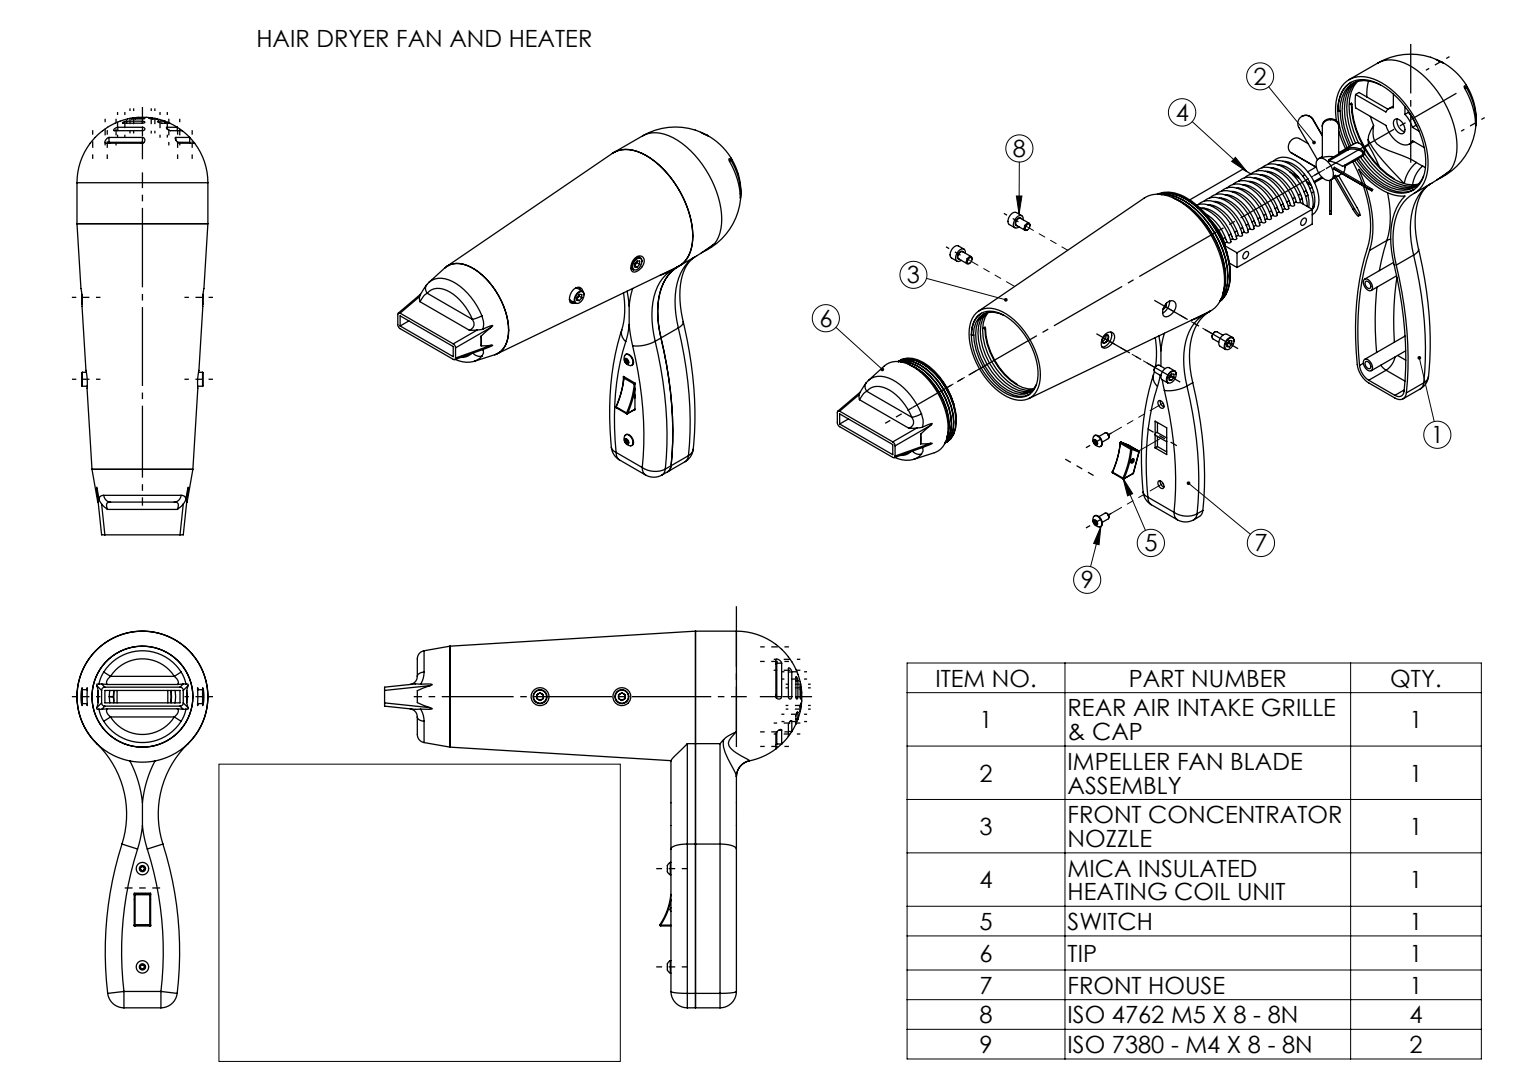
ISO-10303-21;
HEADER;
FILE_DESCRIPTION (('STEP AP214'),
    '1' );
FILE_NAME ('BR-835',
    '2026-10-04T13:31:42',
    ( '' ),
    ( '' ),
    'SwSTEP 2.0',
    'SolidWorks 2026',
    '' );
FILE_SCHEMA (( 'AUTOMOTIVE_DESIGN' ));
ENDSEC;

DATA;
#1 = CARTESIAN_POINT ( 'NONE',  ( -19.03943276465977164, 0.05219959533909376836, 71.24890960531435269 ) ) ;
#2 = CARTESIAN_POINT ( 'NONE',  ( 4.379528057220339221, -16.55341960407611168, 72.70724293864769550 ) ) ;
#3 = CARTESIAN_POINT ( 'NONE',  ( 19.05341960407617918, -5.049401038297876454, 86.04275706135233293 ) ) ;
#4 = CARTESIAN_POINT ( 'NONE',  ( 21.53943276465977519, -0.05219959533907433946, 43.74890960531435979 ) ) ;
#5 = ORIENTED_EDGE ( 'NONE', *, *, #6876, .T. ) ;
#6 = CARTESIAN_POINT ( 'NONE',  ( -19.05341960407611168, -5.049401038298163336, 21.45724293864768839 ) ) ;
#7 = CARTESIAN_POINT ( 'NONE',  ( -16.18388926212240264, -7.379444403734405356, 30.43953151366152809 ) ) ;
#9 = CARTESIAN_POINT ( 'NONE',  ( 21.53943276465977519, -0.05219959533907433946, 73.74890960531433848 ) ) ;
#8 = CARTESIAN_POINT ( 'NONE',  ( 5.049401038298161559, -19.05341960407611168, 77.70724293864765286 ) ) ;
#11 = CARTESIAN_POINT ( 'NONE',  ( -5.049401038298153566, 19.05341960407611168, 75.20724293864769550 ) ) ;
#10 = CARTESIAN_POINT ( 'NONE',  ( -8.314922557961024197, 14.29746914071037800, 97.91775706135236135 ) ) ;
#12 = CARTESIAN_POINT ( 'NONE',  ( -9.564922557961040184, 16.46253265017147172, 72.91775706135233293 ) ) ;
#13 = CARTESIAN_POINT ( 'NONE',  ( 5.823673210054444382, -21.52544592524334988, 85.20942372801901854 ) ) ;
#14 = CARTESIAN_POINT ( 'NONE',  ( -15.80617190586745835, -15.72974639402198527, 56.87390960531436690 ) ) ;
#15 = CARTESIAN_POINT ( 'NONE',  ( 21.52544592524344225, -5.823673210054117533, 23.54057627198102765 ) ) ;
#16 = CARTESIAN_POINT ( 'NONE',  ( -19.02544592524342804, 5.153800228976336051, 36.04057627198100988 ) ) ;
#17 = CARTESIAN_POINT ( 'NONE',  ( -4.379528057220086978, -16.55341960407618274, 94.79275706135234714 ) ) ;
#18 = CARTESIAN_POINT ( 'NONE',  ( -19.05341960407611168, -5.049401038298163336, 56.45724293864768129 ) ) ;
#19 = CARTESIAN_POINT ( 'NONE',  ( 14.29746914071037800, 8.314922557961029526, 26.66775706135235424 ) ) ;
#20 = CARTESIAN_POINT ( 'NONE',  ( 0.000000000000000000, 0.000000000000000000, -45.64921306006598201 ) ) ;
#21 = CARTESIAN_POINT ( 'NONE',  ( 18.67979575497194134, -10.72451020669871369, 110.8344237280190043 ) ) ;
#22 = CARTESIAN_POINT ( 'NONE',  ( -14.29746914071049879, 8.314922557960819915, 55.83224293864770260 ) ) ;
#23 = CARTESIAN_POINT ( 'NONE',  ( -0.05219959533907301413, -21.53943276465977519, 102.4989096053143811 ) ) ;
#24 = CARTESIAN_POINT ( 'NONE',  ( 10.81492255796078972, 18.62759615963270932, 99.58224293864770971 ) ) ;
#25 = CARTESIAN_POINT ( 'NONE',  ( -3.573655867282028392E-15, 2.428612866367529932E-14, -24.99999999999997868 ) ) ;
#26 = CARTESIAN_POINT ( 'NONE',  ( -15.72974639402197994, 15.80617190586746368, 40.62390960531435269 ) ) ;
#27 = CARTESIAN_POINT ( 'NONE',  ( -12.06949235617739369, -12.14591786802326823, 74.37609039468568994 ) ) ;
#28 = CARTESIAN_POINT ( 'NONE',  ( -4.483927247898539470, -16.52544592524342804, 92.29057627198103830 ) ) ;
#29 = CARTESIAN_POINT ( 'NONE',  ( 19.03943276465977164, -0.05219959533909143690, 58.74890960531435979 ) ) ;
#30 = SHAPE_REPRESENTATION_RELATIONSHIP ( 'NONE' , 'NONE' ,  #65015, #146166 ) ;
#31 = DIRECTION ( 'NONE',  ( 0.000000000000000000, 0.000000000000000000, 1.000000000000000000 ) ) ;
#32 = CARTESIAN_POINT ( 'NONE',  ( -12.06949235617739369, -12.14591786802326823, 109.3760903946857042 ) ) ;
#33 = CARTESIAN_POINT ( 'NONE',  ( -5.719274019375665041, -21.55341960407619695, 34.79275706135235424 ) ) ;
#34 = CARTESIAN_POINT ( 'NONE',  ( -19.05341960407611168, -5.049401038298163336, 91.45724293864766707 ) ) ;
#35 = CARTESIAN_POINT ( 'NONE',  ( 21.55341960407619695, -5.719274019375665929, 71.04275706135234714 ) ) ;
#36 = CARTESIAN_POINT ( 'NONE',  ( 0.000000000000000000, 0.000000000000000000, 0.000000000000000000 ) ) ;
#37 = CARTESIAN_POINT ( 'NONE',  ( 0.000000000000000000, -0.7216878364870318308, 1.249999999999999778 ) ) ;
#38 = ORIENTED_EDGE ( 'NONE', *, *, #138549, .T. ) ;
#39 = CARTESIAN_POINT ( 'NONE',  ( 10.72451020669871369, 18.67979575497193778, 57.08442372801901854 ) ) ;
#40 = CARTESIAN_POINT ( 'NONE',  ( -0.05219959533909027116, -19.03943276465977164, 57.49890960531435979 ) ) ;
#41 = CARTESIAN_POINT ( 'NONE',  ( 9.564922557960805705, 16.46253265017160317, 84.58224293864769550 ) ) ;
#42 = CARTESIAN_POINT ( 'NONE',  ( -9.564922557961040184, 16.46253265017147172, 67.91775706135233293 ) ) ;
#43 = CARTESIAN_POINT ( 'NONE',  ( 5.719274019375673035, 21.55341960407619339, 47.29275706135234003 ) ) ;
#44 = CARTESIAN_POINT ( 'NONE',  ( -19.05341960407617563, 5.049401038297882671, 103.5427570613523329 ) ) ;
#45 = CARTESIAN_POINT ( 'NONE',  ( -5.049401038297874678, -19.05341960407617918, 69.79275706135233293 ) ) ;
#46 = CARTESIAN_POINT ( 'NONE',  ( 13.89961937509977652, -13.97604488694527269, 38.12390960531436690 ) ) ;
#47 = CARTESIAN_POINT ( 'NONE',  ( 19.05341960407617918, -5.049401038297876454, 86.04275706135233293 ) ) ;
#48 = CARTESIAN_POINT ( 'NONE',  ( -16.52544592524335698, -4.483927247898792601, 98.95942372801903275 ) ) ;
#49 = CARTESIAN_POINT ( 'NONE',  ( 0.05219959533936267826, -19.03943276465977164, 80.00109039468567573 ) ) ;
#50 = CARTESIAN_POINT ( 'NONE',  ( -12.14591786802309592, -12.06949235617757132, 31.87390960531435979 ) ) ;
#51 = CARTESIAN_POINT ( 'NONE',  ( 16.51473224551083163, -9.474510206698727899, 45.83442372801900433 ) ) ;
#52 = CARTESIAN_POINT ( 'NONE',  ( 15.80617190586769283, -15.72974639402175789, 100.6260903946857184 ) ) ;
#53 = PRODUCT_DEFINITION_SHAPE ( 'NONE', 'NONE',  #200200 ) ;
#55 = EDGE_CURVE ( 'NONE', #141361, #196966, #36036, .T. ) ;
#54 = CARTESIAN_POINT ( 'NONE',  ( 19.05341960407617918, -5.049401038297876454, 21.04275706135232582 ) ) ;
#56 = CARTESIAN_POINT ( 'NONE',  ( 0.05219959533909260263, 19.03943276465977164, 24.99890960531435269 ) ) ;
#57 = CARTESIAN_POINT ( 'NONE',  ( -21.53943276465977519, -0.05219959533937600094, 83.75109039468568994 ) ) ;
#58 = CARTESIAN_POINT ( 'NONE',  ( 8.314922557961029526, -14.29746914071037800, 30.41775706135234358 ) ) ;
#59 = CARTESIAN_POINT ( 'NONE',  ( 19.02544592524343514, -5.153800228976328945, 98.54057627198100988 ) ) ;
#60 = CARTESIAN_POINT ( 'NONE',  ( -8.571926809382608425, 26.38167802310805854, 144.4750000027312069 ) ) ;
#61 = CARTESIAN_POINT ( 'NONE',  ( 0.05219959533909260263, 19.03943276465977164, 79.99890960531436690 ) ) ;
#62 = DIRECTION ( 'NONE',  ( -0.000000000000000000, -0.000000000000000000, 1.000000000000000000 ) ) ;
#63 = ORIENTED_EDGE ( 'NONE', *, *, #98272, .F. ) ;
#64 = CARTESIAN_POINT ( 'NONE',  ( -16.51473224551082808, 9.474510206698731452, 83.33442372801899012 ) ) ;
#66 = CARTESIAN_POINT ( 'NONE',  ( 0.05219959533909260263, 19.03943276465977164, 114.9989096053143669 ) ) ;
#65 = CIRCLE ( 'NONE', #138924, 4.000000000000000888 ) ;
#68 = CARTESIAN_POINT ( 'NONE',  ( -13.97604488694547697, 13.89961937509957934, 103.1260903946856473 ) ) ;
#67 = CARTESIAN_POINT ( 'NONE',  ( -10.72451020669870658, -18.67979575497194134, 109.5844237280190328 ) ) ;
#69 = CARTESIAN_POINT ( 'NONE',  ( -4.483927247898539470, -16.52544592524342804, 97.29057627198105251 ) ) ;
#70 = CARTESIAN_POINT ( 'NONE',  ( -5.153800228976328057, -19.02544592524343514, 22.29057627198102765 ) ) ;
#71 = CARTESIAN_POINT ( 'NONE',  ( -5.823673210054116645, -21.52544592524344225, 62.29057627198102409 ) ) ;
#72 =( BOUNDED_CURVE ( )  B_SPLINE_CURVE ( 2, ( #135553, #193227, #149715, #197225, #132546, #194235, #55701, #58687, #117374, #179071, #182049 ),
 .UNSPECIFIED., .F., .T. ) 
 B_SPLINE_CURVE_WITH_KNOTS ( ( 3, 2, 2, 2, 2, 3 ),
 ( 0.1000000000000000888, 0.1200000000000001343, 0.1400000000000001799, 0.1600000000000001976, 0.1800000000000002431, 0.2000000000000001776 ),
 .UNSPECIFIED. ) 
 CURVE ( )  GEOMETRIC_REPRESENTATION_ITEM ( )  RATIONAL_B_SPLINE_CURVE ( ( 0.9999999999999997780, 0.9510565162951537532, 1.000000000000000000, 0.9510565162951535312, 1.000000000000000000, 0.9510565162951535312, 1.000000000000000000, 0.9510565162951535312, 1.000000000000000000, 0.9510565162951529761, 1.000000000000000444 ) ) 
 REPRESENTATION_ITEM ( '' )  );
#73 = CARTESIAN_POINT ( 'NONE',  ( 10.72451020669898902, -18.67979575497178502, 47.91557627198102409 ) ) ;
#74 = CARTESIAN_POINT ( 'NONE',  ( 13.89961937509977652, -13.97604488694527269, 28.12390960531435624 ) ) ;
#75 = CARTESIAN_POINT ( 'NONE',  ( 27.73933785331498569, 2.768321779492822058E-14, 140.3750000027311842 ) ) ;
#76 = CARTESIAN_POINT ( 'NONE',  ( 16.51473224551083163, -9.474510206698727899, 55.83442372801899722 ) ) ;
#77 = CARTESIAN_POINT ( 'NONE',  ( -14.29746914071049879, 8.314922557960819915, 35.83224293864768839 ) ) ;
#78 = CARTESIAN_POINT ( 'NONE',  ( 9.474510206698971260, -16.51473224551069308, 112.9155762719810383 ) ) ;
#79 = CARTESIAN_POINT ( 'NONE',  ( -15.80617190586768217, 15.72974639402176855, 83.12609039468568994 ) ) ;
#80 = CARTESIAN_POINT ( 'NONE',  ( -10.72451020669898014, 18.67979575497178502, 65.41557627198102409 ) ) ;
#81 = CARTESIAN_POINT ( 'NONE',  ( 18.67979575497194134, -10.72451020669871369, 55.83442372801901854 ) ) ;
#82 = CARTESIAN_POINT ( 'NONE',  ( 15.80617190586769283, -15.72974639402175789, 45.62609039468567573 ) ) ;
#83 = CARTESIAN_POINT ( 'NONE',  ( 13.89961937509977652, -13.97604488694527269, 78.12390960531433848 ) ) ;
#84 = CARTESIAN_POINT ( 'NONE',  ( -8.314922557961024197, 14.29746914071037800, 97.91775706135236135 ) ) ;
#85 = CARTESIAN_POINT ( 'NONE',  ( -5.049401038298153566, 19.05341960407611168, 25.20724293864768484 ) ) ;
#86 = CARTESIAN_POINT ( 'NONE',  ( -31.23840969660177791, 7.314650797970922547, 96.67552899226033958 ) ) ;
#87 = CARTESIAN_POINT ( 'NONE',  ( -14.29746914071049879, 8.314922557960819915, 70.83224293864770971 ) ) ;
#88 = CARTESIAN_POINT ( 'NONE',  ( 8.224510206698953496, -14.34966873604960469, 37.91557627198102409 ) ) ;
#89 = CARTESIAN_POINT ( 'NONE',  ( 19.05341960407611168, 5.049401038298154454, 63.95724293864769550 ) ) ;
#90 = CARTESIAN_POINT ( 'NONE',  ( -19.03943276465977164, 0.05219959533909376836, 36.24890960531436690 ) ) ;
#91 = CARTESIAN_POINT ( 'NONE',  ( 15.72974639402199770, -15.80617190586745480, 43.12390960531435269 ) ) ;
#92 = CARTESIAN_POINT ( 'NONE',  ( -19.02544592524334988, -5.153800228976617603, 33.95942372801897591 ) ) ;
#94 = CARTESIAN_POINT ( 'NONE',  ( 16.55341960407611168, 4.379528057220329451, 48.95724293864770971 ) ) ;
#93 = CARTESIAN_POINT ( 'NONE',  ( 25.38276140623240096, 4.833717845876353891, 166.7901960806512136 ) ) ;
#96 = AXIS2_PLACEMENT_3D ( 'NONE', #158680, #174858, #36324 ) ;
#95 = CARTESIAN_POINT ( 'NONE',  ( -10.72451020669898014, 18.67979575497178502, 30.41557627198101699 ) ) ;
#97 = CARTESIAN_POINT ( 'NONE',  ( 7.656827144875921753, -71.74905178543389184, -15.00000000000000178 ) ) ;
#98 = CARTESIAN_POINT ( 'NONE',  ( -8.314922557961024197, 14.29746914071037800, 72.91775706135234714 ) ) ;
#99 = CARTESIAN_POINT ( 'NONE',  ( 13.97604488694548053, -13.89961937509957401, 70.62609039468567573 ) ) ;
#100 = CARTESIAN_POINT ( 'NONE',  ( 16.53943276465976808, -0.05219959533910856209, 43.74890960531435979 ) ) ;
#101 = CARTESIAN_POINT ( 'NONE',  ( 28.79475375365586132, 2.781246896534039337E-14, 145.2656553485623760 ) ) ;
#102 = CARTESIAN_POINT ( 'NONE',  ( -8.314922557960811034, -14.29746914071050412, 27.08224293864769550 ) ) ;
#103 = CARTESIAN_POINT ( 'NONE',  ( 16.46253265017160672, -9.564922557960803928, 48.33224293864769550 ) ) ;
#104 = CARTESIAN_POINT ( 'NONE',  ( 19.05341960407611168, 5.049401038298154454, 73.95724293864768129 ) ) ;
#105 = CARTESIAN_POINT ( 'NONE',  ( -5.049401038298153566, 19.05341960407611168, 35.20724293864768839 ) ) ;
#106 = CARTESIAN_POINT ( 'NONE',  ( 21.55341960407619695, -5.719274019375665929, 41.04275706135236135 ) ) ;
#107 = CARTESIAN_POINT ( 'NONE',  ( 16.46253265017160672, -9.564922557960803928, 63.33224293864769550 ) ) ;
#108 = DIRECTION ( 'NONE',  ( -0.000000000000000000, -0.000000000000000000, -1.000000000000000000 ) ) ;
#109 = CARTESIAN_POINT ( 'NONE',  ( -19.03943276465977164, 0.05219959533909376836, 46.24890960531435979 ) ) ;
#110 = CARTESIAN_POINT ( 'NONE',  ( -0.05219959533907301413, -21.53943276465977519, 32.49890960531435979 ) ) ;
#111 = B_SPLINE_CURVE_WITH_KNOTS ( 'NONE', 3,
 ( #132361, #22184, #54519, #149527, #68676, #38352 ),
 .UNSPECIFIED., .F., .F.,
 ( 4, 2, 4 ),
 ( 0.007228050697041336729, 0.007608510107494812283, 0.007988969517948286969 ),
 .UNSPECIFIED. ) ;
#113 = CARTESIAN_POINT ( 'NONE',  ( 12.06949235617757843, -12.14591786802309237, 113.1239096053143953 ) ) ;
#112 = CARTESIAN_POINT ( 'NONE',  ( 10.72451020669871369, 18.67979575497193778, 67.08442372801901854 ) ) ;
#114 = CARTESIAN_POINT ( 'NONE',  ( -21.55341960407610458, -5.719274019375992779, 31.45724293864769550 ) ) ;
#115 = CARTESIAN_POINT ( 'NONE',  ( 8.314922557961029526, -14.29746914071037800, 95.41775706135234714 ) ) ;
#116 = CARTESIAN_POINT ( 'NONE',  ( 10.81492255796106328, -18.62759615963255655, 110.4177570613523756 ) ) ;
#117 = CARTESIAN_POINT ( 'NONE',  ( -8.314922557961024197, 14.29746914071037800, 67.91775706135234714 ) ) ;
#118 = CARTESIAN_POINT ( 'NONE',  ( -9.564922557960796823, -16.46253265017161027, 112.0822429386476955 ) ) ;
#119 = CARTESIAN_POINT ( 'NONE',  ( -14.29746914071037622, -8.314922557961029526, 59.16775706135234714 ) ) ;
#120 = CARTESIAN_POINT ( 'NONE',  ( -8.314922557961024197, 14.29746914071037800, 37.91775706135235424 ) ) ;
#121 = CARTESIAN_POINT ( 'NONE',  ( -0.05219959533934338120, 16.53943276465976808, 102.5010903946856899 ) ) ;
#122 = CARTESIAN_POINT ( 'NONE',  ( -15.72974639402176322, -15.80617190586768395, 54.37609039468568994 ) ) ;
#123 = CARTESIAN_POINT ( 'NONE',  ( 4.379528057220092307, 16.55341960407617563, 22.29275706135235069 ) ) ;
#124 = CARTESIAN_POINT ( 'NONE',  ( 5.719274019375991003, -21.55341960407610458, 112.7072429386476955 ) ) ;
#125 = CARTESIAN_POINT ( 'NONE',  ( 8.224510206698742110, 14.34966873604972548, 27.08442372801901854 ) ) ;
#126 = CARTESIAN_POINT ( 'NONE',  ( -12.14591786802326823, 12.06949235617739902, 83.12609039468568994 ) ) ;
#127 = FACE_OUTER_BOUND ( 'NONE', #92552, .T. ) ;
#128 = CARTESIAN_POINT ( 'NONE',  ( 18.67979575497194134, -10.72451020669871369, 85.83442372801901854 ) ) ;
#129 = CARTESIAN_POINT ( 'NONE',  ( 16.46253265017146816, 9.564922557961045513, 81.66775706135233293 ) ) ;
#130 = CARTESIAN_POINT ( 'NONE',  ( -4.379528057220328563, 16.55341960407611168, 60.20724293864768839 ) ) ;
#131 = CARTESIAN_POINT ( 'NONE',  ( -4.379528057220328563, 16.55341960407611168, 40.20724293864769550 ) ) ;
#132 = CARTESIAN_POINT ( 'NONE',  ( -14.29746914071049879, 8.314922557960819915, 105.8322429386476955 ) ) ;
#134 = CARTESIAN_POINT ( 'NONE',  ( 9.809999999999998721, 0.000000000000000000, 1.999999999999999556 ) ) ;
#133 = CARTESIAN_POINT ( 'NONE',  ( -16.46253265017146816, -9.564922557961047289, 49.16775706135233293 ) ) ;
#135 = CARTESIAN_POINT ( 'NONE',  ( 0.05219959533937995610, -21.53943276465977519, 45.00109039468568284 ) ) ;
#136 = CARTESIAN_POINT ( 'NONE',  ( 0.05219959533934541429, -16.53943276465976808, 20.00109039468568639 ) ) ;
#137 = DIRECTION ( 'NONE',  ( 0.000000000000000000, 0.000000000000000000, -1.000000000000000000 ) ) ;
#138 = CARTESIAN_POINT ( 'NONE',  ( 16.46253265017160672, -9.564922557960803928, 108.3322429386476955 ) ) ;
#139 = CARTESIAN_POINT ( 'NONE',  ( 15.80617190586746368, 15.72974639402197994, 69.37390960531436690 ) ) ;
#140 = CARTESIAN_POINT ( 'NONE',  ( -19.02544592524334988, -5.153800228976617603, 98.95942372801900433 ) ) ;
#141 = CARTESIAN_POINT ( 'NONE',  ( -16.51473224551069308, -9.474510206698971260, 106.6655762719810383 ) ) ;
#142 = CARTESIAN_POINT ( 'NONE',  ( 1.955436445514509014, -27.87083070116242567, 139.9999999999999716 ) ) ;
#143 = CARTESIAN_POINT ( 'NONE',  ( 14.29746914071049879, -8.314922557960816363, 113.3322429386476955 ) ) ;
#144 = CARTESIAN_POINT ( 'NONE',  ( -21.55341960407619339, 5.719274019375674811, 98.54275706135234714 ) ) ;
#145 = CARTESIAN_POINT ( 'NONE',  ( 13.89961937509977652, -13.97604488694527269, 28.12390960531435624 ) ) ;
#146 = CARTESIAN_POINT ( 'NONE',  ( 21.52544592524334988, 5.823673210054432836, 51.45942372801901854 ) ) ;
#147 = CARTESIAN_POINT ( 'NONE',  ( -21.53943276465977519, -0.05219959533937600094, 93.75109039468567573 ) ) ;
#148 = CARTESIAN_POINT ( 'NONE',  ( 14.29746914071037800, 8.314922557961029526, 86.66775706135234714 ) ) ;
#149 = CARTESIAN_POINT ( 'NONE',  ( -5.719274019375665041, -21.55341960407619695, 39.79275706135235424 ) ) ;
#150 = CARTESIAN_POINT ( 'NONE',  ( 21.52544592524334988, 5.823673210054432836, 36.45942372801901143 ) ) ;
#152 = CARTESIAN_POINT ( 'NONE',  ( -16.51473224551069308, -9.474510206698971260, 81.66557627198103830 ) ) ;
#151 = CARTESIAN_POINT ( 'NONE',  ( 5.049401038297881783, 19.05341960407617563, 67.29275706135234714 ) ) ;
#153 = CARTESIAN_POINT ( 'NONE',  ( -0.05219959533910754901, -16.53943276465976808, 107.4989096053143669 ) ) ;
#154 = CARTESIAN_POINT ( 'NONE',  ( -0.05219959533907301413, -21.53943276465977519, 82.49890960531436690 ) ) ;
#155 = CARTESIAN_POINT ( 'NONE',  ( 12.14591786802309770, 12.06949235617756955, 64.37390960531435269 ) ) ;
#156 = CARTESIAN_POINT ( 'NONE',  ( -21.52544592524334988, -5.823673210054445271, 103.9594237280190185 ) ) ;
#157 = CARTESIAN_POINT ( 'NONE',  ( -8.224510206698948167, 14.34966873604960824, 90.41557627198103830 ) ) ;
#158 = CARTESIAN_POINT ( 'NONE',  ( -19.02544592524342804, 5.153800228976336051, 41.04057627198103120 ) ) ;
#159 = CARTESIAN_POINT ( 'NONE',  ( 19.02544592524334988, 5.153800228976608722, 66.45942372801899012 ) ) ;
#161 = CARTESIAN_POINT ( 'NONE',  ( -8.224510206698948167, 14.34966873604960824, 50.41557627198103120 ) ) ;
#160 = AXIS2_PLACEMENT_3D ( 'NONE', #57198, #41025, #151201 ) ;
#162 = CARTESIAN_POINT ( 'NONE',  ( 5.823673210054444382, -21.52544592524334988, 95.20942372801903275 ) ) ;
#163 = CARTESIAN_POINT ( 'NONE',  ( 13.97604488694527802, 13.89961937509977652, 89.37390960531436690 ) ) ;
#164 = CARTESIAN_POINT ( 'NONE',  ( 5.153800228976615827, -19.02544592524334988, 55.20942372801899722 ) ) ;
#165 = CARTESIAN_POINT ( 'NONE',  ( 0.05219959533907565091, 21.53943276465977519, 69.99890960531435269 ) ) ;
#166 = CARTESIAN_POINT ( 'NONE',  ( 18.67979575497178502, 10.72451020669898547, 109.1655762719810383 ) ) ;
#167 = CARTESIAN_POINT ( 'NONE',  ( 5.153800228976615827, -19.02544592524334988, 110.2094237280189901 ) ) ;
#168 = CARTESIAN_POINT ( 'NONE',  ( 0.05219959533934541429, -16.53943276465976808, 80.00109039468568994 ) ) ;
#170 = CARTESIAN_POINT ( 'NONE',  ( -10.72451020669870658, -18.67979575497194134, 24.58442372801901499 ) ) ;
#169 = CARTESIAN_POINT ( 'NONE',  ( -5.153800228976328057, -19.02544592524343514, 22.29057627198102765 ) ) ;
#171 = CARTESIAN_POINT ( 'NONE',  ( -14.29746914071049879, 8.314922557960819915, 110.8322429386476955 ) ) ;
#172 = CARTESIAN_POINT ( 'NONE',  ( -11.40812507854755609, 35.11059874428196537, -7.524999997268813523 ) ) ;
#173 = CARTESIAN_POINT ( 'NONE',  ( 8.314922557961029526, -14.29746914071037800, 45.41775706135234003 ) ) ;
#174 = APPLICATION_CONTEXT ( 'automotive_design' ) ;
#175 = CARTESIAN_POINT ( 'NONE',  ( 16.53943276465976808, -0.05219959533910856209, 78.74890960531436690 ) ) ;
#176 = CARTESIAN_POINT ( 'NONE',  ( -18.67979575497178146, -10.72451020669898902, 81.66557627198103830 ) ) ;
#177 = CARTESIAN_POINT ( 'NONE',  ( -8.224510206698735004, -14.34966873604973081, 104.5844237280190185 ) ) ;
#178 = CARTESIAN_POINT ( 'NONE',  ( -4.483927247898782831, 16.52544592524335698, 32.70942372801900433 ) ) ;
#179 = CARTESIAN_POINT ( 'NONE',  ( 19.03943276465977164, -0.05219959533909143690, 38.74890960531436690 ) ) ;
#180 = CARTESIAN_POINT ( 'NONE',  ( -16.53943276465976808, -0.05219959533934237506, 83.75109039468568994 ) ) ;
#181 = CARTESIAN_POINT ( 'NONE',  ( -5.153800228976607833, 19.02544592524334988, 77.70942372801900433 ) ) ;
#182 = CARTESIAN_POINT ( 'NONE',  ( 21.55341960407610458, 5.719274019375980345, 68.95724293864769550 ) ) ;
#183 = CARTESIAN_POINT ( 'NONE',  ( -4.379528057220086978, -16.55341960407618274, 109.7927570613523613 ) ) ;
#184 = CARTESIAN_POINT ( 'NONE',  ( 15.72974639402176855, 15.80617190586768217, 86.87609039468568994 ) ) ;
#185 = CARTESIAN_POINT ( 'NONE',  ( -18.67979575497178146, -10.72451020669898902, 41.66557627198103120 ) ) ;
#186 = EDGE_LOOP ( 'NONE', ( #96983, #147295, #14374 ) ) ;
#187 = CARTESIAN_POINT ( 'NONE',  ( -14.34966873604972548, 8.224510206698743886, 98.33442372801901854 ) ) ;
#188 = CARTESIAN_POINT ( 'NONE',  ( -18.62759615963270932, 10.81492255796079327, 50.83224293864770971 ) ) ;
#189 = ORIENTED_EDGE ( 'NONE', *, *, #119223, .F. ) ;
#190 = CARTESIAN_POINT ( 'NONE',  ( -0.05219959533907301413, -21.53943276465977519, 22.49890960531436335 ) ) ;
#191 = CARTESIAN_POINT ( 'NONE',  ( 17.50000000000000355, 3.565345528327941160, 108.0750551319352581 ) ) ;
#192 = CARTESIAN_POINT ( 'NONE',  ( -16.46253265017160317, 9.564922557960807481, 25.83224293864769194 ) ) ;
#193 = CARTESIAN_POINT ( 'NONE',  ( 15.72974639402199770, -15.80617190586745480, 78.12390960531436690 ) ) ;
#194 = CARTESIAN_POINT ( 'NONE',  ( 0.05219959533934541429, -16.53943276465976808, 105.0010903946856757 ) ) ;
#195 = CARTESIAN_POINT ( 'NONE',  ( 21.53943276465977519, 0.05219959533937863772, 61.25109039468567573 ) ) ;
#196 = CARTESIAN_POINT ( 'NONE',  ( -14.29746914071037622, -8.314922557961029526, 24.16775706135235424 ) ) ;
#197 = CARTESIAN_POINT ( 'NONE',  ( 12.14591786802309770, 12.06949235617756955, 114.3739096053143527 ) ) ;
#198 = CARTESIAN_POINT ( 'NONE',  ( -19.05341960407617563, 5.049401038297882671, 113.5427570613523471 ) ) ;
#199 = CARTESIAN_POINT ( 'NONE',  ( -5.049401038298153566, 19.05341960407611168, 35.20724293864768839 ) ) ;
#200 = CARTESIAN_POINT ( 'NONE',  ( -23.31738231874055245, -16.94106989632524574, 144.1999999999999886 ) ) ;
#201 = CARTESIAN_POINT ( 'NONE',  ( -19.03943276465977164, 0.05219959533909376836, 111.2489096053143669 ) ) ;
#202 = CARTESIAN_POINT ( 'NONE',  ( 0.05219959533934541429, -16.53943276465976808, 85.00109039468568994 ) ) ;
#203 = CARTESIAN_POINT ( 'NONE',  ( -9.564922557961040184, 16.46253265017147172, 82.91775706135233293 ) ) ;
#204 = CARTESIAN_POINT ( 'NONE',  ( 9.564922557961047289, -16.46253265017146816, 30.41775706135232937 ) ) ;
#205 = CARTESIAN_POINT ( 'NONE',  ( 0.05219959533907565091, 21.53943276465977519, 59.99890960531436690 ) ) ;
#206 = CARTESIAN_POINT ( 'NONE',  ( -14.34966873604972548, 8.224510206698743886, 83.33442372801903275 ) ) ;
#207 = CARTESIAN_POINT ( 'NONE',  ( -16.46253265017146816, -9.564922557961047289, 99.16775706135233293 ) ) ;
#208 = CARTESIAN_POINT ( 'NONE',  ( 19.05341960407611168, 5.049401038298154454, 53.95724293864770260 ) ) ;
#209 = CARTESIAN_POINT ( 'NONE',  ( 16.46253265017160672, -9.564922557960803928, 98.33224293864769550 ) ) ;
#210 = CARTESIAN_POINT ( 'NONE',  ( -0.05219959533937732626, 21.53943276465977519, 47.50109039468568994 ) ) ;
#211 = CARTESIAN_POINT ( 'NONE',  ( -19.05341960407611168, -5.049401038298163336, 41.45724293864769550 ) ) ;
#212 = SPHERICAL_SURFACE ( 'NONE', #37950, 10.00000000000000000 ) ;
#213 = CARTESIAN_POINT ( 'NONE',  ( -13.89961937509977652, 13.97604488694528158, 110.6239096053143243 ) ) ;
#214 = CARTESIAN_POINT ( 'NONE',  ( 8.314922557960818139, 14.29746914071049879, 64.58224293864769550 ) ) ;
#215 = CARTESIAN_POINT ( 'NONE',  ( -5.719274019375978568, 21.55341960407610458, 55.20724293864770260 ) ) ;
#216 = CARTESIAN_POINT ( 'NONE',  ( 23.29544513554940011, 16.92513159979228021, 143.4656553485623647 ) ) ;
#217 = CARTESIAN_POINT ( 'NONE',  ( -16.46253265017146816, -9.564922557961047289, 49.16775706135233293 ) ) ;
#218 = CARTESIAN_POINT ( 'NONE',  ( 19.76513836702801186, -12.18681594171306237, 170.0000000000000000 ) ) ;
#220 = CARTESIAN_POINT ( 'NONE',  ( 5.049401038298161559, -19.05341960407611168, 67.70724293864769550 ) ) ;
#219 = CARTESIAN_POINT ( 'NONE',  ( -16.46253265017160317, 9.564922557960807481, 60.83224293864769550 ) ) ;
#221 = EDGE_CURVE ( 'NONE', #165210, #193478, #178958, .T. ) ;
#222 = CARTESIAN_POINT ( 'NONE',  ( 12.06949235617739724, 12.14591786802326823, 46.87609039468568994 ) ) ;
#223 = CARTESIAN_POINT ( 'NONE',  ( 15.64208950468054127, -40.81369178264755959, -21.33727593494802122 ) ) ;
#224 = CARTESIAN_POINT ( 'NONE',  ( 16.51473224551083163, -9.474510206698727899, 30.83442372801900433 ) ) ;
#225 = CYLINDRICAL_SURFACE ( 'NONE', #105054, 10.00000000000000178 ) ;
#226 = CARTESIAN_POINT ( 'NONE',  ( -0.05219959533934338120, 16.53943276465976808, 92.50109039468567573 ) ) ;
#227 = CARTESIAN_POINT ( 'NONE',  ( 69.65682714487590488, -71.74905178543389184, -4.999999999999999112 ) ) ;
#228 = CARTESIAN_POINT ( 'NONE',  ( 16.52544592524335698, 4.483927247898782831, 81.45942372801900433 ) ) ;
#229 = CARTESIAN_POINT ( 'NONE',  ( 4.483927247898790824, -16.52544592524335698, 60.20942372801902565 ) ) ;
#230 = CARTESIAN_POINT ( 'NONE',  ( -5.823673210054431948, 21.52544592524334988, 112.7094237280190328 ) ) ;
#232 = CARTESIAN_POINT ( 'NONE',  ( 17.25602135761909395, -17.10936820804715808, -56.77278709839602300 ) ) ;
#231 = CARTESIAN_POINT ( 'NONE',  ( -5.049401038298153566, 19.05341960407611168, 50.20724293864770260 ) ) ;
#233 = CARTESIAN_POINT ( 'NONE',  ( -10.72451020669870658, -18.67979575497194134, 69.58442372801900433 ) ) ;
#234 = CARTESIAN_POINT ( 'NONE',  ( -19.03943276465977164, -0.05219959533935918106, 73.75109039468566152 ) ) ;
#235 = CARTESIAN_POINT ( 'NONE',  ( -18.67979575497193778, 10.72451020669871902, 113.3344237280190328 ) ) ;
#236 = CARTESIAN_POINT ( 'NONE',  ( 16.51473224551069308, 9.474510206698969483, 29.16557627198103475 ) ) ;
#237 = CARTESIAN_POINT ( 'NONE',  ( 17.50000000000006750, 5.663021631379938192, 23.82188452050911209 ) ) ;
#238 = CARTESIAN_POINT ( 'NONE',  ( -10.72451020669898014, 18.67979575497178502, 70.41557627198102409 ) ) ;
#239 = CARTESIAN_POINT ( 'NONE',  ( 18.67979575497178502, 10.72451020669898547, 24.16557627198103120 ) ) ;
#240 = CARTESIAN_POINT ( 'NONE',  ( 0.05219959533910956823, 16.53943276465976808, 114.9989096053143669 ) ) ;
#241 = CARTESIAN_POINT ( 'NONE',  ( 4.379528057220092307, 16.55341960407617563, 37.29275706135235424 ) ) ;
#242 = CARTESIAN_POINT ( 'NONE',  ( 14.34966873604960469, 8.224510206698951720, 24.16557627198103120 ) ) ;
#243 = VERTEX_POINT ( 'NONE', #159375 ) ;
#244 = CARTESIAN_POINT ( 'NONE',  ( -15.72974639402176322, -15.80617190586768395, 24.37609039468567573 ) ) ;
#246 = CARTESIAN_POINT ( 'NONE',  ( -30.74264578624800492, -22.33583958711396278, -7.800000000000000711 ) ) ;
#245 = CARTESIAN_POINT ( 'NONE',  ( 4.483927247898545687, 16.52544592524342804, 34.79057627198103120 ) ) ;
#247 = CARTESIAN_POINT ( 'NONE',  ( -13.89961937509957401, -13.97604488694547875, 109.3760903946856331 ) ) ;
#248 = CARTESIAN_POINT ( 'NONE',  ( 16.46253265017146816, 9.564922557961045513, 21.66775706135233648 ) ) ;
#249 = CARTESIAN_POINT ( 'NONE',  ( 12.14591786802309770, 12.06949235617756955, 49.37390960531436690 ) ) ;
#250 = CARTESIAN_POINT ( 'NONE',  ( 18.67979575497178502, 10.72451020669898547, 99.16557627198100988 ) ) ;
#252 = CARTESIAN_POINT ( 'NONE',  ( -15.72974639402197994, 15.80617190586746368, 60.62390960531437401 ) ) ;
#251 = CARTESIAN_POINT ( 'NONE',  ( 17.50000000000000355, 5.622605283950888655, 33.81207310596111881 ) ) ;
#253 = CARTESIAN_POINT ( 'NONE',  ( -0.05219959533909027116, -19.03943276465977164, 77.49890960531435269 ) ) ;
#254 = CARTESIAN_POINT ( 'NONE',  ( 8.314922557960818139, 14.29746914071049879, 49.58224293864769550 ) ) ;
#255 = CARTESIAN_POINT ( 'NONE',  ( 0.05219959533909260263, 19.03943276465977164, 89.99890960531436690 ) ) ;
#256 = B_SPLINE_CURVE_WITH_KNOTS ( 'NONE', 3,
 ( #135702, #179228, #194389, #162034, #102364, #70032, #58838, #148877, #56868, #196396, #118543, #180233, #23530, #41702, #119537, #146865, #181220, #193382, #54858, #116532, #178220, #17313, #108315, #14325, #1126, #186178, #60815, #44673, #78968, #169995, #75990, #62800 ),
 .UNSPECIFIED., .F., .F.,
 ( 4, 2, 2, 2, 2, 2, 2, 2, 2, 2, 2, 2, 2, 2, 2, 4 ),
 ( 1.646036181032119693E-15, 0.0003712461730052185930, 0.0007424923460087911502, 0.001113738519012363653, 0.001484984692015936265, 0.002227477038023079753, 0.002598723211026658653, 0.002969969384030237119, 0.003341215557033815585, 0.003712461730037394485, 0.004083707903040972517, 0.004454954076044551417, 0.004826200249048129449, 0.005197446422051708349, 0.005568692595055286382, 0.005939938768058865282 ),
 .UNSPECIFIED. ) ;
#257 = CARTESIAN_POINT ( 'NONE',  ( -36.88729982035408739, 1.776435236410510043, 50.21758054017369233 ) ) ;
#258 = CARTESIAN_POINT ( 'NONE',  ( 0.05219959533936267826, -19.03943276465977164, 60.00109039468566863 ) ) ;
#259 = CARTESIAN_POINT ( 'NONE',  ( 5.823673210054125526, 21.52544592524343514, 99.79057627198103830 ) ) ;
#260 = CARTESIAN_POINT ( 'NONE',  ( 19.05341960407611168, 5.049401038298154454, 43.95724293864769550 ) ) ;
#261 = CARTESIAN_POINT ( 'NONE',  ( -0.05219959533910754901, -16.53943276465976808, 102.4989096053143811 ) ) ;
#262 = CARTESIAN_POINT ( 'NONE',  ( -10.81492255796105439, 18.62759615963255655, 47.91775706135234714 ) ) ;
#263 = CARTESIAN_POINT ( 'NONE',  ( 22.44159573604009239, 16.30477369853692693, 146.0750000027311728 ) ) ;
#264 = CARTESIAN_POINT ( 'NONE',  ( -16.52544592524342804, 4.483927247898546575, 26.04057627198103475 ) ) ;
#265 = CARTESIAN_POINT ( 'NONE',  ( -13.89961937509977652, 13.97604488694528158, 55.62390960531434558 ) ) ;
#266 = CARTESIAN_POINT ( 'NONE',  ( -13.89961937509977652, 13.97604488694528158, 105.6239096053143527 ) ) ;
#267 = CARTESIAN_POINT ( 'NONE',  ( 5.823673210054125526, 21.52544592524343514, 59.79057627198103120 ) ) ;
#268 = CARTESIAN_POINT ( 'NONE',  ( -5.359611314223446995E-15, 29.16686587814335496, 140.3750000027311842 ) ) ;
#269 = CARTESIAN_POINT ( 'NONE',  ( 0.05219959533909260263, 19.03943276465977164, 34.99890960531435979 ) ) ;
#270 = CARTESIAN_POINT ( 'NONE',  ( -15.72974639402197994, 15.80617190586746368, 50.62390960531435979 ) ) ;
#271 = CARTESIAN_POINT ( 'NONE',  ( 15.72974639402176855, 15.80617190586768217, 91.87609039468568994 ) ) ;
#273 = CARTESIAN_POINT ( 'NONE',  ( -16.52544592524335698, -4.483927247898792601, 83.95942372801900433 ) ) ;
#272 = CARTESIAN_POINT ( 'NONE',  ( 14.16830335033699662, -40.16376294013230819, -20.11902964094307933 ) ) ;
#274 = CARTESIAN_POINT ( 'NONE',  ( 12.06949235617739724, 12.14591786802326823, 91.87609039468568994 ) ) ;
#275 = CARTESIAN_POINT ( 'NONE',  ( 5.153800228976335163, 19.02544592524342804, 54.79057627198103120 ) ) ;
#276 = CARTESIAN_POINT ( 'NONE',  ( 13.89961937509977652, -13.97604488694527269, 68.12390960531436690 ) ) ;
#277 = EDGE_LOOP ( 'NONE', ( #133276, #198078, #94972, #136074, #147190 ) ) ;
#278 = CARTESIAN_POINT ( 'NONE',  ( -19.03943276465977164, -0.05219959533935918106, 28.75109039468566507 ) ) ;
#279 = CARTESIAN_POINT ( 'NONE',  ( 14.29746914071037800, 8.314922557961029526, 76.66775706135234714 ) ) ;
#280 = CARTESIAN_POINT ( 'NONE',  ( -18.67979575497193778, 10.72451020669871902, 113.3344237280190328 ) ) ;
#281 = CARTESIAN_POINT ( 'NONE',  ( -19.05341960407611168, -5.049401038298163336, 71.45724293864766707 ) ) ;
#282 = CARTESIAN_POINT ( 'NONE',  ( -21.52544592524343514, 5.823673210054127303, 36.04057627198102409 ) ) ;
#283 = CARTESIAN_POINT ( 'NONE',  ( 14.34966873604972726, -8.224510206698740333, 25.83442372801901499 ) ) ;
#284 = CARTESIAN_POINT ( 'NONE',  ( 0.05219959533937995610, -21.53943276465977519, 80.00109039468568994 ) ) ;
#285 = CARTESIAN_POINT ( 'NONE',  ( -0.05219959533934338120, 16.53943276465976808, 52.50109039468567573 ) ) ;
#286 = CARTESIAN_POINT ( 'NONE',  ( 10.72451020669898902, -18.67979575497178502, 97.91557627198103830 ) ) ;
#287 = CARTESIAN_POINT ( 'NONE',  ( -16.51473224551082808, 9.474510206698731452, 113.3344237280190043 ) ) ;
#288 = CARTESIAN_POINT ( 'NONE',  ( 13.89961937509977652, -13.97604488694527269, 73.12390960531436690 ) ) ;
#289 = CARTESIAN_POINT ( 'NONE',  ( 4.483927247898790824, -16.52544592524335698, 25.20942372801901854 ) ) ;
#290 = CARTESIAN_POINT ( 'NONE',  ( 13.97604488694527802, 13.89961937509977652, 44.37390960531435269 ) ) ;
#291 = CARTESIAN_POINT ( 'NONE',  ( 16.46253265017146816, 9.564922557961045513, 111.6677570613523329 ) ) ;
#292 = CARTESIAN_POINT ( 'NONE',  ( -12.06949235617756955, 12.14591786802309770, 75.62390960531439532 ) ) ;
#293 = CARTESIAN_POINT ( 'NONE',  ( 4.379528057220092307, 16.55341960407617563, 87.29275706135236135 ) ) ;
#294 = EDGE_CURVE ( 'NONE', #2008, #55198, #134552, .T. ) ;
#296 = CARTESIAN_POINT ( 'NONE',  ( 0.05219959533909260263, 19.03943276465977164, 69.99890960531435269 ) ) ;
#295 = CARTESIAN_POINT ( 'NONE',  ( 21.52544592524334988, 5.823673210054432836, 31.45942372801901854 ) ) ;
#297 = CARTESIAN_POINT ( 'NONE',  ( 13.89961937509977652, -13.97604488694527269, 63.12390960531435979 ) ) ;
#298 = CARTESIAN_POINT ( 'NONE',  ( 4.483927247898790824, -16.52544592524335698, 80.20942372801901854 ) ) ;
#300 = ORIENTED_EDGE ( 'NONE', *, *, #146255, .F. ) ;
#299 = CARTESIAN_POINT ( 'NONE',  ( 33.78191506369888941, -21.41920200728860380, -24.99999999999997868 ) ) ;
#301 = EDGE_LOOP ( 'NONE', ( #33851, #130611, #76912, #84363 ) ) ;
#302 = CARTESIAN_POINT ( 'NONE',  ( -19.02544592524334988, -5.153800228976617603, 28.95942372801900433 ) ) ;
#303 = CARTESIAN_POINT ( 'NONE',  ( -5.049401038298153566, 19.05341960407611168, 35.20724293864768839 ) ) ;
#305 = ORIENTED_EDGE ( 'NONE', *, *, #5230, .T. ) ;
#304 = CARTESIAN_POINT ( 'NONE',  ( 0.05219959533909260263, 19.03943276465977164, 109.9989096053143669 ) ) ;
#306 = CARTESIAN_POINT ( 'NONE',  ( -12.14591786802326823, 12.06949235617739902, 33.12609039468569705 ) ) ;
#308 = CARTESIAN_POINT ( 'NONE',  ( -16.52544592524335698, -4.483927247898792601, 38.95942372801901854 ) ) ;
#307 = CARTESIAN_POINT ( 'NONE',  ( 9.474510206698729675, 16.51473224551082808, 52.08442372801900433 ) ) ;
#309 = CARTESIAN_POINT ( 'NONE',  ( 0.05219959533909260263, 19.03943276465977164, 109.9989096053143669 ) ) ;
#310 = CARTESIAN_POINT ( 'NONE',  ( -0.05219959533909027116, -19.03943276465977164, 67.49890960531436690 ) ) ;
#311 = CARTESIAN_POINT ( 'NONE',  ( 15.80617190586746368, 15.72974639402197994, 99.37390960531436690 ) ) ;
#313 = CARTESIAN_POINT ( 'NONE',  ( 19.02544592524343514, -5.153800228976328945, 23.54057627198102054 ) ) ;
#312 = CARTESIAN_POINT ( 'NONE',  ( 16.51473224551069308, 9.474510206698969483, 94.16557627198103830 ) ) ;
#314 = CARTESIAN_POINT ( 'NONE',  ( -9.564922557960796823, -16.46253265017161027, 67.08224293864769550 ) ) ;
#316 = CARTESIAN_POINT ( 'NONE',  ( 9.474510206698971260, -16.51473224551069308, 27.91557627198103120 ) ) ;
#315 = CARTESIAN_POINT ( 'NONE',  ( -12.06949235617739369, -12.14591786802326823, 109.3760903946857042 ) ) ;
#317 = CARTESIAN_POINT ( 'NONE',  ( -9.474510206698720793, -16.51473224551083518, 34.58442372801899722 ) ) ;
#318 = CARTESIAN_POINT ( 'NONE',  ( 12.14591786802309770, 12.06949235617756955, 59.37390960531436690 ) ) ;
#319 = CARTESIAN_POINT ( 'NONE',  ( 21.55341960407619695, -5.719274019375665929, 101.0427570613523756 ) ) ;
#320 = CARTESIAN_POINT ( 'NONE',  ( 19.05341960407611168, 5.049401038298154454, 38.95724293864767418 ) ) ;
#321 = CARTESIAN_POINT ( 'NONE',  ( -8.224510206698735004, -14.34966873604973081, 54.58442372801901143 ) ) ;
#323 = CARTESIAN_POINT ( 'NONE',  ( 18.67979575497194134, -10.72451020669871369, 85.83442372801901854 ) ) ;
#322 = CARTESIAN_POINT ( 'NONE',  ( -8.224510206698948167, 14.34966873604960824, 45.41557627198103830 ) ) ;
#324 = CARTESIAN_POINT ( 'NONE',  ( 13.89961937509977652, -13.97604488694527269, 83.12390960531436690 ) ) ;
#325 = CARTESIAN_POINT ( 'NONE',  ( 5.049401038298161559, -19.05341960407611168, 92.70724293864769550 ) ) ;
#326 = CARTESIAN_POINT ( 'NONE',  ( 16.53943276465976808, -0.05219959533910856209, 103.7489096053143669 ) ) ;
#327 = CARTESIAN_POINT ( 'NONE',  ( 14.29746914071049879, -8.314922557960816363, 78.33224293864770971 ) ) ;
#328 = CARTESIAN_POINT ( 'NONE',  ( 15.80617190586746368, 15.72974639402197994, 84.37390960531438111 ) ) ;
#329 = CARTESIAN_POINT ( 'NONE',  ( 19.02544592524343514, -5.153800228976328945, 78.54057627198099567 ) ) ;
#330 = CARTESIAN_POINT ( 'NONE',  ( 21.52544592524344225, -5.823673210054117533, 93.54057627198103830 ) ) ;
#331 = CARTESIAN_POINT ( 'NONE',  ( 16.46253265017146816, 9.564922557961045513, 71.66775706135233293 ) ) ;
#333 = CARTESIAN_POINT ( 'NONE',  ( -12.14591786802309592, -12.06949235617757132, 91.87390960531436690 ) ) ;
#332 = CARTESIAN_POINT ( 'NONE',  ( 19.53037848336981952, -5.499999999999893419, 47.35532783611446916 ) ) ;
#334 = CARTESIAN_POINT ( 'NONE',  ( 5.049401038298161559, -19.05341960407611168, 57.70724293864769550 ) ) ;
#335 = CARTESIAN_POINT ( 'NONE',  ( 21.52544592524344225, -5.823673210054117533, 63.54057627198103830 ) ) ;
#336 = CARTESIAN_POINT ( 'NONE',  ( -18.09867054820431775, -5.499999999999926281, 83.98393025253589883 ) ) ;
#338 = CARTESIAN_POINT ( 'NONE',  ( -30.82560697742735911, 2.051108057200722688E-14, 150.0000000000000000 ) ) ;
#337 = CARTESIAN_POINT ( 'NONE',  ( 16.53943276465976808, -0.05219959533910856209, 23.74890960531435269 ) ) ;
#339 = CARTESIAN_POINT ( 'NONE',  ( -0.05219959533934338120, 16.53943276465976808, 22.50109039468567573 ) ) ;
#340 = CARTESIAN_POINT ( 'NONE',  ( -8.314922557960811034, -14.29746914071050412, 77.08224293864769550 ) ) ;
#341 = CARTESIAN_POINT ( 'NONE',  ( -19.20446147854526231, -5.499999999999955591, 94.38999695167676407 ) ) ;
#342 = CARTESIAN_POINT ( 'NONE',  ( -19.03943276465977164, 0.05219959533909376836, 76.24890960531435269 ) ) ;
#343 = CARTESIAN_POINT ( 'NONE',  ( -16.46253265017160317, 9.564922557960807481, 35.83224293864768839 ) ) ;
#344 = CARTESIAN_POINT ( 'NONE',  ( -8.224510206698948167, 14.34966873604960824, 65.41557627198102409 ) ) ;
#345 = CARTESIAN_POINT ( 'NONE',  ( -10.81492255796078084, -18.62759615963271287, 22.08224293864769194 ) ) ;
#346 = CARTESIAN_POINT ( 'NONE',  ( 5.153800228976615827, -19.02544592524334988, 95.20942372801897591 ) ) ;
#347 = CARTESIAN_POINT ( 'NONE',  ( -19.03943276465977164, 0.05219959533909376836, 96.24890960531436690 ) ) ;
#348 = CARTESIAN_POINT ( 'NONE',  ( -10.72451020669898014, 18.67979575497178502, 70.41557627198102409 ) ) ;
#349 = CARTESIAN_POINT ( 'NONE',  ( 8.314922557961029526, -14.29746914071037800, 75.41775706135233293 ) ) ;
#350 = CARTESIAN_POINT ( 'NONE',  ( -16.29526858892909758, 7.335722546919977383, 94.20329402199732272 ) ) ;
#351 = CARTESIAN_POINT ( 'NONE',  ( 16.51473224551069308, 9.474510206698969483, 69.16557627198102409 ) ) ;
#352 = CARTESIAN_POINT ( 'NONE',  ( 18.67979575497178502, 10.72451020669898547, 64.16557627198102409 ) ) ;
#353 = CARTESIAN_POINT ( 'NONE',  ( 19.02544592524334988, 5.153800228976608722, 106.4594237280190185 ) ) ;
#355 = CARTESIAN_POINT ( 'NONE',  ( 18.67979575497194134, -10.72451020669871369, 40.83442372801901854 ) ) ;
#354 = CARTESIAN_POINT ( 'NONE',  ( -8.314922557960811034, -14.29746914071050412, 37.08224293864768129 ) ) ;
#356 = CARTESIAN_POINT ( 'NONE',  ( -23.31738231874055245, -16.94106989632524574, 144.4500000054623854 ) ) ;
#358 = CARTESIAN_POINT ( 'NONE',  ( -0.05219959533909027116, -19.03943276465977164, 102.4989096053143669 ) ) ;
#357 = CARTESIAN_POINT ( 'NONE',  ( 16.53943276465976808, 0.05219959533934440121, 76.25109039468568994 ) ) ;
#359 = CARTESIAN_POINT ( 'NONE',  ( 9.564922557960805705, 16.46253265017160317, 104.5822429386476955 ) ) ;
#360 = CARTESIAN_POINT ( 'NONE',  ( 0.2500000000000002220, 0.000000000000000000, 0.000000000000000000 ) ) ;
#361 = CARTESIAN_POINT ( 'NONE',  ( -12.06949235617739369, -12.14591786802326823, 99.37609039468568994 ) ) ;
#362 = CARTESIAN_POINT ( 'NONE',  ( 12.06949235617739724, 12.14591786802326823, 51.87609039468568284 ) ) ;
#363 = CARTESIAN_POINT ( 'NONE',  ( -19.02544592524342804, 5.153800228976336051, 61.04057627198103120 ) ) ;
#364 = CARTESIAN_POINT ( 'NONE',  ( 0.05219959533909260263, 19.03943276465977164, 69.99890960531435269 ) ) ;
#365 = CARTESIAN_POINT ( 'NONE',  ( -18.62759615963255300, -10.81492255796106328, 54.16775706135235424 ) ) ;
#366 = CARTESIAN_POINT ( 'NONE',  ( 14.34966873604972726, -8.224510206698740333, 65.83442372801900433 ) ) ;
#367 = CARTESIAN_POINT ( 'NONE',  ( -0.05219959533910754901, -16.53943276465976808, 32.49890960531435979 ) ) ;
#368 = CARTESIAN_POINT ( 'NONE',  ( -16.46253265017160317, 9.564922557960807481, 40.83224293864769550 ) ) ;
#369 = CARTESIAN_POINT ( 'NONE',  ( -9.474510206698964154, 16.51473224551069663, 30.41557627198102054 ) ) ;
#370 = CARTESIAN_POINT ( 'NONE',  ( -12.06949235617739369, -12.14591786802326823, 24.37609039468567573 ) ) ;
#371 = CARTESIAN_POINT ( 'NONE',  ( 19.05341960407617918, -5.049401038297876454, 76.04275706135230450 ) ) ;
#372 = CARTESIAN_POINT ( 'NONE',  ( -14.34966873604960291, -8.224510206698953496, 81.66557627198103830 ) ) ;
#373 = CARTESIAN_POINT ( 'NONE',  ( -16.46253265017160317, 9.564922557960807481, 55.83224293864769550 ) ) ;
#375 = CYLINDRICAL_SURFACE ( 'NONE', #121053, 37.99626262588765968 ) ;
#374 = CARTESIAN_POINT ( 'NONE',  ( 0.05219959533936267826, -19.03943276465977164, 85.00109039468567573 ) ) ;
#376 = CARTESIAN_POINT ( 'NONE',  ( -21.52544592524334988, -5.823673210054445271, 93.95942372801903275 ) ) ;
#377 = CARTESIAN_POINT ( 'NONE',  ( -14.34966873604972548, 8.224510206698743886, 48.33442372801902565 ) ) ;
#378 = FACE_OUTER_BOUND ( 'NONE', #8839, .T. ) ;
#379 = CARTESIAN_POINT ( 'NONE',  ( -15.80617190586745835, -15.72974639402198527, 51.87390960531437401 ) ) ;
#380 = CARTESIAN_POINT ( 'NONE',  ( 16.55341960407618274, -4.379528057220086978, 36.04275706135234714 ) ) ;
#381 = CARTESIAN_POINT ( 'NONE',  ( -19.35633801406909527, 5.499999999999580780, 69.13373818172763663 ) ) ;
#382 = CARTESIAN_POINT ( 'NONE',  ( 9.564922557961047289, -16.46253265017146816, 45.41775706135232582 ) ) ;
#383 = CARTESIAN_POINT ( 'NONE',  ( -19.03943276465977164, 0.05219959533909376836, 76.24890960531435269 ) ) ;
#384 = CARTESIAN_POINT ( 'NONE',  ( 13.89961937509977652, -13.97604488694527269, 58.12390960531436690 ) ) ;
#385 = CARTESIAN_POINT ( 'NONE',  ( 16.46253265017160672, -9.564922557960803928, 73.33224293864769550 ) ) ;
#386 = CARTESIAN_POINT ( 'NONE',  ( -16.51473224551069308, -9.474510206698971260, 91.66557627198103830 ) ) ;
#387 = CARTESIAN_POINT ( 'NONE',  ( -9.474510206698720793, -16.51473224551083518, 39.58442372801899722 ) ) ;
#388 = CARTESIAN_POINT ( 'NONE',  ( 9.564922557961047289, -16.46253265017146816, 20.41775706135233293 ) ) ;
#389 = CARTESIAN_POINT ( 'NONE',  ( -14.34966873604960291, -8.224510206698953496, 41.66557627198103120 ) ) ;
#390 = CARTESIAN_POINT ( 'NONE',  ( 13.89961937509977652, -13.97604488694527269, 38.12390960531436690 ) ) ;
#391 = CARTESIAN_POINT ( 'NONE',  ( -5.049401038298153566, 19.05341960407611168, 105.2072429386476671 ) ) ;
#392 = CARTESIAN_POINT ( 'NONE',  ( -0.05219959533937732626, 21.53943276465977519, 82.50109039468568994 ) ) ;
#393 = CARTESIAN_POINT ( 'NONE',  ( -13.97604488694527625, -13.89961937509977652, 56.87390960531434558 ) ) ;
#394 = ADVANCED_FACE ( 'NONE', ( #34064 ), #127044, .F. ) ;
#395 = CARTESIAN_POINT ( 'NONE',  ( 18.67979575497194134, -10.72451020669871369, 85.83442372801901854 ) ) ;
#396 = CARTESIAN_POINT ( 'NONE',  ( 18.67979575497178502, 10.72451020669898547, 39.16557627198102409 ) ) ;
#397 = CARTESIAN_POINT ( 'NONE',  ( -15.80617190586768217, 15.72974639402176855, 23.12609039468567573 ) ) ;
#398 = CARTESIAN_POINT ( 'NONE',  ( 19.05341960407617918, -5.049401038297876454, 51.04275706135231871 ) ) ;
#399 = CARTESIAN_POINT ( 'NONE',  ( -0.05219959533909027116, -19.03943276465977164, 22.49890960531436690 ) ) ;
#400 = CARTESIAN_POINT ( 'NONE',  ( 19.05341960407611168, 5.049401038298154454, 78.95724293864769550 ) ) ;
#401 = CARTESIAN_POINT ( 'NONE',  ( 12.14591786802327356, -12.06949235617739191, 30.62609039468567929 ) ) ;
#402 = CARTESIAN_POINT ( 'NONE',  ( -12.06949235617756955, 12.14591786802309770, 90.62390960531436690 ) ) ;
#403 = CARTESIAN_POINT ( 'NONE',  ( -19.03943276465977164, 0.05219959533909376836, 56.24890960531435979 ) ) ;
#404 = CARTESIAN_POINT ( 'NONE',  ( 0.05219959533907565091, 21.53943276465977519, 34.99890960531435979 ) ) ;
#405 = CARTESIAN_POINT ( 'NONE',  ( -16.51473224551082808, 9.474510206698731452, 103.3344237280190043 ) ) ;
#406 = CARTESIAN_POINT ( 'NONE',  ( -21.55341960407610458, -5.719274019375992779, 101.4572429386476955 ) ) ;
#407 = CARTESIAN_POINT ( 'NONE',  ( 18.62759615963255655, 10.81492255796105972, 61.66775706135235424 ) ) ;
#408 = CARTESIAN_POINT ( 'NONE',  ( -8.314922557961024197, 14.29746914071037800, 52.91775706135235424 ) ) ;
#409 = CARTESIAN_POINT ( 'NONE',  ( -16.53943276465976808, -0.05219959533934237506, 73.75109039468567573 ) ) ;
#410 = CARTESIAN_POINT ( 'NONE',  ( -13.89961937509977652, 13.97604488694528158, 60.62390960531436690 ) ) ;
#411 = CARTESIAN_POINT ( 'NONE',  ( -16.53943276465976808, -0.05219959533934237506, 83.75109039468568994 ) ) ;
#412 = CARTESIAN_POINT ( 'NONE',  ( -10.72451020669898014, 18.67979575497178502, 115.4155762719810241 ) ) ;
#413 = CARTESIAN_POINT ( 'NONE',  ( -14.34966873604960291, -8.224510206698953496, 66.66557627198102409 ) ) ;
#414 = CARTESIAN_POINT ( 'NONE',  ( 9.564922557960805705, 16.46253265017160317, 84.58224293864769550 ) ) ;
#415 = CARTESIAN_POINT ( 'NONE',  ( 0.05219959533934541429, -16.53943276465976808, 75.00109039468568994 ) ) ;
#416 = CARTESIAN_POINT ( 'NONE',  ( -5.719274019375665041, -21.55341960407619695, 54.79275706135235424 ) ) ;
#417 = CARTESIAN_POINT ( 'NONE',  ( -0.05219959533934338120, 16.53943276465976808, 22.50109039468567573 ) ) ;
#418 = CARTESIAN_POINT ( 'NONE',  ( -21.53943276465977519, -0.05219959533937600094, 18.75109039468568639 ) ) ;
#419 = CARTESIAN_POINT ( 'NONE',  ( -4.379528057220328563, 16.55341960407611168, 60.20724293864768839 ) ) ;
#420 = ORIENTED_EDGE ( 'NONE', *, *, #46651, .T. ) ;
#421 = CARTESIAN_POINT ( 'NONE',  ( -17.26058549869091863, 6.457015423128480869, 73.62254162523936429 ) ) ;
#422 = CARTESIAN_POINT ( 'NONE',  ( 21.53943276465977519, -0.05219959533907433946, 88.74890960531436690 ) ) ;
#423 = CARTESIAN_POINT ( 'NONE',  ( 12.14591786802309770, 12.06949235617756955, 34.37390960531435979 ) ) ;
#424 = ORIENTED_EDGE ( 'NONE', *, *, #57992, .F. ) ;
#425 = CARTESIAN_POINT ( 'NONE',  ( 35.67631076299766590, 1.230297745838647261, 37.59750771353019871 ) ) ;
#426 = CARTESIAN_POINT ( 'NONE',  ( -10.81492255796078084, -18.62759615963271287, 112.0822429386477097 ) ) ;
#427 = CARTESIAN_POINT ( 'NONE',  ( -9.474510206698964154, 16.51473224551069663, 110.4155762719810383 ) ) ;
#428 = CARTESIAN_POINT ( 'NONE',  ( 21.55341960407619695, -5.719274019375665929, 21.04275706135234714 ) ) ;
#429 = CARTESIAN_POINT ( 'NONE',  ( -16.52544592524342804, 4.483927247898546575, 56.04057627198102409 ) ) ;
#430 = CARTESIAN_POINT ( 'NONE',  ( -12.14591786802326823, 12.06949235617739902, 68.12609039468567573 ) ) ;
#431 = CARTESIAN_POINT ( 'NONE',  ( -5.153800228976328057, -19.02544592524343514, 57.29057627198103120 ) ) ;
#432 = CARTESIAN_POINT ( 'NONE',  ( -19.02544592524334988, -5.153800228976617603, 68.95942372801896170 ) ) ;
#433 = CARTESIAN_POINT ( 'NONE',  ( -16.46253265017160317, 9.564922557960807481, 75.83224293864769550 ) ) ;
#434 = CARTESIAN_POINT ( 'NONE',  ( -18.62759615963270932, 10.81492255796079327, 45.83224293864769550 ) ) ;
#435 = CARTESIAN_POINT ( 'NONE',  ( -8.139631411200216604, -37.86970803905148131, -24.01681473740524808 ) ) ;
#436 = CARTESIAN_POINT ( 'NONE',  ( 5.049401038298161559, -19.05341960407611168, 62.70724293864769550 ) ) ;
#437 = CARTESIAN_POINT ( 'NONE',  ( -4.379528057220086978, -16.55341960407618274, 29.79275706135234358 ) ) ;
#438 = CARTESIAN_POINT ( 'NONE',  ( -19.02544592524334988, -5.153800228976617603, 63.95942372801899012 ) ) ;
#439 = CARTESIAN_POINT ( 'NONE',  ( 21.55341960407610458, 5.719274019375980345, 113.9572429386477239 ) ) ;
#440 = CARTESIAN_POINT ( 'NONE',  ( 0.05219959533910956823, 16.53943276465976808, 49.99890960531437401 ) ) ;
#441 = CARTESIAN_POINT ( 'NONE',  ( -16.46253265017160317, 9.564922557960807481, 95.83224293864769550 ) ) ;
#442 = CARTESIAN_POINT ( 'NONE',  ( 21.55341960407610458, 5.719274019375980345, 58.95724293864770971 ) ) ;
#444 = CARTESIAN_POINT ( 'NONE',  ( -0.05219959533934338120, 16.53943276465976808, 32.50109039468568284 ) ) ;
#443 = CARTESIAN_POINT ( 'NONE',  ( 21.52544592524344225, -5.823673210054117533, 93.54057627198103830 ) ) ;
#445 = CARTESIAN_POINT ( 'NONE',  ( -21.55341960407610458, -5.719274019375992779, 41.45724293864769550 ) ) ;
#446 = CARTESIAN_POINT ( 'NONE',  ( -0.05219959533937732626, 21.53943276465977519, 82.50109039468568994 ) ) ;
#447 = CARTESIAN_POINT ( 'NONE',  ( -13.97604488694527625, -13.89961937509977652, 81.87390960531436690 ) ) ;
#448 = CARTESIAN_POINT ( 'NONE',  ( -9.564922557960796823, -16.46253265017161027, 37.08224293864768839 ) ) ;
#449 = CARTESIAN_POINT ( 'NONE',  ( -16.51473224551069308, -9.474510206698971260, 101.6655762719810241 ) ) ;
#450 = CARTESIAN_POINT ( 'NONE',  ( 16.52544592524342804, -4.483927247898539470, 103.5405762719810383 ) ) ;
#451 = CARTESIAN_POINT ( 'NONE',  ( -9.474510206698964154, 16.51473224551069663, 65.41557627198102409 ) ) ;
#452 = CARTESIAN_POINT ( 'NONE',  ( -19.05341960407617563, 5.049401038297882671, 113.5427570613523471 ) ) ;
#453 = CARTESIAN_POINT ( 'NONE',  ( 17.50000000000001776, 3.471454075611646761, 33.01667418855640790 ) ) ;
#455 = CARTESIAN_POINT ( 'NONE',  ( -0.05219959533907301413, -21.53943276465977519, 32.49890960531435979 ) ) ;
#454 = CARTESIAN_POINT ( 'NONE',  ( 10.72451020669871369, 18.67979575497193778, 97.08442372801904696 ) ) ;
#456 = CARTESIAN_POINT ( 'NONE',  ( -4.483927247898782831, 16.52544592524335698, 87.70942372801901854 ) ) ;
#457 = CARTESIAN_POINT ( 'NONE',  ( 22.90195793322444473, -20.95683088396668481, -46.91699765554876222 ) ) ;
#458 = CARTESIAN_POINT ( 'NONE',  ( -19.03943276465977164, -0.05219959533935918106, 63.75109039468566863 ) ) ;
#459 = CARTESIAN_POINT ( 'NONE',  ( -19.02544592524334988, -5.153800228976617603, 33.95942372801897591 ) ) ;
#460 = CARTESIAN_POINT ( 'NONE',  ( 27.74036206688027661, 1.797278685356906491, 140.0000000000000000 ) ) ;
#461 = CARTESIAN_POINT ( 'NONE',  ( 19.02544592524343514, -5.153800228976328945, 28.54057627198102409 ) ) ;
#462 = CARTESIAN_POINT ( 'NONE',  ( -8.314922557960811034, -14.29746914071050412, 37.08224293864768129 ) ) ;
#463 = CARTESIAN_POINT ( 'NONE',  ( -19.03943276465977164, 0.05219959533909376836, 21.24890960531436335 ) ) ;
#464 = CARTESIAN_POINT ( 'NONE',  ( -14.29746914071049879, 8.314922557960819915, 25.83224293864769194 ) ) ;
#465 = DIRECTION ( 'NONE',  ( 0.000000000000000000, 0.000000000000000000, -1.000000000000000000 ) ) ;
#466 = CARTESIAN_POINT ( 'NONE',  ( 8.224510206698742110, 14.34966873604972548, 92.08442372801901854 ) ) ;
#467 = CARTESIAN_POINT ( 'NONE',  ( -16.51473224551069308, -9.474510206698971260, 31.66557627198102054 ) ) ;
#468 = EDGE_CURVE ( 'NONE', #150285, #194492, #147057, .T. ) ;
#469 = CARTESIAN_POINT ( 'NONE',  ( -19.03943276465977164, -0.05219959533935918106, 18.75109039468567218 ) ) ;
#470 = CARTESIAN_POINT ( 'NONE',  ( -12.06949235617739369, -12.14591786802326823, 24.37609039468567573 ) ) ;
#471 = CARTESIAN_POINT ( 'NONE',  ( 15.72974639402176855, 15.80617190586768217, 81.87609039468568994 ) ) ;
#472 = CARTESIAN_POINT ( 'NONE',  ( -19.02544592524334988, -5.153800228976617603, 53.95942372801898301 ) ) ;
#473 = CARTESIAN_POINT ( 'NONE',  ( 19.03943276465977164, -0.05219959533909143690, 93.74890960531435269 ) ) ;
#474 = CARTESIAN_POINT ( 'NONE',  ( 13.89961937509977652, -13.97604488694527269, 73.12390960531436690 ) ) ;
#475 = CARTESIAN_POINT ( 'NONE',  ( -18.22780087662122028, 5.500000000000031086, 38.51540105326107266 ) ) ;
#476 = CARTESIAN_POINT ( 'NONE',  ( -10.81492255796078084, -18.62759615963271287, 102.0822429386476955 ) ) ;
#477 = CARTESIAN_POINT ( 'NONE',  ( 16.53943276465976808, -0.05219959533910856209, 68.74890960531435269 ) ) ;
#478 = CARTESIAN_POINT ( 'NONE',  ( -18.67979575497178146, -10.72451020669898902, 56.66557627198103830 ) ) ;
#479 = CARTESIAN_POINT ( 'NONE',  ( -9.564922557960796823, -16.46253265017161027, 62.08224293864769550 ) ) ;
#481 = CARTESIAN_POINT ( 'NONE',  ( 14.29746914071037800, 8.314922557961029526, 76.66775706135234714 ) ) ;
#480 = CARTESIAN_POINT ( 'NONE',  ( 0.05219959533907565091, 21.53943276465977519, 89.99890960531438111 ) ) ;
#482 = EDGE_CURVE ( 'NONE', #89587, #45951, #50207, .T. ) ;
#483 = EDGE_LOOP ( 'NONE', ( #165279, #110182, #164294, #124142 ) ) ;
#484 = CARTESIAN_POINT ( 'NONE',  ( -16.46253265017160317, 9.564922557960807481, 50.83224293864770260 ) ) ;
#486 = CARTESIAN_POINT ( 'NONE',  ( 21.65431292632186100, -8.856125861401146437, 168.9593721673316793 ) ) ;
#485 = CARTESIAN_POINT ( 'NONE',  ( -16.55341960407611168, -4.379528057220339221, 91.45724293864769550 ) ) ;
#487 = CARTESIAN_POINT ( 'NONE',  ( 16.51473224551069308, 9.474510206698969483, 44.16557627198103120 ) ) ;
#488 = CARTESIAN_POINT ( 'NONE',  ( 14.34966873604960469, 8.224510206698951720, 114.1655762719810383 ) ) ;
#489 = CARTESIAN_POINT ( 'NONE',  ( -5.153800228976607833, 19.02544592524334988, 62.70942372801899722 ) ) ;
#490 = CARTESIAN_POINT ( 'NONE',  ( -8.314922557960811034, -14.29746914071050412, 87.08224293864769550 ) ) ;
#491 = CARTESIAN_POINT ( 'NONE',  ( 5.823673210054444382, -21.52544592524334988, 45.20942372801901854 ) ) ;
#493 = CARTESIAN_POINT ( 'NONE',  ( 15.80617190586746368, 15.72974639402197994, 109.3739096053143811 ) ) ;
#492 = CARTESIAN_POINT ( 'NONE',  ( 19.03943276465977164, -0.05219959533909143690, 38.74890960531436690 ) ) ;
#494 = CARTESIAN_POINT ( 'NONE',  ( 16.53943276465976808, -0.05219959533910856209, 83.74890960531435269 ) ) ;
#495 = CARTESIAN_POINT ( 'NONE',  ( 5.136056113497502906, -40.38396894446272967, -25.53196577693411840 ) ) ;
#496 = B_SPLINE_CURVE_WITH_KNOTS ( 'NONE', 3,
 ( #116941, #89601, #151289, #149289, #100764, #162446, #23947, #117955, #85601, #178634, #147288, #70447, #132113, #86606, #55272, #148289, #9783, #123892, #138089, #105763, #32904, #171418, #125899, #139075, #1553, #61237 ),
 .UNSPECIFIED., .F., .F.,
 ( 4, 2, 2, 2, 2, 2, 2, 2, 2, 2, 2, 2, 4 ),
 ( 0.000000000000000000, 0.0004878035110667099800, 0.0007317052666000649699, 0.0009756070221334199599, 0.001097557899900097455, 0.001219508777666774950, 0.001341459655433452445, 0.001463410533200129940, 0.001707312288733484930, 0.001951214044266839920, 0.002439017555333544696, 0.002926821066400249038, 0.003902428088533665095 ),
 .UNSPECIFIED. ) ;
#497 = CARTESIAN_POINT ( 'NONE',  ( 13.97604488694527802, 13.89961937509977652, 64.37390960531436690 ) ) ;
#498 = CARTESIAN_POINT ( 'NONE',  ( 19.39056639909671276, 5.500000000000041744, 48.28948781074346641 ) ) ;
#500 = CARTESIAN_POINT ( 'NONE',  ( 13.89961937509977652, -13.97604488694527269, 103.1239096053143527 ) ) ;
#499 = CARTESIAN_POINT ( 'NONE',  ( 19.03943276465977164, 0.05219959533936151252, 96.25109039468567573 ) ) ;
#501 = CARTESIAN_POINT ( 'NONE',  ( 5.823673210054444382, -21.52544592524334988, 30.20942372801902565 ) ) ;
#502 = CARTESIAN_POINT ( 'NONE',  ( 16.46253265017160672, -9.564922557960803928, 88.33224293864769550 ) ) ;
#503 = CARTESIAN_POINT ( 'NONE',  ( -16.46253265017146816, -9.564922557961047289, 69.16775706135233293 ) ) ;
#504 = CARTESIAN_POINT ( 'NONE',  ( 9.564922557960805705, 16.46253265017160317, 59.58224293864769550 ) ) ;
#505 = CARTESIAN_POINT ( 'NONE',  ( -14.34966873604960291, -8.224510206698953496, 71.66557627198100988 ) ) ;
#506 = CARTESIAN_POINT ( 'NONE',  ( -0.05219959533910754901, -16.53943276465976808, 67.49890960531436690 ) ) ;
#507 = CARTESIAN_POINT ( 'NONE',  ( 0.05219959533909260263, 19.03943276465977164, 89.99890960531436690 ) ) ;
#508 = CARTESIAN_POINT ( 'NONE',  ( 5.823673210054125526, 21.52544592524343514, 104.7905762719810241 ) ) ;
#509 = CARTESIAN_POINT ( 'NONE',  ( -5.049401038298153566, 19.05341960407611168, 90.20724293864766707 ) ) ;
#510 = CARTESIAN_POINT ( 'NONE',  ( -5.153800228976607833, 19.02544592524334988, 27.70942372801899722 ) ) ;
#513 = CARTESIAN_POINT ( 'NONE',  ( 14.34966873604960469, 8.224510206698951720, 114.1655762719810383 ) ) ;
#512 = CARTESIAN_POINT ( 'NONE',  ( 16.53943276465976808, -0.05219959533910856209, 28.74890960531435624 ) ) ;
#511 = CARTESIAN_POINT ( 'NONE',  ( -9.474510206698964154, 16.51473224551069663, 30.41557627198102054 ) ) ;
#514 = CARTESIAN_POINT ( 'NONE',  ( 19.03943276465977164, 0.05219959533936151252, 106.2510903946856615 ) ) ;
#515 = VERTEX_POINT ( 'NONE', #119633 ) ;
#516 = CARTESIAN_POINT ( 'NONE',  ( -0.05219959533937732626, 21.53943276465977519, 32.50109039468568284 ) ) ;
#517 = CARTESIAN_POINT ( 'NONE',  ( 19.02544592524334988, 5.153800228976608722, 71.45942372801900433 ) ) ;
#518 = CARTESIAN_POINT ( 'NONE',  ( -16.55341960407611168, -4.379528057220339221, 26.45724293864768839 ) ) ;
#519 = CARTESIAN_POINT ( 'NONE',  ( 18.67979575497178502, 10.72451020669898547, 84.16557627198103830 ) ) ;
#520 = CARTESIAN_POINT ( 'NONE',  ( -13.89961937509977652, 13.97604488694528158, 115.6239096053143669 ) ) ;
#521 = CARTESIAN_POINT ( 'NONE',  ( 12.14591786802309770, 12.06949235617756955, 64.37390960531435269 ) ) ;
#522 = CARTESIAN_POINT ( 'NONE',  ( -0.05219959533909027116, -19.03943276465977164, 32.49890960531435979 ) ) ;
#523 = CARTESIAN_POINT ( 'NONE',  ( -5.153800228976607833, 19.02544592524334988, 27.70942372801899722 ) ) ;
#524 = CARTESIAN_POINT ( 'NONE',  ( -4.483927247898782831, 16.52544592524335698, 92.70942372801901854 ) ) ;
#525 = CARTESIAN_POINT ( 'NONE',  ( 14.34966873604972726, -8.224510206698740333, 50.83442372801901143 ) ) ;
#526 = CARTESIAN_POINT ( 'NONE',  ( -21.55341960407610458, -5.719274019375992779, 21.45724293864769550 ) ) ;
#527 = CARTESIAN_POINT ( 'NONE',  ( -18.67979575497193778, 10.72451020669871902, 113.3344237280190328 ) ) ;
#528 = CARTESIAN_POINT ( 'NONE',  ( 9.564922557960805705, 16.46253265017160317, 79.58224293864769550 ) ) ;
#529 = CARTESIAN_POINT ( 'NONE',  ( 0.05219959533934541429, -16.53943276465976808, 60.00109039468568284 ) ) ;
#530 = CARTESIAN_POINT ( 'NONE',  ( -9.564922557960796823, -16.46253265017161027, 27.08224293864769550 ) ) ;
#531 = CARTESIAN_POINT ( 'NONE',  ( 16.52544592524342804, -4.483927247898539470, 33.54057627198102409 ) ) ;
#532 = CARTESIAN_POINT ( 'NONE',  ( -17.97161686093727795, 5.499999999999975131, 70.99637206859166838 ) ) ;
#534 = CARTESIAN_POINT ( 'NONE',  ( 13.97604488694527802, 13.89961937509977652, 89.37390960531436690 ) ) ;
#533 = CARTESIAN_POINT ( 'NONE',  ( -19.05341960407611168, -5.049401038298163336, 106.4572429386476955 ) ) ;
#535 = CARTESIAN_POINT ( 'NONE',  ( 19.05341960407611168, 5.049401038298154454, 113.9572429386477097 ) ) ;
#536 = CARTESIAN_POINT ( 'NONE',  ( -8.314922557960811034, -14.29746914071050412, 57.08224293864769550 ) ) ;
#537 = CARTESIAN_POINT ( 'NONE',  ( 16.55341960407611168, 4.379528057220329451, 33.95724293864769550 ) ) ;
#538 = CARTESIAN_POINT ( 'NONE',  ( 16.52544592524342804, -4.483927247898539470, 58.54057627198103120 ) ) ;
#540 = DIRECTION ( 'NONE',  ( 1.000000000000000000, 0.000000000000000000, 0.000000000000000000 ) ) ;
#539 = CARTESIAN_POINT ( 'NONE',  ( -14.29746914071037622, -8.314922557961029526, 44.16775706135234714 ) ) ;
#541 = CARTESIAN_POINT ( 'NONE',  ( -13.89961937509957401, -13.97604488694547875, 54.37609039468565442 ) ) ;
#542 = CARTESIAN_POINT ( 'NONE',  ( 16.51473224551069308, 9.474510206698969483, 74.16557627198103830 ) ) ;
#543 = CARTESIAN_POINT ( 'NONE',  ( 19.03943276465977164, 0.05219959533936151252, 66.25109039468567573 ) ) ;
#544 = CARTESIAN_POINT ( 'NONE',  ( -17.14385361876520619, 23.59649016807275856, 143.0750000027311444 ) ) ;
#545 = CARTESIAN_POINT ( 'NONE',  ( 16.51473224551083163, -9.474510206698727899, 55.83442372801899722 ) ) ;
#547 = CARTESIAN_POINT ( 'NONE',  ( -16.55341960407617563, 4.379528057220093196, 78.54275706135236135 ) ) ;
#546 = CARTESIAN_POINT ( 'NONE',  ( 5.153800228976615827, -19.02544592524334988, 100.2094237280190043 ) ) ;
#548 = CARTESIAN_POINT ( 'NONE',  ( -17.14385361876520264, -23.59649016807271593, 143.6750000027311671 ) ) ;
#549 = CARTESIAN_POINT ( 'NONE',  ( 19.02544592524343514, -5.153800228976328945, 23.54057627198102054 ) ) ;
#550 = CARTESIAN_POINT ( 'NONE',  ( -13.89961937509977652, 13.97604488694528158, 105.6239096053143527 ) ) ;
#551 = CARTESIAN_POINT ( 'NONE',  ( -21.55341960407619339, 5.719274019375674811, 43.54275706135235424 ) ) ;
#552 = CARTESIAN_POINT ( 'NONE',  ( 0.05219959533936267826, -19.03943276465977164, 100.0010903946856757 ) ) ;
#554 = CARTESIAN_POINT ( 'NONE',  ( 9.474510206698971260, -16.51473224551069308, 57.91557627198103120 ) ) ;
#553 = DIRECTION ( 'NONE',  ( -0.000000000000000000, -0.000000000000000000, -1.000000000000000000 ) ) ;
#555 = CARTESIAN_POINT ( 'NONE',  ( -0.05219959533909027116, -19.03943276465977164, 102.4989096053143669 ) ) ;
#557 = CARTESIAN_POINT ( 'NONE',  ( -13.97604488694527625, -13.89961937509977652, 56.87390960531434558 ) ) ;
#556 = CARTESIAN_POINT ( 'NONE',  ( -12.06949235617756955, 12.14591786802309770, 65.62390960531436690 ) ) ;
#558 = CARTESIAN_POINT ( 'NONE',  ( 13.89961937509977652, -13.97604488694527269, 58.12390960531436690 ) ) ;
#559 = CARTESIAN_POINT ( 'NONE',  ( 13.89961937509957401, 13.97604488694547697, 81.87609039468564731 ) ) ;
#560 = CARTESIAN_POINT ( 'NONE',  ( -15.80617190586745835, -15.72974639402198527, 51.87390960531437401 ) ) ;
#561 = CARTESIAN_POINT ( 'NONE',  ( -9.474510206698720793, -16.51473224551083518, 49.58442372801899722 ) ) ;
#562 = CARTESIAN_POINT ( 'NONE',  ( -13.97604488694527625, -13.89961937509977652, 76.87390960531433848 ) ) ;
#563 = CARTESIAN_POINT ( 'NONE',  ( -18.62759615963270932, 10.81492255796079327, 80.83224293864769550 ) ) ;
#565 = CARTESIAN_POINT ( 'NONE',  ( -9.564922557961040184, 16.46253265017147172, 37.91775706135233293 ) ) ;
#564 = CARTESIAN_POINT ( 'NONE',  ( 16.53943276465976808, -0.05219959533910856209, 83.74890960531435269 ) ) ;
#566 = CARTESIAN_POINT ( 'NONE',  ( 0.05219959533907565091, 21.53943276465977519, 54.99890960531435269 ) ) ;
#567 = CARTESIAN_POINT ( 'NONE',  ( 15.80617190586746368, 15.72974639402197994, 39.37390960531436690 ) ) ;
#568 = CARTESIAN_POINT ( 'NONE',  ( -13.89961937509977652, 13.97604488694528158, 70.62390960531432427 ) ) ;
#569 = CARTESIAN_POINT ( 'NONE',  ( 16.53943276465976808, -0.05219959533910856209, 108.7489096053143669 ) ) ;
#570 = CARTESIAN_POINT ( 'NONE',  ( -21.53943276465977519, -0.05219959533937600094, 23.75109039468567929 ) ) ;
#571 = CARTESIAN_POINT ( 'NONE',  ( -18.22780087662126647, -5.499999999999827693, 48.98236817873107185 ) ) ;
#572 = CARTESIAN_POINT ( 'NONE',  ( 15.80617190586769283, -15.72974639402175789, 45.62609039468567573 ) ) ;
#573 = CARTESIAN_POINT ( 'NONE',  ( -19.03943276465977164, 0.05219959533909376836, 31.24890960531435979 ) ) ;
#574 = CARTESIAN_POINT ( 'NONE',  ( -18.67979575497178146, -10.72451020669898902, 111.6655762719810525 ) ) ;
#575 = CARTESIAN_POINT ( 'NONE',  ( -13.97604488694547697, 13.89961937509957934, 43.12609039468566152 ) ) ;
#576 = CARTESIAN_POINT ( 'NONE',  ( 0.05219959533909260263, 19.03943276465977164, 24.99890960531435269 ) ) ;
#577 = CARTESIAN_POINT ( 'NONE',  ( 19.35633801406909171, -5.499999999999570122, 76.63373818172759400 ) ) ;
#578 = CARTESIAN_POINT ( 'NONE',  ( 17.35746358384380628, -5.713263725054876119, 21.25662004187655185 ) ) ;
#579 = CARTESIAN_POINT ( 'NONE',  ( 16.53943276465976808, 0.05219959533934440121, 56.25109039468568284 ) ) ;
#580 = CARTESIAN_POINT ( 'NONE',  ( -9.564922557960796823, -16.46253265017161027, 22.08224293864768839 ) ) ;
#581 = CARTESIAN_POINT ( 'NONE',  ( -24.42783677680811749, -12.30119602009749613, 169.8172178118632587 ) ) ;
#582 = CARTESIAN_POINT ( 'NONE',  ( 5.153800228976335163, 19.02544592524342804, 74.79057627198103830 ) ) ;
#583 = CARTESIAN_POINT ( 'NONE',  ( 16.53943276465976808, -0.05219959533910856209, 103.7489096053143669 ) ) ;
#584 = AXIS2_PLACEMENT_3D ( 'NONE', #105275, #147807, #196325 ) ;
#585 = CARTESIAN_POINT ( 'NONE',  ( 0.05219959533907565091, 21.53943276465977519, 64.99890960531435269 ) ) ;
#586 = CARTESIAN_POINT ( 'NONE',  ( -4.379528057220086978, -16.55341960407618274, 39.79275706135235424 ) ) ;
#587 = CARTESIAN_POINT ( 'NONE',  ( -0.05219959533937732626, 21.53943276465977519, 102.5010903946856899 ) ) ;
#588 = EDGE_CURVE ( 'NONE', #47139, #178804, #190478, .T. ) ;
#589 = CARTESIAN_POINT ( 'NONE',  ( -30.00000000000000355, 0.3535533905932703447, 5.353553390593268624 ) ) ;
#590 = CARTESIAN_POINT ( 'NONE',  ( 4.483927247898545687, 16.52544592524342804, 24.79057627198103120 ) ) ;
#591 = CARTESIAN_POINT ( 'NONE',  ( 16.53943276465976808, -0.05219959533910856209, 48.74890960531435979 ) ) ;
#592 = CARTESIAN_POINT ( 'NONE',  ( 16.46253265017160672, -9.564922557960803928, 48.33224293864769550 ) ) ;
#593 = CARTESIAN_POINT ( 'NONE',  ( -21.52544592524334988, -5.823673210054445271, 93.95942372801903275 ) ) ;
#594 = CARTESIAN_POINT ( 'NONE',  ( -5.823673210054116645, -21.52544592524344225, 112.2905762719810241 ) ) ;
#595 = CARTESIAN_POINT ( 'NONE',  ( 10.72451020669871369, 18.67979575497193778, 67.08442372801901854 ) ) ;
#596 = CARTESIAN_POINT ( 'NONE',  ( 14.29746914071037800, 8.314922557961029526, 56.66775706135235424 ) ) ;
#598 = CARTESIAN_POINT ( 'NONE',  ( -5.719274019375665041, -21.55341960407619695, 104.7927570613523898 ) ) ;
#597 = CARTESIAN_POINT ( 'NONE',  ( 16.55341960407611168, 4.379528057220329451, 73.95724293864769550 ) ) ;
#599 = EDGE_CURVE ( 'NONE', #42462, #65926, #197470, .T. ) ;
#600 = CARTESIAN_POINT ( 'NONE',  ( -8.314922557961024197, 14.29746914071037800, 112.9177570613523329 ) ) ;
#601 = CARTESIAN_POINT ( 'NONE',  ( -17.79613651744293890, -24.49428055684528260, 140.5656553485623022 ) ) ;
#602 = CARTESIAN_POINT ( 'NONE',  ( -14.29746914071037622, -8.314922557961029526, 44.16775706135234714 ) ) ;
#603 = CARTESIAN_POINT ( 'NONE',  ( -12.06949235617756955, 12.14591786802309770, 40.62390960531435269 ) ) ;
#604 = CARTESIAN_POINT ( 'NONE',  ( 16.55341960407618274, -4.379528057220086978, 81.04275706135236135 ) ) ;
#605 = CARTESIAN_POINT ( 'NONE',  ( 5.153800228976335163, 19.02544592524342804, 94.79057627198103830 ) ) ;
#606 = CARTESIAN_POINT ( 'NONE',  ( 5.153800228976335163, 19.02544592524342804, 109.7905762719810099 ) ) ;
#607 = CARTESIAN_POINT ( 'NONE',  ( 10.81492255796106328, -18.62759615963255655, 95.41775706135234714 ) ) ;
#608 = CARTESIAN_POINT ( 'NONE',  ( 16.53943276465976808, 0.05219959533934440121, 96.25109039468568994 ) ) ;
#609 = CARTESIAN_POINT ( 'NONE',  ( -4.379528057220328563, 16.55341960407611168, 75.20724293864769550 ) ) ;
#610 = CARTESIAN_POINT ( 'NONE',  ( -19.05341960407611168, -5.049401038298163336, 76.45724293864769550 ) ) ;
#611 = ORIENTED_EDGE ( 'NONE', *, *, #28066, .F. ) ;
#612 = CARTESIAN_POINT ( 'NONE',  ( 12.06949235617739724, 12.14591786802326823, 31.87609039468567929 ) ) ;
#613 = CARTESIAN_POINT ( 'NONE',  ( -16.51473224551069308, -9.474510206698971260, 26.66557627198103120 ) ) ;
#614 = CARTESIAN_POINT ( 'NONE',  ( 13.89961937509977652, -13.97604488694527269, 88.12390960531438111 ) ) ;
#616 = CARTESIAN_POINT ( 'NONE',  ( 36.91746825000000598, -11.99521256947793546, -3.724999997268812812 ) ) ;
#615 = CARTESIAN_POINT ( 'NONE',  ( -8.224510206698735004, -14.34966873604973081, 34.58442372801900433 ) ) ;
#617 = CARTESIAN_POINT ( 'NONE',  ( -9.564922557961040184, 16.46253265017147172, 37.91775706135233293 ) ) ;
#618 = CARTESIAN_POINT ( 'NONE',  ( -4.379528057220086978, -16.55341960407618274, 89.79275706135236135 ) ) ;
#619 = CARTESIAN_POINT ( 'NONE',  ( 16.46253265017160672, -9.564922557960803928, 28.33224293864769550 ) ) ;
#620 = CARTESIAN_POINT ( 'NONE',  ( 16.53943276465976808, 0.05219959533934440121, 81.25109039468568994 ) ) ;
#621 = CARTESIAN_POINT ( 'NONE',  ( 16.52544592524335698, 4.483927247898782831, 71.45942372801901854 ) ) ;
#622 = CARTESIAN_POINT ( 'NONE',  ( -16.51473224551082808, 9.474510206698731452, 88.33442372801900433 ) ) ;
#623 = CARTESIAN_POINT ( 'NONE',  ( -16.46253265017146816, -9.564922557961047289, 34.16775706135233293 ) ) ;
#624 = CARTESIAN_POINT ( 'NONE',  ( 5.049401038298161559, -19.05341960407611168, 42.70724293864767418 ) ) ;
#625 = CARTESIAN_POINT ( 'NONE',  ( 16.53943276465976808, -0.05219959533910856209, 88.74890960531436690 ) ) ;
#626 = CARTESIAN_POINT ( 'NONE',  ( 5.153800228976615827, -19.02544592524334988, 50.20942372801897591 ) ) ;
#627 = CARTESIAN_POINT ( 'NONE',  ( 5.719274019375991003, -21.55341960407610458, 47.70724293864770260 ) ) ;
#628 = CARTESIAN_POINT ( 'NONE',  ( -16.46253265017146816, -9.564922557961047289, 34.16775706135233293 ) ) ;
#629 = CARTESIAN_POINT ( 'NONE',  ( 9.474510206698971260, -16.51473224551069308, 102.9155762719810241 ) ) ;
#630 = EDGE_CURVE ( 'NONE', #182346, #12418, #12467, .T. ) ;
#631 = CARTESIAN_POINT ( 'NONE',  ( -10.72451020669898014, 18.67979575497178502, 75.41557627198102409 ) ) ;
#632 = CARTESIAN_POINT ( 'NONE',  ( 9.564922557960805705, 16.46253265017160317, 114.5822429386476955 ) ) ;
#633 = CARTESIAN_POINT ( 'NONE',  ( -5.153800228976607833, 19.02544592524334988, 92.70942372801901854 ) ) ;
#634 = CARTESIAN_POINT ( 'NONE',  ( -17.49999999999999645, 3.565345528327981128, 109.4249448680647561 ) ) ;
#635 = CARTESIAN_POINT ( 'NONE',  ( -19.05341960407617563, 5.049401038297882671, 108.5427570613523187 ) ) ;
#636 = CARTESIAN_POINT ( 'NONE',  ( -19.05341960407611168, -5.049401038298163336, 31.45724293864769550 ) ) ;
#637 = CARTESIAN_POINT ( 'NONE',  ( -9.564922557960796823, -16.46253265017161027, 92.08224293864769550 ) ) ;
#638 = CARTESIAN_POINT ( 'NONE',  ( -18.62759615963270932, 10.81492255796079327, 80.83224293864769550 ) ) ;
#639 = CARTESIAN_POINT ( 'NONE',  ( 4.379528057220092307, 16.55341960407617563, 42.29275706135235424 ) ) ;
#640 = CARTESIAN_POINT ( 'NONE',  ( -5.823673210054431948, 21.52544592524334988, 42.70942372801901854 ) ) ;
#642 = CARTESIAN_POINT ( 'NONE',  ( 16.46253265017146816, 9.564922557961045513, 21.66775706135233648 ) ) ;
#641 = CARTESIAN_POINT ( 'NONE',  ( -9.564922557961040184, 16.46253265017147172, 87.91775706135233293 ) ) ;
#643 = CARTESIAN_POINT ( 'NONE',  ( -8.224510206698735004, -14.34966873604973081, 104.5844237280190185 ) ) ;
#644 = CARTESIAN_POINT ( 'NONE',  ( 0.05219959533909260263, 19.03943276465977164, 104.9989096053143669 ) ) ;
#645 = CARTESIAN_POINT ( 'NONE',  ( -14.29746914071049879, 8.314922557960819915, 85.83224293864768129 ) ) ;
#646 = CARTESIAN_POINT ( 'NONE',  ( 16.55341960407611168, 4.379528057220329451, 38.95724293864768839 ) ) ;
#647 = CARTESIAN_POINT ( 'NONE',  ( -19.02544592524334988, -5.153800228976617603, 83.95942372801901854 ) ) ;
#648 = CARTESIAN_POINT ( 'NONE',  ( -21.52544592524334988, -5.823673210054445271, 63.95942372801901854 ) ) ;
#649 = CARTESIAN_POINT ( 'NONE',  ( -19.05341960407617563, 5.049401038297882671, 23.54275706135233648 ) ) ;
#650 = CARTESIAN_POINT ( 'NONE',  ( 4.379528057220339221, -16.55341960407611168, 107.7072429386476955 ) ) ;
#651 = CARTESIAN_POINT ( 'NONE',  ( -10.72451020669898014, 18.67979575497178502, 35.41557627198102409 ) ) ;
#652 = CARTESIAN_POINT ( 'NONE',  ( -14.34966873604960291, -8.224510206698953496, 26.66557627198103475 ) ) ;
#653 = CARTESIAN_POINT ( 'NONE',  ( 21.55341960407619695, -5.719274019375665929, 101.0427570613523756 ) ) ;
#654 = CARTESIAN_POINT ( 'NONE',  ( 4.483927247898790824, -16.52544592524335698, 55.20942372801902565 ) ) ;
#655 = CARTESIAN_POINT ( 'NONE',  ( -14.34966873604960291, -8.224510206698953496, 21.66557627198102409 ) ) ;
#656 = CARTESIAN_POINT ( 'NONE',  ( 10.72451020669871369, 18.67979575497193778, 57.08442372801901854 ) ) ;
#657 = CARTESIAN_POINT ( 'NONE',  ( 21.53943276465977519, 0.05219959533937863772, 56.25109039468568284 ) ) ;
#658 = VERTEX_POINT ( 'NONE', #196492 ) ;
#659 = CARTESIAN_POINT ( 'NONE',  ( 16.46253265017160672, -9.564922557960803928, 63.33224293864769550 ) ) ;
#660 = CARTESIAN_POINT ( 'NONE',  ( 21.52544592524334988, 5.823673210054432836, 31.45942372801901854 ) ) ;
#661 = CARTESIAN_POINT ( 'NONE',  ( -8.314922557960811034, -14.29746914071050412, 102.0822429386476955 ) ) ;
#662 = CARTESIAN_POINT ( 'NONE',  ( -13.89961937509977652, 13.97604488694528158, 30.62390960531435269 ) ) ;
#663 = CARTESIAN_POINT ( 'NONE',  ( -4.379528057220328563, 16.55341960407611168, 85.20724293864770971 ) ) ;
#664 = CARTESIAN_POINT ( 'NONE',  ( 9.474510206698971260, -16.51473224551069308, 67.91557627198102409 ) ) ;
#665 = CARTESIAN_POINT ( 'NONE',  ( 14.29746914071049879, -8.314922557960816363, 28.33224293864769550 ) ) ;
#666 = CARTESIAN_POINT ( 'NONE',  ( -18.67979575497178146, -10.72451020669898902, 51.66557627198102409 ) ) ;
#667 = CARTESIAN_POINT ( 'NONE',  ( 4.483927247898545687, 16.52544592524342804, 89.79057627198103830 ) ) ;
#668 = CARTESIAN_POINT ( 'NONE',  ( -21.52544592524343514, 5.823673210054127303, 91.04057627198103830 ) ) ;
#669 = CARTESIAN_POINT ( 'NONE',  ( 19.03943276465977164, -0.05219959533909143690, 103.7489096053143669 ) ) ;
#671 = CARTESIAN_POINT ( 'NONE',  ( -9.564922557961040184, 16.46253265017147172, 102.9177570613523329 ) ) ;
#670 = CARTESIAN_POINT ( 'NONE',  ( -19.05341960407611168, -5.049401038298163336, 46.45724293864768129 ) ) ;
#672 = CARTESIAN_POINT ( 'NONE',  ( -10.81492255796078084, -18.62759615963271287, 42.08224293864769550 ) ) ;
#673 = CARTESIAN_POINT ( 'NONE',  ( 21.55341960407619695, -5.719274019375665929, 86.04275706135236135 ) ) ;
#674 = CARTESIAN_POINT ( 'NONE',  ( 9.474510206698971260, -16.51473224551069308, 72.91557627198102409 ) ) ;
#675 = CARTESIAN_POINT ( 'NONE',  ( 13.89961937509977652, -13.97604488694527269, 103.1239096053143527 ) ) ;
#676 = CARTESIAN_POINT ( 'NONE',  ( 16.52544592524335698, 4.483927247898782831, 76.45942372801901854 ) ) ;
#677 = CARTESIAN_POINT ( 'NONE',  ( 10.72451020669871369, 18.67979575497193778, 57.08442372801901854 ) ) ;
#678 = CARTESIAN_POINT ( 'NONE',  ( 15.72974639402176855, 15.80617190586768217, 86.87609039468568994 ) ) ;
#679 = CARTESIAN_POINT ( 'NONE',  ( -15.72974639402176322, -15.80617190586768395, 19.37609039468568639 ) ) ;
#681 = CARTESIAN_POINT ( 'NONE',  ( -14.29746914071037622, -8.314922557961029526, 79.16775706135234714 ) ) ;
#680 = CARTESIAN_POINT ( 'NONE',  ( -18.67979575497193778, 10.72451020669871902, 43.33442372801901143 ) ) ;
#682 = CARTESIAN_POINT ( 'NONE',  ( -21.55341960407610458, -5.719274019375992779, 76.45724293864769550 ) ) ;
#683 = CARTESIAN_POINT ( 'NONE',  ( -5.153800228976607833, 19.02544592524334988, 32.70942372801899722 ) ) ;
#684 = CARTESIAN_POINT ( 'NONE',  ( 21.52544592524344225, -5.823673210054117533, 43.54057627198103830 ) ) ;
#686 = CARTESIAN_POINT ( 'NONE',  ( -12.14591786802309592, -12.06949235617757132, 26.87390960531435979 ) ) ;
#685 = CARTESIAN_POINT ( 'NONE',  ( -16.46253265017160317, 9.564922557960807481, 75.83224293864769550 ) ) ;
#687 = CARTESIAN_POINT ( 'NONE',  ( -17.44270441346512612, 5.991230190323082461, 63.63664920735770636 ) ) ;
#688 = CARTESIAN_POINT ( 'NONE',  ( -19.02544592524342804, 5.153800228976336051, 106.0405762719810241 ) ) ;
#689 = CARTESIAN_POINT ( 'NONE',  ( -3.181980515339399851, 6.791538853603101167, 8.889087296526001936 ) ) ;
#690 = CARTESIAN_POINT ( 'NONE',  ( 16.46253265017146816, 9.564922557961045513, 96.66775706135233293 ) ) ;
#691 = CARTESIAN_POINT ( 'NONE',  ( -21.52544592524343514, 5.823673210054127303, 76.04057627198102409 ) ) ;
#692 = CARTESIAN_POINT ( 'NONE',  ( 14.34966873604960469, 8.224510206698951720, 44.16557627198103120 ) ) ;
#693 = CARTESIAN_POINT ( 'NONE',  ( -16.51473224551082808, 9.474510206698731452, 113.3344237280190043 ) ) ;
#694 = CARTESIAN_POINT ( 'NONE',  ( -5.049401038298153566, 19.05341960407611168, 30.20724293864768839 ) ) ;
#695 = CARTESIAN_POINT ( 'NONE',  ( -4.379528057220086978, -16.55341960407618274, 19.79275706135235069 ) ) ;
#697 = CARTESIAN_POINT ( 'NONE',  ( -5.049401038297874678, -19.05341960407617918, 64.79275706135233293 ) ) ;
#696 = CARTESIAN_POINT ( 'NONE',  ( -5.823673210054116645, -21.52544592524344225, 97.29057627198105251 ) ) ;
#698 = CARTESIAN_POINT ( 'NONE',  ( 16.53943276465976808, 0.05219959533934440121, 76.25109039468568994 ) ) ;
#699 = CARTESIAN_POINT ( 'NONE',  ( 19.05341960407611168, 5.049401038298154454, 83.95724293864766707 ) ) ;
#700 = CARTESIAN_POINT ( 'NONE',  ( 16.55341960407611168, 4.379528057220329451, 73.95724293864769550 ) ) ;
#701 = CARTESIAN_POINT ( 'NONE',  ( -9.474510206698964154, 16.51473224551069663, 55.41557627198103120 ) ) ;
#702 = CARTESIAN_POINT ( 'NONE',  ( -8.314922557960811034, -14.29746914071050412, 72.08224293864769550 ) ) ;
#703 = CARTESIAN_POINT ( 'NONE',  ( -19.02544592524342804, 5.153800228976336051, 31.04057627198102409 ) ) ;
#704 = CARTESIAN_POINT ( 'NONE',  ( -36.77423900702709858, -4.677204790287845526, 47.89930394225362420 ) ) ;
#705 = CARTESIAN_POINT ( 'NONE',  ( -8.224510206698948167, 14.34966873604960824, 40.41557627198103120 ) ) ;
#706 = CARTESIAN_POINT ( 'NONE',  ( 13.89961937509977652, -13.97604488694527269, 73.12390960531436690 ) ) ;
#707 = CARTESIAN_POINT ( 'NONE',  ( -1.429200727443362906, -15.66521691804238436, -59.59145728475412795 ) ) ;
#708 = CARTESIAN_POINT ( 'NONE',  ( 9.474510206698729675, 16.51473224551082808, 52.08442372801900433 ) ) ;
#709 = CARTESIAN_POINT ( 'NONE',  ( 16.55341960407618274, -4.379528057220086978, 61.04275706135234714 ) ) ;
#710 = CARTESIAN_POINT ( 'NONE',  ( 15.72974639402199770, -15.80617190586745480, 68.12390960531436690 ) ) ;
#711 = CARTESIAN_POINT ( 'NONE',  ( 9.474510206698729675, 16.51473224551082808, 22.08442372801899722 ) ) ;
#712 = CARTESIAN_POINT ( 'NONE',  ( -16.46253265017160317, 9.564922557960807481, 90.83224293864769550 ) ) ;
#713 = CARTESIAN_POINT ( 'NONE',  ( 0.9827870232946694928, 21.65019873939048267, -58.62068706038626686 ) ) ;
#714 = CARTESIAN_POINT ( 'NONE',  ( 10.81492255796078972, 18.62759615963270932, 24.58224293864768839 ) ) ;
#715 = CARTESIAN_POINT ( 'NONE',  ( 19.02544592524343514, -5.153800228976328945, 63.54057627198103830 ) ) ;
#716 = CARTESIAN_POINT ( 'NONE',  ( 5.823673210054444382, -21.52544592524334988, 50.20942372801901854 ) ) ;
#717 = CARTESIAN_POINT ( 'NONE',  ( 0.05219959533910956823, 16.53943276465976808, 109.9989096053143527 ) ) ;
#720 = EDGE_LOOP ( 'NONE', ( #54967, #73852, #188508, #135992 ) ) ;
#719 = CARTESIAN_POINT ( 'NONE',  ( 19.03943276465977164, -0.05219959533909143690, 93.74890960531435269 ) ) ;
#718 = CARTESIAN_POINT ( 'NONE',  ( -10.81492255796078084, -18.62759615963271287, 97.08224293864770971 ) ) ;
#721 = CARTESIAN_POINT ( 'NONE',  ( 0.05219959533937995610, -21.53943276465977519, 45.00109039468568284 ) ) ;
#722 = ADVANCED_FACE ( 'NONE', ( #57962 ), #165143, .F. ) ;
#723 = VERTEX_POINT ( 'NONE', #107411 ) ;
#724 = CARTESIAN_POINT ( 'NONE',  ( -19.05341960407611168, -5.049401038298163336, 91.45724293864766707 ) ) ;
#725 = CARTESIAN_POINT ( 'NONE',  ( 19.36337904590692460, -5.499999999999940492, 82.91494137495615746 ) ) ;
#726 = CARTESIAN_POINT ( 'NONE',  ( 15.72974639402199770, -15.80617190586745480, 88.12390960531436690 ) ) ;
#727 = CARTESIAN_POINT ( 'NONE',  ( 16.51473224551069308, 9.474510206698969483, 49.16557627198102409 ) ) ;
#728 = CARTESIAN_POINT ( 'NONE',  ( 4.379528057220092307, 16.55341960407617563, 27.29275706135234358 ) ) ;
#729 = CARTESIAN_POINT ( 'NONE',  ( 37.99999999999999289, 2.893978650043524126E-14, -10.74999999453762811 ) ) ;
#730 = CARTESIAN_POINT ( 'NONE',  ( 19.03943276465977164, -0.05219959533909143690, 28.74890960531435624 ) ) ;
#731 = CARTESIAN_POINT ( 'NONE',  ( 21.53943276465977519, 0.05219959533937863772, 86.25109039468568994 ) ) ;
#733 = CARTESIAN_POINT ( 'NONE',  ( -18.62759615963255300, -10.81492255796106328, 49.16775706135234003 ) ) ;
#732 = CARTESIAN_POINT ( 'NONE',  ( 13.89961937509977652, -13.97604488694527269, 78.12390960531433848 ) ) ;
#734 = CARTESIAN_POINT ( 'NONE',  ( 15.72974639402176855, 15.80617190586768217, 26.87609039468567218 ) ) ;
#735 = CARTESIAN_POINT ( 'NONE',  ( 17.14385361876520264, -23.59649016807271238, 146.0750000027311728 ) ) ;
#736 = CARTESIAN_POINT ( 'NONE',  ( 16.51473224551069308, 9.474510206698969483, 99.16557627198102409 ) ) ;
#737 = CARTESIAN_POINT ( 'NONE',  ( 19.53091890409951858, 5.500000000000028422, 62.56097431831421574 ) ) ;
#740 = CARTESIAN_POINT ( 'NONE',  ( -10.72451020669870658, -18.67979575497194134, 44.58442372801901854 ) ) ;
#739 = CARTESIAN_POINT ( 'NONE',  ( 16.52544592524335698, 4.483927247898782831, 66.45942372801903275 ) ) ;
#738 = CARTESIAN_POINT ( 'NONE',  ( -8.314922557961024197, 14.29746914071037800, 42.91775706135235424 ) ) ;
#741 = CARTESIAN_POINT ( 'NONE',  ( -18.67979575497193778, 10.72451020669871902, 73.33442372801901854 ) ) ;
#742 = CARTESIAN_POINT ( 'NONE',  ( 3.915344532211609163, 5.773958127068983259, -62.35465819465156301 ) ) ;
#743 = CARTESIAN_POINT ( 'NONE',  ( -9.474510206698720793, -16.51473224551083518, 109.5844237280190043 ) ) ;
#744 = CARTESIAN_POINT ( 'NONE',  ( -13.97604488694527625, -13.89961937509977652, 61.87390960531435979 ) ) ;
#745 = CARTESIAN_POINT ( 'NONE',  ( 13.89961937509977652, -13.97604488694527269, 98.12390960531433848 ) ) ;
#746 = CARTESIAN_POINT ( 'NONE',  ( 8.224510206698953496, -14.34966873604960469, 112.9155762719810383 ) ) ;
#747 = CARTESIAN_POINT ( 'NONE',  ( 4.483927247898545687, 16.52544592524342804, 99.79057627198103830 ) ) ;
#749 = EDGE_CURVE ( 'NONE', #58211, #154964, #98211, .T. ) ;
#748 = CARTESIAN_POINT ( 'NONE',  ( -5.823673210054116645, -21.52544592524344225, 32.29057627198102409 ) ) ;
#750 = CARTESIAN_POINT ( 'NONE',  ( -8.314922557961024197, 14.29746914071037800, 82.91775706135234714 ) ) ;
#752 = CARTESIAN_POINT ( 'NONE',  ( 5.153800228976335163, 19.02544592524342804, 49.79057627198100988 ) ) ;
#751 = CARTESIAN_POINT ( 'NONE',  ( 16.55341960407611168, 4.379528057220329451, 73.95724293864769550 ) ) ;
#753 = CARTESIAN_POINT ( 'NONE',  ( 15.80617190586769283, -15.72974639402175789, 80.62609039468567573 ) ) ;
#754 = CARTESIAN_POINT ( 'NONE',  ( -21.52544592524334988, -5.823673210054445271, 68.95942372801901854 ) ) ;
#755 = CARTESIAN_POINT ( 'NONE',  ( -19.03943276465977164, -0.05219959533935918106, 108.7510903946856615 ) ) ;
#756 = CARTESIAN_POINT ( 'NONE',  ( -14.34966873604960291, -8.224510206698953496, 71.66557627198100988 ) ) ;
#757 = CARTESIAN_POINT ( 'NONE',  ( -15.80617190586768217, 15.72974639402176855, 23.12609039468567573 ) ) ;
#758 = CARTESIAN_POINT ( 'NONE',  ( 21.52544592524344225, -5.823673210054117533, 58.54057627198103120 ) ) ;
#759 = CARTESIAN_POINT ( 'NONE',  ( -17.44270441346516520, -5.991230190323039828, 106.3633507926423363 ) ) ;
#760 = CARTESIAN_POINT ( 'NONE',  ( 28.82186960331499392, -9.364793116373510529, 145.1500000054623456 ) ) ;
#761 = CARTESIAN_POINT ( 'NONE',  ( 13.89961937509977652, -13.97604488694527269, 68.12390960531436690 ) ) ;
#762 = CARTESIAN_POINT ( 'NONE',  ( 4.483927247898545687, 16.52544592524342804, 49.79057627198102409 ) ) ;
#763 = CARTESIAN_POINT ( 'NONE',  ( 14.29746914071037800, 8.314922557961029526, 111.6677570613523613 ) ) ;
#764 = CARTESIAN_POINT ( 'NONE',  ( 12.14591786802327356, -12.06949235617739191, 90.62609039468567573 ) ) ;
#765 = CARTESIAN_POINT ( 'NONE',  ( -16.51473224551082808, 9.474510206698731452, 53.33442372801900433 ) ) ;
#766 = CARTESIAN_POINT ( 'NONE',  ( -24.20533859822809220, -9.236745700548658178, 166.4300890397318540 ) ) ;
#767 = CARTESIAN_POINT ( 'NONE',  ( -9.474510206698964154, 16.51473224551069663, 105.4155762719810383 ) ) ;
#768 = CARTESIAN_POINT ( 'NONE',  ( 0.05219959533910956823, 16.53943276465976808, 74.99890960531435269 ) ) ;
#769 = CARTESIAN_POINT ( 'NONE',  ( -9.564922557961040184, 16.46253265017147172, 42.91775706135234003 ) ) ;
#771 = CARTESIAN_POINT ( 'NONE',  ( 10.72451020669898902, -18.67979575497178502, 37.91557627198102409 ) ) ;
#770 = CARTESIAN_POINT ( 'NONE',  ( 5.153800228976335163, 19.02544592524342804, 34.79057627198102409 ) ) ;
#773 = EDGE_LOOP ( 'NONE', ( #134371, #137023, #169429, #7764 ) ) ;
#772 = CARTESIAN_POINT ( 'NONE',  ( 10.81492255796078972, 18.62759615963270932, 54.58224293864769550 ) ) ;
#774 = CARTESIAN_POINT ( 'NONE',  ( -16.52544592524342804, 4.483927247898546575, 101.0405762719810383 ) ) ;
#775 = CARTESIAN_POINT ( 'NONE',  ( 8.314922557961029526, -14.29746914071037800, 50.41775706135235424 ) ) ;
#776 = CARTESIAN_POINT ( 'NONE',  ( 14.34966873604960469, 8.224510206698951720, 89.16557627198102409 ) ) ;
#777 = CARTESIAN_POINT ( 'NONE',  ( 30.00000000000000000, -5.510910596163089556E-15, 45.00000000000000000 ) ) ;
#778 = CARTESIAN_POINT ( 'NONE',  ( -11.40812507854754720, -35.11059874428192273, -8.724999997268813701 ) ) ;
#779 = CARTESIAN_POINT ( 'NONE',  ( -15.80617190586745835, -15.72974639402198527, 21.87390960531436690 ) ) ;
#780 = DIRECTION ( 'NONE',  ( 0.000000000000000000, 0.000000000000000000, 1.000000000000000000 ) ) ;
#781 = CARTESIAN_POINT ( 'NONE',  ( 8.906447517083057264, -27.41122689804191026, 142.5999999999999943 ) ) ;
#782 = ORIENTED_EDGE ( 'NONE', *, *, #187478, .F. ) ;
#784 = CARTESIAN_POINT ( 'NONE',  ( 12.06949235617757843, -12.14591786802309237, 28.12390960531435979 ) ) ;
#783 = CARTESIAN_POINT ( 'NONE',  ( 16.55341960407618274, -4.379528057220086978, 41.04275706135236135 ) ) ;
#785 = CARTESIAN_POINT ( 'NONE',  ( 10.81492255796078972, 18.62759615963270932, 59.58224293864770260 ) ) ;
#786 = CARTESIAN_POINT ( 'NONE',  ( 13.97604488694548053, -13.89961937509957401, 80.62609039468567573 ) ) ;
#787 = CARTESIAN_POINT ( 'NONE',  ( 10.72451020669898902, -18.67979575497178502, 57.91557627198103120 ) ) ;
#788 = CARTESIAN_POINT ( 'NONE',  ( 15.80617190586769283, -15.72974639402175789, 75.62609039468567573 ) ) ;
#789 = CARTESIAN_POINT ( 'NONE',  ( -11.74323870453920549, 9.621741624713935792, -62.00714677346291381 ) ) ;
#790 = CARTESIAN_POINT ( 'NONE',  ( -0.05219959533934338120, 16.53943276465976808, 52.50109039468567573 ) ) ;
#792 = CARTESIAN_POINT ( 'NONE',  ( -19.05341960407611168, -5.049401038298163336, 101.4572429386476955 ) ) ;
#791 = CARTESIAN_POINT ( 'NONE',  ( 9.564922557960805705, 16.46253265017160317, 34.58224293864770260 ) ) ;
#793 = CARTESIAN_POINT ( 'NONE',  ( -16.51473224551069308, -9.474510206698971260, 41.66557627198103120 ) ) ;
#794 = CARTESIAN_POINT ( 'NONE',  ( -16.55341960407611168, -4.379528057220339221, 106.4572429386477097 ) ) ;
#795 =( LENGTH_UNIT ( ) NAMED_UNIT ( * ) SI_UNIT ( .MILLI., .METRE. ) );
#796 = CARTESIAN_POINT ( 'NONE',  ( -16.46253265017160317, 9.564922557960807481, 95.83224293864769550 ) ) ;
#797 = ORIENTED_EDGE ( 'NONE', *, *, #148993, .T. ) ;
#798 = CARTESIAN_POINT ( 'NONE',  ( 14.29746914071037800, 8.314922557961029526, 71.66775706135234714 ) ) ;
#799 = CARTESIAN_POINT ( 'NONE',  ( -10.81492255796078084, -18.62759615963271287, 92.08224293864769550 ) ) ;
#800 = CARTESIAN_POINT ( 'NONE',  ( -13.89961937509977652, 13.97604488694528158, 60.62390960531436690 ) ) ;
#801 = CARTESIAN_POINT ( 'NONE',  ( -5.823673210054431948, 21.52544592524334988, 22.70942372801901499 ) ) ;
#802 = CARTESIAN_POINT ( 'NONE',  ( -5.049401038298153566, 19.05341960407611168, 85.20724293864766707 ) ) ;
#803 = CARTESIAN_POINT ( 'NONE',  ( -33.52048507002410105, -21.84028095222511823, -24.62089730557312350 ) ) ;
#804 = ORIENTED_EDGE ( 'NONE', *, *, #97826, .F. ) ;
#805 = CARTESIAN_POINT ( 'NONE',  ( -21.55341960407610458, -5.719274019375992779, 111.4572429386476813 ) ) ;
#808 = CARTESIAN_POINT ( 'NONE',  ( 19.05341960407617918, -5.049401038297876454, 71.04275706135234714 ) ) ;
#807 = CARTESIAN_POINT ( 'NONE',  ( 5.153800228976335163, 19.02544592524342804, 109.7905762719810099 ) ) ;
#806 = CARTESIAN_POINT ( 'NONE',  ( -16.51473224551069308, -9.474510206698971260, 26.66557627198103120 ) ) ;
#809 = CARTESIAN_POINT ( 'NONE',  ( -0.05219959533936034679, 19.03943276465977164, 27.50109039468566507 ) ) ;
#810 = CARTESIAN_POINT ( 'NONE',  ( 15.80617190586746368, 15.72974639402197994, 99.37390960531436690 ) ) ;
#811 = CARTESIAN_POINT ( 'NONE',  ( 5.049401038297881783, 19.05341960407617563, 42.29275706135234003 ) ) ;
#812 = CARTESIAN_POINT ( 'NONE',  ( -0.05219959533934338120, 16.53943276465976808, 77.50109039468567573 ) ) ;
#813 = CARTESIAN_POINT ( 'NONE',  ( 9.474510206698971260, -16.51473224551069308, 102.9155762719810241 ) ) ;
#814 = CARTESIAN_POINT ( 'NONE',  ( -0.05219959533909027116, -19.03943276465977164, 52.49890960531436690 ) ) ;
#815 = CARTESIAN_POINT ( 'NONE',  ( 10.81492255796106328, -18.62759615963255655, 60.41775706135235424 ) ) ;
#816 = CARTESIAN_POINT ( 'NONE',  ( 18.67979575497194134, -10.72451020669871369, 75.83442372801900433 ) ) ;
#817 = CARTESIAN_POINT ( 'NONE',  ( 16.46253265017160672, -9.564922557960803928, 68.33224293864770971 ) ) ;
#818 = CARTESIAN_POINT ( 'NONE',  ( 21.52544592524334988, 5.823673210054432836, 46.45942372801901854 ) ) ;
#819 = CARTESIAN_POINT ( 'NONE',  ( 13.89961937509957401, 13.97604488694547697, 91.87609039468567573 ) ) ;
#820 = CARTESIAN_POINT ( 'NONE',  ( -5.153800228976328057, -19.02544592524343514, 47.29057627198102409 ) ) ;
#821 = CARTESIAN_POINT ( 'NONE',  ( 0.05219959533909260263, 19.03943276465977164, 99.99890960531436690 ) ) ;
#822 = CARTESIAN_POINT ( 'NONE',  ( -19.05341960407611168, -5.049401038298163336, 71.45724293864766707 ) ) ;
#823 = CARTESIAN_POINT ( 'NONE',  ( 37.99626262588763836, 12.34573411038918955, -2.647842220587803386 ) ) ;
#824 = CARTESIAN_POINT ( 'NONE',  ( 16.46253265017160672, -9.564922557960803928, 53.33224293864768839 ) ) ;
#825 = CARTESIAN_POINT ( 'NONE',  ( 15.72974639402199770, -15.80617190586745480, 98.12390960531436690 ) ) ;
#826 = CARTESIAN_POINT ( 'NONE',  ( -12.06949235617739369, -12.14591786802326823, 69.37609039468567573 ) ) ;
#827 = CARTESIAN_POINT ( 'NONE',  ( -23.91168844458654164, 8.792376985861425354, 168.9858545422794975 ) ) ;
#828 = CARTESIAN_POINT ( 'NONE',  ( -16.51473224551082808, 9.474510206698731452, 38.33442372801899722 ) ) ;
#829 = EDGE_CURVE ( 'NONE', #120001, #168590, #75101, .T. ) ;
#830 = CARTESIAN_POINT ( 'NONE',  ( -5.049401038298153566, 19.05341960407611168, 70.20724293864769550 ) ) ;
#831 = CARTESIAN_POINT ( 'NONE',  ( 12.06949235617757843, -12.14591786802309237, 53.12390960531436690 ) ) ;
#832 = CARTESIAN_POINT ( 'NONE',  ( 12.14591786802309770, 12.06949235617756955, 89.37390960531435269 ) ) ;
#833 = CARTESIAN_POINT ( 'NONE',  ( -19.05341960407611168, -5.049401038298163336, 111.4572429386476671 ) ) ;
#834 = ORIENTED_EDGE ( 'NONE', *, *, #188269, .F. ) ;
#835 = CARTESIAN_POINT ( 'NONE',  ( -19.05341960407611168, -5.049401038298163336, 86.45724293864769550 ) ) ;
#836 = CARTESIAN_POINT ( 'NONE',  ( 5.153800228976335163, 19.02544592524342804, 104.7905762719809957 ) ) ;
#837 = CARTESIAN_POINT ( 'NONE',  ( -15.80617190586768217, 15.72974639402176855, 108.1260903946856757 ) ) ;
#838 = CARTESIAN_POINT ( 'NONE',  ( -0.05219959533934338120, 16.53943276465976808, 87.50109039468568994 ) ) ;
#839 = CARTESIAN_POINT ( 'NONE',  ( -16.46253265017160317, 9.564922557960807481, 75.83224293864769550 ) ) ;
#840 = CARTESIAN_POINT ( 'NONE',  ( -21.55341960407619339, 5.719274019375674811, 33.54275706135234714 ) ) ;
#841 = CARTESIAN_POINT ( 'NONE',  ( -5.823673210054116645, -21.52544592524344225, 27.29057627198103120 ) ) ;
#842 = CARTESIAN_POINT ( 'NONE',  ( -0.05219959533907301413, -21.53943276465977519, 97.49890960531436690 ) ) ;
#843 = CARTESIAN_POINT ( 'NONE',  ( 12.14591786802309770, 12.06949235617756955, 64.37390960531435269 ) ) ;
#844 = CARTESIAN_POINT ( 'NONE',  ( 16.51473224551069308, 9.474510206698969483, 54.16557627198103120 ) ) ;
#845 = CARTESIAN_POINT ( 'NONE',  ( -16.53943276465976808, 0.05219959533911058130, 86.24890960531436690 ) ) ;
#846 = CARTESIAN_POINT ( 'NONE',  ( 13.97604488694548053, -13.89961937509957401, 45.62609039468566863 ) ) ;
#847 = CARTESIAN_POINT ( 'NONE',  ( 12.14591786802309770, 12.06949235617756955, 109.3739096053143811 ) ) ;
#848 = CARTESIAN_POINT ( 'NONE',  ( 16.55341960407618274, -4.379528057220086978, 66.04275706135236135 ) ) ;
#849 = CARTESIAN_POINT ( 'NONE',  ( 19.05341960407611168, 5.049401038298154454, 83.95724293864766707 ) ) ;
#850 = CARTESIAN_POINT ( 'NONE',  ( 8.571926809382603096, -26.38167802310801235, 145.4750000027311785 ) ) ;
#851 = CARTESIAN_POINT ( 'NONE',  ( -4.483927247898539470, -16.52544592524342804, 102.2905762719810383 ) ) ;
#852 = ORIENTED_EDGE ( 'NONE', *, *, #79706, .T. ) ;
#853 = CARTESIAN_POINT ( 'NONE',  ( -4.483927247898782831, 16.52544592524335698, 112.7094237280190328 ) ) ;
#854 = CARTESIAN_POINT ( 'NONE',  ( -0.05219959533934338120, 16.53943276465976808, 27.50109039468567929 ) ) ;
#855 = CARTESIAN_POINT ( 'NONE',  ( 15.72974639402176855, 15.80617190586768217, 91.87609039468568994 ) ) ;
#856 = CARTESIAN_POINT ( 'NONE',  ( -13.89961937509977652, 13.97604488694528158, 85.62390960531433848 ) ) ;
#857 = CARTESIAN_POINT ( 'NONE',  ( 18.67979575497194134, -10.72451020669871369, 25.83442372801901499 ) ) ;
#858 = CARTESIAN_POINT ( 'NONE',  ( 0.05219959533909260263, 19.03943276465977164, 29.99890960531435979 ) ) ;
#859 = CARTESIAN_POINT ( 'NONE',  ( -16.55341960407617563, 4.379528057220093196, 33.54275706135234714 ) ) ;
#860 = CARTESIAN_POINT ( 'NONE',  ( -9.564922557961040184, 16.46253265017147172, 92.91775706135233293 ) ) ;
#861 = CARTESIAN_POINT ( 'NONE',  ( 10.81492255796078972, 18.62759615963270932, 89.58224293864768129 ) ) ;
#862 = CARTESIAN_POINT ( 'NONE',  ( 5.049401038297881783, 19.05341960407617563, 72.29275706135234714 ) ) ;
#863 = CARTESIAN_POINT ( 'NONE',  ( -17.97058386085787163, -5.500000000000058620, 64.00390968646217971 ) ) ;
#864 = CARTESIAN_POINT ( 'NONE',  ( 18.67979575497194134, -10.72451020669871369, 25.83442372801901499 ) ) ;
#865 = DIRECTION ( 'NONE',  ( -1.000000000000000000, 0.000000000000000000, 0.000000000000000000 ) ) ;
#866 = CARTESIAN_POINT ( 'NONE',  ( -0.05219959533909027116, -19.03943276465977164, 87.49890960531436690 ) ) ;
#867 = CARTESIAN_POINT ( 'NONE',  ( -0.05219959533934338120, 16.53943276465976808, 27.50109039468567929 ) ) ;
#868 = CARTESIAN_POINT ( 'NONE',  ( 11.74149087413294268, 36.13659316521247433, -6.602157773949822506 ) ) ;
#869 = CARTESIAN_POINT ( 'NONE',  ( -19.03943276465977164, -0.05219959533935918106, 53.75109039468566863 ) ) ;
#871 = CARTESIAN_POINT ( 'NONE',  ( 14.29746914071049879, -8.314922557960816363, 73.33224293864769550 ) ) ;
#870 = CARTESIAN_POINT ( 'NONE',  ( -21.52544592524343514, 5.823673210054127303, 116.0405762719810383 ) ) ;
#872 = CARTESIAN_POINT ( 'NONE',  ( -19.05341960407611168, -5.049401038298163336, 81.45724293864769550 ) ) ;
#874 = CARTESIAN_POINT ( 'NONE',  ( 13.97604488694548053, -13.89961937509957401, 55.62609039468566863 ) ) ;
#873 = CARTESIAN_POINT ( 'NONE',  ( 8.224510206698742110, 14.34966873604972548, 52.08442372801901854 ) ) ;
#875 = CARTESIAN_POINT ( 'NONE',  ( 10.72451020669871369, 18.67979575497193778, 72.08442372801899012 ) ) ;
#876 = CARTESIAN_POINT ( 'NONE',  ( -4.483927247898782831, 16.52544592524335698, 22.70942372801901499 ) ) ;
#877 = CARTESIAN_POINT ( 'NONE',  ( 19.03943276465977164, -0.05219959533909143690, 68.74890960531436690 ) ) ;
#878 = CARTESIAN_POINT ( 'NONE',  ( -19.03943276465977164, -0.05219959533935918106, 83.75109039468567573 ) ) ;
#879 = CARTESIAN_POINT ( 'NONE',  ( -14.34966873604972548, 8.224510206698743886, 58.33442372801901143 ) ) ;
#880 = CARTESIAN_POINT ( 'NONE',  ( -18.62759615963255300, -10.81492255796106328, 99.16775706135234714 ) ) ;
#881 = CARTESIAN_POINT ( 'NONE',  ( 16.51473224551083163, -9.474510206698727899, 65.83442372801900433 ) ) ;
#882 = CARTESIAN_POINT ( 'NONE',  ( 9.474510206698971260, -16.51473224551069308, 52.91557627198102409 ) ) ;
#883 = CARTESIAN_POINT ( 'NONE',  ( -21.53943276465977519, 0.05219959533907696930, 71.24890960531435269 ) ) ;
#885 = CARTESIAN_POINT ( 'NONE',  ( -19.03943276465977164, -0.05219959533935918106, 83.75109039468567573 ) ) ;
#884 = CARTESIAN_POINT ( 'NONE',  ( -8.224510206698948167, 14.34966873604960824, 70.41557627198102409 ) ) ;
#886 = CARTESIAN_POINT ( 'NONE',  ( 16.88567814943160172, -6.947325034625743356, 61.20998877347415856 ) ) ;
#887 = CARTESIAN_POINT ( 'NONE',  ( 19.03943276465977164, 0.05219959533936151252, 46.25109039468566863 ) ) ;
#888 = CARTESIAN_POINT ( 'NONE',  ( -8.314922557961024197, 14.29746914071037800, 102.9177570613523756 ) ) ;
#889 = CARTESIAN_POINT ( 'NONE',  ( -12.14591786802309592, -12.06949235617757132, 66.87390960531436690 ) ) ;
#891 = CARTESIAN_POINT ( 'NONE',  ( 1.784210473542230573E-15, -29.16686587814331588, 147.3750000027311842 ) ) ;
#890 = CARTESIAN_POINT ( 'NONE',  ( 0.05219959533937995610, -21.53943276465977519, 100.0010903946857042 ) ) ;
#892 = CARTESIAN_POINT ( 'NONE',  ( -18.67979575497178146, -10.72451020669898902, 106.6655762719810383 ) ) ;
#893 =( BOUNDED_SURFACE ( )  B_SPLINE_SURFACE ( 3, 2, ( 
 ( #10534, #53015, #163206, #193554, #178386, #114694, #23699, #69191, #130857, #72198, #68187, #86359, #133872, #40861, #191538, #115706, #99522, #71201, #39850, #161204, #176389, #195562, #8524, #57036, #100522, #7507, #118709, #22699, #70202, #84346, #162201, #85347, #146024, #9534, #177394, #147040, #180399, #41871, #131869, #101516, #24710, #148044, #129839, #103537, #132864, #194553, #56023, #117701, #165212, #88347, #6507, #156744, #198526, #59997, #89353, #166209, #136842, #134884, #28698, #121664, #125407, #79892, #3051, #32402, #126389, #187104, #110227, #48574, #18238, #171908, #120672, #135867, #111220, #167200, #33396, #17233, #74198, #105515, #155735, #64727, #58031, #78885, #140564, #27710, #119701, #95055, #2053, #141562, #75170, #183359, #188086, #94057, #11545, #63732, #49557, #73213, #181384, #182372, #13505, #172913, #197538, #34391, #150040, #196560, #42862, #104528, #151043, #12533, #59006, #44841, #43849, #90334, #152019, #106497, #168174, #53531, #65709, #66705, #116209, #176902, #174892, #38373, #21203, #175893, #142553, #4031, #54536, #20201, #143535, #127375, #23210, #19227, #113203, #160713, #81847, #6023, #5022, #36358, #68696, #22204, #128368, #51540, #99022, #8022, #189086, #83854, #145535, #173910, #50559, #130351, #7014, #100028, #82859, #144537, #131371, #37364, #157738, #192050, #193060, #80876, #112220, #190064, #159705, #177899, #98010, #96050, #115209, #161715, #35379, #84853, #146530, #97030, #69704, #67702, #158711, #129360, #191056, #52528, #114189, #197060, #9042, #10044, #59508, #120194, #118218, #181884, #164724, #119216, #85867, #147556, #198041, #163726, #86869, #70712, #166717, #162712, #56541, #104039, #25228, #149546, #148553, #43362, #101027, #180901, #105033, #73717, #24217, #71704, #132380, #165719, #11041, #194073, #55535, #28221, #41376, #58528, #133372, #40369, #89862, #117208, #103042, #178901, #195062, #179910, #102042, #42376, #26218, #87858, #12054, #151544, #72716, #134389, #196075, #57547, #27215, #135390, #88861, #150555, #13034, #74700, #136364, #121183, #39368, #186871, #31176, #92826, #122175, #199030, #169680, #167703, #61497, #154512, #155506, #109995, #33164, #62488, #156501, #17001, #140328, #78653, #48340, #1818, #153512, #168677, #141325, #60499, #152518, #63498, #47345, #125173, #107994, #16008, #18003, #124159, #44358, #109001, #79656, #106017, #14006, #15009, #46338, #2814, #30177, #64492, #171675, #93826, #29200, #94824, #182877, #75673, #90834, #77666, #170681, #32169, #137350, #91820, #76670, #183866, #45352, #138348, #107004, #200028, #123166, #184854, #139335, #185859, #814, #172670, #84617, #50328, #173675, #34155, #53293, #49324, #143297, #190820, #111983, #36126, #35142, #6782, #187855, #5790, #68461, #160479, #110984, #96795, #157501, #52295, #97778, #18994, #95815, #114972, #128134, #145299, #19971, #127137, #176664, #80640, #189835, #142317, #81614, #4783, #3797, #129121, #65475, #158483, #98786, #38141, #188844, #66472, #51308, #112968, #174661, #21970, #159465, #144299, #20961, #113952, #83622, #82618, #67463, #130115, #175651, #37126, #191811, #99794, #161481, #22969, #146296, #7783, #126160, #196826, #119962, #149311, #43127, #42143, #26980, #165484, #135153, #103804, #40120, #55295, #27982, #86629, #88623, #134148, #193830, #24983, #72474, #181648, #177663, #195836, #57308, #89621, #54303, #179669, #117979, #131134, #23971, #150321, #41139, #87625, #10805, #11816, #192821, #151310, #118984, #69467, #115975, #25982, #180667, #163486, #147313, #73480, #58293, #166484, #104795, #39132, #8802, #100787, #162470, #116967, #85627, #70472, #132138, #102803, #178658, #101799, #148312, #9806, #164489, #194824, #71468, #133133, #56296, #59272, #169433, #199789, #61257, #120941, #29942, #75440, #137114, #171434, #170434, #78403, #92585, #28965, #140079, #184615, #123908, #91581, #153270, #32921, #108758, #74464, #44124 ),
 ( #182641, #183632, #94576, #93580, #14772, #155265, #138108, #154273, #105783, #167470, #12799, #198801, #60266, #90606, #1570, #136130, #76432, #77423, #121937, #122927, #45114, #16755, #197806, #15764, #63246, #47097, #152288, #106771, #13772, #139095, #46096, #168446, #107751, #124925, #30938, #31926, #569, #62240, #186622, #185607, #48094, #109750, #50079, #34896, #172423, #159220, #95569, #3554, #128878, #6535, #49085, #125917, #111740, #96552, #33911, #20715, #157255, #65232, #190578, #68215, #110742, #142068, #18749, #80396, #17756, #52054, #158239, #174417, #126892, #144060, #113710, #51062, #79413, #160234, #4534, #66226, #188598, #173427, #143055, #141083, #19730, #127887, #175407, #83377, #129867, #35886, #191565, #36875, #98540, #21724, #145054, #53044, #81371, #189590, #114724, #112724, #176417, #82371, #97533, #5541, #67220, #37892, #64250, #156254, #2568, #187615, #69220, #133900, #164247, #41899, #24737, #86387, #134909, #40889, #161232, #25742, #196586, #22726, #130888, #70230, #163237, #119727, #85377, #58056, #195591, #10561, #84374, #57063, #72225, #192578, #118738, #71228, #87388, #149073, #180426, #147070, #131898, #103565, #54061, #193582, #181410, #165240, #178414, #26734, #148071, #179424, #146051, #7535, #99550, #23728, #8554, #115735, #88373, #177422, #116725, #150067, #55054, #9562, #39878, #11572, #38893, #102562, #73238, #100550, #162229, #101545, #132891, #194580, #56050, #117729, #151067, #170188, #44868, #61995, #136868, #43875, #31682, #89378, #106524, #122683, #16512, #15520, #327, #138847, #108509, #77177, #13531, #28724, #1317, #60023, #123661, #107506, #167226, #198553, #45853, #155016, #12558, #169182, #30688, #120698, #74224, #185358, #92339, #46849, #168201, #29698, #78160, #184372, #104553, #154025, #139828, #166235, #135892, #75197, #91329, #62996, #90361, #124674, #93331, #42888, #27735, #197564, #59031, #182397, #105540, #14520, #152046, #121690, #183386, #153021, #76181, #137861, #199541, #61011, #6292, #66976, #64988, #128636, #111491, #65977, #32674, #94327, #144809, #110492, #33659, #156005, #113466, #109503, #3315, #50824, #172174, #96311, #95320, #190330, #47850, #127646, #51807, #20469, #171185, #157005, #17502, #112481, #157997, #79159, #140830, #175160, #188349, #5293, #80151, #187369, #36627, #2319, #49827, #64001, #141822, #126646, #125671, #189346, #48838, #18503, #158977, #98284, #173176, #34652, #19489, #81134, #142815, #82119, #4295, #174174, #35644, #97290, #143811, #159985, #21472, #83133, #67971, #186371, #68974, #145807, #116484, #114465, #8308, #39638, #102317, #56821, #180186, #37637, #132654, #117482, #7290, #99301, #164007, #194342, #71976, #54809, #178173, #164999, #70986, #191320, #55810, #26493, #52797, #160986, #100307, #193335, #149819, #115489, #88135, #25503, #40648, #176167, #87147, #148830, #22480, #10320, #101299, #179180, #133650, #195341, #177177, #161985, #118495, #84128, #23481, #11325, #41655, #69985, #103319, #162988, #9321, #130638, #192333, #129625, #53814, #38650, #85130, #146814, #131653, #24493, #86144, #147835, #183143, #197327, #153782, #134664, #152785, #15277, #107269, #57818, #182150, #104311, #137620, #44628, #165994, #181172, #88, #74962, #92094, #166985, #73987, #61758, #119490, #136624, #42649, #28488, #151806, #89137, #75946, #12322, #120459, #45617, #123426, #27495, #58791, #150825, #135656, #196350, #168940, #198305, #91097, #43635, #60771, #30447, #167965, #105297, #76937, #121451, #106280, #90122, #13297, #59783, #29464, #14276, #199304, #138606, #185119, #46609, #122443, #108271, #169949, #31440, #93094, #154778, #72995, #184135, #2087, #174930, #33430, #189121, #80909, #140597, #171941, #19263, #128403, #155769, #63767, #50593, #66742, #109265, #125440, #94090, #17267, #77927, #112252, #18271, #34424, #187136, #4065, #173944, #111254, #139594, #20234, #64760, #126422, #78920, #32436 ),
 ( #35411, #48608, #110260, #36393, #95089, #97063, #142586, #156778, #79924, #65743, #190100, #124436, #127411, #158745, #141597, #186132, #81882, #143574, #5057, #51575, #3084, #113239, #98047, #96083, #188120, #16275, #49591, #1080, #172946, #157772, #62755, #47611, #170944, #191093, #59306, #53572, #10838, #119018, #180701, #192089, #44157, #42177, #52568, #115249, #161753, #23248, #82896, #176941, #119995, #43162, #151344, #11851, #37405, #120975, #28016, #38411, #182673, #149342, #104829, #159745, #165518, #100068, #166518, #136165, #99063, #150354, #21242, #27014, #72508, #87657, #196861, #160751, #88658, #58327, #181681, #134183, #83892, #114228, #68734, #144574, #73516, #195870, #89658, #57343, #175933, #135187, #103837, #6061, #22243, #12833, #74499, #197840, #67739, #129397, #145575, #7052, #130392, #171467, #154307, #75473, #78439, #167504, #31959, #141116, #28999, #137146, #76466, #169468, #125950, #91616, #2605, #140113, #16789, #90639, #1604, #63280, #198834, #124960, #77456, #170469, #155299, #186657, #153304, #138143, #48127, #60298, #199823, #187648, #109784, #184648, #32955, #30969, #185640, #152321, #13807, #64283, #29977, #14805, #121972, #94610, #183664, #122961, #93614, #61291, #15796, #46130, #156289, #45149, #47132, #17790, #79446, #106805, #107783, #168479, #105817, #139127, #92616, #604, #62274, #123942, #108790, #143091, #50113, #37924, #95603, #112758, #18784, #4570, #127922, #65266, #52088, #188633, #96586, #21758, #99584, #142103, #34933, #126926, #111773, #110776, #83410, #51098, #67254, #158275, #36911, #145087, #144093, #172458, #53079, #97566, #159254, #173461, #19764, #35920, #33945, #189624, #20750, #6570, #176451, #161265, #128912, #22759, #68249, #129900, #191600, #114757, #84408, #81405, #66262, #7569, #174451, #146085, #113745, #82405, #5574, #175441, #69255, #157288, #98574, #160268, #190613, #130921, #49119, #80430, #3588, #24776, #150107, #73276, #181447, #41936, #70265, #151105, #58093, #9600, #12597, #179462, #134946, #74261, #195629, #71265, #196623, #166275, #131934, #180464, #192612, #57102, #102600, #86423, #26771, #193617, #118776, #88411, #11608, #56088, #116760, #23765, #101586, #54094, #103602, #132929, #119763, #148109, #85414, #165277, #194616, #115768, #147106, #42925, #25779, #87425, #104589, #117769, #40927, #27773, #89416, #149110, #177456, #38926, #164286, #10600, #100583, #8591, #162265, #72261, #133939, #55089, #178451, #39918, #163274, #77213, #135931, #197601, #92374, #62033, #29733, #13566, #138882, #362, #32710, #123697, #185395, #75233, #31718, #156041, #183419, #17538, #124711, #182433, #107542, #46886, #136904, #105575, #94362, #169218, #61046, #184408, #108546, #93366, #43913, #154060, #122718, #45889, #167261, #153057, #186409, #109539, #30727, #47886, #1354, #15555, #152081, #63033, #170225, #155053, #14559, #76217, #59067, #16548, #120734, #28760, #90397, #91366, #78195, #139865, #171221, #168237, #198591, #60059, #121727, #44903, #106560, #137896, #199578, #125707, #49861, #175197, #98321, #158032, #36662, #190367, #189381, #172210, #51843, #142850, #159012, #111527, #173212, #83169, #82153, #140867, #48874, #21508, #188384, #19523, #127681, #50858, #126680, #144843, #112516, #110529, #34688, #96345, #81168, #2356, #65024, #143849, #67012, #160021, #97326, #33694, #79198, #64037, #4329, #187406, #174210, #95357, #157042, #113502, #35678, #18539, #80186, #66013, #141858, #3349, #20505, #5328, #128671, #94023, #137553, #186064, #155704, #17199, #123362, #184066, #91032, #168874, #121388, #47547, #19, #140532, #92024, #152718, #32370, #15212, #183080, #14209, #110195, #93027, #154715, #78853, #138541, #46543, #170879, #2021, #16208, #18203, #44563, #169884, #108203, #106218, #75877, #63700, #31377, #77863, #1013, #125375, #167902, #141529, #62687, #59716, #29402, #139530, #109200, #153716, #199236, #124369, #187071 ),
 ( #48541, #171873, #45549, #76871, #33362, #95021, #60701, #156710, #79861, #107204, #61693, #122377, #30379, #185055, #23172, #83819, #81813, #145499, #128334, #82822, #49522, #111185, #161676, #127338, #50525, #172875, #130315, #126355, #20168, #67667, #189050, #113169, #112187, #6980, #64694, #144503, #68660, #37329, #188052, #173875, #34356, #129325, #174857, #96017, #157702, #192012, #4985, #22169, #96996, #3997, #53496, #19192, #66671, #80841, #158679, #143501, #142518, #5987, #65676, #35345, #175857, #115173, #190033, #51507, #36323, #97977, #159670, #98988, #21166, #191020, #52495, #114155, #160677, #176866, #38335, #99991, #84816, #3017, #85832, #162676, #133336, #131336, #25191, #56504, #119182, #73682, #197026, #26183, #120159, #180867, #104005, #42343, #12020, #165683, #117170, #132344, #104997, #163689, #27181, #11006, #70678, #102007, #149509, #58493, #54501, #72680, #134355, #24182, #116173, #88828, #196039, #150521, #135354, #195027, #177863, #181850, #7986, #57514, #43329, #69669, #39332, #178865, #10009, #166684, #194036, #28186, #146495, #193024, #100991, #147522, #9010, #55500, #40332, #118182, #86833, #148519, #71669, #179873, #41341, #103003, #164688, #87823, #34119, #50290, #52258, #96756, #51271, #17965, #79620, #130075, #95778, #18957, #141288, #98749, #94784, #188807, #36090, #157464, #81576, #80602, #113916, #33128, #112931, #175614, #5751, #156465, #142279, #2778, #97741, #143261, #64454, #126124, #160442, #173636, #190784, #65437, #172631, #21932, #187819, #35105, #49288, #127098, #111947, #110946, #174625, #3760, #158446, #144264, #83583, #19934, #4745, #66434, #128095, #189799, #67427, #159429, #20925, #82583, #129084, #37090, #145262, #6744, #68423, #191774, #53256, #171638, #131096, #101764, #99757, #193793, #24949, #87593, #42111, #165452, #194789, #88591, #149279, #72439, #10774, #180636, #134115, #85590, #100753, #73448, #132102, #195804, #179635, #39097, #70436, #117945, #26949, #22933, #41105, #102769, #192784, #84579, #57276, #164456, #118950, #103773, #163451, #146259, #150289, #176627, #25950, #11784, #38102, #7743, #147277, #178623, #135121, #162435, #196795, #114934, #161441, #69429, #54267, #115939, #177629, #23936, #86596, #8767, #55261, #116930, #40086, #148279, #9772, #71436, #56262, #133100, #104765, #16727, #182608, #105751, #166453, #185578, #181617, #75409, #122896, #44093, #168415, #167437, #139063, #119932, #138077, #541, #92555, #43096, #28934, #89591, #184585, #29910, #151278, #27950, #47069, #60235, #77393, #152256, #59240, #108729, #12767, #121906, #74431, #13741, #137081, #136098, #61225, #197774, #90575, #30907, #170406, #120909, #198769, #183599, #45083, #106740, #154243, #91550, #76401, #153237, #46066, #15734, #14740, #199758, #62212, #107720, #169401, #123880, #31898, #93551, #155237, #78375, #140051, #58263, #131616, #54775, #81345, #178137, #174390, #159192, #97506, #69951, #35860, #172394, #187588, #162953, #18720, #23447, #66197, #125888, #157228, #4507, #116449, #109724, #127860, #189564, #79386, #171408, #85094, #51036, #146779, #193300, #50050, #32894, #8273, #63217, #112698, #39604, #124897, #94546, #33883, #65204, #24459, #49057, #101263, #86109, #1541, #186596, #48068, #156227, #17728, #141055, #173398, #2541, #64223, #110712, #95540, #80367, #142040, #3528, #34869, #126863, #96523, #188570, #111712, #158213, #19703, #143029, #9285, #179146, #44595, #41622, #196317, #104279, #165961, #180153, #29433, #27462, #40614, #103286, #149787, #11290, #72963, #198274, #194307, #135623, #136594, #197294, #25470, #106251, #13268, #164966, #167933, #134632, #28457, #147800, #150794, #26459, #151775, #121421, #87110, #58757, #70950, #12290, #57786, #88102, #182117, #148796, #73955, #43603, #105268, #119457, #71944, #102284, #56789, #132620, #120426, #181141, #90093, #42615, #163973, #166954, #89103, #55773, #10286, #59751, #74931 ),
 ( #183113, #117447, #133614, #195308, #118461, #152751, #172914, #32403, #91064, #14241, #47579, #17234, #185087, #168907, #94058, #155736, #188087, #78886, #140565, #30413, #187105, #111221, #138574, #75912, #79893, #137586, #62720, #2055, #92060, #60737, #49558, #124403, #16243, #139563, #63733, #48575, #199269, #109231, #77895, #1047, #122410, #108237, #141563, #64728, #186097, #3052, #156745, #170910, #107236, #126390, #153749, #125408, #184100, #110228, #171909, #123395, #33397, #15244, #95056, #18240, #45583, #154747, #76903, #52, #61727, #46576, #169917, #31409, #93060, #66707, #65710, #7015, #190065, #157739, #189087, #84854, #67703, #129361, #68697, #113204, #21204, #145536, #130352, #191057, #193061, #19228, #144538, #82861, #96051, #50561, #192051, #6024, #52529, #175894, #176903, #80877, #116210, #37366, #34393, #142554, #114190, #160714, #128369, #112221, #99024, #22205, #131373, #83855, #53533, #173911, #115210, #54537, #81848, #4032, #23211, #127376, #38374, #100029, #35380, #97031, #158712, #161716, #20202, #146531, #143536, #8024, #69706, #5023, #51541, #174893, #36359, #98011, #159706, #26219, #147558, #150557, #39369, #104040, #13035, #101028, #9043, #148554, #41377, #198042, #163728, #74701, #12056, #88863, #162713, #73718, #135391, #70713, #197061, #149547, #42377, #27216, #58529, #25229, #10045, #120195, #181885, #11042, #165720, #40370, #56543, #43363, #103043, #57548, #24219, #85869, #136365, #102044, #86870, #132381, #105035, #194074, #166719, #179911, #196077, #71705, #28223, #89863, #72718, #55536, #151545, #87859, #134391, #117209, #178902, #164725, #133373, #118220, #119217, #59509, #177900, #195063, #180902, #94825, #93827, #78654, #17002, #186872, #155507, #91821, #107005, #79658, #138349, #140329, #185861, #32171, #44360, #168678, #77667, #29201, #124160, #109003, #199032, #90835, #1819, #47347, #63500, #48342, #169682, #152519, #125175, #182878, #170682, #156502, #106018, #14007, #153514, #184855, #141327, #30178, #18004, #109996, #171676, #167705, #33165, #2815, #75674, #121185, #92828, #137352, #60501, #122176, #15011, #76672, #183868, #45353, #154513, #200030, #61498, #123167, #46339, #107995, #815, #31177, #16010, #139336, #62489, #111985, #172671, #191813, #187856, #81615, #129123, #50329, #174662, #188845, #145300, #126161, #144301, #6783, #98787, #49325, #173676, #95817, #190821, #36127, #157502, #34156, #53294, #66473, #83623, #158484, #65476, #114973, #110985, #128136, #18995, #19972, #143298, #80641, #67464, #3798, #35143, #37127, #176666, #142318, #96797, #127138, #4784, #189836, #20962, #52296, #51309, #112970, #113953, #5791, #161482, #175653, #160481, #97779, #21971, #84618, #159467, #146297, #38142, #82619, #68462, #130116, #99795, #22970, #64494, #27983, #178659, #134149, #118985, #165485, #54304, #164490, #194825, #56298, #115976, #24985, #58295, #181649, #117980, #119963, #73482, #87626, #23973, #135154, #179670, #180668, #86630, #148313, #89623, #103805, #69468, #39133, #104797, #101800, #41141, #25983, #149312, #40122, #7785, #10806, #100788, #163487, #9808, #71469, #133134, #43128, #177664, #195837, #196827, #57310, #85628, #166485, #131135, #102804, #192823, #72476, #88625, #162471, #42145, #26981, #11817, #147314, #8804, #150322, #70473, #132139, #193832, #55296, #116968, #28966, #77424, #47098, #185609, #14773, #75441, #182642, #60267, #12800, #139096, #91582, #31927, #183633, #44125, #123910, #106773, #74466, #105785, #1572, #184616, #46097, #108759, #29943, #138110, #62241, #170436, #107752, #109751, #136131, #61258, #199790, #197807, #167471, #93581, #122928, #169435, #92586, #155266, #59273, #32922, #154275, #151311, #120943, #570, #90608, #171435, #16756, #168448, #152289, #30939, #78404, #13773, #15765, #153272, #140080, #124926, #137116, #63247, #198802, #186624, #48095, #45115, #121939, #76433, #20716, #190579, #128879, #158240 ),
 ( #188599, #173428, #110743, #97534, #33913, #142069, #67221, #145055, #187616, #80397, #172424, #95570, #156255, #52055, #96553, #112725, #3555, #82373, #113711, #189591, #17758, #98542, #143057, #4535, #157256, #18751, #81372, #79414, #34898, #66228, #175408, #21725, #6536, #174418, #68216, #36876, #160235, #83378, #129868, #191566, #65233, #126893, #53045, #111741, #114725, #159221, #5542, #141084, #50080, #51064, #2570, #144061, #176418, #19731, #64251, #94577, #125918, #49086, #127888, #35887, #7536, #10562, #99551, #164248, #73239, #161233, #69221, #8555, #101546, #58057, #23729, #134910, #72226, #149074, #22727, #133901, #195592, #130889, #57064, #9563, #102563, #87389, #118739, #85378, #70231, #180427, #41900, #71229, #25743, #100551, #116726, #103566, #39879, #56051, #147071, #165241, #26735, #132892, #84375, #88374, #86388, #148072, #177423, #54062, #24738, #146052, #178415, #194581, #150068, #11573, #196587, #117730, #119728, #37893, #192579, #115736, #38894, #162230, #131899, #193583, #55055, #163238, #179425, #40890, #92340, #104554, #167227, #137862, #89379, #184373, #169183, #59032, #151068, #15521, #45854, #123662, #46850, #29699, #12559, #154026, #42889, #107507, #16513, #166236, #74225, #152047, #44869, #1318, #28725, #78161, #77178, #138848, #27736, #328, #61996, #135893, #185359, #153022, #30689, #108510, #170189, #90362, #13532, #31683, #93332, #14521, #155017, #43876, #60024, #139829, #106525, #61012, #197565, #120699, #62997, #105541, #75198, #182398, #181411, #136869, #198554, #121691, #183387, #91330, #168202, #76182, #199542, #122684, #5294, #158978, #109504, #33660, #156006, #189347, #34653, #17503, #32675, #51808, #126647, #143812, #18504, #125672, #113467, #171186, #188350, #94328, #80152, #3316, #140831, #127647, #64002, #172175, #97291, #175161, #79160, #110493, #2320, #187370, #186372, #64989, #48839, #50825, #95321, #157006, #20470, #36628, #141823, #49828, #111492, #173177, #47851, #82120, #96312, #142816, #157998, #112482, #66977, #19490, #81135, #128637, #4296, #65978, #174175, #35645, #190331, #98285, #159986, #21473, #83134, #144810, #6293, #124675, #41656, #40649, #25504, #164008, #133651, #102318, #38651, #53815, #26494, #85131, #87148, #132655, #179181, #191321, #115490, #24494, #176168, #70987, #55811, #145808, #37638, #148831, #194343, #10321, #195342, #116485, #99302, #71977, #129626, #117483, #103320, #52798, #160987, #100308, #131654, #88136, #177178, #165000, #56822, #118496, #114466, #180187, #149820, #22481, #67972, #39639, #84129, #7291, #68975, #161986, #23482, #130639, #192334, #101300, #146815, #8309, #69986, #193336, #54810, #147836, #178174, #162989, #86145, #9322, #58792, #119491, #141358, #134665, #28489, #78683, #197328, #121452, #135657, #94854, #72996, #91098, #156535, #48371, #196351, #120460, #42650, #140359, #183144, #104312, #181173, #2845, #13298, #33195, #105298, #12323, #64523, #57819, #74963, #165995, #166986, #90123, #198306, #125204, #110028, #167966, #172702, #27496, #44629, #59784, #89138, #150826, #186900, #106281, #29465, #152786, #18034, #73988, #95847, #14277, #11326, #182151, #1847, #63529, #151807, #43636, #171706, #79688, #111015, #126190, #187886, #136625, #49353, #34186, #4815, #177693, #146326, #3827, #129153, #98816, #96829, #127167, #145331, #39161, #128165, #83653, #68491, #115003, #65506, #113984, #144331, #5820, #188876, #174693, #7815, #131164, #67496, #69499, #23003, #37157, #173706, #84649, #190850, #130146, #36157, #97809, #157531, #53324, #19025, #50358, #54333, #51339, #52327, #175682, #160510, #189865, #80671, #22000, #112017, #112999, #159498, #20994, #82649, #192854, #35174, #6813, #116004, #191843, #158513, #142347, #20001, #176697, #81644, #38171, #99826, #143328, #161511, #66502, #104830, #74500, #178692, #88659, #59307, #165519, #10839, #133165, #135188, #40154, #27015, #196862, #58328 ),
 ( #55326, #151345, #134184, #195871, #119996, #120976, #89659, #147346, #72509, #42178, #101830, #70502, #150355, #182674, #71498, #11852, #73517, #181682, #8834, #57344, #87658, #149343, #132170, #118011, #12834, #136166, #119019, #197841, #166519, #180702, #116997, #28017, #103838, #43163, #179700, #41172, #100819, #162502, #24003, #193861, #85659, #194856, #163517, #25016, #86659, #56329, #148343, #9839, #102835, #164521, #26014, #46131, #107784, #94611, #90640, #31960, #32956, #93615, #121973, #2606, #109785, #61292, #64284, #30970, #124961, #125951, #47133, #122962, #48128, #17791, #183665, #155300, #44158, #108791, #154308, #76467, #78440, #45150, #170470, #140114, #1605, #169469, #168480, #75474, #153305, #105818, #16790, #184649, #186658, #138144, #137147, #63281, #199824, #167505, #198835, #156290, #77457, #139128, #171468, #92617, #15797, #79447, #141117, #605, #29000, #152322, #62275, #123943, #13808, #60299, #106806, #185641, #29978, #91617, #14806, #49120, #69256, #128913, #187649, #110777, #144094, #113746, #81406, #65267, #190614, #52089, #84409, #175442, #36912, #126927, #83411, #7570, #34934, #19765, #21759, #188634, #98575, #145088, #6571, #51099, #111774, #18785, #96587, #172459, #160269, #127923, #68250, #143092, #80431, #129901, #4571, #33946, #142104, #37925, #20751, #82406, #191601, #66263, #174452, #53080, #114758, #5575, #146086, #95604, #97567, #35921, #157289, #3589, #176452, #159255, #67255, #99585, #161266, #50114, #173462, #22760, #158276, #189625, #112759, #57103, #24777, #8592, #133940, #72262, #27774, #118777, #180465, #70266, #26772, #151106, #178452, #12598, #119764, #177457, #102601, #195630, #131935, #100584, #41937, #130922, #101587, #103603, #165278, #88412, #38927, #87426, #117770, #179463, #162266, #148110, #181448, #104590, #40928, #42926, #196624, #10601, #147107, #58094, #164287, #150108, #9601, #71266, #192613, #11609, #54095, #73277, #115769, #134947, #166276, #23766, #89417, #25780, #85415, #193618, #55090, #116761, #163275, #39919, #86424, #149111, #132930, #194617, #56089, #155054, #199579, #154061, #120735, #182434, #32711, #198592, #121728, #43914, #1355, #197602, #91367, #138883, #60060, #184409, #183420, #16549, #139866, #122719, #105576, #46887, #135932, #363, #109540, #59068, #167262, #44904, #137897, #94363, #63034, #28761, #90398, #62034, #152082, #170226, #108547, #13567, #31719, #45890, #123698, #185396, #78196, #106561, #168238, #93367, #124712, #107543, #186410, #136905, #153058, #47887, #61047, #15556, #75234, #29734, #156042, #14560, #76218, #169219, #171222, #30728, #92375, #74262, #77214, #127682, #141859, #98322, #79199, #97327, #160022, #51844, #2357, #126681, #48875, #82154, #189382, #110530, #125708, #144844, #19524, #36663, #111528, #18540, #6327, #64038, #81169, #187407, #173213, #96346, #33695, #20506, #157043, #65025, #190369, #68007, #172211, #3350, #95358, #80187, #140868, #113503, #142851, #35679, #188385, #5329, #175198, #112517, #49862, #21509, #66014, #50859, #34689, #158033, #4330, #174211, #159013, #143850, #83170, #129659, #191355, #67013, #52833, #114502, #176204, #37673, #99338, #17539, #128672, #162021, #103355, #131688, #102351, #194376, #40681, #84162, #23517, #147869, #7324, #55843, #117517, #115525, #69008, #164040, #179215, #10355, #192368, #85163, #177213, #38686, #22515, #25539, #116519, #9355, #146851, #87183, #148864, #86179, #145842, #72012, #101333, #163022, #100342, #53851, #24528, #130674, #193369, #71020, #133685, #195378, #56856, #132688, #118531, #180220, #41690, #165033, #26526, #161021, #8344, #70019, #54845, #178207, #39671, #5988, #52496, #64695, #127339, #97978, #49523, #144504, #129326, #19193, #111186, #175858, #67668, #83820, #6981, #190034, #172876, #114156, #3018, #191021, #176867, #126356, #34357, #112188, #4986, #161677, #68661, #188053, #157703, #37330, #96018, #98989, #160678 ) ),
 .UNSPECIFIED., .T., .F., .F. ) 
 B_SPLINE_SURFACE_WITH_KNOTS ( ( 4, 3, 4 ),
 ( 3, 2, 2, 2, 2, 2, 2, 2, 2, 2, 2, 2, 2, 2, 2, 2, 2, 2, 2, 2, 2, 2, 2, 2, 2, 2, 2, 2, 2, 2, 2, 2, 2, 2, 2, 2, 2, 2, 2, 2, 2, 2, 2, 2, 2, 2, 2, 2, 2, 2, 2, 2, 2, 2, 2, 2, 2, 2, 2, 2, 2, 2, 2, 2, 2, 2, 2, 2, 2, 2, 2, 2, 2, 2, 2, 2, 2, 2, 2, 2, 2, 2, 2, 2, 2, 2, 2, 2, 2, 2, 2, 2, 2, 2, 2, 2, 2, 2, 2, 2, 2, 2, 2, 2, 2, 2, 2, 2, 2, 2, 2, 2, 2, 2, 2, 2, 2, 2, 2, 2, 2, 2, 2, 2, 2, 2, 2, 2, 2, 2, 2, 2, 2, 2, 2, 2, 2, 2, 2, 2, 2, 2, 2, 2, 2, 2, 2, 2, 2, 2, 2, 2, 2, 2, 2, 2, 2, 2, 2, 2, 2, 2, 2, 2, 2, 2, 2, 2, 2, 2, 2, 2, 2, 2, 2, 2, 2, 2, 2, 2, 2, 2, 2, 2, 2, 2, 2, 2, 2, 2, 2, 2, 2, 2, 2, 2, 2, 2, 2, 2, 2, 2, 2, 2, 2, 2, 2, 2, 2, 2, 2, 2, 2, 2, 2, 2, 2, 2, 2, 2, 2, 2, 2, 2, 2, 2, 2, 2, 3 ),
 ( 0.000000000000000000, 0.5000000000000000000, 1.000000000000000000 ),
 ( 0.000000000000000000, 0.004385964912280701511, 0.008771929824561403022, 0.01315789473684210453, 0.01754385964912280604, 0.02192982456140350755, 0.02631578947368420907, 0.03070175438596491058, 0.03508771929824561209, 0.03947368421052631360, 0.04385964912280701511, 0.04824561403508771662, 0.05263157894736841813, 0.05701754385964911964, 0.06140350877192982115, 0.06578947368421052266, 0.07017543859649122417, 0.07456140350877192569, 0.07894736842105262720, 0.08333333333333332871, 0.08771929824561403022, 0.09210526315789473173, 0.09649122807017543324, 0.1008771929824561348, 0.1052631578947368363, 0.1096491228070175378, 0.1140350877192982393, 0.1184210526315789408, 0.1228070175438596423, 0.1271929824561403577, 0.1315789473684210453, 0.1359649122807017607, 0.1403508771929824483, 0.1447368421052631637, 0.1491228070175438514, 0.1535087719298245668, 0.1578947368421052544, 0.1622807017543859698, 0.1666666666666666574, 0.1710526315789473728, 0.1754385964912280604, 0.1798245614035087758, 0.1842105263157894635, 0.1885964912280701788, 0.1929824561403508665, 0.1973684210526315819, 0.2017543859649122695, 0.2061403508771929849, 0.2105263157894736725, 0.2149122807017543879, 0.2192982456140350755, 0.2236842105263157909, 0.2280701754385964786, 0.2324561403508771940, 0.2368421052631578816, 0.2412280701754385970, 0.2456140350877192846, 0.2500000000000000000, 0.2543859649122807154, 0.2587719298245614308, 0.2631578947368420907, 0.2675438596491228060, 0.2719298245614035214, 0.2763157894736842368, 0.2807017543859648967, 0.2850877192982456121, 0.2894736842105263275, 0.2938596491228070429, 0.2982456140350877027, 0.3026315789473684181, 0.3070175438596491335, 0.3114035087719298489, 0.3157894736842105088, 0.3201754385964912242, 0.3245614035087719396, 0.3289473684210526550, 0.3333333333333333148, 0.3377192982456140302, 0.3421052631578947456, 0.3464912280701754610, 0.3508771929824561209, 0.3552631578947368363, 0.3596491228070175517, 0.3640350877192982670, 0.3684210526315789269, 0.3728070175438596423, 0.3771929824561403577, 0.3815789473684210731, 0.3859649122807017330, 0.3903508771929824483, 0.3947368421052631637, 0.3991228070175438791, 0.4035087719298245390, 0.4078947368421052544, 0.4122807017543859698, 0.4166666666666666852, 0.4210526315789473450, 0.4254385964912280604, 0.4298245614035087758, 0.4342105263157894912, 0.4385964912280701511, 0.4429824561403508665, 0.4473684210526315819, 0.4517543859649122973, 0.4561403508771929571, 0.4605263157894736725, 0.4649122807017543879, 0.4692982456140351033, 0.4736842105263157632, 0.4780701754385964786, 0.4824561403508771940, 0.4868421052631579093, 0.4912280701754385692, 0.4956140350877192846, 0.5000000000000000000, 0.5043859649122807154, 0.5087719298245614308, 0.5131578947368421462, 0.5175438596491228616, 0.5219298245614034659, 0.5263157894736841813, 0.5307017543859648967, 0.5350877192982456121, 0.5394736842105263275, 0.5438596491228070429, 0.5482456140350877583, 0.5526315789473684736, 0.5570175438596490780, 0.5614035087719297934, 0.5657894736842105088, 0.5701754385964912242, 0.5745614035087719396, 0.5789473684210526550, 0.5833333333333333703, 0.5877192982456140857, 0.5921052631578946901, 0.5964912280701754055, 0.6008771929824561209, 0.6052631578947368363, 0.6096491228070175517, 0.6140350877192982670, 0.6184210526315789824, 0.6228070175438596978, 0.6271929824561403022, 0.6315789473684210176, 0.6359649122807017330, 0.6403508771929824483, 0.6447368421052631637, 0.6491228070175438791, 0.6535087719298245945, 0.6578947368421053099, 0.6622807017543859143, 0.6666666666666666297, 0.6710526315789473450, 0.6754385964912280604, 0.6798245614035087758, 0.6842105263157894912, 0.6885964912280702066, 0.6929824561403509220, 0.6973684210526315264, 0.7017543859649122417, 0.7061403508771929571, 0.7105263157894736725, 0.7149122807017543879, 0.7192982456140351033, 0.7236842105263158187, 0.7280701754385965341, 0.7324561403508771384, 0.7368421052631578538, 0.7412280701754385692, 0.7456140350877192846, 0.7500000000000000000, 0.7543859649122807154, 0.7587719298245614308, 0.7631578947368421462, 0.7675438596491228616, 0.7719298245614034659, 0.7763157894736841813, 0.7807017543859648967, 0.7850877192982456121, 0.7894736842105263275, 0.7938596491228070429, 0.7982456140350877583, 0.8026315789473684736, 0.8070175438596490780, 0.8114035087719297934, 0.8157894736842105088, 0.8201754385964912242, 0.8245614035087719396, 0.8289473684210526550, 0.8333333333333333703, 0.8377192982456140857, 0.8421052631578946901, 0.8464912280701754055, 0.8508771929824561209, 0.8552631578947368363, 0.8596491228070175517, 0.8640350877192982670, 0.8684210526315789824, 0.8728070175438596978, 0.8771929824561403022, 0.8815789473684210176, 0.8859649122807017330, 0.8903508771929824483, 0.8947368421052631637, 0.8991228070175438791, 0.9035087719298245945, 0.9078947368421053099, 0.9122807017543859143, 0.9166666666666666297, 0.9210526315789473450, 0.9254385964912280604, 0.9298245614035087758, 0.9342105263157894912, 0.9385964912280702066, 0.9429824561403509220, 0.9473684210526315264, 0.9517543859649122417, 0.9561403508771929571, 0.9605263157894736725, 0.9649122807017543879, 0.9692982456140351033, 0.9736842105263158187, 0.9780701754385965341, 0.9824561403508771384, 0.9868421052631578538, 0.9912280701754385692, 0.9956140350877192846, 1.000000000000000000 ),
 .UNSPECIFIED. ) 
 GEOMETRIC_REPRESENTATION_ITEM ( )  RATIONAL_B_SPLINE_SURFACE ( (
 ( 1.000000000000000000, 0.9659258262890683122, 1.000000000000000000, 0.9659258262890683122, 1.000000000000000000, 0.9659258262890683122, 1.000000000000000000, 0.9659258262890683122, 1.000000000000000000, 0.9659258262890683122, 1.000000000000000000, 0.9659258262890683122, 1.000000000000000000, 0.9659258262890683122, 1.000000000000000000, 0.9659258262890683122, 1.000000000000000000, 0.9659258262890683122, 1.000000000000000000, 0.9659258262890683122, 1.000000000000000000, 0.9659258262890683122, 1.000000000000000000, 0.9659258262890683122, 1.000000000000000000, 0.9659258262890683122, 1.000000000000000000, 0.9659258262890683122, 1.000000000000000000, 0.9659258262890683122, 1.000000000000000000, 0.9659258262890683122, 1.000000000000000000, 0.9659258262890683122, 1.000000000000000000, 0.9659258262890683122, 1.000000000000000000, 0.9659258262890683122, 1.000000000000000000, 0.9659258262890683122, 1.000000000000000000, 0.9659258262890683122, 1.000000000000000000, 0.9659258262890683122, 1.000000000000000000, 0.9659258262890683122, 1.000000000000000000, 0.9659258262890683122, 1.000000000000000000, 0.9659258262890683122, 1.000000000000000000, 0.9659258262890683122, 1.000000000000000000, 0.9659258262890683122, 1.000000000000000000, 0.9659258262890683122, 1.000000000000000000, 0.9659258262890683122, 1.000000000000000000, 0.9659258262890683122, 1.000000000000000000, 0.9659258262890683122, 1.000000000000000000, 0.9659258262890683122, 1.000000000000000000, 0.9659258262890683122, 1.000000000000000000, 0.9659258262890683122, 1.000000000000000000, 0.9659258262890683122, 1.000000000000000000, 0.9659258262890683122, 1.000000000000000000, 0.9659258262890683122, 1.000000000000000000, 0.9659258262890683122, 1.000000000000000000, 0.9659258262890683122, 1.000000000000000000, 0.9659258262890683122, 1.000000000000000000, 0.9659258262890683122, 1.000000000000000000, 0.9659258262890683122, 1.000000000000000000, 0.9659258262890683122, 1.000000000000000000, 0.9659258262890683122, 1.000000000000000000, 0.9659258262890683122, 1.000000000000000000, 0.9659258262890683122, 1.000000000000000000, 0.9659258262890683122, 1.000000000000000000, 0.9659258262890683122, 1.000000000000000000, 0.9659258262890683122, 1.000000000000000000, 0.9659258262890683122, 1.000000000000000000, 0.9659258262890683122, 1.000000000000000000, 0.9659258262890683122, 1.000000000000000000, 0.9659258262890683122, 1.000000000000000000, 0.9659258262890683122, 1.000000000000000000, 0.9659258262890683122, 1.000000000000000000, 0.9659258262890683122, 1.000000000000000000, 0.9659258262890683122, 1.000000000000000000, 0.9659258262890683122, 1.000000000000000000, 0.9659258262890683122, 1.000000000000000000, 0.9659258262890683122, 1.000000000000000000, 0.9659258262890683122, 1.000000000000000000, 0.9659258262890683122, 1.000000000000000000, 0.9659258262890683122, 1.000000000000000000, 0.9659258262890683122, 1.000000000000000000, 0.9659258262890683122, 1.000000000000000000, 0.9659258262890683122, 1.000000000000000000, 0.9659258262890683122, 1.000000000000000000, 0.9659258262890683122, 1.000000000000000000, 0.9659258262890683122, 1.000000000000000000, 0.9659258262890683122, 1.000000000000000000, 0.9659258262890683122, 1.000000000000000000, 0.9659258262890683122, 1.000000000000000000, 0.9659258262890683122, 1.000000000000000000, 0.9659258262890683122, 1.000000000000000000, 0.9659258262890683122, 1.000000000000000000, 0.9659258262890683122, 1.000000000000000000, 0.9659258262890683122, 1.000000000000000000, 0.9659258262890683122, 1.000000000000000000, 0.9659258262890683122, 1.000000000000000000, 0.9659258262890683122, 1.000000000000000000, 0.9659258262890683122, 1.000000000000000000, 0.9659258262890683122, 1.000000000000000000, 0.9659258262890683122, 1.000000000000000000, 0.9659258262890683122, 1.000000000000000000, 0.9659258262890683122, 1.000000000000000000, 0.9659258262890683122, 1.000000000000000000, 0.9659258262890683122, 1.000000000000000000, 0.9659258262890683122, 1.000000000000000000, 0.9659258262890683122, 1.000000000000000000, 0.9659258262890683122, 1.000000000000000000, 0.9659258262890683122, 1.000000000000000000, 0.9659258262890683122, 1.000000000000000000, 0.9659258262890683122, 1.000000000000000000, 0.9659258262890683122, 1.000000000000000000, 0.9659258262890683122, 1.000000000000000000, 0.9659258262890683122, 1.000000000000000000, 0.9659258262890683122, 1.000000000000000000, 0.9659258262890683122, 1.000000000000000000, 0.9659258262890683122, 1.000000000000000000, 0.9659258262890683122, 1.000000000000000000, 0.9659258262890683122, 1.000000000000000000, 0.9659258262890683122, 1.000000000000000000, 0.9659258262890683122, 1.000000000000000000, 0.9659258262890683122, 1.000000000000000000, 0.9659258262890683122, 1.000000000000000000, 0.9659258262890683122, 1.000000000000000000, 0.9659258262890683122, 1.000000000000000000, 0.9659258262890683122, 1.000000000000000000, 0.9659258262890683122, 1.000000000000000000, 0.9659258262890683122, 1.000000000000000000, 0.9659258262890683122, 1.000000000000000000, 0.9659258262890683122, 1.000000000000000000, 0.9659258262890683122, 1.000000000000000000, 0.9659258262890683122, 1.000000000000000000, 0.9659258262890683122, 1.000000000000000000, 0.9659258262890683122, 1.000000000000000000, 0.9659258262890683122, 1.000000000000000000, 0.9659258262890683122, 1.000000000000000000, 0.9659258262890683122, 1.000000000000000000, 0.9659258262890683122, 1.000000000000000000, 0.9659258262890683122, 1.000000000000000000, 0.9659258262890683122, 1.000000000000000000, 0.9659258262890683122, 1.000000000000000000, 0.9659258262890683122, 1.000000000000000000, 0.9659258262890683122, 1.000000000000000000, 0.9659258262890683122, 1.000000000000000000, 0.9659258262890683122, 1.000000000000000000, 0.9659258262890683122, 1.000000000000000000, 0.9659258262890683122, 1.000000000000000000, 0.9659258262890683122, 1.000000000000000000, 0.9659258262890683122, 1.000000000000000000, 0.9659258262890683122, 1.000000000000000000, 0.9659258262890683122, 1.000000000000000000, 0.9659258262890683122, 1.000000000000000000, 0.9659258262890683122, 1.000000000000000000, 0.9659258262890683122, 1.000000000000000000, 0.9659258262890683122, 1.000000000000000000, 0.9659258262890683122, 1.000000000000000000, 0.9659258262890683122, 1.000000000000000000, 0.9659258262890683122, 1.000000000000000000, 0.9659258262890683122, 1.000000000000000000, 0.9659258262890683122, 1.000000000000000000, 0.9659258262890683122, 1.000000000000000000, 0.9659258262890683122, 1.000000000000000000, 0.9659258262890683122, 1.000000000000000000, 0.9659258262890683122, 1.000000000000000000, 0.9659258262890683122, 1.000000000000000000, 0.9659258262890683122, 1.000000000000000000, 0.9659258262890683122, 1.000000000000000000, 0.9659258262890683122, 1.000000000000000000, 0.9659258262890683122, 1.000000000000000000, 0.9659258262890683122, 1.000000000000000000, 0.9659258262890683122, 1.000000000000000000, 0.9659258262890683122, 1.000000000000000000, 0.9659258262890683122, 1.000000000000000000, 0.9659258262890683122, 1.000000000000000000, 0.9659258262890683122, 1.000000000000000000, 0.9659258262890683122, 1.000000000000000000, 0.9659258262890683122, 1.000000000000000000, 0.9659258262890683122, 1.000000000000000000, 0.9659258262890683122, 1.000000000000000000, 0.9659258262890683122, 1.000000000000000000, 0.9659258262890683122, 1.000000000000000000, 0.9659258262890683122, 1.000000000000000000, 0.9659258262890683122, 1.000000000000000000, 0.9659258262890683122, 1.000000000000000000, 0.9659258262890683122, 1.000000000000000000, 0.9659258262890683122, 1.000000000000000000, 0.9659258262890683122, 1.000000000000000000, 0.9659258262890683122, 1.000000000000000000, 0.9659258262890683122, 1.000000000000000000, 0.9659258262890683122, 1.000000000000000000, 0.9659258262890683122, 1.000000000000000000, 0.9659258262890683122, 1.000000000000000000, 0.9659258262890683122, 1.000000000000000000, 0.9659258262890683122, 1.000000000000000000, 0.9659258262890683122, 1.000000000000000000, 0.9659258262890683122, 1.000000000000000000, 0.9659258262890683122, 1.000000000000000000, 0.9659258262890683122, 1.000000000000000000, 0.9659258262890683122, 1.000000000000000000, 0.9659258262890683122, 1.000000000000000000, 0.9659258262890683122, 1.000000000000000000, 0.9659258262890683122, 1.000000000000000000, 0.9659258262890683122, 1.000000000000000000, 0.9659258262890683122, 1.000000000000000000, 0.9659258262890683122, 1.000000000000000000, 0.9659258262890683122, 1.000000000000000000, 0.9659258262890683122, 1.000000000000000000, 0.9659258262890683122, 1.000000000000000000, 0.9659258262890683122, 1.000000000000000000, 0.9659258262890683122, 1.000000000000000000, 0.9659258262890683122, 1.000000000000000000, 0.9659258262890683122, 1.000000000000000000, 0.9659258262890683122, 1.000000000000000000, 0.9659258262890683122, 1.000000000000000000, 0.9659258262890683122, 1.000000000000000000, 0.9659258262890683122, 1.000000000000000000, 0.9659258262890683122, 1.000000000000000000, 0.9659258262890683122, 1.000000000000000000, 0.9659258262890683122, 1.000000000000000000, 0.9659258262890683122, 1.000000000000000000, 0.9659258262890683122, 1.000000000000000000, 0.9659258262890683122, 1.000000000000000000, 0.9659258262890683122, 1.000000000000000000, 0.9659258262890683122, 1.000000000000000000, 0.9659258262890683122, 1.000000000000000000, 0.9659258262890683122, 1.000000000000000000, 0.9659258262890683122, 1.000000000000000000, 0.9659258262890683122, 1.000000000000000000, 0.9659258262890683122, 1.000000000000000000, 0.9659258262890683122, 1.000000000000000000, 0.9659258262890683122, 1.000000000000000000, 0.9659258262890683122, 1.000000000000000000, 0.9659258262890683122, 1.000000000000000000, 0.9659258262890683122, 1.000000000000000000, 0.9659258262890683122, 1.000000000000000000, 0.9659258262890683122, 1.000000000000000000, 0.9659258262890683122, 1.000000000000000000, 0.9659258262890683122, 1.000000000000000000, 0.9659258262890683122, 1.000000000000000000, 0.9659258262890683122, 1.000000000000000000, 0.9659258262890683122, 1.000000000000000000, 0.9659258262890683122, 1.000000000000000000, 0.9659258262890683122, 1.000000000000000000, 0.9659258262890683122, 1.000000000000000000, 0.9659258262890683122, 1.000000000000000000, 0.9659258262890683122, 1.000000000000000000),
 ( 0.3333333333333333703, 0.3219752754296894559, 0.3333333333333333703, 0.3219752754296894559, 0.3333333333333333703, 0.3219752754296894559, 0.3333333333333333703, 0.3219752754296894559, 0.3333333333333333703, 0.3219752754296894559, 0.3333333333333333703, 0.3219752754296894559, 0.3333333333333333703, 0.3219752754296894559, 0.3333333333333333703, 0.3219752754296894559, 0.3333333333333333703, 0.3219752754296894559, 0.3333333333333333703, 0.3219752754296894559, 0.3333333333333333703, 0.3219752754296894559, 0.3333333333333333703, 0.3219752754296894559, 0.3333333333333333703, 0.3219752754296894559, 0.3333333333333333703, 0.3219752754296894559, 0.3333333333333333703, 0.3219752754296894559, 0.3333333333333333703, 0.3219752754296894559, 0.3333333333333333703, 0.3219752754296894559, 0.3333333333333333703, 0.3219752754296894559, 0.3333333333333333703, 0.3219752754296894559, 0.3333333333333333703, 0.3219752754296894559, 0.3333333333333333703, 0.3219752754296894559, 0.3333333333333333703, 0.3219752754296894559, 0.3333333333333333703, 0.3219752754296894559, 0.3333333333333333703, 0.3219752754296894559, 0.3333333333333333703, 0.3219752754296894559, 0.3333333333333333703, 0.3219752754296894559, 0.3333333333333333703, 0.3219752754296894559, 0.3333333333333333703, 0.3219752754296894559, 0.3333333333333333703, 0.3219752754296894559, 0.3333333333333333703, 0.3219752754296894559, 0.3333333333333333703, 0.3219752754296894559, 0.3333333333333333703, 0.3219752754296894559, 0.3333333333333333703, 0.3219752754296894559, 0.3333333333333333703, 0.3219752754296894559, 0.3333333333333333703, 0.3219752754296894559, 0.3333333333333333703, 0.3219752754296894559, 0.3333333333333333703, 0.3219752754296894559, 0.3333333333333333703, 0.3219752754296894559, 0.3333333333333333703, 0.3219752754296894559, 0.3333333333333333703, 0.3219752754296894559, 0.3333333333333333703, 0.3219752754296894559, 0.3333333333333333703, 0.3219752754296894559, 0.3333333333333333703, 0.3219752754296894559, 0.3333333333333333703, 0.3219752754296894559, 0.3333333333333333703, 0.3219752754296894559, 0.3333333333333333703, 0.3219752754296894559, 0.3333333333333333703, 0.3219752754296894559, 0.3333333333333333703, 0.3219752754296894559, 0.3333333333333333703, 0.3219752754296894559, 0.3333333333333333703, 0.3219752754296894559, 0.3333333333333333703, 0.3219752754296894559, 0.3333333333333333703, 0.3219752754296894559, 0.3333333333333333703, 0.3219752754296894559, 0.3333333333333333703, 0.3219752754296894559, 0.3333333333333333703, 0.3219752754296894559, 0.3333333333333333703, 0.3219752754296894559, 0.3333333333333333703, 0.3219752754296894559, 0.3333333333333333703, 0.3219752754296894559, 0.3333333333333333703, 0.3219752754296894559, 0.3333333333333333703, 0.3219752754296894559, 0.3333333333333333703, 0.3219752754296894559, 0.3333333333333333703, 0.3219752754296894559, 0.3333333333333333703, 0.3219752754296894559, 0.3333333333333333703, 0.3219752754296894559, 0.3333333333333333703, 0.3219752754296894559, 0.3333333333333333703, 0.3219752754296894559, 0.3333333333333333703, 0.3219752754296894559, 0.3333333333333333703, 0.3219752754296894559, 0.3333333333333333703, 0.3219752754296894559, 0.3333333333333333703, 0.3219752754296894559, 0.3333333333333333703, 0.3219752754296894559, 0.3333333333333333703, 0.3219752754296894559, 0.3333333333333333703, 0.3219752754296894559, 0.3333333333333333703, 0.3219752754296894559, 0.3333333333333333703, 0.3219752754296894559, 0.3333333333333333703, 0.3219752754296894559, 0.3333333333333333703, 0.3219752754296894559, 0.3333333333333333703, 0.3219752754296894559, 0.3333333333333333703, 0.3219752754296894559, 0.3333333333333333703, 0.3219752754296894559, 0.3333333333333333703, 0.3219752754296894559, 0.3333333333333333703, 0.3219752754296894559, 0.3333333333333333703, 0.3219752754296894559, 0.3333333333333333703, 0.3219752754296894559, 0.3333333333333333703, 0.3219752754296894559, 0.3333333333333333703, 0.3219752754296894559, 0.3333333333333333703, 0.3219752754296894559, 0.3333333333333333703, 0.3219752754296894559, 0.3333333333333333703, 0.3219752754296894559, 0.3333333333333333703, 0.3219752754296894559, 0.3333333333333333703, 0.3219752754296894559, 0.3333333333333333703, 0.3219752754296894559, 0.3333333333333333703, 0.3219752754296894559, 0.3333333333333333703, 0.3219752754296894559, 0.3333333333333333703, 0.3219752754296894559, 0.3333333333333333703, 0.3219752754296894559, 0.3333333333333333703, 0.3219752754296894559, 0.3333333333333333703, 0.3219752754296894559, 0.3333333333333333703, 0.3219752754296894559, 0.3333333333333333703, 0.3219752754296894559, 0.3333333333333333703, 0.3219752754296894559, 0.3333333333333333703, 0.3219752754296894559, 0.3333333333333333703, 0.3219752754296894559, 0.3333333333333333703, 0.3219752754296894559, 0.3333333333333333703, 0.3219752754296894559, 0.3333333333333333703, 0.3219752754296894559, 0.3333333333333333703, 0.3219752754296894559, 0.3333333333333333703, 0.3219752754296894559, 0.3333333333333333703, 0.3219752754296894559, 0.3333333333333333703, 0.3219752754296894559, 0.3333333333333333703, 0.3219752754296894559, 0.3333333333333333703, 0.3219752754296894559, 0.3333333333333333703, 0.3219752754296894559, 0.3333333333333333703, 0.3219752754296894559, 0.3333333333333333703, 0.3219752754296894559, 0.3333333333333333703, 0.3219752754296894559, 0.3333333333333333703, 0.3219752754296894559, 0.3333333333333333703, 0.3219752754296894559, 0.3333333333333333703, 0.3219752754296894559, 0.3333333333333333703, 0.3219752754296894559, 0.3333333333333333703, 0.3219752754296894559, 0.3333333333333333703, 0.3219752754296894559, 0.3333333333333333703, 0.3219752754296894559, 0.3333333333333333703, 0.3219752754296894559, 0.3333333333333333703, 0.3219752754296894559, 0.3333333333333333703, 0.3219752754296894559, 0.3333333333333333703, 0.3219752754296894559, 0.3333333333333333703, 0.3219752754296894559, 0.3333333333333333703, 0.3219752754296894559, 0.3333333333333333703, 0.3219752754296894559, 0.3333333333333333703, 0.3219752754296894559, 0.3333333333333333703, 0.3219752754296894559, 0.3333333333333333703, 0.3219752754296894559, 0.3333333333333333703, 0.3219752754296894559, 0.3333333333333333703, 0.3219752754296894559, 0.3333333333333333703, 0.3219752754296894559, 0.3333333333333333703, 0.3219752754296894559, 0.3333333333333333703, 0.3219752754296894559, 0.3333333333333333703, 0.3219752754296894559, 0.3333333333333333703, 0.3219752754296894559, 0.3333333333333333703, 0.3219752754296894559, 0.3333333333333333703, 0.3219752754296894559, 0.3333333333333333703, 0.3219752754296894559, 0.3333333333333333703, 0.3219752754296894559, 0.3333333333333333703, 0.3219752754296894559, 0.3333333333333333703, 0.3219752754296894559, 0.3333333333333333703, 0.3219752754296894559, 0.3333333333333333703, 0.3219752754296894559, 0.3333333333333333703, 0.3219752754296894559, 0.3333333333333333703, 0.3219752754296894559, 0.3333333333333333703, 0.3219752754296894559, 0.3333333333333333703, 0.3219752754296894559, 0.3333333333333333703, 0.3219752754296894559, 0.3333333333333333703, 0.3219752754296894559, 0.3333333333333333703, 0.3219752754296894559, 0.3333333333333333703, 0.3219752754296894559, 0.3333333333333333703, 0.3219752754296894559, 0.3333333333333333703, 0.3219752754296894559, 0.3333333333333333703, 0.3219752754296894559, 0.3333333333333333703, 0.3219752754296894559, 0.3333333333333333703, 0.3219752754296894559, 0.3333333333333333703, 0.3219752754296894559, 0.3333333333333333703, 0.3219752754296894559, 0.3333333333333333703, 0.3219752754296894559, 0.3333333333333333703, 0.3219752754296894559, 0.3333333333333333703, 0.3219752754296894559, 0.3333333333333333703, 0.3219752754296894559, 0.3333333333333333703, 0.3219752754296894559, 0.3333333333333333703, 0.3219752754296894559, 0.3333333333333333703, 0.3219752754296894559, 0.3333333333333333703, 0.3219752754296894559, 0.3333333333333333703, 0.3219752754296894559, 0.3333333333333333703, 0.3219752754296894559, 0.3333333333333333703, 0.3219752754296894559, 0.3333333333333333703, 0.3219752754296894559, 0.3333333333333333703, 0.3219752754296894559, 0.3333333333333333703, 0.3219752754296894559, 0.3333333333333333703, 0.3219752754296894559, 0.3333333333333333703, 0.3219752754296894559, 0.3333333333333333703, 0.3219752754296894559, 0.3333333333333333703, 0.3219752754296894559, 0.3333333333333333703, 0.3219752754296894559, 0.3333333333333333703, 0.3219752754296894559, 0.3333333333333333703, 0.3219752754296894559, 0.3333333333333333703, 0.3219752754296894559, 0.3333333333333333703, 0.3219752754296894559, 0.3333333333333333703, 0.3219752754296894559, 0.3333333333333333703, 0.3219752754296894559, 0.3333333333333333703, 0.3219752754296894559, 0.3333333333333333703, 0.3219752754296894559, 0.3333333333333333703, 0.3219752754296894559, 0.3333333333333333703, 0.3219752754296894559, 0.3333333333333333703, 0.3219752754296894559, 0.3333333333333333703, 0.3219752754296894559, 0.3333333333333333703, 0.3219752754296894559, 0.3333333333333333703, 0.3219752754296894559, 0.3333333333333333703, 0.3219752754296894559, 0.3333333333333333703, 0.3219752754296894559, 0.3333333333333333703, 0.3219752754296894559, 0.3333333333333333703, 0.3219752754296894559, 0.3333333333333333703, 0.3219752754296894559, 0.3333333333333333703, 0.3219752754296894559, 0.3333333333333333703, 0.3219752754296894559, 0.3333333333333333703, 0.3219752754296894559, 0.3333333333333333703, 0.3219752754296894559, 0.3333333333333333703, 0.3219752754296894559, 0.3333333333333333703, 0.3219752754296894559, 0.3333333333333333703, 0.3219752754296894559, 0.3333333333333333703, 0.3219752754296894559, 0.3333333333333333703, 0.3219752754296894559, 0.3333333333333333703, 0.3219752754296894559, 0.3333333333333333703, 0.3219752754296894559, 0.3333333333333333703, 0.3219752754296894559, 0.3333333333333333703, 0.3219752754296894559, 0.3333333333333333703, 0.3219752754296894559, 0.3333333333333333703, 0.3219752754296894559, 0.3333333333333333703, 0.3219752754296894559, 0.3333333333333333703, 0.3219752754296894559, 0.3333333333333333703, 0.3219752754296894559, 0.3333333333333333703, 0.3219752754296894559, 0.3333333333333333703, 0.3219752754296894559, 0.3333333333333333703, 0.3219752754296894559, 0.3333333333333333703, 0.3219752754296894559, 0.3333333333333333703, 0.3219752754296894559, 0.3333333333333333703, 0.3219752754296894559, 0.3333333333333333703, 0.3219752754296894559, 0.3333333333333333703, 0.3219752754296894559, 0.3333333333333333703, 0.3219752754296894559, 0.3333333333333333703),
 ( 0.3333333333333333703, 0.3219752754296894559, 0.3333333333333333703, 0.3219752754296894559, 0.3333333333333333703, 0.3219752754296894559, 0.3333333333333333703, 0.3219752754296894559, 0.3333333333333333703, 0.3219752754296894559, 0.3333333333333333703, 0.3219752754296894559, 0.3333333333333333703, 0.3219752754296894559, 0.3333333333333333703, 0.3219752754296894559, 0.3333333333333333703, 0.3219752754296894559, 0.3333333333333333703, 0.3219752754296894559, 0.3333333333333333703, 0.3219752754296894559, 0.3333333333333333703, 0.3219752754296894559, 0.3333333333333333703, 0.3219752754296894559, 0.3333333333333333703, 0.3219752754296894559, 0.3333333333333333703, 0.3219752754296894559, 0.3333333333333333703, 0.3219752754296894559, 0.3333333333333333703, 0.3219752754296894559, 0.3333333333333333703, 0.3219752754296894559, 0.3333333333333333703, 0.3219752754296894559, 0.3333333333333333703, 0.3219752754296894559, 0.3333333333333333703, 0.3219752754296894559, 0.3333333333333333703, 0.3219752754296894559, 0.3333333333333333703, 0.3219752754296894559, 0.3333333333333333703, 0.3219752754296894559, 0.3333333333333333703, 0.3219752754296894559, 0.3333333333333333703, 0.3219752754296894559, 0.3333333333333333703, 0.3219752754296894559, 0.3333333333333333703, 0.3219752754296894559, 0.3333333333333333703, 0.3219752754296894559, 0.3333333333333333703, 0.3219752754296894559, 0.3333333333333333703, 0.3219752754296894559, 0.3333333333333333703, 0.3219752754296894559, 0.3333333333333333703, 0.3219752754296894559, 0.3333333333333333703, 0.3219752754296894559, 0.3333333333333333703, 0.3219752754296894559, 0.3333333333333333703, 0.3219752754296894559, 0.3333333333333333703, 0.3219752754296894559, 0.3333333333333333703, 0.3219752754296894559, 0.3333333333333333703, 0.3219752754296894559, 0.3333333333333333703, 0.3219752754296894559, 0.3333333333333333703, 0.3219752754296894559, 0.3333333333333333703, 0.3219752754296894559, 0.3333333333333333703, 0.3219752754296894559, 0.3333333333333333703, 0.3219752754296894559, 0.3333333333333333703, 0.3219752754296894559, 0.3333333333333333703, 0.3219752754296894559, 0.3333333333333333703, 0.3219752754296894559, 0.3333333333333333703, 0.3219752754296894559, 0.3333333333333333703, 0.3219752754296894559, 0.3333333333333333703, 0.3219752754296894559, 0.3333333333333333703, 0.3219752754296894559, 0.3333333333333333703, 0.3219752754296894559, 0.3333333333333333703, 0.3219752754296894559, 0.3333333333333333703, 0.3219752754296894559, 0.3333333333333333703, 0.3219752754296894559, 0.3333333333333333703, 0.3219752754296894559, 0.3333333333333333703, 0.3219752754296894559, 0.3333333333333333703, 0.3219752754296894559, 0.3333333333333333703, 0.3219752754296894559, 0.3333333333333333703, 0.3219752754296894559, 0.3333333333333333703, 0.3219752754296894559, 0.3333333333333333703, 0.3219752754296894559, 0.3333333333333333703, 0.3219752754296894559, 0.3333333333333333703, 0.3219752754296894559, 0.3333333333333333703, 0.3219752754296894559, 0.3333333333333333703, 0.3219752754296894559, 0.3333333333333333703, 0.3219752754296894559, 0.3333333333333333703, 0.3219752754296894559, 0.3333333333333333703, 0.3219752754296894559, 0.3333333333333333703, 0.3219752754296894559, 0.3333333333333333703, 0.3219752754296894559, 0.3333333333333333703, 0.3219752754296894559, 0.3333333333333333703, 0.3219752754296894559, 0.3333333333333333703, 0.3219752754296894559, 0.3333333333333333703, 0.3219752754296894559, 0.3333333333333333703, 0.3219752754296894559, 0.3333333333333333703, 0.3219752754296894559, 0.3333333333333333703, 0.3219752754296894559, 0.3333333333333333703, 0.3219752754296894559, 0.3333333333333333703, 0.3219752754296894559, 0.3333333333333333703, 0.3219752754296894559, 0.3333333333333333703, 0.3219752754296894559, 0.3333333333333333703, 0.3219752754296894559, 0.3333333333333333703, 0.3219752754296894559, 0.3333333333333333703, 0.3219752754296894559, 0.3333333333333333703, 0.3219752754296894559, 0.3333333333333333703, 0.3219752754296894559, 0.3333333333333333703, 0.3219752754296894559, 0.3333333333333333703, 0.3219752754296894559, 0.3333333333333333703, 0.3219752754296894559, 0.3333333333333333703, 0.3219752754296894559, 0.3333333333333333703, 0.3219752754296894559, 0.3333333333333333703, 0.3219752754296894559, 0.3333333333333333703, 0.3219752754296894559, 0.3333333333333333703, 0.3219752754296894559, 0.3333333333333333703, 0.3219752754296894559, 0.3333333333333333703, 0.3219752754296894559, 0.3333333333333333703, 0.3219752754296894559, 0.3333333333333333703, 0.3219752754296894559, 0.3333333333333333703, 0.3219752754296894559, 0.3333333333333333703, 0.3219752754296894559, 0.3333333333333333703, 0.3219752754296894559, 0.3333333333333333703, 0.3219752754296894559, 0.3333333333333333703, 0.3219752754296894559, 0.3333333333333333703, 0.3219752754296894559, 0.3333333333333333703, 0.3219752754296894559, 0.3333333333333333703, 0.3219752754296894559, 0.3333333333333333703, 0.3219752754296894559, 0.3333333333333333703, 0.3219752754296894559, 0.3333333333333333703, 0.3219752754296894559, 0.3333333333333333703, 0.3219752754296894559, 0.3333333333333333703, 0.3219752754296894559, 0.3333333333333333703, 0.3219752754296894559, 0.3333333333333333703, 0.3219752754296894559, 0.3333333333333333703, 0.3219752754296894559, 0.3333333333333333703, 0.3219752754296894559, 0.3333333333333333703, 0.3219752754296894559, 0.3333333333333333703, 0.3219752754296894559, 0.3333333333333333703, 0.3219752754296894559, 0.3333333333333333703, 0.3219752754296894559, 0.3333333333333333703, 0.3219752754296894559, 0.3333333333333333703, 0.3219752754296894559, 0.3333333333333333703, 0.3219752754296894559, 0.3333333333333333703, 0.3219752754296894559, 0.3333333333333333703, 0.3219752754296894559, 0.3333333333333333703, 0.3219752754296894559, 0.3333333333333333703, 0.3219752754296894559, 0.3333333333333333703, 0.3219752754296894559, 0.3333333333333333703, 0.3219752754296894559, 0.3333333333333333703, 0.3219752754296894559, 0.3333333333333333703, 0.3219752754296894559, 0.3333333333333333703, 0.3219752754296894559, 0.3333333333333333703, 0.3219752754296894559, 0.3333333333333333703, 0.3219752754296894559, 0.3333333333333333703, 0.3219752754296894559, 0.3333333333333333703, 0.3219752754296894559, 0.3333333333333333703, 0.3219752754296894559, 0.3333333333333333703, 0.3219752754296894559, 0.3333333333333333703, 0.3219752754296894559, 0.3333333333333333703, 0.3219752754296894559, 0.3333333333333333703, 0.3219752754296894559, 0.3333333333333333703, 0.3219752754296894559, 0.3333333333333333703, 0.3219752754296894559, 0.3333333333333333703, 0.3219752754296894559, 0.3333333333333333703, 0.3219752754296894559, 0.3333333333333333703, 0.3219752754296894559, 0.3333333333333333703, 0.3219752754296894559, 0.3333333333333333703, 0.3219752754296894559, 0.3333333333333333703, 0.3219752754296894559, 0.3333333333333333703, 0.3219752754296894559, 0.3333333333333333703, 0.3219752754296894559, 0.3333333333333333703, 0.3219752754296894559, 0.3333333333333333703, 0.3219752754296894559, 0.3333333333333333703, 0.3219752754296894559, 0.3333333333333333703, 0.3219752754296894559, 0.3333333333333333703, 0.3219752754296894559, 0.3333333333333333703, 0.3219752754296894559, 0.3333333333333333703, 0.3219752754296894559, 0.3333333333333333703, 0.3219752754296894559, 0.3333333333333333703, 0.3219752754296894559, 0.3333333333333333703, 0.3219752754296894559, 0.3333333333333333703, 0.3219752754296894559, 0.3333333333333333703, 0.3219752754296894559, 0.3333333333333333703, 0.3219752754296894559, 0.3333333333333333703, 0.3219752754296894559, 0.3333333333333333703, 0.3219752754296894559, 0.3333333333333333703, 0.3219752754296894559, 0.3333333333333333703, 0.3219752754296894559, 0.3333333333333333703, 0.3219752754296894559, 0.3333333333333333703, 0.3219752754296894559, 0.3333333333333333703, 0.3219752754296894559, 0.3333333333333333703, 0.3219752754296894559, 0.3333333333333333703, 0.3219752754296894559, 0.3333333333333333703, 0.3219752754296894559, 0.3333333333333333703, 0.3219752754296894559, 0.3333333333333333703, 0.3219752754296894559, 0.3333333333333333703, 0.3219752754296894559, 0.3333333333333333703, 0.3219752754296894559, 0.3333333333333333703, 0.3219752754296894559, 0.3333333333333333703, 0.3219752754296894559, 0.3333333333333333703, 0.3219752754296894559, 0.3333333333333333703, 0.3219752754296894559, 0.3333333333333333703, 0.3219752754296894559, 0.3333333333333333703, 0.3219752754296894559, 0.3333333333333333703, 0.3219752754296894559, 0.3333333333333333703, 0.3219752754296894559, 0.3333333333333333703, 0.3219752754296894559, 0.3333333333333333703, 0.3219752754296894559, 0.3333333333333333703, 0.3219752754296894559, 0.3333333333333333703, 0.3219752754296894559, 0.3333333333333333703, 0.3219752754296894559, 0.3333333333333333703, 0.3219752754296894559, 0.3333333333333333703, 0.3219752754296894559, 0.3333333333333333703, 0.3219752754296894559, 0.3333333333333333703, 0.3219752754296894559, 0.3333333333333333703, 0.3219752754296894559, 0.3333333333333333703, 0.3219752754296894559, 0.3333333333333333703, 0.3219752754296894559, 0.3333333333333333703, 0.3219752754296894559, 0.3333333333333333703, 0.3219752754296894559, 0.3333333333333333703, 0.3219752754296894559, 0.3333333333333333703, 0.3219752754296894559, 0.3333333333333333703, 0.3219752754296894559, 0.3333333333333333703, 0.3219752754296894559, 0.3333333333333333703, 0.3219752754296894559, 0.3333333333333333703, 0.3219752754296894559, 0.3333333333333333703, 0.3219752754296894559, 0.3333333333333333703, 0.3219752754296894559, 0.3333333333333333703, 0.3219752754296894559, 0.3333333333333333703, 0.3219752754296894559, 0.3333333333333333703, 0.3219752754296894559, 0.3333333333333333703, 0.3219752754296894559, 0.3333333333333333703, 0.3219752754296894559, 0.3333333333333333703, 0.3219752754296894559, 0.3333333333333333703, 0.3219752754296894559, 0.3333333333333333703, 0.3219752754296894559, 0.3333333333333333703, 0.3219752754296894559, 0.3333333333333333703, 0.3219752754296894559, 0.3333333333333333703, 0.3219752754296894559, 0.3333333333333333703, 0.3219752754296894559, 0.3333333333333333703, 0.3219752754296894559, 0.3333333333333333703, 0.3219752754296894559, 0.3333333333333333703, 0.3219752754296894559, 0.3333333333333333703, 0.3219752754296894559, 0.3333333333333333703, 0.3219752754296894559, 0.3333333333333333703, 0.3219752754296894559, 0.3333333333333333703, 0.3219752754296894559, 0.3333333333333333703, 0.3219752754296894559, 0.3333333333333333703),
 ( 1.000000000000000000, 0.9659258262890683122, 1.000000000000000000, 0.9659258262890683122, 1.000000000000000000, 0.9659258262890683122, 1.000000000000000000, 0.9659258262890683122, 1.000000000000000000, 0.9659258262890683122, 1.000000000000000000, 0.9659258262890683122, 1.000000000000000000, 0.9659258262890683122, 1.000000000000000000, 0.9659258262890683122, 1.000000000000000000, 0.9659258262890683122, 1.000000000000000000, 0.9659258262890683122, 1.000000000000000000, 0.9659258262890683122, 1.000000000000000000, 0.9659258262890683122, 1.000000000000000000, 0.9659258262890683122, 1.000000000000000000, 0.9659258262890683122, 1.000000000000000000, 0.9659258262890683122, 1.000000000000000000, 0.9659258262890683122, 1.000000000000000000, 0.9659258262890683122, 1.000000000000000000, 0.9659258262890683122, 1.000000000000000000, 0.9659258262890683122, 1.000000000000000000, 0.9659258262890683122, 1.000000000000000000, 0.9659258262890683122, 1.000000000000000000, 0.9659258262890683122, 1.000000000000000000, 0.9659258262890683122, 1.000000000000000000, 0.9659258262890683122, 1.000000000000000000, 0.9659258262890683122, 1.000000000000000000, 0.9659258262890683122, 1.000000000000000000, 0.9659258262890683122, 1.000000000000000000, 0.9659258262890683122, 1.000000000000000000, 0.9659258262890683122, 1.000000000000000000, 0.9659258262890683122, 1.000000000000000000, 0.9659258262890683122, 1.000000000000000000, 0.9659258262890683122, 1.000000000000000000, 0.9659258262890683122, 1.000000000000000000, 0.9659258262890683122, 1.000000000000000000, 0.9659258262890683122, 1.000000000000000000, 0.9659258262890683122, 1.000000000000000000, 0.9659258262890683122, 1.000000000000000000, 0.9659258262890683122, 1.000000000000000000, 0.9659258262890683122, 1.000000000000000000, 0.9659258262890683122, 1.000000000000000000, 0.9659258262890683122, 1.000000000000000000, 0.9659258262890683122, 1.000000000000000000, 0.9659258262890683122, 1.000000000000000000, 0.9659258262890683122, 1.000000000000000000, 0.9659258262890683122, 1.000000000000000000, 0.9659258262890683122, 1.000000000000000000, 0.9659258262890683122, 1.000000000000000000, 0.9659258262890683122, 1.000000000000000000, 0.9659258262890683122, 1.000000000000000000, 0.9659258262890683122, 1.000000000000000000, 0.9659258262890683122, 1.000000000000000000, 0.9659258262890683122, 1.000000000000000000, 0.9659258262890683122, 1.000000000000000000, 0.9659258262890683122, 1.000000000000000000, 0.9659258262890683122, 1.000000000000000000, 0.9659258262890683122, 1.000000000000000000, 0.9659258262890683122, 1.000000000000000000, 0.9659258262890683122, 1.000000000000000000, 0.9659258262890683122, 1.000000000000000000, 0.9659258262890683122, 1.000000000000000000, 0.9659258262890683122, 1.000000000000000000, 0.9659258262890683122, 1.000000000000000000, 0.9659258262890683122, 1.000000000000000000, 0.9659258262890683122, 1.000000000000000000, 0.9659258262890683122, 1.000000000000000000, 0.9659258262890683122, 1.000000000000000000, 0.9659258262890683122, 1.000000000000000000, 0.9659258262890683122, 1.000000000000000000, 0.9659258262890683122, 1.000000000000000000, 0.9659258262890683122, 1.000000000000000000, 0.9659258262890683122, 1.000000000000000000, 0.9659258262890683122, 1.000000000000000000, 0.9659258262890683122, 1.000000000000000000, 0.9659258262890683122, 1.000000000000000000, 0.9659258262890683122, 1.000000000000000000, 0.9659258262890683122, 1.000000000000000000, 0.9659258262890683122, 1.000000000000000000, 0.9659258262890683122, 1.000000000000000000, 0.9659258262890683122, 1.000000000000000000, 0.9659258262890683122, 1.000000000000000000, 0.9659258262890683122, 1.000000000000000000, 0.9659258262890683122, 1.000000000000000000, 0.9659258262890683122, 1.000000000000000000, 0.9659258262890683122, 1.000000000000000000, 0.9659258262890683122, 1.000000000000000000, 0.9659258262890683122, 1.000000000000000000, 0.9659258262890683122, 1.000000000000000000, 0.9659258262890683122, 1.000000000000000000, 0.9659258262890683122, 1.000000000000000000, 0.9659258262890683122, 1.000000000000000000, 0.9659258262890683122, 1.000000000000000000, 0.9659258262890683122, 1.000000000000000000, 0.9659258262890683122, 1.000000000000000000, 0.9659258262890683122, 1.000000000000000000, 0.9659258262890683122, 1.000000000000000000, 0.9659258262890683122, 1.000000000000000000, 0.9659258262890683122, 1.000000000000000000, 0.9659258262890683122, 1.000000000000000000, 0.9659258262890683122, 1.000000000000000000, 0.9659258262890683122, 1.000000000000000000, 0.9659258262890683122, 1.000000000000000000, 0.9659258262890683122, 1.000000000000000000, 0.9659258262890683122, 1.000000000000000000, 0.9659258262890683122, 1.000000000000000000, 0.9659258262890683122, 1.000000000000000000, 0.9659258262890683122, 1.000000000000000000, 0.9659258262890683122, 1.000000000000000000, 0.9659258262890683122, 1.000000000000000000, 0.9659258262890683122, 1.000000000000000000, 0.9659258262890683122, 1.000000000000000000, 0.9659258262890683122, 1.000000000000000000, 0.9659258262890683122, 1.000000000000000000, 0.9659258262890683122, 1.000000000000000000, 0.9659258262890683122, 1.000000000000000000, 0.9659258262890683122, 1.000000000000000000, 0.9659258262890683122, 1.000000000000000000, 0.9659258262890683122, 1.000000000000000000, 0.9659258262890683122, 1.000000000000000000, 0.9659258262890683122, 1.000000000000000000, 0.9659258262890683122, 1.000000000000000000, 0.9659258262890683122, 1.000000000000000000, 0.9659258262890683122, 1.000000000000000000, 0.9659258262890683122, 1.000000000000000000, 0.9659258262890683122, 1.000000000000000000, 0.9659258262890683122, 1.000000000000000000, 0.9659258262890683122, 1.000000000000000000, 0.9659258262890683122, 1.000000000000000000, 0.9659258262890683122, 1.000000000000000000, 0.9659258262890683122, 1.000000000000000000, 0.9659258262890683122, 1.000000000000000000, 0.9659258262890683122, 1.000000000000000000, 0.9659258262890683122, 1.000000000000000000, 0.9659258262890683122, 1.000000000000000000, 0.9659258262890683122, 1.000000000000000000, 0.9659258262890683122, 1.000000000000000000, 0.9659258262890683122, 1.000000000000000000, 0.9659258262890683122, 1.000000000000000000, 0.9659258262890683122, 1.000000000000000000, 0.9659258262890683122, 1.000000000000000000, 0.9659258262890683122, 1.000000000000000000, 0.9659258262890683122, 1.000000000000000000, 0.9659258262890683122, 1.000000000000000000, 0.9659258262890683122, 1.000000000000000000, 0.9659258262890683122, 1.000000000000000000, 0.9659258262890683122, 1.000000000000000000, 0.9659258262890683122, 1.000000000000000000, 0.9659258262890683122, 1.000000000000000000, 0.9659258262890683122, 1.000000000000000000, 0.9659258262890683122, 1.000000000000000000, 0.9659258262890683122, 1.000000000000000000, 0.9659258262890683122, 1.000000000000000000, 0.9659258262890683122, 1.000000000000000000, 0.9659258262890683122, 1.000000000000000000, 0.9659258262890683122, 1.000000000000000000, 0.9659258262890683122, 1.000000000000000000, 0.9659258262890683122, 1.000000000000000000, 0.9659258262890683122, 1.000000000000000000, 0.9659258262890683122, 1.000000000000000000, 0.9659258262890683122, 1.000000000000000000, 0.9659258262890683122, 1.000000000000000000, 0.9659258262890683122, 1.000000000000000000, 0.9659258262890683122, 1.000000000000000000, 0.9659258262890683122, 1.000000000000000000, 0.9659258262890683122, 1.000000000000000000, 0.9659258262890683122, 1.000000000000000000, 0.9659258262890683122, 1.000000000000000000, 0.9659258262890683122, 1.000000000000000000, 0.9659258262890683122, 1.000000000000000000, 0.9659258262890683122, 1.000000000000000000, 0.9659258262890683122, 1.000000000000000000, 0.9659258262890683122, 1.000000000000000000, 0.9659258262890683122, 1.000000000000000000, 0.9659258262890683122, 1.000000000000000000, 0.9659258262890683122, 1.000000000000000000, 0.9659258262890683122, 1.000000000000000000, 0.9659258262890683122, 1.000000000000000000, 0.9659258262890683122, 1.000000000000000000, 0.9659258262890683122, 1.000000000000000000, 0.9659258262890683122, 1.000000000000000000, 0.9659258262890683122, 1.000000000000000000, 0.9659258262890683122, 1.000000000000000000, 0.9659258262890683122, 1.000000000000000000, 0.9659258262890683122, 1.000000000000000000, 0.9659258262890683122, 1.000000000000000000, 0.9659258262890683122, 1.000000000000000000, 0.9659258262890683122, 1.000000000000000000, 0.9659258262890683122, 1.000000000000000000, 0.9659258262890683122, 1.000000000000000000, 0.9659258262890683122, 1.000000000000000000, 0.9659258262890683122, 1.000000000000000000, 0.9659258262890683122, 1.000000000000000000, 0.9659258262890683122, 1.000000000000000000, 0.9659258262890683122, 1.000000000000000000, 0.9659258262890683122, 1.000000000000000000, 0.9659258262890683122, 1.000000000000000000, 0.9659258262890683122, 1.000000000000000000, 0.9659258262890683122, 1.000000000000000000, 0.9659258262890683122, 1.000000000000000000, 0.9659258262890683122, 1.000000000000000000, 0.9659258262890683122, 1.000000000000000000, 0.9659258262890683122, 1.000000000000000000, 0.9659258262890683122, 1.000000000000000000, 0.9659258262890683122, 1.000000000000000000, 0.9659258262890683122, 1.000000000000000000, 0.9659258262890683122, 1.000000000000000000, 0.9659258262890683122, 1.000000000000000000, 0.9659258262890683122, 1.000000000000000000, 0.9659258262890683122, 1.000000000000000000, 0.9659258262890683122, 1.000000000000000000, 0.9659258262890683122, 1.000000000000000000, 0.9659258262890683122, 1.000000000000000000, 0.9659258262890683122, 1.000000000000000000, 0.9659258262890683122, 1.000000000000000000, 0.9659258262890683122, 1.000000000000000000, 0.9659258262890683122, 1.000000000000000000, 0.9659258262890683122, 1.000000000000000000, 0.9659258262890683122, 1.000000000000000000, 0.9659258262890683122, 1.000000000000000000, 0.9659258262890683122, 1.000000000000000000, 0.9659258262890683122, 1.000000000000000000, 0.9659258262890683122, 1.000000000000000000, 0.9659258262890683122, 1.000000000000000000, 0.9659258262890683122, 1.000000000000000000, 0.9659258262890683122, 1.000000000000000000, 0.9659258262890683122, 1.000000000000000000, 0.9659258262890683122, 1.000000000000000000, 0.9659258262890683122, 1.000000000000000000, 0.9659258262890683122, 1.000000000000000000),
 ( 0.3333333333333333703, 0.3219752754296894559, 0.3333333333333333703, 0.3219752754296894559, 0.3333333333333333703, 0.3219752754296894559, 0.3333333333333333703, 0.3219752754296894559, 0.3333333333333333703, 0.3219752754296894559, 0.3333333333333333703, 0.3219752754296894559, 0.3333333333333333703, 0.3219752754296894559, 0.3333333333333333703, 0.3219752754296894559, 0.3333333333333333703, 0.3219752754296894559, 0.3333333333333333703, 0.3219752754296894559, 0.3333333333333333703, 0.3219752754296894559, 0.3333333333333333703, 0.3219752754296894559, 0.3333333333333333703, 0.3219752754296894559, 0.3333333333333333703, 0.3219752754296894559, 0.3333333333333333703, 0.3219752754296894559, 0.3333333333333333703, 0.3219752754296894559, 0.3333333333333333703, 0.3219752754296894559, 0.3333333333333333703, 0.3219752754296894559, 0.3333333333333333703, 0.3219752754296894559, 0.3333333333333333703, 0.3219752754296894559, 0.3333333333333333703, 0.3219752754296894559, 0.3333333333333333703, 0.3219752754296894559, 0.3333333333333333703, 0.3219752754296894559, 0.3333333333333333703, 0.3219752754296894559, 0.3333333333333333703, 0.3219752754296894559, 0.3333333333333333703, 0.3219752754296894559, 0.3333333333333333703, 0.3219752754296894559, 0.3333333333333333703, 0.3219752754296894559, 0.3333333333333333703, 0.3219752754296894559, 0.3333333333333333703, 0.3219752754296894559, 0.3333333333333333703, 0.3219752754296894559, 0.3333333333333333703, 0.3219752754296894559, 0.3333333333333333703, 0.3219752754296894559, 0.3333333333333333703, 0.3219752754296894559, 0.3333333333333333703, 0.3219752754296894559, 0.3333333333333333703, 0.3219752754296894559, 0.3333333333333333703, 0.3219752754296894559, 0.3333333333333333703, 0.3219752754296894559, 0.3333333333333333703, 0.3219752754296894559, 0.3333333333333333703, 0.3219752754296894559, 0.3333333333333333703, 0.3219752754296894559, 0.3333333333333333703, 0.3219752754296894559, 0.3333333333333333703, 0.3219752754296894559, 0.3333333333333333703, 0.3219752754296894559, 0.3333333333333333703, 0.3219752754296894559, 0.3333333333333333703, 0.3219752754296894559, 0.3333333333333333703, 0.3219752754296894559, 0.3333333333333333703, 0.3219752754296894559, 0.3333333333333333703, 0.3219752754296894559, 0.3333333333333333703, 0.3219752754296894559, 0.3333333333333333703, 0.3219752754296894559, 0.3333333333333333703, 0.3219752754296894559, 0.3333333333333333703, 0.3219752754296894559, 0.3333333333333333703, 0.3219752754296894559, 0.3333333333333333703, 0.3219752754296894559, 0.3333333333333333703, 0.3219752754296894559, 0.3333333333333333703, 0.3219752754296894559, 0.3333333333333333703, 0.3219752754296894559, 0.3333333333333333703, 0.3219752754296894559, 0.3333333333333333703, 0.3219752754296894559, 0.3333333333333333703, 0.3219752754296894559, 0.3333333333333333703, 0.3219752754296894559, 0.3333333333333333703, 0.3219752754296894559, 0.3333333333333333703, 0.3219752754296894559, 0.3333333333333333703, 0.3219752754296894559, 0.3333333333333333703, 0.3219752754296894559, 0.3333333333333333703, 0.3219752754296894559, 0.3333333333333333703, 0.3219752754296894559, 0.3333333333333333703, 0.3219752754296894559, 0.3333333333333333703, 0.3219752754296894559, 0.3333333333333333703, 0.3219752754296894559, 0.3333333333333333703, 0.3219752754296894559, 0.3333333333333333703, 0.3219752754296894559, 0.3333333333333333703, 0.3219752754296894559, 0.3333333333333333703, 0.3219752754296894559, 0.3333333333333333703, 0.3219752754296894559, 0.3333333333333333703, 0.3219752754296894559, 0.3333333333333333703, 0.3219752754296894559, 0.3333333333333333703, 0.3219752754296894559, 0.3333333333333333703, 0.3219752754296894559, 0.3333333333333333703, 0.3219752754296894559, 0.3333333333333333703, 0.3219752754296894559, 0.3333333333333333703, 0.3219752754296894559, 0.3333333333333333703, 0.3219752754296894559, 0.3333333333333333703, 0.3219752754296894559, 0.3333333333333333703, 0.3219752754296894559, 0.3333333333333333703, 0.3219752754296894559, 0.3333333333333333703, 0.3219752754296894559, 0.3333333333333333703, 0.3219752754296894559, 0.3333333333333333703, 0.3219752754296894559, 0.3333333333333333703, 0.3219752754296894559, 0.3333333333333333703, 0.3219752754296894559, 0.3333333333333333703, 0.3219752754296894559, 0.3333333333333333703, 0.3219752754296894559, 0.3333333333333333703, 0.3219752754296894559, 0.3333333333333333703, 0.3219752754296894559, 0.3333333333333333703, 0.3219752754296894559, 0.3333333333333333703, 0.3219752754296894559, 0.3333333333333333703, 0.3219752754296894559, 0.3333333333333333703, 0.3219752754296894559, 0.3333333333333333703, 0.3219752754296894559, 0.3333333333333333703, 0.3219752754296894559, 0.3333333333333333703, 0.3219752754296894559, 0.3333333333333333703, 0.3219752754296894559, 0.3333333333333333703, 0.3219752754296894559, 0.3333333333333333703, 0.3219752754296894559, 0.3333333333333333703, 0.3219752754296894559, 0.3333333333333333703, 0.3219752754296894559, 0.3333333333333333703, 0.3219752754296894559, 0.3333333333333333703, 0.3219752754296894559, 0.3333333333333333703, 0.3219752754296894559, 0.3333333333333333703, 0.3219752754296894559, 0.3333333333333333703, 0.3219752754296894559, 0.3333333333333333703, 0.3219752754296894559, 0.3333333333333333703, 0.3219752754296894559, 0.3333333333333333703, 0.3219752754296894559, 0.3333333333333333703, 0.3219752754296894559, 0.3333333333333333703, 0.3219752754296894559, 0.3333333333333333703, 0.3219752754296894559, 0.3333333333333333703, 0.3219752754296894559, 0.3333333333333333703, 0.3219752754296894559, 0.3333333333333333703, 0.3219752754296894559, 0.3333333333333333703, 0.3219752754296894559, 0.3333333333333333703, 0.3219752754296894559, 0.3333333333333333703, 0.3219752754296894559, 0.3333333333333333703, 0.3219752754296894559, 0.3333333333333333703, 0.3219752754296894559, 0.3333333333333333703, 0.3219752754296894559, 0.3333333333333333703, 0.3219752754296894559, 0.3333333333333333703, 0.3219752754296894559, 0.3333333333333333703, 0.3219752754296894559, 0.3333333333333333703, 0.3219752754296894559, 0.3333333333333333703, 0.3219752754296894559, 0.3333333333333333703, 0.3219752754296894559, 0.3333333333333333703, 0.3219752754296894559, 0.3333333333333333703, 0.3219752754296894559, 0.3333333333333333703, 0.3219752754296894559, 0.3333333333333333703, 0.3219752754296894559, 0.3333333333333333703, 0.3219752754296894559, 0.3333333333333333703, 0.3219752754296894559, 0.3333333333333333703, 0.3219752754296894559, 0.3333333333333333703, 0.3219752754296894559, 0.3333333333333333703, 0.3219752754296894559, 0.3333333333333333703, 0.3219752754296894559, 0.3333333333333333703, 0.3219752754296894559, 0.3333333333333333703, 0.3219752754296894559, 0.3333333333333333703, 0.3219752754296894559, 0.3333333333333333703, 0.3219752754296894559, 0.3333333333333333703, 0.3219752754296894559, 0.3333333333333333703, 0.3219752754296894559, 0.3333333333333333703, 0.3219752754296894559, 0.3333333333333333703, 0.3219752754296894559, 0.3333333333333333703, 0.3219752754296894559, 0.3333333333333333703, 0.3219752754296894559, 0.3333333333333333703, 0.3219752754296894559, 0.3333333333333333703, 0.3219752754296894559, 0.3333333333333333703, 0.3219752754296894559, 0.3333333333333333703, 0.3219752754296894559, 0.3333333333333333703, 0.3219752754296894559, 0.3333333333333333703, 0.3219752754296894559, 0.3333333333333333703, 0.3219752754296894559, 0.3333333333333333703, 0.3219752754296894559, 0.3333333333333333703, 0.3219752754296894559, 0.3333333333333333703, 0.3219752754296894559, 0.3333333333333333703, 0.3219752754296894559, 0.3333333333333333703, 0.3219752754296894559, 0.3333333333333333703, 0.3219752754296894559, 0.3333333333333333703, 0.3219752754296894559, 0.3333333333333333703, 0.3219752754296894559, 0.3333333333333333703, 0.3219752754296894559, 0.3333333333333333703, 0.3219752754296894559, 0.3333333333333333703, 0.3219752754296894559, 0.3333333333333333703, 0.3219752754296894559, 0.3333333333333333703, 0.3219752754296894559, 0.3333333333333333703, 0.3219752754296894559, 0.3333333333333333703, 0.3219752754296894559, 0.3333333333333333703, 0.3219752754296894559, 0.3333333333333333703, 0.3219752754296894559, 0.3333333333333333703, 0.3219752754296894559, 0.3333333333333333703, 0.3219752754296894559, 0.3333333333333333703, 0.3219752754296894559, 0.3333333333333333703, 0.3219752754296894559, 0.3333333333333333703, 0.3219752754296894559, 0.3333333333333333703, 0.3219752754296894559, 0.3333333333333333703, 0.3219752754296894559, 0.3333333333333333703, 0.3219752754296894559, 0.3333333333333333703, 0.3219752754296894559, 0.3333333333333333703, 0.3219752754296894559, 0.3333333333333333703, 0.3219752754296894559, 0.3333333333333333703, 0.3219752754296894559, 0.3333333333333333703, 0.3219752754296894559, 0.3333333333333333703, 0.3219752754296894559, 0.3333333333333333703, 0.3219752754296894559, 0.3333333333333333703, 0.3219752754296894559, 0.3333333333333333703, 0.3219752754296894559, 0.3333333333333333703, 0.3219752754296894559, 0.3333333333333333703, 0.3219752754296894559, 0.3333333333333333703, 0.3219752754296894559, 0.3333333333333333703, 0.3219752754296894559, 0.3333333333333333703, 0.3219752754296894559, 0.3333333333333333703, 0.3219752754296894559, 0.3333333333333333703, 0.3219752754296894559, 0.3333333333333333703, 0.3219752754296894559, 0.3333333333333333703, 0.3219752754296894559, 0.3333333333333333703, 0.3219752754296894559, 0.3333333333333333703, 0.3219752754296894559, 0.3333333333333333703, 0.3219752754296894559, 0.3333333333333333703, 0.3219752754296894559, 0.3333333333333333703, 0.3219752754296894559, 0.3333333333333333703, 0.3219752754296894559, 0.3333333333333333703, 0.3219752754296894559, 0.3333333333333333703, 0.3219752754296894559, 0.3333333333333333703, 0.3219752754296894559, 0.3333333333333333703, 0.3219752754296894559, 0.3333333333333333703, 0.3219752754296894559, 0.3333333333333333703, 0.3219752754296894559, 0.3333333333333333703, 0.3219752754296894559, 0.3333333333333333703, 0.3219752754296894559, 0.3333333333333333703, 0.3219752754296894559, 0.3333333333333333703, 0.3219752754296894559, 0.3333333333333333703, 0.3219752754296894559, 0.3333333333333333703, 0.3219752754296894559, 0.3333333333333333703, 0.3219752754296894559, 0.3333333333333333703, 0.3219752754296894559, 0.3333333333333333703, 0.3219752754296894559, 0.3333333333333333703, 0.3219752754296894559, 0.3333333333333333703, 0.3219752754296894559, 0.3333333333333333703, 0.3219752754296894559, 0.3333333333333333703),
 ( 0.3333333333333333703, 0.3219752754296894559, 0.3333333333333333703, 0.3219752754296894559, 0.3333333333333333703, 0.3219752754296894559, 0.3333333333333333703, 0.3219752754296894559, 0.3333333333333333703, 0.3219752754296894559, 0.3333333333333333703, 0.3219752754296894559, 0.3333333333333333703, 0.3219752754296894559, 0.3333333333333333703, 0.3219752754296894559, 0.3333333333333333703, 0.3219752754296894559, 0.3333333333333333703, 0.3219752754296894559, 0.3333333333333333703, 0.3219752754296894559, 0.3333333333333333703, 0.3219752754296894559, 0.3333333333333333703, 0.3219752754296894559, 0.3333333333333333703, 0.3219752754296894559, 0.3333333333333333703, 0.3219752754296894559, 0.3333333333333333703, 0.3219752754296894559, 0.3333333333333333703, 0.3219752754296894559, 0.3333333333333333703, 0.3219752754296894559, 0.3333333333333333703, 0.3219752754296894559, 0.3333333333333333703, 0.3219752754296894559, 0.3333333333333333703, 0.3219752754296894559, 0.3333333333333333703, 0.3219752754296894559, 0.3333333333333333703, 0.3219752754296894559, 0.3333333333333333703, 0.3219752754296894559, 0.3333333333333333703, 0.3219752754296894559, 0.3333333333333333703, 0.3219752754296894559, 0.3333333333333333703, 0.3219752754296894559, 0.3333333333333333703, 0.3219752754296894559, 0.3333333333333333703, 0.3219752754296894559, 0.3333333333333333703, 0.3219752754296894559, 0.3333333333333333703, 0.3219752754296894559, 0.3333333333333333703, 0.3219752754296894559, 0.3333333333333333703, 0.3219752754296894559, 0.3333333333333333703, 0.3219752754296894559, 0.3333333333333333703, 0.3219752754296894559, 0.3333333333333333703, 0.3219752754296894559, 0.3333333333333333703, 0.3219752754296894559, 0.3333333333333333703, 0.3219752754296894559, 0.3333333333333333703, 0.3219752754296894559, 0.3333333333333333703, 0.3219752754296894559, 0.3333333333333333703, 0.3219752754296894559, 0.3333333333333333703, 0.3219752754296894559, 0.3333333333333333703, 0.3219752754296894559, 0.3333333333333333703, 0.3219752754296894559, 0.3333333333333333703, 0.3219752754296894559, 0.3333333333333333703, 0.3219752754296894559, 0.3333333333333333703, 0.3219752754296894559, 0.3333333333333333703, 0.3219752754296894559, 0.3333333333333333703, 0.3219752754296894559, 0.3333333333333333703, 0.3219752754296894559, 0.3333333333333333703, 0.3219752754296894559, 0.3333333333333333703, 0.3219752754296894559, 0.3333333333333333703, 0.3219752754296894559, 0.3333333333333333703, 0.3219752754296894559, 0.3333333333333333703, 0.3219752754296894559, 0.3333333333333333703, 0.3219752754296894559, 0.3333333333333333703, 0.3219752754296894559, 0.3333333333333333703, 0.3219752754296894559, 0.3333333333333333703, 0.3219752754296894559, 0.3333333333333333703, 0.3219752754296894559, 0.3333333333333333703, 0.3219752754296894559, 0.3333333333333333703, 0.3219752754296894559, 0.3333333333333333703, 0.3219752754296894559, 0.3333333333333333703, 0.3219752754296894559, 0.3333333333333333703, 0.3219752754296894559, 0.3333333333333333703, 0.3219752754296894559, 0.3333333333333333703, 0.3219752754296894559, 0.3333333333333333703, 0.3219752754296894559, 0.3333333333333333703, 0.3219752754296894559, 0.3333333333333333703, 0.3219752754296894559, 0.3333333333333333703, 0.3219752754296894559, 0.3333333333333333703, 0.3219752754296894559, 0.3333333333333333703, 0.3219752754296894559, 0.3333333333333333703, 0.3219752754296894559, 0.3333333333333333703, 0.3219752754296894559, 0.3333333333333333703, 0.3219752754296894559, 0.3333333333333333703, 0.3219752754296894559, 0.3333333333333333703, 0.3219752754296894559, 0.3333333333333333703, 0.3219752754296894559, 0.3333333333333333703, 0.3219752754296894559, 0.3333333333333333703, 0.3219752754296894559, 0.3333333333333333703, 0.3219752754296894559, 0.3333333333333333703, 0.3219752754296894559, 0.3333333333333333703, 0.3219752754296894559, 0.3333333333333333703, 0.3219752754296894559, 0.3333333333333333703, 0.3219752754296894559, 0.3333333333333333703, 0.3219752754296894559, 0.3333333333333333703, 0.3219752754296894559, 0.3333333333333333703, 0.3219752754296894559, 0.3333333333333333703, 0.3219752754296894559, 0.3333333333333333703, 0.3219752754296894559, 0.3333333333333333703, 0.3219752754296894559, 0.3333333333333333703, 0.3219752754296894559, 0.3333333333333333703, 0.3219752754296894559, 0.3333333333333333703, 0.3219752754296894559, 0.3333333333333333703, 0.3219752754296894559, 0.3333333333333333703, 0.3219752754296894559, 0.3333333333333333703, 0.3219752754296894559, 0.3333333333333333703, 0.3219752754296894559, 0.3333333333333333703, 0.3219752754296894559, 0.3333333333333333703, 0.3219752754296894559, 0.3333333333333333703, 0.3219752754296894559, 0.3333333333333333703, 0.3219752754296894559, 0.3333333333333333703, 0.3219752754296894559, 0.3333333333333333703, 0.3219752754296894559, 0.3333333333333333703, 0.3219752754296894559, 0.3333333333333333703, 0.3219752754296894559, 0.3333333333333333703, 0.3219752754296894559, 0.3333333333333333703, 0.3219752754296894559, 0.3333333333333333703, 0.3219752754296894559, 0.3333333333333333703, 0.3219752754296894559, 0.3333333333333333703, 0.3219752754296894559, 0.3333333333333333703, 0.3219752754296894559, 0.3333333333333333703, 0.3219752754296894559, 0.3333333333333333703, 0.3219752754296894559, 0.3333333333333333703, 0.3219752754296894559, 0.3333333333333333703, 0.3219752754296894559, 0.3333333333333333703, 0.3219752754296894559, 0.3333333333333333703, 0.3219752754296894559, 0.3333333333333333703, 0.3219752754296894559, 0.3333333333333333703, 0.3219752754296894559, 0.3333333333333333703, 0.3219752754296894559, 0.3333333333333333703, 0.3219752754296894559, 0.3333333333333333703, 0.3219752754296894559, 0.3333333333333333703, 0.3219752754296894559, 0.3333333333333333703, 0.3219752754296894559, 0.3333333333333333703, 0.3219752754296894559, 0.3333333333333333703, 0.3219752754296894559, 0.3333333333333333703, 0.3219752754296894559, 0.3333333333333333703, 0.3219752754296894559, 0.3333333333333333703, 0.3219752754296894559, 0.3333333333333333703, 0.3219752754296894559, 0.3333333333333333703, 0.3219752754296894559, 0.3333333333333333703, 0.3219752754296894559, 0.3333333333333333703, 0.3219752754296894559, 0.3333333333333333703, 0.3219752754296894559, 0.3333333333333333703, 0.3219752754296894559, 0.3333333333333333703, 0.3219752754296894559, 0.3333333333333333703, 0.3219752754296894559, 0.3333333333333333703, 0.3219752754296894559, 0.3333333333333333703, 0.3219752754296894559, 0.3333333333333333703, 0.3219752754296894559, 0.3333333333333333703, 0.3219752754296894559, 0.3333333333333333703, 0.3219752754296894559, 0.3333333333333333703, 0.3219752754296894559, 0.3333333333333333703, 0.3219752754296894559, 0.3333333333333333703, 0.3219752754296894559, 0.3333333333333333703, 0.3219752754296894559, 0.3333333333333333703, 0.3219752754296894559, 0.3333333333333333703, 0.3219752754296894559, 0.3333333333333333703, 0.3219752754296894559, 0.3333333333333333703, 0.3219752754296894559, 0.3333333333333333703, 0.3219752754296894559, 0.3333333333333333703, 0.3219752754296894559, 0.3333333333333333703, 0.3219752754296894559, 0.3333333333333333703, 0.3219752754296894559, 0.3333333333333333703, 0.3219752754296894559, 0.3333333333333333703, 0.3219752754296894559, 0.3333333333333333703, 0.3219752754296894559, 0.3333333333333333703, 0.3219752754296894559, 0.3333333333333333703, 0.3219752754296894559, 0.3333333333333333703, 0.3219752754296894559, 0.3333333333333333703, 0.3219752754296894559, 0.3333333333333333703, 0.3219752754296894559, 0.3333333333333333703, 0.3219752754296894559, 0.3333333333333333703, 0.3219752754296894559, 0.3333333333333333703, 0.3219752754296894559, 0.3333333333333333703, 0.3219752754296894559, 0.3333333333333333703, 0.3219752754296894559, 0.3333333333333333703, 0.3219752754296894559, 0.3333333333333333703, 0.3219752754296894559, 0.3333333333333333703, 0.3219752754296894559, 0.3333333333333333703, 0.3219752754296894559, 0.3333333333333333703, 0.3219752754296894559, 0.3333333333333333703, 0.3219752754296894559, 0.3333333333333333703, 0.3219752754296894559, 0.3333333333333333703, 0.3219752754296894559, 0.3333333333333333703, 0.3219752754296894559, 0.3333333333333333703, 0.3219752754296894559, 0.3333333333333333703, 0.3219752754296894559, 0.3333333333333333703, 0.3219752754296894559, 0.3333333333333333703, 0.3219752754296894559, 0.3333333333333333703, 0.3219752754296894559, 0.3333333333333333703, 0.3219752754296894559, 0.3333333333333333703, 0.3219752754296894559, 0.3333333333333333703, 0.3219752754296894559, 0.3333333333333333703, 0.3219752754296894559, 0.3333333333333333703, 0.3219752754296894559, 0.3333333333333333703, 0.3219752754296894559, 0.3333333333333333703, 0.3219752754296894559, 0.3333333333333333703, 0.3219752754296894559, 0.3333333333333333703, 0.3219752754296894559, 0.3333333333333333703, 0.3219752754296894559, 0.3333333333333333703, 0.3219752754296894559, 0.3333333333333333703, 0.3219752754296894559, 0.3333333333333333703, 0.3219752754296894559, 0.3333333333333333703, 0.3219752754296894559, 0.3333333333333333703, 0.3219752754296894559, 0.3333333333333333703, 0.3219752754296894559, 0.3333333333333333703, 0.3219752754296894559, 0.3333333333333333703, 0.3219752754296894559, 0.3333333333333333703, 0.3219752754296894559, 0.3333333333333333703, 0.3219752754296894559, 0.3333333333333333703, 0.3219752754296894559, 0.3333333333333333703, 0.3219752754296894559, 0.3333333333333333703, 0.3219752754296894559, 0.3333333333333333703, 0.3219752754296894559, 0.3333333333333333703, 0.3219752754296894559, 0.3333333333333333703, 0.3219752754296894559, 0.3333333333333333703, 0.3219752754296894559, 0.3333333333333333703, 0.3219752754296894559, 0.3333333333333333703, 0.3219752754296894559, 0.3333333333333333703, 0.3219752754296894559, 0.3333333333333333703, 0.3219752754296894559, 0.3333333333333333703, 0.3219752754296894559, 0.3333333333333333703, 0.3219752754296894559, 0.3333333333333333703, 0.3219752754296894559, 0.3333333333333333703, 0.3219752754296894559, 0.3333333333333333703, 0.3219752754296894559, 0.3333333333333333703, 0.3219752754296894559, 0.3333333333333333703, 0.3219752754296894559, 0.3333333333333333703, 0.3219752754296894559, 0.3333333333333333703, 0.3219752754296894559, 0.3333333333333333703, 0.3219752754296894559, 0.3333333333333333703, 0.3219752754296894559, 0.3333333333333333703, 0.3219752754296894559, 0.3333333333333333703, 0.3219752754296894559, 0.3333333333333333703, 0.3219752754296894559, 0.3333333333333333703),
 ( 1.000000000000000000, 0.9659258262890683122, 1.000000000000000000, 0.9659258262890683122, 1.000000000000000000, 0.9659258262890683122, 1.000000000000000000, 0.9659258262890683122, 1.000000000000000000, 0.9659258262890683122, 1.000000000000000000, 0.9659258262890683122, 1.000000000000000000, 0.9659258262890683122, 1.000000000000000000, 0.9659258262890683122, 1.000000000000000000, 0.9659258262890683122, 1.000000000000000000, 0.9659258262890683122, 1.000000000000000000, 0.9659258262890683122, 1.000000000000000000, 0.9659258262890683122, 1.000000000000000000, 0.9659258262890683122, 1.000000000000000000, 0.9659258262890683122, 1.000000000000000000, 0.9659258262890683122, 1.000000000000000000, 0.9659258262890683122, 1.000000000000000000, 0.9659258262890683122, 1.000000000000000000, 0.9659258262890683122, 1.000000000000000000, 0.9659258262890683122, 1.000000000000000000, 0.9659258262890683122, 1.000000000000000000, 0.9659258262890683122, 1.000000000000000000, 0.9659258262890683122, 1.000000000000000000, 0.9659258262890683122, 1.000000000000000000, 0.9659258262890683122, 1.000000000000000000, 0.9659258262890683122, 1.000000000000000000, 0.9659258262890683122, 1.000000000000000000, 0.9659258262890683122, 1.000000000000000000, 0.9659258262890683122, 1.000000000000000000, 0.9659258262890683122, 1.000000000000000000, 0.9659258262890683122, 1.000000000000000000, 0.9659258262890683122, 1.000000000000000000, 0.9659258262890683122, 1.000000000000000000, 0.9659258262890683122, 1.000000000000000000, 0.9659258262890683122, 1.000000000000000000, 0.9659258262890683122, 1.000000000000000000, 0.9659258262890683122, 1.000000000000000000, 0.9659258262890683122, 1.000000000000000000, 0.9659258262890683122, 1.000000000000000000, 0.9659258262890683122, 1.000000000000000000, 0.9659258262890683122, 1.000000000000000000, 0.9659258262890683122, 1.000000000000000000, 0.9659258262890683122, 1.000000000000000000, 0.9659258262890683122, 1.000000000000000000, 0.9659258262890683122, 1.000000000000000000, 0.9659258262890683122, 1.000000000000000000, 0.9659258262890683122, 1.000000000000000000, 0.9659258262890683122, 1.000000000000000000, 0.9659258262890683122, 1.000000000000000000, 0.9659258262890683122, 1.000000000000000000, 0.9659258262890683122, 1.000000000000000000, 0.9659258262890683122, 1.000000000000000000, 0.9659258262890683122, 1.000000000000000000, 0.9659258262890683122, 1.000000000000000000, 0.9659258262890683122, 1.000000000000000000, 0.9659258262890683122, 1.000000000000000000, 0.9659258262890683122, 1.000000000000000000, 0.9659258262890683122, 1.000000000000000000, 0.9659258262890683122, 1.000000000000000000, 0.9659258262890683122, 1.000000000000000000, 0.9659258262890683122, 1.000000000000000000, 0.9659258262890683122, 1.000000000000000000, 0.9659258262890683122, 1.000000000000000000, 0.9659258262890683122, 1.000000000000000000, 0.9659258262890683122, 1.000000000000000000, 0.9659258262890683122, 1.000000000000000000, 0.9659258262890683122, 1.000000000000000000, 0.9659258262890683122, 1.000000000000000000, 0.9659258262890683122, 1.000000000000000000, 0.9659258262890683122, 1.000000000000000000, 0.9659258262890683122, 1.000000000000000000, 0.9659258262890683122, 1.000000000000000000, 0.9659258262890683122, 1.000000000000000000, 0.9659258262890683122, 1.000000000000000000, 0.9659258262890683122, 1.000000000000000000, 0.9659258262890683122, 1.000000000000000000, 0.9659258262890683122, 1.000000000000000000, 0.9659258262890683122, 1.000000000000000000, 0.9659258262890683122, 1.000000000000000000, 0.9659258262890683122, 1.000000000000000000, 0.9659258262890683122, 1.000000000000000000, 0.9659258262890683122, 1.000000000000000000, 0.9659258262890683122, 1.000000000000000000, 0.9659258262890683122, 1.000000000000000000, 0.9659258262890683122, 1.000000000000000000, 0.9659258262890683122, 1.000000000000000000, 0.9659258262890683122, 1.000000000000000000, 0.9659258262890683122, 1.000000000000000000, 0.9659258262890683122, 1.000000000000000000, 0.9659258262890683122, 1.000000000000000000, 0.9659258262890683122, 1.000000000000000000, 0.9659258262890683122, 1.000000000000000000, 0.9659258262890683122, 1.000000000000000000, 0.9659258262890683122, 1.000000000000000000, 0.9659258262890683122, 1.000000000000000000, 0.9659258262890683122, 1.000000000000000000, 0.9659258262890683122, 1.000000000000000000, 0.9659258262890683122, 1.000000000000000000, 0.9659258262890683122, 1.000000000000000000, 0.9659258262890683122, 1.000000000000000000, 0.9659258262890683122, 1.000000000000000000, 0.9659258262890683122, 1.000000000000000000, 0.9659258262890683122, 1.000000000000000000, 0.9659258262890683122, 1.000000000000000000, 0.9659258262890683122, 1.000000000000000000, 0.9659258262890683122, 1.000000000000000000, 0.9659258262890683122, 1.000000000000000000, 0.9659258262890683122, 1.000000000000000000, 0.9659258262890683122, 1.000000000000000000, 0.9659258262890683122, 1.000000000000000000, 0.9659258262890683122, 1.000000000000000000, 0.9659258262890683122, 1.000000000000000000, 0.9659258262890683122, 1.000000000000000000, 0.9659258262890683122, 1.000000000000000000, 0.9659258262890683122, 1.000000000000000000, 0.9659258262890683122, 1.000000000000000000, 0.9659258262890683122, 1.000000000000000000, 0.9659258262890683122, 1.000000000000000000, 0.9659258262890683122, 1.000000000000000000, 0.9659258262890683122, 1.000000000000000000, 0.9659258262890683122, 1.000000000000000000, 0.9659258262890683122, 1.000000000000000000, 0.9659258262890683122, 1.000000000000000000, 0.9659258262890683122, 1.000000000000000000, 0.9659258262890683122, 1.000000000000000000, 0.9659258262890683122, 1.000000000000000000, 0.9659258262890683122, 1.000000000000000000, 0.9659258262890683122, 1.000000000000000000, 0.9659258262890683122, 1.000000000000000000, 0.9659258262890683122, 1.000000000000000000, 0.9659258262890683122, 1.000000000000000000, 0.9659258262890683122, 1.000000000000000000, 0.9659258262890683122, 1.000000000000000000, 0.9659258262890683122, 1.000000000000000000, 0.9659258262890683122, 1.000000000000000000, 0.9659258262890683122, 1.000000000000000000, 0.9659258262890683122, 1.000000000000000000, 0.9659258262890683122, 1.000000000000000000, 0.9659258262890683122, 1.000000000000000000, 0.9659258262890683122, 1.000000000000000000, 0.9659258262890683122, 1.000000000000000000, 0.9659258262890683122, 1.000000000000000000, 0.9659258262890683122, 1.000000000000000000, 0.9659258262890683122, 1.000000000000000000, 0.9659258262890683122, 1.000000000000000000, 0.9659258262890683122, 1.000000000000000000, 0.9659258262890683122, 1.000000000000000000, 0.9659258262890683122, 1.000000000000000000, 0.9659258262890683122, 1.000000000000000000, 0.9659258262890683122, 1.000000000000000000, 0.9659258262890683122, 1.000000000000000000, 0.9659258262890683122, 1.000000000000000000, 0.9659258262890683122, 1.000000000000000000, 0.9659258262890683122, 1.000000000000000000, 0.9659258262890683122, 1.000000000000000000, 0.9659258262890683122, 1.000000000000000000, 0.9659258262890683122, 1.000000000000000000, 0.9659258262890683122, 1.000000000000000000, 0.9659258262890683122, 1.000000000000000000, 0.9659258262890683122, 1.000000000000000000, 0.9659258262890683122, 1.000000000000000000, 0.9659258262890683122, 1.000000000000000000, 0.9659258262890683122, 1.000000000000000000, 0.9659258262890683122, 1.000000000000000000, 0.9659258262890683122, 1.000000000000000000, 0.9659258262890683122, 1.000000000000000000, 0.9659258262890683122, 1.000000000000000000, 0.9659258262890683122, 1.000000000000000000, 0.9659258262890683122, 1.000000000000000000, 0.9659258262890683122, 1.000000000000000000, 0.9659258262890683122, 1.000000000000000000, 0.9659258262890683122, 1.000000000000000000, 0.9659258262890683122, 1.000000000000000000, 0.9659258262890683122, 1.000000000000000000, 0.9659258262890683122, 1.000000000000000000, 0.9659258262890683122, 1.000000000000000000, 0.9659258262890683122, 1.000000000000000000, 0.9659258262890683122, 1.000000000000000000, 0.9659258262890683122, 1.000000000000000000, 0.9659258262890683122, 1.000000000000000000, 0.9659258262890683122, 1.000000000000000000, 0.9659258262890683122, 1.000000000000000000, 0.9659258262890683122, 1.000000000000000000, 0.9659258262890683122, 1.000000000000000000, 0.9659258262890683122, 1.000000000000000000, 0.9659258262890683122, 1.000000000000000000, 0.9659258262890683122, 1.000000000000000000, 0.9659258262890683122, 1.000000000000000000, 0.9659258262890683122, 1.000000000000000000, 0.9659258262890683122, 1.000000000000000000, 0.9659258262890683122, 1.000000000000000000, 0.9659258262890683122, 1.000000000000000000, 0.9659258262890683122, 1.000000000000000000, 0.9659258262890683122, 1.000000000000000000, 0.9659258262890683122, 1.000000000000000000, 0.9659258262890683122, 1.000000000000000000, 0.9659258262890683122, 1.000000000000000000, 0.9659258262890683122, 1.000000000000000000, 0.9659258262890683122, 1.000000000000000000, 0.9659258262890683122, 1.000000000000000000, 0.9659258262890683122, 1.000000000000000000, 0.9659258262890683122, 1.000000000000000000, 0.9659258262890683122, 1.000000000000000000, 0.9659258262890683122, 1.000000000000000000, 0.9659258262890683122, 1.000000000000000000, 0.9659258262890683122, 1.000000000000000000, 0.9659258262890683122, 1.000000000000000000, 0.9659258262890683122, 1.000000000000000000, 0.9659258262890683122, 1.000000000000000000, 0.9659258262890683122, 1.000000000000000000, 0.9659258262890683122, 1.000000000000000000, 0.9659258262890683122, 1.000000000000000000, 0.9659258262890683122, 1.000000000000000000, 0.9659258262890683122, 1.000000000000000000, 0.9659258262890683122, 1.000000000000000000, 0.9659258262890683122, 1.000000000000000000, 0.9659258262890683122, 1.000000000000000000, 0.9659258262890683122, 1.000000000000000000, 0.9659258262890683122, 1.000000000000000000, 0.9659258262890683122, 1.000000000000000000, 0.9659258262890683122, 1.000000000000000000, 0.9659258262890683122, 1.000000000000000000, 0.9659258262890683122, 1.000000000000000000, 0.9659258262890683122, 1.000000000000000000, 0.9659258262890683122, 1.000000000000000000, 0.9659258262890683122, 1.000000000000000000, 0.9659258262890683122, 1.000000000000000000, 0.9659258262890683122, 1.000000000000000000, 0.9659258262890683122, 1.000000000000000000) ) ) 
 REPRESENTATION_ITEM ( '' )  SURFACE ( )  );
#894 = CARTESIAN_POINT ( 'NONE',  ( 5.049401038298161559, -19.05341960407611168, 62.70724293864769550 ) ) ;
#895 = CARTESIAN_POINT ( 'NONE',  ( 21.52544592524334988, 5.823673210054432836, 66.45942372801903275 ) ) ;
#896 = CARTESIAN_POINT ( 'NONE',  ( 13.89961937509977652, -13.97604488694527269, 53.12390960531434558 ) ) ;
#897 = CARTESIAN_POINT ( 'NONE',  ( 19.03943276465977164, -0.05219959533909143690, 28.74890960531435624 ) ) ;
#898 = CARTESIAN_POINT ( 'NONE',  ( 9.564922557960805705, 16.46253265017160317, 114.5822429386476955 ) ) ;
#899 = CARTESIAN_POINT ( 'NONE',  ( -4.379528057220328563, 16.55341960407611168, 65.20724293864768129 ) ) ;
#900 = CARTESIAN_POINT ( 'NONE',  ( 19.05341960407611168, 5.049401038298154454, 23.95724293864769194 ) ) ;
#901 = CARTESIAN_POINT ( 'NONE',  ( -8.314922557960811034, -14.29746914071050412, 87.08224293864769550 ) ) ;
#902 = CARTESIAN_POINT ( 'NONE',  ( -21.55341960407610458, -5.719274019375992779, 101.4572429386476955 ) ) ;
#903 = CARTESIAN_POINT ( 'NONE',  ( 5.719274019375673035, 21.55341960407619339, 37.29275706135235424 ) ) ;
#904 = CARTESIAN_POINT ( 'NONE',  ( -8.906447517083060816, 27.41122689804195645, 149.5999999999999943 ) ) ;
#905 = CARTESIAN_POINT ( 'NONE',  ( 16.53943276465976808, 0.05219959533934440121, 46.25109039468567573 ) ) ;
#906 = CARTESIAN_POINT ( 'NONE',  ( 18.62759615963271287, -10.81492255796078972, 98.33224293864769550 ) ) ;
#907 = CARTESIAN_POINT ( 'NONE',  ( 9.564922557961047289, -16.46253265017146816, 30.41775706135232937 ) ) ;
#908 = CARTESIAN_POINT ( 'NONE',  ( 5.049401038298161559, -19.05341960407611168, 112.7072429386476813 ) ) ;
#909 = CARTESIAN_POINT ( 'NONE',  ( -5.719274019375665041, -21.55341960407619695, 44.79275706135234714 ) ) ;
#910 = CIRCLE ( 'NONE', #26805, 5.000000000000000000 ) ;
#911 = CARTESIAN_POINT ( 'NONE',  ( -10.72451020669898014, 18.67979575497178502, 40.41557627198103120 ) ) ;
#912 = CARTESIAN_POINT ( 'NONE',  ( -12.14591786802309592, -12.06949235617757132, 21.87390960531436690 ) ) ;
#914 = CARTESIAN_POINT ( 'NONE',  ( 18.62759615963255655, 10.81492255796105972, 96.66775706135234714 ) ) ;
#913 = CARTESIAN_POINT ( 'NONE',  ( 21.53943276465977519, 0.05219959533937863772, 61.25109039468567573 ) ) ;
#915 = CARTESIAN_POINT ( 'NONE',  ( 0.05219959533936267826, -19.03943276465977164, 25.00109039468566152 ) ) ;
#916 = CARTESIAN_POINT ( 'NONE',  ( -14.34966873604972548, 8.224510206698743886, 83.33442372801903275 ) ) ;
#917 = CARTESIAN_POINT ( 'NONE',  ( 0.05219959533937995610, -21.53943276465977519, 50.00109039468568994 ) ) ;
#918 = CARTESIAN_POINT ( 'NONE',  ( -19.03943276465977164, 0.05219959533909376836, 46.24890960531435979 ) ) ;
#919 = CARTESIAN_POINT ( 'NONE',  ( -19.03943276465977164, -0.05219959533935918106, 23.75109039468566152 ) ) ;
#920 = CARTESIAN_POINT ( 'NONE',  ( -0.05219959533907301413, -21.53943276465977519, 27.49890960531435269 ) ) ;
#921 = CARTESIAN_POINT ( 'NONE',  ( 10.81492255796078972, 18.62759615963270932, 114.5822429386477097 ) ) ;
#922 = CARTESIAN_POINT ( 'NONE',  ( -5.823673210054116645, -21.52544592524344225, 72.29057627198102409 ) ) ;
#923 = CARTESIAN_POINT ( 'NONE',  ( -8.224510206698735004, -14.34966873604973081, 39.58442372801901143 ) ) ;
#925 = CARTESIAN_POINT ( 'NONE',  ( 18.67979575497178502, 10.72451020669898547, 74.16557627198102409 ) ) ;
#924 = FACE_BOUND ( 'NONE', #178509, .T. ) ;
#927 = CARTESIAN_POINT ( 'NONE',  ( -4.483927247898539470, -16.52544592524342804, 57.29057627198103120 ) ) ;
#926 = CARTESIAN_POINT ( 'NONE',  ( -16.53943276465976808, -0.05219959533934237506, 68.75109039468568994 ) ) ;
#928 = CARTESIAN_POINT ( 'NONE',  ( -22.90350128981420141, 22.02608267474392179, -45.83983912514964487 ) ) ;
#929 = CARTESIAN_POINT ( 'NONE',  ( 19.05341960407617918, -5.049401038297876454, 106.0427570613523471 ) ) ;
#930 = CARTESIAN_POINT ( 'NONE',  ( 6.685465210013314952, -6.128229644718811819, -61.90241664256964782 ) ) ;
#931 = CARTESIAN_POINT ( 'NONE',  ( 4.483927247898790824, -16.52544592524335698, 45.20942372801901854 ) ) ;
#932 = CARTESIAN_POINT ( 'NONE',  ( -21.53943276465977519, 0.05219959533907696930, 106.2489096053143811 ) ) ;
#933 = CARTESIAN_POINT ( 'NONE',  ( 10.81492255796078972, 18.62759615963270932, 29.58224293864769905 ) ) ;
#934 = CARTESIAN_POINT ( 'NONE',  ( 16.55341960407618274, -4.379528057220086978, 51.04275706135234714 ) ) ;
#935 = CARTESIAN_POINT ( 'NONE',  ( -16.51473224551069308, -9.474510206698971260, 71.66557627198102409 ) ) ;
#937 = CARTESIAN_POINT ( 'NONE',  ( -19.05341960407617563, 5.049401038297882671, 113.5427570613523471 ) ) ;
#936 = CARTESIAN_POINT ( 'NONE',  ( -0.05219959533937732626, 21.53943276465977519, 42.50109039468567573 ) ) ;
#938 = CARTESIAN_POINT ( 'NONE',  ( -0.05219959533907301413, -21.53943276465977519, 22.49890960531436335 ) ) ;
#939 = CARTESIAN_POINT ( 'NONE',  ( -19.02544592524334988, -5.153800228976617603, 23.95942372801900078 ) ) ;
#940 = CARTESIAN_POINT ( 'NONE',  ( 4.483927247898790824, -16.52544592524335698, 40.20942372801901854 ) ) ;
#941 = CARTESIAN_POINT ( 'NONE',  ( -9.564922557960796823, -16.46253265017161027, 107.0822429386476955 ) ) ;
#942 = CARTESIAN_POINT ( 'NONE',  ( 21.53943276465977519, -0.05219959533907433946, 98.74890960531438111 ) ) ;
#943 = CARTESIAN_POINT ( 'NONE',  ( -9.474510206698964154, 16.51473224551069663, 70.41557627198102409 ) ) ;
#944 = CARTESIAN_POINT ( 'NONE',  ( -17.48847506799967988, 5.747544572773784388, 25.82697437843280497 ) ) ;
#945 = CARTESIAN_POINT ( 'NONE',  ( 16.53943276465976808, -0.05219959533910856209, 78.74890960531436690 ) ) ;
#946 = CARTESIAN_POINT ( 'NONE',  ( -16.51473224551069308, -9.474510206698971260, 111.6655762719810383 ) ) ;
#947 = LINE ( 'NONE', #122312, #12055 ) ;
#948 = CARTESIAN_POINT ( 'NONE',  ( 0.05219959533934541429, -16.53943276465976808, 70.00109039468568994 ) ) ;
#949 = CARTESIAN_POINT ( 'NONE',  ( 15.80617190586746368, 15.72974639402197994, 99.37390960531436690 ) ) ;
#950 = CARTESIAN_POINT ( 'NONE',  ( 5.049401038297881783, 19.05341960407617563, 67.29275706135234714 ) ) ;
#951 = CARTESIAN_POINT ( 'NONE',  ( -15.80617190586745835, -15.72974639402198527, 26.87390960531435979 ) ) ;
#952 = CARTESIAN_POINT ( 'NONE',  ( 9.564922557960805705, 16.46253265017160317, 29.58224293864769550 ) ) ;
#953 = CARTESIAN_POINT ( 'NONE',  ( 15.80617190586746368, 15.72974639402197994, 74.37390960531436690 ) ) ;
#954 = CARTESIAN_POINT ( 'NONE',  ( 5.049401038298161559, -19.05341960407611168, 102.7072429386476955 ) ) ;
#955 = EDGE_CURVE ( 'NONE', #12036, #40598, #167128, .T. ) ;
#956 = CARTESIAN_POINT ( 'NONE',  ( -18.67979575497193778, 10.72451020669871902, 93.33442372801901854 ) ) ;
#957 = CARTESIAN_POINT ( 'NONE',  ( -0.05219959533909027116, -19.03943276465977164, 52.49890960531436690 ) ) ;
#958 = CARTESIAN_POINT ( 'NONE',  ( -4.483927247898539470, -16.52544592524342804, 92.29057627198103830 ) ) ;
#959 = CARTESIAN_POINT ( 'NONE',  ( 14.29746914071037800, 8.314922557961029526, 41.66775706135235424 ) ) ;
#960 = CARTESIAN_POINT ( 'NONE',  ( -5.049401038298153566, 19.05341960407611168, 60.20724293864768129 ) ) ;
#961 = CARTESIAN_POINT ( 'NONE',  ( 0.05219959533937995610, -21.53943276465977519, 80.00109039468568994 ) ) ;
#962 = EDGE_LOOP ( 'NONE', ( #189631, #4030 ) ) ;
#963 = CARTESIAN_POINT ( 'NONE',  ( -19.02544592524334988, -5.153800228976617603, 38.95942372801900433 ) ) ;
#964 = CARTESIAN_POINT ( 'NONE',  ( 19.03943276465977164, 0.05219959533936151252, 41.25109039468566152 ) ) ;
#965 = CARTESIAN_POINT ( 'NONE',  ( 18.62759615963255655, 10.81492255796105972, 31.66775706135234358 ) ) ;
#966 = CARTESIAN_POINT ( 'NONE',  ( -8.724588103088155577, 0.9974278668898441946, -61.97156292062780381 ) ) ;
#967 = CARTESIAN_POINT ( 'NONE',  ( 16.51473224551083163, -9.474510206698727899, 35.83442372801899722 ) ) ;
#968 = CARTESIAN_POINT ( 'NONE',  ( -13.97604488694527625, -13.89961937509977652, 81.87390960531436690 ) ) ;
#969 = CARTESIAN_POINT ( 'NONE',  ( 5.153800228976335163, 19.02544592524342804, 74.79057627198103830 ) ) ;
#970 = CARTESIAN_POINT ( 'NONE',  ( -8.224510206698948167, 14.34966873604960824, 30.41557627198101699 ) ) ;
#972 = CARTESIAN_POINT ( 'NONE',  ( -15.80617190586768217, 15.72974639402176855, 83.12609039468568994 ) ) ;
#971 = CARTESIAN_POINT ( 'NONE',  ( -16.46253265017160317, 9.564922557960807481, 110.8322429386476955 ) ) ;
#973 = CARTESIAN_POINT ( 'NONE',  ( 3.556970738554033499E-15, -38.81732327939057825, -2.124999997268813612 ) ) ;
#974 = CARTESIAN_POINT ( 'NONE',  ( -34.51819068884489639, 0.7175229865516564720, 89.53493623002425750 ) ) ;
#975 = CARTESIAN_POINT ( 'NONE',  ( 0.05219959533937995610, -21.53943276465977519, 100.0010903946857042 ) ) ;
#976 = CARTESIAN_POINT ( 'NONE',  ( 17.40805194822031154, -6.112264579159331745, 43.33371272510611760 ) ) ;
#977 = CARTESIAN_POINT ( 'NONE',  ( 13.97604488694527802, 13.89961937509977652, 114.3739096053143669 ) ) ;
#978 = CARTESIAN_POINT ( 'NONE',  ( -25.28179187713397269, -11.97099003546684415, 166.1915553108511290 ) ) ;
#979 = CARTESIAN_POINT ( 'NONE',  ( 14.34966873604972726, -8.224510206698740333, 50.83442372801901143 ) ) ;
#981 = EDGE_CURVE ( 'NONE', #31363, #49313, #26634, .T. ) ;
#980 = CARTESIAN_POINT ( 'NONE',  ( -15.72974639402197994, 15.80617190586746368, 75.62390960531439532 ) ) ;
#982 = CARTESIAN_POINT ( 'NONE',  ( 8.314922557960818139, 14.29746914071049879, 29.58224293864769905 ) ) ;
#984 = CARTESIAN_POINT ( 'NONE',  ( 9.564922557960805705, 16.46253265017160317, 99.58224293864770971 ) ) ;
#983 = CARTESIAN_POINT ( 'NONE',  ( 4.483927247898545687, 16.52544592524342804, 114.7905762719810383 ) ) ;
#985 = CARTESIAN_POINT ( 'NONE',  ( 19.03943276465977164, 0.05219959533936151252, 26.25109039468566507 ) ) ;
#986 = CARTESIAN_POINT ( 'NONE',  ( 9.564922557960805705, 16.46253265017160317, 24.58224293864769194 ) ) ;
#987 = CARTESIAN_POINT ( 'NONE',  ( -5.719274019375665041, -21.55341960407619695, 64.79275706135234714 ) ) ;
#988 = CARTESIAN_POINT ( 'NONE',  ( -16.46253265017160317, 9.564922557960807481, 110.8322429386476955 ) ) ;
#989 = CARTESIAN_POINT ( 'NONE',  ( -8.314922557961024197, 14.29746914071037800, 107.9177570613523471 ) ) ;
#990 = CARTESIAN_POINT ( 'NONE',  ( 9.564922557961047289, -16.46253265017146816, 65.41775706135233293 ) ) ;
#991 = CARTESIAN_POINT ( 'NONE',  ( 29.86685920354754487, 21.69954338932564752, -3.924999997268812990 ) ) ;
#992 = CARTESIAN_POINT ( 'NONE',  ( -19.05341960407611168, -5.049401038298163336, 106.4572429386476955 ) ) ;
#993 = CARTESIAN_POINT ( 'NONE',  ( 16.55341960407611168, 4.379528057220329451, 93.95724293864770971 ) ) ;
#994 = CARTESIAN_POINT ( 'NONE',  ( 19.02544592524334988, 5.153800228976608722, 61.45942372801900433 ) ) ;
#995 = CARTESIAN_POINT ( 'NONE',  ( 13.89961937509977652, -13.97604488694527269, 83.12390960531436690 ) ) ;
#996 = CARTESIAN_POINT ( 'NONE',  ( -12.14591786802309592, -12.06949235617757132, 66.87390960531436690 ) ) ;
#997 = CARTESIAN_POINT ( 'NONE',  ( 9.474510206698729675, 16.51473224551082808, 97.08442372801900433 ) ) ;
#998 = CARTESIAN_POINT ( 'NONE',  ( -5.719274019375978568, 21.55341960407610458, 55.20724293864770260 ) ) ;
#999 = ORIENTED_EDGE ( 'NONE', *, *, #31053, .F. ) ;
#1000 = CARTESIAN_POINT ( 'NONE',  ( -13.89961937509977652, 13.97604488694528158, 25.62390960531434558 ) ) ;
#1001 = CARTESIAN_POINT ( 'NONE',  ( -9.474510206698720793, -16.51473224551083518, 99.58442372801900433 ) ) ;
#1003 = CARTESIAN_POINT ( 'NONE',  ( -18.67979575497178146, -10.72451020669898902, 81.66557627198103830 ) ) ;
#1002 = CARTESIAN_POINT ( 'NONE',  ( -19.03943276465977164, 0.05219959533909376836, 71.24890960531435269 ) ) ;
#1005 = CARTESIAN_POINT ( 'NONE',  ( 9.474510206698971260, -16.51473224551069308, 67.91557627198102409 ) ) ;
#1004 = CARTESIAN_POINT ( 'NONE',  ( 4.379528057220092307, 16.55341960407617563, 92.29275706135236135 ) ) ;
#1006 = CARTESIAN_POINT ( 'NONE',  ( -0.05219959533936034679, 19.03943276465977164, 67.50109039468566152 ) ) ;
#1007 = CARTESIAN_POINT ( 'NONE',  ( 5.823673210054444382, -21.52544592524334988, 75.20942372801901854 ) ) ;
#1008 = CARTESIAN_POINT ( 'NONE',  ( -15.80617190586745835, -15.72974639402198527, 66.87390960531436690 ) ) ;
#1009 = CARTESIAN_POINT ( 'NONE',  ( 15.72974639402199770, -15.80617190586745480, 23.12390960531436335 ) ) ;
#1010 = CARTESIAN_POINT ( 'NONE',  ( -5.153800228976328057, -19.02544592524343514, 42.29057627198101699 ) ) ;
#1011 = CARTESIAN_POINT ( 'NONE',  ( 0.05219959533934541429, -16.53943276465976808, 105.0010903946856757 ) ) ;
#1012 = CARTESIAN_POINT ( 'NONE',  ( 0.05219959533909260263, 19.03943276465977164, 54.99890960531435979 ) ) ;
#1013 = CARTESIAN_POINT ( 'NONE',  ( 16.53943276465976808, 0.05219959533934440121, 21.25109039468567218 ) ) ;
#1014 = CARTESIAN_POINT ( 'NONE',  ( -3.573655867282028392E-15, 2.428612866367529932E-14, 139.9999999999999716 ) ) ;
#1015 = CARTESIAN_POINT ( 'NONE',  ( -21.52544592524334988, -5.823673210054445271, 108.9594237280190185 ) ) ;
#1016 = CARTESIAN_POINT ( 'NONE',  ( 12.14591786802309770, 12.06949235617756955, 59.37390960531436690 ) ) ;
#1017 = VECTOR ( 'NONE', #142739, 1000.000000000000000 ) ;
#1018 = CARTESIAN_POINT ( 'NONE',  ( -10.72451020669898014, 18.67979575497178502, 100.4155762719810241 ) ) ;
#1019 = CARTESIAN_POINT ( 'NONE',  ( -15.80617190586745835, -15.72974639402198527, 106.8739096053143811 ) ) ;
#1020 = CARTESIAN_POINT ( 'NONE',  ( 17.48853670773245383, -5.747243402303092275, 96.16671299749991420 ) ) ;
#1021 = CARTESIAN_POINT ( 'NONE',  ( -10.72451020669898014, 18.67979575497178502, 50.41557627198103120 ) ) ;
#1022 = CARTESIAN_POINT ( 'NONE',  ( 14.29746914071037800, 8.314922557961029526, 76.66775706135234714 ) ) ;
#1023 = CARTESIAN_POINT ( 'NONE',  ( -14.29746914071049879, 8.314922557960819915, 85.83224293864768129 ) ) ;
#1024 = CARTESIAN_POINT ( 'NONE',  ( -19.02544592524342804, 5.153800228976336051, 46.04057627198101699 ) ) ;
#1025 =( NAMED_UNIT ( * ) PLANE_ANGLE_UNIT ( ) SI_UNIT ( $, .RADIAN. ) );
#1026 = CARTESIAN_POINT ( 'NONE',  ( -10.65638358537376007, -44.90791467878717924, -23.56120423312990297 ) ) ;
#1027 = CARTESIAN_POINT ( 'NONE',  ( 4.379528057220339221, -16.55341960407611168, 22.70724293864769194 ) ) ;
#1028 = CARTESIAN_POINT ( 'NONE',  ( -0.05219959533937732626, 21.53943276465977519, 27.50109039468567929 ) ) ;
#1029 = CARTESIAN_POINT ( 'NONE',  ( -13.97604488694527625, -13.89961937509977652, 91.87390960531432427 ) ) ;
#1030 = CARTESIAN_POINT ( 'NONE',  ( 10.72451020669871369, 18.67979575497193778, 62.08442372801901143 ) ) ;
#1031 = DIRECTION ( 'NONE',  ( 0.000000000000000000, 0.000000000000000000, 1.000000000000000000 ) ) ;
#1032 = CARTESIAN_POINT ( 'NONE',  ( 9.564922557960805705, 16.46253265017160317, 29.58224293864769550 ) ) ;
#1033 = ORIENTED_EDGE ( 'NONE', *, *, #63840, .F. ) ;
#1034 = CARTESIAN_POINT ( 'NONE',  ( 18.67979575497194134, -10.72451020669871369, 60.83442372801901854 ) ) ;
#1036 = CARTESIAN_POINT ( 'NONE',  ( -19.05341960407611168, -5.049401038298163336, 111.4572429386476671 ) ) ;
#1035 = CARTESIAN_POINT ( 'NONE',  ( -19.02544592524342804, 5.153800228976336051, 56.04057627198100988 ) ) ;
#1037 = CARTESIAN_POINT ( 'NONE',  ( 16.46253265017160672, -9.564922557960803928, 93.33224293864769550 ) ) ;
#1038 = CARTESIAN_POINT ( 'NONE',  ( -19.02544592524334988, -5.153800228976617603, 68.95942372801896170 ) ) ;
#1039 = CARTESIAN_POINT ( 'NONE',  ( -10.72451020669870658, -18.67979575497194134, 39.58442372801901143 ) ) ;
#1040 = CARTESIAN_POINT ( 'NONE',  ( -13.97604488694547697, 13.89961937509957934, 103.1260903946856473 ) ) ;
#1041 = CARTESIAN_POINT ( 'NONE',  ( -19.02544592524334988, -5.153800228976617603, 78.95942372801900433 ) ) ;
#1042 = CARTESIAN_POINT ( 'NONE',  ( 19.03943276465977164, -0.05219959533909143690, 43.74890960531435979 ) ) ;
#1043 = CARTESIAN_POINT ( 'NONE',  ( -16.52544592524335698, -4.483927247898792601, 103.9594237280190185 ) ) ;
#1044 = CARTESIAN_POINT ( 'NONE',  ( 9.564922557961047289, -16.46253265017146816, 70.41775706135233293 ) ) ;
#1045 = CARTESIAN_POINT ( 'NONE',  ( -14.29746914071049879, 8.314922557960819915, 25.83224293864769194 ) ) ;
#1046 = CARTESIAN_POINT ( 'NONE',  ( 0.05219959533936267826, -19.03943276465977164, 45.00109039468566863 ) ) ;
#1047 = CARTESIAN_POINT ( 'NONE',  ( 15.80617190586769283, -15.72974639402175789, 105.6260903946856899 ) ) ;
#1048 = CARTESIAN_POINT ( 'NONE',  ( 16.51473224551083163, -9.474510206698727899, 30.83442372801900433 ) ) ;
#1049 = CARTESIAN_POINT ( 'NONE',  ( -16.46253265017160317, 9.564922557960807481, 30.83224293864769550 ) ) ;
#1050 = CARTESIAN_POINT ( 'NONE',  ( -21.55341960407619339, 5.719274019375674811, 93.54275706135234714 ) ) ;
#1051 = CARTESIAN_POINT ( 'NONE',  ( 14.29746914071037800, 8.314922557961029526, 26.66775706135235424 ) ) ;
#1052 = CARTESIAN_POINT ( 'NONE',  ( -5.153800228976328057, -19.02544592524343514, 87.29057627198103830 ) ) ;
#1053 = AXIS2_PLACEMENT_3D ( 'NONE', #11334, #147844, #73005 ) ;
#1054 = CARTESIAN_POINT ( 'NONE',  ( 27.73933785331498214, 9.013057229001095294, 145.9750000027311785 ) ) ;
#1055 = CARTESIAN_POINT ( 'NONE',  ( 19.05341960407611168, 5.049401038298154454, 83.95724293864766707 ) ) ;
#1056 = CARTESIAN_POINT ( 'NONE',  ( -17.05587630539706367, 6.762274262136686254, 100.7418030903728408 ) ) ;
#1057 = CARTESIAN_POINT ( 'NONE',  ( 13.89961937509957401, 13.97604488694547697, 81.87609039468564731 ) ) ;
#1058 = CARTESIAN_POINT ( 'NONE',  ( -9.474510206698964154, 16.51473224551069663, 110.4155762719810383 ) ) ;
#1059 = CARTESIAN_POINT ( 'NONE',  ( -18.67979575497193778, 10.72451020669871902, 98.33442372801901854 ) ) ;
#1060 = CARTESIAN_POINT ( 'NONE',  ( 14.34966873604960469, 8.224510206698951720, 104.1655762719810241 ) ) ;
#1061 = CARTESIAN_POINT ( 'NONE',  ( 20.69372460268722236, -10.84650605405300539, 168.1714143675833668 ) ) ;
#1062 = CARTESIAN_POINT ( 'NONE',  ( 0.05219959533907565091, 21.53943276465977519, 59.99890960531436690 ) ) ;
#1063 = CARTESIAN_POINT ( 'NONE',  ( 10.72451020669898902, -18.67979575497178502, 42.91557627198103120 ) ) ;
#1064 = CARTESIAN_POINT ( 'NONE',  ( -9.564922557960796823, -16.46253265017161027, 22.08224293864768839 ) ) ;
#1065 = CARTESIAN_POINT ( 'NONE',  ( -0.4881926659581863892, -9.021779378622676759, -61.91041879129567604 ) ) ;
#1066 = CARTESIAN_POINT ( 'NONE',  ( -16.46253265017146816, -9.564922557961047289, 54.16775706135234003 ) ) ;
#1067 = CARTESIAN_POINT ( 'NONE',  ( -4.379528057220328563, 16.55341960407611168, 40.20724293864769550 ) ) ;
#1068 = CARTESIAN_POINT ( 'NONE',  ( 5.719274019375991003, -21.55341960407610458, 22.70724293864769194 ) ) ;
#1069 = CARTESIAN_POINT ( 'NONE',  ( -15.72974639402176322, -15.80617190586768395, 74.37609039468568994 ) ) ;
#1070 = CARTESIAN_POINT ( 'NONE',  ( -10.81492255796078084, -18.62759615963271287, 72.08224293864769550 ) ) ;
#1071 = CARTESIAN_POINT ( 'NONE',  ( -18.62759615963255300, -10.81492255796106328, 54.16775706135235424 ) ) ;
#1072 = CARTESIAN_POINT ( 'NONE',  ( -5.823673210054116645, -21.52544592524344225, 97.29057627198105251 ) ) ;
#1073 = CARTESIAN_POINT ( 'NONE',  ( -0.05219959533937732626, 21.53943276465977519, 52.50109039468567573 ) ) ;
#1074 = CARTESIAN_POINT ( 'NONE',  ( -5.153800228976328057, -19.02544592524343514, 32.29057627198102409 ) ) ;
#1075 = CARTESIAN_POINT ( 'NONE',  ( -13.97604488694527625, -13.89961937509977652, 76.87390960531433848 ) ) ;
#1076 = CARTESIAN_POINT ( 'NONE',  ( 0.05219959533934541429, -16.53943276465976808, 85.00109039468568994 ) ) ;
#1077 = CARTESIAN_POINT ( 'NONE',  ( 19.03943276465977164, -0.05219959533909143690, 28.74890960531435624 ) ) ;
#1078 = CARTESIAN_POINT ( 'NONE',  ( -32.23033374730685807, 4.573250637950163622, 89.03582022910542548 ) ) ;
#1079 = CARTESIAN_POINT ( 'NONE',  ( -16.52544592524342804, 4.483927247898546575, 56.04057627198102409 ) ) ;
#1080 = CARTESIAN_POINT ( 'NONE',  ( -12.14591786802326823, 12.06949235617739902, 108.1260903946856757 ) ) ;
#1081 = CARTESIAN_POINT ( 'NONE',  ( -19.02544592524342804, 5.153800228976336051, 71.04057627198099567 ) ) ;
#1082 = CARTESIAN_POINT ( 'NONE',  ( 19.02544592524343514, -5.153800228976328945, 38.54057627198103120 ) ) ;
#1083 = CARTESIAN_POINT ( 'NONE',  ( 5.823673210054125526, 21.52544592524343514, 49.79057627198102409 ) ) ;
#1084 = CARTESIAN_POINT ( 'NONE',  ( 9.474510206698729675, 16.51473224551082808, 42.08442372801900433 ) ) ;
#1086 = CARTESIAN_POINT ( 'NONE',  ( 8.314922557960818139, 14.29746914071049879, 49.58224293864769550 ) ) ;
#1085 = CARTESIAN_POINT ( 'NONE',  ( 2.973862142520697471, -93.04182470242777470, -4.999999999999999112 ) ) ;
#1087 = CARTESIAN_POINT ( 'NONE',  ( 5.823673210054125526, 21.52544592524343514, 29.79057627198102409 ) ) ;
#1088 = CARTESIAN_POINT ( 'NONE',  ( -28.82186960331480208, 9.364793116373830273, 140.1500000054623740 ) ) ;
#1089 = CARTESIAN_POINT ( 'NONE',  ( -16.53943276465976808, -0.05219959533934237506, 68.75109039468568994 ) ) ;
#1090 = CARTESIAN_POINT ( 'NONE',  ( -19.05341960407617563, 5.049401038297882671, 63.54275706135234003 ) ) ;
#1091 = CARTESIAN_POINT ( 'NONE',  ( -16.55341960407611168, -4.379528057220339221, 36.45724293864768839 ) ) ;
#1092 = CARTESIAN_POINT ( 'NONE',  ( 0.000000000000000000, 0.000000000000000000, -64.92279855667830191 ) ) ;
#1093 = CARTESIAN_POINT ( 'NONE',  ( -14.29746914071049879, 8.314922557960819915, 30.83224293864770260 ) ) ;
#1094 = CARTESIAN_POINT ( 'NONE',  ( -16.46253265017160317, 9.564922557960807481, 40.83224293864769550 ) ) ;
#1095 = CARTESIAN_POINT ( 'NONE',  ( 5.049401038298161559, -19.05341960407611168, 62.70724293864769550 ) ) ;
#1096 = CARTESIAN_POINT ( 'NONE',  ( -19.05341960407611168, -5.049401038298163336, 21.45724293864768839 ) ) ;
#1097 = CARTESIAN_POINT ( 'NONE',  ( 21.55341960407619695, -5.719274019375665929, 36.04275706135234714 ) ) ;
#1098 = CARTESIAN_POINT ( 'NONE',  ( 16.46253265017160672, -9.564922557960803928, 58.33224293864769550 ) ) ;
#1099 = CYLINDRICAL_SURFACE ( 'NONE', #19317, 2.649999999999999467 ) ;
#1100 = CARTESIAN_POINT ( 'NONE',  ( 13.97604488694527802, 13.89961937509977652, 44.37390960531435269 ) ) ;
#1101 = CARTESIAN_POINT ( 'NONE',  ( -10.72451020669898014, 18.67979575497178502, 35.41557627198102409 ) ) ;
#1103 = CARTESIAN_POINT ( 'NONE',  ( -19.05341960407611168, -5.049401038298163336, 21.45724293864768839 ) ) ;
#1102 = CARTESIAN_POINT ( 'NONE',  ( 10.81492255796106328, -18.62759615963255655, 60.41775706135235424 ) ) ;
#1104 = CARTESIAN_POINT ( 'NONE',  ( 15.80617190586746368, 15.72974639402197994, 24.37390960531435979 ) ) ;
#1105 = AXIS2_PLACEMENT_3D ( 'NONE', #147719, #164887, #181061 ) ;
#1106 = CARTESIAN_POINT ( 'NONE',  ( 16.52544592524335698, 4.483927247898782831, 96.45942372801901854 ) ) ;
#1107 = EDGE_CURVE ( 'NONE', #17186, #144635, #184276, .T. ) ;
#1108 = CARTESIAN_POINT ( 'NONE',  ( -21.52544592524334988, -5.823673210054445271, 108.9594237280190185 ) ) ;
#1109 = CARTESIAN_POINT ( 'NONE',  ( -12.14591786802326823, 12.06949235617739902, 63.12609039468568994 ) ) ;
#1110 = CARTESIAN_POINT ( 'NONE',  ( -9.474510206698964154, 16.51473224551069663, 110.4155762719810383 ) ) ;
#1111 = CARTESIAN_POINT ( 'NONE',  ( 16.53943276465976808, 0.05219959533934440121, 51.25109039468568994 ) ) ;
#1112 = CARTESIAN_POINT ( 'NONE',  ( 4.379528057220092307, 16.55341960407617563, 32.29275706135235424 ) ) ;
#1113 = CARTESIAN_POINT ( 'NONE',  ( -14.29746914071037622, -8.314922557961029526, 94.16775706135237556 ) ) ;
#1114 = CARTESIAN_POINT ( 'NONE',  ( -18.62759615963255300, -10.81492255796106328, 49.16775706135234003 ) ) ;
#1115 = CARTESIAN_POINT ( 'NONE',  ( 0.05219959533934541429, -16.53943276465976808, 20.00109039468568639 ) ) ;
#1116 = CARTESIAN_POINT ( 'NONE',  ( 18.62759615963271287, -10.81492255796078972, 113.3322429386476955 ) ) ;
#1117 = CARTESIAN_POINT ( 'NONE',  ( 4.379528057220092307, 16.55341960407617563, 27.29275706135234358 ) ) ;
#1118 = CARTESIAN_POINT ( 'NONE',  ( -16.55341960407617563, 4.379528057220093196, 88.54275706135236135 ) ) ;
#1119 = DIRECTION ( 'NONE',  ( -0.8164965809277249242, 0.000000000000000000, 0.5773502691896271743 ) ) ;
#1120 = CARTESIAN_POINT ( 'NONE',  ( -21.53943276465977519, -0.05219959533937600094, 93.75109039468567573 ) ) ;
#1121 = CARTESIAN_POINT ( 'NONE',  ( -9.564922557961040184, 16.46253265017147172, 87.91775706135233293 ) ) ;
#1122 = CARTESIAN_POINT ( 'NONE',  ( 4.379528057220339221, -16.55341960407611168, 62.70724293864769550 ) ) ;
#1123 = CARTESIAN_POINT ( 'NONE',  ( -4.483927247898539470, -16.52544592524342804, 37.29057627198102409 ) ) ;
#1124 = CARTESIAN_POINT ( 'NONE',  ( -12.14591786802309592, -12.06949235617757132, 111.8739096053143669 ) ) ;
#1126 = CARTESIAN_POINT ( 'NONE',  ( 17.12812012977052589, -6.668231424565583154, 56.14051240676855059 ) ) ;
#1125 = CARTESIAN_POINT ( 'NONE',  ( 19.05341960407617918, -5.049401038297876454, 51.04275706135231871 ) ) ;
#1127 = CARTESIAN_POINT ( 'NONE',  ( -18.67979575497193778, 10.72451020669871902, 53.33442372801901854 ) ) ;
#1128 = CARTESIAN_POINT ( 'NONE',  ( 16.46253265017146816, 9.564922557961045513, 106.6677570613523471 ) ) ;
#1129 = DIRECTION ( 'NONE',  ( -0.000000000000000000, 0.000000000000000000, 1.000000000000000000 ) ) ;
#1130 = CARTESIAN_POINT ( 'NONE',  ( -19.02544592524342804, 5.153800228976336051, 101.0405762719810241 ) ) ;
#1131 = CARTESIAN_POINT ( 'NONE',  ( 15.72974639402199770, -15.80617190586745480, 63.12390960531435979 ) ) ;
#1132 = CARTESIAN_POINT ( 'NONE',  ( 0.05219959533936267826, -19.03943276465977164, 100.0010903946856757 ) ) ;
#1133 = CARTESIAN_POINT ( 'NONE',  ( 13.97604488694527802, 13.89961937509977652, 89.37390960531436690 ) ) ;
#1134 = CARTESIAN_POINT ( 'NONE',  ( -18.62759615963270932, 10.81492255796079327, 50.83224293864770971 ) ) ;
#1135 = CARTESIAN_POINT ( 'NONE',  ( -12.06949235617756955, 12.14591786802309770, 110.6239096053143669 ) ) ;
#1136 = CARTESIAN_POINT ( 'NONE',  ( -19.03943276465977164, 0.05219959533909376836, 76.24890960531435269 ) ) ;
#1137 = CARTESIAN_POINT ( 'NONE',  ( 5.049401038298161559, -19.05341960407611168, 32.70724293864768129 ) ) ;
#1138 = CARTESIAN_POINT ( 'NONE',  ( 10.81492255796106328, -18.62759615963255655, 35.41775706135234003 ) ) ;
#1139 = CARTESIAN_POINT ( 'NONE',  ( 21.55341960407619695, -5.719274019375665929, 86.04275706135236135 ) ) ;
#1140 = CARTESIAN_POINT ( 'NONE',  ( 14.34966873604972726, -8.224510206698740333, 95.83442372801903275 ) ) ;
#1141 = CARTESIAN_POINT ( 'NONE',  ( -15.72974639402176322, -15.80617190586768395, 34.37609039468568284 ) ) ;
#1142 = CARTESIAN_POINT ( 'NONE',  ( 5.719274019375673035, 21.55341960407619339, 37.29275706135235424 ) ) ;
#1144 = CARTESIAN_POINT ( 'NONE',  ( -5.049401038298153566, 19.05341960407611168, 75.20724293864769550 ) ) ;
#1143 = CARTESIAN_POINT ( 'NONE',  ( 5.153800228976615827, -19.02544592524334988, 60.20942372801899012 ) ) ;
#1145 = CARTESIAN_POINT ( 'NONE',  ( 18.67979575497194134, -10.72451020669871369, 80.83442372801901854 ) ) ;
#1146 = CARTESIAN_POINT ( 'NONE',  ( 15.80617190586746368, 15.72974639402197994, 89.37390960531435269 ) ) ;
#1147 = CARTESIAN_POINT ( 'NONE',  ( -14.29746914071049879, 8.314922557960819915, 65.83224293864769550 ) ) ;
#1148 = CARTESIAN_POINT ( 'NONE',  ( -5.823673210054431948, 21.52544592524334988, 107.7094237280190328 ) ) ;
#1149 = CARTESIAN_POINT ( 'NONE',  ( -16.53943276465976808, 0.05219959533911058130, 86.24890960531436690 ) ) ;
#1150 = CARTESIAN_POINT ( 'NONE',  ( -13.97604488694527625, -13.89961937509977652, 31.87390960531435979 ) ) ;
#1151 = CARTESIAN_POINT ( 'NONE',  ( 0.05219959533936267826, -19.03943276465977164, 65.00109039468567573 ) ) ;
#1152 = CARTESIAN_POINT ( 'NONE',  ( -12.06949235617756955, 12.14591786802309770, 30.62390960531436335 ) ) ;
#1153 = CARTESIAN_POINT ( 'NONE',  ( -10.81492255796105439, 18.62759615963255655, 92.91775706135236135 ) ) ;
#1154 = CARTESIAN_POINT ( 'NONE',  ( 9.564922557960805705, 16.46253265017160317, 94.58224293864769550 ) ) ;
#1155 = CARTESIAN_POINT ( 'NONE',  ( 9.564922557961047289, -16.46253265017146816, 65.41775706135233293 ) ) ;
#1156 = CARTESIAN_POINT ( 'NONE',  ( 10.81492255796078972, 18.62759615963270932, 64.58224293864769550 ) ) ;
#1157 = CARTESIAN_POINT ( 'NONE',  ( -18.62759615963255300, -10.81492255796106328, 19.16775706135234714 ) ) ;
#1158 = CARTESIAN_POINT ( 'NONE',  ( 19.05341960407617918, -5.049401038297876454, 106.0427570613523471 ) ) ;
#1159 = CARTESIAN_POINT ( 'NONE',  ( 12.14591786802327356, -12.06949235617739191, 85.62609039468568994 ) ) ;
#1161 = CARTESIAN_POINT ( 'NONE',  ( -10.81492255796105439, 18.62759615963255655, 22.91775706135235069 ) ) ;
#1160 = CARTESIAN_POINT ( 'NONE',  ( 16.31925111598459210, 7.325300261831489301, 62.33575461032749132 ) ) ;
#1162 = CARTESIAN_POINT ( 'NONE',  ( -16.53943276465976808, 0.05219959533911058130, 101.2489096053143669 ) ) ;
#1163 = CARTESIAN_POINT ( 'NONE',  ( -36.91746825000000598, 2.428612866367529932E-14, -7.124999997268813168 ) ) ;
#1164 = CARTESIAN_POINT ( 'NONE',  ( -12.14591786802326823, 12.06949235617739902, 43.12609039468568284 ) ) ;
#1165 = CARTESIAN_POINT ( 'NONE',  ( 15.72974639402199770, -15.80617190586745480, 68.12390960531436690 ) ) ;
#1166 = CARTESIAN_POINT ( 'NONE',  ( 14.34966873604972726, -8.224510206698740333, 110.8344237280190043 ) ) ;
#1167 = CARTESIAN_POINT ( 'NONE',  ( -0.05219959533934338120, 16.53943276465976808, 42.50109039468567573 ) ) ;
#1168 = CARTESIAN_POINT ( 'NONE',  ( 16.46253265017160672, -9.564922557960803928, 48.33224293864769550 ) ) ;
#1169 = CARTESIAN_POINT ( 'NONE',  ( 14.29746914071037800, 8.314922557961029526, 81.66775706135236135 ) ) ;
#1170 = CARTESIAN_POINT ( 'NONE',  ( -16.51473224551082808, 9.474510206698731452, 78.33442372801900433 ) ) ;
#1171 = CARTESIAN_POINT ( 'NONE',  ( 18.67979575497178502, 10.72451020669898547, 69.16557627198102409 ) ) ;
#1172 = CARTESIAN_POINT ( 'NONE',  ( 16.52544592524335698, 4.483927247898782831, 91.45942372801901854 ) ) ;
#1173 = CARTESIAN_POINT ( 'NONE',  ( 5.719274019375673035, 21.55341960407619339, 82.29275706135234714 ) ) ;
#1174 = CARTESIAN_POINT ( 'NONE',  ( 15.80617190586746368, 15.72974639402197994, 64.37390960531435269 ) ) ;
#1175 = CARTESIAN_POINT ( 'NONE',  ( -0.05219959533907301413, -21.53943276465977519, 52.49890960531435979 ) ) ;
#1176 = VERTEX_POINT ( 'NONE', #135799 ) ;
#1177 = CARTESIAN_POINT ( 'NONE',  ( -8.314922557961024197, 14.29746914071037800, 77.91775706135231871 ) ) ;
#1178 = CARTESIAN_POINT ( 'NONE',  ( -10.81492255796078084, -18.62759615963271287, 47.08224293864770260 ) ) ;
#1179 = ORIENTED_EDGE ( 'NONE', *, *, #88509, .T. ) ;
#1180 = CARTESIAN_POINT ( 'NONE',  ( -19.02544592524342804, 5.153800228976336051, 116.0405762719810383 ) ) ;
#1181 = DIRECTION ( 'NONE',  ( -0.000000000000000000, -0.000000000000000000, 1.000000000000000000 ) ) ;
#1182 = CARTESIAN_POINT ( 'NONE',  ( -5.153800228976328057, -19.02544592524343514, 22.29057627198102765 ) ) ;
#1183 = CARTESIAN_POINT ( 'NONE',  ( 10.81492255796078972, 18.62759615963270932, 74.58224293864768129 ) ) ;
#1184 = CARTESIAN_POINT ( 'NONE',  ( -16.52544592524335698, -4.483927247898792601, 98.95942372801903275 ) ) ;
#1185 = CARTESIAN_POINT ( 'NONE',  ( 21.52544592524334988, 5.823673210054432836, 51.45942372801901854 ) ) ;
#1186 = CARTESIAN_POINT ( 'NONE',  ( -5.153800228976607833, 19.02544592524334988, 107.7094237280189759 ) ) ;
#1187 = CARTESIAN_POINT ( 'NONE',  ( 12.06949235617757843, -12.14591786802309237, 113.1239096053143953 ) ) ;
#1188 = CARTESIAN_POINT ( 'NONE',  ( 0.05219959533936267826, -19.03943276465977164, 105.0010903946856615 ) ) ;
#1189 = CARTESIAN_POINT ( 'NONE',  ( -5.153800228976328057, -19.02544592524343514, 42.29057627198101699 ) ) ;
#1190 = EDGE_CURVE ( 'NONE', #113441, #194207, #182299, .T. ) ;
#1191 = CARTESIAN_POINT ( 'NONE',  ( -17.81289503416611808, 24.51734667627700404, 143.7000000000000171 ) ) ;
#1192 = CARTESIAN_POINT ( 'NONE',  ( 5.153800228976335163, 19.02544592524342804, 94.79057627198103830 ) ) ;
#1193 = CARTESIAN_POINT ( 'NONE',  ( 12.14591786802327356, -12.06949235617739191, 70.62609039468567573 ) ) ;
#1194 = CARTESIAN_POINT ( 'NONE',  ( -16.46253265017146816, -9.564922557961047289, 84.16775706135233293 ) ) ;
#1195 = CARTESIAN_POINT ( 'NONE',  ( 0.05219959533936267826, -19.03943276465977164, 20.00109039468567218 ) ) ;
#1196 = CARTESIAN_POINT ( 'NONE',  ( 5.823673210054125526, 21.52544592524343514, 59.79057627198103120 ) ) ;
#1197 = CARTESIAN_POINT ( 'NONE',  ( 12.06949235617739724, 12.14591786802326823, 81.87609039468568994 ) ) ;
#1198 = AXIS2_PLACEMENT_3D ( 'NONE', #589, #95589, #143077 ) ;
#1199 = CARTESIAN_POINT ( 'NONE',  ( 19.02544592524334988, 5.153800228976608722, 81.45942372801897591 ) ) ;
#1200 = CARTESIAN_POINT ( 'NONE',  ( -0.05219959533909027116, -19.03943276465977164, 37.49890960531436690 ) ) ;
#1201 = CARTESIAN_POINT ( 'NONE',  ( 5.049401038298161559, -19.05341960407611168, 97.70724293864766707 ) ) ;
#1202 = CARTESIAN_POINT ( 'NONE',  ( -18.62759615963255300, -10.81492255796106328, 54.16775706135235424 ) ) ;
#1203 = CARTESIAN_POINT ( 'NONE',  ( -16.51473224551069308, -9.474510206698971260, 46.66557627198102409 ) ) ;
#1204 = CARTESIAN_POINT ( 'NONE',  ( 24.18299921989822820, -12.77492350451709235, 169.7822198539309966 ) ) ;
#1205 = CARTESIAN_POINT ( 'NONE',  ( -0.05219959533909027116, -19.03943276465977164, 112.4989096053143669 ) ) ;
#1206 = CARTESIAN_POINT ( 'NONE',  ( -14.29746914071049879, 8.314922557960819915, 70.83224293864770971 ) ) ;
#1207 = CARTESIAN_POINT ( 'NONE',  ( 5.823673210054125526, 21.52544592524343514, 64.79057627198103830 ) ) ;
#1208 = CARTESIAN_POINT ( 'NONE',  ( -193.3062444957834884, -155.7167183371838064, -4.999999999999999112 ) ) ;
#1209 = CARTESIAN_POINT ( 'NONE',  ( 5.049401038297881783, 19.05341960407617563, 42.29275706135234003 ) ) ;
#1210 = CARTESIAN_POINT ( 'NONE',  ( 21.34799762026584702, -10.44447989802409893, 170.3878604776606096 ) ) ;
#1212 = CARTESIAN_POINT ( 'NONE',  ( -19.05341960407611168, -5.049401038298163336, 76.45724293864769550 ) ) ;
#1211 = CARTESIAN_POINT ( 'NONE',  ( 19.05341960407611168, 5.049401038298154454, 58.95724293864768129 ) ) ;
#1213 = CARTESIAN_POINT ( 'NONE',  ( 8.224510206698742110, 14.34966873604972548, 52.08442372801901854 ) ) ;
#1214 = CARTESIAN_POINT ( 'NONE',  ( -24.74823625077143774, 6.005039613785521091, 168.8763313249075964 ) ) ;
#1215 = CARTESIAN_POINT ( 'NONE',  ( 26.46959431505284499, -27.26463967846488146, -15.00000000000000178 ) ) ;
#1216 = CARTESIAN_POINT ( 'NONE',  ( -16.53943276465976808, -0.05219959533934237506, 83.75109039468568994 ) ) ;
#1217 = CARTESIAN_POINT ( 'NONE',  ( -1.227931366032057224E-14, -24.30000000000003268, -54.21489346206828230 ) ) ;
#1218 = CARTESIAN_POINT ( 'NONE',  ( -8.224510206698735004, -14.34966873604973081, 84.58442372801903275 ) ) ;
#1219 = CARTESIAN_POINT ( 'NONE',  ( 12.14591786802327356, -12.06949235617739191, 50.62609039468568994 ) ) ;
#1220 = CARTESIAN_POINT ( 'NONE',  ( -5.049401038297874678, -19.05341960407617918, 29.79275706135232227 ) ) ;
#1222 = CARTESIAN_POINT ( 'NONE',  ( 17.61359324038537721, -16.30702395557608142, -56.99769869564799052 ) ) ;
#1221 = CARTESIAN_POINT ( 'NONE',  ( 19.03943276465977164, -0.05219959533909143690, 48.74890960531435979 ) ) ;
#1223 = CARTESIAN_POINT ( 'NONE',  ( 0.05219959533937995610, -21.53943276465977519, 55.00109039468568284 ) ) ;
#1224 = CARTESIAN_POINT ( 'NONE',  ( 13.97604488694548053, -13.89961937509957401, 55.62609039468566863 ) ) ;
#1225 = CARTESIAN_POINT ( 'NONE',  ( -5.719274019375665041, -21.55341960407619695, 109.7927570613523613 ) ) ;
#1226 = CARTESIAN_POINT ( 'NONE',  ( -0.05219959533909027116, -19.03943276465977164, 32.49890960531435979 ) ) ;
#1227 = CARTESIAN_POINT ( 'NONE',  ( -17.26089242801066348, 17.10449713765558499, -56.77278709839601589 ) ) ;
#1228 = CARTESIAN_POINT ( 'NONE',  ( 0.05219959533907565091, 21.53943276465977519, 69.99890960531435269 ) ) ;
#1229 = CARTESIAN_POINT ( 'NONE',  ( 9.474510206698971260, -16.51473224551069308, 112.9155762719810383 ) ) ;
#1230 = CARTESIAN_POINT ( 'NONE',  ( 8.224510206698953496, -14.34966873604960469, 107.9155762719810241 ) ) ;
#1231 = CARTESIAN_POINT ( 'NONE',  ( 8.224510206698742110, 14.34966873604972548, 37.08442372801901143 ) ) ;
#1232 = CARTESIAN_POINT ( 'NONE',  ( -8.314922557960811034, -14.29746914071050412, 32.08224293864769550 ) ) ;
#1233 = VERTEX_POINT ( 'NONE', #44770 ) ;
#1234 = CARTESIAN_POINT ( 'NONE',  ( -21.53943276465977519, 0.05219959533907696930, 116.2489096053143669 ) ) ;
#1236 = CARTESIAN_POINT ( 'NONE',  ( 19.05341960407611168, 5.049401038298154454, 113.9572429386477097 ) ) ;
#1235 = CARTESIAN_POINT ( 'NONE',  ( -4.483927247898539470, -16.52544592524342804, 42.29057627198103120 ) ) ;
#1237 = CARTESIAN_POINT ( 'NONE',  ( 0.05219959533936267826, -19.03943276465977164, 110.0010903946856757 ) ) ;
#1238 = CARTESIAN_POINT ( 'NONE',  ( -5.153800228976607833, 19.02544592524334988, 22.70942372801899012 ) ) ;
#1239 = CARTESIAN_POINT ( 'NONE',  ( -12.06949235617756955, 12.14591786802309770, 30.62390960531436335 ) ) ;
#1240 = CARTESIAN_POINT ( 'NONE',  ( 21.52544592524344225, -5.823673210054117533, 103.5405762719810383 ) ) ;
#1242 = CARTESIAN_POINT ( 'NONE',  ( -0.05219959533907301413, -21.53943276465977519, 62.49890960531436690 ) ) ;
#1241 = DIRECTION ( 'NONE',  ( 0.000000000000000000, 0.000000000000000000, -1.000000000000000000 ) ) ;
#1243 = CARTESIAN_POINT ( 'NONE',  ( -5.049401038298153566, 19.05341960407611168, 75.20724293864769550 ) ) ;
#1244 = CARTESIAN_POINT ( 'NONE',  ( 8.314922557960818139, 14.29746914071049879, 54.58224293864769550 ) ) ;
#1245 = CARTESIAN_POINT ( 'NONE',  ( 5.153800228976335163, 19.02544592524342804, 84.79057627198099567 ) ) ;
#1246 = DIRECTION ( 'NONE',  ( 0.000000000000000000, 0.000000000000000000, -1.000000000000000000 ) ) ;
#1247 = CARTESIAN_POINT ( 'NONE',  ( -19.02544592524334988, -5.153800228976617603, 58.95942372801900433 ) ) ;
#1248 = CARTESIAN_POINT ( 'NONE',  ( 0.05219959533907565091, 21.53943276465977519, 99.99890960531436690 ) ) ;
#1249 = CARTESIAN_POINT ( 'NONE',  ( 14.29746914071049879, -8.314922557960816363, 98.33224293864769550 ) ) ;
#1250 = AXIS2_PLACEMENT_3D ( 'NONE', #88283, #13443, #89288 ) ;
#1251 =( BOUNDED_CURVE ( )  B_SPLINE_CURVE ( 3, ( #125567, #152909, #47741, #154906 ),
 .UNSPECIFIED., .F., .T. ) 
 B_SPLINE_CURVE_WITH_KNOTS ( ( 4, 4 ),
 ( 2.008945357379067431, 2.115944711806982514 ),
 .UNSPECIFIED. ) 
 CURVE ( )  GEOMETRIC_REPRESENTATION_ITEM ( )  RATIONAL_B_SPLINE_CURVE ( ( 1.000000000000000000, 0.9990461557208837329, 0.9990461557208837329, 1.000000000000000000 ) ) 
 REPRESENTATION_ITEM ( '' )  );
#1252 = CARTESIAN_POINT ( 'NONE',  ( 0.05219959533937995610, -21.53943276465977519, 55.00109039468568284 ) ) ;
#1253 = CARTESIAN_POINT ( 'NONE',  ( 22.44159573604009594, -16.30477369853687364, 148.1750000027311671 ) ) ;
#1254 = CARTESIAN_POINT ( 'NONE',  ( 4.379528057220339221, -16.55341960407611168, 27.70724293864769905 ) ) ;
#1255 = CARTESIAN_POINT ( 'NONE',  ( -9.474510206698964154, 16.51473224551069663, 35.41557627198102409 ) ) ;
#1256 = CARTESIAN_POINT ( 'NONE',  ( 16.51473224551069308, 9.474510206698969483, 99.16557627198102409 ) ) ;
#1257 = CARTESIAN_POINT ( 'NONE',  ( -10.81492255796078084, -18.62759615963271287, 67.08224293864770971 ) ) ;
#1258 = CARTESIAN_POINT ( 'NONE',  ( -27.73933785331498925, -9.013057229001049109, 140.9750000027311501 ) ) ;
#1259 = CARTESIAN_POINT ( 'NONE',  ( -0.05219959533909027116, -19.03943276465977164, 27.49890960531435624 ) ) ;
#1260 = CARTESIAN_POINT ( 'NONE',  ( 15.80617190586746368, 15.72974639402197994, 54.37390960531435979 ) ) ;
#1261 = CARTESIAN_POINT ( 'NONE',  ( 18.67979575497194134, -10.72451020669871369, 70.83442372801901854 ) ) ;
#1263 = CARTESIAN_POINT ( 'NONE',  ( 16.53943276465976808, 0.05219959533934440121, 76.25109039468568994 ) ) ;
#1262 = CARTESIAN_POINT ( 'NONE',  ( 17.93416671128860784, -36.08982269496112139, -18.53391066944393728 ) ) ;
#1264 = CARTESIAN_POINT ( 'NONE',  ( -9.564922557960796823, -16.46253265017161027, 57.08224293864769550 ) ) ;
#1265 = CARTESIAN_POINT ( 'NONE',  ( 13.97604488694527802, 13.89961937509977652, 59.37390960531434558 ) ) ;
#1266 = ORIENTED_EDGE ( 'NONE', *, *, #147318, .T. ) ;
#1267 = CARTESIAN_POINT ( 'NONE',  ( 13.89961937509957401, 13.97604488694547697, 21.87609039468566152 ) ) ;
#1268 = CARTESIAN_POINT ( 'NONE',  ( 16.53943276465976808, 0.05219959533934440121, 81.25109039468568994 ) ) ;
#1269 = CARTESIAN_POINT ( 'NONE',  ( 10.72451020669871369, 18.67979575497193778, 102.0844237280190185 ) ) ;
#1270 = CARTESIAN_POINT ( 'NONE',  ( 13.89961937509977652, -13.97604488694527269, 73.12390960531436690 ) ) ;
#1271 = CARTESIAN_POINT ( 'NONE',  ( -10.72451020669898014, 18.67979575497178502, 40.41557627198103120 ) ) ;
#1272 = CARTESIAN_POINT ( 'NONE',  ( -19.03943276465977164, -0.05219959533935918106, 108.7510903946856615 ) ) ;
#1273 = CARTESIAN_POINT ( 'NONE',  ( -10.72451020669870658, -18.67979575497194134, 79.58442372801903275 ) ) ;
#1274 = CARTESIAN_POINT ( 'NONE',  ( -8.314922557961024197, 14.29746914071037800, 47.91775706135234714 ) ) ;
#1275 = CARTESIAN_POINT ( 'NONE',  ( 15.80617190586746368, 15.72974639402197994, 94.37390960531436690 ) ) ;
#1276 = CARTESIAN_POINT ( 'NONE',  ( -19.03943276465977164, -0.05219959533935918106, 113.7510903946856757 ) ) ;
#1277 = CARTESIAN_POINT ( 'NONE',  ( -5.049401038298153566, 19.05341960407611168, 80.20724293864769550 ) ) ;
#1278 = CARTESIAN_POINT ( 'NONE',  ( 9.474510206698729675, 16.51473224551082808, 112.0844237280190043 ) ) ;
#1279 = CARTESIAN_POINT ( 'NONE',  ( 19.03943276465977164, -0.05219959533909143690, 43.74890960531435979 ) ) ;
#1280 = VECTOR ( 'NONE', #85682, 1000.000000000000000 ) ;
#1281 = CARTESIAN_POINT ( 'NONE',  ( 19.03943276465977164, 0.05219959533936151252, 111.2510903946856757 ) ) ;
#1282 = CARTESIAN_POINT ( 'NONE',  ( -12.14591786802309592, -12.06949235617757132, 71.87390960531438111 ) ) ;
#1283 = CARTESIAN_POINT ( 'NONE',  ( 16.55341960407618274, -4.379528057220086978, 71.04275706135234714 ) ) ;
#1285 = CARTESIAN_POINT ( 'NONE',  ( 13.89961937509977652, -13.97604488694527269, 53.12390960531434558 ) ) ;
#1284 = CARTESIAN_POINT ( 'NONE',  ( -10.81492255796105439, 18.62759615963255655, 27.91775706135234358 ) ) ;
#1286 = CARTESIAN_POINT ( 'NONE',  ( 0.05219959533909260263, 19.03943276465977164, 69.99890960531435269 ) ) ;
#1287 = CARTESIAN_POINT ( 'NONE',  ( 4.483927247898790824, -16.52544592524335698, 75.20942372801901854 ) ) ;
#1288 = CARTESIAN_POINT ( 'NONE',  ( -17.50000000000000711, -5.499999999999944045, 81.28230962303565832 ) ) ;
#1289 = ORIENTED_EDGE ( 'NONE', *, *, #38432, .T. ) ;
#1290 = CARTESIAN_POINT ( 'NONE',  ( -19.02544592524334988, -5.153800228976617603, 23.95942372801900078 ) ) ;
#1291 = CARTESIAN_POINT ( 'NONE',  ( 19.03943276465977164, -0.05219959533909143690, 33.74890960531435979 ) ) ;
#1293 = ORIENTED_EDGE ( 'NONE', *, *, #171007, .T. ) ;
#1292 = CARTESIAN_POINT ( 'NONE',  ( 17.50000000000000000, 5.499999999999992895, 66.70309617465828467 ) ) ;
#1294 = CARTESIAN_POINT ( 'NONE',  ( -16.55341960407617563, 4.379528057220093196, 28.54275706135234358 ) ) ;
#1296 = CARTESIAN_POINT ( 'NONE',  ( -8.314922557961024197, 14.29746914071037800, 37.91775706135235424 ) ) ;
#1295 = CARTESIAN_POINT ( 'NONE',  ( -19.05341960407617563, 5.049401038297882671, 58.54275706135234003 ) ) ;
#1297 = CARTESIAN_POINT ( 'NONE',  ( 5.049401038298161559, -19.05341960407611168, 37.70724293864768839 ) ) ;
#1298 = CARTESIAN_POINT ( 'NONE',  ( 19.02544592524343514, -5.153800228976328945, 108.5405762719810383 ) ) ;
#1299 = CARTESIAN_POINT ( 'NONE',  ( 13.97604488694527802, 13.89961937509977652, 59.37390960531434558 ) ) ;
#1300 = CARTESIAN_POINT ( 'NONE',  ( 15.80617190586746368, 15.72974639402197994, 94.37390960531436690 ) ) ;
#1302 = DIRECTION ( 'NONE',  ( 0.000000000000000000, 0.000000000000000000, 1.000000000000000000 ) ) ;
#1301 = CARTESIAN_POINT ( 'NONE',  ( 9.474510206698971260, -16.51473224551069308, 87.91557627198102409 ) ) ;
#1303 = CARTESIAN_POINT ( 'NONE',  ( 19.02544592524343514, -5.153800228976328945, 68.54057627198103830 ) ) ;
#1305 = CARTESIAN_POINT ( 'NONE',  ( 1.784210473542230573E-15, -29.16686587814331588, 147.8750000027311273 ) ) ;
#1304 = CARTESIAN_POINT ( 'NONE',  ( 14.34966873604972726, -8.224510206698740333, 110.8344237280190043 ) ) ;
#1306 = CARTESIAN_POINT ( 'NONE',  ( -16.46253265017146816, -9.564922557961047289, 99.16775706135233293 ) ) ;
#1307 = EDGE_CURVE ( 'NONE', #113002, #29646, #193703, .T. ) ;
#1308 = CARTESIAN_POINT ( 'NONE',  ( 9.474510206698729675, 16.51473224551082808, 22.08442372801899722 ) ) ;
#1309 = CARTESIAN_POINT ( 'NONE',  ( 4.379528057220339221, -16.55341960407611168, 62.70724293864769550 ) ) ;
#1310 = CARTESIAN_POINT ( 'NONE',  ( 18.67979575497194134, -10.72451020669871369, 95.83442372801903275 ) ) ;
#1311 = CARTESIAN_POINT ( 'NONE',  ( 16.51473224551069308, 9.474510206698969483, 44.16557627198103120 ) ) ;
#1313 = CARTESIAN_POINT ( 'NONE',  ( -15.72974639402176322, -15.80617190586768395, 84.37609039468570415 ) ) ;
#1312 = CARTESIAN_POINT ( 'NONE',  ( 4.379528057220339221, -16.55341960407611168, 27.70724293864769905 ) ) ;
#1314 = CARTESIAN_POINT ( 'NONE',  ( -19.02544592524342804, 5.153800228976336051, 81.04057627198103830 ) ) ;
#1315 = CARTESIAN_POINT ( 'NONE',  ( 19.05341960407611168, 5.049401038298154454, 93.95724293864769550 ) ) ;
#1316 = CARTESIAN_POINT ( 'NONE',  ( 8.314922557960818139, 14.29746914071049879, 89.58224293864768129 ) ) ;
#1317 = CARTESIAN_POINT ( 'NONE',  ( -8.314922557960811034, -14.29746914071050412, 77.08224293864769550 ) ) ;
#1318 = CARTESIAN_POINT ( 'NONE',  ( -15.72974639402197994, 15.80617190586746368, 85.62390960531436690 ) ) ;
#1319 = CARTESIAN_POINT ( 'NONE',  ( 13.89961937509977652, -13.97604488694527269, 78.12390960531433848 ) ) ;
#1320 = CARTESIAN_POINT ( 'NONE',  ( 18.67979575497178502, 10.72451020669898547, 79.16557627198103830 ) ) ;
#1321 = CARTESIAN_POINT ( 'NONE',  ( -13.97604488694547697, 13.89961937509957934, 73.12609039468568994 ) ) ;
#1323 = CARTESIAN_POINT ( 'NONE',  ( -14.34966873604960291, -8.224510206698953496, 86.66557627198102409 ) ) ;
#1322 = FACE_OUTER_BOUND ( 'NONE', #192429, .T. ) ;
#1324 = CARTESIAN_POINT ( 'NONE',  ( 5.049401038298161559, -19.05341960407611168, 62.70724293864769550 ) ) ;
#1325 = CARTESIAN_POINT ( 'NONE',  ( 21.53943276465977519, -0.05219959533907433946, 63.74890960531435979 ) ) ;
#1326 = CARTESIAN_POINT ( 'NONE',  ( -25.66012929990208136, -7.783344152590475851, 170.2244316400881701 ) ) ;
#1328 =( LENGTH_UNIT ( ) NAMED_UNIT ( * ) SI_UNIT ( .MILLI., .METRE. ) );
#1327 = CARTESIAN_POINT ( 'NONE',  ( -12.14591786802309592, -12.06949235617757132, 21.87390960531436690 ) ) ;
#1329 = CARTESIAN_POINT ( 'NONE',  ( 5.049401038297881783, 19.05341960407617563, 112.2927570613523471 ) ) ;
#1330 = CARTESIAN_POINT ( 'NONE',  ( -4.483927247898539470, -16.52544592524342804, 82.29057627198103830 ) ) ;
#1331 = CARTESIAN_POINT ( 'NONE',  ( -19.35543954521080323, -5.499999999999531042, 94.58901960356449479 ) ) ;
#1332 = CARTESIAN_POINT ( 'NONE',  ( -16.46253265017160317, 9.564922557960807481, 70.83224293864770971 ) ) ;
#1333 = CARTESIAN_POINT ( 'NONE',  ( 19.02544592524343514, -5.153800228976328945, 38.54057627198103120 ) ) ;
#1334 = CARTESIAN_POINT ( 'NONE',  ( -8.314922557960811034, -14.29746914071050412, 72.08224293864769550 ) ) ;
#1335 = CARTESIAN_POINT ( 'NONE',  ( -19.02544592524342804, 5.153800228976336051, 101.0405762719810241 ) ) ;
#1337 = CARTESIAN_POINT ( 'NONE',  ( -9.564922557960796823, -16.46253265017161027, 82.08224293864768129 ) ) ;
#1336 = CARTESIAN_POINT ( 'NONE',  ( -13.89961937509957401, -13.97604488694547875, 84.37609039468567573 ) ) ;
#1338 = CARTESIAN_POINT ( 'NONE',  ( -19.03943276465977164, 0.05219959533909376836, 86.24890960531436690 ) ) ;
#1339 = CARTESIAN_POINT ( 'NONE',  ( 5.823673210054125526, 21.52544592524343514, 79.79057627198102409 ) ) ;
#1340 = CARTESIAN_POINT ( 'NONE',  ( -4.483927247898782831, 16.52544592524335698, 67.70942372801901854 ) ) ;
#1341 = CARTESIAN_POINT ( 'NONE',  ( 13.89961937509957579, 13.97604488694547520, 111.8760903946856757 ) ) ;
#1342 = CARTESIAN_POINT ( 'NONE',  ( 19.05341960407611168, 5.049401038298154454, 68.95724293864769550 ) ) ;
#1343 = CARTESIAN_POINT ( 'NONE',  ( -21.55341960407610458, -5.719274019375992779, 66.45724293864768129 ) ) ;
#1344 = CARTESIAN_POINT ( 'NONE',  ( 13.89961937509957401, 13.97604488694547697, 91.87609039468567573 ) ) ;
#1346 = CARTESIAN_POINT ( 'NONE',  ( 21.52544592524334988, 5.823673210054432836, 46.45942372801901854 ) ) ;
#1345 = CARTESIAN_POINT ( 'NONE',  ( 8.314922557960818139, 14.29746914071049879, 44.58224293864769550 ) ) ;
#1347 = EDGE_CURVE ( 'NONE', #15917, #80087, #46585, .T. ) ;
#1348 = LINE ( 'NONE', #110523, #66983 ) ;
#1350 = CARTESIAN_POINT ( 'NONE',  ( 16.46253265017160672, -9.564922557960803928, 103.3322429386476955 ) ) ;
#1349 = CARTESIAN_POINT ( 'NONE',  ( -14.34966873604972548, 8.224510206698743886, 73.33442372801901854 ) ) ;
#1351 = LINE ( 'NONE', #17535, #30677 ) ;
#1352 = FACE_OUTER_BOUND ( 'NONE', #80306, .T. ) ;
#1353 = CARTESIAN_POINT ( 'NONE',  ( -16.53943276465976808, -0.05219959533934237506, 88.75109039468567573 ) ) ;
#1354 = CARTESIAN_POINT ( 'NONE',  ( 8.314922557961029526, -14.29746914071037800, 45.41775706135234003 ) ) ;
#1355 = CARTESIAN_POINT ( 'NONE',  ( 19.03943276465977164, -0.05219959533909143690, 63.74890960531435979 ) ) ;
#1356 = CARTESIAN_POINT ( 'NONE',  ( 0.05219959533909260263, 19.03943276465977164, 59.99890960531436690 ) ) ;
#1357 = CARTESIAN_POINT ( 'NONE',  ( -15.80617190586768217, 15.72974639402176855, 53.12609039468568284 ) ) ;
#1358 = CARTESIAN_POINT ( 'NONE',  ( 4.379528057220092307, 16.55341960407617563, 62.29275706135236845 ) ) ;
#1359 = CARTESIAN_POINT ( 'NONE',  ( -16.55341960407611168, -4.379528057220339221, 31.45724293864769550 ) ) ;
#1360 = CARTESIAN_POINT ( 'NONE',  ( -16.46253265017160317, 9.564922557960807481, 35.83224293864768839 ) ) ;
#1361 = CARTESIAN_POINT ( 'NONE',  ( 19.02544592524343514, -5.153800228976328945, 28.54057627198102409 ) ) ;
#1362 = CARTESIAN_POINT ( 'NONE',  ( -12.14591786802326823, 12.06949235617739902, 28.12609039468568284 ) ) ;
#1363 = CARTESIAN_POINT ( 'NONE',  ( 5.049401038297881783, 19.05341960407617563, 87.29275706135234714 ) ) ;
#1364 = CARTESIAN_POINT ( 'NONE',  ( 8.224510206698953496, -14.34966873604960469, 82.91557627198103830 ) ) ;
#1365 = CARTESIAN_POINT ( 'NONE',  ( -0.05219959533909027116, -19.03943276465977164, 52.49890960531436690 ) ) ;
#1367 = CARTESIAN_POINT ( 'NONE',  ( 0.3535533905935857035, 30.00000000000000000, 5.353553390593269512 ) ) ;
#1366 = CARTESIAN_POINT ( 'NONE',  ( -13.89961937509957401, -13.97604488694547875, 84.37609039468567573 ) ) ;
#1368 = CARTESIAN_POINT ( 'NONE',  ( 21.52544592524334988, 5.823673210054432836, 91.45942372801901854 ) ) ;
#1369 = CARTESIAN_POINT ( 'NONE',  ( 8.224510206698742110, 14.34966873604972548, 52.08442372801901854 ) ) ;
#1370 = PLANE ( 'NONE',  #27795 ) ;
#1371 = CARTESIAN_POINT ( 'NONE',  ( 10.72451020669898902, -18.67979575497178502, 47.91557627198102409 ) ) ;
#1372 = CARTESIAN_POINT ( 'NONE',  ( -8.224510206698735004, -14.34966873604973081, 44.58442372801901854 ) ) ;
#1373 = CARTESIAN_POINT ( 'NONE',  ( -0.05219959533909027116, -19.03943276465977164, 32.49890960531435979 ) ) ;
#1374 = CARTESIAN_POINT ( 'NONE',  ( 16.46253265017146816, 9.564922557961045513, 31.66775706135232937 ) ) ;
#1375 = CARTESIAN_POINT ( 'NONE',  ( 13.89961937509977652, -13.97604488694527269, 73.12390960531436690 ) ) ;
#1376 = CARTESIAN_POINT ( 'NONE',  ( 17.50000000000000000, -5.499999999999992895, 66.21769037696435589 ) ) ;
#1377 = CARTESIAN_POINT ( 'NONE',  ( 19.02544592524343514, -5.153800228976328945, 58.54057627198102409 ) ) ;
#1378 = CARTESIAN_POINT ( 'NONE',  ( -20.01995586163601715, -21.79717389941245287, -51.90954606063881016 ) ) ;
#1379 = CARTESIAN_POINT ( 'NONE',  ( 19.05341960407611168, 5.049401038298154454, 73.95724293864768129 ) ) ;
#1380 = CARTESIAN_POINT ( 'NONE',  ( 17.50000000000014921, -3.292511757969696973, 112.5652027021053669 ) ) ;
#1381 = CARTESIAN_POINT ( 'NONE',  ( -16.46253265017146816, -9.564922557961047289, 29.16775706135232937 ) ) ;
#1382 = CARTESIAN_POINT ( 'NONE',  ( -13.89961937509957401, -13.97604488694547875, 19.37609039468566507 ) ) ;
#1383 = CARTESIAN_POINT ( 'NONE',  ( -8.314922557960811034, -14.29746914071050412, 32.08224293864769550 ) ) ;
#1384 = CARTESIAN_POINT ( 'NONE',  ( 13.89961937509977652, -13.97604488694527269, 48.12390960531435979 ) ) ;
#1385 = CARTESIAN_POINT ( 'NONE',  ( -9.564922557960796823, -16.46253265017161027, 107.0822429386476955 ) ) ;
#1386 = CARTESIAN_POINT ( 'NONE',  ( 15.72974639402176855, 15.80617190586768217, 66.87609039468568994 ) ) ;
#1387 = CARTESIAN_POINT ( 'NONE',  ( 0.05219959533909260263, 19.03943276465977164, 49.99890960531435979 ) ) ;
#1388 = CARTESIAN_POINT ( 'NONE',  ( -15.72974639402176322, -15.80617190586768395, 74.37609039468568994 ) ) ;
#1389 = CARTESIAN_POINT ( 'NONE',  ( -10.81492255796078084, -18.62759615963271287, 27.08224293864769550 ) ) ;
#1390 = CARTESIAN_POINT ( 'NONE',  ( 16.51473224551069308, 9.474510206698969483, 34.16557627198102409 ) ) ;
#1391 = CARTESIAN_POINT ( 'NONE',  ( -15.72974639402176322, -15.80617190586768395, 29.37609039468568284 ) ) ;
#1392 = CARTESIAN_POINT ( 'NONE',  ( 0.05219959533936267826, -19.03943276465977164, 50.00109039468566863 ) ) ;
#1393 = CARTESIAN_POINT ( 'NONE',  ( 16.51473224551069308, 9.474510206698969483, 34.16557627198102409 ) ) ;
#1394 = CARTESIAN_POINT ( 'NONE',  ( -16.46253265017160317, 9.564922557960807481, 80.83224293864769550 ) ) ;
#1396 = AXIS2_PLACEMENT_3D ( 'NONE', #152271, #151292, #11796 ) ;
#1395 = CARTESIAN_POINT ( 'NONE',  ( 16.55341960407618274, -4.379528057220086978, 21.04275706135234714 ) ) ;
#1397 = CARTESIAN_POINT ( 'NONE',  ( 12.14591786802309770, 12.06949235617756955, 69.37390960531436690 ) ) ;
#1398 = CARTESIAN_POINT ( 'NONE',  ( -21.53943276465977519, 0.05219959533907696930, 36.24890960531435979 ) ) ;
#1399 = CARTESIAN_POINT ( 'NONE',  ( 19.05341960407617918, -5.049401038297876454, 106.0427570613523471 ) ) ;
#1400 = CARTESIAN_POINT ( 'NONE',  ( 5.823673210054125526, 21.52544592524343514, 104.7905762719810241 ) ) ;
#1401 = CARTESIAN_POINT ( 'NONE',  ( 18.62759615963255655, 10.81492255796105972, 56.66775706135235424 ) ) ;
#1403 = CARTESIAN_POINT ( 'NONE',  ( -0.05219959533934338120, 16.53943276465976808, 57.50109039468568994 ) ) ;
#1402 = B_SPLINE_CURVE_WITH_KNOTS ( 'NONE', 3,
 ( #110750, #139103, #2578, #64258, #187623, #33920, #577, #123917, #81380, #159229, #23738, #191575, #192587, #22735, #98550, #160244, #99559, #144069, #20724, #65241 ),
 .UNSPECIFIED., .F., .F.,
 ( 4, 2, 2, 2, 2, 2, 2, 2, 2, 4 ),
 ( 0.004000878361811950439, 0.004499404418915936912, 0.004997930476019924254, 0.005496456533123910727, 0.005994982590227897201, 0.006244245618779890872, 0.006493508647331884542, 0.006992034704435875353, 0.007490560761539866164, 0.007989086818643856974 ),
 .UNSPECIFIED. ) ;
#1404 = CARTESIAN_POINT ( 'NONE',  ( 16.53943276465976808, 0.05219959533934440121, 56.25109039468568284 ) ) ;
#1405 = CARTESIAN_POINT ( 'NONE',  ( 19.03943276465977164, -0.05219959533909143690, 53.74890960531436690 ) ) ;
#1406 = CARTESIAN_POINT ( 'NONE',  ( 12.14591786802327356, -12.06949235617739191, 85.62609039468568994 ) ) ;
#1407 = CARTESIAN_POINT ( 'NONE',  ( -18.62759615963270932, 10.81492255796079327, 110.8322429386476955 ) ) ;
#1408 = CARTESIAN_POINT ( 'NONE',  ( -8.314922557960811034, -14.29746914071050412, 47.08224293864770260 ) ) ;
#1409 = CARTESIAN_POINT ( 'NONE',  ( 5.153800228976335163, 19.02544592524342804, 84.79057627198099567 ) ) ;
#1410 = CARTESIAN_POINT ( 'NONE',  ( -12.06949235617739369, -12.14591786802326823, 69.37609039468567573 ) ) ;
#1411 = CARTESIAN_POINT ( 'NONE',  ( 15.72974639402176855, 15.80617190586768217, 46.87609039468568994 ) ) ;
#1412 = CARTESIAN_POINT ( 'NONE',  ( -5.153800228976607833, 19.02544592524334988, 107.7094237280189759 ) ) ;
#1413 = CARTESIAN_POINT ( 'NONE',  ( 10.81492255796106328, -18.62759615963255655, 20.41775706135234714 ) ) ;
#1414 = CARTESIAN_POINT ( 'NONE',  ( -0.05219959533910754901, -16.53943276465976808, 47.49890960531435979 ) ) ;
#1415 = VERTEX_POINT ( 'NONE', #56964 ) ;
#1416 = CARTESIAN_POINT ( 'NONE',  ( -17.49999999999999645, 5.499999999999992895, 73.71769037696435589 ) ) ;
#1417 = CARTESIAN_POINT ( 'NONE',  ( -18.67979575497178146, -10.72451020669898902, 91.66557627198103830 ) ) ;
#1418 = CARTESIAN_POINT ( 'NONE',  ( -12.14591786802309592, -12.06949235617757132, 26.87390960531435979 ) ) ;
#1419 = ORIENTED_EDGE ( 'NONE', *, *, #80402, .F. ) ;
#1420 = CARTESIAN_POINT ( 'NONE',  ( 34.67490207739297148, 3.335485537672782552, 51.73549893453298409 ) ) ;
#1421 = CARTESIAN_POINT ( 'NONE',  ( 5.719274019375673035, 21.55341960407619339, 22.29275706135235069 ) ) ;
#1422 = CARTESIAN_POINT ( 'NONE',  ( -0.05219959533909027116, -19.03943276465977164, 107.4989096053143527 ) ) ;
#1423 = CARTESIAN_POINT ( 'NONE',  ( -10.72451020669870658, -18.67979575497194134, 19.58442372801901143 ) ) ;
#1424 = CARTESIAN_POINT ( 'NONE',  ( -12.06949235617756955, 12.14591786802309770, 50.62390960531435979 ) ) ;
#1426 = CARTESIAN_POINT ( 'NONE',  ( 4.483927247898790824, -16.52544592524335698, 60.20942372801902565 ) ) ;
#1425 = AXIS2_PLACEMENT_3D ( 'NONE', #179920, #53542, #83864 ) ;
#1427 = CARTESIAN_POINT ( 'NONE',  ( -19.02544592524342804, 5.153800228976336051, 66.04057627198103830 ) ) ;
#1428 = CARTESIAN_POINT ( 'NONE',  ( 19.03943276465977164, 0.05219959533936151252, 71.25109039468566152 ) ) ;
#1429 = CARTESIAN_POINT ( 'NONE',  ( 5.049401038298161559, -19.05341960407611168, 77.70724293864765286 ) ) ;
#1430 = EDGE_CURVE ( 'NONE', #122419, #49313, #11102, .T. ) ;
#1431 = CARTESIAN_POINT ( 'NONE',  ( 18.67979575497178502, 10.72451020669898547, 34.16557627198102409 ) ) ;
#1432 = CARTESIAN_POINT ( 'NONE',  ( -17.48462780208382128, -33.70920939566911301, -26.63509803227388062 ) ) ;
#1433 = CARTESIAN_POINT ( 'NONE',  ( -19.05341960407611168, -5.049401038298163336, 41.45724293864769550 ) ) ;
#1434 = CARTESIAN_POINT ( 'NONE',  ( 16.53943276465976808, 0.05219959533934440121, 21.25109039468567218 ) ) ;
#1435 = CARTESIAN_POINT ( 'NONE',  ( 0.05219959533936267826, -19.03943276465977164, 60.00109039468566863 ) ) ;
#1436 = CARTESIAN_POINT ( 'NONE',  ( -5.719274019375978568, 21.55341960407610458, 105.2072429386477097 ) ) ;
#1437 = CARTESIAN_POINT ( 'NONE',  ( 16.52544592524342804, -4.483927247898539470, 38.54057627198103120 ) ) ;
#1438 = CARTESIAN_POINT ( 'NONE',  ( -19.05341960407611168, -5.049401038298163336, 86.45724293864769550 ) ) ;
#1439 = CARTESIAN_POINT ( 'NONE',  ( 21.53943276465977519, -0.05219959533907433946, 53.74890960531437401 ) ) ;
#1441 = CARTESIAN_POINT ( 'NONE',  ( -8.314922557961024197, 14.29746914071037800, 37.91775706135235424 ) ) ;
#1440 = CARTESIAN_POINT ( 'NONE',  ( 15.80617190586746368, 15.72974639402197994, 99.37390960531436690 ) ) ;
#1442 = CARTESIAN_POINT ( 'NONE',  ( -5.823673210054116645, -21.52544592524344225, 37.29057627198102409 ) ) ;
#1443 = CARTESIAN_POINT ( 'NONE',  ( 5.719274019375673035, 21.55341960407619339, 82.29275706135234714 ) ) ;
#1444 = CARTESIAN_POINT ( 'NONE',  ( -5.153800228976328057, -19.02544592524343514, 92.29057627198099567 ) ) ;
#1445 = CARTESIAN_POINT ( 'NONE',  ( 5.049401038298161559, -19.05341960407611168, 32.70724293864768129 ) ) ;
#1446 = CARTESIAN_POINT ( 'NONE',  ( -13.89961937509977652, 13.97604488694528158, 90.62390960531432427 ) ) ;
#1447 = CARTESIAN_POINT ( 'NONE',  ( -14.29746914071049879, 8.314922557960819915, 105.8322429386476955 ) ) ;
#1448 = CARTESIAN_POINT ( 'NONE',  ( 13.97604488694527802, 13.89961937509977652, 64.37390960531436690 ) ) ;
#1449 = CARTESIAN_POINT ( 'NONE',  ( -4.483927247898782831, 16.52544592524335698, 27.70942372801901854 ) ) ;
#1450 = CARTESIAN_POINT ( 'NONE',  ( 17.62203461105333702, -16.12203461105326951, -57.08650645001478097 ) ) ;
#1452 = CARTESIAN_POINT ( 'NONE',  ( -19.03943276465977164, 0.05219959533909376836, 111.2489096053143669 ) ) ;
#1451 = CARTESIAN_POINT ( 'NONE',  ( 21.55341960407619695, -5.719274019375665929, 101.0427570613523756 ) ) ;
#1453 = CARTESIAN_POINT ( 'NONE',  ( 8.314922557961029526, -14.29746914071037800, 85.41775706135236135 ) ) ;
#1454 = CARTESIAN_POINT ( 'NONE',  ( 22.14710224105762748, -20.13854895287483515, -48.40914604263300447 ) ) ;
#1455 = CARTESIAN_POINT ( 'NONE',  ( 9.474510206698729675, 16.51473224551082808, 67.08442372801900433 ) ) ;
#1456 = CARTESIAN_POINT ( 'NONE',  ( -19.05341960407617563, 5.049401038297882671, 28.54275706135232937 ) ) ;
#1457 = CARTESIAN_POINT ( 'NONE',  ( 27.38287604894768634, -4.524378969001820572, 139.9999999999999716 ) ) ;
#1458 = CARTESIAN_POINT ( 'NONE',  ( 16.51473224551069308, 9.474510206698969483, 24.16557627198102765 ) ) ;
#1459 = CARTESIAN_POINT ( 'NONE',  ( 0.05219959533910956823, 16.53943276465976808, 34.99890960531435979 ) ) ;
#1460 = CARTESIAN_POINT ( 'NONE',  ( 13.97604488694527802, 13.89961937509977652, 24.37390960531435624 ) ) ;
#1461 = CARTESIAN_POINT ( 'NONE',  ( -12.06949235617756955, 12.14591786802309770, 30.62390960531436335 ) ) ;
#1462 = CARTESIAN_POINT ( 'NONE',  ( 6.685389299484707948, -6.128353407782586082, -63.95879637121625194 ) ) ;
#1463 = CARTESIAN_POINT ( 'NONE',  ( -12.06949235617739369, -12.14591786802326823, 94.37609039468568994 ) ) ;
#1464 = CARTESIAN_POINT ( 'NONE',  ( -19.02544592524342804, 5.153800228976336051, 41.04057627198103120 ) ) ;
#1465 = CARTESIAN_POINT ( 'NONE',  ( 15.80617190586769283, -15.72974639402175789, 90.62609039468567573 ) ) ;
#1466 = CARTESIAN_POINT ( 'NONE',  ( -19.03943276465977164, -0.05219959533935918106, 98.75109039468567573 ) ) ;
#1467 = CARTESIAN_POINT ( 'NONE',  ( -15.80617190586768217, 15.72974639402176855, 78.12609039468570415 ) ) ;
#1468 = CARTESIAN_POINT ( 'NONE',  ( -19.05341960407617563, 5.049401038297882671, 53.54275706135231871 ) ) ;
#1469 = CARTESIAN_POINT ( 'NONE',  ( 19.03943276465977164, -0.05219959533909143690, 98.74890960531436690 ) ) ;
#1470 = CARTESIAN_POINT ( 'NONE',  ( 16.46253265017160672, -9.564922557960803928, 68.33224293864770971 ) ) ;
#1471 = CARTESIAN_POINT ( 'NONE',  ( 16.61371651742599909, 7.165104196376162804, 73.64584930007004004 ) ) ;
#1472 = CARTESIAN_POINT ( 'NONE',  ( -12.14591786802309592, -12.06949235617757132, 66.87390960531436690 ) ) ;
#1473 = CARTESIAN_POINT ( 'NONE',  ( 5.719274019375991003, -21.55341960407610458, 67.70724293864769550 ) ) ;
#1474 = CARTESIAN_POINT ( 'NONE',  ( 5.049401038298161559, -19.05341960407611168, 57.70724293864769550 ) ) ;
#1476 = CARTESIAN_POINT ( 'NONE',  ( -14.29746914071037622, -8.314922557961029526, 74.16775706135231871 ) ) ;
#1475 = CARTESIAN_POINT ( 'NONE',  ( -15.72974639402197994, 15.80617190586746368, 80.62390960531438111 ) ) ;
#1477 = ORIENTED_EDGE ( 'NONE', *, *, #126618, .F. ) ;
#1478 = CARTESIAN_POINT ( 'NONE',  ( 19.05341960407611168, 5.049401038298154454, 48.95724293864768129 ) ) ;
#1479 = AXIS2_PLACEMENT_3D ( 'NONE', #153769, #105284, #28475 ) ;
#1481 = CARTESIAN_POINT ( 'NONE',  ( 11.40812507854754365, 35.11059874428196537, -1.224999997268813479 ) ) ;
#1480 = CARTESIAN_POINT ( 'NONE',  ( -12.06949235617756955, 12.14591786802309770, 75.62390960531439532 ) ) ;
#1482 = CARTESIAN_POINT ( 'NONE',  ( -9.474510206698964154, 16.51473224551069663, 50.41557627198102409 ) ) ;
#1483 = CARTESIAN_POINT ( 'NONE',  ( -16.51473224551069308, -9.474510206698971260, 21.66557627198102765 ) ) ;
#1484 = CARTESIAN_POINT ( 'NONE',  ( -13.89961937509957401, -13.97604488694547875, 69.37609039468564731 ) ) ;
#1485 = CARTESIAN_POINT ( 'NONE',  ( -8.314922557960811034, -14.29746914071050412, 82.08224293864768129 ) ) ;
#1486 = CARTESIAN_POINT ( 'NONE',  ( 21.55341960407619695, -5.719274019375665929, 41.04275706135236135 ) ) ;
#1488 = CARTESIAN_POINT ( 'NONE',  ( -15.72974639402197994, 15.80617190586746368, 100.6239096053143811 ) ) ;
#1487 = CARTESIAN_POINT ( 'NONE',  ( -5.153800228976328057, -19.02544592524343514, 37.29057627198102409 ) ) ;
#1489 = CARTESIAN_POINT ( 'NONE',  ( 5.049401038298161559, -19.05341960407611168, 112.7072429386476813 ) ) ;
#1490 = CARTESIAN_POINT ( 'NONE',  ( 8.224510206698953496, -14.34966873604960469, 87.91557627198103830 ) ) ;
#1491 = CARTESIAN_POINT ( 'NONE',  ( 21.53686564358446631, -33.52628202222955167, -20.57266355564622629 ) ) ;
#1492 = CARTESIAN_POINT ( 'NONE',  ( 9.564922557960805705, 16.46253265017160317, 44.58224293864769550 ) ) ;
#1493 = CARTESIAN_POINT ( 'NONE',  ( 16.88567814943161238, 6.947325034625693618, 113.7900112265259054 ) ) ;
#1495 = CARTESIAN_POINT ( 'NONE',  ( 5.049401038298161559, -19.05341960407611168, 92.70724293864769550 ) ) ;
#1494 = CARTESIAN_POINT ( 'NONE',  ( -0.05219959533936034679, 19.03943276465977164, 97.50109039468567573 ) ) ;
#1496 = CARTESIAN_POINT ( 'NONE',  ( -15.72974639402176322, -15.80617190586768395, 39.37609039468567573 ) ) ;
#1497 = CARTESIAN_POINT ( 'NONE',  ( -19.02544592524342804, 5.153800228976336051, 81.04057627198103830 ) ) ;
#1498 = CARTESIAN_POINT ( 'NONE',  ( -5.049401038297874678, -19.05341960407617918, 69.79275706135233293 ) ) ;
#1499 = CARTESIAN_POINT ( 'NONE',  ( -13.97604488694527625, -13.89961937509977652, 41.87390960531435979 ) ) ;
#1500 = CARTESIAN_POINT ( 'NONE',  ( -8.224510206698948167, 14.34966873604960824, 70.41557627198102409 ) ) ;
#1501 = CARTESIAN_POINT ( 'NONE',  ( 0.05219959533910956823, 16.53943276465976808, 69.99890960531435269 ) ) ;
#1502 = CARTESIAN_POINT ( 'NONE',  ( 5.049401038298161559, -19.05341960407611168, 77.70724293864765286 ) ) ;
#1503 = CARTESIAN_POINT ( 'NONE',  ( -10.72451020669898014, 18.67979575497178502, 100.4155762719810241 ) ) ;
#1504 = CARTESIAN_POINT ( 'NONE',  ( -19.02544592524342804, 5.153800228976336051, 66.04057627198103830 ) ) ;
#1505 = VECTOR ( 'NONE', #166542, 1000.000000000000000 ) ;
#1506 = CARTESIAN_POINT ( 'NONE',  ( 5.049401038297881783, 19.05341960407617563, 22.29275706135233648 ) ) ;
#1509 = CARTESIAN_POINT ( 'NONE',  ( -14.34966873604960291, -8.224510206698953496, 106.6655762719810383 ) ) ;
#1508 = CARTESIAN_POINT ( 'NONE',  ( -4.483927247898539470, -16.52544592524342804, 27.29057627198103120 ) ) ;
#1507 = CARTESIAN_POINT ( 'NONE',  ( -19.05341960407611168, -5.049401038298163336, 36.45724293864766707 ) ) ;
#1510 = CARTESIAN_POINT ( 'NONE',  ( 5.049401038297881783, 19.05341960407617563, 102.2927570613523045 ) ) ;
#1511 = ORIENTED_EDGE ( 'NONE', *, *, #22791, .F. ) ;
#1512 = CARTESIAN_POINT ( 'NONE',  ( 18.67979575497194134, -10.72451020669871369, 25.83442372801901499 ) ) ;
#1513 = CARTESIAN_POINT ( 'NONE',  ( -13.97604488694547697, 13.89961937509957934, 63.12609039468566152 ) ) ;
#1514 = CARTESIAN_POINT ( 'NONE',  ( -12.14591786802326823, 12.06949235617739902, 113.1260903946856899 ) ) ;
#1515 = CARTESIAN_POINT ( 'NONE',  ( 15.72974639402199770, -15.80617190586745480, 68.12390960531436690 ) ) ;
#1516 = CARTESIAN_POINT ( 'NONE',  ( -16.46253265017160317, 9.564922557960807481, 110.8322429386476955 ) ) ;
#1517 = CARTESIAN_POINT ( 'NONE',  ( 4.379528057220339221, -16.55341960407611168, 57.70724293864770260 ) ) ;
#1518 = CARTESIAN_POINT ( 'NONE',  ( 13.97604488694527802, 13.89961937509977652, 29.37390960531435979 ) ) ;
#1519 = CARTESIAN_POINT ( 'NONE',  ( 13.97604488694548053, -13.89961937509957401, 20.62609039468567573 ) ) ;
#1520 = CARTESIAN_POINT ( 'NONE',  ( -16.53943276465976808, -0.05219959533934237506, 83.75109039468568994 ) ) ;
#1521 = CARTESIAN_POINT ( 'NONE',  ( -0.05219959533934338120, 16.53943276465976808, 52.50109039468567573 ) ) ;
#1522 = CARTESIAN_POINT ( 'NONE',  ( 10.81492255796078972, 18.62759615963270932, 24.58224293864768839 ) ) ;
#1523 = CARTESIAN_POINT ( 'NONE',  ( 5.719274019375673035, 21.55341960407619339, 112.2927570613523471 ) ) ;
#1524 = CARTESIAN_POINT ( 'NONE',  ( -13.97604488694527625, -13.89961937509977652, 81.87390960531436690 ) ) ;
#1525 = CARTESIAN_POINT ( 'NONE',  ( 16.55341960407618274, -4.379528057220086978, 66.04275706135236135 ) ) ;
#1526 = CARTESIAN_POINT ( 'NONE',  ( -14.34966873604960291, -8.224510206698953496, 111.6655762719810525 ) ) ;
#1527 = CARTESIAN_POINT ( 'NONE',  ( -4.483927247898539470, -16.52544592524342804, 22.29057627198102765 ) ) ;
#1528 = CARTESIAN_POINT ( 'NONE',  ( 26.99873734152944138, 22.49873734152883387, 1.110912703473986074 ) ) ;
#1531 = CARTESIAN_POINT ( 'NONE',  ( 19.02544592524343514, -5.153800228976328945, 83.54057627198100988 ) ) ;
#1530 = CARTESIAN_POINT ( 'NONE',  ( -19.05341960407611168, -5.049401038298163336, 91.45724293864766707 ) ) ;
#1529 = CARTESIAN_POINT ( 'NONE',  ( -10.81492255796105439, 18.62759615963255655, 67.91775706135234714 ) ) ;
#1532 = CARTESIAN_POINT ( 'NONE',  ( -5.049401038298153566, 19.05341960407611168, 105.2072429386476671 ) ) ;
#1533 = VECTOR ( 'NONE', #54192, 1000.000000000000000 ) ;
#1534 = CARTESIAN_POINT ( 'NONE',  ( 4.379528057220339221, -16.55341960407611168, 57.70724293864770260 ) ) ;
#1535 = EDGE_CURVE ( 'NONE', #136214, #11685, #2227, .T. ) ;
#1536 = CARTESIAN_POINT ( 'NONE',  ( -14.34966873604972548, 8.224510206698743886, 108.3344237280190185 ) ) ;
#1537 = CARTESIAN_POINT ( 'NONE',  ( 12.06949235617757843, -12.14591786802309237, 48.12390960531436690 ) ) ;
#1540 = CIRCLE ( 'NONE', #59712, 5.000000000000000888 ) ;
#1539 = CARTESIAN_POINT ( 'NONE',  ( 18.22780087662125226, -5.499999999999864997, 61.01540105326109398 ) ) ;
#1538 = CARTESIAN_POINT ( 'NONE',  ( 0.05219959533934541429, -16.53943276465976808, 40.00109039468567573 ) ) ;
#1541 = CARTESIAN_POINT ( 'NONE',  ( 9.564922557961047289, -16.46253265017146816, 35.41775706135233293 ) ) ;
#1542 = CARTESIAN_POINT ( 'NONE',  ( -9.564922557960796823, -16.46253265017161027, 82.08224293864768129 ) ) ;
#1543 = CARTESIAN_POINT ( 'NONE',  ( 13.89961937509957401, 13.97604488694547697, 56.87609039468564731 ) ) ;
#1544 = CARTESIAN_POINT ( 'NONE',  ( -9.564922557961040184, 16.46253265017147172, 57.91775706135233293 ) ) ;
#1546 = CARTESIAN_POINT ( 'NONE',  ( 14.34966873604972726, -8.224510206698740333, 80.83442372801901854 ) ) ;
#1545 = CARTESIAN_POINT ( 'NONE',  ( 9.474510206698729675, 16.51473224551082808, 97.08442372801900433 ) ) ;
#1547 = CARTESIAN_POINT ( 'NONE',  ( 22.44159573604009239, 16.30477369853692693, 148.5750000027312012 ) ) ;
#1549 = CARTESIAN_POINT ( 'NONE',  ( -16.51473224551069308, -9.474510206698971260, 26.66557627198103120 ) ) ;
#1548 = AXIS2_PLACEMENT_3D ( 'NONE', #164704, #183844, #184835 ) ;
#1550 = CARTESIAN_POINT ( 'NONE',  ( 19.05341960407611168, 5.049401038298154454, 103.9572429386476671 ) ) ;
#1551 = CARTESIAN_POINT ( 'NONE',  ( -5.823673210054431948, 21.52544592524334988, 37.70942372801900433 ) ) ;
#1552 = CARTESIAN_POINT ( 'NONE',  ( -13.89961937509957401, -13.97604488694547875, 84.37609039468567573 ) ) ;
#1554 = CARTESIAN_POINT ( 'NONE',  ( -19.03943276465977164, 0.05219959533909376836, 61.24890960531436690 ) ) ;
#1553 = CARTESIAN_POINT ( 'NONE',  ( 17.50000000000000355, 5.185212231016174123, 23.70589219561835392 ) ) ;
#1555 = CARTESIAN_POINT ( 'NONE',  ( -9.564922557960796823, -16.46253265017161027, 102.0822429386477097 ) ) ;
#1557 = CARTESIAN_POINT ( 'NONE',  ( -16.46253265017160317, 9.564922557960807481, 65.83224293864769550 ) ) ;
#1556 = CARTESIAN_POINT ( 'NONE',  ( -12.14591786802309592, -12.06949235617757132, 61.87390960531436690 ) ) ;
#1558 = CARTESIAN_POINT ( 'NONE',  ( -16.51473224551069308, -9.474510206698971260, 61.66557627198103120 ) ) ;
#1559 = CARTESIAN_POINT ( 'NONE',  ( -16.46253265017146816, -9.564922557961047289, 59.16775706135233293 ) ) ;
#1560 = CARTESIAN_POINT ( 'NONE',  ( 18.67979575497178502, 10.72451020669898547, 49.16557627198102409 ) ) ;
#1561 = CARTESIAN_POINT ( 'NONE',  ( 5.049401038297881783, 19.05341960407617563, 42.29275706135234003 ) ) ;
#1562 = CARTESIAN_POINT ( 'NONE',  ( -16.46253265017160317, 9.564922557960807481, 75.83224293864769550 ) ) ;
#1563 = CARTESIAN_POINT ( 'NONE',  ( 5.719274019375991003, -21.55341960407610458, 82.70724293864770971 ) ) ;
#1565 = CARTESIAN_POINT ( 'NONE',  ( 0.05219959533936267826, -19.03943276465977164, 35.00109039468566863 ) ) ;
#1564 = CARTESIAN_POINT ( 'NONE',  ( 8.314922557960818139, 14.29746914071049879, 84.58224293864769550 ) ) ;
#1566 = CARTESIAN_POINT ( 'NONE',  ( -18.67979575497178146, -10.72451020669898902, 46.66557627198102409 ) ) ;
#1567 = CARTESIAN_POINT ( 'NONE',  ( 10.81492255796078972, 18.62759615963270932, 34.58224293864770260 ) ) ;
#1568 = CARTESIAN_POINT ( 'NONE',  ( -19.03943276465977164, 0.05219959533909376836, 66.24890960531436690 ) ) ;
#1569 = CARTESIAN_POINT ( 'NONE',  ( -13.97604488694527625, -13.89961937509977652, 56.87390960531434558 ) ) ;
#1570 = CARTESIAN_POINT ( 'NONE',  ( 14.29746914071049879, -8.314922557960816363, 113.3322429386476955 ) ) ;
#1571 = AXIS2_PLACEMENT_3D ( 'NONE', #136288, #181809, #132303 ) ;
#1572 = CARTESIAN_POINT ( 'NONE',  ( -21.52544592524334988, -5.823673210054445271, 28.95942372801902209 ) ) ;
#1573 = CARTESIAN_POINT ( 'NONE',  ( -9.474510206698964154, 16.51473224551069663, 110.4155762719810383 ) ) ;
#1574 = CARTESIAN_POINT ( 'NONE',  ( -21.53943276465977519, -0.05219959533937600094, 33.75109039468568284 ) ) ;
#1575 = CARTESIAN_POINT ( 'NONE',  ( 13.89961937509977652, -13.97604488694527269, 33.12390960531434558 ) ) ;
#1576 = CARTESIAN_POINT ( 'NONE',  ( -10.81492255796078084, -18.62759615963271287, 112.0822429386477097 ) ) ;
#1577 = CARTESIAN_POINT ( 'NONE',  ( -19.05341960407617563, 5.049401038297882671, 43.54275706135232582 ) ) ;
#1578 = CARTESIAN_POINT ( 'NONE',  ( 13.89961937509977652, -13.97604488694527269, 28.12390960531435624 ) ) ;
#1579 = DIRECTION ( 'NONE',  ( 1.000000000000000000, -0.000000000000000000, 6.982962677686266711E-15 ) ) ;
#1580 = CARTESIAN_POINT ( 'NONE',  ( 17.15686820162335025, -6.332220283772392655, 21.21893983122704341 ) ) ;
#1581 = CARTESIAN_POINT ( 'NONE',  ( 4.379528057220092307, 16.55341960407617563, 62.29275706135236845 ) ) ;
#1582 = CARTESIAN_POINT ( 'NONE',  ( -13.97604488694527625, -13.89961937509977652, 31.87390960531435979 ) ) ;
#1583 = CARTESIAN_POINT ( 'NONE',  ( 34.02657648861390527, -4.769071838117370454, 92.23683055719311596 ) ) ;
#1584 = CARTESIAN_POINT ( 'NONE',  ( 13.97604488694527802, 13.89961937509977652, 69.37390960531436690 ) ) ;
#1585 = CARTESIAN_POINT ( 'NONE',  ( -12.14591786802309592, -12.06949235617757132, 111.8739096053143669 ) ) ;
#1586 = CARTESIAN_POINT ( 'NONE',  ( -21.53943276465977519, 0.05219959533907696930, 66.24890960531436690 ) ) ;
#1587 = CARTESIAN_POINT ( 'NONE',  ( 4.379528057220339221, -16.55341960407611168, 82.70724293864770971 ) ) ;
#1588 = CARTESIAN_POINT ( 'NONE',  ( -16.52544592524335698, -4.483927247898792601, 28.95942372801902209 ) ) ;
#1589 = CARTESIAN_POINT ( 'NONE',  ( 5.719274019375673035, 21.55341960407619339, 92.29275706135236135 ) ) ;
#1590 = CARTESIAN_POINT ( 'NONE',  ( 16.46253265017160672, -9.564922557960803928, 28.33224293864769550 ) ) ;
#1591 = CARTESIAN_POINT ( 'NONE',  ( 0.05219959533934541429, -16.53943276465976808, 110.0010903946856757 ) ) ;
#1592 = CARTESIAN_POINT ( 'NONE',  ( 16.55341960407611168, 4.379528057220329451, 58.95724293864770971 ) ) ;
#1593 = CARTESIAN_POINT ( 'NONE',  ( -5.153800228976328057, -19.02544592524343514, 52.29057627198100988 ) ) ;
#1594 = CARTESIAN_POINT ( 'NONE',  ( 21.53943276465977519, 0.05219959533937863772, 96.25109039468568994 ) ) ;
#1595 = CARTESIAN_POINT ( 'NONE',  ( -5.719274019375978568, 21.55341960407610458, 110.2072429386477239 ) ) ;
#1596 = CARTESIAN_POINT ( 'NONE',  ( 10.72451020669871369, 18.67979575497193778, 72.08442372801899012 ) ) ;
#1597 = CARTESIAN_POINT ( 'NONE',  ( 12.14591786802327356, -12.06949235617739191, 45.62609039468567573 ) ) ;
#1599 = CARTESIAN_POINT ( 'NONE',  ( 5.719274019375673035, 21.55341960407619339, 87.29275706135236135 ) ) ;
#1598 = CARTESIAN_POINT ( 'NONE',  ( -14.34966873604960291, -8.224510206698953496, 76.66557627198103830 ) ) ;
#1600 = CARTESIAN_POINT ( 'NONE',  ( -14.34966873604960291, -8.224510206698953496, 26.66557627198103475 ) ) ;
#1601 = CARTESIAN_POINT ( 'NONE',  ( -17.40861289039002457, 6.110651285853324843, 113.6276752917256800 ) ) ;
#1602 = CARTESIAN_POINT ( 'NONE',  ( 16.55341960407618274, -4.379528057220086978, 46.04275706135234714 ) ) ;
#1603 = CARTESIAN_POINT ( 'NONE',  ( 12.06949235617757843, -12.14591786802309237, 38.12390960531436690 ) ) ;
#1604 = CARTESIAN_POINT ( 'NONE',  ( 0.05219959533934541429, -16.53943276465976808, 90.00109039468567573 ) ) ;
#1605 = CARTESIAN_POINT ( 'NONE',  ( 9.564922557960805705, 16.46253265017160317, 99.58224293864770971 ) ) ;
#1606 = CARTESIAN_POINT ( 'NONE',  ( -0.05219959533907301413, -21.53943276465977519, 22.49890960531436335 ) ) ;
#1607 = CARTESIAN_POINT ( 'NONE',  ( -5.823673210054431948, 21.52544592524334988, 102.7094237280190185 ) ) ;
#1608 = CARTESIAN_POINT ( 'NONE',  ( 12.06949235617739724, 12.14591786802326823, 106.8760903946856899 ) ) ;
#1609 = CARTESIAN_POINT ( 'NONE',  ( 14.29746914071049879, -8.314922557960816363, 73.33224293864769550 ) ) ;
#1610 = CARTESIAN_POINT ( 'NONE',  ( 9.474510206698971260, -16.51473224551069308, 87.91557627198102409 ) ) ;
#1611 = VERTEX_POINT ( 'NONE', #4204 ) ;
#1612 = CARTESIAN_POINT ( 'NONE',  ( 4.483927247898790824, -16.52544592524335698, 25.20942372801901854 ) ) ;
#1613 = CARTESIAN_POINT ( 'NONE',  ( 13.89961937509977652, -13.97604488694527269, 33.12390960531434558 ) ) ;
#1614 = CARTESIAN_POINT ( 'NONE',  ( 19.02544592524343514, -5.153800228976328945, 88.54057627198102409 ) ) ;
#1616 = CARTESIAN_POINT ( 'NONE',  ( -29.86685920354755197, -21.69954338932560134, -4.424999997268812990 ) ) ;
#1615 = CARTESIAN_POINT ( 'NONE',  ( -8.314922557961024197, 14.29746914071037800, 37.91775706135235424 ) ) ;
#1617 = CARTESIAN_POINT ( 'NONE',  ( 19.03943276465977164, 0.05219959533936151252, 41.25109039468566152 ) ) ;
#1618 = CARTESIAN_POINT ( 'NONE',  ( 16.55341960407618274, -4.379528057220086978, 96.04275706135236135 ) ) ;
#1619 = CARTESIAN_POINT ( 'NONE',  ( 13.97604488694548053, -13.89961937509957401, 110.6260903946856615 ) ) ;
#1620 = CARTESIAN_POINT ( 'NONE',  ( -9.564922557960796823, -16.46253265017161027, 32.08224293864769550 ) ) ;
#1621 = CARTESIAN_POINT ( 'NONE',  ( -14.34966873604972548, 8.224510206698743886, 83.33442372801903275 ) ) ;
#1622 = CARTESIAN_POINT ( 'NONE',  ( 14.29746914071037800, 8.314922557961029526, 71.66775706135234714 ) ) ;
#1623 = CARTESIAN_POINT ( 'NONE',  ( 9.564922557961047289, -16.46253265017146816, 85.41775706135233293 ) ) ;
#1624 = AXIS2_PLACEMENT_3D ( 'NONE', #95423, #190434, #66079 ) ;
#1625 = CARTESIAN_POINT ( 'NONE',  ( -21.53943276465977519, -0.05219959533937600094, 108.7510903946857042 ) ) ;
#1626 = CARTESIAN_POINT ( 'NONE',  ( -19.05341960407611168, -5.049401038298163336, 41.45724293864769550 ) ) ;
#1627 = CARTESIAN_POINT ( 'NONE',  ( -19.02544592524342804, 5.153800228976336051, 91.04057627198100988 ) ) ;
#1628 = CARTESIAN_POINT ( 'NONE',  ( -8.224510206698948167, 14.34966873604960824, 80.41557627198103830 ) ) ;
#1629 = EDGE_CURVE ( 'NONE', #185763, #46465, #128478, .T. ) ;
#1630 = CARTESIAN_POINT ( 'NONE',  ( -9.474510206698720793, -16.51473224551083518, 49.58442372801899722 ) ) ;
#1631 = CARTESIAN_POINT ( 'NONE',  ( -21.53943276465977519, 0.05219959533907696930, 51.24890960531436690 ) ) ;
#1632 = CARTESIAN_POINT ( 'NONE',  ( -5.153800228976607833, 19.02544592524334988, 27.70942372801899722 ) ) ;
#1633 = CARTESIAN_POINT ( 'NONE',  ( -13.97604488694527625, -13.89961937509977652, 86.87390960531436690 ) ) ;
#1634 = CARTESIAN_POINT ( 'NONE',  ( -13.97604488694547697, 13.89961937509957934, 28.12609039468565797 ) ) ;
#1635 = CARTESIAN_POINT ( 'NONE',  ( 5.823673210054125526, 21.52544592524343514, 69.79057627198102409 ) ) ;
#1636 = CARTESIAN_POINT ( 'NONE',  ( 5.049401038298161559, -19.05341960407611168, 107.7072429386476955 ) ) ;
#1637 = CARTESIAN_POINT ( 'NONE',  ( 19.05341960407617918, -5.049401038297876454, 91.04275706135234714 ) ) ;
#1638 = CARTESIAN_POINT ( 'NONE',  ( -17.50000000000002132, 4.049696124445919310, 109.1803967066594794 ) ) ;
#1639 = CARTESIAN_POINT ( 'NONE',  ( 0.05219959533936267826, -19.03943276465977164, 105.0010903946856615 ) ) ;
#1640 = CARTESIAN_POINT ( 'NONE',  ( 13.97604488694527802, 13.89961937509977652, 29.37390960531435979 ) ) ;
#1641 = CARTESIAN_POINT ( 'NONE',  ( -19.02544592524342804, 5.153800228976336051, 91.04057627198100988 ) ) ;
#1642 = CARTESIAN_POINT ( 'NONE',  ( 10.72451020669898902, -18.67979575497178502, 82.91557627198103830 ) ) ;
#1643 = CARTESIAN_POINT ( 'NONE',  ( 16.52544592524335698, 4.483927247898782831, 46.45942372801901854 ) ) ;
#1644 = CARTESIAN_POINT ( 'NONE',  ( 18.62759615963255655, 10.81492255796105972, 51.66775706135234714 ) ) ;
#1646 = CARTESIAN_POINT ( 'NONE',  ( 15.80617190586769283, -15.72974639402175789, 100.6260903946857184 ) ) ;
#1645 = CARTESIAN_POINT ( 'NONE',  ( 16.51473224551083163, -9.474510206698727899, 95.83442372801900433 ) ) ;
#1647 = CARTESIAN_POINT ( 'NONE',  ( -16.53943276465976808, -0.05219959533934237506, 93.75109039468567573 ) ) ;
#1648 = CARTESIAN_POINT ( 'NONE',  ( -16.46253265017160317, 9.564922557960807481, 105.8322429386476955 ) ) ;
#1649 = CARTESIAN_POINT ( 'NONE',  ( 0.05219959533910956823, 16.53943276465976808, 84.99890960531436690 ) ) ;
#1650 = CARTESIAN_POINT ( 'NONE',  ( 4.379528057220339221, -16.55341960407611168, 32.70724293864770260 ) ) ;
#1651 = CARTESIAN_POINT ( 'NONE',  ( -16.46253265017146816, -9.564922557961047289, 74.16775706135234714 ) ) ;
#1652 = CARTESIAN_POINT ( 'NONE',  ( 15.80617190586769283, -15.72974639402175789, 55.62609039468568284 ) ) ;
#1653 = CARTESIAN_POINT ( 'NONE',  ( 16.46253265017146816, 9.564922557961045513, 31.66775706135232937 ) ) ;
#1654 = CARTESIAN_POINT ( 'NONE',  ( 16.53943276465976808, -0.05219959533910856209, 93.74890960531436690 ) ) ;
#1655 = CARTESIAN_POINT ( 'NONE',  ( 15.72974639402199770, -15.80617190586745480, 33.12390960531435979 ) ) ;
#1656 = CARTESIAN_POINT ( 'NONE',  ( -0.05219959533934338120, 16.53943276465976808, 112.5010903946857042 ) ) ;
#1657 = VECTOR ( 'NONE', #198444, 1000.000000000000000 ) ;
#1658 = CARTESIAN_POINT ( 'NONE',  ( -18.67979575497193778, 10.72451020669871902, 103.3344237280190043 ) ) ;
#1659 = CARTESIAN_POINT ( 'NONE',  ( -4.379528057220086978, -16.55341960407618274, 59.79275706135234714 ) ) ;
#1660 = CARTESIAN_POINT ( 'NONE',  ( -12.06949235617739369, -12.14591786802326823, 109.3760903946857042 ) ) ;
#1661 = CARTESIAN_POINT ( 'NONE',  ( -18.62759615963255300, -10.81492255796106328, 49.16775706135234003 ) ) ;
#1662 = CARTESIAN_POINT ( 'NONE',  ( 15.80617190586769283, -15.72974639402175789, 60.62609039468567573 ) ) ;
#1663 = ORIENTED_EDGE ( 'NONE', *, *, #80326, .T. ) ;
#1664 = CARTESIAN_POINT ( 'NONE',  ( -10.81492255796105439, 18.62759615963255655, 32.91775706135234714 ) ) ;
#1665 = CARTESIAN_POINT ( 'NONE',  ( 14.34966873604960469, 8.224510206698951720, 99.16557627198100988 ) ) ;
#1666 = CARTESIAN_POINT ( 'NONE',  ( 13.89961937509977652, -13.97604488694527269, 23.12390960531436335 ) ) ;
#1667 = CARTESIAN_POINT ( 'NONE',  ( -0.05219959533910754901, -16.53943276465976808, 62.49890960531436690 ) ) ;
#1668 = CARTESIAN_POINT ( 'NONE',  ( 5.049401038298161559, -19.05341960407611168, 72.70724293864768129 ) ) ;
#1669 = CARTESIAN_POINT ( 'NONE',  ( 14.34966873604972726, -8.224510206698740333, 110.8344237280190043 ) ) ;
#1670 = CARTESIAN_POINT ( 'NONE',  ( 10.81492255796078972, 18.62759615963270932, 54.58224293864769550 ) ) ;
#1671 = CARTESIAN_POINT ( 'NONE',  ( -12.14591786802309592, -12.06949235617757132, 96.87390960531436690 ) ) ;
#1672 = CARTESIAN_POINT ( 'NONE',  ( -5.823673210054116645, -21.52544592524344225, 87.29057627198103830 ) ) ;
#1673 = CARTESIAN_POINT ( 'NONE',  ( 19.02544592524343514, -5.153800228976328945, 103.5405762719809957 ) ) ;
#1675 = CARTESIAN_POINT ( 'NONE',  ( 19.05341960407617918, -5.049401038297876454, 111.0427570613523329 ) ) ;
#1674 = CARTESIAN_POINT ( 'NONE',  ( -13.89961937509977652, 13.97604488694528158, 45.62390960531433848 ) ) ;
#1676 = CARTESIAN_POINT ( 'NONE',  ( 15.72974639402199770, -15.80617190586745480, 48.12390960531436690 ) ) ;
#1677 = CARTESIAN_POINT ( 'NONE',  ( 5.823673210054444382, -21.52544592524334988, 70.20942372801904696 ) ) ;
#1678 = CARTESIAN_POINT ( 'NONE',  ( 5.153800228976335163, 19.02544592524342804, 69.79057627198103830 ) ) ;
#1679 = CARTESIAN_POINT ( 'NONE',  ( 19.02544592524343514, -5.153800228976328945, 93.54057627198102409 ) ) ;
#1680 = CARTESIAN_POINT ( 'NONE',  ( -14.34966873604972548, 8.224510206698743886, 68.33442372801900433 ) ) ;
#1681 = CARTESIAN_POINT ( 'NONE',  ( -0.05219959533937732626, 21.53943276465977519, 47.50109039468568994 ) ) ;
#1682 = CARTESIAN_POINT ( 'NONE',  ( -18.67979575497193778, 10.72451020669871902, 83.33442372801903275 ) ) ;
#1683 = CARTESIAN_POINT ( 'NONE',  ( -21.53943276465977519, 0.05219959533907696930, 96.24890960531435269 ) ) ;
#1684 = AXIS2_PLACEMENT_3D ( 'NONE', #76193, #63008, #124687 ) ;
#1686 = CARTESIAN_POINT ( 'NONE',  ( 14.34966873604972726, -8.224510206698740333, 80.83442372801901854 ) ) ;
#1685 = CARTESIAN_POINT ( 'NONE',  ( 10.81492255796106328, -18.62759615963255655, 40.41775706135234714 ) ) ;
#1687 = CARTESIAN_POINT ( 'NONE',  ( -0.05219959533907301413, -21.53943276465977519, 77.49890960531433848 ) ) ;
#1688 = CARTESIAN_POINT ( 'NONE',  ( -19.05341960407617563, 5.049401038297882671, 38.54275706135233293 ) ) ;
#1689 = CIRCLE ( 'NONE', #85550, 2.500000000000002220 ) ;
#1691 = CARTESIAN_POINT ( 'NONE',  ( 8.224510206698742110, 14.34966873604972548, 112.0844237280190185 ) ) ;
#1690 = CARTESIAN_POINT ( 'NONE',  ( 0.05219959533909260263, 19.03943276465977164, 79.99890960531436690 ) ) ;
#1692 = DIRECTION ( 'NONE',  ( 0.000000000000000000, 0.000000000000000000, -1.000000000000000000 ) ) ;
#1693 = CARTESIAN_POINT ( 'NONE',  ( 13.89961937509977652, -13.97604488694527269, 98.12390960531433848 ) ) ;
#1694 = DIRECTION ( 'NONE',  ( 1.000000000000000000, 0.000000000000000000, -0.000000000000000000 ) ) ;
#1695 = CARTESIAN_POINT ( 'NONE',  ( -9.564922557961040184, 16.46253265017147172, 97.91775706135233293 ) ) ;
#1696 = CARTESIAN_POINT ( 'NONE',  ( 5.823673210054125526, 21.52544592524343514, 54.79057627198104541 ) ) ;
#1697 = CARTESIAN_POINT ( 'NONE',  ( 12.06949235617757843, -12.14591786802309237, 38.12390960531436690 ) ) ;
#1698 = CARTESIAN_POINT ( 'NONE',  ( -9.564922557961040184, 16.46253265017147172, 107.9177570613523471 ) ) ;
#1699 = CARTESIAN_POINT ( 'NONE',  ( 0.05219959533909260263, 19.03943276465977164, 24.99890960531435269 ) ) ;
#1700 = CARTESIAN_POINT ( 'NONE',  ( -19.03943276465977164, -0.05219959533935918106, 108.7510903946856615 ) ) ;
#1702 = CARTESIAN_POINT ( 'NONE',  ( 19.05341960407617918, -5.049401038297876454, 76.04275706135230450 ) ) ;
#1701 = CARTESIAN_POINT ( 'NONE',  ( -15.80617190586745835, -15.72974639402198527, 101.8739096053143811 ) ) ;
#1703 = CARTESIAN_POINT ( 'NONE',  ( 16.52544592524335698, 4.483927247898782831, 86.45942372801901854 ) ) ;
#1704 = CARTESIAN_POINT ( 'NONE',  ( 9.564922557960805705, 16.46253265017160317, 64.58224293864769550 ) ) ;
#1705 = CARTESIAN_POINT ( 'NONE',  ( -4.379528057220328563, 16.55341960407611168, 80.20724293864769550 ) ) ;
#1706 = CARTESIAN_POINT ( 'NONE',  ( -19.05341960407611168, -5.049401038298163336, 56.45724293864768129 ) ) ;
#1707 = CARTESIAN_POINT ( 'NONE',  ( 14.34966873604960469, 8.224510206698951720, 64.16557627198102409 ) ) ;
#1708 = CARTESIAN_POINT ( 'NONE',  ( 16.46253265017160672, -9.564922557960803928, 23.33224293864769194 ) ) ;
#1709 = CARTESIAN_POINT ( 'NONE',  ( -36.91128768240056957, -0.3593773198236934197, 50.50000000000003553 ) ) ;
#1710 = CARTESIAN_POINT ( 'NONE',  ( 8.224510206698953496, -14.34966873604960469, 47.91557627198102409 ) ) ;
#1711 = CARTESIAN_POINT ( 'NONE',  ( -13.89961937509977652, 13.97604488694528158, 75.62390960531438111 ) ) ;
#1712 = CARTESIAN_POINT ( 'NONE',  ( -0.2055526423334300690, -16.68934465457932959, -59.13845350790287370 ) ) ;
#1713 = CARTESIAN_POINT ( 'NONE',  ( 19.05341960407617918, -5.049401038297876454, 36.04275706135234003 ) ) ;
#1714 = CARTESIAN_POINT ( 'NONE',  ( 8.224510206698742110, 14.34966873604972548, 62.08442372801901143 ) ) ;
#1715 = CARTESIAN_POINT ( 'NONE',  ( 21.53943276465977519, -0.05219959533907433946, 68.74890960531435269 ) ) ;
#1716 = CARTESIAN_POINT ( 'NONE',  ( 5.719274019375673035, 21.55341960407619339, 112.2927570613523471 ) ) ;
#1717 = CARTESIAN_POINT ( 'NONE',  ( -9.564922557960796823, -16.46253265017161027, 72.08224293864770971 ) ) ;
#1718 = CARTESIAN_POINT ( 'NONE',  ( 2.200000000000000178, 4.653657836759941744E-16, -3.799999999999999378 ) ) ;
#1719 = CARTESIAN_POINT ( 'NONE',  ( -21.53943276465977519, 0.05219959533907696930, 21.24890960531436690 ) ) ;
#1720 = CARTESIAN_POINT ( 'NONE',  ( 16.51473224551069308, 9.474510206698969483, 64.16557627198102409 ) ) ;
#1721 = CARTESIAN_POINT ( 'NONE',  ( -21.52544592524334988, -5.823673210054445271, 38.95942372801901854 ) ) ;
#1722 = CARTESIAN_POINT ( 'NONE',  ( -8.224510206698948167, 14.34966873604960824, 110.4155762719810383 ) ) ;
#1725 = ORIENTED_EDGE ( 'NONE', *, *, #84050, .T. ) ;
#1724 = CARTESIAN_POINT ( 'NONE',  ( 19.02544592524343514, -5.153800228976328945, 93.54057627198102409 ) ) ;
#1723 = CARTESIAN_POINT ( 'NONE',  ( 18.62759615963271287, -10.81492255796078972, 103.3322429386476955 ) ) ;
#1726 = CARTESIAN_POINT ( 'NONE',  ( -0.05219959533937732626, 21.53943276465977519, 22.50109039468567573 ) ) ;
#1727 = ORIENTED_EDGE ( 'NONE', *, *, #192158, .T. ) ;
#1728 = CARTESIAN_POINT ( 'NONE',  ( -5.153800228976328057, -19.02544592524343514, 82.29057627198103830 ) ) ;
#1729 = CARTESIAN_POINT ( 'NONE',  ( -31.74999999999995737, 0.000000000000000000, 0.000000000000000000 ) ) ;
#1730 = CARTESIAN_POINT ( 'NONE',  ( 10.81492255796078972, 18.62759615963270932, 99.58224293864770971 ) ) ;
#1731 = CARTESIAN_POINT ( 'NONE',  ( -13.89961937509977652, 13.97604488694528158, 50.62390960531435979 ) ) ;
#1732 = CARTESIAN_POINT ( 'NONE',  ( 9.474510206698729675, 16.51473224551082808, 102.0844237280190043 ) ) ;
#1733 = CARTESIAN_POINT ( 'NONE',  ( 3.556970738554033499E-15, -38.81732327939057825, -10.62499999726881050 ) ) ;
#1734 = CARTESIAN_POINT ( 'NONE',  ( -19.02544592524342804, 5.153800228976336051, 31.04057627198102409 ) ) ;
#1735 = CARTESIAN_POINT ( 'NONE',  ( 21.52544592524334988, 5.823673210054432836, 91.45942372801901854 ) ) ;
#1737 = CARTESIAN_POINT ( 'NONE',  ( 15.72974639402176855, 15.80617190586768217, 41.87609039468568284 ) ) ;
#1736 = CARTESIAN_POINT ( 'NONE',  ( -9.564922557960796823, -16.46253265017161027, 72.08224293864770971 ) ) ;
#1738 = CARTESIAN_POINT ( 'NONE',  ( -10.81492255796105439, 18.62759615963255655, 27.91775706135234358 ) ) ;
#1739 = CARTESIAN_POINT ( 'NONE',  ( -28.82186960331499037, 2.428612866367529932E-14, 150.0000000000000000 ) ) ;
#1740 = CARTESIAN_POINT ( 'NONE',  ( -16.51473224551069308, -9.474510206698971260, 86.66557627198102409 ) ) ;
#1741 = CARTESIAN_POINT ( 'NONE',  ( 19.49671883438228193, 5.499999999999968914, 62.39279849105682985 ) ) ;
#1744 = CARTESIAN_POINT ( 'NONE',  ( -10.72451020669870658, -18.67979575497194134, 39.58442372801901143 ) ) ;
#1743 = CARTESIAN_POINT ( 'NONE',  ( -21.55341960407610458, -5.719274019375992779, 46.45724293864769550 ) ) ;
#1742 = CARTESIAN_POINT ( 'NONE',  ( -12.06949235617739369, -12.14591786802326823, 44.37609039468567573 ) ) ;
#1745 = CARTESIAN_POINT ( 'NONE',  ( -5.823673210054431948, 21.52544592524334988, 77.70942372801900433 ) ) ;
#1746 = CARTESIAN_POINT ( 'NONE',  ( -193.3062444957834884, -155.7167183371838064, -15.00000000000000178 ) ) ;
#1747 = CARTESIAN_POINT ( 'NONE',  ( 0.05219959533936267826, -19.03943276465977164, 110.0010903946856757 ) ) ;
#1748 = CARTESIAN_POINT ( 'NONE',  ( -19.02544592524342804, 5.153800228976336051, 56.04057627198100988 ) ) ;
#1749 = CARTESIAN_POINT ( 'NONE',  ( 19.03943276465977164, -0.05219959533909143690, 88.74890960531436690 ) ) ;
#1750 = CARTESIAN_POINT ( 'NONE',  ( 14.34966873604960469, 8.224510206698951720, 104.1655762719810241 ) ) ;
#1751 = CARTESIAN_POINT ( 'NONE',  ( 16.53943276465976808, -0.05219959533910856209, 103.7489096053143669 ) ) ;
#1752 = CARTESIAN_POINT ( 'NONE',  ( -15.80617190586745835, -15.72974639402198527, 21.87390960531436690 ) ) ;
#1753 = CARTESIAN_POINT ( 'NONE',  ( -0.05219959533934338120, 16.53943276465976808, 82.50109039468568994 ) ) ;
#1755 = CARTESIAN_POINT ( 'NONE',  ( -16.46253265017160317, 9.564922557960807481, 55.83224293864769550 ) ) ;
#1754 = CARTESIAN_POINT ( 'NONE',  ( -16.52544592524342804, 4.483927247898546575, 76.04057627198102409 ) ) ;
#1756 = CARTESIAN_POINT ( 'NONE',  ( -10.72451020669870658, -18.67979575497194134, 79.58442372801903275 ) ) ;
#1757 = CARTESIAN_POINT ( 'NONE',  ( 18.62759615963255655, 10.81492255796105972, 71.66775706135234714 ) ) ;
#1758 = CARTESIAN_POINT ( 'NONE',  ( 19.05341960407617918, -5.049401038297876454, 106.0427570613523471 ) ) ;
#1759 = CARTESIAN_POINT ( 'NONE',  ( -8.224510206698948167, 14.34966873604960824, 65.41557627198102409 ) ) ;
#1760 = CARTESIAN_POINT ( 'NONE',  ( 5.823673210054444382, -21.52544592524334988, 30.20942372801902565 ) ) ;
#1761 = CARTESIAN_POINT ( 'NONE',  ( -10.81492255796078084, -18.62759615963271287, 67.08224293864770971 ) ) ;
#1763 = CARTESIAN_POINT ( 'NONE',  ( 19.25176906914650843, 5.499999999999742428, 73.49927264242276692 ) ) ;
#1762 = AXIS2_PLACEMENT_3D ( 'NONE', #110360, #81011, #66842 ) ;
#1764 = CARTESIAN_POINT ( 'NONE',  ( -8.906447517083060816, 27.41122689804195645, 147.8500000054623627 ) ) ;
#1765 = CARTESIAN_POINT ( 'NONE',  ( 13.89961937509977652, -13.97604488694527269, 73.12390960531436690 ) ) ;
#1766 = CARTESIAN_POINT ( 'NONE',  ( 14.34966873604960469, 8.224510206698951720, 39.16557627198102409 ) ) ;
#1767 = CARTESIAN_POINT ( 'NONE',  ( 0.05219959533934541429, -16.53943276465976808, 110.0010903946856757 ) ) ;
#1768 = CARTESIAN_POINT ( 'NONE',  ( -16.55341960407617563, 4.379528057220093196, 93.54275706135234714 ) ) ;
#1769 = CARTESIAN_POINT ( 'NONE',  ( 5.153800228976615827, -19.02544592524334988, 55.20942372801899722 ) ) ;
#1770 = CARTESIAN_POINT ( 'NONE',  ( 16.19135201231368981, 7.376712067591808974, 47.68680854052031748 ) ) ;
#1771 = CARTESIAN_POINT ( 'NONE',  ( -5.153800228976328057, -19.02544592524343514, 102.2905762719810383 ) ) ;
#1772 = CARTESIAN_POINT ( 'NONE',  ( -14.29746914071049879, 8.314922557960819915, 80.83224293864769550 ) ) ;
#1773 = CARTESIAN_POINT ( 'NONE',  ( 0.05219959533936267826, -19.03943276465977164, 40.00109039468566152 ) ) ;
#1775 = CARTESIAN_POINT ( 'NONE',  ( 18.62759615963271287, -10.81492255796078972, 28.33224293864769550 ) ) ;
#1774 = CARTESIAN_POINT ( 'NONE',  ( -16.51473224551069308, -9.474510206698971260, 21.66557627198102765 ) ) ;
#1776 = CARTESIAN_POINT ( 'NONE',  ( 10.72451020669898902, -18.67979575497178502, 57.91557627198103120 ) ) ;
#1777 = CARTESIAN_POINT ( 'NONE',  ( 8.314922557960818139, 14.29746914071049879, 94.58224293864769550 ) ) ;
#1778 = CARTESIAN_POINT ( 'NONE',  ( -4.379528057220086978, -16.55341960407618274, 49.79275706135234714 ) ) ;
#1779 = ADVANCED_FACE ( 'NONE', ( #62900 ), #3223, .T. ) ;
#1780 = CARTESIAN_POINT ( 'NONE',  ( -16.52544592524342804, 4.483927247898546575, 96.04057627198102409 ) ) ;
#1781 = DIRECTION ( 'NONE',  ( 0.000000000000000000, -0.000000000000000000, -1.000000000000000000 ) ) ;
#1782 = CARTESIAN_POINT ( 'NONE',  ( -16.21995358207306381, 7.366697692864089042, 49.93551001512157939 ) ) ;
#1783 = CARTESIAN_POINT ( 'NONE',  ( 0.05219959533909260263, 19.03943276465977164, 109.9989096053143669 ) ) ;
#1784 = CARTESIAN_POINT ( 'NONE',  ( 22.81625015709509441, 31.40387420917330275, -3.824999997268813345 ) ) ;
#1785 = CARTESIAN_POINT ( 'NONE',  ( 4.500000000000000000, 0.000000000000000000, 0.000000000000000000 ) ) ;
#1786 = ORIENTED_EDGE ( 'NONE', *, *, #121976, .F. ) ;
#1788 = CARTESIAN_POINT ( 'NONE',  ( 4.379528057220339221, -16.55341960407611168, 27.70724293864769905 ) ) ;
#1787 = CARTESIAN_POINT ( 'NONE',  ( -8.314922557961024197, 14.29746914071037800, 42.91775706135235424 ) ) ;
#1789 = CARTESIAN_POINT ( 'NONE',  ( -18.62759615963270932, 10.81492255796079327, 55.83224293864770260 ) ) ;
#1790 = CARTESIAN_POINT ( 'NONE',  ( 0.05219959533936267826, -19.03943276465977164, 90.00109039468567573 ) ) ;
#1791 = CARTESIAN_POINT ( 'NONE',  ( 21.53943276465977519, -0.05219959533907433946, 53.74890960531437401 ) ) ;
#1792 = CARTESIAN_POINT ( 'NONE',  ( -18.62759615963255300, -10.81492255796106328, 84.16775706135234714 ) ) ;
#1793 = CARTESIAN_POINT ( 'NONE',  ( 17.10305700086941272, -33.88765926517208982, -26.94085628989243730 ) ) ;
#1794 = CARTESIAN_POINT ( 'NONE',  ( -4.483927247898782831, 16.52544592524335698, 37.70942372801900433 ) ) ;
#1796 = CARTESIAN_POINT ( 'NONE',  ( 9.474510206698971260, -16.51473224551069308, 97.91557627198102409 ) ) ;
#1795 = CARTESIAN_POINT ( 'NONE',  ( -19.02544592524342804, 5.153800228976336051, 41.04057627198103120 ) ) ;
#1797 = CARTESIAN_POINT ( 'NONE',  ( -5.153800228976328057, -19.02544592524343514, 32.29057627198102409 ) ) ;
#1798 = CARTESIAN_POINT ( 'NONE',  ( -16.52544592524342804, 4.483927247898546575, 101.0405762719810383 ) ) ;
#1799 = CARTESIAN_POINT ( 'NONE',  ( -5.049401038298153566, 19.05341960407611168, 95.20724293864770971 ) ) ;
#1800 = ORIENTED_EDGE ( 'NONE', *, *, #195432, .F. ) ;
#1801 = CARTESIAN_POINT ( 'NONE',  ( 12.06949235617739724, 12.14591786802326823, 51.87609039468568284 ) ) ;
#1802 = CARTESIAN_POINT ( 'NONE',  ( -21.55341960407610458, -5.719274019375992779, 96.45724293864770971 ) ) ;
#1803 = CARTESIAN_POINT ( 'NONE',  ( -19.02544592524342804, 5.153800228976336051, 61.04057627198103120 ) ) ;
#1804 = CARTESIAN_POINT ( 'NONE',  ( -10.72451020669870658, -18.67979575497194134, 24.58442372801901499 ) ) ;
#1805 = CARTESIAN_POINT ( 'NONE',  ( 19.03943276465977164, -0.05219959533909143690, 83.74890960531436690 ) ) ;
#1806 = CARTESIAN_POINT ( 'NONE',  ( -8.898068258721474777, 27.38543819252877043, 145.5843446569000150 ) ) ;
#1807 = ORIENTED_EDGE ( 'NONE', *, *, #14345, .F. ) ;
#1808 = CARTESIAN_POINT ( 'NONE',  ( 16.53943276465976808, 0.05219959533934440121, 41.25109039468568284 ) ) ;
#1809 = CARTESIAN_POINT ( 'NONE',  ( 0.05219959533937995610, -21.53943276465977519, 25.00109039468567218 ) ) ;
#1812 = CARTESIAN_POINT ( 'NONE',  ( 0.05219959533936267826, -19.03943276465977164, 70.00109039468566152 ) ) ;
#1811 = CARTESIAN_POINT ( 'NONE',  ( 9.474510206698971260, -16.51473224551069308, 102.9155762719810241 ) ) ;
#1810 = CARTESIAN_POINT ( 'NONE',  ( 5.153800228976335163, 19.02544592524342804, 24.79057627198102765 ) ) ;
#1813 = CARTESIAN_POINT ( 'NONE',  ( 9.474510206698729675, 16.51473224551082808, 32.08442372801900433 ) ) ;
#1814 = CARTESIAN_POINT ( 'NONE',  ( -21.53943276465977519, 0.05219959533907696930, 86.24890960531436690 ) ) ;
#1815 = CARTESIAN_POINT ( 'NONE',  ( -16.46253265017146816, -9.564922557961047289, 39.16775706135234003 ) ) ;
#1816 = CARTESIAN_POINT ( 'NONE',  ( -8.224510206698735004, -14.34966873604973081, 74.58442372801901854 ) ) ;
#1817 = CARTESIAN_POINT ( 'NONE',  ( -9.564922557960796823, -16.46253265017161027, 112.0822429386476955 ) ) ;
#1818 = CARTESIAN_POINT ( 'NONE',  ( -13.97604488694527625, -13.89961937509977652, 61.87390960531435979 ) ) ;
#1819 = CARTESIAN_POINT ( 'NONE',  ( -18.67979575497193778, 10.72451020669871902, 68.33442372801900433 ) ) ;
#1820 = CARTESIAN_POINT ( 'NONE',  ( 21.53943276465977519, 0.05219959533937863772, 86.25109039468568994 ) ) ;
#1821 = CARTESIAN_POINT ( 'NONE',  ( -19.03943276465977164, 0.05219959533909376836, 71.24890960531435269 ) ) ;
#1822 = CARTESIAN_POINT ( 'NONE',  ( 21.52544592524334988, 5.823673210054432836, 51.45942372801901854 ) ) ;
#1823 = CARTESIAN_POINT ( 'NONE',  ( -19.05341960407617563, 5.049401038297882671, 93.54275706135234714 ) ) ;
#1824 = CARTESIAN_POINT ( 'NONE',  ( -13.97604488694527625, -13.89961937509977652, 56.87390960531434558 ) ) ;
#1825 = CARTESIAN_POINT ( 'NONE',  ( 19.02544592524343514, -5.153800228976328945, 103.5405762719809957 ) ) ;
#1826 = CARTESIAN_POINT ( 'NONE',  ( -9.564922557960796823, -16.46253265017161027, 62.08224293864769550 ) ) ;
#1827 = CARTESIAN_POINT ( 'NONE',  ( 16.46253265017160672, -9.564922557960803928, 113.3322429386476955 ) ) ;
#1828 = CARTESIAN_POINT ( 'NONE',  ( -5.153800228976328057, -19.02544592524343514, 47.29057627198102409 ) ) ;
#1829 = CARTESIAN_POINT ( 'NONE',  ( -5.823673210054116645, -21.52544592524344225, 102.2905762719810383 ) ) ;
#1830 = CARTESIAN_POINT ( 'NONE',  ( -12.14591786802326823, 12.06949235617739902, 73.12609039468567573 ) ) ;
#1831 = CARTESIAN_POINT ( 'NONE',  ( -21.70479006154311108, 8.695791278452229989, 169.0563666577074287 ) ) ;
#1832 = CARTESIAN_POINT ( 'NONE',  ( 16.51473224551083163, -9.474510206698727899, 30.83442372801900433 ) ) ;
#1833 = CARTESIAN_POINT ( 'NONE',  ( -0.05219959533909027116, -19.03943276465977164, 72.49890960531435269 ) ) ;
#1834 = CARTESIAN_POINT ( 'NONE',  ( -8.224510206698948167, 14.34966873604960824, 60.41557627198102409 ) ) ;
#1835 = CARTESIAN_POINT ( 'NONE',  ( -8.314922557960811034, -14.29746914071050412, 92.08224293864769550 ) ) ;
#1836 = CARTESIAN_POINT ( 'NONE',  ( 0.05219959533909260263, 19.03943276465977164, 94.99890960531436690 ) ) ;
#1837 = CARTESIAN_POINT ( 'NONE',  ( 9.474510206698971260, -16.51473224551069308, 97.91557627198102409 ) ) ;
#1838 = CARTESIAN_POINT ( 'NONE',  ( -16.46253265017160317, 9.564922557960807481, 105.8322429386476955 ) ) ;
#1839 = CARTESIAN_POINT ( 'NONE',  ( 19.03943276465977164, 0.05219959533936151252, 21.25109039468565797 ) ) ;
#1840 = CARTESIAN_POINT ( 'NONE',  ( -14.29746914071037622, -8.314922557961029526, 94.16775706135237556 ) ) ;
#1841 = CARTESIAN_POINT ( 'NONE',  ( -10.81492255796105439, 18.62759615963255655, 37.91775706135235424 ) ) ;
#1842 = CARTESIAN_POINT ( 'NONE',  ( 10.81492255796078972, 18.62759615963270932, 29.58224293864769905 ) ) ;
#1843 = CARTESIAN_POINT ( 'NONE',  ( -5.823673210054116645, -21.52544592524344225, 102.2905762719810383 ) ) ;
#1844 = CARTESIAN_POINT ( 'NONE',  ( -12.06949235617756955, 12.14591786802309770, 65.62390960531436690 ) ) ;
#1845 = CARTESIAN_POINT ( 'NONE',  ( 0.05219959533909260263, 19.03943276465977164, 49.99890960531435979 ) ) ;
#1846 = CARTESIAN_POINT ( 'NONE',  ( -16.52544592524342804, 4.483927247898546575, 81.04057627198102409 ) ) ;
#1847 = CARTESIAN_POINT ( 'NONE',  ( 10.81492255796078972, 18.62759615963270932, 39.58224293864769550 ) ) ;
#1848 = CARTESIAN_POINT ( 'NONE',  ( -5.049401038297874678, -19.05341960407617918, 49.79275706135231871 ) ) ;
#1849 = CARTESIAN_POINT ( 'NONE',  ( -12.14591786802309592, -12.06949235617757132, 111.8739096053143669 ) ) ;
#1850 = VERTEX_POINT ( 'NONE', #97199 ) ;
#1851 = CARTESIAN_POINT ( 'NONE',  ( 8.224510206698742110, 14.34966873604972548, 67.08442372801901854 ) ) ;
#1852 = CARTESIAN_POINT ( 'NONE',  ( 5.153800228976335163, 19.02544592524342804, 64.79057627198100988 ) ) ;
#1853 = CARTESIAN_POINT ( 'NONE',  ( 27.73933785331498569, 2.768321779492822058E-14, 145.8750000027311842 ) ) ;
#1854 = CARTESIAN_POINT ( 'NONE',  ( -16.55341960407611168, -4.379528057220339221, 86.45724293864770971 ) ) ;
#1855 = CARTESIAN_POINT ( 'NONE',  ( -5.823673210054116645, -21.52544592524344225, 37.29057627198102409 ) ) ;
#1856 = ORIENTED_EDGE ( 'NONE', *, *, #13659, .T. ) ;
#1857 = CARTESIAN_POINT ( 'NONE',  ( 16.55341960407618274, -4.379528057220086978, 106.0427570613523471 ) ) ;
#1858 = CARTESIAN_POINT ( 'NONE',  ( 16.53943276465976808, 0.05219959533934440121, 31.25109039468568639 ) ) ;
#1859 = CARTESIAN_POINT ( 'NONE',  ( -18.62759615963255300, -10.81492255796106328, 99.16775706135234714 ) ) ;
#1860 = CARTESIAN_POINT ( 'NONE',  ( -19.02544592524342804, 5.153800228976336051, 86.04057627198103830 ) ) ;
#1861 = CARTESIAN_POINT ( 'NONE',  ( -21.53943276465977519, 0.05219959533907696930, 116.2489096053143669 ) ) ;
#1862 = CARTESIAN_POINT ( 'NONE',  ( -19.02544592524342804, 5.153800228976336051, 31.04057627198102409 ) ) ;
#1863 = CARTESIAN_POINT ( 'NONE',  ( -8.224510206698735004, -14.34966873604973081, 24.58442372801901499 ) ) ;
#1864 = ADVANCED_FACE ( 'NONE', ( #142724 ), #159574, .T. ) ;
#1865 = CARTESIAN_POINT ( 'NONE',  ( -13.89961937509957401, -13.97604488694547875, 89.37609039468563310 ) ) ;
#1866 = CARTESIAN_POINT ( 'NONE',  ( 21.55341960407610458, 5.719274019375980345, 88.95724293864769550 ) ) ;
#1867 = CARTESIAN_POINT ( 'NONE',  ( 13.97604488694548053, -13.89961937509957401, 65.62609039468567573 ) ) ;
#1868 = FACE_OUTER_BOUND ( 'NONE', #166626, .T. ) ;
#1869 = CARTESIAN_POINT ( 'NONE',  ( 15.80617190586746368, 15.72974639402197994, 114.3739096053143527 ) ) ;
#1870 = CARTESIAN_POINT ( 'NONE',  ( 18.22780087662123805, -5.499999999999976019, 73.51763182126894947 ) ) ;
#1871 = CARTESIAN_POINT ( 'NONE',  ( -9.474510206698964154, 16.51473224551069663, 80.41557627198103830 ) ) ;
#1872 = CARTESIAN_POINT ( 'NONE',  ( 8.224510206698742110, 14.34966873604972548, 27.08442372801901854 ) ) ;
#1873 = CARTESIAN_POINT ( 'NONE',  ( 18.50421606877890923, -35.46346162465770391, -8.316515678940758605 ) ) ;
#1874 = CARTESIAN_POINT ( 'NONE',  ( 9.564922557961047289, -16.46253265017146816, 65.41775706135233293 ) ) ;
#1876 = CARTESIAN_POINT ( 'NONE',  ( -16.55341960407611168, -4.379528057220339221, 71.45724293864769550 ) ) ;
#1875 = CARTESIAN_POINT ( 'NONE',  ( -15.80617190586768217, 15.72974639402176855, 23.12609039468567573 ) ) ;
#1877 = CARTESIAN_POINT ( 'NONE',  ( 0.05219959533909260263, 19.03943276465977164, 79.99890960531436690 ) ) ;
#1879 = CARTESIAN_POINT ( 'NONE',  ( -16.51473224551082808, 9.474510206698731452, 38.33442372801899722 ) ) ;
#1878 = CARTESIAN_POINT ( 'NONE',  ( -12.14591786802326823, 12.06949235617739902, 43.12609039468568284 ) ) ;
#1880 = CARTESIAN_POINT ( 'NONE',  ( -21.55341960407619339, 5.719274019375674811, 68.54275706135234714 ) ) ;
#1881 = CARTESIAN_POINT ( 'NONE',  ( -9.474510206698720793, -16.51473224551083518, 104.5844237280190043 ) ) ;
#1882 = CARTESIAN_POINT ( 'NONE',  ( 9.564922557960805705, 16.46253265017160317, 59.58224293864769550 ) ) ;
#1883 = CARTESIAN_POINT ( 'NONE',  ( -19.03943276465977164, -0.05219959533935918106, 88.75109039468567573 ) ) ;
#1884 = CARTESIAN_POINT ( 'NONE',  ( -16.53943276465976808, -0.05219959533934237506, 53.75109039468568994 ) ) ;
#1885 = CARTESIAN_POINT ( 'NONE',  ( 10.81492255796106328, -18.62759615963255655, 100.4177570613523471 ) ) ;
#1886 = CARTESIAN_POINT ( 'NONE',  ( -9.474510206698720793, -16.51473224551083518, 64.58442372801900433 ) ) ;
#1887 = CARTESIAN_POINT ( 'NONE',  ( -19.05341960407611168, -5.049401038298163336, 56.45724293864768129 ) ) ;
#1888 = CARTESIAN_POINT ( 'NONE',  ( -18.67979575497178146, -10.72451020669898902, 66.66557627198102409 ) ) ;
#1890 = CARTESIAN_POINT ( 'NONE',  ( -19.03943276465977164, -0.05219959533935918106, 63.75109039468566863 ) ) ;
#1889 = CARTESIAN_POINT ( 'NONE',  ( 16.55341960407611168, 4.379528057220329451, 68.95724293864769550 ) ) ;
#1891 = DIRECTION ( 'NONE',  ( 1.000000000000000000, 0.000000000000000000, 0.000000000000000000 ) ) ;
#1893 = EDGE_CURVE ( 'NONE', #82035, #127301, #31585, .T. ) ;
#1892 = CARTESIAN_POINT ( 'NONE',  ( 0.05219959533936267826, -19.03943276465977164, 40.00109039468566152 ) ) ;
#1894 = CARTESIAN_POINT ( 'NONE',  ( -4.379528057220086978, -16.55341960407618274, 94.79275706135234714 ) ) ;
#1895 = CARTESIAN_POINT ( 'NONE',  ( 12.06949235617757843, -12.14591786802309237, 68.12390960531436690 ) ) ;
#1897 = CARTESIAN_POINT ( 'NONE',  ( 8.571926809382603096, -26.38167802310801235, 139.4750000027311785 ) ) ;
#1896 = CARTESIAN_POINT ( 'NONE',  ( 10.81492255796106328, -18.62759615963255655, 90.41775706135236135 ) ) ;
#1898 = CARTESIAN_POINT ( 'NONE',  ( -10.81492255796078084, -18.62759615963271287, 92.08224293864769550 ) ) ;
#1899 = CARTESIAN_POINT ( 'NONE',  ( 13.89961937509977652, -13.97604488694527269, 48.12390960531435979 ) ) ;
#1900 = CARTESIAN_POINT ( 'NONE',  ( 18.62759615963255655, 10.81492255796105972, 76.66775706135234714 ) ) ;
#1901 = CARTESIAN_POINT ( 'NONE',  ( 19.03943276465977164, -0.05219959533909143690, 53.74890960531436690 ) ) ;
#1902 = ORIENTED_EDGE ( 'NONE', *, *, #135350, .T. ) ;
#1903 = CARTESIAN_POINT ( 'NONE',  ( 5.153800228976335163, 19.02544592524342804, 64.79057627198100988 ) ) ;
#1904 = CARTESIAN_POINT ( 'NONE',  ( 12.14591786802309770, 12.06949235617756955, 114.3739096053143527 ) ) ;
#1905 = CARTESIAN_POINT ( 'NONE',  ( -21.53943276465977519, 0.05219959533907696930, 21.24890960531436690 ) ) ;
#1906 = VECTOR ( 'NONE', #11374, 1000.000000000000000 ) ;
#1907 = CARTESIAN_POINT ( 'NONE',  ( 14.34966873604960469, 8.224510206698951720, 49.16557627198102409 ) ) ;
#1908 = CARTESIAN_POINT ( 'NONE',  ( 9.474510206698971260, -16.51473224551069308, 27.91557627198103120 ) ) ;
#1909 = CARTESIAN_POINT ( 'NONE',  ( -16.53943276465976808, 0.05219959533911058130, 86.24890960531436690 ) ) ;
#1910 = CARTESIAN_POINT ( 'NONE',  ( -10.81492255796078084, -18.62759615963271287, 102.0822429386476955 ) ) ;
#1911 = CARTESIAN_POINT ( 'NONE',  ( 21.53943276465977519, 0.05219959533937863772, 31.25109039468568639 ) ) ;
#1912 = CARTESIAN_POINT ( 'NONE',  ( 1.425040633100159937, 7.121692137566853376, -62.29960613186693763 ) ) ;
#1913 = CARTESIAN_POINT ( 'NONE',  ( -14.29746914071037622, -8.314922557961029526, 49.16775706135234003 ) ) ;
#1914 = CARTESIAN_POINT ( 'NONE',  ( -18.62759615963270932, 10.81492255796079327, 90.83224293864769550 ) ) ;
#1915 = CARTESIAN_POINT ( 'NONE',  ( -21.53943276465977519, -0.05219959533937600094, 108.7510903946857042 ) ) ;
#1916 = CARTESIAN_POINT ( 'NONE',  ( 0.05219959533909260263, 19.03943276465977164, 109.9989096053143669 ) ) ;
#1917 = CARTESIAN_POINT ( 'NONE',  ( 0.05219959533937995610, -21.53943276465977519, 50.00109039468568994 ) ) ;
#1918 = CARTESIAN_POINT ( 'NONE',  ( -18.62759615963270932, 10.81492255796079327, 40.83224293864769550 ) ) ;
#1919 = CARTESIAN_POINT ( 'NONE',  ( 4.483927247898790824, -16.52544592524335698, 100.2094237280190043 ) ) ;
#1921 = CARTESIAN_POINT ( 'NONE',  ( 0.05219959533937995610, -21.53943276465977519, 100.0010903946857042 ) ) ;
#1920 = CARTESIAN_POINT ( 'NONE',  ( 5.823673210054444382, -21.52544592524334988, 60.20942372801902565 ) ) ;
#1922 = CARTESIAN_POINT ( 'NONE',  ( 16.46253265017146816, 9.564922557961045513, 36.66775706135233293 ) ) ;
#1923 = CARTESIAN_POINT ( 'NONE',  ( -14.34966873604972548, 8.224510206698743886, 93.33442372801901854 ) ) ;
#1924 = CARTESIAN_POINT ( 'NONE',  ( 15.72974639402176855, 15.80617190586768217, 36.87609039468568994 ) ) ;
#1925 = CARTESIAN_POINT ( 'NONE',  ( -0.05219959533909027116, -19.03943276465977164, 42.49890960531435269 ) ) ;
#1926 = CARTESIAN_POINT ( 'NONE',  ( -5.153800228976607833, 19.02544592524334988, 27.70942372801899722 ) ) ;
#1927 = CARTESIAN_POINT ( 'NONE',  ( 21.52544592524344225, -5.823673210054117533, 23.54057627198102765 ) ) ;
#1928 = CARTESIAN_POINT ( 'NONE',  ( -18.67979575497178146, -10.72451020669898902, 111.6655762719810525 ) ) ;
#1929 = CARTESIAN_POINT ( 'NONE',  ( 21.53943276465977519, -0.05219959533907433946, 78.74890960531436690 ) ) ;
#1930 = CARTESIAN_POINT ( 'NONE',  ( 12.06949235617739724, 12.14591786802326823, 36.87609039468568994 ) ) ;
#1932 = CARTESIAN_POINT ( 'NONE',  ( -15.80617190586745835, -15.72974639402198527, 76.87390960531439532 ) ) ;
#1931 = CARTESIAN_POINT ( 'NONE',  ( -17.49999999999999645, -7.500000000000000888, 22.00000000000000711 ) ) ;
#1934 = CARTESIAN_POINT ( 'NONE',  ( 14.34966873604960469, 8.224510206698951720, 64.16557627198102409 ) ) ;
#1933 = CARTESIAN_POINT ( 'NONE',  ( -4.379528057220086978, -16.55341960407618274, 69.79275706135234714 ) ) ;
#1935 = CARTESIAN_POINT ( 'NONE',  ( 1.366360357771132517, 29.77508901761298787, -48.57104573785031221 ) ) ;
#1936 = CARTESIAN_POINT ( 'NONE',  ( -0.05219959533936034679, 19.03943276465977164, 97.50109039468567573 ) ) ;
#1937 = CARTESIAN_POINT ( 'NONE',  ( -24.11542121825890561, 0.7284999611697620114, -54.35861002160294930 ) ) ;
#1938 = CARTESIAN_POINT ( 'NONE',  ( 16.55341960407618274, -4.379528057220086978, 41.04275706135236135 ) ) ;
#1939 = CARTESIAN_POINT ( 'NONE',  ( 5.823673210054125526, 21.52544592524343514, 114.7905762719810383 ) ) ;
#1940 = CARTESIAN_POINT ( 'NONE',  ( 18.67979575497178502, 10.72451020669898547, 69.16557627198102409 ) ) ;
#1941 = CARTESIAN_POINT ( 'NONE',  ( -13.89961937509977652, 13.97604488694528158, 115.6239096053143669 ) ) ;
#1942 = CARTESIAN_POINT ( 'NONE',  ( 12.14591786802327356, -12.06949235617739191, 60.62609039468567573 ) ) ;
#1943 = CARTESIAN_POINT ( 'NONE',  ( 5.153800228976335163, 19.02544592524342804, 74.79057627198103830 ) ) ;
#1945 = CARTESIAN_POINT ( 'NONE',  ( 13.89961937509957401, 13.97604488694547697, 111.8760903946856757 ) ) ;
#1944 = CARTESIAN_POINT ( 'NONE',  ( -21.52544592524334988, -5.823673210054445271, 43.95942372801902565 ) ) ;
#1946 = CARTESIAN_POINT ( 'NONE',  ( -19.02544592524342804, 5.153800228976336051, 106.0405762719810241 ) ) ;
#1947 = VERTEX_POINT ( 'NONE', #111400 ) ;
#1948 = CARTESIAN_POINT ( 'NONE',  ( 19.02544592524334988, 5.153800228976608722, 26.45942372801899722 ) ) ;
#1949 = CARTESIAN_POINT ( 'NONE',  ( -16.53943276465976808, -0.05219959533934237506, 38.75109039468567573 ) ) ;
#1950 = CARTESIAN_POINT ( 'NONE',  ( 13.97604488694527802, 13.89961937509977652, 104.3739096053143385 ) ) ;
#1951 = CARTESIAN_POINT ( 'NONE',  ( 18.67979575497178502, 10.72451020669898547, 99.16557627198100988 ) ) ;
#1952 = CARTESIAN_POINT ( 'NONE',  ( -5.153800228976328057, -19.02544592524343514, 57.29057627198103120 ) ) ;
#1953 = CARTESIAN_POINT ( 'NONE',  ( -16.61371651742603461, 7.165104196376024248, 23.85415069992998482 ) ) ;
#1954 = CARTESIAN_POINT ( 'NONE',  ( 8.224510206698953496, -14.34966873604960469, 77.91557627198102409 ) ) ;
#1955 = CARTESIAN_POINT ( 'NONE',  ( 21.52544592524344225, -5.823673210054117533, 23.54057627198102765 ) ) ;
#1956 = CARTESIAN_POINT ( 'NONE',  ( -16.18388926212241685, 7.379444403734376046, 34.56046848633846480 ) ) ;
#1957 = CARTESIAN_POINT ( 'NONE',  ( 18.67979575497178502, 10.72451020669898547, 109.1655762719810383 ) ) ;
#1958 = CARTESIAN_POINT ( 'NONE',  ( 19.03943276465977164, 0.05219959533936151252, 61.25109039468566863 ) ) ;
#1959 = CARTESIAN_POINT ( 'NONE',  ( 21.53943276465977519, -0.05219959533907433946, 33.74890960531436690 ) ) ;
#1960 = CARTESIAN_POINT ( 'NONE',  ( 13.97604488694527802, 13.89961937509977652, 29.37390960531435979 ) ) ;
#1961 = CARTESIAN_POINT ( 'NONE',  ( 18.67979575497178502, 10.72451020669898547, 49.16557627198102409 ) ) ;
#1962 = CARTESIAN_POINT ( 'NONE',  ( -19.03943276465977164, 0.05219959533909376836, 101.2489096053143669 ) ) ;
#1963 = CARTESIAN_POINT ( 'NONE',  ( 10.72451020669871369, 18.67979575497193778, 82.08442372801901854 ) ) ;
#1964 = CARTESIAN_POINT ( 'NONE',  ( 0.05219959533909260263, 19.03943276465977164, 49.99890960531435979 ) ) ;
#1965 = CARTESIAN_POINT ( 'NONE',  ( 16.53943276465976808, -0.05219959533910856209, 88.74890960531436690 ) ) ;
#1966 = CARTESIAN_POINT ( 'NONE',  ( 4.483927247898790824, -16.52544592524335698, 30.20942372801902565 ) ) ;
#1967 = CARTESIAN_POINT ( 'NONE',  ( 5.153800228976335163, 19.02544592524342804, 54.79057627198103120 ) ) ;
#1968 = CARTESIAN_POINT ( 'NONE',  ( 18.67979575497194134, -10.72451020669871369, 65.83442372801900433 ) ) ;
#1969 = ORIENTED_EDGE ( 'NONE', *, *, #146153, .T. ) ;
#1970 = CARTESIAN_POINT ( 'NONE',  ( 5.153800228976615827, -19.02544592524334988, 25.20942372801900433 ) ) ;
#1971 = CARTESIAN_POINT ( 'NONE',  ( 5.049401038297881783, 19.05341960407617563, 42.29275706135234003 ) ) ;
#1972 = CARTESIAN_POINT ( 'NONE',  ( 4.500000000000000888, -126.2936762853306902, 8.011306146643438097 ) ) ;
#1973 = CARTESIAN_POINT ( 'NONE',  ( -21.52544592524334988, -5.823673210054445271, 38.95942372801901854 ) ) ;
#1974 = ADVANCED_FACE ( 'NONE', ( #188258, #93235, #49732, #35552, #138750, #32579, #47755, #94232, #173085, #34564, #96220, #155913, #15422, #140738, #16418, #19399, #154920, #127556 ), #125579, .F. ) ;
#1975 = LINE ( 'NONE', #106172, #114116 ) ;
#1976 = CARTESIAN_POINT ( 'NONE',  ( 5.049401038297881783, 19.05341960407617563, 32.29275706135233293 ) ) ;
#1977 = CARTESIAN_POINT ( 'NONE',  ( -16.46253265017160317, 9.564922557960807481, 85.83224293864769550 ) ) ;
#1978 = CARTESIAN_POINT ( 'NONE',  ( -19.03943276465977164, 0.05219959533909376836, 66.24890960531436690 ) ) ;
#1979 = CARTESIAN_POINT ( 'NONE',  ( 12.06949235617757843, -12.14591786802309237, 23.12390960531436335 ) ) ;
#1981 = CARTESIAN_POINT ( 'NONE',  ( 15.80617190586769283, -15.72974639402175789, 80.62609039468567573 ) ) ;
#1980 = CARTESIAN_POINT ( 'NONE',  ( 0.05219959533909260263, 19.03943276465977164, 114.9989096053143669 ) ) ;
#1982 = CARTESIAN_POINT ( 'NONE',  ( 11.40812507854755253, -35.11059874428192273, -10.52499999726881263 ) ) ;
#1983 = CARTESIAN_POINT ( 'NONE',  ( 16.36317988757058473, 7.306389748694949837, 58.40210391636776421 ) ) ;
#1984 = CARTESIAN_POINT ( 'NONE',  ( 21.53943276465977519, 0.05219959533937863772, 81.25109039468568994 ) ) ;
#1985 = CARTESIAN_POINT ( 'NONE',  ( 16.61371651742598843, -7.165104196376272938, 41.35415069992997417 ) ) ;
#1986 = CARTESIAN_POINT ( 'NONE',  ( 5.153800228976335163, 19.02544592524342804, 104.7905762719809957 ) ) ;
#1987 = EDGE_CURVE ( 'NONE', #137596, #48134, #24393, .T. ) ;
#1988 = CARTESIAN_POINT ( 'NONE',  ( 33.68482864984028424, 4.779698632210292786, 97.74495643025990432 ) ) ;
#1989 = CARTESIAN_POINT ( 'NONE',  ( 21.55341960407610458, 5.719274019375980345, 63.95724293864770260 ) ) ;
#1990 = CARTESIAN_POINT ( 'NONE',  ( -8.314922557960811034, -14.29746914071050412, 22.08224293864769194 ) ) ;
#1992 = CARTESIAN_POINT ( 'NONE',  ( 5.049401038298161559, -19.05341960407611168, 97.70724293864766707 ) ) ;
#1991 = CARTESIAN_POINT ( 'NONE',  ( 0.05219959533910956823, 16.53943276465976808, 109.9989096053143527 ) ) ;
#1993 = CARTESIAN_POINT ( 'NONE',  ( 10.72451020669871369, 18.67979575497193778, 112.0844237280190185 ) ) ;
#1994 = CARTESIAN_POINT ( 'NONE',  ( -8.224510206698948167, 14.34966873604960824, 105.4155762719810383 ) ) ;
#1995 = CARTESIAN_POINT ( 'NONE',  ( 21.52544592524334988, 5.823673210054432836, 66.45942372801903275 ) ) ;
#1996 = CARTESIAN_POINT ( 'NONE',  ( 9.474510206698971260, -16.51473224551069308, 112.9155762719810383 ) ) ;
#1997 = CARTESIAN_POINT ( 'NONE',  ( 8.314922557961029526, -14.29746914071037800, 105.4177570613523613 ) ) ;
#1998 = CARTESIAN_POINT ( 'NONE',  ( -13.89961937509957401, -13.97604488694547875, 64.37609039468567573 ) ) ;
#1999 = CARTESIAN_POINT ( 'NONE',  ( -29.86685920354755552, 21.69954338932564397, -5.324999997268814234 ) ) ;
#2000 = CARTESIAN_POINT ( 'NONE',  ( 19.02544592524343514, -5.153800228976328945, 103.5405762719809957 ) ) ;
#2001 = CARTESIAN_POINT ( 'NONE',  ( 12.14591786802309770, 12.06949235617756955, 74.37390960531436690 ) ) ;
#2003 = CARTESIAN_POINT ( 'NONE',  ( -13.89961937509957401, -13.97604488694547875, 59.37609039468566863 ) ) ;
#2002 = TOROIDAL_SURFACE ( 'NONE', #8512, 40.49999999999999289, 0.5000000000000000000 ) ;
#2004 = CARTESIAN_POINT ( 'NONE',  ( 5.153800228976335163, 19.02544592524342804, 79.79057627198102409 ) ) ;
#2005 = CARTESIAN_POINT ( 'NONE',  ( -16.52544592524342804, 4.483927247898546575, 66.04057627198103830 ) ) ;
#2006 = CARTESIAN_POINT ( 'NONE',  ( -0.05219959533936034679, 19.03943276465977164, 97.50109039468567573 ) ) ;
#2007 = CARTESIAN_POINT ( 'NONE',  ( 15.72974639402199770, -15.80617190586745480, 48.12390960531436690 ) ) ;
#2008 = VERTEX_POINT ( 'NONE', #18414 ) ;
#2009 = CARTESIAN_POINT ( 'NONE',  ( -13.97604488694527625, -13.89961937509977652, 21.87390960531435979 ) ) ;
#2010 = CARTESIAN_POINT ( 'NONE',  ( 30.00000000000000000, -1.163414459189985801E-14, 92.50000000000000000 ) ) ;
#2012 = CARTESIAN_POINT ( 'NONE',  ( -15.72974639402197994, 15.80617190586746368, 65.62390960531436690 ) ) ;
#2011 = CARTESIAN_POINT ( 'NONE',  ( -16.51473224551069308, -9.474510206698971260, 76.66557627198103830 ) ) ;
#2014 = CARTESIAN_POINT ( 'NONE',  ( 16.46253265017160672, -9.564922557960803928, 78.33224293864769550 ) ) ;
#2013 = CARTESIAN_POINT ( 'NONE',  ( -12.06949235617739369, -12.14591786802326823, 94.37609039468568994 ) ) ;
#2015 = CARTESIAN_POINT ( 'NONE',  ( 0.05219959533936267826, -19.03943276465977164, 50.00109039468566863 ) ) ;
#2016 = CARTESIAN_POINT ( 'NONE',  ( 0.05219959533937995610, -21.53943276465977519, 80.00109039468568994 ) ) ;
#2017 = CARTESIAN_POINT ( 'NONE',  ( -5.719274019375978568, 21.55341960407610458, 65.20724293864768129 ) ) ;
#2018 = CARTESIAN_POINT ( 'NONE',  ( -5.153800228976328057, -19.02544592524343514, 112.2905762719810099 ) ) ;
#2019 = CARTESIAN_POINT ( 'NONE',  ( 5.153800228976335163, 19.02544592524342804, 34.79057627198102409 ) ) ;
#2020 = CARTESIAN_POINT ( 'NONE',  ( 4.379528057220092307, 16.55341960407617563, 107.2927570613523471 ) ) ;
#2021 = CARTESIAN_POINT ( 'NONE',  ( -16.55341960407617563, 4.379528057220093196, 23.54275706135235424 ) ) ;
#2022 = CARTESIAN_POINT ( 'NONE',  ( 16.61371651742603817, 7.165104196376042012, 53.64584930007004715 ) ) ;
#2023 = CARTESIAN_POINT ( 'NONE',  ( -18.67979575497193778, 10.72451020669871902, 103.3344237280190043 ) ) ;
#2024 = CARTESIAN_POINT ( 'NONE',  ( 16.55341960407611168, 4.379528057220329451, 53.95724293864770260 ) ) ;
#2025 = CARTESIAN_POINT ( 'NONE',  ( 5.823673210054125526, 21.52544592524343514, 89.79057627198103830 ) ) ;
#2026 = CARTESIAN_POINT ( 'NONE',  ( 18.62759615963271287, -10.81492255796078972, 88.33224293864769550 ) ) ;
#2027 = CARTESIAN_POINT ( 'NONE',  ( 1.221313414957698099E-14, -31.90000000000003411, -45.64921306006598201 ) ) ;
#2028 = CARTESIAN_POINT ( 'NONE',  ( 0.05219959533907565091, 21.53943276465977519, 39.99890960531436690 ) ) ;
#2029 = CARTESIAN_POINT ( 'NONE',  ( 14.29746914071037800, 8.314922557961029526, 61.66775706135235424 ) ) ;
#2030 = CARTESIAN_POINT ( 'NONE',  ( 12.14591786802309770, 12.06949235617756955, 89.37390960531435269 ) ) ;
#2031 = CARTESIAN_POINT ( 'NONE',  ( -16.51473224551069308, -9.474510206698971260, 51.66557627198102409 ) ) ;
#2032 = CARTESIAN_POINT ( 'NONE',  ( 34.45224964297659653, -5.970420695714325099, 49.56603145559587631 ) ) ;
#2033 = CARTESIAN_POINT ( 'NONE',  ( 16.52544592524335698, 4.483927247898782831, 101.4594237280190185 ) ) ;
#2034 = CARTESIAN_POINT ( 'NONE',  ( -18.62759615963255300, -10.81492255796106328, 34.16775706135234714 ) ) ;
#2035 = CARTESIAN_POINT ( 'NONE',  ( -0.05219959533909027116, -19.03943276465977164, 102.4989096053143669 ) ) ;
#2036 = CARTESIAN_POINT ( 'NONE',  ( -5.823673210054431948, 21.52544592524334988, 67.70942372801901854 ) ) ;
#2037 = PLANE ( 'NONE',  #40540 ) ;
#2038 = CARTESIAN_POINT ( 'NONE',  ( -0.05219959533909027116, -19.03943276465977164, 27.49890960531435624 ) ) ;
#2039 = ORIENTED_EDGE ( 'NONE', *, *, #94568, .T. ) ;
#2040 = CARTESIAN_POINT ( 'NONE',  ( 5.719274019375673035, 21.55341960407619339, 57.29275706135234714 ) ) ;
#2042 = CARTESIAN_POINT ( 'NONE',  ( 19.03943276465977164, -0.05219959533909143690, 113.7489096053143669 ) ) ;
#2041 = CARTESIAN_POINT ( 'NONE',  ( 5.153800228976335163, 19.02544592524342804, 49.79057627198100988 ) ) ;
#2043 = CARTESIAN_POINT ( 'NONE',  ( 0.05219959533909260263, 19.03943276465977164, 89.99890960531436690 ) ) ;
#2044 = CARTESIAN_POINT ( 'NONE',  ( 16.46253265017146816, 9.564922557961045513, 61.66775706135234003 ) ) ;
#2045 = CARTESIAN_POINT ( 'NONE',  ( -5.823673210054431948, 21.52544592524334988, 47.70942372801902565 ) ) ;
#2046 = AXIS2_PLACEMENT_3D ( 'NONE', #73162, #149985, #85294 ) ;
#2047 = CARTESIAN_POINT ( 'NONE',  ( 16.46253265017146816, 9.564922557961045513, 56.66775706135233293 ) ) ;
#2048 = CARTESIAN_POINT ( 'NONE',  ( 13.97604488694527802, 13.89961937509977652, 39.37390960531435269 ) ) ;
#2049 = CARTESIAN_POINT ( 'NONE',  ( -12.06949235617739369, -12.14591786802326823, 104.3760903946856899 ) ) ;
#2050 = CARTESIAN_POINT ( 'NONE',  ( -9.474510206698720793, -16.51473224551083518, 74.58442372801900433 ) ) ;
#2051 = CARTESIAN_POINT ( 'NONE',  ( -8.224510206698948167, 14.34966873604960824, 30.41557627198101699 ) ) ;
#2052 = CARTESIAN_POINT ( 'NONE',  ( -5.049401038297874678, -19.05341960407617918, 49.79275706135231871 ) ) ;
#2053 = CARTESIAN_POINT ( 'NONE',  ( 16.46253265017160672, -9.564922557960803928, 98.33224293864769550 ) ) ;
#2054 = AXIS2_PLACEMENT_3D ( 'NONE', #17433, #106450, #168129 ) ;
#2055 = CARTESIAN_POINT ( 'NONE',  ( -15.80617190586768217, 15.72974639402176855, 108.1260903946856757 ) ) ;
#2056 = CARTESIAN_POINT ( 'NONE',  ( 19.03943276465977164, 0.05219959533936151252, 31.25109039468566863 ) ) ;
#2057 = CARTESIAN_POINT ( 'NONE',  ( 19.03943276465977164, -0.05219959533909143690, 33.74890960531435979 ) ) ;
#2058 = CARTESIAN_POINT ( 'NONE',  ( 0.05219959533937995610, -21.53943276465977519, 90.00109039468567573 ) ) ;
#2059 = CARTESIAN_POINT ( 'NONE',  ( -4.379528057220086978, -16.55341960407618274, 29.79275706135234358 ) ) ;
#2060 = CARTESIAN_POINT ( 'NONE',  ( 5.049401038298161559, -19.05341960407611168, 92.70724293864769550 ) ) ;
#2061 = CARTESIAN_POINT ( 'NONE',  ( -27.73933785331498925, 2.428612866367529932E-14, 140.8750000027311842 ) ) ;
#2062 = CARTESIAN_POINT ( 'NONE',  ( 19.03943276465977164, -0.05219959533909143690, 73.74890960531435269 ) ) ;
#2063 = CARTESIAN_POINT ( 'NONE',  ( -17.97161686094259636, 5.499999999999976907, 95.99637206859250682 ) ) ;
#2064 = CARTESIAN_POINT ( 'NONE',  ( -19.02544592524334988, -5.153800228976617603, 88.95942372801897591 ) ) ;
#2065 = CARTESIAN_POINT ( 'NONE',  ( 19.03943276465977164, -0.05219959533909143690, 103.7489096053143669 ) ) ;
#2066 = CARTESIAN_POINT ( 'NONE',  ( -15.72974639402176322, -15.80617190586768395, 104.3760903946856899 ) ) ;
#2067 = CARTESIAN_POINT ( 'NONE',  ( 8.314922557960818139, 14.29746914071049879, 99.58224293864770971 ) ) ;
#2068 = FACE_OUTER_BOUND ( 'NONE', #96703, .T. ) ;
#2069 = CARTESIAN_POINT ( 'NONE',  ( -10.81492255796078084, -18.62759615963271287, 52.08224293864768839 ) ) ;
#2070 = CARTESIAN_POINT ( 'NONE',  ( 18.67979575497178502, 10.72451020669898547, 39.16557627198102409 ) ) ;
#2071 = CARTESIAN_POINT ( 'NONE',  ( -12.14591786802309592, -12.06949235617757132, 111.8739096053143669 ) ) ;
#2072 = CYLINDRICAL_SURFACE ( 'NONE', #98302, 1.500000000000001332 ) ;
#2073 = CARTESIAN_POINT ( 'NONE',  ( -9.564922557961040184, 16.46253265017147172, 62.91775706135233293 ) ) ;
#2074 = CARTESIAN_POINT ( 'NONE',  ( 4.379528057220339221, -16.55341960407611168, 37.70724293864769550 ) ) ;
#2075 = CARTESIAN_POINT ( 'NONE',  ( 0.05219959533907565091, 21.53943276465977519, 24.99890960531435624 ) ) ;
#2076 = CARTESIAN_POINT ( 'NONE',  ( -0.05219959533937732626, 21.53943276465977519, 82.50109039468568994 ) ) ;
#2077 = CARTESIAN_POINT ( 'NONE',  ( -18.67979575497178146, -10.72451020669898902, 76.66557627198103830 ) ) ;
#2078 = CARTESIAN_POINT ( 'NONE',  ( -10.72451020669870658, -18.67979575497194134, 49.58442372801901143 ) ) ;
#2079 = CARTESIAN_POINT ( 'NONE',  ( 15.72974639402199770, -15.80617190586745480, 93.12390960531436690 ) ) ;
#2080 = CARTESIAN_POINT ( 'NONE',  ( 18.67979575497194134, -10.72451020669871369, 50.83442372801901143 ) ) ;
#2081 = CARTESIAN_POINT ( 'NONE',  ( 19.03943276465977164, -0.05219959533909143690, 23.74890960531435269 ) ) ;
#2082 = CARTESIAN_POINT ( 'NONE',  ( 19.05341960407611168, 5.049401038298154454, 83.95724293864766707 ) ) ;
#2083 = CARTESIAN_POINT ( 'NONE',  ( -16.55341960407617563, 4.379528057220093196, 83.54275706135234714 ) ) ;
#2084 = CARTESIAN_POINT ( 'NONE',  ( -16.53943276465976808, 0.05219959533911058130, 111.2489096053143669 ) ) ;
#2085 = CARTESIAN_POINT ( 'NONE',  ( 19.05341960407611168, 5.049401038298154454, 108.9572429386477097 ) ) ;
#2086 = CARTESIAN_POINT ( 'NONE',  ( 4.483927247898545687, 16.52544592524342804, 59.79057627198103120 ) ) ;
#2087 = CARTESIAN_POINT ( 'NONE',  ( -0.05219959533910754901, -16.53943276465976808, 27.49890960531435269 ) ) ;
#2088 = CARTESIAN_POINT ( 'NONE',  ( -5.049401038298153566, 19.05341960407611168, 70.20724293864769550 ) ) ;
#2089 = CARTESIAN_POINT ( 'NONE',  ( 13.97604488694527802, 13.89961937509977652, 34.37390960531436690 ) ) ;
#2090 = CARTESIAN_POINT ( 'NONE',  ( -21.53943276465977519, 0.05219959533907696930, 51.24890960531436690 ) ) ;
#2091 = CARTESIAN_POINT ( 'NONE',  ( -9.474510206698720793, -16.51473224551083518, 34.58442372801899722 ) ) ;
#2093 = CARTESIAN_POINT ( 'NONE',  ( -8.314922557960811034, -14.29746914071050412, 32.08224293864769550 ) ) ;
#2092 = CARTESIAN_POINT ( 'NONE',  ( -17.49999999999998579, -5.500000000000015099, 41.28230962303565832 ) ) ;
#2094 = CARTESIAN_POINT ( 'NONE',  ( 13.89961937509977652, -13.97604488694527269, 103.1239096053143527 ) ) ;
#2095 = CARTESIAN_POINT ( 'NONE',  ( 21.52544592524334988, 5.823673210054432836, 66.45942372801903275 ) ) ;
#2096 = CARTESIAN_POINT ( 'NONE',  ( 17.78921395495479629, -1.086248361263877582, 37.49999999999999289 ) ) ;
#2097 = CARTESIAN_POINT ( 'NONE',  ( 16.53943276465976808, 0.05219959533934440121, 56.25109039468568284 ) ) ;
#2098 = CARTESIAN_POINT ( 'NONE',  ( 19.02544592524334988, 5.153800228976608722, 56.45942372801898301 ) ) ;
#2099 = CARTESIAN_POINT ( 'NONE',  ( -14.34966873604960291, -8.224510206698953496, 36.66557627198103120 ) ) ;
#2100 = CARTESIAN_POINT ( 'NONE',  ( 16.79531203550644136, -7.028104445595668714, 51.24755011779560476 ) ) ;
#2101 = CARTESIAN_POINT ( 'NONE',  ( 14.34966873604972726, -8.224510206698740333, 105.8344237280190328 ) ) ;
#2102 = CARTESIAN_POINT ( 'NONE',  ( 5.153800228976335163, 19.02544592524342804, 39.79057627198100988 ) ) ;
#2103 = CARTESIAN_POINT ( 'NONE',  ( -13.97604488694527625, -13.89961937509977652, 66.87390960531436690 ) ) ;
#2104 = CARTESIAN_POINT ( 'NONE',  ( 9.564922557960805705, 16.46253265017160317, 29.58224293864769550 ) ) ;
#2105 = CARTESIAN_POINT ( 'NONE',  ( 21.53943276465977519, 0.05219959533937863772, 26.25109039468567573 ) ) ;
#2106 = CARTESIAN_POINT ( 'NONE',  ( -19.05341960407611168, -5.049401038298163336, 61.45724293864769550 ) ) ;
#2107 = CARTESIAN_POINT ( 'NONE',  ( 16.51473224551069308, 9.474510206698969483, 114.1655762719810241 ) ) ;
#2108 = CARTESIAN_POINT ( 'NONE',  ( 13.89961937509977652, -13.97604488694527269, 43.12390960531434558 ) ) ;
#2109 = CARTESIAN_POINT ( 'NONE',  ( -21.55341960407610458, -5.719274019375992779, 26.45724293864768839 ) ) ;
#2111 = CARTESIAN_POINT ( 'NONE',  ( 16.46253265017160672, -9.564922557960803928, 23.33224293864769194 ) ) ;
#2110 = CARTESIAN_POINT ( 'NONE',  ( -21.53943276465977519, -0.05219959533937600094, 53.75109039468568994 ) ) ;
#2112 = CARTESIAN_POINT ( 'NONE',  ( 21.52544592524344225, -5.823673210054117533, 33.54057627198102409 ) ) ;
#2113 = CARTESIAN_POINT ( 'NONE',  ( -4.483927247898782831, 16.52544592524335698, 72.70942372801901854 ) ) ;
#2114 = CARTESIAN_POINT ( 'NONE',  ( -15.80617190586768217, 15.72974639402176855, 103.1260903946856757 ) ) ;
#2115 = CARTESIAN_POINT ( 'NONE',  ( 14.34966873604972726, -8.224510206698740333, 70.83442372801901854 ) ) ;
#2116 = CARTESIAN_POINT ( 'NONE',  ( -19.03943276465977164, 0.05219959533909376836, 101.2489096053143669 ) ) ;
#2117 = CARTESIAN_POINT ( 'NONE',  ( -14.34966873604972548, 8.224510206698743886, 48.33442372801902565 ) ) ;
#2118 = CARTESIAN_POINT ( 'NONE',  ( 8.224510206698742110, 14.34966873604972548, 32.08442372801901854 ) ) ;
#2119 = CARTESIAN_POINT ( 'NONE',  ( 8.224510206698742110, 14.34966873604972548, 102.0844237280190185 ) ) ;
#2120 = CARTESIAN_POINT ( 'NONE',  ( -15.80617190586768217, 15.72974639402176855, 48.12609039468568284 ) ) ;
#2121 = CARTESIAN_POINT ( 'NONE',  ( -19.02544592524334988, -5.153800228976617603, 108.9594237280189759 ) ) ;
#2122 = CARTESIAN_POINT ( 'NONE',  ( -21.55341960407610458, -5.719274019375992779, 111.4572429386476813 ) ) ;
#2124 = CARTESIAN_POINT ( 'NONE',  ( 5.049401038297881783, 19.05341960407617563, 107.2927570613523187 ) ) ;
#2123 = CARTESIAN_POINT ( 'NONE',  ( 4.379528057220339221, -16.55341960407611168, 102.7072429386476955 ) ) ;
#2125 = CARTESIAN_POINT ( 'NONE',  ( -16.53943276465976808, -0.05219959533934237506, 83.75109039468568994 ) ) ;
#2126 = FACE_OUTER_BOUND ( 'NONE', #140551, .T. ) ;
#2128 = EDGE_CURVE ( 'NONE', #35378, #51307, #33569, .T. ) ;
#2127 = CARTESIAN_POINT ( 'NONE',  ( -16.51473224551082808, 9.474510206698731452, 88.33442372801900433 ) ) ;
#2129 = CARTESIAN_POINT ( 'NONE',  ( -16.52544592524342804, 4.483927247898546575, 41.04057627198103120 ) ) ;
#2130 = CARTESIAN_POINT ( 'NONE',  ( -4.483927247898539470, -16.52544592524342804, 47.29057627198103120 ) ) ;
#2131 = CARTESIAN_POINT ( 'NONE',  ( 12.06949235617757843, -12.14591786802309237, 108.1239096053143811 ) ) ;
#2133 = CARTESIAN_POINT ( 'NONE',  ( -17.49999999999998579, 5.500000000000031974, 90.79690382534171533 ) ) ;
#2132 = CARTESIAN_POINT ( 'NONE',  ( 13.89961937509957401, 13.97604488694547697, 46.87609039468565442 ) ) ;
#2134 = CARTESIAN_POINT ( 'NONE',  ( 0.05219959533937995610, -21.53943276465977519, 40.00109039468567573 ) ) ;
#2135 = CARTESIAN_POINT ( 'NONE',  ( 8.314922557961029526, -14.29746914071037800, 20.41775706135234714 ) ) ;
#2136 = DIRECTION ( 'NONE',  ( -0.7071067811865466846, 2.468850131082262583E-15, 0.7071067811865484609 ) ) ;
#2137 = CARTESIAN_POINT ( 'NONE',  ( -13.89961937509977652, 13.97604488694528158, 105.6239096053143527 ) ) ;
#2138 = CARTESIAN_POINT ( 'NONE',  ( -10.72451020669898014, 18.67979575497178502, 60.41557627198102409 ) ) ;
#2139 = CARTESIAN_POINT ( 'NONE',  ( 16.51473224551069308, 9.474510206698969483, 84.16557627198102409 ) ) ;
#2140 = CARTESIAN_POINT ( 'NONE',  ( -21.52544592524343514, 5.823673210054127303, 51.04057627198103120 ) ) ;
#2141 = CARTESIAN_POINT ( 'NONE',  ( 16.52544592524342804, -4.483927247898539470, 113.5405762719810383 ) ) ;
#2142 = CARTESIAN_POINT ( 'NONE',  ( -9.474510206698964154, 16.51473224551069663, 70.41557627198102409 ) ) ;
#2143 = EDGE_CURVE ( 'NONE', #18425, #66087, #76032, .T. ) ;
#2144 = CARTESIAN_POINT ( 'NONE',  ( -0.05219959533909027116, -19.03943276465977164, 32.49890960531435979 ) ) ;
#2145 = CIRCLE ( 'NONE', #140835, 61.99999999999998579 ) ;
#2146 = CARTESIAN_POINT ( 'NONE',  ( 18.67979575497194134, -10.72451020669871369, 40.83442372801901854 ) ) ;
#2147 = CARTESIAN_POINT ( 'NONE',  ( 18.62759615963255655, 10.81492255796105972, 76.66775706135234714 ) ) ;
#2148 = CARTESIAN_POINT ( 'NONE',  ( -16.52544592524335698, -4.483927247898792601, 93.95942372801903275 ) ) ;
#2149 = CARTESIAN_POINT ( 'NONE',  ( 21.52544592524334988, 5.823673210054432836, 31.45942372801901854 ) ) ;
#2150 = CARTESIAN_POINT ( 'NONE',  ( -0.05219959533937732626, 21.53943276465977519, 32.50109039468568284 ) ) ;
#2152 = CARTESIAN_POINT ( 'NONE',  ( 16.51473224551069308, 9.474510206698969483, 79.16557627198103830 ) ) ;
#2151 = CARTESIAN_POINT ( 'NONE',  ( 9.564922557961047289, -16.46253265017146816, 70.41775706135233293 ) ) ;
#2153 = CARTESIAN_POINT ( 'NONE',  ( 21.53943276465977519, 0.05219959533937863772, 86.25109039468568994 ) ) ;
#2154 = CARTESIAN_POINT ( 'NONE',  ( 10.72451020669898902, -18.67979575497178502, 87.91557627198103830 ) ) ;
#2155 = CARTESIAN_POINT ( 'NONE',  ( -12.06949235617756955, 12.14591786802309770, 60.62390960531437401 ) ) ;
#2156 = CARTESIAN_POINT ( 'NONE',  ( -21.53943276465977519, -0.05219959533937600094, 98.75109039468568994 ) ) ;
#2157 = CARTESIAN_POINT ( 'NONE',  ( 8.314922557960818139, 14.29746914071049879, 79.58224293864769550 ) ) ;
#2158 = CARTESIAN_POINT ( 'NONE',  ( -9.564922557960796823, -16.46253265017161027, 27.08224293864769550 ) ) ;
#2159 = CARTESIAN_POINT ( 'NONE',  ( -13.89961937509957401, -13.97604488694547875, 74.37609039468566152 ) ) ;
#2160 = CARTESIAN_POINT ( 'NONE',  ( -14.34966873604960291, -8.224510206698953496, 31.66557627198102054 ) ) ;
#2161 = CARTESIAN_POINT ( 'NONE',  ( -18.67979575497193778, 10.72451020669871902, 88.33442372801901854 ) ) ;
#2162 = CARTESIAN_POINT ( 'NONE',  ( 13.89961937509977652, -13.97604488694527269, 88.12390960531438111 ) ) ;
#2163 = CARTESIAN_POINT ( 'NONE',  ( 13.97604488694548053, -13.89961937509957401, 60.62609039468564731 ) ) ;
#2164 = CARTESIAN_POINT ( 'NONE',  ( -21.55341960407610458, -5.719274019375992779, 71.45724293864769550 ) ) ;
#2165 = CARTESIAN_POINT ( 'NONE',  ( -21.55341960407610458, -5.719274019375992779, 111.4572429386476813 ) ) ;
#2166 = CARTESIAN_POINT ( 'NONE',  ( -19.02544592524334988, -5.153800228976617603, 108.9594237280189759 ) ) ;
#2167 = CARTESIAN_POINT ( 'NONE',  ( 14.29746914071037800, 8.314922557961029526, 81.66775706135236135 ) ) ;
#2169 = CARTESIAN_POINT ( 'NONE',  ( -5.719274019375665041, -21.55341960407619695, 24.79275706135235779 ) ) ;
#2168 = CARTESIAN_POINT ( 'NONE',  ( 17.31747979337950127, 6.344076630961019703, 63.87944868065186199 ) ) ;
#2170 = CARTESIAN_POINT ( 'NONE',  ( -12.14591786802309592, -12.06949235617757132, 106.8739096053143811 ) ) ;
#2171 = CARTESIAN_POINT ( 'NONE',  ( 11.40812507854754365, 35.11059874428196537, -7.724999997268813701 ) ) ;
#2172 = CARTESIAN_POINT ( 'NONE',  ( -0.05219959533934338120, 16.53943276465976808, 32.50109039468568284 ) ) ;
#2173 = CARTESIAN_POINT ( 'NONE',  ( -15.80617190586745835, -15.72974639402198527, 56.87390960531436690 ) ) ;
#2174 = CARTESIAN_POINT ( 'NONE',  ( -12.06949235617739369, -12.14591786802326823, 109.3760903946857042 ) ) ;
#2175 = CARTESIAN_POINT ( 'NONE',  ( 16.55341960407618274, -4.379528057220086978, 36.04275706135234714 ) ) ;
#2176 = CARTESIAN_POINT ( 'NONE',  ( -9.564922557960796823, -16.46253265017161027, 37.08224293864768839 ) ) ;
#2177 = CARTESIAN_POINT ( 'NONE',  ( -8.314922557961024197, 14.29746914071037800, 77.91775706135231871 ) ) ;
#2178 = CARTESIAN_POINT ( 'NONE',  ( 13.97604488694548053, -13.89961937509957401, 75.62609039468564731 ) ) ;
#2179 = CARTESIAN_POINT ( 'NONE',  ( 15.80617190586746368, 15.72974639402197994, 74.37390960531436690 ) ) ;
#2180 = CARTESIAN_POINT ( 'NONE',  ( 16.53943276465976808, 0.05219959533934440121, 101.2510903946856757 ) ) ;
#2181 = CARTESIAN_POINT ( 'NONE',  ( -18.67979575497193778, 10.72451020669871902, 88.33442372801901854 ) ) ;
#2182 = CARTESIAN_POINT ( 'NONE',  ( -15.72974639402197994, 15.80617190586746368, 55.62390960531436690 ) ) ;
#2183 = CARTESIAN_POINT ( 'NONE',  ( -5.823673210054116645, -21.52544592524344225, 47.29057627198103120 ) ) ;
#2184 = CARTESIAN_POINT ( 'NONE',  ( -16.55341960407617563, 4.379528057220093196, 73.54275706135234714 ) ) ;
#2185 = CARTESIAN_POINT ( 'NONE',  ( 5.823673210054125526, 21.52544592524343514, 49.79057627198102409 ) ) ;
#2186 = ORIENTED_EDGE ( 'NONE', *, *, #107130, .T. ) ;
#2187 = CARTESIAN_POINT ( 'NONE',  ( -5.153800228976328057, -19.02544592524343514, 112.2905762719810099 ) ) ;
#2188 = CARTESIAN_POINT ( 'NONE',  ( 0.000000000000000000, -165.0000000000000000, 12.00000000000000355 ) ) ;
#2189 = CARTESIAN_POINT ( 'NONE',  ( 9.564922557960805705, 16.46253265017160317, 24.58224293864769194 ) ) ;
#2190 = CARTESIAN_POINT ( 'NONE',  ( -21.52544592524343514, 5.823673210054127303, 56.04057627198102409 ) ) ;
#2191 = CARTESIAN_POINT ( 'NONE',  ( 16.55341960407618274, -4.379528057220086978, 101.0427570613523756 ) ) ;
#2192 = CARTESIAN_POINT ( 'NONE',  ( 5.823673210054444382, -21.52544592524334988, 40.20942372801901854 ) ) ;
#2193 = CARTESIAN_POINT ( 'NONE',  ( -5.153800228976607833, 19.02544592524334988, 97.70942372801900433 ) ) ;
#2194 = CARTESIAN_POINT ( 'NONE',  ( 4.483927247898545687, 16.52544592524342804, 114.7905762719810383 ) ) ;
#2195 = CARTESIAN_POINT ( 'NONE',  ( 16.51473224551083163, -9.474510206698727899, 105.8344237280190043 ) ) ;
#2196 = VECTOR ( 'NONE', #7013, 1000.000000000000000 ) ;
#2197 = CARTESIAN_POINT ( 'NONE',  ( 13.97604488694527802, 13.89961937509977652, 39.37390960531435269 ) ) ;
#2198 = CARTESIAN_POINT ( 'NONE',  ( -5.429308488886486681E-15, 30.30510711980690175, 143.4999999999999432 ) ) ;
#2199 = CARTESIAN_POINT ( 'NONE',  ( 5.049401038298161559, -19.05341960407611168, 87.70724293864769550 ) ) ;
#2200 = CARTESIAN_POINT ( 'NONE',  ( 8.224510206698742110, 14.34966873604972548, 72.08442372801899012 ) ) ;
#2201 = CARTESIAN_POINT ( 'NONE',  ( -9.474510206698720793, -16.51473224551083518, 84.58442372801900433 ) ) ;
#2202 = CARTESIAN_POINT ( 'NONE',  ( 5.049401038297881783, 19.05341960407617563, 22.29275706135233648 ) ) ;
#2203 = CARTESIAN_POINT ( 'NONE',  ( -21.53943276465977519, 0.05219959533907696930, 56.24890960531436690 ) ) ;
#2204 = CARTESIAN_POINT ( 'NONE',  ( -14.34966873604972548, 8.224510206698743886, 88.33442372801901854 ) ) ;
#2205 = CARTESIAN_POINT ( 'NONE',  ( 19.03943276465977164, 0.05219959533936151252, 76.25109039468566152 ) ) ;
#2206 = CARTESIAN_POINT ( 'NONE',  ( 0.05219959533909260263, 19.03943276465977164, 39.99890960531436690 ) ) ;
#2207 = CARTESIAN_POINT ( 'NONE',  ( -5.049401038298153566, 19.05341960407611168, 75.20724293864769550 ) ) ;
#2208 = CARTESIAN_POINT ( 'NONE',  ( -10.72451020669870658, -18.67979575497194134, 54.58442372801901143 ) ) ;
#2209 = CARTESIAN_POINT ( 'NONE',  ( -13.89961937509977652, 13.97604488694528158, 45.62390960531433848 ) ) ;
#2210 = CARTESIAN_POINT ( 'NONE',  ( -13.89961937509957401, -13.97604488694547875, 74.37609039468566152 ) ) ;
#2211 = CARTESIAN_POINT ( 'NONE',  ( 25.86526910843990379, -7.630673861715740358, 173.3900163844746771 ) ) ;
#2212 = CARTESIAN_POINT ( 'NONE',  ( 0.05219959533909260263, 19.03943276465977164, 109.9989096053143669 ) ) ;
#2213 = CARTESIAN_POINT ( 'NONE',  ( -12.14591786802309592, -12.06949235617757132, 66.87390960531436690 ) ) ;
#2214 = CARTESIAN_POINT ( 'NONE',  ( 5.823673210054125526, 21.52544592524343514, 59.79057627198103120 ) ) ;
#2215 = DIRECTION ( 'NONE',  ( 0.000000000000000000, 0.000000000000000000, 1.000000000000000000 ) ) ;
#2216 = CARTESIAN_POINT ( 'NONE',  ( 19.03943276465977164, 0.05219959533936151252, 31.25109039468566863 ) ) ;
#2218 = CARTESIAN_POINT ( 'NONE',  ( 19.02544592524343514, -5.153800228976328945, 78.54057627198099567 ) ) ;
#2217 = CARTESIAN_POINT ( 'NONE',  ( 5.049401038298161559, -19.05341960407611168, 57.70724293864769550 ) ) ;
#2219 = CARTESIAN_POINT ( 'NONE',  ( -4.379528057220086978, -16.55341960407618274, 44.79275706135234714 ) ) ;
#2220 = CARTESIAN_POINT ( 'NONE',  ( 13.50000934768028671, -42.70547949999480153, -22.37447973961942793 ) ) ;
#2221 = CARTESIAN_POINT ( 'NONE',  ( -17.40805194822031510, 6.112264579159313982, 110.8337127251061247 ) ) ;
#2222 = CARTESIAN_POINT ( 'NONE',  ( -14.29746914071037622, -8.314922557961029526, 89.16775706135236135 ) ) ;
#2223 = CARTESIAN_POINT ( 'NONE',  ( -17.49999999999999645, 5.499999999999992895, 78.71769037696437010 ) ) ;
#2224 = CARTESIAN_POINT ( 'NONE',  ( 0.05219959533934541429, -16.53943276465976808, 65.00109039468568994 ) ) ;
#2225 = CARTESIAN_POINT ( 'NONE',  ( -16.52544592524335698, -4.483927247898792601, 38.95942372801901854 ) ) ;
#2227 = LINE ( 'NONE', #170091, #198734 ) ;
#2226 = CARTESIAN_POINT ( 'NONE',  ( 9.564922557960805705, 16.46253265017160317, 59.58224293864769550 ) ) ;
#2228 = CARTESIAN_POINT ( 'NONE',  ( 21.55341960407619695, -5.719274019375665929, 56.04275706135235424 ) ) ;
#2229 = CARTESIAN_POINT ( 'NONE',  ( 9.564922557961047289, -16.46253265017146816, 60.41775706135233293 ) ) ;
#2230 = CARTESIAN_POINT ( 'NONE',  ( 0.05219959533937995610, -21.53943276465977519, 105.0010903946856757 ) ) ;
#2231 = CARTESIAN_POINT ( 'NONE',  ( -19.02544592524342804, 5.153800228976336051, 36.04057627198100988 ) ) ;
#2232 = DIRECTION ( 'NONE',  ( 0.000000000000000000, 0.000000000000000000, 1.000000000000000000 ) ) ;
#2233 = CARTESIAN_POINT ( 'NONE',  ( 15.80617190586746368, 15.72974639402197994, 49.37390960531436690 ) ) ;
#2234 = CARTESIAN_POINT ( 'NONE',  ( -19.05341960407611168, -5.049401038298163336, 111.4572429386476671 ) ) ;
#2235 = CARTESIAN_POINT ( 'NONE',  ( -4.379528057220328563, 16.55341960407611168, 105.2072429386477097 ) ) ;
#2236 = CARTESIAN_POINT ( 'NONE',  ( 16.53943276465976808, 0.05219959533934440121, 36.25109039468567573 ) ) ;
#2237 = CARTESIAN_POINT ( 'NONE',  ( -16.55341960407611168, -4.379528057220339221, 31.45724293864769550 ) ) ;
#2238 = ORIENTED_EDGE ( 'NONE', *, *, #185422, .T. ) ;
#2239 = CARTESIAN_POINT ( 'NONE',  ( -18.67979575497193778, 10.72451020669871902, 23.33442372801901499 ) ) ;
#2241 = CARTESIAN_POINT ( 'NONE',  ( 5.049401038298161559, -19.05341960407611168, 107.7072429386476955 ) ) ;
#2240 = CARTESIAN_POINT ( 'NONE',  ( -4.379528057220328563, 16.55341960407611168, 40.20724293864769550 ) ) ;
#2242 = CARTESIAN_POINT ( 'NONE',  ( -13.97604488694547697, 13.89961937509957934, 113.1260903946856757 ) ) ;
#2243 = CARTESIAN_POINT ( 'NONE',  ( -19.03943276465977164, -0.05219959533935918106, 23.75109039468566152 ) ) ;
#2244 = CARTESIAN_POINT ( 'NONE',  ( 4.483927247898545687, 16.52544592524342804, 34.79057627198103120 ) ) ;
#2245 = CARTESIAN_POINT ( 'NONE',  ( 21.53943276465977519, -0.05219959533907433946, 103.7489096053143669 ) ) ;
#2246 = CARTESIAN_POINT ( 'NONE',  ( 18.62759615963271287, -10.81492255796078972, 63.33224293864770260 ) ) ;
#2247 = CARTESIAN_POINT ( 'NONE',  ( -13.89961937509977652, 13.97604488694528158, 70.62390960531432427 ) ) ;
#2248 = CARTESIAN_POINT ( 'NONE',  ( -12.14591786802309592, -12.06949235617757132, 51.87390960531437401 ) ) ;
#2249 = CARTESIAN_POINT ( 'NONE',  ( 19.03943276465977164, -0.05219959533909143690, 93.74890960531435269 ) ) ;
#2250 = B_SPLINE_CURVE_WITH_KNOTS ( 'NONE', 3,
 ( #76551, #27097, #62361, #16875, #170556, #81491 ),
 .UNSPECIFIED., .F., .F.,
 ( 4, 2, 4 ),
 ( 0.003989672132298188560, 0.004372778065220606601, 0.004755883998143024642 ),
 .UNSPECIFIED. ) ;
#2251 = CARTESIAN_POINT ( 'NONE',  ( 0.05219959533909260263, 19.03943276465977164, 79.99890960531436690 ) ) ;
#2252 = CARTESIAN_POINT ( 'NONE',  ( 19.02544592524334988, 5.153800228976608722, 41.45942372801900433 ) ) ;
#2253 = CARTESIAN_POINT ( 'NONE',  ( -15.72974639402197994, 15.80617190586746368, 90.62390960531436690 ) ) ;
#2254 = CARTESIAN_POINT ( 'NONE',  ( 14.29746914071049879, -8.314922557960816363, 93.33224293864769550 ) ) ;
#2255 = CARTESIAN_POINT ( 'NONE',  ( -5.823673210054431948, 21.52544592524334988, 32.70942372801900433 ) ) ;
#2256 = CARTESIAN_POINT ( 'NONE',  ( 8.571926809382597767, 26.38167802310806209, 142.2750000027311899 ) ) ;
#2257 = CARTESIAN_POINT ( 'NONE',  ( 16.55341960407611168, 4.379528057220329451, 23.95724293864769550 ) ) ;
#2258 = CARTESIAN_POINT ( 'NONE',  ( 0.05219959533909260263, 19.03943276465977164, 29.99890960531435979 ) ) ;
#2259 = CARTESIAN_POINT ( 'NONE',  ( 16.46253265017160672, -9.564922557960803928, 88.33224293864769550 ) ) ;
#2260 = CARTESIAN_POINT ( 'NONE',  ( -21.55341960407610458, -5.719274019375992779, 61.45724293864770260 ) ) ;
#2261 = CARTESIAN_POINT ( 'NONE',  ( 1.784210473542230573E-15, -29.16686587814331588, 139.3750000027311842 ) ) ;
#2262 = CARTESIAN_POINT ( 'NONE',  ( -5.049401038298153566, 19.05341960407611168, 25.20724293864768484 ) ) ;
#2263 = CARTESIAN_POINT ( 'NONE',  ( 5.719274019375991003, -21.55341960407610458, 57.70724293864770260 ) ) ;
#2264 = CARTESIAN_POINT ( 'NONE',  ( 21.52544592524334988, 5.823673210054432836, 76.45942372801901854 ) ) ;
#2266 = CARTESIAN_POINT ( 'NONE',  ( -8.224510206698735004, -14.34966873604973081, 69.58442372801900433 ) ) ;
#2265 = CARTESIAN_POINT ( 'NONE',  ( 9.164641033550608995, -36.31047332450842902, -31.46032839770289513 ) ) ;
#2267 = CARTESIAN_POINT ( 'NONE',  ( -9.474510206698964154, 16.51473224551069663, 55.41557627198103120 ) ) ;
#2268 = CARTESIAN_POINT ( 'NONE',  ( -9.474510206698964154, 16.51473224551069663, 70.41557627198102409 ) ) ;
#2269 = EDGE_LOOP ( 'NONE', ( #119206, #10771, #58766, #37881 ) ) ;
#2270 = CARTESIAN_POINT ( 'NONE',  ( -21.53943276465977519, -0.05219959533937600094, 113.7510903946856757 ) ) ;
#2271 = CARTESIAN_POINT ( 'NONE',  ( 16.55341960407618274, -4.379528057220086978, 81.04275706135236135 ) ) ;
#2272 = CARTESIAN_POINT ( 'NONE',  ( -21.55341960407619339, 5.719274019375674811, 103.5427570613523613 ) ) ;
#2273 = CARTESIAN_POINT ( 'NONE',  ( 0.05219959533909260263, 19.03943276465977164, 59.99890960531436690 ) ) ;
#2274 = CARTESIAN_POINT ( 'NONE',  ( 18.67979575497178502, 10.72451020669898547, 29.16557627198103120 ) ) ;
#2275 = CARTESIAN_POINT ( 'NONE',  ( -9.564922557961040184, 16.46253265017147172, 102.9177570613523329 ) ) ;
#2276 = CARTESIAN_POINT ( 'NONE',  ( 5.823673210054444382, -21.52544592524334988, 85.20942372801901854 ) ) ;
#2277 = CARTESIAN_POINT ( 'NONE',  ( -8.314922557961024197, 14.29746914071037800, 42.91775706135235424 ) ) ;
#2278 = CARTESIAN_POINT ( 'NONE',  ( -21.55341960407610458, -5.719274019375992779, 101.4572429386476955 ) ) ;
#2279 = CARTESIAN_POINT ( 'NONE',  ( -19.03943276465977164, -0.05219959533935918106, 98.75109039468567573 ) ) ;
#2280 = CARTESIAN_POINT ( 'NONE',  ( -16.46253265017160317, 9.564922557960807481, 80.83224293864769550 ) ) ;
#2281 = CARTESIAN_POINT ( 'NONE',  ( 16.46253265017146816, 9.564922557961045513, 106.6677570613523471 ) ) ;
#2282 = CARTESIAN_POINT ( 'NONE',  ( 0.05219959533909260263, 19.03943276465977164, 34.99890960531435979 ) ) ;
#2283 = CIRCLE ( 'NONE', #5446, 0.2000000000000057288 ) ;
#2284 = CARTESIAN_POINT ( 'NONE',  ( 0.05219959533934541429, -16.53943276465976808, 20.00109039468568639 ) ) ;
#2285 = CARTESIAN_POINT ( 'NONE',  ( -16.52544592524342804, 4.483927247898546575, 61.04057627198103120 ) ) ;
#2286 = CARTESIAN_POINT ( 'NONE',  ( 0.05219959533934541429, -16.53943276465976808, 75.00109039468568994 ) ) ;
#2288 = CARTESIAN_POINT ( 'NONE',  ( -13.97604488694527625, -13.89961937509977652, 56.87390960531434558 ) ) ;
#2287 = CARTESIAN_POINT ( 'NONE',  ( 0.05219959533937995610, -21.53943276465977519, 30.00109039468568284 ) ) ;
#2289 = CARTESIAN_POINT ( 'NONE',  ( 5.049401038298161559, -19.05341960407611168, 67.70724293864769550 ) ) ;
#2290 = CARTESIAN_POINT ( 'NONE',  ( -16.53943276465976808, -0.05219959533934237506, 73.75109039468567573 ) ) ;
#2291 = CARTESIAN_POINT ( 'NONE',  ( -5.429308488886486681E-15, 30.30510711980690175, 147.7500000054623683 ) ) ;
#2292 = ORIENTED_EDGE ( 'NONE', *, *, #135320, .T. ) ;
#2293 = CARTESIAN_POINT ( 'NONE',  ( 5.049401038297881783, 19.05341960407617563, 22.29275706135233648 ) ) ;
#2294 = AXIS2_PLACEMENT_3D ( 'NONE', #133017, #26862, #120823 ) ;
#2295 = CARTESIAN_POINT ( 'NONE',  ( 9.564922557960805705, 16.46253265017160317, 29.58224293864769550 ) ) ;
#2296 = VERTEX_POINT ( 'NONE', #80063 ) ;
#2297 = CARTESIAN_POINT ( 'NONE',  ( 16.55341960407618274, -4.379528057220086978, 26.04275706135235779 ) ) ;
#2299 = CARTESIAN_POINT ( 'NONE',  ( 12.06949235617739724, 12.14591786802326823, 41.87609039468568284 ) ) ;
#2298 = CARTESIAN_POINT ( 'NONE',  ( 19.03943276465977164, 0.05219959533936151252, 46.25109039468566863 ) ) ;
#2300 = CARTESIAN_POINT ( 'NONE',  ( 19.02544592524343514, -5.153800228976328945, 48.54057627198103120 ) ) ;
#2301 = CARTESIAN_POINT ( 'NONE',  ( -13.97604488694527625, -13.89961937509977652, 101.8739096053143811 ) ) ;
#2302 = CARTESIAN_POINT ( 'NONE',  ( -0.05219959533909027116, -19.03943276465977164, 57.49890960531435979 ) ) ;
#2303 = CARTESIAN_POINT ( 'NONE',  ( -5.719274019375978568, 21.55341960407610458, 90.20724293864770971 ) ) ;
#2305 = CARTESIAN_POINT ( 'NONE',  ( -16.46253265017160317, 9.564922557960807481, 115.8322429386477097 ) ) ;
#2304 = CARTESIAN_POINT ( 'NONE',  ( -19.05341960407611168, -5.049401038298163336, 76.45724293864769550 ) ) ;
#2306 = CARTESIAN_POINT ( 'NONE',  ( 16.46253265017160672, -9.564922557960803928, 63.33224293864769550 ) ) ;
#2307 = DIRECTION ( 'NONE',  ( 1.000000000000000000, 0.000000000000000000, 0.000000000000000000 ) ) ;
#2308 = CARTESIAN_POINT ( 'NONE',  ( -16.46253265017146816, -9.564922557961047289, 94.16775706135233293 ) ) ;
#2309 = CARTESIAN_POINT ( 'NONE',  ( 19.05341960407617918, -5.049401038297876454, 21.04275706135232582 ) ) ;
#2310 = CARTESIAN_POINT ( 'NONE',  ( -14.34966873604960291, -8.224510206698953496, 56.66557627198103830 ) ) ;
#2311 = CARTESIAN_POINT ( 'NONE',  ( -10.72451020669870658, -18.67979575497194134, 89.58442372801901854 ) ) ;
#2312 = CARTESIAN_POINT ( 'NONE',  ( -16.53943276465976808, 0.05219959533911058130, 116.2489096053143669 ) ) ;
#2314 = CARTESIAN_POINT ( 'NONE',  ( 21.52544592524334988, 5.823673210054432836, 91.45942372801901854 ) ) ;
#2313 = CARTESIAN_POINT ( 'NONE',  ( -12.14591786802309592, -12.06949235617757132, 26.87390960531435979 ) ) ;
#2315 = CARTESIAN_POINT ( 'NONE',  ( 9.564922557960805705, 16.46253265017160317, 74.58224293864769550 ) ) ;
#2316 = CARTESIAN_POINT ( 'NONE',  ( -10.72451020669870658, -18.67979575497194134, 44.58442372801901854 ) ) ;
#2317 = CARTESIAN_POINT ( 'NONE',  ( 19.03943276465977164, -0.05219959533909143690, 78.74890960531436690 ) ) ;
#2318 = CARTESIAN_POINT ( 'NONE',  ( 4.483927247898545687, 16.52544592524342804, 89.79057627198103830 ) ) ;
#2319 = CARTESIAN_POINT ( 'NONE',  ( 4.483927247898545687, 16.52544592524342804, 59.79057627198103120 ) ) ;
#2320 = CARTESIAN_POINT ( 'NONE',  ( -21.53943276465977519, 0.05219959533907696930, 71.24890960531435269 ) ) ;
#2321 = CARTESIAN_POINT ( 'NONE',  ( 19.03943276465977164, -0.05219959533909143690, 78.74890960531436690 ) ) ;
#2322 = CARTESIAN_POINT ( 'NONE',  ( -21.53943276465977519, 0.05219959533907696930, 91.24890960531436690 ) ) ;
#2323 = CARTESIAN_POINT ( 'NONE',  ( 0.05219959533936267826, -19.03943276465977164, 80.00109039468567573 ) ) ;
#2325 = CARTESIAN_POINT ( 'NONE',  ( 12.14591786802309770, 12.06949235617756955, 79.37390960531436690 ) ) ;
#2324 = CARTESIAN_POINT ( 'NONE',  ( 13.89961937509957579, 13.97604488694547520, 36.87609039468566863 ) ) ;
#2327 = CARTESIAN_POINT ( 'NONE',  ( -13.89961937509977652, 13.97604488694528158, 60.62390960531436690 ) ) ;
#2326 = AXIS2_PLACEMENT_3D ( 'NONE', #102933, #86762, #132273 ) ;
#2328 = CARTESIAN_POINT ( 'NONE',  ( -5.823673210054116645, -21.52544592524344225, 72.29057627198102409 ) ) ;
#2329 = CARTESIAN_POINT ( 'NONE',  ( 16.79531203550645202, -7.028104445595743321, 26.24755011779557989 ) ) ;
#2331 = CARTESIAN_POINT ( 'NONE',  ( 8.571926809382603096, -26.38167802310801235, 143.9750000027312069 ) ) ;
#2330 = CARTESIAN_POINT ( 'NONE',  ( 8.314922557961029526, -14.29746914071037800, 110.4177570613523756 ) ) ;
#2332 = CARTESIAN_POINT ( 'NONE',  ( 19.05341960407617918, -5.049401038297876454, 106.0427570613523471 ) ) ;
#2333 = CARTESIAN_POINT ( 'NONE',  ( 4.379528057220339221, -16.55341960407611168, 87.70724293864769550 ) ) ;
#2334 = CARTESIAN_POINT ( 'NONE',  ( -17.49999999999998579, 4.640572885337610920, 35.63788164548841308 ) ) ;
#2335 = CARTESIAN_POINT ( 'NONE',  ( 5.153800228976335163, 19.02544592524342804, 79.79057627198102409 ) ) ;
#2336 = CARTESIAN_POINT ( 'NONE',  ( -13.97604488694527625, -13.89961937509977652, 31.87390960531435979 ) ) ;
#2337 = CARTESIAN_POINT ( 'NONE',  ( 0.05219959533910956823, 16.53943276465976808, 64.99890960531435269 ) ) ;
#2338 = CARTESIAN_POINT ( 'NONE',  ( -19.03943276465977164, 0.05219959533909376836, 96.24890960531436690 ) ) ;
#2340 = CARTESIAN_POINT ( 'NONE',  ( -19.05341960407611168, -5.049401038298163336, 61.45724293864769550 ) ) ;
#2339 = CARTESIAN_POINT ( 'NONE',  ( 9.564922557961047289, -16.46253265017146816, 95.41775706135233293 ) ) ;
#2341 = CARTESIAN_POINT ( 'NONE',  ( 9.564922557960805705, 16.46253265017160317, 89.58224293864769550 ) ) ;
#2342 = CARTESIAN_POINT ( 'NONE',  ( 5.719274019375991003, -21.55341960407610458, 77.70724293864770971 ) ) ;
#2343 = CARTESIAN_POINT ( 'NONE',  ( 14.29746914071037800, 8.314922557961029526, 71.66775706135234714 ) ) ;
#2344 = CARTESIAN_POINT ( 'NONE',  ( -19.05341960407617918, 5.049401038297883559, 108.5427570613523329 ) ) ;
#2345 = CARTESIAN_POINT ( 'NONE',  ( 5.049401038298161559, -19.05341960407611168, 62.70724293864769550 ) ) ;
#2346 = CARTESIAN_POINT ( 'NONE',  ( 18.67979575497178502, 10.72451020669898547, 74.16557627198102409 ) ) ;
#2347 = CARTESIAN_POINT ( 'NONE',  ( -5.153800228976607833, 19.02544592524334988, 97.70942372801900433 ) ) ;
#2349 = CARTESIAN_POINT ( 'NONE',  ( 21.55341960407619695, -5.719274019375665929, 46.04275706135234714 ) ) ;
#2348 = CARTESIAN_POINT ( 'NONE',  ( 16.55341960407611168, 4.379528057220329451, 38.95724293864768839 ) ) ;
#2350 = CARTESIAN_POINT ( 'NONE',  ( -38.00000000000000711, 2.428612866367529932E-14, -3.749999994537626780 ) ) ;
#2352 = CARTESIAN_POINT ( 'NONE',  ( -0.05219959533909027116, -19.03943276465977164, 112.4989096053143669 ) ) ;
#2351 = CARTESIAN_POINT ( 'NONE',  ( 16.52544592524335698, 4.483927247898782831, 76.45942372801901854 ) ) ;
#2353 = CARTESIAN_POINT ( 'NONE',  ( -5.049401038298153566, 19.05341960407611168, 105.2072429386476813 ) ) ;
#2354 = CARTESIAN_POINT ( 'NONE',  ( -16.18388926212235290, -7.379444403734648716, 35.43953151366154941 ) ) ;
#2355 = CARTESIAN_POINT ( 'NONE',  ( -16.53943276465976808, -0.05219959533934237506, 98.75109039468568994 ) ) ;
#2356 = CARTESIAN_POINT ( 'NONE',  ( -16.52544592524335698, -4.483927247898792601, 33.95942372801901143 ) ) ;
#2357 = CARTESIAN_POINT ( 'NONE',  ( -16.46253265017160317, 9.564922557960807481, 50.83224293864770260 ) ) ;
#2358 = CARTESIAN_POINT ( 'NONE',  ( -9.474510206698964154, 16.51473224551069663, 55.41557627198103120 ) ) ;
#2359 = CARTESIAN_POINT ( 'NONE',  ( 16.51473224551069308, 9.474510206698969483, 59.16557627198102409 ) ) ;
#2360 = CARTESIAN_POINT ( 'NONE',  ( 15.80617190586769283, -15.72974639402175789, 50.62609039468568994 ) ) ;
#2361 = CARTESIAN_POINT ( 'NONE',  ( -16.55341960407617563, 4.379528057220093196, 58.54275706135235424 ) ) ;
#2362 = CARTESIAN_POINT ( 'NONE',  ( 14.34966873604960469, 8.224510206698951720, 34.16557627198102409 ) ) ;
#2363 = CARTESIAN_POINT ( 'NONE',  ( -19.03943276465977164, 0.05219959533909376836, 46.24890960531435979 ) ) ;
#2364 = CARTESIAN_POINT ( 'NONE',  ( -13.97604488694527625, -13.89961937509977652, 36.87390960531436690 ) ) ;
#2366 = EDGE_CURVE ( 'NONE', #144904, #188934, #66351, .T. ) ;
#2365 = CARTESIAN_POINT ( 'NONE',  ( 14.34966873604972726, -8.224510206698740333, 25.83442372801901499 ) ) ;
#2367 = CARTESIAN_POINT ( 'NONE',  ( 16.51473224551083163, -9.474510206698727899, 80.83442372801899012 ) ) ;
#2368 = CARTESIAN_POINT ( 'NONE',  ( 14.34966873604960469, 8.224510206698951720, 79.16557627198103830 ) ) ;
#2369 = CARTESIAN_POINT ( 'NONE',  ( -13.97604488694527625, -13.89961937509977652, 56.87390960531434558 ) ) ;
#2371 = DIRECTION ( 'NONE',  ( 0.000000000000000000, 0.000000000000000000, -1.000000000000000000 ) ) ;
#2370 = CARTESIAN_POINT ( 'NONE',  ( 9.474510206698729675, 16.51473224551082808, 82.08442372801899012 ) ) ;
#2372 = CARTESIAN_POINT ( 'NONE',  ( -5.719274019375665041, -21.55341960407619695, 79.79275706135236135 ) ) ;
#2373 = CARTESIAN_POINT ( 'NONE',  ( -16.55341960407617563, 4.379528057220093196, 58.54275706135235424 ) ) ;
#2374 = CARTESIAN_POINT ( 'NONE',  ( 21.23184647844206197, -181.1785498424364675, 0.000000000000000000 ) ) ;
#2375 = CARTESIAN_POINT ( 'NONE',  ( -18.62759615963270932, 10.81492255796079327, 55.83224293864770260 ) ) ;
#2376 = CARTESIAN_POINT ( 'NONE',  ( -0.05219959533934338120, 16.53943276465976808, 37.50109039468568284 ) ) ;
#2377 = CARTESIAN_POINT ( 'NONE',  ( 19.05341960407611168, 5.049401038298154454, 23.95724293864769194 ) ) ;
#2378 = CARTESIAN_POINT ( 'NONE',  ( -13.97604488694547697, 13.89961937509957934, 23.12609039468565442 ) ) ;
#2379 = CARTESIAN_POINT ( 'NONE',  ( 19.02544592524343514, -5.153800228976328945, 83.54057627198100988 ) ) ;
#2380 = CARTESIAN_POINT ( 'NONE',  ( 3.766062262543149401E-15, -39.95556452105413570, -7.500000000000000888 ) ) ;
#2381 = CARTESIAN_POINT ( 'NONE',  ( 9.474510206698971260, -16.51473224551069308, 47.91557627198102409 ) ) ;
#2382 = CARTESIAN_POINT ( 'NONE',  ( -21.29652154493212990, -22.98910344481098988, -49.85957558946837054 ) ) ;
#2383 = CARTESIAN_POINT ( 'NONE',  ( 5.153800228976335163, 19.02544592524342804, 69.79057627198103830 ) ) ;
#2384 = CARTESIAN_POINT ( 'NONE',  ( 17.50000000000000355, -5.068104630630377194, 113.2281840534003265 ) ) ;
#2385 = CARTESIAN_POINT ( 'NONE',  ( 19.03943276465977164, 0.05219959533936151252, 21.25109039468565797 ) ) ;
#2386 = CARTESIAN_POINT ( 'NONE',  ( 12.06949235617757843, -12.14591786802309237, 38.12390960531436690 ) ) ;
#2387 = CARTESIAN_POINT ( 'NONE',  ( 19.05341960407611168, 5.049401038298154454, 43.95724293864769550 ) ) ;
#2388 = CARTESIAN_POINT ( 'NONE',  ( -13.89961937509977652, 13.97604488694528158, 110.6239096053143243 ) ) ;
#2389 = CARTESIAN_POINT ( 'NONE',  ( -5.719274019375665041, -21.55341960407619695, 74.79275706135234714 ) ) ;
#2390 = CARTESIAN_POINT ( 'NONE',  ( 13.97604488694527802, 13.89961937509977652, 54.37390960531435979 ) ) ;
#2391 = CARTESIAN_POINT ( 'NONE',  ( -10.72451020669870658, -18.67979575497194134, 69.58442372801900433 ) ) ;
#2392 = CARTESIAN_POINT ( 'NONE',  ( 21.52544592524344225, -5.823673210054117533, 28.54057627198103120 ) ) ;
#2393 = CARTESIAN_POINT ( 'NONE',  ( -5.049401038298153566, 19.05341960407611168, 40.20724293864768839 ) ) ;
#2394 = CARTESIAN_POINT ( 'NONE',  ( 15.80617190586769283, -15.72974639402175789, 30.62609039468567929 ) ) ;
#2395 = CARTESIAN_POINT ( 'NONE',  ( -19.03943276465977164, -0.05219959533935918106, 48.75109039468566863 ) ) ;
#2396 = CARTESIAN_POINT ( 'NONE',  ( -13.97604488694527625, -13.89961937509977652, 26.87390960531434558 ) ) ;
#2397 = CARTESIAN_POINT ( 'NONE',  ( -19.05341960407611168, -5.049401038298163336, 71.45724293864766707 ) ) ;
#2398 = CARTESIAN_POINT ( 'NONE',  ( 9.564922557961047289, -16.46253265017146816, 105.4177570613523471 ) ) ;
#2399 = CARTESIAN_POINT ( 'NONE',  ( -14.34966873604960291, -8.224510206698953496, 71.66557627198100988 ) ) ;
#2401 = B_SPLINE_CURVE_WITH_KNOTS ( 'NONE', 3,
 ( #185497, #49966, #125805, #48974, #110629, #172310, #78294, #18640, #139968, #80286, #46988, #31817, #63135, #143950, #37777, #52933, #51944, #193471, #159112, #5430, #7426, #19624, #113604, #189481, #116620, #175298 ),
 .UNSPECIFIED., .F., .F.,
 ( 4, 2, 2, 2, 2, 2, 2, 2, 2, 2, 2, 2, 4 ),
 ( 2.788292423116888737E-07, 0.0002961032055655192312, 0.0005919275818887267775, 0.0008877519582119342695, 0.001183576334535141545, 0.001775225087181556095, 0.002366873839827970862, 0.002662698216151183558, 0.002958522592474396255, 0.003254346968797609384, 0.003550171345120822081, 0.004141820097767247473, 0.004733468850413673733 ),
 .UNSPECIFIED. ) ;
#2400 = CARTESIAN_POINT ( 'NONE',  ( 15.72974639402199770, -15.80617190586745480, 43.12390960531435269 ) ) ;
#2402 = CARTESIAN_POINT ( 'NONE',  ( -9.474510206698720793, -16.51473224551083518, 99.58442372801900433 ) ) ;
#2403 = CARTESIAN_POINT ( 'NONE',  ( 21.53943276465977519, -0.05219959533907433946, 103.7489096053143669 ) ) ;
#2404 = CARTESIAN_POINT ( 'NONE',  ( 0.05219959533937995610, -21.53943276465977519, 55.00109039468568284 ) ) ;
#2405 = CARTESIAN_POINT ( 'NONE',  ( 4.379528057220092307, 16.55341960407617563, 62.29275706135236845 ) ) ;
#2406 = CARTESIAN_POINT ( 'NONE',  ( 16.53943276465976808, 0.05219959533934440121, 61.25109039468567573 ) ) ;
#2407 = CARTESIAN_POINT ( 'NONE',  ( 5.823673210054125526, 21.52544592524343514, 69.79057627198102409 ) ) ;
#2408 = CARTESIAN_POINT ( 'NONE',  ( 16.46253265017160672, -9.564922557960803928, 43.33224293864769550 ) ) ;
#2409 = CARTESIAN_POINT ( 'NONE',  ( 16.52544592524335698, 4.483927247898782831, 91.45942372801901854 ) ) ;
#2410 = CARTESIAN_POINT ( 'NONE',  ( -15.80617190586745835, -15.72974639402198527, 106.8739096053143811 ) ) ;
#2411 = CARTESIAN_POINT ( 'NONE',  ( -8.314922557960811034, -14.29746914071050412, 57.08224293864769550 ) ) ;
#2412 = CARTESIAN_POINT ( 'NONE',  ( -5.153800228976328057, -19.02544592524343514, 77.29057627198099567 ) ) ;
#2413 = CARTESIAN_POINT ( 'NONE',  ( -12.14591786802326823, 12.06949235617739902, 78.12609039468570415 ) ) ;
#2414 = CARTESIAN_POINT ( 'NONE',  ( -0.05219959533936034679, 19.03943276465977164, 112.5010903946856757 ) ) ;
#2415 = CARTESIAN_POINT ( 'NONE',  ( -21.52544592524343514, 5.823673210054127303, 106.0405762719810525 ) ) ;
#2416 = CARTESIAN_POINT ( 'NONE',  ( -14.29746914071049879, 8.314922557960819915, 45.83224293864769550 ) ) ;
#2417 = ORIENTED_EDGE ( 'NONE', *, *, #165213, .F. ) ;
#2418 = CARTESIAN_POINT ( 'NONE',  ( -17.26058549869092573, 6.457015423128486198, 68.62254162523935008 ) ) ;
#2419 = CARTESIAN_POINT ( 'NONE',  ( 10.72451020669898902, -18.67979575497178502, 87.91557627198103830 ) ) ;
#2420 = ORIENTED_EDGE ( 'NONE', *, *, #94263, .F. ) ;
#2421 = CARTESIAN_POINT ( 'NONE',  ( -16.52544592524342804, 4.483927247898546575, 26.04057627198103475 ) ) ;
#2422 = ORIENTED_EDGE ( 'NONE', *, *, #150310, .F. ) ;
#2423 = DIRECTION ( 'NONE',  ( -9.445700745138859830E-17, 1.000000000000000000, 0.000000000000000000 ) ) ;
#2424 = CARTESIAN_POINT ( 'NONE',  ( -21.53943276465977519, 0.05219959533907696930, 101.2489096053143669 ) ) ;
#2425 = CARTESIAN_POINT ( 'NONE',  ( -13.89961937509977652, 13.97604488694528158, 105.6239096053143527 ) ) ;
#2426 = CARTESIAN_POINT ( 'NONE',  ( 10.81492255796106328, -18.62759615963255655, 20.41775706135234714 ) ) ;
#2427 = CARTESIAN_POINT ( 'NONE',  ( -8.224510206698948167, 14.34966873604960824, 50.41557627198103120 ) ) ;
#2428 = CARTESIAN_POINT ( 'NONE',  ( 4.379528057220092307, 16.55341960407617563, 52.29275706135236135 ) ) ;
#2429 = AXIS2_PLACEMENT_3D ( 'NONE', #118960, #58273, #120921 ) ;
#2430 = CARTESIAN_POINT ( 'NONE',  ( -9.474510206698964154, 16.51473224551069663, 55.41557627198103120 ) ) ;
#2431 = CARTESIAN_POINT ( 'NONE',  ( 16.51473224551083163, -9.474510206698727899, 50.83442372801899722 ) ) ;
#2432 = CARTESIAN_POINT ( 'NONE',  ( 5.153800228976335163, 19.02544592524342804, 79.79057627198102409 ) ) ;
#2433 = CARTESIAN_POINT ( 'NONE',  ( 18.62759615963271287, -10.81492255796078972, 38.33224293864768839 ) ) ;
#2434 = CARTESIAN_POINT ( 'NONE',  ( -9.474510206698964154, 16.51473224551069663, 40.41557627198103120 ) ) ;
#2435 = CARTESIAN_POINT ( 'NONE',  ( -19.03943276465977164, -0.05219959533935918106, 113.7510903946856757 ) ) ;
#2436 = CARTESIAN_POINT ( 'NONE',  ( 9.564922557961047289, -16.46253265017146816, 60.41775706135233293 ) ) ;
#2437 = CARTESIAN_POINT ( 'NONE',  ( 15.80617190586746368, 15.72974639402197994, 104.3739096053143669 ) ) ;
#2438 = CARTESIAN_POINT ( 'NONE',  ( -14.29746914071049879, 8.314922557960819915, 35.83224293864768839 ) ) ;
#2439 = CARTESIAN_POINT ( 'NONE',  ( 9.564922557960805705, 16.46253265017160317, 74.58224293864769550 ) ) ;
#2440 = CARTESIAN_POINT ( 'NONE',  ( -10.72451020669898014, 18.67979575497178502, 65.41557627198102409 ) ) ;
#2442 = CARTESIAN_POINT ( 'NONE',  ( 4.483927247898790824, -16.52544592524335698, 25.20942372801901854 ) ) ;
#2441 = CARTESIAN_POINT ( 'NONE',  ( -15.72974639402197994, 15.80617190586746368, 95.62390960531436690 ) ) ;
#2443 = CARTESIAN_POINT ( 'NONE',  ( 9.474510206698971260, -16.51473224551069308, 112.9155762719810383 ) ) ;
#2444 = CARTESIAN_POINT ( 'NONE',  ( -18.67979575497193778, 10.72451020669871902, 88.33442372801901854 ) ) ;
#2445 = CARTESIAN_POINT ( 'NONE',  ( -19.02544592524342804, 5.153800228976336051, 81.04057627198103830 ) ) ;
#2446 = CARTESIAN_POINT ( 'NONE',  ( -16.51473224551069308, -9.474510206698971260, 26.66557627198103120 ) ) ;
#2447 = CARTESIAN_POINT ( 'NONE',  ( -19.02544592524342804, 5.153800228976336051, 81.04057627198103830 ) ) ;
#2448 = CARTESIAN_POINT ( 'NONE',  ( 8.314922557960818139, 14.29746914071049879, 109.5822429386476955 ) ) ;
#2449 = CARTESIAN_POINT ( 'NONE',  ( 19.02544592524343514, -5.153800228976328945, 68.54057627198103830 ) ) ;
#2450 = CARTESIAN_POINT ( 'NONE',  ( 0.05219959533934541429, -16.53943276465976808, 25.00109039468567218 ) ) ;
#2451 = CARTESIAN_POINT ( 'NONE',  ( 5.049401038297881783, 19.05341960407617918, 42.29275706135234003 ) ) ;
#2452 = CIRCLE ( 'NONE', #137990, 2.500000000000000444 ) ;
#2454 = CARTESIAN_POINT ( 'NONE',  ( -19.03943276465977164, 0.05219959533909376836, 116.2489096053143669 ) ) ;
#2453 = CARTESIAN_POINT ( 'NONE',  ( 21.53943276465977519, 0.05219959533937863772, 91.25109039468568994 ) ) ;
#2455 = CARTESIAN_POINT ( 'NONE',  ( 14.29746914071037800, 8.314922557961029526, 86.66775706135234714 ) ) ;
#2456 = CARTESIAN_POINT ( 'NONE',  ( 21.60633875066715959, -19.99157099255409165, -49.03222299240194815 ) ) ;
#2457 = CARTESIAN_POINT ( 'NONE',  ( -13.97604488694547697, 13.89961937509957934, 73.12609039468568994 ) ) ;
#2458 = CARTESIAN_POINT ( 'NONE',  ( 9.564922557961047289, -16.46253265017146816, 25.41775706135234003 ) ) ;
#2459 = CARTESIAN_POINT ( 'NONE',  ( 18.35237201590196676, -20.87933371662905202, 140.0000000000000284 ) ) ;
#2460 = CARTESIAN_POINT ( 'NONE',  ( -5.049401038298153566, 19.05341960407611168, 30.20724293864768839 ) ) ;
#2461 = CARTESIAN_POINT ( 'NONE',  ( -16.52544592524342804, 4.483927247898546575, 36.04057627198102409 ) ) ;
#2462 = DIRECTION ( 'NONE',  ( 0.000000000000000000, 0.000000000000000000, 1.000000000000000000 ) ) ;
#2463 = CARTESIAN_POINT ( 'NONE',  ( 16.52544592524335698, 4.483927247898782831, 111.4594237280190328 ) ) ;
#2464 = CARTESIAN_POINT ( 'NONE',  ( 16.62475595723700650, 7.163666690055261910, 66.97286648189530922 ) ) ;
#2465 = CARTESIAN_POINT ( 'NONE',  ( -0.05219959533934338120, 16.53943276465976808, 82.50109039468568994 ) ) ;
#2466 = CARTESIAN_POINT ( 'NONE',  ( 9.474510206698971260, -16.51473224551069308, 37.91557627198102409 ) ) ;
#2467 = CARTESIAN_POINT ( 'NONE',  ( -15.72974639402176322, -15.80617190586768395, 99.37609039468568994 ) ) ;
#2468 = CARTESIAN_POINT ( 'NONE',  ( 5.049401038297881783, 19.05341960407617563, 97.29275706135233293 ) ) ;
#2469 = CARTESIAN_POINT ( 'NONE',  ( 0.05219959533937995610, -21.53943276465977519, 85.00109039468568994 ) ) ;
#2470 = CARTESIAN_POINT ( 'NONE',  ( 13.97604488694548053, -13.89961937509957401, 50.62609039468566152 ) ) ;
#2471 = CARTESIAN_POINT ( 'NONE',  ( -9.564922557960796823, -16.46253265017161027, 92.08224293864769550 ) ) ;
#2472 = CARTESIAN_POINT ( 'NONE',  ( 19.02544592524343514, -5.153800228976328945, 73.54057627198103830 ) ) ;
#2473 = CARTESIAN_POINT ( 'NONE',  ( 17.44279575226822843, 5.990770900252481823, 71.66442432485683867 ) ) ;
#2474 = AXIS2_PLACEMENT_3D ( 'NONE', #196952, #104924, #28113 ) ;
#2475 = CARTESIAN_POINT ( 'NONE',  ( -14.29746914071049879, 8.314922557960819915, 65.83224293864769550 ) ) ;
#2476 = CARTESIAN_POINT ( 'NONE',  ( -5.719274019375978568, 21.55341960407610458, 55.20724293864770260 ) ) ;
#2477 = CARTESIAN_POINT ( 'NONE',  ( 9.564922557960805705, 16.46253265017160317, 49.58224293864770260 ) ) ;
#2479 = CARTESIAN_POINT ( 'NONE',  ( -8.224510206698735004, -14.34966873604973081, 74.58442372801901854 ) ) ;
#2478 = CARTESIAN_POINT ( 'NONE',  ( 10.81492255796078972, 18.62759615963270932, 84.58224293864769550 ) ) ;
#2480 = VERTEX_POINT ( 'NONE', #101200 ) ;
#2481 = CARTESIAN_POINT ( 'NONE',  ( 16.46253265017160672, -9.564922557960803928, 43.33224293864769550 ) ) ;
#2483 = CARTESIAN_POINT ( 'NONE',  ( 22.81625015709510151, -31.40387420917324590, -3.924999997268811658 ) ) ;
#2482 = CARTESIAN_POINT ( 'NONE',  ( 14.29746914071049879, -8.314922557960816363, 73.33224293864769550 ) ) ;
#2484 = CARTESIAN_POINT ( 'NONE',  ( 9.564922557960805705, 16.46253265017160317, 49.58224293864770260 ) ) ;
#2485 = CARTESIAN_POINT ( 'NONE',  ( -19.02544592524342804, 5.153800228976336051, 26.04057627198103120 ) ) ;
#2486 = CARTESIAN_POINT ( 'NONE',  ( 13.97604488694548053, -13.89961937509957401, 70.62609039468567573 ) ) ;
#2487 = CARTESIAN_POINT ( 'NONE',  ( 14.34966873604960469, 8.224510206698951720, 74.16557627198102409 ) ) ;
#2488 = CARTESIAN_POINT ( 'NONE',  ( -5.823673210054431948, 21.52544592524334988, 47.70942372801902565 ) ) ;
#2490 = CARTESIAN_POINT ( 'NONE',  ( 18.62759615963271287, -10.81492255796078972, 103.3322429386476955 ) ) ;
#2489 = CARTESIAN_POINT ( 'NONE',  ( -9.564922557960796823, -16.46253265017161027, 37.08224293864768839 ) ) ;
#2491 = CARTESIAN_POINT ( 'NONE',  ( -5.049401038298153566, 19.05341960407611168, 115.2072429386477097 ) ) ;
#2492 = CARTESIAN_POINT ( 'NONE',  ( 4.379528057220339221, -16.55341960407611168, 82.70724293864770971 ) ) ;
#2493 = CARTESIAN_POINT ( 'NONE',  ( 24.80109738229595351, -30.87060611836716717, -19.02242571536587334 ) ) ;
#2494 = CARTESIAN_POINT ( 'NONE',  ( -19.03943276465977164, 0.05219959533909376836, 51.24890960531436690 ) ) ;
#2495 = CARTESIAN_POINT ( 'NONE',  ( 19.25918095147781273, 5.499999999999579892, 46.95284276293937609 ) ) ;
#2496 = CARTESIAN_POINT ( 'NONE',  ( 19.05341960407617918, -5.049401038297876454, 91.04275706135234714 ) ) ;
#2497 = CARTESIAN_POINT ( 'NONE',  ( -21.53943276465977519, -0.05219959533937600094, 38.75109039468567573 ) ) ;
#2498 = CARTESIAN_POINT ( 'NONE',  ( -19.03943276465977164, 0.05219959533909376836, 81.24890960531436690 ) ) ;
#2499 = CARTESIAN_POINT ( 'NONE',  ( -19.03943276465977164, -0.05219959533935918106, 68.75109039468566152 ) ) ;
#2500 = CARTESIAN_POINT ( 'NONE',  ( -9.474510206698964154, 16.51473224551069663, 40.41557627198103120 ) ) ;
#2501 = EDGE_CURVE ( 'NONE', #144635, #114656, #107792, .T. ) ;
#2502 = CARTESIAN_POINT ( 'NONE',  ( -14.34966873604960291, -8.224510206698953496, 61.66557627198103120 ) ) ;
#2503 = CARTESIAN_POINT ( 'NONE',  ( 4.379528057220339221, -16.55341960407611168, 67.70724293864769550 ) ) ;
#2504 = CARTESIAN_POINT ( 'NONE',  ( -19.05341960407611168, -5.049401038298163336, 71.45724293864766707 ) ) ;
#2505 = CARTESIAN_POINT ( 'NONE',  ( 10.81492255796078972, 18.62759615963270932, 99.58224293864770971 ) ) ;
#2506 = CARTESIAN_POINT ( 'NONE',  ( 0.05219959533909260263, 19.03943276465977164, 74.99890960531435269 ) ) ;
#2507 = CARTESIAN_POINT ( 'NONE',  ( -18.67979575497193778, 10.72451020669871902, 108.3344237280190185 ) ) ;
#2510 = CARTESIAN_POINT ( 'NONE',  ( -16.53943276465976808, 0.05219959533911058130, 111.2489096053143669 ) ) ;
#2509 = CARTESIAN_POINT ( 'NONE',  ( -16.53943276465976808, 0.05219959533911058130, 21.24890960531436690 ) ) ;
#2508 = CARTESIAN_POINT ( 'NONE',  ( 13.97604488694527802, 13.89961937509977652, 39.37390960531435269 ) ) ;
#2511 = CARTESIAN_POINT ( 'NONE',  ( -9.474510206698720793, -16.51473224551083518, 99.58442372801900433 ) ) ;
#2512 = ORIENTED_EDGE ( 'NONE', *, *, #55964, .F. ) ;
#2513 = CARTESIAN_POINT ( 'NONE',  ( 10.72451020669871369, 18.67979575497193778, 37.08442372801901143 ) ) ;
#2514 = CARTESIAN_POINT ( 'NONE',  ( 5.153800228976615827, -19.02544592524334988, 55.20942372801899722 ) ) ;
#2515 = CARTESIAN_POINT ( 'NONE',  ( -8.314922557960811034, -14.29746914071050412, 22.08224293864769194 ) ) ;
#2516 = CARTESIAN_POINT ( 'NONE',  ( -10.72451020669898014, 18.67979575497178502, 75.41557627198102409 ) ) ;
#2517 = CARTESIAN_POINT ( 'NONE',  ( 18.67979575497178502, 10.72451020669898547, 24.16557627198103120 ) ) ;
#2518 = CARTESIAN_POINT ( 'NONE',  ( -12.14591786802309592, -12.06949235617757132, 56.87390960531436690 ) ) ;
#2519 = CARTESIAN_POINT ( 'NONE',  ( 19.03943276465977164, -0.05219959533909143690, 28.74890960531435624 ) ) ;
#2520 = CARTESIAN_POINT ( 'NONE',  ( -19.03943276465977164, 0.05219959533909376836, 36.24890960531436690 ) ) ;
#2521 = CARTESIAN_POINT ( 'NONE',  ( -19.02544592524334988, -5.153800228976617603, 28.95942372801900433 ) ) ;
#2522 = CARTESIAN_POINT ( 'NONE',  ( 12.14591786802327356, -12.06949235617739191, 90.62609039468567573 ) ) ;
#2523 = CARTESIAN_POINT ( 'NONE',  ( 16.53943276465976808, 0.05219959533934440121, 46.25109039468567573 ) ) ;
#2524 = CARTESIAN_POINT ( 'NONE',  ( 5.823673210054125526, 21.52544592524343514, 24.79057627198103120 ) ) ;
#2526 = CARTESIAN_POINT ( 'NONE',  ( -21.53943276465977519, -0.05219959533937600094, 88.75109039468567573 ) ) ;
#2525 = CARTESIAN_POINT ( 'NONE',  ( 0.05219959533909260263, 19.03943276465977164, 59.99890960531436690 ) ) ;
#2527 = CARTESIAN_POINT ( 'NONE',  ( -16.51473224551069308, -9.474510206698971260, 81.66557627198103830 ) ) ;
#2528 = CARTESIAN_POINT ( 'NONE',  ( -14.29746914071037622, -8.314922557961029526, 64.16775706135234714 ) ) ;
#2529 = CARTESIAN_POINT ( 'NONE',  ( 8.314922557960818139, 14.29746914071049879, 109.5822429386476955 ) ) ;
#2530 = CARTESIAN_POINT ( 'NONE',  ( 8.314922557961029526, -14.29746914071037800, 110.4177570613523756 ) ) ;
#2531 = DIRECTION ( 'NONE',  ( -0.7071067811865467956, 2.468850131082262977E-15, 0.7071067811865483499 ) ) ;
#2534 = CARTESIAN_POINT ( 'NONE',  ( -16.51473224551069308, -9.474510206698971260, 71.66557627198102409 ) ) ;
#2533 = CARTESIAN_POINT ( 'NONE',  ( -13.97604488694527625, -13.89961937509977652, 86.87390960531436690 ) ) ;
#2532 = CARTESIAN_POINT ( 'NONE',  ( 10.72451020669871369, 18.67979575497193778, 67.08442372801901854 ) ) ;
#2535 = CARTESIAN_POINT ( 'NONE',  ( 16.51473224551069308, 9.474510206698969483, 114.1655762719810241 ) ) ;
#2536 = CARTESIAN_POINT ( 'NONE',  ( -14.34966873604960291, -8.224510206698953496, 61.66557627198103120 ) ) ;
#2537 = CARTESIAN_POINT ( 'NONE',  ( 12.06949235617739724, 12.14591786802326823, 111.8760903946856615 ) ) ;
#2538 = CARTESIAN_POINT ( 'NONE',  ( 0.05219959533910956823, 16.53943276465976808, 34.99890960531435979 ) ) ;
#2540 = CARTESIAN_POINT ( 'NONE',  ( -16.15948758285046338, -17.62941224709156529, -54.53140136687973438 ) ) ;
#2539 = CARTESIAN_POINT ( 'NONE',  ( -16.53943276465976808, -0.05219959533934237506, 43.75109039468568284 ) ) ;
#2541 = CARTESIAN_POINT ( 'NONE',  ( -19.02544592524334988, -5.153800228976617603, 33.95942372801897591 ) ) ;
#2542 = CARTESIAN_POINT ( 'NONE',  ( 5.153800228976335163, 19.02544592524342804, 74.79057627198103830 ) ) ;
#2543 = CARTESIAN_POINT ( 'NONE',  ( 16.46253265017146816, 9.564922557961045513, 51.66775706135233293 ) ) ;
#2544 = CARTESIAN_POINT ( 'NONE',  ( 11.40812507854755253, -35.11059874428192273, -8.524999997268814411 ) ) ;
#2545 = CARTESIAN_POINT ( 'NONE',  ( 23.48529157249599564, 32.32473071737754111, -2.449999994537626513 ) ) ;
#2547 = CARTESIAN_POINT ( 'NONE',  ( 4.483927247898790824, -16.52544592524335698, 80.20942372801901854 ) ) ;
#2546 = CARTESIAN_POINT ( 'NONE',  ( 0.05219959533936267826, -19.03943276465977164, 80.00109039468567573 ) ) ;
#2548 = CARTESIAN_POINT ( 'NONE',  ( -28.79475375365586842, 2.428612866367529932E-14, 155.0000000000000000 ) ) ;
#2549 = CARTESIAN_POINT ( 'NONE',  ( -9.474510206698964154, 16.51473224551069663, 110.4155762719810383 ) ) ;
#2550 = CARTESIAN_POINT ( 'NONE',  ( 0.05219959533937995610, -21.53943276465977519, 45.00109039468568284 ) ) ;
#2551 = CARTESIAN_POINT ( 'NONE',  ( 5.153800228976615827, -19.02544592524334988, 95.20942372801897591 ) ) ;
#2553 = CARTESIAN_POINT ( 'NONE',  ( -19.05341960407611168, -5.049401038298163336, 41.45724293864769550 ) ) ;
#2552 = FACE_OUTER_BOUND ( 'NONE', #116365, .T. ) ;
#2554 = CARTESIAN_POINT ( 'NONE',  ( 19.05341960407611168, 5.049401038298154454, 108.9572429386477097 ) ) ;
#2556 = CARTESIAN_POINT ( 'NONE',  ( 19.05341960407611168, 5.049401038298154454, 53.95724293864770260 ) ) ;
#2555 = CARTESIAN_POINT ( 'NONE',  ( -0.05219959533910754901, -16.53943276465976808, 62.49890960531436690 ) ) ;
#2557 = CARTESIAN_POINT ( 'NONE',  ( 5.049401038298161559, -19.05341960407611168, 62.70724293864769550 ) ) ;
#2558 = CARTESIAN_POINT ( 'NONE',  ( -13.97604488694547697, 13.89961937509957934, 58.12609039468566863 ) ) ;
#2559 = CARTESIAN_POINT ( 'NONE',  ( 19.05341960407617918, -5.049401038297876454, 46.04275706135233293 ) ) ;
#2560 = CARTESIAN_POINT ( 'NONE',  ( 9.564922557960805705, 16.46253265017160317, 69.58224293864770971 ) ) ;
#2561 = CARTESIAN_POINT ( 'NONE',  ( 5.823673210054125526, 21.52544592524343514, 74.79057627198105251 ) ) ;
#2563 = CARTESIAN_POINT ( 'NONE',  ( 5.153800228976615827, -19.02544592524334988, 40.20942372801898301 ) ) ;
#2562 = CARTESIAN_POINT ( 'NONE',  ( -4.483927247898539470, -16.52544592524342804, 72.29057627198102409 ) ) ;
#2564 = CARTESIAN_POINT ( 'NONE',  ( -21.52544592524343514, 5.823673210054127303, 46.04057627198103830 ) ) ;
#2565 = CARTESIAN_POINT ( 'NONE',  ( -21.52544592524343514, 5.823673210054127303, 36.04057627198102409 ) ) ;
#2566 = CARTESIAN_POINT ( 'NONE',  ( -19.03943276465977164, 0.05219959533909376836, 61.24890960531436690 ) ) ;
#2567 = CARTESIAN_POINT ( 'NONE',  ( -13.89961937509977652, 13.97604488694528158, 40.62390960531435979 ) ) ;
#2568 = CARTESIAN_POINT ( 'NONE',  ( 8.314922557960818139, 14.29746914071049879, 94.58224293864769550 ) ) ;
#2569 = AXIS2_PLACEMENT_3D ( 'NONE', #195043, #118200, #101008 ) ;
#2570 = CARTESIAN_POINT ( 'NONE',  ( -18.62759615963270932, 10.81492255796079327, 105.8322429386476955 ) ) ;
#2571 = CARTESIAN_POINT ( 'NONE',  ( -0.05219959533909027116, -19.03943276465977164, 112.4989096053143669 ) ) ;
#2572 = CARTESIAN_POINT ( 'NONE',  ( 10.72451020669871369, 18.67979575497193778, 27.08442372801901854 ) ) ;
#2573 = CARTESIAN_POINT ( 'NONE',  ( -19.03943276465977164, 0.05219959533909376836, 41.24890960531435269 ) ) ;
#2574 = CARTESIAN_POINT ( 'NONE',  ( 10.81492255796078972, 18.62759615963270932, 109.5822429386476955 ) ) ;
#2575 = ADVANCED_FACE ( 'NONE', ( #39541 ), #193239, .T. ) ;
#2576 = CARTESIAN_POINT ( 'NONE',  ( -9.474510206698720793, -16.51473224551083518, 49.58442372801899722 ) ) ;
#2577 = CARTESIAN_POINT ( 'NONE',  ( 0.05219959533909260263, 19.03943276465977164, 29.99890960531435979 ) ) ;
#2578 = CARTESIAN_POINT ( 'NONE',  ( 18.56197773271727414, -5.500000000000073719, 76.05066217314451649 ) ) ;
#2579 = SURFACE_SIDE_STYLE ('',( #75448 ) ) ;
#2580 = CARTESIAN_POINT ( 'NONE',  ( -16.55341960407617563, 4.379528057220093196, 48.54275706135234714 ) ) ;
#2581 = CARTESIAN_POINT ( 'NONE',  ( -19.02544592524342804, 5.153800228976336051, 26.04057627198103120 ) ) ;
#2582 = CARTESIAN_POINT ( 'NONE',  ( 34.37111623004059169, -2.754365613946268443, 90.23597232697532888 ) ) ;
#2583 = CARTESIAN_POINT ( 'NONE',  ( 5.153800228976335163, 19.02544592524342804, 69.79057627198103830 ) ) ;
#2584 = CARTESIAN_POINT ( 'NONE',  ( -12.06949235617756955, 12.14591786802309770, 110.6239096053143669 ) ) ;
#2585 = CARTESIAN_POINT ( 'NONE',  ( -5.823673210054116645, -21.52544592524344225, 52.29057627198102409 ) ) ;
#2586 = CARTESIAN_POINT ( 'NONE',  ( -14.34966873604960291, -8.224510206698953496, 81.66557627198103830 ) ) ;
#2587 = CARTESIAN_POINT ( 'NONE',  ( -4.483927247898782831, 16.52544592524335698, 37.70942372801900433 ) ) ;
#2588 = CARTESIAN_POINT ( 'NONE',  ( 18.67979575497194134, -10.72451020669871369, 80.83442372801901854 ) ) ;
#2589 = CARTESIAN_POINT ( 'NONE',  ( -19.03943276465977164, 0.05219959533909376836, 26.24890960531435624 ) ) ;
#2590 = ADVANCED_FACE ( 'NONE', ( #83038 ), #179085, .F. ) ;
#2591 = CARTESIAN_POINT ( 'NONE',  ( -4.483927247898782831, 16.52544592524335698, 107.7094237280190328 ) ) ;
#2592 = CARTESIAN_POINT ( 'NONE',  ( -16.55341960407611168, -4.379528057220339221, 56.45724293864768839 ) ) ;
#2593 = CARTESIAN_POINT ( 'NONE',  ( -16.46253265017160317, 9.564922557960807481, 50.83224293864770260 ) ) ;
#2594 = CARTESIAN_POINT ( 'NONE',  ( -5.719274019375665041, -21.55341960407619695, 94.79275706135234714 ) ) ;
#2595 = CARTESIAN_POINT ( 'NONE',  ( 21.52544592524344225, -5.823673210054117533, 103.5405762719810383 ) ) ;
#2596 = CARTESIAN_POINT ( 'NONE',  ( -15.80617190586768217, 15.72974639402176855, 73.12609039468567573 ) ) ;
#2597 = CARTESIAN_POINT ( 'NONE',  ( 16.55341960407618274, -4.379528057220086978, 36.04275706135234714 ) ) ;
#2599 = CARTESIAN_POINT ( 'NONE',  ( 18.62759615963255655, 10.81492255796105972, 91.66775706135234714 ) ) ;
#2598 = CARTESIAN_POINT ( 'NONE',  ( -16.55341960407611168, -4.379528057220339221, 81.45724293864769550 ) ) ;
#2600 = CIRCLE ( 'NONE', #60618, 214.0437394197456342 ) ;
#2601 = CARTESIAN_POINT ( 'NONE',  ( 12.14591786802309770, 12.06949235617756955, 24.37390960531435979 ) ) ;
#2602 = CARTESIAN_POINT ( 'NONE',  ( 18.22780087662125226, -5.499999999999864997, 61.01540105326109398 ) ) ;
#2603 = CARTESIAN_POINT ( 'NONE',  ( 12.14591786802327356, -12.06949235617739191, 45.62609039468567573 ) ) ;
#2604 = CARTESIAN_POINT ( 'NONE',  ( -16.53943276465976808, 0.05219959533911058130, 36.24890960531435979 ) ) ;
#2605 = CARTESIAN_POINT ( 'NONE',  ( 14.34966873604972726, -8.224510206698740333, 90.83442372801901854 ) ) ;
#2606 = CARTESIAN_POINT ( 'NONE',  ( 19.05341960407611168, 5.049401038298154454, 103.9572429386476671 ) ) ;
#2607 = CIRCLE ( 'NONE', #18786, 216.0437394197456911 ) ;
#2608 = CARTESIAN_POINT ( 'NONE',  ( 9.564922557960805705, 16.46253265017160317, 94.58224293864769550 ) ) ;
#2609 = CARTESIAN_POINT ( 'NONE',  ( 15.80617190586769283, -15.72974639402175789, 100.6260903946857184 ) ) ;
#2610 = CARTESIAN_POINT ( 'NONE',  ( -16.52544592524335698, -4.483927247898792601, 98.95942372801903275 ) ) ;
#2611 = CARTESIAN_POINT ( 'NONE',  ( -12.06949235617756955, 12.14591786802309770, 70.62390960531436690 ) ) ;
#2612 = CARTESIAN_POINT ( 'NONE',  ( 16.46253265017160672, -9.564922557960803928, 83.33224293864768129 ) ) ;
#2613 = ORIENTED_EDGE ( 'NONE', *, *, #47794, .T. ) ;
#2614 = CARTESIAN_POINT ( 'NONE',  ( 14.29746914071037800, 8.314922557961029526, 31.66775706135234358 ) ) ;
#2615 = CARTESIAN_POINT ( 'NONE',  ( 5.153800228976335163, 19.02544592524342804, 24.79057627198102765 ) ) ;
#2616 = CARTESIAN_POINT ( 'NONE',  ( -19.05341960407611168, -5.049401038298163336, 91.45724293864766707 ) ) ;
#2618 = CARTESIAN_POINT ( 'NONE',  ( -11.40812507854755609, 35.11059874428196537, -3.024999997268813523 ) ) ;
#2617 = CARTESIAN_POINT ( 'NONE',  ( 16.53943276465976808, 0.05219959533934440121, 36.25109039468567573 ) ) ;
#2619 = CARTESIAN_POINT ( 'NONE',  ( 0.05219959533936267826, -19.03943276465977164, 30.00109039468566863 ) ) ;
#2620 = CARTESIAN_POINT ( 'NONE',  ( -14.34966873604972548, 8.224510206698743886, 93.33442372801901854 ) ) ;
#2621 = CARTESIAN_POINT ( 'NONE',  ( 13.89961937509957401, 13.97604488694547697, 111.8760903946856757 ) ) ;
#2622 = CARTESIAN_POINT ( 'NONE',  ( 13.97604488694527802, 13.89961937509977652, 29.37390960531435979 ) ) ;
#2623 = CARTESIAN_POINT ( 'NONE',  ( -8.314922557961024197, 14.29746914071037800, 77.91775706135231871 ) ) ;
#2624 = CARTESIAN_POINT ( 'NONE',  ( -16.52544592524335698, -4.483927247898792601, 63.95942372801901854 ) ) ;
#2625 = CARTESIAN_POINT ( 'NONE',  ( -19.02544592524342804, 5.153800228976336051, 26.04057627198103120 ) ) ;
#2626 = CARTESIAN_POINT ( 'NONE',  ( -13.97604488694547697, 13.89961937509957934, 68.12609039468563310 ) ) ;
#2627 = CARTESIAN_POINT ( 'NONE',  ( -18.67979575497193778, 10.72451020669871902, 113.3344237280190328 ) ) ;
#2628 = CARTESIAN_POINT ( 'NONE',  ( 5.049401038298161559, -19.05341960407611168, 47.70724293864770260 ) ) ;
#2629 = CARTESIAN_POINT ( 'NONE',  ( 16.46253265017160672, -9.564922557960803928, 88.33224293864769550 ) ) ;
#2630 = CARTESIAN_POINT ( 'NONE',  ( 14.34966873604960469, 8.224510206698951720, 84.16557627198103830 ) ) ;
#2631 = B_SPLINE_CURVE_WITH_KNOTS ( 'NONE', 3,
 ( #184968, #62602, #138458, #91937, #183979, #170795, #107119, #153630 ),
 .UNSPECIFIED., .F., .F.,
 ( 4, 2, 2, 4 ),
 ( 2.244678719545345876E-07, 0.002115167047690978165, 0.004230109627510002419, 0.008459994787147971998 ),
 .UNSPECIFIED. ) ;
#2632 = CARTESIAN_POINT ( 'NONE',  ( 5.153800228976615827, -19.02544592524334988, 60.20942372801899012 ) ) ;
#2633 = CARTESIAN_POINT ( 'NONE',  ( 21.53943276465977519, -0.05219959533907433946, 53.74890960531437401 ) ) ;
#2634 = CARTESIAN_POINT ( 'NONE',  ( -19.02544592524334988, -5.153800228976617603, 18.95942372801899722 ) ) ;
#2635 = CARTESIAN_POINT ( 'NONE',  ( 9.564922557960805705, 16.46253265017160317, 94.58224293864769550 ) ) ;
#2636 = CARTESIAN_POINT ( 'NONE',  ( -13.97604488694547697, 13.89961937509957934, 23.12609039468565442 ) ) ;
#2637 = CARTESIAN_POINT ( 'NONE',  ( -21.55341960407610458, -5.719274019375992779, 61.45724293864770260 ) ) ;
#2638 = CARTESIAN_POINT ( 'NONE',  ( 19.05341960407611168, 5.049401038298154454, 113.9572429386477097 ) ) ;
#2639 = CARTESIAN_POINT ( 'NONE',  ( 16.46253265017146816, 9.564922557961045513, 86.66775706135233293 ) ) ;
#2640 = CARTESIAN_POINT ( 'NONE',  ( -17.50000000000148148, 3.202012800152246097, 109.9282241602726202 ) ) ;
#2641 = CARTESIAN_POINT ( 'NONE',  ( -9.474510206698720793, -16.51473224551083518, 104.5844237280190043 ) ) ;
#2642 = CARTESIAN_POINT ( 'NONE',  ( -8.224510206698948167, 14.34966873604960824, 110.4155762719810383 ) ) ;
#2643 = CARTESIAN_POINT ( 'NONE',  ( 9.474510206698971260, -16.51473224551069308, 97.91557627198102409 ) ) ;
#2644 = CARTESIAN_POINT ( 'NONE',  ( 15.72974639402199770, -15.80617190586745480, 73.12390960531436690 ) ) ;
#2645 = CARTESIAN_POINT ( 'NONE',  ( -4.483927247898782831, 16.52544592524335698, 42.70942372801901854 ) ) ;
#2646 = CARTESIAN_POINT ( 'NONE',  ( 5.719274019375673035, 21.55341960407619339, 47.29275706135234003 ) ) ;
#2647 = CARTESIAN_POINT ( 'NONE',  ( 10.81492255796106328, -18.62759615963255655, 95.41775706135234714 ) ) ;
#2648 = CARTESIAN_POINT ( 'NONE',  ( -16.53943276465976808, -0.05219959533934237506, 98.75109039468568994 ) ) ;
#2649 = CARTESIAN_POINT ( 'NONE',  ( 19.02544592524343514, -5.153800228976328945, 93.54057627198102409 ) ) ;
#2650 = CARTESIAN_POINT ( 'NONE',  ( -16.55341960407611168, -4.379528057220339221, 96.45724293864770971 ) ) ;
#2651 = CARTESIAN_POINT ( 'NONE',  ( -14.34966873604960291, -8.224510206698953496, 36.66557627198103120 ) ) ;
#2652 = CARTESIAN_POINT ( 'NONE',  ( -19.05341960407617563, 5.049401038297882671, 68.54275706135230450 ) ) ;
#2653 = CARTESIAN_POINT ( 'NONE',  ( -5.719274019375665041, -21.55341960407619695, 44.79275706135234714 ) ) ;
#2654 = CARTESIAN_POINT ( 'NONE',  ( -13.97604488694547697, 13.89961937509957934, 33.12609039468566863 ) ) ;
#2655 = CARTESIAN_POINT ( 'NONE',  ( 12.14591786802309770, 12.06949235617756955, 89.37390960531435269 ) ) ;
#2656 = CARTESIAN_POINT ( 'NONE',  ( -16.51473224551069308, -9.474510206698971260, 111.6655762719810383 ) ) ;
#2657 = CARTESIAN_POINT ( 'NONE',  ( 16.53943276465976808, 0.05219959533934440121, 111.2510903946856899 ) ) ;
#2658 = CARTESIAN_POINT ( 'NONE',  ( -0.05219959533937732626, 21.53943276465977519, 87.50109039468568994 ) ) ;
#2659 = CARTESIAN_POINT ( 'NONE',  ( 4.379528057220092307, 16.55341960407617563, 62.29275706135236845 ) ) ;
#2660 = CARTESIAN_POINT ( 'NONE',  ( -16.55341960407617563, 4.379528057220093196, 103.5427570613523613 ) ) ;
#2661 = CARTESIAN_POINT ( 'NONE',  ( -15.80617190586768217, 15.72974639402176855, 48.12609039468568284 ) ) ;
#2662 = EDGE_LOOP ( 'NONE', ( #45263, #157409, #181382, #132862 ) ) ;
#2663 = CARTESIAN_POINT ( 'NONE',  ( -21.52544592524334988, -5.823673210054445271, 28.95942372801902209 ) ) ;
#2664 = CARTESIAN_POINT ( 'NONE',  ( 12.06949235617757843, -12.14591786802309237, 103.1239096053143811 ) ) ;
#2665 = CARTESIAN_POINT ( 'NONE',  ( -19.03943276465977164, 0.05219959533909376836, 21.24890960531436335 ) ) ;
#2666 = CARTESIAN_POINT ( 'NONE',  ( -16.52544592524342804, 4.483927247898546575, 66.04057627198103830 ) ) ;
#2667 = CARTESIAN_POINT ( 'NONE',  ( 16.51473224551069308, 9.474510206698969483, 74.16557627198103830 ) ) ;
#2668 = CARTESIAN_POINT ( 'NONE',  ( 16.53943276465976808, 0.05219959533934440121, 101.2510903946856757 ) ) ;
#2669 = CARTESIAN_POINT ( 'NONE',  ( -0.05219959533909027116, -19.03943276465977164, 42.49890960531435269 ) ) ;
#2670 = CARTESIAN_POINT ( 'NONE',  ( 10.72451020669898902, -18.67979575497178502, 52.91557627198103830 ) ) ;
#2671 = CARTESIAN_POINT ( 'NONE',  ( -0.05219959533910754901, -16.53943276465976808, 97.49890960531436690 ) ) ;
#2672 = CARTESIAN_POINT ( 'NONE',  ( -10.81492255796078084, -18.62759615963271287, 97.08224293864770971 ) ) ;
#2673 = CARTESIAN_POINT ( 'NONE',  ( 0.05219959533909260263, 19.03943276465977164, 94.99890960531436690 ) ) ;
#2675 = CARTESIAN_POINT ( 'NONE',  ( -5.153800228976607833, 19.02544592524334988, 97.70942372801900433 ) ) ;
#2674 = CARTESIAN_POINT ( 'NONE',  ( 13.89961937509977652, -13.97604488694527269, 48.12390960531435979 ) ) ;
#2676 = CARTESIAN_POINT ( 'NONE',  ( -15.72974639402197994, 15.80617190586746368, 40.62390960531435269 ) ) ;
#2677 = CARTESIAN_POINT ( 'NONE',  ( 0.05219959533937995610, -21.53943276465977519, 65.00109039468568994 ) ) ;
#2678 = CARTESIAN_POINT ( 'NONE',  ( 13.97604488694527802, 13.89961937509977652, 59.37390960531434558 ) ) ;
#2679 = CARTESIAN_POINT ( 'NONE',  ( 19.05341960407611168, 5.049401038298154454, 88.95724293864769550 ) ) ;
#2680 = CARTESIAN_POINT ( 'NONE',  ( -0.05219959533934338120, 16.53943276465976808, 67.50109039468568994 ) ) ;
#2681 = CARTESIAN_POINT ( 'NONE',  ( 0.05219959533937995610, -21.53943276465977519, 50.00109039468568994 ) ) ;
#2682 = CARTESIAN_POINT ( 'NONE',  ( -5.823673210054431948, 21.52544592524334988, 92.70942372801901854 ) ) ;
#2683 = CARTESIAN_POINT ( 'NONE',  ( 21.55341960407610458, 5.719274019375980345, 98.95724293864770971 ) ) ;
#2685 = CARTESIAN_POINT ( 'NONE',  ( 14.34966873604972726, -8.224510206698740333, 65.83442372801900433 ) ) ;
#2684 = CARTESIAN_POINT ( 'NONE',  ( -10.72451020669870658, -18.67979575497194134, 39.58442372801901143 ) ) ;
#2686 = CARTESIAN_POINT ( 'NONE',  ( 15.72974639402199770, -15.80617190586745480, 63.12390960531435979 ) ) ;
#2687 = CARTESIAN_POINT ( 'NONE',  ( 9.474510206698729675, 16.51473224551082808, 32.08442372801900433 ) ) ;
#2689 = CARTESIAN_POINT ( 'NONE',  ( 14.34966873604972726, -8.224510206698740333, 110.8344237280190043 ) ) ;
#2688 = CARTESIAN_POINT ( 'NONE',  ( -9.564922557960796823, -16.46253265017161027, 62.08224293864769550 ) ) ;
#2690 = CARTESIAN_POINT ( 'NONE',  ( -17.50000000000000000, -5.500000000000000000, 106.2823096230357010 ) ) ;
#2691 = CARTESIAN_POINT ( 'NONE',  ( -19.05341960407611168, -5.049401038298163336, 96.45724293864769550 ) ) ;
#2693 = B_SPLINE_CURVE_WITH_KNOTS ( 'NONE', 3,
 ( #139494, #65640, #46503, #108163, #142482, #141494, #49487, #63665, #200187, #111149, #153678, #172839, #140497, #186027, #169845, #45512, #110160, #34318, #80804, #77825, #32336, #15175, #48506, #3960 ),
 .UNSPECIFIED., .F., .F.,
 ( 4, 2, 2, 2, 2, 2, 2, 2, 2, 2, 2, 4 ),
 ( 1.968491852713559257E-07, 0.0003260565056757782384, 0.0006519161621662850634, 0.0009777758186567920510, 0.001303635475147298930, 0.001955354788128312472, 0.002607074101109326230, 0.003258793414090339988, 0.003910512727071354180, 0.004562232040052368806, 0.004888091696542873517, 0.005213951353033378228 ),
 .UNSPECIFIED. ) ;
#2692 = CARTESIAN_POINT ( 'NONE',  ( -3.660253528765552655, 6.551653823223177575, 8.410814283099849575 ) ) ;
#2694 = CARTESIAN_POINT ( 'NONE',  ( 9.564922557961047289, -16.46253265017146816, 85.41775706135233293 ) ) ;
#2695 = CARTESIAN_POINT ( 'NONE',  ( 0.05219959533907565091, 21.53943276465977519, 54.99890960531435269 ) ) ;
#2696 = CARTESIAN_POINT ( 'NONE',  ( -8.224510206698948167, 14.34966873604960824, 40.41557627198103120 ) ) ;
#2697 = CARTESIAN_POINT ( 'NONE',  ( 5.153800228976615827, -19.02544592524334988, 110.2094237280189901 ) ) ;
#2698 = CARTESIAN_POINT ( 'NONE',  ( -16.51473224551069308, -9.474510206698971260, 26.66557627198103120 ) ) ;
#2699 = CARTESIAN_POINT ( 'NONE',  ( 5.153800228976615827, -19.02544592524334988, 110.2094237280189901 ) ) ;
#2701 = CARTESIAN_POINT ( 'NONE',  ( 9.474510206698729675, 16.51473224551082808, 67.08442372801900433 ) ) ;
#2700 = CARTESIAN_POINT ( 'NONE',  ( -10.72451020669898014, 18.67979575497178502, 105.4155762719810383 ) ) ;
#2702 = CARTESIAN_POINT ( 'NONE',  ( 4.483927247898790824, -16.52544592524335698, 75.20942372801901854 ) ) ;
#2703 = CARTESIAN_POINT ( 'NONE',  ( 16.46253265017160672, -9.564922557960803928, 73.33224293864769550 ) ) ;
#2704 = CARTESIAN_POINT ( 'NONE',  ( -4.483927247898539470, -16.52544592524342804, 82.29057627198103830 ) ) ;
#2705 = CARTESIAN_POINT ( 'NONE',  ( -19.02544592524342804, 5.153800228976336051, 61.04057627198103120 ) ) ;
#2706 = CARTESIAN_POINT ( 'NONE',  ( 12.06949235617757843, -12.14591786802309237, 63.12390960531435979 ) ) ;
#2707 = CARTESIAN_POINT ( 'NONE',  ( -37.99626262588766679, 2.428612866367529932E-14, -5.747842220587803475 ) ) ;
#2708 = CARTESIAN_POINT ( 'NONE',  ( -37.19790397533368775, -4.369830079088519170, 41.64077531718623248 ) ) ;
#2709 = CARTESIAN_POINT ( 'NONE',  ( -4.483927247898539470, -16.52544592524342804, 47.29057627198103120 ) ) ;
#2710 = CARTESIAN_POINT ( 'NONE',  ( -13.89961937509977652, 13.97604488694528158, 70.62390960531432427 ) ) ;
#2711 = LINE ( 'NONE', #121077, #57362 ) ;
#2712 = CARTESIAN_POINT ( 'NONE',  ( -16.46253265017146816, -9.564922557961047289, 44.16775706135232582 ) ) ;
#2713 = CARTESIAN_POINT ( 'NONE',  ( 14.34966873604972726, -8.224510206698740333, 50.83442372801901143 ) ) ;
#2714 = CARTESIAN_POINT ( 'NONE',  ( -5.719274019375978568, 21.55341960407610458, 60.20724293864768839 ) ) ;
#2715 = CARTESIAN_POINT ( 'NONE',  ( -9.474510206698720793, -16.51473224551083518, 29.58442372801900433 ) ) ;
#2716 = CARTESIAN_POINT ( 'NONE',  ( 19.02544592524343514, -5.153800228976328945, 78.54057627198099567 ) ) ;
#2717 = CARTESIAN_POINT ( 'NONE',  ( -24.81835880841865816, 6.052260367207988878, 168.4265213779230521 ) ) ;
#2718 = CARTESIAN_POINT ( 'NONE',  ( -16.51473224551069308, -9.474510206698971260, 111.6655762719810383 ) ) ;
#2719 = CARTESIAN_POINT ( 'NONE',  ( -10.81492255796105439, 18.62759615963255655, 42.91775706135235424 ) ) ;
#2720 = CARTESIAN_POINT ( 'NONE',  ( 8.224510206698953496, -14.34966873604960469, 112.9155762719810383 ) ) ;
#2723 = EDGE_LOOP ( 'NONE', ( #5934, #77789, #146194, #159845 ) ) ;
#2722 = CARTESIAN_POINT ( 'NONE',  ( 16.51473224551069308, 9.474510206698969483, 79.16557627198103830 ) ) ;
#2721 = CARTESIAN_POINT ( 'NONE',  ( -18.62759615963270932, 10.81492255796079327, 95.83224293864770971 ) ) ;
#2724 = CARTESIAN_POINT ( 'NONE',  ( 0.05219959533937995610, -21.53943276465977519, 30.00109039468568284 ) ) ;
#2725 = ORIENTED_EDGE ( 'NONE', *, *, #92972, .T. ) ;
#2726 = CARTESIAN_POINT ( 'NONE',  ( -19.03943276465977164, 0.05219959533909376836, 91.24890960531436690 ) ) ;
#2727 = CARTESIAN_POINT ( 'NONE',  ( -17.97214573761834799, -5.500000000000021316, 76.46970049038655759 ) ) ;
#2728 = CARTESIAN_POINT ( 'NONE',  ( 13.89961937509977652, -13.97604488694527269, 28.12390960531435624 ) ) ;
#2729 = CARTESIAN_POINT ( 'NONE',  ( -13.97604488694547697, 13.89961937509957934, 103.1260903946856473 ) ) ;
#2730 = CARTESIAN_POINT ( 'NONE',  ( -22.81625015709509441, -31.40387420917324590, -10.82499999726881157 ) ) ;
#2731 = CARTESIAN_POINT ( 'NONE',  ( -8.224510206698948167, 14.34966873604960824, 110.4155762719810383 ) ) ;
#2732 = CARTESIAN_POINT ( 'NONE',  ( -21.52544592524334988, -5.823673210054445271, 78.95942372801901854 ) ) ;
#2734 = CARTESIAN_POINT ( 'NONE',  ( 5.823673210054444382, -21.52544592524334988, 45.20942372801901854 ) ) ;
#2733 = CARTESIAN_POINT ( 'NONE',  ( -5.049401038298153566, 19.05341960407611168, 80.20724293864769550 ) ) ;
#2735 = CARTESIAN_POINT ( 'NONE',  ( 10.81492255796106328, -18.62759615963255655, 30.41775706135234358 ) ) ;
#2736 = CARTESIAN_POINT ( 'NONE',  ( 28.82186960331499392, -9.364793116373510529, 148.9000000000000057 ) ) ;
#2737 = CARTESIAN_POINT ( 'NONE',  ( -19.05341960407611168, -5.049401038298163336, 86.45724293864769550 ) ) ;
#2738 = CARTESIAN_POINT ( 'NONE',  ( 3.796749449783271668, 28.08088322626615607, 140.0000000000000000 ) ) ;
#2740 = CARTESIAN_POINT ( 'NONE',  ( 18.62759615963271287, -10.81492255796078972, 38.33224293864768839 ) ) ;
#2739 = CARTESIAN_POINT ( 'NONE',  ( 16.55341960407618274, -4.379528057220086978, 41.04275706135236135 ) ) ;
#2741 = CARTESIAN_POINT ( 'NONE',  ( 15.72974639402176855, 15.80617190586768217, 76.87609039468567573 ) ) ;
#2742 = CARTESIAN_POINT ( 'NONE',  ( 4.381595247748339084, 6.502951376627817304, -62.18229462841636490 ) ) ;
#2743 = CARTESIAN_POINT ( 'NONE',  ( 13.89961937509957401, 13.97604488694547697, 111.8760903946856757 ) ) ;
#2744 = CARTESIAN_POINT ( 'NONE',  ( -16.51473224551069308, -9.474510206698971260, 66.66557627198102409 ) ) ;
#2745 = CARTESIAN_POINT ( 'NONE',  ( -16.46253265017160317, 9.564922557960807481, 85.83224293864769550 ) ) ;
#2746 = EDGE_CURVE ( 'NONE', #167830, #92192, #92435, .T. ) ;
#2747 = CARTESIAN_POINT ( 'NONE',  ( -16.53943276465976808, 0.05219959533911058130, 106.2489096053143811 ) ) ;
#2748 = CARTESIAN_POINT ( 'NONE',  ( 8.224510206698953496, -14.34966873604960469, 102.9155762719810383 ) ) ;
#2749 = CARTESIAN_POINT ( 'NONE',  ( -9.474510206698964154, 16.51473224551069663, 105.4155762719810383 ) ) ;
#2750 = CARTESIAN_POINT ( 'NONE',  ( 8.224510206698742110, 14.34966873604972548, 77.08442372801901854 ) ) ;
#2752 = CARTESIAN_POINT ( 'NONE',  ( 13.89961937509977652, -13.97604488694527269, 48.12390960531435979 ) ) ;
#2751 = CARTESIAN_POINT ( 'NONE',  ( 14.34966873604960469, 8.224510206698951720, 54.16557627198103120 ) ) ;
#2753 = CARTESIAN_POINT ( 'NONE',  ( 21.53943276465977519, 0.05219959533937863772, 76.25109039468568994 ) ) ;
#2754 = CARTESIAN_POINT ( 'NONE',  ( 5.719274019375673035, 21.55341960407619339, 77.29275706135234714 ) ) ;
#2755 = CARTESIAN_POINT ( 'NONE',  ( -9.564922557961040184, 16.46253265017147172, 107.9177570613523471 ) ) ;
#2756 = CARTESIAN_POINT ( 'NONE',  ( 16.55341960407611168, 4.379528057220329451, 68.95724293864769550 ) ) ;
#2757 = CARTESIAN_POINT ( 'NONE',  ( -0.05219959533907301413, -21.53943276465977519, 107.4989096053143669 ) ) ;
#2758 = CARTESIAN_POINT ( 'NONE',  ( -21.53943276465977519, 0.05219959533907696930, 66.24890960531436690 ) ) ;
#2759 = CARTESIAN_POINT ( 'NONE',  ( 19.34837522270366961, 5.499999999999741540, 73.36337684832578532 ) ) ;
#2760 = CARTESIAN_POINT ( 'NONE',  ( -27.73933785331498925, 9.013057229001089965, 148.7750000027311899 ) ) ;
#2761 = CARTESIAN_POINT ( 'NONE',  ( 16.46253265017160672, -9.564922557960803928, 63.33224293864769550 ) ) ;
#2762 = CARTESIAN_POINT ( 'NONE',  ( 14.29746914071049879, -8.314922557960816363, 43.33224293864769550 ) ) ;
#2763 = CARTESIAN_POINT ( 'NONE',  ( 8.314922557960818139, 14.29746914071049879, 24.58224293864768839 ) ) ;
#2764 = CARTESIAN_POINT ( 'NONE',  ( -4.483927247898782831, 16.52544592524335698, 97.70942372801904696 ) ) ;
#2765 = CARTESIAN_POINT ( 'NONE',  ( -19.02544592524334988, -5.153800228976617603, 48.95942372801900433 ) ) ;
#2766 = CARTESIAN_POINT ( 'NONE',  ( -17.49999999999999645, -5.500000000000000888, 120.0000000000000142 ) ) ;
#2767 = CARTESIAN_POINT ( 'NONE',  ( -16.51473224551069308, -9.474510206698971260, 86.66557627198102409 ) ) ;
#2768 = ADVANCED_FACE ( 'NONE', ( #20375 ), #134223, .F. ) ;
#2769 = CARTESIAN_POINT ( 'NONE',  ( -8.224510206698948167, 14.34966873604960824, 60.41557627198102409 ) ) ;
#2771 = CARTESIAN_POINT ( 'NONE',  ( -15.72974639402197994, 15.80617190586746368, 25.62390960531435624 ) ) ;
#2770 = CARTESIAN_POINT ( 'NONE',  ( 16.51473224551069308, 9.474510206698969483, 24.16557627198102765 ) ) ;
#2773 = VERTEX_POINT ( 'NONE', #175067 ) ;
#2772 = CARTESIAN_POINT ( 'NONE',  ( 15.80617190586746368, 15.72974639402197994, 49.37390960531436690 ) ) ;
#2774 = CARTESIAN_POINT ( 'NONE',  ( 14.29746914071049879, -8.314922557960816363, 93.33224293864769550 ) ) ;
#2775 = CARTESIAN_POINT ( 'NONE',  ( 12.06949235617739724, 12.14591786802326823, 56.87609039468568994 ) ) ;
#2776 = CARTESIAN_POINT ( 'NONE',  ( -12.14591786802309592, -12.06949235617757132, 76.87390960531439532 ) ) ;
#2777 = DIRECTION ( 'NONE',  ( 0.000000000000000000, 0.000000000000000000, 1.000000000000000000 ) ) ;
#2778 = CARTESIAN_POINT ( 'NONE',  ( -19.02544592524334988, -5.153800228976617603, 78.95942372801900433 ) ) ;
#2779 = CARTESIAN_POINT ( 'NONE',  ( -19.02544592524342804, 5.153800228976336051, 116.0405762719810383 ) ) ;
#2780 = CARTESIAN_POINT ( 'NONE',  ( 22.81625015709510151, -31.40387420917324590, -2.424999997268812546 ) ) ;
#2781 = CARTESIAN_POINT ( 'NONE',  ( 19.17291183240702779, 5.499999999999965361, 101.8490549527296452 ) ) ;
#2783 = CARTESIAN_POINT ( 'NONE',  ( 16.52544592524342804, -4.483927247898539470, 28.54057627198103120 ) ) ;
#2782 = CARTESIAN_POINT ( 'NONE',  ( -12.06949235617739369, -12.14591786802326823, 49.37609039468569705 ) ) ;
#2784 = CARTESIAN_POINT ( 'NONE',  ( -18.67979575497178146, -10.72451020669898902, 61.66557627198103120 ) ) ;
#2785 = CARTESIAN_POINT ( 'NONE',  ( 9.564922557961047289, -16.46253265017146816, 80.41775706135234714 ) ) ;
#2786 = CARTESIAN_POINT ( 'NONE',  ( 18.62759615963271287, -10.81492255796078972, 43.33224293864769550 ) ) ;
#2787 = CARTESIAN_POINT ( 'NONE',  ( -21.55341960407619339, 5.719274019375674811, 78.54275706135236135 ) ) ;
#2788 = CARTESIAN_POINT ( 'NONE',  ( -17.49999999999999289, 5.500000000000036415, 85.79690382534171533 ) ) ;
#2789 = CARTESIAN_POINT ( 'NONE',  ( 14.34966873604972726, -8.224510206698740333, 30.83442372801902209 ) ) ;
#2791 = CARTESIAN_POINT ( 'NONE',  ( 16.51473224551069308, 9.474510206698969483, 104.1655762719810241 ) ) ;
#2790 = CARTESIAN_POINT ( 'NONE',  ( -9.564922557960796823, -16.46253265017161027, 37.08224293864768839 ) ) ;
#2792 = CARTESIAN_POINT ( 'NONE',  ( -16.46253265017160317, 9.564922557960807481, 35.83224293864768839 ) ) ;
#2793 = CARTESIAN_POINT ( 'NONE',  ( -12.14591786802309592, -12.06949235617757132, 106.8739096053143811 ) ) ;
#2794 = DIRECTION ( 'NONE',  ( 1.000000000000000000, 9.714451465470120961E-17, 5.551115123125775923E-17 ) ) ;
#2795 = CARTESIAN_POINT ( 'NONE',  ( 5.049401038298161559, -19.05341960407611168, 107.7072429386476955 ) ) ;
#2796 = ORIENTED_EDGE ( 'NONE', *, *, #152637, .F. ) ;
#2797 = CARTESIAN_POINT ( 'NONE',  ( -4.379528057220086978, -16.55341960407618274, 49.79275706135234714 ) ) ;
#2798 = CARTESIAN_POINT ( 'NONE',  ( -5.719274019375978568, 21.55341960407610458, 90.20724293864770971 ) ) ;
#2799 = CARTESIAN_POINT ( 'NONE',  ( -19.03943276465977164, 0.05219959533909376836, 41.24890960531435269 ) ) ;
#2800 = CARTESIAN_POINT ( 'NONE',  ( -21.53943276465977519, -0.05219959533937600094, 33.75109039468568284 ) ) ;
#2801 = CARTESIAN_POINT ( 'NONE',  ( 5.049401038298161559, -19.05341960407611168, 87.70724293864769550 ) ) ;
#2802 = CARTESIAN_POINT ( 'NONE',  ( -28.79475375365603185, 9.355982642739006039, 145.8843446568999980 ) ) ;
#2803 = ORIENTED_EDGE ( 'NONE', *, *, #179291, .F. ) ;
#2804 = CARTESIAN_POINT ( 'NONE',  ( -14.34966873604972548, 8.224510206698743886, 48.33442372801902565 ) ) ;
#2805 = CARTESIAN_POINT ( 'NONE',  ( -21.52544592524343514, 5.823673210054127303, 111.0405762719810525 ) ) ;
#2808 = CARTESIAN_POINT ( 'NONE',  ( -19.03943276465977164, -0.05219959533935918106, 68.75109039468566152 ) ) ;
#2807 = CARTESIAN_POINT ( 'NONE',  ( 19.02544592524343514, -5.153800228976328945, 98.54057627198100988 ) ) ;
#2806 = CARTESIAN_POINT ( 'NONE',  ( 4.379528057220339221, -16.55341960407611168, 102.7072429386476955 ) ) ;
#2809 = CARTESIAN_POINT ( 'NONE',  ( -13.97604488694547697, 13.89961937509957934, 33.12609039468566863 ) ) ;
#2810 = CARTESIAN_POINT ( 'NONE',  ( -10.81492255796078084, -18.62759615963271287, 82.08224293864768129 ) ) ;
#2811 = CARTESIAN_POINT ( 'NONE',  ( 9.474510206698729675, 16.51473224551082808, 27.08442372801900433 ) ) ;
#2812 = CARTESIAN_POINT ( 'NONE',  ( -12.14591786802326823, 12.06949235617739902, 78.12609039468570415 ) ) ;
#2813 = CARTESIAN_POINT ( 'NONE',  ( -16.51473224551069308, -9.474510206698971260, 101.6655762719810241 ) ) ;
#2814 = CARTESIAN_POINT ( 'NONE',  ( 5.049401038298161559, -19.05341960407611168, 57.70724293864769550 ) ) ;
#2815 = CARTESIAN_POINT ( 'NONE',  ( -21.52544592524334988, -5.823673210054445271, 63.95942372801901854 ) ) ;
#2816 = CARTESIAN_POINT ( 'NONE',  ( 21.52544592524334988, 5.823673210054432836, 61.45942372801901854 ) ) ;
#2817 = CARTESIAN_POINT ( 'NONE',  ( -5.049401038298153566, 19.05341960407611168, 70.20724293864769550 ) ) ;
#2818 = CARTESIAN_POINT ( 'NONE',  ( -0.05219959533937732626, 21.53943276465977519, 47.50109039468568994 ) ) ;
#2819 = EDGE_CURVE ( 'NONE', #146728, #77030, #14249, .T. ) ;
#2820 = CARTESIAN_POINT ( 'NONE',  ( -16.46253265017146816, -9.564922557961047289, 94.16775706135233293 ) ) ;
#2821 = CARTESIAN_POINT ( 'NONE',  ( 16.51473224551069308, 9.474510206698969483, 49.16557627198102409 ) ) ;
#2822 = CARTESIAN_POINT ( 'NONE',  ( 16.51473224551069308, 9.474510206698969483, 94.16557627198103830 ) ) ;
#2823 = CARTESIAN_POINT ( 'NONE',  ( 5.049401038298161559, -19.05341960407611168, 62.70724293864769550 ) ) ;
#2824 = CARTESIAN_POINT ( 'NONE',  ( 9.564922557960805705, 16.46253265017160317, 114.5822429386476955 ) ) ;
#2825 = CARTESIAN_POINT ( 'NONE',  ( 0.05219959533909260263, 19.03943276465977164, 49.99890960531435979 ) ) ;
#2826 = CARTESIAN_POINT ( 'NONE',  ( -15.72974639402197994, 15.80617190586746368, 80.62390960531438111 ) ) ;
#2827 = CARTESIAN_POINT ( 'NONE',  ( -16.53943276465976808, -0.05219959533934237506, 78.75109039468568994 ) ) ;
#2828 = CARTESIAN_POINT ( 'NONE',  ( -23.14613071126281341, 10.96668486446900381, 168.1016194467972014 ) ) ;
#2829 = CARTESIAN_POINT ( 'NONE',  ( 13.97604488694548053, -13.89961937509957401, 25.62609039468566507 ) ) ;
#2830 = CARTESIAN_POINT ( 'NONE',  ( -19.02544592524342804, 5.153800228976336051, 71.04057627198099567 ) ) ;
#2831 = CARTESIAN_POINT ( 'NONE',  ( 4.483927247898545687, 16.52544592524342804, 59.79057627198103120 ) ) ;
#2832 = CARTESIAN_POINT ( 'NONE',  ( -4.483927247898539470, -16.52544592524342804, 92.29057627198103830 ) ) ;
#2833 = CARTESIAN_POINT ( 'NONE',  ( -19.03943276465977164, 0.05219959533909376836, 96.24890960531436690 ) ) ;
#2834 = CARTESIAN_POINT ( 'NONE',  ( 16.46253265017160672, -9.564922557960803928, 98.33224293864769550 ) ) ;
#2835 = CARTESIAN_POINT ( 'NONE',  ( 0.05219959533937995610, -21.53943276465977519, 45.00109039468568284 ) ) ;
#2836 = CARTESIAN_POINT ( 'NONE',  ( 16.46253265017160672, -9.564922557960803928, 103.3322429386476955 ) ) ;
#2837 = CARTESIAN_POINT ( 'NONE',  ( 5.719274019375673035, 21.55341960407619339, 112.2927570613523471 ) ) ;
#2838 = CARTESIAN_POINT ( 'NONE',  ( 14.34966873604972726, -8.224510206698740333, 75.83442372801900433 ) ) ;
#2839 = CARTESIAN_POINT ( 'NONE',  ( -21.55341960407619339, 5.719274019375674811, 43.54275706135235424 ) ) ;
#2840 = CARTESIAN_POINT ( 'NONE',  ( -10.72451020669898014, 18.67979575497178502, 25.41557627198103120 ) ) ;
#2841 = CARTESIAN_POINT ( 'NONE',  ( 5.719274019375991003, -21.55341960407610458, 97.70724293864772392 ) ) ;
#2842 = CARTESIAN_POINT ( 'NONE',  ( -14.29746914071049879, 8.314922557960819915, 60.83224293864769550 ) ) ;
#2843 = CARTESIAN_POINT ( 'NONE',  ( 16.46253265017160672, -9.564922557960803928, 58.33224293864769550 ) ) ;
#2844 = CARTESIAN_POINT ( 'NONE',  ( -8.314922557960811034, -14.29746914071050412, 77.08224293864769550 ) ) ;
#2845 = CARTESIAN_POINT ( 'NONE',  ( -21.52544592524343514, 5.823673210054127303, 46.04057627198103830 ) ) ;
#2846 = CARTESIAN_POINT ( 'NONE',  ( 5.049401038297881783, 19.05341960407617563, 47.29275706135231161 ) ) ;
#2847 = CARTESIAN_POINT ( 'NONE',  ( -13.97604488694527625, -13.89961937509977652, 21.87390960531435979 ) ) ;
#2848 = ORIENTED_EDGE ( 'NONE', *, *, #192109, .F. ) ;
#2849 = CARTESIAN_POINT ( 'NONE',  ( 4.483927247898790824, -16.52544592524335698, 70.20942372801904696 ) ) ;
#2850 = CARTESIAN_POINT ( 'NONE',  ( 13.89961937509977652, -13.97604488694527269, 73.12390960531436690 ) ) ;
#2851 = CARTESIAN_POINT ( 'NONE',  ( -5.359611314223446995E-15, 29.16686587814335851, 144.3750000027311842 ) ) ;
#2852 = CARTESIAN_POINT ( 'NONE',  ( -16.55341960407611168, -4.379528057220339221, 91.45724293864769550 ) ) ;
#2853 = CARTESIAN_POINT ( 'NONE',  ( -0.05219959533907301413, -21.53943276465977519, 42.49890960531435979 ) ) ;
#2854 = VERTEX_POINT ( 'NONE', #99206 ) ;
#2855 = CARTESIAN_POINT ( 'NONE',  ( -16.55341960407617563, 4.379528057220093196, 103.5427570613523613 ) ) ;
#2856 = CARTESIAN_POINT ( 'NONE',  ( -19.03943276465977164, -0.05219959533935918106, 108.7510903946856615 ) ) ;
#2857 = CARTESIAN_POINT ( 'NONE',  ( -21.53943276465977519, -0.05219959533937600094, 73.75109039468567573 ) ) ;
#2858 = CARTESIAN_POINT ( 'NONE',  ( 13.89961937509977652, -13.97604488694527269, 93.12390960531436690 ) ) ;
#2859 = CARTESIAN_POINT ( 'NONE',  ( -15.80617190586745835, -15.72974639402198527, 101.8739096053143811 ) ) ;
#2860 = CARTESIAN_POINT ( 'NONE',  ( 16.53943276465976808, 0.05219959533934440121, 56.25109039468568284 ) ) ;
#2861 = CARTESIAN_POINT ( 'NONE',  ( 0.05219959533909260263, 19.03943276465977164, 34.99890960531435979 ) ) ;
#2862 = CARTESIAN_POINT ( 'NONE',  ( -8.314922557961024197, 14.29746914071037800, 32.91775706135234714 ) ) ;
#2863 = CARTESIAN_POINT ( 'NONE',  ( -19.03943276465977164, -0.05219959533935918106, 98.75109039468567573 ) ) ;
#2864 = B_SPLINE_CURVE_WITH_KNOTS ( 'NONE', 3,
 ( #190179, #24336, #51654, #25347, #83975, #85986 ),
 .UNSPECIFIED., .F., .F.,
 ( 4, 2, 4 ),
 ( 0.000000000000000000, 0.0003837532665634992165, 0.0007675065331269984329 ),
 .UNSPECIFIED. ) ;
#2865 = CARTESIAN_POINT ( 'NONE',  ( -15.72974639402197994, 15.80617190586746368, 90.62390960531436690 ) ) ;
#2866 = CARTESIAN_POINT ( 'NONE',  ( -16.51473224551082808, 9.474510206698731452, 53.33442372801900433 ) ) ;
#2867 = DIRECTION ( 'NONE',  ( 0.000000000000000000, -1.000000000000000000, 0.000000000000000000 ) ) ;
#2868 = CARTESIAN_POINT ( 'NONE',  ( -5.823673210054116645, -21.52544592524344225, 107.2905762719810525 ) ) ;
#2869 = CARTESIAN_POINT ( 'NONE',  ( 28.82186960331518222, 9.364793116373306248, 141.3500000054623911 ) ) ;
#2870 = CARTESIAN_POINT ( 'NONE',  ( 19.03943276465977164, -0.05219959533909143690, 73.74890960531435269 ) ) ;
#2871 = CARTESIAN_POINT ( 'NONE',  ( -12.06949235617739369, -12.14591786802326823, 39.37609039468567573 ) ) ;
#2872 = CARTESIAN_POINT ( 'NONE',  ( -18.09805431107524143, 5.499999999999980460, 101.0160622929189032 ) ) ;
#2873 = CARTESIAN_POINT ( 'NONE',  ( -19.05341960407617563, 5.049401038297882671, 58.54275706135234003 ) ) ;
#2875 = CARTESIAN_POINT ( 'NONE',  ( -8.224510206698948167, 14.34966873604960824, 60.41557627198102409 ) ) ;
#2874 = CARTESIAN_POINT ( 'NONE',  ( 5.719274019375673035, 21.55341960407619339, 22.29275706135235069 ) ) ;
#2876 = CARTESIAN_POINT ( 'NONE',  ( -0.05219959533909027116, -19.03943276465977164, 72.49890960531435269 ) ) ;
#2878 = CARTESIAN_POINT ( 'NONE',  ( 13.89961937509957401, 13.97604488694547697, 41.87609039468566152 ) ) ;
#2877 = CARTESIAN_POINT ( 'NONE',  ( 16.52544592524335698, 4.483927247898782831, 41.45942372801901143 ) ) ;
#2879 = CARTESIAN_POINT ( 'NONE',  ( 5.719274019375673035, 21.55341960407619339, 47.29275706135234003 ) ) ;
#2880 = CARTESIAN_POINT ( 'NONE',  ( 16.51473224551083163, -9.474510206698727899, 110.8344237280190043 ) ) ;
#2881 = CARTESIAN_POINT ( 'NONE',  ( 9.474510206698971260, -16.51473224551069308, 52.91557627198102409 ) ) ;
#2882 = CARTESIAN_POINT ( 'NONE',  ( 16.51473224551083163, -9.474510206698727899, 75.83442372801900433 ) ) ;
#2883 = CARTESIAN_POINT ( 'NONE',  ( -5.823673210054431948, 21.52544592524334988, 97.70942372801904696 ) ) ;
#2884 = CARTESIAN_POINT ( 'NONE',  ( 13.89961937509957401, 13.97604488694547697, 66.87609039468567573 ) ) ;
#2885 = CARTESIAN_POINT ( 'NONE',  ( 5.049401038298161559, -19.05341960407611168, 42.70724293864767418 ) ) ;
#2886 = CARTESIAN_POINT ( 'NONE',  ( -10.72451020669898014, 18.67979575497178502, 75.41557627198102409 ) ) ;
#2888 = CARTESIAN_POINT ( 'NONE',  ( -16.46253265017146816, -9.564922557961047289, 64.16775706135233293 ) ) ;
#2887 = CARTESIAN_POINT ( 'NONE',  ( 14.34966873604960469, 8.224510206698951720, 59.16557627198103120 ) ) ;
#2889 = CARTESIAN_POINT ( 'NONE',  ( -1.040834085586084257E-14, 30.40000000000003766, -65.00100000000003320 ) ) ;
#2890 = CARTESIAN_POINT ( 'NONE',  ( 19.05341960407617918, -5.049401038297876454, 26.04275706135233293 ) ) ;
#2891 = CARTESIAN_POINT ( 'NONE',  ( 4.379528057220092307, 16.55341960407617563, 92.29275706135236135 ) ) ;
#2892 = CARTESIAN_POINT ( 'NONE',  ( -16.52544592524342804, 4.483927247898546575, 51.04057627198103120 ) ) ;
#2894 = CARTESIAN_POINT ( 'NONE',  ( 22.44159573604009239, 16.30477369853692693, 142.0750000027311728 ) ) ;
#2893 = CARTESIAN_POINT ( 'NONE',  ( -15.72974639402176322, -15.80617190586768395, 84.37609039468570415 ) ) ;
#2895 = CARTESIAN_POINT ( 'NONE',  ( 21.55341960407610458, 5.719274019375980345, 93.95724293864770971 ) ) ;
#2896 = CARTESIAN_POINT ( 'NONE',  ( 19.05341960407611168, 5.049401038298154454, 48.95724293864768129 ) ) ;
#2897 = CARTESIAN_POINT ( 'NONE',  ( 5.823673210054444382, -21.52544592524334988, 65.20942372801901854 ) ) ;
#2898 = CARTESIAN_POINT ( 'NONE',  ( 16.51473224551069308, 9.474510206698969483, 44.16557627198103120 ) ) ;
#2899 = ORIENTED_EDGE ( 'NONE', *, *, #115308, .F. ) ;
#2900 = CARTESIAN_POINT ( 'NONE',  ( 16.46253265017160672, -9.564922557960803928, 63.33224293864769550 ) ) ;
#2901 = CARTESIAN_POINT ( 'NONE',  ( 16.52544592524342804, -4.483927247898539470, 108.5405762719810241 ) ) ;
#2902 = CARTESIAN_POINT ( 'NONE',  ( -13.89961937509977652, 13.97604488694528158, 105.6239096053143527 ) ) ;
#2903 = CARTESIAN_POINT ( 'NONE',  ( 4.483927247898545687, 16.52544592524342804, 59.79057627198103120 ) ) ;
#2904 = CARTESIAN_POINT ( 'NONE',  ( -5.153800228976328057, -19.02544592524343514, 32.29057627198102409 ) ) ;
#2905 = CARTESIAN_POINT ( 'NONE',  ( 16.52544592524342804, -4.483927247898539470, 88.54057627198103830 ) ) ;
#2906 = CARTESIAN_POINT ( 'NONE',  ( -15.80617190586745835, -15.72974639402198527, 96.87390960531436690 ) ) ;
#2907 = CARTESIAN_POINT ( 'NONE',  ( -21.52544592524334988, -5.823673210054445271, 28.95942372801902209 ) ) ;
#2908 = DIRECTION ( 'NONE',  ( 0.8164965809277261455, 0.000000000000000000, 0.5773502691896257311 ) ) ;
#2909 = CARTESIAN_POINT ( 'NONE',  ( -16.52544592524335698, -4.483927247898792601, 48.95942372801902565 ) ) ;
#2910 = CARTESIAN_POINT ( 'NONE',  ( -21.53943276465977519, 0.05219959533907696930, 86.24890960531436690 ) ) ;
#2911 = CARTESIAN_POINT ( 'NONE',  ( -18.62759615963255300, -10.81492255796106328, 104.1677570613523471 ) ) ;
#2912 = CARTESIAN_POINT ( 'NONE',  ( -19.03943276465977164, 0.05219959533909376836, 96.24890960531436690 ) ) ;
#2913 = CARTESIAN_POINT ( 'NONE',  ( -21.55341960407619339, 5.719274019375674811, 48.54275706135234714 ) ) ;
#2914 = EDGE_CURVE ( 'NONE', #152202, #186287, #21179, .T. ) ;
#2915 = CARTESIAN_POINT ( 'NONE',  ( -18.62759615963270932, 10.81492255796079327, 35.83224293864768839 ) ) ;
#2916 = CARTESIAN_POINT ( 'NONE',  ( -8.314922557961024197, 14.29746914071037800, 102.9177570613523756 ) ) ;
#2918 = CARTESIAN_POINT ( 'NONE',  ( 21.53943276465977519, 0.05219959533937863772, 81.25109039468568994 ) ) ;
#2917 = CARTESIAN_POINT ( 'NONE',  ( 0.05219959533937995610, -21.53943276465977519, 60.00109039468568284 ) ) ;
#2919 = CARTESIAN_POINT ( 'NONE',  ( 5.049401038297881783, 19.05341960407617563, 37.29275706135232582 ) ) ;
#2920 = CARTESIAN_POINT ( 'NONE',  ( -8.314922557961024197, 14.29746914071037800, 87.91775706135234714 ) ) ;
#2921 = CARTESIAN_POINT ( 'NONE',  ( 5.719274019375673035, 21.55341960407619339, 42.29275706135235424 ) ) ;
#2922 = CARTESIAN_POINT ( 'NONE',  ( 19.03943276465977164, -0.05219959533909143690, 43.74890960531435979 ) ) ;
#2923 = CARTESIAN_POINT ( 'NONE',  ( -18.67979575497193778, 10.72451020669871902, 108.3344237280190185 ) ) ;
#2924 = CARTESIAN_POINT ( 'NONE',  ( -21.55341960407610458, -5.719274019375992779, 21.45724293864769550 ) ) ;
#2925 = CARTESIAN_POINT ( 'NONE',  ( 0.05219959533907565091, 21.53943276465977519, 114.9989096053143669 ) ) ;
#2926 = CARTESIAN_POINT ( 'NONE',  ( 18.67979575497178502, 10.72451020669898547, 79.16557627198103830 ) ) ;
#2928 = CARTESIAN_POINT ( 'NONE',  ( 0.05219959533907565091, 21.53943276465977519, 69.99890960531435269 ) ) ;
#2927 = DIRECTION ( 'NONE',  ( 0.000000000000000000, 0.000000000000000000, 1.000000000000000000 ) ) ;
#2930 = CARTESIAN_POINT ( 'NONE',  ( 14.29746914071049879, -8.314922557960816363, 58.33224293864768839 ) ) ;
#2929 = CARTESIAN_POINT ( 'NONE',  ( -16.52544592524335698, -4.483927247898792601, 53.95942372801900433 ) ) ;
#2931 = CARTESIAN_POINT ( 'NONE',  ( -1.304248841091933035E-15, -21.30000000000002913, -64.92279855667830191 ) ) ;
#2932 = CARTESIAN_POINT ( 'NONE',  ( -19.03943276465977164, -0.05219959533935918106, 93.75109039468566152 ) ) ;
#2933 = CARTESIAN_POINT ( 'NONE',  ( 2.500000000000000000, 1.178949249685212974, -2.042000000000001148 ) ) ;
#2934 = CARTESIAN_POINT ( 'NONE',  ( 14.29746914071037800, 8.314922557961029526, 26.66775706135235424 ) ) ;
#2935 = CARTESIAN_POINT ( 'NONE',  ( 0.05219959533907565091, 21.53943276465977519, 99.99890960531436690 ) ) ;
#2936 = CARTESIAN_POINT ( 'NONE',  ( -15.80617190586745835, -15.72974639402198527, 71.87390960531438111 ) ) ;
#2937 = CARTESIAN_POINT ( 'NONE',  ( -16.51473224551069308, -9.474510206698971260, 111.6655762719810383 ) ) ;
#2938 = CARTESIAN_POINT ( 'NONE',  ( 0.05219959533934541429, -16.53943276465976808, 55.00109039468568284 ) ) ;
#2939 = CARTESIAN_POINT ( 'NONE',  ( -5.153800228976328057, -19.02544592524343514, 72.29057627198102409 ) ) ;
#2941 = CARTESIAN_POINT ( 'NONE',  ( -4.379528057220086978, -16.55341960407618274, 19.79275706135235069 ) ) ;
#2940 = CARTESIAN_POINT ( 'NONE',  ( 15.80617190586769283, -15.72974639402175789, 45.62609039468567573 ) ) ;
#2942 = CARTESIAN_POINT ( 'NONE',  ( -13.89961937509977652, 13.97604488694528158, 110.6239096053143243 ) ) ;
#2943 = CARTESIAN_POINT ( 'NONE',  ( -19.02544592524334988, -5.153800228976617603, 28.95942372801900433 ) ) ;
#2944 = CARTESIAN_POINT ( 'NONE',  ( 0.05219959533909260263, 19.03943276465977164, 104.9989096053143669 ) ) ;
#2945 = CARTESIAN_POINT ( 'NONE',  ( -10.72451020669898014, 18.67979575497178502, 105.4155762719810383 ) ) ;
#2946 = CARTESIAN_POINT ( 'NONE',  ( 5.153800228976335163, 19.02544592524342804, 64.79057627198100988 ) ) ;
#2947 = CARTESIAN_POINT ( 'NONE',  ( -3.874011537017814977, -5.276842784226742467, -62.43202641272173992 ) ) ;
#2948 = CARTESIAN_POINT ( 'NONE',  ( 12.06949235617757843, -12.14591786802309237, 83.12390960531436690 ) ) ;
#2949 = CARTESIAN_POINT ( 'NONE',  ( -0.05219959533909027116, -19.03943276465977164, 112.4989096053143669 ) ) ;
#2950 = CARTESIAN_POINT ( 'NONE',  ( -16.79531203550644491, 7.028104445595745098, 33.74755011779555502 ) ) ;
#2951 = CARTESIAN_POINT ( 'NONE',  ( -10.81492255796078084, -18.62759615963271287, 107.0822429386476955 ) ) ;
#2952 = CARTESIAN_POINT ( 'NONE',  ( -19.03943276465977164, -0.05219959533935918106, 63.75109039468566863 ) ) ;
#2953 = CARTESIAN_POINT ( 'NONE',  ( 13.97604488694527802, 13.89961937509977652, 109.3739096053143669 ) ) ;
#2954 = CARTESIAN_POINT ( 'NONE',  ( -9.564922557960796823, -16.46253265017161027, 32.08224293864769550 ) ) ;
#2955 = CARTESIAN_POINT ( 'NONE',  ( -0.05219959533907301413, -21.53943276465977519, 57.49890960531435979 ) ) ;
#2956 = CARTESIAN_POINT ( 'NONE',  ( -9.474510206698964154, 16.51473224551069663, 95.41557627198102409 ) ) ;
#2957 = CARTESIAN_POINT ( 'NONE',  ( -18.62759615963255300, -10.81492255796106328, 79.16775706135234714 ) ) ;
#2958 = CARTESIAN_POINT ( 'NONE',  ( -13.97604488694527625, -13.89961937509977652, 46.87390960531435979 ) ) ;
#2959 = CARTESIAN_POINT ( 'NONE',  ( 4.483927247898545687, 16.52544592524342804, 84.79057627198102409 ) ) ;
#2960 = CARTESIAN_POINT ( 'NONE',  ( -16.53943276465976808, -0.05219959533934237506, 33.75109039468568284 ) ) ;
#2961 = CARTESIAN_POINT ( 'NONE',  ( 5.823673210054444382, -21.52544592524334988, 70.20942372801904696 ) ) ;
#2962 = ORIENTED_EDGE ( 'NONE', *, *, #57363, .F. ) ;
#2963 = CARTESIAN_POINT ( 'NONE',  ( -16.51473224551082808, 9.474510206698731452, 23.33442372801900078 ) ) ;
#2964 = CARTESIAN_POINT ( 'NONE',  ( -5.153800228976607833, 19.02544592524334988, 82.70942372801897591 ) ) ;
#2965 = CARTESIAN_POINT ( 'NONE',  ( 5.049401038297881783, 19.05341960407617563, 37.29275706135232582 ) ) ;
#2966 = DIRECTION ( 'NONE',  ( -0.000000000000000000, -0.000000000000000000, -1.000000000000000000 ) ) ;
#2967 = CARTESIAN_POINT ( 'NONE',  ( 15.72974639402176855, 15.80617190586768217, 36.87609039468568994 ) ) ;
#2968 = CARTESIAN_POINT ( 'NONE',  ( -19.52851543214742946, -5.500000000000037303, 45.39357721762583964 ) ) ;
#2969 = CARTESIAN_POINT ( 'NONE',  ( -9.564922557961040184, 16.46253265017147172, 27.91775706135232582 ) ) ;
#2970 = CARTESIAN_POINT ( 'NONE',  ( -5.153800228976328057, -19.02544592524343514, 72.29057627198102409 ) ) ;
#2971 = CARTESIAN_POINT ( 'NONE',  ( -8.224510206698948167, 14.34966873604960824, 25.41557627198103120 ) ) ;
#2973 = CARTESIAN_POINT ( 'NONE',  ( -5.719274019375665041, -21.55341960407619695, 89.79275706135236135 ) ) ;
#2972 = CARTESIAN_POINT ( 'NONE',  ( -10.81492255796078084, -18.62759615963271287, 27.08224293864769550 ) ) ;
#2974 = CIRCLE ( 'NONE', #183833, 2.500000000000002220 ) ;
#2975 = CARTESIAN_POINT ( 'NONE',  ( 29.86685920354754487, 21.69954338932564752, -5.424999997268813878 ) ) ;
#2976 = CARTESIAN_POINT ( 'NONE',  ( -17.50000000000015277, -3.292511757969575292, 34.93479729789483201 ) ) ;
#2977 = CARTESIAN_POINT ( 'NONE',  ( 15.80617190586769283, -15.72974639402175789, 80.62609039468567573 ) ) ;
#2978 = CARTESIAN_POINT ( 'NONE',  ( 17.13100169013300089, -6.664070546373147330, 43.26789835699850784 ) ) ;
#2979 = CARTESIAN_POINT ( 'NONE',  ( -19.05341960407611168, -5.049401038298163336, 106.4572429386476955 ) ) ;
#2980 = CARTESIAN_POINT ( 'NONE',  ( -1.029908246020144968, -31.49504140153652898, -49.63772645510944415 ) ) ;
#2981 = CARTESIAN_POINT ( 'NONE',  ( 13.89961937509977652, -13.97604488694527269, 48.12390960531435979 ) ) ;
#2982 = CARTESIAN_POINT ( 'NONE',  ( -5.823673210054116645, -21.52544592524344225, 52.29057627198102409 ) ) ;
#2983 = CARTESIAN_POINT ( 'NONE',  ( -0.05219959533910754901, -16.53943276465976808, 32.49890960531435979 ) ) ;
#2985 = CARTESIAN_POINT ( 'NONE',  ( 19.02544592524343514, -5.153800228976328945, 88.54057627198102409 ) ) ;
#2984 = CARTESIAN_POINT ( 'NONE',  ( -14.29746914071049879, 8.314922557960819915, 110.8322429386476955 ) ) ;
#2986 = CARTESIAN_POINT ( 'NONE',  ( 19.02544592524334988, 5.153800228976608722, 26.45942372801899722 ) ) ;
#2987 = EDGE_CURVE ( 'NONE', #118975, #96409, #59563, .T. ) ;
#2988 = CARTESIAN_POINT ( 'NONE',  ( -16.53943276465976808, 0.05219959533911058130, 96.24890960531435269 ) ) ;
#2989 = CARTESIAN_POINT ( 'NONE',  ( -21.53943276465977519, -0.05219959533937600094, 58.75109039468568994 ) ) ;
#2990 = CARTESIAN_POINT ( 'NONE',  ( -0.05219959533909027116, -19.03943276465977164, 112.4989096053143669 ) ) ;
#2991 = CARTESIAN_POINT ( 'NONE',  ( -16.52544592524335698, -4.483927247898792601, 103.9594237280190185 ) ) ;
#2992 = CARTESIAN_POINT ( 'NONE',  ( -19.03943276465977164, -0.05219959533935918106, 63.75109039468566863 ) ) ;
#2993 = CARTESIAN_POINT ( 'NONE',  ( 22.81625015709509441, 31.40387420917330275, -7.824999997268813345 ) ) ;
#2994 = CARTESIAN_POINT ( 'NONE',  ( 16.51473224551069308, 9.474510206698969483, 114.1655762719810241 ) ) ;
#2995 = CARTESIAN_POINT ( 'NONE',  ( -16.53943276465976808, 0.05219959533911058130, 76.24890960531435269 ) ) ;
#2996 = CARTESIAN_POINT ( 'NONE',  ( -13.97604488694547697, 13.89961937509957934, 63.12609039468566152 ) ) ;
#2998 = CIRCLE ( 'NONE', #35325, 5.000000000000000000 ) ;
#2997 = CARTESIAN_POINT ( 'NONE',  ( 13.97604488694527802, 13.89961937509977652, 64.37390960531436690 ) ) ;
#2999 = CARTESIAN_POINT ( 'NONE',  ( -16.52544592524342804, 4.483927247898546575, 56.04057627198102409 ) ) ;
#3000 = CARTESIAN_POINT ( 'NONE',  ( -9.474510206698720793, -16.51473224551083518, 94.58442372801900433 ) ) ;
#3001 = CARTESIAN_POINT ( 'NONE',  ( 21.53943276465977519, -0.05219959533907433946, 53.74890960531437401 ) ) ;
#3002 = EDGE_LOOP ( 'NONE', ( #73351, #153883, #149706, #79021 ) ) ;
#3003 = EDGE_CURVE ( 'NONE', #196688, #171715, #100113, .T. ) ;
#3004 = CARTESIAN_POINT ( 'NONE',  ( -16.55341960407611168, -4.379528057220339221, 101.4572429386476955 ) ) ;
#3005 = CARTESIAN_POINT ( 'NONE',  ( -16.36317988757057762, -7.306389748694950725, 30.90210391636774290 ) ) ;
#3007 = CARTESIAN_POINT ( 'NONE',  ( 5.719274019375991003, -21.55341960407610458, 57.70724293864770260 ) ) ;
#3006 = CARTESIAN_POINT ( 'NONE',  ( 5.153800228976335163, 19.02544592524342804, 64.79057627198100988 ) ) ;
#3009 = CARTESIAN_POINT ( 'NONE',  ( 0.05219959533909260263, 19.03943276465977164, 79.99890960531436690 ) ) ;
#3008 = CARTESIAN_POINT ( 'NONE',  ( 12.14591786802327356, -12.06949235617739191, 90.62609039468567573 ) ) ;
#3010 = CARTESIAN_POINT ( 'NONE',  ( -9.474510206698720793, -16.51473224551083518, 59.58442372801900433 ) ) ;
#3011 = CARTESIAN_POINT ( 'NONE',  ( 15.72974639402176855, 15.80617190586768217, 81.87609039468568994 ) ) ;
#3012 = ORIENTED_EDGE ( 'NONE', *, *, #25923, .F. ) ;
#3013 = CARTESIAN_POINT ( 'NONE',  ( -18.62759615963270932, 10.81492255796079327, 65.83224293864769550 ) ) ;
#3014 = CARTESIAN_POINT ( 'NONE',  ( -19.02544592524342804, 5.153800228976336051, 101.0405762719810241 ) ) ;
#3015 = CARTESIAN_POINT ( 'NONE',  ( -19.03943276465977164, 0.05219959533909376836, 41.24890960531435269 ) ) ;
#3016 = CARTESIAN_POINT ( 'NONE',  ( -14.29746914071037622, -8.314922557961029526, 89.16775706135236135 ) ) ;
#3017 = CARTESIAN_POINT ( 'NONE',  ( -5.153800228976607833, 19.02544592524334988, 97.70942372801900433 ) ) ;
#3018 = CARTESIAN_POINT ( 'NONE',  ( 16.51473224551069308, 9.474510206698969483, 24.16557627198102765 ) ) ;
#3019 = CARTESIAN_POINT ( 'NONE',  ( 17.05116617787827238, 6.768360034955700932, 53.84324446740803438 ) ) ;
#3020 = CARTESIAN_POINT ( 'NONE',  ( 10.72451020669871369, 18.67979575497193778, 92.08442372801901854 ) ) ;
#3021 = ORIENTED_EDGE ( 'NONE', *, *, #106786, .F. ) ;
#3022 = CARTESIAN_POINT ( 'NONE',  ( 16.52544592524342804, -4.483927247898539470, 63.54057627198103830 ) ) ;
#3023 = CARTESIAN_POINT ( 'NONE',  ( -16.53943276465976808, 0.05219959533911058130, 71.24890960531435269 ) ) ;
#3024 = CARTESIAN_POINT ( 'NONE',  ( 10.81492255796078972, 18.62759615963270932, 94.58224293864769550 ) ) ;
#3025 = CARTESIAN_POINT ( 'NONE',  ( -10.72451020669898014, 18.67979575497178502, 90.41557627198103830 ) ) ;
#3026 = CARTESIAN_POINT ( 'NONE',  ( 16.29526858892875296, -7.335722546920107945, 96.70329402199793378 ) ) ;
#3027 = CARTESIAN_POINT ( 'NONE',  ( 15.80617190586746368, 15.72974639402197994, 49.37390960531436690 ) ) ;
#3028 = CARTESIAN_POINT ( 'NONE',  ( 8.314922557961029526, -14.29746914071037800, 65.41775706135234714 ) ) ;
#3029 = CARTESIAN_POINT ( 'NONE',  ( -16.53943276465976808, 0.05219959533911058130, 91.24890960531436690 ) ) ;
#3030 = CARTESIAN_POINT ( 'NONE',  ( -13.89961937509977652, 13.97604488694528158, 40.62390960531435979 ) ) ;
#3031 = CARTESIAN_POINT ( 'NONE',  ( 34.75592306271658316, -1.707766843171824478, 52.30709029423474732 ) ) ;
#3032 = CARTESIAN_POINT ( 'NONE',  ( -4.483927247898782831, 16.52544592524335698, 92.70942372801901854 ) ) ;
#3033 = CARTESIAN_POINT ( 'NONE',  ( -15.72974639402176322, -15.80617190586768395, 34.37609039468568284 ) ) ;
#3034 = CARTESIAN_POINT ( 'NONE',  ( 13.97604488694527802, 13.89961937509977652, 79.37390960531435269 ) ) ;
#3035 = CARTESIAN_POINT ( 'NONE',  ( -5.823673210054431948, 21.52544592524334988, 72.70942372801901854 ) ) ;
#3036 = DIRECTION ( 'NONE',  ( 0.000000000000000000, 0.000000000000000000, 1.000000000000000000 ) ) ;
#3037 = CARTESIAN_POINT ( 'NONE',  ( 0.000000000000000000, 0.000000000000000000, -18.00000000000000000 ) ) ;
#3038 = ORIENTED_EDGE ( 'NONE', *, *, #106448, .F. ) ;
#3039 = CARTESIAN_POINT ( 'NONE',  ( 10.81492255796106328, -18.62759615963255655, 55.41775706135234714 ) ) ;
#3041 = CARTESIAN_POINT ( 'NONE',  ( 16.46253265017160672, -9.564922557960803928, 113.3322429386476955 ) ) ;
#3040 = CARTESIAN_POINT ( 'NONE',  ( -19.05341960407611168, -5.049401038298163336, 36.45724293864766707 ) ) ;
#3042 = CARTESIAN_POINT ( 'NONE',  ( 16.46253265017160672, -9.564922557960803928, 88.33224293864769550 ) ) ;
#3043 = CARTESIAN_POINT ( 'NONE',  ( 13.97604488694548053, -13.89961937509957401, 60.62609039468564731 ) ) ;
#3044 = CARTESIAN_POINT ( 'NONE',  ( 15.80617190586769283, -15.72974639402175789, 30.62609039468567929 ) ) ;
#3045 = CARTESIAN_POINT ( 'NONE',  ( -16.46253265017146816, -9.564922557961047289, 54.16775706135234003 ) ) ;
#3046 = CARTESIAN_POINT ( 'NONE',  ( 16.46253265017160672, -9.564922557960803928, 43.33224293864769550 ) ) ;
#3047 = CARTESIAN_POINT ( 'NONE',  ( -16.55341960407617563, 4.379528057220093196, 98.54275706135234714 ) ) ;
#3048 = CARTESIAN_POINT ( 'NONE',  ( -13.89961937509957401, -13.97604488694547875, 69.37609039468564731 ) ) ;
#3049 = CARTESIAN_POINT ( 'NONE',  ( -4.379528057220328563, 16.55341960407611168, 25.20724293864769550 ) ) ;
#3050 = CARTESIAN_POINT ( 'NONE',  ( -19.03943276465977164, -0.05219959533935918106, 53.75109039468566863 ) ) ;
#3051 = CARTESIAN_POINT ( 'NONE',  ( 16.46253265017160672, -9.564922557960803928, 103.3322429386476955 ) ) ;
#3052 = CARTESIAN_POINT ( 'NONE',  ( -15.72974639402176322, -15.80617190586768395, 104.3760903946856899 ) ) ;
#3053 = CARTESIAN_POINT ( 'NONE',  ( -18.67979575497193778, 10.72451020669871902, 108.3344237280190185 ) ) ;
#3054 = DIRECTION ( 'NONE',  ( -0.000000000000000000, -0.000000000000000000, 1.000000000000000000 ) ) ;
#3055 = CARTESIAN_POINT ( 'NONE',  ( 21.55341960407619695, -5.719274019375665929, 86.04275706135236135 ) ) ;
#3056 = CARTESIAN_POINT ( 'NONE',  ( -12.06949235617739369, -12.14591786802326823, 29.37609039468568284 ) ) ;
#3057 = CARTESIAN_POINT ( 'NONE',  ( -5.153800228976328057, -19.02544592524343514, 97.29057627198099567 ) ) ;
#3058 = CARTESIAN_POINT ( 'NONE',  ( -27.60098488412532802, 5.861468761074982936, 164.8187539380761564 ) ) ;
#3059 = CARTESIAN_POINT ( 'NONE',  ( -5.049401038298153566, 19.05341960407611168, 85.20724293864766707 ) ) ;
#3060 = DIRECTION ( 'NONE',  ( -1.000000000000000000, -0.000000000000000000, -0.000000000000000000 ) ) ;
#3061 = CARTESIAN_POINT ( 'NONE',  ( -0.05219959533936034679, 19.03943276465977164, 67.50109039468566152 ) ) ;
#3062 = CARTESIAN_POINT ( 'NONE',  ( -9.564922557960796823, -16.46253265017161027, 112.0822429386476955 ) ) ;
#3063 = CARTESIAN_POINT ( 'NONE',  ( 21.53943276465977519, 0.05219959533937863772, 101.2510903946856757 ) ) ;
#3064 = CARTESIAN_POINT ( 'NONE',  ( 14.34966873604960469, 8.224510206698951720, 99.16557627198100988 ) ) ;
#3065 = CARTESIAN_POINT ( 'NONE',  ( -15.72974639402197994, 15.80617190586746368, 50.62390960531435979 ) ) ;
#3066 = CARTESIAN_POINT ( 'NONE',  ( -21.55341960407610458, -5.719274019375992779, 31.45724293864769550 ) ) ;
#3067 = CARTESIAN_POINT ( 'NONE',  ( -8.314922557960811034, -14.29746914071050412, 102.0822429386476955 ) ) ;
#3068 = CARTESIAN_POINT ( 'NONE',  ( -13.70000000000001528, 0.2066332630088025535, -62.58071313852362039 ) ) ;
#3069 = CARTESIAN_POINT ( 'NONE',  ( -19.02544592524334988, -5.153800228976617603, 53.95942372801898301 ) ) ;
#3070 = CARTESIAN_POINT ( 'NONE',  ( -12.06949235617756955, 12.14591786802309770, 30.62390960531436335 ) ) ;
#3071 = B_SPLINE_CURVE_WITH_KNOTS ( 'NONE', 3,
 ( #188981, #130245, #82752, #4917, #145428, #37259, #66600, #116102, #175785, #34287, #80772, #98917, #160609, #128264, #189962, #53425, #115102, #131265, #176794, #38267, #142450, #99921, #23100, #69598, #51437, #3928, #127268, #146423, #113097, #174788, #7914, #192953 ),
 .UNSPECIFIED., .F., .F.,
 ( 4, 2, 2, 2, 2, 2, 2, 2, 2, 2, 2, 2, 2, 2, 2, 4 ),
 ( 2.969368287472575283E-17, 0.0003712461730036993547, 0.0007424923460073690022, 0.001113738519011038758, 0.001484984692014708297, 0.002227477038022045424, 0.002598723211025721468, 0.002969969384029397079, 0.003341215557033072690, 0.003712461730036748300, 0.004083707903040423477, 0.004454954076044099522, 0.004826200249047774699, 0.005197446422051450743, 0.005568692595055125920, 0.005939938768058801964 ),
 .UNSPECIFIED. ) ;
#3072 = CARTESIAN_POINT ( 'NONE',  ( -19.02544592524342804, 5.153800228976336051, 106.0405762719810241 ) ) ;
#3073 = CARTESIAN_POINT ( 'NONE',  ( 15.72974639402176855, 15.80617190586768217, 81.87609039468568994 ) ) ;
#3074 = CARTESIAN_POINT ( 'NONE',  ( 18.67979575497178502, 10.72451020669898547, 69.16557627198102409 ) ) ;
#3075 = CARTESIAN_POINT ( 'NONE',  ( 15.72974639402176855, 15.80617190586768217, 41.87609039468568284 ) ) ;
#3076 = CARTESIAN_POINT ( 'NONE',  ( 15.80617190586746368, 15.72974639402197994, 99.37390960531436690 ) ) ;
#3077 = CARTESIAN_POINT ( 'NONE',  ( -15.72974639402176322, -15.80617190586768395, 49.37609039468569705 ) ) ;
#3078 = CARTESIAN_POINT ( 'NONE',  ( 9.564922557960805705, 16.46253265017160317, 29.58224293864769550 ) ) ;
#3079 = CARTESIAN_POINT ( 'NONE',  ( 19.03943276465977164, -0.05219959533909143690, 88.74890960531436690 ) ) ;
#3080 = CARTESIAN_POINT ( 'NONE',  ( -14.29746914071037622, -8.314922557961029526, 79.16775706135234714 ) ) ;
#3081 = CARTESIAN_POINT ( 'NONE',  ( -16.55341960407611168, -4.379528057220339221, 106.4572429386477097 ) ) ;
#3082 = CARTESIAN_POINT ( 'NONE',  ( 19.02544592524343514, -5.153800228976328945, 113.5405762719810241 ) ) ;
#3083 = CARTESIAN_POINT ( 'NONE',  ( 8.314922557960818139, 14.29746914071049879, 59.58224293864770260 ) ) ;
#3084 = CARTESIAN_POINT ( 'NONE',  ( -8.224510206698735004, -14.34966873604973081, 109.5844237280190328 ) ) ;
#3085 = CARTESIAN_POINT ( 'NONE',  ( 5.153800228976335163, 19.02544592524342804, 49.79057627198100988 ) ) ;
#3086 = CARTESIAN_POINT ( 'NONE',  ( -19.02544592524342804, 5.153800228976336051, 31.04057627198102409 ) ) ;
#3087 = CARTESIAN_POINT ( 'NONE',  ( -10.81492255796078084, -18.62759615963271287, 47.08224293864770260 ) ) ;
#3088 = CARTESIAN_POINT ( 'NONE',  ( -19.03943276465977164, -0.05219959533935918106, 33.75109039468566863 ) ) ;
#3090 = CARTESIAN_POINT ( 'NONE',  ( 0.05219959533910956823, 16.53943276465976808, 29.99890960531435979 ) ) ;
#3089 = LINE ( 'NONE', #34429, #184950 ) ;
#3091 = CARTESIAN_POINT ( 'NONE',  ( -21.52544592524334988, -5.823673210054445271, 43.95942372801902565 ) ) ;
#3092 = CARTESIAN_POINT ( 'NONE',  ( -10.46900522708356895, -36.04764466666199496, -30.96889465344750292 ) ) ;
#3093 = CARTESIAN_POINT ( 'NONE',  ( -4.379528057220086978, -16.55341960407618274, 54.79275706135235424 ) ) ;
#3094 = CARTESIAN_POINT ( 'NONE',  ( -16.46253265017146816, -9.564922557961047289, 64.16775706135233293 ) ) ;
#3095 = CARTESIAN_POINT ( 'NONE',  ( -12.06949235617756955, 12.14591786802309770, 25.62390960531435624 ) ) ;
#3096 = CARTESIAN_POINT ( 'NONE',  ( -18.22780087662123094, -5.499999999999984901, 76.48459894673894155 ) ) ;
#3097 = CARTESIAN_POINT ( 'NONE',  ( -8.314922557961024197, 14.29746914071037800, 102.9177570613523756 ) ) ;
#3098 = CARTESIAN_POINT ( 'NONE',  ( 19.03943276465977164, -0.05219959533909143690, 33.74890960531435979 ) ) ;
#3099 = CARTESIAN_POINT ( 'NONE',  ( 0.05219959533909260263, 19.03943276465977164, 64.99890960531436690 ) ) ;
#3100 = CARTESIAN_POINT ( 'NONE',  ( -13.89961937509977652, 13.97604488694528158, 30.62390960531435269 ) ) ;
#3101 = CARTESIAN_POINT ( 'NONE',  ( -18.67979575497193778, 10.72451020669871902, 38.33442372801900433 ) ) ;
#3102 = CARTESIAN_POINT ( 'NONE',  ( 5.049401038298161559, -19.05341960407611168, 42.70724293864767418 ) ) ;
#3103 = CARTESIAN_POINT ( 'NONE',  ( -5.153800228976328057, -19.02544592524343514, 112.2905762719810099 ) ) ;
#3104 = CARTESIAN_POINT ( 'NONE',  ( -5.153800228976328057, -19.02544592524343514, 42.29057627198101699 ) ) ;
#3105 = EDGE_CURVE ( 'NONE', #165429, #128792, #7889, .T. ) ;
#3106 = CARTESIAN_POINT ( 'NONE',  ( 16.46253265017160672, -9.564922557960803928, 113.3322429386476955 ) ) ;
#3107 = AXIS2_PLACEMENT_3D ( 'NONE', #176431, #145067, #162243 ) ;
#3109 = CARTESIAN_POINT ( 'NONE',  ( -8.224510206698948167, 14.34966873604960824, 115.4155762719810241 ) ) ;
#3108 = CARTESIAN_POINT ( 'NONE',  ( 15.80617190586769283, -15.72974639402175789, 55.62609039468568284 ) ) ;
#3110 = CARTESIAN_POINT ( 'NONE',  ( 0.05219959533907565091, 21.53943276465977519, 29.99890960531435979 ) ) ;
#3111 = CARTESIAN_POINT ( 'NONE',  ( 14.29746914071037800, 8.314922557961029526, 71.66775706135234714 ) ) ;
#3112 = CARTESIAN_POINT ( 'NONE',  ( 10.72451020669871369, 18.67979575497193778, 97.08442372801904696 ) ) ;
#3113 = CARTESIAN_POINT ( 'NONE',  ( 0.05219959533934541429, -16.53943276465976808, 50.00109039468568994 ) ) ;
#3114 = CARTESIAN_POINT ( 'NONE',  ( 9.474510206698971260, -16.51473224551069308, 92.91557627198103830 ) ) ;
#3115 = ADVANCED_FACE ( 'NONE', ( #114370 ), #176313, .T. ) ;
#3116 = CARTESIAN_POINT ( 'NONE',  ( -0.05219959533934338120, 16.53943276465976808, 47.50109039468568994 ) ) ;
#3117 = CARTESIAN_POINT ( 'NONE',  ( -8.224510206698735004, -14.34966873604973081, 24.58442372801901499 ) ) ;
#3118 = CARTESIAN_POINT ( 'NONE',  ( 12.14591786802327356, -12.06949235617739191, 95.62609039468568994 ) ) ;
#3119 = CARTESIAN_POINT ( 'NONE',  ( 15.72974639402176855, 15.80617190586768217, 56.87609039468568994 ) ) ;
#3120 = CARTESIAN_POINT ( 'NONE',  ( 19.03943276465977164, 0.05219959533936151252, 101.2510903946856757 ) ) ;
#3121 = CARTESIAN_POINT ( 'NONE',  ( 5.719274019375991003, -21.55341960407610458, 107.7072429386476955 ) ) ;
#3123 = CARTESIAN_POINT ( 'NONE',  ( -19.03943276465977164, -0.05219959533935918106, 103.7510903946856757 ) ) ;
#3122 = CARTESIAN_POINT ( 'NONE',  ( -4.483927247898539470, -16.52544592524342804, 97.29057627198105251 ) ) ;
#3124 = CARTESIAN_POINT ( 'NONE',  ( -4.379528057220086978, -16.55341960407618274, 74.79275706135234714 ) ) ;
#3125 = CARTESIAN_POINT ( 'NONE',  ( -17.49999999999999645, 5.499999999999992895, 43.71769037696436300 ) ) ;
#3126 = CARTESIAN_POINT ( 'NONE',  ( 9.474510206698729675, 16.51473224551082808, 77.08442372801900433 ) ) ;
#3127 = CARTESIAN_POINT ( 'NONE',  ( -14.34966873604960291, -8.224510206698953496, 46.66557627198102409 ) ) ;
#3128 = CARTESIAN_POINT ( 'NONE',  ( 14.29746914071049879, -8.314922557960816363, 48.33224293864770260 ) ) ;
#3129 = CARTESIAN_POINT ( 'NONE',  ( -16.55341960407611168, -4.379528057220339221, 96.45724293864770971 ) ) ;
#3131 = CARTESIAN_POINT ( 'NONE',  ( -17.50000000000001066, 5.622605283950872668, 88.68792689403889540 ) ) ;
#3130 = CARTESIAN_POINT ( 'NONE',  ( 19.02544592524334988, 5.153800228976608722, 31.45942372801900433 ) ) ;
#3132 = CARTESIAN_POINT ( 'NONE',  ( -15.72974639402176322, -15.80617190586768395, 34.37609039468568284 ) ) ;
#3133 = CARTESIAN_POINT ( 'NONE',  ( 19.03943276465977164, 0.05219959533936151252, 101.2510903946856757 ) ) ;
#3134 = DIRECTION ( 'NONE',  ( 1.000000000000000000, 0.000000000000000000, 0.000000000000000000 ) ) ;
#3135 = CARTESIAN_POINT ( 'NONE',  ( 19.02544592524343514, -5.153800228976328945, 93.54057627198102409 ) ) ;
#3136 = CARTESIAN_POINT ( 'NONE',  ( 16.46253265017160672, -9.564922557960803928, 93.33224293864769550 ) ) ;
#3137 = CARTESIAN_POINT ( 'NONE',  ( 21.55341960407610458, 5.719274019375980345, 58.95724293864770971 ) ) ;
#3138 = CARTESIAN_POINT ( 'NONE',  ( -16.52544592524342804, 4.483927247898546575, 96.04057627198102409 ) ) ;
#3139 = CARTESIAN_POINT ( 'NONE',  ( -16.51473224551069308, -9.474510206698971260, 76.66557627198103830 ) ) ;
#3140 = CARTESIAN_POINT ( 'NONE',  ( -19.02544592524342804, 5.153800228976336051, 26.04057627198103120 ) ) ;
#3141 = CARTESIAN_POINT ( 'NONE',  ( 21.53943276465977519, 0.05219959533937863772, 41.25109039468568284 ) ) ;
#3142 = AXIS2_PLACEMENT_3D ( 'NONE', #21155, #119173, #40320 ) ;
#3143 = CARTESIAN_POINT ( 'NONE',  ( -5.719274019375665041, -21.55341960407619695, 69.79275706135234714 ) ) ;
#3144 = CARTESIAN_POINT ( 'NONE',  ( 0.05219959533934541429, -16.53943276465976808, 90.00109039468567573 ) ) ;
#3145 = CARTESIAN_POINT ( 'NONE',  ( 18.67979575497194134, -10.72451020669871369, 30.83442372801902209 ) ) ;
#3146 = CARTESIAN_POINT ( 'NONE',  ( 10.81492255796106328, -18.62759615963255655, 30.41775706135234358 ) ) ;
#3148 = CARTESIAN_POINT ( 'NONE',  ( -19.02544592524342804, 5.153800228976336051, 81.04057627198103830 ) ) ;
#3147 = CARTESIAN_POINT ( 'NONE',  ( -9.564922557961040184, 16.46253265017147172, 57.91775706135233293 ) ) ;
#3149 = CARTESIAN_POINT ( 'NONE',  ( -10.72451020669870658, -18.67979575497194134, 89.58442372801901854 ) ) ;
#3150 = EDGE_CURVE ( 'NONE', #42832, #9747, #47569, .T. ) ;
#3151 = CARTESIAN_POINT ( 'NONE',  ( 10.81492255796078972, 18.62759615963270932, 79.58224293864769550 ) ) ;
#3152 = CARTESIAN_POINT ( 'NONE',  ( 14.29746914071049879, -8.314922557960816363, 53.33224293864769550 ) ) ;
#3154 = CARTESIAN_POINT ( 'NONE',  ( -0.05219959533936034679, 19.03943276465977164, 32.50109039468566863 ) ) ;
#3153 = CARTESIAN_POINT ( 'NONE',  ( 5.719274019375673035, 21.55341960407619339, 97.29275706135234714 ) ) ;
#3155 = CARTESIAN_POINT ( 'NONE',  ( -16.55341960407611168, -4.379528057220339221, 71.45724293864769550 ) ) ;
#3156 = CARTESIAN_POINT ( 'NONE',  ( -0.05219959533910754901, -16.53943276465976808, 112.4989096053143669 ) ) ;
#3157 = CARTESIAN_POINT ( 'NONE',  ( 16.51473224551083163, -9.474510206698727899, 70.83442372801900433 ) ) ;
#3158 = CARTESIAN_POINT ( 'NONE',  ( 8.314922557960818139, 14.29746914071049879, 39.58224293864769550 ) ) ;
#3159 = CARTESIAN_POINT ( 'NONE',  ( 5.719274019375673035, 21.55341960407619339, 82.29275706135234714 ) ) ;
#3160 = CARTESIAN_POINT ( 'NONE',  ( 19.03943276465977164, -0.05219959533909143690, 78.74890960531436690 ) ) ;
#3161 = CARTESIAN_POINT ( 'NONE',  ( -9.564922557961040184, 16.46253265017147172, 62.91775706135233293 ) ) ;
#3162 = CARTESIAN_POINT ( 'NONE',  ( 5.719274019375991003, -21.55341960407610458, 62.70724293864769550 ) ) ;
#3163 = CARTESIAN_POINT ( 'NONE',  ( 21.52544592524344225, -5.823673210054117533, 113.5405762719810383 ) ) ;
#3164 = CARTESIAN_POINT ( 'NONE',  ( -9.474510206698720793, -16.51473224551083518, 109.5844237280190043 ) ) ;
#3165 = CARTESIAN_POINT ( 'NONE',  ( -16.55341960407617563, 4.379528057220093196, 78.54275706135236135 ) ) ;
#3167 = CARTESIAN_POINT ( 'NONE',  ( 21.53943276465977519, 0.05219959533937863772, 21.25109039468567218 ) ) ;
#3166 = CARTESIAN_POINT ( 'NONE',  ( 16.79531203550650176, 7.028104445595486638, 63.75244988220443787 ) ) ;
#3168 = CARTESIAN_POINT ( 'NONE',  ( 14.34966873604960469, 8.224510206698951720, 104.1655762719810241 ) ) ;
#3169 = CARTESIAN_POINT ( 'NONE',  ( 11.40812507854755253, -35.11059874428192273, -10.52499999726881263 ) ) ;
#3170 = CARTESIAN_POINT ( 'NONE',  ( -16.55341960407617563, 4.379528057220093196, 33.54275706135234714 ) ) ;
#3171 = CARTESIAN_POINT ( 'NONE',  ( 5.719274019375991003, -21.55341960407610458, 62.70724293864769550 ) ) ;
#3172 = CARTESIAN_POINT ( 'NONE',  ( 8.314922557961029526, -14.29746914071037800, 110.4177570613523756 ) ) ;
#3173 = CARTESIAN_POINT ( 'NONE',  ( -13.89961937509977652, 13.97604488694528158, 35.62390960531435269 ) ) ;
#3174 = CARTESIAN_POINT ( 'NONE',  ( 14.34966873604972726, -8.224510206698740333, 60.83442372801901854 ) ) ;
#3175 = CARTESIAN_POINT ( 'NONE',  ( 5.049401038297881783, 19.05341960407617563, 77.29275706135231871 ) ) ;
#3176 = CARTESIAN_POINT ( 'NONE',  ( 10.72451020669871369, 18.67979575497193778, 47.08442372801901854 ) ) ;
#3177 = CARTESIAN_POINT ( 'NONE',  ( 5.823673210054125526, 21.52544592524343514, 54.79057627198104541 ) ) ;
#3178 = CARTESIAN_POINT ( 'NONE',  ( -16.53943276465976808, -0.05219959533934237506, 98.75109039468568994 ) ) ;
#3179 = CARTESIAN_POINT ( 'NONE',  ( 21.53943276465977519, 0.05219959533937863772, 86.25109039468568994 ) ) ;
#3180 = CARTESIAN_POINT ( 'NONE',  ( 10.81492255796078972, 18.62759615963270932, 49.58224293864769550 ) ) ;
#3181 = CARTESIAN_POINT ( 'NONE',  ( -5.823673210054116645, -21.52544592524344225, 52.29057627198102409 ) ) ;
#3182 = CARTESIAN_POINT ( 'NONE',  ( 12.14591786802327356, -12.06949235617739191, 75.62609039468567573 ) ) ;
#3183 = CARTESIAN_POINT ( 'NONE',  ( 21.53943276465977519, -0.05219959533907433946, 48.74890960531435979 ) ) ;
#3184 = ORIENTED_EDGE ( 'NONE', *, *, #51790, .T. ) ;
#3185 = CARTESIAN_POINT ( 'NONE',  ( 13.89961937509977652, -13.97604488694527269, 103.1239096053143527 ) ) ;
#3186 = CARTESIAN_POINT ( 'NONE',  ( -4.999999999999999112, -140.0000000000000000, -15.00000000000000000 ) ) ;
#3187 = CARTESIAN_POINT ( 'NONE',  ( -16.46253265017160317, 9.564922557960807481, 30.83224293864769550 ) ) ;
#3188 = CARTESIAN_POINT ( 'NONE',  ( 5.719274019375991003, -21.55341960407610458, 62.70724293864769550 ) ) ;
#3189 = CARTESIAN_POINT ( 'NONE',  ( 16.53943276465976808, 0.05219959533934440121, 91.25109039468568994 ) ) ;
#3190 = CARTESIAN_POINT ( 'NONE',  ( 21.53943276465977519, 0.05219959533937863772, 46.25109039468567573 ) ) ;
#3191 = CARTESIAN_POINT ( 'NONE',  ( -19.02544592524334988, -5.153800228976617603, 108.9594237280189759 ) ) ;
#3192 = CARTESIAN_POINT ( 'NONE',  ( 14.34966873604960469, 8.224510206698951720, 104.1655762719810241 ) ) ;
#3193 = CARTESIAN_POINT ( 'NONE',  ( 0.05219959533934541429, -16.53943276465976808, 20.00109039468568639 ) ) ;
#3194 = CARTESIAN_POINT ( 'NONE',  ( 9.564922557960805705, 16.46253265017160317, 44.58224293864769550 ) ) ;
#3195 = CARTESIAN_POINT ( 'NONE',  ( 15.29519331188521747, -1.499966876285990347, -61.92990168432670828 ) ) ;
#3196 = CARTESIAN_POINT ( 'NONE',  ( -9.564922557960796823, -16.46253265017161027, 92.08224293864769550 ) ) ;
#3197 = CARTESIAN_POINT ( 'NONE',  ( -0.05219959533934338120, 16.53943276465976808, 77.50109039468567573 ) ) ;
#3198 = CARTESIAN_POINT ( 'NONE',  ( -10.72451020669870658, -18.67979575497194134, 104.5844237280190185 ) ) ;
#3199 = CARTESIAN_POINT ( 'NONE',  ( 18.62759615963271287, -10.81492255796078972, 68.33224293864769550 ) ) ;
#3200 = CARTESIAN_POINT ( 'NONE',  ( 4.379528057220092307, 16.55341960407617563, 87.29275706135236135 ) ) ;
#3201 = CARTESIAN_POINT ( 'NONE',  ( 16.51473224551083163, -9.474510206698727899, 80.83442372801899012 ) ) ;
#3202 = CARTESIAN_POINT ( 'NONE',  ( -19.03943276465977164, 0.05219959533909376836, 31.24890960531435979 ) ) ;
#3203 = CARTESIAN_POINT ( 'NONE',  ( 5.153800228976335163, 19.02544592524342804, 79.79057627198102409 ) ) ;
#3204 = CARTESIAN_POINT ( 'NONE',  ( 9.564922557960805705, 16.46253265017160317, 29.58224293864769550 ) ) ;
#3205 = CARTESIAN_POINT ( 'NONE',  ( 5.049401038297881783, 19.05341960407617563, 67.29275706135234714 ) ) ;
#3206 = CARTESIAN_POINT ( 'NONE',  ( 21.35462415990438245, -10.43496131973849117, 170.3924512066481043 ) ) ;
#3207 = CARTESIAN_POINT ( 'NONE',  ( -0.05219959533909027116, -19.03943276465977164, 107.4989096053143527 ) ) ;
#3208 = CARTESIAN_POINT ( 'NONE',  ( -4.379528057220328563, 16.55341960407611168, 70.20724293864769550 ) ) ;
#3209 = CARTESIAN_POINT ( 'NONE',  ( -5.719274019375978568, 21.55341960407610458, 60.20724293864768839 ) ) ;
#3210 = CARTESIAN_POINT ( 'NONE',  ( -28.82186960331499037, 2.428612866367529932E-14, 149.1250000027311842 ) ) ;
#3211 = CARTESIAN_POINT ( 'NONE',  ( 13.89961937509957401, 13.97604488694547697, 31.87609039468566863 ) ) ;
#3212 = CARTESIAN_POINT ( 'NONE',  ( 21.97181142354051531, -8.379174292515184419, 172.0076905927031419 ) ) ;
#3214 = CARTESIAN_POINT ( 'NONE',  ( -13.97604488694527625, -13.89961937509977652, 76.87390960531433848 ) ) ;
#3213 = CARTESIAN_POINT ( 'NONE',  ( 13.89961937509977652, -13.97604488694527269, 68.12390960531436690 ) ) ;
#3215 = CARTESIAN_POINT ( 'NONE',  ( -4.483927247898782831, 16.52544592524335698, 52.70942372801902565 ) ) ;
#3216 = CARTESIAN_POINT ( 'NONE',  ( -33.83559363775140838, -1.430799499857056789, 100.3228003899267975 ) ) ;
#3217 = CARTESIAN_POINT ( 'NONE',  ( -16.62475595723701005, 7.163666690055290331, 110.5271335181047760 ) ) ;
#3218 = CARTESIAN_POINT ( 'NONE',  ( -16.55341960407617563, 4.379528057220093196, 73.54275706135234714 ) ) ;
#3219 = LINE ( 'NONE', #11975, #188941 ) ;
#3220 = CARTESIAN_POINT ( 'NONE',  ( -12.14591786802326823, 12.06949235617739902, 63.12609039468568994 ) ) ;
#3221 = CARTESIAN_POINT ( 'NONE',  ( 14.34966873604972726, -8.224510206698740333, 35.83442372801901143 ) ) ;
#3223 = CYLINDRICAL_SURFACE ( 'NONE', #72438, 28.79475375365586487 ) ;
#3222 = CARTESIAN_POINT ( 'NONE',  ( -5.049401038298153566, 19.05341960407611168, 60.20724293864768129 ) ) ;
#3224 = CARTESIAN_POINT ( 'NONE',  ( -15.72974639402176322, -15.80617190586768395, 54.37609039468568994 ) ) ;
#3225 = CARTESIAN_POINT ( 'NONE',  ( -19.05341960407617563, 5.049401038297882671, 63.54275706135234003 ) ) ;
#3226 = CARTESIAN_POINT ( 'NONE',  ( 10.72451020669871369, 18.67979575497193778, 112.0844237280190185 ) ) ;
#3227 = CARTESIAN_POINT ( 'NONE',  ( 19.05341960407611168, 5.049401038298154454, 28.95724293864769550 ) ) ;
#3228 = CARTESIAN_POINT ( 'NONE',  ( -15.50344475828858748, 14.75151636811253120, -58.79419791951499974 ) ) ;
#3229 = CARTESIAN_POINT ( 'NONE',  ( 10.72451020669898902, -18.67979575497178502, 57.91557627198103120 ) ) ;
#3230 = CARTESIAN_POINT ( 'NONE',  ( -19.03943276465977164, 0.05219959533909376836, 106.2489096053143669 ) ) ;
#3231 = CARTESIAN_POINT ( 'NONE',  ( 14.34966873604960469, 8.224510206698951720, 104.1655762719810241 ) ) ;
#3232 = CARTESIAN_POINT ( 'NONE',  ( -0.05219959533934338120, 16.53943276465976808, 42.50109039468567573 ) ) ;
#3233 = CARTESIAN_POINT ( 'NONE',  ( 8.224510206698953496, -14.34966873604960469, 27.91557627198103830 ) ) ;
#3234 = ORIENTED_EDGE ( 'NONE', *, *, #131252, .T. ) ;
#3235 = CARTESIAN_POINT ( 'NONE',  ( 5.719274019375991003, -21.55341960407610458, 97.70724293864772392 ) ) ;
#3237 = CARTESIAN_POINT ( 'NONE',  ( 16.46253265017160672, -9.564922557960803928, 113.3322429386476955 ) ) ;
#3236 = CARTESIAN_POINT ( 'NONE',  ( -14.29746914071049879, 8.314922557960819915, 40.83224293864769550 ) ) ;
#3238 = CARTESIAN_POINT ( 'NONE',  ( 9.564922557961047289, -16.46253265017146816, 90.41775706135234714 ) ) ;
#3239 = CARTESIAN_POINT ( 'NONE',  ( -19.05341960407617563, 5.049401038297882671, 23.54275706135233648 ) ) ;
#3240 = CARTESIAN_POINT ( 'NONE',  ( -4.483927247898539470, -16.52544592524342804, 27.29057627198103120 ) ) ;
#3241 = CARTESIAN_POINT ( 'NONE',  ( -21.52544592524343514, 5.823673210054127303, 101.0405762719810383 ) ) ;
#3242 = CARTESIAN_POINT ( 'NONE',  ( 15.80617190586746368, 15.72974639402197994, 49.37390960531436690 ) ) ;
#3243 = CARTESIAN_POINT ( 'NONE',  ( -19.03943276465977164, 0.05219959533909376836, 76.24890960531435269 ) ) ;
#3244 = CARTESIAN_POINT ( 'NONE',  ( -0.05219959533910754901, -16.53943276465976808, 42.49890960531435979 ) ) ;
#3245 = CARTESIAN_POINT ( 'NONE',  ( -5.153800228976328057, -19.02544592524343514, 92.29057627198099567 ) ) ;
#3246 = VECTOR ( 'NONE', #122823, 1000.000000000000000 ) ;
#3247 = VERTEX_POINT ( 'NONE', #81837 ) ;
#3248 = FACE_OUTER_BOUND ( 'NONE', #133845, .T. ) ;
#3249 = CARTESIAN_POINT ( 'NONE',  ( 9.474510206698729675, 16.51473224551082808, 37.08442372801899722 ) ) ;
#3250 = CARTESIAN_POINT ( 'NONE',  ( 21.53943276465977519, -0.05219959533907433946, 83.74890960531435269 ) ) ;
#3251 = CARTESIAN_POINT ( 'NONE',  ( 0.05219959533910956823, 16.53943276465976808, 104.9989096053143669 ) ) ;
#3252 = CARTESIAN_POINT ( 'NONE',  ( -18.67979575497193778, 10.72451020669871902, 33.33442372801900433 ) ) ;
#3253 = CARTESIAN_POINT ( 'NONE',  ( 17.14385361876520264, 23.59649016807275856, 148.6750000027311387 ) ) ;
#3254 = CARTESIAN_POINT ( 'NONE',  ( -8.314922557961024197, 14.29746914071037800, 112.9177570613523329 ) ) ;
#3255 = CARTESIAN_POINT ( 'NONE',  ( -16.51473224551069308, -9.474510206698971260, 41.66557627198103120 ) ) ;
#3256 = CARTESIAN_POINT ( 'NONE',  ( -16.51473224551069308, -9.474510206698971260, 81.66557627198103830 ) ) ;
#3257 = CARTESIAN_POINT ( 'NONE',  ( -19.52217212775657273, 5.500000000000115463, 44.93993709005262360 ) ) ;
#3258 = CARTESIAN_POINT ( 'NONE',  ( 19.03943276465977164, -0.05219959533909143690, 33.74890960531435979 ) ) ;
#3259 = CARTESIAN_POINT ( 'NONE',  ( -0.05219959533910754901, -16.53943276465976808, 37.49890960531436690 ) ) ;
#3260 = EDGE_CURVE ( 'NONE', #40834, #66675, #157727, .T. ) ;
#3261 = CARTESIAN_POINT ( 'NONE',  ( -0.05219959533937732626, 21.53943276465977519, 72.50109039468568994 ) ) ;
#3263 = CARTESIAN_POINT ( 'NONE',  ( -14.29746914071037622, -8.314922557961029526, 69.16775706135234714 ) ) ;
#3262 = CARTESIAN_POINT ( 'NONE',  ( 24.50241233882493219, -28.74340065771663433, -20.80149134687501089 ) ) ;
#3264 = CARTESIAN_POINT ( 'NONE',  ( 5.049401038298161559, -19.05341960407611168, 57.70724293864769550 ) ) ;
#3265 = CARTESIAN_POINT ( 'NONE',  ( -16.51473224551069308, -9.474510206698971260, 66.66557627198102409 ) ) ;
#3266 =( BOUNDED_CURVE ( )  B_SPLINE_CURVE ( 2, ( #65961, #49812, #125658, #82104, #110478, #172161, #127632, #112467, #5279, #66961, #128622, #190315, #32661, #3301, #175144, #1305, #62984, #124663, #18490, #64973, #94315, #155993, #17489, #140818, #95307, #156991, #102301, #85114, #83118, #38634, #84113, #176152, #39622, #146798, #178157, #101282, #37622, #115472, #36612, #8291, #192317, #6278, #161969, #7275, #116468, #163990, #162972, #193319, #145792, #25487, #68959, #130621, #147818, #194326, #55794, #179164, #40632, #24477, #99284, #23465, #86127, #117466, #9304, #195326, #70970, #132638, #21457, #53797, #118480, #87129, #148814, #131635, #10304, #71961, #133635, #177161, #100291, #54793, #56806, #69969, #67956, #98268, #191306, #22465, #144795, #129611, #159970, #52782, #114451, #160971, #75, #166972, #13284, #137606, #72980 ),
 .UNSPECIFIED., .F., .F. ) 
 B_SPLINE_CURVE_WITH_KNOTS ( ( 3, 2, 2, 2, 2, 2, 2, 2, 2, 2, 2, 2, 2, 2, 2, 2, 2, 2, 2, 2, 2, 2, 2, 2, 2, 2, 2, 2, 2, 2, 2, 2, 2, 2, 2, 2, 2, 2, 2, 2, 2, 2, 2, 2, 2, 2, 2, 3 ),
 ( 0.000000000000000000, 0.02000000000000000042, 0.04000000000000000083, 0.05999999999999999778, 0.08000000000000000167, 0.1000000000000000056, 0.1199999999999999956, 0.1400000000000000133, 0.1600000000000000033, 0.1799999999999999933, 0.2000000000000000111, 0.2200000000000000011, 0.2399999999999999911, 0.2600000000000000089, 0.2800000000000000266, 0.2999999999999999889, 0.3200000000000000067, 0.3400000000000000244, 0.3599999999999999867, 0.3800000000000000044, 0.4000000000000000222, 0.4199999999999999845, 0.4400000000000000022, 0.4599999999999999645, 0.4799999999999999822, 0.5000000000000000000, 0.5200000000000000178, 0.5400000000000000355, 0.5600000000000000533, 0.5800000000000000711, 0.5999999999999999778, 0.6199999999999999956, 0.6400000000000000133, 0.6600000000000000311, 0.6800000000000000488, 0.6999999999999999556, 0.7199999999999999734, 0.7399999999999999911, 0.7600000000000000089, 0.7800000000000000266, 0.8000000000000000444, 0.8199999999999999512, 0.8399999999999999689, 0.8599999999999999867, 0.8800000000000000044, 0.9000000000000000222, 0.9199999999999999289, 0.9374174419963630100 ),
 .UNSPECIFIED. ) 
 CURVE ( )  GEOMETRIC_REPRESENTATION_ITEM ( )  RATIONAL_B_SPLINE_CURVE ( ( 1.000000000000000000, 0.9510565162951535312, 1.000000000000000000, 0.9510565162951535312, 1.000000000000000000, 0.9510565162951535312, 1.000000000000000000, 0.9510565162951535312, 1.000000000000000000, 0.9510565162951535312, 1.000000000000000000, 0.9510565162951535312, 1.000000000000000000, 0.9510565162951535312, 1.000000000000000000, 0.9510565162951535312, 1.000000000000000000, 0.9510565162951535312, 1.000000000000000000, 0.9510565162951535312, 1.000000000000000000, 0.9510565162951535312, 1.000000000000000000, 0.9510565162951535312, 1.000000000000000000, 0.9510565162951535312, 1.000000000000000000, 0.9510565162951535312, 1.000000000000000000, 0.9510565162951535312, 1.000000000000000000, 0.9510565162951535312, 1.000000000000000000, 0.9510565162951535312, 1.000000000000000000, 0.9510565162951535312, 1.000000000000000000, 0.9510565162951535312, 1.000000000000000000, 0.9510565162951535312, 1.000000000000000000, 0.9510565162951535312, 1.000000000000000000, 0.9510565162951535312, 1.000000000000000000, 0.9510565162951535312, 1.000000000000000000, 0.9510565162951535312, 1.000000000000000000, 0.9510565162951535312, 1.000000000000000000, 0.9510565162951535312, 1.000000000000000000, 0.9510565162951535312, 1.000000000000000000, 0.9510565162951535312, 1.000000000000000000, 0.9510565162951535312, 1.000000000000000000, 0.9510565162951535312, 1.000000000000000000, 0.9510565162951535312, 1.000000000000000000, 0.9510565162951535312, 1.000000000000000000, 0.9510565162951535312, 1.000000000000000000, 0.9510565162951535312, 1.000000000000000000, 0.9510565162951535312, 1.000000000000000000, 0.9510565162951535312, 1.000000000000000000, 0.9510565162951535312, 1.000000000000000000, 0.9510565162951535312, 1.000000000000000000, 0.9510565162951535312, 1.000000000000000000, 0.9510565162951535312, 1.000000000000000000, 0.9510565162951535312, 1.000000000000000000, 0.9510565162951535312, 1.000000000000000000, 0.9510565162951535312, 1.000000000000000000, 0.9510565162951535312, 1.000000000000000000, 0.9510565162951535312, 1.000000000000000000, 0.9510565162951535312, 1.000000000000000000, 0.9573764855735448220, 0.9889922301674822780 ) ) 
 REPRESENTATION_ITEM ( '' )  );
#3267 = ORIENTED_EDGE ( 'NONE', *, *, #14918, .T. ) ;
#3268 = CARTESIAN_POINT ( 'NONE',  ( 5.719274019375673035, 21.55341960407619339, 102.2927570613523613 ) ) ;
#3269 = CARTESIAN_POINT ( 'NONE',  ( -12.06949235617739369, -12.14591786802326823, 69.37609039468567573 ) ) ;
#3270 = CARTESIAN_POINT ( 'NONE',  ( -15.72974639402176322, -15.80617190586768395, 99.37609039468568994 ) ) ;
#3271 = CARTESIAN_POINT ( 'NONE',  ( -19.03943276465977164, 0.05219959533909376836, 61.24890960531436690 ) ) ;
#3272 = CARTESIAN_POINT ( 'NONE',  ( 5.719274019375991003, -21.55341960407610458, 32.70724293864770260 ) ) ;
#3273 = CARTESIAN_POINT ( 'NONE',  ( 13.97604488694548053, -13.89961937509957401, 100.6260903946856615 ) ) ;
#3274 = CARTESIAN_POINT ( 'NONE',  ( 21.55341960407619695, -5.719274019375665929, 66.04275706135236135 ) ) ;
#3275 = CARTESIAN_POINT ( 'NONE',  ( -4.379528057220086978, -16.55341960407618274, 54.79275706135235424 ) ) ;
#3276 = CARTESIAN_POINT ( 'NONE',  ( -15.80617190586745835, -15.72974639402198527, 101.8739096053143811 ) ) ;
#3277 = CARTESIAN_POINT ( 'NONE',  ( -19.02544592524334988, -5.153800228976617603, 103.9594237280190043 ) ) ;
#3278 = CARTESIAN_POINT ( 'NONE',  ( 5.049401038298161559, -19.05341960407611168, 77.70724293864765286 ) ) ;
#3279 = CARTESIAN_POINT ( 'NONE',  ( -9.474510206698720793, -16.51473224551083518, 104.5844237280190043 ) ) ;
#3280 = AXIS2_PLACEMENT_3D ( 'NONE', #188040, #19180, #186051 ) ;
#3281 = CARTESIAN_POINT ( 'NONE',  ( -19.03943276465977164, -0.05219959533935918106, 113.7510903946856757 ) ) ;
#3282 = CARTESIAN_POINT ( 'NONE',  ( -12.14591786802309592, -12.06949235617757132, 61.87390960531436690 ) ) ;
#3283 = CARTESIAN_POINT ( 'NONE',  ( -0.05219959533934338120, 16.53943276465976808, 67.50109039468568994 ) ) ;
#3285 = CARTESIAN_POINT ( 'NONE',  ( -19.05341960407611168, -5.049401038298163336, 46.45724293864768129 ) ) ;
#3284 = CARTESIAN_POINT ( 'NONE',  ( 5.823673210054444382, -21.52544592524334988, 20.20942372801900788 ) ) ;
#3286 = CARTESIAN_POINT ( 'NONE',  ( -0.05219959533909027116, -19.03943276465977164, 67.49890960531436690 ) ) ;
#3287 = CARTESIAN_POINT ( 'NONE',  ( -4.379528057220086978, -16.55341960407618274, 74.79275706135234714 ) ) ;
#3288 = DIRECTION ( 'NONE',  ( 1.000000000000000000, 0.000000000000000000, 0.000000000000000000 ) ) ;
#3289 = ORIENTED_EDGE ( 'NONE', *, *, #133011, .T. ) ;
#3290 = CARTESIAN_POINT ( 'NONE',  ( -19.05341960407617563, 5.049401038297882671, 23.54275706135233648 ) ) ;
#3291 = CARTESIAN_POINT ( 'NONE',  ( -16.46253265017160317, 9.564922557960807481, 40.83224293864769550 ) ) ;
#3292 = EDGE_LOOP ( 'NONE', ( #165342, #121879, #135522, #133598 ) ) ;
#3293 = CARTESIAN_POINT ( 'NONE',  ( 8.224510206698742110, 14.34966873604972548, 22.08442372801901143 ) ) ;
#3295 = CARTESIAN_POINT ( 'NONE',  ( -14.29746914071037622, -8.314922557961029526, 29.16775706135234003 ) ) ;
#3294 = CARTESIAN_POINT ( 'NONE',  ( 0.05219959533936267826, -19.03943276465977164, 40.00109039468566152 ) ) ;
#3296 = CARTESIAN_POINT ( 'NONE',  ( 19.02544592524343514, -5.153800228976328945, 38.54057627198103120 ) ) ;
#3297 = CARTESIAN_POINT ( 'NONE',  ( 19.05341960407611168, 5.049401038298154454, 68.95724293864769550 ) ) ;
#3298 = CARTESIAN_POINT ( 'NONE',  ( -18.67979575497178146, -10.72451020669898902, 86.66557627198102409 ) ) ;
#3299 = CARTESIAN_POINT ( 'NONE',  ( 16.51473224551069308, 9.474510206698969483, 114.1655762719810241 ) ) ;
#3300 = CARTESIAN_POINT ( 'NONE',  ( -9.474510206698964154, 16.51473224551069663, 55.41557627198103120 ) ) ;
#3301 = CARTESIAN_POINT ( 'NONE',  ( 17.14385361876520264, -23.59649016807270883, 148.0750000027312012 ) ) ;
#3302 = CARTESIAN_POINT ( 'NONE',  ( 16.51473224551083163, -9.474510206698727899, 95.83442372801900433 ) ) ;
#3303 = CARTESIAN_POINT ( 'NONE',  ( -10.72451020669898014, 18.67979575497178502, 70.41557627198102409 ) ) ;
#3304 = CARTESIAN_POINT ( 'NONE',  ( -16.51473224551082808, 9.474510206698731452, 23.33442372801900078 ) ) ;
#3305 = CARTESIAN_POINT ( 'NONE',  ( 8.224510206698953496, -14.34966873604960469, 62.91557627198102409 ) ) ;
#3306 = CARTESIAN_POINT ( 'NONE',  ( 15.72974639402176855, 15.80617190586768217, 91.87609039468568994 ) ) ;
#3307 = CARTESIAN_POINT ( 'NONE',  ( 13.97604488694527802, 13.89961937509977652, 29.37390960531435979 ) ) ;
#3308 = CARTESIAN_POINT ( 'NONE',  ( -18.62759615963255300, -10.81492255796106328, 94.16775706135237556 ) ) ;
#3310 = CARTESIAN_POINT ( 'NONE',  ( -10.81492255796105439, 18.62759615963255655, 87.91775706135234714 ) ) ;
#3309 = CARTESIAN_POINT ( 'NONE',  ( 0.05219959533910956823, 16.53943276465976808, 24.99890960531435624 ) ) ;
#3311 = CARTESIAN_POINT ( 'NONE',  ( 19.03943276465977164, -0.05219959533909143690, 73.74890960531435269 ) ) ;
#3312 = CARTESIAN_POINT ( 'NONE',  ( -18.62759615963255300, -10.81492255796106328, 39.16775706135235424 ) ) ;
#3313 = CARTESIAN_POINT ( 'NONE',  ( -16.46253265017160317, 9.564922557960807481, 75.83224293864769550 ) ) ;
#3314 = CARTESIAN_POINT ( 'NONE',  ( -16.55341960407611168, -4.379528057220339221, 96.45724293864770971 ) ) ;
#3315 = CARTESIAN_POINT ( 'NONE',  ( 8.314922557960818139, 14.29746914071049879, 64.58224293864769550 ) ) ;
#3316 = CARTESIAN_POINT ( 'NONE',  ( 15.72974639402199770, -15.80617190586745480, 73.12390960531436690 ) ) ;
#3317 = CARTESIAN_POINT ( 'NONE',  ( -9.474510206698964154, 16.51473224551069663, 75.41557627198103830 ) ) ;
#3318 = CARTESIAN_POINT ( 'NONE',  ( -10.72451020669898014, 18.67979575497178502, 90.41557627198103830 ) ) ;
#3319 = CARTESIAN_POINT ( 'NONE',  ( -9.564922557961040184, 16.46253265017147172, 82.91775706135233293 ) ) ;
#3321 = CARTESIAN_POINT ( 'NONE',  ( -8.314922557960811034, -14.29746914071050412, 82.08224293864768129 ) ) ;
#3320 = CARTESIAN_POINT ( 'NONE',  ( 16.51473224551083163, -9.474510206698727899, 30.83442372801900433 ) ) ;
#3322 = CARTESIAN_POINT ( 'NONE',  ( -21.55341960407610458, -5.719274019375992779, 51.45724293864770260 ) ) ;
#3323 = DIRECTION ( 'NONE',  ( -0.000000000000000000, -0.000000000000000000, -1.000000000000000000 ) ) ;
#3325 = CARTESIAN_POINT ( 'NONE',  ( -22.44159573604010305, 16.30477369853692338, 145.1750000027311671 ) ) ;
#3324 = CARTESIAN_POINT ( 'NONE',  ( -12.14591786802326823, 12.06949235617739902, 103.1260903946856757 ) ) ;
#3326 = CARTESIAN_POINT ( 'NONE',  ( -0.05219959533936034679, 19.03943276465977164, 107.5010903946856615 ) ) ;
#3327 = CARTESIAN_POINT ( 'NONE',  ( 8.224510206698953496, -14.34966873604960469, 67.91557627198102409 ) ) ;
#3328 = CARTESIAN_POINT ( 'NONE',  ( 8.348819774032595120, -1.314123079931750926, -62.04874212273342948 ) ) ;
#3329 = CARTESIAN_POINT ( 'NONE',  ( -16.46253265017160317, 9.564922557960807481, 60.83224293864769550 ) ) ;
#3330 = CARTESIAN_POINT ( 'NONE',  ( -12.14591786802309592, -12.06949235617757132, 56.87390960531436690 ) ) ;
#3331 = CARTESIAN_POINT ( 'NONE',  ( 19.02544592524343514, -5.153800228976328945, 103.5405762719809957 ) ) ;
#3333 = CARTESIAN_POINT ( 'NONE',  ( -0.05219959533909027116, -19.03943276465977164, 62.49890960531435979 ) ) ;
#3332 = CARTESIAN_POINT ( 'NONE',  ( 9.564922557961047289, -16.46253265017146816, 90.41775706135234714 ) ) ;
#3334 = CARTESIAN_POINT ( 'NONE',  ( -19.02544592524342804, 5.153800228976336051, 86.04057627198103830 ) ) ;
#3335 = CARTESIAN_POINT ( 'NONE',  ( 13.89961937509977652, -13.97604488694527269, 83.12390960531436690 ) ) ;
#3336 = CARTESIAN_POINT ( 'NONE',  ( 18.67979575497178502, 10.72451020669898547, 59.16557627198103120 ) ) ;
#3337 = CARTESIAN_POINT ( 'NONE',  ( -14.34966873604972548, 8.224510206698743886, 58.33442372801901143 ) ) ;
#3338 = CARTESIAN_POINT ( 'NONE',  ( -13.89961937509957401, -13.97604488694547697, 104.3760903946856757 ) ) ;
#3339 = CARTESIAN_POINT ( 'NONE',  ( -19.03943276465977164, 0.05219959533909376836, 61.24890960531436690 ) ) ;
#3340 = CARTESIAN_POINT ( 'NONE',  ( -18.62759615963270932, 10.81492255796079327, 65.83224293864769550 ) ) ;
#3341 = CARTESIAN_POINT ( 'NONE',  ( 16.51473224551083163, -9.474510206698727899, 95.83442372801900433 ) ) ;
#3343 = CARTESIAN_POINT ( 'NONE',  ( 0.05219959533937995610, -21.53943276465977519, 50.00109039468568994 ) ) ;
#3342 = CARTESIAN_POINT ( 'NONE',  ( -14.34966873604960291, -8.224510206698953496, 26.66557627198103475 ) ) ;
#3344 = CARTESIAN_POINT ( 'NONE',  ( -4.071997446883320215, -4.622768748654204174, -62.49744614497421935 ) ) ;
#3346 = CARTESIAN_POINT ( 'NONE',  ( -8.314922557961024197, 14.29746914071037800, 97.91775706135236135 ) ) ;
#3345 = CARTESIAN_POINT ( 'NONE',  ( -16.55341960407617563, 4.379528057220093196, 68.54275706135234714 ) ) ;
#3347 = CARTESIAN_POINT ( 'NONE',  ( 19.52837319214027900, -5.499999999999891642, 42.10471352585535953 ) ) ;
#3348 = CARTESIAN_POINT ( 'NONE',  ( -16.52544592524335698, -4.483927247898792601, 78.95942372801901854 ) ) ;
#3349 = CARTESIAN_POINT ( 'NONE',  ( -4.379528057220086978, -16.55341960407618274, 29.79275706135234358 ) ) ;
#3350 = CARTESIAN_POINT ( 'NONE',  ( -13.89961937509977652, 13.97604488694528158, 45.62390960531433848 ) ) ;
#3351 = CARTESIAN_POINT ( 'NONE',  ( 5.153800228976335163, 19.02544592524342804, 54.79057627198103120 ) ) ;
#3352 = CARTESIAN_POINT ( 'NONE',  ( -19.03943276465977164, 0.05219959533909376836, 61.24890960531436690 ) ) ;
#3353 = CARTESIAN_POINT ( 'NONE',  ( 18.62759615963255655, 10.81492255796105972, 51.66775706135234714 ) ) ;
#3354 = CARTESIAN_POINT ( 'NONE',  ( 16.55341960407618274, -4.379528057220086978, 46.04275706135234714 ) ) ;
#3355 = CARTESIAN_POINT ( 'NONE',  ( 16.55341960407611168, 4.379528057220329451, 38.95724293864768839 ) ) ;
#3356 = CARTESIAN_POINT ( 'NONE',  ( 19.03943276465977164, -0.05219959533909143690, 33.74890960531435979 ) ) ;
#3357 = CARTESIAN_POINT ( 'NONE',  ( 0.05219959533909260263, 19.03943276465977164, 39.99890960531436690 ) ) ;
#3358 = CARTESIAN_POINT ( 'NONE',  ( 16.52544592524335698, 4.483927247898782831, 31.45942372801901854 ) ) ;
#3359 = CARTESIAN_POINT ( 'NONE',  ( 5.049401038297881783, 19.05341960407617563, 82.29275706135229029 ) ) ;
#3360 = CARTESIAN_POINT ( 'NONE',  ( 12.06949235617757843, -12.14591786802309237, 88.12390960531436690 ) ) ;
#3361 = CARTESIAN_POINT ( 'NONE',  ( -0.05219959533909027116, -19.03943276465977164, 57.49890960531435979 ) ) ;
#3363 = CARTESIAN_POINT ( 'NONE',  ( 17.44279575226822132, 5.990770900252482711, 76.66442432485679603 ) ) ;
#3362 = CARTESIAN_POINT ( 'NONE',  ( -9.474510206698720793, -16.51473224551083518, 79.58442372801899012 ) ) ;
#3364 = CARTESIAN_POINT ( 'NONE',  ( -21.53943276465977519, -0.05219959533937600094, 78.75109039468568994 ) ) ;
#3365 = CARTESIAN_POINT ( 'NONE',  ( -16.55341960407617563, 4.379528057220093196, 53.54275706135234714 ) ) ;
#3366 = CARTESIAN_POINT ( 'NONE',  ( 17.31728774477273092, 6.344390552232407998, 36.68093348310681279 ) ) ;
#3367 = CARTESIAN_POINT ( 'NONE',  ( -15.80617190586745835, -15.72974639402198527, 36.87390960531435979 ) ) ;
#3368 = CARTESIAN_POINT ( 'NONE',  ( 8.224510206698742110, 14.34966873604972548, 32.08442372801901854 ) ) ;
#3369 = CARTESIAN_POINT ( 'NONE',  ( -28.82186960331494419, 9.364793116373629545, 147.8999999999999773 ) ) ;
#3370 = CARTESIAN_POINT ( 'NONE',  ( 19.03943276465977164, 0.05219959533936151252, 26.25109039468566507 ) ) ;
#3371 = CARTESIAN_POINT ( 'NONE',  ( 9.456233179636212682, 11.51622829137495074, -59.95663916823115613 ) ) ;
#3372 = CARTESIAN_POINT ( 'NONE',  ( -13.97604488694527625, -13.89961937509977652, 41.87390960531435979 ) ) ;
#3373 = DIRECTION ( 'NONE',  ( -1.000000000000000000, 0.000000000000000000, 0.000000000000000000 ) ) ;
#3374 = CARTESIAN_POINT ( 'NONE',  ( 19.05341960407611168, 5.049401038298154454, 68.95724293864769550 ) ) ;
#3375 = CARTESIAN_POINT ( 'NONE',  ( -19.49190055781010145, -5.500000000000053291, 55.56116087098782685 ) ) ;
#3376 = CARTESIAN_POINT ( 'NONE',  ( 15.80617190586769283, -15.72974639402175789, 110.6260903946857042 ) ) ;
#3377 = CARTESIAN_POINT ( 'NONE',  ( 8.314922557960818139, 14.29746914071049879, 34.58224293864770260 ) ) ;
#3378 = CARTESIAN_POINT ( 'NONE',  ( 19.05341960407611168, 5.049401038298154454, 38.95724293864767418 ) ) ;
#3379 = CARTESIAN_POINT ( 'NONE',  ( -19.05341960407611168, -5.049401038298163336, 111.4572429386476671 ) ) ;
#3380 = CARTESIAN_POINT ( 'NONE',  ( 18.67979575497194134, -10.72451020669871369, 75.83442372801900433 ) ) ;
#3381 = CARTESIAN_POINT ( 'NONE',  ( -13.89961937509977652, 13.97604488694528158, 55.62390960531434558 ) ) ;
#3382 = CARTESIAN_POINT ( 'NONE',  ( 21.53943276465977519, 0.05219959533937863772, 71.25109039468568994 ) ) ;
#3383 = CARTESIAN_POINT ( 'NONE',  ( 5.049401038298161559, -19.05341960407611168, 112.7072429386476813 ) ) ;
#3384 = CARTESIAN_POINT ( 'NONE',  ( 19.03943276465977164, -0.05219959533909143690, 38.74890960531436690 ) ) ;
#3385 = CARTESIAN_POINT ( 'NONE',  ( -21.55341960407619339, 5.719274019375674811, 23.54275706135235424 ) ) ;
#3386 = CARTESIAN_POINT ( 'NONE',  ( 5.049401038297881783, 19.05341960407617563, 42.29275706135234003 ) ) ;
#3387 = CARTESIAN_POINT ( 'NONE',  ( -12.14591786802309592, -12.06949235617757132, 106.8739096053143811 ) ) ;
#3388 = CARTESIAN_POINT ( 'NONE',  ( -9.474510206698964154, 16.51473224551069663, 65.41557627198102409 ) ) ;
#3389 = CARTESIAN_POINT ( 'NONE',  ( 14.29746914071037800, 8.314922557961029526, 21.66775706135235069 ) ) ;
#3390 = CARTESIAN_POINT ( 'NONE',  ( -8.224510206698948167, 14.34966873604960824, 75.41557627198102409 ) ) ;
#3391 = CARTESIAN_POINT ( 'NONE',  ( 18.62759615963271287, -10.81492255796078972, 28.33224293864769550 ) ) ;
#3392 = CARTESIAN_POINT ( 'NONE',  ( -9.564922557961040184, 16.46253265017147172, 107.9177570613523471 ) ) ;
#3393 = CARTESIAN_POINT ( 'NONE',  ( -15.72974639402197994, 15.80617190586746368, 110.6239096053143669 ) ) ;
#3394 = CARTESIAN_POINT ( 'NONE',  ( -10.81492255796105439, 18.62759615963255655, 52.91775706135235424 ) ) ;
#3395 = CARTESIAN_POINT ( 'NONE',  ( 16.53943276465976808, 0.05219959533934440121, 61.25109039468567573 ) ) ;
#3396 = CARTESIAN_POINT ( 'NONE',  ( 14.29746914071037800, 8.314922557961029526, 56.66775706135235424 ) ) ;
#3397 = CARTESIAN_POINT ( 'NONE',  ( -5.823673210054116645, -21.52544592524344225, 52.29057627198102409 ) ) ;
#3398 = CARTESIAN_POINT ( 'NONE',  ( -5.049401038298153566, 19.05341960407611168, 50.20724293864770260 ) ) ;
#3399 = CARTESIAN_POINT ( 'NONE',  ( 16.55341960407618274, -4.379528057220086978, 81.04275706135236135 ) ) ;
#3400 = CARTESIAN_POINT ( 'NONE',  ( -21.52544592524343514, 5.823673210054127303, 96.04057627198102409 ) ) ;
#3401 = CARTESIAN_POINT ( 'NONE',  ( 16.55341960407611168, 4.379528057220329451, 48.95724293864770971 ) ) ;
#3402 = CARTESIAN_POINT ( 'NONE',  ( -19.02544592524342804, 5.153800228976336051, 71.04057627198099567 ) ) ;
#3403 = CARTESIAN_POINT ( 'NONE',  ( -4.483927247898782831, 16.52544592524335698, 77.70942372801900433 ) ) ;
#3404 = CARTESIAN_POINT ( 'NONE',  ( -19.03943276465977164, -0.05219959533935918106, 113.7510903946856757 ) ) ;
#3405 = CARTESIAN_POINT ( 'NONE',  ( -15.72974639402197994, 15.80617190586746368, 100.6239096053143811 ) ) ;
#3406 = CARTESIAN_POINT ( 'NONE',  ( 8.224510206698953496, -14.34966873604960469, 47.91557627198102409 ) ) ;
#3407 = ORIENTED_EDGE ( 'NONE', *, *, #43390, .F. ) ;
#3408 = CARTESIAN_POINT ( 'NONE',  ( -16.62475595723698518, 7.163666690055228159, 75.52713351810470499 ) ) ;
#3409 = CARTESIAN_POINT ( 'NONE',  ( -15.72974639402197994, 15.80617190586746368, 85.62390960531436690 ) ) ;
#3410 = CARTESIAN_POINT ( 'NONE',  ( 12.06949235617757843, -12.14591786802309237, 23.12390960531436335 ) ) ;
#3411 = ORIENTED_EDGE ( 'NONE', *, *, #139086, .F. ) ;
#3412 = PLANE ( 'NONE',  #166342 ) ;
#3413 = CARTESIAN_POINT ( 'NONE',  ( -15.80617190586745835, -15.72974639402198527, 101.8739096053143811 ) ) ;
#3414 = CARTESIAN_POINT ( 'NONE',  ( 19.02544592524343514, -5.153800228976328945, 98.54057627198100988 ) ) ;
#3415 = CARTESIAN_POINT ( 'NONE',  ( -5.823673210054431948, 21.52544592524334988, 22.70942372801901499 ) ) ;
#3416 = CARTESIAN_POINT ( 'NONE',  ( 12.06949235617757843, -12.14591786802309237, 33.12390960531435979 ) ) ;
#3417 = CARTESIAN_POINT ( 'NONE',  ( -12.06949235617739369, -12.14591786802326823, 44.37609039468567573 ) ) ;
#3418 = CARTESIAN_POINT ( 'NONE',  ( 5.153800228976335163, 19.02544592524342804, 44.79057627198103830 ) ) ;
#3419 = CARTESIAN_POINT ( 'NONE',  ( 16.46253265017146816, 9.564922557961045513, 46.66775706135233293 ) ) ;
#3420 = CARTESIAN_POINT ( 'NONE',  ( 9.564922557960805705, 16.46253265017160317, 79.58224293864769550 ) ) ;
#3421 = CARTESIAN_POINT ( 'NONE',  ( 10.81492255796078972, 18.62759615963270932, 34.58224293864770260 ) ) ;
#3422 = CARTESIAN_POINT ( 'NONE',  ( -25.83444802367754178, -27.47999234037504834, -20.36589038153027076 ) ) ;
#3423 = CARTESIAN_POINT ( 'NONE',  ( -4.483927247898782831, 16.52544592524335698, 22.70942372801901499 ) ) ;
#3424 = CARTESIAN_POINT ( 'NONE',  ( 0.05219959533936267826, -19.03943276465977164, 50.00109039468566863 ) ) ;
#3425 = CARTESIAN_POINT ( 'NONE',  ( 18.62759615963271287, -10.81492255796078972, 103.3322429386476955 ) ) ;
#3426 = CARTESIAN_POINT ( 'NONE',  ( -8.224510206698948167, 14.34966873604960824, 35.41557627198102409 ) ) ;
#3427 = CARTESIAN_POINT ( 'NONE',  ( -16.46253265017160317, 9.564922557960807481, 80.83224293864769550 ) ) ;
#3428 = CARTESIAN_POINT ( 'NONE',  ( -21.52544592524343514, 5.823673210054127303, 66.04057627198103830 ) ) ;
#3430 = CARTESIAN_POINT ( 'NONE',  ( -16.53943276465976808, -0.05219959533934237506, 28.75109039468567929 ) ) ;
#3429 = CARTESIAN_POINT ( 'NONE',  ( -18.67979575497178146, -10.72451020669898902, 101.6655762719810383 ) ) ;
#3431 = CARTESIAN_POINT ( 'NONE',  ( 18.67979575497178502, 10.72451020669898547, 29.16557627198103120 ) ) ;
#3432 = CARTESIAN_POINT ( 'NONE',  ( -0.05219959533937732626, 21.53943276465977519, 87.50109039468568994 ) ) ;
#3433 = CARTESIAN_POINT ( 'NONE',  ( 5.049401038298161559, -19.05341960407611168, 82.70724293864770971 ) ) ;
#3434 = CARTESIAN_POINT ( 'NONE',  ( 19.05341960407611168, 5.049401038298154454, 23.95724293864769194 ) ) ;
#3435 = CARTESIAN_POINT ( 'NONE',  ( 19.02544592524343514, -5.153800228976328945, 88.54057627198102409 ) ) ;
#3436 = CARTESIAN_POINT ( 'NONE',  ( 14.29746914071049879, -8.314922557960816363, 108.3322429386477097 ) ) ;
#3437 = CARTESIAN_POINT ( 'NONE',  ( -16.51473224551069308, -9.474510206698971260, 66.66557627198102409 ) ) ;
#3438 = CARTESIAN_POINT ( 'NONE',  ( 14.29746914071037800, 8.314922557961029526, 26.66775706135235424 ) ) ;
#3439 = CARTESIAN_POINT ( 'NONE',  ( 17.50000000000147082, 3.202012800152225669, 32.57177583972737978 ) ) ;
#3440 = CARTESIAN_POINT ( 'NONE',  ( 5.049401038298161559, -19.05341960407611168, 72.70724293864768129 ) ) ;
#3442 = CARTESIAN_POINT ( 'NONE',  ( 5.719274019375991003, -21.55341960407610458, 22.70724293864769194 ) ) ;
#3441 = CARTESIAN_POINT ( 'NONE',  ( -15.80617190586768217, 15.72974639402176855, 103.1260903946856757 ) ) ;
#3443 = CARTESIAN_POINT ( 'NONE',  ( -8.224510206698735004, -14.34966873604973081, 89.58442372801901854 ) ) ;
#3444 = CARTESIAN_POINT ( 'NONE',  ( -22.55670631985092456, 22.55670631985084995, -45.64921306006598201 ) ) ;
#3445 = CARTESIAN_POINT ( 'NONE',  ( 5.049401038297881783, 19.05341960407617563, 72.29275706135234714 ) ) ;
#3446 = CARTESIAN_POINT ( 'NONE',  ( 18.67979575497194134, -10.72451020669871369, 110.8344237280190043 ) ) ;
#3447 = CARTESIAN_POINT ( 'NONE',  ( -17.40861289039002813, -6.110651285853281323, 46.37232470827434838 ) ) ;
#3448 = CARTESIAN_POINT ( 'NONE',  ( -5.049401038298153566, 19.05341960407611168, 25.20724293864768484 ) ) ;
#3449 = CARTESIAN_POINT ( 'NONE',  ( -12.14591786802309592, -12.06949235617757132, 31.87390960531435979 ) ) ;
#3450 = CARTESIAN_POINT ( 'NONE',  ( 2.500000000000000000, -165.0000000000000000, 7.000000000000003553 ) ) ;
#3451 = CARTESIAN_POINT ( 'NONE',  ( -12.14591786802326823, 12.06949235617739902, 103.1260903946856757 ) ) ;
#3452 = CARTESIAN_POINT ( 'NONE',  ( -18.87255363501902750, -5.500000000000067502, 86.32513748171830059 ) ) ;
#3453 = CARTESIAN_POINT ( 'NONE',  ( 8.314922557961029526, -14.29746914071037800, 80.41775706135234714 ) ) ;
#3454 = CARTESIAN_POINT ( 'NONE',  ( -9.564922557960796823, -16.46253265017161027, 37.08224293864768839 ) ) ;
#3455 = CARTESIAN_POINT ( 'NONE',  ( 21.53943276465977519, 0.05219959533937863772, 96.25109039468568994 ) ) ;
#3456 = CARTESIAN_POINT ( 'NONE',  ( 13.97604488694548053, -13.89961937509957401, 95.62609039468563310 ) ) ;
#3457 = CARTESIAN_POINT ( 'NONE',  ( -18.67979575497193778, 10.72451020669871902, 78.33442372801901854 ) ) ;
#3458 = CARTESIAN_POINT ( 'NONE',  ( -16.51473224551082808, 9.474510206698731452, 48.33442372801900433 ) ) ;
#3459 = CARTESIAN_POINT ( 'NONE',  ( -5.153800228976328057, -19.02544592524343514, 77.29057627198099567 ) ) ;
#3460 = CARTESIAN_POINT ( 'NONE',  ( 5.153800228976335163, 19.02544592524342804, 69.79057627198103830 ) ) ;
#3461 = CARTESIAN_POINT ( 'NONE',  ( 17.50000000000000000, 5.499999999999997335, 120.0000000000000142 ) ) ;
#3462 = CARTESIAN_POINT ( 'NONE',  ( 8.224510206698953496, -14.34966873604960469, 67.91557627198102409 ) ) ;
#3463 = CARTESIAN_POINT ( 'NONE',  ( 18.62759615963271287, -10.81492255796078972, 53.33224293864769550 ) ) ;
#3464 = CARTESIAN_POINT ( 'NONE',  ( 5.049401038298161559, -19.05341960407611168, 47.70724293864770260 ) ) ;
#3466 = CARTESIAN_POINT ( 'NONE',  ( 16.52544592524335698, 4.483927247898782831, 81.45942372801900433 ) ) ;
#3465 = CARTESIAN_POINT ( 'NONE',  ( 15.80617190586746368, 15.72974639402197994, 84.37390960531438111 ) ) ;
#3467 = ORIENTED_EDGE ( 'NONE', *, *, #68507, .F. ) ;
#3469 = CARTESIAN_POINT ( 'NONE',  ( -22.81625015709510507, 31.40387420917330275, -4.924999997268813878 ) ) ;
#3468 = CARTESIAN_POINT ( 'NONE',  ( 8.224510206698953496, -14.34966873604960469, 77.91557627198102409 ) ) ;
#3470 = CARTESIAN_POINT ( 'NONE',  ( -8.224510206698735004, -14.34966873604973081, 44.58442372801901854 ) ) ;
#3471 = CARTESIAN_POINT ( 'NONE',  ( -14.29746914071049879, 8.314922557960819915, 110.8322429386476955 ) ) ;
#3472 = CARTESIAN_POINT ( 'NONE',  ( -0.05219959533936034679, 19.03943276465977164, 72.50109039468566152 ) ) ;
#3473 = CARTESIAN_POINT ( 'NONE',  ( -12.06949235617756955, 12.14591786802309770, 65.62390960531436690 ) ) ;
#3474 = CARTESIAN_POINT ( 'NONE',  ( -5.719274019375665041, -21.55341960407619695, 44.79275706135234714 ) ) ;
#3476 = CARTESIAN_POINT ( 'NONE',  ( -21.52544592524343514, 5.823673210054127303, 96.04057627198102409 ) ) ;
#3475 = DIRECTION ( 'NONE',  ( 0.000000000000000000, -1.000000000000000000, 0.000000000000000000 ) ) ;
#3477 = CARTESIAN_POINT ( 'NONE',  ( 17.50000000000000000, 5.499999999999992895, 91.70309617465828467 ) ) ;
#3478 = CARTESIAN_POINT ( 'NONE',  ( -14.34966873604960291, -8.224510206698953496, 81.66557627198103830 ) ) ;
#3479 = CARTESIAN_POINT ( 'NONE',  ( 22.60381889853746173, -32.71308136366295827, -20.00853410804237242 ) ) ;
#3480 = CARTESIAN_POINT ( 'NONE',  ( 9.564922557960805705, 16.46253265017160317, 39.58224293864768839 ) ) ;
#3481 = CARTESIAN_POINT ( 'NONE',  ( -36.91746825000000598, 2.428612866367529932E-14, -4.624999997268814056 ) ) ;
#3482 = CARTESIAN_POINT ( 'NONE',  ( -19.02544592524334988, -5.153800228976617603, 78.95942372801900433 ) ) ;
#3483 = CARTESIAN_POINT ( 'NONE',  ( -21.53943276465977519, -0.05219959533937600094, 33.75109039468568284 ) ) ;
#3484 = CARTESIAN_POINT ( 'NONE',  ( 19.03943276465977164, -0.05219959533909143690, 68.74890960531436690 ) ) ;
#3485 = CARTESIAN_POINT ( 'NONE',  ( 0.05219959533936267826, -19.03943276465977164, 55.00109039468566863 ) ) ;
#3486 = CARTESIAN_POINT ( 'NONE',  ( -13.89961937509977652, 13.97604488694528158, 50.62390960531435979 ) ) ;
#3487 = CARTESIAN_POINT ( 'NONE',  ( 16.52544592524342804, -4.483927247898539470, 58.54057627198103120 ) ) ;
#3488 = CARTESIAN_POINT ( 'NONE',  ( -4.483927247898539470, -16.52544592524342804, 57.29057627198103120 ) ) ;
#3489 = CARTESIAN_POINT ( 'NONE',  ( 5.153800228976335163, 19.02544592524342804, 69.79057627198103830 ) ) ;
#3490 = CARTESIAN_POINT ( 'NONE',  ( -21.55341960407610458, -5.719274019375992779, 101.4572429386476955 ) ) ;
#3491 = CARTESIAN_POINT ( 'NONE',  ( -13.97604488694527625, -13.89961937509977652, 66.87390960531436690 ) ) ;
#3492 = CARTESIAN_POINT ( 'NONE',  ( -15.72974639402197994, 15.80617190586746368, 80.62390960531438111 ) ) ;
#3493 = EDGE_CURVE ( 'NONE', #90870, #121091, #171835, .T. ) ;
#3494 = CARTESIAN_POINT ( 'NONE',  ( -18.67979575497193778, 10.72451020669871902, 113.3344237280190328 ) ) ;
#3497 = CARTESIAN_POINT ( 'NONE',  ( -4.379528057220328563, 16.55341960407611168, 100.2072429386476955 ) ) ;
#3496 = CARTESIAN_POINT ( 'NONE',  ( -12.06949235617739369, -12.14591786802326823, 104.3760903946856899 ) ) ;
#3495 = CARTESIAN_POINT ( 'NONE',  ( -0.05219959533909027116, -19.03943276465977164, 32.49890960531435979 ) ) ;
#3498 = CARTESIAN_POINT ( 'NONE',  ( 13.97604488694548053, -13.89961937509957401, 110.6260903946856615 ) ) ;
#3499 = ORIENTED_EDGE ( 'NONE', *, *, #136656, .T. ) ;
#3500 = CARTESIAN_POINT ( 'NONE',  ( 0.05219959533937995610, -21.53943276465977519, 30.00109039468568284 ) ) ;
#3501 = CARTESIAN_POINT ( 'NONE',  ( -5.049401038297874678, -19.05341960407617918, 59.79275706135231871 ) ) ;
#3502 = CARTESIAN_POINT ( 'NONE',  ( -12.14591786802309592, -12.06949235617757132, 26.87390960531435979 ) ) ;
#3503 = CARTESIAN_POINT ( 'NONE',  ( -21.52544592524343514, 5.823673210054127303, 76.04057627198102409 ) ) ;
#3504 = CARTESIAN_POINT ( 'NONE',  ( -13.97604488694527625, -13.89961937509977652, 101.8739096053143811 ) ) ;
#3505 = CARTESIAN_POINT ( 'NONE',  ( -16.52544592524342804, 4.483927247898546575, 61.04057627198103120 ) ) ;
#3506 = CARTESIAN_POINT ( 'NONE',  ( -5.153800228976328057, -19.02544592524343514, 27.29057627198103120 ) ) ;
#3507 = CARTESIAN_POINT ( 'NONE',  ( -9.474510206698964154, 16.51473224551069663, 40.41557627198103120 ) ) ;
#3508 = CARTESIAN_POINT ( 'NONE',  ( 5.153800228976615827, -19.02544592524334988, 30.20942372801900433 ) ) ;
#3509 = CARTESIAN_POINT ( 'NONE',  ( -0.05219959533934338120, 16.53943276465976808, 92.50109039468567573 ) ) ;
#3510 = CARTESIAN_POINT ( 'NONE',  ( 10.81492255796106328, -18.62759615963255655, 40.41775706135234714 ) ) ;
#3511 = CARTESIAN_POINT ( 'NONE',  ( -8.314922557961024197, 14.29746914071037800, 47.91775706135234714 ) ) ;
#3512 = CARTESIAN_POINT ( 'NONE',  ( 21.55341960407610458, 5.719274019375980345, 28.95724293864769905 ) ) ;
#3514 = CARTESIAN_POINT ( 'NONE',  ( -0.05219959533937732626, 21.53943276465977519, 92.50109039468567573 ) ) ;
#3513 = CARTESIAN_POINT ( 'NONE',  ( 5.049401038298161559, -19.05341960407611168, 47.70724293864770260 ) ) ;
#3515 = CARTESIAN_POINT ( 'NONE',  ( -5.049401038298153566, 19.05341960407611168, 75.20724293864769550 ) ) ;
#3516 = CARTESIAN_POINT ( 'NONE',  ( -14.34966873604972548, 8.224510206698743886, 58.33442372801901143 ) ) ;
#3517 = CARTESIAN_POINT ( 'NONE',  ( -16.52544592524342804, 4.483927247898546575, 101.0405762719810383 ) ) ;
#3518 = CARTESIAN_POINT ( 'NONE',  ( -4.379528057220086978, -16.55341960407618274, 109.7927570613523613 ) ) ;
#3519 = DIRECTION ( 'NONE',  ( 0.000000000000000000, 0.000000000000000000, 1.000000000000000000 ) ) ;
#3522 = CARTESIAN_POINT ( 'NONE',  ( -19.03943276465977164, 0.05219959533909376836, 81.24890960531436690 ) ) ;
#3521 = CARTESIAN_POINT ( 'NONE',  ( 9.474510206698971260, -16.51473224551069308, 97.91557627198102409 ) ) ;
#3520 = CARTESIAN_POINT ( 'NONE',  ( 10.72451020669871369, 18.67979575497193778, 62.08442372801901143 ) ) ;
#3523 = CARTESIAN_POINT ( 'NONE',  ( 16.46253265017160672, -9.564922557960803928, 113.3322429386476955 ) ) ;
#3524 = CARTESIAN_POINT ( 'NONE',  ( 0.05219959533910956823, 16.53943276465976808, 44.99890960531435979 ) ) ;
#3525 = CARTESIAN_POINT ( 'NONE',  ( 8.314922557960818139, 14.29746914071049879, 24.58224293864768839 ) ) ;
#3526 = CARTESIAN_POINT ( 'NONE',  ( 4.379528057220339221, -16.55341960407611168, 37.70724293864769550 ) ) ;
#3527 = CARTESIAN_POINT ( 'NONE',  ( 8.673617379884035472E-16, 1.899999999999999689, 0.000000000000000000 ) ) ;
#3528 = CARTESIAN_POINT ( 'NONE',  ( -5.153800228976607833, 19.02544592524334988, 32.70942372801899722 ) ) ;
#3529 = CARTESIAN_POINT ( 'NONE',  ( 5.153800228976335163, 19.02544592524342804, 79.79057627198102409 ) ) ;
#3530 = CARTESIAN_POINT ( 'NONE',  ( -0.05219959533936034679, 19.03943276465977164, 57.50109039468566863 ) ) ;
#3531 = CARTESIAN_POINT ( 'NONE',  ( 11.40812507854754365, 35.11059874428196537, -3.224999997268813701 ) ) ;
#3533 = CARTESIAN_POINT ( 'NONE',  ( -12.14591786802326823, 12.06949235617739902, 73.12609039468567573 ) ) ;
#3532 = CARTESIAN_POINT ( 'NONE',  ( -0.05219959533936034679, 19.03943276465977164, 82.50109039468567573 ) ) ;
#3534 = FACE_OUTER_BOUND ( 'NONE', #60688, .T. ) ;
#3535 = CARTESIAN_POINT ( 'NONE',  ( 0.05219959533909260263, 19.03943276465977164, 109.9989096053143669 ) ) ;
#3536 = CARTESIAN_POINT ( 'NONE',  ( 18.62759615963255655, 10.81492255796105972, 26.66775706135235424 ) ) ;
#3537 = CARTESIAN_POINT ( 'NONE',  ( 19.05341960407617918, -5.049401038297876454, 96.04275706135231871 ) ) ;
#3538 = CARTESIAN_POINT ( 'NONE',  ( 19.05341960407611168, 5.049401038298154454, 53.95724293864770260 ) ) ;
#3539 = CARTESIAN_POINT ( 'NONE',  ( -16.46253265017160317, 9.564922557960807481, 95.83224293864769550 ) ) ;
#3541 = CARTESIAN_POINT ( 'NONE',  ( 5.049401038298161559, -19.05341960407611168, 52.70724293864767418 ) ) ;
#3540 = CARTESIAN_POINT ( 'NONE',  ( -12.14591786802309592, -12.06949235617757132, 56.87390960531436690 ) ) ;
#3542 = CARTESIAN_POINT ( 'NONE',  ( 5.153800228976335163, 19.02544592524342804, 59.79057627198100988 ) ) ;
#3543 = CARTESIAN_POINT ( 'NONE',  ( 9.474510206698729675, 16.51473224551082808, 67.08442372801900433 ) ) ;
#3544 = CARTESIAN_POINT ( 'NONE',  ( -19.03943276465977164, -0.05219959533935918106, 28.75109039468566507 ) ) ;
#3545 = CARTESIAN_POINT ( 'NONE',  ( -13.89961937509977652, 13.97604488694528158, 60.62390960531436690 ) ) ;
#3546 = CARTESIAN_POINT ( 'NONE',  ( -0.05219959533907301413, -21.53943276465977519, 67.49890960531436690 ) ) ;
#3548 = CARTESIAN_POINT ( 'NONE',  ( 9.564922557961047289, -16.46253265017146816, 30.41775706135232937 ) ) ;
#3547 = CARTESIAN_POINT ( 'NONE',  ( -14.34966873604960291, -8.224510206698953496, 71.66557627198100988 ) ) ;
#3549 = CARTESIAN_POINT ( 'NONE',  ( 30.00000000000000000, -5.204748896376250896E-15, 47.50000000000000000 ) ) ;
#3550 = CARTESIAN_POINT ( 'NONE',  ( 15.72974639402199770, -15.80617190586745480, 48.12390960531436690 ) ) ;
#3551 = CARTESIAN_POINT ( 'NONE',  ( 18.62759615963271287, -10.81492255796078972, 23.33224293864769194 ) ) ;
#3552 = CARTESIAN_POINT ( 'NONE',  ( 13.97604488694527802, 13.89961937509977652, 54.37390960531435979 ) ) ;
#3553 = CARTESIAN_POINT ( 'NONE',  ( -19.03943276465977164, 0.05219959533909376836, 41.24890960531435269 ) ) ;
#3554 = CARTESIAN_POINT ( 'NONE',  ( -16.55341960407611168, -4.379528057220339221, 106.4572429386477097 ) ) ;
#3555 = CARTESIAN_POINT ( 'NONE',  ( 10.72451020669898902, -18.67979575497178502, 112.9155762719810383 ) ) ;
#3556 = CARTESIAN_POINT ( 'NONE',  ( 13.89961937509977652, -13.97604488694527269, 108.1239096053143669 ) ) ;
#3557 = CARTESIAN_POINT ( 'NONE',  ( -21.55341960407619339, 5.719274019375674811, 33.54275706135234714 ) ) ;
#3558 = CARTESIAN_POINT ( 'NONE',  ( 12.06949235617757843, -12.14591786802309237, 113.1239096053143953 ) ) ;
#3559 = CARTESIAN_POINT ( 'NONE',  ( -10.72451020669870658, -18.67979575497194134, 84.58442372801903275 ) ) ;
#3560 = CARTESIAN_POINT ( 'NONE',  ( 10.72451020669898902, -18.67979575497178502, 87.91557627198103830 ) ) ;
#3561 = CARTESIAN_POINT ( 'NONE',  ( -16.46253265017146816, -9.564922557961047289, 39.16775706135234003 ) ) ;
#3562 = DIRECTION ( 'NONE',  ( 0.000000000000000000, 0.000000000000000000, 1.000000000000000000 ) ) ;
#3563 = CARTESIAN_POINT ( 'NONE',  ( 9.564922557960805705, 16.46253265017160317, 24.58224293864769194 ) ) ;
#3564 = CARTESIAN_POINT ( 'NONE',  ( 29.61737564226525876, -1.282731051913165388, -51.85482277101435500 ) ) ;
#3565 = CARTESIAN_POINT ( 'NONE',  ( 16.55341960407618274, -4.379528057220086978, 41.04275706135236135 ) ) ;
#3566 = CARTESIAN_POINT ( 'NONE',  ( -9.474510206698964154, 16.51473224551069663, 30.41557627198102054 ) ) ;
#3567 = CARTESIAN_POINT ( 'NONE',  ( 33.68444218968561188, -5.327119193238885053, 96.41491933019777605 ) ) ;
#3568 = CARTESIAN_POINT ( 'NONE',  ( -0.05219959533909027116, -19.03943276465977164, 67.49890960531436690 ) ) ;
#3569 = CARTESIAN_POINT ( 'NONE',  ( 4.379528057220339221, -16.55341960407611168, 87.70724293864769550 ) ) ;
#3570 = CARTESIAN_POINT ( 'NONE',  ( -10.72451020669898014, 18.67979575497178502, 50.41557627198103120 ) ) ;
#3571 = CARTESIAN_POINT ( 'NONE',  ( 8.224510206698953496, -14.34966873604960469, 82.91557627198103830 ) ) ;
#3572 = CARTESIAN_POINT ( 'NONE',  ( 0.05219959533934541429, -16.53943276465976808, 30.00109039468568284 ) ) ;
#3573 = CARTESIAN_POINT ( 'NONE',  ( -21.52544592524334988, -5.823673210054445271, 83.95942372801900433 ) ) ;
#3574 = CARTESIAN_POINT ( 'NONE',  ( 5.049401038298161559, -19.05341960407611168, 32.70724293864768129 ) ) ;
#3575 = CARTESIAN_POINT ( 'NONE',  ( 16.52544592524335698, 4.483927247898782831, 101.4594237280190185 ) ) ;
#3576 = CARTESIAN_POINT ( 'NONE',  ( -8.314922557960811034, -14.29746914071050412, 47.08224293864770260 ) ) ;
#3577 = CARTESIAN_POINT ( 'NONE',  ( -0.05219959533909027116, -19.03943276465977164, 52.49890960531436690 ) ) ;
#3578 = CARTESIAN_POINT ( 'NONE',  ( -5.823673210054431948, 21.52544592524334988, 97.70942372801904696 ) ) ;
#3579 = CARTESIAN_POINT ( 'NONE',  ( -10.81492255796078084, -18.62759615963271287, 102.0822429386476955 ) ) ;
#3580 = CARTESIAN_POINT ( 'NONE',  ( -18.62759615963255300, -10.81492255796106328, 54.16775706135235424 ) ) ;
#3581 = CARTESIAN_POINT ( 'NONE',  ( 4.483927247898790824, -16.52544592524335698, 35.20942372801901854 ) ) ;
#3583 = CARTESIAN_POINT ( 'NONE',  ( -5.823673210054431948, 21.52544592524334988, 92.70942372801901854 ) ) ;
#3582 = CARTESIAN_POINT ( 'NONE',  ( -14.29746914071049879, 8.314922557960819915, 60.83224293864769550 ) ) ;
#3584 = CARTESIAN_POINT ( 'NONE',  ( 12.06949235617757843, -12.14591786802309237, 23.12390960531436335 ) ) ;
#3585 = CARTESIAN_POINT ( 'NONE',  ( 16.21995358207275117, -7.366697692864356384, 47.43551001512066989 ) ) ;
#3586 = CARTESIAN_POINT ( 'NONE',  ( -19.25176906914649422, -5.499999999999740652, 65.99927264242279534 ) ) ;
#3587 = CARTESIAN_POINT ( 'NONE',  ( 4.483927247898545687, 16.52544592524342804, 39.79057627198103830 ) ) ;
#3588 = CARTESIAN_POINT ( 'NONE',  ( 8.224510206698742110, 14.34966873604972548, 67.08442372801901854 ) ) ;
#3589 = CARTESIAN_POINT ( 'NONE',  ( -19.05341960407611168, -5.049401038298163336, 81.45724293864769550 ) ) ;
#3590 = CARTESIAN_POINT ( 'NONE',  ( -19.03943276465977164, 0.05219959533909376836, 106.2489096053143669 ) ) ;
#3591 = CARTESIAN_POINT ( 'NONE',  ( -18.62759615963255300, -10.81492255796106328, 84.16775706135234714 ) ) ;
#3592 = CARTESIAN_POINT ( 'NONE',  ( -4.379528057220086978, -16.55341960407618274, 84.79275706135234714 ) ) ;
#3593 = CARTESIAN_POINT ( 'NONE',  ( 16.52544592524342804, -4.483927247898539470, 73.54057627198102409 ) ) ;
#3594 = CARTESIAN_POINT ( 'NONE',  ( 19.02544592524343514, -5.153800228976328945, 78.54057627198099567 ) ) ;
#3595 = EDGE_LOOP ( 'NONE', ( #36208, #123149, #70849, #193266 ) ) ;
#3596 = CARTESIAN_POINT ( 'NONE',  ( -8.224510206698735004, -14.34966873604973081, 29.58442372801901854 ) ) ;
#3597 = CARTESIAN_POINT ( 'NONE',  ( 19.03943276465977164, -0.05219959533909143690, 23.74890960531435269 ) ) ;
#3598 = CARTESIAN_POINT ( 'NONE',  ( 5.049401038298161559, -19.05341960407611168, 97.70724293864766707 ) ) ;
#3600 = CARTESIAN_POINT ( 'NONE',  ( 3.556970738554033499E-15, -38.81732327939057825, -8.124999997268814056 ) ) ;
#3599 = CARTESIAN_POINT ( 'NONE',  ( -8.314922557961024197, 14.29746914071037800, 27.91775706135234358 ) ) ;
#3601 = CARTESIAN_POINT ( 'NONE',  ( 21.52544592524334988, 5.823673210054432836, 111.4594237280190328 ) ) ;
#3602 = CARTESIAN_POINT ( 'NONE',  ( -12.06949235617739369, -12.14591786802326823, 89.37609039468568994 ) ) ;
#3603 = CARTESIAN_POINT ( 'NONE',  ( 16.46253265017146816, 9.564922557961045513, 106.6677570613523471 ) ) ;
#3604 = CARTESIAN_POINT ( 'NONE',  ( 0.05219959533909260263, 19.03943276465977164, 29.99890960531435979 ) ) ;
#3605 = CARTESIAN_POINT ( 'NONE',  ( 14.34966873604972726, -8.224510206698740333, 80.83442372801901854 ) ) ;
#3606 = CARTESIAN_POINT ( 'NONE',  ( 0.05219959533934541429, -16.53943276465976808, 70.00109039468568994 ) ) ;
#3607 = CARTESIAN_POINT ( 'NONE',  ( 22.30855676328228654, -33.25042073255080766, -9.512168350472055778 ) ) ;
#3608 = CARTESIAN_POINT ( 'NONE',  ( 16.46253265017146816, 9.564922557961045513, 66.66775706135233293 ) ) ;
#3609 = CARTESIAN_POINT ( 'NONE',  ( 16.46253265017146816, 9.564922557961045513, 21.66775706135233648 ) ) ;
#3610 = CARTESIAN_POINT ( 'NONE',  ( -16.51473224551069308, -9.474510206698971260, 46.66557627198102409 ) ) ;
#3611 = CARTESIAN_POINT ( 'NONE',  ( -16.46253265017160317, 9.564922557960807481, 95.83224293864769550 ) ) ;
#3612 = CARTESIAN_POINT ( 'NONE',  ( -16.53943276465976808, 0.05219959533911058130, 91.24890960531436690 ) ) ;
#3613 = CARTESIAN_POINT ( 'NONE',  ( 16.46253265017146816, 9.564922557961045513, 51.66775706135233293 ) ) ;
#3614 = CARTESIAN_POINT ( 'NONE',  ( -18.67979575497178146, -10.72451020669898902, 46.66557627198102409 ) ) ;
#3615 = CARTESIAN_POINT ( 'NONE',  ( -15.72974639402176322, -15.80617190586768395, 104.3760903946856899 ) ) ;
#3616 = CARTESIAN_POINT ( 'NONE',  ( -9.564922557960796823, -16.46253265017161027, 87.08224293864769550 ) ) ;
#3617 = CARTESIAN_POINT ( 'NONE',  ( -10.72451020669870658, -18.67979575497194134, 109.5844237280190328 ) ) ;
#3618 = CARTESIAN_POINT ( 'NONE',  ( 21.53943276465977519, -0.05219959533907433946, 68.74890960531435269 ) ) ;
#3619 = CARTESIAN_POINT ( 'NONE',  ( -0.05219959533909027116, -19.03943276465977164, 92.49890960531436690 ) ) ;
#3620 = CARTESIAN_POINT ( 'NONE',  ( 0.05219959533936267826, -19.03943276465977164, 85.00109039468567573 ) ) ;
#3621 = CARTESIAN_POINT ( 'NONE',  ( 13.89961937509977652, -13.97604488694527269, 108.1239096053143669 ) ) ;
#3622 = CARTESIAN_POINT ( 'NONE',  ( -16.46253265017146816, -9.564922557961047289, 104.1677570613523329 ) ) ;
#3623 = CARTESIAN_POINT ( 'NONE',  ( -12.14591786802309592, -12.06949235617757132, 111.8739096053143669 ) ) ;
#3624 = CARTESIAN_POINT ( 'NONE',  ( 0.05219959533909260263, 19.03943276465977164, 79.99890960531436690 ) ) ;
#3625 = CARTESIAN_POINT ( 'NONE',  ( -21.53943276465977519, 0.05219959533907696930, 76.24890960531435269 ) ) ;
#3626 = CARTESIAN_POINT ( 'NONE',  ( -0.05219959533934338120, 16.53943276465976808, 42.50109039468567573 ) ) ;
#3627 = CARTESIAN_POINT ( 'NONE',  ( -5.823673210054431948, 21.52544592524334988, 47.70942372801902565 ) ) ;
#3628 = CARTESIAN_POINT ( 'NONE',  ( -10.81492255796105439, 18.62759615963255655, 102.9177570613523756 ) ) ;
#3629 = CARTESIAN_POINT ( 'NONE',  ( -4.379528057220086978, -16.55341960407618274, 89.79275706135236135 ) ) ;
#3630 = CARTESIAN_POINT ( 'NONE',  ( -9.474510206698964154, 16.51473224551069663, 85.41557627198102409 ) ) ;
#3631 = CARTESIAN_POINT ( 'NONE',  ( -0.05219959533910754901, -16.53943276465976808, 97.49890960531436690 ) ) ;
#3632 = CARTESIAN_POINT ( 'NONE',  ( 4.379528057220339221, -16.55341960407611168, 27.70724293864769905 ) ) ;
#3633 = CARTESIAN_POINT ( 'NONE',  ( -19.03943276465977164, -0.05219959533935918106, 63.75109039468566863 ) ) ;
#3634 = ADVANCED_FACE ( 'NONE', ( #17223 ), #51107, .T. ) ;
#3635 = CARTESIAN_POINT ( 'NONE',  ( 21.53943276465977519, 0.05219959533937863772, 41.25109039468568284 ) ) ;
#3636 = CARTESIAN_POINT ( 'NONE',  ( -9.474510206698720793, -16.51473224551083518, 24.58442372801900078 ) ) ;
#3637 = CARTESIAN_POINT ( 'NONE',  ( -8.314922557960811034, -14.29746914071050412, 97.08224293864770971 ) ) ;
#3638 = CARTESIAN_POINT ( 'NONE',  ( 13.89961937509977652, -13.97604488694527269, 113.1239096053143527 ) ) ;
#3639 = CARTESIAN_POINT ( 'NONE',  ( -8.224510206698948167, 14.34966873604960824, 25.41557627198103120 ) ) ;
#3640 = CARTESIAN_POINT ( 'NONE',  ( -21.52544592524334988, -5.823673210054445271, 78.95942372801901854 ) ) ;
#3641 = CARTESIAN_POINT ( 'NONE',  ( -4.483927247898782831, 16.52544592524335698, 52.70942372801902565 ) ) ;
#3642 = CARTESIAN_POINT ( 'NONE',  ( 0.05219959533934541429, -16.53943276465976808, 100.0010903946857042 ) ) ;
#3643 = CARTESIAN_POINT ( 'NONE',  ( 18.67979575497194134, -10.72451020669871369, 55.83442372801901854 ) ) ;
#3644 = ORIENTED_EDGE ( 'NONE', *, *, #152669, .F. ) ;
#3645 = CARTESIAN_POINT ( 'NONE',  ( 18.67979575497194134, -10.72451020669871369, 25.83442372801901499 ) ) ;
#3646 = CARTESIAN_POINT ( 'NONE',  ( -16.53943276465976808, 0.05219959533911058130, 101.2489096053143669 ) ) ;
#3647 = CARTESIAN_POINT ( 'NONE',  ( 19.05341960407611168, 5.049401038298154454, 28.95724293864769550 ) ) ;
#3648 = CARTESIAN_POINT ( 'NONE',  ( -8.314922557960811034, -14.29746914071050412, 72.08224293864769550 ) ) ;
#3649 = CARTESIAN_POINT ( 'NONE',  ( 19.02544592524343514, -5.153800228976328945, 68.54057627198103830 ) ) ;
#3650 = CARTESIAN_POINT ( 'NONE',  ( 8.224510206698742110, 14.34966873604972548, 102.0844237280190185 ) ) ;
#3651 = CARTESIAN_POINT ( 'NONE',  ( -5.153800228976328057, -19.02544592524343514, 37.29057627198102409 ) ) ;
#3652 = CARTESIAN_POINT ( 'NONE',  ( -10.72451020669898014, 18.67979575497178502, 50.41557627198103120 ) ) ;
#3653 = CARTESIAN_POINT ( 'NONE',  ( 12.06949235617757843, -12.14591786802309237, 88.12390960531436690 ) ) ;
#3654 = CARTESIAN_POINT ( 'NONE',  ( 21.53943276465977519, -0.05219959533907433946, 88.74890960531436690 ) ) ;
#3655 = CARTESIAN_POINT ( 'NONE',  ( 0.05219959533909260263, 19.03943276465977164, 89.99890960531436690 ) ) ;
#3657 = CARTESIAN_POINT ( 'NONE',  ( 19.02544592524334988, 5.153800228976608722, 86.45942372801900433 ) ) ;
#3656 = CARTESIAN_POINT ( 'NONE',  ( -19.02544592524342804, 5.153800228976336051, 46.04057627198101699 ) ) ;
#3658 = CARTESIAN_POINT ( 'NONE',  ( 15.80617190586746368, 15.72974639402197994, 39.37390960531436690 ) ) ;
#3659 = CARTESIAN_POINT ( 'NONE',  ( -18.62759615963255300, -10.81492255796106328, 74.16775706135231871 ) ) ;
#3660 = CARTESIAN_POINT ( 'NONE',  ( 9.474510206698971260, -16.51473224551069308, 57.91557627198103120 ) ) ;
#3661 = CARTESIAN_POINT ( 'NONE',  ( 5.049401038298161559, -19.05341960407611168, 87.70724293864769550 ) ) ;
#3662 = CARTESIAN_POINT ( 'NONE',  ( 16.52544592524335698, 4.483927247898782831, 66.45942372801903275 ) ) ;
#3663 = CARTESIAN_POINT ( 'NONE',  ( -10.81492255796105439, 18.62759615963255655, 37.91775706135235424 ) ) ;
#3664 = CARTESIAN_POINT ( 'NONE',  ( 5.719274019375673035, 21.55341960407619339, 72.29275706135236135 ) ) ;
#3665 = CARTESIAN_POINT ( 'NONE',  ( 9.564922557960805705, 16.46253265017160317, 114.5822429386476955 ) ) ;
#3666 = CARTESIAN_POINT ( 'NONE',  ( 18.62759615963271287, -10.81492255796078972, 103.3322429386476955 ) ) ;
#3668 = CARTESIAN_POINT ( 'NONE',  ( 0.05219959533934541429, -16.53943276465976808, 70.00109039468568994 ) ) ;
#3667 = CARTESIAN_POINT ( 'NONE',  ( -21.55341960407619339, 5.719274019375674811, 33.54275706135234714 ) ) ;
#3669 = CARTESIAN_POINT ( 'NONE',  ( 21.53943276465977519, -0.05219959533907433946, 68.74890960531435269 ) ) ;
#3670 = CARTESIAN_POINT ( 'NONE',  ( -19.03943276465977164, -0.05219959533935918106, 38.75109039468566152 ) ) ;
#3672 = CARTESIAN_POINT ( 'NONE',  ( -12.06949235617739369, -12.14591786802326823, 109.3760903946857042 ) ) ;
#3671 = CARTESIAN_POINT ( 'NONE',  ( 19.03943276465977164, -0.05219959533909143690, 68.74890960531436690 ) ) ;
#3673 = CARTESIAN_POINT ( 'NONE',  ( -3.573655867282028392E-15, 2.428612866367529932E-14, 2.000000000000000000 ) ) ;
#3674 = CARTESIAN_POINT ( 'NONE',  ( 5.153800228976335163, 19.02544592524342804, 104.7905762719809957 ) ) ;
#3675 = CARTESIAN_POINT ( 'NONE',  ( 17.50000000000000000, 5.499999999999992895, 96.70309617465829888 ) ) ;
#3676 = CARTESIAN_POINT ( 'NONE',  ( 16.46253265017146816, 9.564922557961045513, 81.66775706135233293 ) ) ;
#3677 = CARTESIAN_POINT ( 'NONE',  ( -5.719274019375978568, 21.55341960407610458, 60.20724293864768839 ) ) ;
#3678 = CARTESIAN_POINT ( 'NONE',  ( -8.314922557960811034, -14.29746914071050412, 37.08224293864768129 ) ) ;
#3679 = CARTESIAN_POINT ( 'NONE',  ( -9.564922557961040184, 16.46253265017147172, 112.9177570613523329 ) ) ;
#3680 = CARTESIAN_POINT ( 'NONE',  ( 9.474510206698971260, -16.51473224551069308, 37.91557627198102409 ) ) ;
#3681 = CARTESIAN_POINT ( 'NONE',  ( 13.89961937509957401, 13.97604488694547697, 106.8760903946856757 ) ) ;
#3683 = CARTESIAN_POINT ( 'NONE',  ( -5.153800228976607833, 19.02544592524334988, 62.70942372801899722 ) ) ;
#3682 = CARTESIAN_POINT ( 'NONE',  ( 10.72451020669898902, -18.67979575497178502, 92.91557627198103830 ) ) ;
#3684 = CARTESIAN_POINT ( 'NONE',  ( 8.314922557961029526, -14.29746914071037800, 75.41775706135233293 ) ) ;
#3685 = CARTESIAN_POINT ( 'NONE',  ( -19.05341960407611168, -5.049401038298163336, 66.45724293864769550 ) ) ;
#3686 = CARTESIAN_POINT ( 'NONE',  ( -8.314922557960811034, -14.29746914071050412, 72.08224293864769550 ) ) ;
#3687 = CARTESIAN_POINT ( 'NONE',  ( -19.03943276465977164, 0.05219959533909376836, 51.24890960531436690 ) ) ;
#3688 = CARTESIAN_POINT ( 'NONE',  ( -16.53943276465976808, 0.05219959533911058130, 51.24890960531436690 ) ) ;
#3689 = CARTESIAN_POINT ( 'NONE',  ( 19.03943276465977164, -0.05219959533909143690, 23.74890960531435269 ) ) ;
#3690 = CARTESIAN_POINT ( 'NONE',  ( 1.342408831710876438, 22.10627130652513017, -55.87976878746020759 ) ) ;
#3691 = CARTESIAN_POINT ( 'NONE',  ( 12.06949235617757843, -12.14591786802309237, 23.12390960531436335 ) ) ;
#3692 = CARTESIAN_POINT ( 'NONE',  ( 19.03943276465977164, -0.05219959533909143690, 73.74890960531435269 ) ) ;
#3693 = CARTESIAN_POINT ( 'NONE',  ( -21.99873734152892268, 27.49873734152935967, 1.818019484660534424 ) ) ;
#3694 = CARTESIAN_POINT ( 'NONE',  ( -5.153800228976607833, 19.02544592524334988, 42.70942372801901143 ) ) ;
#3695 = CARTESIAN_POINT ( 'NONE',  ( 8.314922557961029526, -14.29746914071037800, 40.41775706135234714 ) ) ;
#3696 = CARTESIAN_POINT ( 'NONE',  ( 18.62759615963271287, -10.81492255796078972, 63.33224293864770260 ) ) ;
#3697 = CARTESIAN_POINT ( 'NONE',  ( 19.05341960407617918, -5.049401038297876454, 21.04275706135232582 ) ) ;
#3698 = CARTESIAN_POINT ( 'NONE',  ( -9.474510206698964154, 16.51473224551069663, 80.41557627198103830 ) ) ;
#3699 = LINE ( 'NONE', #80542, #50035 ) ;
#3700 = CARTESIAN_POINT ( 'NONE',  ( 19.05341960407611168, 5.049401038298154454, 103.9572429386476671 ) ) ;
#3701 = CARTESIAN_POINT ( 'NONE',  ( -18.67979575497193778, 10.72451020669871902, 38.33442372801900433 ) ) ;
#3702 = CARTESIAN_POINT ( 'NONE',  ( 16.53943276465976808, -0.05219959533910856209, 108.7489096053143669 ) ) ;
#3703 = EDGE_CURVE ( 'NONE', #70870, #68071, #179075, .T. ) ;
#3706 = CARTESIAN_POINT ( 'NONE',  ( 3.181980515339348337, -35.00000000000001421, 8.889087296526001936 ) ) ;
#3705 = CARTESIAN_POINT ( 'NONE',  ( 9.474510206698971260, -16.51473224551069308, 82.91557627198103830 ) ) ;
#3704 = CARTESIAN_POINT ( 'NONE',  ( -5.823673210054116645, -21.52544592524344225, 102.2905762719810383 ) ) ;
#3707 = CARTESIAN_POINT ( 'NONE',  ( -0.05219959533937732626, 21.53943276465977519, 27.50109039468567929 ) ) ;
#3708 = ORIENTED_EDGE ( 'NONE', *, *, #21762, .T. ) ;
#3709 = CARTESIAN_POINT ( 'NONE',  ( -0.05219959533909027116, -19.03943276465977164, 82.49890960531436690 ) ) ;
#3710 = CARTESIAN_POINT ( 'NONE',  ( 18.87075004821567603, -5.500000000000079936, 81.17408112101045958 ) ) ;
#3711 = B_SPLINE_CURVE_WITH_KNOTS ( 'NONE', 3,
 ( #6941, #68620, #140734, #100949, #49728, #176825, #162633, #187273 ),
 .UNSPECIFIED., .F., .F.,
 ( 4, 2, 2, 4 ),
 ( 0.005020700917424133526, 0.005703339821162721132, 0.006044659273032013634, 0.006385978724901306136 ),
 .UNSPECIFIED. ) ;
#3713 = CARTESIAN_POINT ( 'NONE',  ( -0.05219959533909027116, -19.03943276465977164, 27.49890960531435624 ) ) ;
#3712 = CARTESIAN_POINT ( 'NONE',  ( -14.29746914071049879, 8.314922557960819915, 115.8322429386477097 ) ) ;
#3714 = CARTESIAN_POINT ( 'NONE',  ( -19.03943276465977164, -0.05219959533935918106, 103.7510903946856757 ) ) ;
#3715 = CARTESIAN_POINT ( 'NONE',  ( 36.91746824999999887, 11.99521256947799053, -8.024999997268814411 ) ) ;
#3716 = CARTESIAN_POINT ( 'NONE',  ( 16.52544592524342804, -4.483927247898539470, 108.5405762719810241 ) ) ;
#3717 = CARTESIAN_POINT ( 'NONE',  ( 5.823673210054444382, -21.52544592524334988, 85.20942372801901854 ) ) ;
#3719 = CARTESIAN_POINT ( 'NONE',  ( 0.05219959533937995610, -21.53943276465977519, 50.00109039468568994 ) ) ;
#3718 = CARTESIAN_POINT ( 'NONE',  ( 19.03943276465977164, -0.05219959533909143690, 68.74890960531436690 ) ) ;
#3720 = CARTESIAN_POINT ( 'NONE',  ( 18.62759615963255655, 10.81492255796105972, 26.66775706135235424 ) ) ;
#3721 = CARTESIAN_POINT ( 'NONE',  ( -28.82186960331499037, 2.428612866367529932E-14, 148.0000000000000000 ) ) ;
#3722 = CARTESIAN_POINT ( 'NONE',  ( 13.89961937509977652, -13.97604488694527269, 88.12390960531438111 ) ) ;
#3723 = CARTESIAN_POINT ( 'NONE',  ( 27.89898386898346772, 7.496946767014385671, 160.9847407629968359 ) ) ;
#3725 = CARTESIAN_POINT ( 'NONE',  ( -18.62759615963270932, 10.81492255796079327, 40.83224293864769550 ) ) ;
#3724 = CARTESIAN_POINT ( 'NONE',  ( 14.29746914071037800, 8.314922557961029526, 31.66775706135234358 ) ) ;
#3726 = CARTESIAN_POINT ( 'NONE',  ( 5.719274019375673035, 21.55341960407619339, 77.29275706135234714 ) ) ;
#3727 = CARTESIAN_POINT ( 'NONE',  ( 13.97604488694527802, 13.89961937509977652, 109.3739096053143669 ) ) ;
#3728 = CARTESIAN_POINT ( 'NONE',  ( -0.05219959533936034679, 19.03943276465977164, 102.5010903946856757 ) ) ;
#3729 = CARTESIAN_POINT ( 'NONE',  ( -9.564922557960796823, -16.46253265017161027, 62.08224293864769550 ) ) ;
#3730 = CARTESIAN_POINT ( 'NONE',  ( 19.05341960407611168, 5.049401038298154454, 88.95724293864769550 ) ) ;
#3731 = CARTESIAN_POINT ( 'NONE',  ( -4.379528057220328563, 16.55341960407611168, 105.2072429386477097 ) ) ;
#3732 = CARTESIAN_POINT ( 'NONE',  ( 0.05219959533910956823, 16.53943276465976808, 104.9989096053143669 ) ) ;
#3733 = CARTESIAN_POINT ( 'NONE',  ( -16.46253265017160317, 9.564922557960807481, 115.8322429386477097 ) ) ;
#3734 = CARTESIAN_POINT ( 'NONE',  ( 16.52544592524335698, 4.483927247898782831, 76.45942372801901854 ) ) ;
#3736 = CARTESIAN_POINT ( 'NONE',  ( -19.03943276465977164, 0.05219959533909376836, 36.24890960531436690 ) ) ;
#3735 = CARTESIAN_POINT ( 'NONE',  ( -14.34966873604960291, -8.224510206698953496, 61.66557627198103120 ) ) ;
#3737 = CARTESIAN_POINT ( 'NONE',  ( -5.823673210054431948, 21.52544592524334988, 72.70942372801901854 ) ) ;
#3738 = CARTESIAN_POINT ( 'NONE',  ( -16.51473224551082808, 9.474510206698731452, 88.33442372801900433 ) ) ;
#3739 = CARTESIAN_POINT ( 'NONE',  ( 4.379528057220339221, -16.55341960407611168, 67.70724293864769550 ) ) ;
#3740 = CARTESIAN_POINT ( 'NONE',  ( -18.62759615963255300, -10.81492255796106328, 19.16775706135234714 ) ) ;
#3741 = CARTESIAN_POINT ( 'NONE',  ( 5.823673210054125526, 21.52544592524343514, 49.79057627198102409 ) ) ;
#3742 = LINE ( 'NONE', #186814, #122762 ) ;
#3743 = CARTESIAN_POINT ( 'NONE',  ( 27.73933785331498569, 2.768321779492822058E-14, 147.8750000027311842 ) ) ;
#3744 = CARTESIAN_POINT ( 'NONE',  ( 5.153800228976335163, 19.02544592524342804, 69.79057627198103830 ) ) ;
#3745 = CARTESIAN_POINT ( 'NONE',  ( 12.06949235617757843, -12.14591786802309237, 43.12390960531435269 ) ) ;
#3746 = CARTESIAN_POINT ( 'NONE',  ( 4.379528057220339221, -16.55341960407611168, 22.70724293864769194 ) ) ;
#3747 = CARTESIAN_POINT ( 'NONE',  ( -16.55341960407617563, 4.379528057220093196, 83.54275706135234714 ) ) ;
#3748 = CARTESIAN_POINT ( 'NONE',  ( -5.049401038297874678, -19.05341960407617918, 44.79275706135232582 ) ) ;
#3749 = CARTESIAN_POINT ( 'NONE',  ( 0.000000000000000000, 0.000000000000000000, -18.00000000000000000 ) ) ;
#3750 = CARTESIAN_POINT ( 'NONE',  ( 13.89961937509977652, -13.97604488694527269, 98.12390960531433848 ) ) ;
#3751 = CARTESIAN_POINT ( 'NONE',  ( -12.14591786802309592, -12.06949235617757132, 56.87390960531436690 ) ) ;
#3753 = CARTESIAN_POINT ( 'NONE',  ( -19.02544592524342804, 5.153800228976336051, 116.0405762719810383 ) ) ;
#3752 = CARTESIAN_POINT ( 'NONE',  ( 16.20579543436678094, -7.371946100355078357, 101.9347916582813127 ) ) ;
#3755 = VERTEX_POINT ( 'NONE', #40545 ) ;
#3754 = CARTESIAN_POINT ( 'NONE',  ( -15.72974639402197994, 15.80617190586746368, 50.62390960531435979 ) ) ;
#3756 = CARTESIAN_POINT ( 'NONE',  ( -16.53943276465976808, 0.05219959533911058130, 101.2489096053143669 ) ) ;
#3757 = CARTESIAN_POINT ( 'NONE',  ( -8.224510206698735004, -14.34966873604973081, 39.58442372801901143 ) ) ;
#3758 = CARTESIAN_POINT ( 'NONE',  ( 4.483927247898545687, 16.52544592524342804, 84.79057627198102409 ) ) ;
#3759 = DIRECTION ( 'NONE',  ( -1.000000000000000000, 1.246178594180516623E-14, 0.000000000000000000 ) ) ;
#3760 = CARTESIAN_POINT ( 'NONE',  ( 5.153800228976615827, -19.02544592524334988, 75.20942372801896170 ) ) ;
#3761 = CARTESIAN_POINT ( 'NONE',  ( -0.05219959533907301413, -21.53943276465977519, 27.49890960531435269 ) ) ;
#3762 = CARTESIAN_POINT ( 'NONE',  ( -36.91746825000000598, 2.428612866367529932E-14, -3.124999997268813168 ) ) ;
#3763 = CARTESIAN_POINT ( 'NONE',  ( -21.85243030949941456, 20.02676387111000622, -51.86007293692900078 ) ) ;
#3765 = CARTESIAN_POINT ( 'NONE',  ( -16.55341960407611168, -4.379528057220339221, 31.45724293864769550 ) ) ;
#3764 = CARTESIAN_POINT ( 'NONE',  ( 14.34966873604972726, -8.224510206698740333, 35.83442372801901143 ) ) ;
#3766 = CARTESIAN_POINT ( 'NONE',  ( -21.55341960407610458, -5.719274019375992779, 51.45724293864770260 ) ) ;
#3767 = CARTESIAN_POINT ( 'NONE',  ( -9.564922557961040184, 16.46253265017147172, 72.91775706135233293 ) ) ;
#3768 = CARTESIAN_POINT ( 'NONE',  ( 18.62759615963271287, -10.81492255796078972, 53.33224293864769550 ) ) ;
#3769 = CARTESIAN_POINT ( 'NONE',  ( -10.81492255796105439, 18.62759615963255655, 62.91775706135236135 ) ) ;
#3770 = DIRECTION ( 'NONE',  ( 0.000000000000000000, 0.000000000000000000, 1.000000000000000000 ) ) ;
#3771 = CARTESIAN_POINT ( 'NONE',  ( -16.53943276465976808, -0.05219959533934237506, 38.75109039468567573 ) ) ;
#3773 = CARTESIAN_POINT ( 'NONE',  ( -16.46253265017160317, 9.564922557960807481, 90.83224293864769550 ) ) ;
#3772 = CARTESIAN_POINT ( 'NONE',  ( -13.89961937509977652, 13.97604488694528158, 30.62390960531435269 ) ) ;
#3774 = CARTESIAN_POINT ( 'NONE',  ( -16.51473224551069308, -9.474510206698971260, 31.66557627198102054 ) ) ;
#3775 = CARTESIAN_POINT ( 'NONE',  ( -0.05219959533910754901, -16.53943276465976808, 102.4989096053143811 ) ) ;
#3776 = PRODUCT_CONTEXT ( 'NONE', #173204, 'mechanical' ) ;
#3777 = CARTESIAN_POINT ( 'NONE',  ( 0.05219959533909260263, 19.03943276465977164, 99.99890960531436690 ) ) ;
#3778 = VERTEX_POINT ( 'NONE', #101192 ) ;
#3779 = CARTESIAN_POINT ( 'NONE',  ( -4.379528057220086978, -16.55341960407618274, 59.79275706135234714 ) ) ;
#3780 = CARTESIAN_POINT ( 'NONE',  ( -21.52544592524343514, 5.823673210054127303, 91.04057627198103830 ) ) ;
#3781 = CARTESIAN_POINT ( 'NONE',  ( 13.97604488694527802, 13.89961937509977652, 49.37390960531434558 ) ) ;
#3783 = CARTESIAN_POINT ( 'NONE',  ( 18.62759615963255655, 10.81492255796105972, 31.66775706135234358 ) ) ;
#3782 = CARTESIAN_POINT ( 'NONE',  ( 0.05219959533936267826, -19.03943276465977164, 75.00109039468566152 ) ) ;
#3784 = CARTESIAN_POINT ( 'NONE',  ( 19.03943276465977164, -0.05219959533909143690, 73.74890960531435269 ) ) ;
#3785 = CARTESIAN_POINT ( 'NONE',  ( -13.89961937509977652, 13.97604488694528158, 100.6239096053143669 ) ) ;
#3786 = ORIENTED_EDGE ( 'NONE', *, *, #177460, .F. ) ;
#3787 = CARTESIAN_POINT ( 'NONE',  ( -4.483927247898782831, 16.52544592524335698, 37.70942372801900433 ) ) ;
#3788 = CARTESIAN_POINT ( 'NONE',  ( 5.719274019375673035, 21.55341960407619339, 22.29275706135235069 ) ) ;
#3791 = CARTESIAN_POINT ( 'NONE',  ( 19.02544592524334988, 5.153800228976608722, 71.45942372801900433 ) ) ;
#3790 = CARTESIAN_POINT ( 'NONE',  ( -19.02544592524342804, 5.153800228976336051, 96.04057627198103830 ) ) ;
#3789 = CARTESIAN_POINT ( 'NONE',  ( -4.379528057220328563, 16.55341960407611168, 105.2072429386477097 ) ) ;
#3792 = CARTESIAN_POINT ( 'NONE',  ( 18.67979575497178502, 10.72451020669898547, 89.16557627198102409 ) ) ;
#3793 = CARTESIAN_POINT ( 'NONE',  ( 0.05219959533910956823, 16.53943276465976808, 49.99890960531437401 ) ) ;
#3794 = CARTESIAN_POINT ( 'NONE',  ( 19.03943276465977164, 0.05219959533936151252, 26.25109039468566507 ) ) ;
#3795 = CARTESIAN_POINT ( 'NONE',  ( -12.06949235617739369, -12.14591786802326823, 74.37609039468568994 ) ) ;
#3796 = CARTESIAN_POINT ( 'NONE',  ( 5.153800228976335163, 19.02544592524342804, 89.79057627198102409 ) ) ;
#3797 = CARTESIAN_POINT ( 'NONE',  ( 0.05219959533909260263, 19.03943276465977164, 44.99890960531435979 ) ) ;
#3798 = CARTESIAN_POINT ( 'NONE',  ( 5.719274019375673035, 21.55341960407619339, 52.29275706135236135 ) ) ;
#3799 = CARTESIAN_POINT ( 'NONE',  ( 21.53943276465977519, 0.05219959533937863772, 71.25109039468568994 ) ) ;
#3800 = CARTESIAN_POINT ( 'NONE',  ( -9.474510206698964154, 16.51473224551069663, 55.41557627198103120 ) ) ;
#3801 = CARTESIAN_POINT ( 'NONE',  ( 10.72451020669871369, 18.67979575497193778, 37.08442372801901143 ) ) ;
#3802 = CARTESIAN_POINT ( 'NONE',  ( -19.03943276465977164, -0.05219959533935918106, 83.75109039468567573 ) ) ;
#3803 = CARTESIAN_POINT ( 'NONE',  ( -9.564922557960796823, -16.46253265017161027, 37.08224293864768839 ) ) ;
#3804 = CARTESIAN_POINT ( 'NONE',  ( 8.224510206698742110, 14.34966873604972548, 92.08442372801901854 ) ) ;
#3805 = CARTESIAN_POINT ( 'NONE',  ( -9.564922557960796823, -16.46253265017161027, 67.08224293864769550 ) ) ;
#3806 = CARTESIAN_POINT ( 'NONE',  ( -9.474510206698964154, 16.51473224551069663, 110.4155762719810383 ) ) ;
#3807 = CARTESIAN_POINT ( 'NONE',  ( -16.46253265017160317, 9.564922557960807481, 50.83224293864770260 ) ) ;
#3808 = CARTESIAN_POINT ( 'NONE',  ( 0.05219959533907565091, 21.53943276465977519, 89.99890960531438111 ) ) ;
#3809 = CARTESIAN_POINT ( 'NONE',  ( -8.314922557961024197, 14.29746914071037800, 77.91775706135231871 ) ) ;
#3810 = CARTESIAN_POINT ( 'NONE',  ( -21.92083080610932910, 6.374575339255513562, 171.4095429173270020 ) ) ;
#3811 = CARTESIAN_POINT ( 'NONE',  ( 5.049401038297881783, 19.05341960407617563, 32.29275706135233293 ) ) ;
#3812 = CARTESIAN_POINT ( 'NONE',  ( -16.51473224551069308, -9.474510206698971260, 61.66557627198103120 ) ) ;
#3813 = CARTESIAN_POINT ( 'NONE',  ( -4.483927247898539470, -16.52544592524342804, 52.29057627198102409 ) ) ;
#3814 = CARTESIAN_POINT ( 'NONE',  ( 12.06949235617757843, -12.14591786802309237, 78.12390960531436690 ) ) ;
#3815 = CARTESIAN_POINT ( 'NONE',  ( -9.474510206698964154, 16.51473224551069663, 100.4155762719810241 ) ) ;
#3816 = CARTESIAN_POINT ( 'NONE',  ( 16.46253265017160672, -9.564922557960803928, 93.33224293864769550 ) ) ;
#3817 = CARTESIAN_POINT ( 'NONE',  ( 18.62759615963255655, 10.81492255796105972, 51.66775706135234714 ) ) ;
#3818 = CARTESIAN_POINT ( 'NONE',  ( 19.03943276465977164, -0.05219959533909143690, 108.7489096053143527 ) ) ;
#3819 = CARTESIAN_POINT ( 'NONE',  ( 5.823673210054444382, -21.52544592524334988, 110.2094237280190185 ) ) ;
#3820 = CARTESIAN_POINT ( 'NONE',  ( 16.52544592524335698, 4.483927247898782831, 76.45942372801901854 ) ) ;
#3821 = CARTESIAN_POINT ( 'NONE',  ( 15.72974639402176855, 15.80617190586768217, 36.87609039468568994 ) ) ;
#3822 = CARTESIAN_POINT ( 'NONE',  ( 19.02544592524343514, -5.153800228976328945, 108.5405762719810383 ) ) ;
#3823 = CARTESIAN_POINT ( 'NONE',  ( 21.53943276465977519, -0.05219959533907433946, 108.7489096053143669 ) ) ;
#3824 = CARTESIAN_POINT ( 'NONE',  ( 12.14591786802309770, 12.06949235617756955, 54.37390960531435979 ) ) ;
#3825 = CARTESIAN_POINT ( 'NONE',  ( 19.02544592524343514, -5.153800228976328945, 58.54057627198102409 ) ) ;
#3826 = CARTESIAN_POINT ( 'NONE',  ( 14.34966873604960469, 8.224510206698951720, 79.16557627198103830 ) ) ;
#3827 = CARTESIAN_POINT ( 'NONE',  ( -21.55341960407610458, -5.719274019375992779, 36.45724293864768839 ) ) ;
#3828 = CARTESIAN_POINT ( 'NONE',  ( -19.02544592524334988, -5.153800228976617603, 38.95942372801900433 ) ) ;
#3829 = CARTESIAN_POINT ( 'NONE',  ( 8.224510206698953496, -14.34966873604960469, 112.9155762719810383 ) ) ;
#3830 = VERTEX_POINT ( 'NONE', #148727 ) ;
#3831 = CARTESIAN_POINT ( 'NONE',  ( -16.53943276465976808, -0.05219959533934237506, 63.75109039468568284 ) ) ;
#3832 = CARTESIAN_POINT ( 'NONE',  ( -9.474510206698964154, 16.51473224551069663, 65.41557627198102409 ) ) ;
#3833 = CARTESIAN_POINT ( 'NONE',  ( 22.44159573604009594, -16.30477369853687364, 145.6750000027311671 ) ) ;
#3834 = CARTESIAN_POINT ( 'NONE',  ( -16.52544592524342804, 4.483927247898546575, 91.04057627198103830 ) ) ;
#3835 = CARTESIAN_POINT ( 'NONE',  ( -21.52544592524343514, 5.823673210054127303, 41.04057627198103120 ) ) ;
#3836 = ORIENTED_EDGE ( 'NONE', *, *, #177334, .F. ) ;
#3837 = CARTESIAN_POINT ( 'NONE',  ( -14.34966873604972548, 8.224510206698743886, 108.3344237280190185 ) ) ;
#3838 = CARTESIAN_POINT ( 'NONE',  ( -13.89961937509957401, -13.97604488694547875, 104.3760903946856757 ) ) ;
#3839 = CARTESIAN_POINT ( 'NONE',  ( -15.80617190586768217, 15.72974639402176855, 78.12609039468570415 ) ) ;
#3840 = CARTESIAN_POINT ( 'NONE',  ( 16.46253265017160672, -9.564922557960803928, 88.33224293864769550 ) ) ;
#3841 = CARTESIAN_POINT ( 'NONE',  ( 15.80617190586746368, 15.72974639402197994, 104.3739096053143669 ) ) ;
#3842 = CARTESIAN_POINT ( 'NONE',  ( -14.29746914071037622, -8.314922557961029526, 49.16775706135234003 ) ) ;
#3843 = CARTESIAN_POINT ( 'NONE',  ( 13.89961937509977652, -13.97604488694527269, 28.12390960531435624 ) ) ;
#3844 = CARTESIAN_POINT ( 'NONE',  ( 8.224510206698742110, 14.34966873604972548, 27.08442372801901854 ) ) ;
#3845 = CARTESIAN_POINT ( 'NONE',  ( 5.153800228976615827, -19.02544592524334988, 95.20942372801897591 ) ) ;
#3846 = CARTESIAN_POINT ( 'NONE',  ( 21.53943276465977519, -0.05219959533907433946, 93.74890960531436690 ) ) ;
#3847 = CARTESIAN_POINT ( 'NONE',  ( -13.89961937509957401, -13.97604488694547875, 59.37609039468566863 ) ) ;
#3848 = CARTESIAN_POINT ( 'NONE',  ( -17.49999999999999645, 5.499999999999997335, 120.0000000000000142 ) ) ;
#3849 = CARTESIAN_POINT ( 'NONE',  ( 21.55341960407610458, 5.719274019375980345, 108.9572429386476955 ) ) ;
#3850 = CARTESIAN_POINT ( 'NONE',  ( 16.46253265017160672, -9.564922557960803928, 73.33224293864769550 ) ) ;
#3851 = CARTESIAN_POINT ( 'NONE',  ( 5.049401038298161559, -19.05341960407611168, 72.70724293864768129 ) ) ;
#3852 = LINE ( 'NONE', #20027, #140137 ) ;
#3853 = CARTESIAN_POINT ( 'NONE',  ( -16.55341960407617563, 4.379528057220093196, 33.54275706135234714 ) ) ;
#3854 = CARTESIAN_POINT ( 'NONE',  ( -37.99626262588766679, 2.428612866367529932E-14, -6.002157773949822861 ) ) ;
#3856 = CARTESIAN_POINT ( 'NONE',  ( 8.224510206698953496, -14.34966873604960469, 62.91557627198102409 ) ) ;
#3855 = CARTESIAN_POINT ( 'NONE',  ( -10.72451020669870658, -18.67979575497194134, 24.58442372801901499 ) ) ;
#3857 = CARTESIAN_POINT ( 'NONE',  ( 5.153800228976335163, 19.02544592524342804, 74.79057627198103830 ) ) ;
#3859 = CARTESIAN_POINT ( 'NONE',  ( 16.46253265017146816, 9.564922557961045513, 46.66775706135233293 ) ) ;
#3858 = CARTESIAN_POINT ( 'NONE',  ( -14.34966873604972548, 8.224510206698743886, 43.33442372801901143 ) ) ;
#3860 = CARTESIAN_POINT ( 'NONE',  ( 5.719274019375673035, 21.55341960407619339, 57.29275706135234714 ) ) ;
#3861 = CARTESIAN_POINT ( 'NONE',  ( -16.46253265017146816, -9.564922557961047289, 104.1677570613523329 ) ) ;
#3863 = EDGE_CURVE ( 'NONE', #25133, #53699, #36920, .T. ) ;
#3862 = CARTESIAN_POINT ( 'NONE',  ( -19.05341960407611168, -5.049401038298163336, 56.45724293864768129 ) ) ;
#3864 = CARTESIAN_POINT ( 'NONE',  ( -19.02544592524334988, -5.153800228976617603, 83.95942372801901854 ) ) ;
#3865 = CARTESIAN_POINT ( 'NONE',  ( 5.823673210054444382, -21.52544592524334988, 85.20942372801901854 ) ) ;
#3866 = CARTESIAN_POINT ( 'NONE',  ( 19.02544592524334988, 5.153800228976608722, 66.45942372801899012 ) ) ;
#3867 = CARTESIAN_POINT ( 'NONE',  ( 13.89961937509977652, -13.97604488694527269, 38.12390960531436690 ) ) ;
#3868 = CARTESIAN_POINT ( 'NONE',  ( -21.55341960407610458, -5.719274019375992779, 56.45724293864768839 ) ) ;
#3870 = CARTESIAN_POINT ( 'NONE',  ( -9.474510206698720793, -16.51473224551083518, 64.58442372801900433 ) ) ;
#3869 = CARTESIAN_POINT ( 'NONE',  ( -16.55341960407611168, -4.379528057220339221, 61.45724293864770260 ) ) ;
#3871 = CARTESIAN_POINT ( 'NONE',  ( -16.18388926212235646, -7.379444403734649605, 25.43953151366155296 ) ) ;
#3872 = CARTESIAN_POINT ( 'NONE',  ( 13.97604488694548053, -13.89961937509957401, 25.62609039468566507 ) ) ;
#3873 = CARTESIAN_POINT ( 'NONE',  ( -4.379528057220086978, -16.55341960407618274, 99.79275706135234714 ) ) ;
#3874 = CARTESIAN_POINT ( 'NONE',  ( 12.06949235617757843, -12.14591786802309237, 58.12390960531435979 ) ) ;
#3876 = CARTESIAN_POINT ( 'NONE',  ( -22.44159573604010305, 16.30477369853692338, 149.1750000027311671 ) ) ;
#3875 = CARTESIAN_POINT ( 'NONE',  ( -21.55341960407619339, 5.719274019375674811, 93.54275706135234714 ) ) ;
#3877 = CARTESIAN_POINT ( 'NONE',  ( -18.67979575497193778, 10.72451020669871902, 93.33442372801901854 ) ) ;
#3878 = CARTESIAN_POINT ( 'NONE',  ( 0.05219959533907565091, 21.53943276465977519, 94.99890960531436690 ) ) ;
#3879 = CARTESIAN_POINT ( 'NONE',  ( 9.564922557960805705, 16.46253265017160317, 54.58224293864769550 ) ) ;
#3880 = CARTESIAN_POINT ( 'NONE',  ( 21.53943276465977519, 0.05219959533937863772, 66.25109039468567573 ) ) ;
#3881 = CARTESIAN_POINT ( 'NONE',  ( 5.153800228976335163, 19.02544592524342804, 54.79057627198103120 ) ) ;
#3882 = CARTESIAN_POINT ( 'NONE',  ( -5.049401038298153566, 19.05341960407611168, 70.20724293864769550 ) ) ;
#3883 = CARTESIAN_POINT ( 'NONE',  ( -12.06949235617756955, 12.14591786802309770, 110.6239096053143669 ) ) ;
#3884 = CARTESIAN_POINT ( 'NONE',  ( 10.72451020669898902, -18.67979575497178502, 22.91557627198102765 ) ) ;
#3885 = CARTESIAN_POINT ( 'NONE',  ( -8.314922557960811034, -14.29746914071050412, 52.08224293864768839 ) ) ;
#3886 = CARTESIAN_POINT ( 'NONE',  ( -16.51473224551069308, -9.474510206698971260, 26.66557627198103120 ) ) ;
#3887 = CARTESIAN_POINT ( 'NONE',  ( -8.314922557960811034, -14.29746914071050412, 77.08224293864769550 ) ) ;
#3888 = CARTESIAN_POINT ( 'NONE',  ( -21.53943276465977519, 0.05219959533907696930, 91.24890960531436690 ) ) ;
#3889 = CARTESIAN_POINT ( 'NONE',  ( 21.53943276465977519, 0.05219959533937863772, 36.25109039468567573 ) ) ;
#3890 = CARTESIAN_POINT ( 'NONE',  ( 23.31738231874054534, 16.94106989632529192, 149.1999999999999886 ) ) ;
#3891 = CARTESIAN_POINT ( 'NONE',  ( -14.29746914071037622, -8.314922557961029526, 39.16775706135235424 ) ) ;
#3892 = CARTESIAN_POINT ( 'NONE',  ( 15.80617190586746368, 15.72974639402197994, 84.37390960531438111 ) ) ;
#3894 = CARTESIAN_POINT ( 'NONE',  ( -21.55341960407619339, 5.719274019375674811, 113.5427570613523756 ) ) ;
#3893 = PRODUCT_DEFINITION_CONTEXT ( 'detailed design', #36479, 'design' ) ;
#3895 = CARTESIAN_POINT ( 'NONE',  ( 5.049401038298161559, -19.05341960407611168, 87.70724293864769550 ) ) ;
#3896 = CARTESIAN_POINT ( 'NONE',  ( 10.72451020669871369, 18.67979575497193778, 47.08442372801901854 ) ) ;
#3897 = CARTESIAN_POINT ( 'NONE',  ( -18.62759615963270932, 10.81492255796079327, 25.83224293864769194 ) ) ;
#3898 = CARTESIAN_POINT ( 'NONE',  ( -16.53943276465976808, -0.05219959533934237506, 98.75109039468568994 ) ) ;
#3900 = CARTESIAN_POINT ( 'NONE',  ( -21.53943276465977519, -0.05219959533937600094, 88.75109039468567573 ) ) ;
#3899 = CARTESIAN_POINT ( 'NONE',  ( -15.72974639402176322, -15.80617190586768395, 49.37609039468569705 ) ) ;
#3901 = CARTESIAN_POINT ( 'NONE',  ( -13.89961937509957401, -13.97604488694547875, 29.37609039468565797 ) ) ;
#3902 = CARTESIAN_POINT ( 'NONE',  ( -4.379528057220086978, -16.55341960407618274, 89.79275706135236135 ) ) ;
#3903 = CARTESIAN_POINT ( 'NONE',  ( 10.81492255796106328, -18.62759615963255655, 45.41775706135234003 ) ) ;
#3904 = CARTESIAN_POINT ( 'NONE',  ( -5.153800228976328057, -19.02544592524343514, 32.29057627198102409 ) ) ;
#3905 = CARTESIAN_POINT ( 'NONE',  ( -21.55341960407619339, 5.719274019375674811, 98.54275706135234714 ) ) ;
#3906 = CARTESIAN_POINT ( 'NONE',  ( 5.153800228976335163, 19.02544592524342804, 104.7905762719809957 ) ) ;
#3907 = CARTESIAN_POINT ( 'NONE',  ( 5.719274019375991003, -21.55341960407610458, 107.7072429386476955 ) ) ;
#3908 = CARTESIAN_POINT ( 'NONE',  ( -18.67979575497178146, -10.72451020669898902, 61.66557627198103120 ) ) ;
#3910 = CARTESIAN_POINT ( 'NONE',  ( 10.72451020669898902, -18.67979575497178502, 62.91557627198102409 ) ) ;
#3909 = DIRECTION ( 'NONE',  ( 0.000000000000000000, -1.000000000000000000, 0.000000000000000000 ) ) ;
#3912 = CARTESIAN_POINT ( 'NONE',  ( -12.14591786802309592, -12.06949235617757132, 56.87390960531436690 ) ) ;
#3911 = CARTESIAN_POINT ( 'NONE',  ( 12.06949235617739724, 12.14591786802326823, 46.87609039468568994 ) ) ;
#3913 = CARTESIAN_POINT ( 'NONE',  ( -7.500000000000000888, 1.380023386739105407, 4.327083394447439169 ) ) ;
#3914 = CARTESIAN_POINT ( 'NONE',  ( 19.02544592524334988, 5.153800228976608722, 96.45942372801897591 ) ) ;
#3915 = FACE_OUTER_BOUND ( 'NONE', #114573, .T. ) ;
#3916 = CARTESIAN_POINT ( 'NONE',  ( 16.52544592524335698, 4.483927247898782831, 21.45942372801901499 ) ) ;
#3917 = CARTESIAN_POINT ( 'NONE',  ( -0.05219959533907301413, -21.53943276465977519, 92.49890960531436690 ) ) ;
#3918 = CARTESIAN_POINT ( 'NONE',  ( -21.53943276465977519, 0.05219959533907696930, 76.24890960531435269 ) ) ;
#3919 = CARTESIAN_POINT ( 'NONE',  ( -5.049401038298153566, 19.05341960407611168, 110.2072429386476671 ) ) ;
#3920 = CARTESIAN_POINT ( 'NONE',  ( -8.314922557961024197, 14.29746914071037800, 52.91775706135235424 ) ) ;
#3921 = CARTESIAN_POINT ( 'NONE',  ( 19.03943276465977164, -0.05219959533909143690, 73.74890960531435269 ) ) ;
#3923 = CARTESIAN_POINT ( 'NONE',  ( 16.51473224551083163, -9.474510206698727899, 105.8344237280190043 ) ) ;
#3922 = CARTESIAN_POINT ( 'NONE',  ( -5.719274019375665041, -21.55341960407619695, 29.79275706135234358 ) ) ;
#3924 = CARTESIAN_POINT ( 'NONE',  ( -13.97604488694527625, -13.89961937509977652, 106.8739096053143669 ) ) ;
#3925 = CARTESIAN_POINT ( 'NONE',  ( 16.51473224551069308, 9.474510206698969483, 84.16557627198102409 ) ) ;
#3926 = CARTESIAN_POINT ( 'NONE',  ( -5.719274019375978568, 21.55341960407610458, 85.20724293864770971 ) ) ;
#3927 = CARTESIAN_POINT ( 'NONE',  ( 5.049401038298161559, -19.05341960407611168, 62.70724293864769550 ) ) ;
#3928 = CARTESIAN_POINT ( 'NONE',  ( -17.26058549869089376, -6.457015423128632747, 61.37745837476070676 ) ) ;
#3929 = CARTESIAN_POINT ( 'NONE',  ( 14.34966873604960469, 8.224510206698951720, 64.16557627198102409 ) ) ;
#3930 = CARTESIAN_POINT ( 'NONE',  ( -16.46253265017160317, 9.564922557960807481, 115.8322429386477097 ) ) ;
#3931 = CARTESIAN_POINT ( 'NONE',  ( 16.53812085701073187, -14.65432885500447746, -55.91693222716156697 ) ) ;
#3932 = CARTESIAN_POINT ( 'NONE',  ( 15.72974639402199770, -15.80617190586745480, 108.1239096053143811 ) ) ;
#3933 = CARTESIAN_POINT ( 'NONE',  ( 16.51473224551083163, -9.474510206698727899, 60.83442372801900433 ) ) ;
#3934 = CARTESIAN_POINT ( 'NONE',  ( 19.02544592524343514, -5.153800228976328945, 108.5405762719810383 ) ) ;
#3935 = CARTESIAN_POINT ( 'NONE',  ( 9.474510206698971260, -16.51473224551069308, 27.91557627198103120 ) ) ;
#3936 = CARTESIAN_POINT ( 'NONE',  ( 21.52544592524344225, -5.823673210054117533, 58.54057627198103120 ) ) ;
#3937 = CARTESIAN_POINT ( 'NONE',  ( -13.97604488694527625, -13.89961937509977652, 86.87390960531436690 ) ) ;
#3938 = CARTESIAN_POINT ( 'NONE',  ( 5.719274019375673035, 21.55341960407619339, 82.29275706135234714 ) ) ;
#3939 = CARTESIAN_POINT ( 'NONE',  ( -19.02544592524342804, 5.153800228976336051, 56.04057627198100988 ) ) ;
#3940 = EDGE_CURVE ( 'NONE', #118127, #27924, #43421, .T. ) ;
#3941 = CARTESIAN_POINT ( 'NONE',  ( -16.55341960407611168, -4.379528057220339221, 81.45724293864769550 ) ) ;
#3942 = CARTESIAN_POINT ( 'NONE',  ( -14.29746914071037622, -8.314922557961029526, 34.16775706135234714 ) ) ;
#3943 = CARTESIAN_POINT ( 'NONE',  ( -15.72974639402176322, -15.80617190586768395, 69.37609039468567573 ) ) ;
#3944 = ORIENTED_EDGE ( 'NONE', *, *, #32795, .T. ) ;
#3945 = CARTESIAN_POINT ( 'NONE',  ( -19.02544592524334988, -5.153800228976617603, 23.95942372801900078 ) ) ;
#3946 = CARTESIAN_POINT ( 'NONE',  ( 5.049401038297881783, 19.05341960407617563, 77.29275706135231871 ) ) ;
#3947 = CARTESIAN_POINT ( 'NONE',  ( -19.03943276465977164, -0.05219959533935918106, 38.75109039468566152 ) ) ;
#3948 = DIRECTION ( 'NONE',  ( -1.000000000000000000, 0.000000000000000000, 0.000000000000000000 ) ) ;
#3949 = CARTESIAN_POINT ( 'NONE',  ( -18.67979575497193778, 10.72451020669871902, 43.33442372801901143 ) ) ;
#3950 = DIRECTION ( 'NONE',  ( 4.336808689942018229E-16, -1.000000000000000000, -0.000000000000000000 ) ) ;
#3951 = CARTESIAN_POINT ( 'NONE',  ( -0.05219959533936034679, 19.03943276465977164, 32.50109039468566863 ) ) ;
#3952 = CARTESIAN_POINT ( 'NONE',  ( -9.474510206698964154, 16.51473224551069663, 50.41557627198102409 ) ) ;
#3953 = CARTESIAN_POINT ( 'NONE',  ( -5.049401038297874678, -19.05341960407617918, 29.79275706135232227 ) ) ;
#3954 = CARTESIAN_POINT ( 'NONE',  ( -16.52544592524335698, -4.483927247898792601, 98.95942372801903275 ) ) ;
#3956 = CARTESIAN_POINT ( 'NONE',  ( -0.05219959533937732626, 21.53943276465977519, 82.50109039468568994 ) ) ;
#3955 = CARTESIAN_POINT ( 'NONE',  ( 13.97604488694527802, 13.89961937509977652, 109.3739096053143669 ) ) ;
#3957 = CARTESIAN_POINT ( 'NONE',  ( 36.91746824999999887, 11.99521256947799053, -3.524999997268813079 ) ) ;
#3958 = CARTESIAN_POINT ( 'NONE',  ( -33.83915642739259511, 1.250096592814743612, 100.3591031859434395 ) ) ;
#3959 = CARTESIAN_POINT ( 'NONE',  ( -15.72974639402176322, -15.80617190586768395, 89.37609039468568994 ) ) ;
#3960 = CARTESIAN_POINT ( 'NONE',  ( 21.30000000000002913, -7.567280135845077329E-14, -58.85720012050612837 ) ) ;
#3961 = CARTESIAN_POINT ( 'NONE',  ( -16.51473224551069308, -9.474510206698971260, 106.6655762719810383 ) ) ;
#3962 = CARTESIAN_POINT ( 'NONE',  ( 27.48145228890733094, -25.86941904439665052, -20.55877432051690690 ) ) ;
#3963 = CARTESIAN_POINT ( 'NONE',  ( -13.89961937509977652, 13.97604488694528158, 55.62390960531434558 ) ) ;
#3964 = CARTESIAN_POINT ( 'NONE',  ( 21.53943276465977519, -0.05219959533907433946, 53.74890960531437401 ) ) ;
#3965 = CARTESIAN_POINT ( 'NONE',  ( 14.34966873604960469, 8.224510206698951720, 24.16557627198103120 ) ) ;
#3967 = CARTESIAN_POINT ( 'NONE',  ( 13.89961937509977652, -13.97604488694527269, 93.12390960531436690 ) ) ;
#3966 = CARTESIAN_POINT ( 'NONE',  ( 12.06949235617757843, -12.14591786802309237, 98.12390960531436690 ) ) ;
#3968 = CARTESIAN_POINT ( 'NONE',  ( 9.564922557961047289, -16.46253265017146816, 25.41775706135234003 ) ) ;
#3969 = CARTESIAN_POINT ( 'NONE',  ( -19.03943276465977164, 0.05219959533909376836, 36.24890960531436690 ) ) ;
#3970 = CARTESIAN_POINT ( 'NONE',  ( 4.379528057220339221, -16.55341960407611168, 107.7072429386476955 ) ) ;
#3971 = CARTESIAN_POINT ( 'NONE',  ( -15.80617190586768217, 15.72974639402176855, 53.12609039468568284 ) ) ;
#3972 = CARTESIAN_POINT ( 'NONE',  ( -16.53943276465976808, -0.05219959533934237506, 108.7510903946857042 ) ) ;
#3973 = CARTESIAN_POINT ( 'NONE',  ( 5.049401038297881783, 19.05341960407617563, 62.29275706135234003 ) ) ;
#3974 = PLANE ( 'NONE',  #72309 ) ;
#3975 = CARTESIAN_POINT ( 'NONE',  ( -16.46253265017160317, 9.564922557960807481, 110.8322429386476955 ) ) ;
#3976 = CARTESIAN_POINT ( 'NONE',  ( 14.34966873604960469, 8.224510206698951720, 79.16557627198103830 ) ) ;
#3977 = CARTESIAN_POINT ( 'NONE',  ( -19.05341960407617563, 5.049401038297882671, 43.54275706135232582 ) ) ;
#3978 = CARTESIAN_POINT ( 'NONE',  ( 0.05219959533909260263, 19.03943276465977164, 64.99890960531436690 ) ) ;
#3979 = CARTESIAN_POINT ( 'NONE',  ( -4.483927247898539470, -16.52544592524342804, 57.29057627198103120 ) ) ;
#3980 = CARTESIAN_POINT ( 'NONE',  ( 5.153800228976615827, -19.02544592524334988, 85.20942372801900433 ) ) ;
#3981 = CARTESIAN_POINT ( 'NONE',  ( -21.55341960407610458, -5.719274019375992779, 36.45724293864768839 ) ) ;
#3982 = ORIENTED_EDGE ( 'NONE', *, *, #6380, .F. ) ;
#3983 = CARTESIAN_POINT ( 'NONE',  ( 8.224510206698953496, -14.34966873604960469, 107.9155762719810241 ) ) ;
#3984 = DIRECTION ( 'NONE',  ( -0.7071067811865467956, 0.000000000000000000, 0.7071067811865483499 ) ) ;
#3986 = CARTESIAN_POINT ( 'NONE',  ( 5.823673210054125526, 21.52544592524343514, 59.79057627198103120 ) ) ;
#3985 = CARTESIAN_POINT ( 'NONE',  ( 16.51473224551069308, 9.474510206698969483, 59.16557627198102409 ) ) ;
#3987 = CARTESIAN_POINT ( 'NONE',  ( -13.97604488694527625, -13.89961937509977652, 41.87390960531435979 ) ) ;
#3989 = CARTESIAN_POINT ( 'NONE',  ( 13.89961937509977652, -13.97604488694527269, 78.12390960531433848 ) ) ;
#3988 = CARTESIAN_POINT ( 'NONE',  ( 16.52544592524335698, 4.483927247898782831, 91.45942372801901854 ) ) ;
#3990 = CARTESIAN_POINT ( 'NONE',  ( -5.049401038297874678, -19.05341960407617918, 59.79275706135231871 ) ) ;
#3991 = CARTESIAN_POINT ( 'NONE',  ( -15.80617190586768217, 15.72974639402176855, 73.12609039468567573 ) ) ;
#3992 = CARTESIAN_POINT ( 'NONE',  ( -5.719274019375978568, 21.55341960407610458, 45.20724293864769550 ) ) ;
#3993 = CARTESIAN_POINT ( 'NONE',  ( -0.05219959533909027116, -19.03943276465977164, 102.4989096053143669 ) ) ;
#3994 = CARTESIAN_POINT ( 'NONE',  ( 9.564922557960805705, 16.46253265017160317, 29.58224293864769550 ) ) ;
#3995 = CARTESIAN_POINT ( 'NONE',  ( -14.34966873604972548, 8.224510206698743886, 88.33442372801901854 ) ) ;
#3997 = CARTESIAN_POINT ( 'NONE',  ( -19.05341960407617563, 5.049401038297882671, 103.5427570613523329 ) ) ;
#3996 = B_SPLINE_CURVE_WITH_KNOTS ( 'NONE', 3,
 ( #16571, #139889, #1378, #171245, #14584, #32734, #94386, #156065, #183444, #17563, #76241, #2382, #106584, #137919, #168261, #199603, #29757, #91392 ),
 .UNSPECIFIED., .F., .F.,
 ( 4, 2, 2, 2, 2, 2, 2, 2, 4 ),
 ( 0.001292559216902551241, 0.001886468742252372498, 0.002480378267602193973, 0.003074287792952015014, 0.003668197318301836922, 0.004262106843651657963, 0.004856016369001479004, 0.005449925894351300912, 0.006043835419701121953 ),
 .UNSPECIFIED. ) ;
#3998 = DIRECTION ( 'NONE',  ( -0.1178549842436482503, 0.9930308165857338887, -1.226674847570000151E-16 ) ) ;
#3999 = CARTESIAN_POINT ( 'NONE',  ( 0.000000000000000000, -105.0000000000000000, 7.000000000000003553 ) ) ;
#4000 = CARTESIAN_POINT ( 'NONE',  ( 21.52544592524334988, 5.823673210054432836, 96.45942372801901854 ) ) ;
#4001 = CARTESIAN_POINT ( 'NONE',  ( 16.52544592524342804, -4.483927247898539470, 58.54057627198103120 ) ) ;
#4002 = CARTESIAN_POINT ( 'NONE',  ( 16.52544592524342804, -4.483927247898539470, 68.54057627198103830 ) ) ;
#4003 = CARTESIAN_POINT ( 'NONE',  ( 5.719274019375991003, -21.55341960407610458, 97.70724293864772392 ) ) ;
#4004 = CARTESIAN_POINT ( 'NONE',  ( 10.72451020669898902, -18.67979575497178502, 82.91557627198103830 ) ) ;
#4005 = CARTESIAN_POINT ( 'NONE',  ( -5.427562675786936573E-15, 30.27659582821221207, 149.4843446568999923 ) ) ;
#4006 = CARTESIAN_POINT ( 'NONE',  ( 21.55341960407610458, 5.719274019375980345, 38.95724293864768839 ) ) ;
#4007 = CARTESIAN_POINT ( 'NONE',  ( -4.483927247898782831, 16.52544592524335698, 62.70942372801902565 ) ) ;
#4008 = CARTESIAN_POINT ( 'NONE',  ( 8.314922557960818139, 14.29746914071049879, 89.58224293864768129 ) ) ;
#4009 = CARTESIAN_POINT ( 'NONE',  ( 0.05219959533909260263, 19.03943276465977164, 39.99890960531436690 ) ) ;
#4010 =( NAMED_UNIT ( * ) SI_UNIT ( $, .STERADIAN. ) SOLID_ANGLE_UNIT ( ) );
#4011 = CARTESIAN_POINT ( 'NONE',  ( 34.36934878537046956, -7.254149193659900519, 46.92043707032848943 ) ) ;
#4012 = CARTESIAN_POINT ( 'NONE',  ( 14.29746914071037800, 8.314922557961029526, 96.66775706135234714 ) ) ;
#4013 = CARTESIAN_POINT ( 'NONE',  ( 15.72974639402176855, 15.80617190586768217, 31.87609039468567929 ) ) ;
#4014 = CARTESIAN_POINT ( 'NONE',  ( 19.05341960407611168, 5.049401038298154454, 78.95724293864769550 ) ) ;
#4015 = CARTESIAN_POINT ( 'NONE',  ( 15.80617190586769283, -15.72974639402175789, 65.62609039468568994 ) ) ;
#4016 = CARTESIAN_POINT ( 'NONE',  ( 9.564922557960805705, 16.46253265017160317, 109.5822429386476955 ) ) ;
#4017 = CARTESIAN_POINT ( 'NONE',  ( -2.802625768539468432, -39.09149893265184517, -33.00000000000000000 ) ) ;
#4018 = ORIENTED_EDGE ( 'NONE', *, *, #130470, .T. ) ;
#4019 = CARTESIAN_POINT ( 'NONE',  ( -18.67979575497193778, 10.72451020669871902, 63.33442372801900433 ) ) ;
#4021 = CARTESIAN_POINT ( 'NONE',  ( 5.153800228976335163, 19.02544592524342804, 114.7905762719810241 ) ) ;
#4020 = CARTESIAN_POINT ( 'NONE',  ( -19.03943276465977164, 0.05219959533909376836, 41.24890960531435269 ) ) ;
#4022 = CARTESIAN_POINT ( 'NONE',  ( 0.05219959533936267826, -19.03943276465977164, 65.00109039468567573 ) ) ;
#4023 = CARTESIAN_POINT ( 'NONE',  ( -5.823673210054431948, 21.52544592524334988, 22.70942372801901499 ) ) ;
#4024 = CARTESIAN_POINT ( 'NONE',  ( -9.474510206698720793, -16.51473224551083518, 54.58442372801899722 ) ) ;
#4025 = CARTESIAN_POINT ( 'NONE',  ( 5.049401038298161559, -19.05341960407611168, 27.70724293864769550 ) ) ;
#4026 = CARTESIAN_POINT ( 'NONE',  ( -12.14591786802326823, 12.06949235617739902, 98.12609039468570415 ) ) ;
#4027 = CARTESIAN_POINT ( 'NONE',  ( -19.02544592524334988, -5.153800228976617603, 63.95942372801899012 ) ) ;
#4028 = CARTESIAN_POINT ( 'NONE',  ( 4.379528057220339221, -16.55341960407611168, 22.70724293864769194 ) ) ;
#4030 = ORIENTED_EDGE ( 'NONE', *, *, #121810, .F. ) ;
#4029 = CARTESIAN_POINT ( 'NONE',  ( 16.46253265017146816, 9.564922557961045513, 46.66775706135233293 ) ) ;
#4031 = CARTESIAN_POINT ( 'NONE',  ( -5.049401038298153566, 19.05341960407611168, 90.20724293864766707 ) ) ;
#4032 = CARTESIAN_POINT ( 'NONE',  ( 5.823673210054444382, -21.52544592524334988, 90.20942372801903275 ) ) ;
#4033 = CARTESIAN_POINT ( 'NONE',  ( -18.67979575497193778, 10.72451020669871902, 113.3344237280190328 ) ) ;
#4034 = CARTESIAN_POINT ( 'NONE',  ( -22.00000000000000000, -1.163414459189985801E-14, 95.00000000000000000 ) ) ;
#4035 = CARTESIAN_POINT ( 'NONE',  ( -18.62759615963255300, -10.81492255796106328, 89.16775706135236135 ) ) ;
#4036 = CARTESIAN_POINT ( 'NONE',  ( 14.29746914071037800, 8.314922557961029526, 36.66775706135234714 ) ) ;
#4037 = CARTESIAN_POINT ( 'NONE',  ( 9.474510206698971260, -16.51473224551069308, 87.91557627198102409 ) ) ;
#4039 = EDGE_CURVE ( 'NONE', #135144, #122542, #15177, .T. ) ;
#4038 = CARTESIAN_POINT ( 'NONE',  ( -0.05219959533907301413, -21.53943276465977519, 32.49890960531435979 ) ) ;
#4040 = CARTESIAN_POINT ( 'NONE',  ( -27.18966431762778058, 4.276553394869404556, 168.7322077152510928 ) ) ;
#4041 = CARTESIAN_POINT ( 'NONE',  ( -13.97604488694527625, -13.89961937509977652, 81.87390960531436690 ) ) ;
#4042 = CARTESIAN_POINT ( 'NONE',  ( -19.25176906914649777, -5.499999999999744205, 40.99927264242279534 ) ) ;
#4043 = CARTESIAN_POINT ( 'NONE',  ( 19.05341960407617918, -5.049401038297876454, 66.04275706135233293 ) ) ;
#4044 = CARTESIAN_POINT ( 'NONE',  ( -13.89961937509977652, 13.97604488694528158, 100.6239096053143669 ) ) ;
#4045 = CARTESIAN_POINT ( 'NONE',  ( -21.53943276465977519, -0.05219959533937600094, 103.7510903946857042 ) ) ;
#4046 = CARTESIAN_POINT ( 'NONE',  ( 12.14591786802309770, 12.06949235617756955, 99.37390960531436690 ) ) ;
#4047 = CARTESIAN_POINT ( 'NONE',  ( -21.55341960407610458, -5.719274019375992779, 46.45724293864769550 ) ) ;
#4048 = CARTESIAN_POINT ( 'NONE',  ( -10.72451020669898014, 18.67979575497178502, 35.41557627198102409 ) ) ;
#4049 = CARTESIAN_POINT ( 'NONE',  ( 16.55341960407611168, 4.379528057220329451, 108.9572429386476955 ) ) ;
#4050 = DIRECTION ( 'NONE',  ( -1.047444401652940164E-14, -1.000000000000000000, -0.000000000000000000 ) ) ;
#4051 = CARTESIAN_POINT ( 'NONE',  ( 19.02544592524334988, 5.153800228976608722, 61.45942372801900433 ) ) ;
#4052 = CARTESIAN_POINT ( 'NONE',  ( -14.34966873604972548, 8.224510206698743886, 113.3344237280190328 ) ) ;
#4053 = CARTESIAN_POINT ( 'NONE',  ( -19.05341960407611168, -5.049401038298163336, 96.45724293864769550 ) ) ;
#4054 = CARTESIAN_POINT ( 'NONE',  ( -18.67979575497193778, 10.72451020669871902, 78.33442372801901854 ) ) ;
#4055 = CARTESIAN_POINT ( 'NONE',  ( -21.53943276465977519, 0.05219959533907696930, 61.24890960531435979 ) ) ;
#4056 = CARTESIAN_POINT ( 'NONE',  ( 21.53943276465977519, 0.05219959533937863772, 41.25109039468568284 ) ) ;
#4057 = CARTESIAN_POINT ( 'NONE',  ( 10.81492255796078972, 18.62759615963270932, 94.58224293864769550 ) ) ;
#4058 = CARTESIAN_POINT ( 'NONE',  ( -10.72451020669870658, -18.67979575497194134, 39.58442372801901143 ) ) ;
#4059 = CARTESIAN_POINT ( 'NONE',  ( 9.474510206698971260, -16.51473224551069308, 27.91557627198103120 ) ) ;
#4060 = CARTESIAN_POINT ( 'NONE',  ( -9.474510206698964154, 16.51473224551069663, 80.41557627198103830 ) ) ;
#4061 = CARTESIAN_POINT ( 'NONE',  ( 8.224510206698742110, 14.34966873604972548, 77.08442372801901854 ) ) ;
#4062 = CARTESIAN_POINT ( 'NONE',  ( -14.34966873604960291, -8.224510206698953496, 101.6655762719810383 ) ) ;
#4063 = CARTESIAN_POINT ( 'NONE',  ( 13.89961937509977652, -13.97604488694527269, 113.1239096053143527 ) ) ;
#4064 = CARTESIAN_POINT ( 'NONE',  ( -16.53943276465976808, 0.05219959533911058130, 56.24890960531436690 ) ) ;
#4065 = CARTESIAN_POINT ( 'NONE',  ( 8.224510206698953496, -14.34966873604960469, 22.91557627198102765 ) ) ;
#4066 = CARTESIAN_POINT ( 'NONE',  ( 9.474510206698971260, -16.51473224551069308, 47.91557627198102409 ) ) ;
#4067 = CARTESIAN_POINT ( 'NONE',  ( -13.89961937509977652, 13.97604488694528158, 30.62390960531435269 ) ) ;
#4068 = CARTESIAN_POINT ( 'NONE',  ( -18.67979575497178146, -10.72451020669898902, 41.66557627198103120 ) ) ;
#4069 = EDGE_CURVE ( 'NONE', #163981, #33758, #46734, .T. ) ;
#4070 = CARTESIAN_POINT ( 'NONE',  ( 19.02544592524334988, 5.153800228976608722, 21.45942372801899012 ) ) ;
#4072 = CARTESIAN_POINT ( 'NONE',  ( 4.379528057220339221, -16.55341960407611168, 32.70724293864770260 ) ) ;
#4071 = CARTESIAN_POINT ( 'NONE',  ( -17.49999999999998934, -5.622605283950890431, 41.31207310596112592 ) ) ;
#4073 = CARTESIAN_POINT ( 'NONE',  ( -5.719274019375665041, -21.55341960407619695, 49.79275706135234714 ) ) ;
#4074 = CARTESIAN_POINT ( 'NONE',  ( 16.51473224551069308, 9.474510206698969483, 114.1655762719810241 ) ) ;
#4075 = CARTESIAN_POINT ( 'NONE',  ( -8.314922557961024197, 14.29746914071037800, 62.91775706135236135 ) ) ;
#4076 = CARTESIAN_POINT ( 'NONE',  ( 19.05341960407617918, -5.049401038297876454, 66.04275706135233293 ) ) ;
#4077 = CARTESIAN_POINT ( 'NONE',  ( -14.34966873604960291, -8.224510206698953496, 31.66557627198102054 ) ) ;
#4078 = CARTESIAN_POINT ( 'NONE',  ( 12.14591786802327356, -12.06949235617739191, 100.6260903946857184 ) ) ;
#4079 = CARTESIAN_POINT ( 'NONE',  ( -0.05219959533909027116, -19.03943276465977164, 37.49890960531436690 ) ) ;
#4080 = CARTESIAN_POINT ( 'NONE',  ( 5.153800228976335163, 19.02544592524342804, 59.79057627198100988 ) ) ;
#4081 = CARTESIAN_POINT ( 'NONE',  ( -9.474510206698964154, 16.51473224551069663, 25.41557627198103120 ) ) ;
#4082 = CARTESIAN_POINT ( 'NONE',  ( 15.80617190586769283, -15.72974639402175789, 30.62609039468567929 ) ) ;
#4083 = CARTESIAN_POINT ( 'NONE',  ( -19.03943276465977164, 0.05219959533909376836, 51.24890960531436690 ) ) ;
#4084 = FACE_OUTER_BOUND ( 'NONE', #127362, .T. ) ;
#4085 = CARTESIAN_POINT ( 'NONE',  ( -9.564922557960796823, -16.46253265017161027, 47.08224293864769550 ) ) ;
#4086 = CARTESIAN_POINT ( 'NONE',  ( 13.97604488694527802, 13.89961937509977652, 114.3739096053143669 ) ) ;
#4088 = CARTESIAN_POINT ( 'NONE',  ( -8.224510206698948167, 14.34966873604960824, 110.4155762719810383 ) ) ;
#4087 = CARTESIAN_POINT ( 'NONE',  ( 10.72451020669871369, 18.67979575497193778, 62.08442372801901143 ) ) ;
#4089 = CARTESIAN_POINT ( 'NONE',  ( 19.03943276465977164, -0.05219959533909143690, 108.7489096053143527 ) ) ;
#4090 = CARTESIAN_POINT ( 'NONE',  ( 16.53943276465976808, 0.05219959533934440121, 81.25109039468568994 ) ) ;
#4091 = CARTESIAN_POINT ( 'NONE',  ( 15.72974639402176855, 15.80617190586768217, 86.87609039468568994 ) ) ;
#4092 = CARTESIAN_POINT ( 'NONE',  ( -8.224510206698735004, -14.34966873604973081, 49.58442372801901143 ) ) ;
#4093 = CARTESIAN_POINT ( 'NONE',  ( -5.049401038298153566, 19.05341960407611168, 100.2072429386476955 ) ) ;
#4094 = CARTESIAN_POINT ( 'NONE',  ( -14.29746914071037622, -8.314922557961029526, 44.16775706135234714 ) ) ;
#4095 = CARTESIAN_POINT ( 'NONE',  ( 14.29746914071037800, 8.314922557961029526, 26.66775706135235424 ) ) ;
#4096 = CARTESIAN_POINT ( 'NONE',  ( 12.06949235617739724, 12.14591786802326823, 86.87609039468568994 ) ) ;
#4097 = CARTESIAN_POINT ( 'NONE',  ( 13.97604488694548053, -13.89961937509957401, 110.6260903946856615 ) ) ;
#4098 = CARTESIAN_POINT ( 'NONE',  ( 21.55341960407610458, 5.719274019375980345, 103.9572429386476813 ) ) ;
#4100 = CARTESIAN_POINT ( 'NONE',  ( -16.46253265017146816, -9.564922557961047289, 99.16775706135233293 ) ) ;
#4099 = CARTESIAN_POINT ( 'NONE',  ( 4.483927247898545687, 16.52544592524342804, 109.7905762719810383 ) ) ;
#4101 = CARTESIAN_POINT ( 'NONE',  ( -12.14591786802326823, 12.06949235617739902, 68.12609039468567573 ) ) ;
#4102 = CARTESIAN_POINT ( 'NONE',  ( 24.06756124613832171, 8.142616467494580235, 169.4332804344653312 ) ) ;
#4103 = CARTESIAN_POINT ( 'NONE',  ( 5.153800228976615827, -19.02544592524334988, 65.20942372801900433 ) ) ;
#4104 = CARTESIAN_POINT ( 'NONE',  ( 8.224510206698953496, -14.34966873604960469, 42.91557627198103120 ) ) ;
#4105 = CARTESIAN_POINT ( 'NONE',  ( 0.05219959533910956823, 16.53943276465976808, 34.99890960531435979 ) ) ;
#4106 = CARTESIAN_POINT ( 'NONE',  ( -16.52544592524342804, 4.483927247898546575, 91.04057627198103830 ) ) ;
#4108 = DIRECTION ( 'NONE',  ( -1.000000000000000000, 0.000000000000000000, 0.000000000000000000 ) ) ;
#4107 = CARTESIAN_POINT ( 'NONE',  ( -5.049401038297874678, -19.05341960407617918, 29.79275706135232227 ) ) ;
#4109 = CARTESIAN_POINT ( 'NONE',  ( 18.67979575497194134, -10.72451020669871369, 40.83442372801901854 ) ) ;
#4110 = CARTESIAN_POINT ( 'NONE',  ( 0.05219959533936267826, -19.03943276465977164, 100.0010903946856757 ) ) ;
#4111 = CARTESIAN_POINT ( 'NONE',  ( 13.70000000000001528, -4.867217739956692332E-14, -64.92279855667830191 ) ) ;
#4112 = CARTESIAN_POINT ( 'NONE',  ( 9.474510206698971260, -16.51473224551069308, 87.91557627198102409 ) ) ;
#4113 = CARTESIAN_POINT ( 'NONE',  ( 0.05219959533909260263, 19.03943276465977164, 89.99890960531436690 ) ) ;
#4114 = CARTESIAN_POINT ( 'NONE',  ( -10.72451020669898014, 18.67979575497178502, 55.41557627198102409 ) ) ;
#4115 = CARTESIAN_POINT ( 'NONE',  ( 14.29746914071049879, -8.314922557960816363, 88.33224293864769550 ) ) ;
#4116 = CARTESIAN_POINT ( 'NONE',  ( -5.049401038298153566, 19.05341960407611168, 75.20724293864769550 ) ) ;
#4117 = CARTESIAN_POINT ( 'NONE',  ( 19.02544592524343514, -5.153800228976328945, 33.54057627198102409 ) ) ;
#4118 = CARTESIAN_POINT ( 'NONE',  ( 15.80617190586769283, -15.72974639402175789, 35.62609039468568994 ) ) ;
#4119 = CARTESIAN_POINT ( 'NONE',  ( 5.719274019375673035, 21.55341960407619339, 77.29275706135234714 ) ) ;
#4120 = CARTESIAN_POINT ( 'NONE',  ( 13.97604488694527802, 13.89961937509977652, 59.37390960531434558 ) ) ;
#4121 = CARTESIAN_POINT ( 'NONE',  ( -16.55341960407617563, 4.379528057220093196, 78.54275706135236135 ) ) ;
#4122 = ADVANCED_FACE ( 'NONE', ( #197229 ), #62878, .F. ) ;
#4123 = CARTESIAN_POINT ( 'NONE',  ( 10.72451020669871369, 18.67979575497193778, 32.08442372801901854 ) ) ;
#4124 = CARTESIAN_POINT ( 'NONE',  ( 0.05219959533937995610, -21.53943276465977519, 20.00109039468568639 ) ) ;
#4126 = CARTESIAN_POINT ( 'NONE',  ( 13.89961937509977652, -13.97604488694527269, 78.12390960531433848 ) ) ;
#4125 = CARTESIAN_POINT ( 'NONE',  ( -19.05341960407617563, 5.049401038297882671, 48.54275706135233293 ) ) ;
#4127 = CARTESIAN_POINT ( 'NONE',  ( -19.05341960407617563, 5.049401038297882671, 28.54275706135232937 ) ) ;
#4128 = CARTESIAN_POINT ( 'NONE',  ( -10.72451020669870658, -18.67979575497194134, 84.58442372801903275 ) ) ;
#4129 = CARTESIAN_POINT ( 'NONE',  ( 18.67979575497178502, 10.72451020669898547, 69.16557627198102409 ) ) ;
#4130 = CARTESIAN_POINT ( 'NONE',  ( -16.53943276465976808, 0.05219959533911058130, 56.24890960531436690 ) ) ;
#4132 = CARTESIAN_POINT ( 'NONE',  ( 13.97604488694548053, -13.89961937509957401, 25.62609039468566507 ) ) ;
#4131 = CARTESIAN_POINT ( 'NONE',  ( 0.05219959533937995610, -21.53943276465977519, 95.00109039468568994 ) ) ;
#4133 = CARTESIAN_POINT ( 'NONE',  ( 4.379528057220339221, -16.55341960407611168, 72.70724293864769550 ) ) ;
#4134 = CARTESIAN_POINT ( 'NONE',  ( 9.474510206698971260, -16.51473224551069308, 27.91557627198103120 ) ) ;
#4135 = CARTESIAN_POINT ( 'NONE',  ( 0.05219959533936267826, -19.03943276465977164, 75.00109039468566152 ) ) ;
#4136 = CARTESIAN_POINT ( 'NONE',  ( -4.379528057220328563, 16.55341960407611168, 40.20724293864769550 ) ) ;
#4137 = CARTESIAN_POINT ( 'NONE',  ( -15.72974639402176322, -15.80617190586768395, 79.37609039468567573 ) ) ;
#4138 = CARTESIAN_POINT ( 'NONE',  ( -9.564922557960796823, -16.46253265017161027, 77.08224293864769550 ) ) ;
#4139 = CARTESIAN_POINT ( 'NONE',  ( -13.89961937509957401, -13.97604488694547875, 44.37609039468566863 ) ) ;
#4140 = CARTESIAN_POINT ( 'NONE',  ( -10.81492255796078084, -18.62759615963271287, 52.08224293864768839 ) ) ;
#4141 = CARTESIAN_POINT ( 'NONE',  ( -21.52544592524334988, -5.823673210054445271, 18.95942372801901143 ) ) ;
#4142 = CARTESIAN_POINT ( 'NONE',  ( 16.52544592524335698, 4.483927247898782831, 21.45942372801901499 ) ) ;
#4143 = CARTESIAN_POINT ( 'NONE',  ( -4.483927247898782831, 16.52544592524335698, 72.70942372801901854 ) ) ;
#4145 = CARTESIAN_POINT ( 'NONE',  ( -15.80617190586745835, -15.72974639402198527, 111.8739096053143669 ) ) ;
#4144 = CARTESIAN_POINT ( 'NONE',  ( -6.412877669190335972, 3.889087296526014814, 1.818019484660534424 ) ) ;
#4146 = CARTESIAN_POINT ( 'NONE',  ( -14.34966873604960291, -8.224510206698953496, 106.6655762719810383 ) ) ;
#4147 = CARTESIAN_POINT ( 'NONE',  ( -17.49999999999998579, -3.237210098469594399, 30.28763012620448691 ) ) ;
#4148 = CARTESIAN_POINT ( 'NONE',  ( 16.53943276465976808, 0.05219959533934440121, 41.25109039468568284 ) ) ;
#4149 = CARTESIAN_POINT ( 'NONE',  ( -18.67979575497178146, -10.72451020669898902, 66.66557627198102409 ) ) ;
#4150 = CARTESIAN_POINT ( 'NONE',  ( 4.483927247898790824, -16.52544592524335698, 105.2094237280190328 ) ) ;
#4151 = CARTESIAN_POINT ( 'NONE',  ( -0.05219959533909027116, -19.03943276465977164, 37.49890960531436690 ) ) ;
#4152 = CARTESIAN_POINT ( 'NONE',  ( -14.34966873604972548, 8.224510206698743886, 68.33442372801900433 ) ) ;
#4153 = CARTESIAN_POINT ( 'NONE',  ( -16.51473224551082808, 9.474510206698731452, 58.33442372801900433 ) ) ;
#4154 = CARTESIAN_POINT ( 'NONE',  ( -5.719274019375665041, -21.55341960407619695, 39.79275706135235424 ) ) ;
#4155 = CARTESIAN_POINT ( 'NONE',  ( -10.81492255796078084, -18.62759615963271287, 62.08224293864769550 ) ) ;
#4156 = CARTESIAN_POINT ( 'NONE',  ( 14.29746914071037800, 8.314922557961029526, 101.6677570613523613 ) ) ;
#4157 = CARTESIAN_POINT ( 'NONE',  ( 21.55341960407619695, -5.719274019375665929, 81.04275706135236135 ) ) ;
#4158 = CARTESIAN_POINT ( 'NONE',  ( 21.53943276465977519, -0.05219959533907433946, 58.74890960531436690 ) ) ;
#4159 = CARTESIAN_POINT ( 'NONE',  ( -21.52544592524343514, 5.823673210054127303, 41.04057627198103120 ) ) ;
#4160 = ORIENTED_EDGE ( 'NONE', *, *, #91683, .T. ) ;
#4161 = CARTESIAN_POINT ( 'NONE',  ( -4.483927247898782831, 16.52544592524335698, 82.70942372801900433 ) ) ;
#4162 = CARTESIAN_POINT ( 'NONE',  ( 15.72974639402199770, -15.80617190586745480, 43.12390960531435269 ) ) ;
#4163 = VERTEX_POINT ( 'NONE', #90027 ) ;
#4164 = CARTESIAN_POINT ( 'NONE',  ( -19.05341960407611168, -5.049401038298163336, 96.45724293864769550 ) ) ;
#4165 = CARTESIAN_POINT ( 'NONE',  ( 12.06949235617739724, 12.14591786802326823, 111.8760903946856615 ) ) ;
#4166 = DIRECTION ( 'NONE',  ( -0.000000000000000000, -0.000000000000000000, -1.000000000000000000 ) ) ;
#4167 = CARTESIAN_POINT ( 'NONE',  ( -19.03943276465977164, 0.05219959533909376836, 26.24890960531435624 ) ) ;
#4168 = CARTESIAN_POINT ( 'NONE',  ( -18.67979575497178146, -10.72451020669898902, 61.66557627198103120 ) ) ;
#4169 = CARTESIAN_POINT ( 'NONE',  ( -16.55341960407617563, 4.379528057220093196, 88.54275706135236135 ) ) ;
#4170 = CARTESIAN_POINT ( 'NONE',  ( -21.55341960407619339, 5.719274019375674811, 43.54275706135235424 ) ) ;
#4171 = CARTESIAN_POINT ( 'NONE',  ( -16.51473224551082808, 9.474510206698731452, 108.3344237280190043 ) ) ;
#4172 = CARTESIAN_POINT ( 'NONE',  ( 12.06949235617757843, -12.14591786802309237, 103.1239096053143811 ) ) ;
#4173 = CARTESIAN_POINT ( 'NONE',  ( 0.05219959533936267826, -19.03943276465977164, 110.0010903946856757 ) ) ;
#4174 = CARTESIAN_POINT ( 'NONE',  ( 16.46253265017160672, -9.564922557960803928, 38.33224293864768839 ) ) ;
#4175 = FACE_OUTER_BOUND ( 'NONE', #83053, .T. ) ;
#4176 = CARTESIAN_POINT ( 'NONE',  ( -19.05341960407611168, -5.049401038298163336, 91.45724293864766707 ) ) ;
#4177 = CARTESIAN_POINT ( 'NONE',  ( 12.06949235617739724, 12.14591786802326823, 71.87609039468568994 ) ) ;
#4178 = CARTESIAN_POINT ( 'NONE',  ( 15.72974639402176855, 15.80617190586768217, 101.8760903946857042 ) ) ;
#4179 = CARTESIAN_POINT ( 'NONE',  ( 18.62759615963271287, -10.81492255796078972, 58.33224293864768839 ) ) ;
#4180 = CARTESIAN_POINT ( 'NONE',  ( 14.29746914071037800, 8.314922557961029526, 91.66775706135234714 ) ) ;
#4181 = CARTESIAN_POINT ( 'NONE',  ( -19.02544592524334988, -5.153800228976617603, 78.95942372801900433 ) ) ;
#4182 = CARTESIAN_POINT ( 'NONE',  ( -19.02544592524342804, 5.153800228976336051, 31.04057627198102409 ) ) ;
#4183 = CARTESIAN_POINT ( 'NONE',  ( 19.05341960407611168, 5.049401038298154454, 83.95724293864766707 ) ) ;
#4184 = CARTESIAN_POINT ( 'NONE',  ( 13.89961937509977652, -13.97604488694527269, 28.12390960531435624 ) ) ;
#4185 = CARTESIAN_POINT ( 'NONE',  ( -13.97604488694547697, 13.89961937509957934, 68.12609039468563310 ) ) ;
#4186 = CARTESIAN_POINT ( 'NONE',  ( 24.05407591190871130, -13.01182159662947413, 169.7785964492052244 ) ) ;
#4187 = CARTESIAN_POINT ( 'NONE',  ( 9.564922557960805705, 16.46253265017160317, 94.58224293864769550 ) ) ;
#4188 = CARTESIAN_POINT ( 'NONE',  ( -0.05219959533910754901, -16.53943276465976808, 47.49890960531435979 ) ) ;
#4189 = CARTESIAN_POINT ( 'NONE',  ( -18.67979575497178146, -10.72451020669898902, 56.66557627198103830 ) ) ;
#4190 = CARTESIAN_POINT ( 'NONE',  ( 17.50000000000000000, -5.499999999999992895, 91.21769037696437010 ) ) ;
#4191 =( BOUNDED_SURFACE ( )  B_SPLINE_SURFACE ( 3, 2, ( 
 ( #118549, #161040, #22534, #147888, #41708, #84181, #148883, #165051, #145861, #53870, #115544, #193388, #24548, #177232, #38704, #100361, #23536, #40700, #164059, #39690, #85182, #70038, #86198, #8363, #9374, #116538, #178226, #71039, #55862, #25558, #87202, #10374, #136678, #90175, #106333, #168993, #16328, #92148, #42703, #105350, #166048, #44680, #30497, #121504, #45669, #122496, #141, #135709, #138660, #77978, #15331, #76989, #75997, #153834, #14332, #107320, #119544, #137671, #198360, #27548, #59835, #61810, #197380, #89189, #123480, #12375, #168019, #152838, #75013, #199357, #60822, #184187, #28539, #196402, #74038, #46663, #185172, #170002, #29515, #108322, #91149, #57872, #31493, #151858, #181227, #93146, #183198, #154830, #104364, #150881, #58845, #13349, #120512, #182204, #43688, #167037, #65792, #173991, #79978, #18321, #110311, #95139, #141646, #188170, #80959, #125491, #66787, #51622, #98097, #50639, #3136, #112301, #157821, #156828, #19311, #49643, #35460, #111306, #189167, #34473, #96132, #36442, #190147, #126472, #97111, #142635, #4113, #47666, #158794, #1133, #109318, #127461, #128451, #62807, #20283, #5106, #32490, #159795, #94143, #64811, #172995, #186185, #155822, #139645, #113287, #81929, #143621, #174978, #21290, #124489, #170998, #17319, #78974, #140649, #2139, #63818, #187188, #48659, #171993, #33481, #23295, #176991, #193145, #55620, #103130, #178988, #129446, #192141, #52619, #131458, #117293, #8112, #132465, #9131, #86957, #22293, #25315, #164811, #102129, #163813, #162796, #40455, #101110, #148641, #41465, #82947, #24305, #191145, #70797, #179998, #53622, #177982, #39449, #144625, #133461, #69790, #10131, #85954, #147642, #114281, #71792, #6108, #175984, #194156, #195151, #67789, #56632, #118306, #37452, #99113, #160805, #161800, #54617, #83944, #145624, #7103, #68785, #130442, #115298, #116292, #38461, #100117, #84939, #146620, #121267, #104125, #28305, #45431, #138427, #149634, #165807, #44444, #166805, #120276, #136445, #199113, #46420, #122256, #72807, #135475, #196162, #74783, #60580, #151626, #75756, #152599, #30259, #27304, #168756, #108078, #107084, #91902, #106098, #183946, #167784, #137433, #200107, #61575, #26306, #59593, #90914, #76752, #14090, #57636, #182961, #153594, #29283, #87946, #42461, #15092, #197143, #105119, #13119, #88951, #11132, #123244, #134477, #184935, #119302, #181968, #180985, #150642, #12138, #73802, #58610, #43451, #89945, #198126, #127220, #92907, #157583, #34238, #78736, #80724, #139413, #3881, #33249, #124247, #77747, #81696, #1901, #126242, #31257, #896, #169762, #143379, #51391, #35227, #63581, #185942, #142402, #64577, #47427, #171760, #188933, #4871, #154593, #109083, #187937, #110080, #125255, #79741, #65560, #189916, #50411, #16089, #140412, #62570, #18086, #112071, #94907, #19076, #95900, #173759, #170762, #96880, #32251, #158564, #20053, #49406, #66555, #111069, #128219, #93909, #155587, #17082, #2898, #186954, #48424, #156591, #141410, #172758, #132223, #131218, #174744, #129206, #147400, #83705, #191895, #38223, #114037, #113052, #193916, #194908, #117049, #86712, #6865, #177747, #55379, #71552, #148397, #24059, #101887, #36207, #178744, #70556, #97861, #100872, #39216, #22054, #85714, #82702, #8888, #176749, #67548, #21048, #25069, #145383, #69554, #159551, #144386, #5872, #9891, #190904, #40208, #68544, #52380, #163569, #133217, #175735, #37213, #54386, #98869, #162554, #160565, #130200, #7868, #192909, #53379, #115057, #99878, #161562, #116059, #23055, #84700, #146380, #118065, #26065, #151397, #45205, #179755, #152375, #122029, #149394, #153360, #10889, #135241, #166571, #102886, #72562, #56383, #183719, #121030, #182728, #43215, #76523, #73568, #28071, #14862, #74550, #196913, #150409, #89712, #29052, #138200, #13860, #164571, #165569, #87708, #104883, #90692, #181734, #105871, #44212, #60356, #195922, #198888 ),
 ( #167558, #134237, #12887, #75527, #136217, #41225, #57398, #137202, #27068, #58380, #197892, #119070, #180752, #106859, #42228, #168533, #30031, #11904, #91669, #103889, #88714, #120047, #59361, #188691, #199882, #18843, #157348, #123017, #187705, #64341, #108848, #110835, #169524, #34004, #63343, #154362, #107840, #111829, #32018, #156348, #61346, #31024, #184702, #173517, #81461, #65324, #93676, #15856, #172519, #80488, #158331, #46187, #141174, #92674, #49177, #96643, #170528, #94669, #17848, #19820, #50172, #186716, #95660, #2664, #126010, #77514, #142162, #139186, #661, #79505, #34989, #62331, #3646, #126984, #124001, #185699, #47188, #78499, #109841, #155359, #16848, #140172, #1665, #125020, #48186, #171526, #33014, #160327, #53138, #42737, #37987, #20807, #145146, #165084, #57905, #66318, #82463, #180272, #113803, #21817, #68308, #144149, #143147, #26578, #27584, #149905, #119577, #36971, #7630, #88221, #104399, #181260, #54154, #134753, #4628, #11412, #103406, #127979, #130980, #69314, #52146, #118582, #112815, #41742, #6629, #97622, #51154, #166081, #175498, #99643, #189682, #174508, #35975, #159312, #5634, #73082, #98632, #67311, #196435, #128970, #190670, #83469, #84465, #129959, #192671, #191659, #114817, #161326, #22819, #176509, #146143, #168051, #92183, #60854, #122529, #135742, #15365, #150916, #197413, #14365, #123512, #12409, #153867, #61843, #120545, #170036, #58879, #121537, #91181, #74071, #43723, #89222, #154864, #77021, #138693, #184220, #182238, #137706, #107352, #105384, #175, #183232, #45701, #93179, #167071, #90209, #44713, #185205, #169025, #199390, #30530, #31526, #28573, #151892, #198393, #46696, #106369, #108357, #13382, #75046, #136712, #59870, #29548, #152870, #76030, #63383, #60393, #168570, #33055, #154403, #153403, #44250, #702, #61385, #152410, #123057, #78539, #122065, #13898, #32060, #137240, #31066, #77555, #199922, #139227, #94710, #105907, #198925, #62374, #184743, #14901, #92714, #93716, #141216, #16888, #167593, #30068, #90727, #169569, #155398, #46228, #170569, #47231, #125060, #186757, #29088, #75564, #183757, #140214, #124044, #1707, #185743, #48227, #156388, #17892, #2706, #15897, #108890, #171566, #109882, #45243, #79546, #121072, #182766, #106897, #91709, #76563, #138238, #107882, #189726, #65367, #64383, #83511, #146186, #68350, #38030, #158375, #129014, #145188, #22861, #99686, #175541, #53185, #126051, #6672, #21861, #187748, #52187, #190714, #173563, #37016, #34047, #98677, #128024, #18885, #172561, #176555, #96687, #20854, #49218, #95704, #110876, #161370, #157392, #130001, #19864, #80531, #160370, #191701, #84508, #142205, #5678, #3688, #113845, #127027, #35032, #159356, #82510, #188734, #114860, #51199, #50219, #67354, #111873, #81504, #143192, #4672, #66364, #144192, #112860, #174551, #36018, #97667, #100682, #104693, #162364, #86524, #117873, #54197, #23865, #7671, #135051, #72366, #134040, #194720, #27877, #24875, #179563, #166381, #102699, #85516, #9702, #26876, #148208, #196727, #71366, #133030, #56190, #195733, #42039, #41033, #164387, #178550, #163378, #25880, #87525, #149212, #193722, #58195, #119863, #89518, #118881, #10703, #180565, #57206, #103703, #165383, #88519, #115869, #132033, #69355, #131024, #150215, #181548, #11712, #43027, #73379, #192713, #177558, #39027, #147204, #8695, #70365, #55190, #116859, #40016, #101689, #186518, #155159, #76324, #60162, #14663, #138001, #199685, #197702, #93472, #61150, #15659, #170329, #77318, #47992, #1461, #105679, #92479, #183525, #184512, #137006, #122822, #198696, #16651, #120837, #123803, #78298, #31822, #63139, #45992, #109646, #138986, #107647, #151208, #91474, #139972, #44018, #90503, #464, #121831, #182536, #124818, #32816, #74362, #171328, #152185, #45008, #12696, #169324, #106668, #136028, #30831, #153162, #167365, #154168, #108651, #13669, #28863, #62139, #75336, #185501 ),
 ( #168341, #46992, #59168, #29837, #129764, #5435, #83275, #94467, #113609, #51949, #17646, #2463, #175303, #156148, #64145, #189485, #144949, #79306, #190476, #160129, #187512, #191460, #48978, #173319, #4432, #140975, #110633, #125809, #21617, #159117, #20612, #81270, #114612, #111634, #66120, #52938, #50963, #172314, #96449, #36769, #6430, #33803, #95463, #112622, #34794, #188491, #127785, #67119, #176311, #98433, #157149, #3451, #18644, #142952, #128777, #19628, #143955, #82263, #68112, #80290, #141962, #65128, #126785, #49970, #174314, #158136, #35784, #97431, #11468, #149962, #57959, #71125, #102457, #88274, #164145, #7431, #132791, #56961, #55950, #99446, #53956, #72121, #8451, #116624, #163131, #38791, #37782, #118634, #119630, #41794, #73139, #131796, #25642, #180326, #196489, #134809, #148971, #26631, #161126, #103461, #195486, #22622, #87287, #10460, #146963, #133794, #69115, #165140, #101440, #192473, #145950, #84269, #70124, #194478, #130781, #115631, #177320, #100448, #162128, #23624, #193475, #85272, #54952, #178313, #39776, #24634, #179324, #86282, #147973, #9462, #117626, #40788, #137757, #78061, #31581, #168101, #15418, #184272, #45755, #153924, #1218, #77076, #27639, #90262, #150970, #29599, #138746, #106420, #30586, #107407, #185261, #46753, #166137, #89280, #12465, #228, #60909, #61896, #199441, #92238, #154916, #93231, #62895, #14417, #169080, #16414, #123566, #74125, #76081, #108412, #122585, #42792, #197467, #170087, #151945, #59922, #91230, #182296, #181313, #139729, #104454, #135796, #58933, #75098, #120602, #43776, #105440, #167125, #28625, #13434, #136765, #198451, #121590, #183285, #44767, #152921, #33566, #38298, #94228, #161638, #188255, #79062, #32575, #39293, #156914, #81044, #186272, #155909, #124576, #100950, #8969, #192986, #18411, #140735, #99952, #146455, #85793, #47751, #65878, #171084, #115134, #24141, #95228, #19395, #142720, #147479, #177823, #111397, #23132, #127552, #189253, #17405, #7948, #109405, #2224, #4200, #116134, #63906, #84777, #54464, #125576, #187274, #48743, #3220, #34559, #110397, #172079, #80060, #162634, #53458, #176826, #173082, #141730, #64894, #96217, #126555, #69631, #49729, #157906, #131297, #182802, #193996, #148479, #88788, #10965, #164648, #180826, #178822, #89785, #150481, #28145, #11976, #120119, #44285, #105943, #90763, #103965, #135312, #121108, #196985, #40293, #165643, #151470, #73641, #132304, #86792, #104957, #41302, #149470, #196000, #71630, #70638, #12959, #152446, #74623, #167628, #26143, #58451, #136289, #29125, #55458, #181810, #59435, #117129, #197965, #101967, #163648, #43288, #166643, #179832, #25150, #9970, #133296, #134314, #194986, #56464, #118142, #102963, #27141, #87785, #72639, #57473, #119145, #42304, #79581, #46264, #30104, #125095, #33089, #172595, #95739, #155433, #60427, #1742, #110909, #184778, #108925, #170605, #34081, #64416, #738, #48264, #16923, #78576, #122101, #94745, #75599, #183791, #32095, #2739, #137278, #109918, #141250, #106931, #13932, #168604, #92750, #124080, #45278, #91744, #198960, #126085, #140250, #63420, #62410, #153439, #31102, #185781, #14937, #93752, #76597, #15932, #156425, #187781, #138273, #199956, #186793, #154438, #107919, #47268, #171601, #61421, #17926, #123092, #169604, #77591, #49251, #139262, #82547, #6706, #83545, #161403, #22895, #142239, #3724, #113879, #20889, #80564, #96721, #190748, #98712, #192747, #65401, #111909, #50253, #54230, #84541, #144229, #66398, #5713, #67390, #129047, #127062, #99719, #52222, #21895, #176589, #145224, #115901, #7706, #173597, #160406, #189762, #175576, #143226, #37053, #4708, #146218, #188769, #130036, #69389, #38063, #131058, #68384, #177591, #191735, #53217, #157425, #97703, #39058, #35066, #158409, #114895, #128060, #19898, #18919, #81539, #51234, #112895, #174589, #36054, #159394, #134075, #133063, #23899, #180597, #41068 ),
 ( #194753, #100716, #178585, #151238, #27909, #74393, #149244, #12727, #195765, #162396, #42071, #56225, #85552, #89552, #179596, #136058, #182568, #57239, #58225, #117907, #197733, #102731, #164420, #87557, #26908, #135082, #25913, #10735, #71399, #72399, #118913, #103735, #165415, #86557, #59199, #120868, #147238, #11744, #88551, #73411, #150250, #196758, #119894, #181579, #8730, #24910, #70399, #132067, #43057, #193756, #104723, #55224, #166415, #116893, #40049, #101725, #163414, #148241, #9735, #137037, #183556, #108684, #153193, #75367, #186551, #125842, #167398, #48023, #45042, #91506, #156181, #77352, #76359, #28894, #123835, #184543, #198728, #46023, #1494, #106700, #60194, #155193, #121864, #154201, #499, #122855, #62171, #185533, #170362, #138036, #44051, #168373, #94499, #171361, #17680, #92512, #79338, #139019, #105711, #47026, #199717, #90534, #32849, #107679, #141008, #152216, #31854, #63172, #61183, #2496, #169356, #30866, #15691, #93507, #78332, #16682, #140005, #14697, #124851, #109680, #64177, #13700, #29869, #114644, #99475, #145978, #98465, #66151, #160159, #5467, #142984, #67149, #97460, #33835, #111666, #187544, #7460, #128807, #176342, #143986, #37814, #21650, #190506, #50992, #110666, #126818, #20642, #51980, #22652, #172346, #141994, #80321, #84299, #191489, #112653, #96479, #174344, #35814, #159146, #95495, #129792, #82295, #113638, #6460, #175333, #69144, #161156, #3482, #36800, #19659, #83303, #173353, #144980, #34824, #52967, #157181, #68141, #49011, #18675, #65159, #188524, #50001, #158167, #81300, #4462, #127814, #189519, #70154, #164173, #72149, #166167, #115659, #85300, #23652, #27668, #134838, #55979, #39804, #194506, #117656, #179353, #177349, #73168, #40816, #195516, #149991, #56989, #89308, #181341, #146992, #133825, #163160, #25671, #116651, #102486, #178342, #196517, #100477, #103490, #57988, #11497, #42820, #87316, #151001, #118663, #149000, #130811, #71154, #119659, #8479, #131824, #180354, #101470, #162156, #104483, #12492, #53986, #192502, #193505, #24663, #38819, #10489, #86312, #54982, #41823, #132820, #148001, #165168, #88303, #9491, #26661, #185290, #90290, #184304, #30616, #152949, #92269, #153953, #258, #106451, #74154, #151974, #124606, #1247, #47781, #122614, #186301, #107437, #135825, #15449, #168130, #197495, #62926, #14448, #109433, #155938, #169109, #31611, #91258, #171115, #76111, #137788, #60939, #61927, #108441, #199472, #45785, #44796, #29626, #77107, #138777, #123596, #59952, #32605, #94258, #58962, #46782, #170117, #93261, #154947, #16443, #78092, #139761, #120630, #198480, #182327, #43806, #105469, #167155, #28655, #13462, #75126, #136794, #121619, #183314, #64922, #129560, #50760, #49758, #140763, #97225, #157933, #48772, #19424, #175093, #156941, #110427, #128570, #33594, #127582, #174109, #96245, #35579, #158912, #143746, #111426, #17434, #95258, #67907, #144741, #191259, #65909, #52734, #112417, #79090, #20403, #173112, #2252, #6228, #81071, #114401, #99235, #82051, #36562, #34588, #176102, #142750, #4230, #189282, #5225, #51742, #66907, #190265, #188284, #113403, #98217, #159920, #21409, #3249, #37572, #63934, #125603, #83066, #187301, #172108, #18438, #80089, #141757, #126582, #7225, #85063, #160922, #119425, #179115, #88069, #117417, #149755, #71912, #40583, #24428, #84065, #100239, #194276, #102253, #196286, #145744, #115423, #53749, #57755, #164936, #86076, #69918, #147767, #9253, #70920, #68910, #103254, #132587, #25438, #180122, #87079, #181109, #11258, #177112, #163941, #193268, #55743, #146745, #148764, #8240, #26429, #130570, #133584, #72931, #41590, #134600, #10253, #42583, #195274, #56757, #22415, #101231, #192267, #38583, #161921, #118429, #131584, #23415, #54742, #116414, #178104, #39572, #162919, #77865, #16210, #124371, #137555, #168876, #154717, #30381, #73922, #199238, #123364, #122379, #165929, #120395, #138543 ),
 ( #198245, #27426, #93029, #183082, #31379, #186066, #60703, #61695, #121390, #139532, #44565, #106220, #91034, #92026, #21, #167904, #29404, #74901, #59718, #152720, #14211, #45551, #90063, #1015, #62689, #104246, #15214, #75879, #76873, #184068, #107206, #153718, #185057, #150762, #28426, #89071, #12259, #46545, #135592, #108205, #197264, #169886, #58726, #182089, #43572, #105237, #166925, #151745, #13238, #136564, #2023, #140534, #82826, #51510, #172878, #156712, #111188, #34359, #96020, #94025, #190036, #157705, #112190, #66674, #173878, #144507, #97981, #63702, #189053, #79863, #80844, #33364, #19195, #95023, #113172, #17201, #20170, #174861, #128337, #159674, #142521, #5991, #35348, #4000, #47549, #188055, #36327, #125377, #187073, #96999, #18205, #78855, #21170, #129329, #170881, #67671, #49525, #64697, #65679, #158682, #81816, #127341, #126358, #141532, #3020, #50528, #143504, #4988, #109202, #32372, #155706, #48543, #110197, #171875, #163694, #9015, #146500, #70683, #100996, #37333, #115178, #191024, #149514, #132349, #118187, #147527, #179878, #102012, #194041, #54506, #114159, #130320, #24187, #55505, #26188, #175861, #145504, #83823, #87828, #195032, #116178, #99996, #177868, #39337, #162681, #98992, #133341, #85837, #117175, #10014, #178870, #11011, #41346, #6985, #40337, #23177, #25196, #176871, #86838, #38340, #56509, #160681, #148524, #103008, #71674, #164693, #72685, #52499, #22173, #68665, #192017, #131341, #53501, #161681, #84821, #7991, #69674, #193029, #79375, #18712, #57519, #141046, #73687, #181855, #49047, #170397, #166688, #119187, #16716, #74668, #165688, #136335, #94535, #135359, #27186, #48059, #150526, #44329, #93542, #13005, #155227, #78366, #63208, #28191, #134360, #12025, #187579, #64213, #110702, #182846, #172382, #31888, #196044, #140040, #89833, #180872, #125879, #198009, #33873, #42348, #1529, #156217, #151513, #95532, #2532, #17717, #157219, #124888, #104010, #186587, #109715, #88833, #59479, #197031, #58498, #120164, #171398, #43334, #105002, #121153, #108720, #32885, #22690, #19695, #127851, #192541, #113675, #112689, #3520, #160197, #20678, #111704, #82333, #37854, #81337, #173390, #191529, #96515, #190542, #36837, #159183, #98502, #21687, #6498, #174381, #80359, #158205, #130849, #7499, #54024, #128843, #115697, #175369, #142032, #83340, #35851, #65196, #69183, #144023, #177386, #162193, #145017, #99513, #97497, #38857, #5504, #67186, #52016, #68178, #114685, #129830, #53006, #51028, #176380, #161194, #84337, #146016, #66189, #100514, #126855, #188561, #50040, #34860, #143020, #4498, #189556, #103529, #133863, #70194, #148037, #23691, #182363, #41863, #151036, #180392, #12526, #134876, #165204, #87352, #147032, #163198, #57028, #26699, #58999, #8516, #178378, #116688, #120665, #27702, #149038, #132856, #10526, #72189, #195554, #131861, #166201, #118701, #88339, #42855, #150030, #43841, #74191, #39842, #11537, #56015, #73205, #9526, #196553, #71192, #89345, #193545, #58024, #119694, #181377, #85339, #164210, #135860, #101508, #24702, #104520, #194544, #55018, #197531, #105506, #86351, #117693, #179390, #40853, #102527, #25707, #199509, #90326, #46816, #107472, #198517, #169149, #124641, #106488, #59988, #78127, #183350, #77144, #123630, #45821, #185326, #108476, #93296, #60975, #167193, #44833, #17469, #94293, #140798, #15487, #79125, #295, #28690, #170154, #122651, #152011, #155972, #30653, #2287, #48806, #61963, #186336, #184339, #63969, #92307, #153990, #138814, #154982, #1284, #31647, #16477, #137826, #139795, #62960, #47818, #109467, #152986, #125639, #187336, #13497, #171151, #32639, #75162, #136834, #121656, #168166, #29663, #91295, #14485, #76147, #52764, #158944, #144775, #20433, #83099, #190296, #97256, #65943, #33628, #126614, #35611, #82084, #129592, #95290, #141790, #3284, #191288, #159951, #189314, #34620, #127614, #67939, #6259 ),
 ( #36593, #114433, #172141, #64955, #143777, #4263, #19457, #112450, #51773, #176134, #5258, #110460, #66941, #156974, #98249, #128603, #174139, #188316, #96279, #113433, #175126, #18471, #49794, #111460, #173145, #80121, #157965, #21439, #81104, #142782, #50791, #63630, #47475, #76803, #77793, #155637, #110129, #17132, #126286, #141461, #45480, #32303, #123293, #124295, #138474, #16138, #200155, #94954, #60632, #125306, #156638, #171807, #2945, #185992, #49453, #78784, #109132, #90963, #31304, #79788, #183997, #30310, #140461, #61625, #122306, #33295, #172804, #14140, #18134, #91953, #184985, #64624, #170810, #46469, #75807, #93958, #92957, #107136, #154643, #48472, #153646, #168806, #1951, #15141, #942, #187002, #169813, #187983, #111115, #152650, #108129, #137485, #139462, #199165, #62617, #7912, #82750, #146421, #67593, #34285, #114082, #128262, #95945, #23098, #113095, #161604, #116100, #129252, #191939, #51435, #84745, #174786, #36252, #21093, #160607, #68587, #97905, #159596, #4915, #189960, #144430, #5916, #175783, #20098, #69596, #131263, #192951, #145426, #190947, #6909, #52424, #37257, #98915, #22097, #80770, #158608, #157631, #83747, #66598, #130243, #53423, #115100, #176792, #81742, #54430, #19120, #142448, #38265, #99919, #3926, #65606, #127266, #188979, #50455, #112114, #143429, #173806, #35271, #96926, #104922, #134278, #166609, #88754, #195966, #41266, #100914, #117093, #10931, #119111, #12922, #162599, #132268, #70601, #74586, #181773, #102928, #86757, #164613, #135278, #150447, #57438, #163612, #26107, #42271, #196950, #103929, #136254, #28111, #193959, #180792, #9935, #72604, #25113, #87750, #148440, #43254, #147444, #11943, #89749, #58418, #151435, #165609, #197930, #27108, #73607, #177788, #118108, #59398, #55422, #178788, #120085, #71594, #8932, #39258, #24103, #85757, #40257, #101930, #133260, #194951, #56428, #179797, #149435, #40567, #149740, #72916, #104231, #90048, #165912, #9237, #134585, #58710, #57740, #101214, #55727, #73907, #10236, #118413, #164919, #102237, #39557, #120380, #121373, #43556, #13223, #133567, #27410, #182073, #198229, #74886, #150747, #28411, #162903, #105222, #197249, #24412, #89056, #12245, #148748, #135577, #70904, #166910, #103237, #194260, #147750, #86061, #151730, #180106, #136548, #132571, #196271, #59701, #56742, #117400, #41574, #26413, #88052, #179098, #163925, #11241, #119410, #71896, #195258, #181093, #42568, #25421, #87063, #110181, #95007, #141515, #94009, #61678, #155690, #998, #138526, #62672, #93012, #29387, #107188, #183066, #3001, #124353, #171860, #139515, #33348, #17185, #186048, #46527, #106204, #122362, #16193, #47531, #18189, #167888, #137539, #75863, #79846, #187057, #108187, #92007, #169868, #140517, #78839, #109186, #168859, #31362, #170865, #2007, #32356, #64678, #156695, #199221, #63686, #15196, #77848, #30364, #154698, #153701, #48527, #152704, #125360, #44549, #91018, #14193, #60687, #184051, #45534, #76855, #4, #123347, #185040, #19177, #65661, #191006, #35329, #157686, #68647, #7973, #49507, #130303, #127323, #173861, #38323, #159656, #158663, #52482, #6967, #20154, #114141, #128320, #83807, #189035, #80825, #37316, #142503, #36309, #82808, #4971, #144490, #5973, #175842, #81799, #126340, #3981, #176854, #53483, #99979, #174844, #161664, #21153, #188037, #67653, #143486, #23160, #129310, #50510, #190019, #145487, #84803, #111170, #112173, #98974, #66657, #51493, #97964, #160664, #146482, #22156, #172860, #96982, #96002, #191997, #115161, #113154, #34341, #196027, #73669, #135341, #54489, #116161, #177851, #88817, #149498, #27170, #87812, #147507, #39320, #70665, #179860, #102990, #134344, #120147, #57502, #100979, #164676, #150510, #10995, #131323, #85820, #103992, #40318, #148507, #195015, #132332, #69656, #12008, #151497, #197015, #43318, #163676, #119171, #58480, #28174, #104985, #180855, #181838, #193012 ),
 ( #101994, #25178, #71657, #118169, #72667, #55486, #166672, #89816, #162663, #42331, #9997, #165671, #24169, #86820, #8997, #41330, #194023, #117156, #178852, #133324, #56491, #26171, #169634, #140279, #124111, #31130, #76624, #136318, #152474, #46291, #154468, #48292, #197993, #167657, #105972, #109948, #16951, #138302, #122130, #199983, #170634, #185811, #92779, #198987, #61450, #77620, #32123, #139290, #171629, #63449, #29153, #123120, #767, #93780, #62437, #33117, #125125, #90790, #15960, #45307, #107948, #60455, #184805, #183817, #78605, #182831, #47297, #1771, #155461, #186822, #108954, #94774, #12989, #74652, #59464, #153467, #121137, #13960, #75627, #44313, #106957, #137306, #168631, #30131, #91773, #14964, #95767, #3750, #68411, #189789, #188797, #20915, #37080, #50280, #144254, #158436, #113905, #157453, #49278, #67417, #172622, #66424, #112920, #35094, #174615, #36080, #82573, #111937, #156456, #34110, #6733, #83573, #130064, #4735, #191763, #51260, #17955, #97729, #173624, #79608, #145252, #96746, #53246, #38092, #159419, #175603, #19923, #114924, #81565, #143251, #128085, #5741, #190773, #129072, #52248, #127088, #98739, #160432, #21922, #176617, #142267, #141278, #2767, #64443, #126114, #187809, #110936, #18947, #80592, #65427, #9760, #146247, #23925, #99747, #58252, #117934, #26936, #56252, #88578, #10762, #179623, #163441, #22923, #39087, #133088, #41095, #135108, #84569, #54258, #192774, #196784, #103762, #24938, #8756, #86584, #57266, #72426, #102759, #85580, #161431, #164446, #193782, #7733, #150276, #178612, #11772, #181606, #194778, #118940, #116919, #73437, #40075, #101753, #148268, #25940, #134104, #71424, #87583, #70427, #55251, #149270, #195794, #180625, #147266, #119920, #69419, #131085, #42097, #165441, #115929, #177619, #100743, #162424, #132093, #92288, #170134, #43084, #4245, #63951, #173128, #2268, #34603, #156956, #125620, #109449, #169130, #185307, #79106, #187318, #81087, #30635, #276, #138795, #142765, #49776, #171132, #154963, #32621, #3265, #18453, #48789, #31628, #94275, #110443, #64938, #172124, #65925, #96262, #61945, #33610, #78108, #140779, #93278, #155953, #16459, #111441, #15469, #80104, #157948, #126597, #19439, #95273, #127598, #141772, #188299, #104751, #186317, #153972, #123612, #46798, #77126, #139777, #108457, #1265, #62942, #124622, #47799, #17450, #36576, #101246, #22428, #21421, #53762, #69934, #83081, #177127, #191271, #146760, #128585, #82067, #100254, #5241, #99249, #145757, #67921, #7239, #68924, #115436, #144757, #189297, #66921, #39587, #116431, #162935, #37587, #24442, #84078, #175107, #193283, #158928, #161935, #54757, #8254, #86091, #130586, #147782, #38598, #192281, #50774, #129574, #178119, #143760, #190279, #23430, #98231, #20417, #131598, #70934, #112434, #9268, #51755, #159934, #174123, #85077, #6242, #35594, #97240, #52746, #113416, #114415, #176116, #160936, #25454, #43587, #148779, #42598, #89086, #11272, #150778, #12273, #58741, #164949, #132601, #10268, #183098, #59735, #106235, #181124, #44579, #165944, #194291, #73938, #26442, #55757, #121404, #72945, #167918, #14226, #27444, #90077, #149770, #29418, #134615, #196299, #119439, #120410, #166939, #57769, #104261, #103269, #88084, #135607, #197278, #182102, #118442, #91049, #152736, #117431, #105253, #28442, #151760, #13253, #74916, #136579, #198259, #179129, #56770, #40597, #102268, #163956, #87094, #71927, #133597, #195289, #180135, #41604, #199254, #15229, #109217, #17218, #111205, #60721, #30397, #168892, #172897, #79879, #1032, #185072, #139547, #33381, #48560, #32388, #61710, #62704, #140550, #95039, #2038, #34376, #126375, #92044, #78870, #108222, #170896, #123380, #124387, #96036, #46560, #94043, #155721, #157723, #188072, #186082, #110213, #63718, #125393, #184084, #156730, #137571, #45568, #187090, #64713, #122395, #171894, #141548, #153733, #75896, #76888 ) ),
 .UNSPECIFIED., .T., .F., .F. ) 
 B_SPLINE_SURFACE_WITH_KNOTS ( ( 4, 3, 4 ),
 ( 3, 2, 2, 2, 2, 2, 2, 2, 2, 2, 2, 2, 2, 2, 2, 2, 2, 2, 2, 2, 2, 2, 2, 2, 2, 2, 2, 2, 2, 2, 2, 2, 2, 2, 2, 2, 2, 2, 2, 2, 2, 2, 2, 2, 2, 2, 2, 2, 2, 2, 2, 2, 2, 2, 2, 2, 2, 2, 2, 2, 2, 2, 2, 2, 2, 2, 2, 2, 2, 2, 2, 2, 2, 2, 2, 2, 2, 2, 2, 2, 2, 2, 2, 2, 2, 2, 2, 2, 2, 2, 2, 2, 2, 2, 2, 2, 2, 2, 2, 2, 2, 2, 2, 2, 2, 2, 2, 2, 2, 2, 2, 2, 2, 2, 2, 2, 2, 2, 2, 2, 2, 2, 2, 2, 2, 2, 2, 2, 2, 2, 2, 2, 2, 2, 2, 2, 2, 2, 2, 2, 2, 2, 2, 2, 2, 2, 2, 2, 2, 2, 2, 2, 2, 2, 2, 2, 2, 2, 2, 2, 2, 2, 2, 2, 2, 2, 2, 2, 2, 2, 2, 2, 2, 2, 2, 2, 2, 2, 2, 2, 2, 2, 2, 2, 2, 2, 2, 2, 2, 2, 2, 2, 2, 2, 2, 2, 2, 2, 2, 2, 2, 2, 2, 2, 2, 2, 2, 2, 2, 2, 2, 2, 2, 2, 2, 2, 2, 2, 2, 2, 2, 2, 2, 2, 2, 2, 2, 2, 3 ),
 ( 0.000000000000000000, 0.5000000000000000000, 1.000000000000000000 ),
 ( 0.000000000000000000, 0.004385964912280701511, 0.008771929824561403022, 0.01315789473684210453, 0.01754385964912280604, 0.02192982456140350755, 0.02631578947368420907, 0.03070175438596491058, 0.03508771929824561209, 0.03947368421052631360, 0.04385964912280701511, 0.04824561403508771662, 0.05263157894736841813, 0.05701754385964911964, 0.06140350877192982115, 0.06578947368421052266, 0.07017543859649122417, 0.07456140350877192569, 0.07894736842105262720, 0.08333333333333332871, 0.08771929824561403022, 0.09210526315789473173, 0.09649122807017543324, 0.1008771929824561348, 0.1052631578947368363, 0.1096491228070175378, 0.1140350877192982393, 0.1184210526315789408, 0.1228070175438596423, 0.1271929824561403577, 0.1315789473684210453, 0.1359649122807017607, 0.1403508771929824483, 0.1447368421052631637, 0.1491228070175438514, 0.1535087719298245668, 0.1578947368421052544, 0.1622807017543859698, 0.1666666666666666574, 0.1710526315789473728, 0.1754385964912280604, 0.1798245614035087758, 0.1842105263157894635, 0.1885964912280701788, 0.1929824561403508665, 0.1973684210526315819, 0.2017543859649122695, 0.2061403508771929849, 0.2105263157894736725, 0.2149122807017543879, 0.2192982456140350755, 0.2236842105263157909, 0.2280701754385964786, 0.2324561403508771940, 0.2368421052631578816, 0.2412280701754385970, 0.2456140350877192846, 0.2500000000000000000, 0.2543859649122807154, 0.2587719298245614308, 0.2631578947368420907, 0.2675438596491228060, 0.2719298245614035214, 0.2763157894736842368, 0.2807017543859648967, 0.2850877192982456121, 0.2894736842105263275, 0.2938596491228070429, 0.2982456140350877027, 0.3026315789473684181, 0.3070175438596491335, 0.3114035087719298489, 0.3157894736842105088, 0.3201754385964912242, 0.3245614035087719396, 0.3289473684210526550, 0.3333333333333333148, 0.3377192982456140302, 0.3421052631578947456, 0.3464912280701754610, 0.3508771929824561209, 0.3552631578947368363, 0.3596491228070175517, 0.3640350877192982670, 0.3684210526315789269, 0.3728070175438596423, 0.3771929824561403577, 0.3815789473684210731, 0.3859649122807017330, 0.3903508771929824483, 0.3947368421052631637, 0.3991228070175438791, 0.4035087719298245390, 0.4078947368421052544, 0.4122807017543859698, 0.4166666666666666852, 0.4210526315789473450, 0.4254385964912280604, 0.4298245614035087758, 0.4342105263157894912, 0.4385964912280701511, 0.4429824561403508665, 0.4473684210526315819, 0.4517543859649122973, 0.4561403508771929571, 0.4605263157894736725, 0.4649122807017543879, 0.4692982456140351033, 0.4736842105263157632, 0.4780701754385964786, 0.4824561403508771940, 0.4868421052631579093, 0.4912280701754385692, 0.4956140350877192846, 0.5000000000000000000, 0.5043859649122807154, 0.5087719298245614308, 0.5131578947368421462, 0.5175438596491228616, 0.5219298245614034659, 0.5263157894736841813, 0.5307017543859648967, 0.5350877192982456121, 0.5394736842105263275, 0.5438596491228070429, 0.5482456140350877583, 0.5526315789473684736, 0.5570175438596490780, 0.5614035087719297934, 0.5657894736842105088, 0.5701754385964912242, 0.5745614035087719396, 0.5789473684210526550, 0.5833333333333333703, 0.5877192982456140857, 0.5921052631578946901, 0.5964912280701754055, 0.6008771929824561209, 0.6052631578947368363, 0.6096491228070175517, 0.6140350877192982670, 0.6184210526315789824, 0.6228070175438596978, 0.6271929824561403022, 0.6315789473684210176, 0.6359649122807017330, 0.6403508771929824483, 0.6447368421052631637, 0.6491228070175438791, 0.6535087719298245945, 0.6578947368421053099, 0.6622807017543859143, 0.6666666666666666297, 0.6710526315789473450, 0.6754385964912280604, 0.6798245614035087758, 0.6842105263157894912, 0.6885964912280702066, 0.6929824561403509220, 0.6973684210526315264, 0.7017543859649122417, 0.7061403508771929571, 0.7105263157894736725, 0.7149122807017543879, 0.7192982456140351033, 0.7236842105263158187, 0.7280701754385965341, 0.7324561403508771384, 0.7368421052631578538, 0.7412280701754385692, 0.7456140350877192846, 0.7500000000000000000, 0.7543859649122807154, 0.7587719298245614308, 0.7631578947368421462, 0.7675438596491228616, 0.7719298245614034659, 0.7763157894736841813, 0.7807017543859648967, 0.7850877192982456121, 0.7894736842105263275, 0.7938596491228070429, 0.7982456140350877583, 0.8026315789473684736, 0.8070175438596490780, 0.8114035087719297934, 0.8157894736842105088, 0.8201754385964912242, 0.8245614035087719396, 0.8289473684210526550, 0.8333333333333333703, 0.8377192982456140857, 0.8421052631578946901, 0.8464912280701754055, 0.8508771929824561209, 0.8552631578947368363, 0.8596491228070175517, 0.8640350877192982670, 0.8684210526315789824, 0.8728070175438596978, 0.8771929824561403022, 0.8815789473684210176, 0.8859649122807017330, 0.8903508771929824483, 0.8947368421052631637, 0.8991228070175438791, 0.9035087719298245945, 0.9078947368421053099, 0.9122807017543859143, 0.9166666666666666297, 0.9210526315789473450, 0.9254385964912280604, 0.9298245614035087758, 0.9342105263157894912, 0.9385964912280702066, 0.9429824561403509220, 0.9473684210526315264, 0.9517543859649122417, 0.9561403508771929571, 0.9605263157894736725, 0.9649122807017543879, 0.9692982456140351033, 0.9736842105263158187, 0.9780701754385965341, 0.9824561403508771384, 0.9868421052631578538, 0.9912280701754385692, 0.9956140350877192846, 1.000000000000000000 ),
 .UNSPECIFIED. ) 
 GEOMETRIC_REPRESENTATION_ITEM ( )  RATIONAL_B_SPLINE_SURFACE ( (
 ( 1.000000000000000000, 0.9659258262890683122, 1.000000000000000000, 0.9659258262890683122, 1.000000000000000000, 0.9659258262890683122, 1.000000000000000000, 0.9659258262890683122, 1.000000000000000000, 0.9659258262890683122, 1.000000000000000000, 0.9659258262890683122, 1.000000000000000000, 0.9659258262890683122, 1.000000000000000000, 0.9659258262890683122, 1.000000000000000000, 0.9659258262890683122, 1.000000000000000000, 0.9659258262890683122, 1.000000000000000000, 0.9659258262890683122, 1.000000000000000000, 0.9659258262890683122, 1.000000000000000000, 0.9659258262890683122, 1.000000000000000000, 0.9659258262890683122, 1.000000000000000000, 0.9659258262890683122, 1.000000000000000000, 0.9659258262890683122, 1.000000000000000000, 0.9659258262890683122, 1.000000000000000000, 0.9659258262890683122, 1.000000000000000000, 0.9659258262890683122, 1.000000000000000000, 0.9659258262890683122, 1.000000000000000000, 0.9659258262890683122, 1.000000000000000000, 0.9659258262890683122, 1.000000000000000000, 0.9659258262890683122, 1.000000000000000000, 0.9659258262890683122, 1.000000000000000000, 0.9659258262890683122, 1.000000000000000000, 0.9659258262890683122, 1.000000000000000000, 0.9659258262890683122, 1.000000000000000000, 0.9659258262890683122, 1.000000000000000000, 0.9659258262890683122, 1.000000000000000000, 0.9659258262890683122, 1.000000000000000000, 0.9659258262890683122, 1.000000000000000000, 0.9659258262890683122, 1.000000000000000000, 0.9659258262890683122, 1.000000000000000000, 0.9659258262890683122, 1.000000000000000000, 0.9659258262890683122, 1.000000000000000000, 0.9659258262890683122, 1.000000000000000000, 0.9659258262890683122, 1.000000000000000000, 0.9659258262890683122, 1.000000000000000000, 0.9659258262890683122, 1.000000000000000000, 0.9659258262890683122, 1.000000000000000000, 0.9659258262890683122, 1.000000000000000000, 0.9659258262890683122, 1.000000000000000000, 0.9659258262890683122, 1.000000000000000000, 0.9659258262890683122, 1.000000000000000000, 0.9659258262890683122, 1.000000000000000000, 0.9659258262890683122, 1.000000000000000000, 0.9659258262890683122, 1.000000000000000000, 0.9659258262890683122, 1.000000000000000000, 0.9659258262890683122, 1.000000000000000000, 0.9659258262890683122, 1.000000000000000000, 0.9659258262890683122, 1.000000000000000000, 0.9659258262890683122, 1.000000000000000000, 0.9659258262890683122, 1.000000000000000000, 0.9659258262890683122, 1.000000000000000000, 0.9659258262890683122, 1.000000000000000000, 0.9659258262890683122, 1.000000000000000000, 0.9659258262890683122, 1.000000000000000000, 0.9659258262890683122, 1.000000000000000000, 0.9659258262890683122, 1.000000000000000000, 0.9659258262890683122, 1.000000000000000000, 0.9659258262890683122, 1.000000000000000000, 0.9659258262890683122, 1.000000000000000000, 0.9659258262890683122, 1.000000000000000000, 0.9659258262890683122, 1.000000000000000000, 0.9659258262890683122, 1.000000000000000000, 0.9659258262890683122, 1.000000000000000000, 0.9659258262890683122, 1.000000000000000000, 0.9659258262890683122, 1.000000000000000000, 0.9659258262890683122, 1.000000000000000000, 0.9659258262890683122, 1.000000000000000000, 0.9659258262890683122, 1.000000000000000000, 0.9659258262890683122, 1.000000000000000000, 0.9659258262890683122, 1.000000000000000000, 0.9659258262890683122, 1.000000000000000000, 0.9659258262890683122, 1.000000000000000000, 0.9659258262890683122, 1.000000000000000000, 0.9659258262890683122, 1.000000000000000000, 0.9659258262890683122, 1.000000000000000000, 0.9659258262890683122, 1.000000000000000000, 0.9659258262890683122, 1.000000000000000000, 0.9659258262890683122, 1.000000000000000000, 0.9659258262890683122, 1.000000000000000000, 0.9659258262890683122, 1.000000000000000000, 0.9659258262890683122, 1.000000000000000000, 0.9659258262890683122, 1.000000000000000000, 0.9659258262890683122, 1.000000000000000000, 0.9659258262890683122, 1.000000000000000000, 0.9659258262890683122, 1.000000000000000000, 0.9659258262890683122, 1.000000000000000000, 0.9659258262890683122, 1.000000000000000000, 0.9659258262890683122, 1.000000000000000000, 0.9659258262890683122, 1.000000000000000000, 0.9659258262890683122, 1.000000000000000000, 0.9659258262890683122, 1.000000000000000000, 0.9659258262890683122, 1.000000000000000000, 0.9659258262890683122, 1.000000000000000000, 0.9659258262890683122, 1.000000000000000000, 0.9659258262890683122, 1.000000000000000000, 0.9659258262890683122, 1.000000000000000000, 0.9659258262890683122, 1.000000000000000000, 0.9659258262890683122, 1.000000000000000000, 0.9659258262890683122, 1.000000000000000000, 0.9659258262890683122, 1.000000000000000000, 0.9659258262890683122, 1.000000000000000000, 0.9659258262890683122, 1.000000000000000000, 0.9659258262890683122, 1.000000000000000000, 0.9659258262890683122, 1.000000000000000000, 0.9659258262890683122, 1.000000000000000000, 0.9659258262890683122, 1.000000000000000000, 0.9659258262890683122, 1.000000000000000000, 0.9659258262890683122, 1.000000000000000000, 0.9659258262890683122, 1.000000000000000000, 0.9659258262890683122, 1.000000000000000000, 0.9659258262890683122, 1.000000000000000000, 0.9659258262890683122, 1.000000000000000000, 0.9659258262890683122, 1.000000000000000000, 0.9659258262890683122, 1.000000000000000000, 0.9659258262890683122, 1.000000000000000000, 0.9659258262890683122, 1.000000000000000000, 0.9659258262890683122, 1.000000000000000000, 0.9659258262890683122, 1.000000000000000000, 0.9659258262890683122, 1.000000000000000000, 0.9659258262890683122, 1.000000000000000000, 0.9659258262890683122, 1.000000000000000000, 0.9659258262890683122, 1.000000000000000000, 0.9659258262890683122, 1.000000000000000000, 0.9659258262890683122, 1.000000000000000000, 0.9659258262890683122, 1.000000000000000000, 0.9659258262890683122, 1.000000000000000000, 0.9659258262890683122, 1.000000000000000000, 0.9659258262890683122, 1.000000000000000000, 0.9659258262890683122, 1.000000000000000000, 0.9659258262890683122, 1.000000000000000000, 0.9659258262890683122, 1.000000000000000000, 0.9659258262890683122, 1.000000000000000000, 0.9659258262890683122, 1.000000000000000000, 0.9659258262890683122, 1.000000000000000000, 0.9659258262890683122, 1.000000000000000000, 0.9659258262890683122, 1.000000000000000000, 0.9659258262890683122, 1.000000000000000000, 0.9659258262890683122, 1.000000000000000000, 0.9659258262890683122, 1.000000000000000000, 0.9659258262890683122, 1.000000000000000000, 0.9659258262890683122, 1.000000000000000000, 0.9659258262890683122, 1.000000000000000000, 0.9659258262890683122, 1.000000000000000000, 0.9659258262890683122, 1.000000000000000000, 0.9659258262890683122, 1.000000000000000000, 0.9659258262890683122, 1.000000000000000000, 0.9659258262890683122, 1.000000000000000000, 0.9659258262890683122, 1.000000000000000000, 0.9659258262890683122, 1.000000000000000000, 0.9659258262890683122, 1.000000000000000000, 0.9659258262890683122, 1.000000000000000000, 0.9659258262890683122, 1.000000000000000000, 0.9659258262890683122, 1.000000000000000000, 0.9659258262890683122, 1.000000000000000000, 0.9659258262890683122, 1.000000000000000000, 0.9659258262890683122, 1.000000000000000000, 0.9659258262890683122, 1.000000000000000000, 0.9659258262890683122, 1.000000000000000000, 0.9659258262890683122, 1.000000000000000000, 0.9659258262890683122, 1.000000000000000000, 0.9659258262890683122, 1.000000000000000000, 0.9659258262890683122, 1.000000000000000000, 0.9659258262890683122, 1.000000000000000000, 0.9659258262890683122, 1.000000000000000000, 0.9659258262890683122, 1.000000000000000000, 0.9659258262890683122, 1.000000000000000000, 0.9659258262890683122, 1.000000000000000000, 0.9659258262890683122, 1.000000000000000000, 0.9659258262890683122, 1.000000000000000000, 0.9659258262890683122, 1.000000000000000000, 0.9659258262890683122, 1.000000000000000000, 0.9659258262890683122, 1.000000000000000000, 0.9659258262890683122, 1.000000000000000000, 0.9659258262890683122, 1.000000000000000000, 0.9659258262890683122, 1.000000000000000000, 0.9659258262890683122, 1.000000000000000000, 0.9659258262890683122, 1.000000000000000000, 0.9659258262890683122, 1.000000000000000000, 0.9659258262890683122, 1.000000000000000000, 0.9659258262890683122, 1.000000000000000000, 0.9659258262890683122, 1.000000000000000000, 0.9659258262890683122, 1.000000000000000000, 0.9659258262890683122, 1.000000000000000000, 0.9659258262890683122, 1.000000000000000000, 0.9659258262890683122, 1.000000000000000000, 0.9659258262890683122, 1.000000000000000000, 0.9659258262890683122, 1.000000000000000000, 0.9659258262890683122, 1.000000000000000000, 0.9659258262890683122, 1.000000000000000000, 0.9659258262890683122, 1.000000000000000000, 0.9659258262890683122, 1.000000000000000000, 0.9659258262890683122, 1.000000000000000000, 0.9659258262890683122, 1.000000000000000000, 0.9659258262890683122, 1.000000000000000000, 0.9659258262890683122, 1.000000000000000000, 0.9659258262890683122, 1.000000000000000000, 0.9659258262890683122, 1.000000000000000000, 0.9659258262890683122, 1.000000000000000000, 0.9659258262890683122, 1.000000000000000000, 0.9659258262890683122, 1.000000000000000000, 0.9659258262890683122, 1.000000000000000000, 0.9659258262890683122, 1.000000000000000000, 0.9659258262890683122, 1.000000000000000000, 0.9659258262890683122, 1.000000000000000000, 0.9659258262890683122, 1.000000000000000000, 0.9659258262890683122, 1.000000000000000000, 0.9659258262890683122, 1.000000000000000000, 0.9659258262890683122, 1.000000000000000000, 0.9659258262890683122, 1.000000000000000000, 0.9659258262890683122, 1.000000000000000000, 0.9659258262890683122, 1.000000000000000000, 0.9659258262890683122, 1.000000000000000000, 0.9659258262890683122, 1.000000000000000000, 0.9659258262890683122, 1.000000000000000000, 0.9659258262890683122, 1.000000000000000000, 0.9659258262890683122, 1.000000000000000000, 0.9659258262890683122, 1.000000000000000000, 0.9659258262890683122, 1.000000000000000000, 0.9659258262890683122, 1.000000000000000000, 0.9659258262890683122, 1.000000000000000000, 0.9659258262890683122, 1.000000000000000000, 0.9659258262890683122, 1.000000000000000000, 0.9659258262890683122, 1.000000000000000000, 0.9659258262890683122, 1.000000000000000000, 0.9659258262890683122, 1.000000000000000000),
 ( 0.3333333333333333703, 0.3219752754296894559, 0.3333333333333333703, 0.3219752754296894559, 0.3333333333333333703, 0.3219752754296894559, 0.3333333333333333703, 0.3219752754296894559, 0.3333333333333333703, 0.3219752754296894559, 0.3333333333333333703, 0.3219752754296894559, 0.3333333333333333703, 0.3219752754296894559, 0.3333333333333333703, 0.3219752754296894559, 0.3333333333333333703, 0.3219752754296894559, 0.3333333333333333703, 0.3219752754296894559, 0.3333333333333333703, 0.3219752754296894559, 0.3333333333333333703, 0.3219752754296894559, 0.3333333333333333703, 0.3219752754296894559, 0.3333333333333333703, 0.3219752754296894559, 0.3333333333333333703, 0.3219752754296894559, 0.3333333333333333703, 0.3219752754296894559, 0.3333333333333333703, 0.3219752754296894559, 0.3333333333333333703, 0.3219752754296894559, 0.3333333333333333703, 0.3219752754296894559, 0.3333333333333333703, 0.3219752754296894559, 0.3333333333333333703, 0.3219752754296894559, 0.3333333333333333703, 0.3219752754296894559, 0.3333333333333333703, 0.3219752754296894559, 0.3333333333333333703, 0.3219752754296894559, 0.3333333333333333703, 0.3219752754296894559, 0.3333333333333333703, 0.3219752754296894559, 0.3333333333333333703, 0.3219752754296894559, 0.3333333333333333703, 0.3219752754296894559, 0.3333333333333333703, 0.3219752754296894559, 0.3333333333333333703, 0.3219752754296894559, 0.3333333333333333703, 0.3219752754296894559, 0.3333333333333333703, 0.3219752754296894559, 0.3333333333333333703, 0.3219752754296894559, 0.3333333333333333703, 0.3219752754296894559, 0.3333333333333333703, 0.3219752754296894559, 0.3333333333333333703, 0.3219752754296894559, 0.3333333333333333703, 0.3219752754296894559, 0.3333333333333333703, 0.3219752754296894559, 0.3333333333333333703, 0.3219752754296894559, 0.3333333333333333703, 0.3219752754296894559, 0.3333333333333333703, 0.3219752754296894559, 0.3333333333333333703, 0.3219752754296894559, 0.3333333333333333703, 0.3219752754296894559, 0.3333333333333333703, 0.3219752754296894559, 0.3333333333333333703, 0.3219752754296894559, 0.3333333333333333703, 0.3219752754296894559, 0.3333333333333333703, 0.3219752754296894559, 0.3333333333333333703, 0.3219752754296894559, 0.3333333333333333703, 0.3219752754296894559, 0.3333333333333333703, 0.3219752754296894559, 0.3333333333333333703, 0.3219752754296894559, 0.3333333333333333703, 0.3219752754296894559, 0.3333333333333333703, 0.3219752754296894559, 0.3333333333333333703, 0.3219752754296894559, 0.3333333333333333703, 0.3219752754296894559, 0.3333333333333333703, 0.3219752754296894559, 0.3333333333333333703, 0.3219752754296894559, 0.3333333333333333703, 0.3219752754296894559, 0.3333333333333333703, 0.3219752754296894559, 0.3333333333333333703, 0.3219752754296894559, 0.3333333333333333703, 0.3219752754296894559, 0.3333333333333333703, 0.3219752754296894559, 0.3333333333333333703, 0.3219752754296894559, 0.3333333333333333703, 0.3219752754296894559, 0.3333333333333333703, 0.3219752754296894559, 0.3333333333333333703, 0.3219752754296894559, 0.3333333333333333703, 0.3219752754296894559, 0.3333333333333333703, 0.3219752754296894559, 0.3333333333333333703, 0.3219752754296894559, 0.3333333333333333703, 0.3219752754296894559, 0.3333333333333333703, 0.3219752754296894559, 0.3333333333333333703, 0.3219752754296894559, 0.3333333333333333703, 0.3219752754296894559, 0.3333333333333333703, 0.3219752754296894559, 0.3333333333333333703, 0.3219752754296894559, 0.3333333333333333703, 0.3219752754296894559, 0.3333333333333333703, 0.3219752754296894559, 0.3333333333333333703, 0.3219752754296894559, 0.3333333333333333703, 0.3219752754296894559, 0.3333333333333333703, 0.3219752754296894559, 0.3333333333333333703, 0.3219752754296894559, 0.3333333333333333703, 0.3219752754296894559, 0.3333333333333333703, 0.3219752754296894559, 0.3333333333333333703, 0.3219752754296894559, 0.3333333333333333703, 0.3219752754296894559, 0.3333333333333333703, 0.3219752754296894559, 0.3333333333333333703, 0.3219752754296894559, 0.3333333333333333703, 0.3219752754296894559, 0.3333333333333333703, 0.3219752754296894559, 0.3333333333333333703, 0.3219752754296894559, 0.3333333333333333703, 0.3219752754296894559, 0.3333333333333333703, 0.3219752754296894559, 0.3333333333333333703, 0.3219752754296894559, 0.3333333333333333703, 0.3219752754296894559, 0.3333333333333333703, 0.3219752754296894559, 0.3333333333333333703, 0.3219752754296894559, 0.3333333333333333703, 0.3219752754296894559, 0.3333333333333333703, 0.3219752754296894559, 0.3333333333333333703, 0.3219752754296894559, 0.3333333333333333703, 0.3219752754296894559, 0.3333333333333333703, 0.3219752754296894559, 0.3333333333333333703, 0.3219752754296894559, 0.3333333333333333703, 0.3219752754296894559, 0.3333333333333333703, 0.3219752754296894559, 0.3333333333333333703, 0.3219752754296894559, 0.3333333333333333703, 0.3219752754296894559, 0.3333333333333333703, 0.3219752754296894559, 0.3333333333333333703, 0.3219752754296894559, 0.3333333333333333703, 0.3219752754296894559, 0.3333333333333333703, 0.3219752754296894559, 0.3333333333333333703, 0.3219752754296894559, 0.3333333333333333703, 0.3219752754296894559, 0.3333333333333333703, 0.3219752754296894559, 0.3333333333333333703, 0.3219752754296894559, 0.3333333333333333703, 0.3219752754296894559, 0.3333333333333333703, 0.3219752754296894559, 0.3333333333333333703, 0.3219752754296894559, 0.3333333333333333703, 0.3219752754296894559, 0.3333333333333333703, 0.3219752754296894559, 0.3333333333333333703, 0.3219752754296894559, 0.3333333333333333703, 0.3219752754296894559, 0.3333333333333333703, 0.3219752754296894559, 0.3333333333333333703, 0.3219752754296894559, 0.3333333333333333703, 0.3219752754296894559, 0.3333333333333333703, 0.3219752754296894559, 0.3333333333333333703, 0.3219752754296894559, 0.3333333333333333703, 0.3219752754296894559, 0.3333333333333333703, 0.3219752754296894559, 0.3333333333333333703, 0.3219752754296894559, 0.3333333333333333703, 0.3219752754296894559, 0.3333333333333333703, 0.3219752754296894559, 0.3333333333333333703, 0.3219752754296894559, 0.3333333333333333703, 0.3219752754296894559, 0.3333333333333333703, 0.3219752754296894559, 0.3333333333333333703, 0.3219752754296894559, 0.3333333333333333703, 0.3219752754296894559, 0.3333333333333333703, 0.3219752754296894559, 0.3333333333333333703, 0.3219752754296894559, 0.3333333333333333703, 0.3219752754296894559, 0.3333333333333333703, 0.3219752754296894559, 0.3333333333333333703, 0.3219752754296894559, 0.3333333333333333703, 0.3219752754296894559, 0.3333333333333333703, 0.3219752754296894559, 0.3333333333333333703, 0.3219752754296894559, 0.3333333333333333703, 0.3219752754296894559, 0.3333333333333333703, 0.3219752754296894559, 0.3333333333333333703, 0.3219752754296894559, 0.3333333333333333703, 0.3219752754296894559, 0.3333333333333333703, 0.3219752754296894559, 0.3333333333333333703, 0.3219752754296894559, 0.3333333333333333703, 0.3219752754296894559, 0.3333333333333333703, 0.3219752754296894559, 0.3333333333333333703, 0.3219752754296894559, 0.3333333333333333703, 0.3219752754296894559, 0.3333333333333333703, 0.3219752754296894559, 0.3333333333333333703, 0.3219752754296894559, 0.3333333333333333703, 0.3219752754296894559, 0.3333333333333333703, 0.3219752754296894559, 0.3333333333333333703, 0.3219752754296894559, 0.3333333333333333703, 0.3219752754296894559, 0.3333333333333333703, 0.3219752754296894559, 0.3333333333333333703, 0.3219752754296894559, 0.3333333333333333703, 0.3219752754296894559, 0.3333333333333333703, 0.3219752754296894559, 0.3333333333333333703, 0.3219752754296894559, 0.3333333333333333703, 0.3219752754296894559, 0.3333333333333333703, 0.3219752754296894559, 0.3333333333333333703, 0.3219752754296894559, 0.3333333333333333703, 0.3219752754296894559, 0.3333333333333333703, 0.3219752754296894559, 0.3333333333333333703, 0.3219752754296894559, 0.3333333333333333703, 0.3219752754296894559, 0.3333333333333333703, 0.3219752754296894559, 0.3333333333333333703, 0.3219752754296894559, 0.3333333333333333703, 0.3219752754296894559, 0.3333333333333333703, 0.3219752754296894559, 0.3333333333333333703, 0.3219752754296894559, 0.3333333333333333703, 0.3219752754296894559, 0.3333333333333333703, 0.3219752754296894559, 0.3333333333333333703, 0.3219752754296894559, 0.3333333333333333703, 0.3219752754296894559, 0.3333333333333333703, 0.3219752754296894559, 0.3333333333333333703, 0.3219752754296894559, 0.3333333333333333703, 0.3219752754296894559, 0.3333333333333333703, 0.3219752754296894559, 0.3333333333333333703, 0.3219752754296894559, 0.3333333333333333703, 0.3219752754296894559, 0.3333333333333333703, 0.3219752754296894559, 0.3333333333333333703, 0.3219752754296894559, 0.3333333333333333703, 0.3219752754296894559, 0.3333333333333333703, 0.3219752754296894559, 0.3333333333333333703, 0.3219752754296894559, 0.3333333333333333703, 0.3219752754296894559, 0.3333333333333333703, 0.3219752754296894559, 0.3333333333333333703, 0.3219752754296894559, 0.3333333333333333703, 0.3219752754296894559, 0.3333333333333333703, 0.3219752754296894559, 0.3333333333333333703, 0.3219752754296894559, 0.3333333333333333703, 0.3219752754296894559, 0.3333333333333333703, 0.3219752754296894559, 0.3333333333333333703, 0.3219752754296894559, 0.3333333333333333703, 0.3219752754296894559, 0.3333333333333333703, 0.3219752754296894559, 0.3333333333333333703, 0.3219752754296894559, 0.3333333333333333703, 0.3219752754296894559, 0.3333333333333333703, 0.3219752754296894559, 0.3333333333333333703, 0.3219752754296894559, 0.3333333333333333703, 0.3219752754296894559, 0.3333333333333333703, 0.3219752754296894559, 0.3333333333333333703, 0.3219752754296894559, 0.3333333333333333703, 0.3219752754296894559, 0.3333333333333333703, 0.3219752754296894559, 0.3333333333333333703, 0.3219752754296894559, 0.3333333333333333703, 0.3219752754296894559, 0.3333333333333333703, 0.3219752754296894559, 0.3333333333333333703, 0.3219752754296894559, 0.3333333333333333703, 0.3219752754296894559, 0.3333333333333333703, 0.3219752754296894559, 0.3333333333333333703, 0.3219752754296894559, 0.3333333333333333703, 0.3219752754296894559, 0.3333333333333333703, 0.3219752754296894559, 0.3333333333333333703, 0.3219752754296894559, 0.3333333333333333703, 0.3219752754296894559, 0.3333333333333333703, 0.3219752754296894559, 0.3333333333333333703, 0.3219752754296894559, 0.3333333333333333703, 0.3219752754296894559, 0.3333333333333333703, 0.3219752754296894559, 0.3333333333333333703, 0.3219752754296894559, 0.3333333333333333703),
 ( 0.3333333333333333703, 0.3219752754296894559, 0.3333333333333333703, 0.3219752754296894559, 0.3333333333333333703, 0.3219752754296894559, 0.3333333333333333703, 0.3219752754296894559, 0.3333333333333333703, 0.3219752754296894559, 0.3333333333333333703, 0.3219752754296894559, 0.3333333333333333703, 0.3219752754296894559, 0.3333333333333333703, 0.3219752754296894559, 0.3333333333333333703, 0.3219752754296894559, 0.3333333333333333703, 0.3219752754296894559, 0.3333333333333333703, 0.3219752754296894559, 0.3333333333333333703, 0.3219752754296894559, 0.3333333333333333703, 0.3219752754296894559, 0.3333333333333333703, 0.3219752754296894559, 0.3333333333333333703, 0.3219752754296894559, 0.3333333333333333703, 0.3219752754296894559, 0.3333333333333333703, 0.3219752754296894559, 0.3333333333333333703, 0.3219752754296894559, 0.3333333333333333703, 0.3219752754296894559, 0.3333333333333333703, 0.3219752754296894559, 0.3333333333333333703, 0.3219752754296894559, 0.3333333333333333703, 0.3219752754296894559, 0.3333333333333333703, 0.3219752754296894559, 0.3333333333333333703, 0.3219752754296894559, 0.3333333333333333703, 0.3219752754296894559, 0.3333333333333333703, 0.3219752754296894559, 0.3333333333333333703, 0.3219752754296894559, 0.3333333333333333703, 0.3219752754296894559, 0.3333333333333333703, 0.3219752754296894559, 0.3333333333333333703, 0.3219752754296894559, 0.3333333333333333703, 0.3219752754296894559, 0.3333333333333333703, 0.3219752754296894559, 0.3333333333333333703, 0.3219752754296894559, 0.3333333333333333703, 0.3219752754296894559, 0.3333333333333333703, 0.3219752754296894559, 0.3333333333333333703, 0.3219752754296894559, 0.3333333333333333703, 0.3219752754296894559, 0.3333333333333333703, 0.3219752754296894559, 0.3333333333333333703, 0.3219752754296894559, 0.3333333333333333703, 0.3219752754296894559, 0.3333333333333333703, 0.3219752754296894559, 0.3333333333333333703, 0.3219752754296894559, 0.3333333333333333703, 0.3219752754296894559, 0.3333333333333333703, 0.3219752754296894559, 0.3333333333333333703, 0.3219752754296894559, 0.3333333333333333703, 0.3219752754296894559, 0.3333333333333333703, 0.3219752754296894559, 0.3333333333333333703, 0.3219752754296894559, 0.3333333333333333703, 0.3219752754296894559, 0.3333333333333333703, 0.3219752754296894559, 0.3333333333333333703, 0.3219752754296894559, 0.3333333333333333703, 0.3219752754296894559, 0.3333333333333333703, 0.3219752754296894559, 0.3333333333333333703, 0.3219752754296894559, 0.3333333333333333703, 0.3219752754296894559, 0.3333333333333333703, 0.3219752754296894559, 0.3333333333333333703, 0.3219752754296894559, 0.3333333333333333703, 0.3219752754296894559, 0.3333333333333333703, 0.3219752754296894559, 0.3333333333333333703, 0.3219752754296894559, 0.3333333333333333703, 0.3219752754296894559, 0.3333333333333333703, 0.3219752754296894559, 0.3333333333333333703, 0.3219752754296894559, 0.3333333333333333703, 0.3219752754296894559, 0.3333333333333333703, 0.3219752754296894559, 0.3333333333333333703, 0.3219752754296894559, 0.3333333333333333703, 0.3219752754296894559, 0.3333333333333333703, 0.3219752754296894559, 0.3333333333333333703, 0.3219752754296894559, 0.3333333333333333703, 0.3219752754296894559, 0.3333333333333333703, 0.3219752754296894559, 0.3333333333333333703, 0.3219752754296894559, 0.3333333333333333703, 0.3219752754296894559, 0.3333333333333333703, 0.3219752754296894559, 0.3333333333333333703, 0.3219752754296894559, 0.3333333333333333703, 0.3219752754296894559, 0.3333333333333333703, 0.3219752754296894559, 0.3333333333333333703, 0.3219752754296894559, 0.3333333333333333703, 0.3219752754296894559, 0.3333333333333333703, 0.3219752754296894559, 0.3333333333333333703, 0.3219752754296894559, 0.3333333333333333703, 0.3219752754296894559, 0.3333333333333333703, 0.3219752754296894559, 0.3333333333333333703, 0.3219752754296894559, 0.3333333333333333703, 0.3219752754296894559, 0.3333333333333333703, 0.3219752754296894559, 0.3333333333333333703, 0.3219752754296894559, 0.3333333333333333703, 0.3219752754296894559, 0.3333333333333333703, 0.3219752754296894559, 0.3333333333333333703, 0.3219752754296894559, 0.3333333333333333703, 0.3219752754296894559, 0.3333333333333333703, 0.3219752754296894559, 0.3333333333333333703, 0.3219752754296894559, 0.3333333333333333703, 0.3219752754296894559, 0.3333333333333333703, 0.3219752754296894559, 0.3333333333333333703, 0.3219752754296894559, 0.3333333333333333703, 0.3219752754296894559, 0.3333333333333333703, 0.3219752754296894559, 0.3333333333333333703, 0.3219752754296894559, 0.3333333333333333703, 0.3219752754296894559, 0.3333333333333333703, 0.3219752754296894559, 0.3333333333333333703, 0.3219752754296894559, 0.3333333333333333703, 0.3219752754296894559, 0.3333333333333333703, 0.3219752754296894559, 0.3333333333333333703, 0.3219752754296894559, 0.3333333333333333703, 0.3219752754296894559, 0.3333333333333333703, 0.3219752754296894559, 0.3333333333333333703, 0.3219752754296894559, 0.3333333333333333703, 0.3219752754296894559, 0.3333333333333333703, 0.3219752754296894559, 0.3333333333333333703, 0.3219752754296894559, 0.3333333333333333703, 0.3219752754296894559, 0.3333333333333333703, 0.3219752754296894559, 0.3333333333333333703, 0.3219752754296894559, 0.3333333333333333703, 0.3219752754296894559, 0.3333333333333333703, 0.3219752754296894559, 0.3333333333333333703, 0.3219752754296894559, 0.3333333333333333703, 0.3219752754296894559, 0.3333333333333333703, 0.3219752754296894559, 0.3333333333333333703, 0.3219752754296894559, 0.3333333333333333703, 0.3219752754296894559, 0.3333333333333333703, 0.3219752754296894559, 0.3333333333333333703, 0.3219752754296894559, 0.3333333333333333703, 0.3219752754296894559, 0.3333333333333333703, 0.3219752754296894559, 0.3333333333333333703, 0.3219752754296894559, 0.3333333333333333703, 0.3219752754296894559, 0.3333333333333333703, 0.3219752754296894559, 0.3333333333333333703, 0.3219752754296894559, 0.3333333333333333703, 0.3219752754296894559, 0.3333333333333333703, 0.3219752754296894559, 0.3333333333333333703, 0.3219752754296894559, 0.3333333333333333703, 0.3219752754296894559, 0.3333333333333333703, 0.3219752754296894559, 0.3333333333333333703, 0.3219752754296894559, 0.3333333333333333703, 0.3219752754296894559, 0.3333333333333333703, 0.3219752754296894559, 0.3333333333333333703, 0.3219752754296894559, 0.3333333333333333703, 0.3219752754296894559, 0.3333333333333333703, 0.3219752754296894559, 0.3333333333333333703, 0.3219752754296894559, 0.3333333333333333703, 0.3219752754296894559, 0.3333333333333333703, 0.3219752754296894559, 0.3333333333333333703, 0.3219752754296894559, 0.3333333333333333703, 0.3219752754296894559, 0.3333333333333333703, 0.3219752754296894559, 0.3333333333333333703, 0.3219752754296894559, 0.3333333333333333703, 0.3219752754296894559, 0.3333333333333333703, 0.3219752754296894559, 0.3333333333333333703, 0.3219752754296894559, 0.3333333333333333703, 0.3219752754296894559, 0.3333333333333333703, 0.3219752754296894559, 0.3333333333333333703, 0.3219752754296894559, 0.3333333333333333703, 0.3219752754296894559, 0.3333333333333333703, 0.3219752754296894559, 0.3333333333333333703, 0.3219752754296894559, 0.3333333333333333703, 0.3219752754296894559, 0.3333333333333333703, 0.3219752754296894559, 0.3333333333333333703, 0.3219752754296894559, 0.3333333333333333703, 0.3219752754296894559, 0.3333333333333333703, 0.3219752754296894559, 0.3333333333333333703, 0.3219752754296894559, 0.3333333333333333703, 0.3219752754296894559, 0.3333333333333333703, 0.3219752754296894559, 0.3333333333333333703, 0.3219752754296894559, 0.3333333333333333703, 0.3219752754296894559, 0.3333333333333333703, 0.3219752754296894559, 0.3333333333333333703, 0.3219752754296894559, 0.3333333333333333703, 0.3219752754296894559, 0.3333333333333333703, 0.3219752754296894559, 0.3333333333333333703, 0.3219752754296894559, 0.3333333333333333703, 0.3219752754296894559, 0.3333333333333333703, 0.3219752754296894559, 0.3333333333333333703, 0.3219752754296894559, 0.3333333333333333703, 0.3219752754296894559, 0.3333333333333333703, 0.3219752754296894559, 0.3333333333333333703, 0.3219752754296894559, 0.3333333333333333703, 0.3219752754296894559, 0.3333333333333333703, 0.3219752754296894559, 0.3333333333333333703, 0.3219752754296894559, 0.3333333333333333703, 0.3219752754296894559, 0.3333333333333333703, 0.3219752754296894559, 0.3333333333333333703, 0.3219752754296894559, 0.3333333333333333703, 0.3219752754296894559, 0.3333333333333333703, 0.3219752754296894559, 0.3333333333333333703, 0.3219752754296894559, 0.3333333333333333703, 0.3219752754296894559, 0.3333333333333333703, 0.3219752754296894559, 0.3333333333333333703, 0.3219752754296894559, 0.3333333333333333703, 0.3219752754296894559, 0.3333333333333333703, 0.3219752754296894559, 0.3333333333333333703, 0.3219752754296894559, 0.3333333333333333703, 0.3219752754296894559, 0.3333333333333333703, 0.3219752754296894559, 0.3333333333333333703, 0.3219752754296894559, 0.3333333333333333703, 0.3219752754296894559, 0.3333333333333333703, 0.3219752754296894559, 0.3333333333333333703, 0.3219752754296894559, 0.3333333333333333703, 0.3219752754296894559, 0.3333333333333333703, 0.3219752754296894559, 0.3333333333333333703, 0.3219752754296894559, 0.3333333333333333703, 0.3219752754296894559, 0.3333333333333333703, 0.3219752754296894559, 0.3333333333333333703, 0.3219752754296894559, 0.3333333333333333703, 0.3219752754296894559, 0.3333333333333333703, 0.3219752754296894559, 0.3333333333333333703, 0.3219752754296894559, 0.3333333333333333703, 0.3219752754296894559, 0.3333333333333333703, 0.3219752754296894559, 0.3333333333333333703, 0.3219752754296894559, 0.3333333333333333703, 0.3219752754296894559, 0.3333333333333333703, 0.3219752754296894559, 0.3333333333333333703, 0.3219752754296894559, 0.3333333333333333703, 0.3219752754296894559, 0.3333333333333333703, 0.3219752754296894559, 0.3333333333333333703, 0.3219752754296894559, 0.3333333333333333703, 0.3219752754296894559, 0.3333333333333333703, 0.3219752754296894559, 0.3333333333333333703, 0.3219752754296894559, 0.3333333333333333703, 0.3219752754296894559, 0.3333333333333333703, 0.3219752754296894559, 0.3333333333333333703, 0.3219752754296894559, 0.3333333333333333703, 0.3219752754296894559, 0.3333333333333333703, 0.3219752754296894559, 0.3333333333333333703, 0.3219752754296894559, 0.3333333333333333703, 0.3219752754296894559, 0.3333333333333333703, 0.3219752754296894559, 0.3333333333333333703, 0.3219752754296894559, 0.3333333333333333703),
 ( 1.000000000000000000, 0.9659258262890683122, 1.000000000000000000, 0.9659258262890683122, 1.000000000000000000, 0.9659258262890683122, 1.000000000000000000, 0.9659258262890683122, 1.000000000000000000, 0.9659258262890683122, 1.000000000000000000, 0.9659258262890683122, 1.000000000000000000, 0.9659258262890683122, 1.000000000000000000, 0.9659258262890683122, 1.000000000000000000, 0.9659258262890683122, 1.000000000000000000, 0.9659258262890683122, 1.000000000000000000, 0.9659258262890683122, 1.000000000000000000, 0.9659258262890683122, 1.000000000000000000, 0.9659258262890683122, 1.000000000000000000, 0.9659258262890683122, 1.000000000000000000, 0.9659258262890683122, 1.000000000000000000, 0.9659258262890683122, 1.000000000000000000, 0.9659258262890683122, 1.000000000000000000, 0.9659258262890683122, 1.000000000000000000, 0.9659258262890683122, 1.000000000000000000, 0.9659258262890683122, 1.000000000000000000, 0.9659258262890683122, 1.000000000000000000, 0.9659258262890683122, 1.000000000000000000, 0.9659258262890683122, 1.000000000000000000, 0.9659258262890683122, 1.000000000000000000, 0.9659258262890683122, 1.000000000000000000, 0.9659258262890683122, 1.000000000000000000, 0.9659258262890683122, 1.000000000000000000, 0.9659258262890683122, 1.000000000000000000, 0.9659258262890683122, 1.000000000000000000, 0.9659258262890683122, 1.000000000000000000, 0.9659258262890683122, 1.000000000000000000, 0.9659258262890683122, 1.000000000000000000, 0.9659258262890683122, 1.000000000000000000, 0.9659258262890683122, 1.000000000000000000, 0.9659258262890683122, 1.000000000000000000, 0.9659258262890683122, 1.000000000000000000, 0.9659258262890683122, 1.000000000000000000, 0.9659258262890683122, 1.000000000000000000, 0.9659258262890683122, 1.000000000000000000, 0.9659258262890683122, 1.000000000000000000, 0.9659258262890683122, 1.000000000000000000, 0.9659258262890683122, 1.000000000000000000, 0.9659258262890683122, 1.000000000000000000, 0.9659258262890683122, 1.000000000000000000, 0.9659258262890683122, 1.000000000000000000, 0.9659258262890683122, 1.000000000000000000, 0.9659258262890683122, 1.000000000000000000, 0.9659258262890683122, 1.000000000000000000, 0.9659258262890683122, 1.000000000000000000, 0.9659258262890683122, 1.000000000000000000, 0.9659258262890683122, 1.000000000000000000, 0.9659258262890683122, 1.000000000000000000, 0.9659258262890683122, 1.000000000000000000, 0.9659258262890683122, 1.000000000000000000, 0.9659258262890683122, 1.000000000000000000, 0.9659258262890683122, 1.000000000000000000, 0.9659258262890683122, 1.000000000000000000, 0.9659258262890683122, 1.000000000000000000, 0.9659258262890683122, 1.000000000000000000, 0.9659258262890683122, 1.000000000000000000, 0.9659258262890683122, 1.000000000000000000, 0.9659258262890683122, 1.000000000000000000, 0.9659258262890683122, 1.000000000000000000, 0.9659258262890683122, 1.000000000000000000, 0.9659258262890683122, 1.000000000000000000, 0.9659258262890683122, 1.000000000000000000, 0.9659258262890683122, 1.000000000000000000, 0.9659258262890683122, 1.000000000000000000, 0.9659258262890683122, 1.000000000000000000, 0.9659258262890683122, 1.000000000000000000, 0.9659258262890683122, 1.000000000000000000, 0.9659258262890683122, 1.000000000000000000, 0.9659258262890683122, 1.000000000000000000, 0.9659258262890683122, 1.000000000000000000, 0.9659258262890683122, 1.000000000000000000, 0.9659258262890683122, 1.000000000000000000, 0.9659258262890683122, 1.000000000000000000, 0.9659258262890683122, 1.000000000000000000, 0.9659258262890683122, 1.000000000000000000, 0.9659258262890683122, 1.000000000000000000, 0.9659258262890683122, 1.000000000000000000, 0.9659258262890683122, 1.000000000000000000, 0.9659258262890683122, 1.000000000000000000, 0.9659258262890683122, 1.000000000000000000, 0.9659258262890683122, 1.000000000000000000, 0.9659258262890683122, 1.000000000000000000, 0.9659258262890683122, 1.000000000000000000, 0.9659258262890683122, 1.000000000000000000, 0.9659258262890683122, 1.000000000000000000, 0.9659258262890683122, 1.000000000000000000, 0.9659258262890683122, 1.000000000000000000, 0.9659258262890683122, 1.000000000000000000, 0.9659258262890683122, 1.000000000000000000, 0.9659258262890683122, 1.000000000000000000, 0.9659258262890683122, 1.000000000000000000, 0.9659258262890683122, 1.000000000000000000, 0.9659258262890683122, 1.000000000000000000, 0.9659258262890683122, 1.000000000000000000, 0.9659258262890683122, 1.000000000000000000, 0.9659258262890683122, 1.000000000000000000, 0.9659258262890683122, 1.000000000000000000, 0.9659258262890683122, 1.000000000000000000, 0.9659258262890683122, 1.000000000000000000, 0.9659258262890683122, 1.000000000000000000, 0.9659258262890683122, 1.000000000000000000, 0.9659258262890683122, 1.000000000000000000, 0.9659258262890683122, 1.000000000000000000, 0.9659258262890683122, 1.000000000000000000, 0.9659258262890683122, 1.000000000000000000, 0.9659258262890683122, 1.000000000000000000, 0.9659258262890683122, 1.000000000000000000, 0.9659258262890683122, 1.000000000000000000, 0.9659258262890683122, 1.000000000000000000, 0.9659258262890683122, 1.000000000000000000, 0.9659258262890683122, 1.000000000000000000, 0.9659258262890683122, 1.000000000000000000, 0.9659258262890683122, 1.000000000000000000, 0.9659258262890683122, 1.000000000000000000, 0.9659258262890683122, 1.000000000000000000, 0.9659258262890683122, 1.000000000000000000, 0.9659258262890683122, 1.000000000000000000, 0.9659258262890683122, 1.000000000000000000, 0.9659258262890683122, 1.000000000000000000, 0.9659258262890683122, 1.000000000000000000, 0.9659258262890683122, 1.000000000000000000, 0.9659258262890683122, 1.000000000000000000, 0.9659258262890683122, 1.000000000000000000, 0.9659258262890683122, 1.000000000000000000, 0.9659258262890683122, 1.000000000000000000, 0.9659258262890683122, 1.000000000000000000, 0.9659258262890683122, 1.000000000000000000, 0.9659258262890683122, 1.000000000000000000, 0.9659258262890683122, 1.000000000000000000, 0.9659258262890683122, 1.000000000000000000, 0.9659258262890683122, 1.000000000000000000, 0.9659258262890683122, 1.000000000000000000, 0.9659258262890683122, 1.000000000000000000, 0.9659258262890683122, 1.000000000000000000, 0.9659258262890683122, 1.000000000000000000, 0.9659258262890683122, 1.000000000000000000, 0.9659258262890683122, 1.000000000000000000, 0.9659258262890683122, 1.000000000000000000, 0.9659258262890683122, 1.000000000000000000, 0.9659258262890683122, 1.000000000000000000, 0.9659258262890683122, 1.000000000000000000, 0.9659258262890683122, 1.000000000000000000, 0.9659258262890683122, 1.000000000000000000, 0.9659258262890683122, 1.000000000000000000, 0.9659258262890683122, 1.000000000000000000, 0.9659258262890683122, 1.000000000000000000, 0.9659258262890683122, 1.000000000000000000, 0.9659258262890683122, 1.000000000000000000, 0.9659258262890683122, 1.000000000000000000, 0.9659258262890683122, 1.000000000000000000, 0.9659258262890683122, 1.000000000000000000, 0.9659258262890683122, 1.000000000000000000, 0.9659258262890683122, 1.000000000000000000, 0.9659258262890683122, 1.000000000000000000, 0.9659258262890683122, 1.000000000000000000, 0.9659258262890683122, 1.000000000000000000, 0.9659258262890683122, 1.000000000000000000, 0.9659258262890683122, 1.000000000000000000, 0.9659258262890683122, 1.000000000000000000, 0.9659258262890683122, 1.000000000000000000, 0.9659258262890683122, 1.000000000000000000, 0.9659258262890683122, 1.000000000000000000, 0.9659258262890683122, 1.000000000000000000, 0.9659258262890683122, 1.000000000000000000, 0.9659258262890683122, 1.000000000000000000, 0.9659258262890683122, 1.000000000000000000, 0.9659258262890683122, 1.000000000000000000, 0.9659258262890683122, 1.000000000000000000, 0.9659258262890683122, 1.000000000000000000, 0.9659258262890683122, 1.000000000000000000, 0.9659258262890683122, 1.000000000000000000, 0.9659258262890683122, 1.000000000000000000, 0.9659258262890683122, 1.000000000000000000, 0.9659258262890683122, 1.000000000000000000, 0.9659258262890683122, 1.000000000000000000, 0.9659258262890683122, 1.000000000000000000, 0.9659258262890683122, 1.000000000000000000, 0.9659258262890683122, 1.000000000000000000, 0.9659258262890683122, 1.000000000000000000, 0.9659258262890683122, 1.000000000000000000, 0.9659258262890683122, 1.000000000000000000, 0.9659258262890683122, 1.000000000000000000, 0.9659258262890683122, 1.000000000000000000, 0.9659258262890683122, 1.000000000000000000, 0.9659258262890683122, 1.000000000000000000, 0.9659258262890683122, 1.000000000000000000, 0.9659258262890683122, 1.000000000000000000, 0.9659258262890683122, 1.000000000000000000, 0.9659258262890683122, 1.000000000000000000, 0.9659258262890683122, 1.000000000000000000, 0.9659258262890683122, 1.000000000000000000, 0.9659258262890683122, 1.000000000000000000, 0.9659258262890683122, 1.000000000000000000, 0.9659258262890683122, 1.000000000000000000, 0.9659258262890683122, 1.000000000000000000, 0.9659258262890683122, 1.000000000000000000, 0.9659258262890683122, 1.000000000000000000, 0.9659258262890683122, 1.000000000000000000, 0.9659258262890683122, 1.000000000000000000, 0.9659258262890683122, 1.000000000000000000, 0.9659258262890683122, 1.000000000000000000, 0.9659258262890683122, 1.000000000000000000, 0.9659258262890683122, 1.000000000000000000, 0.9659258262890683122, 1.000000000000000000, 0.9659258262890683122, 1.000000000000000000, 0.9659258262890683122, 1.000000000000000000, 0.9659258262890683122, 1.000000000000000000, 0.9659258262890683122, 1.000000000000000000, 0.9659258262890683122, 1.000000000000000000, 0.9659258262890683122, 1.000000000000000000, 0.9659258262890683122, 1.000000000000000000, 0.9659258262890683122, 1.000000000000000000, 0.9659258262890683122, 1.000000000000000000, 0.9659258262890683122, 1.000000000000000000, 0.9659258262890683122, 1.000000000000000000, 0.9659258262890683122, 1.000000000000000000, 0.9659258262890683122, 1.000000000000000000, 0.9659258262890683122, 1.000000000000000000, 0.9659258262890683122, 1.000000000000000000, 0.9659258262890683122, 1.000000000000000000, 0.9659258262890683122, 1.000000000000000000, 0.9659258262890683122, 1.000000000000000000, 0.9659258262890683122, 1.000000000000000000, 0.9659258262890683122, 1.000000000000000000),
 ( 0.3333333333333333703, 0.3219752754296894559, 0.3333333333333333703, 0.3219752754296894559, 0.3333333333333333703, 0.3219752754296894559, 0.3333333333333333703, 0.3219752754296894559, 0.3333333333333333703, 0.3219752754296894559, 0.3333333333333333703, 0.3219752754296894559, 0.3333333333333333703, 0.3219752754296894559, 0.3333333333333333703, 0.3219752754296894559, 0.3333333333333333703, 0.3219752754296894559, 0.3333333333333333703, 0.3219752754296894559, 0.3333333333333333703, 0.3219752754296894559, 0.3333333333333333703, 0.3219752754296894559, 0.3333333333333333703, 0.3219752754296894559, 0.3333333333333333703, 0.3219752754296894559, 0.3333333333333333703, 0.3219752754296894559, 0.3333333333333333703, 0.3219752754296894559, 0.3333333333333333703, 0.3219752754296894559, 0.3333333333333333703, 0.3219752754296894559, 0.3333333333333333703, 0.3219752754296894559, 0.3333333333333333703, 0.3219752754296894559, 0.3333333333333333703, 0.3219752754296894559, 0.3333333333333333703, 0.3219752754296894559, 0.3333333333333333703, 0.3219752754296894559, 0.3333333333333333703, 0.3219752754296894559, 0.3333333333333333703, 0.3219752754296894559, 0.3333333333333333703, 0.3219752754296894559, 0.3333333333333333703, 0.3219752754296894559, 0.3333333333333333703, 0.3219752754296894559, 0.3333333333333333703, 0.3219752754296894559, 0.3333333333333333703, 0.3219752754296894559, 0.3333333333333333703, 0.3219752754296894559, 0.3333333333333333703, 0.3219752754296894559, 0.3333333333333333703, 0.3219752754296894559, 0.3333333333333333703, 0.3219752754296894559, 0.3333333333333333703, 0.3219752754296894559, 0.3333333333333333703, 0.3219752754296894559, 0.3333333333333333703, 0.3219752754296894559, 0.3333333333333333703, 0.3219752754296894559, 0.3333333333333333703, 0.3219752754296894559, 0.3333333333333333703, 0.3219752754296894559, 0.3333333333333333703, 0.3219752754296894559, 0.3333333333333333703, 0.3219752754296894559, 0.3333333333333333703, 0.3219752754296894559, 0.3333333333333333703, 0.3219752754296894559, 0.3333333333333333703, 0.3219752754296894559, 0.3333333333333333703, 0.3219752754296894559, 0.3333333333333333703, 0.3219752754296894559, 0.3333333333333333703, 0.3219752754296894559, 0.3333333333333333703, 0.3219752754296894559, 0.3333333333333333703, 0.3219752754296894559, 0.3333333333333333703, 0.3219752754296894559, 0.3333333333333333703, 0.3219752754296894559, 0.3333333333333333703, 0.3219752754296894559, 0.3333333333333333703, 0.3219752754296894559, 0.3333333333333333703, 0.3219752754296894559, 0.3333333333333333703, 0.3219752754296894559, 0.3333333333333333703, 0.3219752754296894559, 0.3333333333333333703, 0.3219752754296894559, 0.3333333333333333703, 0.3219752754296894559, 0.3333333333333333703, 0.3219752754296894559, 0.3333333333333333703, 0.3219752754296894559, 0.3333333333333333703, 0.3219752754296894559, 0.3333333333333333703, 0.3219752754296894559, 0.3333333333333333703, 0.3219752754296894559, 0.3333333333333333703, 0.3219752754296894559, 0.3333333333333333703, 0.3219752754296894559, 0.3333333333333333703, 0.3219752754296894559, 0.3333333333333333703, 0.3219752754296894559, 0.3333333333333333703, 0.3219752754296894559, 0.3333333333333333703, 0.3219752754296894559, 0.3333333333333333703, 0.3219752754296894559, 0.3333333333333333703, 0.3219752754296894559, 0.3333333333333333703, 0.3219752754296894559, 0.3333333333333333703, 0.3219752754296894559, 0.3333333333333333703, 0.3219752754296894559, 0.3333333333333333703, 0.3219752754296894559, 0.3333333333333333703, 0.3219752754296894559, 0.3333333333333333703, 0.3219752754296894559, 0.3333333333333333703, 0.3219752754296894559, 0.3333333333333333703, 0.3219752754296894559, 0.3333333333333333703, 0.3219752754296894559, 0.3333333333333333703, 0.3219752754296894559, 0.3333333333333333703, 0.3219752754296894559, 0.3333333333333333703, 0.3219752754296894559, 0.3333333333333333703, 0.3219752754296894559, 0.3333333333333333703, 0.3219752754296894559, 0.3333333333333333703, 0.3219752754296894559, 0.3333333333333333703, 0.3219752754296894559, 0.3333333333333333703, 0.3219752754296894559, 0.3333333333333333703, 0.3219752754296894559, 0.3333333333333333703, 0.3219752754296894559, 0.3333333333333333703, 0.3219752754296894559, 0.3333333333333333703, 0.3219752754296894559, 0.3333333333333333703, 0.3219752754296894559, 0.3333333333333333703, 0.3219752754296894559, 0.3333333333333333703, 0.3219752754296894559, 0.3333333333333333703, 0.3219752754296894559, 0.3333333333333333703, 0.3219752754296894559, 0.3333333333333333703, 0.3219752754296894559, 0.3333333333333333703, 0.3219752754296894559, 0.3333333333333333703, 0.3219752754296894559, 0.3333333333333333703, 0.3219752754296894559, 0.3333333333333333703, 0.3219752754296894559, 0.3333333333333333703, 0.3219752754296894559, 0.3333333333333333703, 0.3219752754296894559, 0.3333333333333333703, 0.3219752754296894559, 0.3333333333333333703, 0.3219752754296894559, 0.3333333333333333703, 0.3219752754296894559, 0.3333333333333333703, 0.3219752754296894559, 0.3333333333333333703, 0.3219752754296894559, 0.3333333333333333703, 0.3219752754296894559, 0.3333333333333333703, 0.3219752754296894559, 0.3333333333333333703, 0.3219752754296894559, 0.3333333333333333703, 0.3219752754296894559, 0.3333333333333333703, 0.3219752754296894559, 0.3333333333333333703, 0.3219752754296894559, 0.3333333333333333703, 0.3219752754296894559, 0.3333333333333333703, 0.3219752754296894559, 0.3333333333333333703, 0.3219752754296894559, 0.3333333333333333703, 0.3219752754296894559, 0.3333333333333333703, 0.3219752754296894559, 0.3333333333333333703, 0.3219752754296894559, 0.3333333333333333703, 0.3219752754296894559, 0.3333333333333333703, 0.3219752754296894559, 0.3333333333333333703, 0.3219752754296894559, 0.3333333333333333703, 0.3219752754296894559, 0.3333333333333333703, 0.3219752754296894559, 0.3333333333333333703, 0.3219752754296894559, 0.3333333333333333703, 0.3219752754296894559, 0.3333333333333333703, 0.3219752754296894559, 0.3333333333333333703, 0.3219752754296894559, 0.3333333333333333703, 0.3219752754296894559, 0.3333333333333333703, 0.3219752754296894559, 0.3333333333333333703, 0.3219752754296894559, 0.3333333333333333703, 0.3219752754296894559, 0.3333333333333333703, 0.3219752754296894559, 0.3333333333333333703, 0.3219752754296894559, 0.3333333333333333703, 0.3219752754296894559, 0.3333333333333333703, 0.3219752754296894559, 0.3333333333333333703, 0.3219752754296894559, 0.3333333333333333703, 0.3219752754296894559, 0.3333333333333333703, 0.3219752754296894559, 0.3333333333333333703, 0.3219752754296894559, 0.3333333333333333703, 0.3219752754296894559, 0.3333333333333333703, 0.3219752754296894559, 0.3333333333333333703, 0.3219752754296894559, 0.3333333333333333703, 0.3219752754296894559, 0.3333333333333333703, 0.3219752754296894559, 0.3333333333333333703, 0.3219752754296894559, 0.3333333333333333703, 0.3219752754296894559, 0.3333333333333333703, 0.3219752754296894559, 0.3333333333333333703, 0.3219752754296894559, 0.3333333333333333703, 0.3219752754296894559, 0.3333333333333333703, 0.3219752754296894559, 0.3333333333333333703, 0.3219752754296894559, 0.3333333333333333703, 0.3219752754296894559, 0.3333333333333333703, 0.3219752754296894559, 0.3333333333333333703, 0.3219752754296894559, 0.3333333333333333703, 0.3219752754296894559, 0.3333333333333333703, 0.3219752754296894559, 0.3333333333333333703, 0.3219752754296894559, 0.3333333333333333703, 0.3219752754296894559, 0.3333333333333333703, 0.3219752754296894559, 0.3333333333333333703, 0.3219752754296894559, 0.3333333333333333703, 0.3219752754296894559, 0.3333333333333333703, 0.3219752754296894559, 0.3333333333333333703, 0.3219752754296894559, 0.3333333333333333703, 0.3219752754296894559, 0.3333333333333333703, 0.3219752754296894559, 0.3333333333333333703, 0.3219752754296894559, 0.3333333333333333703, 0.3219752754296894559, 0.3333333333333333703, 0.3219752754296894559, 0.3333333333333333703, 0.3219752754296894559, 0.3333333333333333703, 0.3219752754296894559, 0.3333333333333333703, 0.3219752754296894559, 0.3333333333333333703, 0.3219752754296894559, 0.3333333333333333703, 0.3219752754296894559, 0.3333333333333333703, 0.3219752754296894559, 0.3333333333333333703, 0.3219752754296894559, 0.3333333333333333703, 0.3219752754296894559, 0.3333333333333333703, 0.3219752754296894559, 0.3333333333333333703, 0.3219752754296894559, 0.3333333333333333703, 0.3219752754296894559, 0.3333333333333333703, 0.3219752754296894559, 0.3333333333333333703, 0.3219752754296894559, 0.3333333333333333703, 0.3219752754296894559, 0.3333333333333333703, 0.3219752754296894559, 0.3333333333333333703, 0.3219752754296894559, 0.3333333333333333703, 0.3219752754296894559, 0.3333333333333333703, 0.3219752754296894559, 0.3333333333333333703, 0.3219752754296894559, 0.3333333333333333703, 0.3219752754296894559, 0.3333333333333333703, 0.3219752754296894559, 0.3333333333333333703, 0.3219752754296894559, 0.3333333333333333703, 0.3219752754296894559, 0.3333333333333333703, 0.3219752754296894559, 0.3333333333333333703, 0.3219752754296894559, 0.3333333333333333703, 0.3219752754296894559, 0.3333333333333333703, 0.3219752754296894559, 0.3333333333333333703, 0.3219752754296894559, 0.3333333333333333703, 0.3219752754296894559, 0.3333333333333333703, 0.3219752754296894559, 0.3333333333333333703, 0.3219752754296894559, 0.3333333333333333703, 0.3219752754296894559, 0.3333333333333333703, 0.3219752754296894559, 0.3333333333333333703, 0.3219752754296894559, 0.3333333333333333703, 0.3219752754296894559, 0.3333333333333333703, 0.3219752754296894559, 0.3333333333333333703, 0.3219752754296894559, 0.3333333333333333703, 0.3219752754296894559, 0.3333333333333333703, 0.3219752754296894559, 0.3333333333333333703, 0.3219752754296894559, 0.3333333333333333703, 0.3219752754296894559, 0.3333333333333333703, 0.3219752754296894559, 0.3333333333333333703, 0.3219752754296894559, 0.3333333333333333703, 0.3219752754296894559, 0.3333333333333333703, 0.3219752754296894559, 0.3333333333333333703, 0.3219752754296894559, 0.3333333333333333703, 0.3219752754296894559, 0.3333333333333333703, 0.3219752754296894559, 0.3333333333333333703, 0.3219752754296894559, 0.3333333333333333703, 0.3219752754296894559, 0.3333333333333333703, 0.3219752754296894559, 0.3333333333333333703, 0.3219752754296894559, 0.3333333333333333703, 0.3219752754296894559, 0.3333333333333333703, 0.3219752754296894559, 0.3333333333333333703, 0.3219752754296894559, 0.3333333333333333703, 0.3219752754296894559, 0.3333333333333333703),
 ( 0.3333333333333333703, 0.3219752754296894559, 0.3333333333333333703, 0.3219752754296894559, 0.3333333333333333703, 0.3219752754296894559, 0.3333333333333333703, 0.3219752754296894559, 0.3333333333333333703, 0.3219752754296894559, 0.3333333333333333703, 0.3219752754296894559, 0.3333333333333333703, 0.3219752754296894559, 0.3333333333333333703, 0.3219752754296894559, 0.3333333333333333703, 0.3219752754296894559, 0.3333333333333333703, 0.3219752754296894559, 0.3333333333333333703, 0.3219752754296894559, 0.3333333333333333703, 0.3219752754296894559, 0.3333333333333333703, 0.3219752754296894559, 0.3333333333333333703, 0.3219752754296894559, 0.3333333333333333703, 0.3219752754296894559, 0.3333333333333333703, 0.3219752754296894559, 0.3333333333333333703, 0.3219752754296894559, 0.3333333333333333703, 0.3219752754296894559, 0.3333333333333333703, 0.3219752754296894559, 0.3333333333333333703, 0.3219752754296894559, 0.3333333333333333703, 0.3219752754296894559, 0.3333333333333333703, 0.3219752754296894559, 0.3333333333333333703, 0.3219752754296894559, 0.3333333333333333703, 0.3219752754296894559, 0.3333333333333333703, 0.3219752754296894559, 0.3333333333333333703, 0.3219752754296894559, 0.3333333333333333703, 0.3219752754296894559, 0.3333333333333333703, 0.3219752754296894559, 0.3333333333333333703, 0.3219752754296894559, 0.3333333333333333703, 0.3219752754296894559, 0.3333333333333333703, 0.3219752754296894559, 0.3333333333333333703, 0.3219752754296894559, 0.3333333333333333703, 0.3219752754296894559, 0.3333333333333333703, 0.3219752754296894559, 0.3333333333333333703, 0.3219752754296894559, 0.3333333333333333703, 0.3219752754296894559, 0.3333333333333333703, 0.3219752754296894559, 0.3333333333333333703, 0.3219752754296894559, 0.3333333333333333703, 0.3219752754296894559, 0.3333333333333333703, 0.3219752754296894559, 0.3333333333333333703, 0.3219752754296894559, 0.3333333333333333703, 0.3219752754296894559, 0.3333333333333333703, 0.3219752754296894559, 0.3333333333333333703, 0.3219752754296894559, 0.3333333333333333703, 0.3219752754296894559, 0.3333333333333333703, 0.3219752754296894559, 0.3333333333333333703, 0.3219752754296894559, 0.3333333333333333703, 0.3219752754296894559, 0.3333333333333333703, 0.3219752754296894559, 0.3333333333333333703, 0.3219752754296894559, 0.3333333333333333703, 0.3219752754296894559, 0.3333333333333333703, 0.3219752754296894559, 0.3333333333333333703, 0.3219752754296894559, 0.3333333333333333703, 0.3219752754296894559, 0.3333333333333333703, 0.3219752754296894559, 0.3333333333333333703, 0.3219752754296894559, 0.3333333333333333703, 0.3219752754296894559, 0.3333333333333333703, 0.3219752754296894559, 0.3333333333333333703, 0.3219752754296894559, 0.3333333333333333703, 0.3219752754296894559, 0.3333333333333333703, 0.3219752754296894559, 0.3333333333333333703, 0.3219752754296894559, 0.3333333333333333703, 0.3219752754296894559, 0.3333333333333333703, 0.3219752754296894559, 0.3333333333333333703, 0.3219752754296894559, 0.3333333333333333703, 0.3219752754296894559, 0.3333333333333333703, 0.3219752754296894559, 0.3333333333333333703, 0.3219752754296894559, 0.3333333333333333703, 0.3219752754296894559, 0.3333333333333333703, 0.3219752754296894559, 0.3333333333333333703, 0.3219752754296894559, 0.3333333333333333703, 0.3219752754296894559, 0.3333333333333333703, 0.3219752754296894559, 0.3333333333333333703, 0.3219752754296894559, 0.3333333333333333703, 0.3219752754296894559, 0.3333333333333333703, 0.3219752754296894559, 0.3333333333333333703, 0.3219752754296894559, 0.3333333333333333703, 0.3219752754296894559, 0.3333333333333333703, 0.3219752754296894559, 0.3333333333333333703, 0.3219752754296894559, 0.3333333333333333703, 0.3219752754296894559, 0.3333333333333333703, 0.3219752754296894559, 0.3333333333333333703, 0.3219752754296894559, 0.3333333333333333703, 0.3219752754296894559, 0.3333333333333333703, 0.3219752754296894559, 0.3333333333333333703, 0.3219752754296894559, 0.3333333333333333703, 0.3219752754296894559, 0.3333333333333333703, 0.3219752754296894559, 0.3333333333333333703, 0.3219752754296894559, 0.3333333333333333703, 0.3219752754296894559, 0.3333333333333333703, 0.3219752754296894559, 0.3333333333333333703, 0.3219752754296894559, 0.3333333333333333703, 0.3219752754296894559, 0.3333333333333333703, 0.3219752754296894559, 0.3333333333333333703, 0.3219752754296894559, 0.3333333333333333703, 0.3219752754296894559, 0.3333333333333333703, 0.3219752754296894559, 0.3333333333333333703, 0.3219752754296894559, 0.3333333333333333703, 0.3219752754296894559, 0.3333333333333333703, 0.3219752754296894559, 0.3333333333333333703, 0.3219752754296894559, 0.3333333333333333703, 0.3219752754296894559, 0.3333333333333333703, 0.3219752754296894559, 0.3333333333333333703, 0.3219752754296894559, 0.3333333333333333703, 0.3219752754296894559, 0.3333333333333333703, 0.3219752754296894559, 0.3333333333333333703, 0.3219752754296894559, 0.3333333333333333703, 0.3219752754296894559, 0.3333333333333333703, 0.3219752754296894559, 0.3333333333333333703, 0.3219752754296894559, 0.3333333333333333703, 0.3219752754296894559, 0.3333333333333333703, 0.3219752754296894559, 0.3333333333333333703, 0.3219752754296894559, 0.3333333333333333703, 0.3219752754296894559, 0.3333333333333333703, 0.3219752754296894559, 0.3333333333333333703, 0.3219752754296894559, 0.3333333333333333703, 0.3219752754296894559, 0.3333333333333333703, 0.3219752754296894559, 0.3333333333333333703, 0.3219752754296894559, 0.3333333333333333703, 0.3219752754296894559, 0.3333333333333333703, 0.3219752754296894559, 0.3333333333333333703, 0.3219752754296894559, 0.3333333333333333703, 0.3219752754296894559, 0.3333333333333333703, 0.3219752754296894559, 0.3333333333333333703, 0.3219752754296894559, 0.3333333333333333703, 0.3219752754296894559, 0.3333333333333333703, 0.3219752754296894559, 0.3333333333333333703, 0.3219752754296894559, 0.3333333333333333703, 0.3219752754296894559, 0.3333333333333333703, 0.3219752754296894559, 0.3333333333333333703, 0.3219752754296894559, 0.3333333333333333703, 0.3219752754296894559, 0.3333333333333333703, 0.3219752754296894559, 0.3333333333333333703, 0.3219752754296894559, 0.3333333333333333703, 0.3219752754296894559, 0.3333333333333333703, 0.3219752754296894559, 0.3333333333333333703, 0.3219752754296894559, 0.3333333333333333703, 0.3219752754296894559, 0.3333333333333333703, 0.3219752754296894559, 0.3333333333333333703, 0.3219752754296894559, 0.3333333333333333703, 0.3219752754296894559, 0.3333333333333333703, 0.3219752754296894559, 0.3333333333333333703, 0.3219752754296894559, 0.3333333333333333703, 0.3219752754296894559, 0.3333333333333333703, 0.3219752754296894559, 0.3333333333333333703, 0.3219752754296894559, 0.3333333333333333703, 0.3219752754296894559, 0.3333333333333333703, 0.3219752754296894559, 0.3333333333333333703, 0.3219752754296894559, 0.3333333333333333703, 0.3219752754296894559, 0.3333333333333333703, 0.3219752754296894559, 0.3333333333333333703, 0.3219752754296894559, 0.3333333333333333703, 0.3219752754296894559, 0.3333333333333333703, 0.3219752754296894559, 0.3333333333333333703, 0.3219752754296894559, 0.3333333333333333703, 0.3219752754296894559, 0.3333333333333333703, 0.3219752754296894559, 0.3333333333333333703, 0.3219752754296894559, 0.3333333333333333703, 0.3219752754296894559, 0.3333333333333333703, 0.3219752754296894559, 0.3333333333333333703, 0.3219752754296894559, 0.3333333333333333703, 0.3219752754296894559, 0.3333333333333333703, 0.3219752754296894559, 0.3333333333333333703, 0.3219752754296894559, 0.3333333333333333703, 0.3219752754296894559, 0.3333333333333333703, 0.3219752754296894559, 0.3333333333333333703, 0.3219752754296894559, 0.3333333333333333703, 0.3219752754296894559, 0.3333333333333333703, 0.3219752754296894559, 0.3333333333333333703, 0.3219752754296894559, 0.3333333333333333703, 0.3219752754296894559, 0.3333333333333333703, 0.3219752754296894559, 0.3333333333333333703, 0.3219752754296894559, 0.3333333333333333703, 0.3219752754296894559, 0.3333333333333333703, 0.3219752754296894559, 0.3333333333333333703, 0.3219752754296894559, 0.3333333333333333703, 0.3219752754296894559, 0.3333333333333333703, 0.3219752754296894559, 0.3333333333333333703, 0.3219752754296894559, 0.3333333333333333703, 0.3219752754296894559, 0.3333333333333333703, 0.3219752754296894559, 0.3333333333333333703, 0.3219752754296894559, 0.3333333333333333703, 0.3219752754296894559, 0.3333333333333333703, 0.3219752754296894559, 0.3333333333333333703, 0.3219752754296894559, 0.3333333333333333703, 0.3219752754296894559, 0.3333333333333333703, 0.3219752754296894559, 0.3333333333333333703, 0.3219752754296894559, 0.3333333333333333703, 0.3219752754296894559, 0.3333333333333333703, 0.3219752754296894559, 0.3333333333333333703, 0.3219752754296894559, 0.3333333333333333703, 0.3219752754296894559, 0.3333333333333333703, 0.3219752754296894559, 0.3333333333333333703, 0.3219752754296894559, 0.3333333333333333703, 0.3219752754296894559, 0.3333333333333333703, 0.3219752754296894559, 0.3333333333333333703, 0.3219752754296894559, 0.3333333333333333703, 0.3219752754296894559, 0.3333333333333333703, 0.3219752754296894559, 0.3333333333333333703, 0.3219752754296894559, 0.3333333333333333703, 0.3219752754296894559, 0.3333333333333333703, 0.3219752754296894559, 0.3333333333333333703, 0.3219752754296894559, 0.3333333333333333703, 0.3219752754296894559, 0.3333333333333333703, 0.3219752754296894559, 0.3333333333333333703, 0.3219752754296894559, 0.3333333333333333703, 0.3219752754296894559, 0.3333333333333333703, 0.3219752754296894559, 0.3333333333333333703, 0.3219752754296894559, 0.3333333333333333703, 0.3219752754296894559, 0.3333333333333333703, 0.3219752754296894559, 0.3333333333333333703, 0.3219752754296894559, 0.3333333333333333703, 0.3219752754296894559, 0.3333333333333333703, 0.3219752754296894559, 0.3333333333333333703, 0.3219752754296894559, 0.3333333333333333703, 0.3219752754296894559, 0.3333333333333333703, 0.3219752754296894559, 0.3333333333333333703, 0.3219752754296894559, 0.3333333333333333703, 0.3219752754296894559, 0.3333333333333333703, 0.3219752754296894559, 0.3333333333333333703, 0.3219752754296894559, 0.3333333333333333703, 0.3219752754296894559, 0.3333333333333333703, 0.3219752754296894559, 0.3333333333333333703, 0.3219752754296894559, 0.3333333333333333703, 0.3219752754296894559, 0.3333333333333333703, 0.3219752754296894559, 0.3333333333333333703, 0.3219752754296894559, 0.3333333333333333703, 0.3219752754296894559, 0.3333333333333333703),
 ( 1.000000000000000000, 0.9659258262890683122, 1.000000000000000000, 0.9659258262890683122, 1.000000000000000000, 0.9659258262890683122, 1.000000000000000000, 0.9659258262890683122, 1.000000000000000000, 0.9659258262890683122, 1.000000000000000000, 0.9659258262890683122, 1.000000000000000000, 0.9659258262890683122, 1.000000000000000000, 0.9659258262890683122, 1.000000000000000000, 0.9659258262890683122, 1.000000000000000000, 0.9659258262890683122, 1.000000000000000000, 0.9659258262890683122, 1.000000000000000000, 0.9659258262890683122, 1.000000000000000000, 0.9659258262890683122, 1.000000000000000000, 0.9659258262890683122, 1.000000000000000000, 0.9659258262890683122, 1.000000000000000000, 0.9659258262890683122, 1.000000000000000000, 0.9659258262890683122, 1.000000000000000000, 0.9659258262890683122, 1.000000000000000000, 0.9659258262890683122, 1.000000000000000000, 0.9659258262890683122, 1.000000000000000000, 0.9659258262890683122, 1.000000000000000000, 0.9659258262890683122, 1.000000000000000000, 0.9659258262890683122, 1.000000000000000000, 0.9659258262890683122, 1.000000000000000000, 0.9659258262890683122, 1.000000000000000000, 0.9659258262890683122, 1.000000000000000000, 0.9659258262890683122, 1.000000000000000000, 0.9659258262890683122, 1.000000000000000000, 0.9659258262890683122, 1.000000000000000000, 0.9659258262890683122, 1.000000000000000000, 0.9659258262890683122, 1.000000000000000000, 0.9659258262890683122, 1.000000000000000000, 0.9659258262890683122, 1.000000000000000000, 0.9659258262890683122, 1.000000000000000000, 0.9659258262890683122, 1.000000000000000000, 0.9659258262890683122, 1.000000000000000000, 0.9659258262890683122, 1.000000000000000000, 0.9659258262890683122, 1.000000000000000000, 0.9659258262890683122, 1.000000000000000000, 0.9659258262890683122, 1.000000000000000000, 0.9659258262890683122, 1.000000000000000000, 0.9659258262890683122, 1.000000000000000000, 0.9659258262890683122, 1.000000000000000000, 0.9659258262890683122, 1.000000000000000000, 0.9659258262890683122, 1.000000000000000000, 0.9659258262890683122, 1.000000000000000000, 0.9659258262890683122, 1.000000000000000000, 0.9659258262890683122, 1.000000000000000000, 0.9659258262890683122, 1.000000000000000000, 0.9659258262890683122, 1.000000000000000000, 0.9659258262890683122, 1.000000000000000000, 0.9659258262890683122, 1.000000000000000000, 0.9659258262890683122, 1.000000000000000000, 0.9659258262890683122, 1.000000000000000000, 0.9659258262890683122, 1.000000000000000000, 0.9659258262890683122, 1.000000000000000000, 0.9659258262890683122, 1.000000000000000000, 0.9659258262890683122, 1.000000000000000000, 0.9659258262890683122, 1.000000000000000000, 0.9659258262890683122, 1.000000000000000000, 0.9659258262890683122, 1.000000000000000000, 0.9659258262890683122, 1.000000000000000000, 0.9659258262890683122, 1.000000000000000000, 0.9659258262890683122, 1.000000000000000000, 0.9659258262890683122, 1.000000000000000000, 0.9659258262890683122, 1.000000000000000000, 0.9659258262890683122, 1.000000000000000000, 0.9659258262890683122, 1.000000000000000000, 0.9659258262890683122, 1.000000000000000000, 0.9659258262890683122, 1.000000000000000000, 0.9659258262890683122, 1.000000000000000000, 0.9659258262890683122, 1.000000000000000000, 0.9659258262890683122, 1.000000000000000000, 0.9659258262890683122, 1.000000000000000000, 0.9659258262890683122, 1.000000000000000000, 0.9659258262890683122, 1.000000000000000000, 0.9659258262890683122, 1.000000000000000000, 0.9659258262890683122, 1.000000000000000000, 0.9659258262890683122, 1.000000000000000000, 0.9659258262890683122, 1.000000000000000000, 0.9659258262890683122, 1.000000000000000000, 0.9659258262890683122, 1.000000000000000000, 0.9659258262890683122, 1.000000000000000000, 0.9659258262890683122, 1.000000000000000000, 0.9659258262890683122, 1.000000000000000000, 0.9659258262890683122, 1.000000000000000000, 0.9659258262890683122, 1.000000000000000000, 0.9659258262890683122, 1.000000000000000000, 0.9659258262890683122, 1.000000000000000000, 0.9659258262890683122, 1.000000000000000000, 0.9659258262890683122, 1.000000000000000000, 0.9659258262890683122, 1.000000000000000000, 0.9659258262890683122, 1.000000000000000000, 0.9659258262890683122, 1.000000000000000000, 0.9659258262890683122, 1.000000000000000000, 0.9659258262890683122, 1.000000000000000000, 0.9659258262890683122, 1.000000000000000000, 0.9659258262890683122, 1.000000000000000000, 0.9659258262890683122, 1.000000000000000000, 0.9659258262890683122, 1.000000000000000000, 0.9659258262890683122, 1.000000000000000000, 0.9659258262890683122, 1.000000000000000000, 0.9659258262890683122, 1.000000000000000000, 0.9659258262890683122, 1.000000000000000000, 0.9659258262890683122, 1.000000000000000000, 0.9659258262890683122, 1.000000000000000000, 0.9659258262890683122, 1.000000000000000000, 0.9659258262890683122, 1.000000000000000000, 0.9659258262890683122, 1.000000000000000000, 0.9659258262890683122, 1.000000000000000000, 0.9659258262890683122, 1.000000000000000000, 0.9659258262890683122, 1.000000000000000000, 0.9659258262890683122, 1.000000000000000000, 0.9659258262890683122, 1.000000000000000000, 0.9659258262890683122, 1.000000000000000000, 0.9659258262890683122, 1.000000000000000000, 0.9659258262890683122, 1.000000000000000000, 0.9659258262890683122, 1.000000000000000000, 0.9659258262890683122, 1.000000000000000000, 0.9659258262890683122, 1.000000000000000000, 0.9659258262890683122, 1.000000000000000000, 0.9659258262890683122, 1.000000000000000000, 0.9659258262890683122, 1.000000000000000000, 0.9659258262890683122, 1.000000000000000000, 0.9659258262890683122, 1.000000000000000000, 0.9659258262890683122, 1.000000000000000000, 0.9659258262890683122, 1.000000000000000000, 0.9659258262890683122, 1.000000000000000000, 0.9659258262890683122, 1.000000000000000000, 0.9659258262890683122, 1.000000000000000000, 0.9659258262890683122, 1.000000000000000000, 0.9659258262890683122, 1.000000000000000000, 0.9659258262890683122, 1.000000000000000000, 0.9659258262890683122, 1.000000000000000000, 0.9659258262890683122, 1.000000000000000000, 0.9659258262890683122, 1.000000000000000000, 0.9659258262890683122, 1.000000000000000000, 0.9659258262890683122, 1.000000000000000000, 0.9659258262890683122, 1.000000000000000000, 0.9659258262890683122, 1.000000000000000000, 0.9659258262890683122, 1.000000000000000000, 0.9659258262890683122, 1.000000000000000000, 0.9659258262890683122, 1.000000000000000000, 0.9659258262890683122, 1.000000000000000000, 0.9659258262890683122, 1.000000000000000000, 0.9659258262890683122, 1.000000000000000000, 0.9659258262890683122, 1.000000000000000000, 0.9659258262890683122, 1.000000000000000000, 0.9659258262890683122, 1.000000000000000000, 0.9659258262890683122, 1.000000000000000000, 0.9659258262890683122, 1.000000000000000000, 0.9659258262890683122, 1.000000000000000000, 0.9659258262890683122, 1.000000000000000000, 0.9659258262890683122, 1.000000000000000000, 0.9659258262890683122, 1.000000000000000000, 0.9659258262890683122, 1.000000000000000000, 0.9659258262890683122, 1.000000000000000000, 0.9659258262890683122, 1.000000000000000000, 0.9659258262890683122, 1.000000000000000000, 0.9659258262890683122, 1.000000000000000000, 0.9659258262890683122, 1.000000000000000000, 0.9659258262890683122, 1.000000000000000000, 0.9659258262890683122, 1.000000000000000000, 0.9659258262890683122, 1.000000000000000000, 0.9659258262890683122, 1.000000000000000000, 0.9659258262890683122, 1.000000000000000000, 0.9659258262890683122, 1.000000000000000000, 0.9659258262890683122, 1.000000000000000000, 0.9659258262890683122, 1.000000000000000000, 0.9659258262890683122, 1.000000000000000000, 0.9659258262890683122, 1.000000000000000000, 0.9659258262890683122, 1.000000000000000000, 0.9659258262890683122, 1.000000000000000000, 0.9659258262890683122, 1.000000000000000000, 0.9659258262890683122, 1.000000000000000000, 0.9659258262890683122, 1.000000000000000000, 0.9659258262890683122, 1.000000000000000000, 0.9659258262890683122, 1.000000000000000000, 0.9659258262890683122, 1.000000000000000000, 0.9659258262890683122, 1.000000000000000000, 0.9659258262890683122, 1.000000000000000000, 0.9659258262890683122, 1.000000000000000000, 0.9659258262890683122, 1.000000000000000000, 0.9659258262890683122, 1.000000000000000000, 0.9659258262890683122, 1.000000000000000000, 0.9659258262890683122, 1.000000000000000000, 0.9659258262890683122, 1.000000000000000000, 0.9659258262890683122, 1.000000000000000000, 0.9659258262890683122, 1.000000000000000000, 0.9659258262890683122, 1.000000000000000000, 0.9659258262890683122, 1.000000000000000000, 0.9659258262890683122, 1.000000000000000000, 0.9659258262890683122, 1.000000000000000000, 0.9659258262890683122, 1.000000000000000000, 0.9659258262890683122, 1.000000000000000000, 0.9659258262890683122, 1.000000000000000000, 0.9659258262890683122, 1.000000000000000000, 0.9659258262890683122, 1.000000000000000000, 0.9659258262890683122, 1.000000000000000000, 0.9659258262890683122, 1.000000000000000000, 0.9659258262890683122, 1.000000000000000000, 0.9659258262890683122, 1.000000000000000000, 0.9659258262890683122, 1.000000000000000000, 0.9659258262890683122, 1.000000000000000000, 0.9659258262890683122, 1.000000000000000000, 0.9659258262890683122, 1.000000000000000000, 0.9659258262890683122, 1.000000000000000000, 0.9659258262890683122, 1.000000000000000000, 0.9659258262890683122, 1.000000000000000000, 0.9659258262890683122, 1.000000000000000000, 0.9659258262890683122, 1.000000000000000000, 0.9659258262890683122, 1.000000000000000000, 0.9659258262890683122, 1.000000000000000000, 0.9659258262890683122, 1.000000000000000000, 0.9659258262890683122, 1.000000000000000000, 0.9659258262890683122, 1.000000000000000000, 0.9659258262890683122, 1.000000000000000000, 0.9659258262890683122, 1.000000000000000000, 0.9659258262890683122, 1.000000000000000000, 0.9659258262890683122, 1.000000000000000000, 0.9659258262890683122, 1.000000000000000000, 0.9659258262890683122, 1.000000000000000000, 0.9659258262890683122, 1.000000000000000000, 0.9659258262890683122, 1.000000000000000000, 0.9659258262890683122, 1.000000000000000000, 0.9659258262890683122, 1.000000000000000000, 0.9659258262890683122, 1.000000000000000000, 0.9659258262890683122, 1.000000000000000000) ) ) 
 REPRESENTATION_ITEM ( '' )  SURFACE ( )  );
#4192 = CARTESIAN_POINT ( 'NONE',  ( -16.51473224551082808, 9.474510206698731452, 28.33442372801900433 ) ) ;
#4193 = CARTESIAN_POINT ( 'NONE',  ( 21.96405779611664855, -8.831116573701658368, 171.4809137887048962 ) ) ;
#4195 = CARTESIAN_POINT ( 'NONE',  ( 19.02544592524343514, -5.153800228976328945, 68.54057627198103830 ) ) ;
#4194 = CARTESIAN_POINT ( 'NONE',  ( -13.97604488694527625, -13.89961937509977652, 51.87390960531436690 ) ) ;
#4196 = CARTESIAN_POINT ( 'NONE',  ( 8.224510206698742110, 14.34966873604972548, 32.08442372801901854 ) ) ;
#4197 = DIRECTION ( 'NONE',  ( -1.000000000000000000, 0.000000000000000000, 0.000000000000000000 ) ) ;
#4198 = CARTESIAN_POINT ( 'NONE',  ( -16.79531203550645913, 7.028104445595614536, 108.7475501177955834 ) ) ;
#4199 = CARTESIAN_POINT ( 'NONE',  ( 8.314922557961029526, -14.29746914071037800, 80.41775706135234714 ) ) ;
#4201 = CARTESIAN_POINT ( 'NONE',  ( -5.719274019375978568, 21.55341960407610458, 90.20724293864770971 ) ) ;
#4200 = CARTESIAN_POINT ( 'NONE',  ( -4.379528057220086978, -16.55341960407618274, 64.79275706135234714 ) ) ;
#4202 = CARTESIAN_POINT ( 'NONE',  ( -8.314922557961024197, 14.29746914071037800, 47.91775706135234714 ) ) ;
#4204 = CARTESIAN_POINT ( 'NONE',  ( 1.221313414957698099E-14, -31.90000000000003411, -45.64921306006598201 ) ) ;
#4203 = CARTESIAN_POINT ( 'NONE',  ( -16.51473224551069308, -9.474510206698971260, 41.66557627198103120 ) ) ;
#4205 = CARTESIAN_POINT ( 'NONE',  ( -21.53943276465977519, -0.05219959533937600094, 58.75109039468568994 ) ) ;
#4206 = CARTESIAN_POINT ( 'NONE',  ( -13.97604488694547697, 13.89961937509957934, 68.12609039468563310 ) ) ;
#4207 = CARTESIAN_POINT ( 'NONE',  ( -10.81492255796105439, 18.62759615963255655, 97.91775706135236135 ) ) ;
#4208 = CARTESIAN_POINT ( 'NONE',  ( 5.049401038298161559, -19.05341960407611168, 32.70724293864768129 ) ) ;
#4209 = CARTESIAN_POINT ( 'NONE',  ( -15.29496450215403058, 1.499960427298884680, -59.75377357153833913 ) ) ;
#4210 = CARTESIAN_POINT ( 'NONE',  ( -21.52544592524343514, 5.823673210054127303, 56.04057627198102409 ) ) ;
#4211 = CARTESIAN_POINT ( 'NONE',  ( 5.153800228976335163, 19.02544592524342804, 99.79057627198102409 ) ) ;
#4212 = CARTESIAN_POINT ( 'NONE',  ( 12.06949235617757843, -12.14591786802309237, 103.1239096053143811 ) ) ;
#4213 = CARTESIAN_POINT ( 'NONE',  ( 4.379528057220092307, 16.55341960407617563, 42.29275706135235424 ) ) ;
#4214 = CARTESIAN_POINT ( 'NONE',  ( -16.55341960407617563, 4.379528057220093196, 108.5427570613523756 ) ) ;
#4215 = VERTEX_POINT ( 'NONE', #91986 ) ;
#4216 = CARTESIAN_POINT ( 'NONE',  ( 18.62759615963271287, -10.81492255796078972, 108.3322429386477097 ) ) ;
#4217 = AXIS2_PLACEMENT_3D ( 'NONE', #86911, #8069, #40413 ) ;
#4219 = CARTESIAN_POINT ( 'NONE',  ( -19.02544592524342804, 5.153800228976336051, 111.0405762719810099 ) ) ;
#4218 = CARTESIAN_POINT ( 'NONE',  ( 0.05219959533910956823, 16.53943276465976808, 34.99890960531435979 ) ) ;
#4220 = CARTESIAN_POINT ( 'NONE',  ( 9.564922557961047289, -16.46253265017146816, 95.41775706135233293 ) ) ;
#4221 = CARTESIAN_POINT ( 'NONE',  ( -0.05219959533936034679, 19.03943276465977164, 22.50109039468566152 ) ) ;
#4222 = CARTESIAN_POINT ( 'NONE',  ( -8.224510206698948167, 14.34966873604960824, 25.41557627198103120 ) ) ;
#4223 = CARTESIAN_POINT ( 'NONE',  ( 0.05219959533907565091, 21.53943276465977519, 94.99890960531436690 ) ) ;
#4224 = CARTESIAN_POINT ( 'NONE',  ( 10.72451020669898902, -18.67979575497178502, 52.91557627198103830 ) ) ;
#4225 = CARTESIAN_POINT ( 'NONE',  ( -9.474510206698964154, 16.51473224551069663, 60.41557627198102409 ) ) ;
#4226 = CARTESIAN_POINT ( 'NONE',  ( -8.224510206698948167, 14.34966873604960824, 35.41557627198102409 ) ) ;
#4227 = CARTESIAN_POINT ( 'NONE',  ( -5.049401038298153566, 19.05341960407611168, 85.20724293864766707 ) ) ;
#4228 = ORIENTED_EDGE ( 'NONE', *, *, #72173, .F. ) ;
#4229 = CARTESIAN_POINT ( 'NONE',  ( 18.22780087662125226, -5.499999999999864997, 61.01540105326109398 ) ) ;
#4230 = CARTESIAN_POINT ( 'NONE',  ( -13.89961937509957401, -13.97604488694547875, 39.37609039468566152 ) ) ;
#4231 = CARTESIAN_POINT ( 'NONE',  ( -21.52544592524343514, 5.823673210054127303, 86.04057627198102409 ) ) ;
#4232 = CARTESIAN_POINT ( 'NONE',  ( 4.379528057220339221, -16.55341960407611168, 97.70724293864772392 ) ) ;
#4233 = CARTESIAN_POINT ( 'NONE',  ( 10.72451020669871369, 18.67979575497193778, 37.08442372801901143 ) ) ;
#4234 = CARTESIAN_POINT ( 'NONE',  ( -27.73933785331498925, 2.428612866367529932E-14, 138.8750000027311842 ) ) ;
#4235 = CARTESIAN_POINT ( 'NONE',  ( -12.06949235617739369, -12.14591786802326823, 104.3760903946856899 ) ) ;
#4236 = CARTESIAN_POINT ( 'NONE',  ( 5.049401038298161559, -19.05341960407611168, 37.70724293864768839 ) ) ;
#4237 = CARTESIAN_POINT ( 'NONE',  ( -16.46253265017160317, 9.564922557960807481, 85.83224293864769550 ) ) ;
#4238 = CARTESIAN_POINT ( 'NONE',  ( -19.26498983726237313, 5.499999999999599432, 45.55319577422005750 ) ) ;
#4239 = CARTESIAN_POINT ( 'NONE',  ( 9.564922557960805705, 16.46253265017160317, 29.58224293864769550 ) ) ;
#4240 = CARTESIAN_POINT ( 'NONE',  ( 8.224510206698953496, -14.34966873604960469, 47.91557627198102409 ) ) ;
#4241 = CARTESIAN_POINT ( 'NONE',  ( -5.823673210054431948, 21.52544592524334988, 67.70942372801901854 ) ) ;
#4243 = CARTESIAN_POINT ( 'NONE',  ( -12.14591786802326823, 12.06949235617739902, 73.12609039468567573 ) ) ;
#4242 = CARTESIAN_POINT ( 'NONE',  ( -67.00000000000000000, -1.096058885236868847E-14, 100.5000000000010232 ) ) ;
#4244 = CARTESIAN_POINT ( 'NONE',  ( 13.97604488694527802, 13.89961937509977652, 54.37390960531435979 ) ) ;
#4245 = CARTESIAN_POINT ( 'NONE',  ( -19.02544592524342804, 5.153800228976336051, 71.04057627198099567 ) ) ;
#4246 = VERTEX_POINT ( 'NONE', #76836 ) ;
#4247 = CARTESIAN_POINT ( 'NONE',  ( 21.52544592524334988, 5.823673210054432836, 106.4594237280190328 ) ) ;
#4248 = CARTESIAN_POINT ( 'NONE',  ( -16.55341960407617563, 4.379528057220093196, 78.54275706135236135 ) ) ;
#4249 = B_SPLINE_CURVE_WITH_KNOTS ( 'NONE', 3,
 ( #199002, #121154, #154481, #199997, #182847, #186838 ),
 .UNSPECIFIED., .F., .F.,
 ( 4, 2, 4 ),
 ( 0.003239945802372220466, 0.003620412082092073526, 0.004000878361811927020 ),
 .UNSPECIFIED. ) ;
#4250 = CARTESIAN_POINT ( 'NONE',  ( -18.67979575497193778, 10.72451020669871902, 98.33442372801901854 ) ) ;
#4251 = CARTESIAN_POINT ( 'NONE',  ( -13.97604488694527625, -13.89961937509977652, 56.87390960531434558 ) ) ;
#4252 = CARTESIAN_POINT ( 'NONE',  ( 21.53943276465977519, -0.05219959533907433946, 33.74890960531436690 ) ) ;
#4253 = CARTESIAN_POINT ( 'NONE',  ( 5.153800228976615827, -19.02544592524334988, 110.2094237280189901 ) ) ;
#4254 = CARTESIAN_POINT ( 'NONE',  ( -18.62759615963255300, -10.81492255796106328, 69.16775706135234714 ) ) ;
#4255 = CARTESIAN_POINT ( 'NONE',  ( -16.52544592524335698, -4.483927247898792601, 48.95942372801902565 ) ) ;
#4256 = CARTESIAN_POINT ( 'NONE',  ( 21.55341960407610458, 5.719274019375980345, 98.95724293864770971 ) ) ;
#4257 = CARTESIAN_POINT ( 'NONE',  ( -9.564922557961040184, 16.46253265017147172, 92.91775706135233293 ) ) ;
#4258 = CARTESIAN_POINT ( 'NONE',  ( -5.049401038298153566, 19.05341960407611168, 75.20724293864769550 ) ) ;
#4259 = CARTESIAN_POINT ( 'NONE',  ( -19.05341960407617563, 5.049401038297882671, 103.5427570613523329 ) ) ;
#4260 = CARTESIAN_POINT ( 'NONE',  ( -19.03943276465977164, -0.05219959533935918106, 108.7510903946856615 ) ) ;
#4261 = CARTESIAN_POINT ( 'NONE',  ( -16.55341960407611168, -4.379528057220339221, 61.45724293864770260 ) ) ;
#4262 = CARTESIAN_POINT ( 'NONE',  ( -0.05219959533934338120, 16.53943276465976808, 77.50109039468567573 ) ) ;
#4264 = CARTESIAN_POINT ( 'NONE',  ( 16.46253265017160672, -9.564922557960803928, 48.33224293864769550 ) ) ;
#4263 = CARTESIAN_POINT ( 'NONE',  ( -5.719274019375978568, 21.55341960407610458, 115.2072429386476955 ) ) ;
#4265 = CARTESIAN_POINT ( 'NONE',  ( 5.153800228976335163, 19.02544592524342804, 59.79057627198100988 ) ) ;
#4266 = CARTESIAN_POINT ( 'NONE',  ( 0.05219959533934541429, -16.53943276465976808, 75.00109039468568994 ) ) ;
#4267 = ADVANCED_FACE ( 'NONE', ( #27388 ), #85950, .T. ) ;
#4268 = CARTESIAN_POINT ( 'NONE',  ( -28.82186960331499392, 9.364793116373565596, 148.1500000054624024 ) ) ;
#4269 = VERTEX_POINT ( 'NONE', #96770 ) ;
#4270 = CARTESIAN_POINT ( 'NONE',  ( 19.03943276465977164, 0.05219959533936151252, 21.25109039468565797 ) ) ;
#4271 = CARTESIAN_POINT ( 'NONE',  ( 5.049401038298161559, -19.05341960407611168, 22.70724293864769194 ) ) ;
#4272 = CARTESIAN_POINT ( 'NONE',  ( 14.29746914071037800, 8.314922557961029526, 21.66775706135235069 ) ) ;
#4274 = CARTESIAN_POINT ( 'NONE',  ( -16.55341960407617563, 4.379528057220093196, 23.54275706135235424 ) ) ;
#4273 = CARTESIAN_POINT ( 'NONE',  ( 19.05341960407617918, -5.049401038297876454, 46.04275706135233293 ) ) ;
#4275 = CARTESIAN_POINT ( 'NONE',  ( -0.05219959533909027116, -19.03943276465977164, 37.49890960531436690 ) ) ;
#4276 = B_SPLINE_CURVE_WITH_KNOTS ( 'NONE', 3,
 ( #133701, #28535, #45665, #168015, #199353, #10371, #13345, #135705, #165048, #30493, #148880, #59830, #12371, #73044, #137666, #90171, #72028, #26541, #182199, #103370, #29511, #121500, #91145, #60818, #75009, #195393, #151854, #197376, #122492, #89185, #104360, #149869 ),
 .UNSPECIFIED., .F., .F.,
 ( 4, 2, 2, 2, 2, 2, 2, 2, 2, 2, 2, 2, 2, 2, 2, 4 ),
 ( 2.453269466693398313E-17, 0.0003712461730037028783, 0.0007424923460073811453, 0.001113738519011059358, 0.001484984692014737788, 0.002227477038022087925, 0.002598723211025748790, 0.002969969384029409656, 0.003341215557033070088, 0.003712461730036730519, 0.004083707903040390517, 0.004454954076044050949, 0.004826200249047711381, 0.005197446422051372680, 0.005568692595055032245, 0.005939938768058692677 ),
 .UNSPECIFIED. ) ;
#4277 = CARTESIAN_POINT ( 'NONE',  ( 5.153800228976335163, 19.02544592524342804, 59.79057627198100988 ) ) ;
#4278 = CARTESIAN_POINT ( 'NONE',  ( -18.62759615963270932, 10.81492255796079327, 85.83224293864768129 ) ) ;
#4279 = CARTESIAN_POINT ( 'NONE',  ( 5.153800228976335163, 19.02544592524342804, 114.7905762719810241 ) ) ;
#4280 = CARTESIAN_POINT ( 'NONE',  ( -16.51473224551069308, -9.474510206698971260, 46.66557627198102409 ) ) ;
#4281 = CARTESIAN_POINT ( 'NONE',  ( -0.3535533905933930798, -35.00000000000000000, 5.353553390593270400 ) ) ;
#4282 = CARTESIAN_POINT ( 'NONE',  ( 13.89961937509957401, 13.97604488694547697, 101.8760903946856331 ) ) ;
#4283 = CARTESIAN_POINT ( 'NONE',  ( -16.55341960407611168, -4.379528057220339221, 66.45724293864768129 ) ) ;
#4284 = CARTESIAN_POINT ( 'NONE',  ( 13.97604488694548053, -13.89961937509957401, 20.62609039468567573 ) ) ;
#4285 = CARTESIAN_POINT ( 'NONE',  ( -16.53943276465976808, 0.05219959533911058130, 61.24890960531435979 ) ) ;
#4286 = CARTESIAN_POINT ( 'NONE',  ( 0.05219959533937995610, -21.53943276465977519, 90.00109039468567573 ) ) ;
#4287 = CARTESIAN_POINT ( 'NONE',  ( 13.89961937509977652, -13.97604488694527269, 28.12390960531435624 ) ) ;
#4288 = CARTESIAN_POINT ( 'NONE',  ( -0.05219959533937732626, 21.53943276465977519, 97.50109039468567573 ) ) ;
#4290 = CARTESIAN_POINT ( 'NONE',  ( 10.81492255796106328, -18.62759615963255655, 70.41775706135236135 ) ) ;
#4289 = CARTESIAN_POINT ( 'NONE',  ( 14.29746914071049879, -8.314922557960816363, 23.33224293864769194 ) ) ;
#4291 = CARTESIAN_POINT ( 'NONE',  ( -19.02544592524342804, 5.153800228976336051, 86.04057627198103830 ) ) ;
#4292 = CARTESIAN_POINT ( 'NONE',  ( -21.55341960407619339, 5.719274019375674811, 48.54275706135234714 ) ) ;
#4293 = CARTESIAN_POINT ( 'NONE',  ( -16.51473224551069308, -9.474510206698971260, 81.66557627198103830 ) ) ;
#4294 = CARTESIAN_POINT ( 'NONE',  ( 14.34966873604960469, 8.224510206698951720, 94.16557627198103830 ) ) ;
#4295 = CARTESIAN_POINT ( 'NONE',  ( -16.53943276465976808, 0.05219959533911058130, 56.24890960531436690 ) ) ;
#4296 = CARTESIAN_POINT ( 'NONE',  ( -21.53943276465977519, 0.05219959533907696930, 66.24890960531436690 ) ) ;
#4297 = CARTESIAN_POINT ( 'NONE',  ( 16.51473224551069308, 9.474510206698969483, 74.16557627198103830 ) ) ;
#4298 = CARTESIAN_POINT ( 'NONE',  ( 0.05219959533907565091, 21.53943276465977519, 79.99890960531435269 ) ) ;
#4299 = CARTESIAN_POINT ( 'NONE',  ( -16.46253265017146816, -9.564922557961047289, 64.16775706135233293 ) ) ;
#4301 = CARTESIAN_POINT ( 'NONE',  ( -8.314922557960811034, -14.29746914071050412, 72.08224293864769550 ) ) ;
#4300 = CARTESIAN_POINT ( 'NONE',  ( -13.97604488694547520, 13.89961937509957934, 28.12609039468566152 ) ) ;
#4302 = CARTESIAN_POINT ( 'NONE',  ( 15.72974639402199770, -15.80617190586745480, 48.12390960531436690 ) ) ;
#4303 = CYLINDRICAL_SURFACE ( 'NONE', #49564, 38.00000000000000000 ) ;
#4305 = CARTESIAN_POINT ( 'NONE',  ( 27.73933785331498569, 9.013057229001093518, 142.4750000027312069 ) ) ;
#4304 = CARTESIAN_POINT ( 'NONE',  ( -4.379528057220086978, -16.55341960407618274, 99.79275706135234714 ) ) ;
#4306 = CARTESIAN_POINT ( 'NONE',  ( 9.474510206698729675, 16.51473224551082808, 97.08442372801900433 ) ) ;
#4307 = CARTESIAN_POINT ( 'NONE',  ( 14.34966873604960469, 8.224510206698951720, 64.16557627198102409 ) ) ;
#4308 = CARTESIAN_POINT ( 'NONE',  ( -17.50000000000001776, 3.305555262949595452, 34.62517152156593170 ) ) ;
#4309 = CARTESIAN_POINT ( 'NONE',  ( 0.05219959533909260263, 19.03943276465977164, 54.99890960531435979 ) ) ;
#4310 = CARTESIAN_POINT ( 'NONE',  ( 14.29746914071049879, -8.314922557960816363, 53.33224293864769550 ) ) ;
#4311 = CARTESIAN_POINT ( 'NONE',  ( 9.564922557960805705, 16.46253265017160317, 99.58224293864770971 ) ) ;
#4313 = CARTESIAN_POINT ( 'NONE',  ( -13.89961937509977652, 13.97604488694528158, 70.62390960531432427 ) ) ;
#4312 = CARTESIAN_POINT ( 'NONE',  ( 19.02544592524334988, 5.153800228976608722, 81.45942372801897591 ) ) ;
#4314 = CARTESIAN_POINT ( 'NONE',  ( -13.97604488694527625, -13.89961937509977652, 91.87390960531432427 ) ) ;
#4315 = CARTESIAN_POINT ( 'NONE',  ( -16.46253265017160317, 9.564922557960807481, 80.83224293864769550 ) ) ;
#4316 = CARTESIAN_POINT ( 'NONE',  ( 5.719274019375991003, -21.55341960407610458, 67.70724293864769550 ) ) ;
#4317 = CARTESIAN_POINT ( 'NONE',  ( -4.379528057220086978, -16.55341960407618274, 54.79275706135235424 ) ) ;
#4318 = CARTESIAN_POINT ( 'NONE',  ( -9.141470119588765426E-16, -69.45486021086043138, -22.99263613531268291 ) ) ;
#4319 = CARTESIAN_POINT ( 'NONE',  ( -19.05341960407611168, -5.049401038298163336, 46.45724293864768129 ) ) ;
#4320 = CARTESIAN_POINT ( 'NONE',  ( 5.719274019375991003, -21.55341960407610458, 52.70724293864769550 ) ) ;
#4321 = CARTESIAN_POINT ( 'NONE',  ( -9.474510206698720793, -16.51473224551083518, 99.58442372801900433 ) ) ;
#4323 = CARTESIAN_POINT ( 'NONE',  ( 18.62759615963255655, 10.81492255796105972, 46.66775706135234714 ) ) ;
#4322 = CARTESIAN_POINT ( 'NONE',  ( -4.379528057220328563, 16.55341960407611168, 30.20724293864769550 ) ) ;
#4324 = CARTESIAN_POINT ( 'NONE',  ( 5.049401038297881783, 19.05341960407617563, 37.29275706135232582 ) ) ;
#4326 = CARTESIAN_POINT ( 'NONE',  ( -16.53943276465976808, -0.05219959533934237506, 93.75109039468567573 ) ) ;
#4325 = CARTESIAN_POINT ( 'NONE',  ( -12.06949235617739369, -12.14591786802326823, 54.37609039468568994 ) ) ;
#4327 = CARTESIAN_POINT ( 'NONE',  ( 18.87580814761073711, -5.500000000000038192, 43.37172394265759579 ) ) ;
#4328 = CARTESIAN_POINT ( 'NONE',  ( 12.14591786802327356, -12.06949235617739191, 75.62609039468567573 ) ) ;
#4329 = CARTESIAN_POINT ( 'NONE',  ( 8.224510206698742110, 14.34966873604972548, 32.08442372801901854 ) ) ;
#4330 = CARTESIAN_POINT ( 'NONE',  ( -9.564922557960796823, -16.46253265017161027, 42.08224293864769550 ) ) ;
#4331 = CARTESIAN_POINT ( 'NONE',  ( 9.474510206698971260, -16.51473224551069308, 52.91557627198102409 ) ) ;
#4332 = CARTESIAN_POINT ( 'NONE',  ( -16.51473224551069308, -9.474510206698971260, 61.66557627198103120 ) ) ;
#4333 = CARTESIAN_POINT ( 'NONE',  ( -15.72974639402176322, -15.80617190586768395, 54.37609039468568994 ) ) ;
#4334 = CARTESIAN_POINT ( 'NONE',  ( 4.483927247898790824, -16.52544592524335698, 50.20942372801901854 ) ) ;
#4335 = CARTESIAN_POINT ( 'NONE',  ( -8.314922557961024197, 14.29746914071037800, 112.9177570613523329 ) ) ;
#4336 = CARTESIAN_POINT ( 'NONE',  ( -0.05219959533909027116, -19.03943276465977164, 22.49890960531436690 ) ) ;
#4337 = CARTESIAN_POINT ( 'NONE',  ( -9.474510206698720793, -16.51473224551083518, 19.58442372801899722 ) ) ;
#4338 = CARTESIAN_POINT ( 'NONE',  ( 9.474510206698729675, 16.51473224551082808, 112.0844237280190043 ) ) ;
#4339 = CARTESIAN_POINT ( 'NONE',  ( -13.89961937509957401, -13.97604488694547875, 69.37609039468564731 ) ) ;
#4340 = CARTESIAN_POINT ( 'NONE',  ( -12.14591786802309592, -12.06949235617757132, 81.87390960531435269 ) ) ;
#4341 = CARTESIAN_POINT ( 'NONE',  ( 0.05219959533909260263, 19.03943276465977164, 39.99890960531436690 ) ) ;
#4343 = CARTESIAN_POINT ( 'NONE',  ( -30.00000000000000355, 0.3535533905932729537, 5.353553390593267736 ) ) ;
#4342 = CARTESIAN_POINT ( 'NONE',  ( 16.46253265017146816, 9.564922557961045513, 76.66775706135234714 ) ) ;
#4344 = CARTESIAN_POINT ( 'NONE',  ( -10.81492255796105439, 18.62759615963255655, 82.91775706135234714 ) ) ;
#4345 = CARTESIAN_POINT ( 'NONE',  ( 8.314922557961029526, -14.29746914071037800, 35.41775706135234003 ) ) ;
#4346 = CARTESIAN_POINT ( 'NONE',  ( -17.50000000000000711, 4.049696124445808287, 24.18039670665952201 ) ) ;
#4347 = CARTESIAN_POINT ( 'NONE',  ( -10.72451020669898014, 18.67979575497178502, 40.41557627198103120 ) ) ;
#4348 = CARTESIAN_POINT ( 'NONE',  ( -4.379528057220086978, -16.55341960407618274, 24.79275706135235779 ) ) ;
#4349 = CARTESIAN_POINT ( 'NONE',  ( 9.564922557960805705, 16.46253265017160317, 29.58224293864769550 ) ) ;
#4350 = CARTESIAN_POINT ( 'NONE',  ( -19.03943276465977164, -0.05219959533935918106, 33.75109039468566863 ) ) ;
#4351 = CARTESIAN_POINT ( 'NONE',  ( 37.99999999999999289, 2.893978650043524126E-14, -7.000000000000000000 ) ) ;
#4352 = CARTESIAN_POINT ( 'NONE',  ( -5.049401038298153566, 19.05341960407611168, 35.20724293864768839 ) ) ;
#4353 = FACE_OUTER_BOUND ( 'NONE', #24443, .T. ) ;
#4354 = CARTESIAN_POINT ( 'NONE',  ( 0.05219959533909260263, 19.03943276465977164, 64.99890960531436690 ) ) ;
#4355 = CARTESIAN_POINT ( 'NONE',  ( 17.50000000000000355, -3.345213924137376171, 112.0876862309434756 ) ) ;
#4356 = CARTESIAN_POINT ( 'NONE',  ( -21.52544592524334988, -5.823673210054445271, 108.9594237280190185 ) ) ;
#4357 = CARTESIAN_POINT ( 'NONE',  ( 14.29746914071049879, -8.314922557960816363, 33.33224293864769550 ) ) ;
#4358 = CARTESIAN_POINT ( 'NONE',  ( 9.474510206698971260, -16.51473224551069308, 47.91557627198102409 ) ) ;
#4359 = EDGE_CURVE ( 'NONE', #122084, #114881, #130090, .T. ) ;
#4360 = CARTESIAN_POINT ( 'NONE',  ( -5.049401038298153566, 19.05341960407611168, 90.20724293864766707 ) ) ;
#4361 = CARTESIAN_POINT ( 'NONE',  ( -5.823673210054431948, 21.52544592524334988, 67.70942372801901854 ) ) ;
#4362 = CARTESIAN_POINT ( 'NONE',  ( 16.51473224551069308, 9.474510206698969483, 49.16557627198102409 ) ) ;
#4363 = CIRCLE ( 'NONE', #120577, 4.500000000000000000 ) ;
#4364 = CARTESIAN_POINT ( 'NONE',  ( -15.72974639402176322, -15.80617190586768395, 69.37609039468567573 ) ) ;
#4365 = CARTESIAN_POINT ( 'NONE',  ( 15.80617190586746368, 15.72974639402197994, 24.37390960531435979 ) ) ;
#4366 = CARTESIAN_POINT ( 'NONE',  ( 13.97604488694527802, 13.89961937509977652, 34.37390960531436690 ) ) ;
#4367 = CARTESIAN_POINT ( 'NONE',  ( 5.823673210054125526, 21.52544592524343514, 114.7905762719810383 ) ) ;
#4368 = CARTESIAN_POINT ( 'NONE',  ( 19.05341960407617918, -5.049401038297876454, 31.04275706135232227 ) ) ;
#4369 = CARTESIAN_POINT ( 'NONE',  ( -0.05219959533910754901, -16.53943276465976808, 107.4989096053143669 ) ) ;
#4370 = CARTESIAN_POINT ( 'NONE',  ( -13.97604488694527625, -13.89961937509977652, 66.87390960531436690 ) ) ;
#4371 = CARTESIAN_POINT ( 'NONE',  ( -16.52544592524335698, -4.483927247898792601, 18.95942372801901143 ) ) ;
#4372 = CARTESIAN_POINT ( 'NONE',  ( 8.314922557960818139, 14.29746914071049879, 74.58224293864768129 ) ) ;
#4373 = CARTESIAN_POINT ( 'NONE',  ( -21.53943276465977519, 0.05219959533907696930, 26.24890960531435624 ) ) ;
#4374 = CARTESIAN_POINT ( 'NONE',  ( 16.46253265017146816, 9.564922557961045513, 86.66775706135233293 ) ) ;
#4375 = CARTESIAN_POINT ( 'NONE',  ( -18.67979575497178146, -10.72451020669898902, 111.6655762719810525 ) ) ;
#4376 = CARTESIAN_POINT ( 'NONE',  ( 21.55341960407619695, -5.719274019375665929, 56.04275706135235424 ) ) ;
#4377 = CARTESIAN_POINT ( 'NONE',  ( 14.29746914071037800, 8.314922557961029526, 61.66775706135235424 ) ) ;
#4378 = CARTESIAN_POINT ( 'NONE',  ( -4.483927247898782831, 16.52544592524335698, 57.70942372801901143 ) ) ;
#4379 = CARTESIAN_POINT ( 'NONE',  ( -10.81492255796078084, -18.62759615963271287, 52.08224293864768839 ) ) ;
#4380 = CARTESIAN_POINT ( 'NONE',  ( -19.02544592524342804, 5.153800228976336051, 51.04057627198103120 ) ) ;
#4381 = CARTESIAN_POINT ( 'NONE',  ( 30.74264578624799782, 22.33583958711400541, -2.549999994537626602 ) ) ;
#4382 = CARTESIAN_POINT ( 'NONE',  ( -0.05219959533934338120, 16.53943276465976808, 77.50109039468567573 ) ) ;
#4383 = CARTESIAN_POINT ( 'NONE',  ( -18.62759615963270932, 10.81492255796079327, 100.8322429386477097 ) ) ;
#4384 = CARTESIAN_POINT ( 'NONE',  ( -0.05219959533910754901, -16.53943276465976808, 52.49890960531435979 ) ) ;
#4385 = CARTESIAN_POINT ( 'NONE',  ( 14.29746914071037800, 8.314922557961029526, 76.66775706135234714 ) ) ;
#4386 = CARTESIAN_POINT ( 'NONE',  ( 16.51473224551083163, -9.474510206698727899, 105.8344237280190043 ) ) ;
#4387 = CARTESIAN_POINT ( 'NONE',  ( 18.67979575497178502, 10.72451020669898547, 94.16557627198103830 ) ) ;
#4388 = CARTESIAN_POINT ( 'NONE',  ( -0.05219959533910754901, -16.53943276465976808, 42.49890960531435979 ) ) ;
#4389 = EDGE_CURVE ( 'NONE', #70174, #115376, #63320, .T. ) ;
#4390 = EDGE_LOOP ( 'NONE', ( #44839, #29813, #144030, #184763 ) ) ;
#4391 = CARTESIAN_POINT ( 'NONE',  ( -16.29526858892875651, 7.335722546920117715, 69.20329402199793378 ) ) ;
#4392 = CARTESIAN_POINT ( 'NONE',  ( 18.67979575497178502, 10.72451020669898547, 79.16557627198103830 ) ) ;
#4393 = CARTESIAN_POINT ( 'NONE',  ( -14.34966873604972548, 8.224510206698743886, 113.3344237280190328 ) ) ;
#4394 = EDGE_LOOP ( 'NONE', ( #77649, #111972, #192802, #188802 ) ) ;
#4395 = CARTESIAN_POINT ( 'NONE',  ( -17.31728774477271671, -6.344390552232407110, 54.18093348310682700 ) ) ;
#4396 = CARTESIAN_POINT ( 'NONE',  ( -18.62759615963270932, 10.81492255796079327, 95.83224293864770971 ) ) ;
#4397 = CARTESIAN_POINT ( 'NONE',  ( -5.719274019375665041, -21.55341960407619695, 24.79275706135235779 ) ) ;
#4398 = CARTESIAN_POINT ( 'NONE',  ( 4.483927247898545687, 16.52544592524342804, 34.79057627198103120 ) ) ;
#4399 = CARTESIAN_POINT ( 'NONE',  ( -4.483927247898782831, 16.52544592524335698, 47.70942372801902565 ) ) ;
#4400 = CARTESIAN_POINT ( 'NONE',  ( 19.03943276465977164, -0.05219959533909143690, 53.74890960531436690 ) ) ;
#4401 = CARTESIAN_POINT ( 'NONE',  ( -13.97604488694527625, -13.89961937509977652, 81.87390960531436690 ) ) ;
#4402 = ORIENTED_EDGE ( 'NONE', *, *, #164677, .T. ) ;
#4403 = CARTESIAN_POINT ( 'NONE',  ( 21.53943276465977519, -0.05219959533907433946, 28.74890960531435624 ) ) ;
#4404 = CARTESIAN_POINT ( 'NONE',  ( -37.02045864137325992, -17.72559658019849138, -19.07609595512615996 ) ) ;
#4405 = CARTESIAN_POINT ( 'NONE',  ( 12.06949235617739724, 12.14591786802326823, 21.87609039468567573 ) ) ;
#4406 = CARTESIAN_POINT ( 'NONE',  ( -9.474510206698720793, -16.51473224551083518, 49.58442372801899722 ) ) ;
#4407 = CARTESIAN_POINT ( 'NONE',  ( 5.719274019375991003, -21.55341960407610458, 97.70724293864772392 ) ) ;
#4408 = CARTESIAN_POINT ( 'NONE',  ( 0.05219959533910956823, 16.53943276465976808, 34.99890960531435979 ) ) ;
#4409 = CARTESIAN_POINT ( 'NONE',  ( 0.05219959533909260263, 19.03943276465977164, 79.99890960531436690 ) ) ;
#4410 = CARTESIAN_POINT ( 'NONE',  ( 5.719274019375991003, -21.55341960407610458, 57.70724293864770260 ) ) ;
#4412 = CARTESIAN_POINT ( 'NONE',  ( 16.55341960407618274, -4.379528057220086978, 26.04275706135235779 ) ) ;
#4411 = CARTESIAN_POINT ( 'NONE',  ( 5.823673210054125526, 21.52544592524343514, 99.79057627198103830 ) ) ;
#4413 = CARTESIAN_POINT ( 'NONE',  ( 5.049401038298161559, -19.05341960407611168, 112.7072429386476813 ) ) ;
#4414 = CARTESIAN_POINT ( 'NONE',  ( -15.80617190586768217, 15.72974639402176855, 83.12609039468568994 ) ) ;
#4415 = CARTESIAN_POINT ( 'NONE',  ( -5.153800228976328057, -19.02544592524343514, 77.29057627198099567 ) ) ;
#4416 = CARTESIAN_POINT ( 'NONE',  ( -19.03943276465977164, 0.05219959533909376836, 31.24890960531435979 ) ) ;
#4417 = CARTESIAN_POINT ( 'NONE',  ( -13.97604488694527625, -13.89961937509977652, 86.87390960531436690 ) ) ;
#4418 = CARTESIAN_POINT ( 'NONE',  ( 4.483927247898545687, 16.52544592524342804, 99.79057627198103830 ) ) ;
#4419 = CARTESIAN_POINT ( 'NONE',  ( 5.153800228976615827, -19.02544592524334988, 110.2094237280189901 ) ) ;
#4420 = CIRCLE ( 'NONE', #36755, 16.70000000000002061 ) ;
#4421 = DIRECTION ( 'NONE',  ( 1.000000000000000000, 0.000000000000000000, 0.000000000000000000 ) ) ;
#4422 = CARTESIAN_POINT ( 'NONE',  ( 9.564922557960805705, 16.46253265017160317, 74.58224293864769550 ) ) ;
#4424 = CARTESIAN_POINT ( 'NONE',  ( -21.55341960407610458, -5.719274019375992779, 21.45724293864769550 ) ) ;
#4423 = CARTESIAN_POINT ( 'NONE',  ( -5.719274019375665041, -21.55341960407619695, 94.79275706135234714 ) ) ;
#4425 = CARTESIAN_POINT ( 'NONE',  ( -4.483927247898782831, 16.52544592524335698, 92.70942372801901854 ) ) ;
#4426 = CARTESIAN_POINT ( 'NONE',  ( -31.77050690183224546, 0.6194686979414664174, -45.83912112027729080 ) ) ;
#4427 = CARTESIAN_POINT ( 'NONE',  ( -5.153800228976607833, 19.02544592524334988, 57.70942372801899012 ) ) ;
#4428 = CARTESIAN_POINT ( 'NONE',  ( -19.05341960407617563, 5.049401038297882671, 23.54275706135233648 ) ) ;
#4429 = CARTESIAN_POINT ( 'NONE',  ( -19.05341960407611168, -5.049401038298163336, 26.45724293864769550 ) ) ;
#4430 = CARTESIAN_POINT ( 'NONE',  ( -16.55341960407611168, -4.379528057220339221, 26.45724293864768839 ) ) ;
#4431 = CARTESIAN_POINT ( 'NONE',  ( 32.00000000000000000, -1.230770033143102596E-14, 100.5000000000010232 ) ) ;
#4432 = CARTESIAN_POINT ( 'NONE',  ( -16.53943276465976808, -0.05219959533934237506, 108.7510903946857042 ) ) ;
#4433 = CARTESIAN_POINT ( 'NONE',  ( -4.622231866529366047E-30, -105.0000000000000000, -15.00000000000000000 ) ) ;
#4434 = CARTESIAN_POINT ( 'NONE',  ( 0.05219959533934541429, -16.53943276465976808, 80.00109039468568994 ) ) ;
#4435 = CARTESIAN_POINT ( 'NONE',  ( -9.564922557960796823, -16.46253265017161027, 22.08224293864768839 ) ) ;
#4436 = CARTESIAN_POINT ( 'NONE',  ( -15.72974639402176322, -15.80617190586768395, 89.37609039468568994 ) ) ;
#4437 = CARTESIAN_POINT ( 'NONE',  ( 0.05219959533936267826, -19.03943276465977164, 105.0010903946856615 ) ) ;
#4438 = CARTESIAN_POINT ( 'NONE',  ( -10.72451020669870658, -18.67979575497194134, 64.58442372801900433 ) ) ;
#4439 = CARTESIAN_POINT ( 'NONE',  ( 0.05219959533936267826, -19.03943276465977164, 35.00109039468566863 ) ) ;
#4440 = CARTESIAN_POINT ( 'NONE',  ( 0.05219959533909260263, 19.03943276465977164, 84.99890960531436690 ) ) ;
#4441 = CARTESIAN_POINT ( 'NONE',  ( -16.51473224551069308, -9.474510206698971260, 76.66557627198103830 ) ) ;
#4442 = CARTESIAN_POINT ( 'NONE',  ( -7.652493125962417153, -39.26116846143397510, -13.00000000000000000 ) ) ;
#4443 = CARTESIAN_POINT ( 'NONE',  ( 5.719274019375991003, -21.55341960407610458, 52.70724293864769550 ) ) ;
#4444 = CARTESIAN_POINT ( 'NONE',  ( 9.474510206698971260, -16.51473224551069308, 47.91557627198102409 ) ) ;
#4445 = CARTESIAN_POINT ( 'NONE',  ( -8.224510206698735004, -14.34966873604973081, 79.58442372801903275 ) ) ;
#4446 = ORIENTED_EDGE ( 'NONE', *, *, #59341, .T. ) ;
#4448 = CARTESIAN_POINT ( 'NONE',  ( 36.91746825000000598, -11.99521256947793546, -1.724999997268813479 ) ) ;
#4447 = CARTESIAN_POINT ( 'NONE',  ( -4.379528057220328563, 16.55341960407611168, 75.20724293864769550 ) ) ;
#4449 = CARTESIAN_POINT ( 'NONE',  ( -16.52544592524335698, -4.483927247898792601, 43.95942372801902565 ) ) ;
#4450 = CARTESIAN_POINT ( 'NONE',  ( -16.52544592524342804, 4.483927247898546575, 116.0405762719810383 ) ) ;
#4451 = CARTESIAN_POINT ( 'NONE',  ( -0.05219959533936034679, 19.03943276465977164, 62.50109039468566863 ) ) ;
#4452 = CARTESIAN_POINT ( 'NONE',  ( -14.34966873604960291, -8.224510206698953496, 71.66557627198100988 ) ) ;
#4454 = EDGE_CURVE ( 'NONE', #48994, #85047, #178636, .T. ) ;
#4453 = CARTESIAN_POINT ( 'NONE',  ( -21.55341960407619339, 5.719274019375674811, 48.54275706135234714 ) ) ;
#4456 = CARTESIAN_POINT ( 'NONE',  ( 21.55341960407610458, 5.719274019375980345, 88.95724293864769550 ) ) ;
#4455 = CYLINDRICAL_SURFACE ( 'NONE', #82707, 2.000000000000001776 ) ;
#4457 = CARTESIAN_POINT ( 'NONE',  ( 19.02544592524343514, -5.153800228976328945, 113.5405762719810241 ) ) ;
#4458 = CARTESIAN_POINT ( 'NONE',  ( 14.34966873604960469, 8.224510206698951720, 69.16557627198102409 ) ) ;
#4459 = CARTESIAN_POINT ( 'NONE',  ( 13.37225149056123108, -38.04021455641917271, -24.47500528307575252 ) ) ;
#4460 = CARTESIAN_POINT ( 'NONE',  ( 0.05219959533909260263, 19.03943276465977164, 39.99890960531436690 ) ) ;
#4461 = CARTESIAN_POINT ( 'NONE',  ( -22.81625015709510507, 31.40387420917330275, -6.924999997268812990 ) ) ;
#4462 = CARTESIAN_POINT ( 'NONE',  ( 9.564922557961047289, -16.46253265017146816, 75.41775706135234714 ) ) ;
#4463 = CARTESIAN_POINT ( 'NONE',  ( -10.81492255796105439, 18.62759615963255655, 22.91775706135235069 ) ) ;
#4464 = CARTESIAN_POINT ( 'NONE',  ( 9.564922557960805705, 16.46253265017160317, 74.58224293864769550 ) ) ;
#4465 = CARTESIAN_POINT ( 'NONE',  ( 9.564922557961047289, -16.46253265017146816, 50.41775706135233293 ) ) ;
#4466 = CARTESIAN_POINT ( 'NONE',  ( -16.51473224551069308, -9.474510206698971260, 41.66557627198103120 ) ) ;
#4467 = CARTESIAN_POINT ( 'NONE',  ( 14.29746914071049879, -8.314922557960816363, 58.33224293864768839 ) ) ;
#4468 = CARTESIAN_POINT ( 'NONE',  ( 14.34966873604960469, 8.224510206698951720, 54.16557627198103120 ) ) ;
#4469 = CARTESIAN_POINT ( 'NONE',  ( 0.05219959533909260263, 19.03943276465977164, 79.99890960531436690 ) ) ;
#4470 = CARTESIAN_POINT ( 'NONE',  ( 21.55341960407610458, 5.719274019375980345, 83.95724293864770971 ) ) ;
#4471 = CARTESIAN_POINT ( 'NONE',  ( -13.97604488694527625, -13.89961937509977652, 76.87390960531433848 ) ) ;
#4472 = CARTESIAN_POINT ( 'NONE',  ( -0.05219959533907301413, -21.53943276465977519, 77.49890960531433848 ) ) ;
#4473 = CARTESIAN_POINT ( 'NONE',  ( 5.153800228976615827, -19.02544592524334988, 20.20942372801899722 ) ) ;
#4476 = CARTESIAN_POINT ( 'NONE',  ( 8.224510206698953496, -14.34966873604960469, 102.9155762719810383 ) ) ;
#4475 = CARTESIAN_POINT ( 'NONE',  ( -12.14591786802326823, 12.06949235617739902, 103.1260903946856757 ) ) ;
#4474 = CARTESIAN_POINT ( 'NONE',  ( 16.51473224551069308, 9.474510206698969483, 24.16557627198102765 ) ) ;
#4477 = CARTESIAN_POINT ( 'NONE',  ( -19.05341960407617563, 5.049401038297882671, 108.5427570613523187 ) ) ;
#4478 = ORIENTED_EDGE ( 'NONE', *, *, #588, .F. ) ;
#4479 = CARTESIAN_POINT ( 'NONE',  ( 21.53943276465977519, 0.05219959533937863772, 36.25109039468567573 ) ) ;
#4480 = CARTESIAN_POINT ( 'NONE',  ( -0.05219959533936034679, 19.03943276465977164, 47.50109039468566863 ) ) ;
#4481 = CARTESIAN_POINT ( 'NONE',  ( 4.379528057220339221, -16.55341960407611168, 22.70724293864769194 ) ) ;
#4482 = CARTESIAN_POINT ( 'NONE',  ( -18.62759615963270932, 10.81492255796079327, 70.83224293864770971 ) ) ;
#4483 = CARTESIAN_POINT ( 'NONE',  ( 19.03943276465977164, -0.05219959533909143690, 103.7489096053143669 ) ) ;
#4484 = CARTESIAN_POINT ( 'NONE',  ( -4.483927247898539470, -16.52544592524342804, 62.29057627198102409 ) ) ;
#4485 = CARTESIAN_POINT ( 'NONE',  ( 0.000000000000000000, 0.000000000000000000, -64.92279855667830191 ) ) ;
#4486 = CARTESIAN_POINT ( 'NONE',  ( -16.51473224551069308, -9.474510206698971260, 36.66557627198102409 ) ) ;
#4487 = CARTESIAN_POINT ( 'NONE',  ( -21.55341960407619339, 5.719274019375674811, 103.5427570613523613 ) ) ;
#4488 = CARTESIAN_POINT ( 'NONE',  ( 14.34966873604972726, -8.224510206698740333, 85.83442372801901854 ) ) ;
#4489 = CARTESIAN_POINT ( 'NONE',  ( 5.719274019375673035, 21.55341960407619339, 42.29275706135235424 ) ) ;
#4490 = CARTESIAN_POINT ( 'NONE',  ( 14.34966873604972726, -8.224510206698740333, 45.83442372801901854 ) ) ;
#4491 = CARTESIAN_POINT ( 'NONE',  ( 18.67979575497178502, 10.72451020669898547, 29.16557627198103120 ) ) ;
#4492 = CARTESIAN_POINT ( 'NONE',  ( 0.05219959533909260263, 19.03943276465977164, 49.99890960531435979 ) ) ;
#4493 = CARTESIAN_POINT ( 'NONE',  ( 0.05219959533909260263, 19.03943276465977164, 69.99890960531435269 ) ) ;
#4494 = CARTESIAN_POINT ( 'NONE',  ( 14.29746914071037800, 8.314922557961029526, 56.66775706135235424 ) ) ;
#4495 = CARTESIAN_POINT ( 'NONE',  ( 14.29746914071049879, -8.314922557960816363, 103.3322429386476955 ) ) ;
#4496 = CARTESIAN_POINT ( 'NONE',  ( -8.224510206698735004, -14.34966873604973081, 109.5844237280190328 ) ) ;
#4497 = DIRECTION ( 'NONE',  ( -1.000000000000000000, -0.000000000000000000, -0.000000000000000000 ) ) ;
#4500 = CARTESIAN_POINT ( 'NONE',  ( 16.51473224551069308, 9.474510206698969483, 84.16557627198102409 ) ) ;
#4499 = CARTESIAN_POINT ( 'NONE',  ( 0.05219959533909260263, 19.03943276465977164, 94.99890960531436690 ) ) ;
#4498 = CARTESIAN_POINT ( 'NONE',  ( 10.81492255796106328, -18.62759615963255655, 50.41775706135235424 ) ) ;
#4501 = CARTESIAN_POINT ( 'NONE',  ( 0.05219959533909260263, 19.03943276465977164, 99.99890960531436690 ) ) ;
#4502 = CARTESIAN_POINT ( 'NONE',  ( -8.224510206698948167, 14.34966873604960824, 50.41557627198103120 ) ) ;
#4503 = CARTESIAN_POINT ( 'NONE',  ( -16.55341960407617563, 4.379528057220093196, 113.5427570613523756 ) ) ;
#4504 = CIRCLE ( 'NONE', #14199, 0.5000000000000005551 ) ;
#4505 = CARTESIAN_POINT ( 'NONE',  ( -14.29746914071049879, 8.314922557960819915, 40.83224293864769550 ) ) ;
#4506 = CARTESIAN_POINT ( 'NONE',  ( -16.00800591765002778, -17.62450045179643254, -54.61670405711556242 ) ) ;
#4507 = CARTESIAN_POINT ( 'NONE',  ( 13.97604488694548053, -13.89961937509957401, 40.62609039468564731 ) ) ;
#4508 = CARTESIAN_POINT ( 'NONE',  ( -16.51473224551069308, -9.474510206698971260, 71.66557627198102409 ) ) ;
#4509 = CARTESIAN_POINT ( 'NONE',  ( -19.02544592524334988, -5.153800228976617603, 58.95942372801900433 ) ) ;
#4510 = CARTESIAN_POINT ( 'NONE',  ( 3.556970738554033499E-15, -38.81732327939057825, -8.624999997268814056 ) ) ;
#4511 = FACE_OUTER_BOUND ( 'NONE', #127744, .T. ) ;
#4513 = CARTESIAN_POINT ( 'NONE',  ( 16.53943276465976808, 0.05219959533934440121, 71.25109039468568994 ) ) ;
#4512 = CARTESIAN_POINT ( 'NONE',  ( 5.153800228976615827, -19.02544592524334988, 80.20942372801901854 ) ) ;
#4514 = CARTESIAN_POINT ( 'NONE',  ( -24.43796699203916845, 7.704306453272268485, 171.8420650787743966 ) ) ;
#4515 = CARTESIAN_POINT ( 'NONE',  ( 9.564922557960805705, 16.46253265017160317, 104.5822429386476955 ) ) ;
#4516 = CARTESIAN_POINT ( 'NONE',  ( 15.80617190586769283, -15.72974639402175789, 30.62609039468567929 ) ) ;
#4517 = CARTESIAN_POINT ( 'NONE',  ( -19.02544592524334988, -5.153800228976617603, 88.95942372801897591 ) ) ;
#4519 = CARTESIAN_POINT ( 'NONE',  ( 19.05341960407611168, 5.049401038298154454, 48.95724293864768129 ) ) ;
#4518 = CARTESIAN_POINT ( 'NONE',  ( 16.18388926212237067, 7.379444403734554569, 87.93953151366153520 ) ) ;
#4520 = CARTESIAN_POINT ( 'NONE',  ( -16.51473224551069308, -9.474510206698971260, 86.66557627198102409 ) ) ;
#4522 = CARTESIAN_POINT ( 'NONE',  ( 16.46253265017160672, -9.564922557960803928, 53.33224293864768839 ) ) ;
#4521 = CARTESIAN_POINT ( 'NONE',  ( -12.06949235617756955, 12.14591786802309770, 45.62390960531436690 ) ) ;
#4523 = CARTESIAN_POINT ( 'NONE',  ( -0.05219959533936034679, 19.03943276465977164, 67.50109039468566152 ) ) ;
#4524 = CARTESIAN_POINT ( 'NONE',  ( 16.46253265017146816, 9.564922557961045513, 26.66775706135234003 ) ) ;
#4525 = CARTESIAN_POINT ( 'NONE',  ( -16.46253265017160317, 9.564922557960807481, 60.83224293864769550 ) ) ;
#4526 = AXIS2_PLACEMENT_3D ( 'NONE', #70715, #118222, #178904 ) ;
#4527 = CARTESIAN_POINT ( 'NONE',  ( 5.823673210054125526, 21.52544592524343514, 59.79057627198103120 ) ) ;
#4529 = CARTESIAN_POINT ( 'NONE',  ( 5.719274019375673035, 21.55341960407619339, 112.2927570613523471 ) ) ;
#4528 = CARTESIAN_POINT ( 'NONE',  ( 14.34966873604960469, 8.224510206698951720, 69.16557627198102409 ) ) ;
#4530 = DIRECTION ( 'NONE',  ( 0.000000000000000000, 0.000000000000000000, -1.000000000000000000 ) ) ;
#4531 = CARTESIAN_POINT ( 'NONE',  ( -16.46253265017160317, 9.564922557960807481, 115.8322429386477097 ) ) ;
#4532 = CARTESIAN_POINT ( 'NONE',  ( 19.02544592524343514, -5.153800228976328945, 53.54057627198102409 ) ) ;
#4533 = CARTESIAN_POINT ( 'NONE',  ( -5.153800228976328057, -19.02544592524343514, 37.29057627198102409 ) ) ;
#4534 = CARTESIAN_POINT ( 'NONE',  ( -14.29746914071049879, 8.314922557960819915, 100.8322429386477097 ) ) ;
#4535 = CARTESIAN_POINT ( 'NONE',  ( -21.55341960407610458, -5.719274019375992779, 111.4572429386476813 ) ) ;
#4536 = CARTESIAN_POINT ( 'NONE',  ( 25.90244409532897762, -6.509810826857640897, 161.8457455760359949 ) ) ;
#4537 = CARTESIAN_POINT ( 'NONE',  ( 5.823673210054444382, -21.52544592524334988, 30.20942372801902565 ) ) ;
#4538 = CARTESIAN_POINT ( 'NONE',  ( -19.03943276465977164, 0.05219959533909376836, 26.24890960531435624 ) ) ;
#4539 = CARTESIAN_POINT ( 'NONE',  ( -18.67979575497193778, 10.72451020669871902, 78.33442372801901854 ) ) ;
#4540 = CARTESIAN_POINT ( 'NONE',  ( 15.72974639402199770, -15.80617190586745480, 93.12390960531436690 ) ) ;
#4541 = CARTESIAN_POINT ( 'NONE',  ( 13.89961937509957401, 13.97604488694547697, 36.87609039468565442 ) ) ;
#4542 = CARTESIAN_POINT ( 'NONE',  ( -16.51473224551069308, -9.474510206698971260, 21.66557627198102765 ) ) ;
#4543 = CARTESIAN_POINT ( 'NONE',  ( -69.65682714487590488, -71.74905178543390605, -15.00000000000000000 ) ) ;
#4544 = CARTESIAN_POINT ( 'NONE',  ( 12.21143611141174468, -11.13220115481712646, -61.42794421580953212 ) ) ;
#4545 = CARTESIAN_POINT ( 'NONE',  ( -14.29746914071037622, -8.314922557961029526, 49.16775706135234003 ) ) ;
#4547 = AXIS2_PLACEMENT_3D ( 'NONE', #182810, #104965, #93502 ) ;
#4546 = CARTESIAN_POINT ( 'NONE',  ( 4.379528057220339221, -16.55341960407611168, 102.7072429386476955 ) ) ;
#4548 = CARTESIAN_POINT ( 'NONE',  ( 34.11707783341799427, -4.368959606072635005, 91.63974055655047835 ) ) ;
#4549 = CARTESIAN_POINT ( 'NONE',  ( 16.51473224551069308, 9.474510206698969483, 74.16557627198103830 ) ) ;
#4550 = CARTESIAN_POINT ( 'NONE',  ( -14.34966873604960291, -8.224510206698953496, 96.66557627198102409 ) ) ;
#4551 = CARTESIAN_POINT ( 'NONE',  ( -21.55341960407610458, -5.719274019375992779, 51.45724293864770260 ) ) ;
#4552 = CARTESIAN_POINT ( 'NONE',  ( 14.34966873604960469, 8.224510206698951720, 69.16557627198102409 ) ) ;
#4553 = CARTESIAN_POINT ( 'NONE',  ( 12.14591786802327356, -12.06949235617739191, 30.62609039468567929 ) ) ;
#4554 = CARTESIAN_POINT ( 'NONE',  ( -21.53943276465977519, -0.05219959533937600094, 83.75109039468568994 ) ) ;
#4555 = CLOSED_SHELL ( 'NONE', ( #90232, #12376, #39790, #49765, #196807, #195802, #5067, #178847, #90906, #29062, #71683, #37608, #132806, #83460, #86746, #142950, #9900, #188345, #21736, #102737, #129324, #36223, #83487, #180359, #110651, #151179, #135829, #116056, #163838, #21395, #184629, #66098, #113969, #161198, #91600, #44781, #54625, #152525, #139324, #99460, #181205, #19000, #32262, #11988, #77426, #192893, #49369, #139173, #138390, #165381, #24013, #108264, #157224, #194354, #83980, #9700, #103342, #135698, #72433, #186703, #66135, #146997, #103745, #47351, #199677, #22379, #63505, #38617, #191100, #189772, #111561, #137258, #44759, #98675, #18130, #51870, #110625, #156274, #9092, #133714, #77296, #1864 ) ) ;
#4556 = DIRECTION ( 'NONE',  ( 0.000000000000000000, 1.000000000000000000, 0.000000000000000000 ) ) ;
#4557 = CARTESIAN_POINT ( 'NONE',  ( 12.06949235617739724, 12.14591786802326823, 91.87609039468568994 ) ) ;
#4558 = CARTESIAN_POINT ( 'NONE',  ( 4.483927247898545687, 16.52544592524342804, 44.79057627198103120 ) ) ;
#4559 = CARTESIAN_POINT ( 'NONE',  ( -19.02544592524342804, 5.153800228976336051, 36.04057627198100988 ) ) ;
#4560 = CARTESIAN_POINT ( 'NONE',  ( 9.474510206698971260, -16.51473224551069308, 82.91557627198103830 ) ) ;
#4561 = CARTESIAN_POINT ( 'NONE',  ( 15.80617190586746368, 15.72974639402197994, 114.3739096053143527 ) ) ;
#4562 = CARTESIAN_POINT ( 'NONE',  ( 18.62759615963255655, 10.81492255796105972, 56.66775706135235424 ) ) ;
#4563 = CARTESIAN_POINT ( 'NONE',  ( -8.314922557961024197, 14.29746914071037800, 37.91775706135235424 ) ) ;
#4565 = CARTESIAN_POINT ( 'NONE',  ( 0.05219959533937995610, -21.53943276465977519, 85.00109039468568994 ) ) ;
#4564 = CARTESIAN_POINT ( 'NONE',  ( -16.53943276465976808, 0.05219959533911058130, 61.24890960531435979 ) ) ;
#4566 = CARTESIAN_POINT ( 'NONE',  ( -12.06949235617739369, -12.14591786802326823, 99.37609039468568994 ) ) ;
#4567 = CARTESIAN_POINT ( 'NONE',  ( 16.18388926212245948, -7.379444403734571445, 47.06046848633767610 ) ) ;
#4568 = CARTESIAN_POINT ( 'NONE',  ( -17.49999999999999645, 5.499999999999992895, 48.71769037696437010 ) ) ;
#4569 = CARTESIAN_POINT ( 'NONE',  ( 12.14591786802309770, 12.06949235617756955, 34.37390960531435979 ) ) ;
#4570 = CARTESIAN_POINT ( 'NONE',  ( -16.52544592524335698, -4.483927247898792601, 78.95942372801901854 ) ) ;
#4571 = CARTESIAN_POINT ( 'NONE',  ( 0.05219959533909260263, 19.03943276465977164, 84.99890960531436690 ) ) ;
#4572 = CARTESIAN_POINT ( 'NONE',  ( -9.564922557960796823, -16.46253265017161027, 97.08224293864769550 ) ) ;
#4573 = CARTESIAN_POINT ( 'NONE',  ( -5.719274019375665041, -21.55341960407619695, 79.79275706135236135 ) ) ;
#4574 = CARTESIAN_POINT ( 'NONE',  ( 16.53943276465976808, 0.05219959533934440121, 91.25109039468568994 ) ) ;
#4575 = CARTESIAN_POINT ( 'NONE',  ( 16.52544592524342804, -4.483927247898539470, 58.54057627198103120 ) ) ;
#4576 = CARTESIAN_POINT ( 'NONE',  ( 13.89961937509977652, -13.97604488694527269, 73.12390960531436690 ) ) ;
#4577 = VERTEX_POINT ( 'NONE', #180648 ) ;
#4578 = CARTESIAN_POINT ( 'NONE',  ( 14.34966873604972726, -8.224510206698740333, 25.83442372801901499 ) ) ;
#4579 = CARTESIAN_POINT ( 'NONE',  ( -19.05341960407611168, -5.049401038298163336, 31.45724293864769550 ) ) ;
#4580 = CARTESIAN_POINT ( 'NONE',  ( -16.51473224551069308, -9.474510206698971260, 81.66557627198103830 ) ) ;
#4582 = CARTESIAN_POINT ( 'NONE',  ( -36.91746825000001309, 11.99521256947798342, -6.724999997268813701 ) ) ;
#4581 = CARTESIAN_POINT ( 'NONE',  ( -5.153800228976607833, 19.02544592524334988, 112.7094237280190043 ) ) ;
#4583 = CARTESIAN_POINT ( 'NONE',  ( 16.46253265017146816, 9.564922557961045513, 21.66775706135233648 ) ) ;
#4584 = CARTESIAN_POINT ( 'NONE',  ( 8.224510206698742110, 14.34966873604972548, 87.08442372801901854 ) ) ;
#4585 = CARTESIAN_POINT ( 'NONE',  ( 5.153800228976615827, -19.02544592524334988, 110.2094237280189901 ) ) ;
#4586 = CARTESIAN_POINT ( 'NONE',  ( 16.46253265017160672, -9.564922557960803928, 23.33224293864769194 ) ) ;
#4587 = CARTESIAN_POINT ( 'NONE',  ( -16.53943276465976808, -0.05219959533934237506, 63.75109039468568284 ) ) ;
#4588 = CARTESIAN_POINT ( 'NONE',  ( 16.55341960407618274, -4.379528057220086978, 56.04275706135235424 ) ) ;
#4589 = CARTESIAN_POINT ( 'NONE',  ( 19.05341960407611168, 5.049401038298154454, 23.95724293864769194 ) ) ;
#4590 = CARTESIAN_POINT ( 'NONE',  ( -9.474510206698720793, -16.51473224551083518, 74.58442372801900433 ) ) ;
#4591 = CARTESIAN_POINT ( 'NONE',  ( -0.05219959533937732626, 21.53943276465977519, 107.5010903946856899 ) ) ;
#4592 = CARTESIAN_POINT ( 'NONE',  ( -13.89961937509977652, 13.97604488694528158, 30.62390960531435269 ) ) ;
#4593 = CARTESIAN_POINT ( 'NONE',  ( 9.564922557960805705, 16.46253265017160317, 84.58224293864769550 ) ) ;
#4594 = CARTESIAN_POINT ( 'NONE',  ( -0.05219959533910754901, -16.53943276465976808, 77.49890960531433848 ) ) ;
#4595 = CIRCLE ( 'NONE', #146625, 24.30000000000003268 ) ;
#4596 = CARTESIAN_POINT ( 'NONE',  ( -19.03943276465977164, -0.05219959533935918106, 38.75109039468566152 ) ) ;
#4597 = CARTESIAN_POINT ( 'NONE',  ( -15.80617190586745835, -15.72974639402198527, 41.87390960531435979 ) ) ;
#4598 = CARTESIAN_POINT ( 'NONE',  ( -5.049401038297874678, -19.05341960407617918, 19.79275706135233293 ) ) ;
#4599 = CARTESIAN_POINT ( 'NONE',  ( 5.153800228976335163, 19.02544592524342804, 89.79057627198102409 ) ) ;
#4600 = CARTESIAN_POINT ( 'NONE',  ( -21.55341960407619339, 5.719274019375674811, 103.5427570613523613 ) ) ;
#4601 = CARTESIAN_POINT ( 'NONE',  ( 15.80617190586746368, 15.72974639402197994, 59.37390960531436690 ) ) ;
#4602 = CARTESIAN_POINT ( 'NONE',  ( -9.564922557960796823, -16.46253265017161027, 102.0822429386477097 ) ) ;
#4603 = CARTESIAN_POINT ( 'NONE',  ( -9.564922557961040184, 16.46253265017147172, 82.91775706135233293 ) ) ;
#4604 = CARTESIAN_POINT ( 'NONE',  ( -13.97604488694527625, -13.89961937509977652, 101.8739096053143811 ) ) ;
#4605 = CARTESIAN_POINT ( 'NONE',  ( -5.153800228976607833, 19.02544592524334988, 97.70942372801900433 ) ) ;
#4606 = CARTESIAN_POINT ( 'NONE',  ( -8.224510206698948167, 14.34966873604960824, 115.4155762719810241 ) ) ;
#4607 = CARTESIAN_POINT ( 'NONE',  ( 5.049401038298161559, -19.05341960407611168, 82.70724293864770971 ) ) ;
#4608 = CARTESIAN_POINT ( 'NONE',  ( 21.55341960407610458, 5.719274019375980345, 63.95724293864770260 ) ) ;
#4609 = CARTESIAN_POINT ( 'NONE',  ( -12.14591786802326823, 12.06949235617739902, 43.12609039468568284 ) ) ;
#4610 = CARTESIAN_POINT ( 'NONE',  ( 0.05219959533937995610, -21.53943276465977519, 50.00109039468568994 ) ) ;
#4611 = CARTESIAN_POINT ( 'NONE',  ( 10.81492255796106328, -18.62759615963255655, 100.4177570613523471 ) ) ;
#4612 = CARTESIAN_POINT ( 'NONE',  ( 4.379528057220092307, 16.55341960407617563, 92.29275706135236135 ) ) ;
#4613 = CARTESIAN_POINT ( 'NONE',  ( 9.564922557960805705, 16.46253265017160317, 89.58224293864769550 ) ) ;
#4614 = CARTESIAN_POINT ( 'NONE',  ( -8.314922557960811034, -14.29746914071050412, 87.08224293864769550 ) ) ;
#4615 = CARTESIAN_POINT ( 'NONE',  ( -16.52544592524342804, 4.483927247898546575, 26.04057627198103475 ) ) ;
#4616 = CARTESIAN_POINT ( 'NONE',  ( -13.97604488694547697, 13.89961937509957934, 63.12609039468566152 ) ) ;
#4617 = CARTESIAN_POINT ( 'NONE',  ( -10.72451020669870658, -18.67979575497194134, 39.58442372801901143 ) ) ;
#4619 = CARTESIAN_POINT ( 'NONE',  ( -4.379528057220328563, 16.55341960407611168, 95.20724293864769550 ) ) ;
#4618 = VECTOR ( 'NONE', #144945, 1000.000000000000000 ) ;
#4620 = CARTESIAN_POINT ( 'NONE',  ( -13.97604488694527625, -13.89961937509977652, 106.8739096053143669 ) ) ;
#4621 = CARTESIAN_POINT ( 'NONE',  ( 8.314922557961029526, -14.29746914071037800, 110.4177570613523756 ) ) ;
#4622 = CARTESIAN_POINT ( 'NONE',  ( 21.53943276465977519, 0.05219959533937863772, 91.25109039468568994 ) ) ;
#4623 = CARTESIAN_POINT ( 'NONE',  ( -14.29746914071037622, -8.314922557961029526, 64.16775706135234714 ) ) ;
#4624 = CARTESIAN_POINT ( 'NONE',  ( 5.719274019375673035, 21.55341960407619339, 42.29275706135235424 ) ) ;
#4625 = EDGE_CURVE ( 'NONE', #192038, #188447, #191917, .T. ) ;
#4626 = VERTEX_POINT ( 'NONE', #89603 ) ;
#4627 = CARTESIAN_POINT ( 'NONE',  ( 0.05219959533937995610, -21.53943276465977519, 35.00109039468568284 ) ) ;
#4628 = CARTESIAN_POINT ( 'NONE',  ( -0.05219959533910754901, -16.53943276465976808, 92.49890960531436690 ) ) ;
#4629 = CARTESIAN_POINT ( 'NONE',  ( 19.05341960407611168, 5.049401038298154454, 23.95724293864769194 ) ) ;
#4630 = CARTESIAN_POINT ( 'NONE',  ( 12.14591786802309770, 12.06949235617756955, 64.37390960531435269 ) ) ;
#4631 = CARTESIAN_POINT ( 'NONE',  ( -5.049401038298153566, 19.05341960407611168, 60.20724293864768129 ) ) ;
#4632 = CARTESIAN_POINT ( 'NONE',  ( 16.52544592524335698, 4.483927247898782831, 111.4594237280190328 ) ) ;
#4633 = CARTESIAN_POINT ( 'NONE',  ( 16.46253265017160672, -9.564922557960803928, 38.33224293864768839 ) ) ;
#4634 = CARTESIAN_POINT ( 'NONE',  ( 18.67979575497178502, 10.72451020669898547, 49.16557627198102409 ) ) ;
#4635 = CARTESIAN_POINT ( 'NONE',  ( -16.53943276465976808, 0.05219959533911058130, 76.24890960531435269 ) ) ;
#4636 = CARTESIAN_POINT ( 'NONE',  ( 18.62759615963271287, -10.81492255796078972, 88.33224293864769550 ) ) ;
#4637 = CARTESIAN_POINT ( 'NONE',  ( -9.564922557960796823, -16.46253265017161027, 82.08224293864768129 ) ) ;
#4639 = CARTESIAN_POINT ( 'NONE',  ( 16.46253265017146816, 9.564922557961045513, 91.66775706135234714 ) ) ;
#4638 = CARTESIAN_POINT ( 'NONE',  ( -5.049401038298153566, 19.05341960407611168, 50.20724293864770260 ) ) ;
#4640 = CARTESIAN_POINT ( 'NONE',  ( 18.67979575497178502, 10.72451020669898547, 44.16557627198103120 ) ) ;
#4641 = CARTESIAN_POINT ( 'NONE',  ( -15.72974639402176322, -15.80617190586768395, 74.37609039468568994 ) ) ;
#4642 = CARTESIAN_POINT ( 'NONE',  ( 16.46253265017160672, -9.564922557960803928, 48.33224293864769550 ) ) ;
#4643 = CARTESIAN_POINT ( 'NONE',  ( 19.02544592524343514, -5.153800228976328945, 88.54057627198102409 ) ) ;
#4644 = VERTEX_POINT ( 'NONE', #59254 ) ;
#4645 = CARTESIAN_POINT ( 'NONE',  ( 12.06949235617739724, 12.14591786802326823, 61.87609039468568284 ) ) ;
#4646 = CARTESIAN_POINT ( 'NONE',  ( 18.67979575497194134, -10.72451020669871369, 40.83442372801901854 ) ) ;
#4647 = CARTESIAN_POINT ( 'NONE',  ( -0.05219959533937732626, 21.53943276465977519, 67.50109039468568994 ) ) ;
#4648 = CARTESIAN_POINT ( 'NONE',  ( 10.72451020669898902, -18.67979575497178502, 22.91557627198102765 ) ) ;
#4649 = CARTESIAN_POINT ( 'NONE',  ( -18.62759615963270932, 10.81492255796079327, 100.8322429386477097 ) ) ;
#4651 = CARTESIAN_POINT ( 'NONE',  ( 16.52544592524335698, 4.483927247898782831, 71.45942372801901854 ) ) ;
#4650 = CARTESIAN_POINT ( 'NONE',  ( 15.72974639402176855, 15.80617190586768217, 31.87609039468567929 ) ) ;
#4652 = CARTESIAN_POINT ( 'NONE',  ( -5.719274019375978568, 21.55341960407610458, 60.20724293864768839 ) ) ;
#4653 = CARTESIAN_POINT ( 'NONE',  ( 19.05341960407617918, -5.049401038297876454, 36.04275706135234003 ) ) ;
#4655 = CARTESIAN_POINT ( 'NONE',  ( 12.14591786802327356, -12.06949235617739191, 105.6260903946856899 ) ) ;
#4654 = CARTESIAN_POINT ( 'NONE',  ( -16.46253265017160317, 9.564922557960807481, 65.83224293864769550 ) ) ;
#4656 = CARTESIAN_POINT ( 'NONE',  ( 18.22780087662123805, -5.499999999999976019, 83.51763182126894947 ) ) ;
#4657 = CARTESIAN_POINT ( 'NONE',  ( -16.46253265017160317, 9.564922557960807481, 100.8322429386477097 ) ) ;
#4658 = FACE_OUTER_BOUND ( 'NONE', #43791, .T. ) ;
#4659 = CARTESIAN_POINT ( 'NONE',  ( -0.05219959533936034679, 19.03943276465977164, 87.50109039468567573 ) ) ;
#4660 = CARTESIAN_POINT ( 'NONE',  ( -15.80617190586745835, -15.72974639402198527, 51.87390960531437401 ) ) ;
#4661 = CARTESIAN_POINT ( 'NONE',  ( 4.379528057220339221, -16.55341960407611168, 32.70724293864770260 ) ) ;
#4662 = CARTESIAN_POINT ( 'NONE',  ( -9.474510206698720793, -16.51473224551083518, 104.5844237280190043 ) ) ;
#4663 = CARTESIAN_POINT ( 'NONE',  ( -4.999999999999999112, -140.0000000000000000, -15.00000000000000000 ) ) ;
#4664 = CARTESIAN_POINT ( 'NONE',  ( -19.02544592524334988, -5.153800228976617603, 93.95942372801900433 ) ) ;
#4666 = CARTESIAN_POINT ( 'NONE',  ( -16.51473224551082808, 9.474510206698731452, 63.33442372801900433 ) ) ;
#4665 = CARTESIAN_POINT ( 'NONE',  ( -10.81492255796078084, -18.62759615963271287, 82.08224293864768129 ) ) ;
#4667 = CARTESIAN_POINT ( 'NONE',  ( 16.55341960407618274, -4.379528057220086978, 76.04275706135237556 ) ) ;
#4668 = CARTESIAN_POINT ( 'NONE',  ( 19.03943276465977164, -0.05219959533909143690, 63.74890960531435979 ) ) ;
#4669 = CARTESIAN_POINT ( 'NONE',  ( 4.379528057220339221, -16.55341960407611168, 62.70724293864769550 ) ) ;
#4670 = VECTOR ( 'NONE', #189946, 1000.000000000000000 ) ;
#4671 = CARTESIAN_POINT ( 'NONE',  ( 9.474510206698971260, -16.51473224551069308, 52.91557627198102409 ) ) ;
#4672 = CARTESIAN_POINT ( 'NONE',  ( 14.29746914071049879, -8.314922557960816363, 48.33224293864770260 ) ) ;
#4673 = CARTESIAN_POINT ( 'NONE',  ( -19.05341960407611168, -5.049401038298163336, 21.45724293864768839 ) ) ;
#4674 = CARTESIAN_POINT ( 'NONE',  ( 31.26372923869871201, -6.750542664803641735, 98.30470173274461843 ) ) ;
#4675 = CARTESIAN_POINT ( 'NONE',  ( 14.34966873604960469, 8.224510206698951720, 34.16557627198102409 ) ) ;
#4676 = CARTESIAN_POINT ( 'NONE',  ( -0.05219959533909027116, -19.03943276465977164, 77.49890960531435269 ) ) ;
#4677 = CARTESIAN_POINT ( 'NONE',  ( -18.22780087662122028, 5.500000000000031086, 73.51540105326107266 ) ) ;
#4678 = CARTESIAN_POINT ( 'NONE',  ( -19.03943276465977164, -0.05219959533935918106, 43.75109039468566863 ) ) ;
#4679 = CARTESIAN_POINT ( 'NONE',  ( 4.379528057220092307, 16.55341960407617563, 52.29275706135236135 ) ) ;
#4680 = CARTESIAN_POINT ( 'NONE',  ( 18.67979575497178502, 10.72451020669898547, 54.16557627198103120 ) ) ;
#4681 = CARTESIAN_POINT ( 'NONE',  ( 0.05219959533937995610, -21.53943276465977519, 100.0010903946857042 ) ) ;
#4682 = CARTESIAN_POINT ( 'NONE',  ( 5.049401038298161559, -19.05341960407611168, 72.70724293864768129 ) ) ;
#4683 = LINE ( 'NONE', #52198, #69514 ) ;
#4684 = CARTESIAN_POINT ( 'NONE',  ( -13.89961937509977652, 13.97604488694528158, 105.6239096053143527 ) ) ;
#4685 = CARTESIAN_POINT ( 'NONE',  ( 15.72974639402176855, 15.80617190586768217, 41.87609039468568284 ) ) ;
#4686 = CARTESIAN_POINT ( 'NONE',  ( 0.05219959533910956823, 16.53943276465976808, 94.99890960531436690 ) ) ;
#4689 = VERTEX_POINT ( 'NONE', #24962 ) ;
#4688 = CARTESIAN_POINT ( 'NONE',  ( -19.02544592524342804, 5.153800228976336051, 86.04057627198103830 ) ) ;
#4687 = CARTESIAN_POINT ( 'NONE',  ( 21.52544592524344225, -5.823673210054117533, 83.54057627198102409 ) ) ;
#4690 = CARTESIAN_POINT ( 'NONE',  ( -21.52544592524334988, -5.823673210054445271, 28.95942372801902209 ) ) ;
#4691 = AXIS2_PLACEMENT_3D ( 'NONE', #148800, #166959, #28461 ) ;
#4692 = ORIENTED_EDGE ( 'NONE', *, *, #3003, .F. ) ;
#4693 = CARTESIAN_POINT ( 'NONE',  ( 9.564922557960805705, 16.46253265017160317, 84.58224293864769550 ) ) ;
#4694 = FACE_OUTER_BOUND ( 'NONE', #155307, .T. ) ;
#4696 = CARTESIAN_POINT ( 'NONE',  ( -9.564922557960796823, -16.46253265017161027, 37.08224293864768839 ) ) ;
#4695 = CARTESIAN_POINT ( 'NONE',  ( 16.51473224551069308, 9.474510206698969483, 24.16557627198102765 ) ) ;
#4697 = CARTESIAN_POINT ( 'NONE',  ( -9.564922557961040184, 16.46253265017147172, 112.9177570613523329 ) ) ;
#4698 = CARTESIAN_POINT ( 'NONE',  ( -36.91746825000001309, -11.99521256947794789, -7.024999997268812635 ) ) ;
#4699 = STYLED_ITEM ( 'NONE', ( #184623 ), #5735 ) ;
#4700 = CARTESIAN_POINT ( 'NONE',  ( 14.34966873604960469, 8.224510206698951720, 109.1655762719810383 ) ) ;
#4701 = CARTESIAN_POINT ( 'NONE',  ( 21.53943276465977519, 0.05219959533937863772, 91.25109039468568994 ) ) ;
#4703 = CARTESIAN_POINT ( 'NONE',  ( 15.72974639402176855, 15.80617190586768217, 31.87609039468567929 ) ) ;
#4702 = CARTESIAN_POINT ( 'NONE',  ( -5.153800228976328057, -19.02544592524343514, 62.29057627198100988 ) ) ;
#4704 = CARTESIAN_POINT ( 'NONE',  ( 5.719274019375673035, 21.55341960407619339, 32.29275706135235424 ) ) ;
#4705 = CARTESIAN_POINT ( 'NONE',  ( -28.82186960331499392, -9.364793116373526516, 146.1000000000000227 ) ) ;
#4706 = CARTESIAN_POINT ( 'NONE',  ( -5.153800228976328057, -19.02544592524343514, 87.29057627198103830 ) ) ;
#4707 = CARTESIAN_POINT ( 'NONE',  ( 27.96890437653522099, 7.184031643483238305, 161.0522725792803556 ) ) ;
#4709 = CARTESIAN_POINT ( 'NONE',  ( 18.67979575497178502, 10.72451020669898547, 49.16557627198102409 ) ) ;
#4708 = CARTESIAN_POINT ( 'NONE',  ( 0.05219959533934541429, -16.53943276465976808, 25.00109039468567218 ) ) ;
#4710 = CARTESIAN_POINT ( 'NONE',  ( 5.719274019375673035, 21.55341960407619339, 57.29275706135234714 ) ) ;
#4711 = AXIS2_PLACEMENT_3D ( 'NONE', #123147, #109975, #105997 ) ;
#4712 = CARTESIAN_POINT ( 'NONE',  ( 0.05219959533909260263, 19.03943276465977164, 109.9989096053143669 ) ) ;
#4713 = CARTESIAN_POINT ( 'NONE',  ( -0.05219959533936034679, 19.03943276465977164, 97.50109039468567573 ) ) ;
#4714 = CARTESIAN_POINT ( 'NONE',  ( -13.97604488694527625, -13.89961937509977652, 66.87390960531436690 ) ) ;
#4715 = CARTESIAN_POINT ( 'NONE',  ( -16.46253265017160317, 9.564922557960807481, 90.83224293864769550 ) ) ;
#4716 = CARTESIAN_POINT ( 'NONE',  ( -0.05219959533910754901, -16.53943276465976808, 92.49890960531436690 ) ) ;
#4717 = CARTESIAN_POINT ( 'NONE',  ( -0.05219959533910754901, -16.53943276465976808, 107.4989096053143669 ) ) ;
#4718 = CARTESIAN_POINT ( 'NONE',  ( 13.89961937509977652, -13.97604488694527269, 113.1239096053143527 ) ) ;
#4720 = CARTESIAN_POINT ( 'NONE',  ( -16.46253265017160317, 9.564922557960807481, 35.83224293864768839 ) ) ;
#4719 = CARTESIAN_POINT ( 'NONE',  ( -16.55341960407611168, -4.379528057220339221, 51.45724293864770260 ) ) ;
#4721 = CARTESIAN_POINT ( 'NONE',  ( -10.72451020669870658, -18.67979575497194134, 74.58442372801901854 ) ) ;
#4722 = CARTESIAN_POINT ( 'NONE',  ( 16.51473224551083163, -9.474510206698727899, 90.83442372801900433 ) ) ;
#4723 = CARTESIAN_POINT ( 'NONE',  ( -8.224510206698948167, 14.34966873604960824, 60.41557627198102409 ) ) ;
#4724 = CARTESIAN_POINT ( 'NONE',  ( -15.80617190586745835, -15.72974639402198527, 106.8739096053143811 ) ) ;
#4725 = CARTESIAN_POINT ( 'NONE',  ( 15.80617190586746368, 15.72974639402197994, 44.37390960531435979 ) ) ;
#4726 = CARTESIAN_POINT ( 'NONE',  ( -16.51473224551069308, -9.474510206698971260, 111.6655762719810383 ) ) ;
#4727 = CARTESIAN_POINT ( 'NONE',  ( -8.571926809382608425, 26.38167802310805854, 148.4750000027311785 ) ) ;
#4728 = CARTESIAN_POINT ( 'NONE',  ( -13.89961937509977652, 13.97604488694528158, 70.62390960531432427 ) ) ;
#4729 = CARTESIAN_POINT ( 'NONE',  ( 14.34966873604960469, 8.224510206698951720, 34.16557627198102409 ) ) ;
#4730 = CIRCLE ( 'NONE', #36937, 214.0437394197456911 ) ;
#4731 = CARTESIAN_POINT ( 'NONE',  ( 16.53943276465976808, 0.05219959533934440121, 106.2510903946856757 ) ) ;
#4732 = CARTESIAN_POINT ( 'NONE',  ( 16.52544592524335698, 4.483927247898782831, 86.45942372801901854 ) ) ;
#4733 = CARTESIAN_POINT ( 'NONE',  ( -9.474510206698720793, -16.51473224551083518, 44.58442372801900433 ) ) ;
#4734 = CARTESIAN_POINT ( 'NONE',  ( -22.77340942535178314, 12.66915129224426906, 165.5704402759699008 ) ) ;
#4735 = CARTESIAN_POINT ( 'NONE',  ( 5.049401038298161559, -19.05341960407611168, 92.70724293864769550 ) ) ;
#4736 = CARTESIAN_POINT ( 'NONE',  ( 13.97604488694527802, 13.89961937509977652, 44.37390960531435269 ) ) ;
#4737 = CARTESIAN_POINT ( 'NONE',  ( 14.34966873604960469, 8.224510206698951720, 59.16557627198103120 ) ) ;
#4739 = CARTESIAN_POINT ( 'NONE',  ( 5.719274019375991003, -21.55341960407610458, 22.70724293864769194 ) ) ;
#4738 = CARTESIAN_POINT ( 'NONE',  ( 17.13100169013300444, -6.664070546373146442, 103.2678983569984581 ) ) ;
#4740 = CARTESIAN_POINT ( 'NONE',  ( 15.72974639402199770, -15.80617190586745480, 58.12390960531435979 ) ) ;
#4741 = CARTESIAN_POINT ( 'NONE',  ( -16.55341960407611168, -4.379528057220339221, 81.45724293864769550 ) ) ;
#4742 = CARTESIAN_POINT ( 'NONE',  ( -16.55341960407617563, 4.379528057220093196, 33.54275706135234714 ) ) ;
#4743 = CARTESIAN_POINT ( 'NONE',  ( 14.29746914071049879, -8.314922557960816363, 83.33224293864769550 ) ) ;
#4744 = CARTESIAN_POINT ( 'NONE',  ( -19.49149378614657735, 5.499999999999777955, 64.43757513605362419 ) ) ;
#4745 = CARTESIAN_POINT ( 'NONE',  ( -16.46253265017146816, -9.564922557961047289, 74.16775706135234714 ) ) ;
#4746 = CARTESIAN_POINT ( 'NONE',  ( 13.89961937509977652, -13.97604488694527269, 113.1239096053143527 ) ) ;
#4747 = CARTESIAN_POINT ( 'NONE',  ( 36.91746825000000598, -11.99521256947793546, -2.224999997268813701 ) ) ;
#4748 = CARTESIAN_POINT ( 'NONE',  ( -20.61667489342692150, 20.25409705915558689, -52.65483682830181777 ) ) ;
#4750 = CARTESIAN_POINT ( 'NONE',  ( 12.14591786802327356, -12.06949235617739191, 105.6260903946856899 ) ) ;
#4749 = CARTESIAN_POINT ( 'NONE',  ( -16.55341960407617563, 4.379528057220093196, 33.54275706135234714 ) ) ;
#4751 = CARTESIAN_POINT ( 'NONE',  ( -13.89961937509957401, -13.97604488694547875, 69.37609039468564731 ) ) ;
#4752 = CARTESIAN_POINT ( 'NONE',  ( -21.55341960407610458, -5.719274019375992779, 46.45724293864769550 ) ) ;
#4753 = CARTESIAN_POINT ( 'NONE',  ( -21.52544592524334988, -5.823673210054445271, 73.95942372801901854 ) ) ;
#4754 = CARTESIAN_POINT ( 'NONE',  ( -28.82186960331499037, 2.428612866367529932E-14, 146.2500000054623683 ) ) ;
#4755 = CARTESIAN_POINT ( 'NONE',  ( 12.06949235617739724, 12.14591786802326823, 31.87609039468567929 ) ) ;
#4758 = EDGE_CURVE ( 'NONE', #21601, #200018, #57632, .T. ) ;
#4757 = CARTESIAN_POINT ( 'NONE',  ( -19.05341960407611168, -5.049401038298163336, 91.45724293864766707 ) ) ;
#4756 = DIRECTION ( 'NONE',  ( -0.4999999999999967804, 0.5000000000000019984, 0.7071067811865484609 ) ) ;
#4759 = CARTESIAN_POINT ( 'NONE',  ( -9.564922557960796823, -16.46253265017161027, 22.08224293864768839 ) ) ;
#4760 = CARTESIAN_POINT ( 'NONE',  ( -0.05219959533910754901, -16.53943276465976808, 97.49890960531436690 ) ) ;
#4761 = SHAPE_DEFINITION_REPRESENTATION ( #137256, #9542 ) ;
#4762 = CARTESIAN_POINT ( 'NONE',  ( 19.03943276465977164, -0.05219959533909143690, 103.7489096053143669 ) ) ;
#4763 = ORIENTED_EDGE ( 'NONE', *, *, #39724, .F. ) ;
#4764 = CARTESIAN_POINT ( 'NONE',  ( -12.06949235617739369, -12.14591786802326823, 59.37609039468568284 ) ) ;
#4765 = CARTESIAN_POINT ( 'NONE',  ( -5.153800228976607833, 19.02544592524334988, 102.7094237280189759 ) ) ;
#4766 = CARTESIAN_POINT ( 'NONE',  ( 18.62759615963271287, -10.81492255796078972, 83.33224293864769550 ) ) ;
#4767 = CARTESIAN_POINT ( 'NONE',  ( 5.153800228976335163, 19.02544592524342804, 44.79057627198103830 ) ) ;
#4769 = CARTESIAN_POINT ( 'NONE',  ( -21.52544592524334988, -5.823673210054445271, 18.95942372801901143 ) ) ;
#4768 = CARTESIAN_POINT ( 'NONE',  ( 5.049401038297881783, 19.05341960407617563, 72.29275706135234714 ) ) ;
#4770 = CARTESIAN_POINT ( 'NONE',  ( 16.51473224551069308, 9.474510206698969483, 69.16557627198102409 ) ) ;
#4771 = CARTESIAN_POINT ( 'NONE',  ( 19.03943276465977164, -0.05219959533909143690, 108.7489096053143527 ) ) ;
#4772 = ORIENTED_EDGE ( 'NONE', *, *, #189415, .T. ) ;
#4773 = CARTESIAN_POINT ( 'NONE',  ( -8.224510206698735004, -14.34966873604973081, 29.58442372801901854 ) ) ;
#4774 = CARTESIAN_POINT ( 'NONE',  ( 21.55341960407610458, 5.719274019375980345, 103.9572429386476813 ) ) ;
#4777 = CARTESIAN_POINT ( 'NONE',  ( -19.03943276465977164, -0.05219959533935918106, 73.75109039468566152 ) ) ;
#4776 = CARTESIAN_POINT ( 'NONE',  ( -9.474510206698964154, 16.51473224551069663, 95.41557627198102409 ) ) ;
#4775 = CARTESIAN_POINT ( 'NONE',  ( -0.05219959533910754901, -16.53943276465976808, 107.4989096053143669 ) ) ;
#4778 = CARTESIAN_POINT ( 'NONE',  ( 0.05219959533907565091, 21.53943276465977519, 84.99890960531436690 ) ) ;
#4779 = CARTESIAN_POINT ( 'NONE',  ( 14.29746914071049879, -8.314922557960816363, 43.33224293864769550 ) ) ;
#4780 = CARTESIAN_POINT ( 'NONE',  ( -10.81492255796105439, 18.62759615963255655, 112.9177570613523329 ) ) ;
#4781 = CARTESIAN_POINT ( 'NONE',  ( -12.14591786802326823, 12.06949235617739902, 68.12609039468567573 ) ) ;
#4782 = CARTESIAN_POINT ( 'NONE',  ( -9.474510206698964154, 16.51473224551069663, 90.41557627198103830 ) ) ;
#4783 = CARTESIAN_POINT ( 'NONE',  ( -5.049401038298153566, 19.05341960407611168, 45.20724293864769550 ) ) ;
#4784 = CARTESIAN_POINT ( 'NONE',  ( 18.67979575497194134, -10.72451020669871369, 50.83442372801901143 ) ) ;
#4785 = CARTESIAN_POINT ( 'NONE',  ( 15.72974639402176855, 15.80617190586768217, 61.87609039468568284 ) ) ;
#4786 = CARTESIAN_POINT ( 'NONE',  ( 5.153800228976335163, 19.02544592524342804, 59.79057627198100988 ) ) ;
#4787 = CARTESIAN_POINT ( 'NONE',  ( 21.52544592524334988, 5.823673210054432836, 31.45942372801901854 ) ) ;
#4788 = CARTESIAN_POINT ( 'NONE',  ( 9.564922557961047289, -16.46253265017146816, 70.41775706135233293 ) ) ;
#4789 = CARTESIAN_POINT ( 'NONE',  ( -19.02544592524342804, 5.153800228976336051, 41.04057627198103120 ) ) ;
#4790 = CARTESIAN_POINT ( 'NONE',  ( -8.224510206698735004, -14.34966873604973081, 84.58442372801903275 ) ) ;
#4791 = CARTESIAN_POINT ( 'NONE',  ( -16.46253265017160317, 9.564922557960807481, 50.83224293864770260 ) ) ;
#4792 = CARTESIAN_POINT ( 'NONE',  ( -19.05341960407611168, -5.049401038298163336, 106.4572429386476955 ) ) ;
#4793 = CARTESIAN_POINT ( 'NONE',  ( -19.02544592524342804, 5.153800228976336051, 41.04057627198103120 ) ) ;
#4794 = AXIS2_PLACEMENT_3D ( 'NONE', #35630, #97275, #157983 ) ;
#4795 = CARTESIAN_POINT ( 'NONE',  ( -21.52544592524343514, 5.823673210054127303, 81.04057627198102409 ) ) ;
#4796 = CARTESIAN_POINT ( 'NONE',  ( -14.34966873604972548, 8.224510206698743886, 78.33442372801901854 ) ) ;
#4797 = FACE_OUTER_BOUND ( 'NONE', #30547, .T. ) ;
#4798 = CARTESIAN_POINT ( 'NONE',  ( -9.564922557961040184, 16.46253265017147172, 32.91775706135233293 ) ) ;
#4799 = CARTESIAN_POINT ( 'NONE',  ( -9.564922557960796823, -16.46253265017161027, 57.08224293864769550 ) ) ;
#4800 = CARTESIAN_POINT ( 'NONE',  ( 14.29746914071049879, -8.314922557960816363, 43.33224293864769550 ) ) ;
#4801 = CARTESIAN_POINT ( 'NONE',  ( 8.314922557960818139, 14.29746914071049879, 79.58224293864769550 ) ) ;
#4802 = CARTESIAN_POINT ( 'NONE',  ( -16.51473224551069308, -9.474510206698971260, 106.6655762719810383 ) ) ;
#4803 = CARTESIAN_POINT ( 'NONE',  ( 9.564922557960805705, 16.46253265017160317, 79.58224293864769550 ) ) ;
#4804 = CARTESIAN_POINT ( 'NONE',  ( -15.72974639402176322, -15.80617190586768395, 54.37609039468568994 ) ) ;
#4805 = CARTESIAN_POINT ( 'NONE',  ( 19.03943276465977164, -0.05219959533909143690, 98.74890960531436690 ) ) ;
#4806 = CARTESIAN_POINT ( 'NONE',  ( -0.05219959533937732626, 21.53943276465977519, 102.5010903946856899 ) ) ;
#4807 = CARTESIAN_POINT ( 'NONE',  ( 16.53943276465976808, 0.05219959533934440121, 81.25109039468568994 ) ) ;
#4808 = ADVANCED_FACE ( 'NONE', ( #75423 ), #167452, .T. ) ;
#4809 = CARTESIAN_POINT ( 'NONE',  ( 18.67979575497194134, -10.72451020669871369, 25.83442372801901499 ) ) ;
#4810 = CARTESIAN_POINT ( 'NONE',  ( 18.67979575497178502, 10.72451020669898547, 109.1655762719810383 ) ) ;
#4811 = CARTESIAN_POINT ( 'NONE',  ( -4.379528057220328563, 16.55341960407611168, 55.20724293864770260 ) ) ;
#4813 = CARTESIAN_POINT ( 'NONE',  ( -16.46253265017160317, 9.564922557960807481, 40.83224293864769550 ) ) ;
#4812 = AXIS2_PLACEMENT_3D ( 'NONE', #26522, #196381, #195373 ) ;
#4814 = CARTESIAN_POINT ( 'NONE',  ( -4.379528057220328563, 16.55341960407611168, 65.20724293864768129 ) ) ;
#4815 = CARTESIAN_POINT ( 'NONE',  ( -10.81492255796078084, -18.62759615963271287, 37.08224293864768129 ) ) ;
#4816 = CARTESIAN_POINT ( 'NONE',  ( 9.474510206698729675, 16.51473224551082808, 37.08442372801899722 ) ) ;
#4817 = CARTESIAN_POINT ( 'NONE',  ( -16.55341960407611168, -4.379528057220339221, 96.45724293864770971 ) ) ;
#4818 = ORIENTED_EDGE ( 'NONE', *, *, #137018, .F. ) ;
#4819 = CARTESIAN_POINT ( 'NONE',  ( 16.53943276465976808, 0.05219959533934440121, 66.25109039468567573 ) ) ;
#4820 = CARTESIAN_POINT ( 'NONE',  ( 19.03943276465977164, -0.05219959533909143690, 68.74890960531436690 ) ) ;
#4821 = CARTESIAN_POINT ( 'NONE',  ( -16.99472585857189699, -5.499999999999960032, 20.67116795353343051 ) ) ;
#4822 = CARTESIAN_POINT ( 'NONE',  ( 16.55341960407611168, 4.379528057220329451, 83.95724293864770971 ) ) ;
#4823 = CARTESIAN_POINT ( 'NONE',  ( -21.55341960407610458, -5.719274019375992779, 31.45724293864769550 ) ) ;
#4824 = CARTESIAN_POINT ( 'NONE',  ( 12.14591786802327356, -12.06949235617739191, 90.62609039468567573 ) ) ;
#4825 = CARTESIAN_POINT ( 'NONE',  ( 4.483927247898790824, -16.52544592524335698, 20.20942372801900788 ) ) ;
#4826 = CARTESIAN_POINT ( 'NONE',  ( -18.67979575497193778, 10.72451020669871902, 73.33442372801901854 ) ) ;
#4827 = CARTESIAN_POINT ( 'NONE',  ( 13.97604488694527802, 13.89961937509977652, 94.37390960531436690 ) ) ;
#4828 = CARTESIAN_POINT ( 'NONE',  ( 0.05219959533907565091, 21.53943276465977519, 104.9989096053143669 ) ) ;
#4829 = CARTESIAN_POINT ( 'NONE',  ( -14.29746914071037622, -8.314922557961029526, 59.16775706135234714 ) ) ;
#4831 = CARTESIAN_POINT ( 'NONE',  ( 16.53943276465976808, -0.05219959533910856209, 108.7489096053143669 ) ) ;
#4830 = VECTOR ( 'NONE', #8942, 1000.000000000000000 ) ;
#4832 = CARTESIAN_POINT ( 'NONE',  ( -14.29746914071037622, -8.314922557961029526, 19.16775706135234714 ) ) ;
#4833 = CARTESIAN_POINT ( 'NONE',  ( 0.05219959533936267826, -19.03943276465977164, 75.00109039468566152 ) ) ;
#4834 = CARTESIAN_POINT ( 'NONE',  ( 5.719274019375991003, -21.55341960407610458, 92.70724293864770971 ) ) ;
#4835 = CARTESIAN_POINT ( 'NONE',  ( 19.02544592524334988, 5.153800228976608722, 51.45942372801900433 ) ) ;
#4836 = CARTESIAN_POINT ( 'NONE',  ( 19.49149378614661998, -5.499999999999574563, 86.93757513605363840 ) ) ;
#4837 = CARTESIAN_POINT ( 'NONE',  ( -21.53943276465977519, 0.05219959533907696930, 106.2489096053143811 ) ) ;
#4838 = CARTESIAN_POINT ( 'NONE',  ( -17.49999999999999289, 5.500000000000036415, 85.79690382534171533 ) ) ;
#4839 = CARTESIAN_POINT ( 'NONE',  ( -9.564922557960796823, -16.46253265017161027, 77.08224293864769550 ) ) ;
#4840 = AXIS2_PLACEMENT_3D ( 'NONE', #167237, #77188, #47861 ) ;
#4841 = CARTESIAN_POINT ( 'NONE',  ( 0.000000000000000000, 0.000000000000000000, -56.77278709839600879 ) ) ;
#4842 = CARTESIAN_POINT ( 'NONE',  ( 4.483927247898790824, -16.52544592524335698, 35.20942372801901854 ) ) ;
#4843 = DIRECTION ( 'NONE',  ( -0.000000000000000000, -0.000000000000000000, 1.000000000000000000 ) ) ;
#4845 = CARTESIAN_POINT ( 'NONE',  ( -4.379528057220328563, 16.55341960407611168, 65.20724293864768129 ) ) ;
#4844 = CARTESIAN_POINT ( 'NONE',  ( 21.53943276465977519, -0.05219959533907433946, 98.74890960531438111 ) ) ;
#4846 = CARTESIAN_POINT ( 'NONE',  ( 5.153800228976335163, 19.02544592524342804, 64.79057627198100988 ) ) ;
#4847 = VECTOR ( 'NONE', #61893, 1000.000000000000000 ) ;
#4848 = CARTESIAN_POINT ( 'NONE',  ( 21.55341960407619695, -5.719274019375665929, 91.04275706135236135 ) ) ;
#4849 = CARTESIAN_POINT ( 'NONE',  ( -4.379528057220328563, 16.55341960407611168, 95.20724293864769550 ) ) ;
#4851 = CARTESIAN_POINT ( 'NONE',  ( 16.46253265017146816, 9.564922557961045513, 41.66775706135234003 ) ) ;
#4850 = CARTESIAN_POINT ( 'NONE',  ( -16.52544592524335698, -4.483927247898792601, 43.95942372801902565 ) ) ;
#4852 = CARTESIAN_POINT ( 'NONE',  ( -5.719274019375665041, -21.55341960407619695, 54.79275706135235424 ) ) ;
#4853 = CARTESIAN_POINT ( 'NONE',  ( -13.97604488694547697, 13.89961937509957934, 113.1260903946856757 ) ) ;
#4854 = CARTESIAN_POINT ( 'NONE',  ( -0.05219959533909027116, -19.03943276465977164, 52.49890960531436690 ) ) ;
#4855 = CARTESIAN_POINT ( 'NONE',  ( 19.02544592524334988, 5.153800228976608722, 81.45942372801897591 ) ) ;
#4856 = CARTESIAN_POINT ( 'NONE',  ( 18.67979575497194134, -10.72451020669871369, 80.83442372801901854 ) ) ;
#4857 = CARTESIAN_POINT ( 'NONE',  ( -0.05219959533936034679, 19.03943276465977164, 72.50109039468566152 ) ) ;
#4858 = CARTESIAN_POINT ( 'NONE',  ( 16.51473224551069308, 9.474510206698969483, 34.16557627198102409 ) ) ;
#4859 = CARTESIAN_POINT ( 'NONE',  ( -10.72451020669898014, 18.67979575497178502, 60.41557627198102409 ) ) ;
#4860 = CARTESIAN_POINT ( 'NONE',  ( 4.379528057220339221, -16.55341960407611168, 62.70724293864769550 ) ) ;
#4861 = CARTESIAN_POINT ( 'NONE',  ( 21.96329795405619834, 8.386426352705248277, 172.0132153625898468 ) ) ;
#4862 = CARTESIAN_POINT ( 'NONE',  ( -9.564922557961040184, 16.46253265017147172, 27.91775706135232582 ) ) ;
#4863 = CARTESIAN_POINT ( 'NONE',  ( -12.06949235617739369, -12.14591786802326823, 99.37609039468568994 ) ) ;
#4864 = CARTESIAN_POINT ( 'NONE',  ( 8.314922557960818139, 14.29746914071049879, 59.58224293864770260 ) ) ;
#4865 = CARTESIAN_POINT ( 'NONE',  ( -21.53943276465977519, -0.05219959533937600094, 88.75109039468567573 ) ) ;
#4866 = CARTESIAN_POINT ( 'NONE',  ( -18.67979575497193778, 10.72451020669871902, 78.33442372801901854 ) ) ;
#4867 = CARTESIAN_POINT ( 'NONE',  ( -18.62759615963270932, 10.81492255796079327, 90.83224293864769550 ) ) ;
#4868 = EDGE_CURVE ( 'NONE', #192734, #168486, #104777, .T. ) ;
#4869 = CARTESIAN_POINT ( 'NONE',  ( 19.03943276465977164, -0.05219959533909143690, 53.74890960531436690 ) ) ;
#4870 = CARTESIAN_POINT ( 'NONE',  ( 15.80617190586769283, -15.72974639402175789, 75.62609039468567573 ) ) ;
#4871 = CARTESIAN_POINT ( 'NONE',  ( -13.89961937509977652, 13.97604488694528158, 50.62390960531435979 ) ) ;
#4872 = ORIENTED_EDGE ( 'NONE', *, *, #119692, .T. ) ;
#4873 = CARTESIAN_POINT ( 'NONE',  ( 0.05219959533909260263, 19.03943276465977164, 69.99890960531435269 ) ) ;
#4874 = CARTESIAN_POINT ( 'NONE',  ( 12.06949235617757843, -12.14591786802309237, 108.1239096053143811 ) ) ;
#4875 = CARTESIAN_POINT ( 'NONE',  ( 9.474510206698971260, -16.51473224551069308, 92.91557627198103830 ) ) ;
#4876 = CARTESIAN_POINT ( 'NONE',  ( 0.05219959533910956823, 16.53943276465976808, 59.99890960531436690 ) ) ;
#4877 = CARTESIAN_POINT ( 'NONE',  ( 16.55341960407611168, 4.379528057220329451, 108.9572429386476955 ) ) ;
#4878 = VECTOR ( 'NONE', #141249, 1000.000000000000000 ) ;
#4879 = CARTESIAN_POINT ( 'NONE',  ( 10.72451020669898902, -18.67979575497178502, 82.91557627198103830 ) ) ;
#4880 = CARTESIAN_POINT ( 'NONE',  ( -21.52544592524334988, -5.823673210054445271, 33.95942372801901143 ) ) ;
#4881 = CARTESIAN_POINT ( 'NONE',  ( 27.77694149905228471, -7.633451960439483486, 161.4496143021105183 ) ) ;
#4882 = CARTESIAN_POINT ( 'NONE',  ( 16.55341960407618274, -4.379528057220086978, 36.04275706135234714 ) ) ;
#4883 = CARTESIAN_POINT ( 'NONE',  ( -5.823673210054116645, -21.52544592524344225, 82.29057627198103830 ) ) ;
#4884 = CARTESIAN_POINT ( 'NONE',  ( 21.53943276465977519, 0.05219959533937863772, 111.2510903946856899 ) ) ;
#4885 = CARTESIAN_POINT ( 'NONE',  ( 16.51473224551069308, 9.474510206698969483, 94.16557627198103830 ) ) ;
#4886 = CARTESIAN_POINT ( 'NONE',  ( -5.823673210054431948, 21.52544592524334988, 27.70942372801901854 ) ) ;
#4887 = CARTESIAN_POINT ( 'NONE',  ( 21.55341960407610458, 5.719274019375980345, 28.95724293864769905 ) ) ;
#4888 = CARTESIAN_POINT ( 'NONE',  ( -4.379528057220086978, -16.55341960407618274, 99.79275706135234714 ) ) ;
#4890 = CARTESIAN_POINT ( 'NONE',  ( -0.05219959533937732626, 21.53943276465977519, 87.50109039468568994 ) ) ;
#4889 = CARTESIAN_POINT ( 'NONE',  ( -0.05219959533937732626, 21.53943276465977519, 47.50109039468568994 ) ) ;
#4891 = CARTESIAN_POINT ( 'NONE',  ( -21.53943276465977519, -0.05219959533937600094, 113.7510903946856757 ) ) ;
#4892 = CARTESIAN_POINT ( 'NONE',  ( 0.05219959533934541429, -16.53943276465976808, 70.00109039468568994 ) ) ;
#4893 = CARTESIAN_POINT ( 'NONE',  ( 15.72974639402176855, 15.80617190586768217, 46.87609039468568994 ) ) ;
#4894 = CARTESIAN_POINT ( 'NONE',  ( -13.97604488694527625, -13.89961937509977652, 36.87390960531436690 ) ) ;
#4895 = CARTESIAN_POINT ( 'NONE',  ( 21.53943276465977519, 0.05219959533937863772, 106.2510903946856757 ) ) ;
#4896 = CARTESIAN_POINT ( 'NONE',  ( 19.03943276465977164, -0.05219959533909143690, 103.7489096053143669 ) ) ;
#4897 = CARTESIAN_POINT ( 'NONE',  ( 15.80617190586746368, 15.72974639402197994, 99.37390960531436690 ) ) ;
#4899 = CARTESIAN_POINT ( 'NONE',  ( 21.52544592524344225, -5.823673210054117533, 73.54057627198102409 ) ) ;
#4898 = DIRECTION ( 'NONE',  ( -0.000000000000000000, 0.000000000000000000, 1.000000000000000000 ) ) ;
#4901 = CARTESIAN_POINT ( 'NONE',  ( 16.52544592524342804, -4.483927247898539470, 43.54057627198103830 ) ) ;
#4900 = CARTESIAN_POINT ( 'NONE',  ( 16.53943276465976808, 0.05219959533934440121, 56.25109039468568284 ) ) ;
#4902 = CARTESIAN_POINT ( 'NONE',  ( 18.41295718396491310, -5.500000000000023093, 101.0176815517915969 ) ) ;
#4903 = CARTESIAN_POINT ( 'NONE',  ( 9.564922557961047289, -16.46253265017146816, 95.41775706135233293 ) ) ;
#4904 = DIRECTION ( 'NONE',  ( 0.000000000000000000, -1.000000000000000000, 1.287488025362403787E-15 ) ) ;
#4905 = CARTESIAN_POINT ( 'NONE',  ( 16.53943276465976808, 0.05219959533934440121, 26.25109039468567573 ) ) ;
#4906 = CARTESIAN_POINT ( 'NONE',  ( 15.80617190586746368, 15.72974639402197994, 104.3739096053143669 ) ) ;
#4907 = CARTESIAN_POINT ( 'NONE',  ( 0.05219959533907565091, 21.53943276465977519, 74.99890960531435269 ) ) ;
#4908 = CARTESIAN_POINT ( 'NONE',  ( -9.474510206698964154, 16.51473224551069663, 110.4155762719810383 ) ) ;
#4909 = CARTESIAN_POINT ( 'NONE',  ( 16.55341960407618274, -4.379528057220086978, 46.04275706135234714 ) ) ;
#4910 = CARTESIAN_POINT ( 'NONE',  ( 19.05341960407611168, 5.049401038298154454, 73.95724293864768129 ) ) ;
#4912 = CARTESIAN_POINT ( 'NONE',  ( 13.89961937509957401, 13.97604488694547697, 101.8760903946856331 ) ) ;
#4911 = CARTESIAN_POINT ( 'NONE',  ( -18.62759615963255300, -10.81492255796106328, 24.16775706135235424 ) ) ;
#4913 = CARTESIAN_POINT ( 'NONE',  ( 5.153800228976335163, 19.02544592524342804, 114.7905762719810241 ) ) ;
#4914 = CARTESIAN_POINT ( 'NONE',  ( 9.564922557960805705, 16.46253265017160317, 89.58224293864769550 ) ) ;
#4915 = CARTESIAN_POINT ( 'NONE',  ( -18.67979575497178146, -10.72451020669898902, 91.66557627198103830 ) ) ;
#4916 = CARTESIAN_POINT ( 'NONE',  ( 9.564922557960805705, 16.46253265017160317, 54.58224293864769550 ) ) ;
#4917 = CARTESIAN_POINT ( 'NONE',  ( -17.44279575226822487, -5.990770900252486264, 59.16442432485682446 ) ) ;
#4918 = CARTESIAN_POINT ( 'NONE',  ( -4.483927247898539470, -16.52544592524342804, 62.29057627198102409 ) ) ;
#4919 = CARTESIAN_POINT ( 'NONE',  ( -18.67979575497178146, -10.72451020669898902, 21.66557627198102409 ) ) ;
#4920 = CARTESIAN_POINT ( 'NONE',  ( -30.26186088262143059, 1.502453648625585281, -51.11561252063849281 ) ) ;
#4921 = CIRCLE ( 'NONE', #117974, 3.799999999999999378 ) ;
#4922 = CARTESIAN_POINT ( 'NONE',  ( -10.81492255796078084, -18.62759615963271287, 92.08224293864769550 ) ) ;
#4923 = CARTESIAN_POINT ( 'NONE',  ( -5.049401038297874678, -19.05341960407617918, 69.79275706135233293 ) ) ;
#4924 = CARTESIAN_POINT ( 'NONE',  ( 21.52544592524344225, -5.823673210054117533, 23.54057627198102765 ) ) ;
#4925 = CARTESIAN_POINT ( 'NONE',  ( 19.49671883438228548, 5.499999999999968026, 67.39279849105682274 ) ) ;
#4926 = CARTESIAN_POINT ( 'NONE',  ( -21.52544592524343514, 5.823673210054127303, 61.04057627198103120 ) ) ;
#4927 = CARTESIAN_POINT ( 'NONE',  ( 19.05341960407611168, 5.049401038298154454, 83.95724293864766707 ) ) ;
#4928 = CARTESIAN_POINT ( 'NONE',  ( -18.62759615963255300, -10.81492255796106328, 84.16775706135234714 ) ) ;
#4929 = CARTESIAN_POINT ( 'NONE',  ( -13.89961937509977652, 13.97604488694528158, 50.62390960531435979 ) ) ;
#4930 = CARTESIAN_POINT ( 'NONE',  ( -8.314922557960811034, -14.29746914071050412, 77.08224293864769550 ) ) ;
#4931 = CARTESIAN_POINT ( 'NONE',  ( -4.483927247898782831, 16.52544592524335698, 32.70942372801900433 ) ) ;
#4932 = CARTESIAN_POINT ( 'NONE',  ( 21.53943276465977519, 0.05219959533937863772, 71.25109039468568994 ) ) ;
#4933 = EDGE_LOOP ( 'NONE', ( #151041, #193866, #198494, #130742, #179815 ) ) ;
#4934 = CARTESIAN_POINT ( 'NONE',  ( -13.89961937509957401, -13.97604488694547875, 19.37609039468566507 ) ) ;
#4935 = CARTESIAN_POINT ( 'NONE',  ( 16.51473224551083163, -9.474510206698727899, 75.83442372801900433 ) ) ;
#4936 = CARTESIAN_POINT ( 'NONE',  ( -18.62759615963255300, -10.81492255796106328, 39.16775706135235424 ) ) ;
#4937 = CARTESIAN_POINT ( 'NONE',  ( 37.99999999999999289, 2.893978650043524126E-14, -2.749999994537626780 ) ) ;
#4938 = CARTESIAN_POINT ( 'NONE',  ( 5.049401038297881783, 19.05341960407617563, 27.29275706135232937 ) ) ;
#4939 = CARTESIAN_POINT ( 'NONE',  ( -19.02544592524342804, 5.153800228976336051, 56.04057627198100988 ) ) ;
#4940 = CARTESIAN_POINT ( 'NONE',  ( -16.51473224551082808, 9.474510206698731452, 28.33442372801900433 ) ) ;
#4941 = CARTESIAN_POINT ( 'NONE',  ( -8.314922557961024197, 14.29746914071037800, 107.9177570613523471 ) ) ;
#4943 = CARTESIAN_POINT ( 'NONE',  ( -0.05219959533937732626, 21.53943276465977519, 72.50109039468568994 ) ) ;
#4942 = CARTESIAN_POINT ( 'NONE',  ( 0.05219959533909260263, 19.03943276465977164, 99.99890960531436690 ) ) ;
#4944 = CARTESIAN_POINT ( 'NONE',  ( 11.40812507854755253, -35.11059874428192273, -8.024999997268814411 ) ) ;
#4945 = CARTESIAN_POINT ( 'NONE',  ( -33.81930014798969353, 1.942787237620518859, 100.1485738335251341 ) ) ;
#4946 = CARTESIAN_POINT ( 'NONE',  ( -15.72974639402176322, -15.80617190586768395, 84.37609039468570415 ) ) ;
#4947 = DIRECTION ( 'NONE',  ( 0.000000000000000000, 0.000000000000000000, 1.000000000000000000 ) ) ;
#4948 = CARTESIAN_POINT ( 'NONE',  ( 5.153800228976335163, 19.02544592524342804, 99.79057627198102409 ) ) ;
#4949 = CARTESIAN_POINT ( 'NONE',  ( -9.564922557961040184, 16.46253265017147172, 27.91775706135232582 ) ) ;
#4950 = CARTESIAN_POINT ( 'NONE',  ( -26.58496454516998853, -7.626754437231455519, 167.9682100371138915 ) ) ;
#4951 = CARTESIAN_POINT ( 'NONE',  ( 5.153800228976335163, 19.02544592524342804, 34.79057627198102409 ) ) ;
#4952 = CARTESIAN_POINT ( 'NONE',  ( 21.52544592524344225, -5.823673210054117533, 53.54057627198103120 ) ) ;
#4953 = CARTESIAN_POINT ( 'NONE',  ( 12.14591786802309770, 12.06949235617756955, 24.37390960531435979 ) ) ;
#4955 = CARTESIAN_POINT ( 'NONE',  ( -9.474510206698964154, 16.51473224551069663, 75.41557627198103830 ) ) ;
#4954 = CARTESIAN_POINT ( 'NONE',  ( -14.34966873604960291, -8.224510206698953496, 91.66557627198103830 ) ) ;
#4956 = CARTESIAN_POINT ( 'NONE',  ( 21.55341960407619695, -5.719274019375665929, 101.0427570613523756 ) ) ;
#4957 = CARTESIAN_POINT ( 'NONE',  ( -9.474510206698964154, 16.51473224551069663, 35.41557627198102409 ) ) ;
#4958 = CARTESIAN_POINT ( 'NONE',  ( 4.483927247898545687, 16.52544592524342804, 104.7905762719810241 ) ) ;
#4959 = CARTESIAN_POINT ( 'NONE',  ( -0.05219959533937732626, 21.53943276465977519, 57.50109039468568994 ) ) ;
#4960 = CARTESIAN_POINT ( 'NONE',  ( -15.72974639402197994, 15.80617190586746368, 80.62390960531438111 ) ) ;
#4961 = CARTESIAN_POINT ( 'NONE',  ( 5.153800228976615827, -19.02544592524334988, 50.20942372801897591 ) ) ;
#4962 = CARTESIAN_POINT ( 'NONE',  ( -3.573655867282028392E-15, 2.428612866367529932E-14, 155.0000000000000000 ) ) ;
#4963 = CARTESIAN_POINT ( 'NONE',  ( -9.474510206698964154, 16.51473224551069663, 105.4155762719810383 ) ) ;
#4964 = CARTESIAN_POINT ( 'NONE',  ( -8.314922557960811034, -14.29746914071050412, 82.08224293864768129 ) ) ;
#4965 = AXIS2_PLACEMENT_3D ( 'NONE', #90039, #28400, #135568 ) ;
#4966 = CARTESIAN_POINT ( 'NONE',  ( -5.049401038297874678, -19.05341960407617918, 44.79275706135232582 ) ) ;
#4967 = CARTESIAN_POINT ( 'NONE',  ( -13.97604488694527625, -13.89961937509977652, 61.87390960531435979 ) ) ;
#4968 = CARTESIAN_POINT ( 'NONE',  ( -16.53943276465976808, 0.05219959533911058130, 56.24890960531436690 ) ) ;
#4969 = CARTESIAN_POINT ( 'NONE',  ( -19.05341960407617563, 5.049401038297882671, 73.54275706135233293 ) ) ;
#4970 = FACE_OUTER_BOUND ( 'NONE', #19771, .T. ) ;
#4971 = CARTESIAN_POINT ( 'NONE',  ( 5.719274019375991003, -21.55341960407610458, 37.70724293864769550 ) ) ;
#4972 = VERTEX_POINT ( 'NONE', #44107 ) ;
#4973 = CARTESIAN_POINT ( 'NONE',  ( 12.06949235617757843, -12.14591786802309237, 98.12390960531436690 ) ) ;
#4974 = CARTESIAN_POINT ( 'NONE',  ( -17.49999999999997158, -3.805241302050501151, 24.62647527217407628 ) ) ;
#4976 = CARTESIAN_POINT ( 'NONE',  ( 5.719274019375991003, -21.55341960407610458, 67.70724293864769550 ) ) ;
#4975 = CARTESIAN_POINT ( 'NONE',  ( 9.474510206698971260, -16.51473224551069308, 62.91557627198102409 ) ) ;
#4977 = CARTESIAN_POINT ( 'NONE',  ( 19.05341960407611168, 5.049401038298154454, 33.95724293864769550 ) ) ;
#4979 = CARTESIAN_POINT ( 'NONE',  ( -13.97604488694527625, -13.89961937509977652, 66.87390960531436690 ) ) ;
#4978 = CARTESIAN_POINT ( 'NONE',  ( -4.483927247898782831, 16.52544592524335698, 77.70942372801900433 ) ) ;
#4980 = CARTESIAN_POINT ( 'NONE',  ( 5.153800228976615827, -19.02544592524334988, 50.20942372801897591 ) ) ;
#4981 = CARTESIAN_POINT ( 'NONE',  ( 21.52544592524334988, 5.823673210054432836, 66.45942372801903275 ) ) ;
#4982 = CARTESIAN_POINT ( 'NONE',  ( 18.67979575497178502, 10.72451020669898547, 44.16557627198103120 ) ) ;
#4983 = CARTESIAN_POINT ( 'NONE',  ( 5.153800228976335163, 19.02544592524342804, 29.79057627198102409 ) ) ;
#4984 = CARTESIAN_POINT ( 'NONE',  ( 12.14591786802327356, -12.06949235617739191, 85.62609039468568994 ) ) ;
#4985 = CARTESIAN_POINT ( 'NONE',  ( -16.46253265017146816, -9.564922557961047289, 104.1677570613523329 ) ) ;
#4986 = CARTESIAN_POINT ( 'NONE',  ( 9.474510206698971260, -16.51473224551069308, 22.91557627198102765 ) ) ;
#4987 = DIRECTION ( 'NONE',  ( -1.000000000000000000, 0.000000000000000000, 0.000000000000000000 ) ) ;
#4988 = CARTESIAN_POINT ( 'NONE',  ( 21.52544592524334988, 5.823673210054432836, 91.45942372801901854 ) ) ;
#4990 = ORIENTED_EDGE ( 'NONE', *, *, #133302, .T. ) ;
#4989 = CIRCLE ( 'NONE', #117593, 0.5000000000000004441 ) ;
#4991 = CARTESIAN_POINT ( 'NONE',  ( -4.379528057220328563, 16.55341960407611168, 40.20724293864769550 ) ) ;
#4992 = CARTESIAN_POINT ( 'NONE',  ( -4.379528057220328563, 16.55341960407611168, 55.20724293864770260 ) ) ;
#4993 = CARTESIAN_POINT ( 'NONE',  ( 21.52544592524344225, -5.823673210054117533, 93.54057627198103830 ) ) ;
#4994 = CARTESIAN_POINT ( 'NONE',  ( 18.62759615963271287, -10.81492255796078972, 93.33224293864769550 ) ) ;
#4995 = CARTESIAN_POINT ( 'NONE',  ( -1.278449583442071713, -31.20457203169705096, -46.64972497815391250 ) ) ;
#4997 = ADVANCED_FACE ( 'NONE', ( #193808 ), #113093, .T. ) ;
#4996 = CARTESIAN_POINT ( 'NONE',  ( -15.72974639402197994, 15.80617190586746368, 35.62390960531437401 ) ) ;
#4999 = AXIS2_PLACEMENT_3D ( 'NONE', #194247, #161891, #192238 ) ;
#4998 = CARTESIAN_POINT ( 'NONE',  ( -8.314922557961024197, 14.29746914071037800, 72.91775706135234714 ) ) ;
#5000 = CARTESIAN_POINT ( 'NONE',  ( 14.34966873604960469, 8.224510206698951720, 84.16557627198103830 ) ) ;
#5001 = CARTESIAN_POINT ( 'NONE',  ( -9.564922557960796823, -16.46253265017161027, 47.08224293864769550 ) ) ;
#5002 = LINE ( 'NONE', #17212, #21917 ) ;
#5003 = ORIENTED_EDGE ( 'NONE', *, *, #126225, .F. ) ;
#5004 = CARTESIAN_POINT ( 'NONE',  ( 14.34966873604972726, -8.224510206698740333, 100.8344237280190185 ) ) ;
#5005 = CARTESIAN_POINT ( 'NONE',  ( 21.53943276465977519, -0.05219959533907433946, 113.7489096053143527 ) ) ;
#5006 = CARTESIAN_POINT ( 'NONE',  ( -16.46253265017160317, 9.564922557960807481, 80.83224293864769550 ) ) ;
#5007 = CARTESIAN_POINT ( 'NONE',  ( 21.52544592524334988, 5.823673210054432836, 51.45942372801901854 ) ) ;
#5008 = CARTESIAN_POINT ( 'NONE',  ( 0.05219959533909260263, 19.03943276465977164, 104.9989096053143669 ) ) ;
#5009 = CARTESIAN_POINT ( 'NONE',  ( -9.646990561631263006, -38.22155086790370149, -31.80034568179328858 ) ) ;
#5010 = VERTEX_POINT ( 'NONE', #89630 ) ;
#5011 = CARTESIAN_POINT ( 'NONE',  ( 5.823673210054444382, -21.52544592524334988, 45.20942372801901854 ) ) ;
#5013 = CARTESIAN_POINT ( 'NONE',  ( -19.05341960407611168, -5.049401038298163336, 21.45724293864768839 ) ) ;
#5012 = CARTESIAN_POINT ( 'NONE',  ( 0.05219959533909260263, 19.03943276465977164, 39.99890960531436690 ) ) ;
#5014 = CARTESIAN_POINT ( 'NONE',  ( -13.89961937509957401, -13.97604488694547875, 59.37609039468566863 ) ) ;
#5015 = CARTESIAN_POINT ( 'NONE',  ( -5.823673210054431948, 21.52544592524334988, 27.70942372801901854 ) ) ;
#5016 = CARTESIAN_POINT ( 'NONE',  ( -9.474510206698720793, -16.51473224551083518, 64.58442372801900433 ) ) ;
#5017 = CARTESIAN_POINT ( 'NONE',  ( -16.46253265017160317, 9.564922557960807481, 30.83224293864769550 ) ) ;
#5018 = CARTESIAN_POINT ( 'NONE',  ( 16.55341960407618274, -4.379528057220086978, 96.04275706135236135 ) ) ;
#5019 = CARTESIAN_POINT ( 'NONE',  ( 19.05341960407617918, -5.049401038297876454, 66.04275706135233293 ) ) ;
#5020 = CARTESIAN_POINT ( 'NONE',  ( 14.34966873604972726, -8.224510206698740333, 110.8344237280190043 ) ) ;
#5021 = PLANE ( 'NONE',  #137868 ) ;
#5022 = CARTESIAN_POINT ( 'NONE',  ( 9.474510206698971260, -16.51473224551069308, 87.91557627198102409 ) ) ;
#5023 = CARTESIAN_POINT ( 'NONE',  ( 5.719274019375673035, 21.55341960407619339, 87.29275706135236135 ) ) ;
#5024 = CARTESIAN_POINT ( 'NONE',  ( -21.55341960407619339, 5.719274019375674811, 103.5427570613523613 ) ) ;
#5025 = DIRECTION ( 'NONE',  ( -0.7071067811865466846, 7.406550393246786959E-15, -0.7071067811865484609 ) ) ;
#5026 = CARTESIAN_POINT ( 'NONE',  ( 0.05219959533909260263, 19.03943276465977164, 94.99890960531436690 ) ) ;
#5027 = CARTESIAN_POINT ( 'NONE',  ( 15.72974639402176855, 15.80617190586768217, 71.87609039468568994 ) ) ;
#5028 = CARTESIAN_POINT ( 'NONE',  ( 0.05219959533934541429, -16.53943276465976808, 25.00109039468567218 ) ) ;
#5029 = CARTESIAN_POINT ( 'NONE',  ( 16.46253265017160672, -9.564922557960803928, 78.33224293864769550 ) ) ;
#5030 = CARTESIAN_POINT ( 'NONE',  ( -15.80617190586745835, -15.72974639402198527, 31.87390960531435979 ) ) ;
#5031 = CARTESIAN_POINT ( 'NONE',  ( -27.39399371936807270, 5.109217719441145000, 166.7881433183807189 ) ) ;
#5032 = CARTESIAN_POINT ( 'NONE',  ( 13.97604488694527802, 13.89961937509977652, 59.37390960531434558 ) ) ;
#5033 = CARTESIAN_POINT ( 'NONE',  ( 16.55341960407618274, -4.379528057220086978, 111.0427570613523613 ) ) ;
#5034 = CARTESIAN_POINT ( 'NONE',  ( -16.19135201231352639, 7.376712067591985722, 99.81319145947878724 ) ) ;
#5035 = CARTESIAN_POINT ( 'NONE',  ( 19.02544592524334988, 5.153800228976608722, 71.45942372801900433 ) ) ;
#5036 = CARTESIAN_POINT ( 'NONE',  ( -19.03943276465977164, 0.05219959533909376836, 101.2489096053143669 ) ) ;
#5037 = CARTESIAN_POINT ( 'NONE',  ( 10.72451020669871369, 18.67979575497193778, 102.0844237280190185 ) ) ;
#5038 = CARTESIAN_POINT ( 'NONE',  ( 8.314922557960818139, 14.29746914071049879, 84.58224293864769550 ) ) ;
#5039 = CARTESIAN_POINT ( 'NONE',  ( -15.80617190586745835, -15.72974639402198527, 51.87390960531437401 ) ) ;
#5040 = CARTESIAN_POINT ( 'NONE',  ( -15.72974639402197994, 15.80617190586746368, 35.62390960531437401 ) ) ;
#5041 = CARTESIAN_POINT ( 'NONE',  ( -14.29746914071049879, 8.314922557960819915, 110.8322429386476955 ) ) ;
#5042 = CARTESIAN_POINT ( 'NONE',  ( -1.351304681146049624, -6.941592873960400922, -62.33628431810817716 ) ) ;
#5043 = CARTESIAN_POINT ( 'NONE',  ( 19.03943276465977164, 0.05219959533936151252, 41.25109039468566152 ) ) ;
#5044 = CARTESIAN_POINT ( 'NONE',  ( 8.224510206698953496, -14.34966873604960469, 22.91557627198102765 ) ) ;
#5045 = CARTESIAN_POINT ( 'NONE',  ( 9.564922557960805705, 16.46253265017160317, 99.58224293864770971 ) ) ;
#5046 = CARTESIAN_POINT ( 'NONE',  ( 15.80617190586769283, -15.72974639402175789, 70.62609039468567573 ) ) ;
#5047 = CARTESIAN_POINT ( 'NONE',  ( 15.80617190586746368, 15.72974639402197994, 54.37390960531435979 ) ) ;
#5048 = CARTESIAN_POINT ( 'NONE',  ( -5.719274019375665041, -21.55341960407619695, 44.79275706135234714 ) ) ;
#5049 = CARTESIAN_POINT ( 'NONE',  ( 5.719274019375991003, -21.55341960407610458, 97.70724293864772392 ) ) ;
#5050 = CARTESIAN_POINT ( 'NONE',  ( -18.67979575497193778, 10.72451020669871902, 33.33442372801900433 ) ) ;
#5051 = CARTESIAN_POINT ( 'NONE',  ( 16.46253265017160672, -9.564922557960803928, 28.33224293864769550 ) ) ;
#5052 = CARTESIAN_POINT ( 'NONE',  ( 0.05219959533936267826, -19.03943276465977164, 65.00109039468567573 ) ) ;
#5053 = CARTESIAN_POINT ( 'NONE',  ( -8.224510206698948167, 14.34966873604960824, 110.4155762719810383 ) ) ;
#5054 = CARTESIAN_POINT ( 'NONE',  ( -19.05341960407611168, -5.049401038298163336, 106.4572429386476955 ) ) ;
#5055 = TOROIDAL_SURFACE ( 'NONE', #179484, 206.0437394197456342, 10.00000000000000000 ) ;
#5056 = CARTESIAN_POINT ( 'NONE',  ( 8.224510206698953496, -14.34966873604960469, 57.91557627198103120 ) ) ;
#5057 = CARTESIAN_POINT ( 'NONE',  ( 0.05219959533934541429, -16.53943276465976808, 110.0010903946856757 ) ) ;
#5058 = CARTESIAN_POINT ( 'NONE',  ( -19.05341960407611168, -5.049401038298163336, 46.45724293864768129 ) ) ;
#5059 = CARTESIAN_POINT ( 'NONE',  ( 16.53943276465976808, -0.05219959533910856209, 113.7489096053143527 ) ) ;
#5060 = CARTESIAN_POINT ( 'NONE',  ( -15.72974639402197994, 15.80617190586746368, 30.62390960531436335 ) ) ;
#5061 = CARTESIAN_POINT ( 'NONE',  ( -5.049401038297874678, -19.05341960407617918, 29.79275706135232227 ) ) ;
#5063 = CARTESIAN_POINT ( 'NONE',  ( 16.53943276465976808, -0.05219959533910856209, 33.74890960531436690 ) ) ;
#5062 = CARTESIAN_POINT ( 'NONE',  ( -2.500000000000000000, -165.0000000000000000, 7.000000000000003553 ) ) ;
#5064 = CARTESIAN_POINT ( 'NONE',  ( 10.72451020669871369, 18.67979575497193778, 47.08442372801901854 ) ) ;
#5065 = CARTESIAN_POINT ( 'NONE',  ( 17.50000000000000000, -7.500000000000000888, 120.0000000000000142 ) ) ;
#5066 = CARTESIAN_POINT ( 'NONE',  ( 8.224510206698742110, 14.34966873604972548, 62.08442372801901143 ) ) ;
#5067 = ADVANCED_FACE ( 'NONE', ( #165492 ), #104804, .F. ) ;
#5068 = CARTESIAN_POINT ( 'NONE',  ( 9.474510206698729675, 16.51473224551082808, 62.08442372801899722 ) ) ;
#5069 = CARTESIAN_POINT ( 'NONE',  ( 4.483927247898545687, 16.52544592524342804, 29.79057627198102409 ) ) ;
#5070 = CARTESIAN_POINT ( 'NONE',  ( 4.379528057220092307, 16.55341960407617563, 107.2927570613523471 ) ) ;
#5071 = CARTESIAN_POINT ( 'NONE',  ( 19.05341960407611168, 5.049401038298154454, 33.95724293864769550 ) ) ;
#5072 = CARTESIAN_POINT ( 'NONE',  ( 9.474510206698971260, -16.51473224551069308, 67.91557627198102409 ) ) ;
#5073 = CARTESIAN_POINT ( 'NONE',  ( -5.153800228976328057, -19.02544592524343514, 27.29057627198103120 ) ) ;
#5074 = CARTESIAN_POINT ( 'NONE',  ( 18.67979575497194134, -10.72451020669871369, 30.83442372801902209 ) ) ;
#5075 = CARTESIAN_POINT ( 'NONE',  ( 19.03943276465977164, -0.05219959533909143690, 48.74890960531435979 ) ) ;
#5076 = DIRECTION ( 'NONE',  ( 1.000000000000000000, -5.392603844284257652E-33, 0.000000000000000000 ) ) ;
#5077 = CARTESIAN_POINT ( 'NONE',  ( 19.03943276465977164, -0.05219959533909143690, 33.74890960531435979 ) ) ;
#5078 = CARTESIAN_POINT ( 'NONE',  ( -0.05219959533909027116, -19.03943276465977164, 112.4989096053143669 ) ) ;
#5079 = ADVANCED_FACE ( 'NONE', ( #148320 ), #71476, .T. ) ;
#5081 = CARTESIAN_POINT ( 'NONE',  ( -16.53943276465976808, 0.05219959533911058130, 101.2489096053143669 ) ) ;
#5080 = CARTESIAN_POINT ( 'NONE',  ( -10.72451020669870658, -18.67979575497194134, 64.58442372801900433 ) ) ;
#5082 = CARTESIAN_POINT ( 'NONE',  ( -16.46253265017160317, 9.564922557960807481, 115.8322429386477097 ) ) ;
#5083 = CARTESIAN_POINT ( 'NONE',  ( -14.29746914071037622, -8.314922557961029526, 84.16775706135234714 ) ) ;
#5084 = CARTESIAN_POINT ( 'NONE',  ( -5.719274019375665041, -21.55341960407619695, 94.79275706135234714 ) ) ;
#5085 = CARTESIAN_POINT ( 'NONE',  ( -12.14591786802326823, 12.06949235617739902, 48.12609039468568284 ) ) ;
#5086 = CARTESIAN_POINT ( 'NONE',  ( 13.97604488694527802, 13.89961937509977652, 94.37390960531436690 ) ) ;
#5087 = CARTESIAN_POINT ( 'NONE',  ( 16.55341960407618274, -4.379528057220086978, 36.04275706135234714 ) ) ;
#5088 = CARTESIAN_POINT ( 'NONE',  ( 16.52544592524335698, 4.483927247898782831, 21.45942372801901499 ) ) ;
#5089 = CARTESIAN_POINT ( 'NONE',  ( 16.52544592524335698, 4.483927247898782831, 81.45942372801900433 ) ) ;
#5090 = CARTESIAN_POINT ( 'NONE',  ( -13.89961937509957401, -13.97604488694547875, 109.3760903946856331 ) ) ;
#5091 = CARTESIAN_POINT ( 'NONE',  ( 18.62759615963271287, -10.81492255796078972, 93.33224293864769550 ) ) ;
#5093 = CARTESIAN_POINT ( 'NONE',  ( -16.51473224551082808, 9.474510206698731452, 98.33442372801900433 ) ) ;
#5092 = CARTESIAN_POINT ( 'NONE',  ( 16.55341960407611168, 4.379528057220329451, 103.9572429386476813 ) ) ;
#5094 = CARTESIAN_POINT ( 'NONE',  ( 4.379528057220092307, 16.55341960407617563, 77.29275706135234714 ) ) ;
#5095 = CARTESIAN_POINT ( 'NONE',  ( 24.29042230868054020, 8.936166115089967832, 166.5611006352800132 ) ) ;
#5096 = CARTESIAN_POINT ( 'NONE',  ( -19.02544592524334988, -5.153800228976617603, 63.95942372801899012 ) ) ;
#5097 = CARTESIAN_POINT ( 'NONE',  ( -8.224510206698948167, 14.34966873604960824, 45.41557627198103830 ) ) ;
#5098 = CARTESIAN_POINT ( 'NONE',  ( 8.224510206698953496, -14.34966873604960469, 92.91557627198103830 ) ) ;
#5100 = CARTESIAN_POINT ( 'NONE',  ( -19.49149378614659867, 5.499999999999578115, 89.43757513605359577 ) ) ;
#5099 = CARTESIAN_POINT ( 'NONE',  ( 5.153800228976615827, -19.02544592524334988, 35.20942372801899722 ) ) ;
#5101 = CARTESIAN_POINT ( 'NONE',  ( 5.823673210054444382, -21.52544592524334988, 40.20942372801901854 ) ) ;
#5102 = CARTESIAN_POINT ( 'NONE',  ( 16.51473224551083163, -9.474510206698727899, 95.83442372801900433 ) ) ;
#5103 = CARTESIAN_POINT ( 'NONE',  ( -19.05341960407611168, -5.049401038298163336, 111.4572429386476671 ) ) ;
#5104 = CARTESIAN_POINT ( 'NONE',  ( 16.51473224551069308, 9.474510206698969483, 94.16557627198103830 ) ) ;
#5105 = CARTESIAN_POINT ( 'NONE',  ( 21.52544592524334988, 5.823673210054432836, 111.4594237280190328 ) ) ;
#5106 = CARTESIAN_POINT ( 'NONE',  ( 13.89961937509977652, -13.97604488694527269, 88.12390960531438111 ) ) ;
#5107 = CARTESIAN_POINT ( 'NONE',  ( -21.53943276465977519, 0.05219959533907696930, 61.24890960531435979 ) ) ;
#5108 = CARTESIAN_POINT ( 'NONE',  ( 4.379528057220339221, -16.55341960407611168, 87.70724293864769550 ) ) ;
#5109 = CARTESIAN_POINT ( 'NONE',  ( -19.05341960407611168, -5.049401038298163336, 66.45724293864769550 ) ) ;
#5110 = CARTESIAN_POINT ( 'NONE',  ( 12.06949235617757843, -12.14591786802309237, 108.1239096053143811 ) ) ;
#5111 = CARTESIAN_POINT ( 'NONE',  ( -21.52544592524334988, -5.823673210054445271, 43.95942372801902565 ) ) ;
#5112 = CARTESIAN_POINT ( 'NONE',  ( -18.67979575497193778, 10.72451020669871902, 78.33442372801901854 ) ) ;
#5113 = CARTESIAN_POINT ( 'NONE',  ( 5.153800228976335163, 19.02544592524342804, 49.79057627198100988 ) ) ;
#5114 = CARTESIAN_POINT ( 'NONE',  ( -8.314922557961024197, 14.29746914071037800, 72.91775706135234714 ) ) ;
#5115 = CARTESIAN_POINT ( 'NONE',  ( 21.53943276465977519, 0.05219959533937863772, 36.25109039468567573 ) ) ;
#5116 = CARTESIAN_POINT ( 'NONE',  ( 21.55341960407619695, -5.719274019375665929, 26.04275706135235779 ) ) ;
#5118 = CARTESIAN_POINT ( 'NONE',  ( -13.97604488694527625, -13.89961937509977652, 66.87390960531436690 ) ) ;
#5117 = CARTESIAN_POINT ( 'NONE',  ( -16.51473224551082808, 9.474510206698731452, 53.33442372801900433 ) ) ;
#5119 = CARTESIAN_POINT ( 'NONE',  ( 16.46253265017146816, 9.564922557961045513, 26.66775706135234003 ) ) ;
#5120 = CARTESIAN_POINT ( 'NONE',  ( -0.05219959533937732626, 21.53943276465977519, 87.50109039468568994 ) ) ;
#5121 = CARTESIAN_POINT ( 'NONE',  ( 21.53943276465977519, -0.05219959533907433946, 73.74890960531433848 ) ) ;
#5122 = CARTESIAN_POINT ( 'NONE',  ( 8.314922557960818139, 14.29746914071049879, 49.58224293864769550 ) ) ;
#5124 = CARTESIAN_POINT ( 'NONE',  ( -16.46253265017146816, -9.564922557961047289, 24.16775706135233648 ) ) ;
#5123 = CARTESIAN_POINT ( 'NONE',  ( 10.81492255796106328, -18.62759615963255655, 85.41775706135236135 ) ) ;
#5125 = CARTESIAN_POINT ( 'NONE',  ( -12.14591786802309592, -12.06949235617757132, 76.87390960531439532 ) ) ;
#5126 = CARTESIAN_POINT ( 'NONE',  ( -16.46253265017160317, 9.564922557960807481, 25.83224293864769194 ) ) ;
#5127 = CARTESIAN_POINT ( 'NONE',  ( -16.46253265017146816, -9.564922557961047289, 54.16775706135234003 ) ) ;
#5128 = CARTESIAN_POINT ( 'NONE',  ( -12.14591786802309592, -12.06949235617757132, 31.87390960531435979 ) ) ;
#5129 = CARTESIAN_POINT ( 'NONE',  ( 18.62759615963255655, 10.81492255796105972, 86.66775706135234714 ) ) ;
#5130 = CARTESIAN_POINT ( 'NONE',  ( 16.51473224551069308, 9.474510206698969483, 79.16557627198103830 ) ) ;
#5131 = CARTESIAN_POINT ( 'NONE',  ( 13.89961937509957401, 13.97604488694547697, 51.87609039468566863 ) ) ;
#5132 = CARTESIAN_POINT ( 'NONE',  ( -18.67979575497178146, -10.72451020669898902, 46.66557627198102409 ) ) ;
#5134 = CARTESIAN_POINT ( 'NONE',  ( -21.55341960407619339, 5.719274019375674811, 48.54275706135234714 ) ) ;
#5133 = B_SPLINE_CURVE_WITH_KNOTS ( 'NONE', 3,
 ( #22604, #131776, #54935, #86265, #72103, #147955, #191443, #116607, #40770, #39759, #83256, #37764, #55931, #53938, #100430, #146946, #84250, #144931, #164126, #101422, #38774, #161108, #145931, #9442, #71107, #117606, #162111, #23608, #7413, #163114, #115613, #85254, #24617, #69096, #148953, #133776, #180309, #132773, #8435, #194460, #179306, #103443, #102439, #68094 ),
 .UNSPECIFIED., .F., .F.,
 ( 4, 2, 2, 2, 2, 2, 2, 2, 2, 2, 2, 2, 2, 2, 2, 2, 2, 2, 2, 2, 2, 4 ),
 ( 0.01750047681075387815, 0.01897230708297379873, 0.01970822221908375901, 0.02044413735519371930, 0.02191596762741363988, 0.02338779789963356393, 0.02485962817185348450, 0.02559554330796346561, 0.02633145844407343977, 0.02706737358018342088, 0.02780328871629339851, 0.02927511898851335725, 0.03074694926073331253, 0.03221877953295326780, 0.03295469466906326972, 0.03369060980517327164, 0.03516244007739326854, 0.03663427034961326545, 0.03737018548572325349, 0.03810610062183324154, 0.03957793089405323150, 0.04104976116627322147 ),
 .UNSPECIFIED. ) ;
#5135 = CARTESIAN_POINT ( 'NONE',  ( -21.55341960407610458, -5.719274019375992779, 96.45724293864770971 ) ) ;
#5136 = CARTESIAN_POINT ( 'NONE',  ( 13.97604488694548053, -13.89961937509957401, 100.6260903946856615 ) ) ;
#5137 = CARTESIAN_POINT ( 'NONE',  ( 8.224510206698742110, 14.34966873604972548, 62.08442372801901143 ) ) ;
#5139 = CARTESIAN_POINT ( 'NONE',  ( 15.72974639402199770, -15.80617190586745480, 108.1239096053143811 ) ) ;
#5138 = DIRECTION ( 'NONE',  ( -1.000000000000000000, 0.000000000000000000, 0.000000000000000000 ) ) ;
#5140 = CARTESIAN_POINT ( 'NONE',  ( -12.14591786802309592, -12.06949235617757132, 96.87390960531436690 ) ) ;
#5141 = DIRECTION ( 'NONE',  ( 0.000000000000000000, 0.000000000000000000, -1.000000000000000000 ) ) ;
#5142 = CARTESIAN_POINT ( 'NONE',  ( 16.55341960407618274, -4.379528057220086978, 31.04275706135234714 ) ) ;
#5143 = CARTESIAN_POINT ( 'NONE',  ( -10.72451020669898014, 18.67979575497178502, 65.41557627198102409 ) ) ;
#5144 = CARTESIAN_POINT ( 'NONE',  ( -12.14591786802326823, 12.06949235617739902, 98.12609039468570415 ) ) ;
#5145 = CARTESIAN_POINT ( 'NONE',  ( 13.89961937509977652, -13.97604488694527269, 28.12390960531435624 ) ) ;
#5146 = CARTESIAN_POINT ( 'NONE',  ( -8.224510206698735004, -14.34966873604973081, 64.58442372801900433 ) ) ;
#5147 = CARTESIAN_POINT ( 'NONE',  ( -16.46253265017146816, -9.564922557961047289, 59.16775706135233293 ) ) ;
#5148 = CARTESIAN_POINT ( 'NONE',  ( -18.67979575497193778, 10.72451020669871902, 43.33442372801901143 ) ) ;
#5149 = CARTESIAN_POINT ( 'NONE',  ( 21.55341960407610458, 5.719274019375980345, 58.95724293864770971 ) ) ;
#5150 = CARTESIAN_POINT ( 'NONE',  ( -4.483927247898782831, 16.52544592524335698, 87.70942372801901854 ) ) ;
#5151 = CARTESIAN_POINT ( 'NONE',  ( -21.53943276465977519, -0.05219959533937600094, 73.75109039468567573 ) ) ;
#5152 = CARTESIAN_POINT ( 'NONE',  ( 5.719274019375991003, -21.55341960407610458, 57.70724293864770260 ) ) ;
#5153 = CARTESIAN_POINT ( 'NONE',  ( 0.05219959533907565091, 21.53943276465977519, 39.99890960531436690 ) ) ;
#5154 = CARTESIAN_POINT ( 'NONE',  ( 4.483927247898790824, -16.52544592524335698, 60.20942372801902565 ) ) ;
#5155 = CARTESIAN_POINT ( 'NONE',  ( -18.62759615963270932, 10.81492255796079327, 35.83224293864768839 ) ) ;
#5156 = ORIENTED_EDGE ( 'NONE', *, *, #165915, .T. ) ;
#5157 = CARTESIAN_POINT ( 'NONE',  ( 19.05341960407611168, 5.049401038298154454, 93.95724293864769550 ) ) ;
#5158 = CARTESIAN_POINT ( 'NONE',  ( -12.14591786802326823, 12.06949235617739902, 113.1260903946856899 ) ) ;
#5159 = DIRECTION ( 'NONE',  ( 0.5000000000000004441, 0.4999999999999987232, -0.7071067811865482389 ) ) ;
#5160 = CARTESIAN_POINT ( 'NONE',  ( 8.224510206698953496, -14.34966873604960469, 102.9155762719810383 ) ) ;
#5161 = CARTESIAN_POINT ( 'NONE',  ( -15.72974639402197994, 15.80617190586746368, 65.62390960531436690 ) ) ;
#5162 = CARTESIAN_POINT ( 'NONE',  ( 14.34966873604972726, -8.224510206698740333, 85.83442372801901854 ) ) ;
#5163 = CARTESIAN_POINT ( 'NONE',  ( -15.72974639402176322, -15.80617190586768395, 49.37609039468569705 ) ) ;
#5164 = CARTESIAN_POINT ( 'NONE',  ( -0.05219959533936034679, 19.03943276465977164, 107.5010903946856615 ) ) ;
#5165 = CARTESIAN_POINT ( 'NONE',  ( 4.379528057220339221, -16.55341960407611168, 102.7072429386476955 ) ) ;
#5166 = CARTESIAN_POINT ( 'NONE',  ( -9.564922557960796823, -16.46253265017161027, 52.08224293864768839 ) ) ;
#5167 = AXIS2_PLACEMENT_3D ( 'NONE', #72107, #11455, #147960 ) ;
#5168 = CARTESIAN_POINT ( 'NONE',  ( 9.564922557960805705, 16.46253265017160317, 29.58224293864769550 ) ) ;
#5169 = DIRECTION ( 'NONE',  ( -1.000000000000000000, 0.000000000000000000, 0.000000000000000000 ) ) ;
#5170 = CARTESIAN_POINT ( 'NONE',  ( 5.153800228976335163, 19.02544592524342804, 89.79057627198102409 ) ) ;
#5171 = CARTESIAN_POINT ( 'NONE',  ( -8.314922557961024197, 14.29746914071037800, 77.91775706135231871 ) ) ;
#5172 = CARTESIAN_POINT ( 'NONE',  ( -5.719274019375665041, -21.55341960407619695, 99.79275706135234714 ) ) ;
#5173 = CARTESIAN_POINT ( 'NONE',  ( 10.72451020669898902, -18.67979575497178502, 47.91557627198102409 ) ) ;
#5174 = EDGE_CURVE ( 'NONE', #71503, #154069, #101569, .T. ) ;
#5175 = CARTESIAN_POINT ( 'NONE',  ( -14.34966873604972548, 8.224510206698743886, 78.33442372801901854 ) ) ;
#5176 = CARTESIAN_POINT ( 'NONE',  ( 13.97604488694548053, -13.89961937509957401, 80.62609039468567573 ) ) ;
#5177 = ORIENTED_EDGE ( 'NONE', *, *, #34776, .T. ) ;
#5178 = CARTESIAN_POINT ( 'NONE',  ( -13.97604488694527625, -13.89961937509977652, 36.87390960531436690 ) ) ;
#5179 = CARTESIAN_POINT ( 'NONE',  ( -13.89961937509977652, 13.97604488694528158, 80.62390960531436690 ) ) ;
#5180 = CARTESIAN_POINT ( 'NONE',  ( 13.89961937509977652, -13.97604488694527269, 38.12390960531436690 ) ) ;
#5181 = CARTESIAN_POINT ( 'NONE',  ( -13.97604488694547697, 13.89961937509957934, 78.12609039468567573 ) ) ;
#5182 = CARTESIAN_POINT ( 'NONE',  ( 25.11239783071230747, -12.35465959874983533, 166.1131185557732124 ) ) ;
#5183 = CARTESIAN_POINT ( 'NONE',  ( -0.05219959533909027116, -19.03943276465977164, 102.4989096053143669 ) ) ;
#5184 = CARTESIAN_POINT ( 'NONE',  ( -12.06949235617756955, 12.14591786802309770, 55.62390960531436690 ) ) ;
#5185 = CARTESIAN_POINT ( 'NONE',  ( -10.72451020669898014, 18.67979575497178502, 50.41557627198103120 ) ) ;
#5186 = CARTESIAN_POINT ( 'NONE',  ( -17.50000000000000000, 3.209263204892625954, 104.7619682560627297 ) ) ;
#5187 = CARTESIAN_POINT ( 'NONE',  ( 9.564922557961047289, -16.46253265017146816, 30.41775706135232937 ) ) ;
#5188 = CARTESIAN_POINT ( 'NONE',  ( -17.50000000000000711, -5.499999999999944045, 81.28230962303565832 ) ) ;
#5189 = CARTESIAN_POINT ( 'NONE',  ( -5.153800228976328057, -19.02544592524343514, 47.29057627198102409 ) ) ;
#5190 = CARTESIAN_POINT ( 'NONE',  ( 16.55341960407618274, -4.379528057220086978, 36.04275706135234714 ) ) ;
#5191 = CARTESIAN_POINT ( 'NONE',  ( -18.56399227203342051, -5.499999999999968914, 98.97830131249901342 ) ) ;
#5192 = CYLINDRICAL_SURFACE ( 'NONE', #117906, 0.5000000000000004441 ) ;
#5193 = CARTESIAN_POINT ( 'NONE',  ( 4.379528057220092307, 16.55341960407617563, 82.29275706135234714 ) ) ;
#5194 = CARTESIAN_POINT ( 'NONE',  ( 21.55341960407610458, 5.719274019375980345, 93.95724293864770971 ) ) ;
#5195 = CARTESIAN_POINT ( 'NONE',  ( -0.05219959533934338120, 16.53943276465976808, 42.50109039468567573 ) ) ;
#5197 = CARTESIAN_POINT ( 'NONE',  ( -5.049401038298153566, 19.05341960407611168, 115.2072429386477097 ) ) ;
#5196 = CARTESIAN_POINT ( 'NONE',  ( 13.89961937509977652, -13.97604488694527269, 38.12390960531436690 ) ) ;
#5198 = CARTESIAN_POINT ( 'NONE',  ( -21.55341960407619339, 5.719274019375674811, 38.54275706135234714 ) ) ;
#5199 = CARTESIAN_POINT ( 'NONE',  ( 19.05341960407617918, -5.049401038297876454, 56.04275706135234714 ) ) ;
#5200 = CARTESIAN_POINT ( 'NONE',  ( 21.55341960407619695, -5.719274019375665929, 96.04275706135236135 ) ) ;
#5201 = AXIS2_PLACEMENT_3D ( 'NONE', #184358, #1302, #42874 ) ;
#5202 = CARTESIAN_POINT ( 'NONE',  ( -23.22614267028769319, -5.670187745555518077, 172.0618673401326646 ) ) ;
#5203 = CARTESIAN_POINT ( 'NONE',  ( -4.379528057220328563, 16.55341960407611168, 35.20724293864768839 ) ) ;
#5204 = CARTESIAN_POINT ( 'NONE',  ( 0.000000000000000000, 0.000000000000000000, -45.64921306006598201 ) ) ;
#5205 = CARTESIAN_POINT ( 'NONE',  ( -15.80617190586745835, -15.72974639402198527, 56.87390960531436690 ) ) ;
#5206 = CARTESIAN_POINT ( 'NONE',  ( 22.44159573604009239, 16.30477369853692693, 140.0750000027311728 ) ) ;
#5207 = CARTESIAN_POINT ( 'NONE',  ( -16.51473224551069308, -9.474510206698971260, 106.6655762719810383 ) ) ;
#5208 = CARTESIAN_POINT ( 'NONE',  ( 14.29746914071049879, -8.314922557960816363, 108.3322429386477097 ) ) ;
#5209 = CARTESIAN_POINT ( 'NONE',  ( -12.06949235617739369, -12.14591786802326823, 19.37609039468568639 ) ) ;
#5210 = CARTESIAN_POINT ( 'NONE',  ( -4.379528057220086978, -16.55341960407618274, 109.7927570613523613 ) ) ;
#5211 = ORIENTED_EDGE ( 'NONE', *, *, #139086, .T. ) ;
#5213 = CARTESIAN_POINT ( 'NONE',  ( 5.719274019375991003, -21.55341960407610458, 102.7072429386476955 ) ) ;
#5212 = CARTESIAN_POINT ( 'NONE',  ( 19.02544592524343514, -5.153800228976328945, 103.5405762719809957 ) ) ;
#5215 = CARTESIAN_POINT ( 'NONE',  ( -13.97604488694527625, -13.89961937509977652, 111.8739096053143243 ) ) ;
#5214 = CARTESIAN_POINT ( 'NONE',  ( -16.53943276465976808, 0.05219959533911058130, 31.24890960531435979 ) ) ;
#5216 = CARTESIAN_POINT ( 'NONE',  ( 13.97604488694548053, -13.89961937509957401, 90.62609039468567573 ) ) ;
#5217 = CARTESIAN_POINT ( 'NONE',  ( 5.719274019375673035, 21.55341960407619339, 102.2927570613523613 ) ) ;
#5218 = CARTESIAN_POINT ( 'NONE',  ( -4.379528057220328563, 16.55341960407611168, 30.20724293864769550 ) ) ;
#5219 = CARTESIAN_POINT ( 'NONE',  ( -18.67979575497178146, -10.72451020669898902, 86.66557627198102409 ) ) ;
#5220 = CARTESIAN_POINT ( 'NONE',  ( 21.55341960407610458, 5.719274019375980345, 48.95724293864770971 ) ) ;
#5221 = CARTESIAN_POINT ( 'NONE',  ( 16.46253265017160672, -9.564922557960803928, 63.33224293864769550 ) ) ;
#5222 = CARTESIAN_POINT ( 'NONE',  ( 0.05219959533910956823, 16.53943276465976808, 29.99890960531435979 ) ) ;
#5223 = CARTESIAN_POINT ( 'NONE',  ( 5.049401038298161559, -19.05341960407611168, 77.70724293864765286 ) ) ;
#5224 = CARTESIAN_POINT ( 'NONE',  ( 19.53037848336977333, -5.500000000000093259, 62.35532783611444074 ) ) ;
#5225 = CARTESIAN_POINT ( 'NONE',  ( -19.02544592524334988, -5.153800228976617603, 38.95942372801900433 ) ) ;
#5226 = CARTESIAN_POINT ( 'NONE',  ( -10.81492255796078084, -18.62759615963271287, 87.08224293864769550 ) ) ;
#5227 = CARTESIAN_POINT ( 'NONE',  ( 0.05219959533910956823, 16.53943276465976808, 84.99890960531436690 ) ) ;
#5228 = CARTESIAN_POINT ( 'NONE',  ( 10.72451020669871369, 18.67979575497193778, 42.08442372801901854 ) ) ;
#5229 = CARTESIAN_POINT ( 'NONE',  ( 17.14385361876520264, -23.59649016807271238, 141.5750000027312012 ) ) ;
#5230 = EDGE_CURVE ( 'NONE', #13916, #15707, #123918, .T. ) ;
#5231 = CARTESIAN_POINT ( 'NONE',  ( -14.34966873604972548, 8.224510206698743886, 108.3344237280190185 ) ) ;
#5232 = CARTESIAN_POINT ( 'NONE',  ( -0.05219959533909027116, -19.03943276465977164, 22.49890960531436690 ) ) ;
#5233 = CARTESIAN_POINT ( 'NONE',  ( -16.46253265017160317, 9.564922557960807481, 90.83224293864769550 ) ) ;
#5234 = LINE ( 'NONE', #97233, #43292 ) ;
#5235 = CARTESIAN_POINT ( 'NONE',  ( 5.000000000000001776, -120.0000000000000142, 0.0009999999999992653654 ) ) ;
#5236 = CARTESIAN_POINT ( 'NONE',  ( -16.52544592524342804, 4.483927247898546575, 41.04057627198103120 ) ) ;
#5237 = CARTESIAN_POINT ( 'NONE',  ( 10.72451020669871369, 18.67979575497193778, 77.08442372801901854 ) ) ;
#5239 = CARTESIAN_POINT ( 'NONE',  ( -4.379528057220086978, -16.55341960407618274, 69.79275706135234714 ) ) ;
#5238 = CARTESIAN_POINT ( 'NONE',  ( 3.660253528765602393, -6.551653823223149153, 8.410814283099844246 ) ) ;
#5240 = CARTESIAN_POINT ( 'NONE',  ( -16.46253265017160317, 9.564922557960807481, 40.83224293864769550 ) ) ;
#5241 = CARTESIAN_POINT ( 'NONE',  ( -13.89961937509977652, 13.97604488694528158, 55.62390960531434558 ) ) ;
#5242 = ORIENTED_EDGE ( 'NONE', *, *, #113163, .T. ) ;
#5243 = CARTESIAN_POINT ( 'NONE',  ( 5.823673210054444382, -21.52544592524334988, 110.2094237280190185 ) ) ;
#5244 = CARTESIAN_POINT ( 'NONE',  ( 14.34966873604972726, -8.224510206698740333, 65.83442372801900433 ) ) ;
#5245 = CARTESIAN_POINT ( 'NONE',  ( 5.823673210054444382, -21.52544592524334988, 95.20942372801903275 ) ) ;
#5246 = CARTESIAN_POINT ( 'NONE',  ( -13.89961937509977652, 13.97604488694528158, 115.6239096053143669 ) ) ;
#5247 = CARTESIAN_POINT ( 'NONE',  ( -5.153800228976607833, 19.02544592524334988, 102.7094237280189759 ) ) ;
#5248 = CARTESIAN_POINT ( 'NONE',  ( -5.823673210054431948, 21.52544592524334988, 72.70942372801901854 ) ) ;
#5249 = CARTESIAN_POINT ( 'NONE',  ( 16.52544592524335698, 4.483927247898782831, 31.45942372801901854 ) ) ;
#5250 = CARTESIAN_POINT ( 'NONE',  ( -10.81492255796078084, -18.62759615963271287, 92.08224293864769550 ) ) ;
#5251 = CARTESIAN_POINT ( 'NONE',  ( -16.46253265017146816, -9.564922557961047289, 99.16775706135233293 ) ) ;
#5252 = CARTESIAN_POINT ( 'NONE',  ( -19.03943276465977164, 0.05219959533909376836, 66.24890960531436690 ) ) ;
#5253 = CARTESIAN_POINT ( 'NONE',  ( 5.153800228976615827, -19.02544592524334988, 110.2094237280189901 ) ) ;
#5254 = CARTESIAN_POINT ( 'NONE',  ( 13.97604488694548053, -13.89961937509957401, 100.6260903946856615 ) ) ;
#5255 = CARTESIAN_POINT ( 'NONE',  ( -4.483927247898539470, -16.52544592524342804, 62.29057627198102409 ) ) ;
#5256 = CARTESIAN_POINT ( 'NONE',  ( 5.049401038297881783, 19.05341960407617563, 82.29275706135229029 ) ) ;
#5257 = CARTESIAN_POINT ( 'NONE',  ( -4.483927247898782831, 16.52544592524335698, 72.70942372801901854 ) ) ;
#5259 = CARTESIAN_POINT ( 'NONE',  ( -9.474510206698964154, 16.51473224551069663, 35.41557627198102409 ) ) ;
#5258 = CARTESIAN_POINT ( 'NONE',  ( 18.67979575497178502, 10.72451020669898547, 114.1655762719810383 ) ) ;
#5261 = EDGE_CURVE ( 'NONE', #139926, #193517, #14400, .T. ) ;
#5260 = CARTESIAN_POINT ( 'NONE',  ( -9.564922557960796823, -16.46253265017161027, 52.08224293864768839 ) ) ;
#5262 = CARTESIAN_POINT ( 'NONE',  ( -16.53943276465976808, -0.05219959533934237506, 78.75109039468568994 ) ) ;
#5263 = CARTESIAN_POINT ( 'NONE',  ( 1.784210473542230573E-15, -29.16686587814331588, 141.8750000027311842 ) ) ;
#5264 = CARTESIAN_POINT ( 'NONE',  ( 17.81289503416611453, -24.51734667627695785, 146.9500000054623570 ) ) ;
#5265 = ORIENTED_EDGE ( 'NONE', *, *, #135302, .F. ) ;
#5266 = CARTESIAN_POINT ( 'NONE',  ( -5.153800228976607833, 19.02544592524334988, 22.70942372801899012 ) ) ;
#5267 = FACE_OUTER_BOUND ( 'NONE', #180808, .T. ) ;
#5268 = ORIENTED_EDGE ( 'NONE', *, *, #8681, .F. ) ;
#5269 = CARTESIAN_POINT ( 'NONE',  ( 4.379528057220092307, 16.55341960407617563, 22.29275706135235069 ) ) ;
#5270 = B_SPLINE_CURVE_WITH_KNOTS ( 'NONE', 3,
 ( #154319, #121986, #64295, #157300, #139139, #155312 ),
 .UNSPECIFIED., .F., .F.,
 ( 4, 2, 4 ),
 ( 0.007228050697041574386, 0.007608510107495053409, 0.007988969517948531565 ),
 .UNSPECIFIED. ) ;
#5271 = CARTESIAN_POINT ( 'NONE',  ( -15.72974639402197994, 15.80617190586746368, 45.62390960531436690 ) ) ;
#5273 = CARTESIAN_POINT ( 'NONE',  ( -16.52544592524335698, -4.483927247898792601, 33.95942372801901143 ) ) ;
#5272 = CARTESIAN_POINT ( 'NONE',  ( -9.564922557961040184, 16.46253265017147172, 47.91775706135233293 ) ) ;
#5274 = CARTESIAN_POINT ( 'NONE',  ( 13.89961937509977652, -13.97604488694527269, 48.12390960531435979 ) ) ;
#5275 = CARTESIAN_POINT ( 'NONE',  ( -9.474510206698964154, 16.51473224551069663, 55.41557627198103120 ) ) ;
#5276 = CARTESIAN_POINT ( 'NONE',  ( 5.823673210054125526, 21.52544592524343514, 89.79057627198103830 ) ) ;
#5277 = CARTESIAN_POINT ( 'NONE',  ( -19.03943276465977164, 0.05219959533909376836, 106.2489096053143669 ) ) ;
#5278 = CARTESIAN_POINT ( 'NONE',  ( 19.05341960407611168, 5.049401038298154454, 48.95724293864768129 ) ) ;
#5279 = CARTESIAN_POINT ( 'NONE',  ( 22.44159573604009239, 16.30477369853692693, 148.5750000027312012 ) ) ;
#5280 = CARTESIAN_POINT ( 'NONE',  ( -5.153800228976607833, 19.02544592524334988, 92.70942372801901854 ) ) ;
#5281 = CARTESIAN_POINT ( 'NONE',  ( -4.483927247898539470, -16.52544592524342804, 62.29057627198102409 ) ) ;
#5282 = CARTESIAN_POINT ( 'NONE',  ( -9.474510206698720793, -16.51473224551083518, 19.58442372801899722 ) ) ;
#5283 = CARTESIAN_POINT ( 'NONE',  ( 5.823673210054125526, 21.52544592524343514, 99.79057627198103830 ) ) ;
#5284 = CARTESIAN_POINT ( 'NONE',  ( 18.62759615963255655, 10.81492255796105972, 81.66775706135236135 ) ) ;
#5285 = CARTESIAN_POINT ( 'NONE',  ( 16.46253265017160672, -9.564922557960803928, 23.33224293864769194 ) ) ;
#5286 = CARTESIAN_POINT ( 'NONE',  ( -18.62759615963255300, -10.81492255796106328, 84.16775706135234714 ) ) ;
#5288 = CARTESIAN_POINT ( 'NONE',  ( 18.62759615963255655, 10.81492255796105972, 76.66775706135234714 ) ) ;
#5287 = CARTESIAN_POINT ( 'NONE',  ( -14.34966873604972548, 8.224510206698743886, 113.3344237280190328 ) ) ;
#5289 = CARTESIAN_POINT ( 'NONE',  ( -5.049401038298153566, 19.05341960407611168, 65.20724293864765286 ) ) ;
#5290 = CARTESIAN_POINT ( 'NONE',  ( -10.81492255796105439, 18.62759615963255655, 37.91775706135235424 ) ) ;
#5291 = CARTESIAN_POINT ( 'NONE',  ( 16.46253265017160672, -9.564922557960803928, 78.33224293864769550 ) ) ;
#5292 = CARTESIAN_POINT ( 'NONE',  ( 8.224510206698953496, -14.34966873604960469, 92.91557627198103830 ) ) ;
#5293 = CARTESIAN_POINT ( 'NONE',  ( -12.06949235617756955, 12.14591786802309770, 60.62390960531437401 ) ) ;
#5294 = CARTESIAN_POINT ( 'NONE',  ( -10.81492255796078084, -18.62759615963271287, 77.08224293864769550 ) ) ;
#5295 = CARTESIAN_POINT ( 'NONE',  ( -13.89961937509977652, 13.97604488694528158, 60.62390960531436690 ) ) ;
#5296 = CARTESIAN_POINT ( 'NONE',  ( 10.81492255796078972, 18.62759615963270932, 89.58224293864768129 ) ) ;
#5297 = CARTESIAN_POINT ( 'NONE',  ( 16.51473224551083163, -9.474510206698727899, 60.83442372801900433 ) ) ;
#5299 = CARTESIAN_POINT ( 'NONE',  ( -8.314922557960811034, -14.29746914071050412, 77.08224293864769550 ) ) ;
#5298 = CARTESIAN_POINT ( 'NONE',  ( 17.50000000000000000, 5.499999999999997335, 36.70309617465829177 ) ) ;
#5300 = CARTESIAN_POINT ( 'NONE',  ( -5.719274019375978568, 21.55341960407610458, 50.20724293864769550 ) ) ;
#5301 = DIRECTION ( 'NONE',  ( -0.000000000000000000, 0.000000000000000000, 1.000000000000000000 ) ) ;
#5303 = CARTESIAN_POINT ( 'NONE',  ( -17.14385361876520975, 23.59649016807275856, 147.0750000027312012 ) ) ;
#5302 = CARTESIAN_POINT ( 'NONE',  ( 16.53943276465976808, 0.05219959533934440121, 96.25109039468568994 ) ) ;
#5304 = CARTESIAN_POINT ( 'NONE',  ( 16.46253265017146816, 9.564922557961045513, 96.66775706135233293 ) ) ;
#5305 = CARTESIAN_POINT ( 'NONE',  ( 14.29746914071049879, -8.314922557960816363, 68.33224293864769550 ) ) ;
#5306 = CARTESIAN_POINT ( 'NONE',  ( -17.50000000000001066, -5.499999999999943157, 86.28230962303568674 ) ) ;
#5307 = CARTESIAN_POINT ( 'NONE',  ( -5.049401038298153566, 19.05341960407611168, 55.20724293864769550 ) ) ;
#5308 = CARTESIAN_POINT ( 'NONE',  ( 14.29746914071049879, -8.314922557960816363, 58.33224293864768839 ) ) ;
#5309 = CARTESIAN_POINT ( 'NONE',  ( -13.89961937509977652, 13.97604488694528158, 105.6239096053143527 ) ) ;
#5311 = CARTESIAN_POINT ( 'NONE',  ( -19.02544592524342804, 5.153800228976336051, 66.04057627198103830 ) ) ;
#5310 = CARTESIAN_POINT ( 'NONE',  ( -13.97604488694547697, 13.89961937509957934, 73.12609039468568994 ) ) ;
#5312 = CARTESIAN_POINT ( 'NONE',  ( 13.89961937509977652, -13.97604488694527269, 88.12390960531438111 ) ) ;
#5313 = CARTESIAN_POINT ( 'NONE',  ( 19.05341960407611168, 5.049401038298154454, 78.95724293864769550 ) ) ;
#5314 = CARTESIAN_POINT ( 'NONE',  ( -5.823673210054116645, -21.52544592524344225, 67.29057627198103830 ) ) ;
#5315 = CARTESIAN_POINT ( 'NONE',  ( -12.14591786802326823, 12.06949235617739902, 63.12609039468568994 ) ) ;
#5316 = CARTESIAN_POINT ( 'NONE',  ( 2.044528755335677683, -7.220908937440018605, 1.589185716900141321 ) ) ;
#5317 = CARTESIAN_POINT ( 'NONE',  ( 9.564922557960805705, 16.46253265017160317, 44.58224293864769550 ) ) ;
#5318 = CARTESIAN_POINT ( 'NONE',  ( 5.823673210054125526, 21.52544592524343514, 49.79057627198102409 ) ) ;
#5319 = CARTESIAN_POINT ( 'NONE',  ( 9.474510206698729675, 16.51473224551082808, 92.08442372801900433 ) ) ;
#5321 = CARTESIAN_POINT ( 'NONE',  ( -10.72451020669870658, -18.67979575497194134, 29.58442372801901854 ) ) ;
#5320 = CARTESIAN_POINT ( 'NONE',  ( -16.52544592524342804, 4.483927247898546575, 31.04057627198102409 ) ) ;
#5322 = CARTESIAN_POINT ( 'NONE',  ( 19.02544592524334988, 5.153800228976608722, 31.45942372801900433 ) ) ;
#5324 = CARTESIAN_POINT ( 'NONE',  ( -0.05219959533934338120, 16.53943276465976808, 97.50109039468567573 ) ) ;
#5323 = CARTESIAN_POINT ( 'NONE',  ( -0.05219959533934338120, 16.53943276465976808, 62.50109039468568284 ) ) ;
#5325 = CARTESIAN_POINT ( 'NONE',  ( -23.29544513554941076, 16.92513159979227666, 148.0656553485623590 ) ) ;
#5326 = CARTESIAN_POINT ( 'NONE',  ( 4.483927247898790824, -16.52544592524335698, 80.20942372801901854 ) ) ;
#5328 = CARTESIAN_POINT ( 'NONE',  ( -12.06949235617739369, -12.14591786802326823, 29.37609039468568284 ) ) ;
#5327 = CARTESIAN_POINT ( 'NONE',  ( 21.52544592524344225, -5.823673210054117533, 23.54057627198102765 ) ) ;
#5329 = CARTESIAN_POINT ( 'NONE',  ( 19.05341960407611168, 5.049401038298154454, 43.95724293864769550 ) ) ;
#5330 = CARTESIAN_POINT ( 'NONE',  ( 9.564922557960805705, 16.46253265017160317, 49.58224293864770260 ) ) ;
#5331 = CARTESIAN_POINT ( 'NONE',  ( 19.05341960407611168, 5.049401038298154454, 63.95724293864769550 ) ) ;
#5332 = CARTESIAN_POINT ( 'NONE',  ( -0.05219959533937732626, 21.53943276465977519, 42.50109039468567573 ) ) ;
#5333 = CARTESIAN_POINT ( 'NONE',  ( -8.224510206698735004, -14.34966873604973081, 49.58442372801901143 ) ) ;
#5334 = CARTESIAN_POINT ( 'NONE',  ( -14.29746914071037622, -8.314922557961029526, 109.1677570613523613 ) ) ;
#5335 = CARTESIAN_POINT ( 'NONE',  ( -19.02544592524342804, 5.153800228976336051, 31.04057627198102409 ) ) ;
#5336 = CARTESIAN_POINT ( 'NONE',  ( -0.05219959533937732626, 21.53943276465977519, 107.5010903946856899 ) ) ;
#5337 = CARTESIAN_POINT ( 'NONE',  ( -13.89961937509957401, -13.97604488694547875, 109.3760903946856331 ) ) ;
#5338 = CARTESIAN_POINT ( 'NONE',  ( -19.03943276465977164, -0.05219959533935918106, 63.75109039468566863 ) ) ;
#5339 = CARTESIAN_POINT ( 'NONE',  ( 12.14591786802309770, 12.06949235617756955, 64.37390960531435269 ) ) ;
#5340 = CARTESIAN_POINT ( 'NONE',  ( 16.46253265017160672, -9.564922557960803928, 33.33224293864770260 ) ) ;
#5342 = CARTESIAN_POINT ( 'NONE',  ( 17.48853670773245028, -5.747243402303091386, 91.16671299749991420 ) ) ;
#5341 = CARTESIAN_POINT ( 'NONE',  ( -0.05219959533936034679, 19.03943276465977164, 67.50109039468566152 ) ) ;
#5343 = CARTESIAN_POINT ( 'NONE',  ( -10.72451020669870658, -18.67979575497194134, 79.58442372801903275 ) ) ;
#5344 = CARTESIAN_POINT ( 'NONE',  ( -4.379528057220086978, -16.55341960407618274, 34.79275706135235424 ) ) ;
#5345 = CARTESIAN_POINT ( 'NONE',  ( 18.22780087662119897, -5.500000000000096811, 58.51763182126894947 ) ) ;
#5346 = CARTESIAN_POINT ( 'NONE',  ( 10.81492255796078972, 18.62759615963270932, 39.58224293864769550 ) ) ;
#5347 = CARTESIAN_POINT ( 'NONE',  ( -0.05219959533934338120, 16.53943276465976808, 32.50109039468568284 ) ) ;
#5348 = CARTESIAN_POINT ( 'NONE',  ( 19.03943276465977164, -0.05219959533909143690, 23.74890960531435269 ) ) ;
#5349 = CARTESIAN_POINT ( 'NONE',  ( 13.97604488694548053, -13.89961937509957401, 30.62609039468566863 ) ) ;
#5350 = CARTESIAN_POINT ( 'NONE',  ( -11.74264578624799782, -36.14014761921581709, -7.599999999999999645 ) ) ;
#5351 = CARTESIAN_POINT ( 'NONE',  ( -19.03943276465977164, 0.05219959533909376836, 36.24890960531436690 ) ) ;
#5352 = CARTESIAN_POINT ( 'NONE',  ( 13.89961937509957579, 13.97604488694547520, 56.87609039468566863 ) ) ;
#5353 = CARTESIAN_POINT ( 'NONE',  ( -19.02544592524342804, 5.153800228976336051, 61.04057627198103120 ) ) ;
#5355 = CARTESIAN_POINT ( 'NONE',  ( -19.25176906914649422, -5.499999999999741540, 55.99927264242278824 ) ) ;
#5354 = CIRCLE ( 'NONE', #118409, 40.00000000000002132 ) ;
#5356 = CARTESIAN_POINT ( 'NONE',  ( -21.55341960407619339, 5.719274019375674811, 113.5427570613523756 ) ) ;
#5357 = CARTESIAN_POINT ( 'NONE',  ( 14.34966873604960469, 8.224510206698951720, 24.16557627198103120 ) ) ;
#5358 = CARTESIAN_POINT ( 'NONE',  ( -13.97604488694527625, -13.89961937509977652, 31.87390960531435979 ) ) ;
#5359 = CARTESIAN_POINT ( 'NONE',  ( -19.03943276465977164, 0.05219959533909376836, 96.24890960531436690 ) ) ;
#5360 = CARTESIAN_POINT ( 'NONE',  ( 21.52544592524334988, 5.823673210054432836, 71.45942372801901854 ) ) ;
#5361 = CARTESIAN_POINT ( 'NONE',  ( 16.51473224551069308, 9.474510206698969483, 44.16557627198103120 ) ) ;
#5362 = CARTESIAN_POINT ( 'NONE',  ( -15.72974639402176322, -15.80617190586768395, 64.37609039468568994 ) ) ;
#5364 = CARTESIAN_POINT ( 'NONE',  ( 10.72451020669898902, -18.67979575497178502, 22.91557627198102765 ) ) ;
#5363 = CARTESIAN_POINT ( 'NONE',  ( 13.97604488694548053, -13.89961937509957401, 95.62609039468563310 ) ) ;
#5365 = CARTESIAN_POINT ( 'NONE',  ( -16.46253265017160317, 9.564922557960807481, 30.83224293864769550 ) ) ;
#5366 = CARTESIAN_POINT ( 'NONE',  ( -18.67979575497178146, -10.72451020669898902, 106.6655762719810383 ) ) ;
#5367 = CARTESIAN_POINT ( 'NONE',  ( 19.03943276465977164, 0.05219959533936151252, 31.25109039468566863 ) ) ;
#5368 = CARTESIAN_POINT ( 'NONE',  ( 14.34966873604960469, 8.224510206698951720, 104.1655762719810241 ) ) ;
#5369 = CARTESIAN_POINT ( 'NONE',  ( -19.03943276465977164, 0.05219959533909376836, 61.24890960531436690 ) ) ;
#5370 = CARTESIAN_POINT ( 'NONE',  ( -5.153800228976607833, 19.02544592524334988, 107.7094237280189759 ) ) ;
#5371 = CARTESIAN_POINT ( 'NONE',  ( 4.379528057220339221, -16.55341960407611168, 72.70724293864769550 ) ) ;
#5372 = CARTESIAN_POINT ( 'NONE',  ( -5.049401038298153566, 19.05341960407611168, 115.2072429386477097 ) ) ;
#5373 = CARTESIAN_POINT ( 'NONE',  ( -13.97604488694547697, 13.89961937509957934, 83.12609039468564731 ) ) ;
#5374 = CARTESIAN_POINT ( 'NONE',  ( 21.52544592524344225, -5.823673210054117533, 88.54057627198103830 ) ) ;
#5375 = CARTESIAN_POINT ( 'NONE',  ( 21.52544592524334988, 5.823673210054432836, 41.45942372801901143 ) ) ;
#5376 = CARTESIAN_POINT ( 'NONE',  ( -8.224510206698735004, -14.34966873604973081, 49.58442372801901143 ) ) ;
#5378 = CARTESIAN_POINT ( 'NONE',  ( 5.823673210054444382, -21.52544592524334988, 55.20942372801902565 ) ) ;
#5377 = CARTESIAN_POINT ( 'NONE',  ( 4.483927247898790824, -16.52544592524335698, 50.20942372801901854 ) ) ;
#5379 = CARTESIAN_POINT ( 'NONE',  ( -21.53943276465977519, 0.05219959533907696930, 61.24890960531435979 ) ) ;
#5380 =( BOUNDED_CURVE ( )  B_SPLINE_CURVE ( 2, ( #51492, #21152, #144489, #25177, #86819, #148506, #52481, #66656, #115160, #99978, #113153, #114140, #37315 ),
 .UNSPECIFIED., .F., .F. ) 
 B_SPLINE_CURVE_WITH_KNOTS ( ( 3, 2, 2, 2, 2, 2, 3 ),
 ( 0.2393182215122932333, 0.2412280701754385970, 0.2456140350877192846, 0.2500000000000000000, 0.2543859649122807154, 0.2587719298245614308, 0.2607274583097970999 ),
 .UNSPECIFIED. ) 
 CURVE ( )  GEOMETRIC_REPRESENTATION_ITEM ( )  RATIONAL_B_SPLINE_CURVE ( ( 0.9832469066685285419, 0.9851625545550100060, 1.000000000000000000, 0.9659258262890683122, 1.000000000000000000, 0.9659258262890683122, 1.000000000000000000, 0.9659258262890683122, 1.000000000000000000, 0.9659258262890683122, 1.000000000000000000, 0.9848076720550081875, 0.9831626618144004848 ) ) 
 REPRESENTATION_ITEM ( '' )  );
#5381 = CARTESIAN_POINT ( 'NONE',  ( 9.564922557960805705, 16.46253265017160317, 49.58224293864770260 ) ) ;
#5382 = CARTESIAN_POINT ( 'NONE',  ( 23.48529157249600630, -32.32473071737749137, -7.049999994537626158 ) ) ;
#5383 = CARTESIAN_POINT ( 'NONE',  ( 14.34966873604972726, -8.224510206698740333, 75.83442372801900433 ) ) ;
#5384 = CARTESIAN_POINT ( 'NONE',  ( -5.823673210054116645, -21.52544592524344225, 102.2905762719810383 ) ) ;
#5385 = CARTESIAN_POINT ( 'NONE',  ( -12.14591786802309592, -12.06949235617757132, 56.87390960531436690 ) ) ;
#5386 = CARTESIAN_POINT ( 'NONE',  ( 14.29746914071037800, 8.314922557961029526, 66.66775706135234714 ) ) ;
#5387 = CARTESIAN_POINT ( 'NONE',  ( 19.02544592524334988, 5.153800228976608722, 96.45942372801897591 ) ) ;
#5388 = CARTESIAN_POINT ( 'NONE',  ( -10.72451020669898014, 18.67979575497178502, 100.4155762719810241 ) ) ;
#5389 = CARTESIAN_POINT ( 'NONE',  ( -8.224510206698948167, 14.34966873604960824, 45.41557627198103830 ) ) ;
#5390 = ORIENTED_EDGE ( 'NONE', *, *, #176309, .T. ) ;
#5391 = CARTESIAN_POINT ( 'NONE',  ( 18.22780087662123805, -5.499999999999976019, 93.51763182126896368 ) ) ;
#5392 = CARTESIAN_POINT ( 'NONE',  ( 18.62759615963271287, -10.81492255796078972, 78.33224293864770971 ) ) ;
#5393 = CARTESIAN_POINT ( 'NONE',  ( -8.224510206698948167, 14.34966873604960824, 25.41557627198103120 ) ) ;
#5394 = ORIENTED_EDGE ( 'NONE', *, *, #47533, .T. ) ;
#5395 = CARTESIAN_POINT ( 'NONE',  ( 4.500000000000000888, -130.0000000000000000, 12.49999999999999645 ) ) ;
#5396 = CARTESIAN_POINT ( 'NONE',  ( 5.719274019375991003, -21.55341960407610458, 107.7072429386476955 ) ) ;
#5397 = CARTESIAN_POINT ( 'NONE',  ( -18.67979575497178146, -10.72451020669898902, 111.6655762719810525 ) ) ;
#5398 = CARTESIAN_POINT ( 'NONE',  ( 8.224510206698953496, -14.34966873604960469, 42.91557627198103120 ) ) ;
#5399 = CARTESIAN_POINT ( 'NONE',  ( 12.14591786802327356, -12.06949235617739191, 50.62609039468568994 ) ) ;
#5400 = CARTESIAN_POINT ( 'NONE',  ( 19.02544592524343514, -5.153800228976328945, 53.54057627198102409 ) ) ;
#5401 = CARTESIAN_POINT ( 'NONE',  ( 0.05219959533909260263, 19.03943276465977164, 69.99890960531435269 ) ) ;
#5402 = ORIENTED_EDGE ( 'NONE', *, *, #181788, .T. ) ;
#5403 = CARTESIAN_POINT ( 'NONE',  ( 10.72451020669898902, -18.67979575497178502, 37.91557627198102409 ) ) ;
#5404 = CARTESIAN_POINT ( 'NONE',  ( -27.37900830011268027, -26.18142635053349210, -16.57177559434630609 ) ) ;
#5405 = CARTESIAN_POINT ( 'NONE',  ( -5.153800228976607833, 19.02544592524334988, 107.7094237280189759 ) ) ;
#5406 = CARTESIAN_POINT ( 'NONE',  ( -13.97604488694547697, 13.89961937509957934, 53.12609039468565442 ) ) ;
#5407 = CARTESIAN_POINT ( 'NONE',  ( 21.53943276465977519, -0.05219959533907433946, 103.7489096053143669 ) ) ;
#5408 = EDGE_CURVE ( 'NONE', #57684, #116458, #31935, .T. ) ;
#5409 = CARTESIAN_POINT ( 'NONE',  ( -8.314922557960811034, -14.29746914071050412, 32.08224293864769550 ) ) ;
#5410 = CARTESIAN_POINT ( 'NONE',  ( 19.02544592524343514, -5.153800228976328945, 78.54057627198099567 ) ) ;
#5411 = CARTESIAN_POINT ( 'NONE',  ( 21.52544592524344225, -5.823673210054117533, 43.54057627198103830 ) ) ;
#5413 = CARTESIAN_POINT ( 'NONE',  ( 8.224510206698742110, 14.34966873604972548, 22.08442372801901143 ) ) ;
#5412 = CARTESIAN_POINT ( 'NONE',  ( -0.05219959533907301413, -21.53943276465977519, 87.49890960531436690 ) ) ;
#5414 = CARTESIAN_POINT ( 'NONE',  ( -9.474510206698964154, 16.51473224551069663, 115.4155762719810241 ) ) ;
#5415 = CARTESIAN_POINT ( 'NONE',  ( 15.80617190586769283, -15.72974639402175789, 70.62609039468567573 ) ) ;
#5416 = CARTESIAN_POINT ( 'NONE',  ( 16.46253265017160672, -9.564922557960803928, 78.33224293864769550 ) ) ;
#5417 = CARTESIAN_POINT ( 'NONE',  ( 5.153800228976335163, 19.02544592524342804, 24.79057627198102765 ) ) ;
#5418 = CARTESIAN_POINT ( 'NONE',  ( 0.05219959533909260263, 19.03943276465977164, 79.99890960531436690 ) ) ;
#5419 = CARTESIAN_POINT ( 'NONE',  ( 8.314922557960818139, 14.29746914071049879, 94.58224293864769550 ) ) ;
#5420 = ORIENTED_EDGE ( 'NONE', *, *, #58231, .F. ) ;
#5421 = CARTESIAN_POINT ( 'NONE',  ( -19.05341960407617563, 5.049401038297882671, 103.5427570613523329 ) ) ;
#5422 = DIRECTION ( 'NONE',  ( 0.000000000000000000, 0.000000000000000000, 1.000000000000000000 ) ) ;
#5423 = CARTESIAN_POINT ( 'NONE',  ( 16.46253265017160672, -9.564922557960803928, 78.33224293864769550 ) ) ;
#5425 = CARTESIAN_POINT ( 'NONE',  ( -16.46253265017160317, 9.564922557960807481, 110.8322429386476955 ) ) ;
#5424 = CARTESIAN_POINT ( 'NONE',  ( 10.72451020669871369, 18.67979575497193778, 82.08442372801901854 ) ) ;
#5426 = CARTESIAN_POINT ( 'NONE',  ( -16.55341960407617563, 4.379528057220093196, 78.54275706135236135 ) ) ;
#5427 = CARTESIAN_POINT ( 'NONE',  ( -17.26172910966779384, -6.454744622555833367, 74.19353091350777163 ) ) ;
#5428 = CARTESIAN_POINT ( 'NONE',  ( -5.153800228976607833, 19.02544592524334988, 52.70942372801900433 ) ) ;
#5429 = CARTESIAN_POINT ( 'NONE',  ( -0.05219959533936034679, 19.03943276465977164, 22.50109039468566152 ) ) ;
#5430 = CARTESIAN_POINT ( 'NONE',  ( 5.170161995863685966, 6.863278975470355370, -64.06628402976478753 ) ) ;
#5431 = CARTESIAN_POINT ( 'NONE',  ( -9.656827144875922642, -71.74905178543390605, -25.00000000000000000 ) ) ;
#5432 = CARTESIAN_POINT ( 'NONE',  ( 11.40812507854754365, 35.11059874428196537, -3.724999997268813701 ) ) ;
#5433 = CARTESIAN_POINT ( 'NONE',  ( 12.06949235617757843, -12.14591786802309237, 28.12390960531435979 ) ) ;
#5434 = CARTESIAN_POINT ( 'NONE',  ( -4.718528363748727840E-30, -105.0000000000000000, -13.00000000000000000 ) ) ;
#5435 = CARTESIAN_POINT ( 'NONE',  ( -4.483927247898782831, 16.52544592524335698, 112.7094237280190328 ) ) ;
#5436 = DIRECTION ( 'NONE',  ( 1.000000000000000000, 0.000000000000000000, 0.000000000000000000 ) ) ;
#5437 = CARTESIAN_POINT ( 'NONE',  ( -0.05219959533934338120, 16.53943276465976808, 87.50109039468568994 ) ) ;
#5438 = CARTESIAN_POINT ( 'NONE',  ( 15.80617190586769283, -15.72974639402175789, 100.6260903946857184 ) ) ;
#5439 = CARTESIAN_POINT ( 'NONE',  ( 13.89961937509957401, 13.97604488694547697, 101.8760903946856331 ) ) ;
#5440 = CARTESIAN_POINT ( 'NONE',  ( 21.55341960407619695, -5.719274019375665929, 61.04275706135234714 ) ) ;
#5441 = CARTESIAN_POINT ( 'NONE',  ( 13.89961937509957401, 13.97604488694547697, 41.87609039468566152 ) ) ;
#5442 = CARTESIAN_POINT ( 'NONE',  ( 16.46253265017160672, -9.564922557960803928, 83.33224293864768129 ) ) ;
#5443 = CARTESIAN_POINT ( 'NONE',  ( -13.97604488694527625, -13.89961937509977652, 51.87390960531436690 ) ) ;
#5444 = CARTESIAN_POINT ( 'NONE',  ( -10.96632750431057879, -38.47313893329367573, -12.60384275245237617 ) ) ;
#5445 = CARTESIAN_POINT ( 'NONE',  ( -0.05219959533907301413, -21.53943276465977519, 92.49890960531436690 ) ) ;
#5446 = AXIS2_PLACEMENT_3D ( 'NONE', #181467, #58113, #41956 ) ;
#5447 = CARTESIAN_POINT ( 'NONE',  ( 18.67979575497178502, 10.72451020669898547, 49.16557627198102409 ) ) ;
#5448 = CARTESIAN_POINT ( 'NONE',  ( 13.97604488694527802, 13.89961937509977652, 44.37390960531435269 ) ) ;
#5449 = CARTESIAN_POINT ( 'NONE',  ( 14.29746914071037800, 8.314922557961029526, 66.66775706135234714 ) ) ;
#5450 = UNCERTAINTY_MEASURE_WITH_UNIT (LENGTH_MEASURE( 1.000000000000000082E-05 ), #162691, 'distance_accuracy_value', 'NONE');
#5451 = ORIENTED_EDGE ( 'NONE', *, *, #13659, .F. ) ;
#5452 = CARTESIAN_POINT ( 'NONE',  ( -21.53943276465977519, -0.05219959533937600094, 38.75109039468567573 ) ) ;
#5454 = CARTESIAN_POINT ( 'NONE',  ( -36.91746825000001309, -11.99521256947794789, -4.524999997268813523 ) ) ;
#5453 = CARTESIAN_POINT ( 'NONE',  ( -16.52544592524342804, 4.483927247898546575, 81.04057627198102409 ) ) ;
#5455 = CARTESIAN_POINT ( 'NONE',  ( -4.483927247898782831, 16.52544592524335698, 42.70942372801901854 ) ) ;
#5456 = CARTESIAN_POINT ( 'NONE',  ( 8.224510206698953496, -14.34966873604960469, 107.9155762719810241 ) ) ;
#5457 = CARTESIAN_POINT ( 'NONE',  ( 19.02544592524334988, 5.153800228976608722, 51.45942372801900433 ) ) ;
#5458 = VECTOR ( 'NONE', #88989, 1000.000000000000000 ) ;
#5459 = CARTESIAN_POINT ( 'NONE',  ( -16.52544592524342804, 4.483927247898546575, 71.04057627198103830 ) ) ;
#5460 = CARTESIAN_POINT ( 'NONE',  ( 21.52544592524334988, 5.823673210054432836, 36.45942372801901143 ) ) ;
#5462 = CARTESIAN_POINT ( 'NONE',  ( 5.823673210054125526, 21.52544592524343514, 84.79057627198102409 ) ) ;
#5461 = CARTESIAN_POINT ( 'NONE',  ( 19.05341960407611168, 5.049401038298154454, 28.95724293864769550 ) ) ;
#5463 = CARTESIAN_POINT ( 'NONE',  ( 0.05219959533909260263, 19.03943276465977164, 99.99890960531436690 ) ) ;
#5464 = CARTESIAN_POINT ( 'NONE',  ( 14.29746914071049879, -8.314922557960816363, 68.33224293864769550 ) ) ;
#5465 = CARTESIAN_POINT ( 'NONE',  ( 18.40487137061644418, -35.48337831122941566, -26.72115582345234941 ) ) ;
#5466 = CARTESIAN_POINT ( 'NONE',  ( 11.40812507854755253, -35.11059874428192273, -2.024999997268813079 ) ) ;
#5467 = CARTESIAN_POINT ( 'NONE',  ( 13.89961937509957401, 13.97604488694547697, 86.87609039468567573 ) ) ;
#5468 = CARTESIAN_POINT ( 'NONE',  ( -21.53943276465977519, -0.05219959533937600094, 28.75109039468567929 ) ) ;
#5469 = CARTESIAN_POINT ( 'NONE',  ( -19.02544592524342804, 5.153800228976336051, 66.04057627198103830 ) ) ;
#5470 = CARTESIAN_POINT ( 'NONE',  ( 0.05219959533936267826, -19.03943276465977164, 60.00109039468566863 ) ) ;
#5471 = CARTESIAN_POINT ( 'NONE',  ( 9.564922557960805705, 16.46253265017160317, 44.58224293864769550 ) ) ;
#5472 = CARTESIAN_POINT ( 'NONE',  ( -8.224510206698948167, 14.34966873604960824, 60.41557627198102409 ) ) ;
#5473 = CARTESIAN_POINT ( 'NONE',  ( -8.224510206698948167, 14.34966873604960824, 55.41557627198102409 ) ) ;
#5474 = CARTESIAN_POINT ( 'NONE',  ( 13.89961937509977652, -13.97604488694527269, 73.12390960531436690 ) ) ;
#5475 = CARTESIAN_POINT ( 'NONE',  ( 18.67979575497178502, 10.72451020669898547, 89.16557627198102409 ) ) ;
#5476 = CARTESIAN_POINT ( 'NONE',  ( 13.89961937509977652, -13.97604488694527269, 68.12390960531436690 ) ) ;
#5477 = CARTESIAN_POINT ( 'NONE',  ( -18.62759615963270932, 10.81492255796079327, 85.83224293864768129 ) ) ;
#5478 = CARTESIAN_POINT ( 'NONE',  ( -0.05219959533937732626, 21.53943276465977519, 112.5010903946857042 ) ) ;
#5481 = CARTESIAN_POINT ( 'NONE',  ( -0.05219959533910754901, -16.53943276465976808, 97.49890960531436690 ) ) ;
#5480 = CARTESIAN_POINT ( 'NONE',  ( -0.05219959533910754901, -16.53943276465976808, 22.49890960531436335 ) ) ;
#5479 = CARTESIAN_POINT ( 'NONE',  ( -17.49999999999999645, -7.500000000000000888, 120.0000000000000142 ) ) ;
#5482 = CARTESIAN_POINT ( 'NONE',  ( 13.89961937509957401, 13.97604488694547697, 91.87609039468567573 ) ) ;
#5483 = EDGE_LOOP ( 'NONE', ( #52442, #128612, #179339 ) ) ;
#5484 = CARTESIAN_POINT ( 'NONE',  ( 21.52544592524334988, 5.823673210054432836, 21.45942372801901499 ) ) ;
#5485 = CARTESIAN_POINT ( 'NONE',  ( 9.564922557961047289, -16.46253265017146816, 50.41775706135233293 ) ) ;
#5486 = CARTESIAN_POINT ( 'NONE',  ( -14.34966873604972548, 8.224510206698743886, 108.3344237280190185 ) ) ;
#5487 = CARTESIAN_POINT ( 'NONE',  ( 16.46253265017146816, 9.564922557961045513, 46.66775706135233293 ) ) ;
#5488 = CARTESIAN_POINT ( 'NONE',  ( 5.049401038298161559, -19.05341960407611168, 107.7072429386476955 ) ) ;
#5489 = CARTESIAN_POINT ( 'NONE',  ( -8.314922557960811034, -14.29746914071050412, 62.08224293864769550 ) ) ;
#5490 = CARTESIAN_POINT ( 'NONE',  ( -19.53037848336980886, 5.499999999999898748, 49.85532783611443364 ) ) ;
#5491 = CARTESIAN_POINT ( 'NONE',  ( 13.89961937509977652, -13.97604488694527269, 33.12390960531434558 ) ) ;
#5492 = CARTESIAN_POINT ( 'NONE',  ( 21.52544592524334988, 5.823673210054432836, 111.4594237280190328 ) ) ;
#5493 = CARTESIAN_POINT ( 'NONE',  ( -4.379528057220086978, -16.55341960407618274, 79.79275706135236135 ) ) ;
#5494 = CARTESIAN_POINT ( 'NONE',  ( -21.53943276465977519, -0.05219959533937600094, 43.75109039468568284 ) ) ;
#5495 = CARTESIAN_POINT ( 'NONE',  ( -14.34966873604972548, 8.224510206698743886, 43.33442372801901143 ) ) ;
#5496 = CARTESIAN_POINT ( 'NONE',  ( -9.564922557960796823, -16.46253265017161027, 102.0822429386477097 ) ) ;
#5497 = CARTESIAN_POINT ( 'NONE',  ( 0.05219959533909260263, 19.03943276465977164, 54.99890960531435979 ) ) ;
#5498 = CARTESIAN_POINT ( 'NONE',  ( -9.474510206698964154, 16.51473224551069663, 70.41557627198102409 ) ) ;
#5499 = AXIS2_PLACEMENT_3D ( 'NONE', #65195, #36836, #37853 ) ;
#5500 = CARTESIAN_POINT ( 'NONE',  ( -12.06949235617739369, -12.14591786802326823, 49.37609039468569705 ) ) ;
#5501 = CARTESIAN_POINT ( 'NONE',  ( 16.55341960407611168, 4.379528057220329451, 103.9572429386476813 ) ) ;
#5502 = CARTESIAN_POINT ( 'NONE',  ( 12.14591786802309770, 12.06949235617756955, 24.37390960531435979 ) ) ;
#5503 = CARTESIAN_POINT ( 'NONE',  ( 3.181980515339782212, 29.99999999999996803, 1.110912703473986074 ) ) ;
#5506 = CARTESIAN_POINT ( 'NONE',  ( -9.474510206698964154, 16.51473224551069663, 65.41557627198102409 ) ) ;
#5505 = CARTESIAN_POINT ( 'NONE',  ( 16.46253265017160672, -9.564922557960803928, 88.33224293864769550 ) ) ;
#5504 = CARTESIAN_POINT ( 'NONE',  ( -15.72974639402176322, -15.80617190586768395, 54.37609039468568994 ) ) ;
#5508 = EDGE_CURVE ( 'NONE', #66459, #145335, #32930, .T. ) ;
#5507 = CARTESIAN_POINT ( 'NONE',  ( -5.153800228976328057, -19.02544592524343514, 97.29057627198099567 ) ) ;
#5509 = CARTESIAN_POINT ( 'NONE',  ( 14.29746914071049879, -8.314922557960816363, 48.33224293864770260 ) ) ;
#5510 = CARTESIAN_POINT ( 'NONE',  ( 4.379528057220339221, -16.55341960407611168, 22.70724293864769194 ) ) ;
#5511 = CARTESIAN_POINT ( 'NONE',  ( -16.55341960407611168, -4.379528057220339221, 36.45724293864768839 ) ) ;
#5512 = VERTEX_POINT ( 'NONE', #91590 ) ;
#5513 = DIRECTION ( 'NONE',  ( 0.7071067811865414665, -0.7071067811865536790, -0.000000000000000000 ) ) ;
#5514 = CARTESIAN_POINT ( 'NONE',  ( -5.153800228976328057, -19.02544592524343514, 67.29057627198102409 ) ) ;
#5515 = CARTESIAN_POINT ( 'NONE',  ( 19.05341960407617918, -5.049401038297876454, 36.04275706135234003 ) ) ;
#5516 = CARTESIAN_POINT ( 'NONE',  ( 36.91746825000000598, -11.99521256947793546, -10.22499999726881548 ) ) ;
#5517 = CARTESIAN_POINT ( 'NONE',  ( -5.153800228976328057, -19.02544592524343514, 67.29057627198102409 ) ) ;
#5519 = CARTESIAN_POINT ( 'NONE',  ( -8.314922557961024197, 14.29746914071037800, 62.91775706135236135 ) ) ;
#5518 = CARTESIAN_POINT ( 'NONE',  ( -16.51473224551082808, 9.474510206698731452, 88.33442372801900433 ) ) ;
#5520 = CARTESIAN_POINT ( 'NONE',  ( -23.58955696227030074, 7.613471476246056469, 172.7063021553927911 ) ) ;
#5521 = CARTESIAN_POINT ( 'NONE',  ( -19.03943276465977164, 0.05219959533909376836, 96.24890960531436690 ) ) ;
#5522 = CARTESIAN_POINT ( 'NONE',  ( 18.67979575497194134, -10.72451020669871369, 25.83442372801901499 ) ) ;
#5523 = CARTESIAN_POINT ( 'NONE',  ( 16.46253265017146816, 9.564922557961045513, 86.66775706135233293 ) ) ;
#5525 = CARTESIAN_POINT ( 'NONE',  ( -9.564922557960796823, -16.46253265017161027, 42.08224293864769550 ) ) ;
#5524 = CARTESIAN_POINT ( 'NONE',  ( 19.05341960407611168, 5.049401038298154454, 113.9572429386477097 ) ) ;
#5526 = CARTESIAN_POINT ( 'NONE',  ( -13.97604488694527625, -13.89961937509977652, 86.87390960531436690 ) ) ;
#5528 = CARTESIAN_POINT ( 'NONE',  ( -9.474510206698964154, 16.51473224551069663, 50.41557627198102409 ) ) ;
#5527 = CARTESIAN_POINT ( 'NONE',  ( 12.06949235617757843, -12.14591786802309237, 53.12390960531436690 ) ) ;
#5529 = CARTESIAN_POINT ( 'NONE',  ( -5.049401038297874678, -19.05341960407617918, 69.79275706135233293 ) ) ;
#5530 = ORIENTED_EDGE ( 'NONE', *, *, #127855, .T. ) ;
#5531 = CARTESIAN_POINT ( 'NONE',  ( 12.06949235617757843, -12.14591786802309237, 83.12390960531436690 ) ) ;
#5532 = CARTESIAN_POINT ( 'NONE',  ( -9.474510206698720793, -16.51473224551083518, 24.58442372801900078 ) ) ;
#5533 = CARTESIAN_POINT ( 'NONE',  ( -9.564922557960796823, -16.46253265017161027, 72.08224293864770971 ) ) ;
#5534 = CARTESIAN_POINT ( 'NONE',  ( -0.05219959533907301413, -21.53943276465977519, 57.49890960531435979 ) ) ;
#5536 = CARTESIAN_POINT ( 'NONE',  ( -9.474510206698720793, -16.51473224551083518, 24.58442372801900078 ) ) ;
#5535 = CARTESIAN_POINT ( 'NONE',  ( -8.314922557960811034, -14.29746914071050412, 72.08224293864769550 ) ) ;
#5537 = CARTESIAN_POINT ( 'NONE',  ( 0.05219959533909260263, 19.03943276465977164, 109.9989096053143669 ) ) ;
#5538 = CARTESIAN_POINT ( 'NONE',  ( 10.72451020669898902, -18.67979575497178502, 27.91557627198103830 ) ) ;
#5539 = CARTESIAN_POINT ( 'NONE',  ( 19.02544592524343514, -5.153800228976328945, 48.54057627198103120 ) ) ;
#5540 = CARTESIAN_POINT ( 'NONE',  ( 19.02544592524343514, -5.153800228976328945, 38.54057627198103120 ) ) ;
#5541 = CARTESIAN_POINT ( 'NONE',  ( -12.06949235617756955, 12.14591786802309770, 95.62390960531436690 ) ) ;
#5542 = CARTESIAN_POINT ( 'NONE',  ( -18.67979575497178146, -10.72451020669898902, 106.6655762719810383 ) ) ;
#5543 = CARTESIAN_POINT ( 'NONE',  ( -19.03943276465977164, 0.05219959533909376836, 111.2489096053143669 ) ) ;
#5544 = CARTESIAN_POINT ( 'NONE',  ( -15.80617190586768217, 15.72974639402176855, 23.12609039468567573 ) ) ;
#5545 = CARTESIAN_POINT ( 'NONE',  ( -5.049401038298153566, 19.05341960407611168, 105.2072429386476671 ) ) ;
#5546 = CARTESIAN_POINT ( 'NONE',  ( 9.474510206698971260, -16.51473224551069308, 22.91557627198102765 ) ) ;
#5547 = CARTESIAN_POINT ( 'NONE',  ( 10.72451020669871369, 18.67979575497193778, 72.08442372801899012 ) ) ;
#5548 = CARTESIAN_POINT ( 'NONE',  ( 5.719274019375991003, -21.55341960407610458, 92.70724293864770971 ) ) ;
#5549 = CARTESIAN_POINT ( 'NONE',  ( 17.50000000000000000, -5.500000000000000888, 33.29690382534174375 ) ) ;
#5550 = CARTESIAN_POINT ( 'NONE',  ( -5.153800228976328057, -19.02544592524343514, 52.29057627198101699 ) ) ;
#5551 = CARTESIAN_POINT ( 'NONE',  ( 23.48529157249600630, -32.32473071737748427, -1.299999999999999822 ) ) ;
#5552 = CARTESIAN_POINT ( 'NONE',  ( 8.314922557961029526, -14.29746914071037800, 50.41775706135235424 ) ) ;
#5553 = CARTESIAN_POINT ( 'NONE',  ( -4.379528057220328563, 16.55341960407611168, 110.2072429386477239 ) ) ;
#5554 = CARTESIAN_POINT ( 'NONE',  ( 33.67956615508441587, -5.223713096473153072, 96.75862529643663379 ) ) ;
#5555 = CARTESIAN_POINT ( 'NONE',  ( -9.564922557960796823, -16.46253265017161027, 57.08224293864769550 ) ) ;
#5556 = CARTESIAN_POINT ( 'NONE',  ( -14.34966873604960291, -8.224510206698953496, 91.66557627198103830 ) ) ;
#5557 = CARTESIAN_POINT ( 'NONE',  ( 15.72974639402199770, -15.80617190586745480, 43.12390960531435269 ) ) ;
#5558 = CARTESIAN_POINT ( 'NONE',  ( 14.29746914071049879, -8.314922557960816363, 68.33224293864769550 ) ) ;
#5559 = CARTESIAN_POINT ( 'NONE',  ( -0.05219959533934338120, 16.53943276465976808, 22.50109039468567573 ) ) ;
#5560 = CARTESIAN_POINT ( 'NONE',  ( 15.72974639402176855, 15.80617190586768217, 81.87609039468568994 ) ) ;
#5561 = CARTESIAN_POINT ( 'NONE',  ( 17.40861289039004944, -6.110651285853252901, 76.12767529172570846 ) ) ;
#5562 = CARTESIAN_POINT ( 'NONE',  ( -0.05219959533934338120, 16.53943276465976808, 97.50109039468567573 ) ) ;
#5563 = CARTESIAN_POINT ( 'NONE',  ( -8.314922557960811034, -14.29746914071050412, 37.08224293864768129 ) ) ;
#5564 = CARTESIAN_POINT ( 'NONE',  ( 19.03943276465977164, -0.05219959533909143690, 38.74890960531436690 ) ) ;
#5565 = CARTESIAN_POINT ( 'NONE',  ( -16.51473224551069308, -9.474510206698971260, 86.66557627198102409 ) ) ;
#5566 = CARTESIAN_POINT ( 'NONE',  ( 10.81492255796078972, 18.62759615963270932, 89.58224293864768129 ) ) ;
#5567 = CARTESIAN_POINT ( 'NONE',  ( 8.314922557961029526, -14.29746914071037800, 45.41775706135234003 ) ) ;
#5569 = CARTESIAN_POINT ( 'NONE',  ( 18.67979575497194134, -10.72451020669871369, 80.83442372801901854 ) ) ;
#5568 = CARTESIAN_POINT ( 'NONE',  ( 4.483927247898545687, 16.52544592524342804, 69.79057627198102409 ) ) ;
#5570 = CARTESIAN_POINT ( 'NONE',  ( -12.06949235617739369, -12.14591786802326823, 94.37609039468568994 ) ) ;
#5571 = CARTESIAN_POINT ( 'NONE',  ( 17.31728774477213051, -6.344390552233675429, 48.31906651689307353 ) ) ;
#5572 = CARTESIAN_POINT ( 'NONE',  ( -19.01529144963331674, -5.500000000000166978, 66.23431955728440812 ) ) ;
#5573 = CARTESIAN_POINT ( 'NONE',  ( 16.53943276465976808, -0.05219959533910856209, 33.74890960531436690 ) ) ;
#5574 = CARTESIAN_POINT ( 'NONE',  ( -14.29746914071037622, -8.314922557961029526, 69.16775706135234714 ) ) ;
#5575 = CARTESIAN_POINT ( 'NONE',  ( 5.049401038298161559, -19.05341960407611168, 82.70724293864770971 ) ) ;
#5576 = CARTESIAN_POINT ( 'NONE',  ( -19.02544592524342804, 5.153800228976336051, 96.04057627198103830 ) ) ;
#5577 = CARTESIAN_POINT ( 'NONE',  ( 10.72451020669871369, 18.67979575497193778, 87.08442372801901854 ) ) ;
#5578 = CARTESIAN_POINT ( 'NONE',  ( 8.224510206698742110, 14.34966873604972548, 87.08442372801901854 ) ) ;
#5579 = CARTESIAN_POINT ( 'NONE',  ( -8.224510206698948167, 14.34966873604960824, 55.41557627198102409 ) ) ;
#5580 = CARTESIAN_POINT ( 'NONE',  ( 13.89961937509977652, -13.97604488694527269, 63.12390960531435979 ) ) ;
#5581 = ORIENTED_EDGE ( 'NONE', *, *, #50316, .F. ) ;
#5582 = CARTESIAN_POINT ( 'NONE',  ( 19.03943276465977164, 0.05219959533936151252, 106.2510903946856615 ) ) ;
#5583 = CARTESIAN_POINT ( 'NONE',  ( -4.379528057220328563, 16.55341960407611168, 110.2072429386477239 ) ) ;
#5584 = CARTESIAN_POINT ( 'NONE',  ( -0.05219959533909027116, -19.03943276465977164, 72.49890960531435269 ) ) ;
#5586 = CARTESIAN_POINT ( 'NONE',  ( -29.86685920354755552, 21.69954338932564397, -8.824999997268815122 ) ) ;
#5585 = CARTESIAN_POINT ( 'NONE',  ( -16.52544592524335698, -4.483927247898792601, 18.95942372801901143 ) ) ;
#5587 = CARTESIAN_POINT ( 'NONE',  ( 5.153800228976615827, -19.02544592524334988, 20.20942372801899722 ) ) ;
#5588 = CARTESIAN_POINT ( 'NONE',  ( -12.06949235617739369, -12.14591786802326823, 74.37609039468568994 ) ) ;
#5589 = CARTESIAN_POINT ( 'NONE',  ( 19.02544592524334988, 5.153800228976608722, 106.4594237280190185 ) ) ;
#5590 = CARTESIAN_POINT ( 'NONE',  ( -8.224510206698948167, 14.34966873604960824, 110.4155762719810383 ) ) ;
#5591 = CARTESIAN_POINT ( 'NONE',  ( 0.05219959533934541429, -16.53943276465976808, 60.00109039468568284 ) ) ;
#5592 = CARTESIAN_POINT ( 'NONE',  ( 4.379528057220092307, 16.55341960407617563, 52.29275706135236135 ) ) ;
#5593 = CARTESIAN_POINT ( 'NONE',  ( -5.153800228976328057, -19.02544592524343514, 22.29057627198102765 ) ) ;
#5594 = CARTESIAN_POINT ( 'NONE',  ( -16.46253265017146816, -9.564922557961047289, 64.16775706135233293 ) ) ;
#5595 = CARTESIAN_POINT ( 'NONE',  ( -15.72974639402176322, -15.80617190586768395, 109.3760903946857042 ) ) ;
#5596 = CARTESIAN_POINT ( 'NONE',  ( 19.05341960407611168, 5.049401038298154454, 33.95724293864769550 ) ) ;
#5597 = CARTESIAN_POINT ( 'NONE',  ( 0.05219959533909260263, 19.03943276465977164, 84.99890960531436690 ) ) ;
#5598 = CARTESIAN_POINT ( 'NONE',  ( 8.314922557960818139, 14.29746914071049879, 74.58224293864768129 ) ) ;
#5599 = AXIS2_PLACEMENT_3D ( 'NONE', #147019, #83327, #192528 ) ;
#5600 = CARTESIAN_POINT ( 'NONE',  ( 5.153800228976615827, -19.02544592524334988, 35.20942372801899722 ) ) ;
#5601 = CARTESIAN_POINT ( 'NONE',  ( -5.823673210054116645, -21.52544592524344225, 32.29057627198102409 ) ) ;
#5602 = CARTESIAN_POINT ( 'NONE',  ( -16.46253265017146816, -9.564922557961047289, 19.16775706135233293 ) ) ;
#5603 = CARTESIAN_POINT ( 'NONE',  ( -19.03943276465977164, 0.05219959533909376836, 86.24890960531436690 ) ) ;
#5604 = CARTESIAN_POINT ( 'NONE',  ( -0.05219959533937732626, 21.53943276465977519, 112.5010903946857042 ) ) ;
#5605 = CARTESIAN_POINT ( 'NONE',  ( -0.05219959533907301413, -21.53943276465977519, 62.49890960531436690 ) ) ;
#5606 = CARTESIAN_POINT ( 'NONE',  ( -16.46253265017160317, 9.564922557960807481, 90.83224293864769550 ) ) ;
#5607 = CARTESIAN_POINT ( 'NONE',  ( -19.03943276465977164, -0.05219959533935918106, 78.75109039468567573 ) ) ;
#5608 = CARTESIAN_POINT ( 'NONE',  ( 19.03943276465977164, -0.05219959533909143690, 98.74890960531436690 ) ) ;
#5609 = EDGE_CURVE ( 'NONE', #62967, #140310, #11253, .T. ) ;
#5610 = CARTESIAN_POINT ( 'NONE',  ( 9.474510206698729675, 16.51473224551082808, 102.0844237280190043 ) ) ;
#5611 = CARTESIAN_POINT ( 'NONE',  ( 8.224510206698742110, 14.34966873604972548, 57.08442372801901854 ) ) ;
#5612 = CARTESIAN_POINT ( 'NONE',  ( -16.53943276465976808, 0.05219959533911058130, 111.2489096053143669 ) ) ;
#5613 = CARTESIAN_POINT ( 'NONE',  ( 9.564922557960805705, 16.46253265017160317, 79.58224293864769550 ) ) ;
#5614 = CARTESIAN_POINT ( 'NONE',  ( 21.52544592524344225, -5.823673210054117533, 68.54057627198103830 ) ) ;
#5615 = CARTESIAN_POINT ( 'NONE',  ( -4.379528057220086978, -16.55341960407618274, 34.79275706135235424 ) ) ;
#5616 = CARTESIAN_POINT ( 'NONE',  ( -21.52544592524334988, -5.823673210054445271, 28.95942372801902209 ) ) ;
#5617 = CARTESIAN_POINT ( 'NONE',  ( -15.72974639402176322, -15.80617190586768395, 84.37609039468570415 ) ) ;
#5618 = CARTESIAN_POINT ( 'NONE',  ( -16.55341960407617563, 4.379528057220093196, 93.54275706135234714 ) ) ;
#5619 = CARTESIAN_POINT ( 'NONE',  ( 16.46253265017160672, -9.564922557960803928, 93.33224293864769550 ) ) ;
#5620 = CARTESIAN_POINT ( 'NONE',  ( -4.379528057220328563, 16.55341960407611168, 80.20724293864769550 ) ) ;
#5621 = CARTESIAN_POINT ( 'NONE',  ( -16.53943276465976808, 0.05219959533911058130, 26.24890960531435624 ) ) ;
#5622 = CARTESIAN_POINT ( 'NONE',  ( 9.564922557961047289, -16.46253265017146816, 75.41775706135234714 ) ) ;
#5623 = STYLED_ITEM ( 'NONE', ( #178064 ), #74599 ) ;
#5624 = CARTESIAN_POINT ( 'NONE',  ( -18.67979575497193778, 10.72451020669871902, 43.33442372801901143 ) ) ;
#5625 = EDGE_CURVE ( 'NONE', #199940, #38283, #53651, .T. ) ;
#5626 = CARTESIAN_POINT ( 'NONE',  ( -0.05219959533910754901, -16.53943276465976808, 87.49890960531436690 ) ) ;
#5627 = CARTESIAN_POINT ( 'NONE',  ( -13.97604488694527625, -13.89961937509977652, 111.8739096053143243 ) ) ;
#5628 = CARTESIAN_POINT ( 'NONE',  ( 12.14591786802327356, -12.06949235617739191, 105.6260903946856899 ) ) ;
#5629 = CARTESIAN_POINT ( 'NONE',  ( -21.55341960407619339, 5.719274019375674811, 83.54275706135234714 ) ) ;
#5630 = CARTESIAN_POINT ( 'NONE',  ( 0.05219959533934541429, -16.53943276465976808, 45.00109039468568284 ) ) ;
#5631 = CARTESIAN_POINT ( 'NONE',  ( -18.67979575497193778, 10.72451020669871902, 43.33442372801901143 ) ) ;
#5632 = ORIENTED_EDGE ( 'NONE', *, *, #5625, .T. ) ;
#5633 = CARTESIAN_POINT ( 'NONE',  ( 18.62759615963255655, 10.81492255796105972, 21.66775706135235069 ) ) ;
#5634 = CARTESIAN_POINT ( 'NONE',  ( 14.29746914071049879, -8.314922557960816363, 88.33224293864769550 ) ) ;
#5635 = CARTESIAN_POINT ( 'NONE',  ( 0.000000000000000000, 0.000000000000000000, -59.13370768023891344 ) ) ;
#5636 = CARTESIAN_POINT ( 'NONE',  ( 12.06949235617757843, -12.14591786802309237, 63.12390960531435979 ) ) ;
#5637 = CARTESIAN_POINT ( 'NONE',  ( -4.379528057220086978, -16.55341960407618274, 104.7927570613523898 ) ) ;
#5638 = CARTESIAN_POINT ( 'NONE',  ( 16.51473224551069308, 9.474510206698969483, 34.16557627198102409 ) ) ;
#5639 = CARTESIAN_POINT ( 'NONE',  ( -10.72451020669898014, 18.67979575497178502, 45.41557627198103830 ) ) ;
#5640 = CARTESIAN_POINT ( 'NONE',  ( 4.379528057220339221, -16.55341960407611168, 72.70724293864769550 ) ) ;
#5641 = CARTESIAN_POINT ( 'NONE',  ( -10.81492255796078084, -18.62759615963271287, 82.08224293864768129 ) ) ;
#5642 = CARTESIAN_POINT ( 'NONE',  ( 5.153800228976335163, 19.02544592524342804, 84.79057627198099567 ) ) ;
#5644 = CARTESIAN_POINT ( 'NONE',  ( 19.03943276465977164, 0.05219959533936151252, 96.25109039468567573 ) ) ;
#5643 = CARTESIAN_POINT ( 'NONE',  ( -13.97604488694527625, -13.89961937509977652, 36.87390960531436690 ) ) ;
#5645 = CARTESIAN_POINT ( 'NONE',  ( -10.81492255796078084, -18.62759615963271287, 37.08224293864768129 ) ) ;
#5646 = CARTESIAN_POINT ( 'NONE',  ( -21.52544592524334988, -5.823673210054445271, 73.95942372801901854 ) ) ;
#5647 = CARTESIAN_POINT ( 'NONE',  ( 16.51473224551069308, 9.474510206698969483, 59.16557627198102409 ) ) ;
#5648 = CARTESIAN_POINT ( 'NONE',  ( -9.474510206698964154, 16.51473224551069663, 90.41557627198103830 ) ) ;
#5649 = ORIENTED_EDGE ( 'NONE', *, *, #90472, .F. ) ;
#5650 = CARTESIAN_POINT ( 'NONE',  ( 12.06949235617739724, 12.14591786802326823, 66.87609039468568994 ) ) ;
#5651 = CARTESIAN_POINT ( 'NONE',  ( -21.53943276465977519, -0.05219959533937600094, 48.75109039468568284 ) ) ;
#5652 = ADVANCED_FACE ( 'NONE', ( #169444 ), #46105, .F. ) ;
#5653 = CARTESIAN_POINT ( 'NONE',  ( 21.53943276465977519, 0.05219959533937863772, 76.25109039468568994 ) ) ;
#5654 = CARTESIAN_POINT ( 'NONE',  ( 15.72974639402199770, -15.80617190586745480, 28.12390960531435979 ) ) ;
#5655 = CARTESIAN_POINT ( 'NONE',  ( 0.05219959533907565091, 21.53943276465977519, 89.99890960531438111 ) ) ;
#5657 = CARTESIAN_POINT ( 'NONE',  ( -16.53943276465976808, -0.05219959533934237506, 58.75109039468568994 ) ) ;
#5656 = CARTESIAN_POINT ( 'NONE',  ( 18.67979575497194134, -10.72451020669871369, 25.83442372801901499 ) ) ;
#5658 = CARTESIAN_POINT ( 'NONE',  ( 18.62759615963271287, -10.81492255796078972, 63.33224293864770260 ) ) ;
#5659 = CARTESIAN_POINT ( 'NONE',  ( -19.02544592524334988, -5.153800228976617603, 18.95942372801899722 ) ) ;
#5661 = CARTESIAN_POINT ( 'NONE',  ( -16.52544592524335698, -4.483927247898792601, 103.9594237280190185 ) ) ;
#5660 = CARTESIAN_POINT ( 'NONE',  ( -19.02544592524342804, 5.153800228976336051, 71.04057627198099567 ) ) ;
#5662 = LINE ( 'NONE', #189711, #146711 ) ;
#5663 = CARTESIAN_POINT ( 'NONE',  ( 16.46253265017160672, -9.564922557960803928, 88.33224293864769550 ) ) ;
#5664 = CARTESIAN_POINT ( 'NONE',  ( 4.379528057220092307, 16.55341960407617563, 37.29275706135235424 ) ) ;
#5665 = CARTESIAN_POINT ( 'NONE',  ( 17.49999999999999645, 3.190838340304485321, 102.6087687570488498 ) ) ;
#5666 = CARTESIAN_POINT ( 'NONE',  ( 5.153800228976615827, -19.02544592524334988, 80.20942372801901854 ) ) ;
#5667 = CARTESIAN_POINT ( 'NONE',  ( 15.72974639402199770, -15.80617190586745480, 63.12390960531435979 ) ) ;
#5668 = CARTESIAN_POINT ( 'NONE',  ( -8.314922557960811034, -14.29746914071050412, 22.08224293864769194 ) ) ;
#5669 = CARTESIAN_POINT ( 'NONE',  ( 19.03943276465977164, 0.05219959533936151252, 96.25109039468567573 ) ) ;
#5670 = CARTESIAN_POINT ( 'NONE',  ( -17.58332526062525858, 7.635886036038558977, 40.92334959558466778 ) ) ;
#5671 = CARTESIAN_POINT ( 'NONE',  ( -5.153800228976607833, 19.02544592524334988, 97.70942372801900433 ) ) ;
#5673 = CARTESIAN_POINT ( 'NONE',  ( 19.02544592524334988, 5.153800228976608722, 61.45942372801900433 ) ) ;
#5672 = CARTESIAN_POINT ( 'NONE',  ( -15.80617190586745835, -15.72974639402198527, 86.87390960531438111 ) ) ;
#5674 = DIRECTION ( 'NONE',  ( -0.000000000000000000, -0.000000000000000000, -1.000000000000000000 ) ) ;
#5675 = CARTESIAN_POINT ( 'NONE',  ( 5.153800228976335163, 19.02544592524342804, 54.79057627198103120 ) ) ;
#5676 = CARTESIAN_POINT ( 'NONE',  ( 8.224510206698953496, -14.34966873604960469, 57.91557627198103120 ) ) ;
#5677 = CARTESIAN_POINT ( 'NONE',  ( 19.03943276465977164, -0.05219959533909143690, 48.74890960531435979 ) ) ;
#5678 = CARTESIAN_POINT ( 'NONE',  ( -16.55341960407611168, -4.379528057220339221, 51.45724293864770260 ) ) ;
#5679 = DIRECTION ( 'NONE',  ( -0.000000000000000000, -0.000000000000000000, 1.000000000000000000 ) ) ;
#5680 = CARTESIAN_POINT ( 'NONE',  ( 31.34418352700886601, -5.970234417100042101, 99.56646813413777863 ) ) ;
#5681 = CARTESIAN_POINT ( 'NONE',  ( -16.55341960407611168, -4.379528057220339221, 31.45724293864769550 ) ) ;
#5682 = CARTESIAN_POINT ( 'NONE',  ( -9.474510206698964154, 16.51473224551069663, 60.41557627198102409 ) ) ;
#5683 = CARTESIAN_POINT ( 'NONE',  ( -13.97604488694547520, 13.89961937509957934, 73.12609039468567573 ) ) ;
#5684 = CARTESIAN_POINT ( 'NONE',  ( 0.05219959533936267826, -19.03943276465977164, 45.00109039468566863 ) ) ;
#5685 = CARTESIAN_POINT ( 'NONE',  ( 8.224510206698742110, 14.34966873604972548, 52.08442372801901854 ) ) ;
#5686 = CARTESIAN_POINT ( 'NONE',  ( 10.72451020669898902, -18.67979575497178502, 47.91557627198102409 ) ) ;
#5687 = CARTESIAN_POINT ( 'NONE',  ( -21.52544592524334988, -5.823673210054445271, 108.9594237280190185 ) ) ;
#5688 = CARTESIAN_POINT ( 'NONE',  ( -19.02544592524342804, 5.153800228976336051, 71.04057627198099567 ) ) ;
#5689 = CARTESIAN_POINT ( 'NONE',  ( 1.577468763857913883E-14, -78.62686331009493301, -24.99999901254159695 ) ) ;
#5690 = CARTESIAN_POINT ( 'NONE',  ( -16.46253265017160317, 9.564922557960807481, 105.8322429386476955 ) ) ;
#5691 = CARTESIAN_POINT ( 'NONE',  ( 0.000000000000000000, 0.000000000000000000, -61.34707691135562868 ) ) ;
#5692 = CARTESIAN_POINT ( 'NONE',  ( 15.72974639402176855, 15.80617190586768217, 36.87609039468568994 ) ) ;
#5693 = CARTESIAN_POINT ( 'NONE',  ( 4.379528057220339221, -16.55341960407611168, 87.70724293864769550 ) ) ;
#5695 = CARTESIAN_POINT ( 'NONE',  ( 9.474510206698971260, -16.51473224551069308, 87.91557627198102409 ) ) ;
#5694 = CARTESIAN_POINT ( 'NONE',  ( -10.81492255796078084, -18.62759615963271287, 82.08224293864768129 ) ) ;
#5696 = CARTESIAN_POINT ( 'NONE',  ( 13.89961937509977652, -13.97604488694527269, 93.12390960531436690 ) ) ;
#5697 = CARTESIAN_POINT ( 'NONE',  ( -18.62759615963255300, -10.81492255796106328, 29.16775706135234003 ) ) ;
#5698 = ORIENTED_EDGE ( 'NONE', *, *, #139940, .F. ) ;
#5699 = CARTESIAN_POINT ( 'NONE',  ( 5.153800228976335163, 19.02544592524342804, 74.79057627198103830 ) ) ;
#5700 = CARTESIAN_POINT ( 'NONE',  ( 28.79475375365586132, 2.781246896534039337E-14, 146.9843446568999923 ) ) ;
#5702 = CARTESIAN_POINT ( 'NONE',  ( -9.474510206698964154, 16.51473224551069663, 30.41557627198102054 ) ) ;
#5701 = CARTESIAN_POINT ( 'NONE',  ( 19.02544592524343514, -5.153800228976328945, 23.54057627198102054 ) ) ;
#5703 = CARTESIAN_POINT ( 'NONE',  ( 19.02544592524334988, 5.153800228976608722, 111.4594237280190043 ) ) ;
#5704 = CARTESIAN_POINT ( 'NONE',  ( -29.86685920354755552, 21.69954338932564397, -9.324999997268813345 ) ) ;
#5705 = CARTESIAN_POINT ( 'NONE',  ( 14.29746914071049879, -8.314922557960816363, 108.3322429386477097 ) ) ;
#5706 = CARTESIAN_POINT ( 'NONE',  ( -5.823673210054431948, 21.52544592524334988, 77.70942372801900433 ) ) ;
#5708 = CARTESIAN_POINT ( 'NONE',  ( 10.81492255796106328, -18.62759615963255655, 30.41775706135234358 ) ) ;
#5707 = CARTESIAN_POINT ( 'NONE',  ( 9.474510206698971260, -16.51473224551069308, 62.91557627198102409 ) ) ;
#5709 = CARTESIAN_POINT ( 'NONE',  ( 18.62759615963271287, -10.81492255796078972, 113.3322429386476955 ) ) ;
#5710 = CARTESIAN_POINT ( 'NONE',  ( -23.31738231874055600, 16.94106989632528837, 149.7999999999999829 ) ) ;
#5711 = CARTESIAN_POINT ( 'NONE',  ( 5.049401038298161559, -19.05341960407611168, 87.70724293864769550 ) ) ;
#5712 = CARTESIAN_POINT ( 'NONE',  ( 22.12969251635687229, 16.97230210225939118, 139.9999999999999432 ) ) ;
#5714 = CARTESIAN_POINT ( 'NONE',  ( 21.52544592524344225, -5.823673210054117533, 38.54057627198103120 ) ) ;
#5713 = CARTESIAN_POINT ( 'NONE',  ( -16.55341960407617563, 4.379528057220093196, 28.54275706135234358 ) ) ;
#5715 = CARTESIAN_POINT ( 'NONE',  ( 5.719274019375673035, 21.55341960407619339, 67.29275706135234714 ) ) ;
#5716 = CARTESIAN_POINT ( 'NONE',  ( -9.474510206698964154, 16.51473224551069663, 110.4155762719810383 ) ) ;
#5717 = CARTESIAN_POINT ( 'NONE',  ( 13.97604488694548053, -13.89961937509957401, 100.6260903946856615 ) ) ;
#5718 = CARTESIAN_POINT ( 'NONE',  ( -0.05219959533909027116, -19.03943276465977164, 47.49890960531435979 ) ) ;
#5719 = CARTESIAN_POINT ( 'NONE',  ( -0.05219959533909027116, -19.03943276465977164, 82.49890960531436690 ) ) ;
#5720 = CARTESIAN_POINT ( 'NONE',  ( -8.314922557960811034, -14.29746914071050412, 92.08224293864769550 ) ) ;
#5721 = CARTESIAN_POINT ( 'NONE',  ( 12.06949235617757843, -12.14591786802309237, 93.12390960531436690 ) ) ;
#5722 = CARTESIAN_POINT ( 'NONE',  ( 19.02544592524343514, -5.153800228976328945, 108.5405762719810383 ) ) ;
#5724 = CARTESIAN_POINT ( 'NONE',  ( -19.05341960407611168, -5.049401038298163336, 46.45724293864768129 ) ) ;
#5723 = CARTESIAN_POINT ( 'NONE',  ( 0.05219959533910956823, 16.53943276465976808, 54.99890960531435269 ) ) ;
#5725 = CARTESIAN_POINT ( 'NONE',  ( 15.80617190586769283, -15.72974639402175789, 60.62609039468567573 ) ) ;
#5726 = CARTESIAN_POINT ( 'NONE',  ( -5.049401038297874678, -19.05341960407617918, 99.79275706135234714 ) ) ;
#5727 = CARTESIAN_POINT ( 'NONE',  ( 16.55341960407611168, 4.379528057220329451, 58.95724293864770971 ) ) ;
#5728 = CARTESIAN_POINT ( 'NONE',  ( -15.72974639402197994, 15.80617190586746368, 110.6239096053143669 ) ) ;
#5729 = CARTESIAN_POINT ( 'NONE',  ( -18.67979575497178146, -10.72451020669898902, 46.66557627198102409 ) ) ;
#5730 = CARTESIAN_POINT ( 'NONE',  ( -19.02544592524342804, 5.153800228976336051, 116.0405762719810383 ) ) ;
#5731 = CARTESIAN_POINT ( 'NONE',  ( -8.906447517083060816, 27.41122689804195645, 139.8500000054623911 ) ) ;
#5732 = CARTESIAN_POINT ( 'NONE',  ( -16.46253265017160317, 9.564922557960807481, 55.83224293864769550 ) ) ;
#5733 = CARTESIAN_POINT ( 'NONE',  ( -4.483927247898539470, -16.52544592524342804, 32.29057627198102409 ) ) ;
#5734 = AXIS2_PLACEMENT_3D ( 'NONE', #61704, #10514, #133851 ) ;
#5735 = MANIFOLD_SOLID_BREP ( 'Fillet1', #195579 ) ;
#5736 = CARTESIAN_POINT ( 'NONE',  ( 16.52544592524335698, 4.483927247898782831, 106.4594237280190328 ) ) ;
#5737 = CARTESIAN_POINT ( 'NONE',  ( -4.379528057220086978, -16.55341960407618274, 89.79275706135236135 ) ) ;
#5739 = EDGE_CURVE ( 'NONE', #109599, #48040, #198809, .T. ) ;
#5738 = CARTESIAN_POINT ( 'NONE',  ( -5.049401038297874678, -19.05341960407617918, 34.79275706135233293 ) ) ;
#5740 = CARTESIAN_POINT ( 'NONE',  ( -21.99873734152930638, -27.49873734152905413, 8.181980515339454030 ) ) ;
#5741 = CARTESIAN_POINT ( 'NONE',  ( 19.05341960407611168, 5.049401038298154454, 88.95724293864769550 ) ) ;
#5742 = CARTESIAN_POINT ( 'NONE',  ( -0.05219959533909027116, -19.03943276465977164, 52.49890960531436690 ) ) ;
#5743 = CARTESIAN_POINT ( 'NONE',  ( -14.29746914071049879, 8.314922557960819915, 60.83224293864769550 ) ) ;
#5745 = CARTESIAN_POINT ( 'NONE',  ( -21.52544592524343514, 5.823673210054127303, 26.04057627198103475 ) ) ;
#5744 = CARTESIAN_POINT ( 'NONE',  ( 16.52216118717207394, -7.221426719304488984, 101.4240097895301034 ) ) ;
#5746 = CARTESIAN_POINT ( 'NONE',  ( -15.80617190586745835, -15.72974639402198527, 46.87390960531435979 ) ) ;
#5747 = CARTESIAN_POINT ( 'NONE',  ( -14.34966873604960291, -8.224510206698953496, 81.66557627198103830 ) ) ;
#5748 = CARTESIAN_POINT ( 'NONE',  ( -0.05219959533934338120, 16.53943276465976808, 32.50109039468568284 ) ) ;
#5749 = CARTESIAN_POINT ( 'NONE',  ( -16.55341960407611168, -4.379528057220339221, 76.45724293864769550 ) ) ;
#5750 = CARTESIAN_POINT ( 'NONE',  ( 31.90000000000003411, -9.916512055951908821E-14, -45.64921306006598201 ) ) ;
#5751 = CARTESIAN_POINT ( 'NONE',  ( -9.474510206698720793, -16.51473224551083518, 79.58442372801899012 ) ) ;
#5752 = CARTESIAN_POINT ( 'NONE',  ( 5.049401038298161559, -19.05341960407611168, 107.7072429386476955 ) ) ;
#5753 = CARTESIAN_POINT ( 'NONE',  ( 22.81625015709509441, 31.40387420917330275, -1.824999997268813567 ) ) ;
#5754 = CARTESIAN_POINT ( 'NONE',  ( -0.05219959533909027116, -19.03943276465977164, 42.49890960531435269 ) ) ;
#5756 = CARTESIAN_POINT ( 'NONE',  ( -16.53943276465976808, -0.05219959533934237506, 103.7510903946857042 ) ) ;
#5755 = CARTESIAN_POINT ( 'NONE',  ( -8.224510206698735004, -14.34966873604973081, 29.58442372801901854 ) ) ;
#5757 = CARTESIAN_POINT ( 'NONE',  ( -19.05341960407617563, 5.049401038297882671, 68.54275706135230450 ) ) ;
#5758 = CARTESIAN_POINT ( 'NONE',  ( 18.67979575497178502, 10.72451020669898547, 44.16557627198103120 ) ) ;
#5759 = CARTESIAN_POINT ( 'NONE',  ( -15.72974639402176322, -15.80617190586768395, 69.37609039468567573 ) ) ;
#5760 = CARTESIAN_POINT ( 'NONE',  ( -17.81289503416611097, -24.51734667627696496, 146.5500000054623513 ) ) ;
#5761 = CARTESIAN_POINT ( 'NONE',  ( 16.55341960407618274, -4.379528057220086978, 41.04275706135236135 ) ) ;
#5763 = CARTESIAN_POINT ( 'NONE',  ( -16.51473224551069308, -9.474510206698971260, 81.66557627198103830 ) ) ;
#5762 = CARTESIAN_POINT ( 'NONE',  ( 0.05219959533909260263, 19.03943276465977164, 29.99890960531435979 ) ) ;
#5764 = AXIS2_PLACEMENT_3D ( 'NONE', #10969, #196003, #74627 ) ;
#5765 = CARTESIAN_POINT ( 'NONE',  ( -19.05341960407611168, -5.049401038298163336, 26.45724293864769550 ) ) ;
#5766 = CARTESIAN_POINT ( 'NONE',  ( 4.483927247898545687, 16.52544592524342804, 84.79057627198102409 ) ) ;
#5767 = SHAPE_DEFINITION_REPRESENTATION ( #167934, #112845 ) ;
#5768 = CARTESIAN_POINT ( 'NONE',  ( 0.05219959533909260263, 19.03943276465977164, 84.99890960531436690 ) ) ;
#5769 = ORIENTED_EDGE ( 'NONE', *, *, #148652, .F. ) ;
#5770 = CARTESIAN_POINT ( 'NONE',  ( 19.05341960407617918, -5.049401038297876454, 101.0427570613523045 ) ) ;
#5771 = CARTESIAN_POINT ( 'NONE',  ( 21.53943276465977519, -0.05219959533907433946, 78.74890960531436690 ) ) ;
#5772 = CARTESIAN_POINT ( 'NONE',  ( -19.02544592524342804, 5.153800228976336051, 46.04057627198101699 ) ) ;
#5774 = CARTESIAN_POINT ( 'NONE',  ( 5.719274019375991003, -21.55341960407610458, 112.7072429386476955 ) ) ;
#5773 = CARTESIAN_POINT ( 'NONE',  ( -5.049401038297874678, -19.05341960407617918, 69.79275706135233293 ) ) ;
#5775 = CARTESIAN_POINT ( 'NONE',  ( 5.153800228976335163, 19.02544592524342804, 64.79057627198100988 ) ) ;
#5777 = EDGE_CURVE ( 'NONE', #113441, #35858, #44000, .T. ) ;
#5776 = CARTESIAN_POINT ( 'NONE',  ( 5.153800228976335163, 19.02544592524342804, 109.7905762719810099 ) ) ;
#5778 = EDGE_LOOP ( 'NONE', ( #158950, #3267, #104526 ) ) ;
#5779 = CARTESIAN_POINT ( 'NONE',  ( -16.53943276465976808, -0.05219959533934237506, 33.75109039468568284 ) ) ;
#5780 = CARTESIAN_POINT ( 'NONE',  ( -10.72451020669898014, 18.67979575497178502, 105.4155762719810383 ) ) ;
#5783 = CARTESIAN_POINT ( 'NONE',  ( 5.153800228976615827, -19.02544592524334988, 55.20942372801899722 ) ) ;
#5782 = CARTESIAN_POINT ( 'NONE',  ( -19.02544592524342804, 5.153800228976336051, 91.04057627198100988 ) ) ;
#5781 = CARTESIAN_POINT ( 'NONE',  ( -0.05219959533910754901, -16.53943276465976808, 112.4989096053143669 ) ) ;
#5784 = CARTESIAN_POINT ( 'NONE',  ( 10.72451020669898902, -18.67979575497178502, 82.91557627198103830 ) ) ;
#5785 = CARTESIAN_POINT ( 'NONE',  ( -12.06949235617756955, 12.14591786802309770, 45.62390960531436690 ) ) ;
#5786 = CARTESIAN_POINT ( 'NONE',  ( -13.89961937509957401, -13.97604488694547875, 24.37609039468565442 ) ) ;
#5787 = CARTESIAN_POINT ( 'NONE',  ( -14.29746914071037622, -8.314922557961029526, 64.16775706135234714 ) ) ;
#5788 = EDGE_CURVE ( 'NONE', #135024, #43345, #75504, .T. ) ;
#5789 = CARTESIAN_POINT ( 'NONE',  ( 19.05341960407611168, 5.049401038298154454, 98.95724293864766707 ) ) ;
#5790 = CARTESIAN_POINT ( 'NONE',  ( 13.97604488694527802, 13.89961937509977652, 49.37390960531434558 ) ) ;
#5791 = CARTESIAN_POINT ( 'NONE',  ( -15.72974639402176322, -15.80617190586768395, 49.37609039468569705 ) ) ;
#5792 = CARTESIAN_POINT ( 'NONE',  ( -5.823673210054431948, 21.52544592524334988, 67.70942372801901854 ) ) ;
#5793 = CARTESIAN_POINT ( 'NONE',  ( -19.05341960407611168, -5.049401038298163336, 66.45724293864769550 ) ) ;
#5794 = CARTESIAN_POINT ( 'NONE',  ( 15.80617190586769283, -15.72974639402175789, 30.62609039468567929 ) ) ;
#5795 = CARTESIAN_POINT ( 'NONE',  ( -16.51473224551082808, 9.474510206698731452, 73.33442372801900433 ) ) ;
#5796 = CARTESIAN_POINT ( 'NONE',  ( -13.97604488694547697, 13.89961937509957934, 73.12609039468568994 ) ) ;
#5797 = CARTESIAN_POINT ( 'NONE',  ( 19.05341960407611168, 5.049401038298154454, 33.95724293864769550 ) ) ;
#5798 = CARTESIAN_POINT ( 'NONE',  ( -4.379528057220086978, -16.55341960407618274, 89.79275706135236135 ) ) ;
#5799 = CARTESIAN_POINT ( 'NONE',  ( 19.02544592524343514, -5.153800228976328945, 48.54057627198103120 ) ) ;
#5800 = CARTESIAN_POINT ( 'NONE',  ( 5.153800228976335163, 19.02544592524342804, 24.79057627198102765 ) ) ;
#5801 = CARTESIAN_POINT ( 'NONE',  ( -5.153800228976328057, -19.02544592524343514, 102.2905762719810383 ) ) ;
#5802 = CARTESIAN_POINT ( 'NONE',  ( -5.153800228976328057, -19.02544592524343514, 32.29057627198102409 ) ) ;
#5803 = CARTESIAN_POINT ( 'NONE',  ( -5.719274019375978568, 21.55341960407610458, 90.20724293864770971 ) ) ;
#5804 = CARTESIAN_POINT ( 'NONE',  ( 8.314922557961029526, -14.29746914071037800, 60.41775706135235424 ) ) ;
#5805 = CARTESIAN_POINT ( 'NONE',  ( 19.02544592524334988, 5.153800228976608722, 36.45942372801900433 ) ) ;
#5806 = CARTESIAN_POINT ( 'NONE',  ( -13.97604488694527625, -13.89961937509977652, 46.87390960531435979 ) ) ;
#5807 = CARTESIAN_POINT ( 'NONE',  ( 8.314922557960818139, 14.29746914071049879, 39.58224293864769550 ) ) ;
#5808 = CARTESIAN_POINT ( 'NONE',  ( -16.52544592524342804, 4.483927247898546575, 76.04057627198102409 ) ) ;
#5809 = CARTESIAN_POINT ( 'NONE',  ( -19.05341960407611168, -5.049401038298163336, 81.45724293864769550 ) ) ;
#5810 = CARTESIAN_POINT ( 'NONE',  ( -9.564922557960796823, -16.46253265017161027, 77.08224293864769550 ) ) ;
#5811 = CARTESIAN_POINT ( 'NONE',  ( 10.72451020669871369, 18.67979575497193778, 32.08442372801901854 ) ) ;
#5812 = CARTESIAN_POINT ( 'NONE',  ( -9.564922557960796823, -16.46253265017161027, 87.08224293864769550 ) ) ;
#5813 = CARTESIAN_POINT ( 'NONE',  ( -21.52544592524334988, -5.823673210054445271, 103.9594237280190185 ) ) ;
#5814 = CARTESIAN_POINT ( 'NONE',  ( 16.53943276465976808, 0.05219959533934440121, 76.25109039468568994 ) ) ;
#5815 = CARTESIAN_POINT ( 'NONE',  ( 5.719274019375673035, 21.55341960407619339, 22.29275706135235069 ) ) ;
#5816 = CARTESIAN_POINT ( 'NONE',  ( 10.72451020669898902, -18.67979575497178502, 87.91557627198103830 ) ) ;
#5817 = CARTESIAN_POINT ( 'NONE',  ( 8.224510206698953496, -14.34966873604960469, 47.91557627198102409 ) ) ;
#5818 = CARTESIAN_POINT ( 'NONE',  ( -19.05341960407611168, -5.049401038298163336, 41.45724293864769550 ) ) ;
#5819 = CARTESIAN_POINT ( 'NONE',  ( 12.06949235617757843, -12.14591786802309237, 73.12390960531436690 ) ) ;
#5820 = CARTESIAN_POINT ( 'NONE',  ( 21.52544592524344225, -5.823673210054117533, 33.54057627198102409 ) ) ;
#5821 = CARTESIAN_POINT ( 'NONE',  ( -5.049401038297874678, -19.05341960407617918, 29.79275706135232227 ) ) ;
#5822 = CARTESIAN_POINT ( 'NONE',  ( -16.53943276465976808, 0.05219959533911058130, 106.2489096053143811 ) ) ;
#5823 = CARTESIAN_POINT ( 'NONE',  ( -13.97604488694527625, -13.89961937509977652, 106.8739096053143669 ) ) ;
#5824 = EDGE_LOOP ( 'NONE', ( #66134, #59358 ) ) ;
#5825 = CARTESIAN_POINT ( 'NONE',  ( 16.55341960407618274, -4.379528057220086978, 51.04275706135234714 ) ) ;
#5826 = CARTESIAN_POINT ( 'NONE',  ( 13.89961937509977652, -13.97604488694527269, 63.12390960531435979 ) ) ;
#5827 = CARTESIAN_POINT ( 'NONE',  ( -17.14385361876520264, -23.59649016807271238, 139.1750000027311671 ) ) ;
#5828 = CARTESIAN_POINT ( 'NONE',  ( 15.72974639402199770, -15.80617190586745480, 23.12390960531436335 ) ) ;
#5829 = CARTESIAN_POINT ( 'NONE',  ( -12.06949235617739369, -12.14591786802326823, 89.37609039468568994 ) ) ;
#5830 = CARTESIAN_POINT ( 'NONE',  ( -8.224510206698735004, -14.34966873604973081, 19.58442372801901143 ) ) ;
#5831 = CARTESIAN_POINT ( 'NONE',  ( 21.55341960407619695, -5.719274019375665929, 86.04275706135236135 ) ) ;
#5832 = CARTESIAN_POINT ( 'NONE',  ( -9.474510206698964154, 16.51473224551069663, 75.41557627198103830 ) ) ;
#5833 = CARTESIAN_POINT ( 'NONE',  ( 15.72974639402199770, -15.80617190586745480, 103.1239096053143811 ) ) ;
#5834 = CARTESIAN_POINT ( 'NONE',  ( 16.53943276465976808, 0.05219959533934440121, 61.25109039468567573 ) ) ;
#5835 = CARTESIAN_POINT ( 'NONE',  ( 12.14591786802309770, 12.06949235617756955, 114.3739096053143527 ) ) ;
#5836 = CARTESIAN_POINT ( 'NONE',  ( 14.29746914071037800, 8.314922557961029526, 21.66775706135235069 ) ) ;
#5837 = CARTESIAN_POINT ( 'NONE',  ( 9.564922557961047289, -16.46253265017146816, 85.41775706135233293 ) ) ;
#5838 = CARTESIAN_POINT ( 'NONE',  ( -10.72451020669898014, 18.67979575497178502, 80.41557627198103830 ) ) ;
#5839 = CARTESIAN_POINT ( 'NONE',  ( 19.05341960407617918, -5.049401038297876454, 56.04275706135234714 ) ) ;
#5840 = CARTESIAN_POINT ( 'NONE',  ( -21.98685479826777112, -13.98560643873833875, 165.5209445330007441 ) ) ;
#5841 = CARTESIAN_POINT ( 'NONE',  ( -15.80617190586745835, -15.72974639402198527, 101.8739096053143811 ) ) ;
#5842 = FACE_OUTER_BOUND ( 'NONE', #173760, .T. ) ;
#5843 = CARTESIAN_POINT ( 'NONE',  ( 19.02544592524343514, -5.153800228976328945, 78.54057627198099567 ) ) ;
#5844 = DIRECTION ( 'NONE',  ( 0.000000000000000000, -0.9396926207859095381, 0.3420201433256656043 ) ) ;
#5845 = CARTESIAN_POINT ( 'NONE',  ( 16.53943276465976808, 0.05219959533934440121, 21.25109039468567218 ) ) ;
#5846 = CARTESIAN_POINT ( 'NONE',  ( 14.06517603784871007, -37.45098900586879154, -11.50478690063030562 ) ) ;
#5848 = CARTESIAN_POINT ( 'NONE',  ( -4.379528057220328563, 16.55341960407611168, 70.20724293864769550 ) ) ;
#5847 = CARTESIAN_POINT ( 'NONE',  ( -10.81492255796078084, -18.62759615963271287, 97.08224293864770971 ) ) ;
#5849 = CARTESIAN_POINT ( 'NONE',  ( 19.05341960407611168, 5.049401038298154454, 63.95724293864769550 ) ) ;
#5850 = CARTESIAN_POINT ( 'NONE',  ( 0.05219959533937995610, -21.53943276465977519, 75.00109039468568994 ) ) ;
#5852 = CARTESIAN_POINT ( 'NONE',  ( -0.05219959533936034679, 19.03943276465977164, 37.50109039468567573 ) ) ;
#5851 = CARTESIAN_POINT ( 'NONE',  ( -0.05219959533934338120, 16.53943276465976808, 37.50109039468568284 ) ) ;
#5853 = CARTESIAN_POINT ( 'NONE',  ( 21.53943276465977519, 0.05219959533937863772, 56.25109039468568284 ) ) ;
#5854 = CARTESIAN_POINT ( 'NONE',  ( -5.719274019375978568, 21.55341960407610458, 65.20724293864768129 ) ) ;
#5855 = CARTESIAN_POINT ( 'NONE',  ( 19.03943276465977164, 0.05219959533936151252, 106.2510903946856615 ) ) ;
#5856 = CARTESIAN_POINT ( 'NONE',  ( -19.02544592524342804, 5.153800228976336051, 51.04057627198103120 ) ) ;
#5857 = CARTESIAN_POINT ( 'NONE',  ( -9.474510206698720793, -16.51473224551083518, 74.58442372801900433 ) ) ;
#5858 = CARTESIAN_POINT ( 'NONE',  ( -15.80617190586768217, 15.72974639402176855, 78.12609039468570415 ) ) ;
#5859 = CARTESIAN_POINT ( 'NONE',  ( -13.97604488694547697, 13.89961937509957934, 48.12609039468566863 ) ) ;
#5860 = CARTESIAN_POINT ( 'NONE',  ( -19.05341960407611168, -5.049401038298163336, 41.45724293864769550 ) ) ;
#5861 = CARTESIAN_POINT ( 'NONE',  ( 21.55341960407610458, 5.719274019375980345, 63.95724293864770260 ) ) ;
#5862 = CARTESIAN_POINT ( 'NONE',  ( -16.55341960407611168, -4.379528057220339221, 46.45724293864769550 ) ) ;
#5863 = FACE_OUTER_BOUND ( 'NONE', #105488, .T. ) ;
#5864 = CARTESIAN_POINT ( 'NONE',  ( 9.564922557961047289, -16.46253265017146816, 25.41775706135234003 ) ) ;
#5865 = CARTESIAN_POINT ( 'NONE',  ( 14.29746914071037800, 8.314922557961029526, 91.66775706135234714 ) ) ;
#5866 = CARTESIAN_POINT ( 'NONE',  ( -0.05219959533910754901, -16.53943276465976808, 57.49890960531435979 ) ) ;
#5867 = CARTESIAN_POINT ( 'NONE',  ( -18.67979575497193778, 10.72451020669871902, 83.33442372801903275 ) ) ;
#5868 = CARTESIAN_POINT ( 'NONE',  ( -15.72974639402176322, -15.80617190586768395, 79.37609039468567573 ) ) ;
#5869 = CARTESIAN_POINT ( 'NONE',  ( -21.52544592524343514, 5.823673210054127303, 76.04057627198102409 ) ) ;
#5870 = CARTESIAN_POINT ( 'NONE',  ( 16.51473224551069308, 9.474510206698969483, 54.16557627198103120 ) ) ;
#5871 = CARTESIAN_POINT ( 'NONE',  ( 21.55341960407619695, -5.719274019375665929, 56.04275706135235424 ) ) ;
#5872 = CARTESIAN_POINT ( 'NONE',  ( 5.153800228976335163, 19.02544592524342804, 34.79057627198102409 ) ) ;
#5873 = CARTESIAN_POINT ( 'NONE',  ( -9.474510206698964154, 16.51473224551069663, 50.41557627198102409 ) ) ;
#5874 = CARTESIAN_POINT ( 'NONE',  ( 0.05219959533910956823, 16.53943276465976808, 109.9989096053143527 ) ) ;
#5875 = CARTESIAN_POINT ( 'NONE',  ( -5.153800228976328057, -19.02544592524343514, 97.29057627198099567 ) ) ;
#5876 = CARTESIAN_POINT ( 'NONE',  ( -4.483927247898539470, -16.52544592524342804, 47.29057627198103120 ) ) ;
#5877 = CARTESIAN_POINT ( 'NONE',  ( 14.29746914071049879, -8.314922557960816363, 108.3322429386477097 ) ) ;
#5878 = CARTESIAN_POINT ( 'NONE',  ( -0.05219959533907301413, -21.53943276465977519, 82.49890960531436690 ) ) ;
#5879 = CARTESIAN_POINT ( 'NONE',  ( 15.80617190586769283, -15.72974639402175789, 20.62609039468568639 ) ) ;
#5880 = DIRECTION ( 'NONE',  ( -0.000000000000000000, 0.000000000000000000, 1.000000000000000000 ) ) ;
#5881 = CARTESIAN_POINT ( 'NONE',  ( 8.224510206698742110, 14.34966873604972548, 42.08442372801901854 ) ) ;
#5882 = EDGE_LOOP ( 'NONE', ( #15030, #54670, #59880, #149688, #178120, #2796, #66506, #131779 ) ) ;
#5883 = CARTESIAN_POINT ( 'NONE',  ( 10.72451020669898902, -18.67979575497178502, 67.91557627198102409 ) ) ;
#5885 = CARTESIAN_POINT ( 'NONE',  ( 15.72974639402176855, 15.80617190586768217, 106.8760903946856899 ) ) ;
#5884 = PRODUCT_DEFINITION_CONTEXT ( 'detailed design', #143659, 'design' ) ;
#5886 = CARTESIAN_POINT ( 'NONE',  ( -19.02544592524342804, 5.153800228976336051, 96.04057627198103830 ) ) ;
#5887 = CARTESIAN_POINT ( 'NONE',  ( 5.719274019375673035, 21.55341960407619339, 27.29275706135234358 ) ) ;
#5888 = CARTESIAN_POINT ( 'NONE',  ( 5.823673210054125526, 21.52544592524343514, 29.79057627198102409 ) ) ;
#5889 = CARTESIAN_POINT ( 'NONE',  ( 8.314922557961029526, -14.29746914071037800, 105.4177570613523613 ) ) ;
#5891 = CARTESIAN_POINT ( 'NONE',  ( -18.67979575497193778, 10.72451020669871902, 78.33442372801901854 ) ) ;
#5890 = CARTESIAN_POINT ( 'NONE',  ( -18.67979575497193778, 10.72451020669871902, 53.33442372801901854 ) ) ;
#5892 = CARTESIAN_POINT ( 'NONE',  ( 10.81492255796106328, -18.62759615963255655, 110.4177570613523756 ) ) ;
#5893 = CARTESIAN_POINT ( 'NONE',  ( 12.14591786802327356, -12.06949235617739191, 70.62609039468567573 ) ) ;
#5894 = CARTESIAN_POINT ( 'NONE',  ( 21.53943276465977519, 0.05219959533937863772, 36.25109039468567573 ) ) ;
#5895 = CARTESIAN_POINT ( 'NONE',  ( 9.474510206698971260, -16.51473224551069308, 27.91557627198103120 ) ) ;
#5896 = CARTESIAN_POINT ( 'NONE',  ( -5.823673210054431948, 21.52544592524334988, 107.7094237280190328 ) ) ;
#5897 = CARTESIAN_POINT ( 'NONE',  ( -19.02544592524342804, 5.153800228976336051, 106.0405762719810241 ) ) ;
#5898 = CARTESIAN_POINT ( 'NONE',  ( 18.62759615963271287, -10.81492255796078972, 108.3322429386477097 ) ) ;
#5900 = CARTESIAN_POINT ( 'NONE',  ( -21.52544592524343514, 5.823673210054127303, 71.04057627198103830 ) ) ;
#5899 = CARTESIAN_POINT ( 'NONE',  ( -7.980598154334920480, -36.52039581308733318, -31.83703727319203125 ) ) ;
#5902 = CARTESIAN_POINT ( 'NONE',  ( 16.53943276465976808, -0.05219959533910856209, 43.74890960531435979 ) ) ;
#5901 = CARTESIAN_POINT ( 'NONE',  ( -16.53943276465976808, -0.05219959533934237506, 53.75109039468568994 ) ) ;
#5903 = CARTESIAN_POINT ( 'NONE',  ( 8.898068258721473001, -27.38543819252872069, 146.8656553485623704 ) ) ;
#5904 = CARTESIAN_POINT ( 'NONE',  ( 9.564922557961047289, -16.46253265017146816, 85.41775706135233293 ) ) ;
#5905 = CARTESIAN_POINT ( 'NONE',  ( -0.1032682159774158670, -16.70000000000002061, -61.34707691135562868 ) ) ;
#5906 = CARTESIAN_POINT ( 'NONE',  ( -16.53943276465976808, -0.05219959533934237506, 23.75109039468567929 ) ) ;
#5907 = CARTESIAN_POINT ( 'NONE',  ( 21.52544592524344225, -5.823673210054117533, 93.54057627198103830 ) ) ;
#5908 = CARTESIAN_POINT ( 'NONE',  ( 15.80617190586746368, 15.72974639402197994, 69.37390960531436690 ) ) ;
#5909 = CARTESIAN_POINT ( 'NONE',  ( 9.474510206698971260, -16.51473224551069308, 107.9155762719810383 ) ) ;
#5910 = CARTESIAN_POINT ( 'NONE',  ( -8.314922557961024197, 14.29746914071037800, 47.91775706135234714 ) ) ;
#5911 = CARTESIAN_POINT ( 'NONE',  ( -9.474510206698964154, 16.51473224551069663, 55.41557627198103120 ) ) ;
#5913 = CARTESIAN_POINT ( 'NONE',  ( -0.05219959533936034679, 19.03943276465977164, 92.50109039468566152 ) ) ;
#5912 = CARTESIAN_POINT ( 'NONE',  ( 18.67979575497194134, -10.72451020669871369, 35.83442372801901143 ) ) ;
#5914 = CARTESIAN_POINT ( 'NONE',  ( 16.46253265017160672, -9.564922557960803928, 103.3322429386476955 ) ) ;
#5915 = CARTESIAN_POINT ( 'NONE',  ( 16.51473224551069308, 9.474510206698969483, 94.16557627198103830 ) ) ;
#5916 = CARTESIAN_POINT ( 'NONE',  ( -21.52544592524343514, 5.823673210054127303, 91.04057627198103830 ) ) ;
#5917 = CARTESIAN_POINT ( 'NONE',  ( -5.153800228976328057, -19.02544592524343514, 62.29057627198100988 ) ) ;
#5918 = CARTESIAN_POINT ( 'NONE',  ( -6.791538853603066528, 3.181980515339468241, 1.110912703473986074 ) ) ;
#5919 = CARTESIAN_POINT ( 'NONE',  ( 8.314922557960818139, 14.29746914071049879, 69.58224293864769550 ) ) ;
#5920 = CARTESIAN_POINT ( 'NONE',  ( 19.02544592524343514, -5.153800228976328945, 98.54057627198100988 ) ) ;
#5921 = CARTESIAN_POINT ( 'NONE',  ( 15.32289026290833611, -14.84183971327400542, -56.44770181572976497 ) ) ;
#5922 = CARTESIAN_POINT ( 'NONE',  ( -5.049401038297874678, -19.05341960407617918, 79.79275706135233293 ) ) ;
#5923 = CARTESIAN_POINT ( 'NONE',  ( -18.67979575497178146, -10.72451020669898902, 86.66557627198102409 ) ) ;
#5924 = CARTESIAN_POINT ( 'NONE',  ( 19.03943276465977164, 0.05219959533936151252, 46.25109039468566863 ) ) ;
#5925 = CARTESIAN_POINT ( 'NONE',  ( 15.80617190586746368, 15.72974639402197994, 24.37390960531435979 ) ) ;
#5926 = SURFACE_STYLE_USAGE ( .BOTH. , #173815 ) ;
#5927 = CARTESIAN_POINT ( 'NONE',  ( 21.55341960407610458, 5.719274019375980345, 58.95724293864770971 ) ) ;
#5928 = CARTESIAN_POINT ( 'NONE',  ( 13.89961937509977652, -13.97604488694527269, 88.12390960531438111 ) ) ;
#5929 = CARTESIAN_POINT ( 'NONE',  ( 21.53943276465977519, 0.05219959533937863772, 76.25109039468568994 ) ) ;
#5930 = CARTESIAN_POINT ( 'NONE',  ( 5.049401038298161559, -19.05341960407611168, 37.70724293864768839 ) ) ;
#5931 = CARTESIAN_POINT ( 'NONE',  ( -8.314922557960811034, -14.29746914071050412, 72.08224293864769550 ) ) ;
#5932 = CARTESIAN_POINT ( 'NONE',  ( 4.379528057220092307, 16.55341960407617563, 27.29275706135234358 ) ) ;
#5933 = CARTESIAN_POINT ( 'NONE',  ( 15.80617190586769283, -15.72974639402175789, 60.62609039468567573 ) ) ;
#5934 = ORIENTED_EDGE ( 'NONE', *, *, #160165, .T. ) ;
#5935 = CARTESIAN_POINT ( 'NONE',  ( -13.97604488694547697, 13.89961937509957934, 28.12609039468565797 ) ) ;
#5936 = CARTESIAN_POINT ( 'NONE',  ( 19.05341960407617918, -5.049401038297876454, 81.04275706135231871 ) ) ;
#5937 = CARTESIAN_POINT ( 'NONE',  ( -17.60779699588841751, -5.499999999999947597, 91.34981316670105400 ) ) ;
#5938 = CARTESIAN_POINT ( 'NONE',  ( -21.52544592524334988, -5.823673210054445271, 23.95942372801901143 ) ) ;
#5939 = CARTESIAN_POINT ( 'NONE',  ( 2.500000000000000000, -1.178949249685214307, 2.042000000000002036 ) ) ;
#5940 = CARTESIAN_POINT ( 'NONE',  ( 10.81492255796106328, -18.62759615963255655, 110.4177570613523756 ) ) ;
#5941 = CARTESIAN_POINT ( 'NONE',  ( -5.153800228976328057, -19.02544592524343514, 57.29057627198103120 ) ) ;
#5942 = CARTESIAN_POINT ( 'NONE',  ( 19.03943276465977164, 0.05219959533936151252, 21.25109039468565797 ) ) ;
#5943 = CARTESIAN_POINT ( 'NONE',  ( -8.224510206698735004, -14.34966873604973081, 104.5844237280190185 ) ) ;
#5945 = CARTESIAN_POINT ( 'NONE',  ( -21.55341960407619339, 5.719274019375674811, 78.54275706135236135 ) ) ;
#5944 = CARTESIAN_POINT ( 'NONE',  ( -9.474510206698964154, 16.51473224551069663, 105.4155762719810383 ) ) ;
#5946 = CARTESIAN_POINT ( 'NONE',  ( 36.91746825000000598, -11.99521256947793546, -5.724999997268813701 ) ) ;
#5947 = CARTESIAN_POINT ( 'NONE',  ( -33.90110335395768715, 5.206480924673157595, 93.21819085016213080 ) ) ;
#5948 = CARTESIAN_POINT ( 'NONE',  ( 18.67979575497194134, -10.72451020669871369, 90.83442372801901854 ) ) ;
#5949 = CARTESIAN_POINT ( 'NONE',  ( 21.52544592524334988, 5.823673210054432836, 101.4594237280190185 ) ) ;
#5950 = DIRECTION ( 'NONE',  ( 0.000000000000000000, -0.5000000000000011102, -0.8660254037844379305 ) ) ;
#5951 = CARTESIAN_POINT ( 'NONE',  ( 9.474510206698971260, -16.51473224551069308, 102.9155762719810241 ) ) ;
#5952 = CARTESIAN_POINT ( 'NONE',  ( 9.564922557961047289, -16.46253265017146816, 20.41775706135233293 ) ) ;
#5953 = CARTESIAN_POINT ( 'NONE',  ( 39.99999999999999289, 2.428612866367529932E-14, -25.00000000000000000 ) ) ;
#5954 = CARTESIAN_POINT ( 'NONE',  ( -19.05341960407611168, -5.049401038298163336, 36.45724293864766707 ) ) ;
#5955 = CARTESIAN_POINT ( 'NONE',  ( 10.72451020669898902, -18.67979575497178502, 57.91557627198103120 ) ) ;
#5956 = CARTESIAN_POINT ( 'NONE',  ( 12.14591786802327356, -12.06949235617739191, 105.6260903946856899 ) ) ;
#5958 = CARTESIAN_POINT ( 'NONE',  ( 5.049401038298161559, -19.05341960407611168, 87.70724293864769550 ) ) ;
#5957 = CARTESIAN_POINT ( 'NONE',  ( -14.29746914071049879, 8.314922557960819915, 100.8322429386477097 ) ) ;
#5959 = CARTESIAN_POINT ( 'NONE',  ( -21.53943276465977519, -0.05219959533937600094, 103.7510903946857042 ) ) ;
#5960 = CARTESIAN_POINT ( 'NONE',  ( -5.049401038298153566, 19.05341960407611168, 35.20724293864768839 ) ) ;
#5961 = CARTESIAN_POINT ( 'NONE',  ( 4.379528057220339221, -16.55341960407611168, 97.70724293864772392 ) ) ;
#5962 = CARTESIAN_POINT ( 'NONE',  ( 15.80617190586769283, -15.72974639402175789, 60.62609039468567573 ) ) ;
#5963 = CARTESIAN_POINT ( 'NONE',  ( 18.62759615963271287, -10.81492255796078972, 93.33224293864769550 ) ) ;
#5964 = CARTESIAN_POINT ( 'NONE',  ( -9.474510206698720793, -16.51473224551083518, 54.58442372801899722 ) ) ;
#5965 = CARTESIAN_POINT ( 'NONE',  ( 17.58332526062526568, -7.635886036038552760, 48.42334959558466778 ) ) ;
#5966 = CARTESIAN_POINT ( 'NONE',  ( -16.51473224551069308, -9.474510206698971260, 96.66557627198102409 ) ) ;
#5967 = CARTESIAN_POINT ( 'NONE',  ( -16.55341960407611168, -4.379528057220339221, 71.45724293864769550 ) ) ;
#5968 = CARTESIAN_POINT ( 'NONE',  ( -16.51473224551082808, 9.474510206698731452, 38.33442372801899722 ) ) ;
#5969 = CARTESIAN_POINT ( 'NONE',  ( -13.89961937509977652, 13.97604488694528158, 60.62390960531436690 ) ) ;
#5970 = CARTESIAN_POINT ( 'NONE',  ( -8.314922557960811034, -14.29746914071050412, 47.08224293864770260 ) ) ;
#5971 = CARTESIAN_POINT ( 'NONE',  ( -19.03943276465977164, -0.05219959533935918106, 73.75109039468566152 ) ) ;
#5972 = CARTESIAN_POINT ( 'NONE',  ( 17.50000000000000000, -5.499999999999992895, 101.2176903769643559 ) ) ;
#5973 = CARTESIAN_POINT ( 'NONE',  ( -5.823673210054116645, -21.52544592524344225, 37.29057627198102409 ) ) ;
#5974 = CARTESIAN_POINT ( 'NONE',  ( -16.52544592524342804, 4.483927247898546575, 101.0405762719810383 ) ) ;
#5975 = CARTESIAN_POINT ( 'NONE',  ( -11.30153831258470731, -180.0000000000000568, -15.00000000000000178 ) ) ;
#5977 = CARTESIAN_POINT ( 'NONE',  ( 21.55341960407610458, 5.719274019375980345, 58.95724293864770971 ) ) ;
#5976 = CARTESIAN_POINT ( 'NONE',  ( 5.049401038298161559, -19.05341960407611168, 57.70724293864769550 ) ) ;
#5978 = CARTESIAN_POINT ( 'NONE',  ( -19.02544592524342804, 5.153800228976336051, 31.04057627198102409 ) ) ;
#5980 = CARTESIAN_POINT ( 'NONE',  ( -19.03943276465977164, 0.05219959533909376836, 61.24890960531436690 ) ) ;
#5979 = CARTESIAN_POINT ( 'NONE',  ( -0.05219959533934338120, 16.53943276465976808, 72.50109039468568994 ) ) ;
#5981 = CARTESIAN_POINT ( 'NONE',  ( 0.05219959533936267826, -19.03943276465977164, 55.00109039468566863 ) ) ;
#5982 = CARTESIAN_POINT ( 'NONE',  ( -18.62759615963255300, -10.81492255796106328, 74.16775706135231871 ) ) ;
#5983 = ORIENTED_EDGE ( 'NONE', *, *, #3150, .T. ) ;
#5984 = CARTESIAN_POINT ( 'NONE',  ( 5.719274019375991003, -21.55341960407610458, 47.70724293864770260 ) ) ;
#5985 = CARTESIAN_POINT ( 'NONE',  ( 13.97604488694527802, 13.89961937509977652, 29.37390960531435979 ) ) ;
#5986 = CARTESIAN_POINT ( 'NONE',  ( 4.379528057220092307, 16.55341960407617563, 82.29275706135234714 ) ) ;
#5987 = CARTESIAN_POINT ( 'NONE',  ( 13.89961937509957401, 13.97604488694547697, 101.8760903946856331 ) ) ;
#5988 = CARTESIAN_POINT ( 'NONE',  ( 5.049401038298161559, -19.05341960407611168, 27.70724293864769550 ) ) ;
#5990 = CARTESIAN_POINT ( 'NONE',  ( -15.80617190586745835, -15.72974639402198527, 56.87390960531436690 ) ) ;
#5989 = CARTESIAN_POINT ( 'NONE',  ( -4.500000000000001776, -120.9970989573719038, 14.58956564881030182 ) ) ;
#5991 = CARTESIAN_POINT ( 'NONE',  ( 15.72974639402176855, 15.80617190586768217, 96.87609039468568994 ) ) ;
#5992 = ORIENTED_EDGE ( 'NONE', *, *, #183981, .T. ) ;
#5993 = CARTESIAN_POINT ( 'NONE',  ( 8.224510206698953496, -14.34966873604960469, 47.91557627198102409 ) ) ;
#5994 = CARTESIAN_POINT ( 'NONE',  ( -16.55341960407611168, -4.379528057220339221, 51.45724293864770260 ) ) ;
#5995 = CARTESIAN_POINT ( 'NONE',  ( -15.72974639402197994, 15.80617190586746368, 85.62390960531436690 ) ) ;
#5996 = CARTESIAN_POINT ( 'NONE',  ( 15.72974639402199770, -15.80617190586745480, 93.12390960531436690 ) ) ;
#5997 = CARTESIAN_POINT ( 'NONE',  ( -1.135674102528219320, -29.41559601785655076, -49.03020479230151807 ) ) ;
#5998 = CARTESIAN_POINT ( 'NONE',  ( 21.52544592524344225, -5.823673210054117533, 28.54057627198103120 ) ) ;
#5999 = CARTESIAN_POINT ( 'NONE',  ( 8.224510206698742110, 14.34966873604972548, 67.08442372801901854 ) ) ;
#6000 = CARTESIAN_POINT ( 'NONE',  ( 8.224510206698953496, -14.34966873604960469, 77.91557627198102409 ) ) ;
#6001 = CARTESIAN_POINT ( 'NONE',  ( -5.153800228976328057, -19.02544592524343514, 32.29057627198102409 ) ) ;
#6002 =( NAMED_UNIT ( * ) PLANE_ANGLE_UNIT ( ) SI_UNIT ( $, .RADIAN. ) );
#6003 = DIRECTION ( 'NONE',  ( -7.709882115452472644E-15, 0.000000000000000000, 1.000000000000000000 ) ) ;
#6004 = CARTESIAN_POINT ( 'NONE',  ( 8.314922557961029526, -14.29746914071037800, 90.41775706135236135 ) ) ;
#6005 = CARTESIAN_POINT ( 'NONE',  ( -21.53943276465977519, 0.05219959533907696930, 116.2489096053143669 ) ) ;
#6006 = CARTESIAN_POINT ( 'NONE',  ( 5.049401038298161559, -19.05341960407611168, 77.70724293864765286 ) ) ;
#6007 = CARTESIAN_POINT ( 'NONE',  ( -21.52544592524334988, -5.823673210054445271, 53.95942372801900433 ) ) ;
#6008 = CARTESIAN_POINT ( 'NONE',  ( 5.049401038298161559, -19.05341960407611168, 107.7072429386476955 ) ) ;
#6010 = ADVANCED_FACE ( 'NONE', ( #112734 ), #110751, .T. ) ;
#6009 = CARTESIAN_POINT ( 'NONE',  ( -2.919401842228618094, -40.72031138817900597, -24.99999999999999289 ) ) ;
#6011 = ORIENTED_EDGE ( 'NONE', *, *, #13792, .F. ) ;
#6012 = CARTESIAN_POINT ( 'NONE',  ( 21.53943276465977519, 0.05219959533937863772, 41.25109039468568284 ) ) ;
#6014 = CARTESIAN_POINT ( 'NONE',  ( 9.474510206698971260, -16.51473224551069308, 97.91557627198102409 ) ) ;
#6013 = CARTESIAN_POINT ( 'NONE',  ( 16.51473224551069308, 9.474510206698969483, 39.16557627198103120 ) ) ;
#6015 = CARTESIAN_POINT ( 'NONE',  ( 19.03943276465977164, 0.05219959533936151252, 56.25109039468566863 ) ) ;
#6016 = CARTESIAN_POINT ( 'NONE',  ( -18.62759615963255300, -10.81492255796106328, 29.16775706135234003 ) ) ;
#6017 = CARTESIAN_POINT ( 'NONE',  ( 9.564922557961047289, -16.46253265017146816, 45.41775706135232582 ) ) ;
#6018 = CARTESIAN_POINT ( 'NONE',  ( 13.97604488694527802, 13.89961937509977652, 29.37390960531435979 ) ) ;
#6019 = CARTESIAN_POINT ( 'NONE',  ( 16.52544592524335698, 4.483927247898782831, 96.45942372801901854 ) ) ;
#6020 = CARTESIAN_POINT ( 'NONE',  ( 5.049401038297881783, 19.05341960407617563, 57.29275706135231871 ) ) ;
#6021 = CARTESIAN_POINT ( 'NONE',  ( -16.53943276465976808, -0.05219959533934237506, 108.7510903946857042 ) ) ;
#6022 = CARTESIAN_POINT ( 'NONE',  ( 17.72560187377285601, 5.500000000000046185, 86.57814504131317790 ) ) ;
#6023 = CARTESIAN_POINT ( 'NONE',  ( 13.89961937509977652, -13.97604488694527269, 88.12390960531438111 ) ) ;
#6024 = CARTESIAN_POINT ( 'NONE',  ( -5.719274019375665041, -21.55341960407619695, 94.79275706135234714 ) ) ;
#6025 = CARTESIAN_POINT ( 'NONE',  ( 10.72451020669871369, 18.67979575497193778, 107.0844237280190043 ) ) ;
#6026 = CARTESIAN_POINT ( 'NONE',  ( -30.73962218707678673, 22.33364281372846705, -4.202157773949823927 ) ) ;
#6027 = CARTESIAN_POINT ( 'NONE',  ( -9.564922557960796823, -16.46253265017161027, 107.0822429386476955 ) ) ;
#6028 = CARTESIAN_POINT ( 'NONE',  ( -21.55341960407619339, 5.719274019375674811, 73.54275706135234714 ) ) ;
#6029 = CARTESIAN_POINT ( 'NONE',  ( -5.153800228976607833, 19.02544592524334988, 112.7094237280190043 ) ) ;
#6030 = CARTESIAN_POINT ( 'NONE',  ( 5.049401038298161559, -19.05341960407611168, 82.70724293864770971 ) ) ;
#6031 = CARTESIAN_POINT ( 'NONE',  ( 21.52544592524344225, -5.823673210054117533, 33.54057627198102409 ) ) ;
#6032 = CARTESIAN_POINT ( 'NONE',  ( -0.05219959533909027116, -19.03943276465977164, 92.49890960531436690 ) ) ;
#6033 = CARTESIAN_POINT ( 'NONE',  ( -40.00200000000003087, -1.071565949253934124E-14, 102.5000000000000142 ) ) ;
#6034 = CARTESIAN_POINT ( 'NONE',  ( 5.049401038298161559, -19.05341960407611168, 77.70724293864765286 ) ) ;
#6035 = CARTESIAN_POINT ( 'NONE',  ( -9.564922557960796823, -16.46253265017161027, 62.08224293864769550 ) ) ;
#6036 = CARTESIAN_POINT ( 'NONE',  ( 14.29746914071037800, 8.314922557961029526, 111.6677570613523613 ) ) ;
#6037 = CARTESIAN_POINT ( 'NONE',  ( -16.20579543436698700, 7.371946100355027731, 99.43479165828048849 ) ) ;
#6038 = CARTESIAN_POINT ( 'NONE',  ( -5.153800228976607833, 19.02544592524334988, 67.70942372801900433 ) ) ;
#6039 = CARTESIAN_POINT ( 'NONE',  ( 9.564922557960805705, 16.46253265017160317, 99.58224293864770971 ) ) ;
#6040 = CARTESIAN_POINT ( 'NONE',  ( 8.314922557960818139, 14.29746914071049879, 89.58224293864768129 ) ) ;
#6041 = B_SPLINE_CURVE_WITH_KNOTS ( 'NONE', 3,
 ( #29383, #75859, #10232, #40563, #148744, #71892, #133563, #106031, #72734, #73732, #199044, #198056, #181899, #151560, #137365, #58543, #153527, #165735, #89877, #167717, #11058, #118235, #42392, #44375, #60514, #57563 ),
 .UNSPECIFIED., .F., .F.,
 ( 4, 2, 2, 2, 2, 2, 2, 2, 2, 2, 2, 2, 4 ),
 ( 1.971416325814069830E-07, 0.0002960211146592699161, 0.0005918450876859584521, 0.0008876690607126472591, 0.001183493033739336066, 0.001775140979792709343, 0.002366788925846082838, 0.002662612898872765248, 0.002958436871899448525, 0.003254260844926130936, 0.003550084817952813779, 0.004141732764006179034, 0.004733380710059543854 ),
 .UNSPECIFIED. ) ;
#6042 = CARTESIAN_POINT ( 'NONE',  ( 10.72451020669898902, -18.67979575497178502, 47.91557627198102409 ) ) ;
#6043 = CARTESIAN_POINT ( 'NONE',  ( 18.67979575497178502, 10.72451020669898547, 29.16557627198103120 ) ) ;
#6044 = CARTESIAN_POINT ( 'NONE',  ( -12.14591786802309592, -12.06949235617757132, 106.8739096053143811 ) ) ;
#6045 = CARTESIAN_POINT ( 'NONE',  ( -17.44270441346513678, 5.991230190323085125, 53.63664920735775610 ) ) ;
#6046 = CARTESIAN_POINT ( 'NONE',  ( 5.049401038297881783, 19.05341960407617563, 42.29275706135234003 ) ) ;
#6047 = CARTESIAN_POINT ( 'NONE',  ( -4.379528057220328563, 16.55341960407611168, 30.20724293864769550 ) ) ;
#6048 = CARTESIAN_POINT ( 'NONE',  ( -13.97604488694527625, -13.89961937509977652, 106.8739096053143669 ) ) ;
#6049 = CARTESIAN_POINT ( 'NONE',  ( 15.72974639402176855, 15.80617190586768217, 71.87609039468568994 ) ) ;
#6050 = CARTESIAN_POINT ( 'NONE',  ( -18.67979575497178146, -10.72451020669898902, 61.66557627198103120 ) ) ;
#6051 = CARTESIAN_POINT ( 'NONE',  ( 18.67979575497194134, -10.72451020669871369, 50.83442372801901143 ) ) ;
#6052 = CARTESIAN_POINT ( 'NONE',  ( -5.823673210054116645, -21.52544592524344225, 82.29057627198103830 ) ) ;
#6053 = CARTESIAN_POINT ( 'NONE',  ( 18.62759615963255655, 10.81492255796105972, 41.66775706135235424 ) ) ;
#6054 = CARTESIAN_POINT ( 'NONE',  ( 12.06949235617757843, -12.14591786802309237, 113.1239096053143953 ) ) ;
#6055 = CARTESIAN_POINT ( 'NONE',  ( -5.049401038297874678, -19.05341960407617918, 74.79275706135231871 ) ) ;
#6056 = CARTESIAN_POINT ( 'NONE',  ( 16.51473224551069308, 9.474510206698969483, 39.16557627198103120 ) ) ;
#6057 = CARTESIAN_POINT ( 'NONE',  ( -16.53943276465976808, 0.05219959533911058130, 86.24890960531436690 ) ) ;
#6058 = CARTESIAN_POINT ( 'NONE',  ( 16.51473224551069308, 9.474510206698969483, 104.1655762719810241 ) ) ;
#6059 = CARTESIAN_POINT ( 'NONE',  ( -19.05341960407611168, -5.049401038298163336, 26.45724293864769550 ) ) ;
#6060 = CARTESIAN_POINT ( 'NONE',  ( 16.52544592524342804, -4.483927247898539470, 43.54057627198103830 ) ) ;
#6061 = CARTESIAN_POINT ( 'NONE',  ( 12.14591786802327356, -12.06949235617739191, 95.62609039468568994 ) ) ;
#6062 = CARTESIAN_POINT ( 'NONE',  ( 5.049401038298161559, -19.05341960407611168, 57.70724293864769550 ) ) ;
#6063 = CARTESIAN_POINT ( 'NONE',  ( -13.89961937509977652, 13.97604488694528158, 25.62390960531434558 ) ) ;
#6064 = CARTESIAN_POINT ( 'NONE',  ( -13.97604488694547697, 13.89961937509957934, 28.12609039468565797 ) ) ;
#6066 = CARTESIAN_POINT ( 'NONE',  ( -14.29746914071049879, 8.314922557960819915, 35.83224293864768839 ) ) ;
#6065 = CARTESIAN_POINT ( 'NONE',  ( 0.05219959533909260263, 19.03943276465977164, 109.9989096053143669 ) ) ;
#6067 = CARTESIAN_POINT ( 'NONE',  ( 21.55341960407619695, -5.719274019375665929, 46.04275706135234714 ) ) ;
#6068 = CARTESIAN_POINT ( 'NONE',  ( -14.61778469963293325, -34.91027835867548390, -28.77367925216612576 ) ) ;
#6069 = CARTESIAN_POINT ( 'NONE',  ( 14.29746914071037800, 8.314922557961029526, 61.66775706135235424 ) ) ;
#6070 = CARTESIAN_POINT ( 'NONE',  ( 4.379528057220339221, -16.55341960407611168, 22.70724293864769194 ) ) ;
#6071 = CARTESIAN_POINT ( 'NONE',  ( -4.379528057220086978, -16.55341960407618274, 109.7927570613523613 ) ) ;
#6072 = CARTESIAN_POINT ( 'NONE',  ( -16.53943276465976808, -0.05219959533934237506, 23.75109039468567929 ) ) ;
#6073 = CARTESIAN_POINT ( 'NONE',  ( -5.049401038298153566, 19.05341960407611168, 50.20724293864770260 ) ) ;
#6074 = CARTESIAN_POINT ( 'NONE',  ( 16.53943276465976808, -0.05219959533910856209, 108.7489096053143669 ) ) ;
#6075 = CARTESIAN_POINT ( 'NONE',  ( 5.823673210054125526, 21.52544592524343514, 114.7905762719810383 ) ) ;
#6076 = CARTESIAN_POINT ( 'NONE',  ( -5.049401038298153566, 19.05341960407611168, 50.20724293864770260 ) ) ;
#6077 = CARTESIAN_POINT ( 'NONE',  ( -3.874011537017815865, -5.668178584001447362, -62.37582247038324823 ) ) ;
#6078 = CARTESIAN_POINT ( 'NONE',  ( 9.474510206698971260, -16.51473224551069308, 27.91557627198103120 ) ) ;
#6079 = CARTESIAN_POINT ( 'NONE',  ( -18.67979575497178146, -10.72451020669898902, 21.66557627198102409 ) ) ;
#6080 = CARTESIAN_POINT ( 'NONE',  ( -17.44270441346516876, -5.991230190323022065, 36.36335079264227232 ) ) ;
#6081 = CARTESIAN_POINT ( 'NONE',  ( 16.46253265017160672, -9.564922557960803928, 98.33224293864769550 ) ) ;
#6083 = CARTESIAN_POINT ( 'NONE',  ( -8.314922557960811034, -14.29746914071050412, 102.0822429386476955 ) ) ;
#6082 = CARTESIAN_POINT ( 'NONE',  ( 5.719274019375673035, 21.55341960407619339, 47.29275706135234003 ) ) ;
#6084 = CARTESIAN_POINT ( 'NONE',  ( -5.049401038298153566, 19.05341960407611168, 105.2072429386476671 ) ) ;
#6085 = CARTESIAN_POINT ( 'NONE',  ( -27.91252812235343228, -7.473505457753331527, 160.9450913315372986 ) ) ;
#6086 = CARTESIAN_POINT ( 'NONE',  ( 4.379528057220092307, 16.55341960407617563, 77.29275706135234714 ) ) ;
#6087 = CARTESIAN_POINT ( 'NONE',  ( -21.53943276465977519, -0.05219959533937600094, 98.75109039468568994 ) ) ;
#6088 = CARTESIAN_POINT ( 'NONE',  ( -12.06949235617739369, -12.14591786802326823, 54.37609039468568994 ) ) ;
#6089 = CARTESIAN_POINT ( 'NONE',  ( 16.46253265017160672, -9.564922557960803928, 98.33224293864769550 ) ) ;
#6090 = CARTESIAN_POINT ( 'NONE',  ( 0.05219959533934541429, -16.53943276465976808, 40.00109039468567573 ) ) ;
#6091 = CARTESIAN_POINT ( 'NONE',  ( -5.153800228976607833, 19.02544592524334988, 107.7094237280189759 ) ) ;
#6092 = CARTESIAN_POINT ( 'NONE',  ( -8.224510206698735004, -14.34966873604973081, 79.58442372801903275 ) ) ;
#6093 = CARTESIAN_POINT ( 'NONE',  ( -16.46253265017146816, -9.564922557961047289, 109.1677570613523471 ) ) ;
#6094 = CARTESIAN_POINT ( 'NONE',  ( -5.049401038298153566, 19.05341960407611168, 75.20724293864769550 ) ) ;
#6095 = CARTESIAN_POINT ( 'NONE',  ( 18.62759615963271287, -10.81492255796078972, 103.3322429386476955 ) ) ;
#6097 = CARTESIAN_POINT ( 'NONE',  ( 16.46253265017146816, 9.564922557961045513, 106.6677570613523471 ) ) ;
#6096 = CARTESIAN_POINT ( 'NONE',  ( 16.53943276465976808, -0.05219959533910856209, 103.7489096053143669 ) ) ;
#6098 = CARTESIAN_POINT ( 'NONE',  ( -14.29746914071037622, -8.314922557961029526, 69.16775706135234714 ) ) ;
#6099 = CARTESIAN_POINT ( 'NONE',  ( 19.02544592524334988, 5.153800228976608722, 76.45942372801897591 ) ) ;
#6100 = CARTESIAN_POINT ( 'NONE',  ( 4.483927247898545687, 16.52544592524342804, 34.79057627198103120 ) ) ;
#6101 = CARTESIAN_POINT ( 'NONE',  ( 8.314922557960818139, 14.29746914071049879, 99.58224293864770971 ) ) ;
#6102 = CARTESIAN_POINT ( 'NONE',  ( -19.03943276465977164, -0.05219959533935918106, 33.75109039468566863 ) ) ;
#6103 = CARTESIAN_POINT ( 'NONE',  ( -5.823673210054431948, 21.52544592524334988, 42.70942372801901854 ) ) ;
#6104 = CARTESIAN_POINT ( 'NONE',  ( -13.89961937509957401, -13.97604488694547875, 94.37609039468566152 ) ) ;
#6105 = CARTESIAN_POINT ( 'NONE',  ( 13.89961937509977652, -13.97604488694527269, 113.1239096053143527 ) ) ;
#6106 = CARTESIAN_POINT ( 'NONE',  ( 19.02544592524343514, -5.153800228976328945, 88.54057627198102409 ) ) ;
#6107 = CARTESIAN_POINT ( 'NONE',  ( -18.62759615963255300, -10.81492255796106328, 109.1677570613523613 ) ) ;
#6108 = CARTESIAN_POINT ( 'NONE',  ( 13.97604488694527802, 13.89961937509977652, 74.37390960531436690 ) ) ;
#6109 = CARTESIAN_POINT ( 'NONE',  ( 21.52544592524344225, -5.823673210054117533, 43.54057627198103830 ) ) ;
#6110 = CARTESIAN_POINT ( 'NONE',  ( 12.14591786802309770, 12.06949235617756955, 94.37390960531436690 ) ) ;
#6111 = CARTESIAN_POINT ( 'NONE',  ( 9.564922557960805705, 16.46253265017160317, 59.58224293864769550 ) ) ;
#6112 = CARTESIAN_POINT ( 'NONE',  ( -14.29746914071049879, 8.314922557960819915, 115.8322429386477097 ) ) ;
#6113 = CARTESIAN_POINT ( 'NONE',  ( -0.05219959533937732626, 21.53943276465977519, 27.50109039468567929 ) ) ;
#6114 = CARTESIAN_POINT ( 'NONE',  ( 15.80617190586769283, -15.72974639402175789, 80.62609039468567573 ) ) ;
#6115 = CARTESIAN_POINT ( 'NONE',  ( -0.05219959533909027116, -19.03943276465977164, 42.49890960531435269 ) ) ;
#6116 = CARTESIAN_POINT ( 'NONE',  ( 16.52544592524335698, 4.483927247898782831, 81.45942372801900433 ) ) ;
#6117 = CARTESIAN_POINT ( 'NONE',  ( -15.72974639402176322, -15.80617190586768395, 19.37609039468568639 ) ) ;
#6118 = ORIENTED_EDGE ( 'NONE', *, *, #178686, .F. ) ;
#6119 = CARTESIAN_POINT ( 'NONE',  ( -5.719274019375665041, -21.55341960407619695, 29.79275706135234358 ) ) ;
#6121 = CARTESIAN_POINT ( 'NONE',  ( -13.97604488694527625, -13.89961937509977652, 61.87390960531435979 ) ) ;
#6120 = CARTESIAN_POINT ( 'NONE',  ( -13.97604488694547697, 13.89961937509957934, 48.12609039468566863 ) ) ;
#6122 = CARTESIAN_POINT ( 'NONE',  ( -0.05219959533936034679, 19.03943276465977164, 32.50109039468566863 ) ) ;
#6123 = CARTESIAN_POINT ( 'NONE',  ( 5.719274019375673035, 21.55341960407619339, 77.29275706135234714 ) ) ;
#6124 = CARTESIAN_POINT ( 'NONE',  ( 21.55341960407610458, 5.719274019375980345, 68.95724293864769550 ) ) ;
#6125 = CARTESIAN_POINT ( 'NONE',  ( -16.53943276465976808, 0.05219959533911058130, 46.24890960531435979 ) ) ;
#6127 = CARTESIAN_POINT ( 'NONE',  ( 19.02544592524334988, 5.153800228976608722, 31.45942372801900433 ) ) ;
#6126 = CARTESIAN_POINT ( 'NONE',  ( 21.52544592524334988, 5.823673210054432836, 86.45942372801901854 ) ) ;
#6128 = CARTESIAN_POINT ( 'NONE',  ( -4.379528057220328563, 16.55341960407611168, 75.20724293864769550 ) ) ;
#6129 = CARTESIAN_POINT ( 'NONE',  ( -19.05341960407611168, -5.049401038298163336, 26.45724293864769550 ) ) ;
#6130 = CARTESIAN_POINT ( 'NONE',  ( 13.89961937509957401, 13.97604488694547697, 61.87609039468566863 ) ) ;
#6131 = CARTESIAN_POINT ( 'NONE',  ( -14.34966873604960291, -8.224510206698953496, 26.66557627198103475 ) ) ;
#6132 = CARTESIAN_POINT ( 'NONE',  ( 18.67979575497194134, -10.72451020669871369, 80.83442372801901854 ) ) ;
#6133 = CARTESIAN_POINT ( 'NONE',  ( -5.049401038297874678, -19.05341960407617918, 44.79275706135232582 ) ) ;
#6134 = CARTESIAN_POINT ( 'NONE',  ( -15.80617190586745835, -15.72974639402198527, 56.87390960531436690 ) ) ;
#6135 = CARTESIAN_POINT ( 'NONE',  ( 21.53943276465977519, 0.05219959533937863772, 41.25109039468568284 ) ) ;
#6136 = AXIS2_PLACEMENT_3D ( 'NONE', #66629, #172837, #37289 ) ;
#6137 = CARTESIAN_POINT ( 'NONE',  ( 18.62759615963271287, -10.81492255796078972, 98.33224293864769550 ) ) ;
#6138 = CARTESIAN_POINT ( 'NONE',  ( 16.51473224551083163, -9.474510206698727899, 100.8344237280190043 ) ) ;
#6139 = CARTESIAN_POINT ( 'NONE',  ( 12.14591786802327356, -12.06949235617739191, 70.62609039468567573 ) ) ;
#6141 = CARTESIAN_POINT ( 'NONE',  ( -21.52544592524343514, 5.823673210054127303, 106.0405762719810525 ) ) ;
#6140 = CARTESIAN_POINT ( 'NONE',  ( 17.50000000000000000, -5.500000000000031086, 98.29690382534174375 ) ) ;
#6142 = CARTESIAN_POINT ( 'NONE',  ( -4.379528057220328563, 16.55341960407611168, 95.20724293864769550 ) ) ;
#6143 = LINE ( 'NONE', #113321, #114368 ) ;
#6144 = CARTESIAN_POINT ( 'NONE',  ( 12.06949235617739724, 12.14591786802326823, 41.87609039468568284 ) ) ;
#6145 = EDGE_CURVE ( 'NONE', #27850, #11421, #169810, .T. ) ;
#6146 = CARTESIAN_POINT ( 'NONE',  ( 15.72974639402199770, -15.80617190586745480, 43.12390960531435269 ) ) ;
#6147 = CARTESIAN_POINT ( 'NONE',  ( 16.53943276465976808, 0.05219959533934440121, 96.25109039468568994 ) ) ;
#6148 = CARTESIAN_POINT ( 'NONE',  ( 13.97604488694527802, 13.89961937509977652, 24.37390960531435624 ) ) ;
#6149 = B_SPLINE_CURVE_WITH_KNOTS ( 'NONE', 3,
 ( #55086, #194613, #23762, #131931, #118773, #56085, #85411, #180461, #11605, #71262, #10597, #8588, #165274, #26768 ),
 .UNSPECIFIED., .F., .F.,
 ( 4, 2, 2, 2, 2, 2, 4 ),
 ( 0.000000000000000000, 0.002096066633256107002, 0.003144099949884150962, 0.004192133266512195790, 0.006288199899768283710, 0.007336233216396328971, 0.008384266533024374232 ),
 .UNSPECIFIED. ) ;
#6150 = CARTESIAN_POINT ( 'NONE',  ( -16.53943276465976808, -0.05219959533934237506, 63.75109039468568284 ) ) ;
#6151 = CARTESIAN_POINT ( 'NONE',  ( 0.05219959533937995610, -21.53943276465977519, 40.00109039468567573 ) ) ;
#6152 = CARTESIAN_POINT ( 'NONE',  ( 18.62759615963271287, -10.81492255796078972, 63.33224293864770260 ) ) ;
#6153 = CARTESIAN_POINT ( 'NONE',  ( 8.314922557961029526, -14.29746914071037800, 80.41775706135234714 ) ) ;
#6154 = CARTESIAN_POINT ( 'NONE',  ( 18.67979575497194134, -10.72451020669871369, 70.83442372801901854 ) ) ;
#6155 = CARTESIAN_POINT ( 'NONE',  ( 15.72974639402199770, -15.80617190586745480, 58.12390960531435979 ) ) ;
#6156 = CARTESIAN_POINT ( 'NONE',  ( 15.72974639402199770, -15.80617190586745480, 38.12390960531436690 ) ) ;
#6157 = CARTESIAN_POINT ( 'NONE',  ( 0.05219959533934541429, -16.53943276465976808, 60.00109039468568284 ) ) ;
#6158 = CARTESIAN_POINT ( 'NONE',  ( -21.55341960407610458, -5.719274019375992779, 36.45724293864768839 ) ) ;
#6159 = ORIENTED_EDGE ( 'NONE', *, *, #78263, .T. ) ;
#6160 = CARTESIAN_POINT ( 'NONE',  ( -0.05219959533909027116, -19.03943276465977164, 102.4989096053143669 ) ) ;
#6161 = CARTESIAN_POINT ( 'NONE',  ( 8.224510206698742110, 14.34966873604972548, 107.0844237280190043 ) ) ;
#6162 = CARTESIAN_POINT ( 'NONE',  ( -18.09867054820431775, -5.499999999999927169, 78.98393025253584199 ) ) ;
#6163 = CARTESIAN_POINT ( 'NONE',  ( 0.05219959533910956823, 16.53943276465976808, 114.9989096053143669 ) ) ;
#6164 = CARTESIAN_POINT ( 'NONE',  ( 18.67979575497178502, 10.72451020669898547, 59.16557627198103120 ) ) ;
#6165 = CARTESIAN_POINT ( 'NONE',  ( 19.05341960407611168, 5.049401038298154454, 38.95724293864767418 ) ) ;
#6166 = CARTESIAN_POINT ( 'NONE',  ( 16.53943276465976808, 0.05219959533934440121, 96.25109039468568994 ) ) ;
#6167 = CARTESIAN_POINT ( 'NONE',  ( 10.72451020669871369, 18.67979575497193778, 37.08442372801901143 ) ) ;
#6168 = CARTESIAN_POINT ( 'NONE',  ( 0.05219959533936267826, -19.03943276465977164, 95.00109039468567573 ) ) ;
#6169 = CARTESIAN_POINT ( 'NONE',  ( 12.06949235617757843, -12.14591786802309237, 108.1239096053143811 ) ) ;
#6170 = CARTESIAN_POINT ( 'NONE',  ( 9.564922557960805705, 16.46253265017160317, 59.58224293864769550 ) ) ;
#6171 = CARTESIAN_POINT ( 'NONE',  ( -6.856101608890801443E-16, -71.74905178543389184, -22.99263613531268291 ) ) ;
#6172 = FACE_BOUND ( 'NONE', #14736, .T. ) ;
#6173 = CARTESIAN_POINT ( 'NONE',  ( 9.564922557960805705, 16.46253265017160317, 79.58224293864769550 ) ) ;
#6174 = CARTESIAN_POINT ( 'NONE',  ( 16.52544592524335698, 4.483927247898782831, 61.45942372801901854 ) ) ;
#6175 = CARTESIAN_POINT ( 'NONE',  ( 10.81492255796106328, -18.62759615963255655, 100.4177570613523471 ) ) ;
#6176 = CARTESIAN_POINT ( 'NONE',  ( 21.53943276465977519, -0.05219959533907433946, 48.74890960531435979 ) ) ;
#6177 = CARTESIAN_POINT ( 'NONE',  ( -0.05219959533934338120, 16.53943276465976808, 72.50109039468568994 ) ) ;
#6178 = CARTESIAN_POINT ( 'NONE',  ( -16.46253265017146816, -9.564922557961047289, 64.16775706135233293 ) ) ;
#6179 = VERTEX_POINT ( 'NONE', #111749 ) ;
#6180 = CARTESIAN_POINT ( 'NONE',  ( -15.72974639402176322, -15.80617190586768395, 69.37609039468567573 ) ) ;
#6181 = CARTESIAN_POINT ( 'NONE',  ( 5.153800228976335163, 19.02544592524342804, 69.79057627198103830 ) ) ;
#6182 = CARTESIAN_POINT ( 'NONE',  ( 9.474510206698971260, -16.51473224551069308, 32.91557627198102409 ) ) ;
#6183 = CARTESIAN_POINT ( 'NONE',  ( 9.474510206698729675, 16.51473224551082808, 62.08442372801899722 ) ) ;
#6184 = CARTESIAN_POINT ( 'NONE',  ( 5.153800228976335163, 19.02544592524342804, 109.7905762719810099 ) ) ;
#6185 = CARTESIAN_POINT ( 'NONE',  ( 13.97604488694527802, 13.89961937509977652, 99.37390960531436690 ) ) ;
#6186 = CARTESIAN_POINT ( 'NONE',  ( -16.52544592524342804, 4.483927247898546575, 56.04057627198102409 ) ) ;
#6187 = CARTESIAN_POINT ( 'NONE',  ( -10.81492255796078084, -18.62759615963271287, 52.08224293864768839 ) ) ;
#6188 = CARTESIAN_POINT ( 'NONE',  ( 0.000000000000000000, 0.000000000000000000, -23.00000000000000355 ) ) ;
#6189 = CARTESIAN_POINT ( 'NONE',  ( 5.153800228976615827, -19.02544592524334988, 30.20942372801900433 ) ) ;
#6190 = DIRECTION ( 'NONE',  ( 0.000000000000000000, 0.000000000000000000, -1.000000000000000000 ) ) ;
#6191 = CARTESIAN_POINT ( 'NONE',  ( 9.564922557960805705, 16.46253265017160317, 49.58224293864770260 ) ) ;
#6192 = CARTESIAN_POINT ( 'NONE',  ( 12.14591786802327356, -12.06949235617739191, 35.62609039468568994 ) ) ;
#6193 = CARTESIAN_POINT ( 'NONE',  ( 14.18669005401828187, -34.08280046153741694, -8.000000000000001776 ) ) ;
#6194 = DIRECTION ( 'NONE',  ( 0.000000000000000000, 0.000000000000000000, 1.000000000000000000 ) ) ;
#6195 = CARTESIAN_POINT ( 'NONE',  ( -14.29746914071037622, -8.314922557961029526, 74.16775706135231871 ) ) ;
#6196 = CARTESIAN_POINT ( 'NONE',  ( -15.80617190586745835, -15.72974639402198527, 96.87390960531436690 ) ) ;
#6197 =( BOUNDED_CURVE ( )  B_SPLINE_CURVE ( 2, ( #81814, #143502, #159671, #66672, #82823, #72681, #162677, #54502, #119183, #149510, #27182, #150522, #133337, #116174, #57515, #146496, #11007, #120160, #7987, #177864, #55501, #102008, #180868, #134356, #40333, #39333, #181851, #178866, #195028, #41342, #103004, #117171, #166685, #164689, #100992, #163690, #86834, #148520, #10010, #135355, #131337, #147523, #25192, #165684, #71670, #26184, #193025, #24183, #43330, #9011, #132345, #85833, #12021, #69670, #56505, #196040, #70679, #118183, #194037, #88829, #179874, #42344, #87824, #104006, #73683, #197027, #58494, #104998, #84817, #137318, #89829, #15971, #168643, #108964, #60466, #59476, #778, #183829, #151510, #182843, #78616, #44326, #31142, #167669, #75640, #62449, #140291, #121150, #13973, #105985, #29167, #13002, #124123, #30142, #46303, #198999, #77631, #185822, #123132, #74665, #32133 ),
 .UNSPECIFIED., .F., .F. ) 
 B_SPLINE_CURVE_WITH_KNOTS ( ( 3, 2, 2, 2, 2, 2, 2, 2, 2, 2, 2, 2, 2, 2, 2, 2, 2, 2, 2, 2, 2, 2, 2, 2, 2, 2, 2, 2, 2, 2, 2, 2, 2, 2, 2, 2, 2, 2, 2, 2, 2, 2, 2, 2, 2, 2, 2, 2, 2, 2, 3 ),
 ( 0.000000000000000000, 0.02000000000000000042, 0.04000000000000000083, 0.05999999999999999778, 0.08000000000000000167, 0.1000000000000000056, 0.1199999999999999956, 0.1400000000000000133, 0.1600000000000000033, 0.1799999999999999933, 0.2000000000000000111, 0.2200000000000000011, 0.2399999999999999911, 0.2600000000000000089, 0.2800000000000000266, 0.2999999999999999889, 0.3200000000000000067, 0.3400000000000000244, 0.3599999999999999867, 0.3800000000000000044, 0.4000000000000000222, 0.4199999999999999845, 0.4400000000000000022, 0.4600000000000000200, 0.4799999999999999822, 0.5000000000000000000, 0.5200000000000000178, 0.5400000000000000355, 0.5600000000000000533, 0.5799999999999999600, 0.5999999999999999778, 0.6199999999999999956, 0.6400000000000000133, 0.6600000000000000311, 0.6800000000000000488, 0.6999999999999999556, 0.7199999999999999734, 0.7399999999999999911, 0.7600000000000000089, 0.7800000000000000266, 0.8000000000000000444, 0.8199999999999999512, 0.8399999999999999689, 0.8599999999999999867, 0.8800000000000000044, 0.9000000000000000222, 0.9200000000000000400, 0.9399999999999999467, 0.9599999999999999645, 0.9799999999999999822, 1.000000000000000000 ),
 .UNSPECIFIED. ) 
 CURVE ( )  GEOMETRIC_REPRESENTATION_ITEM ( )  RATIONAL_B_SPLINE_CURVE ( ( 1.000000000000000000, 0.9510565162951535312, 1.000000000000000000, 0.9510565162951535312, 1.000000000000000000, 0.9510565162951535312, 1.000000000000000000, 0.9510565162951535312, 1.000000000000000000, 0.9510565162951535312, 1.000000000000000000, 0.9510565162951535312, 1.000000000000000000, 0.9510565162951535312, 1.000000000000000000, 0.9510565162951535312, 1.000000000000000000, 0.9510565162951535312, 1.000000000000000000, 0.9510565162951535312, 1.000000000000000000, 0.9510565162951535312, 1.000000000000000000, 0.9510565162951535312, 1.000000000000000000, 0.9510565162951535312, 1.000000000000000000, 0.9510565162951535312, 1.000000000000000000, 0.9510565162951535312, 1.000000000000000000, 0.9510565162951535312, 1.000000000000000000, 0.9510565162951535312, 1.000000000000000000, 0.9510565162951535312, 1.000000000000000000, 0.9510565162951535312, 1.000000000000000000, 0.9510565162951535312, 1.000000000000000000, 0.9510565162951535312, 1.000000000000000000, 0.9510565162951535312, 1.000000000000000000, 0.9510565162951535312, 1.000000000000000000, 0.9510565162951535312, 1.000000000000000000, 0.9510565162951535312, 1.000000000000000000, 0.9510565162951535312, 1.000000000000000000, 0.9510565162951535312, 1.000000000000000000, 0.9510565162951535312, 1.000000000000000000, 0.9510565162951535312, 1.000000000000000000, 0.9510565162951535312, 1.000000000000000000, 0.9510565162951535312, 1.000000000000000000, 0.9510565162951535312, 1.000000000000000000, 0.9510565162951535312, 1.000000000000000000, 0.9510565162951535312, 1.000000000000000000, 0.9510565162951535312, 1.000000000000000000, 0.9510565162951535312, 1.000000000000000000, 0.9510565162951535312, 1.000000000000000000, 0.9510565162951535312, 1.000000000000000000, 0.9510565162951535312, 1.000000000000000000, 0.9510565162951535312, 1.000000000000000000, 0.9510565162951535312, 1.000000000000000000, 0.9510565162951535312, 1.000000000000000000, 0.9510565162951535312, 1.000000000000000000, 0.9510565162951535312, 1.000000000000000000, 0.9510565162951535312, 1.000000000000000000, 0.9510565162951535312, 1.000000000000000000, 0.9510565162951535312, 1.000000000000000000, 0.9510565162951535312, 1.000000000000000000, 0.9510565162951535312, 1.000000000000000000, 0.9510565162951535312, 1.000000000000000000 ) ) 
 REPRESENTATION_ITEM ( '' )  );
#6199 = CARTESIAN_POINT ( 'NONE',  ( -38.00000000000000711, 2.428612866367529932E-14, -5.749999994537626336 ) ) ;
#6198 = CARTESIAN_POINT ( 'NONE',  ( -19.05341960407611168, -5.049401038298163336, 36.45724293864766707 ) ) ;
#6200 = CARTESIAN_POINT ( 'NONE',  ( 5.719274019375673035, 21.55341960407619339, 37.29275706135235424 ) ) ;
#6201 = CARTESIAN_POINT ( 'NONE',  ( -19.05341960407617563, 5.049401038297882671, 48.54275706135233293 ) ) ;
#6202 = CARTESIAN_POINT ( 'NONE',  ( 9.564922557960805705, 16.46253265017160317, 44.58224293864769550 ) ) ;
#6203 = CARTESIAN_POINT ( 'NONE',  ( 21.53943276465977519, 0.05219959533937863772, 101.2510903946856757 ) ) ;
#6204 = CARTESIAN_POINT ( 'NONE',  ( 16.52216118717209525, 7.221426719304514741, 98.57599021046996768 ) ) ;
#6205 = CARTESIAN_POINT ( 'NONE',  ( 8.314922557960818139, 14.29746914071049879, 34.58224293864770260 ) ) ;
#6206 = CARTESIAN_POINT ( 'NONE',  ( 18.56399227203344893, 5.499999999999817923, 41.47830131249902763 ) ) ;
#6207 = CARTESIAN_POINT ( 'NONE',  ( -0.05219959533907301413, -21.53943276465977519, 57.49890960531435979 ) ) ;
#6208 = CARTESIAN_POINT ( 'NONE',  ( -22.44159573604009950, -16.30477369853688430, 141.0750000027311728 ) ) ;
#6209 = CARTESIAN_POINT ( 'NONE',  ( -16.51473224551069308, -9.474510206698971260, 96.66557627198102409 ) ) ;
#6210 = CARTESIAN_POINT ( 'NONE',  ( -4.483927247898539470, -16.52544592524342804, 92.29057627198103830 ) ) ;
#6211 = CARTESIAN_POINT ( 'NONE',  ( -19.03943276465977164, -0.05219959533935918106, 113.7510903946856757 ) ) ;
#6212 = EDGE_CURVE ( 'NONE', #48812, #162452, #31629, .T. ) ;
#6213 = CARTESIAN_POINT ( 'NONE',  ( -16.53943276465976808, -0.05219959533934237506, 103.7510903946857042 ) ) ;
#6214 = ORIENTED_EDGE ( 'NONE', *, *, #121040, .F. ) ;
#6216 = CARTESIAN_POINT ( 'NONE',  ( 5.823673210054125526, 21.52544592524343514, 99.79057627198103830 ) ) ;
#6215 = CARTESIAN_POINT ( 'NONE',  ( 9.474510206698971260, -16.51473224551069308, 97.91557627198102409 ) ) ;
#6218 = CARTESIAN_POINT ( 'NONE',  ( 9.474510206698971260, -16.51473224551069308, 97.91557627198102409 ) ) ;
#6217 = CARTESIAN_POINT ( 'NONE',  ( -14.34966873604960291, -8.224510206698953496, 21.66557627198102409 ) ) ;
#6219 = CARTESIAN_POINT ( 'NONE',  ( -9.474510206698720793, -16.51473224551083518, 99.58442372801900433 ) ) ;
#6220 = CARTESIAN_POINT ( 'NONE',  ( -21.52544592524334988, -5.823673210054445271, 108.9594237280190185 ) ) ;
#6221 = CARTESIAN_POINT ( 'NONE',  ( 21.55341960407610458, 5.719274019375980345, 83.95724293864770971 ) ) ;
#6222 = CARTESIAN_POINT ( 'NONE',  ( -10.72451020669898014, 18.67979575497178502, 45.41557627198103830 ) ) ;
#6223 = CARTESIAN_POINT ( 'NONE',  ( 13.89961937509977652, -13.97604488694527269, 58.12390960531436690 ) ) ;
#6224 = CARTESIAN_POINT ( 'NONE',  ( 12.06949235617757843, -12.14591786802309237, 38.12390960531436690 ) ) ;
#6225 = CARTESIAN_POINT ( 'NONE',  ( 16.46253265017160672, -9.564922557960803928, 83.33224293864768129 ) ) ;
#6226 = EDGE_LOOP ( 'NONE', ( #121374, #45710 ) ) ;
#6227 = CARTESIAN_POINT ( 'NONE',  ( 18.87255363501903105, 5.499999999999944045, 58.82513748171828638 ) ) ;
#6228 = CARTESIAN_POINT ( 'NONE',  ( 19.03943276465977164, 0.05219959533936151252, 41.25109039468566152 ) ) ;
#6229 = CARTESIAN_POINT ( 'NONE',  ( -5.719274019375978568, 21.55341960407610458, 80.20724293864769550 ) ) ;
#6230 = CARTESIAN_POINT ( 'NONE',  ( -8.224510206698948167, 14.34966873604960824, 80.41557627198103830 ) ) ;
#6231 = CARTESIAN_POINT ( 'NONE',  ( -5.719274019375978568, 21.55341960407610458, 115.2072429386476955 ) ) ;
#6232 = CARTESIAN_POINT ( 'NONE',  ( 22.44159573604009239, 16.30477369853692693, 146.5750000027312012 ) ) ;
#6233 = CARTESIAN_POINT ( 'NONE',  ( -4.483927247898782831, 16.52544592524335698, 112.7094237280190328 ) ) ;
#6234 = CARTESIAN_POINT ( 'NONE',  ( 19.03943276465977164, -0.05219959533909143690, 28.74890960531435624 ) ) ;
#6235 = CARTESIAN_POINT ( 'NONE',  ( -0.05219959533909027116, -19.03943276465977164, 92.49890960531436690 ) ) ;
#6236 = SURFACE_SIDE_STYLE ('',( #127591 ) ) ;
#6237 = DIRECTION ( 'NONE',  ( -5.392603844284257652E-33, 1.000000000000000000, 0.000000000000000000 ) ) ;
#6238 = CARTESIAN_POINT ( 'NONE',  ( 16.52544592524342804, -4.483927247898539470, 48.54057627198103120 ) ) ;
#6239 = CARTESIAN_POINT ( 'NONE',  ( -15.80617190586768217, 15.72974639402176855, 63.12609039468568994 ) ) ;
#6240 = CARTESIAN_POINT ( 'NONE',  ( 24.94736998983877285, -28.55544918295356638, -16.60430580961556402 ) ) ;
#6241 = CARTESIAN_POINT ( 'NONE',  ( 9.474510206698971260, -16.51473224551069308, 37.91557627198102409 ) ) ;
#6242 = CARTESIAN_POINT ( 'NONE',  ( -16.51473224551069308, -9.474510206698971260, 46.66557627198102409 ) ) ;
#6243 = ORIENTED_EDGE ( 'NONE', *, *, #128983, .F. ) ;
#6244 = CARTESIAN_POINT ( 'NONE',  ( 21.53943276465977519, 0.05219959533937863772, 111.2510903946856899 ) ) ;
#6245 = CARTESIAN_POINT ( 'NONE',  ( -16.52544592524335698, -4.483927247898792601, 63.95942372801901854 ) ) ;
#6246 = CARTESIAN_POINT ( 'NONE',  ( 15.72974639402176855, 15.80617190586768217, 86.87609039468568994 ) ) ;
#6247 = CARTESIAN_POINT ( 'NONE',  ( 13.97604488694527802, 13.89961937509977652, 114.3739096053143669 ) ) ;
#6248 = CARTESIAN_POINT ( 'NONE',  ( 16.46253265017146816, 9.564922557961045513, 96.66775706135233293 ) ) ;
#6249 = CARTESIAN_POINT ( 'NONE',  ( -21.55341960407619339, 5.719274019375674811, 63.54275706135234003 ) ) ;
#6250 = CARTESIAN_POINT ( 'NONE',  ( -8.224510206698735004, -14.34966873604973081, 29.58442372801901854 ) ) ;
#6251 = CARTESIAN_POINT ( 'NONE',  ( -18.67979575497178146, -10.72451020669898902, 81.66557627198103830 ) ) ;
#6252 = CARTESIAN_POINT ( 'NONE',  ( -16.51473224551082808, 9.474510206698731452, 103.3344237280190043 ) ) ;
#6253 = CARTESIAN_POINT ( 'NONE',  ( -5.153800228976328057, -19.02544592524343514, 62.29057627198100988 ) ) ;
#6254 = CARTESIAN_POINT ( 'NONE',  ( 5.049401038297881783, 19.05341960407617563, 97.29275706135233293 ) ) ;
#6255 = CARTESIAN_POINT ( 'NONE',  ( 16.51473224551083163, -9.474510206698727899, 100.8344237280190043 ) ) ;
#6256 = CARTESIAN_POINT ( 'NONE',  ( -14.34966873604960291, -8.224510206698953496, 56.66557627198103830 ) ) ;
#6257 = CARTESIAN_POINT ( 'NONE',  ( 0.05219959533936267826, -19.03943276465977164, 80.00109039468567573 ) ) ;
#6258 = CARTESIAN_POINT ( 'NONE',  ( -12.14591786802326823, 12.06949235617739902, 63.12609039468568994 ) ) ;
#6260 = CARTESIAN_POINT ( 'NONE',  ( -9.564922557960796823, -16.46253265017161027, 32.08224293864769550 ) ) ;
#6259 = CARTESIAN_POINT ( 'NONE',  ( -21.53943276465977519, -0.05219959533937600094, 18.75109039468568639 ) ) ;
#6261 = CARTESIAN_POINT ( 'NONE',  ( 16.51473224551069308, 9.474510206698969483, 54.16557627198103120 ) ) ;
#6262 = CARTESIAN_POINT ( 'NONE',  ( -8.314922557961024197, 14.29746914071037800, 62.91775706135236135 ) ) ;
#6263 = LINE ( 'NONE', #191292, #46725 ) ;
#6264 = CARTESIAN_POINT ( 'NONE',  ( -28.82186960331499392, -9.364793116373526516, 146.3500000054623627 ) ) ;
#6265 = CARTESIAN_POINT ( 'NONE',  ( 9.564922557960805705, 16.46253265017160317, 104.5822429386476955 ) ) ;
#6266 = CYLINDRICAL_SURFACE ( 'NONE', #130179, 59.99999999999998579 ) ;
#6267 = ORIENTED_EDGE ( 'NONE', *, *, #21840, .T. ) ;
#6268 = CARTESIAN_POINT ( 'NONE',  ( 19.05341960407617918, -5.049401038297876454, 111.0427570613523329 ) ) ;
#6270 = CARTESIAN_POINT ( 'NONE',  ( 18.62759615963271287, -10.81492255796078972, 38.33224293864768839 ) ) ;
#6269 = TOROIDAL_SURFACE ( 'NONE', #22456, 1.500000000000001776, 0.5000000000000000000 ) ;
#6272 = CARTESIAN_POINT ( 'NONE',  ( 16.55341960407618274, -4.379528057220086978, 26.04275706135235779 ) ) ;
#6271 = CARTESIAN_POINT ( 'NONE',  ( -0.05219959533936034679, 19.03943276465977164, 42.50109039468566152 ) ) ;
#6273 = CARTESIAN_POINT ( 'NONE',  ( 19.05341960407611168, 5.049401038298154454, 23.95724293864769194 ) ) ;
#6274 = CARTESIAN_POINT ( 'NONE',  ( -19.02544592524342804, 5.153800228976336051, 51.04057627198103120 ) ) ;
#6275 = CARTESIAN_POINT ( 'NONE',  ( -21.55341960407610458, -5.719274019375992779, 86.45724293864770971 ) ) ;
#6276 = CARTESIAN_POINT ( 'NONE',  ( -16.46253265017160317, 9.564922557960807481, 110.8322429386476955 ) ) ;
#6277 = CARTESIAN_POINT ( 'NONE',  ( 16.51473224551069308, 9.474510206698969483, 54.16557627198103120 ) ) ;
#6278 = CARTESIAN_POINT ( 'NONE',  ( -27.73933785331498925, 9.013057229001088189, 145.2750000027311899 ) ) ;
#6279 = CARTESIAN_POINT ( 'NONE',  ( -16.51473224551082808, 9.474510206698731452, 83.33442372801899012 ) ) ;
#6280 = CARTESIAN_POINT ( 'NONE',  ( -4.483927247898539470, -16.52544592524342804, 67.29057627198103830 ) ) ;
#6281 = CARTESIAN_POINT ( 'NONE',  ( 21.55341960407619695, -5.719274019375665929, 106.0427570613523471 ) ) ;
#6282 = CARTESIAN_POINT ( 'NONE',  ( 18.67979575497178502, 10.72451020669898547, 104.1655762719810241 ) ) ;
#6283 = CARTESIAN_POINT ( 'NONE',  ( 21.55341960407619695, -5.719274019375665929, 86.04275706135236135 ) ) ;
#6284 = CARTESIAN_POINT ( 'NONE',  ( 21.52544592524334988, 5.823673210054432836, 81.45942372801900433 ) ) ;
#6285 = CARTESIAN_POINT ( 'NONE',  ( 16.46253265017160672, -9.564922557960803928, 103.3322429386476955 ) ) ;
#6287 = CARTESIAN_POINT ( 'NONE',  ( 5.823673210054444382, -21.52544592524334988, 80.20942372801901854 ) ) ;
#6286 = CARTESIAN_POINT ( 'NONE',  ( 8.314922557961029526, -14.29746914071037800, 110.4177570613523756 ) ) ;
#6288 = CARTESIAN_POINT ( 'NONE',  ( -19.05341960407611168, -5.049401038298163336, 61.45724293864769550 ) ) ;
#6289 = CARTESIAN_POINT ( 'NONE',  ( 21.55341960407619695, -5.719274019375665929, 46.04275706135234714 ) ) ;
#6290 = CARTESIAN_POINT ( 'NONE',  ( 5.153800228976335163, 19.02544592524342804, 84.79057627198099567 ) ) ;
#6291 = CARTESIAN_POINT ( 'NONE',  ( 14.29746914071049879, -8.314922557960816363, 83.33224293864769550 ) ) ;
#6292 = CARTESIAN_POINT ( 'NONE',  ( -0.05219959533910754901, -16.53943276465976808, 67.49890960531436690 ) ) ;
#6293 = CARTESIAN_POINT ( 'NONE',  ( 18.67979575497178502, 10.72451020669898547, 64.16557627198102409 ) ) ;
#6294 = CARTESIAN_POINT ( 'NONE',  ( -19.03943276465977164, 0.05219959533909376836, 56.24890960531435979 ) ) ;
#6295 = CARTESIAN_POINT ( 'NONE',  ( -21.52544592524343514, 5.823673210054127303, 71.04057627198103830 ) ) ;
#6296 = CARTESIAN_POINT ( 'NONE',  ( -19.02544592524334988, -5.153800228976617603, 58.95942372801900433 ) ) ;
#6298 = CARTESIAN_POINT ( 'NONE',  ( 12.06949235617757843, -12.14591786802309237, 73.12390960531436690 ) ) ;
#6297 = CARTESIAN_POINT ( 'NONE',  ( 9.474510206698729675, 16.51473224551082808, 37.08442372801899722 ) ) ;
#6300 = AXIS2_PLACEMENT_3D ( 'NONE', #67822, #132498, #161831 ) ;
#6299 = CARTESIAN_POINT ( 'NONE',  ( -15.80617190586745835, -15.72974639402198527, 51.87390960531437401 ) ) ;
#6301 = CARTESIAN_POINT ( 'NONE',  ( -32.00000000000000711, -5.510910596163089556E-15, 45.00000000000000000 ) ) ;
#6303 = CARTESIAN_POINT ( 'NONE',  ( -5.359611314223446995E-15, 29.16686587814335851, 144.8750000027311842 ) ) ;
#6302 = CARTESIAN_POINT ( 'NONE',  ( 12.14591786802327356, -12.06949235617739191, 100.6260903946857184 ) ) ;
#6304 = CARTESIAN_POINT ( 'NONE',  ( -5.153800228976607833, 19.02544592524334988, 107.7094237280189759 ) ) ;
#6305 = CARTESIAN_POINT ( 'NONE',  ( -4.379528057220328563, 16.55341960407611168, 65.20724293864768129 ) ) ;
#6306 = CARTESIAN_POINT ( 'NONE',  ( -17.49999999999999645, 5.499999999999992895, 68.71769037696435589 ) ) ;
#6307 = CARTESIAN_POINT ( 'NONE',  ( 13.89961937509977652, -13.97604488694527269, 63.12390960531435979 ) ) ;
#6308 = CARTESIAN_POINT ( 'NONE',  ( 14.34966873604960469, 8.224510206698951720, 49.16557627198102409 ) ) ;
#6309 = CARTESIAN_POINT ( 'NONE',  ( 19.05341960407611168, 5.049401038298154454, 88.95724293864769550 ) ) ;
#6311 = CARTESIAN_POINT ( 'NONE',  ( 5.153800228976335163, 19.02544592524342804, 64.79057627198100988 ) ) ;
#6310 = CARTESIAN_POINT ( 'NONE',  ( 5.049401038297881783, 19.05341960407617563, 77.29275706135231871 ) ) ;
#6312 = CARTESIAN_POINT ( 'NONE',  ( 19.03943276465977164, -0.05219959533909143690, 83.74890960531436690 ) ) ;
#6313 = CARTESIAN_POINT ( 'NONE',  ( 5.049401038298161559, -19.05341960407611168, 67.70724293864769550 ) ) ;
#6314 = CARTESIAN_POINT ( 'NONE',  ( -15.80617190586745835, -15.72974639402198527, 61.87390960531436690 ) ) ;
#6315 = CARTESIAN_POINT ( 'NONE',  ( -0.05219959533934338120, 16.53943276465976808, 62.50109039468568284 ) ) ;
#6316 = CARTESIAN_POINT ( 'NONE',  ( -9.474510206698720793, -16.51473224551083518, 104.5844237280190043 ) ) ;
#6317 = CARTESIAN_POINT ( 'NONE',  ( -5.049401038298153566, 19.05341960407611168, 55.20724293864769550 ) ) ;
#6318 = CARTESIAN_POINT ( 'NONE',  ( 0.05219959533907565091, 21.53943276465977519, 54.99890960531435269 ) ) ;
#6319 = CARTESIAN_POINT ( 'NONE',  ( 5.049401038297881783, 19.05341960407617563, 82.29275706135229029 ) ) ;
#6320 = CARTESIAN_POINT ( 'NONE',  ( -0.05219959533934338120, 16.53943276465976808, 112.5010903946857042 ) ) ;
#6321 = CARTESIAN_POINT ( 'NONE',  ( -0.05219959533936034679, 19.03943276465977164, 42.50109039468566152 ) ) ;
#6323 = CARTESIAN_POINT ( 'NONE',  ( -0.05219959533934338120, 16.53943276465976808, 92.50109039468567573 ) ) ;
#6322 = CARTESIAN_POINT ( 'NONE',  ( -12.06949235617739369, -12.14591786802326823, 64.37609039468568994 ) ) ;
#6324 = CARTESIAN_POINT ( 'NONE',  ( 35.00000000000000000, -3.181980515339468241, 1.110912703473986074 ) ) ;
#6325 = CARTESIAN_POINT ( 'NONE',  ( 12.06949235617739724, 12.14591786802326823, 81.87609039468568994 ) ) ;
#6326 = CARTESIAN_POINT ( 'NONE',  ( 15.72974639402199770, -15.80617190586745480, 28.12390960531435979 ) ) ;
#6327 = CARTESIAN_POINT ( 'NONE',  ( 16.46253265017160672, -9.564922557960803928, 48.33224293864769550 ) ) ;
#6328 = CARTESIAN_POINT ( 'NONE',  ( -9.564922557960796823, -16.46253265017161027, 47.08224293864769550 ) ) ;
#6329 = CARTESIAN_POINT ( 'NONE',  ( -5.153800228976328057, -19.02544592524343514, 47.29057627198102409 ) ) ;
#6330 = CARTESIAN_POINT ( 'NONE',  ( 18.67979575497194134, -10.72451020669871369, 35.83442372801901143 ) ) ;
#6331 = CARTESIAN_POINT ( 'NONE',  ( 16.52544592524335698, 4.483927247898782831, 51.45942372801901854 ) ) ;
#6332 = CARTESIAN_POINT ( 'NONE',  ( -12.06949235617756955, 12.14591786802309770, 25.62390960531435624 ) ) ;
#6333 = CARTESIAN_POINT ( 'NONE',  ( -5.153800228976328057, -19.02544592524343514, 27.29057627198103120 ) ) ;
#6334 = CARTESIAN_POINT ( 'NONE',  ( 9.564922557961047289, -16.46253265017146816, 20.41775706135233293 ) ) ;
#6335 = CARTESIAN_POINT ( 'NONE',  ( -9.564922557961040184, 16.46253265017147172, 112.9177570613523329 ) ) ;
#6336 = CARTESIAN_POINT ( 'NONE',  ( -13.97604488694547697, 13.89961937509957934, 63.12609039468566152 ) ) ;
#6337 = CARTESIAN_POINT ( 'NONE',  ( -12.06949235617756955, 12.14591786802309770, 65.62390960531436690 ) ) ;
#6338 = CARTESIAN_POINT ( 'NONE',  ( -5.049401038298153566, 19.05341960407611168, 40.20724293864768839 ) ) ;
#6340 = CARTESIAN_POINT ( 'NONE',  ( 16.81555441253551564, 7.025013491695499823, 76.86314554665744936 ) ) ;
#6339 = CARTESIAN_POINT ( 'NONE',  ( 9.474510206698729675, 16.51473224551082808, 77.08442372801900433 ) ) ;
#6341 = CARTESIAN_POINT ( 'NONE',  ( -18.62759615963255300, -10.81492255796106328, 79.16775706135234714 ) ) ;
#6342 = CARTESIAN_POINT ( 'NONE',  ( -8.224510206698735004, -14.34966873604973081, 39.58442372801901143 ) ) ;
#6343 = CARTESIAN_POINT ( 'NONE',  ( -31.80000000000000782, -1.130348995613007185E-14, 97.69999999999998863 ) ) ;
#6344 = CARTESIAN_POINT ( 'NONE',  ( 21.52544592524344225, -5.823673210054117533, 33.54057627198102409 ) ) ;
#6345 = CARTESIAN_POINT ( 'NONE',  ( 14.29746914071037800, 8.314922557961029526, 31.66775706135234358 ) ) ;
#6346 = CARTESIAN_POINT ( 'NONE',  ( 17.97214573761835510, 5.499999999999910294, 88.96970049038655759 ) ) ;
#6347 = CARTESIAN_POINT ( 'NONE',  ( 0.05219959533937995610, -21.53943276465977519, 110.0010903946856757 ) ) ;
#6348 = CARTESIAN_POINT ( 'NONE',  ( -25.55222625260934066, 11.31436996698904629, 166.3494238031456405 ) ) ;
#6349 = CARTESIAN_POINT ( 'NONE',  ( 0.05219959533909260263, 19.03943276465977164, 34.99890960531435979 ) ) ;
#6350 = CARTESIAN_POINT ( 'NONE',  ( -20.03497210076587010, -21.14457701270107037, -52.41383543719814497 ) ) ;
#6351 = CARTESIAN_POINT ( 'NONE',  ( -19.03943276465977164, 0.05219959533909376836, 51.24890960531436690 ) ) ;
#6352 = CARTESIAN_POINT ( 'NONE',  ( 21.55341960407619695, -5.719274019375665929, 66.04275706135236135 ) ) ;
#6353 = CARTESIAN_POINT ( 'NONE',  ( 5.049401038297881783, 19.05341960407617563, 22.29275706135233648 ) ) ;
#6354 = CARTESIAN_POINT ( 'NONE',  ( 0.05219959533910956823, 16.53943276465976808, 29.99890960531435979 ) ) ;
#6355 = CARTESIAN_POINT ( 'NONE',  ( 9.564922557960805705, 16.46253265017160317, 29.58224293864769550 ) ) ;
#6356 = CARTESIAN_POINT ( 'NONE',  ( -5.153800228976328057, -19.02544592524343514, 97.29057627198099567 ) ) ;
#6357 = CARTESIAN_POINT ( 'NONE',  ( 5.823673210054444382, -21.52544592524334988, 50.20942372801901854 ) ) ;
#6358 = CARTESIAN_POINT ( 'NONE',  ( 9.474510206698971260, -16.51473224551069308, 37.91557627198102409 ) ) ;
#6359 = CARTESIAN_POINT ( 'NONE',  ( -21.52544592524334988, -5.823673210054445271, 63.95942372801901854 ) ) ;
#6361 = CARTESIAN_POINT ( 'NONE',  ( 5.153800228976335163, 19.02544592524342804, 109.7905762719810099 ) ) ;
#6360 = CARTESIAN_POINT ( 'NONE',  ( 9.564922557961047289, -16.46253265017146816, 90.41775706135234714 ) ) ;
#6362 = CARTESIAN_POINT ( 'NONE',  ( -16.51473224551069308, -9.474510206698971260, 21.66557627198102765 ) ) ;
#6363 = CARTESIAN_POINT ( 'NONE',  ( -21.53943276465977519, 0.05219959533907696930, 106.2489096053143811 ) ) ;
#6364 = CARTESIAN_POINT ( 'NONE',  ( -9.564922557961040184, 16.46253265017147172, 32.91775706135233293 ) ) ;
#6365 = CARTESIAN_POINT ( 'NONE',  ( 16.55341960407611168, 4.379528057220329451, 108.9572429386476955 ) ) ;
#6366 = CARTESIAN_POINT ( 'NONE',  ( 5.153800228976335163, 19.02544592524342804, 59.79057627198100988 ) ) ;
#6367 = CARTESIAN_POINT ( 'NONE',  ( 5.153800228976615827, -19.02544592524334988, 100.2094237280190043 ) ) ;
#6368 = CARTESIAN_POINT ( 'NONE',  ( 14.34966873604960469, 8.224510206698951720, 64.16557627198102409 ) ) ;
#6369 = CARTESIAN_POINT ( 'NONE',  ( 0.05219959533907565091, 21.53943276465977519, 24.99890960531435624 ) ) ;
#6370 = CARTESIAN_POINT ( 'NONE',  ( 19.03943276465977164, 0.05219959533936151252, 91.25109039468566152 ) ) ;
#6371 = CARTESIAN_POINT ( 'NONE',  ( -10.81492255796078084, -18.62759615963271287, 97.08224293864770971 ) ) ;
#6372 = CARTESIAN_POINT ( 'NONE',  ( 10.72451020669871369, 18.67979575497193778, 42.08442372801901854 ) ) ;
#6373 = CARTESIAN_POINT ( 'NONE',  ( -16.55341960407617563, 4.379528057220093196, 38.54275706135234714 ) ) ;
#6375 = CARTESIAN_POINT ( 'NONE',  ( 15.80617190586769283, -15.72974639402175789, 55.62609039468568284 ) ) ;
#6374 = CARTESIAN_POINT ( 'NONE',  ( 12.06949235617739724, 12.14591786802326823, 41.87609039468568284 ) ) ;
#6376 = CARTESIAN_POINT ( 'NONE',  ( 18.62759615963271287, -10.81492255796078972, 53.33224293864769550 ) ) ;
#6377 = CARTESIAN_POINT ( 'NONE',  ( 13.97604488694527802, 13.89961937509977652, 34.37390960531436690 ) ) ;
#6378 = CARTESIAN_POINT ( 'NONE',  ( 30.74264578624799782, 22.33583958711400541, -6.549999994537627046 ) ) ;
#6379 = CARTESIAN_POINT ( 'NONE',  ( 0.05219959533934541429, -16.53943276465976808, 70.00109039468568994 ) ) ;
#6380 = EDGE_CURVE ( 'NONE', #65463, #186347, #182275, .T. ) ;
#6381 = CARTESIAN_POINT ( 'NONE',  ( 10.81492255796078972, 18.62759615963270932, 104.5822429386477097 ) ) ;
#6382 = CARTESIAN_POINT ( 'NONE',  ( -8.314922557960811034, -14.29746914071050412, 42.08224293864769550 ) ) ;
#6383 = CARTESIAN_POINT ( 'NONE',  ( 14.29746914071037800, 8.314922557961029526, 61.66775706135235424 ) ) ;
#6384 = CARTESIAN_POINT ( 'NONE',  ( 19.02544592524334988, 5.153800228976608722, 101.4594237280189759 ) ) ;
#6385 = CARTESIAN_POINT ( 'NONE',  ( 21.55341960407610458, 5.719274019375980345, 93.95724293864770971 ) ) ;
#6386 = CARTESIAN_POINT ( 'NONE',  ( -14.34966873604960291, -8.224510206698953496, 31.66557627198102054 ) ) ;
#6387 = ORIENTED_EDGE ( 'NONE', *, *, #121040, .T. ) ;
#6388 = CARTESIAN_POINT ( 'NONE',  ( -12.06949235617739369, -12.14591786802326823, 74.37609039468568994 ) ) ;
#6389 = CARTESIAN_POINT ( 'NONE',  ( 23.64874990377914799, 15.04272038711346049, 165.8682408883346397 ) ) ;
#6390 = CARTESIAN_POINT ( 'NONE',  ( -5.719274019375978568, 21.55341960407610458, 70.20724293864769550 ) ) ;
#6391 = CARTESIAN_POINT ( 'NONE',  ( 14.29746914071037800, 8.314922557961029526, 111.6677570613523613 ) ) ;
#6392 = ORIENTED_EDGE ( 'NONE', *, *, #134059, .T. ) ;
#6393 = CARTESIAN_POINT ( 'NONE',  ( 11.74264578624800315, -36.14014761921581709, -3.400000000000000355 ) ) ;
#6394 = CARTESIAN_POINT ( 'NONE',  ( -10.72451020669898014, 18.67979575497178502, 105.4155762719810383 ) ) ;
#6395 = CARTESIAN_POINT ( 'NONE',  ( -0.05219959533907301413, -21.53943276465977519, 112.4989096053143669 ) ) ;
#6396 = CARTESIAN_POINT ( 'NONE',  ( -4.379528057220328563, 16.55341960407611168, 35.20724293864768839 ) ) ;
#6397 = CARTESIAN_POINT ( 'NONE',  ( -14.34966873604972548, 8.224510206698743886, 43.33442372801901143 ) ) ;
#6398 = CARTESIAN_POINT ( 'NONE',  ( 13.89961937509977652, -13.97604488694527269, 53.12390960531434558 ) ) ;
#6399 = CARTESIAN_POINT ( 'NONE',  ( 9.474510206698971260, -16.51473224551069308, 67.91557627198102409 ) ) ;
#6400 = CARTESIAN_POINT ( 'NONE',  ( -19.02544592524342804, 5.153800228976336051, 111.0405762719810099 ) ) ;
#6401 = CARTESIAN_POINT ( 'NONE',  ( -25.53334702086137042, -27.44079366658189301, -18.45201707417109915 ) ) ;
#6402 = CARTESIAN_POINT ( 'NONE',  ( 19.03943276465977164, 0.05219959533936151252, 101.2510903946856757 ) ) ;
#6403 = CARTESIAN_POINT ( 'NONE',  ( 9.564922557961047289, -16.46253265017146816, 50.41775706135233293 ) ) ;
#6404 = CARTESIAN_POINT ( 'NONE',  ( 18.62759615963271287, -10.81492255796078972, 93.33224293864769550 ) ) ;
#6405 = CARTESIAN_POINT ( 'NONE',  ( -8.314922557961024197, 14.29746914071037800, 112.9177570613523329 ) ) ;
#6406 = CARTESIAN_POINT ( 'NONE',  ( 0.05219959533907565091, 21.53943276465977519, 49.99890960531437401 ) ) ;
#6408 = CARTESIAN_POINT ( 'NONE',  ( 19.03943276465977164, 0.05219959533936151252, 111.2510903946856757 ) ) ;
#6407 = CARTESIAN_POINT ( 'NONE',  ( -10.81492255796078084, -18.62759615963271287, 77.08224293864769550 ) ) ;
#6409 = CARTESIAN_POINT ( 'NONE',  ( 16.46253265017160672, -9.564922557960803928, 113.3322429386476955 ) ) ;
#6410 = CARTESIAN_POINT ( 'NONE',  ( -15.72974639402176322, -15.80617190586768395, 79.37609039468567573 ) ) ;
#6411 = CARTESIAN_POINT ( 'NONE',  ( -19.02544592524342804, 5.153800228976336051, 76.04057627198102409 ) ) ;
#6412 = VECTOR ( 'NONE', #39028, 1000.000000000000114 ) ;
#6413 = FACE_OUTER_BOUND ( 'NONE', #20333, .T. ) ;
#6414 = CARTESIAN_POINT ( 'NONE',  ( 5.153800228976335163, 19.02544592524342804, 69.79057627198103830 ) ) ;
#6415 = CARTESIAN_POINT ( 'NONE',  ( -14.29746914071049879, 8.314922557960819915, 85.83224293864768129 ) ) ;
#6416 = ORIENTED_EDGE ( 'NONE', *, *, #152623, .F. ) ;
#6417 = CARTESIAN_POINT ( 'NONE',  ( 13.97604488694548053, -13.89961937509957401, 110.6260903946856615 ) ) ;
#6418 = LINE ( 'NONE', #131782, #102043 ) ;
#6419 = CARTESIAN_POINT ( 'NONE',  ( -9.564922557960796823, -16.46253265017161027, 77.08224293864769550 ) ) ;
#6421 = CARTESIAN_POINT ( 'NONE',  ( -19.03943276465977164, 0.05219959533909376836, 106.2489096053143669 ) ) ;
#6420 = CARTESIAN_POINT ( 'NONE',  ( -5.719274019375665041, -21.55341960407619695, 89.79275706135236135 ) ) ;
#6422 = CARTESIAN_POINT ( 'NONE',  ( 12.14591786802327356, -12.06949235617739191, 80.62609039468567573 ) ) ;
#6423 = CARTESIAN_POINT ( 'NONE',  ( -16.61371651742603106, -7.165104196376148593, 76.14584930007006847 ) ) ;
#6424 = CARTESIAN_POINT ( 'NONE',  ( 19.03943276465977164, 0.05219959533936151252, 51.25109039468567573 ) ) ;
#6425 = CARTESIAN_POINT ( 'NONE',  ( -5.719274019375665041, -21.55341960407619695, 109.7927570613523613 ) ) ;
#6426 = CARTESIAN_POINT ( 'NONE',  ( -17.79613651744293890, -24.49428055684527550, 144.2843446568999752 ) ) ;
#6427 = CARTESIAN_POINT ( 'NONE',  ( -22.81625015709509441, -31.40387420917324590, -6.824999997268814234 ) ) ;
#6428 = CARTESIAN_POINT ( 'NONE',  ( -8.224510206698948167, 14.34966873604960824, 25.41557627198103120 ) ) ;
#6429 = DIRECTION ( 'NONE',  ( 0.000000000000000000, 0.000000000000000000, -1.000000000000000000 ) ) ;
#6430 = CARTESIAN_POINT ( 'NONE',  ( 8.314922557961029526, -14.29746914071037800, 105.4177570613523613 ) ) ;
#6431 = CARTESIAN_POINT ( 'NONE',  ( -5.427562675786936573E-15, 30.27659582821221207, 145.7656553485623192 ) ) ;
#6432 = CARTESIAN_POINT ( 'NONE',  ( 16.55341960407618274, -4.379528057220086978, 81.04275706135236135 ) ) ;
#6433 = CARTESIAN_POINT ( 'NONE',  ( -18.62759615963255300, -10.81492255796106328, 79.16775706135234714 ) ) ;
#6434 = CARTESIAN_POINT ( 'NONE',  ( -5.049401038297874678, -19.05341960407617918, 89.79275706135230450 ) ) ;
#6435 = CARTESIAN_POINT ( 'NONE',  ( -16.51473224551082808, 9.474510206698731452, 33.33442372801899722 ) ) ;
#6436 = CARTESIAN_POINT ( 'NONE',  ( 9.564922557960805705, 16.46253265017160317, 74.58224293864769550 ) ) ;
#6437 = CARTESIAN_POINT ( 'NONE',  ( 16.51473224551069308, 9.474510206698969483, 54.16557627198103120 ) ) ;
#6438 = CARTESIAN_POINT ( 'NONE',  ( 17.50000000000000711, -5.499999999999978684, 41.21769037696436300 ) ) ;
#6439 = CARTESIAN_POINT ( 'NONE',  ( 5.823673210054125526, 21.52544592524343514, 89.79057627198103830 ) ) ;
#6440 = AXIS2_PLACEMENT_3D ( 'NONE', #168862, #94012, #61681 ) ;
#6441 = CARTESIAN_POINT ( 'NONE',  ( 5.823673210054125526, 21.52544592524343514, 44.79057627198103120 ) ) ;
#6442 = CARTESIAN_POINT ( 'NONE',  ( 19.02544592524343514, -5.153800228976328945, 43.54057627198103120 ) ) ;
#6443 = CARTESIAN_POINT ( 'NONE',  ( -0.05219959533934338120, 16.53943276465976808, 67.50109039468568994 ) ) ;
#6444 = EDGE_CURVE ( 'NONE', #40791, #194062, #8567, .T. ) ;
#6445 = ORIENTED_EDGE ( 'NONE', *, *, #56848, .T. ) ;
#6446 = CARTESIAN_POINT ( 'NONE',  ( 10.72451020669871369, 18.67979575497193778, 47.08442372801901854 ) ) ;
#6448 = CARTESIAN_POINT ( 'NONE',  ( 11.74264578624800315, -36.14014761921581709, -1.399999999999999689 ) ) ;
#6447 = CARTESIAN_POINT ( 'NONE',  ( 4.379528057220339221, -16.55341960407611168, 67.70724293864769550 ) ) ;
#6449 = CARTESIAN_POINT ( 'NONE',  ( -12.14591786802326823, 12.06949235617739902, 33.12609039468569705 ) ) ;
#6450 = CARTESIAN_POINT ( 'NONE',  ( -8.314922557960811034, -14.29746914071050412, 97.08224293864770971 ) ) ;
#6451 = CARTESIAN_POINT ( 'NONE',  ( 13.89961937509957401, 13.97604488694547697, 46.87609039468565442 ) ) ;
#6452 = CARTESIAN_POINT ( 'NONE',  ( -8.314922557960811034, -14.29746914071050412, 77.08224293864769550 ) ) ;
#6453 = CARTESIAN_POINT ( 'NONE',  ( 21.52544592524334988, 5.823673210054432836, 31.45942372801901854 ) ) ;
#6455 = CARTESIAN_POINT ( 'NONE',  ( -15.72974639402197994, 15.80617190586746368, 95.62390960531436690 ) ) ;
#6454 = CARTESIAN_POINT ( 'NONE',  ( -19.02544592524342804, 5.153800228976336051, 26.04057627198103120 ) ) ;
#6456 = CARTESIAN_POINT ( 'NONE',  ( -13.89961937509977652, 13.97604488694528158, 100.6239096053143669 ) ) ;
#6457 = CARTESIAN_POINT ( 'NONE',  ( -14.29746914071049879, 8.314922557960819915, 70.83224293864770971 ) ) ;
#6458 = CARTESIAN_POINT ( 'NONE',  ( -9.474510206698964154, 16.51473224551069663, 115.4155762719810241 ) ) ;
#6459 = CARTESIAN_POINT ( 'NONE',  ( -29.86685920354755552, 21.69954338932564397, -2.824999997268813345 ) ) ;
#6460 = CARTESIAN_POINT ( 'NONE',  ( -5.049401038297874678, -19.05341960407617918, 79.79275706135233293 ) ) ;
#6461 = CARTESIAN_POINT ( 'NONE',  ( -21.55341960407619339, 5.719274019375674811, 23.54275706135235424 ) ) ;
#6462 = CARTESIAN_POINT ( 'NONE',  ( -19.05341960407611168, -5.049401038298163336, 66.45724293864769550 ) ) ;
#6463 = CARTESIAN_POINT ( 'NONE',  ( 5.049401038297881783, 19.05341960407617563, 52.29275706135234003 ) ) ;
#6464 = CARTESIAN_POINT ( 'NONE',  ( -16.46253265017160317, 9.564922557960807481, 30.83224293864769550 ) ) ;
#6465 = CARTESIAN_POINT ( 'NONE',  ( 10.72451020669871369, 18.67979575497193778, 77.08442372801901854 ) ) ;
#6466 = CARTESIAN_POINT ( 'NONE',  ( 0.05219959533910956823, 16.53943276465976808, 64.99890960531435269 ) ) ;
#6467 = CARTESIAN_POINT ( 'NONE',  ( 16.52544592524342804, -4.483927247898539470, 53.54057627198103120 ) ) ;
#6468 = CARTESIAN_POINT ( 'NONE',  ( -5.153800228976328057, -19.02544592524343514, 62.29057627198100988 ) ) ;
#6469 = CARTESIAN_POINT ( 'NONE',  ( 10.72451020669898902, -18.67979575497178502, 82.91557627198103830 ) ) ;
#6470 = CARTESIAN_POINT ( 'NONE',  ( 13.97604488694527802, 13.89961937509977652, 54.37390960531435979 ) ) ;
#6471 = ORIENTED_EDGE ( 'NONE', *, *, #12002, .T. ) ;
#6472 = CARTESIAN_POINT ( 'NONE',  ( -15.80617190586745835, -15.72974639402198527, 76.87390960531439532 ) ) ;
#6473 = CARTESIAN_POINT ( 'NONE',  ( 15.80617190586769283, -15.72974639402175789, 100.6260903946857184 ) ) ;
#6476 = CARTESIAN_POINT ( 'NONE',  ( -16.55341960407611168, -4.379528057220339221, 101.4572429386476955 ) ) ;
#6475 = CARTESIAN_POINT ( 'NONE',  ( 14.34966873604972726, -8.224510206698740333, 110.8344237280190043 ) ) ;
#6474 = FACE_BOUND ( 'NONE', #962, .T. ) ;
#6477 = CARTESIAN_POINT ( 'NONE',  ( 19.05341960407617918, -5.049401038297876454, 91.04275706135234714 ) ) ;
#6478 = ORIENTED_EDGE ( 'NONE', *, *, #129249, .T. ) ;
#6479 = CARTESIAN_POINT ( 'NONE',  ( 15.72974639402176855, 15.80617190586768217, 21.87609039468567573 ) ) ;
#6480 = CARTESIAN_POINT ( 'NONE',  ( -13.89961937509957401, -13.97604488694547875, 59.37609039468566863 ) ) ;
#6481 = CARTESIAN_POINT ( 'NONE',  ( -16.55341960407617563, 4.379528057220093196, 98.54275706135234714 ) ) ;
#6482 = CARTESIAN_POINT ( 'NONE',  ( 9.474510206698729675, 16.51473224551082808, 37.08442372801899722 ) ) ;
#6483 = CARTESIAN_POINT ( 'NONE',  ( 16.46253265017160672, -9.564922557960803928, 98.33224293864769550 ) ) ;
#6484 = CARTESIAN_POINT ( 'NONE',  ( 5.719274019375991003, -21.55341960407610458, 67.70724293864769550 ) ) ;
#6485 = DIRECTION ( 'NONE',  ( 0.9526137857479310966, -0.3041824702427718408, 0.000000000000000000 ) ) ;
#6486 = CARTESIAN_POINT ( 'NONE',  ( 13.97604488694527802, 13.89961937509977652, 29.37390960531435979 ) ) ;
#6487 = CARTESIAN_POINT ( 'NONE',  ( -15.72974639402176322, -15.80617190586768395, 109.3760903946857042 ) ) ;
#6488 = CARTESIAN_POINT ( 'NONE',  ( 12.14591786802327356, -12.06949235617739191, 70.62609039468567573 ) ) ;
#6489 = CARTESIAN_POINT ( 'NONE',  ( 10.81492255796106328, -18.62759615963255655, 25.41775706135235779 ) ) ;
#6490 = CARTESIAN_POINT ( 'NONE',  ( -14.34966873604972548, 8.224510206698743886, 48.33442372801902565 ) ) ;
#6491 = CARTESIAN_POINT ( 'NONE',  ( 13.89961937509977652, -13.97604488694527269, 108.1239096053143669 ) ) ;
#6492 = CARTESIAN_POINT ( 'NONE',  ( 16.51473224551069308, 9.474510206698969483, 54.16557627198103120 ) ) ;
#6493 = CARTESIAN_POINT ( 'NONE',  ( -19.05341960407611168, -5.049401038298163336, 71.45724293864766707 ) ) ;
#6494 = CARTESIAN_POINT ( 'NONE',  ( 16.55341960407618274, -4.379528057220086978, 41.04275706135236135 ) ) ;
#6495 = CARTESIAN_POINT ( 'NONE',  ( -16.55341960407611168, -4.379528057220339221, 96.45724293864770971 ) ) ;
#6496 = CARTESIAN_POINT ( 'NONE',  ( 16.52544592524335698, 4.483927247898782831, 106.4594237280190328 ) ) ;
#6497 = DIRECTION ( 'NONE',  ( -1.000000000000000000, -4.336808689942018352E-17, 3.574525976782710619E-31 ) ) ;
#6500 = CARTESIAN_POINT ( 'NONE',  ( 13.89961937509977652, -13.97604488694527269, 63.12390960531435979 ) ) ;
#6499 = CARTESIAN_POINT ( 'NONE',  ( 16.46253265017160672, -9.564922557960803928, 78.33224293864769550 ) ) ;
#6498 = CARTESIAN_POINT ( 'NONE',  ( -21.52544592524334988, -5.823673210054445271, 58.95942372801902565 ) ) ;
#6501 = CARTESIAN_POINT ( 'NONE',  ( -13.97604488694527625, -13.89961937509977652, 96.87390960531433848 ) ) ;
#6502 = CARTESIAN_POINT ( 'NONE',  ( -16.53943276465976808, 0.05219959533911058130, 51.24890960531436690 ) ) ;
#6503 = CARTESIAN_POINT ( 'NONE',  ( 14.34966873604972726, -8.224510206698740333, 95.83442372801903275 ) ) ;
#6504 = CARTESIAN_POINT ( 'NONE',  ( 8.224510206698953496, -14.34966873604960469, 42.91557627198103120 ) ) ;
#6505 = ORIENTED_EDGE ( 'NONE', *, *, #136550, .T. ) ;
#6506 = CARTESIAN_POINT ( 'NONE',  ( -16.51473224551082808, 9.474510206698731452, 38.33442372801899722 ) ) ;
#6507 = CARTESIAN_POINT ( 'NONE',  ( -16.46253265017160317, 9.564922557960807481, 105.8322429386476955 ) ) ;
#6508 = CARTESIAN_POINT ( 'NONE',  ( -19.05341960407611168, -5.049401038298163336, 66.45724293864769550 ) ) ;
#6509 = CARTESIAN_POINT ( 'NONE',  ( 16.46253265017146816, 9.564922557961045513, 41.66775706135234003 ) ) ;
#6510 = B_SPLINE_CURVE_WITH_KNOTS ( 'NONE', 3,
 ( #75257, #90421, #186434, #122741, #47910, #64061, #15578, #169243, #45912, #152106, #140893, #198616, #13590, #184432, #154084, #44928, #109564, #77236, #182457, #46911 ),
 .UNSPECIFIED., .F., .F.,
 ( 4, 2, 2, 2, 2, 2, 2, 2, 2, 4 ),
 ( 2.784207231387392883E-07, 0.0003311547508960732472, 0.0006620310810690078346, 0.0009929074112419423136, 0.001323783741414876793, 0.002647289062106605601, 0.003309041722452476294, 0.003970794382798350022, 0.004632547043144224184, 0.005294299703490098347 ),
 .UNSPECIFIED. ) ;
#6511 = CARTESIAN_POINT ( 'NONE',  ( 36.91746825000000598, -11.99521256947793546, -8.224999997268810148 ) ) ;
#6512 = CARTESIAN_POINT ( 'NONE',  ( 17.72662750342724891, 5.500000000000079048, 58.90179492283742491 ) ) ;
#6514 = CARTESIAN_POINT ( 'NONE',  ( 16.55341960407618274, -4.379528057220086978, 71.04275706135234714 ) ) ;
#6513 = CARTESIAN_POINT ( 'NONE',  ( 16.51473224551083163, -9.474510206698727899, 90.83442372801900433 ) ) ;
#6515 = DIRECTION ( 'NONE',  ( -1.000000000000000000, 0.000000000000000000, 0.000000000000000000 ) ) ;
#6516 = CARTESIAN_POINT ( 'NONE',  ( 9.474510206698971260, -16.51473224551069308, 87.91557627198102409 ) ) ;
#6517 = CARTESIAN_POINT ( 'NONE',  ( -15.72974639402176322, -15.80617190586768395, 34.37609039468568284 ) ) ;
#6518 = CARTESIAN_POINT ( 'NONE',  ( -16.46253265017146816, -9.564922557961047289, 79.16775706135234714 ) ) ;
#6520 = CARTESIAN_POINT ( 'NONE',  ( -13.97604488694527625, -13.89961937509977652, 41.87390960531435979 ) ) ;
#6519 = FACE_OUTER_BOUND ( 'NONE', #134586, .T. ) ;
#6521 = CARTESIAN_POINT ( 'NONE',  ( 9.474510206698971260, -16.51473224551069308, 92.91557627198103830 ) ) ;
#6523 = CARTESIAN_POINT ( 'NONE',  ( 9.564922557960805705, 16.46253265017160317, 34.58224293864770260 ) ) ;
#6522 = CARTESIAN_POINT ( 'NONE',  ( -16.52544592524342804, 4.483927247898546575, 51.04057627198103120 ) ) ;
#6524 = CARTESIAN_POINT ( 'NONE',  ( -9.564922557961040184, 16.46253265017147172, 47.91775706135233293 ) ) ;
#6525 = CARTESIAN_POINT ( 'NONE',  ( -4.483927247898539470, -16.52544592524342804, 92.29057627198103830 ) ) ;
#6526 = CARTESIAN_POINT ( 'NONE',  ( -9.474510206698720793, -16.51473224551083518, 29.58442372801900433 ) ) ;
#6527 = CARTESIAN_POINT ( 'NONE',  ( 19.05341960407611168, 5.049401038298154454, 63.95724293864769550 ) ) ;
#6528 = CARTESIAN_POINT ( 'NONE',  ( 5.823673210054125526, 21.52544592524343514, 69.79057627198102409 ) ) ;
#6530 = CARTESIAN_POINT ( 'NONE',  ( -16.46253265017146816, -9.564922557961047289, 19.16775706135233293 ) ) ;
#6529 = CARTESIAN_POINT ( 'NONE',  ( 16.53943276465976808, -0.05219959533910856209, 68.74890960531435269 ) ) ;
#6531 = CARTESIAN_POINT ( 'NONE',  ( 0.05219959533909260263, 19.03943276465977164, 99.99890960531436690 ) ) ;
#6532 = CARTESIAN_POINT ( 'NONE',  ( -21.52544592524343514, 5.823673210054127303, 26.04057627198103475 ) ) ;
#6533 = CARTESIAN_POINT ( 'NONE',  ( 16.51473224551069308, 9.474510206698969483, 49.16557627198102409 ) ) ;
#6534 = CARTESIAN_POINT ( 'NONE',  ( -9.474510206698964154, 16.51473224551069663, 35.41557627198102409 ) ) ;
#6535 = CARTESIAN_POINT ( 'NONE',  ( -16.52544592524342804, 4.483927247898546575, 106.0405762719810525 ) ) ;
#6536 = CARTESIAN_POINT ( 'NONE',  ( 10.81492255796078972, 18.62759615963270932, 109.5822429386476955 ) ) ;
#6537 = CARTESIAN_POINT ( 'NONE',  ( -5.049401038298153566, 19.05341960407611168, 95.20724293864770971 ) ) ;
#6538 = CARTESIAN_POINT ( 'NONE',  ( 10.81492255796078972, 18.62759615963270932, 109.5822429386476955 ) ) ;
#6539 = CARTESIAN_POINT ( 'NONE',  ( 9.564922557960805705, 16.46253265017160317, 104.5822429386476955 ) ) ;
#6540 = CARTESIAN_POINT ( 'NONE',  ( -16.53943276465976808, 0.05219959533911058130, 116.2489096053143669 ) ) ;
#6541 = CARTESIAN_POINT ( 'NONE',  ( -21.53943276465977519, -0.05219959533937600094, 83.75109039468568994 ) ) ;
#6542 = CARTESIAN_POINT ( 'NONE',  ( -10.72451020669898014, 18.67979575497178502, 90.41557627198103830 ) ) ;
#6543 = CARTESIAN_POINT ( 'NONE',  ( -3.573655867282028392E-15, 2.428612866367529932E-14, 150.0000000000000000 ) ) ;
#6544 = CARTESIAN_POINT ( 'NONE',  ( -19.03943276465977164, -0.05219959533935918106, 18.75109039468567218 ) ) ;
#6545 = CARTESIAN_POINT ( 'NONE',  ( 5.153800228976335163, 19.02544592524342804, 59.79057627198101699 ) ) ;
#6546 = CARTESIAN_POINT ( 'NONE',  ( 16.53943276465976808, 0.05219959533934440121, 46.25109039468567573 ) ) ;
#6547 = CARTESIAN_POINT ( 'NONE',  ( 14.34966873604960469, 8.224510206698951720, 109.1655762719810383 ) ) ;
#6548 = CARTESIAN_POINT ( 'NONE',  ( -17.50000000000147082, -3.202012800152271854, 110.0717758397273798 ) ) ;
#6549 = CARTESIAN_POINT ( 'NONE',  ( -5.153800228976328057, -19.02544592524343514, 57.29057627198103120 ) ) ;
#6551 = EDGE_CURVE ( 'NONE', #147696, #97386, #74235, .T. ) ;
#6550 = CARTESIAN_POINT ( 'NONE',  ( -8.224510206698948167, 14.34966873604960824, 100.4155762719810241 ) ) ;
#6552 = CARTESIAN_POINT ( 'NONE',  ( 18.62759615963271287, -10.81492255796078972, 43.33224293864769550 ) ) ;
#6553 = CARTESIAN_POINT ( 'NONE',  ( -16.55341960407611168, -4.379528057220339221, 66.45724293864768129 ) ) ;
#6554 = CARTESIAN_POINT ( 'NONE',  ( -16.51473224551082808, 9.474510206698731452, 113.3344237280190043 ) ) ;
#6555 = CARTESIAN_POINT ( 'NONE',  ( -18.67979575497193778, 10.72451020669871902, 68.33442372801900433 ) ) ;
#6556 = DIRECTION ( 'NONE',  ( 0.000000000000000000, 0.000000000000000000, -1.000000000000000000 ) ) ;
#6557 = CARTESIAN_POINT ( 'NONE',  ( -16.52544592524335698, -4.483927247898792601, 103.9594237280190185 ) ) ;
#6558 = CARTESIAN_POINT ( 'NONE',  ( -16.53943276465976808, 0.05219959533911058130, 41.24890960531435269 ) ) ;
#6559 = CARTESIAN_POINT ( 'NONE',  ( -9.564922557960796823, -16.46253265017161027, 42.08224293864769550 ) ) ;
#6560 = CARTESIAN_POINT ( 'NONE',  ( 19.03943276465977164, -0.05219959533909143690, 93.74890960531435269 ) ) ;
#6561 = CARTESIAN_POINT ( 'NONE',  ( 18.67979575497178502, 10.72451020669898547, 94.16557627198103830 ) ) ;
#6562 =( BOUNDED_SURFACE ( )  B_SPLINE_SURFACE ( 3, 2, ( 
 ( #143243, #5730, #54248, #146237, #11506, #73177, #68402, #175595, #99737, #81557, #36072, #196526, #21913, #97721, #57997, #26671, #52240, #88312, #35085, #160424, #98731, #83564, #4726, #66416, #7724, #150000, #159411, #69410, #114914, #115920, #53237, #119667, #96738, #20906, #190765, #158427, #84559, #128077, #192765, #130054, #131076, #177610, #113897, #145243, #189780, #82565, #144246, #67409, #6724, #30624, #169119, #266, #13471, #90298, #93269, #137797, #58970, #16450, #75134, #61934, #120638, #31619, #60947, #154954, #92277, #74162, #44804, #122622, #42828, #138785, #104493, #181349, #78099, #170124, #199481, #76119, #106459, #184312, #29634, #166175, #27676, #182336, #1256, #168138, #153961, #14456, #123603, #89316, #135834, #197503, #139768, #45793, #15459, #151009, #107445, #12500, #91267, #62933, #108448, #43814, #77115, #185298, #167164, #105477, #28663, #46789, #151983, #136804, #198488, #59961, #121627, #183323, #152958, #36569, #6235, #35586, #96253, #189289, #187309, #141764, #49768, #155945, #5233, #48780, #17441, #34595, #95265, #157940, #79097, #50767, #140770, #19431, #128578, #81078, #2259, #126589, #63942, #159927, #110434, #125610, #82059, #124613, #142757, #97232, #51749, #172116, #4237, #113410, #112425, #175101, #158920, #65917, #94266, #127590, #98224, #21416, #83074, #143753, #156948, #33602, #174116, #18445, #80096, #20410, #66914, #144750, #3256, #47789, #111433, #64930, #188291, #186308, #173120, #190272, #109440, #171123, #32612, #37578, #71920, #25446, #69925, #39579, #84071, #54749, #52740, #146752, #178111, #40590, #195282, #149763, #179122, #101238, #132594, #130578, #85070, #193276, #99241, #148771, #192273, #160930, #162927, #38591, #24435, #22421, #194284, #145750, #86083, #133591, #147774, #7231, #131591, #68916, #103261, #53755, #115429, #87086, #67914, #9261, #102261, #56764, #177120, #70927, #118436, #55750, #180129, #163948, #117424, #100246, #10260, #41597, #164943, #26436, #88077, #161928, #23422, #129567, #8247, #116423, #191265, #114407, #176108, #73931, #134607, #198253, #135600, #120404, #169894, #59728, #30389, #61703, #90071, #105246, #181117, #15222, #168884, #13246, #183091, #27436, #121398, #196293, #151753, #44573, #184076, #138552, #123372, #91042, #185065, #199246, #104254, #74909, #152729, #72938, #92036, #57763, #11266, #46553, #29, #167912, #106228, #136573, #29412, #14219, #119433, #42591, #12267, #31388, #75888, #60713, #137563, #153726, #165937, #89079, #150770, #108215, #122387, #45560, #197272, #107214, #58734, #76881, #93037, #182097, #43581, #166933, #28435, #140543, #16220, #155714, #20180, #170889, #2031, #173889, #128346, #63711, #51519, #66684, #190045, #35358, #65688, #113181, #174871, #188064, #95032, #19205, #139540, #17210, #36337, #141541, #78863, #154725, #143513, #171886, #5001, #77873, #79872, #18214, #156722, #1024, #62697, #127352, #124379, #32381, #189066, #34368, #97009, #172889, #186074, #96029, #111197, #80854, #81826, #47557, #112199, #125386, #94035, #157715, #187083, #48552, #142531, #126368, #109210, #110206, #33374, #3030, #64706, #49535, #4009, #50537, #158691, #148534, #176881, #192027, #67680, #102022, #55515, #100006, #69685, #114168, #84831, #82836, #38351, #8001, #70693, #25207, #10025, #177879, #71685, #85846, #191033, #161693, #39347, #159684, #117186, #21181, #97990, #133351, #86849, #54518, #193040, #23188, #116190, #146511, #144516, #6001, #99001, #118197, #131352, #147536, #101006, #40347, #129338, #52508, #175871, #195042, #162690, #9024, #37343, #24196, #160691, #132360, #179889, #56519, #22182, #194052, #178880, #83832, #145513, #6994, #163705, #68675, #130330, #53511, #115188, #88842, #138328, #153493, #14989, #123146, #152498, #13014, #105996, #104019, #58507, #166697, #74678, #73697, #44339, #26199, #30156, #89842, #167683, #150534, #136345, #91799, #164703, #137330, #134369 ),
 ( #76650, #149525, #60479, #199011, #197040, #87838, #11021, #122154, #198020, #200009, #105013, #61475, #72694, #29179, #59489, #196053, #12034, #183843, #13986, #41356, #103020, #121164, #181864, #90815, #57528, #42357, #119197, #28200, #165698, #180882, #27196, #120173, #135369, #43343, #151523, #182857, #75652, #45332, #106982, #168656, #173651, #62466, #157480, #64472, #65452, #2793, #46319, #794, #18972, #155486, #143276, #110962, #111961, #142295, #17981, #79635, #80618, #63476, #78632, #184833, #77646, #187834, #31157, #140307, #34134, #172646, #3775, #16978, #93807, #96771, #141304, #124139, #19949, #1798, #127115, #185838, #47325, #188821, #126139, #95793, #125151, #108981, #49304, #50304, #81590, #35119, #158460, #186850, #48319, #107974, #4760, #169661, #109974, #92806, #66448, #170661, #171654, #154493, #15988, #33143, #139315, #32149, #94801, #156480, #146273, #86609, #68437, #83597, #163466, #162449, #129098, #24963, #36104, #147291, #23950, #145277, #174639, #97756, #85605, #22947, #148292, #191789, #178637, #159444, #115954, #161456, #20939, #98763, #8781, #39111, #101778, #9786, #84593, #130091, #192799, #112946, #190798, #128109, #114948, #52272, #189814, #116944, #6758, #40100, #51285, #53270, #176641, #38117, #82596, #144278, #100767, #5766, #67441, #70451, #7760, #132116, #69443, #113930, #175630, #193809, #160456, #37104, #54282, #55274, #21948, #131111, #177643, #99771, #150301, #165466, #71448, #164469, #74447, #117958, #26962, #120924, #59255, #90590, #103786, #180649, #183615, #27963, #149292, #106755, #88605, #152272, #10786, #72453, #75424, #89604, #197789, #11797, #134128, #136113, #12781, #168430, #182623, #137098, #73461, #135135, #194801, #44108, #56275, #196809, #179649, #105766, #195817, #58276, #198784, #167453, #119945, #151293, #60250, #43110, #181630, #28949, #41119, #121921, #104778, #13756, #118965, #166466, #45098, #102783, #29926, #25963, #91565, #153253, #133113, #87606, #57289, #42124, #32907, #64237, #122912, #79399, #184600, #140065, #34883, #142054, #46081, #141070, #187602, #556, #76416, #15749, #80382, #30922, #62227, #33897, #188584, #123895, #111726, #126878, #50065, #96538, #125903, #186609, #2555, #77408, #31912, #1556, #107736, #95554, #139078, #169417, #124911, #185594, #48081, #92570, #49071, #154258, #109737, #18735, #171421, #47083, #16740, #108744, #173412, #170420, #93565, #172408, #14755, #94561, #110727, #3540, #155251, #156240, #65218, #157241, #138092, #199773, #78389, #17742, #61240, #63232, #85363, #55041, #115721, #128865, #174405, #161218, #97520, #5527, #37878, #129854, #131884, #20701, #81359, #145040, #82357, #67207, #116711, #6522, #177409, #8539, #36860, #52040, #127874, #162216, #38880, #160220, #191552, #35874, #68201, #143043, #98527, #53029, #130874, #147055, #70217, #99536, #193569, #146038, #51050, #21710, #22713, #19717, #100537, #4521, #158227, #178401, #39865, #114710, #176403, #83364, #84360, #7522, #66214, #189578, #159207, #112712, #69206, #192564, #54047, #23715, #144045, #190565, #113696, #175392, #181398, #73226, #75183, #164233, #24724, #88361, #25729, #10548, #60011, #150054, #120686, #152033, #180413, #195577, #71215, #105528, #59019, #103552, #134897, #117715, #11560, #86373, #41885, #196574, #74212, #28711, #13518, #42876, #136855, #89366, #194567, #165227, #104541, #163223, #182385, #148058, #101531, #198540, #90347, #58044, #119714, #26722, #166222, #27723, #9549, #132878, #102549, #121678, #151055, #12546, #135880, #43863, #56037, #179411, #40876, #183374, #197551, #167214, #87375, #149060, #72212, #133886, #57050, #118725, #153008, #171173, #20211, #30674, #106511, #45841, #113216, #60999, #92327, #66719, #21216, #154013, #144551, #159719, #82873, #129373, #155992, #16500, #109490, #107493, #61983, #170176, #76169, #128380, #169170, #137849, #155003, #15508, #78148, #199530, #32660, #122671, #139817 ),
 ( #36370, #184360, #81859, #124662, #190076, #62983, #168188, #77165, #143547, #138835, #6036, #94314, #174906, #5033, #1304, #186358, #51552, #47838, #185347, #98024, #29685, #315, #67715, #31669, #123649, #44855, #91317, #46837, #14507, #108497, #93319, #54550, #193075, #175907, #37379, #102057, #179924, #68709, #163742, #70727, #71718, #9056, #52542, #7027, #25242, #161728, #149560, #117222, #118233, #148568, #24232, #85883, #86883, #69719, #84866, #191069, #83867, #194087, #99036, #146544, #40383, #178916, #10058, #23223, #100042, #103056, #147571, #130366, #26233, #8037, #133386, #192063, #53545, #195077, #132394, #56556, #131386, #115223, #55549, #41391, #87872, #164738, #11056, #116223, #177914, #114203, #72731, #160726, #39382, #22218, #145549, #176915, #101041, #38386, #162727, #182891, #152532, #138360, #106030, #166732, #137364, #119231, #123179, #44374, #199043, #181898, #29214, #184868, #57561, #30191, #27229, #167716, #200041, #16021, #61510, #88877, #104053, #14019, #92839, #74715, #89876, #169693, #168690, #135404, #31187, #42390, #153526, #91833, #151559, #180915, #165733, #15023, #90847, #154524, #198055, #46350, #150570, #122188, #75685, #12069, #105048, #76684, #45365, #108008, #134404, #196091, #60513, #183880, #59521, #107018, #73731, #197075, #58542, #120208, #43376, #121198, #28236, #13048, #136378, #62501, #32182, #170693, #112982, #95829, #127149, #185873, #142329, #47359, #2827, #97792, #4796, #109014, #3809, #50340, #63512, #139347, #78665, #143309, #93838, #125187, #96810, #51321, #186883, #174675, #189847, #36140, #159481, #188857, #49335, #65487, #140342, #94836, #64505, #155518, #158496, #1830, #17013, #187867, #48353, #110997, #110007, #111997, #171688, #172683, #81626, #34167, #33177, #79669, #156515, #77678, #18016, #141340, #35154, #826, #157513, #173688, #66485, #126172, #19007, #128147, #19983, #124172, #80653, #99809, #39146, #177678, #147329, #148327, #117995, #178673, #191827, #37141, #23986, #160494, #68475, #100801, #192836, #194839, #83636, #144314, #7799, #145313, #130130, #179684, #69483, #40137, #71483, #161495, #114986, #190834, #25000, #101814, #22983, #54317, #98800, #131148, #5804, #84633, #115989, #193845, #9822, #133148, #162485, #56312, #8816, #113967, #146310, #85643, #82632, #163502, #67477, #20975, #41156, #102819, #129137, #52310, #175666, #132152, #70486, #55309, #6797, #38155, #116981, #21984, #86644, #53308, #176679, #74481, #135169, #197822, #195852, #28981, #57324, #59288, #168462, #120957, #180683, #166500, #103819, #199806, #150336, #42159, #121954, #164504, #182656, #75455, #91597, #88640, #44140, #153287, #152304, #14788, #198816, #43142, #105799, #167485, #90622, #76448, #61273, #183647, #196842, #165499, #13789, #26995, #11831, #137129, #136146, #138125, #73497, #87640, #151326, #58309, #119977, #122943, #12814, #45129, #184632, #104811, #181663, #134163, #29960, #106788, #27998, #60281, #89637, #46113, #149326, #25998, #10820, #72490, #119000, #158258, #187632, #19748, #95587, #586, #171451, #49102, #169451, #65250, #30953, #107766, #81389, #96570, #64267, #2587, #32939, #125933, #156272, #92600, #154290, #108774, #127906, #94594, #157271, #141100, #50097, #15780, #62258, #123926, #143075, #110760, #18767, #77439, #172441, #139111, #17774, #189608, #34914, #185624, #33929, #80414, #93597, #47115, #170452, #173446, #31943, #155283, #126910, #4553, #16773, #142086, #3572, #78421, #188616, #140097, #79429, #1588, #66246, #63263, #111757, #124943, #186640, #48111, #109767, #116744, #67238, #36894, #70250, #24760, #98559, #148092, #163258, #86407, #132913, #162250, #22744, #115753, #113729, #68232, #176436, #82390, #131918, #175426, #144078, #161250, #21743, #84393, #5559, #177441, #128897, #146069, #55074, #7554, #190596, #53063, #52073, #9583, #160253, #83395, #69240, #23749, #35905, #85398, #39902, #145072, #147091 ),
 ( #8575, #129885, #6554, #51082, #191585, #54079, #97551, #114742, #100568, #38911, #193602, #37910, #99569, #71249, #130906, #192596, #112742, #178434, #101567, #174435, #159239, #20733, #151088, #120718, #88395, #72245, #197584, #135913, #91349, #182416, #198573, #196606, #58077, #117752, #59051, #179445, #119747, #102584, #167245, #133922, #134929, #60043, #43896, #42908, #12579, #121711, #166256, #26755, #105559, #40911, #183404, #104574, #28744, #41920, #89399, #44887, #164268, #90380, #25763, #149094, #87409, #29717, #74244, #152065, #10584, #13550, #195613, #181430, #14540, #106544, #57085, #75216, #136888, #180448, #56072, #118759, #168220, #103586, #165261, #153041, #76201, #150088, #194600, #11592, #73260, #27756, #48856, #109522, #2339, #346, #155036, #63016, #169202, #18522, #62015, #30708, #47869, #108529, #171204, #92358, #64020, #154044, #32694, #141841, #94345, #15539, #139847, #77197, #173194, #123679, #107525, #126663, #3332, #137880, #110511, #65006, #185378, #156024, #188367, #125689, #49844, #172192, #16531, #17521, #79179, #187388, #111508, #34670, #95339, #170208, #138866, #140850, #46868, #31701, #33677, #157024, #96328, #93350, #61030, #124695, #78178, #1336, #158015, #186392, #80169, #19506, #199561, #122702, #184392, #45872, #7308, #175178, #144826, #174192, #21491, #4312, #113484, #83152, #22499, #53834, #177196, #191338, #38669, #37656, #112498, #98303, #52816, #81151, #68993, #65995, #142833, #23499, #162003, #114484, #176187, #6310, #99321, #67988, #189364, #35660, #143830, #127664, #129642, #130658, #161005, #100324, #50841, #97308, #84146, #158994, #20487, #145825, #85147, #192351, #146833, #5310, #82136, #66994, #115508, #128653, #190348, #51824, #36644, #160003, #77840, #95993, #32348, #20145, #188029, #189026, #19168, #95000, #156686, #157678, #140509, #155682, #61670, #154690, #64670, #108178, #17177, #111162, #49500, #80817, #94001, #170857, #173853, #18180, #139507, #96973, #78831, #142495, #990, #62664, #65653, #79837, #172851, #1998, #124344, #126332, #2992, #158654, #34332, #127315, #63677, #125352, #185032, #3973, #46519, #187049, #169859, #50500, #186039, #48519, #112164, #35319, #110173, #141507, #81790, #33340, #171852, #143477, #31353, #123339, #93004, #16185, #109178, #47522, #194015, #128309, #100970, #97955, #38316, #70657, #86812, #132323, #159647, #174835, #23151, #163668, #145477, #160655, #40311, #39311, #5964, #101987, #113145, #24161, #162655, #22147, #51483, #36300, #85812, #99971, #25170, #68638, #55478, #21143, #193005, #161655, #82798, #175833, #147498, #116152, #178843, #4961, #84795, #6958, #69649, #190009, #67642, #66647, #191988, #129301, #177843, #190997, #144480, #52473, #117148, #114132, #37306, #8989, #98965, #83797, #130294, #53475, #115152, #176845, #146474, #7966, #131315, #54482, #165663, #73661, #179851, #29145, #72659, #41322, #58472, #119163, #181830, #102982, #12980, #164667, #43309, #152466, #104977, #26163, #150501, #87804, #183810, #134334, #118161, #137298, #13952, #148498, #59455, #75618, #196018, #166664, #198979, #136310, #60446, #182823, #27161, #28165, #89807, #74644, #122121, #45298, #105964, #180846, #149490, #151489, #10986, #57494, #197985, #120139, #106950, #42323, #71649, #135333, #103984, #88809, #168623, #197006, #167649, #30123, #11998, #121129, #44305, #9989, #90782, #133316, #195005, #56483, #181944, #58587, #64312, #29259, #167761, #125980, #16817, #32986, #28283, #89922, #149610, #93644, #11108, #151604, #134453, #1634, #165784, #166782, #94639, #155329, #74761, #44421, #156320, #198103, #120253, #78468, #72783, #17820, #136423, #140142, #73778, #121244, #79478, #196138, #124990, #119278, #59569, #141146, #110806, #2636, #180961, #57609, #106074, #187678, #13095, #43427, #27279, #88927, #49148, #26281, #105096, #182938, #87923, #63311, #186686, #42438, #48156, #104101, #109814, #171497, #150619 ),
 ( #12115, #135451, #197120, #192642, #35949, #160299, #5604, #114789, #157319, #126955, #65296, #7600, #190643, #21789, #80459, #36943, #142133, #97595, #54125, #99616, #3617, #98605, #145118, #158305, #33976, #173491, #37958, #188664, #19793, #191631, #146116, #81434, #69286, #84438, #130952, #172488, #83440, #144123, #6602, #34964, #189655, #159283, #50143, #53111, #96616, #111803, #82435, #143120, #67284, #4600, #68281, #66292, #128942, #176482, #52119, #127951, #174482, #51128, #95632, #112788, #20780, #161296, #22792, #18815, #129932, #113775, #175471, #133972, #42958, #103635, #166310, #150141, #194650, #195663, #72293, #41968, #104621, #12628, #73309, #86455, #131964, #118810, #55121, #163308, #57134, #87456, #89448, #178482, #38957, #102632, #39948, #24806, #74293, #164317, #134980, #27807, #56120, #9631, #85446, #119795, #148140, #135962, #165312, #151137, #196657, #149142, #10633, #11643, #117802, #71298, #115798, #8624, #180496, #162296, #132961, #26806, #88446, #58126, #179495, #40960, #197632, #181479, #193649, #177488, #25810, #100614, #116790, #101619, #23796, #147136, #70296, #91403, #94396, #62067, #395, #156077, #46921, #63069, #61079, #122752, #182465, #123732, #43946, #184442, #167296, #31752, #198627, #199613, #124748, #185431, #107576, #77246, #186444, #30761, #153091, #108581, #105608, #47920, #169254, #170258, #106595, #154094, #109574, #28792, #155087, #152117, #92408, #171257, #140905, #32744, #13600, #90431, #138914, #17573, #45922, #14595, #79234, #93401, #60093, #59099, #75268, #78229, #16581, #76251, #136938, #121761, #139900, #15588, #120764, #1388, #183454, #44939, #168271, #29768, #137929, #173246, #21542, #113536, #176236, #37707, #35712, #142882, #67046, #187440, #3382, #99369, #189416, #65057, #161052, #191388, #19557, #52865, #2391, #4364, #51877, #159045, #175230, #48908, #36695, #114536, #80220, #98356, #82188, #83202, #20539, #64070, #18573, #160055, #125740, #144877, #129691, #22547, #143881, #84193, #190401, #95391, #66047, #5362, #110562, #6359, #172243, #33730, #157077, #141891, #128704, #97359, #127714, #68039, #50891, #126714, #188418, #49895, #111562, #112549, #34721, #96379, #158066, #81201, #174244, #38716, #181237, #164069, #195407, #53882, #10384, #115557, #71050, #166058, #73058, #177244, #72041, #118559, #131719, #7356, #146884, #11388, #162052, #193401, #165061, #119554, #54876, #42713, #57882, #104375, #27559, #56885, #117547, #133715, #8376, #163052, #132716, #100374, #26555, #70051, #23548, #55874, #116550, #179246, #85196, #180249, #178239, #40712, #149882, #102381, #39700, #147898, #101363, #145873, #24559, #86208, #134730, #196412, #69041, #41719, #130706, #9384, #25568, #192400, #103383, #194404, #88198, #87212, #148894, #45678, #15342, #16338, #186195, #46672, #59847, #105361, #92157, #28549, #136688, #169002, #60831, #62816, #151869, #12386, #76007, #13359, #198370, #47676, #137682, #108332, #139654, #168028, #183209, #58855, #93156, #170012, #91158, #122506, #167048, #30506, #89199, #171009, #107329, #154841, #184196, #121514, #153844, #74048, #77987, #199367, #76998, #44690, #138670, #1142, #135719, #185182, #182215, #150, #124500, #150892, #109327, #43699, #120522, #61819, #197390, #29525, #106344, #90186, #123489, #75023, #152847, #14341, #31503, #128461, #188180, #78983, #2150, #190157, #127471, #67802, #96142, #82959, #140658, #20293, #65803, #63828, #3146, #51633, #143632, #6119, #129457, #189177, #173005, #97121, #17328, #33490, #191156, #19322, #95148, #52629, #21302, #49652, #144636, #32500, #34484, #81941, #50650, #5116, #125500, #66798, #114293, #110321, #113297, #112311, #174988, #174001, #94152, #48669, #36452, #64820, #155831, #158804, #159807, #98110, #35472, #187198, #172002, #111316, #126482, #156837, #18332, #79987, #141655, #157831, #80969, #142645, #4124, #8123, #84949, #87958, #132477, #53634, #11144 ),
 ( #180009, #177992, #39459, #99126, #40467, #160816, #101120, #83955, #148654, #115311, #116303, #41476, #102139, #24315, #177003, #103140, #164822, #131469, #69801, #72818, #178999, #117303, #134487, #163824, #26318, #162806, #85964, #22304, #25325, #145635, #147653, #7115, #10142, #38472, #9141, #149646, #86967, #70808, #194166, #196174, #55630, #193156, #71802, #68797, #57646, #133471, #195162, #23305, #56643, #175995, #130456, #118316, #192153, #37465, #100129, #161810, #146631, #54628, #88963, #137447, #77758, #59607, #74794, #154605, #153607, #120288, #16100, #27316, #138437, #15103, #136456, #165819, #150653, #76764, #14101, #139424, #182973, #169774, #12151, #107096, #152611, #73816, #89957, #200118, #30269, #92919, #906, #75769, #121280, #183956, #104137, #181981, #119312, #106111, #43463, #180998, #108090, #135486, #91914, #105131, #197156, #31268, #123255, #42474, #61587, #46431, #166817, #199126, #58621, #168766, #28318, #184946, #198137, #60593, #122268, #45443, #151637, #13132, #44457, #167795, #29295, #90925, #1914, #110093, #142414, #34251, #36218, #125268, #185954, #49419, #186966, #171771, #21061, #111081, #81708, #113062, #141423, #156604, #32264, #66565, #20064, #64588, #144398, #155599, #2910, #112082, #19087, #35238, #47438, #173772, #51402, #140424, #96892, #3892, #143392, #80735, #124259, #78747, #158575, #33260, #82715, #188946, #189927, #4883, #95911, #157595, #128230, #126253, #18098, #62581, #17094, #65572, #109095, #79753, #174754, #50423, #97871, #94918, #187950, #159562, #127231, #63593, #170774, #172771, #93921, #48436, #145394, #9903, #71563, #161573, #38233, #41236, #8899, #147411, #102897, #193927, #133228, #7878, #69564, #129218, #70567, #190915, #131230, #114049, #178755, #6877, #146390, #194919, #132235, #54397, #24069, #56394, #177757, #99888, #55390, #52392, #118077, #116069, #117060, #53391, #100882, #179767, #175747, #101898, #98882, #39226, #164582, #87720, #26076, #160576, #37225, #85724, #5883, #192919, #23066, #67560, #40220, #68555, #22065, #83716, #25080, #163580, #84712, #130211, #191906, #86723, #162565, #115069, #148408, #176761, #195935, #137212, #182740, #57409, #120058, #168543, #60367, #123028, #184714, #44224, #89723, #13870, #134248, #150421, #46198, #136228, #11916, #107851, #29063, #196924, #61357, #31036, #122039, #121044, #75537, #73580, #166583, #74561, #180763, #30041, #135252, #42239, #59372, #181745, #105882, #103900, #198899, #165581, #167569, #153372, #90702, #27079, #138211, #119081, #183729, #58391, #88725, #199893, #14874, #149405, #45215, #76535, #43227, #152385, #169536, #106870, #10900, #91680, #28083, #72573, #104894, #151409, #12897, #197903, #50185, #63354, #108860, #95675, #32029, #140184, #172531, #64353, #66331, #155370, #15867, #79517, #16859, #1676, #51168, #141187, #111842, #143160, #171537, #186727, #62343, #96656, #173532, #94680, #126022, #170539, #34017, #92685, #174520, #154373, #65336, #19832, #4640, #157361, #127992, #80501, #185710, #156359, #18855, #77525, #35001, #139197, #672, #189695, #81473, #49189, #187718, #17862, #110847, #2676, #124012, #47200, #93687, #112828, #142174, #3658, #126996, #158343, #78510, #125031, #48198, #109852, #188703, #33025, #144160, #103420, #5645, #161337, #58894, #166097, #67322, #165099, #11426, #21828, #97634, #36983, #104414, #52157, #83480, #57920, #12424, #145158, #135757, #150931, #56922, #197428, #176522, #191670, #74087, #73096, #98645, #120560, #128984, #119591, #134767, #53149, #82475, #190682, #196450, #133753, #35987, #99653, #89237, #113814, #26592, #72079, #175509, #6642, #181274, #149920, #159323, #20819, #195447, #37998, #88235, #160339, #68320, #129970, #22829, #114828, #84476, #118597, #148931, #10421, #180287, #41755, #42751, #27599, #154880, #167086, #93195, #171047, #59886, #16378, #61859, #62857, #190, #43739, #198409, #78025, #152885, #140697, #108376 ),
 ( #170052, #1180, #14380, #91195, #94190, #138709, #121552, #17367, #76046, #124539, #183248, #44729, #186236, #47715, #137722, #199406, #79022, #185222, #123528, #2187, #31543, #109365, #184236, #45717, #105400, #46713, #28588, #107370, #90224, #139694, #106385, #122546, #32537, #155870, #30548, #63869, #182254, #153884, #60869, #151908, #13397, #75061, #92200, #136727, #29564, #77038, #168066, #169042, #15381, #18373, #158846, #191195, #7158, #52670, #80025, #95190, #175030, #113338, #144675, #157872, #34523, #37504, #81983, #3185, #160856, #19361, #6160, #64858, #126520, #129496, #114333, #81010, #142685, #22346, #128503, #66840, #83997, #36495, #176036, #127512, #189216, #48706, #190198, #110359, #50695, #33528, #98149, #188219, #65842, #99166, #51676, #174044, #143676, #145676, #97161, #4164, #159849, #172041, #125540, #35513, #21342, #173046, #20334, #187236, #156876, #83000, #141694, #5157, #49692, #111357, #96183, #112353, #67840, #87011, #27357, #9185, #24357, #104179, #103185, #69844, #165861, #177045, #88001, #164866, #86008, #115355, #38515, #26361, #163870, #89003, #132519, #119357, #100171, #56686, #102182, #161853, #39502, #149689, #180053, #42516, #150694, #25369, #70850, #133514, #53678, #131512, #68841, #55673, #193198, #130500, #148697, #116345, #192196, #23347, #194208, #118360, #10185, #41522, #84992, #11187, #57689, #146673, #72862, #71845, #134532, #195206, #8168, #54671, #196219, #101162, #178034, #181041, #162850, #147697, #117347, #179043, #40511, #90964, #106152, #12192, #105170, #15142, #58660, #167834, #120326, #138475, #184986, #198176, #73857, #13171, #77794, #28358, #59646, #31305, #185993, #121320, #109133, #124296, #47476, #93959, #123294, #183998, #76804, #74834, #29335, #137486, #43504, #92958, #136496, #166856, #122307, #183012, #45481, #89996, #200156, #151678, #107137, #16139, #168807, #44496, #943, #182021, #46470, #152651, #14141, #62618, #139463, #135526, #108130, #170811, #75808, #30311, #32304, #61626, #197197, #169814, #199166, #91954, #153647, #154644, #60633, #52425, #113096, #126287, #171808, #158609, #94955, #2946, #35272, #127267, #129253, #18135, #78785, #142449, #79789, #64625, #114083, #3927, #174787, #5917, #34286, #49454, #125307, #159597, #36253, #157632, #188980, #33296, #96927, #155638, #37258, #17133, #128263, #82751, #67594, #20099, #190948, #143430, #48473, #19121, #81743, #140462, #97906, #1952, #63631, #175784, #144431, #112115, #50456, #80771, #173807, #65607, #187003, #110130, #156639, #141462, #4916, #66599, #189961, #21094, #187984, #111116, #172805, #95946, #51436, #148441, #6910, #163613, #68588, #24104, #119112, #26108, #87751, #23099, #117094, #149436, #86758, #10932, #133261, #177789, #178789, #55423, #25114, #72605, #195967, #56429, #69597, #115101, #101931, #38266, #146422, #40258, #70602, #134279, #161605, #22098, #85758, #84746, #7913, #57439, #147445, #118109, #180793, #39259, #192952, #130244, #102929, #179798, #100915, #132269, #176793, #9936, #98916, #160608, #83748, #71595, #145427, #191940, #194952, #53424, #41267, #99920, #162600, #164614, #131264, #54431, #116101, #8933, #193960, #31067, #198926, #137241, #105908, #60394, #90728, #103930, #88755, #43255, #62375, #167594, #30069, #75565, #184744, #27109, #196951, #135279, #77556, #122066, #91710, #150448, #106898, #11944, #29089, #124045, #169570, #73608, #168571, #14902, #28112, #165610, #104923, #107883, #58419, #89750, #61386, #15898, #151436, #139228, #154404, #703, #42272, #153404, #13899, #76564, #166610, #59399, #152411, #120086, #123058, #12923, #181774, #183758, #74587, #45244, #136255, #138239, #197931, #199923, #46229, #92715, #121073, #182767, #44251, #96688, #109883, #155399, #174552, #189727, #185744, #158376, #63384, #19865, #65368, #66365, #3689, #47232, #1708, #81505, #156389, #144193, #111874, #112861, #143193, #18886, #80532, #4673, #64384 ) ),
 .UNSPECIFIED., .T., .F., .T. ) 
 B_SPLINE_SURFACE_WITH_KNOTS ( ( 4, 3, 4 ),
 ( 3, 2, 2, 2, 2, 2, 2, 2, 2, 2, 2, 2, 2, 2, 2, 2, 2, 2, 2, 2, 2, 2, 2, 2, 2, 2, 2, 2, 2, 2, 2, 2, 2, 2, 2, 2, 2, 2, 2, 2, 2, 2, 2, 2, 2, 2, 2, 2, 2, 2, 2, 2, 2, 2, 2, 2, 2, 2, 2, 2, 2, 2, 2, 2, 2, 2, 2, 2, 2, 2, 2, 2, 2, 2, 2, 2, 2, 2, 2, 2, 2, 2, 2, 2, 2, 2, 2, 2, 2, 2, 2, 2, 2, 2, 2, 2, 2, 2, 2, 2, 2, 2, 2, 2, 2, 2, 2, 2, 2, 2, 2, 2, 2, 2, 2, 2, 2, 2, 2, 2, 2, 2, 2, 2, 2, 2, 2, 2, 2, 2, 2, 2, 2, 2, 2, 2, 2, 2, 2, 2, 2, 2, 2, 2, 2, 2, 2, 2, 2, 2, 2, 2, 2, 2, 2, 2, 2, 2, 2, 2, 2, 2, 2, 2, 2, 2, 2, 2, 2, 2, 2, 2, 2, 2, 2, 2, 2, 2, 2, 2, 2, 2, 2, 2, 2, 2, 2, 2, 2, 2, 2, 2, 2, 2, 2, 2, 2, 2, 2, 2, 2, 2, 2, 2, 2, 2, 2, 2, 2, 2, 2, 2, 2, 2, 2, 2, 2, 2, 2, 2, 2, 2, 2, 2, 2, 2, 2, 2, 3 ),
 ( 0.000000000000000000, 0.5000000000000000000, 1.000000000000000000 ),
 ( 0.000000000000000000, 0.004385964912280701511, 0.008771929824561403022, 0.01315789473684210453, 0.01754385964912280604, 0.02192982456140350755, 0.02631578947368420907, 0.03070175438596491058, 0.03508771929824561209, 0.03947368421052631360, 0.04385964912280701511, 0.04824561403508771662, 0.05263157894736841813, 0.05701754385964911964, 0.06140350877192982115, 0.06578947368421052266, 0.07017543859649122417, 0.07456140350877192569, 0.07894736842105262720, 0.08333333333333332871, 0.08771929824561403022, 0.09210526315789473173, 0.09649122807017543324, 0.1008771929824561348, 0.1052631578947368363, 0.1096491228070175378, 0.1140350877192982393, 0.1184210526315789408, 0.1228070175438596423, 0.1271929824561403577, 0.1315789473684210453, 0.1359649122807017607, 0.1403508771929824483, 0.1447368421052631637, 0.1491228070175438514, 0.1535087719298245668, 0.1578947368421052544, 0.1622807017543859698, 0.1666666666666666574, 0.1710526315789473728, 0.1754385964912280604, 0.1798245614035087758, 0.1842105263157894635, 0.1885964912280701788, 0.1929824561403508665, 0.1973684210526315819, 0.2017543859649122695, 0.2061403508771929849, 0.2105263157894736725, 0.2149122807017543879, 0.2192982456140350755, 0.2236842105263157909, 0.2280701754385964786, 0.2324561403508771940, 0.2368421052631578816, 0.2412280701754385970, 0.2456140350877192846, 0.2500000000000000000, 0.2543859649122807154, 0.2587719298245614308, 0.2631578947368420907, 0.2675438596491228060, 0.2719298245614035214, 0.2763157894736842368, 0.2807017543859648967, 0.2850877192982456121, 0.2894736842105263275, 0.2938596491228070429, 0.2982456140350877027, 0.3026315789473684181, 0.3070175438596491335, 0.3114035087719298489, 0.3157894736842105088, 0.3201754385964912242, 0.3245614035087719396, 0.3289473684210526550, 0.3333333333333333148, 0.3377192982456140302, 0.3421052631578947456, 0.3464912280701754610, 0.3508771929824561209, 0.3552631578947368363, 0.3596491228070175517, 0.3640350877192982670, 0.3684210526315789269, 0.3728070175438596423, 0.3771929824561403577, 0.3815789473684210731, 0.3859649122807017330, 0.3903508771929824483, 0.3947368421052631637, 0.3991228070175438791, 0.4035087719298245390, 0.4078947368421052544, 0.4122807017543859698, 0.4166666666666666852, 0.4210526315789473450, 0.4254385964912280604, 0.4298245614035087758, 0.4342105263157894912, 0.4385964912280701511, 0.4429824561403508665, 0.4473684210526315819, 0.4517543859649122973, 0.4561403508771929571, 0.4605263157894736725, 0.4649122807017543879, 0.4692982456140351033, 0.4736842105263157632, 0.4780701754385964786, 0.4824561403508771940, 0.4868421052631579093, 0.4912280701754385692, 0.4956140350877192846, 0.5000000000000000000, 0.5043859649122807154, 0.5087719298245614308, 0.5131578947368421462, 0.5175438596491228616, 0.5219298245614034659, 0.5263157894736841813, 0.5307017543859648967, 0.5350877192982456121, 0.5394736842105263275, 0.5438596491228070429, 0.5482456140350877583, 0.5526315789473684736, 0.5570175438596490780, 0.5614035087719297934, 0.5657894736842105088, 0.5701754385964912242, 0.5745614035087719396, 0.5789473684210526550, 0.5833333333333333703, 0.5877192982456140857, 0.5921052631578946901, 0.5964912280701754055, 0.6008771929824561209, 0.6052631578947368363, 0.6096491228070175517, 0.6140350877192982670, 0.6184210526315789824, 0.6228070175438596978, 0.6271929824561403022, 0.6315789473684210176, 0.6359649122807017330, 0.6403508771929824483, 0.6447368421052631637, 0.6491228070175438791, 0.6535087719298245945, 0.6578947368421053099, 0.6622807017543859143, 0.6666666666666666297, 0.6710526315789473450, 0.6754385964912280604, 0.6798245614035087758, 0.6842105263157894912, 0.6885964912280702066, 0.6929824561403509220, 0.6973684210526315264, 0.7017543859649122417, 0.7061403508771929571, 0.7105263157894736725, 0.7149122807017543879, 0.7192982456140351033, 0.7236842105263158187, 0.7280701754385965341, 0.7324561403508771384, 0.7368421052631578538, 0.7412280701754385692, 0.7456140350877192846, 0.7500000000000000000, 0.7543859649122807154, 0.7587719298245614308, 0.7631578947368421462, 0.7675438596491228616, 0.7719298245614034659, 0.7763157894736841813, 0.7807017543859648967, 0.7850877192982456121, 0.7894736842105263275, 0.7938596491228070429, 0.7982456140350877583, 0.8026315789473684736, 0.8070175438596490780, 0.8114035087719297934, 0.8157894736842105088, 0.8201754385964912242, 0.8245614035087719396, 0.8289473684210526550, 0.8333333333333333703, 0.8377192982456140857, 0.8421052631578946901, 0.8464912280701754055, 0.8508771929824561209, 0.8552631578947368363, 0.8596491228070175517, 0.8640350877192982670, 0.8684210526315789824, 0.8728070175438596978, 0.8771929824561403022, 0.8815789473684210176, 0.8859649122807017330, 0.8903508771929824483, 0.8947368421052631637, 0.8991228070175438791, 0.9035087719298245945, 0.9078947368421053099, 0.9122807017543859143, 0.9166666666666666297, 0.9210526315789473450, 0.9254385964912280604, 0.9298245614035087758, 0.9342105263157894912, 0.9385964912280702066, 0.9429824561403509220, 0.9473684210526315264, 0.9517543859649122417, 0.9561403508771929571, 0.9605263157894736725, 0.9649122807017543879, 0.9692982456140351033, 0.9736842105263158187, 0.9780701754385965341, 0.9824561403508771384, 0.9868421052631578538, 0.9912280701754385692, 0.9956140350877192846, 1.000000000000000000 ),
 .UNSPECIFIED. ) 
 GEOMETRIC_REPRESENTATION_ITEM ( )  RATIONAL_B_SPLINE_SURFACE ( (
 ( 1.000000000000000000, 0.9659258262890683122, 1.000000000000000000, 0.9659258262890683122, 1.000000000000000000, 0.9659258262890683122, 1.000000000000000000, 0.9659258262890683122, 1.000000000000000000, 0.9659258262890683122, 1.000000000000000000, 0.9659258262890683122, 1.000000000000000000, 0.9659258262890683122, 1.000000000000000000, 0.9659258262890683122, 1.000000000000000000, 0.9659258262890683122, 1.000000000000000000, 0.9659258262890683122, 1.000000000000000000, 0.9659258262890683122, 1.000000000000000000, 0.9659258262890683122, 1.000000000000000000, 0.9659258262890683122, 1.000000000000000000, 0.9659258262890683122, 1.000000000000000000, 0.9659258262890683122, 1.000000000000000000, 0.9659258262890683122, 1.000000000000000000, 0.9659258262890683122, 1.000000000000000000, 0.9659258262890683122, 1.000000000000000000, 0.9659258262890683122, 1.000000000000000000, 0.9659258262890683122, 1.000000000000000000, 0.9659258262890683122, 1.000000000000000000, 0.9659258262890683122, 1.000000000000000000, 0.9659258262890683122, 1.000000000000000000, 0.9659258262890683122, 1.000000000000000000, 0.9659258262890683122, 1.000000000000000000, 0.9659258262890683122, 1.000000000000000000, 0.9659258262890683122, 1.000000000000000000, 0.9659258262890683122, 1.000000000000000000, 0.9659258262890683122, 1.000000000000000000, 0.9659258262890683122, 1.000000000000000000, 0.9659258262890683122, 1.000000000000000000, 0.9659258262890683122, 1.000000000000000000, 0.9659258262890683122, 1.000000000000000000, 0.9659258262890683122, 1.000000000000000000, 0.9659258262890683122, 1.000000000000000000, 0.9659258262890683122, 1.000000000000000000, 0.9659258262890683122, 1.000000000000000000, 0.9659258262890683122, 1.000000000000000000, 0.9659258262890683122, 1.000000000000000000, 0.9659258262890683122, 1.000000000000000000, 0.9659258262890683122, 1.000000000000000000, 0.9659258262890683122, 1.000000000000000000, 0.9659258262890683122, 1.000000000000000000, 0.9659258262890683122, 1.000000000000000000, 0.9659258262890683122, 1.000000000000000000, 0.9659258262890683122, 1.000000000000000000, 0.9659258262890683122, 1.000000000000000000, 0.9659258262890683122, 1.000000000000000000, 0.9659258262890683122, 1.000000000000000000, 0.9659258262890683122, 1.000000000000000000, 0.9659258262890683122, 1.000000000000000000, 0.9659258262890683122, 1.000000000000000000, 0.9659258262890683122, 1.000000000000000000, 0.9659258262890683122, 1.000000000000000000, 0.9659258262890683122, 1.000000000000000000, 0.9659258262890683122, 1.000000000000000000, 0.9659258262890683122, 1.000000000000000000, 0.9659258262890683122, 1.000000000000000000, 0.9659258262890683122, 1.000000000000000000, 0.9659258262890683122, 1.000000000000000000, 0.9659258262890683122, 1.000000000000000000, 0.9659258262890683122, 1.000000000000000000, 0.9659258262890683122, 1.000000000000000000, 0.9659258262890683122, 1.000000000000000000, 0.9659258262890683122, 1.000000000000000000, 0.9659258262890683122, 1.000000000000000000, 0.9659258262890683122, 1.000000000000000000, 0.9659258262890683122, 1.000000000000000000, 0.9659258262890683122, 1.000000000000000000, 0.9659258262890683122, 1.000000000000000000, 0.9659258262890683122, 1.000000000000000000, 0.9659258262890683122, 1.000000000000000000, 0.9659258262890683122, 1.000000000000000000, 0.9659258262890683122, 1.000000000000000000, 0.9659258262890683122, 1.000000000000000000, 0.9659258262890683122, 1.000000000000000000, 0.9659258262890683122, 1.000000000000000000, 0.9659258262890683122, 1.000000000000000000, 0.9659258262890683122, 1.000000000000000000, 0.9659258262890683122, 1.000000000000000000, 0.9659258262890683122, 1.000000000000000000, 0.9659258262890683122, 1.000000000000000000, 0.9659258262890683122, 1.000000000000000000, 0.9659258262890683122, 1.000000000000000000, 0.9659258262890683122, 1.000000000000000000, 0.9659258262890683122, 1.000000000000000000, 0.9659258262890683122, 1.000000000000000000, 0.9659258262890683122, 1.000000000000000000, 0.9659258262890683122, 1.000000000000000000, 0.9659258262890683122, 1.000000000000000000, 0.9659258262890683122, 1.000000000000000000, 0.9659258262890683122, 1.000000000000000000, 0.9659258262890683122, 1.000000000000000000, 0.9659258262890683122, 1.000000000000000000, 0.9659258262890683122, 1.000000000000000000, 0.9659258262890683122, 1.000000000000000000, 0.9659258262890683122, 1.000000000000000000, 0.9659258262890683122, 1.000000000000000000, 0.9659258262890683122, 1.000000000000000000, 0.9659258262890683122, 1.000000000000000000, 0.9659258262890683122, 1.000000000000000000, 0.9659258262890683122, 1.000000000000000000, 0.9659258262890683122, 1.000000000000000000, 0.9659258262890683122, 1.000000000000000000, 0.9659258262890683122, 1.000000000000000000, 0.9659258262890683122, 1.000000000000000000, 0.9659258262890683122, 1.000000000000000000, 0.9659258262890683122, 1.000000000000000000, 0.9659258262890683122, 1.000000000000000000, 0.9659258262890683122, 1.000000000000000000, 0.9659258262890683122, 1.000000000000000000, 0.9659258262890683122, 1.000000000000000000, 0.9659258262890683122, 1.000000000000000000, 0.9659258262890683122, 1.000000000000000000, 0.9659258262890683122, 1.000000000000000000, 0.9659258262890683122, 1.000000000000000000, 0.9659258262890683122, 1.000000000000000000, 0.9659258262890683122, 1.000000000000000000, 0.9659258262890683122, 1.000000000000000000, 0.9659258262890683122, 1.000000000000000000, 0.9659258262890683122, 1.000000000000000000, 0.9659258262890683122, 1.000000000000000000, 0.9659258262890683122, 1.000000000000000000, 0.9659258262890683122, 1.000000000000000000, 0.9659258262890683122, 1.000000000000000000, 0.9659258262890683122, 1.000000000000000000, 0.9659258262890683122, 1.000000000000000000, 0.9659258262890683122, 1.000000000000000000, 0.9659258262890683122, 1.000000000000000000, 0.9659258262890683122, 1.000000000000000000, 0.9659258262890683122, 1.000000000000000000, 0.9659258262890683122, 1.000000000000000000, 0.9659258262890683122, 1.000000000000000000, 0.9659258262890683122, 1.000000000000000000, 0.9659258262890683122, 1.000000000000000000, 0.9659258262890683122, 1.000000000000000000, 0.9659258262890683122, 1.000000000000000000, 0.9659258262890683122, 1.000000000000000000, 0.9659258262890683122, 1.000000000000000000, 0.9659258262890683122, 1.000000000000000000, 0.9659258262890683122, 1.000000000000000000, 0.9659258262890683122, 1.000000000000000000, 0.9659258262890683122, 1.000000000000000000, 0.9659258262890683122, 1.000000000000000000, 0.9659258262890683122, 1.000000000000000000, 0.9659258262890683122, 1.000000000000000000, 0.9659258262890683122, 1.000000000000000000, 0.9659258262890683122, 1.000000000000000000, 0.9659258262890683122, 1.000000000000000000, 0.9659258262890683122, 1.000000000000000000, 0.9659258262890683122, 1.000000000000000000, 0.9659258262890683122, 1.000000000000000000, 0.9659258262890683122, 1.000000000000000000, 0.9659258262890683122, 1.000000000000000000, 0.9659258262890683122, 1.000000000000000000, 0.9659258262890683122, 1.000000000000000000, 0.9659258262890683122, 1.000000000000000000, 0.9659258262890683122, 1.000000000000000000, 0.9659258262890683122, 1.000000000000000000, 0.9659258262890683122, 1.000000000000000000, 0.9659258262890683122, 1.000000000000000000, 0.9659258262890683122, 1.000000000000000000, 0.9659258262890683122, 1.000000000000000000, 0.9659258262890683122, 1.000000000000000000, 0.9659258262890683122, 1.000000000000000000, 0.9659258262890683122, 1.000000000000000000, 0.9659258262890683122, 1.000000000000000000, 0.9659258262890683122, 1.000000000000000000, 0.9659258262890683122, 1.000000000000000000, 0.9659258262890683122, 1.000000000000000000, 0.9659258262890683122, 1.000000000000000000, 0.9659258262890683122, 1.000000000000000000, 0.9659258262890683122, 1.000000000000000000, 0.9659258262890683122, 1.000000000000000000, 0.9659258262890683122, 1.000000000000000000, 0.9659258262890683122, 1.000000000000000000, 0.9659258262890683122, 1.000000000000000000, 0.9659258262890683122, 1.000000000000000000, 0.9659258262890683122, 1.000000000000000000, 0.9659258262890683122, 1.000000000000000000, 0.9659258262890683122, 1.000000000000000000, 0.9659258262890683122, 1.000000000000000000, 0.9659258262890683122, 1.000000000000000000, 0.9659258262890683122, 1.000000000000000000, 0.9659258262890683122, 1.000000000000000000, 0.9659258262890683122, 1.000000000000000000, 0.9659258262890683122, 1.000000000000000000, 0.9659258262890683122, 1.000000000000000000, 0.9659258262890683122, 1.000000000000000000, 0.9659258262890683122, 1.000000000000000000, 0.9659258262890683122, 1.000000000000000000, 0.9659258262890683122, 1.000000000000000000, 0.9659258262890683122, 1.000000000000000000, 0.9659258262890683122, 1.000000000000000000, 0.9659258262890683122, 1.000000000000000000, 0.9659258262890683122, 1.000000000000000000, 0.9659258262890683122, 1.000000000000000000, 0.9659258262890683122, 1.000000000000000000, 0.9659258262890683122, 1.000000000000000000, 0.9659258262890683122, 1.000000000000000000, 0.9659258262890683122, 1.000000000000000000, 0.9659258262890683122, 1.000000000000000000, 0.9659258262890683122, 1.000000000000000000, 0.9659258262890683122, 1.000000000000000000, 0.9659258262890683122, 1.000000000000000000, 0.9659258262890683122, 1.000000000000000000, 0.9659258262890683122, 1.000000000000000000, 0.9659258262890683122, 1.000000000000000000, 0.9659258262890683122, 1.000000000000000000, 0.9659258262890683122, 1.000000000000000000, 0.9659258262890683122, 1.000000000000000000, 0.9659258262890683122, 1.000000000000000000, 0.9659258262890683122, 1.000000000000000000, 0.9659258262890683122, 1.000000000000000000, 0.9659258262890683122, 1.000000000000000000, 0.9659258262890683122, 1.000000000000000000, 0.9659258262890683122, 1.000000000000000000, 0.9659258262890683122, 1.000000000000000000, 0.9659258262890683122, 1.000000000000000000, 0.9659258262890683122, 1.000000000000000000, 0.9659258262890683122, 1.000000000000000000, 0.9659258262890683122, 1.000000000000000000, 0.9659258262890683122, 1.000000000000000000, 0.9659258262890683122, 1.000000000000000000, 0.9659258262890683122, 1.000000000000000000, 0.9659258262890683122, 1.000000000000000000, 0.9659258262890683122, 1.000000000000000000, 0.9659258262890683122, 1.000000000000000000),
 ( 0.3333333333333333703, 0.3219752754296894559, 0.3333333333333333703, 0.3219752754296894559, 0.3333333333333333703, 0.3219752754296894559, 0.3333333333333333703, 0.3219752754296894559, 0.3333333333333333703, 0.3219752754296894559, 0.3333333333333333703, 0.3219752754296894559, 0.3333333333333333703, 0.3219752754296894559, 0.3333333333333333703, 0.3219752754296894559, 0.3333333333333333703, 0.3219752754296894559, 0.3333333333333333703, 0.3219752754296894559, 0.3333333333333333703, 0.3219752754296894559, 0.3333333333333333703, 0.3219752754296894559, 0.3333333333333333703, 0.3219752754296894559, 0.3333333333333333703, 0.3219752754296894559, 0.3333333333333333703, 0.3219752754296894559, 0.3333333333333333703, 0.3219752754296894559, 0.3333333333333333703, 0.3219752754296894559, 0.3333333333333333703, 0.3219752754296894559, 0.3333333333333333703, 0.3219752754296894559, 0.3333333333333333703, 0.3219752754296894559, 0.3333333333333333703, 0.3219752754296894559, 0.3333333333333333703, 0.3219752754296894559, 0.3333333333333333703, 0.3219752754296894559, 0.3333333333333333703, 0.3219752754296894559, 0.3333333333333333703, 0.3219752754296894559, 0.3333333333333333703, 0.3219752754296894559, 0.3333333333333333703, 0.3219752754296894559, 0.3333333333333333703, 0.3219752754296894559, 0.3333333333333333703, 0.3219752754296894559, 0.3333333333333333703, 0.3219752754296894559, 0.3333333333333333703, 0.3219752754296894559, 0.3333333333333333703, 0.3219752754296894559, 0.3333333333333333703, 0.3219752754296894559, 0.3333333333333333703, 0.3219752754296894559, 0.3333333333333333703, 0.3219752754296894559, 0.3333333333333333703, 0.3219752754296894559, 0.3333333333333333703, 0.3219752754296894559, 0.3333333333333333703, 0.3219752754296894559, 0.3333333333333333703, 0.3219752754296894559, 0.3333333333333333703, 0.3219752754296894559, 0.3333333333333333703, 0.3219752754296894559, 0.3333333333333333703, 0.3219752754296894559, 0.3333333333333333703, 0.3219752754296894559, 0.3333333333333333703, 0.3219752754296894559, 0.3333333333333333703, 0.3219752754296894559, 0.3333333333333333703, 0.3219752754296894559, 0.3333333333333333703, 0.3219752754296894559, 0.3333333333333333703, 0.3219752754296894559, 0.3333333333333333703, 0.3219752754296894559, 0.3333333333333333703, 0.3219752754296894559, 0.3333333333333333703, 0.3219752754296894559, 0.3333333333333333703, 0.3219752754296894559, 0.3333333333333333703, 0.3219752754296894559, 0.3333333333333333703, 0.3219752754296894559, 0.3333333333333333703, 0.3219752754296894559, 0.3333333333333333703, 0.3219752754296894559, 0.3333333333333333703, 0.3219752754296894559, 0.3333333333333333703, 0.3219752754296894559, 0.3333333333333333703, 0.3219752754296894559, 0.3333333333333333703, 0.3219752754296894559, 0.3333333333333333703, 0.3219752754296894559, 0.3333333333333333703, 0.3219752754296894559, 0.3333333333333333703, 0.3219752754296894559, 0.3333333333333333703, 0.3219752754296894559, 0.3333333333333333703, 0.3219752754296894559, 0.3333333333333333703, 0.3219752754296894559, 0.3333333333333333703, 0.3219752754296894559, 0.3333333333333333703, 0.3219752754296894559, 0.3333333333333333703, 0.3219752754296894559, 0.3333333333333333703, 0.3219752754296894559, 0.3333333333333333703, 0.3219752754296894559, 0.3333333333333333703, 0.3219752754296894559, 0.3333333333333333703, 0.3219752754296894559, 0.3333333333333333703, 0.3219752754296894559, 0.3333333333333333703, 0.3219752754296894559, 0.3333333333333333703, 0.3219752754296894559, 0.3333333333333333703, 0.3219752754296894559, 0.3333333333333333703, 0.3219752754296894559, 0.3333333333333333703, 0.3219752754296894559, 0.3333333333333333703, 0.3219752754296894559, 0.3333333333333333703, 0.3219752754296894559, 0.3333333333333333703, 0.3219752754296894559, 0.3333333333333333703, 0.3219752754296894559, 0.3333333333333333703, 0.3219752754296894559, 0.3333333333333333703, 0.3219752754296894559, 0.3333333333333333703, 0.3219752754296894559, 0.3333333333333333703, 0.3219752754296894559, 0.3333333333333333703, 0.3219752754296894559, 0.3333333333333333703, 0.3219752754296894559, 0.3333333333333333703, 0.3219752754296894559, 0.3333333333333333703, 0.3219752754296894559, 0.3333333333333333703, 0.3219752754296894559, 0.3333333333333333703, 0.3219752754296894559, 0.3333333333333333703, 0.3219752754296894559, 0.3333333333333333703, 0.3219752754296894559, 0.3333333333333333703, 0.3219752754296894559, 0.3333333333333333703, 0.3219752754296894559, 0.3333333333333333703, 0.3219752754296894559, 0.3333333333333333703, 0.3219752754296894559, 0.3333333333333333703, 0.3219752754296894559, 0.3333333333333333703, 0.3219752754296894559, 0.3333333333333333703, 0.3219752754296894559, 0.3333333333333333703, 0.3219752754296894559, 0.3333333333333333703, 0.3219752754296894559, 0.3333333333333333703, 0.3219752754296894559, 0.3333333333333333703, 0.3219752754296894559, 0.3333333333333333703, 0.3219752754296894559, 0.3333333333333333703, 0.3219752754296894559, 0.3333333333333333703, 0.3219752754296894559, 0.3333333333333333703, 0.3219752754296894559, 0.3333333333333333703, 0.3219752754296894559, 0.3333333333333333703, 0.3219752754296894559, 0.3333333333333333703, 0.3219752754296894559, 0.3333333333333333703, 0.3219752754296894559, 0.3333333333333333703, 0.3219752754296894559, 0.3333333333333333703, 0.3219752754296894559, 0.3333333333333333703, 0.3219752754296894559, 0.3333333333333333703, 0.3219752754296894559, 0.3333333333333333703, 0.3219752754296894559, 0.3333333333333333703, 0.3219752754296894559, 0.3333333333333333703, 0.3219752754296894559, 0.3333333333333333703, 0.3219752754296894559, 0.3333333333333333703, 0.3219752754296894559, 0.3333333333333333703, 0.3219752754296894559, 0.3333333333333333703, 0.3219752754296894559, 0.3333333333333333703, 0.3219752754296894559, 0.3333333333333333703, 0.3219752754296894559, 0.3333333333333333703, 0.3219752754296894559, 0.3333333333333333703, 0.3219752754296894559, 0.3333333333333333703, 0.3219752754296894559, 0.3333333333333333703, 0.3219752754296894559, 0.3333333333333333703, 0.3219752754296894559, 0.3333333333333333703, 0.3219752754296894559, 0.3333333333333333703, 0.3219752754296894559, 0.3333333333333333703, 0.3219752754296894559, 0.3333333333333333703, 0.3219752754296894559, 0.3333333333333333703, 0.3219752754296894559, 0.3333333333333333703, 0.3219752754296894559, 0.3333333333333333703, 0.3219752754296894559, 0.3333333333333333703, 0.3219752754296894559, 0.3333333333333333703, 0.3219752754296894559, 0.3333333333333333703, 0.3219752754296894559, 0.3333333333333333703, 0.3219752754296894559, 0.3333333333333333703, 0.3219752754296894559, 0.3333333333333333703, 0.3219752754296894559, 0.3333333333333333703, 0.3219752754296894559, 0.3333333333333333703, 0.3219752754296894559, 0.3333333333333333703, 0.3219752754296894559, 0.3333333333333333703, 0.3219752754296894559, 0.3333333333333333703, 0.3219752754296894559, 0.3333333333333333703, 0.3219752754296894559, 0.3333333333333333703, 0.3219752754296894559, 0.3333333333333333703, 0.3219752754296894559, 0.3333333333333333703, 0.3219752754296894559, 0.3333333333333333703, 0.3219752754296894559, 0.3333333333333333703, 0.3219752754296894559, 0.3333333333333333703, 0.3219752754296894559, 0.3333333333333333703, 0.3219752754296894559, 0.3333333333333333703, 0.3219752754296894559, 0.3333333333333333703, 0.3219752754296894559, 0.3333333333333333703, 0.3219752754296894559, 0.3333333333333333703, 0.3219752754296894559, 0.3333333333333333703, 0.3219752754296894559, 0.3333333333333333703, 0.3219752754296894559, 0.3333333333333333703, 0.3219752754296894559, 0.3333333333333333703, 0.3219752754296894559, 0.3333333333333333703, 0.3219752754296894559, 0.3333333333333333703, 0.3219752754296894559, 0.3333333333333333703, 0.3219752754296894559, 0.3333333333333333703, 0.3219752754296894559, 0.3333333333333333703, 0.3219752754296894559, 0.3333333333333333703, 0.3219752754296894559, 0.3333333333333333703, 0.3219752754296894559, 0.3333333333333333703, 0.3219752754296894559, 0.3333333333333333703, 0.3219752754296894559, 0.3333333333333333703, 0.3219752754296894559, 0.3333333333333333703, 0.3219752754296894559, 0.3333333333333333703, 0.3219752754296894559, 0.3333333333333333703, 0.3219752754296894559, 0.3333333333333333703, 0.3219752754296894559, 0.3333333333333333703, 0.3219752754296894559, 0.3333333333333333703, 0.3219752754296894559, 0.3333333333333333703, 0.3219752754296894559, 0.3333333333333333703, 0.3219752754296894559, 0.3333333333333333703, 0.3219752754296894559, 0.3333333333333333703, 0.3219752754296894559, 0.3333333333333333703, 0.3219752754296894559, 0.3333333333333333703, 0.3219752754296894559, 0.3333333333333333703, 0.3219752754296894559, 0.3333333333333333703, 0.3219752754296894559, 0.3333333333333333703, 0.3219752754296894559, 0.3333333333333333703, 0.3219752754296894559, 0.3333333333333333703, 0.3219752754296894559, 0.3333333333333333703, 0.3219752754296894559, 0.3333333333333333703, 0.3219752754296894559, 0.3333333333333333703, 0.3219752754296894559, 0.3333333333333333703, 0.3219752754296894559, 0.3333333333333333703, 0.3219752754296894559, 0.3333333333333333703, 0.3219752754296894559, 0.3333333333333333703, 0.3219752754296894559, 0.3333333333333333703, 0.3219752754296894559, 0.3333333333333333703, 0.3219752754296894559, 0.3333333333333333703, 0.3219752754296894559, 0.3333333333333333703, 0.3219752754296894559, 0.3333333333333333703, 0.3219752754296894559, 0.3333333333333333703, 0.3219752754296894559, 0.3333333333333333703, 0.3219752754296894559, 0.3333333333333333703, 0.3219752754296894559, 0.3333333333333333703, 0.3219752754296894559, 0.3333333333333333703, 0.3219752754296894559, 0.3333333333333333703, 0.3219752754296894559, 0.3333333333333333703, 0.3219752754296894559, 0.3333333333333333703, 0.3219752754296894559, 0.3333333333333333703, 0.3219752754296894559, 0.3333333333333333703, 0.3219752754296894559, 0.3333333333333333703, 0.3219752754296894559, 0.3333333333333333703, 0.3219752754296894559, 0.3333333333333333703, 0.3219752754296894559, 0.3333333333333333703, 0.3219752754296894559, 0.3333333333333333703, 0.3219752754296894559, 0.3333333333333333703, 0.3219752754296894559, 0.3333333333333333703, 0.3219752754296894559, 0.3333333333333333703, 0.3219752754296894559, 0.3333333333333333703, 0.3219752754296894559, 0.3333333333333333703, 0.3219752754296894559, 0.3333333333333333703, 0.3219752754296894559, 0.3333333333333333703, 0.3219752754296894559, 0.3333333333333333703, 0.3219752754296894559, 0.3333333333333333703),
 ( 0.3333333333333333703, 0.3219752754296894559, 0.3333333333333333703, 0.3219752754296894559, 0.3333333333333333703, 0.3219752754296894559, 0.3333333333333333703, 0.3219752754296894559, 0.3333333333333333703, 0.3219752754296894559, 0.3333333333333333703, 0.3219752754296894559, 0.3333333333333333703, 0.3219752754296894559, 0.3333333333333333703, 0.3219752754296894559, 0.3333333333333333703, 0.3219752754296894559, 0.3333333333333333703, 0.3219752754296894559, 0.3333333333333333703, 0.3219752754296894559, 0.3333333333333333703, 0.3219752754296894559, 0.3333333333333333703, 0.3219752754296894559, 0.3333333333333333703, 0.3219752754296894559, 0.3333333333333333703, 0.3219752754296894559, 0.3333333333333333703, 0.3219752754296894559, 0.3333333333333333703, 0.3219752754296894559, 0.3333333333333333703, 0.3219752754296894559, 0.3333333333333333703, 0.3219752754296894559, 0.3333333333333333703, 0.3219752754296894559, 0.3333333333333333703, 0.3219752754296894559, 0.3333333333333333703, 0.3219752754296894559, 0.3333333333333333703, 0.3219752754296894559, 0.3333333333333333703, 0.3219752754296894559, 0.3333333333333333703, 0.3219752754296894559, 0.3333333333333333703, 0.3219752754296894559, 0.3333333333333333703, 0.3219752754296894559, 0.3333333333333333703, 0.3219752754296894559, 0.3333333333333333703, 0.3219752754296894559, 0.3333333333333333703, 0.3219752754296894559, 0.3333333333333333703, 0.3219752754296894559, 0.3333333333333333703, 0.3219752754296894559, 0.3333333333333333703, 0.3219752754296894559, 0.3333333333333333703, 0.3219752754296894559, 0.3333333333333333703, 0.3219752754296894559, 0.3333333333333333703, 0.3219752754296894559, 0.3333333333333333703, 0.3219752754296894559, 0.3333333333333333703, 0.3219752754296894559, 0.3333333333333333703, 0.3219752754296894559, 0.3333333333333333703, 0.3219752754296894559, 0.3333333333333333703, 0.3219752754296894559, 0.3333333333333333703, 0.3219752754296894559, 0.3333333333333333703, 0.3219752754296894559, 0.3333333333333333703, 0.3219752754296894559, 0.3333333333333333703, 0.3219752754296894559, 0.3333333333333333703, 0.3219752754296894559, 0.3333333333333333703, 0.3219752754296894559, 0.3333333333333333703, 0.3219752754296894559, 0.3333333333333333703, 0.3219752754296894559, 0.3333333333333333703, 0.3219752754296894559, 0.3333333333333333703, 0.3219752754296894559, 0.3333333333333333703, 0.3219752754296894559, 0.3333333333333333703, 0.3219752754296894559, 0.3333333333333333703, 0.3219752754296894559, 0.3333333333333333703, 0.3219752754296894559, 0.3333333333333333703, 0.3219752754296894559, 0.3333333333333333703, 0.3219752754296894559, 0.3333333333333333703, 0.3219752754296894559, 0.3333333333333333703, 0.3219752754296894559, 0.3333333333333333703, 0.3219752754296894559, 0.3333333333333333703, 0.3219752754296894559, 0.3333333333333333703, 0.3219752754296894559, 0.3333333333333333703, 0.3219752754296894559, 0.3333333333333333703, 0.3219752754296894559, 0.3333333333333333703, 0.3219752754296894559, 0.3333333333333333703, 0.3219752754296894559, 0.3333333333333333703, 0.3219752754296894559, 0.3333333333333333703, 0.3219752754296894559, 0.3333333333333333703, 0.3219752754296894559, 0.3333333333333333703, 0.3219752754296894559, 0.3333333333333333703, 0.3219752754296894559, 0.3333333333333333703, 0.3219752754296894559, 0.3333333333333333703, 0.3219752754296894559, 0.3333333333333333703, 0.3219752754296894559, 0.3333333333333333703, 0.3219752754296894559, 0.3333333333333333703, 0.3219752754296894559, 0.3333333333333333703, 0.3219752754296894559, 0.3333333333333333703, 0.3219752754296894559, 0.3333333333333333703, 0.3219752754296894559, 0.3333333333333333703, 0.3219752754296894559, 0.3333333333333333703, 0.3219752754296894559, 0.3333333333333333703, 0.3219752754296894559, 0.3333333333333333703, 0.3219752754296894559, 0.3333333333333333703, 0.3219752754296894559, 0.3333333333333333703, 0.3219752754296894559, 0.3333333333333333703, 0.3219752754296894559, 0.3333333333333333703, 0.3219752754296894559, 0.3333333333333333703, 0.3219752754296894559, 0.3333333333333333703, 0.3219752754296894559, 0.3333333333333333703, 0.3219752754296894559, 0.3333333333333333703, 0.3219752754296894559, 0.3333333333333333703, 0.3219752754296894559, 0.3333333333333333703, 0.3219752754296894559, 0.3333333333333333703, 0.3219752754296894559, 0.3333333333333333703, 0.3219752754296894559, 0.3333333333333333703, 0.3219752754296894559, 0.3333333333333333703, 0.3219752754296894559, 0.3333333333333333703, 0.3219752754296894559, 0.3333333333333333703, 0.3219752754296894559, 0.3333333333333333703, 0.3219752754296894559, 0.3333333333333333703, 0.3219752754296894559, 0.3333333333333333703, 0.3219752754296894559, 0.3333333333333333703, 0.3219752754296894559, 0.3333333333333333703, 0.3219752754296894559, 0.3333333333333333703, 0.3219752754296894559, 0.3333333333333333703, 0.3219752754296894559, 0.3333333333333333703, 0.3219752754296894559, 0.3333333333333333703, 0.3219752754296894559, 0.3333333333333333703, 0.3219752754296894559, 0.3333333333333333703, 0.3219752754296894559, 0.3333333333333333703, 0.3219752754296894559, 0.3333333333333333703, 0.3219752754296894559, 0.3333333333333333703, 0.3219752754296894559, 0.3333333333333333703, 0.3219752754296894559, 0.3333333333333333703, 0.3219752754296894559, 0.3333333333333333703, 0.3219752754296894559, 0.3333333333333333703, 0.3219752754296894559, 0.3333333333333333703, 0.3219752754296894559, 0.3333333333333333703, 0.3219752754296894559, 0.3333333333333333703, 0.3219752754296894559, 0.3333333333333333703, 0.3219752754296894559, 0.3333333333333333703, 0.3219752754296894559, 0.3333333333333333703, 0.3219752754296894559, 0.3333333333333333703, 0.3219752754296894559, 0.3333333333333333703, 0.3219752754296894559, 0.3333333333333333703, 0.3219752754296894559, 0.3333333333333333703, 0.3219752754296894559, 0.3333333333333333703, 0.3219752754296894559, 0.3333333333333333703, 0.3219752754296894559, 0.3333333333333333703, 0.3219752754296894559, 0.3333333333333333703, 0.3219752754296894559, 0.3333333333333333703, 0.3219752754296894559, 0.3333333333333333703, 0.3219752754296894559, 0.3333333333333333703, 0.3219752754296894559, 0.3333333333333333703, 0.3219752754296894559, 0.3333333333333333703, 0.3219752754296894559, 0.3333333333333333703, 0.3219752754296894559, 0.3333333333333333703, 0.3219752754296894559, 0.3333333333333333703, 0.3219752754296894559, 0.3333333333333333703, 0.3219752754296894559, 0.3333333333333333703, 0.3219752754296894559, 0.3333333333333333703, 0.3219752754296894559, 0.3333333333333333703, 0.3219752754296894559, 0.3333333333333333703, 0.3219752754296894559, 0.3333333333333333703, 0.3219752754296894559, 0.3333333333333333703, 0.3219752754296894559, 0.3333333333333333703, 0.3219752754296894559, 0.3333333333333333703, 0.3219752754296894559, 0.3333333333333333703, 0.3219752754296894559, 0.3333333333333333703, 0.3219752754296894559, 0.3333333333333333703, 0.3219752754296894559, 0.3333333333333333703, 0.3219752754296894559, 0.3333333333333333703, 0.3219752754296894559, 0.3333333333333333703, 0.3219752754296894559, 0.3333333333333333703, 0.3219752754296894559, 0.3333333333333333703, 0.3219752754296894559, 0.3333333333333333703, 0.3219752754296894559, 0.3333333333333333703, 0.3219752754296894559, 0.3333333333333333703, 0.3219752754296894559, 0.3333333333333333703, 0.3219752754296894559, 0.3333333333333333703, 0.3219752754296894559, 0.3333333333333333703, 0.3219752754296894559, 0.3333333333333333703, 0.3219752754296894559, 0.3333333333333333703, 0.3219752754296894559, 0.3333333333333333703, 0.3219752754296894559, 0.3333333333333333703, 0.3219752754296894559, 0.3333333333333333703, 0.3219752754296894559, 0.3333333333333333703, 0.3219752754296894559, 0.3333333333333333703, 0.3219752754296894559, 0.3333333333333333703, 0.3219752754296894559, 0.3333333333333333703, 0.3219752754296894559, 0.3333333333333333703, 0.3219752754296894559, 0.3333333333333333703, 0.3219752754296894559, 0.3333333333333333703, 0.3219752754296894559, 0.3333333333333333703, 0.3219752754296894559, 0.3333333333333333703, 0.3219752754296894559, 0.3333333333333333703, 0.3219752754296894559, 0.3333333333333333703, 0.3219752754296894559, 0.3333333333333333703, 0.3219752754296894559, 0.3333333333333333703, 0.3219752754296894559, 0.3333333333333333703, 0.3219752754296894559, 0.3333333333333333703, 0.3219752754296894559, 0.3333333333333333703, 0.3219752754296894559, 0.3333333333333333703, 0.3219752754296894559, 0.3333333333333333703, 0.3219752754296894559, 0.3333333333333333703, 0.3219752754296894559, 0.3333333333333333703, 0.3219752754296894559, 0.3333333333333333703, 0.3219752754296894559, 0.3333333333333333703, 0.3219752754296894559, 0.3333333333333333703, 0.3219752754296894559, 0.3333333333333333703, 0.3219752754296894559, 0.3333333333333333703, 0.3219752754296894559, 0.3333333333333333703, 0.3219752754296894559, 0.3333333333333333703, 0.3219752754296894559, 0.3333333333333333703, 0.3219752754296894559, 0.3333333333333333703, 0.3219752754296894559, 0.3333333333333333703, 0.3219752754296894559, 0.3333333333333333703, 0.3219752754296894559, 0.3333333333333333703, 0.3219752754296894559, 0.3333333333333333703, 0.3219752754296894559, 0.3333333333333333703, 0.3219752754296894559, 0.3333333333333333703, 0.3219752754296894559, 0.3333333333333333703, 0.3219752754296894559, 0.3333333333333333703, 0.3219752754296894559, 0.3333333333333333703, 0.3219752754296894559, 0.3333333333333333703, 0.3219752754296894559, 0.3333333333333333703, 0.3219752754296894559, 0.3333333333333333703, 0.3219752754296894559, 0.3333333333333333703, 0.3219752754296894559, 0.3333333333333333703, 0.3219752754296894559, 0.3333333333333333703, 0.3219752754296894559, 0.3333333333333333703, 0.3219752754296894559, 0.3333333333333333703, 0.3219752754296894559, 0.3333333333333333703, 0.3219752754296894559, 0.3333333333333333703, 0.3219752754296894559, 0.3333333333333333703, 0.3219752754296894559, 0.3333333333333333703, 0.3219752754296894559, 0.3333333333333333703, 0.3219752754296894559, 0.3333333333333333703, 0.3219752754296894559, 0.3333333333333333703, 0.3219752754296894559, 0.3333333333333333703, 0.3219752754296894559, 0.3333333333333333703, 0.3219752754296894559, 0.3333333333333333703, 0.3219752754296894559, 0.3333333333333333703, 0.3219752754296894559, 0.3333333333333333703, 0.3219752754296894559, 0.3333333333333333703, 0.3219752754296894559, 0.3333333333333333703, 0.3219752754296894559, 0.3333333333333333703, 0.3219752754296894559, 0.3333333333333333703),
 ( 1.000000000000000000, 0.9659258262890683122, 1.000000000000000000, 0.9659258262890683122, 1.000000000000000000, 0.9659258262890683122, 1.000000000000000000, 0.9659258262890683122, 1.000000000000000000, 0.9659258262890683122, 1.000000000000000000, 0.9659258262890683122, 1.000000000000000000, 0.9659258262890683122, 1.000000000000000000, 0.9659258262890683122, 1.000000000000000000, 0.9659258262890683122, 1.000000000000000000, 0.9659258262890683122, 1.000000000000000000, 0.9659258262890683122, 1.000000000000000000, 0.9659258262890683122, 1.000000000000000000, 0.9659258262890683122, 1.000000000000000000, 0.9659258262890683122, 1.000000000000000000, 0.9659258262890683122, 1.000000000000000000, 0.9659258262890683122, 1.000000000000000000, 0.9659258262890683122, 1.000000000000000000, 0.9659258262890683122, 1.000000000000000000, 0.9659258262890683122, 1.000000000000000000, 0.9659258262890683122, 1.000000000000000000, 0.9659258262890683122, 1.000000000000000000, 0.9659258262890683122, 1.000000000000000000, 0.9659258262890683122, 1.000000000000000000, 0.9659258262890683122, 1.000000000000000000, 0.9659258262890683122, 1.000000000000000000, 0.9659258262890683122, 1.000000000000000000, 0.9659258262890683122, 1.000000000000000000, 0.9659258262890683122, 1.000000000000000000, 0.9659258262890683122, 1.000000000000000000, 0.9659258262890683122, 1.000000000000000000, 0.9659258262890683122, 1.000000000000000000, 0.9659258262890683122, 1.000000000000000000, 0.9659258262890683122, 1.000000000000000000, 0.9659258262890683122, 1.000000000000000000, 0.9659258262890683122, 1.000000000000000000, 0.9659258262890683122, 1.000000000000000000, 0.9659258262890683122, 1.000000000000000000, 0.9659258262890683122, 1.000000000000000000, 0.9659258262890683122, 1.000000000000000000, 0.9659258262890683122, 1.000000000000000000, 0.9659258262890683122, 1.000000000000000000, 0.9659258262890683122, 1.000000000000000000, 0.9659258262890683122, 1.000000000000000000, 0.9659258262890683122, 1.000000000000000000, 0.9659258262890683122, 1.000000000000000000, 0.9659258262890683122, 1.000000000000000000, 0.9659258262890683122, 1.000000000000000000, 0.9659258262890683122, 1.000000000000000000, 0.9659258262890683122, 1.000000000000000000, 0.9659258262890683122, 1.000000000000000000, 0.9659258262890683122, 1.000000000000000000, 0.9659258262890683122, 1.000000000000000000, 0.9659258262890683122, 1.000000000000000000, 0.9659258262890683122, 1.000000000000000000, 0.9659258262890683122, 1.000000000000000000, 0.9659258262890683122, 1.000000000000000000, 0.9659258262890683122, 1.000000000000000000, 0.9659258262890683122, 1.000000000000000000, 0.9659258262890683122, 1.000000000000000000, 0.9659258262890683122, 1.000000000000000000, 0.9659258262890683122, 1.000000000000000000, 0.9659258262890683122, 1.000000000000000000, 0.9659258262890683122, 1.000000000000000000, 0.9659258262890683122, 1.000000000000000000, 0.9659258262890683122, 1.000000000000000000, 0.9659258262890683122, 1.000000000000000000, 0.9659258262890683122, 1.000000000000000000, 0.9659258262890683122, 1.000000000000000000, 0.9659258262890683122, 1.000000000000000000, 0.9659258262890683122, 1.000000000000000000, 0.9659258262890683122, 1.000000000000000000, 0.9659258262890683122, 1.000000000000000000, 0.9659258262890683122, 1.000000000000000000, 0.9659258262890683122, 1.000000000000000000, 0.9659258262890683122, 1.000000000000000000, 0.9659258262890683122, 1.000000000000000000, 0.9659258262890683122, 1.000000000000000000, 0.9659258262890683122, 1.000000000000000000, 0.9659258262890683122, 1.000000000000000000, 0.9659258262890683122, 1.000000000000000000, 0.9659258262890683122, 1.000000000000000000, 0.9659258262890683122, 1.000000000000000000, 0.9659258262890683122, 1.000000000000000000, 0.9659258262890683122, 1.000000000000000000, 0.9659258262890683122, 1.000000000000000000, 0.9659258262890683122, 1.000000000000000000, 0.9659258262890683122, 1.000000000000000000, 0.9659258262890683122, 1.000000000000000000, 0.9659258262890683122, 1.000000000000000000, 0.9659258262890683122, 1.000000000000000000, 0.9659258262890683122, 1.000000000000000000, 0.9659258262890683122, 1.000000000000000000, 0.9659258262890683122, 1.000000000000000000, 0.9659258262890683122, 1.000000000000000000, 0.9659258262890683122, 1.000000000000000000, 0.9659258262890683122, 1.000000000000000000, 0.9659258262890683122, 1.000000000000000000, 0.9659258262890683122, 1.000000000000000000, 0.9659258262890683122, 1.000000000000000000, 0.9659258262890683122, 1.000000000000000000, 0.9659258262890683122, 1.000000000000000000, 0.9659258262890683122, 1.000000000000000000, 0.9659258262890683122, 1.000000000000000000, 0.9659258262890683122, 1.000000000000000000, 0.9659258262890683122, 1.000000000000000000, 0.9659258262890683122, 1.000000000000000000, 0.9659258262890683122, 1.000000000000000000, 0.9659258262890683122, 1.000000000000000000, 0.9659258262890683122, 1.000000000000000000, 0.9659258262890683122, 1.000000000000000000, 0.9659258262890683122, 1.000000000000000000, 0.9659258262890683122, 1.000000000000000000, 0.9659258262890683122, 1.000000000000000000, 0.9659258262890683122, 1.000000000000000000, 0.9659258262890683122, 1.000000000000000000, 0.9659258262890683122, 1.000000000000000000, 0.9659258262890683122, 1.000000000000000000, 0.9659258262890683122, 1.000000000000000000, 0.9659258262890683122, 1.000000000000000000, 0.9659258262890683122, 1.000000000000000000, 0.9659258262890683122, 1.000000000000000000, 0.9659258262890683122, 1.000000000000000000, 0.9659258262890683122, 1.000000000000000000, 0.9659258262890683122, 1.000000000000000000, 0.9659258262890683122, 1.000000000000000000, 0.9659258262890683122, 1.000000000000000000, 0.9659258262890683122, 1.000000000000000000, 0.9659258262890683122, 1.000000000000000000, 0.9659258262890683122, 1.000000000000000000, 0.9659258262890683122, 1.000000000000000000, 0.9659258262890683122, 1.000000000000000000, 0.9659258262890683122, 1.000000000000000000, 0.9659258262890683122, 1.000000000000000000, 0.9659258262890683122, 1.000000000000000000, 0.9659258262890683122, 1.000000000000000000, 0.9659258262890683122, 1.000000000000000000, 0.9659258262890683122, 1.000000000000000000, 0.9659258262890683122, 1.000000000000000000, 0.9659258262890683122, 1.000000000000000000, 0.9659258262890683122, 1.000000000000000000, 0.9659258262890683122, 1.000000000000000000, 0.9659258262890683122, 1.000000000000000000, 0.9659258262890683122, 1.000000000000000000, 0.9659258262890683122, 1.000000000000000000, 0.9659258262890683122, 1.000000000000000000, 0.9659258262890683122, 1.000000000000000000, 0.9659258262890683122, 1.000000000000000000, 0.9659258262890683122, 1.000000000000000000, 0.9659258262890683122, 1.000000000000000000, 0.9659258262890683122, 1.000000000000000000, 0.9659258262890683122, 1.000000000000000000, 0.9659258262890683122, 1.000000000000000000, 0.9659258262890683122, 1.000000000000000000, 0.9659258262890683122, 1.000000000000000000, 0.9659258262890683122, 1.000000000000000000, 0.9659258262890683122, 1.000000000000000000, 0.9659258262890683122, 1.000000000000000000, 0.9659258262890683122, 1.000000000000000000, 0.9659258262890683122, 1.000000000000000000, 0.9659258262890683122, 1.000000000000000000, 0.9659258262890683122, 1.000000000000000000, 0.9659258262890683122, 1.000000000000000000, 0.9659258262890683122, 1.000000000000000000, 0.9659258262890683122, 1.000000000000000000, 0.9659258262890683122, 1.000000000000000000, 0.9659258262890683122, 1.000000000000000000, 0.9659258262890683122, 1.000000000000000000, 0.9659258262890683122, 1.000000000000000000, 0.9659258262890683122, 1.000000000000000000, 0.9659258262890683122, 1.000000000000000000, 0.9659258262890683122, 1.000000000000000000, 0.9659258262890683122, 1.000000000000000000, 0.9659258262890683122, 1.000000000000000000, 0.9659258262890683122, 1.000000000000000000, 0.9659258262890683122, 1.000000000000000000, 0.9659258262890683122, 1.000000000000000000, 0.9659258262890683122, 1.000000000000000000, 0.9659258262890683122, 1.000000000000000000, 0.9659258262890683122, 1.000000000000000000, 0.9659258262890683122, 1.000000000000000000, 0.9659258262890683122, 1.000000000000000000, 0.9659258262890683122, 1.000000000000000000, 0.9659258262890683122, 1.000000000000000000, 0.9659258262890683122, 1.000000000000000000, 0.9659258262890683122, 1.000000000000000000, 0.9659258262890683122, 1.000000000000000000, 0.9659258262890683122, 1.000000000000000000, 0.9659258262890683122, 1.000000000000000000, 0.9659258262890683122, 1.000000000000000000, 0.9659258262890683122, 1.000000000000000000, 0.9659258262890683122, 1.000000000000000000, 0.9659258262890683122, 1.000000000000000000, 0.9659258262890683122, 1.000000000000000000, 0.9659258262890683122, 1.000000000000000000, 0.9659258262890683122, 1.000000000000000000, 0.9659258262890683122, 1.000000000000000000, 0.9659258262890683122, 1.000000000000000000, 0.9659258262890683122, 1.000000000000000000, 0.9659258262890683122, 1.000000000000000000, 0.9659258262890683122, 1.000000000000000000, 0.9659258262890683122, 1.000000000000000000, 0.9659258262890683122, 1.000000000000000000, 0.9659258262890683122, 1.000000000000000000, 0.9659258262890683122, 1.000000000000000000, 0.9659258262890683122, 1.000000000000000000, 0.9659258262890683122, 1.000000000000000000, 0.9659258262890683122, 1.000000000000000000, 0.9659258262890683122, 1.000000000000000000, 0.9659258262890683122, 1.000000000000000000, 0.9659258262890683122, 1.000000000000000000, 0.9659258262890683122, 1.000000000000000000, 0.9659258262890683122, 1.000000000000000000, 0.9659258262890683122, 1.000000000000000000, 0.9659258262890683122, 1.000000000000000000, 0.9659258262890683122, 1.000000000000000000, 0.9659258262890683122, 1.000000000000000000, 0.9659258262890683122, 1.000000000000000000, 0.9659258262890683122, 1.000000000000000000, 0.9659258262890683122, 1.000000000000000000, 0.9659258262890683122, 1.000000000000000000, 0.9659258262890683122, 1.000000000000000000, 0.9659258262890683122, 1.000000000000000000, 0.9659258262890683122, 1.000000000000000000, 0.9659258262890683122, 1.000000000000000000, 0.9659258262890683122, 1.000000000000000000, 0.9659258262890683122, 1.000000000000000000, 0.9659258262890683122, 1.000000000000000000, 0.9659258262890683122, 1.000000000000000000),
 ( 0.3333333333333333703, 0.3219752754296894559, 0.3333333333333333703, 0.3219752754296894559, 0.3333333333333333703, 0.3219752754296894559, 0.3333333333333333703, 0.3219752754296894559, 0.3333333333333333703, 0.3219752754296894559, 0.3333333333333333703, 0.3219752754296894559, 0.3333333333333333703, 0.3219752754296894559, 0.3333333333333333703, 0.3219752754296894559, 0.3333333333333333703, 0.3219752754296894559, 0.3333333333333333703, 0.3219752754296894559, 0.3333333333333333703, 0.3219752754296894559, 0.3333333333333333703, 0.3219752754296894559, 0.3333333333333333703, 0.3219752754296894559, 0.3333333333333333703, 0.3219752754296894559, 0.3333333333333333703, 0.3219752754296894559, 0.3333333333333333703, 0.3219752754296894559, 0.3333333333333333703, 0.3219752754296894559, 0.3333333333333333703, 0.3219752754296894559, 0.3333333333333333703, 0.3219752754296894559, 0.3333333333333333703, 0.3219752754296894559, 0.3333333333333333703, 0.3219752754296894559, 0.3333333333333333703, 0.3219752754296894559, 0.3333333333333333703, 0.3219752754296894559, 0.3333333333333333703, 0.3219752754296894559, 0.3333333333333333703, 0.3219752754296894559, 0.3333333333333333703, 0.3219752754296894559, 0.3333333333333333703, 0.3219752754296894559, 0.3333333333333333703, 0.3219752754296894559, 0.3333333333333333703, 0.3219752754296894559, 0.3333333333333333703, 0.3219752754296894559, 0.3333333333333333703, 0.3219752754296894559, 0.3333333333333333703, 0.3219752754296894559, 0.3333333333333333703, 0.3219752754296894559, 0.3333333333333333703, 0.3219752754296894559, 0.3333333333333333703, 0.3219752754296894559, 0.3333333333333333703, 0.3219752754296894559, 0.3333333333333333703, 0.3219752754296894559, 0.3333333333333333703, 0.3219752754296894559, 0.3333333333333333703, 0.3219752754296894559, 0.3333333333333333703, 0.3219752754296894559, 0.3333333333333333703, 0.3219752754296894559, 0.3333333333333333703, 0.3219752754296894559, 0.3333333333333333703, 0.3219752754296894559, 0.3333333333333333703, 0.3219752754296894559, 0.3333333333333333703, 0.3219752754296894559, 0.3333333333333333703, 0.3219752754296894559, 0.3333333333333333703, 0.3219752754296894559, 0.3333333333333333703, 0.3219752754296894559, 0.3333333333333333703, 0.3219752754296894559, 0.3333333333333333703, 0.3219752754296894559, 0.3333333333333333703, 0.3219752754296894559, 0.3333333333333333703, 0.3219752754296894559, 0.3333333333333333703, 0.3219752754296894559, 0.3333333333333333703, 0.3219752754296894559, 0.3333333333333333703, 0.3219752754296894559, 0.3333333333333333703, 0.3219752754296894559, 0.3333333333333333703, 0.3219752754296894559, 0.3333333333333333703, 0.3219752754296894559, 0.3333333333333333703, 0.3219752754296894559, 0.3333333333333333703, 0.3219752754296894559, 0.3333333333333333703, 0.3219752754296894559, 0.3333333333333333703, 0.3219752754296894559, 0.3333333333333333703, 0.3219752754296894559, 0.3333333333333333703, 0.3219752754296894559, 0.3333333333333333703, 0.3219752754296894559, 0.3333333333333333703, 0.3219752754296894559, 0.3333333333333333703, 0.3219752754296894559, 0.3333333333333333703, 0.3219752754296894559, 0.3333333333333333703, 0.3219752754296894559, 0.3333333333333333703, 0.3219752754296894559, 0.3333333333333333703, 0.3219752754296894559, 0.3333333333333333703, 0.3219752754296894559, 0.3333333333333333703, 0.3219752754296894559, 0.3333333333333333703, 0.3219752754296894559, 0.3333333333333333703, 0.3219752754296894559, 0.3333333333333333703, 0.3219752754296894559, 0.3333333333333333703, 0.3219752754296894559, 0.3333333333333333703, 0.3219752754296894559, 0.3333333333333333703, 0.3219752754296894559, 0.3333333333333333703, 0.3219752754296894559, 0.3333333333333333703, 0.3219752754296894559, 0.3333333333333333703, 0.3219752754296894559, 0.3333333333333333703, 0.3219752754296894559, 0.3333333333333333703, 0.3219752754296894559, 0.3333333333333333703, 0.3219752754296894559, 0.3333333333333333703, 0.3219752754296894559, 0.3333333333333333703, 0.3219752754296894559, 0.3333333333333333703, 0.3219752754296894559, 0.3333333333333333703, 0.3219752754296894559, 0.3333333333333333703, 0.3219752754296894559, 0.3333333333333333703, 0.3219752754296894559, 0.3333333333333333703, 0.3219752754296894559, 0.3333333333333333703, 0.3219752754296894559, 0.3333333333333333703, 0.3219752754296894559, 0.3333333333333333703, 0.3219752754296894559, 0.3333333333333333703, 0.3219752754296894559, 0.3333333333333333703, 0.3219752754296894559, 0.3333333333333333703, 0.3219752754296894559, 0.3333333333333333703, 0.3219752754296894559, 0.3333333333333333703, 0.3219752754296894559, 0.3333333333333333703, 0.3219752754296894559, 0.3333333333333333703, 0.3219752754296894559, 0.3333333333333333703, 0.3219752754296894559, 0.3333333333333333703, 0.3219752754296894559, 0.3333333333333333703, 0.3219752754296894559, 0.3333333333333333703, 0.3219752754296894559, 0.3333333333333333703, 0.3219752754296894559, 0.3333333333333333703, 0.3219752754296894559, 0.3333333333333333703, 0.3219752754296894559, 0.3333333333333333703, 0.3219752754296894559, 0.3333333333333333703, 0.3219752754296894559, 0.3333333333333333703, 0.3219752754296894559, 0.3333333333333333703, 0.3219752754296894559, 0.3333333333333333703, 0.3219752754296894559, 0.3333333333333333703, 0.3219752754296894559, 0.3333333333333333703, 0.3219752754296894559, 0.3333333333333333703, 0.3219752754296894559, 0.3333333333333333703, 0.3219752754296894559, 0.3333333333333333703, 0.3219752754296894559, 0.3333333333333333703, 0.3219752754296894559, 0.3333333333333333703, 0.3219752754296894559, 0.3333333333333333703, 0.3219752754296894559, 0.3333333333333333703, 0.3219752754296894559, 0.3333333333333333703, 0.3219752754296894559, 0.3333333333333333703, 0.3219752754296894559, 0.3333333333333333703, 0.3219752754296894559, 0.3333333333333333703, 0.3219752754296894559, 0.3333333333333333703, 0.3219752754296894559, 0.3333333333333333703, 0.3219752754296894559, 0.3333333333333333703, 0.3219752754296894559, 0.3333333333333333703, 0.3219752754296894559, 0.3333333333333333703, 0.3219752754296894559, 0.3333333333333333703, 0.3219752754296894559, 0.3333333333333333703, 0.3219752754296894559, 0.3333333333333333703, 0.3219752754296894559, 0.3333333333333333703, 0.3219752754296894559, 0.3333333333333333703, 0.3219752754296894559, 0.3333333333333333703, 0.3219752754296894559, 0.3333333333333333703, 0.3219752754296894559, 0.3333333333333333703, 0.3219752754296894559, 0.3333333333333333703, 0.3219752754296894559, 0.3333333333333333703, 0.3219752754296894559, 0.3333333333333333703, 0.3219752754296894559, 0.3333333333333333703, 0.3219752754296894559, 0.3333333333333333703, 0.3219752754296894559, 0.3333333333333333703, 0.3219752754296894559, 0.3333333333333333703, 0.3219752754296894559, 0.3333333333333333703, 0.3219752754296894559, 0.3333333333333333703, 0.3219752754296894559, 0.3333333333333333703, 0.3219752754296894559, 0.3333333333333333703, 0.3219752754296894559, 0.3333333333333333703, 0.3219752754296894559, 0.3333333333333333703, 0.3219752754296894559, 0.3333333333333333703, 0.3219752754296894559, 0.3333333333333333703, 0.3219752754296894559, 0.3333333333333333703, 0.3219752754296894559, 0.3333333333333333703, 0.3219752754296894559, 0.3333333333333333703, 0.3219752754296894559, 0.3333333333333333703, 0.3219752754296894559, 0.3333333333333333703, 0.3219752754296894559, 0.3333333333333333703, 0.3219752754296894559, 0.3333333333333333703, 0.3219752754296894559, 0.3333333333333333703, 0.3219752754296894559, 0.3333333333333333703, 0.3219752754296894559, 0.3333333333333333703, 0.3219752754296894559, 0.3333333333333333703, 0.3219752754296894559, 0.3333333333333333703, 0.3219752754296894559, 0.3333333333333333703, 0.3219752754296894559, 0.3333333333333333703, 0.3219752754296894559, 0.3333333333333333703, 0.3219752754296894559, 0.3333333333333333703, 0.3219752754296894559, 0.3333333333333333703, 0.3219752754296894559, 0.3333333333333333703, 0.3219752754296894559, 0.3333333333333333703, 0.3219752754296894559, 0.3333333333333333703, 0.3219752754296894559, 0.3333333333333333703, 0.3219752754296894559, 0.3333333333333333703, 0.3219752754296894559, 0.3333333333333333703, 0.3219752754296894559, 0.3333333333333333703, 0.3219752754296894559, 0.3333333333333333703, 0.3219752754296894559, 0.3333333333333333703, 0.3219752754296894559, 0.3333333333333333703, 0.3219752754296894559, 0.3333333333333333703, 0.3219752754296894559, 0.3333333333333333703, 0.3219752754296894559, 0.3333333333333333703, 0.3219752754296894559, 0.3333333333333333703, 0.3219752754296894559, 0.3333333333333333703, 0.3219752754296894559, 0.3333333333333333703, 0.3219752754296894559, 0.3333333333333333703, 0.3219752754296894559, 0.3333333333333333703, 0.3219752754296894559, 0.3333333333333333703, 0.3219752754296894559, 0.3333333333333333703, 0.3219752754296894559, 0.3333333333333333703, 0.3219752754296894559, 0.3333333333333333703, 0.3219752754296894559, 0.3333333333333333703, 0.3219752754296894559, 0.3333333333333333703, 0.3219752754296894559, 0.3333333333333333703, 0.3219752754296894559, 0.3333333333333333703, 0.3219752754296894559, 0.3333333333333333703, 0.3219752754296894559, 0.3333333333333333703, 0.3219752754296894559, 0.3333333333333333703, 0.3219752754296894559, 0.3333333333333333703, 0.3219752754296894559, 0.3333333333333333703, 0.3219752754296894559, 0.3333333333333333703, 0.3219752754296894559, 0.3333333333333333703, 0.3219752754296894559, 0.3333333333333333703, 0.3219752754296894559, 0.3333333333333333703, 0.3219752754296894559, 0.3333333333333333703, 0.3219752754296894559, 0.3333333333333333703, 0.3219752754296894559, 0.3333333333333333703, 0.3219752754296894559, 0.3333333333333333703, 0.3219752754296894559, 0.3333333333333333703, 0.3219752754296894559, 0.3333333333333333703, 0.3219752754296894559, 0.3333333333333333703, 0.3219752754296894559, 0.3333333333333333703, 0.3219752754296894559, 0.3333333333333333703, 0.3219752754296894559, 0.3333333333333333703, 0.3219752754296894559, 0.3333333333333333703, 0.3219752754296894559, 0.3333333333333333703, 0.3219752754296894559, 0.3333333333333333703, 0.3219752754296894559, 0.3333333333333333703, 0.3219752754296894559, 0.3333333333333333703, 0.3219752754296894559, 0.3333333333333333703, 0.3219752754296894559, 0.3333333333333333703, 0.3219752754296894559, 0.3333333333333333703, 0.3219752754296894559, 0.3333333333333333703, 0.3219752754296894559, 0.3333333333333333703, 0.3219752754296894559, 0.3333333333333333703, 0.3219752754296894559, 0.3333333333333333703),
 ( 0.3333333333333333703, 0.3219752754296894559, 0.3333333333333333703, 0.3219752754296894559, 0.3333333333333333703, 0.3219752754296894559, 0.3333333333333333703, 0.3219752754296894559, 0.3333333333333333703, 0.3219752754296894559, 0.3333333333333333703, 0.3219752754296894559, 0.3333333333333333703, 0.3219752754296894559, 0.3333333333333333703, 0.3219752754296894559, 0.3333333333333333703, 0.3219752754296894559, 0.3333333333333333703, 0.3219752754296894559, 0.3333333333333333703, 0.3219752754296894559, 0.3333333333333333703, 0.3219752754296894559, 0.3333333333333333703, 0.3219752754296894559, 0.3333333333333333703, 0.3219752754296894559, 0.3333333333333333703, 0.3219752754296894559, 0.3333333333333333703, 0.3219752754296894559, 0.3333333333333333703, 0.3219752754296894559, 0.3333333333333333703, 0.3219752754296894559, 0.3333333333333333703, 0.3219752754296894559, 0.3333333333333333703, 0.3219752754296894559, 0.3333333333333333703, 0.3219752754296894559, 0.3333333333333333703, 0.3219752754296894559, 0.3333333333333333703, 0.3219752754296894559, 0.3333333333333333703, 0.3219752754296894559, 0.3333333333333333703, 0.3219752754296894559, 0.3333333333333333703, 0.3219752754296894559, 0.3333333333333333703, 0.3219752754296894559, 0.3333333333333333703, 0.3219752754296894559, 0.3333333333333333703, 0.3219752754296894559, 0.3333333333333333703, 0.3219752754296894559, 0.3333333333333333703, 0.3219752754296894559, 0.3333333333333333703, 0.3219752754296894559, 0.3333333333333333703, 0.3219752754296894559, 0.3333333333333333703, 0.3219752754296894559, 0.3333333333333333703, 0.3219752754296894559, 0.3333333333333333703, 0.3219752754296894559, 0.3333333333333333703, 0.3219752754296894559, 0.3333333333333333703, 0.3219752754296894559, 0.3333333333333333703, 0.3219752754296894559, 0.3333333333333333703, 0.3219752754296894559, 0.3333333333333333703, 0.3219752754296894559, 0.3333333333333333703, 0.3219752754296894559, 0.3333333333333333703, 0.3219752754296894559, 0.3333333333333333703, 0.3219752754296894559, 0.3333333333333333703, 0.3219752754296894559, 0.3333333333333333703, 0.3219752754296894559, 0.3333333333333333703, 0.3219752754296894559, 0.3333333333333333703, 0.3219752754296894559, 0.3333333333333333703, 0.3219752754296894559, 0.3333333333333333703, 0.3219752754296894559, 0.3333333333333333703, 0.3219752754296894559, 0.3333333333333333703, 0.3219752754296894559, 0.3333333333333333703, 0.3219752754296894559, 0.3333333333333333703, 0.3219752754296894559, 0.3333333333333333703, 0.3219752754296894559, 0.3333333333333333703, 0.3219752754296894559, 0.3333333333333333703, 0.3219752754296894559, 0.3333333333333333703, 0.3219752754296894559, 0.3333333333333333703, 0.3219752754296894559, 0.3333333333333333703, 0.3219752754296894559, 0.3333333333333333703, 0.3219752754296894559, 0.3333333333333333703, 0.3219752754296894559, 0.3333333333333333703, 0.3219752754296894559, 0.3333333333333333703, 0.3219752754296894559, 0.3333333333333333703, 0.3219752754296894559, 0.3333333333333333703, 0.3219752754296894559, 0.3333333333333333703, 0.3219752754296894559, 0.3333333333333333703, 0.3219752754296894559, 0.3333333333333333703, 0.3219752754296894559, 0.3333333333333333703, 0.3219752754296894559, 0.3333333333333333703, 0.3219752754296894559, 0.3333333333333333703, 0.3219752754296894559, 0.3333333333333333703, 0.3219752754296894559, 0.3333333333333333703, 0.3219752754296894559, 0.3333333333333333703, 0.3219752754296894559, 0.3333333333333333703, 0.3219752754296894559, 0.3333333333333333703, 0.3219752754296894559, 0.3333333333333333703, 0.3219752754296894559, 0.3333333333333333703, 0.3219752754296894559, 0.3333333333333333703, 0.3219752754296894559, 0.3333333333333333703, 0.3219752754296894559, 0.3333333333333333703, 0.3219752754296894559, 0.3333333333333333703, 0.3219752754296894559, 0.3333333333333333703, 0.3219752754296894559, 0.3333333333333333703, 0.3219752754296894559, 0.3333333333333333703, 0.3219752754296894559, 0.3333333333333333703, 0.3219752754296894559, 0.3333333333333333703, 0.3219752754296894559, 0.3333333333333333703, 0.3219752754296894559, 0.3333333333333333703, 0.3219752754296894559, 0.3333333333333333703, 0.3219752754296894559, 0.3333333333333333703, 0.3219752754296894559, 0.3333333333333333703, 0.3219752754296894559, 0.3333333333333333703, 0.3219752754296894559, 0.3333333333333333703, 0.3219752754296894559, 0.3333333333333333703, 0.3219752754296894559, 0.3333333333333333703, 0.3219752754296894559, 0.3333333333333333703, 0.3219752754296894559, 0.3333333333333333703, 0.3219752754296894559, 0.3333333333333333703, 0.3219752754296894559, 0.3333333333333333703, 0.3219752754296894559, 0.3333333333333333703, 0.3219752754296894559, 0.3333333333333333703, 0.3219752754296894559, 0.3333333333333333703, 0.3219752754296894559, 0.3333333333333333703, 0.3219752754296894559, 0.3333333333333333703, 0.3219752754296894559, 0.3333333333333333703, 0.3219752754296894559, 0.3333333333333333703, 0.3219752754296894559, 0.3333333333333333703, 0.3219752754296894559, 0.3333333333333333703, 0.3219752754296894559, 0.3333333333333333703, 0.3219752754296894559, 0.3333333333333333703, 0.3219752754296894559, 0.3333333333333333703, 0.3219752754296894559, 0.3333333333333333703, 0.3219752754296894559, 0.3333333333333333703, 0.3219752754296894559, 0.3333333333333333703, 0.3219752754296894559, 0.3333333333333333703, 0.3219752754296894559, 0.3333333333333333703, 0.3219752754296894559, 0.3333333333333333703, 0.3219752754296894559, 0.3333333333333333703, 0.3219752754296894559, 0.3333333333333333703, 0.3219752754296894559, 0.3333333333333333703, 0.3219752754296894559, 0.3333333333333333703, 0.3219752754296894559, 0.3333333333333333703, 0.3219752754296894559, 0.3333333333333333703, 0.3219752754296894559, 0.3333333333333333703, 0.3219752754296894559, 0.3333333333333333703, 0.3219752754296894559, 0.3333333333333333703, 0.3219752754296894559, 0.3333333333333333703, 0.3219752754296894559, 0.3333333333333333703, 0.3219752754296894559, 0.3333333333333333703, 0.3219752754296894559, 0.3333333333333333703, 0.3219752754296894559, 0.3333333333333333703, 0.3219752754296894559, 0.3333333333333333703, 0.3219752754296894559, 0.3333333333333333703, 0.3219752754296894559, 0.3333333333333333703, 0.3219752754296894559, 0.3333333333333333703, 0.3219752754296894559, 0.3333333333333333703, 0.3219752754296894559, 0.3333333333333333703, 0.3219752754296894559, 0.3333333333333333703, 0.3219752754296894559, 0.3333333333333333703, 0.3219752754296894559, 0.3333333333333333703, 0.3219752754296894559, 0.3333333333333333703, 0.3219752754296894559, 0.3333333333333333703, 0.3219752754296894559, 0.3333333333333333703, 0.3219752754296894559, 0.3333333333333333703, 0.3219752754296894559, 0.3333333333333333703, 0.3219752754296894559, 0.3333333333333333703, 0.3219752754296894559, 0.3333333333333333703, 0.3219752754296894559, 0.3333333333333333703, 0.3219752754296894559, 0.3333333333333333703, 0.3219752754296894559, 0.3333333333333333703, 0.3219752754296894559, 0.3333333333333333703, 0.3219752754296894559, 0.3333333333333333703, 0.3219752754296894559, 0.3333333333333333703, 0.3219752754296894559, 0.3333333333333333703, 0.3219752754296894559, 0.3333333333333333703, 0.3219752754296894559, 0.3333333333333333703, 0.3219752754296894559, 0.3333333333333333703, 0.3219752754296894559, 0.3333333333333333703, 0.3219752754296894559, 0.3333333333333333703, 0.3219752754296894559, 0.3333333333333333703, 0.3219752754296894559, 0.3333333333333333703, 0.3219752754296894559, 0.3333333333333333703, 0.3219752754296894559, 0.3333333333333333703, 0.3219752754296894559, 0.3333333333333333703, 0.3219752754296894559, 0.3333333333333333703, 0.3219752754296894559, 0.3333333333333333703, 0.3219752754296894559, 0.3333333333333333703, 0.3219752754296894559, 0.3333333333333333703, 0.3219752754296894559, 0.3333333333333333703, 0.3219752754296894559, 0.3333333333333333703, 0.3219752754296894559, 0.3333333333333333703, 0.3219752754296894559, 0.3333333333333333703, 0.3219752754296894559, 0.3333333333333333703, 0.3219752754296894559, 0.3333333333333333703, 0.3219752754296894559, 0.3333333333333333703, 0.3219752754296894559, 0.3333333333333333703, 0.3219752754296894559, 0.3333333333333333703, 0.3219752754296894559, 0.3333333333333333703, 0.3219752754296894559, 0.3333333333333333703, 0.3219752754296894559, 0.3333333333333333703, 0.3219752754296894559, 0.3333333333333333703, 0.3219752754296894559, 0.3333333333333333703, 0.3219752754296894559, 0.3333333333333333703, 0.3219752754296894559, 0.3333333333333333703, 0.3219752754296894559, 0.3333333333333333703, 0.3219752754296894559, 0.3333333333333333703, 0.3219752754296894559, 0.3333333333333333703, 0.3219752754296894559, 0.3333333333333333703, 0.3219752754296894559, 0.3333333333333333703, 0.3219752754296894559, 0.3333333333333333703, 0.3219752754296894559, 0.3333333333333333703, 0.3219752754296894559, 0.3333333333333333703, 0.3219752754296894559, 0.3333333333333333703, 0.3219752754296894559, 0.3333333333333333703, 0.3219752754296894559, 0.3333333333333333703, 0.3219752754296894559, 0.3333333333333333703, 0.3219752754296894559, 0.3333333333333333703, 0.3219752754296894559, 0.3333333333333333703, 0.3219752754296894559, 0.3333333333333333703, 0.3219752754296894559, 0.3333333333333333703, 0.3219752754296894559, 0.3333333333333333703, 0.3219752754296894559, 0.3333333333333333703, 0.3219752754296894559, 0.3333333333333333703, 0.3219752754296894559, 0.3333333333333333703, 0.3219752754296894559, 0.3333333333333333703, 0.3219752754296894559, 0.3333333333333333703, 0.3219752754296894559, 0.3333333333333333703, 0.3219752754296894559, 0.3333333333333333703, 0.3219752754296894559, 0.3333333333333333703, 0.3219752754296894559, 0.3333333333333333703, 0.3219752754296894559, 0.3333333333333333703, 0.3219752754296894559, 0.3333333333333333703, 0.3219752754296894559, 0.3333333333333333703, 0.3219752754296894559, 0.3333333333333333703, 0.3219752754296894559, 0.3333333333333333703, 0.3219752754296894559, 0.3333333333333333703, 0.3219752754296894559, 0.3333333333333333703, 0.3219752754296894559, 0.3333333333333333703, 0.3219752754296894559, 0.3333333333333333703, 0.3219752754296894559, 0.3333333333333333703, 0.3219752754296894559, 0.3333333333333333703, 0.3219752754296894559, 0.3333333333333333703, 0.3219752754296894559, 0.3333333333333333703, 0.3219752754296894559, 0.3333333333333333703, 0.3219752754296894559, 0.3333333333333333703, 0.3219752754296894559, 0.3333333333333333703, 0.3219752754296894559, 0.3333333333333333703),
 ( 1.000000000000000000, 0.9659258262890683122, 1.000000000000000000, 0.9659258262890683122, 1.000000000000000000, 0.9659258262890683122, 1.000000000000000000, 0.9659258262890683122, 1.000000000000000000, 0.9659258262890683122, 1.000000000000000000, 0.9659258262890683122, 1.000000000000000000, 0.9659258262890683122, 1.000000000000000000, 0.9659258262890683122, 1.000000000000000000, 0.9659258262890683122, 1.000000000000000000, 0.9659258262890683122, 1.000000000000000000, 0.9659258262890683122, 1.000000000000000000, 0.9659258262890683122, 1.000000000000000000, 0.9659258262890683122, 1.000000000000000000, 0.9659258262890683122, 1.000000000000000000, 0.9659258262890683122, 1.000000000000000000, 0.9659258262890683122, 1.000000000000000000, 0.9659258262890683122, 1.000000000000000000, 0.9659258262890683122, 1.000000000000000000, 0.9659258262890683122, 1.000000000000000000, 0.9659258262890683122, 1.000000000000000000, 0.9659258262890683122, 1.000000000000000000, 0.9659258262890683122, 1.000000000000000000, 0.9659258262890683122, 1.000000000000000000, 0.9659258262890683122, 1.000000000000000000, 0.9659258262890683122, 1.000000000000000000, 0.9659258262890683122, 1.000000000000000000, 0.9659258262890683122, 1.000000000000000000, 0.9659258262890683122, 1.000000000000000000, 0.9659258262890683122, 1.000000000000000000, 0.9659258262890683122, 1.000000000000000000, 0.9659258262890683122, 1.000000000000000000, 0.9659258262890683122, 1.000000000000000000, 0.9659258262890683122, 1.000000000000000000, 0.9659258262890683122, 1.000000000000000000, 0.9659258262890683122, 1.000000000000000000, 0.9659258262890683122, 1.000000000000000000, 0.9659258262890683122, 1.000000000000000000, 0.9659258262890683122, 1.000000000000000000, 0.9659258262890683122, 1.000000000000000000, 0.9659258262890683122, 1.000000000000000000, 0.9659258262890683122, 1.000000000000000000, 0.9659258262890683122, 1.000000000000000000, 0.9659258262890683122, 1.000000000000000000, 0.9659258262890683122, 1.000000000000000000, 0.9659258262890683122, 1.000000000000000000, 0.9659258262890683122, 1.000000000000000000, 0.9659258262890683122, 1.000000000000000000, 0.9659258262890683122, 1.000000000000000000, 0.9659258262890683122, 1.000000000000000000, 0.9659258262890683122, 1.000000000000000000, 0.9659258262890683122, 1.000000000000000000, 0.9659258262890683122, 1.000000000000000000, 0.9659258262890683122, 1.000000000000000000, 0.9659258262890683122, 1.000000000000000000, 0.9659258262890683122, 1.000000000000000000, 0.9659258262890683122, 1.000000000000000000, 0.9659258262890683122, 1.000000000000000000, 0.9659258262890683122, 1.000000000000000000, 0.9659258262890683122, 1.000000000000000000, 0.9659258262890683122, 1.000000000000000000, 0.9659258262890683122, 1.000000000000000000, 0.9659258262890683122, 1.000000000000000000, 0.9659258262890683122, 1.000000000000000000, 0.9659258262890683122, 1.000000000000000000, 0.9659258262890683122, 1.000000000000000000, 0.9659258262890683122, 1.000000000000000000, 0.9659258262890683122, 1.000000000000000000, 0.9659258262890683122, 1.000000000000000000, 0.9659258262890683122, 1.000000000000000000, 0.9659258262890683122, 1.000000000000000000, 0.9659258262890683122, 1.000000000000000000, 0.9659258262890683122, 1.000000000000000000, 0.9659258262890683122, 1.000000000000000000, 0.9659258262890683122, 1.000000000000000000, 0.9659258262890683122, 1.000000000000000000, 0.9659258262890683122, 1.000000000000000000, 0.9659258262890683122, 1.000000000000000000, 0.9659258262890683122, 1.000000000000000000, 0.9659258262890683122, 1.000000000000000000, 0.9659258262890683122, 1.000000000000000000, 0.9659258262890683122, 1.000000000000000000, 0.9659258262890683122, 1.000000000000000000, 0.9659258262890683122, 1.000000000000000000, 0.9659258262890683122, 1.000000000000000000, 0.9659258262890683122, 1.000000000000000000, 0.9659258262890683122, 1.000000000000000000, 0.9659258262890683122, 1.000000000000000000, 0.9659258262890683122, 1.000000000000000000, 0.9659258262890683122, 1.000000000000000000, 0.9659258262890683122, 1.000000000000000000, 0.9659258262890683122, 1.000000000000000000, 0.9659258262890683122, 1.000000000000000000, 0.9659258262890683122, 1.000000000000000000, 0.9659258262890683122, 1.000000000000000000, 0.9659258262890683122, 1.000000000000000000, 0.9659258262890683122, 1.000000000000000000, 0.9659258262890683122, 1.000000000000000000, 0.9659258262890683122, 1.000000000000000000, 0.9659258262890683122, 1.000000000000000000, 0.9659258262890683122, 1.000000000000000000, 0.9659258262890683122, 1.000000000000000000, 0.9659258262890683122, 1.000000000000000000, 0.9659258262890683122, 1.000000000000000000, 0.9659258262890683122, 1.000000000000000000, 0.9659258262890683122, 1.000000000000000000, 0.9659258262890683122, 1.000000000000000000, 0.9659258262890683122, 1.000000000000000000, 0.9659258262890683122, 1.000000000000000000, 0.9659258262890683122, 1.000000000000000000, 0.9659258262890683122, 1.000000000000000000, 0.9659258262890683122, 1.000000000000000000, 0.9659258262890683122, 1.000000000000000000, 0.9659258262890683122, 1.000000000000000000, 0.9659258262890683122, 1.000000000000000000, 0.9659258262890683122, 1.000000000000000000, 0.9659258262890683122, 1.000000000000000000, 0.9659258262890683122, 1.000000000000000000, 0.9659258262890683122, 1.000000000000000000, 0.9659258262890683122, 1.000000000000000000, 0.9659258262890683122, 1.000000000000000000, 0.9659258262890683122, 1.000000000000000000, 0.9659258262890683122, 1.000000000000000000, 0.9659258262890683122, 1.000000000000000000, 0.9659258262890683122, 1.000000000000000000, 0.9659258262890683122, 1.000000000000000000, 0.9659258262890683122, 1.000000000000000000, 0.9659258262890683122, 1.000000000000000000, 0.9659258262890683122, 1.000000000000000000, 0.9659258262890683122, 1.000000000000000000, 0.9659258262890683122, 1.000000000000000000, 0.9659258262890683122, 1.000000000000000000, 0.9659258262890683122, 1.000000000000000000, 0.9659258262890683122, 1.000000000000000000, 0.9659258262890683122, 1.000000000000000000, 0.9659258262890683122, 1.000000000000000000, 0.9659258262890683122, 1.000000000000000000, 0.9659258262890683122, 1.000000000000000000, 0.9659258262890683122, 1.000000000000000000, 0.9659258262890683122, 1.000000000000000000, 0.9659258262890683122, 1.000000000000000000, 0.9659258262890683122, 1.000000000000000000, 0.9659258262890683122, 1.000000000000000000, 0.9659258262890683122, 1.000000000000000000, 0.9659258262890683122, 1.000000000000000000, 0.9659258262890683122, 1.000000000000000000, 0.9659258262890683122, 1.000000000000000000, 0.9659258262890683122, 1.000000000000000000, 0.9659258262890683122, 1.000000000000000000, 0.9659258262890683122, 1.000000000000000000, 0.9659258262890683122, 1.000000000000000000, 0.9659258262890683122, 1.000000000000000000, 0.9659258262890683122, 1.000000000000000000, 0.9659258262890683122, 1.000000000000000000, 0.9659258262890683122, 1.000000000000000000, 0.9659258262890683122, 1.000000000000000000, 0.9659258262890683122, 1.000000000000000000, 0.9659258262890683122, 1.000000000000000000, 0.9659258262890683122, 1.000000000000000000, 0.9659258262890683122, 1.000000000000000000, 0.9659258262890683122, 1.000000000000000000, 0.9659258262890683122, 1.000000000000000000, 0.9659258262890683122, 1.000000000000000000, 0.9659258262890683122, 1.000000000000000000, 0.9659258262890683122, 1.000000000000000000, 0.9659258262890683122, 1.000000000000000000, 0.9659258262890683122, 1.000000000000000000, 0.9659258262890683122, 1.000000000000000000, 0.9659258262890683122, 1.000000000000000000, 0.9659258262890683122, 1.000000000000000000, 0.9659258262890683122, 1.000000000000000000, 0.9659258262890683122, 1.000000000000000000, 0.9659258262890683122, 1.000000000000000000, 0.9659258262890683122, 1.000000000000000000, 0.9659258262890683122, 1.000000000000000000, 0.9659258262890683122, 1.000000000000000000, 0.9659258262890683122, 1.000000000000000000, 0.9659258262890683122, 1.000000000000000000, 0.9659258262890683122, 1.000000000000000000, 0.9659258262890683122, 1.000000000000000000, 0.9659258262890683122, 1.000000000000000000, 0.9659258262890683122, 1.000000000000000000, 0.9659258262890683122, 1.000000000000000000, 0.9659258262890683122, 1.000000000000000000, 0.9659258262890683122, 1.000000000000000000, 0.9659258262890683122, 1.000000000000000000, 0.9659258262890683122, 1.000000000000000000, 0.9659258262890683122, 1.000000000000000000, 0.9659258262890683122, 1.000000000000000000, 0.9659258262890683122, 1.000000000000000000, 0.9659258262890683122, 1.000000000000000000, 0.9659258262890683122, 1.000000000000000000, 0.9659258262890683122, 1.000000000000000000, 0.9659258262890683122, 1.000000000000000000, 0.9659258262890683122, 1.000000000000000000, 0.9659258262890683122, 1.000000000000000000, 0.9659258262890683122, 1.000000000000000000, 0.9659258262890683122, 1.000000000000000000, 0.9659258262890683122, 1.000000000000000000, 0.9659258262890683122, 1.000000000000000000, 0.9659258262890683122, 1.000000000000000000, 0.9659258262890683122, 1.000000000000000000, 0.9659258262890683122, 1.000000000000000000, 0.9659258262890683122, 1.000000000000000000, 0.9659258262890683122, 1.000000000000000000, 0.9659258262890683122, 1.000000000000000000, 0.9659258262890683122, 1.000000000000000000, 0.9659258262890683122, 1.000000000000000000, 0.9659258262890683122, 1.000000000000000000, 0.9659258262890683122, 1.000000000000000000, 0.9659258262890683122, 1.000000000000000000, 0.9659258262890683122, 1.000000000000000000, 0.9659258262890683122, 1.000000000000000000, 0.9659258262890683122, 1.000000000000000000, 0.9659258262890683122, 1.000000000000000000, 0.9659258262890683122, 1.000000000000000000, 0.9659258262890683122, 1.000000000000000000, 0.9659258262890683122, 1.000000000000000000, 0.9659258262890683122, 1.000000000000000000, 0.9659258262890683122, 1.000000000000000000, 0.9659258262890683122, 1.000000000000000000, 0.9659258262890683122, 1.000000000000000000, 0.9659258262890683122, 1.000000000000000000, 0.9659258262890683122, 1.000000000000000000, 0.9659258262890683122, 1.000000000000000000, 0.9659258262890683122, 1.000000000000000000, 0.9659258262890683122, 1.000000000000000000, 0.9659258262890683122, 1.000000000000000000, 0.9659258262890683122, 1.000000000000000000) ) ) 
 REPRESENTATION_ITEM ( '' )  SURFACE ( )  );
#6563 = CARTESIAN_POINT ( 'NONE',  ( -8.314922557961024197, 14.29746914071037800, 27.91775706135234358 ) ) ;
#6565 = CARTESIAN_POINT ( 'NONE',  ( 15.72974639402176855, 15.80617190586768217, 76.87609039468567573 ) ) ;
#6564 = CARTESIAN_POINT ( 'NONE',  ( -14.29746914071049879, 8.314922557960819915, 65.83224293864769550 ) ) ;
#6566 = CARTESIAN_POINT ( 'NONE',  ( 4.483927247898790824, -16.52544592524335698, 100.2094237280190043 ) ) ;
#6567 = CARTESIAN_POINT ( 'NONE',  ( 17.40861289039011339, -6.110651285853056613, 46.12767529172570136 ) ) ;
#6568 = CARTESIAN_POINT ( 'NONE',  ( -18.56399227203345959, -5.499999999999829470, 63.97830131249904184 ) ) ;
#6569 = CARTESIAN_POINT ( 'NONE',  ( -16.52544592524342804, 4.483927247898546575, 26.04057627198103475 ) ) ;
#6570 = CARTESIAN_POINT ( 'NONE',  ( -4.483927247898782831, 16.52544592524335698, 72.70942372801901854 ) ) ;
#6571 = CARTESIAN_POINT ( 'NONE',  ( -0.05219959533909027116, -19.03943276465977164, 87.49890960531436690 ) ) ;
#6572 = CARTESIAN_POINT ( 'NONE',  ( 16.46253265017160672, -9.564922557960803928, 98.33224293864769550 ) ) ;
#6573 = CARTESIAN_POINT ( 'NONE',  ( -10.81492255796105439, 18.62759615963255655, 82.91775706135234714 ) ) ;
#6574 = CARTESIAN_POINT ( 'NONE',  ( -14.29746914071037622, -8.314922557961029526, 94.16775706135237556 ) ) ;
#6575 = CARTESIAN_POINT ( 'NONE',  ( -14.29746914071049879, 8.314922557960819915, 60.83224293864769550 ) ) ;
#6576 = CARTESIAN_POINT ( 'NONE',  ( -13.89961937509977652, 13.97604488694528158, 65.62390960531436690 ) ) ;
#6577 = ORIENTED_EDGE ( 'NONE', *, *, #25423, .F. ) ;
#6578 = CARTESIAN_POINT ( 'NONE',  ( -19.05341960407617563, 5.049401038297882671, 108.5427570613523187 ) ) ;
#6579 = CARTESIAN_POINT ( 'NONE',  ( -16.53943276465976808, 0.05219959533911058130, 111.2489096053143669 ) ) ;
#6580 = CARTESIAN_POINT ( 'NONE',  ( 19.05341960407611168, 5.049401038298154454, 73.95724293864768129 ) ) ;
#6582 = CARTESIAN_POINT ( 'NONE',  ( -22.81625015709510507, 31.40387420917330275, -6.924999997268812990 ) ) ;
#6581 = CARTESIAN_POINT ( 'NONE',  ( -4.379528057220086978, -16.55341960407618274, 19.79275706135235069 ) ) ;
#6583 = CARTESIAN_POINT ( 'NONE',  ( -19.03943276465977164, -0.05219959533935918106, 23.75109039468566152 ) ) ;
#6584 = CARTESIAN_POINT ( 'NONE',  ( 4.379528057220092307, 16.55341960407617563, 77.29275706135234714 ) ) ;
#6585 = CARTESIAN_POINT ( 'NONE',  ( -13.97604488694547697, 13.89961937509957934, 98.12609039468566152 ) ) ;
#6586 = CARTESIAN_POINT ( 'NONE',  ( 19.03943276465977164, -0.05219959533909143690, 23.74890960531435269 ) ) ;
#6587 = CARTESIAN_POINT ( 'NONE',  ( 0.05219959533934541429, -16.53943276465976808, 65.00109039468568994 ) ) ;
#6588 = CARTESIAN_POINT ( 'NONE',  ( 0.05219959533934541429, -16.53943276465976808, 50.00109039468568994 ) ) ;
#6589 = CARTESIAN_POINT ( 'NONE',  ( -5.153800228976328057, -19.02544592524343514, 27.29057627198103120 ) ) ;
#6590 = CARTESIAN_POINT ( 'NONE',  ( 13.89961937509957401, 13.97604488694547697, 51.87609039468566863 ) ) ;
#6591 = CARTESIAN_POINT ( 'NONE',  ( -5.823673210054431948, 21.52544592524334988, 92.70942372801901854 ) ) ;
#6592 = CARTESIAN_POINT ( 'NONE',  ( -19.02544592524342804, 5.153800228976336051, 31.04057627198102409 ) ) ;
#6593 = CARTESIAN_POINT ( 'NONE',  ( 5.153800228976335163, 19.02544592524342804, 74.79057627198103830 ) ) ;
#6594 = CARTESIAN_POINT ( 'NONE',  ( -8.314922557960811034, -14.29746914071050412, 72.08224293864769550 ) ) ;
#6595 = VECTOR ( 'NONE', #69761, 1000.000000000000000 ) ;
#6596 = CARTESIAN_POINT ( 'NONE',  ( 21.55341960407619695, -5.719274019375665929, 96.04275706135236135 ) ) ;
#6597 = CARTESIAN_POINT ( 'NONE',  ( 0.05219959533936267826, -19.03943276465977164, 60.00109039468566863 ) ) ;
#6598 = CARTESIAN_POINT ( 'NONE',  ( 13.97604488694548053, -13.89961937509957401, 40.62609039468564731 ) ) ;
#6599 = CARTESIAN_POINT ( 'NONE',  ( 10.72451020669898902, -18.67979575497178502, 37.91557627198102409 ) ) ;
#6600 = CARTESIAN_POINT ( 'NONE',  ( 21.53943276465977519, 0.05219959533937863772, 106.2510903946856757 ) ) ;
#6601 = CARTESIAN_POINT ( 'NONE',  ( -13.97604488694527625, -13.89961937509977652, 71.87390960531433848 ) ) ;
#6602 = CARTESIAN_POINT ( 'NONE',  ( 18.67979575497194134, -10.72451020669871369, 105.8344237280190328 ) ) ;
#6603 = CARTESIAN_POINT ( 'NONE',  ( -5.719274019375978568, 21.55341960407610458, 45.20724293864769550 ) ) ;
#6604 = CARTESIAN_POINT ( 'NONE',  ( 9.474510206698971260, -16.51473224551069308, 102.9155762719810241 ) ) ;
#6605 = CARTESIAN_POINT ( 'NONE',  ( -5.049401038297874678, -19.05341960407617918, 69.79275706135233293 ) ) ;
#6606 = CARTESIAN_POINT ( 'NONE',  ( -19.03943276465977164, 0.05219959533909376836, 106.2489096053143669 ) ) ;
#6607 = CARTESIAN_POINT ( 'NONE',  ( -16.51473224551082808, 9.474510206698731452, 98.33442372801900433 ) ) ;
#6608 = CARTESIAN_POINT ( 'NONE',  ( 16.53943276465976808, 0.05219959533934440121, 41.25109039468568284 ) ) ;
#6609 = CARTESIAN_POINT ( 'NONE',  ( -16.46253265017160317, 9.564922557960807481, 25.83224293864769194 ) ) ;
#6610 = CARTESIAN_POINT ( 'NONE',  ( 13.89961937509977652, -13.97604488694527269, 78.12390960531433848 ) ) ;
#6611 = CARTESIAN_POINT ( 'NONE',  ( 18.62759615963271287, -10.81492255796078972, 68.33224293864769550 ) ) ;
#6612 = CARTESIAN_POINT ( 'NONE',  ( -12.14591786802326823, 12.06949235617739902, 38.12609039468567573 ) ) ;
#6613 = CARTESIAN_POINT ( 'NONE',  ( 5.823673210054444382, -21.52544592524334988, 40.20942372801901854 ) ) ;
#6614 = CARTESIAN_POINT ( 'NONE',  ( 5.823673210054444382, -21.52544592524334988, 80.20942372801901854 ) ) ;
#6615 = CARTESIAN_POINT ( 'NONE',  ( -12.06949235617739369, -12.14591786802326823, 79.37609039468567573 ) ) ;
#6616 = CARTESIAN_POINT ( 'NONE',  ( 16.51473224551069308, 9.474510206698969483, 89.16557627198103830 ) ) ;
#6617 = CARTESIAN_POINT ( 'NONE',  ( -16.55341960407611168, -4.379528057220339221, 71.45724293864769550 ) ) ;
#6618 = CARTESIAN_POINT ( 'NONE',  ( 8.224510206698953496, -14.34966873604960469, 27.91557627198103830 ) ) ;
#6619 = CARTESIAN_POINT ( 'NONE',  ( -19.03943276465977164, -0.05219959533935918106, 53.75109039468566863 ) ) ;
#6620 = CARTESIAN_POINT ( 'NONE',  ( -15.80617190586768217, 15.72974639402176855, 43.12609039468568284 ) ) ;
#6621 = CARTESIAN_POINT ( 'NONE',  ( 16.53943276465976808, -0.05219959533910856209, 83.74890960531435269 ) ) ;
#6622 = CARTESIAN_POINT ( 'NONE',  ( 15.72974639402199770, -15.80617190586745480, 23.12390960531436335 ) ) ;
#6623 = CARTESIAN_POINT ( 'NONE',  ( 16.52544592524335698, 4.483927247898782831, 96.45942372801901854 ) ) ;
#6624 = CARTESIAN_POINT ( 'NONE',  ( 10.81492255796106328, -18.62759615963255655, 80.41775706135234714 ) ) ;
#6625 = CARTESIAN_POINT ( 'NONE',  ( 0.05219959533934541429, -16.53943276465976808, 50.00109039468568994 ) ) ;
#6626 = CARTESIAN_POINT ( 'NONE',  ( -21.55341960407619339, 5.719274019375674811, 43.54275706135235424 ) ) ;
#6627 = VERTEX_POINT ( 'NONE', #57076 ) ;
#6628 = CARTESIAN_POINT ( 'NONE',  ( 18.67979575497178502, 10.72451020669898547, 109.1655762719810383 ) ) ;
#6629 = CARTESIAN_POINT ( 'NONE',  ( -8.224510206698948167, 14.34966873604960824, 90.41557627198103830 ) ) ;
#6630 = EDGE_CURVE ( 'NONE', #122538, #2008, #46499, .T. ) ;
#6631 = DIRECTION ( 'NONE',  ( 0.000000000000000000, 0.000000000000000000, -1.000000000000000000 ) ) ;
#6632 = CARTESIAN_POINT ( 'NONE',  ( 8.314922557960818139, 14.29746914071049879, 49.58224293864769550 ) ) ;
#6633 = CARTESIAN_POINT ( 'NONE',  ( -14.29746914071037622, -8.314922557961029526, 94.16775706135237556 ) ) ;
#6634 = CARTESIAN_POINT ( 'NONE',  ( -9.564922557960796823, -16.46253265017161027, 42.08224293864769550 ) ) ;
#6635 = CARTESIAN_POINT ( 'NONE',  ( 15.80617190586746368, 15.72974639402197994, 44.37390960531435979 ) ) ;
#6636 = CARTESIAN_POINT ( 'NONE',  ( -14.34966873604960291, -8.224510206698953496, 71.66557627198100988 ) ) ;
#6637 = CARTESIAN_POINT ( 'NONE',  ( -21.53943276465977519, 0.05219959533907696930, 76.24890960531435269 ) ) ;
#6638 = CARTESIAN_POINT ( 'NONE',  ( -16.51473224551069308, -9.474510206698971260, 86.66557627198102409 ) ) ;
#6640 = CARTESIAN_POINT ( 'NONE',  ( 0.05219959533936267826, -19.03943276465977164, 95.00109039468567573 ) ) ;
#6639 = CARTESIAN_POINT ( 'NONE',  ( 5.153800228976335163, 19.02544592524342804, 34.79057627198102409 ) ) ;
#6641 = EDGE_CURVE ( 'NONE', #36560, #198744, #104764, .T. ) ;
#6642 = CARTESIAN_POINT ( 'NONE',  ( 21.52544592524344225, -5.823673210054117533, 28.54057627198103120 ) ) ;
#6643 = CARTESIAN_POINT ( 'NONE',  ( 15.72974639402176855, 15.80617190586768217, 56.87609039468568994 ) ) ;
#6644 = CARTESIAN_POINT ( 'NONE',  ( 9.564922557960805705, 16.46253265017160317, 49.58224293864770260 ) ) ;
#6645 = CARTESIAN_POINT ( 'NONE',  ( 0.05219959533909260263, 19.03943276465977164, 84.99890960531436690 ) ) ;
#6646 = ORIENTED_EDGE ( 'NONE', *, *, #14461, .F. ) ;
#6647 = CARTESIAN_POINT ( 'NONE',  ( -16.53943276465976808, -0.05219959533934237506, 53.75109039468568994 ) ) ;
#6648 = CARTESIAN_POINT ( 'NONE',  ( 10.72451020669871369, 18.67979575497193778, 32.08442372801901854 ) ) ;
#6649 = CARTESIAN_POINT ( 'NONE',  ( 21.55341960407619695, -5.719274019375665929, 71.04275706135234714 ) ) ;
#6650 = CARTESIAN_POINT ( 'NONE',  ( -10.81492255796078084, -18.62759615963271287, 27.08224293864769550 ) ) ;
#6651 = CARTESIAN_POINT ( 'NONE',  ( 15.72974639402199770, -15.80617190586745480, 83.12390960531436690 ) ) ;
#6653 = CARTESIAN_POINT ( 'NONE',  ( 12.06949235617739724, 12.14591786802326823, 61.87609039468568284 ) ) ;
#6652 = CARTESIAN_POINT ( 'NONE',  ( -21.52544592524334988, -5.823673210054445271, 18.95942372801901143 ) ) ;
#6654 = CARTESIAN_POINT ( 'NONE',  ( -15.72974639402197994, 15.80617190586746368, 65.62390960531436690 ) ) ;
#6655 = CARTESIAN_POINT ( 'NONE',  ( -16.46253265017146816, -9.564922557961047289, 19.16775706135233293 ) ) ;
#6656 = CARTESIAN_POINT ( 'NONE',  ( -5.153800228976328057, -19.02544592524343514, 67.29057627198102409 ) ) ;
#6657 = CARTESIAN_POINT ( 'NONE',  ( 16.51473224551069308, 9.474510206698969483, 104.1655762719810241 ) ) ;
#6658 = CARTESIAN_POINT ( 'NONE',  ( 19.05341960407611168, 5.049401038298154454, 88.95724293864769550 ) ) ;
#6659 = CARTESIAN_POINT ( 'NONE',  ( -23.96320343559627375, 18.46320343559663257, 8.181980515339452253 ) ) ;
#6660 = CARTESIAN_POINT ( 'NONE',  ( -19.05341960407617563, 5.049401038297882671, 63.54275706135234003 ) ) ;
#6661 = CARTESIAN_POINT ( 'NONE',  ( -10.72451020669898014, 18.67979575497178502, 50.41557627198103120 ) ) ;
#6662 = CARTESIAN_POINT ( 'NONE',  ( 16.52544592524342804, -4.483927247898539470, 23.54057627198102765 ) ) ;
#6663 = CARTESIAN_POINT ( 'NONE',  ( -16.46253265017146816, -9.564922557961047289, 104.1677570613523329 ) ) ;
#6664 = CARTESIAN_POINT ( 'NONE',  ( 9.474510206698971260, -16.51473224551069308, 22.91557627198102765 ) ) ;
#6665 = CARTESIAN_POINT ( 'NONE',  ( 19.02544592524334988, 5.153800228976608722, 101.4594237280189759 ) ) ;
#6667 = CARTESIAN_POINT ( 'NONE',  ( -13.97604488694547697, 13.89961937509957934, 53.12609039468565442 ) ) ;
#6666 = CARTESIAN_POINT ( 'NONE',  ( 5.823673210054125526, 21.52544592524343514, 84.79057627198102409 ) ) ;
#6668 = CARTESIAN_POINT ( 'NONE',  ( 17.26172910966779739, 6.454744622555832478, 106.6935309135077432 ) ) ;
#6669 = CARTESIAN_POINT ( 'NONE',  ( -13.97604488694527625, -13.89961937509977652, 51.87390960531436690 ) ) ;
#6670 = CARTESIAN_POINT ( 'NONE',  ( 12.14591786802309770, 12.06949235617756955, 64.37390960531435269 ) ) ;
#6671 = CARTESIAN_POINT ( 'NONE',  ( 19.03943276465977164, -0.05219959533909143690, 43.74890960531435979 ) ) ;
#6672 = CARTESIAN_POINT ( 'NONE',  ( -8.314922557960811034, -14.29746914071050412, 57.08224293864769550 ) ) ;
#6673 = CARTESIAN_POINT ( 'NONE',  ( -28.45933917494770427, -27.69424206401140864, -20.18904788101069769 ) ) ;
#6674 = CARTESIAN_POINT ( 'NONE',  ( -16.53943276465976808, 0.05219959533911058130, 26.24890960531435624 ) ) ;
#6675 = CARTESIAN_POINT ( 'NONE',  ( 9.564922557960805705, 16.46253265017160317, 64.58224293864769550 ) ) ;
#6676 = CARTESIAN_POINT ( 'NONE',  ( -17.72517630440429670, 5.500000000000146549, 50.92175719257211597 ) ) ;
#6677 = CARTESIAN_POINT ( 'NONE',  ( 13.89961937509957401, 13.97604488694547697, 31.87609039468566863 ) ) ;
#6678 = CARTESIAN_POINT ( 'NONE',  ( 8.224510206698742110, 14.34966873604972548, 42.08442372801901854 ) ) ;
#6679 = CARTESIAN_POINT ( 'NONE',  ( -18.62759615963270932, 10.81492255796079327, 55.83224293864770260 ) ) ;
#6681 = VERTEX_POINT ( 'NONE', #26746 ) ;
#6680 = CARTESIAN_POINT ( 'NONE',  ( 18.62759615963255655, 10.81492255796105972, 106.6677570613523756 ) ) ;
#6682 = CARTESIAN_POINT ( 'NONE',  ( -0.05219959533909027116, -19.03943276465977164, 57.49890960531435979 ) ) ;
#6683 = DIRECTION ( 'NONE',  ( 1.000000000000000000, 0.000000000000000000, 0.000000000000000000 ) ) ;
#6684 = CARTESIAN_POINT ( 'NONE',  ( 5.049401038298161559, -19.05341960407611168, 102.7072429386476955 ) ) ;
#6685 = CARTESIAN_POINT ( 'NONE',  ( -17.60691670004650433, -5.500000000000067502, 44.13333313366439370 ) ) ;
#6686 = CARTESIAN_POINT ( 'NONE',  ( 18.67979575497194134, -10.72451020669871369, 25.83442372801901499 ) ) ;
#6687 = CARTESIAN_POINT ( 'NONE',  ( 12.06949235617757843, -12.14591786802309237, 98.12390960531436690 ) ) ;
#6689 = CARTESIAN_POINT ( 'NONE',  ( 16.46253265017160672, -9.564922557960803928, 88.33224293864769550 ) ) ;
#6688 = CARTESIAN_POINT ( 'NONE',  ( -5.823673210054116645, -21.52544592524344225, 87.29057627198103830 ) ) ;
#6690 = CARTESIAN_POINT ( 'NONE',  ( -19.02544592524342804, 5.153800228976336051, 91.04057627198100988 ) ) ;
#6691 = CARTESIAN_POINT ( 'NONE',  ( 5.823673210054125526, 21.52544592524343514, 114.7905762719810383 ) ) ;
#6692 = ORIENTED_EDGE ( 'NONE', *, *, #32808, .T. ) ;
#6693 = CARTESIAN_POINT ( 'NONE',  ( 19.03943276465977164, -0.05219959533909143690, 68.74890960531436690 ) ) ;
#6694 = CARTESIAN_POINT ( 'NONE',  ( 18.22780087662122384, -5.500000000000022204, 96.01540105326108687 ) ) ;
#6696 = CARTESIAN_POINT ( 'NONE',  ( 19.02544592524343514, -5.153800228976328945, 38.54057627198103120 ) ) ;
#6695 = CARTESIAN_POINT ( 'NONE',  ( -8.224510206698948167, 14.34966873604960824, 100.4155762719810241 ) ) ;
#6697 = CARTESIAN_POINT ( 'NONE',  ( 13.97604488694548053, -13.89961937509957401, 95.62609039468563310 ) ) ;
#6698 = CARTESIAN_POINT ( 'NONE',  ( 16.53943276465976808, -0.05219959533910856209, 108.7489096053143669 ) ) ;
#6699 = CARTESIAN_POINT ( 'NONE',  ( 15.80617190586769283, -15.72974639402175789, 75.62609039468567573 ) ) ;
#6701 = CARTESIAN_POINT ( 'NONE',  ( 10.72451020669871369, 18.67979575497193778, 37.08442372801901143 ) ) ;
#6700 = CARTESIAN_POINT ( 'NONE',  ( 9.474510206698971260, -16.51473224551069308, 57.91557627198103120 ) ) ;
#6702 = CARTESIAN_POINT ( 'NONE',  ( -5.719274019375978568, 21.55341960407610458, 105.2072429386477097 ) ) ;
#6703 = CARTESIAN_POINT ( 'NONE',  ( -8.906447517083053711, -27.41122689804191026, 144.4000000000000057 ) ) ;
#6704 = CARTESIAN_POINT ( 'NONE',  ( 5.153800228976335163, 19.02544592524342804, 69.79057627198103830 ) ) ;
#6705 = CARTESIAN_POINT ( 'NONE',  ( 12.50000000000001066, -90.00000000000005684, -25.00000000000000000 ) ) ;
#6707 = CARTESIAN_POINT ( 'NONE',  ( 18.67979575497178502, 10.72451020669898547, 29.16557627198103120 ) ) ;
#6706 = CARTESIAN_POINT ( 'NONE',  ( -4.483927247898782831, 16.52544592524335698, 32.70942372801900433 ) ) ;
#6708 = CARTESIAN_POINT ( 'NONE',  ( -5.823673210054431948, 21.52544592524334988, 62.70942372801902565 ) ) ;
#6709 = CARTESIAN_POINT ( 'NONE',  ( 19.02544592524343514, -5.153800228976328945, 113.5405762719810241 ) ) ;
#6710 = CARTESIAN_POINT ( 'NONE',  ( 9.474510206698729675, 16.51473224551082808, 92.08442372801900433 ) ) ;
#6711 = CARTESIAN_POINT ( 'NONE',  ( -9.564922557960796823, -16.46253265017161027, 52.08224293864768839 ) ) ;
#6712 = CARTESIAN_POINT ( 'NONE',  ( 5.153800228976335163, 19.02544592524342804, 74.79057627198103830 ) ) ;
#6713 = CARTESIAN_POINT ( 'NONE',  ( -12.06949235617756955, 12.14591786802309770, 100.6239096053143811 ) ) ;
#6714 = CARTESIAN_POINT ( 'NONE',  ( 16.51473224551069308, 9.474510206698969483, 104.1655762719810241 ) ) ;
#6715 = CARTESIAN_POINT ( 'NONE',  ( 16.55341960407611168, 4.379528057220329451, 88.95724293864769550 ) ) ;
#6716 = CARTESIAN_POINT ( 'NONE',  ( 19.03943276465977164, -0.05219959533909143690, 103.7489096053143669 ) ) ;
#6718 = CARTESIAN_POINT ( 'NONE',  ( -16.51473224551069308, -9.474510206698971260, 36.66557627198102409 ) ) ;
#6717 = CARTESIAN_POINT ( 'NONE',  ( -8.314922557960811034, -14.29746914071050412, 57.08224293864769550 ) ) ;
#6719 = CARTESIAN_POINT ( 'NONE',  ( -18.62759615963255300, -10.81492255796106328, 64.16775706135234714 ) ) ;
#6720 = CARTESIAN_POINT ( 'NONE',  ( 16.51473224551083163, -9.474510206698727899, 95.83442372801900433 ) ) ;
#6721 = CARTESIAN_POINT ( 'NONE',  ( 0.05219959533910956823, 16.53943276465976808, 54.99890960531435269 ) ) ;
#6722 = CARTESIAN_POINT ( 'NONE',  ( -21.55341960407610458, -5.719274019375992779, 111.4572429386476813 ) ) ;
#6723 = CARTESIAN_POINT ( 'NONE',  ( -21.55341960407610458, -5.719274019375992779, 46.45724293864769550 ) ) ;
#6725 = CARTESIAN_POINT ( 'NONE',  ( 12.06949235617757843, -12.14591786802309237, 83.12390960531436690 ) ) ;
#6724 = CARTESIAN_POINT ( 'NONE',  ( -19.03943276465977164, 0.05219959533909376836, 106.2489096053143669 ) ) ;
#6726 = CARTESIAN_POINT ( 'NONE',  ( -8.906447517083053711, -27.41122689804191026, 142.6500000054623740 ) ) ;
#6727 = CARTESIAN_POINT ( 'NONE',  ( -19.05341960407611168, -5.049401038298163336, 56.45724293864768129 ) ) ;
#6728 = CARTESIAN_POINT ( 'NONE',  ( 16.55341960407611168, 4.379528057220329451, 23.95724293864769550 ) ) ;
#6729 = CARTESIAN_POINT ( 'NONE',  ( 8.224510206698742110, 14.34966873604972548, 97.08442372801904696 ) ) ;
#6730 = CARTESIAN_POINT ( 'NONE',  ( 16.55341960407618274, -4.379528057220086978, 81.04275706135236135 ) ) ;
#6731 = CARTESIAN_POINT ( 'NONE',  ( -13.89961937509957401, -13.97604488694547875, 44.37609039468566863 ) ) ;
#6732 = CARTESIAN_POINT ( 'NONE',  ( -24.66673051387562410, 7.254129419879411955, 167.4978569920363611 ) ) ;
#6733 = CARTESIAN_POINT ( 'NONE',  ( 16.46253265017160672, -9.564922557960803928, 93.33224293864769550 ) ) ;
#6734 = CARTESIAN_POINT ( 'NONE',  ( 9.564922557960805705, 16.46253265017160317, 49.58224293864770260 ) ) ;
#6735 = CARTESIAN_POINT ( 'NONE',  ( -14.34966873604960291, -8.224510206698953496, 61.66557627198103120 ) ) ;
#6737 = CARTESIAN_POINT ( 'NONE',  ( -9.564922557960796823, -16.46253265017161027, 107.0822429386476955 ) ) ;
#6736 = SURFACE_STYLE_FILL_AREA ( #179627 ) ;
#6738 = CARTESIAN_POINT ( 'NONE',  ( -15.72974639402197994, 15.80617190586746368, 40.62390960531435269 ) ) ;
#6739 = CARTESIAN_POINT ( 'NONE',  ( -16.55341960407611168, -4.379528057220339221, 91.45724293864769550 ) ) ;
#6740 = CARTESIAN_POINT ( 'NONE',  ( -16.52544592524335698, -4.483927247898792601, 43.95942372801902565 ) ) ;
#6741 = CARTESIAN_POINT ( 'NONE',  ( 12.14591786802309770, 12.06949235617756955, 84.37390960531438111 ) ) ;
#6742 = EDGE_CURVE ( 'NONE', #143487, #74970, #177432, .T. ) ;
#6743 = CARTESIAN_POINT ( 'NONE',  ( -18.22780087662121673, -5.500000000000063061, 51.48459894673893444 ) ) ;
#6744 = CARTESIAN_POINT ( 'NONE',  ( 13.89961937509957401, 13.97604488694547697, 71.87609039468567573 ) ) ;
#6745 = CARTESIAN_POINT ( 'NONE',  ( 13.89961937509977652, -13.97604488694527269, 103.1239096053143527 ) ) ;
#6746 = CARTESIAN_POINT ( 'NONE',  ( -19.02544592524334988, -5.153800228976617603, 73.95942372801900433 ) ) ;
#6747 = CARTESIAN_POINT ( 'NONE',  ( 2.500000000000000000, -1.178949249685214307, 2.042000000000002036 ) ) ;
#6749 = CARTESIAN_POINT ( 'NONE',  ( -14.34966873604972548, 8.224510206698743886, 113.3344237280190328 ) ) ;
#6748 = CARTESIAN_POINT ( 'NONE',  ( 16.52544592524335698, 4.483927247898782831, 26.45942372801901854 ) ) ;
#6750 = CARTESIAN_POINT ( 'NONE',  ( -0.05219959533936034679, 19.03943276465977164, 72.50109039468566152 ) ) ;
#6751 = CARTESIAN_POINT ( 'NONE',  ( 21.52544592524344225, -5.823673210054117533, 33.54057627198102409 ) ) ;
#6752 = CARTESIAN_POINT ( 'NONE',  ( -21.53943276465977519, -0.05219959533937600094, 73.75109039468567573 ) ) ;
#6753 = CARTESIAN_POINT ( 'NONE',  ( -19.49401214000074489, -12.39993551617566325, 167.9999999999999716 ) ) ;
#6754 = CARTESIAN_POINT ( 'NONE',  ( 16.53943276465976808, 0.05219959533934440121, 26.25109039468567573 ) ) ;
#6756 = CARTESIAN_POINT ( 'NONE',  ( -13.97604488694527625, -13.89961937509977652, 86.87390960531436690 ) ) ;
#6755 = CARTESIAN_POINT ( 'NONE',  ( 13.89961937509977652, -13.97604488694527269, 28.12390960531435624 ) ) ;
#6757 = CARTESIAN_POINT ( 'NONE',  ( 19.05341960407611168, 5.049401038298154454, 23.95724293864769194 ) ) ;
#6760 = ADVANCED_FACE ( 'NONE', ( #38903 ), #132903, .T. ) ;
#6759 = CARTESIAN_POINT ( 'NONE',  ( -19.03943276465977164, 0.05219959533909376836, 86.24890960531436690 ) ) ;
#6758 = CARTESIAN_POINT ( 'NONE',  ( -14.34966873604960291, -8.224510206698953496, 86.66557627198102409 ) ) ;
#6761 = CARTESIAN_POINT ( 'NONE',  ( -9.564922557960796823, -16.46253265017161027, 82.08224293864768129 ) ) ;
#6762 = ORIENTED_EDGE ( 'NONE', *, *, #100373, .T. ) ;
#6763 = CARTESIAN_POINT ( 'NONE',  ( 13.89961937509957401, 13.97604488694547697, 91.87609039468567573 ) ) ;
#6764 = CARTESIAN_POINT ( 'NONE',  ( -18.67979575497178146, -10.72451020669898902, 81.66557627198103830 ) ) ;
#6765 = CARTESIAN_POINT ( 'NONE',  ( -16.46253265017160317, 9.564922557960807481, 40.83224293864769550 ) ) ;
#6767 = CARTESIAN_POINT ( 'NONE',  ( 21.55341960407610458, 5.719274019375980345, 113.9572429386477239 ) ) ;
#6766 = CARTESIAN_POINT ( 'NONE',  ( -19.05341960407617563, 5.049401038297882671, 73.54275706135233293 ) ) ;
#6768 = CARTESIAN_POINT ( 'NONE',  ( -0.05219959533909027116, -19.03943276465977164, 72.49890960531435269 ) ) ;
#6769 = CARTESIAN_POINT ( 'NONE',  ( -19.02544592524342804, 5.153800228976336051, 111.0405762719810099 ) ) ;
#6770 = EDGE_LOOP ( 'NONE', ( #148749, #114399 ) ) ;
#6771 = CARTESIAN_POINT ( 'NONE',  ( -16.53943276465976808, -0.05219959533934237506, 38.75109039468567573 ) ) ;
#6772 = CARTESIAN_POINT ( 'NONE',  ( 5.719274019375991003, -21.55341960407610458, 102.7072429386476955 ) ) ;
#6775 = CARTESIAN_POINT ( 'NONE',  ( -9.564922557961040184, 16.46253265017147172, 57.91775706135233293 ) ) ;
#6774 = CARTESIAN_POINT ( 'NONE',  ( -9.564922557960796823, -16.46253265017161027, 87.08224293864769550 ) ) ;
#6773 = CARTESIAN_POINT ( 'NONE',  ( 14.34966873604960469, 8.224510206698951720, 109.1655762719810383 ) ) ;
#6776 = CARTESIAN_POINT ( 'NONE',  ( 18.62759615963271287, -10.81492255796078972, 88.33224293864769550 ) ) ;
#6777 = CARTESIAN_POINT ( 'NONE',  ( 0.05219959533907565091, 21.53943276465977519, 69.99890960531435269 ) ) ;
#6778 = CARTESIAN_POINT ( 'NONE',  ( -16.52544592524342804, 4.483927247898546575, 51.04057627198103120 ) ) ;
#6779 = CARTESIAN_POINT ( 'NONE',  ( -5.823673210054431948, 21.52544592524334988, 112.7094237280190328 ) ) ;
#6780 = CARTESIAN_POINT ( 'NONE',  ( 0.05219959533934541429, -16.53943276465976808, 60.00109039468568284 ) ) ;
#6781 = CARTESIAN_POINT ( 'NONE',  ( 5.049401038298161559, -19.05341960407611168, 97.70724293864766707 ) ) ;
#6782 = CARTESIAN_POINT ( 'NONE',  ( 5.153800228976335163, 19.02544592524342804, 49.79057627198100988 ) ) ;
#6783 = CARTESIAN_POINT ( 'NONE',  ( 15.72974639402176855, 15.80617190586768217, 56.87609039468568994 ) ) ;
#6784 = CARTESIAN_POINT ( 'NONE',  ( 15.80617190586769283, -15.72974639402175789, 65.62609039468568994 ) ) ;
#6785 = CARTESIAN_POINT ( 'NONE',  ( -19.02544592524342804, 5.153800228976336051, 61.04057627198103120 ) ) ;
#6786 = CARTESIAN_POINT ( 'NONE',  ( -18.67979575497193778, 10.72451020669871902, 38.33442372801900433 ) ) ;
#6787 = CARTESIAN_POINT ( 'NONE',  ( 19.03943276465977164, 0.05219959533936151252, 71.25109039468566152 ) ) ;
#6788 = CARTESIAN_POINT ( 'NONE',  ( -19.03943276465977164, -0.05219959533935918106, 68.75109039468566152 ) ) ;
#6789 = CARTESIAN_POINT ( 'NONE',  ( 9.474510206698971260, -16.51473224551069308, 32.91557627198102409 ) ) ;
#6790 = CARTESIAN_POINT ( 'NONE',  ( 14.34966873604972726, -8.224510206698740333, 90.83442372801901854 ) ) ;
#6791 = CARTESIAN_POINT ( 'NONE',  ( 13.89961937509977652, -13.97604488694527269, 58.12390960531436690 ) ) ;
#6792 = CARTESIAN_POINT ( 'NONE',  ( 21.73861122199297569, -5.803778330637474170, 172.6157762304496828 ) ) ;
#6793 = CARTESIAN_POINT ( 'NONE',  ( 19.05341960407611168, 5.049401038298154454, 98.95724293864766707 ) ) ;
#6795 = EDGE_CURVE ( 'NONE', #140935, #23953, #150090, .T. ) ;
#6794 = CARTESIAN_POINT ( 'NONE',  ( 13.89961937509977652, -13.97604488694527269, 38.12390960531436690 ) ) ;
#6796 = CARTESIAN_POINT ( 'NONE',  ( 10.81492255796078972, 18.62759615963270932, 84.58224293864769550 ) ) ;
#6797 = CARTESIAN_POINT ( 'NONE',  ( 8.314922557961029526, -14.29746914071037800, 55.41775706135234714 ) ) ;
#6798 = CARTESIAN_POINT ( 'NONE',  ( 5.823673210054444382, -21.52544592524334988, 110.2094237280190185 ) ) ;
#6799 = CARTESIAN_POINT ( 'NONE',  ( 16.51473224551069308, 9.474510206698969483, 59.16557627198102409 ) ) ;
#6800 = CARTESIAN_POINT ( 'NONE',  ( -14.34966873604960291, -8.224510206698953496, 51.66557627198102409 ) ) ;
#6801 = CARTESIAN_POINT ( 'NONE',  ( 16.55341960407611168, 4.379528057220329451, 78.95724293864769550 ) ) ;
#6802 = CARTESIAN_POINT ( 'NONE',  ( 13.97604488694527802, 13.89961937509977652, 84.37390960531433848 ) ) ;
#6803 = CARTESIAN_POINT ( 'NONE',  ( -5.719274019375665041, -21.55341960407619695, 39.79275706135235424 ) ) ;
#6804 = CARTESIAN_POINT ( 'NONE',  ( 5.153800228976335163, 19.02544592524342804, 89.79057627198102409 ) ) ;
#6805 = CARTESIAN_POINT ( 'NONE',  ( 15.72974639402176855, 15.80617190586768217, 96.87609039468568994 ) ) ;
#6806 = CARTESIAN_POINT ( 'NONE',  ( -14.34966873604972548, 8.224510206698743886, 78.33442372801901854 ) ) ;
#6807 = CARTESIAN_POINT ( 'NONE',  ( -5.823673210054431948, 21.52544592524334988, 27.70942372801901854 ) ) ;
#6808 = CARTESIAN_POINT ( 'NONE',  ( -19.03943276465977164, 0.05219959533909376836, 111.2489096053143669 ) ) ;
#6809 = CARTESIAN_POINT ( 'NONE',  ( 0.05219959533907565091, 21.53943276465977519, 84.99890960531436690 ) ) ;
#6810 = CARTESIAN_POINT ( 'NONE',  ( 16.53943276465976808, -0.05219959533910856209, 53.74890960531437401 ) ) ;
#6811 = CARTESIAN_POINT ( 'NONE',  ( 13.89961937509977652, -13.97604488694527269, 38.12390960531436690 ) ) ;
#6812 = CARTESIAN_POINT ( 'NONE',  ( 16.52544592524342804, -4.483927247898539470, 73.54057627198102409 ) ) ;
#6813 = CARTESIAN_POINT ( 'NONE',  ( -21.55341960407610458, -5.719274019375992779, 26.45724293864768839 ) ) ;
#6814 = CARTESIAN_POINT ( 'NONE',  ( 13.97604488694548053, -13.89961937509957401, 30.62609039468566863 ) ) ;
#6815 = CARTESIAN_POINT ( 'NONE',  ( 16.55341960407611168, 4.379528057220329451, 93.95724293864770971 ) ) ;
#6816 = CARTESIAN_POINT ( 'NONE',  ( -9.564922557960796823, -16.46253265017161027, 112.0822429386476955 ) ) ;
#6817 = VERTEX_POINT ( 'NONE', #56062 ) ;
#6818 = CARTESIAN_POINT ( 'NONE',  ( -4.379528057220086978, -16.55341960407618274, 49.79275706135234714 ) ) ;
#6819 = CARTESIAN_POINT ( 'NONE',  ( -19.02544592524342804, 5.153800228976336051, 61.04057627198103120 ) ) ;
#6820 = FACE_OUTER_BOUND ( 'NONE', #145721, .T. ) ;
#6821 = CARTESIAN_POINT ( 'NONE',  ( 12.14591786802327356, -12.06949235617739191, 95.62609039468568994 ) ) ;
#6822 = CARTESIAN_POINT ( 'NONE',  ( -19.03943276465977164, -0.05219959533935918106, 103.7510903946856757 ) ) ;
#6823 = CARTESIAN_POINT ( 'NONE',  ( 10.72451020669871369, 18.67979575497193778, 77.08442372801901854 ) ) ;
#6824 = CARTESIAN_POINT ( 'NONE',  ( -13.89961937509977652, 13.97604488694528158, 75.62390960531438111 ) ) ;
#6825 = CARTESIAN_POINT ( 'NONE',  ( 10.81492255796078972, 18.62759615963270932, 109.5822429386476955 ) ) ;
#6826 = CARTESIAN_POINT ( 'NONE',  ( -0.05219959533934338120, 16.53943276465976808, 57.50109039468568994 ) ) ;
#6827 = CARTESIAN_POINT ( 'NONE',  ( 5.049401038298161559, -19.05341960407611168, 22.70724293864769194 ) ) ;
#6828 = CARTESIAN_POINT ( 'NONE',  ( -16.51473224551082808, 9.474510206698731452, 113.3344237280190043 ) ) ;
#6829 = CARTESIAN_POINT ( 'NONE',  ( 16.46253265017146816, 9.564922557961045513, 81.66775706135233293 ) ) ;
#6830 = CARTESIAN_POINT ( 'NONE',  ( -21.53943276465977519, 0.05219959533907696930, 81.24890960531436690 ) ) ;
#6831 = CARTESIAN_POINT ( 'NONE',  ( -0.05219959533936034679, 19.03943276465977164, 57.50109039468566863 ) ) ;
#6832 = CARTESIAN_POINT ( 'NONE',  ( -13.97604488694527625, -13.89961937509977652, 111.8739096053143243 ) ) ;
#6833 = CARTESIAN_POINT ( 'NONE',  ( 10.81492255796078972, 18.62759615963270932, 104.5822429386477097 ) ) ;
#6834 = CARTESIAN_POINT ( 'NONE',  ( 23.31738231874054890, -16.94106989632523508, 148.7999999999999829 ) ) ;
#6835 = CARTESIAN_POINT ( 'NONE',  ( -19.03943276465977164, 0.05219959533909376836, 71.24890960531435269 ) ) ;
#6836 = DIRECTION ( 'NONE',  ( -1.000000000000000000, 0.000000000000000000, 0.000000000000000000 ) ) ;
#6837 = CARTESIAN_POINT ( 'NONE',  ( -0.05219959533936034679, 19.03943276465977164, 112.5010903946856757 ) ) ;
#6838 = CARTESIAN_POINT ( 'NONE',  ( 32.00000000000000000, -1.163414459189985801E-14, 92.35000000000000853 ) ) ;
#6839 = CARTESIAN_POINT ( 'NONE',  ( -0.05219959533937732626, 21.53943276465977519, 57.50109039468568994 ) ) ;
#6841 = CARTESIAN_POINT ( 'NONE',  ( 16.53943276465976808, -0.05219959533910856209, 68.74890960531435269 ) ) ;
#6840 = CARTESIAN_POINT ( 'NONE',  ( -21.55341960407610458, -5.719274019375992779, 106.4572429386477097 ) ) ;
#6842 = CARTESIAN_POINT ( 'NONE',  ( -5.049401038298153566, 19.05341960407611168, 75.20724293864769550 ) ) ;
#6843 = CARTESIAN_POINT ( 'NONE',  ( -15.80617190586768217, 15.72974639402176855, 68.12609039468567573 ) ) ;
#6845 = CARTESIAN_POINT ( 'NONE',  ( -19.05341960407617563, 5.049401038297882671, 33.54275706135231871 ) ) ;
#6844 = CARTESIAN_POINT ( 'NONE',  ( 12.14591786802327356, -12.06949235617739191, 30.62609039468567929 ) ) ;
#6846 = CARTESIAN_POINT ( 'NONE',  ( 21.52544592524334988, 5.823673210054432836, 56.45942372801902565 ) ) ;
#6847 = CARTESIAN_POINT ( 'NONE',  ( 10.72451020669898902, -18.67979575497178502, 112.9155762719810383 ) ) ;
#6848 = CARTESIAN_POINT ( 'NONE',  ( 15.80617190586746368, 15.72974639402197994, 64.37390960531435269 ) ) ;
#6849 = CARTESIAN_POINT ( 'NONE',  ( -16.46253265017146816, -9.564922557961047289, 99.16775706135233293 ) ) ;
#6850 = CARTESIAN_POINT ( 'NONE',  ( -16.51473224551082808, 9.474510206698731452, 68.33442372801900433 ) ) ;
#6851 = CARTESIAN_POINT ( 'NONE',  ( -18.62759615963255300, -10.81492255796106328, 89.16775706135236135 ) ) ;
#6852 = CARTESIAN_POINT ( 'NONE',  ( -0.05219959533936034679, 19.03943276465977164, 57.50109039468566863 ) ) ;
#6853 = CARTESIAN_POINT ( 'NONE',  ( -19.05341960407611168, -5.049401038298163336, 31.45724293864769550 ) ) ;
#6854 = CARTESIAN_POINT ( 'NONE',  ( -21.53943276465977519, 0.05219959533907696930, 51.24890960531436690 ) ) ;
#6855 = CARTESIAN_POINT ( 'NONE',  ( -16.52544592524342804, 4.483927247898546575, 46.04057627198103830 ) ) ;
#6856 = CARTESIAN_POINT ( 'NONE',  ( -19.02130022317636104, 5.499999999999802824, 95.78188669246574705 ) ) ;
#6857 = CARTESIAN_POINT ( 'NONE',  ( -16.51473224551082808, 9.474510206698731452, 33.33442372801899722 ) ) ;
#6858 = CARTESIAN_POINT ( 'NONE',  ( -14.34966873604972548, 8.224510206698743886, 88.33442372801901854 ) ) ;
#6859 = CARTESIAN_POINT ( 'NONE',  ( -16.52544592524342804, 4.483927247898546575, 56.04057627198102409 ) ) ;
#6860 = CARTESIAN_POINT ( 'NONE',  ( 21.53943276465977519, 0.05219959533937863772, 81.25109039468568994 ) ) ;
#6861 = CARTESIAN_POINT ( 'NONE',  ( 5.823673210054444382, -21.52544592524334988, 80.20942372801901854 ) ) ;
#6862 = CARTESIAN_POINT ( 'NONE',  ( -21.53943276465977519, 0.05219959533907696930, 81.24890960531436690 ) ) ;
#6863 = CARTESIAN_POINT ( 'NONE',  ( 9.474510206698971260, -16.51473224551069308, 37.91557627198102409 ) ) ;
#6864 = CARTESIAN_POINT ( 'NONE',  ( 21.53943276465977519, 0.05219959533937863772, 51.25109039468568994 ) ) ;
#6865 = CARTESIAN_POINT ( 'NONE',  ( 0.05219959533909260263, 19.03943276465977164, 39.99890960531436690 ) ) ;
#6866 = CARTESIAN_POINT ( 'NONE',  ( -5.153800228976328057, -19.02544592524343514, 47.29057627198102409 ) ) ;
#6867 = CARTESIAN_POINT ( 'NONE',  ( -14.29746914071049879, 8.314922557960819915, 110.8322429386476955 ) ) ;
#6868 = CARTESIAN_POINT ( 'NONE',  ( 9.564922557960805705, 16.46253265017160317, 104.5822429386476955 ) ) ;
#6869 = CARTESIAN_POINT ( 'NONE',  ( -4.379528057220328563, 16.55341960407611168, 40.20724293864769550 ) ) ;
#6870 = CARTESIAN_POINT ( 'NONE',  ( 0.05219959533910956823, 16.53943276465976808, 114.9989096053143669 ) ) ;
#6871 = CARTESIAN_POINT ( 'NONE',  ( -18.62759615963270932, 10.81492255796079327, 85.83224293864768129 ) ) ;
#6872 = CARTESIAN_POINT ( 'NONE',  ( 21.53943276465977519, 0.05219959533937863772, 21.25109039468567218 ) ) ;
#6873 = LINE ( 'NONE', #190912, #159839 ) ;
#6874 = CARTESIAN_POINT ( 'NONE',  ( -16.55341960407617563, 4.379528057220093196, 33.54275706135234714 ) ) ;
#6875 = ORIENTED_EDGE ( 'NONE', *, *, #116835, .F. ) ;
#6876 = EDGE_CURVE ( 'NONE', #157949, #129810, #101294, .T. ) ;
#6877 = CARTESIAN_POINT ( 'NONE',  ( 21.52544592524344225, -5.823673210054117533, 73.54057627198102409 ) ) ;
#6878 = CARTESIAN_POINT ( 'NONE',  ( -10.81492255796105439, 18.62759615963255655, 97.91775706135236135 ) ) ;
#6879 = CARTESIAN_POINT ( 'NONE',  ( 9.564922557960805705, 16.46253265017160317, 89.58224293864769550 ) ) ;
#6880 = CARTESIAN_POINT ( 'NONE',  ( 21.52544592524334988, 5.823673210054432836, 36.45942372801901143 ) ) ;
#6881 = CARTESIAN_POINT ( 'NONE',  ( -21.52544592524343514, 5.823673210054127303, 26.04057627198103475 ) ) ;
#6882 = CARTESIAN_POINT ( 'NONE',  ( 14.29746914071037800, 8.314922557961029526, 86.66775706135234714 ) ) ;
#6883 = CARTESIAN_POINT ( 'NONE',  ( -21.52544592524334988, -5.823673210054445271, 78.95942372801901854 ) ) ;
#6884 = CARTESIAN_POINT ( 'NONE',  ( -9.474510206698720793, -16.51473224551083518, 19.58442372801899722 ) ) ;
#6885 = CARTESIAN_POINT ( 'NONE',  ( -8.314922557961024197, 14.29746914071037800, 72.91775706135234714 ) ) ;
#6886 = CARTESIAN_POINT ( 'NONE',  ( -21.55341960407619339, 5.719274019375674811, 23.54275706135235424 ) ) ;
#6887 = CARTESIAN_POINT ( 'NONE',  ( -9.564922557960796823, -16.46253265017161027, 37.08224293864768839 ) ) ;
#6888 = CARTESIAN_POINT ( 'NONE',  ( 15.80617190586769283, -15.72974639402175789, 100.6260903946857184 ) ) ;
#6889 = CARTESIAN_POINT ( 'NONE',  ( -5.153800228976328057, -19.02544592524343514, 112.2905762719810099 ) ) ;
#6890 = CARTESIAN_POINT ( 'NONE',  ( 15.72974639402199770, -15.80617190586745480, 98.12390960531436690 ) ) ;
#6892 = CARTESIAN_POINT ( 'NONE',  ( -21.53943276465977519, 0.05219959533907696930, 61.24890960531435979 ) ) ;
#6891 = CARTESIAN_POINT ( 'NONE',  ( 17.97161686094262123, -5.499999999999981348, 88.49637206859249261 ) ) ;
#6894 = CARTESIAN_POINT ( 'NONE',  ( -8.224510206698948167, 14.34966873604960824, 50.41557627198103120 ) ) ;
#6893 = CARTESIAN_POINT ( 'NONE',  ( -4.379528057220086978, -16.55341960407618274, 54.79275706135235424 ) ) ;
#6895 = CARTESIAN_POINT ( 'NONE',  ( 19.15291303114473820, -5.500000000000005329, 101.3916229363312311 ) ) ;
#6896 = CARTESIAN_POINT ( 'NONE',  ( 5.153800228976615827, -19.02544592524334988, 75.20942372801896170 ) ) ;
#6897 = CARTESIAN_POINT ( 'NONE',  ( -16.38665767535054485, 7.295008042176108987, 105.2640086421455266 ) ) ;
#6898 = CARTESIAN_POINT ( 'NONE',  ( -0.05219959533934338120, 16.53943276465976808, 32.50109039468568284 ) ) ;
#6899 = CARTESIAN_POINT ( 'NONE',  ( 18.62759615963271287, -10.81492255796078972, 93.33224293864769550 ) ) ;
#6900 = CARTESIAN_POINT ( 'NONE',  ( 16.55341960407611168, 4.379528057220329451, 58.95724293864770971 ) ) ;
#6901 = CARTESIAN_POINT ( 'NONE',  ( 19.05341960407611168, 5.049401038298154454, 98.95724293864766707 ) ) ;
#6902 = CARTESIAN_POINT ( 'NONE',  ( 0.05219959533934541429, -16.53943276465976808, 50.00109039468568994 ) ) ;
#6903 = CARTESIAN_POINT ( 'NONE',  ( 13.89961937509977652, -13.97604488694527269, 53.12390960531434558 ) ) ;
#6905 = CARTESIAN_POINT ( 'NONE',  ( -5.049401038297874678, -19.05341960407617918, 94.79275706135230450 ) ) ;
#6904 = CARTESIAN_POINT ( 'NONE',  ( -18.67979575497193778, 10.72451020669871902, 28.33442372801902209 ) ) ;
#6906 = EDGE_CURVE ( 'NONE', #84463, #144635, #114277, .T. ) ;
#6907 = CARTESIAN_POINT ( 'NONE',  ( -13.89961937509977652, 13.97604488694528158, 90.62390960531432427 ) ) ;
#6908 = CARTESIAN_POINT ( 'NONE',  ( -19.02544592524342804, 5.153800228976336051, 91.04057627198100988 ) ) ;
#6909 = CARTESIAN_POINT ( 'NONE',  ( 15.80617190586746368, 15.72974639402197994, 89.37390960531435269 ) ) ;
#6910 = CARTESIAN_POINT ( 'NONE',  ( -0.05219959533909027116, -19.03943276465977164, 52.49890960531436690 ) ) ;
#6911 = DIRECTION ( 'NONE',  ( 0.000000000000000000, 0.4999999999999993894, -0.8660254037844389297 ) ) ;
#6912 = CARTESIAN_POINT ( 'NONE',  ( -16.55341960407611168, -4.379528057220339221, 66.45724293864768129 ) ) ;
#6913 = CARTESIAN_POINT ( 'NONE',  ( -0.05219959533909027116, -19.03943276465977164, 97.49890960531436690 ) ) ;
#6914 = CARTESIAN_POINT ( 'NONE',  ( 16.24127373534237861, -14.59486009359520509, -56.10187840754844757 ) ) ;
#6915 = CARTESIAN_POINT ( 'NONE',  ( -16.51473224551082808, 9.474510206698731452, 83.33442372801899012 ) ) ;
#6916 = CARTESIAN_POINT ( 'NONE',  ( -21.52544592524343514, 5.823673210054127303, 86.04057627198102409 ) ) ;
#6917 = CARTESIAN_POINT ( 'NONE',  ( 5.153800228976615827, -19.02544592524334988, 50.20942372801897591 ) ) ;
#6918 = CARTESIAN_POINT ( 'NONE',  ( 21.53943276465977519, -0.05219959533907433946, 23.74890960531435269 ) ) ;
#6919 = CARTESIAN_POINT ( 'NONE',  ( 18.09867054820430710, 5.500000000000001776, 76.48393025253584199 ) ) ;
#6920 = CARTESIAN_POINT ( 'NONE',  ( -10.81492255796078084, -18.62759615963271287, 42.08224293864769550 ) ) ;
#6921 = CARTESIAN_POINT ( 'NONE',  ( 16.46253265017160672, -9.564922557960803928, 83.33224293864768129 ) ) ;
#6922 = CARTESIAN_POINT ( 'NONE',  ( -15.80617190586768217, 15.72974639402176855, 68.12609039468567573 ) ) ;
#6923 = CARTESIAN_POINT ( 'NONE',  ( 13.97604488694527802, 13.89961937509977652, 34.37390960531436690 ) ) ;
#6924 = CARTESIAN_POINT ( 'NONE',  ( -14.34966873604960291, -8.224510206698953496, 71.66557627198100988 ) ) ;
#6925 = CARTESIAN_POINT ( 'NONE',  ( -19.03943276465977164, -0.05219959533935918106, 113.7510903946856757 ) ) ;
#6926 = CARTESIAN_POINT ( 'NONE',  ( -5.823673210054431948, 21.52544592524334988, 52.70942372801902565 ) ) ;
#6927 = VERTEX_POINT ( 'NONE', #148083 ) ;
#6928 = CARTESIAN_POINT ( 'NONE',  ( 16.51473224551069308, 9.474510206698969483, 109.1655762719810383 ) ) ;
#6929 = CARTESIAN_POINT ( 'NONE',  ( -13.97604488694547697, 13.89961937509957934, 78.12609039468567573 ) ) ;
#6930 = CARTESIAN_POINT ( 'NONE',  ( 26.37337922943876123, -29.71119707698740697, -20.32121347158684799 ) ) ;
#6931 = CARTESIAN_POINT ( 'NONE',  ( -5.719274019375665041, -21.55341960407619695, 24.79275706135235779 ) ) ;
#6932 = CARTESIAN_POINT ( 'NONE',  ( -15.06137443927361019, -15.06137443927335440, -64.92279855667830191 ) ) ;
#6933 = CARTESIAN_POINT ( 'NONE',  ( 21.55341960407619695, -5.719274019375665929, 111.0427570613523613 ) ) ;
#6934 = CARTESIAN_POINT ( 'NONE',  ( -5.049401038298153566, 19.05341960407611168, 50.20724293864770260 ) ) ;
#6935 = CARTESIAN_POINT ( 'NONE',  ( 21.55341960407619695, -5.719274019375665929, 111.0427570613523613 ) ) ;
#6936 = CARTESIAN_POINT ( 'NONE',  ( 16.53943276465976808, 0.05219959533934440121, 106.2510903946856757 ) ) ;
#6938 = CARTESIAN_POINT ( 'NONE',  ( -5.719274019375665041, -21.55341960407619695, 74.79275706135234714 ) ) ;
#6937 = CARTESIAN_POINT ( 'NONE',  ( 16.46253265017160672, -9.564922557960803928, 98.33224293864769550 ) ) ;
#6939 = CARTESIAN_POINT ( 'NONE',  ( -29.86685920354755552, 21.69954338932564397, -8.824999997268815122 ) ) ;
#6940 = CARTESIAN_POINT ( 'NONE',  ( -17.72696623605162713, 5.499999999999965361, 98.59811031808418136 ) ) ;
#6941 = CARTESIAN_POINT ( 'NONE',  ( 22.99604614807110181, -21.49604614807103786, -46.28618945597792589 ) ) ;
#6942 = CARTESIAN_POINT ( 'NONE',  ( -5.823673210054431948, 21.52544592524334988, 72.70942372801901854 ) ) ;
#6943 = CARTESIAN_POINT ( 'NONE',  ( -18.67979575497193778, 10.72451020669871902, 108.3344237280190185 ) ) ;
#6944 = CARTESIAN_POINT ( 'NONE',  ( 5.000000000000000000, -139.5000000000000000, 21.32407087589996308 ) ) ;
#6945 = CARTESIAN_POINT ( 'NONE',  ( -5.049401038298153566, 19.05341960407611168, 90.20724293864766707 ) ) ;
#6946 = CARTESIAN_POINT ( 'NONE',  ( -16.46253265017146816, -9.564922557961047289, 24.16775706135233648 ) ) ;
#6947 = CARTESIAN_POINT ( 'NONE',  ( 22.19904868473526705, -30.74855836414197086, -22.45812049023449219 ) ) ;
#6948 = CARTESIAN_POINT ( 'NONE',  ( -9.474510206698964154, 16.51473224551069663, 35.41557627198102409 ) ) ;
#6949 = CARTESIAN_POINT ( 'NONE',  ( 21.55341960407610458, 5.719274019375980345, 53.95724293864770260 ) ) ;
#6950 = CARTESIAN_POINT ( 'NONE',  ( 16.55341960407618274, -4.379528057220086978, 106.0427570613523471 ) ) ;
#6952 = CARTESIAN_POINT ( 'NONE',  ( -16.51473224551069308, -9.474510206698971260, 81.66557627198103830 ) ) ;
#6951 = CARTESIAN_POINT ( 'NONE',  ( 8.224510206698953496, -14.34966873604960469, 102.9155762719810383 ) ) ;
#6953 = CARTESIAN_POINT ( 'NONE',  ( -18.67979575497193778, 10.72451020669871902, 103.3344237280190043 ) ) ;
#6954 = CARTESIAN_POINT ( 'NONE',  ( -16.51473224551069308, -9.474510206698971260, 41.66557627198103120 ) ) ;
#6955 = CARTESIAN_POINT ( 'NONE',  ( 4.483927247898545687, 16.52544592524342804, 89.79057627198103830 ) ) ;
#6956 = CARTESIAN_POINT ( 'NONE',  ( -15.72974639402176322, -15.80617190586768395, 49.37609039468569705 ) ) ;
#6957 = CARTESIAN_POINT ( 'NONE',  ( -15.80617190586745835, -15.72974639402198527, 86.87390960531438111 ) ) ;
#6958 = CARTESIAN_POINT ( 'NONE',  ( -5.049401038297874678, -19.05341960407617918, 49.79275706135231871 ) ) ;
#6959 = CARTESIAN_POINT ( 'NONE',  ( -9.720620470091368759, -38.81506340700470048, -14.89813575833734305 ) ) ;
#6960 = CARTESIAN_POINT ( 'NONE',  ( -9.564922557960796823, -16.46253265017161027, 92.08224293864769550 ) ) ;
#6961 = CARTESIAN_POINT ( 'NONE',  ( 14.29746914071049879, -8.314922557960816363, 63.33224293864770260 ) ) ;
#6962 = CARTESIAN_POINT ( 'NONE',  ( 13.89961937509957401, 13.97604488694547697, 46.87609039468565442 ) ) ;
#6963 = CARTESIAN_POINT ( 'NONE',  ( 19.03943276465977164, -0.05219959533909143690, 53.74890960531436690 ) ) ;
#6964 = CARTESIAN_POINT ( 'NONE',  ( 12.06949235617757843, -12.14591786802309237, 43.12390960531435269 ) ) ;
#6965 = CARTESIAN_POINT ( 'NONE',  ( 5.049401038297881783, 19.05341960407617563, 82.29275706135229029 ) ) ;
#6966 = DIRECTION ( 'NONE',  ( 1.000000000000000000, 0.000000000000000000, 3.469446951953612217E-15 ) ) ;
#6967 = CARTESIAN_POINT ( 'NONE',  ( 0.05219959533907565091, 21.53943276465977519, 39.99890960531436690 ) ) ;
#6968 = CARTESIAN_POINT ( 'NONE',  ( -16.52544592524342804, 4.483927247898546575, 96.04057627198102409 ) ) ;
#6969 = CARTESIAN_POINT ( 'NONE',  ( -17.49999999999996447, -4.013004640162789904, 24.55394279005590619 ) ) ;
#6971 = CARTESIAN_POINT ( 'NONE',  ( 15.80617190586746368, 15.72974639402197994, 54.37390960531435979 ) ) ;
#6970 = CARTESIAN_POINT ( 'NONE',  ( 19.03943276465977164, -0.05219959533909143690, 58.74890960531435979 ) ) ;
#6972 = CARTESIAN_POINT ( 'NONE',  ( -19.02544592524342804, 5.153800228976336051, 36.04057627198100988 ) ) ;
#6974 = CARTESIAN_POINT ( 'NONE',  ( 13.97604488694527802, 13.89961937509977652, 54.37390960531435979 ) ) ;
#6973 = CARTESIAN_POINT ( 'NONE',  ( -12.06949235617739369, -12.14591786802326823, 79.37609039468567573 ) ) ;
#6975 = CARTESIAN_POINT ( 'NONE',  ( 9.474510206698729675, 16.51473224551082808, 37.08442372801899722 ) ) ;
#6976 = CARTESIAN_POINT ( 'NONE',  ( 5.823673210054444382, -21.52544592524334988, 70.20942372801904696 ) ) ;
#6977 = CARTESIAN_POINT ( 'NONE',  ( -15.80617190586745835, -15.72974639402198527, 51.87390960531437401 ) ) ;
#6978 = CARTESIAN_POINT ( 'NONE',  ( 19.05341960407611168, 5.049401038298154454, 28.95724293864769550 ) ) ;
#6979 = EDGE_CURVE ( 'NONE', #198657, #243, #178426, .T. ) ;
#6980 = CARTESIAN_POINT ( 'NONE',  ( 13.89961937509957401, 13.97604488694547697, 106.8760903946856757 ) ) ;
#6981 = CARTESIAN_POINT ( 'NONE',  ( 0.05219959533909260263, 19.03943276465977164, 24.99890960531435269 ) ) ;
#6983 = CARTESIAN_POINT ( 'NONE',  ( 10.72451020669898902, -18.67979575497178502, 42.91557627198103120 ) ) ;
#6982 = CARTESIAN_POINT ( 'NONE',  ( -1.499560036715100075, -22.98313974082796918, -57.70434786042496000 ) ) ;
#6984 = CARTESIAN_POINT ( 'NONE',  ( 16.36317988757059894, -7.306389748694922304, 66.59789608363222158 ) ) ;
#6985 = CARTESIAN_POINT ( 'NONE',  ( 15.72974639402176855, 15.80617190586768217, 81.87609039468568994 ) ) ;
#6986 = CARTESIAN_POINT ( 'NONE',  ( 14.34966873604960469, 8.224510206698951720, 49.16557627198102409 ) ) ;
#6987 = CARTESIAN_POINT ( 'NONE',  ( -12.14591786802309592, -12.06949235617757132, 61.87390960531436690 ) ) ;
#6988 = CARTESIAN_POINT ( 'NONE',  ( 18.62759615963271287, -10.81492255796078972, 78.33224293864770971 ) ) ;
#6989 = CARTESIAN_POINT ( 'NONE',  ( -5.719274019375978568, 21.55341960407610458, 80.20724293864769550 ) ) ;
#6990 = PLANE ( 'NONE',  #143579 ) ;
#6991 = CARTESIAN_POINT ( 'NONE',  ( 0.05219959533907565091, 21.53943276465977519, 29.99890960531435979 ) ) ;
#6992 = CARTESIAN_POINT ( 'NONE',  ( -14.34966873604972548, 8.224510206698743886, 48.33442372801902565 ) ) ;
#6993 = CARTESIAN_POINT ( 'NONE',  ( 16.55341960407611168, 4.379528057220329451, 78.95724293864769550 ) ) ;
#6994 = CARTESIAN_POINT ( 'NONE',  ( -5.153800228976328057, -19.02544592524343514, 27.29057627198103120 ) ) ;
#6995 = DIRECTION ( 'NONE',  ( 0.000000000000000000, 0.000000000000000000, -1.000000000000000000 ) ) ;
#6996 = CARTESIAN_POINT ( 'NONE',  ( -16.55341960407617563, 4.379528057220093196, 78.54275706135236135 ) ) ;
#6997 = CARTESIAN_POINT ( 'NONE',  ( 5.719274019375673035, 21.55341960407619339, 22.29275706135235069 ) ) ;
#6998 = CARTESIAN_POINT ( 'NONE',  ( 9.474510206698971260, -16.51473224551069308, 87.91557627198102409 ) ) ;
#6999 = CARTESIAN_POINT ( 'NONE',  ( -5.823673210054431948, 21.52544592524334988, 57.70942372801901143 ) ) ;
#7000 = CARTESIAN_POINT ( 'NONE',  ( -19.02544592524342804, 5.153800228976336051, 116.0405762719810383 ) ) ;
#7001 = CARTESIAN_POINT ( 'NONE',  ( -12.33280382558396404, -43.64415646941903049, -22.88837716264928801 ) ) ;
#7002 = ORIENTED_EDGE ( 'NONE', *, *, #173288, .T. ) ;
#7003 = CARTESIAN_POINT ( 'NONE',  ( 10.81492255796106328, -18.62759615963255655, 50.41775706135235424 ) ) ;
#7005 = CARTESIAN_POINT ( 'NONE',  ( -5.049401038298153566, 19.05341960407611168, 105.2072429386476671 ) ) ;
#7004 = CARTESIAN_POINT ( 'NONE',  ( 5.153800228976335163, 19.02544592524342804, 34.79057627198102409 ) ) ;
#7006 = CARTESIAN_POINT ( 'NONE',  ( 5.153800228976615827, -19.02544592524334988, 55.20942372801899722 ) ) ;
#7007 = CARTESIAN_POINT ( 'NONE',  ( 18.67979575497194134, -10.72451020669871369, 30.83442372801902209 ) ) ;
#7008 = CARTESIAN_POINT ( 'NONE',  ( 19.05341960407617918, -5.049401038297876454, 46.04275706135233293 ) ) ;
#7009 = CARTESIAN_POINT ( 'NONE',  ( -5.153800228976328057, -19.02544592524343514, 27.29057627198103120 ) ) ;
#7010 = CARTESIAN_POINT ( 'NONE',  ( 16.53943276465976808, 0.05219959533934440121, 96.25109039468568994 ) ) ;
#7011 = CARTESIAN_POINT ( 'NONE',  ( -16.51473224551082808, 9.474510206698731452, 63.33442372801900433 ) ) ;
#7012 = CARTESIAN_POINT ( 'NONE',  ( -14.29746914071037622, -8.314922557961029526, 99.16775706135234714 ) ) ;
#7013 = DIRECTION ( 'NONE',  ( 0.000000000000000000, 0.000000000000000000, 1.000000000000000000 ) ) ;
#7014 = CARTESIAN_POINT ( 'NONE',  ( 0.05219959533909260263, 19.03943276465977164, 84.99890960531436690 ) ) ;
#7015 = CARTESIAN_POINT ( 'NONE',  ( -21.52544592524334988, -5.823673210054445271, 98.95942372801903275 ) ) ;
#7016 = CARTESIAN_POINT ( 'NONE',  ( 21.52544592524334988, 5.823673210054432836, 111.4594237280190328 ) ) ;
#7017 = DIRECTION ( 'NONE',  ( 1.000000000000000000, 0.000000000000000000, 0.000000000000000000 ) ) ;
#7018 = CARTESIAN_POINT ( 'NONE',  ( 9.564922557960805705, 16.46253265017160317, 104.5822429386476955 ) ) ;
#7019 = CARTESIAN_POINT ( 'NONE',  ( -0.05219959533937732626, 21.53943276465977519, 72.50109039468568994 ) ) ;
#7020 = CARTESIAN_POINT ( 'NONE',  ( 13.97604488694548053, -13.89961937509957401, 110.6260903946856615 ) ) ;
#7021 = CARTESIAN_POINT ( 'NONE',  ( -5.049401038298153566, 19.05341960407611168, 80.20724293864769550 ) ) ;
#7022 = CARTESIAN_POINT ( 'NONE',  ( -10.81492255796078084, -18.62759615963271287, 32.08224293864769550 ) ) ;
#7023 = CARTESIAN_POINT ( 'NONE',  ( 16.46253265017160672, -9.564922557960803928, 88.33224293864769550 ) ) ;
#7024 = CARTESIAN_POINT ( 'NONE',  ( -16.36317988757058828, -7.306389748694930297, 90.90210391636776421 ) ) ;
#7025 = CARTESIAN_POINT ( 'NONE',  ( -16.51473224551069308, -9.474510206698971260, 76.66557627198103830 ) ) ;
#7026 = CARTESIAN_POINT ( 'NONE',  ( -16.51473224551069308, -9.474510206698971260, 66.66557627198102409 ) ) ;
#7027 = CARTESIAN_POINT ( 'NONE',  ( -4.379528057220086978, -16.55341960407618274, 104.7927570613523898 ) ) ;
#7028 = FACE_OUTER_BOUND ( 'NONE', #115842, .T. ) ;
#7029 = CARTESIAN_POINT ( 'NONE',  ( 13.89961937509957401, 13.97604488694547697, 71.87609039468567573 ) ) ;
#7030 = CARTESIAN_POINT ( 'NONE',  ( -19.02544592524342804, 5.153800228976336051, 91.04057627198100988 ) ) ;
#7031 = CARTESIAN_POINT ( 'NONE',  ( 4.483927247898545687, 16.52544592524342804, 79.79057627198102409 ) ) ;
#7032 = CARTESIAN_POINT ( 'NONE',  ( 21.53943276465977519, -0.05219959533907433946, 33.74890960531436690 ) ) ;
#7033 = CARTESIAN_POINT ( 'NONE',  ( 0.05219959533909260263, 19.03943276465977164, 114.9989096053143669 ) ) ;
#7034 = CARTESIAN_POINT ( 'NONE',  ( -14.29746914071049879, 8.314922557960819915, 95.83224293864770971 ) ) ;
#7035 = DIRECTION ( 'NONE',  ( -0.000000000000000000, -0.000000000000000000, 1.000000000000000000 ) ) ;
#7036 = CARTESIAN_POINT ( 'NONE',  ( 9.474510206698729675, 16.51473224551082808, 42.08442372801900433 ) ) ;
#7037 = CARTESIAN_POINT ( 'NONE',  ( -16.52544592524342804, 4.483927247898546575, 31.04057627198102409 ) ) ;
#7038 = CARTESIAN_POINT ( 'NONE',  ( 5.153800228976335163, 19.02544592524342804, 104.7905762719809957 ) ) ;
#7039 = CARTESIAN_POINT ( 'NONE',  ( 5.823673210054444382, -21.52544592524334988, 60.20942372801902565 ) ) ;
#7040 = CARTESIAN_POINT ( 'NONE',  ( -5.719274019375978568, 21.55341960407610458, 60.20724293864768839 ) ) ;
#7041 = CARTESIAN_POINT ( 'NONE',  ( -15.80617190586768217, 15.72974639402176855, 33.12609039468569705 ) ) ;
#7042 = CARTESIAN_POINT ( 'NONE',  ( -10.81492255796078084, -18.62759615963271287, 77.08224293864769550 ) ) ;
#7043 = CARTESIAN_POINT ( 'NONE',  ( 10.81492255796106328, -18.62759615963255655, 40.41775706135234714 ) ) ;
#7044 = CARTESIAN_POINT ( 'NONE',  ( 8.314922557960818139, 14.29746914071049879, 104.5822429386477097 ) ) ;
#7045 = CARTESIAN_POINT ( 'NONE',  ( -19.03943276465977164, -0.05219959533935918106, 73.75109039468566152 ) ) ;
#7046 = CARTESIAN_POINT ( 'NONE',  ( 16.46253265017160672, -9.564922557960803928, 48.33224293864769550 ) ) ;
#7048 = CARTESIAN_POINT ( 'NONE',  ( -5.153800228976328057, -19.02544592524343514, 92.29057627198099567 ) ) ;
#7047 = CARTESIAN_POINT ( 'NONE',  ( -16.52544592524342804, 4.483927247898546575, 96.04057627198102409 ) ) ;
#7049 = CARTESIAN_POINT ( 'NONE',  ( -16.46253265017160317, 9.564922557960807481, 95.83224293864769550 ) ) ;
#7050 = CARTESIAN_POINT ( 'NONE',  ( 4.483927247898545687, 16.52544592524342804, 114.7905762719810383 ) ) ;
#7051 = CARTESIAN_POINT ( 'NONE',  ( -16.55341960407611168, -4.379528057220339221, 36.45724293864768839 ) ) ;
#7052 = CARTESIAN_POINT ( 'NONE',  ( -16.52544592524335698, -4.483927247898792601, 93.95942372801903275 ) ) ;
#7053 = CARTESIAN_POINT ( 'NONE',  ( -13.97604488694527625, -13.89961937509977652, 56.87390960531434558 ) ) ;
#7054 = CARTESIAN_POINT ( 'NONE',  ( 13.89961937509977652, -13.97604488694527269, 23.12390960531436335 ) ) ;
#7055 = CARTESIAN_POINT ( 'NONE',  ( 5.153800228976615827, -19.02544592524334988, 25.20942372801900433 ) ) ;
#7057 = CARTESIAN_POINT ( 'NONE',  ( -8.314922557960811034, -14.29746914071050412, 27.08224293864769550 ) ) ;
#7056 = CARTESIAN_POINT ( 'NONE',  ( -3.181980515339590365, -34.99999999999999289, 1.110912703473986074 ) ) ;
#7058 = MANIFOLD_SOLID_BREP ( 'AdvancedHole1', #101418 ) ;
#7059 = CARTESIAN_POINT ( 'NONE',  ( -15.80617190586768217, 15.72974639402176855, 48.12609039468568284 ) ) ;
#7060 = CARTESIAN_POINT ( 'NONE',  ( -9.474510206698964154, 16.51473224551069663, 115.4155762719810241 ) ) ;
#7061 = CARTESIAN_POINT ( 'NONE',  ( 4.483927247898790824, -16.52544592524335698, 50.20942372801901854 ) ) ;
#7062 = CARTESIAN_POINT ( 'NONE',  ( -14.34966873604960291, -8.224510206698953496, 21.66557627198102409 ) ) ;
#7063 = CARTESIAN_POINT ( 'NONE',  ( 19.02544592524343514, -5.153800228976328945, 48.54057627198103120 ) ) ;
#7064 = CARTESIAN_POINT ( 'NONE',  ( 12.06949235617739724, 12.14591786802326823, 91.87609039468568994 ) ) ;
#7065 = CARTESIAN_POINT ( 'NONE',  ( 0.05219959533934541429, -16.53943276465976808, 20.00109039468568639 ) ) ;
#7066 = CARTESIAN_POINT ( 'NONE',  ( 9.474510206698971260, -16.51473224551069308, 42.91557627198103120 ) ) ;
#7067 = CARTESIAN_POINT ( 'NONE',  ( 16.53943276465976808, -0.05219959533910856209, 103.7489096053143669 ) ) ;
#7068 = CARTESIAN_POINT ( 'NONE',  ( -21.55341960407610458, -5.719274019375992779, 111.4572429386476813 ) ) ;
#7069 = CARTESIAN_POINT ( 'NONE',  ( -9.474510206698964154, 16.51473224551069663, 50.41557627198102409 ) ) ;
#7070 = AXIS2_PLACEMENT_3D ( 'NONE', #152759, #109240, #140573 ) ;
#7071 = CARTESIAN_POINT ( 'NONE',  ( 19.05341960407611168, 5.049401038298154454, 108.9572429386477097 ) ) ;
#7072 = CARTESIAN_POINT ( 'NONE',  ( 19.05341960407611168, 5.049401038298154454, 38.95724293864767418 ) ) ;
#7073 = CARTESIAN_POINT ( 'NONE',  ( 5.153800228976335163, 19.02544592524342804, 104.7905762719809957 ) ) ;
#7074 = CARTESIAN_POINT ( 'NONE',  ( 1.221313414957698099E-14, -31.90000000000003411, -64.92279855667830191 ) ) ;
#7075 = CARTESIAN_POINT ( 'NONE',  ( -9.564922557960796823, -16.46253265017161027, 92.08224293864769550 ) ) ;
#7077 = CARTESIAN_POINT ( 'NONE',  ( 12.14591786802309770, 12.06949235617756955, 104.3739096053143669 ) ) ;
#7076 = CARTESIAN_POINT ( 'NONE',  ( 10.72451020669871369, 18.67979575497193778, 42.08442372801901854 ) ) ;
#7078 = CARTESIAN_POINT ( 'NONE',  ( -16.51473224551069308, -9.474510206698971260, 106.6655762719810383 ) ) ;
#7079 = CARTESIAN_POINT ( 'NONE',  ( -17.58332526062526213, -7.635886036038624702, 69.07665040441534643 ) ) ;
#7080 = CARTESIAN_POINT ( 'NONE',  ( -16.53943276465976808, -0.05219959533934237506, 63.75109039468568284 ) ) ;
#7081 = CARTESIAN_POINT ( 'NONE',  ( -5.719274019375665041, -21.55341960407619695, 89.79275706135236135 ) ) ;
#7082 = CARTESIAN_POINT ( 'NONE',  ( 14.29746914071037800, 8.314922557961029526, 51.66775706135234714 ) ) ;
#7083 = CARTESIAN_POINT ( 'NONE',  ( 19.03943276465977164, -0.05219959533909143690, 83.74890960531436690 ) ) ;
#7084 = CARTESIAN_POINT ( 'NONE',  ( -8.224510206698735004, -14.34966873604973081, 44.58442372801901854 ) ) ;
#7085 = CARTESIAN_POINT ( 'NONE',  ( -9.564922557961040184, 16.46253265017147172, 102.9177570613523329 ) ) ;
#7086 = CARTESIAN_POINT ( 'NONE',  ( -16.55341960407617563, 4.379528057220093196, 78.54275706135236135 ) ) ;
#7087 = CARTESIAN_POINT ( 'NONE',  ( 0.05219959533936267826, -19.03943276465977164, 95.00109039468567573 ) ) ;
#7088 = CARTESIAN_POINT ( 'NONE',  ( 0.05219959533909260263, 19.03943276465977164, 79.99890960531436690 ) ) ;
#7089 = CARTESIAN_POINT ( 'NONE',  ( -18.67979575497178146, -10.72451020669898902, 96.66557627198102409 ) ) ;
#7091 = CARTESIAN_POINT ( 'NONE',  ( -9.564922557961040184, 16.46253265017147172, 87.91775706135233293 ) ) ;
#7090 = CARTESIAN_POINT ( 'NONE',  ( 0.05219959533910956823, 16.53943276465976808, 84.99890960531436690 ) ) ;
#7092 = CARTESIAN_POINT ( 'NONE',  ( -16.52544592524335698, -4.483927247898792601, 78.95942372801901854 ) ) ;
#7093 = CARTESIAN_POINT ( 'NONE',  ( 23.84827716990778512, 9.022217638662837658, 168.8513102586128127 ) ) ;
#7094 = CARTESIAN_POINT ( 'NONE',  ( 9.564922557961047289, -16.46253265017146816, 75.41775706135234714 ) ) ;
#7095 = CARTESIAN_POINT ( 'NONE',  ( 8.314922557960818139, 14.29746914071049879, 29.58224293864769905 ) ) ;
#7096 = CARTESIAN_POINT ( 'NONE',  ( 4.379528057220339221, -16.55341960407611168, 97.70724293864772392 ) ) ;
#7098 = CARTESIAN_POINT ( 'NONE',  ( -17.31747979337962562, 6.344076630960745256, 38.62055131934819485 ) ) ;
#7097 = CARTESIAN_POINT ( 'NONE',  ( 13.89961937509957401, 13.97604488694547697, 36.87609039468565442 ) ) ;
#7099 = CARTESIAN_POINT ( 'NONE',  ( -21.53943276465977519, 0.05219959533907696930, 116.2489096053143669 ) ) ;
#7100 = CARTESIAN_POINT ( 'NONE',  ( -9.474510206698964154, 16.51473224551069663, 110.4155762719810383 ) ) ;
#7101 = CARTESIAN_POINT ( 'NONE',  ( 16.46253265017160672, -9.564922557960803928, 93.33224293864769550 ) ) ;
#7102 = CARTESIAN_POINT ( 'NONE',  ( 21.53943276465977519, 0.05219959533937863772, 96.25109039468568994 ) ) ;
#7103 = CARTESIAN_POINT ( 'NONE',  ( -19.05341960407611168, -5.049401038298163336, 71.45724293864766707 ) ) ;
#7104 = ORIENTED_EDGE ( 'NONE', *, *, #128488, .T. ) ;
#7105 = CARTESIAN_POINT ( 'NONE',  ( 10.72451020669898902, -18.67979575497178502, 42.91557627198103120 ) ) ;
#7106 = CARTESIAN_POINT ( 'NONE',  ( 8.314922557960818139, 14.29746914071049879, 99.58224293864770971 ) ) ;
#7107 = CARTESIAN_POINT ( 'NONE',  ( -19.05341960407611168, -5.049401038298163336, 61.45724293864769550 ) ) ;
#7108 = CARTESIAN_POINT ( 'NONE',  ( -12.06949235617756955, 12.14591786802309770, 110.6239096053143669 ) ) ;
#7109 = CARTESIAN_POINT ( 'NONE',  ( 5.823673210054444382, -21.52544592524334988, 30.20942372801902565 ) ) ;
#7110 = CARTESIAN_POINT ( 'NONE',  ( -15.80617190586768217, 15.72974639402176855, 58.12609039468568994 ) ) ;
#7111 = CARTESIAN_POINT ( 'NONE',  ( 13.89961937509977652, -13.97604488694527269, 38.12390960531436690 ) ) ;
#7112 = CARTESIAN_POINT ( 'NONE',  ( 8.224510206698742110, 14.34966873604972548, 77.08442372801901854 ) ) ;
#7113 = CARTESIAN_POINT ( 'NONE',  ( 21.52544592524344225, -5.823673210054117533, 113.5405762719810383 ) ) ;
#7114 = ORIENTED_EDGE ( 'NONE', *, *, #149935, .F. ) ;
#7115 = CARTESIAN_POINT ( 'NONE',  ( 5.823673210054125526, 21.52544592524343514, 109.7905762719810383 ) ) ;
#7117 = CARTESIAN_POINT ( 'NONE',  ( -19.05341960407611168, -5.049401038298163336, 71.45724293864766707 ) ) ;
#7116 = CARTESIAN_POINT ( 'NONE',  ( -5.049401038297874678, -19.05341960407617918, 54.79275706135234003 ) ) ;
#7118 = CARTESIAN_POINT ( 'NONE',  ( -0.05219959533936034679, 19.03943276465977164, 37.50109039468567573 ) ) ;
#7119 = CARTESIAN_POINT ( 'NONE',  ( 21.52544592524334988, 5.823673210054432836, 76.45942372801901854 ) ) ;
#7120 = CARTESIAN_POINT ( 'NONE',  ( 0.05219959533907565091, 21.53943276465977519, 74.99890960531435269 ) ) ;
#7121 = CARTESIAN_POINT ( 'NONE',  ( -8.224510206698948167, 14.34966873604960824, 55.41557627198102409 ) ) ;
#7123 = CARTESIAN_POINT ( 'NONE',  ( -5.049401038297874678, -19.05341960407617918, 34.79275706135233293 ) ) ;
#7122 = CARTESIAN_POINT ( 'NONE',  ( -15.72974639402176322, -15.80617190586768395, 84.37609039468570415 ) ) ;
#7124 = CARTESIAN_POINT ( 'NONE',  ( -12.14591786802309592, -12.06949235617757132, 66.87390960531436690 ) ) ;
#7125 = CARTESIAN_POINT ( 'NONE',  ( 12.14591786802309770, 12.06949235617756955, 109.3739096053143811 ) ) ;
#7126 = CARTESIAN_POINT ( 'NONE',  ( 16.46253265017146816, 9.564922557961045513, 51.66775706135233293 ) ) ;
#7127 = CARTESIAN_POINT ( 'NONE',  ( -16.53943276465976808, -0.05219959533934237506, 108.7510903946857042 ) ) ;
#7128 = CARTESIAN_POINT ( 'NONE',  ( 0.05219959533937995610, -21.53943276465977519, 75.00109039468568994 ) ) ;
#7129 = CARTESIAN_POINT ( 'NONE',  ( 5.049401038298161559, -19.05341960407611168, 72.70724293864768129 ) ) ;
#7130 = CARTESIAN_POINT ( 'NONE',  ( 13.89961937509957401, 13.97604488694547697, 46.87609039468565442 ) ) ;
#7131 = CARTESIAN_POINT ( 'NONE',  ( 0.05219959533907565091, 21.53943276465977519, 54.99890960531435269 ) ) ;
#7132 = CARTESIAN_POINT ( 'NONE',  ( 0.05219959533937995610, -21.53943276465977519, 45.00109039468568284 ) ) ;
#7133 = CARTESIAN_POINT ( 'NONE',  ( 21.53943276465977519, -0.05219959533907433946, 103.7489096053143669 ) ) ;
#7134 = CARTESIAN_POINT ( 'NONE',  ( 5.049401038297881783, 19.05341960407617563, 97.29275706135233293 ) ) ;
#7135 = CARTESIAN_POINT ( 'NONE',  ( 8.314922557961029526, -14.29746914071037800, 60.41775706135235424 ) ) ;
#7137 = CARTESIAN_POINT ( 'NONE',  ( -10.81492255796078084, -18.62759615963271287, 102.0822429386476955 ) ) ;
#7136 = CARTESIAN_POINT ( 'NONE',  ( -15.35002835867562432, -17.41572776432974479, -57.57448828401508933 ) ) ;
#7138 = CARTESIAN_POINT ( 'NONE',  ( -4.379528057220328563, 16.55341960407611168, 90.20724293864770971 ) ) ;
#7139 = DIRECTION ( 'NONE',  ( 1.000000000000000000, 0.000000000000000000, 0.000000000000000000 ) ) ;
#7140 = CARTESIAN_POINT ( 'NONE',  ( 16.53943276465976808, 0.05219959533934440121, 21.25109039468567218 ) ) ;
#7141 = CARTESIAN_POINT ( 'NONE',  ( 18.67979575497178502, 10.72451020669898547, 49.16557627198102409 ) ) ;
#7142 = CARTESIAN_POINT ( 'NONE',  ( 4.483927247898790824, -16.52544592524335698, 85.20942372801901854 ) ) ;
#7143 = CARTESIAN_POINT ( 'NONE',  ( 36.44859680441125960, 5.987861874135487206, -7.999999999999996447 ) ) ;
#7144 = CARTESIAN_POINT ( 'NONE',  ( -0.05219959533934338120, 16.53943276465976808, 62.50109039468568284 ) ) ;
#7145 = CARTESIAN_POINT ( 'NONE',  ( 10.81492255796106328, -18.62759615963255655, 35.41775706135234003 ) ) ;
#7146 = CARTESIAN_POINT ( 'NONE',  ( 10.81492255796078972, 18.62759615963270932, 64.58224293864769550 ) ) ;
#7147 = CARTESIAN_POINT ( 'NONE',  ( -12.14591786802326823, 12.06949235617739902, 88.12609039468570415 ) ) ;
#7148 = CARTESIAN_POINT ( 'NONE',  ( 9.474510206698971260, -16.51473224551069308, 92.91557627198103830 ) ) ;
#7149 = CARTESIAN_POINT ( 'NONE',  ( 15.72974639402176855, 15.80617190586768217, 71.87609039468568994 ) ) ;
#7150 = EDGE_CURVE ( 'NONE', #179366, #27205, #179436, .T. ) ;
#7151 = CARTESIAN_POINT ( 'NONE',  ( -21.52544592524343514, 5.823673210054127303, 46.04057627198103830 ) ) ;
#7152 = CARTESIAN_POINT ( 'NONE',  ( -21.55341960407610458, -5.719274019375992779, 31.45724293864769550 ) ) ;
#7153 = EDGE_LOOP ( 'NONE', ( #32159, #159327, #16906, #182605 ) ) ;
#7154 = CARTESIAN_POINT ( 'NONE',  ( -16.51473224551082808, 9.474510206698731452, 48.33442372801900433 ) ) ;
#7155 = CARTESIAN_POINT ( 'NONE',  ( 0.05219959533934541429, -16.53943276465976808, 70.00109039468568994 ) ) ;
#7156 = CARTESIAN_POINT ( 'NONE',  ( 5.823673210054125526, 21.52544592524343514, 34.79057627198103120 ) ) ;
#7157 = VERTEX_POINT ( 'NONE', #106535 ) ;
#7158 = CARTESIAN_POINT ( 'NONE',  ( -9.474510206698964154, 16.51473224551069663, 105.4155762719810383 ) ) ;
#7159 = CARTESIAN_POINT ( 'NONE',  ( 8.224510206698742110, 14.34966873604972548, 112.0844237280190185 ) ) ;
#7160 = DIRECTION ( 'NONE',  ( 1.000000000000000000, 0.000000000000000000, 0.000000000000000000 ) ) ;
#7161 = CARTESIAN_POINT ( 'NONE',  ( 4.379528057220339221, -16.55341960407611168, 112.7072429386476955 ) ) ;
#7162 = CARTESIAN_POINT ( 'NONE',  ( 21.52544592524344225, -5.823673210054117533, 53.54057627198103120 ) ) ;
#7163 = CARTESIAN_POINT ( 'NONE',  ( -19.02544592524342804, 5.153800228976336051, 51.04057627198103120 ) ) ;
#7164 = CARTESIAN_POINT ( 'NONE',  ( 8.314922557961029526, -14.29746914071037800, 95.41775706135234714 ) ) ;
#7165 = CARTESIAN_POINT ( 'NONE',  ( -21.53943276465977519, -0.05219959533937600094, 28.75109039468567929 ) ) ;
#7166 = CARTESIAN_POINT ( 'NONE',  ( 13.89961937509957401, 13.97604488694547697, 91.87609039468567573 ) ) ;
#7167 = CARTESIAN_POINT ( 'NONE',  ( -14.29746914071049879, 8.314922557960819915, 95.83224293864770971 ) ) ;
#7168 = CARTESIAN_POINT ( 'NONE',  ( 13.89961937509977652, -13.97604488694527269, 53.12390960531434558 ) ) ;
#7169 = CARTESIAN_POINT ( 'NONE',  ( -0.05219959533909027116, -19.03943276465977164, 32.49890960531435979 ) ) ;
#7170 = FACE_BOUND ( 'NONE', #125078, .T. ) ;
#7171 = CARTESIAN_POINT ( 'NONE',  ( -13.97604488694527625, -13.89961937509977652, 71.87390960531433848 ) ) ;
#7172 = CARTESIAN_POINT ( 'NONE',  ( 16.52544592524335698, 4.483927247898782831, 56.45942372801902565 ) ) ;
#7173 = CARTESIAN_POINT ( 'NONE',  ( 15.80617190586769283, -15.72974639402175789, 110.6260903946857042 ) ) ;
#7174 = CARTESIAN_POINT ( 'NONE',  ( 5.719274019375991003, -21.55341960407610458, 52.70724293864769550 ) ) ;
#7175 = CARTESIAN_POINT ( 'NONE',  ( -12.14591786802326823, 12.06949235617739902, 73.12609039468567573 ) ) ;
#7176 = CARTESIAN_POINT ( 'NONE',  ( 16.46253265017146816, 9.564922557961045513, 46.66775706135233293 ) ) ;
#7177 = CARTESIAN_POINT ( 'NONE',  ( 19.03943276465977164, 0.05219959533936151252, 61.25109039468566863 ) ) ;
#7178 = CARTESIAN_POINT ( 'NONE',  ( 15.80617190586769283, -15.72974639402175789, 65.62609039468568994 ) ) ;
#7179 = CARTESIAN_POINT ( 'NONE',  ( -5.049401038298153566, 19.05341960407611168, 70.20724293864769550 ) ) ;
#7180 = CARTESIAN_POINT ( 'NONE',  ( 16.51473224551069308, 9.474510206698969483, 34.16557627198102409 ) ) ;
#7181 = CARTESIAN_POINT ( 'NONE',  ( 5.049401038297881783, 19.05341960407617563, 62.29275706135234003 ) ) ;
#7182 = CARTESIAN_POINT ( 'NONE',  ( -9.474510206698964154, 16.51473224551069663, 110.4155762719810383 ) ) ;
#7183 = CARTESIAN_POINT ( 'NONE',  ( -19.05341960407611168, -5.049401038298163336, 91.45724293864766707 ) ) ;
#7184 = CARTESIAN_POINT ( 'NONE',  ( 16.53943276465976808, -0.05219959533910856209, 48.74890960531435979 ) ) ;
#7185 = CARTESIAN_POINT ( 'NONE',  ( -5.823673210054116645, -21.52544592524344225, 42.29057627198103120 ) ) ;
#7186 = DIRECTION ( 'NONE',  ( 0.000000000000000000, 0.000000000000000000, 1.000000000000000000 ) ) ;
#7187 = CARTESIAN_POINT ( 'NONE',  ( -21.55341960407619339, 5.719274019375674811, 108.5427570613523756 ) ) ;
#7188 = DIRECTION ( 'NONE',  ( -1.000000000000000000, 0.000000000000000000, -0.000000000000000000 ) ) ;
#7189 = CARTESIAN_POINT ( 'NONE',  ( 5.049401038298161559, -19.05341960407611168, 52.70724293864767418 ) ) ;
#7190 = CARTESIAN_POINT ( 'NONE',  ( -18.22780087662122028, -5.500000000000014211, 101.4845989467389273 ) ) ;
#7191 = CARTESIAN_POINT ( 'NONE',  ( 9.138071159678322175, -35.85733837751254782, -7.999999999999996447 ) ) ;
#7192 = CARTESIAN_POINT ( 'NONE',  ( 12.14591786802327356, -12.06949235617739191, 70.62609039468567573 ) ) ;
#7193 = CARTESIAN_POINT ( 'NONE',  ( 10.81492255796078972, 18.62759615963270932, 99.58224293864770971 ) ) ;
#7194 = CARTESIAN_POINT ( 'NONE',  ( 12.06949235617757843, -12.14591786802309237, 48.12390960531436690 ) ) ;
#7196 = DIRECTION ( 'NONE',  ( -1.000000000000000000, -0.000000000000000000, -0.000000000000000000 ) ) ;
#7195 = CARTESIAN_POINT ( 'NONE',  ( -13.89961937509977652, 13.97604488694528158, 35.62390960531435269 ) ) ;
#7197 = CARTESIAN_POINT ( 'NONE',  ( 5.823673210054444382, -21.52544592524334988, 35.20942372801901854 ) ) ;
#7198 = CARTESIAN_POINT ( 'NONE',  ( -9.564922557961040184, 16.46253265017147172, 52.91775706135233293 ) ) ;
#7199 = CARTESIAN_POINT ( 'NONE',  ( 9.474510206698971260, -16.51473224551069308, 52.91557627198102409 ) ) ;
#7200 = CARTESIAN_POINT ( 'NONE',  ( -18.62759615963255300, -10.81492255796106328, 99.16775706135234714 ) ) ;
#7201 = CARTESIAN_POINT ( 'NONE',  ( 16.31925111598457079, 7.325300261831539927, 97.33575461032749843 ) ) ;
#7202 = ORIENTED_EDGE ( 'NONE', *, *, #67479, .F. ) ;
#7203 = CARTESIAN_POINT ( 'NONE',  ( 8.314922557960818139, 14.29746914071049879, 39.58224293864769550 ) ) ;
#7204 = CARTESIAN_POINT ( 'NONE',  ( 18.39639308325437383, 5.500000000000037303, 43.98252246182197922 ) ) ;
#7205 = CARTESIAN_POINT ( 'NONE',  ( -21.52544592524343514, 5.823673210054127303, 36.04057627198102409 ) ) ;
#7206 = CARTESIAN_POINT ( 'NONE',  ( 17.14385361876520264, -23.59649016807270883, 141.5750000027311728 ) ) ;
#7207 = CARTESIAN_POINT ( 'NONE',  ( 19.03943276465977164, -0.05219959533909143690, 98.74890960531436690 ) ) ;
#7208 = CARTESIAN_POINT ( 'NONE',  ( -8.224510206698948167, 14.34966873604960824, 85.41557627198102409 ) ) ;
#7209 = CARTESIAN_POINT ( 'NONE',  ( -16.52544592524335698, -4.483927247898792601, 23.95942372801901143 ) ) ;
#7210 = CARTESIAN_POINT ( 'NONE',  ( 16.52544592524335698, 4.483927247898782831, 111.4594237280190328 ) ) ;
#7211 = ORIENTED_EDGE ( 'NONE', *, *, #183499, .T. ) ;
#7213 = CARTESIAN_POINT ( 'NONE',  ( 5.823673210054125526, 21.52544592524343514, 104.7905762719810241 ) ) ;
#7212 = CARTESIAN_POINT ( 'NONE',  ( 16.51473224551069308, 9.474510206698969483, 94.16557627198103830 ) ) ;
#7215 = CARTESIAN_POINT ( 'NONE',  ( 16.51473224551069308, 9.474510206698969483, 94.16557627198103830 ) ) ;
#7214 = CARTESIAN_POINT ( 'NONE',  ( -8.314922557961024197, 14.29746914071037800, 112.9177570613523329 ) ) ;
#7216 = CARTESIAN_POINT ( 'NONE',  ( -13.89961937509957401, -13.97604488694547875, 94.37609039468566152 ) ) ;
#7217 = CARTESIAN_POINT ( 'NONE',  ( 18.67979575497194134, -10.72451020669871369, 110.8344237280190043 ) ) ;
#7218 = CARTESIAN_POINT ( 'NONE',  ( 21.53943276465977519, -0.05219959533907433946, 93.74890960531436690 ) ) ;
#7219 = CARTESIAN_POINT ( 'NONE',  ( -10.81492255796078084, -18.62759615963271287, 52.08224293864768839 ) ) ;
#7220 = CARTESIAN_POINT ( 'NONE',  ( -19.02544592524342804, 5.153800228976336051, 66.04057627198103830 ) ) ;
#7221 = CARTESIAN_POINT ( 'NONE',  ( -8.314922557960811034, -14.29746914071050412, 32.08224293864769550 ) ) ;
#7222 = CARTESIAN_POINT ( 'NONE',  ( -16.51473224551069308, -9.474510206698971260, 76.66557627198103830 ) ) ;
#7223 = ORIENTED_EDGE ( 'NONE', *, *, #175162, .T. ) ;
#7224 = DIRECTION ( 'NONE',  ( 1.000000000000000000, 0.000000000000000000, 0.000000000000000000 ) ) ;
#7225 = CARTESIAN_POINT ( 'NONE',  ( -5.049401038297874678, -19.05341960407617918, 34.79275706135233293 ) ) ;
#7226 = CARTESIAN_POINT ( 'NONE',  ( -16.52544592524342804, 4.483927247898546575, 86.04057627198102409 ) ) ;
#7227 = CARTESIAN_POINT ( 'NONE',  ( -15.72974639402176322, -15.80617190586768395, 24.37609039468567573 ) ) ;
#7228 = CARTESIAN_POINT ( 'NONE',  ( 27.73933785331498214, 9.013057229001095294, 142.4750000027311785 ) ) ;
#7229 = CARTESIAN_POINT ( 'NONE',  ( 14.34966873604972726, -8.224510206698740333, 100.8344237280190185 ) ) ;
#7230 = CARTESIAN_POINT ( 'NONE',  ( 4.379528057220339221, -16.55341960407611168, 112.7072429386476955 ) ) ;
#7231 = CARTESIAN_POINT ( 'NONE',  ( 5.049401038298161559, -19.05341960407611168, 72.70724293864768129 ) ) ;
#7232 = FILL_AREA_STYLE ('',( #69926 ) ) ;
#7233 = CARTESIAN_POINT ( 'NONE',  ( -5.153800228976328057, -19.02544592524343514, 22.29057627198102765 ) ) ;
#7234 = CARTESIAN_POINT ( 'NONE',  ( -4.483927247898539470, -16.52544592524342804, 32.29057627198102409 ) ) ;
#7235 = CARTESIAN_POINT ( 'NONE',  ( -21.55341960407619339, 5.719274019375674811, 53.54275706135234714 ) ) ;
#7236 = CARTESIAN_POINT ( 'NONE',  ( 3.889087296525994830, -6.412877669190346630, 8.181980515339454030 ) ) ;
#7237 = CARTESIAN_POINT ( 'NONE',  ( 18.62759615963255655, 10.81492255796105972, 96.66775706135234714 ) ) ;
#7238 = CARTESIAN_POINT ( 'NONE',  ( -9.474510206698964154, 16.51473224551069663, 45.41557627198103120 ) ) ;
#7239 = CARTESIAN_POINT ( 'NONE',  ( 5.153800228976335163, 19.02544592524342804, 54.79057627198103120 ) ) ;
#7240 = ORIENTED_EDGE ( 'NONE', *, *, #34091, .F. ) ;
#7241 = CARTESIAN_POINT ( 'NONE',  ( -18.62759615963255300, -10.81492255796106328, 89.16775706135236135 ) ) ;
#7242 = CARTESIAN_POINT ( 'NONE',  ( -4.483927247898782831, 16.52544592524335698, 67.70942372801901854 ) ) ;
#7243 = CARTESIAN_POINT ( 'NONE',  ( 10.72451020669871369, 18.67979575497193778, 87.08442372801901854 ) ) ;
#7244 = CARTESIAN_POINT ( 'NONE',  ( -5.049401038298153566, 19.05341960407611168, 110.2072429386476671 ) ) ;
#7245 = CARTESIAN_POINT ( 'NONE',  ( -5.049401038297874678, -19.05341960407617918, 99.79275706135234714 ) ) ;
#7246 = CARTESIAN_POINT ( 'NONE',  ( -15.72974639402176322, -15.80617190586768395, 69.37609039468567573 ) ) ;
#7247 = CARTESIAN_POINT ( 'NONE',  ( 8.224510206698742110, 14.34966873604972548, 42.08442372801901854 ) ) ;
#7248 = CARTESIAN_POINT ( 'NONE',  ( 10.81492255796078972, 18.62759615963270932, 84.58224293864769550 ) ) ;
#7249 = CARTESIAN_POINT ( 'NONE',  ( 19.05341960407617918, -5.049401038297876454, 81.04275706135231871 ) ) ;
#7250 = CARTESIAN_POINT ( 'NONE',  ( -5.049401038298153566, 19.05341960407611168, 70.20724293864769550 ) ) ;
#7251 = CARTESIAN_POINT ( 'NONE',  ( -0.05219959533936034679, 19.03943276465977164, 97.50109039468567573 ) ) ;
#7252 = CARTESIAN_POINT ( 'NONE',  ( 0.05219959533936267826, -19.03943276465977164, 105.0010903946856615 ) ) ;
#7253 = CARTESIAN_POINT ( 'NONE',  ( -16.52544592524342804, 4.483927247898546575, 46.04057627198103830 ) ) ;
#7254 = CARTESIAN_POINT ( 'NONE',  ( -9.564922557961040184, 16.46253265017147172, 82.91775706135233293 ) ) ;
#7255 = CARTESIAN_POINT ( 'NONE',  ( 16.52544592524335698, 4.483927247898782831, 66.45942372801903275 ) ) ;
#7256 = CARTESIAN_POINT ( 'NONE',  ( -0.05219959533909027116, -19.03943276465977164, 42.49890960531435269 ) ) ;
#7257 = CARTESIAN_POINT ( 'NONE',  ( -5.153800228976328057, -19.02544592524343514, 62.29057627198100988 ) ) ;
#7258 = CARTESIAN_POINT ( 'NONE',  ( 14.34966873604972726, -8.224510206698740333, 65.83442372801900433 ) ) ;
#7259 = CARTESIAN_POINT ( 'NONE',  ( 17.14385361876520264, 23.59649016807275856, 140.6750000027311387 ) ) ;
#7260 = CARTESIAN_POINT ( 'NONE',  ( 17.81289503416610742, 24.51734667627700404, 141.5500000054623797 ) ) ;
#7261 = CARTESIAN_POINT ( 'NONE',  ( -19.02544592524342804, 5.153800228976336051, 111.0405762719810099 ) ) ;
#7262 = CARTESIAN_POINT ( 'NONE',  ( -15.06137443927351249, 15.06137443927345210, -58.85720012050612837 ) ) ;
#7263 = ORIENTED_EDGE ( 'NONE', *, *, #66362, .F. ) ;
#7264 = CARTESIAN_POINT ( 'NONE',  ( 19.03943276465977164, 0.05219959533936151252, 111.2510903946856757 ) ) ;
#7265 = B_SPLINE_CURVE_WITH_KNOTS ( 'NONE', 3,
 ( #180380, #153727, #148025, #9514, #87340, #15223, #57015, #76882 ),
 .UNSPECIFIED., .F., .F.,
 ( 4, 2, 2, 4 ),
 ( 0.01263483034531142669, 0.01686471550494896693, 0.01897965808476773791, 0.02109460066458650543 ),
 .UNSPECIFIED. ) ;
#7266 = CARTESIAN_POINT ( 'NONE',  ( -10.81492255796078084, -18.62759615963271287, 37.08224293864768129 ) ) ;
#7268 = CARTESIAN_POINT ( 'NONE',  ( -16.55341960407617563, 4.379528057220093196, 33.54275706135234714 ) ) ;
#7267 = CARTESIAN_POINT ( 'NONE',  ( -5.049401038297874678, -19.05341960407617918, 34.79275706135233293 ) ) ;
#7269 = CARTESIAN_POINT ( 'NONE',  ( 19.03943276465977164, -0.05219959533909143690, 28.74890960531435624 ) ) ;
#7270 = CARTESIAN_POINT ( 'NONE',  ( -16.51473224551069308, -9.474510206698971260, 51.66557627198102409 ) ) ;
#7271 = CARTESIAN_POINT ( 'NONE',  ( 10.72451020669898902, -18.67979575497178502, 77.91557627198102409 ) ) ;
#7272 = CARTESIAN_POINT ( 'NONE',  ( -13.97604488694527625, -13.89961937509977652, 96.87390960531433848 ) ) ;
#7273 = EDGE_CURVE ( 'NONE', #179892, #165007, #168212, .T. ) ;
#7274 = CARTESIAN_POINT ( 'NONE',  ( -13.97604488694527625, -13.89961937509977652, 46.87390960531435979 ) ) ;
#7275 = CARTESIAN_POINT ( 'NONE',  ( -17.14385361876520975, 23.59649016807275856, 145.0750000027311444 ) ) ;
#7276 = CARTESIAN_POINT ( 'NONE',  ( 9.474510206698729675, 16.51473224551082808, 82.08442372801899012 ) ) ;
#7277 = CARTESIAN_POINT ( 'NONE',  ( 4.483927247898545687, 16.52544592524342804, 64.79057627198103830 ) ) ;
#7278 = CARTESIAN_POINT ( 'NONE',  ( -10.81492255796078084, -18.62759615963271287, 42.08224293864769550 ) ) ;
#7279 = CARTESIAN_POINT ( 'NONE',  ( 5.719274019375673035, 21.55341960407619339, 112.2927570613523471 ) ) ;
#7280 = CARTESIAN_POINT ( 'NONE',  ( -15.72974639402197994, 15.80617190586746368, 100.6239096053143811 ) ) ;
#7281 = CARTESIAN_POINT ( 'NONE',  ( 5.719274019375673035, 21.55341960407619339, 72.29275706135236135 ) ) ;
#7282 = CARTESIAN_POINT ( 'NONE',  ( 18.67979575497194134, -10.72451020669871369, 80.83442372801901854 ) ) ;
#7283 = CARTESIAN_POINT ( 'NONE',  ( -13.89961937509977652, 13.97604488694528158, 115.6239096053143669 ) ) ;
#7285 = CARTESIAN_POINT ( 'NONE',  ( -5.823673210054431948, 21.52544592524334988, 72.70942372801901854 ) ) ;
#7284 = CARTESIAN_POINT ( 'NONE',  ( -12.14591786802326823, 12.06949235617739902, 103.1260903946856757 ) ) ;
#7286 = CARTESIAN_POINT ( 'NONE',  ( -13.97604488694527625, -13.89961937509977652, 71.87390960531433848 ) ) ;
#7287 = CARTESIAN_POINT ( 'NONE',  ( 21.53943276465977519, 0.05219959533937863772, 31.25109039468568639 ) ) ;
#7288 = CARTESIAN_POINT ( 'NONE',  ( -19.02544592524342804, 5.153800228976336051, 66.04057627198103830 ) ) ;
#7289 = CARTESIAN_POINT ( 'NONE',  ( -8.314922557960811034, -14.29746914071050412, 77.08224293864769550 ) ) ;
#7290 = CARTESIAN_POINT ( 'NONE',  ( -14.34966873604960291, -8.224510206698953496, 51.66557627198102409 ) ) ;
#7291 = CARTESIAN_POINT ( 'NONE',  ( 21.55341960407610458, 5.719274019375980345, 53.95724293864770260 ) ) ;
#7292 = CARTESIAN_POINT ( 'NONE',  ( 19.05341960407611168, 5.049401038298154454, 58.95724293864768129 ) ) ;
#7293 = CARTESIAN_POINT ( 'NONE',  ( -18.67979575497178146, -10.72451020669898902, 76.66557627198103830 ) ) ;
#7294 = CARTESIAN_POINT ( 'NONE',  ( 19.02544592524334988, 5.153800228976608722, 61.45942372801900433 ) ) ;
#7296 = CARTESIAN_POINT ( 'NONE',  ( 14.34966873604960469, 8.224510206698951720, 69.16557627198102409 ) ) ;
#7295 = CARTESIAN_POINT ( 'NONE',  ( -13.89961937509957401, -13.97604488694547697, 19.37609039468566863 ) ) ;
#7297 = CARTESIAN_POINT ( 'NONE',  ( 15.72974639402199770, -15.80617190586745480, 38.12390960531436690 ) ) ;
#7298 = ORIENTED_EDGE ( 'NONE', *, *, #35651, .T. ) ;
#7299 = LINE ( 'NONE', #52807, #17240 ) ;
#7301 = CARTESIAN_POINT ( 'NONE',  ( 17.14385361876520264, -23.59649016807270883, 142.0750000027311444 ) ) ;
#7300 = CARTESIAN_POINT ( 'NONE',  ( 8.224510206698742110, 14.34966873604972548, 102.0844237280190185 ) ) ;
#7302 = CARTESIAN_POINT ( 'NONE',  ( -19.02544592524334988, -5.153800228976617603, 83.95942372801901854 ) ) ;
#7303 = CARTESIAN_POINT ( 'NONE',  ( 14.29746914071049879, -8.314922557960816363, 73.33224293864769550 ) ) ;
#7304 = DIRECTION ( 'NONE',  ( -1.000000000000000000, 0.000000000000000000, 0.000000000000000000 ) ) ;
#7305 = CARTESIAN_POINT ( 'NONE',  ( -5.153800228976328057, -19.02544592524343514, 57.29057627198103120 ) ) ;
#7306 = CARTESIAN_POINT ( 'NONE',  ( -8.314922557960811034, -14.29746914071050412, 52.08224293864768839 ) ) ;
#7307 = CARTESIAN_POINT ( 'NONE',  ( -0.05219959533909027116, -19.03943276465977164, 82.49890960531436690 ) ) ;
#7309 = CARTESIAN_POINT ( 'NONE',  ( -13.97604488694527625, -13.89961937509977652, 56.87390960531434558 ) ) ;
#7308 = CARTESIAN_POINT ( 'NONE',  ( -0.05219959533936034679, 19.03943276465977164, 82.50109039468567573 ) ) ;
#7310 = CARTESIAN_POINT ( 'NONE',  ( -19.02544592524342804, 5.153800228976336051, 81.04057627198103830 ) ) ;
#7311 = CARTESIAN_POINT ( 'NONE',  ( -16.51473224551069308, -9.474510206698971260, 66.66557627198102409 ) ) ;
#7312 = CARTESIAN_POINT ( 'NONE',  ( -5.823673210054116645, -21.52544592524344225, 62.29057627198102409 ) ) ;
#7313 = CARTESIAN_POINT ( 'NONE',  ( -9.474510206698964154, 16.51473224551069663, 50.41557627198102409 ) ) ;
#7314 = CARTESIAN_POINT ( 'NONE',  ( 10.72451020669898902, -18.67979575497178502, 52.91557627198103830 ) ) ;
#7315 = CARTESIAN_POINT ( 'NONE',  ( 19.05341960407617918, -5.049401038297876454, 76.04275706135230450 ) ) ;
#7316 = CARTESIAN_POINT ( 'NONE',  ( 4.483927247898545687, 16.52544592524342804, 29.79057627198102409 ) ) ;
#7317 = EDGE_CURVE ( 'NONE', #142110, #123757, #172728, .T. ) ;
#7318 = CARTESIAN_POINT ( 'NONE',  ( -0.05219959533936034679, 19.03943276465977164, 32.50109039468566863 ) ) ;
#7320 = CARTESIAN_POINT ( 'NONE',  ( 14.29746914071037800, 8.314922557961029526, 96.66775706135234714 ) ) ;
#7319 = CARTESIAN_POINT ( 'NONE',  ( 14.29746914071037800, 8.314922557961029526, 61.66775706135235424 ) ) ;
#7321 = CARTESIAN_POINT ( 'NONE',  ( 18.56197773271726348, -5.499999999999867661, 41.05066217314450938 ) ) ;
#7322 = CARTESIAN_POINT ( 'NONE',  ( 16.52544592524335698, 4.483927247898782831, 81.45942372801900433 ) ) ;
#7323 = CARTESIAN_POINT ( 'NONE',  ( 10.72451020669898902, -18.67979575497178502, 32.91557627198102409 ) ) ;
#7324 = CARTESIAN_POINT ( 'NONE',  ( -9.564922557960796823, -16.46253265017161027, 37.08224293864768839 ) ) ;
#7325 = CARTESIAN_POINT ( 'NONE',  ( -14.29746914071037622, -8.314922557961029526, 34.16775706135234714 ) ) ;
#7326 = CARTESIAN_POINT ( 'NONE',  ( 5.049401038298161559, -19.05341960407611168, 47.70724293864770260 ) ) ;
#7327 = CARTESIAN_POINT ( 'NONE',  ( -10.81492255796105439, 18.62759615963255655, 42.91775706135235424 ) ) ;
#7328 = CARTESIAN_POINT ( 'NONE',  ( 8.224510206698742110, 14.34966873604972548, 47.08442372801901854 ) ) ;
#7329 = CARTESIAN_POINT ( 'NONE',  ( 14.29746914071049879, -8.314922557960816363, 23.33224293864769194 ) ) ;
#7330 = CARTESIAN_POINT ( 'NONE',  ( 19.02544592524343514, -5.153800228976328945, 23.54057627198102054 ) ) ;
#7331 = CARTESIAN_POINT ( 'NONE',  ( -19.02544592524334988, -5.153800228976617603, 23.95942372801900078 ) ) ;
#7332 = CARTESIAN_POINT ( 'NONE',  ( 5.153800228976615827, -19.02544592524334988, 110.2094237280189901 ) ) ;
#7333 = CARTESIAN_POINT ( 'NONE',  ( -5.049401038297874678, -19.05341960407617918, 74.79275706135231871 ) ) ;
#7334 = CARTESIAN_POINT ( 'NONE',  ( 14.34966873604960469, 8.224510206698951720, 74.16557627198102409 ) ) ;
#7335 = CARTESIAN_POINT ( 'NONE',  ( -5.049401038298153566, 19.05341960407611168, 35.20724293864768839 ) ) ;
#7337 = CARTESIAN_POINT ( 'NONE',  ( 17.50000000000000355, -5.622605283950865562, 91.18792689403888119 ) ) ;
#7336 = CARTESIAN_POINT ( 'NONE',  ( -13.89961937509957401, -13.97604488694547875, 69.37609039468564731 ) ) ;
#7338 = CARTESIAN_POINT ( 'NONE',  ( 0.05219959533937995610, -21.53943276465977519, 70.00109039468568994 ) ) ;
#7339 = CARTESIAN_POINT ( 'NONE',  ( 4.483927247898790824, -16.52544592524335698, 45.20942372801901854 ) ) ;
#7340 = CARTESIAN_POINT ( 'NONE',  ( -28.26900468436335245, -28.30519395875711552, -15.36550801296253432 ) ) ;
#7341 = CARTESIAN_POINT ( 'NONE',  ( -18.67979575497178146, -10.72451020669898902, 31.66557627198102054 ) ) ;
#7342 = CARTESIAN_POINT ( 'NONE',  ( -8.314922557961024197, 14.29746914071037800, 27.91775706135234358 ) ) ;
#7343 = DIRECTION ( 'NONE',  ( 0.000000000000000000, 0.000000000000000000, 1.000000000000000000 ) ) ;
#7344 = CARTESIAN_POINT ( 'NONE',  ( -25.75939503182791768, 8.559839547494505041, 171.7912139782359588 ) ) ;
#7345 = CARTESIAN_POINT ( 'NONE',  ( 19.03943276465977164, -0.05219959533909143690, 38.74890960531436690 ) ) ;
#7346 = CARTESIAN_POINT ( 'NONE',  ( -5.153800228976607833, 19.02544592524335343, 57.70942372801899722 ) ) ;
#7347 = CARTESIAN_POINT ( 'NONE',  ( -13.97604488694527625, -13.89961937509977652, 61.87390960531435979 ) ) ;
#7348 = CARTESIAN_POINT ( 'NONE',  ( -15.72974639402176322, -15.80617190586768395, 59.37609039468568284 ) ) ;
#7349 = ADVANCED_FACE ( 'NONE', ( #109514 ), #171196, .T. ) ;
#7350 = CARTESIAN_POINT ( 'NONE',  ( 10.81492255796106328, -18.62759615963255655, 100.4177570613523471 ) ) ;
#7351 = CARTESIAN_POINT ( 'NONE',  ( 16.53943276465976808, -0.05219959533910856209, 28.74890960531435624 ) ) ;
#7352 = CARTESIAN_POINT ( 'NONE',  ( 19.03943276465977164, -0.05219959533909143690, 28.74890960531435624 ) ) ;
#7353 = CARTESIAN_POINT ( 'NONE',  ( 16.46253265017160672, -9.564922557960803928, 93.33224293864769550 ) ) ;
#7354 = CARTESIAN_POINT ( 'NONE',  ( 21.55341960407619695, -5.719274019375665929, 56.04275706135235424 ) ) ;
#7355 = CARTESIAN_POINT ( 'NONE',  ( 5.153800228976335163, 19.02544592524342804, 34.79057627198102409 ) ) ;
#7356 = CARTESIAN_POINT ( 'NONE',  ( 15.72974639402176855, 15.80617190586768217, 56.87609039468568994 ) ) ;
#7358 = CARTESIAN_POINT ( 'NONE',  ( 13.97604488694527802, 13.89961937509977652, 104.3739096053143385 ) ) ;
#7357 = CARTESIAN_POINT ( 'NONE',  ( -5.153800228976607833, 19.02544592524334988, 97.70942372801900433 ) ) ;
#7359 = CARTESIAN_POINT ( 'NONE',  ( -19.05341960407611168, -5.049401038298163336, 21.45724293864768839 ) ) ;
#7360 = CARTESIAN_POINT ( 'NONE',  ( -5.823673210054116645, -21.52544592524344225, 107.2905762719810525 ) ) ;
#7361 = CARTESIAN_POINT ( 'NONE',  ( -19.02544592524334988, -5.153800228976617603, 38.95942372801900433 ) ) ;
#7362 = CARTESIAN_POINT ( 'NONE',  ( -9.564922557960796823, -16.46253265017161027, 22.08224293864768839 ) ) ;
#7363 = CARTESIAN_POINT ( 'NONE',  ( -9.564922557960796823, -16.46253265017161027, 67.08224293864769550 ) ) ;
#7364 = CARTESIAN_POINT ( 'NONE',  ( 16.51473224551083163, -9.474510206698727899, 100.8344237280190043 ) ) ;
#7365 = CARTESIAN_POINT ( 'NONE',  ( 16.53943276465976808, -0.05219959533910856209, 68.74890960531435269 ) ) ;
#7366 = CARTESIAN_POINT ( 'NONE',  ( 19.02544592524334988, 5.153800228976608722, 26.45942372801899722 ) ) ;
#7367 = CARTESIAN_POINT ( 'NONE',  ( 10.81492255796078972, 18.62759615963270932, 24.58224293864768839 ) ) ;
#7368 = CARTESIAN_POINT ( 'NONE',  ( -19.05341960407617563, 5.049401038297882671, 93.54275706135234714 ) ) ;
#7369 = CARTESIAN_POINT ( 'NONE',  ( -0.05219959533907301413, -21.53943276465977519, 92.49890960531436690 ) ) ;
#7370 = CARTESIAN_POINT ( 'NONE',  ( 10.81492255796106328, -18.62759615963255655, 40.41775706135234714 ) ) ;
#7371 = CARTESIAN_POINT ( 'NONE',  ( 16.52544592524335698, 4.483927247898782831, 36.45942372801901143 ) ) ;
#7372 = CARTESIAN_POINT ( 'NONE',  ( -8.314922557961024197, 14.29746914071037800, 102.9177570613523756 ) ) ;
#7374 = CARTESIAN_POINT ( 'NONE',  ( 10.72451020669871369, 18.67979575497193778, 52.08442372801901854 ) ) ;
#7373 = CARTESIAN_POINT ( 'NONE',  ( 4.483927247898790824, -16.52544592524335698, 35.20942372801901854 ) ) ;
#7375 = CARTESIAN_POINT ( 'NONE',  ( -15.72974639402197994, 15.80617190586746368, 50.62390960531435979 ) ) ;
#7376 = CARTESIAN_POINT ( 'NONE',  ( 16.46253265017160672, -9.564922557960803928, 28.33224293864769550 ) ) ;
#7377 = CARTESIAN_POINT ( 'NONE',  ( -11.74264578624799782, -36.14014761921581709, -3.349999994537626868 ) ) ;
#7379 = VECTOR ( 'NONE', #45031, 1000.000000000000000 ) ;
#7378 = CARTESIAN_POINT ( 'NONE',  ( 16.53943276465976808, 0.05219959533934440121, 56.25109039468568284 ) ) ;
#7380 = CARTESIAN_POINT ( 'NONE',  ( -10.72451020669898014, 18.67979575497178502, 90.41557627198103830 ) ) ;
#7381 = CARTESIAN_POINT ( 'NONE',  ( 8.224510206698953496, -14.34966873604960469, 32.91557627198102409 ) ) ;
#7382 = CARTESIAN_POINT ( 'NONE',  ( 12.14591786802327356, -12.06949235617739191, 60.62609039468567573 ) ) ;
#7383 = CARTESIAN_POINT ( 'NONE',  ( -16.46253265017146816, -9.564922557961047289, 104.1677570613523329 ) ) ;
#7384 = CARTESIAN_POINT ( 'NONE',  ( 21.55341960407610458, 5.719274019375980345, 98.95724293864770971 ) ) ;
#7385 = CARTESIAN_POINT ( 'NONE',  ( 0.05219959533910956823, 16.53943276465976808, 24.99890960531435624 ) ) ;
#7386 = EDGE_LOOP ( 'NONE', ( #176353, #78348, #99493, #52023, #74607 ) ) ;
#7387 = CARTESIAN_POINT ( 'NONE',  ( 14.34966873604972726, -8.224510206698740333, 75.83442372801900433 ) ) ;
#7388 = CARTESIAN_POINT ( 'NONE',  ( 25.66129429279843066, 9.008087060820804126, 171.3163768196993431 ) ) ;
#7389 =( BOUNDED_SURFACE ( )  B_SPLINE_SURFACE ( 3, 2, ( 
 ( #25226, #12052, #135388, #148552, #182876, #57546, #28220, #121182, #10043, #71703, #197058, #134387, #198039, #196073, #59507, #90833, #186870, #154511, #138347, #63496, #1817, #157500, #48339, #170680, #183864, #169679, #124158, #45351, #18993, #31175, #107993, #140327, #109994, #46337, #61496, #171674, #153511, #142316, #33163, #141324, #47344, #172669, #60498, #16007, #184853, #77665, #122174, #123165, #92825, #80639, #18002, #126158, #125171, #76668, #187854, #30176, #49323, #16999, #62486, #139334, #107003, #94822, #110983, #168676, #813, #108999, #78652, #200027, #15008, #185858, #2813, #32168, #93825, #34154, #155505, #156500, #91819, #79655, #64491, #95814, #53292, #81612, #162469, #5789, #161480, #160478, #96793, #84616, #23970, #6781, #20960, #7782, #177662, #143296, #191810, #68460, #112967, #131133, #130114, #99793, #115974, #39131, #100786, #38140, #67462, #128133, #35141, #65473, #37125, #113951, #176663, #146295, #36125, #158482, #22968, #129120, #114971, #127136, #85626, #174660, #51306, #83621, #69466, #189834, #4782, #192820, #19970, #3796, #54302, #188842, #190819, #50327, #111982, #97777, #159464, #82617, #173674, #66470, #144298, #52294, #175650, #98785, #145298, #21969, #12798, #116966, #74463, #103803, #149310, #9805, #8801, #73479, #136129, #44123, #41138, #195835, #165483, #86628, #101798, #71467, #89620, #163485, #24982, #197805, #148311, #133132, #105782, #70471, #25981, #59271, #196825, #194823, #167469, #10804, #104794, #26979, #40119, #27981, #28964, #150320, #164488, #151309, #120940, #56295, #135152, #11815, #117978, #182640, #58292, #43126, #147312, #132137, #193829, #181647, #72473, #179668, #178657, #55294, #180666, #57307, #119961, #102802, #87624, #134147, #166483, #118983, #42142, #88622, #153269, #187613, #106770, #171432, #16753, #14771, #141081, #125915, #186620, #49083, #75439, #568, #139094, #121936, #156252, #30937, #78401, #94574, #137113, #198800, #77422, #172421, #31924, #90605, #152287, #47096, #140077, #184614, #168445, #93578, #155263, #110740, #1568, #62239, #13771, #199788, #154272, #183631, #17754, #92584, #63244, #79411, #60265, #45113, #123907, #29941, #124923, #91580, #76431, #108756, #48092, #46095, #138107, #109748, #32919, #61256, #2566, #185606, #122926, #107750, #15763, #169432, #170432, #64248, #81369, #113708, #160232, #19728, #34894, #145052, #126890, #115733, #21722, #114722, #20713, #146049, #33909, #127885, #158237, #189588, #95567, #96550, #143053, #192576, #191563, #99548, #175405, #50077, #161230, #3552, #22724, #190576, #35884, #4532, #157253, #83375, #84372, #130886, #51060, #82369, #52052, #173425, #188596, #66224, #176415, #111738, #112722, #7533, #174415, #97531, #54059, #18747, #159218, #69218, #6533, #144058, #80394, #5539, #53042, #36873, #67218, #37890, #142066, #98538, #128876, #65230, #68213, #129865, #165238, #180424, #86385, #104551, #41897, #73236, #89376, #12556, #151065, #11570, #40887, #101543, #8552, #38891, #10559, #87386, #150065, #58054, #9560, #70228, #134907, #102560, #103563, #72223, #39876, #74222, #193580, #119725, #26732, #163235, #27733, #135890, #196584, #197562, #162227, #149071, #25740, #88371, #133898, #24735, #59029, #55052, #181408, #42886, #148069, #177420, #100548, #166233, #23726, #85375, #195589, #57061, #131896, #147068, #117727, #116723, #178412, #71226, #132889, #164245, #194578, #118736, #56048, #179422, #79918, #49585, #17261, #1074, #126416, #64754, #20229, #111248, #33424, #43873, #32430, #187130, #105538, #81877, #94084, #170938, #3078, #172939, #109259, #124429, #34418, #13529, #5051, #96077, #4059, #110254, #35406, #120696, #78914, #47605, #140591, #182395, #186125, #155763, #143569, #80903, #189114, #188113, #136866, #50587, #90359, #112247, #141590, #125434, #2081, #167224, #157766, #173938, #28722, #63760, #171935, #19256, #62749, #75195, #48602, #65737, #95083 ),
 ( #156771, #18265, #142580, #127405, #152044, #97057, #158740, #83884, #131403, #52559, #176933, #114220, #38403, #144568, #194104, #6054, #193091, #162743, #101058, #130383, #191086, #98041, #128397, #100060, #161745, #39398, #147589, #99055, #159738, #24251, #192081, #175925, #21235, #54567, #23240, #82890, #163759, #146563, #67732, #53563, #160743, #129390, #55566, #113233, #51569, #174923, #115241, #85901, #37396, #116239, #9074, #178933, #84884, #70744, #22235, #145566, #7044, #68726, #190094, #132412, #8058, #69735, #177931, #36387, #117240, #40403, #102074, #25259, #86902, #148585, #66737, #26251, #197092, #195094, #88895, #120225, #182907, #137381, #60529, #89893, #122204, #59538, #198072, #71735, #165753, #57579, #119249, #196109, #133405, #43395, #14036, #121217, #10077, #28254, #56577, #152548, #103074, #105066, #166750, #151576, #45381, #168706, #149578, #44391, #135421, #58559, #107034, #13065, #118251, #136395, #30208, #179942, #74731, #106046, #91850, #41409, #12086, #11074, #87892, #181915, #164756, #167732, #29230, #72752, #90863, #134423, #75701, #199060, #180933, #183896, #42408, #104071, #27246, #150587, #73749, #76701, #32200, #34185, #78682, #33194, #47376, #93857, #140358, #110027, #845, #61526, #80670, #138377, #170710, #18033, #139364, #63528, #62518, #125203, #31205, #142346, #95846, #187885, #200057, #77696, #184885, #15040, #186899, #48370, #126189, #157530, #185891, #46367, #49352, #1846, #79687, #171705, #16038, #50357, #169712, #19024, #141357, #124190, #3826, #188875, #111014, #112016, #123195, #94853, #156534, #108025, #65505, #155534, #2844, #127166, #92856, #154543, #64522, #35173, #172701, #153543, #109031, #173705, #17029, #190849, #174692, #99825, #38170, #193860, #84648, #6812, #19999, #5819, #160509, #81643, #55325, #67495, #144330, #176696, #23002, #82647, #97808, #7814, #189864, #178691, #146325, #177692, #83652, #8833, #96828, #52326, #20993, #113983, #158512, #159497, #129152, #116996, #54332, #162501, #161510, #112998, #24002, #66501, #85658, #53323, #98815, #175681, #143327, #69498, #147345, #4814, #37156, #145330, #115002, #36156, #51338, #21999, #39160, #68490, #130145, #70501, #191842, #131163, #128164, #192853, #116003, #132169, #100818, #118010, #198833, #42176, #197839, #196860, #133163, #120974, #60297, #43161, #57342, #44156, #13806, #179699, #28015, #104828, #149341, #167503, #166517, #74498, #41171, #89657, #136164, #59305, #103836, #28998, #151343, #182672, #102834, #12832, #105816, #90638, #165517, #164520, #71497, #101829, #73515, #150353, #152320, #75472, #72507, #194855, #137145, #27013, #121971, #135186, #26013, #40153, #56328, #163516, #25015, #87656, #86658, #148342, #9838, #10837, #134182, #11850, #88657, #195869, #119017, #180700, #58326, #119994, #181680, #168478, #170468, #65265, #124959, #183663, #45148, #140112, #109783, #77455, #61290, #186656, #48126, #80429, #171466, #93613, #106804, #92615, #47131, #29976, #142102, #154306, #30968, #63279, #32954, #169467, #184647, #94609, #76465, #91615, #156288, #64282, #31958, #95602, #153303, #139126, #107782, #603, #14804, #46128, #15795, #3587, #141115, #49118, #17789, #199822, #110775, #138142, #172457, #1603, #185639, #62273, #122960, #79445, #33944, #123941, #108789, #155298, #2604, #16788, #78438, #125949, #187647, #157287, #18783, #115767, #81404, #4569, #85413, #50112, #5573, #177455, #176450, #66261, #147105, #128911, #84407, #83409, #19763, #7568, #8590, #129899, #144092, #130920, #100582, #127921, #114756, #191599, #35919, #173460, #111772, #34932, #175440, #161264, #112757, #37923, #99583, #38925, #160267, #146084, #143090, #97565, #189623, #51097, #188632, #22758, #174450, #6569, #145086, #96585, #159253, #69254, #192611, #82404, #36910, #98573, #20749, #67253, #113744, #158274, #190612, #21757, #54093, #162264, #23764, #68248, #126925, #52087, #53078, #131933, #25778 ),
 ( #165276, #26770, #105574, #28759, #9599, #42924, #195628, #57101, #167260, #11607, #193616, #196622, #90396, #55088, #88410, #134945, #152080, #116759, #72260, #71264, #86422, #41935, #178450, #166274, #104588, #39917, #58092, #70264, #73275, #197600, #101585, #119762, #12596, #40926, #118775, #181446, #27772, #163273, #149109, #151104, #180463, #150106, #164285, #10599, #103601, #89415, #117768, #24775, #59066, #148108, #87424, #74260, #56087, #135930, #179461, #120733, #132928, #182432, #43912, #194615, #102599, #133938, #44902, #78194, #123696, #106559, #110528, #93365, #14558, #361, #107541, #76216, #2355, #95356, #169217, #137895, #30726, #13565, #199577, #61045, #172209, #171220, #79197, #155052, #29732, #140866, #183418, #64036, #170224, #15554, #122717, #75232, #139864, #125706, #33693, #92373, #62032, #31717, #153056, #168236, #184407, #156040, #91365, #45888, #187405, #154059, #77212, #136903, #198590, #138881, #48873, #63032, #185394, #60058, #46885, #32709, #16547, #108545, #94361, #121726, #1353, #124710, #17537, #186408, #47885, #109538, #160019, #66012, #84160, #21506, #191353, #34687, #83167, #52831, #114500, #20503, #81167, #188383, #18538, #190365, #67010, #129657, #37671, #189380, #49860, #176202, #82151, #144841, #51841, #19522, #53849, #173211, #99336, #6325, #142849, #7322, #192366, #161019, #115523, #141857, #128669, #5326, #111526, #22513, #97324, #68005, #145840, #3348, #65023, #143847, #38684, #98319, #157041, #80185, #113500, #69006, #50857, #96344, #130672, #177211, #126679, #158031, #175195, #4328, #127680, #36660, #112515, #174208, #35676, #159010, #180217, #26523, #86177, #101331, #11356, #193367, #182182, #88168, #181206, #87180, #12354, #149852, #162019, #55841, #147867, #9353, #71018, #23515, #133682, #104343, #73027, #100340, #118528, #85161, #42682, #54843, #195374, #56853, #41687, #135687, #58824, #39669, #134699, #25536, #148861, #197359, #103352, #146848, #196382, #120491, #8342, #165030, #57851, #70017, #131686, #102349, #163019, #116517, #72009, #178205, #119523, #166027, #24526, #27527, #132686, #89168, #150860, #194374, #74017, #117515, #179212, #10352, #40679, #164038, #167017, #122474, #124466, #168970, #123458, #137649, #184165, #30475, #119, #91127, #151837, #170975, #28518, #60801, #108300, #29494, #153813, #152817, #15308, #121483, #32468, #186163, #77956, #90154, #14310, #74992, #169980, #76967, #136657, #140627, #185150, #44659, #92126, #199336, #106312, #94121, #13327, #198337, #59813, #138638, #139623, #75976, #31471, #16306, #155800, #61788, #1111, #183177, #45647, #167998, #107298, #105329, #62785, #46640, #93123, #154808, #47645, #109296, #17298, #78952, #2117, #63799, #125472, #43667, #3116, #173972, #171973, #65773, #97092, #159775, #114260, #37433, #66769, #99093, #36422, #143603, #79957, #67769, #7084, #190127, #4094, #191124, #160785, #64791, #174958, #51602, #96113, #175964, #113266, #21270, #126452, #98077, #82927, #144605, #50621, #111285, #18301, #48639, #20264, #158776, #6090, #129426, #19292, #141626, #52598, #112282, #22273, #81910, #49623, #83924, #188150, #145605, #68765, #172975, #187168, #110291, #33461, #95119, #156809, #5087, #35440, #34454, #157801, #127442, #80940, #142615, #189148, #128430, #120021, #14835, #74526, #130423, #192122, #89685, #59333, #27041, #10864, #136191, #197866, #30007, #121003, #43187, #53603, #42203, #196887, #118037, #91645, #103863, #180727, #12861, #182701, #119045, #134210, #44186, #26038, #179728, #105845, #13834, #181706, #45180, #41198, #88687, #57372, #150383, #102860, #195897, #165544, #153334, #90667, #198862, #167532, #149368, #60329, #164545, #122003, #151370, #135215, #11879, #87683, #29027, #183694, #72534, #73542, #104856, #152349, #58354, #166545, #28044, #75500, #137174, #106834, #168509, #30998, #154336, #34969, #199855, #155334, #65301, #125985, #15827, #96621, #78473, #33981 ),
 ( #185672, #107815, #141152, #186691, #169499, #173496, #156325, #77488, #63316, #170501, #139158, #126960, #122992, #61321, #184678, #124996, #110811, #62305, #64317, #49153, #188669, #109819, #95637, #92647, #47163, #635, #123975, #138174, #172494, #108822, #17825, #32991, #46161, #31991, #157325, #18820, #93649, #48161, #171502, #16823, #140147, #94645, #1639, #79483, #2641, #80464, #3622, #50149, #187683, #111808, #142138, #158310, #76498, #175476, #67289, #128947, #5610, #81439, #53116, #23801, #69291, #19798, #37963, #143125, #162301, #112793, #114794, #176487, #99621, #55126, #178487, #159288, #192647, #145123, #6607, #116796, #161302, #4605, #146121, #39954, #66297, #22797, #84443, #101625, #127957, #21794, #20785, #35954, #191636, #189660, #115803, #54130, #51133, #7605, #174487, #130957, #147141, #97600, #177493, #85451, #190648, #68286, #38963, #100619, #82440, #98610, #8629, #129937, #70301, #113780, #160304, #131970, #193654, #52124, #144128, #36948, #83446, #149149, #118816, #9637, #103641, #163314, #40966, #41974, #133978, #71304, #165319, #102638, #57140, #87462, #132967, #180502, #24812, #72300, #164323, #86461, #148146, #25816, #194657, #56126, #10639, #117808, #179501, #195669, #21436, #69949, #39602, #178135, #7254, #67937, #175124, #5256, #177142, #53777, #116447, #24457, #176132, #36591, #101261, #68939, #8270, #38613, #6257, #40612, #159949, #86107, #131614, #129590, #194305, #179144, #162951, #102282, #128600, #115452, #192298, #98247, #9283, #84094, #193298, #147798, #190294, #51771, #130603, #25468, #85092, #143775, #66938, #100269, #54773, #37602, #83097, #146777, #70948, #163971, #132618, #161950, #113431, #52762, #23445, #144772, #191286, #114431, #99265, #55771, #117445, #160951, #22444, #145772, #180151, #168906, #74929, #167931, #73953, #199268, #87108, #181139, #11288, #42613, #148794, #149785, #72961, #45582, #44593, #152749, #166952, #103284, #14239, #56787, #75911, #43601, #89101, #134630, #10284, #13266, #137585, #184099, #104277, #135621, #105266, #26457, #41620, #196315, #29431, #197292, #28455, #88099, #164964, #57784, #91062, #119455, #71942, #90091, #60736, #165959, #107235, #133612, #27460, #122409, #136592, #150792, #195306, #12288, #106249, #151773, #58755, #118459, #120424, #198272, #182115, #59749, #121419, #183111, #18237, #33395, #139562, #157736, #95054, #64726, #108236, #156743, #126388, #188085, #94056, #154746, #61726, #92059, #63731, #140563, #3050, #111219, #62719, #123394, #49556, #155734, #79891, #125406, #93059, #127373, #46575, #172911, #141561, #16242, #80875, #65707, #34389, #189085, #15243, #2052, #78884, #185086, #96049, #170909, #19225, #142551, #76902, #138573, #17232, #112218, #171907, #30412, #153748, #187103, #4029, #124402, #169916, #50558, #51, #31408, #77894, #48573, #1046, #186096, #110226, #47578, #109230, #32401, #49856, #111521, #21502, #192362, #37667, #188379, #6321, #173207, #130668, #81163, #83163, #144837, #68001, #23511, #146844, #127676, #161015, #113496, #175191, #85158, #129653, #34683, #114496, #8338, #96340, #191349, #52827, #70013, #158027, #190361, #189376, #4324, #160015, #19518, #142845, #66008, #98315, #36657, #50853, #53845, #128665, #176198, #115519, #112511, #174204, #99332, #35672, #22509, #97320, #159006, #84156, #145836, #82147, #20499, #7318, #69002, #143843, #177207, #38680, #5322, #67006, #51837, #100336, #162014, #148857, #193363, #11352, #57847, #117510, #132682, #42678, #24522, #13324, #119519, #12350, #118524, #43664, #131682, #25532, #55837, #87176, #54839, #194370, #179208, #90151, #89164, #197355, #73023, #147863, #58819, #101327, #120487, #88164, #133678, #40675, #116514, #181201, #182178, #28515, #10348, #180213, #149848, #71014, #86173, #102345, #74013, #9349, #178201, #134695, #135683, #164034, #151834, #39665, #72005, #105326, #104339, #195369, #163015, #56849, #150855, #196378 ),
 ( #166023, #41683, #27523, #167014, #103347, #165026, #26519, #106309, #136653, #108297, #185147, #47640, #155797, #107295, #167995, #109293, #116, #139620, #169976, #137646, #171970, #91124, #17295, #1108, #199333, #125468, #110288, #170972, #63795, #121480, #59810, #183173, #123455, #32465, #60798, #62782, #94118, #187165, #31468, #78949, #29491, #45644, #152814, #14306, #198334, #140624, #75973, #154805, #93120, #44656, #122471, #2114, #48636, #30472, #46637, #16303, #184162, #168967, #61785, #92122, #153810, #77953, #33458, #95116, #156806, #124463, #74989, #186160, #15304, #76964, #138635, #50618, #6087, #79953, #141623, #51599, #22270, #67766, #18298, #36418, #3112, #160781, #111282, #113263, #174955, #98074, #53600, #176969, #157798, #191121, #143600, #5084, #115276, #159772, #64788, #144601, #38439, #126449, #21267, #82924, #100095, #188147, #20261, #19289, #34451, #190124, #49620, #114256, #52595, #172972, #129423, #96109, #175961, #145602, #128427, #7081, #81907, #80936, #66766, #37430, #99090, #142612, #97089, #83921, #68762, #130420, #112278, #158772, #192118, #4091, #65770, #127439, #189145, #173969, #35437, #26283, #147621, #71769, #9108, #133439, #39429, #88929, #42440, #196140, #146598, #70775, #193123, #87925, #195129, #54597, #58589, #41442, #162775, #148618, #55599, #24283, #163791, #85932, #23274, #149612, #150621, #120255, #117273, #10109, #118284, #101089, #116271, #132444, #104103, #177961, #84918, #179975, #165786, #194135, #181946, #8091, #40434, #12117, #11110, #178967, #43429, #25292, #119280, #103108, #102106, #27283, #161779, #164789, #86935, #73780, #135453, #56610, #72785, #134455, #57611, #197122, #180963, #69769, #131437, #31237, #875, #139393, #168735, #29262, #136425, #166784, #138406, #15070, #77727, #185922, #137412, #198106, #62550, #30239, #169742, #200087, #167764, #1880, #121247, #47407, #92886, #90893, #155567, #140392, #124226, #63561, #89924, #76731, #153573, #59572, #170741, #45411, #154573, #109063, #151606, #13098, #91882, #186933, #46399, #105098, #28285, #61555, #16069, #199093, #182941, #108058, #32231, #125235, #93889, #123224, #74763, #14069, #184915, #17062, #44424, #122235, #106077, #78716, #152579, #75736, #60560, #183926, #107064, #130180, #36188, #129186, #35208, #160545, #48403, #142382, #172738, #3860, #110060, #111050, #34218, #6846, #5853, #114017, #128200, #64558, #175714, #18067, #37193, #4852, #190884, #173739, #189897, #65540, #188913, #96861, #66536, #95881, #156572, #98850, #171740, #127199, #113033, #157564, #158545, #19057, #20035, #126222, #22034, #52360, #82682, #33229, #80704, #79722, #174725, #81677, #141391, #145364, #51372, #49387, #143360, #50391, #112051, #83686, #94888, #2879, #187918, #97842, #144366, #159530, #21029, #67529, #68525, #27810, #152120, #84681, #162535, #69535, #131199, #53360, #28795, #192889, #74296, #151140, #115037, #177728, #13602, #75270, #147380, #42961, #104624, #54367, #7848, #181483, #176730, #70536, #166313, #167299, #121763, #44942, #135965, #106597, #43949, #182468, #38203, #89451, #24039, #105611, #99859, #161543, #12631, #198629, #90434, #191876, #197636, #23036, #136940, #146361, #59102, #120767, #60095, #29770, #153093, #116039, #183456, #119798, #168273, #91405, #14597, #39197, #76253, #100853, #85694, #8869, #132205, #196660, #58129, #139902, #77248, #154096, #109577, #199615, #33733, #110565, #107579, #2394, #96382, #79237, #65060, #47923, #126717, #1391, #45924, #63072, #64073, #95394, #61081, #16583, #80223, #30763, #122754, #94399, #141894, #15590, #158069, #184444, #78231, #188421, #187443, #138916, #19560, #124751, #157080, #156080, #92410, #18576, #137931, #140908, #155089, #3385, #111565, #397, #125743, #48911, #46923, #49898, #172246, #173249, #62069, #34724, #169256, #123734, #186447, #185433, #108583, #170260, #171260, #32748, #31754, #93403, #17576, #112553, #53886 ),
 ( #159049, #20543, #142885, #115561, #82192, #161056, #37711, #4367, #67050, #100378, #162056, #36699, #129695, #191392, #143885, #97363, #68043, #66050, #160059, #52869, #177248, #8380, #131723, #22551, #193405, #130710, #69045, #127718, #114540, #113540, #192404, #189420, #50895, #176240, #85200, #38720, #81204, #99373, #174248, #23552, #35716, #84197, #145877, #7360, #116554, #39704, #5366, #146888, #6363, #70055, #178243, #54880, #128708, #101367, #163056, #190405, #51881, #175234, #98360, #21546, #83206, #144881, #40716, #196416, #86212, #120526, #197394, #194408, #89203, #183213, #166062, #58860, #55878, #150896, #44694, #27563, #151873, #134734, #13363, #26559, #132720, #149886, #12390, #182219, #147902, #103387, #105365, #11392, #104379, #118563, #165065, #73062, #181241, #72045, #117551, #75027, #9388, #41723, #74052, #10388, #57886, #133719, #119558, #102385, #136693, #167052, #43703, #71054, #195411, #179250, #135723, #42717, #164073, #121518, #28553, #25572, #90190, #180253, #87216, #198374, #148898, #56889, #88202, #59851, #106348, #24563, #155835, #140662, #79991, #1146, #125505, #60835, #138674, #45682, #107333, #29529, #2154, #169006, #47681, #124504, #91162, #153848, #187202, #48673, #123493, #16342, #77991, #30510, #184200, #154845, #152851, #46677, #139658, #63832, #95153, #18336, #109331, #141659, #17332, #78988, #14346, #62821, #154, #110325, #76011, #137686, #186199, #172006, #33494, #168032, #171013, #199371, #156841, #122510, #32504, #94156, #3151, #64824, #126486, #92162, #188184, #93160, #49656, #15346, #77002, #61823, #185186, #108336, #170017, #31507, #176001, #193161, #96147, #113302, #50655, #127477, #82964, #173010, #7120, #52634, #111320, #34489, #67807, #37470, #5121, #189182, #114299, #99131, #8129, #160821, #21307, #157836, #20298, #174993, #191161, #146636, #128466, #19327, #22309, #83960, #97126, #144641, #80975, #129462, #142650, #53639, #4129, #6124, #145640, #68802, #69807, #131474, #112316, #130461, #36458, #98115, #65808, #192159, #174006, #115316, #35477, #158810, #177008, #38477, #81946, #143638, #159812, #66803, #190162, #100134, #51638, #161815, #23310, #84954, #119317, #13137, #196179, #181986, #164827, #43468, #56648, #162811, #180014, #181004, #12156, #177997, #133475, #135491, #41481, #134492, #148659, #195167, #103146, #11149, #102144, #24320, #105136, #39464, #71807, #42479, #40472, #26323, #163829, #87963, #132482, #166822, #197161, #88968, #101125, #25331, #85969, #104142, #149651, #147659, #151642, #57651, #55635, #72823, #10147, #117308, #28323, #9146, #70813, #194171, #165824, #150658, #86972, #27321, #73821, #89962, #58627, #120293, #179004, #118321, #74799, #136462, #116308, #54633, #137452, #77762, #154609, #59612, #183961, #17099, #78751, #153612, #108094, #45448, #169779, #75774, #125273, #140428, #32268, #182978, #107102, #29300, #62585, #31272, #90930, #94923, #139428, #199131, #184951, #91920, #60598, #186970, #44462, #106116, #167800, #46435, #93925, #168772, #185958, #170778, #110097, #92923, #155603, #152616, #30274, #122273, #15108, #121285, #1918, #76769, #911, #16104, #14107, #138441, #63597, #48440, #200122, #124263, #47443, #61591, #123259, #109099, #171775, #33264, #156608, #18103, #79757, #198142, #21065, #53395, #190919, #129222, #2915, #128234, #173776, #52396, #64593, #143398, #50427, #51406, #174758, #141428, #159567, #126257, #83720, #34256, #36224, #97876, #82721, #176765, #99892, #80740, #114055, #66569, #189931, #38237, #144402, #187954, #67564, #161577, #49424, #5888, #175752, #23070, #111085, #4887, #142418, #157600, #113066, #172775, #37229, #98886, #95915, #160580, #19091, #22069, #68559, #145399, #130216, #6881, #3897, #191911, #115073, #65577, #127236, #20069, #188950, #112086, #35242, #96896, #81713, #158580, #41240, #132239, #192923, #11919, #7883, #101902, #149409, #70571, #43231, #26080, #73583 ),
 ( #25085, #9907, #102902, #193931, #54401, #135255, #69569, #163584, #10905, #55394, #194924, #117064, #56399, #162570, #196927, #165585, #119086, #131235, #178760, #116073, #72578, #118081, #177761, #181749, #164586, #85728, #71567, #40225, #147416, #58395, #39230, #100886, #24073, #133232, #180768, #86727, #134252, #57413, #120061, #179771, #42243, #8903, #148412, #87724, #195939, #146394, #103904, #27083, #88729, #150424, #104897, #166586, #84716, #47204, #183732, #76538, #138214, #167572, #44228, #14877, #12900, #106873, #199896, #675, #155373, #78513, #107855, #140187, #77528, #15870, #89726, #61360, #60370, #139200, #151412, #30044, #137215, #123031, #184717, #28086, #46201, #74564, #170542, #121048, #169540, #31039, #92688, #63357, #186730, #29066, #62346, #153375, #154376, #125034, #124016, #136232, #185713, #48201, #197906, #108863, #32033, #109855, #59376, #91685, #90705, #105885, #93690, #182743, #16862, #1679, #152388, #13874, #75541, #198902, #122042, #45218, #168546, #145161, #49192, #159326, #174523, #80504, #98648, #35990, #5648, #110850, #97637, #67325, #128987, #35004, #95678, #2679, #33028, #4643, #81476, #144163, #52160, #3661, #64356, #190685, #96659, #20822, #66334, #34020, #68323, #187721, #113817, #82479, #157364, #21831, #6645, #175512, #129973, #156362, #143163, #19835, #126025, #36986, #111845, #160342, #83483, #17865, #79520, #158346, #53153, #112831, #171540, #94683, #127995, #191673, #65339, #172534, #141190, #18858, #142177, #126999, #189698, #188706, #50188, #51171, #173535, #150183, #132005, #176526, #84480, #195704, #130993, #38002, #25853, #7643, #196698, #102672, #57176, #101660, #26847, #114832, #8665, #38999, #70338, #99657, #177530, #100655, #73350, #72337, #180536, #194692, #192685, #42010, #146157, #103675, #71339, #116831, #162337, #161341, #41005, #165353, #11684, #193693, #163351, #133002, #54168, #69327, #23838, #118853, #115841, #22833, #56162, #88488, #85487, #135023, #147176, #55161, #178522, #164357, #39989, #24847, #86496, #134012, #117844, #148181, #87496, #9674, #179536, #149185, #10673, #137972, #93442, #75307, #119835, #27849, #138957, #74336, #181520, #169295, #151181, #139943, #45963, #436, #44979, #170300, #58168, #152157, #182507, #13640, #42999, #120808, #43987, #16622, #15630, #123774, #199654, #136002, #185473, #89490, #46963, #14635, #60134, #105648, #104666, #184484, #108622, #155129, #136978, #106639, #76294, #197673, #12669, #167337, #62111, #59138, #166351, #61120, #31793, #28834, #78270, #90475, #198667, #121802, #107617, #183495, #168312, #29808, #77287, #122794, #91444, #153132, #30801, #92450, #154138, #8173, #178039, #79277, #192201, #7163, #113343, #131517, #68846, #38520, #140947, #130505, #100176, #161858, #67845, #125781, #32786, #63111, #37509, #114338, #177050, #84997, #36500, #94438, #23352, #129500, #53683, #99171, #64116, #101167, #17618, #146678, #115360, #187483, #54676, #39507, #69849, #162855, #186488, #176041, #52675, #156119, #193203, #144680, #116350, #24362, #47964, #109616, #191200, #86013, #145681, #1433, #124789, #160861, #171300, #98154, #2434, #51681, #175035, #159854, #21347, #22351, #83005, #6165, #84002, #147702, #104184, #73862, #41527, #25374, #150699, #89008, #44501, #135531, #57694, #70855, #56691, #11192, #27362, #183017, #164871, #9190, #117352, #28363, #163875, #132524, #58665, #40516, #29340, #197202, #90001, #134536, #59651, #194213, #103190, #71850, #26366, #55678, #10190, #133519, #106157, #105175, #13175, #12197, #87016, #74838, #179048, #136501, #165866, #149694, #195211, #102187, #120331, #198181, #167839, #88006, #196224, #182026, #148702, #118365, #180058, #151683, #72867, #119362, #43509, #121325, #181046, #42521, #166861, #169818, #79793, #140466, #168811, #49458, #92962, #48477, #47480, #184003, #171812, #111120, #93962, #108134, #94959, #64629, #30315, #78789, #155642, #200160, #18139 ) ),
 .UNSPECIFIED., .T., .F., .F. ) 
 B_SPLINE_SURFACE_WITH_KNOTS ( ( 4, 3, 4 ),
 ( 3, 2, 2, 2, 2, 2, 2, 2, 2, 2, 2, 2, 2, 2, 2, 2, 2, 2, 2, 2, 2, 2, 2, 2, 2, 2, 2, 2, 2, 2, 2, 2, 2, 2, 2, 2, 2, 2, 2, 2, 2, 2, 2, 2, 2, 2, 2, 2, 2, 2, 2, 2, 2, 2, 2, 2, 2, 2, 2, 2, 2, 2, 2, 2, 2, 2, 2, 2, 2, 2, 2, 2, 2, 2, 2, 2, 2, 2, 2, 2, 2, 2, 2, 2, 2, 2, 2, 2, 2, 2, 2, 2, 2, 2, 2, 2, 2, 2, 2, 2, 2, 2, 2, 2, 2, 2, 2, 2, 2, 2, 2, 2, 2, 2, 2, 2, 2, 2, 2, 2, 2, 2, 2, 2, 2, 2, 2, 2, 2, 2, 2, 2, 2, 2, 2, 2, 2, 2, 2, 2, 2, 2, 2, 2, 2, 2, 2, 2, 2, 2, 2, 2, 2, 2, 2, 2, 2, 2, 2, 2, 2, 2, 2, 2, 2, 2, 2, 2, 2, 2, 2, 2, 2, 2, 2, 2, 2, 2, 2, 2, 2, 2, 2, 2, 2, 2, 2, 2, 2, 2, 2, 2, 2, 2, 2, 2, 2, 2, 2, 2, 2, 2, 2, 2, 2, 2, 2, 2, 2, 2, 2, 2, 2, 2, 2, 2, 2, 2, 2, 2, 2, 2, 2, 2, 2, 2, 2, 2, 3 ),
 ( 0.000000000000000000, 0.5000000000000000000, 1.000000000000000000 ),
 ( 0.000000000000000000, 0.004385964912280701511, 0.008771929824561403022, 0.01315789473684210453, 0.01754385964912280604, 0.02192982456140350755, 0.02631578947368420907, 0.03070175438596491058, 0.03508771929824561209, 0.03947368421052631360, 0.04385964912280701511, 0.04824561403508771662, 0.05263157894736841813, 0.05701754385964911964, 0.06140350877192982115, 0.06578947368421052266, 0.07017543859649122417, 0.07456140350877192569, 0.07894736842105262720, 0.08333333333333332871, 0.08771929824561403022, 0.09210526315789473173, 0.09649122807017543324, 0.1008771929824561348, 0.1052631578947368363, 0.1096491228070175378, 0.1140350877192982393, 0.1184210526315789408, 0.1228070175438596423, 0.1271929824561403577, 0.1315789473684210453, 0.1359649122807017607, 0.1403508771929824483, 0.1447368421052631637, 0.1491228070175438514, 0.1535087719298245668, 0.1578947368421052544, 0.1622807017543859698, 0.1666666666666666574, 0.1710526315789473728, 0.1754385964912280604, 0.1798245614035087758, 0.1842105263157894635, 0.1885964912280701788, 0.1929824561403508665, 0.1973684210526315819, 0.2017543859649122695, 0.2061403508771929849, 0.2105263157894736725, 0.2149122807017543879, 0.2192982456140350755, 0.2236842105263157909, 0.2280701754385964786, 0.2324561403508771940, 0.2368421052631578816, 0.2412280701754385970, 0.2456140350877192846, 0.2500000000000000000, 0.2543859649122807154, 0.2587719298245614308, 0.2631578947368420907, 0.2675438596491228060, 0.2719298245614035214, 0.2763157894736842368, 0.2807017543859648967, 0.2850877192982456121, 0.2894736842105263275, 0.2938596491228070429, 0.2982456140350877027, 0.3026315789473684181, 0.3070175438596491335, 0.3114035087719298489, 0.3157894736842105088, 0.3201754385964912242, 0.3245614035087719396, 0.3289473684210526550, 0.3333333333333333148, 0.3377192982456140302, 0.3421052631578947456, 0.3464912280701754610, 0.3508771929824561209, 0.3552631578947368363, 0.3596491228070175517, 0.3640350877192982670, 0.3684210526315789269, 0.3728070175438596423, 0.3771929824561403577, 0.3815789473684210731, 0.3859649122807017330, 0.3903508771929824483, 0.3947368421052631637, 0.3991228070175438791, 0.4035087719298245390, 0.4078947368421052544, 0.4122807017543859698, 0.4166666666666666852, 0.4210526315789473450, 0.4254385964912280604, 0.4298245614035087758, 0.4342105263157894912, 0.4385964912280701511, 0.4429824561403508665, 0.4473684210526315819, 0.4517543859649122973, 0.4561403508771929571, 0.4605263157894736725, 0.4649122807017543879, 0.4692982456140351033, 0.4736842105263157632, 0.4780701754385964786, 0.4824561403508771940, 0.4868421052631579093, 0.4912280701754385692, 0.4956140350877192846, 0.5000000000000000000, 0.5043859649122807154, 0.5087719298245614308, 0.5131578947368421462, 0.5175438596491228616, 0.5219298245614034659, 0.5263157894736841813, 0.5307017543859648967, 0.5350877192982456121, 0.5394736842105263275, 0.5438596491228070429, 0.5482456140350877583, 0.5526315789473684736, 0.5570175438596490780, 0.5614035087719297934, 0.5657894736842105088, 0.5701754385964912242, 0.5745614035087719396, 0.5789473684210526550, 0.5833333333333333703, 0.5877192982456140857, 0.5921052631578946901, 0.5964912280701754055, 0.6008771929824561209, 0.6052631578947368363, 0.6096491228070175517, 0.6140350877192982670, 0.6184210526315789824, 0.6228070175438596978, 0.6271929824561403022, 0.6315789473684210176, 0.6359649122807017330, 0.6403508771929824483, 0.6447368421052631637, 0.6491228070175438791, 0.6535087719298245945, 0.6578947368421053099, 0.6622807017543859143, 0.6666666666666666297, 0.6710526315789473450, 0.6754385964912280604, 0.6798245614035087758, 0.6842105263157894912, 0.6885964912280702066, 0.6929824561403509220, 0.6973684210526315264, 0.7017543859649122417, 0.7061403508771929571, 0.7105263157894736725, 0.7149122807017543879, 0.7192982456140351033, 0.7236842105263158187, 0.7280701754385965341, 0.7324561403508771384, 0.7368421052631578538, 0.7412280701754385692, 0.7456140350877192846, 0.7500000000000000000, 0.7543859649122807154, 0.7587719298245614308, 0.7631578947368421462, 0.7675438596491228616, 0.7719298245614034659, 0.7763157894736841813, 0.7807017543859648967, 0.7850877192982456121, 0.7894736842105263275, 0.7938596491228070429, 0.7982456140350877583, 0.8026315789473684736, 0.8070175438596490780, 0.8114035087719297934, 0.8157894736842105088, 0.8201754385964912242, 0.8245614035087719396, 0.8289473684210526550, 0.8333333333333333703, 0.8377192982456140857, 0.8421052631578946901, 0.8464912280701754055, 0.8508771929824561209, 0.8552631578947368363, 0.8596491228070175517, 0.8640350877192982670, 0.8684210526315789824, 0.8728070175438596978, 0.8771929824561403022, 0.8815789473684210176, 0.8859649122807017330, 0.8903508771929824483, 0.8947368421052631637, 0.8991228070175438791, 0.9035087719298245945, 0.9078947368421053099, 0.9122807017543859143, 0.9166666666666666297, 0.9210526315789473450, 0.9254385964912280604, 0.9298245614035087758, 0.9342105263157894912, 0.9385964912280702066, 0.9429824561403509220, 0.9473684210526315264, 0.9517543859649122417, 0.9561403508771929571, 0.9605263157894736725, 0.9649122807017543879, 0.9692982456140351033, 0.9736842105263158187, 0.9780701754385965341, 0.9824561403508771384, 0.9868421052631578538, 0.9912280701754385692, 0.9956140350877192846, 1.000000000000000000 ),
 .UNSPECIFIED. ) 
 GEOMETRIC_REPRESENTATION_ITEM ( )  RATIONAL_B_SPLINE_SURFACE ( (
 ( 1.000000000000000000, 0.9659258262890683122, 1.000000000000000000, 0.9659258262890683122, 1.000000000000000000, 0.9659258262890683122, 1.000000000000000000, 0.9659258262890683122, 1.000000000000000000, 0.9659258262890683122, 1.000000000000000000, 0.9659258262890683122, 1.000000000000000000, 0.9659258262890683122, 1.000000000000000000, 0.9659258262890683122, 1.000000000000000000, 0.9659258262890683122, 1.000000000000000000, 0.9659258262890683122, 1.000000000000000000, 0.9659258262890683122, 1.000000000000000000, 0.9659258262890683122, 1.000000000000000000, 0.9659258262890683122, 1.000000000000000000, 0.9659258262890683122, 1.000000000000000000, 0.9659258262890683122, 1.000000000000000000, 0.9659258262890683122, 1.000000000000000000, 0.9659258262890683122, 1.000000000000000000, 0.9659258262890683122, 1.000000000000000000, 0.9659258262890683122, 1.000000000000000000, 0.9659258262890683122, 1.000000000000000000, 0.9659258262890683122, 1.000000000000000000, 0.9659258262890683122, 1.000000000000000000, 0.9659258262890683122, 1.000000000000000000, 0.9659258262890683122, 1.000000000000000000, 0.9659258262890683122, 1.000000000000000000, 0.9659258262890683122, 1.000000000000000000, 0.9659258262890683122, 1.000000000000000000, 0.9659258262890683122, 1.000000000000000000, 0.9659258262890683122, 1.000000000000000000, 0.9659258262890683122, 1.000000000000000000, 0.9659258262890683122, 1.000000000000000000, 0.9659258262890683122, 1.000000000000000000, 0.9659258262890683122, 1.000000000000000000, 0.9659258262890683122, 1.000000000000000000, 0.9659258262890683122, 1.000000000000000000, 0.9659258262890683122, 1.000000000000000000, 0.9659258262890683122, 1.000000000000000000, 0.9659258262890683122, 1.000000000000000000, 0.9659258262890683122, 1.000000000000000000, 0.9659258262890683122, 1.000000000000000000, 0.9659258262890683122, 1.000000000000000000, 0.9659258262890683122, 1.000000000000000000, 0.9659258262890683122, 1.000000000000000000, 0.9659258262890683122, 1.000000000000000000, 0.9659258262890683122, 1.000000000000000000, 0.9659258262890683122, 1.000000000000000000, 0.9659258262890683122, 1.000000000000000000, 0.9659258262890683122, 1.000000000000000000, 0.9659258262890683122, 1.000000000000000000, 0.9659258262890683122, 1.000000000000000000, 0.9659258262890683122, 1.000000000000000000, 0.9659258262890683122, 1.000000000000000000, 0.9659258262890683122, 1.000000000000000000, 0.9659258262890683122, 1.000000000000000000, 0.9659258262890683122, 1.000000000000000000, 0.9659258262890683122, 1.000000000000000000, 0.9659258262890683122, 1.000000000000000000, 0.9659258262890683122, 1.000000000000000000, 0.9659258262890683122, 1.000000000000000000, 0.9659258262890683122, 1.000000000000000000, 0.9659258262890683122, 1.000000000000000000, 0.9659258262890683122, 1.000000000000000000, 0.9659258262890683122, 1.000000000000000000, 0.9659258262890683122, 1.000000000000000000, 0.9659258262890683122, 1.000000000000000000, 0.9659258262890683122, 1.000000000000000000, 0.9659258262890683122, 1.000000000000000000, 0.9659258262890683122, 1.000000000000000000, 0.9659258262890683122, 1.000000000000000000, 0.9659258262890683122, 1.000000000000000000, 0.9659258262890683122, 1.000000000000000000, 0.9659258262890683122, 1.000000000000000000, 0.9659258262890683122, 1.000000000000000000, 0.9659258262890683122, 1.000000000000000000, 0.9659258262890683122, 1.000000000000000000, 0.9659258262890683122, 1.000000000000000000, 0.9659258262890683122, 1.000000000000000000, 0.9659258262890683122, 1.000000000000000000, 0.9659258262890683122, 1.000000000000000000, 0.9659258262890683122, 1.000000000000000000, 0.9659258262890683122, 1.000000000000000000, 0.9659258262890683122, 1.000000000000000000, 0.9659258262890683122, 1.000000000000000000, 0.9659258262890683122, 1.000000000000000000, 0.9659258262890683122, 1.000000000000000000, 0.9659258262890683122, 1.000000000000000000, 0.9659258262890683122, 1.000000000000000000, 0.9659258262890683122, 1.000000000000000000, 0.9659258262890683122, 1.000000000000000000, 0.9659258262890683122, 1.000000000000000000, 0.9659258262890683122, 1.000000000000000000, 0.9659258262890683122, 1.000000000000000000, 0.9659258262890683122, 1.000000000000000000, 0.9659258262890683122, 1.000000000000000000, 0.9659258262890683122, 1.000000000000000000, 0.9659258262890683122, 1.000000000000000000, 0.9659258262890683122, 1.000000000000000000, 0.9659258262890683122, 1.000000000000000000, 0.9659258262890683122, 1.000000000000000000, 0.9659258262890683122, 1.000000000000000000, 0.9659258262890683122, 1.000000000000000000, 0.9659258262890683122, 1.000000000000000000, 0.9659258262890683122, 1.000000000000000000, 0.9659258262890683122, 1.000000000000000000, 0.9659258262890683122, 1.000000000000000000, 0.9659258262890683122, 1.000000000000000000, 0.9659258262890683122, 1.000000000000000000, 0.9659258262890683122, 1.000000000000000000, 0.9659258262890683122, 1.000000000000000000, 0.9659258262890683122, 1.000000000000000000, 0.9659258262890683122, 1.000000000000000000, 0.9659258262890683122, 1.000000000000000000, 0.9659258262890683122, 1.000000000000000000, 0.9659258262890683122, 1.000000000000000000, 0.9659258262890683122, 1.000000000000000000, 0.9659258262890683122, 1.000000000000000000, 0.9659258262890683122, 1.000000000000000000, 0.9659258262890683122, 1.000000000000000000, 0.9659258262890683122, 1.000000000000000000, 0.9659258262890683122, 1.000000000000000000, 0.9659258262890683122, 1.000000000000000000, 0.9659258262890683122, 1.000000000000000000, 0.9659258262890683122, 1.000000000000000000, 0.9659258262890683122, 1.000000000000000000, 0.9659258262890683122, 1.000000000000000000, 0.9659258262890683122, 1.000000000000000000, 0.9659258262890683122, 1.000000000000000000, 0.9659258262890683122, 1.000000000000000000, 0.9659258262890683122, 1.000000000000000000, 0.9659258262890683122, 1.000000000000000000, 0.9659258262890683122, 1.000000000000000000, 0.9659258262890683122, 1.000000000000000000, 0.9659258262890683122, 1.000000000000000000, 0.9659258262890683122, 1.000000000000000000, 0.9659258262890683122, 1.000000000000000000, 0.9659258262890683122, 1.000000000000000000, 0.9659258262890683122, 1.000000000000000000, 0.9659258262890683122, 1.000000000000000000, 0.9659258262890683122, 1.000000000000000000, 0.9659258262890683122, 1.000000000000000000, 0.9659258262890683122, 1.000000000000000000, 0.9659258262890683122, 1.000000000000000000, 0.9659258262890683122, 1.000000000000000000, 0.9659258262890683122, 1.000000000000000000, 0.9659258262890683122, 1.000000000000000000, 0.9659258262890683122, 1.000000000000000000, 0.9659258262890683122, 1.000000000000000000, 0.9659258262890683122, 1.000000000000000000, 0.9659258262890683122, 1.000000000000000000, 0.9659258262890683122, 1.000000000000000000, 0.9659258262890683122, 1.000000000000000000, 0.9659258262890683122, 1.000000000000000000, 0.9659258262890683122, 1.000000000000000000, 0.9659258262890683122, 1.000000000000000000, 0.9659258262890683122, 1.000000000000000000, 0.9659258262890683122, 1.000000000000000000, 0.9659258262890683122, 1.000000000000000000, 0.9659258262890683122, 1.000000000000000000, 0.9659258262890683122, 1.000000000000000000, 0.9659258262890683122, 1.000000000000000000, 0.9659258262890683122, 1.000000000000000000, 0.9659258262890683122, 1.000000000000000000, 0.9659258262890683122, 1.000000000000000000, 0.9659258262890683122, 1.000000000000000000, 0.9659258262890683122, 1.000000000000000000, 0.9659258262890683122, 1.000000000000000000, 0.9659258262890683122, 1.000000000000000000, 0.9659258262890683122, 1.000000000000000000, 0.9659258262890683122, 1.000000000000000000, 0.9659258262890683122, 1.000000000000000000, 0.9659258262890683122, 1.000000000000000000, 0.9659258262890683122, 1.000000000000000000, 0.9659258262890683122, 1.000000000000000000, 0.9659258262890683122, 1.000000000000000000, 0.9659258262890683122, 1.000000000000000000, 0.9659258262890683122, 1.000000000000000000, 0.9659258262890683122, 1.000000000000000000, 0.9659258262890683122, 1.000000000000000000, 0.9659258262890683122, 1.000000000000000000, 0.9659258262890683122, 1.000000000000000000, 0.9659258262890683122, 1.000000000000000000, 0.9659258262890683122, 1.000000000000000000, 0.9659258262890683122, 1.000000000000000000, 0.9659258262890683122, 1.000000000000000000, 0.9659258262890683122, 1.000000000000000000, 0.9659258262890683122, 1.000000000000000000, 0.9659258262890683122, 1.000000000000000000, 0.9659258262890683122, 1.000000000000000000, 0.9659258262890683122, 1.000000000000000000, 0.9659258262890683122, 1.000000000000000000, 0.9659258262890683122, 1.000000000000000000, 0.9659258262890683122, 1.000000000000000000, 0.9659258262890683122, 1.000000000000000000, 0.9659258262890683122, 1.000000000000000000, 0.9659258262890683122, 1.000000000000000000, 0.9659258262890683122, 1.000000000000000000, 0.9659258262890683122, 1.000000000000000000, 0.9659258262890683122, 1.000000000000000000, 0.9659258262890683122, 1.000000000000000000, 0.9659258262890683122, 1.000000000000000000, 0.9659258262890683122, 1.000000000000000000, 0.9659258262890683122, 1.000000000000000000, 0.9659258262890683122, 1.000000000000000000, 0.9659258262890683122, 1.000000000000000000, 0.9659258262890683122, 1.000000000000000000, 0.9659258262890683122, 1.000000000000000000, 0.9659258262890683122, 1.000000000000000000, 0.9659258262890683122, 1.000000000000000000, 0.9659258262890683122, 1.000000000000000000, 0.9659258262890683122, 1.000000000000000000, 0.9659258262890683122, 1.000000000000000000, 0.9659258262890683122, 1.000000000000000000, 0.9659258262890683122, 1.000000000000000000, 0.9659258262890683122, 1.000000000000000000, 0.9659258262890683122, 1.000000000000000000, 0.9659258262890683122, 1.000000000000000000, 0.9659258262890683122, 1.000000000000000000, 0.9659258262890683122, 1.000000000000000000, 0.9659258262890683122, 1.000000000000000000, 0.9659258262890683122, 1.000000000000000000, 0.9659258262890683122, 1.000000000000000000, 0.9659258262890683122, 1.000000000000000000, 0.9659258262890683122, 1.000000000000000000, 0.9659258262890683122, 1.000000000000000000, 0.9659258262890683122, 1.000000000000000000, 0.9659258262890683122, 1.000000000000000000, 0.9659258262890683122, 1.000000000000000000, 0.9659258262890683122, 1.000000000000000000),
 ( 0.3333333333333333703, 0.3219752754296894559, 0.3333333333333333703, 0.3219752754296894559, 0.3333333333333333703, 0.3219752754296894559, 0.3333333333333333703, 0.3219752754296894559, 0.3333333333333333703, 0.3219752754296894559, 0.3333333333333333703, 0.3219752754296894559, 0.3333333333333333703, 0.3219752754296894559, 0.3333333333333333703, 0.3219752754296894559, 0.3333333333333333703, 0.3219752754296894559, 0.3333333333333333703, 0.3219752754296894559, 0.3333333333333333703, 0.3219752754296894559, 0.3333333333333333703, 0.3219752754296894559, 0.3333333333333333703, 0.3219752754296894559, 0.3333333333333333703, 0.3219752754296894559, 0.3333333333333333703, 0.3219752754296894559, 0.3333333333333333703, 0.3219752754296894559, 0.3333333333333333703, 0.3219752754296894559, 0.3333333333333333703, 0.3219752754296894559, 0.3333333333333333703, 0.3219752754296894559, 0.3333333333333333703, 0.3219752754296894559, 0.3333333333333333703, 0.3219752754296894559, 0.3333333333333333703, 0.3219752754296894559, 0.3333333333333333703, 0.3219752754296894559, 0.3333333333333333703, 0.3219752754296894559, 0.3333333333333333703, 0.3219752754296894559, 0.3333333333333333703, 0.3219752754296894559, 0.3333333333333333703, 0.3219752754296894559, 0.3333333333333333703, 0.3219752754296894559, 0.3333333333333333703, 0.3219752754296894559, 0.3333333333333333703, 0.3219752754296894559, 0.3333333333333333703, 0.3219752754296894559, 0.3333333333333333703, 0.3219752754296894559, 0.3333333333333333703, 0.3219752754296894559, 0.3333333333333333703, 0.3219752754296894559, 0.3333333333333333703, 0.3219752754296894559, 0.3333333333333333703, 0.3219752754296894559, 0.3333333333333333703, 0.3219752754296894559, 0.3333333333333333703, 0.3219752754296894559, 0.3333333333333333703, 0.3219752754296894559, 0.3333333333333333703, 0.3219752754296894559, 0.3333333333333333703, 0.3219752754296894559, 0.3333333333333333703, 0.3219752754296894559, 0.3333333333333333703, 0.3219752754296894559, 0.3333333333333333703, 0.3219752754296894559, 0.3333333333333333703, 0.3219752754296894559, 0.3333333333333333703, 0.3219752754296894559, 0.3333333333333333703, 0.3219752754296894559, 0.3333333333333333703, 0.3219752754296894559, 0.3333333333333333703, 0.3219752754296894559, 0.3333333333333333703, 0.3219752754296894559, 0.3333333333333333703, 0.3219752754296894559, 0.3333333333333333703, 0.3219752754296894559, 0.3333333333333333703, 0.3219752754296894559, 0.3333333333333333703, 0.3219752754296894559, 0.3333333333333333703, 0.3219752754296894559, 0.3333333333333333703, 0.3219752754296894559, 0.3333333333333333703, 0.3219752754296894559, 0.3333333333333333703, 0.3219752754296894559, 0.3333333333333333703, 0.3219752754296894559, 0.3333333333333333703, 0.3219752754296894559, 0.3333333333333333703, 0.3219752754296894559, 0.3333333333333333703, 0.3219752754296894559, 0.3333333333333333703, 0.3219752754296894559, 0.3333333333333333703, 0.3219752754296894559, 0.3333333333333333703, 0.3219752754296894559, 0.3333333333333333703, 0.3219752754296894559, 0.3333333333333333703, 0.3219752754296894559, 0.3333333333333333703, 0.3219752754296894559, 0.3333333333333333703, 0.3219752754296894559, 0.3333333333333333703, 0.3219752754296894559, 0.3333333333333333703, 0.3219752754296894559, 0.3333333333333333703, 0.3219752754296894559, 0.3333333333333333703, 0.3219752754296894559, 0.3333333333333333703, 0.3219752754296894559, 0.3333333333333333703, 0.3219752754296894559, 0.3333333333333333703, 0.3219752754296894559, 0.3333333333333333703, 0.3219752754296894559, 0.3333333333333333703, 0.3219752754296894559, 0.3333333333333333703, 0.3219752754296894559, 0.3333333333333333703, 0.3219752754296894559, 0.3333333333333333703, 0.3219752754296894559, 0.3333333333333333703, 0.3219752754296894559, 0.3333333333333333703, 0.3219752754296894559, 0.3333333333333333703, 0.3219752754296894559, 0.3333333333333333703, 0.3219752754296894559, 0.3333333333333333703, 0.3219752754296894559, 0.3333333333333333703, 0.3219752754296894559, 0.3333333333333333703, 0.3219752754296894559, 0.3333333333333333703, 0.3219752754296894559, 0.3333333333333333703, 0.3219752754296894559, 0.3333333333333333703, 0.3219752754296894559, 0.3333333333333333703, 0.3219752754296894559, 0.3333333333333333703, 0.3219752754296894559, 0.3333333333333333703, 0.3219752754296894559, 0.3333333333333333703, 0.3219752754296894559, 0.3333333333333333703, 0.3219752754296894559, 0.3333333333333333703, 0.3219752754296894559, 0.3333333333333333703, 0.3219752754296894559, 0.3333333333333333703, 0.3219752754296894559, 0.3333333333333333703, 0.3219752754296894559, 0.3333333333333333703, 0.3219752754296894559, 0.3333333333333333703, 0.3219752754296894559, 0.3333333333333333703, 0.3219752754296894559, 0.3333333333333333703, 0.3219752754296894559, 0.3333333333333333703, 0.3219752754296894559, 0.3333333333333333703, 0.3219752754296894559, 0.3333333333333333703, 0.3219752754296894559, 0.3333333333333333703, 0.3219752754296894559, 0.3333333333333333703, 0.3219752754296894559, 0.3333333333333333703, 0.3219752754296894559, 0.3333333333333333703, 0.3219752754296894559, 0.3333333333333333703, 0.3219752754296894559, 0.3333333333333333703, 0.3219752754296894559, 0.3333333333333333703, 0.3219752754296894559, 0.3333333333333333703, 0.3219752754296894559, 0.3333333333333333703, 0.3219752754296894559, 0.3333333333333333703, 0.3219752754296894559, 0.3333333333333333703, 0.3219752754296894559, 0.3333333333333333703, 0.3219752754296894559, 0.3333333333333333703, 0.3219752754296894559, 0.3333333333333333703, 0.3219752754296894559, 0.3333333333333333703, 0.3219752754296894559, 0.3333333333333333703, 0.3219752754296894559, 0.3333333333333333703, 0.3219752754296894559, 0.3333333333333333703, 0.3219752754296894559, 0.3333333333333333703, 0.3219752754296894559, 0.3333333333333333703, 0.3219752754296894559, 0.3333333333333333703, 0.3219752754296894559, 0.3333333333333333703, 0.3219752754296894559, 0.3333333333333333703, 0.3219752754296894559, 0.3333333333333333703, 0.3219752754296894559, 0.3333333333333333703, 0.3219752754296894559, 0.3333333333333333703, 0.3219752754296894559, 0.3333333333333333703, 0.3219752754296894559, 0.3333333333333333703, 0.3219752754296894559, 0.3333333333333333703, 0.3219752754296894559, 0.3333333333333333703, 0.3219752754296894559, 0.3333333333333333703, 0.3219752754296894559, 0.3333333333333333703, 0.3219752754296894559, 0.3333333333333333703, 0.3219752754296894559, 0.3333333333333333703, 0.3219752754296894559, 0.3333333333333333703, 0.3219752754296894559, 0.3333333333333333703, 0.3219752754296894559, 0.3333333333333333703, 0.3219752754296894559, 0.3333333333333333703, 0.3219752754296894559, 0.3333333333333333703, 0.3219752754296894559, 0.3333333333333333703, 0.3219752754296894559, 0.3333333333333333703, 0.3219752754296894559, 0.3333333333333333703, 0.3219752754296894559, 0.3333333333333333703, 0.3219752754296894559, 0.3333333333333333703, 0.3219752754296894559, 0.3333333333333333703, 0.3219752754296894559, 0.3333333333333333703, 0.3219752754296894559, 0.3333333333333333703, 0.3219752754296894559, 0.3333333333333333703, 0.3219752754296894559, 0.3333333333333333703, 0.3219752754296894559, 0.3333333333333333703, 0.3219752754296894559, 0.3333333333333333703, 0.3219752754296894559, 0.3333333333333333703, 0.3219752754296894559, 0.3333333333333333703, 0.3219752754296894559, 0.3333333333333333703, 0.3219752754296894559, 0.3333333333333333703, 0.3219752754296894559, 0.3333333333333333703, 0.3219752754296894559, 0.3333333333333333703, 0.3219752754296894559, 0.3333333333333333703, 0.3219752754296894559, 0.3333333333333333703, 0.3219752754296894559, 0.3333333333333333703, 0.3219752754296894559, 0.3333333333333333703, 0.3219752754296894559, 0.3333333333333333703, 0.3219752754296894559, 0.3333333333333333703, 0.3219752754296894559, 0.3333333333333333703, 0.3219752754296894559, 0.3333333333333333703, 0.3219752754296894559, 0.3333333333333333703, 0.3219752754296894559, 0.3333333333333333703, 0.3219752754296894559, 0.3333333333333333703, 0.3219752754296894559, 0.3333333333333333703, 0.3219752754296894559, 0.3333333333333333703, 0.3219752754296894559, 0.3333333333333333703, 0.3219752754296894559, 0.3333333333333333703, 0.3219752754296894559, 0.3333333333333333703, 0.3219752754296894559, 0.3333333333333333703, 0.3219752754296894559, 0.3333333333333333703, 0.3219752754296894559, 0.3333333333333333703, 0.3219752754296894559, 0.3333333333333333703, 0.3219752754296894559, 0.3333333333333333703, 0.3219752754296894559, 0.3333333333333333703, 0.3219752754296894559, 0.3333333333333333703, 0.3219752754296894559, 0.3333333333333333703, 0.3219752754296894559, 0.3333333333333333703, 0.3219752754296894559, 0.3333333333333333703, 0.3219752754296894559, 0.3333333333333333703, 0.3219752754296894559, 0.3333333333333333703, 0.3219752754296894559, 0.3333333333333333703, 0.3219752754296894559, 0.3333333333333333703, 0.3219752754296894559, 0.3333333333333333703, 0.3219752754296894559, 0.3333333333333333703, 0.3219752754296894559, 0.3333333333333333703, 0.3219752754296894559, 0.3333333333333333703, 0.3219752754296894559, 0.3333333333333333703, 0.3219752754296894559, 0.3333333333333333703, 0.3219752754296894559, 0.3333333333333333703, 0.3219752754296894559, 0.3333333333333333703, 0.3219752754296894559, 0.3333333333333333703, 0.3219752754296894559, 0.3333333333333333703, 0.3219752754296894559, 0.3333333333333333703, 0.3219752754296894559, 0.3333333333333333703, 0.3219752754296894559, 0.3333333333333333703, 0.3219752754296894559, 0.3333333333333333703, 0.3219752754296894559, 0.3333333333333333703, 0.3219752754296894559, 0.3333333333333333703, 0.3219752754296894559, 0.3333333333333333703, 0.3219752754296894559, 0.3333333333333333703, 0.3219752754296894559, 0.3333333333333333703, 0.3219752754296894559, 0.3333333333333333703, 0.3219752754296894559, 0.3333333333333333703, 0.3219752754296894559, 0.3333333333333333703, 0.3219752754296894559, 0.3333333333333333703, 0.3219752754296894559, 0.3333333333333333703, 0.3219752754296894559, 0.3333333333333333703, 0.3219752754296894559, 0.3333333333333333703, 0.3219752754296894559, 0.3333333333333333703, 0.3219752754296894559, 0.3333333333333333703, 0.3219752754296894559, 0.3333333333333333703, 0.3219752754296894559, 0.3333333333333333703, 0.3219752754296894559, 0.3333333333333333703, 0.3219752754296894559, 0.3333333333333333703, 0.3219752754296894559, 0.3333333333333333703, 0.3219752754296894559, 0.3333333333333333703, 0.3219752754296894559, 0.3333333333333333703),
 ( 0.3333333333333333703, 0.3219752754296894559, 0.3333333333333333703, 0.3219752754296894559, 0.3333333333333333703, 0.3219752754296894559, 0.3333333333333333703, 0.3219752754296894559, 0.3333333333333333703, 0.3219752754296894559, 0.3333333333333333703, 0.3219752754296894559, 0.3333333333333333703, 0.3219752754296894559, 0.3333333333333333703, 0.3219752754296894559, 0.3333333333333333703, 0.3219752754296894559, 0.3333333333333333703, 0.3219752754296894559, 0.3333333333333333703, 0.3219752754296894559, 0.3333333333333333703, 0.3219752754296894559, 0.3333333333333333703, 0.3219752754296894559, 0.3333333333333333703, 0.3219752754296894559, 0.3333333333333333703, 0.3219752754296894559, 0.3333333333333333703, 0.3219752754296894559, 0.3333333333333333703, 0.3219752754296894559, 0.3333333333333333703, 0.3219752754296894559, 0.3333333333333333703, 0.3219752754296894559, 0.3333333333333333703, 0.3219752754296894559, 0.3333333333333333703, 0.3219752754296894559, 0.3333333333333333703, 0.3219752754296894559, 0.3333333333333333703, 0.3219752754296894559, 0.3333333333333333703, 0.3219752754296894559, 0.3333333333333333703, 0.3219752754296894559, 0.3333333333333333703, 0.3219752754296894559, 0.3333333333333333703, 0.3219752754296894559, 0.3333333333333333703, 0.3219752754296894559, 0.3333333333333333703, 0.3219752754296894559, 0.3333333333333333703, 0.3219752754296894559, 0.3333333333333333703, 0.3219752754296894559, 0.3333333333333333703, 0.3219752754296894559, 0.3333333333333333703, 0.3219752754296894559, 0.3333333333333333703, 0.3219752754296894559, 0.3333333333333333703, 0.3219752754296894559, 0.3333333333333333703, 0.3219752754296894559, 0.3333333333333333703, 0.3219752754296894559, 0.3333333333333333703, 0.3219752754296894559, 0.3333333333333333703, 0.3219752754296894559, 0.3333333333333333703, 0.3219752754296894559, 0.3333333333333333703, 0.3219752754296894559, 0.3333333333333333703, 0.3219752754296894559, 0.3333333333333333703, 0.3219752754296894559, 0.3333333333333333703, 0.3219752754296894559, 0.3333333333333333703, 0.3219752754296894559, 0.3333333333333333703, 0.3219752754296894559, 0.3333333333333333703, 0.3219752754296894559, 0.3333333333333333703, 0.3219752754296894559, 0.3333333333333333703, 0.3219752754296894559, 0.3333333333333333703, 0.3219752754296894559, 0.3333333333333333703, 0.3219752754296894559, 0.3333333333333333703, 0.3219752754296894559, 0.3333333333333333703, 0.3219752754296894559, 0.3333333333333333703, 0.3219752754296894559, 0.3333333333333333703, 0.3219752754296894559, 0.3333333333333333703, 0.3219752754296894559, 0.3333333333333333703, 0.3219752754296894559, 0.3333333333333333703, 0.3219752754296894559, 0.3333333333333333703, 0.3219752754296894559, 0.3333333333333333703, 0.3219752754296894559, 0.3333333333333333703, 0.3219752754296894559, 0.3333333333333333703, 0.3219752754296894559, 0.3333333333333333703, 0.3219752754296894559, 0.3333333333333333703, 0.3219752754296894559, 0.3333333333333333703, 0.3219752754296894559, 0.3333333333333333703, 0.3219752754296894559, 0.3333333333333333703, 0.3219752754296894559, 0.3333333333333333703, 0.3219752754296894559, 0.3333333333333333703, 0.3219752754296894559, 0.3333333333333333703, 0.3219752754296894559, 0.3333333333333333703, 0.3219752754296894559, 0.3333333333333333703, 0.3219752754296894559, 0.3333333333333333703, 0.3219752754296894559, 0.3333333333333333703, 0.3219752754296894559, 0.3333333333333333703, 0.3219752754296894559, 0.3333333333333333703, 0.3219752754296894559, 0.3333333333333333703, 0.3219752754296894559, 0.3333333333333333703, 0.3219752754296894559, 0.3333333333333333703, 0.3219752754296894559, 0.3333333333333333703, 0.3219752754296894559, 0.3333333333333333703, 0.3219752754296894559, 0.3333333333333333703, 0.3219752754296894559, 0.3333333333333333703, 0.3219752754296894559, 0.3333333333333333703, 0.3219752754296894559, 0.3333333333333333703, 0.3219752754296894559, 0.3333333333333333703, 0.3219752754296894559, 0.3333333333333333703, 0.3219752754296894559, 0.3333333333333333703, 0.3219752754296894559, 0.3333333333333333703, 0.3219752754296894559, 0.3333333333333333703, 0.3219752754296894559, 0.3333333333333333703, 0.3219752754296894559, 0.3333333333333333703, 0.3219752754296894559, 0.3333333333333333703, 0.3219752754296894559, 0.3333333333333333703, 0.3219752754296894559, 0.3333333333333333703, 0.3219752754296894559, 0.3333333333333333703, 0.3219752754296894559, 0.3333333333333333703, 0.3219752754296894559, 0.3333333333333333703, 0.3219752754296894559, 0.3333333333333333703, 0.3219752754296894559, 0.3333333333333333703, 0.3219752754296894559, 0.3333333333333333703, 0.3219752754296894559, 0.3333333333333333703, 0.3219752754296894559, 0.3333333333333333703, 0.3219752754296894559, 0.3333333333333333703, 0.3219752754296894559, 0.3333333333333333703, 0.3219752754296894559, 0.3333333333333333703, 0.3219752754296894559, 0.3333333333333333703, 0.3219752754296894559, 0.3333333333333333703, 0.3219752754296894559, 0.3333333333333333703, 0.3219752754296894559, 0.3333333333333333703, 0.3219752754296894559, 0.3333333333333333703, 0.3219752754296894559, 0.3333333333333333703, 0.3219752754296894559, 0.3333333333333333703, 0.3219752754296894559, 0.3333333333333333703, 0.3219752754296894559, 0.3333333333333333703, 0.3219752754296894559, 0.3333333333333333703, 0.3219752754296894559, 0.3333333333333333703, 0.3219752754296894559, 0.3333333333333333703, 0.3219752754296894559, 0.3333333333333333703, 0.3219752754296894559, 0.3333333333333333703, 0.3219752754296894559, 0.3333333333333333703, 0.3219752754296894559, 0.3333333333333333703, 0.3219752754296894559, 0.3333333333333333703, 0.3219752754296894559, 0.3333333333333333703, 0.3219752754296894559, 0.3333333333333333703, 0.3219752754296894559, 0.3333333333333333703, 0.3219752754296894559, 0.3333333333333333703, 0.3219752754296894559, 0.3333333333333333703, 0.3219752754296894559, 0.3333333333333333703, 0.3219752754296894559, 0.3333333333333333703, 0.3219752754296894559, 0.3333333333333333703, 0.3219752754296894559, 0.3333333333333333703, 0.3219752754296894559, 0.3333333333333333703, 0.3219752754296894559, 0.3333333333333333703, 0.3219752754296894559, 0.3333333333333333703, 0.3219752754296894559, 0.3333333333333333703, 0.3219752754296894559, 0.3333333333333333703, 0.3219752754296894559, 0.3333333333333333703, 0.3219752754296894559, 0.3333333333333333703, 0.3219752754296894559, 0.3333333333333333703, 0.3219752754296894559, 0.3333333333333333703, 0.3219752754296894559, 0.3333333333333333703, 0.3219752754296894559, 0.3333333333333333703, 0.3219752754296894559, 0.3333333333333333703, 0.3219752754296894559, 0.3333333333333333703, 0.3219752754296894559, 0.3333333333333333703, 0.3219752754296894559, 0.3333333333333333703, 0.3219752754296894559, 0.3333333333333333703, 0.3219752754296894559, 0.3333333333333333703, 0.3219752754296894559, 0.3333333333333333703, 0.3219752754296894559, 0.3333333333333333703, 0.3219752754296894559, 0.3333333333333333703, 0.3219752754296894559, 0.3333333333333333703, 0.3219752754296894559, 0.3333333333333333703, 0.3219752754296894559, 0.3333333333333333703, 0.3219752754296894559, 0.3333333333333333703, 0.3219752754296894559, 0.3333333333333333703, 0.3219752754296894559, 0.3333333333333333703, 0.3219752754296894559, 0.3333333333333333703, 0.3219752754296894559, 0.3333333333333333703, 0.3219752754296894559, 0.3333333333333333703, 0.3219752754296894559, 0.3333333333333333703, 0.3219752754296894559, 0.3333333333333333703, 0.3219752754296894559, 0.3333333333333333703, 0.3219752754296894559, 0.3333333333333333703, 0.3219752754296894559, 0.3333333333333333703, 0.3219752754296894559, 0.3333333333333333703, 0.3219752754296894559, 0.3333333333333333703, 0.3219752754296894559, 0.3333333333333333703, 0.3219752754296894559, 0.3333333333333333703, 0.3219752754296894559, 0.3333333333333333703, 0.3219752754296894559, 0.3333333333333333703, 0.3219752754296894559, 0.3333333333333333703, 0.3219752754296894559, 0.3333333333333333703, 0.3219752754296894559, 0.3333333333333333703, 0.3219752754296894559, 0.3333333333333333703, 0.3219752754296894559, 0.3333333333333333703, 0.3219752754296894559, 0.3333333333333333703, 0.3219752754296894559, 0.3333333333333333703, 0.3219752754296894559, 0.3333333333333333703, 0.3219752754296894559, 0.3333333333333333703, 0.3219752754296894559, 0.3333333333333333703, 0.3219752754296894559, 0.3333333333333333703, 0.3219752754296894559, 0.3333333333333333703, 0.3219752754296894559, 0.3333333333333333703, 0.3219752754296894559, 0.3333333333333333703, 0.3219752754296894559, 0.3333333333333333703, 0.3219752754296894559, 0.3333333333333333703, 0.3219752754296894559, 0.3333333333333333703, 0.3219752754296894559, 0.3333333333333333703, 0.3219752754296894559, 0.3333333333333333703, 0.3219752754296894559, 0.3333333333333333703, 0.3219752754296894559, 0.3333333333333333703, 0.3219752754296894559, 0.3333333333333333703, 0.3219752754296894559, 0.3333333333333333703, 0.3219752754296894559, 0.3333333333333333703, 0.3219752754296894559, 0.3333333333333333703, 0.3219752754296894559, 0.3333333333333333703, 0.3219752754296894559, 0.3333333333333333703, 0.3219752754296894559, 0.3333333333333333703, 0.3219752754296894559, 0.3333333333333333703, 0.3219752754296894559, 0.3333333333333333703, 0.3219752754296894559, 0.3333333333333333703, 0.3219752754296894559, 0.3333333333333333703, 0.3219752754296894559, 0.3333333333333333703, 0.3219752754296894559, 0.3333333333333333703, 0.3219752754296894559, 0.3333333333333333703, 0.3219752754296894559, 0.3333333333333333703, 0.3219752754296894559, 0.3333333333333333703, 0.3219752754296894559, 0.3333333333333333703, 0.3219752754296894559, 0.3333333333333333703, 0.3219752754296894559, 0.3333333333333333703, 0.3219752754296894559, 0.3333333333333333703, 0.3219752754296894559, 0.3333333333333333703, 0.3219752754296894559, 0.3333333333333333703, 0.3219752754296894559, 0.3333333333333333703, 0.3219752754296894559, 0.3333333333333333703, 0.3219752754296894559, 0.3333333333333333703, 0.3219752754296894559, 0.3333333333333333703, 0.3219752754296894559, 0.3333333333333333703, 0.3219752754296894559, 0.3333333333333333703, 0.3219752754296894559, 0.3333333333333333703, 0.3219752754296894559, 0.3333333333333333703, 0.3219752754296894559, 0.3333333333333333703, 0.3219752754296894559, 0.3333333333333333703, 0.3219752754296894559, 0.3333333333333333703, 0.3219752754296894559, 0.3333333333333333703, 0.3219752754296894559, 0.3333333333333333703, 0.3219752754296894559, 0.3333333333333333703),
 ( 1.000000000000000000, 0.9659258262890683122, 1.000000000000000000, 0.9659258262890683122, 1.000000000000000000, 0.9659258262890683122, 1.000000000000000000, 0.9659258262890683122, 1.000000000000000000, 0.9659258262890683122, 1.000000000000000000, 0.9659258262890683122, 1.000000000000000000, 0.9659258262890683122, 1.000000000000000000, 0.9659258262890683122, 1.000000000000000000, 0.9659258262890683122, 1.000000000000000000, 0.9659258262890683122, 1.000000000000000000, 0.9659258262890683122, 1.000000000000000000, 0.9659258262890683122, 1.000000000000000000, 0.9659258262890683122, 1.000000000000000000, 0.9659258262890683122, 1.000000000000000000, 0.9659258262890683122, 1.000000000000000000, 0.9659258262890683122, 1.000000000000000000, 0.9659258262890683122, 1.000000000000000000, 0.9659258262890683122, 1.000000000000000000, 0.9659258262890683122, 1.000000000000000000, 0.9659258262890683122, 1.000000000000000000, 0.9659258262890683122, 1.000000000000000000, 0.9659258262890683122, 1.000000000000000000, 0.9659258262890683122, 1.000000000000000000, 0.9659258262890683122, 1.000000000000000000, 0.9659258262890683122, 1.000000000000000000, 0.9659258262890683122, 1.000000000000000000, 0.9659258262890683122, 1.000000000000000000, 0.9659258262890683122, 1.000000000000000000, 0.9659258262890683122, 1.000000000000000000, 0.9659258262890683122, 1.000000000000000000, 0.9659258262890683122, 1.000000000000000000, 0.9659258262890683122, 1.000000000000000000, 0.9659258262890683122, 1.000000000000000000, 0.9659258262890683122, 1.000000000000000000, 0.9659258262890683122, 1.000000000000000000, 0.9659258262890683122, 1.000000000000000000, 0.9659258262890683122, 1.000000000000000000, 0.9659258262890683122, 1.000000000000000000, 0.9659258262890683122, 1.000000000000000000, 0.9659258262890683122, 1.000000000000000000, 0.9659258262890683122, 1.000000000000000000, 0.9659258262890683122, 1.000000000000000000, 0.9659258262890683122, 1.000000000000000000, 0.9659258262890683122, 1.000000000000000000, 0.9659258262890683122, 1.000000000000000000, 0.9659258262890683122, 1.000000000000000000, 0.9659258262890683122, 1.000000000000000000, 0.9659258262890683122, 1.000000000000000000, 0.9659258262890683122, 1.000000000000000000, 0.9659258262890683122, 1.000000000000000000, 0.9659258262890683122, 1.000000000000000000, 0.9659258262890683122, 1.000000000000000000, 0.9659258262890683122, 1.000000000000000000, 0.9659258262890683122, 1.000000000000000000, 0.9659258262890683122, 1.000000000000000000, 0.9659258262890683122, 1.000000000000000000, 0.9659258262890683122, 1.000000000000000000, 0.9659258262890683122, 1.000000000000000000, 0.9659258262890683122, 1.000000000000000000, 0.9659258262890683122, 1.000000000000000000, 0.9659258262890683122, 1.000000000000000000, 0.9659258262890683122, 1.000000000000000000, 0.9659258262890683122, 1.000000000000000000, 0.9659258262890683122, 1.000000000000000000, 0.9659258262890683122, 1.000000000000000000, 0.9659258262890683122, 1.000000000000000000, 0.9659258262890683122, 1.000000000000000000, 0.9659258262890683122, 1.000000000000000000, 0.9659258262890683122, 1.000000000000000000, 0.9659258262890683122, 1.000000000000000000, 0.9659258262890683122, 1.000000000000000000, 0.9659258262890683122, 1.000000000000000000, 0.9659258262890683122, 1.000000000000000000, 0.9659258262890683122, 1.000000000000000000, 0.9659258262890683122, 1.000000000000000000, 0.9659258262890683122, 1.000000000000000000, 0.9659258262890683122, 1.000000000000000000, 0.9659258262890683122, 1.000000000000000000, 0.9659258262890683122, 1.000000000000000000, 0.9659258262890683122, 1.000000000000000000, 0.9659258262890683122, 1.000000000000000000, 0.9659258262890683122, 1.000000000000000000, 0.9659258262890683122, 1.000000000000000000, 0.9659258262890683122, 1.000000000000000000, 0.9659258262890683122, 1.000000000000000000, 0.9659258262890683122, 1.000000000000000000, 0.9659258262890683122, 1.000000000000000000, 0.9659258262890683122, 1.000000000000000000, 0.9659258262890683122, 1.000000000000000000, 0.9659258262890683122, 1.000000000000000000, 0.9659258262890683122, 1.000000000000000000, 0.9659258262890683122, 1.000000000000000000, 0.9659258262890683122, 1.000000000000000000, 0.9659258262890683122, 1.000000000000000000, 0.9659258262890683122, 1.000000000000000000, 0.9659258262890683122, 1.000000000000000000, 0.9659258262890683122, 1.000000000000000000, 0.9659258262890683122, 1.000000000000000000, 0.9659258262890683122, 1.000000000000000000, 0.9659258262890683122, 1.000000000000000000, 0.9659258262890683122, 1.000000000000000000, 0.9659258262890683122, 1.000000000000000000, 0.9659258262890683122, 1.000000000000000000, 0.9659258262890683122, 1.000000000000000000, 0.9659258262890683122, 1.000000000000000000, 0.9659258262890683122, 1.000000000000000000, 0.9659258262890683122, 1.000000000000000000, 0.9659258262890683122, 1.000000000000000000, 0.9659258262890683122, 1.000000000000000000, 0.9659258262890683122, 1.000000000000000000, 0.9659258262890683122, 1.000000000000000000, 0.9659258262890683122, 1.000000000000000000, 0.9659258262890683122, 1.000000000000000000, 0.9659258262890683122, 1.000000000000000000, 0.9659258262890683122, 1.000000000000000000, 0.9659258262890683122, 1.000000000000000000, 0.9659258262890683122, 1.000000000000000000, 0.9659258262890683122, 1.000000000000000000, 0.9659258262890683122, 1.000000000000000000, 0.9659258262890683122, 1.000000000000000000, 0.9659258262890683122, 1.000000000000000000, 0.9659258262890683122, 1.000000000000000000, 0.9659258262890683122, 1.000000000000000000, 0.9659258262890683122, 1.000000000000000000, 0.9659258262890683122, 1.000000000000000000, 0.9659258262890683122, 1.000000000000000000, 0.9659258262890683122, 1.000000000000000000, 0.9659258262890683122, 1.000000000000000000, 0.9659258262890683122, 1.000000000000000000, 0.9659258262890683122, 1.000000000000000000, 0.9659258262890683122, 1.000000000000000000, 0.9659258262890683122, 1.000000000000000000, 0.9659258262890683122, 1.000000000000000000, 0.9659258262890683122, 1.000000000000000000, 0.9659258262890683122, 1.000000000000000000, 0.9659258262890683122, 1.000000000000000000, 0.9659258262890683122, 1.000000000000000000, 0.9659258262890683122, 1.000000000000000000, 0.9659258262890683122, 1.000000000000000000, 0.9659258262890683122, 1.000000000000000000, 0.9659258262890683122, 1.000000000000000000, 0.9659258262890683122, 1.000000000000000000, 0.9659258262890683122, 1.000000000000000000, 0.9659258262890683122, 1.000000000000000000, 0.9659258262890683122, 1.000000000000000000, 0.9659258262890683122, 1.000000000000000000, 0.9659258262890683122, 1.000000000000000000, 0.9659258262890683122, 1.000000000000000000, 0.9659258262890683122, 1.000000000000000000, 0.9659258262890683122, 1.000000000000000000, 0.9659258262890683122, 1.000000000000000000, 0.9659258262890683122, 1.000000000000000000, 0.9659258262890683122, 1.000000000000000000, 0.9659258262890683122, 1.000000000000000000, 0.9659258262890683122, 1.000000000000000000, 0.9659258262890683122, 1.000000000000000000, 0.9659258262890683122, 1.000000000000000000, 0.9659258262890683122, 1.000000000000000000, 0.9659258262890683122, 1.000000000000000000, 0.9659258262890683122, 1.000000000000000000, 0.9659258262890683122, 1.000000000000000000, 0.9659258262890683122, 1.000000000000000000, 0.9659258262890683122, 1.000000000000000000, 0.9659258262890683122, 1.000000000000000000, 0.9659258262890683122, 1.000000000000000000, 0.9659258262890683122, 1.000000000000000000, 0.9659258262890683122, 1.000000000000000000, 0.9659258262890683122, 1.000000000000000000, 0.9659258262890683122, 1.000000000000000000, 0.9659258262890683122, 1.000000000000000000, 0.9659258262890683122, 1.000000000000000000, 0.9659258262890683122, 1.000000000000000000, 0.9659258262890683122, 1.000000000000000000, 0.9659258262890683122, 1.000000000000000000, 0.9659258262890683122, 1.000000000000000000, 0.9659258262890683122, 1.000000000000000000, 0.9659258262890683122, 1.000000000000000000, 0.9659258262890683122, 1.000000000000000000, 0.9659258262890683122, 1.000000000000000000, 0.9659258262890683122, 1.000000000000000000, 0.9659258262890683122, 1.000000000000000000, 0.9659258262890683122, 1.000000000000000000, 0.9659258262890683122, 1.000000000000000000, 0.9659258262890683122, 1.000000000000000000, 0.9659258262890683122, 1.000000000000000000, 0.9659258262890683122, 1.000000000000000000, 0.9659258262890683122, 1.000000000000000000, 0.9659258262890683122, 1.000000000000000000, 0.9659258262890683122, 1.000000000000000000, 0.9659258262890683122, 1.000000000000000000, 0.9659258262890683122, 1.000000000000000000, 0.9659258262890683122, 1.000000000000000000, 0.9659258262890683122, 1.000000000000000000, 0.9659258262890683122, 1.000000000000000000, 0.9659258262890683122, 1.000000000000000000, 0.9659258262890683122, 1.000000000000000000, 0.9659258262890683122, 1.000000000000000000, 0.9659258262890683122, 1.000000000000000000, 0.9659258262890683122, 1.000000000000000000, 0.9659258262890683122, 1.000000000000000000, 0.9659258262890683122, 1.000000000000000000, 0.9659258262890683122, 1.000000000000000000, 0.9659258262890683122, 1.000000000000000000, 0.9659258262890683122, 1.000000000000000000, 0.9659258262890683122, 1.000000000000000000, 0.9659258262890683122, 1.000000000000000000, 0.9659258262890683122, 1.000000000000000000, 0.9659258262890683122, 1.000000000000000000, 0.9659258262890683122, 1.000000000000000000, 0.9659258262890683122, 1.000000000000000000, 0.9659258262890683122, 1.000000000000000000, 0.9659258262890683122, 1.000000000000000000, 0.9659258262890683122, 1.000000000000000000, 0.9659258262890683122, 1.000000000000000000, 0.9659258262890683122, 1.000000000000000000, 0.9659258262890683122, 1.000000000000000000, 0.9659258262890683122, 1.000000000000000000, 0.9659258262890683122, 1.000000000000000000, 0.9659258262890683122, 1.000000000000000000, 0.9659258262890683122, 1.000000000000000000, 0.9659258262890683122, 1.000000000000000000, 0.9659258262890683122, 1.000000000000000000, 0.9659258262890683122, 1.000000000000000000, 0.9659258262890683122, 1.000000000000000000, 0.9659258262890683122, 1.000000000000000000, 0.9659258262890683122, 1.000000000000000000, 0.9659258262890683122, 1.000000000000000000, 0.9659258262890683122, 1.000000000000000000),
 ( 0.3333333333333333703, 0.3219752754296894559, 0.3333333333333333703, 0.3219752754296894559, 0.3333333333333333703, 0.3219752754296894559, 0.3333333333333333703, 0.3219752754296894559, 0.3333333333333333703, 0.3219752754296894559, 0.3333333333333333703, 0.3219752754296894559, 0.3333333333333333703, 0.3219752754296894559, 0.3333333333333333703, 0.3219752754296894559, 0.3333333333333333703, 0.3219752754296894559, 0.3333333333333333703, 0.3219752754296894559, 0.3333333333333333703, 0.3219752754296894559, 0.3333333333333333703, 0.3219752754296894559, 0.3333333333333333703, 0.3219752754296894559, 0.3333333333333333703, 0.3219752754296894559, 0.3333333333333333703, 0.3219752754296894559, 0.3333333333333333703, 0.3219752754296894559, 0.3333333333333333703, 0.3219752754296894559, 0.3333333333333333703, 0.3219752754296894559, 0.3333333333333333703, 0.3219752754296894559, 0.3333333333333333703, 0.3219752754296894559, 0.3333333333333333703, 0.3219752754296894559, 0.3333333333333333703, 0.3219752754296894559, 0.3333333333333333703, 0.3219752754296894559, 0.3333333333333333703, 0.3219752754296894559, 0.3333333333333333703, 0.3219752754296894559, 0.3333333333333333703, 0.3219752754296894559, 0.3333333333333333703, 0.3219752754296894559, 0.3333333333333333703, 0.3219752754296894559, 0.3333333333333333703, 0.3219752754296894559, 0.3333333333333333703, 0.3219752754296894559, 0.3333333333333333703, 0.3219752754296894559, 0.3333333333333333703, 0.3219752754296894559, 0.3333333333333333703, 0.3219752754296894559, 0.3333333333333333703, 0.3219752754296894559, 0.3333333333333333703, 0.3219752754296894559, 0.3333333333333333703, 0.3219752754296894559, 0.3333333333333333703, 0.3219752754296894559, 0.3333333333333333703, 0.3219752754296894559, 0.3333333333333333703, 0.3219752754296894559, 0.3333333333333333703, 0.3219752754296894559, 0.3333333333333333703, 0.3219752754296894559, 0.3333333333333333703, 0.3219752754296894559, 0.3333333333333333703, 0.3219752754296894559, 0.3333333333333333703, 0.3219752754296894559, 0.3333333333333333703, 0.3219752754296894559, 0.3333333333333333703, 0.3219752754296894559, 0.3333333333333333703, 0.3219752754296894559, 0.3333333333333333703, 0.3219752754296894559, 0.3333333333333333703, 0.3219752754296894559, 0.3333333333333333703, 0.3219752754296894559, 0.3333333333333333703, 0.3219752754296894559, 0.3333333333333333703, 0.3219752754296894559, 0.3333333333333333703, 0.3219752754296894559, 0.3333333333333333703, 0.3219752754296894559, 0.3333333333333333703, 0.3219752754296894559, 0.3333333333333333703, 0.3219752754296894559, 0.3333333333333333703, 0.3219752754296894559, 0.3333333333333333703, 0.3219752754296894559, 0.3333333333333333703, 0.3219752754296894559, 0.3333333333333333703, 0.3219752754296894559, 0.3333333333333333703, 0.3219752754296894559, 0.3333333333333333703, 0.3219752754296894559, 0.3333333333333333703, 0.3219752754296894559, 0.3333333333333333703, 0.3219752754296894559, 0.3333333333333333703, 0.3219752754296894559, 0.3333333333333333703, 0.3219752754296894559, 0.3333333333333333703, 0.3219752754296894559, 0.3333333333333333703, 0.3219752754296894559, 0.3333333333333333703, 0.3219752754296894559, 0.3333333333333333703, 0.3219752754296894559, 0.3333333333333333703, 0.3219752754296894559, 0.3333333333333333703, 0.3219752754296894559, 0.3333333333333333703, 0.3219752754296894559, 0.3333333333333333703, 0.3219752754296894559, 0.3333333333333333703, 0.3219752754296894559, 0.3333333333333333703, 0.3219752754296894559, 0.3333333333333333703, 0.3219752754296894559, 0.3333333333333333703, 0.3219752754296894559, 0.3333333333333333703, 0.3219752754296894559, 0.3333333333333333703, 0.3219752754296894559, 0.3333333333333333703, 0.3219752754296894559, 0.3333333333333333703, 0.3219752754296894559, 0.3333333333333333703, 0.3219752754296894559, 0.3333333333333333703, 0.3219752754296894559, 0.3333333333333333703, 0.3219752754296894559, 0.3333333333333333703, 0.3219752754296894559, 0.3333333333333333703, 0.3219752754296894559, 0.3333333333333333703, 0.3219752754296894559, 0.3333333333333333703, 0.3219752754296894559, 0.3333333333333333703, 0.3219752754296894559, 0.3333333333333333703, 0.3219752754296894559, 0.3333333333333333703, 0.3219752754296894559, 0.3333333333333333703, 0.3219752754296894559, 0.3333333333333333703, 0.3219752754296894559, 0.3333333333333333703, 0.3219752754296894559, 0.3333333333333333703, 0.3219752754296894559, 0.3333333333333333703, 0.3219752754296894559, 0.3333333333333333703, 0.3219752754296894559, 0.3333333333333333703, 0.3219752754296894559, 0.3333333333333333703, 0.3219752754296894559, 0.3333333333333333703, 0.3219752754296894559, 0.3333333333333333703, 0.3219752754296894559, 0.3333333333333333703, 0.3219752754296894559, 0.3333333333333333703, 0.3219752754296894559, 0.3333333333333333703, 0.3219752754296894559, 0.3333333333333333703, 0.3219752754296894559, 0.3333333333333333703, 0.3219752754296894559, 0.3333333333333333703, 0.3219752754296894559, 0.3333333333333333703, 0.3219752754296894559, 0.3333333333333333703, 0.3219752754296894559, 0.3333333333333333703, 0.3219752754296894559, 0.3333333333333333703, 0.3219752754296894559, 0.3333333333333333703, 0.3219752754296894559, 0.3333333333333333703, 0.3219752754296894559, 0.3333333333333333703, 0.3219752754296894559, 0.3333333333333333703, 0.3219752754296894559, 0.3333333333333333703, 0.3219752754296894559, 0.3333333333333333703, 0.3219752754296894559, 0.3333333333333333703, 0.3219752754296894559, 0.3333333333333333703, 0.3219752754296894559, 0.3333333333333333703, 0.3219752754296894559, 0.3333333333333333703, 0.3219752754296894559, 0.3333333333333333703, 0.3219752754296894559, 0.3333333333333333703, 0.3219752754296894559, 0.3333333333333333703, 0.3219752754296894559, 0.3333333333333333703, 0.3219752754296894559, 0.3333333333333333703, 0.3219752754296894559, 0.3333333333333333703, 0.3219752754296894559, 0.3333333333333333703, 0.3219752754296894559, 0.3333333333333333703, 0.3219752754296894559, 0.3333333333333333703, 0.3219752754296894559, 0.3333333333333333703, 0.3219752754296894559, 0.3333333333333333703, 0.3219752754296894559, 0.3333333333333333703, 0.3219752754296894559, 0.3333333333333333703, 0.3219752754296894559, 0.3333333333333333703, 0.3219752754296894559, 0.3333333333333333703, 0.3219752754296894559, 0.3333333333333333703, 0.3219752754296894559, 0.3333333333333333703, 0.3219752754296894559, 0.3333333333333333703, 0.3219752754296894559, 0.3333333333333333703, 0.3219752754296894559, 0.3333333333333333703, 0.3219752754296894559, 0.3333333333333333703, 0.3219752754296894559, 0.3333333333333333703, 0.3219752754296894559, 0.3333333333333333703, 0.3219752754296894559, 0.3333333333333333703, 0.3219752754296894559, 0.3333333333333333703, 0.3219752754296894559, 0.3333333333333333703, 0.3219752754296894559, 0.3333333333333333703, 0.3219752754296894559, 0.3333333333333333703, 0.3219752754296894559, 0.3333333333333333703, 0.3219752754296894559, 0.3333333333333333703, 0.3219752754296894559, 0.3333333333333333703, 0.3219752754296894559, 0.3333333333333333703, 0.3219752754296894559, 0.3333333333333333703, 0.3219752754296894559, 0.3333333333333333703, 0.3219752754296894559, 0.3333333333333333703, 0.3219752754296894559, 0.3333333333333333703, 0.3219752754296894559, 0.3333333333333333703, 0.3219752754296894559, 0.3333333333333333703, 0.3219752754296894559, 0.3333333333333333703, 0.3219752754296894559, 0.3333333333333333703, 0.3219752754296894559, 0.3333333333333333703, 0.3219752754296894559, 0.3333333333333333703, 0.3219752754296894559, 0.3333333333333333703, 0.3219752754296894559, 0.3333333333333333703, 0.3219752754296894559, 0.3333333333333333703, 0.3219752754296894559, 0.3333333333333333703, 0.3219752754296894559, 0.3333333333333333703, 0.3219752754296894559, 0.3333333333333333703, 0.3219752754296894559, 0.3333333333333333703, 0.3219752754296894559, 0.3333333333333333703, 0.3219752754296894559, 0.3333333333333333703, 0.3219752754296894559, 0.3333333333333333703, 0.3219752754296894559, 0.3333333333333333703, 0.3219752754296894559, 0.3333333333333333703, 0.3219752754296894559, 0.3333333333333333703, 0.3219752754296894559, 0.3333333333333333703, 0.3219752754296894559, 0.3333333333333333703, 0.3219752754296894559, 0.3333333333333333703, 0.3219752754296894559, 0.3333333333333333703, 0.3219752754296894559, 0.3333333333333333703, 0.3219752754296894559, 0.3333333333333333703, 0.3219752754296894559, 0.3333333333333333703, 0.3219752754296894559, 0.3333333333333333703, 0.3219752754296894559, 0.3333333333333333703, 0.3219752754296894559, 0.3333333333333333703, 0.3219752754296894559, 0.3333333333333333703, 0.3219752754296894559, 0.3333333333333333703, 0.3219752754296894559, 0.3333333333333333703, 0.3219752754296894559, 0.3333333333333333703, 0.3219752754296894559, 0.3333333333333333703, 0.3219752754296894559, 0.3333333333333333703, 0.3219752754296894559, 0.3333333333333333703, 0.3219752754296894559, 0.3333333333333333703, 0.3219752754296894559, 0.3333333333333333703, 0.3219752754296894559, 0.3333333333333333703, 0.3219752754296894559, 0.3333333333333333703, 0.3219752754296894559, 0.3333333333333333703, 0.3219752754296894559, 0.3333333333333333703, 0.3219752754296894559, 0.3333333333333333703, 0.3219752754296894559, 0.3333333333333333703, 0.3219752754296894559, 0.3333333333333333703, 0.3219752754296894559, 0.3333333333333333703, 0.3219752754296894559, 0.3333333333333333703, 0.3219752754296894559, 0.3333333333333333703, 0.3219752754296894559, 0.3333333333333333703, 0.3219752754296894559, 0.3333333333333333703, 0.3219752754296894559, 0.3333333333333333703, 0.3219752754296894559, 0.3333333333333333703, 0.3219752754296894559, 0.3333333333333333703, 0.3219752754296894559, 0.3333333333333333703, 0.3219752754296894559, 0.3333333333333333703, 0.3219752754296894559, 0.3333333333333333703, 0.3219752754296894559, 0.3333333333333333703, 0.3219752754296894559, 0.3333333333333333703, 0.3219752754296894559, 0.3333333333333333703, 0.3219752754296894559, 0.3333333333333333703, 0.3219752754296894559, 0.3333333333333333703, 0.3219752754296894559, 0.3333333333333333703, 0.3219752754296894559, 0.3333333333333333703, 0.3219752754296894559, 0.3333333333333333703, 0.3219752754296894559, 0.3333333333333333703, 0.3219752754296894559, 0.3333333333333333703, 0.3219752754296894559, 0.3333333333333333703, 0.3219752754296894559, 0.3333333333333333703, 0.3219752754296894559, 0.3333333333333333703, 0.3219752754296894559, 0.3333333333333333703, 0.3219752754296894559, 0.3333333333333333703),
 ( 0.3333333333333333703, 0.3219752754296894559, 0.3333333333333333703, 0.3219752754296894559, 0.3333333333333333703, 0.3219752754296894559, 0.3333333333333333703, 0.3219752754296894559, 0.3333333333333333703, 0.3219752754296894559, 0.3333333333333333703, 0.3219752754296894559, 0.3333333333333333703, 0.3219752754296894559, 0.3333333333333333703, 0.3219752754296894559, 0.3333333333333333703, 0.3219752754296894559, 0.3333333333333333703, 0.3219752754296894559, 0.3333333333333333703, 0.3219752754296894559, 0.3333333333333333703, 0.3219752754296894559, 0.3333333333333333703, 0.3219752754296894559, 0.3333333333333333703, 0.3219752754296894559, 0.3333333333333333703, 0.3219752754296894559, 0.3333333333333333703, 0.3219752754296894559, 0.3333333333333333703, 0.3219752754296894559, 0.3333333333333333703, 0.3219752754296894559, 0.3333333333333333703, 0.3219752754296894559, 0.3333333333333333703, 0.3219752754296894559, 0.3333333333333333703, 0.3219752754296894559, 0.3333333333333333703, 0.3219752754296894559, 0.3333333333333333703, 0.3219752754296894559, 0.3333333333333333703, 0.3219752754296894559, 0.3333333333333333703, 0.3219752754296894559, 0.3333333333333333703, 0.3219752754296894559, 0.3333333333333333703, 0.3219752754296894559, 0.3333333333333333703, 0.3219752754296894559, 0.3333333333333333703, 0.3219752754296894559, 0.3333333333333333703, 0.3219752754296894559, 0.3333333333333333703, 0.3219752754296894559, 0.3333333333333333703, 0.3219752754296894559, 0.3333333333333333703, 0.3219752754296894559, 0.3333333333333333703, 0.3219752754296894559, 0.3333333333333333703, 0.3219752754296894559, 0.3333333333333333703, 0.3219752754296894559, 0.3333333333333333703, 0.3219752754296894559, 0.3333333333333333703, 0.3219752754296894559, 0.3333333333333333703, 0.3219752754296894559, 0.3333333333333333703, 0.3219752754296894559, 0.3333333333333333703, 0.3219752754296894559, 0.3333333333333333703, 0.3219752754296894559, 0.3333333333333333703, 0.3219752754296894559, 0.3333333333333333703, 0.3219752754296894559, 0.3333333333333333703, 0.3219752754296894559, 0.3333333333333333703, 0.3219752754296894559, 0.3333333333333333703, 0.3219752754296894559, 0.3333333333333333703, 0.3219752754296894559, 0.3333333333333333703, 0.3219752754296894559, 0.3333333333333333703, 0.3219752754296894559, 0.3333333333333333703, 0.3219752754296894559, 0.3333333333333333703, 0.3219752754296894559, 0.3333333333333333703, 0.3219752754296894559, 0.3333333333333333703, 0.3219752754296894559, 0.3333333333333333703, 0.3219752754296894559, 0.3333333333333333703, 0.3219752754296894559, 0.3333333333333333703, 0.3219752754296894559, 0.3333333333333333703, 0.3219752754296894559, 0.3333333333333333703, 0.3219752754296894559, 0.3333333333333333703, 0.3219752754296894559, 0.3333333333333333703, 0.3219752754296894559, 0.3333333333333333703, 0.3219752754296894559, 0.3333333333333333703, 0.3219752754296894559, 0.3333333333333333703, 0.3219752754296894559, 0.3333333333333333703, 0.3219752754296894559, 0.3333333333333333703, 0.3219752754296894559, 0.3333333333333333703, 0.3219752754296894559, 0.3333333333333333703, 0.3219752754296894559, 0.3333333333333333703, 0.3219752754296894559, 0.3333333333333333703, 0.3219752754296894559, 0.3333333333333333703, 0.3219752754296894559, 0.3333333333333333703, 0.3219752754296894559, 0.3333333333333333703, 0.3219752754296894559, 0.3333333333333333703, 0.3219752754296894559, 0.3333333333333333703, 0.3219752754296894559, 0.3333333333333333703, 0.3219752754296894559, 0.3333333333333333703, 0.3219752754296894559, 0.3333333333333333703, 0.3219752754296894559, 0.3333333333333333703, 0.3219752754296894559, 0.3333333333333333703, 0.3219752754296894559, 0.3333333333333333703, 0.3219752754296894559, 0.3333333333333333703, 0.3219752754296894559, 0.3333333333333333703, 0.3219752754296894559, 0.3333333333333333703, 0.3219752754296894559, 0.3333333333333333703, 0.3219752754296894559, 0.3333333333333333703, 0.3219752754296894559, 0.3333333333333333703, 0.3219752754296894559, 0.3333333333333333703, 0.3219752754296894559, 0.3333333333333333703, 0.3219752754296894559, 0.3333333333333333703, 0.3219752754296894559, 0.3333333333333333703, 0.3219752754296894559, 0.3333333333333333703, 0.3219752754296894559, 0.3333333333333333703, 0.3219752754296894559, 0.3333333333333333703, 0.3219752754296894559, 0.3333333333333333703, 0.3219752754296894559, 0.3333333333333333703, 0.3219752754296894559, 0.3333333333333333703, 0.3219752754296894559, 0.3333333333333333703, 0.3219752754296894559, 0.3333333333333333703, 0.3219752754296894559, 0.3333333333333333703, 0.3219752754296894559, 0.3333333333333333703, 0.3219752754296894559, 0.3333333333333333703, 0.3219752754296894559, 0.3333333333333333703, 0.3219752754296894559, 0.3333333333333333703, 0.3219752754296894559, 0.3333333333333333703, 0.3219752754296894559, 0.3333333333333333703, 0.3219752754296894559, 0.3333333333333333703, 0.3219752754296894559, 0.3333333333333333703, 0.3219752754296894559, 0.3333333333333333703, 0.3219752754296894559, 0.3333333333333333703, 0.3219752754296894559, 0.3333333333333333703, 0.3219752754296894559, 0.3333333333333333703, 0.3219752754296894559, 0.3333333333333333703, 0.3219752754296894559, 0.3333333333333333703, 0.3219752754296894559, 0.3333333333333333703, 0.3219752754296894559, 0.3333333333333333703, 0.3219752754296894559, 0.3333333333333333703, 0.3219752754296894559, 0.3333333333333333703, 0.3219752754296894559, 0.3333333333333333703, 0.3219752754296894559, 0.3333333333333333703, 0.3219752754296894559, 0.3333333333333333703, 0.3219752754296894559, 0.3333333333333333703, 0.3219752754296894559, 0.3333333333333333703, 0.3219752754296894559, 0.3333333333333333703, 0.3219752754296894559, 0.3333333333333333703, 0.3219752754296894559, 0.3333333333333333703, 0.3219752754296894559, 0.3333333333333333703, 0.3219752754296894559, 0.3333333333333333703, 0.3219752754296894559, 0.3333333333333333703, 0.3219752754296894559, 0.3333333333333333703, 0.3219752754296894559, 0.3333333333333333703, 0.3219752754296894559, 0.3333333333333333703, 0.3219752754296894559, 0.3333333333333333703, 0.3219752754296894559, 0.3333333333333333703, 0.3219752754296894559, 0.3333333333333333703, 0.3219752754296894559, 0.3333333333333333703, 0.3219752754296894559, 0.3333333333333333703, 0.3219752754296894559, 0.3333333333333333703, 0.3219752754296894559, 0.3333333333333333703, 0.3219752754296894559, 0.3333333333333333703, 0.3219752754296894559, 0.3333333333333333703, 0.3219752754296894559, 0.3333333333333333703, 0.3219752754296894559, 0.3333333333333333703, 0.3219752754296894559, 0.3333333333333333703, 0.3219752754296894559, 0.3333333333333333703, 0.3219752754296894559, 0.3333333333333333703, 0.3219752754296894559, 0.3333333333333333703, 0.3219752754296894559, 0.3333333333333333703, 0.3219752754296894559, 0.3333333333333333703, 0.3219752754296894559, 0.3333333333333333703, 0.3219752754296894559, 0.3333333333333333703, 0.3219752754296894559, 0.3333333333333333703, 0.3219752754296894559, 0.3333333333333333703, 0.3219752754296894559, 0.3333333333333333703, 0.3219752754296894559, 0.3333333333333333703, 0.3219752754296894559, 0.3333333333333333703, 0.3219752754296894559, 0.3333333333333333703, 0.3219752754296894559, 0.3333333333333333703, 0.3219752754296894559, 0.3333333333333333703, 0.3219752754296894559, 0.3333333333333333703, 0.3219752754296894559, 0.3333333333333333703, 0.3219752754296894559, 0.3333333333333333703, 0.3219752754296894559, 0.3333333333333333703, 0.3219752754296894559, 0.3333333333333333703, 0.3219752754296894559, 0.3333333333333333703, 0.3219752754296894559, 0.3333333333333333703, 0.3219752754296894559, 0.3333333333333333703, 0.3219752754296894559, 0.3333333333333333703, 0.3219752754296894559, 0.3333333333333333703, 0.3219752754296894559, 0.3333333333333333703, 0.3219752754296894559, 0.3333333333333333703, 0.3219752754296894559, 0.3333333333333333703, 0.3219752754296894559, 0.3333333333333333703, 0.3219752754296894559, 0.3333333333333333703, 0.3219752754296894559, 0.3333333333333333703, 0.3219752754296894559, 0.3333333333333333703, 0.3219752754296894559, 0.3333333333333333703, 0.3219752754296894559, 0.3333333333333333703, 0.3219752754296894559, 0.3333333333333333703, 0.3219752754296894559, 0.3333333333333333703, 0.3219752754296894559, 0.3333333333333333703, 0.3219752754296894559, 0.3333333333333333703, 0.3219752754296894559, 0.3333333333333333703, 0.3219752754296894559, 0.3333333333333333703, 0.3219752754296894559, 0.3333333333333333703, 0.3219752754296894559, 0.3333333333333333703, 0.3219752754296894559, 0.3333333333333333703, 0.3219752754296894559, 0.3333333333333333703, 0.3219752754296894559, 0.3333333333333333703, 0.3219752754296894559, 0.3333333333333333703, 0.3219752754296894559, 0.3333333333333333703, 0.3219752754296894559, 0.3333333333333333703, 0.3219752754296894559, 0.3333333333333333703, 0.3219752754296894559, 0.3333333333333333703, 0.3219752754296894559, 0.3333333333333333703, 0.3219752754296894559, 0.3333333333333333703, 0.3219752754296894559, 0.3333333333333333703, 0.3219752754296894559, 0.3333333333333333703, 0.3219752754296894559, 0.3333333333333333703, 0.3219752754296894559, 0.3333333333333333703, 0.3219752754296894559, 0.3333333333333333703, 0.3219752754296894559, 0.3333333333333333703, 0.3219752754296894559, 0.3333333333333333703, 0.3219752754296894559, 0.3333333333333333703, 0.3219752754296894559, 0.3333333333333333703, 0.3219752754296894559, 0.3333333333333333703, 0.3219752754296894559, 0.3333333333333333703, 0.3219752754296894559, 0.3333333333333333703, 0.3219752754296894559, 0.3333333333333333703, 0.3219752754296894559, 0.3333333333333333703, 0.3219752754296894559, 0.3333333333333333703, 0.3219752754296894559, 0.3333333333333333703, 0.3219752754296894559, 0.3333333333333333703, 0.3219752754296894559, 0.3333333333333333703, 0.3219752754296894559, 0.3333333333333333703, 0.3219752754296894559, 0.3333333333333333703, 0.3219752754296894559, 0.3333333333333333703, 0.3219752754296894559, 0.3333333333333333703, 0.3219752754296894559, 0.3333333333333333703, 0.3219752754296894559, 0.3333333333333333703, 0.3219752754296894559, 0.3333333333333333703, 0.3219752754296894559, 0.3333333333333333703, 0.3219752754296894559, 0.3333333333333333703, 0.3219752754296894559, 0.3333333333333333703, 0.3219752754296894559, 0.3333333333333333703, 0.3219752754296894559, 0.3333333333333333703, 0.3219752754296894559, 0.3333333333333333703, 0.3219752754296894559, 0.3333333333333333703, 0.3219752754296894559, 0.3333333333333333703),
 ( 1.000000000000000000, 0.9659258262890683122, 1.000000000000000000, 0.9659258262890683122, 1.000000000000000000, 0.9659258262890683122, 1.000000000000000000, 0.9659258262890683122, 1.000000000000000000, 0.9659258262890683122, 1.000000000000000000, 0.9659258262890683122, 1.000000000000000000, 0.9659258262890683122, 1.000000000000000000, 0.9659258262890683122, 1.000000000000000000, 0.9659258262890683122, 1.000000000000000000, 0.9659258262890683122, 1.000000000000000000, 0.9659258262890683122, 1.000000000000000000, 0.9659258262890683122, 1.000000000000000000, 0.9659258262890683122, 1.000000000000000000, 0.9659258262890683122, 1.000000000000000000, 0.9659258262890683122, 1.000000000000000000, 0.9659258262890683122, 1.000000000000000000, 0.9659258262890683122, 1.000000000000000000, 0.9659258262890683122, 1.000000000000000000, 0.9659258262890683122, 1.000000000000000000, 0.9659258262890683122, 1.000000000000000000, 0.9659258262890683122, 1.000000000000000000, 0.9659258262890683122, 1.000000000000000000, 0.9659258262890683122, 1.000000000000000000, 0.9659258262890683122, 1.000000000000000000, 0.9659258262890683122, 1.000000000000000000, 0.9659258262890683122, 1.000000000000000000, 0.9659258262890683122, 1.000000000000000000, 0.9659258262890683122, 1.000000000000000000, 0.9659258262890683122, 1.000000000000000000, 0.9659258262890683122, 1.000000000000000000, 0.9659258262890683122, 1.000000000000000000, 0.9659258262890683122, 1.000000000000000000, 0.9659258262890683122, 1.000000000000000000, 0.9659258262890683122, 1.000000000000000000, 0.9659258262890683122, 1.000000000000000000, 0.9659258262890683122, 1.000000000000000000, 0.9659258262890683122, 1.000000000000000000, 0.9659258262890683122, 1.000000000000000000, 0.9659258262890683122, 1.000000000000000000, 0.9659258262890683122, 1.000000000000000000, 0.9659258262890683122, 1.000000000000000000, 0.9659258262890683122, 1.000000000000000000, 0.9659258262890683122, 1.000000000000000000, 0.9659258262890683122, 1.000000000000000000, 0.9659258262890683122, 1.000000000000000000, 0.9659258262890683122, 1.000000000000000000, 0.9659258262890683122, 1.000000000000000000, 0.9659258262890683122, 1.000000000000000000, 0.9659258262890683122, 1.000000000000000000, 0.9659258262890683122, 1.000000000000000000, 0.9659258262890683122, 1.000000000000000000, 0.9659258262890683122, 1.000000000000000000, 0.9659258262890683122, 1.000000000000000000, 0.9659258262890683122, 1.000000000000000000, 0.9659258262890683122, 1.000000000000000000, 0.9659258262890683122, 1.000000000000000000, 0.9659258262890683122, 1.000000000000000000, 0.9659258262890683122, 1.000000000000000000, 0.9659258262890683122, 1.000000000000000000, 0.9659258262890683122, 1.000000000000000000, 0.9659258262890683122, 1.000000000000000000, 0.9659258262890683122, 1.000000000000000000, 0.9659258262890683122, 1.000000000000000000, 0.9659258262890683122, 1.000000000000000000, 0.9659258262890683122, 1.000000000000000000, 0.9659258262890683122, 1.000000000000000000, 0.9659258262890683122, 1.000000000000000000, 0.9659258262890683122, 1.000000000000000000, 0.9659258262890683122, 1.000000000000000000, 0.9659258262890683122, 1.000000000000000000, 0.9659258262890683122, 1.000000000000000000, 0.9659258262890683122, 1.000000000000000000, 0.9659258262890683122, 1.000000000000000000, 0.9659258262890683122, 1.000000000000000000, 0.9659258262890683122, 1.000000000000000000, 0.9659258262890683122, 1.000000000000000000, 0.9659258262890683122, 1.000000000000000000, 0.9659258262890683122, 1.000000000000000000, 0.9659258262890683122, 1.000000000000000000, 0.9659258262890683122, 1.000000000000000000, 0.9659258262890683122, 1.000000000000000000, 0.9659258262890683122, 1.000000000000000000, 0.9659258262890683122, 1.000000000000000000, 0.9659258262890683122, 1.000000000000000000, 0.9659258262890683122, 1.000000000000000000, 0.9659258262890683122, 1.000000000000000000, 0.9659258262890683122, 1.000000000000000000, 0.9659258262890683122, 1.000000000000000000, 0.9659258262890683122, 1.000000000000000000, 0.9659258262890683122, 1.000000000000000000, 0.9659258262890683122, 1.000000000000000000, 0.9659258262890683122, 1.000000000000000000, 0.9659258262890683122, 1.000000000000000000, 0.9659258262890683122, 1.000000000000000000, 0.9659258262890683122, 1.000000000000000000, 0.9659258262890683122, 1.000000000000000000, 0.9659258262890683122, 1.000000000000000000, 0.9659258262890683122, 1.000000000000000000, 0.9659258262890683122, 1.000000000000000000, 0.9659258262890683122, 1.000000000000000000, 0.9659258262890683122, 1.000000000000000000, 0.9659258262890683122, 1.000000000000000000, 0.9659258262890683122, 1.000000000000000000, 0.9659258262890683122, 1.000000000000000000, 0.9659258262890683122, 1.000000000000000000, 0.9659258262890683122, 1.000000000000000000, 0.9659258262890683122, 1.000000000000000000, 0.9659258262890683122, 1.000000000000000000, 0.9659258262890683122, 1.000000000000000000, 0.9659258262890683122, 1.000000000000000000, 0.9659258262890683122, 1.000000000000000000, 0.9659258262890683122, 1.000000000000000000, 0.9659258262890683122, 1.000000000000000000, 0.9659258262890683122, 1.000000000000000000, 0.9659258262890683122, 1.000000000000000000, 0.9659258262890683122, 1.000000000000000000, 0.9659258262890683122, 1.000000000000000000, 0.9659258262890683122, 1.000000000000000000, 0.9659258262890683122, 1.000000000000000000, 0.9659258262890683122, 1.000000000000000000, 0.9659258262890683122, 1.000000000000000000, 0.9659258262890683122, 1.000000000000000000, 0.9659258262890683122, 1.000000000000000000, 0.9659258262890683122, 1.000000000000000000, 0.9659258262890683122, 1.000000000000000000, 0.9659258262890683122, 1.000000000000000000, 0.9659258262890683122, 1.000000000000000000, 0.9659258262890683122, 1.000000000000000000, 0.9659258262890683122, 1.000000000000000000, 0.9659258262890683122, 1.000000000000000000, 0.9659258262890683122, 1.000000000000000000, 0.9659258262890683122, 1.000000000000000000, 0.9659258262890683122, 1.000000000000000000, 0.9659258262890683122, 1.000000000000000000, 0.9659258262890683122, 1.000000000000000000, 0.9659258262890683122, 1.000000000000000000, 0.9659258262890683122, 1.000000000000000000, 0.9659258262890683122, 1.000000000000000000, 0.9659258262890683122, 1.000000000000000000, 0.9659258262890683122, 1.000000000000000000, 0.9659258262890683122, 1.000000000000000000, 0.9659258262890683122, 1.000000000000000000, 0.9659258262890683122, 1.000000000000000000, 0.9659258262890683122, 1.000000000000000000, 0.9659258262890683122, 1.000000000000000000, 0.9659258262890683122, 1.000000000000000000, 0.9659258262890683122, 1.000000000000000000, 0.9659258262890683122, 1.000000000000000000, 0.9659258262890683122, 1.000000000000000000, 0.9659258262890683122, 1.000000000000000000, 0.9659258262890683122, 1.000000000000000000, 0.9659258262890683122, 1.000000000000000000, 0.9659258262890683122, 1.000000000000000000, 0.9659258262890683122, 1.000000000000000000, 0.9659258262890683122, 1.000000000000000000, 0.9659258262890683122, 1.000000000000000000, 0.9659258262890683122, 1.000000000000000000, 0.9659258262890683122, 1.000000000000000000, 0.9659258262890683122, 1.000000000000000000, 0.9659258262890683122, 1.000000000000000000, 0.9659258262890683122, 1.000000000000000000, 0.9659258262890683122, 1.000000000000000000, 0.9659258262890683122, 1.000000000000000000, 0.9659258262890683122, 1.000000000000000000, 0.9659258262890683122, 1.000000000000000000, 0.9659258262890683122, 1.000000000000000000, 0.9659258262890683122, 1.000000000000000000, 0.9659258262890683122, 1.000000000000000000, 0.9659258262890683122, 1.000000000000000000, 0.9659258262890683122, 1.000000000000000000, 0.9659258262890683122, 1.000000000000000000, 0.9659258262890683122, 1.000000000000000000, 0.9659258262890683122, 1.000000000000000000, 0.9659258262890683122, 1.000000000000000000, 0.9659258262890683122, 1.000000000000000000, 0.9659258262890683122, 1.000000000000000000, 0.9659258262890683122, 1.000000000000000000, 0.9659258262890683122, 1.000000000000000000, 0.9659258262890683122, 1.000000000000000000, 0.9659258262890683122, 1.000000000000000000, 0.9659258262890683122, 1.000000000000000000, 0.9659258262890683122, 1.000000000000000000, 0.9659258262890683122, 1.000000000000000000, 0.9659258262890683122, 1.000000000000000000, 0.9659258262890683122, 1.000000000000000000, 0.9659258262890683122, 1.000000000000000000, 0.9659258262890683122, 1.000000000000000000, 0.9659258262890683122, 1.000000000000000000, 0.9659258262890683122, 1.000000000000000000, 0.9659258262890683122, 1.000000000000000000, 0.9659258262890683122, 1.000000000000000000, 0.9659258262890683122, 1.000000000000000000, 0.9659258262890683122, 1.000000000000000000, 0.9659258262890683122, 1.000000000000000000, 0.9659258262890683122, 1.000000000000000000, 0.9659258262890683122, 1.000000000000000000, 0.9659258262890683122, 1.000000000000000000, 0.9659258262890683122, 1.000000000000000000, 0.9659258262890683122, 1.000000000000000000, 0.9659258262890683122, 1.000000000000000000, 0.9659258262890683122, 1.000000000000000000, 0.9659258262890683122, 1.000000000000000000, 0.9659258262890683122, 1.000000000000000000, 0.9659258262890683122, 1.000000000000000000, 0.9659258262890683122, 1.000000000000000000, 0.9659258262890683122, 1.000000000000000000, 0.9659258262890683122, 1.000000000000000000, 0.9659258262890683122, 1.000000000000000000, 0.9659258262890683122, 1.000000000000000000, 0.9659258262890683122, 1.000000000000000000, 0.9659258262890683122, 1.000000000000000000, 0.9659258262890683122, 1.000000000000000000, 0.9659258262890683122, 1.000000000000000000, 0.9659258262890683122, 1.000000000000000000, 0.9659258262890683122, 1.000000000000000000, 0.9659258262890683122, 1.000000000000000000, 0.9659258262890683122, 1.000000000000000000, 0.9659258262890683122, 1.000000000000000000, 0.9659258262890683122, 1.000000000000000000, 0.9659258262890683122, 1.000000000000000000, 0.9659258262890683122, 1.000000000000000000, 0.9659258262890683122, 1.000000000000000000, 0.9659258262890683122, 1.000000000000000000, 0.9659258262890683122, 1.000000000000000000, 0.9659258262890683122, 1.000000000000000000, 0.9659258262890683122, 1.000000000000000000, 0.9659258262890683122, 1.000000000000000000, 0.9659258262890683122, 1.000000000000000000) ) ) 
 REPRESENTATION_ITEM ( '' )  SURFACE ( )  );
#7390 = CARTESIAN_POINT ( 'NONE',  ( 18.67979575497178502, 10.72451020669898547, 69.16557627198102409 ) ) ;
#7391 = CARTESIAN_POINT ( 'NONE',  ( 8.314922557961029526, -14.29746914071037800, 110.4177570613523756 ) ) ;
#7392 = ORIENTED_EDGE ( 'NONE', *, *, #132031, .F. ) ;
#7393 = DIRECTION ( 'NONE',  ( -0.000000000000000000, -0.000000000000000000, 1.000000000000000000 ) ) ;
#7394 = CARTESIAN_POINT ( 'NONE',  ( -10.72451020669898014, 18.67979575497178502, 90.41557627198103830 ) ) ;
#7395 = CARTESIAN_POINT ( 'NONE',  ( 5.719274019375991003, -21.55341960407610458, 112.7072429386476955 ) ) ;
#7396 = CARTESIAN_POINT ( 'NONE',  ( -16.55341960407611168, -4.379528057220339221, 41.45724293864769550 ) ) ;
#7397 = CARTESIAN_POINT ( 'NONE',  ( -8.224510206698735004, -14.34966873604973081, 29.58442372801901854 ) ) ;
#7398 = CARTESIAN_POINT ( 'NONE',  ( 19.05341960407611168, 5.049401038298154454, 53.95724293864770260 ) ) ;
#7399 = CARTESIAN_POINT ( 'NONE',  ( -0.05219959533909027116, -19.03943276465977164, 67.49890960531436690 ) ) ;
#7400 = CARTESIAN_POINT ( 'NONE',  ( -10.72451020669898014, 18.67979575497178502, 25.41557627198103120 ) ) ;
#7401 = CARTESIAN_POINT ( 'NONE',  ( -17.49999999999999645, 5.499999999999997335, 22.00000000000000711 ) ) ;
#7402 = CARTESIAN_POINT ( 'NONE',  ( -19.02544592524334988, -5.153800228976617603, 98.95942372801900433 ) ) ;
#7403 = CARTESIAN_POINT ( 'NONE',  ( 19.05341960407617918, -5.049401038297876454, 51.04275706135231871 ) ) ;
#7404 = CARTESIAN_POINT ( 'NONE',  ( 5.823673210054125526, 21.52544592524343514, 89.79057627198103830 ) ) ;
#7405 = CARTESIAN_POINT ( 'NONE',  ( 4.379528057220092307, 16.55341960407617563, 107.2927570613523471 ) ) ;
#7406 = CIRCLE ( 'NONE', #188271, 28.90000000000004476 ) ;
#7407 = CARTESIAN_POINT ( 'NONE',  ( -0.05219959533907301413, -21.53943276465977519, 47.49890960531435979 ) ) ;
#7409 = CARTESIAN_POINT ( 'NONE',  ( -13.97604488694547697, 13.89961937509957934, 103.1260903946856473 ) ) ;
#7408 = CARTESIAN_POINT ( 'NONE',  ( -15.72974639402197994, 15.80617190586746368, 75.62390960531439532 ) ) ;
#7410 = CARTESIAN_POINT ( 'NONE',  ( -19.02544592524342804, 5.153800228976336051, 101.0405762719810241 ) ) ;
#7411 = CARTESIAN_POINT ( 'NONE',  ( -10.72451020669870658, -18.67979575497194134, 69.58442372801900433 ) ) ;
#7412 = CARTESIAN_POINT ( 'NONE',  ( 19.02544592524343514, -5.153800228976328945, 68.54057627198103830 ) ) ;
#7413 = CARTESIAN_POINT ( 'NONE',  ( 31.68669428337295102, 6.716517432552111977, 91.65365426639641555 ) ) ;
#7414 = CARTESIAN_POINT ( 'NONE',  ( -16.46253265017160317, 9.564922557960807481, 70.83224293864770971 ) ) ;
#7415 = CARTESIAN_POINT ( 'NONE',  ( -14.29746914071049879, 8.314922557960819915, 90.83224293864769550 ) ) ;
#7416 = ORIENTED_EDGE ( 'NONE', *, *, #68419, .F. ) ;
#7417 = CARTESIAN_POINT ( 'NONE',  ( 19.03943276465977164, 0.05219959533936151252, 106.2510903946856615 ) ) ;
#7418 = CARTESIAN_POINT ( 'NONE',  ( 17.44279575226823908, -5.990770900252459619, 83.33557567514316133 ) ) ;
#7419 = CARTESIAN_POINT ( 'NONE',  ( 5.153800228976335163, 19.02544592524342804, 69.79057627198103830 ) ) ;
#7421 = CARTESIAN_POINT ( 'NONE',  ( 0.05219959533909260263, 19.03943276465977164, 99.99890960531436690 ) ) ;
#7420 = CARTESIAN_POINT ( 'NONE',  ( 5.719274019375673035, 21.55341960407619339, 87.29275706135236135 ) ) ;
#7422 = CARTESIAN_POINT ( 'NONE',  ( 4.379528057220092307, 16.55341960407617563, 72.29275706135236135 ) ) ;
#7423 = CARTESIAN_POINT ( 'NONE',  ( -29.15849868437705439, -10.00000000000000000, 150.0000000000000000 ) ) ;
#7424 = CARTESIAN_POINT ( 'NONE',  ( 13.97604488694548053, -13.89961937509957401, 50.62609039468566152 ) ) ;
#7425 = CARTESIAN_POINT ( 'NONE',  ( -15.80617190586768217, 15.72974639402176855, 108.1260903946856757 ) ) ;
#7426 = CARTESIAN_POINT ( 'NONE',  ( 5.267258167721604600, 6.873473828371179373, -64.05152134952703591 ) ) ;
#7427 = DIRECTION ( 'NONE',  ( 0.7071067811865483499, 0.000000000000000000, -0.7071067811865465735 ) ) ;
#7428 = CARTESIAN_POINT ( 'NONE',  ( -36.91746825000000598, 2.428612866367529932E-14, -5.124999997268813168 ) ) ;
#7429 = CARTESIAN_POINT ( 'NONE',  ( 8.314922557961029526, -14.29746914071037800, 110.4177570613523756 ) ) ;
#7430 = CARTESIAN_POINT ( 'NONE',  ( 16.51473224551083163, -9.474510206698727899, 75.83442372801900433 ) ) ;
#7431 = CARTESIAN_POINT ( 'NONE',  ( -12.14591786802326823, 12.06949235617739902, 98.12609039468570415 ) ) ;
#7432 = CARTESIAN_POINT ( 'NONE',  ( 33.67159378368906175, -21.59246066468708847, -24.63947658914731420 ) ) ;
#7433 = CARTESIAN_POINT ( 'NONE',  ( 14.34966873604972726, -8.224510206698740333, 70.83442372801901854 ) ) ;
#7434 = CARTESIAN_POINT ( 'NONE',  ( -15.80617190586768217, 15.72974639402176855, 78.12609039468570415 ) ) ;
#7435 = CARTESIAN_POINT ( 'NONE',  ( -19.02544592524334988, -5.153800228976617603, 88.95942372801897591 ) ) ;
#7436 = CARTESIAN_POINT ( 'NONE',  ( -13.97604488694547697, 13.89961937509957934, 38.12609039468566152 ) ) ;
#7437 = CARTESIAN_POINT ( 'NONE',  ( -5.049401038298153566, 19.05341960407611168, 85.20724293864766707 ) ) ;
#7438 = CARTESIAN_POINT ( 'NONE',  ( -5.153800228976328057, -19.02544592524343514, 57.29057627198103120 ) ) ;
#7439 = CARTESIAN_POINT ( 'NONE',  ( -18.39635199886966177, 5.500000000000103029, 41.01967076359999709 ) ) ;
#7440 = CARTESIAN_POINT ( 'NONE',  ( -5.823673210054116645, -21.52544592524344225, 77.29057627198102409 ) ) ;
#7441 = CARTESIAN_POINT ( 'NONE',  ( 10.81492255796078972, 18.62759615963270932, 54.58224293864769550 ) ) ;
#7442 = CARTESIAN_POINT ( 'NONE',  ( -19.03943276465977164, 0.05219959533909376836, 31.24890960531435979 ) ) ;
#7443 = CARTESIAN_POINT ( 'NONE',  ( -14.29746914071037622, -8.314922557961029526, 64.16775706135234714 ) ) ;
#7444 = UNCERTAINTY_MEASURE_WITH_UNIT (LENGTH_MEASURE( 1.000000000000000082E-05 ), #170444, 'distance_accuracy_value', 'NONE');
#7445 = EDGE_LOOP ( 'NONE', ( #130021, #155977, #65948, #134955 ) ) ;
#7446 = CARTESIAN_POINT ( 'NONE',  ( 21.53943276465977519, 0.05219959533937863772, 51.25109039468568994 ) ) ;
#7448 = CARTESIAN_POINT ( 'NONE',  ( -36.91746825000000598, 2.428612866367529932E-14, -10.62499999726881406 ) ) ;
#7447 = CARTESIAN_POINT ( 'NONE',  ( -16.53943276465976808, 0.05219959533911058130, 71.24890960531435269 ) ) ;
#7449 = CARTESIAN_POINT ( 'NONE',  ( -16.52544592524335698, -4.483927247898792601, 38.95942372801901854 ) ) ;
#7450 = CARTESIAN_POINT ( 'NONE',  ( -14.34966873604960291, -8.224510206698953496, 106.6655762719810383 ) ) ;
#7451 = CARTESIAN_POINT ( 'NONE',  ( -9.474510206698720793, -16.51473224551083518, 54.58442372801899722 ) ) ;
#7452 = CARTESIAN_POINT ( 'NONE',  ( 8.224510206698953496, -14.34966873604960469, 62.91557627198102409 ) ) ;
#7453 = CARTESIAN_POINT ( 'NONE',  ( -21.55341960407619339, 5.719274019375674811, 38.54275706135234714 ) ) ;
#7455 = CARTESIAN_POINT ( 'NONE',  ( 18.62759615963271287, -10.81492255796078972, 88.33224293864769550 ) ) ;
#7454 = LINE ( 'NONE', #67143, #166615 ) ;
#7456 = CARTESIAN_POINT ( 'NONE',  ( 16.51473224551069308, 9.474510206698969483, 109.1655762719810383 ) ) ;
#7457 = CARTESIAN_POINT ( 'NONE',  ( 16.55341960407611168, 4.379528057220329451, 73.95724293864769550 ) ) ;
#7458 = CARTESIAN_POINT ( 'NONE',  ( 30.87493573979816119, -25.21320017017430715, -21.56479137965274973 ) ) ;
#7459 = CARTESIAN_POINT ( 'NONE',  ( -22.81625015709509441, -31.40387420917324590, -2.324999997268813345 ) ) ;
#7460 = CARTESIAN_POINT ( 'NONE',  ( 9.564922557961047289, -16.46253265017146816, 85.41775706135233293 ) ) ;
#7461 = CARTESIAN_POINT ( 'NONE',  ( 21.52544592524334988, 5.823673210054432836, 26.45942372801901854 ) ) ;
#7462 = CARTESIAN_POINT ( 'NONE',  ( 19.02544592524343514, -5.153800228976328945, 63.54057627198103830 ) ) ;
#7463 = CARTESIAN_POINT ( 'NONE',  ( -13.97604488694547697, 13.89961937509957934, 53.12609039468565442 ) ) ;
#7464 = CARTESIAN_POINT ( 'NONE',  ( -16.51473224551069308, -9.474510206698971260, 36.66557627198102409 ) ) ;
#7465 = CARTESIAN_POINT ( 'NONE',  ( -18.62759615963255300, -10.81492255796106328, 69.16775706135234714 ) ) ;
#7466 = ADVANCED_FACE ( 'NONE', ( #43887 ), #170200, .T. ) ;
#7467 = CARTESIAN_POINT ( 'NONE',  ( -17.40805194822030089, -6.112264579159311317, 69.16628727489386108 ) ) ;
#7468 = CARTESIAN_POINT ( 'NONE',  ( -0.05219959533910754901, -16.53943276465976808, 52.49890960531435979 ) ) ;
#7469 = CARTESIAN_POINT ( 'NONE',  ( 13.89961937509977652, -13.97604488694527269, 58.12390960531436690 ) ) ;
#7470 = CARTESIAN_POINT ( 'NONE',  ( -21.52544592524343514, 5.823673210054127303, 91.04057627198103830 ) ) ;
#7471 = CARTESIAN_POINT ( 'NONE',  ( -9.564922557960796823, -16.46253265017161027, 57.08224293864769550 ) ) ;
#7472 = ORIENTED_EDGE ( 'NONE', *, *, #110611, .F. ) ;
#7473 = CARTESIAN_POINT ( 'NONE',  ( 21.55341960407610458, 5.719274019375980345, 78.95724293864769550 ) ) ;
#7474 = CARTESIAN_POINT ( 'NONE',  ( -21.53943276465977519, -0.05219959533937600094, 93.75109039468567573 ) ) ;
#7477 = CARTESIAN_POINT ( 'NONE',  ( 4.483927247898545687, 16.52544592524342804, 99.79057627198103830 ) ) ;
#7476 = CARTESIAN_POINT ( 'NONE',  ( -14.34966873604972548, 8.224510206698743886, 98.33442372801901854 ) ) ;
#7475 = CARTESIAN_POINT ( 'NONE',  ( -5.049401038298153566, 19.05341960407611168, 25.20724293864768484 ) ) ;
#7478 = CARTESIAN_POINT ( 'NONE',  ( 5.049401038297881783, 19.05341960407617563, 87.29275706135234714 ) ) ;
#7479 = ORIENTED_EDGE ( 'NONE', *, *, #86511, .F. ) ;
#7480 = CARTESIAN_POINT ( 'NONE',  ( -15.80617190586745835, -15.72974639402198527, 111.8739096053143669 ) ) ;
#7481 = CARTESIAN_POINT ( 'NONE',  ( 0.05219959533936267826, -19.03943276465977164, 40.00109039468566152 ) ) ;
#7482 = CARTESIAN_POINT ( 'NONE',  ( 0.05219959533934541429, -16.53943276465976808, 100.0010903946857042 ) ) ;
#7483 = CARTESIAN_POINT ( 'NONE',  ( -9.474510206698720793, -16.51473224551083518, 24.58442372801900078 ) ) ;
#7484 = CARTESIAN_POINT ( 'NONE',  ( -16.51473224551069308, -9.474510206698971260, 101.6655762719810241 ) ) ;
#7485 = CARTESIAN_POINT ( 'NONE',  ( 21.52544592524344225, -5.823673210054117533, 58.54057627198103120 ) ) ;
#7486 = CARTESIAN_POINT ( 'NONE',  ( -24.02706313830240603, 14.44797190822832711, 165.8682408883346113 ) ) ;
#7487 = CARTESIAN_POINT ( 'NONE',  ( -13.97604488694527625, -13.89961937509977652, 26.87390960531434558 ) ) ;
#7488 = CARTESIAN_POINT ( 'NONE',  ( 5.823673210054444382, -21.52544592524334988, 110.2094237280190185 ) ) ;
#7489 = CARTESIAN_POINT ( 'NONE',  ( -8.224510206698735004, -14.34966873604973081, 69.58442372801900433 ) ) ;
#7490 = CARTESIAN_POINT ( 'NONE',  ( -5.823673210054431948, 21.52544592524334988, 22.70942372801901499 ) ) ;
#7491 = CARTESIAN_POINT ( 'NONE',  ( 16.52544592524335698, 4.483927247898782831, 36.45942372801901143 ) ) ;
#7492 = CARTESIAN_POINT ( 'NONE',  ( -19.02544592524342804, 5.153800228976336051, 106.0405762719810241 ) ) ;
#7493 = CARTESIAN_POINT ( 'NONE',  ( 19.05341960407611168, 5.049401038298154454, 43.95724293864769550 ) ) ;
#7494 = CARTESIAN_POINT ( 'NONE',  ( -16.51473224551069308, -9.474510206698971260, 71.66557627198102409 ) ) ;
#7495 = CARTESIAN_POINT ( 'NONE',  ( -16.55341960407617563, 4.379528057220093196, 53.54275706135234714 ) ) ;
#7496 = CARTESIAN_POINT ( 'NONE',  ( 14.29746914071049879, -8.314922557960816363, 88.33224293864769550 ) ) ;
#7497 = CARTESIAN_POINT ( 'NONE',  ( -16.53943276465976808, -0.05219959533934237506, 103.7510903946857042 ) ) ;
#7498 = CARTESIAN_POINT ( 'NONE',  ( -30.00000000000000000, -1.130961319012580892E-14, 92.35000000000000853 ) ) ;
#7501 = CARTESIAN_POINT ( 'NONE',  ( 16.51473224551069308, 9.474510206698969483, 59.16557627198102409 ) ) ;
#7500 = CARTESIAN_POINT ( 'NONE',  ( 13.97604488694527802, 13.89961937509977652, 74.37390960531436690 ) ) ;
#7499 = CARTESIAN_POINT ( 'NONE',  ( -10.81492255796105439, 18.62759615963255655, 57.91775706135234714 ) ) ;
#7502 = CARTESIAN_POINT ( 'NONE',  ( 5.049401038298161559, -19.05341960407611168, 92.70724293864769550 ) ) ;
#7503 = CARTESIAN_POINT ( 'NONE',  ( -0.05219959533910754901, -16.53943276465976808, 42.49890960531435979 ) ) ;
#7504 = CARTESIAN_POINT ( 'NONE',  ( 16.53943276465976808, 0.05219959533934440121, 101.2510903946856757 ) ) ;
#7505 = EDGE_LOOP ( 'NONE', ( #18975, #111133, #32322, #195295, #124314, #19951 ) ) ;
#7506 = CARTESIAN_POINT ( 'NONE',  ( 9.474510206698729675, 16.51473224551082808, 42.08442372801900433 ) ) ;
#7507 = CARTESIAN_POINT ( 'NONE',  ( -19.02544592524342804, 5.153800228976336051, 111.0405762719810099 ) ) ;
#7508 = CARTESIAN_POINT ( 'NONE',  ( -16.46253265017160317, 9.564922557960807481, 65.83224293864769550 ) ) ;
#7509 = CARTESIAN_POINT ( 'NONE',  ( -19.03943276465977164, -0.05219959533935918106, 33.75109039468566863 ) ) ;
#7510 = CARTESIAN_POINT ( 'NONE',  ( 29.86685920354754842, -21.69954338932559068, -7.824999997268813345 ) ) ;
#7511 = CARTESIAN_POINT ( 'NONE',  ( 19.01533133064925352, -5.499999999999438671, 71.26586590595739779 ) ) ;
#7513 = CARTESIAN_POINT ( 'NONE',  ( 14.29746914071037800, 8.314922557961029526, 66.66775706135234714 ) ) ;
#7512 = CARTESIAN_POINT ( 'NONE',  ( 13.97604488694548053, -13.89961937509957401, 65.62609039468567573 ) ) ;
#7514 = CARTESIAN_POINT ( 'NONE',  ( 17.40861289039003523, 6.110651285853315962, 93.87232470827436259 ) ) ;
#7515 = CARTESIAN_POINT ( 'NONE',  ( 9.564922557960805705, 16.46253265017160317, 84.58224293864769550 ) ) ;
#7516 = CARTESIAN_POINT ( 'NONE',  ( -18.62759615963255300, -10.81492255796106328, 29.16775706135234003 ) ) ;
#7517 = CARTESIAN_POINT ( 'NONE',  ( -19.05341960407617563, 5.049401038297882671, 78.54275706135233293 ) ) ;
#7519 = CARTESIAN_POINT ( 'NONE',  ( 0.05219959533909260263, 19.03943276465977164, 39.99890960531436690 ) ) ;
#7518 = CARTESIAN_POINT ( 'NONE',  ( 13.97604488694527802, 13.89961937509977652, 114.3739096053143669 ) ) ;
#7520 = EDGE_CURVE ( 'NONE', #167413, #66922, #31693, .T. ) ;
#7521 = CARTESIAN_POINT ( 'NONE',  ( -9.474510206698964154, 16.51473224551069663, 85.41557627198102409 ) ) ;
#7523 = CARTESIAN_POINT ( 'NONE',  ( -5.049401038298153566, 19.05341960407611168, 35.20724293864768839 ) ) ;
#7522 = CARTESIAN_POINT ( 'NONE',  ( 16.55341960407611168, 4.379528057220329451, 43.95724293864769550 ) ) ;
#7524 = CARTESIAN_POINT ( 'NONE',  ( 13.97604488694548053, -13.89961937509957401, 45.62609039468566863 ) ) ;
#7525 = CARTESIAN_POINT ( 'NONE',  ( -16.55341960407611168, -4.379528057220339221, 81.45724293864769550 ) ) ;
#7526 = CARTESIAN_POINT ( 'NONE',  ( 5.719274019375673035, 21.55341960407619339, 107.2927570613523471 ) ) ;
#7527 = CARTESIAN_POINT ( 'NONE',  ( 13.89961937509977652, -13.97604488694527269, 53.12390960531434558 ) ) ;
#7528 = CARTESIAN_POINT ( 'NONE',  ( -5.719274019375978568, 21.55341960407610458, 60.20724293864768839 ) ) ;
#7530 = CARTESIAN_POINT ( 'NONE',  ( -13.89961937509957401, -13.97604488694547875, 24.37609039468565442 ) ) ;
#7529 = CARTESIAN_POINT ( 'NONE',  ( -4.483927247898539470, -16.52544592524342804, 57.29057627198103120 ) ) ;
#7531 = CARTESIAN_POINT ( 'NONE',  ( -13.97604488694527625, -13.89961937509977652, 106.8739096053143669 ) ) ;
#7532 = CARTESIAN_POINT ( 'NONE',  ( -15.80617190586745835, -15.72974639402198527, 21.87390960531436690 ) ) ;
#7533 = CARTESIAN_POINT ( 'NONE',  ( -13.89961937509977652, 13.97604488694528158, 50.62390960531435979 ) ) ;
#7534 = CARTESIAN_POINT ( 'NONE',  ( -16.46253265017160317, 9.564922557960807481, 25.83224293864769194 ) ) ;
#7535 = CARTESIAN_POINT ( 'NONE',  ( -12.06949235617756955, 12.14591786802309770, 85.62390960531436690 ) ) ;
#7536 = CARTESIAN_POINT ( 'NONE',  ( 21.53943276465977519, -0.05219959533907433946, 103.7489096053143669 ) ) ;
#7537 = CARTESIAN_POINT ( 'NONE',  ( 5.049401038298161559, -19.05341960407611168, 107.7072429386476955 ) ) ;
#7538 = CARTESIAN_POINT ( 'NONE',  ( -15.72974639402197994, 15.80617190586746368, 115.6239096053143669 ) ) ;
#7539 = CARTESIAN_POINT ( 'NONE',  ( 19.03943276465977164, -0.05219959533909143690, 103.7489096053143669 ) ) ;
#7540 = CARTESIAN_POINT ( 'NONE',  ( -16.51473224551069308, -9.474510206698971260, 21.66557627198102765 ) ) ;
#7541 = CARTESIAN_POINT ( 'NONE',  ( -5.719274019375665041, -21.55341960407619695, 74.79275706135234714 ) ) ;
#7542 = CARTESIAN_POINT ( 'NONE',  ( -15.80617190586745835, -15.72974639402198527, 91.87390960531436690 ) ) ;
#7543 = DIRECTION ( 'NONE',  ( 1.000000000000000000, 0.000000000000000000, 0.000000000000000000 ) ) ;
#7544 = CARTESIAN_POINT ( 'NONE',  ( 21.49604614807111602, 21.49604614807102720, -64.92279855667830191 ) ) ;
#7545 = CARTESIAN_POINT ( 'NONE',  ( 11.80868324581538253, -11.80868324581533457, -61.34707691135562868 ) ) ;
#7546 = CARTESIAN_POINT ( 'NONE',  ( -14.34966873604972548, 8.224510206698743886, 38.33442372801900433 ) ) ;
#7547 = CARTESIAN_POINT ( 'NONE',  ( -8.224510206698948167, 14.34966873604960824, 105.4155762719810383 ) ) ;
#7548 = CARTESIAN_POINT ( 'NONE',  ( 19.01533133064921799, -5.499999999999651834, 51.26586590595738357 ) ) ;
#7549 = CARTESIAN_POINT ( 'NONE',  ( -9.564922557960796823, -16.46253265017161027, 62.08224293864769550 ) ) ;
#7550 = CARTESIAN_POINT ( 'NONE',  ( -0.05219959533910754901, -16.53943276465976808, 97.49890960531436690 ) ) ;
#7551 = VECTOR ( 'NONE', #58066, 1000.000000000000114 ) ;
#7552 = CARTESIAN_POINT ( 'NONE',  ( 15.80617190586746368, 15.72974639402197994, 29.37390960531435269 ) ) ;
#7553 = CARTESIAN_POINT ( 'NONE',  ( 0.05219959533910956823, 16.53943276465976808, 69.99890960531435269 ) ) ;
#7554 = CARTESIAN_POINT ( 'NONE',  ( 16.52544592524335698, 4.483927247898782831, 21.45942372801901499 ) ) ;
#7555 = CARTESIAN_POINT ( 'NONE',  ( 5.719274019375673035, 21.55341960407619339, 67.29275706135234714 ) ) ;
#7556 = CARTESIAN_POINT ( 'NONE',  ( 16.81555441253551919, -7.025013491695474954, 78.13685445334255064 ) ) ;
#7557 = CARTESIAN_POINT ( 'NONE',  ( -16.46253265017160317, 9.564922557960807481, 110.8322429386476955 ) ) ;
#7558 = CARTESIAN_POINT ( 'NONE',  ( -0.05219959533934338120, 16.53943276465976808, 102.5010903946856899 ) ) ;
#7559 = CARTESIAN_POINT ( 'NONE',  ( 13.89961937509977652, -13.97604488694527269, 43.12390960531434558 ) ) ;
#7560 = CARTESIAN_POINT ( 'NONE',  ( -19.05341960407611168, -5.049401038298163336, 86.45724293864769550 ) ) ;
#7561 = CARTESIAN_POINT ( 'NONE',  ( 0.05219959533907565091, 21.53943276465977519, 99.99890960531436690 ) ) ;
#7562 = CARTESIAN_POINT ( 'NONE',  ( 4.483927247898790824, -16.52544592524335698, 20.20942372801900788 ) ) ;
#7564 = CARTESIAN_POINT ( 'NONE',  ( -21.55341960407619339, 5.719274019375674811, 78.54275706135236135 ) ) ;
#7563 = CARTESIAN_POINT ( 'NONE',  ( 16.52544592524342804, -4.483927247898539470, 63.54057627198103830 ) ) ;
#7565 = CARTESIAN_POINT ( 'NONE',  ( -4.379528057220086978, -16.55341960407618274, 104.7927570613523898 ) ) ;
#7566 = CARTESIAN_POINT ( 'NONE',  ( 16.88567814943192857, -6.947325034625397855, 46.20998877347406619 ) ) ;
#7567 = CARTESIAN_POINT ( 'NONE',  ( 3.181980515339834614, 34.99999999999997158, 1.110912703473986074 ) ) ;
#7568 = CARTESIAN_POINT ( 'NONE',  ( -12.14591786802309592, -12.06949235617757132, 31.87390960531435979 ) ) ;
#7569 = CARTESIAN_POINT ( 'NONE',  ( 4.483927247898790824, -16.52544592524335698, 70.20942372801904696 ) ) ;
#7570 = CARTESIAN_POINT ( 'NONE',  ( 19.05341960407611168, 5.049401038298154454, 88.95724293864769550 ) ) ;
#7571 = CARTESIAN_POINT ( 'NONE',  ( 0.05219959533909260263, 19.03943276465977164, 84.99890960531436690 ) ) ;
#7572 = CARTESIAN_POINT ( 'NONE',  ( -21.53943276465977519, -0.05219959533937600094, 83.75109039468568994 ) ) ;
#7573 = CARTESIAN_POINT ( 'NONE',  ( 8.314922557961029526, -14.29746914071037800, 90.41775706135236135 ) ) ;
#7574 = CARTESIAN_POINT ( 'NONE',  ( -16.53943276465976808, 0.05219959533911058130, 66.24890960531436690 ) ) ;
#7575 = CARTESIAN_POINT ( 'NONE',  ( 9.474510206698971260, -16.51473224551069308, 67.91557627198102409 ) ) ;
#7576 = ORIENTED_EDGE ( 'NONE', *, *, #27260, .F. ) ;
#7577 = CARTESIAN_POINT ( 'NONE',  ( -13.89961937509957401, -13.97604488694547875, 109.3760903946856331 ) ) ;
#7578 = CARTESIAN_POINT ( 'NONE',  ( 12.06949235617757843, -12.14591786802309237, 108.1239096053143811 ) ) ;
#7579 = CARTESIAN_POINT ( 'NONE',  ( -19.03943276465977164, 0.05219959533909376836, 81.24890960531436690 ) ) ;
#7581 = CARTESIAN_POINT ( 'NONE',  ( 36.91746825000000598, -11.99521256947793546, -5.724999997268813701 ) ) ;
#7580 = CARTESIAN_POINT ( 'NONE',  ( -13.97604488694547697, 13.89961937509957934, 113.1260903946856757 ) ) ;
#7582 = CARTESIAN_POINT ( 'NONE',  ( 16.51473224551083163, -9.474510206698727899, 20.83442372801899722 ) ) ;
#7583 = CARTESIAN_POINT ( 'NONE',  ( 16.55341960407618274, -4.379528057220086978, 81.04275706135236135 ) ) ;
#7584 = CARTESIAN_POINT ( 'NONE',  ( -13.97604488694547697, 13.89961937509957934, 93.12609039468566152 ) ) ;
#7585 = CARTESIAN_POINT ( 'NONE',  ( 5.049401038298161559, -19.05341960407611168, 22.70724293864769194 ) ) ;
#7586 = CARTESIAN_POINT ( 'NONE',  ( -4.379528057220086978, -16.55341960407618274, 64.79275706135234714 ) ) ;
#7587 = CARTESIAN_POINT ( 'NONE',  ( -69.65682714487590488, -71.74905178543390605, 0.000000000000000000 ) ) ;
#7588 = CARTESIAN_POINT ( 'NONE',  ( -5.049401038297874678, -19.05341960407617918, 49.79275706135231871 ) ) ;
#7589 = CARTESIAN_POINT ( 'NONE',  ( 18.67979575497194134, -10.72451020669871369, 100.8344237280190185 ) ) ;
#7590 = CARTESIAN_POINT ( 'NONE',  ( 0.05219959533909260263, 19.03943276465977164, 34.99890960531435979 ) ) ;
#7591 = CARTESIAN_POINT ( 'NONE',  ( 16.46253265017160672, -9.564922557960803928, 78.33224293864769550 ) ) ;
#7592 = CARTESIAN_POINT ( 'NONE',  ( 16.53943276465976808, -0.05219959533910856209, 68.74890960531435269 ) ) ;
#7593 = CARTESIAN_POINT ( 'NONE',  ( -15.72974639402176322, -15.80617190586768395, 84.37609039468570415 ) ) ;
#7594 = EDGE_CURVE ( 'NONE', #181556, #117432, #185718, .T. ) ;
#7595 = CARTESIAN_POINT ( 'NONE',  ( 5.153800228976615827, -19.02544592524334988, 60.20942372801899012 ) ) ;
#7596 = CARTESIAN_POINT ( 'NONE',  ( -5.049401038297874678, -19.05341960407617918, 39.79275706135232582 ) ) ;
#7597 = CARTESIAN_POINT ( 'NONE',  ( 21.53943276465977519, -0.05219959533907433946, 33.74890960531436690 ) ) ;
#7598 = CARTESIAN_POINT ( 'NONE',  ( 15.72974639402176855, 15.80617190586768217, 96.87609039468568994 ) ) ;
#7599 = CARTESIAN_POINT ( 'NONE',  ( 13.97604488694527802, 13.89961937509977652, 74.37390960531436690 ) ) ;
#7600 = CARTESIAN_POINT ( 'NONE',  ( 21.52544592524334988, 5.823673210054432836, 111.4594237280190328 ) ) ;
#7601 = CARTESIAN_POINT ( 'NONE',  ( -21.53943276465977519, 0.05219959533907696930, 51.24890960531436690 ) ) ;
#7602 = CARTESIAN_POINT ( 'NONE',  ( 13.89961937509977652, -13.97604488694527269, 93.12390960531436690 ) ) ;
#7603 = CARTESIAN_POINT ( 'NONE',  ( 9.564922557961047289, -16.46253265017146816, 80.41775706135234714 ) ) ;
#7604 = CARTESIAN_POINT ( 'NONE',  ( 19.02544592524343514, -5.153800228976328945, 108.5405762719810383 ) ) ;
#7605 = CARTESIAN_POINT ( 'NONE',  ( -13.89961937509957401, -13.97604488694547875, 94.37609039468566152 ) ) ;
#7606 = CARTESIAN_POINT ( 'NONE',  ( -14.34966873604972548, 8.224510206698743886, 48.33442372801902565 ) ) ;
#7607 = CARTESIAN_POINT ( 'NONE',  ( -12.06949235617756955, 12.14591786802309770, 100.6239096053143811 ) ) ;
#7608 = CARTESIAN_POINT ( 'NONE',  ( 13.89961937509977652, -13.97604488694527269, 88.12390960531438111 ) ) ;
#7609 = EDGE_CURVE ( 'NONE', #24124, #177464, #30709, .T. ) ;
#7610 = CARTESIAN_POINT ( 'NONE',  ( -15.80617190586745835, -15.72974639402198527, 61.87390960531436690 ) ) ;
#7611 = CARTESIAN_POINT ( 'NONE',  ( 8.224510206698742110, 14.34966873604972548, 37.08442372801901143 ) ) ;
#7612 = CARTESIAN_POINT ( 'NONE',  ( 18.62759615963255655, 10.81492255796105972, 36.66775706135234714 ) ) ;
#7613 = CARTESIAN_POINT ( 'NONE',  ( -15.72974639402176322, -15.80617190586768395, 79.37609039468567573 ) ) ;
#7614 = CARTESIAN_POINT ( 'NONE',  ( 14.34966873604972726, -8.224510206698740333, 80.83442372801901854 ) ) ;
#7615 = AXIS2_PLACEMENT_3D ( 'NONE', #110151, #93979, #124319 ) ;
#7616 = CARTESIAN_POINT ( 'NONE',  ( 19.02544592524343514, -5.153800228976328945, 78.54057627198099567 ) ) ;
#7617 = CARTESIAN_POINT ( 'NONE',  ( 16.52544592524342804, -4.483927247898539470, 73.54057627198102409 ) ) ;
#7618 = CARTESIAN_POINT ( 'NONE',  ( -4.379528057220086978, -16.55341960407618274, 109.7927570613523613 ) ) ;
#7619 = CARTESIAN_POINT ( 'NONE',  ( 9.564922557961047289, -16.46253265017146816, 60.41775706135233293 ) ) ;
#7620 = CARTESIAN_POINT ( 'NONE',  ( 21.55341960407619695, -5.719274019375665929, 31.04275706135234714 ) ) ;
#7621 = CARTESIAN_POINT ( 'NONE',  ( -4.483927247898539470, -16.52544592524342804, 77.29057627198102409 ) ) ;
#7622 = CARTESIAN_POINT ( 'NONE',  ( 0.05219959533909260263, 19.03943276465977164, 99.99890960531436690 ) ) ;
#7623 = CARTESIAN_POINT ( 'NONE',  ( -16.55341960407617563, 4.379528057220093196, 108.5427570613523756 ) ) ;
#7624 = CARTESIAN_POINT ( 'NONE',  ( -15.72974639402176322, -15.80617190586768395, 74.37609039468568994 ) ) ;
#7625 = CARTESIAN_POINT ( 'NONE',  ( -0.05219959533934338120, 16.53943276465976808, 47.50109039468568994 ) ) ;
#7626 = CARTESIAN_POINT ( 'NONE',  ( -10.72451020669870658, -18.67979575497194134, 34.58442372801900433 ) ) ;
#7627 = CARTESIAN_POINT ( 'NONE',  ( -16.55341960407611168, -4.379528057220339221, 71.45724293864769550 ) ) ;
#7628 = ORIENTED_EDGE ( 'NONE', *, *, #49174, .T. ) ;
#7629 = CARTESIAN_POINT ( 'NONE',  ( -5.719274019375978568, 21.55341960407610458, 110.2072429386477239 ) ) ;
#7630 = CARTESIAN_POINT ( 'NONE',  ( 16.53943276465976808, -0.05219959533910856209, 93.74890960531436690 ) ) ;
#7631 = CARTESIAN_POINT ( 'NONE',  ( -19.52851543214742236, -5.500000000000036415, 50.39357721762583964 ) ) ;
#7632 = CARTESIAN_POINT ( 'NONE',  ( -4.379528057220328563, 16.55341960407611168, 55.20724293864770260 ) ) ;
#7633 = CARTESIAN_POINT ( 'NONE',  ( -5.049401038298153566, 19.05341960407611168, 30.20724293864768839 ) ) ;
#7634 = CARTESIAN_POINT ( 'NONE',  ( -10.81492255796078084, -18.62759615963271287, 47.08224293864770260 ) ) ;
#7635 = CARTESIAN_POINT ( 'NONE',  ( 16.55341960407611168, 4.379528057220329451, 83.95724293864770971 ) ) ;
#7636 = CARTESIAN_POINT ( 'NONE',  ( 18.67979575497178502, 10.72451020669898547, 84.16557627198103830 ) ) ;
#7637 = CARTESIAN_POINT ( 'NONE',  ( 19.03943276465977164, -0.05219959533909143690, 93.74890960531435269 ) ) ;
#7639 = CARTESIAN_POINT ( 'NONE',  ( -16.46253265017146816, -9.564922557961047289, 79.16775706135234714 ) ) ;
#7638 = CARTESIAN_POINT ( 'NONE',  ( 19.05341960407611168, 5.049401038298154454, 38.95724293864767418 ) ) ;
#7641 = CARTESIAN_POINT ( 'NONE',  ( 0.05219959533907565091, 21.53943276465977519, 64.99890960531435269 ) ) ;
#7640 = CARTESIAN_POINT ( 'NONE',  ( -18.62759615963255300, -10.81492255796106328, 59.16775706135234714 ) ) ;
#7642 = CARTESIAN_POINT ( 'NONE',  ( 0.05219959533909260263, 19.03943276465977164, 34.99890960531435979 ) ) ;
#7643 = CARTESIAN_POINT ( 'NONE',  ( -13.97604488694527625, -13.89961937509977652, 76.87390960531433848 ) ) ;
#7644 = ORIENTED_EDGE ( 'NONE', *, *, #25526, .F. ) ;
#7645 = CARTESIAN_POINT ( 'NONE',  ( 14.29746914071037800, 8.314922557961029526, 56.66775706135235424 ) ) ;
#7646 = CARTESIAN_POINT ( 'NONE',  ( 5.719274019375673035, 21.55341960407619339, 37.29275706135235424 ) ) ;
#7647 = CARTESIAN_POINT ( 'NONE',  ( 15.72974639402176855, 15.80617190586768217, 76.87609039468567573 ) ) ;
#7648 = CARTESIAN_POINT ( 'NONE',  ( 5.049401038298161559, -19.05341960407611168, 112.7072429386476813 ) ) ;
#7649 = CARTESIAN_POINT ( 'NONE',  ( -18.62759615963270932, 10.81492255796079327, 80.83224293864769550 ) ) ;
#7651 = CARTESIAN_POINT ( 'NONE',  ( 4.483927247898790824, -16.52544592524335698, 55.20942372801902565 ) ) ;
#7650 = CARTESIAN_POINT ( 'NONE',  ( 18.67979575497194134, -10.72451020669871369, 20.83442372801901143 ) ) ;
#7652 = CARTESIAN_POINT ( 'NONE',  ( 18.62759615963271287, -10.81492255796078972, 48.33224293864770260 ) ) ;
#7653 = CARTESIAN_POINT ( 'NONE',  ( 5.823673210054444382, -21.52544592524334988, 110.2094237280190185 ) ) ;
#7654 = CARTESIAN_POINT ( 'NONE',  ( 16.51473224551069308, 9.474510206698969483, 54.16557627198103120 ) ) ;
#7655 = CARTESIAN_POINT ( 'NONE',  ( -16.46253265017160317, 9.564922557960807481, 110.8322429386476955 ) ) ;
#7656 = CARTESIAN_POINT ( 'NONE',  ( -5.049401038298153566, 19.05341960407611168, 90.20724293864766707 ) ) ;
#7657 = CARTESIAN_POINT ( 'NONE',  ( 22.46063206192303241, 22.65278057777875986, -45.64921306006598911 ) ) ;
#7658 = CARTESIAN_POINT ( 'NONE',  ( -13.97604488694547697, 13.89961937509957934, 63.12609039468566152 ) ) ;
#7659 = CARTESIAN_POINT ( 'NONE',  ( 10.72451020669898902, -18.67979575497178502, 47.91557627198102409 ) ) ;
#7660 = CARTESIAN_POINT ( 'NONE',  ( 12.06949235617757843, -12.14591786802309237, 28.12390960531435979 ) ) ;
#7661 = CARTESIAN_POINT ( 'NONE',  ( 19.05341960407617918, -5.049401038297876454, 106.0427570613523471 ) ) ;
#7662 = CARTESIAN_POINT ( 'NONE',  ( 17.49999999999999289, 5.500000000000007994, 83.78230962303564411 ) ) ;
#7663 = CARTESIAN_POINT ( 'NONE',  ( 5.153800228976615827, -19.02544592524334988, 20.20942372801899722 ) ) ;
#7664 = CARTESIAN_POINT ( 'NONE',  ( -19.03943276465977164, -0.05219959533935918106, 98.75109039468567573 ) ) ;
#7666 = CARTESIAN_POINT ( 'NONE',  ( -13.97604488694547697, 13.89961937509957934, 58.12609039468566863 ) ) ;
#7665 = CARTESIAN_POINT ( 'NONE',  ( -0.05219959533907301413, -21.53943276465977519, 82.49890960531436690 ) ) ;
#7667 = LINE ( 'NONE', #113841, #95061 ) ;
#7668 = CARTESIAN_POINT ( 'NONE',  ( -19.05341960407611168, -5.049401038298163336, 61.45724293864769550 ) ) ;
#7669 = CARTESIAN_POINT ( 'NONE',  ( 16.52544592524342804, -4.483927247898539470, 68.54057627198103830 ) ) ;
#7670 = CARTESIAN_POINT ( 'NONE',  ( 13.89961937509977652, -13.97604488694527269, 48.12390960531435979 ) ) ;
#7671 = CARTESIAN_POINT ( 'NONE',  ( -8.224510206698948167, 14.34966873604960824, 45.41557627198103830 ) ) ;
#7672 = PLANE ( 'NONE',  #93602 ) ;
#7673 = CARTESIAN_POINT ( 'NONE',  ( -14.34966873604960291, -8.224510206698953496, 31.66557627198102054 ) ) ;
#7674 = CARTESIAN_POINT ( 'NONE',  ( 19.03943276465977164, -0.05219959533909143690, 58.74890960531435979 ) ) ;
#7675 = CARTESIAN_POINT ( 'NONE',  ( 13.97604488694548053, -13.89961937509957401, 30.62609039468566863 ) ) ;
#7676 = CARTESIAN_POINT ( 'NONE',  ( -4.483927247898782831, 16.52544592524335698, 37.70942372801900433 ) ) ;
#7677 = CARTESIAN_POINT ( 'NONE',  ( -21.53943276465977519, 0.05219959533907696930, 56.24890960531436690 ) ) ;
#7679 = VERTEX_POINT ( 'NONE', #61022 ) ;
#7678 = CARTESIAN_POINT ( 'NONE',  ( -21.55341960407619339, 5.719274019375674811, 103.5427570613523613 ) ) ;
#7680 = CARTESIAN_POINT ( 'NONE',  ( -16.46253265017160317, 9.564922557960807481, 65.83224293864769550 ) ) ;
#7681 = CARTESIAN_POINT ( 'NONE',  ( -9.474510206698964154, 16.51473224551069663, 115.4155762719810241 ) ) ;
#7682 = CARTESIAN_POINT ( 'NONE',  ( -16.46253265017160317, 9.564922557960807481, 90.83224293864769550 ) ) ;
#7683 = CARTESIAN_POINT ( 'NONE',  ( -11.40812507854755609, 35.11059874428196537, -1.024999997268813301 ) ) ;
#7684 = CARTESIAN_POINT ( 'NONE',  ( 18.62759615963255655, 10.81492255796105972, 31.66775706135234358 ) ) ;
#7685 = CARTESIAN_POINT ( 'NONE',  ( -16.53943276465976808, 0.05219959533911058130, 96.24890960531435269 ) ) ;
#7687 = CARTESIAN_POINT ( 'NONE',  ( -19.02544592524342804, 5.153800228976336051, 66.04057627198103830 ) ) ;
#7686 = CARTESIAN_POINT ( 'NONE',  ( 15.72974639402199770, -15.80617190586745480, 93.12390960531436690 ) ) ;
#7688 = CARTESIAN_POINT ( 'NONE',  ( 19.05341960407611168, 5.049401038298154454, 73.95724293864768129 ) ) ;
#7689 = CARTESIAN_POINT ( 'NONE',  ( -10.81492255796078084, -18.62759615963271287, 112.0822429386477097 ) ) ;
#7690 = ORIENTED_EDGE ( 'NONE', *, *, #48933, .F. ) ;
#7691 = CARTESIAN_POINT ( 'NONE',  ( 0.05219959533909260263, 19.03943276465977164, 74.99890960531435269 ) ) ;
#7692 = EDGE_CURVE ( 'NONE', #11205, #144964, #15531, .T. ) ;
#7693 = AXIS2_PLACEMENT_3D ( 'NONE', #192247, #178083, #22396 ) ;
#7694 = CARTESIAN_POINT ( 'NONE',  ( -13.70000000000001528, 1.443387660838688656E-13, -62.58071313852362039 ) ) ;
#7696 = CARTESIAN_POINT ( 'NONE',  ( -19.03943276465977164, 0.05219959533909376836, 26.24890960531435624 ) ) ;
#7695 = CARTESIAN_POINT ( 'NONE',  ( 16.55341960407611168, 4.379528057220329451, 108.9572429386476955 ) ) ;
#7697 = CARTESIAN_POINT ( 'NONE',  ( -9.564922557961040184, 16.46253265017147172, 97.91775706135233293 ) ) ;
#7698 = CARTESIAN_POINT ( 'NONE',  ( -8.314922557960811034, -14.29746914071050412, 102.0822429386476955 ) ) ;
#7699 = CARTESIAN_POINT ( 'NONE',  ( 18.67979575497194134, -10.72451020669871369, 70.83442372801901854 ) ) ;
#7701 = CARTESIAN_POINT ( 'NONE',  ( 21.52544592524334988, 5.823673210054432836, 36.45942372801901143 ) ) ;
#7700 = CARTESIAN_POINT ( 'NONE',  ( -0.05219959533909027116, -19.03943276465977164, 67.49890960531436690 ) ) ;
#7702 = CARTESIAN_POINT ( 'NONE',  ( 10.72451020669898902, -18.67979575497178502, 112.9155762719810383 ) ) ;
#7703 = CARTESIAN_POINT ( 'NONE',  ( -28.82186960331499037, 2.428612866367529932E-14, 139.9999999999999716 ) ) ;
#7704 = CARTESIAN_POINT ( 'NONE',  ( 9.474510206698971260, -16.51473224551069308, 77.91557627198103830 ) ) ;
#7705 = CARTESIAN_POINT ( 'NONE',  ( 26.82869043059737635, 7.693057566823323867, 166.5358880480721098 ) ) ;
#7707 = CARTESIAN_POINT ( 'NONE',  ( 15.80617190586746368, 15.72974639402197994, 24.37390960531435979 ) ) ;
#7706 = CARTESIAN_POINT ( 'NONE',  ( 16.52544592524335698, 4.483927247898782831, 26.45942372801901854 ) ) ;
#7708 = CARTESIAN_POINT ( 'NONE',  ( -0.05219959533937732626, 21.53943276465977519, 67.50109039468568994 ) ) ;
#7709 = CARTESIAN_POINT ( 'NONE',  ( -9.474510206698964154, 16.51473224551069663, 105.4155762719810383 ) ) ;
#7710 = CARTESIAN_POINT ( 'NONE',  ( -5.049401038297874678, -19.05341960407617918, 94.79275706135230450 ) ) ;
#7711 = CARTESIAN_POINT ( 'NONE',  ( 5.153800228976335163, 19.02544592524342804, 49.79057627198100988 ) ) ;
#7712 = CARTESIAN_POINT ( 'NONE',  ( 19.05341960407611168, 5.049401038298154454, 73.95724293864768129 ) ) ;
#7713 = CARTESIAN_POINT ( 'NONE',  ( 14.34966873604960469, 8.224510206698951720, 99.16557627198100988 ) ) ;
#7714 = CARTESIAN_POINT ( 'NONE',  ( 13.97604488694527802, 13.89961937509977652, 99.37390960531436690 ) ) ;
#7715 = CARTESIAN_POINT ( 'NONE',  ( -4.483927247898539470, -16.52544592524342804, 97.29057627198105251 ) ) ;
#7716 = CARTESIAN_POINT ( 'NONE',  ( 9.564922557960805705, 16.46253265017160317, 104.5822429386476955 ) ) ;
#7718 = CARTESIAN_POINT ( 'NONE',  ( 19.05341960407611168, 5.049401038298154454, 43.95724293864769550 ) ) ;
#7717 = CARTESIAN_POINT ( 'NONE',  ( -8.224510206698948167, 14.34966873604960824, 45.41557627198103830 ) ) ;
#7719 = CARTESIAN_POINT ( 'NONE',  ( -0.05219959533937732626, 21.53943276465977519, 52.50109039468567573 ) ) ;
#7720 = CARTESIAN_POINT ( 'NONE',  ( 13.89961937509957401, 13.97604488694547697, 96.87609039468566152 ) ) ;
#7721 = CARTESIAN_POINT ( 'NONE',  ( 14.34966873604960469, 8.224510206698951720, 44.16557627198103120 ) ) ;
#7722 = CARTESIAN_POINT ( 'NONE',  ( 18.67979575497178502, 10.72451020669898547, 104.1655762719810241 ) ) ;
#7723 = CARTESIAN_POINT ( 'NONE',  ( -0.05219959533907301413, -21.53943276465977519, 52.49890960531435979 ) ) ;
#7725 = CARTESIAN_POINT ( 'NONE',  ( -14.29746914071049879, 8.314922557960819915, 85.83224293864768129 ) ) ;
#7724 = CARTESIAN_POINT ( 'NONE',  ( -19.03943276465977164, 0.05219959533909376836, 111.2489096053143669 ) ) ;
#7726 = CARTESIAN_POINT ( 'NONE',  ( -19.03943276465977164, 0.05219959533909376836, 51.24890960531436690 ) ) ;
#7727 = CARTESIAN_POINT ( 'NONE',  ( -8.224510206698735004, -14.34966873604973081, 109.5844237280190328 ) ) ;
#7728 = CARTESIAN_POINT ( 'NONE',  ( 8.314922557961029526, -14.29746914071037800, 100.4177570613523471 ) ) ;
#7729 = CARTESIAN_POINT ( 'NONE',  ( 14.29746914071037800, 8.314922557961029526, 86.66775706135234714 ) ) ;
#7730 = CARTESIAN_POINT ( 'NONE',  ( 5.153800228976615827, -19.02544592524334988, 45.20942372801901143 ) ) ;
#7732 = CARTESIAN_POINT ( 'NONE',  ( 5.153800228976335163, 19.02544592524342804, 104.7905762719809957 ) ) ;
#7731 = LINE ( 'NONE', #22921, #105403 ) ;
#7733 = CARTESIAN_POINT ( 'NONE',  ( 16.46253265017160672, -9.564922557960803928, 78.33224293864769550 ) ) ;
#7734 = CARTESIAN_POINT ( 'NONE',  ( -16.46253265017160317, 9.564922557960807481, 35.83224293864768839 ) ) ;
#7735 = CARTESIAN_POINT ( 'NONE',  ( 14.29746914071049879, -8.314922557960816363, 43.33224293864769550 ) ) ;
#7737 = CARTESIAN_POINT ( 'NONE',  ( 19.03943276465977164, -0.05219959533909143690, 103.7489096053143669 ) ) ;
#7736 = CARTESIAN_POINT ( 'NONE',  ( 13.97604488694527802, 13.89961937509977652, 114.3739096053143669 ) ) ;
#7738 = CARTESIAN_POINT ( 'NONE',  ( 18.67979575497178502, 10.72451020669898547, 34.16557627198102409 ) ) ;
#7739 = CARTESIAN_POINT ( 'NONE',  ( -0.05219959533910754901, -16.53943276465976808, 87.49890960531436690 ) ) ;
#7740 = CARTESIAN_POINT ( 'NONE',  ( 16.53943276465976808, 0.05219959533934440121, 36.25109039468567573 ) ) ;
#7741 = CARTESIAN_POINT ( 'NONE',  ( -12.14591786802309592, -12.06949235617757132, 61.87390960531436690 ) ) ;
#7742 = CARTESIAN_POINT ( 'NONE',  ( 29.87692619418715267, -1.408284774589644517, -48.43935853184048312 ) ) ;
#7743 = CARTESIAN_POINT ( 'NONE',  ( 5.049401038297881783, 19.05341960407617563, 62.29275706135234003 ) ) ;
#7744 = CARTESIAN_POINT ( 'NONE',  ( 19.03943276465977164, -0.05219959533909143690, 98.74890960531436690 ) ) ;
#7745 = CARTESIAN_POINT ( 'NONE',  ( 13.97604488694548053, -13.89961937509957401, 75.62609039468564731 ) ) ;
#7746 = CARTESIAN_POINT ( 'NONE',  ( 17.14385361876520264, -23.59649016807271238, 148.0750000027311728 ) ) ;
#7748 = CARTESIAN_POINT ( 'NONE',  ( -12.14591786802326823, 12.06949235617739902, 103.1260903946856757 ) ) ;
#7747 = CARTESIAN_POINT ( 'NONE',  ( 16.55341960407618274, -4.379528057220086978, 36.04275706135234714 ) ) ;
#7750 = CARTESIAN_POINT ( 'NONE',  ( 9.564922557961047289, -16.46253265017146816, 70.41775706135233293 ) ) ;
#7749 = VECTOR ( 'NONE', #34804, 1000.000000000000000 ) ;
#7751 =( BOUNDED_CURVE ( )  B_SPLINE_CURVE ( 2, ( #44363, #121187, #110737, #174413, #30180 ),
 .UNSPECIFIED., .F., .F. ) 
 B_SPLINE_CURVE_WITH_KNOTS ( ( 3, 2, 3 ),
 ( 0.9000000000000000222, 0.9200000000000000400, 0.9255006513465138251 ),
 .UNSPECIFIED. ) 
 CURVE ( )  GEOMETRIC_REPRESENTATION_ITEM ( )  RATIONAL_B_SPLINE_CURVE ( ( 1.000000000000000000, 0.9510565162951535312, 1.000000000000000000, 0.9865389480227928498, 0.9804823514139773266 ) ) 
 REPRESENTATION_ITEM ( '' )  );
#7752 = CARTESIAN_POINT ( 'NONE',  ( -15.72974639402197994, 15.80617190586746368, 30.62390960531436335 ) ) ;
#7753 = CARTESIAN_POINT ( 'NONE',  ( -18.67979575497193778, 10.72451020669871902, 73.33442372801901854 ) ) ;
#7754 = CARTESIAN_POINT ( 'NONE',  ( -23.19706360625325559, -11.80427776162532538, 165.7059442611694067 ) ) ;
#7755 = CARTESIAN_POINT ( 'NONE',  ( 19.02544592524334988, 5.153800228976608722, 111.4594237280190043 ) ) ;
#7757 = CARTESIAN_POINT ( 'NONE',  ( 5.153800228976335163, 19.02544592524342804, 74.79057627198103830 ) ) ;
#7756 = CARTESIAN_POINT ( 'NONE',  ( -9.564922557960796823, -16.46253265017161027, 27.08224293864769550 ) ) ;
#7758 = EDGE_CURVE ( 'NONE', #162084, #62156, #27421, .T. ) ;
#7759 = CARTESIAN_POINT ( 'NONE',  ( 14.62341493535845416, 16.00195535827008442, -58.61703605924742533 ) ) ;
#7761 = CARTESIAN_POINT ( 'NONE',  ( 5.049401038298161559, -19.05341960407611168, 72.70724293864768129 ) ) ;
#7760 = CARTESIAN_POINT ( 'NONE',  ( 14.34966873604960469, 8.224510206698951720, 84.16557627198103830 ) ) ;
#7762 = SHAPE_DEFINITION_REPRESENTATION ( #187433, #31381 ) ;
#7763 = CARTESIAN_POINT ( 'NONE',  ( 16.46253265017160672, -9.564922557960803928, 93.33224293864769550 ) ) ;
#7764 = ORIENTED_EDGE ( 'NONE', *, *, #187248, .F. ) ;
#7765 = CARTESIAN_POINT ( 'NONE',  ( -5.153800228976607833, 19.02544592524334988, 87.70942372801897591 ) ) ;
#7766 = CARTESIAN_POINT ( 'NONE',  ( -21.55341960407610458, -5.719274019375992779, 81.45724293864769550 ) ) ;
#7767 = CARTESIAN_POINT ( 'NONE',  ( -5.153800228976328057, -19.02544592524343514, 27.29057627198103120 ) ) ;
#7769 = CARTESIAN_POINT ( 'NONE',  ( 15.80617190586746368, 15.72974639402197994, 109.3739096053143811 ) ) ;
#7768 = CARTESIAN_POINT ( 'NONE',  ( -19.02544592524334988, -5.153800228976617603, 68.95942372801896170 ) ) ;
#7770 = CARTESIAN_POINT ( 'NONE',  ( 9.564922557960805705, 16.46253265017160317, 69.58224293864770971 ) ) ;
#7771 = CARTESIAN_POINT ( 'NONE',  ( 9.564922557960805705, 16.46253265017160317, 104.5822429386476955 ) ) ;
#7772 = ORIENTED_EDGE ( 'NONE', *, *, #98256, .F. ) ;
#7773 = CARTESIAN_POINT ( 'NONE',  ( -5.719274019375978568, 21.55341960407610458, 100.2072429386476955 ) ) ;
#7776 = CARTESIAN_POINT ( 'NONE',  ( -19.03943276465977164, -0.05219959533935918106, 63.75109039468566863 ) ) ;
#7775 = CARTESIAN_POINT ( 'NONE',  ( -19.05341960407611168, -5.049401038298163336, 81.45724293864769550 ) ) ;
#7774 = CARTESIAN_POINT ( 'NONE',  ( 14.29746914071049879, -8.314922557960816363, 88.33224293864769550 ) ) ;
#7777 = CARTESIAN_POINT ( 'NONE',  ( -15.80617190586745835, -15.72974639402198527, 91.87390960531436690 ) ) ;
#7778 = CARTESIAN_POINT ( 'NONE',  ( 10.81492255796078972, 18.62759615963270932, 74.58224293864768129 ) ) ;
#7779 = CARTESIAN_POINT ( 'NONE',  ( -8.224510206698948167, 14.34966873604960824, 40.41557627198103120 ) ) ;
#7780 = CARTESIAN_POINT ( 'NONE',  ( 18.62759615963255655, 10.81492255796105972, 101.6677570613523613 ) ) ;
#7781 = CARTESIAN_POINT ( 'NONE',  ( -14.29746914071037622, -8.314922557961029526, 69.16775706135234714 ) ) ;
#7782 = CARTESIAN_POINT ( 'NONE',  ( -5.153800228976328057, -19.02544592524343514, 97.29057627198099567 ) ) ;
#7783 = CARTESIAN_POINT ( 'NONE',  ( 13.97604488694527802, 13.89961937509977652, 39.37390960531435269 ) ) ;
#7784 = CIRCLE ( 'NONE', #130448, 38.00000000000000000 ) ;
#7785 = CARTESIAN_POINT ( 'NONE',  ( -18.62759615963255300, -10.81492255796106328, 39.16775706135235424 ) ) ;
#7786 = CARTESIAN_POINT ( 'NONE',  ( 0.05219959533937995610, -21.53943276465977519, 50.00109039468568994 ) ) ;
#7787 = CARTESIAN_POINT ( 'NONE',  ( 0.05219959533909260263, 19.03943276465977164, 64.99890960531436690 ) ) ;
#7788 = CARTESIAN_POINT ( 'NONE',  ( -0.05219959533937732626, 21.53943276465977519, 37.50109039468568284 ) ) ;
#7789 = CARTESIAN_POINT ( 'NONE',  ( 13.97604488694548053, -13.89961937509957401, 80.62609039468567573 ) ) ;
#7790 = EDGE_CURVE ( 'NONE', #6179, #40990, #17513, .T. ) ;
#7791 = CARTESIAN_POINT ( 'NONE',  ( 19.02544592524334988, 5.153800228976608722, 71.45942372801900433 ) ) ;
#7792 = CARTESIAN_POINT ( 'NONE',  ( -16.51473224551069308, -9.474510206698971260, 41.66557627198103120 ) ) ;
#7793 = CARTESIAN_POINT ( 'NONE',  ( -12.14591786802326823, 12.06949235617739902, 93.12609039468568994 ) ) ;
#7794 = CARTESIAN_POINT ( 'NONE',  ( -19.02544592524342804, 5.153800228976336051, 51.04057627198103120 ) ) ;
#7795 = CARTESIAN_POINT ( 'NONE',  ( 22.00000000000000000, -5.204748896376250896E-15, 47.50000000000000000 ) ) ;
#7796 = CARTESIAN_POINT ( 'NONE',  ( 19.05341960407611168, 5.049401038298154454, 103.9572429386476671 ) ) ;
#7797 = CARTESIAN_POINT ( 'NONE',  ( 9.564922557960805705, 16.46253265017160317, 39.58224293864768839 ) ) ;
#7798 = CARTESIAN_POINT ( 'NONE',  ( 21.52544592524344225, -5.823673210054117533, 68.54057627198103830 ) ) ;
#7799 = CARTESIAN_POINT ( 'NONE',  ( -16.53943276465976808, -0.05219959533934237506, 63.75109039468568284 ) ) ;
#7800 = CARTESIAN_POINT ( 'NONE',  ( 5.153800228976615827, -19.02544592524334988, 20.20942372801899722 ) ) ;
#7801 = CARTESIAN_POINT ( 'NONE',  ( 19.02544592524343514, -5.153800228976328945, 48.54057627198103120 ) ) ;
#7802 = CARTESIAN_POINT ( 'NONE',  ( -4.483927247898539470, -16.52544592524342804, 47.29057627198103120 ) ) ;
#7803 = CARTESIAN_POINT ( 'NONE',  ( -14.34966873604960291, -8.224510206698953496, 81.66557627198103830 ) ) ;
#7804 = CARTESIAN_POINT ( 'NONE',  ( -19.05341960407611168, -5.049401038298163336, 81.45724293864769550 ) ) ;
#7805 = CARTESIAN_POINT ( 'NONE',  ( -15.72974639402176322, -15.80617190586768395, 34.37609039468568284 ) ) ;
#7806 = CARTESIAN_POINT ( 'NONE',  ( 16.46253265017160672, -9.564922557960803928, 98.33224293864769550 ) ) ;
#7807 = CARTESIAN_POINT ( 'NONE',  ( -21.52544592524334988, -5.823673210054445271, 93.95942372801903275 ) ) ;
#7808 = CARTESIAN_POINT ( 'NONE',  ( -4.379528057220086978, -16.55341960407618274, 64.79275706135234714 ) ) ;
#7809 = CARTESIAN_POINT ( 'NONE',  ( -21.52544592524334988, -5.823673210054445271, 28.95942372801902209 ) ) ;
#7810 = CARTESIAN_POINT ( 'NONE',  ( -0.05219959533909027116, -19.03943276465977164, 102.4989096053143669 ) ) ;
#7811 = CARTESIAN_POINT ( 'NONE',  ( 0.05219959533907565091, 21.53943276465977519, 89.99890960531438111 ) ) ;
#7812 = CARTESIAN_POINT ( 'NONE',  ( -12.06949235617756955, 12.14591786802309770, 40.62390960531435269 ) ) ;
#7813 = CARTESIAN_POINT ( 'NONE',  ( -13.89961937509977652, 13.97604488694528158, 35.62390960531435269 ) ) ;
#7814 = CARTESIAN_POINT ( 'NONE',  ( -16.52544592524342804, 4.483927247898546575, 71.04057627198103830 ) ) ;
#7815 = CARTESIAN_POINT ( 'NONE',  ( 10.72451020669898902, -18.67979575497178502, 32.91557627198102409 ) ) ;
#7816 = CARTESIAN_POINT ( 'NONE',  ( 19.05341960407617918, -5.049401038297876454, 31.04275706135232227 ) ) ;
#7817 = CARTESIAN_POINT ( 'NONE',  ( -14.34966873604960291, -8.224510206698953496, 96.66557627198102409 ) ) ;
#7818 = CARTESIAN_POINT ( 'NONE',  ( -0.05219959533909027116, -19.03943276465977164, 112.4989096053143669 ) ) ;
#7819 = ORIENTED_EDGE ( 'NONE', *, *, #40745, .F. ) ;
#7820 = CARTESIAN_POINT ( 'NONE',  ( -8.314922557961024197, 14.29746914071037800, 57.91775706135234714 ) ) ;
#7821 = CARTESIAN_POINT ( 'NONE',  ( 19.05341960407611168, 5.049401038298154454, 48.95724293864768129 ) ) ;
#7822 = DIRECTION ( 'NONE',  ( -0.000000000000000000, -0.000000000000000000, 1.000000000000000000 ) ) ;
#7823 = CARTESIAN_POINT ( 'NONE',  ( -14.34966873604972548, 8.224510206698743886, 93.33442372801901854 ) ) ;
#7824 = CARTESIAN_POINT ( 'NONE',  ( 13.97604488694548053, -13.89961937509957401, 95.62609039468563310 ) ) ;
#7825 = CARTESIAN_POINT ( 'NONE',  ( 18.62759615963255655, 10.81492255796105972, 66.66775706135234714 ) ) ;
#7826 = CARTESIAN_POINT ( 'NONE',  ( 19.02544592524343514, -5.153800228976328945, 73.54057627198103830 ) ) ;
#7827 = CARTESIAN_POINT ( 'NONE',  ( -18.67979575497178146, -10.72451020669898902, 86.66557627198102409 ) ) ;
#7828 = CARTESIAN_POINT ( 'NONE',  ( 4.483927247898790824, -16.52544592524335698, 45.20942372801901854 ) ) ;
#7829 = CARTESIAN_POINT ( 'NONE',  ( 9.474510206698971260, -16.51473224551069308, 22.91557627198102765 ) ) ;
#7830 = CARTESIAN_POINT ( 'NONE',  ( 9.474510206698729675, 16.51473224551082808, 77.08442372801900433 ) ) ;
#7831 = CARTESIAN_POINT ( 'NONE',  ( 21.52544592524344225, -5.823673210054117533, 73.54057627198102409 ) ) ;
#7832 = CARTESIAN_POINT ( 'NONE',  ( -16.51473224551082808, 9.474510206698731452, 43.33442372801900433 ) ) ;
#7833 = CARTESIAN_POINT ( 'NONE',  ( -9.564922557960796823, -16.46253265017161027, 112.0822429386476955 ) ) ;
#7834 = CARTESIAN_POINT ( 'NONE',  ( -10.72451020669898014, 18.67979575497178502, 90.41557627198103830 ) ) ;
#7835 = CARTESIAN_POINT ( 'NONE',  ( 17.50000000000000000, 5.499999999999992895, 61.70309617465829177 ) ) ;
#7836 = CARTESIAN_POINT ( 'NONE',  ( -9.474510206698964154, 16.51473224551069663, 60.41557627198102409 ) ) ;
#7837 = FACE_OUTER_BOUND ( 'NONE', #8950, .T. ) ;
#7838 = CARTESIAN_POINT ( 'NONE',  ( -4.379528057220086978, -16.55341960407618274, 24.79275706135235779 ) ) ;
#7839 = CARTESIAN_POINT ( 'NONE',  ( -1.221313414957698099E-14, 31.90000000000003411, -65.00100000000003320 ) ) ;
#7840 = CARTESIAN_POINT ( 'NONE',  ( -5.049401038298153566, 19.05341960407611168, 50.20724293864770260 ) ) ;
#7842 = CARTESIAN_POINT ( 'NONE',  ( 8.314922557960818139, 14.29746914071049879, 49.58224293864769550 ) ) ;
#7841 = CARTESIAN_POINT ( 'NONE',  ( -5.823673210054116645, -21.52544592524344225, 107.2905762719810525 ) ) ;
#7843 = CARTESIAN_POINT ( 'NONE',  ( 5.153800228976335163, 19.02544592524342804, 54.79057627198103120 ) ) ;
#7844 = CARTESIAN_POINT ( 'NONE',  ( -15.72974639402176322, -15.80617190586768395, 79.37609039468567573 ) ) ;
#7846 = CARTESIAN_POINT ( 'NONE',  ( -5.153800228976607833, 19.02544592524334988, 27.70942372801899722 ) ) ;
#7845 = CARTESIAN_POINT ( 'NONE',  ( -19.03943276465977164, -0.05219959533935918106, 113.7510903946856757 ) ) ;
#7847 = CARTESIAN_POINT ( 'NONE',  ( -12.06949235617756955, 12.14591786802309770, 25.62390960531435624 ) ) ;
#7848 = CARTESIAN_POINT ( 'NONE',  ( 18.62759615963255655, 10.81492255796105972, 41.66775706135235424 ) ) ;
#7849 = CARTESIAN_POINT ( 'NONE',  ( 5.823673210054444382, -21.52544592524334988, 20.20942372801900788 ) ) ;
#7850 = CARTESIAN_POINT ( 'NONE',  ( 18.62759615963271287, -10.81492255796078972, 58.33224293864768839 ) ) ;
#7851 = CARTESIAN_POINT ( 'NONE',  ( 19.05341960407617918, -5.049401038297876454, 96.04275706135231871 ) ) ;
#7852 = CARTESIAN_POINT ( 'NONE',  ( -9.474510206698720793, -16.51473224551083518, 69.58442372801901854 ) ) ;
#7853 = CARTESIAN_POINT ( 'NONE',  ( -18.67979575497193778, 10.72451020669871902, 78.33442372801901854 ) ) ;
#7854 = CARTESIAN_POINT ( 'NONE',  ( -16.46253265017146816, -9.564922557961047289, 59.16775706135233293 ) ) ;
#7855 = CARTESIAN_POINT ( 'NONE',  ( -16.51473224551069308, -9.474510206698971260, 21.66557627198102765 ) ) ;
#7856 = CARTESIAN_POINT ( 'NONE',  ( 10.72451020669898902, -18.67979575497178502, 62.91557627198102409 ) ) ;
#7857 = CARTESIAN_POINT ( 'NONE',  ( -8.224510206698948167, 14.34966873604960824, 50.41557627198103120 ) ) ;
#7858 = CARTESIAN_POINT ( 'NONE',  ( -17.50000000000001421, -5.499999999999956479, 26.28230962303566542 ) ) ;
#7859 = CARTESIAN_POINT ( 'NONE',  ( 16.51473224551083163, -9.474510206698727899, 20.83442372801899722 ) ) ;
#7860 = CARTESIAN_POINT ( 'NONE',  ( -4.379528057220086978, -16.55341960407618274, 79.79275706135236135 ) ) ;
#7861 = CARTESIAN_POINT ( 'NONE',  ( 16.55341960407611168, 4.379528057220329451, 43.95724293864769550 ) ) ;
#7862 = CARTESIAN_POINT ( 'NONE',  ( -10.81492255796105439, 18.62759615963255655, 72.91775706135234714 ) ) ;
#7863 = CARTESIAN_POINT ( 'NONE',  ( 15.80617190586769283, -15.72974639402175789, 75.62609039468567573 ) ) ;
#7864 = CARTESIAN_POINT ( 'NONE',  ( -5.823673210054116645, -21.52544592524344225, 87.29057627198103830 ) ) ;
#7865 = VECTOR ( 'NONE', #42257, 1000.000000000000114 ) ;
#7866 = CARTESIAN_POINT ( 'NONE',  ( 5.153800228976335163, 19.02544592524342804, 34.79057627198102409 ) ) ;
#7867 = CARTESIAN_POINT ( 'NONE',  ( 10.72451020669871369, 18.67979575497193778, 62.08442372801901143 ) ) ;
#7868 = CARTESIAN_POINT ( 'NONE',  ( -16.51473224551069308, -9.474510206698971260, 31.66557627198102054 ) ) ;
#7869 = CARTESIAN_POINT ( 'NONE',  ( 19.02544592524343514, -5.153800228976328945, 58.54057627198102409 ) ) ;
#7870 = CARTESIAN_POINT ( 'NONE',  ( 16.53943276465976808, -0.05219959533910856209, 93.74890960531436690 ) ) ;
#7871 = CARTESIAN_POINT ( 'NONE',  ( 13.97604488694527802, 13.89961937509977652, 99.37390960531436690 ) ) ;
#7872 = CARTESIAN_POINT ( 'NONE',  ( 16.52544592524342804, -4.483927247898539470, 43.54057627198103830 ) ) ;
#7873 = CARTESIAN_POINT ( 'NONE',  ( 16.53943276465976808, -0.05219959533910856209, 108.7489096053143669 ) ) ;
#7874 = CARTESIAN_POINT ( 'NONE',  ( 15.72974639402199770, -15.80617190586745480, 83.12390960531436690 ) ) ;
#7875 = CARTESIAN_POINT ( 'NONE',  ( -15.80617190586768217, 15.72974639402176855, 28.12609039468568284 ) ) ;
#7876 = DIRECTION ( 'NONE',  ( 0.000000000000000000, 0.000000000000000000, -1.000000000000000000 ) ) ;
#7877 = CARTESIAN_POINT ( 'NONE',  ( 4.379528057220092307, 16.55341960407617563, 37.29275706135235424 ) ) ;
#7878 = CARTESIAN_POINT ( 'NONE',  ( -5.719274019375978568, 21.55341960407610458, 75.20724293864769550 ) ) ;
#7879 = VECTOR ( 'NONE', #129440, 1000.000000000000000 ) ;
#7880 = CARTESIAN_POINT ( 'NONE',  ( -21.55341960407619339, 5.719274019375674811, 98.54275706135234714 ) ) ;
#7881 = CARTESIAN_POINT ( 'NONE',  ( -19.05341960407611168, -5.049401038298163336, 76.45724293864769550 ) ) ;
#7882 = CARTESIAN_POINT ( 'NONE',  ( -10.72451020669870658, -18.67979575497194134, 24.58442372801901499 ) ) ;
#7883 = CARTESIAN_POINT ( 'NONE',  ( -0.05219959533907301413, -21.53943276465977519, 22.49890960531436335 ) ) ;
#7884 = CARTESIAN_POINT ( 'NONE',  ( -16.52544592524335698, -4.483927247898792601, 88.95942372801901854 ) ) ;
#7885 = CARTESIAN_POINT ( 'NONE',  ( -21.53943276465977519, -0.05219959533937600094, 73.75109039468567573 ) ) ;
#7886 = CARTESIAN_POINT ( 'NONE',  ( -19.02544592524334988, -5.153800228976617603, 23.95942372801900078 ) ) ;
#7887 = CARTESIAN_POINT ( 'NONE',  ( 4.483927247898790824, -16.52544592524335698, 80.20942372801901854 ) ) ;
#7888 = CARTESIAN_POINT ( 'NONE',  ( -5.823673210054431948, 21.52544592524334988, 27.70942372801901854 ) ) ;
#7889 = CIRCLE ( 'NONE', #130564, 5.000000000000000000 ) ;
#7890 = CARTESIAN_POINT ( 'NONE',  ( -13.97604488694527625, -13.89961937509977652, 26.87390960531434558 ) ) ;
#7891 = CARTESIAN_POINT ( 'NONE',  ( -10.72451020669870658, -18.67979575497194134, 89.58442372801901854 ) ) ;
#7892 = CARTESIAN_POINT ( 'NONE',  ( -13.97604488694527625, -13.89961937509977652, 101.8739096053143811 ) ) ;
#7893 = CARTESIAN_POINT ( 'NONE',  ( 15.80617190586746368, 15.72974639402197994, 104.3739096053143669 ) ) ;
#7895 = CARTESIAN_POINT ( 'NONE',  ( -5.823673210054116645, -21.52544592524344225, 52.29057627198102409 ) ) ;
#7894 = LINE ( 'NONE', #21076, #90322 ) ;
#7897 = CARTESIAN_POINT ( 'NONE',  ( -8.314922557960811034, -14.29746914071050412, 52.08224293864768839 ) ) ;
#7896 = CARTESIAN_POINT ( 'NONE',  ( 19.02544592524343514, -5.153800228976328945, 93.54057627198102409 ) ) ;
#7898 = CARTESIAN_POINT ( 'NONE',  ( 9.921929963571523459, -9.486473617298056382, -62.57108492361744823 ) ) ;
#7899 = CARTESIAN_POINT ( 'NONE',  ( -19.02544592524334988, -5.153800228976617603, 73.95942372801900433 ) ) ;
#7900 = STYLED_ITEM ( 'NONE', ( #152730 ), #117169 ) ;
#7901 = CARTESIAN_POINT ( 'NONE',  ( -17.13100169013301155, 6.664070546373146442, 105.7678983569985007 ) ) ;
#7902 = CARTESIAN_POINT ( 'NONE',  ( 16.51473224551083163, -9.474510206698727899, 110.8344237280190043 ) ) ;
#7903 = CARTESIAN_POINT ( 'NONE',  ( -10.72451020669898014, 18.67979575497178502, 85.41557627198102409 ) ) ;
#7904 = CARTESIAN_POINT ( 'NONE',  ( -14.34966873604960291, -8.224510206698953496, 61.66557627198103120 ) ) ;
#7905 = CARTESIAN_POINT ( 'NONE',  ( -19.03943276465977164, 0.05219959533909376836, 101.2489096053143669 ) ) ;
#7906 = CARTESIAN_POINT ( 'NONE',  ( 8.314922557961029526, -14.29746914071037800, 40.41775706135234714 ) ) ;
#7907 = CARTESIAN_POINT ( 'NONE',  ( 5.153800228976335163, 19.02544592524342804, 59.79057627198100988 ) ) ;
#7909 = CARTESIAN_POINT ( 'NONE',  ( -19.02544592524334988, -5.153800228976617603, 98.95942372801900433 ) ) ;
#7908 = CARTESIAN_POINT ( 'NONE',  ( 10.72451020669871369, 18.67979575497193778, 27.08442372801901854 ) ) ;
#7910 = CARTESIAN_POINT ( 'NONE',  ( -13.89961937509977652, 13.97604488694528158, 100.6239096053143669 ) ) ;
#7911 = CARTESIAN_POINT ( 'NONE',  ( 9.474510206698971260, -16.51473224551069308, 82.91557627198103830 ) ) ;
#7912 = CARTESIAN_POINT ( 'NONE',  ( -21.55341960407610458, -5.719274019375992779, 96.45724293864770971 ) ) ;
#7913 = CARTESIAN_POINT ( 'NONE',  ( -16.46253265017160317, 9.564922557960807481, 45.83224293864769550 ) ) ;
#7914 = CARTESIAN_POINT ( 'NONE',  ( -17.49999999999999645, -5.622605283950893096, 61.31207310596114723 ) ) ;
#7915 = CARTESIAN_POINT ( 'NONE',  ( 16.53943276465976808, -0.05219959533910856209, 73.74890960531433848 ) ) ;
#7916 = CARTESIAN_POINT ( 'NONE',  ( -13.97604488694527625, -13.89961937509977652, 101.8739096053143811 ) ) ;
#7917 = CARTESIAN_POINT ( 'NONE',  ( -29.32058373238548654, 1.046637022531065719, -52.18867397238356887 ) ) ;
#7918 = CARTESIAN_POINT ( 'NONE',  ( 0.05219959533936267826, -19.03943276465977164, 60.00109039468566863 ) ) ;
#7919 = CARTESIAN_POINT ( 'NONE',  ( -15.80617190586745835, -15.72974639402198527, 91.87390960531436690 ) ) ;
#7920 = CARTESIAN_POINT ( 'NONE',  ( -9.474510206698720793, -16.51473224551083518, 54.58442372801899722 ) ) ;
#7921 = CARTESIAN_POINT ( 'NONE',  ( 5.049401038298161559, -19.05341960407611168, 97.70724293864766707 ) ) ;
#7922 = FILL_AREA_STYLE ('',( #81751 ) ) ;
#7923 = CARTESIAN_POINT ( 'NONE',  ( -5.719274019375978568, 21.55341960407610458, 45.20724293864769550 ) ) ;
#7924 = CARTESIAN_POINT ( 'NONE',  ( 16.51473224551069308, 9.474510206698969483, 89.16557627198103830 ) ) ;
#7925 = CARTESIAN_POINT ( 'NONE',  ( 5.719274019375673035, 21.55341960407619339, 67.29275706135234714 ) ) ;
#7927 = CARTESIAN_POINT ( 'NONE',  ( -0.05219959533909027116, -19.03943276465977164, 42.49890960531435269 ) ) ;
#7926 = PRODUCT_DEFINITION_SHAPE ( 'NONE', 'NONE',  #25201 ) ;
#7928 = CARTESIAN_POINT ( 'NONE',  ( 8.224510206698953496, -14.34966873604960469, 77.91557627198102409 ) ) ;
#7929 = CARTESIAN_POINT ( 'NONE',  ( -16.52544592524335698, -4.483927247898792601, 23.95942372801901143 ) ) ;
#7930 = CARTESIAN_POINT ( 'NONE',  ( -18.62759615963255300, -10.81492255796106328, 59.16775706135234714 ) ) ;
#7931 = EDGE_LOOP ( 'NONE', ( #62477, #72857 ) ) ;
#7932 = CARTESIAN_POINT ( 'NONE',  ( -13.89961937509977652, 13.97604488694528158, 115.6239096053143669 ) ) ;
#7934 = EDGE_CURVE ( 'NONE', #98202, #176832, #121982, .T. ) ;
#7933 = CARTESIAN_POINT ( 'NONE',  ( 13.89961937509957401, 13.97604488694547697, 66.87609039468567573 ) ) ;
#7935 = CARTESIAN_POINT ( 'NONE',  ( -19.49401214000077331, 12.39993551617566681, 167.9999999999999716 ) ) ;
#7936 = CARTESIAN_POINT ( 'NONE',  ( -15.80617190586768217, 15.72974639402176855, 28.12609039468568284 ) ) ;
#7937 = CARTESIAN_POINT ( 'NONE',  ( 19.02544592524343514, -5.153800228976328945, 58.54057627198102409 ) ) ;
#7938 = CARTESIAN_POINT ( 'NONE',  ( 38.00000000000000711, -12.34694845685040754, -6.849999994537626868 ) ) ;
#7939 = CARTESIAN_POINT ( 'NONE',  ( 21.53943276465977519, 0.05219959533937863772, 111.2510903946856899 ) ) ;
#7940 = CARTESIAN_POINT ( 'NONE',  ( 0.05219959533909260263, 19.03943276465977164, 49.99890960531435979 ) ) ;
#7941 = CARTESIAN_POINT ( 'NONE',  ( 9.474510206698729675, 16.51473224551082808, 22.08442372801899722 ) ) ;
#7942 = CARTESIAN_POINT ( 'NONE',  ( -16.53943276465976808, -0.05219959533934237506, 108.7510903946857042 ) ) ;
#7944 = CARTESIAN_POINT ( 'NONE',  ( -18.67979575497193778, 10.72451020669871902, 73.33442372801901854 ) ) ;
#7943 = CARTESIAN_POINT ( 'NONE',  ( -16.46253265017160317, 9.564922557960807481, 100.8322429386477097 ) ) ;
#7945 = CARTESIAN_POINT ( 'NONE',  ( -17.14385361876520619, 23.59649016807275856, 149.0750000027311728 ) ) ;
#7946 = CARTESIAN_POINT ( 'NONE',  ( 9.564922557960805705, 16.46253265017160317, 114.5822429386476955 ) ) ;
#7947 = CARTESIAN_POINT ( 'NONE',  ( 18.09867054820431420, 5.499999999999960032, 96.48393025253585620 ) ) ;
#7949 = CARTESIAN_POINT ( 'NONE',  ( 10.81492255796106328, -18.62759615963255655, 65.41775706135234714 ) ) ;
#7948 = CARTESIAN_POINT ( 'NONE',  ( 8.314922557961029526, -14.29746914071037800, 65.41775706135234714 ) ) ;
#7950 = CARTESIAN_POINT ( 'NONE',  ( 18.62759615963255655, 10.81492255796105972, 101.6677570613523613 ) ) ;
#7951 = DIRECTION ( 'NONE',  ( -0.000000000000000000, -0.000000000000000000, -1.000000000000000000 ) ) ;
#7952 = CARTESIAN_POINT ( 'NONE',  ( 19.02544592524343514, -5.153800228976328945, 83.54057627198100988 ) ) ;
#7953 = CARTESIAN_POINT ( 'NONE',  ( -9.564922557960796823, -16.46253265017161027, 112.0822429386476955 ) ) ;
#7954 = EDGE_LOOP ( 'NONE', ( #143380, #17846, #35752, #95480 ) ) ;
#7955 = CARTESIAN_POINT ( 'NONE',  ( -0.6023940538448385729, -29.02171288343480882, -52.52077797743537957 ) ) ;
#7956 = CARTESIAN_POINT ( 'NONE',  ( 9.564922557960805705, 16.46253265017160317, 34.58224293864770260 ) ) ;
#7957 = CARTESIAN_POINT ( 'NONE',  ( 5.719274019375991003, -21.55341960407610458, 42.70724293864770260 ) ) ;
#7958 = CARTESIAN_POINT ( 'NONE',  ( 16.53943276465976808, 0.05219959533934440121, 106.2510903946856757 ) ) ;
#7960 = CARTESIAN_POINT ( 'NONE',  ( -5.153800228976328057, -19.02544592524343514, 77.29057627198099567 ) ) ;
#7959 = CARTESIAN_POINT ( 'NONE',  ( -14.29746914071049879, 8.314922557960819915, 95.83224293864770971 ) ) ;
#7961 = CARTESIAN_POINT ( 'NONE',  ( -5.719274019375665041, -21.55341960407619695, 104.7927570613523898 ) ) ;
#7962 = CARTESIAN_POINT ( 'NONE',  ( 0.05219959533909260263, 19.03943276465977164, 34.99890960531435979 ) ) ;
#7963 = CARTESIAN_POINT ( 'NONE',  ( -16.55341960407611168, -4.379528057220339221, 86.45724293864770971 ) ) ;
#7964 = CARTESIAN_POINT ( 'NONE',  ( 15.80617190586769283, -15.72974639402175789, 45.62609039468567573 ) ) ;
#7965 = CARTESIAN_POINT ( 'NONE',  ( 10.72451020669898902, -18.67979575497178502, 82.91557627198103830 ) ) ;
#7966 = CARTESIAN_POINT ( 'NONE',  ( 5.153800228976615827, -19.02544592524334988, 45.20942372801901143 ) ) ;
#7967 = CARTESIAN_POINT ( 'NONE',  ( 9.564922557960805705, 16.46253265017160317, 44.58224293864769550 ) ) ;
#7968 = CARTESIAN_POINT ( 'NONE',  ( 0.05219959533909260263, 19.03943276465977164, 89.99890960531436690 ) ) ;
#7969 = CARTESIAN_POINT ( 'NONE',  ( 12.14591786802309770, 12.06949235617756955, 59.37390960531436690 ) ) ;
#7970 = CARTESIAN_POINT ( 'NONE',  ( -4.483927247898539470, -16.52544592524342804, 52.29057627198102409 ) ) ;
#7971 = CARTESIAN_POINT ( 'NONE',  ( -5.153800228976607833, 19.02544592524334988, 77.70942372801900433 ) ) ;
#7972 = CARTESIAN_POINT ( 'NONE',  ( -19.36337904590693526, 5.499999999999953815, 85.41494137495625694 ) ) ;
#7973 = CARTESIAN_POINT ( 'NONE',  ( -15.80617190586745835, -15.72974639402198527, 41.87390960531435979 ) ) ;
#7974 = CARTESIAN_POINT ( 'NONE',  ( 12.14591786802309770, 12.06949235617756955, 94.37390960531436690 ) ) ;
#7975 = DIRECTION ( 'NONE',  ( 0.000000000000000000, 0.000000000000000000, 1.000000000000000000 ) ) ;
#7977 = CARTESIAN_POINT ( 'NONE',  ( 5.823673210054125526, 21.52544592524343514, 49.79057627198102409 ) ) ;
#7976 = CARTESIAN_POINT ( 'NONE',  ( -13.97604488694527625, -13.89961937509977652, 46.87390960531435979 ) ) ;
#7978 = CARTESIAN_POINT ( 'NONE',  ( -16.51473224551069308, -9.474510206698971260, 31.66557627198102054 ) ) ;
#7980 = CARTESIAN_POINT ( 'NONE',  ( -16.46253265017160317, 9.564922557960807481, 65.83224293864769550 ) ) ;
#7979 = CARTESIAN_POINT ( 'NONE',  ( 12.14591786802327356, -12.06949235617739191, 75.62609039468567573 ) ) ;
#7981 = CARTESIAN_POINT ( 'NONE',  ( -16.46253265017146816, -9.564922557961047289, 39.16775706135234003 ) ) ;
#7982 = CIRCLE ( 'NONE', #120998, 0.1999999999999987899 ) ;
#7983 = CARTESIAN_POINT ( 'NONE',  ( -15.72974639402176322, -15.80617190586768395, 74.37609039468568994 ) ) ;
#7984 = CARTESIAN_POINT ( 'NONE',  ( 15.80617190586746368, 15.72974639402197994, 49.37390960531436690 ) ) ;
#7985 = CARTESIAN_POINT ( 'NONE',  ( 8.224510206698953496, -14.34966873604960469, 112.9155762719810383 ) ) ;
#7986 = CARTESIAN_POINT ( 'NONE',  ( -9.474510206698720793, -16.51473224551083518, 89.58442372801900433 ) ) ;
#7987 = CARTESIAN_POINT ( 'NONE',  ( -29.86685920354755197, -21.69954338932560134, -2.924999997268813878 ) ) ;
#7989 = CARTESIAN_POINT ( 'NONE',  ( 18.67979575497178502, 10.72451020669898547, 44.16557627198103120 ) ) ;
#7988 = CARTESIAN_POINT ( 'NONE',  ( -1.240847218223085413, -23.66491666289340401, -57.22545927231450946 ) ) ;
#7990 = CARTESIAN_POINT ( 'NONE',  ( 16.31925111598459210, -7.325300261831447557, 67.66424538967254421 ) ) ;
#7991 = CARTESIAN_POINT ( 'NONE',  ( 5.719274019375673035, 21.55341960407619339, 77.29275706135234714 ) ) ;
#7992 = CARTESIAN_POINT ( 'NONE',  ( -0.05219959533910754901, -16.53943276465976808, 52.49890960531435979 ) ) ;
#7993 = CARTESIAN_POINT ( 'NONE',  ( -16.52544592524342804, 4.483927247898546575, 56.04057627198102409 ) ) ;
#7994 = CARTESIAN_POINT ( 'NONE',  ( -21.52544592524343514, 5.823673210054127303, 86.04057627198102409 ) ) ;
#7995 = CARTESIAN_POINT ( 'NONE',  ( -10.72451020669898014, 18.67979575497178502, 75.41557627198102409 ) ) ;
#7996 = CARTESIAN_POINT ( 'NONE',  ( -0.2690448904508037087, -28.91886483090992854, -49.65045026909250225 ) ) ;
#7997 = CARTESIAN_POINT ( 'NONE',  ( 5.823673210054125526, 21.52544592524343514, 34.79057627198103120 ) ) ;
#7998 = CARTESIAN_POINT ( 'NONE',  ( -8.224510206698735004, -14.34966873604973081, 59.58442372801901854 ) ) ;
#7999 = CARTESIAN_POINT ( 'NONE',  ( -14.34966873604960291, -8.224510206698953496, 76.66557627198103830 ) ) ;
#8000 = CARTESIAN_POINT ( 'NONE',  ( -13.97604488694527625, -13.89961937509977652, 61.87390960531435979 ) ) ;
#8001 = CARTESIAN_POINT ( 'NONE',  ( -13.97604488694527625, -13.89961937509977652, 36.87390960531436690 ) ) ;
#8002 = DIRECTION ( 'NONE',  ( -0.000000000000000000, -0.000000000000000000, -1.000000000000000000 ) ) ;
#8004 = CARTESIAN_POINT ( 'NONE',  ( 0.05219959533934541429, -16.53943276465976808, 85.00109039468568994 ) ) ;
#8003 = AXIS2_PLACEMENT_3D ( 'NONE', #45886, #186406, #129656 ) ;
#8005 = CARTESIAN_POINT ( 'NONE',  ( -10.81492255796105439, 18.62759615963255655, 22.91775706135235069 ) ) ;
#8006 = CARTESIAN_POINT ( 'NONE',  ( 19.02544592524343514, -5.153800228976328945, 63.54057627198103830 ) ) ;
#8007 = CARTESIAN_POINT ( 'NONE',  ( -5.719274019375665041, -21.55341960407619695, 54.79275706135235424 ) ) ;
#8008 = CARTESIAN_POINT ( 'NONE',  ( -13.97604488694527625, -13.89961937509977652, 111.8739096053143243 ) ) ;
#8009 = CARTESIAN_POINT ( 'NONE',  ( -6.004573588232718251, -47.77740467397597968, -24.84605846612137725 ) ) ;
#8010 = EDGE_LOOP ( 'NONE', ( #184344, #148536, #25787, #20628 ) ) ;
#8011 = CARTESIAN_POINT ( 'NONE',  ( 21.55341960407619695, -5.719274019375665929, 46.04275706135234714 ) ) ;
#8013 = CARTESIAN_POINT ( 'NONE',  ( -13.97604488694527625, -13.89961937509977652, 106.8739096053143669 ) ) ;
#8012 = CARTESIAN_POINT ( 'NONE',  ( -19.03943276465977164, 0.05219959533909376836, 116.2489096053143669 ) ) ;
#8014 = CARTESIAN_POINT ( 'NONE',  ( 0.05219959533936267826, -19.03943276465977164, 60.00109039468566863 ) ) ;
#8015 = CARTESIAN_POINT ( 'NONE',  ( 18.62759615963271287, -10.81492255796078972, 108.3322429386477097 ) ) ;
#8016 = CARTESIAN_POINT ( 'NONE',  ( 9.564922557961047289, -16.46253265017146816, 40.41775706135234003 ) ) ;
#8017 = CARTESIAN_POINT ( 'NONE',  ( -4.379528057220086978, -16.55341960407618274, 94.79275706135234714 ) ) ;
#8018 = CARTESIAN_POINT ( 'NONE',  ( -9.564922557961040184, 16.46253265017147172, 67.91775706135233293 ) ) ;
#8019 = CARTESIAN_POINT ( 'NONE',  ( -4.483927247898782831, 16.52544592524335698, 102.7094237280190185 ) ) ;
#8021 = ORIENTED_EDGE ( 'NONE', *, *, #60920, .F. ) ;
#8020 = DIRECTION ( 'NONE',  ( -1.000000000000000000, -5.267352820763006950E-15, 0.000000000000000000 ) ) ;
#8022 = CARTESIAN_POINT ( 'NONE',  ( -19.05341960407611168, -5.049401038298163336, 86.45724293864769550 ) ) ;
#8023 = AXIS2_PLACEMENT_3D ( 'NONE', #149445, #135288, #120095 ) ;
#8024 = CARTESIAN_POINT ( 'NONE',  ( -5.823673210054431948, 21.52544592524334988, 87.70942372801901854 ) ) ;
#8025 = CARTESIAN_POINT ( 'NONE',  ( -0.05219959533937732626, 21.53943276465977519, 97.50109039468567573 ) ) ;
#8026 = CARTESIAN_POINT ( 'NONE',  ( 21.65895526037594010, -0.9928668394655185692, -56.20821996642038698 ) ) ;
#8027 = CARTESIAN_POINT ( 'NONE',  ( 19.02544592524343514, -5.153800228976328945, 98.54057627198100988 ) ) ;
#8028 = CARTESIAN_POINT ( 'NONE',  ( 10.81492255796106328, -18.62759615963255655, 80.41775706135234714 ) ) ;
#8029 = CARTESIAN_POINT ( 'NONE',  ( -16.53943276465976808, -0.05219959533934237506, 23.75109039468567929 ) ) ;
#8030 = EDGE_CURVE ( 'NONE', #120176, #111780, #137786, .T. ) ;
#8031 = CARTESIAN_POINT ( 'NONE',  ( -16.46253265017160317, 9.564922557960807481, 75.83224293864769550 ) ) ;
#8032 = CARTESIAN_POINT ( 'NONE',  ( -18.62759615963270932, 10.81492255796079327, 30.83224293864770260 ) ) ;
#8033 = CARTESIAN_POINT ( 'NONE',  ( -19.05341960407611168, -5.049401038298163336, 91.45724293864766707 ) ) ;
#8034 = CARTESIAN_POINT ( 'NONE',  ( -17.48847506799968698, -5.747544572773761296, 89.17302562156721990 ) ) ;
#8035 = CARTESIAN_POINT ( 'NONE',  ( 13.89961937509977652, -13.97604488694527269, 83.12390960531436690 ) ) ;
#8036 = CARTESIAN_POINT ( 'NONE',  ( 5.153800228976335163, 19.02544592524342804, 64.79057627198100988 ) ) ;
#8037 = CARTESIAN_POINT ( 'NONE',  ( -12.06949235617739369, -12.14591786802326823, 99.37609039468568994 ) ) ;
#8038 = CARTESIAN_POINT ( 'NONE',  ( -19.19724070472090816, -5.500000000000166978, 41.06193348274383226 ) ) ;
#8039 = VECTOR ( 'NONE', #46142, 1000.000000000000000 ) ;
#8040 = CARTESIAN_POINT ( 'NONE',  ( 13.97604488694548053, -13.89961937509957401, 60.62609039468564731 ) ) ;
#8041 = CARTESIAN_POINT ( 'NONE',  ( 19.05341960407611168, 5.049401038298154454, 88.95724293864769550 ) ) ;
#8042 = CARTESIAN_POINT ( 'NONE',  ( 16.52544592524342804, -4.483927247898539470, 88.54057627198103830 ) ) ;
#8043 = TOROIDAL_SURFACE ( 'NONE', #111384, 40.49999999999999289, 0.5000000000000000000 ) ;
#8044 = CARTESIAN_POINT ( 'NONE',  ( -21.55341960407610458, -5.719274019375992779, 26.45724293864768839 ) ) ;
#8045 = COLOUR_RGB ( '', 0.72549020, 0.75294118, 0.79215686) ;
#8046 = CARTESIAN_POINT ( 'NONE',  ( -0.05219959533909027116, -19.03943276465977164, 112.4989096053143669 ) ) ;
#8047 = CARTESIAN_POINT ( 'NONE',  ( 12.14591786802309770, 12.06949235617756955, 89.37390960531435269 ) ) ;
#8048 = CARTESIAN_POINT ( 'NONE',  ( -1.136345303629771264, -6.615873399348758177, -62.40252569733547716 ) ) ;
#8049 = CARTESIAN_POINT ( 'NONE',  ( -19.05341960407617563, 5.049401038297882671, 48.54275706135233293 ) ) ;
#8050 = CARTESIAN_POINT ( 'NONE',  ( 12.14591786802327356, -12.06949235617739191, 105.6260903946856899 ) ) ;
#8051 = CARTESIAN_POINT ( 'NONE',  ( 16.46253265017160672, -9.564922557960803928, 88.33224293864769550 ) ) ;
#8052 = CARTESIAN_POINT ( 'NONE',  ( 18.62759615963255655, 10.81492255796105972, 71.66775706135234714 ) ) ;
#8053 = CARTESIAN_POINT ( 'NONE',  ( -18.67979575497178146, -10.72451020669898902, 51.66557627198102409 ) ) ;
#8055 = ORIENTED_EDGE ( 'NONE', *, *, #1107, .F. ) ;
#8054 = CARTESIAN_POINT ( 'NONE',  ( -5.719274019375665041, -21.55341960407619695, 29.79275706135234358 ) ) ;
#8056 = CARTESIAN_POINT ( 'NONE',  ( -15.80617190586745835, -15.72974639402198527, 86.87390960531438111 ) ) ;
#8057 = CARTESIAN_POINT ( 'NONE',  ( -21.55341960407619339, 5.719274019375674811, 38.54275706135234714 ) ) ;
#8058 = CARTESIAN_POINT ( 'NONE',  ( 16.53943276465976808, -0.05219959533910856209, 103.7489096053143669 ) ) ;
#8059 = CARTESIAN_POINT ( 'NONE',  ( -16.51473224551082808, 9.474510206698731452, 68.33442372801900433 ) ) ;
#8060 = CARTESIAN_POINT ( 'NONE',  ( -5.153800228976328057, -19.02544592524343514, 47.29057627198102409 ) ) ;
#8061 = CARTESIAN_POINT ( 'NONE',  ( -9.564922557960796823, -16.46253265017161027, 102.0822429386477097 ) ) ;
#8062 = CARTESIAN_POINT ( 'NONE',  ( 16.51473224551069308, 9.474510206698969483, 94.16557627198103830 ) ) ;
#8063 = CARTESIAN_POINT ( 'NONE',  ( 19.05341960407611168, 5.049401038298154454, 23.95724293864769194 ) ) ;
#8064 = CARTESIAN_POINT ( 'NONE',  ( -4.379528057220328563, 16.55341960407611168, 35.20724293864768839 ) ) ;
#8065 = CARTESIAN_POINT ( 'NONE',  ( -8.314922557961024197, 14.29746914071037800, 42.91775706135235424 ) ) ;
#8066 = CARTESIAN_POINT ( 'NONE',  ( -14.29746914071049879, 8.314922557960819915, 115.8322429386477097 ) ) ;
#8068 = VECTOR ( 'NONE', #126784, 1000.000000000000000 ) ;
#8067 = CARTESIAN_POINT ( 'NONE',  ( -5.153800228976607833, 19.02544592524334988, 27.70942372801899722 ) ) ;
#8070 = CARTESIAN_POINT ( 'NONE',  ( 4.483927247898545687, 16.52544592524342804, 24.79057627198103120 ) ) ;
#8069 = DIRECTION ( 'NONE',  ( -0.000000000000000000, -0.000000000000000000, 1.000000000000000000 ) ) ;
#8071 = CARTESIAN_POINT ( 'NONE',  ( 0.05219959533937995610, -21.53943276465977519, 30.00109039468568284 ) ) ;
#8072 = CARTESIAN_POINT ( 'NONE',  ( -5.049401038298153566, 19.05341960407611168, 105.2072429386476671 ) ) ;
#8073 = CARTESIAN_POINT ( 'NONE',  ( -16.52544592524335698, -4.483927247898792601, 43.95942372801902565 ) ) ;
#8074 = CARTESIAN_POINT ( 'NONE',  ( -12.06949235617739369, -12.14591786802326823, 109.3760903946857042 ) ) ;
#8075 = CARTESIAN_POINT ( 'NONE',  ( 4.379528057220092307, 16.55341960407617563, 87.29275706135236135 ) ) ;
#8076 = CARTESIAN_POINT ( 'NONE',  ( 12.06949235617739724, 12.14591786802326823, 31.87609039468567929 ) ) ;
#8077 = CARTESIAN_POINT ( 'NONE',  ( -5.049401038298153566, 19.05341960407611168, 45.20724293864769550 ) ) ;
#8078 = CARTESIAN_POINT ( 'NONE',  ( 14.34966873604960469, 8.224510206698951720, 104.1655762719810241 ) ) ;
#8079 = CARTESIAN_POINT ( 'NONE',  ( 5.719274019375673035, 21.55341960407619339, 22.29275706135235069 ) ) ;
#8080 = CARTESIAN_POINT ( 'NONE',  ( 13.89961937509977652, -13.97604488694527269, 33.12390960531434558 ) ) ;
#8081 = CARTESIAN_POINT ( 'NONE',  ( 9.564922557960805705, 16.46253265017160317, 99.58224293864770971 ) ) ;
#8082 = CARTESIAN_POINT ( 'NONE',  ( -5.153800228976328057, -19.02544592524343514, 37.29057627198102409 ) ) ;
#8083 = CARTESIAN_POINT ( 'NONE',  ( 19.02544592524343514, -5.153800228976328945, 98.54057627198100988 ) ) ;
#8084 = DIRECTION ( 'NONE',  ( 0.000000000000000000, 0.000000000000000000, 1.000000000000000000 ) ) ;
#8085 = CARTESIAN_POINT ( 'NONE',  ( 5.049401038298161559, -19.05341960407611168, 97.70724293864766707 ) ) ;
#8087 = CARTESIAN_POINT ( 'NONE',  ( -8.224510206698948167, 14.34966873604960824, 85.41557627198102409 ) ) ;
#8086 = CARTESIAN_POINT ( 'NONE',  ( 18.67979575497194134, -10.72451020669871369, 50.83442372801901143 ) ) ;
#8088 = CARTESIAN_POINT ( 'NONE',  ( -13.97604488694527625, -13.89961937509977652, 111.8739096053143243 ) ) ;
#8089 = CARTESIAN_POINT ( 'NONE',  ( -27.96890437653549455, -7.184031643498222763, 161.0522725792576182 ) ) ;
#8090 = CARTESIAN_POINT ( 'NONE',  ( 4.379528057220092307, 16.55341960407617563, 67.29275706135234714 ) ) ;
#8091 = CARTESIAN_POINT ( 'NONE',  ( 5.719274019375673035, 21.55341960407619339, 77.29275706135234714 ) ) ;
#8092 = CARTESIAN_POINT ( 'NONE',  ( -12.06949235617739369, -12.14591786802326823, 34.37609039468568284 ) ) ;
#8093 = CARTESIAN_POINT ( 'NONE',  ( -13.89961937509977652, 13.97604488694528158, 80.62390960531436690 ) ) ;
#8094 = CARTESIAN_POINT ( 'NONE',  ( 19.03943276465977164, 0.05219959533936151252, 106.2510903946856615 ) ) ;
#8095 = CARTESIAN_POINT ( 'NONE',  ( 16.53943276465976808, 0.05219959533934440121, 76.25109039468568994 ) ) ;
#8096 = CARTESIAN_POINT ( 'NONE',  ( 0.05219959533936267826, -19.03943276465977164, 90.00109039468567573 ) ) ;
#8097 = CARTESIAN_POINT ( 'NONE',  ( 0.05219959533909260263, 19.03943276465977164, 64.99890960531436690 ) ) ;
#8098 = CARTESIAN_POINT ( 'NONE',  ( 10.72451020669898902, -18.67979575497178502, 92.91557627198103830 ) ) ;
#8100 = CARTESIAN_POINT ( 'NONE',  ( -19.03943276465977164, -0.05219959533935918106, 93.75109039468566152 ) ) ;
#8099 = CARTESIAN_POINT ( 'NONE',  ( -0.05219959533910754901, -16.53943276465976808, 92.49890960531436690 ) ) ;
#8101 = CARTESIAN_POINT ( 'NONE',  ( 16.53943276465976808, 0.05219959533934440121, 61.25109039468567573 ) ) ;
#8102 = CARTESIAN_POINT ( 'NONE',  ( -18.39635199886971151, 5.499999999999982236, 81.01967076360003261 ) ) ;
#8103 = CARTESIAN_POINT ( 'NONE',  ( -16.51473224551082808, 9.474510206698731452, 68.33442372801900433 ) ) ;
#8104 = CARTESIAN_POINT ( 'NONE',  ( -16.55341960407611168, -4.379528057220339221, 26.45724293864768839 ) ) ;
#8105 = CARTESIAN_POINT ( 'NONE',  ( 16.52544592524342804, -4.483927247898539470, 83.54057627198102409 ) ) ;
#8107 = CARTESIAN_POINT ( 'NONE',  ( -17.12812012977050458, 6.668231424565584042, 38.64051240676854349 ) ) ;
#8106 = CARTESIAN_POINT ( 'NONE',  ( 19.05341960407617918, -5.049401038297876454, 26.04275706135233293 ) ) ;
#8108 = CARTESIAN_POINT ( 'NONE',  ( 21.53943276465977519, 0.05219959533937863772, 21.25109039468567218 ) ) ;
#8109 = CARTESIAN_POINT ( 'NONE',  ( -3.573655867282028392E-15, 2.428612866367529932E-14, 164.9999999999999716 ) ) ;
#8110 = CARTESIAN_POINT ( 'NONE',  ( 9.564922557960805705, 16.46253265017160317, 79.58224293864769550 ) ) ;
#8111 = CARTESIAN_POINT ( 'NONE',  ( -21.53943276465977519, -0.05219959533937600094, 93.75109039468567573 ) ) ;
#8112 = CARTESIAN_POINT ( 'NONE',  ( -13.89961937509977652, 13.97604488694528158, 80.62390960531436690 ) ) ;
#8113 = CARTESIAN_POINT ( 'NONE',  ( -18.67979575497178146, -10.72451020669898902, 41.66557627198103120 ) ) ;
#8114 = AXIS2_PLACEMENT_3D ( 'NONE', #68843, #71847, #148699 ) ;
#8115 = CARTESIAN_POINT ( 'NONE',  ( 16.53943276465976808, -0.05219959533910856209, 83.74890960531435269 ) ) ;
#8116 = CARTESIAN_POINT ( 'NONE',  ( -16.51473224551069308, -9.474510206698971260, 56.66557627198103120 ) ) ;
#8117 = CARTESIAN_POINT ( 'NONE',  ( -14.29746914071049879, 8.314922557960819915, 105.8322429386476955 ) ) ;
#8118 = CARTESIAN_POINT ( 'NONE',  ( 0.05219959533937995610, -21.53943276465977519, 30.00109039468568284 ) ) ;
#8119 = CARTESIAN_POINT ( 'NONE',  ( 21.53943276465977519, 0.05219959533937863772, 56.25109039468568284 ) ) ;
#8120 = CARTESIAN_POINT ( 'NONE',  ( 13.97604488694527802, 13.89961937509977652, 49.37390960531434558 ) ) ;
#8121 = CARTESIAN_POINT ( 'NONE',  ( 4.379528057220092307, 16.55341960407617563, 72.29275706135236135 ) ) ;
#8122 = CARTESIAN_POINT ( 'NONE',  ( 0.05219959533907565091, 21.53943276465977519, 114.9989096053143669 ) ) ;
#8123 = CARTESIAN_POINT ( 'NONE',  ( -5.719274019375665041, -21.55341960407619695, 19.79275706135235069 ) ) ;
#8125 = CARTESIAN_POINT ( 'NONE',  ( 19.02544592524343514, -5.153800228976328945, 63.54057627198103830 ) ) ;
#8124 = CARTESIAN_POINT ( 'NONE',  ( 0.05219959533936267826, -19.03943276465977164, 35.00109039468566863 ) ) ;
#8126 = CARTESIAN_POINT ( 'NONE',  ( 9.474510206698729675, 16.51473224551082808, 32.08442372801900433 ) ) ;
#8127 = CARTESIAN_POINT ( 'NONE',  ( -0.05219959533937732626, 21.53943276465977519, 72.50109039468568994 ) ) ;
#8128 = AXIS2_PLACEMENT_3D ( 'NONE', #113217, #146545, #159720 ) ;
#8129 = CARTESIAN_POINT ( 'NONE',  ( 10.72451020669898902, -18.67979575497178502, 72.91557627198103830 ) ) ;
#8130 = CARTESIAN_POINT ( 'NONE',  ( -12.06949235617756955, 12.14591786802309770, 35.62390960531437401 ) ) ;
#8132 = CARTESIAN_POINT ( 'NONE',  ( -18.67979575497193778, 10.72451020669871902, 108.3344237280190185 ) ) ;
#8131 = CARTESIAN_POINT ( 'NONE',  ( -5.823673210054431948, 21.52544592524334988, 87.70942372801901854 ) ) ;
#8133 = CARTESIAN_POINT ( 'NONE',  ( 8.314922557960818139, 14.29746914071049879, 59.58224293864770260 ) ) ;
#8134 = CARTESIAN_POINT ( 'NONE',  ( 4.379528057220339221, -16.55341960407611168, 102.7072429386476955 ) ) ;
#8135 = CARTESIAN_POINT ( 'NONE',  ( 9.474510206698729675, 16.51473224551082808, 57.08442372801900433 ) ) ;
#8136 = CARTESIAN_POINT ( 'NONE',  ( -14.29746914071049879, 8.314922557960819915, 25.83224293864769194 ) ) ;
#8138 = EDGE_CURVE ( 'NONE', #13627, #4626, #1540, .T. ) ;
#8137 = CARTESIAN_POINT ( 'NONE',  ( 5.719274019375673035, 21.55341960407619339, 67.29275706135234714 ) ) ;
#8139 = CARTESIAN_POINT ( 'NONE',  ( -16.46253265017160317, 9.564922557960807481, 75.83224293864769550 ) ) ;
#8140 = CARTESIAN_POINT ( 'NONE',  ( -19.03943276465977164, -0.05219959533935918106, 48.75109039468566863 ) ) ;
#8141 = CARTESIAN_POINT ( 'NONE',  ( 5.823673210054125526, 21.52544592524343514, 49.79057627198102409 ) ) ;
#8142 = CARTESIAN_POINT ( 'NONE',  ( -5.823673210054431948, 21.52544592524334988, 42.70942372801901854 ) ) ;
#8143 = CARTESIAN_POINT ( 'NONE',  ( 21.55341960407610458, 5.719274019375980345, 103.9572429386476813 ) ) ;
#8144 = CARTESIAN_POINT ( 'NONE',  ( 9.564922557961047289, -16.46253265017146816, 100.4177570613523329 ) ) ;
#8145 = CARTESIAN_POINT ( 'NONE',  ( -12.14591786802326823, 12.06949235617739902, 63.12609039468568994 ) ) ;
#8147 = CARTESIAN_POINT ( 'NONE',  ( -21.55341960407610458, -5.719274019375992779, 96.45724293864770971 ) ) ;
#8146 = CARTESIAN_POINT ( 'NONE',  ( 37.99626262588765258, -12.34573411038911672, -5.102157773949822506 ) ) ;
#8148 = CARTESIAN_POINT ( 'NONE',  ( -16.53943276465976808, 0.05219959533911058130, 91.24890960531436690 ) ) ;
#8149 = CARTESIAN_POINT ( 'NONE',  ( -27.03637221620033770, -26.30952996081082773, -20.42959548696012462 ) ) ;
#8150 = CARTESIAN_POINT ( 'NONE',  ( 14.34966873604972726, -8.224510206698740333, 20.83442372801901143 ) ) ;
#8151 = CARTESIAN_POINT ( 'NONE',  ( -0.05219959533907301413, -21.53943276465977519, 52.49890960531435979 ) ) ;
#8152 = CARTESIAN_POINT ( 'NONE',  ( 16.55341960407618274, -4.379528057220086978, 96.04275706135236135 ) ) ;
#8153 = CARTESIAN_POINT ( 'NONE',  ( 29.32033176666156393, -22.46488766722420749, -8.000000000000003553 ) ) ;
#8154 = EDGE_CURVE ( 'NONE', #53763, #106856, #120793, .T. ) ;
#8155 = CARTESIAN_POINT ( 'NONE',  ( -8.314922557961024197, 14.29746914071037800, 47.91775706135234714 ) ) ;
#8156 = CARTESIAN_POINT ( 'NONE',  ( 18.67979575497194134, -10.72451020669871369, 30.83442372801902209 ) ) ;
#8157 = CARTESIAN_POINT ( 'NONE',  ( 10.81492255796078972, 18.62759615963270932, 39.58224293864769550 ) ) ;
#8158 = CARTESIAN_POINT ( 'NONE',  ( 4.379528057220092307, 16.55341960407617563, 87.29275706135236135 ) ) ;
#8159 = CARTESIAN_POINT ( 'NONE',  ( 0.05219959533909260263, 19.03943276465977164, 94.99890960531436690 ) ) ;
#8160 = CARTESIAN_POINT ( 'NONE',  ( -21.52544592524334988, -5.823673210054445271, 68.95942372801901854 ) ) ;
#8161 = CARTESIAN_POINT ( 'NONE',  ( -21.53943276465977519, 0.05219959533907696930, 41.24890960531435269 ) ) ;
#8162 = CARTESIAN_POINT ( 'NONE',  ( 18.67979575497178502, 10.72451020669898547, 34.16557627198102409 ) ) ;
#8163 = ORIENTED_EDGE ( 'NONE', *, *, #26705, .F. ) ;
#8164 = CARTESIAN_POINT ( 'NONE',  ( -5.049401038297874678, -19.05341960407617918, 54.79275706135234003 ) ) ;
#8165 = CARTESIAN_POINT ( 'NONE',  ( -14.34966873604972548, 8.224510206698743886, 63.33442372801900433 ) ) ;
#8166 = CARTESIAN_POINT ( 'NONE',  ( 18.62759615963271287, -10.81492255796078972, 28.33224293864769550 ) ) ;
#8167 = EDGE_LOOP ( 'NONE', ( #3184, #164472 ) ) ;
#8168 = CARTESIAN_POINT ( 'NONE',  ( -16.51473224551069308, -9.474510206698971260, 81.66557627198103830 ) ) ;
#8169 = CARTESIAN_POINT ( 'NONE',  ( 12.14591786802327356, -12.06949235617739191, 110.6260903946857042 ) ) ;
#8170 = CARTESIAN_POINT ( 'NONE',  ( 11.78083973539067486, -37.76997396076107805, -30.94638762609303129 ) ) ;
#8171 = CARTESIAN_POINT ( 'NONE',  ( -8.224510206698948167, 14.34966873604960824, 105.4155762719810383 ) ) ;
#8172 = CARTESIAN_POINT ( 'NONE',  ( 18.62759615963271287, -10.81492255796078972, 43.33224293864769550 ) ) ;
#8173 = CARTESIAN_POINT ( 'NONE',  ( -13.97604488694527625, -13.89961937509977652, 51.87390960531436690 ) ) ;
#8174 = CARTESIAN_POINT ( 'NONE',  ( -16.55341960407617563, 4.379528057220093196, 73.54275706135234714 ) ) ;
#8175 = CARTESIAN_POINT ( 'NONE',  ( -0.05219959533937732626, 21.53943276465977519, 37.50109039468568284 ) ) ;
#8176 = CARTESIAN_POINT ( 'NONE',  ( -16.51473224551082808, 9.474510206698731452, 93.33442372801900433 ) ) ;
#8177 = CARTESIAN_POINT ( 'NONE',  ( -16.55341960407611168, -4.379528057220339221, 91.45724293864769550 ) ) ;
#8178 = CARTESIAN_POINT ( 'NONE',  ( 19.05341960407611168, 5.049401038298154454, 48.95724293864768129 ) ) ;
#8179 = AXIS2_PLACEMENT_3D ( 'NONE', #36261, #97915, #22107 ) ;
#8180 = CARTESIAN_POINT ( 'NONE',  ( 19.05341960407611168, 5.049401038298154454, 23.95724293864769194 ) ) ;
#8181 = CARTESIAN_POINT ( 'NONE',  ( 5.719274019375673035, 21.55341960407619339, 107.2927570613523471 ) ) ;
#8182 = CARTESIAN_POINT ( 'NONE',  ( -19.03943276465977164, 0.05219959533909376836, 81.24890960531436690 ) ) ;
#8183 = CARTESIAN_POINT ( 'NONE',  ( -4.379528057220086978, -16.55341960407618274, 59.79275706135234714 ) ) ;
#8184 = CARTESIAN_POINT ( 'NONE',  ( 5.823673210054444382, -21.52544592524334988, 95.20942372801903275 ) ) ;
#8185 = CARTESIAN_POINT ( 'NONE',  ( 5.719274019375991003, -21.55341960407610458, 47.70724293864770260 ) ) ;
#8186 = CARTESIAN_POINT ( 'NONE',  ( 4.379528057220092307, 16.55341960407617563, 77.29275706135234714 ) ) ;
#8187 = CARTESIAN_POINT ( 'NONE',  ( 19.05341960407617918, -5.049401038297876454, 46.04275706135233293 ) ) ;
#8188 = EDGE_CURVE ( 'NONE', #144904, #70166, #146333, .T. ) ;
#8189 = CARTESIAN_POINT ( 'NONE',  ( 5.049401038297881783, 19.05341960407617563, 72.29275706135234714 ) ) ;
#8190 = ORIENTED_EDGE ( 'NONE', *, *, #124207, .T. ) ;
#8191 = CARTESIAN_POINT ( 'NONE',  ( -21.52544592524334988, -5.823673210054445271, 68.95942372801901854 ) ) ;
#8192 = CARTESIAN_POINT ( 'NONE',  ( 5.049401038298161559, -19.05341960407611168, 67.70724293864769550 ) ) ;
#8193 = CARTESIAN_POINT ( 'NONE',  ( -16.46253265017160317, 9.564922557960807481, 25.83224293864769194 ) ) ;
#8194 = CARTESIAN_POINT ( 'NONE',  ( -9.564922557961040184, 16.46253265017147172, 52.91775706135233293 ) ) ;
#8195 = CARTESIAN_POINT ( 'NONE',  ( -13.97604488694527625, -13.89961937509977652, 106.8739096053143669 ) ) ;
#8196 = CARTESIAN_POINT ( 'NONE',  ( 19.03943276465977164, -0.05219959533909143690, 93.74890960531435269 ) ) ;
#8197 = CARTESIAN_POINT ( 'NONE',  ( -16.52544592524342804, 4.483927247898546575, 51.04057627198103120 ) ) ;
#8198 = CARTESIAN_POINT ( 'NONE',  ( 10.72451020669898902, -18.67979575497178502, 47.91557627198102409 ) ) ;
#8199 = DIRECTION ( 'NONE',  ( 1.000000000000000000, -0.000000000000000000, -0.000000000000000000 ) ) ;
#8200 = CARTESIAN_POINT ( 'NONE',  ( 19.03943276465977164, 0.05219959533936151252, 21.25109039468565797 ) ) ;
#8201 = CARTESIAN_POINT ( 'NONE',  ( 18.22780087662126647, 5.499999999999818812, 46.48236817873107185 ) ) ;
#8202 = CARTESIAN_POINT ( 'NONE',  ( 19.05341960407611168, 5.049401038298154454, 48.95724293864768129 ) ) ;
#8203 = CARTESIAN_POINT ( 'NONE',  ( 13.97604488694527802, 13.89961937509977830, 84.37390960531435269 ) ) ;
#8204 = CARTESIAN_POINT ( 'NONE',  ( 30.74264578624799782, 22.33583958711400541, -4.800000000000000711 ) ) ;
#8205 = FACE_OUTER_BOUND ( 'NONE', #27654, .T. ) ;
#8206 = CARTESIAN_POINT ( 'NONE',  ( 14.29746914071037800, 8.314922557961029526, 66.66775706135234714 ) ) ;
#8207 = CARTESIAN_POINT ( 'NONE',  ( 5.719274019375991003, -21.55341960407610458, 82.70724293864770971 ) ) ;
#8208 = CARTESIAN_POINT ( 'NONE',  ( 14.29746914071049879, -8.314922557960816363, 58.33224293864768839 ) ) ;
#8210 = CARTESIAN_POINT ( 'NONE',  ( 37.99999999999999289, 2.893978650043524126E-14, -4.749999994537627224 ) ) ;
#8209 = CARTESIAN_POINT ( 'NONE',  ( 0.05219959533909260263, 19.03943276465977164, 39.99890960531436690 ) ) ;
#8211 = CARTESIAN_POINT ( 'NONE',  ( -18.62759615963255300, -10.81492255796106328, 34.16775706135234714 ) ) ;
#8212 = CARTESIAN_POINT ( 'NONE',  ( -16.46253265017146816, -9.564922557961047289, 54.16775706135234003 ) ) ;
#8213 = CARTESIAN_POINT ( 'NONE',  ( -16.51473224551069308, -9.474510206698971260, 36.66557627198102409 ) ) ;
#8214 = CARTESIAN_POINT ( 'NONE',  ( 18.67979575497194134, -10.72451020669871369, 100.8344237280190185 ) ) ;
#8215 = CARTESIAN_POINT ( 'NONE',  ( 17.40805194822032931, 6.112264579159340627, 96.66628727489391792 ) ) ;
#8216 = ORIENTED_EDGE ( 'NONE', *, *, #29165, .T. ) ;
#8217 = CARTESIAN_POINT ( 'NONE',  ( -16.55341960407611168, -4.379528057220339221, 36.45724293864768839 ) ) ;
#8218 = DIRECTION ( 'NONE',  ( 0.000000000000000000, -1.224646799147353454E-16, 1.000000000000000000 ) ) ;
#8219 = CARTESIAN_POINT ( 'NONE',  ( -5.719274019375978568, 21.55341960407610458, 40.20724293864769550 ) ) ;
#8220 = CARTESIAN_POINT ( 'NONE',  ( 17.14385361876520264, 23.59649016807275856, 140.1750000027311671 ) ) ;
#8221 = CARTESIAN_POINT ( 'NONE',  ( -16.51473224551069308, -9.474510206698971260, 86.66557627198102409 ) ) ;
#8222 = CARTESIAN_POINT ( 'NONE',  ( 12.06949235617757843, -12.14591786802309237, 83.12390960531436690 ) ) ;
#8223 = CARTESIAN_POINT ( 'NONE',  ( 14.34966873604972726, -8.224510206698740333, 20.83442372801901143 ) ) ;
#8224 = CARTESIAN_POINT ( 'NONE',  ( 4.379528057220339221, -16.55341960407611168, 22.70724293864769194 ) ) ;
#8225 = ORIENTED_EDGE ( 'NONE', *, *, #128791, .T. ) ;
#8226 = CARTESIAN_POINT ( 'NONE',  ( -0.05219959533909027116, -19.03943276465977164, 42.49890960531435269 ) ) ;
#8228 = CARTESIAN_POINT ( 'NONE',  ( 15.80617190586746368, 15.72974639402197994, 84.37390960531438111 ) ) ;
#8227 = CARTESIAN_POINT ( 'NONE',  ( -5.049401038298153566, 19.05341960407611168, 85.20724293864766707 ) ) ;
#8230 = CARTESIAN_POINT ( 'NONE',  ( -13.89961937509977652, 13.97604488694528158, 100.6239096053143669 ) ) ;
#8229 = CARTESIAN_POINT ( 'NONE',  ( 4.379528057220339221, -16.55341960407611168, 27.70724293864769905 ) ) ;
#8231 = CARTESIAN_POINT ( 'NONE',  ( -19.05341960407617563, 5.049401038297882671, 83.54275706135233293 ) ) ;
#8232 = CARTESIAN_POINT ( 'NONE',  ( -21.55341960407619339, 5.719274019375674811, 108.5427570613523756 ) ) ;
#8233 = CARTESIAN_POINT ( 'NONE',  ( -21.53943276465977519, 0.05219959533907696930, 86.24890960531436690 ) ) ;
#8234 = CARTESIAN_POINT ( 'NONE',  ( -10.72451020669898014, 18.67979575497178502, 40.41557627198103120 ) ) ;
#8235 = CARTESIAN_POINT ( 'NONE',  ( -5.049401038298153566, 19.05341960407611168, 70.20724293864769550 ) ) ;
#8236 = CARTESIAN_POINT ( 'NONE',  ( -12.14591786802309592, -12.06949235617757132, 36.87390960531435979 ) ) ;
#8237 = CARTESIAN_POINT ( 'NONE',  ( 5.153800228976335163, 19.02544592524342804, 74.79057627198103830 ) ) ;
#8238 = VERTEX_POINT ( 'NONE', #130153 ) ;
#8239 = CARTESIAN_POINT ( 'NONE',  ( 18.22780087662122739, 5.500000000000000888, 76.48236817873106475 ) ) ;
#8240 = CARTESIAN_POINT ( 'NONE',  ( 19.02544592524334988, 5.153800228976608722, 26.45942372801899722 ) ) ;
#8241 = CARTESIAN_POINT ( 'NONE',  ( -14.34966873604960291, -8.224510206698953496, 81.66557627198103830 ) ) ;
#8242 = CARTESIAN_POINT ( 'NONE',  ( -21.53943276465977519, -0.05219959533937600094, 23.75109039468567929 ) ) ;
#8243 = CARTESIAN_POINT ( 'NONE',  ( -22.44159573604010305, 16.30477369853692338, 143.1750000027311671 ) ) ;
#8244 = CARTESIAN_POINT ( 'NONE',  ( -5.823673210054116645, -21.52544592524344225, 72.29057627198102409 ) ) ;
#8245 = CARTESIAN_POINT ( 'NONE',  ( -8.224510206698735004, -14.34966873604973081, 99.58442372801900433 ) ) ;
#8246 = CARTESIAN_POINT ( 'NONE',  ( 19.05341960407611168, 5.049401038298154454, 28.95724293864769550 ) ) ;
#8247 = CARTESIAN_POINT ( 'NONE',  ( -9.564922557960796823, -16.46253265017161027, 67.08224293864769550 ) ) ;
#8248 = CARTESIAN_POINT ( 'NONE',  ( -37.99626262588765968, -12.34573411038913626, -5.647842220587802942 ) ) ;
#8249 = CARTESIAN_POINT ( 'NONE',  ( 4.379528057220339221, -16.55341960407611168, 32.70724293864770260 ) ) ;
#8250 = CARTESIAN_POINT ( 'NONE',  ( 5.823673210054444382, -21.52544592524334988, 65.20942372801901854 ) ) ;
#8251 = CARTESIAN_POINT ( 'NONE',  ( 24.54856932378043410, -28.36614238946604161, -18.58410241723692025 ) ) ;
#8252 = CARTESIAN_POINT ( 'NONE',  ( 10.72451020669871369, 18.67979575497193778, 97.08442372801904696 ) ) ;
#8253 = CARTESIAN_POINT ( 'NONE',  ( 19.05341960407611168, 5.049401038298154454, 48.95724293864768129 ) ) ;
#8254 = CARTESIAN_POINT ( 'NONE',  ( -19.03943276465977164, 0.05219959533909376836, 51.24890960531436690 ) ) ;
#8255 = ORIENTED_EDGE ( 'NONE', *, *, #28811, .T. ) ;
#8256 = CARTESIAN_POINT ( 'NONE',  ( -21.53943276465977519, -0.05219959533937600094, 98.75109039468568994 ) ) ;
#8257 = CARTESIAN_POINT ( 'NONE',  ( -0.05219959533934338120, 16.53943276465976808, 57.50109039468568994 ) ) ;
#8258 = CARTESIAN_POINT ( 'NONE',  ( 10.81492255796106328, -18.62759615963255655, 80.41775706135234714 ) ) ;
#8259 = CARTESIAN_POINT ( 'NONE',  ( 0.05219959533907565091, 21.53943276465977519, 24.99890960531435624 ) ) ;
#8260 = CARTESIAN_POINT ( 'NONE',  ( -16.51473224551082808, 9.474510206698731452, 93.33442372801900433 ) ) ;
#8261 = CARTESIAN_POINT ( 'NONE',  ( 10.81492255796106328, -18.62759615963255655, 50.41775706135235424 ) ) ;
#8262 = CARTESIAN_POINT ( 'NONE',  ( -16.55341960407617563, 4.379528057220093196, 38.54275706135234714 ) ) ;
#8264 = CARTESIAN_POINT ( 'NONE',  ( -0.05219959533907301413, -21.53943276465977519, 87.49890960531436690 ) ) ;
#8263 = AXIS2_PLACEMENT_3D ( 'NONE', #15571, #11625, #198607 ) ;
#8265 = CARTESIAN_POINT ( 'NONE',  ( 9.474510206698729675, 16.51473224551082808, 92.08442372801900433 ) ) ;
#8266 = CARTESIAN_POINT ( 'NONE',  ( 16.46253265017160672, -9.564922557960803928, 68.33224293864770971 ) ) ;
#8267 = CARTESIAN_POINT ( 'NONE',  ( 5.153800228976615827, -19.02544592524334988, 100.2094237280190043 ) ) ;
#8268 = CARTESIAN_POINT ( 'NONE',  ( -5.153800228976607833, 19.02544592524334988, 107.7094237280189759 ) ) ;
#8269 = CARTESIAN_POINT ( 'NONE',  ( -8.314922557960811034, -14.29746914071050412, 52.08224293864768839 ) ) ;
#8271 = ORIENTED_EDGE ( 'NONE', *, *, #74210, .F. ) ;
#8270 = CARTESIAN_POINT ( 'NONE',  ( 9.564922557961047289, -16.46253265017146816, 80.41775706135234714 ) ) ;
#8272 = CARTESIAN_POINT ( 'NONE',  ( -4.483927247898782831, 16.52544592524335698, 57.70942372801901143 ) ) ;
#8273 = CARTESIAN_POINT ( 'NONE',  ( -9.564922557961040184, 16.46253265017147172, 37.91775706135233293 ) ) ;
#8274 = CARTESIAN_POINT ( 'NONE',  ( -16.51473224551069308, -9.474510206698971260, 36.66557627198102409 ) ) ;
#8275 = CARTESIAN_POINT ( 'NONE',  ( 13.89961937509977652, -13.97604488694527269, 53.12390960531434558 ) ) ;
#8276 = CARTESIAN_POINT ( 'NONE',  ( -12.06949235617739369, -12.14591786802326823, 54.37609039468568994 ) ) ;
#8277 = CARTESIAN_POINT ( 'NONE',  ( -27.73933785331498925, 2.428612866367529932E-14, 141.3750000027311842 ) ) ;
#8278 = CARTESIAN_POINT ( 'NONE',  ( -17.14385361876520619, 23.59649016807275856, 148.5750000027311444 ) ) ;
#8279 = CARTESIAN_POINT ( 'NONE',  ( -19.05341960407611168, -5.049401038298163336, 106.4572429386476955 ) ) ;
#8280 = CARTESIAN_POINT ( 'NONE',  ( 19.03943276465977164, -0.05219959533909143690, 28.74890960531435624 ) ) ;
#8281 = VERTEX_POINT ( 'NONE', #97815 ) ;
#8282 = CARTESIAN_POINT ( 'NONE',  ( 13.89961937509957401, 13.97604488694547697, 101.8760903946856331 ) ) ;
#8283 = CARTESIAN_POINT ( 'NONE',  ( -21.52544592524343514, 5.823673210054127303, 36.04057627198102409 ) ) ;
#8285 = CARTESIAN_POINT ( 'NONE',  ( 12.14591786802327356, -12.06949235617739191, 20.62609039468568639 ) ) ;
#8284 = CARTESIAN_POINT ( 'NONE',  ( -0.05219959533936034679, 19.03943276465977164, 27.50109039468566507 ) ) ;
#8286 = CARTESIAN_POINT ( 'NONE',  ( -9.474510206698964154, 16.51473224551069663, 30.41557627198102054 ) ) ;
#8287 = CARTESIAN_POINT ( 'NONE',  ( -19.02544592524342804, 5.153800228976336051, 46.04057627198101699 ) ) ;
#8288 = CARTESIAN_POINT ( 'NONE',  ( 0.05219959533907565091, 21.53943276465977519, 69.99890960531435269 ) ) ;
#8289 = CARTESIAN_POINT ( 'NONE',  ( 16.46253265017160672, -9.564922557960803928, 103.3322429386476955 ) ) ;
#8290 = CARTESIAN_POINT ( 'NONE',  ( 9.564922557960805705, 16.46253265017160317, 34.58224293864770260 ) ) ;
#8291 = CARTESIAN_POINT ( 'NONE',  ( -27.73933785331498925, -9.013057229001049109, 145.4750000027311785 ) ) ;
#8292 = CARTESIAN_POINT ( 'NONE',  ( 13.89961937509957401, 13.97604488694547697, 86.87609039468567573 ) ) ;
#8293 = CARTESIAN_POINT ( 'NONE',  ( -0.05219959533910754901, -16.53943276465976808, 72.49890960531435269 ) ) ;
#8294 = CARTESIAN_POINT ( 'NONE',  ( 15.80617190586746368, 15.72974639402197994, 44.37390960531435979 ) ) ;
#8295 = CARTESIAN_POINT ( 'NONE',  ( 21.55341960407619695, -5.719274019375665929, 111.0427570613523613 ) ) ;
#8296 = CARTESIAN_POINT ( 'NONE',  ( 10.72451020669898902, -18.67979575497178502, 97.91557627198103830 ) ) ;
#8297 = CARTESIAN_POINT ( 'NONE',  ( 15.72974639402176855, 15.80617190586768217, 66.87609039468568994 ) ) ;
#8298 = CARTESIAN_POINT ( 'NONE',  ( 10.81492255796106328, -18.62759615963255655, 80.41775706135234714 ) ) ;
#8299 = ADVANCED_FACE ( 'NONE', ( #6820 ), #108199, .F. ) ;
#8300 = CARTESIAN_POINT ( 'NONE',  ( -19.03943276465977164, 0.05219959533909376836, 111.2489096053143669 ) ) ;
#8302 = CARTESIAN_POINT ( 'NONE',  ( 21.55341960407619695, -5.719274019375665929, 76.04275706135237556 ) ) ;
#8301 = CARTESIAN_POINT ( 'NONE',  ( -8.314922557961024197, 14.29746914071037800, 102.9177570613523756 ) ) ;
#8303 = CARTESIAN_POINT ( 'NONE',  ( 9.474510206698971260, -16.51473224551069308, 67.91557627198102409 ) ) ;
#8304 = CARTESIAN_POINT ( 'NONE',  ( -16.46253265017146816, -9.564922557961047289, 34.16775706135233293 ) ) ;
#8305 = CARTESIAN_POINT ( 'NONE',  ( 21.52544592524334988, 5.823673210054432836, 31.45942372801901854 ) ) ;
#8306 = CARTESIAN_POINT ( 'NONE',  ( -16.51473224551069308, -9.474510206698971260, 61.66557627198103120 ) ) ;
#8307 = CARTESIAN_POINT ( 'NONE',  ( 12.14591786802309770, 12.06949235617756955, 79.37390960531436690 ) ) ;
#8308 = CARTESIAN_POINT ( 'NONE',  ( 14.29746914071049879, -8.314922557960816363, 53.33224293864769550 ) ) ;
#8309 = CARTESIAN_POINT ( 'NONE',  ( -5.823673210054116645, -21.52544592524344225, 52.29057627198102409 ) ) ;
#8310 = EDGE_CURVE ( 'NONE', #132987, #99125, #22008, .T. ) ;
#8311 = CARTESIAN_POINT ( 'NONE',  ( 13.97604488694527802, 13.89961937509977652, 59.37390960531434558 ) ) ;
#8312 = CARTESIAN_POINT ( 'NONE',  ( -5.719274019375978568, 21.55341960407610458, 70.20724293864769550 ) ) ;
#8313 = CARTESIAN_POINT ( 'NONE',  ( 13.89961937509957401, 13.97604488694547697, 61.87609039468566863 ) ) ;
#8315 = CARTESIAN_POINT ( 'NONE',  ( 16.53943276465976808, -0.05219959533910856209, 63.74890960531435979 ) ) ;
#8314 = CARTESIAN_POINT ( 'NONE',  ( -19.02544592524335343, -5.153800228976618492, 23.95942372801900078 ) ) ;
#8316 = CARTESIAN_POINT ( 'NONE',  ( 15.80617190586746368, 15.72974639402197994, 39.37390960531436690 ) ) ;
#8317 = EDGE_LOOP ( 'NONE', ( #155924, #169926 ) ) ;
#8318 = CARTESIAN_POINT ( 'NONE',  ( 16.19135201231366850, 7.376712067591939537, 102.6868085405203459 ) ) ;
#8320 = CARTESIAN_POINT ( 'NONE',  ( -27.73933785331498925, 9.013057229001088189, 141.2750000027311899 ) ) ;
#8319 = CARTESIAN_POINT ( 'NONE',  ( 4.483927247898790824, -16.52544592524335698, 85.20942372801901854 ) ) ;
#8321 = CARTESIAN_POINT ( 'NONE',  ( -0.05219959533936034679, 19.03943276465977164, 82.50109039468567573 ) ) ;
#8322 = CARTESIAN_POINT ( 'NONE',  ( 0.05219959533910956823, 16.53943276465976808, 54.99890960531435269 ) ) ;
#8323 = DIRECTION ( 'NONE',  ( 0.000000000000000000, 1.000000000000000000, 0.000000000000000000 ) ) ;
#8324 = CARTESIAN_POINT ( 'NONE',  ( 19.02544592524343514, -5.153800228976328945, 48.54057627198103120 ) ) ;
#8325 = CARTESIAN_POINT ( 'NONE',  ( -16.52544592524342804, 4.483927247898546575, 46.04057627198103830 ) ) ;
#8326 = CARTESIAN_POINT ( 'NONE',  ( 5.049401038298161559, -19.05341960407611168, 87.70724293864769550 ) ) ;
#8327 = CARTESIAN_POINT ( 'NONE',  ( 19.05341960407611168, 5.049401038298154454, 58.95724293864768129 ) ) ;
#8328 = CARTESIAN_POINT ( 'NONE',  ( 21.55341960407619695, -5.719274019375665929, 66.04275706135236135 ) ) ;
#8329 = CARTESIAN_POINT ( 'NONE',  ( 9.564922557960805705, 16.46253265017160317, 74.58224293864769550 ) ) ;
#8330 = CARTESIAN_POINT ( 'NONE',  ( 13.89961937509977652, -13.97604488694527269, 33.12390960531434558 ) ) ;
#8331 = CARTESIAN_POINT ( 'NONE',  ( 19.05341960407611168, 5.049401038298154454, 73.95724293864768129 ) ) ;
#8332 = CARTESIAN_POINT ( 'NONE',  ( 21.53943276465977519, -0.05219959533907433946, 48.74890960531435979 ) ) ;
#8333 = CARTESIAN_POINT ( 'NONE',  ( 0.05219959533909260263, 19.03943276465977164, 54.99890960531435979 ) ) ;
#8334 = CARTESIAN_POINT ( 'NONE',  ( 18.67979575497178502, 10.72451020669898547, 54.16557627198103120 ) ) ;
#8335 = SHAPE_REPRESENTATION ( 'Impeller Fan Blade Assembly', ( #82054 ), #65912 ) ;
#8336 = CARTESIAN_POINT ( 'NONE',  ( 16.51473224551083163, -9.474510206698727899, 80.83442372801899012 ) ) ;
#8337 = CARTESIAN_POINT ( 'NONE',  ( -4.483927247898782831, 16.52544592524335698, 102.7094237280190185 ) ) ;
#8338 = CARTESIAN_POINT ( 'NONE',  ( -19.02544592524334988, -5.153800228976617603, 38.95942372801900433 ) ) ;
#8340 = CARTESIAN_POINT ( 'NONE',  ( 4.379528057220092307, 16.55341960407617563, 82.29275706135234714 ) ) ;
#8339 = CARTESIAN_POINT ( 'NONE',  ( -8.224510206698735004, -14.34966873604973081, 64.58442372801900433 ) ) ;
#8341 = CARTESIAN_POINT ( 'NONE',  ( 11.80868324581538253, -11.80868324581533457, -61.34707691135562868 ) ) ;
#8342 = CARTESIAN_POINT ( 'NONE',  ( 14.34966873604972726, -8.224510206698740333, 65.83442372801900433 ) ) ;
#8343 = CARTESIAN_POINT ( 'NONE',  ( -18.67979575497178146, -10.72451020669898902, 26.66557627198103475 ) ) ;
#8344 = CARTESIAN_POINT ( 'NONE',  ( 19.03943276465977164, -0.05219959533909143690, 28.74890960531435624 ) ) ;
#8345 = CARTESIAN_POINT ( 'NONE',  ( -14.34966873604972548, 8.224510206698743886, 43.33442372801901143 ) ) ;
#8346 = CARTESIAN_POINT ( 'NONE',  ( -5.049401038298153566, 19.05341960407611168, 50.20724293864770260 ) ) ;
#8347 = CARTESIAN_POINT ( 'NONE',  ( 21.52544592524334988, 5.823673210054432836, 41.45942372801901143 ) ) ;
#8348 = CARTESIAN_POINT ( 'NONE',  ( -8.224510206698735004, -14.34966873604973081, 29.58442372801901854 ) ) ;
#8349 = CARTESIAN_POINT ( 'NONE',  ( -12.14591786802326823, 12.06949235617739902, 103.1260903946856757 ) ) ;
#8350 = CARTESIAN_POINT ( 'NONE',  ( -17.60779699588842462, -5.499999999999949374, 71.34981316670105400 ) ) ;
#8351 = CARTESIAN_POINT ( 'NONE',  ( 21.52544592524334988, 5.823673210054432836, 111.4594237280190328 ) ) ;
#8352 = CARTESIAN_POINT ( 'NONE',  ( 19.05341960407617918, -5.049401038297876454, 111.0427570613523329 ) ) ;
#8353 = CARTESIAN_POINT ( 'NONE',  ( 5.153800228976615827, -19.02544592524334988, 65.20942372801900433 ) ) ;
#8354 = CARTESIAN_POINT ( 'NONE',  ( -16.53943276465976808, 0.05219959533911058130, 76.24890960531435269 ) ) ;
#8355 = CARTESIAN_POINT ( 'NONE',  ( -9.474510206698964154, 16.51473224551069663, 35.41557627198102409 ) ) ;
#8357 = CARTESIAN_POINT ( 'NONE',  ( 17.31747979337949062, 6.344076630961017926, 78.87944868065184778 ) ) ;
#8356 = CARTESIAN_POINT ( 'NONE',  ( -16.51473224551082808, 9.474510206698731452, 63.33442372801900433 ) ) ;
#8358 = CARTESIAN_POINT ( 'NONE',  ( -21.52544592524334988, -5.823673210054445271, 58.95942372801902565 ) ) ;
#8359 = CARTESIAN_POINT ( 'NONE',  ( 12.06949235617739724, 12.14591786802326823, 36.87609039468568994 ) ) ;
#8360 = CARTESIAN_POINT ( 'NONE',  ( 24.81835718235489807, 6.052279806424484931, 168.4265042179603142 ) ) ;
#8361 = CARTESIAN_POINT ( 'NONE',  ( -10.81492255796078084, -18.62759615963271287, 22.08224293864769194 ) ) ;
#8362 = CARTESIAN_POINT ( 'NONE',  ( -5.049401038297874678, -19.05341960407617918, 104.7927570613523471 ) ) ;
#8363 = CARTESIAN_POINT ( 'NONE',  ( -19.05341960407611168, -5.049401038298163336, 111.4572429386476671 ) ) ;
#8364 = CARTESIAN_POINT ( 'NONE',  ( -19.49401214000077687, 12.39993551617566681, 169.9999999999999716 ) ) ;
#8365 = CARTESIAN_POINT ( 'NONE',  ( 9.474510206698971260, -16.51473224551069308, 27.91557627198103120 ) ) ;
#8366 = CARTESIAN_POINT ( 'NONE',  ( 15.72974639402176855, 15.80617190586768217, 111.8760903946856615 ) ) ;
#8367 = CARTESIAN_POINT ( 'NONE',  ( 5.153800228976335163, 19.02544592524342804, 59.79057627198100988 ) ) ;
#8368 = CIRCLE ( 'NONE', #104487, 69.99999999999997158 ) ;
#8369 = CARTESIAN_POINT ( 'NONE',  ( 18.67979575497194134, -10.72451020669871369, 60.83442372801901854 ) ) ;
#8370 = CARTESIAN_POINT ( 'NONE',  ( 10.72451020669871369, 18.67979575497193778, 97.08442372801904696 ) ) ;
#8371 = CARTESIAN_POINT ( 'NONE',  ( 4.483927247898545687, 16.52544592524342804, 24.79057627198103120 ) ) ;
#8372 = CARTESIAN_POINT ( 'NONE',  ( 16.46253265017160672, -9.564922557960803928, 33.33224293864770260 ) ) ;
#8373 = CARTESIAN_POINT ( 'NONE',  ( -13.97604488694527625, -13.89961937509977652, 96.87390960531433848 ) ) ;
#8374 = CARTESIAN_POINT ( 'NONE',  ( -5.823673210054431948, 21.52544592524334988, 57.70942372801901143 ) ) ;
#8375 = CARTESIAN_POINT ( 'NONE',  ( 19.03943276465977164, -0.05219959533909143690, 38.74890960531436690 ) ) ;
#8376 = CARTESIAN_POINT ( 'NONE',  ( -21.53943276465977519, -0.05219959533937600094, 53.75109039468568994 ) ) ;
#8378 = CARTESIAN_POINT ( 'NONE',  ( 13.97604488694527802, 13.89961937509977652, 99.37390960531436690 ) ) ;
#8377 = CARTESIAN_POINT ( 'NONE',  ( -19.03943276465977164, -0.05219959533935918106, 83.75109039468567573 ) ) ;
#8379 = CARTESIAN_POINT ( 'NONE',  ( 16.53943276465976808, -0.05219959533910856209, 113.7489096053143527 ) ) ;
#8380 = CARTESIAN_POINT ( 'NONE',  ( -15.80617190586745835, -15.72974639402198527, 111.8739096053143669 ) ) ;
#8381 = CARTESIAN_POINT ( 'NONE',  ( 9.474510206698729675, 16.51473224551082808, 37.08442372801899722 ) ) ;
#8382 = CARTESIAN_POINT ( 'NONE',  ( 16.52544592524342804, -4.483927247898539470, 93.54057627198103830 ) ) ;
#8383 = CARTESIAN_POINT ( 'NONE',  ( -16.46253265017160317, 9.564922557960807481, 55.83224293864769550 ) ) ;
#8384 = CARTESIAN_POINT ( 'NONE',  ( -13.89961937509957401, -13.97604488694547875, 104.3760903946856757 ) ) ;
#8385 = CARTESIAN_POINT ( 'NONE',  ( 16.53943276465976808, -0.05219959533910856209, 58.74890960531436690 ) ) ;
#8386 = CARTESIAN_POINT ( 'NONE',  ( -5.719274019375665041, -21.55341960407619695, 104.7927570613523898 ) ) ;
#8387 = CARTESIAN_POINT ( 'NONE',  ( -16.46253265017160317, 9.564922557960807481, 100.8322429386477097 ) ) ;
#8388 = CARTESIAN_POINT ( 'NONE',  ( -16.46253265017146816, -9.564922557961047289, 94.16775706135233293 ) ) ;
#8389 = CARTESIAN_POINT ( 'NONE',  ( -18.62759615963270932, 10.81492255796079327, 90.83224293864769550 ) ) ;
#8390 = CARTESIAN_POINT ( 'NONE',  ( -21.53943276465977519, -0.05219959533937600094, 43.75109039468568284 ) ) ;
#8391 = CARTESIAN_POINT ( 'NONE',  ( 14.29746914071037800, 8.314922557961029526, 46.66775706135234714 ) ) ;
#8392 = CARTESIAN_POINT ( 'NONE',  ( -16.55341960407617563, 4.379528057220093196, 108.5427570613523756 ) ) ;
#8394 = CARTESIAN_POINT ( 'NONE',  ( 5.823673210054444382, -21.52544592524334988, 45.20942372801901854 ) ) ;
#8393 = CARTESIAN_POINT ( 'NONE',  ( 16.52544592524335698, 4.483927247898782831, 46.45942372801901854 ) ) ;
#8395 = CARTESIAN_POINT ( 'NONE',  ( -21.53943276465977519, 0.05219959533907696930, 41.24890960531435269 ) ) ;
#8396 = CARTESIAN_POINT ( 'NONE',  ( 0.05219959533909260263, 19.03943276465977164, 34.99890960531435979 ) ) ;
#8397 = CARTESIAN_POINT ( 'NONE',  ( -30.74264578624800492, -22.33583958711396278, -7.549999994537627934 ) ) ;
#8398 = CARTESIAN_POINT ( 'NONE',  ( 4.483927247898790824, -16.52544592524335698, 65.20942372801901854 ) ) ;
#8399 = CARTESIAN_POINT ( 'NONE',  ( 21.52544592524344225, -5.823673210054117533, 83.54057627198102409 ) ) ;
#8400 = CARTESIAN_POINT ( 'NONE',  ( -16.52544592524342804, 4.483927247898546575, 41.04057627198103120 ) ) ;
#8401 = CARTESIAN_POINT ( 'NONE',  ( -14.29746914071037622, -8.314922557961029526, 59.16775706135234714 ) ) ;
#8402 = CARTESIAN_POINT ( 'NONE',  ( -13.97604488694527625, -13.89961937509977652, 56.87390960531434558 ) ) ;
#8403 = CARTESIAN_POINT ( 'NONE',  ( 16.51473224551083163, -9.474510206698727899, 95.83442372801900433 ) ) ;
#8404 = CARTESIAN_POINT ( 'NONE',  ( 0.05219959533907565091, 21.53943276465977519, 79.99890960531435269 ) ) ;
#8405 = CARTESIAN_POINT ( 'NONE',  ( -12.14591786802309592, -12.06949235617757132, 31.87390960531435979 ) ) ;
#8406 = ORIENTED_EDGE ( 'NONE', *, *, #70616, .F. ) ;
#8407 = CARTESIAN_POINT ( 'NONE',  ( 14.29746914071037800, 8.314922557961029526, 76.66775706135234714 ) ) ;
#8408 = CARTESIAN_POINT ( 'NONE',  ( 24.18299921989880730, 12.77492350451764125, 169.7822198539310250 ) ) ;
#8409 = CARTESIAN_POINT ( 'NONE',  ( -5.823673210054116645, -21.52544592524344225, 77.29057627198102409 ) ) ;
#8410 = ORIENTED_EDGE ( 'NONE', *, *, #1629, .T. ) ;
#8411 = CARTESIAN_POINT ( 'NONE',  ( 16.53943276465976808, 0.05219959533934440121, 111.2510903946856899 ) ) ;
#8412 = ORIENTED_EDGE ( 'NONE', *, *, #195701, .F. ) ;
#8413 = DIRECTION ( 'NONE',  ( -1.000000000000000000, 0.000000000000000000, 0.000000000000000000 ) ) ;
#8414 = CARTESIAN_POINT ( 'NONE',  ( 10.81492255796078972, 18.62759615963270932, 94.58224293864769550 ) ) ;
#8415 = CIRCLE ( 'NONE', #73099, 2.500000000000002220 ) ;
#8416 = CARTESIAN_POINT ( 'NONE',  ( 5.719274019375991003, -21.55341960407610458, 107.7072429386476955 ) ) ;
#8417 = CARTESIAN_POINT ( 'NONE',  ( -8.224510206698948167, 14.34966873604960824, 30.41557627198101699 ) ) ;
#8418 = CARTESIAN_POINT ( 'NONE',  ( -16.53943276465976808, -0.05219959533934237506, 28.75109039468567929 ) ) ;
#8419 = CARTESIAN_POINT ( 'NONE',  ( -16.46253265017160317, 9.564922557960807481, 30.83224293864769550 ) ) ;
#8420 = CARTESIAN_POINT ( 'NONE',  ( -19.02544592524342804, 5.153800228976336051, 71.04057627198099567 ) ) ;
#8421 = CARTESIAN_POINT ( 'NONE',  ( 8.906447517083050158, 27.41122689804195645, 147.4000000000000057 ) ) ;
#8422 = CARTESIAN_POINT ( 'NONE',  ( 5.719274019375991003, -21.55341960407610458, 22.70724293864769194 ) ) ;
#8423 = CARTESIAN_POINT ( 'NONE',  ( 18.22780087662121673, 5.500000000000056843, 63.98459894673894155 ) ) ;
#8424 = CARTESIAN_POINT ( 'NONE',  ( 5.153800228976615827, -19.02544592524334988, 105.2094237280190185 ) ) ;
#8425 = CARTESIAN_POINT ( 'NONE',  ( 9.564922557961047289, -16.46253265017146816, 40.41775706135234003 ) ) ;
#8426 = CARTESIAN_POINT ( 'NONE',  ( 21.52544592524344225, -5.823673210054117533, 88.54057627198103830 ) ) ;
#8427 = CARTESIAN_POINT ( 'NONE',  ( 14.29746914071037800, 8.314922557961029526, 111.6677570613523613 ) ) ;
#8428 = CARTESIAN_POINT ( 'NONE',  ( -21.55341960407610458, -5.719274019375992779, 46.45724293864769550 ) ) ;
#8430 = CARTESIAN_POINT ( 'NONE',  ( -5.049401038297874678, -19.05341960407617918, 104.7927570613523471 ) ) ;
#8429 = CARTESIAN_POINT ( 'NONE',  ( -5.823673210054116645, -21.52544592524344225, 87.29057627198103830 ) ) ;
#8431 = CARTESIAN_POINT ( 'NONE',  ( -16.51473224551069308, -9.474510206698971260, 106.6655762719810383 ) ) ;
#8432 = CARTESIAN_POINT ( 'NONE',  ( 18.62759615963255655, 10.81492255796105972, 81.66775706135236135 ) ) ;
#8433 = CARTESIAN_POINT ( 'NONE',  ( 5.153800228976335163, 19.02544592524342804, 69.79057627198103830 ) ) ;
#8434 = CARTESIAN_POINT ( 'NONE',  ( -14.34966873604960291, -8.224510206698953496, 101.6655762719810383 ) ) ;
#8435 = CARTESIAN_POINT ( 'NONE',  ( 32.45668260148360673, 3.101559039593180689, 88.16695215365970739 ) ) ;
#8436 = CARTESIAN_POINT ( 'NONE',  ( -0.05219959533909027116, -19.03943276465977164, 72.49890960531435269 ) ) ;
#8437 = CARTESIAN_POINT ( 'NONE',  ( -0.05219959533910754901, -16.53943276465976808, 87.49890960531436690 ) ) ;
#8438 = ORIENTED_EDGE ( 'NONE', *, *, #48191, .F. ) ;
#8439 = CARTESIAN_POINT ( 'NONE',  ( -13.97604488694547697, 13.89961937509957934, 103.1260903946856473 ) ) ;
#8440 = CARTESIAN_POINT ( 'NONE',  ( 19.05341960407611168, 5.049401038298154454, 53.95724293864770260 ) ) ;
#8442 = CARTESIAN_POINT ( 'NONE',  ( -16.51473224551069308, -9.474510206698971260, 96.66557627198102409 ) ) ;
#8441 = CARTESIAN_POINT ( 'NONE',  ( 15.80617190586769283, -15.72974639402175789, 85.62609039468568994 ) ) ;
#8443 = CARTESIAN_POINT ( 'NONE',  ( -14.34966873604972548, 8.224510206698743886, 78.33442372801901854 ) ) ;
#8444 = PLANE ( 'NONE',  #103538 ) ;
#8445 = CARTESIAN_POINT ( 'NONE',  ( -16.51473224551082808, 9.474510206698731452, 58.33442372801900433 ) ) ;
#8446 = CARTESIAN_POINT ( 'NONE',  ( -10.81492255796105439, 18.62759615963255655, 102.9177570613523756 ) ) ;
#8447 = CARTESIAN_POINT ( 'NONE',  ( 17.79613651744294245, -24.49428055684527195, 144.6843446569000093 ) ) ;
#8448 = DIRECTION ( 'NONE',  ( -0.000000000000000000, -0.000000000000000000, -1.000000000000000000 ) ) ;
#8449 = CARTESIAN_POINT ( 'NONE',  ( 8.314922557960818139, 14.29746914071049879, 24.58224293864768839 ) ) ;
#8450 = CARTESIAN_POINT ( 'NONE',  ( 16.70000000000002061, 0.000000000000000000, -59.13370768023891344 ) ) ;
#8451 = CARTESIAN_POINT ( 'NONE',  ( 14.29746914071037800, 8.314922557961029526, 96.66775706135234714 ) ) ;
#8452 = CARTESIAN_POINT ( 'NONE',  ( 17.79613651744293534, 24.49428055684532524, 145.5656553485623590 ) ) ;
#8453 = CARTESIAN_POINT ( 'NONE',  ( -8.314922557961024197, 14.29746914071037800, 67.91775706135234714 ) ) ;
#8454 = DIRECTION ( 'NONE',  ( -1.000000000000000000, 0.000000000000000000, 0.000000000000000000 ) ) ;
#8455 = CARTESIAN_POINT ( 'NONE',  ( 15.80617190586769283, -15.72974639402175789, 85.62609039468568994 ) ) ;
#8456 = CARTESIAN_POINT ( 'NONE',  ( 13.89961937509957401, 13.97604488694547697, 86.87609039468567573 ) ) ;
#8457 = CARTESIAN_POINT ( 'NONE',  ( 16.46253265017146816, 9.564922557961045513, 36.66775706135233293 ) ) ;
#8458 = CARTESIAN_POINT ( 'NONE',  ( 16.51473224551069308, 9.474510206698969483, 69.16557627198102409 ) ) ;
#8459 = CARTESIAN_POINT ( 'NONE',  ( 13.89961937509977652, -13.97604488694527269, 58.12390960531436690 ) ) ;
#8460 = CARTESIAN_POINT ( 'NONE',  ( 37.66961640367472341, -4.999999999999976019, -18.00000000000000355 ) ) ;
#8461 = CARTESIAN_POINT ( 'NONE',  ( -21.55341960407610458, -5.719274019375992779, 76.45724293864769550 ) ) ;
#8462 = CARTESIAN_POINT ( 'NONE',  ( 10.72451020669898902, -18.67979575497178502, 32.91557627198102409 ) ) ;
#8463 = CARTESIAN_POINT ( 'NONE',  ( 9.474510206698971260, -16.51473224551069308, 37.91557627198102409 ) ) ;
#8464 = CARTESIAN_POINT ( 'NONE',  ( 4.379528057220092307, 16.55341960407617563, 67.29275706135234714 ) ) ;
#8465 = EDGE_LOOP ( 'NONE', ( #183152, #145287 ) ) ;
#8466 = CARTESIAN_POINT ( 'NONE',  ( -0.05219959533937732626, 21.53943276465977519, 27.50109039468567929 ) ) ;
#8468 = CARTESIAN_POINT ( 'NONE',  ( 36.91746824999999177, 2.880721459617395097E-14, -7.624999997268813168 ) ) ;
#8467 = CARTESIAN_POINT ( 'NONE',  ( 4.483927247898545687, 16.52544592524342804, 69.79057627198102409 ) ) ;
#8469 = CARTESIAN_POINT ( 'NONE',  ( 0.05219959533934541429, -16.53943276465976808, 25.00109039468567218 ) ) ;
#8470 = CARTESIAN_POINT ( 'NONE',  ( 19.05341960407617918, -5.049401038297876454, 56.04275706135234714 ) ) ;
#8471 = CARTESIAN_POINT ( 'NONE',  ( 8.314922557960818139, 14.29746914071049879, 59.58224293864770260 ) ) ;
#8472 = CARTESIAN_POINT ( 'NONE',  ( -21.52544592524334988, -5.823673210054445271, 28.95942372801902209 ) ) ;
#8474 = CARTESIAN_POINT ( 'NONE',  ( -18.67979575497178146, -10.72451020669898902, 71.66557627198100988 ) ) ;
#8473 = CARTESIAN_POINT ( 'NONE',  ( 0.000000000000000000, 0.000000000000000000, -64.92279855667830191 ) ) ;
#8475 = CARTESIAN_POINT ( 'NONE',  ( -19.03943276465977164, 0.05219959533909376836, 101.2489096053143669 ) ) ;
#8476 = CARTESIAN_POINT ( 'NONE',  ( -4.483927247898539470, -16.52544592524342804, 72.29057627198102409 ) ) ;
#8477 = CARTESIAN_POINT ( 'NONE',  ( 33.17138627372818860, -22.14683228597266762, -20.77970695692249237 ) ) ;
#8478 = CARTESIAN_POINT ( 'NONE',  ( 17.60779699588838199, 5.500000000000005329, 43.84981316670103979 ) ) ;
#8479 = CARTESIAN_POINT ( 'NONE',  ( 19.05341960407617918, -5.049401038297876454, 66.04275706135233293 ) ) ;
#8480 = CARTESIAN_POINT ( 'NONE',  ( -18.62759615963255300, -10.81492255796106328, 29.16775706135234003 ) ) ;
#8481 = CARTESIAN_POINT ( 'NONE',  ( 16.46253265017160672, -9.564922557960803928, 63.33224293864769550 ) ) ;
#8482 = CARTESIAN_POINT ( 'NONE',  ( -13.97604488694547697, 13.89961937509957934, 43.12609039468566152 ) ) ;
#8483 = CARTESIAN_POINT ( 'NONE',  ( 13.89961937509977652, -13.97604488694527269, 28.12390960531435624 ) ) ;
#8484 = CARTESIAN_POINT ( 'NONE',  ( -18.62759615963255300, -10.81492255796106328, 64.16775706135234714 ) ) ;
#8485 = CYLINDRICAL_SURFACE ( 'NONE', #27165, 28.79475375365586487 ) ;
#8486 = CARTESIAN_POINT ( 'NONE',  ( 0.05219959533910956823, 16.53943276465976808, 39.99890960531436690 ) ) ;
#8487 = CARTESIAN_POINT ( 'NONE',  ( 19.03943276465977164, -0.05219959533909143690, 68.74890960531436690 ) ) ;
#8488 = CARTESIAN_POINT ( 'NONE',  ( -18.62759615963270932, 10.81492255796079327, 85.83224293864768129 ) ) ;
#8489 = CARTESIAN_POINT ( 'NONE',  ( -0.05219959533909027116, -19.03943276465977164, 62.49890960531435979 ) ) ;
#8490 = ORIENTED_EDGE ( 'NONE', *, *, #15491, .T. ) ;
#8491 = CARTESIAN_POINT ( 'NONE',  ( -21.55341960407610458, -5.719274019375992779, 61.45724293864770260 ) ) ;
#8492 = CARTESIAN_POINT ( 'NONE',  ( -10.72451020669870658, -18.67979575497194134, 104.5844237280190185 ) ) ;
#8495 = CARTESIAN_POINT ( 'NONE',  ( -4.483927247898539470, -16.52544592524342804, 77.29057627198102409 ) ) ;
#8494 = CARTESIAN_POINT ( 'NONE',  ( 14.29746914071037800, 8.314922557961029526, 91.66775706135234714 ) ) ;
#8493 = CARTESIAN_POINT ( 'NONE',  ( -3.573655867282028392E-15, 2.428612866367529932E-14, -23.00000000000000000 ) ) ;
#8496 = CARTESIAN_POINT ( 'NONE',  ( 16.46253265017146816, 9.564922557961045513, 91.66775706135234714 ) ) ;
#8497 = ORIENTED_EDGE ( 'NONE', *, *, #57626, .F. ) ;
#8498 = CARTESIAN_POINT ( 'NONE',  ( -10.72451020669898014, 18.67979575497178502, 110.4155762719810383 ) ) ;
#8499 = CARTESIAN_POINT ( 'NONE',  ( -9.474510206698720793, -16.51473224551083518, 34.58442372801899722 ) ) ;
#8500 = CARTESIAN_POINT ( 'NONE',  ( 8.224510206698742110, 14.34966873604972548, 102.0844237280190185 ) ) ;
#8501 = CARTESIAN_POINT ( 'NONE',  ( -16.46253265017146816, -9.564922557961047289, 34.16775706135233293 ) ) ;
#8502 = CARTESIAN_POINT ( 'NONE',  ( -16.46253265017160317, 9.564922557960807481, 85.83224293864769550 ) ) ;
#8503 = CARTESIAN_POINT ( 'NONE',  ( 21.53943276465977519, -0.05219959533907433946, 63.74890960531435979 ) ) ;
#8504 = CARTESIAN_POINT ( 'NONE',  ( 4.379528057220339221, -16.55341960407611168, 112.7072429386476955 ) ) ;
#8505 = CARTESIAN_POINT ( 'NONE',  ( 18.62759615963255655, 10.81492255796105972, 111.6677570613523613 ) ) ;
#8506 = CARTESIAN_POINT ( 'NONE',  ( 8.314922557961029526, -14.29746914071037800, 80.41775706135234714 ) ) ;
#8507 = CARTESIAN_POINT ( 'NONE',  ( 5.823673210054444382, -21.52544592524334988, 30.20942372801902565 ) ) ;
#8508 = CARTESIAN_POINT ( 'NONE',  ( -4.379528057220086978, -16.55341960407618274, 34.79275706135235424 ) ) ;
#8509 = CARTESIAN_POINT ( 'NONE',  ( 9.564922557960805705, 16.46253265017160317, 99.58224293864770971 ) ) ;
#8510 = CARTESIAN_POINT ( 'NONE',  ( -16.46253265017160317, 9.564922557960807481, 40.83224293864769550 ) ) ;
#8511 = CARTESIAN_POINT ( 'NONE',  ( -16.51473224551069308, -9.474510206698971260, 61.66557627198103120 ) ) ;
#8512 = AXIS2_PLACEMENT_3D ( 'NONE', #12362, #182190, #164046 ) ;
#8513 = CARTESIAN_POINT ( 'NONE',  ( -12.06949235617739369, -12.14591786802326823, 44.37609039468567573 ) ) ;
#8514 = CARTESIAN_POINT ( 'NONE',  ( -14.34966873604960291, -8.224510206698953496, 96.66557627198102409 ) ) ;
#8515 = CARTESIAN_POINT ( 'NONE',  ( -14.34966873604972548, 8.224510206698743886, 103.3344237280190043 ) ) ;
#8518 = CARTESIAN_POINT ( 'NONE',  ( 5.153800228976335163, 19.02544592524342804, 69.79057627198103830 ) ) ;
#8517 = CARTESIAN_POINT ( 'NONE',  ( 19.03943276465977164, -0.05219959533909143690, 78.74890960531436690 ) ) ;
#8516 = CARTESIAN_POINT ( 'NONE',  ( 21.53943276465977519, 0.05219959533937863772, 46.25109039468567573 ) ) ;
#8519 = CARTESIAN_POINT ( 'NONE',  ( -5.153800228976328057, -19.02544592524343514, 102.2905762719810383 ) ) ;
#8520 = CARTESIAN_POINT ( 'NONE',  ( 14.34966873604960469, 8.224510206698951720, 34.16557627198102409 ) ) ;
#8521 = CARTESIAN_POINT ( 'NONE',  ( -4.483927247898782831, 16.52544592524335698, 92.70942372801901854 ) ) ;
#8522 = ORIENTED_EDGE ( 'NONE', *, *, #6979, .T. ) ;
#8523 = CARTESIAN_POINT ( 'NONE',  ( 16.51473224551083163, -9.474510206698727899, 40.83442372801900433 ) ) ;
#8524 = CARTESIAN_POINT ( 'NONE',  ( -16.51473224551069308, -9.474510206698971260, 111.6655762719810383 ) ) ;
#8525 = CARTESIAN_POINT ( 'NONE',  ( 16.51473224551069308, 9.474510206698969483, 64.16557627198102409 ) ) ;
#8526 = CARTESIAN_POINT ( 'NONE',  ( -19.03943276465977164, -0.05219959533935918106, 38.75109039468566152 ) ) ;
#8527 = CARTESIAN_POINT ( 'NONE',  ( 29.86685920354754842, -21.69954338932559068, -5.824999997268813345 ) ) ;
#8528 = CARTESIAN_POINT ( 'NONE',  ( 19.53037848336980886, -5.499999999999890754, 72.35532783611448338 ) ) ;
#8529 = CARTESIAN_POINT ( 'NONE',  ( 4.483927247898790824, -16.52544592524335698, 55.20942372801902565 ) ) ;
#8531 = CARTESIAN_POINT ( 'NONE',  ( -4.379528057220086978, -16.55341960407618274, 54.79275706135235424 ) ) ;
#8530 = CARTESIAN_POINT ( 'NONE',  ( 5.153800228976615827, -19.02544592524334988, 65.20942372801900433 ) ) ;
#8532 = CARTESIAN_POINT ( 'NONE',  ( -19.05341960407611168, -5.049401038298163336, 91.45724293864766707 ) ) ;
#8533 = CARTESIAN_POINT ( 'NONE',  ( -21.55341960407610458, -5.719274019375992779, 111.4572429386476813 ) ) ;
#8534 = CARTESIAN_POINT ( 'NONE',  ( 5.049401038297881783, 19.05341960407617563, 77.29275706135231871 ) ) ;
#8536 = CARTESIAN_POINT ( 'NONE',  ( 19.02544592524343514, -5.153800228976328945, 28.54057627198102409 ) ) ;
#8535 = CARTESIAN_POINT ( 'NONE',  ( -19.05341960407611168, -5.049401038298163336, 106.4572429386476955 ) ) ;
#8537 = EDGE_CURVE ( 'NONE', #42462, #143427, #37181, .T. ) ;
#8538 = CARTESIAN_POINT ( 'NONE',  ( 9.474510206698971260, -16.51473224551069308, 82.91557627198103830 ) ) ;
#8540 = CARTESIAN_POINT ( 'NONE',  ( -19.05341960407611168, -5.049401038298163336, 36.45724293864766707 ) ) ;
#8539 = CARTESIAN_POINT ( 'NONE',  ( -12.06949235617756955, 12.14591786802309770, 50.62390960531435979 ) ) ;
#8541 = CARTESIAN_POINT ( 'NONE',  ( 19.02544592524334988, 5.153800228976608722, 56.45942372801898301 ) ) ;
#8542 = CARTESIAN_POINT ( 'NONE',  ( 16.55341960407611168, 4.379528057220329451, 88.95724293864769550 ) ) ;
#8543 = CARTESIAN_POINT ( 'NONE',  ( 10.72451020669871369, 18.67979575497193778, 107.0844237280190043 ) ) ;
#8544 = CARTESIAN_POINT ( 'NONE',  ( 16.51473224551069308, 9.474510206698969483, 49.16557627198102409 ) ) ;
#8545 = EDGE_CURVE ( 'NONE', #129803, #55277, #158519, .T. ) ;
#8546 = CARTESIAN_POINT ( 'NONE',  ( 5.823673210054125526, 21.52544592524343514, 54.79057627198104541 ) ) ;
#8548 = CARTESIAN_POINT ( 'NONE',  ( -9.474510206698720793, -16.51473224551083518, 19.58442372801899722 ) ) ;
#8547 = CARTESIAN_POINT ( 'NONE',  ( -0.05219959533910754901, -16.53943276465976808, 47.49890960531435979 ) ) ;
#8549 = CARTESIAN_POINT ( 'NONE',  ( -13.97604488694527625, -13.89961937509977652, 101.8739096053143811 ) ) ;
#8550 = CIRCLE ( 'NONE', #157064, 12.50000000000000000 ) ;
#8551 = CARTESIAN_POINT ( 'NONE',  ( 9.564922557960805705, 16.46253265017160317, 114.5822429386476955 ) ) ;
#8552 = CARTESIAN_POINT ( 'NONE',  ( 19.03943276465977164, -0.05219959533909143690, 43.74890960531435979 ) ) ;
#8553 = CARTESIAN_POINT ( 'NONE',  ( -16.51473224551069308, -9.474510206698971260, 31.66557627198102054 ) ) ;
#8554 = CARTESIAN_POINT ( 'NONE',  ( 0.05219959533910956823, 16.53943276465976808, 84.99890960531436690 ) ) ;
#8555 = CARTESIAN_POINT ( 'NONE',  ( -5.823673210054116645, -21.52544592524344225, 102.2905762719810383 ) ) ;
#8556 = CARTESIAN_POINT ( 'NONE',  ( -0.05219959533909027116, -19.03943276465977164, 97.49890960531436690 ) ) ;
#8557 = CARTESIAN_POINT ( 'NONE',  ( -5.823673210054116645, -21.52544592524344225, 107.2905762719810525 ) ) ;
#8558 = CARTESIAN_POINT ( 'NONE',  ( 9.564922557960805705, 16.46253265017160317, 99.58224293864770971 ) ) ;
#8560 = CARTESIAN_POINT ( 'NONE',  ( 0.05219959533910956823, 16.53943276465976808, 99.99890960531436690 ) ) ;
#8559 = DIRECTION ( 'NONE',  ( -1.000000000000000000, 0.000000000000000000, 0.000000000000000000 ) ) ;
#8562 = CARTESIAN_POINT ( 'NONE',  ( 0.05219959533909260263, 19.03943276465977164, 69.99890960531435269 ) ) ;
#8561 = AXIS2_PLACEMENT_3D ( 'NONE', #20, #13237, #15213 ) ;
#8563 = CARTESIAN_POINT ( 'NONE',  ( 21.52544592524344225, -5.823673210054117533, 78.54057627198103830 ) ) ;
#8564 = DIRECTION ( 'NONE',  ( 0.000000000000000000, -0.7071067811865483499, -0.7071067811865467956 ) ) ;
#8565 = CARTESIAN_POINT ( 'NONE',  ( -21.93208748025632460, -6.437649280788580342, 171.3046185016227412 ) ) ;
#8567 = LINE ( 'NONE', #134920, #185577 ) ;
#8566 = CARTESIAN_POINT ( 'NONE',  ( -21.53943276465977519, 0.05219959533907696930, 26.24890960531435624 ) ) ;
#8568 = CARTESIAN_POINT ( 'NONE',  ( 4.483927247898790824, -16.52544592524335698, 30.20942372801902565 ) ) ;
#8569 = CARTESIAN_POINT ( 'NONE',  ( 14.29746914071049879, -8.314922557960816363, 108.3322429386477097 ) ) ;
#8570 = FACE_OUTER_BOUND ( 'NONE', #24783, .T. ) ;
#8571 = CARTESIAN_POINT ( 'NONE',  ( 5.153800228976335163, 19.02544592524342804, 64.79057627198100988 ) ) ;
#8572 = CARTESIAN_POINT ( 'NONE',  ( -8.314922557960811034, -14.29746914071050412, 77.08224293864769550 ) ) ;
#8573 = CARTESIAN_POINT ( 'NONE',  ( -0.05219959533907301413, -21.53943276465977519, 27.49890960531435269 ) ) ;
#8574 = CARTESIAN_POINT ( 'NONE',  ( 4.379528057220339221, -16.55341960407611168, 62.70724293864769550 ) ) ;
#8575 = CARTESIAN_POINT ( 'NONE',  ( -19.03943276465977164, -0.05219959533935918106, 113.7510903946856757 ) ) ;
#8576 = CARTESIAN_POINT ( 'NONE',  ( -10.72451020669870658, -18.67979575497194134, 74.58442372801901854 ) ) ;
#8577 = CARTESIAN_POINT ( 'NONE',  ( 17.44279575226823198, -5.990770900252457842, 78.33557567514317554 ) ) ;
#8578 = CARTESIAN_POINT ( 'NONE',  ( -18.67979575497178146, -10.72451020669898902, 21.66557627198102409 ) ) ;
#8579 = CARTESIAN_POINT ( 'NONE',  ( 16.55341960407618274, -4.379528057220086978, 81.04275706135236135 ) ) ;
#8580 = B_SPLINE_CURVE_WITH_KNOTS ( 'NONE', 3,
 ( #163921, #72911, #166905, #105218, #180102, #182069, #134580, #183061, #73903, #195253, #152700, #149736, #198225, #56738, #118408, #121369, #135573, #43552, #196267, #41570, #120376, #44545, #167884, #197245 ),
 .UNSPECIFIED., .F., .F.,
 ( 4, 2, 2, 2, 2, 2, 2, 2, 2, 2, 2, 4 ),
 ( 0.000000000000000000, 0.002199680649073693962, 0.004399361298147387925, 0.006599041947221081887, 0.008798722596294775850, 0.01319808389444217418, 0.01759744519258957252, 0.02199680649073697605, 0.02639616778888437959, 0.03079552908703178313, 0.03299520973610547969, 0.03519489038517917973 ),
 .UNSPECIFIED. ) ;
#8581 = CARTESIAN_POINT ( 'NONE',  ( 13.97604488694527802, 13.89961937509977652, 39.37390960531435269 ) ) ;
#8582 = CARTESIAN_POINT ( 'NONE',  ( 19.02544592524343514, -5.153800228976328945, 88.54057627198102409 ) ) ;
#8583 = CARTESIAN_POINT ( 'NONE',  ( -15.72974639402197994, 15.80617190586746368, 90.62390960531436690 ) ) ;
#8584 = CARTESIAN_POINT ( 'NONE',  ( -8.224510206698735004, -14.34966873604973081, 19.58442372801901143 ) ) ;
#8586 = CARTESIAN_POINT ( 'NONE',  ( 5.719274019375673035, 21.55341960407619339, 77.29275706135234714 ) ) ;
#8585 = CARTESIAN_POINT ( 'NONE',  ( -4.483927247898539470, -16.52544592524342804, 52.29057627198102409 ) ) ;
#8587 = CARTESIAN_POINT ( 'NONE',  ( -8.314922557961024197, 14.29746914071037800, 102.9177570613523756 ) ) ;
#8588 = CARTESIAN_POINT ( 'NONE',  ( 26.47570757000580954, 8.223507928023316538, 167.6031463996532409 ) ) ;
#8589 = FACE_BOUND ( 'NONE', #92313, .T. ) ;
#8590 = CARTESIAN_POINT ( 'NONE',  ( -14.34966873604960291, -8.224510206698953496, 31.66557627198102054 ) ) ;
#8591 = CARTESIAN_POINT ( 'NONE',  ( 4.483927247898790824, -16.52544592524335698, 55.20942372801902565 ) ) ;
#8593 = VERTEX_POINT ( 'NONE', #115010 ) ;
#8592 = CARTESIAN_POINT ( 'NONE',  ( 19.02544592524343514, -5.153800228976328945, 78.54057627198099567 ) ) ;
#8594 = CARTESIAN_POINT ( 'NONE',  ( 5.049401038298161559, -19.05341960407611168, 82.70724293864770971 ) ) ;
#8595 = CARTESIAN_POINT ( 'NONE',  ( 21.52544592524334988, 5.823673210054432836, 66.45942372801903275 ) ) ;
#8596 = CARTESIAN_POINT ( 'NONE',  ( 8.314922557961029526, -14.29746914071037800, 70.41775706135236135 ) ) ;
#8597 = CARTESIAN_POINT ( 'NONE',  ( 16.52544592524342804, -4.483927247898539470, 53.54057627198103120 ) ) ;
#8598 = CARTESIAN_POINT ( 'NONE',  ( 19.02544592524343514, -5.153800228976328945, 68.54057627198103830 ) ) ;
#8599 = ORIENTED_EDGE ( 'NONE', *, *, #37462, .T. ) ;
#8601 = CARTESIAN_POINT ( 'NONE',  ( 19.05341960407617918, -5.049401038297876454, 106.0427570613523471 ) ) ;
#8600 =( BOUNDED_CURVE ( )  B_SPLINE_CURVE ( 2, ( #149282, #26952, #69432, #162438, #54270, #115943, #99760, #72442, #178626, #194792, #23939, #164459, #134118 ),
 .UNSPECIFIED., .F., .F. ) 
 B_SPLINE_CURVE_WITH_KNOTS ( ( 3, 2, 2, 2, 2, 2, 3 ),
 ( 0.1866866425649248151, 0.1885964912280701788, 0.1929824561403508665, 0.1973684210526315819, 0.2017543859649122695, 0.2061403508771929849, 0.2080958793624286540 ),
 .UNSPECIFIED. ) 
 CURVE ( )  GEOMETRIC_REPRESENTATION_ITEM ( )  RATIONAL_B_SPLINE_CURVE ( ( 0.9832469066685285419, 0.9851625545550100060, 1.000000000000000000, 0.9659258262890683122, 1.000000000000000000, 0.9659258262890683122, 1.000000000000000000, 0.9659258262890683122, 1.000000000000000000, 0.9659258262890683122, 1.000000000000000000, 0.9848076720550082985, 0.9831626618144004848 ) ) 
 REPRESENTATION_ITEM ( '' )  );
#8602 = CARTESIAN_POINT ( 'NONE',  ( -14.29746914071049879, 8.314922557960819915, 115.8322429386477097 ) ) ;
#8603 = CARTESIAN_POINT ( 'NONE',  ( 13.97604488694527802, 13.89961937509977652, 84.37390960531433848 ) ) ;
#8605 = CARTESIAN_POINT ( 'NONE',  ( 30.74264578624800137, -22.33583958711395212, -3.200000000000000178 ) ) ;
#8604 = CARTESIAN_POINT ( 'NONE',  ( -12.14591786802326823, 12.06949235617739902, 23.12609039468567573 ) ) ;
#8606 = CARTESIAN_POINT ( 'NONE',  ( -10.72451020669870658, -18.67979575497194134, 109.5844237280190328 ) ) ;
#8607 = CARTESIAN_POINT ( 'NONE',  ( -8.224510206698735004, -14.34966873604973081, 84.58442372801903275 ) ) ;
#8608 = CARTESIAN_POINT ( 'NONE',  ( -5.049401038297874678, -19.05341960407617918, 94.79275706135230450 ) ) ;
#8609 = CARTESIAN_POINT ( 'NONE',  ( 0.05219959533910956823, 16.53943276465976808, 114.9989096053143669 ) ) ;
#8610 = CARTESIAN_POINT ( 'NONE',  ( 16.52544592524335698, 4.483927247898782831, 61.45942372801901854 ) ) ;
#8611 = CARTESIAN_POINT ( 'NONE',  ( 27.86273085795036408, -28.69962071417356242, 0.000000000000000000 ) ) ;
#8612 = CARTESIAN_POINT ( 'NONE',  ( 5.049401038297881783, 19.05341960407617563, 52.29275706135234003 ) ) ;
#8613 = CARTESIAN_POINT ( 'NONE',  ( -18.62759615963255300, -10.81492255796106328, 94.16775706135237556 ) ) ;
#8614 = CARTESIAN_POINT ( 'NONE',  ( 16.46253265017160672, -9.564922557960803928, 33.33224293864770260 ) ) ;
#8615 = CARTESIAN_POINT ( 'NONE',  ( 19.03943276465977164, -0.05219959533909143690, 73.74890960531435269 ) ) ;
#8616 = CARTESIAN_POINT ( 'NONE',  ( 0.05219959533910956823, 16.53943276465976808, 69.99890960531435269 ) ) ;
#8617 = B_SPLINE_CURVE_WITH_KNOTS ( 'NONE', 3,
 ( #36357, #98009, #144536, #6022, #129359, #191054 ),
 .UNSPECIFIED., .F., .F.,
 ( 4, 2, 4 ),
 ( 0.003989672132298169478, 0.004372778065220577978, 0.004755883998142986478 ),
 .UNSPECIFIED. ) ;
#8618 = CARTESIAN_POINT ( 'NONE',  ( -10.72451020669870658, -18.67979575497194134, 84.58442372801903275 ) ) ;
#8619 = CARTESIAN_POINT ( 'NONE',  ( 19.03943276465977164, 0.05219959533936151252, 46.25109039468566863 ) ) ;
#8620 = CARTESIAN_POINT ( 'NONE',  ( -9.564922557961040184, 16.46253265017147172, 47.91775706135233293 ) ) ;
#8621 = CARTESIAN_POINT ( 'NONE',  ( -21.55341960407610458, -5.719274019375992779, 36.45724293864768839 ) ) ;
#8622 = CARTESIAN_POINT ( 'NONE',  ( -21.52544592524334988, -5.823673210054445271, 98.95942372801903275 ) ) ;
#8623 = CARTESIAN_POINT ( 'NONE',  ( -16.51473224551069308, -9.474510206698971260, 81.66557627198103830 ) ) ;
#8624 = CARTESIAN_POINT ( 'NONE',  ( 15.80617190586769283, -15.72974639402175789, 90.62609039468567573 ) ) ;
#8625 = CARTESIAN_POINT ( 'NONE',  ( 21.55341960407610458, 5.719274019375980345, 43.95724293864769550 ) ) ;
#8626 = CARTESIAN_POINT ( 'NONE',  ( 9.564922557960805705, 16.46253265017160317, 89.58224293864769550 ) ) ;
#8627 = CARTESIAN_POINT ( 'NONE',  ( -19.02544592524334988, -5.153800228976617603, 73.95942372801900433 ) ) ;
#8628 = CARTESIAN_POINT ( 'NONE',  ( 9.564922557960805705, 16.46253265017160317, 94.58224293864769550 ) ) ;
#8629 = CARTESIAN_POINT ( 'NONE',  ( 16.46253265017146816, 9.564922557961045513, 91.66775706135234714 ) ) ;
#8630 = CARTESIAN_POINT ( 'NONE',  ( 14.29746914071037800, 8.314922557961029526, 36.66775706135234714 ) ) ;
#8631 = CARTESIAN_POINT ( 'NONE',  ( -8.224510206698948167, 14.34966873604960824, 105.4155762719810383 ) ) ;
#8632 = CARTESIAN_POINT ( 'NONE',  ( -9.564922557960796823, -16.46253265017161027, 72.08224293864770971 ) ) ;
#8633 = CARTESIAN_POINT ( 'NONE',  ( 15.80617190586746368, 15.72974639402197994, 69.37390960531436690 ) ) ;
#8634 = CARTESIAN_POINT ( 'NONE',  ( 14.34966873604972726, -8.224510206698740333, 30.83442372801902209 ) ) ;
#8635 = CARTESIAN_POINT ( 'NONE',  ( -21.52544592524334988, -5.823673210054445271, 33.95942372801901143 ) ) ;
#8636 = CARTESIAN_POINT ( 'NONE',  ( 21.52544592524334988, 5.823673210054432836, 86.45942372801901854 ) ) ;
#8637 = CARTESIAN_POINT ( 'NONE',  ( 12.06949235617739724, 12.14591786802326823, 81.87609039468568994 ) ) ;
#8638 = CARTESIAN_POINT ( 'NONE',  ( 16.46253265017160672, -9.564922557960803928, 68.33224293864770971 ) ) ;
#8639 = CARTESIAN_POINT ( 'NONE',  ( 4.379528057220339221, -16.55341960407611168, 82.70724293864770971 ) ) ;
#8640 = CARTESIAN_POINT ( 'NONE',  ( 4.379528057220092307, 16.55341960407617563, 97.29275706135234714 ) ) ;
#8641 = CARTESIAN_POINT ( 'NONE',  ( -13.89961937509957401, -13.97604488694547875, 49.37609039468567573 ) ) ;
#8642 = CARTESIAN_POINT ( 'NONE',  ( 10.81492255796106328, -18.62759615963255655, 25.41775706135235779 ) ) ;
#8643 = CARTESIAN_POINT ( 'NONE',  ( 14.29746914071049879, -8.314922557960816363, 73.33224293864769550 ) ) ;
#8644 = CARTESIAN_POINT ( 'NONE',  ( 9.474510206698971260, -16.51473224551069308, 97.91557627198102409 ) ) ;
#8645 = CARTESIAN_POINT ( 'NONE',  ( 4.379528057220092307, 16.55341960407617563, 107.2927570613523471 ) ) ;
#8646 = CARTESIAN_POINT ( 'NONE',  ( 18.62759615963255655, 10.81492255796105972, 66.66775706135234714 ) ) ;
#8647 = CARTESIAN_POINT ( 'NONE',  ( -8.314922557961024197, 14.29746914071037800, 42.91775706135235424 ) ) ;
#8648 = CARTESIAN_POINT ( 'NONE',  ( 10.72451020669871369, 18.67979575497193778, 42.08442372801901854 ) ) ;
#8649 = CARTESIAN_POINT ( 'NONE',  ( -12.14591786802309592, -12.06949235617757132, 71.87390960531438111 ) ) ;
#8650 = VERTEX_POINT ( 'NONE', #85667 ) ;
#8651 = CARTESIAN_POINT ( 'NONE',  ( 15.72974639402199770, -15.80617190586745480, 113.1239096053143953 ) ) ;
#8652 = CARTESIAN_POINT ( 'NONE',  ( -19.25918095147780207, -5.499999999999583444, 49.45284276293934056 ) ) ;
#8653 = CARTESIAN_POINT ( 'NONE',  ( -8.314922557960811034, -14.29746914071050412, 47.08224293864770260 ) ) ;
#8654 = DIRECTION ( 'NONE',  ( 0.000000000000000000, 0.000000000000000000, 1.000000000000000000 ) ) ;
#8655 = CARTESIAN_POINT ( 'NONE',  ( 10.72451020669898902, -18.67979575497178502, 42.91557627198103120 ) ) ;
#8656 = CARTESIAN_POINT ( 'NONE',  ( 4.483927247898545687, 16.52544592524342804, 74.79057627198105251 ) ) ;
#8657 = VECTOR ( 'NONE', #192387, 1000.000000000000000 ) ;
#8658 = CARTESIAN_POINT ( 'NONE',  ( -5.719274019375978568, 21.55341960407610458, 85.20724293864770971 ) ) ;
#8659 = CARTESIAN_POINT ( 'NONE',  ( 19.03943276465977164, -0.05219959533909143690, 73.74890960531435269 ) ) ;
#8661 = CARTESIAN_POINT ( 'NONE',  ( -0.05219959533936034679, 19.03943276465977164, 72.50109039468566152 ) ) ;
#8660 = CARTESIAN_POINT ( 'NONE',  ( 13.89961937509977652, -13.97604488694527269, 43.12390960531434558 ) ) ;
#8663 = CARTESIAN_POINT ( 'NONE',  ( 10.72451020669898902, -18.67979575497178502, 57.91557627198103120 ) ) ;
#8662 = CARTESIAN_POINT ( 'NONE',  ( 21.52544592524334988, 5.823673210054432836, 51.45942372801901854 ) ) ;
#8664 = CARTESIAN_POINT ( 'NONE',  ( 5.153800228976335163, 19.02544592524342804, 39.79057627198100988 ) ) ;
#8665 = CARTESIAN_POINT ( 'NONE',  ( -9.474510206698964154, 16.51473224551069663, 75.41557627198103830 ) ) ;
#8666 = ORIENTED_EDGE ( 'NONE', *, *, #178067, .T. ) ;
#8667 = CARTESIAN_POINT ( 'NONE',  ( 0.05219959533934541429, -16.53943276465976808, 50.00109039468568994 ) ) ;
#8668 = CARTESIAN_POINT ( 'NONE',  ( -10.81492255796105439, 18.62759615963255655, 32.91775706135234714 ) ) ;
#8669 = CARTESIAN_POINT ( 'NONE',  ( -5.719274019375665041, -21.55341960407619695, 59.79275706135234714 ) ) ;
#8670 = CARTESIAN_POINT ( 'NONE',  ( -19.02544592524342804, 5.153800228976336051, 106.0405762719810241 ) ) ;
#8671 = CARTESIAN_POINT ( 'NONE',  ( 10.72451020669898902, -18.67979575497178502, 82.91557627198103830 ) ) ;
#8673 = CARTESIAN_POINT ( 'NONE',  ( 8.314922557961029526, -14.29746914071037800, 45.41775706135234003 ) ) ;
#8672 = CARTESIAN_POINT ( 'NONE',  ( 10.81492255796106328, -18.62759615963255655, 25.41775706135235779 ) ) ;
#8675 = CARTESIAN_POINT ( 'NONE',  ( -10.72451020669898014, 18.67979575497178502, 45.41557627198103830 ) ) ;
#8674 = B_SPLINE_CURVE_WITH_KNOTS ( 'NONE', 3,
 ( #85040, #129539, #142729, #69894, #193246, #128546, #175073, #23394, #189263, #35557, #99213, #143724, #65887, #177090, #4209, #113383, #98195, #22394, #131562, #160901, #52713, #84044, #145723, #50738 ),
 .UNSPECIFIED., .F., .F.,
 ( 4, 2, 2, 2, 2, 2, 2, 2, 2, 2, 2, 4 ),
 ( 1.970462154608161142E-07, 0.0003069708713091477670, 0.0006137446964028346478, 0.001227292346590209060, 0.001534066171683895561, 0.001840839996777582496, 0.002147613821871268997, 0.002454387646964955282, 0.003067935297152315274, 0.003681482947339676133, 0.004295030597527037426, 0.004908578247714397852 ),
 .UNSPECIFIED. ) ;
#8676 = CARTESIAN_POINT ( 'NONE',  ( 19.03943276465977164, 0.05219959533936151252, 26.25109039468566507 ) ) ;
#8677 = CARTESIAN_POINT ( 'NONE',  ( -9.474510206698964154, 16.51473224551069663, 50.41557627198102409 ) ) ;
#8678 = CARTESIAN_POINT ( 'NONE',  ( 5.153800228976335163, 19.02544592524342804, 109.7905762719810099 ) ) ;
#8679 = CARTESIAN_POINT ( 'NONE',  ( -13.97604488694527625, -13.89961937509977652, 91.87390960531432427 ) ) ;
#8680 = CARTESIAN_POINT ( 'NONE',  ( -18.22780087662122028, 5.500000000000031086, 53.51540105326106556 ) ) ;
#8681 = EDGE_CURVE ( 'NONE', #167085, #7157, #101715, .T. ) ;
#8682 = CARTESIAN_POINT ( 'NONE',  ( 9.474510206698729675, 16.51473224551082808, 72.08442372801900433 ) ) ;
#8683 = CARTESIAN_POINT ( 'NONE',  ( -15.72974639402197994, 15.80617190586746368, 50.62390960531435979 ) ) ;
#8684 = CARTESIAN_POINT ( 'NONE',  ( -12.06949235617756955, 12.14591786802309770, 30.62390960531436335 ) ) ;
#8685 = CARTESIAN_POINT ( 'NONE',  ( 5.049401038297881783, 19.05341960407617563, 92.29275706135234714 ) ) ;
#8686 = EDGE_CURVE ( 'NONE', #132603, #17083, #89459, .T. ) ;
#8687 = CARTESIAN_POINT ( 'NONE',  ( -30.00000000000000355, -0.3535533905932729537, 4.646446609406719830 ) ) ;
#8688 = CARTESIAN_POINT ( 'NONE',  ( 9.474510206698729675, 16.51473224551082808, 27.08442372801900433 ) ) ;
#8689 = CARTESIAN_POINT ( 'NONE',  ( 13.89961937509957401, 13.97604488694547697, 91.87609039468567573 ) ) ;
#8690 = CARTESIAN_POINT ( 'NONE',  ( 5.153800228976615827, -19.02544592524334988, 40.20942372801898301 ) ) ;
#8691 = CARTESIAN_POINT ( 'NONE',  ( 11.45643923738959735, 5.000000000000007105, -18.00000000000000000 ) ) ;
#8692 = CARTESIAN_POINT ( 'NONE',  ( -19.02544592524342804, 5.153800228976336051, 56.04057627198100988 ) ) ;
#8693 = CARTESIAN_POINT ( 'NONE',  ( 16.52544592524342804, -4.483927247898539470, 58.54057627198103120 ) ) ;
#8694 = CARTESIAN_POINT ( 'NONE',  ( 5.153800228976335163, 19.02544592524342804, 29.79057627198102409 ) ) ;
#8695 = CARTESIAN_POINT ( 'NONE',  ( 4.483927247898545687, 16.52544592524342804, 34.79057627198103120 ) ) ;
#8696 = CARTESIAN_POINT ( 'NONE',  ( 17.50000000000000000, -5.499999999999992895, 56.21769037696436300 ) ) ;
#8697 = CARTESIAN_POINT ( 'NONE',  ( 8.314922557961029526, -14.29746914071037800, 105.4177570613523613 ) ) ;
#8698 = CARTESIAN_POINT ( 'NONE',  ( 5.049401038298161559, -19.05341960407611168, 57.70724293864769550 ) ) ;
#8699 = CARTESIAN_POINT ( 'NONE',  ( 19.03943276465977164, 0.05219959533936151252, 26.25109039468566507 ) ) ;
#8700 = CARTESIAN_POINT ( 'NONE',  ( -8.314922557961024197, 14.29746914071037800, 27.91775706135234358 ) ) ;
#8701 = CARTESIAN_POINT ( 'NONE',  ( -21.53943276465977519, 0.05219959533907696930, 51.24890960531436690 ) ) ;
#8703 = ORIENTED_EDGE ( 'NONE', *, *, #135435, .T. ) ;
#8702 = CARTESIAN_POINT ( 'NONE',  ( -5.823673210054431948, 21.52544592524334988, 107.7094237280190328 ) ) ;
#8704 = CARTESIAN_POINT ( 'NONE',  ( 16.51473224551069308, 9.474510206698969483, 64.16557627198102409 ) ) ;
#8705 = CARTESIAN_POINT ( 'NONE',  ( 0.05219959533909260263, 19.03943276465977164, 104.9989096053143669 ) ) ;
#8706 = CARTESIAN_POINT ( 'NONE',  ( 19.03943276465977164, -0.05219959533909143690, 98.74890960531436690 ) ) ;
#8707 = CARTESIAN_POINT ( 'NONE',  ( 22.81625015709510151, -31.40387420917324590, -1.924999997268813212 ) ) ;
#8708 = CARTESIAN_POINT ( 'NONE',  ( -15.80617190586768217, 15.72974639402176855, 23.12609039468567573 ) ) ;
#8709 = AXIS2_PLACEMENT_3D ( 'NONE', #11039, #179908, #106016 ) ;
#8710 = CARTESIAN_POINT ( 'NONE',  ( -14.29746914071049879, 8.314922557960819915, 95.83224293864770971 ) ) ;
#8712 = CARTESIAN_POINT ( 'NONE',  ( -0.05219959533909027116, -19.03943276465977164, 62.49890960531435979 ) ) ;
#8711 = CARTESIAN_POINT ( 'NONE',  ( -21.52544592524343514, 5.823673210054127303, 86.04057627198102409 ) ) ;
#8713 = CARTESIAN_POINT ( 'NONE',  ( -13.89961937509977652, 13.97604488694528158, 70.62390960531432427 ) ) ;
#8714 = CARTESIAN_POINT ( 'NONE',  ( -5.719274019375978568, 21.55341960407610458, 110.2072429386477239 ) ) ;
#8715 = ORIENTED_EDGE ( 'NONE', *, *, #22998, .F. ) ;
#8716 = CARTESIAN_POINT ( 'NONE',  ( 19.03943276465977164, -0.05219959533909143690, 73.74890960531435269 ) ) ;
#8717 = CARTESIAN_POINT ( 'NONE',  ( 19.02130022317637525, -5.499999999999793943, 98.28188669246577547 ) ) ;
#8719 = FACE_BOUND ( 'NONE', #63868, .T. ) ;
#8718 = CARTESIAN_POINT ( 'NONE',  ( -16.52544592524342804, 4.483927247898546575, 111.0405762719810525 ) ) ;
#8720 = CARTESIAN_POINT ( 'NONE',  ( 5.153800228976335163, 19.02544592524342804, 69.79057627198103830 ) ) ;
#8721 = CARTESIAN_POINT ( 'NONE',  ( 5.049401038297881783, 19.05341960407617563, 92.29275706135234714 ) ) ;
#8722 = CARTESIAN_POINT ( 'NONE',  ( -8.224510206698948167, 14.34966873604960824, 100.4155762719810241 ) ) ;
#8723 = CARTESIAN_POINT ( 'NONE',  ( -18.62759615963255300, -10.81492255796106328, 69.16775706135234714 ) ) ;
#8725 = CARTESIAN_POINT ( 'NONE',  ( -5.823673210054431948, 21.52544592524334988, 27.70942372801901854 ) ) ;
#8724 = CARTESIAN_POINT ( 'NONE',  ( 19.05341960407611168, 5.049401038298154454, 43.95724293864769550 ) ) ;
#8726 = CARTESIAN_POINT ( 'NONE',  ( -21.52544592524343514, 5.823673210054127303, 111.0405762719810525 ) ) ;
#8727 = CARTESIAN_POINT ( 'NONE',  ( -28.82186960331499392, 9.364793116373565596, 148.1500000054624024 ) ) ;
#8728 = CARTESIAN_POINT ( 'NONE',  ( 13.89961937509977652, -13.97604488694527269, 73.12390960531436690 ) ) ;
#8729 = CARTESIAN_POINT ( 'NONE',  ( 17.81289503416610742, 24.51734667627700404, 143.5500000054623513 ) ) ;
#8731 = CARTESIAN_POINT ( 'NONE',  ( 18.67979575497178502, 10.72451020669898547, 34.16557627198102409 ) ) ;
#8730 = CARTESIAN_POINT ( 'NONE',  ( -9.474510206698720793, -16.51473224551083518, 104.5844237280190043 ) ) ;
#8732 = CARTESIAN_POINT ( 'NONE',  ( -10.72451020669870658, -18.67979575497194134, 69.58442372801900433 ) ) ;
#8733 = CARTESIAN_POINT ( 'NONE',  ( -19.05341960407611168, -5.049401038298163336, 91.45724293864766707 ) ) ;
#8734 = CARTESIAN_POINT ( 'NONE',  ( -16.51473224551082808, 9.474510206698731452, 78.33442372801900433 ) ) ;
#8735 = CARTESIAN_POINT ( 'NONE',  ( 9.474510206698971260, -16.51473224551069308, 42.91557627198103120 ) ) ;
#8736 = CARTESIAN_POINT ( 'NONE',  ( 16.46253265017160672, -9.564922557960803928, 68.33224293864770971 ) ) ;
#8737 = CARTESIAN_POINT ( 'NONE',  ( 14.29746914071049879, -8.314922557960816363, 98.33224293864769550 ) ) ;
#8738 = CARTESIAN_POINT ( 'NONE',  ( 9.564922557960805705, 16.46253265017160317, 104.5822429386476955 ) ) ;
#8739 = CARTESIAN_POINT ( 'NONE',  ( -8.314922557960811034, -14.29746914071050412, 87.08224293864769550 ) ) ;
#8740 = CARTESIAN_POINT ( 'NONE',  ( 16.51473224551069308, 9.474510206698969483, 94.16557627198103830 ) ) ;
#8742 = CARTESIAN_POINT ( 'NONE',  ( -5.049401038298153566, 19.05341960407611168, 25.20724293864768484 ) ) ;
#8741 = CARTESIAN_POINT ( 'NONE',  ( 8.224510206698953496, -14.34966873604960469, 37.91557627198102409 ) ) ;
#8743 = VERTEX_POINT ( 'NONE', #105828 ) ;
#8744 = CARTESIAN_POINT ( 'NONE',  ( -15.72974639402176322, -15.80617190586768395, 64.37609039468568994 ) ) ;
#8745 = CARTESIAN_POINT ( 'NONE',  ( 16.51473224551083163, -9.474510206698727899, 80.83442372801899012 ) ) ;
#8746 = CARTESIAN_POINT ( 'NONE',  ( 4.483927247898545687, 16.52544592524342804, 44.79057627198103120 ) ) ;
#8747 = CARTESIAN_POINT ( 'NONE',  ( -5.719274019375978568, 21.55341960407610458, 95.20724293864769550 ) ) ;
#8748 = CARTESIAN_POINT ( 'NONE',  ( 15.72974639402199770, -15.80617190586745480, 28.12390960531435979 ) ) ;
#8749 = CARTESIAN_POINT ( 'NONE',  ( -4.483927247898539470, -16.52544592524342804, 77.29057627198102409 ) ) ;
#8750 = CARTESIAN_POINT ( 'NONE',  ( 5.049401038298161559, -19.05341960407611168, 57.70724293864769550 ) ) ;
#8751 = CARTESIAN_POINT ( 'NONE',  ( -0.05219959533910754901, -16.53943276465976808, 22.49890960531436335 ) ) ;
#8752 = CARTESIAN_POINT ( 'NONE',  ( -16.55341960407617563, 4.379528057220093196, 98.54275706135234714 ) ) ;
#8753 = CARTESIAN_POINT ( 'NONE',  ( 14.29746914071037800, 8.314922557961029526, 71.66775706135234714 ) ) ;
#8754 = CARTESIAN_POINT ( 'NONE',  ( 16.46253265017146816, 9.564922557961045513, 31.66775706135232937 ) ) ;
#8755 = CARTESIAN_POINT ( 'NONE',  ( 13.89961937509977652, -13.97604488694527269, 103.1239096053143527 ) ) ;
#8756 = CARTESIAN_POINT ( 'NONE',  ( -5.049401038298153566, 19.05341960407611168, 80.20724293864769550 ) ) ;
#8757 = CARTESIAN_POINT ( 'NONE',  ( -19.05341960407611168, -5.049401038298163336, 31.45724293864769550 ) ) ;
#8758 = ADVANCED_FACE ( 'NONE', ( #117005 ), #40162, .F. ) ;
#8759 = CARTESIAN_POINT ( 'NONE',  ( -12.06949235617756955, 12.14591786802309770, 50.62390960531435979 ) ) ;
#8761 = CARTESIAN_POINT ( 'NONE',  ( -13.89961937509977652, 13.97604488694528158, 105.6239096053143527 ) ) ;
#8760 = SURFACE_SIDE_STYLE ('',( #6736 ) ) ;
#8762 = CARTESIAN_POINT ( 'NONE',  ( 15.80617190586746368, 15.72974639402197994, 39.37390960531436690 ) ) ;
#8763 = CARTESIAN_POINT ( 'NONE',  ( 14.34966873604960469, 8.224510206698951720, 79.16557627198103830 ) ) ;
#8764 = CARTESIAN_POINT ( 'NONE',  ( 12.14591786802327356, -12.06949235617739191, 25.62609039468567929 ) ) ;
#8765 = CARTESIAN_POINT ( 'NONE',  ( 12.06949235617757843, -12.14591786802309237, 68.12390960531436690 ) ) ;
#8766 = CARTESIAN_POINT ( 'NONE',  ( 31.61347055016709007, -0.9086318102906248972, -46.06737158113914177 ) ) ;
#8767 = CARTESIAN_POINT ( 'NONE',  ( -13.89961937509957401, -13.97604488694547875, 59.37609039468566863 ) ) ;
#8768 = CARTESIAN_POINT ( 'NONE',  ( -19.02544592524342804, 5.153800228976336051, 106.0405762719810241 ) ) ;
#8769 = CARTESIAN_POINT ( 'NONE',  ( -5.049401038297874678, -19.05341960407617918, 79.79275706135233293 ) ) ;
#8770 = FACE_OUTER_BOUND ( 'NONE', #32591, .T. ) ;
#8772 = CARTESIAN_POINT ( 'NONE',  ( 12.06949235617739724, 12.14591786802326823, 106.8760903946856899 ) ) ;
#8771 = CARTESIAN_POINT ( 'NONE',  ( 0.05219959533936267826, -19.03943276465977164, 110.0010903946856757 ) ) ;
#8773 = CARTESIAN_POINT ( 'NONE',  ( 16.46253265017160672, -9.564922557960803928, 38.33224293864768839 ) ) ;
#8774 = CARTESIAN_POINT ( 'NONE',  ( -21.55341960407610458, -5.719274019375992779, 36.45724293864768839 ) ) ;
#8775 = CARTESIAN_POINT ( 'NONE',  ( 0.05219959533937995610, -21.53943276465977519, 55.00109039468568284 ) ) ;
#8776 = CARTESIAN_POINT ( 'NONE',  ( -24.29042230868021690, -8.936166115090793838, 166.5611006352801553 ) ) ;
#8777 = CARTESIAN_POINT ( 'NONE',  ( 14.34966873604972726, -8.224510206698740333, 25.83442372801901499 ) ) ;
#8779 = CARTESIAN_POINT ( 'NONE',  ( -9.474510206698964154, 16.51473224551069663, 75.41557627198103830 ) ) ;
#8778 = DIRECTION ( 'NONE',  ( 0.000000000000000000, 1.000000000000000000, -1.471414886128461669E-15 ) ) ;
#8780 = CARTESIAN_POINT ( 'NONE',  ( 16.44579809102488710, 17.60164288208763850, -56.93377352129066082 ) ) ;
#8782 = CARTESIAN_POINT ( 'NONE',  ( -5.153800228976328057, -19.02544592524343514, 72.29057627198102409 ) ) ;
#8781 = CARTESIAN_POINT ( 'NONE',  ( 8.314922557960818139, 14.29746914071049879, 89.58224293864768129 ) ) ;
#8783 = CARTESIAN_POINT ( 'NONE',  ( -16.51473224551069308, -9.474510206698971260, 91.66557627198103830 ) ) ;
#8784 = ORIENTED_EDGE ( 'NONE', *, *, #41117, .T. ) ;
#8785 = CARTESIAN_POINT ( 'NONE',  ( -5.049401038297874678, -19.05341960407617918, 89.79275706135230450 ) ) ;
#8786 = CARTESIAN_POINT ( 'NONE',  ( 0.05219959533907565091, 21.53943276465977519, 79.99890960531435269 ) ) ;
#8787 = CARTESIAN_POINT ( 'NONE',  ( 5.153800228976335163, 19.02544592524342804, 34.79057627198102409 ) ) ;
#8788 = CARTESIAN_POINT ( 'NONE',  ( -16.46253265017146816, -9.564922557961047289, 54.16775706135234003 ) ) ;
#8789 = CARTESIAN_POINT ( 'NONE',  ( -5.153800228976328057, -19.02544592524343514, 52.29057627198100988 ) ) ;
#8790 = CARTESIAN_POINT ( 'NONE',  ( -0.05219959533909027116, -19.03943276465977164, 92.49890960531436690 ) ) ;
#8791 = ORIENTED_EDGE ( 'NONE', *, *, #84741, .T. ) ;
#8792 = CARTESIAN_POINT ( 'NONE',  ( 18.67979575497178502, 10.72451020669898547, 99.16557627198100988 ) ) ;
#8795 = CARTESIAN_POINT ( 'NONE',  ( 13.97604488694548053, -13.89961937509957401, 60.62609039468564731 ) ) ;
#8794 = CARTESIAN_POINT ( 'NONE',  ( 19.03943276465977164, -0.05219959533909143690, 83.74890960531436690 ) ) ;
#8793 = CARTESIAN_POINT ( 'NONE',  ( -8.224510206698948167, 14.34966873604960824, 95.41557627198102409 ) ) ;
#8796 = CARTESIAN_POINT ( 'NONE',  ( 5.823673210054125526, 21.52544592524343514, 84.79057627198102409 ) ) ;
#8797 = CARTESIAN_POINT ( 'NONE',  ( 21.52544592524344225, -5.823673210054117533, 73.54057627198102409 ) ) ;
#8798 = CARTESIAN_POINT ( 'NONE',  ( -4.483927247898539470, -16.52544592524342804, 32.29057627198102409 ) ) ;
#8799 = CARTESIAN_POINT ( 'NONE',  ( -18.67979575497193778, 10.72451020669871902, 98.33442372801901854 ) ) ;
#8800 = CARTESIAN_POINT ( 'NONE',  ( -14.34966873604972548, 8.224510206698743886, 63.33442372801900433 ) ) ;
#8801 = CARTESIAN_POINT ( 'NONE',  ( 0.05219959533909260263, 19.03943276465977164, 84.99890960531436690 ) ) ;
#8802 = CARTESIAN_POINT ( 'NONE',  ( 16.51473224551069308, 9.474510206698969483, 29.16557627198103475 ) ) ;
#8803 = AXIS2_PLACEMENT_3D ( 'NONE', #44105, #64234, #152268 ) ;
#8804 = CARTESIAN_POINT ( 'NONE',  ( -18.62759615963255300, -10.81492255796106328, 34.16775706135234714 ) ) ;
#8805 = CARTESIAN_POINT ( 'NONE',  ( -21.55341960407619339, 5.719274019375674811, 53.54275706135234714 ) ) ;
#8806 = CARTESIAN_POINT ( 'NONE',  ( 16.51473224551069308, 9.474510206698969483, 49.16557627198102409 ) ) ;
#8807 = CARTESIAN_POINT ( 'NONE',  ( 21.52544592524334988, 5.823673210054432836, 21.45942372801901499 ) ) ;
#8808 = CARTESIAN_POINT ( 'NONE',  ( 16.51473224551083163, -9.474510206698727899, 70.83442372801900433 ) ) ;
#8809 = CARTESIAN_POINT ( 'NONE',  ( -13.97604488694547697, 13.89961937509957934, 78.12609039468567573 ) ) ;
#8810 = CARTESIAN_POINT ( 'NONE',  ( -16.51473224551069308, -9.474510206698971260, 31.66557627198102054 ) ) ;
#8811 = CARTESIAN_POINT ( 'NONE',  ( -14.34966873604972548, 8.224510206698743886, 68.33442372801900433 ) ) ;
#8812 = CARTESIAN_POINT ( 'NONE',  ( -9.564922557960796823, -16.46253265017161027, 57.08224293864769550 ) ) ;
#8813 = CARTESIAN_POINT ( 'NONE',  ( -5.153800228976328057, -19.02544592524343514, 97.29057627198099567 ) ) ;
#8814 = CARTESIAN_POINT ( 'NONE',  ( 0.05219959533909260263, 19.03943276465977164, 39.99890960531436690 ) ) ;
#8815 = CARTESIAN_POINT ( 'NONE',  ( -5.719274019375978568, 21.55341960407610458, 75.20724293864769550 ) ) ;
#8816 = CARTESIAN_POINT ( 'NONE',  ( -16.53943276465976808, -0.05219959533934237506, 58.75109039468568994 ) ) ;
#8817 = CIRCLE ( 'NONE', #41014, 4.999999999999999112 ) ;
#8818 = CARTESIAN_POINT ( 'NONE',  ( 10.81492255796106328, -18.62759615963255655, 110.4177570613523756 ) ) ;
#8819 = CARTESIAN_POINT ( 'NONE',  ( -19.05341960407611168, -5.049401038298163336, 56.45724293864768129 ) ) ;
#8820 = CARTESIAN_POINT ( 'NONE',  ( 12.14591786802309770, 12.06949235617756955, 39.37390960531436690 ) ) ;
#8821 = CARTESIAN_POINT ( 'NONE',  ( -4.483927247898539470, -16.52544592524342804, 72.29057627198102409 ) ) ;
#8822 = CARTESIAN_POINT ( 'NONE',  ( -13.97604488694527625, -13.89961937509977652, 76.87390960531433848 ) ) ;
#8823 = CARTESIAN_POINT ( 'NONE',  ( 15.72974639402176855, 15.80617190586768217, 36.87609039468568994 ) ) ;
#8824 = CARTESIAN_POINT ( 'NONE',  ( 9.474510206698971260, -16.51473224551069308, 87.91557627198102409 ) ) ;
#8825 = CARTESIAN_POINT ( 'NONE',  ( -15.80617190586768217, 15.72974639402176855, 103.1260903946856757 ) ) ;
#8826 = CARTESIAN_POINT ( 'NONE',  ( 4.379528057220092307, 16.55341960407617563, 72.29275706135236135 ) ) ;
#8827 = CARTESIAN_POINT ( 'NONE',  ( 19.02544592524343514, -5.153800228976328945, 108.5405762719810383 ) ) ;
#8828 = VECTOR ( 'NONE', #50723, 1000.000000000000000 ) ;
#8829 = CARTESIAN_POINT ( 'NONE',  ( 18.62759615963271287, -10.81492255796078972, 88.33224293864769550 ) ) ;
#8830 = CARTESIAN_POINT ( 'NONE',  ( 4.483927247898545687, 16.52544592524342804, 49.79057627198102409 ) ) ;
#8831 = CARTESIAN_POINT ( 'NONE',  ( 9.564922557960805705, 16.46253265017160317, 44.58224293864769550 ) ) ;
#8832 = CARTESIAN_POINT ( 'NONE',  ( 16.52544592524335698, 4.483927247898782831, 56.45942372801902565 ) ) ;
#8833 = CARTESIAN_POINT ( 'NONE',  ( 4.483927247898545687, 16.52544592524342804, 69.79057627198102409 ) ) ;
#8834 = CARTESIAN_POINT ( 'NONE',  ( -0.05219959533909027116, -19.03943276465977164, 112.4989096053143669 ) ) ;
#8835 = CARTESIAN_POINT ( 'NONE',  ( 21.53943276465977519, -0.05219959533907433946, 33.74890960531436690 ) ) ;
#8836 = CARTESIAN_POINT ( 'NONE',  ( 9.564922557961047289, -16.46253265017146816, 35.41775706135233293 ) ) ;
#8837 = CARTESIAN_POINT ( 'NONE',  ( 4.483927247898545687, 16.52544592524342804, 104.7905762719810241 ) ) ;
#8838 = CARTESIAN_POINT ( 'NONE',  ( 5.153800228976335163, 19.02544592524342804, 114.7905762719810241 ) ) ;
#8839 = EDGE_LOOP ( 'NONE', ( #48329, #140518, #172705 ) ) ;
#8840 = CARTESIAN_POINT ( 'NONE',  ( 14.34966873604972726, -8.224510206698740333, 55.83442372801901854 ) ) ;
#8841 = CARTESIAN_POINT ( 'NONE',  ( -16.51473224551069308, -9.474510206698971260, 61.66557627198103120 ) ) ;
#8842 = CARTESIAN_POINT ( 'NONE',  ( -16.68133157960667035, -6.285544323925044807, 20.58868060224343211 ) ) ;
#8843 = CARTESIAN_POINT ( 'NONE',  ( -16.46253265017146816, -9.564922557961047289, 54.16775706135234003 ) ) ;
#8844 = CARTESIAN_POINT ( 'NONE',  ( -8.224510206698735004, -14.34966873604973081, 99.58442372801900433 ) ) ;
#8845 = CARTESIAN_POINT ( 'NONE',  ( 13.89961937509957401, 13.97604488694547697, 96.87609039468566152 ) ) ;
#8846 = CARTESIAN_POINT ( 'NONE',  ( -5.823673210054431948, 21.52544592524334988, 72.70942372801901854 ) ) ;
#8847 = CARTESIAN_POINT ( 'NONE',  ( -19.02544592524342804, 5.153800228976336051, 71.04057627198099567 ) ) ;
#8848 = CARTESIAN_POINT ( 'NONE',  ( -21.55341960407610458, -5.719274019375992779, 96.45724293864770971 ) ) ;
#8849 = CARTESIAN_POINT ( 'NONE',  ( -16.52544592524342804, 4.483927247898546575, 111.0405762719810525 ) ) ;
#8850 = CIRCLE ( 'NONE', #154180, 35.99626262588765258 ) ;
#8851 = CARTESIAN_POINT ( 'NONE',  ( -19.03943276465977164, -0.05219959533935918106, 83.75109039468567573 ) ) ;
#8852 = CARTESIAN_POINT ( 'NONE',  ( 15.80617190586746368, 15.72974639402197994, 74.37390960531436690 ) ) ;
#8853 = CARTESIAN_POINT ( 'NONE',  ( -9.474510206698720793, -16.51473224551083518, 39.58442372801899722 ) ) ;
#8854 = FACE_BOUND ( 'NONE', #86092, .T. ) ;
#8855 = CARTESIAN_POINT ( 'NONE',  ( 5.719274019375991003, -21.55341960407610458, 87.70724293864769550 ) ) ;
#8856 = CARTESIAN_POINT ( 'NONE',  ( -18.56197773271732387, 5.499999999999902300, 53.55066217314453780 ) ) ;
#8857 = CARTESIAN_POINT ( 'NONE',  ( -0.05219959533909027116, -19.03943276465977164, 67.49890960531436690 ) ) ;
#8858 = DIRECTION ( 'NONE',  ( -1.000000000000000000, 0.000000000000000000, 0.000000000000000000 ) ) ;
#8859 = CARTESIAN_POINT ( 'NONE',  ( -16.52544592524335698, -4.483927247898792601, 18.95942372801901143 ) ) ;
#8860 = CARTESIAN_POINT ( 'NONE',  ( -26.03370437638687918, 6.875205692009823011, 160.5968874236874910 ) ) ;
#8861 = CARTESIAN_POINT ( 'NONE',  ( 5.153800228976335163, 19.02544592524342804, 49.79057627198100988 ) ) ;
#8862 = CARTESIAN_POINT ( 'NONE',  ( -16.51473224551069308, -9.474510206698971260, 111.6655762719810383 ) ) ;
#8864 = CARTESIAN_POINT ( 'NONE',  ( -14.29746914071049879, 8.314922557960819915, 45.83224293864769550 ) ) ;
#8863 = CARTESIAN_POINT ( 'NONE',  ( 5.719274019375991003, -21.55341960407610458, 102.7072429386476955 ) ) ;
#8865 = CARTESIAN_POINT ( 'NONE',  ( 18.62759615963255655, 10.81492255796105972, 76.66775706135234714 ) ) ;
#8867 = CARTESIAN_POINT ( 'NONE',  ( -0.05219959533936034679, 19.03943276465977164, 27.50109039468566507 ) ) ;
#8866 = CARTESIAN_POINT ( 'NONE',  ( -16.53943276465976808, -0.05219959533934237506, 28.75109039468567929 ) ) ;
#8868 = CARTESIAN_POINT ( 'NONE',  ( -8.224510206698948167, 14.34966873604960824, 30.41557627198101699 ) ) ;
#8869 = CARTESIAN_POINT ( 'NONE',  ( -15.80617190586768217, 15.72974639402176855, 33.12609039468569705 ) ) ;
#8870 = CARTESIAN_POINT ( 'NONE',  ( 18.62759615963271287, -10.81492255796078972, 113.3322429386476955 ) ) ;
#8871 = CARTESIAN_POINT ( 'NONE',  ( 14.29746914071049879, -8.314922557960816363, 43.33224293864769550 ) ) ;
#8872 = CARTESIAN_POINT ( 'NONE',  ( 13.89961937509957401, 13.97604488694547697, 101.8760903946856331 ) ) ;
#8873 = CARTESIAN_POINT ( 'NONE',  ( -19.02544592524334988, -5.153800228976617603, 73.95942372801900433 ) ) ;
#8874 = CARTESIAN_POINT ( 'NONE',  ( -21.52544592524334988, -5.823673210054445271, 73.95942372801901854 ) ) ;
#8875 = CARTESIAN_POINT ( 'NONE',  ( 16.51473224551083163, -9.474510206698727899, 55.83442372801899722 ) ) ;
#8876 = CARTESIAN_POINT ( 'NONE',  ( 19.03943276465977164, -0.05219959533909143690, 28.74890960531435624 ) ) ;
#8877 = CARTESIAN_POINT ( 'NONE',  ( 21.52544592524344225, -5.823673210054117533, 48.54057627198103120 ) ) ;
#8878 = CARTESIAN_POINT ( 'NONE',  ( -16.52544592524342804, 4.483927247898546575, 56.04057627198102409 ) ) ;
#8879 = CARTESIAN_POINT ( 'NONE',  ( 17.50000000000002487, -5.499999999999880984, 53.29690382534172244 ) ) ;
#8880 = CARTESIAN_POINT ( 'NONE',  ( 10.81492255796106328, -18.62759615963255655, 110.4177570613523756 ) ) ;
#8881 = CARTESIAN_POINT ( 'NONE',  ( 12.06949235617739724, 12.14591786802326823, 81.87609039468568994 ) ) ;
#8882 = CARTESIAN_POINT ( 'NONE',  ( -14.29746914071049879, 8.314922557960819915, 35.83224293864768839 ) ) ;
#8883 = CARTESIAN_POINT ( 'NONE',  ( -10.72451020669870658, -18.67979575497194134, 69.58442372801900433 ) ) ;
#8884 = CARTESIAN_POINT ( 'NONE',  ( 5.719274019375673035, 21.55341960407619339, 87.29275706135236135 ) ) ;
#8885 = CARTESIAN_POINT ( 'NONE',  ( 10.81492255796078972, 18.62759615963270932, 79.58224293864769550 ) ) ;
#8886 = CARTESIAN_POINT ( 'NONE',  ( -13.97604488694527625, -13.89961937509977652, 31.87390960531435979 ) ) ;
#8887 = CARTESIAN_POINT ( 'NONE',  ( -15.80617190586768217, 15.72974639402176855, 63.12609039468568994 ) ) ;
#8888 = CARTESIAN_POINT ( 'NONE',  ( -16.51473224551069308, -9.474510206698971260, 36.66557627198102409 ) ) ;
#8889 = CARTESIAN_POINT ( 'NONE',  ( 16.46253265017160672, -9.564922557960803928, 53.33224293864768839 ) ) ;
#8890 = CARTESIAN_POINT ( 'NONE',  ( -14.34966873604960291, -8.224510206698953496, 86.66557627198102409 ) ) ;
#8891 = CARTESIAN_POINT ( 'NONE',  ( 5.153800228976335163, 19.02544592524342804, 94.79057627198103830 ) ) ;
#8892 = CARTESIAN_POINT ( 'NONE',  ( 16.53943276465976808, -0.05219959533910856209, 43.74890960531435979 ) ) ;
#8893 = CARTESIAN_POINT ( 'NONE',  ( -4.379528057220328563, 16.55341960407611168, 115.2072429386476955 ) ) ;
#8894 = CARTESIAN_POINT ( 'NONE',  ( -21.52544592524343514, 5.823673210054127303, 86.04057627198102409 ) ) ;
#8895 = CARTESIAN_POINT ( 'NONE',  ( -18.62759615963270932, 10.81492255796079327, 115.8322429386477097 ) ) ;
#8896 = CARTESIAN_POINT ( 'NONE',  ( -15.22666363356483821, 14.91361452257038422, -56.46021433273639190 ) ) ;
#8898 = CARTESIAN_POINT ( 'NONE',  ( 16.55341960407618274, -4.379528057220086978, 21.04275706135234714 ) ) ;
#8897 = CARTESIAN_POINT ( 'NONE',  ( -9.474510206698964154, 16.51473224551069663, 80.41557627198103830 ) ) ;
#8899 = CARTESIAN_POINT ( 'NONE',  ( -21.53943276465977519, 0.05219959533907696930, 76.24890960531435269 ) ) ;
#8900 = CARTESIAN_POINT ( 'NONE',  ( -10.72451020669870658, -18.67979575497194134, 99.58442372801900433 ) ) ;
#8901 = CARTESIAN_POINT ( 'NONE',  ( -5.153800228976328057, -19.02544592524343514, 77.29057627198099567 ) ) ;
#8902 = CARTESIAN_POINT ( 'NONE',  ( 10.72451020669871369, 18.67979575497193778, 37.08442372801901143 ) ) ;
#8903 = CARTESIAN_POINT ( 'NONE',  ( 5.049401038298161559, -19.05341960407611168, 107.7072429386476955 ) ) ;
#8904 = CARTESIAN_POINT ( 'NONE',  ( 12.06949235617739724, 12.14591786802326823, 96.87609039468568994 ) ) ;
#8905 = CARTESIAN_POINT ( 'NONE',  ( -18.62759615963255300, -10.81492255796106328, 74.16775706135231871 ) ) ;
#8906 = CARTESIAN_POINT ( 'NONE',  ( -15.72974639402176322, -15.80617190586768395, 109.3760903946857042 ) ) ;
#8907 = CARTESIAN_POINT ( 'NONE',  ( 14.34966873604972726, -8.224510206698740333, 75.83442372801900433 ) ) ;
#8908 = CARTESIAN_POINT ( 'NONE',  ( 0.05219959533937995610, -21.53943276465977519, 25.00109039468567218 ) ) ;
#8909 = CARTESIAN_POINT ( 'NONE',  ( -5.049401038298153566, 19.05341960407611168, 25.20724293864768484 ) ) ;
#8910 = CARTESIAN_POINT ( 'NONE',  ( 18.62759615963255655, 10.81492255796105972, 86.66775706135234714 ) ) ;
#8911 = CARTESIAN_POINT ( 'NONE',  ( -13.89961937509977652, 13.97604488694528158, 90.62390960531432427 ) ) ;
#8912 = CARTESIAN_POINT ( 'NONE',  ( 10.81492255796078972, 18.62759615963270932, 89.58224293864768129 ) ) ;
#8913 = CARTESIAN_POINT ( 'NONE',  ( 13.89961937509957401, 13.97604488694547697, 61.87609039468566863 ) ) ;
#8915 = CARTESIAN_POINT ( 'NONE',  ( -5.719274019375978568, 21.55341960407610458, 55.20724293864770260 ) ) ;
#8914 = CARTESIAN_POINT ( 'NONE',  ( -3.620324696388704577, -38.95353743397183166, -23.38767721380492048 ) ) ;
#8917 = CARTESIAN_POINT ( 'NONE',  ( -16.55341960407611168, -4.379528057220339221, 56.45724293864768839 ) ) ;
#8916 = CARTESIAN_POINT ( 'NONE',  ( 0.05219959533909260263, 19.03943276465977164, 89.99890960531436690 ) ) ;
#8918 = LINE ( 'NONE', #11931, #7865 ) ;
#8919 = CARTESIAN_POINT ( 'NONE',  ( -19.03943276465977164, -0.05219959533935918106, 83.75109039468567573 ) ) ;
#8920 = CARTESIAN_POINT ( 'NONE',  ( -17.49999999999999645, 5.499999999999997335, 105.7969038253417153 ) ) ;
#8921 = EDGE_CURVE ( 'NONE', #11483, #170159, #195880, .T. ) ;
#8922 = CARTESIAN_POINT ( 'NONE',  ( -5.153800228976607833, 19.02544592524334988, 112.7094237280190043 ) ) ;
#8923 = CARTESIAN_POINT ( 'NONE',  ( -18.62759615963270932, 10.81492255796079327, 80.83224293864769550 ) ) ;
#8924 = CARTESIAN_POINT ( 'NONE',  ( -12.06949235617756955, 12.14591786802309770, 65.62390960531436690 ) ) ;
#8925 = CARTESIAN_POINT ( 'NONE',  ( -19.02544592524342804, 5.153800228976336051, 101.0405762719810241 ) ) ;
#8926 = CARTESIAN_POINT ( 'NONE',  ( -0.05219959533934338120, 16.53943276465976808, 47.50109039468568994 ) ) ;
#8927 = CARTESIAN_POINT ( 'NONE',  ( -9.474510206698964154, 16.51473224551069663, 60.41557627198102409 ) ) ;
#8929 = CARTESIAN_POINT ( 'NONE',  ( -16.51473224551082808, 9.474510206698731452, 103.3344237280190043 ) ) ;
#8928 = CARTESIAN_POINT ( 'NONE',  ( 21.52544592524344225, -5.823673210054117533, 113.5405762719810383 ) ) ;
#8930 = CARTESIAN_POINT ( 'NONE',  ( 9.564922557960805705, 16.46253265017160317, 99.58224293864770971 ) ) ;
#8931 = CARTESIAN_POINT ( 'NONE',  ( 13.89961937509977652, -13.97604488694527269, 73.12390960531436690 ) ) ;
#8932 = CARTESIAN_POINT ( 'NONE',  ( -10.81492255796078084, -18.62759615963271287, 72.08224293864769550 ) ) ;
#8933 = CARTESIAN_POINT ( 'NONE',  ( 5.153800228976335163, 19.02544592524342804, 39.79057627198100988 ) ) ;
#8934 = CARTESIAN_POINT ( 'NONE',  ( 28.83912964652353494, 23.35006605898203347, -8.000000000000001776 ) ) ;
#8935 = CARTESIAN_POINT ( 'NONE',  ( -4.483927247898539470, -16.52544592524342804, 57.29057627198103120 ) ) ;
#8936 = CARTESIAN_POINT ( 'NONE',  ( -5.153800228976328057, -19.02544592524343514, 97.29057627198099567 ) ) ;
#8937 = CARTESIAN_POINT ( 'NONE',  ( 17.50000000000000000, 5.499999999999992895, 38.78230962303566542 ) ) ;
#8938 = CARTESIAN_POINT ( 'NONE',  ( -19.02544592524334988, -5.153800228976617603, 58.95942372801900433 ) ) ;
#8939 = CARTESIAN_POINT ( 'NONE',  ( -10.81492255796078084, -18.62759615963271287, 97.08224293864770971 ) ) ;
#8940 = CARTESIAN_POINT ( 'NONE',  ( -9.474510206698720793, -16.51473224551083518, 49.58442372801899722 ) ) ;
#8941 = CARTESIAN_POINT ( 'NONE',  ( 0.05219959533909260263, 19.03943276465977164, 94.99890960531436690 ) ) ;
#8942 = DIRECTION ( 'NONE',  ( -0.7071067811865561215, -0.7071067811865389130, -0.000000000000000000 ) ) ;
#8943 = CARTESIAN_POINT ( 'NONE',  ( 15.72974639402199770, -15.80617190586745480, 48.12390960531436690 ) ) ;
#8944 = AXIS2_PLACEMENT_3D ( 'NONE', #117188, #55516, #86851 ) ;
#8945 = CARTESIAN_POINT ( 'NONE',  ( 16.51473224551069308, 9.474510206698969483, 79.16557627198103830 ) ) ;
#8946 = CARTESIAN_POINT ( 'NONE',  ( -21.52544592524334988, -5.823673210054445271, 58.95942372801902565 ) ) ;
#8947 = CARTESIAN_POINT ( 'NONE',  ( -13.97604488694527625, -13.89961937509977652, 36.87390960531436690 ) ) ;
#8948 = ADVANCED_FACE ( 'NONE', ( #56337 ), #72517, .T. ) ;
#8950 = EDGE_LOOP ( 'NONE', ( #154421, #38535, #18480, #137340 ) ) ;
#8949 = CARTESIAN_POINT ( 'NONE',  ( -14.29746914071049879, 8.314922557960819915, 75.83224293864769550 ) ) ;
#8951 = CARTESIAN_POINT ( 'NONE',  ( -12.06949235617739369, -12.14591786802326823, 24.37609039468567573 ) ) ;
#8952 = CARTESIAN_POINT ( 'NONE',  ( 10.72451020669871369, 18.67979575497193778, 52.08442372801901854 ) ) ;
#8953 = EDGE_LOOP ( 'NONE', ( #122779, #89234, #12743, #137387 ) ) ;
#8954 = CARTESIAN_POINT ( 'NONE',  ( 19.02544592524343514, -5.153800228976328945, 108.5405762719810383 ) ) ;
#8955 = CARTESIAN_POINT ( 'NONE',  ( -9.564922557961040184, 16.46253265017147172, 62.91775706135233293 ) ) ;
#8956 = DIRECTION ( 'NONE',  ( 1.000000000000000000, 0.000000000000000000, 0.000000000000000000 ) ) ;
#8957 = CARTESIAN_POINT ( 'NONE',  ( -18.67979575497193778, 10.72451020669871902, 23.33442372801901499 ) ) ;
#8958 = CARTESIAN_POINT ( 'NONE',  ( 13.89961937509977652, -13.97604488694527269, 58.12390960531436690 ) ) ;
#8959 = CARTESIAN_POINT ( 'NONE',  ( 30.74264578624799782, 22.33583958711400541, -6.549999994537627046 ) ) ;
#8960 = CARTESIAN_POINT ( 'NONE',  ( -18.67979575497193778, 10.72451020669871902, 108.3344237280190185 ) ) ;
#8961 = CARTESIAN_POINT ( 'NONE',  ( 16.51473224551069308, 9.474510206698969483, 44.16557627198103120 ) ) ;
#8962 = CARTESIAN_POINT ( 'NONE',  ( -19.03943276465977164, -0.05219959533935918106, 18.75109039468567218 ) ) ;
#8963 = CARTESIAN_POINT ( 'NONE',  ( -0.05219959533934338120, 16.53943276465976808, 87.50109039468568994 ) ) ;
#8965 = CARTESIAN_POINT ( 'NONE',  ( -21.52544592524334988, -5.823673210054445271, 68.95942372801901854 ) ) ;
#8964 = CARTESIAN_POINT ( 'NONE',  ( 19.05341960407611168, 5.049401038298154454, 103.9572429386476671 ) ) ;
#8966 = CARTESIAN_POINT ( 'NONE',  ( 11.40812507854754365, 35.11059874428196537, -9.224999997268813701 ) ) ;
#8967 = CARTESIAN_POINT ( 'NONE',  ( -16.51473224551069308, -9.474510206698971260, 106.6655762719810383 ) ) ;
#8968 = CARTESIAN_POINT ( 'NONE',  ( 2.500000000000000000, -1.178949249685214307, 2.042000000000002036 ) ) ;
#8970 = CARTESIAN_POINT ( 'NONE',  ( -15.72974639402176322, -15.80617190586768395, 69.37609039468567573 ) ) ;
#8969 = CARTESIAN_POINT ( 'NONE',  ( 0.05219959533934541429, -16.53943276465976808, 70.00109039468568994 ) ) ;
#8971 = CARTESIAN_POINT ( 'NONE',  ( 18.67979575497194134, -10.72451020669871369, 105.8344237280190328 ) ) ;
#8972 = CARTESIAN_POINT ( 'NONE',  ( 5.000000000000000888, -130.0000000000000000, 15.50000000000000000 ) ) ;
#8973 = CARTESIAN_POINT ( 'NONE',  ( 16.55341960407618274, -4.379528057220086978, 41.04275706135236135 ) ) ;
#8974 = CARTESIAN_POINT ( 'NONE',  ( -0.05219959533909027116, -19.03943276465977164, 87.49890960531436690 ) ) ;
#8975 = CARTESIAN_POINT ( 'NONE',  ( -19.03943276465977164, 0.05219959533909376836, 111.2489096053143669 ) ) ;
#8976 = EDGE_LOOP ( 'NONE', ( #101835, #70618, #40159, #782 ) ) ;
#8977 = AXIS2_PLACEMENT_3D ( 'NONE', #29250, #183915, #153562 ) ;
#8978 = CARTESIAN_POINT ( 'NONE',  ( 16.61371651742603461, 7.165104196376041124, 43.64584930007006136 ) ) ;
#8979 = CARTESIAN_POINT ( 'NONE',  ( 0.05219959533909260263, 19.03943276465977164, 34.99890960531435979 ) ) ;
#8980 = CARTESIAN_POINT ( 'NONE',  ( -18.67979575497178146, -10.72451020669898902, 46.66557627198102409 ) ) ;
#8981 = CARTESIAN_POINT ( 'NONE',  ( -14.29746914071037622, -8.314922557961029526, 104.1677570613523471 ) ) ;
#8983 = CARTESIAN_POINT ( 'NONE',  ( 9.474510206698971260, -16.51473224551069308, 77.91557627198103830 ) ) ;
#8982 = CARTESIAN_POINT ( 'NONE',  ( 12.06949235617757843, -12.14591786802309237, 88.12390960531436690 ) ) ;
#8984 = CARTESIAN_POINT ( 'NONE',  ( 15.80617190586769283, -15.72974639402175789, 100.6260903946857184 ) ) ;
#8985 = CARTESIAN_POINT ( 'NONE',  ( -0.05219959533934338120, 16.53943276465976808, 22.50109039468567573 ) ) ;
#8986 = CARTESIAN_POINT ( 'NONE',  ( -14.34966873604960291, -8.224510206698953496, 86.66557627198102409 ) ) ;
#8987 = CARTESIAN_POINT ( 'NONE',  ( 15.80617190586769283, -15.72974639402175789, 35.62609039468568994 ) ) ;
#8988 = CARTESIAN_POINT ( 'NONE',  ( 10.72451020669898902, -18.67979575497178502, 87.91557627198103830 ) ) ;
#8989 = CARTESIAN_POINT ( 'NONE',  ( 13.89961937509957401, 13.97604488694547697, 46.87609039468565442 ) ) ;
#8990 = CARTESIAN_POINT ( 'NONE',  ( -34.40742850069382541, 7.501893140248845349, 45.46088305597102419 ) ) ;
#8991 = CARTESIAN_POINT ( 'NONE',  ( -19.05341960407611168, -5.049401038298163336, 101.4572429386476955 ) ) ;
#8992 = CARTESIAN_POINT ( 'NONE',  ( 8.224510206698953496, -14.34966873604960469, 62.91557627198102409 ) ) ;
#8993 = CARTESIAN_POINT ( 'NONE',  ( -4.379528057220328563, 16.55341960407611168, 45.20724293864769550 ) ) ;
#8994 = CARTESIAN_POINT ( 'NONE',  ( -16.52544592524335698, -4.483927247898792601, 103.9594237280190185 ) ) ;
#8995 = CARTESIAN_POINT ( 'NONE',  ( -19.05341960407617563, 5.049401038297882671, 63.54275706135234003 ) ) ;
#8996 = CARTESIAN_POINT ( 'NONE',  ( 30.00000000000000000, -1.130961319012580892E-14, 97.65000000000000568 ) ) ;
#8997 = CARTESIAN_POINT ( 'NONE',  ( 16.46253265017160672, -9.564922557960803928, 113.3322429386476955 ) ) ;
#8998 = EDGE_CURVE ( 'NONE', #133171, #50923, #118019, .T. ) ;
#8999 = CARTESIAN_POINT ( 'NONE',  ( -4.483927247898539470, -16.52544592524342804, 87.29057627198103830 ) ) ;
#9000 = CARTESIAN_POINT ( 'NONE',  ( -0.3431728551240714742, -71.74905178543389184, -4.999999999999999112 ) ) ;
#9002 = CARTESIAN_POINT ( 'NONE',  ( -10.72451020669898014, 18.67979575497178502, 45.41557627198103830 ) ) ;
#9001 = CARTESIAN_POINT ( 'NONE',  ( -5.153800228976328057, -19.02544592524343514, 52.29057627198100988 ) ) ;
#9003 = CARTESIAN_POINT ( 'NONE',  ( -19.02544592524342804, 5.153800228976336051, 26.04057627198103120 ) ) ;
#9005 = CARTESIAN_POINT ( 'NONE',  ( -13.89961937509977652, 13.97604488694528158, 60.62390960531436690 ) ) ;
#9004 = CARTESIAN_POINT ( 'NONE',  ( -8.224510206698735004, -14.34966873604973081, 84.58442372801903275 ) ) ;
#9006 = CARTESIAN_POINT ( 'NONE',  ( -5.153800228976607833, 19.02544592524334988, 42.70942372801901143 ) ) ;
#9007 = CARTESIAN_POINT ( 'NONE',  ( 18.62759615963255655, 10.81492255796105972, 51.66775706135234714 ) ) ;
#9008 = CARTESIAN_POINT ( 'NONE',  ( 5.719274019375991003, -21.55341960407610458, 32.70724293864770260 ) ) ;
#9009 = CARTESIAN_POINT ( 'NONE',  ( -8.314922557960811034, -14.29746914071050412, 102.0822429386476955 ) ) ;
#9010 = CARTESIAN_POINT ( 'NONE',  ( 16.46253265017146816, 9.564922557961045513, 86.66775706135233293 ) ) ;
#9011 = CARTESIAN_POINT ( 'NONE',  ( 36.91746824999999177, 11.99521256947799230, -6.024999997268812635 ) ) ;
#9013 = CARTESIAN_POINT ( 'NONE',  ( 10.72451020669898902, -18.67979575497178502, 52.91557627198103830 ) ) ;
#9012 = DIRECTION ( 'NONE',  ( -0.000000000000000000, -0.000000000000000000, 1.000000000000000000 ) ) ;
#9014 = CARTESIAN_POINT ( 'NONE',  ( 13.89961937509977652, -13.97604488694527269, 23.12390960531436335 ) ) ;
#9015 = CARTESIAN_POINT ( 'NONE',  ( -5.719274019375665041, -21.55341960407619695, 89.79275706135236135 ) ) ;
#9016 = CARTESIAN_POINT ( 'NONE',  ( 4.379528057220339221, -16.55341960407611168, 52.70724293864769550 ) ) ;
#9018 = CARTESIAN_POINT ( 'NONE',  ( 14.29746914071049879, -8.314922557960816363, 58.33224293864768839 ) ) ;
#9017 = CARTESIAN_POINT ( 'NONE',  ( 8.314922557961029526, -14.29746914071037800, 60.41775706135235424 ) ) ;
#9019 = CARTESIAN_POINT ( 'NONE',  ( -0.05219959533907301413, -21.53943276465977519, 77.49890960531433848 ) ) ;
#9020 = CARTESIAN_POINT ( 'NONE',  ( -15.72974639402197994, 15.80617190586746368, 70.62390960531436690 ) ) ;
#9021 = CARTESIAN_POINT ( 'NONE',  ( 1.300000000000000044, 0.000000000000000000, 0.000000000000000000 ) ) ;
#9022 = CARTESIAN_POINT ( 'NONE',  ( 10.72451020669898902, -18.67979575497178502, 22.91557627198102765 ) ) ;
#9023 = CARTESIAN_POINT ( 'NONE',  ( -16.46253265017160317, 9.564922557960807481, 65.83224293864769550 ) ) ;
#9024 = CARTESIAN_POINT ( 'NONE',  ( 5.153800228976335163, 19.02544592524342804, 29.79057627198102409 ) ) ;
#9025 = CARTESIAN_POINT ( 'NONE',  ( -18.09805431107249873, 5.499999999999980460, 76.01606229291883210 ) ) ;
#9026 = CARTESIAN_POINT ( 'NONE',  ( 8.224510206698742110, 14.34966873604972548, 82.08442372801901854 ) ) ;
#9027 = CARTESIAN_POINT ( 'NONE',  ( 0.05219959533937995610, -21.53943276465977519, 20.00109039468568639 ) ) ;
#9028 = CARTESIAN_POINT ( 'NONE',  ( -13.89961937509977652, 13.97604488694528158, 65.62390960531436690 ) ) ;
#9029 = CARTESIAN_POINT ( 'NONE',  ( 18.67979575497194134, -10.72451020669871369, 55.83442372801901854 ) ) ;
#9030 = CARTESIAN_POINT ( 'NONE',  ( -16.46253265017160317, 9.564922557960807481, 100.8322429386477097 ) ) ;
#9031 = CARTESIAN_POINT ( 'NONE',  ( -26.41049836824041464, -29.67629096701854863, -20.30943395415518182 ) ) ;
#9032 = VERTEX_POINT ( 'NONE', #57353 ) ;
#9033 = CARTESIAN_POINT ( 'NONE',  ( -18.62759615963255300, -10.81492255796106328, 44.16775706135234714 ) ) ;
#9035 = CARTESIAN_POINT ( 'NONE',  ( -5.049401038298153566, 19.05341960407611168, 100.2072429386476955 ) ) ;
#9034 = CARTESIAN_POINT ( 'NONE',  ( -0.05219959533909027116, -19.03943276465977164, 27.49890960531435624 ) ) ;
#9036 = CARTESIAN_POINT ( 'NONE',  ( -13.89961937509957401, -13.97604488694547875, 49.37609039468567573 ) ) ;
#9037 = CARTESIAN_POINT ( 'NONE',  ( -15.80617190586745835, -15.72974639402198527, 111.8739096053143669 ) ) ;
#9038 = CARTESIAN_POINT ( 'NONE',  ( -19.03943276465977164, -0.05219959533935918106, 48.75109039468566863 ) ) ;
#9039 = CARTESIAN_POINT ( 'NONE',  ( 13.89961937509957401, 13.97604488694547697, 46.87609039468565442 ) ) ;
#9040 = CARTESIAN_POINT ( 'NONE',  ( -14.29746914071037622, -8.314922557961029526, 104.1677570613523471 ) ) ;
#9041 = CARTESIAN_POINT ( 'NONE',  ( 193.3062444957835453, -155.7167183371837496, -4.999999999999999112 ) ) ;
#9042 = CARTESIAN_POINT ( 'NONE',  ( 19.03943276465977164, -0.05219959533909143690, 78.74890960531436690 ) ) ;
#9043 = CARTESIAN_POINT ( 'NONE',  ( -10.72451020669870658, -18.67979575497194134, 84.58442372801903275 ) ) ;
#9044 = CARTESIAN_POINT ( 'NONE',  ( 10.81492255796106328, -18.62759615963255655, 100.4177570613523471 ) ) ;
#9045 = CARTESIAN_POINT ( 'NONE',  ( -0.7565710328820600683, -8.898962301217522963, -63.99033069988504963 ) ) ;
#9046 = CARTESIAN_POINT ( 'NONE',  ( -13.97604488694527625, -13.89961937509977652, 96.87390960531433848 ) ) ;
#9047 = CARTESIAN_POINT ( 'NONE',  ( 15.72974639402176855, 15.80617190586768217, 81.87609039468568994 ) ) ;
#9048 = CARTESIAN_POINT ( 'NONE',  ( 16.46253265017146816, 9.564922557961045513, 111.6677570613523329 ) ) ;
#9049 = CARTESIAN_POINT ( 'NONE',  ( -19.05341960407611168, -5.049401038298163336, 76.45724293864769550 ) ) ;
#9050 = CARTESIAN_POINT ( 'NONE',  ( -13.97604488694527625, -13.89961937509977652, 111.8739096053143243 ) ) ;
#9051 = CARTESIAN_POINT ( 'NONE',  ( 5.049401038298161559, -19.05341960407611168, 97.70724293864766707 ) ) ;
#9052 = CARTESIAN_POINT ( 'NONE',  ( 16.46253265017146816, 9.564922557961045513, 86.66775706135233293 ) ) ;
#9053 = CARTESIAN_POINT ( 'NONE',  ( 9.474510206698971260, -16.51473224551069308, 77.91557627198103830 ) ) ;
#9054 = CARTESIAN_POINT ( 'NONE',  ( -16.46253265017160317, 9.564922557960807481, 60.83224293864769550 ) ) ;
#9055 = CARTESIAN_POINT ( 'NONE',  ( -5.823673210054116645, -21.52544592524344225, 107.2905762719810525 ) ) ;
#9056 = CARTESIAN_POINT ( 'NONE',  ( 4.483927247898790824, -16.52544592524335698, 105.2094237280190328 ) ) ;
#9057 = CARTESIAN_POINT ( 'NONE',  ( 1.784589286804253661, -7.284589286804279418, 1.818019484660534424 ) ) ;
#9058 = CARTESIAN_POINT ( 'NONE',  ( -9.474510206698720793, -16.51473224551083518, 64.58442372801900433 ) ) ;
#9059 = B_SPLINE_CURVE_WITH_KNOTS ( 'NONE', 3,
 ( #31329, #123314, #76824, #138495, #90985, #122328, #75829, #28378, #966, #170834, #121340, #74855, #155659, #30333, #17155, #90016, #46492, #200177, #91974, #183033, #13192, #62642, #78808, #108153, #107157, #153668 ),
 .UNSPECIFIED., .F., .F.,
 ( 4, 2, 2, 2, 2, 2, 2, 2, 2, 2, 2, 2, 4 ),
 ( 1.971390914465818311E-07, 0.0002963316798229296048, 0.0005924662205544125584, 0.0008886007612858956746, 0.001184735302017378899, 0.001777004383480341879, 0.002369273464943304642, 0.002665408005674786349, 0.002961542546406268055, 0.003257677087137749328, 0.003553811627869231035, 0.004146080709332196183, 0.004738349790795161331 ),
 .UNSPECIFIED. ) ;
#9060 = CARTESIAN_POINT ( 'NONE',  ( 13.89961937509977652, -13.97604488694527269, 93.12390960531436690 ) ) ;
#9061 = CARTESIAN_POINT ( 'NONE',  ( -8.224510206698948167, 14.34966873604960824, 90.41557627198103830 ) ) ;
#9062 = CARTESIAN_POINT ( 'NONE',  ( -0.05219959533909027116, -19.03943276465977164, 27.49890960531435624 ) ) ;
#9063 = CARTESIAN_POINT ( 'NONE',  ( 10.72451020669898902, -18.67979575497178502, 32.91557627198102409 ) ) ;
#9064 = CARTESIAN_POINT ( 'NONE',  ( 10.81492255796078972, 18.62759615963270932, 24.58224293864768839 ) ) ;
#9065 = CARTESIAN_POINT ( 'NONE',  ( -16.55341960407611168, -4.379528057220339221, 86.45724293864770971 ) ) ;
#9066 = CARTESIAN_POINT ( 'NONE',  ( 30.82560697742735201, 2.428612866367529932E-14, 150.0000000000000000 ) ) ;
#9067 = CARTESIAN_POINT ( 'NONE',  ( -5.049401038297874678, -19.05341960407617918, 44.79275706135232582 ) ) ;
#9068 = CARTESIAN_POINT ( 'NONE',  ( -0.05219959533934338120, 16.53943276465976808, 102.5010903946856899 ) ) ;
#9069 = CARTESIAN_POINT ( 'NONE',  ( -19.02544592524342804, 5.153800228976336051, 91.04057627198100988 ) ) ;
#9070 = CARTESIAN_POINT ( 'NONE',  ( 10.81492255796106328, -18.62759615963255655, 70.41775706135236135 ) ) ;
#9071 = CARTESIAN_POINT ( 'NONE',  ( -21.55341960407610458, -5.719274019375992779, 41.45724293864769550 ) ) ;
#9072 = CARTESIAN_POINT ( 'NONE',  ( 5.823673210054444382, -21.52544592524334988, 35.20942372801901854 ) ) ;
#9073 = CARTESIAN_POINT ( 'NONE',  ( -10.72451020669898014, 18.67979575497178502, 80.41557627198103830 ) ) ;
#9074 = CARTESIAN_POINT ( 'NONE',  ( -14.29746914071049879, 8.314922557960819915, 105.8322429386476955 ) ) ;
#9075 = CARTESIAN_POINT ( 'NONE',  ( 0.05219959533936267826, -19.03943276465977164, 75.00109039468566152 ) ) ;
#9076 = CARTESIAN_POINT ( 'NONE',  ( -13.89961937509977652, 13.97604488694528158, 45.62390960531433848 ) ) ;
#9077 = CARTESIAN_POINT ( 'NONE',  ( 19.03943276465977164, -0.05219959533909143690, 98.74890960531436690 ) ) ;
#9078 = CARTESIAN_POINT ( 'NONE',  ( -9.564922557960796823, -16.46253265017161027, 97.08224293864769550 ) ) ;
#9079 = CARTESIAN_POINT ( 'NONE',  ( 9.474510206698971260, -16.51473224551069308, 22.91557627198102765 ) ) ;
#9080 = CARTESIAN_POINT ( 'NONE',  ( -8.224510206698948167, 14.34966873604960824, 45.41557627198103830 ) ) ;
#9081 = CARTESIAN_POINT ( 'NONE',  ( -8.314922557961024197, 14.29746914071037800, 37.91775706135235424 ) ) ;
#9082 = CARTESIAN_POINT ( 'NONE',  ( 15.80617190586769283, -15.72974639402175789, 105.6260903946856899 ) ) ;
#9085 = CARTESIAN_POINT ( 'NONE',  ( -4.483927247898539470, -16.52544592524342804, 22.29057627198102765 ) ) ;
#9084 = CARTESIAN_POINT ( 'NONE',  ( 18.22780087662123805, -5.499999999999976019, 73.51763182126894947 ) ) ;
#9083 = AXIS2_PLACEMENT_3D ( 'NONE', #99154, #180038, #22332 ) ;
#9086 = MANIFOLD_SOLID_BREP ( 'Extrude-Thin3', #40546 ) ;
#9087 = CARTESIAN_POINT ( 'NONE',  ( -18.67979575497193778, 10.72451020669871902, 38.33442372801900433 ) ) ;
#9088 = CARTESIAN_POINT ( 'NONE',  ( -16.51473224551069308, -9.474510206698971260, 106.6655762719810383 ) ) ;
#9089 = CARTESIAN_POINT ( 'NONE',  ( 8.314922557961029526, -14.29746914071037800, 105.4177570613523613 ) ) ;
#9090 = CARTESIAN_POINT ( 'NONE',  ( 12.06949235617739724, 12.14591786802326823, 96.87609039468568994 ) ) ;
#9091 = CARTESIAN_POINT ( 'NONE',  ( 16.52544592524335698, 4.483927247898782831, 31.45942372801901854 ) ) ;
#9092 = ADVANCED_FACE ( 'NONE', ( #165528 ), #46870, .T. ) ;
#9093 = CARTESIAN_POINT ( 'NONE',  ( 19.03943276465977164, -0.05219959533909143690, 48.74890960531435979 ) ) ;
#9094 = CARTESIAN_POINT ( 'NONE',  ( -12.06949235617756955, 12.14591786802309770, 110.6239096053143669 ) ) ;
#9095 = CARTESIAN_POINT ( 'NONE',  ( -15.72974639402176322, -15.80617190586768395, 19.37609039468568639 ) ) ;
#9096 = CARTESIAN_POINT ( 'NONE',  ( -16.51473224551069308, -9.474510206698971260, 26.66557627198103120 ) ) ;
#9097 = CARTESIAN_POINT ( 'NONE',  ( -19.03943276465977164, 0.05219959533909376836, 111.2489096053143669 ) ) ;
#9098 = CARTESIAN_POINT ( 'NONE',  ( 0.05219959533937995610, -21.53943276465977519, 30.00109039468568284 ) ) ;
#9099 = CARTESIAN_POINT ( 'NONE',  ( 19.05341960407611168, 5.049401038298154454, 28.95724293864769550 ) ) ;
#9100 = CARTESIAN_POINT ( 'NONE',  ( -5.153800228976328057, -19.02544592524343514, 107.2905762719810383 ) ) ;
#9101 = CARTESIAN_POINT ( 'NONE',  ( -17.05587630539787725, -6.762274262135647973, 34.25819690962688213 ) ) ;
#9102 = CARTESIAN_POINT ( 'NONE',  ( -19.05341960407611168, -5.049401038298163336, 101.4572429386476955 ) ) ;
#9104 = CARTESIAN_POINT ( 'NONE',  ( -4.379528057220328563, 16.55341960407611168, 90.20724293864770971 ) ) ;
#9103 = CARTESIAN_POINT ( 'NONE',  ( 21.53943276465977519, 0.05219959533937863772, 41.25109039468568284 ) ) ;
#9105 = CARTESIAN_POINT ( 'NONE',  ( 5.153800228976335163, 19.02544592524342804, 94.79057627198103830 ) ) ;
#9106 = CARTESIAN_POINT ( 'NONE',  ( -27.46944729266723328, -7.746537029273099506, 162.9576794167586797 ) ) ;
#9107 = CARTESIAN_POINT ( 'NONE',  ( 14.34966873604972726, -8.224510206698740333, 70.83442372801901854 ) ) ;
#9108 = CARTESIAN_POINT ( 'NONE',  ( 0.05219959533937995610, -21.53943276465977519, 85.00109039468568994 ) ) ;
#9109 = CIRCLE ( 'NONE', #176970, 0.4999999999999945044 ) ;
#9110 = CARTESIAN_POINT ( 'NONE',  ( -8.314922557961024197, 14.29746914071037800, 37.91775706135235424 ) ) ;
#9111 = CARTESIAN_POINT ( 'NONE',  ( -9.564922557960796823, -16.46253265017161027, 82.08224293864768129 ) ) ;
#9112 = CARTESIAN_POINT ( 'NONE',  ( -13.89961937509957401, -13.97604488694547875, 109.3760903946856331 ) ) ;
#9113 = CARTESIAN_POINT ( 'NONE',  ( -8.314922557961024197, 14.29746914071037800, 67.91775706135234714 ) ) ;
#9114 = CARTESIAN_POINT ( 'NONE',  ( 19.05341960407617918, -5.049401038297876454, 96.04275706135231871 ) ) ;
#9115 = CARTESIAN_POINT ( 'NONE',  ( -5.049401038298153566, 19.05341960407611168, 70.20724293864769550 ) ) ;
#9116 = CARTESIAN_POINT ( 'NONE',  ( -10.81492255796078084, -18.62759615963271287, 87.08224293864769550 ) ) ;
#9118 = CARTESIAN_POINT ( 'NONE',  ( 13.97604488694548053, -13.89961937509957401, 85.62609039468568994 ) ) ;
#9117 = CARTESIAN_POINT ( 'NONE',  ( -16.55341960407611168, -4.379528057220339221, 96.45724293864770971 ) ) ;
#9119 = CARTESIAN_POINT ( 'NONE',  ( -16.52544592524335698, -4.483927247898792601, 53.95942372801900433 ) ) ;
#9120 = CARTESIAN_POINT ( 'NONE',  ( 21.56952297831559662, 5.557039098534931831, 173.4609804364286276 ) ) ;
#9121 = CIRCLE ( 'NONE', #145522, 28.90000000000004476 ) ;
#9122 = CARTESIAN_POINT ( 'NONE',  ( -9.564922557961040184, 16.46253265017147172, 62.91775706135233293 ) ) ;
#9123 = CARTESIAN_POINT ( 'NONE',  ( 4.483927247898545687, 16.52544592524342804, 29.79057627198102409 ) ) ;
#9124 = CARTESIAN_POINT ( 'NONE',  ( -8.224510206698948167, 14.34966873604960824, 75.41557627198102409 ) ) ;
#9126 = CARTESIAN_POINT ( 'NONE',  ( -16.36317988757094710, 7.306389748694859243, 39.09789608363175972 ) ) ;
#9125 = CARTESIAN_POINT ( 'NONE',  ( -9.474510206698720793, -16.51473224551083518, 19.58442372801899722 ) ) ;
#9127 = CARTESIAN_POINT ( 'NONE',  ( -18.67979575497193778, 10.72451020669871902, 23.33442372801901499 ) ) ;
#9128 = CARTESIAN_POINT ( 'NONE',  ( -19.03943276465977164, 0.05219959533909376836, 111.2489096053143669 ) ) ;
#9129 = CARTESIAN_POINT ( 'NONE',  ( -0.05219959533909027116, -19.03943276465977164, 77.49890960531435269 ) ) ;
#9130 = CARTESIAN_POINT ( 'NONE',  ( -21.52544592524334988, -5.823673210054445271, 93.95942372801903275 ) ) ;
#9131 = CARTESIAN_POINT ( 'NONE',  ( -5.049401038298153566, 19.05341960407611168, 80.20724293864769550 ) ) ;
#9132 = CARTESIAN_POINT ( 'NONE',  ( -15.72974639402197994, 15.80617190586746368, 45.62390960531436690 ) ) ;
#9133 = CARTESIAN_POINT ( 'NONE',  ( -16.55341960407611168, -4.379528057220339221, 76.45724293864769550 ) ) ;
#9134 = CARTESIAN_POINT ( 'NONE',  ( 13.97604488694527802, 13.89961937509977652, 59.37390960531434558 ) ) ;
#9135 = CARTESIAN_POINT ( 'NONE',  ( -16.52544592524342804, 4.483927247898546575, 111.0405762719810525 ) ) ;
#9136 = CARTESIAN_POINT ( 'NONE',  ( 21.55341960407619695, -5.719274019375665929, 21.04275706135234714 ) ) ;
#9137 = CARTESIAN_POINT ( 'NONE',  ( -5.823673210054431948, 21.52544592524334988, 62.70942372801902565 ) ) ;
#9138 = CARTESIAN_POINT ( 'NONE',  ( 9.474510206698971260, -16.51473224551069308, 37.91557627198102409 ) ) ;
#9139 = CARTESIAN_POINT ( 'NONE',  ( -16.52544592524335698, -4.483927247898792601, 63.95942372801901854 ) ) ;
#9140 = CARTESIAN_POINT ( 'NONE',  ( 15.80617190586746368, 15.72974639402197994, 109.3739096053143811 ) ) ;
#9141 = CARTESIAN_POINT ( 'NONE',  ( 18.67979575497178502, 10.72451020669898547, 109.1655762719810383 ) ) ;
#9143 = CARTESIAN_POINT ( 'NONE',  ( -5.049401038298153566, 19.05341960407611168, 65.20724293864765286 ) ) ;
#9142 = CARTESIAN_POINT ( 'NONE',  ( -19.02544592524334988, -5.153800228976617603, 38.95942372801900433 ) ) ;
#9144 = DIRECTION ( 'NONE',  ( 1.000000000000000000, 0.000000000000000000, 0.000000000000000000 ) ) ;
#9145 = CARTESIAN_POINT ( 'NONE',  ( -21.52544592524334988, -5.823673210054445271, 73.95942372801901854 ) ) ;
#9146 = CARTESIAN_POINT ( 'NONE',  ( 21.52544592524344225, -5.823673210054117533, 53.54057627198103120 ) ) ;
#9147 = CARTESIAN_POINT ( 'NONE',  ( -16.53943276465976808, 0.05219959533911058130, 36.24890960531435979 ) ) ;
#9149 = CARTESIAN_POINT ( 'NONE',  ( 21.55341960407619695, -5.719274019375665929, 111.0427570613523613 ) ) ;
#9148 = CARTESIAN_POINT ( 'NONE',  ( 18.62759615963255655, 10.81492255796105972, 76.66775706135234714 ) ) ;
#9150 = CARTESIAN_POINT ( 'NONE',  ( 16.53943276465976808, -0.05219959533910856209, 53.74890960531437401 ) ) ;
#9152 = B_SPLINE_CURVE_WITH_KNOTS ( 'NONE', 3,
 ( #131548, #149720, #11220, #72895, #179076, #194240, #134563, #116378, #55707, #40547, #163905, #82673, #114007, #176720, #131188, #54356 ),
 .UNSPECIFIED., .F., .F.,
 ( 4, 2, 2, 2, 2, 2, 2, 4 ),
 ( 0.001191682210564843237, 0.002120961452828536587, 0.002585601073960383696, 0.003050240695092231238, 0.003514880316224078347, 0.003979519937355925456, 0.004444159558487772999, 0.004908799179619620541 ),
 .UNSPECIFIED. ) ;
#9151 = CARTESIAN_POINT ( 'NONE',  ( 16.53943276465976808, -0.05219959533910856209, 103.7489096053143669 ) ) ;
#9153 = CARTESIAN_POINT ( 'NONE',  ( 13.89961937509957401, 13.97604488694547697, 56.87609039468564731 ) ) ;
#9154 = CARTESIAN_POINT ( 'NONE',  ( 12.06949235617739724, 12.14591786802326823, 111.8760903946856615 ) ) ;
#9155 = CARTESIAN_POINT ( 'NONE',  ( 15.72974639402176855, 15.80617190586768217, 61.87609039468568284 ) ) ;
#9156 = CARTESIAN_POINT ( 'NONE',  ( -9.564922557960796823, -16.46253265017161027, 72.08224293864770971 ) ) ;
#9157 = CARTESIAN_POINT ( 'NONE',  ( 5.049401038297881783, 19.05341960407617563, 32.29275706135233293 ) ) ;
#9158 = CARTESIAN_POINT ( 'NONE',  ( 18.67979575497178502, 10.72451020669898547, 44.16557627198103120 ) ) ;
#9159 = CARTESIAN_POINT ( 'NONE',  ( 5.719274019375673035, 21.55341960407619339, 27.29275706135234358 ) ) ;
#9160 = CARTESIAN_POINT ( 'NONE',  ( 15.80617190586746368, 15.72974639402197994, 94.37390960531436690 ) ) ;
#9161 = CARTESIAN_POINT ( 'NONE',  ( -13.97604488694547697, 13.89961937509957934, 98.12609039468566152 ) ) ;
#9162 = CARTESIAN_POINT ( 'NONE',  ( -4.483927247898782831, 16.52544592524335698, 47.70942372801902565 ) ) ;
#9164 = CARTESIAN_POINT ( 'NONE',  ( -18.67979575497178146, -10.72451020669898902, 96.66557627198102409 ) ) ;
#9163 = CARTESIAN_POINT ( 'NONE',  ( -30.74264578624800492, 22.33583958711400186, -6.200000000000001066 ) ) ;
#9165 = CARTESIAN_POINT ( 'NONE',  ( 0.05219959533910956823, 16.53943276465976808, 94.99890960531436690 ) ) ;
#9166 = CARTESIAN_POINT ( 'NONE',  ( -22.19904868473514981, -30.74855836414207744, -22.45812049023462009 ) ) ;
#9167 = CARTESIAN_POINT ( 'NONE',  ( 8.224510206698742110, 14.34966873604972548, 22.08442372801901143 ) ) ;
#9168 = CARTESIAN_POINT ( 'NONE',  ( 10.81492255796078972, 18.62759615963270932, 54.58224293864769550 ) ) ;
#9169 = CARTESIAN_POINT ( 'NONE',  ( -8.224510206698735004, -14.34966873604973081, 89.58442372801901854 ) ) ;
#9170 = DIRECTION ( 'NONE',  ( -0.000000000000000000, 1.000000000000000000, -0.000000000000000000 ) ) ;
#9171 = CARTESIAN_POINT ( 'NONE',  ( 16.53943276465976808, 0.05219959533934440121, 56.25109039468568284 ) ) ;
#9172 = CARTESIAN_POINT ( 'NONE',  ( 21.53943276465977519, 0.05219959533937863772, 31.25109039468568639 ) ) ;
#9173 = CARTESIAN_POINT ( 'NONE',  ( -15.72974639402197994, 15.80617190586746368, 50.62390960531435979 ) ) ;
#9174 = CARTESIAN_POINT ( 'NONE',  ( -8.224510206698735004, -14.34966873604973081, 89.58442372801901854 ) ) ;
#9175 = CARTESIAN_POINT ( 'NONE',  ( -16.46253265017160317, 9.564922557960807481, 100.8322429386477097 ) ) ;
#9176 = CARTESIAN_POINT ( 'NONE',  ( -21.53943276465977519, -0.05219959533937600094, 63.75109039468568284 ) ) ;
#9177 = CARTESIAN_POINT ( 'NONE',  ( 18.62759615963271287, -10.81492255796078972, 33.33224293864769550 ) ) ;
#9178 = CARTESIAN_POINT ( 'NONE',  ( -5.049401038298153566, 19.05341960407611168, 115.2072429386477097 ) ) ;
#9179 = VERTEX_POINT ( 'NONE', #194864 ) ;
#9180 = CARTESIAN_POINT ( 'NONE',  ( -9.474510206698720793, -16.51473224551083518, 54.58442372801899722 ) ) ;
#9181 = CARTESIAN_POINT ( 'NONE',  ( 16.52544592524335698, 4.483927247898782831, 61.45942372801901854 ) ) ;
#9182 = CARTESIAN_POINT ( 'NONE',  ( 18.62759615963271287, -10.81492255796078972, 23.33224293864769194 ) ) ;
#9183 = ORIENTED_EDGE ( 'NONE', *, *, #11833, .F. ) ;
#9184 = EDGE_CURVE ( 'NONE', #150360, #8650, #151354, .T. ) ;
#9185 = CARTESIAN_POINT ( 'NONE',  ( -5.153800228976328057, -19.02544592524343514, 92.29057627198099567 ) ) ;
#9186 = CARTESIAN_POINT ( 'NONE',  ( 16.53943276465976808, 0.05219959533934440121, 106.2510903946856757 ) ) ;
#9187 = CARTESIAN_POINT ( 'NONE',  ( 0.000000000000000000, -105.0000000000000000, 12.00000000000000355 ) ) ;
#9188 = CARTESIAN_POINT ( 'NONE',  ( -16.55341960407611168, -4.379528057220339221, 91.45724293864769550 ) ) ;
#9189 = CARTESIAN_POINT ( 'NONE',  ( 5.719274019375991003, -21.55341960407610458, 47.70724293864770260 ) ) ;
#9190 = CARTESIAN_POINT ( 'NONE',  ( -5.049401038298153566, 19.05341960407611168, 35.20724293864768839 ) ) ;
#9191 = CARTESIAN_POINT ( 'NONE',  ( 8.224510206698742110, 14.34966873604972548, 72.08442372801899012 ) ) ;
#9192 = CARTESIAN_POINT ( 'NONE',  ( -5.823673210054431948, 21.52544592524334988, 37.70942372801900433 ) ) ;
#9193 = CARTESIAN_POINT ( 'NONE',  ( 0.05219959533936267826, -19.03943276465977164, 90.00109039468567573 ) ) ;
#9194 = CARTESIAN_POINT ( 'NONE',  ( 16.53943276465976808, -0.05219959533910856209, 93.74890960531436690 ) ) ;
#9195 = CARTESIAN_POINT ( 'NONE',  ( 9.474510206698971260, -16.51473224551069308, 52.91557627198102409 ) ) ;
#9196 = CARTESIAN_POINT ( 'NONE',  ( 19.03943276465977164, -0.05219959533909143690, 23.74890960531435269 ) ) ;
#9197 = CARTESIAN_POINT ( 'NONE',  ( 18.62759615963255655, 10.81492255796105972, 106.6677570613523756 ) ) ;
#9198 = CARTESIAN_POINT ( 'NONE',  ( 13.89961937509977652, -13.97604488694527269, 78.12390960531433848 ) ) ;
#9199 = ADVANCED_FACE ( 'NONE', ( #12843 ), #74509, .F. ) ;
#9200 = CARTESIAN_POINT ( 'NONE',  ( 12.14591786802327356, -12.06949235617739191, 60.62609039468567573 ) ) ;
#9201 = CARTESIAN_POINT ( 'NONE',  ( 15.72974639402176855, 15.80617190586768217, 96.87609039468568994 ) ) ;
#9202 = CARTESIAN_POINT ( 'NONE',  ( 0.05219959533934541429, -16.53943276465976808, 80.00109039468568994 ) ) ;
#9203 = CARTESIAN_POINT ( 'NONE',  ( -5.153800228976607833, 19.02544592524334988, 57.70942372801899012 ) ) ;
#9204 = CARTESIAN_POINT ( 'NONE',  ( 5.153800228976615827, -19.02544592524334988, 65.20942372801900433 ) ) ;
#9205 = CARTESIAN_POINT ( 'NONE',  ( 0.05219959533937995610, -21.53943276465977519, 60.00109039468568284 ) ) ;
#9206 = CARTESIAN_POINT ( 'NONE',  ( 5.153800228976335163, 19.02544592524342804, 64.79057627198100988 ) ) ;
#9207 = CARTESIAN_POINT ( 'NONE',  ( 13.97604488694548053, -13.89961937509957401, 60.62609039468564731 ) ) ;
#9208 = CARTESIAN_POINT ( 'NONE',  ( -16.51473224551069308, -9.474510206698971260, 111.6655762719810383 ) ) ;
#9209 = CARTESIAN_POINT ( 'NONE',  ( 5.049401038298161559, -19.05341960407611168, 82.70724293864770971 ) ) ;
#9210 = CARTESIAN_POINT ( 'NONE',  ( -16.55341960407611168, -4.379528057220339221, 36.45724293864768839 ) ) ;
#9211 = CARTESIAN_POINT ( 'NONE',  ( 15.72974639402199770, -15.80617190586745480, 48.12390960531436690 ) ) ;
#9212 = CARTESIAN_POINT ( 'NONE',  ( 19.99598863510436786, 21.26972126690560216, -52.34638024103105636 ) ) ;
#9213 = CARTESIAN_POINT ( 'NONE',  ( 15.80617190586769283, -15.72974639402175789, 105.6260903946856899 ) ) ;
#9214 = CARTESIAN_POINT ( 'NONE',  ( -16.19135201231366850, -7.376712067591933319, 80.18680854052030327 ) ) ;
#9215 = CARTESIAN_POINT ( 'NONE',  ( -9.564922557960796823, -16.46253265017161027, 37.08224293864768839 ) ) ;
#9216 = CARTESIAN_POINT ( 'NONE',  ( -9.474510206698964154, 16.51473224551069663, 25.41557627198103120 ) ) ;
#9217 = CARTESIAN_POINT ( 'NONE',  ( -34.40553910806575999, -2.436532241128162468, 90.06585364601160393 ) ) ;
#9218 = CARTESIAN_POINT ( 'NONE',  ( -0.05219959533937732626, 21.53943276465977519, 62.50109039468568284 ) ) ;
#9219 = CARTESIAN_POINT ( 'NONE',  ( -6.782741387738352223, -36.64508735834520081, -7.999999999999996447 ) ) ;
#9220 = CARTESIAN_POINT ( 'NONE',  ( 12.06949235617739724, 12.14591786802326823, 56.87609039468568994 ) ) ;
#9221 = CARTESIAN_POINT ( 'NONE',  ( 21.53943276465977519, -0.05219959533907433946, 88.74890960531436690 ) ) ;
#9222 = CARTESIAN_POINT ( 'NONE',  ( 8.224510206698953496, -14.34966873604960469, 57.91557627198103120 ) ) ;
#9224 = DIRECTION ( 'NONE',  ( 0.000000000000000000, 0.000000000000000000, 1.000000000000000000 ) ) ;
#9223 = CARTESIAN_POINT ( 'NONE',  ( 13.97604488694527802, 13.89961937509977652, 24.37390960531435624 ) ) ;
#9225 = CARTESIAN_POINT ( 'NONE',  ( 18.67979575497194134, -10.72451020669871369, 40.83442372801901854 ) ) ;
#9226 = CARTESIAN_POINT ( 'NONE',  ( 9.564922557961047289, -16.46253265017146816, 45.41775706135232582 ) ) ;
#9227 = CARTESIAN_POINT ( 'NONE',  ( -13.97604488694527625, -13.89961937509977652, 31.87390960531435979 ) ) ;
#9228 = CARTESIAN_POINT ( 'NONE',  ( 15.80617190586769283, -15.72974639402175789, 85.62609039468568994 ) ) ;
#9229 = CARTESIAN_POINT ( 'NONE',  ( -24.71161622716357087, -5.993525217005509553, 168.9855167950506427 ) ) ;
#9230 = CARTESIAN_POINT ( 'NONE',  ( 4.483927247898545687, 16.52544592524342804, 39.79057627198103830 ) ) ;
#9231 = DIRECTION ( 'NONE',  ( 0.000000000000000000, 0.000000000000000000, 1.000000000000000000 ) ) ;
#9232 = CARTESIAN_POINT ( 'NONE',  ( 10.81492255796078972, 18.62759615963270932, 39.58224293864769550 ) ) ;
#9233 = CARTESIAN_POINT ( 'NONE',  ( -27.73933785331498925, 2.428612866367529932E-14, 142.8750000027311842 ) ) ;
#9234 = CARTESIAN_POINT ( 'NONE',  ( 19.02544592524343514, -5.153800228976328945, 83.54057627198100988 ) ) ;
#9235 = CARTESIAN_POINT ( 'NONE',  ( -12.06949235617756955, 12.14591786802309770, 90.62390960531436690 ) ) ;
#9236 = CARTESIAN_POINT ( 'NONE',  ( -12.06949235617739369, -12.14591786802326823, 29.37609039468568284 ) ) ;
#9237 = CARTESIAN_POINT ( 'NONE',  ( 21.52544592524344225, -5.823673210054117533, 68.54057627198103830 ) ) ;
#9238 = VERTEX_POINT ( 'NONE', #13818 ) ;
#9239 = CARTESIAN_POINT ( 'NONE',  ( -5.153800228976328057, -19.02544592524343514, 32.29057627198102409 ) ) ;
#9241 = CARTESIAN_POINT ( 'NONE',  ( 21.53943276465977519, -0.05219959533907433946, 88.74890960531436690 ) ) ;
#9240 = CARTESIAN_POINT ( 'NONE',  ( 5.153800228976335163, 19.02544592524342804, 79.79057627198102409 ) ) ;
#9243 = CARTESIAN_POINT ( 'NONE',  ( -19.05341960407611168, -5.049401038298163336, 96.45724293864769550 ) ) ;
#9242 = CARTESIAN_POINT ( 'NONE',  ( 8.224510206698742110, 14.34966873604972548, 112.0844237280190185 ) ) ;
#9244 = CARTESIAN_POINT ( 'NONE',  ( -13.97604488694547697, 13.89961937509957934, 83.12609039468564731 ) ) ;
#9245 = CARTESIAN_POINT ( 'NONE',  ( -19.02544592524334988, -5.153800228976617603, 18.95942372801899722 ) ) ;
#9246 = CARTESIAN_POINT ( 'NONE',  ( 10.72451020669898902, -18.67979575497178502, 77.91557627198102409 ) ) ;
#9247 = CARTESIAN_POINT ( 'NONE',  ( -18.67979575497178146, -10.72451020669898902, 41.66557627198103120 ) ) ;
#9248 = CARTESIAN_POINT ( 'NONE',  ( -9.474510206698964154, 16.51473224551069663, 55.41557627198103120 ) ) ;
#9249 = CARTESIAN_POINT ( 'NONE',  ( 16.52544592524342804, -4.483927247898539470, 23.54057627198102765 ) ) ;
#9250 = CARTESIAN_POINT ( 'NONE',  ( 19.05341960407611168, 5.049401038298154454, 78.95724293864769550 ) ) ;
#9251 = ORIENTED_EDGE ( 'NONE', *, *, #115825, .T. ) ;
#9252 = DIRECTION ( 'NONE',  ( -1.000000000000000000, -0.000000000000000000, -0.000000000000000000 ) ) ;
#9253 = CARTESIAN_POINT ( 'NONE',  ( -5.049401038297874678, -19.05341960407617918, 29.79275706135232227 ) ) ;
#9254 = CARTESIAN_POINT ( 'NONE',  ( -12.14591786802309592, -12.06949235617757132, 91.87390960531436690 ) ) ;
#9255 = CARTESIAN_POINT ( 'NONE',  ( -10.81492255796105439, 18.62759615963255655, 27.91775706135234358 ) ) ;
#9256 = VECTOR ( 'NONE', #68426, 1000.000000000000000 ) ;
#9257 = CARTESIAN_POINT ( 'NONE',  ( 17.14385361876520264, -23.59649016807271238, 146.0750000027311728 ) ) ;
#9258 = CARTESIAN_POINT ( 'NONE',  ( 15.80617190586746368, 15.72974639402197994, 54.37390960531435979 ) ) ;
#9259 = CARTESIAN_POINT ( 'NONE',  ( -4.483927247898782831, 16.52544592524335698, 87.70942372801901854 ) ) ;
#9260 = CARTESIAN_POINT ( 'NONE',  ( 13.89961937509977652, -13.97604488694527269, 28.12390960531435624 ) ) ;
#9261 = CARTESIAN_POINT ( 'NONE',  ( -19.02544592524342804, 5.153800228976336051, 71.04057627198099567 ) ) ;
#9262 = SPHERICAL_SURFACE ( 'NONE', #151291, 40.00000000000002132 ) ;
#9263 = CARTESIAN_POINT ( 'NONE',  ( 14.34966873604960469, 8.224510206698951720, 34.16557627198102409 ) ) ;
#9264 = CARTESIAN_POINT ( 'NONE',  ( -15.72974639402176322, -15.80617190586768395, 64.37609039468568994 ) ) ;
#9265 = CARTESIAN_POINT ( 'NONE',  ( 5.153800228976335163, 19.02544592524342804, 114.7905762719810241 ) ) ;
#9266 = CARTESIAN_POINT ( 'NONE',  ( -15.80617190586768217, 15.72974639402176855, 98.12609039468570415 ) ) ;
#9267 = CARTESIAN_POINT ( 'NONE',  ( -5.153800228976328057, -19.02544592524343514, 42.29057627198101699 ) ) ;
#9268 = CARTESIAN_POINT ( 'NONE',  ( 5.049401038298161559, -19.05341960407611168, 47.70724293864770260 ) ) ;
#9269 = EDGE_LOOP ( 'NONE', ( #41358, #12246, #83229, #108482, #56522, #89351, #151534, #41754 ) ) ;
#9270 = CARTESIAN_POINT ( 'NONE',  ( 21.53943276465977519, 0.05219959533937863772, 96.25109039468568994 ) ) ;
#9271 = CARTESIAN_POINT ( 'NONE',  ( -14.34966873604972548, 8.224510206698743886, 63.33442372801900433 ) ) ;
#9272 = CARTESIAN_POINT ( 'NONE',  ( 21.55341960407619695, -5.719274019375665929, 91.04275706135236135 ) ) ;
#9273 = CARTESIAN_POINT ( 'NONE',  ( -18.67979575497178146, -10.72451020669898902, 26.66557627198103475 ) ) ;
#9274 = CARTESIAN_POINT ( 'NONE',  ( 13.89961937509957401, 13.97604488694547697, 91.87609039468567573 ) ) ;
#9275 = CARTESIAN_POINT ( 'NONE',  ( -15.72974639402176322, -15.80617190586768395, 49.37609039468569705 ) ) ;
#9276 = CARTESIAN_POINT ( 'NONE',  ( 14.29746914071037800, 8.314922557961029526, 36.66775706135234714 ) ) ;
#9277 = CARTESIAN_POINT ( 'NONE',  ( -5.823673210054116645, -21.52544592524344225, 82.29057627198103830 ) ) ;
#9278 = CARTESIAN_POINT ( 'NONE',  ( 16.46253265017146816, 9.564922557961045513, 91.66775706135234714 ) ) ;
#9279 = CARTESIAN_POINT ( 'NONE',  ( 9.564922557960805705, 16.46253265017160317, 64.58224293864769550 ) ) ;
#9280 = CARTESIAN_POINT ( 'NONE',  ( -0.05219959533936034679, 19.03943276465977164, 102.5010903946856757 ) ) ;
#9281 = CARTESIAN_POINT ( 'NONE',  ( -19.02544592524334988, -5.153800228976617603, 88.95942372801897591 ) ) ;
#9282 = CARTESIAN_POINT ( 'NONE',  ( 8.224510206698953496, -14.34966873604960469, 57.91557627198103120 ) ) ;
#9283 = CARTESIAN_POINT ( 'NONE',  ( 9.474510206698729675, 16.51473224551082808, 77.08442372801900433 ) ) ;
#9284 = CARTESIAN_POINT ( 'NONE',  ( 8.314922557961029526, -14.29746914071037800, 55.41775706135234714 ) ) ;
#9285 = CARTESIAN_POINT ( 'NONE',  ( 16.51473224551083163, -9.474510206698727899, 30.83442372801900433 ) ) ;
#9286 = CARTESIAN_POINT ( 'NONE',  ( -13.97604488694527625, -13.89961937509977652, 36.87390960531436690 ) ) ;
#9287 = CARTESIAN_POINT ( 'NONE',  ( -19.02544592524342804, 5.153800228976336051, 46.04057627198101699 ) ) ;
#9288 = CARTESIAN_POINT ( 'NONE',  ( -14.34966873604972548, 8.224510206698743886, 58.33442372801901143 ) ) ;
#9289 = CARTESIAN_POINT ( 'NONE',  ( -8.571926809382608425, 26.38167802310805854, 140.9750000027312069 ) ) ;
#9290 = CARTESIAN_POINT ( 'NONE',  ( -28.82186960331499392, 9.364793116373565596, 140.1500000054623740 ) ) ;
#9291 = CARTESIAN_POINT ( 'NONE',  ( 9.474510206698971260, -16.51473224551069308, 102.9155762719810241 ) ) ;
#9292 = EDGE_CURVE ( 'NONE', #142736, #40368, #163061, .T. ) ;
#9293 = DIRECTION ( 'NONE',  ( 0.000000000000000000, 0.000000000000000000, -1.000000000000000000 ) ) ;
#9294 = VERTEX_POINT ( 'NONE', #179708 ) ;
#9295 = CARTESIAN_POINT ( 'NONE',  ( -5.049401038297874678, -19.05341960407617918, 99.79275706135234714 ) ) ;
#9296 = CARTESIAN_POINT ( 'NONE',  ( -0.05219959533907301413, -21.53943276465977519, 37.49890960531436690 ) ) ;
#9298 = CARTESIAN_POINT ( 'NONE',  ( 14.29746914071037800, 8.314922557961029526, 21.66775706135235069 ) ) ;
#9297 = CARTESIAN_POINT ( 'NONE',  ( 19.03943276465977164, 0.05219959533936151252, 36.25109039468567573 ) ) ;
#9299 = CARTESIAN_POINT ( 'NONE',  ( 9.474510206698971260, -16.51473224551069308, 32.91557627198102409 ) ) ;
#9300 = CARTESIAN_POINT ( 'NONE',  ( -13.89961937509977652, 13.97604488694528158, 50.62390960531435979 ) ) ;
#9301 = CARTESIAN_POINT ( 'NONE',  ( 18.62759615963271287, -10.81492255796078972, 78.33224293864770971 ) ) ;
#9302 = CARTESIAN_POINT ( 'NONE',  ( 13.89961937509977652, -13.97604488694527269, 103.1239096053143527 ) ) ;
#9303 = CARTESIAN_POINT ( 'NONE',  ( 5.049401038298161559, -19.05341960407611168, 32.70724293864768129 ) ) ;
#9304 = CARTESIAN_POINT ( 'NONE',  ( -22.44159573604010305, 16.30477369853692338, 143.1750000027311671 ) ) ;
#9305 = CARTESIAN_POINT ( 'NONE',  ( -16.51473224551082808, 9.474510206698731452, 88.33442372801900433 ) ) ;
#9306 = CARTESIAN_POINT ( 'NONE',  ( 16.53943276465976808, -0.05219959533910856209, 53.74890960531437401 ) ) ;
#9307 = CARTESIAN_POINT ( 'NONE',  ( -18.62759615963270932, 10.81492255796079327, 30.83224293864770260 ) ) ;
#9308 = CARTESIAN_POINT ( 'NONE',  ( -18.67979575497193778, 10.72451020669871902, 103.3344237280190043 ) ) ;
#9309 = EDGE_CURVE ( 'NONE', #119772, #30365, #17109, .T. ) ;
#9310 = CARTESIAN_POINT ( 'NONE',  ( -21.55341960407610458, -5.719274019375992779, 101.4572429386476955 ) ) ;
#9311 = CARTESIAN_POINT ( 'NONE',  ( -21.53943276465977519, -0.05219959533937600094, 73.75109039468567573 ) ) ;
#9312 = CARTESIAN_POINT ( 'NONE',  ( 5.719274019375673035, 21.55341960407619339, 72.29275706135236135 ) ) ;
#9313 = CARTESIAN_POINT ( 'NONE',  ( 16.46253265017160672, -9.564922557960803928, 108.3322429386476955 ) ) ;
#9315 = CARTESIAN_POINT ( 'NONE',  ( 18.62759615963255655, 10.81492255796105972, 66.66775706135234714 ) ) ;
#9314 = CARTESIAN_POINT ( 'NONE',  ( -16.52544592524335698, -4.483927247898792601, 103.9594237280190185 ) ) ;
#9316 = CARTESIAN_POINT ( 'NONE',  ( 16.51473224551069308, 9.474510206698969483, 59.16557627198102409 ) ) ;
#9317 = CARTESIAN_POINT ( 'NONE',  ( -5.049401038297874678, -19.05341960407617918, 39.79275706135232582 ) ) ;
#9318 = CARTESIAN_POINT ( 'NONE',  ( 21.53943276465977519, 0.05219959533937863772, 26.25109039468567573 ) ) ;
#9319 = CARTESIAN_POINT ( 'NONE',  ( -13.97604488694527625, -13.89961937509977652, 61.87390960531435979 ) ) ;
#9320 = CARTESIAN_POINT ( 'NONE',  ( 16.53943276465976808, -0.05219959533910856209, 78.74890960531436690 ) ) ;
#9321 = CARTESIAN_POINT ( 'NONE',  ( 14.29746914071049879, -8.314922557960816363, 43.33224293864769550 ) ) ;
#9322 = CARTESIAN_POINT ( 'NONE',  ( -15.72974639402197994, 15.80617190586746368, 50.62390960531435979 ) ) ;
#9323 = CARTESIAN_POINT ( 'NONE',  ( 19.02544592524343514, -5.153800228976328945, 63.54057627198103830 ) ) ;
#9324 = CARTESIAN_POINT ( 'NONE',  ( -15.72974639402197994, 15.80617190586746368, 70.62390960531436690 ) ) ;
#9325 = CARTESIAN_POINT ( 'NONE',  ( 9.564922557961047289, -16.46253265017146816, 45.41775706135232582 ) ) ;
#9327 = CARTESIAN_POINT ( 'NONE',  ( -4.379528057220328563, 16.55341960407611168, 65.20724293864768129 ) ) ;
#9326 = CARTESIAN_POINT ( 'NONE',  ( 16.51473224551083163, -9.474510206698727899, 20.83442372801899722 ) ) ;
#9328 = CARTESIAN_POINT ( 'NONE',  ( 5.719274019375991003, -21.55341960407610458, 37.70724293864769550 ) ) ;
#9329 = ORIENTED_EDGE ( 'NONE', *, *, #39985, .T. ) ;
#9330 = CARTESIAN_POINT ( 'NONE',  ( 4.500000000000000000, 0.000000000000000000, -20.00000000000000000 ) ) ;
#9332 = CARTESIAN_POINT ( 'NONE',  ( 22.44159573604009594, -16.30477369853687364, 147.6750000027311671 ) ) ;
#9331 = CARTESIAN_POINT ( 'NONE',  ( 16.53943276465976808, 0.05219959533934440121, 81.25109039468568994 ) ) ;
#9333 = CARTESIAN_POINT ( 'NONE',  ( 0.05219959533936267826, -19.03943276465977164, 90.00109039468567573 ) ) ;
#9334 = CARTESIAN_POINT ( 'NONE',  ( -16.55341960407611168, -4.379528057220339221, 51.45724293864770260 ) ) ;
#9335 = CARTESIAN_POINT ( 'NONE',  ( 2.021687836487040535, 0.000000000000000000, 2.168404344971008868E-16 ) ) ;
#9336 = CARTESIAN_POINT ( 'NONE',  ( 5.049401038298161559, -19.05341960407611168, 52.70724293864767418 ) ) ;
#9337 = CARTESIAN_POINT ( 'NONE',  ( -16.55341960407611168, -4.379528057220339221, 36.45724293864768839 ) ) ;
#9338 = EDGE_CURVE ( 'NONE', #120176, #41844, #186669, .T. ) ;
#9339 = CARTESIAN_POINT ( 'NONE',  ( -5.049401038298153566, 19.05341960407611168, 85.20724293864766707 ) ) ;
#9340 = CARTESIAN_POINT ( 'NONE',  ( -19.03943276465977164, 0.05219959533909376836, 51.24890960531436690 ) ) ;
#9341 = CARTESIAN_POINT ( 'NONE',  ( 21.52544592524334988, 5.823673210054432836, 56.45942372801902565 ) ) ;
#9342 = CARTESIAN_POINT ( 'NONE',  ( 9.474510206698971260, -16.51473224551069308, 72.91557627198102409 ) ) ;
#9343 = CARTESIAN_POINT ( 'NONE',  ( 19.02544592524343514, -5.153800228976328945, 28.54057627198102409 ) ) ;
#9344 = CARTESIAN_POINT ( 'NONE',  ( -16.51473224551069308, -9.474510206698971260, 76.66557627198103830 ) ) ;
#9345 = CARTESIAN_POINT ( 'NONE',  ( -5.823673210054116645, -21.52544592524344225, 52.29057627198102409 ) ) ;
#9346 = CARTESIAN_POINT ( 'NONE',  ( -9.564922557960796823, -16.46253265017161027, 32.08224293864769550 ) ) ;
#9347 = CARTESIAN_POINT ( 'NONE',  ( 15.72974639402199770, -15.80617190586745480, 38.12390960531436690 ) ) ;
#9348 = CARTESIAN_POINT ( 'NONE',  ( 4.483927247898790824, -16.52544592524335698, 110.2094237280190185 ) ) ;
#9349 = CARTESIAN_POINT ( 'NONE',  ( 16.46253265017146816, 9.564922557961045513, 21.66775706135233648 ) ) ;
#9351 = CARTESIAN_POINT ( 'NONE',  ( 16.52544592524335698, 4.483927247898782831, 86.45942372801901854 ) ) ;
#9350 = CARTESIAN_POINT ( 'NONE',  ( -14.29746914071037622, -8.314922557961029526, 49.16775706135234003 ) ) ;
#9352 = FACE_OUTER_BOUND ( 'NONE', #59736, .T. ) ;
#9353 = CARTESIAN_POINT ( 'NONE',  ( 16.55341960407618274, -4.379528057220086978, 71.04275706135234714 ) ) ;
#9354 = CARTESIAN_POINT ( 'NONE',  ( -0.05219959533907301413, -21.53943276465977519, 32.49890960531435979 ) ) ;
#9355 = CARTESIAN_POINT ( 'NONE',  ( 19.05341960407611168, 5.049401038298154454, 33.95724293864769550 ) ) ;
#9356 = CARTESIAN_POINT ( 'NONE',  ( -8.224510206698735004, -14.34966873604973081, 39.58442372801901143 ) ) ;
#9357 = CARTESIAN_POINT ( 'NONE',  ( -19.03943276465977164, 0.05219959533909376836, 51.24890960531436690 ) ) ;
#9358 = CARTESIAN_POINT ( 'NONE',  ( 0.05219959533937995610, -21.53943276465977519, 45.00109039468568284 ) ) ;
#9359 = CARTESIAN_POINT ( 'NONE',  ( -16.53943276465976808, -0.05219959533934237506, 33.75109039468568284 ) ) ;
#9360 = CARTESIAN_POINT ( 'NONE',  ( 8.314922557961029526, -14.29746914071037800, 95.41775706135234714 ) ) ;
#9361 = CARTESIAN_POINT ( 'NONE',  ( -18.22780087662123094, -5.499999999999984901, 71.48459894673891313 ) ) ;
#9362 = CARTESIAN_POINT ( 'NONE',  ( 5.823673210054444382, -21.52544592524334988, 105.2094237280190328 ) ) ;
#9363 = CARTESIAN_POINT ( 'NONE',  ( 0.05219959533936267826, -19.03943276465977164, 100.0010903946856757 ) ) ;
#9364 = CARTESIAN_POINT ( 'NONE',  ( 19.03943276465977164, 0.05219959533936151252, 51.25109039468567573 ) ) ;
#9365 = CARTESIAN_POINT ( 'NONE',  ( -14.34966873604960291, -8.224510206698953496, 76.66557627198103830 ) ) ;
#9366 = CARTESIAN_POINT ( 'NONE',  ( -16.46253265017160317, 9.564922557960807481, 25.83224293864769194 ) ) ;
#9368 = CARTESIAN_POINT ( 'NONE',  ( 30.74264578624800137, -22.33583958711395212, -2.949999994537626957 ) ) ;
#9367 = CARTESIAN_POINT ( 'NONE',  ( 16.51473224551083163, -9.474510206698727899, 55.83442372801899722 ) ) ;
#9369 = CARTESIAN_POINT ( 'NONE',  ( 15.72974639402176855, 15.80617190586768217, 66.87609039468568994 ) ) ;
#9370 = CARTESIAN_POINT ( 'NONE',  ( -12.06949235617739369, -12.14591786802326823, 24.37609039468567573 ) ) ;
#9371 = CARTESIAN_POINT ( 'NONE',  ( 17.48853670773242541, 5.747243402303173987, 38.83328700250009291 ) ) ;
#9372 = CARTESIAN_POINT ( 'NONE',  ( -21.53943276465977519, 0.05219959533907696930, 21.24890960531436690 ) ) ;
#9373 = CARTESIAN_POINT ( 'NONE',  ( -5.153800228976607833, 19.02544592524334988, 102.7094237280189759 ) ) ;
#9374 = CARTESIAN_POINT ( 'NONE',  ( -19.03943276465977164, 0.05219959533909376836, 111.2489096053143669 ) ) ;
#9375 = CARTESIAN_POINT ( 'NONE',  ( -21.51693143705273670, 10.15780255052816550, 170.5200780514257133 ) ) ;
#9376 = CARTESIAN_POINT ( 'NONE',  ( -8.224510206698948167, 14.34966873604960824, 115.4155762719810241 ) ) ;
#9377 = CARTESIAN_POINT ( 'NONE',  ( -21.55341960407619339, 5.719274019375674811, 103.5427570613523613 ) ) ;
#9378 = CARTESIAN_POINT ( 'NONE',  ( 9.564922557960805705, 16.46253265017160317, 54.58224293864769550 ) ) ;
#9379 = CARTESIAN_POINT ( 'NONE',  ( 21.53943276465977519, 0.05219959533937863772, 61.25109039468567573 ) ) ;
#9380 = CARTESIAN_POINT ( 'NONE',  ( -10.72451020669870658, -18.67979575497194134, 104.5844237280190185 ) ) ;
#9381 = CARTESIAN_POINT ( 'NONE',  ( -12.14591786802326823, 12.06949235617739902, 113.1260903946856899 ) ) ;
#9382 = CARTESIAN_POINT ( 'NONE',  ( -9.474510206698964154, 16.51473224551069663, 75.41557627198103830 ) ) ;
#9383 = CARTESIAN_POINT ( 'NONE',  ( -15.72974639402176322, -15.80617190586768395, 54.37609039468568994 ) ) ;
#9384 = CARTESIAN_POINT ( 'NONE',  ( -15.80617190586768217, 15.72974639402176855, 48.12609039468568284 ) ) ;
#9386 = CARTESIAN_POINT ( 'NONE',  ( -13.97604488694527625, -13.89961937509977652, 106.8739096053143669 ) ) ;
#9385 = CARTESIAN_POINT ( 'NONE',  ( 9.564922557961047289, -16.46253265017146816, 75.41775706135234714 ) ) ;
#9387 = CARTESIAN_POINT ( 'NONE',  ( -19.03943276465977164, 0.05219959533909376836, 26.24890960531435624 ) ) ;
#9388 = CARTESIAN_POINT ( 'NONE',  ( -21.53943276465977519, 0.05219959533907696930, 96.24890960531435269 ) ) ;
#9389 = CARTESIAN_POINT ( 'NONE',  ( -13.89961937509957401, -13.97604488694547875, 19.37609039468566507 ) ) ;
#9390 = CARTESIAN_POINT ( 'NONE',  ( 12.14591786802309770, 12.06949235617756955, 99.37390960531436690 ) ) ;
#9391 = CARTESIAN_POINT ( 'NONE',  ( -19.03943276465977164, 0.05219959533909376836, 56.24890960531435979 ) ) ;
#9392 = CARTESIAN_POINT ( 'NONE',  ( -13.89961937509957401, -13.97604488694547875, 99.37609039468567573 ) ) ;
#9393 = CARTESIAN_POINT ( 'NONE',  ( 8.224510206698953496, -14.34966873604960469, 67.91557627198102409 ) ) ;
#9394 = CARTESIAN_POINT ( 'NONE',  ( -19.02544592524334988, -5.153800228976617603, 18.95942372801899722 ) ) ;
#9395 = CARTESIAN_POINT ( 'NONE',  ( 16.51473224551069308, 9.474510206698969483, 99.16557627198102409 ) ) ;
#9396 = CARTESIAN_POINT ( 'NONE',  ( 13.97604488694548053, -13.89961937509957401, 80.62609039468567573 ) ) ;
#9397 = CARTESIAN_POINT ( 'NONE',  ( -10.81492255796078084, -18.62759615963271287, 82.08224293864768129 ) ) ;
#9398 = CARTESIAN_POINT ( 'NONE',  ( -15.80617190586768217, 15.72974639402176855, 43.12609039468568284 ) ) ;
#9399 = CARTESIAN_POINT ( 'NONE',  ( -16.55341960407617563, 4.379528057220093196, 48.54275706135234714 ) ) ;
#9400 = CARTESIAN_POINT ( 'NONE',  ( -14.34966873604972548, 8.224510206698743886, 98.33442372801901854 ) ) ;
#9402 = CARTESIAN_POINT ( 'NONE',  ( 18.67979575497194134, -10.72451020669871369, 35.83442372801901143 ) ) ;
#9401 = CARTESIAN_POINT ( 'NONE',  ( 12.14591786802327356, -12.06949235617739191, 40.62609039468567573 ) ) ;
#9403 = CARTESIAN_POINT ( 'NONE',  ( 15.72974639402199770, -15.80617190586745480, 43.12390960531435269 ) ) ;
#9404 = CARTESIAN_POINT ( 'NONE',  ( 19.03943276465977164, -0.05219959533909143690, 38.74890960531436690 ) ) ;
#9405 = CARTESIAN_POINT ( 'NONE',  ( -38.00000000000001421, 12.34694845685046438, -7.849999994537626868 ) ) ;
#9406 = CARTESIAN_POINT ( 'NONE',  ( -4.483927247898782831, 16.52544592524335698, 57.70942372801901143 ) ) ;
#9407 = CARTESIAN_POINT ( 'NONE',  ( -15.80617190586745835, -15.72974639402198527, 86.87390960531438111 ) ) ;
#9408 = CARTESIAN_POINT ( 'NONE',  ( 4.379528057220339221, -16.55341960407611168, 37.70724293864769550 ) ) ;
#9409 = CARTESIAN_POINT ( 'NONE',  ( 16.55341960407618274, -4.379528057220086978, 51.04275706135234714 ) ) ;
#9410 = CARTESIAN_POINT ( 'NONE',  ( 19.05341960407611168, 5.049401038298154454, 58.95724293864768129 ) ) ;
#9411 = CARTESIAN_POINT ( 'NONE',  ( -5.153800228976607833, 19.02544592524334988, 92.70942372801901854 ) ) ;
#9412 = CARTESIAN_POINT ( 'NONE',  ( 21.53943276465977519, -0.05219959533907433946, 78.74890960531436690 ) ) ;
#9413 = CARTESIAN_POINT ( 'NONE',  ( 0.05219959533910956823, 16.53943276465976808, 34.99890960531435979 ) ) ;
#9414 = ORIENTED_EDGE ( 'NONE', *, *, #119720, .T. ) ;
#9415 = CARTESIAN_POINT ( 'NONE',  ( 19.46398650005389541, -5.500000000000039968, 92.68269651486369298 ) ) ;
#9416 = CARTESIAN_POINT ( 'NONE',  ( 5.719274019375991003, -21.55341960407610458, 62.70724293864769550 ) ) ;
#9417 = ORIENTED_EDGE ( 'NONE', *, *, #177665, .F. ) ;
#9418 = CARTESIAN_POINT ( 'NONE',  ( 0.05219959533934541429, -16.53943276465976808, 110.0010903946856757 ) ) ;
#9419 = ORIENTED_EDGE ( 'NONE', *, *, #92161, .F. ) ;
#9420 = CARTESIAN_POINT ( 'NONE',  ( 19.53091890409951858, 5.500000000000029310, 87.56097431831419442 ) ) ;
#9421 = CARTESIAN_POINT ( 'NONE',  ( -21.55341960407610458, -5.719274019375992779, 91.45724293864769550 ) ) ;
#9422 = CARTESIAN_POINT ( 'NONE',  ( -4.483927247898539470, -16.52544592524342804, 27.29057627198103120 ) ) ;
#9423 = CARTESIAN_POINT ( 'NONE',  ( -14.29746914071037622, -8.314922557961029526, 29.16775706135234003 ) ) ;
#9424 = CARTESIAN_POINT ( 'NONE',  ( -9.474510206698964154, 16.51473224551069663, 35.41557627198102409 ) ) ;
#9425 = CARTESIAN_POINT ( 'NONE',  ( 19.02544592524343514, -5.153800228976328945, 68.54057627198103830 ) ) ;
#9426 = CARTESIAN_POINT ( 'NONE',  ( -8.906447517083060816, 27.41122689804195645, 145.5999999999999943 ) ) ;
#9427 = CARTESIAN_POINT ( 'NONE',  ( -13.97604488694527625, -13.89961937509977652, 111.8739096053143243 ) ) ;
#9428 = CARTESIAN_POINT ( 'NONE',  ( 0.5956237041775711560, 29.01886376551548352, -52.52392249052597606 ) ) ;
#9429 = CARTESIAN_POINT ( 'NONE',  ( -12.06949235617739369, -12.14591786802326823, 104.3760903946856899 ) ) ;
#9430 = CARTESIAN_POINT ( 'NONE',  ( 13.89961937509957401, 13.97604488694547697, 106.8760903946856757 ) ) ;
#9431 = CARTESIAN_POINT ( 'NONE',  ( -5.153800228976607833, 19.02544592524334988, 32.70942372801899722 ) ) ;
#9432 = CARTESIAN_POINT ( 'NONE',  ( -0.05219959533907301413, -21.53943276465977519, 82.49890960531436690 ) ) ;
#9433 = CARTESIAN_POINT ( 'NONE',  ( 14.34966873604960469, 8.224510206698951720, 24.16557627198103120 ) ) ;
#9434 = CARTESIAN_POINT ( 'NONE',  ( -5.823673210054116645, -21.52544592524344225, 47.29057627198103120 ) ) ;
#9436 = CARTESIAN_POINT ( 'NONE',  ( 16.46253265017146816, 9.564922557961045513, 106.6677570613523471 ) ) ;
#9435 = CARTESIAN_POINT ( 'NONE',  ( -15.80617190586745835, -15.72974639402198527, 76.87390960531439532 ) ) ;
#9437 = CARTESIAN_POINT ( 'NONE',  ( 16.51473224551069308, 9.474510206698969483, 109.1655762719810383 ) ) ;
#9438 = CARTESIAN_POINT ( 'NONE',  ( 0.05219959533937995610, -21.53943276465977519, 75.00109039468568994 ) ) ;
#9439 = CARTESIAN_POINT ( 'NONE',  ( -16.46253265017160317, 9.564922557960807481, 65.83224293864769550 ) ) ;
#9440 = B_SPLINE_CURVE_WITH_KNOTS ( 'NONE', 3,
 ( #85746, #5905, #118097, #175771, #147433, #70589, #86745, #194941, #71583, #193948, #148429, #36241, #55411, #9924, #37246, #56417, #97893, #160596, #83736, #145415, #13886, #75552 ),
 .UNSPECIFIED., .F., .F.,
 ( 4, 2, 2, 2, 2, 2, 2, 2, 2, 2, 4 ),
 ( 1.970604704964099883E-07, 0.0003054521314110426400, 0.0006107072023515888737, 0.001221217344232681341, 0.001831727486113774242, 0.002136982557054321018, 0.002442237627994867360, 0.003052747769875972621, 0.003663257911757078315, 0.004273768053638177071, 0.004884278195519273225 ),
 .UNSPECIFIED. ) ;
#9441 = CARTESIAN_POINT ( 'NONE',  ( 0.05219959533910956823, 16.53943276465976808, 99.99890960531436690 ) ) ;
#9442 = CARTESIAN_POINT ( 'NONE',  ( 31.33330333603523954, 7.497710212630238402, 94.47580324309009825 ) ) ;
#9443 = CARTESIAN_POINT ( 'NONE',  ( -19.03943276465977164, 0.05219959533909376836, 71.24890960531435269 ) ) ;
#9444 = CARTESIAN_POINT ( 'NONE',  ( -16.53943276465976808, 0.05219959533911058130, 91.24890960531436690 ) ) ;
#9445 = ORIENTED_EDGE ( 'NONE', *, *, #103944, .F. ) ;
#9446 = CARTESIAN_POINT ( 'NONE',  ( -9.474510206698720793, -16.51473224551083518, 89.58442372801900433 ) ) ;
#9447 = CARTESIAN_POINT ( 'NONE',  ( 12.99999999999999822, 0.000000000000000000, 0.000000000000000000 ) ) ;
#9448 = CARTESIAN_POINT ( 'NONE',  ( -19.03943276465977164, 0.05219959533909376836, 56.24890960531435979 ) ) ;
#9449 = CARTESIAN_POINT ( 'NONE',  ( 31.31738933903719513, -7.498949511226639331, 94.72411213025004884 ) ) ;
#9451 = CARTESIAN_POINT ( 'NONE',  ( 0.05219959533909260263, 19.03943276465977164, 94.99890960531436690 ) ) ;
#9450 = CARTESIAN_POINT ( 'NONE',  ( 18.67979575497194134, -10.72451020669871369, 85.83442372801901854 ) ) ;
#9452 = CARTESIAN_POINT ( 'NONE',  ( -14.34966873604972548, 8.224510206698743886, 73.33442372801901854 ) ) ;
#9453 = CARTESIAN_POINT ( 'NONE',  ( -17.50000000000000355, -5.622605283950894872, 51.31207310596111171 ) ) ;
#9454 = B_SPLINE_CURVE_WITH_KNOTS ( 'NONE', 3,
 ( #130773, #175295, #114605, #49963, #4426, #190468, #158129, #176302, #22615, #21609, #34787, #69107, #192465, #131788, #96442, #67111, #160121, #127778, #81263, #189478, #50956, #174307, #128769, #113601, #83267, #42785 ),
 .UNSPECIFIED., .F., .F.,
 ( 4, 2, 2, 2, 2, 2, 2, 2, 2, 2, 2, 2, 4 ),
 ( 1.969502666224155977E-07, 0.0004009345686709464129, 0.0008016721870752703321, 0.001603147423883922182, 0.002404622660692573924, 0.003206097897501225449, 0.004007573134309877841, 0.004408310752714203820, 0.004809048371118529799, 0.005209785989522855779, 0.005610523607927182625, 0.006011261226331507737, 0.006411998844735834584 ),
 .UNSPECIFIED. ) ;
#9455 = CARTESIAN_POINT ( 'NONE',  ( -16.46253265017146816, -9.564922557961047289, 44.16775706135232582 ) ) ;
#9456 = CARTESIAN_POINT ( 'NONE',  ( 18.67979575497194134, -10.72451020669871369, 105.8344237280190328 ) ) ;
#9457 = CARTESIAN_POINT ( 'NONE',  ( 17.47620519128089711, 5.664886850699101473, 21.69135819420533196 ) ) ;
#9458 = CARTESIAN_POINT ( 'NONE',  ( 31.90000000000003411, -9.916512055951908821E-14, -64.92279855667830191 ) ) ;
#9459 = CARTESIAN_POINT ( 'NONE',  ( -16.52544592524335698, -4.483927247898792601, 108.9594237280190185 ) ) ;
#9460 = EDGE_CURVE ( 'NONE', #69916, #73939, #5270, .T. ) ;
#9461 = CARTESIAN_POINT ( 'NONE',  ( -9.474510206698720793, -16.51473224551083518, 74.58442372801900433 ) ) ;
#9462 = CARTESIAN_POINT ( 'NONE',  ( 12.06949235617739724, 12.14591786802326823, 86.87609039468568994 ) ) ;
#9463 = CARTESIAN_POINT ( 'NONE',  ( 16.61371651742599909, 7.165104196376162804, 68.64584930007004004 ) ) ;
#9464 = CARTESIAN_POINT ( 'NONE',  ( 0.05219959533934541429, -16.53943276465976808, 65.00109039468568994 ) ) ;
#9465 = ORIENTED_EDGE ( 'NONE', *, *, #98300, .F. ) ;
#9466 = CARTESIAN_POINT ( 'NONE',  ( 10.72451020669871369, 18.67979575497193778, 87.08442372801901854 ) ) ;
#9467 = CARTESIAN_POINT ( 'NONE',  ( -0.05219959533936034679, 19.03943276465977164, 92.50109039468566152 ) ) ;
#9468 = CARTESIAN_POINT ( 'NONE',  ( -16.46253265017146816, -9.564922557961047289, 29.16775706135232937 ) ) ;
#9469 = CARTESIAN_POINT ( 'NONE',  ( 5.049401038298161559, -19.05341960407611168, 67.70724293864769550 ) ) ;
#9470 = CARTESIAN_POINT ( 'NONE',  ( 5.049401038298161559, -19.05341960407611168, 52.70724293864767418 ) ) ;
#9471 = CARTESIAN_POINT ( 'NONE',  ( -18.05685959898565685, -35.69332804049738428, -8.787752958456431784 ) ) ;
#9472 = CARTESIAN_POINT ( 'NONE',  ( -5.719274019375978568, 21.55341960407610458, 85.20724293864770971 ) ) ;
#9473 = CARTESIAN_POINT ( 'NONE',  ( -18.67979575497178146, -10.72451020669898902, 31.66557627198102054 ) ) ;
#9474 = CARTESIAN_POINT ( 'NONE',  ( 16.51473224551069308, 9.474510206698969483, 29.16557627198103475 ) ) ;
#9475 = CARTESIAN_POINT ( 'NONE',  ( -4.379528057220086978, -16.55341960407618274, 69.79275706135234714 ) ) ;
#9476 = ORIENTED_EDGE ( 'NONE', *, *, #127759, .T. ) ;
#9477 = CARTESIAN_POINT ( 'NONE',  ( -10.81492255796105439, 18.62759615963255655, 27.91775706135234358 ) ) ;
#9479 = CARTESIAN_POINT ( 'NONE',  ( 36.91746824999999887, 11.99521256947799053, -9.524999997268812635 ) ) ;
#9478 = CARTESIAN_POINT ( 'NONE',  ( -8.314922557960811034, -14.29746914071050412, 67.08224293864770971 ) ) ;
#9480 = CARTESIAN_POINT ( 'NONE',  ( -4.379528057220086978, -16.55341960407618274, 24.79275706135235779 ) ) ;
#9481 = CARTESIAN_POINT ( 'NONE',  ( -5.049401038297874678, -19.05341960407617918, 54.79275706135234003 ) ) ;
#9482 = CARTESIAN_POINT ( 'NONE',  ( -4.379528057220328563, 16.55341960407611168, 60.20724293864768839 ) ) ;
#9483 = CARTESIAN_POINT ( 'NONE',  ( -10.72451020669870658, -18.67979575497194134, 19.58442372801901143 ) ) ;
#9485 = CARTESIAN_POINT ( 'NONE',  ( 10.81492255796078972, 18.62759615963270932, 74.58224293864768129 ) ) ;
#9484 = DIRECTION ( 'NONE',  ( -1.000000000000000000, 4.336808689942018352E-17, 0.000000000000000000 ) ) ;
#9486 = CARTESIAN_POINT ( 'NONE',  ( 19.03943276465977164, -0.05219959533909143690, 108.7489096053143527 ) ) ;
#9487 = CARTESIAN_POINT ( 'NONE',  ( 8.224510206698953496, -14.34966873604960469, 57.91557627198103120 ) ) ;
#9488 = CARTESIAN_POINT ( 'NONE',  ( 28.71286925542251112, -27.61909494970911183, -16.96471949291807135 ) ) ;
#9489 = CIRCLE ( 'NONE', #106305, 48.98979485566358250 ) ;
#9490 = DIRECTION ( 'NONE',  ( -0.7071067811865483499, 7.406550393246807469E-15, 0.7071067811865467956 ) ) ;
#9491 = CARTESIAN_POINT ( 'NONE',  ( 13.89961937509957401, 13.97604488694547697, 61.87609039468566863 ) ) ;
#9492 = CARTESIAN_POINT ( 'NONE',  ( -0.05219959533907301413, -21.53943276465977519, 102.4989096053143811 ) ) ;
#9493 = CARTESIAN_POINT ( 'NONE',  ( 5.153800228976335163, 19.02544592524342804, 59.79057627198100988 ) ) ;
#9494 = CARTESIAN_POINT ( 'NONE',  ( -5.049401038297874678, -19.05341960407617918, 39.79275706135232582 ) ) ;
#9495 = CARTESIAN_POINT ( 'NONE',  ( -13.97604488694527625, -13.89961937509977652, 26.87390960531434558 ) ) ;
#9496 = CARTESIAN_POINT ( 'NONE',  ( 5.719274019375673035, 21.55341960407619339, 67.29275706135234714 ) ) ;
#9497 = CARTESIAN_POINT ( 'NONE',  ( -16.18388926212239554, -7.379444403734528812, 70.43953151366159204 ) ) ;
#9498 = CARTESIAN_POINT ( 'NONE',  ( 8.224510206698953496, -14.34966873604960469, 37.91557627198102409 ) ) ;
#9499 = CARTESIAN_POINT ( 'NONE',  ( 5.153800228976335163, 19.02544592524342804, 64.79057627198100988 ) ) ;
#9500 = CARTESIAN_POINT ( 'NONE',  ( 21.53943276465977519, -0.05219959533907433946, 68.74890960531435269 ) ) ;
#9501 = CARTESIAN_POINT ( 'NONE',  ( -9.564922557960796823, -16.46253265017161027, 62.08224293864769550 ) ) ;
#9502 = CARTESIAN_POINT ( 'NONE',  ( 21.53943276465977519, -0.05219959533907433946, 68.74890960531435269 ) ) ;
#9503 = CARTESIAN_POINT ( 'NONE',  ( -21.53943276465977519, -0.05219959533937600094, 98.75109039468568994 ) ) ;
#9506 = CARTESIAN_POINT ( 'NONE',  ( -14.29746914071049879, 8.314922557960819915, 85.83224293864768129 ) ) ;
#9505 = CARTESIAN_POINT ( 'NONE',  ( 16.53943276465976808, 0.05219959533934440121, 101.2510903946856757 ) ) ;
#9504 = DIRECTION ( 'NONE',  ( -0.4999999999999966693, 0.5000000000000019984, 0.7071067811865484609 ) ) ;
#9507 = CARTESIAN_POINT ( 'NONE',  ( 0.05219959533936267826, -19.03943276465977164, 90.00109039468567573 ) ) ;
#9508 = VERTEX_POINT ( 'NONE', #142115 ) ;
#9509 = CARTESIAN_POINT ( 'NONE',  ( 19.05341960407617918, -5.049401038297876454, 41.04275706135233293 ) ) ;
#9510 = CARTESIAN_POINT ( 'NONE',  ( 16.53943276465976808, 0.05219959533934440121, 101.2510903946856757 ) ) ;
#9511 = CARTESIAN_POINT ( 'NONE',  ( 5.153800228976615827, -19.02544592524334988, 35.20942372801899722 ) ) ;
#9512 = CARTESIAN_POINT ( 'NONE',  ( -19.05341960407611168, -5.049401038298163336, 91.45724293864766707 ) ) ;
#9513 = CARTESIAN_POINT ( 'NONE',  ( -10.81492255796078084, -18.62759615963271287, 57.08224293864769550 ) ) ;
#9514 = CARTESIAN_POINT ( 'NONE',  ( 27.39399371936806560, -5.109217719441128125, 166.7881433183806905 ) ) ;
#9515 = CARTESIAN_POINT ( 'NONE',  ( 9.474510206698971260, -16.51473224551069308, 22.91557627198102765 ) ) ;
#9516 = CARTESIAN_POINT ( 'NONE',  ( 15.80617190586769283, -15.72974639402175789, 100.6260903946857184 ) ) ;
#9517 = CARTESIAN_POINT ( 'NONE',  ( -16.55341960407617563, 4.379528057220093196, 78.54275706135236135 ) ) ;
#9518 = CARTESIAN_POINT ( 'NONE',  ( 5.823673210054444382, -21.52544592524334988, 25.20942372801901854 ) ) ;
#9519 = CARTESIAN_POINT ( 'NONE',  ( 14.34966873604972726, -8.224510206698740333, 35.83442372801901143 ) ) ;
#9520 = CARTESIAN_POINT ( 'NONE',  ( 0.05219959533909260263, 19.03943276465977164, 109.9989096053143669 ) ) ;
#9521 = CARTESIAN_POINT ( 'NONE',  ( 5.153800228976335163, 19.02544592524342804, 34.79057627198102409 ) ) ;
#9522 = CARTESIAN_POINT ( 'NONE',  ( 13.97604488694527802, 13.89961937509977652, 49.37390960531434558 ) ) ;
#9523 = CARTESIAN_POINT ( 'NONE',  ( -8.314922557961024197, 14.29746914071037800, 52.91775706135235424 ) ) ;
#9524 = CARTESIAN_POINT ( 'NONE',  ( 4.483927247898545687, 16.52544592524342804, 94.79057627198105251 ) ) ;
#9525 = CARTESIAN_POINT ( 'NONE',  ( -12.06949235617739369, -12.14591786802326823, 99.37609039468568994 ) ) ;
#9528 = CARTESIAN_POINT ( 'NONE',  ( 5.049401038298161559, -19.05341960407611168, 67.70724293864769550 ) ) ;
#9527 = CARTESIAN_POINT ( 'NONE',  ( -16.46253265017160317, 9.564922557960807481, 80.83224293864769550 ) ) ;
#9526 = CARTESIAN_POINT ( 'NONE',  ( 18.62759615963255655, 10.81492255796105972, 41.66775706135235424 ) ) ;
#9529 = CARTESIAN_POINT ( 'NONE',  ( 19.03943276465977164, -0.05219959533909143690, 83.74890960531436690 ) ) ;
#9530 = CARTESIAN_POINT ( 'NONE',  ( 8.224510206698953496, -14.34966873604960469, 27.91557627198103830 ) ) ;
#9531 = CARTESIAN_POINT ( 'NONE',  ( 8.224510206698742110, 14.34966873604972548, 102.0844237280190185 ) ) ;
#9532 = VERTEX_POINT ( 'NONE', #109796 ) ;
#9533 = CARTESIAN_POINT ( 'NONE',  ( 19.03943276465977164, 0.05219959533936151252, 41.25109039468566152 ) ) ;
#9534 = CARTESIAN_POINT ( 'NONE',  ( 13.97604488694527802, 13.89961937509977652, 109.3739096053143669 ) ) ;
#9535 = CARTESIAN_POINT ( 'NONE',  ( 16.51473224551069308, 9.474510206698969483, 69.16557627198102409 ) ) ;
#9536 = CARTESIAN_POINT ( 'NONE',  ( -5.049401038297874678, -19.05341960407617918, 39.79275706135232582 ) ) ;
#9537 = CARTESIAN_POINT ( 'NONE',  ( 22.81625015709509441, 31.40387420917330275, -5.324999997268812457 ) ) ;
#9538 = CARTESIAN_POINT ( 'NONE',  ( 16.52544592524335698, 4.483927247898782831, 41.45942372801901143 ) ) ;
#9540 = CARTESIAN_POINT ( 'NONE',  ( 8.224510206698742110, 14.34966873604972548, 57.08442372801901854 ) ) ;
#9539 = CARTESIAN_POINT ( 'NONE',  ( -16.51473224551082808, 9.474510206698731452, 68.33442372801900433 ) ) ;
#9541 = CARTESIAN_POINT ( 'NONE',  ( 5.000000000000000888, -140.0000000000000000, 0.0009999999999992653654 ) ) ;
#9542 = SHAPE_REPRESENTATION ( 'socket head cap screw_iso_ISO 4762 M5 x 8 - 8N', ( #82054 ), #85555 ) ;
#9543 = CARTESIAN_POINT ( 'NONE',  ( 19.02544592524343514, -5.153800228976328945, 88.54057627198102409 ) ) ;
#9544 = CARTESIAN_POINT ( 'NONE',  ( 5.719274019375991003, -21.55341960407610458, 107.7072429386476955 ) ) ;
#9545 = CARTESIAN_POINT ( 'NONE',  ( -19.03943276465977164, -0.05219959533935918106, 78.75109039468567573 ) ) ;
#9547 = CARTESIAN_POINT ( 'NONE',  ( 13.97604488694527802, 13.89961937509977652, 34.37390960531436690 ) ) ;
#9546 = CARTESIAN_POINT ( 'NONE',  ( 5.049401038298161559, -19.05341960407611168, 107.7072429386476955 ) ) ;
#9548 = CARTESIAN_POINT ( 'NONE',  ( -0.05219959533909027116, -19.03943276465977164, 77.49890960531435269 ) ) ;
#9550 = CARTESIAN_POINT ( 'NONE',  ( -19.03943276465977164, 0.05219959533909376836, 31.24890960531435979 ) ) ;
#9549 = CARTESIAN_POINT ( 'NONE',  ( -8.314922557960811034, -14.29746914071050412, 32.08224293864769550 ) ) ;
#9551 = CARTESIAN_POINT ( 'NONE',  ( 13.97604488694548053, -13.89961937509957401, 50.62609039468566152 ) ) ;
#9552 = CARTESIAN_POINT ( 'NONE',  ( -4.483927247898539470, -16.52544592524342804, 87.29057627198103830 ) ) ;
#9553 = CARTESIAN_POINT ( 'NONE',  ( 0.05219959533936267826, -19.03943276465977164, 20.00109039468567218 ) ) ;
#9554 = CARTESIAN_POINT ( 'NONE',  ( 19.03943276465977164, -0.05219959533909143690, 48.74890960531435979 ) ) ;
#9555 = CARTESIAN_POINT ( 'NONE',  ( 15.80617190586746368, 15.72974639402197994, 49.37390960531436690 ) ) ;
#9557 = CARTESIAN_POINT ( 'NONE',  ( -10.72451020669870658, -18.67979575497194134, 109.5844237280190328 ) ) ;
#9556 = CARTESIAN_POINT ( 'NONE',  ( 8.314922557960818139, 14.29746914071049879, 54.58224293864769550 ) ) ;
#9558 = CARTESIAN_POINT ( 'NONE',  ( 0.05219959533909260263, 19.03943276465977164, 104.9989096053143669 ) ) ;
#9559 = CARTESIAN_POINT ( 'NONE',  ( 0.05219959533909260263, 19.03943276465977164, 104.9989096053143669 ) ) ;
#9560 = CARTESIAN_POINT ( 'NONE',  ( -0.05219959533909027116, -19.03943276465977164, 42.49890960531435269 ) ) ;
#9561 = CARTESIAN_POINT ( 'NONE',  ( 16.46253265017160672, -9.564922557960803928, 28.33224293864769550 ) ) ;
#9562 = CARTESIAN_POINT ( 'NONE',  ( 16.52544592524342804, -4.483927247898539470, 83.54057627198102409 ) ) ;
#9563 = CARTESIAN_POINT ( 'NONE',  ( 5.823673210054125526, 21.52544592524343514, 99.79057627198103830 ) ) ;
#9564 = CARTESIAN_POINT ( 'NONE',  ( 13.89961937509977652, -13.97604488694527269, 103.1239096053143527 ) ) ;
#9565 = CARTESIAN_POINT ( 'NONE',  ( 18.62759615963271287, -10.81492255796078972, 113.3322429386476955 ) ) ;
#9566 = CARTESIAN_POINT ( 'NONE',  ( -19.05341960407611168, -5.049401038298163336, 86.45724293864769550 ) ) ;
#9568 = CARTESIAN_POINT ( 'NONE',  ( 16.52544592524342804, -4.483927247898539470, 108.5405762719810241 ) ) ;
#9567 = DIRECTION ( 'NONE',  ( 0.000000000000000000, 0.000000000000000000, -1.000000000000000000 ) ) ;
#9569 = CARTESIAN_POINT ( 'NONE',  ( -16.51473224551069308, -9.474510206698971260, 71.66557627198102409 ) ) ;
#9570 = CARTESIAN_POINT ( 'NONE',  ( -18.62759615963270932, 10.81492255796079327, 75.83224293864769550 ) ) ;
#9571 = DIRECTION ( 'NONE',  ( 1.000000000000000000, 0.000000000000000000, 0.000000000000000000 ) ) ;
#9572 = CARTESIAN_POINT ( 'NONE',  ( 20.96320343559639454, -21.46320343559646560, 5.353553390593268624 ) ) ;
#9574 = CARTESIAN_POINT ( 'NONE',  ( 6.791538853603070081, -3.181980515339468241, 1.110912703473986074 ) ) ;
#9573 = CARTESIAN_POINT ( 'NONE',  ( 18.62759615963271287, -10.81492255796078972, 28.33224293864769550 ) ) ;
#9575 = CARTESIAN_POINT ( 'NONE',  ( -14.34966873604972548, 8.224510206698743886, 28.33442372801902209 ) ) ;
#9576 = CARTESIAN_POINT ( 'NONE',  ( -14.29746914071049879, 8.314922557960819915, 95.83224293864770971 ) ) ;
#9577 = CARTESIAN_POINT ( 'NONE',  ( -17.49999999999999645, -5.500000000000000888, 109.2030961746582847 ) ) ;
#9578 = CARTESIAN_POINT ( 'NONE',  ( -5.153800228976328057, -19.02544592524343514, 82.29057627198103830 ) ) ;
#9579 = CARTESIAN_POINT ( 'NONE',  ( -5.049401038298153566, 19.05341960407611168, 65.20724293864765286 ) ) ;
#9580 = CARTESIAN_POINT ( 'NONE',  ( -8.314922557960811034, -14.29746914071050412, 87.08224293864769550 ) ) ;
#9581 = CARTESIAN_POINT ( 'NONE',  ( -21.52544592524343514, 5.823673210054127303, 31.04057627198102409 ) ) ;
#9582 = CARTESIAN_POINT ( 'NONE',  ( -14.34966873604960291, -8.224510206698953496, 51.66557627198102409 ) ) ;
#9583 = CARTESIAN_POINT ( 'NONE',  ( 12.14591786802327356, -12.06949235617739191, 20.62609039468568639 ) ) ;
#9584 = CARTESIAN_POINT ( 'NONE',  ( -10.72451020669870658, -18.67979575497194134, 69.58442372801900433 ) ) ;
#9585 = CARTESIAN_POINT ( 'NONE',  ( 1.784210473542230573E-15, -29.16686587814331588, 145.3750000027311842 ) ) ;
#9586 = CARTESIAN_POINT ( 'NONE',  ( 19.05341960407611168, 5.049401038298154454, 113.9572429386477097 ) ) ;
#9588 = B_SPLINE_CURVE_WITH_KNOTS ( 'NONE', 3,
 ( #76078, #152918, #108409, #153920, #186269, #168098 ),
 .UNSPECIFIED., .F., .F.,
 ( 4, 2, 4 ),
 ( 0.000000000000000000, 0.0003837532665635193284, 0.0007675065331270386568 ),
 .UNSPECIFIED. ) ;
#9587 = CARTESIAN_POINT ( 'NONE',  ( -8.224510206698735004, -14.34966873604973081, 84.58442372801903275 ) ) ;
#9589 = CARTESIAN_POINT ( 'NONE',  ( 5.049401038298161559, -19.05341960407611168, 27.70724293864769550 ) ) ;
#9590 = CARTESIAN_POINT ( 'NONE',  ( -16.46253265017160317, 9.564922557960807481, 80.83224293864769550 ) ) ;
#9591 = CARTESIAN_POINT ( 'NONE',  ( 15.72974639402199770, -15.80617190586745480, 98.12390960531436690 ) ) ;
#9592 = CARTESIAN_POINT ( 'NONE',  ( -0.05219959533934338120, 16.53943276465976808, 27.50109039468567929 ) ) ;
#9594 = CARTESIAN_POINT ( 'NONE',  ( -0.05219959533937732626, 21.53943276465977519, 77.50109039468567573 ) ) ;
#9593 = CARTESIAN_POINT ( 'NONE',  ( 14.29746914071049879, -8.314922557960816363, 48.33224293864770260 ) ) ;
#9596 = CARTESIAN_POINT ( 'NONE',  ( 19.03943276465977164, -0.05219959533909143690, 113.7489096053143669 ) ) ;
#9595 = CARTESIAN_POINT ( 'NONE',  ( -0.05219959533934338120, 16.53943276465976808, 92.50109039468567573 ) ) ;
#9597 = CARTESIAN_POINT ( 'NONE',  ( 17.40861289039004234, 6.110651285853276882, 28.87232470827434128 ) ) ;
#9598 = CARTESIAN_POINT ( 'NONE',  ( 0.000000000000000000, 0.000000000000000000, -60.44446360152740283 ) ) ;
#9599 = CARTESIAN_POINT ( 'NONE',  ( -8.314922557961024197, 14.29746914071037800, 112.9177570613523329 ) ) ;
#9600 = CARTESIAN_POINT ( 'NONE',  ( 4.483927247898790824, -16.52544592524335698, 65.20942372801901854 ) ) ;
#9601 = CARTESIAN_POINT ( 'NONE',  ( -9.474510206698964154, 16.51473224551069663, 70.41557627198102409 ) ) ;
#9602 = CARTESIAN_POINT ( 'NONE',  ( 5.153800228976335163, 19.02544592524342804, 84.79057627198099567 ) ) ;
#9603 = CARTESIAN_POINT ( 'NONE',  ( -21.52544592524334988, -5.823673210054445271, 78.95942372801901854 ) ) ;
#9604 = CARTESIAN_POINT ( 'NONE',  ( -14.29746914071037622, -8.314922557961029526, 79.16775706135234714 ) ) ;
#9605 = CARTESIAN_POINT ( 'NONE',  ( 16.53943276465976808, -0.05219959533910856209, 43.74890960531435979 ) ) ;
#9606 = CARTESIAN_POINT ( 'NONE',  ( -19.05341960407611168, -5.049401038298163336, 51.45724293864770260 ) ) ;
#9607 = CARTESIAN_POINT ( 'NONE',  ( -19.02544592524342804, 5.153800228976336051, 46.04057627198101699 ) ) ;
#9608 = ORIENTED_EDGE ( 'NONE', *, *, #10239, .F. ) ;
#9609 = CARTESIAN_POINT ( 'NONE',  ( 13.89961937509957401, 13.97604488694547697, 106.8760903946856757 ) ) ;
#9610 = CARTESIAN_POINT ( 'NONE',  ( -16.53943276465976808, 0.05219959533911058130, 116.2489096053143669 ) ) ;
#9611 = CARTESIAN_POINT ( 'NONE',  ( -9.474510206698964154, 16.51473224551069663, 65.41557627198102409 ) ) ;
#9613 = CARTESIAN_POINT ( 'NONE',  ( 38.00000000000000000, 12.34694845685046616, -2.900000000000000355 ) ) ;
#9612 = CARTESIAN_POINT ( 'NONE',  ( 5.153800228976615827, -19.02544592524334988, 95.20942372801897591 ) ) ;
#9614 = CARTESIAN_POINT ( 'NONE',  ( 10.81492255796106328, -18.62759615963255655, 100.4177570613523471 ) ) ;
#9615 = CARTESIAN_POINT ( 'NONE',  ( 4.379528057220092307, 16.55341960407617563, 62.29275706135236845 ) ) ;
#9616 = CARTESIAN_POINT ( 'NONE',  ( 19.03943276465977164, 0.05219959533936151252, 91.25109039468566152 ) ) ;
#9617 = CARTESIAN_POINT ( 'NONE',  ( -15.72974639402197994, 15.80617190586746368, 65.62390960531436690 ) ) ;
#9618 = CARTESIAN_POINT ( 'NONE',  ( -14.29746914071037622, -8.314922557961029526, 49.16775706135234003 ) ) ;
#9619 = CARTESIAN_POINT ( 'NONE',  ( 11.73776690369117937, -38.24261239843917082, -14.51832217641615586 ) ) ;
#9620 = CARTESIAN_POINT ( 'NONE',  ( 16.46253265017146816, 9.564922557961045513, 61.66775706135234003 ) ) ;
#9621 = CARTESIAN_POINT ( 'NONE',  ( 5.719274019375673035, 21.55341960407619339, 97.29275706135234714 ) ) ;
#9622 = CARTESIAN_POINT ( 'NONE',  ( -14.29746914071049879, 8.314922557960819915, 115.8322429386477097 ) ) ;
#9623 = CARTESIAN_POINT ( 'NONE',  ( -16.46253265017160317, 9.564922557960807481, 65.83224293864769550 ) ) ;
#9624 = CARTESIAN_POINT ( 'NONE',  ( -0.05219959533910754901, -16.53943276465976808, 62.49890960531436690 ) ) ;
#9625 = CARTESIAN_POINT ( 'NONE',  ( 21.55341960407619695, -5.719274019375665929, 86.04275706135236135 ) ) ;
#9626 = CARTESIAN_POINT ( 'NONE',  ( -5.153800228976607833, 19.02544592524334988, 42.70942372801901143 ) ) ;
#9627 = CARTESIAN_POINT ( 'NONE',  ( 19.02544592524334988, 5.153800228976608722, 31.45942372801900433 ) ) ;
#9628 = CARTESIAN_POINT ( 'NONE',  ( -21.55341960407610458, -5.719274019375992779, 26.45724293864768839 ) ) ;
#9629 = CARTESIAN_POINT ( 'NONE',  ( -10.81492255796105439, 18.62759615963255655, 102.9177570613523756 ) ) ;
#9630 = CARTESIAN_POINT ( 'NONE',  ( -16.51473224551069308, -9.474510206698971260, 76.66557627198103830 ) ) ;
#9631 = CARTESIAN_POINT ( 'NONE',  ( -21.55341960407619339, 5.719274019375674811, 93.54275706135234714 ) ) ;
#9632 = CARTESIAN_POINT ( 'NONE',  ( 5.823673210054125526, 21.52544592524343514, 49.79057627198102409 ) ) ;
#9633 = CARTESIAN_POINT ( 'NONE',  ( 9.564922557960805705, 16.46253265017160317, 79.58224293864769550 ) ) ;
#9634 = CARTESIAN_POINT ( 'NONE',  ( 19.02544592524334988, 5.153800228976608722, 76.45942372801897591 ) ) ;
#9635 = CARTESIAN_POINT ( 'NONE',  ( -9.474510206698964154, 16.51473224551069663, 45.41557627198103120 ) ) ;
#9636 = CARTESIAN_POINT ( 'NONE',  ( 19.05341960407611168, 5.049401038298154454, 83.95724293864766707 ) ) ;
#9637 = CARTESIAN_POINT ( 'NONE',  ( -19.02544592524334988, -5.153800228976617603, 88.95942372801897591 ) ) ;
#9638 = CARTESIAN_POINT ( 'NONE',  ( 0.05219959533934541429, -16.53943276465976808, 40.00109039468567573 ) ) ;
#9639 = CARTESIAN_POINT ( 'NONE',  ( 16.52544592524342804, -4.483927247898539470, 103.5405762719810383 ) ) ;
#9640 = CARTESIAN_POINT ( 'NONE',  ( 5.049401038298161559, -19.05341960407611168, 72.70724293864768129 ) ) ;
#9641 = CARTESIAN_POINT ( 'NONE',  ( -18.67979575497178146, -10.72451020669898902, 46.66557627198102409 ) ) ;
#9642 = VECTOR ( 'NONE', #178187, 1000.000000000000114 ) ;
#9643 = CARTESIAN_POINT ( 'NONE',  ( 12.14591786802327356, -12.06949235617739191, 35.62609039468568994 ) ) ;
#9644 = CARTESIAN_POINT ( 'NONE',  ( 10.81492255796106328, -18.62759615963255655, 35.41775706135234003 ) ) ;
#9645 = CARTESIAN_POINT ( 'NONE',  ( 18.62759615963255655, 10.81492255796105972, 86.66775706135234714 ) ) ;
#9646 = CARTESIAN_POINT ( 'NONE',  ( -16.53943276465976808, -0.05219959533934237506, 83.75109039468568994 ) ) ;
#9647 = CARTESIAN_POINT ( 'NONE',  ( -16.46253265017160317, 9.564922557960807481, 75.83224293864769550 ) ) ;
#9648 = CARTESIAN_POINT ( 'NONE',  ( 4.379528057220092307, 16.55341960407617563, 102.2927570613523613 ) ) ;
#9649 = CARTESIAN_POINT ( 'NONE',  ( -13.97604488694547697, 13.89961937509957934, 53.12609039468565442 ) ) ;
#9650 = CARTESIAN_POINT ( 'NONE',  ( 10.81492255796106328, -18.62759615963255655, 35.41775706135234003 ) ) ;
#9651 = CARTESIAN_POINT ( 'NONE',  ( -16.53943276465976808, 0.05219959533911058130, 81.24890960531436690 ) ) ;
#9652 = CARTESIAN_POINT ( 'NONE',  ( 13.97604488694527802, 13.89961937509977652, 94.37390960531436690 ) ) ;
#9653 = CARTESIAN_POINT ( 'NONE',  ( 0.05219959533934541429, -16.53943276465976808, 105.0010903946856757 ) ) ;
#9654 = CARTESIAN_POINT ( 'NONE',  ( 10.81492255796106328, -18.62759615963255655, 70.41775706135236135 ) ) ;
#9655 = CARTESIAN_POINT ( 'NONE',  ( 8.314922557961029526, -14.29746914071037800, 30.41775706135234358 ) ) ;
#9656 = CARTESIAN_POINT ( 'NONE',  ( 5.823673210054444382, -21.52544592524334988, 25.20942372801901854 ) ) ;
#9657 = CARTESIAN_POINT ( 'NONE',  ( -16.55341960407611168, -4.379528057220339221, 66.45724293864768129 ) ) ;
#9658 = ORIENTED_EDGE ( 'NONE', *, *, #149935, .T. ) ;
#9659 = CARTESIAN_POINT ( 'NONE',  ( -15.80617190586768217, 15.72974639402176855, 23.12609039468567573 ) ) ;
#9660 = CARTESIAN_POINT ( 'NONE',  ( 12.14591786802309770, 12.06949235617756955, 59.37390960531436690 ) ) ;
#9661 = CARTESIAN_POINT ( 'NONE',  ( 9.564922557960805705, 16.46253265017160317, 29.58224293864769550 ) ) ;
#9662 = CARTESIAN_POINT ( 'NONE',  ( -10.72451020669898014, 18.67979575497178502, 25.41557627198103120 ) ) ;
#9663 = CARTESIAN_POINT ( 'NONE',  ( 21.52544592524334988, 5.823673210054432836, 46.45942372801901854 ) ) ;
#9664 = CARTESIAN_POINT ( 'NONE',  ( 14.34966873604960469, 8.224510206698951720, 64.16557627198102409 ) ) ;
#9665 = AXIS2_PLACEMENT_3D ( 'NONE', #94111, #58812, #184156 ) ;
#9666 = CARTESIAN_POINT ( 'NONE',  ( 21.55341960407610458, 5.719274019375980345, 73.95724293864769550 ) ) ;
#9668 = EDGE_CURVE ( 'NONE', #73091, #73471, #91628, .T. ) ;
#9667 = CARTESIAN_POINT ( 'NONE',  ( -16.46253265017160317, 9.564922557960807481, 70.83224293864770971 ) ) ;
#9670 = CARTESIAN_POINT ( 'NONE',  ( -19.03943276465977164, -0.05219959533935918106, 73.75109039468566152 ) ) ;
#9669 = CARTESIAN_POINT ( 'NONE',  ( 13.97604488694527802, 13.89961937509977652, 24.37390960531435624 ) ) ;
#9672 = CARTESIAN_POINT ( 'NONE',  ( 21.55341960407610458, 5.719274019375980345, 63.95724293864770260 ) ) ;
#9671 = CARTESIAN_POINT ( 'NONE',  ( -10.81492255796105439, 18.62759615963255655, 52.91775706135235424 ) ) ;
#9673 = CARTESIAN_POINT ( 'NONE',  ( -19.03943276465977164, 0.05219959533909376836, 41.24890960531435269 ) ) ;
#9674 = CARTESIAN_POINT ( 'NONE',  ( -19.02544592524342804, 5.153800228976336051, 66.04057627198103830 ) ) ;
#9675 = ORIENTED_EDGE ( 'NONE', *, *, #13792, .T. ) ;
#9676 = CARTESIAN_POINT ( 'NONE',  ( 12.14591786802327356, -12.06949235617739191, 45.62609039468567573 ) ) ;
#9677 = CARTESIAN_POINT ( 'NONE',  ( -21.55341960407619339, 5.719274019375674811, 33.54275706135234714 ) ) ;
#9678 = CARTESIAN_POINT ( 'NONE',  ( 0.05219959533937995610, -21.53943276465977519, 55.00109039468568284 ) ) ;
#9679 = CARTESIAN_POINT ( 'NONE',  ( 0.05219959533909260263, 19.03943276465977164, 99.99890960531436690 ) ) ;
#9680 = CARTESIAN_POINT ( 'NONE',  ( -15.80617190586745835, -15.72974639402198527, 86.87390960531438111 ) ) ;
#9682 = CARTESIAN_POINT ( 'NONE',  ( -12.06949235617739369, -12.14591786802326823, 49.37609039468569705 ) ) ;
#9681 = CARTESIAN_POINT ( 'NONE',  ( -21.52544592524334988, -5.823673210054445271, 28.95942372801902209 ) ) ;
#9683 = CARTESIAN_POINT ( 'NONE',  ( 21.53943276465977519, -0.05219959533907433946, 43.74890960531435979 ) ) ;
#9684 = CARTESIAN_POINT ( 'NONE',  ( 19.05341960407617918, -5.049401038297876454, 26.04275706135233293 ) ) ;
#9685 = CARTESIAN_POINT ( 'NONE',  ( 19.03943276465977164, -0.05219959533909143690, 53.74890960531436690 ) ) ;
#9686 = CARTESIAN_POINT ( 'NONE',  ( 16.46253265017160672, -9.564922557960803928, 113.3322429386476955 ) ) ;
#9687 = CARTESIAN_POINT ( 'NONE',  ( -16.51473224551069308, -9.474510206698971260, 91.66557627198103830 ) ) ;
#9688 = CARTESIAN_POINT ( 'NONE',  ( 16.61371651742640410, -7.165104196375910561, 86.35415069992971837 ) ) ;
#9689 = CARTESIAN_POINT ( 'NONE',  ( 19.05341960407617918, -5.049401038297876454, 71.04275706135234714 ) ) ;
#9690 = CARTESIAN_POINT ( 'NONE',  ( -21.52544592524343514, 5.823673210054127303, 51.04057627198103120 ) ) ;
#9691 = CARTESIAN_POINT ( 'NONE',  ( -16.53943276465976808, 0.05219959533911058130, 26.24890960531435624 ) ) ;
#9692 = CARTESIAN_POINT ( 'NONE',  ( 5.153800228976615827, -19.02544592524334988, 85.20942372801900433 ) ) ;
#9693 = CARTESIAN_POINT ( 'NONE',  ( 19.97888994334924107, -34.65319547504297759, 0.000000000000000000 ) ) ;
#9694 = CARTESIAN_POINT ( 'NONE',  ( -19.02544592524334988, -5.153800228976617603, 23.95942372801900078 ) ) ;
#9695 = CARTESIAN_POINT ( 'NONE',  ( 0.05219959533936267826, -19.03943276465977164, 85.00109039468567573 ) ) ;
#9696 = CARTESIAN_POINT ( 'NONE',  ( -19.05341960407617563, 5.049401038297882671, 38.54275706135233293 ) ) ;
#9697 = CARTESIAN_POINT ( 'NONE',  ( 17.97058386085786097, 5.500000000000047073, 71.50390968646219392 ) ) ;
#9698 = CARTESIAN_POINT ( 'NONE',  ( -19.03943276465977164, 0.05219959533909376836, 61.24890960531436690 ) ) ;
#9699 = CARTESIAN_POINT ( 'NONE',  ( -12.06949235617756955, 12.14591786802309770, 50.62390960531435979 ) ) ;
#9700 = ADVANCED_FACE ( 'NONE', ( #80442 ), #71788, .T. ) ;
#9701 = CARTESIAN_POINT ( 'NONE',  ( 16.51473224551069308, 9.474510206698969483, 39.16557627198103120 ) ) ;
#9702 = CARTESIAN_POINT ( 'NONE',  ( 12.06949235617757843, -12.14591786802309237, 43.12390960531435269 ) ) ;
#9703 = DIRECTION ( 'NONE',  ( -0.000000000000000000, 1.000000000000000000, 0.000000000000000000 ) ) ;
#9704 = CARTESIAN_POINT ( 'NONE',  ( -4.483927247898782831, 16.52544592524335698, 112.7094237280190328 ) ) ;
#9705 = CARTESIAN_POINT ( 'NONE',  ( 13.89961937509977652, -13.97604488694527269, 63.12390960531435979 ) ) ;
#9706 = CARTESIAN_POINT ( 'NONE',  ( -13.89961937509957401, -13.97604488694547875, 19.37609039468566507 ) ) ;
#9707 = CARTESIAN_POINT ( 'NONE',  ( -14.29746914071037622, -8.314922557961029526, 34.16775706135234714 ) ) ;
#9708 = CARTESIAN_POINT ( 'NONE',  ( 18.62759615963271287, -10.81492255796078972, 43.33224293864769550 ) ) ;
#9710 = ORIENTED_EDGE ( 'NONE', *, *, #103264, .F. ) ;
#9709 = CARTESIAN_POINT ( 'NONE',  ( 15.72974639402176855, 15.80617190586768217, 86.87609039468568994 ) ) ;
#9711 = CARTESIAN_POINT ( 'NONE',  ( 9.474510206698971260, -16.51473224551069308, 67.91557627198102409 ) ) ;
#9712 = CARTESIAN_POINT ( 'NONE',  ( -19.05341960407611168, -5.049401038298163336, 111.4572429386476671 ) ) ;
#9713 = CARTESIAN_POINT ( 'NONE',  ( 9.474510206698971260, -16.51473224551069308, 97.91557627198102409 ) ) ;
#9714 = CARTESIAN_POINT ( 'NONE',  ( -36.91746825000000598, 2.428612866367529932E-14, -2.624999997268813168 ) ) ;
#9715 = CARTESIAN_POINT ( 'NONE',  ( 10.72451020669871369, 18.67979575497193778, 22.08442372801901143 ) ) ;
#9716 = CARTESIAN_POINT ( 'NONE',  ( 16.53943276465976808, -0.05219959533910856209, 83.74890960531435269 ) ) ;
#9718 = CARTESIAN_POINT ( 'NONE',  ( -0.05219959533909027116, -19.03943276465977164, 72.49890960531435269 ) ) ;
#9717 = CARTESIAN_POINT ( 'NONE',  ( -21.53943276465977519, 0.05219959533907696930, 76.24890960531435269 ) ) ;
#9719 = CARTESIAN_POINT ( 'NONE',  ( -19.02544592524342804, 5.153800228976336051, 71.04057627198099567 ) ) ;
#9720 = CARTESIAN_POINT ( 'NONE',  ( -21.52544592524343514, 5.823673210054127303, 116.0405762719810383 ) ) ;
#9721 = ORIENTED_EDGE ( 'NONE', *, *, #167487, .T. ) ;
#9722 = CARTESIAN_POINT ( 'NONE',  ( 16.46253265017160672, -9.564922557960803928, 73.33224293864769550 ) ) ;
#9724 = DIRECTION ( 'NONE',  ( 0.000000000000000000, 0.000000000000000000, -1.000000000000000000 ) ) ;
#9723 = CARTESIAN_POINT ( 'NONE',  ( -14.34966873604960291, -8.224510206698953496, 106.6655762719810383 ) ) ;
#9725 = CARTESIAN_POINT ( 'NONE',  ( -13.89961937509977652, 13.97604488694528158, 60.62390960531436690 ) ) ;
#9726 = CARTESIAN_POINT ( 'NONE',  ( -5.153800228976607833, 19.02544592524334988, 92.70942372801901854 ) ) ;
#9727 = CARTESIAN_POINT ( 'NONE',  ( -14.29746914071049879, 8.314922557960819915, 95.83224293864770971 ) ) ;
#9728 = CARTESIAN_POINT ( 'NONE',  ( 0.05219959533937995610, -21.53943276465977519, 75.00109039468568994 ) ) ;
#9730 = CARTESIAN_POINT ( 'NONE',  ( 21.52544592524334988, 5.823673210054432836, 21.45942372801901499 ) ) ;
#9729 = CARTESIAN_POINT ( 'NONE',  ( -19.05341960407611168, -5.049401038298163336, 46.45724293864768129 ) ) ;
#9731 = CARTESIAN_POINT ( 'NONE',  ( -14.34966873604960291, -8.224510206698953496, 96.66557627198102409 ) ) ;
#9732 = CARTESIAN_POINT ( 'NONE',  ( -23.31738231874055600, 16.94106989632528837, 143.7999999999999829 ) ) ;
#9733 = CARTESIAN_POINT ( 'NONE',  ( -5.153800228976328057, -19.02544592524343514, 77.29057627198099567 ) ) ;
#9734 = CARTESIAN_POINT ( 'NONE',  ( 16.31925111598457789, 7.325300261831532822, 112.3357546103274132 ) ) ;
#9736 = CARTESIAN_POINT ( 'NONE',  ( -18.62759615963270932, 10.81492255796079327, 30.83224293864770260 ) ) ;
#9735 = CARTESIAN_POINT ( 'NONE',  ( 16.46253265017146816, 9.564922557961045513, 101.6677570613523329 ) ) ;
#9737 = CARTESIAN_POINT ( 'NONE',  ( -21.53943276465977519, -0.05219959533937600094, 53.75109039468568994 ) ) ;
#9738 = CARTESIAN_POINT ( 'NONE',  ( 13.89961937509977652, -13.97604488694527269, 98.12390960531433848 ) ) ;
#9739 = CARTESIAN_POINT ( 'NONE',  ( -5.153800228976607833, 19.02544592524334988, 77.70942372801900433 ) ) ;
#9740 = CARTESIAN_POINT ( 'NONE',  ( -0.05219959533909027116, -19.03943276465977164, 77.49890960531435269 ) ) ;
#9741 = CARTESIAN_POINT ( 'NONE',  ( 16.55341960407611168, 4.379528057220329451, 83.95724293864770971 ) ) ;
#9742 = CARTESIAN_POINT ( 'NONE',  ( 13.97604488694527802, 13.89961937509977652, 109.3739096053143669 ) ) ;
#9743 = CARTESIAN_POINT ( 'NONE',  ( -16.52544592524342804, 4.483927247898546575, 91.04057627198103830 ) ) ;
#9744 = CARTESIAN_POINT ( 'NONE',  ( -16.46253265017160317, 9.564922557960807481, 100.8322429386477097 ) ) ;
#9746 = CARTESIAN_POINT ( 'NONE',  ( -16.51473224551069308, -9.474510206698971260, 21.66557627198102765 ) ) ;
#9745 = CARTESIAN_POINT ( 'NONE',  ( 4.379528057220339221, -16.55341960407611168, 42.70724293864770260 ) ) ;
#9747 = VERTEX_POINT ( 'NONE', #90410 ) ;
#9748 = CARTESIAN_POINT ( 'NONE',  ( -15.80617190586768217, 15.72974639402176855, 53.12609039468568284 ) ) ;
#9749 = CARTESIAN_POINT ( 'NONE',  ( -5.153800228976607833, 19.02544592524334988, 77.70942372801900433 ) ) ;
#9750 = CARTESIAN_POINT ( 'NONE',  ( -14.29746914071049879, 8.314922557960819915, 45.83224293864769550 ) ) ;
#9751 = CARTESIAN_POINT ( 'NONE',  ( -15.72974639402197994, 15.80617190586746368, 105.6239096053143669 ) ) ;
#9752 = CARTESIAN_POINT ( 'NONE',  ( 0.05219959533907565091, 21.53943276465977519, 34.99890960531435979 ) ) ;
#9753 = CARTESIAN_POINT ( 'NONE',  ( 16.55341960407611168, 4.379528057220329451, 83.95724293864770971 ) ) ;
#9754 = CARTESIAN_POINT ( 'NONE',  ( 19.05341960407611168, 5.049401038298154454, 58.95724293864768129 ) ) ;
#9755 = CARTESIAN_POINT ( 'NONE',  ( 8.314922557960818139, 14.29746914071049879, 24.58224293864768839 ) ) ;
#9756 = CARTESIAN_POINT ( 'NONE',  ( -16.52544592524335698, -4.483927247898792601, 93.95942372801903275 ) ) ;
#9757 = CARTESIAN_POINT ( 'NONE',  ( 16.52544592524335698, 4.483927247898782831, 66.45942372801903275 ) ) ;
#9758 = CARTESIAN_POINT ( 'NONE',  ( -5.049401038297874678, -19.05341960407617918, 19.79275706135233293 ) ) ;
#9759 = CARTESIAN_POINT ( 'NONE',  ( -5.153800228976328057, -19.02544592524343514, 92.29057627198099567 ) ) ;
#9760 = CARTESIAN_POINT ( 'NONE',  ( 0.05219959533909260263, 19.03943276465977164, 84.99890960531436690 ) ) ;
#9761 = CARTESIAN_POINT ( 'NONE',  ( 8.224510206698742110, 14.34966873604972548, 82.08442372801901854 ) ) ;
#9762 = CARTESIAN_POINT ( 'NONE',  ( 19.03943276465977164, -0.05219959533909143690, 43.74890960531435979 ) ) ;
#9763 = CARTESIAN_POINT ( 'NONE',  ( -4.483927247898539470, -16.52544592524342804, 52.29057627198102409 ) ) ;
#9765 = CARTESIAN_POINT ( 'NONE',  ( 19.05341960407611168, 5.049401038298154454, 103.9572429386476671 ) ) ;
#9764 = CARTESIAN_POINT ( 'NONE',  ( 0.05219959533909260263, 19.03943276465977164, 114.9989096053143669 ) ) ;
#9766 = CARTESIAN_POINT ( 'NONE',  ( -18.62759615963270932, 10.81492255796079327, 35.83224293864768839 ) ) ;
#9767 = CARTESIAN_POINT ( 'NONE',  ( 12.06949235617757843, -12.14591786802309237, 78.12390960531436690 ) ) ;
#9768 = CARTESIAN_POINT ( 'NONE',  ( -4.379528057220086978, -16.55341960407618274, 19.79275706135235069 ) ) ;
#9769 = VERTEX_POINT ( 'NONE', #14572 ) ;
#9770 = CARTESIAN_POINT ( 'NONE',  ( 16.52544592524342804, -4.483927247898539470, 68.54057627198103830 ) ) ;
#9771 = CARTESIAN_POINT ( 'NONE',  ( 29.64248797448942696, -1.297617798568356573, -48.74145669546051352 ) ) ;
#9772 = CARTESIAN_POINT ( 'NONE',  ( -16.51473224551082808, 9.474510206698731452, 58.33442372801900433 ) ) ;
#9773 = CARTESIAN_POINT ( 'NONE',  ( 5.153800228976335163, 19.02544592524342804, 99.79057627198102409 ) ) ;
#9774 = CARTESIAN_POINT ( 'NONE',  ( -16.51473224551082808, 9.474510206698731452, 83.33442372801899012 ) ) ;
#9775 = CARTESIAN_POINT ( 'NONE',  ( -8.571926809382608425, 26.38167802310805854, 146.9750000027311785 ) ) ;
#9776 = AXIS2_PLACEMENT_3D ( 'NONE', #62764, #199314, #60780 ) ;
#9778 = CARTESIAN_POINT ( 'NONE',  ( -14.29746914071037622, -8.314922557961029526, 99.16775706135234714 ) ) ;
#9777 = CARTESIAN_POINT ( 'NONE',  ( -5.153800228976607833, 19.02544592524334988, 107.7094237280189759 ) ) ;
#9779 = CARTESIAN_POINT ( 'NONE',  ( -9.474510206698964154, 16.51473224551069663, 35.41557627198102409 ) ) ;
#9780 = CARTESIAN_POINT ( 'NONE',  ( 10.81492255796078972, 18.62759615963270932, 29.58224293864769905 ) ) ;
#9781 = CARTESIAN_POINT ( 'NONE',  ( -10.72451020669870658, -18.67979575497194134, 59.58442372801901854 ) ) ;
#9782 = CARTESIAN_POINT ( 'NONE',  ( 4.379528057220092307, 16.55341960407617563, 27.29275706135234358 ) ) ;
#9784 = CARTESIAN_POINT ( 'NONE',  ( 5.153800228976335163, 19.02544592524342804, 79.79057627198102409 ) ) ;
#9783 = CARTESIAN_POINT ( 'NONE',  ( 17.49999999999999289, 3.401555454158704084, 22.96163022339541726 ) ) ;
#9785 = CARTESIAN_POINT ( 'NONE',  ( -6.019987952026120409E-15, 39.95163481335720235, -0.5021577739498228610 ) ) ;
#9787 = CARTESIAN_POINT ( 'NONE',  ( -0.05219959533909027116, -19.03943276465977164, 77.49890960531435269 ) ) ;
#9786 = CARTESIAN_POINT ( 'NONE',  ( 16.55341960407611168, 4.379528057220329451, 88.95724293864769550 ) ) ;
#9788 = CARTESIAN_POINT ( 'NONE',  ( 19.05341960407611168, 5.049401038298154454, 88.95724293864769550 ) ) ;
#9789 = ORIENTED_EDGE ( 'NONE', *, *, #107496, .F. ) ;
#9790 = CARTESIAN_POINT ( 'NONE',  ( -9.474510206698720793, -16.51473224551083518, 89.58442372801900433 ) ) ;
#9791 = CARTESIAN_POINT ( 'NONE',  ( 10.81492255796078972, 18.62759615963270932, 59.58224293864770260 ) ) ;
#9792 = CARTESIAN_POINT ( 'NONE',  ( -19.05341960407611168, -5.049401038298163336, 36.45724293864766707 ) ) ;
#9793 = CARTESIAN_POINT ( 'NONE',  ( 5.153800228976615827, -19.02544592524334988, 50.20942372801897591 ) ) ;
#9794 = CARTESIAN_POINT ( 'NONE',  ( -19.03943276465977164, 0.05219959533909376836, 56.24890960531435979 ) ) ;
#9795 = CARTESIAN_POINT ( 'NONE',  ( -13.97604488694527625, -13.89961937509977652, 86.87390960531436690 ) ) ;
#9796 = ORIENTED_EDGE ( 'NONE', *, *, #93300, .F. ) ;
#9797 = CARTESIAN_POINT ( 'NONE',  ( 18.67979575497178502, 10.72451020669898547, 94.16557627198103830 ) ) ;
#9799 = CARTESIAN_POINT ( 'NONE',  ( -19.05341960407617563, 5.049401038297882671, 48.54275706135233293 ) ) ;
#9798 = CARTESIAN_POINT ( 'NONE',  ( 16.52544592524342804, -4.483927247898539470, 88.54057627198103830 ) ) ;
#9800 = CARTESIAN_POINT ( 'NONE',  ( 15.72974639402199770, -15.80617190586745480, 88.12390960531436690 ) ) ;
#9801 = CARTESIAN_POINT ( 'NONE',  ( 0.05219959533907565091, 21.53943276465977519, 79.99890960531435269 ) ) ;
#9802 = CARTESIAN_POINT ( 'NONE',  ( -4.379528057220328563, 16.55341960407611168, 35.20724293864768839 ) ) ;
#9803 = CARTESIAN_POINT ( 'NONE',  ( 21.53943276465977519, 0.05219959533937863772, 101.2510903946856757 ) ) ;
#9804 = CARTESIAN_POINT ( 'NONE',  ( 4.483927247898790824, -16.52544592524335698, 50.20942372801901854 ) ) ;
#9805 = CARTESIAN_POINT ( 'NONE',  ( -5.049401038298153566, 19.05341960407611168, 85.20724293864766707 ) ) ;
#9806 = CARTESIAN_POINT ( 'NONE',  ( -13.97604488694527625, -13.89961937509977652, 26.87390960531434558 ) ) ;
#9807 = CIRCLE ( 'NONE', #38950, 13.70000000000001528 ) ;
#9808 = CARTESIAN_POINT ( 'NONE',  ( -18.67979575497193778, 10.72451020669871902, 38.33442372801900433 ) ) ;
#9809 = CARTESIAN_POINT ( 'NONE',  ( -21.53943276465977519, -0.05219959533937600094, 53.75109039468568994 ) ) ;
#9810 = CARTESIAN_POINT ( 'NONE',  ( -5.153800228976328057, -19.02544592524343514, 52.29057627198100988 ) ) ;
#9811 = CARTESIAN_POINT ( 'NONE',  ( 10.81492255796106328, -18.62759615963255655, 20.41775706135234714 ) ) ;
#9812 = CARTESIAN_POINT ( 'NONE',  ( 19.02544592524334988, 5.153800228976608722, 66.45942372801899012 ) ) ;
#9813 = CARTESIAN_POINT ( 'NONE',  ( -19.05341960407617563, 5.049401038297882671, 68.54275706135230450 ) ) ;
#9814 = CARTESIAN_POINT ( 'NONE',  ( -16.55341960407617563, 4.379528057220093196, 28.54275706135234358 ) ) ;
#9815 = CARTESIAN_POINT ( 'NONE',  ( 16.51473224551069308, 9.474510206698969483, 24.16557627198102765 ) ) ;
#9816 = CARTESIAN_POINT ( 'NONE',  ( 8.224510206698742110, 14.34966873604972548, 67.08442372801901854 ) ) ;
#9817 = CARTESIAN_POINT ( 'NONE',  ( -0.05219959533909027116, -19.03943276465977164, 42.49890960531435269 ) ) ;
#9818 = CARTESIAN_POINT ( 'NONE',  ( 21.95653654802608301, -6.613221094984325532, 171.0358100525039902 ) ) ;
#9819 = CARTESIAN_POINT ( 'NONE',  ( -13.89961937509977652, 13.97604488694528158, 95.62390960531436690 ) ) ;
#9820 = CARTESIAN_POINT ( 'NONE',  ( 14.34966873604960469, 8.224510206698951720, 114.1655762719810383 ) ) ;
#9821 = CARTESIAN_POINT ( 'NONE',  ( 21.53943276465977519, -0.05219959533907433946, 78.74890960531436690 ) ) ;
#9822 = CARTESIAN_POINT ( 'NONE',  ( -8.224510206698735004, -14.34966873604973081, 59.58442372801901854 ) ) ;
#9823 = CARTESIAN_POINT ( 'NONE',  ( -19.03943276465977164, -0.05219959533935918106, 18.75109039468567218 ) ) ;
#9824 = CARTESIAN_POINT ( 'NONE',  ( 5.153800228976335163, 19.02544592524342804, 44.79057627198103830 ) ) ;
#9825 = CARTESIAN_POINT ( 'NONE',  ( 0.05219959533910956823, 16.53943276465976808, 34.99890960531435979 ) ) ;
#9827 = CARTESIAN_POINT ( 'NONE',  ( 12.06949235617757843, -12.14591786802309237, 63.12390960531435979 ) ) ;
#9826 = B_SPLINE_CURVE_WITH_KNOTS ( 'NONE', 3,
 ( #156724, #141542, #84833, #116192 ),
 .UNSPECIFIED., .F., .F.,
 ( 4, 4 ),
 ( 0.000000000000000000, 0.007966019813519142206 ),
 .UNSPECIFIED. ) ;
#9828 = CARTESIAN_POINT ( 'NONE',  ( 5.153800228976335163, 19.02544592524342804, 69.79057627198103830 ) ) ;
#9829 = CARTESIAN_POINT ( 'NONE',  ( -10.81492255796105439, 18.62759615963255655, 37.91775706135235424 ) ) ;
#9830 = CARTESIAN_POINT ( 'NONE',  ( 16.46253265017160672, -9.564922557960803928, 78.33224293864769550 ) ) ;
#9831 = CARTESIAN_POINT ( 'NONE',  ( -18.67979575497193778, 10.72451020669871902, 83.33442372801903275 ) ) ;
#9832 = CARTESIAN_POINT ( 'NONE',  ( -12.06949235617739369, -12.14591786802326823, 64.37609039468568994 ) ) ;
#9833 = EDGE_CURVE ( 'NONE', #181866, #51216, #142632, .T. ) ;
#9834 = CARTESIAN_POINT ( 'NONE',  ( 5.153800228976335163, 19.02544592524342804, 104.7905762719809957 ) ) ;
#9835 = CARTESIAN_POINT ( 'NONE',  ( -16.52544592524342804, 4.483927247898546575, 51.04057627198103120 ) ) ;
#9836 = CARTESIAN_POINT ( 'NONE',  ( -13.97604488694527625, -13.89961937509977652, 31.87390960531435979 ) ) ;
#9837 = CARTESIAN_POINT ( 'NONE',  ( -0.05219959533934338120, 16.53943276465976808, 57.50109039468568994 ) ) ;
#9838 = CARTESIAN_POINT ( 'NONE',  ( -8.224510206698948167, 14.34966873604960824, 50.41557627198103120 ) ) ;
#9839 = CARTESIAN_POINT ( 'NONE',  ( -19.05341960407611168, -5.049401038298163336, 106.4572429386476955 ) ) ;
#9840 = CARTESIAN_POINT ( 'NONE',  ( -18.67979575497178146, -10.72451020669898902, 31.66557627198102054 ) ) ;
#9841 = CARTESIAN_POINT ( 'NONE',  ( 9.564922557961047289, -16.46253265017146816, 20.41775706135233293 ) ) ;
#9842 = CARTESIAN_POINT ( 'NONE',  ( -4.483927247898539470, -16.52544592524342804, 92.29057627198103830 ) ) ;
#9843 = CARTESIAN_POINT ( 'NONE',  ( 9.474510206698971260, -16.51473224551069308, 92.91557627198103830 ) ) ;
#9844 = ORIENTED_EDGE ( 'NONE', *, *, #64870, .T. ) ;
#9845 = CARTESIAN_POINT ( 'NONE',  ( -12.14591786802326823, 12.06949235617739902, 58.12609039468568994 ) ) ;
#9846 = CARTESIAN_POINT ( 'NONE',  ( -19.03943276465977164, 0.05219959533909376836, 51.24890960531436690 ) ) ;
#9847 = CARTESIAN_POINT ( 'NONE',  ( -28.82186960331499037, 2.781578969918950771E-14, 139.9999999999999716 ) ) ;
#9848 = CARTESIAN_POINT ( 'NONE',  ( -5.153800228976607833, 19.02544592524334988, 42.70942372801901143 ) ) ;
#9849 = CARTESIAN_POINT ( 'NONE',  ( 8.224510206698742110, 14.34966873604972548, 82.08442372801901854 ) ) ;
#9850 = CARTESIAN_POINT ( 'NONE',  ( 5.153800228976615827, -19.02544592524334988, 100.2094237280190043 ) ) ;
#9851 = CARTESIAN_POINT ( 'NONE',  ( 5.823673210054444382, -21.52544592524334988, 60.20942372801902565 ) ) ;
#9852 = CARTESIAN_POINT ( 'NONE',  ( -19.02544592524342804, 5.153800228976336051, 76.04057627198102409 ) ) ;
#9853 = CARTESIAN_POINT ( 'NONE',  ( -10.81492255796078084, -18.62759615963271287, 97.08224293864770971 ) ) ;
#9854 = CARTESIAN_POINT ( 'NONE',  ( -8.224510206698948167, 14.34966873604960824, 100.4155762719810241 ) ) ;
#9855 = CARTESIAN_POINT ( 'NONE',  ( -19.02544592524334988, -5.153800228976617603, 73.95942372801900433 ) ) ;
#9856 = CARTESIAN_POINT ( 'NONE',  ( -18.62759615963270932, 10.81492255796079327, 60.83224293864769550 ) ) ;
#9857 = CARTESIAN_POINT ( 'NONE',  ( 9.474510206698729675, 16.51473224551082808, 37.08442372801899722 ) ) ;
#9858 = FACE_BOUND ( 'NONE', #6770, .T. ) ;
#9859 = CARTESIAN_POINT ( 'NONE',  ( -21.52544592524343514, 5.823673210054127303, 86.04057627198102409 ) ) ;
#9860 = CARTESIAN_POINT ( 'NONE',  ( -19.48894818550243357, 5.500000000000114575, 55.10307310435241135 ) ) ;
#9861 = CARTESIAN_POINT ( 'NONE',  ( -9.564922557960796823, -16.46253265017161027, 67.08224293864769550 ) ) ;
#9862 = CARTESIAN_POINT ( 'NONE',  ( 16.46253265017160672, -9.564922557960803928, 93.33224293864769550 ) ) ;
#9863 = CARTESIAN_POINT ( 'NONE',  ( 9.474510206698729675, 16.51473224551082808, 112.0844237280190043 ) ) ;
#9864 = CARTESIAN_POINT ( 'NONE',  ( -19.46398650005389896, 5.499999999999949374, 60.18269651486372851 ) ) ;
#9865 = CARTESIAN_POINT ( 'NONE',  ( -16.46253265017160317, 9.564922557960807481, 50.83224293864770260 ) ) ;
#9866 = CARTESIAN_POINT ( 'NONE',  ( -0.05219959533909027116, -19.03943276465977164, 107.4989096053143527 ) ) ;
#9868 = CARTESIAN_POINT ( 'NONE',  ( -12.06949235617756955, 12.14591786802309770, 55.62390960531436690 ) ) ;
#9867 = CARTESIAN_POINT ( 'NONE',  ( -0.05219959533907301413, -21.53943276465977519, 87.49890960531436690 ) ) ;
#9869 = CARTESIAN_POINT ( 'NONE',  ( 10.81492255796106328, -18.62759615963255655, 70.41775706135236135 ) ) ;
#9871 = CARTESIAN_POINT ( 'NONE',  ( 16.51473224551083163, -9.474510206698727899, 30.83442372801900433 ) ) ;
#9870 = CARTESIAN_POINT ( 'NONE',  ( -16.52544592524335698, -4.483927247898792601, 28.95942372801902209 ) ) ;
#9872 = CARTESIAN_POINT ( 'NONE',  ( 12.14591786802309770, 12.06949235617756955, 29.37390960531435269 ) ) ;
#9873 = CARTESIAN_POINT ( 'NONE',  ( 18.67979575497178502, 10.72451020669898547, 109.1655762719810383 ) ) ;
#9874 = CARTESIAN_POINT ( 'NONE',  ( 0.05219959533910956823, 16.53943276465976808, 54.99890960531435269 ) ) ;
#9875 = CARTESIAN_POINT ( 'NONE',  ( -13.89961937509957401, -13.97604488694547875, 89.37609039468563310 ) ) ;
#9876 = CARTESIAN_POINT ( 'NONE',  ( 13.97604488694548053, -13.89961937509957401, 65.62609039468567573 ) ) ;
#9877 = CARTESIAN_POINT ( 'NONE',  ( -21.52544592524334988, -5.823673210054445271, 68.95942372801901854 ) ) ;
#9878 = CARTESIAN_POINT ( 'NONE',  ( -16.51473224551082808, 9.474510206698731452, 53.33442372801900433 ) ) ;
#9879 = CARTESIAN_POINT ( 'NONE',  ( 4.379528057220339221, -16.55341960407611168, 112.7072429386476955 ) ) ;
#9880 = CARTESIAN_POINT ( 'NONE',  ( 15.80617190586746368, 15.72974639402197994, 49.37390960531436690 ) ) ;
#9881 = CARTESIAN_POINT ( 'NONE',  ( -14.29746914071049879, 8.314922557960819915, 50.83224293864770971 ) ) ;
#9882 = CARTESIAN_POINT ( 'NONE',  ( -17.31747979337953680, -6.344076630960945096, 26.37944868065185133 ) ) ;
#9883 = CARTESIAN_POINT ( 'NONE',  ( 5.719274019375673035, 21.55341960407619339, 112.2927570613523471 ) ) ;
#9884 = CARTESIAN_POINT ( 'NONE',  ( -4.483927247898782831, 16.52544592524335698, 87.70942372801901854 ) ) ;
#9885 = CARTESIAN_POINT ( 'NONE',  ( 14.29746914071049879, -8.314922557960816363, 38.33224293864768839 ) ) ;
#9886 = CARTESIAN_POINT ( 'NONE',  ( 10.81492255796106328, -18.62759615963255655, 75.41775706135233293 ) ) ;
#9887 = CARTESIAN_POINT ( 'NONE',  ( 0.05219959533937995610, -21.53943276465977519, 65.00109039468568994 ) ) ;
#9888 = CARTESIAN_POINT ( 'NONE',  ( 15.72974639402199770, -15.80617190586745480, 78.12390960531436690 ) ) ;
#9889 = CARTESIAN_POINT ( 'NONE',  ( 9.474510206698971260, -16.51473224551069308, 42.91557627198103120 ) ) ;
#9890 = CARTESIAN_POINT ( 'NONE',  ( -18.67979575497193778, 10.72451020669871902, 53.33442372801901854 ) ) ;
#9891 = CARTESIAN_POINT ( 'NONE',  ( 9.564922557960805705, 16.46253265017160317, 34.58224293864770260 ) ) ;
#9892 = CARTESIAN_POINT ( 'NONE',  ( 19.05341960407611168, 5.049401038298154454, 58.95724293864768129 ) ) ;
#9893 = CARTESIAN_POINT ( 'NONE',  ( 4.483927247898545687, 16.52544592524342804, 94.79057627198105251 ) ) ;
#9894 = CARTESIAN_POINT ( 'NONE',  ( -16.51473224551069308, -9.474510206698971260, 91.66557627198103830 ) ) ;
#9895 = CARTESIAN_POINT ( 'NONE',  ( -14.34966873604960291, -8.224510206698953496, 41.66557627198103120 ) ) ;
#9896 = CARTESIAN_POINT ( 'NONE',  ( -14.34966873604960291, -8.224510206698953496, 101.6655762719810383 ) ) ;
#9897 = CARTESIAN_POINT ( 'NONE',  ( -15.80617190586745835, -15.72974639402198527, 66.87390960531436690 ) ) ;
#9898 = CARTESIAN_POINT ( 'NONE',  ( -21.52544592524343514, 5.823673210054127303, 116.0405762719810383 ) ) ;
#9899 = CARTESIAN_POINT ( 'NONE',  ( -9.474510206698964154, 16.51473224551069663, 115.4155762719810241 ) ) ;
#9900 = ADVANCED_FACE ( 'NONE', ( #169233 ), #375, .T. ) ;
#9902 = CARTESIAN_POINT ( 'NONE',  ( -5.153800228976607833, 19.02544592524334988, 112.7094237280190043 ) ) ;
#9901 = CARTESIAN_POINT ( 'NONE',  ( -16.51473224551069308, -9.474510206698971260, 76.66557627198103830 ) ) ;
#9903 = CARTESIAN_POINT ( 'NONE',  ( -5.823673210054116645, -21.52544592524344225, 77.29057627198102409 ) ) ;
#9904 = CARTESIAN_POINT ( 'NONE',  ( 15.80617190586769283, -15.72974639402175789, 100.6260903946857184 ) ) ;
#9905 = CARTESIAN_POINT ( 'NONE',  ( 16.51473224551069308, 9.474510206698969483, 74.16557627198103830 ) ) ;
#9906 = CARTESIAN_POINT ( 'NONE',  ( -15.72974639402197994, 15.80617190586746368, 115.6239096053143669 ) ) ;
#9907 = CARTESIAN_POINT ( 'NONE',  ( -19.02544592524342804, 5.153800228976336051, 116.0405762719810383 ) ) ;
#9908 = CARTESIAN_POINT ( 'NONE',  ( -8.314922557961024197, 14.29746914071037800, 87.91775706135234714 ) ) ;
#9909 = CARTESIAN_POINT ( 'NONE',  ( -10.81492255796105439, 18.62759615963255655, 72.91775706135234714 ) ) ;
#9910 = CARTESIAN_POINT ( 'NONE',  ( -5.719274019375665041, -21.55341960407619695, 99.79275706135234714 ) ) ;
#9911 = CARTESIAN_POINT ( 'NONE',  ( 14.29746914071037800, 8.314922557961029526, 56.66775706135235424 ) ) ;
#9912 = CARTESIAN_POINT ( 'NONE',  ( 10.72451020669871369, 18.67979575497193778, 22.08442372801901143 ) ) ;
#9913 = CARTESIAN_POINT ( 'NONE',  ( -19.02544592524342804, 5.153800228976336051, 26.04057627198103120 ) ) ;
#9914 = CARTESIAN_POINT ( 'NONE',  ( -10.72451020669870658, -18.67979575497194134, 94.58442372801901854 ) ) ;
#9915 = CARTESIAN_POINT ( 'NONE',  ( 19.02544592524343514, -5.153800228976328945, 98.54057627198100988 ) ) ;
#9916 = CARTESIAN_POINT ( 'NONE',  ( -5.719274019375978568, 21.55341960407610458, 90.20724293864770971 ) ) ;
#9917 = CARTESIAN_POINT ( 'NONE',  ( 9.564922557961047289, -16.46253265017146816, 55.41775706135234003 ) ) ;
#9919 = CARTESIAN_POINT ( 'NONE',  ( -10.81492255796078084, -18.62759615963271287, 52.08224293864768839 ) ) ;
#9918 = CARTESIAN_POINT ( 'NONE',  ( -20.92307141426356409, -31.70153649905130422, -23.60833562326012469 ) ) ;
#9921 = CARTESIAN_POINT ( 'NONE',  ( -12.06949235617756955, 12.14591786802309770, 35.62390960531437401 ) ) ;
#9920 = CARTESIAN_POINT ( 'NONE',  ( 19.03943276465977164, -0.05219959533909143690, 88.74890960531436690 ) ) ;
#9922 = CARTESIAN_POINT ( 'NONE',  ( 20.85011945226400698, 10.59319688750118083, 168.2343749380337954 ) ) ;
#9923 = CARTESIAN_POINT ( 'NONE',  ( 13.89961937509957401, 13.97604488694547697, 71.87609039468567573 ) ) ;
#9924 = CARTESIAN_POINT ( 'NONE',  ( -1.500065973499163041, -15.01118352434400549, -62.04667436142317172 ) ) ;
#9925 = CARTESIAN_POINT ( 'NONE',  ( -19.02544592524334988, -5.153800228976617603, 108.9594237280189759 ) ) ;
#9926 = CARTESIAN_POINT ( 'NONE',  ( 5.719274019375991003, -21.55341960407610458, 82.70724293864770971 ) ) ;
#9927 = CARTESIAN_POINT ( 'NONE',  ( -16.55341960407611168, -4.379528057220339221, 71.45724293864769550 ) ) ;
#9928 = CARTESIAN_POINT ( 'NONE',  ( -13.89961937509977652, 13.97604488694528158, 95.62390960531436690 ) ) ;
#9929 = CARTESIAN_POINT ( 'NONE',  ( 16.55341960407618274, -4.379528057220086978, 36.04275706135234714 ) ) ;
#9930 = CARTESIAN_POINT ( 'NONE',  ( -19.03943276465977164, 0.05219959533909376836, 56.24890960531435979 ) ) ;
#9932 = CARTESIAN_POINT ( 'NONE',  ( -16.46253265017146816, -9.564922557961047289, 79.16775706135234714 ) ) ;
#9931 = CARTESIAN_POINT ( 'NONE',  ( -5.719274019375978568, 21.55341960407610458, 115.2072429386476955 ) ) ;
#9933 = CARTESIAN_POINT ( 'NONE',  ( 9.474510206698971260, -16.51473224551069308, 97.91557627198102409 ) ) ;
#9934 = CARTESIAN_POINT ( 'NONE',  ( 5.049401038298161559, -19.05341960407611168, 72.70724293864768129 ) ) ;
#9935 = CARTESIAN_POINT ( 'NONE',  ( -18.67979575497178146, -10.72451020669898902, 76.66557627198103830 ) ) ;
#9936 = CARTESIAN_POINT ( 'NONE',  ( 13.89961937509977652, -13.97604488694527269, 43.12390960531434558 ) ) ;
#9937 = DIRECTION ( 'NONE',  ( -1.000000000000000000, 0.000000000000000000, 0.000000000000000000 ) ) ;
#9938 = CARTESIAN_POINT ( 'NONE',  ( -4.379528057220328563, 16.55341960407611168, 50.20724293864769550 ) ) ;
#9939 = CARTESIAN_POINT ( 'NONE',  ( -19.05341960407611168, -5.049401038298163336, 106.4572429386476955 ) ) ;
#9940 = CARTESIAN_POINT ( 'NONE',  ( 8.906447517083057264, -27.41122689804191026, 144.5999999999999943 ) ) ;
#9941 = CARTESIAN_POINT ( 'NONE',  ( 19.03943276465977164, 0.05219959533936151252, 66.25109039468567573 ) ) ;
#9942 = CARTESIAN_POINT ( 'NONE',  ( -21.52544592524343514, 5.823673210054127303, 76.04057627198102409 ) ) ;
#9943 = CARTESIAN_POINT ( 'NONE',  ( 19.03943276465977164, 0.05219959533936151252, 51.25109039468567573 ) ) ;
#9944 = CARTESIAN_POINT ( 'NONE',  ( -13.97604488694527625, -13.89961937509977652, 106.8739096053143669 ) ) ;
#9945 = PLANE ( 'NONE',  #95324 ) ;
#9946 = CARTESIAN_POINT ( 'NONE',  ( 10.81492255796078972, 18.62759615963270932, 44.58224293864769550 ) ) ;
#9947 = CARTESIAN_POINT ( 'NONE',  ( 5.049401038298161559, -19.05341960407611168, 67.70724293864769550 ) ) ;
#9948 = CARTESIAN_POINT ( 'NONE',  ( 18.67979575497194134, -10.72451020669871369, 70.83442372801901854 ) ) ;
#9949 = CARTESIAN_POINT ( 'NONE',  ( -13.97604488694527625, -13.89961937509977652, 41.87390960531435979 ) ) ;
#9951 = ORIENTED_EDGE ( 'NONE', *, *, #182035, .F. ) ;
#9950 = CARTESIAN_POINT ( 'NONE',  ( -21.52544592524334988, -5.823673210054445271, 18.95942372801901143 ) ) ;
#9952 = CARTESIAN_POINT ( 'NONE',  ( 21.52544592524334988, 5.823673210054432836, 51.45942372801901854 ) ) ;
#9953 = ORIENTED_EDGE ( 'NONE', *, *, #58299, .T. ) ;
#9954 = CARTESIAN_POINT ( 'NONE',  ( 9.474510206698971260, -16.51473224551069308, 107.9155762719810383 ) ) ;
#9955 = CARTESIAN_POINT ( 'NONE',  ( 19.03943276465977164, 0.05219959533936151252, 71.25109039468566152 ) ) ;
#9956 = CARTESIAN_POINT ( 'NONE',  ( -21.27520710526540526, 9.818903669220862440, 168.4804316999487241 ) ) ;
#9957 = CARTESIAN_POINT ( 'NONE',  ( -15.72974639402176322, -15.80617190586768395, 24.37609039468567573 ) ) ;
#9958 = CARTESIAN_POINT ( 'NONE',  ( 0.05219959533909260263, 19.03943276465977164, 59.99890960531436690 ) ) ;
#9959 = CARTESIAN_POINT ( 'NONE',  ( -8.314922557961024197, 14.29746914071037800, 42.91775706135235424 ) ) ;
#9960 = CARTESIAN_POINT ( 'NONE',  ( -11.74264578624800670, 36.14014761921585972, -6.149999994537627579 ) ) ;
#9961 = CARTESIAN_POINT ( 'NONE',  ( -19.03943276465977164, -0.05219959533935918106, 18.75109039468567218 ) ) ;
#9962 = CARTESIAN_POINT ( 'NONE',  ( 5.049401038298161559, -19.05341960407611168, 37.70724293864768839 ) ) ;
#9963 = CARTESIAN_POINT ( 'NONE',  ( -13.97604488694547697, 13.89961937509957934, 23.12609039468565442 ) ) ;
#9964 = CARTESIAN_POINT ( 'NONE',  ( 14.29746914071037800, 8.314922557961029526, 86.66775706135234714 ) ) ;
#9966 = CARTESIAN_POINT ( 'NONE',  ( 15.72974639402176855, 15.80617190586768217, 56.87609039468568994 ) ) ;
#9965 = CARTESIAN_POINT ( 'NONE',  ( 16.46253265017160672, -9.564922557960803928, 88.33224293864769550 ) ) ;
#9967 = CARTESIAN_POINT ( 'NONE',  ( -11.40812507854754720, -35.11059874428192273, -10.22499999726881548 ) ) ;
#9968 = CARTESIAN_POINT ( 'NONE',  ( 69.65682714487590488, -71.74905178543389184, -15.00000000000000178 ) ) ;
#9969 = CARTESIAN_POINT ( 'NONE',  ( -17.49999999999999645, 5.499999999999992006, 28.71769037696435234 ) ) ;
#9971 = CARTESIAN_POINT ( 'NONE',  ( 21.53943276465977519, 0.05219959533937863772, 71.25109039468568994 ) ) ;
#9970 = CARTESIAN_POINT ( 'NONE',  ( -16.52544592524335698, -4.483927247898792601, 48.95942372801902565 ) ) ;
#9972 = CARTESIAN_POINT ( 'NONE',  ( -18.62759615963255300, -10.81492255796106328, 104.1677570613523471 ) ) ;
#9973 = CARTESIAN_POINT ( 'NONE',  ( -11.51622829137498805, 9.456233179636171826, -59.95663916823117034 ) ) ;
#9974 = CARTESIAN_POINT ( 'NONE',  ( 14.29746914071037800, 8.314922557961029526, 26.66775706135235424 ) ) ;
#9975 = CARTESIAN_POINT ( 'NONE',  ( -19.03943276465977164, 0.05219959533909376836, 91.24890960531436690 ) ) ;
#9976 = CARTESIAN_POINT ( 'NONE',  ( -5.153800228976328057, -19.02544592524343514, 112.2905762719810099 ) ) ;
#9977 = ORIENTED_EDGE ( 'NONE', *, *, #199123, .T. ) ;
#9978 = CARTESIAN_POINT ( 'NONE',  ( 16.19135201231368981, 7.376712067591806310, 42.68680854052031748 ) ) ;
#9979 = CARTESIAN_POINT ( 'NONE',  ( -14.29746914071049879, 8.314922557960819915, 115.8322429386477097 ) ) ;
#9980 = CARTESIAN_POINT ( 'NONE',  ( -10.81492255796078084, -18.62759615963271287, 42.08224293864769550 ) ) ;
#9981 = CARTESIAN_POINT ( 'NONE',  ( 14.29746914071037800, 8.314922557961029526, 101.6677570613523613 ) ) ;
#9983 = CARTESIAN_POINT ( 'NONE',  ( 5.049401038298161559, -19.05341960407611168, 67.70724293864769550 ) ) ;
#9982 = CARTESIAN_POINT ( 'NONE',  ( 0.05219959533910956823, 16.53943276465976808, 79.99890960531435269 ) ) ;
#9984 = CARTESIAN_POINT ( 'NONE',  ( 18.62759615963255655, 10.81492255796105972, 86.66775706135234714 ) ) ;
#9985 = CARTESIAN_POINT ( 'NONE',  ( -14.29746914071037622, -8.314922557961029526, 19.16775706135234714 ) ) ;
#9986 = CARTESIAN_POINT ( 'NONE',  ( -12.06949235617756955, 12.14591786802309770, 95.62390960531436690 ) ) ;
#9987 = CARTESIAN_POINT ( 'NONE',  ( 0.05219959533937995610, -21.53943276465977519, 40.00109039468567573 ) ) ;
#9988 = CARTESIAN_POINT ( 'NONE',  ( 5.719274019375991003, -21.55341960407610458, 77.70724293864770971 ) ) ;
#9989 = CARTESIAN_POINT ( 'NONE',  ( 5.049401038297881783, 19.05341960407617563, 32.29275706135233293 ) ) ;
#9990 = CARTESIAN_POINT ( 'NONE',  ( -34.57898328185102343, 4.579095689294062410, 50.94499274836915248 ) ) ;
#9991 = CARTESIAN_POINT ( 'NONE',  ( -0.05219959533909027116, -19.03943276465977164, 102.4989096053143669 ) ) ;
#9992 = CARTESIAN_POINT ( 'NONE',  ( 8.314922557960818139, 14.29746914071049879, 64.58224293864769550 ) ) ;
#9993 = CARTESIAN_POINT ( 'NONE',  ( 14.34966873604960469, 8.224510206698951720, 44.16557627198103120 ) ) ;
#9994 = CARTESIAN_POINT ( 'NONE',  ( 14.29746914071049879, -8.314922557960816363, 23.33224293864769194 ) ) ;
#9995 = CARTESIAN_POINT ( 'NONE',  ( 19.03943276465977164, 0.05219959533936151252, 66.25109039468567573 ) ) ;
#9996 = CARTESIAN_POINT ( 'NONE',  ( 19.49671883438228903, 5.499999999999973355, 52.39279849105685116 ) ) ;
#9997 = CARTESIAN_POINT ( 'NONE',  ( 16.51473224551069308, 9.474510206698969483, 114.1655762719810241 ) ) ;
#9998 = CARTESIAN_POINT ( 'NONE',  ( 16.55341960407611168, 4.379528057220329451, 88.95724293864769550 ) ) ;
#9999 = CARTESIAN_POINT ( 'NONE',  ( 24.95432927374997689, 4.974562764236792667, 190.0000000000000000 ) ) ;
#10001 = CARTESIAN_POINT ( 'NONE',  ( -15.72974639402197994, 15.80617190586746368, 50.62390960531435979 ) ) ;
#10000 = CARTESIAN_POINT ( 'NONE',  ( -16.51473224551069308, -9.474510206698971260, 46.66557627198102409 ) ) ;
#10002 = CARTESIAN_POINT ( 'NONE',  ( -0.05219959533907301413, -21.53943276465977519, 82.49890960531436690 ) ) ;
#10003 = CARTESIAN_POINT ( 'NONE',  ( 0.05219959533910956823, 16.53943276465976808, 114.9989096053143669 ) ) ;
#10005 = CARTESIAN_POINT ( 'NONE',  ( 5.049401038298161559, -19.05341960407611168, 42.70724293864767418 ) ) ;
#10004 = CARTESIAN_POINT ( 'NONE',  ( 16.55341960407618274, -4.379528057220086978, 66.04275706135236135 ) ) ;
#10006 = CARTESIAN_POINT ( 'NONE',  ( 19.05341960407617918, -5.049401038297876454, 46.04275706135233293 ) ) ;
#10007 = CARTESIAN_POINT ( 'NONE',  ( 18.67979575497194134, -10.72451020669871369, 60.83442372801901854 ) ) ;
#10008 = CARTESIAN_POINT ( 'NONE',  ( 4.379528057220339221, -16.55341960407611168, 102.7072429386476955 ) ) ;
#10009 = CARTESIAN_POINT ( 'NONE',  ( -16.51473224551082808, 9.474510206698731452, 88.33442372801900433 ) ) ;
#10010 = CARTESIAN_POINT ( 'NONE',  ( -29.86685920354755197, -21.69954338932560134, -4.924999997268813878 ) ) ;
#10012 = CARTESIAN_POINT ( 'NONE',  ( 10.72451020669898902, -18.67979575497178502, 47.91557627198102409 ) ) ;
#10011 = CARTESIAN_POINT ( 'NONE',  ( -0.8101246706333771197, -24.06642195515787108, -56.93999021579659825 ) ) ;
#10013 = CARTESIAN_POINT ( 'NONE',  ( 13.89961937509977652, -13.97604488694527269, 28.12390960531435624 ) ) ;
#10014 = CARTESIAN_POINT ( 'NONE',  ( -5.823673210054431948, 21.52544592524334988, 82.70942372801900433 ) ) ;
#10015 = ORIENTED_EDGE ( 'NONE', *, *, #45882, .T. ) ;
#10016 = CARTESIAN_POINT ( 'NONE',  ( -12.14591786802309592, -12.06949235617757132, 36.87390960531435979 ) ) ;
#10018 = CARTESIAN_POINT ( 'NONE',  ( 12.06949235617757843, -12.14591786802309237, 43.12390960531435269 ) ) ;
#10017 = CARTESIAN_POINT ( 'NONE',  ( 8.314922557961029526, -14.29746914071037800, 55.41775706135234714 ) ) ;
#10019 = CARTESIAN_POINT ( 'NONE',  ( -15.72974639402197994, 15.80617190586746368, 75.62390960531439532 ) ) ;
#10020 = CARTESIAN_POINT ( 'NONE',  ( 0.05219959533907565091, 21.53943276465977519, 79.99890960531435269 ) ) ;
#10021 = DIRECTION ( 'NONE',  ( -1.000000000000000000, -0.000000000000000000, -0.000000000000000000 ) ) ;
#10023 = CARTESIAN_POINT ( 'NONE',  ( 13.97604488694527802, 13.89961937509977652, 114.3739096053143669 ) ) ;
#10022 = CARTESIAN_POINT ( 'NONE',  ( 0.05219959533936267826, -19.03943276465977164, 90.00109039468567573 ) ) ;
#10024 = CARTESIAN_POINT ( 'NONE',  ( -16.51473224551069308, -9.474510206698971260, 46.66557627198102409 ) ) ;
#10025 = CARTESIAN_POINT ( 'NONE',  ( -19.03943276465977164, 0.05219959533909376836, 36.24890960531436690 ) ) ;
#10026 = CARTESIAN_POINT ( 'NONE',  ( 7.500000000000000000, 9.184850993605147944E-16, 10.00000000000000000 ) ) ;
#10027 = VERTEX_POINT ( 'NONE', #136917 ) ;
#10028 = CARTESIAN_POINT ( 'NONE',  ( 14.34966873604972726, -8.224510206698740333, 80.83442372801901854 ) ) ;
#10029 = CARTESIAN_POINT ( 'NONE',  ( 10.81492255796078972, 18.62759615963270932, 109.5822429386476955 ) ) ;
#10030 = CARTESIAN_POINT ( 'NONE',  ( -19.03943276465977164, 0.05219959533909376836, 76.24890960531435269 ) ) ;
#10031 = CARTESIAN_POINT ( 'NONE',  ( 10.72451020669871369, 18.67979575497193778, 37.08442372801901143 ) ) ;
#10032 = CARTESIAN_POINT ( 'NONE',  ( -9.564922557960796823, -16.46253265017161027, 102.0822429386477097 ) ) ;
#10033 = CARTESIAN_POINT ( 'NONE',  ( -28.71047547314692849, -27.16362253576033936, -18.60589795198331231 ) ) ;
#10034 = EDGE_LOOP ( 'NONE', ( #88413, #29183, #24215, #173664, #173536, #22454 ) ) ;
#10035 = CARTESIAN_POINT ( 'NONE',  ( -0.05219959533937732626, 21.53943276465977519, 32.50109039468568284 ) ) ;
#10037 = CARTESIAN_POINT ( 'NONE',  ( -13.89961937509977652, 13.97604488694528158, 105.6239096053143527 ) ) ;
#10036 = CARTESIAN_POINT ( 'NONE',  ( 0.05219959533909260263, 19.03943276465977164, 114.9989096053143669 ) ) ;
#10038 = CARTESIAN_POINT ( 'NONE',  ( 9.474510206698729675, 16.51473224551082808, 37.08442372801899722 ) ) ;
#10039 = CARTESIAN_POINT ( 'NONE',  ( 21.52544592524334988, 5.823673210054432836, 21.45942372801901499 ) ) ;
#10040 = CARTESIAN_POINT ( 'NONE',  ( -5.049401038297874678, -19.05341960407617918, 44.79275706135232582 ) ) ;
#10041 = CARTESIAN_POINT ( 'NONE',  ( -19.05341960407617563, 5.049401038297882671, 43.54275706135232582 ) ) ;
#10042 = CARTESIAN_POINT ( 'NONE',  ( 16.55341960407618274, -4.379528057220086978, 96.04275706135236135 ) ) ;
#10043 = CARTESIAN_POINT ( 'NONE',  ( 9.564922557960805705, 16.46253265017160317, 114.5822429386476955 ) ) ;
#10044 = CARTESIAN_POINT ( 'NONE',  ( 19.02544592524343514, -5.153800228976328945, 78.54057627198099567 ) ) ;
#10045 = CARTESIAN_POINT ( 'NONE',  ( 18.67979575497194134, -10.72451020669871369, 80.83442372801901854 ) ) ;
#10046 = CARTESIAN_POINT ( 'NONE',  ( -21.52544592524334988, -5.823673210054445271, 98.95942372801903275 ) ) ;
#10047 = CARTESIAN_POINT ( 'NONE',  ( 24.20415418211126735, -0.5379555815578801470, -54.28961862586979237 ) ) ;
#10048 = CARTESIAN_POINT ( 'NONE',  ( 19.03943276465977164, -0.05219959533909143690, 83.74890960531436690 ) ) ;
#10049 = CARTESIAN_POINT ( 'NONE',  ( -21.52544592524334988, -5.823673210054445271, 63.95942372801901854 ) ) ;
#10050 = CARTESIAN_POINT ( 'NONE',  ( -5.153800228976607833, 19.02544592524334988, 107.7094237280189759 ) ) ;
#10051 = CARTESIAN_POINT ( 'NONE',  ( 16.46253265017160672, -9.564922557960803928, 63.33224293864769550 ) ) ;
#10052 = CARTESIAN_POINT ( 'NONE',  ( 21.52544592524344225, -5.823673210054117533, 23.54057627198102765 ) ) ;
#10053 = CARTESIAN_POINT ( 'NONE',  ( 19.05341960407611168, 5.049401038298154454, 83.95724293864766707 ) ) ;
#10054 = CARTESIAN_POINT ( 'NONE',  ( 28.47622644277404191, -25.16156846422445881, -16.68312038616162241 ) ) ;
#10055 = CARTESIAN_POINT ( 'NONE',  ( -13.97604488694527625, -13.89961937509977652, 61.87390960531435979 ) ) ;
#10056 = CARTESIAN_POINT ( 'NONE',  ( -9.474510206698964154, 16.51473224551069663, 50.41557627198102409 ) ) ;
#10057 = CARTESIAN_POINT ( 'NONE',  ( 10.81492255796078972, 18.62759615963270932, 109.5822429386476955 ) ) ;
#10058 = CARTESIAN_POINT ( 'NONE',  ( 14.34966873604972726, -8.224510206698740333, 100.8344237280190185 ) ) ;
#10059 = CARTESIAN_POINT ( 'NONE',  ( 0.4034547045401649656, 16.64828639225574136, -61.36869763530247468 ) ) ;
#10060 = CARTESIAN_POINT ( 'NONE',  ( 9.564922557961047289, -16.46253265017146816, 60.41775706135233293 ) ) ;
#10061 = CARTESIAN_POINT ( 'NONE',  ( 5.153800228976335163, 19.02544592524342804, 89.79057627198102409 ) ) ;
#10062 = CARTESIAN_POINT ( 'NONE',  ( 16.53943276465976808, -0.05219959533910856209, 73.74890960531433848 ) ) ;
#10063 = CARTESIAN_POINT ( 'NONE',  ( 14.29746914071049879, -8.314922557960816363, 113.3322429386476955 ) ) ;
#10064 = CARTESIAN_POINT ( 'NONE',  ( 15.80617190586746368, 15.72974639402197994, 39.37390960531436690 ) ) ;
#10065 = CARTESIAN_POINT ( 'NONE',  ( 19.03943276465977164, -0.05219959533909143690, 113.7489096053143669 ) ) ;
#10066 = CARTESIAN_POINT ( 'NONE',  ( 14.29746914071049879, -8.314922557960816363, 93.33224293864769550 ) ) ;
#10067 = CARTESIAN_POINT ( 'NONE',  ( 32.00000000000000000, -6.184466335694137604E-15, 50.50000000000002842 ) ) ;
#10068 = CARTESIAN_POINT ( 'NONE',  ( -19.02544592524334988, -5.153800228976617603, 28.95942372801900433 ) ) ;
#10069 = CARTESIAN_POINT ( 'NONE',  ( -8.314922557961024197, 14.29746914071037800, 107.9177570613523471 ) ) ;
#10071 = EDGE_CURVE ( 'NONE', #170287, #25627, #21017, .T. ) ;
#10070 = CARTESIAN_POINT ( 'NONE',  ( -19.03943276465977164, 0.05219959533909376836, 91.24890960531436690 ) ) ;
#10072 = CARTESIAN_POINT ( 'NONE',  ( -21.55341960407619339, 5.719274019375674811, 48.54275706135234714 ) ) ;
#10073 = CARTESIAN_POINT ( 'NONE',  ( 18.62759615963271287, -10.81492255796078972, 43.33224293864769550 ) ) ;
#10075 = ORIENTED_EDGE ( 'NONE', *, *, #1629, .F. ) ;
#10074 = CARTESIAN_POINT ( 'NONE',  ( -18.62759615963255300, -10.81492255796106328, 29.16775706135234003 ) ) ;
#10076 = CARTESIAN_POINT ( 'NONE',  ( 18.67979575497178502, 10.72451020669898547, 79.16557627198103830 ) ) ;
#10077 = CARTESIAN_POINT ( 'NONE',  ( -8.314922557960811034, -14.29746914071050412, 97.08224293864770971 ) ) ;
#10078 = CARTESIAN_POINT ( 'NONE',  ( 19.05341960407617918, -5.049401038297876454, 56.04275706135234714 ) ) ;
#10079 = CARTESIAN_POINT ( 'NONE',  ( -13.89961937509977652, 13.97604488694528158, 50.62390960531435979 ) ) ;
#10080 = CARTESIAN_POINT ( 'NONE',  ( 19.03943276465977164, -0.05219959533909143690, 93.74890960531435269 ) ) ;
#10081 = CARTESIAN_POINT ( 'NONE',  ( -19.05341960407611168, -5.049401038298163336, 96.45724293864769550 ) ) ;
#10082 = CARTESIAN_POINT ( 'NONE',  ( -12.14591786802309592, -12.06949235617757132, 111.8739096053143669 ) ) ;
#10083 = CARTESIAN_POINT ( 'NONE',  ( -16.53943276465976808, 0.05219959533911058130, 46.24890960531435979 ) ) ;
#10084 = CARTESIAN_POINT ( 'NONE',  ( 8.224510206698742110, 14.34966873604972548, 37.08442372801901143 ) ) ;
#10085 = CARTESIAN_POINT ( 'NONE',  ( -5.719274019375665041, -21.55341960407619695, 104.7927570613523898 ) ) ;
#10087 = CARTESIAN_POINT ( 'NONE',  ( 16.52544592524335698, 4.483927247898782831, 111.4594237280190328 ) ) ;
#10086 = CARTESIAN_POINT ( 'NONE',  ( 5.049401038298161559, -19.05341960407611168, 112.7072429386476813 ) ) ;
#10088 = CARTESIAN_POINT ( 'NONE',  ( -21.52544592524334988, -5.823673210054445271, 38.95942372801901854 ) ) ;
#10089 = CARTESIAN_POINT ( 'NONE',  ( 19.02544592524343514, -5.153800228976328945, 103.5405762719809957 ) ) ;
#10090 = CARTESIAN_POINT ( 'NONE',  ( 14.29746914071037800, 8.314922557961029526, 51.66775706135234714 ) ) ;
#10091 = CARTESIAN_POINT ( 'NONE',  ( -8.314922557961024197, 14.29746914071037800, 112.9177570613523329 ) ) ;
#10092 = CARTESIAN_POINT ( 'NONE',  ( 16.52544592524335698, 4.483927247898782831, 96.45942372801901854 ) ) ;
#10093 = CARTESIAN_POINT ( 'NONE',  ( 14.29746914071037800, 8.314922557961029526, 21.66775706135235069 ) ) ;
#10094 = CARTESIAN_POINT ( 'NONE',  ( 16.46253265017160672, -9.564922557960803928, 43.33224293864769550 ) ) ;
#10095 = CARTESIAN_POINT ( 'NONE',  ( 8.314922557960818139, 14.29746914071049879, 114.5822429386477097 ) ) ;
#10096 = CARTESIAN_POINT ( 'NONE',  ( 10.72451020669898902, -18.67979575497178502, 112.9155762719810383 ) ) ;
#10097 = CARTESIAN_POINT ( 'NONE',  ( 19.03943276465977164, -0.05219959533909143690, 33.74890960531435979 ) ) ;
#10098 = CARTESIAN_POINT ( 'NONE',  ( -13.89961937509977652, 13.97604488694528158, 105.6239096053143527 ) ) ;
#10099 = CARTESIAN_POINT ( 'NONE',  ( 18.67979575497194134, -10.72451020669871369, 30.83442372801902209 ) ) ;
#10100 = CARTESIAN_POINT ( 'NONE',  ( 11.74149087413294268, 36.13659316521247433, -2.602157773949823394 ) ) ;
#10101 = CARTESIAN_POINT ( 'NONE',  ( -16.51473224551069308, -9.474510206698971260, 106.6655762719810383 ) ) ;
#10102 = CARTESIAN_POINT ( 'NONE',  ( 17.40805194822032220, -6.112264579159320199, 113.3337127251061389 ) ) ;
#10103 = CARTESIAN_POINT ( 'NONE',  ( 16.51473224551069308, 9.474510206698969483, 94.16557627198103830 ) ) ;
#10105 = CARTESIAN_POINT ( 'NONE',  ( -8.224510206698948167, 14.34966873604960824, 95.41557627198102409 ) ) ;
#10104 = CARTESIAN_POINT ( 'NONE',  ( 21.53943276465977519, 0.05219959533937863772, 51.25109039468568994 ) ) ;
#10106 = CARTESIAN_POINT ( 'NONE',  ( 16.46253265017160672, -9.564922557960803928, 98.33224293864769550 ) ) ;
#10107 = CARTESIAN_POINT ( 'NONE',  ( -27.96784714409843886, -7.240004476342272177, 160.9788157999716702 ) ) ;
#10108 = CARTESIAN_POINT ( 'NONE',  ( -4.483927247898782831, 16.52544592524335698, 62.70942372801902565 ) ) ;
#10109 = CARTESIAN_POINT ( 'NONE',  ( -5.719274019375665041, -21.55341960407619695, 79.79275706135236135 ) ) ;
#10110 = CARTESIAN_POINT ( 'NONE',  ( -16.53943276465976808, -0.05219959533934237506, 43.75109039468568284 ) ) ;
#10111 = CARTESIAN_POINT ( 'NONE',  ( 9.564922557960805705, 16.46253265017160317, 79.58224293864769550 ) ) ;
#10112 = CARTESIAN_POINT ( 'NONE',  ( 19.05341960407617918, -5.049401038297876454, 111.0427570613523329 ) ) ;
#10113 = CARTESIAN_POINT ( 'NONE',  ( 12.06949235617739724, 12.14591786802326823, 66.87609039468568994 ) ) ;
#10114 = CARTESIAN_POINT ( 'NONE',  ( -10.72451020669870658, -18.67979575497194134, 104.5844237280190185 ) ) ;
#10115 = CARTESIAN_POINT ( 'NONE',  ( 9.564922557961047289, -16.46253265017146816, 95.41775706135233293 ) ) ;
#10116 = CARTESIAN_POINT ( 'NONE',  ( -16.46253265017160317, 9.564922557960807481, 65.83224293864769550 ) ) ;
#10117 = CARTESIAN_POINT ( 'NONE',  ( -21.53943276465977519, 0.05219959533907696930, 86.24890960531436690 ) ) ;
#10119 = CARTESIAN_POINT ( 'NONE',  ( 16.46253265017146816, 9.564922557961045513, 96.66775706135233293 ) ) ;
#10118 = CARTESIAN_POINT ( 'NONE',  ( -16.52544592524342804, 4.483927247898546575, 96.04057627198102409 ) ) ;
#10120 = CARTESIAN_POINT ( 'NONE',  ( 16.55341960407618274, -4.379528057220086978, 66.04275706135236135 ) ) ;
#10121 = CARTESIAN_POINT ( 'NONE',  ( 24.10884208241212079, 5.471882726980997980, 173.8287385965645058 ) ) ;
#10122 = CARTESIAN_POINT ( 'NONE',  ( 16.51473224551083163, -9.474510206698727899, 55.83442372801899722 ) ) ;
#10123 = CARTESIAN_POINT ( 'NONE',  ( 16.55341960407611168, 4.379528057220329451, 28.95724293864769905 ) ) ;
#10124 = CARTESIAN_POINT ( 'NONE',  ( 16.55341960407611168, 4.379528057220329451, 83.95724293864770971 ) ) ;
#10126 = CARTESIAN_POINT ( 'NONE',  ( -17.50000000001356781, 5.500000000000039968, 40.79690382535057580 ) ) ;
#10125 = CARTESIAN_POINT ( 'NONE',  ( 9.474510206698729675, 16.51473224551082808, 22.08442372801899722 ) ) ;
#10127 = CARTESIAN_POINT ( 'NONE',  ( 18.62759615963255655, 10.81492255796105972, 26.66775706135235424 ) ) ;
#10128 = CARTESIAN_POINT ( 'NONE',  ( -5.049401038298153566, 19.05341960407611168, 105.2072429386476671 ) ) ;
#10129 = CARTESIAN_POINT ( 'NONE',  ( 5.049401038298161559, -19.05341960407611168, 82.70724293864770971 ) ) ;
#10130 = CARTESIAN_POINT ( 'NONE',  ( 21.53943276465977519, 0.05219959533937863772, 101.2510903946856757 ) ) ;
#10131 = CARTESIAN_POINT ( 'NONE',  ( -9.474510206698964154, 16.51473224551069663, 75.41557627198103830 ) ) ;
#10132 = CARTESIAN_POINT ( 'NONE',  ( -10.72451020669898014, 18.67979575497178502, 45.41557627198103830 ) ) ;
#10133 = CARTESIAN_POINT ( 'NONE',  ( 14.34966873604960469, 8.224510206698951720, 84.16557627198103830 ) ) ;
#10134 = CARTESIAN_POINT ( 'NONE',  ( -16.51473224551069308, -9.474510206698971260, 61.66557627198103120 ) ) ;
#10135 = CARTESIAN_POINT ( 'NONE',  ( 12.14591786802309770, 12.06949235617756955, 94.37390960531436690 ) ) ;
#10136 = CARTESIAN_POINT ( 'NONE',  ( 10.72451020669898902, -18.67979575497178502, 107.9155762719810241 ) ) ;
#10137 = CARTESIAN_POINT ( 'NONE',  ( -18.67979575497193778, 10.72451020669871902, 63.33442372801900433 ) ) ;
#10138 = CARTESIAN_POINT ( 'NONE',  ( -13.89961937509977652, 13.97604488694528158, 30.62390960531435269 ) ) ;
#10139 = EDGE_CURVE ( 'NONE', #35858, #196503, #111377, .T. ) ;
#10140 = CARTESIAN_POINT ( 'NONE',  ( -16.55341960407617563, 4.379528057220093196, 68.54275706135234714 ) ) ;
#10141 = CARTESIAN_POINT ( 'NONE',  ( 21.55341960407619695, -5.719274019375665929, 21.04275706135234714 ) ) ;
#10142 = CARTESIAN_POINT ( 'NONE',  ( 10.81492255796078972, 18.62759615963270932, 109.5822429386476955 ) ) ;
#10144 = CARTESIAN_POINT ( 'NONE',  ( 16.51473224551069308, 9.474510206698969483, 49.16557627198102409 ) ) ;
#10143 = CARTESIAN_POINT ( 'NONE',  ( 0.05219959533936267826, -19.03943276465977164, 45.00109039468566863 ) ) ;
#10145 = LINE ( 'NONE', #149649, #28034 ) ;
#10146 = CARTESIAN_POINT ( 'NONE',  ( 18.67979575497194134, -10.72451020669871369, 65.83442372801900433 ) ) ;
#10147 = CARTESIAN_POINT ( 'NONE',  ( 18.67979575497178502, 10.72451020669898547, 54.16557627198103120 ) ) ;
#10148 = CARTESIAN_POINT ( 'NONE',  ( 16.55341960407611168, 4.379528057220329451, 33.95724293864769550 ) ) ;
#10150 = CARTESIAN_POINT ( 'NONE',  ( 5.823673210054444382, -21.52544592524334988, 105.2094237280190328 ) ) ;
#10149 = CARTESIAN_POINT ( 'NONE',  ( 21.55341960407619695, -5.719274019375665929, 81.04275706135236135 ) ) ;
#10151 = CARTESIAN_POINT ( 'NONE',  ( -4.483927247898539470, -16.52544592524342804, 62.29057627198102409 ) ) ;
#10152 = CARTESIAN_POINT ( 'NONE',  ( 4.483927247898545687, 16.52544592524342804, 109.7905762719810383 ) ) ;
#10153 = CARTESIAN_POINT ( 'NONE',  ( -0.05219959533936034679, 19.03943276465977164, 47.50109039468566863 ) ) ;
#10154 = CARTESIAN_POINT ( 'NONE',  ( -12.06949235617739369, -12.14591786802326823, 109.3760903946857042 ) ) ;
#10155 = CARTESIAN_POINT ( 'NONE',  ( 5.823673210054444382, -21.52544592524334988, 70.20942372801904696 ) ) ;
#10156 = CARTESIAN_POINT ( 'NONE',  ( -16.51473224551069308, -9.474510206698971260, 56.66557627198103120 ) ) ;
#10157 = CARTESIAN_POINT ( 'NONE',  ( -19.02544592524334988, -5.153800228976617603, 33.95942372801897591 ) ) ;
#10158 = CARTESIAN_POINT ( 'NONE',  ( -10.81492255796078084, -18.62759615963271287, 32.08224293864769550 ) ) ;
#10159 = CARTESIAN_POINT ( 'NONE',  ( -5.823673210054431948, 21.52544592524334988, 32.70942372801900433 ) ) ;
#10160 = CARTESIAN_POINT ( 'NONE',  ( 10.72451020669898902, -18.67979575497178502, 87.91557627198103830 ) ) ;
#10161 = CARTESIAN_POINT ( 'NONE',  ( 19.02544592524334988, 5.153800228976608722, 86.45942372801900433 ) ) ;
#10162 = CARTESIAN_POINT ( 'NONE',  ( -14.29746914071037622, -8.314922557961029526, 59.16775706135234714 ) ) ;
#10164 = CARTESIAN_POINT ( 'NONE',  ( 5.719274019375991003, -21.55341960407610458, 87.70724293864769550 ) ) ;
#10163 = DIRECTION ( 'NONE',  ( 3.491481338843133750E-15, 1.000000000000000000, -0.000000000000000000 ) ) ;
#10165 = CARTESIAN_POINT ( 'NONE',  ( -14.29746914071049879, 8.314922557960819915, 90.83224293864769550 ) ) ;
#10166 = DIRECTION ( 'NONE',  ( -0.000000000000000000, 1.000000000000000000, 1.224646799147353207E-16 ) ) ;
#10167 = CARTESIAN_POINT ( 'NONE',  ( -8.224510206698735004, -14.34966873604973081, 19.58442372801901143 ) ) ;
#10168 = CARTESIAN_POINT ( 'NONE',  ( -21.52544592524343514, 5.823673210054127303, 46.04057627198103830 ) ) ;
#10169 = CARTESIAN_POINT ( 'NONE',  ( -4.379528057220086978, -16.55341960407618274, 79.79275706135236135 ) ) ;
#10170 = LINE ( 'NONE', #71830, #164109 ) ;
#10171 = CARTESIAN_POINT ( 'NONE',  ( -14.34966873604972548, 8.224510206698743886, 53.33442372801901854 ) ) ;
#10172 = CARTESIAN_POINT ( 'NONE',  ( 0.05219959533937995610, -21.53943276465977519, 30.00109039468568284 ) ) ;
#10173 = CARTESIAN_POINT ( 'NONE',  ( 21.52544592524344225, -5.823673210054117533, 48.54057627198103120 ) ) ;
#10174 = CARTESIAN_POINT ( 'NONE',  ( 4.379528057220092307, 16.55341960407617563, 72.29275706135236135 ) ) ;
#10175 = CARTESIAN_POINT ( 'NONE',  ( 19.05341960407611168, 5.049401038298154454, 93.95724293864769550 ) ) ;
#10177 = CARTESIAN_POINT ( 'NONE',  ( -5.153800228976328057, -19.02544592524343514, 22.29057627198102765 ) ) ;
#10176 = CARTESIAN_POINT ( 'NONE',  ( 0.05219959533937995610, -21.53943276465977519, 60.00109039468568284 ) ) ;
#10178 = CARTESIAN_POINT ( 'NONE',  ( -0.05219959533907301413, -21.53943276465977519, 37.49890960531436690 ) ) ;
#10179 = CARTESIAN_POINT ( 'NONE',  ( 21.52544592524344225, -5.823673210054117533, 23.54057627198102765 ) ) ;
#10180 = ORIENTED_EDGE ( 'NONE', *, *, #14847, .F. ) ;
#10181 = CARTESIAN_POINT ( 'NONE',  ( 19.03943276465977164, 0.05219959533936151252, 41.25109039468566152 ) ) ;
#10182 = CARTESIAN_POINT ( 'NONE',  ( -8.314922557961024197, 14.29746914071037800, 47.91775706135234714 ) ) ;
#10183 = CARTESIAN_POINT ( 'NONE',  ( 16.46253265017160672, -9.564922557960803928, 113.3322429386476955 ) ) ;
#10184 = VERTEX_POINT ( 'NONE', #31732 ) ;
#10185 = CARTESIAN_POINT ( 'NONE',  ( 19.03943276465977164, -0.05219959533909143690, 83.74890960531436690 ) ) ;
#10186 = CARTESIAN_POINT ( 'NONE',  ( 16.55341960407618274, -4.379528057220086978, 96.04275706135236135 ) ) ;
#10187 = CARTESIAN_POINT ( 'NONE',  ( -1.734723475976807094E-15, 15.20000000000001883, -65.00100000000003320 ) ) ;
#10188 = CARTESIAN_POINT ( 'NONE',  ( -14.29746914071049879, 8.314922557960819915, 90.83224293864769550 ) ) ;
#10189 = CARTESIAN_POINT ( 'NONE',  ( 0.05219959533907565091, 21.53943276465977519, 54.99890960531435269 ) ) ;
#10190 = CARTESIAN_POINT ( 'NONE',  ( -16.51473224551069308, -9.474510206698971260, 31.66557627198102054 ) ) ;
#10191 = CARTESIAN_POINT ( 'NONE',  ( 16.55341960407618274, -4.379528057220086978, 71.04275706135234714 ) ) ;
#10192 = CARTESIAN_POINT ( 'NONE',  ( -15.72974639402176322, -15.80617190586768395, 29.37609039468568284 ) ) ;
#10193 = CARTESIAN_POINT ( 'NONE',  ( 13.89961937509957401, 13.97604488694547697, 86.87609039468567573 ) ) ;
#10194 = CARTESIAN_POINT ( 'NONE',  ( -19.03943276465977164, 0.05219959533909376836, 36.24890960531436690 ) ) ;
#10195 = CARTESIAN_POINT ( 'NONE',  ( -0.05219959533909027116, -19.03943276465977164, 107.4989096053143527 ) ) ;
#10196 = CARTESIAN_POINT ( 'NONE',  ( -10.72451020669870658, -18.67979575497194134, 109.5844237280190328 ) ) ;
#10197 = CARTESIAN_POINT ( 'NONE',  ( 13.97604488694527802, 13.89961937509977652, 84.37390960531433848 ) ) ;
#10198 = CARTESIAN_POINT ( 'NONE',  ( -16.53943276465976808, -0.05219959533934237506, 68.75109039468568994 ) ) ;
#10199 = CARTESIAN_POINT ( 'NONE',  ( -5.823673210054431948, 21.52544592524334988, 92.70942372801901854 ) ) ;
#10200 = CARTESIAN_POINT ( 'NONE',  ( 0.05219959533936267826, -19.03943276465977164, 50.00109039468566863 ) ) ;
#10201 = CARTESIAN_POINT ( 'NONE',  ( 13.89961937509957401, 13.97604488694547697, 66.87609039468567573 ) ) ;
#10202 = ORIENTED_EDGE ( 'NONE', *, *, #2366, .F. ) ;
#10203 = CARTESIAN_POINT ( 'NONE',  ( 15.72974639402176855, 15.80617190586768217, 66.87609039468568994 ) ) ;
#10204 = CARTESIAN_POINT ( 'NONE',  ( 16.46253265017160672, -9.564922557960803928, 63.33224293864769550 ) ) ;
#10205 = CARTESIAN_POINT ( 'NONE',  ( -16.51473224551069308, -9.474510206698971260, 26.66557627198103120 ) ) ;
#10206 = CARTESIAN_POINT ( 'NONE',  ( 5.049401038297881783, 19.05341960407617563, 57.29275706135231871 ) ) ;
#10207 = CARTESIAN_POINT ( 'NONE',  ( 9.474510206698971260, -16.51473224551069308, 112.9155762719810383 ) ) ;
#10208 = CARTESIAN_POINT ( 'NONE',  ( 5.153800228976335163, 19.02544592524342804, 84.79057627198099567 ) ) ;
#10209 = CARTESIAN_POINT ( 'NONE',  ( 14.29746914071049879, -8.314922557960816363, 33.33224293864769550 ) ) ;
#10210 = CARTESIAN_POINT ( 'NONE',  ( -21.53943276465977519, 0.05219959533907696930, 31.24890960531435979 ) ) ;
#10211 = CARTESIAN_POINT ( 'NONE',  ( -17.72662750342726667, -5.499999999999959144, 96.40179492283743912 ) ) ;
#10212 = CARTESIAN_POINT ( 'NONE',  ( -0.05219959533936034679, 19.03943276465977164, 22.50109039468566152 ) ) ;
#10213 = CARTESIAN_POINT ( 'NONE',  ( -7.656827144875921753, -71.74905178543390605, -15.00000000000000000 ) ) ;
#10214 = CARTESIAN_POINT ( 'NONE',  ( 19.03943276465977164, -0.05219959533909143690, 43.74890960531435979 ) ) ;
#10215 = CARTESIAN_POINT ( 'NONE',  ( -16.46253265017160317, 9.564922557960807481, 85.83224293864769550 ) ) ;
#10216 = CARTESIAN_POINT ( 'NONE',  ( -34.48725679702496194, -1.430676605895445430, 89.67714645826994513 ) ) ;
#10217 = CARTESIAN_POINT ( 'NONE',  ( -15.80617190586768217, 15.72974639402176855, 68.12609039468567573 ) ) ;
#10218 = CARTESIAN_POINT ( 'NONE',  ( -34.63926591227897234, -15.08268834117409973, -8.000000000000003553 ) ) ;
#10219 = CARTESIAN_POINT ( 'NONE',  ( -16.53943276465976808, -0.05219959533934237506, 58.75109039468568994 ) ) ;
#10220 = CARTESIAN_POINT ( 'NONE',  ( 5.823673210054125526, 21.52544592524343514, 79.79057627198102409 ) ) ;
#10221 = CARTESIAN_POINT ( 'NONE',  ( -4.379528057220328563, 16.55341960407611168, 50.20724293864769550 ) ) ;
#10223 = CARTESIAN_POINT ( 'NONE',  ( 19.02544592524343514, -5.153800228976328945, 113.5405762719810241 ) ) ;
#10222 = CARTESIAN_POINT ( 'NONE',  ( 19.03943276465977164, -0.05219959533909143690, 33.74890960531435979 ) ) ;
#10224 = CARTESIAN_POINT ( 'NONE',  ( 21.55341960407619695, -5.719274019375665929, 26.04275706135235779 ) ) ;
#10225 = CARTESIAN_POINT ( 'NONE',  ( -16.51473224551082808, 9.474510206698731452, 43.33442372801900433 ) ) ;
#10226 = CARTESIAN_POINT ( 'NONE',  ( -19.03943276465977164, 0.05219959533909376836, 31.24890960531435979 ) ) ;
#10227 = CARTESIAN_POINT ( 'NONE',  ( 5.823673210054444382, -21.52544592524334988, 80.20942372801901854 ) ) ;
#10228 = CARTESIAN_POINT ( 'NONE',  ( 16.31925111598458855, -7.325300261831445781, 32.66424538967252289 ) ) ;
#10229 = CARTESIAN_POINT ( 'NONE',  ( 4.483927247898545687, 16.52544592524342804, 24.79057627198103120 ) ) ;
#10230 = DIRECTION ( 'NONE',  ( 0.000000000000000000, 0.000000000000000000, 1.000000000000000000 ) ) ;
#10231 = CARTESIAN_POINT ( 'NONE',  ( 10.81492255796078972, 18.62759615963270932, 44.58224293864769550 ) ) ;
#10232 = CARTESIAN_POINT ( 'NONE',  ( 9.090093023806478101, -0.1983487321476342102, -63.95305636720453890 ) ) ;
#10233 = CARTESIAN_POINT ( 'NONE',  ( -13.89961937509977652, 13.97604488694528158, 95.62390960531436690 ) ) ;
#10234 = CARTESIAN_POINT ( 'NONE',  ( 16.52544592524342804, -4.483927247898539470, 93.54057627198103830 ) ) ;
#10235 = CARTESIAN_POINT ( 'NONE',  ( 9.474510206698729675, 16.51473224551082808, 112.0844237280190043 ) ) ;
#10236 = CARTESIAN_POINT ( 'NONE',  ( -10.81492255796078084, -18.62759615963271287, 67.08224293864770971 ) ) ;
#10237 = ORIENTED_EDGE ( 'NONE', *, *, #127999, .T. ) ;
#10238 = CARTESIAN_POINT ( 'NONE',  ( 0.05219959533909260263, 19.03943276465977164, 29.99890960531435979 ) ) ;
#10239 = EDGE_CURVE ( 'NONE', #176032, #199255, #155066, .T. ) ;
#10241 = CARTESIAN_POINT ( 'NONE',  ( -21.55341960407610458, -5.719274019375992779, 86.45724293864770971 ) ) ;
#10240 = CARTESIAN_POINT ( 'NONE',  ( 5.049401038298161559, -19.05341960407611168, 82.70724293864770971 ) ) ;
#10243 = CARTESIAN_POINT ( 'NONE',  ( -19.02544592524342804, 5.153800228976336051, 106.0405762719810241 ) ) ;
#10242 = CARTESIAN_POINT ( 'NONE',  ( 14.29746914071037800, 8.314922557961029526, 111.6677570613523613 ) ) ;
#10244 = CARTESIAN_POINT ( 'NONE',  ( 5.049401038297881783, 19.05341960407617563, 77.29275706135231871 ) ) ;
#10245 = CARTESIAN_POINT ( 'NONE',  ( -10.81492255796105439, 18.62759615963255655, 92.91775706135236135 ) ) ;
#10246 = CARTESIAN_POINT ( 'NONE',  ( -18.62759615963270932, 10.81492255796079327, 80.83224293864769550 ) ) ;
#10247 = CARTESIAN_POINT ( 'NONE',  ( 0.05219959533907565091, 21.53943276465977519, 39.99890960531436690 ) ) ;
#10248 = CARTESIAN_POINT ( 'NONE',  ( -13.89961937509977652, 13.97604488694528158, 50.62390960531435979 ) ) ;
#10249 = CARTESIAN_POINT ( 'NONE',  ( 4.483927247898545687, 16.52544592524342804, 24.79057627198103120 ) ) ;
#10250 = CARTESIAN_POINT ( 'NONE',  ( 13.97604488694527802, 13.89961937509977652, 69.37390960531436690 ) ) ;
#10251 = ORIENTED_EDGE ( 'NONE', *, *, #50509, .T. ) ;
#10252 = FACE_OUTER_BOUND ( 'NONE', #20116, .T. ) ;
#10253 = CARTESIAN_POINT ( 'NONE',  ( 0.05219959533936267826, -19.03943276465977164, 25.00109039468566152 ) ) ;
#10254 = CARTESIAN_POINT ( 'NONE',  ( 16.53943276465976808, -0.05219959533910856209, 78.74890960531436690 ) ) ;
#10255 = CARTESIAN_POINT ( 'NONE',  ( 5.823673210054444382, -21.52544592524334988, 30.20942372801902565 ) ) ;
#10256 = CARTESIAN_POINT ( 'NONE',  ( -8.571926809382608425, 26.38167802310805854, 144.9750000027312069 ) ) ;
#10257 = CARTESIAN_POINT ( 'NONE',  ( -18.62759615963270932, 10.81492255796079327, 60.83224293864769550 ) ) ;
#10258 = CARTESIAN_POINT ( 'NONE',  ( 0.05219959533934541429, -16.53943276465976808, 100.0010903946857042 ) ) ;
#10259 = CARTESIAN_POINT ( 'NONE',  ( -12.06949235617756955, 12.14591786802309770, 110.6239096053143669 ) ) ;
#10260 = CARTESIAN_POINT ( 'NONE',  ( 19.03943276465977164, -0.05219959533909143690, 68.74890960531436690 ) ) ;
#10261 =( NAMED_UNIT ( * ) PLANE_ANGLE_UNIT ( ) SI_UNIT ( $, .RADIAN. ) );
#10262 = FACE_OUTER_BOUND ( 'NONE', #193309, .T. ) ;
#10263 = CARTESIAN_POINT ( 'NONE',  ( 16.52544592524342804, -4.483927247898539470, 33.54057627198102409 ) ) ;
#10264 = CARTESIAN_POINT ( 'NONE',  ( 5.823673210054444382, -21.52544592524334988, 45.20942372801901854 ) ) ;
#10265 = CARTESIAN_POINT ( 'NONE',  ( 16.51473224551069308, 9.474510206698969483, 109.1655762719810383 ) ) ;
#10266 = CARTESIAN_POINT ( 'NONE',  ( 15.80617190586769283, -15.72974639402175789, 80.62609039468567573 ) ) ;
#10267 = CARTESIAN_POINT ( 'NONE',  ( 9.474510206698971260, -16.51473224551069308, 32.91557627198102409 ) ) ;
#10268 = CARTESIAN_POINT ( 'NONE',  ( 5.049401038298161559, -19.05341960407611168, 42.70724293864767418 ) ) ;
#10269 = EDGE_LOOP ( 'NONE', ( #111846, #198402 ) ) ;
#10270 = CARTESIAN_POINT ( 'NONE',  ( -5.719274019375665041, -21.55341960407619695, 99.79275706135234714 ) ) ;
#10271 = CARTESIAN_POINT ( 'NONE',  ( 0.05219959533934541429, -16.53943276465976808, 50.00109039468568994 ) ) ;
#10272 = CARTESIAN_POINT ( 'NONE',  ( 15.80617190586769283, -15.72974639402175789, 80.62609039468567573 ) ) ;
#10273 = CARTESIAN_POINT ( 'NONE',  ( 16.46253265017160672, -9.564922557960803928, 108.3322429386476955 ) ) ;
#10274 = CARTESIAN_POINT ( 'NONE',  ( -16.51473224551082808, 9.474510206698731452, 88.33442372801900433 ) ) ;
#10275 = CARTESIAN_POINT ( 'NONE',  ( 18.67979575497194134, -10.72451020669871369, 55.83442372801901854 ) ) ;
#10276 = CARTESIAN_POINT ( 'NONE',  ( 12.14591786802327356, -12.06949235617739191, 25.62609039468567929 ) ) ;
#10277 = CARTESIAN_POINT ( 'NONE',  ( -13.97604488694547697, 13.89961937509957934, 88.12609039468563310 ) ) ;
#10278 = CARTESIAN_POINT ( 'NONE',  ( -16.51473224551069308, -9.474510206698971260, 46.66557627198102409 ) ) ;
#10279 = CARTESIAN_POINT ( 'NONE',  ( -0.05219959533936034679, 19.03943276465977164, 92.50109039468566152 ) ) ;
#10280 = EDGE_CURVE ( 'NONE', #27947, #199067, #69380, .T. ) ;
#10281 = CARTESIAN_POINT ( 'NONE',  ( -12.06949235617756955, 12.14591786802309770, 25.62390960531435624 ) ) ;
#10282 = CARTESIAN_POINT ( 'NONE',  ( 5.049401038297881783, 19.05341960407617563, 87.29275706135234714 ) ) ;
#10283 = CARTESIAN_POINT ( 'NONE',  ( 8.224510206698953496, -14.34966873604960469, 47.91557627198102409 ) ) ;
#10284 = CARTESIAN_POINT ( 'NONE',  ( 9.564922557961047289, -16.46253265017146816, 65.41775706135233293 ) ) ;
#10285 = CARTESIAN_POINT ( 'NONE',  ( 14.29746914071037800, 8.314922557961029526, 66.66775706135234714 ) ) ;
#10286 = CARTESIAN_POINT ( 'NONE',  ( -16.46253265017146816, -9.564922557961047289, 19.16775706135233293 ) ) ;
#10287 = CARTESIAN_POINT ( 'NONE',  ( -12.06949235617756955, 12.14591786802309770, 115.6239096053143669 ) ) ;
#10288 = CARTESIAN_POINT ( 'NONE',  ( -19.03943276465977164, 0.05219959533909376836, 36.24890960531436690 ) ) ;
#10289 = CARTESIAN_POINT ( 'NONE',  ( 16.52544592524335698, 4.483927247898782831, 56.45942372801902565 ) ) ;
#10290 = CARTESIAN_POINT ( 'NONE',  ( 2.021687836487040535, 2.168404344971008868E-16, 0.000000000000000000 ) ) ;
#10292 = AXIS2_PLACEMENT_3D ( 'NONE', #91072, #108246, #169925 ) ;
#10291 = CARTESIAN_POINT ( 'NONE',  ( 27.73933785331498569, 2.768321779492822058E-14, 147.8750000027311842 ) ) ;
#10293 = CARTESIAN_POINT ( 'NONE',  ( 16.46253265017160672, -9.564922557960803928, 108.3322429386476955 ) ) ;
#10294 = DIRECTION ( 'NONE',  ( 0.000000000000000000, 0.000000000000000000, 1.000000000000000000 ) ) ;
#10295 = ORIENTED_EDGE ( 'NONE', *, *, #53802, .T. ) ;
#10296 = CARTESIAN_POINT ( 'NONE',  ( 16.51473224551083163, -9.474510206698727899, 95.83442372801900433 ) ) ;
#10297 = CARTESIAN_POINT ( 'NONE',  ( 5.823673210054125526, 21.52544592524343514, 39.79057627198103830 ) ) ;
#10299 = CARTESIAN_POINT ( 'NONE',  ( -19.03943276465977164, -0.05219959533935918106, 113.7510903946856757 ) ) ;
#10298 = CARTESIAN_POINT ( 'NONE',  ( 19.02544592524334988, 5.153800228976608722, 26.45942372801899722 ) ) ;
#10300 = CARTESIAN_POINT ( 'NONE',  ( 8.314922557960818139, 14.29746914071049879, 109.5822429386476955 ) ) ;
#10301 = CARTESIAN_POINT ( 'NONE',  ( -19.02544592524342804, 5.153800228976336051, 36.04057627198100988 ) ) ;
#10302 = CARTESIAN_POINT ( 'NONE',  ( -0.05219959533907301413, -21.53943276465977519, 72.49890960531435269 ) ) ;
#10303 = CARTESIAN_POINT ( 'NONE',  ( -16.46253265017160317, 9.564922557960807481, 30.83224293864769550 ) ) ;
#10304 = CARTESIAN_POINT ( 'NONE',  ( 22.44159573604009594, -16.30477369853687364, 142.1750000027311671 ) ) ;
#10305 = CARTESIAN_POINT ( 'NONE',  ( 19.02544592524334988, 5.153800228976608722, 81.45942372801897591 ) ) ;
#10306 = CARTESIAN_POINT ( 'NONE',  ( 4.483927247898545687, 16.52544592524342804, 54.79057627198104541 ) ) ;
#10307 = CARTESIAN_POINT ( 'NONE',  ( -18.67979575497178146, -10.72451020669898902, 31.66557627198102054 ) ) ;
#10308 = CARTESIAN_POINT ( 'NONE',  ( -10.81492255796105439, 18.62759615963255655, 97.91775706135236135 ) ) ;
#10309 = CARTESIAN_POINT ( 'NONE',  ( 5.719274019375991003, -21.55341960407610458, 87.70724293864769550 ) ) ;
#10310 = CARTESIAN_POINT ( 'NONE',  ( -10.72451020669870658, -18.67979575497194134, 74.58442372801901854 ) ) ;
#10311 = CARTESIAN_POINT ( 'NONE',  ( 5.823673210054444382, -21.52544592524334988, 60.20942372801902565 ) ) ;
#10312 = CARTESIAN_POINT ( 'NONE',  ( 13.97604488694527802, 13.89961937509977652, 104.3739096053143385 ) ) ;
#10314 = CARTESIAN_POINT ( 'NONE',  ( -5.823673210054431948, 21.52544592524334988, 67.70942372801901854 ) ) ;
#10313 = CARTESIAN_POINT ( 'NONE',  ( 8.314922557961029526, -14.29746914071037800, 100.4177570613523471 ) ) ;
#10315 = CARTESIAN_POINT ( 'NONE',  ( 5.153800228976335163, 19.02544592524342804, 54.79057627198103120 ) ) ;
#10316 = CARTESIAN_POINT ( 'NONE',  ( -9.474510206698720793, -16.51473224551083518, 39.58442372801899722 ) ) ;
#10317 = CARTESIAN_POINT ( 'NONE',  ( -21.53943276465977519, -0.05219959533937600094, 23.75109039468567929 ) ) ;
#10318 = CARTESIAN_POINT ( 'NONE',  ( 13.97604488694527802, 13.89961937509977652, 64.37390960531436690 ) ) ;
#10319 = CARTESIAN_POINT ( 'NONE',  ( -16.53943276465976808, 0.05219959533911058130, 81.24890960531436690 ) ) ;
#10320 = CARTESIAN_POINT ( 'NONE',  ( -16.55341960407611168, -4.379528057220339221, 46.45724293864769550 ) ) ;
#10321 = CARTESIAN_POINT ( 'NONE',  ( 21.55341960407610458, 5.719274019375980345, 58.95724293864770971 ) ) ;
#10322 = CARTESIAN_POINT ( 'NONE',  ( -13.89961937509977652, 13.97604488694528158, 45.62390960531433848 ) ) ;
#10323 = CARTESIAN_POINT ( 'NONE',  ( 10.72451020669898902, -18.67979575497178502, 72.91557627198103830 ) ) ;
#10324 = CARTESIAN_POINT ( 'NONE',  ( 19.05341960407617918, -5.049401038297876454, 56.04275706135234714 ) ) ;
#10326 = CARTESIAN_POINT ( 'NONE',  ( 16.53943276465976808, -0.05219959533910856209, 68.74890960531435269 ) ) ;
#10325 = CARTESIAN_POINT ( 'NONE',  ( -16.51473224551082808, 9.474510206698731452, 23.33442372801900078 ) ) ;
#10327 = CARTESIAN_POINT ( 'NONE',  ( -15.72974639402197994, 15.80617190586746368, 40.62390960531435269 ) ) ;
#10328 = ORIENTED_EDGE ( 'NONE', *, *, #136461, .F. ) ;
#10329 = CARTESIAN_POINT ( 'NONE',  ( 16.36317988757058473, 7.306389748694926745, 103.4021039163677642 ) ) ;
#10331 = CARTESIAN_POINT ( 'NONE',  ( 1.500000000000163203, 7.503014402978025466, -64.26148919578614027 ) ) ;
#10330 = CARTESIAN_POINT ( 'NONE',  ( -0.05219959533934338120, 16.53943276465976808, 82.50109039468568994 ) ) ;
#10332 = CARTESIAN_POINT ( 'NONE',  ( -0.05219959533936034679, 19.03943276465977164, 87.50109039468567573 ) ) ;
#10333 = EDGE_CURVE ( 'NONE', #90405, #14227, #118471, .T. ) ;
#10334 = CARTESIAN_POINT ( 'NONE',  ( 16.53943276465976808, -0.05219959533910856209, 48.74890960531435979 ) ) ;
#10335 = CARTESIAN_POINT ( 'NONE',  ( -19.35543954521081744, -5.499999999999585221, 59.58901960356450900 ) ) ;
#10336 = CARTESIAN_POINT ( 'NONE',  ( -9.474510206698964154, 16.51473224551069663, 50.41557627198102409 ) ) ;
#10337 = CARTESIAN_POINT ( 'NONE',  ( -4.379528057220328563, 16.55341960407611168, 45.20724293864769550 ) ) ;
#10338 = CARTESIAN_POINT ( 'NONE',  ( 9.474510206698971260, -16.51473224551069308, 92.91557627198103830 ) ) ;
#10339 = CARTESIAN_POINT ( 'NONE',  ( 13.97604488694527802, 13.89961937509977652, 49.37390960531434558 ) ) ;
#10340 = CARTESIAN_POINT ( 'NONE',  ( -21.55341960407619339, 5.719274019375674811, 58.54275706135235424 ) ) ;
#10341 = CARTESIAN_POINT ( 'NONE',  ( 13.97604488694527802, 13.89961937509977652, 69.37390960531436690 ) ) ;
#10342 = CARTESIAN_POINT ( 'NONE',  ( -16.46253265017160317, 9.564922557960807481, 25.83224293864769194 ) ) ;
#10343 = CARTESIAN_POINT ( 'NONE',  ( 5.153800228976335163, 19.02544592524342804, 59.79057627198100988 ) ) ;
#10344 = CARTESIAN_POINT ( 'NONE',  ( 18.67979575497178502, 10.72451020669898547, 49.16557627198102409 ) ) ;
#10345 = CARTESIAN_POINT ( 'NONE',  ( -16.51473224551069308, -9.474510206698971260, 41.66557627198103120 ) ) ;
#10346 = CARTESIAN_POINT ( 'NONE',  ( -18.62759615963270932, 10.81492255796079327, 40.83224293864769550 ) ) ;
#10347 = CARTESIAN_POINT ( 'NONE',  ( 12.14591786802327356, -12.06949235617739191, 105.6260903946856899 ) ) ;
#10348 = CARTESIAN_POINT ( 'NONE',  ( -13.97604488694547697, 13.89961937509957934, 23.12609039468565442 ) ) ;
#10350 = CARTESIAN_POINT ( 'NONE',  ( -14.34966873604972548, 8.224510206698743886, 83.33442372801903275 ) ) ;
#10349 = CARTESIAN_POINT ( 'NONE',  ( -4.379528057220086978, -16.55341960407618274, 49.79275706135234714 ) ) ;
#10351 = CARTESIAN_POINT ( 'NONE',  ( 1.300000000000000044, -1.443375672974063884, -3.691112476943992763E-18 ) ) ;
#10352 = CARTESIAN_POINT ( 'NONE',  ( 16.52544592524335698, 4.483927247898782831, 61.45942372801901854 ) ) ;
#10353 = CARTESIAN_POINT ( 'NONE',  ( 8.224510206698742110, 14.34966873604972548, 47.08442372801901854 ) ) ;
#10354 = CARTESIAN_POINT ( 'NONE',  ( 16.46253265017160672, -9.564922557960803928, 108.3322429386476955 ) ) ;
#10355 = CARTESIAN_POINT ( 'NONE',  ( -13.89961937509977652, 13.97604488694528158, 35.62390960531435269 ) ) ;
#10356 = CARTESIAN_POINT ( 'NONE',  ( -12.14591786802326823, 12.06949235617739902, 33.12609039468569705 ) ) ;
#10357 = CARTESIAN_POINT ( 'NONE',  ( -16.46253265017160317, 9.564922557960807481, 45.83224293864769550 ) ) ;
#10358 = CARTESIAN_POINT ( 'NONE',  ( -15.80617190586768217, 15.72974639402176855, 28.12609039468568284 ) ) ;
#10359 = CARTESIAN_POINT ( 'NONE',  ( -12.06949235617739369, -12.14591786802326823, 39.37609039468567573 ) ) ;
#10360 = CARTESIAN_POINT ( 'NONE',  ( -12.14591786802326823, 12.06949235617739902, 93.12609039468568994 ) ) ;
#10361 = FACE_OUTER_BOUND ( 'NONE', #38175, .T. ) ;
#10362 = CARTESIAN_POINT ( 'NONE',  ( -21.55341960407619339, 5.719274019375674811, 103.5427570613523613 ) ) ;
#10363 = CARTESIAN_POINT ( 'NONE',  ( 13.97604488694548053, -13.89961937509957401, 100.6260903946856615 ) ) ;
#10364 = CARTESIAN_POINT ( 'NONE',  ( 0.05219959533936267826, -19.03943276465977164, 60.00109039468566863 ) ) ;
#10365 = CARTESIAN_POINT ( 'NONE',  ( 14.29746914071049879, -8.314922557960816363, 53.33224293864769550 ) ) ;
#10366 = CARTESIAN_POINT ( 'NONE',  ( -19.05341960407611168, -5.049401038298163336, 31.45724293864769550 ) ) ;
#10368 = CARTESIAN_POINT ( 'NONE',  ( 16.61371651742601685, 7.165104196376161916, 78.64584930007005426 ) ) ;
#10367 = CARTESIAN_POINT ( 'NONE',  ( -5.049401038297874678, -19.05341960407617918, 64.79275706135233293 ) ) ;
#10369 = CARTESIAN_POINT ( 'NONE',  ( -15.80617190586768217, 15.72974639402176855, 68.12609039468567573 ) ) ;
#10370 = CARTESIAN_POINT ( 'NONE',  ( 4.379528057220092307, 16.55341960407617563, 32.29275706135235424 ) ) ;
#10371 = CARTESIAN_POINT ( 'NONE',  ( 17.31728774477273092, 6.344390552232407110, 81.68093348310684121 ) ) ;
#10372 = CARTESIAN_POINT ( 'NONE',  ( -13.89961937509977652, 13.97604488694528158, 115.6239096053143669 ) ) ;
#10373 = CARTESIAN_POINT ( 'NONE',  ( 13.97604488694548053, -13.89961937509957401, 110.6260903946856615 ) ) ;
#10374 = CARTESIAN_POINT ( 'NONE',  ( 5.153800228976335163, 19.02544592524342804, 109.7905762719810099 ) ) ;
#10375 = CARTESIAN_POINT ( 'NONE',  ( -25.34721418589319342, 10.09305078451843940, 170.5222919391071912 ) ) ;
#10376 = CARTESIAN_POINT ( 'NONE',  ( -5.153800228976328057, -19.02544592524343514, 27.29057627198103120 ) ) ;
#10377 = CARTESIAN_POINT ( 'NONE',  ( 21.52544592524334988, 5.823673210054432836, 111.4594237280190328 ) ) ;
#10378 = CARTESIAN_POINT ( 'NONE',  ( 0.05219959533909260263, 19.03943276465977164, 44.99890960531435979 ) ) ;
#10379 = CARTESIAN_POINT ( 'NONE',  ( -10.72451020669870658, -18.67979575497194134, 64.58442372801900433 ) ) ;
#10380 = CARTESIAN_POINT ( 'NONE',  ( -21.53943276465977519, -0.05219959533937600094, 103.7510903946857042 ) ) ;
#10381 = CARTESIAN_POINT ( 'NONE',  ( 4.379528057220092307, 16.55341960407617563, 107.2927570613523471 ) ) ;
#10382 = CARTESIAN_POINT ( 'NONE',  ( 9.474510206698971260, -16.51473224551069308, 82.91557627198103830 ) ) ;
#10383 = CARTESIAN_POINT ( 'NONE',  ( 21.55341960407619695, -5.719274019375665929, 51.04275706135234714 ) ) ;
#10384 = CARTESIAN_POINT ( 'NONE',  ( -21.53943276465977519, -0.05219959533937600094, 58.75109039468568994 ) ) ;
#10386 = CARTESIAN_POINT ( 'NONE',  ( -5.153800228976328057, -19.02544592524343514, 102.2905762719810383 ) ) ;
#10385 = CARTESIAN_POINT ( 'NONE',  ( -16.51473224551082808, 9.474510206698731452, 73.33442372801900433 ) ) ;
#10387 = CARTESIAN_POINT ( 'NONE',  ( 14.29746914071049879, -8.314922557960816363, 113.3322429386476955 ) ) ;
#10388 = CARTESIAN_POINT ( 'NONE',  ( -15.72974639402197994, 15.80617190586746368, 95.62390960531436690 ) ) ;
#10389 = CARTESIAN_POINT ( 'NONE',  ( -13.97604488694547697, 13.89961937509957934, 28.12609039468565797 ) ) ;
#10390 = CARTESIAN_POINT ( 'NONE',  ( -14.34966873604960291, -8.224510206698953496, 96.66557627198102409 ) ) ;
#10391 = CARTESIAN_POINT ( 'NONE',  ( -16.46253265017160317, 9.564922557960807481, 50.83224293864770260 ) ) ;
#10392 = CARTESIAN_POINT ( 'NONE',  ( -0.05219959533936034679, 19.03943276465977164, 82.50109039468567573 ) ) ;
#10393 = CARTESIAN_POINT ( 'NONE',  ( -8.224510206698948167, 14.34966873604960824, 60.41557627198102409 ) ) ;
#10394 = CARTESIAN_POINT ( 'NONE',  ( -18.67979575497193778, 10.72451020669871902, 103.3344237280190043 ) ) ;
#10395 = CARTESIAN_POINT ( 'NONE',  ( 5.153800228976335163, 19.02544592524342804, 109.7905762719810099 ) ) ;
#10396 = CARTESIAN_POINT ( 'NONE',  ( 13.97604488694548053, -13.89961937509957401, 70.62609039468567573 ) ) ;
#10397 = CARTESIAN_POINT ( 'NONE',  ( -15.72974639402197994, 15.80617190586746368, 75.62390960531439532 ) ) ;
#10398 = CARTESIAN_POINT ( 'NONE',  ( -21.55341960407619339, 5.719274019375674811, 28.54275706135234358 ) ) ;
#10399 = CARTESIAN_POINT ( 'NONE',  ( 4.483927247898790824, -16.52544592524335698, 35.20942372801901854 ) ) ;
#10400 = CARTESIAN_POINT ( 'NONE',  ( -14.29746914071037622, -8.314922557961029526, 89.16775706135236135 ) ) ;
#10402 = CARTESIAN_POINT ( 'NONE',  ( 18.62759615963255655, 10.81492255796105972, 36.66775706135234714 ) ) ;
#10401 = CARTESIAN_POINT ( 'NONE',  ( -8.314922557961024197, 14.29746914071037800, 47.91775706135234714 ) ) ;
#10403 = CARTESIAN_POINT ( 'NONE',  ( 21.52544592524344225, -5.823673210054117533, 43.54057627198103830 ) ) ;
#10404 = CARTESIAN_POINT ( 'NONE',  ( -19.03943276465977164, 0.05219959533909376836, 41.24890960531435269 ) ) ;
#10405 = CARTESIAN_POINT ( 'NONE',  ( -22.81625015709510507, 31.40387420917330275, -1.424999997268813212 ) ) ;
#10406 = CARTESIAN_POINT ( 'NONE',  ( 8.314922557961029526, -14.29746914071037800, 60.41775706135235424 ) ) ;
#10407 = CARTESIAN_POINT ( 'NONE',  ( -15.80617190586745835, -15.72974639402198527, 91.87390960531436690 ) ) ;
#10408 = CARTESIAN_POINT ( 'NONE',  ( -14.29746914071049879, 8.314922557960819915, 35.83224293864768839 ) ) ;
#10409 = CARTESIAN_POINT ( 'NONE',  ( -0.05219959533934338120, 16.53943276465976808, 47.50109039468568994 ) ) ;
#10410 = CARTESIAN_POINT ( 'NONE',  ( 0.05219959533909260263, 19.03943276465977164, 59.99890960531436690 ) ) ;
#10411 = CARTESIAN_POINT ( 'NONE',  ( -8.224510206698735004, -14.34966873604973081, 89.58442372801901854 ) ) ;
#10412 = CARTESIAN_POINT ( 'NONE',  ( -0.05219959533936034679, 19.03943276465977164, 87.50109039468567573 ) ) ;
#10413 = CARTESIAN_POINT ( 'NONE',  ( 15.80617190586746368, 15.72974639402197994, 89.37390960531435269 ) ) ;
#10414 = CARTESIAN_POINT ( 'NONE',  ( -0.05219959533910754901, -16.53943276465976808, 27.49890960531435269 ) ) ;
#10415 = ORIENTED_EDGE ( 'NONE', *, *, #114658, .T. ) ;
#10416 = DIRECTION ( 'NONE',  ( 0.000000000000000000, 0.000000000000000000, -1.000000000000000000 ) ) ;
#10417 = CARTESIAN_POINT ( 'NONE',  ( -21.55341960407610458, -5.719274019375992779, 56.45724293864768839 ) ) ;
#10418 = VERTEX_POINT ( 'NONE', #141872 ) ;
#10419 = CARTESIAN_POINT ( 'NONE',  ( -8.224510206698735004, -14.34966873604973081, 99.58442372801900433 ) ) ;
#10420 = VERTEX_POINT ( 'NONE', #81182 ) ;
#10421 = CARTESIAN_POINT ( 'NONE',  ( -5.719274019375978568, 21.55341960407610458, 25.20724293864769550 ) ) ;
#10422 = CARTESIAN_POINT ( 'NONE',  ( 17.50000000000000000, -3.270424329311308220, 102.5422648494460987 ) ) ;
#10423 = CARTESIAN_POINT ( 'NONE',  ( -10.81492255796078084, -18.62759615963271287, 82.08224293864768129 ) ) ;
#10424 = CARTESIAN_POINT ( 'NONE',  ( 8.224510206698742110, 14.34966873604972548, 112.0844237280190185 ) ) ;
#10425 = CARTESIAN_POINT ( 'NONE',  ( -8.314922557961024197, 14.29746914071037800, 37.91775706135235424 ) ) ;
#10426 = CARTESIAN_POINT ( 'NONE',  ( -5.049401038298153566, 19.05341960407611168, 35.20724293864768839 ) ) ;
#10427 = CARTESIAN_POINT ( 'NONE',  ( 4.379528057220092307, 16.55341960407617563, 32.29275706135235424 ) ) ;
#10428 = CARTESIAN_POINT ( 'NONE',  ( 13.89961937509977652, -13.97604488694527269, 48.12390960531435979 ) ) ;
#10429 = CARTESIAN_POINT ( 'NONE',  ( -17.81289503416611808, 24.51734667627700404, 149.6999999999999602 ) ) ;
#10430 = CARTESIAN_POINT ( 'NONE',  ( 0.05219959533907565091, 21.53943276465977519, 24.99890960531435624 ) ) ;
#10431 = CARTESIAN_POINT ( 'NONE',  ( 16.51473224551069308, 9.474510206698969483, 114.1655762719810241 ) ) ;
#10432 = CARTESIAN_POINT ( 'NONE',  ( 16.52544592524335698, 4.483927247898782831, 106.4594237280190328 ) ) ;
#10433 = CARTESIAN_POINT ( 'NONE',  ( -5.153800228976607833, 19.02544592524334988, 87.70942372801897591 ) ) ;
#10434 = CARTESIAN_POINT ( 'NONE',  ( -9.564922557961040184, 16.46253265017147172, 42.91775706135234003 ) ) ;
#10435 = CARTESIAN_POINT ( 'NONE',  ( -18.67979575497178146, -10.72451020669898902, 91.66557627198103830 ) ) ;
#10436 = CARTESIAN_POINT ( 'NONE',  ( -8.224510206698735004, -14.34966873604973081, 109.5844237280190328 ) ) ;
#10437 = CARTESIAN_POINT ( 'NONE',  ( -0.05219959533907301413, -21.53943276465977519, 37.49890960531436690 ) ) ;
#10438 = CARTESIAN_POINT ( 'NONE',  ( -16.51473224551082808, 9.474510206698731452, 103.3344237280190043 ) ) ;
#10439 = CARTESIAN_POINT ( 'NONE',  ( 19.05341960407611168, 5.049401038298154454, 103.9572429386476671 ) ) ;
#10440 = CARTESIAN_POINT ( 'NONE',  ( -5.719274019375665041, -21.55341960407619695, 59.79275706135234714 ) ) ;
#10441 = CARTESIAN_POINT ( 'NONE',  ( -13.97604488694527625, -13.89961937509977652, 66.87390960531436690 ) ) ;
#10442 = CARTESIAN_POINT ( 'NONE',  ( -12.06949235617756955, 12.14591786802309770, 100.6239096053143811 ) ) ;
#10443 = DIRECTION ( 'NONE',  ( -1.000000000000000000, 0.000000000000000000, 0.000000000000000000 ) ) ;
#10444 = CARTESIAN_POINT ( 'NONE',  ( -8.314922557960811034, -14.29746914071050412, 72.08224293864769550 ) ) ;
#10445 = EDGE_LOOP ( 'NONE', ( #100057, #148167, #197663, #25841, #94026, #51172, #193489, #48491 ) ) ;
#10446 = CARTESIAN_POINT ( 'NONE',  ( 19.03943276465977164, 0.05219959533936151252, 91.25109039468566152 ) ) ;
#10447 = CARTESIAN_POINT ( 'NONE',  ( 16.88567814943162659, -6.947325034625689177, 81.20998877347412304 ) ) ;
#10448 = CARTESIAN_POINT ( 'NONE',  ( -13.97604488694527625, -13.89961937509977652, 66.87390960531436690 ) ) ;
#10449 = CARTESIAN_POINT ( 'NONE',  ( 5.000000000000000888, -140.0000000000000000, -15.00000000000000000 ) ) ;
#10451 = CARTESIAN_POINT ( 'NONE',  ( 9.474510206698971260, -16.51473224551069308, 102.9155762719810241 ) ) ;
#10450 = CARTESIAN_POINT ( 'NONE',  ( -9.474510206698964154, 16.51473224551069663, 80.41557627198103830 ) ) ;
#10452 = CARTESIAN_POINT ( 'NONE',  ( 12.14591786802327356, -12.06949235617739191, 70.62609039468567573 ) ) ;
#10453 = CARTESIAN_POINT ( 'NONE',  ( -21.38418241377624085, 5.438282248597754887, 174.2683007571264113 ) ) ;
#10454 = CARTESIAN_POINT ( 'NONE',  ( 13.97604488694548053, -13.89961937509957401, 40.62609039468564731 ) ) ;
#10455 = CARTESIAN_POINT ( 'NONE',  ( -15.72974639402176322, -15.80617190586768395, 99.37609039468568994 ) ) ;
#10456 = CARTESIAN_POINT ( 'NONE',  ( 16.62544781628812274, 7.153289815129877383, 22.00000000000000000 ) ) ;
#10457 = CARTESIAN_POINT ( 'NONE',  ( 5.049401038298161559, -19.05341960407611168, 107.7072429386476955 ) ) ;
#10458 = CARTESIAN_POINT ( 'NONE',  ( 4.483927247898790824, -16.52544592524335698, 105.2094237280190328 ) ) ;
#10459 = CYLINDRICAL_SURFACE ( 'NONE', #137253, 216.0437394197456342 ) ;
#10460 = CARTESIAN_POINT ( 'NONE',  ( 4.379528057220092307, 16.55341960407617563, 92.29275706135236135 ) ) ;
#10461 = CARTESIAN_POINT ( 'NONE',  ( 15.50000000000000178, -7.500000000000000888, 22.00000000000000711 ) ) ;
#10462 = CARTESIAN_POINT ( 'NONE',  ( 8.224510206698742110, 14.34966873604972548, 72.08442372801899012 ) ) ;
#10463 = DIRECTION ( 'NONE',  ( 3.491481338843133750E-15, 1.000000000000000000, -0.000000000000000000 ) ) ;
#10464 = CARTESIAN_POINT ( 'NONE',  ( 0.05219959533937995610, -21.53943276465977519, 80.00109039468568994 ) ) ;
#10465 = CARTESIAN_POINT ( 'NONE',  ( -19.02544592524334988, -5.153800228976617603, 93.95942372801900433 ) ) ;
#10466 = CARTESIAN_POINT ( 'NONE',  ( 13.89961937509957401, 13.97604488694547697, 21.87609039468566152 ) ) ;
#10467 = CARTESIAN_POINT ( 'NONE',  ( 13.89961937509977652, -13.97604488694527269, 68.12390960531436690 ) ) ;
#10468 = CARTESIAN_POINT ( 'NONE',  ( -16.51473224551069308, -9.474510206698971260, 46.66557627198102409 ) ) ;
#10469 = CARTESIAN_POINT ( 'NONE',  ( 17.43550251053431666, -6.020693471854104750, 23.33574881071265139 ) ) ;
#10470 = CARTESIAN_POINT ( 'NONE',  ( 15.72974639402199770, -15.80617190586745480, 78.12390960531436690 ) ) ;
#10471 = CARTESIAN_POINT ( 'NONE',  ( 10.81492255796078972, 18.62759615963270932, 34.58224293864770260 ) ) ;
#10472 = CARTESIAN_POINT ( 'NONE',  ( 9.474510206698971260, -16.51473224551069308, 32.91557627198102409 ) ) ;
#10473 = CARTESIAN_POINT ( 'NONE',  ( -8.314922557961024197, 14.29746914071037800, 52.91775706135235424 ) ) ;
#10474 = ORIENTED_EDGE ( 'NONE', *, *, #142789, .T. ) ;
#10475 = EDGE_CURVE ( 'NONE', #137833, #171158, #174224, .T. ) ;
#10476 = CARTESIAN_POINT ( 'NONE',  ( 21.55341960407619695, -5.719274019375665929, 36.04275706135234714 ) ) ;
#10478 = CARTESIAN_POINT ( 'NONE',  ( -5.950531402560715689E-15, 38.81732327939063509, -7.124999997268814944 ) ) ;
#10477 = CARTESIAN_POINT ( 'NONE',  ( 4.379528057220339221, -16.55341960407611168, 57.70724293864770260 ) ) ;
#10479 = CARTESIAN_POINT ( 'NONE',  ( -16.52544592524335698, -4.483927247898792601, 18.95942372801901143 ) ) ;
#10480 = CARTESIAN_POINT ( 'NONE',  ( 5.153800228976615827, -19.02544592524334988, 35.20942372801899722 ) ) ;
#10481 = CARTESIAN_POINT ( 'NONE',  ( -16.53943276465976808, 0.05219959533911058130, 51.24890960531436690 ) ) ;
#10482 = CARTESIAN_POINT ( 'NONE',  ( 18.62759615963255655, 10.81492255796105972, 21.66775706135235069 ) ) ;
#10484 = CARTESIAN_POINT ( 'NONE',  ( -5.823673210054116645, -21.52544592524344225, 77.29057627198102409 ) ) ;
#10483 = DIRECTION ( 'NONE',  ( 0.000000000000000000, -1.000000000000000000, 0.000000000000000000 ) ) ;
#10485 = CARTESIAN_POINT ( 'NONE',  ( 19.03943276465977164, -0.05219959533909143690, 83.74890960531436690 ) ) ;
#10486 = CARTESIAN_POINT ( 'NONE',  ( 4.379528057220339221, -16.55341960407611168, 67.70724293864769550 ) ) ;
#10487 = FACE_OUTER_BOUND ( 'NONE', #49407, .T. ) ;
#10488 = CARTESIAN_POINT ( 'NONE',  ( -17.49999999999999645, 5.499999999999997335, 120.0000000000000142 ) ) ;
#10489 = CARTESIAN_POINT ( 'NONE',  ( -19.05341960407617563, 5.049401038297882671, 63.54275706135234003 ) ) ;
#10490 = CARTESIAN_POINT ( 'NONE',  ( -18.67979575497178146, -10.72451020669898902, 101.6655762719810383 ) ) ;
#10491 = CARTESIAN_POINT ( 'NONE',  ( -19.05341960407611168, -5.049401038298163336, 61.45724293864769550 ) ) ;
#10492 = CARTESIAN_POINT ( 'NONE',  ( 16.51473224551083163, -9.474510206698727899, 45.83442372801900433 ) ) ;
#10493 = CARTESIAN_POINT ( 'NONE',  ( -5.049401038298153566, 19.05341960407611168, 25.20724293864768484 ) ) ;
#10494 = CARTESIAN_POINT ( 'NONE',  ( 15.80617190586769283, -15.72974639402175789, 60.62609039468567573 ) ) ;
#10495 = CARTESIAN_POINT ( 'NONE',  ( -16.36317988757060249, -7.306389748694935626, 70.90210391636776421 ) ) ;
#10496 = CARTESIAN_POINT ( 'NONE',  ( -12.06949235617756955, 12.14591786802309770, 40.62390960531435269 ) ) ;
#10497 = CARTESIAN_POINT ( 'NONE',  ( -0.05219959533909027116, -19.03943276465977164, 57.49890960531435979 ) ) ;
#10498 = CARTESIAN_POINT ( 'NONE',  ( -15.72974639402197994, 15.80617190586746368, 80.62390960531438111 ) ) ;
#10499 = CARTESIAN_POINT ( 'NONE',  ( -8.571926809382608425, 26.38167802310805854, 146.4750000027311785 ) ) ;
#10500 = CARTESIAN_POINT ( 'NONE',  ( -19.03943276465977164, 0.05219959533909376836, 56.24890960531435979 ) ) ;
#10501 = CARTESIAN_POINT ( 'NONE',  ( 21.52544592524344225, -5.823673210054117533, 68.54057627198103830 ) ) ;
#10502 = ORIENTED_EDGE ( 'NONE', *, *, #34682, .T. ) ;
#10503 = CARTESIAN_POINT ( 'NONE',  ( 21.55341960407619695, -5.719274019375665929, 106.0427570613523471 ) ) ;
#10506 = CARTESIAN_POINT ( 'NONE',  ( -14.29746914071049879, 8.314922557960819915, 80.83224293864769550 ) ) ;
#10505 = CARTESIAN_POINT ( 'NONE',  ( 12.06949235617739724, 12.14591786802326823, 101.8760903946857042 ) ) ;
#10504 = CARTESIAN_POINT ( 'NONE',  ( 3.503282210674364627, -48.86437366581479580, -23.00000000000000355 ) ) ;
#10507 = CARTESIAN_POINT ( 'NONE',  ( -9.474510206698964154, 16.51473224551069663, 65.41557627198102409 ) ) ;
#10508 = EDGE_LOOP ( 'NONE', ( #119645, #128968, #130150, #120844, #135238 ) ) ;
#10509 = CARTESIAN_POINT ( 'NONE',  ( 19.05341960407617918, -5.049401038297876454, 36.04275706135234003 ) ) ;
#10510 = CARTESIAN_POINT ( 'NONE',  ( -14.34966873604972548, 8.224510206698743886, 93.33442372801901854 ) ) ;
#10511 = CARTESIAN_POINT ( 'NONE',  ( -9.564922557961040184, 16.46253265017147172, 32.91775706135233293 ) ) ;
#10512 = CARTESIAN_POINT ( 'NONE',  ( 5.049401038298161559, -19.05341960407611168, 82.70724293864770971 ) ) ;
#10513 = CARTESIAN_POINT ( 'NONE',  ( 5.719274019375991003, -21.55341960407610458, 57.70724293864770260 ) ) ;
#10514 = DIRECTION ( 'NONE',  ( 0.000000000000000000, 0.000000000000000000, -1.000000000000000000 ) ) ;
#10515 = CARTESIAN_POINT ( 'NONE',  ( -16.55341960407611168, -4.379528057220339221, 111.4572429386476813 ) ) ;
#10516 = CARTESIAN_POINT ( 'NONE',  ( 15.72974639402176855, 15.80617190586768217, 101.8760903946857042 ) ) ;
#10517 = CARTESIAN_POINT ( 'NONE',  ( 8.224510206698742110, 14.34966873604972548, 62.08442372801901143 ) ) ;
#10518 = CARTESIAN_POINT ( 'NONE',  ( 18.62759615963255655, 10.81492255796105972, 31.66775706135234358 ) ) ;
#10519 = CARTESIAN_POINT ( 'NONE',  ( -12.06949235617739369, -12.14591786802326823, 24.37609039468567573 ) ) ;
#10520 = CARTESIAN_POINT ( 'NONE',  ( -16.46253265017160317, 9.564922557960807481, 95.83224293864769550 ) ) ;
#10521 = CARTESIAN_POINT ( 'NONE',  ( 13.89961937509977652, -13.97604488694527269, 43.12390960531434558 ) ) ;
#10522 = CARTESIAN_POINT ( 'NONE',  ( 19.05341960407611168, 5.049401038298154454, 53.95724293864770260 ) ) ;
#10523 = CARTESIAN_POINT ( 'NONE',  ( -8.224510206698735004, -14.34966873604973081, 39.58442372801901143 ) ) ;
#10524 = CARTESIAN_POINT ( 'NONE',  ( 16.55341960407611168, 4.379528057220329451, 98.95724293864770971 ) ) ;
#10525 = CARTESIAN_POINT ( 'NONE',  ( 16.52544592524335698, 4.483927247898782831, 96.45942372801901854 ) ) ;
#10528 = CARTESIAN_POINT ( 'NONE',  ( 0.05219959533909260263, 19.03943276465977164, 54.99890960531435979 ) ) ;
#10527 = CARTESIAN_POINT ( 'NONE',  ( -13.97604488694527625, -13.89961937509977652, 81.87390960531436690 ) ) ;
#10526 = CARTESIAN_POINT ( 'NONE',  ( -5.719274019375665041, -21.55341960407619695, 44.79275706135234714 ) ) ;
#10529 = CARTESIAN_POINT ( 'NONE',  ( 9.564922557960805705, 16.46253265017160317, 79.58224293864769550 ) ) ;
#10530 = CARTESIAN_POINT ( 'NONE',  ( 16.52544592524342804, -4.483927247898539470, 33.54057627198102409 ) ) ;
#10531 = CARTESIAN_POINT ( 'NONE',  ( -8.314922557961024197, 14.29746914071037800, 97.91775706135236135 ) ) ;
#10532 = ORIENTED_EDGE ( 'NONE', *, *, #7934, .F. ) ;
#10533 = CARTESIAN_POINT ( 'NONE',  ( -0.05219959533936034679, 19.03943276465977164, 47.50109039468566863 ) ) ;
#10534 = CARTESIAN_POINT ( 'NONE',  ( -19.03943276465977164, 0.05219959533909376836, 116.2489096053143669 ) ) ;
#10535 = CARTESIAN_POINT ( 'NONE',  ( 5.049401038298161559, -19.05341960407611168, 52.70724293864767418 ) ) ;
#10536 = CARTESIAN_POINT ( 'NONE',  ( -5.049401038297874678, -19.05341960407617918, 19.79275706135233293 ) ) ;
#10537 = CARTESIAN_POINT ( 'NONE',  ( 36.91746824999999177, 2.880721459617395097E-14, -7.624999997268813168 ) ) ;
#10538 = CARTESIAN_POINT ( 'NONE',  ( -4.483927247898782831, 16.52544592524335698, 37.70942372801900433 ) ) ;
#10540 = CARTESIAN_POINT ( 'NONE',  ( -16.55341960407617563, 4.379528057220093196, 58.54275706135235424 ) ) ;
#10539 = CARTESIAN_POINT ( 'NONE',  ( 5.049401038297881783, 19.05341960407617563, 77.29275706135231871 ) ) ;
#10541 = CARTESIAN_POINT ( 'NONE',  ( 4.802760416696449930, -3.979030490183114388, -64.51105135991079464 ) ) ;
#10542 = CARTESIAN_POINT ( 'NONE',  ( 9.474510206698971260, -16.51473224551069308, 77.91557627198103830 ) ) ;
#10543 = CARTESIAN_POINT ( 'NONE',  ( 21.53943276465977519, 0.05219959533937863772, 21.25109039468567218 ) ) ;
#10544 = CARTESIAN_POINT ( 'NONE',  ( 9.474510206698729675, 16.51473224551082808, 72.08442372801900433 ) ) ;
#10546 = CARTESIAN_POINT ( 'NONE',  ( -5.153800228976328057, -19.02544592524343514, 32.29057627198102409 ) ) ;
#10545 = CARTESIAN_POINT ( 'NONE',  ( -5.153800228976328057, -19.02544592524343514, 107.2905762719810383 ) ) ;
#10547 = CARTESIAN_POINT ( 'NONE',  ( 19.05341960407611168, 5.049401038298154454, 78.95724293864769550 ) ) ;
#10549 = CARTESIAN_POINT ( 'NONE',  ( -19.05341960407611168, -5.049401038298163336, 41.45724293864769550 ) ) ;
#10548 = CARTESIAN_POINT ( 'NONE',  ( 4.483927247898545687, 16.52544592524342804, 39.79057627198103830 ) ) ;
#10550 = CARTESIAN_POINT ( 'NONE',  ( -5.153800228976607833, 19.02544592524334988, 47.70942372801900433 ) ) ;
#10551 = CARTESIAN_POINT ( 'NONE',  ( -12.06949235617756955, 12.14591786802309770, 80.62390960531438111 ) ) ;
#10552 = CARTESIAN_POINT ( 'NONE',  ( -19.02544592524334988, -5.153800228976617603, 18.95942372801899722 ) ) ;
#10553 = CARTESIAN_POINT ( 'NONE',  ( -13.89961937509977652, 13.97604488694528158, 55.62390960531434558 ) ) ;
#10554 = CARTESIAN_POINT ( 'NONE',  ( 5.719274019375991003, -21.55341960407610458, 47.70724293864770260 ) ) ;
#10556 = CARTESIAN_POINT ( 'NONE',  ( -15.80617190586768217, 15.72974639402176855, 108.1260903946856757 ) ) ;
#10555 = CARTESIAN_POINT ( 'NONE',  ( 12.06949235617757843, -12.14591786802309237, 53.12390960531436690 ) ) ;
#10557 = CARTESIAN_POINT ( 'NONE',  ( 19.02544592524343514, -5.153800228976328945, 93.54057627198102409 ) ) ;
#10558 = CARTESIAN_POINT ( 'NONE',  ( -9.564922557960796823, -16.46253265017161027, 112.0822429386476955 ) ) ;
#10559 = CARTESIAN_POINT ( 'NONE',  ( 16.46253265017160672, -9.564922557960803928, 43.33224293864769550 ) ) ;
#10560 = CARTESIAN_POINT ( 'NONE',  ( -13.97604488694527625, -13.89961937509977652, 21.87390960531435979 ) ) ;
#10561 = CARTESIAN_POINT ( 'NONE',  ( -4.379528057220328563, 16.55341960407611168, 90.20724293864770971 ) ) ;
#10562 = CARTESIAN_POINT ( 'NONE',  ( 21.52544592524344225, -5.823673210054117533, 103.5405762719810383 ) ) ;
#10563 = CARTESIAN_POINT ( 'NONE',  ( 19.02544592524343514, -5.153800228976328945, 88.54057627198102409 ) ) ;
#10564 = CARTESIAN_POINT ( 'NONE',  ( 21.52544592524344225, -5.823673210054117533, 113.5405762719810383 ) ) ;
#10565 = CARTESIAN_POINT ( 'NONE',  ( -9.474510206698964154, 16.51473224551069663, 95.41557627198102409 ) ) ;
#10567 = CARTESIAN_POINT ( 'NONE',  ( -4.483927247898539470, -16.52544592524342804, 107.2905762719810525 ) ) ;
#10566 = CARTESIAN_POINT ( 'NONE',  ( -3.573655867282028392E-15, 2.428612866367529932E-14, -25.00000000000000000 ) ) ;
#10568 = CARTESIAN_POINT ( 'NONE',  ( 19.03943276465977164, -0.05219959533909143690, 68.74890960531436690 ) ) ;
#10569 = CARTESIAN_POINT ( 'NONE',  ( 0.05219959533907565091, 21.53943276465977519, 74.99890960531435269 ) ) ;
#10570 = CARTESIAN_POINT ( 'NONE',  ( -31.23718726401125068, 7.254977440570235636, 96.91727682732809512 ) ) ;
#10571 = CARTESIAN_POINT ( 'NONE',  ( 17.81289503416611453, -24.51734667627695785, 146.6999999999999886 ) ) ;
#10573 = DIRECTION ( 'NONE',  ( -1.000000000000000000, 0.000000000000000000, 0.000000000000000000 ) ) ;
#10572 = CARTESIAN_POINT ( 'NONE',  ( 15.80617190586746368, 15.72974639402197994, 29.37390960531435269 ) ) ;
#10574 = CARTESIAN_POINT ( 'NONE',  ( -14.29746914071037622, -8.314922557961029526, 34.16775706135234714 ) ) ;
#10575 = ADVANCED_FACE ( 'NONE', ( #143863 ), #188902, .T. ) ;
#10576 = CARTESIAN_POINT ( 'NONE',  ( 12.06949235617757843, -12.14591786802309237, 88.12390960531436690 ) ) ;
#10577 = B_SPLINE_CURVE_WITH_KNOTS ( 'NONE', 3,
 ( #194721, #10704, #56191, #83512, #190715, #175542, #130002, #149213, #54198, #178551, #162365, #71367, #113846, #145189, #6673, #25881, #147205, #40017, #37017, #193723, #98678, #68351, #132034, #87526 ),
 .UNSPECIFIED., .F., .F.,
 ( 4, 2, 2, 2, 2, 2, 2, 2, 2, 2, 2, 4 ),
 ( 0.02035494470246975926, 0.02303009228666412500, 0.02570523987085848727, 0.02838038745505284954, 0.02971796124715003068, 0.03105553503924721181, 0.03172432193529579891, 0.03239310883134438601, 0.03373068262344156021, 0.03640583020763589472, 0.03908097779183024312, 0.04175612537602457763 ),
 .UNSPECIFIED. ) ;
#10578 = CARTESIAN_POINT ( 'NONE',  ( -17.50000000000002132, -5.499999999999948486, 91.28230962303565832 ) ) ;
#10579 = CARTESIAN_POINT ( 'NONE',  ( -13.89961937509977652, 13.97604488694528158, 90.62390960531432427 ) ) ;
#10580 = CARTESIAN_POINT ( 'NONE',  ( 5.153800228976335163, 19.02544592524342804, 44.79057627198103830 ) ) ;
#10581 = CARTESIAN_POINT ( 'NONE',  ( 14.34966873604960469, 8.224510206698951720, 74.16557627198102409 ) ) ;
#10582 = CARTESIAN_POINT ( 'NONE',  ( -5.823673210054116645, -21.52544592524344225, 32.29057627198102409 ) ) ;
#10583 = CARTESIAN_POINT ( 'NONE',  ( -4.379528057220328563, 16.55341960407611168, 55.20724293864770260 ) ) ;
#10584 = CARTESIAN_POINT ( 'NONE',  ( 9.564922557961047289, -16.46253265017146816, 100.4177570613523329 ) ) ;
#10585 = CARTESIAN_POINT ( 'NONE',  ( -5.823673210054431948, 21.52544592524334988, 72.70942372801901854 ) ) ;
#10586 = CARTESIAN_POINT ( 'NONE',  ( 1.784210473542230573E-15, -29.16686587814331588, 147.3750000027311842 ) ) ;
#10587 = CARTESIAN_POINT ( 'NONE',  ( 19.02544592524343514, -5.153800228976328945, 113.5405762719810241 ) ) ;
#10588 = CARTESIAN_POINT ( 'NONE',  ( 14.34966873604972726, -8.224510206698740333, 90.83442372801901854 ) ) ;
#10589 = CARTESIAN_POINT ( 'NONE',  ( -17.48847506799949159, 5.747544572775296956, 95.82697437843293642 ) ) ;
#10590 = CARTESIAN_POINT ( 'NONE',  ( 19.05341960407611168, 5.049401038298154454, 73.95724293864768129 ) ) ;
#10591 = CARTESIAN_POINT ( 'NONE',  ( -10.81492255796078084, -18.62759615963271287, 82.08224293864768129 ) ) ;
#10592 = CARTESIAN_POINT ( 'NONE',  ( -14.34966873604972548, 8.224510206698743886, 28.33442372801902209 ) ) ;
#10594 = CARTESIAN_POINT ( 'NONE',  ( -21.52544592524334988, -5.823673210054445271, 78.95942372801901854 ) ) ;
#10593 = CARTESIAN_POINT ( 'NONE',  ( 4.379528057220339221, -16.55341960407611168, 52.70724293864769550 ) ) ;
#10596 = CARTESIAN_POINT ( 'NONE',  ( -21.55341960407610458, -5.719274019375992779, 26.45724293864768839 ) ) ;
#10595 = CARTESIAN_POINT ( 'NONE',  ( 0.05219959533934541429, -16.53943276465976808, 85.00109039468568994 ) ) ;
#10597 = CARTESIAN_POINT ( 'NONE',  ( 26.33867313280597600, 8.832717389288090359, 167.2809140985657450 ) ) ;
#10598 = LINE ( 'NONE', #57100, #90607 ) ;
#10599 = CARTESIAN_POINT ( 'NONE',  ( -4.379528057220086978, -16.55341960407618274, 104.7927570613523898 ) ) ;
#10600 = CARTESIAN_POINT ( 'NONE',  ( 12.14591786802327356, -12.06949235617739191, 55.62609039468568284 ) ) ;
#10601 = CARTESIAN_POINT ( 'NONE',  ( -19.05341960407611168, -5.049401038298163336, 71.45724293864766707 ) ) ;
#10602 = CARTESIAN_POINT ( 'NONE',  ( -9.474510206698964154, 16.51473224551069663, 90.41557627198103830 ) ) ;
#10603 = CARTESIAN_POINT ( 'NONE',  ( -10.81492255796105439, 18.62759615963255655, 77.91775706135231871 ) ) ;
#10604 = EDGE_CURVE ( 'NONE', #65926, #12274, #14541, .T. ) ;
#10605 = CARTESIAN_POINT ( 'NONE',  ( 12.06949235617739724, 12.14591786802326823, 76.87609039468567573 ) ) ;
#10606 = CARTESIAN_POINT ( 'NONE',  ( 12.14591786802309770, 12.06949235617756955, 44.37390960531435979 ) ) ;
#10607 = CARTESIAN_POINT ( 'NONE',  ( -5.153800228976328057, -19.02544592524343514, 57.29057627198103120 ) ) ;
#10608 = CARTESIAN_POINT ( 'NONE',  ( -9.564922557960796823, -16.46253265017161027, 42.08224293864769550 ) ) ;
#10609 = ORIENTED_EDGE ( 'NONE', *, *, #136319, .F. ) ;
#10610 = CARTESIAN_POINT ( 'NONE',  ( 16.46253265017146816, 9.564922557961045513, 96.66775706135233293 ) ) ;
#10611 = CARTESIAN_POINT ( 'NONE',  ( 16.53943276465976808, -0.05219959533910856209, 93.74890960531436690 ) ) ;
#10612 = CARTESIAN_POINT ( 'NONE',  ( 9.564922557960805705, 16.46253265017160317, 59.58224293864769550 ) ) ;
#10614 = CARTESIAN_POINT ( 'NONE',  ( -38.00000000000001421, -12.34694845685042708, -5.900000000000000355 ) ) ;
#10613 = CARTESIAN_POINT ( 'NONE',  ( -13.97604488694547697, 13.89961937509957934, 98.12609039468566152 ) ) ;
#10615 = CARTESIAN_POINT ( 'NONE',  ( -15.72974639402176322, -15.80617190586768395, 109.3760903946857042 ) ) ;
#10616 = CARTESIAN_POINT ( 'NONE',  ( -12.14591786802326823, 12.06949235617739902, 68.12609039468567573 ) ) ;
#10617 = CARTESIAN_POINT ( 'NONE',  ( 16.46253265017146816, 9.564922557961045513, 91.66775706135234714 ) ) ;
#10618 = CARTESIAN_POINT ( 'NONE',  ( 10.81492255796078972, 18.62759615963270932, 59.58224293864770260 ) ) ;
#10619 = CARTESIAN_POINT ( 'NONE',  ( 12.14591786802327356, -12.06949235617739191, 55.62609039468568284 ) ) ;
#10620 = DIRECTION ( 'NONE',  ( 1.000000000000000000, 0.000000000000000000, 0.000000000000000000 ) ) ;
#10621 = CARTESIAN_POINT ( 'NONE',  ( -19.05341960407617563, 5.049401038297882671, 53.54275706135231871 ) ) ;
#10622 = CARTESIAN_POINT ( 'NONE',  ( 10.81492255796106328, -18.62759615963255655, 100.4177570613523471 ) ) ;
#10623 = CARTESIAN_POINT ( 'NONE',  ( -16.55341960407611168, -4.379528057220339221, 111.4572429386476813 ) ) ;
#10624 = CARTESIAN_POINT ( 'NONE',  ( -19.02544592524342804, 5.153800228976336051, 71.04057627198099567 ) ) ;
#10625 = CARTESIAN_POINT ( 'NONE',  ( -16.53943276465976808, 0.05219959533911058130, 56.24890960531436690 ) ) ;
#10626 = CARTESIAN_POINT ( 'NONE',  ( -10.81492255796105439, 18.62759615963255655, 92.91775706135236135 ) ) ;
#10627 = CARTESIAN_POINT ( 'NONE',  ( 13.97604488694548053, -13.89961937509957401, 50.62609039468566152 ) ) ;
#10628 = CARTESIAN_POINT ( 'NONE',  ( 16.46253265017146816, 9.564922557961045513, 26.66775706135234003 ) ) ;
#10629 = CARTESIAN_POINT ( 'NONE',  ( 5.719274019375991003, -21.55341960407610458, 27.70724293864769905 ) ) ;
#10630 = CARTESIAN_POINT ( 'NONE',  ( 15.80617190586769283, -15.72974639402175789, 90.62609039468567573 ) ) ;
#10631 = CARTESIAN_POINT ( 'NONE',  ( -19.02544592524342804, 5.153800228976336051, 81.04057627198103830 ) ) ;
#10632 = AXIS2_PLACEMENT_3D ( 'NONE', #1085, #62761, #79930 ) ;
#10633 = CARTESIAN_POINT ( 'NONE',  ( 18.62759615963255655, 10.81492255796105972, 91.66775706135234714 ) ) ;
#10634 = CARTESIAN_POINT ( 'NONE',  ( -18.67979575497178146, -10.72451020669898902, 46.66557627198102409 ) ) ;
#10635 = CARTESIAN_POINT ( 'NONE',  ( 16.46253265017160672, -9.564922557960803928, 83.33224293864768129 ) ) ;
#10636 = CARTESIAN_POINT ( 'NONE',  ( 16.51473224551083163, -9.474510206698727899, 60.83442372801900433 ) ) ;
#10637 = CARTESIAN_POINT ( 'NONE',  ( -5.153800228976328057, -19.02544592524343514, 42.29057627198101699 ) ) ;
#10638 = CARTESIAN_POINT ( 'NONE',  ( -5.049401038298153566, 19.05341960407611168, 90.20724293864766707 ) ) ;
#10639 = CARTESIAN_POINT ( 'NONE',  ( -9.474510206698720793, -16.51473224551083518, 84.58442372801900433 ) ) ;
#10640 = CARTESIAN_POINT ( 'NONE',  ( 14.29746914071037800, 8.314922557961029526, 46.66775706135234714 ) ) ;
#10641 = CARTESIAN_POINT ( 'NONE',  ( 8.224510206698953496, -14.34966873604960469, 102.9155762719810383 ) ) ;
#10642 = CARTESIAN_POINT ( 'NONE',  ( -9.564922557960796823, -16.46253265017161027, 77.08224293864769550 ) ) ;
#10643 = CARTESIAN_POINT ( 'NONE',  ( -21.53943276465977519, 0.05219959533907696930, 56.24890960531436690 ) ) ;
#10644 = CARTESIAN_POINT ( 'NONE',  ( 13.97604488694548053, -13.89961937509957401, 110.6260903946856615 ) ) ;
#10645 = CARTESIAN_POINT ( 'NONE',  ( 5.823673210054444382, -21.52544592524334988, 20.20942372801900788 ) ) ;
#10646 = CARTESIAN_POINT ( 'NONE',  ( -10.81492255796105439, 18.62759615963255655, 72.91775706135234714 ) ) ;
#10647 = CARTESIAN_POINT ( 'NONE',  ( -12.14591786802326823, 12.06949235617739902, 78.12609039468570415 ) ) ;
#10648 = CARTESIAN_POINT ( 'NONE',  ( 13.97604488694527802, 13.89961937509977652, 74.37390960531436690 ) ) ;
#10649 = CARTESIAN_POINT ( 'NONE',  ( 16.52544592524335698, 4.483927247898782831, 101.4594237280190185 ) ) ;
#10650 = CARTESIAN_POINT ( 'NONE',  ( 0.05219959533936267826, -19.03943276465977164, 60.00109039468566863 ) ) ;
#10651 = CARTESIAN_POINT ( 'NONE',  ( -5.823673210054431948, 21.52544592524334988, 37.70942372801900433 ) ) ;
#10652 = CARTESIAN_POINT ( 'NONE',  ( 8.224510206698953496, -14.34966873604960469, 82.91557627198103830 ) ) ;
#10653 = CARTESIAN_POINT ( 'NONE',  ( -9.474510206698964154, 16.51473224551069663, 105.4155762719810383 ) ) ;
#10654 = CARTESIAN_POINT ( 'NONE',  ( -16.53943276465976808, -0.05219959533934237506, 83.75109039468568994 ) ) ;
#10655 = CARTESIAN_POINT ( 'NONE',  ( 15.80617190586769283, -15.72974639402175789, 70.62609039468567573 ) ) ;
#10656 = CARTESIAN_POINT ( 'NONE',  ( 0.05219959533934541429, -16.53943276465976808, 35.00109039468568284 ) ) ;
#10657 = CARTESIAN_POINT ( 'NONE',  ( 0.05219959533937995610, -21.53943276465977519, 30.00109039468568284 ) ) ;
#10658 = CARTESIAN_POINT ( 'NONE',  ( 4.483927247898545687, 16.52544592524342804, 74.79057627198105251 ) ) ;
#10659 = ORIENTED_EDGE ( 'NONE', *, *, #166522, .F. ) ;
#10660 = CARTESIAN_POINT ( 'NONE',  ( -5.719274019375978568, 21.55341960407610458, 100.2072429386476955 ) ) ;
#10661 = CARTESIAN_POINT ( 'NONE',  ( 16.53943276465976808, -0.05219959533910856209, 58.74890960531436690 ) ) ;
#10662 = ORIENTED_EDGE ( 'NONE', *, *, #153660, .F. ) ;
#10663 = CARTESIAN_POINT ( 'NONE',  ( 19.02544592524343514, -5.153800228976328945, 28.54057627198102409 ) ) ;
#10664 = CARTESIAN_POINT ( 'NONE',  ( -21.53943276465977519, 0.05219959533907696930, 31.24890960531435979 ) ) ;
#10665 = CARTESIAN_POINT ( 'NONE',  ( 21.53943276465977519, 0.05219959533937863772, 36.25109039468567573 ) ) ;
#10666 = CARTESIAN_POINT ( 'NONE',  ( -12.06949235617756955, 12.14591786802309770, 65.62390960531436690 ) ) ;
#10667 = CARTESIAN_POINT ( 'NONE',  ( 21.53943276465977519, -0.05219959533907433946, 63.74890960531435979 ) ) ;
#10668 = CARTESIAN_POINT ( 'NONE',  ( -5.049401038298153566, 19.05341960407611168, 70.20724293864769550 ) ) ;
#10670 = CARTESIAN_POINT ( 'NONE',  ( -5.049401038297874678, -19.05341960407617918, 84.79275706135233293 ) ) ;
#10669 = CARTESIAN_POINT ( 'NONE',  ( -9.564922557960796823, -16.46253265017161027, 27.08224293864769550 ) ) ;
#10671 = CARTESIAN_POINT ( 'NONE',  ( 15.72974639402199770, -15.80617190586745480, 58.12390960531435979 ) ) ;
#10672 = CARTESIAN_POINT ( 'NONE',  ( -9.474510206698964154, 16.51473224551069663, 45.41557627198103120 ) ) ;
#10673 = CARTESIAN_POINT ( 'NONE',  ( -9.474510206698964154, 16.51473224551069663, 65.41557627198102409 ) ) ;
#10674 = EDGE_LOOP ( 'NONE', ( #77033, #138944, #32774, #21666 ) ) ;
#10675 = CARTESIAN_POINT ( 'NONE',  ( 14.34966873604972726, -8.224510206698740333, 55.83442372801901854 ) ) ;
#10676 = CARTESIAN_POINT ( 'NONE',  ( -10.81492255796105439, 18.62759615963255655, 27.91775706135234358 ) ) ;
#10677 = CARTESIAN_POINT ( 'NONE',  ( -21.53943276465977519, -0.05219959533937600094, 53.75109039468568994 ) ) ;
#10678 = CARTESIAN_POINT ( 'NONE',  ( -13.97604488694527625, -13.89961937509977652, 106.8739096053143669 ) ) ;
#10679 = CARTESIAN_POINT ( 'NONE',  ( -21.53943276465977519, 0.05219959533907696930, 71.24890960531435269 ) ) ;
#10681 = CARTESIAN_POINT ( 'NONE',  ( 16.53943276465976808, 0.05219959533934440121, 51.25109039468568994 ) ) ;
#10680 = CARTESIAN_POINT ( 'NONE',  ( 5.823673210054125526, 21.52544592524343514, 114.7905762719810383 ) ) ;
#10682 = ADVANCED_FACE ( 'NONE', ( #99351 ), #192219, .F. ) ;
#10683 = CARTESIAN_POINT ( 'NONE',  ( -10.72451020669898014, 18.67979575497178502, 50.41557627198103120 ) ) ;
#10684 = CARTESIAN_POINT ( 'NONE',  ( -5.823673210054431948, 21.52544592524334988, 107.7094237280190328 ) ) ;
#10685 = CARTESIAN_POINT ( 'NONE',  ( -16.46253265017160317, 9.564922557960807481, 60.83224293864769550 ) ) ;
#10686 = CARTESIAN_POINT ( 'NONE',  ( 0.05219959533909260263, 19.03943276465977164, 104.9989096053143669 ) ) ;
#10687 = CARTESIAN_POINT ( 'NONE',  ( -19.05341960407611168, -5.049401038298163336, 76.45724293864769550 ) ) ;
#10688 = CARTESIAN_POINT ( 'NONE',  ( -24.24789025133655329, -29.25582059975612026, -16.65643465479912066 ) ) ;
#10689 = CARTESIAN_POINT ( 'NONE',  ( 5.153800228976615827, -19.02544592524334988, 70.20942372801899012 ) ) ;
#10691 = CARTESIAN_POINT ( 'NONE',  ( 18.62759615963271287, -10.81492255796078972, 43.33224293864769550 ) ) ;
#10690 = CARTESIAN_POINT ( 'NONE',  ( 5.823673210054444382, -21.52544592524334988, 110.2094237280190185 ) ) ;
#10693 = EDGE_CURVE ( 'NONE', #84229, #1850, #127695, .T. ) ;
#10692 = CARTESIAN_POINT ( 'NONE',  ( -4.483927247898782831, 16.52544592524335698, 102.7094237280190185 ) ) ;
#10694 = CARTESIAN_POINT ( 'NONE',  ( -5.153800228976607833, 19.02544592524334988, 92.70942372801901854 ) ) ;
#10695 = CARTESIAN_POINT ( 'NONE',  ( -17.26172910966779028, 6.454744622555848466, 60.80646908649224258 ) ) ;
#10696 = CARTESIAN_POINT ( 'NONE',  ( -18.67979575497193778, 10.72451020669871902, 113.3344237280190328 ) ) ;
#10697 = CARTESIAN_POINT ( 'NONE',  ( 16.46253265017146816, 9.564922557961045513, 86.66775706135233293 ) ) ;
#10698 = CARTESIAN_POINT ( 'NONE',  ( 9.474510206698729675, 16.51473224551082808, 47.08442372801900433 ) ) ;
#10699 = CARTESIAN_POINT ( 'NONE',  ( 17.50000000000000000, 5.499999999999995559, 108.7823096230356867 ) ) ;
#10700 = CARTESIAN_POINT ( 'NONE',  ( 0.05219959533909260263, 19.03943276465977164, 39.99890960531436690 ) ) ;
#10701 = CARTESIAN_POINT ( 'NONE',  ( 4.379528057220339221, -16.55341960407611168, 52.70724293864769550 ) ) ;
#10702 = CARTESIAN_POINT ( 'NONE',  ( 5.049401038298161559, -19.05341960407611168, 37.70724293864768839 ) ) ;
#10703 = CARTESIAN_POINT ( 'NONE',  ( 16.53943276465976808, -0.05219959533910856209, 38.74890960531435979 ) ) ;
#10704 = CARTESIAN_POINT ( 'NONE',  ( -21.02068080879918455, -34.03872152684794372, -24.45646120681623970 ) ) ;
#10705 = CARTESIAN_POINT ( 'NONE',  ( 8.314922557961029526, -14.29746914071037800, 110.4177570613523756 ) ) ;
#10706 = CARTESIAN_POINT ( 'NONE',  ( -19.05341960407611168, -5.049401038298163336, 56.45724293864768129 ) ) ;
#10707 = CARTESIAN_POINT ( 'NONE',  ( 0.05219959533936267826, -19.03943276465977164, 30.00109039468566863 ) ) ;
#10708 = CARTESIAN_POINT ( 'NONE',  ( 16.53943276465976808, 0.05219959533934440121, 36.25109039468567573 ) ) ;
#10709 = CARTESIAN_POINT ( 'NONE',  ( -18.62759615963270932, 10.81492255796079327, 40.83224293864769550 ) ) ;
#10711 = ORIENTED_EDGE ( 'NONE', *, *, #86821, .T. ) ;
#10710 = CARTESIAN_POINT ( 'NONE',  ( -0.05219959533937732626, 21.53943276465977519, 97.50109039468567573 ) ) ;
#10712 = CARTESIAN_POINT ( 'NONE',  ( -13.97604488694527625, -13.89961937509977652, 106.8739096053143669 ) ) ;
#10713 = CARTESIAN_POINT ( 'NONE',  ( -9.564922557960796823, -16.46253265017161027, 92.08224293864769550 ) ) ;
#10714 = CARTESIAN_POINT ( 'NONE',  ( -29.86685920354755197, -21.69954338932560134, -6.424999997268812990 ) ) ;
#10715 = CARTESIAN_POINT ( 'NONE',  ( -18.62759615963255300, -10.81492255796106328, 19.16775706135234714 ) ) ;
#10716 = CARTESIAN_POINT ( 'NONE',  ( 16.53943276465976808, -0.05219959533910856209, 73.74890960531433848 ) ) ;
#10718 = CARTESIAN_POINT ( 'NONE',  ( -0.05219959533909027116, -19.03943276465977164, 67.49890960531436690 ) ) ;
#10717 = CARTESIAN_POINT ( 'NONE',  ( 0.05219959533907565091, 21.53943276465977519, 74.99890960531435269 ) ) ;
#10719 = CARTESIAN_POINT ( 'NONE',  ( -16.51473224551069308, -9.474510206698971260, 76.66557627198103830 ) ) ;
#10720 = CARTESIAN_POINT ( 'NONE',  ( -21.53943276465977519, -0.05219959533937600094, 18.75109039468568639 ) ) ;
#10721 = EDGE_LOOP ( 'NONE', ( #25511, #113334, #196537, #77150 ) ) ;
#10722 = CARTESIAN_POINT ( 'NONE',  ( 19.02544592524343514, -5.153800228976328945, 58.54057627198102409 ) ) ;
#10724 = CYLINDRICAL_SURFACE ( 'NONE', #120397, 38.00000000000000000 ) ;
#10723 = CARTESIAN_POINT ( 'NONE',  ( -14.34966873604960291, -8.224510206698953496, 111.6655762719810525 ) ) ;
#10725 = CARTESIAN_POINT ( 'NONE',  ( 13.97604488694527802, 13.89961937509977652, 59.37390960531434558 ) ) ;
#10726 = CARTESIAN_POINT ( 'NONE',  ( -9.474510206698720793, -16.51473224551083518, 94.58442372801900433 ) ) ;
#10727 = CARTESIAN_POINT ( 'NONE',  ( 16.55341960407611168, 4.379528057220329451, 98.95724293864770971 ) ) ;
#10728 = CARTESIAN_POINT ( 'NONE',  ( -21.55341960407619339, 5.719274019375674811, 53.54275706135234714 ) ) ;
#10730 = CARTESIAN_POINT ( 'NONE',  ( -5.719274019375978568, 21.55341960407610458, 115.2072429386476955 ) ) ;
#10729 = CARTESIAN_POINT ( 'NONE',  ( 13.97604488694527802, 13.89961937509977652, 54.37390960531435979 ) ) ;
#10731 = CARTESIAN_POINT ( 'NONE',  ( -12.06949235617756955, 12.14591786802309770, 95.62390960531436690 ) ) ;
#10732 = CARTESIAN_POINT ( 'NONE',  ( 8.906447517083057264, -27.41122689804191026, 140.5999999999999943 ) ) ;
#10733 = CARTESIAN_POINT ( 'NONE',  ( 19.05341960407611168, 5.049401038298154454, 78.95724293864769550 ) ) ;
#10734 = CARTESIAN_POINT ( 'NONE',  ( 17.13100169013301155, 6.664070546373125126, 111.7321016430014993 ) ) ;
#10736 = CARTESIAN_POINT ( 'NONE',  ( -21.55341960407610458, -5.719274019375992779, 26.45724293864768839 ) ) ;
#10735 = CARTESIAN_POINT ( 'NONE',  ( -13.97604488694547697, 13.89961937509957934, 108.1260903946856331 ) ) ;
#10737 = CARTESIAN_POINT ( 'NONE',  ( 18.67979575497194134, -10.72451020669871369, 55.83442372801901854 ) ) ;
#10738 = CARTESIAN_POINT ( 'NONE',  ( -9.474510206698964154, 16.51473224551069663, 95.41557627198102409 ) ) ;
#10739 = CARTESIAN_POINT ( 'NONE',  ( 9.564922557961047289, -16.46253265017146816, 85.41775706135233293 ) ) ;
#10740 = CARTESIAN_POINT ( 'NONE',  ( -19.05341960407611168, -5.049401038298163336, 71.45724293864766707 ) ) ;
#10741 = CARTESIAN_POINT ( 'NONE',  ( -12.14591786802309592, -12.06949235617757132, 86.87390960531438111 ) ) ;
#10742 = CARTESIAN_POINT ( 'NONE',  ( 5.049401038298161559, -19.05341960407611168, 107.7072429386476955 ) ) ;
#10743 = CARTESIAN_POINT ( 'NONE',  ( 8.314922557960818139, 14.29746914071049879, 74.58224293864768129 ) ) ;
#10744 = CARTESIAN_POINT ( 'NONE',  ( 19.05341960407611168, 5.049401038298154454, 103.9572429386476671 ) ) ;
#10745 = CARTESIAN_POINT ( 'NONE',  ( 9.474510206698729675, 16.51473224551082808, 42.08442372801900433 ) ) ;
#10748 = CARTESIAN_POINT ( 'NONE',  ( 5.049401038298161559, -19.05341960407611168, 27.70724293864769550 ) ) ;
#10747 = CARTESIAN_POINT ( 'NONE',  ( -4.379528057220328563, 16.55341960407611168, 40.20724293864769550 ) ) ;
#10746 = CARTESIAN_POINT ( 'NONE',  ( 13.97604488694527802, 13.89961937509977652, 49.37390960531434558 ) ) ;
#10749 = EDGE_LOOP ( 'NONE', ( #29190, #196064, #83348, #49237, #191422 ) ) ;
#10750 = CARTESIAN_POINT ( 'NONE',  ( 10.81492255796106328, -18.62759615963255655, 40.41775706135234714 ) ) ;
#10751 = CARTESIAN_POINT ( 'NONE',  ( 9.474510206698729675, 16.51473224551082808, 82.08442372801899012 ) ) ;
#10752 = CARTESIAN_POINT ( 'NONE',  ( -14.34966873604960291, -8.224510206698953496, 51.66557627198102409 ) ) ;
#10753 = CARTESIAN_POINT ( 'NONE',  ( 21.52544592524344225, -5.823673210054117533, 103.5405762719810383 ) ) ;
#10754 = CARTESIAN_POINT ( 'NONE',  ( 5.719274019375991003, -21.55341960407610458, 27.70724293864769905 ) ) ;
#10755 = CARTESIAN_POINT ( 'NONE',  ( 0.05219959533910956823, 16.53943276465976808, 89.99890960531438111 ) ) ;
#10756 = CARTESIAN_POINT ( 'NONE',  ( 9.474510206698971260, -16.51473224551069308, 37.91557627198102409 ) ) ;
#10757 = CARTESIAN_POINT ( 'NONE',  ( -16.55341960407611168, -4.379528057220339221, 21.45724293864769550 ) ) ;
#10758 = CARTESIAN_POINT ( 'NONE',  ( 16.53943276465976808, 0.05219959533934440121, 86.25109039468568994 ) ) ;
#10759 = CARTESIAN_POINT ( 'NONE',  ( 8.314922557961029526, -14.29746914071037800, 65.41775706135234714 ) ) ;
#10760 = CARTESIAN_POINT ( 'NONE',  ( 19.05341960407617918, -5.049401038297876454, 31.04275706135232227 ) ) ;
#10761 = CARTESIAN_POINT ( 'NONE',  ( 9.474510206698971260, -16.51473224551069308, 97.91557627198102409 ) ) ;
#10762 = CARTESIAN_POINT ( 'NONE',  ( 13.89961937509977652, -13.97604488694527269, 83.12390960531436690 ) ) ;
#10763 = CARTESIAN_POINT ( 'NONE',  ( -16.55341960407617563, 4.379528057220093196, 73.54275706135234714 ) ) ;
#10764 = CARTESIAN_POINT ( 'NONE',  ( 9.474510206698971260, -16.51473224551069308, 37.91557627198102409 ) ) ;
#10765 = CARTESIAN_POINT ( 'NONE',  ( -8.314922557960811034, -14.29746914071050412, 52.08224293864768839 ) ) ;
#10767 = CARTESIAN_POINT ( 'NONE',  ( 13.89961937509977652, -13.97604488694527269, 103.1239096053143527 ) ) ;
#10766 = FACE_OUTER_BOUND ( 'NONE', #100934, .T. ) ;
#10768 = CARTESIAN_POINT ( 'NONE',  ( 15.72974639402199770, -15.80617190586745480, 33.12390960531435979 ) ) ;
#10769 = CARTESIAN_POINT ( 'NONE',  ( -16.53943276465976808, 0.05219959533911058130, 66.24890960531436690 ) ) ;
#10770 = CIRCLE ( 'NONE', #191582, 69.99999999999997158 ) ;
#10771 = ORIENTED_EDGE ( 'NONE', *, *, #182212, .T. ) ;
#10772 = CARTESIAN_POINT ( 'NONE',  ( -14.34966873604960291, -8.224510206698953496, 61.66557627198103120 ) ) ;
#10773 = CARTESIAN_POINT ( 'NONE',  ( 31.48176515315800117, -1.054302444749900536, -46.25693415911322859 ) ) ;
#10774 = CARTESIAN_POINT ( 'NONE',  ( -16.51473224551082808, 9.474510206698731452, 68.33442372801900433 ) ) ;
#10775 = CARTESIAN_POINT ( 'NONE',  ( 19.03943276465977164, -0.05219959533909143690, 93.74890960531435269 ) ) ;
#10776 = CARTESIAN_POINT ( 'NONE',  ( 19.05341960407617918, -5.049401038297876454, 76.04275706135230450 ) ) ;
#10778 = CARTESIAN_POINT ( 'NONE',  ( 14.29746914071037800, 8.314922557961029526, 96.66775706135234714 ) ) ;
#10777 = CARTESIAN_POINT ( 'NONE',  ( -0.05219959533936034679, 19.03943276465977164, 107.5010903946856615 ) ) ;
#10779 = CARTESIAN_POINT ( 'NONE',  ( -19.05341960407611168, -5.049401038298163336, 41.45724293864769550 ) ) ;
#10780 = CARTESIAN_POINT ( 'NONE',  ( -10.72451020669898014, 18.67979575497178502, 40.41557627198103120 ) ) ;
#10781 = CARTESIAN_POINT ( 'NONE',  ( -15.72974639402176322, -15.80617190586768395, 49.37609039468569705 ) ) ;
#10782 = CARTESIAN_POINT ( 'NONE',  ( 0.05219959533934541429, -16.53943276465976808, 25.00109039468567218 ) ) ;
#10784 = CARTESIAN_POINT ( 'NONE',  ( -0.05219959533909027116, -19.03943276465977164, 77.49890960531435269 ) ) ;
#10783 = DIRECTION ( 'NONE',  ( -0.9945218953682734009, 0.000000000000000000, 0.1045284632676537068 ) ) ;
#10785 = DIRECTION ( 'NONE',  ( -0.5000000000000004441, -0.4999999999999986122, 0.7071067811865481278 ) ) ;
#10787 = CARTESIAN_POINT ( 'NONE',  ( 0.05219959533909260263, 19.03943276465977164, 74.99890960531435269 ) ) ;
#10786 = CARTESIAN_POINT ( 'NONE',  ( -0.05219959533910754901, -16.53943276465976808, 77.49890960531433848 ) ) ;
#10788 = CARTESIAN_POINT ( 'NONE',  ( 19.02544592524343514, -5.153800228976328945, 68.54057627198103830 ) ) ;
#10789 = ORIENTED_EDGE ( 'NONE', *, *, #32449, .T. ) ;
#10790 = CARTESIAN_POINT ( 'NONE',  ( -19.02544592524334988, -5.153800228976617603, 93.95942372801900433 ) ) ;
#10791 = CARTESIAN_POINT ( 'NONE',  ( 10.72451020669898902, -18.67979575497178502, 57.91557627198103120 ) ) ;
#10792 = CARTESIAN_POINT ( 'NONE',  ( 19.05341960407611168, 5.049401038298154454, 33.95724293864769550 ) ) ;
#10793 = CARTESIAN_POINT ( 'NONE',  ( 5.049401038297881783, 19.05341960407617563, 62.29275706135234003 ) ) ;
#10794 = CARTESIAN_POINT ( 'NONE',  ( 5.153800228976335163, 19.02544592524342804, 54.79057627198103120 ) ) ;
#10795 = CARTESIAN_POINT ( 'NONE',  ( 16.51473224551069308, 9.474510206698969483, 94.16557627198103830 ) ) ;
#10796 = ORIENTED_EDGE ( 'NONE', *, *, #66362, .T. ) ;
#10797 = CARTESIAN_POINT ( 'NONE',  ( -5.823673210054116645, -21.52544592524344225, 87.29057627198103830 ) ) ;
#10799 = CARTESIAN_POINT ( 'NONE',  ( 19.03943276465977164, 0.05219959533936151252, 46.25109039468566863 ) ) ;
#10798 = CARTESIAN_POINT ( 'NONE',  ( -12.14591786802309592, -12.06949235617757132, 96.87390960531436690 ) ) ;
#10800 = CARTESIAN_POINT ( 'NONE',  ( -10.81492255796078084, -18.62759615963271287, 87.08224293864769550 ) ) ;
#10801 = CARTESIAN_POINT ( 'NONE',  ( 5.823673210054125526, 21.52544592524343514, 74.79057627198105251 ) ) ;
#10802 = CARTESIAN_POINT ( 'NONE',  ( -16.55341960407611168, -4.379528057220339221, 31.45724293864769550 ) ) ;
#10803 = CARTESIAN_POINT ( 'NONE',  ( 0.05219959533937995610, -21.53943276465977519, 110.0010903946856757 ) ) ;
#10804 = CARTESIAN_POINT ( 'NONE',  ( -5.049401038298153566, 19.05341960407611168, 80.20724293864769550 ) ) ;
#10805 = CARTESIAN_POINT ( 'NONE',  ( -0.05219959533909027116, -19.03943276465977164, 32.49890960531435979 ) ) ;
#10806 = CARTESIAN_POINT ( 'NONE',  ( -21.52544592524334988, -5.823673210054445271, 38.95942372801901854 ) ) ;
#10807 = CARTESIAN_POINT ( 'NONE',  ( 21.55341960407619695, -5.719274019375665929, 51.04275706135234714 ) ) ;
#10808 = CARTESIAN_POINT ( 'NONE',  ( 13.89961937509977652, -13.97604488694527269, 43.12390960531434558 ) ) ;
#10809 = CARTESIAN_POINT ( 'NONE',  ( 18.62759615963271287, -10.81492255796078972, 113.3322429386476955 ) ) ;
#10810 = CARTESIAN_POINT ( 'NONE',  ( -13.97604488694547697, 13.89961937509957934, 58.12609039468566863 ) ) ;
#10811 = CARTESIAN_POINT ( 'NONE',  ( -5.049401038298153566, 19.05341960407611168, 35.20724293864768839 ) ) ;
#10812 = CARTESIAN_POINT ( 'NONE',  ( -16.53943276465976808, -0.05219959533934237506, 23.75109039468567929 ) ) ;
#10813 = CARTESIAN_POINT ( 'NONE',  ( 5.049401038298161559, -19.05341960407611168, 32.70724293864768129 ) ) ;
#10814 = CARTESIAN_POINT ( 'NONE',  ( -8.224510206698735004, -14.34966873604973081, 74.58442372801901854 ) ) ;
#10815 = CARTESIAN_POINT ( 'NONE',  ( 19.05341960407611168, 5.049401038298154454, 43.95724293864769550 ) ) ;
#10816 = CARTESIAN_POINT ( 'NONE',  ( 24.85114155361846144, -5.582993631601040896, 168.8590791472286412 ) ) ;
#10817 = CARTESIAN_POINT ( 'NONE',  ( -16.51473224551069308, -9.474510206698971260, 81.66557627198103830 ) ) ;
#10818 = CARTESIAN_POINT ( 'NONE',  ( 16.51473224551069308, 9.474510206698969483, 29.16557627198103475 ) ) ;
#10819 = CARTESIAN_POINT ( 'NONE',  ( -15.80617190586745835, -15.72974639402198527, 71.87390960531438111 ) ) ;
#10820 = CARTESIAN_POINT ( 'NONE',  ( 16.53943276465976808, 0.05219959533934440121, 41.25109039468568284 ) ) ;
#10821 = CARTESIAN_POINT ( 'NONE',  ( -13.89961937509957401, -13.97604488694547875, 24.37609039468565442 ) ) ;
#10822 = CARTESIAN_POINT ( 'NONE',  ( 19.03943276465977164, -0.05219959533909143690, 33.74890960531435979 ) ) ;
#10823 = CARTESIAN_POINT ( 'NONE',  ( 8.224510206698953496, -14.34966873604960469, 32.91557627198102409 ) ) ;
#10824 = CARTESIAN_POINT ( 'NONE',  ( 12.14591786802309770, 12.06949235617756955, 69.37390960531436690 ) ) ;
#10825 = CARTESIAN_POINT ( 'NONE',  ( 9.564922557960805705, 16.46253265017160317, 64.58224293864769550 ) ) ;
#10826 = CARTESIAN_POINT ( 'NONE',  ( 18.67979575497194134, -10.72451020669871369, 110.8344237280190043 ) ) ;
#10827 = CARTESIAN_POINT ( 'NONE',  ( -10.72451020669898014, 18.67979575497178502, 115.4155762719810241 ) ) ;
#10828 = CARTESIAN_POINT ( 'NONE',  ( 13.89961937509977652, -13.97604488694527269, 78.12390960531433848 ) ) ;
#10829 = CONICAL_SURFACE ( 'NONE', #7615, 38.00373040315628259, 0.06108652381980166773 ) ;
#10830 = CARTESIAN_POINT ( 'NONE',  ( -18.62759615963255300, -10.81492255796106328, 84.16775706135234714 ) ) ;
#10831 = CARTESIAN_POINT ( 'NONE',  ( -0.05219959533934338120, 16.53943276465976808, 62.50109039468568284 ) ) ;
#10833 = CARTESIAN_POINT ( 'NONE',  ( -16.51473224551069308, -9.474510206698971260, 106.6655762719810383 ) ) ;
#10832 = CARTESIAN_POINT ( 'NONE',  ( -0.05219959533910754901, -16.53943276465976808, 87.49890960531436690 ) ) ;
#10834 = CARTESIAN_POINT ( 'NONE',  ( 0.05219959533910956823, 16.53943276465976808, 29.99890960531435979 ) ) ;
#10835 = CARTESIAN_POINT ( 'NONE',  ( -19.05341960407611168, -5.049401038298163336, 26.45724293864769550 ) ) ;
#10836 = CARTESIAN_POINT ( 'NONE',  ( 12.06949235617739724, 12.14591786802326823, 56.87609039468568994 ) ) ;
#10837 = CARTESIAN_POINT ( 'NONE',  ( -4.379528057220328563, 16.55341960407611168, 50.20724293864769550 ) ) ;
#10838 = CARTESIAN_POINT ( 'NONE',  ( 16.53943276465976808, 0.05219959533934440121, 106.2510903946856757 ) ) ;
#10839 = CARTESIAN_POINT ( 'NONE',  ( -0.05219959533907301413, -21.53943276465977519, 22.49890960531436335 ) ) ;
#10840 = CARTESIAN_POINT ( 'NONE',  ( -21.52544592524343514, 5.823673210054127303, 36.04057627198102409 ) ) ;
#10841 = CARTESIAN_POINT ( 'NONE',  ( 21.53943276465977519, 0.05219959533937863772, 106.2510903946856757 ) ) ;
#10842 = EDGE_CURVE ( 'NONE', #178298, #133752, #105049, .T. ) ;
#10843 = CARTESIAN_POINT ( 'NONE',  ( 14.34966873604960469, 8.224510206698951720, 84.16557627198103830 ) ) ;
#10844 = CARTESIAN_POINT ( 'NONE',  ( -19.05341960407611168, -5.049401038298163336, 91.45724293864766707 ) ) ;
#10845 = VERTEX_POINT ( 'NONE', #35693 ) ;
#10846 = CARTESIAN_POINT ( 'NONE',  ( 4.379528057220092307, 16.55341960407617563, 42.29275706135235424 ) ) ;
#10847 = CARTESIAN_POINT ( 'NONE',  ( 9.564922557960805705, 16.46253265017160317, 54.58224293864769550 ) ) ;
#10848 =( NAMED_UNIT ( * ) SI_UNIT ( $, .STERADIAN. ) SOLID_ANGLE_UNIT ( ) );
#10849 = CARTESIAN_POINT ( 'NONE',  ( -13.89961937509957401, -13.97604488694547875, 44.37609039468566863 ) ) ;
#10850 = CARTESIAN_POINT ( 'NONE',  ( -19.05341960407611168, -5.049401038298163336, 51.45724293864770260 ) ) ;
#10851 = CARTESIAN_POINT ( 'NONE',  ( 16.52544592524335698, 4.483927247898782831, 76.45942372801901854 ) ) ;
#10852 = CARTESIAN_POINT ( 'NONE',  ( -0.05219959533936034679, 19.03943276465977164, 97.50109039468567573 ) ) ;
#10853 = CARTESIAN_POINT ( 'NONE',  ( -19.05341960407611168, -5.049401038298163336, 56.45724293864768129 ) ) ;
#10854 = CARTESIAN_POINT ( 'NONE',  ( 18.67979575497178502, 10.72451020669898547, 94.16557627198103830 ) ) ;
#10855 = CARTESIAN_POINT ( 'NONE',  ( 16.53943276465976808, -0.05219959533910856209, 103.7489096053143669 ) ) ;
#10856 = CARTESIAN_POINT ( 'NONE',  ( -9.474510206698720793, -16.51473224551083518, 64.58442372801900433 ) ) ;
#10857 = CARTESIAN_POINT ( 'NONE',  ( 18.67979575497178502, 10.72451020669898547, 59.16557627198103120 ) ) ;
#10858 = CARTESIAN_POINT ( 'NONE',  ( -19.02544592524334988, -5.153800228976617603, 43.95942372801899012 ) ) ;
#10859 = CARTESIAN_POINT ( 'NONE',  ( 0.05219959533909260263, 19.03943276465977164, 114.9989096053143669 ) ) ;
#10860 = CARTESIAN_POINT ( 'NONE',  ( 18.67979575497178502, 10.72451020669898547, 94.16557627198103830 ) ) ;
#10861 = CARTESIAN_POINT ( 'NONE',  ( -18.87075004821571511, 5.499999999999904077, 53.67408112101048800 ) ) ;
#10862 = CARTESIAN_POINT ( 'NONE',  ( 19.05341960407617918, -5.049401038297876454, 106.0427570613523471 ) ) ;
#10863 = CARTESIAN_POINT ( 'NONE',  ( -19.26498983726237313, 5.499999999999599432, 60.55319577422002908 ) ) ;
#10864 = CARTESIAN_POINT ( 'NONE',  ( -0.05219959533934338120, 16.53943276465976808, 32.50109039468568284 ) ) ;
#10865 = CARTESIAN_POINT ( 'NONE',  ( -13.89961937509977652, 13.97604488694528158, 50.62390960531435979 ) ) ;
#10866 = CARTESIAN_POINT ( 'NONE',  ( 5.153800228976335163, 19.02544592524342804, 114.7905762719810241 ) ) ;
#10867 = CARTESIAN_POINT ( 'NONE',  ( 18.67979575497178502, 10.72451020669898547, 84.16557627198103830 ) ) ;
#10868 = CARTESIAN_POINT ( 'NONE',  ( 5.719274019375673035, 21.55341960407619339, 57.29275706135234714 ) ) ;
#10870 = CARTESIAN_POINT ( 'NONE',  ( -16.46253265017146816, -9.564922557961047289, 29.16775706135232937 ) ) ;
#10869 = CARTESIAN_POINT ( 'NONE',  ( 16.55341960407618274, -4.379528057220086978, 31.04275706135234714 ) ) ;
#10871 = CARTESIAN_POINT ( 'NONE',  ( -16.52544592524342804, 4.483927247898546575, 36.04057627198102409 ) ) ;
#10872 = CARTESIAN_POINT ( 'NONE',  ( 0.05219959533937995610, -21.53943276465977519, 20.00109039468568639 ) ) ;
#10873 = CARTESIAN_POINT ( 'NONE',  ( -0.05219959533910754901, -16.53943276465976808, 52.49890960531435979 ) ) ;
#10874 = CARTESIAN_POINT ( 'NONE',  ( -9.564922557961040184, 16.46253265017147172, 97.91775706135233293 ) ) ;
#10875 = CARTESIAN_POINT ( 'NONE',  ( 9.564922557961047289, -16.46253265017146816, 60.41775706135233293 ) ) ;
#10876 = CARTESIAN_POINT ( 'NONE',  ( 21.55341960407619695, -5.719274019375665929, 76.04275706135237556 ) ) ;
#10877 = CARTESIAN_POINT ( 'NONE',  ( -0.05219959533936034679, 19.03943276465977164, 42.50109039468566152 ) ) ;
#10878 = CARTESIAN_POINT ( 'NONE',  ( 5.049401038298161559, -19.05341960407611168, 22.70724293864769194 ) ) ;
#10879 = CARTESIAN_POINT ( 'NONE',  ( 0.05219959533907565091, 21.53943276465977519, 49.99890960531437401 ) ) ;
#10880 = CARTESIAN_POINT ( 'NONE',  ( -16.53943276465976808, 0.05219959533911058130, 31.24890960531435979 ) ) ;
#10881 = CARTESIAN_POINT ( 'NONE',  ( 21.53943276465977519, 0.05219959533937863772, 111.2510903946856899 ) ) ;
#10882 = CARTESIAN_POINT ( 'NONE',  ( 16.52544592524335698, 4.483927247898782831, 71.45942372801901854 ) ) ;
#10883 = CARTESIAN_POINT ( 'NONE',  ( 16.52544592524342804, -4.483927247898539470, 43.54057627198103830 ) ) ;
#10884 = CARTESIAN_POINT ( 'NONE',  ( -0.05219959533937732626, 21.53943276465977519, 72.50109039468568994 ) ) ;
#10885 = CARTESIAN_POINT ( 'NONE',  ( 10.72451020669871369, 18.67979575497193778, 62.08442372801901143 ) ) ;
#10886 = CARTESIAN_POINT ( 'NONE',  ( -15.80617190586745835, -15.72974639402198527, 66.87390960531436690 ) ) ;
#10887 = CARTESIAN_POINT ( 'NONE',  ( 5.049401038298161559, -19.05341960407611168, 42.70724293864767418 ) ) ;
#10888 = CARTESIAN_POINT ( 'NONE',  ( 15.72974639402176855, 15.80617190586768217, 46.87609039468568994 ) ) ;
#10889 = CARTESIAN_POINT ( 'NONE',  ( 5.049401038298161559, -19.05341960407611168, 27.70724293864769550 ) ) ;
#10890 = CARTESIAN_POINT ( 'NONE',  ( -19.05341960407611168, -5.049401038298163336, 41.45724293864769550 ) ) ;
#10891 = CARTESIAN_POINT ( 'NONE',  ( 8.314922557960818139, 14.29746914071049879, 94.58224293864769550 ) ) ;
#10892 = CARTESIAN_POINT ( 'NONE',  ( -13.89961937509977652, 13.97604488694528158, 80.62390960531436690 ) ) ;
#10893 = CARTESIAN_POINT ( 'NONE',  ( 4.483927247898545687, 16.52544592524342804, 34.79057627198103120 ) ) ;
#10894 = CARTESIAN_POINT ( 'NONE',  ( -4.379528057220328563, 16.55341960407611168, 95.20724293864769550 ) ) ;
#10895 = CARTESIAN_POINT ( 'NONE',  ( 18.67979575497178502, 10.72451020669898547, 64.16557627198102409 ) ) ;
#10896 = CARTESIAN_POINT ( 'NONE',  ( -10.81492255796078084, -18.62759615963271287, 112.0822429386477097 ) ) ;
#10897 = CARTESIAN_POINT ( 'NONE',  ( -16.60031353666876797, 14.64731493820422514, -55.88827192845551650 ) ) ;
#10899 = CARTESIAN_POINT ( 'NONE',  ( -8.224510206698735004, -14.34966873604973081, 29.58442372801901854 ) ) ;
#10898 = CARTESIAN_POINT ( 'NONE',  ( -19.03943276465977164, 0.05219959533909376836, 61.24890960531436690 ) ) ;
#10900 = CARTESIAN_POINT ( 'NONE',  ( -0.05219959533907301413, -21.53943276465977519, 52.49890960531435979 ) ) ;
#10901 = CARTESIAN_POINT ( 'NONE',  ( -21.52544592524334988, -5.823673210054445271, 93.95942372801903275 ) ) ;
#10902 = CARTESIAN_POINT ( 'NONE',  ( 19.05341960407611168, 5.049401038298154454, 83.95724293864766707 ) ) ;
#10903 = CARTESIAN_POINT ( 'NONE',  ( -18.62759615963255300, -10.81492255796106328, 19.16775706135234714 ) ) ;
#10904 = TOROIDAL_SURFACE ( 'NONE', #43230, 206.0437394197456342, 8.000000000000000000 ) ;
#10905 = CARTESIAN_POINT ( 'NONE',  ( 9.564922557960805705, 16.46253265017160317, 114.5822429386476955 ) ) ;
#10906 = CARTESIAN_POINT ( 'NONE',  ( 12.06949235617739724, 12.14591786802326823, 91.87609039468568994 ) ) ;
#10907 = CARTESIAN_POINT ( 'NONE',  ( -15.80617190586768217, 15.72974639402176855, 68.12609039468567573 ) ) ;
#10908 = CARTESIAN_POINT ( 'NONE',  ( -21.53943276465977519, -0.05219959533937600094, 98.75109039468568994 ) ) ;
#10909 = CARTESIAN_POINT ( 'NONE',  ( 4.483927247898790824, -16.52544592524335698, 65.20942372801901854 ) ) ;
#10910 = CARTESIAN_POINT ( 'NONE',  ( -18.67979575497193778, 10.72451020669871902, 28.33442372801902209 ) ) ;
#10911 = CARTESIAN_POINT ( 'NONE',  ( 19.03943276465977164, -0.05219959533909143690, 23.74890960531435269 ) ) ;
#10912 = CARTESIAN_POINT ( 'NONE',  ( -21.52544592524334988, -5.823673210054445271, 88.95942372801901854 ) ) ;
#10913 = CARTESIAN_POINT ( 'NONE',  ( -19.03943276465977164, 0.05219959533909376836, 96.24890960531436690 ) ) ;
#10914 = CARTESIAN_POINT ( 'NONE',  ( -18.62759615963270932, 10.81492255796079327, 85.83224293864768129 ) ) ;
#10915 = CARTESIAN_POINT ( 'NONE',  ( -13.97604488694547697, 13.89961937509957934, 63.12609039468566152 ) ) ;
#10916 = CARTESIAN_POINT ( 'NONE',  ( 18.67979575497178502, 10.72451020669898547, 49.16557627198102409 ) ) ;
#10918 = CARTESIAN_POINT ( 'NONE',  ( -8.224510206698948167, 14.34966873604960824, 40.41557627198103120 ) ) ;
#10917 = CARTESIAN_POINT ( 'NONE',  ( 9.474510206698971260, -16.51473224551069308, 92.91557627198103830 ) ) ;
#10919 = CARTESIAN_POINT ( 'NONE',  ( 11.92407319027615920, -9.806099294356528162, -61.90095559709221362 ) ) ;
#10920 = CARTESIAN_POINT ( 'NONE',  ( -0.05219959533936034679, 19.03943276465977164, 62.50109039468566863 ) ) ;
#10921 = CARTESIAN_POINT ( 'NONE',  ( -19.19724070472094013, -5.500000000000079936, 81.06193348274383936 ) ) ;
#10922 = CARTESIAN_POINT ( 'NONE',  ( 13.97604488694548053, -13.89961937509957401, 105.6260903946856757 ) ) ;
#10923 = CARTESIAN_POINT ( 'NONE',  ( 21.52544592524344225, -5.823673210054117533, 78.54057627198103830 ) ) ;
#10924 = CARTESIAN_POINT ( 'NONE',  ( -14.34966873604960291, -8.224510206698953496, 46.66557627198102409 ) ) ;
#10925 = CARTESIAN_POINT ( 'NONE',  ( 14.34966873604972726, -8.224510206698740333, 25.83442372801901499 ) ) ;
#10926 = CARTESIAN_POINT ( 'NONE',  ( -16.46253265017160317, 9.564922557960807481, 50.83224293864770260 ) ) ;
#10928 = CARTESIAN_POINT ( 'NONE',  ( 13.97604488694548053, -13.89961937509957401, 80.62609039468567573 ) ) ;
#10927 = CARTESIAN_POINT ( 'NONE',  ( -10.81492255796105439, 18.62759615963255655, 22.91775706135235069 ) ) ;
#10929 = CARTESIAN_POINT ( 'NONE',  ( -5.049401038298153566, 19.05341960407611168, 90.20724293864766707 ) ) ;
#10930 = CARTESIAN_POINT ( 'NONE',  ( 19.05341960407611168, 5.049401038298154454, 73.95724293864768129 ) ) ;
#10931 = CARTESIAN_POINT ( 'NONE',  ( -21.55341960407610458, -5.719274019375992779, 81.45724293864769550 ) ) ;
#10932 = CARTESIAN_POINT ( 'NONE',  ( -5.049401038298153566, 19.05341960407611168, 50.20724293864770260 ) ) ;
#10933 = CARTESIAN_POINT ( 'NONE',  ( 0.000000000000000000, 0.000000000000000000, -49.67367017693150189 ) ) ;
#10934 = CARTESIAN_POINT ( 'NONE',  ( -8.314922557960811034, -14.29746914071050412, 52.08224293864768839 ) ) ;
#10935 = CARTESIAN_POINT ( 'NONE',  ( 19.03943276465977164, -0.05219959533909143690, 93.74890960531435269 ) ) ;
#10936 = CARTESIAN_POINT ( 'NONE',  ( -30.00000000000000000, -1.163414459189985801E-14, 87.50000000000000000 ) ) ;
#10937 = CARTESIAN_POINT ( 'NONE',  ( 19.02544592524334988, 5.153800228976608722, 71.45942372801900433 ) ) ;
#10938 = CARTESIAN_POINT ( 'NONE',  ( -5.823673210054116645, -21.52544592524344225, 72.29057627198102409 ) ) ;
#10939 = CARTESIAN_POINT ( 'NONE',  ( 5.049401038297881783, 19.05341960407617563, 37.29275706135232582 ) ) ;
#10940 = CARTESIAN_POINT ( 'NONE',  ( 5.153800228976335163, 19.02544592524342804, 99.79057627198102409 ) ) ;
#10941 = CARTESIAN_POINT ( 'NONE',  ( -17.49999999999999645, 3.565345528327948710, 114.4249448680647276 ) ) ;
#10942 = CARTESIAN_POINT ( 'NONE',  ( 10.72451020669898902, -18.67979575497178502, 42.91557627198103120 ) ) ;
#10943 = CARTESIAN_POINT ( 'NONE',  ( 19.02544592524343514, -5.153800228976328945, 78.54057627198099567 ) ) ;
#10944 = CARTESIAN_POINT ( 'NONE',  ( 18.67979575497194134, -10.72451020669871369, 60.83442372801901854 ) ) ;
#10945 = CARTESIAN_POINT ( 'NONE',  ( 13.89961937509977652, -13.97604488694527269, 23.12390960531436335 ) ) ;
#10947 = EDGE_LOOP ( 'NONE', ( #98390, #76097, #93621, #165339 ) ) ;
#10946 = CARTESIAN_POINT ( 'NONE',  ( -10.81492255796105439, 18.62759615963255655, 22.91775706135235069 ) ) ;
#10948 = CARTESIAN_POINT ( 'NONE',  ( -10.72451020669870658, -18.67979575497194134, 49.58442372801901143 ) ) ;
#10949 = ORIENTED_EDGE ( 'NONE', *, *, #115458, .F. ) ;
#10950 = CARTESIAN_POINT ( 'NONE',  ( -16.46253265017160317, 9.564922557960807481, 115.8322429386477097 ) ) ;
#10951 = CARTESIAN_POINT ( 'NONE',  ( 16.46253265017146816, 9.564922557961045513, 61.66775706135234003 ) ) ;
#10952 = CARTESIAN_POINT ( 'NONE',  ( 27.33089735363351735, -28.79505088701976234, -20.09366309423206687 ) ) ;
#10953 = CARTESIAN_POINT ( 'NONE',  ( 21.53943276465977519, -0.05219959533907433946, 103.7489096053143669 ) ) ;
#10954 = CARTESIAN_POINT ( 'NONE',  ( -13.89961937509977652, 13.97604488694528158, 60.62390960531436690 ) ) ;
#10955 = CARTESIAN_POINT ( 'NONE',  ( -8.224510206698735004, -14.34966873604973081, 39.58442372801901143 ) ) ;
#10956 = CARTESIAN_POINT ( 'NONE',  ( -11.74264578624800670, 36.14014761921585972, -10.14999999453762669 ) ) ;
#10957 = CARTESIAN_POINT ( 'NONE',  ( -18.67979575497193778, 10.72451020669871902, 103.3344237280190043 ) ) ;
#10958 = CARTESIAN_POINT ( 'NONE',  ( 19.05341960407611168, 5.049401038298154454, 48.95724293864768129 ) ) ;
#10959 = CARTESIAN_POINT ( 'NONE',  ( 18.67979575497194134, -10.72451020669871369, 95.83442372801903275 ) ) ;
#10961 = CARTESIAN_POINT ( 'NONE',  ( 18.62759615963255655, 10.81492255796105972, 56.66775706135235424 ) ) ;
#10960 = CARTESIAN_POINT ( 'NONE',  ( 13.89961937509977652, -13.97604488694527269, 83.12390960531436690 ) ) ;
#10962 = CARTESIAN_POINT ( 'NONE',  ( 8.571926809382597767, 26.38167802310806209, 148.7750000027311899 ) ) ;
#10963 = CARTESIAN_POINT ( 'NONE',  ( 0.05219959533909260263, 19.03943276465977164, 114.9989096053143669 ) ) ;
#10964 = LINE ( 'NONE', #72638, #92055 ) ;
#10966 = CARTESIAN_POINT ( 'NONE',  ( -21.55341960407619339, 5.719274019375674811, 68.54275706135234714 ) ) ;
#10965 = CARTESIAN_POINT ( 'NONE',  ( -16.53943276465976808, -0.05219959533934237506, 58.75109039468568994 ) ) ;
#10967 = CARTESIAN_POINT ( 'NONE',  ( 0.05219959533937995610, -21.53943276465977519, 95.00109039468568994 ) ) ;
#10968 = AXIS2_PLACEMENT_3D ( 'NONE', #157679, #65654, #190998 ) ;
#10969 = CARTESIAN_POINT ( 'NONE',  ( 11.30153831258470731, -180.0000000000000000, -15.00000000000000178 ) ) ;
#10970 = CARTESIAN_POINT ( 'NONE',  ( -14.29746914071037622, -8.314922557961029526, 24.16775706135235424 ) ) ;
#10971 = CARTESIAN_POINT ( 'NONE',  ( 5.049401038298161559, -19.05341960407611168, 87.70724293864769550 ) ) ;
#10972 = CARTESIAN_POINT ( 'NONE',  ( -16.46253265017160317, 9.564922557960807481, 115.8322429386477097 ) ) ;
#10973 = ORIENTED_EDGE ( 'NONE', *, *, #159157, .F. ) ;
#10974 = CARTESIAN_POINT ( 'NONE',  ( -17.49999999999999645, -5.500000000000000000, 111.2823096230356725 ) ) ;
#10975 = CARTESIAN_POINT ( 'NONE',  ( 4.483927247898545687, 16.52544592524342804, 114.7905762719810383 ) ) ;
#10976 = CARTESIAN_POINT ( 'NONE',  ( -15.72974639402197994, 15.80617190586746368, 45.62390960531436690 ) ) ;
#10977 = CARTESIAN_POINT ( 'NONE',  ( -16.52544592524335698, -4.483927247898792601, 93.95942372801903275 ) ) ;
#10979 = CARTESIAN_POINT ( 'NONE',  ( -16.46253265017160317, 9.564922557960807481, 65.83224293864769550 ) ) ;
#10978 = CARTESIAN_POINT ( 'NONE',  ( -4.483927247898539470, -16.52544592524342804, 82.29057627198103830 ) ) ;
#10980 = CARTESIAN_POINT ( 'NONE',  ( 5.719274019375673035, 21.55341960407619339, 87.29275706135236135 ) ) ;
#10981 = CARTESIAN_POINT ( 'NONE',  ( -21.30000000000002913, 2.244099063931684814E-13, -58.85720012050612837 ) ) ;
#10982 = CARTESIAN_POINT ( 'NONE',  ( -19.03943276465977164, -0.05219959533935918106, 113.7510903946856757 ) ) ;
#10983 = CARTESIAN_POINT ( 'NONE',  ( -4.379528057220328563, 16.55341960407611168, 85.20724293864770971 ) ) ;
#10984 = CARTESIAN_POINT ( 'NONE',  ( 21.55341960407619695, -5.719274019375665929, 41.04275706135236135 ) ) ;
#10985 = CARTESIAN_POINT ( 'NONE',  ( -0.05219959533907301413, -21.53943276465977519, 72.49890960531435269 ) ) ;
#10986 = CARTESIAN_POINT ( 'NONE',  ( 16.51473224551083163, -9.474510206698727899, 35.83442372801899722 ) ) ;
#10987 = CARTESIAN_POINT ( 'NONE',  ( -34.77757469352546593, 0.9858555240219201155, 52.45108825929359142 ) ) ;
#10988 = CARTESIAN_POINT ( 'NONE',  ( -16.51473224551069308, -9.474510206698971260, 81.66557627198103830 ) ) ;
#10989 = CARTESIAN_POINT ( 'NONE',  ( 14.34966873604960469, 8.224510206698951720, 69.16557627198102409 ) ) ;
#10990 = VECTOR ( 'NONE', #185421, 1000.000000000000000 ) ;
#10991 = CARTESIAN_POINT ( 'NONE',  ( -14.34966873604960291, -8.224510206698953496, 36.66557627198103120 ) ) ;
#10992 = CARTESIAN_POINT ( 'NONE',  ( -4.483927247898782831, 16.52544592524335698, 107.7094237280190328 ) ) ;
#10993 = CARTESIAN_POINT ( 'NONE',  ( -13.89961937509957401, -13.97604488694547875, 59.37609039468566863 ) ) ;
#10994 = CARTESIAN_POINT ( 'NONE',  ( 19.49190055781009434, 5.500000000000042633, 53.06116087098784817 ) ) ;
#10995 = CARTESIAN_POINT ( 'NONE',  ( -10.72451020669898014, 18.67979575497178502, 25.41557627198103120 ) ) ;
#10996 = CARTESIAN_POINT ( 'NONE',  ( 12.06949235617757843, -12.14591786802309237, 88.12390960531436690 ) ) ;
#10997 = CARTESIAN_POINT ( 'NONE',  ( 22.96528548301342809, 5.795830589372932273, 190.0000000000000000 ) ) ;
#10999 = CARTESIAN_POINT ( 'NONE',  ( -21.55341960407610458, -5.719274019375992779, 46.45724293864769550 ) ) ;
#10998 = CARTESIAN_POINT ( 'NONE',  ( -0.05219959533909027116, -19.03943276465977164, 47.49890960531435979 ) ) ;
#11000 = CARTESIAN_POINT ( 'NONE',  ( -10.81492255796078084, -18.62759615963271287, 67.08224293864770971 ) ) ;
#11001 = CARTESIAN_POINT ( 'NONE',  ( 4.379528057220339221, -16.55341960407611168, 112.7072429386476955 ) ) ;
#11003 = CARTESIAN_POINT ( 'NONE',  ( 0.05219959533909260263, 19.03943276465977164, 49.99890960531435979 ) ) ;
#11002 = CARTESIAN_POINT ( 'NONE',  ( -8.224510206698735004, -14.34966873604973081, 69.58442372801900433 ) ) ;
#11004 = CARTESIAN_POINT ( 'NONE',  ( 10.72451020669871369, 18.67979575497193778, 57.08442372801901854 ) ) ;
#11005 = CARTESIAN_POINT ( 'NONE',  ( -16.53943276465976808, 0.05219959533911058130, 111.2489096053143669 ) ) ;
#11006 = CARTESIAN_POINT ( 'NONE',  ( -13.97604488694547697, 13.89961937509957934, 93.12609039468566152 ) ) ;
#11007 = CARTESIAN_POINT ( 'NONE',  ( -11.40812507854754720, -35.11059874428192273, -2.724999997268813257 ) ) ;
#11009 = CARTESIAN_POINT ( 'NONE',  ( -21.55341960407610458, -5.719274019375992779, 51.45724293864770260 ) ) ;
#11008 = CARTESIAN_POINT ( 'NONE',  ( 17.49999999999999645, 5.099703775204536882, 36.76678814087944147 ) ) ;
#11010 = CARTESIAN_POINT ( 'NONE',  ( 0.05219959533909260263, 19.03943276465977164, 24.99890960531435269 ) ) ;
#11011 = CARTESIAN_POINT ( 'NONE',  ( 5.719274019375673035, 21.55341960407619339, 82.29275706135234714 ) ) ;
#11012 = CARTESIAN_POINT ( 'NONE',  ( -8.224510206698948167, 14.34966873604960824, 30.41557627198101699 ) ) ;
#11014 = CARTESIAN_POINT ( 'NONE',  ( -8.314922557960811034, -14.29746914071050412, 37.08224293864768129 ) ) ;
#11013 = CARTESIAN_POINT ( 'NONE',  ( -16.55341960407617563, 4.379528057220093196, 58.54275706135235424 ) ) ;
#11015 = CARTESIAN_POINT ( 'NONE',  ( 21.52544592524344225, -5.823673210054117533, 68.54057627198103830 ) ) ;
#11016 = CARTESIAN_POINT ( 'NONE',  ( -21.52544592524343514, 5.823673210054127303, 76.04057627198102409 ) ) ;
#11017 = FACE_OUTER_BOUND ( 'NONE', #161873, .T. ) ;
#11019 = CARTESIAN_POINT ( 'NONE',  ( 5.049401038298161559, -19.05341960407611168, 112.7072429386476813 ) ) ;
#11018 = CARTESIAN_POINT ( 'NONE',  ( 19.02544592524334988, 5.153800228976608722, 86.45942372801900433 ) ) ;
#11020 = CARTESIAN_POINT ( 'NONE',  ( 13.89961937509977652, -13.97604488694527269, 53.12390960531434558 ) ) ;
#11021 = CARTESIAN_POINT ( 'NONE',  ( 0.05219959533910956823, 16.53943276465976808, 114.9989096053143669 ) ) ;
#11022 = DIRECTION ( 'NONE',  ( 0.000000000000000000, 0.000000000000000000, 1.000000000000000000 ) ) ;
#11023 = ORIENTED_EDGE ( 'NONE', *, *, #97826, .T. ) ;
#11024 = CARTESIAN_POINT ( 'NONE',  ( 4.379528057220092307, 16.55341960407617563, 87.29275706135236135 ) ) ;
#11025 = CARTESIAN_POINT ( 'NONE',  ( -15.80617190586745835, -15.72974639402198527, 106.8739096053143811 ) ) ;
#11026 = CARTESIAN_POINT ( 'NONE',  ( -9.474510206698964154, 16.51473224551069663, 65.41557627198102409 ) ) ;
#11027 = CARTESIAN_POINT ( 'NONE',  ( -21.53943276465977519, -0.05219959533937600094, 43.75109039468568284 ) ) ;
#11028 = CARTESIAN_POINT ( 'NONE',  ( -16.51473224551069308, -9.474510206698971260, 91.66557627198103830 ) ) ;
#11029 = CARTESIAN_POINT ( 'NONE',  ( -27.35218628822427434, -28.77384467243344801, -20.10380102094744714 ) ) ;
#11030 = ORIENTED_EDGE ( 'NONE', *, *, #121212, .F. ) ;
#11031 = CARTESIAN_POINT ( 'NONE',  ( 21.53943276465977519, 0.05219959533937863772, 26.25109039468567573 ) ) ;
#11033 = CARTESIAN_POINT ( 'NONE',  ( -16.51473224551082808, 9.474510206698731452, 93.33442372801900433 ) ) ;
#11032 = CARTESIAN_POINT ( 'NONE',  ( 19.02544592524343514, -5.153800228976328945, 23.54057627198102054 ) ) ;
#11034 = CARTESIAN_POINT ( 'NONE',  ( -19.03943276465977164, -0.05219959533935918106, 43.75109039468566863 ) ) ;
#11035 = CARTESIAN_POINT ( 'NONE',  ( 10.72451020669871369, 18.67979575497193778, 22.08442372801901143 ) ) ;
#11036 = CARTESIAN_POINT ( 'NONE',  ( 0.05219959533936267826, -19.03943276465977164, 30.00109039468566863 ) ) ;
#11037 = CARTESIAN_POINT ( 'NONE',  ( -19.03943276465977164, -0.05219959533935918106, 53.75109039468566863 ) ) ;
#11038 = CARTESIAN_POINT ( 'NONE',  ( 14.34966873604972726, -8.224510206698740333, 90.83442372801901854 ) ) ;
#11040 = ORIENTED_EDGE ( 'NONE', *, *, #91376, .T. ) ;
#11039 = CARTESIAN_POINT ( 'NONE',  ( 30.00000000000000000, 5.499999999999992895, 102.5000000000000142 ) ) ;
#11041 = CARTESIAN_POINT ( 'NONE',  ( -0.05219959533909027116, -19.03943276465977164, 72.49890960531435269 ) ) ;
#11042 = CARTESIAN_POINT ( 'NONE',  ( 5.823673210054444382, -21.52544592524334988, 80.20942372801901854 ) ) ;
#11043 = CARTESIAN_POINT ( 'NONE',  ( 18.67979575497194134, -10.72451020669871369, 100.8344237280190185 ) ) ;
#11044 = CARTESIAN_POINT ( 'NONE',  ( 24.23981148858513635, -0.4346045811322880037, -54.26183423998838862 ) ) ;
#11045 = CARTESIAN_POINT ( 'NONE',  ( -19.03943276465977164, 0.05219959533909376836, 86.24890960531436690 ) ) ;
#11046 = CARTESIAN_POINT ( 'NONE',  ( 21.53943276465977519, 0.05219959533937863772, 61.25109039468567573 ) ) ;
#11047 = CARTESIAN_POINT ( 'NONE',  ( 5.153800228976615827, -19.02544592524334988, 95.20942372801897591 ) ) ;
#11048 = CARTESIAN_POINT ( 'NONE',  ( -5.153800228976328057, -19.02544592524343514, 62.29057627198100988 ) ) ;
#11049 = CARTESIAN_POINT ( 'NONE',  ( -5.823673210054116645, -21.52544592524344225, 22.29057627198102765 ) ) ;
#11050 = AXIS2_PLACEMENT_3D ( 'NONE', #86392, #179429, #71233 ) ;
#11051 = CARTESIAN_POINT ( 'NONE',  ( 0.05219959533909260263, 19.03943276465977164, 74.99890960531435269 ) ) ;
#11052 = CARTESIAN_POINT ( 'NONE',  ( -17.50000000000001066, -5.622605283950841581, 91.31207310596107618 ) ) ;
#11053 = CARTESIAN_POINT ( 'NONE',  ( 19.03943276465977164, -0.05219959533909143690, 58.74890960531435979 ) ) ;
#11054 = CARTESIAN_POINT ( 'NONE',  ( -19.02544592524342804, 5.153800228976336051, 56.04057627198100988 ) ) ;
#11055 = CARTESIAN_POINT ( 'NONE',  ( -10.72451020669870658, -18.67979575497194134, 19.58442372801901143 ) ) ;
#11056 = CARTESIAN_POINT ( 'NONE',  ( 14.29746914071037800, 8.314922557961029526, 96.66775706135234714 ) ) ;
#11057 = DIRECTION ( 'NONE',  ( 1.000000000000000000, 0.000000000000000000, 0.000000000000000000 ) ) ;
#11058 = CARTESIAN_POINT ( 'NONE',  ( 6.615299585309121433, -1.135848680322177451, -64.43295106733367561 ) ) ;
#11059 = CARTESIAN_POINT ( 'NONE',  ( 5.049401038297881783, 19.05341960407617563, 52.29275706135234003 ) ) ;
#11060 = CARTESIAN_POINT ( 'NONE',  ( -0.05219959533909027116, -19.03943276465977164, 77.49890960531435269 ) ) ;
#11061 = CARTESIAN_POINT ( 'NONE',  ( -14.34966873604960291, -8.224510206698953496, 76.66557627198103830 ) ) ;
#11062 = CARTESIAN_POINT ( 'NONE',  ( -14.29746914071049879, 8.314922557960819915, 105.8322429386476955 ) ) ;
#11063 = CARTESIAN_POINT ( 'NONE',  ( 15.80617190586746368, 15.72974639402197994, 34.37390960531435979 ) ) ;
#11064 = CARTESIAN_POINT ( 'NONE',  ( -19.03943276465977164, 0.05219959533909376836, 111.2489096053143669 ) ) ;
#11065 = CARTESIAN_POINT ( 'NONE',  ( 0.05219959533910956823, 16.53943276465976808, 94.99890960531436690 ) ) ;
#11066 = CARTESIAN_POINT ( 'NONE',  ( 9.474510206698971260, -16.51473224551069308, 82.91557627198103830 ) ) ;
#11067 = CARTESIAN_POINT ( 'NONE',  ( -0.05219959533936034679, 19.03943276465977164, 27.50109039468566507 ) ) ;
#11068 = CARTESIAN_POINT ( 'NONE',  ( 8.314922557961029526, -14.29746914071037800, 105.4177570613523613 ) ) ;
#11069 = CARTESIAN_POINT ( 'NONE',  ( -9.564922557960796823, -16.46253265017161027, 87.08224293864769550 ) ) ;
#11070 = CARTESIAN_POINT ( 'NONE',  ( -15.80617190586768217, 15.72974639402176855, 53.12609039468568284 ) ) ;
#11071 = CARTESIAN_POINT ( 'NONE',  ( -18.67979575497178146, -10.72451020669898902, 41.66557627198103120 ) ) ;
#11072 = CARTESIAN_POINT ( 'NONE',  ( -0.05219959533907301413, -21.53943276465977519, 112.4989096053143669 ) ) ;
#11073 = CARTESIAN_POINT ( 'NONE',  ( 10.81492255796078972, 18.62759615963270932, 74.58224293864768129 ) ) ;
#11074 = CARTESIAN_POINT ( 'NONE',  ( -12.14591786802309592, -12.06949235617757132, 91.87390960531436690 ) ) ;
#11075 = CARTESIAN_POINT ( 'NONE',  ( -0.05219959533936034679, 19.03943276465977164, 57.50109039468566863 ) ) ;
#11076 = EDGE_CURVE ( 'NONE', #82999, #84229, #111277, .T. ) ;
#11077 = VECTOR ( 'NONE', #116212, 1000.000000000000000 ) ;
#11078 = CARTESIAN_POINT ( 'NONE',  ( -13.97604488694527625, -13.89961937509977652, 31.87390960531435979 ) ) ;
#11079 = CARTESIAN_POINT ( 'NONE',  ( -16.46253265017160317, 9.564922557960807481, 95.83224293864769550 ) ) ;
#11080 = CARTESIAN_POINT ( 'NONE',  ( 16.46253265017160672, -9.564922557960803928, 98.33224293864769550 ) ) ;
#11081 = CARTESIAN_POINT ( 'NONE',  ( 14.34966873604960469, 8.224510206698951720, 109.1655762719810383 ) ) ;
#11082 = CARTESIAN_POINT ( 'NONE',  ( -14.34966873604960291, -8.224510206698953496, 26.66557627198103475 ) ) ;
#11083 = CARTESIAN_POINT ( 'NONE',  ( 16.55341960407618274, -4.379528057220086978, 46.04275706135234714 ) ) ;
#11084 = CARTESIAN_POINT ( 'NONE',  ( -21.52544592524334988, -5.823673210054445271, 103.9594237280190185 ) ) ;
#11086 = CARTESIAN_POINT ( 'NONE',  ( 14.29746914071049879, -8.314922557960816363, 28.33224293864769550 ) ) ;
#11085 = CARTESIAN_POINT ( 'NONE',  ( -9.474510206698964154, 16.51473224551069663, 105.4155762719810383 ) ) ;
#11087 = CARTESIAN_POINT ( 'NONE',  ( -18.62759615963255300, -10.81492255796106328, 29.16775706135234003 ) ) ;
#11088 = CARTESIAN_POINT ( 'NONE',  ( 5.153800228976335163, 19.02544592524342804, 39.79057627198100988 ) ) ;
#11089 = CARTESIAN_POINT ( 'NONE',  ( -0.05219959533934338120, 16.53943276465976808, 47.50109039468568994 ) ) ;
#11090 = CARTESIAN_POINT ( 'NONE',  ( 14.34966873604972726, -8.224510206698740333, 110.8344237280190043 ) ) ;
#11091 = CARTESIAN_POINT ( 'NONE',  ( -14.34966873604972548, 8.224510206698743886, 98.33442372801901854 ) ) ;
#11092 = CIRCLE ( 'NONE', #108041, 5.000000000000000888 ) ;
#11093 = CARTESIAN_POINT ( 'NONE',  ( 0.05219959533936267826, -19.03943276465977164, 105.0010903946856615 ) ) ;
#11094 = CARTESIAN_POINT ( 'NONE',  ( 16.51473224551069308, 9.474510206698969483, 29.16557627198103475 ) ) ;
#11095 = CARTESIAN_POINT ( 'NONE',  ( 14.34966873604960469, 8.224510206698951720, 94.16557627198103830 ) ) ;
#11096 = CARTESIAN_POINT ( 'NONE',  ( -15.80617190586745835, -15.72974639402198527, 106.8739096053143811 ) ) ;
#11097 = CARTESIAN_POINT ( 'NONE',  ( -9.564922557960796823, -16.46253265017161027, 32.08224293864769550 ) ) ;
#11098 = CARTESIAN_POINT ( 'NONE',  ( -5.153800228976328057, -19.02544592524343514, 102.2905762719810383 ) ) ;
#11099 = CARTESIAN_POINT ( 'NONE',  ( -5.823673210054431948, 21.52544592524334988, 27.70942372801901854 ) ) ;
#11100 = CARTESIAN_POINT ( 'NONE',  ( -23.48298174826590667, 32.32155151706776053, -2.302157773949822683 ) ) ;
#11101 = CARTESIAN_POINT ( 'NONE',  ( 19.02544592524343514, -5.153800228976328945, 103.5405762719809957 ) ) ;
#11102 = CIRCLE ( 'NONE', #36896, 40.00000000000000000 ) ;
#11103 = CARTESIAN_POINT ( 'NONE',  ( 17.50000000000000355, -5.624438216177584771, 113.3167034491464307 ) ) ;
#11104 = CARTESIAN_POINT ( 'NONE',  ( 13.97604488694527802, 13.89961937509977652, 79.37390960531435269 ) ) ;
#11106 = CARTESIAN_POINT ( 'NONE',  ( -16.53943276465976808, 0.05219959533911058130, 96.24890960531435269 ) ) ;
#11105 = CARTESIAN_POINT ( 'NONE',  ( 5.719274019375673035, 21.55341960407619339, 37.29275706135235424 ) ) ;
#11107 = CARTESIAN_POINT ( 'NONE',  ( -16.46253265017160317, 9.564922557960807481, 95.83224293864769550 ) ) ;
#11108 = CARTESIAN_POINT ( 'NONE',  ( -19.03943276465977164, -0.05219959533935918106, 28.75109039468566507 ) ) ;
#11109 = CARTESIAN_POINT ( 'NONE',  ( -8.224510206698735004, -14.34966873604973081, 59.58442372801901854 ) ) ;
#11110 = CARTESIAN_POINT ( 'NONE',  ( 18.62759615963255655, 10.81492255796105972, 76.66775706135234714 ) ) ;
#11111 = CARTESIAN_POINT ( 'NONE',  ( 14.29746914071037800, 8.314922557961029526, 36.66775706135234714 ) ) ;
#11112 = CARTESIAN_POINT ( 'NONE',  ( -9.564922557960796823, -16.46253265017161027, 77.08224293864769550 ) ) ;
#11113 = CARTESIAN_POINT ( 'NONE',  ( -13.89961937509957401, -13.97604488694547875, 89.37609039468563310 ) ) ;
#11114 = CARTESIAN_POINT ( 'NONE',  ( -12.14591786802326823, 12.06949235617739902, 63.12609039468568994 ) ) ;
#11115 = CARTESIAN_POINT ( 'NONE',  ( 5.719274019375673035, 21.55341960407619339, 107.2927570613523471 ) ) ;
#11116 = CARTESIAN_POINT ( 'NONE',  ( -13.97604488694547697, 13.89961937509957934, 98.12609039468566152 ) ) ;
#11117 = CARTESIAN_POINT ( 'NONE',  ( -19.05341960407611168, -5.049401038298163336, 66.45724293864769550 ) ) ;
#11118 = CARTESIAN_POINT ( 'NONE',  ( -18.67979575497178146, -10.72451020669898902, 86.66557627198102409 ) ) ;
#11120 = CARTESIAN_POINT ( 'NONE',  ( -9.564922557961040184, 16.46253265017147172, 92.91775706135233293 ) ) ;
#11119 = CARTESIAN_POINT ( 'NONE',  ( 4.379528057220339221, -16.55341960407611168, 92.70724293864770971 ) ) ;
#11121 = CARTESIAN_POINT ( 'NONE',  ( 16.52544592524335698, 4.483927247898782831, 61.45942372801901854 ) ) ;
#11122 = CARTESIAN_POINT ( 'NONE',  ( 21.96844466259091533, 7.174710485416647465, 170.3366942299255413 ) ) ;
#11123 = CARTESIAN_POINT ( 'NONE',  ( 19.02544592524334988, 5.153800228976608722, 61.45942372801900433 ) ) ;
#11124 = CARTESIAN_POINT ( 'NONE',  ( -12.14591786802326823, 12.06949235617739902, 108.1260903946856757 ) ) ;
#11125 = CARTESIAN_POINT ( 'NONE',  ( 8.224510206698953496, -14.34966873604960469, 77.91557627198102409 ) ) ;
#11127 = CARTESIAN_POINT ( 'NONE',  ( -19.52837319214027900, 5.499999999999900524, 89.60471352585535953 ) ) ;
#11126 = CARTESIAN_POINT ( 'NONE',  ( 13.89961937509957401, 13.97604488694547697, 26.87609039468566507 ) ) ;
#11128 = CARTESIAN_POINT ( 'NONE',  ( 5.719274019375673035, 21.55341960407619339, 22.29275706135235069 ) ) ;
#11129 = CARTESIAN_POINT ( 'NONE',  ( 5.049401038298161559, -19.05341960407611168, 107.7072429386476955 ) ) ;
#11130 = CARTESIAN_POINT ( 'NONE',  ( 5.153800228976335163, 19.02544592524342804, 84.79057627198099567 ) ) ;
#11131 = CARTESIAN_POINT ( 'NONE',  ( 5.719274019375673035, 21.55341960407619339, 82.29275706135234714 ) ) ;
#11132 = CARTESIAN_POINT ( 'NONE',  ( 16.51473224551069308, 9.474510206698969483, 59.16557627198102409 ) ) ;
#11133 = ORIENTED_EDGE ( 'NONE', *, *, #149523, .F. ) ;
#11134 = CARTESIAN_POINT ( 'NONE',  ( 15.72974639402199770, -15.80617190586745480, 33.12390960531435979 ) ) ;
#11135 = CARTESIAN_POINT ( 'NONE',  ( -16.53943276465976808, 0.05219959533911058130, 76.24890960531435269 ) ) ;
#11136 = CARTESIAN_POINT ( 'NONE',  ( 0.05219959533909260263, 19.03943276465977164, 39.99890960531436690 ) ) ;
#11137 = CARTESIAN_POINT ( 'NONE',  ( -8.314922557960811034, -14.29746914071050412, 102.0822429386476955 ) ) ;
#11138 = CIRCLE ( 'NONE', #124106, 5.000000000000000000 ) ;
#11139 = CARTESIAN_POINT ( 'NONE',  ( 0.05219959533907565091, 21.53943276465977519, 104.9989096053143669 ) ) ;
#11140 = CARTESIAN_POINT ( 'NONE',  ( 21.53943276465977519, 0.05219959533937863772, 66.25109039468567573 ) ) ;
#11141 = CARTESIAN_POINT ( 'NONE',  ( 19.05341960407611168, 5.049401038298154454, 33.95724293864769550 ) ) ;
#11142 = CARTESIAN_POINT ( 'NONE',  ( -14.34966873604972548, 8.224510206698743886, 68.33442372801900433 ) ) ;
#11143 = CARTESIAN_POINT ( 'NONE',  ( 21.53943276465977519, -0.05219959533907433946, 103.7489096053143669 ) ) ;
#11144 = CARTESIAN_POINT ( 'NONE',  ( -21.53943276465977519, -0.05219959533937600094, 18.75109039468568639 ) ) ;
#11146 = CARTESIAN_POINT ( 'NONE',  ( -5.153800228976328057, -19.02544592524343514, 57.29057627198103120 ) ) ;
#11145 = CARTESIAN_POINT ( 'NONE',  ( 16.51473224551083163, -9.474510206698727899, 40.83442372801900433 ) ) ;
#11147 = CARTESIAN_POINT ( 'NONE',  ( -17.60769864724389677, 5.499999999999980460, 83.65024842019165874 ) ) ;
#11148 = CARTESIAN_POINT ( 'NONE',  ( -15.72974639402176322, -15.80617190586768395, 59.37609039468568284 ) ) ;
#11149 = CARTESIAN_POINT ( 'NONE',  ( 15.80617190586746368, 15.72974639402197994, 59.37390960531436690 ) ) ;
#11150 = CARTESIAN_POINT ( 'NONE',  ( 8.224510206698953496, -14.34966873604960469, 32.91557627198102409 ) ) ;
#11152 = CARTESIAN_POINT ( 'NONE',  ( -21.53943276465977519, -0.05219959533937600094, 113.7510903946856757 ) ) ;
#11151 = CARTESIAN_POINT ( 'NONE',  ( -15.80617190586768217, 15.72974639402176855, 83.12609039468568994 ) ) ;
#11153 = CARTESIAN_POINT ( 'NONE',  ( -16.52544592524342804, 4.483927247898546575, 56.04057627198102409 ) ) ;
#11154 = CARTESIAN_POINT ( 'NONE',  ( 14.29746914071049879, -8.314922557960816363, 108.3322429386477097 ) ) ;
#11155 = CARTESIAN_POINT ( 'NONE',  ( 0.05219959533936267826, -19.03943276465977164, 50.00109039468566863 ) ) ;
#11156 = CARTESIAN_POINT ( 'NONE',  ( -4.379528057220086978, -16.55341960407618274, 104.7927570613523898 ) ) ;
#11157 = CARTESIAN_POINT ( 'NONE',  ( 18.67979575497194134, -10.72451020669871369, 65.83442372801900433 ) ) ;
#11158 = CARTESIAN_POINT ( 'NONE',  ( 19.05341960407611168, 5.049401038298154454, 63.95724293864769550 ) ) ;
#11159 = CARTESIAN_POINT ( 'NONE',  ( 9.474510206698729675, 16.51473224551082808, 37.08442372801899722 ) ) ;
#11160 = CARTESIAN_POINT ( 'NONE',  ( -0.05219959533907301413, -21.53943276465977519, 32.49890960531435979 ) ) ;
#11161 = CARTESIAN_POINT ( 'NONE',  ( -18.62759615963255300, -10.81492255796106328, 29.16775706135234003 ) ) ;
#11162 = CARTESIAN_POINT ( 'NONE',  ( -0.05219959533907301413, -21.53943276465977519, 82.49890960531436690 ) ) ;
#11163 = CARTESIAN_POINT ( 'NONE',  ( -19.05341960407617563, 5.049401038297882671, 83.54275706135233293 ) ) ;
#11164 = CARTESIAN_POINT ( 'NONE',  ( -12.14591786802326823, 12.06949235617739902, 53.12609039468568284 ) ) ;
#11166 = CARTESIAN_POINT ( 'NONE',  ( 21.53943276465977519, -0.05219959533907433946, 88.74890960531436690 ) ) ;
#11165 = CARTESIAN_POINT ( 'NONE',  ( 17.50000000000002132, -3.734851586428651782, 36.81917961330525202 ) ) ;
#11167 = CARTESIAN_POINT ( 'NONE',  ( -8.224510206698948167, 14.34966873604960824, 75.41557627198102409 ) ) ;
#11168 = CARTESIAN_POINT ( 'NONE',  ( -17.05116617787824396, -6.768360034955821725, 101.3432444674080415 ) ) ;
#11169 = CARTESIAN_POINT ( 'NONE',  ( 19.05341960407617918, -5.049401038297876454, 111.0427570613523329 ) ) ;
#11170 = CARTESIAN_POINT ( 'NONE',  ( 18.67979575497178502, 10.72451020669898547, 39.16557627198102409 ) ) ;
#11171 = CARTESIAN_POINT ( 'NONE',  ( -4.483927247898782831, 16.52544592524335698, 82.70942372801900433 ) ) ;
#11172 = CARTESIAN_POINT ( 'NONE',  ( -17.49999999999999645, 7.499999999999998224, 118.0000000000000142 ) ) ;
#11173 = CARTESIAN_POINT ( 'NONE',  ( 16.55341960407618274, -4.379528057220086978, 56.04275706135235424 ) ) ;
#11174 = CARTESIAN_POINT ( 'NONE',  ( -21.55341960407619339, 5.719274019375674811, 33.54275706135234714 ) ) ;
#11175 = CARTESIAN_POINT ( 'NONE',  ( 18.62759615963271287, -10.81492255796078972, 43.33224293864769550 ) ) ;
#11176 = CARTESIAN_POINT ( 'NONE',  ( 4.379528057220092307, 16.55341960407617563, 67.29275706135234714 ) ) ;
#11177 = CARTESIAN_POINT ( 'NONE',  ( 9.564922557960805705, 16.46253265017160317, 89.58224293864769550 ) ) ;
#11179 = CARTESIAN_POINT ( 'NONE',  ( 19.05341960407611168, 5.049401038298154454, 28.95724293864769550 ) ) ;
#11178 = CARTESIAN_POINT ( 'NONE',  ( -15.72974639402176322, -15.80617190586768395, 59.37609039468568284 ) ) ;
#11180 = CARTESIAN_POINT ( 'NONE',  ( -15.80617190586745835, -15.72974639402198527, 36.87390960531435979 ) ) ;
#11181 = CARTESIAN_POINT ( 'NONE',  ( -19.03943276465977164, 0.05219959533909376836, 111.2489096053143669 ) ) ;
#11182 = ORIENTED_EDGE ( 'NONE', *, *, #90658, .T. ) ;
#11183 = CARTESIAN_POINT ( 'NONE',  ( -19.02544592524334988, -5.153800228976617603, 43.95942372801899012 ) ) ;
#11184 = CARTESIAN_POINT ( 'NONE',  ( 16.52544592524335698, 4.483927247898782831, 51.45942372801901854 ) ) ;
#11185 = CARTESIAN_POINT ( 'NONE',  ( 16.46253265017160672, -9.564922557960803928, 108.3322429386476955 ) ) ;
#11186 = EDGE_LOOP ( 'NONE', ( #162167, #2725, #62094, #31894 ) ) ;
#11187 = CARTESIAN_POINT ( 'NONE',  ( 13.89961937509977652, -13.97604488694527269, 83.12390960531436690 ) ) ;
#11188 = CARTESIAN_POINT ( 'NONE',  ( -8.224510206698735004, -14.34966873604973081, 94.58442372801901854 ) ) ;
#11189 = DIRECTION ( 'NONE',  ( -0.000000000000000000, -0.000000000000000000, 1.000000000000000000 ) ) ;
#11190 = CARTESIAN_POINT ( 'NONE',  ( 16.53943276465976808, -0.05219959533910856209, 88.74890960531436690 ) ) ;
#11191 = CARTESIAN_POINT ( 'NONE',  ( 21.52544592524344225, -5.823673210054117533, 33.54057627198102409 ) ) ;
#11192 = CARTESIAN_POINT ( 'NONE',  ( -19.02544592524342804, 5.153800228976336051, 36.04057627198100988 ) ) ;
#11193 = CARTESIAN_POINT ( 'NONE',  ( 12.14591786802327356, -12.06949235617739191, 80.62609039468567573 ) ) ;
#11194 = CARTESIAN_POINT ( 'NONE',  ( 21.53943276465977519, -0.05219959533907433946, 113.7489096053143527 ) ) ;
#11195 = CARTESIAN_POINT ( 'NONE',  ( 5.153800228976615827, -19.02544592524334988, 75.20942372801896170 ) ) ;
#11196 = CARTESIAN_POINT ( 'NONE',  ( 19.03943276465977164, -0.05219959533909143690, 43.74890960531435979 ) ) ;
#11197 = CARTESIAN_POINT ( 'NONE',  ( 19.05341960407611168, 5.049401038298154454, 113.9572429386477097 ) ) ;
#11198 = CARTESIAN_POINT ( 'NONE',  ( -10.81492255796105439, 18.62759615963255655, 107.9177570613523471 ) ) ;
#11199 = CARTESIAN_POINT ( 'NONE',  ( -16.51473224551069308, -9.474510206698971260, 66.66557627198102409 ) ) ;
#11200 = CARTESIAN_POINT ( 'NONE',  ( -4.483927247898782831, 16.52544592524335698, 42.70942372801901854 ) ) ;
#11201 = CARTESIAN_POINT ( 'NONE',  ( -0.05219959533937732626, 21.53943276465977519, 87.50109039468568994 ) ) ;
#11202 = CARTESIAN_POINT ( 'NONE',  ( 13.89961937509957401, 13.97604488694547697, 51.87609039468566863 ) ) ;
#11203 = AXIS2_PLACEMENT_3D ( 'NONE', #132403, #129381, #147580 ) ;
#11204 = CARTESIAN_POINT ( 'NONE',  ( 16.46253265017146816, 9.564922557961045513, 51.66775706135233293 ) ) ;
#11205 = VERTEX_POINT ( 'NONE', #147882 ) ;
#11206 = CARTESIAN_POINT ( 'NONE',  ( 10.72451020669871369, 18.67979575497193778, 47.08442372801901854 ) ) ;
#11207 = CARTESIAN_POINT ( 'NONE',  ( -16.51473224551069308, -9.474510206698971260, 56.66557627198103120 ) ) ;
#11208 = CARTESIAN_POINT ( 'NONE',  ( -0.05219959533936034679, 19.03943276465977164, 42.50109039468566152 ) ) ;
#11209 = CARTESIAN_POINT ( 'NONE',  ( 0.05219959533909260263, 19.03943276465977164, 104.9989096053143669 ) ) ;
#11210 = CARTESIAN_POINT ( 'NONE',  ( -16.51473224551069308, -9.474510206698971260, 81.66557627198103830 ) ) ;
#11211 = CARTESIAN_POINT ( 'NONE',  ( 4.483927247898545687, 16.52544592524342804, 34.79057627198103120 ) ) ;
#11212 = CARTESIAN_POINT ( 'NONE',  ( -5.719274019375978568, 21.55341960407610458, 35.20724293864768839 ) ) ;
#11213 = CARTESIAN_POINT ( 'NONE',  ( 36.91746825000000598, -11.99521256947793546, -4.224999997268812812 ) ) ;
#11214 = LINE ( 'NONE', #24388, #41679 ) ;
#11215 = CARTESIAN_POINT ( 'NONE',  ( -19.02544592524334988, -5.153800228976617603, 18.95942372801899722 ) ) ;
#11216 = DIRECTION ( 'NONE',  ( -1.000000000000000000, 0.000000000000000000, 0.000000000000000000 ) ) ;
#11217 = CARTESIAN_POINT ( 'NONE',  ( -19.03943276465977164, 0.05219959533909376836, 31.24890960531435979 ) ) ;
#11218 = CARTESIAN_POINT ( 'NONE',  ( -9.564922557960796823, -16.46253265017161027, 27.08224293864769550 ) ) ;
#11219 = ADVANCED_FACE ( 'NONE', ( #166041 ), #39684, .T. ) ;
#11220 = CARTESIAN_POINT ( 'NONE',  ( -9.338429343928289939, -11.33503711070567554, -60.04863804042465603 ) ) ;
#11221 = CARTESIAN_POINT ( 'NONE',  ( -37.99533089065118219, -0.2660902954431525469, -7.999999999999996447 ) ) ;
#11222 = CARTESIAN_POINT ( 'NONE',  ( 16.53943276465976808, 0.05219959533934440121, 66.25109039468567573 ) ) ;
#11223 = CARTESIAN_POINT ( 'NONE',  ( -5.719274019375978568, 21.55341960407610458, 80.20724293864769550 ) ) ;
#11224 = CIRCLE ( 'NONE', #104733, 206.0437394197456911 ) ;
#11225 = CARTESIAN_POINT ( 'NONE',  ( 8.314922557960818139, 14.29746914071049879, 54.58224293864769550 ) ) ;
#11227 = CARTESIAN_POINT ( 'NONE',  ( -19.05341960407611168, -5.049401038298163336, 101.4572429386476955 ) ) ;
#11226 = CARTESIAN_POINT ( 'NONE',  ( 5.153800228976335163, 19.02544592524342804, 34.79057627198102409 ) ) ;
#11228 = CARTESIAN_POINT ( 'NONE',  ( -18.67979575497193778, 10.72451020669871902, 33.33442372801900433 ) ) ;
#11229 = CARTESIAN_POINT ( 'NONE',  ( 16.46253265017146816, 9.564922557961045513, 36.66775706135233293 ) ) ;
#11230 = CARTESIAN_POINT ( 'NONE',  ( 5.153800228976335163, 19.02544592524342804, 39.79057627198100988 ) ) ;
#11231 = CARTESIAN_POINT ( 'NONE',  ( -18.67979575497193778, 10.72451020669871902, 78.33442372801901854 ) ) ;
#11232 = CARTESIAN_POINT ( 'NONE',  ( 17.31728774477274158, -6.344390552232386682, 33.31906651689320142 ) ) ;
#11233 = CARTESIAN_POINT ( 'NONE',  ( -16.52544592524342804, 4.483927247898546575, 26.04057627198103475 ) ) ;
#11234 = CARTESIAN_POINT ( 'NONE',  ( 17.50000000000000355, 3.471454075611732915, 113.0166741885564505 ) ) ;
#11235 = CARTESIAN_POINT ( 'NONE',  ( -21.55341960407610458, -5.719274019375992779, 41.45724293864769550 ) ) ;
#11236 = CARTESIAN_POINT ( 'NONE',  ( -4.483927247898539470, -16.52544592524342804, 102.2905762719810383 ) ) ;
#11237 = DIRECTION ( 'NONE',  ( -0.000000000000000000, 0.4999999999999998890, -0.8660254037844387076 ) ) ;
#11238 = CARTESIAN_POINT ( 'NONE',  ( -9.564922557960796823, -16.46253265017161027, 92.08224293864769550 ) ) ;
#11239 = CARTESIAN_POINT ( 'NONE',  ( -0.05219959533910754901, -16.53943276465976808, 72.49890960531435269 ) ) ;
#11240 = CARTESIAN_POINT ( 'NONE',  ( 19.02544592524334988, 5.153800228976608722, 106.4594237280190185 ) ) ;
#11241 = CARTESIAN_POINT ( 'NONE',  ( 15.72974639402199770, -15.80617190586745480, 58.12390960531435979 ) ) ;
#11242 = EDGE_LOOP ( 'NONE', ( #101594, #137434, #105999, #91375 ) ) ;
#11243 = CARTESIAN_POINT ( 'NONE',  ( -19.03943276465977164, 0.05219959533909376836, 31.24890960531435979 ) ) ;
#11244 = AXIS2_PLACEMENT_3D ( 'NONE', #190710, #5674, #51195 ) ;
#11246 = CARTESIAN_POINT ( 'NONE',  ( -21.53943276465977519, 0.05219959533907696930, 91.24890960531436690 ) ) ;
#11245 = CARTESIAN_POINT ( 'NONE',  ( 9.564922557960805705, 16.46253265017160317, 84.58224293864769550 ) ) ;
#11248 = CARTESIAN_POINT ( 'NONE',  ( -16.46253265017160317, 9.564922557960807481, 90.83224293864769550 ) ) ;
#11247 = CARTESIAN_POINT ( 'NONE',  ( 12.14591786802327356, -12.06949235617739191, 105.6260903946856899 ) ) ;
#11249 = CARTESIAN_POINT ( 'NONE',  ( -16.51473224551082808, 9.474510206698731452, 78.33442372801900433 ) ) ;
#11250 = CARTESIAN_POINT ( 'NONE',  ( 5.823673210054444382, -21.52544592524334988, 95.20942372801903275 ) ) ;
#11251 = CARTESIAN_POINT ( 'NONE',  ( -10.72451020669898014, 18.67979575497178502, 75.41557627198102409 ) ) ;
#11252 = CARTESIAN_POINT ( 'NONE',  ( 18.67979575497178502, 10.72451020669898547, 39.16557627198102409 ) ) ;
#11253 = CIRCLE ( 'NONE', #175759, 38.00000000000000000 ) ;
#11254 = CARTESIAN_POINT ( 'NONE',  ( -16.51473224551069308, -9.474510206698971260, 51.66557627198102409 ) ) ;
#11255 = CARTESIAN_POINT ( 'NONE',  ( -8.314922557961024197, 14.29746914071037800, 112.9177570613523329 ) ) ;
#11256 = CARTESIAN_POINT ( 'NONE',  ( -16.51473224551069308, -9.474510206698971260, 61.66557627198103120 ) ) ;
#11257 = DIRECTION ( 'NONE',  ( -1.000000000000000000, -0.000000000000000000, -0.000000000000000000 ) ) ;
#11258 = CARTESIAN_POINT ( 'NONE',  ( -9.564922557961040184, 16.46253265017147172, 27.91775706135232582 ) ) ;
#11259 = CARTESIAN_POINT ( 'NONE',  ( 12.14591786802309770, 12.06949235617756955, 79.37390960531436690 ) ) ;
#11260 = AXIS2_PLACEMENT_3D ( 'NONE', #133352, #179890, #103021 ) ;
#11261 = CARTESIAN_POINT ( 'NONE',  ( -21.52544592524343514, 5.823673210054127303, 106.0405762719810525 ) ) ;
#11262 = CARTESIAN_POINT ( 'NONE',  ( 8.571926809382603096, -26.38167802310801235, 139.9750000027311785 ) ) ;
#11263 = CARTESIAN_POINT ( 'NONE',  ( 21.52544592524344225, -5.823673210054117533, 58.54057627198103120 ) ) ;
#11264 = CARTESIAN_POINT ( 'NONE',  ( -16.52544592524335698, -4.483927247898792601, 98.95942372801903275 ) ) ;
#11265 = CARTESIAN_POINT ( 'NONE',  ( -14.29746914071049879, 8.314922557960819915, 105.8322429386476955 ) ) ;
#11266 = CARTESIAN_POINT ( 'NONE',  ( 16.51473224551069308, 9.474510206698969483, 59.16557627198102409 ) ) ;
#11267 = CARTESIAN_POINT ( 'NONE',  ( -14.34966873604960291, -8.224510206698953496, 26.66557627198103475 ) ) ;
#11268 = CARTESIAN_POINT ( 'NONE',  ( -10.72451020669870658, -18.67979575497194134, 49.58442372801901143 ) ) ;
#11269 = CARTESIAN_POINT ( 'NONE',  ( -19.02544592524342804, 5.153800228976336051, 116.0405762719810383 ) ) ;
#11270 = CARTESIAN_POINT ( 'NONE',  ( 18.62759615963255655, 10.81492255796105972, 86.66775706135234714 ) ) ;
#11271 = CARTESIAN_POINT ( 'NONE',  ( 9.474510206698971260, -16.51473224551069308, 27.91557627198103120 ) ) ;
#11272 = CARTESIAN_POINT ( 'NONE',  ( 19.05341960407611168, 5.049401038298154454, 43.95724293864769550 ) ) ;
#11273 = ORIENTED_EDGE ( 'NONE', *, *, #120239, .F. ) ;
#11274 = CARTESIAN_POINT ( 'NONE',  ( 10.81492255796106328, -18.62759615963255655, 100.4177570613523471 ) ) ;
#11275 = CARTESIAN_POINT ( 'NONE',  ( 14.34966873604972726, -8.224510206698740333, 50.83442372801901143 ) ) ;
#11276 = CARTESIAN_POINT ( 'NONE',  ( 15.72974639402176855, 15.80617190586768217, 71.87609039468568994 ) ) ;
#11277 = CARTESIAN_POINT ( 'NONE',  ( -9.564922557960796823, -16.46253265017161027, 97.08224293864769550 ) ) ;
#11278 = CARTESIAN_POINT ( 'NONE',  ( -5.153800228976607833, 19.02544592524334988, 77.70942372801900433 ) ) ;
#11279 = CARTESIAN_POINT ( 'NONE',  ( -5.823673210054431948, 21.52544592524334988, 52.70942372801902565 ) ) ;
#11280 = CARTESIAN_POINT ( 'NONE',  ( 16.52544592524335698, 4.483927247898782831, 21.45942372801901499 ) ) ;
#11281 = CARTESIAN_POINT ( 'NONE',  ( 5.049401038297881783, 19.05341960407617563, 92.29275706135234714 ) ) ;
#11282 = CARTESIAN_POINT ( 'NONE',  ( -13.97604488694527625, -13.89961937509977652, 56.87390960531434558 ) ) ;
#11283 = CARTESIAN_POINT ( 'NONE',  ( 19.02544592524334988, 5.153800228976608722, 86.45942372801900433 ) ) ;
#11284 = TOROIDAL_SURFACE ( 'NONE', #156599, 69.99999999999998579, 10.00000000000000000 ) ;
#11285 = CARTESIAN_POINT ( 'NONE',  ( 16.55341960407611168, 4.379528057220329451, 23.95724293864769550 ) ) ;
#11286 = CARTESIAN_POINT ( 'NONE',  ( 5.049401038297881783, 19.05341960407617563, 92.29275706135234714 ) ) ;
#11287 = CARTESIAN_POINT ( 'NONE',  ( 12.06949235617757843, -12.14591786802309237, 43.12390960531435269 ) ) ;
#11288 = CARTESIAN_POINT ( 'NONE',  ( -19.03943276465977164, -0.05219959533935918106, 68.75109039468566152 ) ) ;
#11289 = CARTESIAN_POINT ( 'NONE',  ( -12.14591786802326823, 12.06949235617739902, 48.12609039468568284 ) ) ;
#11290 = CARTESIAN_POINT ( 'NONE',  ( -13.97604488694547697, 13.89961937509957934, 28.12609039468565797 ) ) ;
#11291 = EDGE_CURVE ( 'NONE', #174271, #70701, #154452, .T. ) ;
#11292 = CARTESIAN_POINT ( 'NONE',  ( -5.153800228976328057, -19.02544592524343514, 22.29057627198102765 ) ) ;
#11293 = CARTESIAN_POINT ( 'NONE',  ( 16.51473224551069308, 9.474510206698969483, 44.16557627198103120 ) ) ;
#11294 = CARTESIAN_POINT ( 'NONE',  ( 8.224510206698742110, 14.34966873604972548, 47.08442372801901854 ) ) ;
#11295 = DIRECTION ( 'NONE',  ( 0.000000000000000000, 0.000000000000000000, -1.000000000000000000 ) ) ;
#11296 = CARTESIAN_POINT ( 'NONE',  ( 1.993301997531345292E-15, -30.30510711980685912, 142.7500000054623683 ) ) ;
#11297 = B_SPLINE_CURVE_WITH_KNOTS ( 'NONE', 3,
 ( #2027, #50533, #35354, #97005, #63707, #20176, #125382, #4995, #81822, #48548, #66680, #190041, #51515, #113177, #67676, #146506, #37339, #5997, #39343, #84826, #129334, #52504, #85843, #7996, #68671, #175867 ),
 .UNSPECIFIED., .F., .F.,
 ( 4, 2, 2, 2, 2, 2, 2, 2, 2, 2, 2, 2, 4 ),
 ( 1.969502665979568066E-07, 0.0004009345686709217473, 0.0008016721870752456123, 0.001603147423883905052, 0.002404622660692559612, 0.003206097897501214173, 0.004007573134309868300, 0.004408310752714196014, 0.004809048371118523728, 0.005209785989522850574, 0.005610523607927177421, 0.006011261226331506002, 0.006411998844735832849 ),
 .UNSPECIFIED. ) ;
#11298 = CARTESIAN_POINT ( 'NONE',  ( -19.05341960407611168, -5.049401038298163336, 86.45724293864769550 ) ) ;
#11299 = CARTESIAN_POINT ( 'NONE',  ( 17.76566638676866461, -1.079584607091855997, 102.5000000000000284 ) ) ;
#11300 = EDGE_LOOP ( 'NONE', ( #151816, #141478, #142273, #185841, #12704, #153179, #88489, #18190, #109187, #89708, #190461, #153880 ) ) ;
#11301 = CARTESIAN_POINT ( 'NONE',  ( 19.02544592524334988, 5.153800228976608722, 96.45942372801897591 ) ) ;
#11302 = EDGE_CURVE ( 'NONE', #192686, #15160, #43709, .T. ) ;
#11303 = CARTESIAN_POINT ( 'NONE',  ( 5.823673210054125526, 21.52544592524343514, 24.79057627198103120 ) ) ;
#11305 = CARTESIAN_POINT ( 'NONE',  ( -13.97604488694547697, 13.89961937509957934, 113.1260903946856757 ) ) ;
#11304 = CARTESIAN_POINT ( 'NONE',  ( -5.153800228976607833, 19.02544592524334988, 27.70942372801899722 ) ) ;
#11306 = CARTESIAN_POINT ( 'NONE',  ( -0.05219959533909027116, -19.03943276465977164, 22.49890960531436690 ) ) ;
#11307 = CARTESIAN_POINT ( 'NONE',  ( 19.05341960407611168, 5.049401038298154454, 33.95724293864769550 ) ) ;
#11308 = CARTESIAN_POINT ( 'NONE',  ( 21.55341960407610458, 5.719274019375980345, 73.95724293864769550 ) ) ;
#11309 = CARTESIAN_POINT ( 'NONE',  ( -9.474510206698964154, 16.51473224551069663, 40.41557627198103120 ) ) ;
#11310 = CARTESIAN_POINT ( 'NONE',  ( -18.22780087662114212, 5.499999999999995559, 48.51540105326107266 ) ) ;
#11311 = CARTESIAN_POINT ( 'NONE',  ( -13.89961937509957401, -13.97604488694547875, 74.37609039468566152 ) ) ;
#11312 = CARTESIAN_POINT ( 'NONE',  ( 8.224510206698953496, -14.34966873604960469, 52.91557627198103830 ) ) ;
#11313 = CARTESIAN_POINT ( 'NONE',  ( -5.719274019375978568, 21.55341960407610458, 35.20724293864768839 ) ) ;
#11314 = CARTESIAN_POINT ( 'NONE',  ( -15.80617190586768217, 15.72974639402176855, 93.12609039468568994 ) ) ;
#11315 = CARTESIAN_POINT ( 'NONE',  ( -5.719274019375978568, 21.55341960407610458, 85.20724293864770971 ) ) ;
#11316 = CARTESIAN_POINT ( 'NONE',  ( -21.53943276465977519, -0.05219959533937600094, 68.75109039468568994 ) ) ;
#11317 = CARTESIAN_POINT ( 'NONE',  ( -21.55341960407619339, 5.719274019375674811, 63.54275706135234003 ) ) ;
#11318 = CARTESIAN_POINT ( 'NONE',  ( 5.153800228976335163, 19.02544592524342804, 94.79057627198103830 ) ) ;
#11320 = CARTESIAN_POINT ( 'NONE',  ( 21.55341960407619695, -5.719274019375665929, 66.04275706135236135 ) ) ;
#11319 = CARTESIAN_POINT ( 'NONE',  ( -14.29746914071037622, -8.314922557961029526, 94.16775706135237556 ) ) ;
#11321 = CARTESIAN_POINT ( 'NONE',  ( -16.46253265017160317, 9.564922557960807481, 50.83224293864770260 ) ) ;
#11322 = CARTESIAN_POINT ( 'NONE',  ( -5.719274019375665041, -21.55341960407619695, 29.79275706135234358 ) ) ;
#11323 = CARTESIAN_POINT ( 'NONE',  ( -16.51473224551069308, -9.474510206698971260, 71.66557627198102409 ) ) ;
#11324 = CARTESIAN_POINT ( 'NONE',  ( -4.379528057220328563, 16.55341960407611168, 65.20724293864768129 ) ) ;
#11325 = CARTESIAN_POINT ( 'NONE',  ( 12.14591786802309770, 12.06949235617756955, 44.37390960531435979 ) ) ;
#11326 = CARTESIAN_POINT ( 'NONE',  ( 0.05219959533907565091, 21.53943276465977519, 39.99890960531436690 ) ) ;
#11327 = CARTESIAN_POINT ( 'NONE',  ( 19.02544592524343514, -5.153800228976328945, 48.54057627198103120 ) ) ;
#11328 = CARTESIAN_POINT ( 'NONE',  ( 18.67979575497178502, 10.72451020669898547, 59.16557627198103120 ) ) ;
#11329 = CARTESIAN_POINT ( 'NONE',  ( -0.05219959533936034679, 19.03943276465977164, 52.50109039468566863 ) ) ;
#11331 = CARTESIAN_POINT ( 'NONE',  ( -4.483927247898539470, -16.52544592524342804, 57.29057627198103120 ) ) ;
#11330 = CARTESIAN_POINT ( 'NONE',  ( -9.474510206698720793, -16.51473224551083518, 19.58442372801899722 ) ) ;
#11332 = CARTESIAN_POINT ( 'NONE',  ( 21.53943276465977519, -0.05219959533907433946, 33.74890960531436690 ) ) ;
#11333 = ORIENTED_EDGE ( 'NONE', *, *, #58394, .F. ) ;
#11334 = CARTESIAN_POINT ( 'NONE',  ( 15.50000000000000178, -5.500000000000000888, 22.00000000000000000 ) ) ;
#11335 = CARTESIAN_POINT ( 'NONE',  ( 8.314922557961029526, -14.29746914071037800, 80.41775706135234714 ) ) ;
#11336 = CARTESIAN_POINT ( 'NONE',  ( -16.46253265017146816, -9.564922557961047289, 89.16775706135234714 ) ) ;
#11337 = CARTESIAN_POINT ( 'NONE',  ( 12.06949235617757843, -12.14591786802309237, 53.12390960531436690 ) ) ;
#11338 = DIRECTION ( 'NONE',  ( 0.000000000000000000, 0.000000000000000000, 1.000000000000000000 ) ) ;
#11339 = CARTESIAN_POINT ( 'NONE',  ( 19.02544592524343514, -5.153800228976328945, 43.54057627198103120 ) ) ;
#11340 = CARTESIAN_POINT ( 'NONE',  ( -8.224510206698948167, 14.34966873604960824, 40.41557627198103120 ) ) ;
#11341 = CARTESIAN_POINT ( 'NONE',  ( -13.89961937509977652, 13.97604488694528158, 55.62390960531434558 ) ) ;
#11342 = CARTESIAN_POINT ( 'NONE',  ( -19.03943276465977164, 0.05219959533909376836, 71.24890960531435269 ) ) ;
#11343 = CARTESIAN_POINT ( 'NONE',  ( 16.51473224551069308, 9.474510206698969483, 54.16557627198103120 ) ) ;
#11344 = CARTESIAN_POINT ( 'NONE',  ( 18.67979575497194134, -10.72451020669871369, 50.83442372801901143 ) ) ;
#11345 = CARTESIAN_POINT ( 'NONE',  ( 9.564922557960805705, 16.46253265017160317, 69.58224293864770971 ) ) ;
#11346 = CARTESIAN_POINT ( 'NONE',  ( 9.474510206698971260, -16.51473224551069308, 27.91557627198103120 ) ) ;
#11347 = CARTESIAN_POINT ( 'NONE',  ( 0.05219959533909260263, 19.03943276465977164, 54.99890960531435979 ) ) ;
#11348 = CARTESIAN_POINT ( 'NONE',  ( -10.81492255796078084, -18.62759615963271287, 52.08224293864768839 ) ) ;
#11349 = CARTESIAN_POINT ( 'NONE',  ( 9.564922557960805705, 16.46253265017160317, 34.58224293864770260 ) ) ;
#11350 = CARTESIAN_POINT ( 'NONE',  ( 10.72451020669898902, -18.67979575497178502, 37.91557627198102409 ) ) ;
#11351 = CARTESIAN_POINT ( 'NONE',  ( -4.379528057220086978, -16.55341960407618274, 99.79275706135234714 ) ) ;
#11352 = CARTESIAN_POINT ( 'NONE',  ( 0.05219959533936267826, -19.03943276465977164, 30.00109039468566863 ) ) ;
#11354 = CARTESIAN_POINT ( 'NONE',  ( 0.05219959533934541429, -16.53943276465976808, 75.00109039468568994 ) ) ;
#11353 = CARTESIAN_POINT ( 'NONE',  ( 4.483927247898790824, -16.52544592524335698, 40.20942372801901854 ) ) ;
#11355 = LINE ( 'NONE', #146847, #59682 ) ;
#11356 = CARTESIAN_POINT ( 'NONE',  ( -14.34966873604972548, 8.224510206698743886, 73.33442372801901854 ) ) ;
#11357 = CARTESIAN_POINT ( 'NONE',  ( -12.14591786802326823, 12.06949235617739902, 53.12609039468568284 ) ) ;
#11358 = CARTESIAN_POINT ( 'NONE',  ( -19.03943276465977164, 0.05219959533909376836, 106.2489096053143669 ) ) ;
#11359 = AXIS2_PLACEMENT_3D ( 'NONE', #104342, #74016, #72008 ) ;
#11360 = CARTESIAN_POINT ( 'NONE',  ( 14.29746914071037800, 8.314922557961029526, 36.66775706135234714 ) ) ;
#11361 = CARTESIAN_POINT ( 'NONE',  ( 19.05341960407611168, 5.049401038298154454, 33.95724293864769550 ) ) ;
#11362 = CARTESIAN_POINT ( 'NONE',  ( 21.52544592524334988, 5.823673210054432836, 26.45942372801901854 ) ) ;
#11363 = CARTESIAN_POINT ( 'NONE',  ( -12.06949235617739369, -12.14591786802326823, 34.37609039468568284 ) ) ;
#11364 = CARTESIAN_POINT ( 'NONE',  ( 4.379528057220092307, 16.55341960407617563, 102.2927570613523613 ) ) ;
#11365 = DIRECTION ( 'NONE',  ( 0.9526137857479317628, 0.3041824702427701199, 0.000000000000000000 ) ) ;
#11366 = CARTESIAN_POINT ( 'NONE',  ( 5.719274019375673035, 21.55341960407619339, 102.2927570613523613 ) ) ;
#11367 = CARTESIAN_POINT ( 'NONE',  ( 5.153800228976615827, -19.02544592524334988, 95.20942372801897591 ) ) ;
#11368 = CARTESIAN_POINT ( 'NONE',  ( -12.06949235617756955, 12.14591786802309770, 50.62390960531435979 ) ) ;
#11369 = CARTESIAN_POINT ( 'NONE',  ( -9.474510206698964154, 16.51473224551069663, 25.41557627198103120 ) ) ;
#11371 = CARTESIAN_POINT ( 'NONE',  ( 37.99999999999999289, 2.893978650043524126E-14, -2.749999994537626780 ) ) ;
#11370 = CARTESIAN_POINT ( 'NONE',  ( -19.03943276465977164, -0.05219959533935918106, 63.75109039468566863 ) ) ;
#11372 = CARTESIAN_POINT ( 'NONE',  ( -5.719274019375665041, -21.55341960407619695, 64.79275706135234714 ) ) ;
#11373 = CARTESIAN_POINT ( 'NONE',  ( 4.483927247898790824, -16.52544592524335698, 30.20942372801902565 ) ) ;
#11374 = DIRECTION ( 'NONE',  ( 0.000000000000000000, 0.000000000000000000, 1.000000000000000000 ) ) ;
#11375 = CARTESIAN_POINT ( 'NONE',  ( -18.62759615963270932, 10.81492255796079327, 25.83224293864769194 ) ) ;
#11376 = CARTESIAN_POINT ( 'NONE',  ( -13.97604488694547697, 13.89961937509957934, 108.1260903946856331 ) ) ;
#11377 = FACE_OUTER_BOUND ( 'NONE', #154733, .T. ) ;
#11378 = CARTESIAN_POINT ( 'NONE',  ( -25.80209238092448842, 7.370998251475262997, 174.5109820657625619 ) ) ;
#11379 = CARTESIAN_POINT ( 'NONE',  ( 19.03943276465977164, -0.05219959533909143690, 28.74890960531435624 ) ) ;
#11380 = CARTESIAN_POINT ( 'NONE',  ( -5.719274019375665041, -21.55341960407619695, 109.7927570613523613 ) ) ;
#11381 = CARTESIAN_POINT ( 'NONE',  ( -13.89961937509977652, 13.97604488694528158, 45.62390960531433848 ) ) ;
#11382 = AXIS2_PLACEMENT_3D ( 'NONE', #132278, #86767, #89760 ) ;
#11383 = CARTESIAN_POINT ( 'NONE',  ( 18.67979575497194134, -10.72451020669871369, 45.83442372801901854 ) ) ;
#11384 = CARTESIAN_POINT ( 'NONE',  ( -21.52544592524334988, -5.823673210054445271, 103.9594237280190185 ) ) ;
#11385 = CARTESIAN_POINT ( 'NONE',  ( -8.314922557961024197, 14.29746914071037800, 107.9177570613523471 ) ) ;
#11386 = CARTESIAN_POINT ( 'NONE',  ( 16.46253265017160672, -9.564922557960803928, 78.33224293864769550 ) ) ;
#11387 = CARTESIAN_POINT ( 'NONE',  ( -15.72974639402176322, -15.80617190586768395, 44.37609039468567573 ) ) ;
#11388 = CARTESIAN_POINT ( 'NONE',  ( 21.52544592524334988, 5.823673210054432836, 56.45942372801902565 ) ) ;
#11390 = CARTESIAN_POINT ( 'NONE',  ( -19.02544592524342804, 5.153800228976336051, 91.04057627198100988 ) ) ;
#11389 = CARTESIAN_POINT ( 'NONE',  ( -19.03943276465977164, -0.05219959533935918106, 73.75109039468566152 ) ) ;
#11391 = CARTESIAN_POINT ( 'NONE',  ( 4.483927247898545687, 16.52544592524342804, 109.7905762719810383 ) ) ;
#11392 = CARTESIAN_POINT ( 'NONE',  ( 15.72974639402199770, -15.80617190586745480, 98.12390960531436690 ) ) ;
#11393 = CARTESIAN_POINT ( 'NONE',  ( 19.02544592524334988, 5.153800228976608722, 21.45942372801899012 ) ) ;
#11394 = CARTESIAN_POINT ( 'NONE',  ( 14.29746914071049879, -8.314922557960816363, 103.3322429386476955 ) ) ;
#11395 = CARTESIAN_POINT ( 'NONE',  ( -19.03943276465977164, 0.05219959533909376836, 51.24890960531436690 ) ) ;
#11397 = VECTOR ( 'NONE', #120005, 1000.000000000000000 ) ;
#11396 = CARTESIAN_POINT ( 'NONE',  ( -9.474510206698720793, -16.51473224551083518, 89.58442372801900433 ) ) ;
#11398 = CARTESIAN_POINT ( 'NONE',  ( 16.55341960407611168, 4.379528057220329451, 43.95724293864769550 ) ) ;
#11399 = CARTESIAN_POINT ( 'NONE',  ( 5.719274019375673035, 21.55341960407619339, 102.2927570613523613 ) ) ;
#11400 = CARTESIAN_POINT ( 'NONE',  ( -13.89961937509977652, 13.97604488694528158, 110.6239096053143243 ) ) ;
#11401 = CARTESIAN_POINT ( 'NONE',  ( -19.05341960407617563, 5.049401038297882671, 78.54275706135233293 ) ) ;
#11402 = CARTESIAN_POINT ( 'NONE',  ( -5.823673210054116645, -21.52544592524344225, 72.29057627198102409 ) ) ;
#11403 = CARTESIAN_POINT ( 'NONE',  ( -18.67979575497193778, 10.72451020669871902, 28.33442372801902209 ) ) ;
#11404 = CARTESIAN_POINT ( 'NONE',  ( -8.224510206698735004, -14.34966873604973081, 34.58442372801900433 ) ) ;
#11405 = CARTESIAN_POINT ( 'NONE',  ( 14.34966873604972726, -8.224510206698740333, 90.83442372801901854 ) ) ;
#11407 = CARTESIAN_POINT ( 'NONE',  ( 5.719274019375673035, 21.55341960407619339, 32.29275706135235424 ) ) ;
#11406 = CARTESIAN_POINT ( 'NONE',  ( 9.564922557960805705, 16.46253265017160317, 29.58224293864769550 ) ) ;
#11408 = CARTESIAN_POINT ( 'NONE',  ( -21.52544592524343514, 5.823673210054127303, 46.04057627198103830 ) ) ;
#11409 = CARTESIAN_POINT ( 'NONE',  ( -14.34966873604960291, -8.224510206698953496, 111.6655762719810525 ) ) ;
#11410 = CARTESIAN_POINT ( 'NONE',  ( 23.48529157249600630, -32.32473071737749137, -11.04999999453762527 ) ) ;
#11411 = CARTESIAN_POINT ( 'NONE',  ( -16.55341960407617563, 4.379528057220093196, 68.54275706135234714 ) ) ;
#11412 = CARTESIAN_POINT ( 'NONE',  ( -4.483927247898539470, -16.52544592524342804, 92.29057627198103830 ) ) ;
#11413 = CARTESIAN_POINT ( 'NONE',  ( -5.823673210054116645, -21.52544592524344225, 82.29057627198103830 ) ) ;
#11414 = CARTESIAN_POINT ( 'NONE',  ( -8.314922557960811034, -14.29746914071050412, 32.08224293864769550 ) ) ;
#11415 = CARTESIAN_POINT ( 'NONE',  ( 4.483927247898790824, -16.52544592524335698, 45.20942372801901854 ) ) ;
#11416 = CARTESIAN_POINT ( 'NONE',  ( 19.02544592524343514, -5.153800228976328945, 58.54057627198102409 ) ) ;
#11417 = CARTESIAN_POINT ( 'NONE',  ( 4.379528057220092307, 16.55341960407617563, 87.29275706135236135 ) ) ;
#11418 = CARTESIAN_POINT ( 'NONE',  ( -13.97604488694547697, 13.89961937509957934, 93.12609039468566152 ) ) ;
#11419 = CARTESIAN_POINT ( 'NONE',  ( 0.05219959533907565091, 21.53943276465977519, 89.99890960531438111 ) ) ;
#11420 = CARTESIAN_POINT ( 'NONE',  ( -16.52544592524335698, -4.483927247898792601, 108.9594237280190185 ) ) ;
#11421 = VERTEX_POINT ( 'NONE', #25552 ) ;
#11422 = CARTESIAN_POINT ( 'NONE',  ( 13.97604488694527802, 13.89961937509977652, 114.3739096053143669 ) ) ;
#11423 = CARTESIAN_POINT ( 'NONE',  ( -21.52544592524343514, 5.823673210054127303, 66.04057627198103830 ) ) ;
#11424 = CARTESIAN_POINT ( 'NONE',  ( 0.05219959533934541429, -16.53943276465976808, 90.00109039468567573 ) ) ;
#11425 = VERTEX_POINT ( 'NONE', #73041 ) ;
#11426 = CARTESIAN_POINT ( 'NONE',  ( -18.62759615963270932, 10.81492255796079327, 35.83224293864768839 ) ) ;
#11427 = CARTESIAN_POINT ( 'NONE',  ( -19.52217212775661181, 5.499999999999918288, 74.93993709005260939 ) ) ;
#11428 = CARTESIAN_POINT ( 'NONE',  ( -21.55341960407610458, -5.719274019375992779, 86.45724293864770971 ) ) ;
#11429 = CARTESIAN_POINT ( 'NONE',  ( 14.34966873604960469, 8.224510206698951720, 29.16557627198103120 ) ) ;
#11431 = CARTESIAN_POINT ( 'NONE',  ( -4.379528057220086978, -16.55341960407618274, 34.79275706135235424 ) ) ;
#11430 = AXIS2_PLACEMENT_3D ( 'NONE', #150249, #119893, #136057 ) ;
#11432 = CARTESIAN_POINT ( 'NONE',  ( 13.89961937509977652, -13.97604488694527269, 28.12390960531435624 ) ) ;
#11433 = CARTESIAN_POINT ( 'NONE',  ( 8.314922557961029526, -14.29746914071037800, 25.41775706135235779 ) ) ;
#11434 = CARTESIAN_POINT ( 'NONE',  ( 19.05341960407611168, 5.049401038298154454, 53.95724293864770260 ) ) ;
#11435 = CARTESIAN_POINT ( 'NONE',  ( 23.31738231874054890, -16.94106989632523508, 146.7999999999999829 ) ) ;
#11436 = CARTESIAN_POINT ( 'NONE',  ( -19.03943276465977164, 0.05219959533909376836, 106.2489096053143669 ) ) ;
#11437 = CARTESIAN_POINT ( 'NONE',  ( 0.2521225200370412201, 28.91645205756829995, -52.63676493945838075 ) ) ;
#11438 = CARTESIAN_POINT ( 'NONE',  ( -4.483927247898782831, 16.52544592524335698, 102.7094237280190185 ) ) ;
#11439 = CARTESIAN_POINT ( 'NONE',  ( 13.97604488694548053, -13.89961937509957401, 90.62609039468567573 ) ) ;
#11440 = CARTESIAN_POINT ( 'NONE',  ( 9.474510206698729675, 16.51473224551082808, 37.08442372801899722 ) ) ;
#11441 = CARTESIAN_POINT ( 'NONE',  ( -15.80617190586745835, -15.72974639402198527, 81.87390960531435269 ) ) ;
#11442 = CARTESIAN_POINT ( 'NONE',  ( -16.53943276465976808, -0.05219959533934237506, 103.7510903946857042 ) ) ;
#11443 = CARTESIAN_POINT ( 'NONE',  ( 18.67979575497178502, 10.72451020669898547, 29.16557627198103120 ) ) ;
#11444 = CARTESIAN_POINT ( 'NONE',  ( 19.02544592524334988, 5.153800228976608722, 96.45942372801897591 ) ) ;
#11445 = CARTESIAN_POINT ( 'NONE',  ( 19.03943276465977164, -0.05219959533909143690, 53.74890960531436690 ) ) ;
#11446 = CARTESIAN_POINT ( 'NONE',  ( -0.05219959533909027116, -19.03943276465977164, 102.4989096053143669 ) ) ;
#11447 = CARTESIAN_POINT ( 'NONE',  ( -21.53943276465977519, -0.05219959533937600094, 63.75109039468568284 ) ) ;
#11448 = CARTESIAN_POINT ( 'NONE',  ( 13.97604488694527802, 13.89961937509977652, 64.37390960531436690 ) ) ;
#11449 = CARTESIAN_POINT ( 'NONE',  ( 14.34966873604960469, 8.224510206698951720, 94.16557627198103830 ) ) ;
#11450 = CARTESIAN_POINT ( 'NONE',  ( 11.30153831258471797, -180.0000000000000000, -15.00000000000000178 ) ) ;
#11451 = CARTESIAN_POINT ( 'NONE',  ( -16.55341960407611168, -4.379528057220339221, 71.45724293864769550 ) ) ;
#11452 = CARTESIAN_POINT ( 'NONE',  ( 18.67979575497178502, 10.72451020669898547, 69.16557627198102409 ) ) ;
#11453 = ORIENTED_EDGE ( 'NONE', *, *, #92250, .F. ) ;
#11454 = CARTESIAN_POINT ( 'NONE',  ( -16.46253265017146816, -9.564922557961047289, 89.16775706135234714 ) ) ;
#11455 = DIRECTION ( 'NONE',  ( -1.000000000000000000, 0.000000000000000000, 0.000000000000000000 ) ) ;
#11456 = CARTESIAN_POINT ( 'NONE',  ( 19.02544592524343514, -5.153800228976328945, 58.54057627198102409 ) ) ;
#11457 = CARTESIAN_POINT ( 'NONE',  ( 17.50000000000000000, -5.499999999999992895, 71.21769037696435589 ) ) ;
#11459 = CARTESIAN_POINT ( 'NONE',  ( -0.05219959533909027116, -19.03943276465977164, 87.49890960531436690 ) ) ;
#11458 = CARTESIAN_POINT ( 'NONE',  ( 5.049401038298161559, -19.05341960407611168, 72.70724293864768129 ) ) ;
#11460 = EDGE_CURVE ( 'NONE', #121091, #179892, #256, .T. ) ;
#11461 = CARTESIAN_POINT ( 'NONE',  ( -8.314922557961024197, 14.29746914071037800, 67.91775706135234714 ) ) ;
#11462 = CARTESIAN_POINT ( 'NONE',  ( -17.48847506799968343, -5.747544572773812810, 49.17302562156721280 ) ) ;
#11463 = CARTESIAN_POINT ( 'NONE',  ( 9.474510206698729675, 16.51473224551082808, 42.08442372801900433 ) ) ;
#11464 = CARTESIAN_POINT ( 'NONE',  ( 17.37248965764951336, 6.147170618106522433, 21.68035186998432451 ) ) ;
#11465 = CARTESIAN_POINT ( 'NONE',  ( -13.89961937509977652, 13.97604488694528158, 105.6239096053143527 ) ) ;
#11466 = CARTESIAN_POINT ( 'NONE',  ( -16.53943276465976808, -0.05219959533934237506, 98.75109039468568994 ) ) ;
#11467 = CARTESIAN_POINT ( 'NONE',  ( -34.74703293042581009, -1.945922946419438082, 52.24735972161445829 ) ) ;
#11468 = CARTESIAN_POINT ( 'NONE',  ( -8.224510206698735004, -14.34966873604973081, 99.58442372801900433 ) ) ;
#11469 = CARTESIAN_POINT ( 'NONE',  ( -17.48853670773243607, 5.747243402303161552, 28.66671299749991775 ) ) ;
#11470 = CARTESIAN_POINT ( 'NONE',  ( -12.06949235617739369, -12.14591786802326823, 74.37609039468568994 ) ) ;
#11471 = DIRECTION ( 'NONE',  ( 0.000000000000000000, 0.000000000000000000, 1.000000000000000000 ) ) ;
#11472 = CARTESIAN_POINT ( 'NONE',  ( -21.52544592524334988, -5.823673210054445271, 73.95942372801901854 ) ) ;
#11473 = CARTESIAN_POINT ( 'NONE',  ( 5.049401038297881783, 19.05341960407617563, 77.29275706135231871 ) ) ;
#11474 = CARTESIAN_POINT ( 'NONE',  ( 16.51473224551083163, -9.474510206698727899, 25.83442372801900078 ) ) ;
#11475 = CARTESIAN_POINT ( 'NONE',  ( 9.564922557960805705, 16.46253265017160317, 64.58224293864769550 ) ) ;
#11476 = CARTESIAN_POINT ( 'NONE',  ( 19.03943276465977164, -0.05219959533909143690, 43.74890960531435979 ) ) ;
#11477 = CARTESIAN_POINT ( 'NONE',  ( -18.72120804366350555, -35.34920564451201841, -8.063943084929409366 ) ) ;
#11478 = CARTESIAN_POINT ( 'NONE',  ( 15.72974639402199770, -15.80617190586745480, 83.12390960531436690 ) ) ;
#11479 = CARTESIAN_POINT ( 'NONE',  ( 10.72451020669898902, -18.67979575497178502, 37.91557627198102409 ) ) ;
#11480 = CARTESIAN_POINT ( 'NONE',  ( -19.02544592524342804, 5.153800228976336051, 31.04057627198102409 ) ) ;
#11481 = CARTESIAN_POINT ( 'NONE',  ( -12.14591786802326823, 12.06949235617739902, 53.12609039468568284 ) ) ;
#11482 = ADVANCED_FACE ( 'NONE', ( #124482, #93138 ), #137663, .T. ) ;
#11483 = VERTEX_POINT ( 'NONE', #13342 ) ;
#11484 = CARTESIAN_POINT ( 'NONE',  ( -21.52544592524334988, -5.823673210054445271, 33.95942372801901143 ) ) ;
#11486 = CARTESIAN_POINT ( 'NONE',  ( -30.74264578624800492, 22.33583958711400186, -8.200000000000001066 ) ) ;
#11485 = CARTESIAN_POINT ( 'NONE',  ( -16.52544592524342804, 4.483927247898546575, 51.04057627198103120 ) ) ;
#11487 = CARTESIAN_POINT ( 'NONE',  ( 16.52544592524335698, 4.483927247898782831, 26.45942372801901854 ) ) ;
#11488 = CARTESIAN_POINT ( 'NONE',  ( -16.46253265017146816, -9.564922557961047289, 39.16775706135234003 ) ) ;
#11489 = CARTESIAN_POINT ( 'NONE',  ( -0.05219959533910754901, -16.53943276465976808, 62.49890960531436690 ) ) ;
#11490 = CARTESIAN_POINT ( 'NONE',  ( -21.52544592524343514, 5.823673210054127303, 111.0405762719810525 ) ) ;
#11492 = CARTESIAN_POINT ( 'NONE',  ( 15.80617190586746368, 15.72974639402197994, 79.37390960531436690 ) ) ;
#11491 = PLANE ( 'NONE',  #79409 ) ;
#11493 = CARTESIAN_POINT ( 'NONE',  ( -16.51473224551069308, -9.474510206698971260, 91.66557627198103830 ) ) ;
#11494 = CARTESIAN_POINT ( 'NONE',  ( -4.483927247898539470, -16.52544592524342804, 67.29057627198103830 ) ) ;
#11495 = CARTESIAN_POINT ( 'NONE',  ( -16.51473224551069308, -9.474510206698971260, 101.6655762719810241 ) ) ;
#11496 = CARTESIAN_POINT ( 'NONE',  ( -37.11214605083871731, 4.768680519348648339, 42.23634591622183621 ) ) ;
#11497 = CARTESIAN_POINT ( 'NONE',  ( -9.564922557961040184, 16.46253265017147172, 67.91775706135233293 ) ) ;
#11498 = CARTESIAN_POINT ( 'NONE',  ( 5.719274019375991003, -21.55341960407610458, 102.7072429386476955 ) ) ;
#11499 = CARTESIAN_POINT ( 'NONE',  ( -9.474510206698964154, 16.51473224551069663, 60.41557627198102409 ) ) ;
#11500 = CARTESIAN_POINT ( 'NONE',  ( 19.05341960407617918, -5.049401038297876454, 46.04275706135233293 ) ) ;
#11501 = CARTESIAN_POINT ( 'NONE',  ( -12.06949235617756955, 12.14591786802309770, 115.6239096053143669 ) ) ;
#11502 = CARTESIAN_POINT ( 'NONE',  ( -5.823673210054431948, 21.52544592524334988, 62.70942372801902565 ) ) ;
#11503 = CARTESIAN_POINT ( 'NONE',  ( -16.88567814943164436, -6.947325034625695395, 71.29001122652586275 ) ) ;
#11504 = CARTESIAN_POINT ( 'NONE',  ( 4.483927247898545687, 16.52544592524342804, 39.79057627198103830 ) ) ;
#11505 = CARTESIAN_POINT ( 'NONE',  ( 13.97604488694527802, 13.89961937509977652, 54.37390960531435979 ) ) ;
#11506 = CARTESIAN_POINT ( 'NONE',  ( -9.474510206698964154, 16.51473224551069663, 115.4155762719810241 ) ) ;
#11507 = CARTESIAN_POINT ( 'NONE',  ( 18.67979575497178502, 10.72451020669898547, 74.16557627198102409 ) ) ;
#11508 = CARTESIAN_POINT ( 'NONE',  ( 17.14385361876520264, -23.59649016807271238, 145.5750000027312012 ) ) ;
#11509 = CARTESIAN_POINT ( 'NONE',  ( -16.46253265017160317, 9.564922557960807481, 40.83224293864769550 ) ) ;
#11510 = ORIENTED_EDGE ( 'NONE', *, *, #66871, .F. ) ;
#11511 = CARTESIAN_POINT ( 'NONE',  ( -10.72451020669898014, 18.67979575497178502, 60.41557627198102409 ) ) ;
#11512 = ORIENTED_EDGE ( 'NONE', *, *, #90150, .F. ) ;
#11513 = CARTESIAN_POINT ( 'NONE',  ( 21.55341960407619695, -5.719274019375665929, 81.04275706135236135 ) ) ;
#11516 = CARTESIAN_POINT ( 'NONE',  ( -8.314922557960811034, -14.29746914071050412, 77.08224293864769550 ) ) ;
#11515 = CARTESIAN_POINT ( 'NONE',  ( 8.314922557961029526, -14.29746914071037800, 100.4177570613523471 ) ) ;
#11514 = PLANE ( 'NONE',  #138109 ) ;
#11517 = CARTESIAN_POINT ( 'NONE',  ( 16.51473224551069308, 9.474510206698969483, 74.16557627198103830 ) ) ;
#11518 = ORIENTED_EDGE ( 'NONE', *, *, #6742, .T. ) ;
#11519 = CARTESIAN_POINT ( 'NONE',  ( -19.02544592524334988, -5.153800228976617603, 43.95942372801899012 ) ) ;
#11520 = CARTESIAN_POINT ( 'NONE',  ( -8.314922557961024197, 14.29746914071037800, 92.91775706135236135 ) ) ;
#11521 = CARTESIAN_POINT ( 'NONE',  ( -0.05219959533936034679, 19.03943276465977164, 22.50109039468566152 ) ) ;
#11522 = CARTESIAN_POINT ( 'NONE',  ( 16.51473224551069308, 9.474510206698969483, 84.16557627198102409 ) ) ;
#11523 = CARTESIAN_POINT ( 'NONE',  ( 21.55341960407610458, 5.719274019375980345, 43.95724293864769550 ) ) ;
#11524 = CARTESIAN_POINT ( 'NONE',  ( -3.573655867282028392E-15, 2.428612866367529932E-14, 150.0000000000000000 ) ) ;
#11525 = CARTESIAN_POINT ( 'NONE',  ( 21.52544592524334988, 5.823673210054432836, 101.4594237280190185 ) ) ;
#11526 = CARTESIAN_POINT ( 'NONE',  ( -16.55341960407617563, 4.379528057220093196, 58.54275706135235424 ) ) ;
#11527 = CARTESIAN_POINT ( 'NONE',  ( 10.81492255796078972, 18.62759615963270932, 109.5822429386476955 ) ) ;
#11528 = CARTESIAN_POINT ( 'NONE',  ( 16.52544592524335698, 4.483927247898782831, 31.45942372801901854 ) ) ;
#11529 = CARTESIAN_POINT ( 'NONE',  ( 9.564922557960805705, 16.46253265017160317, 89.58224293864769550 ) ) ;
#11530 = CARTESIAN_POINT ( 'NONE',  ( 5.049401038298161559, -19.05341960407611168, 42.70724293864767418 ) ) ;
#11531 = CARTESIAN_POINT ( 'NONE',  ( 19.05341960407611168, 5.049401038298154454, 48.95724293864768129 ) ) ;
#11532 = VECTOR ( 'NONE', #105037, 1000.000000000000000 ) ;
#11533 = CARTESIAN_POINT ( 'NONE',  ( -16.53943276465976808, -0.05219959533934237506, 28.75109039468567929 ) ) ;
#11534 = CARTESIAN_POINT ( 'NONE',  ( 16.55341960407611168, 4.379528057220329451, 73.95724293864769550 ) ) ;
#11535 = CARTESIAN_POINT ( 'NONE',  ( -16.55341960407617563, 4.379528057220093196, 88.54275706135236135 ) ) ;
#11536 = EDGE_CURVE ( 'NONE', #80788, #101588, #114695, .T. ) ;
#11539 = CARTESIAN_POINT ( 'NONE',  ( 19.02544592524343514, -5.153800228976328945, 48.54057627198103120 ) ) ;
#11538 = CARTESIAN_POINT ( 'NONE',  ( -0.05219959533909027116, -19.03943276465977164, 67.49890960531436690 ) ) ;
#11537 = CARTESIAN_POINT ( 'NONE',  ( 5.719274019375673035, 21.55341960407619339, 42.29275706135235424 ) ) ;
#11540 = CARTESIAN_POINT ( 'NONE',  ( -19.05341960407611168, -5.049401038298163336, 76.45724293864769550 ) ) ;
#11541 = CARTESIAN_POINT ( 'NONE',  ( -14.34966873604960291, -8.224510206698953496, 31.66557627198102054 ) ) ;
#11542 = CARTESIAN_POINT ( 'NONE',  ( 8.224510206698742110, 14.34966873604972548, 82.08442372801901854 ) ) ;
#11543 = EDGE_LOOP ( 'NONE', ( #139060, #54030, #101271, #76583, #175395 ) ) ;
#11544 = CARTESIAN_POINT ( 'NONE',  ( 13.97604488694548053, -13.89961937509957401, 25.62609039468566507 ) ) ;
#11545 = CARTESIAN_POINT ( 'NONE',  ( -9.564922557960796823, -16.46253265017161027, 97.08224293864769550 ) ) ;
#11546 = CARTESIAN_POINT ( 'NONE',  ( -16.51473224551069308, -9.474510206698971260, 46.66557627198102409 ) ) ;
#11547 = CARTESIAN_POINT ( 'NONE',  ( 0.05219959533936267826, -19.03943276465977164, 20.00109039468567218 ) ) ;
#11548 = CARTESIAN_POINT ( 'NONE',  ( -29.86685920354755552, 21.69954338932564397, -4.824999997268814234 ) ) ;
#11549 = CARTESIAN_POINT ( 'NONE',  ( -4.379528057220086978, -16.55341960407618274, 44.79275706135234714 ) ) ;
#11550 = AXIS2_PLACEMENT_3D ( 'NONE', #60720, #15228, #76887 ) ;
#11552 = CARTESIAN_POINT ( 'NONE',  ( -12.06949235617739369, -12.14591786802326823, 49.37609039468569705 ) ) ;
#11551 = CARTESIAN_POINT ( 'NONE',  ( 9.564922557961047289, -16.46253265017146816, 75.41775706135234714 ) ) ;
#11553 = CARTESIAN_POINT ( 'NONE',  ( -13.89961937509977652, 13.97604488694528158, 115.6239096053143669 ) ) ;
#11554 = CARTESIAN_POINT ( 'NONE',  ( 5.049401038298161559, -19.05341960407611168, 72.70724293864768129 ) ) ;
#11555 = CARTESIAN_POINT ( 'NONE',  ( 10.81492255796078972, 18.62759615963270932, 109.5822429386476955 ) ) ;
#11556 = CARTESIAN_POINT ( 'NONE',  ( -0.05219959533936034679, 19.03943276465977164, 67.50109039468566152 ) ) ;
#11558 = CARTESIAN_POINT ( 'NONE',  ( -16.46253265017160317, 9.564922557960807481, 40.83224293864769550 ) ) ;
#11557 = CARTESIAN_POINT ( 'NONE',  ( 0.05219959533909260263, 19.03943276465977164, 109.9989096053143669 ) ) ;
#11559 = CARTESIAN_POINT ( 'NONE',  ( -0.05219959533909027116, -19.03943276465977164, 82.49890960531436690 ) ) ;
#11561 = CARTESIAN_POINT ( 'NONE',  ( -18.22780087662123805, 5.499999999999981348, 71.01763182126894947 ) ) ;
#11560 = CARTESIAN_POINT ( 'NONE',  ( -8.314922557960811034, -14.29746914071050412, 37.08224293864768129 ) ) ;
#11562 = CARTESIAN_POINT ( 'NONE',  ( -5.153800228976607833, 19.02544592524334988, 32.70942372801899722 ) ) ;
#11563 = CARTESIAN_POINT ( 'NONE',  ( 8.314922557960818139, 14.29746914071049879, 79.58224293864769550 ) ) ;
#11564 = CARTESIAN_POINT ( 'NONE',  ( 10.81492255796106328, -18.62759615963255655, 110.4177570613523756 ) ) ;
#11565 = CARTESIAN_POINT ( 'NONE',  ( -16.51473224551069308, -9.474510206698971260, 56.66557627198103120 ) ) ;
#11567 = CARTESIAN_POINT ( 'NONE',  ( 0.05219959533937995610, -21.53943276465977519, 105.0010903946856757 ) ) ;
#11566 = CARTESIAN_POINT ( 'NONE',  ( 14.29746914071049879, -8.314922557960816363, 38.33224293864768839 ) ) ;
#11568 = CARTESIAN_POINT ( 'NONE',  ( -19.03943276465977164, 0.05219959533909376836, 91.24890960531436690 ) ) ;
#11569 = CARTESIAN_POINT ( 'NONE',  ( -19.02544592524342804, 5.153800228976336051, 111.0405762719810099 ) ) ;
#11570 = CARTESIAN_POINT ( 'NONE',  ( 13.97604488694527802, 13.89961937509977652, 44.37390960531435269 ) ) ;
#11571 = CARTESIAN_POINT ( 'NONE',  ( 0.05219959533910956823, 16.53943276465976808, 114.9989096053143669 ) ) ;
#11572 = CARTESIAN_POINT ( 'NONE',  ( 12.06949235617757843, -12.14591786802309237, 83.12390960531436690 ) ) ;
#11573 = CARTESIAN_POINT ( 'NONE',  ( 21.52544592524344225, -5.823673210054117533, 93.54057627198103830 ) ) ;
#11574 = CARTESIAN_POINT ( 'NONE',  ( 9.564922557960805705, 16.46253265017160317, 89.58224293864769550 ) ) ;
#11575 = CARTESIAN_POINT ( 'NONE',  ( 21.55341960407610458, 5.719274019375980345, 93.95724293864770971 ) ) ;
#11576 = CARTESIAN_POINT ( 'NONE',  ( -9.474510206698964154, 16.51473224551069663, 85.41557627198102409 ) ) ;
#11578 = CARTESIAN_POINT ( 'NONE',  ( 16.52544592524342804, -4.483927247898539470, 103.5405762719810383 ) ) ;
#11577 = PLANE ( 'NONE',  #52581 ) ;
#11579 = CARTESIAN_POINT ( 'NONE',  ( -5.153800228976328057, -19.02544592524343514, 67.29057627198102409 ) ) ;
#11580 = CARTESIAN_POINT ( 'NONE',  ( 21.52544592524344225, -5.823673210054117533, 73.54057627198102409 ) ) ;
#11581 = PLANE ( 'NONE',  #81712 ) ;
#11583 = DIRECTION ( 'NONE',  ( 0.000000000000000000, 0.000000000000000000, 1.000000000000000000 ) ) ;
#11582 = CARTESIAN_POINT ( 'NONE',  ( 10.72451020669898902, -18.67979575497178502, 22.91557627198102765 ) ) ;
#11584 = CARTESIAN_POINT ( 'NONE',  ( -14.29746914071037622, -8.314922557961029526, 29.16775706135234003 ) ) ;
#11585 = CARTESIAN_POINT ( 'NONE',  ( 8.224510206698953496, -14.34966873604960469, 97.91557627198103830 ) ) ;
#11586 = CARTESIAN_POINT ( 'NONE',  ( 19.02130022317635749, -5.499999999999802824, 53.28188669246574705 ) ) ;
#11587 = CARTESIAN_POINT ( 'NONE',  ( -5.153800228976328057, -19.02544592524343514, 87.29057627198103830 ) ) ;
#11588 = CARTESIAN_POINT ( 'NONE',  ( -19.05341960407611168, -5.049401038298163336, 46.45724293864768129 ) ) ;
#11589 = CARTESIAN_POINT ( 'NONE',  ( 8.224510206698953496, -14.34966873604960469, 77.91557627198102409 ) ) ;
#11590 = CARTESIAN_POINT ( 'NONE',  ( 0.05219959533907565091, 21.53943276465977519, 29.99890960531435979 ) ) ;
#11591 = CARTESIAN_POINT ( 'NONE',  ( -14.29746914071049879, 8.314922557960819915, 55.83224293864770260 ) ) ;
#11592 = CARTESIAN_POINT ( 'NONE',  ( 19.02544592524334988, 5.153800228976608722, 96.45942372801897591 ) ) ;
#11593 = CARTESIAN_POINT ( 'NONE',  ( -18.67979575497193778, 10.72451020669871902, 63.33442372801900433 ) ) ;
#11594 = CARTESIAN_POINT ( 'NONE',  ( 17.14385361876520264, -23.59649016807270883, 147.5750000027311728 ) ) ;
#11595 = CARTESIAN_POINT ( 'NONE',  ( -5.153800228976328057, -19.02544592524343514, 102.2905762719810383 ) ) ;
#11596 = CARTESIAN_POINT ( 'NONE',  ( 4.379528057220092307, 16.55341960407617563, 82.29275706135234714 ) ) ;
#11597 = CARTESIAN_POINT ( 'NONE',  ( 13.89961937509977652, -13.97604488694527269, 28.12390960531435624 ) ) ;
#11598 = CARTESIAN_POINT ( 'NONE',  ( 9.564922557960805705, 16.46253265017160317, 79.58224293864769550 ) ) ;
#11599 = CARTESIAN_POINT ( 'NONE',  ( 0.05219959533907565091, 21.53943276465977519, 79.99890960531435269 ) ) ;
#11600 = CARTESIAN_POINT ( 'NONE',  ( 5.049401038297881783, 19.05341960407617563, 107.2927570613523187 ) ) ;
#11602 = CARTESIAN_POINT ( 'NONE',  ( 5.823673210054444382, -21.52544592524334988, 60.20942372801902565 ) ) ;
#11601 = CARTESIAN_POINT ( 'NONE',  ( 16.53943276465976808, -0.05219959533910856209, 48.74890960531435979 ) ) ;
#11604 = CARTESIAN_POINT ( 'NONE',  ( -5.719274019375978568, 21.55341960407610458, 30.20724293864769550 ) ) ;
#11603 = CARTESIAN_POINT ( 'NONE',  ( -4.483927247898782831, 16.52544592524335698, 82.70942372801900433 ) ) ;
#11605 = CARTESIAN_POINT ( 'NONE',  ( 26.00062938246248478, 10.06977165081871384, 166.7331697587469250 ) ) ;
#11606 = DIRECTION ( 'NONE',  ( -0.000000000000000000, -0.000000000000000000, 1.000000000000000000 ) ) ;
#11607 = CARTESIAN_POINT ( 'NONE',  ( 12.06949235617739724, 12.14591786802326823, 111.8760903946856615 ) ) ;
#11608 = CARTESIAN_POINT ( 'NONE',  ( 16.53943276465976808, 0.05219959533934440121, 61.25109039468567573 ) ) ;
#11609 = CARTESIAN_POINT ( 'NONE',  ( 5.153800228976335163, 19.02544592524342804, 69.79057627198103830 ) ) ;
#11610 = CARTESIAN_POINT ( 'NONE',  ( 19.05341960407611168, 5.049401038298154454, 83.95724293864766707 ) ) ;
#11611 = CARTESIAN_POINT ( 'NONE',  ( -15.80617190586768217, 15.72974639402176855, 68.12609039468567573 ) ) ;
#11612 = CARTESIAN_POINT ( 'NONE',  ( -16.53943276465976808, -0.05219959533934237506, 73.75109039468567573 ) ) ;
#11613 = CARTESIAN_POINT ( 'NONE',  ( -0.05219959533910754901, -16.53943276465976808, 42.49890960531435979 ) ) ;
#11614 = CARTESIAN_POINT ( 'NONE',  ( -19.05341960407611168, -5.049401038298163336, 56.45724293864768129 ) ) ;
#11615 = CARTESIAN_POINT ( 'NONE',  ( -13.89961937509977652, 13.97604488694528158, 50.62390960531435979 ) ) ;
#11617 = ORIENTED_EDGE ( 'NONE', *, *, #69929, .F. ) ;
#11616 = CARTESIAN_POINT ( 'NONE',  ( -12.14591786802326823, 12.06949235617739902, 43.12609039468568284 ) ) ;
#11618 = CARTESIAN_POINT ( 'NONE',  ( 5.153800228976615827, -19.02544592524334988, 100.2094237280190043 ) ) ;
#11619 = CARTESIAN_POINT ( 'NONE',  ( -8.224510206698948167, 14.34966873604960824, 100.4155762719810241 ) ) ;
#11620 = CARTESIAN_POINT ( 'NONE',  ( -16.46253265017160317, 9.564922557960807481, 60.83224293864769550 ) ) ;
#11622 = CARTESIAN_POINT ( 'NONE',  ( -23.48529157249600985, 32.32473071737754111, -6.300000000000000711 ) ) ;
#11621 = CARTESIAN_POINT ( 'NONE',  ( 16.51473224551083163, -9.474510206698727899, 95.83442372801900433 ) ) ;
#11623 = CARTESIAN_POINT ( 'NONE',  ( -15.72974639402176322, -15.80617190586768395, 104.3760903946856899 ) ) ;
#11624 = CARTESIAN_POINT ( 'NONE',  ( -0.05219959533934338120, 16.53943276465976808, 62.50109039468568284 ) ) ;
#11625 = DIRECTION ( 'NONE',  ( 0.000000000000000000, 1.000000000000000000, 0.000000000000000000 ) ) ;
#11626 = CARTESIAN_POINT ( 'NONE',  ( 18.62759615963271287, -10.81492255796078972, 68.33224293864769550 ) ) ;
#11627 = CARTESIAN_POINT ( 'NONE',  ( -0.05219959533934338120, 16.53943276465976808, 47.50109039468568994 ) ) ;
#11628 = CARTESIAN_POINT ( 'NONE',  ( -30.00000000000000000, -1.163414459189985801E-14, 95.00000000000000000 ) ) ;
#11629 = CARTESIAN_POINT ( 'NONE',  ( 16.51473224551083163, -9.474510206698727899, 40.83442372801900433 ) ) ;
#11630 = AXIS2_PLACEMENT_3D ( 'NONE', #120508, #167033, #180236 ) ;
#11631 = CARTESIAN_POINT ( 'NONE',  ( 13.97604488694527802, 13.89961937509977652, 84.37390960531433848 ) ) ;
#11632 = CARTESIAN_POINT ( 'NONE',  ( -19.05341960407611168, -5.049401038298163336, 26.45724293864769550 ) ) ;
#11633 = CARTESIAN_POINT ( 'NONE',  ( 19.05341960407611168, 5.049401038298154454, 58.95724293864768129 ) ) ;
#11634 = CARTESIAN_POINT ( 'NONE',  ( 4.379528057220339221, -16.55341960407611168, 57.70724293864770260 ) ) ;
#11635 = CARTESIAN_POINT ( 'NONE',  ( 0.05219959533937995610, -21.53943276465977519, 80.00109039468568994 ) ) ;
#11636 = CARTESIAN_POINT ( 'NONE',  ( 13.89961937509957401, 13.97604488694547697, 46.87609039468565442 ) ) ;
#11637 = CARTESIAN_POINT ( 'NONE',  ( -13.89961937509957401, -13.97604488694547875, 29.37609039468565797 ) ) ;
#11638 = CARTESIAN_POINT ( 'NONE',  ( -19.05341960407611168, -5.049401038298163336, 51.45724293864770260 ) ) ;
#11639 = CARTESIAN_POINT ( 'NONE',  ( -0.05219959533907301413, -21.53943276465977519, 22.49890960531436335 ) ) ;
#11640 = CARTESIAN_POINT ( 'NONE',  ( 18.67979575497194134, -10.72451020669871369, 100.8344237280190185 ) ) ;
#11641 = CARTESIAN_POINT ( 'NONE',  ( -9.474510206698964154, 16.51473224551069663, 65.41557627198102409 ) ) ;
#11642 = EDGE_CURVE ( 'NONE', #78253, #165007, #123449, .T. ) ;
#11643 = CARTESIAN_POINT ( 'NONE',  ( 21.52544592524334988, 5.823673210054432836, 91.45942372801901854 ) ) ;
#11644 = CARTESIAN_POINT ( 'NONE',  ( -10.72451020669898014, 18.67979575497178502, 35.41557627198102409 ) ) ;
#11645 = CARTESIAN_POINT ( 'NONE',  ( 13.89961937509977652, -13.97604488694527269, 88.12390960531438111 ) ) ;
#11646 = CARTESIAN_POINT ( 'NONE',  ( -13.97604488694547697, 13.89961937509957934, 68.12609039468563310 ) ) ;
#11647 = CARTESIAN_POINT ( 'NONE',  ( 9.474510206698971260, -16.51473224551069308, 42.91557627198103120 ) ) ;
#11648 = CARTESIAN_POINT ( 'NONE',  ( -0.05219959533909027116, -19.03943276465977164, 87.49890960531436690 ) ) ;
#11649 = CARTESIAN_POINT ( 'NONE',  ( 16.52544592524335698, 4.483927247898782831, 31.45942372801901854 ) ) ;
#11650 = CARTESIAN_POINT ( 'NONE',  ( 14.29746914071049879, -8.314922557960816363, 88.33224293864769550 ) ) ;
#11651 = CARTESIAN_POINT ( 'NONE',  ( 13.89961937509977652, -13.97604488694527269, 68.12390960531436690 ) ) ;
#11652 = CARTESIAN_POINT ( 'NONE',  ( 0.05219959533907565091, 21.53943276465977519, 54.99890960531435269 ) ) ;
#11653 = CARTESIAN_POINT ( 'NONE',  ( -19.03943276465977164, -0.05219959533935918106, 113.7510903946856757 ) ) ;
#11654 = CARTESIAN_POINT ( 'NONE',  ( 10.81492255796078972, 18.62759615963270932, 114.5822429386477097 ) ) ;
#11655 = CARTESIAN_POINT ( 'NONE',  ( 5.719274019375673035, 21.55341960407619339, 67.29275706135234714 ) ) ;
#11656 = CARTESIAN_POINT ( 'NONE',  ( -14.34966873604972548, 8.224510206698743886, 68.33442372801900433 ) ) ;
#11657 = CARTESIAN_POINT ( 'NONE',  ( 16.55341960407618274, -4.379528057220086978, 66.04275706135236135 ) ) ;
#11658 = CARTESIAN_POINT ( 'NONE',  ( -5.049401038298153566, 19.05341960407611168, 60.20724293864768129 ) ) ;
#11659 = CARTESIAN_POINT ( 'NONE',  ( -12.14591786802326823, 12.06949235617739902, 108.1260903946856757 ) ) ;
#11660 = CARTESIAN_POINT ( 'NONE',  ( 5.049401038297881783, 19.05341960407617563, 42.29275706135234003 ) ) ;
#11661 = CARTESIAN_POINT ( 'NONE',  ( -15.72974639402176322, -15.80617190586768395, 34.37609039468568284 ) ) ;
#11662 = CARTESIAN_POINT ( 'NONE',  ( 16.53943276465976808, -0.05219959533910856209, 63.74890960531435979 ) ) ;
#11663 = CARTESIAN_POINT ( 'NONE',  ( 0.05219959533909260263, 19.03943276465977164, 104.9989096053143669 ) ) ;
#11664 = CARTESIAN_POINT ( 'NONE',  ( -8.224510206698735004, -14.34966873604973081, 94.58442372801901854 ) ) ;
#11665 = CARTESIAN_POINT ( 'NONE',  ( -21.55341960407619339, 5.719274019375674811, 73.54275706135234714 ) ) ;
#11666 = CARTESIAN_POINT ( 'NONE',  ( 16.52544592524335698, 4.483927247898782831, 26.45942372801901854 ) ) ;
#11667 = CARTESIAN_POINT ( 'NONE',  ( -21.55341960407619339, 5.719274019375674811, 23.54275706135235424 ) ) ;
#11668 = CARTESIAN_POINT ( 'NONE',  ( -14.34966873604960291, -8.224510206698953496, 56.66557627198103830 ) ) ;
#11669 = VERTEX_POINT ( 'NONE', #170990 ) ;
#11670 = CARTESIAN_POINT ( 'NONE',  ( -5.823673210054116645, -21.52544592524344225, 102.2905762719810383 ) ) ;
#11671 = CARTESIAN_POINT ( 'NONE',  ( 16.53943276465976808, -0.05219959533910856209, 43.74890960531435979 ) ) ;
#11672 = VERTEX_POINT ( 'NONE', #2133 ) ;
#11673 = CARTESIAN_POINT ( 'NONE',  ( -19.02544592524342804, 5.153800228976336051, 26.04057627198103120 ) ) ;
#11674 = CARTESIAN_POINT ( 'NONE',  ( -18.62759615963270932, 10.81492255796079327, 30.83224293864770260 ) ) ;
#11675 = CARTESIAN_POINT ( 'NONE',  ( -10.81492255796105439, 18.62759615963255655, 32.91775706135234714 ) ) ;
#11676 = CARTESIAN_POINT ( 'NONE',  ( 14.29746914071049879, -8.314922557960816363, 63.33224293864770260 ) ) ;
#11677 = AXIS2_PLACEMENT_3D ( 'NONE', #24067, #85722, #21057 ) ;
#11678 = CARTESIAN_POINT ( 'NONE',  ( 5.823673210054125526, 21.52544592524343514, 69.79057627198102409 ) ) ;
#11679 = CARTESIAN_POINT ( 'NONE',  ( -13.97604488694527625, -13.89961937509977652, 71.87390960531433848 ) ) ;
#11681 = CARTESIAN_POINT ( 'NONE',  ( -13.97604488694547697, 13.89961937509957934, 83.12609039468564731 ) ) ;
#11680 = CARTESIAN_POINT ( 'NONE',  ( 0.05219959533909260263, 19.03943276465977164, 24.99890960531435269 ) ) ;
#11682 = CARTESIAN_POINT ( 'NONE',  ( -10.72451020669898014, 18.67979575497178502, 45.41557627198103830 ) ) ;
#11683 = CARTESIAN_POINT ( 'NONE',  ( 0.05219959533909260263, 19.03943276465977164, 39.99890960531436690 ) ) ;
#11684 = CARTESIAN_POINT ( 'NONE',  ( -19.03943276465977164, 0.05219959533909376836, 71.24890960531435269 ) ) ;
#11685 = VERTEX_POINT ( 'NONE', #105343 ) ;
#11686 = CARTESIAN_POINT ( 'NONE',  ( -8.314922557961024197, 14.29746914071037800, 37.91775706135235424 ) ) ;
#11687 = CARTESIAN_POINT ( 'NONE',  ( 15.72974639402176855, 15.80617190586768217, 21.87609039468567573 ) ) ;
#11688 = CARTESIAN_POINT ( 'NONE',  ( 8.314922557960818139, 14.29746914071049879, 44.58224293864769550 ) ) ;
#11689 = CARTESIAN_POINT ( 'NONE',  ( 13.89961937509977652, -13.97604488694527269, 108.1239096053143669 ) ) ;
#11690 = CARTESIAN_POINT ( 'NONE',  ( -0.05219959533907301413, -21.53943276465977519, 77.49890960531433848 ) ) ;
#11692 = CARTESIAN_POINT ( 'NONE',  ( 16.52544592524335698, 4.483927247898782831, 46.45942372801901854 ) ) ;
#11691 = CARTESIAN_POINT ( 'NONE',  ( 15.80617190586746368, 15.72974639402197994, 104.3739096053143669 ) ) ;
#11693 = CARTESIAN_POINT ( 'NONE',  ( -0.05219959533907301413, -21.53943276465977519, 47.49890960531435979 ) ) ;
#11694 = CARTESIAN_POINT ( 'NONE',  ( -21.52544592524334988, -5.823673210054445271, 98.95942372801903275 ) ) ;
#11695 = CARTESIAN_POINT ( 'NONE',  ( 9.564922557960805705, 16.46253265017160317, 49.58224293864770260 ) ) ;
#11696 = CARTESIAN_POINT ( 'NONE',  ( 9.564922557960805705, 16.46253265017160317, 94.58224293864769550 ) ) ;
#11697 = CARTESIAN_POINT ( 'NONE',  ( -5.049401038298153566, 19.05341960407611168, 70.20724293864769550 ) ) ;
#11698 = CARTESIAN_POINT ( 'NONE',  ( -17.41079204577539841, -36.66972510653778983, -18.74440029985510137 ) ) ;
#11699 = CARTESIAN_POINT ( 'NONE',  ( 9.564922557961047289, -16.46253265017146816, 55.41775706135234003 ) ) ;
#11701 = CARTESIAN_POINT ( 'NONE',  ( 15.80617190586746368, 15.72974639402197994, 29.37390960531435269 ) ) ;
#11700 = CARTESIAN_POINT ( 'NONE',  ( -21.53943276465977519, -0.05219959533937600094, 113.7510903946856757 ) ) ;
#11702 = CARTESIAN_POINT ( 'NONE',  ( -16.52544592524335698, -4.483927247898792601, 108.9594237280190185 ) ) ;
#11703 = CARTESIAN_POINT ( 'NONE',  ( 13.89961937509957401, 13.97604488694547697, 91.87609039468567573 ) ) ;
#11704 = CARTESIAN_POINT ( 'NONE',  ( -16.20579543436675962, 7.371946100355235565, 59.43479165828123456 ) ) ;
#11705 = CARTESIAN_POINT ( 'NONE',  ( -13.97604488694547697, 13.89961937509957934, 23.12609039468565442 ) ) ;
#11706 = CARTESIAN_POINT ( 'NONE',  ( -13.89961937509957401, -13.97604488694547875, 84.37609039468567573 ) ) ;
#11707 = CARTESIAN_POINT ( 'NONE',  ( -16.46253265017146816, -9.564922557961047289, 44.16775706135232582 ) ) ;
#11708 = DIRECTION ( 'NONE',  ( 0.000000000000000000, 0.000000000000000000, 1.000000000000000000 ) ) ;
#11709 = CARTESIAN_POINT ( 'NONE',  ( -5.153800228976328057, -19.02544592524343514, 47.29057627198102409 ) ) ;
#11710 = CARTESIAN_POINT ( 'NONE',  ( -14.29746914071049879, 8.314922557960819915, 55.83224293864770260 ) ) ;
#11711 = CARTESIAN_POINT ( 'NONE',  ( 9.474510206698971260, -16.51473224551069308, 27.91557627198103120 ) ) ;
#11712 = CARTESIAN_POINT ( 'NONE',  ( -16.53943276465976808, 0.05219959533911058130, 36.24890960531435979 ) ) ;
#11713 = LINE ( 'NONE', #73380, #83913 ) ;
#11714 = CARTESIAN_POINT ( 'NONE',  ( 14.34966873604972726, -8.224510206698740333, 105.8344237280190328 ) ) ;
#11715 = CARTESIAN_POINT ( 'NONE',  ( -19.03943276465977164, 0.05219959533909376836, 51.24890960531436690 ) ) ;
#11716 = CARTESIAN_POINT ( 'NONE',  ( -5.823673210054431948, 21.52544592524334988, 107.7094237280190328 ) ) ;
#11717 = CARTESIAN_POINT ( 'NONE',  ( 4.483927247898790824, -16.52544592524335698, 35.20942372801901854 ) ) ;
#11718 = CARTESIAN_POINT ( 'NONE',  ( 15.72974639402199770, -15.80617190586745480, 38.12390960531436690 ) ) ;
#11719 = CARTESIAN_POINT ( 'NONE',  ( 5.719274019375673035, 21.55341960407619339, 92.29275706135236135 ) ) ;
#11720 = CARTESIAN_POINT ( 'NONE',  ( 0.05219959533909260263, 19.03943276465977164, 99.99890960531436690 ) ) ;
#11721 = CARTESIAN_POINT ( 'NONE',  ( 5.153800228976335163, 19.02544592524342804, 89.79057627198102409 ) ) ;
#11722 = CARTESIAN_POINT ( 'NONE',  ( 3.556970738554034288E-15, -38.81732327939057114, -6.124999997268812280 ) ) ;
#11723 = CARTESIAN_POINT ( 'NONE',  ( 18.62759615963271287, -10.81492255796078972, 108.3322429386477097 ) ) ;
#11724 = AXIS2_PLACEMENT_3D ( 'NONE', #75086, #119618, #27627 ) ;
#11725 = CARTESIAN_POINT ( 'NONE',  ( -8.224510206698948167, 14.34966873604960824, 85.41557627198102409 ) ) ;
#11726 = CARTESIAN_POINT ( 'NONE',  ( 15.80617190586746368, 15.72974639402197994, 79.37390960531436690 ) ) ;
#11727 = CARTESIAN_POINT ( 'NONE',  ( 16.46253265017160672, -9.564922557960803928, 73.33224293864769550 ) ) ;
#11728 = CARTESIAN_POINT ( 'NONE',  ( 10.72451020669898902, -18.67979575497178502, 102.9155762719810383 ) ) ;
#11729 = EDGE_CURVE ( 'NONE', #177464, #140780, #41494, .T. ) ;
#11730 = VERTEX_POINT ( 'NONE', #138653 ) ;
#11731 = CARTESIAN_POINT ( 'NONE',  ( 5.153800228976335163, 19.02544592524342804, 54.79057627198103120 ) ) ;
#11733 = CARTESIAN_POINT ( 'NONE',  ( 16.51473224551069308, 9.474510206698969483, 24.16557627198102765 ) ) ;
#11732 = CARTESIAN_POINT ( 'NONE',  ( -8.314922557960811034, -14.29746914071050412, 92.08224293864769550 ) ) ;
#11734 = CARTESIAN_POINT ( 'NONE',  ( 5.049401038298161559, -19.05341960407611168, 67.70724293864769550 ) ) ;
#11735 = CARTESIAN_POINT ( 'NONE',  ( -5.049401038297874678, -19.05341960407617918, 74.79275706135231871 ) ) ;
#11736 = CARTESIAN_POINT ( 'NONE',  ( -16.52544592524342804, 4.483927247898546575, 101.0405762719810383 ) ) ;
#11737 = CARTESIAN_POINT ( 'NONE',  ( -21.52544592524334988, -5.823673210054445271, 58.95942372801902565 ) ) ;
#11739 = CARTESIAN_POINT ( 'NONE',  ( -21.55341960407619339, 5.719274019375674811, 23.54275706135235424 ) ) ;
#11738 = CARTESIAN_POINT ( 'NONE',  ( -13.97604488694527625, -13.89961937509977652, 46.87390960531435979 ) ) ;
#11740 = CARTESIAN_POINT ( 'NONE',  ( 8.224510206698953496, -14.34966873604960469, 107.9155762719810241 ) ) ;
#11741 = CYLINDRICAL_SURFACE ( 'NONE', #185239, 2.000000000000001776 ) ;
#11742 = CARTESIAN_POINT ( 'NONE',  ( 19.05341960407611168, 5.049401038298154454, 53.95724293864770260 ) ) ;
#11743 = CARTESIAN_POINT ( 'NONE',  ( 1.784589286804354247, 7.284589286804251884, 8.181980515339454030 ) ) ;
#11745 = CARTESIAN_POINT ( 'NONE',  ( -5.153800228976328057, -19.02544592524343514, 112.2905762719810099 ) ) ;
#11744 = CARTESIAN_POINT ( 'NONE',  ( 19.05341960407617918, -5.049401038297876454, 106.0427570613523471 ) ) ;
#11746 = CARTESIAN_POINT ( 'NONE',  ( -21.55341960407619339, 5.719274019375674811, 43.54275706135235424 ) ) ;
#11747 = CARTESIAN_POINT ( 'NONE',  ( -9.564922557960796823, -16.46253265017161027, 97.08224293864769550 ) ) ;
#11748 = CARTESIAN_POINT ( 'NONE',  ( -5.049401038297874678, -19.05341960407617918, 84.79275706135233293 ) ) ;
#11749 = CARTESIAN_POINT ( 'NONE',  ( 13.89961937509977652, -13.97604488694527269, 63.12390960531435979 ) ) ;
#11750 = CARTESIAN_POINT ( 'NONE',  ( 14.34966873604960469, 8.224510206698951720, 79.16557627198103830 ) ) ;
#11751 = CARTESIAN_POINT ( 'NONE',  ( 5.049401038298161559, -19.05341960407611168, 87.70724293864769550 ) ) ;
#11752 = CARTESIAN_POINT ( 'NONE',  ( -16.53943276465976808, 0.05219959533911058130, 76.24890960531435269 ) ) ;
#11753 = CARTESIAN_POINT ( 'NONE',  ( -19.02544592524342804, 5.153800228976336051, 81.04057627198103830 ) ) ;
#11754 = CARTESIAN_POINT ( 'NONE',  ( 19.05341960407617918, -5.049401038297876454, 31.04275706135232227 ) ) ;
#11757 = CARTESIAN_POINT ( 'NONE',  ( 19.02544592524343514, -5.153800228976328945, 23.54057627198102054 ) ) ;
#11756 = CARTESIAN_POINT ( 'NONE',  ( 12.14591786802309770, 12.06949235617756955, 49.37390960531436690 ) ) ;
#11755 = CARTESIAN_POINT ( 'NONE',  ( 19.05341960407611168, 5.049401038298154454, 43.95724293864769550 ) ) ;
#11758 = VERTEX_POINT ( 'NONE', #134 ) ;
#11759 = CARTESIAN_POINT ( 'NONE',  ( 21.52544592524334988, 5.823673210054432836, 46.45942372801901854 ) ) ;
#11760 = CARTESIAN_POINT ( 'NONE',  ( 19.05341960407617918, -5.049401038297876454, 76.04275706135230450 ) ) ;
#11761 = CARTESIAN_POINT ( 'NONE',  ( -4.379528057220328563, 16.55341960407611168, 30.20724293864769550 ) ) ;
#11762 = CARTESIAN_POINT ( 'NONE',  ( 10.72451020669898902, -18.67979575497178502, 97.91557627198103830 ) ) ;
#11763 = CARTESIAN_POINT ( 'NONE',  ( -18.67979575497178146, -10.72451020669898902, 36.66557627198103120 ) ) ;
#11765 = CARTESIAN_POINT ( 'NONE',  ( -8.224510206698948167, 14.34966873604960824, 75.41557627198102409 ) ) ;
#11764 = AXIS2_PLACEMENT_3D ( 'NONE', #8109, #143619, #190143 ) ;
#11766 = CARTESIAN_POINT ( 'NONE',  ( 0.05219959533909260263, 19.03943276465977164, 44.99890960531435979 ) ) ;
#11767 = CARTESIAN_POINT ( 'NONE',  ( -16.55341960407617563, 4.379528057220093196, 108.5427570613523756 ) ) ;
#11768 = MANIFOLD_SOLID_BREP ( 'Hex', #111522 ) ;
#11769 = CARTESIAN_POINT ( 'NONE',  ( 4.379528057220092307, 16.55341960407617563, 67.29275706135234714 ) ) ;
#11770 = CARTESIAN_POINT ( 'NONE',  ( -13.97604488694547697, 13.89961937509957934, 23.12609039468565442 ) ) ;
#11771 = CARTESIAN_POINT ( 'NONE',  ( -9.564922557960796823, -16.46253265017161027, 92.08224293864769550 ) ) ;
#11772 = CARTESIAN_POINT ( 'NONE',  ( 5.049401038298161559, -19.05341960407611168, 77.70724293864765286 ) ) ;
#11773 = CIRCLE ( 'NONE', #89245, 206.0437394197456342 ) ;
#11774 = CARTESIAN_POINT ( 'NONE',  ( -14.34966873604972548, 8.224510206698743886, 78.33442372801901854 ) ) ;
#11775 = CARTESIAN_POINT ( 'NONE',  ( -5.153800228976328057, -19.02544592524343514, 42.29057627198101699 ) ) ;
#11776 = CARTESIAN_POINT ( 'NONE',  ( 16.53943276465976808, -0.05219959533910856209, 48.74890960531435979 ) ) ;
#11778 = CARTESIAN_POINT ( 'NONE',  ( -5.153800228976328057, -19.02544592524343514, 87.29057627198103830 ) ) ;
#11777 = CARTESIAN_POINT ( 'NONE',  ( -19.03943276465977164, 0.05219959533909376836, 101.2489096053143669 ) ) ;
#11779 = CARTESIAN_POINT ( 'NONE',  ( 10.72451020669898902, -18.67979575497178502, 22.91557627198102765 ) ) ;
#11780 = CARTESIAN_POINT ( 'NONE',  ( -8.224510206698948167, 14.34966873604960824, 75.41557627198102409 ) ) ;
#11781 = CARTESIAN_POINT ( 'NONE',  ( 16.52544592524342804, -4.483927247898539470, 63.54057627198103830 ) ) ;
#11783 = CARTESIAN_POINT ( 'NONE',  ( 17.49999999999999289, -3.345213924137297123, 32.08768623094358219 ) ) ;
#11782 = CARTESIAN_POINT ( 'NONE',  ( 8.224510206698742110, 14.34966873604972548, 47.08442372801901854 ) ) ;
#11784 = CARTESIAN_POINT ( 'NONE',  ( -5.153800228976607833, 19.02544592524334988, 62.70942372801899722 ) ) ;
#11785 = CARTESIAN_POINT ( 'NONE',  ( -9.564922557960796823, -16.46253265017161027, 87.08224293864769550 ) ) ;
#11786 = CARTESIAN_POINT ( 'NONE',  ( 16.51473224551083163, -9.474510206698727899, 60.83442372801900433 ) ) ;
#11787 = CARTESIAN_POINT ( 'NONE',  ( 2.400000000000000799, 0.000000000000000000, 1.999999999999999112 ) ) ;
#11789 = CARTESIAN_POINT ( 'NONE',  ( -4.379528057220086978, -16.55341960407618274, 94.79275706135234714 ) ) ;
#11788 = CARTESIAN_POINT ( 'NONE',  ( -8.224510206698735004, -14.34966873604973081, 19.58442372801901143 ) ) ;
#11790 = CARTESIAN_POINT ( 'NONE',  ( 5.049401038298161559, -19.05341960407611168, 37.70724293864768839 ) ) ;
#11791 = CARTESIAN_POINT ( 'NONE',  ( -21.52544592524343514, 5.823673210054127303, 26.04057627198103475 ) ) ;
#11792 = CARTESIAN_POINT ( 'NONE',  ( 5.823673210054444382, -21.52544592524334988, 50.20942372801901854 ) ) ;
#11793 = CARTESIAN_POINT ( 'NONE',  ( 19.05341960407617918, -5.049401038297876454, 106.0427570613523471 ) ) ;
#11795 = CARTESIAN_POINT ( 'NONE',  ( 16.46253265017160672, -9.564922557960803928, 73.33224293864769550 ) ) ;
#11794 = CARTESIAN_POINT ( 'NONE',  ( 1.300000000000000044, 1.443375672974065216, 7.017607234860990640E-28 ) ) ;
#11796 = DIRECTION ( 'NONE',  ( -1.000000000000000000, 5.392603844284257652E-33, 0.000000000000000000 ) ) ;
#11798 = CARTESIAN_POINT ( 'NONE',  ( -13.89961937509977652, 13.97604488694528158, 75.62390960531438111 ) ) ;
#11797 = CARTESIAN_POINT ( 'NONE',  ( -16.55341960407611168, -4.379528057220339221, 76.45724293864769550 ) ) ;
#11799 = CONTEXT_DEPENDENT_SHAPE_REPRESENTATION ( #85501, #174566 ) ;
#11800 = CARTESIAN_POINT ( 'NONE',  ( 5.153800228976335163, 19.02544592524342804, 74.79057627198103830 ) ) ;
#11801 = CARTESIAN_POINT ( 'NONE',  ( -0.05219959533936034679, 19.03943276465977164, 82.50109039468567573 ) ) ;
#11802 = CARTESIAN_POINT ( 'NONE',  ( -5.719274019375978568, 21.55341960407610458, 65.20724293864768129 ) ) ;
#11803 = CARTESIAN_POINT ( 'NONE',  ( 19.03943276465977164, -0.05219959533909143690, 28.74890960531435624 ) ) ;
#11804 = CARTESIAN_POINT ( 'NONE',  ( 13.89961937509957401, 13.97604488694547697, 61.87609039468566863 ) ) ;
#11805 = CARTESIAN_POINT ( 'NONE',  ( 16.46253265017160672, -9.564922557960803928, 58.33224293864769550 ) ) ;
#11806 = CARTESIAN_POINT ( 'NONE',  ( 19.03943276465977164, -0.05219959533909143690, 93.74890960531435269 ) ) ;
#11807 = ORIENTED_EDGE ( 'NONE', *, *, #91315, .F. ) ;
#11808 = CARTESIAN_POINT ( 'NONE',  ( -21.55341960407610458, -5.719274019375992779, 86.45724293864770971 ) ) ;
#11810 = CARTESIAN_POINT ( 'NONE',  ( 5.049401038297881783, 19.05341960407617563, 42.29275706135234003 ) ) ;
#11809 = CARTESIAN_POINT ( 'NONE',  ( -8.224510206698948167, 14.34966873604960824, 90.41557627198103830 ) ) ;
#11811 = CARTESIAN_POINT ( 'NONE',  ( 15.80617190586746368, 15.72974639402197994, 79.37390960531436690 ) ) ;
#11812 = CARTESIAN_POINT ( 'NONE',  ( 10.72451020669898902, -18.67979575497178502, 57.91557627198103120 ) ) ;
#11813 = CARTESIAN_POINT ( 'NONE',  ( 16.53943276465976808, -0.05219959533910856209, 28.74890960531435624 ) ) ;
#11814 = CARTESIAN_POINT ( 'NONE',  ( -18.67979575497193778, 10.72451020669871902, 103.3344237280190043 ) ) ;
#11815 = CARTESIAN_POINT ( 'NONE',  ( 5.049401038298161559, -19.05341960407611168, 77.70724293864765286 ) ) ;
#11816 = CARTESIAN_POINT ( 'NONE',  ( -5.153800228976328057, -19.02544592524343514, 32.29057627198102409 ) ) ;
#11817 = CARTESIAN_POINT ( 'NONE',  ( -10.72451020669870658, -18.67979575497194134, 34.58442372801900433 ) ) ;
#11818 = CARTESIAN_POINT ( 'NONE',  ( 18.62759615963255655, 10.81492255796105972, 46.66775706135234714 ) ) ;
#11819 = CARTESIAN_POINT ( 'NONE',  ( 13.97604488694527802, 13.89961937509977652, 54.37390960531435979 ) ) ;
#11820 = CARTESIAN_POINT ( 'NONE',  ( -10.72451020669870658, -18.67979575497194134, 24.58442372801901499 ) ) ;
#11821 = CARTESIAN_POINT ( 'NONE',  ( -0.05219959533936034679, 19.03943276465977164, 57.50109039468566863 ) ) ;
#11822 = CARTESIAN_POINT ( 'NONE',  ( -19.03943276465977164, 0.05219959533909376836, 31.24890960531435979 ) ) ;
#11823 = CARTESIAN_POINT ( 'NONE',  ( 12.06949235617739724, 12.14591786802326823, 21.87609039468567573 ) ) ;
#11824 = CARTESIAN_POINT ( 'NONE',  ( 16.51473224551069308, 9.474510206698969483, 29.16557627198103475 ) ) ;
#11825 = CARTESIAN_POINT ( 'NONE',  ( 14.34966873604972726, -8.224510206698740333, 75.83442372801900433 ) ) ;
#11826 = CARTESIAN_POINT ( 'NONE',  ( -19.02544592524342804, 5.153800228976336051, 46.04057627198101699 ) ) ;
#11827 = CARTESIAN_POINT ( 'NONE',  ( -19.83801684532646803, -12.12952959760830041, 169.9999999999999716 ) ) ;
#11828 = CARTESIAN_POINT ( 'NONE',  ( -19.02544592524342804, 5.153800228976336051, 81.04057627198103830 ) ) ;
#11829 = CARTESIAN_POINT ( 'NONE',  ( 19.05341960407611168, 5.049401038298154454, 28.95724293864769550 ) ) ;
#11830 = CARTESIAN_POINT ( 'NONE',  ( -0.05219959533907301413, -21.53943276465977519, 77.49890960531433848 ) ) ;
#11831 = CARTESIAN_POINT ( 'NONE',  ( 16.53943276465976808, 0.05219959533934440121, 46.25109039468567573 ) ) ;
#11832 = CARTESIAN_POINT ( 'NONE',  ( -21.53943276465977519, -0.05219959533937600094, 98.75109039468568994 ) ) ;
#11833 = EDGE_CURVE ( 'NONE', #198671, #10418, #185165, .T. ) ;
#11834 = CARTESIAN_POINT ( 'NONE',  ( 16.51473224551069308, 9.474510206698969483, 44.16557627198103120 ) ) ;
#11835 = CARTESIAN_POINT ( 'NONE',  ( 14.29746914071049879, -8.314922557960816363, 28.33224293864769550 ) ) ;
#11836 = CARTESIAN_POINT ( 'NONE',  ( 16.55341960407611168, 4.379528057220329451, 68.95724293864769550 ) ) ;
#11837 = CARTESIAN_POINT ( 'NONE',  ( -13.97604488694527625, -13.89961937509977652, 71.87390960531433848 ) ) ;
#11838 = CARTESIAN_POINT ( 'NONE',  ( 10.72451020669871369, 18.67979575497193778, 112.0844237280190185 ) ) ;
#11839 = CARTESIAN_POINT ( 'NONE',  ( -21.55341960407619339, 5.719274019375674811, 28.54275706135234358 ) ) ;
#11840 = CARTESIAN_POINT ( 'NONE',  ( -0.05219959533909027116, -19.03943276465977164, 77.49890960531435269 ) ) ;
#11841 = CARTESIAN_POINT ( 'NONE',  ( -10.72451020669870658, -18.67979575497194134, 79.58442372801903275 ) ) ;
#11842 = CARTESIAN_POINT ( 'NONE',  ( 12.14591786802327356, -12.06949235617739191, 70.62609039468567573 ) ) ;
#11843 = CARTESIAN_POINT ( 'NONE',  ( 12.14591786802327356, -12.06949235617739191, 35.62609039468568994 ) ) ;
#11845 = CARTESIAN_POINT ( 'NONE',  ( -18.62759615963255300, -10.81492255796106328, 104.1677570613523471 ) ) ;
#11844 = CARTESIAN_POINT ( 'NONE',  ( -4.483927247898539470, -16.52544592524342804, 92.29057627198103830 ) ) ;
#11846 = EDGE_CURVE ( 'NONE', #137572, #36107, #198420, .T. ) ;
#11847 = CARTESIAN_POINT ( 'NONE',  ( -8.314922557960811034, -14.29746914071050412, 37.08224293864768129 ) ) ;
#11848 = CARTESIAN_POINT ( 'NONE',  ( 5.153800228976335163, 19.02544592524342804, 24.79057627198102765 ) ) ;
#11849 = CARTESIAN_POINT ( 'NONE',  ( 16.52544592524335698, 4.483927247898782831, 46.45942372801901854 ) ) ;
#11850 = CARTESIAN_POINT ( 'NONE',  ( 4.483927247898545687, 16.52544592524342804, 49.79057627198102409 ) ) ;
#11851 = CARTESIAN_POINT ( 'NONE',  ( -12.14591786802326823, 12.06949235617739902, 103.1260903946856757 ) ) ;
#11852 = CARTESIAN_POINT ( 'NONE',  ( 13.89961937509977652, -13.97604488694527269, 113.1239096053143527 ) ) ;
#11853 = CARTESIAN_POINT ( 'NONE',  ( 15.72974639402199770, -15.80617190586745480, 33.12390960531435979 ) ) ;
#11854 = CARTESIAN_POINT ( 'NONE',  ( -16.46253265017146816, -9.564922557961047289, 19.16775706135233293 ) ) ;
#11855 = CARTESIAN_POINT ( 'NONE',  ( 8.314922557960818139, 14.29746914071049879, 84.58224293864769550 ) ) ;
#11856 = CARTESIAN_POINT ( 'NONE',  ( -19.02544592524342804, 5.153800228976336051, 91.04057627198100988 ) ) ;
#11857 = VERTEX_POINT ( 'NONE', #95134 ) ;
#11858 = CARTESIAN_POINT ( 'NONE',  ( -14.34966873604972548, 8.224510206698743886, 43.33442372801901143 ) ) ;
#11859 = CARTESIAN_POINT ( 'NONE',  ( -19.05341960407611168, -5.049401038298163336, 36.45724293864766707 ) ) ;
#11861 = CARTESIAN_POINT ( 'NONE',  ( 5.000000000000000888, -140.0000000000000000, 0.0009999999999992653654 ) ) ;
#11860 = CARTESIAN_POINT ( 'NONE',  ( -12.06949235617739369, -12.14591786802326823, 49.37609039468569705 ) ) ;
#11862 = CARTESIAN_POINT ( 'NONE',  ( -19.02544592524334988, -5.153800228976617603, 48.95942372801900433 ) ) ;
#11863 = CARTESIAN_POINT ( 'NONE',  ( -5.049401038298153566, 19.05341960407611168, 40.20724293864768839 ) ) ;
#11864 = CARTESIAN_POINT ( 'NONE',  ( 4.483927247898790824, -16.52544592524335698, 80.20942372801901854 ) ) ;
#11865 = CARTESIAN_POINT ( 'NONE',  ( 19.02544592524334988, 5.153800228976608722, 101.4594237280189759 ) ) ;
#11866 = CARTESIAN_POINT ( 'NONE',  ( -0.05219959533936034679, 19.03943276465977164, 27.50109039468566507 ) ) ;
#11867 = CARTESIAN_POINT ( 'NONE',  ( -9.474510206698964154, 16.51473224551069663, 60.41557627198102409 ) ) ;
#11868 = CARTESIAN_POINT ( 'NONE',  ( 0.05219959533910956823, 16.53943276465976808, 94.99890960531436690 ) ) ;
#11869 = CIRCLE ( 'NONE', #124829, 2.041999999999999815 ) ;
#11870 = CARTESIAN_POINT ( 'NONE',  ( 5.153800228976615827, -19.02544592524334988, 70.20942372801899012 ) ) ;
#11871 = CARTESIAN_POINT ( 'NONE',  ( -18.62759615963270932, 10.81492255796079327, 65.83224293864769550 ) ) ;
#11872 = CARTESIAN_POINT ( 'NONE',  ( 5.153800228976615827, -19.02544592524334988, 35.20942372801899722 ) ) ;
#11873 = CARTESIAN_POINT ( 'NONE',  ( -19.03943276465977164, 0.05219959533909376836, 101.2489096053143669 ) ) ;
#11874 = EDGE_CURVE ( 'NONE', #11672, #142306, #113785, .T. ) ;
#11875 = CARTESIAN_POINT ( 'NONE',  ( 10.72451020669898902, -18.67979575497178502, 92.91557627198103830 ) ) ;
#11876 = CARTESIAN_POINT ( 'NONE',  ( -32.00000000000000000, -1.163414459189985801E-14, 97.65000000000000568 ) ) ;
#11877 = CARTESIAN_POINT ( 'NONE',  ( 5.153800228976615827, -19.02544592524334988, 105.2094237280190185 ) ) ;
#11878 = CARTESIAN_POINT ( 'NONE',  ( 37.57652299961964104, -0.7251171387572892257, 39.53617709569549277 ) ) ;
#11879 = CARTESIAN_POINT ( 'NONE',  ( -16.52544592524335698, -4.483927247898792601, 23.95942372801901143 ) ) ;
#11880 = CARTESIAN_POINT ( 'NONE',  ( 9.474510206698971260, -16.51473224551069308, 52.91557627198102409 ) ) ;
#11881 = CARTESIAN_POINT ( 'NONE',  ( -9.564922557960796823, -16.46253265017161027, 112.0822429386476955 ) ) ;
#11882 = CARTESIAN_POINT ( 'NONE',  ( -21.55341960407610458, -5.719274019375992779, 96.45724293864770971 ) ) ;
#11883 = CARTESIAN_POINT ( 'NONE',  ( 21.52544592524334988, 5.823673210054432836, 56.45942372801902565 ) ) ;
#11885 = CARTESIAN_POINT ( 'NONE',  ( -5.719274019375665041, -21.55341960407619695, 104.7927570613523898 ) ) ;
#11884 = CARTESIAN_POINT ( 'NONE',  ( -19.05341960407617563, 5.049401038297882671, 108.5427570613523187 ) ) ;
#11886 = CARTESIAN_POINT ( 'NONE',  ( 4.483927247898790824, -16.52544592524335698, 110.2094237280190185 ) ) ;
#11887 = CARTESIAN_POINT ( 'NONE',  ( -15.80617190586745835, -15.72974639402198527, 101.8739096053143811 ) ) ;
#11888 = CARTESIAN_POINT ( 'NONE',  ( 16.53943276465976808, -0.05219959533910856209, 53.74890960531437401 ) ) ;
#11889 = CARTESIAN_POINT ( 'NONE',  ( 9.564922557961047289, -16.46253265017146816, 80.41775706135234714 ) ) ;
#11890 = CARTESIAN_POINT ( 'NONE',  ( -9.474510206698720793, -16.51473224551083518, 59.58442372801900433 ) ) ;
#11891 = CARTESIAN_POINT ( 'NONE',  ( 5.823673210054444382, -21.52544592524334988, 75.20942372801901854 ) ) ;
#11892 = CARTESIAN_POINT ( 'NONE',  ( -5.049401038297874678, -19.05341960407617918, 34.79275706135233293 ) ) ;
#11893 = CARTESIAN_POINT ( 'NONE',  ( -13.97604488694527625, -13.89961937509977652, 26.87390960531434558 ) ) ;
#11894 = CARTESIAN_POINT ( 'NONE',  ( -21.55341960407610458, -5.719274019375992779, 41.45724293864769550 ) ) ;
#11895 = CARTESIAN_POINT ( 'NONE',  ( 14.34966873604960469, 8.224510206698951720, 39.16557627198102409 ) ) ;
#11896 = CARTESIAN_POINT ( 'NONE',  ( -21.53943276465977519, -0.05219959533937600094, 108.7510903946857042 ) ) ;
#11897 = CARTESIAN_POINT ( 'NONE',  ( -4.379528057220086978, -16.55341960407618274, 74.79275706135234714 ) ) ;
#11898 = CARTESIAN_POINT ( 'NONE',  ( -14.29746914071049879, 8.314922557960819915, 45.83224293864769550 ) ) ;
#11899 = CARTESIAN_POINT ( 'NONE',  ( 15.80617190586769283, -15.72974639402175789, 65.62609039468568994 ) ) ;
#11900 = CARTESIAN_POINT ( 'NONE',  ( 15.80617190586769283, -15.72974639402175789, 70.62609039468567573 ) ) ;
#11901 = CARTESIAN_POINT ( 'NONE',  ( -10.72451020669898014, 18.67979575497178502, 70.41557627198102409 ) ) ;
#11902 = CARTESIAN_POINT ( 'NONE',  ( -19.03943276465977164, 0.05219959533909376836, 26.24890960531435624 ) ) ;
#11903 = CARTESIAN_POINT ( 'NONE',  ( 15.72974639402176855, 15.80617190586768217, 36.87609039468568994 ) ) ;
#11904 = CARTESIAN_POINT ( 'NONE',  ( 4.379528057220339221, -16.55341960407611168, 112.7072429386476955 ) ) ;
#11905 = CARTESIAN_POINT ( 'NONE',  ( -0.05219959533909027116, -19.03943276465977164, 32.49890960531435979 ) ) ;
#11906 = CARTESIAN_POINT ( 'NONE',  ( -14.34966873604960291, -8.224510206698953496, 91.66557627198103830 ) ) ;
#11907 = CARTESIAN_POINT ( 'NONE',  ( 16.51473224551069308, 9.474510206698969483, 89.16557627198103830 ) ) ;
#11908 = CARTESIAN_POINT ( 'NONE',  ( -4.379528057220328563, 16.55341960407611168, 30.20724293864769550 ) ) ;
#11909 = CARTESIAN_POINT ( 'NONE',  ( -4.379528057220328563, 16.55341960407611168, 105.2072429386477097 ) ) ;
#11910 = CARTESIAN_POINT ( 'NONE',  ( -18.67979575497178146, -10.72451020669898902, 71.66557627198100988 ) ) ;
#11911 = CIRCLE ( 'NONE', #95864, 216.0437394197456911 ) ;
#11912 = CARTESIAN_POINT ( 'NONE',  ( 5.719274019375991003, -21.55341960407610458, 102.7072429386476955 ) ) ;
#11913 = CARTESIAN_POINT ( 'NONE',  ( 19.05341960407611168, 5.049401038298154454, 108.9572429386477097 ) ) ;
#11915 = CARTESIAN_POINT ( 'NONE',  ( -8.224510206698735004, -14.34966873604973081, 24.58442372801901499 ) ) ;
#11914 = CARTESIAN_POINT ( 'NONE',  ( 19.03943276465977164, -0.05219959533909143690, 58.74890960531435979 ) ) ;
#11916 = CARTESIAN_POINT ( 'NONE',  ( -18.62759615963270932, 10.81492255796079327, 60.83224293864769550 ) ) ;
#11917 = CARTESIAN_POINT ( 'NONE',  ( -5.719274019375665041, -21.55341960407619695, 84.79275706135234714 ) ) ;
#11918 = CARTESIAN_POINT ( 'NONE',  ( -5.049401038298153566, 19.05341960407611168, 80.20724293864769550 ) ) ;
#11919 = CARTESIAN_POINT ( 'NONE',  ( 5.719274019375991003, -21.55341960407610458, 22.70724293864769194 ) ) ;
#11920 = CARTESIAN_POINT ( 'NONE',  ( -16.55341960407617563, 4.379528057220093196, 73.54275706135234714 ) ) ;
#11921 = CARTESIAN_POINT ( 'NONE',  ( -21.55341960407619339, 5.719274019375674811, 73.54275706135234714 ) ) ;
#11922 = CARTESIAN_POINT ( 'NONE',  ( -0.05219959533937732626, 21.53943276465977519, 97.50109039468567573 ) ) ;
#11923 = CARTESIAN_POINT ( 'NONE',  ( 16.53943276465976808, 0.05219959533934440121, 66.25109039468567573 ) ) ;
#11924 = CARTESIAN_POINT ( 'NONE',  ( 15.80617190586746368, 15.72974639402197994, 109.3739096053143811 ) ) ;
#11925 = CARTESIAN_POINT ( 'NONE',  ( -16.51473224551069308, -9.474510206698971260, 21.66557627198102765 ) ) ;
#11926 = CARTESIAN_POINT ( 'NONE',  ( -5.719274019375978568, 21.55341960407610458, 95.20724293864769550 ) ) ;
#11927 = CARTESIAN_POINT ( 'NONE',  ( -19.03943276465977164, -0.05219959533935918106, 43.75109039468566863 ) ) ;
#11928 = CARTESIAN_POINT ( 'NONE',  ( -0.05219959533907301413, -21.53943276465977519, 57.49890960531435979 ) ) ;
#11930 = CARTESIAN_POINT ( 'NONE',  ( 4.379528057220339221, -16.55341960407611168, 42.70724293864770260 ) ) ;
#11929 = CARTESIAN_POINT ( 'NONE',  ( -19.02544592524342804, 5.153800228976336051, 91.04057627198100988 ) ) ;
#11931 = CARTESIAN_POINT ( 'NONE',  ( 4.500000000000000888, -120.0000000000000142, 14.99999999999998757 ) ) ;
#11932 =( BOUNDED_CURVE ( )  B_SPLINE_CURVE ( 3, ( #178851, #190018, #191005, #82807 ),
 .UNSPECIFIED., .F., .T. ) 
 B_SPLINE_CURVE_WITH_KNOTS ( ( 4, 4 ),
 ( 1.570796326794896780, 2.008945357379067875 ),
 .UNSPECIFIED. ) 
 CURVE ( )  GEOMETRIC_REPRESENTATION_ITEM ( )  RATIONAL_B_SPLINE_CURVE ( ( 1.000000000000000000, 0.9840659996946589105, 0.9840659996946589105, 1.000000000000000000 ) ) 
 REPRESENTATION_ITEM ( '' )  );
#11933 = CARTESIAN_POINT ( 'NONE',  ( -18.22780087662122028, 5.500000000000031086, 73.51540105326107266 ) ) ;
#11934 = CARTESIAN_POINT ( 'NONE',  ( 13.89961937509957401, 13.97604488694547697, 111.8760903946856757 ) ) ;
#11935 = CARTESIAN_POINT ( 'NONE',  ( 5.823673210054125526, 21.52544592524343514, 89.79057627198103830 ) ) ;
#11936 = CARTESIAN_POINT ( 'NONE',  ( -16.55341960407611168, -4.379528057220339221, 46.45724293864769550 ) ) ;
#11937 = CARTESIAN_POINT ( 'NONE',  ( 12.14591786802327356, -12.06949235617739191, 30.62609039468567929 ) ) ;
#11938 = CARTESIAN_POINT ( 'NONE',  ( -5.049401038298153566, 19.05341960407611168, 50.20724293864770260 ) ) ;
#11940 = CARTESIAN_POINT ( 'NONE',  ( -19.03943276465977164, -0.05219959533935918106, 83.75109039468567573 ) ) ;
#11939 = CARTESIAN_POINT ( 'NONE',  ( -10.81492255796078084, -18.62759615963271287, 112.0822429386477097 ) ) ;
#11941 = CARTESIAN_POINT ( 'NONE',  ( 5.049401038298161559, -19.05341960407611168, 87.70724293864769550 ) ) ;
#11942 = CARTESIAN_POINT ( 'NONE',  ( -16.51473224551069308, -9.474510206698971260, 71.66557627198102409 ) ) ;
#11943 = CARTESIAN_POINT ( 'NONE',  ( -5.719274019375978568, 21.55341960407610458, 75.20724293864769550 ) ) ;
#11944 = CARTESIAN_POINT ( 'NONE',  ( 5.153800228976335163, 19.02544592524342804, 34.79057627198102409 ) ) ;
#11945 = CARTESIAN_POINT ( 'NONE',  ( -3.573655867282028392E-15, 2.428612866367529932E-14, 139.9999999999999716 ) ) ;
#11946 = CARTESIAN_POINT ( 'NONE',  ( 8.314922557960818139, 14.29746914071049879, 59.58224293864770260 ) ) ;
#11947 = CARTESIAN_POINT ( 'NONE',  ( -16.51473224551069308, -9.474510206698971260, 96.66557627198102409 ) ) ;
#11948 = CARTESIAN_POINT ( 'NONE',  ( -4.500000000000001776, -120.0000000000000142, 14.99999999999998757 ) ) ;
#11949 = CARTESIAN_POINT ( 'NONE',  ( -19.05341960407617563, 5.049401038297882671, 63.54275706135234003 ) ) ;
#11950 = CARTESIAN_POINT ( 'NONE',  ( -18.62759615963270932, 10.81492255796079327, 80.83224293864769550 ) ) ;
#11951 = CARTESIAN_POINT ( 'NONE',  ( 13.97604488694548053, -13.89961937509957401, 30.62609039468566863 ) ) ;
#11952 = CARTESIAN_POINT ( 'NONE',  ( 19.05341960407611168, 5.049401038298154454, 93.95724293864769550 ) ) ;
#11953 = FACE_OUTER_BOUND ( 'NONE', #124538, .T. ) ;
#11954 = CARTESIAN_POINT ( 'NONE',  ( 18.62759615963271287, -10.81492255796078972, 28.33224293864769550 ) ) ;
#11955 = CARTESIAN_POINT ( 'NONE',  ( 9.474510206698971260, -16.51473224551069308, 77.91557627198103830 ) ) ;
#11956 = CARTESIAN_POINT ( 'NONE',  ( 15.72974639402176855, 15.80617190586768217, 56.87609039468568994 ) ) ;
#11957 = CARTESIAN_POINT ( 'NONE',  ( 5.153800228976335163, 19.02544592524342804, 24.79057627198102765 ) ) ;
#11959 = ORIENTED_EDGE ( 'NONE', *, *, #131511, .F. ) ;
#11958 = CARTESIAN_POINT ( 'NONE',  ( 21.53943276465977519, 0.05219959533937863772, 21.25109039468567218 ) ) ;
#11960 = CARTESIAN_POINT ( 'NONE',  ( -5.719274019375665041, -21.55341960407619695, 44.79275706135234714 ) ) ;
#11961 = ORIENTED_EDGE ( 'NONE', *, *, #125347, .T. ) ;
#11962 = CARTESIAN_POINT ( 'NONE',  ( -9.474510206698964154, 16.51473224551069663, 95.41557627198102409 ) ) ;
#11963 = CARTESIAN_POINT ( 'NONE',  ( -21.71408805923171315, 8.664832797227232319, 169.0754946983649916 ) ) ;
#11964 = CARTESIAN_POINT ( 'NONE',  ( 21.52544592524344225, -5.823673210054117533, 108.5405762719810241 ) ) ;
#11965 = CARTESIAN_POINT ( 'NONE',  ( 19.02544592524343514, -5.153800228976328945, 63.54057627198103830 ) ) ;
#11966 = CARTESIAN_POINT ( 'NONE',  ( -4.379528057220086978, -16.55341960407618274, 19.79275706135235069 ) ) ;
#11967 = CARTESIAN_POINT ( 'NONE',  ( 11.74264578624799427, 36.14014761921585972, -6.349999994537625980 ) ) ;
#11968 = CARTESIAN_POINT ( 'NONE',  ( -5.823673210054431948, 21.52544592524334988, 107.7094237280190328 ) ) ;
#11969 = CARTESIAN_POINT ( 'NONE',  ( -9.474510206698964154, 16.51473224551069663, 40.41557627198103120 ) ) ;
#11970 = CARTESIAN_POINT ( 'NONE',  ( -10.81492255796105439, 18.62759615963255655, 97.91775706135236135 ) ) ;
#11972 = CARTESIAN_POINT ( 'NONE',  ( -10.81492255796105439, 18.62759615963255655, 57.91775706135234714 ) ) ;
#11971 = CARTESIAN_POINT ( 'NONE',  ( 19.05341960407611168, 5.049401038298154454, 83.95724293864766707 ) ) ;
#11973 = CARTESIAN_POINT ( 'NONE',  ( 8.571926809382603096, -26.38167802310801235, 141.9750000027312069 ) ) ;
#11974 = CARTESIAN_POINT ( 'NONE',  ( -9.564922557960796823, -16.46253265017161027, 107.0822429386476955 ) ) ;
#11975 = CARTESIAN_POINT ( 'NONE',  ( 37.99626262588765258, 2.893932880411085066E-14, 2.000000000000000000 ) ) ;
#11978 = CARTESIAN_POINT ( 'NONE',  ( -5.719274019375665041, -21.55341960407619695, 64.79275706135234714 ) ) ;
#11977 = CARTESIAN_POINT ( 'NONE',  ( -14.29746914071037622, -8.314922557961029526, 64.16775706135234714 ) ) ;
#11976 = CARTESIAN_POINT ( 'NONE',  ( 4.379528057220092307, 16.55341960407617563, 57.29275706135234714 ) ) ;
#11979 = CARTESIAN_POINT ( 'NONE',  ( -21.55341960407619339, 5.719274019375674811, 93.54275706135234714 ) ) ;
#11980 = CARTESIAN_POINT ( 'NONE',  ( 30.00000000000000000, -5.186379194389041255E-15, 47.64999999999999858 ) ) ;
#11981 = CARTESIAN_POINT ( 'NONE',  ( 14.34966873604972726, -8.224510206698740333, 25.83442372801901499 ) ) ;
#11982 = CARTESIAN_POINT ( 'NONE',  ( 19.05341960407611168, 5.049401038298154454, 68.95724293864769550 ) ) ;
#11983 = CARTESIAN_POINT ( 'NONE',  ( 13.97604488694527802, 13.89961937509977652, 114.3739096053143669 ) ) ;
#11984 = CARTESIAN_POINT ( 'NONE',  ( -15.49999999999999822, -5.500000000000000888, 22.00000000000000000 ) ) ;
#11985 = B_SPLINE_CURVE_WITH_KNOTS ( 'NONE', 3,
 ( #86516, #72358, #26868, #133022, #121824, #134032, #10695, #195725, #181540, #136021, #194712, #59161, #165374, #167358, #25872, #44011, #11704, #198688, #24867, #60155, #152178, #197695, #13662, #88511, #73371, #183518, #120829, #56181, #182529, #117864, #179555, #119856 ),
 .UNSPECIFIED., .F., .F.,
 ( 4, 2, 2, 2, 2, 2, 2, 2, 2, 2, 2, 2, 2, 2, 2, 4 ),
 ( 2.539163526713095107E-17, 0.0003712461730037033662, 0.0007424923460073813621, 0.001113738519011059358, 0.001484984692014737354, 0.002227477038022093563, 0.002598723211025767872, 0.002969969384029442182, 0.003341215557033117359, 0.003712461730036790801, 0.004083707903040465111, 0.004454954076044138553, 0.004826200249047812862, 0.005197446422051487172, 0.005568692595055160614, 0.005939938768058834924 ),
 .UNSPECIFIED. ) ;
#11986 = CARTESIAN_POINT ( 'NONE',  ( -9.474510206698964154, 16.51473224551069663, 30.41557627198102054 ) ) ;
#11988 = ADVANCED_FACE ( 'NONE', ( #52612 ), #20278, .T. ) ;
#11987 = CARTESIAN_POINT ( 'NONE',  ( 15.80617190586746368, 15.72974639402197994, 49.37390960531436690 ) ) ;
#11989 = CARTESIAN_POINT ( 'NONE',  ( -8.224510206698735004, -14.34966873604973081, 89.58442372801901854 ) ) ;
#11991 = CARTESIAN_POINT ( 'NONE',  ( -19.05341960407611168, -5.049401038298163336, 61.45724293864769550 ) ) ;
#11990 = CARTESIAN_POINT ( 'NONE',  ( -4.483927247898539470, -16.52544592524342804, 87.29057627198103830 ) ) ;
#11992 = CARTESIAN_POINT ( 'NONE',  ( 21.55341960407619695, -5.719274019375665929, 86.04275706135236135 ) ) ;
#11993 = CARTESIAN_POINT ( 'NONE',  ( 1.988064558232696151E-15, -30.27659582821216588, 144.7656553485623476 ) ) ;
#11994 = CARTESIAN_POINT ( 'NONE',  ( -4.483927247898782831, 16.52544592524335698, 22.70942372801901499 ) ) ;
#11995 = CARTESIAN_POINT ( 'NONE',  ( 8.224510206698953496, -14.34966873604960469, 72.91557627198103830 ) ) ;
#11996 = CARTESIAN_POINT ( 'NONE',  ( 18.67979575497194134, -10.72451020669871369, 35.83442372801901143 ) ) ;
#11997 = CARTESIAN_POINT ( 'NONE',  ( -21.52544592524343514, 5.823673210054127303, 71.04057627198103830 ) ) ;
#11998 = CARTESIAN_POINT ( 'NONE',  ( -9.564922557961040184, 16.46253265017147172, 32.91775706135233293 ) ) ;
#11999 = CARTESIAN_POINT ( 'NONE',  ( 0.05219959533909260263, 19.03943276465977164, 44.99890960531435979 ) ) ;
#12000 = CARTESIAN_POINT ( 'NONE',  ( -13.97604488694527625, -13.89961937509977652, 76.87390960531433848 ) ) ;
#12001 = CARTESIAN_POINT ( 'NONE',  ( -0.05219959533910754901, -16.53943276465976808, 47.49890960531435979 ) ) ;
#12002 = EDGE_CURVE ( 'NONE', #189322, #192521, #104153, .T. ) ;
#12003 = AXIS2_PLACEMENT_3D ( 'NONE', #72281, #70284, #134966 ) ;
#12004 = CARTESIAN_POINT ( 'NONE',  ( -16.55341960407611168, -4.379528057220339221, 31.45724293864769550 ) ) ;
#12005 = CARTESIAN_POINT ( 'NONE',  ( -16.55341960407617563, 4.379528057220093196, 108.5427570613523756 ) ) ;
#12006 = CARTESIAN_POINT ( 'NONE',  ( -13.97604488694547697, 13.89961937509957934, 63.12609039468566152 ) ) ;
#12007 = CARTESIAN_POINT ( 'NONE',  ( 16.81555441253550143, 7.025013491695497159, 46.86314554665745646 ) ) ;
#12008 = CARTESIAN_POINT ( 'NONE',  ( 21.52544592524344225, -5.823673210054117533, 23.54057627198102765 ) ) ;
#12009 = CARTESIAN_POINT ( 'NONE',  ( 16.52544592524342804, -4.483927247898539470, 88.54057627198103830 ) ) ;
#12010 = PLANE ( 'NONE',  #96796 ) ;
#12012 = CARTESIAN_POINT ( 'NONE',  ( -18.67979575497178146, -10.72451020669898902, 31.66557627198102054 ) ) ;
#12011 = CARTESIAN_POINT ( 'NONE',  ( 9.564922557960805705, 16.46253265017160317, 39.58224293864768839 ) ) ;
#12013 = CARTESIAN_POINT ( 'NONE',  ( 18.62759615963271287, -10.81492255796078972, 68.33224293864769550 ) ) ;
#12014 = CARTESIAN_POINT ( 'NONE',  ( 16.55341960407611168, 4.379528057220329451, 113.9572429386477239 ) ) ;
#12016 = CARTESIAN_POINT ( 'NONE',  ( 13.89961937509977652, -13.97604488694527269, 53.12390960531434558 ) ) ;
#12015 = CARTESIAN_POINT ( 'NONE',  ( -12.14591786802326823, 12.06949235617739902, 68.12609039468567573 ) ) ;
#12017 = CARTESIAN_POINT ( 'NONE',  ( -10.72451020669870658, -18.67979575497194134, 54.58442372801901143 ) ) ;
#12018 = AXIS2_PLACEMENT_3D ( 'NONE', #158362, #47218, #108876 ) ;
#12019 = CARTESIAN_POINT ( 'NONE',  ( 14.29746914071049879, -8.314922557960816363, 103.3322429386476955 ) ) ;
#12020 = CARTESIAN_POINT ( 'NONE',  ( -9.474510206698720793, -16.51473224551083518, 94.58442372801900433 ) ) ;
#12021 = CARTESIAN_POINT ( 'NONE',  ( 29.86685920354754842, -21.69954338932559068, -6.324999997268814234 ) ) ;
#12023 = CARTESIAN_POINT ( 'NONE',  ( 18.67979575497178502, 10.72451020669898547, 34.16557627198102409 ) ) ;
#12022 = CARTESIAN_POINT ( 'NONE',  ( -18.10062525802553779, 5.500000000000031974, 38.51383468041921532 ) ) ;
#12024 = PLANE ( 'NONE',  #47024 ) ;
#12025 = CARTESIAN_POINT ( 'NONE',  ( 21.55341960407619695, -5.719274019375665929, 71.04275706135234714 ) ) ;
#12027 = CARTESIAN_POINT ( 'NONE',  ( -14.34966873604960291, -8.224510206698953496, 46.66557627198102409 ) ) ;
#12026 = CARTESIAN_POINT ( 'NONE',  ( 8.314922557961029526, -14.29746914071037800, 50.41775706135235424 ) ) ;
#12028 = CARTESIAN_POINT ( 'NONE',  ( -21.53943276465977519, 0.05219959533907696930, 66.24890960531436690 ) ) ;
#12029 = CARTESIAN_POINT ( 'NONE',  ( -0.05219959533907301413, -21.53943276465977519, 62.49890960531436690 ) ) ;
#12030 = DIRECTION ( 'NONE',  ( -1.000000000000000000, -0.000000000000000000, -0.000000000000000000 ) ) ;
#12032 = CARTESIAN_POINT ( 'NONE',  ( -21.53943276465977519, 0.05219959533907696930, 21.24890960531436690 ) ) ;
#12031 = CARTESIAN_POINT ( 'NONE',  ( 5.049401038297881783, 19.05341960407617563, 87.29275706135234714 ) ) ;
#12033 = CARTESIAN_POINT ( 'NONE',  ( -13.97604488694527625, -13.89961937509977652, 51.87390960531436690 ) ) ;
#12034 = CARTESIAN_POINT ( 'NONE',  ( 8.224510206698953496, -14.34966873604960469, 112.9155762719810383 ) ) ;
#12035 = CARTESIAN_POINT ( 'NONE',  ( 21.23184647844207618, -181.1785498424364675, -4.999999999999999112 ) ) ;
#12036 = VERTEX_POINT ( 'NONE', #40450 ) ;
#12037 = CARTESIAN_POINT ( 'NONE',  ( -16.53943276465976808, -0.05219959533934237506, 73.75109039468567573 ) ) ;
#12038 = CARTESIAN_POINT ( 'NONE',  ( 21.55341960407610458, 5.719274019375980345, 108.9572429386476955 ) ) ;
#12039 = CARTESIAN_POINT ( 'NONE',  ( 0.05219959533909260263, 19.03943276465977164, 69.99890960531435269 ) ) ;
#12040 = CARTESIAN_POINT ( 'NONE',  ( 0.05219959533937995610, -21.53943276465977519, 45.00109039468568284 ) ) ;
#12041 = CARTESIAN_POINT ( 'NONE',  ( -9.474510206698964154, 16.51473224551069663, 95.41557627198102409 ) ) ;
#12042 = CARTESIAN_POINT ( 'NONE',  ( -28.32820575348087644, -27.54591730359596369, -18.54425385669249593 ) ) ;
#12043 = ORIENTED_EDGE ( 'NONE', *, *, #15456, .T. ) ;
#12044 = CARTESIAN_POINT ( 'NONE',  ( -21.55341960407619339, 5.719274019375674811, 38.54275706135234714 ) ) ;
#12046 = CARTESIAN_POINT ( 'NONE',  ( 9.474510206698729675, 16.51473224551082808, 87.08442372801900433 ) ) ;
#12045 = CARTESIAN_POINT ( 'NONE',  ( -13.97604488694527625, -13.89961937509977652, 26.87390960531434558 ) ) ;
#12047 = CARTESIAN_POINT ( 'NONE',  ( 13.89961937509957401, 13.97604488694547697, 41.87609039468566152 ) ) ;
#12048 = CARTESIAN_POINT ( 'NONE',  ( 15.72974639402199770, -15.80617190586745480, 113.1239096053143953 ) ) ;
#12049 = CARTESIAN_POINT ( 'NONE',  ( -19.03943276465977164, -0.05219959533935918106, 33.75109039468566863 ) ) ;
#12050 = CARTESIAN_POINT ( 'NONE',  ( 16.46253265017146816, 9.564922557961045513, 46.66775706135233293 ) ) ;
#12051 = CARTESIAN_POINT ( 'NONE',  ( 12.14591786802327356, -12.06949235617739191, 90.62609039468567573 ) ) ;
#12053 = EDGE_LOOP ( 'NONE', ( #119024, #139035, #83954, #140369 ) ) ;
#12052 = CARTESIAN_POINT ( 'NONE',  ( -19.02544592524342804, 5.153800228976336051, 116.0405762719810383 ) ) ;
#12054 = CARTESIAN_POINT ( 'NONE',  ( 19.03943276465977164, -0.05219959533909143690, 68.74890960531436690 ) ) ;
#12055 = VECTOR ( 'NONE', #187988, 1000.000000000000114 ) ;
#12056 = CARTESIAN_POINT ( 'NONE',  ( -18.67979575497193778, 10.72451020669871902, 83.33442372801903275 ) ) ;
#12057 = CARTESIAN_POINT ( 'NONE',  ( 5.823673210054444382, -21.52544592524334988, 95.20942372801903275 ) ) ;
#12058 = CARTESIAN_POINT ( 'NONE',  ( -1.452908486251138553, -7.214655873249289364, -64.31726809345073548 ) ) ;
#12059 = CARTESIAN_POINT ( 'NONE',  ( 0.05219959533909260263, 19.03943276465977164, 89.99890960531436690 ) ) ;
#12060 = CARTESIAN_POINT ( 'NONE',  ( 10.81492255796106328, -18.62759615963255655, 65.41775706135234714 ) ) ;
#12061 = CARTESIAN_POINT ( 'NONE',  ( -9.474510206698720793, -16.51473224551083518, 99.58442372801900433 ) ) ;
#12062 = CARTESIAN_POINT ( 'NONE',  ( -5.049401038298153566, 19.05341960407611168, 65.20724293864765286 ) ) ;
#12063 = CARTESIAN_POINT ( 'NONE',  ( -19.02544592524342804, 5.153800228976336051, 111.0405762719810099 ) ) ;
#12064 = CARTESIAN_POINT ( 'NONE',  ( -9.474510206698964154, 16.51473224551069663, 85.41557627198102409 ) ) ;
#12065 = CARTESIAN_POINT ( 'NONE',  ( 17.49999999999997513, -3.267433481402603146, 22.16880360417568241 ) ) ;
#12066 = CARTESIAN_POINT ( 'NONE',  ( -13.89961937509977652, 13.97604488694528158, 65.62390960531436690 ) ) ;
#12067 = CARTESIAN_POINT ( 'NONE',  ( -19.05341960407611168, -5.049401038298163336, 46.45724293864768129 ) ) ;
#12068 = CARTESIAN_POINT ( 'NONE',  ( -5.719274019375978568, 21.55341960407610458, 115.2072429386476955 ) ) ;
#12069 = CARTESIAN_POINT ( 'NONE',  ( -4.379528057220086978, -16.55341960407618274, 84.79275706135234714 ) ) ;
#12070 = CARTESIAN_POINT ( 'NONE',  ( -6.434671708797603529, 6.434671708797564449, -65.00100000000003320 ) ) ;
#12071 = CARTESIAN_POINT ( 'NONE',  ( 19.05341960407617918, -5.049401038297876454, 61.04275706135232582 ) ) ;
#12072 = CARTESIAN_POINT ( 'NONE',  ( -5.049401038298153566, 19.05341960407611168, 80.20724293864769550 ) ) ;
#12073 = CARTESIAN_POINT ( 'NONE',  ( -4.379528057220328563, 16.55341960407611168, 75.20724293864769550 ) ) ;
#12074 = CARTESIAN_POINT ( 'NONE',  ( -12.06949235617756955, 12.14591786802309770, 110.6239096053143669 ) ) ;
#12075 = CARTESIAN_POINT ( 'NONE',  ( -0.05219959533909027116, -19.03943276465977164, 112.4989096053143669 ) ) ;
#12076 = CARTESIAN_POINT ( 'NONE',  ( -13.97604488694527625, -13.89961937509977652, 106.8739096053143669 ) ) ;
#12077 = CARTESIAN_POINT ( 'NONE',  ( -4.379528057220328563, 16.55341960407611168, 80.20724293864769550 ) ) ;
#12078 = CARTESIAN_POINT ( 'NONE',  ( -37.45873412500000654, 2.428612866367529932E-14, -0.3124999986344065839 ) ) ;
#12079 = CARTESIAN_POINT ( 'NONE',  ( 9.474510206698729675, 16.51473224551082808, 37.08442372801899722 ) ) ;
#12080 = CARTESIAN_POINT ( 'NONE',  ( -14.34966873604972548, 8.224510206698743886, 103.3344237280190043 ) ) ;
#12081 = CARTESIAN_POINT ( 'NONE',  ( 19.05341960407611168, 5.049401038298154454, 83.95724293864766707 ) ) ;
#12082 = CARTESIAN_POINT ( 'NONE',  ( -18.67979575497193778, 10.72451020669871902, 53.33442372801901854 ) ) ;
#12083 = CARTESIAN_POINT ( 'NONE',  ( -18.62759615963270932, 10.81492255796079327, 50.83224293864770971 ) ) ;
#12084 = CARTESIAN_POINT ( 'NONE',  ( 10.72451020669898902, -18.67979575497178502, 112.9155762719810383 ) ) ;
#12085 = CARTESIAN_POINT ( 'NONE',  ( 21.53943276465977519, -0.05219959533907433946, 63.74890960531435979 ) ) ;
#12086 = CARTESIAN_POINT ( 'NONE',  ( -8.314922557960811034, -14.29746914071050412, 92.08224293864769550 ) ) ;
#12087 = CARTESIAN_POINT ( 'NONE',  ( 19.05341960407617918, -5.049401038297876454, 51.04275706135231871 ) ) ;
#12088 = CARTESIAN_POINT ( 'NONE',  ( -16.46253265017160317, 9.564922557960807481, 25.83224293864769194 ) ) ;
#12089 = CARTESIAN_POINT ( 'NONE',  ( -16.46253265017160317, 9.564922557960807481, 80.83224293864769550 ) ) ;
#12090 = CARTESIAN_POINT ( 'NONE',  ( 16.46253265017160672, -9.564922557960803928, 78.33224293864769550 ) ) ;
#12091 = CARTESIAN_POINT ( 'NONE',  ( -8.314922557960811034, -14.29746914071050412, 102.0822429386476955 ) ) ;
#12092 = VERTEX_POINT ( 'NONE', #101105 ) ;
#12093 = CARTESIAN_POINT ( 'NONE',  ( -16.53943276465976808, 0.05219959533911058130, 26.24890960531435624 ) ) ;
#12094 = CARTESIAN_POINT ( 'NONE',  ( -16.53943276465976808, -0.05219959533934237506, 38.75109039468567573 ) ) ;
#12095 = CARTESIAN_POINT ( 'NONE',  ( 18.67979575497194134, -10.72451020669871369, 105.8344237280190328 ) ) ;
#12096 = CARTESIAN_POINT ( 'NONE',  ( -19.03943276465977164, 0.05219959533909376836, 96.24890960531436690 ) ) ;
#12097 = CARTESIAN_POINT ( 'NONE',  ( -21.53943276465977519, -0.05219959533937600094, 38.75109039468567573 ) ) ;
#12098 = CARTESIAN_POINT ( 'NONE',  ( 16.46253265017160672, -9.564922557960803928, 38.33224293864768839 ) ) ;
#12099 = CARTESIAN_POINT ( 'NONE',  ( 4.483927247898790824, -16.52544592524335698, 40.20942372801901854 ) ) ;
#12100 = CARTESIAN_POINT ( 'NONE',  ( 13.97604488694548053, -13.89961937509957401, 105.6260903946856757 ) ) ;
#12101 = CARTESIAN_POINT ( 'NONE',  ( 16.46253265017160672, -9.564922557960803928, 38.33224293864768839 ) ) ;
#12102 = CARTESIAN_POINT ( 'NONE',  ( -14.34966873604960291, -8.224510206698953496, 91.66557627198103830 ) ) ;
#12103 = CARTESIAN_POINT ( 'NONE',  ( 18.67979575497178502, 10.72451020669898547, 109.1655762719810383 ) ) ;
#12104 = CARTESIAN_POINT ( 'NONE',  ( -5.153800228976607833, 19.02544592524334988, 87.70942372801897591 ) ) ;
#12105 = CARTESIAN_POINT ( 'NONE',  ( 13.89961937509977652, -13.97604488694527269, 28.12390960531435624 ) ) ;
#12106 = CARTESIAN_POINT ( 'NONE',  ( 19.02544592524343514, -5.153800228976328945, 93.54057627198102409 ) ) ;
#12107 = CARTESIAN_POINT ( 'NONE',  ( 15.72974639402176855, 15.80617190586768217, 36.87609039468568994 ) ) ;
#12108 = CARTESIAN_POINT ( 'NONE',  ( -11.74149087413295511, 36.13659316521247433, -4.147842220587803830 ) ) ;
#12109 = CARTESIAN_POINT ( 'NONE',  ( 9.474510206698971260, -16.51473224551069308, 97.91557627198102409 ) ) ;
#12110 = CARTESIAN_POINT ( 'NONE',  ( 16.36317988757056696, -7.306389748694960495, 111.5978960836323068 ) ) ;
#12111 = CARTESIAN_POINT ( 'NONE',  ( 13.89961937509977652, -13.97604488694527269, 88.12390960531438111 ) ) ;
#12113 = CARTESIAN_POINT ( 'NONE',  ( -16.52544592524342804, 4.483927247898546575, 91.04057627198103830 ) ) ;
#12112 = CARTESIAN_POINT ( 'NONE',  ( -0.05219959533937732626, 21.53943276465977519, 32.50109039468568284 ) ) ;
#12114 = CARTESIAN_POINT ( 'NONE',  ( 5.153800228976335163, 19.02544592524342804, 99.79057627198102409 ) ) ;
#12115 = CARTESIAN_POINT ( 'NONE',  ( -21.53943276465977519, -0.05219959533937600094, 113.7510903946856757 ) ) ;
#12116 = CARTESIAN_POINT ( 'NONE',  ( -0.05219959533934338120, 16.53943276465976808, 52.50109039468567573 ) ) ;
#12117 = CARTESIAN_POINT ( 'NONE',  ( 15.72974639402176855, 15.80617190586768217, 76.87609039468567573 ) ) ;
#12118 = CARTESIAN_POINT ( 'NONE',  ( 12.06949235617739724, 12.14591786802326823, 31.87609039468567929 ) ) ;
#12119 = CARTESIAN_POINT ( 'NONE',  ( 13.89961937509977652, -13.97604488694527269, 73.12390960531436690 ) ) ;
#12120 = CARTESIAN_POINT ( 'NONE',  ( -19.05341960407617563, 5.049401038297882671, 93.54275706135234714 ) ) ;
#12121 = CARTESIAN_POINT ( 'NONE',  ( -12.06949235617739369, -12.14591786802326823, 69.37609039468567573 ) ) ;
#12122 = CARTESIAN_POINT ( 'NONE',  ( -19.03943276465977164, -0.05219959533935918106, 18.75109039468567218 ) ) ;
#12123 = CARTESIAN_POINT ( 'NONE',  ( 13.89961937509957401, 13.97604488694547697, 81.87609039468564731 ) ) ;
#12124 = CARTESIAN_POINT ( 'NONE',  ( -16.46253265017160317, 9.564922557960807481, 60.83224293864769550 ) ) ;
#12125 = CARTESIAN_POINT ( 'NONE',  ( 18.62759615963271287, -10.81492255796078972, 88.33224293864769550 ) ) ;
#12127 = CARTESIAN_POINT ( 'NONE',  ( 9.474510206698729675, 16.51473224551082808, 77.08442372801900433 ) ) ;
#12126 = CARTESIAN_POINT ( 'NONE',  ( -14.34966873604960291, -8.224510206698953496, 76.66557627198103830 ) ) ;
#12128 = CARTESIAN_POINT ( 'NONE',  ( -18.56197773271725993, 5.500000000000081712, 78.55066217314451649 ) ) ;
#12129 = CARTESIAN_POINT ( 'NONE',  ( -13.97604488694547697, 13.89961937509957934, 58.12609039468566863 ) ) ;
#12130 = CARTESIAN_POINT ( 'NONE',  ( 4.379528057220339221, -16.55341960407611168, 22.70724293864769194 ) ) ;
#12131 = CARTESIAN_POINT ( 'NONE',  ( -16.55341960407611168, -4.379528057220339221, 81.45724293864769550 ) ) ;
#12133 = CARTESIAN_POINT ( 'NONE',  ( -17.14385361876520264, -23.59649016807271593, 145.1750000027311387 ) ) ;
#12132 = CARTESIAN_POINT ( 'NONE',  ( -5.049401038297874678, -19.05341960407617918, 19.79275706135233293 ) ) ;
#12134 = CARTESIAN_POINT ( 'NONE',  ( -10.81492255796078084, -18.62759615963271287, 112.0822429386477097 ) ) ;
#12135 = CARTESIAN_POINT ( 'NONE',  ( 16.51473224551069308, 9.474510206698969483, 104.1655762719810241 ) ) ;
#12136 = CARTESIAN_POINT ( 'NONE',  ( 13.89961937509977652, -13.97604488694527269, 73.12390960531436690 ) ) ;
#12137 = CARTESIAN_POINT ( 'NONE',  ( 5.823673210054444382, -21.52544592524334988, 80.20942372801901854 ) ) ;
#12138 = CARTESIAN_POINT ( 'NONE',  ( -0.05219959533909027116, -19.03943276465977164, 57.49890960531435979 ) ) ;
#12139 = VERTEX_POINT ( 'NONE', #39445 ) ;
#12140 = CARTESIAN_POINT ( 'NONE',  ( -16.51473224551069308, -9.474510206698971260, 36.66557627198102409 ) ) ;
#12141 = CARTESIAN_POINT ( 'NONE',  ( 5.719274019375991003, -21.55341960407610458, 27.70724293864769905 ) ) ;
#12142 = CARTESIAN_POINT ( 'NONE',  ( -12.14591786802309592, -12.06949235617757132, 81.87390960531435269 ) ) ;
#12143 = CARTESIAN_POINT ( 'NONE',  ( -16.46253265017160317, 9.564922557960807481, 45.83224293864769550 ) ) ;
#12144 = CARTESIAN_POINT ( 'NONE',  ( -16.52544592524342804, 4.483927247898546575, 96.04057627198102409 ) ) ;
#12145 = AXIS2_PLACEMENT_3D ( 'NONE', #194799, #10783, #73458 ) ;
#12146 = CARTESIAN_POINT ( 'NONE',  ( -15.80617190586745835, -15.72974639402198527, 106.8739096053143811 ) ) ;
#12147 = CARTESIAN_POINT ( 'NONE',  ( 0.05219959533937995610, -21.53943276465977519, 45.00109039468568284 ) ) ;
#12148 = CARTESIAN_POINT ( 'NONE',  ( -9.564922557960796823, -16.46253265017161027, 32.08224293864769550 ) ) ;
#12149 = CARTESIAN_POINT ( 'NONE',  ( 16.52544592524335698, 4.483927247898782831, 66.45942372801903275 ) ) ;
#12150 = CARTESIAN_POINT ( 'NONE',  ( -0.05219959533907301413, -21.53943276465977519, 97.49890960531436690 ) ) ;
#12151 = CARTESIAN_POINT ( 'NONE',  ( 0.05219959533907565091, 21.53943276465977519, 99.99890960531436690 ) ) ;
#12153 = CARTESIAN_POINT ( 'NONE',  ( -16.51473224551069308, -9.474510206698971260, 46.66557627198102409 ) ) ;
#12152 = CARTESIAN_POINT ( 'NONE',  ( -9.474510206698720793, -16.51473224551083518, 39.58442372801899722 ) ) ;
#12154 = CARTESIAN_POINT ( 'NONE',  ( -13.89961937509977652, 13.97604488694528158, 115.6239096053143669 ) ) ;
#12155 = CARTESIAN_POINT ( 'NONE',  ( -10.81492255796105439, 18.62759615963255655, 57.91775706135234714 ) ) ;
#12156 = CARTESIAN_POINT ( 'NONE',  ( -21.53943276465977519, 0.05219959533907696930, 61.24890960531435979 ) ) ;
#12157 = CARTESIAN_POINT ( 'NONE',  ( 12.06949235617757843, -12.14591786802309237, 38.12390960531436690 ) ) ;
#12159 = CARTESIAN_POINT ( 'NONE',  ( 13.97604488694548053, -13.89961937509957401, 20.62609039468567573 ) ) ;
#12158 = CARTESIAN_POINT ( 'NONE',  ( 5.823673210054444382, -21.52544592524334988, 75.20942372801901854 ) ) ;
#12160 = CARTESIAN_POINT ( 'NONE',  ( 16.51473224551083163, -9.474510206698727899, 40.83442372801900433 ) ) ;
#12161 = CARTESIAN_POINT ( 'NONE',  ( 14.34966873604972726, -8.224510206698740333, 100.8344237280190185 ) ) ;
#12162 = CARTESIAN_POINT ( 'NONE',  ( -21.53943276465977519, -0.05219959533937600094, 58.75109039468568994 ) ) ;
#12163 = CARTESIAN_POINT ( 'NONE',  ( -16.46253265017160317, 9.564922557960807481, 65.83224293864769550 ) ) ;
#12164 = CARTESIAN_POINT ( 'NONE',  ( -5.049401038297874678, -19.05341960407617918, 39.79275706135232582 ) ) ;
#12165 = CARTESIAN_POINT ( 'NONE',  ( 21.55341960407610458, 5.719274019375980345, 43.95724293864769550 ) ) ;
#12166 = CARTESIAN_POINT ( 'NONE',  ( -15.80617190586768217, 15.72974639402176855, 28.12609039468568284 ) ) ;
#12167 = CARTESIAN_POINT ( 'NONE',  ( 5.719274019375991003, -21.55341960407610458, 87.70724293864769550 ) ) ;
#12168 = CARTESIAN_POINT ( 'NONE',  ( 16.46253265017146816, 9.564922557961045513, 86.66775706135233293 ) ) ;
#12169 = CARTESIAN_POINT ( 'NONE',  ( -16.55341960407617563, 4.379528057220093196, 58.54275706135235424 ) ) ;
#12171 = CARTESIAN_POINT ( 'NONE',  ( 0.05219959533907565091, 21.53943276465977519, 89.99890960531438111 ) ) ;
#12170 = CARTESIAN_POINT ( 'NONE',  ( 17.49999999999998934, -5.047551163040834510, 36.33463913479419460 ) ) ;
#12173 = CARTESIAN_POINT ( 'NONE',  ( -14.34966873604960291, -8.224510206698953496, 76.66557627198103830 ) ) ;
#12172 = CARTESIAN_POINT ( 'NONE',  ( 16.55341960407618274, -4.379528057220086978, 76.04275706135237556 ) ) ;
#12174 = CARTESIAN_POINT ( 'NONE',  ( -16.36317988757058117, -7.306389748694932962, 100.9021039163677500 ) ) ;
#12175 = CARTESIAN_POINT ( 'NONE',  ( -0.05219959533936034679, 19.03943276465977164, 102.5010903946856757 ) ) ;
#12176 = CARTESIAN_POINT ( 'NONE',  ( -15.80617190586745835, -15.72974639402198527, 41.87390960531435979 ) ) ;
#12177 = AXIS2_PLACEMENT_3D ( 'NONE', #82012, #99198, #7188 ) ;
#12178 = FACE_OUTER_BOUND ( 'NONE', #174880, .T. ) ;
#12179 = CARTESIAN_POINT ( 'NONE',  ( 12.14591786802327356, -12.06949235617739191, 55.62609039468568284 ) ) ;
#12180 = CARTESIAN_POINT ( 'NONE',  ( 10.81492255796106328, -18.62759615963255655, 25.41775706135235779 ) ) ;
#12181 = CARTESIAN_POINT ( 'NONE',  ( -18.62759615963270932, 10.81492255796079327, 50.83224293864770971 ) ) ;
#12182 = CARTESIAN_POINT ( 'NONE',  ( 12.06949235617739724, 12.14591786802326823, 66.87609039468568994 ) ) ;
#12183 = CARTESIAN_POINT ( 'NONE',  ( -16.46253265017160317, 9.564922557960807481, 90.83224293864769550 ) ) ;
#12185 = CARTESIAN_POINT ( 'NONE',  ( 16.46253265017160672, -9.564922557960803928, 28.33224293864769550 ) ) ;
#12184 = CARTESIAN_POINT ( 'NONE',  ( -21.52544592524334988, -5.823673210054445271, 53.95942372801900433 ) ) ;
#12186 = CARTESIAN_POINT ( 'NONE',  ( 15.80617190586746368, 15.72974639402197994, 29.37390960531435269 ) ) ;
#12187 = EDGE_LOOP ( 'NONE', ( #74168, #95274, #89424, #11518 ) ) ;
#12188 = CARTESIAN_POINT ( 'NONE',  ( -13.89961937509957401, -13.97604488694547875, 44.37609039468566863 ) ) ;
#12189 = CARTESIAN_POINT ( 'NONE',  ( 8.224510206698742110, 14.34966873604972548, 47.08442372801901854 ) ) ;
#12190 = CARTESIAN_POINT ( 'NONE',  ( -10.81492255796078084, -18.62759615963271287, 22.08224293864769194 ) ) ;
#12191 = ORIENTED_EDGE ( 'NONE', *, *, #62085, .T. ) ;
#12192 = CARTESIAN_POINT ( 'NONE',  ( 19.05341960407611168, 5.049401038298154454, 78.95724293864769550 ) ) ;
#12193 = CARTESIAN_POINT ( 'NONE',  ( 0.05219959533934541429, -16.53943276465976808, 105.0010903946856757 ) ) ;
#12194 = CARTESIAN_POINT ( 'NONE',  ( -17.79613651744294600, 24.49428055684532524, 141.9656553485623647 ) ) ;
#12195 = CARTESIAN_POINT ( 'NONE',  ( 16.55341960407611168, 4.379528057220329451, 98.95724293864770971 ) ) ;
#12196 = CARTESIAN_POINT ( 'NONE',  ( 15.72974639402199770, -15.80617190586745480, 38.12390960531436690 ) ) ;
#12197 = CARTESIAN_POINT ( 'NONE',  ( -13.89961937509977652, 13.97604488694528158, 30.62390960531435269 ) ) ;
#12198 = CARTESIAN_POINT ( 'NONE',  ( 0.05219959533934541429, -16.53943276465976808, 75.00109039468568994 ) ) ;
#12199 = CARTESIAN_POINT ( 'NONE',  ( 10.81492255796106328, -18.62759615963255655, 20.41775706135234714 ) ) ;
#12200 = CARTESIAN_POINT ( 'NONE',  ( 19.02544592524334988, 5.153800228976608722, 81.45942372801897591 ) ) ;
#12201 = CARTESIAN_POINT ( 'NONE',  ( -9.474510206698964154, 16.51473224551069663, 45.41557627198103120 ) ) ;
#12202 = AXIS2_PLACEMENT_3D ( 'NONE', #109134, #184987, #46471 ) ;
#12203 = CARTESIAN_POINT ( 'NONE',  ( 5.153800228976335163, 19.02544592524342804, 114.7905762719810241 ) ) ;
#12204 = EDGE_CURVE ( 'NONE', #184582, #66658, #133796, .T. ) ;
#12205 = CARTESIAN_POINT ( 'NONE',  ( -5.719274019375665041, -21.55341960407619695, 109.7927570613523613 ) ) ;
#12206 = CARTESIAN_POINT ( 'NONE',  ( 19.05341960407611168, 5.049401038298154454, 58.95724293864768129 ) ) ;
#12207 = CARTESIAN_POINT ( 'NONE',  ( 8.224510206698742110, 14.34966873604972548, 52.08442372801901854 ) ) ;
#12208 = CARTESIAN_POINT ( 'NONE',  ( 10.72451020669871369, 18.67979575497193778, 92.08442372801901854 ) ) ;
#12209 = CARTESIAN_POINT ( 'NONE',  ( 13.89961937509957401, 13.97604488694547697, 36.87609039468565442 ) ) ;
#12210 = CARTESIAN_POINT ( 'NONE',  ( 19.05341960407617918, -5.049401038297876454, 56.04275706135234714 ) ) ;
#12211 = ORIENTED_EDGE ( 'NONE', *, *, #124720, .T. ) ;
#12212 = CARTESIAN_POINT ( 'NONE',  ( -18.62759615963255300, -10.81492255796106328, 44.16775706135234714 ) ) ;
#12213 = CARTESIAN_POINT ( 'NONE',  ( -16.46253265017160317, 9.564922557960807481, 55.83224293864769550 ) ) ;
#12214 = CARTESIAN_POINT ( 'NONE',  ( -5.153800228976607833, 19.02544592524334988, 42.70942372801901143 ) ) ;
#12215 = CARTESIAN_POINT ( 'NONE',  ( 13.89961937509977652, -13.97604488694527269, 103.1239096053143527 ) ) ;
#12216 = CARTESIAN_POINT ( 'NONE',  ( 9.474510206698971260, -16.51473224551069308, 77.91557627198103830 ) ) ;
#12217 = CARTESIAN_POINT ( 'NONE',  ( 14.29746914071049879, -8.314922557960816363, 43.33224293864769550 ) ) ;
#12218 = CARTESIAN_POINT ( 'NONE',  ( 21.55341960407610458, 5.719274019375980345, 33.95724293864769550 ) ) ;
#12219 = CARTESIAN_POINT ( 'NONE',  ( -29.86685920354755197, -21.69954338932560134, -4.924999997268813878 ) ) ;
#12220 = CARTESIAN_POINT ( 'NONE',  ( 21.16989542479042186, 22.97168310438076588, -49.98402367076291597 ) ) ;
#12221 = CARTESIAN_POINT ( 'NONE',  ( -18.62759615963255300, -10.81492255796106328, 104.1677570613523471 ) ) ;
#12222 = CARTESIAN_POINT ( 'NONE',  ( -27.95290315088902133, 7.353483241874900322, 160.8982923760598851 ) ) ;
#12223 = CARTESIAN_POINT ( 'NONE',  ( 19.05341960407611168, 5.049401038298154454, 43.95724293864769550 ) ) ;
#12224 = CARTESIAN_POINT ( 'NONE',  ( 19.03943276465977164, -0.05219959533909143690, 108.7489096053143527 ) ) ;
#12225 = CARTESIAN_POINT ( 'NONE',  ( -2.219726742498586258, -37.13270733954487213, -7.999999999999996447 ) ) ;
#12226 = CARTESIAN_POINT ( 'NONE',  ( -14.34966873604972548, 8.224510206698743886, 58.33442372801901143 ) ) ;
#12228 = EDGE_CURVE ( 'NONE', #83853, #179366, #186155, .T. ) ;
#12227 = CARTESIAN_POINT ( 'NONE',  ( 0.05219959533907565091, 21.53943276465977519, 79.99890960531435269 ) ) ;
#12229 = CARTESIAN_POINT ( 'NONE',  ( -16.55341960407611168, -4.379528057220339221, 36.45724293864768839 ) ) ;
#12231 = CARTESIAN_POINT ( 'NONE',  ( -19.02544592524342804, 5.153800228976336051, 106.0405762719810241 ) ) ;
#12230 = CARTESIAN_POINT ( 'NONE',  ( -19.05341960407611168, -5.049401038298163336, 31.45724293864769550 ) ) ;
#12232 = CARTESIAN_POINT ( 'NONE',  ( -5.823673210054431948, 21.52544592524334988, 32.70942372801900433 ) ) ;
#12233 = CARTESIAN_POINT ( 'NONE',  ( -19.03943276465977164, -0.05219959533935918106, 33.75109039468566863 ) ) ;
#12234 = CARTESIAN_POINT ( 'NONE',  ( 0.05219959533909260263, 19.03943276465977164, 34.99890960531435979 ) ) ;
#12235 = CARTESIAN_POINT ( 'NONE',  ( -21.52544592524334988, -5.823673210054445271, 83.95942372801900433 ) ) ;
#12236 = CARTESIAN_POINT ( 'NONE',  ( 16.19135201231363297, -7.376712067592066546, 32.31319145947969673 ) ) ;
#12237 = CARTESIAN_POINT ( 'NONE',  ( 14.34966873604960469, 8.224510206698951720, 29.16557627198103120 ) ) ;
#12238 = DIRECTION ( 'NONE',  ( 6.938893903907222461E-16, -1.000000000000000000, 0.000000000000000000 ) ) ;
#12239 = CARTESIAN_POINT ( 'NONE',  ( -10.72451020669898014, 18.67979575497178502, 30.41557627198101699 ) ) ;
#12240 = CARTESIAN_POINT ( 'NONE',  ( -4.379528057220328563, 16.55341960407611168, 105.2072429386477097 ) ) ;
#12241 = FACE_OUTER_BOUND ( 'NONE', #179038, .T. ) ;
#12242 = CARTESIAN_POINT ( 'NONE',  ( -13.97604488694527625, -13.89961937509977652, 86.87390960531436690 ) ) ;
#12243 = CARTESIAN_POINT ( 'NONE',  ( 16.55341960407611168, 4.379528057220329451, 73.95724293864769550 ) ) ;
#12244 = CARTESIAN_POINT ( 'NONE',  ( -9.474510206698720793, -16.51473224551083518, 104.5844237280190043 ) ) ;
#12245 = CARTESIAN_POINT ( 'NONE',  ( 5.719274019375991003, -21.55341960407610458, 62.70724293864769550 ) ) ;
#12246 = ORIENTED_EDGE ( 'NONE', *, *, #194452, .T. ) ;
#12247 = CARTESIAN_POINT ( 'NONE',  ( 13.89961937509977652, -13.97604488694527269, 28.12390960531435624 ) ) ;
#12249 = CARTESIAN_POINT ( 'NONE',  ( -0.05219959533907301413, -21.53943276465977519, 87.49890960531436690 ) ) ;
#12248 = CARTESIAN_POINT ( 'NONE',  ( -13.89961937509977652, 13.97604488694528158, 80.62390960531436690 ) ) ;
#12251 = CARTESIAN_POINT ( 'NONE',  ( -5.049401038298153566, 19.05341960407611168, 85.20724293864766707 ) ) ;
#12250 = CARTESIAN_POINT ( 'NONE',  ( 14.34966873604972726, -8.224510206698740333, 110.8344237280190043 ) ) ;
#12252 = CARTESIAN_POINT ( 'NONE',  ( 0.05219959533936267826, -19.03943276465977164, 70.00109039468566152 ) ) ;
#12253 = CARTESIAN_POINT ( 'NONE',  ( -10.72451020669870658, -18.67979575497194134, 89.58442372801901854 ) ) ;
#12254 = CARTESIAN_POINT ( 'NONE',  ( -15.80617190586745835, -15.72974639402198527, 71.87390960531438111 ) ) ;
#12255 = CARTESIAN_POINT ( 'NONE',  ( -21.55341960407610458, -5.719274019375992779, 41.45724293864769550 ) ) ;
#12256 = CARTESIAN_POINT ( 'NONE',  ( 16.46253265017160672, -9.564922557960803928, 53.33224293864768839 ) ) ;
#12257 = CARTESIAN_POINT ( 'NONE',  ( 14.29746914071037800, 8.314922557961029526, 111.6677570613523613 ) ) ;
#12258 = CARTESIAN_POINT ( 'NONE',  ( -13.89961937509977652, 13.97604488694528158, 65.62390960531436690 ) ) ;
#12259 = CARTESIAN_POINT ( 'NONE',  ( 21.53943276465977519, 0.05219959533937863772, 106.2510903946856757 ) ) ;
#12260 = CARTESIAN_POINT ( 'NONE',  ( -0.05219959533910754901, -16.53943276465976808, 77.49890960531433848 ) ) ;
#12261 = CARTESIAN_POINT ( 'NONE',  ( -21.53943276465977519, 0.05219959533907696930, 111.2489096053143669 ) ) ;
#12262 = CARTESIAN_POINT ( 'NONE',  ( -21.53943276465977519, 0.05219959533907696930, 101.2489096053143669 ) ) ;
#12263 = CARTESIAN_POINT ( 'NONE',  ( -4.990514878257755527, 3.920520744267788960, -64.49346902751020139 ) ) ;
#12264 = CARTESIAN_POINT ( 'NONE',  ( -21.53943276465977519, 0.05219959533907696930, 56.24890960531436690 ) ) ;
#12265 = CARTESIAN_POINT ( 'NONE',  ( -4.379528057220086978, -16.55341960407618274, 89.79275706135236135 ) ) ;
#12266 = CARTESIAN_POINT ( 'NONE',  ( 12.14591786802309770, 12.06949235617756955, 104.3739096053143669 ) ) ;
#12267 = CARTESIAN_POINT ( 'NONE',  ( -9.564922557960796823, -16.46253265017161027, 57.08224293864769550 ) ) ;
#12268 = CARTESIAN_POINT ( 'NONE',  ( 16.55341960407618274, -4.379528057220086978, 111.0427570613523613 ) ) ;
#12269 = CARTESIAN_POINT ( 'NONE',  ( 15.80617190586769283, -15.72974639402175789, 40.62609039468567573 ) ) ;
#12270 = CARTESIAN_POINT ( 'NONE',  ( 19.02544592524343514, -5.153800228976328945, 103.5405762719809957 ) ) ;
#12271 = CARTESIAN_POINT ( 'NONE',  ( 5.719274019375673035, 21.55341960407619339, 82.29275706135234714 ) ) ;
#12272 = CARTESIAN_POINT ( 'NONE',  ( -19.02544592524342804, 5.153800228976336051, 36.04057627198100988 ) ) ;
#12273 = CARTESIAN_POINT ( 'NONE',  ( 19.02544592524343514, -5.153800228976328945, 43.54057627198103120 ) ) ;
#12274 = VERTEX_POINT ( 'NONE', #56627 ) ;
#12275 = CARTESIAN_POINT ( 'NONE',  ( 21.52544592524334988, 5.823673210054432836, 86.45942372801901854 ) ) ;
#12276 = CARTESIAN_POINT ( 'NONE',  ( -0.05219959533937732626, 21.53943276465977519, 67.50109039468568994 ) ) ;
#12277 = CARTESIAN_POINT ( 'NONE',  ( 5.153800228976335163, 19.02544592524342804, 109.7905762719810099 ) ) ;
#12278 = CARTESIAN_POINT ( 'NONE',  ( -16.46253265017146816, -9.564922557961047289, 74.16775706135234714 ) ) ;
#12279 = CARTESIAN_POINT ( 'NONE',  ( 15.72974639402176855, 15.80617190586768217, 61.87609039468568284 ) ) ;
#12280 = CARTESIAN_POINT ( 'NONE',  ( 8.224510206698742110, 14.34966873604972548, 22.08442372801901143 ) ) ;
#12281 = CARTESIAN_POINT ( 'NONE',  ( -5.153800228976607833, 19.02544592524334988, 77.70942372801900433 ) ) ;
#12282 = CARTESIAN_POINT ( 'NONE',  ( -16.46253265017160317, 9.564922557960807481, 50.83224293864770260 ) ) ;
#12283 = CARTESIAN_POINT ( 'NONE',  ( -19.03943276465977164, -0.05219959533935918106, 88.75109039468567573 ) ) ;
#12284 = AXIS2_PLACEMENT_3D ( 'NONE', #126369, #112200, #6003 ) ;
#12285 = CARTESIAN_POINT ( 'NONE',  ( 16.52544592524342804, -4.483927247898539470, 23.54057627198102765 ) ) ;
#12286 = CARTESIAN_POINT ( 'NONE',  ( -19.02544592524334988, -5.153800228976617603, 93.95942372801900433 ) ) ;
#12287 = CARTESIAN_POINT ( 'NONE',  ( 12.14591786802309770, 12.06949235617756955, 44.37390960531435979 ) ) ;
#12288 = CARTESIAN_POINT ( 'NONE',  ( -13.89961937509957401, -13.97604488694547875, 59.37609039468566863 ) ) ;
#12289 = CARTESIAN_POINT ( 'NONE',  ( -16.53943276465976808, -0.05219959533934237506, 43.75109039468568284 ) ) ;
#12290 = CARTESIAN_POINT ( 'NONE',  ( -19.05341960407617563, 5.049401038297882671, 23.54275706135233648 ) ) ;
#12291 = CARTESIAN_POINT ( 'NONE',  ( -5.049401038298153566, 19.05341960407611168, 40.20724293864768839 ) ) ;
#12292 = CARTESIAN_POINT ( 'NONE',  ( -16.21995358207306026, -7.366697692864124569, 65.06448998487844904 ) ) ;
#12293 = CARTESIAN_POINT ( 'NONE',  ( 16.53943276465976808, 0.05219959533934440121, 41.25109039468568284 ) ) ;
#12294 = DIRECTION ( 'NONE',  ( 0.7071067811865483499, 0.000000000000000000, 0.7071067811865465735 ) ) ;
#12295 = CARTESIAN_POINT ( 'NONE',  ( -22.44159573604010305, 16.30477369853692338, 142.6750000027311671 ) ) ;
#12296 = CARTESIAN_POINT ( 'NONE',  ( 5.049401038298161559, -19.05341960407611168, 97.70724293864766707 ) ) ;
#12297 = FACE_OUTER_BOUND ( 'NONE', #26675, .T. ) ;
#12298 = CARTESIAN_POINT ( 'NONE',  ( 5.153800228976615827, -19.02544592524334988, 95.20942372801897591 ) ) ;
#12299 = CARTESIAN_POINT ( 'NONE',  ( -0.05219959533907301413, -21.53943276465977519, 22.49890960531436335 ) ) ;
#12301 = CARTESIAN_POINT ( 'NONE',  ( 9.474510206698729675, 16.51473224551082808, 112.0844237280190043 ) ) ;
#12300 = CARTESIAN_POINT ( 'NONE',  ( -9.564922557961040184, 16.46253265017147172, 22.91775706135233648 ) ) ;
#12302 = CARTESIAN_POINT ( 'NONE',  ( -4.483927247898539470, -16.52544592524342804, 112.2905762719810241 ) ) ;
#12303 = CARTESIAN_POINT ( 'NONE',  ( -16.51473224551069308, -9.474510206698971260, 31.66557627198102054 ) ) ;
#12304 = CARTESIAN_POINT ( 'NONE',  ( -5.823673210054116645, -21.52544592524344225, 57.29057627198103120 ) ) ;
#12305 = CARTESIAN_POINT ( 'NONE',  ( 19.02544592524343514, -5.153800228976328945, 43.54057627198103120 ) ) ;
#12306 = CARTESIAN_POINT ( 'NONE',  ( 9.474510206698729675, 16.51473224551082808, 47.08442372801900433 ) ) ;
#12307 = CARTESIAN_POINT ( 'NONE',  ( 19.02544592524334988, 5.153800228976608722, 71.45942372801900433 ) ) ;
#12309 = AXIS2_PLACEMENT_3D ( 'NONE', #85796, #147482, #127299 ) ;
#12308 = CARTESIAN_POINT ( 'NONE',  ( -8.314922557960811034, -14.29746914071050412, 52.08224293864768839 ) ) ;
#12310 = CARTESIAN_POINT ( 'NONE',  ( 10.72451020669898902, -18.67979575497178502, 32.91557627198102409 ) ) ;
#12311 = CARTESIAN_POINT ( 'NONE',  ( 18.67979575497194134, -10.72451020669871369, 95.83442372801903275 ) ) ;
#12312 = CARTESIAN_POINT ( 'NONE',  ( 10.81492255796078972, 18.62759615963270932, 84.58224293864769550 ) ) ;
#12313 = CARTESIAN_POINT ( 'NONE',  ( -18.67979575497193778, 10.72451020669871902, 63.33442372801900433 ) ) ;
#12314 = CARTESIAN_POINT ( 'NONE',  ( -21.55341960407619339, 5.719274019375674811, 68.54275706135234714 ) ) ;
#12315 = CARTESIAN_POINT ( 'NONE',  ( 19.03943276465977164, -0.05219959533909143690, 93.74890960531435269 ) ) ;
#12317 = CARTESIAN_POINT ( 'NONE',  ( -21.52544592524334988, -5.823673210054445271, 68.95942372801901854 ) ) ;
#12316 = CARTESIAN_POINT ( 'NONE',  ( -8.224510206698735004, -14.34966873604973081, 89.58442372801901854 ) ) ;
#12318 = CARTESIAN_POINT ( 'NONE',  ( -9.474510206698964154, 16.51473224551069663, 55.41557627198103120 ) ) ;
#12319 = CARTESIAN_POINT ( 'NONE',  ( 19.03943276465977164, -0.05219959533909143690, 23.74890960531435269 ) ) ;
#12320 = CARTESIAN_POINT ( 'NONE',  ( -19.03943276465977164, 0.05219959533909376836, 51.24890960531436690 ) ) ;
#12321 = CARTESIAN_POINT ( 'NONE',  ( 4.379528057220339221, -16.55341960407611168, 62.70724293864769550 ) ) ;
#12322 = CARTESIAN_POINT ( 'NONE',  ( -4.379528057220328563, 16.55341960407611168, 35.20724293864768839 ) ) ;
#12323 = CARTESIAN_POINT ( 'NONE',  ( -5.719274019375978568, 21.55341960407610458, 45.20724293864769550 ) ) ;
#12324 = CARTESIAN_POINT ( 'NONE',  ( 9.474510206698971260, -16.51473224551069308, 47.91557627198102409 ) ) ;
#12325 = CARTESIAN_POINT ( 'NONE',  ( -5.823673210054116645, -21.52544592524344225, 52.29057627198102409 ) ) ;
#12326 = CARTESIAN_POINT ( 'NONE',  ( -19.02544592524334988, -5.153800228976617603, 48.95942372801900433 ) ) ;
#12328 = CARTESIAN_POINT ( 'NONE',  ( 16.53943276465976808, -0.05219959533910856209, 48.74890960531435979 ) ) ;
#12327 = CARTESIAN_POINT ( 'NONE',  ( 2.500000000000000000, -105.0000000000000000, 12.00000000000000355 ) ) ;
#12329 = CARTESIAN_POINT ( 'NONE',  ( -18.62759615963270932, 10.81492255796079327, 25.83224293864769194 ) ) ;
#12330 = ORIENTED_EDGE ( 'NONE', *, *, #34560, .T. ) ;
#12331 = ORIENTED_EDGE ( 'NONE', *, *, #190442, .T. ) ;
#12332 = DIRECTION ( 'NONE',  ( -0.000000000000000000, -0.000000000000000000, 1.000000000000000000 ) ) ;
#12333 = CARTESIAN_POINT ( 'NONE',  ( -12.14591786802326823, 12.06949235617739902, 88.12609039468570415 ) ) ;
#12334 = CARTESIAN_POINT ( 'NONE',  ( -5.049401038297874678, -19.05341960407617918, 74.79275706135231871 ) ) ;
#12335 = CARTESIAN_POINT ( 'NONE',  ( 8.314922557960818139, 14.29746914071049879, 54.58224293864769550 ) ) ;
#12336 = CARTESIAN_POINT ( 'NONE',  ( -18.22780087662126647, -5.499999999999827693, 58.98236817873108606 ) ) ;
#12337 = CARTESIAN_POINT ( 'NONE',  ( -14.34966873604960291, -8.224510206698953496, 46.66557627198102409 ) ) ;
#12338 = CARTESIAN_POINT ( 'NONE',  ( -5.153800228976328057, -19.02544592524343514, 57.29057627198103120 ) ) ;
#12339 = CARTESIAN_POINT ( 'NONE',  ( 16.46253265017160672, -9.564922557960803928, 68.33224293864770971 ) ) ;
#12340 = CARTESIAN_POINT ( 'NONE',  ( -13.89961937509977652, 13.97604488694528158, 35.62390960531435269 ) ) ;
#12341 = CARTESIAN_POINT ( 'NONE',  ( 0.05219959533937995610, -21.53943276465977519, 40.00109039468567573 ) ) ;
#12342 = CARTESIAN_POINT ( 'NONE',  ( 13.97604488694527802, 13.89961937509977652, 74.37390960531436690 ) ) ;
#12343 = CARTESIAN_POINT ( 'NONE',  ( -9.564922557960796823, -16.46253265017161027, 22.08224293864768839 ) ) ;
#12344 = CARTESIAN_POINT ( 'NONE',  ( -5.049401038298153566, 19.05341960407611168, 60.20724293864768129 ) ) ;
#12345 = CARTESIAN_POINT ( 'NONE',  ( 18.62759615963271287, -10.81492255796078972, 53.33224293864769550 ) ) ;
#12346 = CARTESIAN_POINT ( 'NONE',  ( -5.049401038298153566, 19.05341960407611168, 35.20724293864768839 ) ) ;
#12347 = CARTESIAN_POINT ( 'NONE',  ( -21.55341960407610458, -5.719274019375992779, 46.45724293864769550 ) ) ;
#12348 = CARTESIAN_POINT ( 'NONE',  ( 16.53943276465976808, 0.05219959533934440121, 96.25109039468568994 ) ) ;
#12349 = ADVANCED_FACE ( 'NONE', ( #26301 ), #135008, .T. ) ;
#12350 = CARTESIAN_POINT ( 'NONE',  ( -16.51473224551082808, 9.474510206698731452, 28.33442372801900433 ) ) ;
#12352 = CARTESIAN_POINT ( 'NONE',  ( -14.34966873604972548, 8.224510206698743886, 78.33442372801901854 ) ) ;
#12351 = CARTESIAN_POINT ( 'NONE',  ( 16.55341960407618274, -4.379528057220086978, 51.04275706135234714 ) ) ;
#12353 = CARTESIAN_POINT ( 'NONE',  ( -18.22780087662123805, 5.499999999999981348, 101.0176318212689495 ) ) ;
#12354 = CARTESIAN_POINT ( 'NONE',  ( 8.224510206698742110, 14.34966873604972548, 72.08442372801899012 ) ) ;
#12355 = CARTESIAN_POINT ( 'NONE',  ( -16.53943276465976808, -0.05219959533934237506, 38.75109039468567573 ) ) ;
#12356 = CARTESIAN_POINT ( 'NONE',  ( -13.97604488694527625, -13.89961937509977652, 111.8739096053143243 ) ) ;
#12357 = CARTESIAN_POINT ( 'NONE',  ( -8.224510206698735004, -14.34966873604973081, 24.58442372801901499 ) ) ;
#12358 = CARTESIAN_POINT ( 'NONE',  ( 9.564922557960805705, 16.46253265017160317, 29.58224293864769550 ) ) ;
#12359 = CARTESIAN_POINT ( 'NONE',  ( 21.52544592524334988, 5.823673210054432836, 21.45942372801901499 ) ) ;
#12360 = CARTESIAN_POINT ( 'NONE',  ( 14.34966873604972726, -8.224510206698740333, 40.83442372801901854 ) ) ;
#12361 = CARTESIAN_POINT ( 'NONE',  ( 12.06949235617739724, 12.14591786802326823, 96.87609039468568994 ) ) ;
#12362 = CARTESIAN_POINT ( 'NONE',  ( 4.500000000000000888, -116.8122400552013431, 54.87277500418469600 ) ) ;
#12363 = CARTESIAN_POINT ( 'NONE',  ( -18.67979575497193778, 10.72451020669871902, 98.33442372801901854 ) ) ;
#12364 = CARTESIAN_POINT ( 'NONE',  ( 9.564922557961047289, -16.46253265017146816, 95.41775706135233293 ) ) ;
#12365 = CARTESIAN_POINT ( 'NONE',  ( -12.06949235617756955, 12.14591786802309770, 55.62390960531436690 ) ) ;
#12366 = CARTESIAN_POINT ( 'NONE',  ( -5.049401038298153566, 19.05341960407611168, 25.20724293864768484 ) ) ;
#12368 = CARTESIAN_POINT ( 'NONE',  ( 17.12812012977029141, 6.668231424565949972, 78.85948759323146362 ) ) ;
#12367 = CARTESIAN_POINT ( 'NONE',  ( 13.97604488694548053, -13.89961937509957401, 55.62609039468566863 ) ) ;
#12369 = CARTESIAN_POINT ( 'NONE',  ( 15.72974639402176855, 15.80617190586768217, 56.87609039468568994 ) ) ;
#12370 = CARTESIAN_POINT ( 'NONE',  ( 12.06949235617739724, 12.14591786802326823, 31.87609039468567929 ) ) ;
#12371 = CARTESIAN_POINT ( 'NONE',  ( 16.31925111598459210, 7.325300261831483972, 82.33575461032749843 ) ) ;
#12372 = CARTESIAN_POINT ( 'NONE',  ( 21.55341960407610458, 5.719274019375980345, 28.95724293864769905 ) ) ;
#12373 = CARTESIAN_POINT ( 'NONE',  ( 5.823673210054125526, 21.52544592524343514, 69.79057627198102409 ) ) ;
#12374 = CARTESIAN_POINT ( 'NONE',  ( 13.89961937509957401, 13.97604488694547697, 106.8760903946856757 ) ) ;
#12375 = CARTESIAN_POINT ( 'NONE',  ( 5.049401038298161559, -19.05341960407611168, 102.7072429386476955 ) ) ;
#12376 = ADVANCED_FACE ( 'NONE', ( #83104 ), #169393, .T. ) ;
#12377 = CARTESIAN_POINT ( 'NONE',  ( -7.018946318601956058, -27.29839631544761502, 139.9999999999999716 ) ) ;
#12378 = CARTESIAN_POINT ( 'NONE',  ( 16.55341960407611168, 4.379528057220329451, 113.9572429386477239 ) ) ;
#12379 = CARTESIAN_POINT ( 'NONE',  ( 18.62759615963255655, 10.81492255796105972, 96.66775706135234714 ) ) ;
#12380 = CARTESIAN_POINT ( 'NONE',  ( -19.05341960407611168, -5.049401038298163336, 36.45724293864766707 ) ) ;
#12381 = CARTESIAN_POINT ( 'NONE',  ( 10.81492255796106328, -18.62759615963255655, 50.41775706135235424 ) ) ;
#12382 = CARTESIAN_POINT ( 'NONE',  ( -10.72451020669870658, -18.67979575497194134, 94.58442372801901854 ) ) ;
#12383 = CARTESIAN_POINT ( 'NONE',  ( 4.483927247898790824, -16.52544592524335698, 110.2094237280190185 ) ) ;
#12384 = CARTESIAN_POINT ( 'NONE',  ( 13.97604488694527802, 13.89961937509977652, 84.37390960531433848 ) ) ;
#12385 = CARTESIAN_POINT ( 'NONE',  ( 0.05219959533937995610, -21.53943276465977519, 40.00109039468567573 ) ) ;
#12386 = CARTESIAN_POINT ( 'NONE',  ( -21.55341960407619339, 5.719274019375674811, 43.54275706135235424 ) ) ;
#12388 = CARTESIAN_POINT ( 'NONE',  ( 5.049401038298161559, -19.05341960407611168, 92.70724293864769550 ) ) ;
#12387 = CARTESIAN_POINT ( 'NONE',  ( 19.03943276465977164, 0.05219959533936151252, 76.25109039468566152 ) ) ;
#12389 = CARTESIAN_POINT ( 'NONE',  ( 14.29746914071049879, -8.314922557960816363, 103.3322429386476955 ) ) ;
#12390 = CARTESIAN_POINT ( 'NONE',  ( 18.67979575497178502, 10.72451020669898547, 99.16557627198100988 ) ) ;
#12391 = CARTESIAN_POINT ( 'NONE',  ( -8.314922557960811034, -14.29746914071050412, 82.08224293864768129 ) ) ;
#12392 = CARTESIAN_POINT ( 'NONE',  ( -13.89961937509957401, -13.97604488694547875, 24.37609039468565442 ) ) ;
#12393 = CARTESIAN_POINT ( 'NONE',  ( 4.379528057220339221, -16.55341960407611168, 97.70724293864772392 ) ) ;
#12394 = CARTESIAN_POINT ( 'NONE',  ( 13.97604488694527802, 13.89961937509977652, 44.37390960531435269 ) ) ;
#12395 = CARTESIAN_POINT ( 'NONE',  ( -19.05341960407617563, 5.049401038297882671, 88.54275706135230450 ) ) ;
#12396 = CARTESIAN_POINT ( 'NONE',  ( -4.483927247898539470, -16.52544592524342804, 47.29057627198103120 ) ) ;
#12397 = CARTESIAN_POINT ( 'NONE',  ( -16.46253265017146816, -9.564922557961047289, 19.16775706135233293 ) ) ;
#12398 = CARTESIAN_POINT ( 'NONE',  ( -19.02544592524342804, 5.153800228976336051, 106.0405762719810241 ) ) ;
#12399 = CARTESIAN_POINT ( 'NONE',  ( 5.153800228976615827, -19.02544592524334988, 80.20942372801901854 ) ) ;
#12400 = CARTESIAN_POINT ( 'NONE',  ( 5.719274019375991003, -21.55341960407610458, 77.70724293864770971 ) ) ;
#12401 = CARTESIAN_POINT ( 'NONE',  ( 15.80617190586769283, -15.72974639402175789, 25.62609039468567929 ) ) ;
#12402 = CARTESIAN_POINT ( 'NONE',  ( -12.14591786802326823, 12.06949235617739902, 23.12609039468567573 ) ) ;
#12403 = CARTESIAN_POINT ( 'NONE',  ( -0.05219959533934338120, 16.53943276465976808, 92.50109039468567573 ) ) ;
#12405 = CARTESIAN_POINT ( 'NONE',  ( -15.72974639402176322, -15.80617190586768395, 29.37609039468568284 ) ) ;
#12404 = CARTESIAN_POINT ( 'NONE',  ( -19.03943276465977164, 0.05219959533909376836, 21.24890960531436335 ) ) ;
#12406 = CARTESIAN_POINT ( 'NONE',  ( 0.05219959533910956823, 16.53943276465976808, 109.9989096053143527 ) ) ;
#12407 = CARTESIAN_POINT ( 'NONE',  ( 11.40812507854754365, 35.11059874428196537, -1.724999997268813479 ) ) ;
#12408 = CARTESIAN_POINT ( 'NONE',  ( -16.55341960407617563, 4.379528057220093196, 53.54275706135234714 ) ) ;
#12409 = CARTESIAN_POINT ( 'NONE',  ( 4.379528057220339221, -16.55341960407611168, 82.70724293864770971 ) ) ;
#12410 = CARTESIAN_POINT ( 'NONE',  ( 18.62759615963271287, -10.81492255796078972, 78.33224293864770971 ) ) ;
#12411 = CARTESIAN_POINT ( 'NONE',  ( 0.05219959533910956823, 16.53943276465976808, 24.99890960531435624 ) ) ;
#12412 = CARTESIAN_POINT ( 'NONE',  ( 12.14591786802327356, -12.06949235617739191, 50.62609039468568994 ) ) ;
#12413 = CARTESIAN_POINT ( 'NONE',  ( -9.474510206698964154, 16.51473224551069663, 50.41557627198102409 ) ) ;
#12414 = CARTESIAN_POINT ( 'NONE',  ( 4.483927247898790824, -16.52544592524335698, 95.20942372801903275 ) ) ;
#12415 = CARTESIAN_POINT ( 'NONE',  ( 9.474510206698729675, 16.51473224551082808, 87.08442372801900433 ) ) ;
#12416 = CARTESIAN_POINT ( 'NONE',  ( -10.81492255796078084, -18.62759615963271287, 82.08224293864768129 ) ) ;
#12417 = CARTESIAN_POINT ( 'NONE',  ( 8.314922557961029526, -14.29746914071037800, 110.4177570613523756 ) ) ;
#12418 = VERTEX_POINT ( 'NONE', #22450 ) ;
#12419 = CARTESIAN_POINT ( 'NONE',  ( 21.56952297831559662, 7.512152360717371913, 173.9007003117368981 ) ) ;
#12420 = CARTESIAN_POINT ( 'NONE',  ( -21.52544592524343514, 5.823673210054127303, 56.04057627198102409 ) ) ;
#12421 = ORIENTED_EDGE ( 'NONE', *, *, #88897, .T. ) ;
#12422 = CARTESIAN_POINT ( 'NONE',  ( -12.14591786802326823, 12.06949235617739902, 98.12609039468570415 ) ) ;
#12423 = ORIENTED_EDGE ( 'NONE', *, *, #65499, .F. ) ;
#12424 = CARTESIAN_POINT ( 'NONE',  ( 18.67979575497178502, 10.72451020669898547, 34.16557627198102409 ) ) ;
#12425 = CARTESIAN_POINT ( 'NONE',  ( 17.50000000000147793, 3.202012800152216787, 107.5717758397274508 ) ) ;
#12426 = CARTESIAN_POINT ( 'NONE',  ( 18.67979575497178502, 10.72451020669898547, 74.16557627198102409 ) ) ;
#12427 = CARTESIAN_POINT ( 'NONE',  ( -16.53943276465976808, 0.05219959533911058130, 31.24890960531435979 ) ) ;
#12428 = CARTESIAN_POINT ( 'NONE',  ( -19.03943276465977164, -0.05219959533935918106, 113.7510903946856757 ) ) ;
#12429 = CARTESIAN_POINT ( 'NONE',  ( -5.049401038298153566, 19.05341960407611168, 40.20724293864768839 ) ) ;
#12430 = CARTESIAN_POINT ( 'NONE',  ( -4.483927247898782831, 16.52544592524335698, 32.70942372801900433 ) ) ;
#12431 = CARTESIAN_POINT ( 'NONE',  ( 9.564922557960805705, 16.46253265017160317, 49.58224293864770260 ) ) ;
#12432 = EDGE_CURVE ( 'NONE', #166399, #177515, #11092, .T. ) ;
#12433 = CARTESIAN_POINT ( 'NONE',  ( -28.82186960331499392, -9.364793116373526516, 146.1000000000000227 ) ) ;
#12434 = CARTESIAN_POINT ( 'NONE',  ( -19.05341960407611168, -5.049401038298163336, 106.4572429386476955 ) ) ;
#12435 = CARTESIAN_POINT ( 'NONE',  ( 5.049401038298161559, -19.05341960407611168, 102.7072429386476955 ) ) ;
#12436 = CARTESIAN_POINT ( 'NONE',  ( 14.34966873604972726, -8.224510206698740333, 90.83442372801901854 ) ) ;
#12437 = CARTESIAN_POINT ( 'NONE',  ( -5.153800228976607833, 19.02544592524334988, 92.70942372801901854 ) ) ;
#12438 = CARTESIAN_POINT ( 'NONE',  ( 19.05341960407617918, -5.049401038297876454, 36.04275706135234003 ) ) ;
#12439 = CARTESIAN_POINT ( 'NONE',  ( -21.53943276465977519, 0.05219959533907696930, 76.24890960531435269 ) ) ;
#12440 = CARTESIAN_POINT ( 'NONE',  ( 14.29746914071037800, 8.314922557961029526, 101.6677570613523613 ) ) ;
#12441 = CARTESIAN_POINT ( 'NONE',  ( -21.53943276465977519, 0.05219959533907696930, 36.24890960531435979 ) ) ;
#12442 = CARTESIAN_POINT ( 'NONE',  ( 9.474510206698729675, 16.51473224551082808, 97.08442372801900433 ) ) ;
#12443 = CARTESIAN_POINT ( 'NONE',  ( 13.97604488694527802, 13.89961937509977652, 49.37390960531434558 ) ) ;
#12444 = CARTESIAN_POINT ( 'NONE',  ( 9.564922557960805705, 16.46253265017160317, 94.58224293864769550 ) ) ;
#12445 = CARTESIAN_POINT ( 'NONE',  ( 21.53943276465977519, 0.05219959533937863772, 66.25109039468567573 ) ) ;
#12446 = CARTESIAN_POINT ( 'NONE',  ( -13.89961937509977652, 13.97604488694528158, 55.62390960531434558 ) ) ;
#12447 = CARTESIAN_POINT ( 'NONE',  ( 16.55341960407611168, 4.379528057220329451, 103.9572429386476813 ) ) ;
#12448 = CARTESIAN_POINT ( 'NONE',  ( 24.44405923433062355, -13.71792739260136607, 165.9118100595188707 ) ) ;
#12449 = CARTESIAN_POINT ( 'NONE',  ( -8.224510206698948167, 14.34966873604960824, 75.41557627198102409 ) ) ;
#12450 = CARTESIAN_POINT ( 'NONE',  ( -0.05219959533907301413, -21.53943276465977519, 67.49890960531436690 ) ) ;
#12451 = CARTESIAN_POINT ( 'NONE',  ( 16.46253265017146816, 9.564922557961045513, 91.66775706135234714 ) ) ;
#12452 = CARTESIAN_POINT ( 'NONE',  ( 18.56399227203342406, 5.499999999999960032, 91.47830131249901342 ) ) ;
#12453 = CARTESIAN_POINT ( 'NONE',  ( 13.97604488694527802, 13.89961937509977652, 59.37390960531434558 ) ) ;
#12454 = LINE ( 'NONE', #42781, #99287 ) ;
#12455 = CIRCLE ( 'NONE', #177115, 216.0437394197456911 ) ;
#12457 = CARTESIAN_POINT ( 'NONE',  ( -19.02544592524342804, 5.153800228976336051, 81.04057627198103830 ) ) ;
#12456 = CARTESIAN_POINT ( 'NONE',  ( 19.05341960407611168, 5.049401038298154454, 78.95724293864769550 ) ) ;
#12458 = CARTESIAN_POINT ( 'NONE',  ( 0.05219959533934541429, -16.53943276465976808, 70.00109039468568994 ) ) ;
#12459 = FACE_OUTER_BOUND ( 'NONE', #41122, .T. ) ;
#12460 = CARTESIAN_POINT ( 'NONE',  ( -19.05341960407617563, 5.049401038297882671, 38.54275706135233293 ) ) ;
#12461 = CARTESIAN_POINT ( 'NONE',  ( 15.76708390931707093, -14.65644741022703990, -58.71372985409217904 ) ) ;
#12462 = CARTESIAN_POINT ( 'NONE',  ( -19.02544592524342804, 5.153800228976336051, 116.0405762719810383 ) ) ;
#12463 = CARTESIAN_POINT ( 'NONE',  ( 8.224510206698742110, 14.34966873604972548, 97.08442372801904696 ) ) ;
#12464 = CARTESIAN_POINT ( 'NONE',  ( 15.29496450215404479, -1.499960427298778098, -59.75377357153833913 ) ) ;
#12465 = CARTESIAN_POINT ( 'NONE',  ( 14.29746914071037800, 8.314922557961029526, 81.66775706135236135 ) ) ;
#12466 = CARTESIAN_POINT ( 'NONE',  ( -12.06949235617739369, -12.14591786802326823, 49.37609039468569705 ) ) ;
#12467 = LINE ( 'NONE', #30590, #65903 ) ;
#12468 = CARTESIAN_POINT ( 'NONE',  ( 10.72451020669871369, 18.67979575497193778, 62.08442372801901143 ) ) ;
#12469 = CARTESIAN_POINT ( 'NONE',  ( 16.51473224551083163, -9.474510206698727899, 70.83442372801900433 ) ) ;
#12470 = CARTESIAN_POINT ( 'NONE',  ( -16.51473224551082808, 9.474510206698731452, 23.33442372801900078 ) ) ;
#12471 = CARTESIAN_POINT ( 'NONE',  ( 19.03943276465977164, -0.05219959533909143690, 48.74890960531435979 ) ) ;
#12472 = CARTESIAN_POINT ( 'NONE',  ( 9.474510206698971260, -16.51473224551069308, 42.91557627198103120 ) ) ;
#12473 = CARTESIAN_POINT ( 'NONE',  ( -15.76296483128273707, -36.76812510865116934, -10.58138071059118701 ) ) ;
#12474 = CARTESIAN_POINT ( 'NONE',  ( 18.67979575497178502, 10.72451020669898547, 74.16557627198102409 ) ) ;
#12475 = CARTESIAN_POINT ( 'NONE',  ( -21.55341960407610458, -5.719274019375992779, 31.45724293864769550 ) ) ;
#12476 = CARTESIAN_POINT ( 'NONE',  ( -16.46253265017160317, 9.564922557960807481, 25.83224293864769194 ) ) ;
#12477 = CARTESIAN_POINT ( 'NONE',  ( 16.52544592524335698, 4.483927247898782831, 51.45942372801901854 ) ) ;
#12478 = ORIENTED_EDGE ( 'NONE', *, *, #22446, .F. ) ;
#12479 = CARTESIAN_POINT ( 'NONE',  ( 21.53943276465977519, 0.05219959533937863772, 36.25109039468567573 ) ) ;
#12481 = CARTESIAN_POINT ( 'NONE',  ( -30.74264578624800492, -22.33583958711396278, -3.799999999999999822 ) ) ;
#12480 = CARTESIAN_POINT ( 'NONE',  ( 12.14591786802309770, 12.06949235617756955, 54.37390960531435979 ) ) ;
#12482 = CARTESIAN_POINT ( 'NONE',  ( -12.06949235617739369, -12.14591786802326823, 24.37609039468567573 ) ) ;
#12483 = CARTESIAN_POINT ( 'NONE',  ( 19.03943276465977164, 0.05219959533936151252, 36.25109039468567573 ) ) ;
#12484 = CARTESIAN_POINT ( 'NONE',  ( -16.53943276465976808, 0.05219959533911058130, 46.24890960531435979 ) ) ;
#12485 = CARTESIAN_POINT ( 'NONE',  ( 5.823673210054125526, 21.52544592524343514, 114.7905762719810383 ) ) ;
#12487 = CARTESIAN_POINT ( 'NONE',  ( -0.05219959533907301413, -21.53943276465977519, 82.49890960531436690 ) ) ;
#12486 = CARTESIAN_POINT ( 'NONE',  ( 0.1038182526441163017, 16.70000000000002061, -59.13370768023889923 ) ) ;
#12488 = CARTESIAN_POINT ( 'NONE',  ( -19.03943276465977164, 0.05219959533909376836, 91.24890960531436690 ) ) ;
#12489 = CARTESIAN_POINT ( 'NONE',  ( 14.29746914071049879, -8.314922557960816363, 58.33224293864768839 ) ) ;
#12490 = CARTESIAN_POINT ( 'NONE',  ( -19.05341960407611168, -5.049401038298163336, 106.4572429386476955 ) ) ;
#12491 = CARTESIAN_POINT ( 'NONE',  ( -37.43947335741456328, 2.756686112915582854, 40.22705064412460274 ) ) ;
#12492 = CARTESIAN_POINT ( 'NONE',  ( -5.049401038297874678, -19.05341960407617918, 64.79275706135233293 ) ) ;
#12493 = CARTESIAN_POINT ( 'NONE',  ( 0.05219959533907565091, 21.53943276465977519, 109.9989096053143527 ) ) ;
#12494 = CARTESIAN_POINT ( 'NONE',  ( 16.46253265017160672, -9.564922557960803928, 58.33224293864769550 ) ) ;
#12495 = CARTESIAN_POINT ( 'NONE',  ( -16.52544592524342804, 4.483927247898546575, 111.0405762719810525 ) ) ;
#12496 = CARTESIAN_POINT ( 'NONE',  ( 21.53943276465977519, 0.05219959533937863772, 51.25109039468568994 ) ) ;
#12497 = CARTESIAN_POINT ( 'NONE',  ( 8.571926809382603096, -26.38167802310801235, 143.4750000027312069 ) ) ;
#12498 = CARTESIAN_POINT ( 'NONE',  ( -4.483927247898539470, -16.52544592524342804, 37.29057627198102409 ) ) ;
#12499 = CARTESIAN_POINT ( 'NONE',  ( 19.03943276465977164, -0.05219959533909143690, 43.74890960531435979 ) ) ;
#12500 = CARTESIAN_POINT ( 'NONE',  ( -19.05341960407611168, -5.049401038298163336, 96.45724293864769550 ) ) ;
#12501 = CARTESIAN_POINT ( 'NONE',  ( 5.719274019375991003, -21.55341960407610458, 67.70724293864769550 ) ) ;
#12502 = CARTESIAN_POINT ( 'NONE',  ( -8.571926809382608425, 26.38167802310805854, 142.4750000027312069 ) ) ;
#12503 = CARTESIAN_POINT ( 'NONE',  ( 19.05341960407611168, 5.049401038298154454, 43.95724293864769550 ) ) ;
#12504 = CARTESIAN_POINT ( 'NONE',  ( 5.823673210054125526, 21.52544592524343514, 59.79057627198103120 ) ) ;
#12505 = CARTESIAN_POINT ( 'NONE',  ( -10.72451020669870658, -18.67979575497194134, 89.58442372801901854 ) ) ;
#12508 = CARTESIAN_POINT ( 'NONE',  ( -4.483927247898539470, -16.52544592524342804, 82.29057627198103830 ) ) ;
#12507 = CARTESIAN_POINT ( 'NONE',  ( 8.224510206698742110, 14.34966873604972548, 82.08442372801901854 ) ) ;
#12506 = CARTESIAN_POINT ( 'NONE',  ( -20.43538597629143538, -20.43538597629106945, -52.65483682830182488 ) ) ;
#12509 = CARTESIAN_POINT ( 'NONE',  ( -13.97604488694527625, -13.89961937509977652, 71.87390960531433848 ) ) ;
#12510 = ORIENTED_EDGE ( 'NONE', *, *, #158809, .T. ) ;
#12511 = CARTESIAN_POINT ( 'NONE',  ( 5.049401038297881783, 19.05341960407617563, 32.29275706135233293 ) ) ;
#12512 = CARTESIAN_POINT ( 'NONE',  ( 4.483927247898790824, -16.52544592524335698, 85.20942372801901854 ) ) ;
#12513 = CARTESIAN_POINT ( 'NONE',  ( 21.52544592524334988, 5.823673210054432836, 106.4594237280190328 ) ) ;
#12514 = CARTESIAN_POINT ( 'NONE',  ( -19.02544592524342804, 5.153800228976336051, 91.04057627198100988 ) ) ;
#12515 = CARTESIAN_POINT ( 'NONE',  ( -21.52544592524343514, 5.823673210054127303, 46.04057627198103830 ) ) ;
#12516 = CARTESIAN_POINT ( 'NONE',  ( -0.05219959533937732626, 21.53943276465977519, 92.50109039468567573 ) ) ;
#12517 = CARTESIAN_POINT ( 'NONE',  ( -4.483927247898782831, 16.52544592524335698, 57.70942372801901143 ) ) ;
#12518 = CARTESIAN_POINT ( 'NONE',  ( -18.62759615963270932, 10.81492255796079327, 115.8322429386477097 ) ) ;
#12519 = CARTESIAN_POINT ( 'NONE',  ( 12.14591786802327356, -12.06949235617739191, 20.62609039468568639 ) ) ;
#12520 = CARTESIAN_POINT ( 'NONE',  ( 16.51473224551069308, 9.474510206698969483, 89.16557627198103830 ) ) ;
#12521 = CARTESIAN_POINT ( 'NONE',  ( -14.34966873604972548, 8.224510206698743886, 28.33442372801902209 ) ) ;
#12522 = CARTESIAN_POINT ( 'NONE',  ( 9.474510206698971260, -16.51473224551069308, 57.91557627198103120 ) ) ;
#12523 = CARTESIAN_POINT ( 'NONE',  ( 0.05219959533934541429, -16.53943276465976808, 40.00109039468567573 ) ) ;
#12524 = CARTESIAN_POINT ( 'NONE',  ( -4.483927247898539470, -16.52544592524342804, 77.29057627198102409 ) ) ;
#12525 = CARTESIAN_POINT ( 'NONE',  ( 14.34966873604972726, -8.224510206698740333, 90.83442372801901854 ) ) ;
#12527 = CARTESIAN_POINT ( 'NONE',  ( -16.51473224551069308, -9.474510206698971260, 61.66557627198103120 ) ) ;
#12526 = CARTESIAN_POINT ( 'NONE',  ( -15.80617190586768217, 15.72974639402176855, 48.12609039468568284 ) ) ;
#12528 = CARTESIAN_POINT ( 'NONE',  ( 13.97604488694527802, 13.89961937509977652, 79.37390960531435269 ) ) ;
#12529 = CARTESIAN_POINT ( 'NONE',  ( -14.29746914071037622, -8.314922557961029526, 84.16775706135234714 ) ) ;
#12530 = CARTESIAN_POINT ( 'NONE',  ( -24.10884208241212079, -5.471882726981282197, 173.8287385965643637 ) ) ;
#12531 = EDGE_LOOP ( 'NONE', ( #95723, #112577, #18902, #136968, #137957 ) ) ;
#12532 = CARTESIAN_POINT ( 'NONE',  ( -19.03943276465977164, -0.05219959533935918106, 33.75109039468566863 ) ) ;
#12533 = CARTESIAN_POINT ( 'NONE',  ( 19.05341960407611168, 5.049401038298154454, 93.95724293864769550 ) ) ;
#12534 = CARTESIAN_POINT ( 'NONE',  ( -13.89961937509977652, 13.97604488694528158, 55.62390960531434558 ) ) ;
#12535 = CARTESIAN_POINT ( 'NONE',  ( -9.564922557960796823, -16.46253265017161027, 112.0822429386476955 ) ) ;
#12536 = CARTESIAN_POINT ( 'NONE',  ( -16.53943276465976808, -0.05219959533934237506, 38.75109039468567573 ) ) ;
#12538 = CARTESIAN_POINT ( 'NONE',  ( -8.224510206698735004, -14.34966873604973081, 59.58442372801901854 ) ) ;
#12537 = CARTESIAN_POINT ( 'NONE',  ( -5.049401038297874678, -19.05341960407617918, 59.79275706135231871 ) ) ;
#12539 = CARTESIAN_POINT ( 'NONE',  ( -69.65682714487590488, -71.74905178543390605, -23.00000000000000000 ) ) ;
#12540 = CARTESIAN_POINT ( 'NONE',  ( -16.51473224551069308, -9.474510206698971260, 71.66557627198102409 ) ) ;
#12541 = CARTESIAN_POINT ( 'NONE',  ( 21.52544592524344225, -5.823673210054117533, 108.5405762719810241 ) ) ;
#12542 = CARTESIAN_POINT ( 'NONE',  ( 9.474510206698729675, 16.51473224551082808, 62.08442372801899722 ) ) ;
#12544 = CARTESIAN_POINT ( 'NONE',  ( -16.46253265017160317, 9.564922557960807481, 25.83224293864769194 ) ) ;
#12543 = CARTESIAN_POINT ( 'NONE',  ( 19.02544592524343514, -5.153800228976328945, 103.5405762719809957 ) ) ;
#12545 = CARTESIAN_POINT ( 'NONE',  ( -13.89961937509977652, 13.97604488694528158, 70.62390960531432427 ) ) ;
#12547 = CARTESIAN_POINT ( 'NONE',  ( -9.474510206698964154, 16.51473224551069663, 25.41557627198103120 ) ) ;
#12546 = CARTESIAN_POINT ( 'NONE',  ( -16.52544592524342804, 4.483927247898546575, 31.04057627198102409 ) ) ;
#12548 = CARTESIAN_POINT ( 'NONE',  ( 19.02544592524334988, 5.153800228976608722, 31.45942372801900433 ) ) ;
#12549 = CARTESIAN_POINT ( 'NONE',  ( -14.34966873604960291, -8.224510206698953496, 71.66557627198100988 ) ) ;
#12550 = CARTESIAN_POINT ( 'NONE',  ( 21.53943276465977519, 0.05219959533937863772, 101.2510903946856757 ) ) ;
#12551 = CARTESIAN_POINT ( 'NONE',  ( 5.153800228976335163, 19.02544592524342804, 39.79057627198100988 ) ) ;
#12553 = CARTESIAN_POINT ( 'NONE',  ( 5.823673210054444382, -21.52544592524334988, 100.2094237280190043 ) ) ;
#12552 = CARTESIAN_POINT ( 'NONE',  ( -14.34966873604960291, -8.224510206698953496, 46.66557627198102409 ) ) ;
#12554 = CARTESIAN_POINT ( 'NONE',  ( 19.02544592524343514, -5.153800228976328945, 98.54057627198100988 ) ) ;
#12555 = CARTESIAN_POINT ( 'NONE',  ( -19.05341960407611168, -5.049401038298163336, 91.45724293864766707 ) ) ;
#12556 = CARTESIAN_POINT ( 'NONE',  ( 5.153800228976335163, 19.02544592524342804, 44.79057627198103830 ) ) ;
#12557 = CARTESIAN_POINT ( 'NONE',  ( -4.379528057220328563, 16.55341960407611168, 105.2072429386477097 ) ) ;
#12558 = CARTESIAN_POINT ( 'NONE',  ( -8.224510206698948167, 14.34966873604960824, 75.41557627198102409 ) ) ;
#12559 = CARTESIAN_POINT ( 'NONE',  ( -0.05219959533907301413, -21.53943276465977519, 87.49890960531436690 ) ) ;
#12560 = CARTESIAN_POINT ( 'NONE',  ( -19.02544592524342804, 5.153800228976336051, 91.04057627198100988 ) ) ;
#12561 = CARTESIAN_POINT ( 'NONE',  ( -21.53943276465977519, 0.05219959533907696930, 96.24890960531435269 ) ) ;
#12562 = CARTESIAN_POINT ( 'NONE',  ( 19.05341960407611168, 5.049401038298154454, 93.95724293864769550 ) ) ;
#12564 = CARTESIAN_POINT ( 'NONE',  ( -14.29746914071049879, 8.314922557960819915, 100.8322429386477097 ) ) ;
#12563 = CARTESIAN_POINT ( 'NONE',  ( -19.19724070472098276, -5.499999999999896083, 91.06193348274382515 ) ) ;
#12565 = CARTESIAN_POINT ( 'NONE',  ( 5.049401038298161559, -19.05341960407611168, 77.70724293864765286 ) ) ;
#12566 = CARTESIAN_POINT ( 'NONE',  ( -18.62759615963270932, 10.81492255796079327, 85.83224293864768129 ) ) ;
#12567 = CARTESIAN_POINT ( 'NONE',  ( -20.61165082012731986, -10.97245752705834043, 168.1443239908791440 ) ) ;
#12569 = CARTESIAN_POINT ( 'NONE',  ( 3.889087296526082316, 6.412877669190294228, 1.818019484660534424 ) ) ;
#12568 = CARTESIAN_POINT ( 'NONE',  ( -21.52544592524343514, 5.823673210054127303, 26.04057627198103475 ) ) ;
#12570 = CARTESIAN_POINT ( 'NONE',  ( 14.34966873604972726, -8.224510206698740333, 25.83442372801901499 ) ) ;
#12571 = CARTESIAN_POINT ( 'NONE',  ( -8.314922557960811034, -14.29746914071050412, 97.08224293864770971 ) ) ;
#12572 = CARTESIAN_POINT ( 'NONE',  ( -16.36317988757060604, -7.306389748694945396, 95.90210391636779264 ) ) ;
#12573 = CARTESIAN_POINT ( 'NONE',  ( -16.51473224551069308, -9.474510206698971260, 91.66557627198103830 ) ) ;
#12574 = CARTESIAN_POINT ( 'NONE',  ( -16.46253265017160317, 9.564922557960807481, 45.83224293864769550 ) ) ;
#12575 = CARTESIAN_POINT ( 'NONE',  ( 12.14591786802309770, 12.06949235617756955, 84.37390960531438111 ) ) ;
#12576 = B_SPLINE_CURVE_WITH_KNOTS ( 'NONE', 3,
 ( #163542, #134209, #103862, #151369, #121002, #167531, #12860, #29026, #197865, #90666, #152348, #148369, #9864, #26037, #10863, #118036, #57371, #180726, #42202, #165543 ),
 .UNSPECIFIED., .F., .F.,
 ( 4, 2, 2, 2, 2, 2, 2, 2, 2, 4 ),
 ( 0.004000878361811900999, 0.004499404418915920432, 0.004997930476019939866, 0.005496456533123958432, 0.005994982590227977866, 0.006244245618779977608, 0.006493508647331976483, 0.006992034704435960354, 0.007490560761539944226, 0.007989086818643928098 ),
 .UNSPECIFIED. ) ;
#12577 = CARTESIAN_POINT ( 'NONE',  ( 13.97604488694527802, 13.89961937509977652, 114.3739096053143669 ) ) ;
#12578 = CARTESIAN_POINT ( 'NONE',  ( -4.483927247898539470, -16.52544592524342804, 57.29057627198103120 ) ) ;
#12579 = CARTESIAN_POINT ( 'NONE',  ( -9.474510206698720793, -16.51473224551083518, 104.5844237280190043 ) ) ;
#12580 = CARTESIAN_POINT ( 'NONE',  ( 10.81492255796106328, -18.62759615963255655, 55.41775706135234714 ) ) ;
#12581 = CARTESIAN_POINT ( 'NONE',  ( 8.571926809382597767, 26.38167802310806209, 146.2750000027311899 ) ) ;
#12582 = CARTESIAN_POINT ( 'NONE',  ( -9.474510206698964154, 16.51473224551069663, 105.4155762719810383 ) ) ;
#12583 = CARTESIAN_POINT ( 'NONE',  ( 15.80617190586746368, 15.72974639402197994, 89.37390960531435269 ) ) ;
#12584 = CARTESIAN_POINT ( 'NONE',  ( 14.29746914071037800, 8.314922557961029526, 86.66775706135234714 ) ) ;
#12585 = CARTESIAN_POINT ( 'NONE',  ( -9.564922557960796823, -16.46253265017161027, 22.08224293864768839 ) ) ;
#12586 = CARTESIAN_POINT ( 'NONE',  ( 5.153800228976335163, 19.02544592524342804, 79.79057627198102409 ) ) ;
#12587 = CARTESIAN_POINT ( 'NONE',  ( -18.62759615963270932, 10.81492255796079327, 80.83224293864769550 ) ) ;
#12588 = CARTESIAN_POINT ( 'NONE',  ( 0.05219959533936267826, -19.03943276465977164, 110.0010903946856757 ) ) ;
#12590 = CARTESIAN_POINT ( 'NONE',  ( -10.72451020669870658, -18.67979575497194134, 54.58442372801901143 ) ) ;
#12589 = CARTESIAN_POINT ( 'NONE',  ( -12.06949235617756955, 12.14591786802309770, 50.62390960531435979 ) ) ;
#12591 = EDGE_CURVE ( 'NONE', #81412, #115964, #185427, .T. ) ;
#12593 = CARTESIAN_POINT ( 'NONE',  ( 10.81492255796078972, 18.62759615963270932, 29.58224293864769905 ) ) ;
#12592 = CARTESIAN_POINT ( 'NONE',  ( -4.379528057220086978, -16.55341960407618274, 84.79275706135234714 ) ) ;
#12594 = CARTESIAN_POINT ( 'NONE',  ( 13.97604488694527802, 13.89961937509977830, 109.3739096053143385 ) ) ;
#12595 = DIRECTION ( 'NONE',  ( -1.000000000000000000, -0.000000000000000000, -0.000000000000000000 ) ) ;
#12596 = CARTESIAN_POINT ( 'NONE',  ( 8.224510206698742110, 14.34966873604972548, 107.0844237280190043 ) ) ;
#12597 = CARTESIAN_POINT ( 'NONE',  ( 0.05219959533934541429, -16.53943276465976808, 65.00109039468568994 ) ) ;
#12598 = CARTESIAN_POINT ( 'NONE',  ( -19.05341960407611168, -5.049401038298163336, 76.45724293864769550 ) ) ;
#12599 = CARTESIAN_POINT ( 'NONE',  ( -13.97604488694527625, -13.89961937509977652, 76.87390960531433848 ) ) ;
#12600 = CARTESIAN_POINT ( 'NONE',  ( -8.314922557961024197, 14.29746914071037800, 77.91775706135231871 ) ) ;
#12601 = CARTESIAN_POINT ( 'NONE',  ( 16.55341960407611168, 4.379528057220329451, 43.95724293864769550 ) ) ;
#12602 = CARTESIAN_POINT ( 'NONE',  ( -19.03943276465977164, 0.05219959533909376836, 51.24890960531436690 ) ) ;
#12603 = CARTESIAN_POINT ( 'NONE',  ( -19.03943276465977164, 0.05219959533909376836, 51.24890960531436690 ) ) ;
#12605 = ORIENTED_EDGE ( 'NONE', *, *, #121376, .F. ) ;
#12604 = CARTESIAN_POINT ( 'NONE',  ( -8.314922557961024197, 14.29746914071037800, 42.91775706135235424 ) ) ;
#12606 = CARTESIAN_POINT ( 'NONE',  ( -19.02544592524334988, -5.153800228976617603, 98.95942372801900433 ) ) ;
#12607 = CARTESIAN_POINT ( 'NONE',  ( 0.05219959533910956823, 16.53943276465976808, 94.99890960531436690 ) ) ;
#12608 = CARTESIAN_POINT ( 'NONE',  ( 16.51473224551069308, 9.474510206698969483, 64.16557627198102409 ) ) ;
#12610 = CARTESIAN_POINT ( 'NONE',  ( -23.48529157249599919, -32.32473071737750558, -5.700000000000000178 ) ) ;
#12609 = CARTESIAN_POINT ( 'NONE',  ( 5.049401038297881783, 19.05341960407617563, 102.2927570613523045 ) ) ;
#12611 = CARTESIAN_POINT ( 'NONE',  ( -0.05219959533937732626, 21.53943276465977519, 107.5010903946856899 ) ) ;
#12612 = CARTESIAN_POINT ( 'NONE',  ( 12.14591786802327356, -12.06949235617739191, 70.62609039468567573 ) ) ;
#12613 = DIRECTION ( 'NONE',  ( 0.000000000000000000, 0.000000000000000000, 1.000000000000000000 ) ) ;
#12614 = CARTESIAN_POINT ( 'NONE',  ( -18.67979575497178146, -10.72451020669898902, 66.66557627198102409 ) ) ;
#12615 = CARTESIAN_POINT ( 'NONE',  ( 4.379528057220092307, 16.55341960407617563, 52.29275706135236135 ) ) ;
#12616 = CARTESIAN_POINT ( 'NONE',  ( -13.97604488694527625, -13.89961937509977830, 31.87390960531435979 ) ) ;
#12617 = CARTESIAN_POINT ( 'NONE',  ( -19.03943276465977164, -0.05219959533935918106, 38.75109039468566152 ) ) ;
#12618 = CARTESIAN_POINT ( 'NONE',  ( -5.049401038298153566, 19.05341960407611168, 95.20724293864770971 ) ) ;
#12619 = CARTESIAN_POINT ( 'NONE',  ( -12.06949235617756955, 12.14591786802309770, 115.6239096053143669 ) ) ;
#12620 = CARTESIAN_POINT ( 'NONE',  ( 5.049401038298161559, -19.05341960407611168, 67.70724293864769550 ) ) ;
#12621 = CARTESIAN_POINT ( 'NONE',  ( 21.55341960407619695, -5.719274019375665929, 81.04275706135236135 ) ) ;
#12622 = CARTESIAN_POINT ( 'NONE',  ( 16.46253265017146816, 9.564922557961045513, 51.66775706135233293 ) ) ;
#12623 = CARTESIAN_POINT ( 'NONE',  ( 19.03943276465977164, 0.05219959533936151252, 26.25109039468566507 ) ) ;
#12624 = CARTESIAN_POINT ( 'NONE',  ( -9.564922557960796823, -16.46253265017161027, 57.08224293864769550 ) ) ;
#12625 = CARTESIAN_POINT ( 'NONE',  ( -21.52544592524343514, 5.823673210054127303, 26.04057627198103475 ) ) ;
#12626 = CARTESIAN_POINT ( 'NONE',  ( -5.719274019375665041, -21.55341960407619695, 84.79275706135234714 ) ) ;
#12627 = CARTESIAN_POINT ( 'NONE',  ( -9.564922557960796823, -16.46253265017161027, 62.08224293864769550 ) ) ;
#12628 = CARTESIAN_POINT ( 'NONE',  ( -5.823673210054431948, 21.52544592524334988, 97.70942372801904696 ) ) ;
#12629 = CARTESIAN_POINT ( 'NONE',  ( -5.823673210054116645, -21.52544592524344225, 32.29057627198102409 ) ) ;
#12630 = CARTESIAN_POINT ( 'NONE',  ( -9.564922557960796823, -16.46253265017161027, 82.08224293864768129 ) ) ;
#12631 = CARTESIAN_POINT ( 'NONE',  ( -10.81492255796105439, 18.62759615963255655, 37.91775706135235424 ) ) ;
#12632 = CARTESIAN_POINT ( 'NONE',  ( 9.474510206698729675, 16.51473224551082808, 62.08442372801899722 ) ) ;
#12633 = CARTESIAN_POINT ( 'NONE',  ( 16.46253265017160672, -9.564922557960803928, 38.33224293864768839 ) ) ;
#12634 = CARTESIAN_POINT ( 'NONE',  ( -19.02544592524342804, 5.153800228976336051, 86.04057627198103830 ) ) ;
#12635 = CARTESIAN_POINT ( 'NONE',  ( -14.29746914071037622, -8.314922557961029526, 24.16775706135235424 ) ) ;
#12636 = CARTESIAN_POINT ( 'NONE',  ( 14.29746914071049879, -8.314922557960816363, 83.33224293864769550 ) ) ;
#12637 = CARTESIAN_POINT ( 'NONE',  ( -16.46253265017160317, 9.564922557960807481, 70.83224293864770971 ) ) ;
#12638 = CARTESIAN_POINT ( 'NONE',  ( -0.05219959533907301413, -21.53943276465977519, 52.49890960531435979 ) ) ;
#12639 = CARTESIAN_POINT ( 'NONE',  ( -12.14591786802326823, 12.06949235617739902, 23.12609039468567573 ) ) ;
#12640 = CARTESIAN_POINT ( 'NONE',  ( 21.55341960407619695, -5.719274019375665929, 21.04275706135234714 ) ) ;
#12641 = CARTESIAN_POINT ( 'NONE',  ( 0.05219959533937995610, -21.53943276465977519, 70.00109039468568994 ) ) ;
#12642 = CARTESIAN_POINT ( 'NONE',  ( -12.06949235617739369, -12.14591786802326823, 74.37609039468568994 ) ) ;
#12643 = CARTESIAN_POINT ( 'NONE',  ( -0.05219959533934338120, 16.53943276465976808, 62.50109039468568284 ) ) ;
#12644 = CARTESIAN_POINT ( 'NONE',  ( -13.89961937509977652, 13.97604488694528158, 65.62390960531436690 ) ) ;
#12645 = CARTESIAN_POINT ( 'NONE',  ( -8.224510206698735004, -14.34966873604973081, 99.58442372801900433 ) ) ;
#12646 = CARTESIAN_POINT ( 'NONE',  ( 9.564922557961047289, -16.46253265017146816, 45.41775706135232582 ) ) ;
#12647 = CARTESIAN_POINT ( 'NONE',  ( 21.55341960407619695, -5.719274019375665929, 21.04275706135234714 ) ) ;
#12648 = CARTESIAN_POINT ( 'NONE',  ( -12.06949235617756955, 12.14591786802309770, 60.62390960531437401 ) ) ;
#12649 = CARTESIAN_POINT ( 'NONE',  ( 19.05341960407611168, 5.049401038298154454, 88.95724293864769550 ) ) ;
#12650 = CARTESIAN_POINT ( 'NONE',  ( 12.14591786802327356, -12.06949235617739191, 90.62609039468567573 ) ) ;
#12651 = CARTESIAN_POINT ( 'NONE',  ( -10.81492255796105439, 18.62759615963255655, 57.91775706135234714 ) ) ;
#12652 = CARTESIAN_POINT ( 'NONE',  ( 14.29746914071037800, 8.314922557961029526, 31.66775706135234358 ) ) ;
#12653 = CARTESIAN_POINT ( 'NONE',  ( 21.55341960407619695, -5.719274019375665929, 21.04275706135234714 ) ) ;
#12654 = CARTESIAN_POINT ( 'NONE',  ( 14.29746914071049879, -8.314922557960816363, 63.33224293864770260 ) ) ;
#12655 = ORIENTED_EDGE ( 'NONE', *, *, #61124, .F. ) ;
#12656 = CARTESIAN_POINT ( 'NONE',  ( 10.72451020669898902, -18.67979575497178502, 97.91557627198103830 ) ) ;
#12657 = CARTESIAN_POINT ( 'NONE',  ( 12.06949235617757843, -12.14591786802309237, 33.12390960531435979 ) ) ;
#12658 = ORIENTED_EDGE ( 'NONE', *, *, #135901, .T. ) ;
#12659 = CARTESIAN_POINT ( 'NONE',  ( 34.78522506798721992, 2.428612866353961525E-14, 52.50000000000000000 ) ) ;
#12660 = CARTESIAN_POINT ( 'NONE',  ( -21.53943276465977519, 0.05219959533907696930, 36.24890960531435979 ) ) ;
#12661 = CARTESIAN_POINT ( 'NONE',  ( 21.52544592524334988, 5.823673210054432836, 41.45942372801901143 ) ) ;
#12662 = CARTESIAN_POINT ( 'NONE',  ( -16.55341960407611168, -4.379528057220339221, 61.45724293864770260 ) ) ;
#12663 = CARTESIAN_POINT ( 'NONE',  ( 5.823673210054125526, 21.52544592524343514, 64.79057627198103830 ) ) ;
#12664 = CARTESIAN_POINT ( 'NONE',  ( -19.02544592524342804, 5.153800228976336051, 81.04057627198103830 ) ) ;
#12666 = CARTESIAN_POINT ( 'NONE',  ( -16.46253265017146816, -9.564922557961047289, 59.16775706135233293 ) ) ;
#12665 = CARTESIAN_POINT ( 'NONE',  ( 19.03943276465977164, -0.05219959533909143690, 28.74890960531435624 ) ) ;
#12667 = EDGE_CURVE ( 'NONE', #59885, #155722, #67574, .T. ) ;
#12668 = CARTESIAN_POINT ( 'NONE',  ( -10.81492255796078084, -18.62759615963271287, 52.08224293864768839 ) ) ;
#12669 = CARTESIAN_POINT ( 'NONE',  ( -16.51473224551069308, -9.474510206698971260, 56.66557627198103120 ) ) ;
#12670 = CARTESIAN_POINT ( 'NONE',  ( -4.379528057220086978, -16.55341960407618274, 39.79275706135235424 ) ) ;
#12671 = CARTESIAN_POINT ( 'NONE',  ( -21.52544592524334988, -5.823673210054445271, 18.95942372801901143 ) ) ;
#12672 = CARTESIAN_POINT ( 'NONE',  ( -8.314922557960811034, -14.29746914071050412, 52.08224293864768839 ) ) ;
#12673 = CARTESIAN_POINT ( 'NONE',  ( -9.474510206698964154, 16.51473224551069663, 105.4155762719810383 ) ) ;
#12674 = CARTESIAN_POINT ( 'NONE',  ( 15.72974639402199770, -15.80617190586745480, 73.12390960531436690 ) ) ;
#12676 = CARTESIAN_POINT ( 'NONE',  ( -16.53943276465976808, -0.05219959533934237506, 43.75109039468568284 ) ) ;
#12675 = CARTESIAN_POINT ( 'NONE',  ( 18.67979575497178502, 10.72451020669898547, 109.1655762719810383 ) ) ;
#12677 = CARTESIAN_POINT ( 'NONE',  ( 0.05219959533907565091, 21.53943276465977519, 29.99890960531435979 ) ) ;
#12678 = CARTESIAN_POINT ( 'NONE',  ( 21.53943276465977519, 0.05219959533937863772, 96.25109039468568994 ) ) ;
#12679 = AXIS2_PLACEMENT_3D ( 'NONE', #156904, #121577, #76070 ) ;
#12680 = CARTESIAN_POINT ( 'NONE',  ( -5.049401038298153566, 19.05341960407611168, 35.20724293864768839 ) ) ;
#12681 = CARTESIAN_POINT ( 'NONE',  ( 16.51473224551069308, 9.474510206698969483, 94.16557627198103830 ) ) ;
#12682 = CARTESIAN_POINT ( 'NONE',  ( -0.05219959533909027116, -19.03943276465977164, 77.49890960531435269 ) ) ;
#12683 = CARTESIAN_POINT ( 'NONE',  ( -9.444085519387874328, -44.71325174467975216, -21.93802053968664367 ) ) ;
#12684 = CARTESIAN_POINT ( 'NONE',  ( -19.05341960407617563, 5.049401038297882671, 53.54275706135231871 ) ) ;
#12686 = CARTESIAN_POINT ( 'NONE',  ( -21.52544592524343514, 5.823673210054127303, 26.04057627198103475 ) ) ;
#12685 = CARTESIAN_POINT ( 'NONE',  ( 15.80617190586769283, -15.72974639402175789, 110.6260903946857042 ) ) ;
#12687 = CARTESIAN_POINT ( 'NONE',  ( 8.314922557961029526, -14.29746914071037800, 105.4177570613523613 ) ) ;
#12688 = CARTESIAN_POINT ( 'NONE',  ( 19.05341960407617918, -5.049401038297876454, 91.04275706135234714 ) ) ;
#12689 = CARTESIAN_POINT ( 'NONE',  ( -14.62203461105063873, -16.12203461105573865, -58.56003730381080175 ) ) ;
#12690 = CARTESIAN_POINT ( 'NONE',  ( 9.474510206698729675, 16.51473224551082808, 87.08442372801900433 ) ) ;
#12691 = CARTESIAN_POINT ( 'NONE',  ( -5.049401038297874678, -19.05341960407617918, 39.79275706135232582 ) ) ;
#12692 = CARTESIAN_POINT ( 'NONE',  ( -22.00000000000000000, -1.163414459189985801E-14, 95.00000000000000000 ) ) ;
#12693 = CARTESIAN_POINT ( 'NONE',  ( 5.153800228976335163, 19.02544592524342804, 44.79057627198103830 ) ) ;
#12694 = CARTESIAN_POINT ( 'NONE',  ( -14.34966873604960291, -8.224510206698953496, 51.66557627198102409 ) ) ;
#12695 = CARTESIAN_POINT ( 'NONE',  ( -16.51473224551069308, -9.474510206698971260, 26.66557627198103120 ) ) ;
#12696 = CARTESIAN_POINT ( 'NONE',  ( 16.55341960407611168, 4.379528057220329451, 23.95724293864769550 ) ) ;
#12697 = CARTESIAN_POINT ( 'NONE',  ( -4.500000000000001776, -130.0000000000000000, 13.99999999999999822 ) ) ;
#12698 = CARTESIAN_POINT ( 'NONE',  ( 4.483927247898790824, -16.52544592524335698, 95.20942372801903275 ) ) ;
#12699 = CARTESIAN_POINT ( 'NONE',  ( 5.153800228976335163, 19.02544592524342804, 49.79057627198100988 ) ) ;
#12700 = CARTESIAN_POINT ( 'NONE',  ( -21.55341960407619339, 5.719274019375674811, 103.5427570613523613 ) ) ;
#12701 = CARTESIAN_POINT ( 'NONE',  ( -0.05219959533934338120, 16.53943276465976808, 22.50109039468567573 ) ) ;
#12702 = CARTESIAN_POINT ( 'NONE',  ( -10.81492255796078084, -18.62759615963271287, 42.08224293864769550 ) ) ;
#12704 = ORIENTED_EDGE ( 'NONE', *, *, #122987, .T. ) ;
#12703 = CARTESIAN_POINT ( 'NONE',  ( 10.81492255796106328, -18.62759615963255655, 85.41775706135236135 ) ) ;
#12705 = CARTESIAN_POINT ( 'NONE',  ( 13.97604488694527802, 13.89961937509977652, 104.3739096053143385 ) ) ;
#12706 = CARTESIAN_POINT ( 'NONE',  ( 13.97604488694527802, 13.89961937509977652, 79.37390960531435269 ) ) ;
#12707 = CARTESIAN_POINT ( 'NONE',  ( 36.91746824999999887, -11.99521256947793546, -5.724999997268813701 ) ) ;
#12708 = CARTESIAN_POINT ( 'NONE',  ( 18.67979575497178502, 10.72451020669898547, 104.1655762719810241 ) ) ;
#12709 = CARTESIAN_POINT ( 'NONE',  ( -4.483927247898539470, -16.52544592524342804, 82.29057627198103830 ) ) ;
#12710 = CARTESIAN_POINT ( 'NONE',  ( 15.72974639402199770, -15.80617190586745480, 68.12390960531436690 ) ) ;
#12711 = CARTESIAN_POINT ( 'NONE',  ( 19.05341960407611168, 5.049401038298154454, 63.95724293864769550 ) ) ;
#12712 = CARTESIAN_POINT ( 'NONE',  ( -21.53943276465977519, 0.05219959533907696930, 101.2489096053143669 ) ) ;
#12713 = ORIENTED_EDGE ( 'NONE', *, *, #122412, .T. ) ;
#12714 = CARTESIAN_POINT ( 'NONE',  ( 5.153800228976335163, 19.02544592524342804, 59.79057627198100988 ) ) ;
#12716 = CARTESIAN_POINT ( 'NONE',  ( 19.80295450558173442, -12.05995242899444619, 167.9999999999999716 ) ) ;
#12715 = CARTESIAN_POINT ( 'NONE',  ( 16.53943276465976808, -0.05219959533910856209, 88.74890960531436690 ) ) ;
#12717 = CARTESIAN_POINT ( 'NONE',  ( 5.153800228976335163, 19.02544592524342804, 64.79057627198100988 ) ) ;
#12718 = CARTESIAN_POINT ( 'NONE',  ( -19.03943276465977164, -0.05219959533935918106, 73.75109039468566152 ) ) ;
#12719 = CARTESIAN_POINT ( 'NONE',  ( -16.52544592524342804, 4.483927247898546575, 91.04057627198103830 ) ) ;
#12720 = CARTESIAN_POINT ( 'NONE',  ( 18.62759615963255655, 10.81492255796105972, 61.66775706135235424 ) ) ;
#12722 = CARTESIAN_POINT ( 'NONE',  ( 15.80617190586746368, 15.72974639402197994, 114.3739096053143527 ) ) ;
#12721 = CARTESIAN_POINT ( 'NONE',  ( 13.97604488694527802, 13.89961937509977652, 44.37390960531435269 ) ) ;
#12723 = CARTESIAN_POINT ( 'NONE',  ( -16.52544592524342804, 4.483927247898546575, 106.0405762719810525 ) ) ;
#12724 = CARTESIAN_POINT ( 'NONE',  ( 12.33280382558395871, -43.64415646942563853, -22.88837716264674427 ) ) ;
#12725 = CARTESIAN_POINT ( 'NONE',  ( 0.05219959533909260263, 19.03943276465977164, 64.99890960531436690 ) ) ;
#12726 = CARTESIAN_POINT ( 'NONE',  ( 16.36317988757057051, 7.306389748694948949, 113.4021039163677500 ) ) ;
#12728 = CARTESIAN_POINT ( 'NONE',  ( -9.564922557960796823, -16.46253265017161027, 107.0822429386476955 ) ) ;
#12727 = CARTESIAN_POINT ( 'NONE',  ( 5.049401038297881783, 19.05341960407617563, 112.2927570613523471 ) ) ;
#12729 = CARTESIAN_POINT ( 'NONE',  ( -21.52544592524334988, -5.823673210054445271, 48.95942372801902565 ) ) ;
#12730 = CARTESIAN_POINT ( 'NONE',  ( 9.474510206698971260, -16.51473224551069308, 92.91557627198103830 ) ) ;
#12731 = CARTESIAN_POINT ( 'NONE',  ( 19.03943276465977164, 0.05219959533936151252, 81.25109039468567573 ) ) ;
#12732 = CARTESIAN_POINT ( 'NONE',  ( 19.05341960407611168, 5.049401038298154454, 63.95724293864769550 ) ) ;
#12733 = CARTESIAN_POINT ( 'NONE',  ( -14.34966873604960291, -8.224510206698953496, 76.66557627198103830 ) ) ;
#12734 = CARTESIAN_POINT ( 'NONE',  ( -0.05219959533910754901, -16.53943276465976808, 77.49890960531433848 ) ) ;
#12735 = CARTESIAN_POINT ( 'NONE',  ( 19.03943276465977164, -0.05219959533909143690, 93.74890960531435269 ) ) ;
#12736 = CARTESIAN_POINT ( 'NONE',  ( 16.53943276465976808, -0.05219959533910856209, 73.74890960531433848 ) ) ;
#12737 = CARTESIAN_POINT ( 'NONE',  ( 13.89961937509977652, -13.97604488694527269, 83.12390960531436690 ) ) ;
#12738 = CARTESIAN_POINT ( 'NONE',  ( 19.03943276465977164, 0.05219959533936151252, 36.25109039468567573 ) ) ;
#12742 = CARTESIAN_POINT ( 'NONE',  ( -5.049401038298153566, 19.05341960407611168, 30.20724293864768839 ) ) ;
#12741 =( BOUNDED_CURVE ( )  B_SPLINE_CURVE ( 2, ( #52063, #127897, #174426, #113720, #54070, #188607, #100559, #5550, #82381, #34906, #69230, #84383, #67229 ),
 .UNSPECIFIED., .F., .T. ) 
 B_SPLINE_CURVE_WITH_KNOTS ( ( 3, 2, 2, 2, 2, 2, 3 ),
 ( 0.6603251732691504117, 0.6622807017543859143, 0.6666666666666666297, 0.6710526315789473450, 0.6754385964912280604, 0.6798245614035087758, 0.6817344100666542506 ),
 .UNSPECIFIED. ) 
 CURVE ( )  GEOMETRIC_REPRESENTATION_ITEM ( )  RATIONAL_B_SPLINE_CURVE ( ( 0.9831626618144004848, 0.9848076720550091867, 1.000000000000000000, 0.9659258262890683122, 1.000000000000000000, 0.9659258262890683122, 1.000000000000000000, 0.9659258262890683122, 1.000000000000000000, 0.9659258262890683122, 1.000000000000000000, 0.9851625545550091179, 0.9832469066685282089 ) ) 
 REPRESENTATION_ITEM ( '' )  );
#12740 = CARTESIAN_POINT ( 'NONE',  ( 0.05219959533910956823, 16.53943276465976808, 24.99890960531435624 ) ) ;
#12739 = CARTESIAN_POINT ( 'NONE',  ( -19.03943276465977164, 0.05219959533909376836, 56.24890960531435979 ) ) ;
#12743 = ORIENTED_EDGE ( 'NONE', *, *, #108640, .T. ) ;
#12744 = CARTESIAN_POINT ( 'NONE',  ( -15.72974639402176322, -15.80617190586768395, 49.37609039468569705 ) ) ;
#12745 = CARTESIAN_POINT ( 'NONE',  ( 5.049401038297881783, 19.05341960407617563, 77.29275706135231871 ) ) ;
#12746 = CARTESIAN_POINT ( 'NONE',  ( -16.53943276465976808, 0.05219959533911058130, 36.24890960531435979 ) ) ;
#12747 = CARTESIAN_POINT ( 'NONE',  ( -15.80617190586745835, -15.72974639402198527, 91.87390960531436690 ) ) ;
#12748 = CARTESIAN_POINT ( 'NONE',  ( 21.52544592524344225, -5.823673210054117533, 28.54057627198103120 ) ) ;
#12749 = CARTESIAN_POINT ( 'NONE',  ( 0.05219959533910956823, 16.53943276465976808, 74.99890960531435269 ) ) ;
#12750 = CARTESIAN_POINT ( 'NONE',  ( 9.474510206698971260, -16.51473224551069308, 42.91557627198103120 ) ) ;
#12751 = CARTESIAN_POINT ( 'NONE',  ( -12.14591786802326823, 12.06949235617739902, 98.12609039468570415 ) ) ;
#12752 = CARTESIAN_POINT ( 'NONE',  ( 0.05219959533934541429, -16.53943276465976808, 75.00109039468568994 ) ) ;
#12753 = CARTESIAN_POINT ( 'NONE',  ( 21.53943276465977519, -0.05219959533907433946, 38.74890960531435979 ) ) ;
#12754 = CARTESIAN_POINT ( 'NONE',  ( 19.05341960407617918, -5.049401038297876454, 26.04275706135233293 ) ) ;
#12755 = CARTESIAN_POINT ( 'NONE',  ( -5.049401038298153566, 19.05341960407611168, 95.20724293864770971 ) ) ;
#12756 = CARTESIAN_POINT ( 'NONE',  ( -14.34966873604972548, 8.224510206698743886, 68.33442372801900433 ) ) ;
#12757 = CARTESIAN_POINT ( 'NONE',  ( -19.03943276465977164, 0.05219959533909376836, 21.24890960531436335 ) ) ;
#12758 = CARTESIAN_POINT ( 'NONE',  ( 16.55341960407611168, 4.379528057220329451, 38.95724293864768839 ) ) ;
#12760 = CARTESIAN_POINT ( 'NONE',  ( 16.46253265017160672, -9.564922557960803928, 88.33224293864769550 ) ) ;
#12759 = CARTESIAN_POINT ( 'NONE',  ( -16.46253265017160317, 9.564922557960807481, 105.8322429386476955 ) ) ;
#12761 = CARTESIAN_POINT ( 'NONE',  ( -21.53943276465977519, 0.05219959533907696930, 21.24890960531436690 ) ) ;
#12762 = CARTESIAN_POINT ( 'NONE',  ( 4.483927247898545687, 16.52544592524342804, 74.79057627198105251 ) ) ;
#12763 = EDGE_CURVE ( 'NONE', #127568, #188843, #6263, .T. ) ;
#12764 = CARTESIAN_POINT ( 'NONE',  ( 16.53943276465976808, -0.05219959533910856209, 58.74890960531436690 ) ) ;
#12766 = CARTESIAN_POINT ( 'NONE',  ( -17.97214573761829826, -5.500000000000085265, 56.46970049038657180 ) ) ;
#12765 = CARTESIAN_POINT ( 'NONE',  ( -16.52544592524335698, -4.483927247898792601, 58.95942372801902565 ) ) ;
#12767 = CARTESIAN_POINT ( 'NONE',  ( 19.03943276465977164, 0.05219959533936151252, 51.25109039468567573 ) ) ;
#12768 = CARTESIAN_POINT ( 'NONE',  ( 16.46253265017160672, -9.564922557960803928, 93.33224293864769550 ) ) ;
#12769 = CARTESIAN_POINT ( 'NONE',  ( -16.51473224551082808, 9.474510206698731452, 63.33442372801900433 ) ) ;
#12770 = CARTESIAN_POINT ( 'NONE',  ( -5.359611314223446995E-15, 29.16686587814335496, 142.8750000027311842 ) ) ;
#12771 = CARTESIAN_POINT ( 'NONE',  ( 9.474510206698729675, 16.51473224551082808, 57.08442372801900433 ) ) ;
#12773 = CARTESIAN_POINT ( 'NONE',  ( 8.314922557961029526, -14.29746914071037800, 90.41775706135236135 ) ) ;
#12772 = CARTESIAN_POINT ( 'NONE',  ( 8.314922557961029526, -14.29746914071037800, 20.41775706135234714 ) ) ;
#12774 = CARTESIAN_POINT ( 'NONE',  ( 19.03943276465977164, -0.05219959533909143690, 43.74890960531435979 ) ) ;
#12775 = CARTESIAN_POINT ( 'NONE',  ( 9.474510206698971260, -16.51473224551069308, 112.9155762719810383 ) ) ;
#12776 = CARTESIAN_POINT ( 'NONE',  ( -5.719274019375665041, -21.55341960407619695, 59.79275706135234714 ) ) ;
#12777 = CARTESIAN_POINT ( 'NONE',  ( -13.97604488694547697, 13.89961937509957934, 98.12609039468566152 ) ) ;
#12779 = CARTESIAN_POINT ( 'NONE',  ( -16.51473224551069308, -9.474510206698971260, 56.66557627198103120 ) ) ;
#12778 = CARTESIAN_POINT ( 'NONE',  ( 0.05219959533936267826, -19.03943276465977164, 55.00109039468566863 ) ) ;
#12780 = CARTESIAN_POINT ( 'NONE',  ( -19.03943276465977164, 0.05219959533909376836, 111.2489096053143669 ) ) ;
#12782 = CARTESIAN_POINT ( 'NONE',  ( -13.97604488694527625, -13.89961937509977652, 66.87390960531436690 ) ) ;
#12781 = CARTESIAN_POINT ( 'NONE',  ( -14.29746914071049879, 8.314922557960819915, 75.83224293864769550 ) ) ;
#12783 = ITEM_DEFINED_TRANSFORMATION ( 'NONE', 'NONE', #14406,  #82054 ) ;
#12784 = CARTESIAN_POINT ( 'NONE',  ( -0.05219959533909027116, -19.03943276465977164, 72.49890960531435269 ) ) ;
#12785 = CARTESIAN_POINT ( 'NONE',  ( 5.049401038297881783, 19.05341960407617563, 72.29275706135234714 ) ) ;
#12786 = CARTESIAN_POINT ( 'NONE',  ( -0.05219959533907301413, -21.53943276465977519, 62.49890960531436690 ) ) ;
#12787 = CARTESIAN_POINT ( 'NONE',  ( -8.224510206698948167, 14.34966873604960824, 110.4155762719810383 ) ) ;
#12788 = CARTESIAN_POINT ( 'NONE',  ( 5.049401038297881783, 19.05341960407617563, 52.29275706135234003 ) ) ;
#12789 = CARTESIAN_POINT ( 'NONE',  ( 19.03943276465977164, -0.05219959533909143690, 53.74890960531436690 ) ) ;
#12790 = CARTESIAN_POINT ( 'NONE',  ( 9.474510206698971260, -16.51473224551069308, 92.91557627198103830 ) ) ;
#12791 = CARTESIAN_POINT ( 'NONE',  ( 21.52544592524344225, -5.823673210054117533, 93.54057627198103830 ) ) ;
#12793 = CARTESIAN_POINT ( 'NONE',  ( -19.03943276465977164, -0.05219959533935918106, 43.75109039468566863 ) ) ;
#12792 = CARTESIAN_POINT ( 'NONE',  ( 16.55341960407611168, 4.379528057220329451, 83.95724293864770971 ) ) ;
#12794 = CARTESIAN_POINT ( 'NONE',  ( 18.67979575497178502, 10.72451020669898547, 74.16557627198102409 ) ) ;
#12795 = CARTESIAN_POINT ( 'NONE',  ( 5.719274019375991003, -21.55341960407610458, 57.70724293864770260 ) ) ;
#12796 = CARTESIAN_POINT ( 'NONE',  ( -0.05219959533910754901, -16.53943276465976808, 37.49890960531436690 ) ) ;
#12797 = CARTESIAN_POINT ( 'NONE',  ( 5.719274019375673035, 21.55341960407619339, 92.29275706135236135 ) ) ;
#12798 = CARTESIAN_POINT ( 'NONE',  ( -19.03943276465977164, 0.05219959533909376836, 86.24890960531436690 ) ) ;
#12799 = CARTESIAN_POINT ( 'NONE',  ( 14.34966873604960469, 8.224510206698951720, 114.1655762719810383 ) ) ;
#12800 = CARTESIAN_POINT ( 'NONE',  ( 21.55341960407619695, -5.719274019375665929, 31.04275706135234714 ) ) ;
#12801 = CARTESIAN_POINT ( 'NONE',  ( 10.81492255796106328, -18.62759615963255655, 35.41775706135234003 ) ) ;
#12802 = CARTESIAN_POINT ( 'NONE',  ( 16.46253265017160672, -9.564922557960803928, 43.33224293864769550 ) ) ;
#12803 = CARTESIAN_POINT ( 'NONE',  ( -15.72974639402197994, 15.80617190586746368, 115.6239096053143669 ) ) ;
#12804 = CARTESIAN_POINT ( 'NONE',  ( 13.89961937509957401, 13.97604488694547697, 61.87609039468566863 ) ) ;
#12805 = CARTESIAN_POINT ( 'NONE',  ( 5.049401038298161559, -19.05341960407611168, 37.70724293864768839 ) ) ;
#12806 = CARTESIAN_POINT ( 'NONE',  ( 16.55341960407618274, -4.379528057220086978, 26.04275706135235779 ) ) ;
#12807 = CARTESIAN_POINT ( 'NONE',  ( -67.00000000000000000, -5.510910596163089556E-15, 45.00000000000000000 ) ) ;
#12808 = CARTESIAN_POINT ( 'NONE',  ( -16.53943276465976808, -0.05219959533934237506, 68.75109039468568994 ) ) ;
#12809 = CARTESIAN_POINT ( 'NONE',  ( -9.474510206698964154, 16.51473224551069663, 45.41557627198103120 ) ) ;
#12810 = CARTESIAN_POINT ( 'NONE',  ( -21.96844466259036111, -8.667631922774113207, 171.6690673070920354 ) ) ;
#12811 = CARTESIAN_POINT ( 'NONE',  ( 5.153800228976335163, 19.02544592524342804, 89.79057627198102409 ) ) ;
#12812 = CARTESIAN_POINT ( 'NONE',  ( 13.89961937509977652, -13.97604488694527269, 23.12390960531436335 ) ) ;
#12813 = CARTESIAN_POINT ( 'NONE',  ( 21.53943276465977519, -0.05219959533907433946, 63.74890960531435979 ) ) ;
#12814 = CARTESIAN_POINT ( 'NONE',  ( -14.29746914071037622, -8.314922557961029526, 44.16775706135234714 ) ) ;
#12815 = CARTESIAN_POINT ( 'NONE',  ( 21.53943276465977519, 0.05219959533937863772, 106.2510903946856757 ) ) ;
#12816 = CARTESIAN_POINT ( 'NONE',  ( -5.049401038298153566, 19.05341960407611168, 35.20724293864768839 ) ) ;
#12817 = CARTESIAN_POINT ( 'NONE',  ( -12.06949235617756955, 12.14591786802309770, 35.62390960531437401 ) ) ;
#12818 = CARTESIAN_POINT ( 'NONE',  ( 8.314922557960818139, 14.29746914071049879, 64.58224293864769550 ) ) ;
#12819 = VECTOR ( 'NONE', #47624, 1000.000000000000000 ) ;
#12820 = CARTESIAN_POINT ( 'NONE',  ( 9.564922557960805705, 16.46253265017160317, 59.58224293864769550 ) ) ;
#12821 = CARTESIAN_POINT ( 'NONE',  ( 5.719274019375673035, 21.55341960407619339, 107.2927570613523471 ) ) ;
#12822 = CARTESIAN_POINT ( 'NONE',  ( 5.823673210054444382, -21.52544592524334988, 20.20942372801900788 ) ) ;
#12823 = CARTESIAN_POINT ( 'NONE',  ( -19.03943276465977164, 0.05219959533909376836, 76.24890960531435269 ) ) ;
#12824 = CARTESIAN_POINT ( 'NONE',  ( -5.823673210054431948, 21.52544592524334988, 92.70942372801901854 ) ) ;
#12825 = CARTESIAN_POINT ( 'NONE',  ( 0.05219959533934541429, -16.53943276465976808, 50.00109039468568994 ) ) ;
#12826 = CARTESIAN_POINT ( 'NONE',  ( 12.14591786802327356, -12.06949235617739191, 30.62609039468567929 ) ) ;
#12828 = CARTESIAN_POINT ( 'NONE',  ( 18.67979575497194134, -10.72451020669871369, 95.83442372801903275 ) ) ;
#12827 = CARTESIAN_POINT ( 'NONE',  ( -12.14591786802309592, -12.06949235617757132, 91.87390960531436690 ) ) ;
#12829 = CARTESIAN_POINT ( 'NONE',  ( 0.05219959533910956823, 16.53943276465976808, 34.99890960531435979 ) ) ;
#12830 = CARTESIAN_POINT ( 'NONE',  ( -16.51473224551069308, -9.474510206698971260, 26.66557627198103120 ) ) ;
#12831 = CARTESIAN_POINT ( 'NONE',  ( -8.314922557961024197, 14.29746914071037800, 52.91775706135235424 ) ) ;
#12832 = CARTESIAN_POINT ( 'NONE',  ( -12.06949235617756955, 12.14591786802309770, 55.62390960531436690 ) ) ;
#12833 = CARTESIAN_POINT ( 'NONE',  ( 4.483927247898790824, -16.52544592524335698, 95.20942372801903275 ) ) ;
#12834 = CARTESIAN_POINT ( 'NONE',  ( -19.03943276465977164, 0.05219959533909376836, 111.2489096053143669 ) ) ;
#12835 = CARTESIAN_POINT ( 'NONE',  ( -5.049401038298153566, 19.05341960407611168, 115.2072429386477097 ) ) ;
#12836 = CARTESIAN_POINT ( 'NONE',  ( -15.80617190586768217, 15.72974639402176855, 113.1260903946856899 ) ) ;
#12837 = CARTESIAN_POINT ( 'NONE',  ( -16.53943276465976808, 0.05219959533911058130, 91.24890960531436690 ) ) ;
#12838 = CARTESIAN_POINT ( 'NONE',  ( -13.97604488694527625, -13.89961937509977652, 96.87390960531433848 ) ) ;
#12839 = VERTEX_POINT ( 'NONE', #38619 ) ;
#12840 = CARTESIAN_POINT ( 'NONE',  ( 14.34966873604972726, -8.224510206698740333, 45.83442372801901854 ) ) ;
#12841 = CARTESIAN_POINT ( 'NONE',  ( -5.153800228976328057, -19.02544592524343514, 37.29057627198102409 ) ) ;
#12843 = FACE_OUTER_BOUND ( 'NONE', #7386, .T. ) ;
#12842 = CARTESIAN_POINT ( 'NONE',  ( -4.483927247898782831, 16.52544592524335698, 42.70942372801901854 ) ) ;
#12844 = CARTESIAN_POINT ( 'NONE',  ( 16.46253265017146816, 9.564922557961045513, 46.66775706135233293 ) ) ;
#12845 = CARTESIAN_POINT ( 'NONE',  ( 13.89961937509977652, -13.97604488694527269, 43.12390960531434558 ) ) ;
#12846 = CARTESIAN_POINT ( 'NONE',  ( 12.14591786802327356, -12.06949235617739191, 80.62609039468567573 ) ) ;
#12847 = CARTESIAN_POINT ( 'NONE',  ( -16.51473224551082808, 9.474510206698731452, 83.33442372801899012 ) ) ;
#12848 = CARTESIAN_POINT ( 'NONE',  ( 19.03943276465977164, 0.05219959533936151252, 31.25109039468566863 ) ) ;
#12849 = CARTESIAN_POINT ( 'NONE',  ( -9.474510206698964154, 16.51473224551069663, 55.41557627198103120 ) ) ;
#12850 = CARTESIAN_POINT ( 'NONE',  ( 14.34966873604960469, 8.224510206698951720, 94.16557627198103830 ) ) ;
#12851 = AXIS2_PLACEMENT_3D ( 'NONE', #92936, #50438, #200135 ) ;
#12852 = EDGE_CURVE ( 'NONE', #70870, #34628, #145778, .T. ) ;
#12853 = CARTESIAN_POINT ( 'NONE',  ( -0.05219959533936034679, 19.03943276465977164, 72.50109039468566152 ) ) ;
#12854 = CARTESIAN_POINT ( 'NONE',  ( -21.53943276465977519, 0.05219959533907696930, 66.24890960531436690 ) ) ;
#12855 = CARTESIAN_POINT ( 'NONE',  ( -5.049401038297874678, -19.05341960407617918, 29.79275706135232227 ) ) ;
#12856 = CARTESIAN_POINT ( 'NONE',  ( -16.46253265017160317, 9.564922557960807481, 110.8322429386476955 ) ) ;
#12857 = CARTESIAN_POINT ( 'NONE',  ( 10.72451020669898902, -18.67979575497178502, 77.91557627198102409 ) ) ;
#12858 = CARTESIAN_POINT ( 'NONE',  ( -16.20579543436679160, 7.371946100355091680, 84.43479165828125588 ) ) ;
#12859 = CARTESIAN_POINT ( 'NONE',  ( -19.05341960407617563, 5.049401038297882671, 103.5427570613523329 ) ) ;
#12860 = CARTESIAN_POINT ( 'NONE',  ( -19.35633801406906684, 5.499999999999783284, 59.13373818172765084 ) ) ;
#12861 = CARTESIAN_POINT ( 'NONE',  ( -4.379528057220086978, -16.55341960407618274, 29.79275706135234358 ) ) ;
#12862 = CARTESIAN_POINT ( 'NONE',  ( -16.46253265017160317, 9.564922557960807481, 30.83224293864769550 ) ) ;
#12863 = CARTESIAN_POINT ( 'NONE',  ( -0.05219959533909027116, -19.03943276465977164, 112.4989096053143669 ) ) ;
#12864 = CARTESIAN_POINT ( 'NONE',  ( -21.52544592524343514, 5.823673210054127303, 96.04057627198102409 ) ) ;
#12865 = CARTESIAN_POINT ( 'NONE',  ( 15.80617190586769283, -15.72974639402175789, 65.62609039468568994 ) ) ;
#12867 = CARTESIAN_POINT ( 'NONE',  ( 0.05219959533937995610, -21.53943276465977519, 105.0010903946856757 ) ) ;
#12866 = CARTESIAN_POINT ( 'NONE',  ( -0.05219959533936034679, 19.03943276465977164, 107.5010903946856615 ) ) ;
#12868 = CARTESIAN_POINT ( 'NONE',  ( 16.53943276465976808, 0.05219959533934440121, 106.2510903946856757 ) ) ;
#12869 = CARTESIAN_POINT ( 'NONE',  ( 0.05219959533907565091, 21.53943276465977519, 104.9989096053143669 ) ) ;
#12870 = CARTESIAN_POINT ( 'NONE',  ( 16.52544592524342804, -4.483927247898539470, 43.54057627198103830 ) ) ;
#12871 = CARTESIAN_POINT ( 'NONE',  ( -5.049401038297874678, -19.05341960407617918, 84.79275706135233293 ) ) ;
#12872 = CARTESIAN_POINT ( 'NONE',  ( 19.02544592524334988, 5.153800228976608722, 56.45942372801898301 ) ) ;
#12873 = CARTESIAN_POINT ( 'NONE',  ( 0.05219959533937995610, -21.53943276465977519, 60.00109039468568284 ) ) ;
#12874 = CARTESIAN_POINT ( 'NONE',  ( -19.02544592524334988, -5.153800228976617603, 38.95942372801900433 ) ) ;
#12875 = CARTESIAN_POINT ( 'NONE',  ( -14.29746914071049879, 8.314922557960819915, 100.8322429386477097 ) ) ;
#12876 = CARTESIAN_POINT ( 'NONE',  ( 21.55341960407610458, 5.719274019375980345, 48.95724293864770971 ) ) ;
#12877 = CARTESIAN_POINT ( 'NONE',  ( -16.52544592524342804, 4.483927247898546575, 41.04057627198103120 ) ) ;
#12878 = CARTESIAN_POINT ( 'NONE',  ( 15.72974639402176855, 15.80617190586768217, 101.8760903946857042 ) ) ;
#12879 = CARTESIAN_POINT ( 'NONE',  ( -14.34966873604972548, 8.224510206698743886, 78.33442372801901854 ) ) ;
#12880 = CARTESIAN_POINT ( 'NONE',  ( 12.06949235617757843, -12.14591786802309237, 28.12390960531435979 ) ) ;
#12881 = CARTESIAN_POINT ( 'NONE',  ( 15.72974639402176855, 15.80617190586768217, 56.87609039468568994 ) ) ;
#12882 = CARTESIAN_POINT ( 'NONE',  ( -15.80617190586768217, 15.72974639402176855, 63.12609039468568994 ) ) ;
#12883 = CARTESIAN_POINT ( 'NONE',  ( 18.67979575497178502, 10.72451020669898547, 64.16557627198102409 ) ) ;
#12884 = EDGE_LOOP ( 'NONE', ( #97241, #180583, #38933, #34189 ) ) ;
#12885 = CARTESIAN_POINT ( 'NONE',  ( -5.153800228976328057, -19.02544592524343514, 22.29057627198102765 ) ) ;
#12886 = CARTESIAN_POINT ( 'NONE',  ( 0.05219959533937995610, -21.53943276465977519, 50.00109039468568994 ) ) ;
#12887 = CARTESIAN_POINT ( 'NONE',  ( -14.29746914071049879, 8.314922557960819915, 115.8322429386477097 ) ) ;
#12888 = CARTESIAN_POINT ( 'NONE',  ( 19.03943276465977164, -0.05219959533909143690, 43.74890960531435979 ) ) ;
#12889 = CARTESIAN_POINT ( 'NONE',  ( 12.06949235617757843, -12.14591786802309237, 73.12390960531436690 ) ) ;
#12890 = CARTESIAN_POINT ( 'NONE',  ( -19.02544592524342804, 5.153800228976336051, 91.04057627198100988 ) ) ;
#12891 = CARTESIAN_POINT ( 'NONE',  ( -16.53943276465976808, -0.05219959533934237506, 113.7510903946856757 ) ) ;
#12892 = CARTESIAN_POINT ( 'NONE',  ( -8.314922557960811034, -14.29746914071050412, 97.08224293864770971 ) ) ;
#12893 = CARTESIAN_POINT ( 'NONE',  ( 0.05219959533907565091, 21.53943276465977519, 74.99890960531435269 ) ) ;
#12894 = CARTESIAN_POINT ( 'NONE',  ( 0.05219959533907565091, 21.53943276465977519, 109.9989096053143527 ) ) ;
#12896 = CARTESIAN_POINT ( 'NONE',  ( -14.29746914071037622, -8.314922557961029526, 19.16775706135234714 ) ) ;
#12895 = CARTESIAN_POINT ( 'NONE',  ( -19.05341960407611168, -5.049401038298163336, 66.45724293864769550 ) ) ;
#12897 = CARTESIAN_POINT ( 'NONE',  ( -21.53943276465977519, 0.05219959533907696930, 51.24890960531436690 ) ) ;
#12898 = CARTESIAN_POINT ( 'NONE',  ( 15.72974639402176855, 15.80617190586768217, 76.87609039468567573 ) ) ;
#12899 = CARTESIAN_POINT ( 'NONE',  ( -16.51473224551069308, -9.474510206698971260, 61.66557627198103120 ) ) ;
#12900 = CARTESIAN_POINT ( 'NONE',  ( 19.03943276465977164, -0.05219959533909143690, 103.7489096053143669 ) ) ;
#12901 = CARTESIAN_POINT ( 'NONE',  ( -14.29746914071037622, -8.314922557961029526, 79.16775706135234714 ) ) ;
#12902 = CARTESIAN_POINT ( 'NONE',  ( 21.53943276465977519, 0.05219959533937863772, 51.25109039468568994 ) ) ;
#12903 = CARTESIAN_POINT ( 'NONE',  ( 5.823673210054444382, -21.52544592524334988, 95.20942372801903275 ) ) ;
#12904 = CARTESIAN_POINT ( 'NONE',  ( 21.52544592524344225, -5.823673210054117533, 113.5405762719810383 ) ) ;
#12905 = CARTESIAN_POINT ( 'NONE',  ( 5.823673210054125526, 21.52544592524343514, 89.79057627198103830 ) ) ;
#12906 = CARTESIAN_POINT ( 'NONE',  ( 13.89961937509957401, 13.97604488694547697, 41.87609039468566152 ) ) ;
#12907 = CARTESIAN_POINT ( 'NONE',  ( -18.67979575497178146, -10.72451020669898902, 36.66557627198103120 ) ) ;
#12909 = CARTESIAN_POINT ( 'NONE',  ( -16.53943276465976808, 0.05219959533911058130, 31.24890960531435979 ) ) ;
#12908 = CARTESIAN_POINT ( 'NONE',  ( -9.474510206698964154, 16.51473224551069663, 75.41557627198103830 ) ) ;
#12910 = CARTESIAN_POINT ( 'NONE',  ( -16.38665767535054840, 7.295008042176032603, 65.26400864214548392 ) ) ;
#12911 = CYLINDRICAL_SURFACE ( 'NONE', #115324, 31.90000000000003411 ) ;
#12912 = CARTESIAN_POINT ( 'NONE',  ( -16.46253265017146816, -9.564922557961047289, 99.16775706135233293 ) ) ;
#12913 = CARTESIAN_POINT ( 'NONE',  ( -18.67979575497178146, -10.72451020669898902, 66.66557627198102409 ) ) ;
#12914 = CARTESIAN_POINT ( 'NONE',  ( -14.29746914071049879, 8.314922557960819915, 50.83224293864770971 ) ) ;
#12915 = CARTESIAN_POINT ( 'NONE',  ( 4.379528057220092307, 16.55341960407617563, 37.29275706135235424 ) ) ;
#12916 = CARTESIAN_POINT ( 'NONE',  ( 16.46253265017160672, -9.564922557960803928, 48.33224293864769550 ) ) ;
#12918 = CARTESIAN_POINT ( 'NONE',  ( -0.05219959533936034679, 19.03943276465977164, 87.50109039468567573 ) ) ;
#12917 = CARTESIAN_POINT ( 'NONE',  ( -18.62759615963270932, 10.81492255796079327, 110.8322429386476955 ) ) ;
#12919 = CARTESIAN_POINT ( 'NONE',  ( -16.46253265017160317, 9.564922557960807481, 75.83224293864769550 ) ) ;
#12920 = CARTESIAN_POINT ( 'NONE',  ( -12.14591786802309592, -12.06949235617757132, 91.87390960531436690 ) ) ;
#12921 = CARTESIAN_POINT ( 'NONE',  ( 9.474510206698971260, -16.51473224551069308, 67.91557627198102409 ) ) ;
#12922 = CARTESIAN_POINT ( 'NONE',  ( -21.52544592524343514, 5.823673210054127303, 81.04057627198102409 ) ) ;
#12923 = CARTESIAN_POINT ( 'NONE',  ( 19.05341960407611168, 5.049401038298154454, 28.95724293864769550 ) ) ;
#12924 = CARTESIAN_POINT ( 'NONE',  ( -16.59625950682774231, 33.98852600706017313, -7.999999999999994671 ) ) ;
#12925 = CARTESIAN_POINT ( 'NONE',  ( -14.29746914071049879, 8.314922557960819915, 55.83224293864770260 ) ) ;
#12926 = CARTESIAN_POINT ( 'NONE',  ( -5.049401038298153566, 19.05341960407611168, 95.20724293864770971 ) ) ;
#12927 = CARTESIAN_POINT ( 'NONE',  ( -28.82186960331518932, -9.364793116373263615, 140.3500000054623627 ) ) ;
#12928 = CARTESIAN_POINT ( 'NONE',  ( -0.05219959533936034679, 19.03943276465977164, 52.50109039468566863 ) ) ;
#12929 = CARTESIAN_POINT ( 'NONE',  ( 0.05219959533934541429, -16.53943276465976808, 65.00109039468568994 ) ) ;
#12930 = CARTESIAN_POINT ( 'NONE',  ( -5.719274019375978568, 21.55341960407610458, 80.20724293864769550 ) ) ;
#12931 = CARTESIAN_POINT ( 'NONE',  ( 16.46253265017146816, 9.564922557961045513, 41.66775706135234003 ) ) ;
#12932 = CARTESIAN_POINT ( 'NONE',  ( 9.474510206698971260, -16.51473224551069308, 87.91557627198102409 ) ) ;
#12933 = CARTESIAN_POINT ( 'NONE',  ( -3.573655867281984216E-15, 2.428612866367529932E-14, -13.00000000000000000 ) ) ;
#12934 = CARTESIAN_POINT ( 'NONE',  ( 18.62759615963271287, -10.81492255796078972, 23.33224293864769194 ) ) ;
#12935 = CARTESIAN_POINT ( 'NONE',  ( 5.049401038298161559, -19.05341960407611168, 72.70724293864768129 ) ) ;
#12936 = CARTESIAN_POINT ( 'NONE',  ( 10.81492255796106328, -18.62759615963255655, 55.41775706135234714 ) ) ;
#12937 = CARTESIAN_POINT ( 'NONE',  ( -16.51473224551069308, -9.474510206698971260, 21.66557627198102765 ) ) ;
#12940 = ORIENTED_EDGE ( 'NONE', *, *, #141236, .F. ) ;
#12939 = CARTESIAN_POINT ( 'NONE',  ( -19.05341960407611168, -5.049401038298163336, 91.45724293864766707 ) ) ;
#12938 = CARTESIAN_POINT ( 'NONE',  ( 18.67979575497178502, 10.72451020669898547, 114.1655762719810383 ) ) ;
#12941 = CARTESIAN_POINT ( 'NONE',  ( 21.55341960407619695, -5.719274019375665929, 46.04275706135234714 ) ) ;
#12942 = ORIENTED_EDGE ( 'NONE', *, *, #95173, .F. ) ;
#12943 = CARTESIAN_POINT ( 'NONE',  ( 9.474510206698971260, -16.51473224551069308, 102.9155762719810241 ) ) ;
#12944 = B_SPLINE_CURVE_WITH_KNOTS ( 'NONE', 3,
 ( #12991, #133326, #167659, #26173, #74654, #195017, #164679, #87814 ),
 .UNSPECIFIED., .F., .F.,
 ( 4, 2, 2, 4 ),
 ( 0.000000000000000000, 0.0004423531491111659989, 0.0008847062982223319978, 0.001769412596444684812 ),
 .UNSPECIFIED. ) ;
#12945 = CARTESIAN_POINT ( 'NONE',  ( -21.96434091948370337, 6.687777057363587296, 170.9277123045939106 ) ) ;
#12946 = CARTESIAN_POINT ( 'NONE',  ( -18.62759615963270932, 10.81492255796079327, 105.8322429386476955 ) ) ;
#12947 = CARTESIAN_POINT ( 'NONE',  ( 9.564922557960805705, 16.46253265017160317, 49.58224293864770260 ) ) ;
#12948 = CARTESIAN_POINT ( 'NONE',  ( -16.52544592524335698, -4.483927247898792601, 28.95942372801902209 ) ) ;
#12949 = CARTESIAN_POINT ( 'NONE',  ( 36.91746824999999177, 2.880721459617395097E-14, -4.124999997268813168 ) ) ;
#12950 = CARTESIAN_POINT ( 'NONE',  ( -0.05219959533937732626, 21.53943276465977519, 107.5010903946856899 ) ) ;
#12951 = CARTESIAN_POINT ( 'NONE',  ( -9.474510206698964154, 16.51473224551069663, 45.41557627198103120 ) ) ;
#12952 = CARTESIAN_POINT ( 'NONE',  ( -15.80617190586768217, 15.72974639402176855, 93.12609039468568994 ) ) ;
#12954 = CARTESIAN_POINT ( 'NONE',  ( 18.67979575497194134, -10.72451020669871369, 55.83442372801901854 ) ) ;
#12953 = CARTESIAN_POINT ( 'NONE',  ( 19.05341960407611168, 5.049401038298154454, 88.95724293864769550 ) ) ;
#12955 = CIRCLE ( 'NONE', #41979, 10.00000000000000000 ) ;
#12956 = CARTESIAN_POINT ( 'NONE',  ( -17.14385361876520264, -23.59649016807271593, 141.6750000027311103 ) ) ;
#12957 = CARTESIAN_POINT ( 'NONE',  ( 19.05341960407611168, 5.049401038298154454, 98.95724293864766707 ) ) ;
#12958 = CARTESIAN_POINT ( 'NONE',  ( -17.49999999999998224, 3.805241302050397678, 30.37352472782594504 ) ) ;
#12961 = CARTESIAN_POINT ( 'NONE',  ( 18.67979575497194134, -10.72451020669871369, 55.83442372801901854 ) ) ;
#12960 = CARTESIAN_POINT ( 'NONE',  ( -8.314922557961024197, 14.29746914071037800, 62.91775706135236135 ) ) ;
#12959 = CARTESIAN_POINT ( 'NONE',  ( -8.314922557961024197, 14.29746914071037800, 52.91775706135235424 ) ) ;
#12962 = CARTESIAN_POINT ( 'NONE',  ( -21.55341960407619339, 5.719274019375674811, 83.54275706135234714 ) ) ;
#12963 = DIRECTION ( 'NONE',  ( -1.000000000000000000, 0.000000000000000000, 0.000000000000000000 ) ) ;
#12964 = CARTESIAN_POINT ( 'NONE',  ( 0.05219959533934541429, -16.53943276465976808, 30.00109039468568284 ) ) ;
#12965 = CARTESIAN_POINT ( 'NONE',  ( -16.46253265017160317, 9.564922557960807481, 75.83224293864769550 ) ) ;
#12966 = CARTESIAN_POINT ( 'NONE',  ( -5.153800228976328057, -19.02544592524343514, 102.2905762719810383 ) ) ;
#12967 = ADVANCED_FACE ( 'NONE', ( #39608 ), #101267, .T. ) ;
#12968 = CARTESIAN_POINT ( 'NONE',  ( -16.46253265017160317, 9.564922557960807481, 115.8322429386477097 ) ) ;
#12969 = CARTESIAN_POINT ( 'NONE',  ( 19.02544592524343514, -5.153800228976328945, 23.54057627198102054 ) ) ;
#12970 = CARTESIAN_POINT ( 'NONE',  ( 15.80617190586746368, 15.72974639402197994, 29.37390960531435269 ) ) ;
#12971 = CARTESIAN_POINT ( 'NONE',  ( 12.06949235617739724, 12.14591786802326823, 86.87609039468568994 ) ) ;
#12973 = CARTESIAN_POINT ( 'NONE',  ( -5.153800228976328057, -19.02544592524343514, 62.29057627198100988 ) ) ;
#12972 = CARTESIAN_POINT ( 'NONE',  ( -14.34966873604960291, -8.224510206698953496, 86.66557627198102409 ) ) ;
#12974 = CARTESIAN_POINT ( 'NONE',  ( 15.72974639402176855, 15.80617190586768217, 86.87609039468568994 ) ) ;
#12975 = DIRECTION ( 'NONE',  ( -0.000000000000000000, -0.000000000000000000, 1.000000000000000000 ) ) ;
#12976 = CARTESIAN_POINT ( 'NONE',  ( -0.05219959533934338120, 16.53943276465976808, 27.50109039468567929 ) ) ;
#12977 = CARTESIAN_POINT ( 'NONE',  ( 16.55341960407611168, 4.379528057220329451, 73.95724293864769550 ) ) ;
#12978 = CARTESIAN_POINT ( 'NONE',  ( -18.62759615963255300, -10.81492255796106328, 24.16775706135235424 ) ) ;
#12979 = CARTESIAN_POINT ( 'NONE',  ( -15.72974639402197994, 15.80617190586746368, 75.62390960531439532 ) ) ;
#12980 = CARTESIAN_POINT ( 'NONE',  ( -0.05219959533936034679, 19.03943276465977164, 42.50109039468566152 ) ) ;
#12981 = CARTESIAN_POINT ( 'NONE',  ( 28.82186960331498327, 2.781578969918950771E-14, 145.2500000054623683 ) ) ;
#12982 = CARTESIAN_POINT ( 'NONE',  ( 16.46253265017160672, -9.564922557960803928, 83.33224293864768129 ) ) ;
#12983 = CARTESIAN_POINT ( 'NONE',  ( 12.06949235617757843, -12.14591786802309237, 53.12390960531436690 ) ) ;
#12984 = AXIS2_PLACEMENT_3D ( 'NONE', #30466, #31461, #136645 ) ;
#12985 = CARTESIAN_POINT ( 'NONE',  ( -4.379528057220328563, 16.55341960407611168, 40.20724293864769550 ) ) ;
#12986 = CARTESIAN_POINT ( 'NONE',  ( -16.55341960407611168, -4.379528057220339221, 21.45724293864769550 ) ) ;
#12987 = CARTESIAN_POINT ( 'NONE',  ( -5.049401038297874678, -19.05341960407617918, 64.79275706135233293 ) ) ;
#12988 = CARTESIAN_POINT ( 'NONE',  ( 18.89770734986053569, 5.499999999999910294, 51.60214472496640781 ) ) ;
#12989 = CARTESIAN_POINT ( 'NONE',  ( -19.03943276465977164, 0.05219959533909376836, 101.2489096053143669 ) ) ;
#12990 = CARTESIAN_POINT ( 'NONE',  ( 12.14591786802309770, 12.06949235617756955, 69.37390960531436690 ) ) ;
#12991 = CARTESIAN_POINT ( 'NONE',  ( 19.50973618000807619, -5.499999999999992895, 37.50000000000000000 ) ) ;
#12993 = CARTESIAN_POINT ( 'NONE',  ( -5.823673210054116645, -21.52544592524344225, 42.29057627198103120 ) ) ;
#12992 = CARTESIAN_POINT ( 'NONE',  ( -0.05219959533909027116, -19.03943276465977164, 27.49890960531435624 ) ) ;
#12994 = CARTESIAN_POINT ( 'NONE',  ( 15.72974639402199770, -15.80617190586745480, 73.12390960531436690 ) ) ;
#12995 = CARTESIAN_POINT ( 'NONE',  ( -4.379528057220328563, 16.55341960407611168, 110.2072429386477239 ) ) ;
#12997 = CARTESIAN_POINT ( 'NONE',  ( 19.03943276465977164, -0.05219959533909143690, 43.74890960531435979 ) ) ;
#12996 = CARTESIAN_POINT ( 'NONE',  ( 8.314922557961029526, -14.29746914071037800, 65.41775706135234714 ) ) ;
#12998 = EDGE_CURVE ( 'NONE', #189536, #105726, #146730, .T. ) ;
#12999 = CARTESIAN_POINT ( 'NONE',  ( -21.53943276465977519, -0.05219959533937600094, 53.75109039468568994 ) ) ;
#13000 = CARTESIAN_POINT ( 'NONE',  ( -14.29746914071049879, 8.314922557960819915, 110.8322429386476955 ) ) ;
#13001 = CARTESIAN_POINT ( 'NONE',  ( 16.29526858892872454, -7.335722546920260712, 36.70329402199793378 ) ) ;
#13002 = CARTESIAN_POINT ( 'NONE',  ( 36.91746824999999887, -11.99521256947793546, -10.22499999726881548 ) ) ;
#13003 = CARTESIAN_POINT ( 'NONE',  ( 5.823673210054125526, 21.52544592524343514, 34.79057627198103120 ) ) ;
#13004 = CARTESIAN_POINT ( 'NONE',  ( -40.00200000000003087, -5.510910596163089556E-15, 45.00000000000000000 ) ) ;
#13005 = CARTESIAN_POINT ( 'NONE',  ( 5.719274019375673035, 21.55341960407619339, 72.29275706135236135 ) ) ;
#13007 = CARTESIAN_POINT ( 'NONE',  ( 14.34966873604960469, 8.224510206698951720, 39.16557627198102409 ) ) ;
#13006 = CARTESIAN_POINT ( 'NONE',  ( 4.379528057220092307, 16.55341960407617563, 62.29275706135236845 ) ) ;
#13008 = CARTESIAN_POINT ( 'NONE',  ( 5.823673210054125526, 21.52544592524343514, 69.79057627198102409 ) ) ;
#13009 = CARTESIAN_POINT ( 'NONE',  ( -15.72974639402197994, 15.80617190586746368, 65.62390960531436690 ) ) ;
#13010 = CARTESIAN_POINT ( 'NONE',  ( 30.00000000000000000, 5.499999999999992895, 102.5000000000000142 ) ) ;
#13012 = CARTESIAN_POINT ( 'NONE',  ( -15.72974639402197994, 15.80617190586746368, 25.62390960531435624 ) ) ;
#13011 = CARTESIAN_POINT ( 'NONE',  ( -16.46253265017146816, -9.564922557961047289, 79.16775706135234714 ) ) ;
#13013 = CARTESIAN_POINT ( 'NONE',  ( -5.049401038298153566, 19.05341960407611168, 55.20724293864769550 ) ) ;
#13014 = CARTESIAN_POINT ( 'NONE',  ( 5.153800228976335163, 19.02544592524342804, 24.79057627198102765 ) ) ;
#13015 = CARTESIAN_POINT ( 'NONE',  ( 9.474510206698971260, -16.51473224551069308, 107.9155762719810383 ) ) ;
#13016 = EDGE_LOOP ( 'NONE', ( #106007, #37558 ) ) ;
#13017 = CARTESIAN_POINT ( 'NONE',  ( 8.224510206698742110, 14.34966873604972548, 72.08442372801899012 ) ) ;
#13018 = CARTESIAN_POINT ( 'NONE',  ( 18.62759615963271287, -10.81492255796078972, 108.3322429386477097 ) ) ;
#13019 = CARTESIAN_POINT ( 'NONE',  ( -16.46253265017160317, 9.564922557960807481, 55.83224293864769550 ) ) ;
#13020 = CARTESIAN_POINT ( 'NONE',  ( -18.67979575497193778, 10.72451020669871902, 38.33442372801900433 ) ) ;
#13021 = CARTESIAN_POINT ( 'NONE',  ( 19.02544592524343514, -5.153800228976328945, 93.54057627198102409 ) ) ;
#13022 = CARTESIAN_POINT ( 'NONE',  ( -32.73422133880766438, -23.92350924394295575, -17.85299461211518590 ) ) ;
#13023 = EDGE_LOOP ( 'NONE', ( #163707, #150234, #31137, #136726 ) ) ;
#13024 = CARTESIAN_POINT ( 'NONE',  ( 10.72451020669871369, 18.67979575497193778, 32.08442372801901854 ) ) ;
#13026 = CARTESIAN_POINT ( 'NONE',  ( 19.02544592524334988, 5.153800228976608722, 86.45942372801900433 ) ) ;
#13025 = CARTESIAN_POINT ( 'NONE',  ( 13.89961937509977652, -13.97604488694527269, 108.1239096053143669 ) ) ;
#13027 = CARTESIAN_POINT ( 'NONE',  ( 19.02544592524334988, 5.153800228976608722, 41.45942372801900433 ) ) ;
#13028 = CARTESIAN_POINT ( 'NONE',  ( 5.823673210054125526, 21.52544592524343514, 104.7905762719810241 ) ) ;
#13029 = CARTESIAN_POINT ( 'NONE',  ( -16.51473224551082808, 9.474510206698731452, 28.33442372801900433 ) ) ;
#13030 = CARTESIAN_POINT ( 'NONE',  ( 0.05219959533936267826, -19.03943276465977164, 55.00109039468566863 ) ) ;
#13031 = CARTESIAN_POINT ( 'NONE',  ( 8.224510206698742110, 14.34966873604972548, 92.08442372801901854 ) ) ;
#13033 = ORIENTED_EDGE ( 'NONE', *, *, #147612, .T. ) ;
#13032 = CARTESIAN_POINT ( 'NONE',  ( -8.898068258721467672, -27.38543819252872069, 146.3843446568999980 ) ) ;
#13034 = CARTESIAN_POINT ( 'NONE',  ( -16.51473224551069308, -9.474510206698971260, 66.66557627198102409 ) ) ;
#13035 = CARTESIAN_POINT ( 'NONE',  ( 0.05219959533937995610, -21.53943276465977519, 85.00109039468568994 ) ) ;
#13036 = CARTESIAN_POINT ( 'NONE',  ( 15.80617190586769283, -15.72974639402175789, 75.62609039468567573 ) ) ;
#13037 = CARTESIAN_POINT ( 'NONE',  ( 193.3062444957835453, -155.7167183371837496, -15.00000000000000178 ) ) ;
#13038 = CARTESIAN_POINT ( 'NONE',  ( 13.89961937509977652, -13.97604488694527269, 88.12390960531438111 ) ) ;
#13039 = CARTESIAN_POINT ( 'NONE',  ( 18.67979575497194134, -10.72451020669871369, 55.83442372801901854 ) ) ;
#13040 = CARTESIAN_POINT ( 'NONE',  ( -0.05219959533936034679, 19.03943276465977164, 102.5010903946856757 ) ) ;
#13041 = CARTESIAN_POINT ( 'NONE',  ( -0.05219959533909027116, -19.03943276465977164, 67.49890960531436690 ) ) ;
#13042 = CARTESIAN_POINT ( 'NONE',  ( -9.564922557960796823, -16.46253265017161027, 107.0822429386476955 ) ) ;
#13043 = CARTESIAN_POINT ( 'NONE',  ( -19.05341960407611168, -5.049401038298163336, 76.45724293864769550 ) ) ;
#13044 = CARTESIAN_POINT ( 'NONE',  ( 17.50000000000000711, -3.404445912590670087, 22.03715329543141621 ) ) ;
#13045 = CARTESIAN_POINT ( 'NONE',  ( -19.05341960407611168, -5.049401038298163336, 71.45724293864766707 ) ) ;
#13046 = CARTESIAN_POINT ( 'NONE',  ( 5.049401038298161559, -19.05341960407611168, 57.70724293864769550 ) ) ;
#13047 = CARTESIAN_POINT ( 'NONE',  ( -15.72974639402197994, 15.80617190586746368, 95.62390960531436690 ) ) ;
#13048 = CARTESIAN_POINT ( 'NONE',  ( 16.55341960407618274, -4.379528057220086978, 81.04275706135236135 ) ) ;
#13049 = FACE_OUTER_BOUND ( 'NONE', #133371, .T. ) ;
#13050 = CARTESIAN_POINT ( 'NONE',  ( -5.049401038297874678, -19.05341960407617918, 44.79275706135232582 ) ) ;
#13051 = CARTESIAN_POINT ( 'NONE',  ( -5.153800228976328057, -19.02544592524343514, 77.29057627198099567 ) ) ;
#13052 = CARTESIAN_POINT ( 'NONE',  ( -8.314922557960811034, -14.29746914071050412, 77.08224293864769550 ) ) ;
#13053 = CARTESIAN_POINT ( 'NONE',  ( -4.379528057220328563, 16.55341960407611168, 105.2072429386477097 ) ) ;
#13054 = CARTESIAN_POINT ( 'NONE',  ( -18.62759615963270932, 10.81492255796079327, 25.83224293864769194 ) ) ;
#13055 = CARTESIAN_POINT ( 'NONE',  ( 13.97604488694527802, 13.89961937509977652, 104.3739096053143385 ) ) ;
#13056 = CARTESIAN_POINT ( 'NONE',  ( 4.483927247898545687, 16.52544592524342804, 74.79057627198105251 ) ) ;
#13057 = DIRECTION ( 'NONE',  ( 1.000000000000000000, 0.000000000000000000, 3.709348145883536076E-20 ) ) ;
#13058 = CARTESIAN_POINT ( 'NONE',  ( 19.05341960407617918, -5.049401038297876454, 26.04275706135233293 ) ) ;
#13059 = CARTESIAN_POINT ( 'NONE',  ( -12.06949235617739369, -12.14591786802326823, 94.37609039468568994 ) ) ;
#13060 = CARTESIAN_POINT ( 'NONE',  ( -0.05219959533909027116, -19.03943276465977164, 72.49890960531435269 ) ) ;
#13061 = CARTESIAN_POINT ( 'NONE',  ( 21.55341960407619695, -5.719274019375665929, 51.04275706135234714 ) ) ;
#13062 = CARTESIAN_POINT ( 'NONE',  ( -21.53943276465977519, 0.05219959533907696930, 41.24890960531435269 ) ) ;
#13063 = CARTESIAN_POINT ( 'NONE',  ( 5.823673210054125526, 21.52544592524343514, 109.7905762719810383 ) ) ;
#13064 = CARTESIAN_POINT ( 'NONE',  ( 5.823673210054125526, 21.52544592524343514, 69.79057627198102409 ) ) ;
#13065 = CARTESIAN_POINT ( 'NONE',  ( 16.55341960407611168, 4.379528057220329451, 93.95724293864770971 ) ) ;
#13066 = CARTESIAN_POINT ( 'NONE',  ( 5.049401038297881783, 19.05341960407617563, 52.29275706135234003 ) ) ;
#13067 = CARTESIAN_POINT ( 'NONE',  ( -0.05219959533909027116, -19.03943276465977164, 32.49890960531435979 ) ) ;
#13068 = CARTESIAN_POINT ( 'NONE',  ( -13.89961937509977652, 13.97604488694528158, 80.62390960531436690 ) ) ;
#13069 = CARTESIAN_POINT ( 'NONE',  ( 0.05219959533909260263, 19.03943276465977164, 84.99890960531436690 ) ) ;
#13070 = CARTESIAN_POINT ( 'NONE',  ( -14.34966873604960291, -8.224510206698953496, 101.6655762719810383 ) ) ;
#13071 = CARTESIAN_POINT ( 'NONE',  ( -16.53943276465976808, 0.05219959533911058130, 31.24890960531435979 ) ) ;
#13072 = CARTESIAN_POINT ( 'NONE',  ( -4.379528057220086978, -16.55341960407618274, 29.79275706135234358 ) ) ;
#13073 = CARTESIAN_POINT ( 'NONE',  ( 10.81492255796106328, -18.62759615963255655, 90.41775706135236135 ) ) ;
#13074 = CARTESIAN_POINT ( 'NONE',  ( 13.89961937509977652, -13.97604488694527269, 103.1239096053143527 ) ) ;
#13075 = CARTESIAN_POINT ( 'NONE',  ( 21.53943276465977519, 0.05219959533937863772, 26.25109039468567573 ) ) ;
#13076 = CARTESIAN_POINT ( 'NONE',  ( -16.46253265017160317, 9.564922557960807481, 45.83224293864769550 ) ) ;
#13077 = CARTESIAN_POINT ( 'NONE',  ( -12.06949235617739369, -12.14591786802326823, 44.37609039468567573 ) ) ;
#13078 = EDGE_CURVE ( 'NONE', #161515, #82858, #127381, .T. ) ;
#13079 = B_SPLINE_CURVE_WITH_KNOTS ( 'NONE', 3,
 ( #147619, #193121, #162772, #86933, #116269, #176967, #9106, #191119, #133437, #39427, #70773, #192116, #24281, #118282, #6085, #178964, #99088, #132442, #148616, #164787, #10107, #8089, #103106, #179973, #114253, #194133, #55596, #68760 ),
 .UNSPECIFIED., .F., .F.,
 ( 4, 2, 2, 2, 2, 2, 2, 2, 2, 2, 2, 2, 2, 4 ),
 ( 0.000000000000000000, 0.002181393419090842979, 0.004362786838181685958, 0.005453483547727107014, 0.006544180257272528070, 0.006816854434658824353, 0.007089528612045118902, 0.007225865700738303039, 0.007294034245084918960, 0.007362202789431534881, 0.007498539878124766724, 0.007634876966818000300, 0.008180225321591003129, 0.008725573676364006825 ),
 .UNSPECIFIED. ) ;
#13080 = CARTESIAN_POINT ( 'NONE',  ( -5.153800228976607833, 19.02544592524334988, 102.7094237280189759 ) ) ;
#13081 = CARTESIAN_POINT ( 'NONE',  ( -13.89961937509977652, 13.97604488694528158, 40.62390960531435979 ) ) ;
#13082 = CARTESIAN_POINT ( 'NONE',  ( -14.29746914071049879, 8.314922557960819915, 100.8322429386477097 ) ) ;
#13083 = CARTESIAN_POINT ( 'NONE',  ( 10.81492255796078972, 18.62759615963270932, 109.5822429386476955 ) ) ;
#13084 = CARTESIAN_POINT ( 'NONE',  ( -9.564922557961040184, 16.46253265017147172, 77.91775706135234714 ) ) ;
#13085 = CARTESIAN_POINT ( 'NONE',  ( 13.89961937509977652, -13.97604488694527269, 23.12390960531436335 ) ) ;
#13086 = CARTESIAN_POINT ( 'NONE',  ( -16.51473224551069308, -9.474510206698971260, 86.66557627198102409 ) ) ;
#13087 = CARTESIAN_POINT ( 'NONE',  ( 10.72451020669898902, -18.67979575497178502, 112.9155762719810383 ) ) ;
#13088 = CARTESIAN_POINT ( 'NONE',  ( -13.97604488694527625, -13.89961937509977652, 21.87390960531435979 ) ) ;
#13089 = CARTESIAN_POINT ( 'NONE',  ( -13.97604488694527625, -13.89961937509977652, 86.87390960531436690 ) ) ;
#13090 = CARTESIAN_POINT ( 'NONE',  ( -28.79475375365586842, 2.428612866367529932E-14, 141.9843446568999923 ) ) ;
#13091 = CARTESIAN_POINT ( 'NONE',  ( -13.97604488694527625, -13.89961937509977652, 81.87390960531436690 ) ) ;
#13093 = CARTESIAN_POINT ( 'NONE',  ( 4.379528057220339221, -16.55341960407611168, 77.70724293864770971 ) ) ;
#13092 = CARTESIAN_POINT ( 'NONE',  ( -10.81492255796105439, 18.62759615963255655, 27.91775706135234358 ) ) ;
#13094 = CARTESIAN_POINT ( 'NONE',  ( 0.05219959533909260263, 19.03943276465977164, 94.99890960531436690 ) ) ;
#13095 = CARTESIAN_POINT ( 'NONE',  ( 9.474510206698729675, 16.51473224551082808, 22.08442372801899722 ) ) ;
#13097 =( BOUNDED_SURFACE ( )  B_SPLINE_SURFACE ( 3, 2, ( 
 ( #84572, #146250, #42102, #148272, #102763, #176620, #9764, #116922, #178615, #7736, #72430, #69422, #71428, #118944, #131089, #103766, #68414, #192777, #115932, #177622, #39090, #40078, #153227, #184575, #121896, #77385, #137071, #92546, #107711, #139053, #183589, #198761, #108721, #59231, #45074, #46056, #120900, #28926, #90566, #170398, #91539, #89583, #73441, #43088, #169390, #154235, #14731, #533, #196788, #199749, #12759, #76392, #152248, #166445, #104755, #27941, #30899, #123869, #60227, #15725, #138068, #62205, #122887, #167430, #106732, #168406, #61215, #185567, #47061, #88582, #135112, #150280, #11777, #105743, #151269, #74424, #136090, #197765, #29901, #119925, #58256, #182600, #181610, #44085, #13733, #75400, #113676, #48060, #3521, #186588, #51029, #127852, #142033, #81338, #124889, #65197, #189557, #31889, #171399, #159184, #33874, #190543, #4499, #64214, #111705, #80360, #188562, #16717, #109716, #32886, #67187, #50041, #143021, #140041, #96516, #157220, #18713, #78367, #174382, #1530, #158206, #66190, #17718, #173391, #93543, #19696, #112690, #34861, #35852, #97498, #20679, #82334, #126856, #144024, #5505, #128844, #52017, #155228, #63209, #94536, #156218, #2533, #79376, #141047, #125880, #172383, #95533, #187580, #49048, #110703, #160198, #129831, #71193, #179391, #39843, #164211, #83341, #86352, #99514, #178379, #115698, #53007, #191530, #114686, #132857, #10527, #147033, #102528, #163199, #25708, #9527, #54025, #193546, #131862, #101509, #40854, #148038, #87353, #21688, #57029, #8517, #145018, #6499, #133864, #38858, #194545, #24703, #56016, #68179, #146017, #117694, #161195, #130850, #69184, #149039, #177387, #192542, #176381, #72190, #37855, #22691, #7500, #195555, #84338, #100515, #162194, #175370, #23692, #85340, #70195, #36838, #55019, #98503, #116689, #73206, #119695, #104521, #166202, #90327, #150031, #103530, #134877, #296, #106489, #107473, #136835, #118702, #196554, #152012, #58025, #137827, #14486, #28691, #168167, #11538, #13498, #76148, #180393, #181378, #45822, #120666, #77145, #91296, #151037, #198518, #167194, #75163, #165205, #42856, #27703, #153991, #59989, #29664, #26700, #183351, #43842, #105507, #88340, #60976, #89346, #44834, #152987, #12527, #121657, #41864, #199510, #122652, #184340, #169150, #30654, #92308, #15488, #138815, #74192, #135861, #197532, #59000, #182364, #156975, #110461, #82085, #32640, #95291, #157966, #94294, #2288, #63970, #143778, #64956, #62961, #46817, #16478, #19458, #65944, #126615, #50792, #170155, #173146, #186337, #188317, #125640, #139796, #78128, #1285, #81105, #97257, #33629, #189315, #49795, #112451, #96280, #140799, #80122, #18472, #111461, #127615, #34621, #174140, #108477, #61964, #141791, #31648, #93297, #20434, #187337, #142783, #4264, #35612, #172142, #154983, #124642, #123631, #48807, #17470, #158945, #3285, #185327, #47819, #109468, #171152, #155973, #79126, #66942, #100273, #25471, #147801, #190297, #23448, #145775, #99267, #115454, #128604, #83100, #86110, #7256, #84096, #131617, #177144, #37604, #51774, #191289, #159952, #179147, #52765, #116450, #163974, #38615, #85095, #114434, #87111, #98250, #69952, #68941, #40615, #161952, #67940, #22447, #36594, #101264, #178139, #146781, #9286, #8274, #113434, #21440, #39605, #176135, #130605, #5259, #24460, #162954, #70951, #193301, #54776, #192300, #132621, #194308, #55775, #160953, #53779, #117448, #102285, #175127, #144776, #6260, #129593, #31168, #107985, #26460, #186863, #183856, #139327, #45343, #169672, #78645, #124151, #125164, #185850, #91812, #153504, #56790, #171667, #118462, #15001, #180154, #170673, #41623, #103287, #164967, #184846, #806, #32161, #62479, #93818, #140320, #16000, #33156, #92818, #200020, #1810, #76661, #106995, #149788, #46330, #122166, #47337, #88103, #154504, #63488, #71945, #108992, #11292, #77658, #16991, #148797, #30168, #133616 ),
 ( #48332, #155498, #109987, #10287, #138340, #61488, #72964, #195309, #134633, #123158, #196318, #57787, #168668, #126151, #64484, #128125, #144291, #175643, #5781, #37117, #83612, #159457, #176655, #112960, #143289, #145290, #35134, #50320, #95807, #189827, #65466, #190812, #187847, #51299, #6773, #17995, #52287, #49316, #174653, #160470, #94815, #173667, #4775, #141317, #110976, #53283, #96786, #111975, #130106, #36118, #97770, #34148, #158475, #3789, #19963, #20953, #156493, #82610, #114962, #98776, #79648, #67455, #81605, #188835, #66463, #2806, #172661, #21961, #129113, #113944, #68452, #191802, #127129, #157493, #80632, #18986, #142309, #85617, #149304, #196819, #71460, #117970, #147304, #119955, #131124, #102795, #101790, #73473, #194815, #100778, #55286, #69457, #134140, #10798, #179661, #118977, #56288, #99785, #54294, #72467, #8793, #40112, #38132, #57300, #195829, #180660, #164481, #133125, #178649, #41131, #25975, #88616, #193821, #24975, #87618, #115966, #42136, #70463, #163478, #161471, #103797, #165477, #26973, #150313, #11809, #86621, #135146, #58286, #22960, #116958, #148304, #84608, #146287, #9798, #7774, #192812, #177654, #39123, #162461, #23962, #132128, #13765, #169426, #75433, #199782, #108752, #154267, #155259, #15758, #121930, #183625, #89614, #1564, #151303, #45107, #12792, #564, #74457, #136123, #197799, #14764, #30931, #62235, #92579, #123903, #170428, #46090, #63239, #61250, #29935, #31920, #106764, #137107, #182633, #76425, #152281, #77417, #59265, #138101, #93574, #104788, #139089, #120934, #122921, #47091, #181641, #60259, #91574, #27975, #44117, #140073, #168439, #198793, #16749, #184609, #107745, #105776, #153263, #90599, #185602, #78397, #43120, #166476, #167463, #28958, #109744, #143049, #65225, #18742, #34890, #48088, #2562, #5535, #126885, #3547, #51056, #96546, #157248, #171428, #110735, #79406, #98534, #172416, #35880, #83371, #158233, #4528, #33904, #6529, #17750, #189584, #188591, #160227, #81365, #187609, #142061, #156248, #20709, #97527, #66220, #67214, #50072, #144053, #127880, #112718, #32915, #95561, #174411, #49078, #80389, #111733, #159214, #173420, #19724, #94570, #128872, #141077, #82365, #190572, #64244, #125911, #52048, #113704, #175401, #36869, #21718, #145048, #124919, #186616, #57057, #86381, #150061, #84368, #39872, #22720, #87382, #164241, #178408, #117723, #161226, #101539, #25736, #68209, #7529, #195585, #70224, #26728, #40883, #100544, #148065, #116719, #24731, #53038, #146045, #69214, #103559, #9556, #179418, #176410, #132885, #193576, #55048, #114718, #10555, #37886, #194574, #102556, #54055, #71222, #129861, #56044, #149067, #72219, #133894, #118732, #180420, #41893, #163231, #165234, #88367, #191559, #99544, #130882, #192571, #115729, #177416, #38887, #162223, #23722, #85371, #8547, #131892, #147064, #14515, #12552, #196580, #166229, #107501, #15515, #76176, #322, #119721, #122678, #135886, #137856, #152040, #89372, #27729, #151061, #169177, #46844, #183381, #31677, #106518, #29693, #136862, #90355, #91324, #168196, #199536, #77172, #184367, #123656, #58050, #93326, #44863, #181404, #42882, #170183, #75191, #45848, #92334, #61990, #61006, #11566, #153016, #60018, #185353, #13525, #167220, #74218, #30683, #182391, #154020, #104547, #138842, #108504, #134903, #73232, #197558, #59025, #120692, #43869, #198548, #121685, #105534, #28718, #113460, #95314, #110485, #190324, #34646, #157991, #94321, #156999, #63995, #18497, #173170, #16507, #49821, #175154, #97284, #139823, #96305, #80145, #48832, #64982, #78155, #32668, #35638, #141816, #33653, #81128, #126640, #187363, #1312, #140824, #109498, #128630, #2313, #65970, #36621, #188342, #19483, #125665, #155011, #47845, #142809, #3309, #51801, #111485, #17496, #172168, #186366, #50818, #112475, #4289, #189340, #127640, #62991, #171180, #174168, #158971, #20463, #124669, #82113, #143804 ),
 ( #155999, #79153, #5287, #66970, #176161, #133644, #130632, #86137, #192326, #116477, #25496, #70979, #71970, #132647, #38643, #100300, #6286, #118489, #67965, #161978, #129619, #117475, #191314, #52791, #114459, #131646, #147828, #179173, #37631, #99294, #56815, #23474, #40641, #101291, #162981, #83127, #68968, #24486, #22474, #53807, #115482, #194335, #177170, #85123, #160980, #102310, #144803, #9314, #146807, #84122, #145801, #7284, #8301, #69978, #193328, #54802, #178166, #180180, #55803, #87139, #39631, #98278, #164000, #148823, #10313, #195335, #159979, #21465, #91092, #134658, #74958, #199299, #123422, #181166, #168936, #43630, #84, #14271, #73981, #121447, #90118, #198301, #26487, #196344, #57812, #76933, #59778, #152780, #149813, #106276, #166981, #28484, #88129, #184130, #11319, #167961, #75940, #27488, #183139, #41649, #29460, #137615, #44623, #122438, #107265, #60766, #45613, #136620, #30443, #151802, #92089, #153778, #15273, #138602, #13293, #61754, #12316, #103313, #164993, #135650, #182146, #105293, #72989, #119484, #42643, #104305, #165988, #89131, #150819, #197321, #58784, #120453, #64756, #124431, #18267, #78916, #139590, #77923, #1076, #49587, #65739, #48604, #189116, #110256, #95085, #2083, #17263, #156773, #171937, #79920, #34420, #126418, #142582, #108266, #50589, #33426, #154774, #141593, #111250, #185115, #62751, #80905, #63763, #46605, #172941, #140593, #3080, #188115, #96079, #93090, #186128, #47607, #169945, #157768, #19259, #109261, #4061, #127407, #31436, #170940, #16271, #125436, #32432, #94086, #155765, #187132, #165644, #153440, #91745, #122102, #46265, #31103, #30105, #61422, #198961, #154439, #13933, #169605, #184779, #15933, #60428, #75600, #185782, #136290, #183792, #123093, #197966, #105944, #167629, #47269, #168605, #166644, #150482, #120120, #107920, #92751, #14938, #77592, #73642, #76598, #89786, #138274, #29126, #43289, #181811, #104958, #139263, #739, #137279, #27142, #45279, #106932, #90764, #44286, #199957, #62411, #124081, #88789, #11977, #135313, #196986, #58452, #28146, #151471, #12960, #74624, #152447, #59436, #121109, #182803, #48385, #80686, #5834, #83666, #79702, #66517, #143342, #64538, #22014, #19039, #174706, #142362, #4829, #113997, #159511, #160523, #21007, #127181, #188891, #94869, #6826, #156550, #50372, #18049, #67510, #141373, #2860, #126204, #20016, #36170, #129167, #97822, #190864, #175695, #173721, #33210, #52341, #187900, #113013, #82662, #172717, #128179, #186914, #144346, #37170, #189878, #98829, #145344, #51353, #68504, #81659, #110042, #35189, #171721, #49367, #111031, #34200, #96843, #95862, #157545, #3842, #65521, #112032, #158528, #134954, #14567, #135938, #131179, #115016, #84662, #28767, #136912, #197608, #121735, #38184, #43920, #57110, #59074, #73284, #7828, #146340, #69513, #90404, #168245, #104597, #153065, #27781, #151112, #58101, #11616, #12604, #89423, #120741, #198599, #105582, #44911, #176710, #130159, #166284, #99840, #161524, #91374, #196632, #152089, #182440, #191856, #53337, #167268, #119771, #118784, #88421, #26779, #13574, #181455, #150115, #23016, #60067, #195637, #75241, #42933, #180472, #41944, #103610, #165286, #74268, #183427, #106568, #29741, #158041, #64046, #65033, #94370, #76225, #92382, #47894, #30735, #95366, #172219, #186417, #125716, #169226, #109547, #33703, #137904, #15563, #3358, #78203, #34697, #48883, #108554, #156049, #124719, #32718, #61054, #154068, #77221, #111536, #17546, #187415, #184416, #140876, #1362, #157051, #107550, #138890, #45897, #171229, #110538, #18548, #80195, #141867, #126689, #2365, #199586, #79207, #188393, #49870, #16556, #31726, #370, #173221, #46894, #96354, #62041, #122726, #123705, #185403, #170233, #93374, #155061, #139873, #63041, #98330, #129667, #66022, #35687, #178215, #160030, #175206, #54853, #99346, #22523, #159021, #21517, #128680, #83178, #37681 ),
 ( #52841, #115533, #190377, #144852, #6335, #101341, #84170, #20514, #4338, #174219, #177221, #23525, #145850, #8352, #127690, #130682, #143858, #7332, #68015, #97335, #82162, #5337, #38694, #116527, #191363, #39679, #114510, #161029, #176212, #69016, #192376, #53859, #100350, #85171, #162029, #131696, #189390, #19532, #146859, #50867, #112525, #81177, #70027, #193377, #142859, #67021, #51852, #113511, #36671, #87191, #118539, #56864, #197369, #41698, #180228, #132695, #167026, #147877, #89178, #103363, #117525, #164048, #148872, #10363, #134709, #194384, #9363, #179223, #44669, #150870, #196392, #165041, #42692, #166037, #13337, #26534, #73037, #88178, #24536, #149862, #182192, #59823, #55851, #104353, #119533, #40689, #198349, #195386, #12364, #11367, #181216, #90164, #135697, #136667, #58834, #57860, #27537, #71028, #183187, #102358, #74027, #25547, #43677, #72020, #133693, #120501, #105339, #28528, #151847, #75002, #121493, #163030, #86187, #188160, #124476, #154818, #95129, #46650, #61798, #107308, #139633, #76977, #2127, #137659, #1121, #156819, #29504, #63809, #199346, #62795, #171983, #106322, #185160, #16316, #152827, #122484, #64801, #108310, #123468, #141636, #186173, #109306, #45657, #169990, #15318, #31481, #47655, #168008, #170985, #126462, #48649, #91137, #32478, #93133, #129, #77966, #14321, #184175, #187178, #94131, #155810, #17308, #78963, #138648, #75986, #92136, #60811, #79967, #153823, #140638, #168980, #125482, #110301, #33471, #30485, #18311, #3126, #113276, #84930, #6099, #112291, #66779, #80949, #145615, #7094, #21280, #83934, #160795, #111296, #65782, #68775, #20273, #51612, #131449, #130433, #192132, #53613, #114270, #36432, #96122, #115289, #157810, #175974, #22283, #35449, #67779, #49633, #37443, #99103, #129436, #176982, #38452, #100107, #161791, #82937, #23286, #98087, #146610, #8103, #69781, #144615, #159785, #172985, #81919, #191134, #34463, #143612, #190137, #174968, #19301, #52608, #50630, #142624, #4103, #127451, #189157, #173981, #97101, #158785, #5096, #128440, #196153, #133452, #70788, #9122, #132456, #150633, #28297, #164802, #13110, #87938, #11123, #118297, #71782, #72798, #149625, #119293, #197134, #104116, #105110, #177973, #74775, #26297, #101101, #162787, #151618, #56623, #12129, #57625, #193136, #54609, #165798, #179988, #117285, #148632, #86948, #27295, #195142, #10122, #24295, #58601, #39441, #180976, #41456, #147633, #194147, #178979, #40446, #134468, #85944, #55611, #102119, #116283, #42452, #181959, #88942, #163804, #25306, #73793, #103121, #135465, #120267, #43441, #166796, #89937, #169754, #93901, #18078, #75748, #63573, #138419, #94899, #109075, #168747, #16081, #184927, #92899, #121259, #90905, #29274, #171752, #154585, #185934, #44436, #887, #61567, #107076, #31249, #32243, #30251, #76744, #200099, #136437, #139405, #137425, #182953, #152591, #155579, #140404, #62562, #125247, #106090, #47419, #60572, #123236, #198118, #77739, #199105, #153585, #167776, #17074, #78728, #108070, #170754, #1892, #59585, #14082, #186945, #91894, #46411, #122248, #48416, #110072, #33241, #124238, #156583, #183938, #45423, #15083, #130191, #35218, #189908, #158555, #141402, #173750, #98861, #176741, #172749, #159542, #36199, #157575, #115049, #112062, #67540, #96871, #97853, #6857, #52372, #53371, #114029, #20045, #81688, #187929, #99870, #49398, #143370, #111061, #160556, #34230, #95892, #19068, #113044, #129198, #22046, #190896, #83697, #68536, #144377, #161554, #21040, #128211, #191887, #4862, #66547, #80715, #174736, #50402, #175726, #142393, #82693, #38214, #2890, #37205, #3872, #5864, #145375, #79733, #51383, #64569, #126234, #65551, #127210, #188924, #178736, #58371, #102878, #26057, #162546, #163561, #132215, #25061, #41217, #84692, #118057, #43206, #165561, #7859, #164563, #86704, #117041, #133209, #146372, #100864, #103881, #87700, #179747, #149385 ),
 ( #23047, #134229, #148389, #147392, #40199, #101879, #57389, #9883, #71543, #192901, #27058, #69546, #10881, #194900, #177739, #24050, #8880, #70548, #56374, #54378, #131210, #39208, #104873, #72551, #11896, #195914, #116050, #85706, #119062, #193907, #42220, #180744, #88704, #150400, #55371, #73559, #135232, #196904, #120038, #181725, #168526, #125013, #139177, #198879, #46179, #14854, #123009, #151388, #121021, #59352, #1658, #184695, #15847, #74543, #31016, #91662, #153352, #12878, #108840, #136208, #92666, #653, #152366, #107832, #166562, #154354, #77506, #169516, #47181, #32010, #62323, #123993, #199874, #155352, #76515, #170521, #185691, #16842, #61338, #138191, #186709, #137193, #93667, #78492, #60346, #106851, #30024, #48180, #140165, #167549, #197883, #182718, #63336, #28061, #89702, #44203, #105862, #29044, #90684, #13851, #75518, #122020, #183711, #45197, #67306, #145141, #81456, #129954, #4622, #127974, #34985, #188686, #142156, #189677, #36966, #82457, #83464, #144145, #50166, #111824, #17842, #191654, #79500, #173512, #141169, #128965, #2658, #64335, #126004, #143142, #159307, #190665, #20802, #52141, #98627, #174503, #109836, #51149, #158326, #160321, #96638, #65318, #110829, #66313, #80482, #5629, #187700, #112810, #21812, #33008, #113798, #49170, #35970, #175493, #171519, #19815, #97617, #156342, #172513, #68303, #6624, #126977, #94663, #33998, #95654, #157342, #18837, #3640, #55143, #71320, #114812, #148163, #73331, #195685, #37981, #132983, #193672, #147158, #163332, #176504, #130974, #133994, #116814, #131987, #179517, #24828, #85469, #99638, #38981, #7624, #26827, #100637, #164339, #11665, #86478, #194674, #162318, #135003, #146138, #56143, #178505, #53133, #117824, #115821, #70320, #84460, #149165, #10655, #9654, #87478, #25834, #161321, #69308, #72318, #23819, #39971, #22814, #57156, #118835, #180518, #40986, #102654, #101641, #41991, #103657, #165335, #8646, #88468, #150165, #192665, #54148, #177511, #93421, #89472, #76274, #153113, #74318, #31773, #28816, #184465, #45944, #77267, #107599, #138936, #185452, #61102, #78249, #14617, #44962, #46942, #136961, #152140, #197656, #29790, #167320, #92430, #27831, #91426, #108602, #119818, #154117, #151163, #137952, #62090, #196681, #75290, #106620, #42981, #12651, #155108, #198650, #13623, #16602, #199635, #122775, #135985, #60116, #105631, #121784, #169277, #58150, #30783, #181503, #416, #104646, #15610, #183478, #90456, #168294, #166333, #59122, #123753, #170279, #120788, #182488, #43969, #175006, #186467, #128479, #97139, #116320, #190174, #53652, #101137, #176012, #22320, #51650, #24332, #35489, #83971, #67818, #139922, #145651, #5134, #159824, #174018, #38489, #100146, #114310, #177020, #115329, #1411, #158822, #161827, #113314, #144653, #63090, #23322, #84966, #146648, #7132, #37481, #82977, #68815, #130474, #193173, #98127, #52646, #21319, #124769, #36470, #8142, #39476, #20310, #192171, #99143, #81958, #178009, #6135, #69819, #129473, #160832, #131486, #54645, #162823, #50668, #191172, #112328, #143650, #66816, #194183, #149663, #55648, #105146, #117320, #179016, #40484, #119330, #133487, #57663, #102156, #70825, #163842, #167810, #73831, #74810, #104154, #85982, #25343, #181016, #86984, #166832, #181996, #196191, #135501, #148671, #42490, #43479, #147671, #10159, #13147, #87975, #44472, #58637, #118333, #165835, #134505, #27332, #132494, #71819, #195179, #121296, #88978, #197172, #56660, #150668, #11161, #72835, #180026, #28333, #41495, #12166, #120303, #103158, #89972, #9159, #151652, #136472, #198152, #59622, #182988, #106127, #164839, #26335, #18113, #77772, #33274, #48450, #79768, #124273, #139439, #49434, #200132, #62595, #125283, #61601, #169789, #31282, #111095, #32279, #30285, #14117, #183971, #186980, #94933, #93935, #141438, #137462, #140438, #153622, #110108, #91930, #123270, #199142, #107112, #171786, #64603 ),
 ( #156618, #155614, #185969, #92933, #109109, #17110, #2925, #184961, #921, #108105, #90940, #46445, #126267, #187964, #122283, #170788, #47453, #168783, #29310, #154621, #78761, #16114, #1928, #152627, #63607, #75784, #60608, #45458, #15118, #76780, #138451, #54410, #190929, #21075, #161586, #113076, #128244, #173786, #5898, #143409, #68568, #3907, #67575, #23080, #95925, #130225, #65587, #129232, #38246, #172785, #51416, #82731, #19101, #188960, #131244, #174768, #189941, #7893, #52406, #175763, #112096, #36234, #81724, #97886, #114065, #34266, #37239, #192933, #115082, #157610, #98895, #159578, #66579, #144412, #80750, #50437, #53404, #160589, #22078, #83729, #145408, #4897, #142428, #158590, #127247, #146403, #20079, #6890, #35253, #191921, #176774, #99901, #96906, #84725, #69578, #41249, #197911, #195948, #178769, #133241, #147425, #11926, #73590, #87733, #150431, #27091, #177770, #132249, #135263, #86736, #118090, #116082, #196934, #58402, #120068, #180776, #149418, #56409, #57421, #119094, #166593, #71575, #26089, #194933, #39239, #9916, #181756, #12905, #8912, #42251, #72587, #193940, #151418, #148421, #103913, #179780, #134261, #43238, #88737, #89732, #104905, #102911, #164595, #24083, #136237, #85738, #10914, #70580, #28093, #55403, #117073, #40235, #165593, #74569, #100895, #101911, #162579, #163593, #25094, #155380, #169546, #108870, #152393, #92694, #16869, #141197, #198907, #186737, #61366, #17873, #32040, #91691, #139207, #107861, #15877, #44233, #13879, #75546, #94691, #77535, #170550, #167577, #124023, #184723, #46207, #105890, #1687, #29071, #185721, #93697, #45225, #682, #59381, #47211, #78520, #62353, #140194, #125041, #63364, #48208, #154382, #109862, #31045, #171547, #33036, #156369, #79527, #121054, #182749, #30050, #90710, #137221, #153382, #199902, #123037, #60375, #122047, #183738, #106879, #168552, #14883, #76544, #138220, #191682, #110857, #113826, #127007, #83493, #3669, #35013, #172542, #80512, #160351, #38011, #174532, #22842, #97646, #20832, #128005, #81485, #82488, #159335, #128996, #6654, #175521, #114841, #187728, #84489, #35999, #34027, #95685, #161351, #66343, #21841, #5658, #2686, #64363, #36996, #189707, #188715, #158356, #96668, #98657, #143172, #19844, #157372, #68332, #49199, #190694, #4652, #18866, #65347, #50198, #111854, #144172, #142185, #173544, #51180, #126032, #52169, #53163, #67334, #112840, #145170, #129982, #176535, #99667, #164366, #27859, #162346, #117852, #100664, #165363, #42019, #56171, #195713, #39009, #179545, #103684, #146167, #85497, #73360, #148189, #104675, #118862, #178531, #25861, #194702, #102681, #131002, #23847, #147185, #181529, #87505, #57186, #54177, #10683, #71348, #133012, #192694, #88499, #115850, #72347, #180545, #132014, #149193, #7652, #134021, #26857, #150195, #11693, #135032, #196707, #58177, #41015, #119844, #43008, #166362, #69336, #177540, #8675, #70347, #193701, #116841, #55171, #39998, #101670, #86505, #9683, #163360, #24856, #90484, #74344, #43997, #185482, #93451, #154147, #78279, #197682, #445, #13649, #170309, #152166, #121811, #59147, #167346, #46972, #124799, #61130, #109625, #184493, #107626, #14644, #168321, #169304, #45972, #15639, #155139, #62120, #1442, #136010, #171309, #122803, #120817, #182517, #47973, #153142, #108631, #92459, #89500, #151189, #123783, #76304, #75316, #44989, #183506, #31802, #29818, #106649, #105659, #16632, #28843, #77297, #91454, #136987, #198676, #60143, #137982, #30810, #199665, #139952, #63120, #138967, #186497, #12677, #94448, #48958, #67097, #3431, #34773, #114592, #51928, #128756, #113588, #97409, #66099, #173299, #112601, #35763, #83253, #188469, #142932, #111614, #156128, #126765, #175282, #129743, #125790, #174293, #189465, #110612, #68090, #65107, #20590, #49950, #50943, #160107, #36747, #96430, #172294, #159096, #64125, #17627, #187492, #32796, #82242, #21595 ),
 ( #33783, #144928, #158116, #191440, #5414, #19608, #143933, #81250, #190453, #79286, #95443, #157127, #52916, #98411, #6409, #140956, #2443, #4413, #127765, #18623, #80270, #141940, #102435, #148949, #162107, #194456, #176289, #164122, #25620, #132769, #56941, #41773, #40766, #72099, #9437, #165118, #24613, #180305, #195466, #26610, #71102, #86261, #196469, #146941, #55927, #133771, #8431, #116603, #178291, #57939, #179302, #177298, #161105, #130760, #118615, #103438, #87264, #88253, #84247, #10439, #100426, #149939, #38769, #70103, #145927, #53934, #11446, #73118, #193454, #101417, #147951, #134787, #39755, #7410, #37761, #69093, #163110, #192452, #99423, #115609, #23604, #85250, #117601, #22600, #131772, #54930, #209, #108395, #184255, #1201, #137740, #168084, #170072, #59903, #75078, #120581, #152903, #90242, #15400, #150950, #14399, #31563, #42771, #77057, #12444, #76065, #185242, #119610, #198429, #29581, #166116, #135776, #78044, #121571, #136745, #154899, #199424, #122565, #58913, #183266, #28604, #44746, #60889, #181293, #45737, #139713, #61878, #104433, #107389, #106402, #13414, #91212, #27619, #197447, #123548, #169062, #30568, #92219, #153905, #151925, #89258, #105420, #74106, #93214, #167103, #138729, #182274, #46733, #16398, #43756, #144695, #155889, #142704, #188237, #62877, #4183, #125559, #80043, #94210, #158866, #20355, #34542, #97180, #174064, #124558, #79042, #82003, #33548, #64877, #186255, #143696, #5179, #66860, #127533, #96201, #3203, #65862, #189236, #113359, #18392, #173065, #141712, #47733, #156896, #128523, #159871, #17387, #50714, #19379, #140717, #98170, #95209, #112372, #126538, #81028, #190217, #109386, #2207, #51696, #49712, #21363, #35532, #111376, #175051, #157890, #36515, #171066, #63888, #187256, #83021, #32556, #48725, #110378, #172061, #23369, #85014, #191216, #55694, #52690, #101183, #147718, #7179, #116367, #6181, #24380, #86031, #178055, #117367, #179064, #162872, #132540, #193220, #163893, #8192, #40533, #194228, #25389, #54694, #69867, #71864, #53701, #39523, #102204, #115378, #161875, #146695, #67861, #9206, #68863, #114354, #160877, #87031, #148716, #70872, #10204, #176058, #129516, #177066, #37526, #38537, #131536, #145697, #100193, #99189, #22368, #84019, #130522, #192218, #101172, #97170, #51686, #69854, #6170, #37514, #117357, #54681, #131522, #116355, #100181, #68851, #176046, #115365, #38525, #86018, #191205, #145686, #114343, #158855, #129505, #178044, #132529, #128512, #177055, #192206, #113348, #70860, #67850, #23357, #52680, #53688, #162860, #99176, #160866, #7168, #9195, #22356, #143685, #55683, #5166, #84008, #66849, #39512, #190207, #175040, #36505, #130510, #85002, #24367, #146683, #147707, #194218, #161863, #35522, #8178, #98159, #20343, #159859, #81992, #193208, #21352, #83010, #144685, #195215, #150703, #133523, #198185, #74842, #89012, #28367, #71854, #12201, #136505, #60642, #118369, #106161, #181050, #137495, #151688, #11196, #58669, #27366, #135535, #163880, #56695, #180062, #14150, #197206, #90005, #87020, #43513, #104188, #165870, #25378, #121329, #148706, #105179, #13179, #164875, #120335, #179053, #166865, #59655, #182030, #183021, #44505, #167843, #29344, #73866, #90973, #152660, #75817, #199175, #40521, #102192, #10194, #41531, #149698, #103194, #26370, #72871, #119366, #42525, #88010, #134540, #196228, #57698, #76812, #18144, #126295, #187011, #111124, #30319, #33304, #46479, #2954, #123302, #154653, #91962, #200164, #79797, #157640, #93966, #140472, #153655, #124305, #139472, #952, #1960, #78793, #48481, #187992, #94963, #34294, #107145, #3935, #155646, #15150, #138483, #80779, #186003, #141470, #125315, #122316, #184007, #156648, #47484, #108139, #77803, #16148, #64633, #62628, #109141, #61634, #49462, #168815, #110137, #170820, #184995, #172814, #32312, #169823, #171816, #17141, #63639, #31314, #95955, #92967 ) ),
 .UNSPECIFIED., .T., .F., .F. ) 
 B_SPLINE_SURFACE_WITH_KNOTS ( ( 4, 3, 4 ),
 ( 3, 2, 2, 2, 2, 2, 2, 2, 2, 2, 2, 2, 2, 2, 2, 2, 2, 2, 2, 2, 2, 2, 2, 2, 2, 2, 2, 2, 2, 2, 2, 2, 2, 2, 2, 2, 2, 2, 2, 2, 2, 2, 2, 2, 2, 2, 2, 2, 2, 2, 2, 2, 2, 2, 2, 2, 2, 2, 2, 2, 2, 2, 2, 2, 2, 2, 2, 2, 2, 2, 2, 2, 2, 2, 2, 2, 2, 2, 2, 2, 2, 2, 2, 2, 2, 2, 2, 2, 2, 2, 2, 2, 2, 2, 2, 2, 2, 2, 2, 2, 2, 2, 2, 2, 2, 2, 2, 2, 2, 2, 2, 2, 2, 2, 2, 2, 2, 2, 2, 2, 2, 2, 2, 2, 2, 2, 2, 2, 2, 2, 2, 2, 2, 2, 2, 2, 2, 2, 2, 2, 2, 2, 2, 2, 2, 2, 2, 2, 2, 2, 2, 2, 2, 2, 2, 2, 2, 2, 2, 2, 2, 2, 2, 2, 2, 2, 2, 2, 2, 2, 2, 2, 2, 2, 2, 2, 2, 2, 2, 2, 2, 2, 2, 2, 2, 2, 2, 2, 2, 2, 2, 2, 2, 2, 2, 2, 2, 2, 2, 2, 2, 2, 2, 2, 2, 2, 2, 2, 2, 2, 2, 2, 2, 2, 2, 2, 2, 2, 2, 2, 2, 2, 2, 2, 2, 2, 2, 2, 3 ),
 ( 0.000000000000000000, 0.5000000000000000000, 1.000000000000000000 ),
 ( 0.000000000000000000, 0.004385964912280701511, 0.008771929824561403022, 0.01315789473684210453, 0.01754385964912280604, 0.02192982456140350755, 0.02631578947368420907, 0.03070175438596491058, 0.03508771929824561209, 0.03947368421052631360, 0.04385964912280701511, 0.04824561403508771662, 0.05263157894736841813, 0.05701754385964911964, 0.06140350877192982115, 0.06578947368421052266, 0.07017543859649122417, 0.07456140350877192569, 0.07894736842105262720, 0.08333333333333332871, 0.08771929824561403022, 0.09210526315789473173, 0.09649122807017543324, 0.1008771929824561348, 0.1052631578947368363, 0.1096491228070175378, 0.1140350877192982393, 0.1184210526315789408, 0.1228070175438596423, 0.1271929824561403577, 0.1315789473684210453, 0.1359649122807017607, 0.1403508771929824483, 0.1447368421052631637, 0.1491228070175438514, 0.1535087719298245668, 0.1578947368421052544, 0.1622807017543859698, 0.1666666666666666574, 0.1710526315789473728, 0.1754385964912280604, 0.1798245614035087758, 0.1842105263157894635, 0.1885964912280701788, 0.1929824561403508665, 0.1973684210526315819, 0.2017543859649122695, 0.2061403508771929849, 0.2105263157894736725, 0.2149122807017543879, 0.2192982456140350755, 0.2236842105263157909, 0.2280701754385964786, 0.2324561403508771940, 0.2368421052631578816, 0.2412280701754385970, 0.2456140350877192846, 0.2500000000000000000, 0.2543859649122807154, 0.2587719298245614308, 0.2631578947368420907, 0.2675438596491228060, 0.2719298245614035214, 0.2763157894736842368, 0.2807017543859648967, 0.2850877192982456121, 0.2894736842105263275, 0.2938596491228070429, 0.2982456140350877027, 0.3026315789473684181, 0.3070175438596491335, 0.3114035087719298489, 0.3157894736842105088, 0.3201754385964912242, 0.3245614035087719396, 0.3289473684210526550, 0.3333333333333333148, 0.3377192982456140302, 0.3421052631578947456, 0.3464912280701754610, 0.3508771929824561209, 0.3552631578947368363, 0.3596491228070175517, 0.3640350877192982670, 0.3684210526315789269, 0.3728070175438596423, 0.3771929824561403577, 0.3815789473684210731, 0.3859649122807017330, 0.3903508771929824483, 0.3947368421052631637, 0.3991228070175438791, 0.4035087719298245390, 0.4078947368421052544, 0.4122807017543859698, 0.4166666666666666852, 0.4210526315789473450, 0.4254385964912280604, 0.4298245614035087758, 0.4342105263157894912, 0.4385964912280701511, 0.4429824561403508665, 0.4473684210526315819, 0.4517543859649122973, 0.4561403508771929571, 0.4605263157894736725, 0.4649122807017543879, 0.4692982456140351033, 0.4736842105263157632, 0.4780701754385964786, 0.4824561403508771940, 0.4868421052631579093, 0.4912280701754385692, 0.4956140350877192846, 0.5000000000000000000, 0.5043859649122807154, 0.5087719298245614308, 0.5131578947368421462, 0.5175438596491228616, 0.5219298245614034659, 0.5263157894736841813, 0.5307017543859648967, 0.5350877192982456121, 0.5394736842105263275, 0.5438596491228070429, 0.5482456140350877583, 0.5526315789473684736, 0.5570175438596490780, 0.5614035087719297934, 0.5657894736842105088, 0.5701754385964912242, 0.5745614035087719396, 0.5789473684210526550, 0.5833333333333333703, 0.5877192982456140857, 0.5921052631578946901, 0.5964912280701754055, 0.6008771929824561209, 0.6052631578947368363, 0.6096491228070175517, 0.6140350877192982670, 0.6184210526315789824, 0.6228070175438596978, 0.6271929824561403022, 0.6315789473684210176, 0.6359649122807017330, 0.6403508771929824483, 0.6447368421052631637, 0.6491228070175438791, 0.6535087719298245945, 0.6578947368421053099, 0.6622807017543859143, 0.6666666666666666297, 0.6710526315789473450, 0.6754385964912280604, 0.6798245614035087758, 0.6842105263157894912, 0.6885964912280702066, 0.6929824561403509220, 0.6973684210526315264, 0.7017543859649122417, 0.7061403508771929571, 0.7105263157894736725, 0.7149122807017543879, 0.7192982456140351033, 0.7236842105263158187, 0.7280701754385965341, 0.7324561403508771384, 0.7368421052631578538, 0.7412280701754385692, 0.7456140350877192846, 0.7500000000000000000, 0.7543859649122807154, 0.7587719298245614308, 0.7631578947368421462, 0.7675438596491228616, 0.7719298245614034659, 0.7763157894736841813, 0.7807017543859648967, 0.7850877192982456121, 0.7894736842105263275, 0.7938596491228070429, 0.7982456140350877583, 0.8026315789473684736, 0.8070175438596490780, 0.8114035087719297934, 0.8157894736842105088, 0.8201754385964912242, 0.8245614035087719396, 0.8289473684210526550, 0.8333333333333333703, 0.8377192982456140857, 0.8421052631578946901, 0.8464912280701754055, 0.8508771929824561209, 0.8552631578947368363, 0.8596491228070175517, 0.8640350877192982670, 0.8684210526315789824, 0.8728070175438596978, 0.8771929824561403022, 0.8815789473684210176, 0.8859649122807017330, 0.8903508771929824483, 0.8947368421052631637, 0.8991228070175438791, 0.9035087719298245945, 0.9078947368421053099, 0.9122807017543859143, 0.9166666666666666297, 0.9210526315789473450, 0.9254385964912280604, 0.9298245614035087758, 0.9342105263157894912, 0.9385964912280702066, 0.9429824561403509220, 0.9473684210526315264, 0.9517543859649122417, 0.9561403508771929571, 0.9605263157894736725, 0.9649122807017543879, 0.9692982456140351033, 0.9736842105263158187, 0.9780701754385965341, 0.9824561403508771384, 0.9868421052631578538, 0.9912280701754385692, 0.9956140350877192846, 1.000000000000000000 ),
 .UNSPECIFIED. ) 
 GEOMETRIC_REPRESENTATION_ITEM ( )  RATIONAL_B_SPLINE_SURFACE ( (
 ( 1.000000000000000000, 0.9659258262890683122, 1.000000000000000000, 0.9659258262890683122, 1.000000000000000000, 0.9659258262890683122, 1.000000000000000000, 0.9659258262890683122, 1.000000000000000000, 0.9659258262890683122, 1.000000000000000000, 0.9659258262890683122, 1.000000000000000000, 0.9659258262890683122, 1.000000000000000000, 0.9659258262890683122, 1.000000000000000000, 0.9659258262890683122, 1.000000000000000000, 0.9659258262890683122, 1.000000000000000000, 0.9659258262890683122, 1.000000000000000000, 0.9659258262890683122, 1.000000000000000000, 0.9659258262890683122, 1.000000000000000000, 0.9659258262890683122, 1.000000000000000000, 0.9659258262890683122, 1.000000000000000000, 0.9659258262890683122, 1.000000000000000000, 0.9659258262890683122, 1.000000000000000000, 0.9659258262890683122, 1.000000000000000000, 0.9659258262890683122, 1.000000000000000000, 0.9659258262890683122, 1.000000000000000000, 0.9659258262890683122, 1.000000000000000000, 0.9659258262890683122, 1.000000000000000000, 0.9659258262890683122, 1.000000000000000000, 0.9659258262890683122, 1.000000000000000000, 0.9659258262890683122, 1.000000000000000000, 0.9659258262890683122, 1.000000000000000000, 0.9659258262890683122, 1.000000000000000000, 0.9659258262890683122, 1.000000000000000000, 0.9659258262890683122, 1.000000000000000000, 0.9659258262890683122, 1.000000000000000000, 0.9659258262890683122, 1.000000000000000000, 0.9659258262890683122, 1.000000000000000000, 0.9659258262890683122, 1.000000000000000000, 0.9659258262890683122, 1.000000000000000000, 0.9659258262890683122, 1.000000000000000000, 0.9659258262890683122, 1.000000000000000000, 0.9659258262890683122, 1.000000000000000000, 0.9659258262890683122, 1.000000000000000000, 0.9659258262890683122, 1.000000000000000000, 0.9659258262890683122, 1.000000000000000000, 0.9659258262890683122, 1.000000000000000000, 0.9659258262890683122, 1.000000000000000000, 0.9659258262890683122, 1.000000000000000000, 0.9659258262890683122, 1.000000000000000000, 0.9659258262890683122, 1.000000000000000000, 0.9659258262890683122, 1.000000000000000000, 0.9659258262890683122, 1.000000000000000000, 0.9659258262890683122, 1.000000000000000000, 0.9659258262890683122, 1.000000000000000000, 0.9659258262890683122, 1.000000000000000000, 0.9659258262890683122, 1.000000000000000000, 0.9659258262890683122, 1.000000000000000000, 0.9659258262890683122, 1.000000000000000000, 0.9659258262890683122, 1.000000000000000000, 0.9659258262890683122, 1.000000000000000000, 0.9659258262890683122, 1.000000000000000000, 0.9659258262890683122, 1.000000000000000000, 0.9659258262890683122, 1.000000000000000000, 0.9659258262890683122, 1.000000000000000000, 0.9659258262890683122, 1.000000000000000000, 0.9659258262890683122, 1.000000000000000000, 0.9659258262890683122, 1.000000000000000000, 0.9659258262890683122, 1.000000000000000000, 0.9659258262890683122, 1.000000000000000000, 0.9659258262890683122, 1.000000000000000000, 0.9659258262890683122, 1.000000000000000000, 0.9659258262890683122, 1.000000000000000000, 0.9659258262890683122, 1.000000000000000000, 0.9659258262890683122, 1.000000000000000000, 0.9659258262890683122, 1.000000000000000000, 0.9659258262890683122, 1.000000000000000000, 0.9659258262890683122, 1.000000000000000000, 0.9659258262890683122, 1.000000000000000000, 0.9659258262890683122, 1.000000000000000000, 0.9659258262890683122, 1.000000000000000000, 0.9659258262890683122, 1.000000000000000000, 0.9659258262890683122, 1.000000000000000000, 0.9659258262890683122, 1.000000000000000000, 0.9659258262890683122, 1.000000000000000000, 0.9659258262890683122, 1.000000000000000000, 0.9659258262890683122, 1.000000000000000000, 0.9659258262890683122, 1.000000000000000000, 0.9659258262890683122, 1.000000000000000000, 0.9659258262890683122, 1.000000000000000000, 0.9659258262890683122, 1.000000000000000000, 0.9659258262890683122, 1.000000000000000000, 0.9659258262890683122, 1.000000000000000000, 0.9659258262890683122, 1.000000000000000000, 0.9659258262890683122, 1.000000000000000000, 0.9659258262890683122, 1.000000000000000000, 0.9659258262890683122, 1.000000000000000000, 0.9659258262890683122, 1.000000000000000000, 0.9659258262890683122, 1.000000000000000000, 0.9659258262890683122, 1.000000000000000000, 0.9659258262890683122, 1.000000000000000000, 0.9659258262890683122, 1.000000000000000000, 0.9659258262890683122, 1.000000000000000000, 0.9659258262890683122, 1.000000000000000000, 0.9659258262890683122, 1.000000000000000000, 0.9659258262890683122, 1.000000000000000000, 0.9659258262890683122, 1.000000000000000000, 0.9659258262890683122, 1.000000000000000000, 0.9659258262890683122, 1.000000000000000000, 0.9659258262890683122, 1.000000000000000000, 0.9659258262890683122, 1.000000000000000000, 0.9659258262890683122, 1.000000000000000000, 0.9659258262890683122, 1.000000000000000000, 0.9659258262890683122, 1.000000000000000000, 0.9659258262890683122, 1.000000000000000000, 0.9659258262890683122, 1.000000000000000000, 0.9659258262890683122, 1.000000000000000000, 0.9659258262890683122, 1.000000000000000000, 0.9659258262890683122, 1.000000000000000000, 0.9659258262890683122, 1.000000000000000000, 0.9659258262890683122, 1.000000000000000000, 0.9659258262890683122, 1.000000000000000000, 0.9659258262890683122, 1.000000000000000000, 0.9659258262890683122, 1.000000000000000000, 0.9659258262890683122, 1.000000000000000000, 0.9659258262890683122, 1.000000000000000000, 0.9659258262890683122, 1.000000000000000000, 0.9659258262890683122, 1.000000000000000000, 0.9659258262890683122, 1.000000000000000000, 0.9659258262890683122, 1.000000000000000000, 0.9659258262890683122, 1.000000000000000000, 0.9659258262890683122, 1.000000000000000000, 0.9659258262890683122, 1.000000000000000000, 0.9659258262890683122, 1.000000000000000000, 0.9659258262890683122, 1.000000000000000000, 0.9659258262890683122, 1.000000000000000000, 0.9659258262890683122, 1.000000000000000000, 0.9659258262890683122, 1.000000000000000000, 0.9659258262890683122, 1.000000000000000000, 0.9659258262890683122, 1.000000000000000000, 0.9659258262890683122, 1.000000000000000000, 0.9659258262890683122, 1.000000000000000000, 0.9659258262890683122, 1.000000000000000000, 0.9659258262890683122, 1.000000000000000000, 0.9659258262890683122, 1.000000000000000000, 0.9659258262890683122, 1.000000000000000000, 0.9659258262890683122, 1.000000000000000000, 0.9659258262890683122, 1.000000000000000000, 0.9659258262890683122, 1.000000000000000000, 0.9659258262890683122, 1.000000000000000000, 0.9659258262890683122, 1.000000000000000000, 0.9659258262890683122, 1.000000000000000000, 0.9659258262890683122, 1.000000000000000000, 0.9659258262890683122, 1.000000000000000000, 0.9659258262890683122, 1.000000000000000000, 0.9659258262890683122, 1.000000000000000000, 0.9659258262890683122, 1.000000000000000000, 0.9659258262890683122, 1.000000000000000000, 0.9659258262890683122, 1.000000000000000000, 0.9659258262890683122, 1.000000000000000000, 0.9659258262890683122, 1.000000000000000000, 0.9659258262890683122, 1.000000000000000000, 0.9659258262890683122, 1.000000000000000000, 0.9659258262890683122, 1.000000000000000000, 0.9659258262890683122, 1.000000000000000000, 0.9659258262890683122, 1.000000000000000000, 0.9659258262890683122, 1.000000000000000000, 0.9659258262890683122, 1.000000000000000000, 0.9659258262890683122, 1.000000000000000000, 0.9659258262890683122, 1.000000000000000000, 0.9659258262890683122, 1.000000000000000000, 0.9659258262890683122, 1.000000000000000000, 0.9659258262890683122, 1.000000000000000000, 0.9659258262890683122, 1.000000000000000000, 0.9659258262890683122, 1.000000000000000000, 0.9659258262890683122, 1.000000000000000000, 0.9659258262890683122, 1.000000000000000000, 0.9659258262890683122, 1.000000000000000000, 0.9659258262890683122, 1.000000000000000000, 0.9659258262890683122, 1.000000000000000000, 0.9659258262890683122, 1.000000000000000000, 0.9659258262890683122, 1.000000000000000000, 0.9659258262890683122, 1.000000000000000000, 0.9659258262890683122, 1.000000000000000000, 0.9659258262890683122, 1.000000000000000000, 0.9659258262890683122, 1.000000000000000000, 0.9659258262890683122, 1.000000000000000000, 0.9659258262890683122, 1.000000000000000000, 0.9659258262890683122, 1.000000000000000000, 0.9659258262890683122, 1.000000000000000000, 0.9659258262890683122, 1.000000000000000000, 0.9659258262890683122, 1.000000000000000000, 0.9659258262890683122, 1.000000000000000000, 0.9659258262890683122, 1.000000000000000000, 0.9659258262890683122, 1.000000000000000000, 0.9659258262890683122, 1.000000000000000000, 0.9659258262890683122, 1.000000000000000000, 0.9659258262890683122, 1.000000000000000000, 0.9659258262890683122, 1.000000000000000000, 0.9659258262890683122, 1.000000000000000000, 0.9659258262890683122, 1.000000000000000000, 0.9659258262890683122, 1.000000000000000000, 0.9659258262890683122, 1.000000000000000000, 0.9659258262890683122, 1.000000000000000000, 0.9659258262890683122, 1.000000000000000000, 0.9659258262890683122, 1.000000000000000000, 0.9659258262890683122, 1.000000000000000000, 0.9659258262890683122, 1.000000000000000000, 0.9659258262890683122, 1.000000000000000000, 0.9659258262890683122, 1.000000000000000000, 0.9659258262890683122, 1.000000000000000000, 0.9659258262890683122, 1.000000000000000000, 0.9659258262890683122, 1.000000000000000000, 0.9659258262890683122, 1.000000000000000000, 0.9659258262890683122, 1.000000000000000000, 0.9659258262890683122, 1.000000000000000000, 0.9659258262890683122, 1.000000000000000000, 0.9659258262890683122, 1.000000000000000000, 0.9659258262890683122, 1.000000000000000000, 0.9659258262890683122, 1.000000000000000000, 0.9659258262890683122, 1.000000000000000000, 0.9659258262890683122, 1.000000000000000000, 0.9659258262890683122, 1.000000000000000000, 0.9659258262890683122, 1.000000000000000000, 0.9659258262890683122, 1.000000000000000000, 0.9659258262890683122, 1.000000000000000000, 0.9659258262890683122, 1.000000000000000000, 0.9659258262890683122, 1.000000000000000000, 0.9659258262890683122, 1.000000000000000000, 0.9659258262890683122, 1.000000000000000000, 0.9659258262890683122, 1.000000000000000000, 0.9659258262890683122, 1.000000000000000000, 0.9659258262890683122, 1.000000000000000000, 0.9659258262890683122, 1.000000000000000000),
 ( 0.3333333333333333703, 0.3219752754296894559, 0.3333333333333333703, 0.3219752754296894559, 0.3333333333333333703, 0.3219752754296894559, 0.3333333333333333703, 0.3219752754296894559, 0.3333333333333333703, 0.3219752754296894559, 0.3333333333333333703, 0.3219752754296894559, 0.3333333333333333703, 0.3219752754296894559, 0.3333333333333333703, 0.3219752754296894559, 0.3333333333333333703, 0.3219752754296894559, 0.3333333333333333703, 0.3219752754296894559, 0.3333333333333333703, 0.3219752754296894559, 0.3333333333333333703, 0.3219752754296894559, 0.3333333333333333703, 0.3219752754296894559, 0.3333333333333333703, 0.3219752754296894559, 0.3333333333333333703, 0.3219752754296894559, 0.3333333333333333703, 0.3219752754296894559, 0.3333333333333333703, 0.3219752754296894559, 0.3333333333333333703, 0.3219752754296894559, 0.3333333333333333703, 0.3219752754296894559, 0.3333333333333333703, 0.3219752754296894559, 0.3333333333333333703, 0.3219752754296894559, 0.3333333333333333703, 0.3219752754296894559, 0.3333333333333333703, 0.3219752754296894559, 0.3333333333333333703, 0.3219752754296894559, 0.3333333333333333703, 0.3219752754296894559, 0.3333333333333333703, 0.3219752754296894559, 0.3333333333333333703, 0.3219752754296894559, 0.3333333333333333703, 0.3219752754296894559, 0.3333333333333333703, 0.3219752754296894559, 0.3333333333333333703, 0.3219752754296894559, 0.3333333333333333703, 0.3219752754296894559, 0.3333333333333333703, 0.3219752754296894559, 0.3333333333333333703, 0.3219752754296894559, 0.3333333333333333703, 0.3219752754296894559, 0.3333333333333333703, 0.3219752754296894559, 0.3333333333333333703, 0.3219752754296894559, 0.3333333333333333703, 0.3219752754296894559, 0.3333333333333333703, 0.3219752754296894559, 0.3333333333333333703, 0.3219752754296894559, 0.3333333333333333703, 0.3219752754296894559, 0.3333333333333333703, 0.3219752754296894559, 0.3333333333333333703, 0.3219752754296894559, 0.3333333333333333703, 0.3219752754296894559, 0.3333333333333333703, 0.3219752754296894559, 0.3333333333333333703, 0.3219752754296894559, 0.3333333333333333703, 0.3219752754296894559, 0.3333333333333333703, 0.3219752754296894559, 0.3333333333333333703, 0.3219752754296894559, 0.3333333333333333703, 0.3219752754296894559, 0.3333333333333333703, 0.3219752754296894559, 0.3333333333333333703, 0.3219752754296894559, 0.3333333333333333703, 0.3219752754296894559, 0.3333333333333333703, 0.3219752754296894559, 0.3333333333333333703, 0.3219752754296894559, 0.3333333333333333703, 0.3219752754296894559, 0.3333333333333333703, 0.3219752754296894559, 0.3333333333333333703, 0.3219752754296894559, 0.3333333333333333703, 0.3219752754296894559, 0.3333333333333333703, 0.3219752754296894559, 0.3333333333333333703, 0.3219752754296894559, 0.3333333333333333703, 0.3219752754296894559, 0.3333333333333333703, 0.3219752754296894559, 0.3333333333333333703, 0.3219752754296894559, 0.3333333333333333703, 0.3219752754296894559, 0.3333333333333333703, 0.3219752754296894559, 0.3333333333333333703, 0.3219752754296894559, 0.3333333333333333703, 0.3219752754296894559, 0.3333333333333333703, 0.3219752754296894559, 0.3333333333333333703, 0.3219752754296894559, 0.3333333333333333703, 0.3219752754296894559, 0.3333333333333333703, 0.3219752754296894559, 0.3333333333333333703, 0.3219752754296894559, 0.3333333333333333703, 0.3219752754296894559, 0.3333333333333333703, 0.3219752754296894559, 0.3333333333333333703, 0.3219752754296894559, 0.3333333333333333703, 0.3219752754296894559, 0.3333333333333333703, 0.3219752754296894559, 0.3333333333333333703, 0.3219752754296894559, 0.3333333333333333703, 0.3219752754296894559, 0.3333333333333333703, 0.3219752754296894559, 0.3333333333333333703, 0.3219752754296894559, 0.3333333333333333703, 0.3219752754296894559, 0.3333333333333333703, 0.3219752754296894559, 0.3333333333333333703, 0.3219752754296894559, 0.3333333333333333703, 0.3219752754296894559, 0.3333333333333333703, 0.3219752754296894559, 0.3333333333333333703, 0.3219752754296894559, 0.3333333333333333703, 0.3219752754296894559, 0.3333333333333333703, 0.3219752754296894559, 0.3333333333333333703, 0.3219752754296894559, 0.3333333333333333703, 0.3219752754296894559, 0.3333333333333333703, 0.3219752754296894559, 0.3333333333333333703, 0.3219752754296894559, 0.3333333333333333703, 0.3219752754296894559, 0.3333333333333333703, 0.3219752754296894559, 0.3333333333333333703, 0.3219752754296894559, 0.3333333333333333703, 0.3219752754296894559, 0.3333333333333333703, 0.3219752754296894559, 0.3333333333333333703, 0.3219752754296894559, 0.3333333333333333703, 0.3219752754296894559, 0.3333333333333333703, 0.3219752754296894559, 0.3333333333333333703, 0.3219752754296894559, 0.3333333333333333703, 0.3219752754296894559, 0.3333333333333333703, 0.3219752754296894559, 0.3333333333333333703, 0.3219752754296894559, 0.3333333333333333703, 0.3219752754296894559, 0.3333333333333333703, 0.3219752754296894559, 0.3333333333333333703, 0.3219752754296894559, 0.3333333333333333703, 0.3219752754296894559, 0.3333333333333333703, 0.3219752754296894559, 0.3333333333333333703, 0.3219752754296894559, 0.3333333333333333703, 0.3219752754296894559, 0.3333333333333333703, 0.3219752754296894559, 0.3333333333333333703, 0.3219752754296894559, 0.3333333333333333703, 0.3219752754296894559, 0.3333333333333333703, 0.3219752754296894559, 0.3333333333333333703, 0.3219752754296894559, 0.3333333333333333703, 0.3219752754296894559, 0.3333333333333333703, 0.3219752754296894559, 0.3333333333333333703, 0.3219752754296894559, 0.3333333333333333703, 0.3219752754296894559, 0.3333333333333333703, 0.3219752754296894559, 0.3333333333333333703, 0.3219752754296894559, 0.3333333333333333703, 0.3219752754296894559, 0.3333333333333333703, 0.3219752754296894559, 0.3333333333333333703, 0.3219752754296894559, 0.3333333333333333703, 0.3219752754296894559, 0.3333333333333333703, 0.3219752754296894559, 0.3333333333333333703, 0.3219752754296894559, 0.3333333333333333703, 0.3219752754296894559, 0.3333333333333333703, 0.3219752754296894559, 0.3333333333333333703, 0.3219752754296894559, 0.3333333333333333703, 0.3219752754296894559, 0.3333333333333333703, 0.3219752754296894559, 0.3333333333333333703, 0.3219752754296894559, 0.3333333333333333703, 0.3219752754296894559, 0.3333333333333333703, 0.3219752754296894559, 0.3333333333333333703, 0.3219752754296894559, 0.3333333333333333703, 0.3219752754296894559, 0.3333333333333333703, 0.3219752754296894559, 0.3333333333333333703, 0.3219752754296894559, 0.3333333333333333703, 0.3219752754296894559, 0.3333333333333333703, 0.3219752754296894559, 0.3333333333333333703, 0.3219752754296894559, 0.3333333333333333703, 0.3219752754296894559, 0.3333333333333333703, 0.3219752754296894559, 0.3333333333333333703, 0.3219752754296894559, 0.3333333333333333703, 0.3219752754296894559, 0.3333333333333333703, 0.3219752754296894559, 0.3333333333333333703, 0.3219752754296894559, 0.3333333333333333703, 0.3219752754296894559, 0.3333333333333333703, 0.3219752754296894559, 0.3333333333333333703, 0.3219752754296894559, 0.3333333333333333703, 0.3219752754296894559, 0.3333333333333333703, 0.3219752754296894559, 0.3333333333333333703, 0.3219752754296894559, 0.3333333333333333703, 0.3219752754296894559, 0.3333333333333333703, 0.3219752754296894559, 0.3333333333333333703, 0.3219752754296894559, 0.3333333333333333703, 0.3219752754296894559, 0.3333333333333333703, 0.3219752754296894559, 0.3333333333333333703, 0.3219752754296894559, 0.3333333333333333703, 0.3219752754296894559, 0.3333333333333333703, 0.3219752754296894559, 0.3333333333333333703, 0.3219752754296894559, 0.3333333333333333703, 0.3219752754296894559, 0.3333333333333333703, 0.3219752754296894559, 0.3333333333333333703, 0.3219752754296894559, 0.3333333333333333703, 0.3219752754296894559, 0.3333333333333333703, 0.3219752754296894559, 0.3333333333333333703, 0.3219752754296894559, 0.3333333333333333703, 0.3219752754296894559, 0.3333333333333333703, 0.3219752754296894559, 0.3333333333333333703, 0.3219752754296894559, 0.3333333333333333703, 0.3219752754296894559, 0.3333333333333333703, 0.3219752754296894559, 0.3333333333333333703, 0.3219752754296894559, 0.3333333333333333703, 0.3219752754296894559, 0.3333333333333333703, 0.3219752754296894559, 0.3333333333333333703, 0.3219752754296894559, 0.3333333333333333703, 0.3219752754296894559, 0.3333333333333333703, 0.3219752754296894559, 0.3333333333333333703, 0.3219752754296894559, 0.3333333333333333703, 0.3219752754296894559, 0.3333333333333333703, 0.3219752754296894559, 0.3333333333333333703, 0.3219752754296894559, 0.3333333333333333703, 0.3219752754296894559, 0.3333333333333333703, 0.3219752754296894559, 0.3333333333333333703, 0.3219752754296894559, 0.3333333333333333703, 0.3219752754296894559, 0.3333333333333333703, 0.3219752754296894559, 0.3333333333333333703, 0.3219752754296894559, 0.3333333333333333703, 0.3219752754296894559, 0.3333333333333333703, 0.3219752754296894559, 0.3333333333333333703, 0.3219752754296894559, 0.3333333333333333703, 0.3219752754296894559, 0.3333333333333333703, 0.3219752754296894559, 0.3333333333333333703, 0.3219752754296894559, 0.3333333333333333703, 0.3219752754296894559, 0.3333333333333333703, 0.3219752754296894559, 0.3333333333333333703, 0.3219752754296894559, 0.3333333333333333703, 0.3219752754296894559, 0.3333333333333333703, 0.3219752754296894559, 0.3333333333333333703, 0.3219752754296894559, 0.3333333333333333703, 0.3219752754296894559, 0.3333333333333333703, 0.3219752754296894559, 0.3333333333333333703, 0.3219752754296894559, 0.3333333333333333703, 0.3219752754296894559, 0.3333333333333333703, 0.3219752754296894559, 0.3333333333333333703, 0.3219752754296894559, 0.3333333333333333703, 0.3219752754296894559, 0.3333333333333333703, 0.3219752754296894559, 0.3333333333333333703, 0.3219752754296894559, 0.3333333333333333703, 0.3219752754296894559, 0.3333333333333333703, 0.3219752754296894559, 0.3333333333333333703, 0.3219752754296894559, 0.3333333333333333703, 0.3219752754296894559, 0.3333333333333333703, 0.3219752754296894559, 0.3333333333333333703, 0.3219752754296894559, 0.3333333333333333703, 0.3219752754296894559, 0.3333333333333333703, 0.3219752754296894559, 0.3333333333333333703, 0.3219752754296894559, 0.3333333333333333703, 0.3219752754296894559, 0.3333333333333333703, 0.3219752754296894559, 0.3333333333333333703, 0.3219752754296894559, 0.3333333333333333703, 0.3219752754296894559, 0.3333333333333333703, 0.3219752754296894559, 0.3333333333333333703, 0.3219752754296894559, 0.3333333333333333703),
 ( 0.3333333333333333703, 0.3219752754296894559, 0.3333333333333333703, 0.3219752754296894559, 0.3333333333333333703, 0.3219752754296894559, 0.3333333333333333703, 0.3219752754296894559, 0.3333333333333333703, 0.3219752754296894559, 0.3333333333333333703, 0.3219752754296894559, 0.3333333333333333703, 0.3219752754296894559, 0.3333333333333333703, 0.3219752754296894559, 0.3333333333333333703, 0.3219752754296894559, 0.3333333333333333703, 0.3219752754296894559, 0.3333333333333333703, 0.3219752754296894559, 0.3333333333333333703, 0.3219752754296894559, 0.3333333333333333703, 0.3219752754296894559, 0.3333333333333333703, 0.3219752754296894559, 0.3333333333333333703, 0.3219752754296894559, 0.3333333333333333703, 0.3219752754296894559, 0.3333333333333333703, 0.3219752754296894559, 0.3333333333333333703, 0.3219752754296894559, 0.3333333333333333703, 0.3219752754296894559, 0.3333333333333333703, 0.3219752754296894559, 0.3333333333333333703, 0.3219752754296894559, 0.3333333333333333703, 0.3219752754296894559, 0.3333333333333333703, 0.3219752754296894559, 0.3333333333333333703, 0.3219752754296894559, 0.3333333333333333703, 0.3219752754296894559, 0.3333333333333333703, 0.3219752754296894559, 0.3333333333333333703, 0.3219752754296894559, 0.3333333333333333703, 0.3219752754296894559, 0.3333333333333333703, 0.3219752754296894559, 0.3333333333333333703, 0.3219752754296894559, 0.3333333333333333703, 0.3219752754296894559, 0.3333333333333333703, 0.3219752754296894559, 0.3333333333333333703, 0.3219752754296894559, 0.3333333333333333703, 0.3219752754296894559, 0.3333333333333333703, 0.3219752754296894559, 0.3333333333333333703, 0.3219752754296894559, 0.3333333333333333703, 0.3219752754296894559, 0.3333333333333333703, 0.3219752754296894559, 0.3333333333333333703, 0.3219752754296894559, 0.3333333333333333703, 0.3219752754296894559, 0.3333333333333333703, 0.3219752754296894559, 0.3333333333333333703, 0.3219752754296894559, 0.3333333333333333703, 0.3219752754296894559, 0.3333333333333333703, 0.3219752754296894559, 0.3333333333333333703, 0.3219752754296894559, 0.3333333333333333703, 0.3219752754296894559, 0.3333333333333333703, 0.3219752754296894559, 0.3333333333333333703, 0.3219752754296894559, 0.3333333333333333703, 0.3219752754296894559, 0.3333333333333333703, 0.3219752754296894559, 0.3333333333333333703, 0.3219752754296894559, 0.3333333333333333703, 0.3219752754296894559, 0.3333333333333333703, 0.3219752754296894559, 0.3333333333333333703, 0.3219752754296894559, 0.3333333333333333703, 0.3219752754296894559, 0.3333333333333333703, 0.3219752754296894559, 0.3333333333333333703, 0.3219752754296894559, 0.3333333333333333703, 0.3219752754296894559, 0.3333333333333333703, 0.3219752754296894559, 0.3333333333333333703, 0.3219752754296894559, 0.3333333333333333703, 0.3219752754296894559, 0.3333333333333333703, 0.3219752754296894559, 0.3333333333333333703, 0.3219752754296894559, 0.3333333333333333703, 0.3219752754296894559, 0.3333333333333333703, 0.3219752754296894559, 0.3333333333333333703, 0.3219752754296894559, 0.3333333333333333703, 0.3219752754296894559, 0.3333333333333333703, 0.3219752754296894559, 0.3333333333333333703, 0.3219752754296894559, 0.3333333333333333703, 0.3219752754296894559, 0.3333333333333333703, 0.3219752754296894559, 0.3333333333333333703, 0.3219752754296894559, 0.3333333333333333703, 0.3219752754296894559, 0.3333333333333333703, 0.3219752754296894559, 0.3333333333333333703, 0.3219752754296894559, 0.3333333333333333703, 0.3219752754296894559, 0.3333333333333333703, 0.3219752754296894559, 0.3333333333333333703, 0.3219752754296894559, 0.3333333333333333703, 0.3219752754296894559, 0.3333333333333333703, 0.3219752754296894559, 0.3333333333333333703, 0.3219752754296894559, 0.3333333333333333703, 0.3219752754296894559, 0.3333333333333333703, 0.3219752754296894559, 0.3333333333333333703, 0.3219752754296894559, 0.3333333333333333703, 0.3219752754296894559, 0.3333333333333333703, 0.3219752754296894559, 0.3333333333333333703, 0.3219752754296894559, 0.3333333333333333703, 0.3219752754296894559, 0.3333333333333333703, 0.3219752754296894559, 0.3333333333333333703, 0.3219752754296894559, 0.3333333333333333703, 0.3219752754296894559, 0.3333333333333333703, 0.3219752754296894559, 0.3333333333333333703, 0.3219752754296894559, 0.3333333333333333703, 0.3219752754296894559, 0.3333333333333333703, 0.3219752754296894559, 0.3333333333333333703, 0.3219752754296894559, 0.3333333333333333703, 0.3219752754296894559, 0.3333333333333333703, 0.3219752754296894559, 0.3333333333333333703, 0.3219752754296894559, 0.3333333333333333703, 0.3219752754296894559, 0.3333333333333333703, 0.3219752754296894559, 0.3333333333333333703, 0.3219752754296894559, 0.3333333333333333703, 0.3219752754296894559, 0.3333333333333333703, 0.3219752754296894559, 0.3333333333333333703, 0.3219752754296894559, 0.3333333333333333703, 0.3219752754296894559, 0.3333333333333333703, 0.3219752754296894559, 0.3333333333333333703, 0.3219752754296894559, 0.3333333333333333703, 0.3219752754296894559, 0.3333333333333333703, 0.3219752754296894559, 0.3333333333333333703, 0.3219752754296894559, 0.3333333333333333703, 0.3219752754296894559, 0.3333333333333333703, 0.3219752754296894559, 0.3333333333333333703, 0.3219752754296894559, 0.3333333333333333703, 0.3219752754296894559, 0.3333333333333333703, 0.3219752754296894559, 0.3333333333333333703, 0.3219752754296894559, 0.3333333333333333703, 0.3219752754296894559, 0.3333333333333333703, 0.3219752754296894559, 0.3333333333333333703, 0.3219752754296894559, 0.3333333333333333703, 0.3219752754296894559, 0.3333333333333333703, 0.3219752754296894559, 0.3333333333333333703, 0.3219752754296894559, 0.3333333333333333703, 0.3219752754296894559, 0.3333333333333333703, 0.3219752754296894559, 0.3333333333333333703, 0.3219752754296894559, 0.3333333333333333703, 0.3219752754296894559, 0.3333333333333333703, 0.3219752754296894559, 0.3333333333333333703, 0.3219752754296894559, 0.3333333333333333703, 0.3219752754296894559, 0.3333333333333333703, 0.3219752754296894559, 0.3333333333333333703, 0.3219752754296894559, 0.3333333333333333703, 0.3219752754296894559, 0.3333333333333333703, 0.3219752754296894559, 0.3333333333333333703, 0.3219752754296894559, 0.3333333333333333703, 0.3219752754296894559, 0.3333333333333333703, 0.3219752754296894559, 0.3333333333333333703, 0.3219752754296894559, 0.3333333333333333703, 0.3219752754296894559, 0.3333333333333333703, 0.3219752754296894559, 0.3333333333333333703, 0.3219752754296894559, 0.3333333333333333703, 0.3219752754296894559, 0.3333333333333333703, 0.3219752754296894559, 0.3333333333333333703, 0.3219752754296894559, 0.3333333333333333703, 0.3219752754296894559, 0.3333333333333333703, 0.3219752754296894559, 0.3333333333333333703, 0.3219752754296894559, 0.3333333333333333703, 0.3219752754296894559, 0.3333333333333333703, 0.3219752754296894559, 0.3333333333333333703, 0.3219752754296894559, 0.3333333333333333703, 0.3219752754296894559, 0.3333333333333333703, 0.3219752754296894559, 0.3333333333333333703, 0.3219752754296894559, 0.3333333333333333703, 0.3219752754296894559, 0.3333333333333333703, 0.3219752754296894559, 0.3333333333333333703, 0.3219752754296894559, 0.3333333333333333703, 0.3219752754296894559, 0.3333333333333333703, 0.3219752754296894559, 0.3333333333333333703, 0.3219752754296894559, 0.3333333333333333703, 0.3219752754296894559, 0.3333333333333333703, 0.3219752754296894559, 0.3333333333333333703, 0.3219752754296894559, 0.3333333333333333703, 0.3219752754296894559, 0.3333333333333333703, 0.3219752754296894559, 0.3333333333333333703, 0.3219752754296894559, 0.3333333333333333703, 0.3219752754296894559, 0.3333333333333333703, 0.3219752754296894559, 0.3333333333333333703, 0.3219752754296894559, 0.3333333333333333703, 0.3219752754296894559, 0.3333333333333333703, 0.3219752754296894559, 0.3333333333333333703, 0.3219752754296894559, 0.3333333333333333703, 0.3219752754296894559, 0.3333333333333333703, 0.3219752754296894559, 0.3333333333333333703, 0.3219752754296894559, 0.3333333333333333703, 0.3219752754296894559, 0.3333333333333333703, 0.3219752754296894559, 0.3333333333333333703, 0.3219752754296894559, 0.3333333333333333703, 0.3219752754296894559, 0.3333333333333333703, 0.3219752754296894559, 0.3333333333333333703, 0.3219752754296894559, 0.3333333333333333703, 0.3219752754296894559, 0.3333333333333333703, 0.3219752754296894559, 0.3333333333333333703, 0.3219752754296894559, 0.3333333333333333703, 0.3219752754296894559, 0.3333333333333333703, 0.3219752754296894559, 0.3333333333333333703, 0.3219752754296894559, 0.3333333333333333703, 0.3219752754296894559, 0.3333333333333333703, 0.3219752754296894559, 0.3333333333333333703, 0.3219752754296894559, 0.3333333333333333703, 0.3219752754296894559, 0.3333333333333333703, 0.3219752754296894559, 0.3333333333333333703, 0.3219752754296894559, 0.3333333333333333703, 0.3219752754296894559, 0.3333333333333333703, 0.3219752754296894559, 0.3333333333333333703, 0.3219752754296894559, 0.3333333333333333703, 0.3219752754296894559, 0.3333333333333333703, 0.3219752754296894559, 0.3333333333333333703, 0.3219752754296894559, 0.3333333333333333703, 0.3219752754296894559, 0.3333333333333333703, 0.3219752754296894559, 0.3333333333333333703, 0.3219752754296894559, 0.3333333333333333703, 0.3219752754296894559, 0.3333333333333333703, 0.3219752754296894559, 0.3333333333333333703, 0.3219752754296894559, 0.3333333333333333703, 0.3219752754296894559, 0.3333333333333333703, 0.3219752754296894559, 0.3333333333333333703, 0.3219752754296894559, 0.3333333333333333703, 0.3219752754296894559, 0.3333333333333333703, 0.3219752754296894559, 0.3333333333333333703, 0.3219752754296894559, 0.3333333333333333703, 0.3219752754296894559, 0.3333333333333333703, 0.3219752754296894559, 0.3333333333333333703, 0.3219752754296894559, 0.3333333333333333703, 0.3219752754296894559, 0.3333333333333333703, 0.3219752754296894559, 0.3333333333333333703, 0.3219752754296894559, 0.3333333333333333703, 0.3219752754296894559, 0.3333333333333333703, 0.3219752754296894559, 0.3333333333333333703, 0.3219752754296894559, 0.3333333333333333703, 0.3219752754296894559, 0.3333333333333333703, 0.3219752754296894559, 0.3333333333333333703, 0.3219752754296894559, 0.3333333333333333703, 0.3219752754296894559, 0.3333333333333333703, 0.3219752754296894559, 0.3333333333333333703, 0.3219752754296894559, 0.3333333333333333703, 0.3219752754296894559, 0.3333333333333333703, 0.3219752754296894559, 0.3333333333333333703, 0.3219752754296894559, 0.3333333333333333703),
 ( 1.000000000000000000, 0.9659258262890683122, 1.000000000000000000, 0.9659258262890683122, 1.000000000000000000, 0.9659258262890683122, 1.000000000000000000, 0.9659258262890683122, 1.000000000000000000, 0.9659258262890683122, 1.000000000000000000, 0.9659258262890683122, 1.000000000000000000, 0.9659258262890683122, 1.000000000000000000, 0.9659258262890683122, 1.000000000000000000, 0.9659258262890683122, 1.000000000000000000, 0.9659258262890683122, 1.000000000000000000, 0.9659258262890683122, 1.000000000000000000, 0.9659258262890683122, 1.000000000000000000, 0.9659258262890683122, 1.000000000000000000, 0.9659258262890683122, 1.000000000000000000, 0.9659258262890683122, 1.000000000000000000, 0.9659258262890683122, 1.000000000000000000, 0.9659258262890683122, 1.000000000000000000, 0.9659258262890683122, 1.000000000000000000, 0.9659258262890683122, 1.000000000000000000, 0.9659258262890683122, 1.000000000000000000, 0.9659258262890683122, 1.000000000000000000, 0.9659258262890683122, 1.000000000000000000, 0.9659258262890683122, 1.000000000000000000, 0.9659258262890683122, 1.000000000000000000, 0.9659258262890683122, 1.000000000000000000, 0.9659258262890683122, 1.000000000000000000, 0.9659258262890683122, 1.000000000000000000, 0.9659258262890683122, 1.000000000000000000, 0.9659258262890683122, 1.000000000000000000, 0.9659258262890683122, 1.000000000000000000, 0.9659258262890683122, 1.000000000000000000, 0.9659258262890683122, 1.000000000000000000, 0.9659258262890683122, 1.000000000000000000, 0.9659258262890683122, 1.000000000000000000, 0.9659258262890683122, 1.000000000000000000, 0.9659258262890683122, 1.000000000000000000, 0.9659258262890683122, 1.000000000000000000, 0.9659258262890683122, 1.000000000000000000, 0.9659258262890683122, 1.000000000000000000, 0.9659258262890683122, 1.000000000000000000, 0.9659258262890683122, 1.000000000000000000, 0.9659258262890683122, 1.000000000000000000, 0.9659258262890683122, 1.000000000000000000, 0.9659258262890683122, 1.000000000000000000, 0.9659258262890683122, 1.000000000000000000, 0.9659258262890683122, 1.000000000000000000, 0.9659258262890683122, 1.000000000000000000, 0.9659258262890683122, 1.000000000000000000, 0.9659258262890683122, 1.000000000000000000, 0.9659258262890683122, 1.000000000000000000, 0.9659258262890683122, 1.000000000000000000, 0.9659258262890683122, 1.000000000000000000, 0.9659258262890683122, 1.000000000000000000, 0.9659258262890683122, 1.000000000000000000, 0.9659258262890683122, 1.000000000000000000, 0.9659258262890683122, 1.000000000000000000, 0.9659258262890683122, 1.000000000000000000, 0.9659258262890683122, 1.000000000000000000, 0.9659258262890683122, 1.000000000000000000, 0.9659258262890683122, 1.000000000000000000, 0.9659258262890683122, 1.000000000000000000, 0.9659258262890683122, 1.000000000000000000, 0.9659258262890683122, 1.000000000000000000, 0.9659258262890683122, 1.000000000000000000, 0.9659258262890683122, 1.000000000000000000, 0.9659258262890683122, 1.000000000000000000, 0.9659258262890683122, 1.000000000000000000, 0.9659258262890683122, 1.000000000000000000, 0.9659258262890683122, 1.000000000000000000, 0.9659258262890683122, 1.000000000000000000, 0.9659258262890683122, 1.000000000000000000, 0.9659258262890683122, 1.000000000000000000, 0.9659258262890683122, 1.000000000000000000, 0.9659258262890683122, 1.000000000000000000, 0.9659258262890683122, 1.000000000000000000, 0.9659258262890683122, 1.000000000000000000, 0.9659258262890683122, 1.000000000000000000, 0.9659258262890683122, 1.000000000000000000, 0.9659258262890683122, 1.000000000000000000, 0.9659258262890683122, 1.000000000000000000, 0.9659258262890683122, 1.000000000000000000, 0.9659258262890683122, 1.000000000000000000, 0.9659258262890683122, 1.000000000000000000, 0.9659258262890683122, 1.000000000000000000, 0.9659258262890683122, 1.000000000000000000, 0.9659258262890683122, 1.000000000000000000, 0.9659258262890683122, 1.000000000000000000, 0.9659258262890683122, 1.000000000000000000, 0.9659258262890683122, 1.000000000000000000, 0.9659258262890683122, 1.000000000000000000, 0.9659258262890683122, 1.000000000000000000, 0.9659258262890683122, 1.000000000000000000, 0.9659258262890683122, 1.000000000000000000, 0.9659258262890683122, 1.000000000000000000, 0.9659258262890683122, 1.000000000000000000, 0.9659258262890683122, 1.000000000000000000, 0.9659258262890683122, 1.000000000000000000, 0.9659258262890683122, 1.000000000000000000, 0.9659258262890683122, 1.000000000000000000, 0.9659258262890683122, 1.000000000000000000, 0.9659258262890683122, 1.000000000000000000, 0.9659258262890683122, 1.000000000000000000, 0.9659258262890683122, 1.000000000000000000, 0.9659258262890683122, 1.000000000000000000, 0.9659258262890683122, 1.000000000000000000, 0.9659258262890683122, 1.000000000000000000, 0.9659258262890683122, 1.000000000000000000, 0.9659258262890683122, 1.000000000000000000, 0.9659258262890683122, 1.000000000000000000, 0.9659258262890683122, 1.000000000000000000, 0.9659258262890683122, 1.000000000000000000, 0.9659258262890683122, 1.000000000000000000, 0.9659258262890683122, 1.000000000000000000, 0.9659258262890683122, 1.000000000000000000, 0.9659258262890683122, 1.000000000000000000, 0.9659258262890683122, 1.000000000000000000, 0.9659258262890683122, 1.000000000000000000, 0.9659258262890683122, 1.000000000000000000, 0.9659258262890683122, 1.000000000000000000, 0.9659258262890683122, 1.000000000000000000, 0.9659258262890683122, 1.000000000000000000, 0.9659258262890683122, 1.000000000000000000, 0.9659258262890683122, 1.000000000000000000, 0.9659258262890683122, 1.000000000000000000, 0.9659258262890683122, 1.000000000000000000, 0.9659258262890683122, 1.000000000000000000, 0.9659258262890683122, 1.000000000000000000, 0.9659258262890683122, 1.000000000000000000, 0.9659258262890683122, 1.000000000000000000, 0.9659258262890683122, 1.000000000000000000, 0.9659258262890683122, 1.000000000000000000, 0.9659258262890683122, 1.000000000000000000, 0.9659258262890683122, 1.000000000000000000, 0.9659258262890683122, 1.000000000000000000, 0.9659258262890683122, 1.000000000000000000, 0.9659258262890683122, 1.000000000000000000, 0.9659258262890683122, 1.000000000000000000, 0.9659258262890683122, 1.000000000000000000, 0.9659258262890683122, 1.000000000000000000, 0.9659258262890683122, 1.000000000000000000, 0.9659258262890683122, 1.000000000000000000, 0.9659258262890683122, 1.000000000000000000, 0.9659258262890683122, 1.000000000000000000, 0.9659258262890683122, 1.000000000000000000, 0.9659258262890683122, 1.000000000000000000, 0.9659258262890683122, 1.000000000000000000, 0.9659258262890683122, 1.000000000000000000, 0.9659258262890683122, 1.000000000000000000, 0.9659258262890683122, 1.000000000000000000, 0.9659258262890683122, 1.000000000000000000, 0.9659258262890683122, 1.000000000000000000, 0.9659258262890683122, 1.000000000000000000, 0.9659258262890683122, 1.000000000000000000, 0.9659258262890683122, 1.000000000000000000, 0.9659258262890683122, 1.000000000000000000, 0.9659258262890683122, 1.000000000000000000, 0.9659258262890683122, 1.000000000000000000, 0.9659258262890683122, 1.000000000000000000, 0.9659258262890683122, 1.000000000000000000, 0.9659258262890683122, 1.000000000000000000, 0.9659258262890683122, 1.000000000000000000, 0.9659258262890683122, 1.000000000000000000, 0.9659258262890683122, 1.000000000000000000, 0.9659258262890683122, 1.000000000000000000, 0.9659258262890683122, 1.000000000000000000, 0.9659258262890683122, 1.000000000000000000, 0.9659258262890683122, 1.000000000000000000, 0.9659258262890683122, 1.000000000000000000, 0.9659258262890683122, 1.000000000000000000, 0.9659258262890683122, 1.000000000000000000, 0.9659258262890683122, 1.000000000000000000, 0.9659258262890683122, 1.000000000000000000, 0.9659258262890683122, 1.000000000000000000, 0.9659258262890683122, 1.000000000000000000, 0.9659258262890683122, 1.000000000000000000, 0.9659258262890683122, 1.000000000000000000, 0.9659258262890683122, 1.000000000000000000, 0.9659258262890683122, 1.000000000000000000, 0.9659258262890683122, 1.000000000000000000, 0.9659258262890683122, 1.000000000000000000, 0.9659258262890683122, 1.000000000000000000, 0.9659258262890683122, 1.000000000000000000, 0.9659258262890683122, 1.000000000000000000, 0.9659258262890683122, 1.000000000000000000, 0.9659258262890683122, 1.000000000000000000, 0.9659258262890683122, 1.000000000000000000, 0.9659258262890683122, 1.000000000000000000, 0.9659258262890683122, 1.000000000000000000, 0.9659258262890683122, 1.000000000000000000, 0.9659258262890683122, 1.000000000000000000, 0.9659258262890683122, 1.000000000000000000, 0.9659258262890683122, 1.000000000000000000, 0.9659258262890683122, 1.000000000000000000, 0.9659258262890683122, 1.000000000000000000, 0.9659258262890683122, 1.000000000000000000, 0.9659258262890683122, 1.000000000000000000, 0.9659258262890683122, 1.000000000000000000, 0.9659258262890683122, 1.000000000000000000, 0.9659258262890683122, 1.000000000000000000, 0.9659258262890683122, 1.000000000000000000, 0.9659258262890683122, 1.000000000000000000, 0.9659258262890683122, 1.000000000000000000, 0.9659258262890683122, 1.000000000000000000, 0.9659258262890683122, 1.000000000000000000, 0.9659258262890683122, 1.000000000000000000, 0.9659258262890683122, 1.000000000000000000, 0.9659258262890683122, 1.000000000000000000, 0.9659258262890683122, 1.000000000000000000, 0.9659258262890683122, 1.000000000000000000, 0.9659258262890683122, 1.000000000000000000, 0.9659258262890683122, 1.000000000000000000, 0.9659258262890683122, 1.000000000000000000, 0.9659258262890683122, 1.000000000000000000, 0.9659258262890683122, 1.000000000000000000, 0.9659258262890683122, 1.000000000000000000, 0.9659258262890683122, 1.000000000000000000, 0.9659258262890683122, 1.000000000000000000, 0.9659258262890683122, 1.000000000000000000, 0.9659258262890683122, 1.000000000000000000, 0.9659258262890683122, 1.000000000000000000, 0.9659258262890683122, 1.000000000000000000, 0.9659258262890683122, 1.000000000000000000, 0.9659258262890683122, 1.000000000000000000, 0.9659258262890683122, 1.000000000000000000, 0.9659258262890683122, 1.000000000000000000, 0.9659258262890683122, 1.000000000000000000, 0.9659258262890683122, 1.000000000000000000, 0.9659258262890683122, 1.000000000000000000),
 ( 0.3333333333333333703, 0.3219752754296894559, 0.3333333333333333703, 0.3219752754296894559, 0.3333333333333333703, 0.3219752754296894559, 0.3333333333333333703, 0.3219752754296894559, 0.3333333333333333703, 0.3219752754296894559, 0.3333333333333333703, 0.3219752754296894559, 0.3333333333333333703, 0.3219752754296894559, 0.3333333333333333703, 0.3219752754296894559, 0.3333333333333333703, 0.3219752754296894559, 0.3333333333333333703, 0.3219752754296894559, 0.3333333333333333703, 0.3219752754296894559, 0.3333333333333333703, 0.3219752754296894559, 0.3333333333333333703, 0.3219752754296894559, 0.3333333333333333703, 0.3219752754296894559, 0.3333333333333333703, 0.3219752754296894559, 0.3333333333333333703, 0.3219752754296894559, 0.3333333333333333703, 0.3219752754296894559, 0.3333333333333333703, 0.3219752754296894559, 0.3333333333333333703, 0.3219752754296894559, 0.3333333333333333703, 0.3219752754296894559, 0.3333333333333333703, 0.3219752754296894559, 0.3333333333333333703, 0.3219752754296894559, 0.3333333333333333703, 0.3219752754296894559, 0.3333333333333333703, 0.3219752754296894559, 0.3333333333333333703, 0.3219752754296894559, 0.3333333333333333703, 0.3219752754296894559, 0.3333333333333333703, 0.3219752754296894559, 0.3333333333333333703, 0.3219752754296894559, 0.3333333333333333703, 0.3219752754296894559, 0.3333333333333333703, 0.3219752754296894559, 0.3333333333333333703, 0.3219752754296894559, 0.3333333333333333703, 0.3219752754296894559, 0.3333333333333333703, 0.3219752754296894559, 0.3333333333333333703, 0.3219752754296894559, 0.3333333333333333703, 0.3219752754296894559, 0.3333333333333333703, 0.3219752754296894559, 0.3333333333333333703, 0.3219752754296894559, 0.3333333333333333703, 0.3219752754296894559, 0.3333333333333333703, 0.3219752754296894559, 0.3333333333333333703, 0.3219752754296894559, 0.3333333333333333703, 0.3219752754296894559, 0.3333333333333333703, 0.3219752754296894559, 0.3333333333333333703, 0.3219752754296894559, 0.3333333333333333703, 0.3219752754296894559, 0.3333333333333333703, 0.3219752754296894559, 0.3333333333333333703, 0.3219752754296894559, 0.3333333333333333703, 0.3219752754296894559, 0.3333333333333333703, 0.3219752754296894559, 0.3333333333333333703, 0.3219752754296894559, 0.3333333333333333703, 0.3219752754296894559, 0.3333333333333333703, 0.3219752754296894559, 0.3333333333333333703, 0.3219752754296894559, 0.3333333333333333703, 0.3219752754296894559, 0.3333333333333333703, 0.3219752754296894559, 0.3333333333333333703, 0.3219752754296894559, 0.3333333333333333703, 0.3219752754296894559, 0.3333333333333333703, 0.3219752754296894559, 0.3333333333333333703, 0.3219752754296894559, 0.3333333333333333703, 0.3219752754296894559, 0.3333333333333333703, 0.3219752754296894559, 0.3333333333333333703, 0.3219752754296894559, 0.3333333333333333703, 0.3219752754296894559, 0.3333333333333333703, 0.3219752754296894559, 0.3333333333333333703, 0.3219752754296894559, 0.3333333333333333703, 0.3219752754296894559, 0.3333333333333333703, 0.3219752754296894559, 0.3333333333333333703, 0.3219752754296894559, 0.3333333333333333703, 0.3219752754296894559, 0.3333333333333333703, 0.3219752754296894559, 0.3333333333333333703, 0.3219752754296894559, 0.3333333333333333703, 0.3219752754296894559, 0.3333333333333333703, 0.3219752754296894559, 0.3333333333333333703, 0.3219752754296894559, 0.3333333333333333703, 0.3219752754296894559, 0.3333333333333333703, 0.3219752754296894559, 0.3333333333333333703, 0.3219752754296894559, 0.3333333333333333703, 0.3219752754296894559, 0.3333333333333333703, 0.3219752754296894559, 0.3333333333333333703, 0.3219752754296894559, 0.3333333333333333703, 0.3219752754296894559, 0.3333333333333333703, 0.3219752754296894559, 0.3333333333333333703, 0.3219752754296894559, 0.3333333333333333703, 0.3219752754296894559, 0.3333333333333333703, 0.3219752754296894559, 0.3333333333333333703, 0.3219752754296894559, 0.3333333333333333703, 0.3219752754296894559, 0.3333333333333333703, 0.3219752754296894559, 0.3333333333333333703, 0.3219752754296894559, 0.3333333333333333703, 0.3219752754296894559, 0.3333333333333333703, 0.3219752754296894559, 0.3333333333333333703, 0.3219752754296894559, 0.3333333333333333703, 0.3219752754296894559, 0.3333333333333333703, 0.3219752754296894559, 0.3333333333333333703, 0.3219752754296894559, 0.3333333333333333703, 0.3219752754296894559, 0.3333333333333333703, 0.3219752754296894559, 0.3333333333333333703, 0.3219752754296894559, 0.3333333333333333703, 0.3219752754296894559, 0.3333333333333333703, 0.3219752754296894559, 0.3333333333333333703, 0.3219752754296894559, 0.3333333333333333703, 0.3219752754296894559, 0.3333333333333333703, 0.3219752754296894559, 0.3333333333333333703, 0.3219752754296894559, 0.3333333333333333703, 0.3219752754296894559, 0.3333333333333333703, 0.3219752754296894559, 0.3333333333333333703, 0.3219752754296894559, 0.3333333333333333703, 0.3219752754296894559, 0.3333333333333333703, 0.3219752754296894559, 0.3333333333333333703, 0.3219752754296894559, 0.3333333333333333703, 0.3219752754296894559, 0.3333333333333333703, 0.3219752754296894559, 0.3333333333333333703, 0.3219752754296894559, 0.3333333333333333703, 0.3219752754296894559, 0.3333333333333333703, 0.3219752754296894559, 0.3333333333333333703, 0.3219752754296894559, 0.3333333333333333703, 0.3219752754296894559, 0.3333333333333333703, 0.3219752754296894559, 0.3333333333333333703, 0.3219752754296894559, 0.3333333333333333703, 0.3219752754296894559, 0.3333333333333333703, 0.3219752754296894559, 0.3333333333333333703, 0.3219752754296894559, 0.3333333333333333703, 0.3219752754296894559, 0.3333333333333333703, 0.3219752754296894559, 0.3333333333333333703, 0.3219752754296894559, 0.3333333333333333703, 0.3219752754296894559, 0.3333333333333333703, 0.3219752754296894559, 0.3333333333333333703, 0.3219752754296894559, 0.3333333333333333703, 0.3219752754296894559, 0.3333333333333333703, 0.3219752754296894559, 0.3333333333333333703, 0.3219752754296894559, 0.3333333333333333703, 0.3219752754296894559, 0.3333333333333333703, 0.3219752754296894559, 0.3333333333333333703, 0.3219752754296894559, 0.3333333333333333703, 0.3219752754296894559, 0.3333333333333333703, 0.3219752754296894559, 0.3333333333333333703, 0.3219752754296894559, 0.3333333333333333703, 0.3219752754296894559, 0.3333333333333333703, 0.3219752754296894559, 0.3333333333333333703, 0.3219752754296894559, 0.3333333333333333703, 0.3219752754296894559, 0.3333333333333333703, 0.3219752754296894559, 0.3333333333333333703, 0.3219752754296894559, 0.3333333333333333703, 0.3219752754296894559, 0.3333333333333333703, 0.3219752754296894559, 0.3333333333333333703, 0.3219752754296894559, 0.3333333333333333703, 0.3219752754296894559, 0.3333333333333333703, 0.3219752754296894559, 0.3333333333333333703, 0.3219752754296894559, 0.3333333333333333703, 0.3219752754296894559, 0.3333333333333333703, 0.3219752754296894559, 0.3333333333333333703, 0.3219752754296894559, 0.3333333333333333703, 0.3219752754296894559, 0.3333333333333333703, 0.3219752754296894559, 0.3333333333333333703, 0.3219752754296894559, 0.3333333333333333703, 0.3219752754296894559, 0.3333333333333333703, 0.3219752754296894559, 0.3333333333333333703, 0.3219752754296894559, 0.3333333333333333703, 0.3219752754296894559, 0.3333333333333333703, 0.3219752754296894559, 0.3333333333333333703, 0.3219752754296894559, 0.3333333333333333703, 0.3219752754296894559, 0.3333333333333333703, 0.3219752754296894559, 0.3333333333333333703, 0.3219752754296894559, 0.3333333333333333703, 0.3219752754296894559, 0.3333333333333333703, 0.3219752754296894559, 0.3333333333333333703, 0.3219752754296894559, 0.3333333333333333703, 0.3219752754296894559, 0.3333333333333333703, 0.3219752754296894559, 0.3333333333333333703, 0.3219752754296894559, 0.3333333333333333703, 0.3219752754296894559, 0.3333333333333333703, 0.3219752754296894559, 0.3333333333333333703, 0.3219752754296894559, 0.3333333333333333703, 0.3219752754296894559, 0.3333333333333333703, 0.3219752754296894559, 0.3333333333333333703, 0.3219752754296894559, 0.3333333333333333703, 0.3219752754296894559, 0.3333333333333333703, 0.3219752754296894559, 0.3333333333333333703, 0.3219752754296894559, 0.3333333333333333703, 0.3219752754296894559, 0.3333333333333333703, 0.3219752754296894559, 0.3333333333333333703, 0.3219752754296894559, 0.3333333333333333703, 0.3219752754296894559, 0.3333333333333333703, 0.3219752754296894559, 0.3333333333333333703, 0.3219752754296894559, 0.3333333333333333703, 0.3219752754296894559, 0.3333333333333333703, 0.3219752754296894559, 0.3333333333333333703, 0.3219752754296894559, 0.3333333333333333703, 0.3219752754296894559, 0.3333333333333333703, 0.3219752754296894559, 0.3333333333333333703, 0.3219752754296894559, 0.3333333333333333703, 0.3219752754296894559, 0.3333333333333333703, 0.3219752754296894559, 0.3333333333333333703, 0.3219752754296894559, 0.3333333333333333703, 0.3219752754296894559, 0.3333333333333333703, 0.3219752754296894559, 0.3333333333333333703, 0.3219752754296894559, 0.3333333333333333703, 0.3219752754296894559, 0.3333333333333333703, 0.3219752754296894559, 0.3333333333333333703, 0.3219752754296894559, 0.3333333333333333703, 0.3219752754296894559, 0.3333333333333333703, 0.3219752754296894559, 0.3333333333333333703, 0.3219752754296894559, 0.3333333333333333703, 0.3219752754296894559, 0.3333333333333333703, 0.3219752754296894559, 0.3333333333333333703, 0.3219752754296894559, 0.3333333333333333703, 0.3219752754296894559, 0.3333333333333333703, 0.3219752754296894559, 0.3333333333333333703, 0.3219752754296894559, 0.3333333333333333703, 0.3219752754296894559, 0.3333333333333333703, 0.3219752754296894559, 0.3333333333333333703, 0.3219752754296894559, 0.3333333333333333703, 0.3219752754296894559, 0.3333333333333333703, 0.3219752754296894559, 0.3333333333333333703, 0.3219752754296894559, 0.3333333333333333703, 0.3219752754296894559, 0.3333333333333333703, 0.3219752754296894559, 0.3333333333333333703, 0.3219752754296894559, 0.3333333333333333703, 0.3219752754296894559, 0.3333333333333333703, 0.3219752754296894559, 0.3333333333333333703, 0.3219752754296894559, 0.3333333333333333703, 0.3219752754296894559, 0.3333333333333333703, 0.3219752754296894559, 0.3333333333333333703, 0.3219752754296894559, 0.3333333333333333703, 0.3219752754296894559, 0.3333333333333333703, 0.3219752754296894559, 0.3333333333333333703, 0.3219752754296894559, 0.3333333333333333703, 0.3219752754296894559, 0.3333333333333333703, 0.3219752754296894559, 0.3333333333333333703),
 ( 0.3333333333333333703, 0.3219752754296894559, 0.3333333333333333703, 0.3219752754296894559, 0.3333333333333333703, 0.3219752754296894559, 0.3333333333333333703, 0.3219752754296894559, 0.3333333333333333703, 0.3219752754296894559, 0.3333333333333333703, 0.3219752754296894559, 0.3333333333333333703, 0.3219752754296894559, 0.3333333333333333703, 0.3219752754296894559, 0.3333333333333333703, 0.3219752754296894559, 0.3333333333333333703, 0.3219752754296894559, 0.3333333333333333703, 0.3219752754296894559, 0.3333333333333333703, 0.3219752754296894559, 0.3333333333333333703, 0.3219752754296894559, 0.3333333333333333703, 0.3219752754296894559, 0.3333333333333333703, 0.3219752754296894559, 0.3333333333333333703, 0.3219752754296894559, 0.3333333333333333703, 0.3219752754296894559, 0.3333333333333333703, 0.3219752754296894559, 0.3333333333333333703, 0.3219752754296894559, 0.3333333333333333703, 0.3219752754296894559, 0.3333333333333333703, 0.3219752754296894559, 0.3333333333333333703, 0.3219752754296894559, 0.3333333333333333703, 0.3219752754296894559, 0.3333333333333333703, 0.3219752754296894559, 0.3333333333333333703, 0.3219752754296894559, 0.3333333333333333703, 0.3219752754296894559, 0.3333333333333333703, 0.3219752754296894559, 0.3333333333333333703, 0.3219752754296894559, 0.3333333333333333703, 0.3219752754296894559, 0.3333333333333333703, 0.3219752754296894559, 0.3333333333333333703, 0.3219752754296894559, 0.3333333333333333703, 0.3219752754296894559, 0.3333333333333333703, 0.3219752754296894559, 0.3333333333333333703, 0.3219752754296894559, 0.3333333333333333703, 0.3219752754296894559, 0.3333333333333333703, 0.3219752754296894559, 0.3333333333333333703, 0.3219752754296894559, 0.3333333333333333703, 0.3219752754296894559, 0.3333333333333333703, 0.3219752754296894559, 0.3333333333333333703, 0.3219752754296894559, 0.3333333333333333703, 0.3219752754296894559, 0.3333333333333333703, 0.3219752754296894559, 0.3333333333333333703, 0.3219752754296894559, 0.3333333333333333703, 0.3219752754296894559, 0.3333333333333333703, 0.3219752754296894559, 0.3333333333333333703, 0.3219752754296894559, 0.3333333333333333703, 0.3219752754296894559, 0.3333333333333333703, 0.3219752754296894559, 0.3333333333333333703, 0.3219752754296894559, 0.3333333333333333703, 0.3219752754296894559, 0.3333333333333333703, 0.3219752754296894559, 0.3333333333333333703, 0.3219752754296894559, 0.3333333333333333703, 0.3219752754296894559, 0.3333333333333333703, 0.3219752754296894559, 0.3333333333333333703, 0.3219752754296894559, 0.3333333333333333703, 0.3219752754296894559, 0.3333333333333333703, 0.3219752754296894559, 0.3333333333333333703, 0.3219752754296894559, 0.3333333333333333703, 0.3219752754296894559, 0.3333333333333333703, 0.3219752754296894559, 0.3333333333333333703, 0.3219752754296894559, 0.3333333333333333703, 0.3219752754296894559, 0.3333333333333333703, 0.3219752754296894559, 0.3333333333333333703, 0.3219752754296894559, 0.3333333333333333703, 0.3219752754296894559, 0.3333333333333333703, 0.3219752754296894559, 0.3333333333333333703, 0.3219752754296894559, 0.3333333333333333703, 0.3219752754296894559, 0.3333333333333333703, 0.3219752754296894559, 0.3333333333333333703, 0.3219752754296894559, 0.3333333333333333703, 0.3219752754296894559, 0.3333333333333333703, 0.3219752754296894559, 0.3333333333333333703, 0.3219752754296894559, 0.3333333333333333703, 0.3219752754296894559, 0.3333333333333333703, 0.3219752754296894559, 0.3333333333333333703, 0.3219752754296894559, 0.3333333333333333703, 0.3219752754296894559, 0.3333333333333333703, 0.3219752754296894559, 0.3333333333333333703, 0.3219752754296894559, 0.3333333333333333703, 0.3219752754296894559, 0.3333333333333333703, 0.3219752754296894559, 0.3333333333333333703, 0.3219752754296894559, 0.3333333333333333703, 0.3219752754296894559, 0.3333333333333333703, 0.3219752754296894559, 0.3333333333333333703, 0.3219752754296894559, 0.3333333333333333703, 0.3219752754296894559, 0.3333333333333333703, 0.3219752754296894559, 0.3333333333333333703, 0.3219752754296894559, 0.3333333333333333703, 0.3219752754296894559, 0.3333333333333333703, 0.3219752754296894559, 0.3333333333333333703, 0.3219752754296894559, 0.3333333333333333703, 0.3219752754296894559, 0.3333333333333333703, 0.3219752754296894559, 0.3333333333333333703, 0.3219752754296894559, 0.3333333333333333703, 0.3219752754296894559, 0.3333333333333333703, 0.3219752754296894559, 0.3333333333333333703, 0.3219752754296894559, 0.3333333333333333703, 0.3219752754296894559, 0.3333333333333333703, 0.3219752754296894559, 0.3333333333333333703, 0.3219752754296894559, 0.3333333333333333703, 0.3219752754296894559, 0.3333333333333333703, 0.3219752754296894559, 0.3333333333333333703, 0.3219752754296894559, 0.3333333333333333703, 0.3219752754296894559, 0.3333333333333333703, 0.3219752754296894559, 0.3333333333333333703, 0.3219752754296894559, 0.3333333333333333703, 0.3219752754296894559, 0.3333333333333333703, 0.3219752754296894559, 0.3333333333333333703, 0.3219752754296894559, 0.3333333333333333703, 0.3219752754296894559, 0.3333333333333333703, 0.3219752754296894559, 0.3333333333333333703, 0.3219752754296894559, 0.3333333333333333703, 0.3219752754296894559, 0.3333333333333333703, 0.3219752754296894559, 0.3333333333333333703, 0.3219752754296894559, 0.3333333333333333703, 0.3219752754296894559, 0.3333333333333333703, 0.3219752754296894559, 0.3333333333333333703, 0.3219752754296894559, 0.3333333333333333703, 0.3219752754296894559, 0.3333333333333333703, 0.3219752754296894559, 0.3333333333333333703, 0.3219752754296894559, 0.3333333333333333703, 0.3219752754296894559, 0.3333333333333333703, 0.3219752754296894559, 0.3333333333333333703, 0.3219752754296894559, 0.3333333333333333703, 0.3219752754296894559, 0.3333333333333333703, 0.3219752754296894559, 0.3333333333333333703, 0.3219752754296894559, 0.3333333333333333703, 0.3219752754296894559, 0.3333333333333333703, 0.3219752754296894559, 0.3333333333333333703, 0.3219752754296894559, 0.3333333333333333703, 0.3219752754296894559, 0.3333333333333333703, 0.3219752754296894559, 0.3333333333333333703, 0.3219752754296894559, 0.3333333333333333703, 0.3219752754296894559, 0.3333333333333333703, 0.3219752754296894559, 0.3333333333333333703, 0.3219752754296894559, 0.3333333333333333703, 0.3219752754296894559, 0.3333333333333333703, 0.3219752754296894559, 0.3333333333333333703, 0.3219752754296894559, 0.3333333333333333703, 0.3219752754296894559, 0.3333333333333333703, 0.3219752754296894559, 0.3333333333333333703, 0.3219752754296894559, 0.3333333333333333703, 0.3219752754296894559, 0.3333333333333333703, 0.3219752754296894559, 0.3333333333333333703, 0.3219752754296894559, 0.3333333333333333703, 0.3219752754296894559, 0.3333333333333333703, 0.3219752754296894559, 0.3333333333333333703, 0.3219752754296894559, 0.3333333333333333703, 0.3219752754296894559, 0.3333333333333333703, 0.3219752754296894559, 0.3333333333333333703, 0.3219752754296894559, 0.3333333333333333703, 0.3219752754296894559, 0.3333333333333333703, 0.3219752754296894559, 0.3333333333333333703, 0.3219752754296894559, 0.3333333333333333703, 0.3219752754296894559, 0.3333333333333333703, 0.3219752754296894559, 0.3333333333333333703, 0.3219752754296894559, 0.3333333333333333703, 0.3219752754296894559, 0.3333333333333333703, 0.3219752754296894559, 0.3333333333333333703, 0.3219752754296894559, 0.3333333333333333703, 0.3219752754296894559, 0.3333333333333333703, 0.3219752754296894559, 0.3333333333333333703, 0.3219752754296894559, 0.3333333333333333703, 0.3219752754296894559, 0.3333333333333333703, 0.3219752754296894559, 0.3333333333333333703, 0.3219752754296894559, 0.3333333333333333703, 0.3219752754296894559, 0.3333333333333333703, 0.3219752754296894559, 0.3333333333333333703, 0.3219752754296894559, 0.3333333333333333703, 0.3219752754296894559, 0.3333333333333333703, 0.3219752754296894559, 0.3333333333333333703, 0.3219752754296894559, 0.3333333333333333703, 0.3219752754296894559, 0.3333333333333333703, 0.3219752754296894559, 0.3333333333333333703, 0.3219752754296894559, 0.3333333333333333703, 0.3219752754296894559, 0.3333333333333333703, 0.3219752754296894559, 0.3333333333333333703, 0.3219752754296894559, 0.3333333333333333703, 0.3219752754296894559, 0.3333333333333333703, 0.3219752754296894559, 0.3333333333333333703, 0.3219752754296894559, 0.3333333333333333703, 0.3219752754296894559, 0.3333333333333333703, 0.3219752754296894559, 0.3333333333333333703, 0.3219752754296894559, 0.3333333333333333703, 0.3219752754296894559, 0.3333333333333333703, 0.3219752754296894559, 0.3333333333333333703, 0.3219752754296894559, 0.3333333333333333703, 0.3219752754296894559, 0.3333333333333333703, 0.3219752754296894559, 0.3333333333333333703, 0.3219752754296894559, 0.3333333333333333703, 0.3219752754296894559, 0.3333333333333333703, 0.3219752754296894559, 0.3333333333333333703, 0.3219752754296894559, 0.3333333333333333703, 0.3219752754296894559, 0.3333333333333333703, 0.3219752754296894559, 0.3333333333333333703, 0.3219752754296894559, 0.3333333333333333703, 0.3219752754296894559, 0.3333333333333333703, 0.3219752754296894559, 0.3333333333333333703, 0.3219752754296894559, 0.3333333333333333703, 0.3219752754296894559, 0.3333333333333333703, 0.3219752754296894559, 0.3333333333333333703, 0.3219752754296894559, 0.3333333333333333703, 0.3219752754296894559, 0.3333333333333333703, 0.3219752754296894559, 0.3333333333333333703, 0.3219752754296894559, 0.3333333333333333703, 0.3219752754296894559, 0.3333333333333333703, 0.3219752754296894559, 0.3333333333333333703, 0.3219752754296894559, 0.3333333333333333703, 0.3219752754296894559, 0.3333333333333333703, 0.3219752754296894559, 0.3333333333333333703, 0.3219752754296894559, 0.3333333333333333703, 0.3219752754296894559, 0.3333333333333333703, 0.3219752754296894559, 0.3333333333333333703, 0.3219752754296894559, 0.3333333333333333703, 0.3219752754296894559, 0.3333333333333333703, 0.3219752754296894559, 0.3333333333333333703, 0.3219752754296894559, 0.3333333333333333703, 0.3219752754296894559, 0.3333333333333333703, 0.3219752754296894559, 0.3333333333333333703, 0.3219752754296894559, 0.3333333333333333703, 0.3219752754296894559, 0.3333333333333333703, 0.3219752754296894559, 0.3333333333333333703, 0.3219752754296894559, 0.3333333333333333703, 0.3219752754296894559, 0.3333333333333333703, 0.3219752754296894559, 0.3333333333333333703, 0.3219752754296894559, 0.3333333333333333703, 0.3219752754296894559, 0.3333333333333333703, 0.3219752754296894559, 0.3333333333333333703),
 ( 1.000000000000000000, 0.9659258262890683122, 1.000000000000000000, 0.9659258262890683122, 1.000000000000000000, 0.9659258262890683122, 1.000000000000000000, 0.9659258262890683122, 1.000000000000000000, 0.9659258262890683122, 1.000000000000000000, 0.9659258262890683122, 1.000000000000000000, 0.9659258262890683122, 1.000000000000000000, 0.9659258262890683122, 1.000000000000000000, 0.9659258262890683122, 1.000000000000000000, 0.9659258262890683122, 1.000000000000000000, 0.9659258262890683122, 1.000000000000000000, 0.9659258262890683122, 1.000000000000000000, 0.9659258262890683122, 1.000000000000000000, 0.9659258262890683122, 1.000000000000000000, 0.9659258262890683122, 1.000000000000000000, 0.9659258262890683122, 1.000000000000000000, 0.9659258262890683122, 1.000000000000000000, 0.9659258262890683122, 1.000000000000000000, 0.9659258262890683122, 1.000000000000000000, 0.9659258262890683122, 1.000000000000000000, 0.9659258262890683122, 1.000000000000000000, 0.9659258262890683122, 1.000000000000000000, 0.9659258262890683122, 1.000000000000000000, 0.9659258262890683122, 1.000000000000000000, 0.9659258262890683122, 1.000000000000000000, 0.9659258262890683122, 1.000000000000000000, 0.9659258262890683122, 1.000000000000000000, 0.9659258262890683122, 1.000000000000000000, 0.9659258262890683122, 1.000000000000000000, 0.9659258262890683122, 1.000000000000000000, 0.9659258262890683122, 1.000000000000000000, 0.9659258262890683122, 1.000000000000000000, 0.9659258262890683122, 1.000000000000000000, 0.9659258262890683122, 1.000000000000000000, 0.9659258262890683122, 1.000000000000000000, 0.9659258262890683122, 1.000000000000000000, 0.9659258262890683122, 1.000000000000000000, 0.9659258262890683122, 1.000000000000000000, 0.9659258262890683122, 1.000000000000000000, 0.9659258262890683122, 1.000000000000000000, 0.9659258262890683122, 1.000000000000000000, 0.9659258262890683122, 1.000000000000000000, 0.9659258262890683122, 1.000000000000000000, 0.9659258262890683122, 1.000000000000000000, 0.9659258262890683122, 1.000000000000000000, 0.9659258262890683122, 1.000000000000000000, 0.9659258262890683122, 1.000000000000000000, 0.9659258262890683122, 1.000000000000000000, 0.9659258262890683122, 1.000000000000000000, 0.9659258262890683122, 1.000000000000000000, 0.9659258262890683122, 1.000000000000000000, 0.9659258262890683122, 1.000000000000000000, 0.9659258262890683122, 1.000000000000000000, 0.9659258262890683122, 1.000000000000000000, 0.9659258262890683122, 1.000000000000000000, 0.9659258262890683122, 1.000000000000000000, 0.9659258262890683122, 1.000000000000000000, 0.9659258262890683122, 1.000000000000000000, 0.9659258262890683122, 1.000000000000000000, 0.9659258262890683122, 1.000000000000000000, 0.9659258262890683122, 1.000000000000000000, 0.9659258262890683122, 1.000000000000000000, 0.9659258262890683122, 1.000000000000000000, 0.9659258262890683122, 1.000000000000000000, 0.9659258262890683122, 1.000000000000000000, 0.9659258262890683122, 1.000000000000000000, 0.9659258262890683122, 1.000000000000000000, 0.9659258262890683122, 1.000000000000000000, 0.9659258262890683122, 1.000000000000000000, 0.9659258262890683122, 1.000000000000000000, 0.9659258262890683122, 1.000000000000000000, 0.9659258262890683122, 1.000000000000000000, 0.9659258262890683122, 1.000000000000000000, 0.9659258262890683122, 1.000000000000000000, 0.9659258262890683122, 1.000000000000000000, 0.9659258262890683122, 1.000000000000000000, 0.9659258262890683122, 1.000000000000000000, 0.9659258262890683122, 1.000000000000000000, 0.9659258262890683122, 1.000000000000000000, 0.9659258262890683122, 1.000000000000000000, 0.9659258262890683122, 1.000000000000000000, 0.9659258262890683122, 1.000000000000000000, 0.9659258262890683122, 1.000000000000000000, 0.9659258262890683122, 1.000000000000000000, 0.9659258262890683122, 1.000000000000000000, 0.9659258262890683122, 1.000000000000000000, 0.9659258262890683122, 1.000000000000000000, 0.9659258262890683122, 1.000000000000000000, 0.9659258262890683122, 1.000000000000000000, 0.9659258262890683122, 1.000000000000000000, 0.9659258262890683122, 1.000000000000000000, 0.9659258262890683122, 1.000000000000000000, 0.9659258262890683122, 1.000000000000000000, 0.9659258262890683122, 1.000000000000000000, 0.9659258262890683122, 1.000000000000000000, 0.9659258262890683122, 1.000000000000000000, 0.9659258262890683122, 1.000000000000000000, 0.9659258262890683122, 1.000000000000000000, 0.9659258262890683122, 1.000000000000000000, 0.9659258262890683122, 1.000000000000000000, 0.9659258262890683122, 1.000000000000000000, 0.9659258262890683122, 1.000000000000000000, 0.9659258262890683122, 1.000000000000000000, 0.9659258262890683122, 1.000000000000000000, 0.9659258262890683122, 1.000000000000000000, 0.9659258262890683122, 1.000000000000000000, 0.9659258262890683122, 1.000000000000000000, 0.9659258262890683122, 1.000000000000000000, 0.9659258262890683122, 1.000000000000000000, 0.9659258262890683122, 1.000000000000000000, 0.9659258262890683122, 1.000000000000000000, 0.9659258262890683122, 1.000000000000000000, 0.9659258262890683122, 1.000000000000000000, 0.9659258262890683122, 1.000000000000000000, 0.9659258262890683122, 1.000000000000000000, 0.9659258262890683122, 1.000000000000000000, 0.9659258262890683122, 1.000000000000000000, 0.9659258262890683122, 1.000000000000000000, 0.9659258262890683122, 1.000000000000000000, 0.9659258262890683122, 1.000000000000000000, 0.9659258262890683122, 1.000000000000000000, 0.9659258262890683122, 1.000000000000000000, 0.9659258262890683122, 1.000000000000000000, 0.9659258262890683122, 1.000000000000000000, 0.9659258262890683122, 1.000000000000000000, 0.9659258262890683122, 1.000000000000000000, 0.9659258262890683122, 1.000000000000000000, 0.9659258262890683122, 1.000000000000000000, 0.9659258262890683122, 1.000000000000000000, 0.9659258262890683122, 1.000000000000000000, 0.9659258262890683122, 1.000000000000000000, 0.9659258262890683122, 1.000000000000000000, 0.9659258262890683122, 1.000000000000000000, 0.9659258262890683122, 1.000000000000000000, 0.9659258262890683122, 1.000000000000000000, 0.9659258262890683122, 1.000000000000000000, 0.9659258262890683122, 1.000000000000000000, 0.9659258262890683122, 1.000000000000000000, 0.9659258262890683122, 1.000000000000000000, 0.9659258262890683122, 1.000000000000000000, 0.9659258262890683122, 1.000000000000000000, 0.9659258262890683122, 1.000000000000000000, 0.9659258262890683122, 1.000000000000000000, 0.9659258262890683122, 1.000000000000000000, 0.9659258262890683122, 1.000000000000000000, 0.9659258262890683122, 1.000000000000000000, 0.9659258262890683122, 1.000000000000000000, 0.9659258262890683122, 1.000000000000000000, 0.9659258262890683122, 1.000000000000000000, 0.9659258262890683122, 1.000000000000000000, 0.9659258262890683122, 1.000000000000000000, 0.9659258262890683122, 1.000000000000000000, 0.9659258262890683122, 1.000000000000000000, 0.9659258262890683122, 1.000000000000000000, 0.9659258262890683122, 1.000000000000000000, 0.9659258262890683122, 1.000000000000000000, 0.9659258262890683122, 1.000000000000000000, 0.9659258262890683122, 1.000000000000000000, 0.9659258262890683122, 1.000000000000000000, 0.9659258262890683122, 1.000000000000000000, 0.9659258262890683122, 1.000000000000000000, 0.9659258262890683122, 1.000000000000000000, 0.9659258262890683122, 1.000000000000000000, 0.9659258262890683122, 1.000000000000000000, 0.9659258262890683122, 1.000000000000000000, 0.9659258262890683122, 1.000000000000000000, 0.9659258262890683122, 1.000000000000000000, 0.9659258262890683122, 1.000000000000000000, 0.9659258262890683122, 1.000000000000000000, 0.9659258262890683122, 1.000000000000000000, 0.9659258262890683122, 1.000000000000000000, 0.9659258262890683122, 1.000000000000000000, 0.9659258262890683122, 1.000000000000000000, 0.9659258262890683122, 1.000000000000000000, 0.9659258262890683122, 1.000000000000000000, 0.9659258262890683122, 1.000000000000000000, 0.9659258262890683122, 1.000000000000000000, 0.9659258262890683122, 1.000000000000000000, 0.9659258262890683122, 1.000000000000000000, 0.9659258262890683122, 1.000000000000000000, 0.9659258262890683122, 1.000000000000000000, 0.9659258262890683122, 1.000000000000000000, 0.9659258262890683122, 1.000000000000000000, 0.9659258262890683122, 1.000000000000000000, 0.9659258262890683122, 1.000000000000000000, 0.9659258262890683122, 1.000000000000000000, 0.9659258262890683122, 1.000000000000000000, 0.9659258262890683122, 1.000000000000000000, 0.9659258262890683122, 1.000000000000000000, 0.9659258262890683122, 1.000000000000000000, 0.9659258262890683122, 1.000000000000000000, 0.9659258262890683122, 1.000000000000000000, 0.9659258262890683122, 1.000000000000000000, 0.9659258262890683122, 1.000000000000000000, 0.9659258262890683122, 1.000000000000000000, 0.9659258262890683122, 1.000000000000000000, 0.9659258262890683122, 1.000000000000000000, 0.9659258262890683122, 1.000000000000000000, 0.9659258262890683122, 1.000000000000000000, 0.9659258262890683122, 1.000000000000000000, 0.9659258262890683122, 1.000000000000000000, 0.9659258262890683122, 1.000000000000000000, 0.9659258262890683122, 1.000000000000000000, 0.9659258262890683122, 1.000000000000000000, 0.9659258262890683122, 1.000000000000000000, 0.9659258262890683122, 1.000000000000000000, 0.9659258262890683122, 1.000000000000000000, 0.9659258262890683122, 1.000000000000000000, 0.9659258262890683122, 1.000000000000000000, 0.9659258262890683122, 1.000000000000000000, 0.9659258262890683122, 1.000000000000000000, 0.9659258262890683122, 1.000000000000000000, 0.9659258262890683122, 1.000000000000000000, 0.9659258262890683122, 1.000000000000000000, 0.9659258262890683122, 1.000000000000000000, 0.9659258262890683122, 1.000000000000000000, 0.9659258262890683122, 1.000000000000000000, 0.9659258262890683122, 1.000000000000000000, 0.9659258262890683122, 1.000000000000000000, 0.9659258262890683122, 1.000000000000000000, 0.9659258262890683122, 1.000000000000000000, 0.9659258262890683122, 1.000000000000000000, 0.9659258262890683122, 1.000000000000000000, 0.9659258262890683122, 1.000000000000000000, 0.9659258262890683122, 1.000000000000000000, 0.9659258262890683122, 1.000000000000000000, 0.9659258262890683122, 1.000000000000000000, 0.9659258262890683122, 1.000000000000000000) ) ) 
 REPRESENTATION_ITEM ( '' )  SURFACE ( )  );
#13096 = CARTESIAN_POINT ( 'NONE',  ( 4.483927247898790824, -16.52544592524335698, 45.20942372801901854 ) ) ;
#13098 = CARTESIAN_POINT ( 'NONE',  ( -5.719274019375665041, -21.55341960407619695, 64.79275706135234714 ) ) ;
#13099 = CARTESIAN_POINT ( 'NONE',  ( -16.53943276465976808, -0.05219959533934237506, 28.75109039468567929 ) ) ;
#13100 = CARTESIAN_POINT ( 'NONE',  ( 5.049401038298161559, -19.05341960407611168, 72.70724293864768129 ) ) ;
#13101 = CARTESIAN_POINT ( 'NONE',  ( 5.153800228976615827, -19.02544592524334988, 90.20942372801900433 ) ) ;
#13102 = CARTESIAN_POINT ( 'NONE',  ( 8.224510206698742110, 14.34966873604972548, 72.08442372801899012 ) ) ;
#13103 = CARTESIAN_POINT ( 'NONE',  ( 18.62759615963255655, 10.81492255796105972, 106.6677570613523756 ) ) ;
#13104 = CARTESIAN_POINT ( 'NONE',  ( -19.02544592524334988, -5.153800228976617603, 73.95942372801900433 ) ) ;
#13105 = CARTESIAN_POINT ( 'NONE',  ( 19.02544592524343514, -5.153800228976328945, 53.54057627198102409 ) ) ;
#13106 = CARTESIAN_POINT ( 'NONE',  ( -18.62759615963270932, 10.81492255796079327, 85.83224293864768129 ) ) ;
#13108 = CARTESIAN_POINT ( 'NONE',  ( 19.03943276465977164, 0.05219959533936151252, 76.25109039468566152 ) ) ;
#13107 = CARTESIAN_POINT ( 'NONE',  ( -16.53943276465976808, 0.05219959533911058130, 76.24890960531435269 ) ) ;
#13109 = CARTESIAN_POINT ( 'NONE',  ( 19.49401214000076621, 12.39993551617566681, 169.9999999999999716 ) ) ;
#13111 = EDGE_CURVE ( 'NONE', #198713, #191800, #40221, .T. ) ;
#13110 = CARTESIAN_POINT ( 'NONE',  ( 13.89961937509957401, 13.97604488694547697, 61.87609039468566863 ) ) ;
#13112 = CARTESIAN_POINT ( 'NONE',  ( 8.224510206698742110, 14.34966873604972548, 107.0844237280190043 ) ) ;
#13113 = CARTESIAN_POINT ( 'NONE',  ( -16.53943276465976808, 0.05219959533911058130, 66.24890960531436690 ) ) ;
#13115 = CARTESIAN_POINT ( 'NONE',  ( -5.359611314223446995E-15, 29.16686587814335496, 146.3750000027311842 ) ) ;
#13114 = CARTESIAN_POINT ( 'NONE',  ( 18.62759615963255655, 10.81492255796105972, 106.6677570613523756 ) ) ;
#13116 = CARTESIAN_POINT ( 'NONE',  ( -10.72451020669898014, 18.67979575497178502, 105.4155762719810383 ) ) ;
#13117 = CARTESIAN_POINT ( 'NONE',  ( -5.153800228976328057, -19.02544592524343514, 62.29057627198100988 ) ) ;
#13118 = CARTESIAN_POINT ( 'NONE',  ( -15.80617190586768217, 15.72974639402176855, 78.12609039468570415 ) ) ;
#13119 = CARTESIAN_POINT ( 'NONE',  ( 9.564922557960805705, 16.46253265017160317, 59.58224293864769550 ) ) ;
#13120 = ORIENTED_EDGE ( 'NONE', *, *, #12852, .T. ) ;
#13121 = CARTESIAN_POINT ( 'NONE',  ( 13.97604488694527802, 13.89961937509977652, 29.37390960531435979 ) ) ;
#13122 = CARTESIAN_POINT ( 'NONE',  ( 21.53943276465977519, -0.05219959533907433946, 23.74890960531435269 ) ) ;
#13123 = CARTESIAN_POINT ( 'NONE',  ( 14.29746914071049879, -8.314922557960816363, 68.33224293864769550 ) ) ;
#13124 = CARTESIAN_POINT ( 'NONE',  ( -13.89961937509977652, 13.97604488694528158, 40.62390960531435979 ) ) ;
#13125 = CARTESIAN_POINT ( 'NONE',  ( 12.14591786802309770, 12.06949235617756955, 99.37390960531436690 ) ) ;
#13126 = CARTESIAN_POINT ( 'NONE',  ( 21.55341960407610458, 5.719274019375980345, 108.9572429386476955 ) ) ;
#13127 = CONICAL_SURFACE ( 'NONE', #54963, 1.610000000000000098, 0.7853981633974458365 ) ;
#13128 = CARTESIAN_POINT ( 'NONE',  ( -21.52544592524334988, -5.823673210054445271, 48.95942372801902565 ) ) ;
#13129 = CARTESIAN_POINT ( 'NONE',  ( 19.03943276465977164, -0.05219959533909143690, 28.74890960531435624 ) ) ;
#13130 = CARTESIAN_POINT ( 'NONE',  ( 4.483927247898790824, -16.52544592524335698, 60.20942372801902565 ) ) ;
#13131 = CARTESIAN_POINT ( 'NONE',  ( -21.55341960407610458, -5.719274019375992779, 96.45724293864770971 ) ) ;
#13132 = CARTESIAN_POINT ( 'NONE',  ( -15.80617190586745835, -15.72974639402198527, 91.87390960531436690 ) ) ;
#13134 = CARTESIAN_POINT ( 'NONE',  ( -16.46253265017160317, 9.564922557960807481, 50.83224293864770260 ) ) ;
#13133 = CARTESIAN_POINT ( 'NONE',  ( 19.03943276465977164, 0.05219959533936151252, 31.25109039468566863 ) ) ;
#13135 = PLANE ( 'NONE',  #131319 ) ;
#13136 = CARTESIAN_POINT ( 'NONE',  ( -15.80617190586768217, 15.72974639402176855, 63.12609039468568994 ) ) ;
#13137 = CARTESIAN_POINT ( 'NONE',  ( 15.72974639402199770, -15.80617190586745480, 63.12390960531435979 ) ) ;
#13138 = CARTESIAN_POINT ( 'NONE',  ( 16.52544592524342804, -4.483927247898539470, 23.54057627198102765 ) ) ;
#13140 = CARTESIAN_POINT ( 'NONE',  ( -21.55341960407619339, 5.719274019375674811, 98.54275706135234714 ) ) ;
#13139 = CARTESIAN_POINT ( 'NONE',  ( -5.823673210054431948, 21.52544592524334988, 82.70942372801900433 ) ) ;
#13141 = CARTESIAN_POINT ( 'NONE',  ( 13.97604488694548053, -13.89961937509957401, 40.62609039468564731 ) ) ;
#13142 = CARTESIAN_POINT ( 'NONE',  ( -0.05219959533934338120, 16.53943276465976808, 97.50109039468567573 ) ) ;
#13143 = CARTESIAN_POINT ( 'NONE',  ( 10.81492255796106328, -18.62759615963255655, 50.41775706135235424 ) ) ;
#13144 = CARTESIAN_POINT ( 'NONE',  ( 13.89961937509977652, -13.97604488694527269, 53.12390960531434558 ) ) ;
#13145 = CARTESIAN_POINT ( 'NONE',  ( -16.46253265017146816, -9.564922557961047289, 39.16775706135234003 ) ) ;
#13146 = CARTESIAN_POINT ( 'NONE',  ( 15.80617190586746368, 15.72974639402197994, 34.37390960531435979 ) ) ;
#13147 = CARTESIAN_POINT ( 'NONE',  ( -0.05219959533937732626, 21.53943276465977519, 32.50109039468568284 ) ) ;
#13148 = CARTESIAN_POINT ( 'NONE',  ( -21.53943276465977519, 0.05219959533907696930, 91.24890960531436690 ) ) ;
#13149 = CARTESIAN_POINT ( 'NONE',  ( 16.51473224551083163, -9.474510206698727899, 85.83442372801900433 ) ) ;
#13150 = CARTESIAN_POINT ( 'NONE',  ( 14.34966873604972726, -8.224510206698740333, 55.83442372801901854 ) ) ;
#13152 = CARTESIAN_POINT ( 'NONE',  ( -18.62759615963270932, 10.81492255796079327, 85.83224293864768129 ) ) ;
#13151 = CARTESIAN_POINT ( 'NONE',  ( 17.50000000000001776, -3.242565516147306592, 37.50000000000000000 ) ) ;
#13154 = CARTESIAN_POINT ( 'NONE',  ( 14.34966873604960469, 8.224510206698951720, 74.16557627198102409 ) ) ;
#13153 = CARTESIAN_POINT ( 'NONE',  ( -8.314922557961024197, 14.29746914071037800, 77.91775706135231871 ) ) ;
#13155 = PLANE ( 'NONE',  #56380 ) ;
#13156 = CARTESIAN_POINT ( 'NONE',  ( -16.51473224551082808, 9.474510206698731452, 98.33442372801900433 ) ) ;
#13157 = CARTESIAN_POINT ( 'NONE',  ( 15.80617190586746368, 15.72974639402197994, 29.37390960531435269 ) ) ;
#13158 = DIRECTION ( 'NONE',  ( 1.000000000000000000, 0.000000000000000000, 0.000000000000000000 ) ) ;
#13159 = CARTESIAN_POINT ( 'NONE',  ( -0.05219959533934338120, 16.53943276465976808, 37.50109039468568284 ) ) ;
#13160 = CARTESIAN_POINT ( 'NONE',  ( -21.52544592524343514, 5.823673210054127303, 111.0405762719810525 ) ) ;
#13161 = CARTESIAN_POINT ( 'NONE',  ( 15.80617190586746368, 15.72974639402197994, 29.37390960531435269 ) ) ;
#13162 = CARTESIAN_POINT ( 'NONE',  ( 16.53943276465976808, 0.05219959533934440121, 66.25109039468567573 ) ) ;
#13163 = CARTESIAN_POINT ( 'NONE',  ( 19.05341960407611168, 5.049401038298154454, 83.95724293864766707 ) ) ;
#13165 = CARTESIAN_POINT ( 'NONE',  ( 0.05219959533909260263, 19.03943276465977164, 29.99890960531435979 ) ) ;
#13164 = CARTESIAN_POINT ( 'NONE',  ( 21.52544592524334988, 5.823673210054432836, 51.45942372801901854 ) ) ;
#13166 = CARTESIAN_POINT ( 'NONE',  ( -10.81492255796078084, -18.62759615963271287, 22.08224293864769194 ) ) ;
#13167 = ORIENTED_EDGE ( 'NONE', *, *, #59429, .F. ) ;
#13168 = CARTESIAN_POINT ( 'NONE',  ( 13.89961937509957401, 13.97604488694547697, 41.87609039468566152 ) ) ;
#13169 = CARTESIAN_POINT ( 'NONE',  ( 12.14591786802327356, -12.06949235617739191, 55.62609039468568284 ) ) ;
#13170 = CARTESIAN_POINT ( 'NONE',  ( 10.81492255796078972, 18.62759615963270932, 24.58224293864768839 ) ) ;
#13171 = CARTESIAN_POINT ( 'NONE',  ( -13.97604488694527625, -13.89961937509977652, 76.87390960531433848 ) ) ;
#13172 = CARTESIAN_POINT ( 'NONE',  ( -16.55341960407617563, 4.379528057220093196, 98.54275706135234714 ) ) ;
#13173 = CARTESIAN_POINT ( 'NONE',  ( 4.483927247898545687, 16.52544592524342804, 94.79057627198105251 ) ) ;
#13174 = CARTESIAN_POINT ( 'NONE',  ( -18.67979575497178146, -10.72451020669898902, 36.66557627198103120 ) ) ;
#13175 = CARTESIAN_POINT ( 'NONE',  ( -16.46253265017160317, 9.564922557960807481, 30.83224293864769550 ) ) ;
#13176 = CARTESIAN_POINT ( 'NONE',  ( -16.52544592524335698, -4.483927247898792601, 63.95942372801901854 ) ) ;
#13177 = CARTESIAN_POINT ( 'NONE',  ( 10.81492255796106328, -18.62759615963255655, 25.41775706135235779 ) ) ;
#13178 = CARTESIAN_POINT ( 'NONE',  ( 13.89961937509957401, 13.97604488694547697, 76.87609039468566152 ) ) ;
#13179 = CARTESIAN_POINT ( 'NONE',  ( 0.05219959533909260263, 19.03943276465977164, 39.99890960531436690 ) ) ;
#13180 = CARTESIAN_POINT ( 'NONE',  ( 15.72974639402199770, -15.80617190586745480, 68.12390960531436690 ) ) ;
#13181 = CARTESIAN_POINT ( 'NONE',  ( -5.049401038298153566, 19.05341960407611168, 110.2072429386476671 ) ) ;
#13182 = CARTESIAN_POINT ( 'NONE',  ( -0.05219959533937732626, 21.53943276465977519, 97.50109039468567573 ) ) ;
#13183 = CARTESIAN_POINT ( 'NONE',  ( -19.03943276465977164, 0.05219959533909376836, 66.24890960531436690 ) ) ;
#13184 = CARTESIAN_POINT ( 'NONE',  ( 8.224510206698742110, 14.34966873604972548, 47.08442372801901854 ) ) ;
#13185 = CARTESIAN_POINT ( 'NONE',  ( -13.89961937509977652, 13.97604488694528158, 65.62390960531436690 ) ) ;
#13186 = CARTESIAN_POINT ( 'NONE',  ( -18.62759615963255300, -10.81492255796106328, 84.16775706135234714 ) ) ;
#13187 = CARTESIAN_POINT ( 'NONE',  ( -9.474510206698720793, -16.51473224551083518, 44.58442372801900433 ) ) ;
#13188 = CARTESIAN_POINT ( 'NONE',  ( -9.564922557961040184, 16.46253265017147172, 52.91775706135233293 ) ) ;
#13189 = ORIENTED_EDGE ( 'NONE', *, *, #23592, .T. ) ;
#13190 = CARTESIAN_POINT ( 'NONE',  ( -0.05219959533937732626, 21.53943276465977519, 47.50109039468568994 ) ) ;
#13191 = EDGE_CURVE ( 'NONE', #131044, #61621, #118465, .T. ) ;
#13192 = CARTESIAN_POINT ( 'NONE',  ( -6.615873399348746631, 1.136345303629841208, -62.40252569733544874 ) ) ;
#13193 = CARTESIAN_POINT ( 'NONE',  ( -13.89961937509957401, -13.97604488694547875, 44.37609039468566863 ) ) ;
#13194 = CARTESIAN_POINT ( 'NONE',  ( -9.474510206698964154, 16.51473224551069663, 105.4155762719810383 ) ) ;
#13195 = CARTESIAN_POINT ( 'NONE',  ( -19.03943276465977164, 0.05219959533909376836, 76.24890960531435269 ) ) ;
#13196 = CARTESIAN_POINT ( 'NONE',  ( -8.314922557960811034, -14.29746914071050412, 37.08224293864768129 ) ) ;
#13197 = CARTESIAN_POINT ( 'NONE',  ( 21.53943276465977519, -0.05219959533907433946, 38.74890960531435979 ) ) ;
#13198 = CARTESIAN_POINT ( 'NONE',  ( 29.86685920354754842, -21.69954338932559068, -10.32499999726881335 ) ) ;
#13199 = FACE_OUTER_BOUND ( 'NONE', #110358, .T. ) ;
#13200 = CARTESIAN_POINT ( 'NONE',  ( 18.62759615963255655, 10.81492255796105972, 101.6677570613523613 ) ) ;
#13201 = CARTESIAN_POINT ( 'NONE',  ( -1.040834085586084257E-14, 30.40000000000003766, -65.00100000000003320 ) ) ;
#13202 = CARTESIAN_POINT ( 'NONE',  ( 16.46253265017160672, -9.564922557960803928, 33.33224293864770260 ) ) ;
#13203 = CARTESIAN_POINT ( 'NONE',  ( 13.89961937509977652, -13.97604488694527269, 113.1239096053143527 ) ) ;
#13204 = CARTESIAN_POINT ( 'NONE',  ( 34.35276339089875108, 2.907959671212061004, 90.32815265678038941 ) ) ;
#13205 = CARTESIAN_POINT ( 'NONE',  ( 8.314922557961029526, -14.29746914071037800, 50.41775706135235424 ) ) ;
#13206 = CARTESIAN_POINT ( 'NONE',  ( -5.823673210054116645, -21.52544592524344225, 72.29057627198102409 ) ) ;
#13207 = CARTESIAN_POINT ( 'NONE',  ( -8.224510206698948167, 14.34966873604960824, 35.41557627198102409 ) ) ;
#13209 = CARTESIAN_POINT ( 'NONE',  ( 16.51473224551069308, 9.474510206698969483, 114.1655762719810241 ) ) ;
#13208 = CARTESIAN_POINT ( 'NONE',  ( 0.05219959533909260263, 19.03943276465977164, 29.99890960531435979 ) ) ;
#13210 = CARTESIAN_POINT ( 'NONE',  ( -15.80617190586768217, 15.72974639402176855, 28.12609039468568284 ) ) ;
#13211 = CARTESIAN_POINT ( 'NONE',  ( 16.51473224551083163, -9.474510206698727899, 40.83442372801900433 ) ) ;
#13212 = CARTESIAN_POINT ( 'NONE',  ( 16.55341960407611168, 4.379528057220329451, 113.9572429386477239 ) ) ;
#13213 = CARTESIAN_POINT ( 'NONE',  ( 15.80617190586769283, -15.72974639402175789, 75.62609039468567573 ) ) ;
#13214 = CARTESIAN_POINT ( 'NONE',  ( 16.81555441253552985, -7.025013491695479395, 33.13685445334258617 ) ) ;
#13215 = CARTESIAN_POINT ( 'NONE',  ( 12.06949235617757843, -12.14591786802309237, 28.12390960531435979 ) ) ;
#13216 = FACE_OUTER_BOUND ( 'NONE', #165968, .T. ) ;
#13217 = CARTESIAN_POINT ( 'NONE',  ( 5.823673210054125526, 21.52544592524343514, 29.79057627198102409 ) ) ;
#13218 = CARTESIAN_POINT ( 'NONE',  ( -14.29746914071049879, 8.314922557960819915, 95.83224293864770971 ) ) ;
#13219 = CARTESIAN_POINT ( 'NONE',  ( -5.512880932802044498, -6.874811933691526988, -64.01752234774738781 ) ) ;
#13220 = CARTESIAN_POINT ( 'NONE',  ( -13.97604488694527625, -13.89961937509977652, 76.87390960531433848 ) ) ;
#13221 = CARTESIAN_POINT ( 'NONE',  ( -4.379528057220328563, 16.55341960407611168, 80.20724293864769550 ) ) ;
#13222 = CARTESIAN_POINT ( 'NONE',  ( -5.153800228976607833, 19.02544592524334988, 102.7094237280189759 ) ) ;
#13223 = CARTESIAN_POINT ( 'NONE',  ( -10.72451020669898014, 18.67979575497178502, 65.41557627198102409 ) ) ;
#13224 = ORIENTED_EDGE ( 'NONE', *, *, #63994, .F. ) ;
#13225 = CARTESIAN_POINT ( 'NONE',  ( 9.564922557960805705, 16.46253265017160317, 29.58224293864769550 ) ) ;
#13227 = CARTESIAN_POINT ( 'NONE',  ( -18.62759615963270932, 10.81492255796079327, 80.83224293864769550 ) ) ;
#13226 = CARTESIAN_POINT ( 'NONE',  ( -16.46253265017160317, 9.564922557960807481, 70.83224293864770971 ) ) ;
#13229 = CARTESIAN_POINT ( 'NONE',  ( -19.05341960407611168, -5.049401038298163336, 86.45724293864769550 ) ) ;
#13228 = CARTESIAN_POINT ( 'NONE',  ( -8.224510206698735004, -14.34966873604973081, 109.5844237280190328 ) ) ;
#13230 = CARTESIAN_POINT ( 'NONE',  ( 13.97604488694548053, -13.89961937509957401, 65.62609039468567573 ) ) ;
#13231 = CARTESIAN_POINT ( 'NONE',  ( -10.72451020669870658, -18.67979575497194134, 99.58442372801900433 ) ) ;
#13232 = CARTESIAN_POINT ( 'NONE',  ( -5.823673210054116645, -21.52544592524344225, 77.29057627198102409 ) ) ;
#13233 = CARTESIAN_POINT ( 'NONE',  ( -5.719274019375978568, 21.55341960407610458, 30.20724293864769550 ) ) ;
#13234 = CARTESIAN_POINT ( 'NONE',  ( -0.05219959533909027116, -19.03943276465977164, 52.49890960531436690 ) ) ;
#13235 = CARTESIAN_POINT ( 'NONE',  ( 4.483927247898790824, -16.52544592524335698, 95.20942372801903275 ) ) ;
#13236 = CARTESIAN_POINT ( 'NONE',  ( 5.153800228976335163, 19.02544592524342804, 64.79057627198100988 ) ) ;
#13237 = DIRECTION ( 'NONE',  ( 0.000000000000000000, 0.000000000000000000, -1.000000000000000000 ) ) ;
#13238 = CARTESIAN_POINT ( 'NONE',  ( -21.53943276465977519, -0.05219959533937600094, 103.7510903946857042 ) ) ;
#13239 = CARTESIAN_POINT ( 'NONE',  ( 14.29746914071049879, -8.314922557960816363, 68.33224293864769550 ) ) ;
#13240 = CARTESIAN_POINT ( 'NONE',  ( -5.823673210054116645, -21.52544592524344225, 112.2905762719810241 ) ) ;
#13241 = CARTESIAN_POINT ( 'NONE',  ( 10.72451020669898902, -18.67979575497178502, 107.9155762719810241 ) ) ;
#13242 = CARTESIAN_POINT ( 'NONE',  ( -17.14385361876520264, -23.59649016807271593, 139.6750000027311955 ) ) ;
#13243 = CARTESIAN_POINT ( 'NONE',  ( 5.823673210054125526, 21.52544592524343514, 54.79057627198104541 ) ) ;
#13244 = CARTESIAN_POINT ( 'NONE',  ( 16.53943276465976808, 0.05219959533934440121, 86.25109039468568994 ) ) ;
#13245 = CARTESIAN_POINT ( 'NONE',  ( 8.314922557960818139, 14.29746914071049879, 104.5822429386477097 ) ) ;
#13246 = CARTESIAN_POINT ( 'NONE',  ( 13.89961937509977652, -13.97604488694527269, 63.12390960531435979 ) ) ;
#13247 = SURFACE_SIDE_STYLE ('',( #59729 ) ) ;
#13248 = CARTESIAN_POINT ( 'NONE',  ( -12.14591786802309592, -12.06949235617757132, 21.87390960531436690 ) ) ;
#13249 = CARTESIAN_POINT ( 'NONE',  ( 21.53943276465977519, 0.05219959533937863772, 51.25109039468568994 ) ) ;
#13250 = CARTESIAN_POINT ( 'NONE',  ( 13.97604488694527802, 13.89961937509977652, 99.37390960531436690 ) ) ;
#13251 = CARTESIAN_POINT ( 'NONE',  ( 21.52544592524334988, 5.823673210054432836, 81.45942372801900433 ) ) ;
#13252 = CARTESIAN_POINT ( 'NONE',  ( -19.05341960407611168, -5.049401038298163336, 26.45724293864769550 ) ) ;
#13253 = CARTESIAN_POINT ( 'NONE',  ( 5.153800228976335163, 19.02544592524342804, 34.79057627198102409 ) ) ;
#13254 = ORIENTED_EDGE ( 'NONE', *, *, #8188, .F. ) ;
#13255 = CARTESIAN_POINT ( 'NONE',  ( 10.72451020669871369, 18.67979575497193778, 77.08442372801901854 ) ) ;
#13256 = CARTESIAN_POINT ( 'NONE',  ( 19.03943276465977164, -0.05219959533909143690, 108.7489096053143527 ) ) ;
#13257 = CARTESIAN_POINT ( 'NONE',  ( 5.153800228976615827, -19.02544592524334988, 75.20942372801896170 ) ) ;
#13258 = CARTESIAN_POINT ( 'NONE',  ( 15.80617190586769283, -15.72974639402175789, 45.62609039468567573 ) ) ;
#13259 = CARTESIAN_POINT ( 'NONE',  ( -14.29746914071037622, -8.314922557961029526, 19.16775706135234714 ) ) ;
#13260 = CARTESIAN_POINT ( 'NONE',  ( 0.05219959533936267826, -19.03943276465977164, 70.00109039468566152 ) ) ;
#13261 = CARTESIAN_POINT ( 'NONE',  ( 13.89961937509977652, -13.97604488694527269, 53.12390960531434558 ) ) ;
#13262 = CARTESIAN_POINT ( 'NONE',  ( 9.564922557961047289, -16.46253265017146816, 80.41775706135234714 ) ) ;
#13263 = CARTESIAN_POINT ( 'NONE',  ( -14.34966873604960291, -8.224510206698953496, 26.66557627198103475 ) ) ;
#13264 = CARTESIAN_POINT ( 'NONE',  ( 13.89961937509957401, 13.97604488694547697, 91.87609039468567573 ) ) ;
#13265 = CARTESIAN_POINT ( 'NONE',  ( 14.29746914071049879, -8.314922557960816363, 43.33224293864769550 ) ) ;
#13266 = CARTESIAN_POINT ( 'NONE',  ( 5.153800228976615827, -19.02544592524334988, 65.20942372801900433 ) ) ;
#13267 = CARTESIAN_POINT ( 'NONE',  ( -14.34966873604972548, 8.224510206698743886, 53.33442372801901854 ) ) ;
#13268 = CARTESIAN_POINT ( 'NONE',  ( 19.03943276465977164, 0.05219959533936151252, 26.25109039468566507 ) ) ;
#13269 = CARTESIAN_POINT ( 'NONE',  ( 19.03943276465977164, -0.05219959533909143690, 48.74890960531435979 ) ) ;
#13270 = DIRECTION ( 'NONE',  ( 0.000000000000000000, 0.000000000000000000, -1.000000000000000000 ) ) ;
#13271 = CARTESIAN_POINT ( 'NONE',  ( 16.52544592524335698, 4.483927247898782831, 46.45942372801901854 ) ) ;
#13272 = CARTESIAN_POINT ( 'NONE',  ( -0.3535533905933784249, -30.00000000000000000, 5.353553390593268624 ) ) ;
#13273 = CARTESIAN_POINT ( 'NONE',  ( 17.14385361876520264, 23.59649016807275856, 142.1750000027311671 ) ) ;
#13274 = CARTESIAN_POINT ( 'NONE',  ( -9.474510206698964154, 16.51473224551069663, 95.41557627198102409 ) ) ;
#13275 = CARTESIAN_POINT ( 'NONE',  ( -9.474510206698720793, -16.51473224551083518, 84.58442372801900433 ) ) ;
#13276 = CARTESIAN_POINT ( 'NONE',  ( -0.05219959533936034679, 19.03943276465977164, 82.50109039468567573 ) ) ;
#13277 = CARTESIAN_POINT ( 'NONE',  ( 10.72451020669898902, -18.67979575497178502, 27.91557627198103830 ) ) ;
#13279 = CARTESIAN_POINT ( 'NONE',  ( -0.05219959533936034679, 19.03943276465977164, 97.50109039468567573 ) ) ;
#13278 = CARTESIAN_POINT ( 'NONE',  ( -0.05219959533936034679, 19.03943276465977164, 22.50109039468566152 ) ) ;
#13280 = CARTESIAN_POINT ( 'NONE',  ( -8.224510206698948167, 14.34966873604960824, 115.4155762719810241 ) ) ;
#13281 = CARTESIAN_POINT ( 'NONE',  ( 19.02544592524343514, -5.153800228976328945, 38.54057627198103120 ) ) ;
#13282 = CARTESIAN_POINT ( 'NONE',  ( -15.80617190586745835, -15.72974639402198527, 61.87390960531436690 ) ) ;
#13283 = CARTESIAN_POINT ( 'NONE',  ( -16.52544592524342804, 4.483927247898546575, 116.0405762719810383 ) ) ;
#13284 = CARTESIAN_POINT ( 'NONE',  ( 22.44159573604009594, -16.30477369853687364, 140.1750000027311955 ) ) ;
#13285 = CARTESIAN_POINT ( 'NONE',  ( 5.153800228976615827, -19.02544592524334988, 70.20942372801899012 ) ) ;
#13286 = CARTESIAN_POINT ( 'NONE',  ( -8.224510206698948167, 14.34966873604960824, 35.41557627198102409 ) ) ;
#13287 = CARTESIAN_POINT ( 'NONE',  ( -5.823673210054116645, -21.52544592524344225, 37.29057627198102409 ) ) ;
#13288 = CARTESIAN_POINT ( 'NONE',  ( 18.62759615963255655, 10.81492255796105972, 91.66775706135234714 ) ) ;
#13289 = CARTESIAN_POINT ( 'NONE',  ( -21.53943276465977519, 0.05219959533907696930, 86.24890960531436690 ) ) ;
#13290 = CARTESIAN_POINT ( 'NONE',  ( -10.81492255796105439, 18.62759615963255655, 52.91775706135235424 ) ) ;
#13291 = CARTESIAN_POINT ( 'NONE',  ( 5.823673210054444382, -21.52544592524334988, 65.20942372801901854 ) ) ;
#13292 = CARTESIAN_POINT ( 'NONE',  ( 19.05341960407611168, 5.049401038298154454, 93.95724293864769550 ) ) ;
#13294 = CARTESIAN_POINT ( 'NONE',  ( 18.62759615963255655, 10.81492255796105972, 46.66775706135234714 ) ) ;
#13293 = CARTESIAN_POINT ( 'NONE',  ( 0.05219959533934541429, -16.53943276465976808, 90.00109039468567573 ) ) ;
#13295 = CARTESIAN_POINT ( 'NONE',  ( 8.314922557960818139, 14.29746914071049879, 114.5822429386477097 ) ) ;
#13296 = CARTESIAN_POINT ( 'NONE',  ( -12.14591786802309592, -12.06949235617757132, 71.87390960531438111 ) ) ;
#13297 = CARTESIAN_POINT ( 'NONE',  ( -14.29746914071049879, 8.314922557960819915, 30.83224293864770260 ) ) ;
#13298 = CARTESIAN_POINT ( 'NONE',  ( -18.62759615963270932, 10.81492255796079327, 45.83224293864769550 ) ) ;
#13299 = CARTESIAN_POINT ( 'NONE',  ( -19.05341960407611168, -5.049401038298163336, 51.45724293864770260 ) ) ;
#13300 = CARTESIAN_POINT ( 'NONE',  ( 5.823673210054125526, 21.52544592524343514, 64.79057627198103830 ) ) ;
#13301 = CARTESIAN_POINT ( 'NONE',  ( -13.89961937509957401, -13.97604488694547875, 49.37609039468567573 ) ) ;
#13303 = CARTESIAN_POINT ( 'NONE',  ( 0.05219959533910956823, 16.53943276465976808, 54.99890960531435269 ) ) ;
#13302 = CARTESIAN_POINT ( 'NONE',  ( -16.38665767535053774, -7.295008042176053031, 39.73599135785456582 ) ) ;
#13304 = CARTESIAN_POINT ( 'NONE',  ( 5.719274019375991003, -21.55341960407610458, 22.70724293864769194 ) ) ;
#13305 = ORIENTED_EDGE ( 'NONE', *, *, #168447, .F. ) ;
#13306 = CARTESIAN_POINT ( 'NONE',  ( 8.898068258721473001, -27.38543819252872069, 140.5843446569000150 ) ) ;
#13307 = CARTESIAN_POINT ( 'NONE',  ( -4.379528057220086978, -16.55341960407618274, 69.79275706135234714 ) ) ;
#13308 = CARTESIAN_POINT ( 'NONE',  ( -13.97604488694547697, 13.89961937509957934, 78.12609039468567573 ) ) ;
#13309 = CARTESIAN_POINT ( 'NONE',  ( -12.14591786802309592, -12.06949235617757132, 36.87390960531435979 ) ) ;
#13310 = LINE ( 'NONE', #106295, #99949 ) ;
#13311 = CARTESIAN_POINT ( 'NONE',  ( 4.483927247898545687, 16.52544592524342804, 24.79057627198103120 ) ) ;
#13312 = CARTESIAN_POINT ( 'NONE',  ( -0.05219959533909027116, -19.03943276465977164, 57.49890960531435979 ) ) ;
#13313 = CARTESIAN_POINT ( 'NONE',  ( 16.51473224551069308, 9.474510206698969483, 74.16557627198103830 ) ) ;
#13314 = CARTESIAN_POINT ( 'NONE',  ( 16.46253265017160672, -9.564922557960803928, 43.33224293864769550 ) ) ;
#13315 = CARTESIAN_POINT ( 'NONE',  ( -10.72451020669870658, -18.67979575497194134, 49.58442372801901143 ) ) ;
#13316 = CARTESIAN_POINT ( 'NONE',  ( 16.51473224551069308, 9.474510206698969483, 64.16557627198102409 ) ) ;
#13317 = DIRECTION ( 'NONE',  ( -0.000000000000000000, -0.000000000000000000, 1.000000000000000000 ) ) ;
#13318 = CARTESIAN_POINT ( 'NONE',  ( -19.02544592524342804, 5.153800228976336051, 61.04057627198103120 ) ) ;
#13320 = EDGE_CURVE ( 'NONE', #81477, #29557, #156408, .T. ) ;
#13319 = CARTESIAN_POINT ( 'NONE',  ( -21.52544592524343514, 5.823673210054127303, 41.04057627198103120 ) ) ;
#13321 = CARTESIAN_POINT ( 'NONE',  ( -5.049401038298153566, 19.05341960407611168, 40.20724293864768839 ) ) ;
#13322 = CARTESIAN_POINT ( 'NONE',  ( -21.53943276465977519, 0.05219959533907696930, 36.24890960531435979 ) ) ;
#13323 = CARTESIAN_POINT ( 'NONE',  ( 12.06949235617739724, 12.14591786802326823, 91.87609039468568994 ) ) ;
#13324 = CARTESIAN_POINT ( 'NONE',  ( -19.03943276465977164, -0.05219959533935918106, 28.75109039468566507 ) ) ;
#13325 = CARTESIAN_POINT ( 'NONE',  ( 14.29746914071037800, 8.314922557961029526, 71.66775706135234714 ) ) ;
#13326 = CARTESIAN_POINT ( 'NONE',  ( -0.05219959533909027116, -19.03943276465977164, 102.4989096053143669 ) ) ;
#13327 = CARTESIAN_POINT ( 'NONE',  ( -14.34966873604972548, 8.224510206698743886, 53.33442372801901854 ) ) ;
#13328 = CARTESIAN_POINT ( 'NONE',  ( 4.379528057220092307, 16.55341960407617563, 37.29275706135235424 ) ) ;
#13329 = CARTESIAN_POINT ( 'NONE',  ( 13.89961937509977652, -13.97604488694527269, 103.1239096053143527 ) ) ;
#13330 = CARTESIAN_POINT ( 'NONE',  ( 16.53943276465976808, 0.05219959533934440121, 31.25109039468568639 ) ) ;
#13331 = CARTESIAN_POINT ( 'NONE',  ( -19.05341960407611168, -5.049401038298163336, 31.45724293864769550 ) ) ;
#13332 = CARTESIAN_POINT ( 'NONE',  ( -0.05219959533937732626, 21.53943276465977519, 27.50109039468567929 ) ) ;
#13333 = CARTESIAN_POINT ( 'NONE',  ( -12.14591786802326823, 12.06949235617739902, 23.12609039468567573 ) ) ;
#13334 = CARTESIAN_POINT ( 'NONE',  ( -0.05219959533934338120, 16.53943276465976808, 92.50109039468567573 ) ) ;
#13335 = DIRECTION ( 'NONE',  ( 1.000000000000000000, 0.000000000000000000, 0.000000000000000000 ) ) ;
#13336 = CARTESIAN_POINT ( 'NONE',  ( -21.53943276465977519, -0.05219959533937600094, 98.75109039468568994 ) ) ;
#13338 = EDGE_CURVE ( 'NONE', #194693, #87119, #56395, .T. ) ;
#13337 = CARTESIAN_POINT ( 'NONE',  ( -16.51473224551082808, 9.474510206698731452, 98.33442372801900433 ) ) ;
#13339 = CARTESIAN_POINT ( 'NONE',  ( -12.14591786802309592, -12.06949235617757132, 51.87390960531437401 ) ) ;
#13340 = CARTESIAN_POINT ( 'NONE',  ( 19.05341960407611168, 5.049401038298154454, 23.95724293864769194 ) ) ;
#13342 = CARTESIAN_POINT ( 'NONE',  ( -28.82186960331499037, 2.428612866367529932E-14, 148.0000000000000000 ) ) ;
#13341 = CARTESIAN_POINT ( 'NONE',  ( 16.51473224551083163, -9.474510206698727899, 45.83442372801900433 ) ) ;
#13343 = CARTESIAN_POINT ( 'NONE',  ( -5.823673210054431948, 21.52544592524334988, 52.70942372801902565 ) ) ;
#13344 = CARTESIAN_POINT ( 'NONE',  ( 4.379528057220092307, 16.55341960407617563, 22.29275706135235069 ) ) ;
#13345 = CARTESIAN_POINT ( 'NONE',  ( 17.26172910966779028, 6.454744622555872446, 81.69353091350777163 ) ) ;
#13346 = CARTESIAN_POINT ( 'NONE',  ( -19.05341960407611168, -5.049401038298163336, 106.4572429386476955 ) ) ;
#13347 = CARTESIAN_POINT ( 'NONE',  ( 18.62759615963271287, -10.81492255796078972, 73.33224293864769550 ) ) ;
#13348 = CARTESIAN_POINT ( 'NONE',  ( 19.05341960407617918, -5.049401038297876454, 96.04275706135231871 ) ) ;
#13349 = CARTESIAN_POINT ( 'NONE',  ( -5.153800228976328057, -19.02544592524343514, 97.29057627198099567 ) ) ;
#13350 = CARTESIAN_POINT ( 'NONE',  ( -21.56952297831560372, 7.512152360717371913, 173.9007003117368981 ) ) ;
#13351 = CARTESIAN_POINT ( 'NONE',  ( 8.314922557960818139, 14.29746914071049879, 104.5822429386477097 ) ) ;
#13352 = CARTESIAN_POINT ( 'NONE',  ( -21.52544592524334988, -5.823673210054445271, 98.95942372801903275 ) ) ;
#13353 = CARTESIAN_POINT ( 'NONE',  ( 5.049401038298161559, -19.05341960407611168, 47.70724293864770260 ) ) ;
#13354 = CARTESIAN_POINT ( 'NONE',  ( 15.80617190586769283, -15.72974639402175789, 55.62609039468568284 ) ) ;
#13355 = CARTESIAN_POINT ( 'NONE',  ( 18.62759615963255655, 10.81492255796105972, 86.66775706135234714 ) ) ;
#13356 = CARTESIAN_POINT ( 'NONE',  ( -4.379528057220086978, -16.55341960407618274, 104.7927570613523898 ) ) ;
#13357 = CARTESIAN_POINT ( 'NONE',  ( 9.564922557960805705, 16.46253265017160317, 69.58224293864770971 ) ) ;
#13358 = CARTESIAN_POINT ( 'NONE',  ( 18.62759615963255655, 10.81492255796105972, 46.66775706135234714 ) ) ;
#13359 = CARTESIAN_POINT ( 'NONE',  ( -15.80617190586768217, 15.72974639402176855, 43.12609039468568284 ) ) ;
#13361 = CARTESIAN_POINT ( 'NONE',  ( -0.05219959533909027116, -19.03943276465977164, 92.49890960531436690 ) ) ;
#13360 = CARTESIAN_POINT ( 'NONE',  ( -0.05219959533936034679, 19.03943276465977164, 72.50109039468566152 ) ) ;
#13362 = CARTESIAN_POINT ( 'NONE',  ( 14.34966873604960469, 8.224510206698951720, 99.16557627198100988 ) ) ;
#13363 = CARTESIAN_POINT ( 'NONE',  ( 0.05219959533907565091, 21.53943276465977519, 99.99890960531436690 ) ) ;
#13364 = CARTESIAN_POINT ( 'NONE',  ( 14.34966873604960469, 8.224510206698951720, 59.16557627198103120 ) ) ;
#13365 = CARTESIAN_POINT ( 'NONE',  ( -10.81492255796105439, 18.62759615963255655, 112.9177570613523329 ) ) ;
#13366 = CARTESIAN_POINT ( 'NONE',  ( 0.05219959533910956823, 16.53943276465976808, 84.99890960531436690 ) ) ;
#13367 = CARTESIAN_POINT ( 'NONE',  ( -9.564922557960796823, -16.46253265017161027, 32.08224293864769550 ) ) ;
#13368 = CARTESIAN_POINT ( 'NONE',  ( -5.153800228976607833, 19.02544592524334988, 82.70942372801897591 ) ) ;
#13369 = CARTESIAN_POINT ( 'NONE',  ( -16.52544592524342804, 4.483927247898546575, 51.04057627198103120 ) ) ;
#13370 = CARTESIAN_POINT ( 'NONE',  ( 21.53943276465977519, 0.05219959533937863772, 96.25109039468568994 ) ) ;
#13371 = CARTESIAN_POINT ( 'NONE',  ( 16.51473224551069308, 9.474510206698969483, 94.16557627198103830 ) ) ;
#13372 = CARTESIAN_POINT ( 'NONE',  ( 19.05341960407617918, -5.049401038297876454, 71.04275706135234714 ) ) ;
#13373 = CARTESIAN_POINT ( 'NONE',  ( 15.80617190586746368, 15.72974639402197994, 79.37390960531436690 ) ) ;
#13374 = CARTESIAN_POINT ( 'NONE',  ( -21.52544592524334988, -5.823673210054445271, 33.95942372801901143 ) ) ;
#13375 = CARTESIAN_POINT ( 'NONE',  ( -4.379528057220086978, -16.55341960407618274, 24.79275706135235779 ) ) ;
#13376 = CARTESIAN_POINT ( 'NONE',  ( -4.483927247898782831, 16.52544592524335698, 97.70942372801904696 ) ) ;
#13378 = CARTESIAN_POINT ( 'NONE',  ( -5.823673210054431948, 21.52544592524334988, 32.70942372801900433 ) ) ;
#13377 = CARTESIAN_POINT ( 'NONE',  ( -5.049401038298153566, 19.05341960407611168, 25.20724293864768484 ) ) ;
#13379 = CARTESIAN_POINT ( 'NONE',  ( -5.153800228976328057, -19.02544592524343514, 22.29057627198102765 ) ) ;
#13380 = CARTESIAN_POINT ( 'NONE',  ( -36.91746825000001309, 11.99521256947798342, -1.224999997268813035 ) ) ;
#13381 = CARTESIAN_POINT ( 'NONE',  ( 16.53943276465976808, 0.05219959533934440121, 46.25109039468567573 ) ) ;
#13382 = CARTESIAN_POINT ( 'NONE',  ( 0.05219959533910956823, 16.53943276465976808, 74.99890960531435269 ) ) ;
#13383 = CARTESIAN_POINT ( 'NONE',  ( 15.80617190586746368, 15.72974639402197994, 69.37390960531436690 ) ) ;
#13384 = CARTESIAN_POINT ( 'NONE',  ( 16.55341960407611168, 4.379528057220329451, 23.95724293864769550 ) ) ;
#13385 = CARTESIAN_POINT ( 'NONE',  ( -8.314922557961024197, 14.29746914071037800, 47.91775706135234714 ) ) ;
#13386 = CARTESIAN_POINT ( 'NONE',  ( -19.02544592524342804, 5.153800228976336051, 51.04057627198103120 ) ) ;
#13387 = CARTESIAN_POINT ( 'NONE',  ( -14.34966873604972548, 8.224510206698743886, 88.33442372801901854 ) ) ;
#13388 = CARTESIAN_POINT ( 'NONE',  ( 19.05341960407617918, -5.049401038297876454, 81.04275706135231871 ) ) ;
#13389 = CARTESIAN_POINT ( 'NONE',  ( 21.53943276465977519, -0.05219959533907433946, 68.74890960531435269 ) ) ;
#13390 = CARTESIAN_POINT ( 'NONE',  ( 16.53943276465976808, -0.05219959533910856209, 23.74890960531435269 ) ) ;
#13391 = VERTEX_POINT ( 'NONE', #163977 ) ;
#13392 = CARTESIAN_POINT ( 'NONE',  ( -0.05219959533909027116, -19.03943276465977164, 112.4989096053143669 ) ) ;
#13393 = CARTESIAN_POINT ( 'NONE',  ( 10.72451020669898902, -18.67979575497178502, 62.91557627198102409 ) ) ;
#13394 = EDGE_LOOP ( 'NONE', ( #49175, #4990, #164479 ) ) ;
#13395 = CARTESIAN_POINT ( 'NONE',  ( -16.52544592524335698, -4.483927247898792601, 88.95942372801901854 ) ) ;
#13396 = ORIENTED_EDGE ( 'NONE', *, *, #43196, .T. ) ;
#13397 = CARTESIAN_POINT ( 'NONE',  ( 9.474510206698971260, -16.51473224551069308, 107.9155762719810383 ) ) ;
#13398 = CARTESIAN_POINT ( 'NONE',  ( -37.99999999999997158, 12.34694845685052123, -7.849999994537627757 ) ) ;
#13399 = CARTESIAN_POINT ( 'NONE',  ( -5.719274019375978568, 21.55341960407610458, 70.20724293864769550 ) ) ;
#13400 = CARTESIAN_POINT ( 'NONE',  ( -12.14591786802326823, 12.06949235617739902, 108.1260903946856757 ) ) ;
#13401 = CARTESIAN_POINT ( 'NONE',  ( 4.483927247898790824, -16.52544592524335698, 20.20942372801900788 ) ) ;
#13402 = CARTESIAN_POINT ( 'NONE',  ( 5.049401038298161559, -19.05341960407611168, 22.70724293864769194 ) ) ;
#13403 = CARTESIAN_POINT ( 'NONE',  ( 4.379528057220092307, 16.55341960407617563, 27.29275706135234358 ) ) ;
#13404 = CARTESIAN_POINT ( 'NONE',  ( 0.05219959533909260263, 19.03943276465977164, 49.99890960531435979 ) ) ;
#13405 = CARTESIAN_POINT ( 'NONE',  ( -28.82186960331499037, 2.428612866367529932E-14, 142.0000000000000000 ) ) ;
#13406 = CARTESIAN_POINT ( 'NONE',  ( 5.153800228976335163, 19.02544592524342804, 99.79057627198102409 ) ) ;
#13407 = CARTESIAN_POINT ( 'NONE',  ( 12.14591786802327356, -12.06949235617739191, 95.62609039468568994 ) ) ;
#13408 = CARTESIAN_POINT ( 'NONE',  ( -16.51473224551082808, 9.474510206698731452, 88.33442372801900433 ) ) ;
#13409 = CARTESIAN_POINT ( 'NONE',  ( 5.153800228976615827, -19.02544592524334988, 20.20942372801899722 ) ) ;
#13410 = CARTESIAN_POINT ( 'NONE',  ( 0.05219959533907565091, 21.53943276465977519, 69.99890960531435269 ) ) ;
#13411 = CARTESIAN_POINT ( 'NONE',  ( -8.224510206698735004, -14.34966873604973081, 94.58442372801901854 ) ) ;
#13412 = CARTESIAN_POINT ( 'NONE',  ( 16.46253265017146816, 9.564922557961045513, 91.66775706135234714 ) ) ;
#13413 = CARTESIAN_POINT ( 'NONE',  ( 19.03943276465977164, -0.05219959533909143690, 43.74890960531435979 ) ) ;
#13414 = CARTESIAN_POINT ( 'NONE',  ( 16.51473224551069308, 9.474510206698969483, 89.16557627198103830 ) ) ;
#13415 = CARTESIAN_POINT ( 'NONE',  ( 18.62759615963255655, 10.81492255796105972, 56.66775706135235424 ) ) ;
#13416 = CARTESIAN_POINT ( 'NONE',  ( 9.564922557960805705, 16.46253265017160317, 59.58224293864769550 ) ) ;
#13417 = CARTESIAN_POINT ( 'NONE',  ( -4.483927247898539470, -16.52544592524342804, 87.29057627198103830 ) ) ;
#13418 = FACE_OUTER_BOUND ( 'NONE', #195223, .T. ) ;
#13419 = CARTESIAN_POINT ( 'NONE',  ( -4.379528057220328563, 16.55341960407611168, 75.20724293864769550 ) ) ;
#13420 = CARTESIAN_POINT ( 'NONE',  ( 10.81492255796078972, 18.62759615963270932, 79.58224293864769550 ) ) ;
#13421 = CARTESIAN_POINT ( 'NONE',  ( 13.97604488694548053, -13.89961937509957401, 95.62609039468563310 ) ) ;
#13422 = CARTESIAN_POINT ( 'NONE',  ( 19.39720447994794483, 5.500000000000019540, 92.16317477297178584 ) ) ;
#13423 = CARTESIAN_POINT ( 'NONE',  ( -16.46253265017146816, -9.564922557961047289, 39.16775706135234003 ) ) ;
#13424 = CARTESIAN_POINT ( 'NONE',  ( 17.40805194821986035, -6.112264579160785694, 73.33371272510611050 ) ) ;
#13426 = CARTESIAN_POINT ( 'NONE',  ( -16.51473224551069308, -9.474510206698971260, 81.66557627198103830 ) ) ;
#13425 = CARTESIAN_POINT ( 'NONE',  ( 0.05219959533909260263, 19.03943276465977164, 74.99890960531435269 ) ) ;
#13427 = CARTESIAN_POINT ( 'NONE',  ( 4.379528057220092307, 16.55341960407617563, 67.29275706135234714 ) ) ;
#13428 = CARTESIAN_POINT ( 'NONE',  ( -3.889087296526120063, -29.99999999999998579, 1.818019484660534424 ) ) ;
#13429 = CARTESIAN_POINT ( 'NONE',  ( 19.03943276465977164, 0.05219959533936151252, 46.25109039468566863 ) ) ;
#13430 = CARTESIAN_POINT ( 'NONE',  ( 17.45411292087690569, 5.827443620977868832, 21.68149470724943129 ) ) ;
#13431 = CARTESIAN_POINT ( 'NONE',  ( -13.89961937509977652, 13.97604488694528158, 110.6239096053143243 ) ) ;
#13432 = CARTESIAN_POINT ( 'NONE',  ( 0.05219959533934541429, -16.53943276465976808, 95.00109039468568994 ) ) ;
#13433 = CARTESIAN_POINT ( 'NONE',  ( -3.874011537017657769, -5.276777131403250998, -64.46083232413522524 ) ) ;
#13434 = CARTESIAN_POINT ( 'NONE',  ( -12.06949235617739369, -12.14591786802326823, 74.37609039468568994 ) ) ;
#13435 = DIRECTION ( 'NONE',  ( 0.000000000000000000, 0.000000000000000000, -1.000000000000000000 ) ) ;
#13436 = CARTESIAN_POINT ( 'NONE',  ( 8.224510206698742110, 14.34966873604972548, 52.08442372801901854 ) ) ;
#13437 = DIRECTION ( 'NONE',  ( 1.000000000000000000, 0.000000000000000000, 0.000000000000000000 ) ) ;
#13438 = CARTESIAN_POINT ( 'NONE',  ( -10.72451020669870658, -18.67979575497194134, 64.58442372801900433 ) ) ;
#13439 = CARTESIAN_POINT ( 'NONE',  ( -13.89961937509957401, -13.97604488694547875, 69.37609039468564731 ) ) ;
#13440 = CARTESIAN_POINT ( 'NONE',  ( 0.05219959533936267826, -19.03943276465977164, 25.00109039468566152 ) ) ;
#13441 = CARTESIAN_POINT ( 'NONE',  ( 0.05219959533909260263, 19.03943276465977164, 54.99890960531435979 ) ) ;
#13442 = CARTESIAN_POINT ( 'NONE',  ( -16.46253265017160317, 9.564922557960807481, 40.83224293864769550 ) ) ;
#13443 = DIRECTION ( 'NONE',  ( -1.000000000000000000, 0.000000000000000000, 0.000000000000000000 ) ) ;
#13444 = CARTESIAN_POINT ( 'NONE',  ( 21.53943276465977519, -0.05219959533907433946, 63.74890960531435979 ) ) ;
#13445 = CARTESIAN_POINT ( 'NONE',  ( -9.474510206698964154, 16.51473224551069663, 115.4155762719810241 ) ) ;
#13446 = CARTESIAN_POINT ( 'NONE',  ( 13.89961937509977652, -13.97604488694527269, 23.12390960531436335 ) ) ;
#13447 = CARTESIAN_POINT ( 'NONE',  ( 12.14591786802327356, -12.06949235617739191, 45.62609039468567573 ) ) ;
#13448 = VERTEX_POINT ( 'NONE', #10290 ) ;
#13449 = CARTESIAN_POINT ( 'NONE',  ( 18.62759615963271287, -10.81492255796078972, 113.3322429386476955 ) ) ;
#13451 = CARTESIAN_POINT ( 'NONE',  ( -11.74264578624799782, -36.14014761921581709, -3.600000000000000533 ) ) ;
#13450 = CARTESIAN_POINT ( 'NONE',  ( 16.52544592524342804, -4.483927247898539470, 58.54057627198103120 ) ) ;
#13452 = CARTESIAN_POINT ( 'NONE',  ( 5.153800228976615827, -19.02544592524334988, 110.2094237280189901 ) ) ;
#13453 = CARTESIAN_POINT ( 'NONE',  ( -5.153800228976607833, 19.02544592524334988, 42.70942372801901143 ) ) ;
#13454 = CARTESIAN_POINT ( 'NONE',  ( -4.379528057220328563, 16.55341960407611168, 40.20724293864769550 ) ) ;
#13455 = CARTESIAN_POINT ( 'NONE',  ( -0.05219959533907301413, -21.53943276465977519, 112.4989096053143669 ) ) ;
#13457 = CARTESIAN_POINT ( 'NONE',  ( 18.62759615963271287, -10.81492255796078972, 58.33224293864768839 ) ) ;
#13456 = CARTESIAN_POINT ( 'NONE',  ( 16.29526858892879204, 7.335722546919996034, 33.29670597800208043 ) ) ;
#13458 = CARTESIAN_POINT ( 'NONE',  ( -9.564922557960796823, -16.46253265017161027, 87.08224293864769550 ) ) ;
#13459 = CARTESIAN_POINT ( 'NONE',  ( 12.06949235617757843, -12.14591786802309237, 58.12390960531435979 ) ) ;
#13460 = CARTESIAN_POINT ( 'NONE',  ( 13.97604488694527802, 13.89961937509977652, 104.3739096053143385 ) ) ;
#13461 = CARTESIAN_POINT ( 'NONE',  ( -36.90816834587730000, 0.7173862878750039140, 50.46507289210754266 ) ) ;
#13462 = CARTESIAN_POINT ( 'NONE',  ( -16.46253265017146816, -9.564922557961047289, 49.16775706135233293 ) ) ;
#13463 = CARTESIAN_POINT ( 'NONE',  ( 15.72974639402199770, -15.80617190586745480, 103.1239096053143811 ) ) ;
#13464 = CARTESIAN_POINT ( 'NONE',  ( -0.05219959533909027116, -19.03943276465977164, 47.49890960531435979 ) ) ;
#13465 = CARTESIAN_POINT ( 'NONE',  ( 13.97604488694527802, 13.89961937509977652, 24.37390960531435624 ) ) ;
#13466 = EDGE_CURVE ( 'NONE', #80486, #64642, #91865, .T. ) ;
#13467 = CARTESIAN_POINT ( 'NONE',  ( 10.81492255796106328, -18.62759615963255655, 55.41775706135234714 ) ) ;
#13468 = CARTESIAN_POINT ( 'NONE',  ( 27.73933785331498569, 2.768321779492822058E-14, 145.8750000027311842 ) ) ;
#13469 = CARTESIAN_POINT ( 'NONE',  ( -16.53943276465976808, 0.05219959533911058130, 31.24890960531435979 ) ) ;
#13470 = CARTESIAN_POINT ( 'NONE',  ( -19.02544592524342804, 5.153800228976336051, 46.04057627198101699 ) ) ;
#13471 = CARTESIAN_POINT ( 'NONE',  ( -9.474510206698964154, 16.51473224551069663, 105.4155762719810383 ) ) ;
#13472 = CARTESIAN_POINT ( 'NONE',  ( 5.823673210054125526, 21.52544592524343514, 74.79057627198105251 ) ) ;
#13473 = CARTESIAN_POINT ( 'NONE',  ( 22.44159573604009594, -16.30477369853687364, 141.6750000027311671 ) ) ;
#13474 = CARTESIAN_POINT ( 'NONE',  ( -16.51473224551069308, -9.474510206698971260, 41.66557627198103120 ) ) ;
#13475 = CARTESIAN_POINT ( 'NONE',  ( 21.53943276465977519, -0.05219959533907433946, 58.74890960531436690 ) ) ;
#13476 = CARTESIAN_POINT ( 'NONE',  ( 21.53943276465977519, 0.05219959533937863772, 91.25109039468568994 ) ) ;
#13478 = CARTESIAN_POINT ( 'NONE',  ( 4.483927247898545687, 16.52544592524342804, 74.79057627198105251 ) ) ;
#13477 = CARTESIAN_POINT ( 'NONE',  ( -16.55341960407617563, 4.379528057220093196, 83.54275706135234714 ) ) ;
#13479 = CARTESIAN_POINT ( 'NONE',  ( 19.02544592524343514, -5.153800228976328945, 68.54057627198103830 ) ) ;
#13480 = ORIENTED_EDGE ( 'NONE', *, *, #164374, .T. ) ;
#13481 = CARTESIAN_POINT ( 'NONE',  ( -0.05219959533936034679, 19.03943276465977164, 32.50109039468566863 ) ) ;
#13482 = CARTESIAN_POINT ( 'NONE',  ( -4.379528057220086978, -16.55341960407618274, 94.79275706135234714 ) ) ;
#13483 = CARTESIAN_POINT ( 'NONE',  ( -10.81492255796105439, 18.62759615963255655, 112.9177570613523329 ) ) ;
#13484 = CARTESIAN_POINT ( 'NONE',  ( 16.46253265017160672, -9.564922557960803928, 73.33224293864769550 ) ) ;
#13485 = CARTESIAN_POINT ( 'NONE',  ( -18.67979575497178146, -10.72451020669898902, 46.66557627198102409 ) ) ;
#13486 = CARTESIAN_POINT ( 'NONE',  ( -16.53943276465976808, -0.05219959533934237506, 18.75109039468568639 ) ) ;
#13487 = CARTESIAN_POINT ( 'NONE',  ( -21.55341960407619339, 5.719274019375674811, 93.54275706135234714 ) ) ;
#13488 = CARTESIAN_POINT ( 'NONE',  ( 8.224510206698742110, 14.34966873604972548, 67.08442372801901854 ) ) ;
#13489 = CARTESIAN_POINT ( 'NONE',  ( -0.05219959533907301413, -21.53943276465977519, 112.4989096053143669 ) ) ;
#13490 = CARTESIAN_POINT ( 'NONE',  ( -9.564922557961040184, 16.46253265017147172, 112.9177570613523329 ) ) ;
#13491 = CARTESIAN_POINT ( 'NONE',  ( -19.03943276465977164, 0.05219959533909376836, 91.24890960531436690 ) ) ;
#13492 = CARTESIAN_POINT ( 'NONE',  ( 8.224510206698742110, 14.34966873604972548, 22.08442372801901143 ) ) ;
#13493 = CARTESIAN_POINT ( 'NONE',  ( 16.46253265017160672, -9.564922557960803928, 48.33224293864769550 ) ) ;
#13494 = CARTESIAN_POINT ( 'NONE',  ( -0.05219959533934338120, 16.53943276465976808, 37.50109039468568284 ) ) ;
#13495 = CARTESIAN_POINT ( 'NONE',  ( -12.06949235617756955, 12.14591786802309770, 80.62390960531438111 ) ) ;
#13496 = CARTESIAN_POINT ( 'NONE',  ( -4.483927247898782831, 16.52544592524335698, 92.70942372801901854 ) ) ;
#13498 = CARTESIAN_POINT ( 'NONE',  ( -5.153800228976328057, -19.02544592524343514, 67.29057627198102409 ) ) ;
#13497 = CARTESIAN_POINT ( 'NONE',  ( 15.80617190586769283, -15.72974639402175789, 25.62609039468567929 ) ) ;
#13499 = CARTESIAN_POINT ( 'NONE',  ( -0.05219959533909027116, -19.03943276465977164, 77.49890960531435269 ) ) ;
#13500 = CARTESIAN_POINT ( 'NONE',  ( -12.14591786802326823, 12.06949235617739902, 88.12609039468570415 ) ) ;
#13502 = ORIENTED_EDGE ( 'NONE', *, *, #84475, .T. ) ;
#13501 = CARTESIAN_POINT ( 'NONE',  ( -24.27995301597599465, -6.552671593955007978, 171.1165850637241874 ) ) ;
#13503 = ORIENTED_EDGE ( 'NONE', *, *, #26464, .T. ) ;
#13504 = CARTESIAN_POINT ( 'NONE',  ( 19.05341960407617918, -5.049401038297876454, 31.04275706135232227 ) ) ;
#13505 = CARTESIAN_POINT ( 'NONE',  ( -16.46253265017160317, 9.564922557960807481, 95.83224293864769550 ) ) ;
#13506 = CARTESIAN_POINT ( 'NONE',  ( 19.05341960407611168, 5.049401038298154454, 53.95724293864770260 ) ) ;
#13507 = CARTESIAN_POINT ( 'NONE',  ( 8.388830574159379737E-16, 13.70000000000001528, -62.58071313852362039 ) ) ;
#13508 = CARTESIAN_POINT ( 'NONE',  ( 16.55341960407618274, -4.379528057220086978, 36.04275706135234714 ) ) ;
#13510 = CARTESIAN_POINT ( 'NONE',  ( 14.34966873604972726, -8.224510206698740333, 40.83442372801901854 ) ) ;
#13509 = CARTESIAN_POINT ( 'NONE',  ( 13.97604488694548053, -13.89961937509957401, 55.62609039468566863 ) ) ;
#13511 = CARTESIAN_POINT ( 'NONE',  ( 13.97604488694527802, 13.89961937509977652, 109.3739096053143669 ) ) ;
#13512 = CARTESIAN_POINT ( 'NONE',  ( 13.97604488694527802, 13.89961937509977652, 74.37390960531436690 ) ) ;
#13513 = CARTESIAN_POINT ( 'NONE',  ( -21.55341960407610458, -5.719274019375992779, 96.45724293864770971 ) ) ;
#13514 = CARTESIAN_POINT ( 'NONE',  ( 16.46253265017146816, 9.564922557961045513, 61.66775706135234003 ) ) ;
#13516 = CARTESIAN_POINT ( 'NONE',  ( 17.47739027167831694, -4.111523782424557183, 21.69296162454243770 ) ) ;
#13515 = CARTESIAN_POINT ( 'NONE',  ( -5.049401038298153566, 19.05341960407611168, 95.20724293864770971 ) ) ;
#13517 = CARTESIAN_POINT ( 'NONE',  ( 5.049401038298161559, -19.05341960407611168, 62.70724293864769550 ) ) ;
#13519 = CARTESIAN_POINT ( 'NONE',  ( -9.564922557960796823, -16.46253265017161027, 27.08224293864769550 ) ) ;
#13518 = CARTESIAN_POINT ( 'NONE',  ( -14.29746914071049879, 8.314922557960819915, 35.83224293864768839 ) ) ;
#13520 = CARTESIAN_POINT ( 'NONE',  ( -9.564922557961040184, 16.46253265017147172, 37.91775706135233293 ) ) ;
#13521 = CARTESIAN_POINT ( 'NONE',  ( -14.29746914071049879, 8.314922557960819915, 75.83224293864769550 ) ) ;
#13522 = CARTESIAN_POINT ( 'NONE',  ( 18.62759615963255655, 10.81492255796105972, 96.66775706135234714 ) ) ;
#13523 = CARTESIAN_POINT ( 'NONE',  ( 19.03943276465977164, -0.05219959533909143690, 33.74890960531435979 ) ) ;
#13524 = CARTESIAN_POINT ( 'NONE',  ( -8.314922557961024197, 14.29746914071037800, 47.91775706135234714 ) ) ;
#13526 = CARTESIAN_POINT ( 'NONE',  ( -21.52544592524334988, -5.823673210054445271, 108.9594237280190185 ) ) ;
#13525 = CARTESIAN_POINT ( 'NONE',  ( -0.05219959533910754901, -16.53943276465976808, 37.49890960531436690 ) ) ;
#13527 = CARTESIAN_POINT ( 'NONE',  ( 19.03943276465977164, -0.05219959533909143690, 98.74890960531436690 ) ) ;
#13528 = CARTESIAN_POINT ( 'NONE',  ( 16.46253265017160672, -9.564922557960803928, 88.33224293864769550 ) ) ;
#13529 = CARTESIAN_POINT ( 'NONE',  ( 19.02544592524343514, -5.153800228976328945, 28.54057627198102409 ) ) ;
#13530 = CARTESIAN_POINT ( 'NONE',  ( -12.06949235617756955, 12.14591786802309770, 105.6239096053143669 ) ) ;
#13531 = CARTESIAN_POINT ( 'NONE',  ( -0.05219959533910754901, -16.53943276465976808, 77.49890960531433848 ) ) ;
#13532 = CARTESIAN_POINT ( 'NONE',  ( -0.05219959533907301413, -21.53943276465977519, 82.49890960531436690 ) ) ;
#13533 = CARTESIAN_POINT ( 'NONE',  ( -9.474510206698964154, 16.51473224551069663, 90.41557627198103830 ) ) ;
#13534 = CARTESIAN_POINT ( 'NONE',  ( 10.81492255796078972, 18.62759615963270932, 94.58224293864769550 ) ) ;
#13535 = CARTESIAN_POINT ( 'NONE',  ( 0.05219959533909260263, 19.03943276465977164, 94.99890960531436690 ) ) ;
#13537 = CARTESIAN_POINT ( 'NONE',  ( -0.05219959533910754901, -16.53943276465976808, 87.49890960531436690 ) ) ;
#13536 = CARTESIAN_POINT ( 'NONE',  ( 18.39443945427639093, -5.500000000000022204, 46.01745347608652281 ) ) ;
#13538 = CARTESIAN_POINT ( 'NONE',  ( 19.05341960407611168, 5.049401038298154454, 58.95724293864768129 ) ) ;
#13539 = CARTESIAN_POINT ( 'NONE',  ( 10.72451020669898902, -18.67979575497178502, 72.91557627198103830 ) ) ;
#13540 = EDGE_CURVE ( 'NONE', #155869, #53672, #71948, .T. ) ;
#13541 = CARTESIAN_POINT ( 'NONE',  ( -23.31738231874055245, -16.94106989632524574, 146.1999999999999886 ) ) ;
#13542 = CARTESIAN_POINT ( 'NONE',  ( 12.14591786802327356, -12.06949235617739191, 110.6260903946857042 ) ) ;
#13543 = CARTESIAN_POINT ( 'NONE',  ( -14.29746914071037622, -8.314922557961029526, 24.16775706135235424 ) ) ;
#13544 = CARTESIAN_POINT ( 'NONE',  ( -16.53943276465976808, 0.05219959533911058130, 86.24890960531436690 ) ) ;
#13545 = CARTESIAN_POINT ( 'NONE',  ( -17.49999999999999645, -5.624438216177593652, 94.18329655085352670 ) ) ;
#13546 = CARTESIAN_POINT ( 'NONE',  ( 16.46253265017160672, -9.564922557960803928, 78.33224293864769550 ) ) ;
#13547 = CARTESIAN_POINT ( 'NONE',  ( -19.03943276465977164, 0.05219959533909376836, 51.24890960531436690 ) ) ;
#13548 = CARTESIAN_POINT ( 'NONE',  ( 12.06949235617757843, -12.14591786802309237, 68.12390960531436690 ) ) ;
#13549 = CARTESIAN_POINT ( 'NONE',  ( 0.05219959533909260263, 19.03943276465977164, 114.9989096053143669 ) ) ;
#13550 = CARTESIAN_POINT ( 'NONE',  ( 5.153800228976615827, -19.02544592524334988, 100.2094237280190043 ) ) ;
#13551 = CARTESIAN_POINT ( 'NONE',  ( -5.823673210054431948, 21.52544592524334988, 57.70942372801901143 ) ) ;
#13552 = CARTESIAN_POINT ( 'NONE',  ( 19.03943276465977164, -0.05219959533909143690, 103.7489096053143669 ) ) ;
#13553 = CARTESIAN_POINT ( 'NONE',  ( -5.823673210054116645, -21.52544592524344225, 82.29057627198103830 ) ) ;
#13554 = CARTESIAN_POINT ( 'NONE',  ( -16.52544592524335698, -4.483927247898792601, 68.95942372801901854 ) ) ;
#13555 = CARTESIAN_POINT ( 'NONE',  ( -17.44279575226785894, 5.990770900253882481, 95.83557567514318976 ) ) ;
#13556 = CARTESIAN_POINT ( 'NONE',  ( 9.474510206698971260, -16.51473224551069308, 72.91557627198102409 ) ) ;
#13557 = CARTESIAN_POINT ( 'NONE',  ( 21.55341960407610458, 5.719274019375980345, 83.95724293864770971 ) ) ;
#13558 = CARTESIAN_POINT ( 'NONE',  ( -9.564922557961040184, 16.46253265017147172, 102.9177570613523329 ) ) ;
#13560 = CARTESIAN_POINT ( 'NONE',  ( -21.53943276465977519, -0.05219959533937600094, 53.75109039468568994 ) ) ;
#13559 = CARTESIAN_POINT ( 'NONE',  ( -12.14591786802309592, -12.06949235617757132, 41.87390960531435979 ) ) ;
#13562 = CARTESIAN_POINT ( 'NONE',  ( 5.049401038298161559, -19.05341960407611168, 102.7072429386476955 ) ) ;
#13561 = CARTESIAN_POINT ( 'NONE',  ( -14.29746914071037622, -8.314922557961029526, 84.16775706135234714 ) ) ;
#13563 = CARTESIAN_POINT ( 'NONE',  ( -13.97604488694527625, -13.89961937509977830, 101.8739096053143669 ) ) ;
#13564 = CARTESIAN_POINT ( 'NONE',  ( 4.500000000000000888, -140.0000000000000000, 13.35010376910484275 ) ) ;
#13565 = CARTESIAN_POINT ( 'NONE',  ( -4.483927247898782831, 16.52544592524335698, 97.70942372801904696 ) ) ;
#13566 = CARTESIAN_POINT ( 'NONE',  ( 4.379528057220092307, 16.55341960407617563, 52.29275706135236135 ) ) ;
#13567 = CARTESIAN_POINT ( 'NONE',  ( 13.89961937509977652, -13.97604488694527269, 58.12390960531436690 ) ) ;
#13568 = CARTESIAN_POINT ( 'NONE',  ( -0.05219959533909027116, -19.03943276465977164, 67.49890960531436690 ) ) ;
#13569 = CARTESIAN_POINT ( 'NONE',  ( 5.719274019375673035, 21.55341960407619339, 62.29275706135236845 ) ) ;
#13570 = CARTESIAN_POINT ( 'NONE',  ( -8.314922557961024197, 14.29746914071037800, 67.91775706135234714 ) ) ;
#13571 = CARTESIAN_POINT ( 'NONE',  ( -16.55341960407611168, -4.379528057220339221, 51.45724293864770260 ) ) ;
#13572 = CARTESIAN_POINT ( 'NONE',  ( 9.474510206698971260, -16.51473224551069308, 47.91557627198102409 ) ) ;
#13573 = CARTESIAN_POINT ( 'NONE',  ( 13.89961937509977652, -13.97604488694527269, 53.12390960531434558 ) ) ;
#13574 = CARTESIAN_POINT ( 'NONE',  ( -14.34966873604972548, 8.224510206698743886, 38.33442372801900433 ) ) ;
#13575 = CARTESIAN_POINT ( 'NONE',  ( -5.049401038297874678, -19.05341960407617918, 89.79275706135230450 ) ) ;
#13576 = CARTESIAN_POINT ( 'NONE',  ( 12.14591786802309770, 12.06949235617756955, 94.37390960531436690 ) ) ;
#13577 = CARTESIAN_POINT ( 'NONE',  ( 16.51473224551069308, 9.474510206698969483, 69.16557627198102409 ) ) ;
#13579 = CARTESIAN_POINT ( 'NONE',  ( 23.48529157249600630, -32.32473071737749137, -9.300000000000002487 ) ) ;
#13578 = CARTESIAN_POINT ( 'NONE',  ( -0.05219959533936034679, 19.03943276465977164, 102.5010903946856757 ) ) ;
#13580 = CARTESIAN_POINT ( 'NONE',  ( 10.81492255796106328, -18.62759615963255655, 90.41775706135236135 ) ) ;
#13581 = CARTESIAN_POINT ( 'NONE',  ( 16.53943276465976808, 0.05219959533934440121, 61.25109039468567573 ) ) ;
#13582 = FACE_OUTER_BOUND ( 'NONE', #190809, .T. ) ;
#13583 = CARTESIAN_POINT ( 'NONE',  ( 15.72974639402199770, -15.80617190586745480, 58.12390960531435979 ) ) ;
#13584 = CARTESIAN_POINT ( 'NONE',  ( -12.14591786802326823, 12.06949235617739902, 53.12609039468568284 ) ) ;
#13585 = CARTESIAN_POINT ( 'NONE',  ( -9.564922557960796823, -16.46253265017161027, 37.08224293864768839 ) ) ;
#13586 = CARTESIAN_POINT ( 'NONE',  ( -16.46253265017146816, -9.564922557961047289, 49.16775706135233293 ) ) ;
#13587 = CARTESIAN_POINT ( 'NONE',  ( -19.05341960407611168, -5.049401038298163336, 86.45724293864769550 ) ) ;
#13588 = CARTESIAN_POINT ( 'NONE',  ( 19.02544592524343514, -5.153800228976328945, 23.54057627198102054 ) ) ;
#13589 = CARTESIAN_POINT ( 'NONE',  ( -5.049401038298153566, 19.05341960407611168, 70.20724293864769550 ) ) ;
#13590 = CARTESIAN_POINT ( 'NONE',  ( 15.33930553228143800, 17.41439684931609122, -55.09142748592169170 ) ) ;
#13591 = CARTESIAN_POINT ( 'NONE',  ( -15.80617190586768217, 15.72974639402176855, 83.12609039468568994 ) ) ;
#13592 = CARTESIAN_POINT ( 'NONE',  ( -18.22780087662121673, -5.500000000000063061, 56.48459894673892734 ) ) ;
#13593 = CARTESIAN_POINT ( 'NONE',  ( -13.89961937509957401, -13.97604488694547875, 39.37609039468566152 ) ) ;
#13594 = CARTESIAN_POINT ( 'NONE',  ( -5.049401038297874678, -19.05341960407617918, 24.79275706135233648 ) ) ;
#13595 = CARTESIAN_POINT ( 'NONE',  ( 4.379528057220339221, -16.55341960407611168, 52.70724293864769550 ) ) ;
#13596 = CARTESIAN_POINT ( 'NONE',  ( 0.05219959533909260263, 19.03943276465977164, 54.99890960531435979 ) ) ;
#13597 = CARTESIAN_POINT ( 'NONE',  ( 18.67979575497178502, 10.72451020669898547, 24.16557627198103120 ) ) ;
#13598 = CARTESIAN_POINT ( 'NONE',  ( -5.823673210054431948, 21.52544592524334988, 77.70942372801900433 ) ) ;
#13599 = CARTESIAN_POINT ( 'NONE',  ( -16.51473224551069308, -9.474510206698971260, 61.66557627198103120 ) ) ;
#13600 = CARTESIAN_POINT ( 'NONE',  ( -18.67979575497193778, 10.72451020669871902, 78.33442372801901854 ) ) ;
#13601 = CARTESIAN_POINT ( 'NONE',  ( -21.52544592524343514, 5.823673210054127303, 31.04057627198102409 ) ) ;
#13602 = CARTESIAN_POINT ( 'NONE',  ( -10.81492255796105439, 18.62759615963255655, 42.91775706135235424 ) ) ;
#13603 = CARTESIAN_POINT ( 'NONE',  ( 5.153800228976615827, -19.02544592524334988, 55.20942372801899722 ) ) ;
#13604 = CARTESIAN_POINT ( 'NONE',  ( -16.46253265017160317, 9.564922557960807481, 45.83224293864769550 ) ) ;
#13605 = CARTESIAN_POINT ( 'NONE',  ( 13.97604488694527802, 13.89961937509977652, 74.37390960531436690 ) ) ;
#13606 = CARTESIAN_POINT ( 'NONE',  ( -8.314922557961024197, 14.29746914071037800, 32.91775706135234714 ) ) ;
#13607 = CARTESIAN_POINT ( 'NONE',  ( -8.224510206698948167, 14.34966873604960824, 95.41557627198102409 ) ) ;
#13608 = CARTESIAN_POINT ( 'NONE',  ( -19.02544592524342804, 5.153800228976336051, 56.04057627198100988 ) ) ;
#13609 = CARTESIAN_POINT ( 'NONE',  ( 0.05219959533907565091, 21.53943276465977519, 44.99890960531435979 ) ) ;
#13610 = CARTESIAN_POINT ( 'NONE',  ( 0.05219959533934541429, -16.53943276465976808, 25.00109039468567218 ) ) ;
#13611 = CARTESIAN_POINT ( 'NONE',  ( -10.72451020669870658, -18.67979575497194134, 24.58442372801901499 ) ) ;
#13612 = CARTESIAN_POINT ( 'NONE',  ( -10.72451020669870658, -18.67979575497194134, 74.58442372801901854 ) ) ;
#13614 = CARTESIAN_POINT ( 'NONE',  ( -8.314922557961024197, 14.29746914071037800, 67.91775706135234714 ) ) ;
#13613 = B_SPLINE_CURVE_WITH_KNOTS ( 'NONE', 3,
 ( #148994, #12486, #26655, #87310, #54976, #55973, #88297, #134832, #196511, #181335, #57981, #89302, #23646, #164167, #193498, #119653 ),
 .UNSPECIFIED., .F., .F.,
 ( 4, 2, 2, 2, 2, 2, 2, 4 ),
 ( 1.970462154302192724E-07, 0.0003070558431632680260, 0.0006139146401111058486, 0.001227632234006777482, 0.001534491030954616064, 0.001841349827902454645, 0.002148208624850302551, 0.002455067421798150240 ),
 .UNSPECIFIED. ) ;
#13615 = CARTESIAN_POINT ( 'NONE',  ( -8.314922557961024197, 14.29746914071037800, 67.91775706135234714 ) ) ;
#13616 = CARTESIAN_POINT ( 'NONE',  ( -19.03943276465977164, 0.05219959533909376836, 66.24890960531436690 ) ) ;
#13617 = CARTESIAN_POINT ( 'NONE',  ( 14.34966873604972726, -8.224510206698740333, 90.83442372801901854 ) ) ;
#13618 = CARTESIAN_POINT ( 'NONE',  ( -9.564922557961040184, 16.46253265017147172, 37.91775706135233293 ) ) ;
#13619 = CARTESIAN_POINT ( 'NONE',  ( 21.55341960407610458, 5.719274019375980345, 108.9572429386476955 ) ) ;
#13620 = CARTESIAN_POINT ( 'NONE',  ( 4.483927247898545687, 16.52544592524342804, 64.79057627198103830 ) ) ;
#13621 = CARTESIAN_POINT ( 'NONE',  ( 13.89961937509977652, -13.97604488694527269, 88.12390960531438111 ) ) ;
#13622 = CARTESIAN_POINT ( 'NONE',  ( -14.29746914071037622, -8.314922557961029526, 94.16775706135237556 ) ) ;
#13623 = CARTESIAN_POINT ( 'NONE',  ( 5.719274019375673035, 21.55341960407619339, 57.29275706135234714 ) ) ;
#13624 = CARTESIAN_POINT ( 'NONE',  ( 8.314922557961029526, -14.29746914071037800, 35.41775706135234003 ) ) ;
#13625 = CARTESIAN_POINT ( 'NONE',  ( -15.72974639402176322, -15.80617190586768395, 29.37609039468568284 ) ) ;
#13626 = CARTESIAN_POINT ( 'NONE',  ( 14.34966873604960469, 8.224510206698951720, 59.16557627198103120 ) ) ;
#13627 = VERTEX_POINT ( 'NONE', #119460 ) ;
#13628 = CARTESIAN_POINT ( 'NONE',  ( -18.62759615963270932, 10.81492255796079327, 95.83224293864770971 ) ) ;
#13629 = CARTESIAN_POINT ( 'NONE',  ( -4.379528057220328563, 16.55341960407611168, 45.20724293864769550 ) ) ;
#13630 = ORIENTED_EDGE ( 'NONE', *, *, #118352, .T. ) ;
#13631 = CARTESIAN_POINT ( 'NONE',  ( 34.64436006561229675, 3.766901597203519803, 51.50401746017936944 ) ) ;
#13632 = CARTESIAN_POINT ( 'NONE',  ( -5.823673210054116645, -21.52544592524344225, 22.29057627198102765 ) ) ;
#13633 = CARTESIAN_POINT ( 'NONE',  ( -10.81492255796105439, 18.62759615963255655, 42.91775706135235424 ) ) ;
#13634 = CARTESIAN_POINT ( 'NONE',  ( -14.29746914071049879, 8.314922557960819915, 65.83224293864769550 ) ) ;
#13635 = CARTESIAN_POINT ( 'NONE',  ( 9.474510206698971260, -16.51473224551069308, 57.91557627198103120 ) ) ;
#13637 = CARTESIAN_POINT ( 'NONE',  ( -5.049401038297874678, -19.05341960407617918, 64.79275706135233293 ) ) ;
#13636 = CARTESIAN_POINT ( 'NONE',  ( -19.03943276465977164, 0.05219959533909376836, 21.24890960531436335 ) ) ;
#13638 = CARTESIAN_POINT ( 'NONE',  ( 10.81492255796078972, 18.62759615963270932, 54.58224293864769550 ) ) ;
#13639 = CARTESIAN_POINT ( 'NONE',  ( -25.08997344982928013, -28.19247641866677512, -20.54396225644688556 ) ) ;
#13640 = CARTESIAN_POINT ( 'NONE',  ( -19.05341960407611168, -5.049401038298163336, 61.45724293864769550 ) ) ;
#13641 = CARTESIAN_POINT ( 'NONE',  ( 8.224510206698742110, 14.34966873604972548, 37.08442372801901143 ) ) ;
#13642 = CARTESIAN_POINT ( 'NONE',  ( -18.62759615963270932, 10.81492255796079327, 110.8322429386476955 ) ) ;
#13643 = CARTESIAN_POINT ( 'NONE',  ( -12.14591786802309592, -12.06949235617757132, 41.87390960531435979 ) ) ;
#13644 = EDGE_LOOP ( 'NONE', ( #185573, #160143, #79077, #16374 ) ) ;
#13645 = CARTESIAN_POINT ( 'NONE',  ( 19.05341960407611168, 5.049401038298154454, 88.95724293864769550 ) ) ;
#13646 = CARTESIAN_POINT ( 'NONE',  ( 21.55341960407610458, 5.719274019375980345, 78.95724293864769550 ) ) ;
#13648 = CARTESIAN_POINT ( 'NONE',  ( -8.314922557961024197, 14.29746914071037800, 42.91775706135235424 ) ) ;
#13647 = CARTESIAN_POINT ( 'NONE',  ( -10.81492255796078084, -18.62759615963271287, 112.0822429386477097 ) ) ;
#13649 = CARTESIAN_POINT ( 'NONE',  ( -21.53943276465977519, 0.05219959533907696930, 41.24890960531435269 ) ) ;
#13650 = CARTESIAN_POINT ( 'NONE',  ( -10.81492255796105439, 18.62759615963255655, 102.9177570613523756 ) ) ;
#13651 = CARTESIAN_POINT ( 'NONE',  ( 13.89961937509977652, -13.97604488694527269, 103.1239096053143527 ) ) ;
#13652 = CARTESIAN_POINT ( 'NONE',  ( -9.564922557960796823, -16.46253265017161027, 47.08224293864769550 ) ) ;
#13653 = CARTESIAN_POINT ( 'NONE',  ( 9.474510206698971260, -16.51473224551069308, 92.91557627198103830 ) ) ;
#13654 = CARTESIAN_POINT ( 'NONE',  ( 16.46253265017160672, -9.564922557960803928, 73.33224293864769550 ) ) ;
#13655 = CARTESIAN_POINT ( 'NONE',  ( 16.21995358207279381, -7.366697692864220492, 87.43551001512066989 ) ) ;
#13656 = CARTESIAN_POINT ( 'NONE',  ( 19.05341960407617918, -5.049401038297876454, 51.04275706135231871 ) ) ;
#13658 = CARTESIAN_POINT ( 'NONE',  ( -5.719274019375978568, 21.55341960407610458, 25.20724293864769550 ) ) ;
#13657 = CARTESIAN_POINT ( 'NONE',  ( 10.81492255796106328, -18.62759615963255655, 105.4177570613523613 ) ) ;
#13659 = EDGE_CURVE ( 'NONE', #42657, #30159, #117744, .T. ) ;
#13660 = CARTESIAN_POINT ( 'NONE',  ( -8.314922557961024197, 14.29746914071037800, 102.9177570613523756 ) ) ;
#13661 = CARTESIAN_POINT ( 'NONE',  ( -9.474510206698720793, -16.51473224551083518, 74.58442372801900433 ) ) ;
#13662 = CARTESIAN_POINT ( 'NONE',  ( -16.88567814943164080, 6.947325034625569273, 58.70998877347415856 ) ) ;
#13663 = CARTESIAN_POINT ( 'NONE',  ( 13.97604488694548053, -13.89961937509957401, 85.62609039468568994 ) ) ;
#13664 = CARTESIAN_POINT ( 'NONE',  ( 16.46253265017146816, 9.564922557961045513, 36.66775706135233293 ) ) ;
#13665 = CARTESIAN_POINT ( 'NONE',  ( 17.40861289039002102, 6.110651285853324843, 108.8723247082743342 ) ) ;
#13666 = CARTESIAN_POINT ( 'NONE',  ( -16.51473224551069308, -9.474510206698971260, 41.66557627198103120 ) ) ;
#13667 = CARTESIAN_POINT ( 'NONE',  ( 8.314922557960818139, 14.29746914071049879, 44.58224293864769550 ) ) ;
#13668 = CARTESIAN_POINT ( 'NONE',  ( -5.153800228976328057, -19.02544592524343514, 22.29057627198102765 ) ) ;
#13669 = CARTESIAN_POINT ( 'NONE',  ( -8.314922557960811034, -14.29746914071050412, 22.08224293864769194 ) ) ;
#13670 = CARTESIAN_POINT ( 'NONE',  ( 20.82780142840221060, -20.15002084202731680, -52.57152731843168425 ) ) ;
#13671 = CARTESIAN_POINT ( 'NONE',  ( -16.55341960407617563, 4.379528057220093196, 88.54275706135236135 ) ) ;
#13672 = CARTESIAN_POINT ( 'NONE',  ( 13.97604488694527802, 13.89961937509977652, 54.37390960531435979 ) ) ;
#13673 = CARTESIAN_POINT ( 'NONE',  ( -15.72974639402176322, -15.80617190586768395, 109.3760903946857042 ) ) ;
#13674 = CARTESIAN_POINT ( 'NONE',  ( 5.153800228976615827, -19.02544592524334988, 110.2094237280189901 ) ) ;
#13676 = EDGE_LOOP ( 'NONE', ( #5390, #89021, #93737, #165098, #128042 ) ) ;
#13675 = CARTESIAN_POINT ( 'NONE',  ( 5.823673210054444382, -21.52544592524334988, 95.20942372801903275 ) ) ;
#13677 = CARTESIAN_POINT ( 'NONE',  ( -19.05341960407611168, -5.049401038298163336, 91.45724293864766707 ) ) ;
#13678 = CARTESIAN_POINT ( 'NONE',  ( -5.153800228976328057, -19.02544592524343514, 77.29057627198099567 ) ) ;
#13679 = CARTESIAN_POINT ( 'NONE',  ( 11.40812507854755253, -35.11059874428192273, -10.02499999726881441 ) ) ;
#13680 = CARTESIAN_POINT ( 'NONE',  ( 10.72451020669898902, -18.67979575497178502, 107.9155762719810241 ) ) ;
#13681 = CARTESIAN_POINT ( 'NONE',  ( 12.06949235617757843, -12.14591786802309237, 83.12390960531436690 ) ) ;
#13682 = CARTESIAN_POINT ( 'NONE',  ( 18.67979575497178502, 10.72451020669898547, 74.16557627198102409 ) ) ;
#13683 = CARTESIAN_POINT ( 'NONE',  ( -16.51473224551069308, -9.474510206698971260, 61.66557627198103120 ) ) ;
#13685 = CARTESIAN_POINT ( 'NONE',  ( 14.29746914071037800, 8.314922557961029526, 91.66775706135234714 ) ) ;
#13684 = CARTESIAN_POINT ( 'NONE',  ( -15.72974639402197994, 15.80617190586746368, 100.6239096053143811 ) ) ;
#13686 = EDGE_LOOP ( 'NONE', ( #100957, #99162, #122870, #78497, #107366, #112026 ) ) ;
#13687 = CARTESIAN_POINT ( 'NONE',  ( 5.049401038298161559, -19.05341960407611168, 62.70724293864769550 ) ) ;
#13689 = DIRECTION ( 'NONE',  ( -0.1039620511844979306, 0.1039620511844979306, 0.9891328443778538704 ) ) ;
#13688 = CARTESIAN_POINT ( 'NONE',  ( -14.29746914071049879, 8.314922557960819915, 90.83224293864769550 ) ) ;
#13690 = CARTESIAN_POINT ( 'NONE',  ( 9.564922557960805705, 16.46253265017160317, 54.58224293864769550 ) ) ;
#13691 = CARTESIAN_POINT ( 'NONE',  ( 5.049401038297881783, 19.05341960407617563, 82.29275706135229029 ) ) ;
#13692 = CARTESIAN_POINT ( 'NONE',  ( -8.224510206698948167, 14.34966873604960824, 80.41557627198103830 ) ) ;
#13693 = CARTESIAN_POINT ( 'NONE',  ( 21.53943276465977519, 0.05219959533937863772, 61.25109039468567573 ) ) ;
#13695 = CARTESIAN_POINT ( 'NONE',  ( -10.81492255796078084, -18.62759615963271287, 112.0822429386477097 ) ) ;
#13694 = CARTESIAN_POINT ( 'NONE',  ( 5.153800228976335163, 19.02544592524342804, 34.79057627198102409 ) ) ;
#13696 = CARTESIAN_POINT ( 'NONE',  ( 0.05219959533910956823, 16.53943276465976808, 99.99890960531436690 ) ) ;
#13697 = CARTESIAN_POINT ( 'NONE',  ( 11.94140034372758308, -38.57382067147720761, -24.90972908440997458 ) ) ;
#13698 = CARTESIAN_POINT ( 'NONE',  ( 9.474510206698971260, -16.51473224551069308, 52.91557627198102409 ) ) ;
#13699 = CARTESIAN_POINT ( 'NONE',  ( -10.27527212369962406, -12.17889776840641325, -61.68947035941219070 ) ) ;
#13701 = CARTESIAN_POINT ( 'NONE',  ( 0.05219959533909260263, 19.03943276465977164, 114.9989096053143669 ) ) ;
#13700 = CARTESIAN_POINT ( 'NONE',  ( -19.05341960407617563, 5.049401038297882671, 88.54275706135230450 ) ) ;
#13702 = CARTESIAN_POINT ( 'NONE',  ( -5.719274019375665041, -21.55341960407619695, 49.79275706135234714 ) ) ;
#13703 = CARTESIAN_POINT ( 'NONE',  ( 0.05219959533909260263, 19.03943276465977164, 84.99890960531436690 ) ) ;
#13704 = CARTESIAN_POINT ( 'NONE',  ( -19.05341960407617563, 5.049401038297882671, 73.54275706135233293 ) ) ;
#13705 = CARTESIAN_POINT ( 'NONE',  ( 19.03943276465977164, -0.05219959533909143690, 63.74890960531435979 ) ) ;
#13706 = ADVANCED_FACE ( 'NONE', ( #135627 ), #151779, .T. ) ;
#13707 = CARTESIAN_POINT ( 'NONE',  ( 16.55341960407611168, 4.379528057220329451, 73.95724293864769550 ) ) ;
#13708 = CARTESIAN_POINT ( 'NONE',  ( 16.53943276465976808, -0.05219959533910856209, 83.74890960531435269 ) ) ;
#13709 = CARTESIAN_POINT ( 'NONE',  ( -16.46253265017160317, 9.564922557960807481, 85.83224293864769550 ) ) ;
#13710 = CARTESIAN_POINT ( 'NONE',  ( -8.224510206698948167, 14.34966873604960824, 75.41557627198102409 ) ) ;
#13711 = CARTESIAN_POINT ( 'NONE',  ( -19.05341960407611168, -5.049401038298163336, 91.45724293864766707 ) ) ;
#13712 = CARTESIAN_POINT ( 'NONE',  ( 5.049401038297881783, 19.05341960407617563, 32.29275706135233293 ) ) ;
#13715 = CARTESIAN_POINT ( 'NONE',  ( -12.14591786802309592, -12.06949235617757132, 106.8739096053143811 ) ) ;
#13714 = CARTESIAN_POINT ( 'NONE',  ( 16.53943276465976808, -0.05219959533910856209, 23.74890960531435269 ) ) ;
#13713 = CARTESIAN_POINT ( 'NONE',  ( 19.02544592524343514, -5.153800228976328945, 48.54057627198103120 ) ) ;
#13716 = ORIENTED_EDGE ( 'NONE', *, *, #175617, .T. ) ;
#13717 = CARTESIAN_POINT ( 'NONE',  ( 10.81492255796106328, -18.62759615963255655, 45.41775706135234003 ) ) ;
#13718 = CARTESIAN_POINT ( 'NONE',  ( -9.564922557961040184, 16.46253265017147172, 62.91775706135233293 ) ) ;
#13719 = CARTESIAN_POINT ( 'NONE',  ( 8.224510206698953496, -14.34966873604960469, 32.91557627198102409 ) ) ;
#13720 = CARTESIAN_POINT ( 'NONE',  ( -10.72451020669898014, 18.67979575497178502, 80.41557627198103830 ) ) ;
#13721 = CARTESIAN_POINT ( 'NONE',  ( 15.72974639402199770, -15.80617190586745480, 23.12390960531436335 ) ) ;
#13722 = CARTESIAN_POINT ( 'NONE',  ( -12.14591786802309592, -12.06949235617757132, 66.87390960531436690 ) ) ;
#13723 = CARTESIAN_POINT ( 'NONE',  ( 13.97604488694527802, 13.89961937509977652, 49.37390960531434558 ) ) ;
#13724 = CARTESIAN_POINT ( 'NONE',  ( 19.02544592524334988, 5.153800228976608722, 41.45942372801900433 ) ) ;
#13725 = CARTESIAN_POINT ( 'NONE',  ( 4.379528057220092307, 16.55341960407617563, 102.2927570613523613 ) ) ;
#13726 = CARTESIAN_POINT ( 'NONE',  ( 16.52544592524335698, 4.483927247898782831, 51.45942372801901854 ) ) ;
#13727 = CARTESIAN_POINT ( 'NONE',  ( 21.52544592524344225, -5.823673210054117533, 38.54057627198103120 ) ) ;
#13728 = CARTESIAN_POINT ( 'NONE',  ( -0.05219959533937732626, 21.53943276465977519, 102.5010903946856899 ) ) ;
#13729 = CARTESIAN_POINT ( 'NONE',  ( -16.51473224551069308, -9.474510206698971260, 96.66557627198102409 ) ) ;
#13730 = CARTESIAN_POINT ( 'NONE',  ( 0.05219959533934541429, -16.53943276465976808, 75.00109039468568994 ) ) ;
#13731 = CARTESIAN_POINT ( 'NONE',  ( -19.03943276465977164, 0.05219959533909376836, 26.24890960531435624 ) ) ;
#13732 = CARTESIAN_POINT ( 'NONE',  ( 8.224510206698953496, -14.34966873604960469, 37.91557627198102409 ) ) ;
#13734 = CARTESIAN_POINT ( 'NONE',  ( -9.474510206698964154, 16.51473224551069663, 95.41557627198102409 ) ) ;
#13733 = CARTESIAN_POINT ( 'NONE',  ( 19.03943276465977164, -0.05219959533909143690, 98.74890960531436690 ) ) ;
#13735 = CARTESIAN_POINT ( 'NONE',  ( -21.52544592524343514, 5.823673210054127303, 26.04057627198103475 ) ) ;
#13736 = CARTESIAN_POINT ( 'NONE',  ( -14.34966873604960291, -8.224510206698953496, 66.66557627198102409 ) ) ;
#13737 = CARTESIAN_POINT ( 'NONE',  ( 14.34966873604960469, 8.224510206698951720, 49.16557627198102409 ) ) ;
#13738 = ORIENTED_EDGE ( 'NONE', *, *, #199554, .T. ) ;
#13740 = DIRECTION ( 'NONE',  ( -0.000000000000000000, 1.000000000000000000, 0.000000000000000000 ) ) ;
#13739 = CARTESIAN_POINT ( 'NONE',  ( 4.379528057220092307, 16.55341960407617563, 57.29275706135234714 ) ) ;
#13741 = CARTESIAN_POINT ( 'NONE',  ( 13.97604488694548053, -13.89961937509957401, 50.62609039468566152 ) ) ;
#13742 = CARTESIAN_POINT ( 'NONE',  ( 13.97604488694527802, 13.89961937509977652, 89.37390960531436690 ) ) ;
#13743 = CARTESIAN_POINT ( 'NONE',  ( 13.89961937509957401, 13.97604488694547697, 61.87609039468566863 ) ) ;
#13744 = CARTESIAN_POINT ( 'NONE',  ( 17.14385361876520264, 23.59649016807275856, 142.6750000027311103 ) ) ;
#13745 = CARTESIAN_POINT ( 'NONE',  ( 19.05341960407617918, -5.049401038297876454, 51.04275706135231871 ) ) ;
#13747 = CARTESIAN_POINT ( 'NONE',  ( 14.29746914071037800, 8.314922557961029526, 101.6677570613523613 ) ) ;
#13746 = CARTESIAN_POINT ( 'NONE',  ( -19.02544592524334988, -5.153800228976617603, 98.95942372801900433 ) ) ;
#13748 = CARTESIAN_POINT ( 'NONE',  ( 27.73933785331498214, 9.013057229001095294, 146.4750000027311501 ) ) ;
#13749 = CARTESIAN_POINT ( 'NONE',  ( -9.564922557960796823, -16.46253265017161027, 22.08224293864768839 ) ) ;
#13750 = CARTESIAN_POINT ( 'NONE',  ( -0.05219959533907301413, -21.53943276465977519, 22.49890960531436335 ) ) ;
#13751 = CARTESIAN_POINT ( 'NONE',  ( 21.53943276465977519, 0.05219959533937863772, 46.25109039468567573 ) ) ;
#13752 = CARTESIAN_POINT ( 'NONE',  ( 16.51473224551083163, -9.474510206698727899, 105.8344237280190043 ) ) ;
#13754 = CARTESIAN_POINT ( 'NONE',  ( -0.05219959533909027116, -19.03943276465977164, 62.49890960531435979 ) ) ;
#13753 = CARTESIAN_POINT ( 'NONE',  ( -38.00000000000000711, 12.34694845685046438, -2.100000000000000089 ) ) ;
#13755 = DIRECTION ( 'NONE',  ( -5.392603844284257652E-33, -1.000000000000000000, -0.000000000000000000 ) ) ;
#13757 = CARTESIAN_POINT ( 'NONE',  ( 13.97604488694527802, 13.89961937509977652, 69.37390960531436690 ) ) ;
#13756 = CARTESIAN_POINT ( 'NONE',  ( -12.06949235617756955, 12.14591786802309770, 70.62390960531436690 ) ) ;
#13758 = CARTESIAN_POINT ( 'NONE',  ( -16.46253265017160317, 9.564922557960807481, 80.83224293864769550 ) ) ;
#13759 = CARTESIAN_POINT ( 'NONE',  ( 9.564922557961047289, -16.46253265017146816, 80.41775706135234714 ) ) ;
#13760 = CARTESIAN_POINT ( 'NONE',  ( -21.53943276465977519, 0.05219959533907696930, 51.24890960531436690 ) ) ;
#13761 = CARTESIAN_POINT ( 'NONE',  ( 14.29746914071049879, -8.314922557960816363, 108.3322429386477097 ) ) ;
#13762 = CARTESIAN_POINT ( 'NONE',  ( -5.049401038297874678, -19.05341960407617918, 39.79275706135232582 ) ) ;
#13763 = CARTESIAN_POINT ( 'NONE',  ( 16.46253265017160672, -9.564922557960803928, 73.33224293864769550 ) ) ;
#13764 = CARTESIAN_POINT ( 'NONE',  ( 15.80617190586746368, 15.72974639402197994, 84.37390960531438111 ) ) ;
#13766 = CARTESIAN_POINT ( 'NONE',  ( 16.51473224551083163, -9.474510206698727899, 50.83442372801899722 ) ) ;
#13765 = CARTESIAN_POINT ( 'NONE',  ( -12.14591786802309592, -12.06949235617757132, 86.87390960531438111 ) ) ;
#13767 = CARTESIAN_POINT ( 'NONE',  ( 21.53943276465977519, -0.05219959533907433946, 78.74890960531436690 ) ) ;
#13768 = CARTESIAN_POINT ( 'NONE',  ( 21.52544592524344225, -5.823673210054117533, 58.54057627198103120 ) ) ;
#13769 = CARTESIAN_POINT ( 'NONE',  ( 15.72974639402199770, -15.80617190586745480, 38.12390960531436690 ) ) ;
#13770 = CARTESIAN_POINT ( 'NONE',  ( 21.52544592524334988, 5.823673210054432836, 91.45942372801901854 ) ) ;
#13771 = CARTESIAN_POINT ( 'NONE',  ( -16.46253265017160317, 9.564922557960807481, 65.83224293864769550 ) ) ;
#13772 = CARTESIAN_POINT ( 'NONE',  ( -8.224510206698948167, 14.34966873604960824, 110.4155762719810383 ) ) ;
#13773 = CARTESIAN_POINT ( 'NONE',  ( 10.72451020669871369, 18.67979575497193778, 22.08442372801901143 ) ) ;
#13774 = CARTESIAN_POINT ( 'NONE',  ( -15.72974639402176322, -15.80617190586768395, 44.37609039468567573 ) ) ;
#13775 = CARTESIAN_POINT ( 'NONE',  ( -16.46253265017160317, 9.564922557960807481, 30.83224293864769550 ) ) ;
#13776 = CARTESIAN_POINT ( 'NONE',  ( 21.53943276465977519, -0.05219959533907433946, 103.7489096053143669 ) ) ;
#13777 = ADVANCED_FACE ( 'NONE', ( #136598 ), #73959, .T. ) ;
#13778 = CARTESIAN_POINT ( 'NONE',  ( 19.03943276465977164, 0.05219959533936151252, 56.25109039468566863 ) ) ;
#13779 = CARTESIAN_POINT ( 'NONE',  ( 5.153800228976335163, 19.02544592524342804, 34.79057627198102409 ) ) ;
#13780 = CARTESIAN_POINT ( 'NONE',  ( -8.314922557961024197, 14.29746914071037800, 27.91775706135234358 ) ) ;
#13781 = CARTESIAN_POINT ( 'NONE',  ( 16.44184284207323543, -7.208923782155263638, 21.54787411603375702 ) ) ;
#13782 = CARTESIAN_POINT ( 'NONE',  ( 12.06949235617739724, 12.14591786802326823, 61.87609039468568284 ) ) ;
#13783 = CARTESIAN_POINT ( 'NONE',  ( -16.46253265017160317, 9.564922557960807481, 35.83224293864768839 ) ) ;
#13784 = CARTESIAN_POINT ( 'NONE',  ( -25.82893184621037364, -8.167111171438232731, 172.3011985515803701 ) ) ;
#13785 = CARTESIAN_POINT ( 'NONE',  ( 16.51473224551069308, 9.474510206698969483, 84.16557627198102409 ) ) ;
#13786 = CARTESIAN_POINT ( 'NONE',  ( -16.52544592524342804, 4.483927247898546575, 116.0405762719810383 ) ) ;
#13788 = B_SPLINE_CURVE_WITH_KNOTS ( 'NONE', 3,
 ( #61699, #169890, #123368, #15218, #43577, #185061, #12263, #73927, #108211, #107210, #76877, #167908, #104250, #138547, #119429, #196289, #29408, #199242, #59724, #88073, #28430, #134603, #181113, #91038, #197268, #42587 ),
 .UNSPECIFIED., .F., .F.,
 ( 4, 2, 2, 2, 2, 2, 2, 2, 2, 2, 2, 2, 4 ),
 ( 2.788292423116888737E-07, 0.0002961032055655217791, 0.0005919275818887318732, 0.0008877519582119420757, 0.001183576334535152170, 0.001775225087181574743, 0.002366873839827997750, 0.002662698216151209146, 0.002958522592474420107, 0.003254346968797631502, 0.003550171345120842030, 0.004141820097767267422, 0.004733468850413692815 ),
 .UNSPECIFIED. ) ;
#13787 = CARTESIAN_POINT ( 'NONE',  ( -21.55341960407610458, -5.719274019375992779, 56.45724293864768839 ) ) ;
#13789 = CARTESIAN_POINT ( 'NONE',  ( 14.29746914071037800, 8.314922557961029526, 46.66775706135234714 ) ) ;
#13790 = CARTESIAN_POINT ( 'NONE',  ( 5.719274019375673035, 21.55341960407619339, 102.2927570613523613 ) ) ;
#13791 = CARTESIAN_POINT ( 'NONE',  ( -13.97604488694527625, -13.89961937509977652, 41.87390960531435979 ) ) ;
#13792 = EDGE_CURVE ( 'NONE', #56681, #90959, #182815, .T. ) ;
#13793 = CARTESIAN_POINT ( 'NONE',  ( 16.55341960407618274, -4.379528057220086978, 106.0427570613523471 ) ) ;
#13794 = CARTESIAN_POINT ( 'NONE',  ( -14.34966873604960291, -8.224510206698953496, 56.66557627198103830 ) ) ;
#13795 = CARTESIAN_POINT ( 'NONE',  ( -13.89961937509977652, 13.97604488694528158, 70.62390960531432427 ) ) ;
#13796 = CARTESIAN_POINT ( 'NONE',  ( 18.62759615963255655, 10.81492255796105972, 106.6677570613523756 ) ) ;
#13797 = CARTESIAN_POINT ( 'NONE',  ( -18.67979575497193778, 10.72451020669871902, 28.33442372801902209 ) ) ;
#13798 = CARTESIAN_POINT ( 'NONE',  ( 15.72974639402176855, 15.80617190586768217, 86.87609039468568994 ) ) ;
#13799 = CARTESIAN_POINT ( 'NONE',  ( 14.29746914071037800, 8.314922557961029526, 46.66775706135234714 ) ) ;
#13800 = CARTESIAN_POINT ( 'NONE',  ( 12.14591786802327356, -12.06949235617739191, 25.62609039468567929 ) ) ;
#13802 = CARTESIAN_POINT ( 'NONE',  ( -15.72974639402176322, -15.80617190586768395, 94.37609039468568994 ) ) ;
#13801 = CARTESIAN_POINT ( 'NONE',  ( -4.379528057220328563, 16.55341960407611168, 75.20724293864769550 ) ) ;
#13803 = CARTESIAN_POINT ( 'NONE',  ( -12.06949235617756955, 12.14591786802309770, 30.62390960531436335 ) ) ;
#13804 = CARTESIAN_POINT ( 'NONE',  ( 0.05219959533909260263, 19.03943276465977164, 29.99890960531435979 ) ) ;
#13805 = CARTESIAN_POINT ( 'NONE',  ( -12.14591786802326823, 12.06949235617739902, 43.12609039468568284 ) ) ;
#13806 = CARTESIAN_POINT ( 'NONE',  ( 14.34966873604960469, 8.224510206698951720, 59.16557627198103120 ) ) ;
#13807 = CARTESIAN_POINT ( 'NONE',  ( 14.34966873604972726, -8.224510206698740333, 85.83442372801901854 ) ) ;
#13808 = CARTESIAN_POINT ( 'NONE',  ( 19.03943276465977164, -0.05219959533909143690, 93.74890960531435269 ) ) ;
#13809 = CARTESIAN_POINT ( 'NONE',  ( 13.89961937509977652, -13.97604488694527269, 108.1239096053143669 ) ) ;
#13810 = CARTESIAN_POINT ( 'NONE',  ( -10.81492255796105439, 18.62759615963255655, 107.9177570613523471 ) ) ;
#13811 = CARTESIAN_POINT ( 'NONE',  ( 12.06949235617757843, -12.14591786802309237, 83.12390960531436690 ) ) ;
#13812 = CARTESIAN_POINT ( 'NONE',  ( 13.97604488694527802, 13.89961937509977652, 94.37390960531436690 ) ) ;
#13813 = ORIENTED_EDGE ( 'NONE', *, *, #31053, .T. ) ;
#13814 = CARTESIAN_POINT ( 'NONE',  ( 12.06949235617739724, 12.14591786802326823, 46.87609039468568994 ) ) ;
#13815 = CARTESIAN_POINT ( 'NONE',  ( 19.05341960407611168, 5.049401038298154454, 38.95724293864767418 ) ) ;
#13816 = CARTESIAN_POINT ( 'NONE',  ( -9.474510206698964154, 16.51473224551069663, 105.4155762719810383 ) ) ;
#13818 = CARTESIAN_POINT ( 'NONE',  ( -30.00000000000000000, -1.132798289211302014E-14, 92.50000000000000000 ) ) ;
#13817 = CARTESIAN_POINT ( 'NONE',  ( 16.55341960407618274, -4.379528057220086978, 41.04275706135236135 ) ) ;
#13819 = CARTESIAN_POINT ( 'NONE',  ( -19.03943276465977164, -0.05219959533935918106, 38.75109039468566152 ) ) ;
#13820 = CARTESIAN_POINT ( 'NONE',  ( -5.153800228976328057, -19.02544592524343514, 47.29057627198102409 ) ) ;
#13821 = CARTESIAN_POINT ( 'NONE',  ( -16.52544592524335698, -4.483927247898792601, 83.95942372801900433 ) ) ;
#13822 = CARTESIAN_POINT ( 'NONE',  ( 16.46253265017146816, 9.564922557961045513, 81.66775706135233293 ) ) ;
#13823 = CARTESIAN_POINT ( 'NONE',  ( -19.05341960407617563, 5.049401038297882671, 23.54275706135233648 ) ) ;
#13824 = CARTESIAN_POINT ( 'NONE',  ( 19.02544592524343514, -5.153800228976328945, 58.54057627198102409 ) ) ;
#13825 = CARTESIAN_POINT ( 'NONE',  ( -0.05219959533910754901, -16.53943276465976808, 102.4989096053143811 ) ) ;
#13826 = CARTESIAN_POINT ( 'NONE',  ( 9.564922557961047289, -16.46253265017146816, 65.41775706135233293 ) ) ;
#13827 = CARTESIAN_POINT ( 'NONE',  ( 18.62759615963271287, -10.81492255796078972, 63.33224293864770260 ) ) ;
#13828 = CARTESIAN_POINT ( 'NONE',  ( 5.049401038297881783, 19.05341960407617563, 22.29275706135233648 ) ) ;
#13829 = CARTESIAN_POINT ( 'NONE',  ( 9.564922557960805705, 16.46253265017160317, 109.5822429386476955 ) ) ;
#13830 = CARTESIAN_POINT ( 'NONE',  ( 21.52544592524344225, -5.823673210054117533, 78.54057627198103830 ) ) ;
#13831 = CARTESIAN_POINT ( 'NONE',  ( -0.05219959533909027116, -19.03943276465977164, 107.4989096053143527 ) ) ;
#13832 = CARTESIAN_POINT ( 'NONE',  ( 13.97604488694548053, -13.89961937509957401, 100.6260903946856615 ) ) ;
#13833 = CARTESIAN_POINT ( 'NONE',  ( -30.00000000000000000, -1.163414459189985801E-14, 95.00000000000000000 ) ) ;
#13834 = CARTESIAN_POINT ( 'NONE',  ( -12.14591786802326823, 12.06949235617739902, 28.12609039468568284 ) ) ;
#13835 = CARTESIAN_POINT ( 'NONE',  ( -19.02544592524342804, 5.153800228976336051, 36.04057627198100988 ) ) ;
#13836 = CARTESIAN_POINT ( 'NONE',  ( 13.97604488694527802, 13.89961937509977652, 94.37390960531436690 ) ) ;
#13837 = CARTESIAN_POINT ( 'NONE',  ( -5.823673210054116645, -21.52544592524344225, 87.29057627198103830 ) ) ;
#13838 = CARTESIAN_POINT ( 'NONE',  ( -10.81492255796105439, 18.62759615963255655, 62.91775706135236135 ) ) ;
#13840 = CARTESIAN_POINT ( 'NONE',  ( 13.89961937509957401, 13.97604488694547697, 21.87609039468566152 ) ) ;
#13839 = CARTESIAN_POINT ( 'NONE',  ( 19.03943276465977164, 0.05219959533936151252, 106.2510903946856615 ) ) ;
#13841 = CARTESIAN_POINT ( 'NONE',  ( 16.52544592524335698, 4.483927247898782831, 111.4594237280190328 ) ) ;
#13842 = CARTESIAN_POINT ( 'NONE',  ( -21.53943276465977519, 0.05219959533907696930, 96.24890960531435269 ) ) ;
#13843 = CARTESIAN_POINT ( 'NONE',  ( -4.379528057220328563, 16.55341960407611168, 40.20724293864769550 ) ) ;
#13844 = CARTESIAN_POINT ( 'NONE',  ( -19.02544592524334988, -5.153800228976617603, 88.95942372801897591 ) ) ;
#13845 = CARTESIAN_POINT ( 'NONE',  ( 0.05219959533936267826, -19.03943276465977164, 55.00109039468566863 ) ) ;
#13846 = CARTESIAN_POINT ( 'NONE',  ( 0.05219959533937995610, -21.53943276465977519, 55.00109039468568284 ) ) ;
#13847 = CARTESIAN_POINT ( 'NONE',  ( -13.97604488694547697, 13.89961937509957934, 38.12609039468566152 ) ) ;
#13848 = CARTESIAN_POINT ( 'NONE',  ( 16.55341960407611168, 4.379528057220329451, 108.9572429386476955 ) ) ;
#13849 = CARTESIAN_POINT ( 'NONE',  ( 5.823673210054125526, 21.52544592524343514, 29.79057627198102409 ) ) ;
#13850 = CARTESIAN_POINT ( 'NONE',  ( -14.34966873604960291, -8.224510206698953496, 41.66557627198103120 ) ) ;
#13851 = CARTESIAN_POINT ( 'NONE',  ( -15.80617190586768217, 15.72974639402176855, 93.12609039468568994 ) ) ;
#13852 = CARTESIAN_POINT ( 'NONE',  ( -4.379528057220086978, -16.55341960407618274, 69.79275706135234714 ) ) ;
#13853 = CARTESIAN_POINT ( 'NONE',  ( 8.314922557960818139, 14.29746914071049879, 29.58224293864769905 ) ) ;
#13854 = CARTESIAN_POINT ( 'NONE',  ( 10.72451020669871369, 18.67979575497193778, 67.08442372801901854 ) ) ;
#13855 = CARTESIAN_POINT ( 'NONE',  ( -21.53943276465977519, -0.05219959533937600094, 73.75109039468567573 ) ) ;
#13856 = CARTESIAN_POINT ( 'NONE',  ( 10.81492255796078972, 18.62759615963270932, 74.58224293864768129 ) ) ;
#13857 = ORIENTED_EDGE ( 'NONE', *, *, #87886, .F. ) ;
#13858 = CARTESIAN_POINT ( 'NONE',  ( -13.97604488694527625, -13.89961937509977652, 21.87390960531435979 ) ) ;
#13859 = CARTESIAN_POINT ( 'NONE',  ( -18.67979575497193778, 10.72451020669871902, 43.33442372801901143 ) ) ;
#13860 = CARTESIAN_POINT ( 'NONE',  ( 19.02544592524343514, -5.153800228976328945, 23.54057627198102054 ) ) ;
#13861 = CARTESIAN_POINT ( 'NONE',  ( -19.02544592524342804, 5.153800228976336051, 36.04057627198100988 ) ) ;
#13862 = CARTESIAN_POINT ( 'NONE',  ( 8.224510206698953496, -14.34966873604960469, 72.91557627198103830 ) ) ;
#13863 = CARTESIAN_POINT ( 'NONE',  ( -13.97604488694527625, -13.89961937509977652, 81.87390960531436690 ) ) ;
#13864 = CARTESIAN_POINT ( 'NONE',  ( 14.29746914071049879, -8.314922557960816363, 33.33224293864769550 ) ) ;
#13865 = CARTESIAN_POINT ( 'NONE',  ( -0.05219959533907301413, -21.53943276465977519, 72.49890960531435269 ) ) ;
#13866 = CARTESIAN_POINT ( 'NONE',  ( 10.72451020669898902, -18.67979575497178502, 107.9155762719810241 ) ) ;
#13867 = FACE_OUTER_BOUND ( 'NONE', #37797, .T. ) ;
#13869 = CARTESIAN_POINT ( 'NONE',  ( -19.03943276465977164, -0.05219959533935918106, 108.7510903946856615 ) ) ;
#13868 = CARTESIAN_POINT ( 'NONE',  ( -19.03943276465977164, 0.05219959533909376836, 66.24890960531436690 ) ) ;
#13870 = CARTESIAN_POINT ( 'NONE',  ( -15.80617190586745835, -15.72974639402198527, 61.87390960531436690 ) ) ;
#13871 = CARTESIAN_POINT ( 'NONE',  ( -10.81492255796105439, 18.62759615963255655, 77.91775706135231871 ) ) ;
#13872 = CARTESIAN_POINT ( 'NONE',  ( -19.02544592524342804, 5.153800228976336051, 61.04057627198103120 ) ) ;
#13873 = EDGE_CURVE ( 'NONE', #88773, #51008, #143542, .T. ) ;
#13874 = CARTESIAN_POINT ( 'NONE',  ( 13.89961937509977652, -13.97604488694527269, 93.12390960531436690 ) ) ;
#13875 = CARTESIAN_POINT ( 'NONE',  ( 14.34966873604972726, -8.224510206698740333, 70.83442372801901854 ) ) ;
#13876 = CARTESIAN_POINT ( 'NONE',  ( 21.53943276465977519, 0.05219959533937863772, 61.25109039468567573 ) ) ;
#13877 = CARTESIAN_POINT ( 'NONE',  ( -15.72974639402176322, -15.80617190586768395, 84.37609039468570415 ) ) ;
#13878 = CARTESIAN_POINT ( 'NONE',  ( -0.05219959533907301413, -21.53943276465977519, 112.4989096053143669 ) ) ;
#13879 = CARTESIAN_POINT ( 'NONE',  ( 10.81492255796078972, 18.62759615963270932, 79.58224293864769550 ) ) ;
#13880 = CARTESIAN_POINT ( 'NONE',  ( 19.03943276465977164, 0.05219959533936151252, 41.25109039468566152 ) ) ;
#13881 = CARTESIAN_POINT ( 'NONE',  ( -21.52544592524343514, 5.823673210054127303, 41.04057627198103120 ) ) ;
#13883 = CARTESIAN_POINT ( 'NONE',  ( -12.06949235617756955, 12.14591786802309770, 30.62390960531436335 ) ) ;
#13882 = CARTESIAN_POINT ( 'NONE',  ( 5.049401038298161559, -19.05341960407611168, 87.70724293864769550 ) ) ;
#13884 = LINE ( 'NONE', #197916, #17547 ) ;
#13885 = CIRCLE ( 'NONE', #126873, 37.87393738558669298 ) ;
#13886 = CARTESIAN_POINT ( 'NONE',  ( -0.2066332630086595012, -13.70000000000001528, -62.58071313852357775 ) ) ;
#13887 = CARTESIAN_POINT ( 'NONE',  ( -5.153800228976607833, 19.02544592524334988, 92.70942372801901854 ) ) ;
#13888 = CARTESIAN_POINT ( 'NONE',  ( 15.80617190586746368, 15.72974639402197994, 69.37390960531436690 ) ) ;
#13889 = CARTESIAN_POINT ( 'NONE',  ( -16.55341960407611168, -4.379528057220339221, 56.45724293864768839 ) ) ;
#13890 = CARTESIAN_POINT ( 'NONE',  ( 4.483927247898790824, -16.52544592524335698, 30.20942372801902565 ) ) ;
#13891 = CARTESIAN_POINT ( 'NONE',  ( 9.474510206698971260, -16.51473224551069308, 42.91557627198103120 ) ) ;
#13893 = CARTESIAN_POINT ( 'NONE',  ( 19.03943276465977164, 0.05219959533936151252, 66.25109039468567573 ) ) ;
#13892 = CARTESIAN_POINT ( 'NONE',  ( 21.55341960407610458, 5.719274019375980345, 103.9572429386476813 ) ) ;
#13894 = CARTESIAN_POINT ( 'NONE',  ( -0.05219959533909027116, -19.03943276465977164, 87.49890960531436690 ) ) ;
#13895 = CARTESIAN_POINT ( 'NONE',  ( 4.483927247898545687, 16.52544592524342804, 84.79057627198102409 ) ) ;
#13896 =( BOUNDED_SURFACE ( )  B_SPLINE_SURFACE ( 3, 2, ( 
 ( #146460, #53463, #10972, #101973, #24147, #177830, #72645, #117135, #42310, #11983, #163654, #25156, #38303, #147485, #192991, #54469, #88795, #87791, #196006, #9976, #7953, #57479, #86798, #41308, #8975, #70644, #116139, #115139, #56470, #119151, #27148, #85799, #148485, #71636, #133303, #132310, #130282, #194993, #23137, #194002, #55465, #118148, #176831, #179838, #149476, #134320, #180833, #26149, #69636, #150488, #165650, #161643, #84782, #131302, #39299, #100956, #76604, #90770, #77598, #47275, #151476, #61428, #108932, #105950, #74630, #91751, #107926, #12966, #199963, #169611, #31109, #137285, #197972, #104964, #135319, #106938, #183798, #46271, #154445, #167635, #166651, #92757, #45285, #139269, #30111, #184785, #15939, #745, #62417, #58458, #182809, #28152, #138281, #168611, #89792, #170612, #153446, #136296, #60434, #29132, #59442, #124089, #120126, #185788, #44292, #32102, #198967, #121115, #123099, #152454, #13939, #93759, #155440, #75606, #122108, #14944, #73648, #196992, #181817, #43296, #35072, #64422, #4715, #174595, #140257, #19904, #81546, #65407, #127068, #156433, #33096, #3730, #1749, #95746, #188776, #189768, #144235, #67397, #96727, #190754, #51240, #36060, #112901, #82553, #97709, #187787, #2745, #18925, #126091, #50259, #111915, #159400, #125102, #49257, #157431, #109926, #173603, #158415, #143232, #186800, #20895, #66404, #5719, #142245, #128066, #52228, #129053, #78583, #113884, #175582, #63427, #48271, #110915, #80570, #37059, #98718, #17933, #94752, #16930, #171608, #79587, #141256, #172601, #34087, #132073, #24917, #9740, #41073, #146225, #192753, #117912, #130042, #131064, #180602, #102736, #39065, #164425, #85559, #40055, #6712, #68390, #118918, #84547, #7712, #191741, #87562, #83551, #177597, #86563, #69396, #176595, #163420, #99725, #54236, #133068, #10740, #53225, #115907, #38069, #161409, #21901, #194758, #162403, #178592, #100722, #148246, #179601, #145230, #71404, #56230, #8736, #70405, #22901, #23905, #147244, #114901, #193762, #55230, #25918, #149249, #72404, #101732, #134081, #195770, #57244, #42076, #160412, #116899, #74398, #89557, #105716, #12732, #13705, #137042, #138041, #11749, #136063, #182573, #196763, #198733, #60199, #121869, #73416, #199722, #168379, #46028, #28899, #90539, #139024, #45047, #165420, #29874, #504, #26914, #135087, #197738, #167403, #123840, #152221, #43062, #119899, #75372, #88556, #61188, #76364, #58230, #122860, #183561, #91511, #153198, #184548, #151243, #59204, #107684, #181584, #120873, #185538, #169361, #44056, #30871, #106705, #14702, #150255, #104728, #62176, #27914, #92517, #166420, #154207, #15696, #77357, #103740, #32854, #157185, #112657, #3486, #158171, #189523, #127818, #81304, #31859, #156186, #78337, #111670, #18679, #140011, #143990, #126822, #48028, #33839, #141013, #109685, #35818, #93512, #174348, #17685, #50996, #172350, #95499, #80325, #82299, #188528, #108689, #173358, #5471, #170367, #16687, #79343, #110670, #67153, #49015, #186556, #63177, #141998, #155198, #142988, #19663, #1499, #4466, #65163, #34828, #96483, #97464, #94504, #2500, #66155, #124856, #64181, #128811, #159150, #125847, #20646, #50005, #47031, #171366, #187548, #149004, #114648, #37818, #98469, #117660, #113642, #7464, #54986, #176346, #100481, #55983, #146996, #101474, #132824, #71158, #24667, #175337, #99479, #21654, #116655, #162160, #83307, #87320, #70158, #191493, #177353, #84303, #52971, #179357, #36804, #40820, #161160, #194510, #115663, #6464, #193509, #129796, #22656, #163164, #102490, #144984, #145982, #68145, #69148, #51984, #86317, #192506, #8483, #130815, #178346, #148005, #160163, #39808, #9495, #38823, #23656, #53990, #85304, #131828, #164177, #25675, #10493, #72153, #190510, #184307, #13465, #107440, #106454, #91261, #29629, #199475, #168133, #104486, #119662, #135828, #42823, #43809, #167158, #152952, #41827, #166170 ),
 ( #151004, #137791, #169112, #11501, #121622, #30619, #27671, #134842, #151977, #14451, #73172, #59955, #76114, #60942, #197498, #57991, #165172, #195520, #28658, #105472, #122617, #45788, #89311, #26665, #92272, #12495, #75129, #88307, #90293, #136798, #198483, #153956, #74157, #120633, #44799, #15452, #183317, #133829, #118667, #56993, #182330, #180358, #149995, #103494, #196521, #181344, #58965, #96247, #34590, #158914, #18440, #77110, #138780, #33596, #3251, #171117, #154949, #80091, #141759, #174111, #64924, #126584, #16445, #173114, #97227, #124608, #261, #65911, #123598, #46784, #157935, #93263, #61929, #19426, #125605, #32607, #186303, #81073, #63936, #189284, #185292, #187303, #48774, #108443, #94260, #139763, #1249, #35581, #142752, #4232, #156943, #78094, #127584, #110429, #188286, #155940, #17436, #62928, #170119, #49761, #50762, #31613, #79092, #172110, #95260, #111428, #109435, #47783, #112419, #140765, #2254, #22416, #84066, #143748, #52735, #178105, #101232, #9254, #69919, #98219, #179116, #86077, #37573, #40584, #116415, #54743, #145745, #144743, #51744, #82053, #53750, #130571, #193269, #162920, #114402, #113405, #39573, #191260, #100240, #175096, #192268, #115424, #177113, #24429, #99236, #7226, #131585, #147768, #38584, #102254, #5227, #161922, #68911, #66909, #36564, #70921, #23416, #128572, #67909, #132588, #194277, #20405, #85064, #190267, #159922, #146746, #8241, #176103, #21411, #55744, #117418, #83068, #6230, #129562, #160923, #59720, #184069, #11259, #45552, #152721, #10254, #133585, #44566, #180123, #87080, #106221, #12260, #57756, #72932, #167905, #150763, #75880, #163942, #73923, #135593, #71913, #181110, #26430, #88070, #122380, #121391, #29405, #43574, #41591, #91035, #197265, #74902, #42584, #104247, #149756, #25439, #90064, #14212, #60704, #119426, #58727, #120396, #182090, #196287, #148765, #105238, #56758, #165930, #27427, #89072, #195275, #166926, #183083, #137556, #199239, #13239, #103255, #118430, #164937, #28427, #134601, #151746, #136565, #198246, #110198, #124372, #111189, #80846, #185058, #95024, #142523, #139533, #108207, #125378, #141533, #46546, #33366, #18206, #3022, #63703, #65680, #92028, #17202, #155707, #168877, #61696, #79864, #78856, #30382, #154718, #126360, #64698, #189056, #48544, #107207, #153719, #187075, #156714, #1016, #169887, #171877, #188056, #4001, #49526, #172880, #31380, #34360, #127343, #16211, #15215, #96021, #76874, #138544, #157707, #123365, #22, #19197, #140536, #62690, #77866, #93030, #94027, #186067, #47550, #2024, #109203, #170883, #32374, #113173, #174862, #9016, #7992, #116179, #130321, #66676, #177870, #22174, #161682, #129330, #67672, #36329, #112191, #176872, #39338, #147528, #144508, #98993, #6986, #68666, #82827, #132350, #192018, #143505, #5993, #52500, #114160, #173880, #191025, #69675, #131342, #100997, #99997, #128338, #70684, #162682, #175862, #50529, #37335, #193030, #35350, #53502, #160682, #54507, #24188, #190037, #38341, #85838, #83824, #51511, #115179, #84822, #97982, #23179, #146501, #97001, #145505, #159676, #81818, #158683, #20172, #4991, #21172, #77389, #26189, #25197, #169396, #164694, #76396, #86840, #106736, #29905, #91543, #30903, #75404, #183594, #133342, #10016, #45078, #178871, #137076, #168411, #92550, #123874, #47065, #138072, #170402, #154239, #15729, #139058, #62209, #537, #87829, #179879, #198765, #185572, #60231, #108725, #153232, #149515, #41347, #31893, #14735, #93547, #78371, #199753, #61220, #102013, #11012, #56510, #118188, #155232, #16722, #194042, #122891, #71675, #55506, #184579, #107715, #121900, #46061, #103010, #117176, #40338, #163695, #148525, #195033, #188566, #96520, #158210, #172388, #21692, #19700, #32890, #33878, #142037, #3525, #63213, #95537, #97502, #20683, #128848, #189561, #17722, #98507, #5510, #157225, #160202, #126860, #82338, #140045, #143026, #18717 ),
 ( #171403, #4503, #50046, #94541, #36842, #81342, #141051, #111709, #80364, #2537, #190548, #186592, #67191, #49052, #144028, #65201, #156222, #66194, #79381, #187584, #112695, #52021, #64218, #125884, #110707, #173395, #1536, #174386, #34866, #127857, #51033, #35856, #159188, #124893, #113680, #175374, #48064, #109720, #149043, #100519, #41868, #70199, #164215, #103534, #86356, #162198, #87357, #57033, #161200, #71197, #118706, #115702, #84342, #101513, #117698, #22695, #9531, #179395, #40858, #147037, #7504, #114690, #145022, #116694, #193550, #56020, #25712, #177391, #176385, #102532, #54029, #163203, #37859, #55023, #178383, #39847, #10531, #23696, #131866, #194550, #72195, #24707, #165209, #68183, #148042, #132861, #6503, #99518, #133868, #195559, #129835, #130854, #180397, #83346, #191534, #53011, #146021, #69188, #192546, #38863, #85344, #8521, #29666, #168169, #123633, #14488, #76150, #104524, #122654, #46819, #74194, #108479, #15490, #73210, #134881, #61966, #107475, #90329, #169153, #75165, #120668, #135863, #30656, #13500, #138818, #26704, #136837, #198520, #196557, #43844, #89349, #151039, #185329, #184342, #92310, #106492, #42859, #153993, #59991, #137829, #105510, #167196, #12529, #88344, #152989, #77147, #150036, #182366, #121659, #183354, #44836, #59002, #11542, #91298, #119698, #28693, #152014, #199512, #58028, #60979, #45824, #298, #181381, #166205, #27707, #197534, #95293, #156977, #5262, #111463, #31650, #96282, #66944, #93299, #139798, #140801, #33631, #190299, #172145, #109470, #186339, #141793, #154985, #65946, #142785, #1287, #4266, #3287, #34623, #19461, #50794, #155975, #2290, #127618, #62963, #63972, #51776, #112453, #48809, #174142, #18474, #49798, #16481, #78130, #128606, #94297, #17472, #124644, #97259, #47821, #187339, #157968, #79128, #80124, #35614, #126617, #81107, #158947, #20436, #189317, #171154, #125642, #32642, #82087, #64958, #110463, #170157, #173148, #188319, #143780, #7258, #114436, #102287, #159954, #40617, #22449, #194311, #38618, #129595, #116453, #52767, #160956, #86112, #163976, #6262, #99269, #191291, #176137, #175129, #147803, #115456, #131619, #84098, #101266, #70953, #36596, #178141, #39607, #161954, #23450, #37606, #145777, #100275, #98252, #192302, #85097, #9288, #25473, #87113, #193303, #148799, #132623, #55777, #117450, #179149, #10289, #68943, #130607, #177146, #146783, #162956, #71947, #133618, #21442, #53781, #8276, #67942, #69954, #54778, #24462, #83103, #195311, #113436, #144779, #60741, #30417, #134635, #44599, #92065, #89107, #57789, #74934, #91068, #196320, #183116, #152754, #14244, #120429, #181143, #88105, #118464, #90096, #166958, #29436, #137590, #150797, #149790, #75916, #27465, #136597, #11294, #28460, #151778, #13271, #199273, #135626, #43606, #167937, #122415, #198277, #15248, #41625, #59754, #105271, #180156, #72966, #184105, #121424, #103289, #104281, #45587, #107240, #138578, #106254, #56792, #164969, #168911, #153753, #12293, #119459, #76907, #26462, #42617, #165963, #73958, #197297, #58760, #182120, #47583, #20206, #189092, #46580, #108241, #35384, #80881, #63737, #142558, #48579, #94062, #109235, #4036, #187109, #112225, #81852, #110232, #171913, #169921, #17238, #62724, #124408, #158716, #157743, #65714, #79897, #16248, #127380, #33402, #111226, #78890, #140569, #186101, #61731, #126394, #50565, #97035, #155741, #95060, #156750, #18244, #32407, #58, #141567, #93064, #2059, #125412, #3056, #123399, #64733, #19232, #173915, #185091, #49562, #77900, #31413, #154751, #188091, #139567, #172918, #1051, #170914, #34397, #96055, #145541, #82866, #159710, #115215, #5028, #39374, #116215, #113210, #177906, #176908, #8029, #193066, #24224, #129366, #175899, #101033, #174898, #114195, #163733, #85874, #22211, #147563, #68702, #23216, #190070, #51546, #102049, #67708, #191062, #36364, #70718, #66713, #160719, #69711, #52534 ),
 ( #40375, #84859, #144544, #130357, #37371, #6029, #132386, #98016, #194079, #99029, #9048, #192056, #21209, #146536, #83860, #7020, #162718, #55542, #53538, #38379, #100035, #161721, #128374, #117214, #131378, #54542, #178907, #25234, #143541, #10050, #89868, #151550, #135396, #197066, #26224, #103048, #73723, #71710, #165725, #58534, #59513, #14012, #137357, #166724, #60506, #121190, #44366, #182883, #152524, #106023, #57553, #72723, #88869, #150562, #13040, #45358, #167710, #195068, #119222, #27221, #179916, #181890, #43368, #105040, #56548, #29206, #74706, #90840, #12061, #120200, #122181, #28228, #148559, #136370, #183873, #133378, #118225, #180907, #198047, #107010, #41382, #75678, #168683, #164730, #87864, #42382, #199036, #86875, #149552, #11047, #134396, #196082, #104045, #126165, #2820, #200035, #64498, #1823, #94829, #79662, #110990, #16014, #62493, #187860, #61503, #819, #50333, #172675, #109007, #34160, #155511, #110000, #76677, #138353, #188849, #154517, #77671, #123172, #157506, #153519, #47352, #156507, #139340, #140333, #95821, #186876, #141332, #18999, #80646, #49329, #15016, #124164, #184860, #18008, #63504, #46343, #127142, #171680, #31181, #17006, #185865, #92832, #142322, #107999, #3802, #170686, #65480, #78658, #169686, #33170, #32175, #93831, #111990, #30183, #125180, #48346, #91826, #51313, #35147, #7789, #175657, #191818, #20966, #161486, #131139, #96801, #176670, #38146, #21975, #83627, #112974, #189840, #160485, #158489, #52300, #145304, #146301, #100792, #23977, #53298, #147319, #69473, #192827, #54308, #39137, #115980, #144305, #159471, #37131, #98791, #99800, #132143, #177669, #81619, #5795, #113958, #66478, #68466, #130120, #114977, #143302, #162475, #22974, #85632, #6787, #84622, #8808, #70477, #4788, #193836, #55300, #174666, #173680, #67468, #36132, #19976, #128140, #97783, #82623, #129127, #190825, #133138, #119967, #56302, #164494, #89627, #167475, #9812, #102809, #194829, #117984, #178663, #151315, #118989, #135158, #25987, #104801, #74470, #40126, #181653, #43132, #165489, #26985, #179674, #41145, #103809, #101804, #195841, #88630, #12804, #44130, #28970, #196831, #90612, #136136, #197811, #59277, #182646, #120947, #87630, #149316, #180673, #42149, #166490, #75445, #105789, #24990, #10810, #57314, #71473, #11821, #73486, #58300, #86634, #152293, #27988, #13778, #150326, #137120, #198806, #116972, #163491, #148317, #72480, #134153, #29948, #30944, #123915, #80403, #62246, #199796, #76438, #31932, #121944, #156260, #32927, #91587, #94582, #93586, #124932, #109756, #141089, #46102, #92591, #17763, #153277, #154280, #142075, #2576, #139101, #64256, #185614, #140085, #106777, #168452, #18756, #184620, #107757, #14778, #187621, #183637, #77430, #186629, #169441, #170441, #125923, #16761, #171440, #49091, #110748, #79419, #45119, #15770, #138115, #48100, #155272, #78409, #1577, #172429, #575, #47104, #33918, #95575, #63252, #60271, #61263, #157261, #108764, #122933, #34904, #86140, #146810, #65239, #66235, #70982, #9317, #10316, #116480, #3561, #126899, #178169, #147831, #100303, #143063, #162984, #24489, #188605, #132650, #194338, #4541, #55806, #50086, #177173, #111746, #148826, #158247, #19737, #173434, #25499, #54805, #87143, #39634, #8304, #161981, #96559, #117478, #81378, #127895, #179176, #40644, #38646, #102313, #69981, #131649, #192329, #53810, #115485, #23477, #101295, #85126, #193331, #164003, #62898, #1220, #46755, #45757, #113132, #114119, #83785, #78063, #32577, #143464, #4949, #16416, #68625, #66634, #77079, #139731, #186274, #47753, #107409, #124578, #144468, #67629, #175821, #36287, #61898, #145464, #52461, #109407, #6946, #171086, #129289, #184274, #189996, #94230, #190984, #160643, #123568, #174822, #22135, #155911, #185263, #128297, #21131, #108414, #97943, #82786, #5952, #20133, #170089, #15420, #169082, #81778, #51471, #159635, #37294 ),
 ( #30588, #98953, #92240, #153926, #138748, #230, #31583, #154918, #93233, #150706, #26372, #192208, #161865, #27368, #24370, #179055, #87022, #148708, #162862, #12205, #10196, #23359, #86021, #132531, #194220, #53690, #147710, #88012, #11198, #119369, #180065, #8181, #89015, #196231, #9197, #130512, #117359, #72874, #115368, #133525, #70863, #134542, #104190, #69857, #118371, #55685, #195217, #40524, #41533, #57700, #164877, #177057, #39514, #85004, #56698, #102195, #146685, #38527, #71856, #131525, #163883, #25380, #193210, #181052, #100183, #42527, #101174, #165872, #103197, #54684, #149700, #116357, #178046, #46482, #124308, #166869, #59658, #151692, #13182, #135538, #108142, #75820, #91965, #121332, #61637, #31318, #197209, #76815, #138486, #122319, #184011, #74845, #90008, #60645, #58672, #152663, #45493, #169826, #956, #186006, #153658, #47488, #92970, #154656, #16152, #139475, #77806, #44508, #183025, #137498, #199179, #200168, #32316, #62632, #182033, #106164, #14153, #28370, #168818, #30323, #15154, #109144, #120338, #170823, #167847, #93969, #107148, #136508, #123305, #198188, #29347, #155649, #73868, #90976, #184998, #43516, #105182, #78797, #51447, #19132, #35283, #64636, #4928, #174798, #140475, #20110, #81754, #65618, #127278, #156651, #33307, #3938, #1963, #95959, #188991, #189972, #144444, #67605, #96939, #190960, #113108, #36264, #97918, #82763, #159610, #187995, #2957, #80783, #142460, #143442, #175797, #21108, #125318, #49465, #157643, #110140, #112127, #173818, #158620, #187014, #5929, #66611, #129266, #50467, #128275, #52437, #114095, #63643, #37270, #98928, #48485, #171819, #111128, #17144, #94967, #126298, #18147, #79801, #141473, #172817, #34297, #133273, #130256, #194964, #132281, #25128, #9948, #41280, #146435, #192963, #118122, #191952, #131275, #180805, #102942, #39271, #164626, #85770, #40271, #6922, #68600, #119124, #84757, #7925, #53437, #87763, #83760, #177802, #86770, #69610, #70614, #24117, #163625, #193973, #71607, #26120, #56443, #145440, #54443, #115112, #148453, #55435, #176806, #57452, #101944, #161618, #147457, #116113, #23112, #22110, #100928, #179810, #149448, #42284, #10944, #160619, #38278, #117106, #72618, #162612, #99932, #134293, #195979, #8946, #178801, #153418, #181786, #199936, #124058, #151449, #185758, #92728, #150461, #11956, #139241, #184757, #167607, #46242, #152424, #197943, #12936, #107896, #90741, #15911, #103942, #13912, #75578, #73621, #121087, #166622, #28124, #62388, #61399, #169583, #183771, #120098, #31081, #137255, #14916, #182781, #44264, #165622, #123071, #27121, #135291, #716, #59412, #198940, #60407, #122080, #136268, #88768, #45257, #196963, #105922, #29102, #106911, #58431, #168584, #154417, #77569, #43267, #76577, #104936, #89764, #74601, #30082, #91723, #138253, #128037, #67368, #50232, #64396, #51212, #20867, #125074, #35045, #126064, #96699, #173576, #2719, #81517, #186771, #158388, #143204, #4685, #110889, #171580, #78553, #108904, #80544, #157405, #19877, #189739, #79560, #140228, #66377, #17905, #127040, #1721, #18898, #142218, #3701, #112873, #187761, #34060, #174565, #36032, #65380, #5692, #32074, #188747, #95718, #170583, #63397, #97681, #111886, #159370, #16902, #141228, #129027, #82524, #49231, #144206, #172574, #47246, #93730, #155412, #48241, #33068, #94723, #109896, #156401, #113859, #7684, #55203, #176568, #100695, #54210, #193735, #162376, #101701, #71379, #24888, #175555, #99699, #21875, #116872, #23878, #83525, #87537, #70378, #191714, #177571, #84521, #53198, #179576, #37030, #117885, #161383, #133043, #115881, #6686, #178563, #130015, #38043, #163391, #41046, #145203, #22874, #68364, #114873, #52201, #86537, #192726, #8708, #146198, #40028, #148221, #98691, #9715, #194733, #39038, #85529, #69368, #131037, #147217, #160385, #132046, #56203, #102711, #164400, #25892, #149224, #10715, #72378, #190728 ),
 ( #26888, #28873, #90514, #152196, #103715, #168353, #198706, #76337, #59179, #120848, #169335, #75347, #195744, #60173, #30843, #57218, #165395, #104704, #197714, #154179, #119875, #92490, #29849, #45020, #118892, #91486, #106680, #88531, #153173, #105690, #121842, #183536, #14675, #181560, #166393, #150227, #138013, #44029, #11723, #15670, #13680, #135063, #182547, #27889, #196739, #122834, #180577, #61162, #43038, #199697, #167377, #73391, #137016, #58206, #89531, #184523, #46003, #151219, #12708, #74374, #136039, #42051, #107658, #134052, #98185, #127553, #67876, #37539, #476, #83036, #144711, #128538, #190233, #19396, #93483, #66876, #62150, #158882, #51711, #52704, #7193, #130536, #159889, #53715, #114367, #99203, #176072, #145711, #160891, #50730, #65879, #82019, #143715, #6196, #38551, #22383, #185512, #112388, #20371, #170340, #175065, #36531, #21377, #47003, #84033, #129530, #68877, #5194, #113374, #115392, #191230, #138997, #192234, #177080, #123814, #108662, #174080, #100208, #161888, #189254, #77329, #31833, #155170, #81045, #142721, #4201, #35549, #97196, #195240, #88035, #72898, #104214, #9221, #55711, #181076, #193236, #194244, #43539, #165895, #102220, #27392, #148732, #103220, #69882, #131551, #182056, #147734, #70888, #54709, #150728, #146710, #40551, #149723, #132556, #133550, #87047, #26396, #56724, #134566, #89038, #57723, #8207, #117383, #119393, #116381, #179080, #163909, #178071, #118395, #180089, #41557, #39538, #42551, #11223, #12227, #10220, #71880, #58693, #164902, #85030, #196254, #120363, #101196, #162887, #25405, #73890, #105205, #135560, #23383, #197232, #24396, #86045, #62656, #139498, #136531, #980, #138510, #31344, #16176, #47513, #152687, #199204, #124335, #198212, #137522, #187040, #109169, #45517, #170848, #91990, #46510, #13206, #74869, #125342, #91001, #14176, #59684, #93992, #90030, #184035, #92995, #75846, #76839, #30348, #169850, #159881, #77831, #32339, #186031, #151713, #60671, #121355, #154681, #61661, #183048, #63668, #108169, #167870, #153684, #122346, #29370, #155673, #44532, #17168, #107172, #78821, #15180, #106187, #140500, #168843, #123329, #1989, #48510, #185023, #166892, #28392, #188020, #171843, #144471, #112154, #128300, #157670, #97946, #67632, #33331, #113136, #174826, #158644, #20136, #49492, #126323, #96964, #94991, #189017, #81781, #82789, #37297, #160646, #189999, #83788, #5955, #129292, #190988, #175824, #52464, #80807, #95985, #173844, #35310, #36290, #68629, #143468, #21134, #50491, #127306, #130285, #114122, #156676, #141498, #6949, #3964, #4952, #66637, #51474, #142486, #191979, #159638, #2982, #65644, #98956, #22138, #18171, #145467, #110164, #79828, #64661, #111154, #172843, #34323, #19159, #70648, #11987, #40302, #134323, #73651, #56473, #132314, #57484, #27151, #131306, #41313, #194006, #102973, #179842, #8980, #87795, #192996, #164658, #149480, #10976, #117139, #177834, #84786, #115143, #86803, #163658, #26153, #196009, #85803, #146465, #72649, #24152, #133307, #7957, #25161, #148489, #9980, #119154, #55469, #101978, #180836, #42313, #71640, #135323, #38307, #194996, #118152, #176836, #69640, #103974, #165653, #99962, #100960, #88798, #150491, #53466, #161646, #23141, #54473, #116143, #39302, #147489, #162645, #178833, #138284, #93762, #184787, #46273, #74634, #92760, #16933, #44295, #78586, #185791, #43299, #104967, #32105, #77601, #60436, #139272, #45287, #90772, #105954, #748, #183800, #108935, #196995, #106940, #168613, #166654, #13942, #59445, #121118, #155443, #154449, #62420, #76606, #12970, #124092, #30113, #91754, #169615, #47279, #29135, #28155, #31112, #167638, #199965, #89796, #153448, #14946, #61430, #15942, #75608, #123101, #107929, #170616, #58462, #120129, #181820, #151479, #136300, #197975, #182812, #152456, #137287, #198969, #122111, #159403, #97712, #21905, #81549, #140260, #1752, #96730, #66407, #34090 ),
 ( #126094, #142248, #3733, #128069, #98722, #174598, #48274, #172604, #18929, #33099, #35076, #158419, #19907, #109929, #36064, #4718, #82556, #65410, #127071, #175587, #143235, #63430, #189771, #37063, #125106, #171611, #110918, #188779, #160416, #187791, #186804, #20898, #51244, #94755, #144238, #112904, #156436, #5722, #111918, #67400, #129056, #190757, #49260, #95749, #52232, #17936, #157434, #79590, #113889, #80574, #141259, #50262, #2749, #64425, #173606, #42080, #7716, #131068, #191746, #10744, #6716, #100726, #148250, #69401, #193766, #147249, #86567, #55234, #194762, #164429, #117916, #68394, #192757, #114905, #9744, #116903, #176599, #180607, #53229, #162407, #146229, #54240, #103744, #41077, #149253, #163424, #99729, #72408, #178596, #56234, #23909, #85563, #165424, #179605, #145234, #38073, #83555, #177601, #132077, #40059, #101736, #115911, #130046, #24922, #161413, #39069, #8740, #70409, #22905, #71408, #102741, #25922, #134085, #133072, #84551, #87566, #195775, #57248, #118922, #13711, #107689, #47037, #29879, #44061, #30876, #509, #104732, #14708, #105721, #76369, #153203, #182578, #61193, #166424, #138046, #122865, #184553, #90544, #151248, #58235, #88560, #60204, #137047, #199727, #169367, #59209, #119903, #46034, #152226, #196767, #120878, #167408, #43066, #91517, #27919, #74403, #92522, #77362, #181588, #12737, #89562, #136069, #150259, #154212, #28904, #45052, #197743, #15701, #139030, #11753, #62181, #123845, #75377, #198739, #121874, #183567, #106710, #73420, #168384, #185543, #108694, #26918, #135091, #50011, #143995, #142993, #127823, #66161, #35824, #4471, #141019, #156191, #172355, #33844, #96488, #128816, #189529, #78342, #2506, #49020, #63182, #65168, #126827, #188533, #140016, #111676, #173363, #64186, #51989, #34833, #124862, #125852, #95504, #157190, #93517, #187553, #51001, #112662, #159155, #19668, #48033, #190515, #97470, #110675, #170372, #18684, #174354, #31864, #158178, #80331, #20651, #5476, #109690, #81309, #142003, #82305, #67159, #3491, #155203, #171371, #16692, #1504, #186561, #32859, #94509, #17690, #79348, #147003, #23663, #86324, #194516, #145988, #144989, #148011, #69155, #36809, #68151, #164183, #8489, #70165, #9501, #192512, #100487, #24674, #71165, #131834, #72161, #98476, #85312, #162166, #175342, #129802, #132830, #193516, #160169, #161166, #55990, #117667, #195527, #54992, #113648, #21659, #116661, #39815, #7471, #191501, #178352, #101481, #10500, #163170, #179363, #52977, #40826, #133836, #22662, #83312, #102498, #6470, #114655, #149011, #25681, #177359, #87326, #176352, #130821, #84309, #37825, #99485, #53996, #115670, #38829, #43817, #165179, #74165, #119670, #181352, #15462, #14459, #122625, #136807, #73180, #184315, #28666, #168141, #135837, #197506, #77118, #152961, #118675, #88315, #153964, #151012, #105480, #58973, #138788, #167167, #137800, #57000, #59964, #120641, #60950, #30627, #134851, #44807, #182339, #106462, #183326, #12503, #91270, #196529, #29637, #76122, #199484, #90301, #42831, #150003, #180366, #151986, #13474, #45796, #107448, #89319, #11509, #169122, #75138, #41834, #58000, #92280, #198491, #121630, #103502, #26674, #104496, #166178, #27679, #156950, #158921, #185301, #110437, #48783, #61937, #154957, #173122, #172118, #123606, #47792, #19433, #157942, #82061, #141766, #269, #46792, #18447, #126591, #94269, #78102, #3258, #64932, #97234, #188293, #49770, #139771, #96255, #20411, #109443, #108451, #189291, #170127, #31622, #35588, #81080, #63945, #142759, #33604, #155947, #171126, #4239, #187312, #112427, #93272, #95267, #80098, #16453, #17444, #62936, #124616, #1259, #65919, #127592, #111435, #186311, #50768, #34597, #174117, #79100, #140773, #32615, #2262, #125613, #175102, #40591, #37580, #192274, #100248, #161929, #176110, #25447, #23424, #36570, #99243, #145751, #7233, #66916, #160931, #101240, #24436, #132595 ) ),
 .UNSPECIFIED., .T., .F., .T. ) 
 B_SPLINE_SURFACE_WITH_KNOTS ( ( 4, 3, 4 ),
 ( 3, 2, 2, 2, 2, 2, 2, 2, 2, 2, 2, 2, 2, 2, 2, 2, 2, 2, 2, 2, 2, 2, 2, 2, 2, 2, 2, 2, 2, 2, 2, 2, 2, 2, 2, 2, 2, 2, 2, 2, 2, 2, 2, 2, 2, 2, 2, 2, 2, 2, 2, 2, 2, 2, 2, 2, 2, 2, 2, 2, 2, 2, 2, 2, 2, 2, 2, 2, 2, 2, 2, 2, 2, 2, 2, 2, 2, 2, 2, 2, 2, 2, 2, 2, 2, 2, 2, 2, 2, 2, 2, 2, 2, 2, 2, 2, 2, 2, 2, 2, 2, 2, 2, 2, 2, 2, 2, 2, 2, 2, 2, 2, 2, 2, 2, 2, 2, 2, 2, 2, 2, 2, 2, 2, 2, 2, 2, 2, 2, 2, 2, 2, 2, 2, 2, 2, 2, 2, 2, 2, 2, 2, 2, 2, 2, 2, 2, 2, 2, 2, 2, 2, 2, 2, 2, 2, 2, 2, 2, 2, 2, 2, 2, 2, 2, 2, 2, 2, 2, 2, 2, 2, 2, 2, 2, 2, 2, 2, 2, 2, 2, 2, 2, 2, 2, 2, 2, 2, 2, 2, 2, 2, 2, 2, 2, 2, 2, 2, 2, 2, 2, 2, 2, 2, 2, 2, 2, 2, 2, 2, 2, 2, 2, 2, 2, 2, 2, 2, 2, 2, 2, 2, 2, 2, 2, 2, 2, 2, 3 ),
 ( 0.000000000000000000, 0.5000000000000000000, 1.000000000000000000 ),
 ( 0.000000000000000000, 0.004385964912280701511, 0.008771929824561403022, 0.01315789473684210453, 0.01754385964912280604, 0.02192982456140350755, 0.02631578947368420907, 0.03070175438596491058, 0.03508771929824561209, 0.03947368421052631360, 0.04385964912280701511, 0.04824561403508771662, 0.05263157894736841813, 0.05701754385964911964, 0.06140350877192982115, 0.06578947368421052266, 0.07017543859649122417, 0.07456140350877192569, 0.07894736842105262720, 0.08333333333333332871, 0.08771929824561403022, 0.09210526315789473173, 0.09649122807017543324, 0.1008771929824561348, 0.1052631578947368363, 0.1096491228070175378, 0.1140350877192982393, 0.1184210526315789408, 0.1228070175438596423, 0.1271929824561403577, 0.1315789473684210453, 0.1359649122807017607, 0.1403508771929824483, 0.1447368421052631637, 0.1491228070175438514, 0.1535087719298245668, 0.1578947368421052544, 0.1622807017543859698, 0.1666666666666666574, 0.1710526315789473728, 0.1754385964912280604, 0.1798245614035087758, 0.1842105263157894635, 0.1885964912280701788, 0.1929824561403508665, 0.1973684210526315819, 0.2017543859649122695, 0.2061403508771929849, 0.2105263157894736725, 0.2149122807017543879, 0.2192982456140350755, 0.2236842105263157909, 0.2280701754385964786, 0.2324561403508771940, 0.2368421052631578816, 0.2412280701754385970, 0.2456140350877192846, 0.2500000000000000000, 0.2543859649122807154, 0.2587719298245614308, 0.2631578947368420907, 0.2675438596491228060, 0.2719298245614035214, 0.2763157894736842368, 0.2807017543859648967, 0.2850877192982456121, 0.2894736842105263275, 0.2938596491228070429, 0.2982456140350877027, 0.3026315789473684181, 0.3070175438596491335, 0.3114035087719298489, 0.3157894736842105088, 0.3201754385964912242, 0.3245614035087719396, 0.3289473684210526550, 0.3333333333333333148, 0.3377192982456140302, 0.3421052631578947456, 0.3464912280701754610, 0.3508771929824561209, 0.3552631578947368363, 0.3596491228070175517, 0.3640350877192982670, 0.3684210526315789269, 0.3728070175438596423, 0.3771929824561403577, 0.3815789473684210731, 0.3859649122807017330, 0.3903508771929824483, 0.3947368421052631637, 0.3991228070175438791, 0.4035087719298245390, 0.4078947368421052544, 0.4122807017543859698, 0.4166666666666666852, 0.4210526315789473450, 0.4254385964912280604, 0.4298245614035087758, 0.4342105263157894912, 0.4385964912280701511, 0.4429824561403508665, 0.4473684210526315819, 0.4517543859649122973, 0.4561403508771929571, 0.4605263157894736725, 0.4649122807017543879, 0.4692982456140351033, 0.4736842105263157632, 0.4780701754385964786, 0.4824561403508771940, 0.4868421052631579093, 0.4912280701754385692, 0.4956140350877192846, 0.5000000000000000000, 0.5043859649122807154, 0.5087719298245614308, 0.5131578947368421462, 0.5175438596491228616, 0.5219298245614034659, 0.5263157894736841813, 0.5307017543859648967, 0.5350877192982456121, 0.5394736842105263275, 0.5438596491228070429, 0.5482456140350877583, 0.5526315789473684736, 0.5570175438596490780, 0.5614035087719297934, 0.5657894736842105088, 0.5701754385964912242, 0.5745614035087719396, 0.5789473684210526550, 0.5833333333333333703, 0.5877192982456140857, 0.5921052631578946901, 0.5964912280701754055, 0.6008771929824561209, 0.6052631578947368363, 0.6096491228070175517, 0.6140350877192982670, 0.6184210526315789824, 0.6228070175438596978, 0.6271929824561403022, 0.6315789473684210176, 0.6359649122807017330, 0.6403508771929824483, 0.6447368421052631637, 0.6491228070175438791, 0.6535087719298245945, 0.6578947368421053099, 0.6622807017543859143, 0.6666666666666666297, 0.6710526315789473450, 0.6754385964912280604, 0.6798245614035087758, 0.6842105263157894912, 0.6885964912280702066, 0.6929824561403509220, 0.6973684210526315264, 0.7017543859649122417, 0.7061403508771929571, 0.7105263157894736725, 0.7149122807017543879, 0.7192982456140351033, 0.7236842105263158187, 0.7280701754385965341, 0.7324561403508771384, 0.7368421052631578538, 0.7412280701754385692, 0.7456140350877192846, 0.7500000000000000000, 0.7543859649122807154, 0.7587719298245614308, 0.7631578947368421462, 0.7675438596491228616, 0.7719298245614034659, 0.7763157894736841813, 0.7807017543859648967, 0.7850877192982456121, 0.7894736842105263275, 0.7938596491228070429, 0.7982456140350877583, 0.8026315789473684736, 0.8070175438596490780, 0.8114035087719297934, 0.8157894736842105088, 0.8201754385964912242, 0.8245614035087719396, 0.8289473684210526550, 0.8333333333333333703, 0.8377192982456140857, 0.8421052631578946901, 0.8464912280701754055, 0.8508771929824561209, 0.8552631578947368363, 0.8596491228070175517, 0.8640350877192982670, 0.8684210526315789824, 0.8728070175438596978, 0.8771929824561403022, 0.8815789473684210176, 0.8859649122807017330, 0.8903508771929824483, 0.8947368421052631637, 0.8991228070175438791, 0.9035087719298245945, 0.9078947368421053099, 0.9122807017543859143, 0.9166666666666666297, 0.9210526315789473450, 0.9254385964912280604, 0.9298245614035087758, 0.9342105263157894912, 0.9385964912280702066, 0.9429824561403509220, 0.9473684210526315264, 0.9517543859649122417, 0.9561403508771929571, 0.9605263157894736725, 0.9649122807017543879, 0.9692982456140351033, 0.9736842105263158187, 0.9780701754385965341, 0.9824561403508771384, 0.9868421052631578538, 0.9912280701754385692, 0.9956140350877192846, 1.000000000000000000 ),
 .UNSPECIFIED. ) 
 GEOMETRIC_REPRESENTATION_ITEM ( )  RATIONAL_B_SPLINE_SURFACE ( (
 ( 1.000000000000000000, 0.9659258262890683122, 1.000000000000000000, 0.9659258262890683122, 1.000000000000000000, 0.9659258262890683122, 1.000000000000000000, 0.9659258262890683122, 1.000000000000000000, 0.9659258262890683122, 1.000000000000000000, 0.9659258262890683122, 1.000000000000000000, 0.9659258262890683122, 1.000000000000000000, 0.9659258262890683122, 1.000000000000000000, 0.9659258262890683122, 1.000000000000000000, 0.9659258262890683122, 1.000000000000000000, 0.9659258262890683122, 1.000000000000000000, 0.9659258262890683122, 1.000000000000000000, 0.9659258262890683122, 1.000000000000000000, 0.9659258262890683122, 1.000000000000000000, 0.9659258262890683122, 1.000000000000000000, 0.9659258262890683122, 1.000000000000000000, 0.9659258262890683122, 1.000000000000000000, 0.9659258262890683122, 1.000000000000000000, 0.9659258262890683122, 1.000000000000000000, 0.9659258262890683122, 1.000000000000000000, 0.9659258262890683122, 1.000000000000000000, 0.9659258262890683122, 1.000000000000000000, 0.9659258262890683122, 1.000000000000000000, 0.9659258262890683122, 1.000000000000000000, 0.9659258262890683122, 1.000000000000000000, 0.9659258262890683122, 1.000000000000000000, 0.9659258262890683122, 1.000000000000000000, 0.9659258262890683122, 1.000000000000000000, 0.9659258262890683122, 1.000000000000000000, 0.9659258262890683122, 1.000000000000000000, 0.9659258262890683122, 1.000000000000000000, 0.9659258262890683122, 1.000000000000000000, 0.9659258262890683122, 1.000000000000000000, 0.9659258262890683122, 1.000000000000000000, 0.9659258262890683122, 1.000000000000000000, 0.9659258262890683122, 1.000000000000000000, 0.9659258262890683122, 1.000000000000000000, 0.9659258262890683122, 1.000000000000000000, 0.9659258262890683122, 1.000000000000000000, 0.9659258262890683122, 1.000000000000000000, 0.9659258262890683122, 1.000000000000000000, 0.9659258262890683122, 1.000000000000000000, 0.9659258262890683122, 1.000000000000000000, 0.9659258262890683122, 1.000000000000000000, 0.9659258262890683122, 1.000000000000000000, 0.9659258262890683122, 1.000000000000000000, 0.9659258262890683122, 1.000000000000000000, 0.9659258262890683122, 1.000000000000000000, 0.9659258262890683122, 1.000000000000000000, 0.9659258262890683122, 1.000000000000000000, 0.9659258262890683122, 1.000000000000000000, 0.9659258262890683122, 1.000000000000000000, 0.9659258262890683122, 1.000000000000000000, 0.9659258262890683122, 1.000000000000000000, 0.9659258262890683122, 1.000000000000000000, 0.9659258262890683122, 1.000000000000000000, 0.9659258262890683122, 1.000000000000000000, 0.9659258262890683122, 1.000000000000000000, 0.9659258262890683122, 1.000000000000000000, 0.9659258262890683122, 1.000000000000000000, 0.9659258262890683122, 1.000000000000000000, 0.9659258262890683122, 1.000000000000000000, 0.9659258262890683122, 1.000000000000000000, 0.9659258262890683122, 1.000000000000000000, 0.9659258262890683122, 1.000000000000000000, 0.9659258262890683122, 1.000000000000000000, 0.9659258262890683122, 1.000000000000000000, 0.9659258262890683122, 1.000000000000000000, 0.9659258262890683122, 1.000000000000000000, 0.9659258262890683122, 1.000000000000000000, 0.9659258262890683122, 1.000000000000000000, 0.9659258262890683122, 1.000000000000000000, 0.9659258262890683122, 1.000000000000000000, 0.9659258262890683122, 1.000000000000000000, 0.9659258262890683122, 1.000000000000000000, 0.9659258262890683122, 1.000000000000000000, 0.9659258262890683122, 1.000000000000000000, 0.9659258262890683122, 1.000000000000000000, 0.9659258262890683122, 1.000000000000000000, 0.9659258262890683122, 1.000000000000000000, 0.9659258262890683122, 1.000000000000000000, 0.9659258262890683122, 1.000000000000000000, 0.9659258262890683122, 1.000000000000000000, 0.9659258262890683122, 1.000000000000000000, 0.9659258262890683122, 1.000000000000000000, 0.9659258262890683122, 1.000000000000000000, 0.9659258262890683122, 1.000000000000000000, 0.9659258262890683122, 1.000000000000000000, 0.9659258262890683122, 1.000000000000000000, 0.9659258262890683122, 1.000000000000000000, 0.9659258262890683122, 1.000000000000000000, 0.9659258262890683122, 1.000000000000000000, 0.9659258262890683122, 1.000000000000000000, 0.9659258262890683122, 1.000000000000000000, 0.9659258262890683122, 1.000000000000000000, 0.9659258262890683122, 1.000000000000000000, 0.9659258262890683122, 1.000000000000000000, 0.9659258262890683122, 1.000000000000000000, 0.9659258262890683122, 1.000000000000000000, 0.9659258262890683122, 1.000000000000000000, 0.9659258262890683122, 1.000000000000000000, 0.9659258262890683122, 1.000000000000000000, 0.9659258262890683122, 1.000000000000000000, 0.9659258262890683122, 1.000000000000000000, 0.9659258262890683122, 1.000000000000000000, 0.9659258262890683122, 1.000000000000000000, 0.9659258262890683122, 1.000000000000000000, 0.9659258262890683122, 1.000000000000000000, 0.9659258262890683122, 1.000000000000000000, 0.9659258262890683122, 1.000000000000000000, 0.9659258262890683122, 1.000000000000000000, 0.9659258262890683122, 1.000000000000000000, 0.9659258262890683122, 1.000000000000000000, 0.9659258262890683122, 1.000000000000000000, 0.9659258262890683122, 1.000000000000000000, 0.9659258262890683122, 1.000000000000000000, 0.9659258262890683122, 1.000000000000000000, 0.9659258262890683122, 1.000000000000000000, 0.9659258262890683122, 1.000000000000000000, 0.9659258262890683122, 1.000000000000000000, 0.9659258262890683122, 1.000000000000000000, 0.9659258262890683122, 1.000000000000000000, 0.9659258262890683122, 1.000000000000000000, 0.9659258262890683122, 1.000000000000000000, 0.9659258262890683122, 1.000000000000000000, 0.9659258262890683122, 1.000000000000000000, 0.9659258262890683122, 1.000000000000000000, 0.9659258262890683122, 1.000000000000000000, 0.9659258262890683122, 1.000000000000000000, 0.9659258262890683122, 1.000000000000000000, 0.9659258262890683122, 1.000000000000000000, 0.9659258262890683122, 1.000000000000000000, 0.9659258262890683122, 1.000000000000000000, 0.9659258262890683122, 1.000000000000000000, 0.9659258262890683122, 1.000000000000000000, 0.9659258262890683122, 1.000000000000000000, 0.9659258262890683122, 1.000000000000000000, 0.9659258262890683122, 1.000000000000000000, 0.9659258262890683122, 1.000000000000000000, 0.9659258262890683122, 1.000000000000000000, 0.9659258262890683122, 1.000000000000000000, 0.9659258262890683122, 1.000000000000000000, 0.9659258262890683122, 1.000000000000000000, 0.9659258262890683122, 1.000000000000000000, 0.9659258262890683122, 1.000000000000000000, 0.9659258262890683122, 1.000000000000000000, 0.9659258262890683122, 1.000000000000000000, 0.9659258262890683122, 1.000000000000000000, 0.9659258262890683122, 1.000000000000000000, 0.9659258262890683122, 1.000000000000000000, 0.9659258262890683122, 1.000000000000000000, 0.9659258262890683122, 1.000000000000000000, 0.9659258262890683122, 1.000000000000000000, 0.9659258262890683122, 1.000000000000000000, 0.9659258262890683122, 1.000000000000000000, 0.9659258262890683122, 1.000000000000000000, 0.9659258262890683122, 1.000000000000000000, 0.9659258262890683122, 1.000000000000000000, 0.9659258262890683122, 1.000000000000000000, 0.9659258262890683122, 1.000000000000000000, 0.9659258262890683122, 1.000000000000000000, 0.9659258262890683122, 1.000000000000000000, 0.9659258262890683122, 1.000000000000000000, 0.9659258262890683122, 1.000000000000000000, 0.9659258262890683122, 1.000000000000000000, 0.9659258262890683122, 1.000000000000000000, 0.9659258262890683122, 1.000000000000000000, 0.9659258262890683122, 1.000000000000000000, 0.9659258262890683122, 1.000000000000000000, 0.9659258262890683122, 1.000000000000000000, 0.9659258262890683122, 1.000000000000000000, 0.9659258262890683122, 1.000000000000000000, 0.9659258262890683122, 1.000000000000000000, 0.9659258262890683122, 1.000000000000000000, 0.9659258262890683122, 1.000000000000000000, 0.9659258262890683122, 1.000000000000000000, 0.9659258262890683122, 1.000000000000000000, 0.9659258262890683122, 1.000000000000000000, 0.9659258262890683122, 1.000000000000000000, 0.9659258262890683122, 1.000000000000000000, 0.9659258262890683122, 1.000000000000000000, 0.9659258262890683122, 1.000000000000000000, 0.9659258262890683122, 1.000000000000000000, 0.9659258262890683122, 1.000000000000000000, 0.9659258262890683122, 1.000000000000000000, 0.9659258262890683122, 1.000000000000000000, 0.9659258262890683122, 1.000000000000000000, 0.9659258262890683122, 1.000000000000000000, 0.9659258262890683122, 1.000000000000000000, 0.9659258262890683122, 1.000000000000000000, 0.9659258262890683122, 1.000000000000000000, 0.9659258262890683122, 1.000000000000000000, 0.9659258262890683122, 1.000000000000000000, 0.9659258262890683122, 1.000000000000000000, 0.9659258262890683122, 1.000000000000000000, 0.9659258262890683122, 1.000000000000000000, 0.9659258262890683122, 1.000000000000000000, 0.9659258262890683122, 1.000000000000000000, 0.9659258262890683122, 1.000000000000000000, 0.9659258262890683122, 1.000000000000000000, 0.9659258262890683122, 1.000000000000000000, 0.9659258262890683122, 1.000000000000000000, 0.9659258262890683122, 1.000000000000000000, 0.9659258262890683122, 1.000000000000000000, 0.9659258262890683122, 1.000000000000000000, 0.9659258262890683122, 1.000000000000000000, 0.9659258262890683122, 1.000000000000000000, 0.9659258262890683122, 1.000000000000000000, 0.9659258262890683122, 1.000000000000000000, 0.9659258262890683122, 1.000000000000000000, 0.9659258262890683122, 1.000000000000000000, 0.9659258262890683122, 1.000000000000000000, 0.9659258262890683122, 1.000000000000000000, 0.9659258262890683122, 1.000000000000000000, 0.9659258262890683122, 1.000000000000000000, 0.9659258262890683122, 1.000000000000000000, 0.9659258262890683122, 1.000000000000000000, 0.9659258262890683122, 1.000000000000000000, 0.9659258262890683122, 1.000000000000000000, 0.9659258262890683122, 1.000000000000000000, 0.9659258262890683122, 1.000000000000000000, 0.9659258262890683122, 1.000000000000000000, 0.9659258262890683122, 1.000000000000000000, 0.9659258262890683122, 1.000000000000000000, 0.9659258262890683122, 1.000000000000000000, 0.9659258262890683122, 1.000000000000000000, 0.9659258262890683122, 1.000000000000000000, 0.9659258262890683122, 1.000000000000000000),
 ( 0.3333333333333333703, 0.3219752754296894559, 0.3333333333333333703, 0.3219752754296894559, 0.3333333333333333703, 0.3219752754296894559, 0.3333333333333333703, 0.3219752754296894559, 0.3333333333333333703, 0.3219752754296894559, 0.3333333333333333703, 0.3219752754296894559, 0.3333333333333333703, 0.3219752754296894559, 0.3333333333333333703, 0.3219752754296894559, 0.3333333333333333703, 0.3219752754296894559, 0.3333333333333333703, 0.3219752754296894559, 0.3333333333333333703, 0.3219752754296894559, 0.3333333333333333703, 0.3219752754296894559, 0.3333333333333333703, 0.3219752754296894559, 0.3333333333333333703, 0.3219752754296894559, 0.3333333333333333703, 0.3219752754296894559, 0.3333333333333333703, 0.3219752754296894559, 0.3333333333333333703, 0.3219752754296894559, 0.3333333333333333703, 0.3219752754296894559, 0.3333333333333333703, 0.3219752754296894559, 0.3333333333333333703, 0.3219752754296894559, 0.3333333333333333703, 0.3219752754296894559, 0.3333333333333333703, 0.3219752754296894559, 0.3333333333333333703, 0.3219752754296894559, 0.3333333333333333703, 0.3219752754296894559, 0.3333333333333333703, 0.3219752754296894559, 0.3333333333333333703, 0.3219752754296894559, 0.3333333333333333703, 0.3219752754296894559, 0.3333333333333333703, 0.3219752754296894559, 0.3333333333333333703, 0.3219752754296894559, 0.3333333333333333703, 0.3219752754296894559, 0.3333333333333333703, 0.3219752754296894559, 0.3333333333333333703, 0.3219752754296894559, 0.3333333333333333703, 0.3219752754296894559, 0.3333333333333333703, 0.3219752754296894559, 0.3333333333333333703, 0.3219752754296894559, 0.3333333333333333703, 0.3219752754296894559, 0.3333333333333333703, 0.3219752754296894559, 0.3333333333333333703, 0.3219752754296894559, 0.3333333333333333703, 0.3219752754296894559, 0.3333333333333333703, 0.3219752754296894559, 0.3333333333333333703, 0.3219752754296894559, 0.3333333333333333703, 0.3219752754296894559, 0.3333333333333333703, 0.3219752754296894559, 0.3333333333333333703, 0.3219752754296894559, 0.3333333333333333703, 0.3219752754296894559, 0.3333333333333333703, 0.3219752754296894559, 0.3333333333333333703, 0.3219752754296894559, 0.3333333333333333703, 0.3219752754296894559, 0.3333333333333333703, 0.3219752754296894559, 0.3333333333333333703, 0.3219752754296894559, 0.3333333333333333703, 0.3219752754296894559, 0.3333333333333333703, 0.3219752754296894559, 0.3333333333333333703, 0.3219752754296894559, 0.3333333333333333703, 0.3219752754296894559, 0.3333333333333333703, 0.3219752754296894559, 0.3333333333333333703, 0.3219752754296894559, 0.3333333333333333703, 0.3219752754296894559, 0.3333333333333333703, 0.3219752754296894559, 0.3333333333333333703, 0.3219752754296894559, 0.3333333333333333703, 0.3219752754296894559, 0.3333333333333333703, 0.3219752754296894559, 0.3333333333333333703, 0.3219752754296894559, 0.3333333333333333703, 0.3219752754296894559, 0.3333333333333333703, 0.3219752754296894559, 0.3333333333333333703, 0.3219752754296894559, 0.3333333333333333703, 0.3219752754296894559, 0.3333333333333333703, 0.3219752754296894559, 0.3333333333333333703, 0.3219752754296894559, 0.3333333333333333703, 0.3219752754296894559, 0.3333333333333333703, 0.3219752754296894559, 0.3333333333333333703, 0.3219752754296894559, 0.3333333333333333703, 0.3219752754296894559, 0.3333333333333333703, 0.3219752754296894559, 0.3333333333333333703, 0.3219752754296894559, 0.3333333333333333703, 0.3219752754296894559, 0.3333333333333333703, 0.3219752754296894559, 0.3333333333333333703, 0.3219752754296894559, 0.3333333333333333703, 0.3219752754296894559, 0.3333333333333333703, 0.3219752754296894559, 0.3333333333333333703, 0.3219752754296894559, 0.3333333333333333703, 0.3219752754296894559, 0.3333333333333333703, 0.3219752754296894559, 0.3333333333333333703, 0.3219752754296894559, 0.3333333333333333703, 0.3219752754296894559, 0.3333333333333333703, 0.3219752754296894559, 0.3333333333333333703, 0.3219752754296894559, 0.3333333333333333703, 0.3219752754296894559, 0.3333333333333333703, 0.3219752754296894559, 0.3333333333333333703, 0.3219752754296894559, 0.3333333333333333703, 0.3219752754296894559, 0.3333333333333333703, 0.3219752754296894559, 0.3333333333333333703, 0.3219752754296894559, 0.3333333333333333703, 0.3219752754296894559, 0.3333333333333333703, 0.3219752754296894559, 0.3333333333333333703, 0.3219752754296894559, 0.3333333333333333703, 0.3219752754296894559, 0.3333333333333333703, 0.3219752754296894559, 0.3333333333333333703, 0.3219752754296894559, 0.3333333333333333703, 0.3219752754296894559, 0.3333333333333333703, 0.3219752754296894559, 0.3333333333333333703, 0.3219752754296894559, 0.3333333333333333703, 0.3219752754296894559, 0.3333333333333333703, 0.3219752754296894559, 0.3333333333333333703, 0.3219752754296894559, 0.3333333333333333703, 0.3219752754296894559, 0.3333333333333333703, 0.3219752754296894559, 0.3333333333333333703, 0.3219752754296894559, 0.3333333333333333703, 0.3219752754296894559, 0.3333333333333333703, 0.3219752754296894559, 0.3333333333333333703, 0.3219752754296894559, 0.3333333333333333703, 0.3219752754296894559, 0.3333333333333333703, 0.3219752754296894559, 0.3333333333333333703, 0.3219752754296894559, 0.3333333333333333703, 0.3219752754296894559, 0.3333333333333333703, 0.3219752754296894559, 0.3333333333333333703, 0.3219752754296894559, 0.3333333333333333703, 0.3219752754296894559, 0.3333333333333333703, 0.3219752754296894559, 0.3333333333333333703, 0.3219752754296894559, 0.3333333333333333703, 0.3219752754296894559, 0.3333333333333333703, 0.3219752754296894559, 0.3333333333333333703, 0.3219752754296894559, 0.3333333333333333703, 0.3219752754296894559, 0.3333333333333333703, 0.3219752754296894559, 0.3333333333333333703, 0.3219752754296894559, 0.3333333333333333703, 0.3219752754296894559, 0.3333333333333333703, 0.3219752754296894559, 0.3333333333333333703, 0.3219752754296894559, 0.3333333333333333703, 0.3219752754296894559, 0.3333333333333333703, 0.3219752754296894559, 0.3333333333333333703, 0.3219752754296894559, 0.3333333333333333703, 0.3219752754296894559, 0.3333333333333333703, 0.3219752754296894559, 0.3333333333333333703, 0.3219752754296894559, 0.3333333333333333703, 0.3219752754296894559, 0.3333333333333333703, 0.3219752754296894559, 0.3333333333333333703, 0.3219752754296894559, 0.3333333333333333703, 0.3219752754296894559, 0.3333333333333333703, 0.3219752754296894559, 0.3333333333333333703, 0.3219752754296894559, 0.3333333333333333703, 0.3219752754296894559, 0.3333333333333333703, 0.3219752754296894559, 0.3333333333333333703, 0.3219752754296894559, 0.3333333333333333703, 0.3219752754296894559, 0.3333333333333333703, 0.3219752754296894559, 0.3333333333333333703, 0.3219752754296894559, 0.3333333333333333703, 0.3219752754296894559, 0.3333333333333333703, 0.3219752754296894559, 0.3333333333333333703, 0.3219752754296894559, 0.3333333333333333703, 0.3219752754296894559, 0.3333333333333333703, 0.3219752754296894559, 0.3333333333333333703, 0.3219752754296894559, 0.3333333333333333703, 0.3219752754296894559, 0.3333333333333333703, 0.3219752754296894559, 0.3333333333333333703, 0.3219752754296894559, 0.3333333333333333703, 0.3219752754296894559, 0.3333333333333333703, 0.3219752754296894559, 0.3333333333333333703, 0.3219752754296894559, 0.3333333333333333703, 0.3219752754296894559, 0.3333333333333333703, 0.3219752754296894559, 0.3333333333333333703, 0.3219752754296894559, 0.3333333333333333703, 0.3219752754296894559, 0.3333333333333333703, 0.3219752754296894559, 0.3333333333333333703, 0.3219752754296894559, 0.3333333333333333703, 0.3219752754296894559, 0.3333333333333333703, 0.3219752754296894559, 0.3333333333333333703, 0.3219752754296894559, 0.3333333333333333703, 0.3219752754296894559, 0.3333333333333333703, 0.3219752754296894559, 0.3333333333333333703, 0.3219752754296894559, 0.3333333333333333703, 0.3219752754296894559, 0.3333333333333333703, 0.3219752754296894559, 0.3333333333333333703, 0.3219752754296894559, 0.3333333333333333703, 0.3219752754296894559, 0.3333333333333333703, 0.3219752754296894559, 0.3333333333333333703, 0.3219752754296894559, 0.3333333333333333703, 0.3219752754296894559, 0.3333333333333333703, 0.3219752754296894559, 0.3333333333333333703, 0.3219752754296894559, 0.3333333333333333703, 0.3219752754296894559, 0.3333333333333333703, 0.3219752754296894559, 0.3333333333333333703, 0.3219752754296894559, 0.3333333333333333703, 0.3219752754296894559, 0.3333333333333333703, 0.3219752754296894559, 0.3333333333333333703, 0.3219752754296894559, 0.3333333333333333703, 0.3219752754296894559, 0.3333333333333333703, 0.3219752754296894559, 0.3333333333333333703, 0.3219752754296894559, 0.3333333333333333703, 0.3219752754296894559, 0.3333333333333333703, 0.3219752754296894559, 0.3333333333333333703, 0.3219752754296894559, 0.3333333333333333703, 0.3219752754296894559, 0.3333333333333333703, 0.3219752754296894559, 0.3333333333333333703, 0.3219752754296894559, 0.3333333333333333703, 0.3219752754296894559, 0.3333333333333333703, 0.3219752754296894559, 0.3333333333333333703, 0.3219752754296894559, 0.3333333333333333703, 0.3219752754296894559, 0.3333333333333333703, 0.3219752754296894559, 0.3333333333333333703, 0.3219752754296894559, 0.3333333333333333703, 0.3219752754296894559, 0.3333333333333333703, 0.3219752754296894559, 0.3333333333333333703, 0.3219752754296894559, 0.3333333333333333703, 0.3219752754296894559, 0.3333333333333333703, 0.3219752754296894559, 0.3333333333333333703, 0.3219752754296894559, 0.3333333333333333703, 0.3219752754296894559, 0.3333333333333333703, 0.3219752754296894559, 0.3333333333333333703, 0.3219752754296894559, 0.3333333333333333703, 0.3219752754296894559, 0.3333333333333333703, 0.3219752754296894559, 0.3333333333333333703, 0.3219752754296894559, 0.3333333333333333703, 0.3219752754296894559, 0.3333333333333333703, 0.3219752754296894559, 0.3333333333333333703, 0.3219752754296894559, 0.3333333333333333703, 0.3219752754296894559, 0.3333333333333333703, 0.3219752754296894559, 0.3333333333333333703, 0.3219752754296894559, 0.3333333333333333703, 0.3219752754296894559, 0.3333333333333333703, 0.3219752754296894559, 0.3333333333333333703, 0.3219752754296894559, 0.3333333333333333703, 0.3219752754296894559, 0.3333333333333333703, 0.3219752754296894559, 0.3333333333333333703, 0.3219752754296894559, 0.3333333333333333703, 0.3219752754296894559, 0.3333333333333333703, 0.3219752754296894559, 0.3333333333333333703, 0.3219752754296894559, 0.3333333333333333703, 0.3219752754296894559, 0.3333333333333333703),
 ( 0.3333333333333333703, 0.3219752754296894559, 0.3333333333333333703, 0.3219752754296894559, 0.3333333333333333703, 0.3219752754296894559, 0.3333333333333333703, 0.3219752754296894559, 0.3333333333333333703, 0.3219752754296894559, 0.3333333333333333703, 0.3219752754296894559, 0.3333333333333333703, 0.3219752754296894559, 0.3333333333333333703, 0.3219752754296894559, 0.3333333333333333703, 0.3219752754296894559, 0.3333333333333333703, 0.3219752754296894559, 0.3333333333333333703, 0.3219752754296894559, 0.3333333333333333703, 0.3219752754296894559, 0.3333333333333333703, 0.3219752754296894559, 0.3333333333333333703, 0.3219752754296894559, 0.3333333333333333703, 0.3219752754296894559, 0.3333333333333333703, 0.3219752754296894559, 0.3333333333333333703, 0.3219752754296894559, 0.3333333333333333703, 0.3219752754296894559, 0.3333333333333333703, 0.3219752754296894559, 0.3333333333333333703, 0.3219752754296894559, 0.3333333333333333703, 0.3219752754296894559, 0.3333333333333333703, 0.3219752754296894559, 0.3333333333333333703, 0.3219752754296894559, 0.3333333333333333703, 0.3219752754296894559, 0.3333333333333333703, 0.3219752754296894559, 0.3333333333333333703, 0.3219752754296894559, 0.3333333333333333703, 0.3219752754296894559, 0.3333333333333333703, 0.3219752754296894559, 0.3333333333333333703, 0.3219752754296894559, 0.3333333333333333703, 0.3219752754296894559, 0.3333333333333333703, 0.3219752754296894559, 0.3333333333333333703, 0.3219752754296894559, 0.3333333333333333703, 0.3219752754296894559, 0.3333333333333333703, 0.3219752754296894559, 0.3333333333333333703, 0.3219752754296894559, 0.3333333333333333703, 0.3219752754296894559, 0.3333333333333333703, 0.3219752754296894559, 0.3333333333333333703, 0.3219752754296894559, 0.3333333333333333703, 0.3219752754296894559, 0.3333333333333333703, 0.3219752754296894559, 0.3333333333333333703, 0.3219752754296894559, 0.3333333333333333703, 0.3219752754296894559, 0.3333333333333333703, 0.3219752754296894559, 0.3333333333333333703, 0.3219752754296894559, 0.3333333333333333703, 0.3219752754296894559, 0.3333333333333333703, 0.3219752754296894559, 0.3333333333333333703, 0.3219752754296894559, 0.3333333333333333703, 0.3219752754296894559, 0.3333333333333333703, 0.3219752754296894559, 0.3333333333333333703, 0.3219752754296894559, 0.3333333333333333703, 0.3219752754296894559, 0.3333333333333333703, 0.3219752754296894559, 0.3333333333333333703, 0.3219752754296894559, 0.3333333333333333703, 0.3219752754296894559, 0.3333333333333333703, 0.3219752754296894559, 0.3333333333333333703, 0.3219752754296894559, 0.3333333333333333703, 0.3219752754296894559, 0.3333333333333333703, 0.3219752754296894559, 0.3333333333333333703, 0.3219752754296894559, 0.3333333333333333703, 0.3219752754296894559, 0.3333333333333333703, 0.3219752754296894559, 0.3333333333333333703, 0.3219752754296894559, 0.3333333333333333703, 0.3219752754296894559, 0.3333333333333333703, 0.3219752754296894559, 0.3333333333333333703, 0.3219752754296894559, 0.3333333333333333703, 0.3219752754296894559, 0.3333333333333333703, 0.3219752754296894559, 0.3333333333333333703, 0.3219752754296894559, 0.3333333333333333703, 0.3219752754296894559, 0.3333333333333333703, 0.3219752754296894559, 0.3333333333333333703, 0.3219752754296894559, 0.3333333333333333703, 0.3219752754296894559, 0.3333333333333333703, 0.3219752754296894559, 0.3333333333333333703, 0.3219752754296894559, 0.3333333333333333703, 0.3219752754296894559, 0.3333333333333333703, 0.3219752754296894559, 0.3333333333333333703, 0.3219752754296894559, 0.3333333333333333703, 0.3219752754296894559, 0.3333333333333333703, 0.3219752754296894559, 0.3333333333333333703, 0.3219752754296894559, 0.3333333333333333703, 0.3219752754296894559, 0.3333333333333333703, 0.3219752754296894559, 0.3333333333333333703, 0.3219752754296894559, 0.3333333333333333703, 0.3219752754296894559, 0.3333333333333333703, 0.3219752754296894559, 0.3333333333333333703, 0.3219752754296894559, 0.3333333333333333703, 0.3219752754296894559, 0.3333333333333333703, 0.3219752754296894559, 0.3333333333333333703, 0.3219752754296894559, 0.3333333333333333703, 0.3219752754296894559, 0.3333333333333333703, 0.3219752754296894559, 0.3333333333333333703, 0.3219752754296894559, 0.3333333333333333703, 0.3219752754296894559, 0.3333333333333333703, 0.3219752754296894559, 0.3333333333333333703, 0.3219752754296894559, 0.3333333333333333703, 0.3219752754296894559, 0.3333333333333333703, 0.3219752754296894559, 0.3333333333333333703, 0.3219752754296894559, 0.3333333333333333703, 0.3219752754296894559, 0.3333333333333333703, 0.3219752754296894559, 0.3333333333333333703, 0.3219752754296894559, 0.3333333333333333703, 0.3219752754296894559, 0.3333333333333333703, 0.3219752754296894559, 0.3333333333333333703, 0.3219752754296894559, 0.3333333333333333703, 0.3219752754296894559, 0.3333333333333333703, 0.3219752754296894559, 0.3333333333333333703, 0.3219752754296894559, 0.3333333333333333703, 0.3219752754296894559, 0.3333333333333333703, 0.3219752754296894559, 0.3333333333333333703, 0.3219752754296894559, 0.3333333333333333703, 0.3219752754296894559, 0.3333333333333333703, 0.3219752754296894559, 0.3333333333333333703, 0.3219752754296894559, 0.3333333333333333703, 0.3219752754296894559, 0.3333333333333333703, 0.3219752754296894559, 0.3333333333333333703, 0.3219752754296894559, 0.3333333333333333703, 0.3219752754296894559, 0.3333333333333333703, 0.3219752754296894559, 0.3333333333333333703, 0.3219752754296894559, 0.3333333333333333703, 0.3219752754296894559, 0.3333333333333333703, 0.3219752754296894559, 0.3333333333333333703, 0.3219752754296894559, 0.3333333333333333703, 0.3219752754296894559, 0.3333333333333333703, 0.3219752754296894559, 0.3333333333333333703, 0.3219752754296894559, 0.3333333333333333703, 0.3219752754296894559, 0.3333333333333333703, 0.3219752754296894559, 0.3333333333333333703, 0.3219752754296894559, 0.3333333333333333703, 0.3219752754296894559, 0.3333333333333333703, 0.3219752754296894559, 0.3333333333333333703, 0.3219752754296894559, 0.3333333333333333703, 0.3219752754296894559, 0.3333333333333333703, 0.3219752754296894559, 0.3333333333333333703, 0.3219752754296894559, 0.3333333333333333703, 0.3219752754296894559, 0.3333333333333333703, 0.3219752754296894559, 0.3333333333333333703, 0.3219752754296894559, 0.3333333333333333703, 0.3219752754296894559, 0.3333333333333333703, 0.3219752754296894559, 0.3333333333333333703, 0.3219752754296894559, 0.3333333333333333703, 0.3219752754296894559, 0.3333333333333333703, 0.3219752754296894559, 0.3333333333333333703, 0.3219752754296894559, 0.3333333333333333703, 0.3219752754296894559, 0.3333333333333333703, 0.3219752754296894559, 0.3333333333333333703, 0.3219752754296894559, 0.3333333333333333703, 0.3219752754296894559, 0.3333333333333333703, 0.3219752754296894559, 0.3333333333333333703, 0.3219752754296894559, 0.3333333333333333703, 0.3219752754296894559, 0.3333333333333333703, 0.3219752754296894559, 0.3333333333333333703, 0.3219752754296894559, 0.3333333333333333703, 0.3219752754296894559, 0.3333333333333333703, 0.3219752754296894559, 0.3333333333333333703, 0.3219752754296894559, 0.3333333333333333703, 0.3219752754296894559, 0.3333333333333333703, 0.3219752754296894559, 0.3333333333333333703, 0.3219752754296894559, 0.3333333333333333703, 0.3219752754296894559, 0.3333333333333333703, 0.3219752754296894559, 0.3333333333333333703, 0.3219752754296894559, 0.3333333333333333703, 0.3219752754296894559, 0.3333333333333333703, 0.3219752754296894559, 0.3333333333333333703, 0.3219752754296894559, 0.3333333333333333703, 0.3219752754296894559, 0.3333333333333333703, 0.3219752754296894559, 0.3333333333333333703, 0.3219752754296894559, 0.3333333333333333703, 0.3219752754296894559, 0.3333333333333333703, 0.3219752754296894559, 0.3333333333333333703, 0.3219752754296894559, 0.3333333333333333703, 0.3219752754296894559, 0.3333333333333333703, 0.3219752754296894559, 0.3333333333333333703, 0.3219752754296894559, 0.3333333333333333703, 0.3219752754296894559, 0.3333333333333333703, 0.3219752754296894559, 0.3333333333333333703, 0.3219752754296894559, 0.3333333333333333703, 0.3219752754296894559, 0.3333333333333333703, 0.3219752754296894559, 0.3333333333333333703, 0.3219752754296894559, 0.3333333333333333703, 0.3219752754296894559, 0.3333333333333333703, 0.3219752754296894559, 0.3333333333333333703, 0.3219752754296894559, 0.3333333333333333703, 0.3219752754296894559, 0.3333333333333333703, 0.3219752754296894559, 0.3333333333333333703, 0.3219752754296894559, 0.3333333333333333703, 0.3219752754296894559, 0.3333333333333333703, 0.3219752754296894559, 0.3333333333333333703, 0.3219752754296894559, 0.3333333333333333703, 0.3219752754296894559, 0.3333333333333333703, 0.3219752754296894559, 0.3333333333333333703, 0.3219752754296894559, 0.3333333333333333703, 0.3219752754296894559, 0.3333333333333333703, 0.3219752754296894559, 0.3333333333333333703, 0.3219752754296894559, 0.3333333333333333703, 0.3219752754296894559, 0.3333333333333333703, 0.3219752754296894559, 0.3333333333333333703, 0.3219752754296894559, 0.3333333333333333703, 0.3219752754296894559, 0.3333333333333333703, 0.3219752754296894559, 0.3333333333333333703, 0.3219752754296894559, 0.3333333333333333703, 0.3219752754296894559, 0.3333333333333333703, 0.3219752754296894559, 0.3333333333333333703, 0.3219752754296894559, 0.3333333333333333703, 0.3219752754296894559, 0.3333333333333333703, 0.3219752754296894559, 0.3333333333333333703, 0.3219752754296894559, 0.3333333333333333703, 0.3219752754296894559, 0.3333333333333333703, 0.3219752754296894559, 0.3333333333333333703, 0.3219752754296894559, 0.3333333333333333703, 0.3219752754296894559, 0.3333333333333333703, 0.3219752754296894559, 0.3333333333333333703, 0.3219752754296894559, 0.3333333333333333703, 0.3219752754296894559, 0.3333333333333333703, 0.3219752754296894559, 0.3333333333333333703, 0.3219752754296894559, 0.3333333333333333703, 0.3219752754296894559, 0.3333333333333333703, 0.3219752754296894559, 0.3333333333333333703, 0.3219752754296894559, 0.3333333333333333703, 0.3219752754296894559, 0.3333333333333333703, 0.3219752754296894559, 0.3333333333333333703, 0.3219752754296894559, 0.3333333333333333703, 0.3219752754296894559, 0.3333333333333333703, 0.3219752754296894559, 0.3333333333333333703, 0.3219752754296894559, 0.3333333333333333703, 0.3219752754296894559, 0.3333333333333333703, 0.3219752754296894559, 0.3333333333333333703, 0.3219752754296894559, 0.3333333333333333703, 0.3219752754296894559, 0.3333333333333333703),
 ( 1.000000000000000000, 0.9659258262890683122, 1.000000000000000000, 0.9659258262890683122, 1.000000000000000000, 0.9659258262890683122, 1.000000000000000000, 0.9659258262890683122, 1.000000000000000000, 0.9659258262890683122, 1.000000000000000000, 0.9659258262890683122, 1.000000000000000000, 0.9659258262890683122, 1.000000000000000000, 0.9659258262890683122, 1.000000000000000000, 0.9659258262890683122, 1.000000000000000000, 0.9659258262890683122, 1.000000000000000000, 0.9659258262890683122, 1.000000000000000000, 0.9659258262890683122, 1.000000000000000000, 0.9659258262890683122, 1.000000000000000000, 0.9659258262890683122, 1.000000000000000000, 0.9659258262890683122, 1.000000000000000000, 0.9659258262890683122, 1.000000000000000000, 0.9659258262890683122, 1.000000000000000000, 0.9659258262890683122, 1.000000000000000000, 0.9659258262890683122, 1.000000000000000000, 0.9659258262890683122, 1.000000000000000000, 0.9659258262890683122, 1.000000000000000000, 0.9659258262890683122, 1.000000000000000000, 0.9659258262890683122, 1.000000000000000000, 0.9659258262890683122, 1.000000000000000000, 0.9659258262890683122, 1.000000000000000000, 0.9659258262890683122, 1.000000000000000000, 0.9659258262890683122, 1.000000000000000000, 0.9659258262890683122, 1.000000000000000000, 0.9659258262890683122, 1.000000000000000000, 0.9659258262890683122, 1.000000000000000000, 0.9659258262890683122, 1.000000000000000000, 0.9659258262890683122, 1.000000000000000000, 0.9659258262890683122, 1.000000000000000000, 0.9659258262890683122, 1.000000000000000000, 0.9659258262890683122, 1.000000000000000000, 0.9659258262890683122, 1.000000000000000000, 0.9659258262890683122, 1.000000000000000000, 0.9659258262890683122, 1.000000000000000000, 0.9659258262890683122, 1.000000000000000000, 0.9659258262890683122, 1.000000000000000000, 0.9659258262890683122, 1.000000000000000000, 0.9659258262890683122, 1.000000000000000000, 0.9659258262890683122, 1.000000000000000000, 0.9659258262890683122, 1.000000000000000000, 0.9659258262890683122, 1.000000000000000000, 0.9659258262890683122, 1.000000000000000000, 0.9659258262890683122, 1.000000000000000000, 0.9659258262890683122, 1.000000000000000000, 0.9659258262890683122, 1.000000000000000000, 0.9659258262890683122, 1.000000000000000000, 0.9659258262890683122, 1.000000000000000000, 0.9659258262890683122, 1.000000000000000000, 0.9659258262890683122, 1.000000000000000000, 0.9659258262890683122, 1.000000000000000000, 0.9659258262890683122, 1.000000000000000000, 0.9659258262890683122, 1.000000000000000000, 0.9659258262890683122, 1.000000000000000000, 0.9659258262890683122, 1.000000000000000000, 0.9659258262890683122, 1.000000000000000000, 0.9659258262890683122, 1.000000000000000000, 0.9659258262890683122, 1.000000000000000000, 0.9659258262890683122, 1.000000000000000000, 0.9659258262890683122, 1.000000000000000000, 0.9659258262890683122, 1.000000000000000000, 0.9659258262890683122, 1.000000000000000000, 0.9659258262890683122, 1.000000000000000000, 0.9659258262890683122, 1.000000000000000000, 0.9659258262890683122, 1.000000000000000000, 0.9659258262890683122, 1.000000000000000000, 0.9659258262890683122, 1.000000000000000000, 0.9659258262890683122, 1.000000000000000000, 0.9659258262890683122, 1.000000000000000000, 0.9659258262890683122, 1.000000000000000000, 0.9659258262890683122, 1.000000000000000000, 0.9659258262890683122, 1.000000000000000000, 0.9659258262890683122, 1.000000000000000000, 0.9659258262890683122, 1.000000000000000000, 0.9659258262890683122, 1.000000000000000000, 0.9659258262890683122, 1.000000000000000000, 0.9659258262890683122, 1.000000000000000000, 0.9659258262890683122, 1.000000000000000000, 0.9659258262890683122, 1.000000000000000000, 0.9659258262890683122, 1.000000000000000000, 0.9659258262890683122, 1.000000000000000000, 0.9659258262890683122, 1.000000000000000000, 0.9659258262890683122, 1.000000000000000000, 0.9659258262890683122, 1.000000000000000000, 0.9659258262890683122, 1.000000000000000000, 0.9659258262890683122, 1.000000000000000000, 0.9659258262890683122, 1.000000000000000000, 0.9659258262890683122, 1.000000000000000000, 0.9659258262890683122, 1.000000000000000000, 0.9659258262890683122, 1.000000000000000000, 0.9659258262890683122, 1.000000000000000000, 0.9659258262890683122, 1.000000000000000000, 0.9659258262890683122, 1.000000000000000000, 0.9659258262890683122, 1.000000000000000000, 0.9659258262890683122, 1.000000000000000000, 0.9659258262890683122, 1.000000000000000000, 0.9659258262890683122, 1.000000000000000000, 0.9659258262890683122, 1.000000000000000000, 0.9659258262890683122, 1.000000000000000000, 0.9659258262890683122, 1.000000000000000000, 0.9659258262890683122, 1.000000000000000000, 0.9659258262890683122, 1.000000000000000000, 0.9659258262890683122, 1.000000000000000000, 0.9659258262890683122, 1.000000000000000000, 0.9659258262890683122, 1.000000000000000000, 0.9659258262890683122, 1.000000000000000000, 0.9659258262890683122, 1.000000000000000000, 0.9659258262890683122, 1.000000000000000000, 0.9659258262890683122, 1.000000000000000000, 0.9659258262890683122, 1.000000000000000000, 0.9659258262890683122, 1.000000000000000000, 0.9659258262890683122, 1.000000000000000000, 0.9659258262890683122, 1.000000000000000000, 0.9659258262890683122, 1.000000000000000000, 0.9659258262890683122, 1.000000000000000000, 0.9659258262890683122, 1.000000000000000000, 0.9659258262890683122, 1.000000000000000000, 0.9659258262890683122, 1.000000000000000000, 0.9659258262890683122, 1.000000000000000000, 0.9659258262890683122, 1.000000000000000000, 0.9659258262890683122, 1.000000000000000000, 0.9659258262890683122, 1.000000000000000000, 0.9659258262890683122, 1.000000000000000000, 0.9659258262890683122, 1.000000000000000000, 0.9659258262890683122, 1.000000000000000000, 0.9659258262890683122, 1.000000000000000000, 0.9659258262890683122, 1.000000000000000000, 0.9659258262890683122, 1.000000000000000000, 0.9659258262890683122, 1.000000000000000000, 0.9659258262890683122, 1.000000000000000000, 0.9659258262890683122, 1.000000000000000000, 0.9659258262890683122, 1.000000000000000000, 0.9659258262890683122, 1.000000000000000000, 0.9659258262890683122, 1.000000000000000000, 0.9659258262890683122, 1.000000000000000000, 0.9659258262890683122, 1.000000000000000000, 0.9659258262890683122, 1.000000000000000000, 0.9659258262890683122, 1.000000000000000000, 0.9659258262890683122, 1.000000000000000000, 0.9659258262890683122, 1.000000000000000000, 0.9659258262890683122, 1.000000000000000000, 0.9659258262890683122, 1.000000000000000000, 0.9659258262890683122, 1.000000000000000000, 0.9659258262890683122, 1.000000000000000000, 0.9659258262890683122, 1.000000000000000000, 0.9659258262890683122, 1.000000000000000000, 0.9659258262890683122, 1.000000000000000000, 0.9659258262890683122, 1.000000000000000000, 0.9659258262890683122, 1.000000000000000000, 0.9659258262890683122, 1.000000000000000000, 0.9659258262890683122, 1.000000000000000000, 0.9659258262890683122, 1.000000000000000000, 0.9659258262890683122, 1.000000000000000000, 0.9659258262890683122, 1.000000000000000000, 0.9659258262890683122, 1.000000000000000000, 0.9659258262890683122, 1.000000000000000000, 0.9659258262890683122, 1.000000000000000000, 0.9659258262890683122, 1.000000000000000000, 0.9659258262890683122, 1.000000000000000000, 0.9659258262890683122, 1.000000000000000000, 0.9659258262890683122, 1.000000000000000000, 0.9659258262890683122, 1.000000000000000000, 0.9659258262890683122, 1.000000000000000000, 0.9659258262890683122, 1.000000000000000000, 0.9659258262890683122, 1.000000000000000000, 0.9659258262890683122, 1.000000000000000000, 0.9659258262890683122, 1.000000000000000000, 0.9659258262890683122, 1.000000000000000000, 0.9659258262890683122, 1.000000000000000000, 0.9659258262890683122, 1.000000000000000000, 0.9659258262890683122, 1.000000000000000000, 0.9659258262890683122, 1.000000000000000000, 0.9659258262890683122, 1.000000000000000000, 0.9659258262890683122, 1.000000000000000000, 0.9659258262890683122, 1.000000000000000000, 0.9659258262890683122, 1.000000000000000000, 0.9659258262890683122, 1.000000000000000000, 0.9659258262890683122, 1.000000000000000000, 0.9659258262890683122, 1.000000000000000000, 0.9659258262890683122, 1.000000000000000000, 0.9659258262890683122, 1.000000000000000000, 0.9659258262890683122, 1.000000000000000000, 0.9659258262890683122, 1.000000000000000000, 0.9659258262890683122, 1.000000000000000000, 0.9659258262890683122, 1.000000000000000000, 0.9659258262890683122, 1.000000000000000000, 0.9659258262890683122, 1.000000000000000000, 0.9659258262890683122, 1.000000000000000000, 0.9659258262890683122, 1.000000000000000000, 0.9659258262890683122, 1.000000000000000000, 0.9659258262890683122, 1.000000000000000000, 0.9659258262890683122, 1.000000000000000000, 0.9659258262890683122, 1.000000000000000000, 0.9659258262890683122, 1.000000000000000000, 0.9659258262890683122, 1.000000000000000000, 0.9659258262890683122, 1.000000000000000000, 0.9659258262890683122, 1.000000000000000000, 0.9659258262890683122, 1.000000000000000000, 0.9659258262890683122, 1.000000000000000000, 0.9659258262890683122, 1.000000000000000000, 0.9659258262890683122, 1.000000000000000000, 0.9659258262890683122, 1.000000000000000000, 0.9659258262890683122, 1.000000000000000000, 0.9659258262890683122, 1.000000000000000000, 0.9659258262890683122, 1.000000000000000000, 0.9659258262890683122, 1.000000000000000000, 0.9659258262890683122, 1.000000000000000000, 0.9659258262890683122, 1.000000000000000000, 0.9659258262890683122, 1.000000000000000000, 0.9659258262890683122, 1.000000000000000000, 0.9659258262890683122, 1.000000000000000000, 0.9659258262890683122, 1.000000000000000000, 0.9659258262890683122, 1.000000000000000000, 0.9659258262890683122, 1.000000000000000000, 0.9659258262890683122, 1.000000000000000000, 0.9659258262890683122, 1.000000000000000000, 0.9659258262890683122, 1.000000000000000000, 0.9659258262890683122, 1.000000000000000000, 0.9659258262890683122, 1.000000000000000000, 0.9659258262890683122, 1.000000000000000000, 0.9659258262890683122, 1.000000000000000000, 0.9659258262890683122, 1.000000000000000000, 0.9659258262890683122, 1.000000000000000000, 0.9659258262890683122, 1.000000000000000000, 0.9659258262890683122, 1.000000000000000000),
 ( 0.3333333333333333703, 0.3219752754296894559, 0.3333333333333333703, 0.3219752754296894559, 0.3333333333333333703, 0.3219752754296894559, 0.3333333333333333703, 0.3219752754296894559, 0.3333333333333333703, 0.3219752754296894559, 0.3333333333333333703, 0.3219752754296894559, 0.3333333333333333703, 0.3219752754296894559, 0.3333333333333333703, 0.3219752754296894559, 0.3333333333333333703, 0.3219752754296894559, 0.3333333333333333703, 0.3219752754296894559, 0.3333333333333333703, 0.3219752754296894559, 0.3333333333333333703, 0.3219752754296894559, 0.3333333333333333703, 0.3219752754296894559, 0.3333333333333333703, 0.3219752754296894559, 0.3333333333333333703, 0.3219752754296894559, 0.3333333333333333703, 0.3219752754296894559, 0.3333333333333333703, 0.3219752754296894559, 0.3333333333333333703, 0.3219752754296894559, 0.3333333333333333703, 0.3219752754296894559, 0.3333333333333333703, 0.3219752754296894559, 0.3333333333333333703, 0.3219752754296894559, 0.3333333333333333703, 0.3219752754296894559, 0.3333333333333333703, 0.3219752754296894559, 0.3333333333333333703, 0.3219752754296894559, 0.3333333333333333703, 0.3219752754296894559, 0.3333333333333333703, 0.3219752754296894559, 0.3333333333333333703, 0.3219752754296894559, 0.3333333333333333703, 0.3219752754296894559, 0.3333333333333333703, 0.3219752754296894559, 0.3333333333333333703, 0.3219752754296894559, 0.3333333333333333703, 0.3219752754296894559, 0.3333333333333333703, 0.3219752754296894559, 0.3333333333333333703, 0.3219752754296894559, 0.3333333333333333703, 0.3219752754296894559, 0.3333333333333333703, 0.3219752754296894559, 0.3333333333333333703, 0.3219752754296894559, 0.3333333333333333703, 0.3219752754296894559, 0.3333333333333333703, 0.3219752754296894559, 0.3333333333333333703, 0.3219752754296894559, 0.3333333333333333703, 0.3219752754296894559, 0.3333333333333333703, 0.3219752754296894559, 0.3333333333333333703, 0.3219752754296894559, 0.3333333333333333703, 0.3219752754296894559, 0.3333333333333333703, 0.3219752754296894559, 0.3333333333333333703, 0.3219752754296894559, 0.3333333333333333703, 0.3219752754296894559, 0.3333333333333333703, 0.3219752754296894559, 0.3333333333333333703, 0.3219752754296894559, 0.3333333333333333703, 0.3219752754296894559, 0.3333333333333333703, 0.3219752754296894559, 0.3333333333333333703, 0.3219752754296894559, 0.3333333333333333703, 0.3219752754296894559, 0.3333333333333333703, 0.3219752754296894559, 0.3333333333333333703, 0.3219752754296894559, 0.3333333333333333703, 0.3219752754296894559, 0.3333333333333333703, 0.3219752754296894559, 0.3333333333333333703, 0.3219752754296894559, 0.3333333333333333703, 0.3219752754296894559, 0.3333333333333333703, 0.3219752754296894559, 0.3333333333333333703, 0.3219752754296894559, 0.3333333333333333703, 0.3219752754296894559, 0.3333333333333333703, 0.3219752754296894559, 0.3333333333333333703, 0.3219752754296894559, 0.3333333333333333703, 0.3219752754296894559, 0.3333333333333333703, 0.3219752754296894559, 0.3333333333333333703, 0.3219752754296894559, 0.3333333333333333703, 0.3219752754296894559, 0.3333333333333333703, 0.3219752754296894559, 0.3333333333333333703, 0.3219752754296894559, 0.3333333333333333703, 0.3219752754296894559, 0.3333333333333333703, 0.3219752754296894559, 0.3333333333333333703, 0.3219752754296894559, 0.3333333333333333703, 0.3219752754296894559, 0.3333333333333333703, 0.3219752754296894559, 0.3333333333333333703, 0.3219752754296894559, 0.3333333333333333703, 0.3219752754296894559, 0.3333333333333333703, 0.3219752754296894559, 0.3333333333333333703, 0.3219752754296894559, 0.3333333333333333703, 0.3219752754296894559, 0.3333333333333333703, 0.3219752754296894559, 0.3333333333333333703, 0.3219752754296894559, 0.3333333333333333703, 0.3219752754296894559, 0.3333333333333333703, 0.3219752754296894559, 0.3333333333333333703, 0.3219752754296894559, 0.3333333333333333703, 0.3219752754296894559, 0.3333333333333333703, 0.3219752754296894559, 0.3333333333333333703, 0.3219752754296894559, 0.3333333333333333703, 0.3219752754296894559, 0.3333333333333333703, 0.3219752754296894559, 0.3333333333333333703, 0.3219752754296894559, 0.3333333333333333703, 0.3219752754296894559, 0.3333333333333333703, 0.3219752754296894559, 0.3333333333333333703, 0.3219752754296894559, 0.3333333333333333703, 0.3219752754296894559, 0.3333333333333333703, 0.3219752754296894559, 0.3333333333333333703, 0.3219752754296894559, 0.3333333333333333703, 0.3219752754296894559, 0.3333333333333333703, 0.3219752754296894559, 0.3333333333333333703, 0.3219752754296894559, 0.3333333333333333703, 0.3219752754296894559, 0.3333333333333333703, 0.3219752754296894559, 0.3333333333333333703, 0.3219752754296894559, 0.3333333333333333703, 0.3219752754296894559, 0.3333333333333333703, 0.3219752754296894559, 0.3333333333333333703, 0.3219752754296894559, 0.3333333333333333703, 0.3219752754296894559, 0.3333333333333333703, 0.3219752754296894559, 0.3333333333333333703, 0.3219752754296894559, 0.3333333333333333703, 0.3219752754296894559, 0.3333333333333333703, 0.3219752754296894559, 0.3333333333333333703, 0.3219752754296894559, 0.3333333333333333703, 0.3219752754296894559, 0.3333333333333333703, 0.3219752754296894559, 0.3333333333333333703, 0.3219752754296894559, 0.3333333333333333703, 0.3219752754296894559, 0.3333333333333333703, 0.3219752754296894559, 0.3333333333333333703, 0.3219752754296894559, 0.3333333333333333703, 0.3219752754296894559, 0.3333333333333333703, 0.3219752754296894559, 0.3333333333333333703, 0.3219752754296894559, 0.3333333333333333703, 0.3219752754296894559, 0.3333333333333333703, 0.3219752754296894559, 0.3333333333333333703, 0.3219752754296894559, 0.3333333333333333703, 0.3219752754296894559, 0.3333333333333333703, 0.3219752754296894559, 0.3333333333333333703, 0.3219752754296894559, 0.3333333333333333703, 0.3219752754296894559, 0.3333333333333333703, 0.3219752754296894559, 0.3333333333333333703, 0.3219752754296894559, 0.3333333333333333703, 0.3219752754296894559, 0.3333333333333333703, 0.3219752754296894559, 0.3333333333333333703, 0.3219752754296894559, 0.3333333333333333703, 0.3219752754296894559, 0.3333333333333333703, 0.3219752754296894559, 0.3333333333333333703, 0.3219752754296894559, 0.3333333333333333703, 0.3219752754296894559, 0.3333333333333333703, 0.3219752754296894559, 0.3333333333333333703, 0.3219752754296894559, 0.3333333333333333703, 0.3219752754296894559, 0.3333333333333333703, 0.3219752754296894559, 0.3333333333333333703, 0.3219752754296894559, 0.3333333333333333703, 0.3219752754296894559, 0.3333333333333333703, 0.3219752754296894559, 0.3333333333333333703, 0.3219752754296894559, 0.3333333333333333703, 0.3219752754296894559, 0.3333333333333333703, 0.3219752754296894559, 0.3333333333333333703, 0.3219752754296894559, 0.3333333333333333703, 0.3219752754296894559, 0.3333333333333333703, 0.3219752754296894559, 0.3333333333333333703, 0.3219752754296894559, 0.3333333333333333703, 0.3219752754296894559, 0.3333333333333333703, 0.3219752754296894559, 0.3333333333333333703, 0.3219752754296894559, 0.3333333333333333703, 0.3219752754296894559, 0.3333333333333333703, 0.3219752754296894559, 0.3333333333333333703, 0.3219752754296894559, 0.3333333333333333703, 0.3219752754296894559, 0.3333333333333333703, 0.3219752754296894559, 0.3333333333333333703, 0.3219752754296894559, 0.3333333333333333703, 0.3219752754296894559, 0.3333333333333333703, 0.3219752754296894559, 0.3333333333333333703, 0.3219752754296894559, 0.3333333333333333703, 0.3219752754296894559, 0.3333333333333333703, 0.3219752754296894559, 0.3333333333333333703, 0.3219752754296894559, 0.3333333333333333703, 0.3219752754296894559, 0.3333333333333333703, 0.3219752754296894559, 0.3333333333333333703, 0.3219752754296894559, 0.3333333333333333703, 0.3219752754296894559, 0.3333333333333333703, 0.3219752754296894559, 0.3333333333333333703, 0.3219752754296894559, 0.3333333333333333703, 0.3219752754296894559, 0.3333333333333333703, 0.3219752754296894559, 0.3333333333333333703, 0.3219752754296894559, 0.3333333333333333703, 0.3219752754296894559, 0.3333333333333333703, 0.3219752754296894559, 0.3333333333333333703, 0.3219752754296894559, 0.3333333333333333703, 0.3219752754296894559, 0.3333333333333333703, 0.3219752754296894559, 0.3333333333333333703, 0.3219752754296894559, 0.3333333333333333703, 0.3219752754296894559, 0.3333333333333333703, 0.3219752754296894559, 0.3333333333333333703, 0.3219752754296894559, 0.3333333333333333703, 0.3219752754296894559, 0.3333333333333333703, 0.3219752754296894559, 0.3333333333333333703, 0.3219752754296894559, 0.3333333333333333703, 0.3219752754296894559, 0.3333333333333333703, 0.3219752754296894559, 0.3333333333333333703, 0.3219752754296894559, 0.3333333333333333703, 0.3219752754296894559, 0.3333333333333333703, 0.3219752754296894559, 0.3333333333333333703, 0.3219752754296894559, 0.3333333333333333703, 0.3219752754296894559, 0.3333333333333333703, 0.3219752754296894559, 0.3333333333333333703, 0.3219752754296894559, 0.3333333333333333703, 0.3219752754296894559, 0.3333333333333333703, 0.3219752754296894559, 0.3333333333333333703, 0.3219752754296894559, 0.3333333333333333703, 0.3219752754296894559, 0.3333333333333333703, 0.3219752754296894559, 0.3333333333333333703, 0.3219752754296894559, 0.3333333333333333703, 0.3219752754296894559, 0.3333333333333333703, 0.3219752754296894559, 0.3333333333333333703, 0.3219752754296894559, 0.3333333333333333703, 0.3219752754296894559, 0.3333333333333333703, 0.3219752754296894559, 0.3333333333333333703, 0.3219752754296894559, 0.3333333333333333703, 0.3219752754296894559, 0.3333333333333333703, 0.3219752754296894559, 0.3333333333333333703, 0.3219752754296894559, 0.3333333333333333703, 0.3219752754296894559, 0.3333333333333333703, 0.3219752754296894559, 0.3333333333333333703, 0.3219752754296894559, 0.3333333333333333703, 0.3219752754296894559, 0.3333333333333333703, 0.3219752754296894559, 0.3333333333333333703, 0.3219752754296894559, 0.3333333333333333703, 0.3219752754296894559, 0.3333333333333333703, 0.3219752754296894559, 0.3333333333333333703, 0.3219752754296894559, 0.3333333333333333703, 0.3219752754296894559, 0.3333333333333333703, 0.3219752754296894559, 0.3333333333333333703, 0.3219752754296894559, 0.3333333333333333703, 0.3219752754296894559, 0.3333333333333333703, 0.3219752754296894559, 0.3333333333333333703, 0.3219752754296894559, 0.3333333333333333703, 0.3219752754296894559, 0.3333333333333333703, 0.3219752754296894559, 0.3333333333333333703, 0.3219752754296894559, 0.3333333333333333703),
 ( 0.3333333333333333703, 0.3219752754296894559, 0.3333333333333333703, 0.3219752754296894559, 0.3333333333333333703, 0.3219752754296894559, 0.3333333333333333703, 0.3219752754296894559, 0.3333333333333333703, 0.3219752754296894559, 0.3333333333333333703, 0.3219752754296894559, 0.3333333333333333703, 0.3219752754296894559, 0.3333333333333333703, 0.3219752754296894559, 0.3333333333333333703, 0.3219752754296894559, 0.3333333333333333703, 0.3219752754296894559, 0.3333333333333333703, 0.3219752754296894559, 0.3333333333333333703, 0.3219752754296894559, 0.3333333333333333703, 0.3219752754296894559, 0.3333333333333333703, 0.3219752754296894559, 0.3333333333333333703, 0.3219752754296894559, 0.3333333333333333703, 0.3219752754296894559, 0.3333333333333333703, 0.3219752754296894559, 0.3333333333333333703, 0.3219752754296894559, 0.3333333333333333703, 0.3219752754296894559, 0.3333333333333333703, 0.3219752754296894559, 0.3333333333333333703, 0.3219752754296894559, 0.3333333333333333703, 0.3219752754296894559, 0.3333333333333333703, 0.3219752754296894559, 0.3333333333333333703, 0.3219752754296894559, 0.3333333333333333703, 0.3219752754296894559, 0.3333333333333333703, 0.3219752754296894559, 0.3333333333333333703, 0.3219752754296894559, 0.3333333333333333703, 0.3219752754296894559, 0.3333333333333333703, 0.3219752754296894559, 0.3333333333333333703, 0.3219752754296894559, 0.3333333333333333703, 0.3219752754296894559, 0.3333333333333333703, 0.3219752754296894559, 0.3333333333333333703, 0.3219752754296894559, 0.3333333333333333703, 0.3219752754296894559, 0.3333333333333333703, 0.3219752754296894559, 0.3333333333333333703, 0.3219752754296894559, 0.3333333333333333703, 0.3219752754296894559, 0.3333333333333333703, 0.3219752754296894559, 0.3333333333333333703, 0.3219752754296894559, 0.3333333333333333703, 0.3219752754296894559, 0.3333333333333333703, 0.3219752754296894559, 0.3333333333333333703, 0.3219752754296894559, 0.3333333333333333703, 0.3219752754296894559, 0.3333333333333333703, 0.3219752754296894559, 0.3333333333333333703, 0.3219752754296894559, 0.3333333333333333703, 0.3219752754296894559, 0.3333333333333333703, 0.3219752754296894559, 0.3333333333333333703, 0.3219752754296894559, 0.3333333333333333703, 0.3219752754296894559, 0.3333333333333333703, 0.3219752754296894559, 0.3333333333333333703, 0.3219752754296894559, 0.3333333333333333703, 0.3219752754296894559, 0.3333333333333333703, 0.3219752754296894559, 0.3333333333333333703, 0.3219752754296894559, 0.3333333333333333703, 0.3219752754296894559, 0.3333333333333333703, 0.3219752754296894559, 0.3333333333333333703, 0.3219752754296894559, 0.3333333333333333703, 0.3219752754296894559, 0.3333333333333333703, 0.3219752754296894559, 0.3333333333333333703, 0.3219752754296894559, 0.3333333333333333703, 0.3219752754296894559, 0.3333333333333333703, 0.3219752754296894559, 0.3333333333333333703, 0.3219752754296894559, 0.3333333333333333703, 0.3219752754296894559, 0.3333333333333333703, 0.3219752754296894559, 0.3333333333333333703, 0.3219752754296894559, 0.3333333333333333703, 0.3219752754296894559, 0.3333333333333333703, 0.3219752754296894559, 0.3333333333333333703, 0.3219752754296894559, 0.3333333333333333703, 0.3219752754296894559, 0.3333333333333333703, 0.3219752754296894559, 0.3333333333333333703, 0.3219752754296894559, 0.3333333333333333703, 0.3219752754296894559, 0.3333333333333333703, 0.3219752754296894559, 0.3333333333333333703, 0.3219752754296894559, 0.3333333333333333703, 0.3219752754296894559, 0.3333333333333333703, 0.3219752754296894559, 0.3333333333333333703, 0.3219752754296894559, 0.3333333333333333703, 0.3219752754296894559, 0.3333333333333333703, 0.3219752754296894559, 0.3333333333333333703, 0.3219752754296894559, 0.3333333333333333703, 0.3219752754296894559, 0.3333333333333333703, 0.3219752754296894559, 0.3333333333333333703, 0.3219752754296894559, 0.3333333333333333703, 0.3219752754296894559, 0.3333333333333333703, 0.3219752754296894559, 0.3333333333333333703, 0.3219752754296894559, 0.3333333333333333703, 0.3219752754296894559, 0.3333333333333333703, 0.3219752754296894559, 0.3333333333333333703, 0.3219752754296894559, 0.3333333333333333703, 0.3219752754296894559, 0.3333333333333333703, 0.3219752754296894559, 0.3333333333333333703, 0.3219752754296894559, 0.3333333333333333703, 0.3219752754296894559, 0.3333333333333333703, 0.3219752754296894559, 0.3333333333333333703, 0.3219752754296894559, 0.3333333333333333703, 0.3219752754296894559, 0.3333333333333333703, 0.3219752754296894559, 0.3333333333333333703, 0.3219752754296894559, 0.3333333333333333703, 0.3219752754296894559, 0.3333333333333333703, 0.3219752754296894559, 0.3333333333333333703, 0.3219752754296894559, 0.3333333333333333703, 0.3219752754296894559, 0.3333333333333333703, 0.3219752754296894559, 0.3333333333333333703, 0.3219752754296894559, 0.3333333333333333703, 0.3219752754296894559, 0.3333333333333333703, 0.3219752754296894559, 0.3333333333333333703, 0.3219752754296894559, 0.3333333333333333703, 0.3219752754296894559, 0.3333333333333333703, 0.3219752754296894559, 0.3333333333333333703, 0.3219752754296894559, 0.3333333333333333703, 0.3219752754296894559, 0.3333333333333333703, 0.3219752754296894559, 0.3333333333333333703, 0.3219752754296894559, 0.3333333333333333703, 0.3219752754296894559, 0.3333333333333333703, 0.3219752754296894559, 0.3333333333333333703, 0.3219752754296894559, 0.3333333333333333703, 0.3219752754296894559, 0.3333333333333333703, 0.3219752754296894559, 0.3333333333333333703, 0.3219752754296894559, 0.3333333333333333703, 0.3219752754296894559, 0.3333333333333333703, 0.3219752754296894559, 0.3333333333333333703, 0.3219752754296894559, 0.3333333333333333703, 0.3219752754296894559, 0.3333333333333333703, 0.3219752754296894559, 0.3333333333333333703, 0.3219752754296894559, 0.3333333333333333703, 0.3219752754296894559, 0.3333333333333333703, 0.3219752754296894559, 0.3333333333333333703, 0.3219752754296894559, 0.3333333333333333703, 0.3219752754296894559, 0.3333333333333333703, 0.3219752754296894559, 0.3333333333333333703, 0.3219752754296894559, 0.3333333333333333703, 0.3219752754296894559, 0.3333333333333333703, 0.3219752754296894559, 0.3333333333333333703, 0.3219752754296894559, 0.3333333333333333703, 0.3219752754296894559, 0.3333333333333333703, 0.3219752754296894559, 0.3333333333333333703, 0.3219752754296894559, 0.3333333333333333703, 0.3219752754296894559, 0.3333333333333333703, 0.3219752754296894559, 0.3333333333333333703, 0.3219752754296894559, 0.3333333333333333703, 0.3219752754296894559, 0.3333333333333333703, 0.3219752754296894559, 0.3333333333333333703, 0.3219752754296894559, 0.3333333333333333703, 0.3219752754296894559, 0.3333333333333333703, 0.3219752754296894559, 0.3333333333333333703, 0.3219752754296894559, 0.3333333333333333703, 0.3219752754296894559, 0.3333333333333333703, 0.3219752754296894559, 0.3333333333333333703, 0.3219752754296894559, 0.3333333333333333703, 0.3219752754296894559, 0.3333333333333333703, 0.3219752754296894559, 0.3333333333333333703, 0.3219752754296894559, 0.3333333333333333703, 0.3219752754296894559, 0.3333333333333333703, 0.3219752754296894559, 0.3333333333333333703, 0.3219752754296894559, 0.3333333333333333703, 0.3219752754296894559, 0.3333333333333333703, 0.3219752754296894559, 0.3333333333333333703, 0.3219752754296894559, 0.3333333333333333703, 0.3219752754296894559, 0.3333333333333333703, 0.3219752754296894559, 0.3333333333333333703, 0.3219752754296894559, 0.3333333333333333703, 0.3219752754296894559, 0.3333333333333333703, 0.3219752754296894559, 0.3333333333333333703, 0.3219752754296894559, 0.3333333333333333703, 0.3219752754296894559, 0.3333333333333333703, 0.3219752754296894559, 0.3333333333333333703, 0.3219752754296894559, 0.3333333333333333703, 0.3219752754296894559, 0.3333333333333333703, 0.3219752754296894559, 0.3333333333333333703, 0.3219752754296894559, 0.3333333333333333703, 0.3219752754296894559, 0.3333333333333333703, 0.3219752754296894559, 0.3333333333333333703, 0.3219752754296894559, 0.3333333333333333703, 0.3219752754296894559, 0.3333333333333333703, 0.3219752754296894559, 0.3333333333333333703, 0.3219752754296894559, 0.3333333333333333703, 0.3219752754296894559, 0.3333333333333333703, 0.3219752754296894559, 0.3333333333333333703, 0.3219752754296894559, 0.3333333333333333703, 0.3219752754296894559, 0.3333333333333333703, 0.3219752754296894559, 0.3333333333333333703, 0.3219752754296894559, 0.3333333333333333703, 0.3219752754296894559, 0.3333333333333333703, 0.3219752754296894559, 0.3333333333333333703, 0.3219752754296894559, 0.3333333333333333703, 0.3219752754296894559, 0.3333333333333333703, 0.3219752754296894559, 0.3333333333333333703, 0.3219752754296894559, 0.3333333333333333703, 0.3219752754296894559, 0.3333333333333333703, 0.3219752754296894559, 0.3333333333333333703, 0.3219752754296894559, 0.3333333333333333703, 0.3219752754296894559, 0.3333333333333333703, 0.3219752754296894559, 0.3333333333333333703, 0.3219752754296894559, 0.3333333333333333703, 0.3219752754296894559, 0.3333333333333333703, 0.3219752754296894559, 0.3333333333333333703, 0.3219752754296894559, 0.3333333333333333703, 0.3219752754296894559, 0.3333333333333333703, 0.3219752754296894559, 0.3333333333333333703, 0.3219752754296894559, 0.3333333333333333703, 0.3219752754296894559, 0.3333333333333333703, 0.3219752754296894559, 0.3333333333333333703, 0.3219752754296894559, 0.3333333333333333703, 0.3219752754296894559, 0.3333333333333333703, 0.3219752754296894559, 0.3333333333333333703, 0.3219752754296894559, 0.3333333333333333703, 0.3219752754296894559, 0.3333333333333333703, 0.3219752754296894559, 0.3333333333333333703, 0.3219752754296894559, 0.3333333333333333703, 0.3219752754296894559, 0.3333333333333333703, 0.3219752754296894559, 0.3333333333333333703, 0.3219752754296894559, 0.3333333333333333703, 0.3219752754296894559, 0.3333333333333333703, 0.3219752754296894559, 0.3333333333333333703, 0.3219752754296894559, 0.3333333333333333703, 0.3219752754296894559, 0.3333333333333333703, 0.3219752754296894559, 0.3333333333333333703, 0.3219752754296894559, 0.3333333333333333703, 0.3219752754296894559, 0.3333333333333333703, 0.3219752754296894559, 0.3333333333333333703, 0.3219752754296894559, 0.3333333333333333703, 0.3219752754296894559, 0.3333333333333333703, 0.3219752754296894559, 0.3333333333333333703, 0.3219752754296894559, 0.3333333333333333703, 0.3219752754296894559, 0.3333333333333333703, 0.3219752754296894559, 0.3333333333333333703, 0.3219752754296894559, 0.3333333333333333703),
 ( 1.000000000000000000, 0.9659258262890683122, 1.000000000000000000, 0.9659258262890683122, 1.000000000000000000, 0.9659258262890683122, 1.000000000000000000, 0.9659258262890683122, 1.000000000000000000, 0.9659258262890683122, 1.000000000000000000, 0.9659258262890683122, 1.000000000000000000, 0.9659258262890683122, 1.000000000000000000, 0.9659258262890683122, 1.000000000000000000, 0.9659258262890683122, 1.000000000000000000, 0.9659258262890683122, 1.000000000000000000, 0.9659258262890683122, 1.000000000000000000, 0.9659258262890683122, 1.000000000000000000, 0.9659258262890683122, 1.000000000000000000, 0.9659258262890683122, 1.000000000000000000, 0.9659258262890683122, 1.000000000000000000, 0.9659258262890683122, 1.000000000000000000, 0.9659258262890683122, 1.000000000000000000, 0.9659258262890683122, 1.000000000000000000, 0.9659258262890683122, 1.000000000000000000, 0.9659258262890683122, 1.000000000000000000, 0.9659258262890683122, 1.000000000000000000, 0.9659258262890683122, 1.000000000000000000, 0.9659258262890683122, 1.000000000000000000, 0.9659258262890683122, 1.000000000000000000, 0.9659258262890683122, 1.000000000000000000, 0.9659258262890683122, 1.000000000000000000, 0.9659258262890683122, 1.000000000000000000, 0.9659258262890683122, 1.000000000000000000, 0.9659258262890683122, 1.000000000000000000, 0.9659258262890683122, 1.000000000000000000, 0.9659258262890683122, 1.000000000000000000, 0.9659258262890683122, 1.000000000000000000, 0.9659258262890683122, 1.000000000000000000, 0.9659258262890683122, 1.000000000000000000, 0.9659258262890683122, 1.000000000000000000, 0.9659258262890683122, 1.000000000000000000, 0.9659258262890683122, 1.000000000000000000, 0.9659258262890683122, 1.000000000000000000, 0.9659258262890683122, 1.000000000000000000, 0.9659258262890683122, 1.000000000000000000, 0.9659258262890683122, 1.000000000000000000, 0.9659258262890683122, 1.000000000000000000, 0.9659258262890683122, 1.000000000000000000, 0.9659258262890683122, 1.000000000000000000, 0.9659258262890683122, 1.000000000000000000, 0.9659258262890683122, 1.000000000000000000, 0.9659258262890683122, 1.000000000000000000, 0.9659258262890683122, 1.000000000000000000, 0.9659258262890683122, 1.000000000000000000, 0.9659258262890683122, 1.000000000000000000, 0.9659258262890683122, 1.000000000000000000, 0.9659258262890683122, 1.000000000000000000, 0.9659258262890683122, 1.000000000000000000, 0.9659258262890683122, 1.000000000000000000, 0.9659258262890683122, 1.000000000000000000, 0.9659258262890683122, 1.000000000000000000, 0.9659258262890683122, 1.000000000000000000, 0.9659258262890683122, 1.000000000000000000, 0.9659258262890683122, 1.000000000000000000, 0.9659258262890683122, 1.000000000000000000, 0.9659258262890683122, 1.000000000000000000, 0.9659258262890683122, 1.000000000000000000, 0.9659258262890683122, 1.000000000000000000, 0.9659258262890683122, 1.000000000000000000, 0.9659258262890683122, 1.000000000000000000, 0.9659258262890683122, 1.000000000000000000, 0.9659258262890683122, 1.000000000000000000, 0.9659258262890683122, 1.000000000000000000, 0.9659258262890683122, 1.000000000000000000, 0.9659258262890683122, 1.000000000000000000, 0.9659258262890683122, 1.000000000000000000, 0.9659258262890683122, 1.000000000000000000, 0.9659258262890683122, 1.000000000000000000, 0.9659258262890683122, 1.000000000000000000, 0.9659258262890683122, 1.000000000000000000, 0.9659258262890683122, 1.000000000000000000, 0.9659258262890683122, 1.000000000000000000, 0.9659258262890683122, 1.000000000000000000, 0.9659258262890683122, 1.000000000000000000, 0.9659258262890683122, 1.000000000000000000, 0.9659258262890683122, 1.000000000000000000, 0.9659258262890683122, 1.000000000000000000, 0.9659258262890683122, 1.000000000000000000, 0.9659258262890683122, 1.000000000000000000, 0.9659258262890683122, 1.000000000000000000, 0.9659258262890683122, 1.000000000000000000, 0.9659258262890683122, 1.000000000000000000, 0.9659258262890683122, 1.000000000000000000, 0.9659258262890683122, 1.000000000000000000, 0.9659258262890683122, 1.000000000000000000, 0.9659258262890683122, 1.000000000000000000, 0.9659258262890683122, 1.000000000000000000, 0.9659258262890683122, 1.000000000000000000, 0.9659258262890683122, 1.000000000000000000, 0.9659258262890683122, 1.000000000000000000, 0.9659258262890683122, 1.000000000000000000, 0.9659258262890683122, 1.000000000000000000, 0.9659258262890683122, 1.000000000000000000, 0.9659258262890683122, 1.000000000000000000, 0.9659258262890683122, 1.000000000000000000, 0.9659258262890683122, 1.000000000000000000, 0.9659258262890683122, 1.000000000000000000, 0.9659258262890683122, 1.000000000000000000, 0.9659258262890683122, 1.000000000000000000, 0.9659258262890683122, 1.000000000000000000, 0.9659258262890683122, 1.000000000000000000, 0.9659258262890683122, 1.000000000000000000, 0.9659258262890683122, 1.000000000000000000, 0.9659258262890683122, 1.000000000000000000, 0.9659258262890683122, 1.000000000000000000, 0.9659258262890683122, 1.000000000000000000, 0.9659258262890683122, 1.000000000000000000, 0.9659258262890683122, 1.000000000000000000, 0.9659258262890683122, 1.000000000000000000, 0.9659258262890683122, 1.000000000000000000, 0.9659258262890683122, 1.000000000000000000, 0.9659258262890683122, 1.000000000000000000, 0.9659258262890683122, 1.000000000000000000, 0.9659258262890683122, 1.000000000000000000, 0.9659258262890683122, 1.000000000000000000, 0.9659258262890683122, 1.000000000000000000, 0.9659258262890683122, 1.000000000000000000, 0.9659258262890683122, 1.000000000000000000, 0.9659258262890683122, 1.000000000000000000, 0.9659258262890683122, 1.000000000000000000, 0.9659258262890683122, 1.000000000000000000, 0.9659258262890683122, 1.000000000000000000, 0.9659258262890683122, 1.000000000000000000, 0.9659258262890683122, 1.000000000000000000, 0.9659258262890683122, 1.000000000000000000, 0.9659258262890683122, 1.000000000000000000, 0.9659258262890683122, 1.000000000000000000, 0.9659258262890683122, 1.000000000000000000, 0.9659258262890683122, 1.000000000000000000, 0.9659258262890683122, 1.000000000000000000, 0.9659258262890683122, 1.000000000000000000, 0.9659258262890683122, 1.000000000000000000, 0.9659258262890683122, 1.000000000000000000, 0.9659258262890683122, 1.000000000000000000, 0.9659258262890683122, 1.000000000000000000, 0.9659258262890683122, 1.000000000000000000, 0.9659258262890683122, 1.000000000000000000, 0.9659258262890683122, 1.000000000000000000, 0.9659258262890683122, 1.000000000000000000, 0.9659258262890683122, 1.000000000000000000, 0.9659258262890683122, 1.000000000000000000, 0.9659258262890683122, 1.000000000000000000, 0.9659258262890683122, 1.000000000000000000, 0.9659258262890683122, 1.000000000000000000, 0.9659258262890683122, 1.000000000000000000, 0.9659258262890683122, 1.000000000000000000, 0.9659258262890683122, 1.000000000000000000, 0.9659258262890683122, 1.000000000000000000, 0.9659258262890683122, 1.000000000000000000, 0.9659258262890683122, 1.000000000000000000, 0.9659258262890683122, 1.000000000000000000, 0.9659258262890683122, 1.000000000000000000, 0.9659258262890683122, 1.000000000000000000, 0.9659258262890683122, 1.000000000000000000, 0.9659258262890683122, 1.000000000000000000, 0.9659258262890683122, 1.000000000000000000, 0.9659258262890683122, 1.000000000000000000, 0.9659258262890683122, 1.000000000000000000, 0.9659258262890683122, 1.000000000000000000, 0.9659258262890683122, 1.000000000000000000, 0.9659258262890683122, 1.000000000000000000, 0.9659258262890683122, 1.000000000000000000, 0.9659258262890683122, 1.000000000000000000, 0.9659258262890683122, 1.000000000000000000, 0.9659258262890683122, 1.000000000000000000, 0.9659258262890683122, 1.000000000000000000, 0.9659258262890683122, 1.000000000000000000, 0.9659258262890683122, 1.000000000000000000, 0.9659258262890683122, 1.000000000000000000, 0.9659258262890683122, 1.000000000000000000, 0.9659258262890683122, 1.000000000000000000, 0.9659258262890683122, 1.000000000000000000, 0.9659258262890683122, 1.000000000000000000, 0.9659258262890683122, 1.000000000000000000, 0.9659258262890683122, 1.000000000000000000, 0.9659258262890683122, 1.000000000000000000, 0.9659258262890683122, 1.000000000000000000, 0.9659258262890683122, 1.000000000000000000, 0.9659258262890683122, 1.000000000000000000, 0.9659258262890683122, 1.000000000000000000, 0.9659258262890683122, 1.000000000000000000, 0.9659258262890683122, 1.000000000000000000, 0.9659258262890683122, 1.000000000000000000, 0.9659258262890683122, 1.000000000000000000, 0.9659258262890683122, 1.000000000000000000, 0.9659258262890683122, 1.000000000000000000, 0.9659258262890683122, 1.000000000000000000, 0.9659258262890683122, 1.000000000000000000, 0.9659258262890683122, 1.000000000000000000, 0.9659258262890683122, 1.000000000000000000, 0.9659258262890683122, 1.000000000000000000, 0.9659258262890683122, 1.000000000000000000, 0.9659258262890683122, 1.000000000000000000, 0.9659258262890683122, 1.000000000000000000, 0.9659258262890683122, 1.000000000000000000, 0.9659258262890683122, 1.000000000000000000, 0.9659258262890683122, 1.000000000000000000, 0.9659258262890683122, 1.000000000000000000, 0.9659258262890683122, 1.000000000000000000, 0.9659258262890683122, 1.000000000000000000, 0.9659258262890683122, 1.000000000000000000, 0.9659258262890683122, 1.000000000000000000, 0.9659258262890683122, 1.000000000000000000, 0.9659258262890683122, 1.000000000000000000, 0.9659258262890683122, 1.000000000000000000, 0.9659258262890683122, 1.000000000000000000, 0.9659258262890683122, 1.000000000000000000, 0.9659258262890683122, 1.000000000000000000, 0.9659258262890683122, 1.000000000000000000, 0.9659258262890683122, 1.000000000000000000, 0.9659258262890683122, 1.000000000000000000, 0.9659258262890683122, 1.000000000000000000, 0.9659258262890683122, 1.000000000000000000, 0.9659258262890683122, 1.000000000000000000, 0.9659258262890683122, 1.000000000000000000, 0.9659258262890683122, 1.000000000000000000, 0.9659258262890683122, 1.000000000000000000, 0.9659258262890683122, 1.000000000000000000, 0.9659258262890683122, 1.000000000000000000, 0.9659258262890683122, 1.000000000000000000, 0.9659258262890683122, 1.000000000000000000, 0.9659258262890683122, 1.000000000000000000, 0.9659258262890683122, 1.000000000000000000) ) ) 
 REPRESENTATION_ITEM ( '' )  SURFACE ( )  );
#13897 = CARTESIAN_POINT ( 'NONE',  ( -19.05341960407611168, -5.049401038298163336, 66.45724293864769550 ) ) ;
#13898 = CARTESIAN_POINT ( 'NONE',  ( -14.29746914071049879, 8.314922557960819915, 70.83224293864770971 ) ) ;
#13899 = CARTESIAN_POINT ( 'NONE',  ( -9.474510206698964154, 16.51473224551069663, 30.41557627198102054 ) ) ;
#13900 = CARTESIAN_POINT ( 'NONE',  ( -17.19557940625944070, -5.324144293544740947, 20.93786341900914394 ) ) ;
#13901 = CARTESIAN_POINT ( 'NONE',  ( -4.379528057220328563, 16.55341960407611168, 45.20724293864769550 ) ) ;
#13902 = CARTESIAN_POINT ( 'NONE',  ( -13.97604488694527625, -13.89961937509977652, 86.87390960531436690 ) ) ;
#13903 = CARTESIAN_POINT ( 'NONE',  ( -1.315686079477255355, -15.92681084339658781, -59.47631410104520455 ) ) ;
#13904 = CARTESIAN_POINT ( 'NONE',  ( 16.46253265017146816, 9.564922557961045513, 51.66775706135233293 ) ) ;
#13905 = CARTESIAN_POINT ( 'NONE',  ( -14.29746914071037622, -8.314922557961029526, 64.16775706135234714 ) ) ;
#13906 = CARTESIAN_POINT ( 'NONE',  ( -21.53943276465977519, 0.05219959533907696930, 81.24890960531436690 ) ) ;
#13907 = CARTESIAN_POINT ( 'NONE',  ( -13.97604488694547697, 13.89961937509957934, 33.12609039468566863 ) ) ;
#13908 = CARTESIAN_POINT ( 'NONE',  ( 13.89961937509977652, -13.97604488694527269, 88.12390960531438111 ) ) ;
#13909 = CARTESIAN_POINT ( 'NONE',  ( -30.82560697742735911, 2.051108057200722688E-14, 150.0000000000000000 ) ) ;
#13910 = CARTESIAN_POINT ( 'NONE',  ( 5.719274019375991003, -21.55341960407610458, 22.70724293864769194 ) ) ;
#13911 = CARTESIAN_POINT ( 'NONE',  ( 0.05219959533909260263, 19.03943276465977164, 64.99890960531436690 ) ) ;
#13912 = CARTESIAN_POINT ( 'NONE',  ( -15.72974639402176322, -15.80617190586768395, 54.37609039468568994 ) ) ;
#13913 = CARTESIAN_POINT ( 'NONE',  ( 19.02544592524343514, -5.153800228976328945, 28.54057627198102409 ) ) ;
#13916 = VERTEX_POINT ( 'NONE', #88106 ) ;
#13915 = CARTESIAN_POINT ( 'NONE',  ( -13.97604488694527625, -13.89961937509977652, 91.87390960531432427 ) ) ;
#13914 = CARTESIAN_POINT ( 'NONE',  ( -18.62759615963270932, 10.81492255796079327, 115.8322429386477097 ) ) ;
#13917 = CARTESIAN_POINT ( 'NONE',  ( -18.67979575497193778, 10.72451020669871902, 43.33442372801901143 ) ) ;
#13918 = ORIENTED_EDGE ( 'NONE', *, *, #21608, .F. ) ;
#13919 = CARTESIAN_POINT ( 'NONE',  ( 5.049401038298161559, -19.05341960407611168, 97.70724293864766707 ) ) ;
#13920 = CARTESIAN_POINT ( 'NONE',  ( 21.55341960407610458, 5.719274019375980345, 113.9572429386477239 ) ) ;
#13921 = CARTESIAN_POINT ( 'NONE',  ( 13.89961937509977652, -13.97604488694527269, 43.12390960531434558 ) ) ;
#13922 = CARTESIAN_POINT ( 'NONE',  ( 12.14591786802327356, -12.06949235617739191, 25.62609039468567929 ) ) ;
#13923 = CARTESIAN_POINT ( 'NONE',  ( -38.00000000000001421, -12.34694845685042708, -11.64999999453762669 ) ) ;
#13924 = CARTESIAN_POINT ( 'NONE',  ( 18.67979575497194134, -10.72451020669871369, 105.8344237280190328 ) ) ;
#13925 = CARTESIAN_POINT ( 'NONE',  ( 13.89961937509977652, -13.97604488694527269, 33.12390960531434558 ) ) ;
#13926 = CARTESIAN_POINT ( 'NONE',  ( 21.53943276465977519, 0.05219959533937863772, 96.25109039468568994 ) ) ;
#13928 = CARTESIAN_POINT ( 'NONE',  ( 5.823673210054444382, -21.52544592524334988, 55.20942372801902565 ) ) ;
#13927 = CARTESIAN_POINT ( 'NONE',  ( 5.153800228976335163, 19.02544592524342804, 94.79057627198103830 ) ) ;
#13929 = CARTESIAN_POINT ( 'NONE',  ( -5.359611314223446995E-15, 29.16686587814335496, 144.8750000027311557 ) ) ;
#13930 = CARTESIAN_POINT ( 'NONE',  ( 5.153800228976335163, 19.02544592524342804, 94.79057627198103830 ) ) ;
#13931 = CARTESIAN_POINT ( 'NONE',  ( -2.044528755335630166, 7.220908937440031039, 1.589185716900140211 ) ) ;
#13934 = CARTESIAN_POINT ( 'NONE',  ( 21.52544592524334988, 5.823673210054432836, 56.45942372801902565 ) ) ;
#13933 = CARTESIAN_POINT ( 'NONE',  ( -8.314922557961024197, 14.29746914071037800, 72.91775706135234714 ) ) ;
#13932 = CARTESIAN_POINT ( 'NONE',  ( 0.05219959533934541429, -16.53943276465976808, 40.00109039468567573 ) ) ;
#13935 = CARTESIAN_POINT ( 'NONE',  ( -18.67979575497193778, 10.72451020669871902, 83.33442372801903275 ) ) ;
#13936 = CARTESIAN_POINT ( 'NONE',  ( 18.22780087662123805, -5.499999999999989342, 53.51763182126895657 ) ) ;
#13937 = CARTESIAN_POINT ( 'NONE',  ( 16.55341960407618274, -4.379528057220086978, 31.04275706135234714 ) ) ;
#13938 = CARTESIAN_POINT ( 'NONE',  ( -16.46253265017160317, 9.564922557960807481, 70.83224293864770971 ) ) ;
#13939 = CARTESIAN_POINT ( 'NONE',  ( 16.46253265017160672, -9.564922557960803928, 93.33224293864769550 ) ) ;
#13940 = ADVANCED_FACE ( 'NONE', ( #42618 ), #105272, .F. ) ;
#13941 = CARTESIAN_POINT ( 'NONE',  ( -16.52544592524342804, 4.483927247898546575, 116.0405762719810383 ) ) ;
#13942 = CARTESIAN_POINT ( 'NONE',  ( -18.62759615963270932, 10.81492255796079327, 30.83224293864770260 ) ) ;
#13943 = CARTESIAN_POINT ( 'NONE',  ( -16.55341960407617563, 4.379528057220093196, 98.54275706135234714 ) ) ;
#13945 = CARTESIAN_POINT ( 'NONE',  ( -5.049401038298153566, 19.05341960407611168, 65.20724293864765286 ) ) ;
#13944 = CARTESIAN_POINT ( 'NONE',  ( -0.05219959533910754901, -16.53943276465976808, 67.49890960531436690 ) ) ;
#13946 = CARTESIAN_POINT ( 'NONE',  ( -10.72451020669870658, -18.67979575497194134, 94.58442372801901854 ) ) ;
#13947 = CARTESIAN_POINT ( 'NONE',  ( -24.30000000000003268, 0.1103568551768616401, -56.77278709839603010 ) ) ;
#13948 = CARTESIAN_POINT ( 'NONE',  ( -5.049401038297874678, -19.05341960407617918, 104.7927570613523471 ) ) ;
#13949 = CARTESIAN_POINT ( 'NONE',  ( -4.379528057220328563, 16.55341960407611168, 80.20724293864769550 ) ) ;
#13950 = CARTESIAN_POINT ( 'NONE',  ( -0.05219959533937732626, 21.53943276465977519, 22.50109039468567573 ) ) ;
#13951 = CARTESIAN_POINT ( 'NONE',  ( -21.53943276465977519, 0.05219959533907696930, 61.24890960531435979 ) ) ;
#13952 = CARTESIAN_POINT ( 'NONE',  ( 0.05219959533936267826, -19.03943276465977164, 40.00109039468566152 ) ) ;
#13953 = CARTESIAN_POINT ( 'NONE',  ( 17.81289503416611453, -24.51734667627695785, 144.9500000054623854 ) ) ;
#13954 = CARTESIAN_POINT ( 'NONE',  ( -19.03943276465977164, 0.05219959533909376836, 86.24890960531436690 ) ) ;
#13955 = CARTESIAN_POINT ( 'NONE',  ( -4.379528057220328563, 16.55341960407611168, 55.20724293864770260 ) ) ;
#13956 = CARTESIAN_POINT ( 'NONE',  ( -8.314922557960811034, -14.29746914071050412, 37.08224293864768129 ) ) ;
#13957 = CARTESIAN_POINT ( 'NONE',  ( -16.53943276465976808, -0.05219959533934237506, 103.7510903946857042 ) ) ;
#13958 = CARTESIAN_POINT ( 'NONE',  ( 16.51473224551083163, -9.474510206698727899, 55.83442372801899722 ) ) ;
#13959 = DIRECTION ( 'NONE',  ( -0.9945218953682734009, 0.000000000000000000, -0.1045284632676528741 ) ) ;
#13960 = CARTESIAN_POINT ( 'NONE',  ( -5.049401038298153566, 19.05341960407611168, 100.2072429386476955 ) ) ;
#13961 = EDGE_CURVE ( 'NONE', #82818, #68886, #72967, .T. ) ;
#13962 = CARTESIAN_POINT ( 'NONE',  ( -16.53943276465976808, 0.05219959533911058130, 81.24890960531436690 ) ) ;
#13963 = CARTESIAN_POINT ( 'NONE',  ( -5.049401038297874678, -19.05341960407617918, 49.79275706135231871 ) ) ;
#13965 = CARTESIAN_POINT ( 'NONE',  ( 0.05219959533907565091, 21.53943276465977519, 39.99890960531436690 ) ) ;
#13964 = CARTESIAN_POINT ( 'NONE',  ( 16.46253265017160672, -9.564922557960803928, 33.33224293864770260 ) ) ;
#13966 = CARTESIAN_POINT ( 'NONE',  ( 21.53943276465977519, -0.05219959533907433946, 63.74890960531435979 ) ) ;
#13967 = CARTESIAN_POINT ( 'NONE',  ( -4.379528057220328563, 16.55341960407611168, 115.2072429386476955 ) ) ;
#13969 = CARTESIAN_POINT ( 'NONE',  ( 19.03943276465977164, -0.05219959533909143690, 48.74890960531435979 ) ) ;
#13968 = CARTESIAN_POINT ( 'NONE',  ( -14.34966873604972548, 8.224510206698743886, 48.33442372801902565 ) ) ;
#13970 = CARTESIAN_POINT ( 'NONE',  ( -5.823673210054431948, 21.52544592524334988, 42.70942372801901854 ) ) ;
#13971 = CARTESIAN_POINT ( 'NONE',  ( -16.53943276465976808, 0.05219959533911058130, 86.24890960531436690 ) ) ;
#13972 = CARTESIAN_POINT ( 'NONE',  ( -22.73749492396214933, -155.7167183371837496, -15.00000000000000178 ) ) ;
#13973 = CARTESIAN_POINT ( 'NONE',  ( 29.86685920354754487, 21.69954338932564752, -9.924999997268812990 ) ) ;
#13974 = CARTESIAN_POINT ( 'NONE',  ( -5.823673210054116645, -21.52544592524344225, 32.29057627198102409 ) ) ;
#13975 = CARTESIAN_POINT ( 'NONE',  ( -4.500000000000001776, -130.0000000000000000, 12.49999999999999645 ) ) ;
#13976 = CARTESIAN_POINT ( 'NONE',  ( 1.500000000000008438, 22.80000000000002913, -57.83153971412246364 ) ) ;
#13978 = CARTESIAN_POINT ( 'NONE',  ( 14.34966873604960469, 8.224510206698951720, 44.16557627198103120 ) ) ;
#13977 = CARTESIAN_POINT ( 'NONE',  ( -16.55341960407617563, 4.379528057220093196, 38.54275706135234714 ) ) ;
#13979 = CARTESIAN_POINT ( 'NONE',  ( -10.72451020669898014, 18.67979575497178502, 70.41557627198102409 ) ) ;
#13980 = AXIS2_PLACEMENT_3D ( 'NONE', #187769, #127049, #142226 ) ;
#13981 = CARTESIAN_POINT ( 'NONE',  ( 5.719274019375991003, -21.55341960407610458, 57.70724293864770260 ) ) ;
#13982 = CARTESIAN_POINT ( 'NONE',  ( -37.99626262588766679, 2.428612866367529932E-14, -1.747842220587805251 ) ) ;
#13984 = CARTESIAN_POINT ( 'NONE',  ( -16.51473224551069308, -9.474510206698971260, 101.6655762719810241 ) ) ;
#13983 = CARTESIAN_POINT ( 'NONE',  ( 19.02544592524343514, -5.153800228976328945, 43.54057627198103120 ) ) ;
#13985 = CARTESIAN_POINT ( 'NONE',  ( -19.03943276465977164, 0.05219959533909376836, 51.24890960531436690 ) ) ;
#13986 = CARTESIAN_POINT ( 'NONE',  ( -0.05219959533910754901, -16.53943276465976808, 112.4989096053143669 ) ) ;
#13987 = APPLICATION_PROTOCOL_DEFINITION ( 'draft international standard', 'automotive_design', 1998, #183562 ) ;
#13988 = CARTESIAN_POINT ( 'NONE',  ( -13.89961937509977652, 13.97604488694528158, 115.6239096053143669 ) ) ;
#13989 = ORIENTED_EDGE ( 'NONE', *, *, #42025, .F. ) ;
#13990 = CARTESIAN_POINT ( 'NONE',  ( 4.379528057220092307, 16.55341960407617563, 72.29275706135236135 ) ) ;
#13991 = CARTESIAN_POINT ( 'NONE',  ( -10.72451020669898014, 18.67979575497178502, 110.4155762719810383 ) ) ;
#13992 = CARTESIAN_POINT ( 'NONE',  ( -9.564922557960796823, -16.46253265017161027, 62.08224293864769550 ) ) ;
#13993 = CARTESIAN_POINT ( 'NONE',  ( 5.823673210054444382, -21.52544592524334988, 45.20942372801901854 ) ) ;
#13994 = CARTESIAN_POINT ( 'NONE',  ( -16.46253265017160317, 9.564922557960807481, 80.83224293864769550 ) ) ;
#13995 = CARTESIAN_POINT ( 'NONE',  ( -16.46253265017160317, 9.564922557960807481, 115.8322429386477097 ) ) ;
#13996 = EDGE_LOOP ( 'NONE', ( #152884, #135844, #78840, #26414, #124117, #87089 ) ) ;
#13997 = CARTESIAN_POINT ( 'NONE',  ( -18.67979575497193778, 10.72451020669871902, 28.33442372801902209 ) ) ;
#13999 = CARTESIAN_POINT ( 'NONE',  ( -5.153800228976607833, 19.02544592524334988, 87.70942372801897591 ) ) ;
#13998 = CARTESIAN_POINT ( 'NONE',  ( 13.97604488694527802, 13.89961937509977652, 109.3739096053143669 ) ) ;
#14000 = CARTESIAN_POINT ( 'NONE',  ( 19.02544592524334988, 5.153800228976608722, 46.45942372801899012 ) ) ;
#14001 = CARTESIAN_POINT ( 'NONE',  ( -21.55341960407610458, -5.719274019375992779, 101.4572429386476955 ) ) ;
#14002 = CARTESIAN_POINT ( 'NONE',  ( -19.02544592524334988, -5.153800228976617603, 28.95942372801900433 ) ) ;
#14003 = CARTESIAN_POINT ( 'NONE',  ( -0.05219959533936034679, 19.03943276465977164, 32.50109039468566863 ) ) ;
#14004 = CARTESIAN_POINT ( 'NONE',  ( -14.34966873604972548, 8.224510206698743886, 93.33442372801901854 ) ) ;
#14005 = CARTESIAN_POINT ( 'NONE',  ( 24.20534277172198756, -9.236732224056902751, 166.4300944521385190 ) ) ;
#14006 = CARTESIAN_POINT ( 'NONE',  ( 16.46253265017160672, -9.564922557960803928, 58.33224293864769550 ) ) ;
#14007 = CARTESIAN_POINT ( 'NONE',  ( 21.55341960407619695, -5.719274019375665929, 66.04275706135236135 ) ) ;
#14008 = CARTESIAN_POINT ( 'NONE',  ( 10.72451020669871369, 18.67979575497193778, 77.08442372801901854 ) ) ;
#14009 = CARTESIAN_POINT ( 'NONE',  ( -18.46320343559655086, -23.96320343559633059, 8.181980515339455806 ) ) ;
#14010 = CARTESIAN_POINT ( 'NONE',  ( -9.564922557960796823, -16.46253265017161027, 82.08224293864768129 ) ) ;
#14011 = CARTESIAN_POINT ( 'NONE',  ( 18.62759615963255655, 10.81492255796105972, 61.66775706135235424 ) ) ;
#14012 = CARTESIAN_POINT ( 'NONE',  ( 5.153800228976615827, -19.02544592524334988, 105.2094237280190185 ) ) ;
#14013 = CARTESIAN_POINT ( 'NONE',  ( 19.03943276465977164, -0.05219959533909143690, 63.74890960531435979 ) ) ;
#14014 = CARTESIAN_POINT ( 'NONE',  ( -5.049401038298153566, 19.05341960407611168, 95.20724293864770971 ) ) ;
#14015 = CARTESIAN_POINT ( 'NONE',  ( -13.89961937509977652, 13.97604488694528158, 85.62390960531433848 ) ) ;
#14016 = CARTESIAN_POINT ( 'NONE',  ( -40.00200000000003087, -1.071565949253934124E-14, 102.5000000000000142 ) ) ;
#14017 = CARTESIAN_POINT ( 'NONE',  ( -9.474510206698964154, 16.51473224551069663, 70.41557627198102409 ) ) ;
#14018 = CARTESIAN_POINT ( 'NONE',  ( 18.67979575497178502, 10.72451020669898547, 94.16557627198103830 ) ) ;
#14019 = CARTESIAN_POINT ( 'NONE',  ( -12.06949235617739369, -12.14591786802326823, 89.37609039468568994 ) ) ;
#14020 = CARTESIAN_POINT ( 'NONE',  ( 26.03370437638686852, 6.875205692009825675, 160.5968874236875195 ) ) ;
#14021 = CARTESIAN_POINT ( 'NONE',  ( -19.03943276465977164, -0.05219959533935918106, 38.75109039468566152 ) ) ;
#14022 = CARTESIAN_POINT ( 'NONE',  ( 9.474510206698971260, -16.51473224551069308, 77.91557627198103830 ) ) ;
#14023 = CARTESIAN_POINT ( 'NONE',  ( 8.224510206698953496, -14.34966873604960469, 77.91557627198102409 ) ) ;
#14024 = CARTESIAN_POINT ( 'NONE',  ( -8.224510206698948167, 14.34966873604960824, 110.4155762719810383 ) ) ;
#14025 = CARTESIAN_POINT ( 'NONE',  ( -19.03943276465977164, 0.05219959533909376836, 116.2489096053143669 ) ) ;
#14026 = VERTEX_POINT ( 'NONE', #106255 ) ;
#14027 = CARTESIAN_POINT ( 'NONE',  ( -9.474510206698964154, 16.51473224551069663, 105.4155762719810383 ) ) ;
#14028 = CARTESIAN_POINT ( 'NONE',  ( -18.22780087662123094, -5.499999999999984901, 81.48459894673892734 ) ) ;
#14029 = CARTESIAN_POINT ( 'NONE',  ( 16.51473224551083163, -9.474510206698727899, 25.83442372801900078 ) ) ;
#14030 = CARTESIAN_POINT ( 'NONE',  ( -12.06949235617739369, -12.14591786802326823, 89.37609039468568994 ) ) ;
#14031 = CARTESIAN_POINT ( 'NONE',  ( 19.05341960407611168, 5.049401038298154454, 78.95724293864769550 ) ) ;
#14032 = CARTESIAN_POINT ( 'NONE',  ( -10.81492255796105439, 18.62759615963255655, 57.91775706135234714 ) ) ;
#14033 = CARTESIAN_POINT ( 'NONE',  ( 10.81492255796078972, 18.62759615963270932, 34.58224293864770260 ) ) ;
#14034 = CARTESIAN_POINT ( 'NONE',  ( -10.72451020669870658, -18.67979575497194134, 24.58442372801901499 ) ) ;
#14035 = CARTESIAN_POINT ( 'NONE',  ( -10.81492255796078084, -18.62759615963271287, 72.08224293864769550 ) ) ;
#14036 = CARTESIAN_POINT ( 'NONE',  ( -0.05219959533910754901, -16.53943276465976808, 97.49890960531436690 ) ) ;
#14037 = CARTESIAN_POINT ( 'NONE',  ( 19.03943276465977164, 0.05219959533936151252, 61.25109039468566863 ) ) ;
#14038 = CARTESIAN_POINT ( 'NONE',  ( 19.02544592524343514, -5.153800228976328945, 33.54057627198102409 ) ) ;
#14039 = CARTESIAN_POINT ( 'NONE',  ( 19.02544592524343514, -5.153800228976328945, 78.54057627198099567 ) ) ;
#14040 = CARTESIAN_POINT ( 'NONE',  ( 19.05341960407611168, 5.049401038298154454, 78.95724293864769550 ) ) ;
#14041 = CARTESIAN_POINT ( 'NONE',  ( -17.14385361876520975, 23.59649016807275856, 141.0750000027311728 ) ) ;
#14042 = CARTESIAN_POINT ( 'NONE',  ( -0.05219959533910754901, -16.53943276465976808, 107.4989096053143669 ) ) ;
#14043 = ORIENTED_EDGE ( 'NONE', *, *, #118990, .F. ) ;
#14044 = CARTESIAN_POINT ( 'NONE',  ( 16.52544592524342804, -4.483927247898539470, 33.54057627198102409 ) ) ;
#14045 = CARTESIAN_POINT ( 'NONE',  ( -16.52544592524335698, -4.483927247898792601, 28.95942372801902209 ) ) ;
#14046 = CARTESIAN_POINT ( 'NONE',  ( -5.719274019375665041, -21.55341960407619695, 94.79275706135234714 ) ) ;
#14047 = CARTESIAN_POINT ( 'NONE',  ( -16.51473224551069308, -9.474510206698971260, 106.6655762719810383 ) ) ;
#14048 = CARTESIAN_POINT ( 'NONE',  ( -10.72451020669870658, -18.67979575497194134, 19.58442372801901143 ) ) ;
#14049 = CARTESIAN_POINT ( 'NONE',  ( 9.474510206698971260, -16.51473224551069308, 37.91557627198102409 ) ) ;
#14050 = CARTESIAN_POINT ( 'NONE',  ( 8.314922557961029526, -14.29746914071037800, 40.41775706135234714 ) ) ;
#14051 = CARTESIAN_POINT ( 'NONE',  ( 9.564922557961047289, -16.46253265017146816, 105.4177570613523471 ) ) ;
#14052 = CARTESIAN_POINT ( 'NONE',  ( -13.97604488694527625, -13.89961937509977652, 31.87390960531435979 ) ) ;
#14053 = CIRCLE ( 'NONE', #127048, 2.700000000000001066 ) ;
#14054 = CARTESIAN_POINT ( 'NONE',  ( -16.52544592524342804, 4.483927247898546575, 101.0405762719810383 ) ) ;
#14055 = CARTESIAN_POINT ( 'NONE',  ( 5.823673210054125526, 21.52544592524343514, 99.79057627198103830 ) ) ;
#14056 = CARTESIAN_POINT ( 'NONE',  ( -16.51473224551082808, 9.474510206698731452, 68.33442372801900433 ) ) ;
#14057 = CARTESIAN_POINT ( 'NONE',  ( -18.09867054820433907, -5.499999999999827693, 63.98393025253586330 ) ) ;
#14058 = CARTESIAN_POINT ( 'NONE',  ( -10.81492255796078084, -18.62759615963271287, 112.0822429386477097 ) ) ;
#14059 = LINE ( 'NONE', #26274, #159692 ) ;
#14060 = CARTESIAN_POINT ( 'NONE',  ( 16.51473224551069308, 9.474510206698969483, 94.16557627198103830 ) ) ;
#14061 = CARTESIAN_POINT ( 'NONE',  ( 17.50000000000000000, -5.500000000000000888, 120.0000000000000142 ) ) ;
#14062 = B_SPLINE_CURVE_WITH_KNOTS ( 'NONE', 3,
 ( #113867, #160394, #21883, #115889, #100704, #162384, #147226, #85539, #159034, #190390, #34710, #47908 ),
 .UNSPECIFIED., .F., .F.,
 ( 4, 2, 2, 2, 2, 4 ),
 ( -5.955746802939833779E-05, 0.001235637542566280249, 0.002530832553161958733, 0.005121222574353310499, 0.007711612595544660963, 0.01030200261673601056 ),
 .UNSPECIFIED. ) ;
#14063 = CARTESIAN_POINT ( 'NONE',  ( -9.474510206698964154, 16.51473224551069663, 80.41557627198103830 ) ) ;
#14065 = CARTESIAN_POINT ( 'NONE',  ( 0.05219959533910956823, 16.53943276465976808, 74.99890960531435269 ) ) ;
#14064 = CARTESIAN_POINT ( 'NONE',  ( -10.81492255796105439, 18.62759615963255655, 37.91775706135235424 ) ) ;
#14066 = CARTESIAN_POINT ( 'NONE',  ( -16.51473224551069308, -9.474510206698971260, 76.66557627198103830 ) ) ;
#14068 = CARTESIAN_POINT ( 'NONE',  ( -5.153800228976607833, 19.02544592524334988, 57.70942372801899012 ) ) ;
#14067 = CARTESIAN_POINT ( 'NONE',  ( -8.314922557961024197, 14.29746914071037800, 52.91775706135235424 ) ) ;
#14069 = CARTESIAN_POINT ( 'NONE',  ( 21.52544592524334988, 5.823673210054432836, 61.45942372801901854 ) ) ;
#14070 = CARTESIAN_POINT ( 'NONE',  ( -8.314922557961024197, 14.29746914071037800, 27.91775706135234358 ) ) ;
#14071 = CARTESIAN_POINT ( 'NONE',  ( 16.46253265017160672, -9.564922557960803928, 73.33224293864769550 ) ) ;
#14072 = CARTESIAN_POINT ( 'NONE',  ( -19.03943276465977164, -0.05219959533935918106, 93.75109039468566152 ) ) ;
#14073 = CARTESIAN_POINT ( 'NONE',  ( 12.06949235617739724, 12.14591786802326823, 61.87609039468568284 ) ) ;
#14075 = B_SPLINE_CURVE_WITH_KNOTS ( 'NONE', 3,
 ( #94989, #75843, #108166, #63667, #47511, #78820, #74867, #169848, #13204, #167868, #137520, #199202, #186029, #198210, #184033, #14174, #59681, #77829, #140499, #168841, #155672, #44530, #123327, #60669, #122344, #93991, #1988, #31342, #109167, #106185, #183046, #138508, #45515, #92993, #121353, #29368, #17167, #154679, #30346, #90999 ),
 .UNSPECIFIED., .F., .F.,
 ( 4, 2, 2, 2, 2, 2, 2, 2, 2, 2, 2, 2, 2, 2, 2, 2, 2, 2, 2, 4 ),
 ( 0.004339806180219612543, 0.005417599276633671204, 0.006495392373047728998, 0.007034288921254766569, 0.007573185469461804140, 0.008650978565875881016, 0.009728771662289961361, 0.01080656475870404171, 0.01134546130691106020, 0.01188435785511808215, 0.01296215095153212260, 0.01403994404794615958, 0.01511773714436020002, 0.01619553024077424047, 0.01727332333718827745, 0.01835111643360231790, 0.01942890953001635487, 0.01996780607822336642, 0.02050670262643038144, 0.02158449572284441148 ),
 .UNSPECIFIED. ) ;
#14074 = CARTESIAN_POINT ( 'NONE',  ( -10.72451020669870658, -18.67979575497194134, 99.58442372801900433 ) ) ;
#14076 = CARTESIAN_POINT ( 'NONE',  ( -19.02544592524334988, -5.153800228976617603, 83.95942372801901854 ) ) ;
#14077 = CARTESIAN_POINT ( 'NONE',  ( 13.89961937509977652, -13.97604488694527269, 48.12390960531435979 ) ) ;
#14078 = CARTESIAN_POINT ( 'NONE',  ( -5.719274019375978568, 21.55341960407610458, 70.20724293864769550 ) ) ;
#14080 = CARTESIAN_POINT ( 'NONE',  ( -19.05341960407617563, 5.049401038297882671, 78.54275706135233293 ) ) ;
#14079 = CARTESIAN_POINT ( 'NONE',  ( -4.483927247898539470, -16.52544592524342804, 72.29057627198102409 ) ) ;
#14081 = CARTESIAN_POINT ( 'NONE',  ( 17.05116617787822975, -6.768360034955865245, 61.15675553259200115 ) ) ;
#14082 = CARTESIAN_POINT ( 'NONE',  ( -9.474510206698720793, -16.51473224551083518, 39.58442372801899722 ) ) ;
#14083 = CARTESIAN_POINT ( 'NONE',  ( 14.29746914071037800, 8.314922557961029526, 106.6677570613523756 ) ) ;
#14084 = CARTESIAN_POINT ( 'NONE',  ( -12.14591786802309592, -12.06949235617757132, 61.87390960531436690 ) ) ;
#14086 = CARTESIAN_POINT ( 'NONE',  ( -5.359611314223446995E-15, 29.16686587814335496, 148.3750000027311842 ) ) ;
#14085 = CARTESIAN_POINT ( 'NONE',  ( 15.72974639402176855, 15.80617190586768217, 96.87609039468568994 ) ) ;
#14087 = CARTESIAN_POINT ( 'NONE',  ( -18.62759615963270932, 10.81492255796079327, 110.8322429386476955 ) ) ;
#14088 = CARTESIAN_POINT ( 'NONE',  ( 5.153800228976335163, 19.02544592524342804, 69.79057627198103830 ) ) ;
#14089 = CARTESIAN_POINT ( 'NONE',  ( 21.52544592524334988, 5.823673210054432836, 86.45942372801901854 ) ) ;
#14090 = CARTESIAN_POINT ( 'NONE',  ( -16.51473224551069308, -9.474510206698971260, 61.66557627198103120 ) ) ;
#14091 = CARTESIAN_POINT ( 'NONE',  ( -19.05341960407611168, -5.049401038298163336, 26.45724293864769550 ) ) ;
#14092 = CARTESIAN_POINT ( 'NONE',  ( 0.05219959533907565091, 21.53943276465977519, 34.99890960531435979 ) ) ;
#14093 = CARTESIAN_POINT ( 'NONE',  ( 14.29746914071049879, -8.314922557960816363, 73.33224293864769550 ) ) ;
#14094 = CARTESIAN_POINT ( 'NONE',  ( 13.89961937509977652, -13.97604488694527269, 43.12390960531434558 ) ) ;
#14095 = CARTESIAN_POINT ( 'NONE',  ( -14.29746914071049879, 8.314922557960819915, 100.8322429386477097 ) ) ;
#14096 = CARTESIAN_POINT ( 'NONE',  ( -21.53943276465977519, 0.05219959533907696930, 106.2489096053143811 ) ) ;
#14097 = CARTESIAN_POINT ( 'NONE',  ( 18.67979575497194134, -10.72451020669871369, 50.83442372801901143 ) ) ;
#14098 = CARTESIAN_POINT ( 'NONE',  ( -16.46253265017160317, 9.564922557960807481, 35.83224293864768839 ) ) ;
#14099 = CARTESIAN_POINT ( 'NONE',  ( 12.14591786802327356, -12.06949235617739191, 50.62609039468568994 ) ) ;
#14100 = CARTESIAN_POINT ( 'NONE',  ( -5.719274019375978568, 21.55341960407610458, 105.2072429386477097 ) ) ;
#14101 = CARTESIAN_POINT ( 'NONE',  ( -18.62759615963270932, 10.81492255796079327, 100.8322429386477097 ) ) ;
#14103 = CARTESIAN_POINT ( 'NONE',  ( -5.049401038298153566, 19.05341960407611168, 50.20724293864770260 ) ) ;
#14102 = CARTESIAN_POINT ( 'NONE',  ( 13.89961937509957401, 13.97604488694547697, 21.87609039468566152 ) ) ;
#14104 = CARTESIAN_POINT ( 'NONE',  ( -9.564922557960796823, -16.46253265017161027, 112.0822429386476955 ) ) ;
#14105 = CARTESIAN_POINT ( 'NONE',  ( -15.80617190586768217, 15.72974639402176855, 58.12609039468568994 ) ) ;
#14106 = ADVANCED_FACE ( 'NONE', ( #101685 ), #83507, .T. ) ;
#14107 = CARTESIAN_POINT ( 'NONE',  ( 0.05219959533907565091, 21.53943276465977519, 39.99890960531436690 ) ) ;
#14108 = CARTESIAN_POINT ( 'NONE',  ( 4.483927247898545687, 16.52544592524342804, 24.79057627198103120 ) ) ;
#14110 = CARTESIAN_POINT ( 'NONE',  ( 10.72451020669871369, 18.67979575497193778, 97.08442372801904696 ) ) ;
#14109 = CARTESIAN_POINT ( 'NONE',  ( 10.72451020669871369, 18.67979575497193778, 62.08442372801901143 ) ) ;
#14111 = CARTESIAN_POINT ( 'NONE',  ( 9.564922557961047289, -16.46253265017146816, 45.41775706135232582 ) ) ;
#14112 = CARTESIAN_POINT ( 'NONE',  ( 8.314922557961029526, -14.29746914071037800, 105.4177570613523613 ) ) ;
#14113 = CARTESIAN_POINT ( 'NONE',  ( -18.62759615963255300, -10.81492255796106328, 54.16775706135235424 ) ) ;
#14114 = CARTESIAN_POINT ( 'NONE',  ( 9.474510206698971260, -16.51473224551069308, 62.91557627198102409 ) ) ;
#14115 = CARTESIAN_POINT ( 'NONE',  ( 5.823673210054444382, -21.52544592524334988, 110.2094237280190185 ) ) ;
#14116 = CARTESIAN_POINT ( 'NONE',  ( -9.474510206698964154, 16.51473224551069663, 115.4155762719810241 ) ) ;
#14117 = CARTESIAN_POINT ( 'NONE',  ( 15.72974639402176855, 15.80617190586768217, 21.87609039468567573 ) ) ;
#14118 = CARTESIAN_POINT ( 'NONE',  ( 21.52544592524344225, -5.823673210054117533, 73.54057627198102409 ) ) ;
#14119 = CARTESIAN_POINT ( 'NONE',  ( -12.06949235617739369, -12.14591786802326823, 44.37609039468567573 ) ) ;
#14121 = CARTESIAN_POINT ( 'NONE',  ( -15.72974639402197994, 15.80617190586746368, 80.62390960531438111 ) ) ;
#14120 = CARTESIAN_POINT ( 'NONE',  ( -6.502951376627836844, 4.381595247748321320, -62.18229462841632937 ) ) ;
#14123 = CARTESIAN_POINT ( 'NONE',  ( 12.06949235617757843, -12.14591786802309237, 78.12390960531436690 ) ) ;
#14122 = CARTESIAN_POINT ( 'NONE',  ( -16.55341960407617563, 4.379528057220093196, 68.54275706135234714 ) ) ;
#14124 = CARTESIAN_POINT ( 'NONE',  ( -37.58407650405589351, 1.968340676919130544E-14, 39.49999999999996447 ) ) ;
#14125 = CARTESIAN_POINT ( 'NONE',  ( -19.02544592524334988, -5.153800228976617603, 103.9594237280190043 ) ) ;
#14126 = CARTESIAN_POINT ( 'NONE',  ( -21.53943276465977519, 0.05219959533907696930, 41.24890960531435269 ) ) ;
#14127 = CARTESIAN_POINT ( 'NONE',  ( -9.474510206698964154, 16.51473224551069663, 95.41557627198102409 ) ) ;
#14128 = CARTESIAN_POINT ( 'NONE',  ( 14.34966873604972726, -8.224510206698740333, 35.83442372801901143 ) ) ;
#14129 = CARTESIAN_POINT ( 'NONE',  ( 15.80617190586746368, 15.72974639402197994, 109.3739096053143811 ) ) ;
#14130 = CARTESIAN_POINT ( 'NONE',  ( 18.67979575497178502, 10.72451020669898547, 29.16557627198103120 ) ) ;
#14131 = CARTESIAN_POINT ( 'NONE',  ( 16.55341960407618274, -4.379528057220086978, 71.04275706135234714 ) ) ;
#14132 = CARTESIAN_POINT ( 'NONE',  ( -19.05341960407611168, -5.049401038298163336, 91.45724293864766707 ) ) ;
#14134 = CARTESIAN_POINT ( 'NONE',  ( 19.03943276465977164, -0.05219959533909143690, 33.74890960531435979 ) ) ;
#14133 = CARTESIAN_POINT ( 'NONE',  ( 5.719274019375673035, 21.55341960407619339, 52.29275706135236135 ) ) ;
#14135 = CARTESIAN_POINT ( 'NONE',  ( -18.62759615963270932, 10.81492255796079327, 30.83224293864770260 ) ) ;
#14136 = ORIENTED_EDGE ( 'NONE', *, *, #6145, .T. ) ;
#14137 = CARTESIAN_POINT ( 'NONE',  ( -5.153800228976607833, 19.02544592524334988, 42.70942372801901143 ) ) ;
#14138 = CARTESIAN_POINT ( 'NONE',  ( 0.05219959533934541429, -16.53943276465976808, 55.00109039468568284 ) ) ;
#14139 = CARTESIAN_POINT ( 'NONE',  ( 19.05341960407611168, 5.049401038298154454, 103.9572429386476671 ) ) ;
#14140 = CARTESIAN_POINT ( 'NONE',  ( -5.823673210054116645, -21.52544592524344225, 102.2905762719810383 ) ) ;
#14141 = CARTESIAN_POINT ( 'NONE',  ( 9.564922557960805705, 16.46253265017160317, 69.58224293864770971 ) ) ;
#14142 = DIRECTION ( 'NONE',  ( 1.000000000000000000, 0.000000000000000000, 0.000000000000000000 ) ) ;
#14143 = CARTESIAN_POINT ( 'NONE',  ( 28.79475375365685963, 9.355982642737862065, 141.3656553485623704 ) ) ;
#14144 = CARTESIAN_POINT ( 'NONE',  ( -12.06949235617756955, 12.14591786802309770, 75.62390960531439532 ) ) ;
#14145 = CARTESIAN_POINT ( 'NONE',  ( 21.52544592524344225, -5.823673210054117533, 38.54057627198103120 ) ) ;
#14146 = CARTESIAN_POINT ( 'NONE',  ( -17.13100169013300444, 6.664070546373152659, 35.76789835699850784 ) ) ;
#14147 = CARTESIAN_POINT ( 'NONE',  ( 16.55341960407618274, -4.379528057220086978, 66.04275706135236135 ) ) ;
#14148 = CARTESIAN_POINT ( 'NONE',  ( 15.80617190586769283, -15.72974639402175789, 25.62609039468567929 ) ) ;
#14149 = CARTESIAN_POINT ( 'NONE',  ( 19.02544592524334988, 5.153800228976608722, 76.45942372801897591 ) ) ;
#14150 = CARTESIAN_POINT ( 'NONE',  ( -5.153800228976328057, -19.02544592524343514, 42.29057627198101699 ) ) ;
#14151 = CARTESIAN_POINT ( 'NONE',  ( 18.62759615963271287, -10.81492255796078972, 73.33224293864769550 ) ) ;
#14152 = CARTESIAN_POINT ( 'NONE',  ( 19.02544592524343514, -5.153800228976328945, 113.5405762719810241 ) ) ;
#14153 = CARTESIAN_POINT ( 'NONE',  ( -10.72451020669870658, -18.67979575497194134, 89.58442372801901854 ) ) ;
#14154 = CARTESIAN_POINT ( 'NONE',  ( 19.05341960407611168, 5.049401038298154454, 68.95724293864769550 ) ) ;
#14155 = CARTESIAN_POINT ( 'NONE',  ( -12.06949235617739369, -12.14591786802326823, 44.37609039468567573 ) ) ;
#14156 = CARTESIAN_POINT ( 'NONE',  ( 19.02544592524343514, -5.153800228976328945, 58.54057627198102409 ) ) ;
#14157 = CARTESIAN_POINT ( 'NONE',  ( 18.67979575497194134, -10.72451020669871369, 75.83442372801900433 ) ) ;
#14158 = CARTESIAN_POINT ( 'NONE',  ( -16.46253265017146816, -9.564922557961047289, 34.16775706135233293 ) ) ;
#14159 = CARTESIAN_POINT ( 'NONE',  ( -0.05219959533936034679, 19.03943276465977164, 52.50109039468566863 ) ) ;
#14160 = CARTESIAN_POINT ( 'NONE',  ( 21.55341960407619695, -5.719274019375665929, 56.04275706135235424 ) ) ;
#14161 = CARTESIAN_POINT ( 'NONE',  ( -18.39639308325437383, -5.500000000000040856, 46.48252246182197922 ) ) ;
#14162 = CARTESIAN_POINT ( 'NONE',  ( 19.03943276465977164, 0.05219959533936151252, 41.25109039468566152 ) ) ;
#14163 = CARTESIAN_POINT ( 'NONE',  ( -13.89961937509977652, 13.97604488694528158, 105.6239096053143527 ) ) ;
#14164 = CARTESIAN_POINT ( 'NONE',  ( 16.46253265017160672, -9.564922557960803928, 68.33224293864770971 ) ) ;
#14165 = CARTESIAN_POINT ( 'NONE',  ( -12.06949235617756955, 12.14591786802309770, 30.62390960531436335 ) ) ;
#14167 = CARTESIAN_POINT ( 'NONE',  ( -21.55341960407619339, 5.719274019375674811, 103.5427570613523613 ) ) ;
#14166 = CARTESIAN_POINT ( 'NONE',  ( 21.55341960407610458, 5.719274019375980345, 28.95724293864769905 ) ) ;
#14168 = CARTESIAN_POINT ( 'NONE',  ( -22.81625015709510507, 31.40387420917330275, -9.424999997268812990 ) ) ;
#14169 = CARTESIAN_POINT ( 'NONE',  ( 16.19135201231368981, 7.376712067591808086, 57.68680854052030327 ) ) ;
#14170 = CARTESIAN_POINT ( 'NONE',  ( -15.72974639402176322, -15.80617190586768395, 104.3760903946856899 ) ) ;
#14171 = DIRECTION ( 'NONE',  ( 0.000000000000000000, 0.000000000000000000, 1.000000000000000000 ) ) ;
#14172 = CARTESIAN_POINT ( 'NONE',  ( 16.46253265017160672, -9.564922557960803928, 23.33224293864769194 ) ) ;
#14173 = CARTESIAN_POINT ( 'NONE',  ( 0.05219959533909260263, 19.03943276465977164, 114.9989096053143669 ) ) ;
#14174 = CARTESIAN_POINT ( 'NONE',  ( 33.92112623720979059, 5.144804392130072124, 93.04721607740081879 ) ) ;
#14175 = CARTESIAN_POINT ( 'NONE',  ( 8.224510206698742110, 14.34966873604972548, 52.08442372801901854 ) ) ;
#14176 = CARTESIAN_POINT ( 'NONE',  ( -21.55341960407610458, -5.719274019375992779, 71.45724293864769550 ) ) ;
#14177 = CARTESIAN_POINT ( 'NONE',  ( 16.52544592524342804, -4.483927247898539470, 43.54057627198103830 ) ) ;
#14179 = CARTESIAN_POINT ( 'NONE',  ( 9.474510206698971260, -16.51473224551069308, 107.9155762719810383 ) ) ;
#14178 = CARTESIAN_POINT ( 'NONE',  ( 14.29746914071049879, -8.314922557960816363, 113.3322429386476955 ) ) ;
#14180 = CARTESIAN_POINT ( 'NONE',  ( -18.62759615963255300, -10.81492255796106328, 29.16775706135234003 ) ) ;
#14181 = CARTESIAN_POINT ( 'NONE',  ( 19.05341960407617918, -5.049401038297876454, 36.04275706135234003 ) ) ;
#14182 = CARTESIAN_POINT ( 'NONE',  ( -14.29746914071049879, 8.314922557960819915, 110.8322429386476955 ) ) ;
#14183 = CARTESIAN_POINT ( 'NONE',  ( 15.72974639402176855, 15.80617190586768217, 71.87609039468568994 ) ) ;
#14184 = CARTESIAN_POINT ( 'NONE',  ( 17.50000000000000711, -5.499999999999992895, 31.21769037696435589 ) ) ;
#14185 = CARTESIAN_POINT ( 'NONE',  ( 16.55341960407611168, 4.379528057220329451, 28.95724293864769905 ) ) ;
#14186 = CARTESIAN_POINT ( 'NONE',  ( 11.40812507854754365, 35.11059874428196537, -5.724999997268812812 ) ) ;
#14187 = CARTESIAN_POINT ( 'NONE',  ( 21.53943276465977519, -0.05219959533907433946, 33.74890960531436690 ) ) ;
#14188 = CARTESIAN_POINT ( 'NONE',  ( 14.34966873604960469, 8.224510206698951720, 84.16557627198103830 ) ) ;
#14189 = CARTESIAN_POINT ( 'NONE',  ( -3.896019243642140584, -5.669039853121431882, -64.40437979500936194 ) ) ;
#14190 = CARTESIAN_POINT ( 'NONE',  ( -0.05219959533909027116, -19.03943276465977164, 77.49890960531435269 ) ) ;
#14191 = CARTESIAN_POINT ( 'NONE',  ( 4.483927247898545687, 16.52544592524342804, 79.79057627198102409 ) ) ;
#14192 = CARTESIAN_POINT ( 'NONE',  ( 0.05219959533936267826, -19.03943276465977164, 110.0010903946856757 ) ) ;
#14193 = CARTESIAN_POINT ( 'NONE',  ( 5.823673210054125526, 21.52544592524343514, 44.79057627198103120 ) ) ;
#14194 = ORIENTED_EDGE ( 'NONE', *, *, #117570, .F. ) ;
#14195 = EDGE_CURVE ( 'NONE', #96881, #9508, #7667, .T. ) ;
#14196 = CARTESIAN_POINT ( 'NONE',  ( -16.46253265017160317, 9.564922557960807481, 25.83224293864769194 ) ) ;
#14198 = CARTESIAN_POINT ( 'NONE',  ( 21.52544592524344225, -5.823673210054117533, 78.54057627198103830 ) ) ;
#14197 = CARTESIAN_POINT ( 'NONE',  ( -9.564922557960796823, -16.46253265017161027, 77.08224293864769550 ) ) ;
#14199 = AXIS2_PLACEMENT_3D ( 'NONE', #66248, #145074, #177443 ) ;
#14201 = CARTESIAN_POINT ( 'NONE',  ( 19.02544592524343514, -5.153800228976328945, 83.54057627198100988 ) ) ;
#14200 = CARTESIAN_POINT ( 'NONE',  ( -16.53943276465976808, -0.05219959533934237506, 103.7510903946857042 ) ) ;
#14202 = CARTESIAN_POINT ( 'NONE',  ( -13.89961937509957401, -13.97604488694547875, 69.37609039468564731 ) ) ;
#14203 = CARTESIAN_POINT ( 'NONE',  ( 15.72974639402176855, 15.80617190586768217, 91.87609039468568994 ) ) ;
#14204 = CARTESIAN_POINT ( 'NONE',  ( 15.72974639402199770, -15.80617190586745480, 63.12390960531435979 ) ) ;
#14205 = CARTESIAN_POINT ( 'NONE',  ( 18.67979575497178502, 10.72451020669898547, 29.16557627198103120 ) ) ;
#14206 = CARTESIAN_POINT ( 'NONE',  ( -9.474510206698964154, 16.51473224551069663, 30.41557627198102054 ) ) ;
#14207 = CARTESIAN_POINT ( 'NONE',  ( -4.483927247898782831, 16.52544592524335698, 97.70942372801904696 ) ) ;
#14208 = CARTESIAN_POINT ( 'NONE',  ( -5.049401038298153566, 19.05341960407611168, 60.20724293864768129 ) ) ;
#14209 = CARTESIAN_POINT ( 'NONE',  ( 4.483927247898790824, -16.52544592524335698, 25.20942372801901854 ) ) ;
#14210 = CARTESIAN_POINT ( 'NONE',  ( 16.29526858892879915, 7.335722546920000475, 53.29670597800210174 ) ) ;
#14211 = CARTESIAN_POINT ( 'NONE',  ( -10.72451020669870658, -18.67979575497194134, 109.5844237280190328 ) ) ;
#14212 = CARTESIAN_POINT ( 'NONE',  ( -8.314922557960811034, -14.29746914071050412, 72.08224293864769550 ) ) ;
#14213 = CARTESIAN_POINT ( 'NONE',  ( 15.72974639402199770, -15.80617190586745480, 103.1239096053143811 ) ) ;
#14214 = CARTESIAN_POINT ( 'NONE',  ( -21.55341960407610458, -5.719274019375992779, 96.45724293864770971 ) ) ;
#14215 = CARTESIAN_POINT ( 'NONE',  ( -19.99604614807126524, -21.49604614807087799, -49.12629558063592583 ) ) ;
#14216 = CARTESIAN_POINT ( 'NONE',  ( -10.72451020669898014, 18.67979575497178502, 40.41557627198103120 ) ) ;
#14217 = CARTESIAN_POINT ( 'NONE',  ( -16.52544592524335698, -4.483927247898792601, 83.95942372801900433 ) ) ;
#14218 = CARTESIAN_POINT ( 'NONE',  ( -8.224510206698948167, 14.34966873604960824, 100.4155762719810241 ) ) ;
#14219 = CARTESIAN_POINT ( 'NONE',  ( 5.049401038298161559, -19.05341960407611168, 57.70724293864769550 ) ) ;
#14220 =( LENGTH_UNIT ( ) NAMED_UNIT ( * ) SI_UNIT ( .MILLI., .METRE. ) );
#14221 = CARTESIAN_POINT ( 'NONE',  ( 14.29746914071049879, -8.314922557960816363, 23.33224293864769194 ) ) ;
#14222 = CARTESIAN_POINT ( 'NONE',  ( 10.72451020669871369, 18.67979575497193778, 42.08442372801901854 ) ) ;
#14223 = CARTESIAN_POINT ( 'NONE',  ( 19.03943276465977164, -0.05219959533909143690, 98.74890960531436690 ) ) ;
#14224 = CARTESIAN_POINT ( 'NONE',  ( -18.67979575497193778, 10.72451020669871902, 83.33442372801903275 ) ) ;
#14225 = CARTESIAN_POINT ( 'NONE',  ( 19.03943276465977164, -0.05219959533909143690, 28.74890960531435624 ) ) ;
#14226 = CARTESIAN_POINT ( 'NONE',  ( 5.153800228976335163, 19.02544592524342804, 39.79057627198100988 ) ) ;
#14227 = VERTEX_POINT ( 'NONE', #177554 ) ;
#14228 = CARTESIAN_POINT ( 'NONE',  ( 10.81492255796106328, -18.62759615963255655, 75.41775706135233293 ) ) ;
#14229 = CARTESIAN_POINT ( 'NONE',  ( 19.05341960407611168, 5.049401038298154454, 103.9572429386476671 ) ) ;
#14230 = CARTESIAN_POINT ( 'NONE',  ( -9.474510206698720793, -16.51473224551083518, 74.58442372801900433 ) ) ;
#14231 = CARTESIAN_POINT ( 'NONE',  ( 10.72451020669871369, 18.67979575497193778, 37.08442372801901143 ) ) ;
#14232 = CARTESIAN_POINT ( 'NONE',  ( -16.53943276465976808, -0.05219959533934237506, 28.75109039468567929 ) ) ;
#14233 = CARTESIAN_POINT ( 'NONE',  ( 16.46253265017146816, 9.564922557961045513, 66.66775706135233293 ) ) ;
#14234 = CARTESIAN_POINT ( 'NONE',  ( 19.02544592524343514, -5.153800228976328945, 48.54057627198103120 ) ) ;
#14235 = CARTESIAN_POINT ( 'NONE',  ( -9.474510206698720793, -16.51473224551083518, 89.58442372801900433 ) ) ;
#14236 = CARTESIAN_POINT ( 'NONE',  ( -8.314922557960811034, -14.29746914071050412, 32.08224293864769550 ) ) ;
#14237 = CARTESIAN_POINT ( 'NONE',  ( -0.05219959533936034679, 19.03943276465977164, 82.50109039468567573 ) ) ;
#14238 = CARTESIAN_POINT ( 'NONE',  ( 4.483927247898545687, 16.52544592524342804, 34.79057627198103120 ) ) ;
#14239 = CARTESIAN_POINT ( 'NONE',  ( 16.46253265017146816, 9.564922557961045513, 66.66775706135233293 ) ) ;
#14240 = CARTESIAN_POINT ( 'NONE',  ( 16.52544592524335698, 4.483927247898782831, 41.45942372801901143 ) ) ;
#14241 = CARTESIAN_POINT ( 'NONE',  ( 15.72974639402176855, 15.80617190586768217, 111.8760903946856615 ) ) ;
#14242 = CARTESIAN_POINT ( 'NONE',  ( 5.153800228976335163, 19.02544592524342804, 29.79057627198102409 ) ) ;
#14243 = CARTESIAN_POINT ( 'NONE',  ( -16.52216118717208460, -7.221426719304528064, 66.07599021046993926 ) ) ;
#14244 = CARTESIAN_POINT ( 'NONE',  ( 0.05219959533934541429, -16.53943276465976808, 50.00109039468568994 ) ) ;
#14245 = CARTESIAN_POINT ( 'NONE',  ( 2.400000000000000799, 0.000000000000000000, 2.199999999999999289 ) ) ;
#14246 = CARTESIAN_POINT ( 'NONE',  ( -22.44159573604009950, -16.30477369853688430, 147.0750000027312012 ) ) ;
#14247 = CARTESIAN_POINT ( 'NONE',  ( 13.89961937509977652, -13.97604488694527269, 88.12390960531438111 ) ) ;
#14248 = LINE ( 'NONE', #45591, #191110 ) ;
#14249 = CIRCLE ( 'NONE', #127243, 1.500000000000001332 ) ;
#14250 = VERTEX_POINT ( 'NONE', #128020 ) ;
#14251 = CARTESIAN_POINT ( 'NONE',  ( -9.564922557961040184, 16.46253265017147172, 87.91775706135233293 ) ) ;
#14252 = CARTESIAN_POINT ( 'NONE',  ( -19.02544592524342804, 5.153800228976336051, 116.0405762719810383 ) ) ;
#14254 = CARTESIAN_POINT ( 'NONE',  ( -9.474510206698720793, -16.51473224551083518, 99.58442372801900433 ) ) ;
#14253 = CARTESIAN_POINT ( 'NONE',  ( 15.72974639402176855, 15.80617190586768217, 111.8760903946856615 ) ) ;
#14255 = CARTESIAN_POINT ( 'NONE',  ( 16.53943276465976808, -0.05219959533910856209, 113.7489096053143527 ) ) ;
#14256 = CARTESIAN_POINT ( 'NONE',  ( -5.049401038298153566, 19.05341960407611168, 40.20724293864768839 ) ) ;
#14257 = CARTESIAN_POINT ( 'NONE',  ( 10.72451020669898902, -18.67979575497178502, 52.91557627198103830 ) ) ;
#14258 = MECHANICAL_DESIGN_GEOMETRIC_PRESENTATION_REPRESENTATION (  '', ( #166125 ), #191927 ) ;
#14259 =( BOUNDED_CURVE ( )  B_SPLINE_CURVE ( 2, ( #54227, #8727, #193753, #106697, #135079, #181576, #168370, #91503, #150246, #45039, #29866 ),
 .UNSPECIFIED., .F., .F. ) 
 B_SPLINE_CURVE_WITH_KNOTS ( ( 3, 2, 2, 2, 2, 3 ),
 ( 0.000000000000000000, 0.02000000000000001776, 0.04000000000000003553, 0.06000000000000005329, 0.08000000000000007105, 0.1000000000000000888 ),
 .UNSPECIFIED. ) 
 CURVE ( )  GEOMETRIC_REPRESENTATION_ITEM ( )  RATIONAL_B_SPLINE_CURVE ( ( 1.000000000000000000, 0.9510565162951535312, 1.000000000000000000, 0.9510565162951535312, 1.000000000000000000, 0.9510565162951535312, 1.000000000000000000, 0.9510565162951535312, 1.000000000000000000, 0.9510565162951533091, 1.000000000000000222 ) ) 
 REPRESENTATION_ITEM ( '' )  );
#14260 = CARTESIAN_POINT ( 'NONE',  ( 0.05219959533907565091, 21.53943276465977519, 54.99890960531435269 ) ) ;
#14261 = CARTESIAN_POINT ( 'NONE',  ( -16.51473224551069308, -9.474510206698971260, 26.66557627198103120 ) ) ;
#14262 = CARTESIAN_POINT ( 'NONE',  ( -28.82186960331514669, -9.364793116373306248, 142.3500000054623911 ) ) ;
#14263 = CARTESIAN_POINT ( 'NONE',  ( -9.474510206698720793, -16.51473224551083518, 69.58442372801901854 ) ) ;
#14264 = CARTESIAN_POINT ( 'NONE',  ( -12.14591786802309592, -12.06949235617757132, 36.87390960531435979 ) ) ;
#14265 = CARTESIAN_POINT ( 'NONE',  ( -5.823673210054116645, -21.52544592524344225, 22.29057627198102765 ) ) ;
#14266 = CARTESIAN_POINT ( 'NONE',  ( -15.72974639402176322, -15.80617190586768395, 99.37609039468568994 ) ) ;
#14267 = CARTESIAN_POINT ( 'NONE',  ( 5.823673210054125526, 21.52544592524343514, 79.79057627198102409 ) ) ;
#14268 = CARTESIAN_POINT ( 'NONE',  ( -5.823673210054431948, 21.52544592524334988, 62.70942372801902565 ) ) ;
#14269 = CARTESIAN_POINT ( 'NONE',  ( 10.81492255796106328, -18.62759615963255655, 70.41775706135236135 ) ) ;
#14270 = CARTESIAN_POINT ( 'NONE',  ( -19.02544592524342804, 5.153800228976336051, 91.04057627198100988 ) ) ;
#14272 = CARTESIAN_POINT ( 'NONE',  ( 21.55341960407619695, -5.719274019375665929, 46.04275706135234714 ) ) ;
#14271 = CARTESIAN_POINT ( 'NONE',  ( -4.483927247898782831, 16.52544592524335698, 97.70942372801904696 ) ) ;
#14273 = CARTESIAN_POINT ( 'NONE',  ( -19.05341960407611168, -5.049401038298163336, 26.45724293864769550 ) ) ;
#14274 = CARTESIAN_POINT ( 'NONE',  ( -31.64616484836360755, 2.655180720736634026, 102.0186121717492824 ) ) ;
#14275 = CARTESIAN_POINT ( 'NONE',  ( -8.224510206698948167, 14.34966873604960824, 70.41557627198102409 ) ) ;
#14276 = CARTESIAN_POINT ( 'NONE',  ( -4.379528057220328563, 16.55341960407611168, 30.20724293864769550 ) ) ;
#14277 = CARTESIAN_POINT ( 'NONE',  ( -5.719274019375978568, 21.55341960407610458, 40.20724293864769550 ) ) ;
#14278 = CARTESIAN_POINT ( 'NONE',  ( 9.564922557960805705, 16.46253265017160317, 69.58224293864770971 ) ) ;
#14279 = CARTESIAN_POINT ( 'NONE',  ( 5.153800228976335163, 19.02544592524342804, 44.79057627198103830 ) ) ;
#14280 = CARTESIAN_POINT ( 'NONE',  ( 21.52544592524344225, -5.823673210054117533, 58.54057627198103120 ) ) ;
#14282 = VECTOR ( 'NONE', #46913, 1000.000000000000000 ) ;
#14281 = CARTESIAN_POINT ( 'NONE',  ( -16.46253265017146816, -9.564922557961047289, 39.16775706135234003 ) ) ;
#14284 = CARTESIAN_POINT ( 'NONE',  ( -8.224510206698948167, 14.34966873604960824, 50.41557627198103120 ) ) ;
#14283 = CARTESIAN_POINT ( 'NONE',  ( 22.99604614807109826, -21.66199780171331923, -49.53544670972640773 ) ) ;
#14285 = CARTESIAN_POINT ( 'NONE',  ( -16.46253265017160317, 9.564922557960807481, 115.8322429386477097 ) ) ;
#14286 = EDGE_LOOP ( 'NONE', ( #183716, #59594, #152016, #13480 ) ) ;
#14287 = CARTESIAN_POINT ( 'NONE',  ( 17.59632111031587343, 2.707012485675212243, 37.50000000000002842 ) ) ;
#14288 = CARTESIAN_POINT ( 'NONE',  ( 16.52544592524335698, 4.483927247898782831, 66.45942372801903275 ) ) ;
#14289 = CARTESIAN_POINT ( 'NONE',  ( -19.02544592524334988, -5.153800228976617603, 73.95942372801900433 ) ) ;
#14290 = CARTESIAN_POINT ( 'NONE',  ( 4.483927247898545687, 16.52544592524342804, 34.79057627198103120 ) ) ;
#14291 = ORIENTED_EDGE ( 'NONE', *, *, #192660, .T. ) ;
#14292 = CARTESIAN_POINT ( 'NONE',  ( 193.3062444957835453, -155.7167183371837496, -15.00000000000000178 ) ) ;
#14293 = CARTESIAN_POINT ( 'NONE',  ( -16.53943276465976808, -0.05219959533934237506, 113.7510903946856757 ) ) ;
#14294 = CARTESIAN_POINT ( 'NONE',  ( 5.153800228976335163, 19.02544592524342804, 54.79057627198103120 ) ) ;
#14295 = CARTESIAN_POINT ( 'NONE',  ( -13.89961937509977652, 13.97604488694528158, 75.62390960531438111 ) ) ;
#14296 = CARTESIAN_POINT ( 'NONE',  ( -19.05341960407611168, -5.049401038298163336, 36.45724293864766707 ) ) ;
#14297 = CARTESIAN_POINT ( 'NONE',  ( -5.719274019375665041, -21.55341960407619695, 44.79275706135234714 ) ) ;
#14298 = CARTESIAN_POINT ( 'NONE',  ( 0.05219959533909260263, 19.03943276465977164, 64.99890960531436690 ) ) ;
#14299 = CARTESIAN_POINT ( 'NONE',  ( 5.000000000000001776, -130.0000000000000000, -15.00000000000000000 ) ) ;
#14300 = CARTESIAN_POINT ( 'NONE',  ( 16.46253265017160672, -9.564922557960803928, 63.33224293864769550 ) ) ;
#14301 = EDGE_CURVE ( 'NONE', #176889, #29612, #38026, .T. ) ;
#14302 = CARTESIAN_POINT ( 'NONE',  ( -5.823673210054116645, -21.52544592524344225, 37.29057627198102409 ) ) ;
#14303 = CARTESIAN_POINT ( 'NONE',  ( -19.03943276465977164, 0.05219959533909376836, 26.24890960531435624 ) ) ;
#14304 = CARTESIAN_POINT ( 'NONE',  ( 15.80617190586746368, 15.72974639402197994, 29.37390960531435269 ) ) ;
#14305 = CARTESIAN_POINT ( 'NONE',  ( 4.483927247898790824, -16.52544592524335698, 85.20942372801901854 ) ) ;
#14306 = CARTESIAN_POINT ( 'NONE',  ( -5.719274019375665041, -21.55341960407619695, 104.7927570613523898 ) ) ;
#14307 = CARTESIAN_POINT ( 'NONE',  ( 12.06949235617739724, 12.14591786802326823, 61.87609039468568284 ) ) ;
#14308 = CARTESIAN_POINT ( 'NONE',  ( 13.89961937509977652, -13.97604488694527269, 113.1239096053143527 ) ) ;
#14309 = EDGE_CURVE ( 'NONE', #114568, #105306, #48259, .T. ) ;
#14310 = CARTESIAN_POINT ( 'NONE',  ( 14.34966873604972726, -8.224510206698740333, 55.83442372801901854 ) ) ;
#14311 = CARTESIAN_POINT ( 'NONE',  ( -14.34966873604972548, 8.224510206698743886, 43.33442372801901143 ) ) ;
#14312 = CARTESIAN_POINT ( 'NONE',  ( 19.02544592524343514, -5.153800228976328945, 108.5405762719810383 ) ) ;
#14313 = VECTOR ( 'NONE', #102691, 1000.000000000000114 ) ;
#14314 = CARTESIAN_POINT ( 'NONE',  ( -14.29746914071037622, -8.314922557961029526, 24.16775706135235424 ) ) ;
#14315 = CARTESIAN_POINT ( 'NONE',  ( 16.51473224551069308, 9.474510206698969483, 39.16557627198103120 ) ) ;
#14316 = CARTESIAN_POINT ( 'NONE',  ( 5.823673210054444382, -21.52544592524334988, 30.20942372801902565 ) ) ;
#14317 = CARTESIAN_POINT ( 'NONE',  ( 16.52544592524335698, 4.483927247898782831, 21.45942372801901499 ) ) ;
#14318 = CARTESIAN_POINT ( 'NONE',  ( -0.05219959533934338120, 16.53943276465976808, 87.50109039468568994 ) ) ;
#14319 = CARTESIAN_POINT ( 'NONE',  ( -17.49999999999999289, 5.624438216177559013, 45.81670344914643778 ) ) ;
#14320 = CARTESIAN_POINT ( 'NONE',  ( -15.80617190586768217, 15.72974639402176855, 93.12609039468568994 ) ) ;
#14321 = CARTESIAN_POINT ( 'NONE',  ( 19.03943276465977164, 0.05219959533936151252, 81.25109039468567573 ) ) ;
#14322 = CARTESIAN_POINT ( 'NONE',  ( -16.52544592524342804, 4.483927247898546575, 61.04057627198103120 ) ) ;
#14323 = CARTESIAN_POINT ( 'NONE',  ( -0.05219959533910754901, -16.53943276465976808, 112.4989096053143669 ) ) ;
#14325 = CARTESIAN_POINT ( 'NONE',  ( 17.05116617787849620, -6.768360034955525073, 56.15675553259194430 ) ) ;
#14324 = CARTESIAN_POINT ( 'NONE',  ( -13.89961937509957401, -13.97604488694547875, 44.37609039468566863 ) ) ;
#14326 = CARTESIAN_POINT ( 'NONE',  ( 15.72974639402176855, 15.80617190586768217, 46.87609039468568994 ) ) ;
#14327 = CARTESIAN_POINT ( 'NONE',  ( -0.05219959533936034679, 19.03943276465977164, 112.5010903946856757 ) ) ;
#14328 = CARTESIAN_POINT ( 'NONE',  ( -30.00000000000000000, -5.510910596163089556E-15, 45.00000000000000000 ) ) ;
#14329 = CARTESIAN_POINT ( 'NONE',  ( 16.51473224551069308, 9.474510206698969483, 109.1655762719810383 ) ) ;
#14330 = CARTESIAN_POINT ( 'NONE',  ( 15.80617190586746368, 15.72974639402197994, 74.37390960531436690 ) ) ;
#14331 = CARTESIAN_POINT ( 'NONE',  ( -19.05341960407617563, 5.049401038297882671, 93.54275706135234714 ) ) ;
#14332 = CARTESIAN_POINT ( 'NONE',  ( 0.05219959533909260263, 19.03943276465977164, 104.9989096053143669 ) ) ;
#14333 = CARTESIAN_POINT ( 'NONE',  ( -16.46253265017146816, -9.564922557961047289, 49.16775706135233293 ) ) ;
#14334 = CARTESIAN_POINT ( 'NONE',  ( -16.52544592524342804, 4.483927247898546575, 101.0405762719810383 ) ) ;
#14335 = CARTESIAN_POINT ( 'NONE',  ( 5.823673210054444382, -21.52544592524334988, 90.20942372801903275 ) ) ;
#14336 = CARTESIAN_POINT ( 'NONE',  ( -9.474510206698964154, 16.51473224551069663, 45.41557627198103120 ) ) ;
#14337 = CARTESIAN_POINT ( 'NONE',  ( 10.72451020669871369, 18.67979575497193778, 52.08442372801901854 ) ) ;
#14338 = CARTESIAN_POINT ( 'NONE',  ( -21.52544592524334988, -5.823673210054445271, 93.95942372801903275 ) ) ;
#14339 = CARTESIAN_POINT ( 'NONE',  ( -14.29746914071037622, -8.314922557961029526, 94.16775706135237556 ) ) ;
#14340 = CARTESIAN_POINT ( 'NONE',  ( -18.62759615963255300, -10.81492255796106328, 44.16775706135234714 ) ) ;
#14341 = CARTESIAN_POINT ( 'NONE',  ( -21.55341960407619339, 5.719274019375674811, 33.54275706135234714 ) ) ;
#14343 = CARTESIAN_POINT ( 'NONE',  ( 13.97604488694527802, 13.89961937509977652, 89.37390960531436690 ) ) ;
#14342 = CARTESIAN_POINT ( 'NONE',  ( 19.05341960407617918, -5.049401038297876454, 61.04275706135232582 ) ) ;
#14344 = CARTESIAN_POINT ( 'NONE',  ( -4.483927247898539470, -16.52544592524342804, 107.2905762719810525 ) ) ;
#14345 = EDGE_CURVE ( 'NONE', #48561, #19028, #114532, .T. ) ;
#14346 = CARTESIAN_POINT ( 'NONE',  ( 10.72451020669898902, -18.67979575497178502, 82.91557627198103830 ) ) ;
#14347 = CARTESIAN_POINT ( 'NONE',  ( 16.52544592524342804, -4.483927247898539470, 58.54057627198103120 ) ) ;
#14348 = CARTESIAN_POINT ( 'NONE',  ( -21.55341960407619339, 5.719274019375674811, 103.5427570613523613 ) ) ;
#14349 = CARTESIAN_POINT ( 'NONE',  ( 16.53943276465976808, -0.05219959533910856209, 78.74890960531436690 ) ) ;
#14350 = CARTESIAN_POINT ( 'NONE',  ( -9.564922557960796823, -16.46253265017161027, 42.08224293864769550 ) ) ;
#14351 = CARTESIAN_POINT ( 'NONE',  ( -9.474510206698720793, -16.51473224551083518, 84.58442372801900433 ) ) ;
#14352 = CARTESIAN_POINT ( 'NONE',  ( 12.14591786802309770, 12.06949235617756955, 49.37390960531436690 ) ) ;
#14353 = CARTESIAN_POINT ( 'NONE',  ( 15.72974639402176855, 15.80617190586768217, 96.87609039468568994 ) ) ;
#14354 = CARTESIAN_POINT ( 'NONE',  ( -19.05341960407611168, -5.049401038298163336, 86.45724293864769550 ) ) ;
#14355 = CARTESIAN_POINT ( 'NONE',  ( 5.153800228976615827, -19.02544592524334988, 60.20942372801899012 ) ) ;
#14356 = CARTESIAN_POINT ( 'NONE',  ( 18.62759615963271287, -10.81492255796078972, 63.33224293864770260 ) ) ;
#14357 = CARTESIAN_POINT ( 'NONE',  ( -15.72974639402176322, -15.80617190586768395, 24.37609039468567573 ) ) ;
#14358 = CARTESIAN_POINT ( 'NONE',  ( -14.29746914071037622, -8.314922557961029526, 29.16775706135234003 ) ) ;
#14359 = CARTESIAN_POINT ( 'NONE',  ( -8.224510206698735004, -14.34966873604973081, 74.58442372801901854 ) ) ;
#14361 = CARTESIAN_POINT ( 'NONE',  ( 15.80617190586746368, 15.72974639402197994, 114.3739096053143527 ) ) ;
#14360 = CARTESIAN_POINT ( 'NONE',  ( 19.03943276465977164, -0.05219959533909143690, 23.74890960531435269 ) ) ;
#14362 = CARTESIAN_POINT ( 'NONE',  ( -0.05219959533910754901, -16.53943276465976808, 112.4989096053143669 ) ) ;
#14363 = CARTESIAN_POINT ( 'NONE',  ( 11.40812507854755253, -35.11059874428192273, -6.524999997268813523 ) ) ;
#14364 = CARTESIAN_POINT ( 'NONE',  ( -0.05219959533934338120, 16.53943276465976808, 42.50109039468567573 ) ) ;
#14365 = CARTESIAN_POINT ( 'NONE',  ( 12.06949235617757843, -12.14591786802309237, 83.12390960531436690 ) ) ;
#14366 = CARTESIAN_POINT ( 'NONE',  ( -5.719274019375978568, 21.55341960407610458, 80.20724293864769550 ) ) ;
#14367 = CARTESIAN_POINT ( 'NONE',  ( -0.05219959533910754901, -16.53943276465976808, 22.49890960531436335 ) ) ;
#14368 = CARTESIAN_POINT ( 'NONE',  ( 4.483927247898790824, -16.52544592524335698, 35.20942372801901854 ) ) ;
#14369 = CARTESIAN_POINT ( 'NONE',  ( -13.97604488694527625, -13.89961937509977652, 51.87390960531436690 ) ) ;
#14370 = CARTESIAN_POINT ( 'NONE',  ( -12.06949235617739369, -12.14591786802326823, 84.37609039468570415 ) ) ;
#14371 = CARTESIAN_POINT ( 'NONE',  ( -13.97604488694547697, 13.89961937509957934, 73.12609039468568994 ) ) ;
#14372 = CARTESIAN_POINT ( 'NONE',  ( -21.55341960407610458, -5.719274019375992779, 66.45724293864768129 ) ) ;
#14373 = CARTESIAN_POINT ( 'NONE',  ( -8.224510206698735004, -14.34966873604973081, 109.5844237280190328 ) ) ;
#14374 = ORIENTED_EDGE ( 'NONE', *, *, #48933, .T. ) ;
#14375 = CARTESIAN_POINT ( 'NONE',  ( 25.85231681326528985, 7.957828899753591756, 172.6576833274792762 ) ) ;
#14376 = CARTESIAN_POINT ( 'NONE',  ( 5.823673210054125526, 21.52544592524343514, 49.79057627198102409 ) ) ;
#14377 = VERTEX_POINT ( 'NONE', #39023 ) ;
#14378 = CARTESIAN_POINT ( 'NONE',  ( -4.379528057220086978, -16.55341960407618274, 89.79275706135236135 ) ) ;
#14379 = ORIENTED_EDGE ( 'NONE', *, *, #143946, .T. ) ;
#14380 = CARTESIAN_POINT ( 'NONE',  ( -16.46253265017160317, 9.564922557960807481, 115.8322429386477097 ) ) ;
#14381 = CARTESIAN_POINT ( 'NONE',  ( 17.50000000000000000, 5.499999999999997335, 106.7030961746582847 ) ) ;
#14382 = CARTESIAN_POINT ( 'NONE',  ( -21.52544592524343514, 5.823673210054127303, 76.04057627198102409 ) ) ;
#14383 = CARTESIAN_POINT ( 'NONE',  ( -16.52544592524335698, -4.483927247898792601, 108.9594237280190185 ) ) ;
#14384 = CARTESIAN_POINT ( 'NONE',  ( -5.823673210054431948, 21.52544592524334988, 62.70942372801902565 ) ) ;
#14385 = CARTESIAN_POINT ( 'NONE',  ( 4.483927247898790824, -16.52544592524335698, 25.20942372801901854 ) ) ;
#14386 = CARTESIAN_POINT ( 'NONE',  ( 5.153800228976335163, 19.02544592524342804, 24.79057627198102765 ) ) ;
#14387 = CARTESIAN_POINT ( 'NONE',  ( -16.52544592524335698, -4.483927247898792601, 23.95942372801901143 ) ) ;
#14388 = CARTESIAN_POINT ( 'NONE',  ( 13.89961937509977652, -13.97604488694527269, 58.12390960531436690 ) ) ;
#14389 = CARTESIAN_POINT ( 'NONE',  ( 16.64831001466047056, -0.4033639900674985679, -61.36868776158050309 ) ) ;
#14390 = CARTESIAN_POINT ( 'NONE',  ( 5.153800228976335163, 19.02544592524342804, 109.7905762719810099 ) ) ;
#14391 = AXIS2_PLACEMENT_3D ( 'NONE', #152755, #167938, #196321 ) ;
#14392 = CARTESIAN_POINT ( 'NONE',  ( -12.06949235617739369, -12.14591786802326823, 94.37609039468568994 ) ) ;
#14393 = CARTESIAN_POINT ( 'NONE',  ( -13.89961937509957401, -13.97604488694547875, 94.37609039468566152 ) ) ;
#14394 = CARTESIAN_POINT ( 'NONE',  ( 5.153800228976615827, -19.02544592524334988, 25.20942372801900433 ) ) ;
#14395 = CARTESIAN_POINT ( 'NONE',  ( -10.72451020669898014, 18.67979575497178502, 70.41557627198102409 ) ) ;
#14396 = CARTESIAN_POINT ( 'NONE',  ( -16.55341960407617563, 4.379528057220093196, 98.54275706135234714 ) ) ;
#14397 = CARTESIAN_POINT ( 'NONE',  ( -0.05219959533936034679, 19.03943276465977164, 92.50109039468566152 ) ) ;
#14398 = CARTESIAN_POINT ( 'NONE',  ( -19.03943276465977164, 0.05219959533909376836, 56.24890960531435979 ) ) ;
#14400 = CIRCLE ( 'NONE', #49903, 1.000000000000000888 ) ;
#14399 = CARTESIAN_POINT ( 'NONE',  ( -9.474510206698964154, 16.51473224551069663, 95.41557627198102409 ) ) ;
#14401 = CARTESIAN_POINT ( 'NONE',  ( -15.80617190586768217, 15.72974639402176855, 68.12609039468567573 ) ) ;
#14402 = CARTESIAN_POINT ( 'NONE',  ( 16.46253265017160672, -9.564922557960803928, 48.33224293864769550 ) ) ;
#14403 = CARTESIAN_POINT ( 'NONE',  ( -33.78191506369886810, -21.41920200728862511, -24.99999999999999289 ) ) ;
#14404 = CARTESIAN_POINT ( 'NONE',  ( 16.52544592524342804, -4.483927247898539470, 73.54057627198102409 ) ) ;
#14405 = CARTESIAN_POINT ( 'NONE',  ( -18.67979575497178146, -10.72451020669898902, 71.66557627198100988 ) ) ;
#14406 = AXIS2_PLACEMENT_3D ( 'NONE', #17983, #47326, #79636 ) ;
#14407 = CARTESIAN_POINT ( 'NONE',  ( 9.474510206698729675, 16.51473224551082808, 37.08442372801899722 ) ) ;
#14408 = DIRECTION ( 'NONE',  ( 0.000000000000000000, 0.7071067811865467956, -0.7071067811865483499 ) ) ;
#14410 = CARTESIAN_POINT ( 'NONE',  ( -19.02544592524342804, 5.153800228976336051, 91.04057627198100988 ) ) ;
#14409 = CARTESIAN_POINT ( 'NONE',  ( 13.89961937509977652, -13.97604488694527269, 83.12390960531436690 ) ) ;
#14411 = CARTESIAN_POINT ( 'NONE',  ( 8.314922557961029526, -14.29746914071037800, 50.41775706135235424 ) ) ;
#14412 = LINE ( 'NONE', #123561, #1657 ) ;
#14413 = CARTESIAN_POINT ( 'NONE',  ( -5.049401038297874678, -19.05341960407617918, 24.79275706135233648 ) ) ;
#14414 = LINE ( 'NONE', #123563, #33888 ) ;
#14415 = CARTESIAN_POINT ( 'NONE',  ( -8.314922557961024197, 14.29746914071037800, 82.91775706135234714 ) ) ;
#14416 = FACE_OUTER_BOUND ( 'NONE', #72162, .T. ) ;
#14417 = CARTESIAN_POINT ( 'NONE',  ( -4.379528057220086978, -16.55341960407618274, 79.79275706135236135 ) ) ;
#14418 = CARTESIAN_POINT ( 'NONE',  ( -14.34966873604972548, 8.224510206698743886, 53.33442372801901854 ) ) ;
#14420 = CARTESIAN_POINT ( 'NONE',  ( -5.000000000000000000, -139.8289899283371653, 13.46984631039294200 ) ) ;
#14419 = CARTESIAN_POINT ( 'NONE',  ( -19.05341960407611168, -5.049401038298163336, 51.45724293864770260 ) ) ;
#14421 = CARTESIAN_POINT ( 'NONE',  ( -21.55341960407619339, 5.719274019375674811, 63.54275706135234003 ) ) ;
#14422 = CARTESIAN_POINT ( 'NONE',  ( 9.564922557961047289, -16.46253265017146816, 75.41775706135234714 ) ) ;
#14423 = CARTESIAN_POINT ( 'NONE',  ( 15.72974639402176855, 15.80617190586768217, 101.8760903946857042 ) ) ;
#14424 = CARTESIAN_POINT ( 'NONE',  ( 19.03943276465977164, -0.05219959533909143690, 58.74890960531435979 ) ) ;
#14425 = CARTESIAN_POINT ( 'NONE',  ( 5.049401038298161559, -19.05341960407611168, 37.70724293864768839 ) ) ;
#14426 = CARTESIAN_POINT ( 'NONE',  ( 16.35915291253759207, 7.306589564586257524, 22.28015278803768595 ) ) ;
#14427 = CARTESIAN_POINT ( 'NONE',  ( 18.62759615963271287, -10.81492255796078972, 63.33224293864770260 ) ) ;
#14428 = AXIS2_PLACEMENT_3D ( 'NONE', #96766, #158455, #89350 ) ;
#14429 = EDGE_CURVE ( 'NONE', #171876, #150360, #132028, .T. ) ;
#14430 = CARTESIAN_POINT ( 'NONE',  ( 9.564922557960805705, 16.46253265017160317, 114.5822429386476955 ) ) ;
#14431 = CARTESIAN_POINT ( 'NONE',  ( 19.05341960407611168, 5.049401038298154454, 23.95724293864769194 ) ) ;
#14432 = CARTESIAN_POINT ( 'NONE',  ( 12.06949235617739724, 12.14591786802326823, 56.87609039468568994 ) ) ;
#14433 = CARTESIAN_POINT ( 'NONE',  ( -14.34966873604960291, -8.224510206698953496, 26.66557627198103475 ) ) ;
#14434 = ORIENTED_EDGE ( 'NONE', *, *, #137956, .F. ) ;
#14435 = CARTESIAN_POINT ( 'NONE',  ( -5.823673210054431948, 21.52544592524334988, 22.70942372801901499 ) ) ;
#14437 = CARTESIAN_POINT ( 'NONE',  ( -38.00000000000000711, 2.428612866367529932E-14, -6.000000000000000000 ) ) ;
#14436 = CARTESIAN_POINT ( 'NONE',  ( 4.483927247898545687, 16.52544592524342804, 54.79057627198104541 ) ) ;
#14438 = CARTESIAN_POINT ( 'NONE',  ( -9.474510206698720793, -16.51473224551083518, 104.5844237280190043 ) ) ;
#14439 = CARTESIAN_POINT ( 'NONE',  ( -9.474510206698720793, -16.51473224551083518, 44.58442372801900433 ) ) ;
#14440 = CARTESIAN_POINT ( 'NONE',  ( -16.52544592524342804, 4.483927247898546575, 51.04057627198103120 ) ) ;
#14441 = CARTESIAN_POINT ( 'NONE',  ( 21.52544592524344225, -5.823673210054117533, 98.54057627198105251 ) ) ;
#14443 = CARTESIAN_POINT ( 'NONE',  ( 21.53943276465977519, -0.05219959533907433946, 58.74890960531436690 ) ) ;
#14442 = DIRECTION ( 'NONE',  ( 0.000000000000000000, 0.000000000000000000, 1.000000000000000000 ) ) ;
#14444 = CARTESIAN_POINT ( 'NONE',  ( -13.89961937509977652, 13.97604488694528158, 95.62390960531436690 ) ) ;
#14445 = CARTESIAN_POINT ( 'NONE',  ( 12.14591786802309770, 12.06949235617756955, 49.37390960531436690 ) ) ;
#14446 = CARTESIAN_POINT ( 'NONE',  ( -13.97604488694527625, -13.89961937509977652, 106.8739096053143669 ) ) ;
#14447 = CARTESIAN_POINT ( 'NONE',  ( 1.304248841091933035E-15, 21.30000000000002913, -58.85720012050612837 ) ) ;
#14448 = CARTESIAN_POINT ( 'NONE',  ( 13.89961937509957401, 13.97604488694547697, 56.87609039468564731 ) ) ;
#14449 = CARTESIAN_POINT ( 'NONE',  ( -21.52544592524343514, 5.823673210054127303, 96.04057627198102409 ) ) ;
#14450 = CARTESIAN_POINT ( 'NONE',  ( -9.564922557960796823, -16.46253265017161027, 37.08224293864768839 ) ) ;
#14451 = CARTESIAN_POINT ( 'NONE',  ( 12.14591786802309770, 12.06949235617756955, 114.3739096053143527 ) ) ;
#14452 = CARTESIAN_POINT ( 'NONE',  ( 15.72974639402176855, 15.80617190586768217, 56.87609039468568994 ) ) ;
#14453 = CARTESIAN_POINT ( 'NONE',  ( -5.359611314223446995E-15, 29.16686587814335496, 146.3750000027311842 ) ) ;
#14454 = CARTESIAN_POINT ( 'NONE',  ( -14.34966873604960291, -8.224510206698953496, 21.66557627198102409 ) ) ;
#14455 = CARTESIAN_POINT ( 'NONE',  ( 16.46253265017160672, -9.564922557960803928, 48.33224293864769550 ) ) ;
#14456 = CARTESIAN_POINT ( 'NONE',  ( 19.02544592524343514, -5.153800228976328945, 98.54057627198100988 ) ) ;
#14457 = CARTESIAN_POINT ( 'NONE',  ( 15.80617190586746368, 15.72974639402197994, 64.37390960531435269 ) ) ;
#14458 = CARTESIAN_POINT ( 'NONE',  ( 17.14385361876520264, 23.59649016807275856, 142.1750000027311671 ) ) ;
#14459 = CARTESIAN_POINT ( 'NONE',  ( -5.049401038298153566, 19.05341960407611168, 50.20724293864770260 ) ) ;
#14460 = CARTESIAN_POINT ( 'NONE',  ( 5.719274019375991003, -21.55341960407610458, 52.70724293864769550 ) ) ;
#14461 = EDGE_CURVE ( 'NONE', #89527, #45563, #88726, .T. ) ;
#14462 = CARTESIAN_POINT ( 'NONE',  ( 18.67979575497194134, -10.72451020669871369, 90.83442372801901854 ) ) ;
#14465 = CARTESIAN_POINT ( 'NONE',  ( 16.52544592524342804, -4.483927247898539470, 73.54057627198102409 ) ) ;
#14464 = CARTESIAN_POINT ( 'NONE',  ( 14.29746914071037800, 8.314922557961029526, 86.66775706135234714 ) ) ;
#14463 = CARTESIAN_POINT ( 'NONE',  ( 16.29108346408296271, -34.51247628902855524, -22.00899094813389567 ) ) ;
#14466 = CARTESIAN_POINT ( 'NONE',  ( 16.55341960407618274, -4.379528057220086978, 86.04275706135236135 ) ) ;
#14467 = CARTESIAN_POINT ( 'NONE',  ( 9.474510206698971260, -16.51473224551069308, 72.91557627198102409 ) ) ;
#14468 = ORIENTED_EDGE ( 'NONE', *, *, #106967, .T. ) ;
#14469 = CARTESIAN_POINT ( 'NONE',  ( -13.97604488694547697, 13.89961937509957934, 33.12609039468566863 ) ) ;
#14470 = CARTESIAN_POINT ( 'NONE',  ( -8.314922557961024197, 14.29746914071037800, 87.91775706135234714 ) ) ;
#14471 = CARTESIAN_POINT ( 'NONE',  ( -21.52544592524334988, -5.823673210054445271, 108.9594237280190185 ) ) ;
#14472 = CARTESIAN_POINT ( 'NONE',  ( -19.05341960407611168, -5.049401038298163336, 76.45724293864769550 ) ) ;
#14473 = CARTESIAN_POINT ( 'NONE',  ( 21.52544592524344225, -5.823673210054117533, 43.54057627198103830 ) ) ;
#14474 = CARTESIAN_POINT ( 'NONE',  ( -8.314922557961024197, 14.29746914071037800, 22.91775706135235069 ) ) ;
#14475 = CARTESIAN_POINT ( 'NONE',  ( -5.823673210054431948, 21.52544592524334988, 82.70942372801900433 ) ) ;
#14476 = CARTESIAN_POINT ( 'NONE',  ( 12.06949235617739724, 12.14591786802326823, 61.87609039468568284 ) ) ;
#14477 = CARTESIAN_POINT ( 'NONE',  ( 18.67979575497178502, 10.72451020669898547, 114.1655762719810383 ) ) ;
#14478 = CARTESIAN_POINT ( 'NONE',  ( -14.34966873604972548, 8.224510206698743886, 23.33442372801901499 ) ) ;
#14479 = CARTESIAN_POINT ( 'NONE',  ( -13.97604488694527625, -13.89961937509977652, 91.87390960531432427 ) ) ;
#14480 = CARTESIAN_POINT ( 'NONE',  ( 14.29746914071037800, 8.314922557961029526, 21.66775706135235069 ) ) ;
#14481 = CARTESIAN_POINT ( 'NONE',  ( 19.03943276465977164, -0.05219959533909143690, 38.74890960531436690 ) ) ;
#14482 = CARTESIAN_POINT ( 'NONE',  ( 14.34966873604972726, -8.224510206698740333, 35.83442372801901143 ) ) ;
#14483 = CARTESIAN_POINT ( 'NONE',  ( -4.379528057220328563, 16.55341960407611168, 85.20724293864770971 ) ) ;
#14484 = CARTESIAN_POINT ( 'NONE',  ( -12.06949235617739369, -12.14591786802326823, 89.37609039468568994 ) ) ;
#14486 = CARTESIAN_POINT ( 'NONE',  ( 13.89961937509977652, -13.97604488694527269, 68.12390960531436690 ) ) ;
#14485 = CARTESIAN_POINT ( 'NONE',  ( -21.53943276465977519, -0.05219959533937600094, 23.75109039468567929 ) ) ;
#14487 = CARTESIAN_POINT ( 'NONE',  ( -5.153800228976328057, -19.02544592524343514, 72.29057627198102409 ) ) ;
#14488 = CARTESIAN_POINT ( 'NONE',  ( 12.06949235617739724, 12.14591786802326823, 91.87609039468568994 ) ) ;
#14489 = AXIS2_PLACEMENT_3D ( 'NONE', #152770, #138593, #183130 ) ;
#14491 = ORIENTED_EDGE ( 'NONE', *, *, #192849, .T. ) ;
#14490 = CARTESIAN_POINT ( 'NONE',  ( -17.60779699588842107, -5.499999999999944933, 81.34981316670108242 ) ) ;
#14492 = ORIENTED_EDGE ( 'NONE', *, *, #41383, .F. ) ;
#14493 = CARTESIAN_POINT ( 'NONE',  ( -13.97604488694547697, 13.89961937509957934, 28.12609039468565797 ) ) ;
#14494 = CARTESIAN_POINT ( 'NONE',  ( 19.02544592524343514, -5.153800228976328945, 48.54057627198103120 ) ) ;
#14496 = VERTEX_POINT ( 'NONE', #24871 ) ;
#14495 = CARTESIAN_POINT ( 'NONE',  ( -13.89961937509977652, 13.97604488694528158, 115.6239096053143669 ) ) ;
#14497 = CARTESIAN_POINT ( 'NONE',  ( -14.34966873604972548, 8.224510206698743886, 23.33442372801901499 ) ) ;
#14499 = CARTESIAN_POINT ( 'NONE',  ( -16.52544592524335698, -4.483927247898792601, 43.95942372801902565 ) ) ;
#14498 = CARTESIAN_POINT ( 'NONE',  ( 9.564922557961047289, -16.46253265017146816, 55.41775706135234003 ) ) ;
#14500 = CARTESIAN_POINT ( 'NONE',  ( -5.049401038298153566, 19.05341960407611168, 100.2072429386476955 ) ) ;
#14501 = CARTESIAN_POINT ( 'NONE',  ( -16.46253265017160317, 9.564922557960807481, 75.83224293864769550 ) ) ;
#14502 = CARTESIAN_POINT ( 'NONE',  ( -18.67979575497178146, -10.72451020669898902, 101.6655762719810383 ) ) ;
#14503 = CARTESIAN_POINT ( 'NONE',  ( -16.46253265017146816, -9.564922557961047289, 59.16775706135233293 ) ) ;
#14505 = CARTESIAN_POINT ( 'NONE',  ( 17.49281420622803651, -3.774461901019551924, 21.82614614838133349 ) ) ;
#14504 = CARTESIAN_POINT ( 'NONE',  ( -19.03943276465977164, 0.05219959533909376836, 86.24890960531436690 ) ) ;
#14506 = CARTESIAN_POINT ( 'NONE',  ( 5.049401038298161559, -19.05341960407611168, 57.70724293864769550 ) ) ;
#14508 = CARTESIAN_POINT ( 'NONE',  ( -13.97604488694527625, -13.89961937509977652, 26.87390960531434558 ) ) ;
#14507 = CARTESIAN_POINT ( 'NONE',  ( -8.314922557961024197, 14.29746914071037800, 107.9177570613523471 ) ) ;
#14509 = CARTESIAN_POINT ( 'NONE',  ( 16.46253265017146816, 9.564922557961045513, 41.66775706135234003 ) ) ;
#14510 = AXIS2_PLACEMENT_3D ( 'NONE', #119522, #166026, #27526 ) ;
#14511 = CARTESIAN_POINT ( 'NONE',  ( 16.52544592524342804, -4.483927247898539470, 78.54057627198103830 ) ) ;
#14512 = CARTESIAN_POINT ( 'NONE',  ( 0.05219959533937995610, -21.53943276465977519, 100.0010903946857042 ) ) ;
#14513 = CARTESIAN_POINT ( 'NONE',  ( 9.564922557960805705, 16.46253265017160317, 44.58224293864769550 ) ) ;
#14514 = CARTESIAN_POINT ( 'NONE',  ( -16.52544592524335698, -4.483927247898792601, 48.95942372801902565 ) ) ;
#14516 = CARTESIAN_POINT ( 'NONE',  ( -10.81492255796105439, 18.62759615963255655, 92.91775706135236135 ) ) ;
#14515 = CARTESIAN_POINT ( 'NONE',  ( -12.14591786802309592, -12.06949235617757132, 46.87390960531435979 ) ) ;
#14517 = CARTESIAN_POINT ( 'NONE',  ( 9.564922557960805705, 16.46253265017160317, 99.58224293864770971 ) ) ;
#14518 = CARTESIAN_POINT ( 'NONE',  ( 13.97604488694527802, 13.89961937509977652, 99.37390960531436690 ) ) ;
#14519 = CARTESIAN_POINT ( 'NONE',  ( 16.52544592524342804, -4.483927247898539470, 113.5405762719810383 ) ) ;
#14520 = CARTESIAN_POINT ( 'NONE',  ( 12.14591786802309770, 12.06949235617756955, 69.37390960531436690 ) ) ;
#14521 = CARTESIAN_POINT ( 'NONE',  ( -15.80617190586745835, -15.72974639402198527, 81.87390960531435269 ) ) ;
#14522 = CARTESIAN_POINT ( 'NONE',  ( -13.97604488694527625, -13.89961937509977652, 86.87390960531436690 ) ) ;
#14523 = CARTESIAN_POINT ( 'NONE',  ( 10.72451020669898902, -18.67979575497178502, 97.91557627198103830 ) ) ;
#14524 = CIRCLE ( 'NONE', #82328, 5.000000000000000888 ) ;
#14525 = CARTESIAN_POINT ( 'NONE',  ( -5.153800228976607833, 19.02544592524334988, 72.70942372801900433 ) ) ;
#14527 = CARTESIAN_POINT ( 'NONE',  ( -14.29746914071049879, 8.314922557960819915, 90.83224293864769550 ) ) ;
#14526 = CARTESIAN_POINT ( 'NONE',  ( -19.25176906914648356, -5.499999999999852562, 90.99927264242278113 ) ) ;
#14528 = CARTESIAN_POINT ( 'NONE',  ( 19.02544592524343514, -5.153800228976328945, 63.54057627198103830 ) ) ;
#14529 = CARTESIAN_POINT ( 'NONE',  ( -21.52544592524343514, 5.823673210054127303, 71.04057627198103830 ) ) ;
#14530 = CARTESIAN_POINT ( 'NONE',  ( -26.11842041226232780, -7.699311778675193452, 169.4341694154020956 ) ) ;
#14532 = CARTESIAN_POINT ( 'NONE',  ( 2.500000000000000000, 1.178949249685217193, 2.041999999999998483 ) ) ;
#14531 = CARTESIAN_POINT ( 'NONE',  ( -0.05219959533934338120, 16.53943276465976808, 112.5010903946857042 ) ) ;
#14533 = CARTESIAN_POINT ( 'NONE',  ( 12.14591786802327356, -12.06949235617739191, 20.62609039468568639 ) ) ;
#14534 = CARTESIAN_POINT ( 'NONE',  ( -12.06949235617756955, 12.14591786802309770, 80.62390960531438111 ) ) ;
#14535 = CARTESIAN_POINT ( 'NONE',  ( -16.79531203550650531, -7.028104445595562133, 96.25244988220441655 ) ) ;
#14536 = CARTESIAN_POINT ( 'NONE',  ( -9.474510206698964154, 16.51473224551069663, 70.41557627198102409 ) ) ;
#14537 = CARTESIAN_POINT ( 'NONE',  ( 19.02544592524343514, -5.153800228976328945, 33.54057627198102409 ) ) ;
#14538 = CARTESIAN_POINT ( 'NONE',  ( 8.224510206698953496, -14.34966873604960469, 67.91557627198102409 ) ) ;
#14539 = CARTESIAN_POINT ( 'NONE',  ( 9.474510206698971260, -16.51473224551069308, 112.9155762719810383 ) ) ;
#14540 = CARTESIAN_POINT ( 'NONE',  ( -9.474510206698720793, -16.51473224551083518, 99.58442372801900433 ) ) ;
#14541 = CIRCLE ( 'NONE', #66196, 0.5000000000000004441 ) ;
#14542 = CARTESIAN_POINT ( 'NONE',  ( 19.02544592524343514, -5.153800228976328945, 103.5405762719809957 ) ) ;
#14543 = CARTESIAN_POINT ( 'NONE',  ( -10.81492255796078084, -18.62759615963271287, 82.08224293864768129 ) ) ;
#14544 = CARTESIAN_POINT ( 'NONE',  ( 4.483927247898790824, -16.52544592524335698, 70.20942372801904696 ) ) ;
#14545 = VECTOR ( 'NONE', #30827, 1000.000000000000000 ) ;
#14546 = CARTESIAN_POINT ( 'NONE',  ( -16.51473224551082808, 9.474510206698731452, 113.3344237280190043 ) ) ;
#14547 = CARTESIAN_POINT ( 'NONE',  ( 5.153800228976335163, 19.02544592524342804, 64.79057627198100988 ) ) ;
#14548 = CARTESIAN_POINT ( 'NONE',  ( 21.52544592524344225, -5.823673210054117533, 83.54057627198102409 ) ) ;
#14549 = CARTESIAN_POINT ( 'NONE',  ( -21.53943276465977519, 0.05219959533907696930, 26.24890960531435624 ) ) ;
#14550 = CARTESIAN_POINT ( 'NONE',  ( 16.46253265017146816, 9.564922557961045513, 106.6677570613523471 ) ) ;
#14552 = CARTESIAN_POINT ( 'NONE',  ( -10.81492255796105439, 18.62759615963255655, 52.91775706135235424 ) ) ;
#14551 = CARTESIAN_POINT ( 'NONE',  ( 0.05219959533910956823, 16.53943276465976808, 39.99890960531436690 ) ) ;
#14553 = CARTESIAN_POINT ( 'NONE',  ( 18.22780087662121673, 5.500000000000056843, 83.98459894673892734 ) ) ;
#14555 = CARTESIAN_POINT ( 'NONE',  ( -19.02544592524342804, 5.153800228976336051, 101.0405762719810241 ) ) ;
#14554 = CARTESIAN_POINT ( 'NONE',  ( 16.52544592524335698, 4.483927247898782831, 71.45942372801901854 ) ) ;
#14556 = CARTESIAN_POINT ( 'NONE',  ( 13.89961937509978007, -13.97604488694527269, 103.1239096053143385 ) ) ;
#14557 = CARTESIAN_POINT ( 'NONE',  ( 1.500000000000011102, 30.56489079787948882, -50.76047248289020786 ) ) ;
#14558 = CARTESIAN_POINT ( 'NONE',  ( -8.224510206698735004, -14.34966873604973081, 99.58442372801900433 ) ) ;
#14559 = CARTESIAN_POINT ( 'NONE',  ( -14.29746914071037622, -8.314922557961029526, 44.16775706135234714 ) ) ;
#14560 = CARTESIAN_POINT ( 'NONE',  ( 19.05341960407611168, 5.049401038298154454, 53.95724293864770260 ) ) ;
#14561 = CARTESIAN_POINT ( 'NONE',  ( -19.02544592524342804, 5.153800228976336051, 76.04057627198102409 ) ) ;
#14562 = CARTESIAN_POINT ( 'NONE',  ( -21.53943276465977519, -0.05219959533937600094, 68.75109039468568994 ) ) ;
#14563 = CARTESIAN_POINT ( 'NONE',  ( 14.29746914071037800, 8.314922557961029526, 61.66775706135235424 ) ) ;
#14564 = CARTESIAN_POINT ( 'NONE',  ( 4.379528057220339221, -16.55341960407611168, 32.70724293864770260 ) ) ;
#14565 = CARTESIAN_POINT ( 'NONE',  ( -5.049401038298153566, 19.05341960407611168, 40.20724293864768839 ) ) ;
#14566 = CARTESIAN_POINT ( 'NONE',  ( 9.564922557960805705, 16.46253265017160317, 34.58224293864770260 ) ) ;
#14567 = CARTESIAN_POINT ( 'NONE',  ( -12.14591786802326823, 12.06949235617739902, 48.12609039468568284 ) ) ;
#14568 = CARTESIAN_POINT ( 'NONE',  ( 16.46253265017146816, 9.564922557961045513, 91.66775706135234714 ) ) ;
#14569 = CARTESIAN_POINT ( 'NONE',  ( -12.14591786802309592, -12.06949235617757132, 96.87390960531436690 ) ) ;
#14570 = CARTESIAN_POINT ( 'NONE',  ( -9.474510206698964154, 16.51473224551069663, 50.41557627198102409 ) ) ;
#14572 = CARTESIAN_POINT ( 'NONE',  ( -6.100000000000006750, 6.426762577456935076E-14, -62.50719930893269805 ) ) ;
#14571 = CARTESIAN_POINT ( 'NONE',  ( -19.02544592524334988, -5.153800228976617603, 83.95942372801901854 ) ) ;
#14573 = CARTESIAN_POINT ( 'NONE',  ( -18.62759615963255300, -10.81492255796106328, 89.16775706135236135 ) ) ;
#14574 = CARTESIAN_POINT ( 'NONE',  ( 16.52544592524335698, 4.483927247898782831, 51.45942372801901854 ) ) ;
#14575 = CARTESIAN_POINT ( 'NONE',  ( 69.65682714487590488, -71.74905178543389184, -25.00000000000000000 ) ) ;
#14576 = CARTESIAN_POINT ( 'NONE',  ( 21.53943276465977519, -0.05219959533907433946, 53.74890960531437401 ) ) ;
#14577 = CARTESIAN_POINT ( 'NONE',  ( -4.379528057220086978, -16.55341960407618274, 39.79275706135235424 ) ) ;
#14578 = CARTESIAN_POINT ( 'NONE',  ( -19.46398650005391318, 5.499999999999952038, 70.18269651486372140 ) ) ;
#14579 = CARTESIAN_POINT ( 'NONE',  ( 13.97604488694548053, -13.89961937509957401, 40.62609039468564731 ) ) ;
#14580 = CARTESIAN_POINT ( 'NONE',  ( 9.564922557960805705, 16.46253265017160317, 84.58224293864769550 ) ) ;
#14581 = CARTESIAN_POINT ( 'NONE',  ( -14.29746914071049879, 8.314922557960819915, 105.8322429386476955 ) ) ;
#14582 = CARTESIAN_POINT ( 'NONE',  ( -19.03943276465977164, 0.05219959533909376836, 51.24890960531436690 ) ) ;
#14583 = CIRCLE ( 'NONE', #1571, 2.000000000000001776 ) ;
#14584 = CARTESIAN_POINT ( 'NONE',  ( -20.15904164509370489, -22.18854071326290622, -51.48245768792372701 ) ) ;
#14585 = CARTESIAN_POINT ( 'NONE',  ( 21.55341960407619695, -5.719274019375665929, 76.04275706135237556 ) ) ;
#14586 = CARTESIAN_POINT ( 'NONE',  ( 30.00000000000000000, -1.132798289211302014E-14, 97.50000000000000000 ) ) ;
#14587 = PRODUCT ( 'front house', 'front house', '', ( #99773 ) ) ;
#14588 = CARTESIAN_POINT ( 'NONE',  ( -0.05219959533936034679, 19.03943276465977164, 27.50109039468566507 ) ) ;
#14589 = CARTESIAN_POINT ( 'NONE',  ( 10.81492255796106328, -18.62759615963255655, 110.4177570613523756 ) ) ;
#14590 = CARTESIAN_POINT ( 'NONE',  ( -0.05219959533910754901, -16.53943276465976808, 47.49890960531435979 ) ) ;
#14591 = CARTESIAN_POINT ( 'NONE',  ( 13.89961937509977652, -13.97604488694527269, 63.12390960531435979 ) ) ;
#14592 = CARTESIAN_POINT ( 'NONE',  ( -16.46253265017160317, 9.564922557960807481, 110.8322429386476955 ) ) ;
#14593 = CARTESIAN_POINT ( 'NONE',  ( -18.62759615963255300, -10.81492255796106328, 89.16775706135236135 ) ) ;
#14594 = CARTESIAN_POINT ( 'NONE',  ( 19.03943276465977164, -0.05219959533909143690, 58.74890960531435979 ) ) ;
#14595 = CARTESIAN_POINT ( 'NONE',  ( 5.719274019375673035, 21.55341960407619339, 77.29275706135234714 ) ) ;
#14596 = CARTESIAN_POINT ( 'NONE',  ( -21.53943276465977519, 0.05219959533907696930, 41.24890960531435269 ) ) ;
#14597 = CARTESIAN_POINT ( 'NONE',  ( -18.62759615963255300, -10.81492255796106328, 34.16775706135234714 ) ) ;
#14598 = CARTESIAN_POINT ( 'NONE',  ( 5.049401038297881783, 19.05341960407617563, 62.29275706135234003 ) ) ;
#14599 = CARTESIAN_POINT ( 'NONE',  ( 13.89961937509977652, -13.97604488694527269, 33.12390960531434558 ) ) ;
#14600 = CARTESIAN_POINT ( 'NONE',  ( -19.02544592524342804, 5.153800228976336051, 71.04057627198099567 ) ) ;
#14601 = CARTESIAN_POINT ( 'NONE',  ( -16.53943276465976808, -0.05219959533934237506, 23.75109039468567929 ) ) ;
#14602 = CARTESIAN_POINT ( 'NONE',  ( 8.224510206698953496, -14.34966873604960469, 92.91557627198103830 ) ) ;
#14603 = CARTESIAN_POINT ( 'NONE',  ( -9.564922557960796823, -16.46253265017161027, 57.08224293864769550 ) ) ;
#14604 = CARTESIAN_POINT ( 'NONE',  ( 5.719274019375991003, -21.55341960407610458, 42.70724293864770260 ) ) ;
#14605 = CARTESIAN_POINT ( 'NONE',  ( -16.51473224551082808, 9.474510206698731452, 98.33442372801900433 ) ) ;
#14606 = CARTESIAN_POINT ( 'NONE',  ( -15.72974639402197994, 15.80617190586746368, 115.6239096053143669 ) ) ;
#14607 = CARTESIAN_POINT ( 'NONE',  ( 5.823673210054444382, -21.52544592524334988, 65.20942372801901854 ) ) ;
#14608 = CARTESIAN_POINT ( 'NONE',  ( 16.55341960407618274, -4.379528057220086978, 71.04275706135234714 ) ) ;
#14609 = CARTESIAN_POINT ( 'NONE',  ( -16.52544592524335698, -4.483927247898792601, 68.95942372801901854 ) ) ;
#14610 = CARTESIAN_POINT ( 'NONE',  ( 16.46253265017160672, -9.564922557960803928, 58.33224293864769550 ) ) ;
#14611 = CARTESIAN_POINT ( 'NONE',  ( 4.483927247898790824, -16.52544592524335698, 90.20942372801903275 ) ) ;
#14612 = CARTESIAN_POINT ( 'NONE',  ( 5.153800228976615827, -19.02544592524334988, 40.20942372801898301 ) ) ;
#14613 = CARTESIAN_POINT ( 'NONE',  ( -5.823673210054116645, -21.52544592524344225, 112.2905762719810241 ) ) ;
#14614 = CARTESIAN_POINT ( 'NONE',  ( -16.55341960407611168, -4.379528057220339221, 66.45724293864768129 ) ) ;
#14615 = CARTESIAN_POINT ( 'NONE',  ( 19.02544592524343514, -5.153800228976328945, 88.54057627198102409 ) ) ;
#14616 = CARTESIAN_POINT ( 'NONE',  ( 16.53943276465976808, 0.05219959533934440121, 86.25109039468568994 ) ) ;
#14617 = CARTESIAN_POINT ( 'NONE',  ( 5.719274019375673035, 21.55341960407619339, 62.29275706135236845 ) ) ;
#14618 = CARTESIAN_POINT ( 'NONE',  ( -12.06949235617739369, -12.14591786802326823, 19.37609039468568639 ) ) ;
#14619 = CARTESIAN_POINT ( 'NONE',  ( 18.67979575497194134, -10.72451020669871369, 20.83442372801901143 ) ) ;
#14620 = CARTESIAN_POINT ( 'NONE',  ( 0.05219959533910956823, 16.53943276465976808, 59.99890960531436690 ) ) ;
#14621 = VERTEX_POINT ( 'NONE', #69351 ) ;
#14622 = CARTESIAN_POINT ( 'NONE',  ( 21.55341960407610458, 5.719274019375980345, 83.95724293864770971 ) ) ;
#14623 = CARTESIAN_POINT ( 'NONE',  ( 14.34966873604960469, 8.224510206698951720, 44.16557627198103120 ) ) ;
#14624 = EDGE_LOOP ( 'NONE', ( #60138, #151275, #103948, #169903 ) ) ;
#14625 = LINE ( 'NONE', #108611, #92092 ) ;
#14626 = CARTESIAN_POINT ( 'NONE',  ( 0.05219959533907565091, 21.53943276465977519, 109.9989096053143527 ) ) ;
#14627 = CARTESIAN_POINT ( 'NONE',  ( -16.46253265017160317, 9.564922557960807481, 105.8322429386476955 ) ) ;
#14628 = CARTESIAN_POINT ( 'NONE',  ( 18.67979575497194134, -10.72451020669871369, 35.83442372801901143 ) ) ;
#14629 = CARTESIAN_POINT ( 'NONE',  ( 8.314922557960818139, 14.29746914071049879, 54.58224293864769550 ) ) ;
#14630 = CARTESIAN_POINT ( 'NONE',  ( -9.564922557960796823, -16.46253265017161027, 57.08224293864769550 ) ) ;
#14631 = CARTESIAN_POINT ( 'NONE',  ( -9.474510206698720793, -16.51473224551083518, 64.58442372801900433 ) ) ;
#14632 = CARTESIAN_POINT ( 'NONE',  ( -9.474510206698964154, 16.51473224551069663, 90.41557627198103830 ) ) ;
#14633 = CARTESIAN_POINT ( 'NONE',  ( -0.05219959533907301413, -21.53943276465977519, 52.49890960531435979 ) ) ;
#14634 = CARTESIAN_POINT ( 'NONE',  ( -21.12688062493582919, -32.57662631298939715, -17.38946437510490028 ) ) ;
#14635 = CARTESIAN_POINT ( 'NONE',  ( 19.05341960407611168, 5.049401038298154454, 58.95724293864768129 ) ) ;
#14636 = CARTESIAN_POINT ( 'NONE',  ( -12.06949235617739369, -12.14591786802326823, 34.37609039468568284 ) ) ;
#14637 = CARTESIAN_POINT ( 'NONE',  ( -13.89961937509957401, -13.97604488694547875, 59.37609039468566863 ) ) ;
#14638 = CARTESIAN_POINT ( 'NONE',  ( 15.80617190586746368, 15.72974639402197994, 114.3739096053143527 ) ) ;
#14639 = CARTESIAN_POINT ( 'NONE',  ( 4.379528057220339221, -16.55341960407611168, 52.70724293864769550 ) ) ;
#14640 = CARTESIAN_POINT ( 'NONE',  ( -5.049401038298153566, 19.05341960407611168, 85.20724293864766707 ) ) ;
#14641 = CARTESIAN_POINT ( 'NONE',  ( 5.823673210054125526, 21.52544592524343514, 74.79057627198105251 ) ) ;
#14643 = CARTESIAN_POINT ( 'NONE',  ( 12.06949235617739724, 12.14591786802326823, 41.87609039468568284 ) ) ;
#14642 = CARTESIAN_POINT ( 'NONE',  ( -21.52544592524343514, 5.823673210054127303, 106.0405762719810525 ) ) ;
#14644 = CARTESIAN_POINT ( 'NONE',  ( 21.53943276465977519, -0.05219959533907433946, 38.74890960531435979 ) ) ;
#14645 = CARTESIAN_POINT ( 'NONE',  ( -5.823673210054431948, 21.52544592524334988, 102.7094237280190185 ) ) ;
#14646 = CARTESIAN_POINT ( 'NONE',  ( 16.46253265017160672, -9.564922557960803928, 93.33224293864769550 ) ) ;
#14647 = CARTESIAN_POINT ( 'NONE',  ( 19.05341960407611168, 5.049401038298154454, 43.95724293864769550 ) ) ;
#14648 = CARTESIAN_POINT ( 'NONE',  ( 19.03943276465977164, -0.05219959533909143690, 103.7489096053143669 ) ) ;
#14649 = CARTESIAN_POINT ( 'NONE',  ( 19.02544592524343514, -5.153800228976328945, 78.54057627198099567 ) ) ;
#14650 = CARTESIAN_POINT ( 'NONE',  ( 8.314922557961029526, -14.29746914071037800, 25.41775706135235779 ) ) ;
#14651 = DIRECTION ( 'NONE',  ( 1.000000000000000000, 0.000000000000000000, 0.000000000000000000 ) ) ;
#14652 = CARTESIAN_POINT ( 'NONE',  ( -13.89961937509957401, -13.97604488694547875, 54.37609039468565442 ) ) ;
#14654 = CARTESIAN_POINT ( 'NONE',  ( 15.72974639402199770, -15.80617190586745480, 38.12390960531436690 ) ) ;
#14653 = CARTESIAN_POINT ( 'NONE',  ( -18.67979575497193778, 10.72451020669871902, 113.3344237280190328 ) ) ;
#14655 = CARTESIAN_POINT ( 'NONE',  ( 16.55341960407618274, -4.379528057220086978, 106.0427570613523471 ) ) ;
#14656 = CARTESIAN_POINT ( 'NONE',  ( 21.36642364538387540, -19.99951666465409517, -49.23853142240816538 ) ) ;
#14657 = CARTESIAN_POINT ( 'NONE',  ( 13.89961937509957401, 13.97604488694547697, 76.87609039468566152 ) ) ;
#14658 = CARTESIAN_POINT ( 'NONE',  ( 5.153800228976615827, -19.02544592524334988, 35.20942372801899722 ) ) ;
#14659 = CARTESIAN_POINT ( 'NONE',  ( 26.85241745982147421, -7.190459374138095328, 139.9999999999999716 ) ) ;
#14660 = CARTESIAN_POINT ( 'NONE',  ( -19.05341960407611168, -5.049401038298163336, 46.45724293864768129 ) ) ;
#14661 = CARTESIAN_POINT ( 'NONE',  ( 14.29746914071049879, -8.314922557960816363, 33.33224293864769550 ) ) ;
#14662 = CARTESIAN_POINT ( 'NONE',  ( -16.19135201231367915, -7.376712067591919997, 110.1868085405203459 ) ) ;
#14663 = CARTESIAN_POINT ( 'NONE',  ( 4.379528057220339221, -16.55341960407611168, 32.70724293864770260 ) ) ;
#14664 = CARTESIAN_POINT ( 'NONE',  ( 21.08147685851793440, -20.05196361705210961, -52.44995202553442226 ) ) ;
#14665 = CARTESIAN_POINT ( 'NONE',  ( -12.14591786802326823, 12.06949235617739902, 93.12609039468568994 ) ) ;
#14666 = CARTESIAN_POINT ( 'NONE',  ( 16.46253265017160672, -9.564922557960803928, 38.33224293864768839 ) ) ;
#14667 = CARTESIAN_POINT ( 'NONE',  ( -0.05219959533937732626, 21.53943276465977519, 107.5010903946856899 ) ) ;
#14668 = CARTESIAN_POINT ( 'NONE',  ( 8.314922557961029526, -14.29746914071037800, 20.41775706135234714 ) ) ;
#14670 = ORIENTED_EDGE ( 'NONE', *, *, #30090, .T. ) ;
#14669 = CARTESIAN_POINT ( 'NONE',  ( -0.05219959533937732626, 21.53943276465977519, 82.50109039468568994 ) ) ;
#14671 = CARTESIAN_POINT ( 'NONE',  ( -19.02544592524334988, -5.153800228976617603, 63.95942372801899012 ) ) ;
#14672 = CARTESIAN_POINT ( 'NONE',  ( -9.564922557960796823, -16.46253265017161027, 97.08224293864769550 ) ) ;
#14673 = CARTESIAN_POINT ( 'NONE',  ( 9.564922557960805705, 16.46253265017160317, 89.58224293864769550 ) ) ;
#14674 = CARTESIAN_POINT ( 'NONE',  ( -29.86685920354755197, -21.69954338932560134, -10.42499999726881299 ) ) ;
#14675 = CARTESIAN_POINT ( 'NONE',  ( 10.81492255796078972, 18.62759615963270932, 109.5822429386476955 ) ) ;
#14676 = AXIS2_PLACEMENT_3D ( 'NONE', #64731, #192053, #127378 ) ;
#14677 = CARTESIAN_POINT ( 'NONE',  ( -8.314922557960811034, -14.29746914071050412, 67.08224293864770971 ) ) ;
#14678 = CARTESIAN_POINT ( 'NONE',  ( -10.72451020669898014, 18.67979575497178502, 60.41557627198102409 ) ) ;
#14679 = CARTESIAN_POINT ( 'NONE',  ( 16.51473224551069308, 9.474510206698969483, 59.16557627198102409 ) ) ;
#14681 = CARTESIAN_POINT ( 'NONE',  ( -14.34966873604972548, 8.224510206698743886, 88.33442372801901854 ) ) ;
#14680 = CARTESIAN_POINT ( 'NONE',  ( -21.52544592524343514, 5.823673210054127303, 101.0405762719810383 ) ) ;
#14682 = EDGE_LOOP ( 'NONE', ( #50120, #17366 ) ) ;
#14683 = CARTESIAN_POINT ( 'NONE',  ( 16.51473224551069308, 9.474510206698969483, 59.16557627198102409 ) ) ;
#14685 = CARTESIAN_POINT ( 'NONE',  ( -8.673617379884035472E-16, 7.600000000000007638, -65.00100000000003320 ) ) ;
#14684 = CARTESIAN_POINT ( 'NONE',  ( 12.06949235617757843, -12.14591786802309237, 93.12390960531436690 ) ) ;
#14686 = CARTESIAN_POINT ( 'NONE',  ( 19.05341960407611168, 5.049401038298154454, 48.95724293864768129 ) ) ;
#14687 = CARTESIAN_POINT ( 'NONE',  ( 5.153800228976615827, -19.02544592524334988, 75.20942372801896170 ) ) ;
#14688 = CARTESIAN_POINT ( 'NONE',  ( -0.05219959533910754901, -16.53943276465976808, 82.49890960531436690 ) ) ;
#14689 = CARTESIAN_POINT ( 'NONE',  ( -10.81492255796105439, 18.62759615963255655, 57.91775706135234714 ) ) ;
#14691 = CARTESIAN_POINT ( 'NONE',  ( 10.72451020669898902, -18.67979575497178502, 107.9155762719810241 ) ) ;
#14690 = CARTESIAN_POINT ( 'NONE',  ( 16.51473224551069308, 9.474510206698969483, 34.16557627198102409 ) ) ;
#14692 = CARTESIAN_POINT ( 'NONE',  ( -0.05219959533910754901, -16.53943276465976808, 87.49890960531436690 ) ) ;
#14693 = FACE_OUTER_BOUND ( 'NONE', #153595, .T. ) ;
#14694 = CARTESIAN_POINT ( 'NONE',  ( -16.46253265017160317, 9.564922557960807481, 55.83224293864769550 ) ) ;
#14695 = AXIS2_PLACEMENT_3D ( 'NONE', #155720, #171893, #142537 ) ;
#14696 = FACE_OUTER_BOUND ( 'NONE', #81979, .T. ) ;
#14698 = CARTESIAN_POINT ( 'NONE',  ( -10.81492255796078084, -18.62759615963271287, 22.08224293864769194 ) ) ;
#14697 = CARTESIAN_POINT ( 'NONE',  ( -13.89961937509957401, -13.97604488694547875, 89.37609039468563310 ) ) ;
#14699 = CARTESIAN_POINT ( 'NONE',  ( -10.81492255796105439, 18.62759615963255655, 42.91775706135235424 ) ) ;
#14700 = CARTESIAN_POINT ( 'NONE',  ( 16.51473224551069308, 9.474510206698969483, 79.16557627198103830 ) ) ;
#14701 = CARTESIAN_POINT ( 'NONE',  ( -5.049401038297874678, -19.05341960407617918, 74.79275706135231871 ) ) ;
#14702 = CARTESIAN_POINT ( 'NONE',  ( 19.02544592524343514, -5.153800228976328945, 53.54057627198102409 ) ) ;
#14703 = AXIS2_PLACEMENT_3D ( 'NONE', #109409, #112392, #48747 ) ;
#14704 = CARTESIAN_POINT ( 'NONE',  ( -4.379528057220328563, 16.55341960407611168, 75.20724293864769550 ) ) ;
#14705 = CARTESIAN_POINT ( 'NONE',  ( 8.224510206698953496, -14.34966873604960469, 67.91557627198102409 ) ) ;
#14706 = CARTESIAN_POINT ( 'NONE',  ( -9.474510206698964154, 16.51473224551069663, 90.41557627198103830 ) ) ;
#14707 = CARTESIAN_POINT ( 'NONE',  ( 14.29746914071049879, -8.314922557960816363, 73.33224293864769550 ) ) ;
#14708 = CARTESIAN_POINT ( 'NONE',  ( 5.153800228976335163, 19.02544592524342804, 89.79057627198102409 ) ) ;
#14709 = EDGE_CURVE ( 'NONE', #163628, #83320, #66359, .T. ) ;
#14710 = CARTESIAN_POINT ( 'NONE',  ( 19.05341960407617918, -5.049401038297876454, 36.04275706135234003 ) ) ;
#14713 = CARTESIAN_POINT ( 'NONE',  ( 14.29746914071049879, -8.314922557960816363, 108.3322429386477097 ) ) ;
#14712 = CARTESIAN_POINT ( 'NONE',  ( -16.52544592524342804, 4.483927247898546575, 31.04057627198102409 ) ) ;
#14711 = CARTESIAN_POINT ( 'NONE',  ( -0.05219959533909027116, -19.03943276465977164, 42.49890960531435269 ) ) ;
#14714 = ORIENTED_EDGE ( 'NONE', *, *, #107363, .T. ) ;
#14715 = CARTESIAN_POINT ( 'NONE',  ( -18.67979575497193778, 10.72451020669871902, 38.33442372801900433 ) ) ;
#14716 = CARTESIAN_POINT ( 'NONE',  ( 13.97604488694548053, -13.89961937509957401, 60.62609039468564731 ) ) ;
#14717 = CARTESIAN_POINT ( 'NONE',  ( 4.379528057220339221, -16.55341960407611168, 32.70724293864770260 ) ) ;
#14718 = CARTESIAN_POINT ( 'NONE',  ( 21.52544592524344225, -5.823673210054117533, 88.54057627198103830 ) ) ;
#14719 = CARTESIAN_POINT ( 'NONE',  ( -9.474510206698964154, 16.51473224551069663, 115.4155762719810241 ) ) ;
#14720 = CARTESIAN_POINT ( 'NONE',  ( 12.06949235617757843, -12.14591786802309237, 68.12390960531436690 ) ) ;
#14721 = CARTESIAN_POINT ( 'NONE',  ( -5.049401038298153566, 19.05341960407611168, 45.20724293864769550 ) ) ;
#14722 = CARTESIAN_POINT ( 'NONE',  ( 19.05341960407617918, -5.049401038297876454, 26.04275706135233293 ) ) ;
#14723 = CARTESIAN_POINT ( 'NONE',  ( 8.224510206698742110, 14.34966873604972548, 97.08442372801904696 ) ) ;
#14724 = CARTESIAN_POINT ( 'NONE',  ( 8.224510206698742110, 14.34966873604972548, 57.08442372801901854 ) ) ;
#14725 = CARTESIAN_POINT ( 'NONE',  ( 15.80617190586746368, 15.72974639402197994, 34.37390960531435979 ) ) ;
#14726 = CARTESIAN_POINT ( 'NONE',  ( 21.55341960407619695, -5.719274019375665929, 111.0427570613523613 ) ) ;
#14727 = CARTESIAN_POINT ( 'NONE',  ( -5.153800228976328057, -19.02544592524343514, 82.29057627198103830 ) ) ;
#14728 = CARTESIAN_POINT ( 'NONE',  ( -4.483927247898782831, 16.52544592524335698, 67.70942372801901854 ) ) ;
#14729 = CARTESIAN_POINT ( 'NONE',  ( 13.97604488694527802, 13.89961937509977652, 24.37390960531435624 ) ) ;
#14730 = CARTESIAN_POINT ( 'NONE',  ( -8.224510206698948167, 14.34966873604960824, 35.41557627198102409 ) ) ;
#14732 = CARTESIAN_POINT ( 'NONE',  ( -9.474510206698964154, 16.51473224551069663, 90.41557627198103830 ) ) ;
#14731 = CARTESIAN_POINT ( 'NONE',  ( -16.51473224551069308, -9.474510206698971260, 106.6655762719810383 ) ) ;
#14733 = CARTESIAN_POINT ( 'NONE',  ( -5.823673210054116645, -21.52544592524344225, 27.29057627198103120 ) ) ;
#14734 = CARTESIAN_POINT ( 'NONE',  ( -14.34966873604960291, -8.224510206698953496, 56.66557627198103830 ) ) ;
#14735 = CARTESIAN_POINT ( 'NONE',  ( -14.34966873604960291, -8.224510206698953496, 31.66557627198102054 ) ) ;
#14736 = EDGE_LOOP ( 'NONE', ( #183241, #96003 ) ) ;
#14737 = CARTESIAN_POINT ( 'NONE',  ( -0.05219959533910754901, -16.53943276465976808, 52.49890960531435979 ) ) ;
#14739 = CARTESIAN_POINT ( 'NONE',  ( -7.220908937440027486, -2.044528755335643044, 1.589185716900149092 ) ) ;
#14738 = CARTESIAN_POINT ( 'NONE',  ( 14.29746914071037800, 8.314922557961029526, 41.66775706135235424 ) ) ;
#14740 = CARTESIAN_POINT ( 'NONE',  ( 16.46253265017146816, 9.564922557961045513, 46.66775706135233293 ) ) ;
#14741 = CARTESIAN_POINT ( 'NONE',  ( 5.049401038298161559, -19.05341960407611168, 92.70724293864769550 ) ) ;
#14742 = CARTESIAN_POINT ( 'NONE',  ( 16.46253265017146816, 9.564922557961045513, 61.66775706135234003 ) ) ;
#14743 = CARTESIAN_POINT ( 'NONE',  ( 22.44159573604009239, 16.30477369853692693, 144.5750000027311728 ) ) ;
#14744 = CARTESIAN_POINT ( 'NONE',  ( 0.05219959533936267826, -19.03943276465977164, 50.00109039468566863 ) ) ;
#14746 = CARTESIAN_POINT ( 'NONE',  ( 16.52544592524335698, 4.483927247898782831, 76.45942372801901854 ) ) ;
#14745 = CARTESIAN_POINT ( 'NONE',  ( -0.05219959533936034679, 19.03943276465977164, 97.50109039468567573 ) ) ;
#14747 = CARTESIAN_POINT ( 'NONE',  ( -8.571926809382608425, 26.38167802310805854, 148.9750000027311785 ) ) ;
#14748 = CARTESIAN_POINT ( 'NONE',  ( 0.05219959533909260263, 19.03943276465977164, 24.99890960531435269 ) ) ;
#14749 = CARTESIAN_POINT ( 'NONE',  ( 5.153800228976335163, 19.02544592524342804, 114.7905762719810241 ) ) ;
#14750 = CARTESIAN_POINT ( 'NONE',  ( -15.80617190586768217, 15.72974639402176855, 38.12609039468567573 ) ) ;
#14751 = CARTESIAN_POINT ( 'NONE',  ( 5.153800228976615827, -19.02544592524334988, 100.2094237280190043 ) ) ;
#14753 = CARTESIAN_POINT ( 'NONE',  ( 5.153800228976335163, 19.02544592524342804, 59.79057627198100988 ) ) ;
#14752 = CARTESIAN_POINT ( 'NONE',  ( 17.50000000000000000, -3.850315288878792153, 106.7662913060345034 ) ) ;
#14754 = CARTESIAN_POINT ( 'NONE',  ( 13.89961937509977652, -13.97604488694527269, 103.1239096053143527 ) ) ;
#14756 = CARTESIAN_POINT ( 'NONE',  ( 0.05219959533909260263, 19.03943276465977164, 69.99890960531435269 ) ) ;
#14755 = CARTESIAN_POINT ( 'NONE',  ( -0.05219959533910754901, -16.53943276465976808, 57.49890960531435979 ) ) ;
#14757 = CARTESIAN_POINT ( 'NONE',  ( -0.05219959533909027116, -19.03943276465977164, 77.49890960531435269 ) ) ;
#14758 = CARTESIAN_POINT ( 'NONE',  ( 19.02544592524334988, 5.153800228976608722, 76.45942372801897591 ) ) ;
#14759 = CARTESIAN_POINT ( 'NONE',  ( 21.53943276465977519, -0.05219959533907433946, 48.74890960531435979 ) ) ;
#14760 = CARTESIAN_POINT ( 'NONE',  ( 4.379528057220339221, -16.55341960407611168, 107.7072429386476955 ) ) ;
#14761 = CARTESIAN_POINT ( 'NONE',  ( -5.153800228976607833, 19.02544592524334988, 47.70942372801900433 ) ) ;
#14762 = CARTESIAN_POINT ( 'NONE',  ( -16.46253265017160317, 9.564922557960807481, 85.83224293864769550 ) ) ;
#14763 = CARTESIAN_POINT ( 'NONE',  ( 18.67979575497178502, 10.72451020669898547, 79.16557627198103830 ) ) ;
#14765 = CARTESIAN_POINT ( 'NONE',  ( -13.97604488694547697, 13.89961937509957934, 38.12609039468566152 ) ) ;
#14764 = CARTESIAN_POINT ( 'NONE',  ( 8.224510206698953496, -14.34966873604960469, 82.91557627198103830 ) ) ;
#14766 = CARTESIAN_POINT ( 'NONE',  ( -15.80617190586745835, -15.72974639402198527, 81.87390960531435269 ) ) ;
#14767 = CARTESIAN_POINT ( 'NONE',  ( -10.81492255796078084, -18.62759615963271287, 62.08224293864769550 ) ) ;
#14768 = AXIS2_PLACEMENT_3D ( 'NONE', #93141, #154826, #155818 ) ;
#14769 = CARTESIAN_POINT ( 'NONE',  ( 15.80617190586746368, 15.72974639402197994, 44.37390960531435979 ) ) ;
#14770 = CARTESIAN_POINT ( 'NONE',  ( 21.55341960407619695, -5.719274019375665929, 86.04275706135236135 ) ) ;
#14771 = CARTESIAN_POINT ( 'NONE',  ( -13.97604488694527625, -13.89961937509977652, 71.87390960531433848 ) ) ;
#14772 = CARTESIAN_POINT ( 'NONE',  ( -8.224510206698948167, 14.34966873604960824, 115.4155762719810241 ) ) ;
#14773 = CARTESIAN_POINT ( 'NONE',  ( 15.72974639402176855, 15.80617190586768217, 31.87609039468567929 ) ) ;
#14774 = CARTESIAN_POINT ( 'NONE',  ( 0.7794527325549597263, 16.49732430514584536, -61.43175061772111434 ) ) ;
#14775 = CARTESIAN_POINT ( 'NONE',  ( -18.67979575497193778, 10.72451020669871902, 38.33442372801900433 ) ) ;
#14776 = CARTESIAN_POINT ( 'NONE',  ( -5.049401038298153566, 19.05341960407611168, 30.20724293864768839 ) ) ;
#14777 = CARTESIAN_POINT ( 'NONE',  ( 15.80617190586746368, 15.72974639402197994, 104.3739096053143669 ) ) ;
#14778 = CARTESIAN_POINT ( 'NONE',  ( -0.05219959533936034679, 19.03943276465977164, 47.50109039468566863 ) ) ;
#14779 = CARTESIAN_POINT ( 'NONE',  ( -13.89961937509977652, 13.97604488694528158, 40.62390960531435979 ) ) ;
#14780 = CYLINDRICAL_SURFACE ( 'NONE', #68898, 38.00000000000000000 ) ;
#14781 = DIRECTION ( 'NONE',  ( -1.000000000000000000, -0.000000000000000000, -3.709348145883536076E-20 ) ) ;
#14782 = CARTESIAN_POINT ( 'NONE',  ( 12.14591786802327356, -12.06949235617739191, 65.62609039468568994 ) ) ;
#14783 = CARTESIAN_POINT ( 'NONE',  ( -19.02544592524342804, 5.153800228976336051, 31.04057627198102409 ) ) ;
#14784 = CARTESIAN_POINT ( 'NONE',  ( -21.35462415990328822, -10.43496131973800090, 170.3924512066482748 ) ) ;
#14785 = CARTESIAN_POINT ( 'NONE',  ( 13.97604488694527802, 13.89961937509977652, 79.37390960531435269 ) ) ;
#14786 = CARTESIAN_POINT ( 'NONE',  ( -16.55341960407611168, -4.379528057220339221, 106.4572429386477097 ) ) ;
#14787 = CARTESIAN_POINT ( 'NONE',  ( 15.72974639402199770, -15.80617190586745480, 53.12390960531436690 ) ) ;
#14788 = CARTESIAN_POINT ( 'NONE',  ( -16.52544592524335698, -4.483927247898792601, 48.95942372801902565 ) ) ;
#14789 = CARTESIAN_POINT ( 'NONE',  ( -10.81492255796105439, 18.62759615963255655, 102.9177570613523756 ) ) ;
#14790 = CARTESIAN_POINT ( 'NONE',  ( -5.049401038298153566, 19.05341960407611168, 25.20724293864768484 ) ) ;
#14791 = CARTESIAN_POINT ( 'NONE',  ( 8.224510206698742110, 14.34966873604972548, 112.0844237280190185 ) ) ;
#14792 = CARTESIAN_POINT ( 'NONE',  ( -16.52544592524342804, 4.483927247898546575, 51.04057627198103120 ) ) ;
#14793 = CARTESIAN_POINT ( 'NONE',  ( -16.51473224551069308, -9.474510206698971260, 56.66557627198103120 ) ) ;
#14794 = CARTESIAN_POINT ( 'NONE',  ( 21.53943276465977519, 0.05219959533937863772, 106.2510903946856757 ) ) ;
#14795 = CARTESIAN_POINT ( 'NONE',  ( 21.52544592524334988, 5.823673210054432836, 21.45942372801901499 ) ) ;
#14796 = CARTESIAN_POINT ( 'NONE',  ( -18.62759615963255300, -10.81492255796106328, 79.16775706135234714 ) ) ;
#14797 = CARTESIAN_POINT ( 'NONE',  ( -4.379528057220086978, -16.55341960407618274, 49.79275706135234714 ) ) ;
#14798 = CARTESIAN_POINT ( 'NONE',  ( 12.06949235617739724, 12.14591786802326823, 31.87609039468567929 ) ) ;
#14800 = CARTESIAN_POINT ( 'NONE',  ( -21.52544592524334988, -5.823673210054445271, 93.95942372801903275 ) ) ;
#14799 = CARTESIAN_POINT ( 'NONE',  ( 4.379528057220339221, -16.55341960407611168, 72.70724293864769550 ) ) ;
#14801 = CARTESIAN_POINT ( 'NONE',  ( -4.483927247898539470, -16.52544592524342804, 37.29057627198102409 ) ) ;
#14802 = CARTESIAN_POINT ( 'NONE',  ( -17.48853670773244673, 5.747243402303102044, 113.6667129974999710 ) ) ;
#14803 = CARTESIAN_POINT ( 'NONE',  ( 8.314922557961029526, -14.29746914071037800, 40.41775706135234714 ) ) ;
#14804 = CARTESIAN_POINT ( 'NONE',  ( -8.224510206698948167, 14.34966873604960824, 40.41557627198103120 ) ) ;
#14805 = CARTESIAN_POINT ( 'NONE',  ( 4.483927247898790824, -16.52544592524335698, 85.20942372801901854 ) ) ;
#14806 = CARTESIAN_POINT ( 'NONE',  ( -0.05219959533909027116, -19.03943276465977164, 92.49890960531436690 ) ) ;
#14807 = CARTESIAN_POINT ( 'NONE',  ( -19.02544592524342804, 5.153800228976336051, 111.0405762719810099 ) ) ;
#14808 = CARTESIAN_POINT ( 'NONE',  ( 21.52544592524334988, 5.823673210054432836, 101.4594237280190185 ) ) ;
#14809 = CARTESIAN_POINT ( 'NONE',  ( 16.53943276465976808, 0.05219959533934440121, 101.2510903946856757 ) ) ;
#14810 = CARTESIAN_POINT ( 'NONE',  ( 16.55341960407611168, 4.379528057220329451, 73.95724293864769550 ) ) ;
#14811 = CARTESIAN_POINT ( 'NONE',  ( 9.564922557960805705, 16.46253265017160317, 84.58224293864769550 ) ) ;
#14812 = ORIENTED_EDGE ( 'NONE', *, *, #128355, .F. ) ;
#14813 = CARTESIAN_POINT ( 'NONE',  ( -16.55341960407617563, 4.379528057220093196, 38.54275706135234714 ) ) ;
#14814 = CARTESIAN_POINT ( 'NONE',  ( -19.03943276465977164, 0.05219959533909376836, 46.24890960531435979 ) ) ;
#14815 = CARTESIAN_POINT ( 'NONE',  ( -19.03943276465977164, 0.05219959533909376836, 91.24890960531436690 ) ) ;
#14817 = CARTESIAN_POINT ( 'NONE',  ( 36.91746824999999887, 11.99521256947799053, -1.524999997268813745 ) ) ;
#14816 = CARTESIAN_POINT ( 'NONE',  ( 8.224510206698742110, 14.34966873604972548, 37.08442372801901143 ) ) ;
#14818 = CARTESIAN_POINT ( 'NONE',  ( 16.51473224551083163, -9.474510206698727899, 35.83442372801899722 ) ) ;
#14819 = CARTESIAN_POINT ( 'NONE',  ( 16.53943276465976808, 0.05219959533934440121, 111.2510903946856899 ) ) ;
#14820 = CARTESIAN_POINT ( 'NONE',  ( -9.474510206698964154, 16.51473224551069663, 30.41557627198102054 ) ) ;
#14821 = CARTESIAN_POINT ( 'NONE',  ( 16.52544592524335698, 4.483927247898782831, 76.45942372801901854 ) ) ;
#14822 = CARTESIAN_POINT ( 'NONE',  ( 4.379528057220092307, 16.55341960407617563, 67.29275706135234714 ) ) ;
#14823 = CARTESIAN_POINT ( 'NONE',  ( 13.97604488694548053, -13.89961937509957401, 80.62609039468567573 ) ) ;
#14824 = CARTESIAN_POINT ( 'NONE',  ( 5.153800228976615827, -19.02544592524334988, 30.20942372801900433 ) ) ;
#14825 = CARTESIAN_POINT ( 'NONE',  ( 9.564922557960805705, 16.46253265017160317, 59.58224293864769550 ) ) ;
#14826 = CARTESIAN_POINT ( 'NONE',  ( -12.06949235617756955, 12.14591786802309770, 90.62390960531436690 ) ) ;
#14827 = CARTESIAN_POINT ( 'NONE',  ( 19.03943276465977164, 0.05219959533936151252, 61.25109039468566863 ) ) ;
#14828 = CARTESIAN_POINT ( 'NONE',  ( 10.72451020669898902, -18.67979575497178502, 52.91557627198103830 ) ) ;
#14829 = CARTESIAN_POINT ( 'NONE',  ( 9.474510206698729675, 16.51473224551082808, 22.08442372801899722 ) ) ;
#14830 = CARTESIAN_POINT ( 'NONE',  ( -13.97604488694527625, -13.89961937509977652, 106.8739096053143669 ) ) ;
#14831 = CARTESIAN_POINT ( 'NONE',  ( 5.823673210054125526, 21.52544592524343514, 79.79057627198102409 ) ) ;
#14832 = CARTESIAN_POINT ( 'NONE',  ( 13.97604488694527802, 13.89961937509977652, 104.3739096053143385 ) ) ;
#14833 = CARTESIAN_POINT ( 'NONE',  ( 9.564922557961047289, -16.46253265017146816, 95.41775706135233293 ) ) ;
#14834 = CARTESIAN_POINT ( 'NONE',  ( 5.049401038298161559, -19.05341960407611168, 112.7072429386476813 ) ) ;
#14835 = CARTESIAN_POINT ( 'NONE',  ( -16.52544592524335698, -4.483927247898792601, 33.95942372801901143 ) ) ;
#14836 = CARTESIAN_POINT ( 'NONE',  ( -5.153800228976328057, -19.02544592524343514, 32.29057627198102409 ) ) ;
#14837 = CARTESIAN_POINT ( 'NONE',  ( -9.564922557960796823, -16.46253265017161027, 97.08224293864769550 ) ) ;
#14838 = CARTESIAN_POINT ( 'NONE',  ( 10.81492255796078972, 18.62759615963270932, 74.58224293864768129 ) ) ;
#14839 = CARTESIAN_POINT ( 'NONE',  ( 0.05219959533934541429, -16.53943276465976808, 55.00109039468568284 ) ) ;
#14840 = CARTESIAN_POINT ( 'NONE',  ( -18.62759615963255300, -10.81492255796106328, 59.16775706135234714 ) ) ;
#14842 = CARTESIAN_POINT ( 'NONE',  ( -19.03943276465977164, -0.05219959533935918106, 18.75109039468567218 ) ) ;
#14841 = CARTESIAN_POINT ( 'NONE',  ( -5.153800228976607833, 19.02544592524334988, 102.7094237280189759 ) ) ;
#14843 = CARTESIAN_POINT ( 'NONE',  ( 14.34966873604972726, -8.224510206698740333, 110.8344237280190043 ) ) ;
#14844 = CARTESIAN_POINT ( 'NONE',  ( 5.823673210054125526, 21.52544592524343514, 99.79057627198103830 ) ) ;
#14845 = CARTESIAN_POINT ( 'NONE',  ( 8.314922557960818139, 14.29746914071049879, 34.58224293864770260 ) ) ;
#14846 = CARTESIAN_POINT ( 'NONE',  ( -0.05219959533936034679, 19.03943276465977164, 77.50109039468566152 ) ) ;
#14847 = EDGE_CURVE ( 'NONE', #71084, #110784, #112856, .T. ) ;
#14848 = CARTESIAN_POINT ( 'NONE',  ( 5.719274019375673035, 21.55341960407619339, 52.29275706135236135 ) ) ;
#14849 = CARTESIAN_POINT ( 'NONE',  ( -16.51473224551082808, 9.474510206698731452, 38.33442372801899722 ) ) ;
#14850 = CARTESIAN_POINT ( 'NONE',  ( -4.483927247898539470, -16.52544592524342804, 102.2905762719810383 ) ) ;
#14851 = CARTESIAN_POINT ( 'NONE',  ( -18.67979575497178146, -10.72451020669898902, 26.66557627198103475 ) ) ;
#14853 = EDGE_CURVE ( 'NONE', #9532, #107482, #50757, .T. ) ;
#14852 = CARTESIAN_POINT ( 'NONE',  ( 12.06949235617757843, -12.14591786802309237, 43.12390960531435269 ) ) ;
#14854 = CARTESIAN_POINT ( 'NONE',  ( -15.72974639402176322, -15.80617190586768395, 104.3760903946856899 ) ) ;
#14855 = CARTESIAN_POINT ( 'NONE',  ( 0.05219959533934541429, -16.53943276465976808, 75.00109039468568994 ) ) ;
#14856 = CARTESIAN_POINT ( 'NONE',  ( -8.314922557960811034, -14.29746914071050412, 32.08224293864769550 ) ) ;
#14857 = CARTESIAN_POINT ( 'NONE',  ( 21.55341960407619695, -5.719274019375665929, 66.04275706135236135 ) ) ;
#14858 = CARTESIAN_POINT ( 'NONE',  ( -21.53943276465977519, -0.05219959533937600094, 53.75109039468568994 ) ) ;
#14859 = ORIENTED_EDGE ( 'NONE', *, *, #26654, .T. ) ;
#14860 = CARTESIAN_POINT ( 'NONE',  ( -19.02544592524342804, 5.153800228976336051, 26.04057627198103120 ) ) ;
#14861 = CARTESIAN_POINT ( 'NONE',  ( -21.52544592524334988, -5.823673210054445271, 38.95942372801901854 ) ) ;
#14862 = CARTESIAN_POINT ( 'NONE',  ( 0.05219959533909260263, 19.03943276465977164, 24.99890960531435269 ) ) ;
#14863 = CARTESIAN_POINT ( 'NONE',  ( 9.564922557960805705, 16.46253265017160317, 39.58224293864768839 ) ) ;
#14864 = CARTESIAN_POINT ( 'NONE',  ( 16.55341960407611168, 4.379528057220329451, 83.95724293864770971 ) ) ;
#14865 = CARTESIAN_POINT ( 'NONE',  ( 13.97604488694527802, 13.89961937509977652, 74.37390960531436690 ) ) ;
#14866 = CARTESIAN_POINT ( 'NONE',  ( -16.55341960407611168, -4.379528057220339221, 31.45724293864769550 ) ) ;
#14867 = CARTESIAN_POINT ( 'NONE',  ( 5.823673210054125526, 21.52544592524343514, 54.79057627198104541 ) ) ;
#14868 = CARTESIAN_POINT ( 'NONE',  ( -14.29746914071049879, 8.314922557960819915, 90.83224293864769550 ) ) ;
#14869 = AXIS2_PLACEMENT_3D ( 'NONE', #50951, #127773, #66107 ) ;
#14870 = CARTESIAN_POINT ( 'NONE',  ( -18.67979575497178146, -10.72451020669898902, 101.6655762719810383 ) ) ;
#14871 = CARTESIAN_POINT ( 'NONE',  ( -0.05219959533909027116, -19.03943276465977164, 102.4989096053143669 ) ) ;
#14873 = CARTESIAN_POINT ( 'NONE',  ( -13.89961937509957401, -13.97604488694547875, 109.3760903946856331 ) ) ;
#14872 = CARTESIAN_POINT ( 'NONE',  ( -19.05341960407611168, -5.049401038298163336, 61.45724293864769550 ) ) ;
#14874 = CARTESIAN_POINT ( 'NONE',  ( 18.67979575497178502, 10.72451020669898547, 54.16557627198103120 ) ) ;
#14875 = CARTESIAN_POINT ( 'NONE',  ( 0.05219959533937995610, -21.53943276465977519, 75.00109039468568994 ) ) ;
#14876 = CARTESIAN_POINT ( 'NONE',  ( -16.51473224551069308, -9.474510206698971260, 66.66557627198102409 ) ) ;
#14877 = CARTESIAN_POINT ( 'NONE',  ( 19.05341960407611168, 5.049401038298154454, 103.9572429386476671 ) ) ;
#14878 = CARTESIAN_POINT ( 'NONE',  ( -8.224510206698735004, -14.34966873604973081, 74.58442372801901854 ) ) ;
#14879 = CARTESIAN_POINT ( 'NONE',  ( -18.62759615963255300, -10.81492255796106328, 59.16775706135234714 ) ) ;
#14880 = CARTESIAN_POINT ( 'NONE',  ( -21.55341960407619339, 5.719274019375674811, 83.54275706135234714 ) ) ;
#14881 = CARTESIAN_POINT ( 'NONE',  ( 10.72451020669898902, -18.67979575497178502, 107.9155762719810241 ) ) ;
#14882 = CARTESIAN_POINT ( 'NONE',  ( -14.34966873604972548, 8.224510206698743886, 73.33442372801901854 ) ) ;
#14883 = CARTESIAN_POINT ( 'NONE',  ( -10.72451020669898014, 18.67979575497178502, 70.41557627198102409 ) ) ;
#14884 = CARTESIAN_POINT ( 'NONE',  ( 19.05341960407617918, -5.049401038297876454, 51.04275706135231871 ) ) ;
#14885 = CARTESIAN_POINT ( 'NONE',  ( -15.80617190586745835, -15.72974639402198527, 41.87390960531435979 ) ) ;
#14887 = CARTESIAN_POINT ( 'NONE',  ( -12.14591786802309592, -12.06949235617757132, 21.87390960531436690 ) ) ;
#14886 = CARTESIAN_POINT ( 'NONE',  ( -19.02544592524342804, 5.153800228976336051, 76.04057627198102409 ) ) ;
#14888 = CARTESIAN_POINT ( 'NONE',  ( -16.79531203550650531, 7.028104445595468874, 63.74755011779561897 ) ) ;
#14889 = CARTESIAN_POINT ( 'NONE',  ( -9.474510206698964154, 16.51473224551069663, 115.4155762719810241 ) ) ;
#14890 = DIRECTION ( 'NONE',  ( -1.000000000000000000, 6.391086490440866478E-16, 0.000000000000000000 ) ) ;
#14891 = CARTESIAN_POINT ( 'NONE',  ( -0.05219959533936034679, 19.03943276465977164, 92.50109039468566152 ) ) ;
#14892 = CARTESIAN_POINT ( 'NONE',  ( -21.55341960407610458, -5.719274019375992779, 76.45724293864769550 ) ) ;
#14893 = CARTESIAN_POINT ( 'NONE',  ( -8.314922557960811034, -14.29746914071050412, 52.08224293864768839 ) ) ;
#14894 = CARTESIAN_POINT ( 'NONE',  ( 8.224510206698742110, 14.34966873604972548, 22.08442372801901143 ) ) ;
#14895 = CARTESIAN_POINT ( 'NONE',  ( 19.05341960407611168, 5.049401038298154454, 48.95724293864768129 ) ) ;
#14897 = CARTESIAN_POINT ( 'NONE',  ( 9.564922557961047289, -16.46253265017146816, 75.41775706135234714 ) ) ;
#14896 = CARTESIAN_POINT ( 'NONE',  ( -0.05219959533907301413, -21.53943276465977519, 97.49890960531436690 ) ) ;
#14898 = CARTESIAN_POINT ( 'NONE',  ( -0.05219959533909027116, -19.03943276465977164, 82.49890960531436690 ) ) ;
#14899 = CARTESIAN_POINT ( 'NONE',  ( -8.224510206698948167, 14.34966873604960824, 80.41557627198103830 ) ) ;
#14900 = CARTESIAN_POINT ( 'NONE',  ( -13.89961937509977652, 13.97604488694528158, 60.62390960531436690 ) ) ;
#14901 = CARTESIAN_POINT ( 'NONE',  ( 14.29746914071049879, -8.314922557960816363, 68.33224293864769550 ) ) ;
#14902 = CARTESIAN_POINT ( 'NONE',  ( 19.02544592524343514, -5.153800228976328945, 33.54057627198102409 ) ) ;
#14903 = CARTESIAN_POINT ( 'NONE',  ( -22.55670631985108443, -22.55670631985069008, -49.13275782002545355 ) ) ;
#14904 = CARTESIAN_POINT ( 'NONE',  ( 14.29746914071049879, -8.314922557960816363, 43.33224293864769550 ) ) ;
#14905 = CARTESIAN_POINT ( 'NONE',  ( -19.05341960407611168, -5.049401038298163336, 91.45724293864766707 ) ) ;
#14906 = CARTESIAN_POINT ( 'NONE',  ( -1.499960427298724808, -15.29496450215404479, -59.75377357153833913 ) ) ;
#14907 = CARTESIAN_POINT ( 'NONE',  ( -16.51473224551082808, 9.474510206698731452, 48.33442372801900433 ) ) ;
#14908 = CARTESIAN_POINT ( 'NONE',  ( -14.29746914071037622, -8.314922557961029526, 59.16775706135234714 ) ) ;
#14909 = VECTOR ( 'NONE', #140815, 1000.000000000000000 ) ;
#14910 = CARTESIAN_POINT ( 'NONE',  ( -15.72974639402197994, 15.80617190586746368, 60.62390960531437401 ) ) ;
#14911 = CARTESIAN_POINT ( 'NONE',  ( -19.02544592524334988, -5.153800228976617603, 33.95942372801897591 ) ) ;
#14912 = CARTESIAN_POINT ( 'NONE',  ( -5.153800228976328057, -19.02544592524343514, 92.29057627198099567 ) ) ;
#14913 = CARTESIAN_POINT ( 'NONE',  ( -18.22780087662124160, -5.499999999999927169, 83.98236817873107896 ) ) ;
#14914 = CARTESIAN_POINT ( 'NONE',  ( -18.67979575497178146, -10.72451020669898902, 26.66557627198103475 ) ) ;
#14915 = CARTESIAN_POINT ( 'NONE',  ( 5.153800228976335163, 19.02544592524342804, 59.79057627198100988 ) ) ;
#14916 = CARTESIAN_POINT ( 'NONE',  ( 18.62759615963255655, 10.81492255796105972, 51.66775706135234714 ) ) ;
#14917 = CARTESIAN_POINT ( 'NONE',  ( 16.55341960407611168, 4.379528057220329451, 113.9572429386477239 ) ) ;
#14918 = EDGE_CURVE ( 'NONE', #27850, #16723, #196723, .T. ) ;
#14921 = ORIENTED_EDGE ( 'NONE', *, *, #169635, .F. ) ;
#14920 = CARTESIAN_POINT ( 'NONE',  ( -0.05219959533909027116, -19.03943276465977164, 97.49890960531436690 ) ) ;
#14919 = CARTESIAN_POINT ( 'NONE',  ( 21.53943276465977519, -0.05219959533907433946, 98.74890960531438111 ) ) ;
#14922 = CARTESIAN_POINT ( 'NONE',  ( 5.823673210054444382, -21.52544592524334988, 35.20942372801901854 ) ) ;
#14923 = ORIENTED_EDGE ( 'NONE', *, *, #103523, .F. ) ;
#14924 = CARTESIAN_POINT ( 'NONE',  ( 13.97604488694527802, 13.89961937509977652, 104.3739096053143385 ) ) ;
#14925 = DIRECTION ( 'NONE',  ( 0.5000000000000037748, 0.4999999999999950595, 0.7071067811865484609 ) ) ;
#14926 = CARTESIAN_POINT ( 'NONE',  ( 21.55341960407610458, 5.719274019375980345, 88.95724293864769550 ) ) ;
#14927 = CARTESIAN_POINT ( 'NONE',  ( -16.46253265017160317, 9.564922557960807481, 45.83224293864769550 ) ) ;
#14928 = CARTESIAN_POINT ( 'NONE',  ( 16.52544592524335698, 4.483927247898782831, 21.45942372801901499 ) ) ;
#14929 = CARTESIAN_POINT ( 'NONE',  ( 11.40812507854755253, -35.11059874428192273, -4.524999997268813523 ) ) ;
#14930 = CARTESIAN_POINT ( 'NONE',  ( -16.51473224551069308, -9.474510206698971260, 31.66557627198102054 ) ) ;
#14931 = CARTESIAN_POINT ( 'NONE',  ( -0.05219959533937732626, 21.53943276465977519, 102.5010903946856899 ) ) ;
#14933 = CARTESIAN_POINT ( 'NONE',  ( 18.62759615963255655, 10.81492255796105972, 46.66775706135234714 ) ) ;
#14932 = CARTESIAN_POINT ( 'NONE',  ( -16.46253265017160317, 9.564922557960807481, 75.83224293864769550 ) ) ;
#14934 = CARTESIAN_POINT ( 'NONE',  ( 27.73933785331498569, 2.768321779492822058E-14, 144.3750000027311842 ) ) ;
#14935 = CARTESIAN_POINT ( 'NONE',  ( 16.46253265017160672, -9.564922557960803928, 93.33224293864769550 ) ) ;
#14936 = CARTESIAN_POINT ( 'NONE',  ( -15.67939035206521936, 24.07275550605739767, 140.0000000000000000 ) ) ;
#14939 = CARTESIAN_POINT ( 'NONE',  ( -21.55341960407619339, 5.719274019375674811, 53.54275706135234714 ) ) ;
#14938 = CARTESIAN_POINT ( 'NONE',  ( -16.53943276465976808, -0.05219959533934237506, 68.75109039468568994 ) ) ;
#14937 = CARTESIAN_POINT ( 'NONE',  ( 8.224510206698742110, 14.34966873604972548, 37.08442372801901143 ) ) ;
#14940 = CARTESIAN_POINT ( 'NONE',  ( 0.05219959533937995610, -21.53943276465977519, 85.00109039468568994 ) ) ;
#14941 = CARTESIAN_POINT ( 'NONE',  ( 3.875073520655164305, 5.577594645134329454, -62.38867879588715937 ) ) ;
#14942 = CARTESIAN_POINT ( 'NONE',  ( -13.89961937509957401, -13.97604488694547875, 104.3760903946856757 ) ) ;
#14943 = CARTESIAN_POINT ( 'NONE',  ( 19.03943276465977164, -0.05219959533909143690, 78.74890960531436690 ) ) ;
#14944 = CARTESIAN_POINT ( 'NONE',  ( -5.153800228976328057, -19.02544592524343514, 92.29057627198099567 ) ) ;
#14945 = CARTESIAN_POINT ( 'NONE',  ( -12.14591786802309592, -12.06949235617757132, 111.8739096053143669 ) ) ;
#14946 = CARTESIAN_POINT ( 'NONE',  ( -18.67979575497178146, -10.72451020669898902, 26.66557627198103475 ) ) ;
#14947 = CARTESIAN_POINT ( 'NONE',  ( 8.314922557961029526, -14.29746914071037800, 90.41775706135236135 ) ) ;
#14949 = CARTESIAN_POINT ( 'NONE',  ( -9.474510206698964154, 16.51473224551069663, 60.41557627198102409 ) ) ;
#14948 = CARTESIAN_POINT ( 'NONE',  ( 4.483927247898545687, 16.52544592524342804, 74.79057627198105251 ) ) ;
#14950 = CARTESIAN_POINT ( 'NONE',  ( -21.53943276465977519, -0.05219959533937600094, 78.75109039468568994 ) ) ;
#14951 = CARTESIAN_POINT ( 'NONE',  ( 8.898068258721473001, -27.38543819252872069, 144.8656553485623704 ) ) ;
#14952 = CARTESIAN_POINT ( 'NONE',  ( 16.51473224551083163, -9.474510206698727899, 100.8344237280190043 ) ) ;
#14953 = CARTESIAN_POINT ( 'NONE',  ( 16.52544592524342804, -4.483927247898539470, 78.54057627198103830 ) ) ;
#14954 = CARTESIAN_POINT ( 'NONE',  ( -21.55341960407619339, 5.719274019375674811, 33.54275706135234714 ) ) ;
#14955 = CARTESIAN_POINT ( 'NONE',  ( -5.719274019375978568, 21.55341960407610458, 65.20724293864768129 ) ) ;
#14956 = CARTESIAN_POINT ( 'NONE',  ( -16.62475595723698873, -7.163666690055295660, 104.4728664818953519 ) ) ;
#14957 = CARTESIAN_POINT ( 'NONE',  ( -35.68624576866248788, 0.9837712456775835612, 37.56068211393102274 ) ) ;
#14958 = CARTESIAN_POINT ( 'NONE',  ( 13.97604488694527802, 13.89961937509977652, 79.37390960531435269 ) ) ;
#14959 = CARTESIAN_POINT ( 'NONE',  ( -0.05219959533910754901, -16.53943276465976808, 52.49890960531435979 ) ) ;
#14960 = CARTESIAN_POINT ( 'NONE',  ( -12.06949235617756955, 12.14591786802309770, 40.62390960531435269 ) ) ;
#14961 = CARTESIAN_POINT ( 'NONE',  ( -8.224510206698735004, -14.34966873604973081, 99.58442372801900433 ) ) ;
#14962 = CARTESIAN_POINT ( 'NONE',  ( 9.564922557961047289, -16.46253265017146816, 55.41775706135234003 ) ) ;
#14963 = CARTESIAN_POINT ( 'NONE',  ( -21.98685479826777112, -13.98560643873833875, 165.5209445330007441 ) ) ;
#14964 = CARTESIAN_POINT ( 'NONE',  ( 19.02544592524343514, -5.153800228976328945, 98.54057627198100988 ) ) ;
#14965 = CARTESIAN_POINT ( 'NONE',  ( 16.52544592524342804, -4.483927247898539470, 68.54057627198103830 ) ) ;
#14966 = CARTESIAN_POINT ( 'NONE',  ( -5.153800228976607833, 19.02544592524334988, 42.70942372801901143 ) ) ;
#14968 = CARTESIAN_POINT ( 'NONE',  ( 0.05219959533907565091, 21.53943276465977519, 34.99890960531435979 ) ) ;
#14967 = CARTESIAN_POINT ( 'NONE',  ( -13.97604488694527625, -13.89961937509977652, 36.87390960531436690 ) ) ;
#14969 = CARTESIAN_POINT ( 'NONE',  ( -21.53943276465977519, 0.05219959533907696930, 61.24890960531435979 ) ) ;
#14970 = CARTESIAN_POINT ( 'NONE',  ( -8.224510206698948167, 14.34966873604960824, 95.41557627198102409 ) ) ;
#14971 = CARTESIAN_POINT ( 'NONE',  ( -12.06949235617739369, -12.14591786802326823, 49.37609039468569705 ) ) ;
#14972 = CARTESIAN_POINT ( 'NONE',  ( 18.62759615963255655, 10.81492255796105972, 36.66775706135234714 ) ) ;
#14973 = CARTESIAN_POINT ( 'NONE',  ( 12.06949235617757843, -12.14591786802309237, 93.12390960531436690 ) ) ;
#14974 = CARTESIAN_POINT ( 'NONE',  ( 16.62475595723696387, -7.163666690055227271, 38.02713351810466946 ) ) ;
#14975 = CARTESIAN_POINT ( 'NONE',  ( -16.79531203550651242, 7.028104445595470651, 48.74755011779559055 ) ) ;
#14976 = CARTESIAN_POINT ( 'NONE',  ( 15.72974639402199770, -15.80617190586745480, 33.12390960531435979 ) ) ;
#14977 = DIRECTION ( 'NONE',  ( 0.000000000000000000, 1.000000000000000000, 1.224646799147353207E-16 ) ) ;
#14978 = CARTESIAN_POINT ( 'NONE',  ( 1.500000000004810818, 7.599999999999482725, -64.24270632869257724 ) ) ;
#14980 = CARTESIAN_POINT ( 'NONE',  ( 14.34966873604960469, 8.224510206698951720, 29.16557627198103120 ) ) ;
#14979 = CARTESIAN_POINT ( 'NONE',  ( -4.483927247898782831, 16.52544592524335698, 37.70942372801900433 ) ) ;
#14981 = CARTESIAN_POINT ( 'NONE',  ( 21.55341960407610458, 5.719274019375980345, 73.95724293864769550 ) ) ;
#14982 = CARTESIAN_POINT ( 'NONE',  ( -19.05341960407617563, 5.049401038297882671, 83.54275706135233293 ) ) ;
#14983 = CARTESIAN_POINT ( 'NONE',  ( -18.62759615963270932, 10.81492255796079327, 65.83224293864769550 ) ) ;
#14984 = CARTESIAN_POINT ( 'NONE',  ( -21.92716348790883529, -9.076607822308508489, 171.2490935175190998 ) ) ;
#14985 = CARTESIAN_POINT ( 'NONE',  ( -12.06949235617739369, -12.14591786802326823, 49.37609039468569705 ) ) ;
#14987 = CARTESIAN_POINT ( 'NONE',  ( 5.049401038298161559, -19.05341960407611168, 107.7072429386476955 ) ) ;
#14986 = CARTESIAN_POINT ( 'NONE',  ( 19.03943276465977164, -0.05219959533909143690, 33.74890960531435979 ) ) ;
#14988 = CARTESIAN_POINT ( 'NONE',  ( 9.564922557960805705, 16.46253265017160317, 39.58224293864768839 ) ) ;
#14989 = CARTESIAN_POINT ( 'NONE',  ( -9.474510206698964154, 16.51473224551069663, 25.41557627198103120 ) ) ;
#14990 = CARTESIAN_POINT ( 'NONE',  ( 0.000000000000000000, 0.000000000000000000, 0.000000000000000000 ) ) ;
#14991 = CARTESIAN_POINT ( 'NONE',  ( -16.46253265017160317, 9.564922557960807481, 115.8322429386477097 ) ) ;
#14992 = EDGE_LOOP ( 'NONE', ( #82068, #49986, #96774, #10711, #167686 ) ) ;
#14993 = CARTESIAN_POINT ( 'NONE',  ( 12.14591786802327356, -12.06949235617739191, 70.62609039468567573 ) ) ;
#14994 = CARTESIAN_POINT ( 'NONE',  ( -21.55341960407610458, -5.719274019375992779, 91.45724293864769550 ) ) ;
#14995 = CARTESIAN_POINT ( 'NONE',  ( -9.564922557960796823, -16.46253265017161027, 57.08224293864769550 ) ) ;
#14996 = CARTESIAN_POINT ( 'NONE',  ( -5.823673210054431948, 21.52544592524334988, 32.70942372801900433 ) ) ;
#14997 = CARTESIAN_POINT ( 'NONE',  ( 19.02544592524343514, -5.153800228976328945, 83.54057627198100988 ) ) ;
#14998 = CARTESIAN_POINT ( 'NONE',  ( 19.02544592524343514, -5.153800228976328945, 113.5405762719810241 ) ) ;
#14999 = ORIENTED_EDGE ( 'NONE', *, *, #143971, .T. ) ;
#15000 = CARTESIAN_POINT ( 'NONE',  ( -5.823673210054431948, 21.52544592524334988, 22.70942372801901499 ) ) ;
#15003 = CARTESIAN_POINT ( 'NONE',  ( 9.564922557961047289, -16.46253265017146816, 90.41775706135234714 ) ) ;
#15002 = CARTESIAN_POINT ( 'NONE',  ( -13.97604488694527625, -13.89961937509977652, 106.8739096053143669 ) ) ;
#15001 = CARTESIAN_POINT ( 'NONE',  ( 13.89961937509977652, -13.97604488694527269, 28.12390960531435624 ) ) ;
#15004 = CARTESIAN_POINT ( 'NONE',  ( -16.51473224551082808, 9.474510206698731452, 28.33442372801900433 ) ) ;
#15005 = CARTESIAN_POINT ( 'NONE',  ( -10.72451020669898014, 18.67979575497178502, 105.4155762719810383 ) ) ;
#15006 = CARTESIAN_POINT ( 'NONE',  ( -9.564922557961040184, 16.46253265017147172, 37.91775706135233293 ) ) ;
#15007 = CARTESIAN_POINT ( 'NONE',  ( -16.53943276465976808, -0.05219959533934237506, 73.75109039468567573 ) ) ;
#15008 = CARTESIAN_POINT ( 'NONE',  ( -9.564922557960796823, -16.46253265017161027, 102.0822429386477097 ) ) ;
#15009 = CARTESIAN_POINT ( 'NONE',  ( 13.89961937509977652, -13.97604488694527269, 58.12390960531436690 ) ) ;
#15010 = AXIS2_PLACEMENT_3D ( 'NONE', #82346, #158217, #160210 ) ;
#15011 = CARTESIAN_POINT ( 'NONE',  ( -0.05219959533937732626, 21.53943276465977519, 62.50109039468568284 ) ) ;
#15012 = CARTESIAN_POINT ( 'NONE',  ( 21.53943276465977519, 0.05219959533937863772, 81.25109039468568994 ) ) ;
#15013 = CARTESIAN_POINT ( 'NONE',  ( 19.05341960407611168, 5.049401038298154454, 113.9572429386477097 ) ) ;
#15014 = CARTESIAN_POINT ( 'NONE',  ( -5.153800228976328057, -19.02544592524343514, 77.29057627198099567 ) ) ;
#15015 = CARTESIAN_POINT ( 'NONE',  ( -15.72974639402176322, -15.80617190586768395, 49.37609039468569705 ) ) ;
#15016 = CARTESIAN_POINT ( 'NONE',  ( 16.46253265017146816, 9.564922557961045513, 86.66775706135233293 ) ) ;
#15017 = CARTESIAN_POINT ( 'NONE',  ( -19.05341960407611168, -5.049401038298163336, 46.45724293864768129 ) ) ;
#15018 = CARTESIAN_POINT ( 'NONE',  ( 5.153800228976335163, 19.02544592524342804, 104.7905762719809957 ) ) ;
#15019 = CARTESIAN_POINT ( 'NONE',  ( 9.564922557960805705, 16.46253265017160317, 64.58224293864769550 ) ) ;
#15020 = CARTESIAN_POINT ( 'NONE',  ( 17.50000000000000000, -3.556245443207693313, 22.75258077879468388 ) ) ;
#15021 = CARTESIAN_POINT ( 'NONE',  ( 13.89961937509977652, -13.97604488694527269, 58.12390960531436690 ) ) ;
#15022 = CARTESIAN_POINT ( 'NONE',  ( -21.53943276465977519, 0.05219959533907696930, 106.2489096053143811 ) ) ;
#15023 = CARTESIAN_POINT ( 'NONE',  ( 16.52544592524335698, 4.483927247898782831, 86.45942372801901854 ) ) ;
#15024 = CARTESIAN_POINT ( 'NONE',  ( -16.70000000000002061, 1.759457951533292443E-13, -59.13370768023891344 ) ) ;
#15025 = CARTESIAN_POINT ( 'NONE',  ( -13.89961937509957401, -13.97604488694547875, 49.37609039468567573 ) ) ;
#15026 = CARTESIAN_POINT ( 'NONE',  ( -16.46253265017160317, 9.564922557960807481, 80.83224293864769550 ) ) ;
#15027 = CARTESIAN_POINT ( 'NONE',  ( 12.06949235617757843, -12.14591786802309237, 63.12390960531435979 ) ) ;
#15028 = CARTESIAN_POINT ( 'NONE',  ( -8.224510206698948167, 14.34966873604960824, 95.41557627198102409 ) ) ;
#15029 = CARTESIAN_POINT ( 'NONE',  ( 5.049401038298161559, -19.05341960407611168, 112.7072429386476813 ) ) ;
#15030 = ORIENTED_EDGE ( 'NONE', *, *, #126618, .T. ) ;
#15031 = CARTESIAN_POINT ( 'NONE',  ( 9.564922557960805705, 16.46253265017160317, 99.58224293864770971 ) ) ;
#15032 = CARTESIAN_POINT ( 'NONE',  ( -19.05341960407611168, -5.049401038298163336, 111.4572429386476671 ) ) ;
#15033 = CARTESIAN_POINT ( 'NONE',  ( -9.564922557961040184, 16.46253265017147172, 22.91775706135233648 ) ) ;
#15034 = CARTESIAN_POINT ( 'NONE',  ( -4.379528057220086978, -16.55341960407618274, 94.79275706135234714 ) ) ;
#15035 = CARTESIAN_POINT ( 'NONE',  ( 0.05219959533909260263, 19.03943276465977164, 74.99890960531435269 ) ) ;
#15036 = CARTESIAN_POINT ( 'NONE',  ( 21.55341960407619695, -5.719274019375665929, 36.04275706135234714 ) ) ;
#15037 = CARTESIAN_POINT ( 'NONE',  ( 10.72451020669898902, -18.67979575497178502, 32.91557627198102409 ) ) ;
#15038 = CARTESIAN_POINT ( 'NONE',  ( -21.52544592524343514, 5.823673210054127303, 111.0405762719810525 ) ) ;
#15039 = CARTESIAN_POINT ( 'NONE',  ( 15.72974639402199770, -15.80617190586745480, 73.12390960531436690 ) ) ;
#15040 = CARTESIAN_POINT ( 'NONE',  ( 4.379528057220339221, -16.55341960407611168, 82.70724293864770971 ) ) ;
#15041 = CARTESIAN_POINT ( 'NONE',  ( -16.51473224551082808, 9.474510206698731452, 43.33442372801900433 ) ) ;
#15042 = CARTESIAN_POINT ( 'NONE',  ( -16.46253265017160317, 9.564922557960807481, 35.83224293864768839 ) ) ;
#15043 = CARTESIAN_POINT ( 'NONE',  ( 9.474510206698971260, -16.51473224551069308, 77.91557627198103830 ) ) ;
#15044 = CARTESIAN_POINT ( 'NONE',  ( -13.97604488694527625, -13.89961937509977652, 76.87390960531433848 ) ) ;
#15045 = CARTESIAN_POINT ( 'NONE',  ( -17.14385361876520264, -23.59649016807271238, 141.1750000027311671 ) ) ;
#15046 = CARTESIAN_POINT ( 'NONE',  ( -4.379528057220328563, 16.55341960407611168, 95.20724293864769550 ) ) ;
#15047 = ORIENTED_EDGE ( 'NONE', *, *, #92009, .T. ) ;
#15048 = CARTESIAN_POINT ( 'NONE',  ( -8.224510206698948167, 14.34966873604960824, 25.41557627198103120 ) ) ;
#15049 = CARTESIAN_POINT ( 'NONE',  ( -14.29746914071037622, -8.314922557961029526, 24.16775706135235424 ) ) ;
#15050 = CARTESIAN_POINT ( 'NONE',  ( 0.05219959533937995610, -21.53943276465977519, 90.00109039468567573 ) ) ;
#15051 = CARTESIAN_POINT ( 'NONE',  ( -5.049401038298153566, 19.05341960407611168, 100.2072429386476955 ) ) ;
#15052 = CARTESIAN_POINT ( 'NONE',  ( 21.55341960407619695, -5.719274019375665929, 26.04275706135235779 ) ) ;
#15053 = CARTESIAN_POINT ( 'NONE',  ( 9.564922557960805705, 16.46253265017160317, 39.58224293864768839 ) ) ;
#15054 = CIRCLE ( 'NONE', #92542, 10.00000000000000000 ) ;
#15055 = CARTESIAN_POINT ( 'NONE',  ( 14.34966873604972726, -8.224510206698740333, 40.83442372801901854 ) ) ;
#15056 = CARTESIAN_POINT ( 'NONE',  ( -13.97604488694547697, 13.89961937509957934, 103.1260903946856473 ) ) ;
#15057 = CARTESIAN_POINT ( 'NONE',  ( 5.823673210054125526, 21.52544592524343514, 104.7905762719810241 ) ) ;
#15058 = CARTESIAN_POINT ( 'NONE',  ( -16.46253265017146816, -9.564922557961047289, 64.16775706135233293 ) ) ;
#15059 = DIRECTION ( 'NONE',  ( -0.000000000000000000, -0.000000000000000000, 1.000000000000000000 ) ) ;
#15060 = CARTESIAN_POINT ( 'NONE',  ( -5.719274019375665041, -21.55341960407619695, 19.79275706135235069 ) ) ;
#15061 = FACE_OUTER_BOUND ( 'NONE', #145996, .T. ) ;
#15062 = CARTESIAN_POINT ( 'NONE',  ( 9.474510206698971260, -16.51473224551069308, 92.91557627198103830 ) ) ;
#15063 = CARTESIAN_POINT ( 'NONE',  ( 19.97888994334922685, -34.65319547504297759, -5.000000000000000000 ) ) ;
#15064 = CARTESIAN_POINT ( 'NONE',  ( 9.564922557960805705, 16.46253265017160317, 89.58224293864769550 ) ) ;
#15066 = CARTESIAN_POINT ( 'NONE',  ( -16.53943276465976808, 0.05219959533911058130, 76.24890960531435269 ) ) ;
#15065 = CARTESIAN_POINT ( 'NONE',  ( -21.55341960407619339, 5.719274019375674811, 38.54275706135234714 ) ) ;
#15067 = CARTESIAN_POINT ( 'NONE',  ( -19.02544592524342804, 5.153800228976336051, 81.04057627198103830 ) ) ;
#15069 = CARTESIAN_POINT ( 'NONE',  ( -13.97604488694547697, 13.89961937509957934, 53.12609039468565442 ) ) ;
#15068 = CARTESIAN_POINT ( 'NONE',  ( 16.55341960407618274, -4.379528057220086978, 46.04275706135234714 ) ) ;
#15070 = CARTESIAN_POINT ( 'NONE',  ( 15.80617190586769283, -15.72974639402175789, 70.62609039468567573 ) ) ;
#15071 = CARTESIAN_POINT ( 'NONE',  ( -14.34966873604972548, 8.224510206698743886, 28.33442372801902209 ) ) ;
#15073 = EDGE_CURVE ( 'NONE', #27924, #56776, #115942, .T. ) ;
#15072 = CARTESIAN_POINT ( 'NONE',  ( 16.51473224551069308, 9.474510206698969483, 64.16557627198102409 ) ) ;
#15074 = CARTESIAN_POINT ( 'NONE',  ( 9.564922557961047289, -16.46253265017146816, 90.41775706135234714 ) ) ;
#15075 = CARTESIAN_POINT ( 'NONE',  ( 16.53943276465976808, 0.05219959533934440121, 51.25109039468568994 ) ) ;
#15076 = CARTESIAN_POINT ( 'NONE',  ( 15.72974639402176855, 15.80617190586768217, 96.87609039468568994 ) ) ;
#15077 = CARTESIAN_POINT ( 'NONE',  ( -13.97604488694547697, 13.89961937509957934, 83.12609039468564731 ) ) ;
#15078 = CARTESIAN_POINT ( 'NONE',  ( 19.05341960407611168, 5.049401038298154454, 43.95724293864769550 ) ) ;
#15079 = CARTESIAN_POINT ( 'NONE',  ( -15.72974639402197994, 15.80617190586746368, 75.62390960531439532 ) ) ;
#15081 = CARTESIAN_POINT ( 'NONE',  ( -19.02544592524334988, -5.153800228976617603, 78.95942372801900433 ) ) ;
#15080 = CARTESIAN_POINT ( 'NONE',  ( 14.29746914071049879, -8.314922557960816363, 73.33224293864769550 ) ) ;
#15082 = CARTESIAN_POINT ( 'NONE',  ( 15.50000000000000355, 5.499999999999998224, 118.0000000000000142 ) ) ;
#15083 = CARTESIAN_POINT ( 'NONE',  ( 9.474510206698729675, 16.51473224551082808, 37.08442372801899722 ) ) ;
#15084 = CARTESIAN_POINT ( 'NONE',  ( -14.34966873604960291, -8.224510206698953496, 21.66557627198102409 ) ) ;
#15085 = CARTESIAN_POINT ( 'NONE',  ( -8.224510206698948167, 14.34966873604960824, 60.41557627198102409 ) ) ;
#15087 = CARTESIAN_POINT ( 'NONE',  ( 17.14385361876520264, -23.59649016807271238, 147.5750000027311444 ) ) ;
#15086 = CARTESIAN_POINT ( 'NONE',  ( -15.80617190586768217, 15.72974639402176855, 103.1260903946856757 ) ) ;
#15088 = CARTESIAN_POINT ( 'NONE',  ( 15.80617190586746368, 15.72974639402197994, 114.3739096053143527 ) ) ;
#15089 =( BOUNDED_SURFACE ( )  B_SPLINE_SURFACE ( 1, 2, ( 
 ( #135831, #169116, #91264, #151979, #58967, #46786, #104489, #42825, #166172, #106456, #92274, #61931, #199478, #78096, #44801, #152955, #15455, #151006, #28660, #197500, #182332, #119664, #153958, #77112, #43811, #14453, #45790, #105474, #263, #123600, #13468, #168135, #29631, #167161, #74159, #76116, #27673, #198485, #137793, #30621, #185295, #108445, #60944, #170121, #107442, #31616, #89313, #75131, #90295, #59957, #121624, #93265, #154951, #122619, #12497, #184309, #183320, #139765, #65914, #111430, #32609, #172112, #79094, #112422, #34592, #95262, #2256, #190269, #47786, #186305, #109437, #49764, #35583, #5229, #142754, #21413, #188288, #96250, #158917, #94262, #33599, #140767, #63939, #62930, #97229, #20407, #187306, #157937, #189286, #48776, #82056, #143750, #156945, #173117, #19428, #125607, #17438, #81075, #171119, #80093, #4234 ),
 ( #113407, #50764, #174113, #124610, #18442, #110431, #141761, #3253, #175098, #64926, #126586, #127586, #1253, #66911, #155942, #128575, #51746, #36566, #98221, #159924, #83070, #23418, #179118, #195278, #69921, #131587, #180125, #86079, #6232, #70923, #41593, #67911, #101234, #9257, #26432, #129564, #176105, #54745, #87082, #191262, #52737, #40586, #117420, #114404, #10256, #146748, #39575, #103257, #22418, #37575, #116418, #115426, #193272, #132590, #102257, #99238, #85066, #25442, #178107, #24431, #144747, #160926, #8243, #84068, #147770, #55746, #162923, #145747, #194279, #7228, #56760, #118432, #130575, #163944, #68913, #164939, #192270, #148767, #71915, #53752, #177116, #38586, #133587, #100242, #161924, #149758, #184072, #60707, #57759, #153722, #90067, #183086, #46549, #165933, #11262, #198249, #58730, #13242, #152725, #45556, #72934 ) ),
 .UNSPECIFIED., .F., .F., .F. ) 
 B_SPLINE_SURFACE_WITH_KNOTS ( ( 2, 2 ),
 ( 3, 2, 2, 2, 2, 2, 2, 2, 2, 2, 2, 2, 2, 2, 2, 2, 2, 2, 2, 2, 2, 2, 2, 2, 2, 2, 2, 2, 2, 2, 2, 2, 2, 2, 2, 2, 2, 2, 2, 2, 2, 2, 2, 2, 2, 2, 2, 2, 2, 2, 3 ),
 ( 0.000000000000000000, 1.000000000000000000 ),
 ( 0.000000000000000000, 0.02000000000000000042, 0.04000000000000000083, 0.05999999999999999778, 0.08000000000000000167, 0.1000000000000000056, 0.1199999999999999956, 0.1400000000000000133, 0.1600000000000000033, 0.1799999999999999933, 0.2000000000000000111, 0.2200000000000000011, 0.2399999999999999911, 0.2600000000000000089, 0.2800000000000000266, 0.2999999999999999889, 0.3200000000000000067, 0.3400000000000000244, 0.3599999999999999867, 0.3800000000000000044, 0.4000000000000000222, 0.4199999999999999845, 0.4400000000000000022, 0.4600000000000000200, 0.4799999999999999822, 0.5000000000000000000, 0.5200000000000000178, 0.5400000000000000355, 0.5600000000000000533, 0.5799999999999999600, 0.5999999999999999778, 0.6199999999999999956, 0.6400000000000000133, 0.6600000000000000311, 0.6800000000000000488, 0.6999999999999999556, 0.7199999999999999734, 0.7399999999999999911, 0.7600000000000000089, 0.7800000000000000266, 0.8000000000000000444, 0.8199999999999999512, 0.8399999999999999689, 0.8599999999999999867, 0.8800000000000000044, 0.9000000000000000222, 0.9200000000000000400, 0.9399999999999999467, 0.9599999999999999645, 0.9799999999999999822, 1.000000000000000000 ),
 .UNSPECIFIED. ) 
 GEOMETRIC_REPRESENTATION_ITEM ( )  RATIONAL_B_SPLINE_SURFACE ( (
 ( 1.000000000000000000, 0.9510565162951535312, 1.000000000000000000, 0.9510565162951535312, 1.000000000000000000, 0.9510565162951535312, 1.000000000000000000, 0.9510565162951535312, 1.000000000000000000, 0.9510565162951535312, 1.000000000000000000, 0.9510565162951535312, 1.000000000000000000, 0.9510565162951535312, 1.000000000000000000, 0.9510565162951535312, 1.000000000000000000, 0.9510565162951535312, 1.000000000000000000, 0.9510565162951535312, 1.000000000000000000, 0.9510565162951535312, 1.000000000000000000, 0.9510565162951535312, 1.000000000000000000, 0.9510565162951535312, 1.000000000000000000, 0.9510565162951535312, 1.000000000000000000, 0.9510565162951535312, 1.000000000000000000, 0.9510565162951535312, 1.000000000000000000, 0.9510565162951535312, 1.000000000000000000, 0.9510565162951535312, 1.000000000000000000, 0.9510565162951535312, 1.000000000000000000, 0.9510565162951535312, 1.000000000000000000, 0.9510565162951535312, 1.000000000000000000, 0.9510565162951535312, 1.000000000000000000, 0.9510565162951535312, 1.000000000000000000, 0.9510565162951535312, 1.000000000000000000, 0.9510565162951535312, 1.000000000000000000, 0.9510565162951535312, 1.000000000000000000, 0.9510565162951535312, 1.000000000000000000, 0.9510565162951535312, 1.000000000000000000, 0.9510565162951535312, 1.000000000000000000, 0.9510565162951535312, 1.000000000000000000, 0.9510565162951535312, 1.000000000000000000, 0.9510565162951535312, 1.000000000000000000, 0.9510565162951535312, 1.000000000000000000, 0.9510565162951535312, 1.000000000000000000, 0.9510565162951535312, 1.000000000000000000, 0.9510565162951535312, 1.000000000000000000, 0.9510565162951535312, 1.000000000000000000, 0.9510565162951535312, 1.000000000000000000, 0.9510565162951535312, 1.000000000000000000, 0.9510565162951535312, 1.000000000000000000, 0.9510565162951535312, 1.000000000000000000, 0.9510565162951535312, 1.000000000000000000, 0.9510565162951535312, 1.000000000000000000, 0.9510565162951535312, 1.000000000000000000, 0.9510565162951535312, 1.000000000000000000, 0.9510565162951535312, 1.000000000000000000, 0.9510565162951535312, 1.000000000000000000, 0.9510565162951535312, 1.000000000000000000, 0.9510565162951535312, 1.000000000000000000, 0.9510565162951535312, 1.000000000000000000),
 ( 1.000000000000000000, 0.9510565162951535312, 1.000000000000000000, 0.9510565162951535312, 1.000000000000000000, 0.9510565162951535312, 1.000000000000000000, 0.9510565162951535312, 1.000000000000000000, 0.9510565162951535312, 1.000000000000000000, 0.9510565162951535312, 1.000000000000000000, 0.9510565162951535312, 1.000000000000000000, 0.9510565162951535312, 1.000000000000000000, 0.9510565162951535312, 1.000000000000000000, 0.9510565162951535312, 1.000000000000000000, 0.9510565162951535312, 1.000000000000000000, 0.9510565162951535312, 1.000000000000000000, 0.9510565162951535312, 1.000000000000000000, 0.9510565162951535312, 1.000000000000000000, 0.9510565162951535312, 1.000000000000000000, 0.9510565162951535312, 1.000000000000000000, 0.9510565162951535312, 1.000000000000000000, 0.9510565162951535312, 1.000000000000000000, 0.9510565162951535312, 1.000000000000000000, 0.9510565162951535312, 1.000000000000000000, 0.9510565162951535312, 1.000000000000000000, 0.9510565162951535312, 1.000000000000000000, 0.9510565162951535312, 1.000000000000000000, 0.9510565162951535312, 1.000000000000000000, 0.9510565162951535312, 1.000000000000000000, 0.9510565162951535312, 1.000000000000000000, 0.9510565162951535312, 1.000000000000000000, 0.9510565162951535312, 1.000000000000000000, 0.9510565162951535312, 1.000000000000000000, 0.9510565162951535312, 1.000000000000000000, 0.9510565162951535312, 1.000000000000000000, 0.9510565162951535312, 1.000000000000000000, 0.9510565162951535312, 1.000000000000000000, 0.9510565162951535312, 1.000000000000000000, 0.9510565162951535312, 1.000000000000000000, 0.9510565162951535312, 1.000000000000000000, 0.9510565162951535312, 1.000000000000000000, 0.9510565162951535312, 1.000000000000000000, 0.9510565162951535312, 1.000000000000000000, 0.9510565162951535312, 1.000000000000000000, 0.9510565162951535312, 1.000000000000000000, 0.9510565162951535312, 1.000000000000000000, 0.9510565162951535312, 1.000000000000000000, 0.9510565162951535312, 1.000000000000000000, 0.9510565162951535312, 1.000000000000000000, 0.9510565162951535312, 1.000000000000000000, 0.9510565162951535312, 1.000000000000000000, 0.9510565162951535312, 1.000000000000000000, 0.9510565162951535312, 1.000000000000000000, 0.9510565162951535312, 1.000000000000000000) ) ) 
 REPRESENTATION_ITEM ( '' )  SURFACE ( )  );
#15090 = CARTESIAN_POINT ( 'NONE',  ( 9.564922557960805705, 16.46253265017160317, 69.58224293864770971 ) ) ;
#15091 = CARTESIAN_POINT ( 'NONE',  ( -15.72974639402176322, -15.80617190586768395, 84.37609039468570415 ) ) ;
#15092 = CARTESIAN_POINT ( 'NONE',  ( -5.049401038298153566, 19.05341960407611168, 60.20724293864768129 ) ) ;
#15093 = ORIENTED_EDGE ( 'NONE', *, *, #76762, .T. ) ;
#15094 = CARTESIAN_POINT ( 'NONE',  ( 9.564922557960805705, 16.46253265017160317, 29.58224293864769550 ) ) ;
#15095 = CARTESIAN_POINT ( 'NONE',  ( -21.53943276465977519, 0.05219959533907696930, 36.24890960531435979 ) ) ;
#15096 = CARTESIAN_POINT ( 'NONE',  ( -12.06949235617756955, 12.14591786802309770, 60.62390960531437401 ) ) ;
#15097 = CARTESIAN_POINT ( 'NONE',  ( -16.46253265017160317, 9.564922557960807481, 25.83224293864769194 ) ) ;
#15098 = CARTESIAN_POINT ( 'NONE',  ( -12.14591786802309592, -12.06949235617757132, 86.87390960531438111 ) ) ;
#15099 = CARTESIAN_POINT ( 'NONE',  ( 10.81492255796078972, 18.62759615963270932, 99.58224293864770971 ) ) ;
#15100 = CARTESIAN_POINT ( 'NONE',  ( 21.55341960407619695, -5.719274019375665929, 46.04275706135234714 ) ) ;
#15101 = DIRECTION ( 'NONE',  ( 0.000000000000000000, 0.000000000000000000, 1.000000000000000000 ) ) ;
#15102 = CARTESIAN_POINT ( 'NONE',  ( 14.34966873604972726, -8.224510206698740333, 50.83442372801901143 ) ) ;
#15103 = CARTESIAN_POINT ( 'NONE',  ( -15.80617190586745835, -15.72974639402198527, 101.8739096053143811 ) ) ;
#15105 = CARTESIAN_POINT ( 'NONE',  ( -0.05219959533909027116, -19.03943276465977164, 32.49890960531435979 ) ) ;
#15104 = CARTESIAN_POINT ( 'NONE',  ( -5.153800228976607833, 19.02544592524334988, 32.70942372801899722 ) ) ;
#15106 = CARTESIAN_POINT ( 'NONE',  ( 13.89961937509977652, -13.97604488694527269, 103.1239096053143527 ) ) ;
#15107 = CARTESIAN_POINT ( 'NONE',  ( -21.55341960407619339, 5.719274019375674811, 63.54275706135234003 ) ) ;
#15108 = CARTESIAN_POINT ( 'NONE',  ( -21.53943276465977519, 0.05219959533907696930, 41.24890960531435269 ) ) ;
#15109 = CARTESIAN_POINT ( 'NONE',  ( -12.14591786802326823, 12.06949235617739902, 113.1260903946856899 ) ) ;
#15111 = CARTESIAN_POINT ( 'NONE',  ( 10.72451020669871369, 18.67979575497193778, 92.08442372801901854 ) ) ;
#15110 = CARTESIAN_POINT ( 'NONE',  ( 5.823673210054444382, -21.52544592524334988, 70.20942372801904696 ) ) ;
#15112 = CARTESIAN_POINT ( 'NONE',  ( -5.049401038297874678, -19.05341960407617918, 34.79275706135233293 ) ) ;
#15113 = CARTESIAN_POINT ( 'NONE',  ( -12.06949235617739369, -12.14591786802326823, 89.37609039468568994 ) ) ;
#15114 = CARTESIAN_POINT ( 'NONE',  ( 5.823673210054444382, -21.52544592524334988, 55.20942372801902565 ) ) ;
#15115 = CARTESIAN_POINT ( 'NONE',  ( 19.05341960407611168, 5.049401038298154454, 43.95724293864769550 ) ) ;
#15116 = CARTESIAN_POINT ( 'NONE',  ( 13.97604488694548053, -13.89961937509957401, 25.62609039468566507 ) ) ;
#15117 = CARTESIAN_POINT ( 'NONE',  ( 19.05341960407611168, 5.049401038298154454, 113.9572429386477097 ) ) ;
#15118 = CARTESIAN_POINT ( 'NONE',  ( -10.72451020669898014, 18.67979575497178502, 110.4155762719810383 ) ) ;
#15119 = CARTESIAN_POINT ( 'NONE',  ( 18.67979575497178502, 10.72451020669898547, 69.16557627198102409 ) ) ;
#15120 = CARTESIAN_POINT ( 'NONE',  ( 14.29746914071037800, 8.314922557961029526, 41.66775706135235424 ) ) ;
#15122 = CARTESIAN_POINT ( 'NONE',  ( -21.53943276465977519, 0.05219959533907696930, 76.24890960531435269 ) ) ;
#15121 = CARTESIAN_POINT ( 'NONE',  ( -30.00000000000000355, -3.889087296526017479, 8.181980515339454030 ) ) ;
#15124 = CARTESIAN_POINT ( 'NONE',  ( -14.29746914071049879, 8.314922557960819915, 60.83224293864769550 ) ) ;
#15123 = CARTESIAN_POINT ( 'NONE',  ( -0.05219959533934338120, 16.53943276465976808, 67.50109039468568994 ) ) ;
#15125 = CARTESIAN_POINT ( 'NONE',  ( -3.573655867282028392E-15, 2.428612866367529932E-14, 139.9999999999999716 ) ) ;
#15126 = CARTESIAN_POINT ( 'NONE',  ( -9.474510206698720793, -16.51473224551083518, 99.58442372801900433 ) ) ;
#15127 = CARTESIAN_POINT ( 'NONE',  ( 15.72974639402199770, -15.80617190586745480, 38.12390960531436690 ) ) ;
#15128 = DIRECTION ( 'NONE',  ( -3.469446951953611033E-15, 0.000000000000000000, 1.000000000000000000 ) ) ;
#15129 = CARTESIAN_POINT ( 'NONE',  ( -16.52544592524335698, -4.483927247898792601, 33.95942372801901143 ) ) ;
#15130 = CARTESIAN_POINT ( 'NONE',  ( -0.05219959533907301413, -21.53943276465977519, 112.4989096053143669 ) ) ;
#15131 = CARTESIAN_POINT ( 'NONE',  ( 15.72974639402199770, -15.80617190586745480, 38.12390960531436690 ) ) ;
#15132 = CARTESIAN_POINT ( 'NONE',  ( -16.53943276465976808, -0.05219959533934237506, 58.75109039468568994 ) ) ;
#15133 = CARTESIAN_POINT ( 'NONE',  ( 19.02544592524343514, -5.153800228976328945, 78.54057627198099567 ) ) ;
#15135 = CARTESIAN_POINT ( 'NONE',  ( 5.153800228976615827, -19.02544592524334988, 110.2094237280189901 ) ) ;
#15134 = CARTESIAN_POINT ( 'NONE',  ( 0.05219959533937995610, -21.53943276465977519, 40.00109039468567573 ) ) ;
#15136 = CARTESIAN_POINT ( 'NONE',  ( 5.823673210054125526, 21.52544592524343514, 29.79057627198102409 ) ) ;
#15137 = VERTEX_POINT ( 'NONE', #29833 ) ;
#15138 = CARTESIAN_POINT ( 'NONE',  ( 9.474510206698729675, 16.51473224551082808, 27.08442372801900433 ) ) ;
#15139 = CARTESIAN_POINT ( 'NONE',  ( -4.379528057220086978, -16.55341960407618274, 44.79275706135234714 ) ) ;
#15140 = CARTESIAN_POINT ( 'NONE',  ( -19.03943276465977164, 0.05219959533909376836, 96.24890960531436690 ) ) ;
#15141 = CARTESIAN_POINT ( 'NONE',  ( 21.55341960407610458, 5.719274019375980345, 98.95724293864770971 ) ) ;
#15142 = CARTESIAN_POINT ( 'NONE',  ( 19.02544592524343514, -5.153800228976328945, 78.54057627198099567 ) ) ;
#15143 = CYLINDRICAL_SURFACE ( 'NONE', #47671, 2.500000000000000000 ) ;
#15144 = CARTESIAN_POINT ( 'NONE',  ( 14.29746914071049879, -8.314922557960816363, 83.33224293864769550 ) ) ;
#15145 = CARTESIAN_POINT ( 'NONE',  ( 0.05219959533907565091, 21.53943276465977519, 29.99890960531435979 ) ) ;
#15146 = CARTESIAN_POINT ( 'NONE',  ( -17.40805194822030799, 6.112264579159341515, 35.83371272510612471 ) ) ;
#15147 = CARTESIAN_POINT ( 'NONE',  ( 4.483927247898790824, -16.52544592524335698, 70.20942372801904696 ) ) ;
#15148 = CARTESIAN_POINT ( 'NONE',  ( 21.53943276465977519, 0.05219959533937863772, 26.25109039468567573 ) ) ;
#15149 = CARTESIAN_POINT ( 'NONE',  ( -16.51473224551082808, 9.474510206698731452, 78.33442372801900433 ) ) ;
#15150 = CARTESIAN_POINT ( 'NONE',  ( -0.05219959533909027116, -19.03943276465977164, 27.49890960531435624 ) ) ;
#15151 = CARTESIAN_POINT ( 'NONE',  ( -5.719274019375978568, 21.55341960407610458, 70.20724293864769550 ) ) ;
#15152 = VECTOR ( 'NONE', #148657, 1000.000000000000000 ) ;
#15153 = CARTESIAN_POINT ( 'NONE',  ( -5.049401038298153566, 19.05341960407611168, 105.2072429386476671 ) ) ;
#15154 = CARTESIAN_POINT ( 'NONE',  ( -21.53943276465977519, -0.05219959533937600094, 88.75109039468567573 ) ) ;
#15155 = CARTESIAN_POINT ( 'NONE',  ( -13.89961937509977652, 13.97604488694528158, 65.62390960531436690 ) ) ;
#15156 = ADVANCED_FACE ( 'NONE', ( #166377 ), #150081, .T. ) ;
#15157 = CARTESIAN_POINT ( 'NONE',  ( -14.34966873604972548, 8.224510206698743886, 48.33442372801902565 ) ) ;
#15158 = CARTESIAN_POINT ( 'NONE',  ( -13.89961937509977652, 13.97604488694528158, 60.62390960531436690 ) ) ;
#15159 = CARTESIAN_POINT ( 'NONE',  ( 18.67979575497194134, -10.72451020669871369, 85.83442372801901854 ) ) ;
#15160 = VERTEX_POINT ( 'NONE', #179559 ) ;
#15161 = CARTESIAN_POINT ( 'NONE',  ( -13.97604488694547697, 13.89961937509957934, 33.12609039468566863 ) ) ;
#15162 = CARTESIAN_POINT ( 'NONE',  ( -9.474510206698720793, -16.51473224551083518, 49.58442372801899722 ) ) ;
#15163 = CARTESIAN_POINT ( 'NONE',  ( -15.80617190586768217, 15.72974639402176855, 48.12609039468568284 ) ) ;
#15164 = CIRCLE ( 'NONE', #31328, 26.79475375365586487 ) ;
#15165 = CARTESIAN_POINT ( 'NONE',  ( 16.51473224551069308, 9.474510206698969483, 54.16557627198103120 ) ) ;
#15166 = CARTESIAN_POINT ( 'NONE',  ( 19.05341960407617918, -5.049401038297876454, 46.04275706135233293 ) ) ;
#15167 = CARTESIAN_POINT ( 'NONE',  ( 19.02544592524343514, -5.153800228976328945, 98.54057627198100988 ) ) ;
#15168 = CARTESIAN_POINT ( 'NONE',  ( 5.153800228976335163, 19.02544592524342804, 64.79057627198100988 ) ) ;
#15169 = CARTESIAN_POINT ( 'NONE',  ( 0.05219959533910956823, 16.53943276465976808, 24.99890960531435624 ) ) ;
#15171 = CARTESIAN_POINT ( 'NONE',  ( 10.81492255796106328, -18.62759615963255655, 105.4177570613523613 ) ) ;
#15170 = CARTESIAN_POINT ( 'NONE',  ( -21.52544592524343514, 5.823673210054127303, 26.04057627198103475 ) ) ;
#15172 = CARTESIAN_POINT ( 'NONE',  ( 22.81625015709509441, 31.40387420917330275, -7.824999997268813345 ) ) ;
#15173 = CARTESIAN_POINT ( 'NONE',  ( -33.92112623720979059, 5.144804392130072124, 93.04721607740081879 ) ) ;
#15174 = CARTESIAN_POINT ( 'NONE',  ( -5.719274019375665041, -21.55341960407619695, 104.7927570613523898 ) ) ;
#15175 = CARTESIAN_POINT ( 'NONE',  ( 21.31248648291599324, -0.2211803504529610831, -58.84879416108399397 ) ) ;
#15176 = CARTESIAN_POINT ( 'NONE',  ( -13.89961937509977652, 13.97604488694528158, 25.62390960531434558 ) ) ;
#15177 = LINE ( 'NONE', #154678, #56405 ) ;
#15178 = CARTESIAN_POINT ( 'NONE',  ( -26.00062938246246702, -10.06977165081872094, 166.7331697587468682 ) ) ;
#15179 = CARTESIAN_POINT ( 'NONE',  ( -0.05219959533934338120, 16.53943276465976808, 47.50109039468568994 ) ) ;
#15180 = CARTESIAN_POINT ( 'NONE',  ( 0.05219959533907565091, 21.53943276465977519, 64.99890960531435269 ) ) ;
#15181 = CARTESIAN_POINT ( 'NONE',  ( 16.52544592524342804, -4.483927247898539470, 38.54057627198103120 ) ) ;
#15183 = CARTESIAN_POINT ( 'NONE',  ( 19.05341960407611168, 5.049401038298154454, 93.95724293864769550 ) ) ;
#15182 = CARTESIAN_POINT ( 'NONE',  ( -16.55341960407611168, -4.379528057220339221, 106.4572429386477097 ) ) ;
#15184 = CARTESIAN_POINT ( 'NONE',  ( 9.474510206698729675, 16.51473224551082808, 32.08442372801900433 ) ) ;
#15185 = CARTESIAN_POINT ( 'NONE',  ( -12.06949235617756955, 12.14591786802309770, 110.6239096053143669 ) ) ;
#15186 = CARTESIAN_POINT ( 'NONE',  ( 5.823673210054444382, -21.52544592524334988, 70.20942372801904696 ) ) ;
#15187 = CARTESIAN_POINT ( 'NONE',  ( 1.300000000000000044, 0.000000000000000000, 0.000000000000000000 ) ) ;
#15188 = CARTESIAN_POINT ( 'NONE',  ( -16.55341960407617563, 4.379528057220093196, 103.5427570613523613 ) ) ;
#15189 = CARTESIAN_POINT ( 'NONE',  ( 29.86685920354754487, 21.69954338932564752, -7.924999997268814766 ) ) ;
#15190 = CARTESIAN_POINT ( 'NONE',  ( 5.719274019375991003, -21.55341960407610458, 27.70724293864769905 ) ) ;
#15191 = CARTESIAN_POINT ( 'NONE',  ( -16.53943276465976808, 0.05219959533911058130, 96.24890960531435269 ) ) ;
#15192 = CARTESIAN_POINT ( 'NONE',  ( -16.46253265017146816, -9.564922557961047289, 54.16775706135234003 ) ) ;
#15193 = CARTESIAN_POINT ( 'NONE',  ( 16.46253265017160672, -9.564922557960803928, 78.33224293864769550 ) ) ;
#15194 = CARTESIAN_POINT ( 'NONE',  ( 16.52544592524342804, -4.483927247898539470, 73.54057627198102409 ) ) ;
#15195 = CARTESIAN_POINT ( 'NONE',  ( 19.05341960407617918, -5.049401038297876454, 91.04275706135234714 ) ) ;
#15196 = CARTESIAN_POINT ( 'NONE',  ( -15.80617190586745835, -15.72974639402198527, 46.87390960531435979 ) ) ;
#15197 = ORIENTED_EDGE ( 'NONE', *, *, #79032, .F. ) ;
#15198 = CARTESIAN_POINT ( 'NONE',  ( 12.06949235617757843, -12.14591786802309237, 108.1239096053143811 ) ) ;
#15199 = B_SPLINE_CURVE_WITH_KNOTS ( 'NONE', 3,
 ( #40541, #163900, #10211, #87038, #71871, #164894 ),
 .UNSPECIFIED., .F., .F.,
 ( 4, 2, 4 ),
 ( 0.007228050697041583060, 0.007608510107495075961, 0.007988969517948567994 ),
 .UNSPECIFIED. ) ;
#15200 = CARTESIAN_POINT ( 'NONE',  ( -17.40861289039004589, -6.110651285853283987, 31.37232470827432707 ) ) ;
#15202 = CARTESIAN_POINT ( 'NONE',  ( -21.52544592524343514, 5.823673210054127303, 76.04057627198102409 ) ) ;
#15201 = CARTESIAN_POINT ( 'NONE',  ( 19.03943276465977164, -0.05219959533909143690, 68.74890960531436690 ) ) ;
#15204 = CARTESIAN_POINT ( 'NONE',  ( 19.03943276465977164, -0.05219959533909143690, 88.74890960531436690 ) ) ;
#15203 = CARTESIAN_POINT ( 'NONE',  ( 14.34966873604972726, -8.224510206698740333, 90.83442372801901854 ) ) ;
#15205 = CARTESIAN_POINT ( 'NONE',  ( -0.05219959533936034679, 19.03943276465977164, 72.50109039468566152 ) ) ;
#15206 = CARTESIAN_POINT ( 'NONE',  ( 21.53943276465977519, 0.05219959533937863772, 76.25109039468568994 ) ) ;
#15207 = CARTESIAN_POINT ( 'NONE',  ( -15.72974639402197994, 15.80617190586746368, 60.62390960531437401 ) ) ;
#15208 = CARTESIAN_POINT ( 'NONE',  ( -5.823673210054116645, -21.52544592524344225, 27.29057627198103120 ) ) ;
#15209 = CARTESIAN_POINT ( 'NONE',  ( 16.46253265017160672, -9.564922557960803928, 33.33224293864770260 ) ) ;
#15210 = CARTESIAN_POINT ( 'NONE',  ( -16.52544592524335698, -4.483927247898792601, 98.95942372801903275 ) ) ;
#15211 = CARTESIAN_POINT ( 'NONE',  ( -19.03943276465977164, 0.05219959533909376836, 46.24890960531435979 ) ) ;
#15212 = CARTESIAN_POINT ( 'NONE',  ( 12.14591786802327356, -12.06949235617739191, 25.62609039468567929 ) ) ;
#15213 = DIRECTION ( 'NONE',  ( 1.000000000000000000, 2.486899575160350335E-14, 0.000000000000000000 ) ) ;
#15214 = CARTESIAN_POINT ( 'NONE',  ( -18.67979575497193778, 10.72451020669871902, 108.3344237280190185 ) ) ;
#15215 = CARTESIAN_POINT ( 'NONE',  ( -8.314922557960811034, -14.29746914071050412, 57.08224293864769550 ) ) ;
#15216 = CARTESIAN_POINT ( 'NONE',  ( 15.80617190586746368, 15.72974639402197994, 109.3739096053143811 ) ) ;
#15217 = CARTESIAN_POINT ( 'NONE',  ( -5.823673210054116645, -21.52544592524344225, 107.2905762719810525 ) ) ;
#15218 = CARTESIAN_POINT ( 'NONE',  ( -4.624734593510437364, 4.070821633784361460, -64.52277792523199196 ) ) ;
#15219 = CARTESIAN_POINT ( 'NONE',  ( -15.80617190586745835, -15.72974639402198527, 46.87390960531435979 ) ) ;
#15220 = CARTESIAN_POINT ( 'NONE',  ( 16.53943276465976808, 0.05219959533934440121, 76.25109039468568994 ) ) ;
#15221 = CARTESIAN_POINT ( 'NONE',  ( 14.29746914071049879, -8.314922557960816363, 88.33224293864769550 ) ) ;
#15222 = CARTESIAN_POINT ( 'NONE',  ( 19.02544592524343514, -5.153800228976328945, 63.54057627198103830 ) ) ;
#15223 = CARTESIAN_POINT ( 'NONE',  ( 27.18966431762777702, -4.276553394869359259, 168.7322077152510928 ) ) ;
#15224 = CARTESIAN_POINT ( 'NONE',  ( -4.483927247898539470, -16.52544592524342804, 22.29057627198102765 ) ) ;
#15225 = CARTESIAN_POINT ( 'NONE',  ( 10.81492255796106328, -18.62759615963255655, 30.41775706135234358 ) ) ;
#15226 = CARTESIAN_POINT ( 'NONE',  ( -5.153800228976328057, -19.02544592524343514, 97.29057627198099567 ) ) ;
#15227 = CARTESIAN_POINT ( 'NONE',  ( -18.62759615963255300, -10.81492255796106328, 64.16775706135234714 ) ) ;
#15228 = DIRECTION ( 'NONE',  ( -1.000000000000000000, 4.336808689942018352E-17, 0.000000000000000000 ) ) ;
#15229 = CARTESIAN_POINT ( 'NONE',  ( -19.05341960407611168, -5.049401038298163336, 31.45724293864769550 ) ) ;
#15230 = ORIENTED_EDGE ( 'NONE', *, *, #65989, .F. ) ;
#15231 = CARTESIAN_POINT ( 'NONE',  ( -15.80617190586768217, 15.72974639402176855, 53.12609039468568284 ) ) ;
#15232 = CARTESIAN_POINT ( 'NONE',  ( -19.03943276465977164, 0.05219959533909376836, 46.24890960531435979 ) ) ;
#15233 = CARTESIAN_POINT ( 'NONE',  ( -13.89961937509977652, 13.97604488694528158, 95.62390960531436690 ) ) ;
#15234 = CARTESIAN_POINT ( 'NONE',  ( -16.51473224551082808, 9.474510206698731452, 78.33442372801900433 ) ) ;
#15235 = CARTESIAN_POINT ( 'NONE',  ( 21.53943276465977519, 0.05219959533937863772, 36.25109039468567573 ) ) ;
#15236 = CARTESIAN_POINT ( 'NONE',  ( -5.153800228976607833, 19.02544592524334988, 107.7094237280189759 ) ) ;
#15237 = CARTESIAN_POINT ( 'NONE',  ( 16.46253265017146816, 9.564922557961045513, 71.66775706135233293 ) ) ;
#15238 = CARTESIAN_POINT ( 'NONE',  ( -16.51473224551069308, -9.474510206698971260, 36.66557627198102409 ) ) ;
#15239 = CARTESIAN_POINT ( 'NONE',  ( -5.049401038297874678, -19.05341960407617918, 79.79275706135233293 ) ) ;
#15240 = CARTESIAN_POINT ( 'NONE',  ( -4.483927247898782831, 16.52544592524335698, 102.7094237280190185 ) ) ;
#15241 = CARTESIAN_POINT ( 'NONE',  ( 13.97604488694548053, -13.89961937509957401, 80.62609039468567573 ) ) ;
#15242 = CARTESIAN_POINT ( 'NONE',  ( -8.314922557960811034, -14.29746914071050412, 37.08224293864768129 ) ) ;
#15243 = CARTESIAN_POINT ( 'NONE',  ( 0.05219959533936267826, -19.03943276465977164, 50.00109039468566863 ) ) ;
#15244 = CARTESIAN_POINT ( 'NONE',  ( 15.72974639402176855, 15.80617190586768217, 101.8760903946857042 ) ) ;
#15245 = CARTESIAN_POINT ( 'NONE',  ( -13.89961937509957401, -13.97604488694547875, 19.37609039468566507 ) ) ;
#15246 = CARTESIAN_POINT ( 'NONE',  ( -13.89961937509977652, 13.97604488694528158, 35.62390960531435269 ) ) ;
#15247 = CARTESIAN_POINT ( 'NONE',  ( -15.72974639402176322, -15.80617190586768395, 94.37609039468568994 ) ) ;
#15248 = CARTESIAN_POINT ( 'NONE',  ( 0.05219959533934541429, -16.53943276465976808, 45.00109039468568284 ) ) ;
#15249 = CARTESIAN_POINT ( 'NONE',  ( 19.02544592524343514, -5.153800228976328945, 88.54057627198102409 ) ) ;
#15250 = EDGE_CURVE ( 'NONE', #50775, #1947, #163067, .T. ) ;
#15251 = CARTESIAN_POINT ( 'NONE',  ( 8.571926809382597767, 26.38167802310806209, 146.2750000027311899 ) ) ;
#15252 = CARTESIAN_POINT ( 'NONE',  ( 9.564922557960805705, 16.46253265017160317, 84.58224293864769550 ) ) ;
#15253 = CARTESIAN_POINT ( 'NONE',  ( 17.59632111031626067, -2.707012485672555702, 102.5000000000000284 ) ) ;
#15254 = ORIENTED_EDGE ( 'NONE', *, *, #184219, .F. ) ;
#15255 = CARTESIAN_POINT ( 'NONE',  ( -0.05219959533936034679, 19.03943276465977164, 87.50109039468567573 ) ) ;
#15256 = CARTESIAN_POINT ( 'NONE',  ( -18.67979575497178146, -10.72451020669898902, 21.66557627198102409 ) ) ;
#15258 = CARTESIAN_POINT ( 'NONE',  ( 9.564922557961047289, -16.46253265017146816, 95.41775706135233293 ) ) ;
#15257 = CARTESIAN_POINT ( 'NONE',  ( -18.67979575497193778, 10.72451020669871902, 113.3344237280190328 ) ) ;
#15259 = CARTESIAN_POINT ( 'NONE',  ( 16.52544592524342804, -4.483927247898539470, 98.54057627198105251 ) ) ;
#15260 = CARTESIAN_POINT ( 'NONE',  ( -9.474510206698964154, 16.51473224551069663, 30.41557627198102054 ) ) ;
#15261 = CARTESIAN_POINT ( 'NONE',  ( 21.53943276465977519, -0.05219959533907433946, 58.74890960531436690 ) ) ;
#15262 = CARTESIAN_POINT ( 'NONE',  ( -21.52544592524343514, 5.823673210054127303, 51.04057627198103120 ) ) ;
#15263 = CARTESIAN_POINT ( 'NONE',  ( -19.05341960407611168, -5.049401038298163336, 21.45724293864768839 ) ) ;
#15264 = CARTESIAN_POINT ( 'NONE',  ( 193.3062444957835453, -155.7167183371837496, 0.000000000000000000 ) ) ;
#15265 = CARTESIAN_POINT ( 'NONE',  ( -5.153800228976607833, 19.02544592524334988, 67.70942372801900433 ) ) ;
#15266 = CARTESIAN_POINT ( 'NONE',  ( -12.14591786802309592, -12.06949235617757132, 41.87390960531435979 ) ) ;
#15267 = CARTESIAN_POINT ( 'NONE',  ( 13.97604488694527802, 13.89961937509977652, 114.3739096053143669 ) ) ;
#15268 = CARTESIAN_POINT ( 'NONE',  ( 10.72451020669871369, 18.67979575497193778, 77.08442372801901854 ) ) ;
#15269 = CARTESIAN_POINT ( 'NONE',  ( 0.05219959533907565091, 21.53943276465977519, 69.99890960531435269 ) ) ;
#15270 = CARTESIAN_POINT ( 'NONE',  ( -10.72451020669870658, -18.67979575497194134, 64.58442372801900433 ) ) ;
#15271 = CARTESIAN_POINT ( 'NONE',  ( -15.80617190586768217, 15.72974639402176855, 53.12609039468568284 ) ) ;
#15272 = CARTESIAN_POINT ( 'NONE',  ( -9.564922557960796823, -16.46253265017161027, 102.0822429386477097 ) ) ;
#15273 = CARTESIAN_POINT ( 'NONE',  ( 8.314922557961029526, -14.29746914071037800, 90.41775706135236135 ) ) ;
#15274 = CARTESIAN_POINT ( 'NONE',  ( -16.51473224551069308, -9.474510206698971260, 26.66557627198103120 ) ) ;
#15275 = CARTESIAN_POINT ( 'NONE',  ( 1.300000000000000044, 0.7216878364870328300, 1.249999999999999778 ) ) ;
#15276 = CARTESIAN_POINT ( 'NONE',  ( 12.06949235617757843, -12.14591786802309237, 73.12390960531436690 ) ) ;
#15277 = CARTESIAN_POINT ( 'NONE',  ( 4.483927247898545687, 16.52544592524342804, 39.79057627198103830 ) ) ;
#15278 = CARTESIAN_POINT ( 'NONE',  ( -16.46253265017160317, 9.564922557960807481, 60.83224293864769550 ) ) ;
#15279 = CARTESIAN_POINT ( 'NONE',  ( 19.05341960407611168, 5.049401038298154454, 38.95724293864767418 ) ) ;
#15280 = CARTESIAN_POINT ( 'NONE',  ( 18.67979575497178502, 10.72451020669898547, 44.16557627198103120 ) ) ;
#15281 = CARTESIAN_POINT ( 'NONE',  ( 19.05341960407617918, -5.049401038297876454, 36.04275706135234003 ) ) ;
#15284 = CARTESIAN_POINT ( 'NONE',  ( 0.05219959533910956823, 16.53943276465976808, 49.99890960531437401 ) ) ;
#15283 = DIRECTION ( 'NONE',  ( 0.000000000000000000, 0.000000000000000000, 1.000000000000000000 ) ) ;
#15282 = VECTOR ( 'NONE', #95551, 1000.000000000000000 ) ;
#15285 = CARTESIAN_POINT ( 'NONE',  ( 10.72451020669898902, -18.67979575497178502, 27.91557627198103830 ) ) ;
#15286 = DIRECTION ( 'NONE',  ( -1.000000000000000000, 0.000000000000000000, 0.000000000000000000 ) ) ;
#15287 = CARTESIAN_POINT ( 'NONE',  ( -16.52544592524335698, -4.483927247898792601, 73.95942372801901854 ) ) ;
#15288 = CARTESIAN_POINT ( 'NONE',  ( 19.05341960407617918, -5.049401038297876454, 81.04275706135231871 ) ) ;
#15289 = CARTESIAN_POINT ( 'NONE',  ( -16.55341960407611168, -4.379528057220339221, 46.45724293864769550 ) ) ;
#15290 = CARTESIAN_POINT ( 'NONE',  ( 15.50000000000000178, -7.500000000000000888, 20.00000000000000000 ) ) ;
#15291 = CARTESIAN_POINT ( 'NONE',  ( 14.29746914071049879, -8.314922557960816363, 28.33224293864769550 ) ) ;
#15292 = CARTESIAN_POINT ( 'NONE',  ( 16.51473224551069308, 9.474510206698969483, 49.16557627198102409 ) ) ;
#15293 = CARTESIAN_POINT ( 'NONE',  ( 5.153800228976335163, 19.02544592524342804, 79.79057627198102409 ) ) ;
#15294 = CARTESIAN_POINT ( 'NONE',  ( 19.05341960407611168, 5.049401038298154454, 43.95724293864769550 ) ) ;
#15295 = CARTESIAN_POINT ( 'NONE',  ( -5.823673210054431948, 21.52544592524334988, 42.70942372801901854 ) ) ;
#15296 = CARTESIAN_POINT ( 'NONE',  ( 5.153800228976335163, 19.02544592524342804, 64.79057627198100988 ) ) ;
#15297 = CARTESIAN_POINT ( 'NONE',  ( 0.000000000000000000, -165.0000000000000000, 7.000000000000003553 ) ) ;
#15298 = CARTESIAN_POINT ( 'NONE',  ( 0.05219959533909260263, 19.03943276465977164, 44.99890960531435979 ) ) ;
#15299 = CARTESIAN_POINT ( 'NONE',  ( 5.719274019375991003, -21.55341960407610458, 42.70724293864770260 ) ) ;
#15301 = CARTESIAN_POINT ( 'NONE',  ( 14.34966873604960469, 8.224510206698951720, 114.1655762719810383 ) ) ;
#15300 = CARTESIAN_POINT ( 'NONE',  ( -0.05219959533937732626, 21.53943276465977519, 67.50109039468568994 ) ) ;
#15302 = CARTESIAN_POINT ( 'NONE',  ( 18.67979575497178502, 10.72451020669898547, 24.16557627198103120 ) ) ;
#15303 = CARTESIAN_POINT ( 'NONE',  ( -16.52544592524335698, -4.483927247898792601, 88.95942372801901854 ) ) ;
#15304 = CARTESIAN_POINT ( 'NONE',  ( -10.72451020669870658, -18.67979575497194134, 99.58442372801900433 ) ) ;
#15305 = VECTOR ( 'NONE', #129287, 1000.000000000000000 ) ;
#15306 = CARTESIAN_POINT ( 'NONE',  ( 16.52544592524335698, 4.483927247898782831, 66.45942372801903275 ) ) ;
#15307 = CARTESIAN_POINT ( 'NONE',  ( 9.564922557960805705, 16.46253265017160317, 109.5822429386476955 ) ) ;
#15308 = CARTESIAN_POINT ( 'NONE',  ( 8.224510206698742110, 14.34966873604972548, 57.08442372801901854 ) ) ;
#15309 = CARTESIAN_POINT ( 'NONE',  ( -8.224510206698735004, -14.34966873604973081, 44.58442372801901854 ) ) ;
#15310 = CARTESIAN_POINT ( 'NONE',  ( 16.52544592524335698, 4.483927247898782831, 101.4594237280190185 ) ) ;
#15311 = CARTESIAN_POINT ( 'NONE',  ( -15.72974639402176322, -15.80617190586768395, 49.37609039468569705 ) ) ;
#15312 = CARTESIAN_POINT ( 'NONE',  ( 14.29746914071037800, 8.314922557961029526, 21.66775706135235069 ) ) ;
#15313 = CARTESIAN_POINT ( 'NONE',  ( -21.53943276465977519, 0.05219959533907696930, 111.2489096053143669 ) ) ;
#15314 = CARTESIAN_POINT ( 'NONE',  ( 12.06949235617739724, 12.14591786802326823, 21.87609039468567573 ) ) ;
#15315 = CARTESIAN_POINT ( 'NONE',  ( 0.05219959533934541429, -16.53943276465976808, 90.00109039468567573 ) ) ;
#15316 = CARTESIAN_POINT ( 'NONE',  ( -16.62475595723610411, 7.163666690055881858, 45.52713351810403708 ) ) ;
#15317 = CARTESIAN_POINT ( 'NONE',  ( -18.62759615963255300, -10.81492255796106328, 84.16775706135234714 ) ) ;
#15318 = CARTESIAN_POINT ( 'NONE',  ( -19.03943276465977164, -0.05219959533935918106, 83.75109039468567573 ) ) ;
#15319 = CARTESIAN_POINT ( 'NONE',  ( 12.14591786802309770, 12.06949235617756955, 59.37390960531436690 ) ) ;
#15320 = CARTESIAN_POINT ( 'NONE',  ( 12.14591786802309770, 12.06949235617756955, 44.37390960531435979 ) ) ;
#15321 = CARTESIAN_POINT ( 'NONE',  ( -4.483927247898539470, -16.52544592524342804, 112.2905762719810241 ) ) ;
#15323 = CARTESIAN_POINT ( 'NONE',  ( -8.516692751257721739, 1.203296689329442115, -64.06477955746665032 ) ) ;
#15322 = CARTESIAN_POINT ( 'NONE',  ( -16.51473224551082808, 9.474510206698731452, 53.33442372801900433 ) ) ;
#15324 = CARTESIAN_POINT ( 'NONE',  ( -18.62759615963255300, -10.81492255796106328, 49.16775706135234003 ) ) ;
#15325 = CARTESIAN_POINT ( 'NONE',  ( -9.564922557961040184, 16.46253265017147172, 107.9177570613523471 ) ) ;
#15326 = LINE ( 'NONE', #18319, #111594 ) ;
#15327 = CARTESIAN_POINT ( 'NONE',  ( -19.05341960407611168, -5.049401038298163336, 101.4572429386476955 ) ) ;
#15328 = CARTESIAN_POINT ( 'NONE',  ( -21.53943276465977519, 0.05219959533907696930, 76.24890960531435269 ) ) ;
#15329 = CARTESIAN_POINT ( 'NONE',  ( 16.46253265017146816, 9.564922557961045513, 101.6677570613523329 ) ) ;
#15330 = ADVANCED_FACE ( 'NONE', ( #168337 ), #24239, .F. ) ;
#15331 = CARTESIAN_POINT ( 'NONE',  ( -16.46253265017160317, 9.564922557960807481, 105.8322429386476955 ) ) ;
#15332 = CARTESIAN_POINT ( 'NONE',  ( -25.85231681326420272, 7.957828899755264196, 172.6576833274792762 ) ) ;
#15333 = CARTESIAN_POINT ( 'NONE',  ( 14.34966873604960469, 8.224510206698951720, 104.1655762719810241 ) ) ;
#15334 = CARTESIAN_POINT ( 'NONE',  ( 18.67979575497194134, -10.72451020669871369, 100.8344237280190185 ) ) ;
#15335 = CARTESIAN_POINT ( 'NONE',  ( 5.153800228976335163, 19.02544592524342804, 24.79057627198102765 ) ) ;
#15337 = CARTESIAN_POINT ( 'NONE',  ( 10.72451020669871369, 18.67979575497193778, 57.08442372801901854 ) ) ;
#15336 = VECTOR ( 'NONE', #128029, 1000.000000000000000 ) ;
#15338 = CARTESIAN_POINT ( 'NONE',  ( 15.80617190586769283, -15.72974639402175789, 90.62609039468567573 ) ) ;
#15339 = CARTESIAN_POINT ( 'NONE',  ( -4.379528057220086978, -16.55341960407618274, 94.79275706135234714 ) ) ;
#15340 = EDGE_CURVE ( 'NONE', #67326, #33580, #137405, .T. ) ;
#15341 = CARTESIAN_POINT ( 'NONE',  ( 18.62759615963255655, 10.81492255796105972, 41.66775706135235424 ) ) ;
#15342 = CARTESIAN_POINT ( 'NONE',  ( 21.53943276465977519, 0.05219959533937863772, 46.25109039468567573 ) ) ;
#15344 = CARTESIAN_POINT ( 'NONE',  ( -19.05341960407611168, -5.049401038298163336, 96.45724293864769550 ) ) ;
#15343 = CARTESIAN_POINT ( 'NONE',  ( -5.153800228976607833, 19.02544592524334988, 67.70942372801900433 ) ) ;
#15345 = CARTESIAN_POINT ( 'NONE',  ( 16.55341960407611168, 4.379528057220329451, 108.9572429386476955 ) ) ;
#15346 = CARTESIAN_POINT ( 'NONE',  ( 15.72974639402199770, -15.80617190586745480, 78.12390960531436690 ) ) ;
#15347 = CARTESIAN_POINT ( 'NONE',  ( -16.53943276465976808, 0.05219959533911058130, 61.24890960531435979 ) ) ;
#15348 = CARTESIAN_POINT ( 'NONE',  ( -5.823673210054431948, 21.52544592524334988, 97.70942372801904696 ) ) ;
#15349 = CARTESIAN_POINT ( 'NONE',  ( 16.52544592524342804, -4.483927247898539470, 83.54057627198102409 ) ) ;
#15350 = CARTESIAN_POINT ( 'NONE',  ( -19.02544592524342804, 5.153800228976336051, 36.04057627198100988 ) ) ;
#15351 = CARTESIAN_POINT ( 'NONE',  ( -19.03943276465977164, -0.05219959533935918106, 73.75109039468566152 ) ) ;
#15352 = CARTESIAN_POINT ( 'NONE',  ( 8.314922557960818139, 14.29746914071049879, 44.58224293864769550 ) ) ;
#15353 = CARTESIAN_POINT ( 'NONE',  ( 21.53943276465977519, 0.05219959533937863772, 101.2510903946856757 ) ) ;
#15354 = CARTESIAN_POINT ( 'NONE',  ( -9.564922557960796823, -16.46253265017161027, 97.08224293864769550 ) ) ;
#15355 = CARTESIAN_POINT ( 'NONE',  ( 16.51473224551083163, -9.474510206698727899, 55.83442372801899722 ) ) ;
#15356 = CARTESIAN_POINT ( 'NONE',  ( -18.62759615963270932, 10.81492255796079327, 65.83224293864769550 ) ) ;
#15357 = CARTESIAN_POINT ( 'NONE',  ( 10.81492255796106328, -18.62759615963255655, 20.41775706135234714 ) ) ;
#15358 = CARTESIAN_POINT ( 'NONE',  ( -16.52544592524335698, -4.483927247898792601, 18.95942372801901143 ) ) ;
#15359 = CARTESIAN_POINT ( 'NONE',  ( -14.29746914071037622, -8.314922557961029526, 79.16775706135234714 ) ) ;
#15361 = CARTESIAN_POINT ( 'NONE',  ( -15.80617190586768217, 15.72974639402176855, 23.12609039468567573 ) ) ;
#15360 = CARTESIAN_POINT ( 'NONE',  ( -9.474510206698964154, 16.51473224551069663, 25.41557627198103120 ) ) ;
#15362 = CARTESIAN_POINT ( 'NONE',  ( 16.55341960407611168, 4.379528057220329451, 113.9572429386477239 ) ) ;
#15363 = CARTESIAN_POINT ( 'NONE',  ( 29.86685920354754487, 21.69954338932564752, -7.924999997268814766 ) ) ;
#15364 = CARTESIAN_POINT ( 'NONE',  ( -8.224510206698735004, -14.34966873604973081, 49.58442372801901143 ) ) ;
#15365 = CARTESIAN_POINT ( 'NONE',  ( 16.53943276465976808, -0.05219959533910856209, 83.74890960531435269 ) ) ;
#15366 = CARTESIAN_POINT ( 'NONE',  ( -15.80617190586745835, -15.72974639402198527, 76.87390960531439532 ) ) ;
#15367 = CARTESIAN_POINT ( 'NONE',  ( -14.34966873604972548, 8.224510206698743886, 113.3344237280190328 ) ) ;
#15368 = CARTESIAN_POINT ( 'NONE',  ( -16.55341960407617563, 4.379528057220093196, 33.54275706135234714 ) ) ;
#15369 = CARTESIAN_POINT ( 'NONE',  ( 16.51473224551069308, 9.474510206698969483, 39.16557627198103120 ) ) ;
#15370 = CARTESIAN_POINT ( 'NONE',  ( -14.29746914071037622, -8.314922557961029526, 74.16775706135231871 ) ) ;
#15371 = CARTESIAN_POINT ( 'NONE',  ( -13.97604488694547697, 13.89961937509957934, 68.12609039468563310 ) ) ;
#15372 = CARTESIAN_POINT ( 'NONE',  ( -18.62759615963270932, 10.81492255796079327, 75.83224293864769550 ) ) ;
#15373 = CARTESIAN_POINT ( 'NONE',  ( 14.34966873604960469, 8.224510206698951720, 24.16557627198103120 ) ) ;
#15374 = ORIENTED_EDGE ( 'NONE', *, *, #124070, .T. ) ;
#15375 = CARTESIAN_POINT ( 'NONE',  ( 18.67979575497194134, -10.72451020669871369, 85.83442372801901854 ) ) ;
#15376 = CARTESIAN_POINT ( 'NONE',  ( 15.80617190586746368, 15.72974639402197994, 44.37390960531435979 ) ) ;
#15377 = VERTEX_POINT ( 'NONE', #102695 ) ;
#15378 = CARTESIAN_POINT ( 'NONE',  ( 8.224510206698742110, 14.34966873604972548, 92.08442372801901854 ) ) ;
#15379 = CARTESIAN_POINT ( 'NONE',  ( -21.53943276465977519, 0.05219959533907696930, 51.24890960531436690 ) ) ;
#15380 = VERTEX_POINT ( 'NONE', #151204 ) ;
#15381 = CARTESIAN_POINT ( 'NONE',  ( -19.03943276465977164, 0.05219959533909376836, 106.2489096053143669 ) ) ;
#15382 = CARTESIAN_POINT ( 'NONE',  ( 17.50000000000000000, 3.471454075611686729, 108.0166741885564221 ) ) ;
#15383 = CARTESIAN_POINT ( 'NONE',  ( 5.049401038298161559, -19.05341960407611168, 27.70724293864769550 ) ) ;
#15384 = CARTESIAN_POINT ( 'NONE',  ( 10.81492255796078972, 18.62759615963270932, 79.58224293864769550 ) ) ;
#15385 = CARTESIAN_POINT ( 'NONE',  ( 0.05219959533934541429, -16.53943276465976808, 110.0010903946856757 ) ) ;
#15386 = CARTESIAN_POINT ( 'NONE',  ( -10.72451020669870658, -18.67979575497194134, 59.58442372801901854 ) ) ;
#15387 = CARTESIAN_POINT ( 'NONE',  ( -12.14591786802326823, 12.06949235617739902, 23.12609039468567573 ) ) ;
#15388 = CARTESIAN_POINT ( 'NONE',  ( -9.474510206698964154, 16.51473224551069663, 25.41557627198103120 ) ) ;
#15389 = CARTESIAN_POINT ( 'NONE',  ( -9.564922557961040184, 16.46253265017147172, 107.9177570613523471 ) ) ;
#15390 = CARTESIAN_POINT ( 'NONE',  ( -19.02544592524342804, 5.153800228976336051, 36.04057627198100988 ) ) ;
#15391 = CARTESIAN_POINT ( 'NONE',  ( 17.81289503416610742, 24.51734667627700404, 143.2999999999999829 ) ) ;
#15392 = CARTESIAN_POINT ( 'NONE',  ( -16.46253265017160317, 9.564922557960807481, 105.8322429386476955 ) ) ;
#15393 = CARTESIAN_POINT ( 'NONE',  ( 12.14591786802327356, -12.06949235617739191, 90.62609039468567573 ) ) ;
#15394 = CARTESIAN_POINT ( 'NONE',  ( 9.564922557961047289, -16.46253265017146816, 80.41775706135234714 ) ) ;
#15395 = CARTESIAN_POINT ( 'NONE',  ( -5.153800228976607833, 19.02544592524334988, 27.70942372801899722 ) ) ;
#15396 = CARTESIAN_POINT ( 'NONE',  ( -5.719274019375978568, 21.55341960407610458, 75.20724293864769550 ) ) ;
#15397 = CARTESIAN_POINT ( 'NONE',  ( 14.29746914071037800, 8.314922557961029526, 106.6677570613523756 ) ) ;
#15398 = CARTESIAN_POINT ( 'NONE',  ( 19.03943276465977164, 0.05219959533936151252, 91.25109039468566152 ) ) ;
#15399 = CARTESIAN_POINT ( 'NONE',  ( 19.02544592524343514, -5.153800228976328945, 48.54057627198103120 ) ) ;
#15400 = CARTESIAN_POINT ( 'NONE',  ( -16.46253265017160317, 9.564922557960807481, 95.83224293864769550 ) ) ;
#15401 = CARTESIAN_POINT ( 'NONE',  ( 21.53943276465977519, 0.05219959533937863772, 51.25109039468568994 ) ) ;
#15402 = CARTESIAN_POINT ( 'NONE',  ( 5.153800228976335163, 19.02544592524342804, 44.79057627198103830 ) ) ;
#15403 = CARTESIAN_POINT ( 'NONE',  ( -17.31728774477274868, -6.344390552232371583, 84.18093348310685542 ) ) ;
#15404 = CARTESIAN_POINT ( 'NONE',  ( 5.153800228976335163, 19.02544592524342804, 114.7905762719810241 ) ) ;
#15405 = CARTESIAN_POINT ( 'NONE',  ( -0.05219959533910754901, -16.53943276465976808, 67.49890960531436690 ) ) ;
#15406 = CARTESIAN_POINT ( 'NONE',  ( 5.719274019375991003, -21.55341960407610458, 72.70724293864769550 ) ) ;
#15407 = SPHERICAL_SURFACE ( 'NONE', #19151, 0.5000000000000000000 ) ;
#15408 = CARTESIAN_POINT ( 'NONE',  ( 16.46253265017146816, 9.564922557961045513, 46.66775706135233293 ) ) ;
#15409 = DIRECTION ( 'NONE',  ( 0.000000000000000000, 0.000000000000000000, 1.000000000000000000 ) ) ;
#15411 = CARTESIAN_POINT ( 'NONE',  ( -5.153800228976328057, -19.02544592524343514, 92.29057627198099567 ) ) ;
#15410 = CARTESIAN_POINT ( 'NONE',  ( -5.049401038298153566, 19.05341960407611168, 70.20724293864769550 ) ) ;
#15412 = CARTESIAN_POINT ( 'NONE',  ( 16.52544592524335698, 4.483927247898782831, 46.45942372801901854 ) ) ;
#15413 = CARTESIAN_POINT ( 'NONE',  ( -5.429308488886486681E-15, 30.30510711980690175, 143.4999999999999716 ) ) ;
#15414 = CARTESIAN_POINT ( 'NONE',  ( -13.89961937509957401, -13.97604488694547875, 24.37609039468565442 ) ) ;
#15415 = CARTESIAN_POINT ( 'NONE',  ( 17.81289503416610742, 24.51734667627700404, 145.5500000054623797 ) ) ;
#15416 = CARTESIAN_POINT ( 'NONE',  ( -14.34966873604972548, 8.224510206698743886, 93.33442372801901854 ) ) ;
#15417 = CARTESIAN_POINT ( 'NONE',  ( -4.025060008621055729, -4.710691162182125247, -64.51731263004398897 ) ) ;
#15418 = CARTESIAN_POINT ( 'NONE',  ( 8.314922557961029526, -14.29746914071037800, 85.41775706135236135 ) ) ;
#15419 = CARTESIAN_POINT ( 'NONE',  ( -0.05219959533934338120, 16.53943276465976808, 52.50109039468567573 ) ) ;
#15420 = CARTESIAN_POINT ( 'NONE',  ( -5.049401038297874678, -19.05341960407617918, 19.79275706135233293 ) ) ;
#15422 = FACE_BOUND ( 'NONE', #277, .T. ) ;
#15421 = CARTESIAN_POINT ( 'NONE',  ( -5.153800228976328057, -19.02544592524343514, 52.29057627198100988 ) ) ;
#15423 = CARTESIAN_POINT ( 'NONE',  ( 15.72974639402176855, 15.80617190586768217, 66.87609039468568994 ) ) ;
#15424 = CARTESIAN_POINT ( 'NONE',  ( 16.51473224551083163, -9.474510206698727899, 80.83442372801899012 ) ) ;
#15425 = CARTESIAN_POINT ( 'NONE',  ( -5.049401038297874678, -19.05341960407617918, 19.79275706135233293 ) ) ;
#15426 = CARTESIAN_POINT ( 'NONE',  ( 5.153800228976335163, 19.02544592524342804, 34.79057627198102409 ) ) ;
#15427 = CARTESIAN_POINT ( 'NONE',  ( -15.80137536867090908, 14.65320595882610277, -58.69884337265983021 ) ) ;
#15428 = CARTESIAN_POINT ( 'NONE',  ( 18.62759615963271287, -10.81492255796078972, 73.33224293864769550 ) ) ;
#15429 = AXIS2_PLACEMENT_3D ( 'NONE', #41357, #6995, #160693 ) ;
#15430 = CARTESIAN_POINT ( 'NONE',  ( 0.05219959533907565091, 21.53943276465977519, 24.99890960531435624 ) ) ;
#15431 = CARTESIAN_POINT ( 'NONE',  ( 13.97604488694527802, 13.89961937509977652, 24.37390960531435624 ) ) ;
#15432 = CARTESIAN_POINT ( 'NONE',  ( -12.06949235617739369, -12.14591786802326823, 39.37609039468567573 ) ) ;
#15433 = CARTESIAN_POINT ( 'NONE',  ( 16.53943276465976808, -0.05219959533910856209, 28.74890960531435624 ) ) ;
#15434 = EDGE_LOOP ( 'NONE', ( #117415, #7690, #54758, #129558 ) ) ;
#15435 = CARTESIAN_POINT ( 'NONE',  ( -18.62759615963255300, -10.81492255796106328, 24.16775706135235424 ) ) ;
#15437 = CARTESIAN_POINT ( 'NONE',  ( 11.74264578624800315, -36.14014761921581709, -7.400000000000000355 ) ) ;
#15436 = CARTESIAN_POINT ( 'NONE',  ( 16.53943276465976808, -0.05219959533910856209, 43.74890960531435979 ) ) ;
#15438 = CARTESIAN_POINT ( 'NONE',  ( 5.049401038297881783, 19.05341960407617563, 107.2927570613523187 ) ) ;
#15439 = CARTESIAN_POINT ( 'NONE',  ( 13.89961937509957401, 13.97604488694547697, 21.87609039468566152 ) ) ;
#15440 = CARTESIAN_POINT ( 'NONE',  ( -4.483927247898539470, -16.52544592524342804, 42.29057627198103120 ) ) ;
#15442 = EDGE_CURVE ( 'NONE', #193741, #188751, #19240, .T. ) ;
#15441 = CARTESIAN_POINT ( 'NONE',  ( -5.823673210054116645, -21.52544592524344225, 107.2905762719810525 ) ) ;
#15444 = CARTESIAN_POINT ( 'NONE',  ( 10.81492255796078972, 18.62759615963270932, 69.58224293864769550 ) ) ;
#15443 = CARTESIAN_POINT ( 'NONE',  ( 16.62475595723694965, 7.163666690055250363, 31.97286648189535896 ) ) ;
#15445 = CARTESIAN_POINT ( 'NONE',  ( 19.02544592524343514, -5.153800228976328945, 73.54057627198103830 ) ) ;
#15446 = CARTESIAN_POINT ( 'NONE',  ( 14.29746914071049879, -8.314922557960816363, 43.33224293864769550 ) ) ;
#15447 = CARTESIAN_POINT ( 'NONE',  ( 16.51473224551069308, 9.474510206698969483, 94.16557627198103830 ) ) ;
#15448 = DIRECTION ( 'NONE',  ( -0.000000000000000000, -0.000000000000000000, 1.000000000000000000 ) ) ;
#15449 = CARTESIAN_POINT ( 'NONE',  ( -5.153800228976607833, 19.02544592524334988, 57.70942372801899012 ) ) ;
#15450 = CARTESIAN_POINT ( 'NONE',  ( -21.53943276465977519, 0.05219959533907696930, 91.24890960531436690 ) ) ;
#15451 = CARTESIAN_POINT ( 'NONE',  ( 16.51473224551069308, 9.474510206698969483, 39.16557627198103120 ) ) ;
#15452 = CARTESIAN_POINT ( 'NONE',  ( 16.55341960407611168, 4.379528057220329451, 108.9572429386476955 ) ) ;
#15453 = CARTESIAN_POINT ( 'NONE',  ( -21.52544592524334988, -5.823673210054445271, 53.95942372801900433 ) ) ;
#15454 = AXIS2_PLACEMENT_3D ( 'NONE', #90767, #73645, #87788 ) ;
#15455 = CARTESIAN_POINT ( 'NONE',  ( -8.571926809382601320, -26.38167802310801591, 147.2750000027311899 ) ) ;
#15456 = EDGE_CURVE ( 'NONE', #9747, #199879, #95459, .T. ) ;
#15457 = CARTESIAN_POINT ( 'NONE',  ( -12.14591786802309592, -12.06949235617757132, 26.87390960531435979 ) ) ;
#15458 = CARTESIAN_POINT ( 'NONE',  ( -19.03943276465977164, 0.05219959533909376836, 46.24890960531435979 ) ) ;
#15459 = CARTESIAN_POINT ( 'NONE',  ( -9.564922557960796823, -16.46253265017161027, 97.08224293864769550 ) ) ;
#15460 = CARTESIAN_POINT ( 'NONE',  ( 15.72974639402199770, -15.80617190586745480, 58.12390960531435979 ) ) ;
#15461 = CARTESIAN_POINT ( 'NONE',  ( -5.153800228976607833, 19.02544592524335343, 92.70942372801900433 ) ) ;
#15462 = CARTESIAN_POINT ( 'NONE',  ( -9.474510206698964154, 16.51473224551069663, 50.41557627198102409 ) ) ;
#15463 = CARTESIAN_POINT ( 'NONE',  ( 21.53943276465977519, -0.05219959533907433946, 53.74890960531437401 ) ) ;
#15464 = CARTESIAN_POINT ( 'NONE',  ( 21.52544592524334988, 5.823673210054432836, 81.45942372801900433 ) ) ;
#15466 = CARTESIAN_POINT ( 'NONE',  ( -16.55341960407617563, 4.379528057220093196, 88.54275706135236135 ) ) ;
#15465 = CARTESIAN_POINT ( 'NONE',  ( 21.12688062493369756, -32.57662631299258749, -17.38946437510359644 ) ) ;
#15467 = CARTESIAN_POINT ( 'NONE',  ( -0.05219959533934338120, 16.53943276465976808, 92.50109039468567573 ) ) ;
#15468 = CARTESIAN_POINT ( 'NONE',  ( -19.03943276465977164, 0.05219959533909376836, 61.24890960531436690 ) ) ;
#15469 = CARTESIAN_POINT ( 'NONE',  ( 9.474510206698971260, -16.51473224551069308, 62.91557627198102409 ) ) ;
#15470 = EDGE_LOOP ( 'NONE', ( #127977, #132284 ) ) ;
#15471 = CARTESIAN_POINT ( 'NONE',  ( 5.153800228976615827, -19.02544592524334988, 30.20942372801900433 ) ) ;
#15472 = CARTESIAN_POINT ( 'NONE',  ( -8.314922557961024197, 14.29746914071037800, 72.91775706135234714 ) ) ;
#15473 = CARTESIAN_POINT ( 'NONE',  ( -0.05219959533937732626, 21.53943276465977519, 107.5010903946856899 ) ) ;
#15474 = CARTESIAN_POINT ( 'NONE',  ( -0.05219959533909027116, -19.03943276465977164, 72.49890960531435269 ) ) ;
#15475 = CARTESIAN_POINT ( 'NONE',  ( 15.80617190586746368, 15.72974639402197994, 54.37390960531435979 ) ) ;
#15476 = CARTESIAN_POINT ( 'NONE',  ( 12.14591786802327356, -12.06949235617739191, 20.62609039468568639 ) ) ;
#15477 = CARTESIAN_POINT ( 'NONE',  ( 18.62759615963255655, 10.81492255796105972, 86.66775706135234714 ) ) ;
#15478 = CARTESIAN_POINT ( 'NONE',  ( -12.06949235617739369, -12.14591786802326823, 44.37609039468567573 ) ) ;
#15479 = CARTESIAN_POINT ( 'NONE',  ( 21.53943276465977519, -0.05219959533907433946, 113.7489096053143527 ) ) ;
#15480 = CARTESIAN_POINT ( 'NONE',  ( -0.05219959533934338120, 16.53943276465976808, 22.50109039468567573 ) ) ;
#15481 = CARTESIAN_POINT ( 'NONE',  ( 19.02544592524343514, -5.153800228976328945, 83.54057627198100988 ) ) ;
#15482 = CARTESIAN_POINT ( 'NONE',  ( -16.53943276465976808, -0.05219959533934237506, 28.75109039468567929 ) ) ;
#15483 = CARTESIAN_POINT ( 'NONE',  ( 9.564922557960805705, 16.46253265017160317, 39.58224293864768839 ) ) ;
#15484 = CARTESIAN_POINT ( 'NONE',  ( -8.224510206698735004, -14.34966873604973081, 19.58442372801901143 ) ) ;
#15485 = CARTESIAN_POINT ( 'NONE',  ( 8.314922557960818139, 14.29746914071049879, 74.58224293864768129 ) ) ;
#15486 = CARTESIAN_POINT ( 'NONE',  ( -4.483927247898782831, 16.52544592524335698, 87.70942372801901854 ) ) ;
#15488 = CARTESIAN_POINT ( 'NONE',  ( 5.153800228976335163, 19.02544592524342804, 59.79057627198100988 ) ) ;
#15487 = CARTESIAN_POINT ( 'NONE',  ( 15.72974639402176855, 15.80617190586768217, 31.87609039468567929 ) ) ;
#15489 = CARTESIAN_POINT ( 'NONE',  ( 13.89961937509977652, -13.97604488694527269, 68.12390960531436690 ) ) ;
#15490 = CARTESIAN_POINT ( 'NONE',  ( 8.314922557961029526, -14.29746914071037800, 90.41775706135236135 ) ) ;
#15491 = EDGE_CURVE ( 'NONE', #135989, #186347, #126781, .T. ) ;
#15493 = ORIENTED_EDGE ( 'NONE', *, *, #160761, .F. ) ;
#15492 = DIRECTION ( 'NONE',  ( 0.000000000000000000, 0.6427876096865403621, 0.7660444431189770143 ) ) ;
#15494 = VERTEX_POINT ( 'NONE', #47988 ) ;
#15495 = CARTESIAN_POINT ( 'NONE',  ( 5.049401038297881783, 19.05341960407617563, 32.29275706135233293 ) ) ;
#15496 = CARTESIAN_POINT ( 'NONE',  ( -13.97604488694527625, -13.89961937509977652, 31.87390960531435979 ) ) ;
#15498 = VERTEX_POINT ( 'NONE', #157145 ) ;
#15497 = CARTESIAN_POINT ( 'NONE',  ( 0.4080409027416297962, 13.74233039485027774, -62.56360233571632534 ) ) ;
#15499 = CARTESIAN_POINT ( 'NONE',  ( -16.52544592524335698, -4.483927247898792601, 28.95942372801902209 ) ) ;
#15501 = CARTESIAN_POINT ( 'NONE',  ( 16.55341960407618274, -4.379528057220086978, 46.04275706135234714 ) ) ;
#15500 = CARTESIAN_POINT ( 'NONE',  ( -0.05219959533936034679, 19.03943276465977164, 52.50109039468566863 ) ) ;
#15502 = CARTESIAN_POINT ( 'NONE',  ( 9.564922557960805705, 16.46253265017160317, 104.5822429386476955 ) ) ;
#15503 = CARTESIAN_POINT ( 'NONE',  ( 19.05341960407611168, 5.049401038298154454, 63.95724293864769550 ) ) ;
#15504 = CARTESIAN_POINT ( 'NONE',  ( 15.72974639402199770, -15.80617190586745480, 103.1239096053143811 ) ) ;
#15506 = CARTESIAN_POINT ( 'NONE',  ( 17.48933443480910199, -3.858464096052834247, 21.79111074916215784 ) ) ;
#15505 = CARTESIAN_POINT ( 'NONE',  ( 5.153800228976335163, 19.02544592524342804, 94.79057627198103830 ) ) ;
#15507 = CARTESIAN_POINT ( 'NONE',  ( 16.51473224551069308, 9.474510206698969483, 64.16557627198102409 ) ) ;
#15509 = CARTESIAN_POINT ( 'NONE',  ( 5.049401038298161559, -19.05341960407611168, 22.70724293864769194 ) ) ;
#15508 = CARTESIAN_POINT ( 'NONE',  ( -4.483927247898539470, -16.52544592524342804, 22.29057627198102765 ) ) ;
#15510 = CARTESIAN_POINT ( 'NONE',  ( -16.46253265017146816, -9.564922557961047289, 39.16775706135234003 ) ) ;
#15511 = CARTESIAN_POINT ( 'NONE',  ( 4.483927247898545687, 16.52544592524342804, 59.79057627198103120 ) ) ;
#15512 = CARTESIAN_POINT ( 'NONE',  ( -5.719274019375665041, -21.55341960407619695, 104.7927570613523898 ) ) ;
#15513 = CARTESIAN_POINT ( 'NONE',  ( 19.05341960407611168, 5.049401038298154454, 43.95724293864769550 ) ) ;
#15514 = CARTESIAN_POINT ( 'NONE',  ( 4.379528057220092307, 16.55341960407617563, 57.29275706135234714 ) ) ;
#15516 = CARTESIAN_POINT ( 'NONE',  ( -18.62759615963255300, -10.81492255796106328, 94.16775706135237556 ) ) ;
#15515 = CARTESIAN_POINT ( 'NONE',  ( -14.29746914071049879, 8.314922557960819915, 45.83224293864769550 ) ) ;
#15517 = CARTESIAN_POINT ( 'NONE',  ( -13.89961937509977652, 13.97604488694528158, 75.62390960531438111 ) ) ;
#15518 = CARTESIAN_POINT ( 'NONE',  ( 5.153800228976335163, 19.02544592524342804, 94.79057627198103830 ) ) ;
#15519 = CARTESIAN_POINT ( 'NONE',  ( 8.314922557960818139, 14.29746914071049879, 109.5822429386476955 ) ) ;
#15520 = CARTESIAN_POINT ( 'NONE',  ( 16.52544592524342804, -4.483927247898539470, 78.54057627198103830 ) ) ;
#15521 = CARTESIAN_POINT ( 'NONE',  ( 21.52544592524344225, -5.823673210054117533, 88.54057627198103830 ) ) ;
#15522 = CARTESIAN_POINT ( 'NONE',  ( 19.02544592524343514, -5.153800228976328945, 73.54057627198103830 ) ) ;
#15523 = CARTESIAN_POINT ( 'NONE',  ( -10.81492255796078084, -18.62759615963271287, 97.08224293864770971 ) ) ;
#15524 = CARTESIAN_POINT ( 'NONE',  ( -19.02544592524334988, -5.153800228976617603, 83.95942372801901854 ) ) ;
#15526 = CARTESIAN_POINT ( 'NONE',  ( 8.314922557960818139, 14.29746914071049879, 94.58224293864769550 ) ) ;
#15525 = CARTESIAN_POINT ( 'NONE',  ( -28.79475375365586842, 2.428612866367529932E-14, 146.2656553485623760 ) ) ;
#15527 = CARTESIAN_POINT ( 'NONE',  ( 13.89961937509977652, -13.97604488694527269, 63.12390960531435979 ) ) ;
#15528 = CARTESIAN_POINT ( 'NONE',  ( -5.823673210054116645, -21.52544592524344225, 67.29057627198103830 ) ) ;
#15529 = CARTESIAN_POINT ( 'NONE',  ( 17.40805194822030799, -6.112264579159331745, 28.33371272510611760 ) ) ;
#15531 = LINE ( 'NONE', #338, #92020 ) ;
#15530 = CARTESIAN_POINT ( 'NONE',  ( -12.06949235617739369, -12.14591786802326823, 109.3760903946857042 ) ) ;
#15532 = CARTESIAN_POINT ( 'NONE',  ( 0.05219959533936267826, -19.03943276465977164, 110.0010903946856757 ) ) ;
#15533 = CARTESIAN_POINT ( 'NONE',  ( 12.06949235617757843, -12.14591786802309237, 78.12390960531436690 ) ) ;
#15534 = CARTESIAN_POINT ( 'NONE',  ( -17.97214573761830536, -5.500000000000085265, 46.46970049038654338 ) ) ;
#15535 = CARTESIAN_POINT ( 'NONE',  ( 19.03943276465977164, -0.05219959533909143690, 78.74890960531436690 ) ) ;
#15536 = CARTESIAN_POINT ( 'NONE',  ( -16.51473224551069308, -9.474510206698971260, 36.66557627198102409 ) ) ;
#15537 = CARTESIAN_POINT ( 'NONE',  ( -12.14591786802309592, -12.06949235617757132, 66.87390960531436690 ) ) ;
#15538 = CARTESIAN_POINT ( 'NONE',  ( 19.02544592524343514, -5.153800228976328945, 113.5405762719810241 ) ) ;
#15539 = CARTESIAN_POINT ( 'NONE',  ( 13.89961937509957401, 13.97604488694547697, 91.87609039468567573 ) ) ;
#15540 = CARTESIAN_POINT ( 'NONE',  ( -5.153800228976328057, -19.02544592524343514, 97.29057627198099567 ) ) ;
#15541 = CARTESIAN_POINT ( 'NONE',  ( 10.81492255796078972, 18.62759615963270932, 79.58224293864769550 ) ) ;
#15542 = CARTESIAN_POINT ( 'NONE',  ( 8.224510206698742110, 14.34966873604972548, 72.08442372801899012 ) ) ;
#15543 = CARTESIAN_POINT ( 'NONE',  ( 5.049401038297881783, 19.05341960407617918, 112.2927570613523471 ) ) ;
#15544 = CARTESIAN_POINT ( 'NONE',  ( 5.049401038298161559, -19.05341960407611168, 57.70724293864769550 ) ) ;
#15545 = CARTESIAN_POINT ( 'NONE',  ( -18.67979575497178146, -10.72451020669898902, 71.66557627198100988 ) ) ;
#15546 = CARTESIAN_POINT ( 'NONE',  ( 19.02544592524334988, 5.153800228976608722, 101.4594237280189759 ) ) ;
#15548 = CARTESIAN_POINT ( 'NONE',  ( -5.823673210054431948, 21.52544592524334988, 57.70942372801901143 ) ) ;
#15547 = CARTESIAN_POINT ( 'NONE',  ( -4.379528057220328563, 16.55341960407611168, 40.20724293864769550 ) ) ;
#15549 = DIRECTION ( 'NONE',  ( -6.938893903907222067E-15, 0.000000000000000000, 1.000000000000000000 ) ) ;
#15551 = CARTESIAN_POINT ( 'NONE',  ( 5.153800228976335163, 19.02544592524342804, 104.7905762719809957 ) ) ;
#15550 = CARTESIAN_POINT ( 'NONE',  ( 8.224510206698742110, 14.34966873604972548, 67.08442372801901854 ) ) ;
#15552 = CARTESIAN_POINT ( 'NONE',  ( -19.05341960407611168, -5.049401038298164224, 106.4572429386476955 ) ) ;
#15553 = CARTESIAN_POINT ( 'NONE',  ( 30.00000000000000355, -3.889087296526015258, 1.818019484660534646 ) ) ;
#15554 = CARTESIAN_POINT ( 'NONE',  ( 4.483927247898790824, -16.52544592524335698, 95.20942372801903275 ) ) ;
#15555 = CARTESIAN_POINT ( 'NONE',  ( 4.483927247898790824, -16.52544592524335698, 45.20942372801901854 ) ) ;
#15556 = CARTESIAN_POINT ( 'NONE',  ( 5.153800228976335163, 19.02544592524342804, 54.79057627198103120 ) ) ;
#15557 = CARTESIAN_POINT ( 'NONE',  ( -19.05341960407611168, -5.049401038298163336, 71.45724293864766707 ) ) ;
#15558 = CARTESIAN_POINT ( 'NONE',  ( -21.52544592524334988, -5.823673210054445271, 53.95942372801900433 ) ) ;
#15559 = CARTESIAN_POINT ( 'NONE',  ( 8.224510206698742110, 14.34966873604972548, 62.08442372801901143 ) ) ;
#15560 = CARTESIAN_POINT ( 'NONE',  ( 4.379528057220339221, -16.55341960407611168, 27.70724293864769905 ) ) ;
#15561 = CARTESIAN_POINT ( 'NONE',  ( -19.03943276465977164, 0.05219959533909376836, 36.24890960531436690 ) ) ;
#15562 = CARTESIAN_POINT ( 'NONE',  ( -19.02544592524342804, 5.153800228976336051, 31.04057627198102409 ) ) ;
#15563 = CARTESIAN_POINT ( 'NONE',  ( 14.29746914071037800, 8.314922557961029526, 31.66775706135234358 ) ) ;
#15564 = CARTESIAN_POINT ( 'NONE',  ( 0.05219959533936267826, -19.03943276465977164, 80.00109039468567573 ) ) ;
#15565 = CARTESIAN_POINT ( 'NONE',  ( 8.224510206698953496, -14.34966873604960469, 77.91557627198102409 ) ) ;
#15566 = CARTESIAN_POINT ( 'NONE',  ( -13.97604488694527625, -13.89961937509977652, 46.87390960531435979 ) ) ;
#15568 = DIRECTION ( 'NONE',  ( 0.000000000000000000, 0.000000000000000000, -1.000000000000000000 ) ) ;
#15567 = CARTESIAN_POINT ( 'NONE',  ( 19.05341960407617918, -5.049401038297876454, 81.04275706135231871 ) ) ;
#15569 = CARTESIAN_POINT ( 'NONE',  ( 21.53943276465977519, 0.05219959533937863772, 86.25109039468568994 ) ) ;
#15570 = CARTESIAN_POINT ( 'NONE',  ( 4.483927247898790824, -16.52544592524335698, 60.20942372801902565 ) ) ;
#15571 = CARTESIAN_POINT ( 'NONE',  ( -4.500000000000000888, -139.5000000000000000, 21.32407087589996308 ) ) ;
#15572 = CARTESIAN_POINT ( 'NONE',  ( 5.823673210054125526, 21.52544592524343514, 54.79057627198104541 ) ) ;
#15573 = CARTESIAN_POINT ( 'NONE',  ( 12.14591786802327356, -12.06949235617739191, 40.62609039468567573 ) ) ;
#15574 = CARTESIAN_POINT ( 'NONE',  ( -5.153800228976328057, -19.02544592524343514, 37.29057627198102409 ) ) ;
#15575 = CARTESIAN_POINT ( 'NONE',  ( -16.46253265017146816, -9.564922557961047289, 44.16775706135232582 ) ) ;
#15576 = CARTESIAN_POINT ( 'NONE',  ( 16.51473224551069308, 9.474510206698969483, 89.16557627198103830 ) ) ;
#15577 = CARTESIAN_POINT ( 'NONE',  ( -0.05219959533909027116, -19.03943276465977164, 47.49890960531435979 ) ) ;
#15578 = CARTESIAN_POINT ( 'NONE',  ( 14.65109730209616146, 15.81114279943204437, -56.29481432398279139 ) ) ;
#15579 = CARTESIAN_POINT ( 'NONE',  ( 10.72451020669871369, 18.67979575497193778, 82.08442372801901854 ) ) ;
#15580 = CARTESIAN_POINT ( 'NONE',  ( 5.049401038298163336, -19.05341960407611168, 92.70724293864769550 ) ) ;
#15581 = CARTESIAN_POINT ( 'NONE',  ( -16.46253265017146816, -9.564922557961047289, 39.16775706135234003 ) ) ;
#15582 = CARTESIAN_POINT ( 'NONE',  ( 18.62759615963255655, 10.81492255796105972, 106.6677570613523756 ) ) ;
#15583 = CARTESIAN_POINT ( 'NONE',  ( -8.314922557960811034, -14.29746914071050412, 42.08224293864769550 ) ) ;
#15584 = CARTESIAN_POINT ( 'NONE',  ( 5.153800228976335163, 19.02544592524342804, 39.79057627198100988 ) ) ;
#15585 = CARTESIAN_POINT ( 'NONE',  ( 0.05219959533909260263, 19.03943276465977164, 99.99890960531436690 ) ) ;
#15586 = CARTESIAN_POINT ( 'NONE',  ( 0.05219959533937995610, -21.53943276465977519, 80.00109039468568994 ) ) ;
#15587 = CARTESIAN_POINT ( 'NONE',  ( 19.02544592524343514, -5.153800228976328945, 58.54057627198102409 ) ) ;
#15588 = CARTESIAN_POINT ( 'NONE',  ( -5.719274019375665041, -21.55341960407619695, 74.79275706135234714 ) ) ;
#15589 = CARTESIAN_POINT ( 'NONE',  ( 18.62759615963271287, -10.81492255796078972, 43.33224293864769550 ) ) ;
#15590 = CARTESIAN_POINT ( 'NONE',  ( 15.72974639402176855, 15.80617190586768217, 26.87609039468567218 ) ) ;
#15591 = CARTESIAN_POINT ( 'NONE',  ( -16.46253265017146816, -9.564922557961047289, 49.16775706135233293 ) ) ;
#15592 = CARTESIAN_POINT ( 'NONE',  ( 13.89961937509977652, -13.97604488694527269, 23.12390960531436335 ) ) ;
#15593 = CARTESIAN_POINT ( 'NONE',  ( 5.153800228976335163, 19.02544592524342804, 79.79057627198102409 ) ) ;
#15594 = CARTESIAN_POINT ( 'NONE',  ( -16.52544592524335698, -4.483927247898792601, 28.95942372801902209 ) ) ;
#15595 = CARTESIAN_POINT ( 'NONE',  ( -4.379528057220328563, 16.55341960407611168, 95.20724293864769550 ) ) ;
#15596 = CARTESIAN_POINT ( 'NONE',  ( 0.05219959533909260263, 19.03943276465977164, 59.99890960531436690 ) ) ;
#15597 = CARTESIAN_POINT ( 'NONE',  ( -15.72974639402197994, 15.80617190586746368, 35.62390960531437401 ) ) ;
#15598 = CARTESIAN_POINT ( 'NONE',  ( -19.05341960407617563, 5.049401038297882671, 103.5427570613523329 ) ) ;
#15599 = CARTESIAN_POINT ( 'NONE',  ( -18.67979575497178146, -10.72451020669898902, 106.6655762719810383 ) ) ;
#15600 = CARTESIAN_POINT ( 'NONE',  ( -18.67979575497193778, 10.72451020669871902, 63.33442372801900433 ) ) ;
#15601 = CARTESIAN_POINT ( 'NONE',  ( 14.29746914071037800, 8.314922557961029526, 71.66775706135234714 ) ) ;
#15602 = CARTESIAN_POINT ( 'NONE',  ( -8.314922557961024197, 14.29746914071037800, 72.91775706135234714 ) ) ;
#15603 = CARTESIAN_POINT ( 'NONE',  ( -9.564922557960796823, -16.46253265017161027, 67.08224293864769550 ) ) ;
#15604 = CARTESIAN_POINT ( 'NONE',  ( -14.29746914071037622, -8.314922557961029526, 94.16775706135237556 ) ) ;
#15605 = AXIS2_PLACEMENT_3D ( 'NONE', #777, #169645, #122140 ) ;
#15606 = CARTESIAN_POINT ( 'NONE',  ( -15.72974639402197994, 15.80617190586746368, 115.6239096053143669 ) ) ;
#15607 = CARTESIAN_POINT ( 'NONE',  ( -8.224510206698948167, 14.34966873604960824, 70.41557627198102409 ) ) ;
#15608 = CARTESIAN_POINT ( 'NONE',  ( -5.049401038298153566, 19.05341960407611168, 90.20724293864766707 ) ) ;
#15609 = CARTESIAN_POINT ( 'NONE',  ( -14.34966873604972548, 8.224510206698743886, 73.33442372801901854 ) ) ;
#15610 = CARTESIAN_POINT ( 'NONE',  ( -15.72974639402176322, -15.80617190586768395, 54.37609039468568994 ) ) ;
#15611 = CARTESIAN_POINT ( 'NONE',  ( -12.14591786802326823, 12.06949235617739902, 23.12609039468567573 ) ) ;
#15612 = CARTESIAN_POINT ( 'NONE',  ( -10.81492255796078084, -18.62759615963271287, 112.0822429386477097 ) ) ;
#15613 = CARTESIAN_POINT ( 'NONE',  ( 8.224510206698953496, -14.34966873604960469, 52.91557627198103830 ) ) ;
#15614 = EDGE_CURVE ( 'NONE', #126569, #38777, #76319, .T. ) ;
#15615 = ORIENTED_EDGE ( 'NONE', *, *, #157780, .T. ) ;
#15616 = CARTESIAN_POINT ( 'NONE',  ( -18.62759615963270932, 10.81492255796079327, 85.83224293864768129 ) ) ;
#15617 = CARTESIAN_POINT ( 'NONE',  ( -16.55341960407611168, -4.379528057220339221, 36.45724293864768839 ) ) ;
#15618 = ORIENTED_EDGE ( 'NONE', *, *, #124331, .F. ) ;
#15619 = LINE ( 'NONE', #155117, #179331 ) ;
#15620 = CARTESIAN_POINT ( 'NONE',  ( -21.52544592524334988, -5.823673210054445271, 23.95942372801901143 ) ) ;
#15621 = CARTESIAN_POINT ( 'NONE',  ( -9.564922557960796823, -16.46253265017161027, 112.0822429386476955 ) ) ;
#15622 = CARTESIAN_POINT ( 'NONE',  ( 5.719274019375673035, 21.55341960407619339, 27.29275706135234358 ) ) ;
#15623 = CARTESIAN_POINT ( 'NONE',  ( 0.05219959533910956823, 16.53943276465976808, 54.99890960531435269 ) ) ;
#15624 = CARTESIAN_POINT ( 'NONE',  ( -16.53943276465976808, -0.05219959533934237506, 58.75109039468568994 ) ) ;
#15625 = CARTESIAN_POINT ( 'NONE',  ( 9.564922557960805705, 16.46253265017160317, 64.58224293864769550 ) ) ;
#15626 = CARTESIAN_POINT ( 'NONE',  ( 0.05219959533936267826, -19.03943276465977164, 60.00109039468566863 ) ) ;
#15627 = CARTESIAN_POINT ( 'NONE',  ( 5.049401038298161559, -19.05341960407611168, 82.70724293864770971 ) ) ;
#15628 = CARTESIAN_POINT ( 'NONE',  ( -21.55341960407610458, -5.719274019375992779, 46.45724293864769550 ) ) ;
#15629 = CARTESIAN_POINT ( 'NONE',  ( -16.63682861930514889, -37.51503513662309075, -19.06746308534875922 ) ) ;
#15630 = CARTESIAN_POINT ( 'NONE',  ( -9.474510206698964154, 16.51473224551069663, 60.41557627198102409 ) ) ;
#15631 = CARTESIAN_POINT ( 'NONE',  ( -4.483927247898782831, 16.52544592524335698, 37.70942372801900433 ) ) ;
#15632 = CARTESIAN_POINT ( 'NONE',  ( -13.97604488694547697, 13.89961937509957934, 58.12609039468566863 ) ) ;
#15633 = CARTESIAN_POINT ( 'NONE',  ( -15.80617190586768217, 15.72974639402176855, 23.12609039468567573 ) ) ;
#15634 = CARTESIAN_POINT ( 'NONE',  ( 8.224510206698953496, -14.34966873604960469, 42.91557627198103120 ) ) ;
#15635 = CARTESIAN_POINT ( 'NONE',  ( -13.97604488694527625, -13.89961937509977652, 91.87390960531432427 ) ) ;
#15636 = CARTESIAN_POINT ( 'NONE',  ( -15.80617190586745835, -15.72974639402198527, 61.87390960531436690 ) ) ;
#15638 = CARTESIAN_POINT ( 'NONE',  ( 12.06949235617739724, 12.14591786802326823, 36.87609039468568994 ) ) ;
#15637 = CARTESIAN_POINT ( 'NONE',  ( -5.719274019375978568, 21.55341960407610458, 100.2072429386476955 ) ) ;
#15639 = CARTESIAN_POINT ( 'NONE',  ( 10.72451020669898902, -18.67979575497178502, 37.91557627198102409 ) ) ;
#15640 = CARTESIAN_POINT ( 'NONE',  ( -5.823673210054431948, 21.52544592524334988, 87.70942372801901854 ) ) ;
#15641 = CARTESIAN_POINT ( 'NONE',  ( 19.05341960407611168, 5.049401038298154454, 83.95724293864766707 ) ) ;
#15642 = CARTESIAN_POINT ( 'NONE',  ( 5.049401038298161559, -19.05341960407611168, 37.70724293864768839 ) ) ;
#15643 = CARTESIAN_POINT ( 'NONE',  ( 19.03943276465977164, -0.05219959533909143690, 98.74890960531436690 ) ) ;
#15644 = CARTESIAN_POINT ( 'NONE',  ( -14.29746914071049879, 8.314922557960819915, 110.8322429386476955 ) ) ;
#15645 = CARTESIAN_POINT ( 'NONE',  ( 13.97604488694527802, 13.89961937509977652, 69.37390960531436690 ) ) ;
#15646 = CARTESIAN_POINT ( 'NONE',  ( -12.06949235617739369, -12.14591786802326823, 29.37609039468568284 ) ) ;
#15647 = CARTESIAN_POINT ( 'NONE',  ( 17.50000000000000355, 3.305555262949610995, 32.87482847843406830 ) ) ;
#15648 = CARTESIAN_POINT ( 'NONE',  ( 13.97604488694548053, -13.89961937509957401, 60.62609039468564731 ) ) ;
#15650 = CARTESIAN_POINT ( 'NONE',  ( -10.72451020669898014, 18.67979575497178502, 30.41557627198101699 ) ) ;
#15649 = CARTESIAN_POINT ( 'NONE',  ( 18.67979575497194134, -10.72451020669871369, 100.8344237280190185 ) ) ;
#15651 = CARTESIAN_POINT ( 'NONE',  ( 16.53943276465976808, 0.05219959533934440121, 96.25109039468568994 ) ) ;
#15652 = CYLINDRICAL_SURFACE ( 'NONE', #42200, 38.00000000000000000 ) ;
#15653 = CARTESIAN_POINT ( 'NONE',  ( -13.89961937509957401, -13.97604488694547875, 64.37609039468567573 ) ) ;
#15654 = CARTESIAN_POINT ( 'NONE',  ( -9.474510206698720793, -16.51473224551083518, 29.58442372801900433 ) ) ;
#15655 = CARTESIAN_POINT ( 'NONE',  ( 26.32373036410889355, -8.933993968303854061, 140.0000000000000000 ) ) ;
#15656 = CARTESIAN_POINT ( 'NONE',  ( -13.97604488694527625, -13.89961937509977652, 26.87390960531434558 ) ) ;
#15657 = CARTESIAN_POINT ( 'NONE',  ( 8.224510206698953496, -14.34966873604960469, 37.91557627198102409 ) ) ;
#15658 = CARTESIAN_POINT ( 'NONE',  ( -13.89961937509977652, 13.97604488694528158, 25.62390960531434558 ) ) ;
#15659 = CARTESIAN_POINT ( 'NONE',  ( -16.55341960407611168, -4.379528057220339221, 31.45724293864769550 ) ) ;
#15660 = CARTESIAN_POINT ( 'NONE',  ( -18.22780087662124160, -5.499999999999927169, 83.98236817873107896 ) ) ;
#15661 = CARTESIAN_POINT ( 'NONE',  ( 12.06949235617739724, 12.14591786802326823, 96.87609039468568994 ) ) ;
#15662 = CARTESIAN_POINT ( 'NONE',  ( -19.02544592524342804, 5.153800228976336051, 36.04057627198100988 ) ) ;
#15663 = CARTESIAN_POINT ( 'NONE',  ( -10.72451020669870658, -18.67979575497194134, 109.5844237280190328 ) ) ;
#15664 = CARTESIAN_POINT ( 'NONE',  ( -19.05341960407617563, 5.049401038297882671, 113.5427570613523471 ) ) ;
#15665 = CARTESIAN_POINT ( 'NONE',  ( 0.05219959533937995610, -21.53943276465977519, 80.00109039468568994 ) ) ;
#15666 = CARTESIAN_POINT ( 'NONE',  ( -0.05219959533936034679, 19.03943276465977164, 57.50109039468566863 ) ) ;
#15667 = CARTESIAN_POINT ( 'NONE',  ( 9.474510206698971260, -16.51473224551069308, 97.91557627198102409 ) ) ;
#15668 = CARTESIAN_POINT ( 'NONE',  ( 19.03943276465977164, -0.05219959533909143690, 78.74890960531436690 ) ) ;
#15669 = CARTESIAN_POINT ( 'NONE',  ( 17.48847506799967988, 5.747544572773810145, 71.67302562156723411 ) ) ;
#15670 = CARTESIAN_POINT ( 'NONE',  ( 15.72974639402199770, -15.80617190586745480, 108.1239096053143811 ) ) ;
#15671 = CARTESIAN_POINT ( 'NONE',  ( -16.53943276465976808, 0.05219959533911058130, 61.24890960531435979 ) ) ;
#15672 = CARTESIAN_POINT ( 'NONE',  ( -21.53943276465977519, 0.05219959533907696930, 61.24890960531435979 ) ) ;
#15673 = CARTESIAN_POINT ( 'NONE',  ( -13.89961937509977652, 13.97604488694528158, 55.62390960531434558 ) ) ;
#15675 = CARTESIAN_POINT ( 'NONE',  ( 8.224510206698742110, 14.34966873604972548, 92.08442372801901854 ) ) ;
#15674 = CARTESIAN_POINT ( 'NONE',  ( 10.72451020669898902, -18.67979575497178502, 92.91557627198103830 ) ) ;
#15676 = ORIENTED_EDGE ( 'NONE', *, *, #158416, .F. ) ;
#15677 = CARTESIAN_POINT ( 'NONE',  ( 13.89961937509977652, -13.97604488694527269, 53.12390960531434558 ) ) ;
#15679 = CARTESIAN_POINT ( 'NONE',  ( 20.84945647820395109, -10.59429869652066891, 168.2340845703681964 ) ) ;
#15678 = CARTESIAN_POINT ( 'NONE',  ( 4.483927247898545687, 16.52544592524342804, 89.79057627198103830 ) ) ;
#15680 = CARTESIAN_POINT ( 'NONE',  ( -19.03943276465977164, 0.05219959533909376836, 46.24890960531435979 ) ) ;
#15681 = CARTESIAN_POINT ( 'NONE',  ( -16.53943276465976808, 0.05219959533911058130, 116.2489096053143669 ) ) ;
#15682 = CARTESIAN_POINT ( 'NONE',  ( 19.03943276465977164, 0.05219959533936151252, 76.25109039468566152 ) ) ;
#15683 = CARTESIAN_POINT ( 'NONE',  ( -16.53943276465976808, 0.05219959533911058130, 81.24890960531436690 ) ) ;
#15684 = CARTESIAN_POINT ( 'NONE',  ( -18.62759615963255300, -10.81492255796106328, 49.16775706135234003 ) ) ;
#15686 = CARTESIAN_POINT ( 'NONE',  ( 5.823673210054125526, 21.52544592524343514, 104.7905762719810241 ) ) ;
#15685 = CARTESIAN_POINT ( 'NONE',  ( 9.474510206698971260, -16.51473224551069308, 32.91557627198102409 ) ) ;
#15687 = CARTESIAN_POINT ( 'NONE',  ( 8.314922557960818139, 14.29746914071049879, 84.58224293864769550 ) ) ;
#15688 = CARTESIAN_POINT ( 'NONE',  ( 9.646990561632259542, -38.22155086790374412, -31.80034568179171472 ) ) ;
#15689 = CARTESIAN_POINT ( 'NONE',  ( 19.03943276465977164, -0.05219959533909143690, 58.74890960531435979 ) ) ;
#15690 = CARTESIAN_POINT ( 'NONE',  ( 17.26058549869091152, 6.457015423128539489, 113.8774583747606925 ) ) ;
#15692 = CARTESIAN_POINT ( 'NONE',  ( 16.46253265017160672, -9.564922557960803928, 113.3322429386476955 ) ) ;
#15691 = CARTESIAN_POINT ( 'NONE',  ( 9.564922557961047289, -16.46253265017146816, 90.41775706135234714 ) ) ;
#15693 = CARTESIAN_POINT ( 'NONE',  ( 10.81492255796106328, -18.62759615963255655, 30.41775706135234358 ) ) ;
#15694 = CARTESIAN_POINT ( 'NONE',  ( -5.153800228976328057, -19.02544592524343514, 77.29057627198099567 ) ) ;
#15695 = CARTESIAN_POINT ( 'NONE',  ( -5.049401038297874678, -19.05341960407617918, 64.79275706135233293 ) ) ;
#15696 = CARTESIAN_POINT ( 'NONE',  ( -13.97604488694527625, -13.89961937509977652, 51.87390960531436690 ) ) ;
#15697 = CARTESIAN_POINT ( 'NONE',  ( -12.14591786802309592, -12.06949235617757132, 71.87390960531438111 ) ) ;
#15698 = CARTESIAN_POINT ( 'NONE',  ( -12.06949235617756955, 12.14591786802309770, 65.62390960531436690 ) ) ;
#15699 = CARTESIAN_POINT ( 'NONE',  ( -13.97604488694527625, -13.89961937509977652, 91.87390960531432427 ) ) ;
#15700 = CARTESIAN_POINT ( 'NONE',  ( -5.719274019375978568, 21.55341960407610458, 95.20724293864769550 ) ) ;
#15701 = CARTESIAN_POINT ( 'NONE',  ( -19.05341960407611168, -5.049401038298163336, 81.45724293864769550 ) ) ;
#15702 = EDGE_CURVE ( 'NONE', #140232, #144449, #79767, .T. ) ;
#15703 = CARTESIAN_POINT ( 'NONE',  ( -5.153800228976607833, 19.02544592524334988, 32.70942372801899722 ) ) ;
#15706 = CARTESIAN_POINT ( 'NONE',  ( 16.55341960407611168, 4.379528057220329451, 103.9572429386476813 ) ) ;
#15705 = CARTESIAN_POINT ( 'NONE',  ( 0.05219959533910956823, 16.53943276465976808, 29.99890960531435979 ) ) ;
#15704 = CARTESIAN_POINT ( 'NONE',  ( -19.03943276465977164, 0.05219959533909376836, 31.24890960531435979 ) ) ;
#15707 = VERTEX_POINT ( 'NONE', #16647 ) ;
#15708 = CARTESIAN_POINT ( 'NONE',  ( 0.05219959533937995610, -21.53943276465977519, 35.00109039468568284 ) ) ;
#15709 = CARTESIAN_POINT ( 'NONE',  ( 5.049401038297881783, 19.05341960407617563, 62.29275706135234003 ) ) ;
#15710 = CARTESIAN_POINT ( 'NONE',  ( -4.483927247898539470, -16.52544592524342804, 32.29057627198102409 ) ) ;
#15711 = CARTESIAN_POINT ( 'NONE',  ( 21.55341960407610458, 5.719274019375980345, 83.95724293864770971 ) ) ;
#15712 = CARTESIAN_POINT ( 'NONE',  ( 10.81492255796078972, 18.62759615963270932, 24.58224293864768839 ) ) ;
#15713 = CARTESIAN_POINT ( 'NONE',  ( -12.06949235617756955, 12.14591786802309770, 70.62390960531436690 ) ) ;
#15714 = CARTESIAN_POINT ( 'NONE',  ( -19.03943276465977164, 0.05219959533909376836, 31.24890960531435979 ) ) ;
#15715 = CARTESIAN_POINT ( 'NONE',  ( -5.153800228976607833, 19.02544592524334988, 32.70942372801899722 ) ) ;
#15716 = CARTESIAN_POINT ( 'NONE',  ( 8.224510206698742110, 14.34966873604972548, 102.0844237280190185 ) ) ;
#15717 = CARTESIAN_POINT ( 'NONE',  ( -14.34966873604972548, 8.224510206698743886, 58.33442372801901143 ) ) ;
#15718 = CARTESIAN_POINT ( 'NONE',  ( 13.89961937509977652, -13.97604488694527269, 113.1239096053143527 ) ) ;
#15719 = CARTESIAN_POINT ( 'NONE',  ( -5.823673210054431948, 21.52544592524334988, 107.7094237280190328 ) ) ;
#15720 = CARTESIAN_POINT ( 'NONE',  ( 13.97604488694527802, 13.89961937509977652, 79.37390960531435269 ) ) ;
#15721 = CARTESIAN_POINT ( 'NONE',  ( 12.14591786802327356, -12.06949235617739191, 60.62609039468567573 ) ) ;
#15722 = CARTESIAN_POINT ( 'NONE',  ( -4.379528057220328563, 16.55341960407611168, 115.2072429386476955 ) ) ;
#15723 = CARTESIAN_POINT ( 'NONE',  ( -16.55341960407611168, -4.379528057220339221, 36.45724293864768839 ) ) ;
#15724 = DIRECTION ( 'NONE',  ( 0.000000000000000000, 0.000000000000000000, -1.000000000000000000 ) ) ;
#15726 = CARTESIAN_POINT ( 'NONE',  ( -13.97604488694527625, -13.89961937509977652, 96.87390960531433848 ) ) ;
#15725 = CARTESIAN_POINT ( 'NONE',  ( 19.05341960407611168, 5.049401038298154454, 103.9572429386476671 ) ) ;
#15727 = CARTESIAN_POINT ( 'NONE',  ( 9.474510206698971260, -16.51473224551069308, 112.9155762719810383 ) ) ;
#15728 = CARTESIAN_POINT ( 'NONE',  ( 0.05219959533910956823, 16.53943276465976808, 64.99890960531435269 ) ) ;
#15729 = CARTESIAN_POINT ( 'NONE',  ( 8.314922557960818139, 14.29746914071049879, 34.58224293864770260 ) ) ;
#15730 = CARTESIAN_POINT ( 'NONE',  ( -14.29746914071049879, 8.314922557960819915, 55.83224293864770260 ) ) ;
#15731 = ORIENTED_EDGE ( 'NONE', *, *, #141788, .F. ) ;
#15733 = CARTESIAN_POINT ( 'NONE',  ( 17.50000000000000711, -5.499999999999992895, 31.21769037696435589 ) ) ;
#15732 = CARTESIAN_POINT ( 'NONE',  ( 4.379528057220092307, 16.55341960407617563, 37.29275706135235424 ) ) ;
#15734 = CARTESIAN_POINT ( 'NONE',  ( 13.89961937509957401, 13.97604488694547697, 46.87609039468565442 ) ) ;
#15735 = CARTESIAN_POINT ( 'NONE',  ( -9.564922557960796823, -16.46253265017161027, 77.08224293864769550 ) ) ;
#15736 = CARTESIAN_POINT ( 'NONE',  ( 9.474510206698729675, 16.51473224551082808, 67.08442372801900433 ) ) ;
#15737 = CARTESIAN_POINT ( 'NONE',  ( 27.73933785331498925, -9.013057229001033122, 146.2750000027311899 ) ) ;
#15738 = CARTESIAN_POINT ( 'NONE',  ( -16.46253265017146816, -9.564922557961047289, 59.16775706135233293 ) ) ;
#15740 = CARTESIAN_POINT ( 'NONE',  ( -12.14591786802326823, 12.06949235617739902, 83.12609039468568994 ) ) ;
#15739 = CARTESIAN_POINT ( 'NONE',  ( 19.03943276465977164, 0.05219959533936151252, 101.2510903946856757 ) ) ;
#15741 = CARTESIAN_POINT ( 'NONE',  ( 8.571926809382597767, 26.38167802310806209, 148.7750000027311899 ) ) ;
#15742 = CARTESIAN_POINT ( 'NONE',  ( 5.049401038298161559, -19.05341960407611168, 27.70724293864769550 ) ) ;
#15743 = CARTESIAN_POINT ( 'NONE',  ( -19.03943276465977164, 0.05219959533909376836, 106.2489096053143669 ) ) ;
#15744 = CARTESIAN_POINT ( 'NONE',  ( -5.719274019375665041, -21.55341960407619695, 44.79275706135234714 ) ) ;
#15745 = CARTESIAN_POINT ( 'NONE',  ( 5.153800228976615827, -19.02544592524334988, 105.2094237280190185 ) ) ;
#15747 = CARTESIAN_POINT ( 'NONE',  ( 19.02544592524343514, -5.153800228976328945, 58.54057627198102409 ) ) ;
#15746 = CARTESIAN_POINT ( 'NONE',  ( 17.49999999999999645, -3.512728167236924826, 107.7280999518112594 ) ) ;
#15748 = CARTESIAN_POINT ( 'NONE',  ( -19.02544592524342804, 5.153800228976336051, 101.0405762719810241 ) ) ;
#15750 = CARTESIAN_POINT ( 'NONE',  ( 13.89961937509977652, -13.97604488694527269, 68.12390960531436690 ) ) ;
#15749 = CARTESIAN_POINT ( 'NONE',  ( -4.379528057220328563, 16.55341960407611168, 65.20724293864768129 ) ) ;
#15751 = CARTESIAN_POINT ( 'NONE',  ( 19.03943276465977164, -0.05219959533909143690, 63.74890960531435979 ) ) ;
#15752 = CARTESIAN_POINT ( 'NONE',  ( -19.02544592524334988, -5.153800228976617603, 73.95942372801900433 ) ) ;
#15753 = CARTESIAN_POINT ( 'NONE',  ( -15.72974639402197994, 15.80617190586746368, 50.62390960531435979 ) ) ;
#15754 = CARTESIAN_POINT ( 'NONE',  ( 12.14591786802309770, 12.06949235617756955, 114.3739096053143527 ) ) ;
#15755 = CARTESIAN_POINT ( 'NONE',  ( -0.05219959533936034679, 19.03943276465977164, 42.50109039468566152 ) ) ;
#15756 = CARTESIAN_POINT ( 'NONE',  ( 5.049401038298161559, -19.05341960407611168, 82.70724293864770971 ) ) ;
#15757 = CARTESIAN_POINT ( 'NONE',  ( 21.55341960407610458, 5.719274019375980345, 73.95724293864769550 ) ) ;
#15759 = CARTESIAN_POINT ( 'NONE',  ( 13.89961937509957401, 13.97604488694547697, 36.87609039468565442 ) ) ;
#15758 = CARTESIAN_POINT ( 'NONE',  ( -8.224510206698948167, 14.34966873604960824, 85.41557627198102409 ) ) ;
#15760 = CARTESIAN_POINT ( 'NONE',  ( 0.05219959533907565091, 21.53943276465977519, 59.99890960531436690 ) ) ;
#15761 = CARTESIAN_POINT ( 'NONE',  ( 18.62759615963271287, -10.81492255796078972, 38.33224293864768839 ) ) ;
#15762 = CARTESIAN_POINT ( 'NONE',  ( -18.67979575497193778, 10.72451020669871902, 88.33442372801901854 ) ) ;
#15763 = CARTESIAN_POINT ( 'NONE',  ( -9.474510206698964154, 16.51473224551069663, 60.41557627198102409 ) ) ;
#15764 = CARTESIAN_POINT ( 'NONE',  ( -16.55341960407611168, -4.379528057220339221, 111.4572429386476813 ) ) ;
#15765 = CARTESIAN_POINT ( 'NONE',  ( 15.72974639402176855, 15.80617190586768217, 21.87609039468567573 ) ) ;
#15766 = CARTESIAN_POINT ( 'NONE',  ( -17.72560187377285246, -5.500000000000057732, 49.07814504131319211 ) ) ;
#15767 = CARTESIAN_POINT ( 'NONE',  ( 21.52544592524334988, 5.823673210054432836, 36.45942372801901143 ) ) ;
#15768 = CARTESIAN_POINT ( 'NONE',  ( -19.05341960407611168, -5.049401038298163336, 36.45724293864766707 ) ) ;
#15769 = CARTESIAN_POINT ( 'NONE',  ( 21.55341960407610458, 5.719274019375980345, 103.9572429386476813 ) ) ;
#15770 = CARTESIAN_POINT ( 'NONE',  ( -9.474510206698720793, -16.51473224551083518, 44.58442372801900433 ) ) ;
#15771 = DIRECTION ( 'NONE',  ( -1.000000000000000000, 0.000000000000000000, 0.000000000000000000 ) ) ;
#15772 = DIRECTION ( 'NONE',  ( 0.000000000000000000, 0.000000000000000000, 1.000000000000000000 ) ) ;
#15773 = FILL_AREA_STYLE_COLOUR ( '', #114395 ) ;
#15774 = CARTESIAN_POINT ( 'NONE',  ( 8.314922557961029526, -14.29746914071037800, 65.41775706135234714 ) ) ;
#15775 = CARTESIAN_POINT ( 'NONE',  ( 9.564922557960805705, 16.46253265017160317, 29.58224293864769550 ) ) ;
#15776 = CARTESIAN_POINT ( 'NONE',  ( -25.34721418589374764, -10.09305078451760274, 170.5222919391028142 ) ) ;
#15777 = CARTESIAN_POINT ( 'NONE',  ( -0.05219959533909027116, -19.03943276465977164, 77.49890960531435269 ) ) ;
#15778 = CARTESIAN_POINT ( 'NONE',  ( 12.14591786802309770, 12.06949235617756955, 109.3739096053143811 ) ) ;
#15779 = CARTESIAN_POINT ( 'NONE',  ( 21.55341960407610458, 5.719274019375980345, 63.95724293864770260 ) ) ;
#15780 = CARTESIAN_POINT ( 'NONE',  ( 4.483927247898790824, -16.52544592524335698, 35.20942372801901854 ) ) ;
#15781 = CARTESIAN_POINT ( 'NONE',  ( 21.52544592524334988, 5.823673210054432836, 101.4594237280190185 ) ) ;
#15782 = CARTESIAN_POINT ( 'NONE',  ( -5.000000000000000888, 4.999999999999999112, -18.00000000000000000 ) ) ;
#15783 = CARTESIAN_POINT ( 'NONE',  ( -4.483927247898782831, 16.52544592524335698, 112.7094237280190328 ) ) ;
#15784 = CARTESIAN_POINT ( 'NONE',  ( 4.379528057220339221, -16.55341960407611168, 52.70724293864769550 ) ) ;
#15785 = CARTESIAN_POINT ( 'NONE',  ( -13.89961937509977652, 13.97604488694528158, 45.62390960531433848 ) ) ;
#15786 = CARTESIAN_POINT ( 'NONE',  ( -21.52544592524334988, -5.823673210054445271, 98.95942372801903275 ) ) ;
#15787 = CARTESIAN_POINT ( 'NONE',  ( 18.62759615963271287, -10.81492255796078972, 113.3322429386476955 ) ) ;
#15788 = CARTESIAN_POINT ( 'NONE',  ( 18.62759615963255655, 10.81492255796105972, 66.66775706135234714 ) ) ;
#15789 = CARTESIAN_POINT ( 'NONE',  ( -14.29746914071037622, -8.314922557961029526, 59.16775706135234714 ) ) ;
#15791 = CARTESIAN_POINT ( 'NONE',  ( -18.62759615963255300, -10.81492255796106328, 99.16775706135234714 ) ) ;
#15790 = CARTESIAN_POINT ( 'NONE',  ( 16.52544592524342804, -4.483927247898539470, 83.54057627198102409 ) ) ;
#15792 = CARTESIAN_POINT ( 'NONE',  ( 16.53943276465976808, 0.05219959533934440121, 111.2510903946856899 ) ) ;
#15793 = CARTESIAN_POINT ( 'NONE',  ( 18.10062525802556266, -5.499999999999865885, 61.01383468041922953 ) ) ;
#15794 = CARTESIAN_POINT ( 'NONE',  ( -8.314922557961024197, 14.29746914071037800, 37.91775706135235424 ) ) ;
#15795 = CARTESIAN_POINT ( 'NONE',  ( 0.05219959533910956823, 16.53943276465976808, 39.99890960531436690 ) ) ;
#15796 = CARTESIAN_POINT ( 'NONE',  ( -16.53943276465976808, -0.05219959533934237506, 83.75109039468568994 ) ) ;
#15797 = CARTESIAN_POINT ( 'NONE',  ( -9.474510206698964154, 16.51473224551069663, 95.41557627198102409 ) ) ;
#15798 = CARTESIAN_POINT ( 'NONE',  ( -21.53943276465977519, 0.05219959533907696930, 21.24890960531436690 ) ) ;
#15799 = CARTESIAN_POINT ( 'NONE',  ( -0.05219959533937732626, 21.53943276465977519, 92.50109039468567573 ) ) ;
#15800 = CARTESIAN_POINT ( 'NONE',  ( 16.53943276465976808, 0.05219959533934440121, 106.2510903946856757 ) ) ;
#15801 = CARTESIAN_POINT ( 'NONE',  ( 0.05219959533910956823, 16.53943276465976808, 79.99890960531435269 ) ) ;
#15802 = CARTESIAN_POINT ( 'NONE',  ( -5.049401038298153566, 19.05341960407611168, 85.20724293864766707 ) ) ;
#15803 = ORIENTED_EDGE ( 'NONE', *, *, #168981, .T. ) ;
#15804 = CARTESIAN_POINT ( 'NONE',  ( -16.55341960407617563, 4.379528057220093196, 33.54275706135234714 ) ) ;
#15805 = CARTESIAN_POINT ( 'NONE',  ( -9.474510206698964154, 16.51473224551069663, 40.41557627198103120 ) ) ;
#15806 = CARTESIAN_POINT ( 'NONE',  ( 19.05341960407611168, 5.049401038298154454, 88.95724293864769550 ) ) ;
#15808 = CARTESIAN_POINT ( 'NONE',  ( -29.86685920354755197, -21.69954338932560134, -2.424999997268813434 ) ) ;
#15807 = CARTESIAN_POINT ( 'NONE',  ( 0.05219959533934541429, -16.53943276465976808, 30.00109039468568284 ) ) ;
#15809 = CARTESIAN_POINT ( 'NONE',  ( 16.51473224551083163, -9.474510206698727899, 40.83442372801900433 ) ) ;
#15810 = CARTESIAN_POINT ( 'NONE',  ( -16.53943276465976808, -0.05219959533934237506, 88.75109039468567573 ) ) ;
#15811 = CARTESIAN_POINT ( 'NONE',  ( 19.03943276465977164, -0.05219959533909143690, 38.74890960531436690 ) ) ;
#15812 = CARTESIAN_POINT ( 'NONE',  ( 16.53943276465976808, 0.05219959533934440121, 76.25109039468568994 ) ) ;
#15813 = CARTESIAN_POINT ( 'NONE',  ( 8.224510206698742110, 14.34966873604972548, 72.08442372801899012 ) ) ;
#15814 = CARTESIAN_POINT ( 'NONE',  ( 19.05341960407617918, -5.049401038297876454, 86.04275706135233293 ) ) ;
#15815 = CARTESIAN_POINT ( 'NONE',  ( -5.049401038297874678, -19.05341960407617918, 34.79275706135233293 ) ) ;
#15816 = CARTESIAN_POINT ( 'NONE',  ( -5.049401038298153566, 19.05341960407611168, 45.20724293864769550 ) ) ;
#15817 = CARTESIAN_POINT ( 'NONE',  ( -16.55341960407611168, -4.379528057220339221, 91.45724293864769550 ) ) ;
#15818 = EDGE_CURVE ( 'NONE', #15160, #142224, #92027, .T. ) ;
#15819 = CARTESIAN_POINT ( 'NONE',  ( 13.97604488694548053, -13.89961937509957401, 50.62609039468566152 ) ) ;
#15820 = CARTESIAN_POINT ( 'NONE',  ( -15.72974639402197994, 15.80617190586746368, 50.62390960531435979 ) ) ;
#15821 = CARTESIAN_POINT ( 'NONE',  ( -13.89961937509957401, -13.97604488694547875, 29.37609039468565797 ) ) ;
#15822 = CARTESIAN_POINT ( 'NONE',  ( -0.05219959533909027116, -19.03943276465977164, 107.4989096053143527 ) ) ;
#15823 = CARTESIAN_POINT ( 'NONE',  ( -10.72451020669898014, 18.67979575497178502, 80.41557627198103830 ) ) ;
#15824 = CARTESIAN_POINT ( 'NONE',  ( -13.89961937509977652, 13.97604488694528158, 115.6239096053143669 ) ) ;
#15825 = CARTESIAN_POINT ( 'NONE',  ( -19.03943276465977164, -0.05219959533935918106, 83.75109039468567573 ) ) ;
#15826 = CARTESIAN_POINT ( 'NONE',  ( -17.49999999999999645, 3.805241302050257790, 110.3735247278259237 ) ) ;
#15827 = CARTESIAN_POINT ( 'NONE',  ( -12.06949235617739369, -12.14591786802326823, 19.37609039468568639 ) ) ;
#15828 = ADVANCED_BREP_SHAPE_REPRESENTATION ( '', ( #73950, #82054 ), #166266 ) ;
#15829 = CARTESIAN_POINT ( 'NONE',  ( 16.51473224551069308, 9.474510206698969483, 39.16557627198103120 ) ) ;
#15830 = CARTESIAN_POINT ( 'NONE',  ( 13.89961937509977652, -13.97604488694527269, 98.12390960531433848 ) ) ;
#15831 = CARTESIAN_POINT ( 'NONE',  ( -18.62759615963270932, 10.81492255796079327, 75.83224293864769550 ) ) ;
#15832 = AXIS2_PLACEMENT_3D ( 'NONE', #62650, #168836, #123322 ) ;
#15833 = CARTESIAN_POINT ( 'NONE',  ( -14.29746914071037622, -8.314922557961029526, 44.16775706135234714 ) ) ;
#15834 = CARTESIAN_POINT ( 'NONE',  ( -15.72974639402176322, -15.80617190586768395, 49.37609039468569705 ) ) ;
#15836 = CARTESIAN_POINT ( 'NONE',  ( 5.719274019375673035, 21.55341960407619339, 107.2927570613523471 ) ) ;
#15835 = CARTESIAN_POINT ( 'NONE',  ( -16.51473224551082808, 9.474510206698731452, 88.33442372801900433 ) ) ;
#15837 = CARTESIAN_POINT ( 'NONE',  ( 16.53943276465976808, 0.05219959533934440121, 111.2510903946856899 ) ) ;
#15838 = CARTESIAN_POINT ( 'NONE',  ( -19.05341960407611168, -5.049401038298163336, 96.45724293864769550 ) ) ;
#15839 = CARTESIAN_POINT ( 'NONE',  ( -4.379528057220328563, 16.55341960407611168, 90.20724293864770971 ) ) ;
#15840 = CARTESIAN_POINT ( 'NONE',  ( -14.34966873604960291, -8.224510206698953496, 31.66557627198102054 ) ) ;
#15841 = CARTESIAN_POINT ( 'NONE',  ( 0.05219959533936267826, -19.03943276465977164, 85.00109039468567573 ) ) ;
#15842 = CARTESIAN_POINT ( 'NONE',  ( -18.62759615963255300, -10.81492255796106328, 64.16775706135234714 ) ) ;
#15843 = CARTESIAN_POINT ( 'NONE',  ( 13.89961937509957401, 13.97604488694547697, 26.87609039468566507 ) ) ;
#15844 = CARTESIAN_POINT ( 'NONE',  ( -8.224510206698948167, 14.34966873604960824, 105.4155762719810383 ) ) ;
#15845 = CARTESIAN_POINT ( 'NONE',  ( -5.823673210054116645, -21.52544592524344225, 27.29057627198103120 ) ) ;
#15846 = CARTESIAN_POINT ( 'NONE',  ( -16.55341960407617563, 4.379528057220093196, 113.5427570613523756 ) ) ;
#15847 = CARTESIAN_POINT ( 'NONE',  ( -10.81492255796105439, 18.62759615963255655, 102.9177570613523756 ) ) ;
#15848 = CARTESIAN_POINT ( 'NONE',  ( -4.379528057220086978, -16.55341960407618274, 64.79275706135234714 ) ) ;
#15849 = CARTESIAN_POINT ( 'NONE',  ( 0.05219959533910956823, 16.53943276465976808, 24.99890960531435624 ) ) ;
#15850 = CARTESIAN_POINT ( 'NONE',  ( 10.81492255796106328, -18.62759615963255655, 60.41775706135235424 ) ) ;
#15851 = CARTESIAN_POINT ( 'NONE',  ( 15.80617190586769283, -15.72974639402175789, 50.62609039468568994 ) ) ;
#15852 = EDGE_CURVE ( 'NONE', #138825, #77704, #2401, .T. ) ;
#15853 = EDGE_LOOP ( 'NONE', ( #182017, #104263, #40510 ) ) ;
#15854 = CARTESIAN_POINT ( 'NONE',  ( 0.05219959533909260263, 19.03943276465977164, 24.99890960531435269 ) ) ;
#15855 = CARTESIAN_POINT ( 'NONE',  ( -15.80617190586768217, 15.72974639402176855, 33.12609039468569705 ) ) ;
#15856 = CARTESIAN_POINT ( 'NONE',  ( -16.55341960407611168, -4.379528057220339221, 106.4572429386477097 ) ) ;
#15857 = CARTESIAN_POINT ( 'NONE',  ( -19.02544592524342804, 5.153800228976336051, 26.04057627198103120 ) ) ;
#15858 = CARTESIAN_POINT ( 'NONE',  ( -8.314922557960811034, -14.29746914071050412, 77.08224293864769550 ) ) ;
#15859 = CARTESIAN_POINT ( 'NONE',  ( 19.03943276465977164, -0.05219959533909143690, 68.74890960531436690 ) ) ;
#15860 = CARTESIAN_POINT ( 'NONE',  ( 16.52544592524342804, -4.483927247898539470, 23.54057627198102765 ) ) ;
#15861 = CARTESIAN_POINT ( 'NONE',  ( 18.62759615963271287, -10.81492255796078972, 53.33224293864769550 ) ) ;
#15862 = CARTESIAN_POINT ( 'NONE',  ( -16.52544592524342804, 4.483927247898546575, 96.04057627198102409 ) ) ;
#15863 = CARTESIAN_POINT ( 'NONE',  ( 15.72974639402199770, -15.80617190586745480, 93.12390960531436690 ) ) ;
#15864 = CARTESIAN_POINT ( 'NONE',  ( 13.97604488694527802, 13.89961937509977652, 104.3739096053143385 ) ) ;
#15866 = CARTESIAN_POINT ( 'NONE',  ( 16.46253265017146816, 9.564922557961045513, 111.6677570613523329 ) ) ;
#15865 = CARTESIAN_POINT ( 'NONE',  ( -0.05219959533909027116, -19.03943276465977164, 47.49890960531435979 ) ) ;
#15867 = CARTESIAN_POINT ( 'NONE',  ( 21.53943276465977519, -0.05219959533907433946, 48.74890960531435979 ) ) ;
#15868 = CARTESIAN_POINT ( 'NONE',  ( 18.62759615963255655, 10.81492255796105972, 86.66775706135234714 ) ) ;
#15869 = CARTESIAN_POINT ( 'NONE',  ( -19.05341960407611168, -5.049401038298163336, 71.45724293864766707 ) ) ;
#15870 = CARTESIAN_POINT ( 'NONE',  ( -13.97604488694527625, -13.89961937509977652, 101.8739096053143811 ) ) ;
#15871 = CARTESIAN_POINT ( 'NONE',  ( 4.379528057220092307, 16.55341960407617563, 77.29275706135234714 ) ) ;
#15872 = CARTESIAN_POINT ( 'NONE',  ( -21.55341960407619339, 5.719274019375674811, 53.54275706135234714 ) ) ;
#15873 = CARTESIAN_POINT ( 'NONE',  ( 10.81492255796106328, -18.62759615963255655, 80.41775706135234714 ) ) ;
#15874 = CARTESIAN_POINT ( 'NONE',  ( -21.53943276465977519, 0.05219959533907696930, 106.2489096053143811 ) ) ;
#15876 = CARTESIAN_POINT ( 'NONE',  ( -16.53943276465976808, -0.05219959533934237506, 83.75109039468568994 ) ) ;
#15875 = CARTESIAN_POINT ( 'NONE',  ( -5.719274019375665041, -21.55341960407619695, 39.79275706135235424 ) ) ;
#15877 = CARTESIAN_POINT ( 'NONE',  ( 0.05219959533907565091, 21.53943276465977519, 79.99890960531435269 ) ) ;
#15878 = CARTESIAN_POINT ( 'NONE',  ( 13.97604488694548053, -13.89961937509957401, 30.62609039468566863 ) ) ;
#15879 = CARTESIAN_POINT ( 'NONE',  ( -18.67979575497178146, -10.72451020669898902, 46.66557627198102409 ) ) ;
#15881 = CARTESIAN_POINT ( 'NONE',  ( 16.55341960407618274, -4.379528057220086978, 111.0427570613523613 ) ) ;
#15880 = CARTESIAN_POINT ( 'NONE',  ( -19.05341960407611168, -5.049401038298163336, 76.45724293864769550 ) ) ;
#15882 = DIRECTION ( 'NONE',  ( -0.000000000000000000, -0.000000000000000000, 1.000000000000000000 ) ) ;
#15883 = CARTESIAN_POINT ( 'NONE',  ( 5.049401038298161559, -19.05341960407611168, 112.7072429386476813 ) ) ;
#15884 = DIRECTION ( 'NONE',  ( -0.000000000000000000, 0.000000000000000000, 1.000000000000000000 ) ) ;
#15885 = CARTESIAN_POINT ( 'NONE',  ( -16.51473224551082808, 9.474510206698731452, 98.33442372801900433 ) ) ;
#15886 = CARTESIAN_POINT ( 'NONE',  ( -10.72451020669898014, 18.67979575497178502, 75.41557627198102409 ) ) ;
#15887 = CARTESIAN_POINT ( 'NONE',  ( -0.05219959533910754901, -16.53943276465976808, 37.49890960531436690 ) ) ;
#15888 = CARTESIAN_POINT ( 'NONE',  ( -19.05341960407617563, 5.049401038297882671, 108.5427570613523187 ) ) ;
#15889 = CARTESIAN_POINT ( 'NONE',  ( 13.89961937509977652, -13.97604488694527269, 33.12390960531434558 ) ) ;
#15890 = CARTESIAN_POINT ( 'NONE',  ( -9.564922557961040184, 16.46253265017147172, 112.9177570613523329 ) ) ;
#15892 = CARTESIAN_POINT ( 'NONE',  ( 9.564922557961047289, -16.46253265017146816, 65.41775706135233293 ) ) ;
#15891 = CARTESIAN_POINT ( 'NONE',  ( -21.55341960407610458, -5.719274019375992779, 106.4572429386477097 ) ) ;
#15893 = CARTESIAN_POINT ( 'NONE',  ( 12.06949235617739724, 12.14591786802326823, 81.87609039468568994 ) ) ;
#15894 = CARTESIAN_POINT ( 'NONE',  ( -13.89961937509977652, 13.97604488694528158, 85.62390960531433848 ) ) ;
#15895 = CARTESIAN_POINT ( 'NONE',  ( -8.224510206698948167, 14.34966873604960824, 75.41557627198102409 ) ) ;
#15896 = CARTESIAN_POINT ( 'NONE',  ( -16.46253265017160317, 9.564922557960807481, 55.83224293864769550 ) ) ;
#15897 = CARTESIAN_POINT ( 'NONE',  ( 8.224510206698953496, -14.34966873604960469, 62.91557627198102409 ) ) ;
#15898 = CARTESIAN_POINT ( 'NONE',  ( -13.97604488694527625, -13.89961937509977652, 31.87390960531435979 ) ) ;
#15899 = CARTESIAN_POINT ( 'NONE',  ( -36.85371136276476278, -2.758154363750441096, 49.76185830465988147 ) ) ;
#15900 = CARTESIAN_POINT ( 'NONE',  ( 16.52544592524342804, -4.483927247898539470, 43.54057627198103830 ) ) ;
#15901 = CARTESIAN_POINT ( 'NONE',  ( 13.89961937509977652, -13.97604488694527269, 83.12390960531436690 ) ) ;
#15902 = CARTESIAN_POINT ( 'NONE',  ( -0.2077008434174324458, -13.70000000000001705, -60.44446360152740993 ) ) ;
#15903 = CARTESIAN_POINT ( 'NONE',  ( 13.89961937509957401, 13.97604488694547697, 46.87609039468565442 ) ) ;
#15904 = CARTESIAN_POINT ( 'NONE',  ( 16.53943276465976808, 0.05219959533934440121, 56.25109039468568284 ) ) ;
#15905 = CARTESIAN_POINT ( 'NONE',  ( 10.72451020669898902, -18.67979575497178502, 57.91557627198103120 ) ) ;
#15906 = CARTESIAN_POINT ( 'NONE',  ( -9.564922557961040184, 16.46253265017147172, 27.91775706135232582 ) ) ;
#15907 = CARTESIAN_POINT ( 'NONE',  ( -19.05341960407611168, -5.049401038298163336, 86.45724293864769550 ) ) ;
#15908 = CARTESIAN_POINT ( 'NONE',  ( 1.500000000000008438, 22.80000000000002913, -57.83153971412246364 ) ) ;
#15909 = CARTESIAN_POINT ( 'NONE',  ( 21.55341960407610458, 5.719274019375980345, 33.95724293864769550 ) ) ;
#15910 = CARTESIAN_POINT ( 'NONE',  ( 0.05219959533909260263, 19.03943276465977164, 59.99890960531436690 ) ) ;
#15911 = CARTESIAN_POINT ( 'NONE',  ( -5.719274019375665041, -21.55341960407619695, 54.79275706135235424 ) ) ;
#15912 = CARTESIAN_POINT ( 'NONE',  ( -14.29746914071049879, 8.314922557960819915, 100.8322429386477097 ) ) ;
#15915 = ORIENTED_EDGE ( 'NONE', *, *, #94659, .F. ) ;
#15914 = CARTESIAN_POINT ( 'NONE',  ( 13.89961937509977652, -13.97604488694527269, 93.12390960531436690 ) ) ;
#15913 = CARTESIAN_POINT ( 'NONE',  ( -18.62759615963270932, 10.81492255796079327, 105.8322429386476955 ) ) ;
#15916 = CARTESIAN_POINT ( 'NONE',  ( -15.80617190586768217, 15.72974639402176855, 33.12609039468569705 ) ) ;
#15917 = VERTEX_POINT ( 'NONE', #99441 ) ;
#15918 = CARTESIAN_POINT ( 'NONE',  ( 13.89961937509977652, -13.97604488694527269, 88.12390960531438111 ) ) ;
#15919 = CARTESIAN_POINT ( 'NONE',  ( 18.56453257813363678, -5.500000000000045297, 83.49000423690681316 ) ) ;
#15920 = CARTESIAN_POINT ( 'NONE',  ( 21.52544592524344225, -5.823673210054117533, 88.54057627198103830 ) ) ;
#15921 = CARTESIAN_POINT ( 'NONE',  ( -19.05341960407611168, -5.049401038298163336, 51.45724293864770260 ) ) ;
#15922 = CARTESIAN_POINT ( 'NONE',  ( 16.55341960407618274, -4.379528057220086978, 21.04275706135234714 ) ) ;
#15923 = CARTESIAN_POINT ( 'NONE',  ( 22.81625015709509441, 31.40387420917330275, -3.824999997268813345 ) ) ;
#15924 = CARTESIAN_POINT ( 'NONE',  ( 19.02544592524343514, -5.153800228976328945, 23.54057627198102054 ) ) ;
#15925 = CARTESIAN_POINT ( 'NONE',  ( 10.72451020669871369, 18.67979575497193778, 87.08442372801901854 ) ) ;
#15927 = CARTESIAN_POINT ( 'NONE',  ( -15.80617190586768217, 15.72974639402176855, 53.12609039468568284 ) ) ;
#15926 = CARTESIAN_POINT ( 'NONE',  ( -9.474510206698964154, 16.51473224551069663, 70.41557627198102409 ) ) ;
#15928 = CARTESIAN_POINT ( 'NONE',  ( -10.81492255796105439, 18.62759615963255655, 32.91775706135234714 ) ) ;
#15929 = CARTESIAN_POINT ( 'NONE',  ( 8.571926809382603096, -26.38167802310801235, 143.9750000027312069 ) ) ;
#15930 = CARTESIAN_POINT ( 'NONE',  ( -13.89961937509977652, 13.97604488694528158, 95.62390960531436690 ) ) ;
#15931 = DIRECTION ( 'NONE',  ( -0.000000000000000000, 0.4999999999999998890, -0.8660254037844387076 ) ) ;
#15934 = CARTESIAN_POINT ( 'NONE',  ( 15.72974639402176855, 15.80617190586768217, 56.87609039468568994 ) ) ;
#15933 = CARTESIAN_POINT ( 'NONE',  ( 4.379528057220092307, 16.55341960407617563, 72.29275706135236135 ) ) ;
#15932 = CARTESIAN_POINT ( 'NONE',  ( 16.52544592524335698, 4.483927247898782831, 36.45942372801901143 ) ) ;
#15935 = CARTESIAN_POINT ( 'NONE',  ( 0.05219959533937995610, -21.53943276465977519, 75.00109039468568994 ) ) ;
#15936 = FACE_OUTER_BOUND ( 'NONE', #169670, .T. ) ;
#15937 = CARTESIAN_POINT ( 'NONE',  ( -4.379528057220086978, -16.55341960407618274, 19.79275706135235069 ) ) ;
#15938 = CARTESIAN_POINT ( 'NONE',  ( -5.153800228976328057, -19.02544592524343514, 72.29057627198102409 ) ) ;
#15939 = CARTESIAN_POINT ( 'NONE',  ( 16.46253265017160672, -9.564922557960803928, 98.33224293864769550 ) ) ;
#15940 = CARTESIAN_POINT ( 'NONE',  ( 4.379528057220339221, -16.55341960407611168, 102.7072429386476955 ) ) ;
#15941 = CARTESIAN_POINT ( 'NONE',  ( 4.379528057220339221, -16.55341960407611168, 102.7072429386476955 ) ) ;
#15942 = CARTESIAN_POINT ( 'NONE',  ( -21.53943276465977519, 0.05219959533907696930, 26.24890960531435624 ) ) ;
#15943 = CARTESIAN_POINT ( 'NONE',  ( -4.379528057220086978, -16.55341960407618274, 84.79275706135234714 ) ) ;
#15945 = CARTESIAN_POINT ( 'NONE',  ( -5.153800228976328057, -19.02544592524343514, 52.29057627198100988 ) ) ;
#15944 = CARTESIAN_POINT ( 'NONE',  ( -0.05219959533910754901, -16.53943276465976808, 72.49890960531435269 ) ) ;
#15946 = CARTESIAN_POINT ( 'NONE',  ( 15.72974639402176855, 15.80617190586768217, 71.87609039468568994 ) ) ;
#15947 = CARTESIAN_POINT ( 'NONE',  ( 5.719274019375673035, 21.55341960407619339, 72.29275706135236135 ) ) ;
#15948 = CARTESIAN_POINT ( 'NONE',  ( -9.474510206698720793, -16.51473224551083518, 104.5844237280190043 ) ) ;
#15949 = CARTESIAN_POINT ( 'NONE',  ( -0.05219959533910754901, -16.53943276465976808, 72.49890960531435269 ) ) ;
#15950 = CARTESIAN_POINT ( 'NONE',  ( 15.72974639402176855, 15.80617190586768217, 26.87609039468567218 ) ) ;
#15951 = CARTESIAN_POINT ( 'NONE',  ( -21.55341960407610458, -5.719274019375992779, 56.45724293864768839 ) ) ;
#15952 = CARTESIAN_POINT ( 'NONE',  ( -17.26058549869089731, -6.457015423128557252, 106.3774583747607068 ) ) ;
#15953 = FACE_OUTER_BOUND ( 'NONE', #53154, .T. ) ;
#15954 = CARTESIAN_POINT ( 'NONE',  ( -19.02544592524342804, 5.153800228976336051, 71.04057627198099567 ) ) ;
#15955 = CARTESIAN_POINT ( 'NONE',  ( 8.224510206698953496, -14.34966873604960469, 52.91557627198103830 ) ) ;
#15956 = CARTESIAN_POINT ( 'NONE',  ( -14.34966873604972548, 8.224510206698743886, 113.3344237280190328 ) ) ;
#15957 = CARTESIAN_POINT ( 'NONE',  ( 16.55341960407618274, -4.379528057220086978, 96.04275706135236135 ) ) ;
#15958 = CARTESIAN_POINT ( 'NONE',  ( -0.05219959533936034679, 19.03943276465977164, 57.50109039468566863 ) ) ;
#15959 = CARTESIAN_POINT ( 'NONE',  ( -23.42531391676912378, -11.30614932247368287, 165.8025715494068777 ) ) ;
#15960 = CARTESIAN_POINT ( 'NONE',  ( 16.51473224551069308, 9.474510206698969483, 104.1655762719810241 ) ) ;
#15961 = CARTESIAN_POINT ( 'NONE',  ( 4.379528057220339221, -16.55341960407611168, 72.70724293864769550 ) ) ;
#15962 = CARTESIAN_POINT ( 'NONE',  ( -16.51473224551082808, 9.474510206698731452, 48.33442372801900433 ) ) ;
#15964 = CARTESIAN_POINT ( 'NONE',  ( -21.52544592524343514, 5.823673210054127303, 41.04057627198103120 ) ) ;
#15963 = CARTESIAN_POINT ( 'NONE',  ( 5.153800228976335163, 19.02544592524342804, 29.79057627198102409 ) ) ;
#15966 = EDGE_LOOP ( 'NONE', ( #135007, #65086, #24148, #59142 ) ) ;
#15965 = CARTESIAN_POINT ( 'NONE',  ( -5.719274019375978568, 21.55341960407610458, 60.20724293864768839 ) ) ;
#15967 = CARTESIAN_POINT ( 'NONE',  ( -16.53943276465976808, 0.05219959533911058130, 96.24890960531435269 ) ) ;
#15968 = CARTESIAN_POINT ( 'NONE',  ( 16.52544592524335698, 4.483927247898782831, 51.45942372801901854 ) ) ;
#15969 = CARTESIAN_POINT ( 'NONE',  ( 16.53943276465976808, -0.05219959533910856209, 88.74890960531436690 ) ) ;
#15970 = CARTESIAN_POINT ( 'NONE',  ( 16.18388926212235646, -7.379444403734663815, 37.06046848633847901 ) ) ;
#15971 = CARTESIAN_POINT ( 'NONE',  ( 36.91746824999999887, -11.99521256947793546, -8.224999997268811924 ) ) ;
#15972 = CARTESIAN_POINT ( 'NONE',  ( 21.53943276465977519, -0.05219959533907433946, 33.74890960531436690 ) ) ;
#15973 = CARTESIAN_POINT ( 'NONE',  ( -19.97888994334923751, -34.65319547504298470, -10.00000000000000000 ) ) ;
#15974 = CARTESIAN_POINT ( 'NONE',  ( 1.461487595131980566, 7.989588206515827906, -64.16719899660255066 ) ) ;
#15975 = CIRCLE ( 'NONE', #116131, 5.000000000000000000 ) ;
#15977 = CARTESIAN_POINT ( 'NONE',  ( 8.314922557960818139, 14.29746914071049879, 24.58224293864768839 ) ) ;
#15976 = CARTESIAN_POINT ( 'NONE',  ( 14.34966873604972726, -8.224510206698740333, 45.83442372801901854 ) ) ;
#15978 = CARTESIAN_POINT ( 'NONE',  ( -21.53943276465977519, 0.05219959533907696930, 51.24890960531436690 ) ) ;
#15979 = CARTESIAN_POINT ( 'NONE',  ( -13.89961937509957401, -13.97604488694547875, 84.37609039468567573 ) ) ;
#15980 = CARTESIAN_POINT ( 'NONE',  ( 18.62759615963271287, -10.81492255796078972, 58.33224293864768839 ) ) ;
#15981 = CARTESIAN_POINT ( 'NONE',  ( 21.55341960407619695, -5.719274019375665929, 76.04275706135237556 ) ) ;
#15982 = CARTESIAN_POINT ( 'NONE',  ( -11.51446144058598975, 9.455153793104305038, -62.12179458070791327 ) ) ;
#15983 = CARTESIAN_POINT ( 'NONE',  ( 4.379528057220092307, 16.55341960407617563, 42.29275706135235424 ) ) ;
#15986 = EDGE_CURVE ( 'NONE', #140047, #102181, #43573, .T. ) ;
#15985 = CARTESIAN_POINT ( 'NONE',  ( 5.153800228976335163, 19.02544592524342804, 94.79057627198103830 ) ) ;
#15984 = CARTESIAN_POINT ( 'NONE',  ( 13.89961937509977652, -13.97604488694527269, 33.12390960531434558 ) ) ;
#15987 = CARTESIAN_POINT ( 'NONE',  ( -19.03943276465977164, 0.05219959533909376836, 36.24890960531436690 ) ) ;
#15988 = CARTESIAN_POINT ( 'NONE',  ( -14.29746914071049879, 8.314922557960819915, 95.83224293864770971 ) ) ;
#15989 = DIRECTION ( 'NONE',  ( -1.000000000000000000, 0.000000000000000000, -6.982962677686266711E-15 ) ) ;
#15990 = CARTESIAN_POINT ( 'NONE',  ( -0.05219959533909027116, -19.03943276465977164, 112.4989096053143669 ) ) ;
#15991 = VERTEX_POINT ( 'NONE', #158132 ) ;
#15992 = CARTESIAN_POINT ( 'NONE',  ( 4.483927247898790824, -16.52544592524335698, 65.20942372801901854 ) ) ;
#15993 = CARTESIAN_POINT ( 'NONE',  ( -5.719274019375978568, 21.55341960407610458, 85.20724293864770971 ) ) ;
#15994 = CARTESIAN_POINT ( 'NONE',  ( -9.474510206698964154, 16.51473224551069663, 55.41557627198103120 ) ) ;
#15995 = CARTESIAN_POINT ( 'NONE',  ( 18.62759615963255655, 10.81492255796105972, 26.66775706135235424 ) ) ;
#15996 = CARTESIAN_POINT ( 'NONE',  ( -16.51473224551069308, -9.474510206698971260, 76.66557627198103830 ) ) ;
#15997 = CARTESIAN_POINT ( 'NONE',  ( -36.54539699253353291, -20.47674586971619703, -19.42837732572457909 ) ) ;
#15998 = ORIENTED_EDGE ( 'NONE', *, *, #8921, .F. ) ;
#15999 = CARTESIAN_POINT ( 'NONE',  ( 5.719274019375991003, -21.55341960407610458, 112.7072429386476955 ) ) ;
#16002 = CARTESIAN_POINT ( 'NONE',  ( -16.46253265017146816, -9.564922557961047289, 74.16775706135234714 ) ) ;
#16001 = CARTESIAN_POINT ( 'NONE',  ( -16.51473224551069308, -9.474510206698971260, 106.6655762719810383 ) ) ;
#16000 = CARTESIAN_POINT ( 'NONE',  ( -13.89961937509977652, 13.97604488694528158, 25.62390960531434558 ) ) ;
#16003 = CARTESIAN_POINT ( 'NONE',  ( -16.46253265017146816, -9.564922557961047289, 24.16775706135233648 ) ) ;
#16004 = CARTESIAN_POINT ( 'NONE',  ( 5.719274019375991003, -21.55341960407610458, 102.7072429386476955 ) ) ;
#16005 = CARTESIAN_POINT ( 'NONE',  ( 5.153800228976615827, -19.02544592524334988, 30.20942372801900433 ) ) ;
#16006 = CARTESIAN_POINT ( 'NONE',  ( 8.224510206698742110, 14.34966873604972548, 77.08442372801901854 ) ) ;
#16007 = CARTESIAN_POINT ( 'NONE',  ( -5.153800228976328057, -19.02544592524343514, 107.2905762719810383 ) ) ;
#16008 = CARTESIAN_POINT ( 'NONE',  ( 5.153800228976335163, 19.02544592524342804, 59.79057627198100988 ) ) ;
#16009 = CIRCLE ( 'NONE', #183867, 10.00000000000000000 ) ;
#16010 = CARTESIAN_POINT ( 'NONE',  ( 0.05219959533937995610, -21.53943276465977519, 60.00109039468568284 ) ) ;
#16011 = CARTESIAN_POINT ( 'NONE',  ( -5.719274019375665041, -21.55341960407619695, 84.79275706135234714 ) ) ;
#16012 = CARTESIAN_POINT ( 'NONE',  ( 9.474510206698971260, -16.51473224551069308, 72.91557627198102409 ) ) ;
#16013 = CARTESIAN_POINT ( 'NONE',  ( 21.53943276465977519, 0.05219959533937863772, 46.25109039468567573 ) ) ;
#16014 = CARTESIAN_POINT ( 'NONE',  ( -5.153800228976607833, 19.02544592524334988, 92.70942372801901854 ) ) ;
#16015 = CARTESIAN_POINT ( 'NONE',  ( 16.46253265017160672, -9.564922557960803928, 58.33224293864769550 ) ) ;
#16016 = CARTESIAN_POINT ( 'NONE',  ( -9.564922557960796823, -16.46253265017161027, 102.0822429386477097 ) ) ;
#16017 = CARTESIAN_POINT ( 'NONE',  ( 16.46253265017160672, -9.564922557960803928, 63.33224293864769550 ) ) ;
#16018 = CARTESIAN_POINT ( 'NONE',  ( -13.89961937509977652, 13.97604488694528158, 115.6239096053143669 ) ) ;
#16019 = CARTESIAN_POINT ( 'NONE',  ( -16.46253265017160317, 9.564922557960807481, 45.83224293864769550 ) ) ;
#16020 = CARTESIAN_POINT ( 'NONE',  ( -0.05219959533907301413, -21.53943276465977519, 102.4989096053143811 ) ) ;
#16021 = CARTESIAN_POINT ( 'NONE',  ( 4.483927247898790824, -16.52544592524335698, 90.20942372801903275 ) ) ;
#16022 = CARTESIAN_POINT ( 'NONE',  ( -23.03120525563286947, 11.22467059994864336, 168.0473679553712429 ) ) ;
#16023 = CARTESIAN_POINT ( 'NONE',  ( -13.97604488694547697, 13.89961937509957934, 48.12609039468566863 ) ) ;
#16024 = CARTESIAN_POINT ( 'NONE',  ( -13.89961937509977652, 13.97604488694528158, 60.62390960531436690 ) ) ;
#16025 = CARTESIAN_POINT ( 'NONE',  ( 14.29746914071049879, -8.314922557960816363, 58.33224293864768839 ) ) ;
#16026 = CARTESIAN_POINT ( 'NONE',  ( 0.05219959533910956823, 16.53943276465976808, 89.99890960531438111 ) ) ;
#16027 = CARTESIAN_POINT ( 'NONE',  ( -21.55341960407610458, -5.719274019375992779, 21.45724293864769550 ) ) ;
#16028 = CARTESIAN_POINT ( 'NONE',  ( 9.474510206698971260, -16.51473224551069308, 87.91557627198102409 ) ) ;
#16029 = CARTESIAN_POINT ( 'NONE',  ( -19.03943276465977164, 0.05219959533909376836, 106.2489096053143669 ) ) ;
#16030 = CARTESIAN_POINT ( 'NONE',  ( 10.72451020669871369, 18.67979575497193778, 112.0844237280190185 ) ) ;
#16031 = CARTESIAN_POINT ( 'NONE',  ( -14.34966873604972548, 8.224510206698743886, 88.33442372801901854 ) ) ;
#16032 = CARTESIAN_POINT ( 'NONE',  ( -9.474510206698964154, 16.51473224551069663, 80.41557627198103830 ) ) ;
#16033 = CARTESIAN_POINT ( 'NONE',  ( 5.719274019375673035, 21.55341960407619339, 42.29275706135235424 ) ) ;
#16034 = CARTESIAN_POINT ( 'NONE',  ( 5.823673210054125526, 21.52544592524343514, 24.79057627198103120 ) ) ;
#16035 = CARTESIAN_POINT ( 'NONE',  ( -21.55341960407610458, -5.719274019375992779, 106.4572429386477097 ) ) ;
#16036 = CARTESIAN_POINT ( 'NONE',  ( -12.14591786802309592, -12.06949235617757132, 61.87390960531436690 ) ) ;
#16037 = CARTESIAN_POINT ( 'NONE',  ( 9.564922557960805705, 16.46253265017160317, 59.58224293864769550 ) ) ;
#16038 = CARTESIAN_POINT ( 'NONE',  ( -8.224510206698948167, 14.34966873604960824, 80.41557627198103830 ) ) ;
#16039 = CARTESIAN_POINT ( 'NONE',  ( -5.153800228976607833, 19.02544592524334988, 42.70942372801901143 ) ) ;
#16040 = CARTESIAN_POINT ( 'NONE',  ( -8.314922557960811034, -14.29746914071050412, 112.0822429386477097 ) ) ;
#16041 = CARTESIAN_POINT ( 'NONE',  ( -5.049401038298153566, 19.05341960407611168, 85.20724293864766707 ) ) ;
#16042 = CARTESIAN_POINT ( 'NONE',  ( -19.02544592524342804, 5.153800228976336051, 81.04057627198103830 ) ) ;
#16043 = CARTESIAN_POINT ( 'NONE',  ( 8.571926809382597767, 26.38167802310806209, 142.2750000027311899 ) ) ;
#16044 = CARTESIAN_POINT ( 'NONE',  ( 8.314922557960818139, 14.29746914071049879, 94.58224293864769550 ) ) ;
#16045 = ORIENTED_EDGE ( 'NONE', *, *, #125126, .T. ) ;
#16046 = CARTESIAN_POINT ( 'NONE',  ( 4.379528057220092307, 16.55341960407617563, 112.2927570613523471 ) ) ;
#16047 = CARTESIAN_POINT ( 'NONE',  ( -4.379528057220086978, -16.55341960407618274, 24.79275706135235779 ) ) ;
#16048 = CARTESIAN_POINT ( 'NONE',  ( -10.72451020669870658, -18.67979575497194134, 99.58442372801900433 ) ) ;
#16049 = CARTESIAN_POINT ( 'NONE',  ( -5.153800228976328057, -19.02544592524343514, 87.29057627198103830 ) ) ;
#16050 = CARTESIAN_POINT ( 'NONE',  ( -21.53943276465977519, -0.05219959533937600094, 23.75109039468567929 ) ) ;
#16051 = CARTESIAN_POINT ( 'NONE',  ( -13.97604488694527625, -13.89961937509977652, 31.87390960531435979 ) ) ;
#16052 = EDGE_CURVE ( 'NONE', #76856, #89587, #83270, .T. ) ;
#16053 = CARTESIAN_POINT ( 'NONE',  ( 16.52544592524335698, 4.483927247898782831, 36.45942372801901143 ) ) ;
#16054 = CARTESIAN_POINT ( 'NONE',  ( 19.02544592524334988, 5.153800228976608722, 101.4594237280189759 ) ) ;
#16055 = CARTESIAN_POINT ( 'NONE',  ( 5.823673210054125526, 21.52544592524343514, 94.79057627198105251 ) ) ;
#16056 = CARTESIAN_POINT ( 'NONE',  ( -13.97604488694547697, 13.89961937509957934, 73.12609039468568994 ) ) ;
#16057 = CARTESIAN_POINT ( 'NONE',  ( 13.97604488694527802, 13.89961937509977652, 24.37390960531435624 ) ) ;
#16058 = CARTESIAN_POINT ( 'NONE',  ( -18.67979575497193778, 10.72451020669871902, 23.33442372801901499 ) ) ;
#16059 = CARTESIAN_POINT ( 'NONE',  ( -3.573655867282028392E-15, 2.428612866367529932E-14, 155.0000000000000000 ) ) ;
#16060 = CARTESIAN_POINT ( 'NONE',  ( 19.02544592524343514, -5.153800228976328945, 93.54057627198102409 ) ) ;
#16061 = CARTESIAN_POINT ( 'NONE',  ( 4.379528057220092307, 16.55341960407617563, 52.29275706135236135 ) ) ;
#16062 = CARTESIAN_POINT ( 'NONE',  ( 18.71701949505375850, -35.35143465962271137, -8.069197253667519831 ) ) ;
#16063 = CARTESIAN_POINT ( 'NONE',  ( -16.51473224551082808, 9.474510206698731452, 63.33442372801900433 ) ) ;
#16065 = CARTESIAN_POINT ( 'NONE',  ( -0.05219959533910754901, -16.53943276465976808, 77.49890960531433848 ) ) ;
#16064 = CARTESIAN_POINT ( 'NONE',  ( 15.72974639402176855, 15.80617190586768217, 21.87609039468567573 ) ) ;
#16066 = CARTESIAN_POINT ( 'NONE',  ( -13.97604488694527625, -13.89961937509977652, 86.87390960531436690 ) ) ;
#16068 = CARTESIAN_POINT ( 'NONE',  ( -19.03943276465977164, -0.05219959533935918106, 58.75109039468566863 ) ) ;
#16067 = CARTESIAN_POINT ( 'NONE',  ( 8.314922557961029526, -14.29746914071037800, 50.41775706135235424 ) ) ;
#16069 = CARTESIAN_POINT ( 'NONE',  ( -18.67979575497193778, 10.72451020669871902, 63.33442372801900433 ) ) ;
#16070 = CARTESIAN_POINT ( 'NONE',  ( -8.224510206698735004, -14.34966873604973081, 29.58442372801901854 ) ) ;
#16071 = CARTESIAN_POINT ( 'NONE',  ( -9.564922557960796823, -16.46253265017161027, 72.08224293864770971 ) ) ;
#16072 = CARTESIAN_POINT ( 'NONE',  ( 16.46253265017146816, 9.564922557961045513, 81.66775706135233293 ) ) ;
#16073 = CARTESIAN_POINT ( 'NONE',  ( -16.52544592524335698, -4.483927247898792601, 53.95942372801900433 ) ) ;
#16074 = CARTESIAN_POINT ( 'NONE',  ( -21.52544592524334988, -5.823673210054445271, 93.95942372801903275 ) ) ;
#16075 = CARTESIAN_POINT ( 'NONE',  ( 19.03943276465977164, 0.05219959533936151252, 86.25109039468567573 ) ) ;
#16076 = CARTESIAN_POINT ( 'NONE',  ( -16.51473224551069308, -9.474510206698971260, 56.66557627198103120 ) ) ;
#16077 = CARTESIAN_POINT ( 'NONE',  ( -0.05219959533907301413, -21.53943276465977519, 72.49890960531435269 ) ) ;
#16079 = CARTESIAN_POINT ( 'NONE',  ( 19.03943276465977164, 0.05219959533936151252, 81.25109039468567573 ) ) ;
#16078 = CARTESIAN_POINT ( 'NONE',  ( -12.06949235617756955, 12.14591786802309770, 70.62390960531436690 ) ) ;
#16080 = CYLINDRICAL_SURFACE ( 'NONE', #60174, 28.82186960331498682 ) ;
#16081 = CARTESIAN_POINT ( 'NONE',  ( -16.51473224551082808, 9.474510206698731452, 48.33442372801900433 ) ) ;
#16082 = CARTESIAN_POINT ( 'NONE',  ( 0.05219959533934541429, -16.53943276465976808, 100.0010903946857042 ) ) ;
#16083 = CARTESIAN_POINT ( 'NONE',  ( -8.314922557960811034, -14.29746914071050412, 72.08224293864769550 ) ) ;
#16085 = CARTESIAN_POINT ( 'NONE',  ( -22.44159573604009950, -16.30477369853688430, 145.0750000027311728 ) ) ;
#16084 = CARTESIAN_POINT ( 'NONE',  ( -15.80617190586768217, 15.72974639402176855, 108.1260903946856757 ) ) ;
#16086 = CARTESIAN_POINT ( 'NONE',  ( 10.81492255796078972, 18.62759615963270932, 104.5822429386477097 ) ) ;
#16087 = CARTESIAN_POINT ( 'NONE',  ( 0.05219959533909260263, 19.03943276465977164, 59.99890960531436690 ) ) ;
#16088 = CARTESIAN_POINT ( 'NONE',  ( -10.72451020669870658, -18.67979575497194134, 74.58442372801901854 ) ) ;
#16089 = CARTESIAN_POINT ( 'NONE',  ( 19.02544592524343514, -5.153800228976328945, 48.54057627198103120 ) ) ;
#16090 = ORIENTED_EDGE ( 'NONE', *, *, #19851, .F. ) ;
#16091 = CARTESIAN_POINT ( 'NONE',  ( -0.05219959533909027116, -19.03943276465977164, 27.49890960531435624 ) ) ;
#16092 = CARTESIAN_POINT ( 'NONE',  ( -13.89961937509977652, 13.97604488694528158, 110.6239096053143243 ) ) ;
#16093 = CARTESIAN_POINT ( 'NONE',  ( -12.14591786802309592, -12.06949235617757132, 66.87390960531436690 ) ) ;
#16094 = CARTESIAN_POINT ( 'NONE',  ( 9.564922557960805705, 16.46253265017160317, 24.58224293864769194 ) ) ;
#16095 = CARTESIAN_POINT ( 'NONE',  ( 8.314922557960818139, 14.29746914071049879, 79.58224293864769550 ) ) ;
#16096 = CARTESIAN_POINT ( 'NONE',  ( 10.81492255796078972, 18.62759615963270932, 94.58224293864769550 ) ) ;
#16097 = CARTESIAN_POINT ( 'NONE',  ( 18.67979575497194134, -10.72451020669871369, 45.83442372801901854 ) ) ;
#16098 = LINE ( 'NONE', #64586, #153351 ) ;
#16099 = CARTESIAN_POINT ( 'NONE',  ( 12.06949235617739724, 12.14591786802326823, 51.87609039468568284 ) ) ;
#16100 = CARTESIAN_POINT ( 'NONE',  ( -0.05219959533907301413, -21.53943276465977519, 102.4989096053143811 ) ) ;
#16101 = CARTESIAN_POINT ( 'NONE',  ( -9.564922557961040184, 16.46253265017147172, 32.91775706135233293 ) ) ;
#16102 = CARTESIAN_POINT ( 'NONE',  ( -16.46253265017160317, 9.564922557960807481, 105.8322429386476955 ) ) ;
#16103 = CARTESIAN_POINT ( 'NONE',  ( 10.81492255796106328, -18.62759615963255655, 50.41775706135235424 ) ) ;
#16104 = CARTESIAN_POINT ( 'NONE',  ( -5.719274019375978568, 21.55341960407610458, 40.20724293864769550 ) ) ;
#16105 = CARTESIAN_POINT ( 'NONE',  ( -14.29746914071049879, 8.314922557960819915, 25.83224293864769194 ) ) ;
#16107 = CARTESIAN_POINT ( 'NONE',  ( -21.52544592524334988, -5.823673210054445271, 98.95942372801903275 ) ) ;
#16106 = CARTESIAN_POINT ( 'NONE',  ( 18.67979575497194134, -10.72451020669871369, 60.83442372801901854 ) ) ;
#16108 = CARTESIAN_POINT ( 'NONE',  ( 19.03943276465977164, 0.05219959533936151252, 26.25109039468566507 ) ) ;
#16109 = CARTESIAN_POINT ( 'NONE',  ( 8.224510206698742110, 14.34966873604972548, 82.08442372801901854 ) ) ;
#16110 = CARTESIAN_POINT ( 'NONE',  ( 21.52544592524334988, 5.823673210054432836, 51.45942372801901854 ) ) ;
#16111 = CARTESIAN_POINT ( 'NONE',  ( -9.474510206698964154, 16.51473224551069663, 40.41557627198103120 ) ) ;
#16112 = CARTESIAN_POINT ( 'NONE',  ( -19.03943276465977164, -0.05219959533935918106, 18.75109039468567218 ) ) ;
#16113 = CARTESIAN_POINT ( 'NONE',  ( -21.52544592524343514, 5.823673210054127303, 26.04057627198103475 ) ) ;
#16114 = CARTESIAN_POINT ( 'NONE',  ( -15.80617190586745835, -15.72974639402198527, 111.8739096053143669 ) ) ;
#16115 = AXIS2_PLACEMENT_3D ( 'NONE', #109939, #18939, #79600 ) ;
#16116 = CARTESIAN_POINT ( 'NONE',  ( 18.62759615963271287, -10.81492255796078972, 78.33224293864770971 ) ) ;
#16117 = CARTESIAN_POINT ( 'NONE',  ( 4.379528057220092307, 16.55341960407617563, 42.29275706135235424 ) ) ;
#16119 = CARTESIAN_POINT ( 'NONE',  ( -10.81492255796078084, -18.62759615963271287, 82.08224293864768129 ) ) ;
#16118 = FACE_OUTER_BOUND ( 'NONE', #138338, .T. ) ;
#16122 = CARTESIAN_POINT ( 'NONE',  ( -14.34966873604960291, -8.224510206698953496, 61.66557627198103120 ) ) ;
#16121 = B_SPLINE_CURVE_WITH_KNOTS ( 'NONE', 3,
 ( #174272, #35740, #186472, #62095, #158093, #185457, #95418, #110588, #18599, #188444, #49923, #34747, #9415, #113565, #160085, #51906, #102414, #20567, #21571, #5391 ),
 .UNSPECIFIED., .F., .F.,
 ( 4, 2, 2, 2, 2, 2, 2, 2, 2, 4 ),
 ( 0.004000878361811972990, 0.004499404418915994158, 0.004997930476020014459, 0.005496456533124034760, 0.005994982590228055928, 0.006244245618780045262, 0.006493508647332034596, 0.006992034704436017600, 0.007490560761540001472, 0.007989086818643985344 ),
 .UNSPECIFIED. ) ;
#16120 = CARTESIAN_POINT ( 'NONE',  ( 12.06949235617739724, 12.14591786802326823, 66.87609039468568994 ) ) ;
#16123 = CARTESIAN_POINT ( 'NONE',  ( -22.68986043004510833, 20.57406348593920953, -47.49330165217068611 ) ) ;
#16124 = CARTESIAN_POINT ( 'NONE',  ( -19.05341960407617563, 5.049401038297882671, 98.54275706135233293 ) ) ;
#16125 = CARTESIAN_POINT ( 'NONE',  ( -21.30000000000002203, 0.1123844339352012556, -56.46919128290399215 ) ) ;
#16126 = CARTESIAN_POINT ( 'NONE',  ( -4.379528057220086978, -16.55341960407618274, 39.79275706135235424 ) ) ;
#16127 = CARTESIAN_POINT ( 'NONE',  ( -21.52544592524343514, 5.823673210054127303, 106.0405762719810525 ) ) ;
#16128 = CARTESIAN_POINT ( 'NONE',  ( -10.72451020669898014, 18.67979575497178502, 25.41557627198103120 ) ) ;
#16129 = CARTESIAN_POINT ( 'NONE',  ( 14.29746914071037800, 8.314922557961029526, 51.66775706135234714 ) ) ;
#16130 = CARTESIAN_POINT ( 'NONE',  ( -9.564922557960796823, -16.46253265017161027, 77.08224293864769550 ) ) ;
#16132 = CARTESIAN_POINT ( 'NONE',  ( 5.049401038297881783, 19.05341960407617563, 112.2927570613523471 ) ) ;
#16131 = CARTESIAN_POINT ( 'NONE',  ( 5.823673210054444382, -21.52544592524334988, 45.20942372801901854 ) ) ;
#16133 = CARTESIAN_POINT ( 'NONE',  ( -18.62759615963270932, 10.81492255796079327, 25.83224293864769194 ) ) ;
#16134 = VERTEX_POINT ( 'NONE', #178309 ) ;
#16135 = CARTESIAN_POINT ( 'NONE',  ( -16.46253265017146816, -9.564922557961047289, 29.16775706135232937 ) ) ;
#16136 = CARTESIAN_POINT ( 'NONE',  ( 8.314922557961029526, -14.29746914071037800, 40.41775706135234714 ) ) ;
#16137 = CARTESIAN_POINT ( 'NONE',  ( 9.564922557960805705, 16.46253265017160317, 94.58224293864769550 ) ) ;
#16138 = CARTESIAN_POINT ( 'NONE',  ( -15.80617190586745835, -15.72974639402198527, 106.8739096053143811 ) ) ;
#16139 = CARTESIAN_POINT ( 'NONE',  ( -19.02544592524342804, 5.153800228976336051, 71.04057627198099567 ) ) ;
#16140 = CARTESIAN_POINT ( 'NONE',  ( 30.00000000000000000, -1.163414459189985801E-14, 92.35000000000000853 ) ) ;
#16141 = CARTESIAN_POINT ( 'NONE',  ( -12.14591786802309592, -12.06949235617757132, 81.87390960531435269 ) ) ;
#16142 = CARTESIAN_POINT ( 'NONE',  ( 19.03943276465977164, -0.05219959533909143690, 113.7489096053143669 ) ) ;
#16143 = CARTESIAN_POINT ( 'NONE',  ( -17.12812012977024878, 6.668231424566046783, 33.64051240676857191 ) ) ;
#16144 = CARTESIAN_POINT ( 'NONE',  ( 8.314922557961029526, -14.29746914071037800, 65.41775706135234714 ) ) ;
#16145 = CARTESIAN_POINT ( 'NONE',  ( -18.62759615963270932, 10.81492255796079327, 105.8322429386476955 ) ) ;
#16146 = CARTESIAN_POINT ( 'NONE',  ( -9.474510206698720793, -16.51473224551083518, 64.58442372801900433 ) ) ;
#16147 = CARTESIAN_POINT ( 'NONE',  ( 5.719274019375991003, -21.55341960407610458, 27.70724293864769905 ) ) ;
#16148 = CARTESIAN_POINT ( 'NONE',  ( 0.05219959533909260263, 19.03943276465977164, 24.99890960531435269 ) ) ;
#16149 = CARTESIAN_POINT ( 'NONE',  ( -10.81492255796078084, -18.62759615963271287, 67.08224293864770971 ) ) ;
#16150 = CIRCLE ( 'NONE', #90468, 2.500000000000000000 ) ;
#16151 = CARTESIAN_POINT ( 'NONE',  ( 16.46253265017160672, -9.564922557960803928, 93.33224293864769550 ) ) ;
#16152 = CARTESIAN_POINT ( 'NONE',  ( 10.72451020669871369, 18.67979575497193778, 92.08442372801901854 ) ) ;
#16153 = CARTESIAN_POINT ( 'NONE',  ( -19.03943276465977164, 0.05219959533909376836, 56.24890960531435979 ) ) ;
#16154 = CARTESIAN_POINT ( 'NONE',  ( -4.483927247898782831, 16.52544592524335698, 37.70942372801900433 ) ) ;
#16155 = CARTESIAN_POINT ( 'NONE',  ( 0.05219959533909260263, 19.03943276465977164, 54.99890960531435979 ) ) ;
#16156 = CARTESIAN_POINT ( 'NONE',  ( -5.719274019375665041, -21.55341960407619695, 74.79275706135234714 ) ) ;
#16157 = VERTEX_POINT ( 'NONE', #68107 ) ;
#16158 = CARTESIAN_POINT ( 'NONE',  ( 16.51473224551083163, -9.474510206698727899, 40.83442372801900433 ) ) ;
#16159 = CARTESIAN_POINT ( 'NONE',  ( 19.02544592524334988, 5.153800228976608722, 46.45942372801899012 ) ) ;
#16160 = CARTESIAN_POINT ( 'NONE',  ( 0.05219959533937995610, -21.53943276465977519, 35.00109039468568284 ) ) ;
#16161 = CARTESIAN_POINT ( 'NONE',  ( 17.79613651744293534, 24.49428055684532524, 143.2843446568999468 ) ) ;
#16162 = CARTESIAN_POINT ( 'NONE',  ( -5.049401038297874678, -19.05341960407617918, 29.79275706135232227 ) ) ;
#16163 = CARTESIAN_POINT ( 'NONE',  ( -5.153800228976328057, -19.02544592524343514, 87.29057627198103830 ) ) ;
#16164 = CARTESIAN_POINT ( 'NONE',  ( -5.049401038298153566, 19.05341960407611168, 65.20724293864765286 ) ) ;
#16165 = CARTESIAN_POINT ( 'NONE',  ( 16.55341960407611168, 4.379528057220329451, 28.95724293864769905 ) ) ;
#16167 = CARTESIAN_POINT ( 'NONE',  ( -15.72974639402176322, -15.80617190586768395, 84.37609039468570415 ) ) ;
#16166 = CARTESIAN_POINT ( 'NONE',  ( 9.474510206698971260, -16.51473224551069308, 112.9155762719810383 ) ) ;
#16168 = CARTESIAN_POINT ( 'NONE',  ( -36.91746825000000598, 2.428612866367529932E-14, -9.124999997268814056 ) ) ;
#16169 = CARTESIAN_POINT ( 'NONE',  ( 16.38665767535054130, 7.295008042176050367, 57.23599135785458003 ) ) ;
#16170 = CARTESIAN_POINT ( 'NONE',  ( 10.72451020669871369, 18.67979575497193778, 97.08442372801904696 ) ) ;
#16171 = CARTESIAN_POINT ( 'NONE',  ( 17.48847506799967988, -5.747544572773779947, 43.32697437843280852 ) ) ;
#16172 = CARTESIAN_POINT ( 'NONE',  ( -0.05219959533909027116, -19.03943276465977164, 27.49890960531435624 ) ) ;
#16173 = CARTESIAN_POINT ( 'NONE',  ( 5.199999999999996625, 0.000000000000000000, 0.000000000000000000 ) ) ;
#16174 = CARTESIAN_POINT ( 'NONE',  ( -2.662494480112493012, -37.13692398601925504, -32.59999999999999432 ) ) ;
#16175 = CARTESIAN_POINT ( 'NONE',  ( -14.34966873604972548, 8.224510206698743886, 53.33442372801901854 ) ) ;
#16176 = CARTESIAN_POINT ( 'NONE',  ( 0.05219959533907565091, 21.53943276465977519, 74.99890960531435269 ) ) ;
#16177 = CARTESIAN_POINT ( 'NONE',  ( -4.379528057220328563, 16.55341960407611168, 40.20724293864769550 ) ) ;
#16179 = CARTESIAN_POINT ( 'NONE',  ( 16.51473224551069308, 9.474510206698969483, 89.16557627198103830 ) ) ;
#16178 = CARTESIAN_POINT ( 'NONE',  ( 12.06949235617757843, -12.14591786802309237, 108.1239096053143811 ) ) ;
#16180 = CARTESIAN_POINT ( 'NONE',  ( -19.05341960407617563, 5.049401038297882671, 23.54275706135233648 ) ) ;
#16181 = CARTESIAN_POINT ( 'NONE',  ( -19.02544592524342804, 5.153800228976336051, 26.04057627198103120 ) ) ;
#16182 = CARTESIAN_POINT ( 'NONE',  ( 15.80617190586769283, -15.72974639402175789, 70.62609039468567573 ) ) ;
#16183 = FACE_OUTER_BOUND ( 'NONE', #147162, .T. ) ;
#16184 = CARTESIAN_POINT ( 'NONE',  ( -16.55341960407617563, 4.379528057220093196, 113.5427570613523756 ) ) ;
#16185 = CARTESIAN_POINT ( 'NONE',  ( -19.05341960407617563, 5.049401038297882671, 58.54275706135234003 ) ) ;
#16186 = CARTESIAN_POINT ( 'NONE',  ( 11.40812507854755253, -35.11059874428192273, -6.524999997268813523 ) ) ;
#16187 = CARTESIAN_POINT ( 'NONE',  ( -15.72974639402197994, 15.80617190586746368, 25.62390960531435624 ) ) ;
#16188 = CARTESIAN_POINT ( 'NONE',  ( -16.55341960407611168, -4.379528057220339221, 96.45724293864770971 ) ) ;
#16189 = CARTESIAN_POINT ( 'NONE',  ( 13.89961937509957401, 13.97604488694547697, 51.87609039468566863 ) ) ;
#16190 = CARTESIAN_POINT ( 'NONE',  ( -5.049401038298153566, 19.05341960407611168, 70.20724293864769550 ) ) ;
#16191 = CARTESIAN_POINT ( 'NONE',  ( 16.52544592524342804, -4.483927247898539470, 68.54057627198103830 ) ) ;
#16192 = CARTESIAN_POINT ( 'NONE',  ( -5.049401038297874678, -19.05341960407617918, 89.79275706135230450 ) ) ;
#16193 = CARTESIAN_POINT ( 'NONE',  ( -18.67979575497178146, -10.72451020669898902, 51.66557627198102409 ) ) ;
#16194 = EDGE_LOOP ( 'NONE', ( #158664, #51672, #151674, #15230 ) ) ;
#16195 = CARTESIAN_POINT ( 'NONE',  ( -14.34966873604960291, -8.224510206698953496, 111.6655762719810525 ) ) ;
#16196 = PLANE ( 'NONE',  #3280 ) ;
#16198 = CARTESIAN_POINT ( 'NONE',  ( -21.53943276465977519, 0.05219959533907696930, 71.24890960531435269 ) ) ;
#16197 = CARTESIAN_POINT ( 'NONE',  ( 9.474510206698971260, -16.51473224551069308, 72.91557627198102409 ) ) ;
#16200 = CARTESIAN_POINT ( 'NONE',  ( 9.564922557960805705, 16.46253265017160317, 74.58224293864769550 ) ) ;
#16199 = CARTESIAN_POINT ( 'NONE',  ( -16.53943276465976808, -0.05219959533934237506, 93.75109039468567573 ) ) ;
#16201 = CARTESIAN_POINT ( 'NONE',  ( -19.03943276465977164, -0.05219959533935918106, 68.75109039468566152 ) ) ;
#16202 = CARTESIAN_POINT ( 'NONE',  ( 10.81492255796106328, -18.62759615963255655, 75.41775706135233293 ) ) ;
#16203 = CARTESIAN_POINT ( 'NONE',  ( -18.62759615963270932, 10.81492255796079327, 60.83224293864769550 ) ) ;
#16204 = CARTESIAN_POINT ( 'NONE',  ( -5.719274019375978568, 21.55341960407610458, 25.20724293864769550 ) ) ;
#16205 = CARTESIAN_POINT ( 'NONE',  ( 13.89961937509977652, -13.97604488694527269, 33.12390960531434558 ) ) ;
#16206 = CARTESIAN_POINT ( 'NONE',  ( -16.53943276465976808, -0.05219959533934237506, 98.75109039468568994 ) ) ;
#16207 = CARTESIAN_POINT ( 'NONE',  ( -5.153800228976328057, -19.02544592524343514, 47.29057627198102409 ) ) ;
#16208 = CARTESIAN_POINT ( 'NONE',  ( -14.34966873604972548, 8.224510206698743886, 23.33442372801901499 ) ) ;
#16209 = CARTESIAN_POINT ( 'NONE',  ( 5.049401038297881783, 19.05341960407617918, 82.29275706135231871 ) ) ;
#16210 = CARTESIAN_POINT ( 'NONE',  ( 19.03943276465977164, 0.05219959533936151252, 21.25109039468565797 ) ) ;
#16211 = CARTESIAN_POINT ( 'NONE',  ( -4.483927247898539470, -16.52544592524342804, 57.29057627198103120 ) ) ;
#16212 = CARTESIAN_POINT ( 'NONE',  ( -21.53943276465977519, 0.05219959533907696930, 91.24890960531436690 ) ) ;
#16213 = CARTESIAN_POINT ( 'NONE',  ( -15.72974639402197994, 15.80617190586746368, 95.62390960531436690 ) ) ;
#16214 = CARTESIAN_POINT ( 'NONE',  ( 28.79475375365586132, 2.781246896534039337E-14, 148.9843446568999923 ) ) ;
#16216 = EDGE_CURVE ( 'NONE', #83996, #61621, #196998, .T. ) ;
#16215 = CARTESIAN_POINT ( 'NONE',  ( -18.67979575497178146, -10.72451020669898902, 41.66557627198103120 ) ) ;
#16217 = CARTESIAN_POINT ( 'NONE',  ( -8.314922557961024197, 14.29746914071037800, 77.91775706135231871 ) ) ;
#16218 = CARTESIAN_POINT ( 'NONE',  ( -16.52544592524342804, 4.483927247898546575, 86.04057627198102409 ) ) ;
#16219 = B_SPLINE_CURVE_WITH_KNOTS ( 'NONE', 3,
 ( #97040, #128381, #189097, #80886, #67716, #8038, #4042, #65719, #50570, #112230, #35389, #20212, #36371, #98025, #169436, #139097, #46098, #119232, #72732, #164739 ),
 .UNSPECIFIED., .F., .F.,
 ( 4, 2, 2, 2, 2, 2, 2, 2, 2, 4 ),
 ( 0.000000000000000000, 0.0004987090165372827857, 0.0009974180330745655715, 0.001246772541343199809, 0.001496127049611834263, 0.001994836066149079535, 0.002493545082686324590, 0.002742899590954957310, 0.002992254099223589162, 0.003989672132298133049 ),
 .UNSPECIFIED. ) ;
#16220 = CARTESIAN_POINT ( 'NONE',  ( -0.05219959533909027116, -19.03943276465977164, 52.49890960531436690 ) ) ;
#16221 = SURFACE_STYLE_USAGE ( .BOTH. , #18215 ) ;
#16222 = CARTESIAN_POINT ( 'NONE',  ( 28.82186960331498327, 2.781578969918950771E-14, 149.0000000000000000 ) ) ;
#16223 = CARTESIAN_POINT ( 'NONE',  ( 8.224510206698742110, 14.34966873604972548, 107.0844237280190043 ) ) ;
#16224 = CARTESIAN_POINT ( 'NONE',  ( -21.55341960407619339, 5.719274019375674811, 28.54275706135234358 ) ) ;
#16225 = CARTESIAN_POINT ( 'NONE',  ( 0.05219959533909260263, 19.03943276465977164, 99.99890960531436690 ) ) ;
#16226 = CARTESIAN_POINT ( 'NONE',  ( 15.80617190586769283, -15.72974639402175789, 70.62609039468567573 ) ) ;
#16227 = CARTESIAN_POINT ( 'NONE',  ( -19.03943276465977164, 0.05219959533909376836, 21.24890960531436335 ) ) ;
#16228 = FACE_OUTER_BOUND ( 'NONE', #160343, .T. ) ;
#16229 = VERTEX_POINT ( 'NONE', #146959 ) ;
#16230 = CARTESIAN_POINT ( 'NONE',  ( 15.80617190586769283, -15.72974639402175789, 60.62609039468567573 ) ) ;
#16232 = CARTESIAN_POINT ( 'NONE',  ( 19.02544592524343514, -5.153800228976328945, 23.54057627198102054 ) ) ;
#16231 = CARTESIAN_POINT ( 'NONE',  ( 13.97604488694527802, 13.89961937509977652, 54.37390960531435979 ) ) ;
#16233 = CARTESIAN_POINT ( 'NONE',  ( -16.46253265017160317, 9.564922557960807481, 95.83224293864769550 ) ) ;
#16234 = CARTESIAN_POINT ( 'NONE',  ( 19.05341960407617918, -5.049401038297876454, 66.04275706135233293 ) ) ;
#16235 = CARTESIAN_POINT ( 'NONE',  ( 15.72974639402176855, 15.80617190586768217, 41.87609039468568284 ) ) ;
#16236 = CARTESIAN_POINT ( 'NONE',  ( -16.51473224551082808, 9.474510206698731452, 98.33442372801900433 ) ) ;
#16237 = CARTESIAN_POINT ( 'NONE',  ( -9.474510206698720793, -16.51473224551083518, 69.58442372801901854 ) ) ;
#16238 = CARTESIAN_POINT ( 'NONE',  ( -5.153800228976328057, -19.02544592524343514, 32.29057627198102409 ) ) ;
#16239 = CARTESIAN_POINT ( 'NONE',  ( -14.34966873604972548, 8.224510206698743886, 103.3344237280190043 ) ) ;
#16240 = CARTESIAN_POINT ( 'NONE',  ( -13.89961937509957401, -13.97604488694547875, 74.37609039468566152 ) ) ;
#16241 = CARTESIAN_POINT ( 'NONE',  ( -16.53943276465976808, 0.05219959533911058130, 31.24890960531435979 ) ) ;
#16242 = CARTESIAN_POINT ( 'NONE',  ( 19.05341960407617918, -5.049401038297876454, 51.04275706135231871 ) ) ;
#16243 = CARTESIAN_POINT ( 'NONE',  ( 10.72451020669871369, 18.67979575497193778, 107.0844237280190043 ) ) ;
#16244 = PRODUCT_DEFINITION_SHAPE ( 'NONE', 'NONE',  #180876 ) ;
#16245 = CARTESIAN_POINT ( 'NONE',  ( 0.05219959533936267826, -19.03943276465977164, 25.00109039468566152 ) ) ;
#16246 = CARTESIAN_POINT ( 'NONE',  ( 5.049401038298161559, -19.05341960407611168, 22.70724293864769194 ) ) ;
#16247 = CARTESIAN_POINT ( 'NONE',  ( -0.05219959533937732626, 21.53943276465977519, 92.50109039468567573 ) ) ;
#16248 = CARTESIAN_POINT ( 'NONE',  ( -16.53943276465976808, -0.05219959533934237506, 33.75109039468568284 ) ) ;
#16249 = CARTESIAN_POINT ( 'NONE',  ( -19.03943276465977164, 0.05219959533909376836, 96.24890960531436690 ) ) ;
#16250 = CARTESIAN_POINT ( 'NONE',  ( 8.571926809382597767, 26.38167802310806209, 142.2750000027311899 ) ) ;
#16251 = CARTESIAN_POINT ( 'NONE',  ( -13.89961937509977652, 13.97604488694528158, 80.62390960531436690 ) ) ;
#16252 = CARTESIAN_POINT ( 'NONE',  ( -18.09805431107523077, 5.499999999999980460, 96.01606229291888894 ) ) ;
#16253 = CARTESIAN_POINT ( 'NONE',  ( -16.46253265017146816, -9.564922557961047289, 79.16775706135234714 ) ) ;
#16255 = CARTESIAN_POINT ( 'NONE',  ( 5.153800228976335163, 19.02544592524342804, 109.7905762719810099 ) ) ;
#16254 = AXIS2_PLACEMENT_3D ( 'NONE', #86283, #38792, #20613 ) ;
#16256 = CARTESIAN_POINT ( 'NONE',  ( -21.55341960407619339, 5.719274019375674811, 108.5427570613523756 ) ) ;
#16257 = CARTESIAN_POINT ( 'NONE',  ( 8.224510206698953496, -14.34966873604960469, 92.91557627198103830 ) ) ;
#16258 = CARTESIAN_POINT ( 'NONE',  ( 23.34492853952200520, -11.48509598731610737, 165.7658222004385777 ) ) ;
#16259 = CARTESIAN_POINT ( 'NONE',  ( -10.81492255796078084, -18.62759615963271287, 62.08224293864769550 ) ) ;
#16260 = CARTESIAN_POINT ( 'NONE',  ( 0.05219959533907565091, 21.53943276465977519, 39.99890960531436690 ) ) ;
#16261 = CARTESIAN_POINT ( 'NONE',  ( 13.89961937509977652, -13.97604488694527269, 23.12390960531436335 ) ) ;
#16262 = CARTESIAN_POINT ( 'NONE',  ( -2.577820198429831642E-15, -9.100000000000001421, -61.89430850415821794 ) ) ;
#16263 = CARTESIAN_POINT ( 'NONE',  ( 16.46253265017146816, 9.564922557961045513, 56.66775706135233293 ) ) ;
#16264 = CARTESIAN_POINT ( 'NONE',  ( -16.55341960407611168, -4.379528057220339221, 41.45724293864769550 ) ) ;
#16265 = CARTESIAN_POINT ( 'NONE',  ( 0.05219959533909260263, 19.03943276465977164, 109.9989096053143669 ) ) ;
#16266 = CARTESIAN_POINT ( 'NONE',  ( 18.67979575497194134, -10.72451020669871369, 75.83442372801900433 ) ) ;
#16267 = CARTESIAN_POINT ( 'NONE',  ( 18.62759615963271287, -10.81492255796078972, 73.33224293864769550 ) ) ;
#16268 = CARTESIAN_POINT ( 'NONE',  ( -21.53943276465977519, -0.05219959533937600094, 58.75109039468568994 ) ) ;
#16269 = CARTESIAN_POINT ( 'NONE',  ( 5.719274019375673035, 21.55341960407619339, 47.29275706135234003 ) ) ;
#16270 = CARTESIAN_POINT ( 'NONE',  ( 5.153800228976335163, 19.02544592524342804, 84.79057627198099567 ) ) ;
#16271 = CARTESIAN_POINT ( 'NONE',  ( 16.53943276465976808, 0.05219959533934440121, 76.25109039468568994 ) ) ;
#16272 = CARTESIAN_POINT ( 'NONE',  ( -19.03943276465977164, 0.05219959533909376836, 26.24890960531435624 ) ) ;
#16273 = DIRECTION ( 'NONE',  ( 1.000000000000000000, 0.000000000000000000, 0.000000000000000000 ) ) ;
#16274 = CARTESIAN_POINT ( 'NONE',  ( 8.224510206698953496, -14.34966873604960469, 47.91557627198102409 ) ) ;
#16275 = CARTESIAN_POINT ( 'NONE',  ( -16.55341960407617563, 4.379528057220093196, 108.5427570613523756 ) ) ;
#16276 = CARTESIAN_POINT ( 'NONE',  ( 19.02544592524343514, -5.153800228976328945, 63.54057627198103830 ) ) ;
#16277 = CARTESIAN_POINT ( 'NONE',  ( 13.89961937509977652, -13.97604488694527269, 38.12390960531436690 ) ) ;
#16278 = CARTESIAN_POINT ( 'NONE',  ( 5.719274019375991003, -21.55341960407610458, 42.70724293864770260 ) ) ;
#16279 = CARTESIAN_POINT ( 'NONE',  ( -19.02544592524334988, -5.153800228976617603, 38.95942372801900433 ) ) ;
#16281 = CARTESIAN_POINT ( 'NONE',  ( -4.379528057220328563, 16.55341960407611168, 50.20724293864769550 ) ) ;
#16280 = CARTESIAN_POINT ( 'NONE',  ( -17.49999999999998934, -5.624438216177606975, 39.18329655085358354 ) ) ;
#16283 = AXIS2_PLACEMENT_3D ( 'NONE', #142519, #3998, #65677 ) ;
#16282 = CARTESIAN_POINT ( 'NONE',  ( -5.049401038298153566, 19.05341960407611168, 115.2072429386477097 ) ) ;
#16284 = CARTESIAN_POINT ( 'NONE',  ( 28.79475375365586132, 2.781246896534039337E-14, 140.9843446568999923 ) ) ;
#16285 = CARTESIAN_POINT ( 'NONE',  ( -4.483927247898782831, 16.52544592524335698, 72.70942372801901854 ) ) ;
#16286 = EDGE_CURVE ( 'NONE', #15991, #14250, #130721, .T. ) ;
#16287 = CARTESIAN_POINT ( 'NONE',  ( 0.05219959533936267826, -19.03943276465977164, 70.00109039468566152 ) ) ;
#16288 = CARTESIAN_POINT ( 'NONE',  ( 14.34966873604960469, 8.224510206698951720, 39.16557627198102409 ) ) ;
#16289 = CYLINDRICAL_SURFACE ( 'NONE', #189030, 21.30000000000002913 ) ;
#16290 = CARTESIAN_POINT ( 'NONE',  ( 8.314922557960818139, 14.29746914071049879, 24.58224293864768839 ) ) ;
#16291 = CARTESIAN_POINT ( 'NONE',  ( -9.564922557960796823, -16.46253265017161027, 42.08224293864769550 ) ) ;
#16292 = CARTESIAN_POINT ( 'NONE',  ( -0.05219959533909027116, -19.03943276465977164, 57.49890960531435979 ) ) ;
#16293 = CARTESIAN_POINT ( 'NONE',  ( 5.153800228976335163, 19.02544592524342804, 24.79057627198102765 ) ) ;
#16294 = CARTESIAN_POINT ( 'NONE',  ( -15.80617190586768217, 15.72974639402176855, 28.12609039468568284 ) ) ;
#16295 = CARTESIAN_POINT ( 'NONE',  ( -16.46253265017160317, 9.564922557960807481, 55.83224293864769550 ) ) ;
#16296 = DIRECTION ( 'NONE',  ( -1.000000000000000000, 0.000000000000000000, 0.000000000000000000 ) ) ;
#16297 = CARTESIAN_POINT ( 'NONE',  ( 16.51473224551069308, 9.474510206698969483, 44.16557627198103120 ) ) ;
#16298 = CARTESIAN_POINT ( 'NONE',  ( 5.719274019375991003, -21.55341960407610458, 32.70724293864770260 ) ) ;
#16300 = CARTESIAN_POINT ( 'NONE',  ( 5.049401038298161559, -19.05341960407611168, 27.70724293864769550 ) ) ;
#16299 = CARTESIAN_POINT ( 'NONE',  ( -10.81492255796105439, 18.62759615963255655, 57.91775706135234714 ) ) ;
#16301 = CARTESIAN_POINT ( 'NONE',  ( -10.72451020669898014, 18.67979575497178502, 25.41557627198103120 ) ) ;
#16302 = CARTESIAN_POINT ( 'NONE',  ( -16.53943276465976808, -0.05219959533934237506, 88.75109039468567573 ) ) ;
#16303 = CARTESIAN_POINT ( 'NONE',  ( 5.719274019375673035, 21.55341960407619339, 102.2927570613523613 ) ) ;
#16304 = CARTESIAN_POINT ( 'NONE',  ( -8.314922557961024197, 14.29746914071037800, 72.91775706135234714 ) ) ;
#16305 = CARTESIAN_POINT ( 'NONE',  ( 16.46253265017160672, -9.564922557960803928, 113.3322429386476955 ) ) ;
#16306 = CARTESIAN_POINT ( 'NONE',  ( 12.06949235617739724, 12.14591786802326823, 51.87609039468568284 ) ) ;
#16307 = CARTESIAN_POINT ( 'NONE',  ( 4.483927247898790824, -16.52544592524335698, 40.20942372801901854 ) ) ;
#16308 = CARTESIAN_POINT ( 'NONE',  ( 16.53943276465976808, 0.05219959533934440121, 91.25109039468568994 ) ) ;
#16309 = CARTESIAN_POINT ( 'NONE',  ( -21.55341960407619339, 5.719274019375674811, 58.54275706135235424 ) ) ;
#16310 = CARTESIAN_POINT ( 'NONE',  ( 4.483927247898790824, -16.52544592524335698, 25.20942372801901854 ) ) ;
#16311 = CARTESIAN_POINT ( 'NONE',  ( 21.53943276465977519, -0.05219959533907433946, 108.7489096053143669 ) ) ;
#16312 = CARTESIAN_POINT ( 'NONE',  ( -14.29746914071037622, -8.314922557961029526, 24.16775706135235424 ) ) ;
#16313 = CARTESIAN_POINT ( 'NONE',  ( -4.379528057220086978, -16.55341960407618274, 89.79275706135236135 ) ) ;
#16314 = CARTESIAN_POINT ( 'NONE',  ( 18.22780087662122384, -5.500000000000022204, 71.01540105326107266 ) ) ;
#16315 = CARTESIAN_POINT ( 'NONE',  ( 15.72974639402176855, 15.80617190586768217, 86.87609039468568994 ) ) ;
#16316 = CARTESIAN_POINT ( 'NONE',  ( 19.05341960407617918, -5.049401038297876454, 86.04275706135233293 ) ) ;
#16317 = CARTESIAN_POINT ( 'NONE',  ( 14.34966873604960469, 8.224510206698951720, 64.16557627198102409 ) ) ;
#16318 = CARTESIAN_POINT ( 'NONE',  ( -16.52544592524342804, 4.483927247898546575, 46.04057627198103830 ) ) ;
#16319 = CARTESIAN_POINT ( 'NONE',  ( -8.224510206698948167, 14.34966873604960824, 105.4155762719810383 ) ) ;
#16321 = SURFACE_STYLE_FILL_AREA ( #31486 ) ;
#16320 = CARTESIAN_POINT ( 'NONE',  ( 19.05341960407617918, -5.049401038297876454, 46.04275706135233293 ) ) ;
#16322 = CARTESIAN_POINT ( 'NONE',  ( 15.80617190586769283, -15.72974639402175789, 50.62609039468568994 ) ) ;
#16323 = CARTESIAN_POINT ( 'NONE',  ( 16.51473224551083163, -9.474510206698727899, 110.8344237280190043 ) ) ;
#16324 = CARTESIAN_POINT ( 'NONE',  ( 1.251854463851703304E-30, -64.82615989628266107, -13.00000000000000000 ) ) ;
#16325 = CARTESIAN_POINT ( 'NONE',  ( -16.46253265017160317, 9.564922557960807481, 105.8322429386476955 ) ) ;
#16326 = CARTESIAN_POINT ( 'NONE',  ( -10.81492255796078084, -18.62759615963271287, 67.08224293864770971 ) ) ;
#16327 = CARTESIAN_POINT ( 'NONE',  ( -13.97604488694547697, 13.89961937509957934, 93.12609039468566152 ) ) ;
#16328 = CARTESIAN_POINT ( 'NONE',  ( 19.03943276465977164, -0.05219959533909143690, 108.7489096053143527 ) ) ;
#16329 = CARTESIAN_POINT ( 'NONE',  ( -5.823673210054116645, -21.52544592524344225, 62.29057627198102409 ) ) ;
#16330 = CARTESIAN_POINT ( 'NONE',  ( -14.34966873604960291, -8.224510206698953496, 101.6655762719810383 ) ) ;
#16331 = CARTESIAN_POINT ( 'NONE',  ( -0.05219959533909027116, -19.03943276465977164, 67.49890960531436690 ) ) ;
#16332 = CARTESIAN_POINT ( 'NONE',  ( -10.72451020669870658, -18.67979575497194134, 89.58442372801901854 ) ) ;
#16333 = CARTESIAN_POINT ( 'NONE',  ( -5.153800228976328057, -19.02544592524343514, 32.29057627198102409 ) ) ;
#16334 = CARTESIAN_POINT ( 'NONE',  ( 15.72974639402176855, 15.80617190586768217, 41.87609039468568284 ) ) ;
#16335 = CARTESIAN_POINT ( 'NONE',  ( 5.719274019375673035, 21.55341960407619339, 87.29275706135236135 ) ) ;
#16336 = CARTESIAN_POINT ( 'NONE',  ( 4.379528057220092307, 16.55341960407617563, 87.29275706135236135 ) ) ;
#16337 = CARTESIAN_POINT ( 'NONE',  ( 0.05219959533937995610, -21.53943276465977519, 25.00109039468567218 ) ) ;
#16338 = CARTESIAN_POINT ( 'NONE',  ( 21.55341960407619695, -5.719274019375665929, 46.04275706135234714 ) ) ;
#16340 = CARTESIAN_POINT ( 'NONE',  ( 19.05341960407611168, 5.049401038298154454, 83.95724293864766707 ) ) ;
#16339 = CARTESIAN_POINT ( 'NONE',  ( 19.02544592524334988, 5.153800228976608722, 61.45942372801900433 ) ) ;
#16341 = CARTESIAN_POINT ( 'NONE',  ( -18.67979575497193778, 10.72451020669871902, 88.33442372801901854 ) ) ;
#16342 = CARTESIAN_POINT ( 'NONE',  ( -21.52544592524343514, 5.823673210054127303, 86.04057627198102409 ) ) ;
#16343 = CARTESIAN_POINT ( 'NONE',  ( 8.224510206698953496, -14.34966873604960469, 57.91557627198103120 ) ) ;
#16344 = CARTESIAN_POINT ( 'NONE',  ( 21.53943276465977519, 0.05219959533937863772, 106.2510903946856757 ) ) ;
#16345 = CARTESIAN_POINT ( 'NONE',  ( -14.29746914071049879, 8.314922557960819915, 80.83224293864769550 ) ) ;
#16346 = CARTESIAN_POINT ( 'NONE',  ( 13.97604488694527802, 13.89961937509977652, 34.37390960531436690 ) ) ;
#16347 = CARTESIAN_POINT ( 'NONE',  ( 19.05341960407617918, -5.049401038297876454, 71.04275706135234714 ) ) ;
#16349 = CARTESIAN_POINT ( 'NONE',  ( 16.52544592524342804, -4.483927247898539470, 38.54057627198103120 ) ) ;
#16348 = AXIS2_PLACEMENT_3D ( 'NONE', #65120, #110626, #168334 ) ;
#16350 = CARTESIAN_POINT ( 'NONE',  ( -18.62759615963255300, -10.81492255796106328, 94.16775706135237556 ) ) ;
#16351 = CARTESIAN_POINT ( 'NONE',  ( 9.474510206698971260, -16.51473224551069308, 92.91557627198103830 ) ) ;
#16352 = CARTESIAN_POINT ( 'NONE',  ( 0.05219959533936267826, -19.03943276465977164, 65.00109039468567573 ) ) ;
#16353 = CARTESIAN_POINT ( 'NONE',  ( 10.72451020669898902, -18.67979575497178502, 62.91557627198102409 ) ) ;
#16354 = CARTESIAN_POINT ( 'NONE',  ( -18.62759615963270932, 10.81492255796079327, 115.8322429386477097 ) ) ;
#16355 = CARTESIAN_POINT ( 'NONE',  ( 5.049401038297881783, 19.05341960407617563, 107.2927570613523187 ) ) ;
#16356 = CARTESIAN_POINT ( 'NONE',  ( 4.379528057220092307, 16.55341960407617563, 77.29275706135234714 ) ) ;
#16358 = CARTESIAN_POINT ( 'NONE',  ( 18.62759615963255655, 10.81492255796105972, 21.66775706135235069 ) ) ;
#16357 = DIRECTION ( 'NONE',  ( -0.000000000000000000, -0.000000000000000000, 1.000000000000000000 ) ) ;
#16359 = CARTESIAN_POINT ( 'NONE',  ( -16.55341960407611168, -4.379528057220339221, 106.4572429386477097 ) ) ;
#16360 = CARTESIAN_POINT ( 'NONE',  ( 29.86685920354754842, -21.69954338932559068, -6.324999997268814234 ) ) ;
#16361 = CARTESIAN_POINT ( 'NONE',  ( 4.379528057220092307, 16.55341960407617563, 47.29275706135234003 ) ) ;
#16362 = CARTESIAN_POINT ( 'NONE',  ( 5.719274019375991003, -21.55341960407610458, 57.70724293864770260 ) ) ;
#16363 = CARTESIAN_POINT ( 'NONE',  ( 16.53943276465976808, 0.05219959533934440121, 106.2510903946856757 ) ) ;
#16364 = CARTESIAN_POINT ( 'NONE',  ( 16.52544592524335698, 4.483927247898782831, 41.45942372801901143 ) ) ;
#16365 = CARTESIAN_POINT ( 'NONE',  ( 5.153800228976335163, 19.02544592524342804, 44.79057627198103830 ) ) ;
#16366 = CARTESIAN_POINT ( 'NONE',  ( -16.55341960407617563, 4.379528057220093196, 73.54275706135234714 ) ) ;
#16367 = CARTESIAN_POINT ( 'NONE',  ( 5.049401038297881783, 19.05341960407617563, 67.29275706135234714 ) ) ;
#16368 = CARTESIAN_POINT ( 'NONE',  ( 10.81492255796078972, 18.62759615963270932, 69.58224293864769550 ) ) ;
#16369 = CARTESIAN_POINT ( 'NONE',  ( 8.314922557961029526, -14.29746914071037800, 95.41775706135234714 ) ) ;
#16370 = CARTESIAN_POINT ( 'NONE',  ( 5.823673210054444382, -21.52544592524334988, 80.20942372801901854 ) ) ;
#16371 = CARTESIAN_POINT ( 'NONE',  ( 5.719274019375991003, -21.55341960407610458, 72.70724293864769550 ) ) ;
#16372 = CARTESIAN_POINT ( 'NONE',  ( -18.62759615963270932, 10.81492255796079327, 50.83224293864770971 ) ) ;
#16373 = ORIENTED_EDGE ( 'NONE', *, *, #128894, .T. ) ;
#16374 = ORIENTED_EDGE ( 'NONE', *, *, #190638, .T. ) ;
#16375 = CARTESIAN_POINT ( 'NONE',  ( -12.14591786802326823, 12.06949235617739902, 73.12609039468567573 ) ) ;
#16376 = CARTESIAN_POINT ( 'NONE',  ( 15.80617190586746368, 15.72974639402197994, 44.37390960531435979 ) ) ;
#16377 = ORIENTED_EDGE ( 'NONE', *, *, #36572, .F. ) ;
#16378 = CARTESIAN_POINT ( 'NONE',  ( 15.72974639402199770, -15.80617190586745480, 23.12390960531436335 ) ) ;
#16379 = FACE_OUTER_BOUND ( 'NONE', #101788, .T. ) ;
#16380 = CARTESIAN_POINT ( 'NONE',  ( 0.05219959533909260263, 19.03943276465977164, 24.99890960531435269 ) ) ;
#16381 = CARTESIAN_POINT ( 'NONE',  ( -15.72974639402197994, 15.80617190586746368, 80.62390960531438111 ) ) ;
#16382 = CARTESIAN_POINT ( 'NONE',  ( 4.483927247898790824, -16.52544592524335698, 105.2094237280190328 ) ) ;
#16383 = CARTESIAN_POINT ( 'NONE',  ( -15.80617190586768217, 15.72974639402176855, 53.12609039468568284 ) ) ;
#16384 = CARTESIAN_POINT ( 'NONE',  ( 16.51473224551083163, -9.474510206698727899, 110.8344237280190043 ) ) ;
#16385 = CARTESIAN_POINT ( 'NONE',  ( 19.02544592524343514, -5.153800228976328945, 23.54057627198102054 ) ) ;
#16386 = CARTESIAN_POINT ( 'NONE',  ( -8.224510206698735004, -14.34966873604973081, 19.58442372801901143 ) ) ;
#16387 = CARTESIAN_POINT ( 'NONE',  ( -0.05219959533909027116, -19.03943276465977164, 42.49890960531435269 ) ) ;
#16388 = CARTESIAN_POINT ( 'NONE',  ( 23.31738231874054534, 16.94106989632529192, 145.1999999999999886 ) ) ;
#16389 = CARTESIAN_POINT ( 'NONE',  ( -13.89961937509977652, 13.97604488694528158, 85.62390960531433848 ) ) ;
#16390 = CARTESIAN_POINT ( 'NONE',  ( 14.34966873604972726, -8.224510206698740333, 95.83442372801903275 ) ) ;
#16391 = CARTESIAN_POINT ( 'NONE',  ( 0.05219959533936267826, -19.03943276465977164, 75.00109039468566152 ) ) ;
#16392 = CARTESIAN_POINT ( 'NONE',  ( -0.05219959533936034679, 19.03943276465977164, 27.50109039468566507 ) ) ;
#16393 = CARTESIAN_POINT ( 'NONE',  ( -10.72451020669898014, 18.67979575497178502, 55.41557627198102409 ) ) ;
#16394 = EDGE_CURVE ( 'NONE', #63582, #33758, #63021, .T. ) ;
#16395 = CARTESIAN_POINT ( 'NONE',  ( 12.06949235617739724, 12.14591786802326823, 91.87609039468568994 ) ) ;
#16396 = CARTESIAN_POINT ( 'NONE',  ( -19.03943276465977164, -0.05219959533935918106, 83.75109039468567573 ) ) ;
#16397 = CARTESIAN_POINT ( 'NONE',  ( -5.049401038298153566, 19.05341960407611168, 40.20724293864768839 ) ) ;
#16398 = CARTESIAN_POINT ( 'NONE',  ( -9.474510206698964154, 16.51473224551069663, 85.41557627198102409 ) ) ;
#16399 = CARTESIAN_POINT ( 'NONE',  ( 15.72974639402176855, 15.80617190586768217, 46.87609039468568994 ) ) ;
#16400 = CARTESIAN_POINT ( 'NONE',  ( -19.02544592524342804, 5.153800228976336051, 51.04057627198103120 ) ) ;
#16401 = CARTESIAN_POINT ( 'NONE',  ( 26.36463166569300043, -3.076743934664109226, 174.2851114983688490 ) ) ;
#16402 = CARTESIAN_POINT ( 'NONE',  ( -16.46253265017160317, 9.564922557960807481, 110.8322429386476955 ) ) ;
#16403 = CARTESIAN_POINT ( 'NONE',  ( 16.52544592524342804, -4.483927247898539470, 63.54057627198103830 ) ) ;
#16404 = CARTESIAN_POINT ( 'NONE',  ( -21.55341960407610458, -5.719274019375992779, 61.45724293864770260 ) ) ;
#16405 = CARTESIAN_POINT ( 'NONE',  ( 28.79475375365679923, 9.355982642737952659, 143.3656553485623704 ) ) ;
#16406 = CARTESIAN_POINT ( 'NONE',  ( -5.153800228976607833, 19.02544592524334988, 42.70942372801901143 ) ) ;
#16408 = CARTESIAN_POINT ( 'NONE',  ( 19.02544592524343514, -5.153800228976328945, 73.54057627198103830 ) ) ;
#16407 = CARTESIAN_POINT ( 'NONE',  ( 5.153800228976335163, 19.02544592524342804, 59.79057627198100988 ) ) ;
#16409 = CARTESIAN_POINT ( 'NONE',  ( 14.29746914071037800, 8.314922557961029526, 56.66775706135235424 ) ) ;
#16410 = CARTESIAN_POINT ( 'NONE',  ( 9.564922557961047289, -16.46253265017146816, 80.41775706135234714 ) ) ;
#16411 = CARTESIAN_POINT ( 'NONE',  ( -2.552343178074661267, -7.052343178074616858, 8.889087296526001936 ) ) ;
#16412 = CARTESIAN_POINT ( 'NONE',  ( 0.05219959533934541429, -16.53943276465976808, 90.00109039468567573 ) ) ;
#16413 = CARTESIAN_POINT ( 'NONE',  ( -4.313351365237979351, -4.313351365237916291, -64.53213882399992940 ) ) ;
#16414 = CARTESIAN_POINT ( 'NONE',  ( -12.06949235617739369, -12.14591786802326823, 79.37609039468567573 ) ) ;
#16415 = CARTESIAN_POINT ( 'NONE',  ( 12.06949235617739724, 12.14591786802326823, 56.87609039468568994 ) ) ;
#16416 = CARTESIAN_POINT ( 'NONE',  ( -5.153800228976607833, 19.02544592524334988, 27.70942372801899722 ) ) ;
#16418 = FACE_BOUND ( 'NONE', #144674, .T. ) ;
#16417 = CARTESIAN_POINT ( 'NONE',  ( 16.51473224551069308, 9.474510206698969483, 49.16557627198102409 ) ) ;
#16419 = CARTESIAN_POINT ( 'NONE',  ( -18.62759615963255300, -10.81492255796106328, 59.16775706135234714 ) ) ;
#16420 = CARTESIAN_POINT ( 'NONE',  ( -9.474510206698720793, -16.51473224551083518, 59.58442372801900433 ) ) ;
#16421 = CARTESIAN_POINT ( 'NONE',  ( 21.52544592524334988, 5.823673210054432836, 106.4594237280190328 ) ) ;
#16422 = CARTESIAN_POINT ( 'NONE',  ( -16.46253265017160317, 9.564922557960807481, 25.83224293864769194 ) ) ;
#16423 = CARTESIAN_POINT ( 'NONE',  ( -17.33027132694084571, 17.01743274722957011, -56.78176416808770455 ) ) ;
#16424 = CARTESIAN_POINT ( 'NONE',  ( 5.719274019375991003, -21.55341960407610458, 72.70724293864769550 ) ) ;
#16425 = CARTESIAN_POINT ( 'NONE',  ( -18.67979575497178146, -10.72451020669898902, 26.66557627198103475 ) ) ;
#16426 = CARTESIAN_POINT ( 'NONE',  ( 5.049401038298161559, -19.05341960407611168, 22.70724293864769194 ) ) ;
#16427 = CARTESIAN_POINT ( 'NONE',  ( 8.224510206698742110, 14.34966873604972548, 32.08442372801901854 ) ) ;
#16428 = CARTESIAN_POINT ( 'NONE',  ( 16.52544592524342804, -4.483927247898539470, 23.54057627198102765 ) ) ;
#16429 = ORIENTED_EDGE ( 'NONE', *, *, #13540, .T. ) ;
#16430 = CARTESIAN_POINT ( 'NONE',  ( 0.05219959533937995610, -21.53943276465977519, 20.00109039468568639 ) ) ;
#16432 = CARTESIAN_POINT ( 'NONE',  ( -23.48529157249599919, -32.32473071737750558, -9.699999999999999289 ) ) ;
#16431 = CARTESIAN_POINT ( 'NONE',  ( -12.06949235617756955, 12.14591786802309770, 40.62390960531435269 ) ) ;
#16433 = CARTESIAN_POINT ( 'NONE',  ( 13.89961937509957401, 13.97604488694547697, 111.8760903946856757 ) ) ;
#16434 = CARTESIAN_POINT ( 'NONE',  ( 16.46253265017146816, 9.564922557961045513, 31.66775706135232937 ) ) ;
#16435 = CARTESIAN_POINT ( 'NONE',  ( -0.05219959533910754901, -16.53943276465976808, 47.49890960531435979 ) ) ;
#16436 = CARTESIAN_POINT ( 'NONE',  ( -18.62759615963270932, 10.81492255796079327, 105.8322429386476955 ) ) ;
#16438 = CARTESIAN_POINT ( 'NONE',  ( -21.55341960407610458, -5.719274019375992779, 66.45724293864768129 ) ) ;
#16437 = CARTESIAN_POINT ( 'NONE',  ( 16.61371651742603817, 7.165104196376044676, 33.64584930007004004 ) ) ;
#16439 = CARTESIAN_POINT ( 'NONE',  ( -16.46253265017160317, 9.564922557960807481, 70.83224293864770971 ) ) ;
#16440 = CARTESIAN_POINT ( 'NONE',  ( -8.224510206698948167, 14.34966873604960824, 45.41557627198103830 ) ) ;
#16441 = CARTESIAN_POINT ( 'NONE',  ( 5.153800228976335163, 19.02544592524342804, 89.79057627198102409 ) ) ;
#16442 = DIRECTION ( 'NONE',  ( 0.000000000000000000, 0.8660254037844387076, 0.4999999999999998890 ) ) ;
#16443 = CARTESIAN_POINT ( 'NONE',  ( 19.03943276465977164, 0.05219959533936151252, 51.25109039468567573 ) ) ;
#16444 = CARTESIAN_POINT ( 'NONE',  ( 15.72974639402199770, -15.80617190586745480, 98.12390960531436690 ) ) ;
#16445 = CARTESIAN_POINT ( 'NONE',  ( 14.29746914071049879, -8.314922557960816363, 103.3322429386476955 ) ) ;
#16446 = CARTESIAN_POINT ( 'NONE',  ( 0.05219959533937995610, -21.53943276465977519, 45.00109039468568284 ) ) ;
#16447 = CARTESIAN_POINT ( 'NONE',  ( 0.000000000000000000, 0.000000000000000000, -54.21489346206828230 ) ) ;
#16448 = CARTESIAN_POINT ( 'NONE',  ( 16.52544592524342804, -4.483927247898539470, 28.54057627198103120 ) ) ;
#16449 = CARTESIAN_POINT ( 'NONE',  ( -5.153800228976328057, -19.02544592524343514, 37.29057627198102409 ) ) ;
#16450 = CARTESIAN_POINT ( 'NONE',  ( 13.97604488694527802, 13.89961937509977652, 104.3739096053143385 ) ) ;
#16451 = CARTESIAN_POINT ( 'NONE',  ( 10.81492255796078972, 18.62759615963270932, 64.58224293864769550 ) ) ;
#16452 = CARTESIAN_POINT ( 'NONE',  ( -8.571926809382601320, -26.38167802310801591, 139.2750000027311899 ) ) ;
#16453 = CARTESIAN_POINT ( 'NONE',  ( 16.46253265017160672, -9.564922557960803928, 28.33224293864769550 ) ) ;
#16454 = CARTESIAN_POINT ( 'NONE',  ( -5.823673210054116645, -21.52544592524344225, 52.29057627198102409 ) ) ;
#16455 = CARTESIAN_POINT ( 'NONE',  ( -5.823673210054431948, 21.52544592524334988, 77.70942372801900433 ) ) ;
#16457 = CARTESIAN_POINT ( 'NONE',  ( -16.52544592524335698, -4.483927247898792601, 88.95942372801901854 ) ) ;
#16456 = CARTESIAN_POINT ( 'NONE',  ( 14.20416113188340823, -35.58439206127390975, -22.81347619871590027 ) ) ;
#16458 = CARTESIAN_POINT ( 'NONE',  ( -13.97604488694527625, -13.89961937509977652, 56.87390960531434558 ) ) ;
#16459 = CARTESIAN_POINT ( 'NONE',  ( 16.46253265017160672, -9.564922557960803928, 63.33224293864769550 ) ) ;
#16460 = ORIENTED_EDGE ( 'NONE', *, *, #83608, .T. ) ;
#16461 = CARTESIAN_POINT ( 'NONE',  ( -0.05219959533936034679, 19.03943276465977164, 22.50109039468566152 ) ) ;
#16462 = CARTESIAN_POINT ( 'NONE',  ( -16.52544592524335698, -4.483927247898792601, 73.95942372801901854 ) ) ;
#16463 = CARTESIAN_POINT ( 'NONE',  ( 21.52544592524334988, 5.823673210054432836, 96.45942372801901854 ) ) ;
#16464 = CARTESIAN_POINT ( 'NONE',  ( -5.049401038298153566, 19.05341960407611168, 80.20724293864769550 ) ) ;
#16465 = CARTESIAN_POINT ( 'NONE',  ( -18.62759615963270932, 10.81492255796079327, 30.83224293864770260 ) ) ;
#16466 = CARTESIAN_POINT ( 'NONE',  ( -0.05219959533936034679, 19.03943276465977164, 112.5010903946856757 ) ) ;
#16467 = CARTESIAN_POINT ( 'NONE',  ( -10.81492255796105439, 18.62759615963255655, 87.91775706135234714 ) ) ;
#16468 = CARTESIAN_POINT ( 'NONE',  ( -14.34966873604972548, 8.224510206698743886, 53.33442372801901854 ) ) ;
#16469 = CARTESIAN_POINT ( 'NONE',  ( 0.05219959533907565091, 21.53943276465977519, 94.99890960531436690 ) ) ;
#16470 = CARTESIAN_POINT ( 'NONE',  ( -8.314922557961024197, 14.29746914071037800, 22.91775706135235069 ) ) ;
#16471 = CARTESIAN_POINT ( 'NONE',  ( 5.049401038298161559, -19.05341960407611168, 72.70724293864768129 ) ) ;
#16472 = CARTESIAN_POINT ( 'NONE',  ( -4.379528057220086978, -16.55341960407618274, 24.79275706135235779 ) ) ;
#16473 = CARTESIAN_POINT ( 'NONE',  ( -19.05341960407611168, -5.049401038298163336, 36.45724293864766707 ) ) ;
#16474 = CARTESIAN_POINT ( 'NONE',  ( 0.05219959533936267826, -19.03943276465977164, 110.0010903946856757 ) ) ;
#16475 = CARTESIAN_POINT ( 'NONE',  ( 14.29746914071049879, -8.314922557960816363, 68.33224293864769550 ) ) ;
#16476 = CARTESIAN_POINT ( 'NONE',  ( 4.483927247898790824, -16.52544592524335698, 80.20942372801901854 ) ) ;
#16478 = CARTESIAN_POINT ( 'NONE',  ( -13.89961937509977652, 13.97604488694528158, 55.62390960531434558 ) ) ;
#16477 = CARTESIAN_POINT ( 'NONE',  ( -0.05219959533937732626, 21.53943276465977519, 27.50109039468567929 ) ) ;
#16480 = ADVANCED_FACE ( 'NONE', ( #161121 ), #22618, .F. ) ;
#16479 = CARTESIAN_POINT ( 'NONE',  ( -9.564922557960796823, -16.46253265017161027, 72.08224293864770971 ) ) ;
#16481 = CARTESIAN_POINT ( 'NONE',  ( 14.29746914071037800, 8.314922557961029526, 71.66775706135234714 ) ) ;
#16483 = ORIENTED_EDGE ( 'NONE', *, *, #193676, .F. ) ;
#16482 = CARTESIAN_POINT ( 'NONE',  ( -24.68411608548712266, -7.148172978119915477, 167.5704058020797902 ) ) ;
#16484 = ORIENTED_EDGE ( 'NONE', *, *, #8537, .T. ) ;
#16485 = CARTESIAN_POINT ( 'NONE',  ( 9.474510206698729675, 16.51473224551082808, 22.08442372801899722 ) ) ;
#16486 = CARTESIAN_POINT ( 'NONE',  ( -13.97604488694527625, -13.89961937509977652, 36.87390960531436690 ) ) ;
#16488 = ORIENTED_EDGE ( 'NONE', *, *, #50912, .T. ) ;
#16487 = CARTESIAN_POINT ( 'NONE',  ( 1.322633123934117361, 14.46694947601600312, -62.26929068799466904 ) ) ;
#16489 = CARTESIAN_POINT ( 'NONE',  ( -12.14591786802326823, 12.06949235617739902, 28.12609039468568284 ) ) ;
#16491 = CARTESIAN_POINT ( 'NONE',  ( -12.06949235617739369, -12.14591786802326823, 44.37609039468567573 ) ) ;
#16490 = CARTESIAN_POINT ( 'NONE',  ( 19.02544592524334988, 5.153800228976608722, 61.45942372801900433 ) ) ;
#16492 = CARTESIAN_POINT ( 'NONE',  ( 5.153800228976335163, 19.02544592524342804, 44.79057627198103830 ) ) ;
#16493 = CARTESIAN_POINT ( 'NONE',  ( -5.153800228976328057, -19.02544592524343514, 102.2905762719810383 ) ) ;
#16494 = CARTESIAN_POINT ( 'NONE',  ( -9.564922557960796823, -16.46253265017161027, 67.08224293864769550 ) ) ;
#16495 = CARTESIAN_POINT ( 'NONE',  ( -10.72451020669898014, 18.67979575497178502, 95.41557627198102409 ) ) ;
#16497 = CARTESIAN_POINT ( 'NONE',  ( 28.82186960331498327, 2.428612866367529932E-14, 139.9999999999999716 ) ) ;
#16496 = CARTESIAN_POINT ( 'NONE',  ( -16.51473224551069308, -9.474510206698971260, 96.66557627198102409 ) ) ;
#16498 = PRODUCT_RELATED_PRODUCT_CATEGORY ( 'part', '', ( #14587 ) ) ;
#16499 = CARTESIAN_POINT ( 'NONE',  ( 19.03943276465977164, -0.05219959533909143690, 63.74890960531435979 ) ) ;
#16501 = DIRECTION ( 'NONE',  ( -1.000000000000000000, -6.938893903907222461E-16, 0.000000000000000000 ) ) ;
#16500 = CARTESIAN_POINT ( 'NONE',  ( 12.14591786802309770, 12.06949235617756955, 24.37390960531435979 ) ) ;
#16502 = CARTESIAN_POINT ( 'NONE',  ( -19.02544592524334988, -5.153800228976617603, 98.95942372801900433 ) ) ;
#16503 = CARTESIAN_POINT ( 'NONE',  ( 19.02544592524334988, 5.153800228976608722, 26.45942372801899722 ) ) ;
#16504 = CARTESIAN_POINT ( 'NONE',  ( -0.05219959533910754901, -16.53943276465976808, 67.49890960531436690 ) ) ;
#16505 = CARTESIAN_POINT ( 'NONE',  ( 10.72451020669871369, 18.67979575497193778, 102.0844237280190185 ) ) ;
#16506 = CARTESIAN_POINT ( 'NONE',  ( 0.05219959533909260263, 19.03943276465977164, 34.99890960531435979 ) ) ;
#16508 = CARTESIAN_POINT ( 'NONE',  ( -10.72451020669870658, -18.67979575497194134, 94.58442372801901854 ) ) ;
#16507 = CARTESIAN_POINT ( 'NONE',  ( -16.53943276465976808, 0.05219959533911058130, 31.24890960531435979 ) ) ;
#16509 = CARTESIAN_POINT ( 'NONE',  ( -13.97604488694527625, -13.89961937509977652, 76.87390960531433848 ) ) ;
#16510 = CARTESIAN_POINT ( 'NONE',  ( 9.474510206698971260, -16.51473224551069308, 97.91557627198102409 ) ) ;
#16511 = CARTESIAN_POINT ( 'NONE',  ( -4.379528057220328563, 16.55341960407611168, 110.2072429386477239 ) ) ;
#16512 = CARTESIAN_POINT ( 'NONE',  ( 16.53943276465976808, -0.05219959533910856209, 78.74890960531436690 ) ) ;
#16513 = CARTESIAN_POINT ( 'NONE',  ( -18.67979575497178146, -10.72451020669898902, 86.66557627198102409 ) ) ;
#16514 = CARTESIAN_POINT ( 'NONE',  ( -16.46253265017160317, 9.564922557960807481, 80.83224293864769550 ) ) ;
#16515 = CARTESIAN_POINT ( 'NONE',  ( -21.52544592524343514, 5.823673210054127303, 81.04057627198102409 ) ) ;
#16516 = CARTESIAN_POINT ( 'NONE',  ( 16.51473224551083163, -9.474510206698727899, 75.83442372801900433 ) ) ;
#16518 = CARTESIAN_POINT ( 'NONE',  ( -0.05219959533910754901, -16.53943276465976808, 92.49890960531436690 ) ) ;
#16517 = DIRECTION ( 'NONE',  ( -1.000000000000000000, -0.000000000000000000, -0.000000000000000000 ) ) ;
#16519 = CARTESIAN_POINT ( 'NONE',  ( -16.46253265017160317, 9.564922557960807481, 55.83224293864769550 ) ) ;
#16520 = CARTESIAN_POINT ( 'NONE',  ( 15.72974639402199770, -15.80617190586745480, 73.12390960531436690 ) ) ;
#16521 = CARTESIAN_POINT ( 'NONE',  ( -26.24776304279841455, -7.664901067105981625, 169.1545021717929842 ) ) ;
#16523 = DIRECTION ( 'NONE',  ( -0.000000000000000000, -0.000000000000000000, -1.000000000000000000 ) ) ;
#16522 = CARTESIAN_POINT ( 'NONE',  ( -14.29746914071037622, -8.314922557961029526, 109.1677570613523613 ) ) ;
#16524 = CARTESIAN_POINT ( 'NONE',  ( -16.55341960407617563, 4.379528057220093196, 23.54275706135235424 ) ) ;
#16525 = CARTESIAN_POINT ( 'NONE',  ( 14.34966873604960469, 8.224510206698951720, 79.16557627198103830 ) ) ;
#16526 = CARTESIAN_POINT ( 'NONE',  ( 7.794582437828440291, -1.499905742985332191, -62.16226466885329671 ) ) ;
#16527 = CARTESIAN_POINT ( 'NONE',  ( -19.03943276465977164, 0.05219959533909376836, 71.24890960531435269 ) ) ;
#16528 = CARTESIAN_POINT ( 'NONE',  ( -5.153800228976328057, -19.02544592524343514, 27.29057627198103120 ) ) ;
#16529 = CARTESIAN_POINT ( 'NONE',  ( -4.483927247898539470, -16.52544592524342804, 72.29057627198102409 ) ) ;
#16530 = CARTESIAN_POINT ( 'NONE',  ( -19.05341960407611168, -5.049401038298163336, 106.4572429386476955 ) ) ;
#16532 = CARTESIAN_POINT ( 'NONE',  ( -9.474510206698964154, 16.51473224551069663, 80.41557627198103830 ) ) ;
#16531 = CARTESIAN_POINT ( 'NONE',  ( -16.51473224551082808, 9.474510206698731452, 88.33442372801900433 ) ) ;
#16533 = CARTESIAN_POINT ( 'NONE',  ( 13.97604488694527802, 13.89961937509977652, 89.37390960531436690 ) ) ;
#16534 = CARTESIAN_POINT ( 'NONE',  ( -21.55341960407610458, -5.719274019375992779, 81.45724293864769550 ) ) ;
#16535 = CARTESIAN_POINT ( 'NONE',  ( 16.55341960407618274, -4.379528057220086978, 71.04275706135234714 ) ) ;
#16536 = CARTESIAN_POINT ( 'NONE',  ( 19.05341960407618274, -5.049401038297876454, 111.0427570613523329 ) ) ;
#16537 = CARTESIAN_POINT ( 'NONE',  ( -16.46253265017160317, 9.564922557960807481, 65.83224293864769550 ) ) ;
#16538 = CARTESIAN_POINT ( 'NONE',  ( -18.67979575497178146, -10.72451020669898902, 66.66557627198102409 ) ) ;
#16539 = CARTESIAN_POINT ( 'NONE',  ( -13.97604488694547697, 13.89961937509957934, 93.12609039468566152 ) ) ;
#16541 = CARTESIAN_POINT ( 'NONE',  ( 5.823673210054444382, -21.52544592524334988, 40.20942372801901854 ) ) ;
#16540 = CARTESIAN_POINT ( 'NONE',  ( -0.05219959533910754901, -16.53943276465976808, 32.49890960531435979 ) ) ;
#16542 = CARTESIAN_POINT ( 'NONE',  ( -29.15849868437705439, 10.00000000000000000, 150.0000000000000000 ) ) ;
#16544 = CARTESIAN_POINT ( 'NONE',  ( -5.049401038298153566, 19.05341960407611168, 105.2072429386476671 ) ) ;
#16543 = CARTESIAN_POINT ( 'NONE',  ( -14.29746914071037622, -8.314922557961029526, 79.16775706135234714 ) ) ;
#16545 = CARTESIAN_POINT ( 'NONE',  ( 0.000000000000000000, -165.0000000000000000, 7.000000000000003553 ) ) ;
#16546 = DIRECTION ( 'NONE',  ( -0.000000000000000000, -0.000000000000000000, 1.000000000000000000 ) ) ;
#16547 = CARTESIAN_POINT ( 'NONE',  ( -8.224510206698735004, -14.34966873604973081, 89.58442372801901854 ) ) ;
#16548 = CARTESIAN_POINT ( 'NONE',  ( -16.55341960407617563, 4.379528057220093196, 43.54275706135235424 ) ) ;
#16549 = CARTESIAN_POINT ( 'NONE',  ( -5.153800228976328057, -19.02544592524343514, 62.29057627198100988 ) ) ;
#16550 = CARTESIAN_POINT ( 'NONE',  ( 19.03943276465977164, -0.05219959533909143690, 78.74890960531436690 ) ) ;
#16551 = CARTESIAN_POINT ( 'NONE',  ( -5.719274019375665041, -21.55341960407619695, 49.79275706135234714 ) ) ;
#16552 = CARTESIAN_POINT ( 'NONE',  ( 12.14591786802327356, -12.06949235617739191, 60.62609039468567573 ) ) ;
#16553 = CARTESIAN_POINT ( 'NONE',  ( -16.55341960407611168, -4.379528057220339221, 36.45724293864768839 ) ) ;
#16554 = CARTESIAN_POINT ( 'NONE',  ( -5.153800228976328057, -19.02544592524343514, 37.29057627198102409 ) ) ;
#16555 = CARTESIAN_POINT ( 'NONE',  ( -13.89961937509977652, 13.97604488694528158, 30.62390960531435269 ) ) ;
#16556 = CARTESIAN_POINT ( 'NONE',  ( -4.379528057220086978, -16.55341960407618274, 24.79275706135235779 ) ) ;
#16557 = CARTESIAN_POINT ( 'NONE',  ( -5.153800228976607833, 19.02544592524334988, 77.70942372801900433 ) ) ;
#16558 = CARTESIAN_POINT ( 'NONE',  ( -8.224510206698948167, 14.34966873604960824, 85.41557627198102409 ) ) ;
#16559 = CARTESIAN_POINT ( 'NONE',  ( -5.049401038298153566, 19.05341960407611168, 45.20724293864769550 ) ) ;
#16561 = CARTESIAN_POINT ( 'NONE',  ( 15.50000000000000178, 0.000000000000000000, 120.0000000000000142 ) ) ;
#16560 = CARTESIAN_POINT ( 'NONE',  ( 5.153800228976615827, -19.02544592524334988, 90.20942372801900433 ) ) ;
#16562 = CARTESIAN_POINT ( 'NONE',  ( -5.823673210054431948, 21.52544592524334988, 87.70942372801901854 ) ) ;
#16563 = CARTESIAN_POINT ( 'NONE',  ( -8.224510206698735004, -14.34966873604973081, 59.58442372801901854 ) ) ;
#16564 = CARTESIAN_POINT ( 'NONE',  ( -17.49999999999998224, 3.237210098469581521, 24.71236987379559835 ) ) ;
#16565 = CARTESIAN_POINT ( 'NONE',  ( 10.72451020669898902, -18.67979575497178502, 52.91557627198103830 ) ) ;
#16566 = CARTESIAN_POINT ( 'NONE',  ( 16.52544592524335698, 4.483927247898782831, 41.45942372801901143 ) ) ;
#16567 = FACE_OUTER_BOUND ( 'NONE', #110708, .T. ) ;
#16568 = CARTESIAN_POINT ( 'NONE',  ( -19.05341960407617563, 5.049401038297882671, 33.54275706135231871 ) ) ;
#16569 = CARTESIAN_POINT ( 'NONE',  ( -16.51473224551069308, -9.474510206698971260, 76.66557627198103830 ) ) ;
#16570 = CARTESIAN_POINT ( 'NONE',  ( -9.474510206698964154, 16.51473224551069663, 45.41557627198103120 ) ) ;
#16571 = CARTESIAN_POINT ( 'NONE',  ( -19.99604614807126524, -21.49604614807087799, -52.16759353428663104 ) ) ;
#16572 = CARTESIAN_POINT ( 'NONE',  ( 5.153800228976335163, 19.02544592524342804, 74.79057627198103830 ) ) ;
#16573 = CARTESIAN_POINT ( 'NONE',  ( -19.35633801406907040, 5.499999999999674927, 99.13373818172765084 ) ) ;
#16574 = CARTESIAN_POINT ( 'NONE',  ( -16.46253265017146816, -9.564922557961047289, 34.16775706135233293 ) ) ;
#16575 = CARTESIAN_POINT ( 'NONE',  ( -21.52544592524334988, -5.823673210054445271, 103.9594237280190185 ) ) ;
#16576 = CARTESIAN_POINT ( 'NONE',  ( -8.224510206698948167, 14.34966873604960824, 40.41557627198103120 ) ) ;
#16577 = CARTESIAN_POINT ( 'NONE',  ( -16.51473224551069308, -9.474510206698971260, 36.66557627198102409 ) ) ;
#16578 = CARTESIAN_POINT ( 'NONE',  ( 5.153800228976335163, 19.02544592524342804, 109.7905762719810099 ) ) ;
#16579 = CARTESIAN_POINT ( 'NONE',  ( -10.81492255796105439, 18.62759615963255655, 87.91775706135234714 ) ) ;
#16580 = CARTESIAN_POINT ( 'NONE',  ( -19.02544592524342804, 5.153800228976336051, 56.04057627198100988 ) ) ;
#16581 = CARTESIAN_POINT ( 'NONE',  ( 18.67979575497194134, -10.72451020669871369, 75.83442372801900433 ) ) ;
#16582 = CARTESIAN_POINT ( 'NONE',  ( 19.02544592524343514, -5.153800228976328945, 113.5405762719810241 ) ) ;
#16583 = CARTESIAN_POINT ( 'NONE',  ( -15.80617190586768217, 15.72974639402176855, 28.12609039468568284 ) ) ;
#16584 = CARTESIAN_POINT ( 'NONE',  ( -5.153800228976607833, 19.02544592524334988, 47.70942372801900433 ) ) ;
#16585 = CARTESIAN_POINT ( 'NONE',  ( -5.049401038298153566, 19.05341960407611168, 35.20724293864768839 ) ) ;
#16586 = CARTESIAN_POINT ( 'NONE',  ( -19.02544592524342804, 5.153800228976336051, 76.04057627198102409 ) ) ;
#16587 = CARTESIAN_POINT ( 'NONE',  ( 16.46253265017146816, 9.564922557961045513, 111.6677570613523329 ) ) ;
#16588 = CARTESIAN_POINT ( 'NONE',  ( 0.05219959533910956823, 16.53943276465976808, 69.99890960531435269 ) ) ;
#16589 = CARTESIAN_POINT ( 'NONE',  ( 21.55341960407610458, 5.719274019375980345, 38.95724293864768839 ) ) ;
#16590 = CARTESIAN_POINT ( 'NONE',  ( 5.153800228976615827, -19.02544592524334988, 95.20942372801897591 ) ) ;
#16591 = CARTESIAN_POINT ( 'NONE',  ( 18.67979575497178502, 10.72451020669898547, 99.16557627198100988 ) ) ;
#16592 = CARTESIAN_POINT ( 'NONE',  ( 18.67979575497194134, -10.72451020669871369, 50.83442372801901143 ) ) ;
#16593 = CARTESIAN_POINT ( 'NONE',  ( -8.224510206698735004, -14.34966873604973081, 59.58442372801901854 ) ) ;
#16594 = CARTESIAN_POINT ( 'NONE',  ( 0.05219959533934541429, -16.53943276465976808, 60.00109039468568284 ) ) ;
#16595 = CARTESIAN_POINT ( 'NONE',  ( 13.89961937509977652, -13.97604488694527269, 53.12390960531434558 ) ) ;
#16596 = CARTESIAN_POINT ( 'NONE',  ( 4.483927247898790824, -16.52544592524335698, 95.20942372801903275 ) ) ;
#16597 = CARTESIAN_POINT ( 'NONE',  ( 21.53943276465977519, -0.05219959533907433946, 113.7489096053143527 ) ) ;
#16598 = CARTESIAN_POINT ( 'NONE',  ( 16.53943276465976808, -0.05219959533910856209, 48.74890960531435979 ) ) ;
#16599 = CARTESIAN_POINT ( 'NONE',  ( 5.049401038298161559, -19.05341960407611168, 87.70724293864769550 ) ) ;
#16600 = CARTESIAN_POINT ( 'NONE',  ( -4.379528057220086978, -16.55341960407618274, 69.79275706135234714 ) ) ;
#16601 = B_SPLINE_CURVE_WITH_KNOTS ( 'NONE', 3,
 ( #31144, #167671, #182845, #92792, #47311, #135358 ),
 .UNSPECIFIED., .F., .F.,
 ( 4, 2, 4 ),
 ( 0.000000000000000000, 0.0003837532665635264842, 0.0007675065331270529683 ),
 .UNSPECIFIED. ) ;
#16602 = CARTESIAN_POINT ( 'NONE',  ( 10.72451020669871369, 18.67979575497193778, 57.08442372801901854 ) ) ;
#16603 = CARTESIAN_POINT ( 'NONE',  ( 14.29746914071037800, 8.314922557961029526, 21.66775706135235069 ) ) ;
#16604 = CARTESIAN_POINT ( 'NONE',  ( -15.80617190586745835, -15.72974639402198527, 106.8739096053143811 ) ) ;
#16605 = CARTESIAN_POINT ( 'NONE',  ( -12.14591786802309592, -12.06949235617757132, 41.87390960531435979 ) ) ;
#16606 = EDGE_LOOP ( 'NONE', ( #172037, #135664, #86664, #56163 ) ) ;
#16607 = CARTESIAN_POINT ( 'NONE',  ( -17.50000000000000711, 5.622605283950874444, 68.68792689403892382 ) ) ;
#16608 = CARTESIAN_POINT ( 'NONE',  ( -21.55341960407610458, -5.719274019375992779, 91.45724293864769550 ) ) ;
#16609 = CARTESIAN_POINT ( 'NONE',  ( 4.379528057220339221, -16.55341960407611168, 22.70724293864769194 ) ) ;
#16610 = VERTEX_POINT ( 'NONE', #144944 ) ;
#16611 = FACE_OUTER_BOUND ( 'NONE', #95008, .T. ) ;
#16612 = CARTESIAN_POINT ( 'NONE',  ( 21.53943276465977519, -0.05219959533907433946, 113.7489096053143527 ) ) ;
#16613 = CARTESIAN_POINT ( 'NONE',  ( 9.564922557960805705, 16.46253265017160317, 114.5822429386476955 ) ) ;
#16614 = CARTESIAN_POINT ( 'NONE',  ( -10.81492255796105439, 18.62759615963255655, 22.91775706135235069 ) ) ;
#16615 = CARTESIAN_POINT ( 'NONE',  ( 4.379528057220339221, -16.55341960407611168, 52.70724293864769550 ) ) ;
#16616 = CARTESIAN_POINT ( 'NONE',  ( 4.379528057220092307, 16.55341960407617563, 67.29275706135234714 ) ) ;
#16617 = CARTESIAN_POINT ( 'NONE',  ( 19.03943276465977164, -0.05219959533909143690, 63.74890960531435979 ) ) ;
#16618 = CARTESIAN_POINT ( 'NONE',  ( -9.474510206698720793, -16.51473224551083518, 59.58442372801900433 ) ) ;
#16619 = CARTESIAN_POINT ( 'NONE',  ( 9.564922557960805705, 16.46253265017160317, 74.58224293864769550 ) ) ;
#16620 = CARTESIAN_POINT ( 'NONE',  ( -21.52544592524343514, 5.823673210054127303, 31.04057627198102409 ) ) ;
#16621 = CARTESIAN_POINT ( 'NONE',  ( -22.83040865997688229, -30.22555755524879828, -21.93998231254863285 ) ) ;
#16622 = CARTESIAN_POINT ( 'NONE',  ( -13.89961937509977652, 13.97604488694528158, 60.62390960531436690 ) ) ;
#16623 = CARTESIAN_POINT ( 'NONE',  ( -8.314922557961024197, 14.29746914071037800, 22.91775706135235069 ) ) ;
#16624 = CARTESIAN_POINT ( 'NONE',  ( -13.97604488694547697, 13.89961937509957934, 68.12609039468563310 ) ) ;
#16625 = CARTESIAN_POINT ( 'NONE',  ( -0.05219959533907301413, -21.53943276465977519, 102.4989096053143811 ) ) ;
#16626 = EDGE_CURVE ( 'NONE', #184655, #68071, #74756, .T. ) ;
#16627 = CARTESIAN_POINT ( 'NONE',  ( 12.14591786802309770, 12.06949235617756955, 39.37390960531436690 ) ) ;
#16628 = CARTESIAN_POINT ( 'NONE',  ( -13.97604488694527625, -13.89961937509977652, 96.87390960531433848 ) ) ;
#16629 = CARTESIAN_POINT ( 'NONE',  ( 18.62759615963271287, -10.81492255796078972, 63.33224293864770260 ) ) ;
#16631 = CARTESIAN_POINT ( 'NONE',  ( 4.379528057220092307, 16.55341960407617563, 42.29275706135235424 ) ) ;
#16630 = CARTESIAN_POINT ( 'NONE',  ( -5.719274019375978568, 21.55341960407610458, 95.20724293864769550 ) ) ;
#16632 = CARTESIAN_POINT ( 'NONE',  ( 10.72451020669898902, -18.67979575497178502, 32.91557627198102409 ) ) ;
#16633 = CARTESIAN_POINT ( 'NONE',  ( -21.55341960407619339, 5.719274019375674811, 93.54275706135234714 ) ) ;
#16634 = CARTESIAN_POINT ( 'NONE',  ( 5.153800228976335163, 19.02544592524342804, 84.79057627198099567 ) ) ;
#16635 = CARTESIAN_POINT ( 'NONE',  ( -13.97604488694527625, -13.89961937509977652, 36.87390960531436690 ) ) ;
#16636 = CARTESIAN_POINT ( 'NONE',  ( 9.564922557960805705, 16.46253265017160317, 84.58224293864769550 ) ) ;
#16637 = CARTESIAN_POINT ( 'NONE',  ( -8.224510206698948167, 14.34966873604960824, 110.4155762719810383 ) ) ;
#16638 = CARTESIAN_POINT ( 'NONE',  ( 13.89961937509977652, -13.97604488694527269, 63.12390960531435979 ) ) ;
#16639 = CARTESIAN_POINT ( 'NONE',  ( -8.224510206698735004, -14.34966873604973081, 24.58442372801901499 ) ) ;
#16640 = CARTESIAN_POINT ( 'NONE',  ( 17.50000000000001066, -5.622605283950831812, 86.18792689403892382 ) ) ;
#16642 = CARTESIAN_POINT ( 'NONE',  ( 13.97604488694527802, 13.89961937509977652, 114.3739096053143669 ) ) ;
#16641 = CARTESIAN_POINT ( 'NONE',  ( 10.81492255796106328, -18.62759615963255655, 95.41775706135234714 ) ) ;
#16643 = CARTESIAN_POINT ( 'NONE',  ( -14.29746914071037622, -8.314922557961029526, 89.16775706135236135 ) ) ;
#16644 = CARTESIAN_POINT ( 'NONE',  ( 21.02739490616371754, -20.06800196981514262, -49.47723517191376885 ) ) ;
#16645 = CARTESIAN_POINT ( 'NONE',  ( 19.03943276465977164, 0.05219959533936151252, 76.25109039468566152 ) ) ;
#16646 = CARTESIAN_POINT ( 'NONE',  ( -19.02544592524334988, -5.153800228976617603, 28.95942372801900433 ) ) ;
#16647 = CARTESIAN_POINT ( 'NONE',  ( 17.50000000000000000, 5.499999999999998224, 118.0000000000000142 ) ) ;
#16648 = CARTESIAN_POINT ( 'NONE',  ( 0.05219959533909260263, 19.03943276465977164, 34.99890960531435979 ) ) ;
#16649 = CARTESIAN_POINT ( 'NONE',  ( 4.379528057220339221, -16.55341960407611168, 37.70724293864769550 ) ) ;
#16650 = CARTESIAN_POINT ( 'NONE',  ( -13.97604488694527625, -13.89961937509977652, 21.87390960531435979 ) ) ;
#16651 = CARTESIAN_POINT ( 'NONE',  ( 16.55341960407611168, 4.379528057220329451, 28.95724293864769905 ) ) ;
#16652 = CARTESIAN_POINT ( 'NONE',  ( 6.874011537017776341, -5.374011537017756801, -64.03675147074802965 ) ) ;
#16653 = CARTESIAN_POINT ( 'NONE',  ( -12.06949235617739369, -12.14591786802326823, 99.37609039468568994 ) ) ;
#16654 = CARTESIAN_POINT ( 'NONE',  ( 13.89961937509977652, -13.97604488694527269, 43.12390960531434558 ) ) ;
#16655 = CARTESIAN_POINT ( 'NONE',  ( 10.72451020669871369, 18.67979575497193778, 92.08442372801901854 ) ) ;
#16656 = CARTESIAN_POINT ( 'NONE',  ( 19.02544592524334988, 5.153800228976608722, 111.4594237280190043 ) ) ;
#16657 = CARTESIAN_POINT ( 'NONE',  ( -10.72451020669870658, -18.67979575497194134, 84.58442372801903275 ) ) ;
#16658 = CARTESIAN_POINT ( 'NONE',  ( 9.474510206698729675, 16.51473224551082808, 47.08442372801900433 ) ) ;
#16659 = CARTESIAN_POINT ( 'NONE',  ( 19.02544592524343514, -5.153800228976328945, 98.54057627198100988 ) ) ;
#16660 = CARTESIAN_POINT ( 'NONE',  ( 19.03943276465977164, -0.05219959533909143690, 68.74890960531436690 ) ) ;
#16661 = CARTESIAN_POINT ( 'NONE',  ( 17.50000000000000355, 5.622605283950890431, 73.81207310596110460 ) ) ;
#16662 = CARTESIAN_POINT ( 'NONE',  ( -8.314922557960811034, -14.29746914071050412, 72.08224293864769550 ) ) ;
#16663 = CARTESIAN_POINT ( 'NONE',  ( -18.67979575497178146, -10.72451020669898902, 66.66557627198102409 ) ) ;
#16664 = CARTESIAN_POINT ( 'NONE',  ( 0.05219959533909260263, 19.03943276465977164, 64.99890960531436690 ) ) ;
#16666 = CARTESIAN_POINT ( 'NONE',  ( 14.34966873604972726, -8.224510206698740333, 75.83442372801900433 ) ) ;
#16665 = CARTESIAN_POINT ( 'NONE',  ( 10.81492255796078972, 18.62759615963270932, 79.58224293864769550 ) ) ;
#16667 = ORIENTED_EDGE ( 'NONE', *, *, #171253, .T. ) ;
#16668 = CARTESIAN_POINT ( 'NONE',  ( -9.474510206698964154, 16.51473224551069663, 50.41557627198102409 ) ) ;
#16670 = CARTESIAN_POINT ( 'NONE',  ( 21.27520710526538394, -9.818903669220862440, 168.4804316999487526 ) ) ;
#16669 = CARTESIAN_POINT ( 'NONE',  ( 0.05219959533910956823, 16.53943276465976808, 84.99890960531436690 ) ) ;
#16671 = CARTESIAN_POINT ( 'NONE',  ( -19.02544592524342804, 5.153800228976336051, 56.04057627198100988 ) ) ;
#16672 = CARTESIAN_POINT ( 'NONE',  ( 5.049401038298161559, -19.05341960407611168, 27.70724293864769550 ) ) ;
#16673 = CARTESIAN_POINT ( 'NONE',  ( 9.564922557961047289, -16.46253265017146816, 65.41775706135233293 ) ) ;
#16674 = CARTESIAN_POINT ( 'NONE',  ( 4.483927247898545687, 16.52544592524342804, 89.79057627198103830 ) ) ;
#16675 = CARTESIAN_POINT ( 'NONE',  ( 18.62759615963255655, 10.81492255796105972, 41.66775706135235424 ) ) ;
#16677 = CARTESIAN_POINT ( 'NONE',  ( -5.719274019375978568, 21.55341960407610458, 110.2072429386477239 ) ) ;
#16676 = CARTESIAN_POINT ( 'NONE',  ( 5.049401038298161559, -19.05341960407611168, 37.70724293864768839 ) ) ;
#16678 = CARTESIAN_POINT ( 'NONE',  ( 17.60691670004652565, 5.500000000000029310, 91.63333313366439370 ) ) ;
#16679 = CARTESIAN_POINT ( 'NONE',  ( -16.52544592524342804, 4.483927247898546575, 91.04057627198103830 ) ) ;
#16680 = CARTESIAN_POINT ( 'NONE',  ( 20.47811964340659330, -34.28713832286810259, -21.14919058558335507 ) ) ;
#16681 = CARTESIAN_POINT ( 'NONE',  ( -19.05341960407611168, -5.049401038298163336, 46.45724293864768129 ) ) ;
#16683 = CARTESIAN_POINT ( 'NONE',  ( -19.02544592524342804, 5.153800228976336051, 101.0405762719810241 ) ) ;
#16682 = CARTESIAN_POINT ( 'NONE',  ( -5.049401038297874678, -19.05341960407617918, 89.79275706135230450 ) ) ;
#16684 = CARTESIAN_POINT ( 'NONE',  ( 5.823673210054444382, -21.52544592524334988, 35.20942372801901854 ) ) ;
#16685 = CARTESIAN_POINT ( 'NONE',  ( 19.05341960407611168, 5.049401038298154454, 83.95724293864766707 ) ) ;
#16686 = CARTESIAN_POINT ( 'NONE',  ( 19.02544592524334988, 5.153800228976608722, 76.45942372801897591 ) ) ;
#16687 = CARTESIAN_POINT ( 'NONE',  ( 16.51473224551069308, 9.474510206698969483, 44.16557627198103120 ) ) ;
#16688 = CARTESIAN_POINT ( 'NONE',  ( 16.52544592524342804, -4.483927247898539470, 78.54057627198103830 ) ) ;
#16689 = CARTESIAN_POINT ( 'NONE',  ( -12.14591786802309592, -12.06949235617757132, 61.87390960531436690 ) ) ;
#16690 = CARTESIAN_POINT ( 'NONE',  ( 13.97604488694527802, 13.89961937509977652, 79.37390960531435269 ) ) ;
#16691 = CARTESIAN_POINT ( 'NONE',  ( 15.80617190586746368, 15.72974639402197994, 94.37390960531436690 ) ) ;
#16692 = CARTESIAN_POINT ( 'NONE',  ( -19.03943276465977164, 0.05219959533909376836, 66.24890960531436690 ) ) ;
#16693 = CARTESIAN_POINT ( 'NONE',  ( 21.55341960407619695, -5.719274019375665929, 111.0427570613523613 ) ) ;
#16696 = CARTESIAN_POINT ( 'NONE',  ( 8.224510206698953496, -14.34966873604960469, 107.9155762719810241 ) ) ;
#16695 = CARTESIAN_POINT ( 'NONE',  ( -16.53943276465976808, 0.05219959533911058130, 36.24890960531435979 ) ) ;
#16694 = CARTESIAN_POINT ( 'NONE',  ( -9.564922557960796823, -16.46253265017161027, 37.08224293864768839 ) ) ;
#16697 = CARTESIAN_POINT ( 'NONE',  ( -5.049401038297874678, -19.05341960407617918, 104.7927570613523471 ) ) ;
#16698 = ORIENTED_EDGE ( 'NONE', *, *, #175528, .F. ) ;
#16699 = CARTESIAN_POINT ( 'NONE',  ( 18.62759615963255655, 10.81492255796105972, 26.66775706135235424 ) ) ;
#16700 = CARTESIAN_POINT ( 'NONE',  ( 13.97604488694548053, -13.89961937509957401, 65.62609039468567573 ) ) ;
#16701 = CARTESIAN_POINT ( 'NONE',  ( -8.224510206698948167, 14.34966873604960824, 25.41557627198103120 ) ) ;
#16702 = CARTESIAN_POINT ( 'NONE',  ( 5.719274019375991003, -21.55341960407610458, 87.70724293864769550 ) ) ;
#16703 = CARTESIAN_POINT ( 'NONE',  ( -16.46253265017160317, 9.564922557960807481, 115.8322429386477097 ) ) ;
#16704 = CARTESIAN_POINT ( 'NONE',  ( -8.314922557960811034, -14.29746914071050412, 57.08224293864769550 ) ) ;
#16705 = CARTESIAN_POINT ( 'NONE',  ( -13.89961937509977652, 13.97604488694528158, 30.62390960531435269 ) ) ;
#16706 = CARTESIAN_POINT ( 'NONE',  ( 19.03943276465977164, 0.05219959533936151252, 21.25109039468565797 ) ) ;
#16707 = CARTESIAN_POINT ( 'NONE',  ( 16.55341960407618274, -4.379528057220086978, 96.04275706135236135 ) ) ;
#16708 = CARTESIAN_POINT ( 'NONE',  ( 16.53943276465976808, 0.05219959533934440121, 51.25109039468568994 ) ) ;
#16709 = CARTESIAN_POINT ( 'NONE',  ( -19.02544592524342804, 5.153800228976336051, 116.0405762719810383 ) ) ;
#16710 = CARTESIAN_POINT ( 'NONE',  ( -15.72974639402176322, -15.80617190586768395, 109.3760903946857042 ) ) ;
#16711 = CARTESIAN_POINT ( 'NONE',  ( -0.05219959533909027116, -19.03943276465977164, 82.49890960531436690 ) ) ;
#16712 = CARTESIAN_POINT ( 'NONE',  ( 14.29746914071037800, 8.314922557961029526, 61.66775706135235424 ) ) ;
#16713 = CARTESIAN_POINT ( 'NONE',  ( -13.97604488694527625, -13.89961937509977652, 26.87390960531434558 ) ) ;
#16714 = CARTESIAN_POINT ( 'NONE',  ( 14.29746914071049879, -8.314922557960816363, 38.33224293864768839 ) ) ;
#16715 = DIRECTION ( 'NONE',  ( 0.5000000000000014433, 0.4999999999999996114, 0.7071067811865467956 ) ) ;
#16718 = CARTESIAN_POINT ( 'NONE',  ( 0.05219959533909260263, 19.03943276465977164, 79.99890960531436690 ) ) ;
#16717 = CARTESIAN_POINT ( 'NONE',  ( 19.05341960407611168, 5.049401038298154454, 93.95724293864769550 ) ) ;
#16716 = CARTESIAN_POINT ( 'NONE',  ( -10.72451020669870658, -18.67979575497194134, 74.58442372801901854 ) ) ;
#16720 = EDGE_CURVE ( 'NONE', #138331, #1611, #101723, .T. ) ;
#16719 = CARTESIAN_POINT ( 'NONE',  ( 19.02544592524343514, -5.153800228976328945, 108.5405762719810383 ) ) ;
#16721 = CARTESIAN_POINT ( 'NONE',  ( 4.483927247898545687, 16.52544592524342804, 64.79057627198103830 ) ) ;
#16722 = CARTESIAN_POINT ( 'NONE',  ( 8.314922557960818139, 14.29746914071049879, 29.58224293864769905 ) ) ;
#16723 = VERTEX_POINT ( 'NONE', #86278 ) ;
#16724 = CARTESIAN_POINT ( 'NONE',  ( -16.52544592524342804, 4.483927247898546575, 51.04057627198103120 ) ) ;
#16726 = CARTESIAN_POINT ( 'NONE',  ( 6.791538853603062975, 3.181980515339470905, 8.889087296526001936 ) ) ;
#16725 = CARTESIAN_POINT ( 'NONE',  ( 16.53943276465976808, 0.05219959533934440121, 36.25109039468567573 ) ) ;
#16727 = CARTESIAN_POINT ( 'NONE',  ( 5.049401038297881783, 19.05341960407617563, 57.29275706135231871 ) ) ;
#16728 = CARTESIAN_POINT ( 'NONE',  ( -16.51473224551069308, -9.474510206698971260, 76.66557627198103830 ) ) ;
#16729 = CARTESIAN_POINT ( 'NONE',  ( 16.51473224551083163, -9.474510206698727899, 55.83442372801899722 ) ) ;
#16730 = CARTESIAN_POINT ( 'NONE',  ( -13.89961937509957401, -13.97604488694547875, 59.37609039468566863 ) ) ;
#16732 = CARTESIAN_POINT ( 'NONE',  ( -14.34966873604972548, 8.224510206698743886, 83.33442372801903275 ) ) ;
#16731 = CARTESIAN_POINT ( 'NONE',  ( 13.89961937509957401, 13.97604488694547697, 101.8760903946856331 ) ) ;
#16733 = CARTESIAN_POINT ( 'NONE',  ( -27.73933785331498925, -9.013057229001049109, 145.4750000027311501 ) ) ;
#16734 = CARTESIAN_POINT ( 'NONE',  ( -13.97604488694527625, -13.89961937509977652, 26.87390960531434558 ) ) ;
#16735 = CARTESIAN_POINT ( 'NONE',  ( -16.46253265017160317, 9.564922557960807481, 105.8322429386476955 ) ) ;
#16736 = CARTESIAN_POINT ( 'NONE',  ( -21.53943276465977519, -0.05219959533937600094, 38.75109039468567573 ) ) ;
#16737 = CARTESIAN_POINT ( 'NONE',  ( -16.46253265017146816, -9.564922557961047289, 94.16775706135233293 ) ) ;
#16738 = CARTESIAN_POINT ( 'NONE',  ( -5.049401038298153566, 19.05341960407611168, 60.20724293864768129 ) ) ;
#16739 = CARTESIAN_POINT ( 'NONE',  ( 13.97604488694527802, 13.89961937509977652, 99.37390960531436690 ) ) ;
#16741 = CARTESIAN_POINT ( 'NONE',  ( -5.153800228976328057, -19.02544592524343514, 67.29057627198102409 ) ) ;
#16740 = CARTESIAN_POINT ( 'NONE',  ( 16.53943276465976808, -0.05219959533910856209, 58.74890960531436690 ) ) ;
#16742 = CARTESIAN_POINT ( 'NONE',  ( -16.51473224551069308, -9.474510206698971260, 56.66557627198103120 ) ) ;
#16743 = CARTESIAN_POINT ( 'NONE',  ( -16.46253265017146816, -9.564922557961047289, 69.16775706135233293 ) ) ;
#16744 = CARTESIAN_POINT ( 'NONE',  ( 5.719274019375991003, -21.55341960407610458, 47.70724293864770260 ) ) ;
#16745 = CARTESIAN_POINT ( 'NONE',  ( -13.97604488694547697, 13.89961937509957934, 38.12609039468566152 ) ) ;
#16747 = EDGE_CURVE ( 'NONE', #40506, #185763, #94067, .T. ) ;
#16746 = CARTESIAN_POINT ( 'NONE',  ( -19.03943276465977164, 0.05219959533909376836, 76.24890960531435269 ) ) ;
#16748 = CARTESIAN_POINT ( 'NONE',  ( -15.80617190586745835, -15.72974639402198527, 81.87390960531435269 ) ) ;
#16750 = CARTESIAN_POINT ( 'NONE',  ( 13.97604488694548053, -13.89961937509957401, 35.62609039468567573 ) ) ;
#16749 = CARTESIAN_POINT ( 'NONE',  ( -16.52544592524342804, 4.483927247898546575, 76.04057627198102409 ) ) ;
#16751 = CARTESIAN_POINT ( 'NONE',  ( -18.62759615963270932, 10.81492255796079327, 40.83224293864769550 ) ) ;
#16752 = CARTESIAN_POINT ( 'NONE',  ( -15.80617190586745835, -15.72974639402198527, 36.87390960531435979 ) ) ;
#16753 = CARTESIAN_POINT ( 'NONE',  ( -9.564922557960796823, -16.46253265017161027, 72.08224293864770971 ) ) ;
#16754 = CARTESIAN_POINT ( 'NONE',  ( 9.564922557960805705, 16.46253265017160317, 54.58224293864769550 ) ) ;
#16755 = CARTESIAN_POINT ( 'NONE',  ( -12.14591786802309592, -12.06949235617757132, 111.8739096053143669 ) ) ;
#16756 = CARTESIAN_POINT ( 'NONE',  ( -15.80617190586768217, 15.72974639402176855, 23.12609039468567573 ) ) ;
#16757 = CARTESIAN_POINT ( 'NONE',  ( 25.31894786019267229, -4.571304203950320222, 167.3973414147893379 ) ) ;
#16758 = CARTESIAN_POINT ( 'NONE',  ( 15.80617190586769283, -15.72974639402175789, 30.62609039468567929 ) ) ;
#16759 = CARTESIAN_POINT ( 'NONE',  ( 5.153800228976335163, 19.02544592524342804, 29.79057627198102409 ) ) ;
#16760 = CARTESIAN_POINT ( 'NONE',  ( -15.72974639402197994, 15.80617190586746368, 110.6239096053143669 ) ) ;
#16761 = CARTESIAN_POINT ( 'NONE',  ( 16.51473224551083163, -9.474510206698727899, 45.83442372801900433 ) ) ;
#16762 = CARTESIAN_POINT ( 'NONE',  ( 16.46253265017160672, -9.564922557960803928, 28.33224293864769550 ) ) ;
#16763 = CARTESIAN_POINT ( 'NONE',  ( -9.564922557960796823, -16.46253265017161027, 27.08224293864769550 ) ) ;
#16764 = DIRECTION ( 'NONE',  ( -0.000000000000000000, 0.000000000000000000, 1.000000000000000000 ) ) ;
#16765 = CARTESIAN_POINT ( 'NONE',  ( 16.53943276465976808, 0.05219959533934440121, 66.25109039468567573 ) ) ;
#16766 = CARTESIAN_POINT ( 'NONE',  ( -16.51473224551069308, -9.474510206698971260, 26.66557627198103120 ) ) ;
#16767 = DIRECTION ( 'NONE',  ( 0.000000000000000000, 0.000000000000000000, -1.000000000000000000 ) ) ;
#16768 = CARTESIAN_POINT ( 'NONE',  ( -19.03943276465977164, 0.05219959533909376836, 76.24890960531435269 ) ) ;
#16769 = CARTESIAN_POINT ( 'NONE',  ( 16.55341960407611168, 4.379528057220329451, 108.9572429386476955 ) ) ;
#16770 = AXIS2_PLACEMENT_3D ( 'NONE', #25477, #58765, #181147 ) ;
#16771 = CARTESIAN_POINT ( 'NONE',  ( -21.55341960407610458, -5.719274019375992779, 61.45724293864770260 ) ) ;
#16772 = CARTESIAN_POINT ( 'NONE',  ( -16.53943276465976808, 0.05219959533911058130, 76.24890960531435269 ) ) ;
#16773 = CARTESIAN_POINT ( 'NONE',  ( 8.314922557961029526, -14.29746914071037800, 30.41775706135234358 ) ) ;
#16774 = CARTESIAN_POINT ( 'NONE',  ( -0.05219959533937732626, 21.53943276465977519, 87.50109039468568994 ) ) ;
#16775 = CARTESIAN_POINT ( 'NONE',  ( 0.05219959533909260263, 19.03943276465977164, 24.99890960531435269 ) ) ;
#16776 = CARTESIAN_POINT ( 'NONE',  ( 14.29746914071037800, 8.314922557961029526, 111.6677570613523613 ) ) ;
#16777 = CARTESIAN_POINT ( 'NONE',  ( 8.314922557960818139, 14.29746914071049879, 59.58224293864770260 ) ) ;
#16778 = CARTESIAN_POINT ( 'NONE',  ( -5.049401038298153566, 19.05341960407611168, 55.20724293864769550 ) ) ;
#16779 = CARTESIAN_POINT ( 'NONE',  ( 21.55341960407619695, -5.719274019375665929, 96.04275706135236135 ) ) ;
#16780 = CARTESIAN_POINT ( 'NONE',  ( -5.823673210054116645, -21.52544592524344225, 102.2905762719810383 ) ) ;
#16781 = CARTESIAN_POINT ( 'NONE',  ( 15.80617190586769283, -15.72974639402175789, 75.62609039468567573 ) ) ;
#16782 = CARTESIAN_POINT ( 'NONE',  ( -14.34966873604972548, 8.224510206698743886, 38.33442372801900433 ) ) ;
#16784 = CARTESIAN_POINT ( 'NONE',  ( 15.80617190586769283, -15.72974639402175789, 90.62609039468567573 ) ) ;
#16783 = CARTESIAN_POINT ( 'NONE',  ( -12.14591786802309592, -12.06949235617757132, 81.87390960531435269 ) ) ;
#16785 = CARTESIAN_POINT ( 'NONE',  ( -12.14591786802309592, -12.06949235617757132, 26.87390960531435979 ) ) ;
#16786 = CARTESIAN_POINT ( 'NONE',  ( -17.05587630539788435, 6.762274262135666625, 115.7418030903731392 ) ) ;
#16787 = CARTESIAN_POINT ( 'NONE',  ( 4.483927247898790824, -16.52544592524335698, 45.20942372801901854 ) ) ;
#16788 = CARTESIAN_POINT ( 'NONE',  ( -16.52544592524342804, 4.483927247898546575, 36.04057627198102409 ) ) ;
#16789 = CARTESIAN_POINT ( 'NONE',  ( 8.314922557961029526, -14.29746914071037800, 90.41775706135236135 ) ) ;
#16790 = CARTESIAN_POINT ( 'NONE',  ( 16.46253265017160672, -9.564922557960803928, 98.33224293864769550 ) ) ;
#16791 = CARTESIAN_POINT ( 'NONE',  ( 9.564922557960805705, 16.46253265017160317, 109.5822429386476955 ) ) ;
#16792 = CARTESIAN_POINT ( 'NONE',  ( -10.81492255796105439, 18.62759615963255655, 102.9177570613523756 ) ) ;
#16793 = CARTESIAN_POINT ( 'NONE',  ( 12.14591786802327356, -12.06949235617739191, 105.6260903946856899 ) ) ;
#16794 = CARTESIAN_POINT ( 'NONE',  ( 16.53943276465976808, -0.05219959533910856209, 73.74890960531433848 ) ) ;
#16795 = CARTESIAN_POINT ( 'NONE',  ( 0.05219959533909260263, 19.03943276465977164, 79.99890960531436690 ) ) ;
#16796 = ORIENTED_EDGE ( 'NONE', *, *, #105651, .T. ) ;
#16797 = CARTESIAN_POINT ( 'NONE',  ( -16.53943276465976808, -0.05219959533934237506, 28.75109039468567929 ) ) ;
#16798 = CARTESIAN_POINT ( 'NONE',  ( 0.05219959533909260263, 19.03943276465977164, 29.99890960531435979 ) ) ;
#16799 = CARTESIAN_POINT ( 'NONE',  ( -16.51473224551069308, -9.474510206698971260, 86.66557627198102409 ) ) ;
#16801 = CARTESIAN_POINT ( 'NONE',  ( -36.91746825000000598, 2.428612866367529932E-14, -2.624999997268813168 ) ) ;
#16800 = CARTESIAN_POINT ( 'NONE',  ( 16.52544592524335698, 4.483927247898782831, 36.45942372801901143 ) ) ;
#16802 = CARTESIAN_POINT ( 'NONE',  ( 19.02544592524334988, 5.153800228976608722, 36.45942372801900433 ) ) ;
#16803 = CARTESIAN_POINT ( 'NONE',  ( -16.55341960407617563, 4.379528057220093196, 93.54275706135234714 ) ) ;
#16804 = CARTESIAN_POINT ( 'NONE',  ( -16.46253265017146816, -9.564922557961047289, 104.1677570613523329 ) ) ;
#16805 = CARTESIAN_POINT ( 'NONE',  ( -13.89961937509977652, 13.97604488694528158, 30.62390960531435269 ) ) ;
#16806 = CARTESIAN_POINT ( 'NONE',  ( 4.483927247898790824, -16.52544592524335698, 75.20942372801901854 ) ) ;
#16807 = CARTESIAN_POINT ( 'NONE',  ( -14.34966873604972548, 8.224510206698743886, 63.33442372801900433 ) ) ;
#16808 = CARTESIAN_POINT ( 'NONE',  ( -9.564922557961040184, 16.46253265017147172, 77.91775706135234714 ) ) ;
#16809 = CARTESIAN_POINT ( 'NONE',  ( -5.049401038297874678, -19.05341960407617918, 19.79275706135233293 ) ) ;
#16810 = CARTESIAN_POINT ( 'NONE',  ( -13.97604488694527625, -13.89961937509977652, 41.87390960531435979 ) ) ;
#16811 = CARTESIAN_POINT ( 'NONE',  ( -5.153800228976328057, -19.02544592524343514, 87.29057627198103830 ) ) ;
#16812 = CARTESIAN_POINT ( 'NONE',  ( 0.05219959533910956823, 16.53943276465976808, 89.99890960531438111 ) ) ;
#16813 = CARTESIAN_POINT ( 'NONE',  ( 9.474510206698729675, 16.51473224551082808, 52.08442372801900433 ) ) ;
#16814 = CARTESIAN_POINT ( 'NONE',  ( 21.55341960407610458, 5.719274019375980345, 43.95724293864769550 ) ) ;
#16815 = CARTESIAN_POINT ( 'NONE',  ( 5.153800228976615827, -19.02544592524334988, 30.20942372801900433 ) ) ;
#16816 = CARTESIAN_POINT ( 'NONE',  ( 19.02544592524343514, -5.153800228976328945, 93.54057627198102409 ) ) ;
#16817 = CARTESIAN_POINT ( 'NONE',  ( 0.05219959533936267826, -19.03943276465977164, 30.00109039468566863 ) ) ;
#16818 = CARTESIAN_POINT ( 'NONE',  ( 21.55341960407610458, 5.719274019375980345, 78.95724293864769550 ) ) ;
#16819 = CARTESIAN_POINT ( 'NONE',  ( -16.46253265017160317, 9.564922557960807481, 115.8322429386477097 ) ) ;
#16820 = CARTESIAN_POINT ( 'NONE',  ( 9.474510206698729675, 16.51473224551082808, 82.08442372801899012 ) ) ;
#16821 = CARTESIAN_POINT ( 'NONE',  ( -17.49999999999998934, 3.189878218039177149, 109.8705143742875237 ) ) ;
#16822 = EDGE_CURVE ( 'NONE', #168063, #40368, #192932, .T. ) ;
#16823 = CARTESIAN_POINT ( 'NONE',  ( 13.97604488694548053, -13.89961937509957401, 105.6260903946856757 ) ) ;
#16824 = CARTESIAN_POINT ( 'NONE',  ( 9.564922557960805705, 16.46253265017160317, 39.58224293864768839 ) ) ;
#16825 = CARTESIAN_POINT ( 'NONE',  ( -19.05341960407611168, -5.049401038298163336, 91.45724293864766707 ) ) ;
#16826 = CARTESIAN_POINT ( 'NONE',  ( 5.823673210054125526, 21.52544592524343514, 74.79057627198105251 ) ) ;
#16827 = CARTESIAN_POINT ( 'NONE',  ( 14.29746914071037800, 8.314922557961029526, 46.66775706135234714 ) ) ;
#16828 = CARTESIAN_POINT ( 'NONE',  ( 21.55341960407619695, -5.719274019375665929, 46.04275706135234714 ) ) ;
#16830 = CARTESIAN_POINT ( 'NONE',  ( -10.72451020669870658, -18.67979575497194134, 99.58442372801900433 ) ) ;
#16829 = CARTESIAN_POINT ( 'NONE',  ( 9.474510206698729675, 16.51473224551082808, 87.08442372801900433 ) ) ;
#16831 = CARTESIAN_POINT ( 'NONE',  ( 8.224510206698742110, 14.34966873604972548, 92.08442372801901854 ) ) ;
#16832 = CARTESIAN_POINT ( 'NONE',  ( -16.46253265017160317, 9.564922557960807481, 95.83224293864769550 ) ) ;
#16833 = CARTESIAN_POINT ( 'NONE',  ( 12.06949235617757843, -12.14591786802309237, 93.12390960531436690 ) ) ;
#16834 = CARTESIAN_POINT ( 'NONE',  ( 8.224510206698953496, -14.34966873604960469, 32.91557627198102409 ) ) ;
#16835 = CARTESIAN_POINT ( 'NONE',  ( -16.51473224551082808, 9.474510206698731452, 68.33442372801900433 ) ) ;
#16836 = CARTESIAN_POINT ( 'NONE',  ( 21.52544592524334988, 5.823673210054432836, 56.45942372801902565 ) ) ;
#16838 = EDGE_CURVE ( 'NONE', #172390, #19226, #143704, .T. ) ;
#16837 = CARTESIAN_POINT ( 'NONE',  ( -9.564922557961040184, 16.46253265017147172, 27.91775706135232582 ) ) ;
#16839 = CARTESIAN_POINT ( 'NONE',  ( 16.52544592524342804, -4.483927247898539470, 108.5405762719810241 ) ) ;
#16840 = CARTESIAN_POINT ( 'NONE',  ( 10.81492255796078972, 18.62759615963270932, 29.58224293864769905 ) ) ;
#16841 = CARTESIAN_POINT ( 'NONE',  ( -4.483927247898782831, 16.52544592524335698, 112.7094237280190328 ) ) ;
#16842 = CARTESIAN_POINT ( 'NONE',  ( -5.823673210054431948, 21.52544592524334988, 97.70942372801904696 ) ) ;
#16843 = CARTESIAN_POINT ( 'NONE',  ( 12.14591786802327356, -12.06949235617739191, 60.62609039468567573 ) ) ;
#16844 = CARTESIAN_POINT ( 'NONE',  ( -4.483927247898539470, -16.52544592524342804, 22.29057627198102765 ) ) ;
#16845 = CARTESIAN_POINT ( 'NONE',  ( -10.81492255796105439, 18.62759615963255655, 52.91775706135235424 ) ) ;
#16846 = CARTESIAN_POINT ( 'NONE',  ( -18.62759615963255300, -10.81492255796106328, 49.16775706135234003 ) ) ;
#16847 = CARTESIAN_POINT ( 'NONE',  ( -18.67979575497193778, 10.72451020669871902, 28.33442372801902209 ) ) ;
#16848 = CARTESIAN_POINT ( 'NONE',  ( 8.314922557960818139, 14.29746914071049879, 99.58224293864770971 ) ) ;
#16849 = CARTESIAN_POINT ( 'NONE',  ( 5.049401038298161559, -19.05341960407611168, 27.70724293864769550 ) ) ;
#16850 = CARTESIAN_POINT ( 'NONE',  ( 12.14591786802309770, 12.06949235617756955, 74.37390960531436690 ) ) ;
#16851 = CARTESIAN_POINT ( 'NONE',  ( -19.05341960407611168, -5.049401038298163336, 66.45724293864769550 ) ) ;
#16852 = CARTESIAN_POINT ( 'NONE',  ( 4.379528057220092307, 16.55341960407617563, 112.2927570613523471 ) ) ;
#16853 = CARTESIAN_POINT ( 'NONE',  ( 10.72451020669898902, -18.67979575497178502, 57.91557627198103120 ) ) ;
#16854 = CARTESIAN_POINT ( 'NONE',  ( -14.34966873604960291, -8.224510206698953496, 86.66557627198102409 ) ) ;
#16855 = CARTESIAN_POINT ( 'NONE',  ( 10.81492255796078972, 18.62759615963270932, 99.58224293864770971 ) ) ;
#16856 = CARTESIAN_POINT ( 'NONE',  ( 5.049401038298161559, -19.05341960407611168, 97.70724293864766707 ) ) ;
#16858 = CARTESIAN_POINT ( 'NONE',  ( 19.03943276465977164, 0.05219959533936151252, 106.2510903946856615 ) ) ;
#16857 = CARTESIAN_POINT ( 'NONE',  ( 0.05219959533909260263, 19.03943276465977164, 49.99890960531435979 ) ) ;
#16859 = CARTESIAN_POINT ( 'NONE',  ( 18.62759615963271287, -10.81492255796078972, 48.33224293864770260 ) ) ;
#16860 = CARTESIAN_POINT ( 'NONE',  ( 10.72451020669871369, 18.67979575497193778, 72.08442372801899012 ) ) ;
#16861 = CARTESIAN_POINT ( 'NONE',  ( -9.474510206698964154, 16.51473224551069663, 70.41557627198102409 ) ) ;
#16862 = CARTESIAN_POINT ( 'NONE',  ( 19.03943276465977164, -0.05219959533909143690, 93.74890960531435269 ) ) ;
#16863 = CARTESIAN_POINT ( 'NONE',  ( 12.14591786802327356, -12.06949235617739191, 65.62609039468568994 ) ) ;
#16864 = CARTESIAN_POINT ( 'NONE',  ( 18.67979575497194134, -10.72451020669871369, 55.83442372801901854 ) ) ;
#16865 = CARTESIAN_POINT ( 'NONE',  ( -5.823673210054431948, 21.52544592524334988, 87.70942372801901854 ) ) ;
#16866 = CARTESIAN_POINT ( 'NONE',  ( 15.72974639402199770, -15.80617190586745480, 93.12390960531436690 ) ) ;
#16868 = CARTESIAN_POINT ( 'NONE',  ( 8.224510206698742110, 14.34966873604972548, 72.08442372801899012 ) ) ;
#16867 = CARTESIAN_POINT ( 'NONE',  ( 10.81492255796106328, -18.62759615963255655, 35.41775706135234003 ) ) ;
#16869 = CARTESIAN_POINT ( 'NONE',  ( -10.81492255796078084, -18.62759615963271287, 82.08224293864768129 ) ) ;
#16870 = CARTESIAN_POINT ( 'NONE',  ( 5.153800228976615827, -19.02544592524334988, 30.20942372801900433 ) ) ;
#16872 = CARTESIAN_POINT ( 'NONE',  ( -8.314922557960811034, -14.29746914071050412, 22.08224293864769194 ) ) ;
#16871 = CARTESIAN_POINT ( 'NONE',  ( 5.049401038298161559, -19.05341960407611168, 82.70724293864770971 ) ) ;
#16873 = CARTESIAN_POINT ( 'NONE',  ( -4.500000000000000888, -139.5000000000000000, 13.35010376910484275 ) ) ;
#16874 = CARTESIAN_POINT ( 'NONE',  ( 13.89961937509977652, -13.97604488694527269, 103.1239096053143527 ) ) ;
#16875 = CARTESIAN_POINT ( 'NONE',  ( 17.72560187377284535, 5.500000000000042633, 81.57814504131323474 ) ) ;
#16876 = CARTESIAN_POINT ( 'NONE',  ( 16.51473224551083163, -9.474510206698727899, 90.83442372801900433 ) ) ;
#16877 = CARTESIAN_POINT ( 'NONE',  ( 21.52544592524344225, -5.823673210054117533, 58.54057627198103120 ) ) ;
#16878 = CARTESIAN_POINT ( 'NONE',  ( 12.14591786802309770, 12.06949235617756955, 34.37390960531435979 ) ) ;
#16879 = CARTESIAN_POINT ( 'NONE',  ( -16.55341960407617563, 4.379528057220093196, 23.54275706135235424 ) ) ;
#16880 = CARTESIAN_POINT ( 'NONE',  ( 13.89961937509977652, -13.97604488694527269, 38.12390960531436690 ) ) ;
#16881 = CARTESIAN_POINT ( 'NONE',  ( -5.049401038297874678, -19.05341960407617918, 109.7927570613523187 ) ) ;
#16883 = CARTESIAN_POINT ( 'NONE',  ( 9.474510206698729675, 16.51473224551082808, 77.08442372801900433 ) ) ;
#16882 = CARTESIAN_POINT ( 'NONE',  ( 0.05219959533907565091, 21.53943276465977519, 104.9989096053143669 ) ) ;
#16884 = CARTESIAN_POINT ( 'NONE',  ( 4.483927247898790824, -16.52544592524335698, 80.20942372801901854 ) ) ;
#16885 = CARTESIAN_POINT ( 'NONE',  ( -19.02544592524342804, 5.153800228976336051, 66.04057627198103830 ) ) ;
#16886 = CARTESIAN_POINT ( 'NONE',  ( 14.29746914071049879, -8.314922557960816363, 73.33224293864769550 ) ) ;
#16887 = CARTESIAN_POINT ( 'NONE',  ( 0.05219959533909260263, 19.03943276465977164, 54.99890960531435979 ) ) ;
#16888 = CARTESIAN_POINT ( 'NONE',  ( -0.05219959533910754901, -16.53943276465976808, 67.49890960531436690 ) ) ;
#16889 = LINE ( 'NONE', #110877, #51594 ) ;
#16890 = CARTESIAN_POINT ( 'NONE',  ( -36.88736642480385797, -1.774289666830922485, 50.21844423102493948 ) ) ;
#16891 = CARTESIAN_POINT ( 'NONE',  ( -16.53943276465976808, 0.05219959533911058130, 36.24890960531435979 ) ) ;
#16892 = CARTESIAN_POINT ( 'NONE',  ( -19.03943276465977164, 0.05219959533909376836, 81.24890960531436690 ) ) ;
#16893 = CARTESIAN_POINT ( 'NONE',  ( -8.388830574159379737E-16, -13.70000000000001528, -60.44446360152740283 ) ) ;
#16894 = CARTESIAN_POINT ( 'NONE',  ( -13.97604488694547697, 13.89961937509957934, 58.12609039468566863 ) ) ;
#16895 = CARTESIAN_POINT ( 'NONE',  ( 8.224510206698742110, 14.34966873604972548, 57.08442372801901854 ) ) ;
#16896 = CARTESIAN_POINT ( 'NONE',  ( 21.55341960407610458, 5.719274019375980345, 63.95724293864770260 ) ) ;
#16897 = CARTESIAN_POINT ( 'NONE',  ( 9.564922557961047289, -16.46253265017146816, 25.41775706135234003 ) ) ;
#16898 = CARTESIAN_POINT ( 'NONE',  ( -13.89961937509977652, 13.97604488694528158, 80.62390960531436690 ) ) ;
#16899 = CARTESIAN_POINT ( 'NONE',  ( 6.412877669190335972, -3.889087296526014814, 1.818019484660534424 ) ) ;
#16900 = CARTESIAN_POINT ( 'NONE',  ( 16.51473224551069308, 9.474510206698969483, 114.1655762719810241 ) ) ;
#16901 = CARTESIAN_POINT ( 'NONE',  ( -5.049401038298153566, 19.05341960407611168, 65.20724293864765286 ) ) ;
#16902 = CARTESIAN_POINT ( 'NONE',  ( 0.05219959533937995610, -21.53943276465977519, 35.00109039468568284 ) ) ;
#16903 = CARTESIAN_POINT ( 'NONE',  ( 8.314922557960818139, 14.29746914071049879, 104.5822429386477097 ) ) ;
#16906 = ORIENTED_EDGE ( 'NONE', *, *, #197184, .F. ) ;
#16905 = CARTESIAN_POINT ( 'NONE',  ( 9.564922557960805705, 16.46253265017160317, 94.58224293864769550 ) ) ;
#16904 = CARTESIAN_POINT ( 'NONE',  ( -15.80617190586745835, -15.72974639402198527, 96.87390960531436690 ) ) ;
#16907 = CARTESIAN_POINT ( 'NONE',  ( 5.719274019375673035, 21.55341960407619339, 32.29275706135235424 ) ) ;
#16908 = ORIENTED_EDGE ( 'NONE', *, *, #196572, .F. ) ;
#16909 = CARTESIAN_POINT ( 'NONE',  ( 0.05219959533909260263, 19.03943276465977164, 84.99890960531436690 ) ) ;
#16910 = DIRECTION ( 'NONE',  ( 0.000000000000000000, 0.000000000000000000, 1.000000000000000000 ) ) ;
#16911 = CARTESIAN_POINT ( 'NONE',  ( -10.72451020669898014, 18.67979575497178502, 100.4155762719810241 ) ) ;
#16912 = CARTESIAN_POINT ( 'NONE',  ( -13.89961937509977652, 13.97604488694528158, 45.62390960531433848 ) ) ;
#16913 = CARTESIAN_POINT ( 'NONE',  ( 0.05219959533936267826, -19.03943276465977164, 105.0010903946856615 ) ) ;
#16914 = CARTESIAN_POINT ( 'NONE',  ( -11.40812507854754720, -35.11059874428192273, -2.724999997268813257 ) ) ;
#16915 = CARTESIAN_POINT ( 'NONE',  ( 19.05341960407611168, 5.049401038298154454, 23.95724293864769194 ) ) ;
#16916 = CARTESIAN_POINT ( 'NONE',  ( 18.67979575497194134, -10.72451020669871369, 85.83442372801901854 ) ) ;
#16918 = CARTESIAN_POINT ( 'NONE',  ( 10.81492255796106328, -18.62759615963255655, 50.41775706135235424 ) ) ;
#16917 = CARTESIAN_POINT ( 'NONE',  ( -13.97604488694527625, -13.89961937509977652, 71.87390960531433848 ) ) ;
#16919 = CARTESIAN_POINT ( 'NONE',  ( 18.62759615963255655, 10.81492255796105972, 21.66775706135235069 ) ) ;
#16920 = CARTESIAN_POINT ( 'NONE',  ( -5.429308488886486681E-15, 30.30510711980690175, 147.5000000000000000 ) ) ;
#16921 = CARTESIAN_POINT ( 'NONE',  ( -16.46253265017160317, 9.564922557960807481, 100.8322429386477097 ) ) ;
#16922 = CARTESIAN_POINT ( 'NONE',  ( -0.1587466045633683653, 28.39722349821926528, 140.0000000000000000 ) ) ;
#16925 = CARTESIAN_POINT ( 'NONE',  ( 5.823673210054444382, -21.52544592524334988, 40.20942372801901854 ) ) ;
#16924 = CARTESIAN_POINT ( 'NONE',  ( 18.62759615963271287, -10.81492255796078972, 48.33224293864770260 ) ) ;
#16923 = CARTESIAN_POINT ( 'NONE',  ( -0.05219959533934338120, 16.53943276465976808, 42.50109039468567573 ) ) ;
#16926 = CARTESIAN_POINT ( 'NONE',  ( 21.53943276465977519, 0.05219959533937863772, 71.25109039468568994 ) ) ;
#16927 = CARTESIAN_POINT ( 'NONE',  ( 5.266531018137392550, 6.873421141834948678, -62.00040165901308598 ) ) ;
#16928 = CARTESIAN_POINT ( 'NONE',  ( -16.52544592524335698, -4.483927247898792601, 18.95942372801901143 ) ) ;
#16929 = CARTESIAN_POINT ( 'NONE',  ( 19.02544592524343514, -5.153800228976328945, 63.54057627198103830 ) ) ;
#16930 = CARTESIAN_POINT ( 'NONE',  ( 16.51473224551069308, 9.474510206698969483, 79.16557627198103830 ) ) ;
#16931 = CARTESIAN_POINT ( 'NONE',  ( 8.224510206698953496, -14.34966873604960469, 107.9155762719810241 ) ) ;
#16932 = CARTESIAN_POINT ( 'NONE',  ( -16.52544592524342804, 4.483927247898546575, 106.0405762719810525 ) ) ;
#16933 = CARTESIAN_POINT ( 'NONE',  ( 0.05219959533907565091, 21.53943276465977519, 34.99890960531435979 ) ) ;
#16934 = CARTESIAN_POINT ( 'NONE',  ( -4.483927247898782831, 16.52544592524335698, 82.70942372801900433 ) ) ;
#16936 = CARTESIAN_POINT ( 'NONE',  ( 19.05341960407611168, 5.049401038298154454, 48.95724293864768129 ) ) ;
#16935 = CARTESIAN_POINT ( 'NONE',  ( 0.05219959533910956823, 16.53943276465976808, 64.99890960531435269 ) ) ;
#16937 = CARTESIAN_POINT ( 'NONE',  ( -15.80617190586768217, 15.72974639402176855, 73.12609039468567573 ) ) ;
#16938 = CARTESIAN_POINT ( 'NONE',  ( 15.72974639402176855, 15.80617190586768217, 71.87609039468568994 ) ) ;
#16939 = CARTESIAN_POINT ( 'NONE',  ( -19.05341960407617563, 5.049401038297882671, 108.5427570613523187 ) ) ;
#16940 = CARTESIAN_POINT ( 'NONE',  ( 8.224510206698953496, -14.34966873604960469, 57.91557627198103120 ) ) ;
#16941 = CARTESIAN_POINT ( 'NONE',  ( -21.53943276465977519, -0.05219959533937600094, 23.75109039468567929 ) ) ;
#16942 = CARTESIAN_POINT ( 'NONE',  ( -18.62759615963270932, 10.81492255796079327, 65.83224293864769550 ) ) ;
#16943 = CARTESIAN_POINT ( 'NONE',  ( 18.87255363501904526, 5.499999999999952038, 73.82513748171827217 ) ) ;
#16944 = CARTESIAN_POINT ( 'NONE',  ( 23.31738231874054890, -16.94106989632523508, 145.0500000054623513 ) ) ;
#16945 = CARTESIAN_POINT ( 'NONE',  ( 13.89961937509977652, -13.97604488694527269, 63.12390960531435979 ) ) ;
#16946 = CARTESIAN_POINT ( 'NONE',  ( -12.06949235617756955, 12.14591786802309770, 30.62390960531436335 ) ) ;
#16947 = CARTESIAN_POINT ( 'NONE',  ( 4.483927247898790824, -16.52544592524335698, 110.2094237280190185 ) ) ;
#16948 = CARTESIAN_POINT ( 'NONE',  ( -16.52544592524335698, -4.483927247898792601, 93.95942372801903275 ) ) ;
#16949 = CARTESIAN_POINT ( 'NONE',  ( 9.564922557961047289, -16.46253265017146816, 50.41775706135233293 ) ) ;
#16950 = CARTESIAN_POINT ( 'NONE',  ( -6.020228577223754586E-15, 39.95556452105416412, -8.500000000000000000 ) ) ;
#16951 = CARTESIAN_POINT ( 'NONE',  ( 19.03943276465977164, -0.05219959533909143690, 108.7489096053143527 ) ) ;
#16952 = CARTESIAN_POINT ( 'NONE',  ( -8.224510206698948167, 14.34966873604960824, 75.41557627198102409 ) ) ;
#16953 = CARTESIAN_POINT ( 'NONE',  ( -0.05219959533936034679, 19.03943276465977164, 42.50109039468566152 ) ) ;
#16955 = CARTESIAN_POINT ( 'NONE',  ( -0.05219959533907301413, -21.53943276465977519, 22.49890960531436335 ) ) ;
#16954 = CARTESIAN_POINT ( 'NONE',  ( 13.97604488694527802, 13.89961937509977652, 29.37390960531435979 ) ) ;
#16957 = ORIENTED_EDGE ( 'NONE', *, *, #116692, .T. ) ;
#16956 = CARTESIAN_POINT ( 'NONE',  ( 21.55341960407610458, 5.719274019375980345, 58.95724293864770971 ) ) ;
#16958 = CARTESIAN_POINT ( 'NONE',  ( -16.55341960407611168, -4.379528057220339221, 96.45724293864770971 ) ) ;
#16959 = CARTESIAN_POINT ( 'NONE',  ( 8.314922557961029526, -14.29746914071037800, 55.41775706135234714 ) ) ;
#16960 = VERTEX_POINT ( 'NONE', #164141 ) ;
#16961 = CARTESIAN_POINT ( 'NONE',  ( -12.14591786802309592, -12.06949235617757132, 91.87390960531436690 ) ) ;
#16962 = CARTESIAN_POINT ( 'NONE',  ( -12.73749492396214578, -155.7167183371837496, -4.999999999999999112 ) ) ;
#16963 = CARTESIAN_POINT ( 'NONE',  ( -16.31925111598457434, 7.325300261831449333, 50.16424538967250868 ) ) ;
#16964 = CARTESIAN_POINT ( 'NONE',  ( 19.02544592524343514, -5.153800228976328945, 113.5405762719810241 ) ) ;
#16965 = CARTESIAN_POINT ( 'NONE',  ( 3.556970738554033499E-15, -38.81732327939057825, -2.624999997268812724 ) ) ;
#16966 = CARTESIAN_POINT ( 'NONE',  ( 1.338834197008474947, 23.50074569744939978, -57.34146676846842894 ) ) ;
#16968 = CARTESIAN_POINT ( 'NONE',  ( 16.53943276465976808, -0.05219959533910856209, 23.74890960531435269 ) ) ;
#16967 = CARTESIAN_POINT ( 'NONE',  ( 4.483927247898790824, -16.52544592524335698, 45.20942372801901854 ) ) ;
#16969 = CARTESIAN_POINT ( 'NONE',  ( 0.05219959533907565091, 21.53943276465977519, 59.99890960531436690 ) ) ;
#16970 = CARTESIAN_POINT ( 'NONE',  ( 0.05219959533936267826, -19.03943276465977164, 85.00109039468567573 ) ) ;
#16971 = CARTESIAN_POINT ( 'NONE',  ( -21.53943276465977519, 0.05219959533907696930, 46.24890960531435979 ) ) ;
#16972 = CARTESIAN_POINT ( 'NONE',  ( -0.05219959533937732626, 21.53943276465977519, 87.50109039468568994 ) ) ;
#16973 = CARTESIAN_POINT ( 'NONE',  ( -21.38418241377624085, 7.427326039334300134, 174.4773576836617224 ) ) ;
#16974 = CARTESIAN_POINT ( 'NONE',  ( 8.314922557961029526, -14.29746914071037800, 50.41775706135235424 ) ) ;
#16976 = CARTESIAN_POINT ( 'NONE',  ( -5.153800228976328057, -19.02544592524343514, 102.2905762719810383 ) ) ;
#16975 = CARTESIAN_POINT ( 'NONE',  ( 0.05219959533909260263, 19.03943276465977164, 39.99890960531436690 ) ) ;
#16977 = CARTESIAN_POINT ( 'NONE',  ( 19.05341960407611168, 5.049401038298154454, 38.95724293864767418 ) ) ;
#16978 = CARTESIAN_POINT ( 'NONE',  ( -4.483927247898539470, -16.52544592524342804, 102.2905762719810383 ) ) ;
#16979 = APPLICATION_PROTOCOL_DEFINITION ( 'draft international standard', 'automotive_design', 1998, #66005 ) ;
#16980 = CARTESIAN_POINT ( 'NONE',  ( -13.97604488694527625, -13.89961937509977652, 101.8739096053143811 ) ) ;
#16981 = VERTEX_POINT ( 'NONE', #182292 ) ;
#16982 = CARTESIAN_POINT ( 'NONE',  ( 8.314922557961029526, -14.29746914071037800, 60.41775706135235424 ) ) ;
#16983 = CARTESIAN_POINT ( 'NONE',  ( 18.62759615963271287, -10.81492255796078972, 93.33224293864769550 ) ) ;
#16984 = CARTESIAN_POINT ( 'NONE',  ( -5.153800228976328057, -19.02544592524343514, 52.29057627198100988 ) ) ;
#16985 = CARTESIAN_POINT ( 'NONE',  ( -18.62759615963255300, -10.81492255796106328, 29.16775706135234003 ) ) ;
#16986 = CARTESIAN_POINT ( 'NONE',  ( 13.89961937509977652, -13.97604488694527269, 83.12390960531436690 ) ) ;
#16988 = EDGE_CURVE ( 'NONE', #77120, #196218, #25638, .T. ) ;
#16987 = CARTESIAN_POINT ( 'NONE',  ( -19.03943276465977164, 0.05219959533909376836, 116.2489096053143669 ) ) ;
#16989 = VERTEX_POINT ( 'NONE', #43772 ) ;
#16990 = CARTESIAN_POINT ( 'NONE',  ( -5.823673210054116645, -21.52544592524344225, 112.2905762719810241 ) ) ;
#16993 = CARTESIAN_POINT ( 'NONE',  ( 5.153800228976615827, -19.02544592524334988, 75.20942372801896170 ) ) ;
#16992 = CARTESIAN_POINT ( 'NONE',  ( 19.02544592524343514, -5.153800228976328945, 108.5405762719810383 ) ) ;
#16991 = CARTESIAN_POINT ( 'NONE',  ( -13.97604488694527625, -13.89961937509977652, 21.87390960531435979 ) ) ;
#16994 = CARTESIAN_POINT ( 'NONE',  ( -0.05219959533936034679, 19.03943276465977164, 32.50109039468566863 ) ) ;
#16995 = CARTESIAN_POINT ( 'NONE',  ( -15.72974639402197994, 15.80617190586746368, 95.62390960531436690 ) ) ;
#16996 = CARTESIAN_POINT ( 'NONE',  ( -13.89961937509957401, -13.97604488694547875, 39.37609039468566152 ) ) ;
#16997 = CARTESIAN_POINT ( 'NONE',  ( -16.52544592524335698, -4.483927247898792601, 83.95942372801900433 ) ) ;
#16998 = ADVANCED_FACE ( 'NONE', ( #72117 ), #225, .T. ) ;
#17000 = VERTEX_POINT ( 'NONE', #30583 ) ;
#16999 = CARTESIAN_POINT ( 'NONE',  ( 13.97604488694527802, 13.89961937509977652, 104.3739096053143385 ) ) ;
#17001 = CARTESIAN_POINT ( 'NONE',  ( 5.049401038298161559, -19.05341960407611168, 62.70724293864769550 ) ) ;
#17002 = CARTESIAN_POINT ( 'NONE',  ( 10.72451020669871369, 18.67979575497193778, 72.08442372801899012 ) ) ;
#17003 = CARTESIAN_POINT ( 'NONE',  ( -0.05219959533937732626, 21.53943276465977519, 77.50109039468567573 ) ) ;
#17004 = CARTESIAN_POINT ( 'NONE',  ( -5.153800228976328057, -19.02544592524343514, 72.29057627198102409 ) ) ;
#17005 = CARTESIAN_POINT ( 'NONE',  ( -5.719274019375665041, -21.55341960407619695, 54.79275706135235424 ) ) ;
#17006 = CARTESIAN_POINT ( 'NONE',  ( -5.049401038297874678, -19.05341960407617918, 84.79275706135233293 ) ) ;
#17007 = CARTESIAN_POINT ( 'NONE',  ( 13.89961937509977652, -13.97604488694527269, 53.12390960531434558 ) ) ;
#17008 = CARTESIAN_POINT ( 'NONE',  ( -13.97604488694527625, -13.89961937509977652, 96.87390960531433848 ) ) ;
#17009 = CARTESIAN_POINT ( 'NONE',  ( -13.89961937509977652, 13.97604488694528158, 70.62390960531432427 ) ) ;
#17010 = CARTESIAN_POINT ( 'NONE',  ( 23.48298174826589246, 32.32155151706776053, -2.447842220587803652 ) ) ;
#17011 = CARTESIAN_POINT ( 'NONE',  ( 5.049401038298161559, -19.05341960407611168, 57.70724293864769550 ) ) ;
#17012 = CARTESIAN_POINT ( 'NONE',  ( 18.67979575497178502, 10.72451020669898547, 99.16557627198100988 ) ) ;
#17013 = CARTESIAN_POINT ( 'NONE',  ( -8.314922557961024197, 14.29746914071037800, 72.91775706135234714 ) ) ;
#17014 = CARTESIAN_POINT ( 'NONE',  ( -21.75836449082843060, 8.509082329563685931, 169.1767350484841472 ) ) ;
#17015 = CARTESIAN_POINT ( 'NONE',  ( -19.02544592524334988, -5.153800228976617603, 33.95942372801897591 ) ) ;
#17016 = CARTESIAN_POINT ( 'NONE',  ( -13.97604488694527625, -13.89961937509977652, 61.87390960531435979 ) ) ;
#17017 = CARTESIAN_POINT ( 'NONE',  ( 4.483927247898545687, 16.52544592524342804, 54.79057627198104541 ) ) ;
#17018 = CARTESIAN_POINT ( 'NONE',  ( 14.29746914071049879, -8.314922557960816363, 93.33224293864769550 ) ) ;
#17019 = CARTESIAN_POINT ( 'NONE',  ( 5.153800228976335163, 19.02544592524342804, 104.7905762719809957 ) ) ;
#17020 = CARTESIAN_POINT ( 'NONE',  ( -9.564922557960796823, -16.46253265017161027, 92.08224293864769550 ) ) ;
#17021 = CARTESIAN_POINT ( 'NONE',  ( 9.474510206698971260, -16.51473224551069308, 107.9155762719810383 ) ) ;
#17022 = CARTESIAN_POINT ( 'NONE',  ( -18.67979575497193778, 10.72451020669871902, 113.3344237280190328 ) ) ;
#17023 = CARTESIAN_POINT ( 'NONE',  ( -16.55341960407617563, 4.379528057220093196, 88.54275706135236135 ) ) ;
#17024 = CARTESIAN_POINT ( 'NONE',  ( 10.72451020669871369, 18.67979575497193778, 42.08442372801901854 ) ) ;
#17025 = CARTESIAN_POINT ( 'NONE',  ( -18.62759615963270932, 10.81492255796079327, 30.83224293864770260 ) ) ;
#17026 = CARTESIAN_POINT ( 'NONE',  ( 18.67979575497178502, 10.72451020669898547, 104.1655762719810241 ) ) ;
#17027 = CARTESIAN_POINT ( 'NONE',  ( -12.06949235617756955, 12.14591786802309770, 55.62390960531436690 ) ) ;
#17028 = CARTESIAN_POINT ( 'NONE',  ( 13.97604488694527802, 13.89961937509977652, 54.37390960531435979 ) ) ;
#17029 = CARTESIAN_POINT ( 'NONE',  ( 0.05219959533910956823, 16.53943276465976808, 74.99890960531435269 ) ) ;
#17030 = CARTESIAN_POINT ( 'NONE',  ( -13.89961937509957401, -13.97604488694547875, 44.37609039468566863 ) ) ;
#17031 = CARTESIAN_POINT ( 'NONE',  ( -16.52544592524342804, 4.483927247898546575, 116.0405762719810383 ) ) ;
#17032 = VERTEX_POINT ( 'NONE', #1215 ) ;
#17033 = CARTESIAN_POINT ( 'NONE',  ( 16.52544592524335698, 4.483927247898782831, 61.45942372801901854 ) ) ;
#17034 = CARTESIAN_POINT ( 'NONE',  ( -9.474510206698964154, 16.51473224551069663, 70.41557627198102409 ) ) ;
#17035 = CARTESIAN_POINT ( 'NONE',  ( -27.73933785331498925, 9.013057229001088189, 144.7750000027311614 ) ) ;
#17036 = CARTESIAN_POINT ( 'NONE',  ( 0.05219959533910956823, 16.53943276465976808, 89.99890960531438111 ) ) ;
#17037 = CARTESIAN_POINT ( 'NONE',  ( 10.72451020669898902, -18.67979575497178502, 42.91557627198103120 ) ) ;
#17038 = ORIENTED_EDGE ( 'NONE', *, *, #19616, .F. ) ;
#17039 = CARTESIAN_POINT ( 'NONE',  ( 12.14591786802327356, -12.06949235617739191, 110.6260903946857042 ) ) ;
#17040 = CARTESIAN_POINT ( 'NONE',  ( 12.06949235617739724, 12.14591786802326823, 31.87609039468567929 ) ) ;
#17041 = CARTESIAN_POINT ( 'NONE',  ( 18.62759615963255655, 10.81492255796105972, 86.66775706135234714 ) ) ;
#17042 = CARTESIAN_POINT ( 'NONE',  ( -13.89961937509977652, 13.97604488694528158, 90.62390960531432427 ) ) ;
#17043 = CARTESIAN_POINT ( 'NONE',  ( 5.823673210054125526, 21.52544592524343514, 114.7905762719810383 ) ) ;
#17044 = CARTESIAN_POINT ( 'NONE',  ( 19.05341960407611168, 5.049401038298154454, 28.95724293864769550 ) ) ;
#17045 = CARTESIAN_POINT ( 'NONE',  ( -12.06949235617739369, -12.14591786802326823, 34.37609039468568284 ) ) ;
#17046 = CARTESIAN_POINT ( 'NONE',  ( -9.474510206698720793, -16.51473224551083518, 89.58442372801900433 ) ) ;
#17047 = CARTESIAN_POINT ( 'NONE',  ( -5.719274019375978568, 21.55341960407610458, 90.20724293864770971 ) ) ;
#17048 = CARTESIAN_POINT ( 'NONE',  ( 5.153800228976615827, -19.02544592524334988, 70.20942372801899012 ) ) ;
#17049 = CARTESIAN_POINT ( 'NONE',  ( 32.00000000000000000, -5.186379194389041255E-15, 47.64999999999999858 ) ) ;
#17050 = CARTESIAN_POINT ( 'NONE',  ( -15.72974639402176322, -15.80617190586768395, 19.37609039468568639 ) ) ;
#17051 = DIRECTION ( 'NONE',  ( 1.000000000000000000, -5.392603844284257652E-33, 0.000000000000000000 ) ) ;
#17052 = CARTESIAN_POINT ( 'NONE',  ( 16.51473224551069308, 9.474510206698969483, 84.16557627198102409 ) ) ;
#17053 = CARTESIAN_POINT ( 'NONE',  ( -14.34966873604972548, 8.224510206698743886, 33.33442372801900433 ) ) ;
#17054 = FACE_BOUND ( 'NONE', #15470, .T. ) ;
#17055 = CARTESIAN_POINT ( 'NONE',  ( 19.03943276465977164, 0.05219959533936151252, 61.25109039468566863 ) ) ;
#17057 = CARTESIAN_POINT ( 'NONE',  ( -8.314922557960811034, -14.29746914071050412, 72.08224293864769550 ) ) ;
#17056 = CARTESIAN_POINT ( 'NONE',  ( 5.719274019375991003, -21.55341960407610458, 112.7072429386476955 ) ) ;
#17058 = CARTESIAN_POINT ( 'NONE',  ( -0.05219959533909027116, -19.03943276465977164, 82.49890960531436690 ) ) ;
#17060 = CARTESIAN_POINT ( 'NONE',  ( -19.03943276465977164, -0.05219959533935918106, 48.75109039468566863 ) ) ;
#17059 = CARTESIAN_POINT ( 'NONE',  ( -8.224510206698735004, -14.34966873604973081, 39.58442372801901143 ) ) ;
#17061 = AXIS2_PLACEMENT_3D ( 'NONE', #29858, #46012, #199707 ) ;
#17062 = CARTESIAN_POINT ( 'NONE',  ( 21.55341960407619695, -5.719274019375665929, 61.04275706135234714 ) ) ;
#17063 = CARTESIAN_POINT ( 'NONE',  ( 19.05341960407617918, -5.049401038297876454, 111.0427570613523329 ) ) ;
#17064 = CARTESIAN_POINT ( 'NONE',  ( -19.05341960407611168, -5.049401038298163336, 61.45724293864769550 ) ) ;
#17065 = CARTESIAN_POINT ( 'NONE',  ( 13.89961937509957401, 13.97604488694547697, 76.87609039468566152 ) ) ;
#17066 = CARTESIAN_POINT ( 'NONE',  ( -16.55341960407617563, 4.379528057220093196, 53.54275706135234714 ) ) ;
#17067 = CARTESIAN_POINT ( 'NONE',  ( -0.05219959533937732626, 21.53943276465977519, 97.50109039468567573 ) ) ;
#17068 = CARTESIAN_POINT ( 'NONE',  ( -0.05219959533936034679, 19.03943276465977164, 67.50109039468566152 ) ) ;
#17069 = CARTESIAN_POINT ( 'NONE',  ( 19.05341960407611168, 5.049401038298154454, 48.95724293864768129 ) ) ;
#17070 = CARTESIAN_POINT ( 'NONE',  ( 10.81492255796078972, 18.62759615963270932, 74.58224293864768129 ) ) ;
#17072 = CARTESIAN_POINT ( 'NONE',  ( -13.89961937509957401, -13.97604488694547875, 64.37609039468567573 ) ) ;
#17071 = CARTESIAN_POINT ( 'NONE',  ( -14.29746914071049879, 8.314922557960819915, 60.83224293864769550 ) ) ;
#17073 = CARTESIAN_POINT ( 'NONE',  ( 21.76481224609945997, 7.725237430229302760, 173.1951747752679296 ) ) ;
#17074 = CARTESIAN_POINT ( 'NONE',  ( 16.51473224551083163, -9.474510206698727899, 40.83442372801900433 ) ) ;
#17075 = CARTESIAN_POINT ( 'NONE',  ( -14.34966873604972548, 8.224510206698743886, 103.3344237280190043 ) ) ;
#17076 = CARTESIAN_POINT ( 'NONE',  ( -0.05219959533910754901, -16.53943276465976808, 62.49890960531436690 ) ) ;
#17078 = CARTESIAN_POINT ( 'NONE',  ( -17.14385361876520264, -23.59649016807271593, 141.1750000027311671 ) ) ;
#17077 = CARTESIAN_POINT ( 'NONE',  ( -10.81492255796105439, 18.62759615963255655, 102.9177570613523756 ) ) ;
#17079 = CARTESIAN_POINT ( 'NONE',  ( -21.52544592524343514, 5.823673210054127303, 91.04057627198103830 ) ) ;
#17080 = CARTESIAN_POINT ( 'NONE',  ( 19.02544592524343514, -5.153800228976328945, 68.54057627198103830 ) ) ;
#17081 = CARTESIAN_POINT ( 'NONE',  ( -5.719274019375665041, -21.55341960407619695, 64.79275706135234714 ) ) ;
#17082 = CARTESIAN_POINT ( 'NONE',  ( 13.97604488694527802, 13.89961937509977652, 44.37390960531435269 ) ) ;
#17083 = VERTEX_POINT ( 'NONE', #170084 ) ;
#17084 = CARTESIAN_POINT ( 'NONE',  ( 19.05341960407611168, 5.049401038298154454, 68.95724293864769550 ) ) ;
#17085 = CARTESIAN_POINT ( 'NONE',  ( 8.314922557960818139, 14.29746914071049879, 114.5822429386477097 ) ) ;
#17086 = CARTESIAN_POINT ( 'NONE',  ( -5.823673210054116645, -21.52544592524344225, 22.29057627198102765 ) ) ;
#17087 = CARTESIAN_POINT ( 'NONE',  ( 16.53943276465976808, -0.05219959533910856209, 68.74890960531435269 ) ) ;
#17088 = CARTESIAN_POINT ( 'NONE',  ( -9.474510206698964154, 16.51473224551069663, 35.41557627198102409 ) ) ;
#17089 = CARTESIAN_POINT ( 'NONE',  ( 8.314922557960818139, 14.29746914071049879, 84.58224293864769550 ) ) ;
#17090 = CARTESIAN_POINT ( 'NONE',  ( -10.81492255796078084, -18.62759615963271287, 97.08224293864770971 ) ) ;
#17091 = CARTESIAN_POINT ( 'NONE',  ( 15.72974639402176855, 15.80617190586768217, 31.87609039468567929 ) ) ;
#17092 = CARTESIAN_POINT ( 'NONE',  ( -24.81835718235489097, -6.052279806424480491, 168.4265042179603427 ) ) ;
#17093 = CARTESIAN_POINT ( 'NONE',  ( 4.483927247898790824, -16.52544592524335698, 50.20942372801901854 ) ) ;
#17094 = CARTESIAN_POINT ( 'NONE',  ( -18.62759615963270932, 10.81492255796079327, 80.83224293864769550 ) ) ;
#17095 = CARTESIAN_POINT ( 'NONE',  ( 9.474510206698729675, 16.51473224551082808, 27.08442372801900433 ) ) ;
#17096 = CARTESIAN_POINT ( 'NONE',  ( -9.474510206698964154, 16.51473224551069663, 100.4155762719810241 ) ) ;
#17097 = CARTESIAN_POINT ( 'NONE',  ( -18.67979575497193778, 10.72451020669871902, 48.33442372801902565 ) ) ;
#17098 = AXIS2_PLACEMENT_3D ( 'NONE', #199310, #153787, #73992 ) ;
#17099 = CARTESIAN_POINT ( 'NONE',  ( 21.55341960407610458, 5.719274019375980345, 48.95724293864770971 ) ) ;
#17100 = CARTESIAN_POINT ( 'NONE',  ( -0.05219959533934338120, 16.53943276465976808, 112.5010903946857042 ) ) ;
#17102 = CARTESIAN_POINT ( 'NONE',  ( -21.55341960407619339, 5.719274019375674811, 103.5427570613523613 ) ) ;
#17101 = CARTESIAN_POINT ( 'NONE',  ( -15.72974639402176322, -15.80617190586768395, 69.37609039468567573 ) ) ;
#17103 = CARTESIAN_POINT ( 'NONE',  ( 13.97604488694548053, -13.89961937509957401, 35.62609039468567573 ) ) ;
#17104 = CARTESIAN_POINT ( 'NONE',  ( -12.06949235617739369, -12.14591786802326823, 84.37609039468570415 ) ) ;
#17105 = CARTESIAN_POINT ( 'NONE',  ( 15.72974639402176855, 15.80617190586768217, 41.87609039468568284 ) ) ;
#17106 = CARTESIAN_POINT ( 'NONE',  ( 13.97604488694527802, 13.89961937509977652, 44.37390960531435269 ) ) ;
#17107 = CARTESIAN_POINT ( 'NONE',  ( 5.153800228976615827, -19.02544592524334988, 20.20942372801899722 ) ) ;
#17108 = CARTESIAN_POINT ( 'NONE',  ( -5.719274019375978568, 21.55341960407610458, 30.20724293864769550 ) ) ;
#17109 = B_SPLINE_CURVE_WITH_KNOTS ( 'NONE', 3,
 ( #182684, #137157, #198846, #86668, #41180, #148351 ),
 .UNSPECIFIED., .F., .F.,
 ( 4, 2, 4 ),
 ( 0.001769412596444650985, 0.002152742221722609914, 0.002536071847000569059 ),
 .UNSPECIFIED. ) ;
#17110 = CARTESIAN_POINT ( 'NONE',  ( -5.719274019375978568, 21.55341960407610458, 115.2072429386476955 ) ) ;
#17111 = CARTESIAN_POINT ( 'NONE',  ( 10.72451020669898902, -18.67979575497178502, 72.91557627198103830 ) ) ;
#17112 = CARTESIAN_POINT ( 'NONE',  ( 4.379528057220092307, 16.55341960407617563, 37.29275706135235424 ) ) ;
#17114 = CARTESIAN_POINT ( 'NONE',  ( -10.72451020669898014, 18.67979575497178502, 80.41557627198103830 ) ) ;
#17113 = CARTESIAN_POINT ( 'NONE',  ( -38.00000000000000711, 2.893978650043524126E-14, -25.00000000000000000 ) ) ;
#17116 = CARTESIAN_POINT ( 'NONE',  ( 8.224510206698953496, -14.34966873604960469, 67.91557627198102409 ) ) ;
#17115 = CARTESIAN_POINT ( 'NONE',  ( -4.483927247898782831, 16.52544592524335698, 62.70942372801902565 ) ) ;
#17117 = CARTESIAN_POINT ( 'NONE',  ( -22.78165926218177972, 20.70663425419845893, -47.27781451939566892 ) ) ;
#17118 = CARTESIAN_POINT ( 'NONE',  ( -16.46253265017146816, -9.564922557961047289, 89.16775706135234714 ) ) ;
#17119 = CARTESIAN_POINT ( 'NONE',  ( 11.30153831258470731, -190.0000000000000000, -1.787262988391354872E-28 ) ) ;
#17120 = CARTESIAN_POINT ( 'NONE',  ( 12.14591786802327356, -12.06949235617739191, 45.62609039468567573 ) ) ;
#17121 = CARTESIAN_POINT ( 'NONE',  ( -5.719274019375978568, 21.55341960407610458, 115.2072429386476955 ) ) ;
#17122 = CARTESIAN_POINT ( 'NONE',  ( 21.55341960407610458, 5.719274019375980345, 78.95724293864769550 ) ) ;
#17123 = CARTESIAN_POINT ( 'NONE',  ( -15.80617190586745835, -15.72974639402198527, 36.87390960531435979 ) ) ;
#17124 = CARTESIAN_POINT ( 'NONE',  ( -16.55341960407617563, 4.379528057220093196, 63.54275706135234003 ) ) ;
#17125 = CARTESIAN_POINT ( 'NONE',  ( -16.51473224551069308, -9.474510206698971260, 66.66557627198102409 ) ) ;
#17127 = CARTESIAN_POINT ( 'NONE',  ( -5.049401038297874678, -19.05341960407617918, 109.7927570613523187 ) ) ;
#17126 = CARTESIAN_POINT ( 'NONE',  ( 18.67979575497194134, -10.72451020669871369, 45.83442372801901854 ) ) ;
#17128 = CARTESIAN_POINT ( 'NONE',  ( -13.97604488694527625, -13.89961937509977652, 111.8739096053143243 ) ) ;
#17129 = CARTESIAN_POINT ( 'NONE',  ( 9.474510206698729675, 16.51473224551082808, 22.08442372801899722 ) ) ;
#17130 = CARTESIAN_POINT ( 'NONE',  ( -12.06949235617739369, -12.14591786802326823, 39.37609039468567573 ) ) ;
#17131 = CARTESIAN_POINT ( 'NONE',  ( 19.05341960407611168, 5.049401038298154454, 98.95724293864766707 ) ) ;
#17132 = CARTESIAN_POINT ( 'NONE',  ( 21.52544592524344225, -5.823673210054117533, 108.5405762719810241 ) ) ;
#17133 = CARTESIAN_POINT ( 'NONE',  ( 5.153800228976335163, 19.02544592524342804, 59.79057627198100988 ) ) ;
#17134 = FACE_OUTER_BOUND ( 'NONE', #126071, .T. ) ;
#17135 = CARTESIAN_POINT ( 'NONE',  ( -16.52544592524342804, 4.483927247898546575, 81.04057627198102409 ) ) ;
#17136 = CARTESIAN_POINT ( 'NONE',  ( -19.03943276465977164, 0.05219959533909376836, 116.2489096053143669 ) ) ;
#17137 = CARTESIAN_POINT ( 'NONE',  ( -17.05116617787826527, 6.768360034955678728, 33.65675553259197983 ) ) ;
#17138 = CARTESIAN_POINT ( 'NONE',  ( -21.55341960407610458, -5.719274019375992779, 106.4572429386477097 ) ) ;
#17139 = CARTESIAN_POINT ( 'NONE',  ( -5.153800228976607833, 19.02544592524334988, 57.70942372801899012 ) ) ;
#17140 = CARTESIAN_POINT ( 'NONE',  ( 15.72974639402199770, -15.80617190586745480, 33.12390960531435979 ) ) ;
#17141 = CARTESIAN_POINT ( 'NONE',  ( -9.564922557960796823, -16.46253265017161027, 22.08224293864768839 ) ) ;
#17142 = CARTESIAN_POINT ( 'NONE',  ( 18.67979575497178502, 10.72451020669898547, 74.16557627198102409 ) ) ;
#17143 = CARTESIAN_POINT ( 'NONE',  ( 5.153800228976335163, 19.02544592524342804, 104.7905762719809957 ) ) ;
#17144 = CARTESIAN_POINT ( 'NONE',  ( -21.55341960407619339, 5.719274019375674811, 73.54275706135234714 ) ) ;
#17145 = CARTESIAN_POINT ( 'NONE',  ( -9.564922557960796823, -16.46253265017161027, 52.08224293864768839 ) ) ;
#17146 = CARTESIAN_POINT ( 'NONE',  ( 8.224510206698953496, -14.34966873604960469, 92.91557627198103830 ) ) ;
#17147 = CARTESIAN_POINT ( 'NONE',  ( 8.314922557961029526, -14.29746914071037800, 30.41775706135234358 ) ) ;
#17148 = CARTESIAN_POINT ( 'NONE',  ( 16.51473224551069308, 9.474510206698969483, 59.16557627198102409 ) ) ;
#17149 = CARTESIAN_POINT ( 'NONE',  ( -18.62759615963255300, -10.81492255796106328, 69.16775706135234714 ) ) ;
#17150 = ORIENTED_EDGE ( 'NONE', *, *, #173096, .T. ) ;
#17151 = CARTESIAN_POINT ( 'NONE',  ( 0.05219959533936267826, -19.03943276465977164, 25.00109039468566152 ) ) ;
#17152 = CARTESIAN_POINT ( 'NONE',  ( 19.05341960407617918, -5.049401038297876454, 46.04275706135233293 ) ) ;
#17153 = PLANE ( 'NONE',  #118219 ) ;
#17154 = CARTESIAN_POINT ( 'NONE',  ( 5.823673210054444382, -21.52544592524334988, 30.20942372801902565 ) ) ;
#17155 = CARTESIAN_POINT ( 'NONE',  ( -7.405410116723207814, 1.490485923554937697, -62.24175268741322498 ) ) ;
#17156 = CARTESIAN_POINT ( 'NONE',  ( 13.89961937509957401, 13.97604488694547697, 26.87609039468566507 ) ) ;
#17157 = CARTESIAN_POINT ( 'NONE',  ( -16.46253265017160317, 9.564922557960807481, 80.83224293864769550 ) ) ;
#17158 = CARTESIAN_POINT ( 'NONE',  ( 19.03943276465977164, -0.05219959533909143690, 73.74890960531435269 ) ) ;
#17159 = CARTESIAN_POINT ( 'NONE',  ( -0.05219959533910754901, -16.53943276465976808, 27.49890960531435269 ) ) ;
#17161 = CARTESIAN_POINT ( 'NONE',  ( 18.67979575497194134, -10.72451020669871369, 80.83442372801901854 ) ) ;
#17160 = CARTESIAN_POINT ( 'NONE',  ( 18.67979575497178502, 10.72451020669898547, 24.16557627198103120 ) ) ;
#17162 = CARTESIAN_POINT ( 'NONE',  ( 22.81625015709509441, 31.40387420917330275, -9.824999997268811569 ) ) ;
#17163 = CARTESIAN_POINT ( 'NONE',  ( 16.18388926212240619, 7.379444403734400915, 57.93953151366151388 ) ) ;
#17164 = CARTESIAN_POINT ( 'NONE',  ( 15.80617190586769283, -15.72974639402175789, 85.62609039468568994 ) ) ;
#17165 = CARTESIAN_POINT ( 'NONE',  ( 16.20579543436675252, -7.371946100355224907, 41.93479165828123456 ) ) ;
#17166 = CARTESIAN_POINT ( 'NONE',  ( -16.46253265017160317, 9.564922557960807481, 95.83224293864769550 ) ) ;
#17167 = CARTESIAN_POINT ( 'NONE',  ( 33.83915642739259511, 1.250096592814747165, 100.3591031859434395 ) ) ;
#17168 = CARTESIAN_POINT ( 'NONE',  ( -15.72974639402197994, 15.80617190586746368, 65.62390960531436690 ) ) ;
#17169 = CARTESIAN_POINT ( 'NONE',  ( 0.05219959533910956823, 16.53943276465976808, 29.99890960531435979 ) ) ;
#17171 = CARTESIAN_POINT ( 'NONE',  ( -0.05219959533909027116, -19.03943276465977164, 92.49890960531436690 ) ) ;
#17170 = CARTESIAN_POINT ( 'NONE',  ( -4.483927247898539470, -16.52544592524342804, 112.2905762719810241 ) ) ;
#17172 = CARTESIAN_POINT ( 'NONE',  ( -18.67979575497193778, 10.72451020669871902, 113.3344237280190328 ) ) ;
#17173 = CARTESIAN_POINT ( 'NONE',  ( -13.97604488694527625, -13.89961937509977652, 21.87390960531435979 ) ) ;
#17174 = CARTESIAN_POINT ( 'NONE',  ( -5.823673210054431948, 21.52544592524334988, 72.70942372801901854 ) ) ;
#17175 = CARTESIAN_POINT ( 'NONE',  ( 16.46253265017160672, -9.564922557960803928, 113.3322429386476955 ) ) ;
#17176 = CARTESIAN_POINT ( 'NONE',  ( 16.55341960407618274, -4.379528057220086978, 106.0427570613523471 ) ) ;
#17177 = CARTESIAN_POINT ( 'NONE',  ( -9.564922557961040184, 16.46253265017147172, 67.91775706135233293 ) ) ;
#17178 = CARTESIAN_POINT ( 'NONE',  ( 18.22780087662122739, 5.500000000000000888, 66.48236817873106475 ) ) ;
#17179 = CARTESIAN_POINT ( 'NONE',  ( -19.02544592524342804, 5.153800228976336051, 106.0405762719810241 ) ) ;
#17180 = CARTESIAN_POINT ( 'NONE',  ( -12.14591786802309592, -12.06949235617757132, 86.87390960531438111 ) ) ;
#17181 = CARTESIAN_POINT ( 'NONE',  ( -13.89961937509957401, -13.97604488694547875, 64.37609039468567573 ) ) ;
#17182 = CARTESIAN_POINT ( 'NONE',  ( 9.474510206698971260, -16.51473224551069308, 77.91557627198103830 ) ) ;
#17183 = CARTESIAN_POINT ( 'NONE',  ( -8.314922557960811034, -14.29746914071050412, 57.08224293864769550 ) ) ;
#17184 = CARTESIAN_POINT ( 'NONE',  ( 5.153800228976615827, -19.02544592524334988, 95.20942372801897591 ) ) ;
#17185 = CARTESIAN_POINT ( 'NONE',  ( 5.719274019375991003, -21.55341960407610458, 52.70724293864769550 ) ) ;
#17186 = VERTEX_POINT ( 'NONE', #124573 ) ;
#17187 = CARTESIAN_POINT ( 'NONE',  ( 9.474510206698971260, -16.51473224551069308, 22.91557627198102765 ) ) ;
#17188 = CARTESIAN_POINT ( 'NONE',  ( -16.21995358207306737, -7.366697692864124569, 30.06448998487844904 ) ) ;
#17190 = CARTESIAN_POINT ( 'NONE',  ( -10.81492255796078084, -18.62759615963271287, 82.08224293864768129 ) ) ;
#17189 = CARTESIAN_POINT ( 'NONE',  ( -19.03943276465977164, 0.05219959533909376836, 66.24890960531436690 ) ) ;
#17192 = CARTESIAN_POINT ( 'NONE',  ( 16.46253265017160672, -9.564922557960803928, 73.33224293864769550 ) ) ;
#17191 = CARTESIAN_POINT ( 'NONE',  ( -4.483927247898782831, 16.52544592524335698, 97.70942372801904696 ) ) ;
#17193 = CARTESIAN_POINT ( 'NONE',  ( 13.89961937509957401, 13.97604488694547697, 51.87609039468566863 ) ) ;
#17194 = CARTESIAN_POINT ( 'NONE',  ( 10.72451020669871369, 18.67979575497193778, 77.08442372801901854 ) ) ;
#17195 = CARTESIAN_POINT ( 'NONE',  ( -10.72451020669898014, 18.67979575497178502, 60.41557627198102409 ) ) ;
#17196 = CARTESIAN_POINT ( 'NONE',  ( 10.72451020669898902, -18.67979575497178502, 22.91557627198102765 ) ) ;
#17197 = CARTESIAN_POINT ( 'NONE',  ( -13.89961937509977652, 13.97604488694528158, 40.62390960531435979 ) ) ;
#17198 = CARTESIAN_POINT ( 'NONE',  ( 12.06949235617739724, 12.14591786802326823, 96.87609039468568994 ) ) ;
#17199 = CARTESIAN_POINT ( 'NONE',  ( -12.14591786802326823, 12.06949235617739902, 28.12609039468568284 ) ) ;
#17200 = DIRECTION ( 'NONE',  ( 1.387778780781443782E-14, -0.7660444431189784575, 0.6427876096865388078 ) ) ;
#17201 = CARTESIAN_POINT ( 'NONE',  ( -15.80617190586768217, 15.72974639402176855, 98.12609039468570415 ) ) ;
#17202 = CARTESIAN_POINT ( 'NONE',  ( 4.379528057220339221, -16.55341960407611168, 62.70724293864769550 ) ) ;
#17203 = AXIS2_PLACEMENT_3D ( 'NONE', #13004, #46305, #77633 ) ;
#17204 = CARTESIAN_POINT ( 'NONE',  ( -15.72974639402197994, 15.80617190586746368, 90.62390960531436690 ) ) ;
#17205 = CARTESIAN_POINT ( 'NONE',  ( 21.52544592524344225, -5.823673210054117533, 88.54057627198103830 ) ) ;
#17206 = DIRECTION ( 'NONE',  ( -1.084202172485503448E-15, 1.000000000000000000, 0.000000000000000000 ) ) ;
#17207 = CARTESIAN_POINT ( 'NONE',  ( -18.62759615963270932, 10.81492255796079327, 40.83224293864769550 ) ) ;
#17208 = CARTESIAN_POINT ( 'NONE',  ( 12.14591786802327356, -12.06949235617739191, 85.62609039468568994 ) ) ;
#17209 = CARTESIAN_POINT ( 'NONE',  ( -0.05219959533910754901, -16.53943276465976808, 92.49890960531436690 ) ) ;
#17210 = CARTESIAN_POINT ( 'NONE',  ( 19.02544592524343514, -5.153800228976328945, 48.54057627198103120 ) ) ;
#17211 = FILL_AREA_STYLE ('',( #30390 ) ) ;
#17212 = CARTESIAN_POINT ( 'NONE',  ( 2.500000000000000000, 2.357898499370431722, -2.818925648462311528E-15 ) ) ;
#17213 = CARTESIAN_POINT ( 'NONE',  ( -8.314922557961024197, 14.29746914071037800, 92.91775706135236135 ) ) ;
#17214 = CARTESIAN_POINT ( 'NONE',  ( 21.52544592524334988, 5.823673210054432836, 36.45942372801901143 ) ) ;
#17215 = CARTESIAN_POINT ( 'NONE',  ( -13.89961937509977652, 13.97604488694528158, 100.6239096053143669 ) ) ;
#17216 = CARTESIAN_POINT ( 'NONE',  ( -10.72451020669870658, -18.67979575497194134, 64.58442372801900433 ) ) ;
#17217 = DIRECTION ( 'NONE',  ( 1.000000000000000000, 0.000000000000000000, -0.000000000000000000 ) ) ;
#17219 = EDGE_CURVE ( 'NONE', #15494, #90405, #9588, .T. ) ;
#17218 = CARTESIAN_POINT ( 'NONE',  ( -19.02544592524342804, 5.153800228976336051, 31.04057627198102409 ) ) ;
#17220 = ORIENTED_EDGE ( 'NONE', *, *, #112155, .T. ) ;
#17221 = CARTESIAN_POINT ( 'NONE',  ( -15.72974639402176322, -15.80617190586768395, 64.37609039468568994 ) ) ;
#17223 = FACE_OUTER_BOUND ( 'NONE', #41283, .T. ) ;
#17222 = CARTESIAN_POINT ( 'NONE',  ( 13.89961937509977652, -13.97604488694527269, 48.12390960531435979 ) ) ;
#17224 = CARTESIAN_POINT ( 'NONE',  ( 16.51473224551069308, 9.474510206698969483, 94.16557627198103830 ) ) ;
#17225 = CARTESIAN_POINT ( 'NONE',  ( 5.049401038297881783, 19.05341960407617563, 62.29275706135234003 ) ) ;
#17226 = CARTESIAN_POINT ( 'NONE',  ( 10.72451020669871369, 18.67979575497193778, 47.08442372801901854 ) ) ;
#17227 = CARTESIAN_POINT ( 'NONE',  ( -16.46253265017146816, -9.564922557961047289, 64.16775706135233293 ) ) ;
#17228 = CARTESIAN_POINT ( 'NONE',  ( -0.05219959533909027116, -19.03943276465977164, 42.49890960531435269 ) ) ;
#17229 = CARTESIAN_POINT ( 'NONE',  ( 12.14591786802327356, -12.06949235617739191, 100.6260903946857184 ) ) ;
#17230 = CARTESIAN_POINT ( 'NONE',  ( 5.153800228976615827, -19.02544592524334988, 70.20942372801899012 ) ) ;
#17231 = CARTESIAN_POINT ( 'NONE',  ( -16.53943276465976808, -0.05219959533934237506, 113.7510903946856757 ) ) ;
#17232 = CARTESIAN_POINT ( 'NONE',  ( -9.564922557961040184, 16.46253265017147172, 47.91775706135233293 ) ) ;
#17233 = CARTESIAN_POINT ( 'NONE',  ( -13.89961937509977652, 13.97604488694528158, 100.6239096053143669 ) ) ;
#17234 = CARTESIAN_POINT ( 'NONE',  ( 21.52544592524334988, 5.823673210054432836, 111.4594237280190328 ) ) ;
#17235 = CARTESIAN_POINT ( 'NONE',  ( 5.153800228976615827, -19.02544592524334988, 25.20942372801900433 ) ) ;
#17236 = CARTESIAN_POINT ( 'NONE',  ( -9.474510206698964154, 16.51473224551069663, 30.41557627198102054 ) ) ;
#17237 = CARTESIAN_POINT ( 'NONE',  ( -10.72451020669870658, -18.67979575497194134, 94.58442372801901854 ) ) ;
#17238 = CARTESIAN_POINT ( 'NONE',  ( 4.483927247898790824, -16.52544592524335698, 35.20942372801901854 ) ) ;
#17239 = CARTESIAN_POINT ( 'NONE',  ( 13.97604488694527802, 13.89961937509977652, 89.37390960531436690 ) ) ;
#17240 = VECTOR ( 'NONE', #34661, 1000.000000000000000 ) ;
#17241 = CARTESIAN_POINT ( 'NONE',  ( -17.14385361876520264, -23.59649016807271593, 139.1750000027311955 ) ) ;
#17242 = CARTESIAN_POINT ( 'NONE',  ( -19.02544592524342804, 5.153800228976336051, 76.04057627198102409 ) ) ;
#17243 = CARTESIAN_POINT ( 'NONE',  ( 0.000000000000000000, 0.000000000000000000, -25.00000000000000000 ) ) ;
#17244 = CARTESIAN_POINT ( 'NONE',  ( 5.153800228976615827, -19.02544592524334988, 85.20942372801900433 ) ) ;
#17245 = CARTESIAN_POINT ( 'NONE',  ( -19.03943276465977164, 0.05219959533909376836, 111.2489096053143669 ) ) ;
#17246 = CARTESIAN_POINT ( 'NONE',  ( 0.05219959533937995610, -21.53943276465977519, 100.0010903946857042 ) ) ;
#17247 = CARTESIAN_POINT ( 'NONE',  ( -12.06949235617756955, 12.14591786802309770, 95.62390960531436690 ) ) ;
#17248 = CARTESIAN_POINT ( 'NONE',  ( 16.46253265017160672, -9.564922557960803928, 23.33224293864769194 ) ) ;
#17249 = CARTESIAN_POINT ( 'NONE',  ( -15.72974639402197994, 15.80617190586746368, 45.62390960531436690 ) ) ;
#17250 = CARTESIAN_POINT ( 'NONE',  ( -21.53943276465977519, 0.05219959533907696930, 31.24890960531435979 ) ) ;
#17251 = CARTESIAN_POINT ( 'NONE',  ( -19.03943276465977164, 0.05219959533909376836, 26.24890960531435624 ) ) ;
#17252 = DIRECTION ( 'NONE',  ( 0.000000000000000000, 0.000000000000000000, 1.000000000000000000 ) ) ;
#17253 = CARTESIAN_POINT ( 'NONE',  ( 0.05219959533936267826, -19.03943276465977164, 60.00109039468566863 ) ) ;
#17254 = CARTESIAN_POINT ( 'NONE',  ( 14.34966873604960469, 8.224510206698951720, 39.16557627198102409 ) ) ;
#17255 = CARTESIAN_POINT ( 'NONE',  ( -16.51473224551069308, -9.474510206698971260, 111.6655762719810383 ) ) ;
#17256 = CARTESIAN_POINT ( 'NONE',  ( -21.55341960407619339, 5.719274019375674811, 73.54275706135234714 ) ) ;
#17257 = CARTESIAN_POINT ( 'NONE',  ( 15.72974639402199770, -15.80617190586745480, 73.12390960531436690 ) ) ;
#17258 = CARTESIAN_POINT ( 'NONE',  ( 15.72974639402176855, 15.80617190586768217, 46.87609039468568994 ) ) ;
#17259 = CARTESIAN_POINT ( 'NONE',  ( 21.52544592524344225, -5.823673210054117533, 98.54057627198105251 ) ) ;
#17260 = CARTESIAN_POINT ( 'NONE',  ( -21.55341960407619339, 5.719274019375674811, 53.54275706135234714 ) ) ;
#17261 = CARTESIAN_POINT ( 'NONE',  ( -0.05219959533909027116, -19.03943276465977164, 32.49890960531435979 ) ) ;
#17262 = CARTESIAN_POINT ( 'NONE',  ( 5.049401038298161559, -19.05341960407611168, 87.70724293864769550 ) ) ;
#17263 = CARTESIAN_POINT ( 'NONE',  ( -14.34966873604972548, 8.224510206698743886, 83.33442372801903275 ) ) ;
#17264 = CARTESIAN_POINT ( 'NONE',  ( 0.05219959533910956823, 16.53943276465976808, 109.9989096053143527 ) ) ;
#17265 = CARTESIAN_POINT ( 'NONE',  ( 16.46253265017160672, -9.564922557960803928, 108.3322429386476955 ) ) ;
#17266 = CARTESIAN_POINT ( 'NONE',  ( 0.05219959533910956823, 16.53943276465976808, 59.99890960531436690 ) ) ;
#17267 = CARTESIAN_POINT ( 'NONE',  ( 14.34966873604960469, 8.224510206698951720, 24.16557627198103120 ) ) ;
#17268 = CARTESIAN_POINT ( 'NONE',  ( -13.89961937509977652, 13.97604488694528158, 65.62390960531436690 ) ) ;
#17269 = CARTESIAN_POINT ( 'NONE',  ( -0.05219959533909027116, -19.03943276465977164, 37.49890960531436690 ) ) ;
#17270 = CARTESIAN_POINT ( 'NONE',  ( 18.67979575497178502, 10.72451020669898547, 49.16557627198102409 ) ) ;
#17271 = CARTESIAN_POINT ( 'NONE',  ( -9.474510206698720793, -16.51473224551083518, 39.58442372801899722 ) ) ;
#17273 = CARTESIAN_POINT ( 'NONE',  ( 0.05219959533910956823, 16.53943276465976808, 34.99890960531435979 ) ) ;
#17272 = CARTESIAN_POINT ( 'NONE',  ( -17.72662750342727733, -5.500000000000018652, 86.40179492283746754 ) ) ;
#17274 = CARTESIAN_POINT ( 'NONE',  ( 16.51473224551069308, 9.474510206698969483, 114.1655762719810241 ) ) ;
#17275 = CARTESIAN_POINT ( 'NONE',  ( 18.67979575497194134, -10.72451020669871369, 55.83442372801901854 ) ) ;
#17276 = CARTESIAN_POINT ( 'NONE',  ( 5.000000000000000000, -130.0000000000000000, 13.99999999999999822 ) ) ;
#17277 = CARTESIAN_POINT ( 'NONE',  ( -12.14591786802326823, 12.06949235617739902, 68.12609039468567573 ) ) ;
#17278 = CARTESIAN_POINT ( 'NONE',  ( 19.02544592524334988, 5.153800228976608722, 66.45942372801899012 ) ) ;
#17279 = CARTESIAN_POINT ( 'NONE',  ( -4.483927247898539470, -16.52544592524342804, 47.29057627198103120 ) ) ;
#17280 = CARTESIAN_POINT ( 'NONE',  ( 16.61371651742598132, -7.165104196376200996, 51.35415069993000259 ) ) ;
#17281 = CARTESIAN_POINT ( 'NONE',  ( 14.29746914071049879, -8.314922557960816363, 23.33224293864769194 ) ) ;
#17282 = CARTESIAN_POINT ( 'NONE',  ( -13.97604488694527625, -13.89961937509977652, 36.87390960531436690 ) ) ;
#17283 = CARTESIAN_POINT ( 'NONE',  ( -16.46253265017160317, 9.564922557960807481, 55.83224293864769550 ) ) ;
#17284 = CARTESIAN_POINT ( 'NONE',  ( -5.049401038298153566, 19.05341960407611168, 25.20724293864768484 ) ) ;
#17285 = CARTESIAN_POINT ( 'NONE',  ( -5.719274019375665041, -21.55341960407619695, 34.79275706135235424 ) ) ;
#17286 = CARTESIAN_POINT ( 'NONE',  ( 19.05341960407611168, 5.049401038298154454, 53.95724293864770260 ) ) ;
#17287 = CARTESIAN_POINT ( 'NONE',  ( 19.03943276465977164, -0.05219959533909143690, 113.7489096053143669 ) ) ;
#17288 = CARTESIAN_POINT ( 'NONE',  ( -13.89961937509977652, 13.97604488694528158, 45.62390960531433848 ) ) ;
#17289 = CARTESIAN_POINT ( 'NONE',  ( -10.81492255796078084, -18.62759615963271287, 27.08224293864769550 ) ) ;
#17291 = CARTESIAN_POINT ( 'NONE',  ( -13.89961937509977652, 13.97604488694528158, 25.62390960531434558 ) ) ;
#17290 = CARTESIAN_POINT ( 'NONE',  ( -18.62759615963255300, -10.81492255796106328, 54.16775706135235424 ) ) ;
#17292 = CARTESIAN_POINT ( 'NONE',  ( -15.80617190586745835, -15.72974639402198527, 26.87390960531435979 ) ) ;
#17293 = AXIS2_PLACEMENT_3D ( 'NONE', #144454, #3950, #112137 ) ;
#17294 = CARTESIAN_POINT ( 'NONE',  ( 4.483927247898790824, -16.52544592524335698, 75.20942372801901854 ) ) ;
#17295 = CARTESIAN_POINT ( 'NONE',  ( -18.62759615963255300, -10.81492255796106328, 109.1677570613523613 ) ) ;
#17296 = CARTESIAN_POINT ( 'NONE',  ( 8.224510206698742110, 14.34966873604972548, 67.08442372801901854 ) ) ;
#17297 = CARTESIAN_POINT ( 'NONE',  ( 5.153800228976335163, 19.02544592524342804, 109.7905762719810099 ) ) ;
#17298 = CARTESIAN_POINT ( 'NONE',  ( -16.53943276465976808, -0.05219959533934237506, 48.75109039468568284 ) ) ;
#17299 = CARTESIAN_POINT ( 'NONE',  ( -14.34966873604972548, 8.224510206698743886, 28.33442372801902209 ) ) ;
#17300 = CARTESIAN_POINT ( 'NONE',  ( -8.224510206698735004, -14.34966873604973081, 99.58442372801900433 ) ) ;
#17301 = CARTESIAN_POINT ( 'NONE',  ( 15.80617190586769283, -15.72974639402175789, 60.62609039468567573 ) ) ;
#17302 = CARTESIAN_POINT ( 'NONE',  ( 16.51473224551083163, -9.474510206698727899, 105.8344237280190043 ) ) ;
#17303 = CARTESIAN_POINT ( 'NONE',  ( 21.52544592524344225, -5.823673210054117533, 108.5405762719810241 ) ) ;
#17304 = CARTESIAN_POINT ( 'NONE',  ( -14.29746914071037622, -8.314922557961029526, 19.16775706135234714 ) ) ;
#17305 = CARTESIAN_POINT ( 'NONE',  ( -4.379528057220086978, -16.55341960407618274, 84.79275706135234714 ) ) ;
#17306 = LINE ( 'NONE', #170983, #63499 ) ;
#17307 = CARTESIAN_POINT ( 'NONE',  ( 5.719274019375673035, 21.55341960407619339, 82.29275706135234714 ) ) ;
#17308 = CARTESIAN_POINT ( 'NONE',  ( 5.153800228976615827, -19.02544592524334988, 80.20942372801901854 ) ) ;
#17309 = CARTESIAN_POINT ( 'NONE',  ( 4.483927247898545687, 16.52544592524342804, 44.79057627198103120 ) ) ;
#17310 = CARTESIAN_POINT ( 'NONE',  ( 12.14591786802309770, 12.06949235617756955, 39.37390960531436690 ) ) ;
#17311 = CARTESIAN_POINT ( 'NONE',  ( -8.314922557960811034, -14.29746914071050412, 102.0822429386476955 ) ) ;
#17313 = CARTESIAN_POINT ( 'NONE',  ( 16.79531203550682861, -7.028104445595345418, 56.24755011779544134 ) ) ;
#17312 = CARTESIAN_POINT ( 'NONE',  ( -0.05219959533936034679, 19.03943276465977164, 42.50109039468566152 ) ) ;
#17314 = CARTESIAN_POINT ( 'NONE',  ( 0.05219959533937995610, -21.53943276465977519, 35.00109039468568284 ) ) ;
#17315 = CARTESIAN_POINT ( 'NONE',  ( 9.474510206698729675, 16.51473224551082808, 112.0844237280190043 ) ) ;
#17316 = CARTESIAN_POINT ( 'NONE',  ( -69.65682714487590488, -71.74905178543390605, -25.00000000000000000 ) ) ;
#17317 = CARTESIAN_POINT ( 'NONE',  ( 16.46253265017160672, -9.564922557960803928, 98.33224293864769550 ) ) ;
#17318 = CARTESIAN_POINT ( 'NONE',  ( 10.72451020669898902, -18.67979575497178502, 52.91557627198103830 ) ) ;
#17319 = CARTESIAN_POINT ( 'NONE',  ( 5.153800228976335163, 19.02544592524342804, 84.79057627198099567 ) ) ;
#17320 = CARTESIAN_POINT ( 'NONE',  ( 18.62759615963271287, -10.81492255796078972, 63.33224293864770260 ) ) ;
#17321 = CARTESIAN_POINT ( 'NONE',  ( 8.224510206698953496, -14.34966873604960469, 107.9155762719810241 ) ) ;
#17322 = CARTESIAN_POINT ( 'NONE',  ( -16.46253265017160317, 9.564922557960807481, 70.83224293864770971 ) ) ;
#17323 = CARTESIAN_POINT ( 'NONE',  ( 19.05341960407611168, 5.049401038298154454, 23.95724293864769194 ) ) ;
#17324 = CARTESIAN_POINT ( 'NONE',  ( -5.823673210054431948, 21.52544592524334988, 32.70942372801900433 ) ) ;
#17325 = CARTESIAN_POINT ( 'NONE',  ( -21.55341960407619339, 5.719274019375674811, 78.54275706135236135 ) ) ;
#17326 = CARTESIAN_POINT ( 'NONE',  ( 8.314922557961029526, -14.29746914071037800, 85.41775706135236135 ) ) ;
#17327 = CARTESIAN_POINT ( 'NONE',  ( -15.72974639402176322, -15.80617190586768395, 24.37609039468567573 ) ) ;
#17328 = CARTESIAN_POINT ( 'NONE',  ( -21.53943276465977519, -0.05219959533937600094, 28.75109039468567929 ) ) ;
#17330 = CARTESIAN_POINT ( 'NONE',  ( -0.05219959533909027116, -19.03943276465977164, 82.49890960531436690 ) ) ;
#17329 = CARTESIAN_POINT ( 'NONE',  ( 0.05219959533936267826, -19.03943276465977164, 60.00109039468566863 ) ) ;
#17331 = CARTESIAN_POINT ( 'NONE',  ( -10.81492255796105439, 18.62759615963255655, 82.91775706135234714 ) ) ;
#17332 = CARTESIAN_POINT ( 'NONE',  ( 18.62759615963271287, -10.81492255796078972, 83.33224293864769550 ) ) ;
#17333 = CARTESIAN_POINT ( 'NONE',  ( -8.224510206698948167, 14.34966873604960824, 65.41557627198102409 ) ) ;
#17334 = CARTESIAN_POINT ( 'NONE',  ( -10.72451020669870658, -18.67979575497194134, 99.58442372801900433 ) ) ;
#17335 = CARTESIAN_POINT ( 'NONE',  ( 16.52544592524342804, -4.483927247898539470, 88.54057627198103830 ) ) ;
#17336 = CARTESIAN_POINT ( 'NONE',  ( -13.97604488694527625, -13.89961937509977652, 41.87390960531435979 ) ) ;
#17337 = CARTESIAN_POINT ( 'NONE',  ( 0.05219959533936267826, -19.03943276465977164, 70.00109039468566152 ) ) ;
#17338 = CARTESIAN_POINT ( 'NONE',  ( -4.379528057220328563, 16.55341960407611168, 35.20724293864768839 ) ) ;
#17339 = CARTESIAN_POINT ( 'NONE',  ( 5.719274019375673035, 21.55341960407619339, 92.29275706135236135 ) ) ;
#17340 = CARTESIAN_POINT ( 'NONE',  ( -13.89961937509977652, 13.97604488694528158, 90.62390960531432427 ) ) ;
#17341 = CARTESIAN_POINT ( 'NONE',  ( 9.564922557961047289, -16.46253265017146816, 60.41775706135233293 ) ) ;
#17342 = CARTESIAN_POINT ( 'NONE',  ( 21.53943276465977519, -0.05219959533907433946, 63.74890960531435979 ) ) ;
#17343 = CARTESIAN_POINT ( 'NONE',  ( 15.80617190586746368, 15.72974639402197994, 114.3739096053143527 ) ) ;
#17344 = CARTESIAN_POINT ( 'NONE',  ( 16.55341960407618274, -4.379528057220086978, 21.04275706135234714 ) ) ;
#17345 = CARTESIAN_POINT ( 'NONE',  ( 4.483927247898790824, -16.52544592524335698, 75.20942372801901854 ) ) ;
#17347 = CARTESIAN_POINT ( 'NONE',  ( -5.823673210054431948, 21.52544592524334988, 22.70942372801901499 ) ) ;
#17346 = CARTESIAN_POINT ( 'NONE',  ( 17.50000000000001066, 5.622605283950889543, 63.81207310596114013 ) ) ;
#17348 = CARTESIAN_POINT ( 'NONE',  ( 8.314922557960818139, 14.29746914071049879, 99.58224293864770971 ) ) ;
#17349 = CARTESIAN_POINT ( 'NONE',  ( -11.40812507854755609, 35.11059874428196537, -3.524999997268813523 ) ) ;
#17350 = CARTESIAN_POINT ( 'NONE',  ( -0.05219959533934338120, 16.53943276465976808, 37.50109039468568284 ) ) ;
#17351 = EDGE_CURVE ( 'NONE', #69099, #132572, #185724, .T. ) ;
#17352 = CARTESIAN_POINT ( 'NONE',  ( -5.823673210054116645, -21.52544592524344225, 57.29057627198103120 ) ) ;
#17353 = CARTESIAN_POINT ( 'NONE',  ( 16.53943276465976808, 0.05219959533934440121, 111.2510903946856899 ) ) ;
#17354 = CARTESIAN_POINT ( 'NONE',  ( 12.06949235617739724, 12.14591786802326823, 41.87609039468568284 ) ) ;
#17355 = CARTESIAN_POINT ( 'NONE',  ( 9.474510206698971260, -16.51473224551069308, 37.91557627198102409 ) ) ;
#17356 = CARTESIAN_POINT ( 'NONE',  ( 8.314922557961029526, -14.29746914071037800, 85.41775706135236135 ) ) ;
#17357 = CARTESIAN_POINT ( 'NONE',  ( -19.03943276465977164, -0.05219959533935918106, 78.75109039468567573 ) ) ;
#17358 = CARTESIAN_POINT ( 'NONE',  ( -10.72451020669898014, 18.67979575497178502, 75.41557627198102409 ) ) ;
#17359 = CARTESIAN_POINT ( 'NONE',  ( 16.53943276465976808, 0.05219959533934440121, 96.25109039468568994 ) ) ;
#17360 = CARTESIAN_POINT ( 'NONE',  ( -10.72451020669870658, -18.67979575497194134, 79.58442372801903275 ) ) ;
#17361 = CARTESIAN_POINT ( 'NONE',  ( -10.81492255796078084, -18.62759615963271287, 67.08224293864770971 ) ) ;
#17362 = CARTESIAN_POINT ( 'NONE',  ( -21.52544592524343514, 5.823673210054127303, 51.04057627198103120 ) ) ;
#17363 = VERTEX_POINT ( 'NONE', #16411 ) ;
#17364 = CARTESIAN_POINT ( 'NONE',  ( 8.314922557961029526, -14.29746914071037800, 75.41775706135233293 ) ) ;
#17365 = CARTESIAN_POINT ( 'NONE',  ( 21.52544592524344225, -5.823673210054117533, 43.54057627198103830 ) ) ;
#17366 = ORIENTED_EDGE ( 'NONE', *, *, #64977, .T. ) ;
#17367 = CARTESIAN_POINT ( 'NONE',  ( 5.153800228976335163, 19.02544592524342804, 114.7905762719810241 ) ) ;
#17368 = DIRECTION ( 'NONE',  ( -1.000000000000000000, 0.000000000000000000, 0.000000000000000000 ) ) ;
#17369 = CARTESIAN_POINT ( 'NONE',  ( 5.049401038298161559, -19.05341960407611168, 32.70724293864768129 ) ) ;
#17370 = CARTESIAN_POINT ( 'NONE',  ( -15.72974639402197994, 15.80617190586746368, 55.62390960531436690 ) ) ;
#17371 = CARTESIAN_POINT ( 'NONE',  ( -14.34966873604972548, 8.224510206698743886, 108.3344237280190185 ) ) ;
#17372 = CARTESIAN_POINT ( 'NONE',  ( 18.67979575497194134, -10.72451020669871369, 40.83442372801901854 ) ) ;
#17373 = CARTESIAN_POINT ( 'NONE',  ( -13.97604488694547697, 13.89961937509957934, 98.12609039468566152 ) ) ;
#17374 = CARTESIAN_POINT ( 'NONE',  ( -4.379528057220328563, 16.55341960407611168, 115.2072429386476955 ) ) ;
#17375 = CARTESIAN_POINT ( 'NONE',  ( 12.14591786802327356, -12.06949235617739191, 20.62609039468568639 ) ) ;
#17376 = CARTESIAN_POINT ( 'NONE',  ( 5.153800228976335163, 19.02544592524342804, 39.79057627198100988 ) ) ;
#17377 = CARTESIAN_POINT ( 'NONE',  ( 16.70000000000002061, 0.000000000000000000, -61.34707691135562868 ) ) ;
#17378 = CARTESIAN_POINT ( 'NONE',  ( -19.05341960407611168, -5.049401038298163336, 96.45724293864769550 ) ) ;
#17379 = CARTESIAN_POINT ( 'NONE',  ( 14.29746914071037800, 8.314922557961029526, 81.66775706135236135 ) ) ;
#17380 = CARTESIAN_POINT ( 'NONE',  ( -0.05219959533936034679, 19.03943276465977164, 72.50109039468566152 ) ) ;
#17381 = CARTESIAN_POINT ( 'NONE',  ( 0.05219959533936267826, -19.03943276465977164, 25.00109039468566152 ) ) ;
#17382 = CARTESIAN_POINT ( 'NONE',  ( -5.823673210054116645, -21.52544592524344225, 67.29057627198103830 ) ) ;
#17383 = CARTESIAN_POINT ( 'NONE',  ( 12.14591786802327356, -12.06949235617739191, 80.62609039468567573 ) ) ;
#17384 = CIRCLE ( 'NONE', #120715, 6.100000000000006750 ) ;
#17385 = CARTESIAN_POINT ( 'NONE',  ( 19.05341960407617918, -5.049401038297876454, 86.04275706135233293 ) ) ;
#17386 = CARTESIAN_POINT ( 'NONE',  ( -9.474510206698964154, 16.51473224551069663, 35.41557627198102409 ) ) ;
#17387 = CARTESIAN_POINT ( 'NONE',  ( -0.05219959533909027116, -19.03943276465977164, 77.49890960531435269 ) ) ;
#17388 = CARTESIAN_POINT ( 'NONE',  ( 10.72451020669871369, 18.67979575497193778, 52.08442372801901854 ) ) ;
#17389 = CARTESIAN_POINT ( 'NONE',  ( -5.153800228976328057, -19.02544592524343514, 52.29057627198100988 ) ) ;
#17390 = CARTESIAN_POINT ( 'NONE',  ( -19.02544592524334988, -5.153800228976617603, 68.95942372801896170 ) ) ;
#17391 = CARTESIAN_POINT ( 'NONE',  ( 21.88033147701266046, -9.239123595177041182, 171.1226046679831825 ) ) ;
#17392 = CARTESIAN_POINT ( 'NONE',  ( 13.97604488694527802, 13.89961937509977652, 114.3739096053143669 ) ) ;
#17393 = CARTESIAN_POINT ( 'NONE',  ( -14.29746914071049879, 8.314922557960819915, 60.83224293864769550 ) ) ;
#17394 = CARTESIAN_POINT ( 'NONE',  ( 21.53943276465977519, -0.05219959533907433946, 58.74890960531436690 ) ) ;
#17395 = DIRECTION ( 'NONE',  ( -1.000000000000000000, 0.000000000000000000, 0.000000000000000000 ) ) ;
#17396 = CARTESIAN_POINT ( 'NONE',  ( -19.02544592524334988, -5.153800228976617603, 43.95942372801899012 ) ) ;
#17397 = CARTESIAN_POINT ( 'NONE',  ( 0.000000000000000000, 0.000000000000000000, -10.00000000000000000 ) ) ;
#17399 = CARTESIAN_POINT ( 'NONE',  ( -5.049401038298153566, 19.05341960407611168, 80.20724293864769550 ) ) ;
#17398 = CARTESIAN_POINT ( 'NONE',  ( 19.03943276465977164, -0.05219959533909143690, 58.74890960531435979 ) ) ;
#17400 = CARTESIAN_POINT ( 'NONE',  ( -4.379528057220086978, -16.55341960407618274, 54.79275706135235424 ) ) ;
#17401 = CARTESIAN_POINT ( 'NONE',  ( 4.908066780550757180, -48.27782543269306359, -24.94981842180952469 ) ) ;
#17402 = DIRECTION ( 'NONE',  ( 1.000000000000000000, 0.000000000000000000, 0.000000000000000000 ) ) ;
#17403 = CARTESIAN_POINT ( 'NONE',  ( -12.14591786802326823, 12.06949235617739902, 93.12609039468568994 ) ) ;
#17404 = CARTESIAN_POINT ( 'NONE',  ( 24.77450267193474787, 6.022707119490100069, 168.7078695393446424 ) ) ;
#17405 = CARTESIAN_POINT ( 'NONE',  ( 12.14591786802327356, -12.06949235617739191, 65.62609039468568994 ) ) ;
#17406 = CARTESIAN_POINT ( 'NONE',  ( 0.05219959533934541429, -16.53943276465976808, 40.00109039468567573 ) ) ;
#17408 = DIRECTION ( 'NONE',  ( -1.000000000000000000, 0.000000000000000000, 0.000000000000000000 ) ) ;
#17407 = CARTESIAN_POINT ( 'NONE',  ( -19.03943276465977164, 0.05219959533909376836, 56.24890960531435979 ) ) ;
#17409 = CARTESIAN_POINT ( 'NONE',  ( 18.62759615963255655, 10.81492255796105972, 56.66775706135235424 ) ) ;
#17410 = CARTESIAN_POINT ( 'NONE',  ( 16.51473224551083163, -9.474510206698727899, 65.83442372801900433 ) ) ;
#17411 = CARTESIAN_POINT ( 'NONE',  ( -10.72451020669870658, -18.67979575497194134, 109.5844237280190328 ) ) ;
#17412 = CARTESIAN_POINT ( 'NONE',  ( 5.049401038298161559, -19.05341960407611168, 27.70724293864769550 ) ) ;
#17413 = CARTESIAN_POINT ( 'NONE',  ( -37.90990184318192036, -12.46459953034305101, -7.900967680773318236 ) ) ;
#17414 = CARTESIAN_POINT ( 'NONE',  ( 10.81492255796078972, 18.62759615963270932, 59.58224293864770260 ) ) ;
#17415 = CARTESIAN_POINT ( 'NONE',  ( -0.05219959533909027116, -19.03943276465977164, 112.4989096053143669 ) ) ;
#17416 = CARTESIAN_POINT ( 'NONE',  ( -16.53943276465976808, 0.05219959533911058130, 96.24890960531435269 ) ) ;
#17417 = CARTESIAN_POINT ( 'NONE',  ( -8.314922557961024197, 14.29746914071037800, 42.91775706135235424 ) ) ;
#17418 = EDGE_CURVE ( 'NONE', #75343, #15917, #153385, .T. ) ;
#17419 = CARTESIAN_POINT ( 'NONE',  ( 12.06949235617757843, -12.14591786802309237, 28.12390960531435979 ) ) ;
#17420 = ORIENTED_EDGE ( 'NONE', *, *, #28410, .F. ) ;
#17421 = CARTESIAN_POINT ( 'NONE',  ( 10.81492255796078972, 18.62759615963270932, 109.5822429386476955 ) ) ;
#17423 = CARTESIAN_POINT ( 'NONE',  ( 13.89961937509977652, -13.97604488694527269, 108.1239096053143669 ) ) ;
#17422 = CARTESIAN_POINT ( 'NONE',  ( 12.06949235617757843, -12.14591786802309237, 33.12390960531435979 ) ) ;
#17424 = CARTESIAN_POINT ( 'NONE',  ( 16.46253265017146816, 9.564922557961045513, 101.6677570613523329 ) ) ;
#17425 = CARTESIAN_POINT ( 'NONE',  ( -5.153800228976607833, 19.02544592524334988, 32.70942372801899722 ) ) ;
#17426 = CARTESIAN_POINT ( 'NONE',  ( -4.379528057220328563, 16.55341960407611168, 35.20724293864768839 ) ) ;
#17427 = CARTESIAN_POINT ( 'NONE',  ( -10.72451020669898014, 18.67979575497178502, 105.4155762719810383 ) ) ;
#17428 = CARTESIAN_POINT ( 'NONE',  ( 0.05219959533907565091, 21.53943276465977519, 59.99890960531436690 ) ) ;
#17429 = CARTESIAN_POINT ( 'NONE',  ( 13.97604488694527802, 13.89961937509977652, 79.37390960531435269 ) ) ;
#17430 = CARTESIAN_POINT ( 'NONE',  ( 0.05219959533910956823, 16.53943276465976808, 49.99890960531437401 ) ) ;
#17431 = CARTESIAN_POINT ( 'NONE',  ( 16.51473224551069308, 9.474510206698969483, 84.16557627198102409 ) ) ;
#17432 = EDGE_CURVE ( 'NONE', #66168, #48307, #66202, .T. ) ;
#17433 = CARTESIAN_POINT ( 'NONE',  ( -12.73749492396214578, -155.7167183371837496, -15.00000000000000178 ) ) ;
#17434 = CARTESIAN_POINT ( 'NONE',  ( -19.03943276465977164, -0.05219959533935918106, 43.75109039468566863 ) ) ;
#17435 = CARTESIAN_POINT ( 'NONE',  ( 10.72451020669898902, -18.67979575497178502, 97.91557627198103830 ) ) ;
#17436 = CARTESIAN_POINT ( 'NONE',  ( -16.53943276465976808, 0.05219959533911058130, 96.24890960531435269 ) ) ;
#17437 = CARTESIAN_POINT ( 'NONE',  ( 5.823673210054444382, -21.52544592524334988, 35.20942372801901854 ) ) ;
#17438 = CARTESIAN_POINT ( 'NONE',  ( -8.571926809382601320, -26.38167802310801591, 139.2750000027311899 ) ) ;
#17439 = CARTESIAN_POINT ( 'NONE',  ( -4.379528057220328563, 16.55341960407611168, 25.20724293864769550 ) ) ;
#17440 = CARTESIAN_POINT ( 'NONE',  ( -5.049401038298153566, 19.05341960407611168, 30.20724293864768839 ) ) ;
#17441 = CARTESIAN_POINT ( 'NONE',  ( -9.474510206698964154, 16.51473224551069663, 90.41557627198103830 ) ) ;
#17442 = CARTESIAN_POINT ( 'NONE',  ( 0.05219959533907565091, 21.53943276465977519, 64.99890960531435269 ) ) ;
#17443 = CARTESIAN_POINT ( 'NONE',  ( -18.56197773271731677, 5.499999999999904077, 43.55066217314453070 ) ) ;
#17444 = CARTESIAN_POINT ( 'NONE',  ( 13.89961937509977652, -13.97604488694527269, 28.12390960531435624 ) ) ;
#17445 = CARTESIAN_POINT ( 'NONE',  ( 10.72451020669898902, -18.67979575497178502, 52.91557627198103830 ) ) ;
#17446 = CARTESIAN_POINT ( 'NONE',  ( -21.52544592524334988, -5.823673210054445271, 68.95942372801901854 ) ) ;
#17448 = CARTESIAN_POINT ( 'NONE',  ( -16.52544592524335698, -4.483927247898792601, 63.95942372801901854 ) ) ;
#17447 = CARTESIAN_POINT ( 'NONE',  ( 23.65597376186088496, -29.51279439667791138, -21.31698521574967131 ) ) ;
#17449 = CARTESIAN_POINT ( 'NONE',  ( -5.153800228976328057, -19.02544592524343514, 62.29057627198100988 ) ) ;
#17450 = CARTESIAN_POINT ( 'NONE',  ( 19.02544592524343514, -5.153800228976328945, 58.54057627198102409 ) ) ;
#17451 = ORIENTED_EDGE ( 'NONE', *, *, #68080, .T. ) ;
#17452 = CARTESIAN_POINT ( 'NONE',  ( -18.67979575497193778, 10.72451020669871902, 108.3344237280190185 ) ) ;
#17453 = CARTESIAN_POINT ( 'NONE',  ( -4.379528057220086978, -16.55341960407618274, 74.79275706135234714 ) ) ;
#17454 = CARTESIAN_POINT ( 'NONE',  ( -21.52544592524334988, -5.823673210054445271, 98.95942372801903275 ) ) ;
#17455 = CARTESIAN_POINT ( 'NONE',  ( -9.564922557960796823, -16.46253265017161027, 62.08224293864769550 ) ) ;
#17456 = CARTESIAN_POINT ( 'NONE',  ( 10.81492255796078972, 18.62759615963270932, 29.58224293864769905 ) ) ;
#17457 = CARTESIAN_POINT ( 'NONE',  ( -16.51473224551082808, 9.474510206698731452, 108.3344237280190043 ) ) ;
#17458 = CARTESIAN_POINT ( 'NONE',  ( -5.719274019375665041, -21.55341960407619695, 79.79275706135236135 ) ) ;
#17459 = CARTESIAN_POINT ( 'NONE',  ( 16.53943276465976808, 0.05219959533934440121, 46.25109039468567573 ) ) ;
#17460 = CARTESIAN_POINT ( 'NONE',  ( 18.62759615963271287, -10.81492255796078972, 93.33224293864769550 ) ) ;
#17461 = CARTESIAN_POINT ( 'NONE',  ( 13.89961937509957401, 13.97604488694547697, 96.87609039468566152 ) ) ;
#17462 = CARTESIAN_POINT ( 'NONE',  ( 16.51473224551069308, 9.474510206698969483, 74.16557627198103830 ) ) ;
#17463 = CARTESIAN_POINT ( 'NONE',  ( -13.89961937509957401, -13.97604488694547875, 109.3760903946856331 ) ) ;
#17464 = CARTESIAN_POINT ( 'NONE',  ( -13.89961937509977652, 13.97604488694528158, 35.62390960531435269 ) ) ;
#17465 = AXIS2_PLACEMENT_3D ( 'NONE', #16447, #181346, #136801 ) ;
#17466 = CARTESIAN_POINT ( 'NONE',  ( 8.314922557961029526, -14.29746914071037800, 20.41775706135234714 ) ) ;
#17467 = CARTESIAN_POINT ( 'NONE',  ( 12.14591786802309770, 12.06949235617756955, 69.37390960531436690 ) ) ;
#17468 = CARTESIAN_POINT ( 'NONE',  ( -12.06949235617739369, -12.14591786802326823, 69.37609039468567573 ) ) ;
#17470 = CARTESIAN_POINT ( 'NONE',  ( -13.97604488694527625, -13.89961937509977652, 46.87390960531435979 ) ) ;
#17469 = CARTESIAN_POINT ( 'NONE',  ( -0.05219959533937732626, 21.53943276465977519, 32.50109039468568284 ) ) ;
#17471 = CARTESIAN_POINT ( 'NONE',  ( 19.02544592524343514, -5.153800228976328945, 73.54057627198103830 ) ) ;
#17472 = CARTESIAN_POINT ( 'NONE',  ( 14.34966873604972726, -8.224510206698740333, 70.83442372801901854 ) ) ;
#17473 = CARTESIAN_POINT ( 'NONE',  ( 6.938893903907228378E-15, 22.80000000000002913, -65.00100000000003320 ) ) ;
#17474 = ORIENTED_EDGE ( 'NONE', *, *, #177434, .F. ) ;
#17475 = CARTESIAN_POINT ( 'NONE',  ( -5.823673210054431948, 21.52544592524334988, 112.7094237280190328 ) ) ;
#17476 = CARTESIAN_POINT ( 'NONE',  ( -0.05219959533909027116, -19.03943276465977164, 37.49890960531436690 ) ) ;
#17478 = VERTEX_POINT ( 'NONE', #199438 ) ;
#17477 = CARTESIAN_POINT ( 'NONE',  ( 13.97604488694527802, 13.89961937509977652, 99.37390960531436690 ) ) ;
#17479 = CARTESIAN_POINT ( 'NONE',  ( -16.53943276465976808, -0.05219959533934237506, 33.75109039468568284 ) ) ;
#17481 = CARTESIAN_POINT ( 'NONE',  ( -12.14591786802326823, 12.06949235617739902, 48.12609039468568284 ) ) ;
#17480 = CARTESIAN_POINT ( 'NONE',  ( 16.46253265017146816, 9.564922557961045513, 41.66775706135234003 ) ) ;
#17482 = CARTESIAN_POINT ( 'NONE',  ( -19.05341960407611168, -5.049401038298163336, 41.45724293864769550 ) ) ;
#17483 = CARTESIAN_POINT ( 'NONE',  ( -13.89961937509977652, 13.97604488694528158, 100.6239096053143669 ) ) ;
#17484 = CARTESIAN_POINT ( 'NONE',  ( 16.51473224551069308, 9.474510206698969483, 59.16557627198102409 ) ) ;
#17485 = CARTESIAN_POINT ( 'NONE',  ( -21.52544592524343514, 5.823673210054127303, 101.0405762719810383 ) ) ;
#17487 = CARTESIAN_POINT ( 'NONE',  ( 16.46253265017160672, -9.564922557960803928, 108.3322429386476955 ) ) ;
#17486 = CARTESIAN_POINT ( 'NONE',  ( 19.03943276465977164, -0.05219959533909143690, 83.74890960531436690 ) ) ;
#17488 = CARTESIAN_POINT ( 'NONE',  ( -19.05341960407611168, -5.049401038298163336, 66.45724293864769550 ) ) ;
#17489 = CARTESIAN_POINT ( 'NONE',  ( -22.44159573604010305, 16.30477369853692338, 147.1750000027311671 ) ) ;
#17490 = CARTESIAN_POINT ( 'NONE',  ( 5.153800228976615827, -19.02544592524334988, 95.20942372801897591 ) ) ;
#17491 = CARTESIAN_POINT ( 'NONE',  ( -19.03943276465977164, -0.05219959533935918106, 23.75109039468566152 ) ) ;
#17492 = CARTESIAN_POINT ( 'NONE',  ( -4.483927247898539470, -16.52544592524342804, 62.29057627198102409 ) ) ;
#17493 = CARTESIAN_POINT ( 'NONE',  ( -21.53943276465977519, -0.05219959533937600094, 78.75109039468568994 ) ) ;
#17495 = B_SPLINE_CURVE_WITH_KNOTS ( 'NONE', 3,
 ( #103421, #117584, #165100, #52899, #25604, #114574, #99404, #147934, #71085, #177281, #69077, #9420, #132752, #37744, #161087, #22582, #130743, #192435, #194439, #55910 ),
 .UNSPECIFIED., .F., .F.,
 ( 4, 2, 2, 2, 2, 2, 2, 2, 2, 4 ),
 ( 3.469446951953614189E-18, 0.0004987090165372812679, 0.0009974180330745590663, 0.001246772541343198074, 0.001496127049611837082, 0.001994836066149110326, 0.002493545082686384438, 0.002742899590955021061, 0.002992254099223657683, 0.003989672132298169478 ),
 .UNSPECIFIED. ) ;
#17494 = CARTESIAN_POINT ( 'NONE',  ( -9.564922557960796823, -16.46253265017161027, 22.08224293864768839 ) ) ;
#17497 = CARTESIAN_POINT ( 'NONE',  ( -21.55341960407619339, 5.719274019375674811, 93.54275706135234714 ) ) ;
#17496 = CARTESIAN_POINT ( 'NONE',  ( 12.14591786802309770, 12.06949235617756955, 24.37390960531435979 ) ) ;
#17498 = CARTESIAN_POINT ( 'NONE',  ( 5.153800228976335163, 19.02544592524342804, 84.79057627198099567 ) ) ;
#17499 = CARTESIAN_POINT ( 'NONE',  ( 5.823673210054444382, -21.52544592524334988, 50.20942372801901854 ) ) ;
#17500 = CARTESIAN_POINT ( 'NONE',  ( -5.153800228976328057, -19.02544592524343514, 82.29057627198103830 ) ) ;
#17501 = CARTESIAN_POINT ( 'NONE',  ( -4.379528057220328563, 16.55341960407611168, 90.20724293864770971 ) ) ;
#17502 = CARTESIAN_POINT ( 'NONE',  ( -8.314922557960811034, -14.29746914071050412, 62.08224293864769550 ) ) ;
#17503 = CARTESIAN_POINT ( 'NONE',  ( -15.72974639402197994, 15.80617190586746368, 75.62390960531439532 ) ) ;
#17504 = CARTESIAN_POINT ( 'NONE',  ( 19.02544592524343514, -5.153800228976328945, 68.54057627198103830 ) ) ;
#17505 = CARTESIAN_POINT ( 'NONE',  ( -21.52544592524343514, 5.823673210054127303, 86.04057627198102409 ) ) ;
#17506 = CARTESIAN_POINT ( 'NONE',  ( 5.153800228976615827, -19.02544592524334988, 75.20942372801896170 ) ) ;
#17508 = CARTESIAN_POINT ( 'NONE',  ( 14.34966873604960469, 8.224510206698951720, 84.16557627198103830 ) ) ;
#17507 = CARTESIAN_POINT ( 'NONE',  ( -19.20446147854525876, -5.500000000000010658, 89.38999695167676407 ) ) ;
#17509 = CARTESIAN_POINT ( 'NONE',  ( 9.564922557960805705, 16.46253265017160317, 54.58224293864769550 ) ) ;
#17510 = CARTESIAN_POINT ( 'NONE',  ( -0.05219959533907301413, -21.53943276465977519, 62.49890960531436690 ) ) ;
#17511 = CARTESIAN_POINT ( 'NONE',  ( -26.53315420742543651, -7.611574518544844459, 168.2743882774363726 ) ) ;
#17513 = LINE ( 'NONE', #79171, #40385 ) ;
#17512 = CARTESIAN_POINT ( 'NONE',  ( 4.379528057220092307, 16.55341960407617563, 107.2927570613523471 ) ) ;
#17514 = CARTESIAN_POINT ( 'NONE',  ( 13.89961937509957401, 13.97604488694547697, 96.87609039468566152 ) ) ;
#17515 = CARTESIAN_POINT ( 'NONE',  ( -14.34966873604960291, -8.224510206698953496, 81.66557627198103830 ) ) ;
#17516 = CARTESIAN_POINT ( 'NONE',  ( 6.100000000000007638, -0.2002935562469382313, -62.50719930893271226 ) ) ;
#17517 = CARTESIAN_POINT ( 'NONE',  ( 13.97604488694527802, 13.89961937509977652, 74.37390960531436690 ) ) ;
#17518 = CARTESIAN_POINT ( 'NONE',  ( -0.05219959533909027116, -19.03943276465977164, 32.49890960531435979 ) ) ;
#17519 = CARTESIAN_POINT ( 'NONE',  ( -0.05219959533910754901, -16.53943276465976808, 62.49890960531436690 ) ) ;
#17520 = CARTESIAN_POINT ( 'NONE',  ( -13.97604488694527625, -13.89961937509977652, 96.87390960531433848 ) ) ;
#17522 = CARTESIAN_POINT ( 'NONE',  ( -9.564922557960796823, -16.46253265017161027, 67.08224293864769550 ) ) ;
#17521 = CARTESIAN_POINT ( 'NONE',  ( -13.97604488694547697, 13.89961937509957934, 88.12609039468563310 ) ) ;
#17523 = CARTESIAN_POINT ( 'NONE',  ( -19.05341960407611168, -5.049401038298163336, 91.45724293864766707 ) ) ;
#17524 = CARTESIAN_POINT ( 'NONE',  ( 21.53943276465977519, -0.05219959533907433946, 78.74890960531436690 ) ) ;
#17525 = CARTESIAN_POINT ( 'NONE',  ( 4.379528057220092307, 16.55341960407617563, 72.29275706135236135 ) ) ;
#17526 = CARTESIAN_POINT ( 'NONE',  ( -16.36317988757098263, 7.306389748694730457, 94.09789608363175262 ) ) ;
#17527 = CARTESIAN_POINT ( 'NONE',  ( 19.02544592524343514, -5.153800228976328945, 63.54057627198103830 ) ) ;
#17528 = CARTESIAN_POINT ( 'NONE',  ( 10.81492255796078972, 18.62759615963270932, 64.58224293864769550 ) ) ;
#17529 = CARTESIAN_POINT ( 'NONE',  ( 5.153800228976615827, -19.02544592524334988, 100.2094237280190043 ) ) ;
#17531 = CARTESIAN_POINT ( 'NONE',  ( -5.823673210054431948, 21.52544592524334988, 52.70942372801902565 ) ) ;
#17530 = CARTESIAN_POINT ( 'NONE',  ( 16.53943276465976808, -0.05219959533910856209, 43.74890960531435979 ) ) ;
#17532 = CARTESIAN_POINT ( 'NONE',  ( 69.65682714487590488, -71.74905178543389184, -15.00000000000000000 ) ) ;
#17534 = CARTESIAN_POINT ( 'NONE',  ( -9.564922557960796823, -16.46253265017161027, 112.0822429386476955 ) ) ;
#17533 = CARTESIAN_POINT ( 'NONE',  ( -0.05219959533934338120, 16.53943276465976808, 77.50109039468567573 ) ) ;
#17535 = CARTESIAN_POINT ( 'NONE',  ( -38.00000000000000711, 2.893978650043524126E-14, -25.00000000000000000 ) ) ;
#17536 = LINE ( 'NONE', #36413, #145438 ) ;
#17537 = CARTESIAN_POINT ( 'NONE',  ( -14.34966873604972548, 8.224510206698743886, 88.33442372801901854 ) ) ;
#17538 = CARTESIAN_POINT ( 'NONE',  ( 4.483927247898790824, -16.52544592524335698, 50.20942372801901854 ) ) ;
#17539 = CARTESIAN_POINT ( 'NONE',  ( 13.97604488694527802, 13.89961937509977652, 39.37390960531435269 ) ) ;
#17540 = CARTESIAN_POINT ( 'NONE',  ( -19.03943276465977164, 0.05219959533909376836, 56.24890960531435979 ) ) ;
#17541 = CARTESIAN_POINT ( 'NONE',  ( 5.719274019375673035, 21.55341960407619339, 57.29275706135234714 ) ) ;
#17542 = CARTESIAN_POINT ( 'NONE',  ( -16.53943276465976808, -0.05219959533934237506, 58.75109039468568994 ) ) ;
#17543 = CARTESIAN_POINT ( 'NONE',  ( -0.05219959533910754901, -16.53943276465976808, 37.49890960531436690 ) ) ;
#17544 = CARTESIAN_POINT ( 'NONE',  ( 16.46253265017160672, -9.564922557960803928, 48.33224293864769550 ) ) ;
#17545 = CARTESIAN_POINT ( 'NONE',  ( -0.05219959533909027116, -19.03943276465977164, 37.49890960531436690 ) ) ;
#17546 = CARTESIAN_POINT ( 'NONE',  ( -16.52544592524335698, -4.483927247898792601, 28.95942372801902209 ) ) ;
#17547 = VECTOR ( 'NONE', #121060, 1000.000000000000000 ) ;
#17548 = CARTESIAN_POINT ( 'NONE',  ( -5.049401038297874678, -19.05341960407617918, 79.79275706135233293 ) ) ;
#17549 = CARTESIAN_POINT ( 'NONE',  ( -4.379528057220328563, 16.55341960407611168, 80.20724293864769550 ) ) ;
#17550 = CARTESIAN_POINT ( 'NONE',  ( -5.153800228976328057, -19.02544592524343514, 47.29057627198102409 ) ) ;
#17552 = CARTESIAN_POINT ( 'NONE',  ( 3.766062262543149401E-15, -39.95556452105413570, -9.500000000000001776 ) ) ;
#17551 = CARTESIAN_POINT ( 'NONE',  ( -5.153800228976607833, 19.02544592524334988, 87.70942372801897591 ) ) ;
#17553 = CARTESIAN_POINT ( 'NONE',  ( -21.53943276465977519, -0.05219959533937600094, 93.75109039468567573 ) ) ;
#17554 = CARTESIAN_POINT ( 'NONE',  ( -14.34966873604972548, 8.224510206698743886, 53.33442372801901854 ) ) ;
#17555 = CARTESIAN_POINT ( 'NONE',  ( -29.15849868437705439, 7.427326039334300134, 174.4773576836617224 ) ) ;
#17556 = CARTESIAN_POINT ( 'NONE',  ( 15.80617190586746368, 15.72974639402197994, 44.37390960531435979 ) ) ;
#17557 = CARTESIAN_POINT ( 'NONE',  ( 12.06949235617739724, 12.14591786802326823, 41.87609039468568284 ) ) ;
#17558 = DIRECTION ( 'NONE',  ( 1.000000000000000000, 0.000000000000000000, -0.000000000000000000 ) ) ;
#17559 = CARTESIAN_POINT ( 'NONE',  ( -16.46253265017146816, -9.564922557961047289, 24.16775706135233648 ) ) ;
#17560 = CARTESIAN_POINT ( 'NONE',  ( -13.97604488694527625, -13.89961937509977652, 81.87390960531436690 ) ) ;
#17561 = CARTESIAN_POINT ( 'NONE',  ( 18.22780087662122384, -5.500000000000022204, 66.01540105326107266 ) ) ;
#17562 = CARTESIAN_POINT ( 'NONE',  ( 19.05341960407611168, 5.049401038298154454, 48.95724293864768129 ) ) ;
#17563 = CARTESIAN_POINT ( 'NONE',  ( -20.90420839357180682, -22.88042607247932025, -50.28910616114573884 ) ) ;
#17564 = CARTESIAN_POINT ( 'NONE',  ( -19.02544592524342804, 5.153800228976336051, 76.04057627198102409 ) ) ;
#17565 = CARTESIAN_POINT ( 'NONE',  ( -17.49999999999999289, 5.500000000000036415, 65.79690382534171533 ) ) ;
#17566 = CARTESIAN_POINT ( 'NONE',  ( -5.049401038297874678, -19.05341960407617918, 39.79275706135232582 ) ) ;
#17567 = CARTESIAN_POINT ( 'NONE',  ( -19.02544592524334988, -5.153800228976617603, 18.95942372801899722 ) ) ;
#17568 = CARTESIAN_POINT ( 'NONE',  ( 12.14591786802309770, 12.06949235617756955, 44.37390960531435979 ) ) ;
#17569 = CARTESIAN_POINT ( 'NONE',  ( -19.05341960407611168, -5.049401038298163336, 41.45724293864769550 ) ) ;
#17570 = CARTESIAN_POINT ( 'NONE',  ( -9.474510206698964154, 16.51473224551069663, 100.4155762719810241 ) ) ;
#17571 = CARTESIAN_POINT ( 'NONE',  ( 21.55341960407619695, -5.719274019375665929, 71.04275706135234714 ) ) ;
#17572 = CARTESIAN_POINT ( 'NONE',  ( -9.474510206698964154, 16.51473224551069663, 50.41557627198102409 ) ) ;
#17573 = CARTESIAN_POINT ( 'NONE',  ( -5.823673210054431948, 21.52544592524334988, 77.70942372801900433 ) ) ;
#17574 = CARTESIAN_POINT ( 'NONE',  ( -0.05219959533909027116, -19.03943276465977164, 112.4989096053143669 ) ) ;
#17575 = CARTESIAN_POINT ( 'NONE',  ( -19.05341960407611168, -5.049401038298163336, 41.45724293864769550 ) ) ;
#17576 = CARTESIAN_POINT ( 'NONE',  ( -18.62759615963255300, -10.81492255796106328, 19.16775706135234714 ) ) ;
#17577 = CARTESIAN_POINT ( 'NONE',  ( 19.05341960407617918, -5.049401038297876454, 46.04275706135233293 ) ) ;
#17578 = CARTESIAN_POINT ( 'NONE',  ( -5.153800228976328057, -19.02544592524343514, 27.29057627198103120 ) ) ;
#17579 = CARTESIAN_POINT ( 'NONE',  ( -5.153800228976328057, -19.02544592524343514, 72.29057627198102409 ) ) ;
#17581 = AXIS2_PLACEMENT_3D ( 'NONE', #169847, #44528, #28389 ) ;
#17580 = CARTESIAN_POINT ( 'NONE',  ( 19.05341960407617918, -5.049401038297876454, 106.0427570613523471 ) ) ;
#17582 = CARTESIAN_POINT ( 'NONE',  ( 14.29746914071049879, -8.314922557960816363, 78.33224293864770971 ) ) ;
#17583 = CARTESIAN_POINT ( 'NONE',  ( 18.67979575497178502, 10.72451020669898547, 34.16557627198102409 ) ) ;
#17584 = CARTESIAN_POINT ( 'NONE',  ( -5.153800228976607833, 19.02544592524334988, 97.70942372801900433 ) ) ;
#17585 = CARTESIAN_POINT ( 'NONE',  ( 21.55341960407610458, 5.719274019375980345, 108.9572429386476955 ) ) ;
#17586 = CARTESIAN_POINT ( 'NONE',  ( 18.67979575497194134, -10.72451020669871369, 55.83442372801901854 ) ) ;
#17587 = CARTESIAN_POINT ( 'NONE',  ( 4.483927247898790824, -16.52544592524335698, 50.20942372801901854 ) ) ;
#17588 = CARTESIAN_POINT ( 'NONE',  ( 0.05219959533934541429, -16.53943276465976808, 50.00109039468568994 ) ) ;
#17589 = CARTESIAN_POINT ( 'NONE',  ( 10.72451020669898902, -18.67979575497178502, 67.91557627198102409 ) ) ;
#17590 = CARTESIAN_POINT ( 'NONE',  ( 5.153800228976335163, 19.02544592524342804, 44.79057627198103830 ) ) ;
#17591 = CARTESIAN_POINT ( 'NONE',  ( -12.06949235617739369, -12.14591786802326823, 89.37609039468568994 ) ) ;
#17592 = EDGE_CURVE ( 'NONE', #10845, #135262, #45752, .T. ) ;
#17593 = CARTESIAN_POINT ( 'NONE',  ( -18.67979575497178146, -10.72451020669898902, 101.6655762719810383 ) ) ;
#17594 = CARTESIAN_POINT ( 'NONE',  ( -12.06949235617756955, 12.14591786802309770, 45.62390960531436690 ) ) ;
#17595 = CARTESIAN_POINT ( 'NONE',  ( 19.02544592524343514, -5.153800228976328945, 73.54057627198103830 ) ) ;
#17596 = CARTESIAN_POINT ( 'NONE',  ( 8.224510206698742110, 14.34966873604972548, 72.08442372801899012 ) ) ;
#17597 = CARTESIAN_POINT ( 'NONE',  ( 12.06949235617739724, 12.14591786802326823, 21.87609039468567573 ) ) ;
#17598 = CARTESIAN_POINT ( 'NONE',  ( 21.52544592524344225, -5.823673210054117533, 113.5405762719810383 ) ) ;
#17599 = CARTESIAN_POINT ( 'NONE',  ( -14.29746914071049879, 8.314922557960819915, 40.83224293864769550 ) ) ;
#17600 = EDGE_LOOP ( 'NONE', ( #161936, #80105, #14491, #79742 ) ) ;
#17601 = CARTESIAN_POINT ( 'NONE',  ( -17.40861289039003168, 6.110651285853257342, 68.62767529172569425 ) ) ;
#17602 = CARTESIAN_POINT ( 'NONE',  ( -18.62759615963270932, 10.81492255796079327, 90.83224293864769550 ) ) ;
#17603 = CARTESIAN_POINT ( 'NONE',  ( -4.483927247898539470, -16.52544592524342804, 27.29057627198103120 ) ) ;
#17604 = VERTEX_POINT ( 'NONE', #91227 ) ;
#17605 = LINE ( 'NONE', #175263, #59781 ) ;
#17606 = CARTESIAN_POINT ( 'NONE',  ( 15.80617190586746368, 15.72974639402197994, 104.3739096053143669 ) ) ;
#17607 = CARTESIAN_POINT ( 'NONE',  ( 16.51473224551069308, 9.474510206698969483, 109.1655762719810383 ) ) ;
#17608 = CARTESIAN_POINT ( 'NONE',  ( 21.52544592524334988, 5.823673210054432836, 21.45942372801901499 ) ) ;
#17609 = CARTESIAN_POINT ( 'NONE',  ( 16.53943276465976808, -0.05219959533910856209, 53.74890960531437401 ) ) ;
#17611 = CARTESIAN_POINT ( 'NONE',  ( -12.06949235617739369, -12.14591786802326823, 49.37609039468569705 ) ) ;
#17610 = VECTOR ( 'NONE', #40379, 1000.000000000000000 ) ;
#17612 = CARTESIAN_POINT ( 'NONE',  ( 16.46253265017160672, -9.564922557960803928, 63.33224293864769550 ) ) ;
#17613 = CARTESIAN_POINT ( 'NONE',  ( 19.03943276465977164, 0.05219959533936151252, 56.25109039468566863 ) ) ;
#17614 = CARTESIAN_POINT ( 'NONE',  ( -13.89961937509977652, 13.97604488694528158, 80.62390960531436690 ) ) ;
#17615 = EDGE_CURVE ( 'NONE', #85047, #60651, #14414, .T. ) ;
#17616 = CARTESIAN_POINT ( 'NONE',  ( 21.53943276465977519, -0.05219959533907433946, 38.74890960531435979 ) ) ;
#17617 = CARTESIAN_POINT ( 'NONE',  ( -27.29882810768609147, -25.71095057349984714, -18.52182797988006158 ) ) ;
#17618 = CARTESIAN_POINT ( 'NONE',  ( -16.46253265017160317, 9.564922557960807481, 45.83224293864769550 ) ) ;
#17619 = CARTESIAN_POINT ( 'NONE',  ( -14.29746914071037622, -8.314922557961029526, 24.16775706135235424 ) ) ;
#17620 = CARTESIAN_POINT ( 'NONE',  ( -5.153800228976607833, 19.02544592524334988, 62.70942372801899722 ) ) ;
#17621 = CARTESIAN_POINT ( 'NONE',  ( -0.05219959533907301413, -21.53943276465977519, 107.4989096053143669 ) ) ;
#17622 = CARTESIAN_POINT ( 'NONE',  ( -8.224510206698948167, 14.34966873604960824, 40.41557627198103120 ) ) ;
#17623 = CARTESIAN_POINT ( 'NONE',  ( -19.03943276465977164, 0.05219959533909376836, 86.24890960531436690 ) ) ;
#17624 = CARTESIAN_POINT ( 'NONE',  ( 10.81492255796078972, 18.62759615963270932, 59.58224293864770260 ) ) ;
#17626 = CARTESIAN_POINT ( 'NONE',  ( -14.29746914071037622, -8.314922557961029526, 29.16775706135234003 ) ) ;
#17625 = CARTESIAN_POINT ( 'NONE',  ( -10.72451020669898014, 18.67979575497178502, 90.41557627198103830 ) ) ;
#17627 = CARTESIAN_POINT ( 'NONE',  ( -10.81492255796078084, -18.62759615963271287, 22.08224293864769194 ) ) ;
#17628 = CARTESIAN_POINT ( 'NONE',  ( -5.823673210054431948, 21.52544592524334988, 82.70942372801900433 ) ) ;
#17629 = CARTESIAN_POINT ( 'NONE',  ( -16.51473224551069308, -9.474510206698971260, 86.66557627198102409 ) ) ;
#17630 = CARTESIAN_POINT ( 'NONE',  ( 19.05341960407611168, 5.049401038298154454, 33.95724293864769550 ) ) ;
#17631 = CARTESIAN_POINT ( 'NONE',  ( -9.564922557960796823, -16.46253265017161027, 82.08224293864768129 ) ) ;
#17632 = CARTESIAN_POINT ( 'NONE',  ( 8.314922557960818139, 14.29746914071049879, 99.58224293864770971 ) ) ;
#17633 = CARTESIAN_POINT ( 'NONE',  ( -13.89961937509977652, 13.97604488694528158, 65.62390960531436690 ) ) ;
#17634 = CARTESIAN_POINT ( 'NONE',  ( -14.34966873604972548, 8.224510206698743886, 23.33442372801901499 ) ) ;
#17635 = DIRECTION ( 'NONE',  ( -0.000000000000000000, -0.000000000000000000, -1.000000000000000000 ) ) ;
#17637 = CARTESIAN_POINT ( 'NONE',  ( -0.05219959533909027116, -19.03943276465977164, 107.4989096053143527 ) ) ;
#17636 = CARTESIAN_POINT ( 'NONE',  ( 15.72974639402176855, 15.80617190586768217, 91.87609039468568994 ) ) ;
#17638 = CARTESIAN_POINT ( 'NONE',  ( 8.224510206698742110, 14.34966873604972548, 92.08442372801901854 ) ) ;
#17639 = CARTESIAN_POINT ( 'NONE',  ( 22.72298157751957248, -20.62403296052382728, -47.41336191935017297 ) ) ;
#17640 = CARTESIAN_POINT ( 'NONE',  ( -16.51473224551082808, 9.474510206698731452, 68.33442372801900433 ) ) ;
#17641 = CARTESIAN_POINT ( 'NONE',  ( 16.51473224551083163, -9.474510206698727899, 25.83442372801900078 ) ) ;
#17642 = CARTESIAN_POINT ( 'NONE',  ( 12.31437665787661295, -24.87262748924413813, 139.9999999999999716 ) ) ;
#17643 = CARTESIAN_POINT ( 'NONE',  ( 13.89961937509977652, -13.97604488694527269, 33.12390960531434558 ) ) ;
#17644 = CARTESIAN_POINT ( 'NONE',  ( 0.05219959533910956823, 16.53943276465976808, 29.99890960531435979 ) ) ;
#17645 = DIRECTION ( 'NONE',  ( 0.8571673007021135549, 0.000000000000000000, 0.5150380749100520461 ) ) ;
#17646 = CARTESIAN_POINT ( 'NONE',  ( 14.29746914071037800, 8.314922557961029526, 111.6677570613523613 ) ) ;
#17647 = CARTESIAN_POINT ( 'NONE',  ( 17.05587630539785948, 6.762274262135716363, 66.75819690962687503 ) ) ;
#17648 = CARTESIAN_POINT ( 'NONE',  ( 12.06949235617739724, 12.14591786802326823, 76.87609039468567573 ) ) ;
#17649 = CARTESIAN_POINT ( 'NONE',  ( 5.049401038298161559, -19.05341960407611168, 42.70724293864767418 ) ) ;
#17650 = CARTESIAN_POINT ( 'NONE',  ( 21.55341960407619695, -5.719274019375665929, 96.04275706135236135 ) ) ;
#17651 = CARTESIAN_POINT ( 'NONE',  ( -0.05219959533936034679, 19.03943276465977164, 97.50109039468567573 ) ) ;
#17652 = CARTESIAN_POINT ( 'NONE',  ( -15.80617190586768217, 15.72974639402176855, 83.12609039468568994 ) ) ;
#17653 = CARTESIAN_POINT ( 'NONE',  ( -5.153800228976607833, 19.02544592524334988, 52.70942372801900433 ) ) ;
#17654 = CARTESIAN_POINT ( 'NONE',  ( 9.564922557960805705, 16.46253265017160317, 94.58224293864769550 ) ) ;
#17655 = CARTESIAN_POINT ( 'NONE',  ( -9.564922557960796823, -16.46253265017161027, 72.08224293864770971 ) ) ;
#17656 = CARTESIAN_POINT ( 'NONE',  ( -18.56197773271730966, 5.499999999999902300, 38.55066217314451649 ) ) ;
#17657 = CARTESIAN_POINT ( 'NONE',  ( 12.06949235617757843, -12.14591786802309237, 73.12390960531436690 ) ) ;
#17658 = CARTESIAN_POINT ( 'NONE',  ( -10.72451020669898014, 18.67979575497178502, 65.41557627198102409 ) ) ;
#17659 = CARTESIAN_POINT ( 'NONE',  ( -16.51473224551069308, -9.474510206698971260, 41.66557627198103120 ) ) ;
#17661 = CARTESIAN_POINT ( 'NONE',  ( 14.29746914071037800, 8.314922557961029526, 71.66775706135234714 ) ) ;
#17660 = CARTESIAN_POINT ( 'NONE',  ( -5.719274019375978568, 21.55341960407610458, 85.20724293864770971 ) ) ;
#17662 = EDGE_CURVE ( 'NONE', #60305, #126834, #52285, .T. ) ;
#17663 = VERTEX_POINT ( 'NONE', #183281 ) ;
#17664 = CARTESIAN_POINT ( 'NONE',  ( -19.03943276465977164, 0.05219959533909376836, 51.24890960531436690 ) ) ;
#17665 = CIRCLE ( 'NONE', #82280, 10.00000000000000000 ) ;
#17667 = CARTESIAN_POINT ( 'NONE',  ( 11.40812507854755253, -35.11059874428192273, -6.024999997268814411 ) ) ;
#17666 = CARTESIAN_POINT ( 'NONE',  ( 16.53943276465976808, -0.05219959533910856209, 73.74890960531433848 ) ) ;
#17668 = CARTESIAN_POINT ( 'NONE',  ( -5.153800228976328057, -19.02544592524343514, 52.29057627198100988 ) ) ;
#17669 = CARTESIAN_POINT ( 'NONE',  ( 16.51473224551069308, 9.474510206698969483, 24.16557627198102765 ) ) ;
#17670 = CARTESIAN_POINT ( 'NONE',  ( -16.46253265017146816, -9.564922557961047289, 64.16775706135233293 ) ) ;
#17671 = CARTESIAN_POINT ( 'NONE',  ( -4.379528057220328563, 16.55341960407611168, 75.20724293864769550 ) ) ;
#17672 = CARTESIAN_POINT ( 'NONE',  ( 0.05219959533937995610, -21.53943276465977519, 50.00109039468568994 ) ) ;
#17674 = CARTESIAN_POINT ( 'NONE',  ( 21.52544592524344225, -5.823673210054117533, 108.5405762719810241 ) ) ;
#17673 = CARTESIAN_POINT ( 'NONE',  ( -19.05341960407611168, -5.049401038298163336, 41.45724293864769550 ) ) ;
#17675 = CARTESIAN_POINT ( 'NONE',  ( 8.673617379884035472E-16, 0.000000000000000000, 0.000000000000000000 ) ) ;
#17676 = CARTESIAN_POINT ( 'NONE',  ( 16.55341960407611168, 4.379528057220329451, 88.95724293864769550 ) ) ;
#17677 = CARTESIAN_POINT ( 'NONE',  ( 19.65751872600772998, -34.84114385728654639, -25.66966870009445856 ) ) ;
#17678 = CARTESIAN_POINT ( 'NONE',  ( -0.05219959533909027116, -19.03943276465977164, 52.49890960531436690 ) ) ;
#17679 = CARTESIAN_POINT ( 'NONE',  ( 28.82186960331498327, 2.781578969918950771E-14, 145.0000000000000000 ) ) ;
#17681 = CARTESIAN_POINT ( 'NONE',  ( -9.474510206698964154, 16.51473224551069663, 100.4155762719810241 ) ) ;
#17680 = CARTESIAN_POINT ( 'NONE',  ( -16.46253265017146816, -9.564922557961047289, 94.16775706135233293 ) ) ;
#17682 = CARTESIAN_POINT ( 'NONE',  ( 21.55341960407619695, -5.719274019375665929, 36.04275706135234714 ) ) ;
#17683 = CARTESIAN_POINT ( 'NONE',  ( 19.02544592524343514, -5.153800228976328945, 83.54057627198100988 ) ) ;
#17684 = CARTESIAN_POINT ( 'NONE',  ( -16.51473224551082808, 9.474510206698731452, 73.33442372801900433 ) ) ;
#17685 = CARTESIAN_POINT ( 'NONE',  ( -19.05341960407611168, -5.049401038298163336, 46.45724293864768129 ) ) ;
#17686 = CARTESIAN_POINT ( 'NONE',  ( 4.379528057220339221, -16.55341960407611168, 62.70724293864769550 ) ) ;
#17687 = CARTESIAN_POINT ( 'NONE',  ( 12.06949235617757843, -12.14591786802309237, 73.12390960531436690 ) ) ;
#17688 = CARTESIAN_POINT ( 'NONE',  ( 9.564922557960805705, 16.46253265017160317, 74.58224293864769550 ) ) ;
#17689 = CARTESIAN_POINT ( 'NONE',  ( 21.55341960407610458, 5.719274019375980345, 98.95724293864770971 ) ) ;
#17690 = CARTESIAN_POINT ( 'NONE',  ( -5.049401038298153566, 19.05341960407611168, 65.20724293864765286 ) ) ;
#17691 = CIRCLE ( 'NONE', #88710, 4.999999999999998224 ) ;
#17692 = CARTESIAN_POINT ( 'NONE',  ( 0.05219959533937995610, -21.53943276465977519, 110.0010903946856757 ) ) ;
#17695 = CARTESIAN_POINT ( 'NONE',  ( -12.14591786802309592, -12.06949235617757132, 111.8739096053143669 ) ) ;
#17694 = CARTESIAN_POINT ( 'NONE',  ( -14.34966873604972548, 8.224510206698743886, 113.3344237280190328 ) ) ;
#17693 = CARTESIAN_POINT ( 'NONE',  ( 9.474510206698971260, -16.51473224551069308, 32.91557627198102409 ) ) ;
#17696 = CARTESIAN_POINT ( 'NONE',  ( 19.03943276465977164, 0.05219959533936151252, 101.2510903946856757 ) ) ;
#17697 = ORIENTED_EDGE ( 'NONE', *, *, #5625, .F. ) ;
#17698 = CARTESIAN_POINT ( 'NONE',  ( -5.719274019375665041, -21.55341960407619695, 24.79275706135235779 ) ) ;
#17699 = CARTESIAN_POINT ( 'NONE',  ( 9.564922557961047289, -16.46253265017146816, 60.41775706135233293 ) ) ;
#17700 = CARTESIAN_POINT ( 'NONE',  ( -4.379528057220086978, -16.55341960407618274, 109.7927570613523613 ) ) ;
#17701 = CARTESIAN_POINT ( 'NONE',  ( -21.55341960407610458, -5.719274019375992779, 76.45724293864769550 ) ) ;
#17702 = CARTESIAN_POINT ( 'NONE',  ( -15.80617190586745835, -15.72974639402198527, 21.87390960531436690 ) ) ;
#17703 = CARTESIAN_POINT ( 'NONE',  ( -12.06949235617756955, 12.14591786802309770, 50.62390960531435979 ) ) ;
#17704 = CARTESIAN_POINT ( 'NONE',  ( 9.564922557960805705, 16.46253265017160317, 34.58224293864770260 ) ) ;
#17705 = CARTESIAN_POINT ( 'NONE',  ( 19.03943276465977164, -0.05219959533909143690, 38.74890960531436690 ) ) ;
#17706 = CARTESIAN_POINT ( 'NONE',  ( 9.564922557961047289, -16.46253265017146816, 25.41775706135234003 ) ) ;
#17707 = CARTESIAN_POINT ( 'NONE',  ( -14.29746914071037622, -8.314922557961029526, 94.16775706135237556 ) ) ;
#17708 = CARTESIAN_POINT ( 'NONE',  ( 16.53943276465976808, 0.05219959533934440121, 56.25109039468568284 ) ) ;
#17709 = CARTESIAN_POINT ( 'NONE',  ( -5.823673210054116645, -21.52544592524344225, 22.29057627198102765 ) ) ;
#17711 = CARTESIAN_POINT ( 'NONE',  ( 15.72974639402176855, 15.80617190586768217, 111.8760903946856615 ) ) ;
#17710 = CARTESIAN_POINT ( 'NONE',  ( -9.564922557960796823, -16.46253265017161027, 52.08224293864768839 ) ) ;
#17712 = CARTESIAN_POINT ( 'NONE',  ( 13.97604488694527802, 13.89961937509977652, 84.37390960531433848 ) ) ;
#17713 = CARTESIAN_POINT ( 'NONE',  ( -0.05219959533934338120, 16.53943276465976808, 57.50109039468568994 ) ) ;
#17714 = CARTESIAN_POINT ( 'NONE',  ( -12.06949235617756955, 12.14591786802309770, 110.6239096053143669 ) ) ;
#17715 = CARTESIAN_POINT ( 'NONE',  ( 4.483927247898545687, 16.52544592524342804, 24.79057627198103120 ) ) ;
#17716 = CARTESIAN_POINT ( 'NONE',  ( 17.50000000000000000, -5.500000000000000888, 120.0000000000000142 ) ) ;
#17719 = CARTESIAN_POINT ( 'NONE',  ( -16.46253265017160317, 9.564922557960807481, 80.83224293864769550 ) ) ;
#17718 = CARTESIAN_POINT ( 'NONE',  ( -16.46253265017160317, 9.564922557960807481, 90.83224293864769550 ) ) ;
#17717 = CARTESIAN_POINT ( 'NONE',  ( 15.72974639402176855, 15.80617190586768217, 66.87609039468568994 ) ) ;
#17720 = CARTESIAN_POINT ( 'NONE',  ( 16.51473224551069308, 9.474510206698969483, 109.1655762719810383 ) ) ;
#17721 = CARTESIAN_POINT ( 'NONE',  ( 14.34966873604960469, 8.224510206698951720, 64.16557627198102409 ) ) ;
#17722 = CARTESIAN_POINT ( 'NONE',  ( 12.06949235617757843, -12.14591786802309237, 23.12390960531436335 ) ) ;
#17723 = VERTEX_POINT ( 'NONE', #29596 ) ;
#17724 = CARTESIAN_POINT ( 'NONE',  ( 4.379528057220339221, -16.55341960407611168, 32.70724293864770260 ) ) ;
#17727 = VECTOR ( 'NONE', #96835, 1000.000000000000000 ) ;
#17726 = LINE ( 'NONE', #125887, #25441 ) ;
#17725 = CARTESIAN_POINT ( 'NONE',  ( -0.05219959533934338120, 16.53943276465976808, 37.50109039468568284 ) ) ;
#17728 = CARTESIAN_POINT ( 'NONE',  ( -9.474510206698720793, -16.51473224551083518, 34.58442372801899722 ) ) ;
#17729 = CARTESIAN_POINT ( 'NONE',  ( 19.03943276465977164, -0.05219959533909143690, 78.74890960531436690 ) ) ;
#17730 = CARTESIAN_POINT ( 'NONE',  ( 5.049401038297881783, 19.05341960407617563, 52.29275706135234003 ) ) ;
#17731 = CARTESIAN_POINT ( 'NONE',  ( 36.91746824999999887, 11.99521256947799053, -10.02499999726881086 ) ) ;
#17733 = CARTESIAN_POINT ( 'NONE',  ( -16.53943276465976808, -0.05219959533934237506, 78.75109039468568994 ) ) ;
#17732 = CARTESIAN_POINT ( 'NONE',  ( -5.153800228976607833, 19.02544592524334988, 97.70942372801900433 ) ) ;
#17735 = CARTESIAN_POINT ( 'NONE',  ( 5.153800228976335163, 19.02544592524342804, 24.79057627198102765 ) ) ;
#17734 =( GEOMETRIC_REPRESENTATION_CONTEXT ( 3 ) GLOBAL_UNCERTAINTY_ASSIGNED_CONTEXT ( ( #141424 ) ) GLOBAL_UNIT_ASSIGNED_CONTEXT ( ( #198021, #182858, #135370 ) ) REPRESENTATION_CONTEXT ( 'NONE', 'WORKASPACE' ) );
#17736 = CARTESIAN_POINT ( 'NONE',  ( -9.474510206698964154, 16.51473224551069663, 100.4155762719810241 ) ) ;
#17737 = CARTESIAN_POINT ( 'NONE',  ( -10.81492255796105439, 18.62759615963255655, 47.91775706135234714 ) ) ;
#17738 = CARTESIAN_POINT ( 'NONE',  ( -19.02544592524334988, -5.153800228976617603, 83.95942372801901854 ) ) ;
#17740 = CARTESIAN_POINT ( 'NONE',  ( 13.97604488694527802, 13.89961937509977652, 44.37390960531435269 ) ) ;
#17739 = CARTESIAN_POINT ( 'NONE',  ( -38.00000000000000711, 2.428612866367529932E-14, -2.000000000000000000 ) ) ;
#17741 = CARTESIAN_POINT ( 'NONE',  ( -9.564922557960796823, -16.46253265017161027, 97.08224293864769550 ) ) ;
#17743 = CARTESIAN_POINT ( 'NONE',  ( -5.049401038298153566, 19.05341960407611168, 45.20724293864769550 ) ) ;
#17742 = CARTESIAN_POINT ( 'NONE',  ( -4.379528057220328563, 16.55341960407611168, 55.20724293864770260 ) ) ;
#17744 = CARTESIAN_POINT ( 'NONE',  ( 9.564922557960805705, 16.46253265017160317, 64.58224293864769550 ) ) ;
#17745 = CARTESIAN_POINT ( 'NONE',  ( -16.51473224551082808, 9.474510206698731452, 58.33442372801900433 ) ) ;
#17746 = CARTESIAN_POINT ( 'NONE',  ( 9.474510206698729675, 16.51473224551082808, 37.08442372801899722 ) ) ;
#17747 = CARTESIAN_POINT ( 'NONE',  ( 5.049401038297881783, 19.05341960407617563, 47.29275706135231161 ) ) ;
#17748 = CARTESIAN_POINT ( 'NONE',  ( -13.89961937509977652, 13.97604488694528158, 75.62390960531438111 ) ) ;
#17749 = CARTESIAN_POINT ( 'NONE',  ( 21.52544592524344225, -5.823673210054117533, 73.54057627198102409 ) ) ;
#17751 = CARTESIAN_POINT ( 'NONE',  ( 16.46253265017146816, 9.564922557961045513, 31.66775706135232937 ) ) ;
#17750 = CARTESIAN_POINT ( 'NONE',  ( 16.52544592524342804, -4.483927247898539470, 68.54057627198103830 ) ) ;
#17752 = CARTESIAN_POINT ( 'NONE',  ( 18.62759615963271287, -10.81492255796078972, 53.33224293864769550 ) ) ;
#17753 = CARTESIAN_POINT ( 'NONE',  ( -18.62759615963270932, 10.81492255796079327, 45.83224293864769550 ) ) ;
#17754 = CARTESIAN_POINT ( 'NONE',  ( 0.05219959533909260263, 19.03943276465977164, 64.99890960531436690 ) ) ;
#17755 = CARTESIAN_POINT ( 'NONE',  ( 0.05219959533909260263, 19.03943276465977164, 34.99890960531435979 ) ) ;
#17756 = CARTESIAN_POINT ( 'NONE',  ( 8.224510206698953496, -14.34966873604960469, 102.9155762719810383 ) ) ;
#17757 = AXIS2_PLACEMENT_3D ( 'NONE', #99951, #84776, #110396 ) ;
#17758 = CARTESIAN_POINT ( 'NONE',  ( -10.81492255796078084, -18.62759615963271287, 112.0822429386477097 ) ) ;
#17759 = CARTESIAN_POINT ( 'NONE',  ( 19.02544592524343514, -5.153800228976328945, 108.5405762719810383 ) ) ;
#17760 = CARTESIAN_POINT ( 'NONE',  ( 21.55341960407619695, -5.719274019375665929, 26.04275706135235779 ) ) ;
#17761 = CARTESIAN_POINT ( 'NONE',  ( -9.564922557960796823, -16.46253265017161027, 37.08224293864768839 ) ) ;
#17762 = CARTESIAN_POINT ( 'NONE',  ( -5.823673210054116645, -21.52544592524344225, 107.2905762719810525 ) ) ;
#17763 = CARTESIAN_POINT ( 'NONE',  ( 9.564922557961047289, -16.46253265017146816, 50.41775706135233293 ) ) ;
#17764 = CARTESIAN_POINT ( 'NONE',  ( -5.153800228976328057, -19.02544592524343514, 27.29057627198103120 ) ) ;
#17765 = CARTESIAN_POINT ( 'NONE',  ( -19.03943276465977164, 0.05219959533909376836, 21.24890960531436335 ) ) ;
#17766 = CARTESIAN_POINT ( 'NONE',  ( -14.29746914071037622, -8.314922557961029526, 64.16775706135234714 ) ) ;
#17767 = CARTESIAN_POINT ( 'NONE',  ( -5.049401038298153566, 19.05341960407611168, 30.20724293864768839 ) ) ;
#17768 = CARTESIAN_POINT ( 'NONE',  ( 34.35275354914907098, -2.907972467998146460, 90.32821402270533895 ) ) ;
#17769 = CARTESIAN_POINT ( 'NONE',  ( -0.05219959533909027116, -19.03943276465977164, 72.49890960531435269 ) ) ;
#17771 = ADVANCED_FACE ( 'NONE', ( #155906 ), #106417, .F. ) ;
#17770 = CARTESIAN_POINT ( 'NONE',  ( -14.34966873604960291, -8.224510206698953496, 111.6655762719810525 ) ) ;
#17772 = CARTESIAN_POINT ( 'NONE',  ( -18.62759615963270932, 10.81492255796079327, 40.83224293864769550 ) ) ;
#17773 = CARTESIAN_POINT ( 'NONE',  ( 4.483927247898545687, 16.52544592524342804, 79.79057627198102409 ) ) ;
#17774 = CARTESIAN_POINT ( 'NONE',  ( -14.34966873604972548, 8.224510206698743886, 33.33442372801900433 ) ) ;
#17775 = CARTESIAN_POINT ( 'NONE',  ( 5.719274019375673035, 21.55341960407619339, 87.29275706135236135 ) ) ;
#17776 = CARTESIAN_POINT ( 'NONE',  ( 13.89961937509977652, -13.97604488694527269, 28.12390960531435624 ) ) ;
#17777 = CARTESIAN_POINT ( 'NONE',  ( 16.52544592524335698, 4.483927247898782831, 111.4594237280190328 ) ) ;
#17778 = CARTESIAN_POINT ( 'NONE',  ( -12.06949235617756955, 12.14591786802309770, 60.62390960531437401 ) ) ;
#17779 = CARTESIAN_POINT ( 'NONE',  ( 19.03943276465977164, -0.05219959533909143690, 48.74890960531435979 ) ) ;
#17780 = CARTESIAN_POINT ( 'NONE',  ( 10.72451020669871369, 18.67979575497193778, 97.08442372801904696 ) ) ;
#17781 = CARTESIAN_POINT ( 'NONE',  ( -18.62759615963270932, 10.81492255796079327, 105.8322429386476955 ) ) ;
#17782 = CARTESIAN_POINT ( 'NONE',  ( -5.823673210054431948, 21.52544592524334988, 77.70942372801900433 ) ) ;
#17783 = CARTESIAN_POINT ( 'NONE',  ( 12.14591786802327356, -12.06949235617739191, 35.62609039468568994 ) ) ;
#17785 = CARTESIAN_POINT ( 'NONE',  ( 10.81492255796106328, -18.62759615963255655, 85.41775706135236135 ) ) ;
#17784 = CARTESIAN_POINT ( 'NONE',  ( 14.34966873604960469, 8.224510206698951720, 79.16557627198103830 ) ) ;
#17786 = CARTESIAN_POINT ( 'NONE',  ( -16.53943276465976808, -0.05219959533934237506, 108.7510903946857042 ) ) ;
#17787 = CARTESIAN_POINT ( 'NONE',  ( 28.79475375365487366, -9.355982642740542587, 141.1656553485623817 ) ) ;
#17788 = CARTESIAN_POINT ( 'NONE',  ( 14.29746914071037800, 8.314922557961029526, 36.66775706135234714 ) ) ;
#17789 = CARTESIAN_POINT ( 'NONE',  ( 14.34966873604960469, 8.224510206698951720, 39.16557627198102409 ) ) ;
#17790 = CARTESIAN_POINT ( 'NONE',  ( -4.483927247898782831, 16.52544592524335698, 82.70942372801900433 ) ) ;
#17791 = CARTESIAN_POINT ( 'NONE',  ( -13.97604488694527625, -13.89961937509977652, 101.8739096053143811 ) ) ;
#17792 = CARTESIAN_POINT ( 'NONE',  ( 13.97604488694527802, 13.89961937509977652, 104.3739096053143385 ) ) ;
#17793 = CARTESIAN_POINT ( 'NONE',  ( -15.80617190586768217, 15.72974639402176855, 103.1260903946856757 ) ) ;
#17794 = CARTESIAN_POINT ( 'NONE',  ( -12.06949235617739369, -12.14591786802326823, 99.37609039468568994 ) ) ;
#17795 = CARTESIAN_POINT ( 'NONE',  ( 12.06949235617757843, -12.14591786802309237, 73.12390960531436690 ) ) ;
#17796 = CARTESIAN_POINT ( 'NONE',  ( -5.153800228976328057, -19.02544592524343514, 87.29057627198103830 ) ) ;
#17797 = ORIENTED_EDGE ( 'NONE', *, *, #190985, .T. ) ;
#17798 = CARTESIAN_POINT ( 'NONE',  ( -4.379528057220086978, -16.55341960407618274, 29.79275706135234358 ) ) ;
#17799 = CARTESIAN_POINT ( 'NONE',  ( -0.05219959533909027116, -19.03943276465977164, 27.49890960531435624 ) ) ;
#17800 = CARTESIAN_POINT ( 'NONE',  ( -19.02544592524342804, 5.153800228976336051, 91.04057627198100988 ) ) ;
#17802 = CARTESIAN_POINT ( 'NONE',  ( -5.950531402560715689E-15, 38.81732327939063509, -1.124999997268812946 ) ) ;
#17801 = CARTESIAN_POINT ( 'NONE',  ( -12.14591786802326823, 12.06949235617739902, 33.12609039468569705 ) ) ;
#17803 = CARTESIAN_POINT ( 'NONE',  ( 16.51473224551083163, -9.474510206698727899, 30.83442372801900433 ) ) ;
#17804 = CARTESIAN_POINT ( 'NONE',  ( 12.14591786802327356, -12.06949235617739191, 100.6260903946857184 ) ) ;
#17805 = CARTESIAN_POINT ( 'NONE',  ( -0.05219959533936034679, 19.03943276465977164, 102.5010903946856757 ) ) ;
#17806 = CARTESIAN_POINT ( 'NONE',  ( -13.97604488694527625, -13.89961937509977652, 31.87390960531435979 ) ) ;
#17807 = CARTESIAN_POINT ( 'NONE',  ( 14.29746914071037800, 8.314922557961029526, 81.66775706135236135 ) ) ;
#17808 = CARTESIAN_POINT ( 'NONE',  ( -0.05219959533934338120, 16.53943276465976808, 62.50109039468568284 ) ) ;
#17809 = CARTESIAN_POINT ( 'NONE',  ( 16.51473224551069308, 9.474510206698969483, 34.16557627198102409 ) ) ;
#17810 = CARTESIAN_POINT ( 'NONE',  ( -13.89961937509957401, -13.97604488694547875, 69.37609039468564731 ) ) ;
#17811 = AXIS2_PLACEMENT_3D ( 'NONE', #55151, #23827, #8654 ) ;
#17812 = CARTESIAN_POINT ( 'NONE',  ( 13.89961937509957401, 13.97604488694547697, 21.87609039468566152 ) ) ;
#17813 = CARTESIAN_POINT ( 'NONE',  ( 13.89961937509977652, -13.97604488694527269, 53.12390960531434558 ) ) ;
#17814 = CARTESIAN_POINT ( 'NONE',  ( -5.153800228976328057, -19.02544592524343514, 97.29057627198099567 ) ) ;
#17815 = CARTESIAN_POINT ( 'NONE',  ( 4.483927247898545687, 16.52544592524342804, 84.79057627198102409 ) ) ;
#17816 = CARTESIAN_POINT ( 'NONE',  ( -13.97604488694547697, 13.89961937509957934, 58.12609039468566863 ) ) ;
#17817 = CARTESIAN_POINT ( 'NONE',  ( 15.80617190586746368, 15.72974639402197994, 49.37390960531436690 ) ) ;
#17818 = CARTESIAN_POINT ( 'NONE',  ( -5.823673210054431948, 21.52544592524334988, 107.7094237280190328 ) ) ;
#17819 = CARTESIAN_POINT ( 'NONE',  ( -0.05219959533909027116, -19.03943276465977164, 92.49890960531436690 ) ) ;
#17820 = CARTESIAN_POINT ( 'NONE',  ( 13.97604488694548053, -13.89961937509957401, 25.62609039468566507 ) ) ;
#17821 = CARTESIAN_POINT ( 'NONE',  ( -21.53943276465977519, 0.05219959533907696930, 61.24890960531435979 ) ) ;
#17822 = CARTESIAN_POINT ( 'NONE',  ( -19.02544592524342804, 5.153800228976336051, 111.0405762719810099 ) ) ;
#17823 = CARTESIAN_POINT ( 'NONE',  ( -16.46253265017146816, -9.564922557961047289, 89.16775706135234714 ) ) ;
#17824 = CARTESIAN_POINT ( 'NONE',  ( -19.03943276465977164, 0.05219959533909376836, 116.2489096053143669 ) ) ;
#17825 = CARTESIAN_POINT ( 'NONE',  ( -0.05219959533936034679, 19.03943276465977164, 107.5010903946856615 ) ) ;
#17826 = CARTESIAN_POINT ( 'NONE',  ( -16.52544592524342804, 4.483927247898546575, 111.0405762719810525 ) ) ;
#17827 = CARTESIAN_POINT ( 'NONE',  ( 5.153800228976335163, 19.02544592524342804, 94.79057627198103830 ) ) ;
#17828 = CARTESIAN_POINT ( 'NONE',  ( -21.53943276465977519, 0.05219959533907696930, 81.24890960531436690 ) ) ;
#17829 = CARTESIAN_POINT ( 'NONE',  ( 8.224510206698742110, 14.34966873604972548, 52.08442372801901854 ) ) ;
#17830 = CARTESIAN_POINT ( 'NONE',  ( -15.80617190586768217, 15.72974639402176855, 43.12609039468568284 ) ) ;
#17831 = CARTESIAN_POINT ( 'NONE',  ( 21.55341960407619695, -5.719274019375665929, 96.04275706135236135 ) ) ;
#17832 = CARTESIAN_POINT ( 'NONE',  ( 12.06949235617739724, 12.14591786802326823, 101.8760903946857042 ) ) ;
#17833 = CARTESIAN_POINT ( 'NONE',  ( 5.153800228976335163, 19.02544592524342804, 89.79057627198102409 ) ) ;
#17834 = CARTESIAN_POINT ( 'NONE',  ( -14.34966873604960291, -8.224510206698953496, 91.66557627198103830 ) ) ;
#17835 = CARTESIAN_POINT ( 'NONE',  ( -4.483927247898539470, -16.52544592524342804, 37.29057627198102409 ) ) ;
#17836 = CARTESIAN_POINT ( 'NONE',  ( -16.46253265017146816, -9.564922557961047289, 64.16775706135233293 ) ) ;
#17837 = CARTESIAN_POINT ( 'NONE',  ( 18.62759615963255655, 10.81492255796105972, 46.66775706135234714 ) ) ;
#17838 = CARTESIAN_POINT ( 'NONE',  ( -5.049401038297874678, -19.05341960407617918, 29.79275706135232227 ) ) ;
#17839 = CARTESIAN_POINT ( 'NONE',  ( -12.14591786802309592, -12.06949235617757132, 96.87390960531436690 ) ) ;
#17840 = CARTESIAN_POINT ( 'NONE',  ( -21.53943276465977519, 0.05219959533907696930, 31.24890960531435979 ) ) ;
#17841 = CARTESIAN_POINT ( 'NONE',  ( -8.314922557960811034, -14.29746914071050412, 27.08224293864769550 ) ) ;
#17842 = CARTESIAN_POINT ( 'NONE',  ( -21.53943276465977519, -0.05219959533937600094, 88.75109039468567573 ) ) ;
#17843 = CARTESIAN_POINT ( 'NONE',  ( -16.52544592524335698, -4.483927247898792601, 58.95942372801902565 ) ) ;
#17844 = CARTESIAN_POINT ( 'NONE',  ( -8.314922557961024197, 14.29746914071037800, 112.9177570613523329 ) ) ;
#17845 = CARTESIAN_POINT ( 'NONE',  ( -21.55341960407619339, 5.719274019375674811, 48.54275706135234714 ) ) ;
#17846 = ORIENTED_EDGE ( 'NONE', *, *, #166361, .T. ) ;
#17847 = CARTESIAN_POINT ( 'NONE',  ( 21.55341960407619695, -5.719274019375665929, 31.04275706135234714 ) ) ;
#17848 = CARTESIAN_POINT ( 'NONE',  ( 14.34966873604960469, 8.224510206698951720, 104.1655762719810241 ) ) ;
#17849 = EDGE_CURVE ( 'NONE', #61533, #22005, #93569, .T. ) ;
#17850 = CARTESIAN_POINT ( 'NONE',  ( 0.05219959533909260263, 19.03943276465977164, 24.99890960531435269 ) ) ;
#17851 = CARTESIAN_POINT ( 'NONE',  ( -14.29746914071049879, 8.314922557960819915, 65.83224293864769550 ) ) ;
#17852 = CARTESIAN_POINT ( 'NONE',  ( -19.05341960407611168, -5.049401038298163336, 76.45724293864769550 ) ) ;
#17853 = CARTESIAN_POINT ( 'NONE',  ( 12.06949235617739724, 12.14591786802326823, 106.8760903946856899 ) ) ;
#17854 = CARTESIAN_POINT ( 'NONE',  ( 15.80617190586746368, 15.72974639402197994, 54.37390960531435979 ) ) ;
#17855 = CARTESIAN_POINT ( 'NONE',  ( 0.05219959533910956823, 16.53943276465976808, 94.99890960531436690 ) ) ;
#17856 = VECTOR ( 'NONE', #55254, 1000.000000000000000 ) ;
#17857 = CARTESIAN_POINT ( 'NONE',  ( 21.52544592524344225, -5.823673210054117533, 98.54057627198105251 ) ) ;
#17858 = CARTESIAN_POINT ( 'NONE',  ( 5.153800228976335163, 19.02544592524342804, 99.79057627198102409 ) ) ;
#17860 = CARTESIAN_POINT ( 'NONE',  ( -9.474510206698720793, -16.51473224551083518, 94.58442372801900433 ) ) ;
#17859 = CARTESIAN_POINT ( 'NONE',  ( -16.46253265017160317, 9.564922557960807481, 50.83224293864770260 ) ) ;
#17861 = ADVANCED_FACE ( 'NONE', ( #8205 ), #5192, .T. ) ;
#17862 = CARTESIAN_POINT ( 'NONE',  ( -21.52544592524343514, 5.823673210054127303, 41.04057627198103120 ) ) ;
#17863 = CARTESIAN_POINT ( 'NONE',  ( -21.53943276465977519, -0.05219959533937600094, 63.75109039468568284 ) ) ;
#17864 = CARTESIAN_POINT ( 'NONE',  ( -5.049401038298153566, 19.05341960407611168, 55.20724293864769550 ) ) ;
#17865 = CARTESIAN_POINT ( 'NONE',  ( 5.049401038298161559, -19.05341960407611168, 82.70724293864770971 ) ) ;
#17866 = CARTESIAN_POINT ( 'NONE',  ( 8.224510206698742110, 14.34966873604972548, 57.08442372801901854 ) ) ;
#17867 = CARTESIAN_POINT ( 'NONE',  ( -15.72974639402176322, -15.80617190586768395, 44.37609039468567573 ) ) ;
#17868 = CARTESIAN_POINT ( 'NONE',  ( 18.67979575497194134, -10.72451020669871369, 90.83442372801901854 ) ) ;
#17869 = CARTESIAN_POINT ( 'NONE',  ( 21.55341960407610458, 5.719274019375980345, 103.9572429386476813 ) ) ;
#17870 = AXIS2_PLACEMENT_3D ( 'NONE', #4343, #130687, #157056 ) ;
#17872 = CARTESIAN_POINT ( 'NONE',  ( -16.52544592524335698, -4.483927247898792601, 63.95942372801901854 ) ) ;
#17871 = CARTESIAN_POINT ( 'NONE',  ( 5.719274019375673035, 21.55341960407619339, 32.29275706135235424 ) ) ;
#17873 = CARTESIAN_POINT ( 'NONE',  ( -21.52544592524343514, 5.823673210054127303, 81.04057627198102409 ) ) ;
#17874 = CARTESIAN_POINT ( 'NONE',  ( -13.97604488694547697, 13.89961937509957934, 33.12609039468566863 ) ) ;
#17876 = CARTESIAN_POINT ( 'NONE',  ( -0.05219959533934338120, 16.53943276465976808, 112.5010903946857042 ) ) ;
#17875 = CARTESIAN_POINT ( 'NONE',  ( 19.05341960407611168, 5.049401038298154454, 63.95724293864769550 ) ) ;
#17877 = CARTESIAN_POINT ( 'NONE',  ( -17.49999999999999289, -3.209263204892650823, 105.2380317439373982 ) ) ;
#17878 = CARTESIAN_POINT ( 'NONE',  ( -16.51473224551069308, -9.474510206698971260, 96.66557627198102409 ) ) ;
#17879 = CYLINDRICAL_SURFACE ( 'NONE', #60326, 28.82186960331498682 ) ;
#17880 = CARTESIAN_POINT ( 'NONE',  ( 19.05341960407617918, -5.049401038297876454, 81.04275706135231871 ) ) ;
#17881 = CARTESIAN_POINT ( 'NONE',  ( -5.719274019375978568, 21.55341960407610458, 55.20724293864770260 ) ) ;
#17882 = CARTESIAN_POINT ( 'NONE',  ( 16.55341960407611168, 4.379528057220329451, 33.95724293864769550 ) ) ;
#17883 = CARTESIAN_POINT ( 'NONE',  ( 19.05341960407617918, -5.049401038297876454, 111.0427570613523329 ) ) ;
#17884 = CARTESIAN_POINT ( 'NONE',  ( 9.564922557960805705, 16.46253265017160317, 34.58224293864770260 ) ) ;
#17885 = CARTESIAN_POINT ( 'NONE',  ( -19.05341960407617563, 5.049401038297882671, 113.5427570613523471 ) ) ;
#17887 = CARTESIAN_POINT ( 'NONE',  ( 16.46253265017146816, 9.564922557961045513, 76.66775706135234714 ) ) ;
#17886 = CARTESIAN_POINT ( 'NONE',  ( -10.72451020669898014, 18.67979575497178502, 95.41557627198102409 ) ) ;
#17888 = CARTESIAN_POINT ( 'NONE',  ( 0.05219959533934541429, -16.53943276465976808, 85.00109039468568994 ) ) ;
#17889 = CARTESIAN_POINT ( 'NONE',  ( 0.05219959533909260263, 19.03943276465977164, 74.99890960531435269 ) ) ;
#17890 = CARTESIAN_POINT ( 'NONE',  ( 4.379528057220339221, -16.55341960407611168, 82.70724293864770971 ) ) ;
#17891 = CARTESIAN_POINT ( 'NONE',  ( 5.049401038298161559, -19.05341960407611168, 67.70724293864769550 ) ) ;
#17892 = CARTESIAN_POINT ( 'NONE',  ( 14.29746914071049879, -8.314922557960816363, 63.33224293864770260 ) ) ;
#17893 = PLANE ( 'NONE',  #167944 ) ;
#17894 = CARTESIAN_POINT ( 'NONE',  ( -17.26832448383786200, -5.411067243102611890, 21.06455627637857830 ) ) ;
#17895 = CARTESIAN_POINT ( 'NONE',  ( 14.29746914071049879, -8.314922557960816363, 38.33224293864768839 ) ) ;
#17896 = CARTESIAN_POINT ( 'NONE',  ( -9.564922557960796823, -16.46253265017161027, 77.08224293864769550 ) ) ;
#17897 = CARTESIAN_POINT ( 'NONE',  ( -1.359015117358330027, -15.84196527238552754, -59.51370404797111746 ) ) ;
#17898 = CARTESIAN_POINT ( 'NONE',  ( 19.05341960407617918, -5.049401038297876454, 41.04275706135233293 ) ) ;
#17899 = CARTESIAN_POINT ( 'NONE',  ( 16.53943276465976808, 0.05219959533934440121, 41.25109039468568284 ) ) ;
#17900 = CARTESIAN_POINT ( 'NONE',  ( 5.719274019375991003, -21.55341960407610458, 62.70724293864769550 ) ) ;
#17901 = CARTESIAN_POINT ( 'NONE',  ( -5.049401038297874678, -19.05341960407617918, 24.79275706135233648 ) ) ;
#17902 = CARTESIAN_POINT ( 'NONE',  ( -9.474510206698964154, 16.51473224551069663, 70.41557627198102409 ) ) ;
#17903 = DIRECTION ( 'NONE',  ( 0.000000000000000000, 0.000000000000000000, 1.000000000000000000 ) ) ;
#17904 = CARTESIAN_POINT ( 'NONE',  ( -5.153800228976328057, -19.02544592524343514, 112.2905762719810099 ) ) ;
#17905 = CARTESIAN_POINT ( 'NONE',  ( -15.72974639402176322, -15.80617190586768395, 39.37609039468567573 ) ) ;
#17906 = CARTESIAN_POINT ( 'NONE',  ( 12.14591786802309770, 12.06949235617756955, 104.3739096053143669 ) ) ;
#17909 = ORIENTED_EDGE ( 'NONE', *, *, #89293, .T. ) ;
#17908 = CARTESIAN_POINT ( 'NONE',  ( 19.03943276465977164, -0.05219959533909143690, 83.74890960531436690 ) ) ;
#17907 = CARTESIAN_POINT ( 'NONE',  ( -21.52544592524343514, 5.823673210054127303, 96.04057627198102409 ) ) ;
#17910 = CARTESIAN_POINT ( 'NONE',  ( 21.53943276465977519, 0.05219959533937863772, 21.25109039468567218 ) ) ;
#17911 = ORIENTED_EDGE ( 'NONE', *, *, #27194, .F. ) ;
#17912 = CARTESIAN_POINT ( 'NONE',  ( -13.97604488694527625, -13.89961937509977652, 86.87390960531436690 ) ) ;
#17913 = CARTESIAN_POINT ( 'NONE',  ( 30.00000000000000000, -5.499999999999992895, 37.50000000000000000 ) ) ;
#17914 = CARTESIAN_POINT ( 'NONE',  ( 21.52544592524344225, -5.823673210054117533, 93.54057627198103830 ) ) ;
#17915 = CARTESIAN_POINT ( 'NONE',  ( 16.46253265017160672, -9.564922557960803928, 33.33224293864770260 ) ) ;
#17916 = CARTESIAN_POINT ( 'NONE',  ( -9.564922557961040184, 16.46253265017147172, 107.9177570613523471 ) ) ;
#17917 = LINE ( 'NONE', #79572, #120634 ) ;
#17918 = CARTESIAN_POINT ( 'NONE',  ( 5.153800228976335163, 19.02544592524342804, 34.79057627198102409 ) ) ;
#17919 = CARTESIAN_POINT ( 'NONE',  ( 21.52544592524334988, 5.823673210054432836, 86.45942372801901854 ) ) ;
#17921 = CARTESIAN_POINT ( 'NONE',  ( 10.72451020669871369, 18.67979575497193778, 52.08442372801901854 ) ) ;
#17920 = CARTESIAN_POINT ( 'NONE',  ( 19.03943276465977164, -0.05219959533909143690, 73.74890960531435269 ) ) ;
#17922 = CARTESIAN_POINT ( 'NONE',  ( -21.53943276465977519, -0.05219959533937600094, 28.75109039468567929 ) ) ;
#17923 = CARTESIAN_POINT ( 'NONE',  ( -8.906447517083060816, 27.41122689804195645, 145.5999999999999943 ) ) ;
#17924 = CARTESIAN_POINT ( 'NONE',  ( 9.474510206698971260, -16.51473224551069308, 82.91557627198103830 ) ) ;
#17925 = CARTESIAN_POINT ( 'NONE',  ( 18.89770734986051437, 5.499999999999903189, 61.60214472496640781 ) ) ;
#17928 = CARTESIAN_POINT ( 'NONE',  ( -15.80617190586768217, 15.72974639402176855, 43.12609039468568284 ) ) ;
#17927 = CARTESIAN_POINT ( 'NONE',  ( -21.52544592524343514, 5.823673210054127303, 41.04057627198103120 ) ) ;
#17926 = CARTESIAN_POINT ( 'NONE',  ( -14.29746914071037622, -8.314922557961029526, 34.16775706135234714 ) ) ;
#17929 = CARTESIAN_POINT ( 'NONE',  ( -5.719274019375665041, -21.55341960407619695, 69.79275706135234714 ) ) ;
#17930 = DIRECTION ( 'NONE',  ( 0.000000000000000000, -0.7071067811865467956, -0.7071067811865483499 ) ) ;
#17931 = CARTESIAN_POINT ( 'NONE',  ( 19.03943276465977164, 0.05219959533936151252, 106.2510903946856615 ) ) ;
#17932 = CARTESIAN_POINT ( 'NONE',  ( -9.474510206698964154, 16.51473224551069663, 55.41557627198103120 ) ) ;
#17933 = CARTESIAN_POINT ( 'NONE',  ( 9.564922557960805705, 16.46253265017160317, 79.58224293864769550 ) ) ;
#17934 = CARTESIAN_POINT ( 'NONE',  ( -12.14591786802309592, -12.06949235617757132, 106.8739096053143811 ) ) ;
#17935 = CARTESIAN_POINT ( 'NONE',  ( -14.34966873604960291, -8.224510206698953496, 106.6655762719810383 ) ) ;
#17936 = CARTESIAN_POINT ( 'NONE',  ( -13.97604488694527625, -13.89961937509977652, 106.8739096053143669 ) ) ;
#17937 = CARTESIAN_POINT ( 'NONE',  ( -16.55341960407617563, 4.379528057220093196, 83.54275706135234714 ) ) ;
#17939 = CARTESIAN_POINT ( 'NONE',  ( -19.02544592524342804, 5.153800228976336051, 51.04057627198103120 ) ) ;
#17938 = CARTESIAN_POINT ( 'NONE',  ( 16.53943276465976808, -0.05219959533910856209, 58.74890960531436690 ) ) ;
#17940 = CARTESIAN_POINT ( 'NONE',  ( -21.52544592524334988, -5.823673210054445271, 83.95942372801900433 ) ) ;
#17941 = CARTESIAN_POINT ( 'NONE',  ( 0.05219959533937995610, -21.53943276465977519, 65.00109039468568994 ) ) ;
#17942 = CARTESIAN_POINT ( 'NONE',  ( -5.049401038297874678, -19.05341960407617918, 109.7927570613523187 ) ) ;
#17943 = CARTESIAN_POINT ( 'NONE',  ( -14.29746914071049879, 8.314922557960819915, 55.83224293864770260 ) ) ;
#17944 = CARTESIAN_POINT ( 'NONE',  ( 0.05219959533907565091, 21.53943276465977519, 109.9989096053143527 ) ) ;
#17945 = CARTESIAN_POINT ( 'NONE',  ( 10.81492255796078972, 18.62759615963270932, 59.58224293864770260 ) ) ;
#17947 = CARTESIAN_POINT ( 'NONE',  ( -16.79531203550645913, -7.028104445595622529, 106.2524498822044592 ) ) ;
#17946 = CIRCLE ( 'NONE', #134285, 216.0437394197456342 ) ;
#17948 = CARTESIAN_POINT ( 'NONE',  ( 23.31738231874054890, -16.94106989632523508, 139.0500000054623513 ) ) ;
#17949 = CARTESIAN_POINT ( 'NONE',  ( 19.03943276465977164, -0.05219959533909143690, 63.74890960531435979 ) ) ;
#17950 = CARTESIAN_POINT ( 'NONE',  ( -0.05219959533910754901, -16.53943276465976808, 42.49890960531435979 ) ) ;
#17951 = CARTESIAN_POINT ( 'NONE',  ( -8.224510206698735004, -14.34966873604973081, 109.5844237280190328 ) ) ;
#17952 = CARTESIAN_POINT ( 'NONE',  ( -16.55341960407617563, 4.379528057220093196, 103.5427570613523613 ) ) ;
#17953 = CARTESIAN_POINT ( 'NONE',  ( -9.474510206698720793, -16.51473224551083518, 49.58442372801899722 ) ) ;
#17954 = CARTESIAN_POINT ( 'NONE',  ( 17.48853670773242541, 5.747243402303176651, 48.83328700250012133 ) ) ;
#17955 = CARTESIAN_POINT ( 'NONE',  ( -9.564922557960796823, -16.46253265017161027, 92.08224293864769550 ) ) ;
#17956 = CARTESIAN_POINT ( 'NONE',  ( -4.483927247898539470, -16.52544592524342804, 62.29057627198102409 ) ) ;
#17958 = CARTESIAN_POINT ( 'NONE',  ( -13.97604488694527625, -13.89961937509977652, 111.8739096053143243 ) ) ;
#17957 = CARTESIAN_POINT ( 'NONE',  ( 18.22780087662119897, -5.500000000000096811, 48.51763182126894236 ) ) ;
#17959 = CARTESIAN_POINT ( 'NONE',  ( 15.72974639402199770, -15.80617190586745480, 53.12390960531436690 ) ) ;
#17960 = CARTESIAN_POINT ( 'NONE',  ( -4.379528057220328563, 16.55341960407611168, 95.20724293864769550 ) ) ;
#17961 = CARTESIAN_POINT ( 'NONE',  ( 8.314922557961029526, -14.29746914071037800, 45.41775706135234003 ) ) ;
#17962 = CARTESIAN_POINT ( 'NONE',  ( -8.314922557960811034, -14.29746914071050412, 97.08224293864770971 ) ) ;
#17963 = ADVANCED_FACE ( 'NONE', ( #35547 ), #8043, .T. ) ;
#17964 = CARTESIAN_POINT ( 'NONE',  ( 26.58496454516999563, 7.626754437231445749, 167.9682100371138915 ) ) ;
#17965 = CARTESIAN_POINT ( 'NONE',  ( -13.97604488694547697, 13.89961937509957934, 83.12609039468564731 ) ) ;
#17966 = CARTESIAN_POINT ( 'NONE',  ( 5.153800228976335163, 19.02544592524342804, 109.7905762719810099 ) ) ;
#17967 = CARTESIAN_POINT ( 'NONE',  ( 36.91746824999999177, 2.880721459617395097E-14, -2.124999997268813168 ) ) ;
#17968 = CARTESIAN_POINT ( 'NONE',  ( -22.96000461283911065, 21.84063423829466544, -49.40985016368630767 ) ) ;
#17969 = ORIENTED_EDGE ( 'NONE', *, *, #101326, .T. ) ;
#17971 = CARTESIAN_POINT ( 'NONE',  ( -16.53943276465976808, 0.05219959533911058130, 31.24890960531435979 ) ) ;
#17970 = CARTESIAN_POINT ( 'NONE',  ( 0.05219959533934541429, -16.53943276465976808, 40.00109039468567573 ) ) ;
#17972 = CARTESIAN_POINT ( 'NONE',  ( -21.52544592524343514, 5.823673210054127303, 61.04057627198103120 ) ) ;
#17973 = CARTESIAN_POINT ( 'NONE',  ( 16.46253265017146816, 9.564922557961045513, 81.66775706135233293 ) ) ;
#17974 = CARTESIAN_POINT ( 'NONE',  ( 10.81492255796078972, 18.62759615963270932, 49.58224293864769550 ) ) ;
#17975 = CARTESIAN_POINT ( 'NONE',  ( 5.719274019375673035, 21.55341960407619339, 87.29275706135236135 ) ) ;
#17976 = CARTESIAN_POINT ( 'NONE',  ( -21.83922654085339587, 7.858455564366264134, 172.8813051029758299 ) ) ;
#17977 = CARTESIAN_POINT ( 'NONE',  ( -14.29746914071037622, -8.314922557961029526, 39.16775706135235424 ) ) ;
#17979 = CARTESIAN_POINT ( 'NONE',  ( -13.97604488694527625, -13.89961937509977652, 106.8739096053143669 ) ) ;
#17978 = CARTESIAN_POINT ( 'NONE',  ( 19.02544592524343514, -5.153800228976328945, 38.54057627198103120 ) ) ;
#17980 = CARTESIAN_POINT ( 'NONE',  ( 9.564922557960805705, 16.46253265017160317, 29.58224293864769550 ) ) ;
#17982 = EDGE_CURVE ( 'NONE', #18152, #173841, #96073, .T. ) ;
#17981 = CARTESIAN_POINT ( 'NONE',  ( 0.05219959533910956823, 16.53943276465976808, 104.9989096053143669 ) ) ;
#17983 = CARTESIAN_POINT ( 'NONE',  ( -5.008216064084083931E-14, -105.0000000000000000, 17.20000000000000639 ) ) ;
#17984 = CARTESIAN_POINT ( 'NONE',  ( -5.049401038298153566, 19.05341960407611168, 100.2072429386476955 ) ) ;
#17985 = ORIENTED_EDGE ( 'NONE', *, *, #75323, .F. ) ;
#17986 = CARTESIAN_POINT ( 'NONE',  ( -12.14591786802326823, 12.06949235617739902, 53.12609039468568284 ) ) ;
#17987 = CARTESIAN_POINT ( 'NONE',  ( -18.67979575497178146, -10.72451020669898902, 91.66557627198103830 ) ) ;
#17988 = CARTESIAN_POINT ( 'NONE',  ( 16.51473224551069308, 9.474510206698969483, 49.16557627198102409 ) ) ;
#17989 = CARTESIAN_POINT ( 'NONE',  ( -21.52544592524334988, -5.823673210054445271, 33.95942372801901143 ) ) ;
#17990 = CARTESIAN_POINT ( 'NONE',  ( 16.51473224551069308, 9.474510206698969483, 79.16557627198103830 ) ) ;
#17991 = CARTESIAN_POINT ( 'NONE',  ( -33.88770617167997301, -21.25088722958029663, -25.15219191025231993 ) ) ;
#17992 = ORIENTED_EDGE ( 'NONE', *, *, #154702, .T. ) ;
#17993 = CARTESIAN_POINT ( 'NONE',  ( 14.34966873604972726, -8.224510206698740333, 50.83442372801901143 ) ) ;
#17994 = CARTESIAN_POINT ( 'NONE',  ( -18.62759615963270932, 10.81492255796079327, 115.8322429386477097 ) ) ;
#17997 = CARTESIAN_POINT ( 'NONE',  ( -9.474510206698720793, -16.51473224551083518, 74.58442372801900433 ) ) ;
#17996 = CARTESIAN_POINT ( 'NONE',  ( 13.97604488694527802, 13.89961937509977652, 99.37390960531436690 ) ) ;
#17995 = CARTESIAN_POINT ( 'NONE',  ( 16.55341960407611168, 4.379528057220329451, 108.9572429386476955 ) ) ;
#17998 = CARTESIAN_POINT ( 'NONE',  ( -9.564922557961040184, 16.46253265017147172, 22.91775706135233648 ) ) ;
#17999 = CARTESIAN_POINT ( 'NONE',  ( -0.05219959533907301413, -21.53943276465977519, 82.49890960531436690 ) ) ;
#18000 = CARTESIAN_POINT ( 'NONE',  ( 13.89961937509957401, 13.97604488694547697, 36.87609039468565442 ) ) ;
#18001 = CARTESIAN_POINT ( 'NONE',  ( -0.05219959533934338120, 16.53943276465976808, 82.50109039468568994 ) ) ;
#18002 = CARTESIAN_POINT ( 'NONE',  ( -16.46253265017160317, 9.564922557960807481, 105.8322429386476955 ) ) ;
#18003 = CARTESIAN_POINT ( 'NONE',  ( 9.564922557960805705, 16.46253265017160317, 59.58224293864769550 ) ) ;
#18004 = CARTESIAN_POINT ( 'NONE',  ( 0.05219959533937995610, -21.53943276465977519, 65.00109039468568994 ) ) ;
#18005 = CARTESIAN_POINT ( 'NONE',  ( 18.62759615963255655, 10.81492255796105972, 66.66775706135234714 ) ) ;
#18006 = CARTESIAN_POINT ( 'NONE',  ( -13.89961937509977652, 13.97604488694528158, 70.62390960531432427 ) ) ;
#18007 = CARTESIAN_POINT ( 'NONE',  ( -21.53943276465977519, -0.05219959533937600094, 43.75109039468568284 ) ) ;
#18008 = CARTESIAN_POINT ( 'NONE',  ( 19.05341960407617918, -5.049401038297876454, 86.04275706135233293 ) ) ;
#18009 = CARTESIAN_POINT ( 'NONE',  ( 9.564922557960805705, 16.46253265017160317, 49.58224293864770260 ) ) ;
#18010 = CARTESIAN_POINT ( 'NONE',  ( -13.89961937509977652, 13.97604488694528158, 95.62390960531436690 ) ) ;
#18011 = CARTESIAN_POINT ( 'NONE',  ( -9.564922557960796823, -16.46253265017161027, 72.08224293864770971 ) ) ;
#18012 = CARTESIAN_POINT ( 'NONE',  ( 16.51473224551069308, 9.474510206698969483, 109.1655762719810383 ) ) ;
#18014 = EDGE_CURVE ( 'NONE', #159131, #19675, #142718, .T. ) ;
#18013 = CARTESIAN_POINT ( 'NONE',  ( -5.153800228976328057, -19.02544592524343514, 52.29057627198100988 ) ) ;
#18015 = CARTESIAN_POINT ( 'NONE',  ( 15.72974639402199770, -15.80617190586745480, 83.12390960531436690 ) ) ;
#18016 = CARTESIAN_POINT ( 'NONE',  ( 0.05219959533934541429, -16.53943276465976808, 70.00109039468568994 ) ) ;
#18017 = CARTESIAN_POINT ( 'NONE',  ( -23.46037622756033869, 10.21219847193944474, 168.3031241911537279 ) ) ;
#18018 = CARTESIAN_POINT ( 'NONE',  ( -13.89961937509957401, -13.97604488694547875, 34.37609039468566863 ) ) ;
#18019 = CARTESIAN_POINT ( 'NONE',  ( -9.474510206698964154, 16.51473224551069663, 65.41557627198102409 ) ) ;
#18020 = CARTESIAN_POINT ( 'NONE',  ( 8.224510206698953496, -14.34966873604960469, 57.91557627198103120 ) ) ;
#18021 = CARTESIAN_POINT ( 'NONE',  ( 0.05219959533910956823, 16.53943276465976808, 99.99890960531436690 ) ) ;
#18022 = CARTESIAN_POINT ( 'NONE',  ( 16.51473224551069308, 9.474510206698969483, 99.16557627198102409 ) ) ;
#18023 = CARTESIAN_POINT ( 'NONE',  ( 13.89961937509977652, -13.97604488694527269, 93.12390960531436690 ) ) ;
#18024 = CARTESIAN_POINT ( 'NONE',  ( 21.53943276465977519, 0.05219959533937863772, 51.25109039468568994 ) ) ;
#18025 = CARTESIAN_POINT ( 'NONE',  ( 13.89961937509977652, -13.97604488694527269, 108.1239096053143669 ) ) ;
#18026 = CARTESIAN_POINT ( 'NONE',  ( 5.049401038297881783, 19.05341960407617563, 22.29275706135233648 ) ) ;
#18027 = CARTESIAN_POINT ( 'NONE',  ( 8.314922557961029526, -14.29746914071037800, 75.41775706135233293 ) ) ;
#18028 = CARTESIAN_POINT ( 'NONE',  ( 10.72451020669871369, 18.67979575497193778, 37.08442372801901143 ) ) ;
#18029 = CARTESIAN_POINT ( 'NONE',  ( 21.52544592524344225, -5.823673210054117533, 33.54057627198102409 ) ) ;
#18030 = CARTESIAN_POINT ( 'NONE',  ( -5.823673210054116645, -21.52544592524344225, 107.2905762719810525 ) ) ;
#18031 = CARTESIAN_POINT ( 'NONE',  ( -16.55341960407611168, -4.379528057220339221, 61.45724293864770260 ) ) ;
#18032 = CARTESIAN_POINT ( 'NONE',  ( 13.97604488694527802, 13.89961937509977652, 49.37390960531434558 ) ) ;
#18033 = CARTESIAN_POINT ( 'NONE',  ( -4.379528057220328563, 16.55341960407611168, 85.20724293864770971 ) ) ;
#18034 = CARTESIAN_POINT ( 'NONE',  ( -18.62759615963270932, 10.81492255796079327, 40.83224293864769550 ) ) ;
#18035 = CARTESIAN_POINT ( 'NONE',  ( 13.97604488694548053, -13.89961937509957401, 40.62609039468564731 ) ) ;
#18036 = CARTESIAN_POINT ( 'NONE',  ( -4.379528057220328563, 16.55341960407611168, 115.2072429386476955 ) ) ;
#18037 = ORIENTED_EDGE ( 'NONE', *, *, #137185, .T. ) ;
#18038 = CARTESIAN_POINT ( 'NONE',  ( -12.14591786802326823, 12.06949235617739902, 68.12609039468567573 ) ) ;
#18039 = CARTESIAN_POINT ( 'NONE',  ( 9.474510206698971260, -16.51473224551069308, 72.91557627198102409 ) ) ;
#18040 = CARTESIAN_POINT ( 'NONE',  ( 27.73933785331498569, 2.768321779492822058E-14, 141.8750000027311842 ) ) ;
#18041 = CARTESIAN_POINT ( 'NONE',  ( 14.29746914071049879, -8.314922557960816363, 83.33224293864769550 ) ) ;
#18042 = CARTESIAN_POINT ( 'NONE',  ( -18.62759615963270932, 10.81492255796079327, 40.83224293864769550 ) ) ;
#18043 = ORIENTED_EDGE ( 'NONE', *, *, #68656, .F. ) ;
#18044 = CARTESIAN_POINT ( 'NONE',  ( 4.483927247898790824, -16.52544592524335698, 110.2094237280190185 ) ) ;
#18045 = CARTESIAN_POINT ( 'NONE',  ( -12.06949235617739369, -12.14591786802326823, 19.37609039468568639 ) ) ;
#18046 = CARTESIAN_POINT ( 'NONE',  ( 0.05219959533937995610, -21.53943276465977519, 85.00109039468568994 ) ) ;
#18047 = CARTESIAN_POINT ( 'NONE',  ( 19.02544592524343514, -5.153800228976328945, 88.54057627198102409 ) ) ;
#18048 = CARTESIAN_POINT ( 'NONE',  ( -18.62759615963270932, 10.81492255796079327, 100.8322429386477097 ) ) ;
#18049 = CARTESIAN_POINT ( 'NONE',  ( 12.06949235617739724, 12.14591786802326823, 56.87609039468568994 ) ) ;
#18050 = CARTESIAN_POINT ( 'NONE',  ( -19.05341960407611168, -5.049401038298163336, 31.45724293864769550 ) ) ;
#18051 = CIRCLE ( 'NONE', #11724, 13.70000000000001528 ) ;
#18052 = CARTESIAN_POINT ( 'NONE',  ( -4.379528057220086978, -16.55341960407618274, 29.79275706135234358 ) ) ;
#18053 = CARTESIAN_POINT ( 'NONE',  ( 19.02544592524334988, 5.153800228976608722, 96.45942372801897591 ) ) ;
#18054 = CARTESIAN_POINT ( 'NONE',  ( -21.55341960407610458, -5.719274019375992779, 91.45724293864769550 ) ) ;
#18055 = CARTESIAN_POINT ( 'NONE',  ( -5.153800228976607833, 19.02544592524334988, 72.70942372801900433 ) ) ;
#18056 = CARTESIAN_POINT ( 'NONE',  ( 19.53037848336980886, -5.499999999999891642, 87.35532783611442653 ) ) ;
#18057 = CARTESIAN_POINT ( 'NONE',  ( 18.62759615963271287, -10.81492255796078972, 103.3322429386476955 ) ) ;
#18058 = CARTESIAN_POINT ( 'NONE',  ( 0.05219959533909260263, 19.03943276465977164, 79.99890960531436690 ) ) ;
#18059 = CARTESIAN_POINT ( 'NONE',  ( 14.29746914071037800, 8.314922557961029526, 31.66775706135234358 ) ) ;
#18060 = DIRECTION ( 'NONE',  ( -1.000000000000000000, 0.000000000000000000, -0.000000000000000000 ) ) ;
#18061 = CARTESIAN_POINT ( 'NONE',  ( 19.05341960407617918, -5.049401038297876454, 56.04275706135234714 ) ) ;
#18063 = CARTESIAN_POINT ( 'NONE',  ( -14.34966873604960291, -8.224510206698953496, 66.66557627198102409 ) ) ;
#18062 = CARTESIAN_POINT ( 'NONE',  ( 15.80617190586769283, -15.72974639402175789, 20.62609039468568639 ) ) ;
#18064 = CARTESIAN_POINT ( 'NONE',  ( 19.05341960407611168, 5.049401038298154454, 78.95724293864769550 ) ) ;
#18066 = CARTESIAN_POINT ( 'NONE',  ( -9.564922557961040184, 16.46253265017147172, 47.91775706135233293 ) ) ;
#18065 = CARTESIAN_POINT ( 'NONE',  ( 0.05219959533934541429, -16.53943276465976808, 40.00109039468567573 ) ) ;
#18067 = CARTESIAN_POINT ( 'NONE',  ( 5.823673210054444382, -21.52544592524334988, 55.20942372801902565 ) ) ;
#18068 = CARTESIAN_POINT ( 'NONE',  ( -5.049401038297874678, -19.05341960407617918, 109.7927570613523187 ) ) ;
#18069 = CARTESIAN_POINT ( 'NONE',  ( 13.89961937509977652, -13.97604488694527269, 53.12390960531434558 ) ) ;
#18070 = CARTESIAN_POINT ( 'NONE',  ( 19.03943276465977164, 0.05219959533936151252, 76.25109039468566152 ) ) ;
#18071 = CARTESIAN_POINT ( 'NONE',  ( -21.53943276465977519, -0.05219959533937600094, 93.75109039468567573 ) ) ;
#18072 = CARTESIAN_POINT ( 'NONE',  ( -16.46253265017146816, -9.564922557961047289, 69.16775706135233293 ) ) ;
#18073 = CARTESIAN_POINT ( 'NONE',  ( -19.02544592524342804, 5.153800228976336051, 31.04057627198102409 ) ) ;
#18074 = CARTESIAN_POINT ( 'NONE',  ( -5.719274019375978568, 21.55341960407610458, 75.20724293864769550 ) ) ;
#18076 = CARTESIAN_POINT ( 'NONE',  ( -13.97604488694547697, 13.89961937509957934, 68.12609039468563310 ) ) ;
#18075 = CARTESIAN_POINT ( 'NONE',  ( 4.483927247898545687, 16.52544592524342804, 59.79057627198103120 ) ) ;
#18077 = CARTESIAN_POINT ( 'NONE',  ( -17.05587630539788435, -6.762274262135648861, 24.25819690962687858 ) ) ;
#18078 = CARTESIAN_POINT ( 'NONE',  ( -5.049401038297874678, -19.05341960407617918, 49.79275706135231871 ) ) ;
#18079 = CARTESIAN_POINT ( 'NONE',  ( 14.29746914071037800, 8.314922557961029526, 96.66775706135234714 ) ) ;
#18080 = CARTESIAN_POINT ( 'NONE',  ( 4.379528057220339221, -16.55341960407611168, 57.70724293864770260 ) ) ;
#18082 = CARTESIAN_POINT ( 'NONE',  ( -8.571926809382608425, 26.38167802310805854, 142.4750000027312069 ) ) ;
#18081 = CARTESIAN_POINT ( 'NONE',  ( 5.823673210054444382, -21.52544592524334988, 90.20942372801903275 ) ) ;
#18083 = CARTESIAN_POINT ( 'NONE',  ( 0.05219959533907565091, 21.53943276465977519, 99.99890960531436690 ) ) ;
#18084 = CARTESIAN_POINT ( 'NONE',  ( 19.03943276465977164, -0.05219959533909143690, 48.74890960531435979 ) ) ;
#18085 = CARTESIAN_POINT ( 'NONE',  ( 18.67979575497194134, -10.72451020669871369, 70.83442372801901854 ) ) ;
#18086 = CARTESIAN_POINT ( 'NONE',  ( 9.474510206698971260, -16.51473224551069308, 47.91557627198102409 ) ) ;
#18087 = CARTESIAN_POINT ( 'NONE',  ( -16.51473224551069308, -9.474510206698971260, 71.66557627198102409 ) ) ;
#18088 = CARTESIAN_POINT ( 'NONE',  ( 4.483927247898545687, 16.52544592524342804, 104.7905762719810241 ) ) ;
#18089 = CARTESIAN_POINT ( 'NONE',  ( -16.46253265017160317, 9.564922557960807481, 105.8322429386476955 ) ) ;
#18090 = CIRCLE ( 'NONE', #2046, 7.500000000000007105 ) ;
#18091 = CARTESIAN_POINT ( 'NONE',  ( 4.379528057220339221, -16.55341960407611168, 52.70724293864769550 ) ) ;
#18092 = CARTESIAN_POINT ( 'NONE',  ( -19.03943276465977164, 0.05219959533909376836, 36.24890960531436690 ) ) ;
#18093 = CARTESIAN_POINT ( 'NONE',  ( -14.29746914071049879, 8.314922557960819915, 80.83224293864769550 ) ) ;
#18094 = CARTESIAN_POINT ( 'NONE',  ( 18.62759615963271287, -10.81492255796078972, 98.33224293864769550 ) ) ;
#18095 = CARTESIAN_POINT ( 'NONE',  ( -18.62759615963255300, -10.81492255796106328, 29.16775706135234003 ) ) ;
#18096 = CARTESIAN_POINT ( 'NONE',  ( -7.284589286804255437, 1.784589286804319386, 8.181980515339454030 ) ) ;
#18097 = CARTESIAN_POINT ( 'NONE',  ( -16.52544592524335698, -4.483927247898792601, 43.95942372801902565 ) ) ;
#18098 = CARTESIAN_POINT ( 'NONE',  ( -21.53943276465977519, 0.05219959533907696930, 81.24890960531436690 ) ) ;
#18099 = CARTESIAN_POINT ( 'NONE',  ( 21.52544592524334988, 5.823673210054432836, 111.4594237280190328 ) ) ;
#18100 = B_SPLINE_CURVE_WITH_KNOTS ( 'NONE', 3,
 ( #37647, #175169, #68984, #145816, #111499, #50832 ),
 .UNSPECIFIED., .F., .F.,
 ( 4, 2, 4 ),
 ( 0.007228050697041550100, 0.007608510107495039532, 0.007988969517948528096 ),
 .UNSPECIFIED. ) ;
#18101 = CARTESIAN_POINT ( 'NONE',  ( 19.05341960407611168, 5.049401038298154454, 108.9572429386477097 ) ) ;
#18102 = CARTESIAN_POINT ( 'NONE',  ( -10.81492255796105439, 18.62759615963255655, 37.91775706135235424 ) ) ;
#18103 = CARTESIAN_POINT ( 'NONE',  ( -5.823673210054116645, -21.52544592524344225, 37.29057627198102409 ) ) ;
#18104 = CARTESIAN_POINT ( 'NONE',  ( 4.483927247898790824, -16.52544592524335698, 110.2094237280190185 ) ) ;
#18106 = CARTESIAN_POINT ( 'NONE',  ( 15.80617190586769283, -15.72974639402175789, 85.62609039468568994 ) ) ;
#18105 = CARTESIAN_POINT ( 'NONE',  ( -18.62759615963255300, -10.81492255796106328, 69.16775706135234714 ) ) ;
#18107 = CARTESIAN_POINT ( 'NONE',  ( -19.05341960407617563, 5.049401038297882671, 33.54275706135231871 ) ) ;
#18108 = CARTESIAN_POINT ( 'NONE',  ( -8.224510206698735004, -14.34966873604973081, 94.58442372801901854 ) ) ;
#18109 = CARTESIAN_POINT ( 'NONE',  ( -10.81492255796105439, 18.62759615963255655, 37.91775706135235424 ) ) ;
#18110 = CARTESIAN_POINT ( 'NONE',  ( -5.049401038298153566, 19.05341960407611168, 50.20724293864770260 ) ) ;
#18111 = CARTESIAN_POINT ( 'NONE',  ( 15.80617190586769283, -15.72974639402175789, 105.6260903946856899 ) ) ;
#18112 = CARTESIAN_POINT ( 'NONE',  ( 5.823673210054125526, 21.52544592524343514, 24.79057627198103120 ) ) ;
#18113 = CARTESIAN_POINT ( 'NONE',  ( 10.81492255796106328, -18.62759615963255655, 25.41775706135235779 ) ) ;
#18114 = CARTESIAN_POINT ( 'NONE',  ( 15.80617190586746368, 15.72974639402197994, 79.37390960531436690 ) ) ;
#18116 = CARTESIAN_POINT ( 'NONE',  ( -21.55341960407610458, -5.719274019375992779, 66.45724293864768129 ) ) ;
#18115 = CARTESIAN_POINT ( 'NONE',  ( 17.50000000000000000, 5.499999999999997335, 120.0000000000000142 ) ) ;
#18118 = CARTESIAN_POINT ( 'NONE',  ( 4.483927247898545687, 16.52544592524342804, 59.79057627198103120 ) ) ;
#18117 = CARTESIAN_POINT ( 'NONE',  ( 8.224510206698742110, 14.34966873604972548, 57.08442372801901854 ) ) ;
#18119 = CARTESIAN_POINT ( 'NONE',  ( -38.00000000000000711, 2.428612866367529932E-14, -10.87499999726881228 ) ) ;
#18120 = CARTESIAN_POINT ( 'NONE',  ( -9.564922557961040184, 16.46253265017147172, 87.91775706135233293 ) ) ;
#18121 = CARTESIAN_POINT ( 'NONE',  ( -9.443730985155296409, -10.00060863403381006, -60.42334892181182227 ) ) ;
#18122 = CARTESIAN_POINT ( 'NONE',  ( -16.52544592524335698, -4.483927247898792601, 28.95942372801902209 ) ) ;
#18123 = CARTESIAN_POINT ( 'NONE',  ( -18.67979575497178146, -10.72451020669898902, 101.6655762719810383 ) ) ;
#18124 = CARTESIAN_POINT ( 'NONE',  ( 10.72451020669898902, -18.67979575497178502, 72.91557627198103830 ) ) ;
#18125 = CARTESIAN_POINT ( 'NONE',  ( 13.89961937509977652, -13.97604488694527269, 113.1239096053143527 ) ) ;
#18126 = CARTESIAN_POINT ( 'NONE',  ( -12.14591786802326823, 12.06949235617739902, 63.12609039468568994 ) ) ;
#18127 = CARTESIAN_POINT ( 'NONE',  ( -5.049401038298153566, 19.05341960407611168, 70.20724293864769550 ) ) ;
#18129 = CARTESIAN_POINT ( 'NONE',  ( 16.46253265017146816, 9.564922557961045513, 111.6677570613523329 ) ) ;
#18128 = CARTESIAN_POINT ( 'NONE',  ( -5.719274019375665041, -21.55341960407619695, 39.79275706135235424 ) ) ;
#18130 = ADVANCED_FACE ( 'NONE', ( #67874 ), #173079, .F. ) ;
#18131 = CARTESIAN_POINT ( 'NONE',  ( 19.03943276465977164, -0.05219959533909143690, 103.7489096053143669 ) ) ;
#18132 = CARTESIAN_POINT ( 'NONE',  ( 16.51473224551083163, -9.474510206698727899, 30.83442372801900433 ) ) ;
#18133 = CARTESIAN_POINT ( 'NONE',  ( -19.02544592524342804, 5.153800228976336051, 96.04057627198103830 ) ) ;
#18134 = CARTESIAN_POINT ( 'NONE',  ( -10.81492255796078084, -18.62759615963271287, 102.0822429386476955 ) ) ;
#18135 = CARTESIAN_POINT ( 'NONE',  ( 19.05341960407611168, 5.049401038298154454, 63.95724293864769550 ) ) ;
#18136 = CARTESIAN_POINT ( 'NONE',  ( -16.38665767535054485, 7.295008042176029939, 25.26400864214546971 ) ) ;
#18137 = CARTESIAN_POINT ( 'NONE',  ( -14.34966873604960291, -8.224510206698953496, 76.66557627198103830 ) ) ;
#18138 = CARTESIAN_POINT ( 'NONE',  ( -13.89961937509977652, 13.97604488694528158, 110.6239096053143243 ) ) ;
#18139 = CARTESIAN_POINT ( 'NONE',  ( -19.03943276465977164, 0.05219959533909376836, 21.24890960531436335 ) ) ;
#18140 = CARTESIAN_POINT ( 'NONE',  ( 0.05219959533907565091, 21.53943276465977519, 109.9989096053143527 ) ) ;
#18141 = CARTESIAN_POINT ( 'NONE',  ( -16.51473224551082808, 9.474510206698731452, 58.33442372801900433 ) ) ;
#18142 = AXIS2_PLACEMENT_3D ( 'NONE', #86720, #59369, #90699 ) ;
#18143 = CARTESIAN_POINT ( 'NONE',  ( 9.564922557960805705, 16.46253265017160317, 109.5822429386476955 ) ) ;
#18144 = CARTESIAN_POINT ( 'NONE',  ( 19.02544592524343514, -5.153800228976328945, 33.54057627198102409 ) ) ;
#18145 = CARTESIAN_POINT ( 'NONE',  ( 21.52544592524344225, -5.823673210054117533, 53.54057627198103120 ) ) ;
#18146 = CARTESIAN_POINT ( 'NONE',  ( -13.97604488694527625, -13.89961937509977652, 96.87390960531433848 ) ) ;
#18147 = CARTESIAN_POINT ( 'NONE',  ( -10.81492255796105439, 18.62759615963255655, 72.91775706135234714 ) ) ;
#18148 = CARTESIAN_POINT ( 'NONE',  ( -16.46253265017160317, 9.564922557960807481, 55.83224293864769550 ) ) ;
#18149 = CARTESIAN_POINT ( 'NONE',  ( 16.52544592524342804, -4.483927247898539470, 88.54057627198103830 ) ) ;
#18150 = CARTESIAN_POINT ( 'NONE',  ( 8.224510206698742110, 14.34966873604972548, 42.08442372801901854 ) ) ;
#18151 = CARTESIAN_POINT ( 'NONE',  ( 15.72974639402176855, 15.80617190586768217, 61.87609039468568284 ) ) ;
#18152 = VERTEX_POINT ( 'NONE', #99201 ) ;
#18153 = CARTESIAN_POINT ( 'NONE',  ( -5.049401038297874678, -19.05341960407617918, 19.79275706135233293 ) ) ;
#18154 = CARTESIAN_POINT ( 'NONE',  ( 5.153800228976615827, -19.02544592524334988, 80.20942372801901854 ) ) ;
#18155 = CARTESIAN_POINT ( 'NONE',  ( -16.46253265017146816, -9.564922557961047289, 39.16775706135234003 ) ) ;
#18156 = SPHERICAL_SURFACE ( 'NONE', #56879, 2.000000000000000000 ) ;
#18157 = CARTESIAN_POINT ( 'NONE',  ( 21.53943276465977519, 0.05219959533937863772, 36.25109039468567573 ) ) ;
#18158 = CARTESIAN_POINT ( 'NONE',  ( -31.99364916731038022, -1.163414459189985801E-14, 95.00000000000000000 ) ) ;
#18159 = CARTESIAN_POINT ( 'NONE',  ( -9.474510206698720793, -16.51473224551083518, 34.58442372801899722 ) ) ;
#18160 = CARTESIAN_POINT ( 'NONE',  ( -16.46253265017160317, 9.564922557960807481, 65.83224293864769550 ) ) ;
#18161 = CARTESIAN_POINT ( 'NONE',  ( -16.53943276465976808, 0.05219959533911058130, 21.24890960531436690 ) ) ;
#18163 = CARTESIAN_POINT ( 'NONE',  ( 15.80617190586769283, -15.72974639402175789, 90.62609039468567573 ) ) ;
#18162 = CARTESIAN_POINT ( 'NONE',  ( -13.97604488694527625, -13.89961937509977652, 111.8739096053143243 ) ) ;
#18164 = CARTESIAN_POINT ( 'NONE',  ( 11.40812507854755253, -35.11059874428192273, -6.024999997268814411 ) ) ;
#18165 = CARTESIAN_POINT ( 'NONE',  ( -24.95432927374998044, -3.806786798636382585, 190.0000000000000000 ) ) ;
#18166 = CARTESIAN_POINT ( 'NONE',  ( 21.55341960407619695, -5.719274019375665929, 86.04275706135236135 ) ) ;
#18167 = CARTESIAN_POINT ( 'NONE',  ( 23.48298174826590667, -32.32155151706770368, -3.047842220587803741 ) ) ;
#18168 = CARTESIAN_POINT ( 'NONE',  ( -9.474510206698964154, 16.51473224551069663, 95.41557627198102409 ) ) ;
#18169 = CARTESIAN_POINT ( 'NONE',  ( -0.4884129450682956897, -31.82351365011402322, -49.22894560581806900 ) ) ;
#18170 = CARTESIAN_POINT ( 'NONE',  ( -9.474510206698964154, 16.51473224551069663, 50.41557627198102409 ) ) ;
#18171 = CARTESIAN_POINT ( 'NONE',  ( -21.55341960407610458, -5.719274019375992779, 51.45724293864770260 ) ) ;
#18172 = CARTESIAN_POINT ( 'NONE',  ( -12.14591786802309592, -12.06949235617757132, 31.87390960531435979 ) ) ;
#18174 = CARTESIAN_POINT ( 'NONE',  ( -16.46253265017160317, 9.564922557960807481, 90.83224293864769550 ) ) ;
#18173 = CARTESIAN_POINT ( 'NONE',  ( 16.53943276465976808, -0.05219959533910856209, 113.7489096053143527 ) ) ;
#18175 = CARTESIAN_POINT ( 'NONE',  ( 19.02544592524334988, 5.153800228976608722, 21.45942372801899012 ) ) ;
#18176 = CARTESIAN_POINT ( 'NONE',  ( -14.34966873604960291, -8.224510206698953496, 96.66557627198102409 ) ) ;
#18177 = CARTESIAN_POINT ( 'NONE',  ( -21.52544592524334988, -5.823673210054445271, 68.95942372801901854 ) ) ;
#18178 = CARTESIAN_POINT ( 'NONE',  ( 9.474510206698971260, -16.51473224551069308, 97.91557627198102409 ) ) ;
#18179 = CARTESIAN_POINT ( 'NONE',  ( -12.06949235617739369, -12.14591786802326823, 104.3760903946856899 ) ) ;
#18180 = CARTESIAN_POINT ( 'NONE',  ( 19.02544592524334988, 5.153800228976608722, 66.45942372801899012 ) ) ;
#18181 = CARTESIAN_POINT ( 'NONE',  ( 22.81625015709510151, -31.40387420917324590, -6.424999997268811214 ) ) ;
#18182 = CARTESIAN_POINT ( 'NONE',  ( 19.02544592524343514, -5.153800228976328945, 113.5405762719810241 ) ) ;
#18183 = CARTESIAN_POINT ( 'NONE',  ( 4.379528057220339221, -16.55341960407611168, 77.70724293864770971 ) ) ;
#18185 = CARTESIAN_POINT ( 'NONE',  ( 5.153800228976615827, -19.02544592524334988, 55.20942372801899722 ) ) ;
#18184 = AXIS2_PLACEMENT_3D ( 'NONE', #59648, #11189, #72864 ) ;
#18186 = CARTESIAN_POINT ( 'NONE',  ( 9.474510206698971260, -16.51473224551069308, 57.91557627198103120 ) ) ;
#18187 = CARTESIAN_POINT ( 'NONE',  ( -16.53943276465976808, 0.05219959533911058130, 66.24890960531436690 ) ) ;
#18188 = CARTESIAN_POINT ( 'NONE',  ( 13.89961937509957401, 13.97604488694547697, 91.87609039468567573 ) ) ;
#18189 = CARTESIAN_POINT ( 'NONE',  ( -21.53943276465977519, 0.05219959533907696930, 51.24890960531436690 ) ) ;
#18190 = ORIENTED_EDGE ( 'NONE', *, *, #93397, .F. ) ;
#18191 = CARTESIAN_POINT ( 'NONE',  ( 16.55341960407611168, 4.379528057220329451, 108.9572429386476955 ) ) ;
#18192 = CARTESIAN_POINT ( 'NONE',  ( -17.05587630539784172, -6.762274262135713698, 29.25819690962689279 ) ) ;
#18194 = CARTESIAN_POINT ( 'NONE',  ( 21.52544592524344225, -5.823673210054117533, 58.54057627198103120 ) ) ;
#18193 = CARTESIAN_POINT ( 'NONE',  ( -13.97604488694527625, -13.89961937509977652, 61.87390960531435979 ) ) ;
#18196 = CARTESIAN_POINT ( 'NONE',  ( 19.03943276465977164, -0.05219959533909143690, 78.74890960531436690 ) ) ;
#18195 = CARTESIAN_POINT ( 'NONE',  ( 4.379528057220092307, 16.55341960407617563, 97.29275706135234714 ) ) ;
#18197 = CARTESIAN_POINT ( 'NONE',  ( -16.51473224551082808, 9.474510206698731452, 48.33442372801900433 ) ) ;
#18198 = CARTESIAN_POINT ( 'NONE',  ( 10.72451020669871369, 18.67979575497193778, 87.08442372801901854 ) ) ;
#18199 = CARTESIAN_POINT ( 'NONE',  ( 15.80617190586746368, 15.72974639402197994, 59.37390960531436690 ) ) ;
#18200 = CARTESIAN_POINT ( 'NONE',  ( 16.51473224551069308, 9.474510206698969483, 104.1655762719810241 ) ) ;
#18201 = CARTESIAN_POINT ( 'NONE',  ( -0.05219959533909027116, -19.03943276465977164, 37.49890960531436690 ) ) ;
#18202 = CARTESIAN_POINT ( 'NONE',  ( -4.483927247898782831, 16.52544592524335698, 92.70942372801901854 ) ) ;
#18203 = CARTESIAN_POINT ( 'NONE',  ( -12.14591786802326823, 12.06949235617739902, 23.12609039468567573 ) ) ;
#18204 = FACE_OUTER_BOUND ( 'NONE', #181058, .T. ) ;
#18205 = CARTESIAN_POINT ( 'NONE',  ( 0.05219959533937995610, -21.53943276465977519, 95.00109039468568994 ) ) ;
#18206 = CARTESIAN_POINT ( 'NONE',  ( 16.53943276465976808, -0.05219959533910856209, 63.74890960531435979 ) ) ;
#18207 = CARTESIAN_POINT ( 'NONE',  ( 4.379528057220339221, -16.55341960407611168, 67.70724293864769550 ) ) ;
#18208 = CARTESIAN_POINT ( 'NONE',  ( 0.05219959533907565091, 21.53943276465977519, 99.99890960531436690 ) ) ;
#18209 = CARTESIAN_POINT ( 'NONE',  ( 21.55341960407610458, 5.719274019375980345, 88.95724293864769550 ) ) ;
#18210 = CARTESIAN_POINT ( 'NONE',  ( 16.81555441253552630, -7.025013491695473178, 98.13685445334257906 ) ) ;
#18211 = CARTESIAN_POINT ( 'NONE',  ( -21.53943276465977519, 0.05219959533907696930, 46.24890960531435979 ) ) ;
#18212 = CARTESIAN_POINT ( 'NONE',  ( -8.314922557961024197, 14.29746914071037800, 62.91775706135236135 ) ) ;
#18213 = CARTESIAN_POINT ( 'NONE',  ( 0.05219959533910956823, 16.53943276465976808, 89.99890960531438111 ) ) ;
#18214 = CARTESIAN_POINT ( 'NONE',  ( -19.05341960407611168, -5.049401038298163336, 46.45724293864768129 ) ) ;
#18215 = SURFACE_SIDE_STYLE ('',( #60714 ) ) ;
#18216 = CARTESIAN_POINT ( 'NONE',  ( 34.71415419550759651, -2.652640888949069797, 52.01956328305328014 ) ) ;
#18217 = CARTESIAN_POINT ( 'NONE',  ( 12.14591786802327356, -12.06949235617739191, 95.62609039468568994 ) ) ;
#18218 = ORIENTED_EDGE ( 'NONE', *, *, #5788, .T. ) ;
#18219 = CARTESIAN_POINT ( 'NONE',  ( 21.55341960407619695, -5.719274019375665929, 36.04275706135234714 ) ) ;
#18220 = CARTESIAN_POINT ( 'NONE',  ( -16.51473224551069308, -9.474510206698971260, 81.66557627198103830 ) ) ;
#18221 = CARTESIAN_POINT ( 'NONE',  ( -21.52544592524334988, -5.823673210054445271, 63.95942372801901854 ) ) ;
#18222 = FACE_OUTER_BOUND ( 'NONE', #106812, .T. ) ;
#18223 = DIRECTION ( 'NONE',  ( -0.000000000000000000, -1.000000000000000000, -0.000000000000000000 ) ) ;
#18224 = VERTEX_POINT ( 'NONE', #160889 ) ;
#18225 = CARTESIAN_POINT ( 'NONE',  ( -21.55341960407619339, 5.719274019375674811, 63.54275706135234003 ) ) ;
#18227 = CARTESIAN_POINT ( 'NONE',  ( -19.03943276465977164, 0.05219959533909376836, 21.24890960531436335 ) ) ;
#18226 = CARTESIAN_POINT ( 'NONE',  ( 9.474510206698971260, -16.51473224551069308, 32.91557627198102409 ) ) ;
#18228 = CARTESIAN_POINT ( 'NONE',  ( 19.03943276465977164, -0.05219959533909143690, 88.74890960531436690 ) ) ;
#18229 = CARTESIAN_POINT ( 'NONE',  ( -9.474510206698720793, -16.51473224551083518, 64.58442372801900433 ) ) ;
#18230 = CARTESIAN_POINT ( 'NONE',  ( 5.719274019375673035, 21.55341960407619339, 32.29275706135235424 ) ) ;
#18231 = VECTOR ( 'NONE', #64442, 1000.000000000000000 ) ;
#18232 = CARTESIAN_POINT ( 'NONE',  ( 0.05219959533936267826, -19.03943276465977164, 55.00109039468566863 ) ) ;
#18233 = CARTESIAN_POINT ( 'NONE',  ( -0.05219959533909027116, -19.03943276465977164, 32.49890960531435979 ) ) ;
#18234 = CARTESIAN_POINT ( 'NONE',  ( 12.06949235617739724, 12.14591786802326823, 106.8760903946856899 ) ) ;
#18235 = CARTESIAN_POINT ( 'NONE',  ( 19.02544592524334988, 5.153800228976608722, 76.45942372801897591 ) ) ;
#18236 = CARTESIAN_POINT ( 'NONE',  ( -16.55341960407611168, -4.379528057220339221, 21.45724293864769550 ) ) ;
#18237 = CARTESIAN_POINT ( 'NONE',  ( 9.474510206698729675, 16.51473224551082808, 57.08442372801900433 ) ) ;
#18238 = CARTESIAN_POINT ( 'NONE',  ( -9.564922557960796823, -16.46253265017161027, 102.0822429386477097 ) ) ;
#18239 = CIRCLE ( 'NONE', #44081, 2.199999999999999289 ) ;
#18240 = CARTESIAN_POINT ( 'NONE',  ( 21.52544592524334988, 5.823673210054432836, 101.4594237280190185 ) ) ;
#18241 = CARTESIAN_POINT ( 'NONE',  ( 18.67979575497194134, -10.72451020669871369, 105.8344237280190328 ) ) ;
#18242 = CARTESIAN_POINT ( 'NONE',  ( 13.97604488694527802, 13.89961937509977652, 24.37390960531435624 ) ) ;
#18243 = CARTESIAN_POINT ( 'NONE',  ( 15.72974639402176855, 15.80617190586768217, 91.87609039468568994 ) ) ;
#18244 = CARTESIAN_POINT ( 'NONE',  ( 14.34966873604972726, -8.224510206698740333, 30.83442372801902209 ) ) ;
#18245 = CARTESIAN_POINT ( 'NONE',  ( 19.05341960407611168, 5.049401038298154454, 93.95724293864769550 ) ) ;
#18246 = CARTESIAN_POINT ( 'NONE',  ( -17.14385361876520619, 23.59649016807275856, 140.5750000027311728 ) ) ;
#18247 = CARTESIAN_POINT ( 'NONE',  ( 0.05219959533909260263, 19.03943276465977164, 84.99890960531436690 ) ) ;
#18248 = DIRECTION ( 'NONE',  ( 0.000000000000000000, 0.000000000000000000, -1.000000000000000000 ) ) ;
#18249 = CARTESIAN_POINT ( 'NONE',  ( 9.564922557961047289, -16.46253265017146816, 65.41775706135233293 ) ) ;
#18250 = CARTESIAN_POINT ( 'NONE',  ( -5.153800228976328057, -19.02544592524343514, 107.2905762719810383 ) ) ;
#18251 = CARTESIAN_POINT ( 'NONE',  ( 5.823673210054444382, -21.52544592524334988, 105.2094237280190328 ) ) ;
#18252 = CARTESIAN_POINT ( 'NONE',  ( -4.379528057220328563, 16.55341960407611168, 100.2072429386476955 ) ) ;
#18253 = CARTESIAN_POINT ( 'NONE',  ( 18.62759615963271287, -10.81492255796078972, 48.33224293864770260 ) ) ;
#18254 = CARTESIAN_POINT ( 'NONE',  ( -21.53943276465977519, 0.05219959533907696930, 36.24890960531435979 ) ) ;
#18255 = CARTESIAN_POINT ( 'NONE',  ( -4.483927247898539470, -16.52544592524342804, 102.2905762719810383 ) ) ;
#18256 = CARTESIAN_POINT ( 'NONE',  ( -14.46726734353920740, 1.322814319813122808, -62.26916108939693828 ) ) ;
#18257 = CARTESIAN_POINT ( 'NONE',  ( -5.049401038297874678, -19.05341960407617918, 54.79275706135234003 ) ) ;
#18258 = CARTESIAN_POINT ( 'NONE',  ( -16.55341960407617563, 4.379528057220093196, 113.5427570613523756 ) ) ;
#18259 = CARTESIAN_POINT ( 'NONE',  ( -16.46253265017160317, 9.564922557960807481, 110.8322429386476955 ) ) ;
#18260 = CARTESIAN_POINT ( 'NONE',  ( -21.55341960407619339, 5.719274019375674811, 78.54275706135236135 ) ) ;
#18261 = CARTESIAN_POINT ( 'NONE',  ( -5.719274019375978568, 21.55341960407610458, 75.20724293864769550 ) ) ;
#18262 = CARTESIAN_POINT ( 'NONE',  ( 10.81492255796106328, -18.62759615963255655, 40.41775706135234714 ) ) ;
#18263 = CARTESIAN_POINT ( 'NONE',  ( -21.55341960407610458, -5.719274019375992779, 91.45724293864769550 ) ) ;
#18264 = CARTESIAN_POINT ( 'NONE',  ( 10.72451020669871369, 18.67979575497193778, 52.08442372801901854 ) ) ;
#18265 = CARTESIAN_POINT ( 'NONE',  ( -16.52544592524342804, 4.483927247898546575, 116.0405762719810383 ) ) ;
#18266 = CARTESIAN_POINT ( 'NONE',  ( -19.02544592524342804, 5.153800228976336051, 81.04057627198103830 ) ) ;
#18267 = CARTESIAN_POINT ( 'NONE',  ( 14.34966873604972726, -8.224510206698740333, 85.83442372801901854 ) ) ;
#18268 = CARTESIAN_POINT ( 'NONE',  ( 8.224510206698953496, -14.34966873604960469, 102.9155762719810383 ) ) ;
#18269 = CARTESIAN_POINT ( 'NONE',  ( -9.474510206698964154, 16.51473224551069663, 105.4155762719810383 ) ) ;
#18270 = CARTESIAN_POINT ( 'NONE',  ( 16.55341960407611168, 4.379528057220329451, 53.95724293864770260 ) ) ;
#18271 = CARTESIAN_POINT ( 'NONE',  ( 16.52544592524342804, -4.483927247898539470, 23.54057627198102765 ) ) ;
#18272 = CARTESIAN_POINT ( 'NONE',  ( -16.46253265017160317, 9.564922557960807481, 65.83224293864769550 ) ) ;
#18273 = CARTESIAN_POINT ( 'NONE',  ( -9.564922557960796823, -16.46253265017161027, 32.08224293864769550 ) ) ;
#18274 = CARTESIAN_POINT ( 'NONE',  ( 10.81492255796078972, 18.62759615963270932, 49.58224293864769550 ) ) ;
#18275 = CARTESIAN_POINT ( 'NONE',  ( -13.97604488694547697, 13.89961937509957934, 38.12609039468566152 ) ) ;
#18277 = CARTESIAN_POINT ( 'NONE',  ( -16.52544592524342804, 4.483927247898546575, 41.04057627198103120 ) ) ;
#18276 = DIRECTION ( 'NONE',  ( 0.9526137857479322069, -0.3041824702427683991, 0.000000000000000000 ) ) ;
#18278 = CARTESIAN_POINT ( 'NONE',  ( -13.97604488694527625, -13.89961937509977652, 101.8739096053143811 ) ) ;
#18279 = CARTESIAN_POINT ( 'NONE',  ( 15.80617190586769283, -15.72974639402175789, 60.62609039468567573 ) ) ;
#18280 = FACE_OUTER_BOUND ( 'NONE', #95042, .T. ) ;
#18281 = CARTESIAN_POINT ( 'NONE',  ( 8.314922557961029526, -14.29746914071037800, 55.41775706135234714 ) ) ;
#18282 = CARTESIAN_POINT ( 'NONE',  ( 9.564922557961047289, -16.46253265017146816, 60.41775706135233293 ) ) ;
#18283 = CARTESIAN_POINT ( 'NONE',  ( -16.52544592524342804, 4.483927247898546575, 26.04057627198103475 ) ) ;
#18284 = LINE ( 'NONE', #79939, #133748 ) ;
#18285 = CARTESIAN_POINT ( 'NONE',  ( -12.06949235617739369, -12.14591786802326823, 104.3760903946856899 ) ) ;
#18286 = CARTESIAN_POINT ( 'NONE',  ( 9.564922557960805705, 16.46253265017160317, 34.58224293864770260 ) ) ;
#18287 = CARTESIAN_POINT ( 'NONE',  ( -19.02544592524342804, 5.153800228976336051, 66.04057627198103830 ) ) ;
#18288 = CARTESIAN_POINT ( 'NONE',  ( 5.049401038298161559, -19.05341960407611168, 32.70724293864768129 ) ) ;
#18289 = CARTESIAN_POINT ( 'NONE',  ( 10.72451020669871369, 18.67979575497193778, 32.08442372801901854 ) ) ;
#18290 = CARTESIAN_POINT ( 'NONE',  ( 16.51473224551069308, 9.474510206698969483, 49.16557627198102409 ) ) ;
#18291 = CARTESIAN_POINT ( 'NONE',  ( 19.05341960407611168, 5.049401038298154454, 113.9572429386477097 ) ) ;
#18292 = CARTESIAN_POINT ( 'NONE',  ( -5.049401038298153566, 19.05341960407611168, 45.20724293864769550 ) ) ;
#18293 = CARTESIAN_POINT ( 'NONE',  ( 15.72974639402199770, -15.80617190586745480, 23.12390960531436335 ) ) ;
#18295 = CARTESIAN_POINT ( 'NONE',  ( -16.55341960407611168, -4.379528057220339221, 111.4572429386476813 ) ) ;
#18294 = CARTESIAN_POINT ( 'NONE',  ( 21.53943276465977519, 0.05219959533937863772, 61.25109039468567573 ) ) ;
#18296 = CARTESIAN_POINT ( 'NONE',  ( 21.55341960407610458, 5.719274019375980345, 28.95724293864769905 ) ) ;
#18297 = CARTESIAN_POINT ( 'NONE',  ( 4.379528057220092307, 16.55341960407617563, 72.29275706135236135 ) ) ;
#18298 = CARTESIAN_POINT ( 'NONE',  ( -0.05219959533937732626, 21.53943276465977519, 97.50109039468567573 ) ) ;
#18299 = CARTESIAN_POINT ( 'NONE',  ( -14.29746914071037622, -8.314922557961029526, 54.16775706135235424 ) ) ;
#18300 = CARTESIAN_POINT ( 'NONE',  ( 0.05219959533909260263, 19.03943276465977164, 99.99890960531436690 ) ) ;
#18301 = CARTESIAN_POINT ( 'NONE',  ( 14.34966873604972726, -8.224510206698740333, 40.83442372801901854 ) ) ;
#18302 = CARTESIAN_POINT ( 'NONE',  ( 16.52544592524335698, 4.483927247898782831, 26.45942372801901854 ) ) ;
#18303 = CARTESIAN_POINT ( 'NONE',  ( 0.05219959533934541429, -16.53943276465976808, 100.0010903946857042 ) ) ;
#18304 = CARTESIAN_POINT ( 'NONE',  ( -21.52544592524334988, -5.823673210054445271, 58.95942372801902565 ) ) ;
#18305 = CARTESIAN_POINT ( 'NONE',  ( 16.46253265017146816, 9.564922557961045513, 101.6677570613523329 ) ) ;
#18306 = CARTESIAN_POINT ( 'NONE',  ( -21.53943276465977519, 0.05219959533907696930, 106.2489096053143811 ) ) ;
#18308 = CARTESIAN_POINT ( 'NONE',  ( 9.564922557961047289, -16.46253265017146816, 110.4177570613523471 ) ) ;
#18307 = CARTESIAN_POINT ( 'NONE',  ( 8.224510206698953496, -14.34966873604960469, 97.91557627198103830 ) ) ;
#18309 = CARTESIAN_POINT ( 'NONE',  ( -12.06949235617739369, -12.14591786802326823, 79.37609039468567573 ) ) ;
#18310 = CARTESIAN_POINT ( 'NONE',  ( 20.93662873023604121, 10.44628751056226612, 168.2749732860604865 ) ) ;
#18311 = CARTESIAN_POINT ( 'NONE',  ( 5.049401038297881783, 19.05341960407617563, 77.29275706135231871 ) ) ;
#18312 = CARTESIAN_POINT ( 'NONE',  ( -4.483927247898539470, -16.52544592524342804, 47.29057627198103120 ) ) ;
#18313 = CARTESIAN_POINT ( 'NONE',  ( -16.53943276465976808, 0.05219959533911058130, 46.24890960531435979 ) ) ;
#18314 = CARTESIAN_POINT ( 'NONE',  ( 12.06949235617757843, -12.14591786802309237, 98.12390960531436690 ) ) ;
#18316 = CARTESIAN_POINT ( 'NONE',  ( -16.20579543436678449, 7.371946100355088127, 89.43479165828125588 ) ) ;
#18315 = CARTESIAN_POINT ( 'NONE',  ( 13.97604488694548053, -13.89961937509957401, 35.62609039468567573 ) ) ;
#18317 = CARTESIAN_POINT ( 'NONE',  ( -21.53943276465977519, -0.05219959533937600094, 38.75109039468567573 ) ) ;
#18318 = CARTESIAN_POINT ( 'NONE',  ( -16.46253265017146816, -9.564922557961047289, 109.1677570613523471 ) ) ;
#18319 = CARTESIAN_POINT ( 'NONE',  ( 37.99999999999999289, 2.428612866367529932E-14, -25.00000000000000000 ) ) ;
#18320 = CARTESIAN_POINT ( 'NONE',  ( -5.049401038298153566, 19.05341960407611168, 90.20724293864766707 ) ) ;
#18321 = CARTESIAN_POINT ( 'NONE',  ( -13.89961937509977652, 13.97604488694528158, 95.62390960531436690 ) ) ;
#18322 = CARTESIAN_POINT ( 'NONE',  ( -0.05219959533907301413, -21.53943276465977519, 52.49890960531435979 ) ) ;
#18323 = CARTESIAN_POINT ( 'NONE',  ( 12.06949235617757843, -12.14591786802309237, 93.12390960531436690 ) ) ;
#18324 = CARTESIAN_POINT ( 'NONE',  ( 13.97604488694527802, 13.89961937509977652, 74.37390960531436690 ) ) ;
#18325 = CARTESIAN_POINT ( 'NONE',  ( 0.05219959533909260263, 19.03943276465977164, 24.99890960531435269 ) ) ;
#18326 = VECTOR ( 'NONE', #124731, 1000.000000000000000 ) ;
#18327 = CARTESIAN_POINT ( 'NONE',  ( 18.62759615963255655, 10.81492255796105972, 41.66775706135235424 ) ) ;
#18328 = ADVANCED_FACE ( 'NONE', ( #38549 ), #23381, .T. ) ;
#18329 = CARTESIAN_POINT ( 'NONE',  ( 10.81492255796106328, -18.62759615963255655, 70.41775706135236135 ) ) ;
#18330 = CARTESIAN_POINT ( 'NONE',  ( -4.483927247898782831, 16.52544592524335698, 92.70942372801901854 ) ) ;
#18331 = CARTESIAN_POINT ( 'NONE',  ( -21.55341960407619339, 5.719274019375674811, 23.54275706135235424 ) ) ;
#18332 = CARTESIAN_POINT ( 'NONE',  ( 21.53943276465977519, 0.05219959533937863772, 21.25109039468567218 ) ) ;
#18334 = CARTESIAN_POINT ( 'NONE',  ( -9.474510206698964154, 16.51473224551069663, 80.41557627198103830 ) ) ;
#18333 = CARTESIAN_POINT ( 'NONE',  ( 5.153800228976615827, -19.02544592524334988, 55.20942372801899722 ) ) ;
#18335 = CARTESIAN_POINT ( 'NONE',  ( -15.72974639402176322, -15.80617190586768395, 84.37609039468570415 ) ) ;
#18336 = CARTESIAN_POINT ( 'NONE',  ( 21.55341960407610458, 5.719274019375980345, 83.95724293864770971 ) ) ;
#18337 = CARTESIAN_POINT ( 'NONE',  ( 12.14591786802309770, 12.06949235617756955, 54.37390960531435979 ) ) ;
#18339 = CARTESIAN_POINT ( 'NONE',  ( -13.89961937509957401, -13.97604488694547875, 34.37609039468566863 ) ) ;
#18338 = CARTESIAN_POINT ( 'NONE',  ( -18.67979575497193778, 10.72451020669871902, 103.3344237280190043 ) ) ;
#18340 = CARTESIAN_POINT ( 'NONE',  ( -16.52544592524342804, 4.483927247898546575, 76.04057627198102409 ) ) ;
#18341 = CARTESIAN_POINT ( 'NONE',  ( 16.51473224551069308, 9.474510206698969483, 29.16557627198103475 ) ) ;
#18342 = CARTESIAN_POINT ( 'NONE',  ( 5.049401038297881783, 19.05341960407617563, 67.29275706135234714 ) ) ;
#18343 = CARTESIAN_POINT ( 'NONE',  ( 12.14591786802309770, 12.06949235617756955, 29.37390960531435269 ) ) ;
#18344 = CARTESIAN_POINT ( 'NONE',  ( -21.52544592524334988, -5.823673210054445271, 78.95942372801901854 ) ) ;
#18345 = CARTESIAN_POINT ( 'NONE',  ( 13.89961937509977652, -13.97604488694527269, 78.12390960531433848 ) ) ;
#18346 = CARTESIAN_POINT ( 'NONE',  ( 5.049401038297881783, 19.05341960407617563, 57.29275706135231871 ) ) ;
#18347 = CARTESIAN_POINT ( 'NONE',  ( -15.72974639402197994, 15.80617190586746368, 60.62390960531437401 ) ) ;
#18348 = CARTESIAN_POINT ( 'NONE',  ( 18.67979575497178502, 10.72451020669898547, 114.1655762719810383 ) ) ;
#18349 = CARTESIAN_POINT ( 'NONE',  ( 9.474510206698729675, 16.51473224551082808, 112.0844237280190043 ) ) ;
#18350 = CARTESIAN_POINT ( 'NONE',  ( 12.06949235617739724, 12.14591786802326823, 81.87609039468568994 ) ) ;
#18352 = CARTESIAN_POINT ( 'NONE',  ( -5.823673210054431948, 21.52544592524334988, 27.70942372801901854 ) ) ;
#18351 = CARTESIAN_POINT ( 'NONE',  ( 67.00000000000000000, -6.184466335694137604E-15, 50.50000000000002842 ) ) ;
#18353 = CARTESIAN_POINT ( 'NONE',  ( -14.29746914071049879, 8.314922557960819915, 105.8322429386476955 ) ) ;
#18354 = CARTESIAN_POINT ( 'NONE',  ( -22.81625015709510507, 31.40387420917330275, -5.424999997268812990 ) ) ;
#18355 = CARTESIAN_POINT ( 'NONE',  ( 0.05219959533934541429, -16.53943276465976808, 35.00109039468568284 ) ) ;
#18356 = CARTESIAN_POINT ( 'NONE',  ( -18.62759615963270932, 10.81492255796079327, 55.83224293864770260 ) ) ;
#18357 = CARTESIAN_POINT ( 'NONE',  ( -16.53943276465976808, -0.05219959533934237506, 108.7510903946857042 ) ) ;
#18358 = CARTESIAN_POINT ( 'NONE',  ( -16.52544592524335698, -4.483927247898792601, 38.95942372801901854 ) ) ;
#18359 = CARTESIAN_POINT ( 'NONE',  ( -16.46253265017160317, 9.564922557960807481, 30.83224293864769550 ) ) ;
#18360 = B_SPLINE_CURVE_WITH_KNOTS ( 'NONE', 3,
 ( #49859, #37670, #95355, #33692, #18537, #97323 ),
 .UNSPECIFIED., .F., .F.,
 ( 4, 2, 4 ),
 ( 0.003239945802372292023, 0.003620412082092145951, 0.004000878361811999878 ),
 .UNSPECIFIED. ) ;
#18361 = CARTESIAN_POINT ( 'NONE',  ( 14.34966873604972726, -8.224510206698740333, 80.83442372801901854 ) ) ;
#18362 = CARTESIAN_POINT ( 'NONE',  ( 13.97604488694548053, -13.89961937509957401, 70.62609039468567573 ) ) ;
#18363 = CARTESIAN_POINT ( 'NONE',  ( 10.81492255796106328, -18.62759615963255655, 40.41775706135234714 ) ) ;
#18364 = CARTESIAN_POINT ( 'NONE',  ( -5.719274019375978568, 21.55341960407610458, 55.20724293864770260 ) ) ;
#18365 = CARTESIAN_POINT ( 'NONE',  ( 8.224510206698742110, 14.34966873604972548, 97.08442372801904696 ) ) ;
#18366 = CARTESIAN_POINT ( 'NONE',  ( -5.823673210054431948, 21.52544592524334988, 77.70942372801900433 ) ) ;
#18367 = EDGE_CURVE ( 'NONE', #43523, #157920, #76737, .T. ) ;
#18368 = CARTESIAN_POINT ( 'NONE',  ( 18.67979575497178502, 10.72451020669898547, 49.16557627198102409 ) ) ;
#18369 = CARTESIAN_POINT ( 'NONE',  ( 21.55341960407610458, 5.719274019375980345, 43.95724293864769550 ) ) ;
#18370 = CARTESIAN_POINT ( 'NONE',  ( 4.483927247898790824, -16.52544592524335698, 85.20942372801901854 ) ) ;
#18371 = CARTESIAN_POINT ( 'NONE',  ( -18.67979575497178146, -10.72451020669898902, 46.66557627198102409 ) ) ;
#18372 = ORIENTED_EDGE ( 'NONE', *, *, #106434, .T. ) ;
#18373 = CARTESIAN_POINT ( 'NONE',  ( -19.02544592524342804, 5.153800228976336051, 106.0405762719810241 ) ) ;
#18374 = CARTESIAN_POINT ( 'NONE',  ( -25.82634036940375921, 7.758313425001081676, 169.9660385289634519 ) ) ;
#18375 = CARTESIAN_POINT ( 'NONE',  ( -19.03943276465977164, 0.05219959533909376836, 21.24890960531436335 ) ) ;
#18376 = CARTESIAN_POINT ( 'NONE',  ( -5.719274019375978568, 21.55341960407610458, 55.20724293864770260 ) ) ;
#18377 = CARTESIAN_POINT ( 'NONE',  ( 12.06949235617739724, 12.14591786802326823, 96.87609039468568994 ) ) ;
#18378 = CARTESIAN_POINT ( 'NONE',  ( 5.719274019375673035, 21.55341960407619339, 47.29275706135234003 ) ) ;
#18379 = CARTESIAN_POINT ( 'NONE',  ( 16.51473224551083163, -9.474510206698727899, 100.8344237280190043 ) ) ;
#18380 = CARTESIAN_POINT ( 'NONE',  ( -4.483927247898539470, -16.52544592524342804, 107.2905762719810525 ) ) ;
#18381 = CARTESIAN_POINT ( 'NONE',  ( 16.51473224551083163, -9.474510206698727899, 110.8344237280190043 ) ) ;
#18382 = AXIS2_PLACEMENT_3D ( 'NONE', #66188, #143019, #3519 ) ;
#18383 = CARTESIAN_POINT ( 'NONE',  ( 13.89961937509977652, -13.97604488694527269, 38.12390960531436690 ) ) ;
#18384 = CARTESIAN_POINT ( 'NONE',  ( 0.2219041290406811306, 24.28753333320288021, -54.22462712070620228 ) ) ;
#18385 = CARTESIAN_POINT ( 'NONE',  ( -13.97604488694527625, -13.89961937509977652, 91.87390960531432427 ) ) ;
#18386 = CARTESIAN_POINT ( 'NONE',  ( -0.05219959533934338120, 16.53943276465976808, 82.50109039468568994 ) ) ;
#18387 = CARTESIAN_POINT ( 'NONE',  ( 5.719274019375673035, 21.55341960407619339, 107.2927570613523471 ) ) ;
#18388 = CARTESIAN_POINT ( 'NONE',  ( -18.62759615963270932, 10.81492255796079327, 60.83224293864769550 ) ) ;
#18389 = CARTESIAN_POINT ( 'NONE',  ( 14.29746914071037800, 8.314922557961029526, 86.66775706135234714 ) ) ;
#18390 = CARTESIAN_POINT ( 'NONE',  ( -19.02544592524334988, -5.153800228976617603, 73.95942372801900433 ) ) ;
#18391 = CARTESIAN_POINT ( 'NONE',  ( -9.564922557960796823, -16.46253265017161027, 37.08224293864768839 ) ) ;
#18392 = CARTESIAN_POINT ( 'NONE',  ( 19.05341960407611168, 5.049401038298154454, 78.95724293864769550 ) ) ;
#18393 = CARTESIAN_POINT ( 'NONE',  ( -15.80617190586768217, 15.72974639402176855, 48.12609039468568284 ) ) ;
#18394 = CARTESIAN_POINT ( 'NONE',  ( 5.153800228976335163, 19.02544592524342804, 49.79057627198100988 ) ) ;
#18395 = CARTESIAN_POINT ( 'NONE',  ( 19.02544592524334988, 5.153800228976608722, 71.45942372801900433 ) ) ;
#18396 = CARTESIAN_POINT ( 'NONE',  ( 25.93326183087870973, -10.28624940747355510, 166.6531433017868835 ) ) ;
#18397 = CARTESIAN_POINT ( 'NONE',  ( 5.049401038298161559, -19.05341960407611168, 102.7072429386476955 ) ) ;
#18398 = CARTESIAN_POINT ( 'NONE',  ( 12.06949235617757843, -12.14591786802309237, 68.12390960531436690 ) ) ;
#18399 = CARTESIAN_POINT ( 'NONE',  ( 21.53943276465977519, -0.05219959533907433946, 63.74890960531435979 ) ) ;
#18400 = CARTESIAN_POINT ( 'NONE',  ( 0.2500000000000002220, 0.000000000000000000, 0.000000000000000000 ) ) ;
#18401 =( BOUNDED_CURVE ( )  B_SPLINE_CURVE ( 2, ( #1870, #92876, #3850, #76721, #186923, #185912, #157554, #78706, #62540, #47397, #142371, #79712, #141381 ),
 .UNSPECIFIED., .F., .T. ) 
 B_SPLINE_CURVE_WITH_KNOTS ( ( 3, 2, 2, 2, 2, 2, 3 ),
 ( 0.4497988574796767391, 0.4517543859649122973, 0.4561403508771929571, 0.4605263157894736725, 0.4649122807017543879, 0.4692982456140351033, 0.4712080942771805780 ),
 .UNSPECIFIED. ) 
 CURVE ( )  GEOMETRIC_REPRESENTATION_ITEM ( )  RATIONAL_B_SPLINE_CURVE ( ( 0.9831626618144004848, 0.9848076720550091867, 1.000000000000000000, 0.9659258262890683122, 1.000000000000000000, 0.9659258262890683122, 1.000000000000000000, 0.9659258262890683122, 1.000000000000000000, 0.9659258262890683122, 1.000000000000000000, 0.9851625545550088958, 0.9832469066685279868 ) ) 
 REPRESENTATION_ITEM ( '' )  );
#18402 = CARTESIAN_POINT ( 'NONE',  ( -9.474510206698720793, -16.51473224551083518, 24.58442372801900078 ) ) ;
#18403 = SURFACE_STYLE_FILL_AREA ( #31572 ) ;
#18405 = CARTESIAN_POINT ( 'NONE',  ( -19.05341960407611168, -5.049401038298163336, 71.45724293864766707 ) ) ;
#18404 = CARTESIAN_POINT ( 'NONE',  ( 16.46253265017160672, -9.564922557960803928, 63.33224293864769550 ) ) ;
#18406 = CARTESIAN_POINT ( 'NONE',  ( -8.314922557961024197, 14.29746914071037800, 52.91775706135235424 ) ) ;
#18407 = CARTESIAN_POINT ( 'NONE',  ( 16.67568593663829901, -39.83563513005474732, -20.80532163689324676 ) ) ;
#18408 = CARTESIAN_POINT ( 'NONE',  ( -23.31738231874055600, 16.94106989632528837, 146.0500000054623797 ) ) ;
#18409 = CARTESIAN_POINT ( 'NONE',  ( 12.14591786802327356, -12.06949235617739191, 80.62609039468567573 ) ) ;
#18410 = DIRECTION ( 'NONE',  ( -0.000000000000000000, 1.471414886128461471E-15, 1.000000000000000000 ) ) ;
#18411 = CARTESIAN_POINT ( 'NONE',  ( -8.224510206698735004, -14.34966873604973081, 69.58442372801900433 ) ) ;
#18412 = CARTESIAN_POINT ( 'NONE',  ( 16.53943276465976808, 0.05219959533934440121, 36.25109039468567573 ) ) ;
#18414 = CARTESIAN_POINT ( 'NONE',  ( 18.22780087662119897, -5.500000000000096811, 68.51763182126893525 ) ) ;
#18413 = CARTESIAN_POINT ( 'NONE',  ( 9.474510206698971260, -16.51473224551069308, 57.91557627198103120 ) ) ;
#18415 = CARTESIAN_POINT ( 'NONE',  ( 18.67979575497194134, -10.72451020669871369, 55.83442372801901854 ) ) ;
#18416 = CARTESIAN_POINT ( 'NONE',  ( 0.05219959533936267826, -19.03943276465977164, 60.00109039468566863 ) ) ;
#18417 = CARTESIAN_POINT ( 'NONE',  ( -18.67979575497193778, 10.72451020669871902, 108.3344237280190185 ) ) ;
#18418 = CARTESIAN_POINT ( 'NONE',  ( 13.97604488694527802, 13.89961937509977652, 34.37390960531436690 ) ) ;
#18419 = CARTESIAN_POINT ( 'NONE',  ( 11.74149087413295156, -36.13659316521243881, -7.402157773949824104 ) ) ;
#18420 = CARTESIAN_POINT ( 'NONE',  ( -10.72451020669898014, 18.67979575497178502, 55.41557627198102409 ) ) ;
#18421 = CARTESIAN_POINT ( 'NONE',  ( 16.46253265017160672, -9.564922557960803928, 108.3322429386476955 ) ) ;
#18422 = CARTESIAN_POINT ( 'NONE',  ( -14.29746914071049879, 8.314922557960819915, 105.8322429386476955 ) ) ;
#18423 = CARTESIAN_POINT ( 'NONE',  ( 16.55341960407618274, -4.379528057220086978, 41.04275706135236135 ) ) ;
#18424 = CARTESIAN_POINT ( 'NONE',  ( -14.29746914071049879, 8.314922557960819915, 30.83224293864770260 ) ) ;
#18425 = VERTEX_POINT ( 'NONE', #132554 ) ;
#18426 = CARTESIAN_POINT ( 'NONE',  ( 21.55341960407610458, 5.719274019375980345, 108.9572429386476955 ) ) ;
#18428 = CARTESIAN_POINT ( 'NONE',  ( -11.74264578624799782, -36.14014761921581709, -9.600000000000001421 ) ) ;
#18427 = CARTESIAN_POINT ( 'NONE',  ( -12.06949235617756955, 12.14591786802309770, 45.62390960531436690 ) ) ;
#18429 = CARTESIAN_POINT ( 'NONE',  ( 9.474510206698729675, 16.51473224551082808, 92.08442372801900433 ) ) ;
#18430 = CARTESIAN_POINT ( 'NONE',  ( -16.51473224551082808, 9.474510206698731452, 28.33442372801900433 ) ) ;
#18431 = CARTESIAN_POINT ( 'NONE',  ( 12.06949235617757843, -12.14591786802309237, 33.12390960531435979 ) ) ;
#18432 = CARTESIAN_POINT ( 'NONE',  ( -21.53943276465977519, 0.05219959533907696930, 106.2489096053143811 ) ) ;
#18433 = CARTESIAN_POINT ( 'NONE',  ( -21.55341960407610458, -5.719274019375992779, 51.45724293864770260 ) ) ;
#18434 = CARTESIAN_POINT ( 'NONE',  ( 9.564922557960805705, 16.46253265017160317, 79.58224293864769550 ) ) ;
#18435 = CARTESIAN_POINT ( 'NONE',  ( -14.34966873604960291, -8.224510206698953496, 41.66557627198103120 ) ) ;
#18436 = CARTESIAN_POINT ( 'NONE',  ( -13.97604488694527625, -13.89961937509977652, 91.87390960531432427 ) ) ;
#18437 = FACE_OUTER_BOUND ( 'NONE', #72514, .T. ) ;
#18438 = CARTESIAN_POINT ( 'NONE',  ( 13.97604488694548053, -13.89961937509957401, 35.62609039468567573 ) ) ;
#18439 = CARTESIAN_POINT ( 'NONE',  ( -10.72451020669898014, 18.67979575497178502, 100.4155762719810241 ) ) ;
#18440 = CARTESIAN_POINT ( 'NONE',  ( -14.29746914071049879, 8.314922557960819915, 105.8322429386476955 ) ) ;
#18441 = CARTESIAN_POINT ( 'NONE',  ( 18.62759615963255655, 10.81492255796105972, 31.66775706135234358 ) ) ;
#18442 = CARTESIAN_POINT ( 'NONE',  ( -8.571926809382608425, 26.38167802310805854, 148.9750000027311785 ) ) ;
#18443 = CARTESIAN_POINT ( 'NONE',  ( 8.224510206698742110, 14.34966873604972548, 112.0844237280190185 ) ) ;
#18444 = CARTESIAN_POINT ( 'NONE',  ( 16.46253265017160672, -9.564922557960803928, 33.33224293864770260 ) ) ;
#18445 = CARTESIAN_POINT ( 'NONE',  ( 5.049401038298161559, -19.05341960407611168, 82.70724293864770971 ) ) ;
#18446 = CARTESIAN_POINT ( 'NONE',  ( 27.73933785331498925, -9.013057229001033122, 139.7750000027311899 ) ) ;
#18447 = CARTESIAN_POINT ( 'NONE',  ( 9.564922557960805705, 16.46253265017160317, 34.58224293864770260 ) ) ;
#18448 = CARTESIAN_POINT ( 'NONE',  ( 4.379528057220339221, -16.55341960407611168, 37.70724293864769550 ) ) ;
#18449 = CARTESIAN_POINT ( 'NONE',  ( 15.72974639402176855, 15.80617190586768217, 76.87609039468567573 ) ) ;
#18451 = CARTESIAN_POINT ( 'NONE',  ( 14.34966873604972726, -8.224510206698740333, 75.83442372801900433 ) ) ;
#18450 = CARTESIAN_POINT ( 'NONE',  ( 9.554919064906188808, -36.23455639189494804, -31.31948065624977318 ) ) ;
#18452 = CARTESIAN_POINT ( 'NONE',  ( 13.97604488694527802, 13.89961937509977652, 59.37390960531434558 ) ) ;
#18453 = CARTESIAN_POINT ( 'NONE',  ( -19.05341960407611168, -5.049401038298163336, 66.45724293864769550 ) ) ;
#18454 = ORIENTED_EDGE ( 'NONE', *, *, #40331, .T. ) ;
#18455 = CARTESIAN_POINT ( 'NONE',  ( -5.049401038297874678, -19.05341960407617918, 19.79275706135233293 ) ) ;
#18456 = CARTESIAN_POINT ( 'NONE',  ( 4.483927247898790824, -16.52544592524335698, 70.20942372801904696 ) ) ;
#18457 = CARTESIAN_POINT ( 'NONE',  ( 18.67979575497194134, -10.72451020669871369, 100.8344237280190185 ) ) ;
#18458 = CARTESIAN_POINT ( 'NONE',  ( 13.97604488694527802, 13.89961937509977652, 59.37390960531434558 ) ) ;
#18459 = CARTESIAN_POINT ( 'NONE',  ( -18.62759615963270932, 10.81492255796079327, 40.83224293864769550 ) ) ;
#18460 = CARTESIAN_POINT ( 'NONE',  ( 19.05341960407617918, -5.049401038297876454, 101.0427570613523045 ) ) ;
#18461 = CARTESIAN_POINT ( 'NONE',  ( -21.55341960407619339, 5.719274019375674811, 73.54275706135234714 ) ) ;
#18462 = CARTESIAN_POINT ( 'NONE',  ( -0.05219959533934338120, 16.53943276465976808, 47.50109039468568994 ) ) ;
#18463 = CARTESIAN_POINT ( 'NONE',  ( 15.80617190586746368, 15.72974639402197994, 104.3739096053143669 ) ) ;
#18464 = CARTESIAN_POINT ( 'NONE',  ( 5.153800228976615827, -19.02544592524334988, 105.2094237280190185 ) ) ;
#18465 = CARTESIAN_POINT ( 'NONE',  ( 16.46253265017160672, -9.564922557960803928, 78.33224293864769550 ) ) ;
#18466 = CARTESIAN_POINT ( 'NONE',  ( -8.224510206698735004, -14.34966873604973081, 19.58442372801901143 ) ) ;
#18467 = VECTOR ( 'NONE', #74443, 1000.000000000000000 ) ;
#18468 = CARTESIAN_POINT ( 'NONE',  ( -14.34966873604972548, 8.224510206698743886, 23.33442372801901499 ) ) ;
#18469 = CARTESIAN_POINT ( 'NONE',  ( 16.53943276465976808, -0.05219959533910856209, 68.74890960531435269 ) ) ;
#18470 = CARTESIAN_POINT ( 'NONE',  ( -8.224510206698735004, -14.34966873604973081, 79.58442372801903275 ) ) ;
#18472 = CARTESIAN_POINT ( 'NONE',  ( -19.02544592524342804, 5.153800228976336051, 51.04057627198103120 ) ) ;
#18471 = CARTESIAN_POINT ( 'NONE',  ( -15.80617190586745835, -15.72974639402198527, 111.8739096053143669 ) ) ;
#18473 = CARTESIAN_POINT ( 'NONE',  ( -19.02544592524342804, 5.153800228976336051, 71.04057627198099567 ) ) ;
#18474 = CARTESIAN_POINT ( 'NONE',  ( 8.224510206698742110, 14.34966873604972548, 72.08442372801899012 ) ) ;
#18475 = CARTESIAN_POINT ( 'NONE',  ( 8.906447517083050158, 27.41122689804195645, 145.6500000054623740 ) ) ;
#18476 = ORIENTED_EDGE ( 'NONE', *, *, #94811, .F. ) ;
#18477 = CARTESIAN_POINT ( 'NONE',  ( 19.02544592524334988, 5.153800228976608722, 21.45942372801899012 ) ) ;
#18478 = CIRCLE ( 'NONE', #128148, 8.000000000000000000 ) ;
#18479 = CARTESIAN_POINT ( 'NONE',  ( -19.03943276465977164, 0.05219959533909376836, 36.24890960531436690 ) ) ;
#18480 = ORIENTED_EDGE ( 'NONE', *, *, #90150, .T. ) ;
#18481 = CARTESIAN_POINT ( 'NONE',  ( -13.97604488694547697, 13.89961937509957934, 113.1260903946856757 ) ) ;
#18483 = CARTESIAN_POINT ( 'NONE',  ( -12.06949235617739369, -12.14591786802326823, 24.37609039468567573 ) ) ;
#18482 = CARTESIAN_POINT ( 'NONE',  ( 5.153800228976615827, -19.02544592524334988, 40.20942372801898301 ) ) ;
#18484 = CARTESIAN_POINT ( 'NONE',  ( 19.03943276465977164, -0.05219959533909143690, 38.74890960531436690 ) ) ;
#18485 = CARTESIAN_POINT ( 'NONE',  ( -5.153800228976328057, -19.02544592524343514, 67.29057627198102409 ) ) ;
#18486 = CARTESIAN_POINT ( 'NONE',  ( -0.05219959533907301413, -21.53943276465977519, 92.49890960531436690 ) ) ;
#18487 = CARTESIAN_POINT ( 'NONE',  ( 9.564922557960805705, 16.46253265017160317, 109.5822429386476955 ) ) ;
#18488 = EDGE_CURVE ( 'NONE', #185765, #87616, #87045, .T. ) ;
#18489 = CARTESIAN_POINT ( 'NONE',  ( 19.05341960407611168, 5.049401038298154454, 43.95724293864769550 ) ) ;
#18490 = CARTESIAN_POINT ( 'NONE',  ( -22.44159573604009950, -16.30477369853688430, 147.5750000027312012 ) ) ;
#18491 = CARTESIAN_POINT ( 'NONE',  ( -19.03943276465977164, -0.05219959533935918106, 93.75109039468566152 ) ) ;
#18492 = CARTESIAN_POINT ( 'NONE',  ( -21.52544592524343514, 5.823673210054127303, 71.04057627198103830 ) ) ;
#18493 = CARTESIAN_POINT ( 'NONE',  ( -9.564922557961040184, 16.46253265017147172, 27.91775706135232582 ) ) ;
#18494 = CARTESIAN_POINT ( 'NONE',  ( 4.483927247898545687, 16.52544592524342804, 64.79057627198103830 ) ) ;
#18495 = CARTESIAN_POINT ( 'NONE',  ( 5.823673210054444382, -21.52544592524334988, 85.20942372801901854 ) ) ;
#18496 = CARTESIAN_POINT ( 'NONE',  ( -14.29746914071049879, 8.314922557960819915, 115.8322429386477097 ) ) ;
#18498 = CARTESIAN_POINT ( 'NONE',  ( -18.67979575497193778, 10.72451020669871902, 93.33442372801901854 ) ) ;
#18497 = CARTESIAN_POINT ( 'NONE',  ( -14.34966873604960291, -8.224510206698953496, 31.66557627198102054 ) ) ;
#18499 = CARTESIAN_POINT ( 'NONE',  ( -19.03943276465977164, 0.05219959533909376836, 76.24890960531435269 ) ) ;
#18500 = CARTESIAN_POINT ( 'NONE',  ( 21.53943276465977519, 0.05219959533937863772, 41.25109039468568284 ) ) ;
#18501 = CARTESIAN_POINT ( 'NONE',  ( -19.02544592524342804, 5.153800228976336051, 81.04057627198103830 ) ) ;
#18502 = CARTESIAN_POINT ( 'NONE',  ( 16.55341960407611168, 4.379528057220329451, 98.95724293864770971 ) ) ;
#18503 = CARTESIAN_POINT ( 'NONE',  ( 12.06949235617757843, -12.14591786802309237, 58.12390960531435979 ) ) ;
#18504 = CARTESIAN_POINT ( 'NONE',  ( 10.81492255796078972, 18.62759615963270932, 74.58224293864768129 ) ) ;
#18505 = CARTESIAN_POINT ( 'NONE',  ( -9.564922557960796823, -16.46253265017161027, 77.08224293864769550 ) ) ;
#18506 = CARTESIAN_POINT ( 'NONE',  ( 10.81492255796078972, 18.62759615963270932, 84.58224293864769550 ) ) ;
#18507 = CARTESIAN_POINT ( 'NONE',  ( 19.05341960407617918, -5.049401038297876454, 76.04275706135230450 ) ) ;
#18509 = CARTESIAN_POINT ( 'NONE',  ( 8.314922557960818139, 14.29746914071049879, 79.58224293864769550 ) ) ;
#18508 = CARTESIAN_POINT ( 'NONE',  ( 9.474510206698729675, 16.51473224551082808, 32.08442372801900433 ) ) ;
#18510 = AXIS2_PLACEMENT_3D ( 'NONE', #16542, #33689, #46880 ) ;
#18511 = CARTESIAN_POINT ( 'NONE',  ( 18.67979575497178502, 10.72451020669898547, 54.16557627198103120 ) ) ;
#18512 = DIRECTION ( 'NONE',  ( 0.000000000000000000, 0.000000000000000000, -1.000000000000000000 ) ) ;
#18514 = CARTESIAN_POINT ( 'NONE',  ( 27.73933785331498569, 9.013057229001093518, 144.4750000027311785 ) ) ;
#18513 = CARTESIAN_POINT ( 'NONE',  ( 12.06949235617739724, 12.14591786802326823, 101.8760903946857042 ) ) ;
#18515 = CARTESIAN_POINT ( 'NONE',  ( -0.05219959533936034679, 19.03943276465977164, 102.5010903946856757 ) ) ;
#18516 = CARTESIAN_POINT ( 'NONE',  ( -14.34966873604960291, -8.224510206698953496, 66.66557627198102409 ) ) ;
#18517 = CARTESIAN_POINT ( 'NONE',  ( -19.19724070472095079, -5.500000000000031974, 96.06193348274383936 ) ) ;
#18518 = CARTESIAN_POINT ( 'NONE',  ( -16.51473224551069308, -9.474510206698971260, 61.66557627198103120 ) ) ;
#18519 = CARTESIAN_POINT ( 'NONE',  ( 13.89961937509977652, -13.97604488694527269, 28.12390960531435624 ) ) ;
#18520 = CARTESIAN_POINT ( 'NONE',  ( 12.06949235617757843, -12.14591786802309237, 48.12390960531436690 ) ) ;
#18521 = CARTESIAN_POINT ( 'NONE',  ( 19.05341960407611168, 5.049401038298154454, 103.9572429386476671 ) ) ;
#18523 = CARTESIAN_POINT ( 'NONE',  ( -19.03943276465977164, 0.05219959533909376836, 66.24890960531436690 ) ) ;
#18522 = CARTESIAN_POINT ( 'NONE',  ( -13.89961937509957401, -13.97604488694547875, 94.37609039468566152 ) ) ;
#18524 = CARTESIAN_POINT ( 'NONE',  ( 5.153800228976335163, 19.02544592524342804, 79.79057627198102409 ) ) ;
#18525 = CARTESIAN_POINT ( 'NONE',  ( 5.049401038298161559, -19.05341960407611168, 82.70724293864770971 ) ) ;
#18526 = CARTESIAN_POINT ( 'NONE',  ( 5.823673210054125526, 21.52544592524343514, 59.79057627198103120 ) ) ;
#18527 = CARTESIAN_POINT ( 'NONE',  ( -4.483927247898782831, 16.52544592524335698, 57.70942372801901143 ) ) ;
#18528 = CARTESIAN_POINT ( 'NONE',  ( -0.05219959533936034679, 19.03943276465977164, 107.5010903946856615 ) ) ;
#18529 = CARTESIAN_POINT ( 'NONE',  ( -0.05219959533909027116, -19.03943276465977164, 62.49890960531435979 ) ) ;
#18530 = CARTESIAN_POINT ( 'NONE',  ( 18.67979575497178502, 10.72451020669898547, 69.16557627198102409 ) ) ;
#18531 = CARTESIAN_POINT ( 'NONE',  ( -13.97604488694547697, 13.89961937509957934, 88.12609039468563310 ) ) ;
#18533 = CARTESIAN_POINT ( 'NONE',  ( -10.72451020669870658, -18.67979575497194134, 49.58442372801901143 ) ) ;
#18532 = CARTESIAN_POINT ( 'NONE',  ( -8.314922557960811034, -14.29746914071050412, 27.08224293864769550 ) ) ;
#18534 = CARTESIAN_POINT ( 'NONE',  ( -4.180825498786520988, -4.459728486673432357, -62.50521485713754544 ) ) ;
#18536 = CARTESIAN_POINT ( 'NONE',  ( -16.55341960407617563, 4.379528057220093196, 98.54275706135234714 ) ) ;
#18535 = CARTESIAN_POINT ( 'NONE',  ( -0.05219959533934338120, 16.53943276465976808, 67.50109039468568994 ) ) ;
#18537 = CARTESIAN_POINT ( 'NONE',  ( -18.10062525802553424, 5.500000000000031974, 73.51383468041922242 ) ) ;
#18538 = CARTESIAN_POINT ( 'NONE',  ( 0.05219959533934541429, -16.53943276465976808, 85.00109039468568994 ) ) ;
#18539 = CARTESIAN_POINT ( 'NONE',  ( 12.14591786802327356, -12.06949235617739191, 30.62609039468567929 ) ) ;
#18540 = CARTESIAN_POINT ( 'NONE',  ( 19.02544592524343514, -5.153800228976328945, 48.54057627198103120 ) ) ;
#18541 = CARTESIAN_POINT ( 'NONE',  ( -19.02544592524342804, 5.153800228976336051, 56.04057627198100988 ) ) ;
#18542 = CARTESIAN_POINT ( 'NONE',  ( -5.153800228976328057, -19.02544592524343514, 62.29057627198100988 ) ) ;
#18543 = CARTESIAN_POINT ( 'NONE',  ( -21.55341960407619339, 5.719274019375674811, 48.54275706135234714 ) ) ;
#18544 = CARTESIAN_POINT ( 'NONE',  ( 12.06949235617739724, 12.14591786802326823, 51.87609039468568284 ) ) ;
#18545 = CARTESIAN_POINT ( 'NONE',  ( -8.224510206698948167, 14.34966873604960824, 30.41557627198101699 ) ) ;
#18546 = CARTESIAN_POINT ( 'NONE',  ( 13.89961937509977652, -13.97604488694527269, 23.12390960531436335 ) ) ;
#18547 = CARTESIAN_POINT ( 'NONE',  ( 19.02544592524343514, -5.153800228976328945, 38.54057627198103120 ) ) ;
#18548 = CARTESIAN_POINT ( 'NONE',  ( 14.29746914071037800, 8.314922557961029526, 26.66775706135235424 ) ) ;
#18549 = CARTESIAN_POINT ( 'NONE',  ( 9.564922557961047289, -16.46253265017146816, 85.41775706135233293 ) ) ;
#18550 = CARTESIAN_POINT ( 'NONE',  ( 16.52544592524342804, -4.483927247898539470, 78.54057627198103830 ) ) ;
#18551 = CARTESIAN_POINT ( 'NONE',  ( 16.46253265017160672, -9.564922557960803928, 58.33224293864769550 ) ) ;
#18553 = CARTESIAN_POINT ( 'NONE',  ( 16.81555441253551564, -7.025013491695470513, 93.13685445334256485 ) ) ;
#18552 = CARTESIAN_POINT ( 'NONE',  ( -13.97604488694547697, 13.89961937509957934, 93.12609039468566152 ) ) ;
#18554 = CARTESIAN_POINT ( 'NONE',  ( -10.72451020669870658, -18.67979575497194134, 74.58442372801901854 ) ) ;
#18555 = CARTESIAN_POINT ( 'NONE',  ( -4.379528057220086978, -16.55341960407618274, 54.79275706135235424 ) ) ;
#18556 = CARTESIAN_POINT ( 'NONE',  ( 17.13100169013299379, 6.664070546373169535, 36.73210164300151348 ) ) ;
#18557 = CARTESIAN_POINT ( 'NONE',  ( 18.67979575497178502, 10.72451020669898547, 39.16557627198102409 ) ) ;
#18558 = CARTESIAN_POINT ( 'NONE',  ( 12.06949235617739724, 12.14591786802326823, 36.87609039468568994 ) ) ;
#18559 = CARTESIAN_POINT ( 'NONE',  ( -5.429308488886486681E-15, 30.30510711980690175, 147.5000000000000000 ) ) ;
#18560 = CARTESIAN_POINT ( 'NONE',  ( 13.97604488694548053, -13.89961937509957401, 35.62609039468567573 ) ) ;
#18561 = CARTESIAN_POINT ( 'NONE',  ( 10.33027487414777568, 12.20125963778084710, -59.47400725600236626 ) ) ;
#18562 = CARTESIAN_POINT ( 'NONE',  ( 16.51473224551069308, 9.474510206698969483, 54.16557627198103120 ) ) ;
#18563 = CARTESIAN_POINT ( 'NONE',  ( -17.50000000000001421, -5.499999999999944045, 71.28230962303567253 ) ) ;
#18564 = CARTESIAN_POINT ( 'NONE',  ( 13.89961937509977652, -13.97604488694527269, 73.12390960531436690 ) ) ;
#18565 = CARTESIAN_POINT ( 'NONE',  ( -19.53037848336979820, 5.499999999999995559, 99.85532783611445495 ) ) ;
#18566 = EDGE_CURVE ( 'NONE', #4689, #117112, #165893, .T. ) ;
#18567 = CARTESIAN_POINT ( 'NONE',  ( -19.03943276465977164, -0.05219959533935918106, 23.75109039468566152 ) ) ;
#18568 = CARTESIAN_POINT ( 'NONE',  ( -0.05219959533910754901, -16.53943276465976808, 42.49890960531435979 ) ) ;
#18569 = CARTESIAN_POINT ( 'NONE',  ( 19.02544592524343514, -5.153800228976328945, 48.54057627198103120 ) ) ;
#18570 = CARTESIAN_POINT ( 'NONE',  ( 0.05219959533909260263, 19.03943276465977164, 104.9989096053143669 ) ) ;
#18571 = CARTESIAN_POINT ( 'NONE',  ( -21.55341960407619339, 5.719274019375674811, 73.54275706135234714 ) ) ;
#18572 = CARTESIAN_POINT ( 'NONE',  ( 19.05341960407611168, 5.049401038298154454, 48.95724293864768129 ) ) ;
#18573 = CARTESIAN_POINT ( 'NONE',  ( 18.62759615963255655, 10.81492255796105972, 66.66775706135234714 ) ) ;
#18574 = CARTESIAN_POINT ( 'NONE',  ( 9.474510206698971260, -16.51473224551069308, 112.9155762719810383 ) ) ;
#18575 = CARTESIAN_POINT ( 'NONE',  ( -13.97604488694527625, -13.89961937509977652, 41.87390960531435979 ) ) ;
#18576 = CARTESIAN_POINT ( 'NONE',  ( -15.72974639402176322, -15.80617190586768395, 24.37609039468567573 ) ) ;
#18577 = CARTESIAN_POINT ( 'NONE',  ( 16.46253265017146816, 9.564922557961045513, 51.66775706135233293 ) ) ;
#18578 = CARTESIAN_POINT ( 'NONE',  ( -16.46253265017160317, 9.564922557960807481, 25.83224293864769194 ) ) ;
#18579 = CARTESIAN_POINT ( 'NONE',  ( -0.05219959533909027116, -19.03943276465977164, 57.49890960531435979 ) ) ;
#18580 = CARTESIAN_POINT ( 'NONE',  ( -14.29746914071037622, -8.314922557961029526, 19.16775706135234714 ) ) ;
#18581 = CARTESIAN_POINT ( 'NONE',  ( -12.06949235617756955, 12.14591786802309770, 75.62390960531439532 ) ) ;
#18582 = CARTESIAN_POINT ( 'NONE',  ( -10.72451020669898014, 18.67979575497178502, 40.41557627198103120 ) ) ;
#18583 = CARTESIAN_POINT ( 'NONE',  ( 16.46253265017146816, 9.564922557961045513, 106.6677570613523471 ) ) ;
#18584 = CARTESIAN_POINT ( 'NONE',  ( -18.62759615963270932, 10.81492255796079327, 105.8322429386476955 ) ) ;
#18585 = CARTESIAN_POINT ( 'NONE',  ( 5.823673210054444382, -21.52544592524334988, 55.20942372801902565 ) ) ;
#18586 = CARTESIAN_POINT ( 'NONE',  ( 16.53943276465976808, 0.05219959533934440121, 56.25109039468568284 ) ) ;
#18587 = CARTESIAN_POINT ( 'NONE',  ( -14.34966873604972548, 8.224510206698743886, 48.33442372801902565 ) ) ;
#18588 = CARTESIAN_POINT ( 'NONE',  ( -18.62759615963270932, 10.81492255796079327, 55.83224293864770260 ) ) ;
#18589 = CARTESIAN_POINT ( 'NONE',  ( -19.05341960407611168, -5.049401038298163336, 41.45724293864769550 ) ) ;
#18590 = CARTESIAN_POINT ( 'NONE',  ( 4.483927247898790824, -16.52544592524335698, 70.20942372801904696 ) ) ;
#18591 = CARTESIAN_POINT ( 'NONE',  ( 21.52544592524344225, -5.823673210054117533, 103.5405762719810383 ) ) ;
#18592 = CARTESIAN_POINT ( 'NONE',  ( -4.379528057220328563, 16.55341960407611168, 50.20724293864769550 ) ) ;
#18593 = CARTESIAN_POINT ( 'NONE',  ( 5.049401038298161559, -19.05341960407611168, 67.70724293864769550 ) ) ;
#18594 = CARTESIAN_POINT ( 'NONE',  ( -14.34966873604972548, 8.224510206698743886, 78.33442372801901854 ) ) ;
#18595 = CARTESIAN_POINT ( 'NONE',  ( -19.02544592524334988, -5.153800228976617603, 108.9594237280189759 ) ) ;
#18596 = CARTESIAN_POINT ( 'NONE',  ( -5.719274019375978568, 21.55341960407610458, 105.2072429386477097 ) ) ;
#18597 = CARTESIAN_POINT ( 'NONE',  ( 4.483927247898545687, 16.52544592524342804, 39.79057627198103830 ) ) ;
#18598 = ORIENTED_EDGE ( 'NONE', *, *, #48667, .F. ) ;
#18599 = CARTESIAN_POINT ( 'NONE',  ( 19.52837319214027190, -5.499999999999988454, 92.10471352585543059 ) ) ;
#18600 = CARTESIAN_POINT ( 'NONE',  ( -15.80617190586745835, -15.72974639402198527, 86.87390960531438111 ) ) ;
#18601 = CARTESIAN_POINT ( 'NONE',  ( -8.314922557960811034, -14.29746914071050412, 32.08224293864769550 ) ) ;
#18602 = ORIENTED_EDGE ( 'NONE', *, *, #70632, .T. ) ;
#18603 = DIRECTION ( 'NONE',  ( 0.000000000000000000, 0.000000000000000000, -1.000000000000000000 ) ) ;
#18604 = CARTESIAN_POINT ( 'NONE',  ( -10.81492255796078084, -18.62759615963271287, 97.08224293864770971 ) ) ;
#18605 = CARTESIAN_POINT ( 'NONE',  ( -13.97604488694527625, -13.89961937509977652, 101.8739096053143811 ) ) ;
#18606 = CARTESIAN_POINT ( 'NONE',  ( -18.67979575497193778, 10.72451020669871902, 28.33442372801902209 ) ) ;
#18607 = CARTESIAN_POINT ( 'NONE',  ( -0.05219959533910754901, -16.53943276465976808, 52.49890960531435979 ) ) ;
#18608 = CARTESIAN_POINT ( 'NONE',  ( -16.55341960407617563, 4.379528057220093196, 53.54275706135234714 ) ) ;
#18609 = VECTOR ( 'NONE', #153495, 1000.000000000000000 ) ;
#18610 = CARTESIAN_POINT ( 'NONE',  ( -5.153800228976328057, -19.02544592524343514, 47.29057627198102409 ) ) ;
#18611 = CARTESIAN_POINT ( 'NONE',  ( 0.05219959533936267826, -19.03943276465977164, 50.00109039468566863 ) ) ;
#18612 = CARTESIAN_POINT ( 'NONE',  ( -0.05219959533909027116, -19.03943276465977164, 82.49890960531436690 ) ) ;
#18613 = CARTESIAN_POINT ( 'NONE',  ( -5.719274019375978568, 21.55341960407610458, 40.20724293864769550 ) ) ;
#18614 = CARTESIAN_POINT ( 'NONE',  ( 16.51473224551069308, 9.474510206698969483, 64.16557627198102409 ) ) ;
#18615 = CARTESIAN_POINT ( 'NONE',  ( -9.564922557961040184, 16.46253265017147172, 112.9177570613523329 ) ) ;
#18616 = CARTESIAN_POINT ( 'NONE',  ( 5.153800228976615827, -19.02544592524334988, 55.20942372801899722 ) ) ;
#18617 = CARTESIAN_POINT ( 'NONE',  ( 15.72974639402199770, -15.80617190586745480, 98.12390960531436690 ) ) ;
#18618 = CARTESIAN_POINT ( 'NONE',  ( 4.379528057220339221, -16.55341960407611168, 32.70724293864770260 ) ) ;
#18619 = CARTESIAN_POINT ( 'NONE',  ( -9.474510206698964154, 16.51473224551069663, 80.41557627198103830 ) ) ;
#18620 = CARTESIAN_POINT ( 'NONE',  ( -21.52544592524343514, 5.823673210054127303, 56.04057627198102409 ) ) ;
#18622 = CARTESIAN_POINT ( 'NONE',  ( -4.379528057220086978, -16.55341960407618274, 19.79275706135235069 ) ) ;
#18621 = CARTESIAN_POINT ( 'NONE',  ( -21.55341960407610458, -5.719274019375992779, 91.45724293864769550 ) ) ;
#18623 = CARTESIAN_POINT ( 'NONE',  ( -5.153800228976328057, -19.02544592524343514, 112.2905762719810099 ) ) ;
#18624 = CARTESIAN_POINT ( 'NONE',  ( 0.05219959533937995610, -21.53943276465977519, 95.00109039468568994 ) ) ;
#18625 = CARTESIAN_POINT ( 'NONE',  ( 19.05341960407611168, 5.049401038298154454, 88.95724293864769550 ) ) ;
#18626 = CARTESIAN_POINT ( 'NONE',  ( 0.05219959533909260263, 19.03943276465977164, 24.99890960531435269 ) ) ;
#18627 = CARTESIAN_POINT ( 'NONE',  ( 13.89961937509977652, -13.97604488694527269, 78.12390960531433848 ) ) ;
#18628 = CARTESIAN_POINT ( 'NONE',  ( -16.55341960407611168, -4.379528057220339221, 106.4572429386477097 ) ) ;
#18629 = CARTESIAN_POINT ( 'NONE',  ( -16.46253265017160317, 9.564922557960807481, 65.83224293864769550 ) ) ;
#18630 = CARTESIAN_POINT ( 'NONE',  ( 12.14591786802327356, -12.06949235617739191, 20.62609039468568639 ) ) ;
#18631 = CARTESIAN_POINT ( 'NONE',  ( 17.49999999999999645, 4.013004640162663783, 32.05394279005592040 ) ) ;
#18632 = CARTESIAN_POINT ( 'NONE',  ( 9.564922557960805705, 16.46253265017160317, 79.58224293864769550 ) ) ;
#18633 = AXIS2_PLACEMENT_3D ( 'NONE', #169071, #103451, #28614 ) ;
#18635 = CARTESIAN_POINT ( 'NONE',  ( -15.80617190586745835, -15.72974639402198527, 21.87390960531436690 ) ) ;
#18634 = CARTESIAN_POINT ( 'NONE',  ( -21.52544592524334988, -5.823673210054445271, 98.95942372801903275 ) ) ;
#18636 = CARTESIAN_POINT ( 'NONE',  ( 8.224510206698742110, 14.34966873604972548, 97.08442372801904696 ) ) ;
#18637 = CARTESIAN_POINT ( 'NONE',  ( -38.00000000000000711, 2.428612866367529932E-14, -10.00000000000000000 ) ) ;
#18638 = CARTESIAN_POINT ( 'NONE',  ( -19.05341960407617563, 5.049401038297882671, 73.54275706135233293 ) ) ;
#18639 = CARTESIAN_POINT ( 'NONE',  ( 19.05341960407617918, -5.049401038297876454, 21.04275706135232582 ) ) ;
#18640 = CARTESIAN_POINT ( 'NONE',  ( 3.882848763669480618, 5.183909576824676790, -64.47227361656570110 ) ) ;
#18641 = CARTESIAN_POINT ( 'NONE',  ( 5.153800228976335163, 19.02544592524342804, 29.79057627198102409 ) ) ;
#18642 = CARTESIAN_POINT ( 'NONE',  ( 4.379528057220339221, -16.55341960407611168, 42.70724293864770260 ) ) ;
#18643 = DIRECTION ( 'NONE',  ( -1.000000000000000000, 0.000000000000000000, 0.000000000000000000 ) ) ;
#18644 = CARTESIAN_POINT ( 'NONE',  ( -8.314922557961024197, 14.29746914071037800, 102.9177570613523756 ) ) ;
#18645 = DIRECTION ( 'NONE',  ( -1.000000000000000000, 0.000000000000000000, 0.000000000000000000 ) ) ;
#18646 = CARTESIAN_POINT ( 'NONE',  ( 14.29746914071037800, 8.314922557961029526, 76.66775706135234714 ) ) ;
#18647 = CARTESIAN_POINT ( 'NONE',  ( -19.05341960407611168, -5.049401038298163336, 31.45724293864769550 ) ) ;
#18648 = CARTESIAN_POINT ( 'NONE',  ( -0.05219959533937732626, 21.53943276465977519, 97.50109039468567573 ) ) ;
#18649 = CARTESIAN_POINT ( 'NONE',  ( 19.05341960407617918, -5.049401038297876454, 96.04275706135231871 ) ) ;
#18650 = CARTESIAN_POINT ( 'NONE',  ( 10.81492255796106328, -18.62759615963255655, 75.41775706135233293 ) ) ;
#18651 = CARTESIAN_POINT ( 'NONE',  ( -9.474510206698720793, -16.51473224551083518, 49.58442372801899722 ) ) ;
#18652 = CARTESIAN_POINT ( 'NONE',  ( 19.03943276465977164, -0.05219959533909143690, 78.74890960531436690 ) ) ;
#18653 = CARTESIAN_POINT ( 'NONE',  ( 9.564922557960805705, 16.46253265017160317, 74.58224293864769550 ) ) ;
#18654 = DIRECTION ( 'NONE',  ( -1.000000000000000000, 0.000000000000000000, 0.000000000000000000 ) ) ;
#18655 = CARTESIAN_POINT ( 'NONE',  ( 14.29746914071049879, -8.314922557960816363, 63.33224293864770260 ) ) ;
#18656 = CARTESIAN_POINT ( 'NONE',  ( -18.62759615963270932, 10.81492255796079327, 60.83224293864769550 ) ) ;
#18657 = CARTESIAN_POINT ( 'NONE',  ( 16.46253265017160672, -9.564922557960803928, 48.33224293864769550 ) ) ;
#18659 = CARTESIAN_POINT ( 'NONE',  ( -12.14591786802326823, 12.06949235617739902, 73.12609039468567573 ) ) ;
#18658 = CARTESIAN_POINT ( 'NONE',  ( 21.52544592524344225, -5.823673210054117533, 88.54057627198103830 ) ) ;
#18660 = ORIENTED_EDGE ( 'NONE', *, *, #193497, .T. ) ;
#18662 = CARTESIAN_POINT ( 'NONE',  ( -36.91746825000001309, 11.99521256947798342, -6.724999997268813701 ) ) ;
#18661 = CARTESIAN_POINT ( 'NONE',  ( -0.05219959533910754901, -16.53943276465976808, 82.49890960531436690 ) ) ;
#18663 = CARTESIAN_POINT ( 'NONE',  ( 14.34966873604972726, -8.224510206698740333, 35.83442372801901143 ) ) ;
#18664 = CARTESIAN_POINT ( 'NONE',  ( -0.05219959533910754901, -16.53943276465976808, 112.4989096053143669 ) ) ;
#18665 = CARTESIAN_POINT ( 'NONE',  ( 9.474510206698729675, 16.51473224551082808, 72.08442372801900433 ) ) ;
#18666 = CARTESIAN_POINT ( 'NONE',  ( -14.34966873604960291, -8.224510206698953496, 66.66557627198102409 ) ) ;
#18667 = CARTESIAN_POINT ( 'NONE',  ( -15.72974639402176322, -15.80617190586768395, 49.37609039468569705 ) ) ;
#18669 = CARTESIAN_POINT ( 'NONE',  ( -10.72451020669898014, 18.67979575497178502, 110.4155762719810383 ) ) ;
#18668 = CARTESIAN_POINT ( 'NONE',  ( 0.05219959533909260263, 19.03943276465977164, 24.99890960531435269 ) ) ;
#18670 = CARTESIAN_POINT ( 'NONE',  ( 19.05341960407611168, 5.049401038298154454, 113.9572429386477097 ) ) ;
#18671 = CARTESIAN_POINT ( 'NONE',  ( 14.34966873604960469, 8.224510206698951720, 94.16557627198103830 ) ) ;
#18672 = CARTESIAN_POINT ( 'NONE',  ( 23.38344545171973010, -32.96869167543344048, -17.70766473210208858 ) ) ;
#18673 = CARTESIAN_POINT ( 'NONE',  ( 5.153800228976335163, 19.02544592524342804, 39.79057627198100988 ) ) ;
#18674 = CARTESIAN_POINT ( 'NONE',  ( 22.81625015709509441, 31.40387420917330275, -3.324999997268812901 ) ) ;
#18675 = CARTESIAN_POINT ( 'NONE',  ( 16.46253265017146816, 9.564922557961045513, 76.66775706135234714 ) ) ;
#18676 = CARTESIAN_POINT ( 'NONE',  ( -18.62759615963255300, -10.81492255796106328, 39.16775706135235424 ) ) ;
#18677 = CARTESIAN_POINT ( 'NONE',  ( -9.564922557960796823, -16.46253265017161027, 72.08224293864770971 ) ) ;
#18678 = CARTESIAN_POINT ( 'NONE',  ( -9.564922557961040184, 16.46253265017147172, 62.91775706135233293 ) ) ;
#18679 = CARTESIAN_POINT ( 'NONE',  ( 19.03943276465977164, -0.05219959533909143690, 48.74890960531435979 ) ) ;
#18680 = CARTESIAN_POINT ( 'NONE',  ( 12.06949235617757843, -12.14591786802309237, 68.12390960531436690 ) ) ;
#18681 = CARTESIAN_POINT ( 'NONE',  ( 16.53943276465976808, -0.05219959533910856209, 53.74890960531437401 ) ) ;
#18682 = CARTESIAN_POINT ( 'NONE',  ( -19.03943276465977164, 0.05219959533909376836, 71.24890960531435269 ) ) ;
#18683 = CARTESIAN_POINT ( 'NONE',  ( -18.67979575497178146, -10.72451020669898902, 106.6655762719810383 ) ) ;
#18684 = CARTESIAN_POINT ( 'NONE',  ( 13.97604488694527802, 13.89961937509977652, 69.37390960531436690 ) ) ;
#18685 = CARTESIAN_POINT ( 'NONE',  ( -0.05219959533907301413, -21.53943276465977519, 82.49890960531436690 ) ) ;
#18686 = CARTESIAN_POINT ( 'NONE',  ( 13.89961937509957401, 13.97604488694547697, 21.87609039468566152 ) ) ;
#18689 = CARTESIAN_POINT ( 'NONE',  ( -8.224510206698948167, 14.34966873604960824, 100.4155762719810241 ) ) ;
#18688 = CARTESIAN_POINT ( 'NONE',  ( 16.52544592524335698, 4.483927247898782831, 106.4594237280190328 ) ) ;
#18687 = CARTESIAN_POINT ( 'NONE',  ( -19.03943276465977164, 0.05219959533909376836, 41.24890960531435269 ) ) ;
#18690 = CARTESIAN_POINT ( 'NONE',  ( -9.474510206698720793, -16.51473224551083518, 109.5844237280190043 ) ) ;
#18691 = ORIENTED_EDGE ( 'NONE', *, *, #58823, .T. ) ;
#18692 = CARTESIAN_POINT ( 'NONE',  ( -21.52544592524334988, -5.823673210054445271, 33.95942372801901143 ) ) ;
#18693 = CARTESIAN_POINT ( 'NONE',  ( 19.02544592524334988, 5.153800228976608722, 56.45942372801898301 ) ) ;
#18694 = CARTESIAN_POINT ( 'NONE',  ( -16.55341960407617563, 4.379528057220093196, 113.5427570613523756 ) ) ;
#18695 = CARTESIAN_POINT ( 'NONE',  ( -21.53943276465977519, 0.05219959533907696930, 66.24890960531436690 ) ) ;
#18696 = CARTESIAN_POINT ( 'NONE',  ( -0.05219959533909027116, -19.03943276465977164, 102.4989096053143669 ) ) ;
#18697 = CARTESIAN_POINT ( 'NONE',  ( 4.379528057220339221, -16.55341960407611168, 62.70724293864769550 ) ) ;
#18698 = CARTESIAN_POINT ( 'NONE',  ( 19.02544592524343514, -5.153800228976328945, 28.54057627198102409 ) ) ;
#18699 = CARTESIAN_POINT ( 'NONE',  ( 19.05341960407611168, 5.049401038298154454, 38.95724293864767418 ) ) ;
#18700 = CARTESIAN_POINT ( 'NONE',  ( -16.51473224551082808, 9.474510206698731452, 23.33442372801900078 ) ) ;
#18701 = CARTESIAN_POINT ( 'NONE',  ( 4.483927247898790824, -16.52544592524335698, 95.20942372801903275 ) ) ;
#18702 = CARTESIAN_POINT ( 'NONE',  ( -21.52544592524334988, -5.823673210054445271, 38.95942372801901854 ) ) ;
#18703 = CARTESIAN_POINT ( 'NONE',  ( -4.379528057220086978, -16.55341960407618274, 44.79275706135234714 ) ) ;
#18704 = CARTESIAN_POINT ( 'NONE',  ( 10.72451020669898902, -18.67979575497178502, 27.91557627198103830 ) ) ;
#18706 = CARTESIAN_POINT ( 'NONE',  ( 0.05219959533937995610, -21.53943276465977519, 95.00109039468568994 ) ) ;
#18705 = CARTESIAN_POINT ( 'NONE',  ( -16.51473224551069308, -9.474510206698971260, 56.66557627198103120 ) ) ;
#18707 = CARTESIAN_POINT ( 'NONE',  ( -13.89961937509977652, 13.97604488694528158, 75.62390960531438111 ) ) ;
#18708 = CARTESIAN_POINT ( 'NONE',  ( 16.53943276465976808, 0.05219959533934440121, 61.25109039468567573 ) ) ;
#18709 = CARTESIAN_POINT ( 'NONE',  ( -16.53943276465976808, 0.05219959533911058130, 101.2489096053143669 ) ) ;
#18710 = CARTESIAN_POINT ( 'NONE',  ( -8.314922557960811034, -14.29746914071050412, 27.08224293864769550 ) ) ;
#18711 = CARTESIAN_POINT ( 'NONE',  ( 0.000000000000000000, 0.000000000000000000, -18.00000000000000000 ) ) ;
#18714 = CARTESIAN_POINT ( 'NONE',  ( -19.02544592524342804, 5.153800228976336051, 81.04057627198103830 ) ) ;
#18713 = CARTESIAN_POINT ( 'NONE',  ( -9.564922557960796823, -16.46253265017161027, 92.08224293864769550 ) ) ;
#18712 = CARTESIAN_POINT ( 'NONE',  ( 21.52544592524334988, 5.823673210054432836, 76.45942372801901854 ) ) ;
#18715 = CARTESIAN_POINT ( 'NONE',  ( -19.05341960407611168, -5.049401038298163336, 106.4572429386476955 ) ) ;
#18716 = CARTESIAN_POINT ( 'NONE',  ( 16.52544592524342804, -4.483927247898539470, 63.54057627198103830 ) ) ;
#18717 = CARTESIAN_POINT ( 'NONE',  ( -16.53943276465976808, 0.05219959533911058130, 21.24890960531436690 ) ) ;
#18718 = CARTESIAN_POINT ( 'NONE',  ( -0.05219959533910754901, -16.53943276465976808, 42.49890960531435979 ) ) ;
#18719 = LINE ( 'NONE', #113682, #138407 ) ;
#18720 = CARTESIAN_POINT ( 'NONE',  ( 16.46253265017146816, 9.564922557961045513, 41.66775706135234003 ) ) ;
#18721 = CARTESIAN_POINT ( 'NONE',  ( 5.049401038298161559, -19.05341960407611168, 72.70724293864768129 ) ) ;
#18722 = CARTESIAN_POINT ( 'NONE',  ( 19.05341960407617918, -5.049401038297876454, 51.04275706135231871 ) ) ;
#18723 = CARTESIAN_POINT ( 'NONE',  ( -22.81625015709509441, -31.40387420917324590, -2.324999997268813789 ) ) ;
#18724 = CARTESIAN_POINT ( 'NONE',  ( -9.687362902255795660, -9.687362902255630459, -60.44446360152740993 ) ) ;
#18726 = CARTESIAN_POINT ( 'NONE',  ( -8.224510206698735004, -14.34966873604973081, 79.58442372801903275 ) ) ;
#18725 = CARTESIAN_POINT ( 'NONE',  ( 5.153800228976615827, -19.02544592524334988, 85.20942372801900433 ) ) ;
#18727 = CARTESIAN_POINT ( 'NONE',  ( -24.69864643647405344, 7.736333414721471513, 171.5373488951853460 ) ) ;
#18728 = CARTESIAN_POINT ( 'NONE',  ( -19.02544592524342804, 5.153800228976336051, 106.0405762719810241 ) ) ;
#18729 = CARTESIAN_POINT ( 'NONE',  ( -0.05219959533937732626, 21.53943276465977519, 27.50109039468567929 ) ) ;
#18730 = CARTESIAN_POINT ( 'NONE',  ( 9.564922557961047289, -16.46253265017146816, 95.41775706135233293 ) ) ;
#18732 = CARTESIAN_POINT ( 'NONE',  ( 9.474510206698971260, -16.51473224551069308, 47.91557627198102409 ) ) ;
#18731 = CARTESIAN_POINT ( 'NONE',  ( 17.40861289039004234, 6.110651285853279546, 88.87232470827434838 ) ) ;
#18733 = ADVANCED_FACE ( 'NONE', ( #135557 ), #195238, .F. ) ;
#18734 = CARTESIAN_POINT ( 'NONE',  ( 0.05219959533909260263, 19.03943276465977164, 109.9989096053143669 ) ) ;
#18736 = CARTESIAN_POINT ( 'NONE',  ( 16.51473224551069308, 9.474510206698969483, 49.16557627198102409 ) ) ;
#18735 = CARTESIAN_POINT ( 'NONE',  ( 12.14591786802309770, 12.06949235617756955, 59.37390960531436690 ) ) ;
#18737 = CARTESIAN_POINT ( 'NONE',  ( -16.46253265017160317, 9.564922557960807481, 65.83224293864769550 ) ) ;
#18738 = CARTESIAN_POINT ( 'NONE',  ( -9.564922557961040184, 16.46253265017147172, 62.91775706135233293 ) ) ;
#18739 = CARTESIAN_POINT ( 'NONE',  ( 19.03943276465977164, 0.05219959533936151252, 26.25109039468566507 ) ) ;
#18740 = CARTESIAN_POINT ( 'NONE',  ( -16.46253265017160317, 9.564922557960807481, 70.83224293864770971 ) ) ;
#18741 = CARTESIAN_POINT ( 'NONE',  ( -5.823673210054116645, -21.52544592524344225, 62.29057627198102409 ) ) ;
#18743 = CARTESIAN_POINT ( 'NONE',  ( 19.03943276465977164, 0.05219959533936151252, 36.25109039468567573 ) ) ;
#18742 = CARTESIAN_POINT ( 'NONE',  ( 8.224510206698953496, -14.34966873604960469, 72.91557627198103830 ) ) ;
#18744 = CARTESIAN_POINT ( 'NONE',  ( -16.46253265017160317, 9.564922557960807481, 115.8322429386477097 ) ) ;
#18745 = CARTESIAN_POINT ( 'NONE',  ( -10.81492255796078084, -18.62759615963271287, 52.08224293864768839 ) ) ;
#18746 = CARTESIAN_POINT ( 'NONE',  ( 0.05219959533907565091, 21.53943276465977519, 29.99890960531435979 ) ) ;
#18747 = CARTESIAN_POINT ( 'NONE',  ( 5.153800228976335163, 19.02544592524342804, 49.79057627198100988 ) ) ;
#18748 = CARTESIAN_POINT ( 'NONE',  ( 19.02544592524343514, -5.153800228976328945, 43.54057627198103120 ) ) ;
#18749 = CARTESIAN_POINT ( 'NONE',  ( 14.29746914071049879, -8.314922557960816363, 103.3322429386476955 ) ) ;
#18750 = AXIS2_PLACEMENT_3D ( 'NONE', #120314, #42501, #61612 ) ;
#18751 = CARTESIAN_POINT ( 'NONE',  ( -21.52544592524343514, 5.823673210054127303, 111.0405762719810525 ) ) ;
#18752 = CARTESIAN_POINT ( 'NONE',  ( -9.564922557960796823, -16.46253265017161027, 112.0822429386476955 ) ) ;
#18753 = CARTESIAN_POINT ( 'NONE',  ( 18.62759615963255655, 10.81492255796105972, 21.66775706135235069 ) ) ;
#18754 = CARTESIAN_POINT ( 'NONE',  ( 0.05219959533910956823, 16.53943276465976808, 114.9989096053143669 ) ) ;
#18755 = CARTESIAN_POINT ( 'NONE',  ( 5.719274019375991003, -21.55341960407610458, 97.70724293864772392 ) ) ;
#18756 = CARTESIAN_POINT ( 'NONE',  ( -13.97604488694547697, 13.89961937509957934, 48.12609039468566863 ) ) ;
#18757 = CARTESIAN_POINT ( 'NONE',  ( -19.02544592524342804, 5.153800228976336051, 26.04057627198103120 ) ) ;
#18758 = CARTESIAN_POINT ( 'NONE',  ( -16.46253265017160317, 9.564922557960807481, 25.83224293864769194 ) ) ;
#18759 = CARTESIAN_POINT ( 'NONE',  ( 30.74264578624800137, -22.33583958711395212, -1.200000000000000178 ) ) ;
#18760 = CARTESIAN_POINT ( 'NONE',  ( 4.379528057220092307, 16.55341960407617563, 52.29275706135236135 ) ) ;
#18761 = CARTESIAN_POINT ( 'NONE',  ( -4.379528057220328563, 16.55341960407611168, 115.2072429386476955 ) ) ;
#18762 = FACE_OUTER_BOUND ( 'NONE', #179582, .T. ) ;
#18763 = CARTESIAN_POINT ( 'NONE',  ( 13.89961937509977652, -13.97604488694527269, 78.12390960531433848 ) ) ;
#18764 = CARTESIAN_POINT ( 'NONE',  ( 16.52544592524342804, -4.483927247898539470, 103.5405762719810383 ) ) ;
#18765 = CARTESIAN_POINT ( 'NONE',  ( 5.823673210054125526, 21.52544592524343514, 39.79057627198103830 ) ) ;
#18766 = CARTESIAN_POINT ( 'NONE',  ( -0.05219959533910754901, -16.53943276465976808, 82.49890960531436690 ) ) ;
#18767 = CARTESIAN_POINT ( 'NONE',  ( -14.29746914071037622, -8.314922557961029526, 34.16775706135234714 ) ) ;
#18768 = CARTESIAN_POINT ( 'NONE',  ( 21.55341960407619695, -5.719274019375665929, 91.04275706135236135 ) ) ;
#18769 = CARTESIAN_POINT ( 'NONE',  ( 13.97604488694527802, 13.89961937509977652, 29.37390960531435979 ) ) ;
#18770 = CARTESIAN_POINT ( 'NONE',  ( -4.483927247898782831, 16.52544592524335698, 92.70942372801901854 ) ) ;
#18771 = CARTESIAN_POINT ( 'NONE',  ( -12.14591786802309592, -12.06949235617757132, 46.87390960531435979 ) ) ;
#18772 = CARTESIAN_POINT ( 'NONE',  ( 5.049401038298161559, -19.05341960407611168, 52.70724293864767418 ) ) ;
#18773 = CARTESIAN_POINT ( 'NONE',  ( -18.62759615963255300, -10.81492255796106328, 94.16775706135237556 ) ) ;
#18774 = CARTESIAN_POINT ( 'NONE',  ( 21.55341960407610458, 5.719274019375980345, 103.9572429386476813 ) ) ;
#18775 = CARTESIAN_POINT ( 'NONE',  ( 18.62759615963255655, 10.81492255796105972, 76.66775706135234714 ) ) ;
#18776 = CARTESIAN_POINT ( 'NONE',  ( 12.14591786802327356, -12.06949235617739191, 40.62609039468567573 ) ) ;
#18778 = CARTESIAN_POINT ( 'NONE',  ( 21.52544592524334988, 5.823673210054432836, 86.45942372801901854 ) ) ;
#18777 = CARTESIAN_POINT ( 'NONE',  ( 4.483927247898545687, 16.52544592524342804, 59.79057627198103120 ) ) ;
#18779 = AXIS2_PLACEMENT_3D ( 'NONE', #186921, #190871, #172724 ) ;
#18780 = CARTESIAN_POINT ( 'NONE',  ( 12.06949235617739724, 12.14591786802326823, 106.8760903946856899 ) ) ;
#18781 = CARTESIAN_POINT ( 'NONE',  ( 17.12812012977042642, -6.668231424565811416, 46.14051240676854349 ) ) ;
#18782 = DIRECTION ( 'NONE',  ( 0.000000000000000000, 0.000000000000000000, 1.000000000000000000 ) ) ;
#18783 = CARTESIAN_POINT ( 'NONE',  ( 0.05219959533910956823, 16.53943276465976808, 34.99890960531435979 ) ) ;
#18784 = CARTESIAN_POINT ( 'NONE',  ( -14.29746914071037622, -8.314922557961029526, 79.16775706135234714 ) ) ;
#18785 = CARTESIAN_POINT ( 'NONE',  ( -13.97604488694527625, -13.89961937509977652, 86.87390960531436690 ) ) ;
#18786 = AXIS2_PLACEMENT_3D ( 'NONE', #179317, #40781, #103455 ) ;
#18787 = CARTESIAN_POINT ( 'NONE',  ( -16.51473224551069308, -9.474510206698971260, 101.6655762719810241 ) ) ;
#18788 = CARTESIAN_POINT ( 'NONE',  ( 5.823673210054444382, -21.52544592524334988, 105.2094237280190328 ) ) ;
#18789 = CARTESIAN_POINT ( 'NONE',  ( 4.483927247898790824, -16.52544592524335698, 105.2094237280190328 ) ) ;
#18790 = CARTESIAN_POINT ( 'NONE',  ( 16.53943276465976808, -0.05219959533910856209, 78.74890960531436690 ) ) ;
#18791 = CARTESIAN_POINT ( 'NONE',  ( -13.89961937509977652, 13.97604488694528158, 80.62390960531436690 ) ) ;
#18792 = ORIENTED_EDGE ( 'NONE', *, *, #22613, .T. ) ;
#18793 = CARTESIAN_POINT ( 'NONE',  ( 16.52544592524335698, 4.483927247898782831, 31.45942372801901854 ) ) ;
#18794 = CARTESIAN_POINT ( 'NONE',  ( -13.97604488694527625, -13.89961937509977652, 31.87390960531435979 ) ) ;
#18795 = CARTESIAN_POINT ( 'NONE',  ( -9.474510206698964154, 16.51473224551069663, 85.41557627198102409 ) ) ;
#18797 = CARTESIAN_POINT ( 'NONE',  ( 22.81625015709509441, 31.40387420917330275, -5.324999997268812457 ) ) ;
#18796 = CARTESIAN_POINT ( 'NONE',  ( 12.06949235617739724, 12.14591786802326823, 26.87609039468567218 ) ) ;
#18798 = CARTESIAN_POINT ( 'NONE',  ( 9.474510206698729675, 16.51473224551082808, 27.08442372801900433 ) ) ;
#18799 = CARTESIAN_POINT ( 'NONE',  ( 4.483927247898790824, -16.52544592524335698, 90.20942372801903275 ) ) ;
#18800 = CARTESIAN_POINT ( 'NONE',  ( -5.153800228976607833, 19.02544592524334988, 102.7094237280189759 ) ) ;
#18801 = CARTESIAN_POINT ( 'NONE',  ( -16.51473224551069308, -9.474510206698971260, 26.66557627198103120 ) ) ;
#18802 = CARTESIAN_POINT ( 'NONE',  ( -4.483927247898782831, 16.52544592524335698, 77.70942372801900433 ) ) ;
#18803 = CARTESIAN_POINT ( 'NONE',  ( -16.53943276465976808, -0.05219959533934237506, 63.75109039468568284 ) ) ;
#18804 = CARTESIAN_POINT ( 'NONE',  ( -16.46253265017160317, 9.564922557960807481, 25.83224293864769194 ) ) ;
#18805 = CARTESIAN_POINT ( 'NONE',  ( 19.05341960407617918, -5.049401038297876454, 66.04275706135233293 ) ) ;
#18806 = CARTESIAN_POINT ( 'NONE',  ( 16.51473224551083163, -9.474510206698727899, 20.83442372801899722 ) ) ;
#18807 = CARTESIAN_POINT ( 'NONE',  ( -19.05341960407611168, -5.049401038298163336, 51.45724293864770260 ) ) ;
#18808 = CARTESIAN_POINT ( 'NONE',  ( 13.89961937509977652, -13.97604488694527269, 93.12390960531436690 ) ) ;
#18809 = CARTESIAN_POINT ( 'NONE',  ( -12.14591786802309592, -12.06949235617757132, 86.87390960531438111 ) ) ;
#18810 = EDGE_CURVE ( 'NONE', #189055, #21601, #98913, .T. ) ;
#18811 = CARTESIAN_POINT ( 'NONE',  ( -19.05341960407617563, 5.049401038297882671, 53.54275706135231871 ) ) ;
#18812 = CARTESIAN_POINT ( 'NONE',  ( -15.80617190586745835, -15.72974639402198527, 46.87390960531435979 ) ) ;
#18813 = CARTESIAN_POINT ( 'NONE',  ( -10.72451020669870658, -18.67979575497194134, 104.5844237280190185 ) ) ;
#18814 = CARTESIAN_POINT ( 'NONE',  ( -5.153800228976328057, -19.02544592524343514, 92.29057627198099567 ) ) ;
#18815 = CARTESIAN_POINT ( 'NONE',  ( 15.80617190586769283, -15.72974639402175789, 100.6260903946857184 ) ) ;
#18816 = CARTESIAN_POINT ( 'NONE',  ( -10.81492255796078084, -18.62759615963271287, 62.08224293864769550 ) ) ;
#18817 = CARTESIAN_POINT ( 'NONE',  ( 19.02544592524343514, -5.153800228976328945, 93.54057627198102409 ) ) ;
#18818 = CARTESIAN_POINT ( 'NONE',  ( 19.03943276465977164, 0.05219959533936151252, 91.25109039468566152 ) ) ;
#18819 = CARTESIAN_POINT ( 'NONE',  ( -19.02544592524342804, 5.153800228976336051, 111.0405762719810099 ) ) ;
#18820 = CARTESIAN_POINT ( 'NONE',  ( 19.02544592524334988, 5.153800228976608722, 106.4594237280190185 ) ) ;
#18821 = CARTESIAN_POINT ( 'NONE',  ( 12.14591786802309770, 12.06949235617756955, 109.3739096053143811 ) ) ;
#18822 = CARTESIAN_POINT ( 'NONE',  ( -16.46253265017160317, 9.564922557960807481, 80.83224293864769550 ) ) ;
#18823 = CARTESIAN_POINT ( 'NONE',  ( -21.52544592524343514, 5.823673210054127303, 76.04057627198102409 ) ) ;
#18824 = CARTESIAN_POINT ( 'NONE',  ( 12.14591786802327356, -12.06949235617739191, 45.62609039468567573 ) ) ;
#18825 = CARTESIAN_POINT ( 'NONE',  ( -18.67979575497193778, 10.72451020669871902, 53.33442372801901854 ) ) ;
#18826 = CARTESIAN_POINT ( 'NONE',  ( -5.719274019375665041, -21.55341960407619695, 94.79275706135234714 ) ) ;
#18827 = CARTESIAN_POINT ( 'NONE',  ( 16.52544592524335698, 4.483927247898782831, 101.4594237280190185 ) ) ;
#18828 = CARTESIAN_POINT ( 'NONE',  ( 16.51473224551069308, 9.474510206698969483, 94.16557627198103830 ) ) ;
#18829 = CARTESIAN_POINT ( 'NONE',  ( 4.379528057220339221, -16.55341960407611168, 92.70724293864770971 ) ) ;
#18830 = CARTESIAN_POINT ( 'NONE',  ( 12.14591786802309770, 12.06949235617756955, 29.37390960531435269 ) ) ;
#18831 = CARTESIAN_POINT ( 'NONE',  ( -19.02544592524334988, -5.153800228976617603, 73.95942372801900433 ) ) ;
#18832 = CARTESIAN_POINT ( 'NONE',  ( -10.72451020669870658, -18.67979575497194134, 49.58442372801901143 ) ) ;
#18833 = CARTESIAN_POINT ( 'NONE',  ( 19.05341960407617918, -5.049401038297876454, 31.04275706135232227 ) ) ;
#18834 = CARTESIAN_POINT ( 'NONE',  ( -14.34966873604960291, -8.224510206698953496, 86.66557627198102409 ) ) ;
#18835 = CARTESIAN_POINT ( 'NONE',  ( 16.51473224551069308, 9.474510206698969483, 109.1655762719810383 ) ) ;
#18836 = CARTESIAN_POINT ( 'NONE',  ( -14.34966873604960291, -8.224510206698953496, 21.66557627198102409 ) ) ;
#18837 = CARTESIAN_POINT ( 'NONE',  ( -18.62759615963255300, -10.81492255796106328, 79.16775706135234714 ) ) ;
#18838 = CARTESIAN_POINT ( 'NONE',  ( 0.05219959533934541429, -16.53943276465976808, 65.00109039468568994 ) ) ;
#18839 = CARTESIAN_POINT ( 'NONE',  ( -4.483927247898782831, 16.52544592524335698, 112.7094237280190328 ) ) ;
#18840 = CARTESIAN_POINT ( 'NONE',  ( -5.823673210054431948, 21.52544592524334988, 57.70942372801901143 ) ) ;
#18841 = ORIENTED_EDGE ( 'NONE', *, *, #63306, .T. ) ;
#18842 = CARTESIAN_POINT ( 'NONE',  ( -10.81492255796105439, 18.62759615963255655, 27.91775706135234358 ) ) ;
#18843 = CARTESIAN_POINT ( 'NONE',  ( -16.52544592524342804, 4.483927247898546575, 111.0405762719810525 ) ) ;
#18844 = CARTESIAN_POINT ( 'NONE',  ( 17.50000000000000000, -5.500000000000000888, 28.29690382534172244 ) ) ;
#18845 = CARTESIAN_POINT ( 'NONE',  ( -16.53943276465976808, 0.05219959533911058130, 61.24890960531435979 ) ) ;
#18846 = CARTESIAN_POINT ( 'NONE',  ( -0.05219959533909027116, -19.03943276465977164, 77.49890960531435269 ) ) ;
#18847 = CARTESIAN_POINT ( 'NONE',  ( 0.05219959533934541429, -16.53943276465976808, 105.0010903946856757 ) ) ;
#18848 = CARTESIAN_POINT ( 'NONE',  ( 13.89961937509977652, -13.97604488694527269, 38.12390960531436690 ) ) ;
#18849 = CARTESIAN_POINT ( 'NONE',  ( 15.80617190586746368, 15.72974639402197994, 59.37390960531436690 ) ) ;
#18850 = CARTESIAN_POINT ( 'NONE',  ( 12.14591786802309770, 12.06949235617756955, 89.37390960531435269 ) ) ;
#18851 = CARTESIAN_POINT ( 'NONE',  ( 5.823673210054125526, 21.52544592524343514, 89.79057627198103830 ) ) ;
#18852 = CARTESIAN_POINT ( 'NONE',  ( 13.89961937509977652, -13.97604488694527269, 103.1239096053143527 ) ) ;
#18854 = CARTESIAN_POINT ( 'NONE',  ( -19.02544592524334988, -5.153800228976617603, 93.95942372801900433 ) ) ;
#18853 = CARTESIAN_POINT ( 'NONE',  ( -19.05341960407611168, -5.049401038298163336, 56.45724293864768129 ) ) ;
#18855 = CARTESIAN_POINT ( 'NONE',  ( 10.72451020669898902, -18.67979575497178502, 42.91557627198103120 ) ) ;
#18856 = CARTESIAN_POINT ( 'NONE',  ( 5.719274019375673035, 21.55341960407619339, 67.29275706135234714 ) ) ;
#18857 = CARTESIAN_POINT ( 'NONE',  ( 5.153800228976335163, 19.02544592524342804, 59.79057627198100988 ) ) ;
#18858 = CARTESIAN_POINT ( 'NONE',  ( -5.049401038298153566, 19.05341960407611168, 80.20724293864769550 ) ) ;
#18859 = CARTESIAN_POINT ( 'NONE',  ( 14.29746914071037800, 8.314922557961029526, 61.66775706135235424 ) ) ;
#18860 = CARTESIAN_POINT ( 'NONE',  ( 5.719274019375673035, 21.55341960407619339, 42.29275706135235424 ) ) ;
#18861 = CARTESIAN_POINT ( 'NONE',  ( -5.823673210054431948, 21.52544592524334988, 67.70942372801901854 ) ) ;
#18862 = CARTESIAN_POINT ( 'NONE',  ( -16.51473224551069308, -9.474510206698971260, 111.6655762719810383 ) ) ;
#18863 = CARTESIAN_POINT ( 'NONE',  ( 10.81492255796078972, 18.62759615963270932, 94.58224293864769550 ) ) ;
#18865 = CARTESIAN_POINT ( 'NONE',  ( 16.53943276465976808, 0.05219959533934440121, 71.25109039468568994 ) ) ;
#18864 = CARTESIAN_POINT ( 'NONE',  ( 18.67979575497194134, -10.72451020669871369, 35.83442372801901143 ) ) ;
#18866 = CARTESIAN_POINT ( 'NONE',  ( 0.05219959533907565091, 21.53943276465977519, 59.99890960531436690 ) ) ;
#18867 = CARTESIAN_POINT ( 'NONE',  ( 0.05219959533936267826, -19.03943276465977164, 40.00109039468566152 ) ) ;
#18869 = CARTESIAN_POINT ( 'NONE',  ( -4.379528057220086978, -16.55341960407618274, 109.7927570613523613 ) ) ;
#18868 = CARTESIAN_POINT ( 'NONE',  ( 19.05341960407611168, 5.049401038298154454, 68.95724293864769550 ) ) ;
#18870 = CARTESIAN_POINT ( 'NONE',  ( -17.49999999999999645, -3.471454075611748902, 105.5166741885564505 ) ) ;
#18871 = CARTESIAN_POINT ( 'NONE',  ( -19.05341960407611168, -5.049401038298163336, 106.4572429386476955 ) ) ;
#18872 = DIRECTION ( 'NONE',  ( 0.000000000000000000, 0.000000000000000000, 1.000000000000000000 ) ) ;
#18873 = CARTESIAN_POINT ( 'NONE',  ( -9.564922557961040184, 16.46253265017147172, 77.91775706135234714 ) ) ;
#18874 = CARTESIAN_POINT ( 'NONE',  ( 21.53943276465977519, -0.05219959533907433946, 53.74890960531437401 ) ) ;
#18875 = CARTESIAN_POINT ( 'NONE',  ( -16.53943276465976808, 0.05219959533911058130, 36.24890960531435979 ) ) ;
#18876 = CARTESIAN_POINT ( 'NONE',  ( -16.46253265017146816, -9.564922557961047289, 109.1677570613523471 ) ) ;
#18877 = CARTESIAN_POINT ( 'NONE',  ( -19.02544592524342804, 5.153800228976336051, 31.04057627198102409 ) ) ;
#18878 = CARTESIAN_POINT ( 'NONE',  ( 16.52544592524335698, 4.483927247898782831, 21.45942372801901499 ) ) ;
#18880 = CARTESIAN_POINT ( 'NONE',  ( 5.049401038297881783, 19.05341960407617563, 57.29275706135231871 ) ) ;
#18879 = CARTESIAN_POINT ( 'NONE',  ( -10.81492255796078084, -18.62759615963271287, 92.08224293864769550 ) ) ;
#18881 = CARTESIAN_POINT ( 'NONE',  ( 12.14591786802327356, -12.06949235617739191, 80.62609039468567573 ) ) ;
#18882 = CARTESIAN_POINT ( 'NONE',  ( 13.89961937509977652, -13.97604488694527269, 73.12390960531436690 ) ) ;
#18883 = CARTESIAN_POINT ( 'NONE',  ( -12.06949235617756955, 12.14591786802309770, 75.62390960531439532 ) ) ;
#18884 = CARTESIAN_POINT ( 'NONE',  ( 16.46253265017160672, -9.564922557960803928, 43.33224293864769550 ) ) ;
#18885 = CARTESIAN_POINT ( 'NONE',  ( 0.05219959533910956823, 16.53943276465976808, 54.99890960531435269 ) ) ;
#18886 = CARTESIAN_POINT ( 'NONE',  ( -13.97604488694527625, -13.89961937509977652, 21.87390960531435979 ) ) ;
#18887 = CARTESIAN_POINT ( 'NONE',  ( 31.99650548583503351, -5.647492055662687527, 90.04056618753070040 ) ) ;
#18888 = CARTESIAN_POINT ( 'NONE',  ( 0.05219959533910956823, 16.53943276465976808, 29.99890960531435979 ) ) ;
#18889 = CARTESIAN_POINT ( 'NONE',  ( -16.51473224551069308, -9.474510206698971260, 76.66557627198103830 ) ) ;
#18890 = CARTESIAN_POINT ( 'NONE',  ( -8.388830574159379737E-16, -13.70000000000001528, -60.44446360152740283 ) ) ;
#18891 = CARTESIAN_POINT ( 'NONE',  ( -9.474510206698720793, -16.51473224551083518, 44.58442372801900433 ) ) ;
#18892 = CARTESIAN_POINT ( 'NONE',  ( -0.05219959533934338120, 16.53943276465976808, 42.50109039468567573 ) ) ;
#18893 = CARTESIAN_POINT ( 'NONE',  ( 21.55341960407610458, 5.719274019375980345, 68.95724293864769550 ) ) ;
#18894 = CARTESIAN_POINT ( 'NONE',  ( 9.564922557961047289, -16.46253265017146816, 20.41775706135233293 ) ) ;
#18895 = CARTESIAN_POINT ( 'NONE',  ( 13.89961937509977652, -13.97604488694527269, 68.12390960531436690 ) ) ;
#18896 = CARTESIAN_POINT ( 'NONE',  ( 2.019537816779184180E-14, -78.64189009824758614, -24.99999966871768819 ) ) ;
#18897 = CARTESIAN_POINT ( 'NONE',  ( 13.97604488694527802, 13.89961937509977652, 104.3739096053143385 ) ) ;
#18898 = CARTESIAN_POINT ( 'NONE',  ( -21.53943276465977519, -0.05219959533937600094, 38.75109039468567573 ) ) ;
#18899 = CARTESIAN_POINT ( 'NONE',  ( 4.483927247898545687, 16.52544592524342804, 104.7905762719810241 ) ) ;
#18902 = ORIENTED_EDGE ( 'NONE', *, *, #136231, .T. ) ;
#18901 = CARTESIAN_POINT ( 'NONE',  ( -13.97604488694527625, -13.89961937509977652, 81.87390960531436690 ) ) ;
#18900 = CARTESIAN_POINT ( 'NONE',  ( 5.719274019375991003, -21.55341960407610458, 107.7072429386476955 ) ) ;
#18903 = CARTESIAN_POINT ( 'NONE',  ( 0.05219959533937995610, -21.53943276465977519, 25.00109039468567218 ) ) ;
#18904 = ORIENTED_EDGE ( 'NONE', *, *, #42100, .F. ) ;
#18905 = CARTESIAN_POINT ( 'NONE',  ( 5.153800228976335163, 19.02544592524342804, 84.79057627198099567 ) ) ;
#18906 = EDGE_CURVE ( 'NONE', #96881, #27352, #98517, .T. ) ;
#18907 = CYLINDRICAL_SURFACE ( 'NONE', #130279, 31.90000000000003411 ) ;
#18908 = CARTESIAN_POINT ( 'NONE',  ( 13.89961937509977652, -13.97604488694527269, 38.12390960531436690 ) ) ;
#18909 = CARTESIAN_POINT ( 'NONE',  ( 5.049401038297881783, 19.05341960407617563, 107.2927570613523187 ) ) ;
#18910 = CARTESIAN_POINT ( 'NONE',  ( 22.81625015709510151, -31.40387420917324590, -6.424999997268812102 ) ) ;
#18911 = CARTESIAN_POINT ( 'NONE',  ( 12.14591786802309770, 12.06949235617756955, 109.3739096053143811 ) ) ;
#18912 = CARTESIAN_POINT ( 'NONE',  ( -18.62759615963255300, -10.81492255796106328, 89.16775706135236135 ) ) ;
#18914 = CARTESIAN_POINT ( 'NONE',  ( 21.53943276465977519, 0.05219959533937863772, 41.25109039468568284 ) ) ;
#18913 = CARTESIAN_POINT ( 'NONE',  ( -19.03943276465977164, 0.05219959533909376836, 71.24890960531435269 ) ) ;
#18915 = CARTESIAN_POINT ( 'NONE',  ( -15.80617190586768217, 15.72974639402176855, 33.12609039468569705 ) ) ;
#18916 = CARTESIAN_POINT ( 'NONE',  ( 1.784210473542230573E-15, -29.16686587814331588, 139.8750000027311842 ) ) ;
#18917 = CARTESIAN_POINT ( 'NONE',  ( -19.05341960407611168, -5.049401038298163336, 81.45724293864769550 ) ) ;
#18918 = CARTESIAN_POINT ( 'NONE',  ( 27.94727380668107131, 6.976214527048578695, 161.4607934399207920 ) ) ;
#18920 = CARTESIAN_POINT ( 'NONE',  ( -21.55341960407610458, -5.719274019375992779, 41.45724293864769550 ) ) ;
#18919 = CARTESIAN_POINT ( 'NONE',  ( 16.55341960407618274, -4.379528057220086978, 21.04275706135234714 ) ) ;
#18921 = CARTESIAN_POINT ( 'NONE',  ( -5.719274019375665041, -21.55341960407619695, 79.79275706135236135 ) ) ;
#18922 = CARTESIAN_POINT ( 'NONE',  ( 0.05219959533909260263, 19.03943276465977164, 114.9989096053143669 ) ) ;
#18923 = CARTESIAN_POINT ( 'NONE',  ( -13.97604488694547697, 13.89961937509957934, 93.12609039468566152 ) ) ;
#18924 = CARTESIAN_POINT ( 'NONE',  ( 19.03943276465977164, -0.05219959533909143690, 53.74890960531436690 ) ) ;
#18925 = CARTESIAN_POINT ( 'NONE',  ( -13.89961937509977652, 13.97604488694528158, 85.62390960531433848 ) ) ;
#18926 = AXIS2_PLACEMENT_3D ( 'NONE', #94783, #2777, #3759 ) ;
#18927 = CARTESIAN_POINT ( 'NONE',  ( -16.55341960407611168, -4.379528057220339221, 101.4572429386476955 ) ) ;
#18928 = CARTESIAN_POINT ( 'NONE',  ( 8.314922557960818139, 14.29746914071049879, 109.5822429386476955 ) ) ;
#18929 = CARTESIAN_POINT ( 'NONE',  ( 9.564922557960805705, 16.46253265017160317, 114.5822429386476955 ) ) ;
#18930 = CARTESIAN_POINT ( 'NONE',  ( -14.34966873604972548, 8.224510206698743886, 78.33442372801901854 ) ) ;
#18932 = CARTESIAN_POINT ( 'NONE',  ( 9.474510206698971260, -16.51473224551069308, 37.91557627198102409 ) ) ;
#18931 = CARTESIAN_POINT ( 'NONE',  ( 14.29746914071049879, -8.314922557960816363, 53.33224293864769550 ) ) ;
#18933 = CARTESIAN_POINT ( 'NONE',  ( 5.719274019375673035, 21.55341960407619339, 82.29275706135234714 ) ) ;
#18934 = CARTESIAN_POINT ( 'NONE',  ( 0.05219959533937995610, -21.53943276465977519, 75.00109039468568994 ) ) ;
#18935 = CARTESIAN_POINT ( 'NONE',  ( -19.02544592524334988, -5.153800228976617603, 88.95942372801897591 ) ) ;
#18936 = CARTESIAN_POINT ( 'NONE',  ( -4.483927247898539470, -16.52544592524342804, 62.29057627198102409 ) ) ;
#18937 = CARTESIAN_POINT ( 'NONE',  ( -5.823673210054116645, -21.52544592524344225, 107.2905762719810525 ) ) ;
#18938 = CARTESIAN_POINT ( 'NONE',  ( -10.72451020669898014, 18.67979575497178502, 50.41557627198103120 ) ) ;
#18939 = DIRECTION ( 'NONE',  ( 0.000000000000000000, 0.000000000000000000, -1.000000000000000000 ) ) ;
#18940 = CARTESIAN_POINT ( 'NONE',  ( -17.81289503416611097, -24.51734667627696496, 138.5500000054623229 ) ) ;
#18941 = CARTESIAN_POINT ( 'NONE',  ( -9.564922557960796823, -16.46253265017161027, 72.08224293864770971 ) ) ;
#18942 = CARTESIAN_POINT ( 'NONE',  ( -0.05219959533910754901, -16.53943276465976808, 32.49890960531435979 ) ) ;
#18943 = CARTESIAN_POINT ( 'NONE',  ( -4.483927247898539470, -16.52544592524342804, 27.29057627198103120 ) ) ;
#18944 = CARTESIAN_POINT ( 'NONE',  ( -16.53943276465976808, -0.05219959533934237506, 88.75109039468567573 ) ) ;
#18945 = CARTESIAN_POINT ( 'NONE',  ( 9.474510206698729675, 16.51473224551082808, 37.08442372801899722 ) ) ;
#18946 = CARTESIAN_POINT ( 'NONE',  ( 16.79531203550649110, 7.028104445595497296, 48.75244988220443787 ) ) ;
#18947 = CARTESIAN_POINT ( 'NONE',  ( -13.89961937509977652, 13.97604488694528158, 85.62390960531433848 ) ) ;
#18948 = CARTESIAN_POINT ( 'NONE',  ( -4.483927247898539470, -16.52544592524342804, 57.29057627198103120 ) ) ;
#18950 = CARTESIAN_POINT ( 'NONE',  ( -15.80617190586745835, -15.72974639402198527, 26.87390960531435979 ) ) ;
#18949 = CARTESIAN_POINT ( 'NONE',  ( 16.21995358207306381, -7.366697692864171643, 102.4355100151216647 ) ) ;
#18952 = ORIENTED_EDGE ( 'NONE', *, *, #151324, .T. ) ;
#18951 = CARTESIAN_POINT ( 'NONE',  ( 5.823673210054125526, 21.52544592524343514, 59.79057627198103120 ) ) ;
#18953 = CARTESIAN_POINT ( 'NONE',  ( 8.224510206698953496, -14.34966873604960469, 97.91557627198103830 ) ) ;
#18954 = CARTESIAN_POINT ( 'NONE',  ( -8.314922557961024197, 14.29746914071037800, 42.91775706135235424 ) ) ;
#18955 = CARTESIAN_POINT ( 'NONE',  ( 0.05219959533910956823, 16.53943276465976808, 79.99890960531435269 ) ) ;
#18956 = CARTESIAN_POINT ( 'NONE',  ( 25.12471020271277666, 7.795852113654127002, 170.9710663016988974 ) ) ;
#18957 = CARTESIAN_POINT ( 'NONE',  ( 5.049401038297881783, 19.05341960407617563, 82.29275706135229029 ) ) ;
#18958 = CARTESIAN_POINT ( 'NONE',  ( 13.97604488694527802, 13.89961937509977652, 114.3739096053143669 ) ) ;
#18959 = CARTESIAN_POINT ( 'NONE',  ( 11.40812507854755253, -35.11059874428192273, -4.524999997268813523 ) ) ;
#18960 = CARTESIAN_POINT ( 'NONE',  ( -13.97604488694527625, -13.89961937509977830, 41.87390960531435269 ) ) ;
#18962 = CARTESIAN_POINT ( 'NONE',  ( -16.52544592524342804, 4.483927247898546575, 31.04057627198102409 ) ) ;
#18961 = CARTESIAN_POINT ( 'NONE',  ( -8.314922557961024197, 14.29746914071037800, 27.91775706135234358 ) ) ;
#18963 = CARTESIAN_POINT ( 'NONE',  ( -21.53943276465977519, 0.05219959533907696930, 61.24890960531435979 ) ) ;
#18964 = CARTESIAN_POINT ( 'NONE',  ( -16.51473224551082808, 9.474510206698731452, 88.33442372801900433 ) ) ;
#18965 = CARTESIAN_POINT ( 'NONE',  ( 10.81492255796078972, 18.62759615963270932, 54.58224293864769550 ) ) ;
#18966 = CARTESIAN_POINT ( 'NONE',  ( -21.55341960407619339, 5.719274019375674811, 83.54275706135234714 ) ) ;
#18967 = CARTESIAN_POINT ( 'NONE',  ( 7.819668024151653185, -36.54656901728082374, -31.88218832179849116 ) ) ;
#18968 = CARTESIAN_POINT ( 'NONE',  ( 8.224510206698742110, 14.34966873604972548, 37.08442372801901143 ) ) ;
#18970 = CARTESIAN_POINT ( 'NONE',  ( -5.049401038298153566, 19.05341960407611168, 85.20724293864766707 ) ) ;
#18969 = CARTESIAN_POINT ( 'NONE',  ( 16.46253265017160672, -9.564922557960803928, 23.33224293864769194 ) ) ;
#18971 = CARTESIAN_POINT ( 'NONE',  ( 13.89961937509977652, -13.97604488694527269, 38.12390960531436690 ) ) ;
#18972 = CARTESIAN_POINT ( 'NONE',  ( -16.53943276465976808, 0.05219959533911058130, 106.2489096053143811 ) ) ;
#18973 = APPLICATION_PROTOCOL_DEFINITION ( 'draft international standard', 'automotive_design', 1998, #60997 ) ;
#18974 = CARTESIAN_POINT ( 'NONE',  ( -13.97604488694527625, -13.89961937509977652, 106.8739096053143669 ) ) ;
#18975 = ORIENTED_EDGE ( 'NONE', *, *, #73081, .F. ) ;
#18976 = CARTESIAN_POINT ( 'NONE',  ( 8.224510206698742110, 14.34966873604972548, 62.08442372801901143 ) ) ;
#18977 = CARTESIAN_POINT ( 'NONE',  ( 10.81492255796078972, 18.62759615963270932, 94.58224293864769550 ) ) ;
#18978 = CARTESIAN_POINT ( 'NONE',  ( -0.05219959533909027116, -19.03943276465977164, 37.49890960531436690 ) ) ;
#18980 = CARTESIAN_POINT ( 'NONE',  ( 18.67979575497194134, -10.72451020669871369, 30.83442372801902209 ) ) ;
#18979 = CARTESIAN_POINT ( 'NONE',  ( 19.02544592524334988, 5.153800228976608722, 71.45942372801900433 ) ) ;
#18981 = CARTESIAN_POINT ( 'NONE',  ( -13.89961937509977652, 13.97604488694528158, 70.62390960531432427 ) ) ;
#18982 = CARTESIAN_POINT ( 'NONE',  ( -19.02544592524342804, 5.153800228976336051, 101.0405762719810241 ) ) ;
#18983 = VERTEX_POINT ( 'NONE', #86043 ) ;
#18984 = CARTESIAN_POINT ( 'NONE',  ( 4.483927247898790824, -16.52544592524335698, 35.20942372801901854 ) ) ;
#18985 = CARTESIAN_POINT ( 'NONE',  ( 21.53943276465977519, 0.05219959533937863772, 21.25109039468567218 ) ) ;
#18988 = CARTESIAN_POINT ( 'NONE',  ( -19.05341960407617563, 5.049401038297882671, 78.54275706135233293 ) ) ;
#18987 = CARTESIAN_POINT ( 'NONE',  ( -5.049401038298153566, 19.05341960407611168, 90.20724293864766707 ) ) ;
#18986 = CARTESIAN_POINT ( 'NONE',  ( -12.06949235617756955, 12.14591786802309770, 100.6239096053143811 ) ) ;
#18989 = CARTESIAN_POINT ( 'NONE',  ( 15.72974639402199770, -15.80617190586745480, 83.12390960531436690 ) ) ;
#18990 = CARTESIAN_POINT ( 'NONE',  ( -16.55341960407611168, -4.379528057220339221, 46.45724293864769550 ) ) ;
#18991 = CARTESIAN_POINT ( 'NONE',  ( 16.51473224551083163, -9.474510206698727899, 20.83442372801899722 ) ) ;
#18992 = CARTESIAN_POINT ( 'NONE',  ( 14.34966873604972726, -8.224510206698740333, 75.83442372801900433 ) ) ;
#18993 = CARTESIAN_POINT ( 'NONE',  ( -9.474510206698964154, 16.51473224551069663, 110.4155762719810383 ) ) ;
#18994 = CARTESIAN_POINT ( 'NONE',  ( 5.049401038298161559, -19.05341960407611168, 47.70724293864770260 ) ) ;
#18995 = CARTESIAN_POINT ( 'NONE',  ( -18.67979575497193778, 10.72451020669871902, 53.33442372801901854 ) ) ;
#18996 = CARTESIAN_POINT ( 'NONE',  ( -18.67979575497193778, 10.72451020669871902, 63.33442372801900433 ) ) ;
#18997 = CARTESIAN_POINT ( 'NONE',  ( -19.02544592524342804, 5.153800228976336051, 66.04057627198103830 ) ) ;
#18998 = CARTESIAN_POINT ( 'NONE',  ( 18.67979575497194134, -10.72451020669871369, 45.83442372801901854 ) ) ;
#18999 = CARTESIAN_POINT ( 'NONE',  ( 5.049401038297881783, 19.05341960407617563, 87.29275706135234714 ) ) ;
#19000 = ADVANCED_FACE ( 'NONE', ( #147732 ), #194242, .F. ) ;
#19001 = CARTESIAN_POINT ( 'NONE',  ( -16.46253265017160317, 9.564922557960807481, 55.83224293864769550 ) ) ;
#19002 = CARTESIAN_POINT ( 'NONE',  ( 14.29746914071037800, 8.314922557961029526, 86.66775706135234714 ) ) ;
#19003 = CARTESIAN_POINT ( 'NONE',  ( -19.05341960407611168, -5.049401038298163336, 61.45724293864769550 ) ) ;
#19004 = CARTESIAN_POINT ( 'NONE',  ( 19.02544592524343514, -5.153800228976328945, 113.5405762719810241 ) ) ;
#19005 = CARTESIAN_POINT ( 'NONE',  ( 9.474510206698971260, -16.51473224551069308, 47.91557627198102409 ) ) ;
#19006 = CARTESIAN_POINT ( 'NONE',  ( -18.62759615963270932, 10.81492255796079327, 85.83224293864768129 ) ) ;
#19007 = CARTESIAN_POINT ( 'NONE',  ( -14.34966873604972548, 8.224510206698743886, 68.33442372801900433 ) ) ;
#19008 = CARTESIAN_POINT ( 'NONE',  ( -24.83221077041876512, 4.296110748028908688, 170.3917201292316577 ) ) ;
#19009 = CARTESIAN_POINT ( 'NONE',  ( 16.51473224551083163, -9.474510206698727899, 35.83442372801899722 ) ) ;
#19010 = CARTESIAN_POINT ( 'NONE',  ( -13.97604488694527625, -13.89961937509977652, 66.87390960531436690 ) ) ;
#19011 = CARTESIAN_POINT ( 'NONE',  ( 16.53943276465976808, -0.05219959533910856209, 53.74890960531437401 ) ) ;
#19012 = CARTESIAN_POINT ( 'NONE',  ( 4.483927247898545687, 16.52544592524342804, 94.79057627198105251 ) ) ;
#19013 = CARTESIAN_POINT ( 'NONE',  ( -19.05341960407611168, -5.049401038298163336, 106.4572429386476955 ) ) ;
#19014 = CARTESIAN_POINT ( 'NONE',  ( 5.049401038298161559, -19.05341960407611168, 87.70724293864769550 ) ) ;
#19015 = CARTESIAN_POINT ( 'NONE',  ( 15.72974639402176855, 15.80617190586768217, 46.87609039468568994 ) ) ;
#19016 = CARTESIAN_POINT ( 'NONE',  ( 19.02544592524343514, -5.153800228976328945, 103.5405762719809957 ) ) ;
#19017 = CARTESIAN_POINT ( 'NONE',  ( 9.474510206698729675, 16.51473224551082808, 22.08442372801899722 ) ) ;
#19018 = CARTESIAN_POINT ( 'NONE',  ( 8.314922557961029526, -14.29746914071037800, 85.41775706135236135 ) ) ;
#19019 = CARTESIAN_POINT ( 'NONE',  ( 18.67979575497194134, -10.72451020669871369, 45.83442372801901854 ) ) ;
#19020 = CARTESIAN_POINT ( 'NONE',  ( 13.97604488694527802, 13.89961937509977652, 109.3739096053143669 ) ) ;
#19021 = CARTESIAN_POINT ( 'NONE',  ( 15.80617190586746368, 15.72974639402197994, 104.3739096053143669 ) ) ;
#19022 = CARTESIAN_POINT ( 'NONE',  ( -8.224510206698948167, 14.34966873604960824, 65.41557627198102409 ) ) ;
#19023 = CARTESIAN_POINT ( 'NONE',  ( 0.05219959533909260263, 19.03943276465977164, 54.99890960531435979 ) ) ;
#19024 = CARTESIAN_POINT ( 'NONE',  ( 4.483927247898545687, 16.52544592524342804, 79.79057627198102409 ) ) ;
#19025 = CARTESIAN_POINT ( 'NONE',  ( 0.05219959533907565091, 21.53943276465977519, 29.99890960531435979 ) ) ;
#19026 = CARTESIAN_POINT ( 'NONE',  ( 19.05341960407617918, -5.049401038297876454, 46.04275706135233293 ) ) ;
#19027 = CARTESIAN_POINT ( 'NONE',  ( 16.52544592524342804, -4.483927247898539470, 113.5405762719810383 ) ) ;
#19028 = VERTEX_POINT ( 'NONE', #16174 ) ;
#19029 = CARTESIAN_POINT ( 'NONE',  ( -8.314922557961024197, 14.29746914071037800, 62.91775706135236135 ) ) ;
#19030 = CARTESIAN_POINT ( 'NONE',  ( 16.46253265017160672, -9.564922557960803928, 73.33224293864769550 ) ) ;
#19031 = CARTESIAN_POINT ( 'NONE',  ( -17.14385361876520264, -23.59649016807271238, 145.1750000027311387 ) ) ;
#19032 = CARTESIAN_POINT ( 'NONE',  ( -0.05219959533910754901, -16.53943276465976808, 92.49890960531436690 ) ) ;
#19033 = CARTESIAN_POINT ( 'NONE',  ( 21.53943276465977519, -0.05219959533907433946, 33.74890960531436690 ) ) ;
#19034 = CARTESIAN_POINT ( 'NONE',  ( 4.379528057220092307, 16.55341960407617563, 102.2927570613523613 ) ) ;
#19035 = CARTESIAN_POINT ( 'NONE',  ( 16.46253265017146816, 9.564922557961045513, 111.6677570613523329 ) ) ;
#19036 = CARTESIAN_POINT ( 'NONE',  ( -21.55341960407619339, 5.719274019375674811, 83.54275706135234714 ) ) ;
#19037 = CARTESIAN_POINT ( 'NONE',  ( -9.564922557960796823, -16.46253265017161027, 82.08224293864768129 ) ) ;
#19038 = CARTESIAN_POINT ( 'NONE',  ( 21.55341960407610458, 5.719274019375980345, 98.95724293864770971 ) ) ;
#19039 = CARTESIAN_POINT ( 'NONE',  ( -4.379528057220086978, -16.55341960407618274, 59.79275706135234714 ) ) ;
#19040 = CARTESIAN_POINT ( 'NONE',  ( -19.05341960407611168, -5.049401038298163336, 26.45724293864769550 ) ) ;
#19041 = CARTESIAN_POINT ( 'NONE',  ( 8.224510206698742110, 14.34966873604972548, 37.08442372801901143 ) ) ;
#19042 = CARTESIAN_POINT ( 'NONE',  ( -16.46253265017146816, -9.564922557961047289, 99.16775706135233293 ) ) ;
#19043 = CARTESIAN_POINT ( 'NONE',  ( -21.53943276465977519, 0.05219959533907696930, 86.24890960531436690 ) ) ;
#19044 = CARTESIAN_POINT ( 'NONE',  ( -19.05341960407617563, 5.049401038297882671, 58.54275706135234003 ) ) ;
#19045 = CARTESIAN_POINT ( 'NONE',  ( 18.39635199886970440, -5.499999999999976019, 88.51967076360000419 ) ) ;
#19046 = CARTESIAN_POINT ( 'NONE',  ( -18.67979575497178146, -10.72451020669898902, 106.6655762719810383 ) ) ;
#19047 = DIRECTION ( 'NONE',  ( 0.000000000000000000, 0.000000000000000000, 1.000000000000000000 ) ) ;
#19048 = CARTESIAN_POINT ( 'NONE',  ( 19.03943276465977164, -0.05219959533909143690, 83.74890960531436690 ) ) ;
#19049 = CARTESIAN_POINT ( 'NONE',  ( -14.34966873604972548, 8.224510206698743886, 38.33442372801900433 ) ) ;
#19050 = DIRECTION ( 'NONE',  ( -1.000000000000000000, -0.000000000000000000, -0.000000000000000000 ) ) ;
#19051 = CARTESIAN_POINT ( 'NONE',  ( 13.97604488694548053, -13.89961937509957401, 65.62609039468567573 ) ) ;
#19053 = CARTESIAN_POINT ( 'NONE',  ( 14.29746914071049879, -8.314922557960816363, 58.33224293864768839 ) ) ;
#19052 = CARTESIAN_POINT ( 'NONE',  ( -10.81492255796078084, -18.62759615963271287, 112.0822429386477097 ) ) ;
#19054 = CARTESIAN_POINT ( 'NONE',  ( -16.51473224551069308, -9.474510206698971260, 66.66557627198102409 ) ) ;
#19056 = CARTESIAN_POINT ( 'NONE',  ( -9.564922557961040184, 16.46253265017147172, 42.91775706135234003 ) ) ;
#19055 = CARTESIAN_POINT ( 'NONE',  ( 16.53943276465976808, 0.05219959533934440121, 41.25109039468568284 ) ) ;
#19057 = CARTESIAN_POINT ( 'NONE',  ( 21.52544592524334988, 5.823673210054432836, 51.45942372801901854 ) ) ;
#19058 = CARTESIAN_POINT ( 'NONE',  ( 13.97604488694548053, -13.89961937509957401, 105.6260903946856757 ) ) ;
#19059 = CARTESIAN_POINT ( 'NONE',  ( -0.05219959533909027116, -19.03943276465977164, 57.49890960531435979 ) ) ;
#19060 = CARTESIAN_POINT ( 'NONE',  ( -19.05341960407617563, 5.049401038297882671, 83.54275706135233293 ) ) ;
#19061 = CARTESIAN_POINT ( 'NONE',  ( -18.67979575497193778, 10.72451020669871902, 88.33442372801901854 ) ) ;
#19062 = CARTESIAN_POINT ( 'NONE',  ( 5.049401038297881783, 19.05341960407617563, 72.29275706135234714 ) ) ;
#19063 = CARTESIAN_POINT ( 'NONE',  ( -9.474510206698964154, 16.51473224551069663, 30.41557627198102054 ) ) ;
#19064 = CARTESIAN_POINT ( 'NONE',  ( 21.53943276465977519, -0.05219959533907433946, 58.74890960531436690 ) ) ;
#19066 = CARTESIAN_POINT ( 'NONE',  ( 19.03943276465977164, 0.05219959533936151252, 66.25109039468567573 ) ) ;
#19065 = CARTESIAN_POINT ( 'NONE',  ( -0.05219959533910754901, -16.53943276465976808, 62.49890960531436690 ) ) ;
#19067 = CARTESIAN_POINT ( 'NONE',  ( -16.21995358207306737, -7.366697692864065949, 25.06448998487843483 ) ) ;
#19068 = CARTESIAN_POINT ( 'NONE',  ( 9.564922557961047289, -16.46253265017146816, 30.41775706135232937 ) ) ;
#19069 = CARTESIAN_POINT ( 'NONE',  ( 12.06949235617739724, 12.14591786802326823, 91.87609039468568994 ) ) ;
#19070 = CARTESIAN_POINT ( 'NONE',  ( 4.379528057220339221, -16.55341960407611168, 47.70724293864770260 ) ) ;
#19072 = CARTESIAN_POINT ( 'NONE',  ( -27.73933785331498925, -9.013057229001049109, 138.9750000027311785 ) ) ;
#19071 = CARTESIAN_POINT ( 'NONE',  ( 21.53943276465977519, 0.05219959533937863772, 86.25109039468568994 ) ) ;
#19073 = CARTESIAN_POINT ( 'NONE',  ( -10.81492255796078084, -18.62759615963271287, 97.08224293864770971 ) ) ;
#19074 = CARTESIAN_POINT ( 'NONE',  ( -5.049401038298153566, 19.05341960407611168, 45.20724293864769550 ) ) ;
#19075 = CARTESIAN_POINT ( 'NONE',  ( -15.80617190586768217, 15.72974639402176855, 73.12609039468567573 ) ) ;
#19076 = CARTESIAN_POINT ( 'NONE',  ( -5.153800228976328057, -19.02544592524343514, 47.29057627198102409 ) ) ;
#19077 = CARTESIAN_POINT ( 'NONE',  ( -13.97604488694527625, -13.89961937509977652, 61.87390960531435979 ) ) ;
#19078 = CARTESIAN_POINT ( 'NONE',  ( 16.53943276465976808, -0.05219959533910856209, 103.7489096053143669 ) ) ;
#19079 = CARTESIAN_POINT ( 'NONE',  ( 19.03943276465977164, -0.05219959533909143690, 113.7489096053143669 ) ) ;
#19080 = CARTESIAN_POINT ( 'NONE',  ( -16.55341960407611168, -4.379528057220339221, 51.45724293864770260 ) ) ;
#19081 = CARTESIAN_POINT ( 'NONE',  ( 16.46253265017160672, -9.564922557960803928, 28.33224293864769550 ) ) ;
#19082 = CARTESIAN_POINT ( 'NONE',  ( -16.55341960407611168, -4.379528057220339221, 86.45724293864770971 ) ) ;
#19083 = CARTESIAN_POINT ( 'NONE',  ( 5.823673210054125526, 21.52544592524343514, 94.79057627198105251 ) ) ;
#19084 = CARTESIAN_POINT ( 'NONE',  ( -18.62759615963255300, -10.81492255796106328, 39.16775706135235424 ) ) ;
#19085 = CARTESIAN_POINT ( 'NONE',  ( 1.500000000000211831, 7.503099880506102437, -62.22181180016721669 ) ) ;
#19086 = CARTESIAN_POINT ( 'NONE',  ( -4.379528057220086978, -16.55341960407618274, 34.79275706135235424 ) ) ;
#19087 = CARTESIAN_POINT ( 'NONE',  ( -18.62759615963270932, 10.81492255796079327, 85.83224293864768129 ) ) ;
#19088 = CARTESIAN_POINT ( 'NONE',  ( 18.62759615963255655, 10.81492255796105972, 106.6677570613523756 ) ) ;
#19089 = CARTESIAN_POINT ( 'NONE',  ( 9.564922557960805705, 16.46253265017160317, 99.58224293864770971 ) ) ;
#19090 = CARTESIAN_POINT ( 'NONE',  ( -10.72451020669870658, -18.67979575497194134, 39.58442372801901143 ) ) ;
#19091 = CARTESIAN_POINT ( 'NONE',  ( -10.81492255796078084, -18.62759615963271287, 27.08224293864769550 ) ) ;
#19092 = CARTESIAN_POINT ( 'NONE',  ( -12.14591786802326823, 12.06949235617739902, 103.1260903946856757 ) ) ;
#19094 = CARTESIAN_POINT ( 'NONE',  ( -5.719274019375665041, -21.55341960407619695, 89.79275706135236135 ) ) ;
#19093 = CARTESIAN_POINT ( 'NONE',  ( 15.72974639402176855, 15.80617190586768217, 56.87609039468568994 ) ) ;
#19095 = CARTESIAN_POINT ( 'NONE',  ( 13.89961937509957401, 13.97604488694547697, 26.87609039468566507 ) ) ;
#19096 = CARTESIAN_POINT ( 'NONE',  ( 16.52544592524335698, 4.483927247898782831, 86.45942372801901854 ) ) ;
#19097 = CARTESIAN_POINT ( 'NONE',  ( -18.62759615963255300, -10.81492255796106328, 44.16775706135234714 ) ) ;
#19098 = CARTESIAN_POINT ( 'NONE',  ( 5.049401038298161559, -19.05341960407611168, 47.70724293864770260 ) ) ;
#19099 = CARTESIAN_POINT ( 'NONE',  ( -15.80617190586768217, 15.72974639402176855, 98.12609039468570415 ) ) ;
#19100 = CARTESIAN_POINT ( 'NONE',  ( 16.51473224551069308, 9.474510206698969483, 109.1655762719810383 ) ) ;
#19101 = CARTESIAN_POINT ( 'NONE',  ( -10.72451020669898014, 18.67979575497178502, 105.4155762719810383 ) ) ;
#19102 = CARTESIAN_POINT ( 'NONE',  ( 15.72974639402199770, -15.80617190586745480, 63.12390960531435979 ) ) ;
#19104 = CARTESIAN_POINT ( 'NONE',  ( -18.62759615963270932, 10.81492255796079327, 65.83224293864769550 ) ) ;
#19103 = DIRECTION ( 'NONE',  ( 0.000000000000000000, 0.000000000000000000, -1.000000000000000000 ) ) ;
#19106 = CARTESIAN_POINT ( 'NONE',  ( -16.55341960407611168, -4.379528057220339221, 66.45724293864768129 ) ) ;
#19105 = CARTESIAN_POINT ( 'NONE',  ( 4.379528057220092307, 16.55341960407617563, 57.29275706135234714 ) ) ;
#19107 = CARTESIAN_POINT ( 'NONE',  ( -7.128481858827110607, 2.709097808555396281, 2.998008972631150737 ) ) ;
#19108 = CARTESIAN_POINT ( 'NONE',  ( -19.02544592524334988, -5.153800228976617603, 88.95942372801897591 ) ) ;
#19109 = DIRECTION ( 'NONE',  ( 0.7071067811865483499, -2.468850131082268499E-15, 0.7071067811865467956 ) ) ;
#19110 = CARTESIAN_POINT ( 'NONE',  ( 12.14591786802327356, -12.06949235617739191, 20.62609039468568639 ) ) ;
#19111 = CARTESIAN_POINT ( 'NONE',  ( -0.05219959533907301413, -21.53943276465977519, 97.49890960531436690 ) ) ;
#19112 = CARTESIAN_POINT ( 'NONE',  ( 18.62759615963271287, -10.81492255796078972, 68.33224293864769550 ) ) ;
#19113 = CARTESIAN_POINT ( 'NONE',  ( -19.05341960407611168, -5.049401038298163336, 111.4572429386476671 ) ) ;
#19114 = CARTESIAN_POINT ( 'NONE',  ( -14.29746914071037622, -8.314922557961029526, 54.16775706135235424 ) ) ;
#19115 = CARTESIAN_POINT ( 'NONE',  ( -9.474510206698964154, 16.51473224551069663, 70.41557627198102409 ) ) ;
#19117 = CARTESIAN_POINT ( 'NONE',  ( -0.05219959533936034679, 19.03943276465977164, 112.5010903946856757 ) ) ;
#19116 = CARTESIAN_POINT ( 'NONE',  ( 10.81492255796106328, -18.62759615963255655, 45.41775706135234003 ) ) ;
#19118 = CARTESIAN_POINT ( 'NONE',  ( 5.153800228976335163, 19.02544592524342804, 109.7905762719810099 ) ) ;
#19119 = CARTESIAN_POINT ( 'NONE',  ( 13.89961937509977652, -13.97604488694527269, 93.12390960531436690 ) ) ;
#19120 = CARTESIAN_POINT ( 'NONE',  ( -21.52544592524343514, 5.823673210054127303, 86.04057627198102409 ) ) ;
#19121 = CARTESIAN_POINT ( 'NONE',  ( 13.89961937509977652, -13.97604488694527269, 58.12390960531436690 ) ) ;
#19122 = CARTESIAN_POINT ( 'NONE',  ( -23.48529157249600985, 32.32473071737754111, -0.2999999999999999334 ) ) ;
#19123 = CARTESIAN_POINT ( 'NONE',  ( -8.314922557960811034, -14.29746914071050412, 67.08224293864770971 ) ) ;
#19124 = CARTESIAN_POINT ( 'NONE',  ( -0.05219959533907301413, -21.53943276465977519, 22.49890960531436335 ) ) ;
#19125 = CARTESIAN_POINT ( 'NONE',  ( -31.88380457335793849, 0.2515199893715405755, -49.15318026754364666 ) ) ;
#19126 = CARTESIAN_POINT ( 'NONE',  ( 0.05219959533907565091, 21.53943276465977519, 104.9989096053143669 ) ) ;
#19127 = CARTESIAN_POINT ( 'NONE',  ( 5.049401038297881783, 19.05341960407617563, 62.29275706135234003 ) ) ;
#19128 = CARTESIAN_POINT ( 'NONE',  ( -15.72974639402197994, 15.80617190586746368, 25.62390960531435624 ) ) ;
#19129 = CARTESIAN_POINT ( 'NONE',  ( -11.80868324581545714, -11.80868324581525997, -61.34707691135562868 ) ) ;
#19130 = CARTESIAN_POINT ( 'NONE',  ( 21.55341960407610458, 5.719274019375980345, 53.95724293864770260 ) ) ;
#19131 = CARTESIAN_POINT ( 'NONE',  ( -9.564922557960796823, -16.46253265017161027, 92.08224293864769550 ) ) ;
#19132 = CARTESIAN_POINT ( 'NONE',  ( -5.719274019375665041, -21.55341960407619695, 84.79275706135234714 ) ) ;
#19133 = CARTESIAN_POINT ( 'NONE',  ( 5.049401038298161559, -19.05341960407611168, 57.70724293864769550 ) ) ;
#19134 = CARTESIAN_POINT ( 'NONE',  ( 12.06949235617757843, -12.14591786802309237, 83.12390960531436690 ) ) ;
#19135 = CARTESIAN_POINT ( 'NONE',  ( -8.314922557961024197, 14.29746914071037800, 37.91775706135235424 ) ) ;
#19136 = CARTESIAN_POINT ( 'NONE',  ( 5.719274019375673035, 21.55341960407619339, 62.29275706135236845 ) ) ;
#19137 = ORIENTED_EDGE ( 'NONE', *, *, #154603, .F. ) ;
#19138 = CARTESIAN_POINT ( 'NONE',  ( 13.89961937509957401, 13.97604488694547697, 31.87609039468566863 ) ) ;
#19140 = EDGE_CURVE ( 'NONE', #101009, #45569, #1689, .T. ) ;
#19139 = CARTESIAN_POINT ( 'NONE',  ( 13.89961937509957401, 13.97604488694547697, 81.87609039468564731 ) ) ;
#19141 = CARTESIAN_POINT ( 'NONE',  ( 19.03943276465977164, 0.05219959533936151252, 46.25109039468566863 ) ) ;
#19142 = FACE_OUTER_BOUND ( 'NONE', #84103, .T. ) ;
#19143 = CARTESIAN_POINT ( 'NONE',  ( -10.72451020669870658, -18.67979575497194134, 34.58442372801900433 ) ) ;
#19144 = CARTESIAN_POINT ( 'NONE',  ( -19.25918095147781273, -5.499999999999586997, 44.45284276293936188 ) ) ;
#19145 = CARTESIAN_POINT ( 'NONE',  ( 16.46253265017146816, 9.564922557961045513, 36.66775706135233293 ) ) ;
#19146 = CARTESIAN_POINT ( 'NONE',  ( -5.153800228976328057, -19.02544592524343514, 52.29057627198100988 ) ) ;
#19147 = CARTESIAN_POINT ( 'NONE',  ( 5.049401038297881783, 19.05341960407617563, 27.29275706135232937 ) ) ;
#19148 = CARTESIAN_POINT ( 'NONE',  ( 4.379528057220092307, 16.55341960407617563, 102.2927570613523613 ) ) ;
#19150 = CARTESIAN_POINT ( 'NONE',  ( 18.67979575497194134, -10.72451020669871369, 85.83442372801901854 ) ) ;
#19149 = CARTESIAN_POINT ( 'NONE',  ( 0.05219959533909260263, 19.03943276465977164, 109.9989096053143669 ) ) ;
#19151 = AXIS2_PLACEMENT_3D ( 'NONE', #140725, #139720, #123555 ) ;
#19152 = CARTESIAN_POINT ( 'NONE',  ( 29.86685920354754487, 21.69954338932564752, -3.424999997268813434 ) ) ;
#19153 = CARTESIAN_POINT ( 'NONE',  ( -33.86350577294170705, 5.311679113341315706, 93.56182321589967898 ) ) ;
#19154 = CARTESIAN_POINT ( 'NONE',  ( -5.823673210054431948, 21.52544592524334988, 82.70942372801900433 ) ) ;
#19155 = CARTESIAN_POINT ( 'NONE',  ( -24.81835718235489097, -6.052279806424480491, 168.4265042179603427 ) ) ;
#19156 = CARTESIAN_POINT ( 'NONE',  ( 19.05341960407611168, 5.049401038298154454, 103.9572429386476671 ) ) ;
#19157 = CARTESIAN_POINT ( 'NONE',  ( -2.649999999999999911, -165.0000000000000000, -13.00000000000000000 ) ) ;
#19158 = CARTESIAN_POINT ( 'NONE',  ( 19.02544592524343514, -5.153800228976328945, 48.54057627198103120 ) ) ;
#19159 = CARTESIAN_POINT ( 'NONE',  ( 5.823673210054125526, 21.52544592524343514, 49.79057627198102409 ) ) ;
#19160 = CARTESIAN_POINT ( 'NONE',  ( 16.55341960407611168, 4.379528057220329451, 28.95724293864769905 ) ) ;
#19162 = CARTESIAN_POINT ( 'NONE',  ( 19.03943276465977164, -0.05219959533909143690, 93.74890960531435269 ) ) ;
#19161 = CARTESIAN_POINT ( 'NONE',  ( 8.314922557960818139, 14.29746914071049879, 99.58224293864770971 ) ) ;
#19163 = CARTESIAN_POINT ( 'NONE',  ( -19.03943276465977164, -0.05219959533935918106, 18.75109039468567218 ) ) ;
#19164 = CARTESIAN_POINT ( 'NONE',  ( 9.474510206698971260, -16.51473224551069308, 42.91557627198103120 ) ) ;
#19165 = CARTESIAN_POINT ( 'NONE',  ( -8.224510206698948167, 14.34966873604960824, 100.4155762719810241 ) ) ;
#19166 = CARTESIAN_POINT ( 'NONE',  ( 18.62759615963255655, 10.81492255796105972, 56.66775706135235424 ) ) ;
#19167 = CARTESIAN_POINT ( 'NONE',  ( -14.34966873604972548, 8.224510206698743886, 113.3344237280190328 ) ) ;
#19168 = CARTESIAN_POINT ( 'NONE',  ( 0.05219959533936267826, -19.03943276465977164, 70.00109039468566152 ) ) ;
#19169 = CARTESIAN_POINT ( 'NONE',  ( -8.695239111463058279, -39.05792421784926916, -14.99999999999999822 ) ) ;
#19170 = CARTESIAN_POINT ( 'NONE',  ( 13.97604488694527802, 13.89961937509977652, 109.3739096053143669 ) ) ;
#19171 = CARTESIAN_POINT ( 'NONE',  ( -8.314922557960811034, -14.29746914071050412, 77.08224293864769550 ) ) ;
#19172 = CARTESIAN_POINT ( 'NONE',  ( 19.02544592524334988, 5.153800228976608722, 56.45942372801898301 ) ) ;
#19174 = VECTOR ( 'NONE', #3909, 1000.000000000000000 ) ;
#19173 = CARTESIAN_POINT ( 'NONE',  ( 19.03943276465977164, -0.05219959533909143690, 68.74890960531436690 ) ) ;
#19175 = CARTESIAN_POINT ( 'NONE',  ( 4.483927247898545687, 16.52544592524342804, 59.79057627198103120 ) ) ;
#19176 = CARTESIAN_POINT ( 'NONE',  ( 9.474510206698729675, 16.51473224551082808, 92.08442372801900433 ) ) ;
#19177 = CARTESIAN_POINT ( 'NONE',  ( 15.72974639402199770, -15.80617190586745480, 43.12390960531435269 ) ) ;
#19178 = ORIENTED_EDGE ( 'NONE', *, *, #66645, .T. ) ;
#19179 = CARTESIAN_POINT ( 'NONE',  ( 4.379528057220339221, -16.55341960407611168, 97.70724293864772392 ) ) ;
#19180 = DIRECTION ( 'NONE',  ( 0.000000000000000000, 0.000000000000000000, 1.000000000000000000 ) ) ;
#19182 = CARTESIAN_POINT ( 'NONE',  ( 21.53943276465977519, -0.05219959533907433946, 63.74890960531435979 ) ) ;
#19181 = CARTESIAN_POINT ( 'NONE',  ( -5.049401038298153566, 19.05341960407611168, 65.20724293864765286 ) ) ;
#19183 = CARTESIAN_POINT ( 'NONE',  ( 0.05219959533909260263, 19.03943276465977164, 39.99890960531436690 ) ) ;
#19185 = CARTESIAN_POINT ( 'NONE',  ( -19.05341960407611168, -5.049401038298163336, 76.45724293864769550 ) ) ;
#19184 = CARTESIAN_POINT ( 'NONE',  ( 12.06949235617739724, 12.14591786802326823, 96.87609039468568994 ) ) ;
#19186 = CARTESIAN_POINT ( 'NONE',  ( 19.03943276465977164, 0.05219959533936151252, 56.25109039468566863 ) ) ;
#19187 = CARTESIAN_POINT ( 'NONE',  ( 18.67979575497194134, -10.72451020669871369, 80.83442372801901854 ) ) ;
#19188 = CARTESIAN_POINT ( 'NONE',  ( -5.823673210054116645, -21.52544592524344225, 52.29057627198102409 ) ) ;
#19189 = CARTESIAN_POINT ( 'NONE',  ( 16.51473224551069308, 9.474510206698969483, 109.1655762719810383 ) ) ;
#19190 = CARTESIAN_POINT ( 'NONE',  ( -9.564922557960796823, -16.46253265017161027, 22.08224293864768839 ) ) ;
#19191 = CARTESIAN_POINT ( 'NONE',  ( -12.14591786802326823, 12.06949235617739902, 83.12609039468568994 ) ) ;
#19192 = CARTESIAN_POINT ( 'NONE',  ( -13.97604488694547697, 13.89961937509957934, 103.1260903946856473 ) ) ;
#19193 = CARTESIAN_POINT ( 'NONE',  ( -19.02544592524342804, 5.153800228976336051, 26.04057627198103120 ) ) ;
#19194 = CARTESIAN_POINT ( 'NONE',  ( 19.19724070472095789, 5.499999999999972466, 78.56193348274385357 ) ) ;
#19195 = CARTESIAN_POINT ( 'NONE',  ( -21.53943276465977519, -0.05219959533937600094, 98.75109039468568994 ) ) ;
#19196 = ORIENTED_EDGE ( 'NONE', *, *, #82089, .T. ) ;
#19197 = CARTESIAN_POINT ( 'NONE',  ( -12.06949235617756955, 12.14591786802309770, 55.62390960531436690 ) ) ;
#19198 = CARTESIAN_POINT ( 'NONE',  ( 8.314922557960818139, 14.29746914071049879, 64.58224293864769550 ) ) ;
#19199 = CARTESIAN_POINT ( 'NONE',  ( 21.55341960407610458, 5.719274019375980345, 98.95724293864770971 ) ) ;
#19200 = CARTESIAN_POINT ( 'NONE',  ( 0.05219959533907565091, 21.53943276465977519, 94.99890960531436690 ) ) ;
#19201 = CARTESIAN_POINT ( 'NONE',  ( 8.898068258721464119, 27.38543819252877398, 149.3843446568999980 ) ) ;
#19202 = CARTESIAN_POINT ( 'NONE',  ( 15.80617190586746368, 15.72974639402197994, 29.37390960531435269 ) ) ;
#19203 = CARTESIAN_POINT ( 'NONE',  ( -4.483927247898782831, 16.52544592524335698, 67.70942372801901854 ) ) ;
#19204 = CARTESIAN_POINT ( 'NONE',  ( -12.06949235617756955, 12.14591786802309770, 95.62390960531436690 ) ) ;
#19205 = CARTESIAN_POINT ( 'NONE',  ( 19.05341960407611168, 5.049401038298154454, 48.95724293864768129 ) ) ;
#19206 = CARTESIAN_POINT ( 'NONE',  ( 34.80541354469661286, -6.720605140086532536, 41.66184804092134186 ) ) ;
#19207 = CARTESIAN_POINT ( 'NONE',  ( -8.224510206698735004, -14.34966873604973081, 89.58442372801901854 ) ) ;
#19208 = CARTESIAN_POINT ( 'NONE',  ( 15.72974639402176855, 15.80617190586768217, 36.87609039468568994 ) ) ;
#19209 = CARTESIAN_POINT ( 'NONE',  ( 0.05219959533909260263, 19.03943276465977164, 79.99890960531436690 ) ) ;
#19210 = CARTESIAN_POINT ( 'NONE',  ( 10.81492255796106328, -18.62759615963255655, 65.41775706135234714 ) ) ;
#19211 = CARTESIAN_POINT ( 'NONE',  ( -17.49999999999999289, 5.500000000000037303, 80.79690382534172954 ) ) ;
#19212 = CARTESIAN_POINT ( 'NONE',  ( -7.765519415020589733, -39.80263117873666090, -25.57543461820454667 ) ) ;
#19213 = ORIENTED_EDGE ( 'NONE', *, *, #185215, .T. ) ;
#19214 = CARTESIAN_POINT ( 'NONE',  ( -21.55341960407619339, 5.719274019375674811, 53.54275706135234714 ) ) ;
#19216 = CARTESIAN_POINT ( 'NONE',  ( 17.50000000001358202, -5.500000000000038192, 58.29690382535058291 ) ) ;
#19215 = CARTESIAN_POINT ( 'NONE',  ( 13.89961937509977652, -13.97604488694527269, 43.12390960531434558 ) ) ;
#19217 = CARTESIAN_POINT ( 'NONE',  ( -9.564922557960796823, -16.46253265017161027, 87.08224293864769550 ) ) ;
#19218 = CARTESIAN_POINT ( 'NONE',  ( 19.02544592524334988, 5.153800228976608722, 61.45942372801900433 ) ) ;
#19219 = CARTESIAN_POINT ( 'NONE',  ( -5.719274019375665041, -21.55341960407619695, 34.79275706135235424 ) ) ;
#19220 = CARTESIAN_POINT ( 'NONE',  ( -9.564922557961040184, 16.46253265017147172, 57.91775706135233293 ) ) ;
#19221 = CARTESIAN_POINT ( 'NONE',  ( 16.46253265017160672, -9.564922557960803928, 23.33224293864769194 ) ) ;
#19222 = CARTESIAN_POINT ( 'NONE',  ( -0.05219959533934338120, 16.53943276465976808, 107.5010903946856899 ) ) ;
#19223 = CARTESIAN_POINT ( 'NONE',  ( -13.97604488694547697, 13.89961937509957934, 68.12609039468563310 ) ) ;
#19224 = CARTESIAN_POINT ( 'NONE',  ( -12.06949235617756955, 12.14591786802309770, 25.62390960531435624 ) ) ;
#19226 = VERTEX_POINT ( 'NONE', #185021 ) ;
#19225 = CARTESIAN_POINT ( 'NONE',  ( -19.03943276465977164, -0.05219959533935918106, 48.75109039468566863 ) ) ;
#19227 = CARTESIAN_POINT ( 'NONE',  ( 19.05341960407611168, 5.049401038298154454, 88.95724293864769550 ) ) ;
#19228 = CARTESIAN_POINT ( 'NONE',  ( 21.55341960407619695, -5.719274019375665929, 96.04275706135236135 ) ) ;
#19229 = CARTESIAN_POINT ( 'NONE',  ( -15.80617190586768217, 15.72974639402176855, 103.1260903946856757 ) ) ;
#19230 = CARTESIAN_POINT ( 'NONE',  ( 30.73962218707677607, 22.33364281372847060, -4.802157773949822683 ) ) ;
#19231 = CARTESIAN_POINT ( 'NONE',  ( 5.719274019375673035, 21.55341960407619339, 92.29275706135236135 ) ) ;
#19232 = CARTESIAN_POINT ( 'NONE',  ( -16.53943276465976808, -0.05219959533934237506, 28.75109039468567929 ) ) ;
#19233 = EDGE_CURVE ( 'NONE', #70870, #163891, #14075, .T. ) ;
#19234 = CARTESIAN_POINT ( 'NONE',  ( 9.474510206698971260, -16.51473224551069308, 97.91557627198102409 ) ) ;
#19235 = CARTESIAN_POINT ( 'NONE',  ( 21.55341960407610458, 5.719274019375980345, 23.95724293864769550 ) ) ;
#19236 = CARTESIAN_POINT ( 'NONE',  ( 1.784210473542230573E-15, -29.16686587814331588, 139.3750000027311842 ) ) ;
#19237 = CARTESIAN_POINT ( 'NONE',  ( 19.03943276465977164, -0.05219959533909143690, 83.74890960531436690 ) ) ;
#19238 = CARTESIAN_POINT ( 'NONE',  ( -16.18388926212247725, 7.379444403734496838, 99.56046848633765478 ) ) ;
#19239 = CARTESIAN_POINT ( 'NONE',  ( -19.05341960407617563, 5.049401038297882671, 68.54275706135230450 ) ) ;
#19240 = B_SPLINE_CURVE_WITH_KNOTS ( 'NONE', 3,
 ( #87520, #89514, #72362, #134036, #195729, #45004, #103699, #135047, #58191, #57202, #181544, #74358, #43022, #136024, #152181, #167361, #28859, #90499, #173315, #33799, #65123, #122818, #34790, #169320, #186514, #45988, #107643, #3447, #93468, #155155, #124814, #156144 ),
 .UNSPECIFIED., .F., .F.,
 ( 4, 2, 2, 2, 2, 2, 2, 2, 2, 2, 2, 2, 2, 2, 2, 4 ),
 ( 2.969368287472575283E-17, 0.0003712461730036979452, 0.0007424923460073661833, 0.001113738519011034421, 0.001484984692014702659, 0.002227477038022038919, 0.002598723211025717565, 0.002969969384029395778, 0.003341215557033074424, 0.003712461730036753071, 0.004083707903040432151, 0.004454954076044110797, 0.004826200249047790311, 0.005197446422051468957, 0.005568692595055147604, 0.005939938768058825383 ),
 .UNSPECIFIED. ) ;
#19241 = CARTESIAN_POINT ( 'NONE',  ( 5.049401038298161559, -19.05341960407611168, 112.7072429386476813 ) ) ;
#19242 = CARTESIAN_POINT ( 'NONE',  ( 0.05219959533937995610, -21.53943276465977519, 105.0010903946856757 ) ) ;
#19243 = CARTESIAN_POINT ( 'NONE',  ( -4.379528057220328563, 16.55341960407611168, 95.20724293864769550 ) ) ;
#19244 = CARTESIAN_POINT ( 'NONE',  ( -10.72451020669898014, 18.67979575497178502, 40.41557627198103120 ) ) ;
#19245 = CARTESIAN_POINT ( 'NONE',  ( 21.52544592524344225, -5.823673210054117533, 38.54057627198103120 ) ) ;
#19246 = CARTESIAN_POINT ( 'NONE',  ( -14.34966873604960291, -8.224510206698953496, 111.6655762719810525 ) ) ;
#19247 = CARTESIAN_POINT ( 'NONE',  ( -15.57446157010953591, 1.455575599911040019, -61.81477736546834478 ) ) ;
#19248 = CARTESIAN_POINT ( 'NONE',  ( 13.97604488694548053, -13.89961937509957401, 55.62609039468566863 ) ) ;
#19249 = CARTESIAN_POINT ( 'NONE',  ( -12.14591786802309592, -12.06949235617757132, 26.87390960531435979 ) ) ;
#19250 = CARTESIAN_POINT ( 'NONE',  ( -19.02544592524342804, 5.153800228976336051, 101.0405762719810241 ) ) ;
#19251 = CARTESIAN_POINT ( 'NONE',  ( 10.81492255796106328, -18.62759615963255655, 80.41775706135234714 ) ) ;
#19252 = CARTESIAN_POINT ( 'NONE',  ( -15.80617190586745835, -15.72974639402198527, 66.87390960531436690 ) ) ;
#19253 = CARTESIAN_POINT ( 'NONE',  ( -18.62759615963255300, -10.81492255796106328, 39.16775706135235424 ) ) ;
#19254 = CARTESIAN_POINT ( 'NONE',  ( 21.53943276465977519, -0.05219959533907433946, 98.74890960531438111 ) ) ;
#19255 = CARTESIAN_POINT ( 'NONE',  ( -10.72451020669870658, -18.67979575497194134, 54.58442372801901143 ) ) ;
#19256 = CARTESIAN_POINT ( 'NONE',  ( -5.153800228976328057, -19.02544592524343514, 22.29057627198102765 ) ) ;
#19257 = EDGE_CURVE ( 'NONE', #137960, #94779, #107170, .T. ) ;
#19258 = CARTESIAN_POINT ( 'NONE',  ( 19.05341960407611168, 5.049401038298154454, 78.95724293864769550 ) ) ;
#19259 = CARTESIAN_POINT ( 'NONE',  ( -0.05219959533934338120, 16.53943276465976808, 77.50109039468567573 ) ) ;
#19260 = CARTESIAN_POINT ( 'NONE',  ( -12.06949235617756955, 12.14591786802309770, 105.6239096053143669 ) ) ;
#19261 = CARTESIAN_POINT ( 'NONE',  ( -9.564922557960796823, -16.46253265017161027, 102.0822429386477097 ) ) ;
#19262 = CARTESIAN_POINT ( 'NONE',  ( 12.14591786802309770, 12.06949235617756955, 59.37390960531436690 ) ) ;
#19263 = CARTESIAN_POINT ( 'NONE',  ( -16.52544592524342804, 4.483927247898546575, 26.04057627198103475 ) ) ;
#19264 = CARTESIAN_POINT ( 'NONE',  ( -19.05341960407611168, -5.049401038298163336, 56.45724293864768129 ) ) ;
#19265 = CARTESIAN_POINT ( 'NONE',  ( -16.46253265017160317, 9.564922557960807481, 40.83224293864769550 ) ) ;
#19266 = CARTESIAN_POINT ( 'NONE',  ( -15.72974639402197994, 15.80617190586746368, 50.62390960531435979 ) ) ;
#19267 = CARTESIAN_POINT ( 'NONE',  ( -9.564922557961040184, 16.46253265017147172, 22.91775706135233648 ) ) ;
#19269 = CARTESIAN_POINT ( 'NONE',  ( -8.314922557960811034, -14.29746914071050412, 42.08224293864769550 ) ) ;
#19268 = CARTESIAN_POINT ( 'NONE',  ( 18.22780087662126647, 5.499999999999818812, 51.48236817873107896 ) ) ;
#19270 = CARTESIAN_POINT ( 'NONE',  ( 18.62759615963255655, 10.81492255796105972, 46.66775706135234714 ) ) ;
#19271 = FACE_OUTER_BOUND ( 'NONE', #79322, .T. ) ;
#19272 = CARTESIAN_POINT ( 'NONE',  ( 0.05219959533934541429, -16.53943276465976808, 65.00109039468568994 ) ) ;
#19273 = CARTESIAN_POINT ( 'NONE',  ( 16.46253265017146816, 9.564922557961045513, 61.66775706135234003 ) ) ;
#19274 = CARTESIAN_POINT ( 'NONE',  ( 8.314922557960818139, 14.29746914071049879, 29.58224293864769905 ) ) ;
#19275 = CARTESIAN_POINT ( 'NONE',  ( 4.379528057220092307, 16.55341960407617563, 102.2927570613523613 ) ) ;
#19276 = CARTESIAN_POINT ( 'NONE',  ( -5.049401038298153566, 19.05341960407611168, 35.20724293864768839 ) ) ;
#19277 = CARTESIAN_POINT ( 'NONE',  ( -5.153800228976328057, -19.02544592524343514, 67.29057627198102409 ) ) ;
#19278 = CARTESIAN_POINT ( 'NONE',  ( -19.02544592524342804, 5.153800228976336051, 26.04057627198103120 ) ) ;
#19279 = CARTESIAN_POINT ( 'NONE',  ( 21.55341960407619695, -5.719274019375665929, 31.04275706135234714 ) ) ;
#19280 = CARTESIAN_POINT ( 'NONE',  ( 5.153800228976335163, 19.02544592524342804, 39.79057627198100988 ) ) ;
#19281 = DIRECTION ( 'NONE',  ( 0.000000000000000000, 0.000000000000000000, 1.000000000000000000 ) ) ;
#19282 = CARTESIAN_POINT ( 'NONE',  ( 5.049401038298161559, -19.05341960407611168, 42.70724293864767418 ) ) ;
#19283 = CARTESIAN_POINT ( 'NONE',  ( 5.049401038298161559, -19.05341960407611168, 112.7072429386476813 ) ) ;
#19284 = AXIS2_PLACEMENT_3D ( 'NONE', #173440, #34909, #51076 ) ;
#19286 = CARTESIAN_POINT ( 'NONE',  ( 0.05219959533910956823, 16.53943276465976808, 104.9989096053143669 ) ) ;
#19285 = CARTESIAN_POINT ( 'NONE',  ( -5.823673210054431948, 21.52544592524334988, 57.70942372801901143 ) ) ;
#19287 = CARTESIAN_POINT ( 'NONE',  ( 13.89961937509977652, -13.97604488694527269, 113.1239096053143527 ) ) ;
#19288 = CARTESIAN_POINT ( 'NONE',  ( 12.06949235617739724, 12.14591786802326823, 81.87609039468568994 ) ) ;
#19289 = CARTESIAN_POINT ( 'NONE',  ( 5.719274019375673035, 21.55341960407619339, 92.29275706135236135 ) ) ;
#19290 = CARTESIAN_POINT ( 'NONE',  ( -16.52544592524335698, -4.483927247898792601, 48.95942372801902565 ) ) ;
#19291 = CARTESIAN_POINT ( 'NONE',  ( -19.03943276465977164, 0.05219959533909376836, 96.24890960531436690 ) ) ;
#19292 = CARTESIAN_POINT ( 'NONE',  ( -8.224510206698735004, -14.34966873604973081, 39.58442372801901143 ) ) ;
#19293 = CARTESIAN_POINT ( 'NONE',  ( -0.05219959533934338120, 16.53943276465976808, 27.50109039468567929 ) ) ;
#19294 = CARTESIAN_POINT ( 'NONE',  ( -14.34966873604972548, 8.224510206698743886, 98.33442372801901854 ) ) ;
#19295 = CARTESIAN_POINT ( 'NONE',  ( 9.474510206698729675, 16.51473224551082808, 107.0844237280190043 ) ) ;
#19296 = CARTESIAN_POINT ( 'NONE',  ( -5.823673210054116645, -21.52544592524344225, 102.2905762719810383 ) ) ;
#19298 = CARTESIAN_POINT ( 'NONE',  ( 9.564922557961047289, -16.46253265017146816, 100.4177570613523329 ) ) ;
#19297 = CARTESIAN_POINT ( 'NONE',  ( -14.34966873604960291, -8.224510206698953496, 101.6655762719810383 ) ) ;
#19299 = CARTESIAN_POINT ( 'NONE',  ( -16.55341960407617563, 4.379528057220093196, 68.54275706135234714 ) ) ;
#19300 = CARTESIAN_POINT ( 'NONE',  ( 24.68411608548795044, 7.148172978119885279, 167.5704058020753848 ) ) ;
#19301 = CARTESIAN_POINT ( 'NONE',  ( 19.05341960407617918, -5.049401038297876454, 66.04275706135233293 ) ) ;
#19302 = CARTESIAN_POINT ( 'NONE',  ( -16.53943276465976808, 0.05219959533911058130, 51.24890960531436690 ) ) ;
#19303 = CARTESIAN_POINT ( 'NONE',  ( 14.34966873604960469, 8.224510206698951720, 49.16557627198102409 ) ) ;
#19304 = CARTESIAN_POINT ( 'NONE',  ( -16.52544592524342804, 4.483927247898546575, 96.04057627198102409 ) ) ;
#19306 = CARTESIAN_POINT ( 'NONE',  ( -16.61371651742601330, 7.165104196376141488, 88.85415069993000259 ) ) ;
#19305 = CARTESIAN_POINT ( 'NONE',  ( -16.51473224551082808, 9.474510206698731452, 28.33442372801900433 ) ) ;
#19307 = CARTESIAN_POINT ( 'NONE',  ( 15.72974639402176855, 15.80617190586768217, 36.87609039468568994 ) ) ;
#19308 = CARTESIAN_POINT ( 'NONE',  ( -19.03943276465977164, -0.05219959533935918106, 93.75109039468566152 ) ) ;
#19309 = CARTESIAN_POINT ( 'NONE',  ( -3.181980515339399851, 6.791538853603101167, 8.889087296526001936 ) ) ;
#19310 = CARTESIAN_POINT ( 'NONE',  ( -5.049401038298153566, 19.05341960407611168, 95.20724293864770971 ) ) ;
#19311 = CARTESIAN_POINT ( 'NONE',  ( -0.05219959533909027116, -19.03943276465977164, 92.49890960531436690 ) ) ;
#19312 = CARTESIAN_POINT ( 'NONE',  ( -18.62759615963270932, 10.81492255796079327, 60.83224293864769550 ) ) ;
#19313 = CARTESIAN_POINT ( 'NONE',  ( 16.53943276465976808, -0.05219959533910856209, 88.74890960531436690 ) ) ;
#19314 = CARTESIAN_POINT ( 'NONE',  ( -19.02544592524342804, 5.153800228976336051, 76.04057627198102409 ) ) ;
#19315 = CARTESIAN_POINT ( 'NONE',  ( 16.46253265017160672, -9.564922557960803928, 33.33224293864770260 ) ) ;
#19316 = CARTESIAN_POINT ( 'NONE',  ( 15.80617190586769283, -15.72974639402175789, 40.62609039468567573 ) ) ;
#19317 = AXIS2_PLACEMENT_3D ( 'NONE', #122463, #154798, #153803 ) ;
#19318 = CARTESIAN_POINT ( 'NONE',  ( -18.62759615963255300, -10.81492255796106328, 79.16775706135234714 ) ) ;
#19319 = CARTESIAN_POINT ( 'NONE',  ( -19.02544592524342804, 5.153800228976336051, 61.04057627198103120 ) ) ;
#19320 = CARTESIAN_POINT ( 'NONE',  ( 12.06949235617739724, 12.14591786802326823, 81.87609039468568994 ) ) ;
#19321 = CARTESIAN_POINT ( 'NONE',  ( 18.67979575497194134, -10.72451020669871369, 35.83442372801901143 ) ) ;
#19322 = CARTESIAN_POINT ( 'NONE',  ( -15.80617190586768217, 15.72974639402176855, 28.12609039468568284 ) ) ;
#19324 = CARTESIAN_POINT ( 'NONE',  ( 13.97604488694527802, 13.89961937509977652, 79.37390960531435269 ) ) ;
#19323 = CARTESIAN_POINT ( 'NONE',  ( -19.03943276465977164, -0.05219959533935918106, 48.75109039468566863 ) ) ;
#19325 = CARTESIAN_POINT ( 'NONE',  ( -5.049401038297874678, -19.05341960407617918, 29.79275706135232227 ) ) ;
#19326 = CARTESIAN_POINT ( 'NONE',  ( -10.81492255796105439, 18.62759615963255655, 87.91775706135234714 ) ) ;
#19327 = CARTESIAN_POINT ( 'NONE',  ( -21.52544592524343514, 5.823673210054127303, 71.04057627198103830 ) ) ;
#19328 = CARTESIAN_POINT ( 'NONE',  ( -4.483927247898539470, -16.52544592524342804, 57.29057627198103120 ) ) ;
#19330 = CARTESIAN_POINT ( 'NONE',  ( -9.474510206698720793, -16.51473224551083518, 29.58442372801900433 ) ) ;
#19329 = CARTESIAN_POINT ( 'NONE',  ( -0.05219959533937732626, 21.53943276465977519, 87.50109039468568994 ) ) ;
#19331 = CARTESIAN_POINT ( 'NONE',  ( 16.55341960407611168, 4.379528057220329451, 68.95724293864769550 ) ) ;
#19332 = CARTESIAN_POINT ( 'NONE',  ( 16.51473224551069308, 9.474510206698969483, 24.16557627198102765 ) ) ;
#19333 = CARTESIAN_POINT ( 'NONE',  ( 16.46253265017146816, 9.564922557961045513, 66.66775706135233293 ) ) ;
#19334 = CARTESIAN_POINT ( 'NONE',  ( 4.379528057220339221, -16.55341960407611168, 32.70724293864770260 ) ) ;
#19336 = EDGE_CURVE ( 'NONE', #18425, #70413, #187788, .T. ) ;
#19335 = CARTESIAN_POINT ( 'NONE',  ( -21.55341960407619339, 5.719274019375674811, 83.54275706135234714 ) ) ;
#19337 = CARTESIAN_POINT ( 'NONE',  ( 16.51473224551069308, 9.474510206698969483, 74.16557627198103830 ) ) ;
#19338 = CARTESIAN_POINT ( 'NONE',  ( 19.02544592524334988, 5.153800228976608722, 41.45942372801900433 ) ) ;
#19339 = CARTESIAN_POINT ( 'NONE',  ( 15.80617190586746368, 15.72974639402197994, 54.37390960531435979 ) ) ;
#19340 = CARTESIAN_POINT ( 'NONE',  ( 15.72974639402176855, 15.80617190586768217, 21.87609039468567573 ) ) ;
#19341 = CARTESIAN_POINT ( 'NONE',  ( -16.51473224551082808, 9.474510206698731452, 108.3344237280190043 ) ) ;
#19342 = CARTESIAN_POINT ( 'NONE',  ( -12.14591786802326823, 12.06949235617739902, 68.12609039468567573 ) ) ;
#19343 = CARTESIAN_POINT ( 'NONE',  ( 10.72451020669898902, -18.67979575497178502, 102.9155762719810383 ) ) ;
#19344 = CARTESIAN_POINT ( 'NONE',  ( 14.29746914071049879, -8.314922557960816363, 108.3322429386477097 ) ) ;
#19345 = CARTESIAN_POINT ( 'NONE',  ( -17.50000000000149569, -3.202012800152222560, 30.07177583972730517 ) ) ;
#19346 = CARTESIAN_POINT ( 'NONE',  ( 4.483927247898790824, -16.52544592524335698, 35.20942372801901854 ) ) ;
#19347 = CARTESIAN_POINT ( 'NONE',  ( -15.72974639402197994, 15.80617190586746368, 65.62390960531436690 ) ) ;
#19348 = CARTESIAN_POINT ( 'NONE',  ( 16.52544592524335698, 4.483927247898782831, 101.4594237280190185 ) ) ;
#19349 = CARTESIAN_POINT ( 'NONE',  ( -16.51473224551069308, -9.474510206698971260, 31.66557627198102054 ) ) ;
#19350 = CARTESIAN_POINT ( 'NONE',  ( 14.34966873604972726, -8.224510206698740333, 65.83442372801900433 ) ) ;
#19351 = CARTESIAN_POINT ( 'NONE',  ( -5.049401038297874678, -19.05341960407617918, 64.79275706135233293 ) ) ;
#19352 = CARTESIAN_POINT ( 'NONE',  ( 15.80617190586769283, -15.72974639402175789, 40.62609039468567573 ) ) ;
#19353 = CARTESIAN_POINT ( 'NONE',  ( 15.80617190586746368, 15.72974639402197994, 64.37390960531435269 ) ) ;
#19354 = CARTESIAN_POINT ( 'NONE',  ( -0.05219959533934338120, 16.53943276465976808, 97.50109039468567573 ) ) ;
#19355 = CARTESIAN_POINT ( 'NONE',  ( 18.62759615963255655, 10.81492255796105972, 81.66775706135236135 ) ) ;
#19356 = CARTESIAN_POINT ( 'NONE',  ( -18.62759615963270932, 10.81492255796079327, 50.83224293864770971 ) ) ;
#19357 = CARTESIAN_POINT ( 'NONE',  ( 10.81492255796078972, 18.62759615963270932, 29.58224293864769905 ) ) ;
#19358 = CARTESIAN_POINT ( 'NONE',  ( 0.05219959533934541429, -16.53943276465976808, 75.00109039468568994 ) ) ;
#19359 = CARTESIAN_POINT ( 'NONE',  ( -21.52544592524343514, 5.823673210054127303, 41.04057627198103120 ) ) ;
#19360 = ORIENTED_EDGE ( 'NONE', *, *, #9292, .F. ) ;
#19361 = CARTESIAN_POINT ( 'NONE',  ( 5.049401038298161559, -19.05341960407611168, 102.7072429386476955 ) ) ;
#19362 = CYLINDRICAL_SURFACE ( 'NONE', #88954, 4.000000000000000888 ) ;
#19363 = CARTESIAN_POINT ( 'NONE',  ( -16.51473224551069308, -9.474510206698971260, 26.66557627198103120 ) ) ;
#19364 = CARTESIAN_POINT ( 'NONE',  ( -15.80617190586745835, -15.72974639402198527, 61.87390960531436690 ) ) ;
#19365 = CARTESIAN_POINT ( 'NONE',  ( -0.05219959533934338120, 16.53943276465976808, 92.50109039468567573 ) ) ;
#19366 = CARTESIAN_POINT ( 'NONE',  ( -21.52544592524334988, -5.823673210054445271, 43.95942372801902565 ) ) ;
#19367 = CARTESIAN_POINT ( 'NONE',  ( -9.564922557961040184, 16.46253265017147172, 107.9177570613523471 ) ) ;
#19368 = CARTESIAN_POINT ( 'NONE',  ( 12.14591786802309770, 12.06949235617756955, 99.37390960531436690 ) ) ;
#19369 = CARTESIAN_POINT ( 'NONE',  ( 14.34966873604972726, -8.224510206698740333, 20.83442372801901143 ) ) ;
#19370 = CARTESIAN_POINT ( 'NONE',  ( -19.03943276465977164, 0.05219959533909376836, 41.24890960531435269 ) ) ;
#19371 = CARTESIAN_POINT ( 'NONE',  ( 18.22780087662123805, -5.499999999999989342, 63.51763182126896368 ) ) ;
#19372 = CARTESIAN_POINT ( 'NONE',  ( -16.46253265017160317, 9.564922557960807481, 90.83224293864769550 ) ) ;
#19373 = CARTESIAN_POINT ( 'NONE',  ( -12.14591786802326823, 12.06949235617739902, 73.12609039468567573 ) ) ;
#19374 = CARTESIAN_POINT ( 'NONE',  ( 21.55341960407619695, -5.719274019375665929, 106.0427570613523471 ) ) ;
#19375 = CARTESIAN_POINT ( 'NONE',  ( -0.05219959533907301413, -21.53943276465977519, 57.49890960531435979 ) ) ;
#19376 = CARTESIAN_POINT ( 'NONE',  ( -4.483927247898782831, 16.52544592524335698, 87.70942372801901854 ) ) ;
#19377 = CARTESIAN_POINT ( 'NONE',  ( 5.153800228976615827, -19.02544592524334988, 75.20942372801896170 ) ) ;
#19378 = CARTESIAN_POINT ( 'NONE',  ( -16.51473224551069308, -9.474510206698971260, 41.66557627198103120 ) ) ;
#19379 = CARTESIAN_POINT ( 'NONE',  ( -9.564922557960796823, -16.46253265017161027, 77.08224293864769550 ) ) ;
#19380 = CARTESIAN_POINT ( 'NONE',  ( 19.02544592524343514, -5.153800228976328945, 38.54057627198103120 ) ) ;
#19381 = CARTESIAN_POINT ( 'NONE',  ( 19.05341960407617918, -5.049401038297876454, 76.04275706135230450 ) ) ;
#19382 = CARTESIAN_POINT ( 'NONE',  ( 25.82893184620924742, -8.167111171437140271, 172.3011985515803417 ) ) ;
#19383 = CARTESIAN_POINT ( 'NONE',  ( -0.05219959533909027116, -19.03943276465977164, 97.49890960531436690 ) ) ;
#19384 = CARTESIAN_POINT ( 'NONE',  ( -8.314922557960811034, -14.29746914071050412, 52.08224293864768839 ) ) ;
#19385 = CARTESIAN_POINT ( 'NONE',  ( 18.62759615963271287, -10.81492255796078972, 58.33224293864768839 ) ) ;
#19386 = CARTESIAN_POINT ( 'NONE',  ( -17.49999999999998934, 3.805241302050261343, 105.3735247278259237 ) ) ;
#19387 = CARTESIAN_POINT ( 'NONE',  ( 0.05219959533936267826, -19.03943276465977164, 35.00109039468566863 ) ) ;
#19388 = CARTESIAN_POINT ( 'NONE',  ( 17.62203461105333702, -16.12203461105326951, -64.92279855667830191 ) ) ;
#19390 = CARTESIAN_POINT ( 'NONE',  ( -13.89961937509977652, 13.97604488694528158, 75.62390960531438111 ) ) ;
#19389 = CARTESIAN_POINT ( 'NONE',  ( 9.474510206698971260, -16.51473224551069308, 57.91557627198103120 ) ) ;
#19391 = CARTESIAN_POINT ( 'NONE',  ( -14.34966873604972548, 8.224510206698743886, 43.33442372801901143 ) ) ;
#19392 = CARTESIAN_POINT ( 'NONE',  ( -33.85315667487628843, -0.3599896029658122276, 100.5000000000010232 ) ) ;
#19393 = CARTESIAN_POINT ( 'NONE',  ( -16.29526858892874941, 7.335722546920128373, 109.2032940219979622 ) ) ;
#19394 = CARTESIAN_POINT ( 'NONE',  ( -8.224510206698735004, -14.34966873604973081, 79.58442372801903275 ) ) ;
#19396 = CARTESIAN_POINT ( 'NONE',  ( -21.52544592524343514, 5.823673210054127303, 101.0405762719810383 ) ) ;
#19395 = CARTESIAN_POINT ( 'NONE',  ( 4.379528057220092307, 16.55341960407617563, 67.29275706135234714 ) ) ;
#19397 = CARTESIAN_POINT ( 'NONE',  ( 16.55341960407618274, -4.379528057220086978, 46.04275706135234714 ) ) ;
#19399 = FACE_BOUND ( 'NONE', #90520, .T. ) ;
#19398 = CARTESIAN_POINT ( 'NONE',  ( -19.03943276465977164, 0.05219959533909376836, 46.24890960531435979 ) ) ;
#19400 = CARTESIAN_POINT ( 'NONE',  ( -10.72451020669870658, -18.67979575497194134, 49.58442372801901143 ) ) ;
#19401 = CARTESIAN_POINT ( 'NONE',  ( -0.05219959533936034679, 19.03943276465977164, 62.50109039468566863 ) ) ;
#19402 = CARTESIAN_POINT ( 'NONE',  ( 10.72451020669871369, 18.67979575497193778, 92.08442372801901854 ) ) ;
#19403 = CARTESIAN_POINT ( 'NONE',  ( -5.049401038298153566, 19.05341960407611168, 35.20724293864768839 ) ) ;
#19404 = CARTESIAN_POINT ( 'NONE',  ( 18.87255363501902039, 5.499999999999939604, 43.82513748171827928 ) ) ;
#19405 = CARTESIAN_POINT ( 'NONE',  ( -18.67979575497178146, -10.72451020669898902, 51.66557627198102409 ) ) ;
#19406 = CARTESIAN_POINT ( 'NONE',  ( -16.46253265017160317, 9.564922557960807481, 100.8322429386477097 ) ) ;
#19407 = CARTESIAN_POINT ( 'NONE',  ( -16.55341960407611168, -4.379528057220339221, 101.4572429386476955 ) ) ;
#19408 = CARTESIAN_POINT ( 'NONE',  ( 16.52544592524335698, 4.483927247898782831, 41.45942372801901143 ) ) ;
#19409 = CARTESIAN_POINT ( 'NONE',  ( 8.314922557961029526, -14.29746914071037800, 110.4177570613523756 ) ) ;
#19410 = EDGE_LOOP ( 'NONE', ( #154661, #151131, #54818, #72338, #46622 ) ) ;
#19411 = CARTESIAN_POINT ( 'NONE',  ( -21.55341960407610458, -5.719274019375992779, 106.4572429386477097 ) ) ;
#19413 = FACE_OUTER_BOUND ( 'NONE', #174506, .T. ) ;
#19412 = CARTESIAN_POINT ( 'NONE',  ( 14.29746914071049879, -8.314922557960816363, 43.33224293864769550 ) ) ;
#19414 = CARTESIAN_POINT ( 'NONE',  ( 0.05219959533936267826, -19.03943276465977164, 100.0010903946856757 ) ) ;
#19415 = CARTESIAN_POINT ( 'NONE',  ( -9.474510206698720793, -16.51473224551083518, 29.58442372801900433 ) ) ;
#19416 = CARTESIAN_POINT ( 'NONE',  ( 0.05219959533910956823, 16.53943276465976808, 24.99890960531435624 ) ) ;
#19417 = CARTESIAN_POINT ( 'NONE',  ( -15.80617190586745835, -15.72974639402198527, 86.87390960531438111 ) ) ;
#19418 = CARTESIAN_POINT ( 'NONE',  ( -21.53943276465977519, 0.05219959533907696930, 51.24890960531436690 ) ) ;
#19419 = CARTESIAN_POINT ( 'NONE',  ( 0.05219959533909260263, 19.03943276465977164, 69.99890960531435269 ) ) ;
#19420 = CARTESIAN_POINT ( 'NONE',  ( -16.52544592524342804, 4.483927247898546575, 41.04057627198103120 ) ) ;
#19421 = CARTESIAN_POINT ( 'NONE',  ( -13.89961937509977652, 13.97604488694528158, 85.62390960531433848 ) ) ;
#19422 = AXIS2_PLACEMENT_3D ( 'NONE', #80291, #465, #79307 ) ;
#19423 = CARTESIAN_POINT ( 'NONE',  ( 0.000000000000000000, 0.000000000000000000, -60.44446360152740283 ) ) ;
#19424 = CARTESIAN_POINT ( 'NONE',  ( 19.02544592524334988, 5.153800228976608722, 46.45942372801899012 ) ) ;
#19425 = CARTESIAN_POINT ( 'NONE',  ( -5.823673210054116645, -21.52544592524344225, 87.29057627198103830 ) ) ;
#19426 = CARTESIAN_POINT ( 'NONE',  ( -16.52544592524342804, 4.483927247898546575, 101.0405762719810383 ) ) ;
#19427 = CARTESIAN_POINT ( 'NONE',  ( 5.823673210054444382, -21.52544592524334988, 40.20942372801901854 ) ) ;
#19428 = CARTESIAN_POINT ( 'NONE',  ( 8.571926809382603096, -26.38167802310801235, 139.4750000027311785 ) ) ;
#19429 = CARTESIAN_POINT ( 'NONE',  ( 14.29746914071037800, 8.314922557961029526, 101.6677570613523613 ) ) ;
#19430 = CARTESIAN_POINT ( 'NONE',  ( -19.03943276465977164, 0.05219959533909376836, 41.24890960531435269 ) ) ;
#19431 = CARTESIAN_POINT ( 'NONE',  ( 19.05341960407611168, 5.049401038298154454, 88.95724293864769550 ) ) ;
#19432 = CARTESIAN_POINT ( 'NONE',  ( 27.73933785331498569, 2.768321779492822058E-14, 139.8750000027311842 ) ) ;
#19433 = CARTESIAN_POINT ( 'NONE',  ( -16.46253265017160317, 9.564922557960807481, 35.83224293864768839 ) ) ;
#19434 = CARTESIAN_POINT ( 'NONE',  ( -4.483927247898539470, -16.52544592524342804, 42.29057627198103120 ) ) ;
#19435 = CARTESIAN_POINT ( 'NONE',  ( 15.72974639402176855, 15.80617190586768217, 71.87609039468568994 ) ) ;
#19437 = CARTESIAN_POINT ( 'NONE',  ( 4.483927247898790824, -16.52544592524335698, 75.20942372801901854 ) ) ;
#19436 = CARTESIAN_POINT ( 'NONE',  ( 27.37900830011397346, -26.18142635053362000, -16.57177559434128611 ) ) ;
#19438 = CARTESIAN_POINT ( 'NONE',  ( 9.474510206698971260, -16.51473224551069308, 62.91557627198102409 ) ) ;
#19439 = CARTESIAN_POINT ( 'NONE',  ( -9.564922557960796823, -16.46253265017161027, 62.08224293864769550 ) ) ;
#19440 = ORIENTED_EDGE ( 'NONE', *, *, #127434, .F. ) ;
#19441 = CARTESIAN_POINT ( 'NONE',  ( 15.72974639402176855, 15.80617190586768217, 101.8760903946857042 ) ) ;
#19442 = CARTESIAN_POINT ( 'NONE',  ( -14.29746914071037622, -8.314922557961029526, 79.16775706135234714 ) ) ;
#19443 = CARTESIAN_POINT ( 'NONE',  ( -15.80617190586768217, 15.72974639402176855, 98.12609039468570415 ) ) ;
#19444 = CARTESIAN_POINT ( 'NONE',  ( 9.564922557960805705, 16.46253265017160317, 64.58224293864769550 ) ) ;
#19445 = CARTESIAN_POINT ( 'NONE',  ( -15.72974639402197994, 15.80617190586746368, 40.62390960531435269 ) ) ;
#19446 = CARTESIAN_POINT ( 'NONE',  ( 5.049401038297881783, 19.05341960407617563, 112.2927570613523471 ) ) ;
#19447 = CARTESIAN_POINT ( 'NONE',  ( -21.53943276465977519, -0.05219959533937600094, 73.75109039468567573 ) ) ;
#19448 = CARTESIAN_POINT ( 'NONE',  ( 4.483927247898790824, -16.52544592524335698, 50.20942372801901854 ) ) ;
#19449 = CARTESIAN_POINT ( 'NONE',  ( -21.52544592524343514, 5.823673210054127303, 96.04057627198102409 ) ) ;
#19450 = CARTESIAN_POINT ( 'NONE',  ( 16.46253265017146816, 9.564922557961045513, 101.6677570613523329 ) ) ;
#19451 = CARTESIAN_POINT ( 'NONE',  ( -16.46253265017160317, 9.564922557960807481, 75.83224293864769550 ) ) ;
#19452 = CARTESIAN_POINT ( 'NONE',  ( -19.03943276465977164, -0.05219959533935918106, 103.7510903946856757 ) ) ;
#19453 = AXIS2_PLACEMENT_3D ( 'NONE', #116758, #151103, #71263 ) ;
#19454 = CARTESIAN_POINT ( 'NONE',  ( 19.02544592524334988, 5.153800228976608722, 96.45942372801897591 ) ) ;
#19455 = CARTESIAN_POINT ( 'NONE',  ( -0.05219959533910754901, -16.53943276465976808, 62.49890960531436690 ) ) ;
#19456 = CARTESIAN_POINT ( 'NONE',  ( -8.224510206698735004, -14.34966873604973081, 74.58442372801901854 ) ) ;
#19458 = CARTESIAN_POINT ( 'NONE',  ( -9.474510206698964154, 16.51473224551069663, 55.41557627198103120 ) ) ;
#19457 = CARTESIAN_POINT ( 'NONE',  ( 0.05219959533907565091, 21.53943276465977519, 114.9989096053143669 ) ) ;
#19459 = CARTESIAN_POINT ( 'NONE',  ( -9.474510206698964154, 16.51473224551069663, 60.41557627198102409 ) ) ;
#19460 = B_SPLINE_CURVE_WITH_KNOTS ( 'NONE', 3,
 ( #24339, #25350, #194190, #86991, #164846, #146655 ),
 .UNSPECIFIED., .F., .F.,
 ( 4, 2, 4 ),
 ( 0.003989672132298042843, 0.004372778065220470425, 0.004755883998142898875 ),
 .UNSPECIFIED. ) ;
#19461 = CARTESIAN_POINT ( 'NONE',  ( -12.06949235617739369, -12.14591786802326823, 74.37609039468568994 ) ) ;
#19462 = CARTESIAN_POINT ( 'NONE',  ( -17.81289503416611097, -24.51734667627696496, 144.5500000054623513 ) ) ;
#19463 = ORIENTED_EDGE ( 'NONE', *, *, #40331, .F. ) ;
#19464 = CARTESIAN_POINT ( 'NONE',  ( 9.564922557961047289, -16.46253265017146816, 20.41775706135233293 ) ) ;
#19465 = CARTESIAN_POINT ( 'NONE',  ( -0.05219959533909027116, -19.03943276465977164, 32.49890960531435979 ) ) ;
#19466 = VERTEX_POINT ( 'NONE', #19157 ) ;
#19467 = CARTESIAN_POINT ( 'NONE',  ( -19.05341960407617563, 5.049401038297882671, 113.5427570613523471 ) ) ;
#19469 = CARTESIAN_POINT ( 'NONE',  ( 16.55341960407618274, -4.379528057220086978, 31.04275706135234714 ) ) ;
#19468 = CARTESIAN_POINT ( 'NONE',  ( 16.51473224551083163, -9.474510206698727899, 50.83442372801899722 ) ) ;
#19470 = CARTESIAN_POINT ( 'NONE',  ( 16.46253265017160672, -9.564922557960803928, 38.33224293864768839 ) ) ;
#19471 = CARTESIAN_POINT ( 'NONE',  ( 0.05219959533909260263, 19.03943276465977164, 59.99890960531436690 ) ) ;
#19472 = CARTESIAN_POINT ( 'NONE',  ( 15.80617190586746368, 15.72974639402197994, 89.37390960531435269 ) ) ;
#19473 = CARTESIAN_POINT ( 'NONE',  ( 13.89961937509977652, -13.97604488694527269, 53.12390960531434558 ) ) ;
#19474 = LINE ( 'NONE', #109491, #182511 ) ;
#19475 = CARTESIAN_POINT ( 'NONE',  ( -16.51473224551082808, 9.474510206698731452, 98.33442372801900433 ) ) ;
#19476 = CARTESIAN_POINT ( 'NONE',  ( -16.53943276465976808, 0.05219959533911058130, 71.24890960531435269 ) ) ;
#19477 = CARTESIAN_POINT ( 'NONE',  ( 16.51473224551083163, -9.474510206698727899, 20.83442372801899722 ) ) ;
#19478 = CARTESIAN_POINT ( 'NONE',  ( 8.224510206698953496, -14.34966873604960469, 57.91557627198103120 ) ) ;
#19479 = CARTESIAN_POINT ( 'NONE',  ( -0.05219959533937732626, 21.53943276465977519, 82.50109039468568994 ) ) ;
#19480 = CARTESIAN_POINT ( 'NONE',  ( -19.02544592524342804, 5.153800228976336051, 26.04057627198103120 ) ) ;
#19481 = CARTESIAN_POINT ( 'NONE',  ( -5.719274019375665041, -21.55341960407619695, 84.79275706135234714 ) ) ;
#19482 = EDGE_CURVE ( 'NONE', #66692, #186058, #128298, .T. ) ;
#19484 = CARTESIAN_POINT ( 'NONE',  ( 18.67979575497194134, -10.72451020669871369, 70.83442372801901854 ) ) ;
#19483 = CARTESIAN_POINT ( 'NONE',  ( -16.52544592524342804, 4.483927247898546575, 26.04057627198103475 ) ) ;
#19485 = CARTESIAN_POINT ( 'NONE',  ( 19.02544592524343514, -5.153800228976328945, 73.54057627198103830 ) ) ;
#19486 = CARTESIAN_POINT ( 'NONE',  ( 10.81492255796106328, -18.62759615963255655, 40.41775706135234714 ) ) ;
#19487 = CARTESIAN_POINT ( 'NONE',  ( -0.05219959533909027116, -19.03943276465977164, 82.49890960531436690 ) ) ;
#19488 = CARTESIAN_POINT ( 'NONE',  ( 12.06949235617757843, -12.14591786802309237, 98.12390960531436690 ) ) ;
#19489 = CARTESIAN_POINT ( 'NONE',  ( -8.314922557960811034, -14.29746914071050412, 57.08224293864769550 ) ) ;
#19490 = CARTESIAN_POINT ( 'NONE',  ( -15.80617190586745835, -15.72974639402198527, 66.87390960531436690 ) ) ;
#19491 = CARTESIAN_POINT ( 'NONE',  ( -19.02544592524342804, 5.153800228976336051, 81.04057627198103830 ) ) ;
#19492 = CARTESIAN_POINT ( 'NONE',  ( 15.72974639402199770, -15.80617190586745480, 88.12390960531436690 ) ) ;
#19493 = CARTESIAN_POINT ( 'NONE',  ( -19.02544592524334988, -5.153800228976617603, 68.95942372801896170 ) ) ;
#19495 = CARTESIAN_POINT ( 'NONE',  ( 12.06949235617757843, -12.14591786802309237, 83.12390960531436690 ) ) ;
#19494 = CARTESIAN_POINT ( 'NONE',  ( -13.89961937509957401, -13.97604488694547697, 34.37609039468566863 ) ) ;
#19496 = CARTESIAN_POINT ( 'NONE',  ( 21.53943276465977519, -0.05219959533907433946, 48.74890960531435979 ) ) ;
#19497 = DIRECTION ( 'NONE',  ( 6.391086490440865492E-16, 1.000000000000000000, -0.000000000000000000 ) ) ;
#19499 = CARTESIAN_POINT ( 'NONE',  ( 27.73933785331498569, 9.013057229001093518, 146.4750000027311501 ) ) ;
#19498 = CARTESIAN_POINT ( 'NONE',  ( -4.379528057220086978, -16.55341960407618274, 104.7927570613523898 ) ) ;
#19500 = CARTESIAN_POINT ( 'NONE',  ( 13.89961937509957401, 13.97604488694547697, 101.8760903946856331 ) ) ;
#19501 = CARTESIAN_POINT ( 'NONE',  ( 16.55341960407611168, 4.379528057220329451, 63.95724293864770260 ) ) ;
#19502 = CARTESIAN_POINT ( 'NONE',  ( -19.25176906914649777, -5.499999999999796607, 95.99927264242279534 ) ) ;
#19503 = CARTESIAN_POINT ( 'NONE',  ( 16.46253265017160672, -9.564922557960803928, 63.33224293864769550 ) ) ;
#19504 = CARTESIAN_POINT ( 'NONE',  ( -16.53943276465976808, 0.05219959533911058130, 56.24890960531436690 ) ) ;
#19505 = CARTESIAN_POINT ( 'NONE',  ( 0.05219959533909260263, 19.03943276465977164, 94.99890960531436690 ) ) ;
#19507 = CARTESIAN_POINT ( 'NONE',  ( -9.474510206698964154, 16.51473224551069663, 70.41557627198102409 ) ) ;
#19506 = CARTESIAN_POINT ( 'NONE',  ( -19.05341960407617563, 5.049401038297882671, 83.54275706135233293 ) ) ;
#19508 = CARTESIAN_POINT ( 'NONE',  ( -13.89961937509977652, 13.97604488694528158, 85.62390960531433848 ) ) ;
#19509 = CARTESIAN_POINT ( 'NONE',  ( -19.05341960407611168, -5.049401038298163336, 81.45724293864769550 ) ) ;
#19510 = CARTESIAN_POINT ( 'NONE',  ( -0.05219959533907301413, -21.53943276465977519, 57.49890960531435979 ) ) ;
#19511 = CARTESIAN_POINT ( 'NONE',  ( 4.483927247898790824, -16.52544592524335698, 60.20942372801902565 ) ) ;
#19512 = CARTESIAN_POINT ( 'NONE',  ( 18.09918380851993547, 5.500000000000009770, 98.98618307335611632 ) ) ;
#19513 = CARTESIAN_POINT ( 'NONE',  ( 5.049401038298161559, -19.05341960407611168, 52.70724293864767418 ) ) ;
#19514 = CARTESIAN_POINT ( 'NONE',  ( 15.80617190586746368, 15.72974639402197994, 54.37390960531435979 ) ) ;
#19515 = CARTESIAN_POINT ( 'NONE',  ( -19.02544592524334988, -5.153800228976617603, 93.95942372801900433 ) ) ;
#19517 = CARTESIAN_POINT ( 'NONE',  ( 15.72974639402176855, 15.80617190586768217, 41.87609039468568284 ) ) ;
#19516 = CARTESIAN_POINT ( 'NONE',  ( -14.29746914071049879, 8.314922557960819915, 30.83224293864770260 ) ) ;
#19518 = CARTESIAN_POINT ( 'NONE',  ( 13.89961937509957401, 13.97604488694547697, 36.87609039468565442 ) ) ;
#19520 = CARTESIAN_POINT ( 'NONE',  ( 4.483927247898790824, -16.52544592524335698, 100.2094237280190043 ) ) ;
#19519 = CARTESIAN_POINT ( 'NONE',  ( -4.483927247898782831, 16.52544592524335698, 57.70942372801901143 ) ) ;
#19521 = CARTESIAN_POINT ( 'NONE',  ( 19.46398650005391318, -5.499999999999944045, 42.68269651486371430 ) ) ;
#19522 = CARTESIAN_POINT ( 'NONE',  ( -4.483927247898782831, 16.52544592524335698, 82.70942372801900433 ) ) ;
#19523 = CARTESIAN_POINT ( 'NONE',  ( 16.55341960407618274, -4.379528057220086978, 36.04275706135234714 ) ) ;
#19524 = CARTESIAN_POINT ( 'NONE',  ( 16.51473224551069308, 9.474510206698969483, 49.16557627198102409 ) ) ;
#19525 = CARTESIAN_POINT ( 'NONE',  ( -13.89961937509977652, 13.97604488694528158, 45.62390960531433848 ) ) ;
#19526 = CARTESIAN_POINT ( 'NONE',  ( -13.97604488694527625, -13.89961937509977652, 56.87390960531434558 ) ) ;
#19527 = CARTESIAN_POINT ( 'NONE',  ( -21.53943276465977519, -0.05219959533937600094, 58.75109039468568994 ) ) ;
#19528 = CARTESIAN_POINT ( 'NONE',  ( -14.29746914071037622, -8.314922557961029526, 44.16775706135234714 ) ) ;
#19529 = CARTESIAN_POINT ( 'NONE',  ( 8.314922557961029526, -14.29746914071037800, 110.4177570613523756 ) ) ;
#19530 = CARTESIAN_POINT ( 'NONE',  ( 19.05341960407611168, 5.049401038298154454, 23.95724293864769194 ) ) ;
#19531 = CARTESIAN_POINT ( 'NONE',  ( -5.049401038297874678, -19.05341960407617918, 24.79275706135233648 ) ) ;
#19532 = CARTESIAN_POINT ( 'NONE',  ( 19.05341960407617918, -5.049401038297876454, 106.0427570613523471 ) ) ;
#19533 = CARTESIAN_POINT ( 'NONE',  ( -9.474510206698720793, -16.51473224551083518, 79.58442372801899012 ) ) ;
#19534 = CARTESIAN_POINT ( 'NONE',  ( 14.34966873604960469, 8.224510206698951720, 89.16557627198102409 ) ) ;
#19535 = CARTESIAN_POINT ( 'NONE',  ( -19.03943276465977164, 0.05219959533909376836, 41.24890960531435269 ) ) ;
#19537 = CARTESIAN_POINT ( 'NONE',  ( -193.3062444957834884, -155.7167183371838064, -4.999999999999999112 ) ) ;
#19536 = CARTESIAN_POINT ( 'NONE',  ( 19.03943276465977164, 0.05219959533936151252, 71.25109039468566152 ) ) ;
#19538 = CARTESIAN_POINT ( 'NONE',  ( -15.72974639402176322, -15.80617190586768395, 79.37609039468567573 ) ) ;
#19539 = CARTESIAN_POINT ( 'NONE',  ( 12.14591786802327356, -12.06949235617739191, 45.62609039468567573 ) ) ;
#19540 = CARTESIAN_POINT ( 'NONE',  ( -17.50000000000000000, 5.499999999999992895, 23.71769037696436300 ) ) ;
#19541 = CARTESIAN_POINT ( 'NONE',  ( -21.52544592524343514, 5.823673210054127303, 31.04057627198102409 ) ) ;
#19542 = CARTESIAN_POINT ( 'NONE',  ( 14.34966873604972726, -8.224510206698740333, 30.83442372801902209 ) ) ;
#19543 = CARTESIAN_POINT ( 'NONE',  ( -16.51473224551069308, -9.474510206698971260, 26.66557627198103120 ) ) ;
#19544 = CARTESIAN_POINT ( 'NONE',  ( 19.02544592524334988, 5.153800228976608722, 26.45942372801899722 ) ) ;
#19545 = CARTESIAN_POINT ( 'NONE',  ( -38.00000000000000711, -12.34694845685042708, -7.900000000000000355 ) ) ;
#19546 = CARTESIAN_POINT ( 'NONE',  ( 13.97604488694527802, 13.89961937509977652, 44.37390960531435269 ) ) ;
#19547 = CARTESIAN_POINT ( 'NONE',  ( -20.13069416963696057, -20.86710639515136023, -52.55595668995117364 ) ) ;
#19548 = CARTESIAN_POINT ( 'NONE',  ( -5.049401038298153566, 19.05341960407611168, 65.20724293864765286 ) ) ;
#19549 = CARTESIAN_POINT ( 'NONE',  ( 17.50000000000000000, -5.500000000000000888, 113.2969038253417153 ) ) ;
#19550 = PRODUCT_DEFINITION_SHAPE ( 'NONE', 'NONE',  #75840 ) ;
#19551 = CARTESIAN_POINT ( 'NONE',  ( -9.564922557961040184, 16.46253265017147172, 22.91775706135233648 ) ) ;
#19552 = CARTESIAN_POINT ( 'NONE',  ( 8.314922557960818139, 14.29746914071049879, 39.58224293864769550 ) ) ;
#19553 = CARTESIAN_POINT ( 'NONE',  ( 9.474510206698971260, -16.51473224551069308, 42.91557627198103120 ) ) ;
#19554 = CARTESIAN_POINT ( 'NONE',  ( -0.05219959533909027116, -19.03943276465977164, 97.49890960531436690 ) ) ;
#19555 = CARTESIAN_POINT ( 'NONE',  ( 15.80617190586769283, -15.72974639402175789, 70.62609039468567573 ) ) ;
#19556 = CARTESIAN_POINT ( 'NONE',  ( 13.89961937509977652, -13.97604488694527269, 53.12390960531434558 ) ) ;
#19557 = CARTESIAN_POINT ( 'NONE',  ( 0.05219959533937995610, -21.53943276465977519, 70.00109039468568994 ) ) ;
#19558 = CARTESIAN_POINT ( 'NONE',  ( -19.03943276465977164, 0.05219959533909376836, 116.2489096053143669 ) ) ;
#19559 = CARTESIAN_POINT ( 'NONE',  ( -19.03943276465977164, 0.05219959533909376836, 31.24890960531435979 ) ) ;
#19560 = CARTESIAN_POINT ( 'NONE',  ( 10.81492255796106328, -18.62759615963255655, 25.41775706135235779 ) ) ;
#19561 = CARTESIAN_POINT ( 'NONE',  ( -9.564922557961040184, 16.46253265017147172, 42.91775706135234003 ) ) ;
#19562 = CARTESIAN_POINT ( 'NONE',  ( -16.55341960407611168, -4.379528057220339221, 111.4572429386476813 ) ) ;
#19563 = CARTESIAN_POINT ( 'NONE',  ( 9.474510206698971260, -16.51473224551069308, 57.91557627198103120 ) ) ;
#19564 = CARTESIAN_POINT ( 'NONE',  ( -9.474510206698720793, -16.51473224551083518, 109.5844237280190043 ) ) ;
#19565 = CARTESIAN_POINT ( 'NONE',  ( 16.53943276465976808, -0.05219959533910856209, 78.74890960531436690 ) ) ;
#19566 = CARTESIAN_POINT ( 'NONE',  ( 9.474510206698971260, -16.51473224551069308, 112.9155762719810383 ) ) ;
#19567 = CARTESIAN_POINT ( 'NONE',  ( -13.97604488694547697, 13.89961937509957934, 93.12609039468566152 ) ) ;
#19568 = CARTESIAN_POINT ( 'NONE',  ( 21.52544592524344225, -5.823673210054117533, 108.5405762719810241 ) ) ;
#19569 = CARTESIAN_POINT ( 'NONE',  ( -15.72974639402176322, -15.80617190586768395, 54.37609039468568994 ) ) ;
#19570 = CARTESIAN_POINT ( 'NONE',  ( 8.224510206698742110, 14.34966873604972548, 57.08442372801901854 ) ) ;
#19571 = CARTESIAN_POINT ( 'NONE',  ( -16.55341960407617563, 4.379528057220093196, 53.54275706135234714 ) ) ;
#19572 = CARTESIAN_POINT ( 'NONE',  ( 21.53943276465977519, -0.05219959533907433946, 48.74890960531435979 ) ) ;
#19573 =( BOUNDED_SURFACE ( )  B_SPLINE_SURFACE ( 3, 2, ( 
 ( #10504, #194521, #136812 ),
 ( #180370, #86328, #148015 ),
 ( #55993, #25685, #87330 ),
 ( #149016, #72166, #73184 ),
 ( #165183, #41839, #26678 ),
 ( #88318, #58003, #2265 ),
 ( #78105, #91273, #18450 ),
 ( #77122, #123609, #172121 ),
 ( #122628, #47796, #92284 ),
 ( #125617, #154960, #137803 ),
 ( #44810, #30631, #95270 ),
 ( #199487, #152964, #139774 ),
 ( #170131, #153968, #185304 ),
 ( #272, #16456, #168144 ),
 ( #60954, #140776, #138791 ),
 ( #61941, #14463, #29641 ),
 ( #46795, #93275, #45799 ),
 ( #1262, #183329, #62939 ),
 ( #106465, #33607, #108454 ),
 ( #64935, #124619, #63948 ),
 ( #109446, #184318, #107451 ),
 ( #31625, #169126, #76125 ),
 ( #15465, #94272, #186314 ),
 ( #171129, #156953, #32618 ),
 ( #155950, #80101, #17447 ),
 ( #141769, #79103, #187315 ),
 ( #48786, #110440, #3262 ),
 ( #68921, #8251, #65922 ),
 ( #6240, #81084, #67919 ),
 ( #159932, #112431, #51753 ),
 ( #128583, #113414, #144755 ),
 ( #177124, #21419, #34600 ),
 ( #85074, #20414, #66919 ),
 ( #19436, #127595, #191269 ),
 ( #157945, #130583, #98229 ),
 ( #192278, #188296, #174120 ),
 ( #83079, #158925, #126594 ),
 ( #37584, #189294, #146757 ),
 ( #53759, #142762, #173125 ),
 ( #190277, #115433, #38595 ),
 ( #49773, #176113, #96259 ),
 ( #129572, #100251, #52744 ),
 ( #175105, #82064, #114412 ),
 ( #143757, #111438, #161932 ) ),
 .UNSPECIFIED., .F., .F., .T. ) 
 B_SPLINE_SURFACE_WITH_KNOTS ( ( 4, 2, 2, 2, 2, 2, 2, 2, 2, 2, 2, 2, 2, 2, 2, 2, 2, 2, 2, 2, 2, 4 ),
 ( 3, 3 ),
 ( 0.1334715276261013994, 0.1400397817209069751, 0.1416818452446083620, 0.1433239087683097490, 0.1466080358157125230, 0.1498921628631152969, 0.1531762899105180986, 0.1564604169579209003, 0.1597445440053236743, 0.1630286710527264482, 0.1646707345764278352, 0.1663127981001292222, 0.1679548616238306091, 0.1695969251475319961, 0.1712389886712333831, 0.1720600204330841043, 0.1728810521949347978, 0.1745231157186362125, 0.1761651792423375995, 0.1794493062897403735, 0.1827334333371431474, 0.1860175603845459213 ),
 ( 0.000000000000000000, 1.000000000000000000 ),
 .UNSPECIFIED. ) 
 GEOMETRIC_REPRESENTATION_ITEM ( )  RATIONAL_B_SPLINE_SURFACE ( (
 ( 1.000000000000000000, 0.7745966692414831822, 1.000000000000000000),
 ( 1.000000000000000000, 0.7873173169473692834, 1.000000000000000000),
 ( 1.000000000000000000, 0.8012080269095258611, 1.000000000000000000),
 ( 1.000000000000000000, 0.8197272276932416890, 1.000000000000000000),
 ( 1.000000000000000000, 0.8234885421913027415, 1.000000000000000000),
 ( 1.000000000000000000, 0.8311157573375616003, 1.000000000000000000),
 ( 1.000000000000000000, 0.8349728938257290345, 1.000000000000000000),
 ( 1.000000000000000000, 0.8465302108189953767, 1.000000000000000000),
 ( 1.000000000000000000, 0.8542644918355704053, 1.000000000000000000),
 ( 1.000000000000000000, 0.8696747091109493510, 1.000000000000000000),
 ( 1.000000000000000000, 0.8773507960692895624, 1.000000000000000000),
 ( 1.000000000000000000, 0.8925002889087803037, 1.000000000000000000),
 ( 1.000000000000000000, 0.8999891582782625354, 1.000000000000000000),
 ( 1.000000000000000000, 0.9145203485640004404, 1.000000000000000000),
 ( 1.000000000000000000, 0.9215166741119604765, 1.000000000000000000),
 ( 1.000000000000000000, 0.9348196634156800133, 1.000000000000000000),
 ( 1.000000000000000000, 0.9411264847296241243, 1.000000000000000000),
 ( 1.000000000000000000, 0.9528821887672445090, 1.000000000000000000),
 ( 1.000000000000000000, 0.9583320463343323325, 1.000000000000000000),
 ( 1.000000000000000000, 0.9657141226242917931, 1.000000000000000000),
 ( 1.000000000000000000, 0.9680424144921332408, 1.000000000000000000),
 ( 1.000000000000000000, 0.9724014971077671321, 1.000000000000000000),
 ( 1.000000000000000000, 0.9744334801158450743, 1.000000000000000000),
 ( 1.000000000000000000, 0.9781204877085362126, 1.000000000000000000),
 ( 1.000000000000000000, 0.9797809101335807069, 1.000000000000000000),
 ( 1.000000000000000000, 0.9826818083352882871, 1.000000000000000000),
 ( 1.000000000000000000, 0.9839230189806438265, 1.000000000000000000),
 ( 1.000000000000000000, 0.9859013487405716702, 1.000000000000000000),
 ( 1.000000000000000000, 0.9866146582094302842, 1.000000000000000000),
 ( 1.000000000000000000, 0.9872250220265940124, 1.000000000000000000),
 ( 1.000000000000000000, 0.9873522598263612116, 1.000000000000000000),
 ( 1.000000000000000000, 0.9874472609175478643, 1.000000000000000000),
 ( 1.000000000000000000, 0.9874138636738800656, 1.000000000000000000),
 ( 1.000000000000000000, 0.9870735186574125519, 1.000000000000000000),
 ( 1.000000000000000000, 0.9865315217160652850, 1.000000000000000000),
 ( 1.000000000000000000, 0.9848873008857785827, 1.000000000000000000),
 ( 1.000000000000000000, 0.9837743821442975767, 1.000000000000000000),
 ( 1.000000000000000000, 0.9797976954002131089, 1.000000000000000000),
 ( 1.000000000000000000, 0.9763000371664848354, 1.000000000000000000),
 ( 1.000000000000000000, 0.9680363503266696812, 1.000000000000000000),
 ( 1.000000000000000000, 0.9632464763793496809, 1.000000000000000000),
 ( 1.000000000000000000, 0.9526889542241597786, 1.000000000000000000),
 ( 1.000000000000000000, 0.9469283804590763465, 1.000000000000000000),
 ( 1.000000000000000000, 0.9407878411039235500, 1.000000000000000000) ) ) 
 REPRESENTATION_ITEM ( '' )  SURFACE ( )  );
#19574 = CARTESIAN_POINT ( 'NONE',  ( 13.97604488694527802, 13.89961937509977652, 54.37390960531435979 ) ) ;
#19575 = CARTESIAN_POINT ( 'NONE',  ( -38.00000000000000711, 2.428612866367529932E-14, -3.749999994537626780 ) ) ;
#19576 = CARTESIAN_POINT ( 'NONE',  ( -14.29746914071037622, -8.314922557961029526, 79.16775706135234714 ) ) ;
#19577 = CARTESIAN_POINT ( 'NONE',  ( -18.62759615963270932, 10.81492255796079327, 105.8322429386476955 ) ) ;
#19578 = CARTESIAN_POINT ( 'NONE',  ( -0.05219959533910754901, -16.53943276465976808, 57.49890960531435979 ) ) ;
#19579 = CARTESIAN_POINT ( 'NONE',  ( -19.05341960407611168, -5.049401038298163336, 66.45724293864769550 ) ) ;
#19580 = CARTESIAN_POINT ( 'NONE',  ( -16.53943276465976808, -0.05219959533934237506, 78.75109039468568994 ) ) ;
#19581 = CARTESIAN_POINT ( 'NONE',  ( -19.03943276465977164, -0.05219959533935918106, 103.7510903946856757 ) ) ;
#19582 = CARTESIAN_POINT ( 'NONE',  ( -5.823673210054116645, -21.52544592524344225, 97.29057627198105251 ) ) ;
#19583 = CARTESIAN_POINT ( 'NONE',  ( -16.53943276465976808, 0.05219959533911058130, 46.24890960531435979 ) ) ;
#19584 = ORIENTED_EDGE ( 'NONE', *, *, #83145, .T. ) ;
#19585 = CARTESIAN_POINT ( 'NONE',  ( -16.36317988757058828, 7.306389748694926745, 69.09789608363226421 ) ) ;
#19586 = CARTESIAN_POINT ( 'NONE',  ( -21.53943276465977519, 0.05219959533907696930, 76.24890960531435269 ) ) ;
#19587 = CARTESIAN_POINT ( 'NONE',  ( 16.53943276465976808, -0.05219959533910856209, 23.74890960531435269 ) ) ;
#19588 = ORIENTED_EDGE ( 'NONE', *, *, #32449, .F. ) ;
#19589 = CARTESIAN_POINT ( 'NONE',  ( -17.26058549869089020, -6.457015423128631859, 56.37745837476069966 ) ) ;
#19590 = CARTESIAN_POINT ( 'NONE',  ( -21.53943276465977519, 0.05219959533907696930, 96.24890960531435269 ) ) ;
#19591 = CARTESIAN_POINT ( 'NONE',  ( 21.55341960407619695, -5.719274019375665929, 26.04275706135235779 ) ) ;
#19592 = CARTESIAN_POINT ( 'NONE',  ( 8.314922557960818139, 14.29746914071049879, 34.58224293864770260 ) ) ;
#19593 = CARTESIAN_POINT ( 'NONE',  ( -4.379528057220086978, -16.55341960407618274, 49.79275706135234714 ) ) ;
#19594 = AXIS2_PLACEMENT_3D ( 'NONE', #124218, #65533, #93882 ) ;
#19595 = CARTESIAN_POINT ( 'NONE',  ( 16.46253265017160672, -9.564922557960803928, 53.33224293864768839 ) ) ;
#19596 = CARTESIAN_POINT ( 'NONE',  ( -19.03943276465977164, 0.05219959533909376836, 76.24890960531435269 ) ) ;
#19597 = ORIENTED_EDGE ( 'NONE', *, *, #112389, .F. ) ;
#19598 = CARTESIAN_POINT ( 'NONE',  ( -5.719274019375978568, 21.55341960407610458, 35.20724293864768839 ) ) ;
#19599 = CARTESIAN_POINT ( 'NONE',  ( -30.69486229629621832, -23.16037512311192614, -17.06287707313649449 ) ) ;
#19600 = CARTESIAN_POINT ( 'NONE',  ( 4.483927247898790824, -16.52544592524335698, 25.20942372801901854 ) ) ;
#19601 = CARTESIAN_POINT ( 'NONE',  ( -5.153800228976607833, 19.02544592524334988, 52.70942372801900433 ) ) ;
#19602 = CARTESIAN_POINT ( 'NONE',  ( 0.05219959533907565091, 21.53943276465977519, 104.9989096053143669 ) ) ;
#19603 = CARTESIAN_POINT ( 'NONE',  ( -14.29746914071049879, 8.314922557960819915, 40.83224293864769550 ) ) ;
#19604 = CARTESIAN_POINT ( 'NONE',  ( 16.46253265017160672, -9.564922557960803928, 73.33224293864769550 ) ) ;
#19605 = CARTESIAN_POINT ( 'NONE',  ( -5.719274019375978568, 21.55341960407610458, 65.20724293864768129 ) ) ;
#19607 = CARTESIAN_POINT ( 'NONE',  ( 4.483927247898790824, -16.52544592524335698, 20.20942372801900788 ) ) ;
#19606 = CARTESIAN_POINT ( 'NONE',  ( -21.53943276465977519, 0.05219959533907696930, 96.24890960531435269 ) ) ;
#19608 = CARTESIAN_POINT ( 'NONE',  ( -5.049401038298153566, 19.05341960407611168, 115.2072429386477097 ) ) ;
#19609 = CARTESIAN_POINT ( 'NONE',  ( -5.719274019375665041, -21.55341960407619695, 84.79275706135234714 ) ) ;
#19610 = CARTESIAN_POINT ( 'NONE',  ( 5.153800228976335163, 19.02544592524342804, 74.79057627198103830 ) ) ;
#19611 = CARTESIAN_POINT ( 'NONE',  ( -16.46253265017160317, 9.564922557960807481, 25.83224293864769194 ) ) ;
#19612 = CARTESIAN_POINT ( 'NONE',  ( 9.564922557960805705, 16.46253265017160317, 89.58224293864769550 ) ) ;
#19613 = CARTESIAN_POINT ( 'NONE',  ( -16.52544592524342804, 4.483927247898546575, 101.0405762719810383 ) ) ;
#19614 = CARTESIAN_POINT ( 'NONE',  ( 19.02544592524334988, 5.153800228976608722, 101.4594237280189759 ) ) ;
#19615 = DIRECTION ( 'NONE',  ( 1.000000000000000000, 0.000000000000000000, 0.000000000000000000 ) ) ;
#19616 = EDGE_CURVE ( 'NONE', #193677, #25217, #35308, .T. ) ;
#19617 = CARTESIAN_POINT ( 'NONE',  ( 16.51473224551069308, 9.474510206698969483, 79.16557627198103830 ) ) ;
#19619 = CARTESIAN_POINT ( 'NONE',  ( -19.02544592524342804, 5.153800228976336051, 111.0405762719810099 ) ) ;
#19618 = CARTESIAN_POINT ( 'NONE',  ( 5.719274019375673035, 21.55341960407619339, 97.29275706135234714 ) ) ;
#19620 = CARTESIAN_POINT ( 'NONE',  ( -4.379528057220086978, -16.55341960407618274, 94.79275706135234714 ) ) ;
#19621 = CARTESIAN_POINT ( 'NONE',  ( -17.40861289039003879, -6.110651285853241355, 76.37232470827430575 ) ) ;
#19622 = CARTESIAN_POINT ( 'NONE',  ( 9.564922557961047289, -16.46253265017146816, 60.41775706135233293 ) ) ;
#19623 = CARTESIAN_POINT ( 'NONE',  ( -5.823673210054431948, 21.52544592524334988, 107.7094237280190328 ) ) ;
#19624 = CARTESIAN_POINT ( 'NONE',  ( 5.563988007711757611, 6.875025434611794495, -64.01045944195827531 ) ) ;
#19625 = CARTESIAN_POINT ( 'NONE',  ( 5.049401038298161559, -19.05341960407611168, 22.70724293864769194 ) ) ;
#19626 = CARTESIAN_POINT ( 'NONE',  ( 4.483927247898790824, -16.52544592524335698, 110.2094237280190185 ) ) ;
#19627 = CARTESIAN_POINT ( 'NONE',  ( -35.31558682697089324, -4.577067960279682879, 39.03840433125809994 ) ) ;
#19628 = CARTESIAN_POINT ( 'NONE',  ( 4.379528057220092307, 16.55341960407617563, 102.2927570613523613 ) ) ;
#19629 = CARTESIAN_POINT ( 'NONE',  ( -18.39639308325438094, -5.499999999999988454, 86.48252246182198633 ) ) ;
#19630 = CARTESIAN_POINT ( 'NONE',  ( 14.34966873604972726, -8.224510206698740333, 85.83442372801901854 ) ) ;
#19631 = CARTESIAN_POINT ( 'NONE',  ( 16.51473224551069308, 9.474510206698969483, 84.16557627198102409 ) ) ;
#19632 = CARTESIAN_POINT ( 'NONE',  ( -18.67979575497193778, 10.72451020669871902, 93.33442372801901854 ) ) ;
#19633 = CARTESIAN_POINT ( 'NONE',  ( 9.474510206698729675, 16.51473224551082808, 107.0844237280190043 ) ) ;
#19634 = CARTESIAN_POINT ( 'NONE',  ( 5.823673210054444382, -21.52544592524334988, 70.20942372801904696 ) ) ;
#19635 = CARTESIAN_POINT ( 'NONE',  ( 5.049401038297881783, 19.05341960407617563, 57.29275706135231871 ) ) ;
#19636 = CARTESIAN_POINT ( 'NONE',  ( 16.46253265017160672, -9.564922557960803928, 73.33224293864769550 ) ) ;
#19637 = CARTESIAN_POINT ( 'NONE',  ( 0.05219959533909260263, 19.03943276465977164, 64.99890960531436690 ) ) ;
#19638 = CARTESIAN_POINT ( 'NONE',  ( 16.36317988757055630, 7.306389748694925856, 73.40210391636770737 ) ) ;
#19639 = CARTESIAN_POINT ( 'NONE',  ( 15.72974639402199770, -15.80617190586745480, 43.12390960531435269 ) ) ;
#19640 = CARTESIAN_POINT ( 'NONE',  ( -5.049401038298153566, 19.05341960407611168, 40.20724293864768839 ) ) ;
#19642 = CARTESIAN_POINT ( 'NONE',  ( 4.379528057220092307, 16.55341960407617563, 82.29275706135234714 ) ) ;
#19641 = CARTESIAN_POINT ( 'NONE',  ( -0.05219959533907301413, -21.53943276465977519, 87.49890960531436690 ) ) ;
#19643 = UNCERTAINTY_MEASURE_WITH_UNIT (LENGTH_MEASURE( 1.000000000000000082E-05 ), #1328, 'distance_accuracy_value', 'NONE');
#19644 = ORIENTED_EDGE ( 'NONE', *, *, #166964, .T. ) ;
#19646 = CARTESIAN_POINT ( 'NONE',  ( -22.81625015709510507, 31.40387420917330275, -2.924999997268813434 ) ) ;
#19645 = CARTESIAN_POINT ( 'NONE',  ( -12.14591786802309592, -12.06949235617757132, 81.87390960531435269 ) ) ;
#19647 = CARTESIAN_POINT ( 'NONE',  ( 8.224510206698742110, 14.34966873604972548, 32.08442372801901854 ) ) ;
#19648 = CARTESIAN_POINT ( 'NONE',  ( 5.049401038298161559, -19.05341960407611168, 22.70724293864769194 ) ) ;
#19649 = CARTESIAN_POINT ( 'NONE',  ( 13.89961937509957401, 13.97604488694547697, 66.87609039468567573 ) ) ;
#19650 = CARTESIAN_POINT ( 'NONE',  ( -0.05219959533910754901, -16.53943276465976808, 67.49890960531436690 ) ) ;
#19651 = CARTESIAN_POINT ( 'NONE',  ( 21.53943276465977519, 0.05219959533937863772, 46.25109039468567573 ) ) ;
#19653 = CARTESIAN_POINT ( 'NONE',  ( 10.72451020669898902, -18.67979575497178502, 87.91557627198103830 ) ) ;
#19652 = CARTESIAN_POINT ( 'NONE',  ( 2.500000000000000000, 1.178949249685212974, -2.042000000000001148 ) ) ;
#19654 = FACE_OUTER_BOUND ( 'NONE', #166003, .T. ) ;
#19655 = CARTESIAN_POINT ( 'NONE',  ( -4.379528057220328563, 16.55341960407611168, 70.20724293864769550 ) ) ;
#19656 = CARTESIAN_POINT ( 'NONE',  ( 22.23580286100631653, -34.17069428430818334, -18.13567467416763179 ) ) ;
#19657 = CARTESIAN_POINT ( 'NONE',  ( -9.564922557960796823, -16.46253265017161027, 42.08224293864769550 ) ) ;
#19658 = CARTESIAN_POINT ( 'NONE',  ( 11.40812507854754365, 35.11059874428196537, -5.224999997268813701 ) ) ;
#19659 = CARTESIAN_POINT ( 'NONE',  ( -19.05341960407617563, 5.049401038297882671, 78.54275706135233293 ) ) ;
#19660 = CARTESIAN_POINT ( 'NONE',  ( -10.72451020669870658, -18.67979575497194134, 29.58442372801901854 ) ) ;
#19661 = CARTESIAN_POINT ( 'NONE',  ( 13.89961937509977652, -13.97604488694527269, 68.12390960531436690 ) ) ;
#19662 = CARTESIAN_POINT ( 'NONE',  ( 5.153800228976615827, -19.02544592524334988, 55.20942372801899722 ) ) ;
#19663 = CARTESIAN_POINT ( 'NONE',  ( -9.564922557960796823, -16.46253265017161027, 42.08224293864769550 ) ) ;
#19664 = CARTESIAN_POINT ( 'NONE',  ( 16.55341960407611168, 4.379528057220329451, 63.95724293864770260 ) ) ;
#19665 = CARTESIAN_POINT ( 'NONE',  ( 4.483927247898545687, 16.52544592524342804, 49.79057627198102409 ) ) ;
#19666 = CARTESIAN_POINT ( 'NONE',  ( 5.049401038298161559, -19.05341960407611168, 82.70724293864770971 ) ) ;
#19667 = CARTESIAN_POINT ( 'NONE',  ( 5.823673210054125526, 21.52544592524343514, 99.79057627198103830 ) ) ;
#19668 = CARTESIAN_POINT ( 'NONE',  ( -13.89961937509977652, 13.97604488694528158, 70.62390960531432427 ) ) ;
#19669 = CARTESIAN_POINT ( 'NONE',  ( 18.67979575497178502, 10.72451020669898547, 74.16557627198102409 ) ) ;
#19670 = CARTESIAN_POINT ( 'NONE',  ( -21.55341960407619339, 5.719274019375674811, 113.5427570613523756 ) ) ;
#19673 = CARTESIAN_POINT ( 'NONE',  ( 14.34966873604960469, 8.224510206698951720, 99.16557627198100988 ) ) ;
#19672 = CARTESIAN_POINT ( 'NONE',  ( -12.14591786802326823, 12.06949235617739902, 108.1260903946856757 ) ) ;
#19671 = CARTESIAN_POINT ( 'NONE',  ( 19.05341960407611168, 5.049401038298154454, 28.95724293864769550 ) ) ;
#19674 = CARTESIAN_POINT ( 'NONE',  ( -19.02544592524334988, -5.153800228976617603, 108.9594237280189759 ) ) ;
#19675 = VERTEX_POINT ( 'NONE', #144469 ) ;
#19676 = CARTESIAN_POINT ( 'NONE',  ( -18.67979575497193778, 10.72451020669871902, 28.33442372801902209 ) ) ;
#19677 = CARTESIAN_POINT ( 'NONE',  ( 19.02544592524334988, 5.153800228976608722, 51.45942372801900433 ) ) ;
#19678 = CARTESIAN_POINT ( 'NONE',  ( 14.29746914071049879, -8.314922557960816363, 23.33224293864769194 ) ) ;
#19679 = CARTESIAN_POINT ( 'NONE',  ( 10.72451020669898902, -18.67979575497178502, 72.91557627198103830 ) ) ;
#19680 = CARTESIAN_POINT ( 'NONE',  ( -0.05219959533909027116, -19.03943276465977164, 97.49890960531436690 ) ) ;
#19681 = CARTESIAN_POINT ( 'NONE',  ( -16.53943276465976808, 0.05219959533911058130, 56.24890960531436690 ) ) ;
#19682 = CARTESIAN_POINT ( 'NONE',  ( -19.05341960407611168, -5.049401038298163336, 26.45724293864769550 ) ) ;
#19683 = CARTESIAN_POINT ( 'NONE',  ( -5.153800228976328057, -19.02544592524343514, 37.29057627198102409 ) ) ;
#19684 = CARTESIAN_POINT ( 'NONE',  ( 0.05219959533937995610, -21.53943276465977519, 105.0010903946856757 ) ) ;
#19685 = CARTESIAN_POINT ( 'NONE',  ( 14.29746914071037800, 8.314922557961029526, 86.66775706135234714 ) ) ;
#19686 = CARTESIAN_POINT ( 'NONE',  ( -10.72451020669870658, -18.67979575497194134, 44.58442372801901854 ) ) ;
#19687 = CARTESIAN_POINT ( 'NONE',  ( 4.483927247898790824, -16.52544592524335698, 45.20942372801901854 ) ) ;
#19688 = CARTESIAN_POINT ( 'NONE',  ( 5.719274019375991003, -21.55341960407610458, 22.70724293864769194 ) ) ;
#19689 = CARTESIAN_POINT ( 'NONE',  ( 5.153800228976335163, 19.02544592524342804, 54.79057627198103120 ) ) ;
#19690 = CARTESIAN_POINT ( 'NONE',  ( -13.89961937509977652, 13.97604488694528158, 60.62390960531436690 ) ) ;
#19691 = CARTESIAN_POINT ( 'NONE',  ( 8.224510206698742110, 14.34966873604972548, 57.08442372801901854 ) ) ;
#19692 = CARTESIAN_POINT ( 'NONE',  ( -4.483927247898539470, -16.52544592524342804, 112.2905762719810241 ) ) ;
#19693 = CARTESIAN_POINT ( 'NONE',  ( -8.314922557960811034, -14.29746914071050412, 22.08224293864769194 ) ) ;
#19694 = DIRECTION ( 'NONE',  ( 1.000000000000000000, 0.000000000000000000, 0.000000000000000000 ) ) ;
#19697 = CARTESIAN_POINT ( 'NONE',  ( 13.97604488694527802, 13.89961937509977652, 84.37390960531433848 ) ) ;
#19696 = CARTESIAN_POINT ( 'NONE',  ( -5.049401038298153566, 19.05341960407611168, 90.20724293864766707 ) ) ;
#19695 = CARTESIAN_POINT ( 'NONE',  ( -15.80617190586768217, 15.72974639402176855, 63.12609039468568994 ) ) ;
#19698 = CARTESIAN_POINT ( 'NONE',  ( 13.89961937509977652, -13.97604488694527269, 108.1239096053143669 ) ) ;
#19699 = CARTESIAN_POINT ( 'NONE',  ( 8.224510206698953496, -14.34966873604960469, 42.91557627198103120 ) ) ;
#19700 = CARTESIAN_POINT ( 'NONE',  ( -8.224510206698948167, 14.34966873604960824, 25.41557627198103120 ) ) ;
#19701 = CARTESIAN_POINT ( 'NONE',  ( 4.483927247898545687, 16.52544592524342804, 34.79057627198103120 ) ) ;
#19702 = CARTESIAN_POINT ( 'NONE',  ( 17.60691670004651144, 5.500000000000060396, 56.63333313366439370 ) ) ;
#19703 = CARTESIAN_POINT ( 'NONE',  ( 19.03943276465977164, 0.05219959533936151252, 31.25109039468566863 ) ) ;
#19704 = CARTESIAN_POINT ( 'NONE',  ( -13.89961937509977652, 13.97604488694528158, 80.62390960531436690 ) ) ;
#19705 = CARTESIAN_POINT ( 'NONE',  ( -5.153800228976607833, 19.02544592524334988, 47.70942372801900433 ) ) ;
#19706 = CARTESIAN_POINT ( 'NONE',  ( 29.86685920354754842, -21.69954338932559068, -1.824999997268813345 ) ) ;
#19707 = DIRECTION ( 'NONE',  ( -0.000000000000000000, -0.000000000000000000, 1.000000000000000000 ) ) ;
#19709 = CARTESIAN_POINT ( 'NONE',  ( -12.06949235617739369, -12.14591786802326823, 69.37609039468567573 ) ) ;
#19708 = CARTESIAN_POINT ( 'NONE',  ( -16.51473224551082808, 9.474510206698731452, 83.33442372801899012 ) ) ;
#19710 = DIRECTION ( 'NONE',  ( 0.000000000000000000, -0.8164965809277239250, -0.5773502691896288397 ) ) ;
#19711 = CARTESIAN_POINT ( 'NONE',  ( -5.049401038298153566, 19.05341960407611168, 105.2072429386476671 ) ) ;
#19712 = CARTESIAN_POINT ( 'NONE',  ( -5.719274019375665041, -21.55341960407619695, 29.79275706135234358 ) ) ;
#19713 = CARTESIAN_POINT ( 'NONE',  ( 19.05341960407617918, -5.049401038297876454, 91.04275706135234714 ) ) ;
#19715 = CARTESIAN_POINT ( 'NONE',  ( -0.05219959533909027116, -19.03943276465977164, 52.49890960531436690 ) ) ;
#19714 = CARTESIAN_POINT ( 'NONE',  ( 9.474510206698971260, -16.51473224551069308, 112.9155762719810383 ) ) ;
#19716 = CARTESIAN_POINT ( 'NONE',  ( 5.049401038298161559, -19.05341960407611168, 87.70724293864769550 ) ) ;
#19718 = CARTESIAN_POINT ( 'NONE',  ( 16.51473224551069308, 9.474510206698969483, 44.16557627198103120 ) ) ;
#19717 = CARTESIAN_POINT ( 'NONE',  ( -16.52544592524342804, 4.483927247898546575, 46.04057627198103830 ) ) ;
#19719 = CARTESIAN_POINT ( 'NONE',  ( 19.05341960407617918, -5.049401038297876454, 66.04275706135233293 ) ) ;
#19720 = CARTESIAN_POINT ( 'NONE',  ( 16.51473224551083163, -9.474510206698727899, 25.83442372801900078 ) ) ;
#19721 = CARTESIAN_POINT ( 'NONE',  ( -19.05341960407611168, -5.049401038298163336, 71.45724293864766707 ) ) ;
#19722 = ADVANCED_FACE ( 'NONE', ( #142484 ), #97944, .T. ) ;
#19723 = CARTESIAN_POINT ( 'NONE',  ( -5.823673210054116645, -21.52544592524344225, 67.29057627198103830 ) ) ;
#19725 = CARTESIAN_POINT ( 'NONE',  ( -15.80617190586768217, 15.72974639402176855, 113.1260903946856899 ) ) ;
#19724 = CARTESIAN_POINT ( 'NONE',  ( 16.52544592524342804, -4.483927247898539470, 63.54057627198103830 ) ) ;
#19726 = CARTESIAN_POINT ( 'NONE',  ( -0.9271017399331331621, -6.404328268737251584, -64.47359807031668311 ) ) ;
#19727 = CARTESIAN_POINT ( 'NONE',  ( -21.53943276465977519, 0.05219959533907696930, 21.24890960531436690 ) ) ;
#19728 = CARTESIAN_POINT ( 'NONE',  ( 19.05341960407611168, 5.049401038298154454, 58.95724293864768129 ) ) ;
#19729 = CARTESIAN_POINT ( 'NONE',  ( 13.89961937509977652, -13.97604488694527269, 38.12390960531436690 ) ) ;
#19730 = CARTESIAN_POINT ( 'NONE',  ( 8.314922557960818139, 14.29746914071049879, 99.58224293864770971 ) ) ;
#19731 = CARTESIAN_POINT ( 'NONE',  ( -5.719274019375978568, 21.55341960407610458, 105.2072429386477097 ) ) ;
#19732 = CARTESIAN_POINT ( 'NONE',  ( 26.03370437638690049, -6.875205692009868308, 160.5968874236871784 ) ) ;
#19733 = CARTESIAN_POINT ( 'NONE',  ( 18.62759615963255655, 10.81492255796105972, 26.66775706135235424 ) ) ;
#19734 = CARTESIAN_POINT ( 'NONE',  ( -16.51473224551069308, -9.474510206698971260, 26.66557627198103120 ) ) ;
#19735 = CARTESIAN_POINT ( 'NONE',  ( -15.72974639402176322, -15.80617190586768395, 79.37609039468567573 ) ) ;
#19736 = CARTESIAN_POINT ( 'NONE',  ( -10.81492255796078084, -18.62759615963271287, 92.08224293864769550 ) ) ;
#19737 = CARTESIAN_POINT ( 'NONE',  ( 9.564922557961047289, -16.46253265017146816, 35.41775706135233293 ) ) ;
#19738 = CARTESIAN_POINT ( 'NONE',  ( -19.03943276465977164, 0.05219959533909376836, 26.24890960531435624 ) ) ;
#19739 = PLANE ( 'NONE',  #72096 ) ;
#19740 = CARTESIAN_POINT ( 'NONE',  ( 31.62105185743274660, -0.8768460684519197024, -49.48175094143203268 ) ) ;
#19741 = CARTESIAN_POINT ( 'NONE',  ( 4.379528057220092307, 16.55341960407617563, 47.29275706135234003 ) ) ;
#19742 = CARTESIAN_POINT ( 'NONE',  ( -16.53943276465976808, 0.05219959533911058130, 106.2489096053143811 ) ) ;
#19743 = CARTESIAN_POINT ( 'NONE',  ( -21.36928693577339189, -7.422813773936192128, 174.5222352431090087 ) ) ;
#19744 = CARTESIAN_POINT ( 'NONE',  ( 19.02544592524343514, -5.153800228976328945, 73.54057627198103830 ) ) ;
#19745 = CARTESIAN_POINT ( 'NONE',  ( -4.379528057220328563, 16.55341960407611168, 100.2072429386476955 ) ) ;
#19746 = CARTESIAN_POINT ( 'NONE',  ( 18.67979575497178502, 10.72451020669898547, 49.16557627198102409 ) ) ;
#19747 = CARTESIAN_POINT ( 'NONE',  ( 16.55341960407611168, 4.379528057220329451, 68.95724293864769550 ) ) ;
#19748 = CARTESIAN_POINT ( 'NONE',  ( 4.483927247898790824, -16.52544592524335698, 40.20942372801901854 ) ) ;
#19749 = CARTESIAN_POINT ( 'NONE',  ( 15.72974639402176855, 15.80617190586768217, 86.87609039468568994 ) ) ;
#19750 = CARTESIAN_POINT ( 'NONE',  ( 17.05587630539786659, -6.762274262135687053, 78.24180309037315340 ) ) ;
#19751 = CARTESIAN_POINT ( 'NONE',  ( -4.483927247898782831, 16.52544592524335698, 102.7094237280190185 ) ) ;
#19752 = CARTESIAN_POINT ( 'NONE',  ( -16.55341960407611168, -4.379528057220339221, 46.45724293864769550 ) ) ;
#19753 = CARTESIAN_POINT ( 'NONE',  ( 5.049401038298161559, -19.05341960407611168, 42.70724293864767418 ) ) ;
#19754 = CARTESIAN_POINT ( 'NONE',  ( 18.67979575497194134, -10.72451020669871369, 90.83442372801901854 ) ) ;
#19755 = CARTESIAN_POINT ( 'NONE',  ( -21.52544592524343514, 5.823673210054127303, 106.0405762719810525 ) ) ;
#19756 = CARTESIAN_POINT ( 'NONE',  ( -5.719274019375665041, -21.55341960407619695, 59.79275706135234714 ) ) ;
#19757 = CARTESIAN_POINT ( 'NONE',  ( 14.34966873604972726, -8.224510206698740333, 45.83442372801901854 ) ) ;
#19759 = CARTESIAN_POINT ( 'NONE',  ( 5.719274019375673035, 21.55341960407619339, 82.29275706135234714 ) ) ;
#19758 = CARTESIAN_POINT ( 'NONE',  ( 8.224510206698953496, -14.34966873604960469, 62.91557627198102409 ) ) ;
#19760 = CARTESIAN_POINT ( 'NONE',  ( -16.53943276465976808, 0.05219959533911058130, 26.24890960531435624 ) ) ;
#19761 = CARTESIAN_POINT ( 'NONE',  ( 16.52216118717208460, 7.221426719304522734, 28.57599021046994636 ) ) ;
#19762 = CARTESIAN_POINT ( 'NONE',  ( -24.95432927374998044, 0.000000000000000000, 190.0000000000000000 ) ) ;
#19763 = CARTESIAN_POINT ( 'NONE',  ( -8.314922557960811034, -14.29746914071050412, 32.08224293864769550 ) ) ;
#19764 = CARTESIAN_POINT ( 'NONE',  ( -16.53943276465976808, -0.05219959533934237506, 73.75109039468567573 ) ) ;
#19765 = CARTESIAN_POINT ( 'NONE',  ( 19.02544592524343514, -5.153800228976328945, 88.54057627198102409 ) ) ;
#19766 = CARTESIAN_POINT ( 'NONE',  ( -16.46253265017160317, 9.564922557960807481, 105.8322429386476955 ) ) ;
#19767 = CARTESIAN_POINT ( 'NONE',  ( 0.05219959533937995610, -21.53943276465977519, 80.00109039468568994 ) ) ;
#19768 = CARTESIAN_POINT ( 'NONE',  ( -8.224510206698735004, -14.34966873604973081, 84.58442372801903275 ) ) ;
#19769 = CARTESIAN_POINT ( 'NONE',  ( 14.29746914071049879, -8.314922557960816363, 63.33224293864770260 ) ) ;
#19770 = CARTESIAN_POINT ( 'NONE',  ( 16.51473224551069308, 9.474510206698969483, 69.16557627198102409 ) ) ;
#19771 = EDGE_LOOP ( 'NONE', ( #190197, #68449, #74086, #157970 ) ) ;
#19772 = CARTESIAN_POINT ( 'NONE',  ( 12.14591786802327356, -12.06949235617739191, 30.62609039468567929 ) ) ;
#19773 = CARTESIAN_POINT ( 'NONE',  ( -19.03943276465977164, 0.05219959533909376836, 26.24890960531435624 ) ) ;
#19774 = CARTESIAN_POINT ( 'NONE',  ( 19.02544592524343514, -5.153800228976328945, 73.54057627198103830 ) ) ;
#19776 = CARTESIAN_POINT ( 'NONE',  ( -11.40812507854754720, -35.11059874428192273, -8.224999997268813701 ) ) ;
#19775 = CARTESIAN_POINT ( 'NONE',  ( 19.03943276465977164, 0.05219959533936151252, 111.2510903946856757 ) ) ;
#19777 = CARTESIAN_POINT ( 'NONE',  ( 9.564922557961047289, -16.46253265017146816, 25.41775706135234003 ) ) ;
#19778 = CARTESIAN_POINT ( 'NONE',  ( 14.34966873604972726, -8.224510206698740333, 85.83442372801901854 ) ) ;
#19779 = CARTESIAN_POINT ( 'NONE',  ( -9.564922557961040184, 16.46253265017147172, 102.9177570613523329 ) ) ;
#19780 = CARTESIAN_POINT ( 'NONE',  ( 8.224510206698953496, -14.34966873604960469, 112.9155762719810383 ) ) ;
#19781 = CARTESIAN_POINT ( 'NONE',  ( 16.53943276465976808, 0.05219959533934440121, 71.25109039468568994 ) ) ;
#19782 = CARTESIAN_POINT ( 'NONE',  ( 4.483927247898790824, -16.52544592524335698, 55.20942372801902565 ) ) ;
#19783 = CARTESIAN_POINT ( 'NONE',  ( 13.21959898025320967, -37.75582843579748271, -14.12000380663810262 ) ) ;
#19784 = CARTESIAN_POINT ( 'NONE',  ( 13.97604488694548053, -13.89961937509957401, 75.62609039468564731 ) ) ;
#19785 = CARTESIAN_POINT ( 'NONE',  ( -15.80617190586768217, 15.72974639402176855, 108.1260903946856757 ) ) ;
#19786 = CARTESIAN_POINT ( 'NONE',  ( 19.03943276465977164, -0.05219959533909143690, 48.74890960531435979 ) ) ;
#19787 = CARTESIAN_POINT ( 'NONE',  ( -16.51473224551069308, -9.474510206698971260, 81.66557627198103830 ) ) ;
#19788 = CARTESIAN_POINT ( 'NONE',  ( 14.34966873604960469, 8.224510206698951720, 74.16557627198102409 ) ) ;
#19789 = CARTESIAN_POINT ( 'NONE',  ( -16.51473224551082808, 9.474510206698731452, 43.33442372801900433 ) ) ;
#19790 = CARTESIAN_POINT ( 'NONE',  ( -18.62759615963270932, 10.81492255796079327, 30.83224293864770260 ) ) ;
#19791 = CARTESIAN_POINT ( 'NONE',  ( 15.72974639402176855, 15.80617190586768217, 111.8760903946856615 ) ) ;
#19792 = CARTESIAN_POINT ( 'NONE',  ( -16.51473224551069308, -9.474510206698971260, 91.66557627198103830 ) ) ;
#19793 = CARTESIAN_POINT ( 'NONE',  ( -10.81492255796105439, 18.62759615963255655, 107.9177570613523471 ) ) ;
#19794 = CARTESIAN_POINT ( 'NONE',  ( -21.52544592524343514, 5.823673210054127303, 66.04057627198103830 ) ) ;
#19795 = CARTESIAN_POINT ( 'NONE',  ( -19.02544592524342804, 5.153800228976336051, 91.04057627198100988 ) ) ;
#19796 = CARTESIAN_POINT ( 'NONE',  ( -13.89961937509957401, -13.97604488694547875, 89.37609039468563310 ) ) ;
#19797 = CARTESIAN_POINT ( 'NONE',  ( 16.51473224551069308, 9.474510206698969483, 104.1655762719810241 ) ) ;
#19798 = CARTESIAN_POINT ( 'NONE',  ( 19.05341960407617918, -5.049401038297876454, 101.0427570613523045 ) ) ;
#19799 = CARTESIAN_POINT ( 'NONE',  ( -19.05341960407611168, -5.049401038298163336, 21.45724293864768839 ) ) ;
#19800 = CARTESIAN_POINT ( 'NONE',  ( -9.564922557960796823, -16.46253265017161027, 87.08224293864769550 ) ) ;
#19801 = CARTESIAN_POINT ( 'NONE',  ( 10.72451020669898902, -18.67979575497178502, 57.91557627198103120 ) ) ;
#19802 = CARTESIAN_POINT ( 'NONE',  ( -16.53943276465976808, -0.05219959533934237506, 48.75109039468568284 ) ) ;
#19803 = CARTESIAN_POINT ( 'NONE',  ( 5.823673210054444382, -21.52544592524334988, 45.20942372801901854 ) ) ;
#19804 = CARTESIAN_POINT ( 'NONE',  ( 18.62759615963255655, 10.81492255796105972, 91.66775706135234714 ) ) ;
#19805 = CARTESIAN_POINT ( 'NONE',  ( -14.34966873604972548, 8.224510206698743886, 98.33442372801901854 ) ) ;
#19806 = CARTESIAN_POINT ( 'NONE',  ( -9.564922557960796823, -16.46253265017161027, 92.08224293864769550 ) ) ;
#19807 = CARTESIAN_POINT ( 'NONE',  ( 16.55341960407611168, 4.379528057220329451, 93.95724293864770971 ) ) ;
#19808 = CARTESIAN_POINT ( 'NONE',  ( 16.52544592524335698, 4.483927247898782831, 111.4594237280190328 ) ) ;
#19809 = CARTESIAN_POINT ( 'NONE',  ( -9.474510206698720793, -16.51473224551083518, 69.58442372801901854 ) ) ;
#19810 = EDGE_CURVE ( 'NONE', #56239, #23346, #185257, .T. ) ;
#19811 = CARTESIAN_POINT ( 'NONE',  ( 5.823673210054444382, -21.52544592524334988, 40.20942372801901854 ) ) ;
#19812 = CARTESIAN_POINT ( 'NONE',  ( -12.06949235617756955, 12.14591786802309770, 95.62390960531436690 ) ) ;
#19813 = CARTESIAN_POINT ( 'NONE',  ( -10.81492255796078084, -18.62759615963271287, 22.08224293864769194 ) ) ;
#19814 = CARTESIAN_POINT ( 'NONE',  ( -12.06949235617739369, -12.14591786802326823, 109.3760903946857042 ) ) ;
#19815 = CARTESIAN_POINT ( 'NONE',  ( 21.52544592524334988, 5.823673210054432836, 81.45942372801900433 ) ) ;
#19816 = CARTESIAN_POINT ( 'NONE',  ( -8.314922557961024197, 14.29746914071037800, 57.91775706135234714 ) ) ;
#19817 = CARTESIAN_POINT ( 'NONE',  ( 21.55341960407619695, -5.719274019375665929, 46.04275706135234714 ) ) ;
#19818 = VERTEX_POINT ( 'NONE', #5953 ) ;
#19819 = CARTESIAN_POINT ( 'NONE',  ( 18.62759615963255655, 10.81492255796105972, 26.66775706135235424 ) ) ;
#19820 = CARTESIAN_POINT ( 'NONE',  ( 16.55341960407611168, 4.379528057220329451, 103.9572429386476813 ) ) ;
#19821 = CARTESIAN_POINT ( 'NONE',  ( -16.46253265017160317, 9.564922557960807481, 25.83224293864769194 ) ) ;
#19822 = CARTESIAN_POINT ( 'NONE',  ( 4.483927247898545687, 16.52544592524342804, 69.79057627198102409 ) ) ;
#19823 = CARTESIAN_POINT ( 'NONE',  ( 9.564922557960805705, 16.46253265017160317, 59.58224293864769550 ) ) ;
#19824 = CARTESIAN_POINT ( 'NONE',  ( -0.05219959533934338120, 16.53943276465976808, 112.5010903946857042 ) ) ;
#19825 = CARTESIAN_POINT ( 'NONE',  ( 19.05341960407611168, 5.049401038298154454, 38.95724293864767418 ) ) ;
#19826 = CARTESIAN_POINT ( 'NONE',  ( 10.81492255796078972, 18.62759615963270932, 49.58224293864769550 ) ) ;
#19827 = CARTESIAN_POINT ( 'NONE',  ( 16.52544592524342804, -4.483927247898539470, 78.54057627198103830 ) ) ;
#19828 = CARTESIAN_POINT ( 'NONE',  ( -18.67979575497178146, -10.72451020669898902, 86.66557627198102409 ) ) ;
#19829 = CARTESIAN_POINT ( 'NONE',  ( 16.51473224551069308, 9.474510206698969483, 94.16557627198103830 ) ) ;
#19831 = CARTESIAN_POINT ( 'NONE',  ( 16.46253265017146816, 9.564922557961045513, 96.66775706135233293 ) ) ;
#19830 = CARTESIAN_POINT ( 'NONE',  ( -13.97604488694527625, -13.89961937509977652, 51.87390960531436690 ) ) ;
#19832 = CARTESIAN_POINT ( 'NONE',  ( 15.80617190586746368, 15.72974639402197994, 44.37390960531435979 ) ) ;
#19833 = CARTESIAN_POINT ( 'NONE',  ( 10.81492255796106328, -18.62759615963255655, 65.41775706135234714 ) ) ;
#19834 = CARTESIAN_POINT ( 'NONE',  ( 0.05219959533909260263, 19.03943276465977164, 49.99890960531435979 ) ) ;
#19835 = CARTESIAN_POINT ( 'NONE',  ( 19.05341960407611168, 5.049401038298154454, 83.95724293864766707 ) ) ;
#19836 = VERTEX_POINT ( 'NONE', #130283 ) ;
#19837 = CARTESIAN_POINT ( 'NONE',  ( -12.14591786802326823, 12.06949235617739902, 68.12609039468567573 ) ) ;
#19838 = CARTESIAN_POINT ( 'NONE',  ( -5.719274019375665041, -21.55341960407619695, 39.79275706135235424 ) ) ;
#19839 = CARTESIAN_POINT ( 'NONE',  ( -21.52544592524334988, -5.823673210054445271, 73.95942372801901854 ) ) ;
#19840 = CARTESIAN_POINT ( 'NONE',  ( -16.46253265017160317, 9.564922557960807481, 110.8322429386476955 ) ) ;
#19841 = CARTESIAN_POINT ( 'NONE',  ( 21.52544592524344225, -5.823673210054117533, 98.54057627198105251 ) ) ;
#19843 = CARTESIAN_POINT ( 'NONE',  ( -16.53943276465976808, -0.05219959533934237506, 68.75109039468568994 ) ) ;
#19842 = CARTESIAN_POINT ( 'NONE',  ( -15.72974639402176322, -15.80617190586768395, 34.37609039468568284 ) ) ;
#19844 = CARTESIAN_POINT ( 'NONE',  ( -21.53943276465977519, 0.05219959533907696930, 61.24890960531435979 ) ) ;
#19845 = CARTESIAN_POINT ( 'NONE',  ( -9.474510206698720793, -16.51473224551083518, 29.58442372801900433 ) ) ;
#19847 = CARTESIAN_POINT ( 'NONE',  ( -0.05219959533934338120, 16.53943276465976808, 102.5010903946856899 ) ) ;
#19846 = CARTESIAN_POINT ( 'NONE',  ( -19.03943276465977164, 0.05219959533909376836, 66.24890960531436690 ) ) ;
#19848 = CARTESIAN_POINT ( 'NONE',  ( -17.50000000000147793, -3.202012800152224337, 105.0717758397275361 ) ) ;
#19849 = CARTESIAN_POINT ( 'NONE',  ( -19.03943276465977164, 0.05219959533909376836, 106.2489096053143669 ) ) ;
#19850 = CARTESIAN_POINT ( 'NONE',  ( -3.424326230466266718, 6.677994727576254341, 8.646741581399135512 ) ) ;
#19851 = EDGE_CURVE ( 'NONE', #45770, #75663, #191977, .T. ) ;
#19852 = CARTESIAN_POINT ( 'NONE',  ( 16.46253265017146816, 9.564922557961045513, 76.66775706135234714 ) ) ;
#19853 = CARTESIAN_POINT ( 'NONE',  ( 10.72451020669898902, -18.67979575497178502, 62.91557627198102409 ) ) ;
#19854 = CARTESIAN_POINT ( 'NONE',  ( 0.05219959533910956823, 16.53943276465976808, 39.99890960531436690 ) ) ;
#19855 = CARTESIAN_POINT ( 'NONE',  ( 0.05219959533936267826, -19.03943276465977164, 100.0010903946856757 ) ) ;
#19856 = CARTESIAN_POINT ( 'NONE',  ( 2.649999999999999911, -105.0000000000000000, -13.00000000000000000 ) ) ;
#19857 = CARTESIAN_POINT ( 'NONE',  ( -16.51473224551082808, 9.474510206698731452, 113.3344237280190043 ) ) ;
#19859 = CARTESIAN_POINT ( 'NONE',  ( 0.05219959533936267826, -19.03943276465977164, 60.00109039468566863 ) ) ;
#19858 = CARTESIAN_POINT ( 'NONE',  ( 15.72974639402199770, -15.80617190586745480, 83.12390960531436690 ) ) ;
#19860 = CARTESIAN_POINT ( 'NONE',  ( -4.483927247898782831, 16.52544592524335698, 77.70942372801900433 ) ) ;
#19861 = CARTESIAN_POINT ( 'NONE',  ( 13.97604488694527802, 13.89961937509977652, 64.37390960531436690 ) ) ;
#19862 = CARTESIAN_POINT ( 'NONE',  ( 14.34966873604960469, 8.224510206698951720, 69.16557627198102409 ) ) ;
#19863 = CARTESIAN_POINT ( 'NONE',  ( 19.02544592524343514, -5.153800228976328945, 53.54057627198102409 ) ) ;
#19864 = CARTESIAN_POINT ( 'NONE',  ( 4.379528057220339221, -16.55341960407611168, 52.70724293864769550 ) ) ;
#19865 = CARTESIAN_POINT ( 'NONE',  ( 13.97604488694527802, 13.89961937509977652, 24.37390960531435624 ) ) ;
#19866 = CARTESIAN_POINT ( 'NONE',  ( 0.1986149132935111361, 9.090066029660778923, -61.89635500127618428 ) ) ;
#19867 = CARTESIAN_POINT ( 'NONE',  ( 4.483927247898545687, 16.52544592524342804, 29.79057627198102409 ) ) ;
#19868 = CARTESIAN_POINT ( 'NONE',  ( -19.02544592524342804, 5.153800228976336051, 81.04057627198103830 ) ) ;
#19869 = DIRECTION ( 'NONE',  ( -0.000000000000000000, -0.000000000000000000, -1.000000000000000000 ) ) ;
#19870 = CARTESIAN_POINT ( 'NONE',  ( 9.474510206698729675, 16.51473224551082808, 42.08442372801900433 ) ) ;
#19871 = CARTESIAN_POINT ( 'NONE',  ( 12.06949235617739724, 12.14591786802326823, 51.87609039468568284 ) ) ;
#19872 = CARTESIAN_POINT ( 'NONE',  ( -0.05219959533907301413, -21.53943276465977519, 52.49890960531435979 ) ) ;
#19873 = CARTESIAN_POINT ( 'NONE',  ( -18.67979575497193778, 10.72451020669871902, 113.3344237280190328 ) ) ;
#19874 = CARTESIAN_POINT ( 'NONE',  ( 13.97604488694527802, 13.89961937509977652, 74.37390960531436690 ) ) ;
#19875 = CARTESIAN_POINT ( 'NONE',  ( -3.573655867282028392E-15, 2.428612866367529932E-14, 0.000000000000000000 ) ) ;
#19876 = CARTESIAN_POINT ( 'NONE',  ( -19.03943276465977164, 0.05219959533909376836, 106.2489096053143669 ) ) ;
#19877 = CARTESIAN_POINT ( 'NONE',  ( 10.81492255796106328, -18.62759615963255655, 40.41775706135234714 ) ) ;
#19878 = CARTESIAN_POINT ( 'NONE',  ( 14.34966873604960469, 8.224510206698951720, 89.16557627198102409 ) ) ;
#19881 = ORIENTED_EDGE ( 'NONE', *, *, #199458, .T. ) ;
#19880 = CARTESIAN_POINT ( 'NONE',  ( -9.564922557960796823, -16.46253265017161027, 87.08224293864769550 ) ) ;
#19879 = CARTESIAN_POINT ( 'NONE',  ( -21.55341960407610458, -5.719274019375992779, 81.45724293864769550 ) ) ;
#19882 = CARTESIAN_POINT ( 'NONE',  ( 10.72451020669871369, 18.67979575497193778, 22.08442372801901143 ) ) ;
#19883 = ORIENTED_EDGE ( 'NONE', *, *, #32278, .T. ) ;
#19884 = CARTESIAN_POINT ( 'NONE',  ( 5.153800228976335163, 19.02544592524342804, 89.79057627198102409 ) ) ;
#19885 = CARTESIAN_POINT ( 'NONE',  ( -17.72662750342728089, -5.500000000000020428, 76.40179492283743912 ) ) ;
#19887 = CARTESIAN_POINT ( 'NONE',  ( -19.03943276465977164, 0.05219959533909376836, 36.24890960531436690 ) ) ;
#19886 = CARTESIAN_POINT ( 'NONE',  ( 0.05219959533909260263, 19.03943276465977164, 24.99890960531435269 ) ) ;
#19888 = CARTESIAN_POINT ( 'NONE',  ( -5.153800228976607833, 19.02544592524334988, 102.7094237280189759 ) ) ;
#19889 = CARTESIAN_POINT ( 'NONE',  ( 11.40812507854755253, -35.11059874428192273, -6.524999997268813523 ) ) ;
#19890 = CARTESIAN_POINT ( 'NONE',  ( -13.97604488694527625, -13.89961937509977652, 21.87390960531435979 ) ) ;
#19891 = CARTESIAN_POINT ( 'NONE',  ( 10.81492255796106328, -18.62759615963255655, 85.41775706135236135 ) ) ;
#19893 = CARTESIAN_POINT ( 'NONE',  ( 18.62759615963255655, 10.81492255796105972, 36.66775706135234714 ) ) ;
#19892 = CARTESIAN_POINT ( 'NONE',  ( 16.51473224551069308, 9.474510206698969483, 69.16557627198102409 ) ) ;
#19894 = CARTESIAN_POINT ( 'NONE',  ( 21.55341960407619695, -5.719274019375665929, 26.04275706135235779 ) ) ;
#19895 = CARTESIAN_POINT ( 'NONE',  ( 8.906447517083057264, -27.41122689804191026, 146.5999999999999943 ) ) ;
#19896 = CARTESIAN_POINT ( 'NONE',  ( -9.474510206698964154, 16.51473224551069663, 80.41557627198103830 ) ) ;
#19897 = CARTESIAN_POINT ( 'NONE',  ( -2.500000000000000000, -165.0000000000000000, 12.00000000000000355 ) ) ;
#19899 = CARTESIAN_POINT ( 'NONE',  ( 15.72974639402199770, -15.80617190586745480, 48.12390960531436690 ) ) ;
#19898 = CARTESIAN_POINT ( 'NONE',  ( 16.53943276465976808, 0.05219959533934440121, 21.25109039468567218 ) ) ;
#19900 = CARTESIAN_POINT ( 'NONE',  ( -5.823673210054431948, 21.52544592524334988, 57.70942372801901143 ) ) ;
#19901 = CARTESIAN_POINT ( 'NONE',  ( 19.03943276465977164, -0.05219959533909143690, 103.7489096053143669 ) ) ;
#19902 = CARTESIAN_POINT ( 'NONE',  ( -13.89961937509957401, -13.97604488694547875, 94.37609039468566152 ) ) ;
#19903 = CARTESIAN_POINT ( 'NONE',  ( -16.46253265017160317, 9.564922557960807481, 65.83224293864769550 ) ) ;
#19904 = CARTESIAN_POINT ( 'NONE',  ( -5.049401038298153566, 19.05341960407611168, 90.20724293864766707 ) ) ;
#19905 = CARTESIAN_POINT ( 'NONE',  ( -4.379528057220328563, 16.55341960407611168, 95.20724293864769550 ) ) ;
#19906 = CARTESIAN_POINT ( 'NONE',  ( -14.34966873604960291, -8.224510206698953496, 101.6655762719810383 ) ) ;
#19907 = CARTESIAN_POINT ( 'NONE',  ( 19.03943276465977164, -0.05219959533909143690, 113.7489096053143669 ) ) ;
#19909 = CARTESIAN_POINT ( 'NONE',  ( 13.89961937509977652, -13.97604488694527269, 43.12390960531434558 ) ) ;
#19908 = CARTESIAN_POINT ( 'NONE',  ( -14.34966873604960291, -8.224510206698953496, 51.66557627198102409 ) ) ;
#19910 = CARTESIAN_POINT ( 'NONE',  ( 21.52544592524334988, 5.823673210054432836, 76.45942372801901854 ) ) ;
#19911 = CARTESIAN_POINT ( 'NONE',  ( -0.05219959533936034679, 19.03943276465977164, 87.50109039468567573 ) ) ;
#19912 = CARTESIAN_POINT ( 'NONE',  ( 14.34966873604960469, 8.224510206698951720, 59.16557627198103120 ) ) ;
#19913 = CARTESIAN_POINT ( 'NONE',  ( -0.05219959533907301413, -21.53943276465977519, 112.4989096053143669 ) ) ;
#19914 = CARTESIAN_POINT ( 'NONE',  ( 10.72451020669898902, -18.67979575497178502, 52.91557627198103830 ) ) ;
#19915 = CARTESIAN_POINT ( 'NONE',  ( 5.000000000000000888, -131.0000000000000000, -13.99999999999999822 ) ) ;
#19916 = CARTESIAN_POINT ( 'NONE',  ( -22.44159573604010305, 16.30477369853692338, 148.6750000027311671 ) ) ;
#19917 = CARTESIAN_POINT ( 'NONE',  ( 5.049401038298161559, -19.05341960407611168, 67.70724293864769550 ) ) ;
#19918 = CARTESIAN_POINT ( 'NONE',  ( 12.06949235617757843, -12.14591786802309237, 38.12390960531436690 ) ) ;
#19919 = CARTESIAN_POINT ( 'NONE',  ( -16.53943276465976808, 0.05219959533911058130, 21.24890960531436690 ) ) ;
#19920 = CARTESIAN_POINT ( 'NONE',  ( -0.05219959533934338120, 16.53943276465976808, 87.50109039468568994 ) ) ;
#19921 = CARTESIAN_POINT ( 'NONE',  ( 19.02544592524334988, 5.153800228976608722, 36.45942372801900433 ) ) ;
#19922 = CARTESIAN_POINT ( 'NONE',  ( -23.84690145917539894, 10.26550538186637596, 166.0764395470883983 ) ) ;
#19923 = CARTESIAN_POINT ( 'NONE',  ( 0.05219959533909260263, 19.03943276465977164, 89.99890960531436690 ) ) ;
#19924 = CARTESIAN_POINT ( 'NONE',  ( -19.03943276465977164, 0.05219959533909376836, 51.24890960531436690 ) ) ;
#19925 = ADVANCED_FACE ( 'NONE', ( #188018 ), #156674, .T. ) ;
#19926 = CARTESIAN_POINT ( 'NONE',  ( 12.06949235617757843, -12.14591786802309237, 58.12390960531435979 ) ) ;
#19928 = CARTESIAN_POINT ( 'NONE',  ( 10.72451020669898902, -18.67979575497178502, 22.91557627198102765 ) ) ;
#19927 = CARTESIAN_POINT ( 'NONE',  ( -5.049401038298153566, 19.05341960407611168, 25.20724293864768484 ) ) ;
#19929 = CARTESIAN_POINT ( 'NONE',  ( -15.72974639402197994, 15.80617190586746368, 60.62390960531437401 ) ) ;
#19930 = CARTESIAN_POINT ( 'NONE',  ( 14.34966873604960469, 8.224510206698951720, 89.16557627198102409 ) ) ;
#19931 = CARTESIAN_POINT ( 'NONE',  ( -4.483927247898782831, 16.52544592524335698, 37.70942372801900433 ) ) ;
#19932 = CARTESIAN_POINT ( 'NONE',  ( 8.224510206698953496, -14.34966873604960469, 77.91557627198102409 ) ) ;
#19933 = CARTESIAN_POINT ( 'NONE',  ( -19.25663599770061296, 5.499999999999451994, 63.99419308057201050 ) ) ;
#19934 = CARTESIAN_POINT ( 'NONE',  ( -13.89961937509957401, -13.97604488694547875, 74.37609039468566152 ) ) ;
#19935 = CARTESIAN_POINT ( 'NONE',  ( -9.564922557960796823, -16.46253265017161027, 112.0822429386476955 ) ) ;
#19937 = EDGE_CURVE ( 'NONE', #152430, #12139, #72114, .T. ) ;
#19936 = CARTESIAN_POINT ( 'NONE',  ( -22.81625015709509441, -31.40387420917324590, -4.824999997268813345 ) ) ;
#19938 = CARTESIAN_POINT ( 'NONE',  ( -8.906447517083053711, -27.41122689804191026, 142.4000000000000057 ) ) ;
#19940 = CARTESIAN_POINT ( 'NONE',  ( 16.52544592524335698, 4.483927247898782831, 106.4594237280190328 ) ) ;
#19939 = CARTESIAN_POINT ( 'NONE',  ( 4.483927247898790824, -16.52544592524335698, 35.20942372801901854 ) ) ;
#19941 = CARTESIAN_POINT ( 'NONE',  ( 5.153800228976615827, -19.02544592524334988, 75.20942372801896170 ) ) ;
#19942 = CARTESIAN_POINT ( 'NONE',  ( 15.72974639402199770, -15.80617190586745480, 53.12390960531436690 ) ) ;
#19943 = CARTESIAN_POINT ( 'NONE',  ( -10.81492255796105439, 18.62759615963255655, 72.91775706135234714 ) ) ;
#19944 = CARTESIAN_POINT ( 'NONE',  ( -15.49999999999999822, -5.500000000000000888, 120.0000000000000142 ) ) ;
#19945 = CARTESIAN_POINT ( 'NONE',  ( -16.53943276465976808, -0.05219959533934237506, 33.75109039468568284 ) ) ;
#19947 = CARTESIAN_POINT ( 'NONE',  ( -5.153800228976328057, -19.02544592524343514, 87.29057627198103830 ) ) ;
#19946 = CARTESIAN_POINT ( 'NONE',  ( 13.97604488694527802, 13.89961937509977652, 24.37390960531435624 ) ) ;
#19948 = CARTESIAN_POINT ( 'NONE',  ( 15.67660317299531414, 17.56609036915066469, -57.33766855040059340 ) ) ;
#19949 = CARTESIAN_POINT ( 'NONE',  ( -16.53943276465976808, 0.05219959533911058130, 101.2489096053143669 ) ) ;
#19950 = CARTESIAN_POINT ( 'NONE',  ( 5.049401038298161559, -19.05341960407611168, 102.7072429386476955 ) ) ;
#19951 = ORIENTED_EDGE ( 'NONE', *, *, #121376, .T. ) ;
#19952 = CARTESIAN_POINT ( 'NONE',  ( 8.224510206698742110, 14.34966873604972548, 57.08442372801901854 ) ) ;
#19953 = CARTESIAN_POINT ( 'NONE',  ( 19.02544592524334988, 5.153800228976608722, 106.4594237280190185 ) ) ;
#19954 = CARTESIAN_POINT ( 'NONE',  ( 15.72974639402199770, -15.80617190586745480, 78.12390960531436690 ) ) ;
#19955 = CARTESIAN_POINT ( 'NONE',  ( 9.474510206698971260, -16.51473224551069308, 37.91557627198102409 ) ) ;
#19957 = CARTESIAN_POINT ( 'NONE',  ( 0.05219959533907565091, 21.53943276465977519, 109.9989096053143527 ) ) ;
#19956 = CARTESIAN_POINT ( 'NONE',  ( -5.153800228976607833, 19.02544592524334988, 67.70942372801900433 ) ) ;
#19958 = CARTESIAN_POINT ( 'NONE',  ( 16.46253265017160672, -9.564922557960803928, 68.33224293864770971 ) ) ;
#19959 = CARTESIAN_POINT ( 'NONE',  ( 9.474510206698971260, -16.51473224551069308, 102.9155762719810241 ) ) ;
#19960 = EDGE_LOOP ( 'NONE', ( #159693, #6392, #38372, #30787 ) ) ;
#19961 = CARTESIAN_POINT ( 'NONE',  ( -4.379528057220086978, -16.55341960407618274, 29.79275706135234358 ) ) ;
#19962 = CARTESIAN_POINT ( 'NONE',  ( -15.72974639402197994, 15.80617190586746368, 105.6239096053143669 ) ) ;
#19965 = CARTESIAN_POINT ( 'NONE',  ( -19.02544592524334988, -5.153800228976617603, 78.95942372801900433 ) ) ;
#19964 = CARTESIAN_POINT ( 'NONE',  ( 13.97604488694527802, 13.89961937509977652, 94.37390960531436690 ) ) ;
#19963 = CARTESIAN_POINT ( 'NONE',  ( 0.05219959533910956823, 16.53943276465976808, 104.9989096053143669 ) ) ;
#19966 = CARTESIAN_POINT ( 'NONE',  ( -0.05219959533907301413, -21.53943276465977519, 92.49890960531436690 ) ) ;
#19967 = CARTESIAN_POINT ( 'NONE',  ( -14.29746914071049879, 8.314922557960819915, 45.83224293864769550 ) ) ;
#19968 = CARTESIAN_POINT ( 'NONE',  ( -16.46253265017146816, -9.564922557961047289, 24.16775706135233648 ) ) ;
#19969 = CARTESIAN_POINT ( 'NONE',  ( 16.52544592524335698, 4.483927247898782831, 61.45942372801901854 ) ) ;
#19970 = CARTESIAN_POINT ( 'NONE',  ( 0.05219959533909260263, 19.03943276465977164, 89.99890960531436690 ) ) ;
#19971 = CARTESIAN_POINT ( 'NONE',  ( -16.51473224551069308, -9.474510206698971260, 46.66557627198102409 ) ) ;
#19972 = CARTESIAN_POINT ( 'NONE',  ( -15.80617190586768217, 15.72974639402176855, 53.12609039468568284 ) ) ;
#19973 = CARTESIAN_POINT ( 'NONE',  ( -5.719274019375665041, -21.55341960407619695, 69.79275706135234714 ) ) ;
#19974 = CARTESIAN_POINT ( 'NONE',  ( -19.05341960407611168, -5.049401038298163336, 56.45724293864768129 ) ) ;
#19975 = CARTESIAN_POINT ( 'NONE',  ( -21.52544592524334988, -5.823673210054445271, 38.95942372801901854 ) ) ;
#19976 = CARTESIAN_POINT ( 'NONE',  ( -19.02544592524334988, -5.153800228976617603, 68.95942372801896170 ) ) ;
#19977 = CARTESIAN_POINT ( 'NONE',  ( -0.05219959533909027116, -19.03943276465977164, 37.49890960531436690 ) ) ;
#19978 = CARTESIAN_POINT ( 'NONE',  ( -0.05219959533934338120, 16.53943276465976808, 82.50109039468568994 ) ) ;
#19979 = CARTESIAN_POINT ( 'NONE',  ( -13.89961937509977652, 13.97604488694528158, 55.62390960531434558 ) ) ;
#19980 = CARTESIAN_POINT ( 'NONE',  ( -13.97604488694527625, -13.89961937509977652, 106.8739096053143669 ) ) ;
#19981 = CARTESIAN_POINT ( 'NONE',  ( 5.049401038298161559, -19.05341960407611168, 42.70724293864767418 ) ) ;
#19982 = CARTESIAN_POINT ( 'NONE',  ( 21.53943276465977519, -0.05219959533907433946, 88.74890960531436690 ) ) ;
#19983 = CARTESIAN_POINT ( 'NONE',  ( -8.314922557961024197, 14.29746914071037800, 67.91775706135234714 ) ) ;
#19984 = CARTESIAN_POINT ( 'NONE',  ( -67.00000000000000000, -4.837354856632041508E-15, 50.50000000000002842 ) ) ;
#19985 = CARTESIAN_POINT ( 'NONE',  ( 5.153800228976615827, -19.02544592524334988, 35.20942372801899722 ) ) ;
#19986 = CARTESIAN_POINT ( 'NONE',  ( 19.02544592524343514, -5.153800228976328945, 58.54057627198102409 ) ) ;
#19987 = CARTESIAN_POINT ( 'NONE',  ( -8.224510206698948167, 14.34966873604960824, 40.41557627198103120 ) ) ;
#19988 = CARTESIAN_POINT ( 'NONE',  ( -16.53943276465976808, 0.05219959533911058130, 86.24890960531436690 ) ) ;
#19989 = CARTESIAN_POINT ( 'NONE',  ( -13.89961937509977652, 13.97604488694528158, 100.6239096053143669 ) ) ;
#19990 = CARTESIAN_POINT ( 'NONE',  ( 9.564922557960805705, 16.46253265017160317, 89.58224293864769550 ) ) ;
#19991 = CARTESIAN_POINT ( 'NONE',  ( -0.05219959533937732626, 21.53943276465977519, 52.50109039468567573 ) ) ;
#19992 = CARTESIAN_POINT ( 'NONE',  ( -19.05341960407611168, -5.049401038298163336, 96.45724293864769550 ) ) ;
#19993 = CARTESIAN_POINT ( 'NONE',  ( 18.67979575497194134, -10.72451020669871369, 95.83442372801903275 ) ) ;
#19994 = CARTESIAN_POINT ( 'NONE',  ( -0.05219959533934338120, 16.53943276465976808, 82.50109039468568994 ) ) ;
#19995 = CARTESIAN_POINT ( 'NONE',  ( 5.823673210054444382, -21.52544592524334988, 30.20942372801902565 ) ) ;
#19996 = CARTESIAN_POINT ( 'NONE',  ( 5.823673210054125526, 21.52544592524343514, 99.79057627198103830 ) ) ;
#19997 = CARTESIAN_POINT ( 'NONE',  ( 12.14591786802309770, 12.06949235617756955, 59.37390960531436690 ) ) ;
#19998 = CARTESIAN_POINT ( 'NONE',  ( -19.02544592524342804, 5.153800228976336051, 46.04057627198101699 ) ) ;
#19999 = CARTESIAN_POINT ( 'NONE',  ( 14.29746914071049879, -8.314922557960816363, 73.33224293864769550 ) ) ;
#20000 = B_SPLINE_CURVE_WITH_KNOTS ( 'NONE', 3,
 ( #14381, #27600, #136728, #196451, #167087, #59887, #135758, #121553, #57921, #12425, #30549, #122547, #92201, #184237, #153885, #15382, #191, #168067, #74088, #120561, #198410, #58895 ),
 .UNSPECIFIED., .F., .F.,
 ( 4, 2, 2, 2, 2, 2, 2, 2, 2, 2, 4 ),
 ( 8.673617379884035472E-19, 0.001309639967555435757, 0.001964459951333159381, 0.002291869943222021953, 0.002455574939166439794, 0.002619279935110857202, 0.002782984931055275044, 0.002946689926999692885, 0.003274099918888501246, 0.003928919902666100188, 0.005238559870221296336 ),
 .UNSPECIFIED. ) ;
#20001 = CARTESIAN_POINT ( 'NONE',  ( -10.72451020669898014, 18.67979575497178502, 25.41557627198103120 ) ) ;
#20002 = CARTESIAN_POINT ( 'NONE',  ( -13.89961937509957401, -13.97604488694547875, 34.37609039468566863 ) ) ;
#20003 = CARTESIAN_POINT ( 'NONE',  ( 0.05219959533910956823, 16.53943276465976808, 114.9989096053143669 ) ) ;
#20004 = ORIENTED_EDGE ( 'NONE', *, *, #22636, .F. ) ;
#20005 = CARTESIAN_POINT ( 'NONE',  ( 8.224510206698742110, 14.34966873604972548, 62.08442372801901143 ) ) ;
#20006 = CARTESIAN_POINT ( 'NONE',  ( 19.05341960407611168, 5.049401038298154454, 63.95724293864769550 ) ) ;
#20007 = CARTESIAN_POINT ( 'NONE',  ( -16.93440711220026884, -5.601562513631294316, 20.60331890504276942 ) ) ;
#20008 = CARTESIAN_POINT ( 'NONE',  ( 14.34966873604960469, 8.224510206698951720, 94.16557627198103830 ) ) ;
#20009 = CARTESIAN_POINT ( 'NONE',  ( 5.719274019375991003, -21.55341960407610458, 32.70724293864770260 ) ) ;
#20010 = EDGE_LOOP ( 'NONE', ( #136354, #26591, #168948, #151907 ) ) ;
#20011 = CARTESIAN_POINT ( 'NONE',  ( -4.483927247898782831, 16.52544592524335698, 102.7094237280190185 ) ) ;
#20012 = CARTESIAN_POINT ( 'NONE',  ( -16.51473224551082808, 9.474510206698731452, 108.3344237280190043 ) ) ;
#20013 = CARTESIAN_POINT ( 'NONE',  ( -15.72974639402176322, -15.80617190586768395, 74.37609039468568994 ) ) ;
#20014 = CARTESIAN_POINT ( 'NONE',  ( 16.51473224551069308, 9.474510206698969483, 94.16557627198103830 ) ) ;
#20015 = CARTESIAN_POINT ( 'NONE',  ( 15.80617190586746368, 15.72974639402197994, 109.3739096053143811 ) ) ;
#20016 = CARTESIAN_POINT ( 'NONE',  ( 14.34966873604972726, -8.224510206698740333, 55.83442372801901854 ) ) ;
#20017 = CARTESIAN_POINT ( 'NONE',  ( 19.02544592524343514, -5.153800228976328945, 28.54057627198102409 ) ) ;
#20018 = CARTESIAN_POINT ( 'NONE',  ( 14.34966873604972726, -8.224510206698740333, 20.83442372801901143 ) ) ;
#20019 = CARTESIAN_POINT ( 'NONE',  ( -9.564922557961040184, 16.46253265017147172, 97.91775706135233293 ) ) ;
#20020 = EDGE_CURVE ( 'NONE', #40349, #175270, #101863, .T. ) ;
#20021 = CARTESIAN_POINT ( 'NONE',  ( -21.55341960407610458, -5.719274019375992779, 86.45724293864770971 ) ) ;
#20022 = CARTESIAN_POINT ( 'NONE',  ( -19.02544592524334988, -5.153800228976617603, 58.95942372801900433 ) ) ;
#20023 = CARTESIAN_POINT ( 'NONE',  ( 19.48894818550246200, -5.499999999999907629, 87.60307310435239003 ) ) ;
#20024 = CARTESIAN_POINT ( 'NONE',  ( -15.72974639402197994, 15.80617190586746368, 100.6239096053143811 ) ) ;
#20025 = CARTESIAN_POINT ( 'NONE',  ( -23.31738231874055245, -16.94106989632524574, 148.1999999999999886 ) ) ;
#20026 = CARTESIAN_POINT ( 'NONE',  ( 13.97604488694527802, 13.89961937509977652, 84.37390960531433848 ) ) ;
#20027 = CARTESIAN_POINT ( 'NONE',  ( -38.00373040315628970, 1.963201398428686990E-14, -0.1220970790697140096 ) ) ;
#20028 = CARTESIAN_POINT ( 'NONE',  ( 12.14591786802327356, -12.06949235617739191, 30.62609039468567929 ) ) ;
#20029 = CARTESIAN_POINT ( 'NONE',  ( 10.96715308212796458, -38.47291154382241274, -12.60366170504685712 ) ) ;
#20031 = CARTESIAN_POINT ( 'NONE',  ( -16.52544592524342804, 4.483927247898546575, 61.04057627198103120 ) ) ;
#20030 = CARTESIAN_POINT ( 'NONE',  ( -15.72974639402197994, 15.80617190586746368, 110.6239096053143669 ) ) ;
#20032 = CARTESIAN_POINT ( 'NONE',  ( 0.05219959533909260263, 19.03943276465977164, 74.99890960531435269 ) ) ;
#20034 = CARTESIAN_POINT ( 'NONE',  ( -19.05341960407617563, 5.049401038297882671, 43.54275706135232582 ) ) ;
#20033 = CARTESIAN_POINT ( 'NONE',  ( 4.483927247898790824, -16.52544592524335698, 40.20942372801901854 ) ) ;
#20035 = CARTESIAN_POINT ( 'NONE',  ( 21.53943276465977519, 0.05219959533937863772, 51.25109039468568994 ) ) ;
#20036 = CARTESIAN_POINT ( 'NONE',  ( -19.03943276465977164, -0.05219959533935918106, 103.7510903946856757 ) ) ;
#20037 = CARTESIAN_POINT ( 'NONE',  ( 16.46253265017160672, -9.564922557960803928, 53.33224293864768839 ) ) ;
#20038 = CARTESIAN_POINT ( 'NONE',  ( 13.97604488694548053, -13.89961937509957401, 85.62609039468568994 ) ) ;
#20039 = CARTESIAN_POINT ( 'NONE',  ( 5.823673210054444382, -21.52544592524334988, 80.20942372801901854 ) ) ;
#20040 = CARTESIAN_POINT ( 'NONE',  ( 9.564922557961047289, -16.46253265017146816, 60.41775706135233293 ) ) ;
#20041 = CARTESIAN_POINT ( 'NONE',  ( 0.05219959533909260263, 19.03943276465977164, 34.99890960531435979 ) ) ;
#20042 = CARTESIAN_POINT ( 'NONE',  ( 15.72974639402199770, -15.80617190586745480, 53.12390960531436690 ) ) ;
#20043 = CARTESIAN_POINT ( 'NONE',  ( -4.379528057220328563, 16.55341960407611168, 65.20724293864768129 ) ) ;
#20044 = CARTESIAN_POINT ( 'NONE',  ( -17.49999999999999645, -5.500000000000000888, 24.20309617465829533 ) ) ;
#20045 = CARTESIAN_POINT ( 'NONE',  ( -0.05219959533936034679, 19.03943276465977164, 32.50109039468566863 ) ) ;
#20046 = CARTESIAN_POINT ( 'NONE',  ( 8.224510206698742110, 14.34966873604972548, 102.0844237280190185 ) ) ;
#20047 = CARTESIAN_POINT ( 'NONE',  ( -8.314922557960811034, -14.29746914071050412, 47.08224293864770260 ) ) ;
#20048 = CARTESIAN_POINT ( 'NONE',  ( -0.05219959533937732626, 21.53943276465977519, 87.50109039468568994 ) ) ;
#20049 = CARTESIAN_POINT ( 'NONE',  ( -18.62759615963255300, -10.81492255796106328, 79.16775706135234714 ) ) ;
#20050 = CARTESIAN_POINT ( 'NONE',  ( 21.52544592524344225, -5.823673210054117533, 98.54057627198105251 ) ) ;
#20051 = CARTESIAN_POINT ( 'NONE',  ( 13.89961937509977652, -13.97604488694527269, 53.12390960531434558 ) ) ;
#20052 = CARTESIAN_POINT ( 'NONE',  ( -0.05219959533937732626, 21.53943276465977519, 67.50109039468568994 ) ) ;
#20053 = CARTESIAN_POINT ( 'NONE',  ( -16.46253265017160317, 9.564922557960807481, 45.83224293864769550 ) ) ;
#20054 = CARTESIAN_POINT ( 'NONE',  ( 9.474510206698971260, -16.51473224551069308, 62.91557627198102409 ) ) ;
#20055 = CARTESIAN_POINT ( 'NONE',  ( -16.53943276465976808, 0.05219959533911058130, 101.2489096053143669 ) ) ;
#20056 = CARTESIAN_POINT ( 'NONE',  ( -0.05219959533907301413, -21.53943276465977519, 22.49890960531436335 ) ) ;
#20057 = CARTESIAN_POINT ( 'NONE',  ( -0.05219959533910754901, -16.53943276465976808, 47.49890960531435979 ) ) ;
#20058 = CARTESIAN_POINT ( 'NONE',  ( 4.379528057220339221, -16.55341960407611168, 107.7072429386476955 ) ) ;
#20059 = CARTESIAN_POINT ( 'NONE',  ( -4.483927247898539470, -16.52544592524342804, 72.29057627198102409 ) ) ;
#20060 = CARTESIAN_POINT ( 'NONE',  ( -21.55341960407610458, -5.719274019375992779, 86.45724293864770971 ) ) ;
#20061 = CARTESIAN_POINT ( 'NONE',  ( -21.53943276465977519, -0.05219959533937600094, 38.75109039468567573 ) ) ;
#20062 = CARTESIAN_POINT ( 'NONE',  ( 27.46925885783806720, -7.746560145625162264, 162.9586723222894875 ) ) ;
#20063 = CARTESIAN_POINT ( 'NONE',  ( 14.34966873604972726, -8.224510206698740333, 30.83442372801902209 ) ) ;
#20064 = CARTESIAN_POINT ( 'NONE',  ( -10.81492255796078084, -18.62759615963271287, 87.08224293864769550 ) ) ;
#20066 = CARTESIAN_POINT ( 'NONE',  ( -15.80617190586768217, 15.72974639402176855, 103.1260903946856757 ) ) ;
#20065 = PRODUCT_DEFINITION_CONTEXT ( 'detailed design', #129482, 'design' ) ;
#20067 = CARTESIAN_POINT ( 'NONE',  ( 5.049401038298161559, -19.05341960407611168, 97.70724293864766707 ) ) ;
#20068 = CARTESIAN_POINT ( 'NONE',  ( -21.55341960407619339, 5.719274019375674811, 43.54275706135235424 ) ) ;
#20069 = CARTESIAN_POINT ( 'NONE',  ( 5.823673210054125526, 21.52544592524343514, 24.79057627198103120 ) ) ;
#20070 = CARTESIAN_POINT ( 'NONE',  ( -8.224510206698735004, -14.34966873604973081, 109.5844237280190328 ) ) ;
#20072 = CARTESIAN_POINT ( 'NONE',  ( 18.62759615963255655, 10.81492255796105972, 86.66775706135234714 ) ) ;
#20071 = CARTESIAN_POINT ( 'NONE',  ( 21.53943276465977519, 0.05219959533937863772, 51.25109039468568994 ) ) ;
#20073 = CARTESIAN_POINT ( 'NONE',  ( -19.03943276465977164, -0.05219959533935918106, 18.75109039468567218 ) ) ;
#20074 = CARTESIAN_POINT ( 'NONE',  ( 8.224510206698742110, 14.34966873604972548, 72.08442372801899012 ) ) ;
#20075 = CARTESIAN_POINT ( 'NONE',  ( -15.72974639402176322, -15.80617190586768395, 39.37609039468567573 ) ) ;
#20076 = CARTESIAN_POINT ( 'NONE',  ( 13.97604488694527802, 13.89961937509977652, 34.37390960531436690 ) ) ;
#20077 = CARTESIAN_POINT ( 'NONE',  ( 18.67979575497194134, -10.72451020669871369, 100.8344237280190185 ) ) ;
#20078 = CARTESIAN_POINT ( 'NONE',  ( -5.153800228976328057, -19.02544592524343514, 102.2905762719810383 ) ) ;
#20079 = CARTESIAN_POINT ( 'NONE',  ( 18.62759615963271287, -10.81492255796078972, 98.33224293864769550 ) ) ;
#20081 = CARTESIAN_POINT ( 'NONE',  ( -15.80617190586745835, -15.72974639402198527, 61.87390960531436690 ) ) ;
#20080 = CARTESIAN_POINT ( 'NONE',  ( 19.53091890409950793, 5.500000000000031974, 82.56097431831419442 ) ) ;
#20083 = CARTESIAN_POINT ( 'NONE',  ( 12.14591786802309770, 12.06949235617756955, 44.37390960531435979 ) ) ;
#20082 = CARTESIAN_POINT ( 'NONE',  ( -8.314922557961024197, 14.29746914071037800, 47.91775706135234714 ) ) ;
#20084 = CARTESIAN_POINT ( 'NONE',  ( 19.43099193148530190, -5.499999999999960032, 101.7672081453054886 ) ) ;
#20085 = CARTESIAN_POINT ( 'NONE',  ( -5.153800228976607833, 19.02544592524334988, 87.70942372801897591 ) ) ;
#20086 = DIRECTION ( 'NONE',  ( -1.000000000000000000, 0.000000000000000000, -6.982962677686266711E-15 ) ) ;
#20087 = EDGE_CURVE ( 'NONE', #148926, #24966, #25159, .T. ) ;
#20088 = CARTESIAN_POINT ( 'NONE',  ( 0.05219959533934541429, -16.53943276465976808, 30.00109039468568284 ) ) ;
#20089 = CARTESIAN_POINT ( 'NONE',  ( -10.81492255796078084, -18.62759615963271287, 97.08224293864770971 ) ) ;
#20090 = CARTESIAN_POINT ( 'NONE',  ( -10.81492255796078084, -18.62759615963271287, 72.08224293864769550 ) ) ;
#20091 = CARTESIAN_POINT ( 'NONE',  ( -16.46253265017160317, 9.564922557960807481, 115.8322429386477097 ) ) ;
#20092 = CARTESIAN_POINT ( 'NONE',  ( 4.379528057220092307, 16.55341960407617563, 42.29275706135235424 ) ) ;
#20093 = CARTESIAN_POINT ( 'NONE',  ( -13.89961937509977652, 13.97604488694528158, 75.62390960531438111 ) ) ;
#20095 = CARTESIAN_POINT ( 'NONE',  ( 19.03943276465977164, 0.05219959533936151252, 96.25109039468567573 ) ) ;
#20094 = CARTESIAN_POINT ( 'NONE',  ( 18.67979575497194134, -10.72451020669871369, 30.83442372801902209 ) ) ;
#20096 = CARTESIAN_POINT ( 'NONE',  ( 19.02544592524343514, -5.153800228976328945, 108.5405762719810383 ) ) ;
#20097 = CARTESIAN_POINT ( 'NONE',  ( 19.02544592524343514, -5.153800228976328945, 83.54057627198100988 ) ) ;
#20098 = CARTESIAN_POINT ( 'NONE',  ( -15.72974639402197994, 15.80617190586746368, 90.62390960531436690 ) ) ;
#20099 = CARTESIAN_POINT ( 'NONE',  ( 19.05341960407611168, 5.049401038298154454, 58.95724293864768129 ) ) ;
#20100 = PLANE ( 'NONE',  #147708 ) ;
#20101 = CARTESIAN_POINT ( 'NONE',  ( 4.379528057220339221, -16.55341960407611168, 62.70724293864769550 ) ) ;
#20102 = CARTESIAN_POINT ( 'NONE',  ( 19.02544592524343514, -5.153800228976328945, 113.5405762719810241 ) ) ;
#20103 = CARTESIAN_POINT ( 'NONE',  ( -31.62105185743270397, 0.8768460684521839354, -49.48175094143205399 ) ) ;
#20104 = CARTESIAN_POINT ( 'NONE',  ( -5.719274019375978568, 21.55341960407610458, 95.20724293864769550 ) ) ;
#20105 = CARTESIAN_POINT ( 'NONE',  ( -5.153800228976607833, 19.02544592524334988, 67.70942372801900433 ) ) ;
#20106 = CARTESIAN_POINT ( 'NONE',  ( -19.02544592524342804, 5.153800228976336051, 116.0405762719810383 ) ) ;
#20107 = CARTESIAN_POINT ( 'NONE',  ( 19.34837522270367671, 5.499999999999740652, 68.36337684832577111 ) ) ;
#20108 = CARTESIAN_POINT ( 'NONE',  ( -21.55341960407610458, -5.719274019375992779, 51.45724293864770260 ) ) ;
#20109 = CARTESIAN_POINT ( 'NONE',  ( 16.51473224551069308, 9.474510206698969483, 84.16557627198102409 ) ) ;
#20110 = CARTESIAN_POINT ( 'NONE',  ( -21.55341960407619339, 5.719274019375674811, 83.54275706135234714 ) ) ;
#20111 = CARTESIAN_POINT ( 'NONE',  ( 0.05219959533909260263, 19.03943276465977164, 54.99890960531435979 ) ) ;
#20112 = EDGE_CURVE ( 'NONE', #165180, #69839, #178948, .T. ) ;
#20113 = CARTESIAN_POINT ( 'NONE',  ( -8.314922557960811034, -14.29746914071050412, 87.08224293864769550 ) ) ;
#20114 = CARTESIAN_POINT ( 'NONE',  ( -12.14591786802326823, 12.06949235617739902, 33.12609039468569705 ) ) ;
#20115 = CARTESIAN_POINT ( 'NONE',  ( 21.55341960407619695, -5.719274019375665929, 66.04275706135236135 ) ) ;
#20116 = EDGE_LOOP ( 'NONE', ( #193049, #66892, #148714, #150773 ) ) ;
#20117 = CARTESIAN_POINT ( 'NONE',  ( 5.153800228976615827, -19.02544592524334988, 20.20942372801899722 ) ) ;
#20118 = CARTESIAN_POINT ( 'NONE',  ( -16.46253265017146816, -9.564922557961047289, 79.16775706135234714 ) ) ;
#20119 = CARTESIAN_POINT ( 'NONE',  ( 29.23421922662630834, -26.92455035691565257, -20.45761606001068955 ) ) ;
#20120 = CARTESIAN_POINT ( 'NONE',  ( -0.05219959533937732626, 21.53943276465977519, 42.50109039468567573 ) ) ;
#20121 = CARTESIAN_POINT ( 'NONE',  ( 11.74264578624800315, -36.14014761921581709, -3.149999994537626247 ) ) ;
#20122 = CARTESIAN_POINT ( 'NONE',  ( -0.05219959533936034679, 19.03943276465977164, 37.50109039468567573 ) ) ;
#20123 = CARTESIAN_POINT ( 'NONE',  ( 19.03943276465977164, -0.05219959533909143690, 53.74890960531436690 ) ) ;
#20124 = CARTESIAN_POINT ( 'NONE',  ( 16.46253265017146816, 9.564922557961045513, 36.66775706135233293 ) ) ;
#20125 = CARTESIAN_POINT ( 'NONE',  ( -14.34966873604972548, 8.224510206698743886, 103.3344237280190043 ) ) ;
#20127 = CARTESIAN_POINT ( 'NONE',  ( 15.80617190586769283, -15.72974639402175789, 70.62609039468567573 ) ) ;
#20126 = CARTESIAN_POINT ( 'NONE',  ( -0.05219959533909027116, -19.03943276465977164, 102.4989096053143669 ) ) ;
#20128 = CARTESIAN_POINT ( 'NONE',  ( 11.40812507854754365, 35.11059874428196537, -5.224999997268813701 ) ) ;
#20129 = CARTESIAN_POINT ( 'NONE',  ( -17.97182807773873137, 5.499999999999966249, 98.53038844047286204 ) ) ;
#20130 = CARTESIAN_POINT ( 'NONE',  ( 15.72974639402176855, 15.80617190586768217, 86.87609039468568994 ) ) ;
#20131 = CYLINDRICAL_SURFACE ( 'NONE', #134998, 9.100000000000001421 ) ;
#20132 = CARTESIAN_POINT ( 'NONE',  ( -5.153800228976328057, -19.02544592524343514, 102.2905762719810383 ) ) ;
#20133 = CARTESIAN_POINT ( 'NONE',  ( 5.153800228976615827, -19.02544592524334988, 20.20942372801899722 ) ) ;
#20134 = CARTESIAN_POINT ( 'NONE',  ( 0.3535533905935844268, 30.00000000000000000, 5.353553390593268624 ) ) ;
#20135 = CARTESIAN_POINT ( 'NONE',  ( -9.564922557960796823, -16.46253265017161027, 37.08224293864768839 ) ) ;
#20136 = CARTESIAN_POINT ( 'NONE',  ( -10.72451020669898014, 18.67979575497178502, 60.41557627198102409 ) ) ;
#20137 = CARTESIAN_POINT ( 'NONE',  ( -14.29746914071049879, 8.314922557960819915, 25.83224293864769194 ) ) ;
#20139 = CARTESIAN_POINT ( 'NONE',  ( -5.049401038298153566, 19.05341960407611168, 80.20724293864769550 ) ) ;
#20138 = CARTESIAN_POINT ( 'NONE',  ( -16.52544592524342804, 4.483927247898546575, 101.0405762719810383 ) ) ;
#20140 = CARTESIAN_POINT ( 'NONE',  ( -13.97604488694547697, 13.89961937509957934, 28.12609039468565797 ) ) ;
#20141 = CARTESIAN_POINT ( 'NONE',  ( 13.97604488694527802, 13.89961937509977652, 39.37390960531435269 ) ) ;
#20142 = CARTESIAN_POINT ( 'NONE',  ( 4.379528057220339221, -16.55341960407611168, 102.7072429386476955 ) ) ;
#20143 = CARTESIAN_POINT ( 'NONE',  ( 18.62759615963255655, 10.81492255796105972, 51.66775706135234714 ) ) ;
#20144 = CARTESIAN_POINT ( 'NONE',  ( 15.80617190586746368, 15.72974639402197994, 89.37390960531435269 ) ) ;
#20145 = CARTESIAN_POINT ( 'NONE',  ( 13.97604488694548053, -13.89961937509957401, 70.62609039468567573 ) ) ;
#20146 = FACE_OUTER_BOUND ( 'NONE', #121604, .T. ) ;
#20147 = CARTESIAN_POINT ( 'NONE',  ( -13.97604488694527625, -13.89961937509977652, 106.8739096053143669 ) ) ;
#20148 = CARTESIAN_POINT ( 'NONE',  ( 12.14591786802309770, 12.06949235617756955, 79.37390960531436690 ) ) ;
#20149 = CARTESIAN_POINT ( 'NONE',  ( 16.46253265017146816, 9.564922557961045513, 46.66775706135233293 ) ) ;
#20150 = CARTESIAN_POINT ( 'NONE',  ( 13.89961937509977652, -13.97604488694527269, 63.12390960531435979 ) ) ;
#20151 = CARTESIAN_POINT ( 'NONE',  ( -14.29746914071049879, 8.314922557960819915, 60.83224293864769550 ) ) ;
#20152 = CARTESIAN_POINT ( 'NONE',  ( -16.46253265017146816, -9.564922557961047289, 74.16775706135234714 ) ) ;
#20153 = CARTESIAN_POINT ( 'NONE',  ( 17.31747979337948706, 6.344076630961010821, 33.87944868065184068 ) ) ;
#20154 = CARTESIAN_POINT ( 'NONE',  ( 5.823673210054125526, 21.52544592524343514, 39.79057627198103830 ) ) ;
#20155 = EDGE_LOOP ( 'NONE', ( #67839, #81108 ) ) ;
#20156 = CARTESIAN_POINT ( 'NONE',  ( 14.34966873604960469, 8.224510206698951720, 104.1655762719810241 ) ) ;
#20157 = CARTESIAN_POINT ( 'NONE',  ( -17.50000000000001421, -3.565345528327753755, 25.57505513193517999 ) ) ;
#20159 = CARTESIAN_POINT ( 'NONE',  ( -21.53943276465977519, 0.05219959533907696930, 56.24890960531436690 ) ) ;
#20158 = CARTESIAN_POINT ( 'NONE',  ( 9.474510206698971260, -16.51473224551069308, 52.91557627198102409 ) ) ;
#20160 = CARTESIAN_POINT ( 'NONE',  ( 19.03943276465977164, -0.05219959533909143690, 23.74890960531435269 ) ) ;
#20162 = CARTESIAN_POINT ( 'NONE',  ( -13.89961937509977652, 13.97604488694528158, 75.62390960531438111 ) ) ;
#20161 = CARTESIAN_POINT ( 'NONE',  ( 4.483927247898790824, -16.52544592524335698, 85.20942372801901854 ) ) ;
#20163 = CARTESIAN_POINT ( 'NONE',  ( -19.03943276465977164, -0.05219959533935918106, 53.75109039468566863 ) ) ;
#20164 = CARTESIAN_POINT ( 'NONE',  ( -18.67979575497193778, 10.72451020669871902, 63.33442372801900433 ) ) ;
#20165 = CARTESIAN_POINT ( 'NONE',  ( 10.81492255796078972, 18.62759615963270932, 44.58224293864769550 ) ) ;
#20166 = CARTESIAN_POINT ( 'NONE',  ( -19.05341960407611168, -5.049401038298163336, 26.45724293864769550 ) ) ;
#20167 = CARTESIAN_POINT ( 'NONE',  ( 4.483927247898790824, -16.52544592524335698, 90.20942372801903275 ) ) ;
#20168 = CARTESIAN_POINT ( 'NONE',  ( -9.564922557961040184, 16.46253265017147172, 107.9177570613523471 ) ) ;
#20169 = CARTESIAN_POINT ( 'NONE',  ( 0.000000000000000000, -105.0000000000000000, 7.000000000000003553 ) ) ;
#20170 = CARTESIAN_POINT ( 'NONE',  ( -10.81492255796105439, 18.62759615963255655, 97.91775706135236135 ) ) ;
#20171 = ORIENTED_EDGE ( 'NONE', *, *, #132474, .T. ) ;
#20172 = CARTESIAN_POINT ( 'NONE',  ( -8.224510206698948167, 14.34966873604960824, 40.41557627198103120 ) ) ;
#20173 = CARTESIAN_POINT ( 'NONE',  ( -16.52544592524342804, 4.483927247898546575, 71.04057627198103830 ) ) ;
#20174 = CARTESIAN_POINT ( 'NONE',  ( -5.719274019375978568, 21.55341960407610458, 95.20724293864769550 ) ) ;
#20175 = CARTESIAN_POINT ( 'NONE',  ( -5.719274019375978568, 21.55341960407610458, 95.20724293864769550 ) ) ;
#20176 = CARTESIAN_POINT ( 'NONE',  ( -0.9086318102904998861, -31.61347055016711849, -46.06737158113915598 ) ) ;
#20177 = CARTESIAN_POINT ( 'NONE',  ( -5.823673210054116645, -21.52544592524344225, 27.29057627198103120 ) ) ;
#20178 = CARTESIAN_POINT ( 'NONE',  ( -12.14591786802326823, 12.06949235617739902, 63.12609039468568994 ) ) ;
#20179 = CARTESIAN_POINT ( 'NONE',  ( 0.05219959533910956823, 16.53943276465976808, 74.99890960531435269 ) ) ;
#20180 = CARTESIAN_POINT ( 'NONE',  ( -9.564922557960796823, -16.46253265017161027, 52.08224293864768839 ) ) ;
#20181 = CARTESIAN_POINT ( 'NONE',  ( 35.70266437024449147, -0.4905633046376201012, 37.50000000000000000 ) ) ;
#20182 = CARTESIAN_POINT ( 'NONE',  ( -8.224510206698735004, -14.34966873604973081, 94.58442372801901854 ) ) ;
#20183 = CARTESIAN_POINT ( 'NONE',  ( -18.67979575497193778, 10.72451020669871902, 23.33442372801901499 ) ) ;
#20184 = CARTESIAN_POINT ( 'NONE',  ( 16.46253265017160672, -9.564922557960803928, 78.33224293864769550 ) ) ;
#20185 = CARTESIAN_POINT ( 'NONE',  ( 15.80617190586769283, -15.72974639402175789, 55.62609039468568284 ) ) ;
#20186 = CARTESIAN_POINT ( 'NONE',  ( 13.97604488694527802, 13.89961937509977652, 104.3739096053143385 ) ) ;
#20187 = CARTESIAN_POINT ( 'NONE',  ( -19.65751872600893080, -34.84114385728561558, -25.66966870010219637 ) ) ;
#20188 = ORIENTED_EDGE ( 'NONE', *, *, #57355, .T. ) ;
#20189 = CARTESIAN_POINT ( 'NONE',  ( -5.719274019375665041, -21.55341960407619695, 49.79275706135234714 ) ) ;
#20191 = DIRECTION ( 'NONE',  ( -0.4999999999999966693, 0.5000000000000019984, 0.7071067811865483499 ) ) ;
#20190 = CARTESIAN_POINT ( 'NONE',  ( -16.51473224551069308, -9.474510206698971260, 31.66557627198102054 ) ) ;
#20192 = CARTESIAN_POINT ( 'NONE',  ( -19.03943276465977164, -0.05219959533935918106, 53.75109039468566863 ) ) ;
#20193 = CARTESIAN_POINT ( 'NONE',  ( 15.80617190586769283, -15.72974639402175789, 25.62609039468567929 ) ) ;
#20194 = CARTESIAN_POINT ( 'NONE',  ( 9.474510206698729675, 16.51473224551082808, 57.08442372801900433 ) ) ;
#20195 = CARTESIAN_POINT ( 'NONE',  ( 9.474510206698971260, -16.51473224551069308, 22.91557627198102765 ) ) ;
#20196 = CARTESIAN_POINT ( 'NONE',  ( -14.29746914071037622, -8.314922557961029526, 89.16775706135236135 ) ) ;
#20197 = CARTESIAN_POINT ( 'NONE',  ( -19.05341960407617563, 5.049401038297882671, 58.54275706135234003 ) ) ;
#20198 = CARTESIAN_POINT ( 'NONE',  ( -12.14591786802309592, -12.06949235617757132, 26.87390960531435979 ) ) ;
#20200 = ORIENTED_EDGE ( 'NONE', *, *, #149359, .F. ) ;
#20199 = CARTESIAN_POINT ( 'NONE',  ( 11.66256017358946728, 11.95480631804125515, -61.34707691135565710 ) ) ;
#20201 = CARTESIAN_POINT ( 'NONE',  ( 5.153800228976335163, 19.02544592524342804, 89.79057627198102409 ) ) ;
#20202 = CARTESIAN_POINT ( 'NONE',  ( -18.67979575497193778, 10.72451020669871902, 88.33442372801901854 ) ) ;
#20203 = CARTESIAN_POINT ( 'NONE',  ( 10.81492255796106328, -18.62759615963255655, 110.4177570613523756 ) ) ;
#20204 = CARTESIAN_POINT ( 'NONE',  ( -16.99472585857189699, -5.499999999999960032, 20.67116795353343051 ) ) ;
#20205 = CARTESIAN_POINT ( 'NONE',  ( 18.67979575497194134, -10.72451020669871369, 80.83442372801901854 ) ) ;
#20206 = CARTESIAN_POINT ( 'NONE',  ( -16.52544592524335698, -4.483927247898792601, 38.95942372801901854 ) ) ;
#20207 = CARTESIAN_POINT ( 'NONE',  ( 19.02544592524343514, -5.153800228976328945, 73.54057627198103830 ) ) ;
#20208 = CARTESIAN_POINT ( 'NONE',  ( 21.52544592524344225, -5.823673210054117533, 28.54057627198103120 ) ) ;
#20209 = DIRECTION ( 'NONE',  ( -1.000000000000000000, 0.000000000000000000, 0.000000000000000000 ) ) ;
#20210 = CARTESIAN_POINT ( 'NONE',  ( -19.03943276465977164, 0.05219959533909376836, 61.24890960531436690 ) ) ;
#20211 = CARTESIAN_POINT ( 'NONE',  ( -0.05219959533910754901, -16.53943276465976808, 27.49890960531435269 ) ) ;
#20212 = CARTESIAN_POINT ( 'NONE',  ( -19.53091890409952214, -5.500000000000038192, 40.06097431831420863 ) ) ;
#20213 = CARTESIAN_POINT ( 'NONE',  ( -16.46253265017146816, -9.564922557961047289, 74.16775706135234714 ) ) ;
#20214 = CARTESIAN_POINT ( 'NONE',  ( 13.89961937509977652, -13.97604488694527269, 103.1239096053143527 ) ) ;
#20215 = CARTESIAN_POINT ( 'NONE',  ( -0.05219959533937732626, 21.53943276465977519, 102.5010903946856899 ) ) ;
#20216 = CARTESIAN_POINT ( 'NONE',  ( -8.314922557960811034, -14.29746914071050412, 82.08224293864768129 ) ) ;
#20217 = CARTESIAN_POINT ( 'NONE',  ( -5.823673210054116645, -21.52544592524344225, 47.29057627198103120 ) ) ;
#20218 = CARTESIAN_POINT ( 'NONE',  ( 5.719274019375991003, -21.55341960407610458, 37.70724293864769550 ) ) ;
#20219 = CARTESIAN_POINT ( 'NONE',  ( 16.55341960407611168, 4.379528057220329451, 98.95724293864770971 ) ) ;
#20220 = CARTESIAN_POINT ( 'NONE',  ( -1.499905742985305324, -7.794582437828434962, -62.16226466885326118 ) ) ;
#20221 = CARTESIAN_POINT ( 'NONE',  ( 9.474510206698729675, 16.51473224551082808, 52.08442372801900433 ) ) ;
#20222 = CARTESIAN_POINT ( 'NONE',  ( -12.06949235617756955, 12.14591786802309770, 25.62390960531435624 ) ) ;
#20223 = CARTESIAN_POINT ( 'NONE',  ( -9.474510206698964154, 16.51473224551069663, 95.41557627198102409 ) ) ;
#20224 = CARTESIAN_POINT ( 'NONE',  ( -0.05219959533937732626, 21.53943276465977519, 72.50109039468568994 ) ) ;
#20225 = CARTESIAN_POINT ( 'NONE',  ( 18.67979575497178502, 10.72451020669898547, 59.16557627198103120 ) ) ;
#20226 = CARTESIAN_POINT ( 'NONE',  ( -10.81492255796105439, 18.62759615963255655, 47.91775706135234714 ) ) ;
#20227 = CARTESIAN_POINT ( 'NONE',  ( -0.05219959533907301413, -21.53943276465977519, 97.49890960531436690 ) ) ;
#20228 = CARTESIAN_POINT ( 'NONE',  ( -10.81492255796105439, 18.62759615963255655, 37.91775706135235424 ) ) ;
#20229 = CARTESIAN_POINT ( 'NONE',  ( -16.51473224551069308, -9.474510206698971260, 31.66557627198102054 ) ) ;
#20230 = CARTESIAN_POINT ( 'NONE',  ( 5.153800228976615827, -19.02544592524334988, 70.20942372801899012 ) ) ;
#20231 = CARTESIAN_POINT ( 'NONE',  ( -16.55341960407611168, -4.379528057220339221, 101.4572429386476955 ) ) ;
#20232 = CARTESIAN_POINT ( 'NONE',  ( 19.03943276465977164, -0.05219959533909143690, 108.7489096053143527 ) ) ;
#20233 = CARTESIAN_POINT ( 'NONE',  ( -0.05219959533910754901, -16.53943276465976808, 57.49890960531435979 ) ) ;
#20234 = CARTESIAN_POINT ( 'NONE',  ( -8.314922557960811034, -14.29746914071050412, 22.08224293864769194 ) ) ;
#20235 = CARTESIAN_POINT ( 'NONE',  ( -13.97604488694527625, -13.89961937509977652, 51.87390960531436690 ) ) ;
#20236 = CARTESIAN_POINT ( 'NONE',  ( -4.379528057220328563, 16.55341960407611168, 115.2072429386476955 ) ) ;
#20237 = CARTESIAN_POINT ( 'NONE',  ( -10.72451020669898014, 18.67979575497178502, 35.41557627198102409 ) ) ;
#20238 = CARTESIAN_POINT ( 'NONE',  ( -9.474510206698720793, -16.51473224551083518, 29.58442372801900433 ) ) ;
#20240 = CARTESIAN_POINT ( 'NONE',  ( -8.314922557960811034, -14.29746914071050412, 37.08224293864768129 ) ) ;
#20239 = CARTESIAN_POINT ( 'NONE',  ( -16.79531203550648755, -7.028104445595491079, 41.25244988220442366 ) ) ;
#20241 = CARTESIAN_POINT ( 'NONE',  ( 18.67979575497194134, -10.72451020669871369, 40.83442372801901854 ) ) ;
#20242 = CARTESIAN_POINT ( 'NONE',  ( -5.153800228976328057, -19.02544592524343514, 112.2905762719810099 ) ) ;
#20243 = CARTESIAN_POINT ( 'NONE',  ( -8.224510206698735004, -14.34966873604973081, 64.58442372801900433 ) ) ;
#20244 = CARTESIAN_POINT ( 'NONE',  ( -5.153800228976607833, 19.02544592524334988, 67.70942372801900433 ) ) ;
#20245 = CARTESIAN_POINT ( 'NONE',  ( 8.224510206698953496, -14.34966873604960469, 32.91557627198102409 ) ) ;
#20246 = CARTESIAN_POINT ( 'NONE',  ( -4.483927247898782831, 16.52544592524335698, 102.7094237280190185 ) ) ;
#20247 = CARTESIAN_POINT ( 'NONE',  ( -13.89961937509977652, 13.97604488694528158, 40.62390960531435979 ) ) ;
#20248 = EDGE_CURVE ( 'NONE', #178298, #138583, #149478, .T. ) ;
#20249 = CARTESIAN_POINT ( 'NONE',  ( 13.89961937509977652, -13.97604488694527269, 58.12390960531436690 ) ) ;
#20250 = VECTOR ( 'NONE', #119732, 1000.000000000000000 ) ;
#20251 = CARTESIAN_POINT ( 'NONE',  ( -19.03943276465977164, 0.05219959533909376836, 31.24890960531435979 ) ) ;
#20252 = CARTESIAN_POINT ( 'NONE',  ( -18.62759615963255300, -10.81492255796106328, 34.16775706135234714 ) ) ;
#20253 = CARTESIAN_POINT ( 'NONE',  ( 13.97604488694527802, 13.89961937509977652, 39.37390960531435269 ) ) ;
#20254 = CYLINDRICAL_SURFACE ( 'NONE', #67796, 1.499999999999997780 ) ;
#20255 = CARTESIAN_POINT ( 'NONE',  ( 0.05219959533909260263, 19.03943276465977164, 34.99890960531435979 ) ) ;
#20256 = CARTESIAN_POINT ( 'NONE',  ( -13.97604488694527625, -13.89961937509977652, 111.8739096053143243 ) ) ;
#20258 = CARTESIAN_POINT ( 'NONE',  ( -16.52544592524342804, 4.483927247898546575, 101.0405762719810383 ) ) ;
#20257 = CARTESIAN_POINT ( 'NONE',  ( -18.62759615963255300, -10.81492255796106328, 59.16775706135234714 ) ) ;
#20259 = CARTESIAN_POINT ( 'NONE',  ( -9.474510206698964154, 16.51473224551069663, 105.4155762719810383 ) ) ;
#20260 = CARTESIAN_POINT ( 'NONE',  ( 16.53943276465976808, 0.05219959533934440121, 76.25109039468568994 ) ) ;
#20261 = CARTESIAN_POINT ( 'NONE',  ( -0.05219959533937732626, 21.53943276465977519, 92.50109039468567573 ) ) ;
#20262 = CARTESIAN_POINT ( 'NONE',  ( -0.05219959533934338120, 16.53943276465976808, 52.50109039468567573 ) ) ;
#20263 = CARTESIAN_POINT ( 'NONE',  ( -9.564922557960796823, -16.46253265017161027, 92.08224293864769550 ) ) ;
#20264 = CARTESIAN_POINT ( 'NONE',  ( 8.314922557961029526, -14.29746914071037800, 40.41775706135234714 ) ) ;
#20265 = CARTESIAN_POINT ( 'NONE',  ( 14.29746914071037800, 8.314922557961029526, 21.66775706135235069 ) ) ;
#20266 = CARTESIAN_POINT ( 'NONE',  ( 14.34966873604972726, -8.224510206698740333, 85.83442372801901854 ) ) ;
#20267 = CARTESIAN_POINT ( 'NONE',  ( 19.03943276465977164, 0.05219959533936151252, 111.2510903946856757 ) ) ;
#20268 = CARTESIAN_POINT ( 'NONE',  ( 21.53943276465977519, -0.05219959533907433946, 103.7489096053143669 ) ) ;
#20270 = CARTESIAN_POINT ( 'NONE',  ( 19.05341960407617918, -5.049401038297876454, 111.0427570613523329 ) ) ;
#20269 = CARTESIAN_POINT ( 'NONE',  ( 0.05219959533910956823, 16.53943276465976808, 104.9989096053143669 ) ) ;
#20271 = CARTESIAN_POINT ( 'NONE',  ( 16.53943276465976808, 0.05219959533934440121, 66.25109039468567573 ) ) ;
#20272 = CARTESIAN_POINT ( 'NONE',  ( -16.19135201231350507, 7.376712067592058553, 44.81319145947880145 ) ) ;
#20273 = CARTESIAN_POINT ( 'NONE',  ( -19.02544592524334988, -5.153800228976617603, 73.95942372801900433 ) ) ;
#20274 = CARTESIAN_POINT ( 'NONE',  ( -8.314922557960811034, -14.29746914071050412, 42.08224293864769550 ) ) ;
#20275 = CARTESIAN_POINT ( 'NONE',  ( -16.55341960407611168, -4.379528057220339221, 26.45724293864768839 ) ) ;
#20276 = CARTESIAN_POINT ( 'NONE',  ( -0.05219959533910754901, -16.53943276465976808, 87.49890960531436690 ) ) ;
#20278 = CYLINDRICAL_SURFACE ( 'NONE', #162906, 7.500000000000000000 ) ;
#20277 = CARTESIAN_POINT ( 'NONE',  ( -5.153800228976607833, 19.02544592524334988, 32.70942372801899722 ) ) ;
#20279 = CARTESIAN_POINT ( 'NONE',  ( 5.719274019375673035, 21.55341960407619339, 42.29275706135235424 ) ) ;
#20280 = CARTESIAN_POINT ( 'NONE',  ( 19.02544592524334988, 5.153800228976608722, 96.45942372801897591 ) ) ;
#20281 = CARTESIAN_POINT ( 'NONE',  ( 5.049401038298161559, -19.05341960407611168, 112.7072429386476813 ) ) ;
#20282 = CARTESIAN_POINT ( 'NONE',  ( 0.05219959533909260263, 19.03943276465977164, 84.99890960531436690 ) ) ;
#20283 = CARTESIAN_POINT ( 'NONE',  ( 16.46253265017160672, -9.564922557960803928, 88.33224293864769550 ) ) ;
#20284 = CARTESIAN_POINT ( 'NONE',  ( 10.72451020669898902, -18.67979575497178502, 57.91557627198103120 ) ) ;
#20285 = CARTESIAN_POINT ( 'NONE',  ( -0.05219959533910754901, -16.53943276465976808, 97.49890960531436690 ) ) ;
#20286 = CARTESIAN_POINT ( 'NONE',  ( -19.02544592524342804, 5.153800228976336051, 71.04057627198099567 ) ) ;
#20287 = CARTESIAN_POINT ( 'NONE',  ( 0.05219959533910956823, 16.53943276465976808, 114.9989096053143669 ) ) ;
#20288 = CARTESIAN_POINT ( 'NONE',  ( 10.72451020669871369, 18.67979575497193778, 42.08442372801901854 ) ) ;
#20289 = CARTESIAN_POINT ( 'NONE',  ( -21.55341960407619339, 5.719274019375674811, 73.54275706135234714 ) ) ;
#20290 = CARTESIAN_POINT ( 'NONE',  ( -13.89961937509977652, 13.97604488694528158, 55.62390960531434558 ) ) ;
#20291 = CARTESIAN_POINT ( 'NONE',  ( -4.379528057220086978, -16.55341960407618274, 74.79275706135234714 ) ) ;
#20292 = CARTESIAN_POINT ( 'NONE',  ( -21.53943276465977519, -0.05219959533937600094, 28.75109039468567929 ) ) ;
#20293 = CARTESIAN_POINT ( 'NONE',  ( 21.55341960407619695, -5.719274019375665929, 31.04275706135234714 ) ) ;
#20295 = CARTESIAN_POINT ( 'NONE',  ( 5.049401038298161559, -19.05341960407611168, 82.70724293864770971 ) ) ;
#20294 = CARTESIAN_POINT ( 'NONE',  ( 13.97604488694548053, -13.89961937509957401, 55.62609039468566863 ) ) ;
#20296 = CARTESIAN_POINT ( 'NONE',  ( -5.153800228976607833, 19.02544592524334988, 27.70942372801899722 ) ) ;
#20297 = CARTESIAN_POINT ( 'NONE',  ( -5.823673210054431948, 21.52544592524334988, 77.70942372801900433 ) ) ;
#20298 = CARTESIAN_POINT ( 'NONE',  ( -10.81492255796078084, -18.62759615963271287, 72.08224293864769550 ) ) ;
#20299 = CARTESIAN_POINT ( 'NONE',  ( -14.29746914071049879, 8.314922557960819915, 55.83224293864770260 ) ) ;
#20301 = CARTESIAN_POINT ( 'NONE',  ( -19.05341960407617563, 5.049401038297882671, 28.54275706135232937 ) ) ;
#20300 = CARTESIAN_POINT ( 'NONE',  ( -15.80617190586768217, 15.72974639402176855, 88.12609039468570415 ) ) ;
#20302 = CARTESIAN_POINT ( 'NONE',  ( -8.224510206698948167, 14.34966873604960824, 75.41557627198102409 ) ) ;
#20303 = CARTESIAN_POINT ( 'NONE',  ( -19.05341960407611168, -5.049401038298163336, 21.45724293864768839 ) ) ;
#20304 = CARTESIAN_POINT ( 'NONE',  ( 19.05341960407617918, -5.049401038297876454, 56.04275706135234714 ) ) ;
#20305 = CARTESIAN_POINT ( 'NONE',  ( 16.55341960407611168, 4.379528057220329451, 38.95724293864768839 ) ) ;
#20306 = CARTESIAN_POINT ( 'NONE',  ( 10.81492255796106328, -18.62759615963255655, 85.41775706135236135 ) ) ;
#20307 = CARTESIAN_POINT ( 'NONE',  ( -0.05219959533909027116, -19.03943276465977164, 72.49890960531435269 ) ) ;
#20308 = CARTESIAN_POINT ( 'NONE',  ( 9.474510206698729675, 16.51473224551082808, 52.08442372801900433 ) ) ;
#20309 = CARTESIAN_POINT ( 'NONE',  ( -15.80617190586745835, -15.72974639402198527, 46.87390960531435979 ) ) ;
#20310 = CARTESIAN_POINT ( 'NONE',  ( 5.719274019375673035, 21.55341960407619339, 42.29275706135235424 ) ) ;
#20311 = CARTESIAN_POINT ( 'NONE',  ( 5.823673210054125526, 21.52544592524343514, 99.79057627198103830 ) ) ;
#20312 = CARTESIAN_POINT ( 'NONE',  ( 16.51473224551083163, -9.474510206698727899, 95.83442372801900433 ) ) ;
#20313 = CARTESIAN_POINT ( 'NONE',  ( -14.34966873604972548, 8.224510206698743886, 63.33442372801900433 ) ) ;
#20315 = CARTESIAN_POINT ( 'NONE',  ( 21.52544592524344225, -5.823673210054117533, 103.5405762719810383 ) ) ;
#20314 = DIRECTION ( 'NONE',  ( -1.000000000000000000, 6.391086490440866478E-16, 0.000000000000000000 ) ) ;
#20316 = CARTESIAN_POINT ( 'NONE',  ( -8.314922557960811034, -14.29746914071050412, 97.08224293864770971 ) ) ;
#20317 = CARTESIAN_POINT ( 'NONE',  ( -17.49999999999999289, -5.068104630630435814, 29.27181594659970898 ) ) ;
#20318 = CARTESIAN_POINT ( 'NONE',  ( -16.53943276465976808, -0.05219959533934237506, 33.75109039468568284 ) ) ;
#20319 = CARTESIAN_POINT ( 'NONE',  ( 5.823673210054125526, 21.52544592524343514, 64.79057627198103830 ) ) ;
#20320 = CARTESIAN_POINT ( 'NONE',  ( -8.314922557961024197, 14.29746914071037800, 107.9177570613523471 ) ) ;
#20321 = CARTESIAN_POINT ( 'NONE',  ( 9.564922557960805705, 16.46253265017160317, 29.58224293864769550 ) ) ;
#20322 = CARTESIAN_POINT ( 'NONE',  ( -4.483927247898782831, 16.52544592524335698, 67.70942372801901854 ) ) ;
#20323 = CARTESIAN_POINT ( 'NONE',  ( -9.474510206698720793, -16.51473224551083518, 59.58442372801900433 ) ) ;
#20324 = CARTESIAN_POINT ( 'NONE',  ( 21.53943276465977519, 0.05219959533937863772, 36.25109039468567573 ) ) ;
#20325 = CARTESIAN_POINT ( 'NONE',  ( 10.72451020669898902, -18.67979575497178502, 52.91557627198103830 ) ) ;
#20326 = CARTESIAN_POINT ( 'NONE',  ( 4.483927247898790824, -16.52544592524335698, 100.2094237280190043 ) ) ;
#20327 = CARTESIAN_POINT ( 'NONE',  ( -5.719274019375665041, -21.55341960407619695, 74.79275706135234714 ) ) ;
#20328 = CARTESIAN_POINT ( 'NONE',  ( 5.719274019375991003, -21.55341960407610458, 52.70724293864769550 ) ) ;
#20329 = CARTESIAN_POINT ( 'NONE',  ( 10.72451020669898902, -18.67979575497178502, 37.91557627198102409 ) ) ;
#20330 = VERTEX_POINT ( 'NONE', #10974 ) ;
#20331 = CARTESIAN_POINT ( 'NONE',  ( -14.34966873604972548, 8.224510206698743886, 73.33442372801901854 ) ) ;
#20332 = CARTESIAN_POINT ( 'NONE',  ( -21.55341960407610458, -5.719274019375992779, 26.45724293864768839 ) ) ;
#20333 = EDGE_LOOP ( 'NONE', ( #55783, #66471, #28838, #7002, #127753, #65696, #36728, #43976, #135193 ) ) ;
#20334 = CARTESIAN_POINT ( 'NONE',  ( 0.05219959533909260263, 19.03943276465977164, 94.99890960531436690 ) ) ;
#20335 = CARTESIAN_POINT ( 'NONE',  ( -12.14591786802326823, 12.06949235617739902, 108.1260903946856757 ) ) ;
#20336 = DIRECTION ( 'NONE',  ( 0.5000000000000037748, 0.4999999999999950040, 0.7071067811865484609 ) ) ;
#20337 = CARTESIAN_POINT ( 'NONE',  ( 16.53943276465976808, -0.05219959533910856209, 103.7489096053143669 ) ) ;
#20338 = CARTESIAN_POINT ( 'NONE',  ( 5.823673210054125526, 21.52544592524343514, 59.79057627198103120 ) ) ;
#20339 = CARTESIAN_POINT ( 'NONE',  ( 8.224510206698742110, 14.34966873604972548, 97.08442372801904696 ) ) ;
#20340 = CARTESIAN_POINT ( 'NONE',  ( 21.55341960407619695, -5.719274019375665929, 51.04275706135234714 ) ) ;
#20341 = CARTESIAN_POINT ( 'NONE',  ( -16.46253265017146816, -9.564922557961047289, 109.1677570613523471 ) ) ;
#20342 = CARTESIAN_POINT ( 'NONE',  ( -8.224510206698948167, 14.34966873604960824, 105.4155762719810383 ) ) ;
#20343 = CARTESIAN_POINT ( 'NONE',  ( 19.02544592524343514, -5.153800228976328945, 48.54057627198103120 ) ) ;
#20344 = CARTESIAN_POINT ( 'NONE',  ( 9.474510206698971260, -16.51473224551069308, 22.91557627198102765 ) ) ;
#20345 = CARTESIAN_POINT ( 'NONE',  ( 17.50000000000000000, -5.499999999999992895, 38.29690382534171533 ) ) ;
#20346 = CARTESIAN_POINT ( 'NONE',  ( -16.51473224551069308, -9.474510206698971260, 86.66557627198102409 ) ) ;
#20347 = EDGE_CURVE ( 'NONE', #20566, #145773, #158736, .T. ) ;
#20348 = CARTESIAN_POINT ( 'NONE',  ( -12.06949235617739369, -12.14591786802326823, 74.37609039468568994 ) ) ;
#20349 = CARTESIAN_POINT ( 'NONE',  ( 15.72974639402176855, 15.80617190586768217, 106.8760903946856899 ) ) ;
#20350 = CARTESIAN_POINT ( 'NONE',  ( -15.80617190586745835, -15.72974639402198527, 61.87390960531436690 ) ) ;
#20351 = CARTESIAN_POINT ( 'NONE',  ( 4.379528057220092307, 16.55341960407617563, 67.29275706135234714 ) ) ;
#20352 = CARTESIAN_POINT ( 'NONE',  ( 19.02544592524334988, 5.153800228976608722, 86.45942372801900433 ) ) ;
#20353 = ORIENTED_EDGE ( 'NONE', *, *, #14309, .F. ) ;
#20354 = CARTESIAN_POINT ( 'NONE',  ( 9.474510206698971260, -16.51473224551069308, 37.91557627198102409 ) ) ;
#20355 = CARTESIAN_POINT ( 'NONE',  ( 9.474510206698971260, -16.51473224551069308, 82.91557627198103830 ) ) ;
#20356 = CARTESIAN_POINT ( 'NONE',  ( 19.02544592524343514, -5.153800228976328945, 28.54057627198102409 ) ) ;
#20357 = CARTESIAN_POINT ( 'NONE',  ( -5.049401038297874678, -19.05341960407617918, 74.79275706135231871 ) ) ;
#20358 = CARTESIAN_POINT ( 'NONE',  ( 21.51693143705161404, -10.15780255052775161, 170.5200780514259691 ) ) ;
#20359 = CARTESIAN_POINT ( 'NONE',  ( 19.02544592524343514, -5.153800228976328945, 93.54057627198102409 ) ) ;
#20360 = CARTESIAN_POINT ( 'NONE',  ( 4.483927247898545687, 16.52544592524342804, 44.79057627198103120 ) ) ;
#20361 = CARTESIAN_POINT ( 'NONE',  ( -10.72451020669898014, 18.67979575497178502, 55.41557627198102409 ) ) ;
#20362 = LINE ( 'NONE', #34549, #44992 ) ;
#20363 = CIRCLE ( 'NONE', #75225, 10.00000000000000000 ) ;
#20364 = CARTESIAN_POINT ( 'NONE',  ( 5.049401038297881783, 19.05341960407617563, 27.29275706135232937 ) ) ;
#20366 = CARTESIAN_POINT ( 'NONE',  ( 16.51473224551069308, 9.474510206698969483, 59.16557627198102409 ) ) ;
#20365 = CARTESIAN_POINT ( 'NONE',  ( 9.474510206698971260, -16.51473224551069308, 52.91557627198102409 ) ) ;
#20367 = CARTESIAN_POINT ( 'NONE',  ( 14.34966873604972726, -8.224510206698740333, 40.83442372801901854 ) ) ;
#20368 = CARTESIAN_POINT ( 'NONE',  ( -19.52851543214744012, -5.499999999999989342, 100.3935772176258041 ) ) ;
#20369 = CARTESIAN_POINT ( 'NONE',  ( 22.03588254365928378, -7.477584490968436803, 173.9991804579097163 ) ) ;
#20370 = CARTESIAN_POINT ( 'NONE',  ( -12.06949235617739369, -12.14591786802326823, 69.37609039468567573 ) ) ;
#20371 = CARTESIAN_POINT ( 'NONE',  ( -18.62759615963270932, 10.81492255796079327, 95.83224293864770971 ) ) ;
#20372 =( BOUNDED_CURVE ( )  B_SPLINE_CURVE ( 2, ( #65569, #76761, #80733, #138435, #904, #139422, #123253, #140422, #3890, #200116, #50421 ),
 .UNSPECIFIED., .F., .T. ) 
 B_SPLINE_CURVE_WITH_KNOTS ( ( 3, 2, 2, 2, 2, 3 ),
 ( 0.000000000000000000, 0.02000000000000001776, 0.04000000000000003553, 0.06000000000000005329, 0.08000000000000007105, 0.1000000000000000888 ),
 .UNSPECIFIED. ) 
 CURVE ( )  GEOMETRIC_REPRESENTATION_ITEM ( )  RATIONAL_B_SPLINE_CURVE ( ( 1.000000000000000000, 0.9510565162951535312, 1.000000000000000000, 0.9510565162951535312, 1.000000000000000000, 0.9510565162951535312, 1.000000000000000000, 0.9510565162951535312, 1.000000000000000000, 0.9510565162951533091, 1.000000000000000222 ) ) 
 REPRESENTATION_ITEM ( '' )  );
#20373 = CARTESIAN_POINT ( 'NONE',  ( 14.29746914071037800, 8.314922557961029526, 41.66775706135235424 ) ) ;
#20375 = FACE_OUTER_BOUND ( 'NONE', #125535, .T. ) ;
#20374 = CARTESIAN_POINT ( 'NONE',  ( 5.153800228976335163, 19.02544592524342804, 39.79057627198100988 ) ) ;
#20376 = CARTESIAN_POINT ( 'NONE',  ( -21.53943276465977519, -0.05219959533937600094, 53.75109039468568994 ) ) ;
#20377 = CARTESIAN_POINT ( 'NONE',  ( -19.02544592524334988, -5.153800228976617603, 58.95942372801900433 ) ) ;
#20378 = CARTESIAN_POINT ( 'NONE',  ( -10.72451020669870658, -18.67979575497194134, 94.58442372801901854 ) ) ;
#20379 = CARTESIAN_POINT ( 'NONE',  ( -21.38418241377623374, -5.438282248597753110, 174.2683007571264113 ) ) ;
#20380 = CARTESIAN_POINT ( 'NONE',  ( 4.379528057220339221, -16.55341960407611168, 47.70724293864770260 ) ) ;
#20381 = CARTESIAN_POINT ( 'NONE',  ( 19.53091890409951503, 5.500000000000023981, 42.56097431831420863 ) ) ;
#20382 = CARTESIAN_POINT ( 'NONE',  ( -15.72974639402197994, 15.80617190586746368, 60.62390960531437401 ) ) ;
#20383 = CARTESIAN_POINT ( 'NONE',  ( -27.73933785331498925, 9.013057229001088189, 142.7750000027311899 ) ) ;
#20384 = CARTESIAN_POINT ( 'NONE',  ( 19.02544592524343514, -5.153800228976328945, 98.54057627198100988 ) ) ;
#20385 = CARTESIAN_POINT ( 'NONE',  ( 14.34966873604960469, 8.224510206698951720, 99.16557627198100988 ) ) ;
#20386 = CARTESIAN_POINT ( 'NONE',  ( 16.53943276465976808, 0.05219959533934440121, 21.25109039468567218 ) ) ;
#20387 = CARTESIAN_POINT ( 'NONE',  ( 12.14591786802327356, -12.06949235617739191, 105.6260903946856899 ) ) ;
#20388 = EDGE_LOOP ( 'NONE', ( #171344, #83609, #148692 ) ) ;
#20389 = CARTESIAN_POINT ( 'NONE',  ( 18.67979575497178502, 10.72451020669898547, 109.1655762719810383 ) ) ;
#20390 = VECTOR ( 'NONE', #105550, 1000.000000000000000 ) ;
#20392 = CARTESIAN_POINT ( 'NONE',  ( 5.049401038298161559, -19.05341960407611168, 112.7072429386476813 ) ) ;
#20391 = CARTESIAN_POINT ( 'NONE',  ( -8.224510206698948167, 14.34966873604960824, 25.41557627198103120 ) ) ;
#20393 = CARTESIAN_POINT ( 'NONE',  ( 16.46253265017146816, 9.564922557961045513, 91.66775706135234714 ) ) ;
#20394 = CARTESIAN_POINT ( 'NONE',  ( -5.823673210054431948, 21.52544592524334988, 102.7094237280190185 ) ) ;
#20395 = CARTESIAN_POINT ( 'NONE',  ( -14.34966873604960291, -8.224510206698953496, 26.66557627198103475 ) ) ;
#20396 = CARTESIAN_POINT ( 'NONE',  ( 10.72451020669898902, -18.67979575497178502, 87.91557627198103830 ) ) ;
#20397 = CARTESIAN_POINT ( 'NONE',  ( -21.53943276465977519, 0.05219959533907696930, 56.24890960531436690 ) ) ;
#20398 = CARTESIAN_POINT ( 'NONE',  ( 19.05341960407611168, 5.049401038298154454, 58.95724293864768129 ) ) ;
#20399 = CARTESIAN_POINT ( 'NONE',  ( 8.314922557960818139, 14.29746914071049879, 29.58224293864769905 ) ) ;
#20400 = CARTESIAN_POINT ( 'NONE',  ( -9.564922557960796823, -16.46253265017161027, 82.08224293864768129 ) ) ;
#20401 = ORIENTED_EDGE ( 'NONE', *, *, #108955, .T. ) ;
#20402 = DIRECTION ( 'NONE',  ( 1.000000000000000000, 0.000000000000000000, 0.000000000000000000 ) ) ;
#20403 = CARTESIAN_POINT ( 'NONE',  ( 13.89961937509957401, 13.97604488694547697, 41.87609039468566152 ) ) ;
#20404 = CARTESIAN_POINT ( 'NONE',  ( -21.53943276465977519, 0.05219959533907696930, 86.24890960531436690 ) ) ;
#20405 = CARTESIAN_POINT ( 'NONE',  ( 4.379528057220339221, -16.55341960407611168, 82.70724293864770971 ) ) ;
#20406 = CARTESIAN_POINT ( 'NONE',  ( 18.67979575497194134, -10.72451020669871369, 35.83442372801901143 ) ) ;
#20407 = CARTESIAN_POINT ( 'NONE',  ( -5.359611314223446995E-15, 29.16686587814335496, 140.3750000027311842 ) ) ;
#20408 = CARTESIAN_POINT ( 'NONE',  ( -4.379528057220086978, -16.55341960407618274, 109.7927570613523613 ) ) ;
#20409 = CARTESIAN_POINT ( 'NONE',  ( 5.049401038298161559, -19.05341960407611168, 32.70724293864768129 ) ) ;
#20410 = CARTESIAN_POINT ( 'NONE',  ( -5.153800228976328057, -19.02544592524343514, 82.29057627198103830 ) ) ;
#20411 = CARTESIAN_POINT ( 'NONE',  ( -5.153800228976328057, -19.02544592524343514, 32.29057627198102409 ) ) ;
#20412 = CARTESIAN_POINT ( 'NONE',  ( 16.55341960407611168, 4.379528057220329451, 48.95724293864770971 ) ) ;
#20413 = CARTESIAN_POINT ( 'NONE',  ( -21.52544592524334988, -5.823673210054445271, 73.95942372801901854 ) ) ;
#20415 = CARTESIAN_POINT ( 'NONE',  ( 8.314922557961029526, -14.29746914071037800, 65.41775706135234714 ) ) ;
#20414 = CARTESIAN_POINT ( 'NONE',  ( 26.32780677389235890, -26.67379781540241268, -18.43298970368203626 ) ) ;
#20416 = CARTESIAN_POINT ( 'NONE',  ( 9.474510206698971260, -16.51473224551069308, 42.91557627198103120 ) ) ;
#20417 = CARTESIAN_POINT ( 'NONE',  ( 19.02544592524343514, -5.153800228976328945, 48.54057627198103120 ) ) ;
#20418 = ORIENTED_EDGE ( 'NONE', *, *, #116795, .T. ) ;
#20419 = CARTESIAN_POINT ( 'NONE',  ( -9.474510206698720793, -16.51473224551083518, 19.58442372801899722 ) ) ;
#20420 = CARTESIAN_POINT ( 'NONE',  ( 16.52544592524335698, 4.483927247898782831, 56.45942372801902565 ) ) ;
#20421 = CARTESIAN_POINT ( 'NONE',  ( -15.80617190586768217, 15.72974639402176855, 103.1260903946856757 ) ) ;
#20422 = CARTESIAN_POINT ( 'NONE',  ( -5.719274019375978568, 21.55341960407610458, 35.20724293864768839 ) ) ;
#20423 = CARTESIAN_POINT ( 'NONE',  ( -13.89961937509957401, -13.97604488694547875, 109.3760903946856331 ) ) ;
#20424 = CARTESIAN_POINT ( 'NONE',  ( -5.823673210054431948, 21.52544592524334988, 67.70942372801901854 ) ) ;
#20425 = CARTESIAN_POINT ( 'NONE',  ( 4.379528057220092307, 16.55341960407617563, 32.29275706135235424 ) ) ;
#20426 = CARTESIAN_POINT ( 'NONE',  ( 0.05219959533907565091, 21.53943276465977519, 99.99890960531436690 ) ) ;
#20427 = CARTESIAN_POINT ( 'NONE',  ( 16.51473224551083163, -9.474510206698727899, 95.83442372801900433 ) ) ;
#20428 = CARTESIAN_POINT ( 'NONE',  ( -0.05219959533909027116, -19.03943276465977164, 67.49890960531436690 ) ) ;
#20429 = CARTESIAN_POINT ( 'NONE',  ( 16.53943276465976808, 0.05219959533934440121, 21.25109039468567218 ) ) ;
#20430 = CARTESIAN_POINT ( 'NONE',  ( -19.02544592524334988, -5.153800228976617603, 108.9594237280189759 ) ) ;
#20431 = CARTESIAN_POINT ( 'NONE',  ( 16.55341960407611168, 4.379528057220329451, 63.95724293864770260 ) ) ;
#20432 = CARTESIAN_POINT ( 'NONE',  ( -14.34966873604972548, 8.224510206698743886, 73.33442372801901854 ) ) ;
#20434 = CARTESIAN_POINT ( 'NONE',  ( 19.05341960407611168, 5.049401038298154454, 48.95724293864768129 ) ) ;
#20433 = CARTESIAN_POINT ( 'NONE',  ( -5.823673210054431948, 21.52544592524334988, 22.70942372801901499 ) ) ;
#20435 = CARTESIAN_POINT ( 'NONE',  ( 16.46253265017160672, -9.564922557960803928, 53.33224293864768839 ) ) ;
#20436 = CARTESIAN_POINT ( 'NONE',  ( -14.34966873604972548, 8.224510206698743886, 68.33442372801900433 ) ) ;
#20437 = CARTESIAN_POINT ( 'NONE',  ( 17.14385361876520264, 23.59649016807275856, 142.6750000027311103 ) ) ;
#20438 = CARTESIAN_POINT ( 'NONE',  ( -5.429308488886486681E-15, 30.30510711980690175, 143.7500000054623399 ) ) ;
#20439 = ORIENTED_EDGE ( 'NONE', *, *, #173336, .F. ) ;
#20440 = CARTESIAN_POINT ( 'NONE',  ( -19.03943276465977164, -0.05219959533935918106, 23.75109039468566152 ) ) ;
#20441 = ADVANCED_FACE ( 'NONE', ( #58460 ), #143836, .F. ) ;
#20442 = CARTESIAN_POINT ( 'NONE',  ( -19.05341960407611168, -5.049401038298163336, 26.45724293864769550 ) ) ;
#20443 = ORIENTED_EDGE ( 'NONE', *, *, #3493, .T. ) ;
#20444 = CARTESIAN_POINT ( 'NONE',  ( -19.02544592524334988, -5.153800228976617603, 108.9594237280189759 ) ) ;
#20445 = CARTESIAN_POINT ( 'NONE',  ( -21.55341960407610458, -5.719274019375992779, 46.45724293864769550 ) ) ;
#20447 = CARTESIAN_POINT ( 'NONE',  ( 12.14591786802327356, -12.06949235617739191, 35.62609039468568994 ) ) ;
#20446 = CARTESIAN_POINT ( 'NONE',  ( 5.153800228976615827, -19.02544592524334988, 50.20942372801897591 ) ) ;
#20448 = CARTESIAN_POINT ( 'NONE',  ( -16.51473224551069308, -9.474510206698971260, 41.66557627198103120 ) ) ;
#20449 = CARTESIAN_POINT ( 'NONE',  ( -9.564922557960796823, -16.46253265017161027, 47.08224293864769550 ) ) ;
#20450 = CARTESIAN_POINT ( 'NONE',  ( -21.53943276465977519, 0.05219959533907696930, 86.24890960531436690 ) ) ;
#20451 = CARTESIAN_POINT ( 'NONE',  ( 13.97604488694527802, 13.89961937509977652, 109.3739096053143669 ) ) ;
#20452 = AXIS2_PLACEMENT_3D ( 'NONE', #155420, #125082, #16910 ) ;
#20453 = CARTESIAN_POINT ( 'NONE',  ( -13.89961937509977652, 13.97604488694528158, 55.62390960531434558 ) ) ;
#20454 = CARTESIAN_POINT ( 'NONE',  ( -21.49604614807126524, -21.49604614807088154, -64.92279855667830191 ) ) ;
#20455 = CARTESIAN_POINT ( 'NONE',  ( 13.89961937509957401, 13.97604488694547697, 91.87609039468567573 ) ) ;
#20456 = CARTESIAN_POINT ( 'NONE',  ( -16.52544592524342804, 4.483927247898546575, 61.04057627198103120 ) ) ;
#20457 = CARTESIAN_POINT ( 'NONE',  ( 5.153800228976615827, -19.02544592524334988, 25.20942372801900433 ) ) ;
#20458 = EDGE_CURVE ( 'NONE', #101425, #178697, #37334, .T. ) ;
#20459 = CARTESIAN_POINT ( 'NONE',  ( 21.53943276465977519, -0.05219959533907433946, 93.74890960531436690 ) ) ;
#20460 = CARTESIAN_POINT ( 'NONE',  ( 15.72974639402176855, 15.80617190586768217, 86.87609039468568994 ) ) ;
#20461 = CARTESIAN_POINT ( 'NONE',  ( 19.05341960407611168, 5.049401038298154454, 23.95724293864769194 ) ) ;
#20462 = CARTESIAN_POINT ( 'NONE',  ( -18.67979575497193778, 10.72451020669871902, 73.33442372801901854 ) ) ;
#20464 = CARTESIAN_POINT ( 'NONE',  ( 21.53943276465977519, 0.05219959533937863772, 76.25109039468568994 ) ) ;
#20463 = CARTESIAN_POINT ( 'NONE',  ( -12.14591786802309592, -12.06949235617757132, 21.87390960531436690 ) ) ;
#20465 = CARTESIAN_POINT ( 'NONE',  ( 0.05219959533909260263, 19.03943276465977164, 69.99890960531435269 ) ) ;
#20466 = CARTESIAN_POINT ( 'NONE',  ( -15.80617190586768217, 15.72974639402176855, 43.12609039468568284 ) ) ;
#20467 = CARTESIAN_POINT ( 'NONE',  ( 9.474510206698971260, -16.51473224551069308, 87.91557627198102409 ) ) ;
#20468 = CARTESIAN_POINT ( 'NONE',  ( -14.29746914071049879, 8.314922557960819915, 95.83224293864770971 ) ) ;
#20469 = CARTESIAN_POINT ( 'NONE',  ( 4.379528057220339221, -16.55341960407611168, 62.70724293864769550 ) ) ;
#20470 = CARTESIAN_POINT ( 'NONE',  ( 10.81492255796078972, 18.62759615963270932, 69.58224293864769550 ) ) ;
#20471 = CARTESIAN_POINT ( 'NONE',  ( -19.05341960407611168, -5.049401038298163336, 56.45724293864768129 ) ) ;
#20472 = CARTESIAN_POINT ( 'NONE',  ( -5.719274019375978568, 21.55341960407610458, 80.20724293864769550 ) ) ;
#20473 = CARTESIAN_POINT ( 'NONE',  ( 19.03943276465977164, 0.05219959533936151252, 71.25109039468566152 ) ) ;
#20475 = CARTESIAN_POINT ( 'NONE',  ( -14.29746914071049879, 8.314922557960819915, 80.83224293864769550 ) ) ;
#20474 = CARTESIAN_POINT ( 'NONE',  ( -5.049401038297874678, -19.05341960407618274, 34.79275706135233293 ) ) ;
#20476 = CARTESIAN_POINT ( 'NONE',  ( 18.62759615963271287, -10.81492255796078972, 53.33224293864769550 ) ) ;
#20477 = CARTESIAN_POINT ( 'NONE',  ( 17.44279575226824619, 5.990770900252460507, 101.6644243248568245 ) ) ;
#20479 = CARTESIAN_POINT ( 'NONE',  ( -8.571926809382601320, -26.38167802310801591, 147.7750000027311899 ) ) ;
#20478 = CARTESIAN_POINT ( 'NONE',  ( -12.14591786802326823, 12.06949235617739902, 98.12609039468570415 ) ) ;
#20480 = CARTESIAN_POINT ( 'NONE',  ( 19.03943276465977164, 0.05219959533936151252, 96.25109039468567573 ) ) ;
#20481 = CARTESIAN_POINT ( 'NONE',  ( 4.483927247898545687, 16.52544592524342804, 69.79057627198102409 ) ) ;
#20482 = CARTESIAN_POINT ( 'NONE',  ( -19.39056639909676605, -5.500000000000018652, 95.78948781074342378 ) ) ;
#20483 = CARTESIAN_POINT ( 'NONE',  ( -19.02544592524342804, 5.153800228976336051, 61.04057627198103120 ) ) ;
#20484 = CARTESIAN_POINT ( 'NONE',  ( -4.483927247898539470, -16.52544592524342804, 47.29057627198103120 ) ) ;
#20485 = ADVANCED_FACE ( 'NONE', ( #19654 ), #167636, .F. ) ;
#20486 = CARTESIAN_POINT ( 'NONE',  ( -5.153800228976328057, -19.02544592524343514, 102.2905762719810383 ) ) ;
#20488 = CARTESIAN_POINT ( 'NONE',  ( -16.51473224551069308, -9.474510206698971260, 71.66557627198102409 ) ) ;
#20487 = CARTESIAN_POINT ( 'NONE',  ( -16.46253265017146816, -9.564922557961047289, 74.16775706135234714 ) ) ;
#20489 = CARTESIAN_POINT ( 'NONE',  ( -16.51473224551069308, -9.474510206698971260, 91.66557627198103830 ) ) ;
#20490 = CARTESIAN_POINT ( 'NONE',  ( 9.564922557960805705, 16.46253265017160317, 79.58224293864769550 ) ) ;
#20491 = CARTESIAN_POINT ( 'NONE',  ( -18.67979575497178146, -10.72451020669898902, 56.66557627198103830 ) ) ;
#20492 = CARTESIAN_POINT ( 'NONE',  ( -0.05219959533934338120, 16.53943276465976808, 57.50109039468568994 ) ) ;
#20493 = CARTESIAN_POINT ( 'NONE',  ( 9.564922557961047289, -16.46253265017146816, 105.4177570613523471 ) ) ;
#20494 = CARTESIAN_POINT ( 'NONE',  ( -19.03943276465977164, 0.05219959533909376836, 46.24890960531435979 ) ) ;
#20495 = CARTESIAN_POINT ( 'NONE',  ( -21.53943276465977519, 0.05219959533907696930, 61.24890960531435979 ) ) ;
#20496 = CARTESIAN_POINT ( 'NONE',  ( -19.05341960407617563, 5.049401038297882671, 93.54275706135234714 ) ) ;
#20498 = CARTESIAN_POINT ( 'NONE',  ( -5.823673210054431948, 21.52544592524334988, 32.70942372801900433 ) ) ;
#20497 = CARTESIAN_POINT ( 'NONE',  ( 8.314922557960818139, 14.29746914071049879, 29.58224293864769905 ) ) ;
#20499 = CARTESIAN_POINT ( 'NONE',  ( -5.153800228976607833, 19.02544592524334988, 32.70942372801899722 ) ) ;
#20501 = CARTESIAN_POINT ( 'NONE',  ( -14.34966873604972548, 8.224510206698743886, 88.33442372801901854 ) ) ;
#20500 = CARTESIAN_POINT ( 'NONE',  ( 16.53943276465976808, 0.05219959533934440121, 61.25109039468567573 ) ) ;
#20502 = CARTESIAN_POINT ( 'NONE',  ( 18.22780087662114212, -5.499999999999987566, 41.01540105326107977 ) ) ;
#20503 = CARTESIAN_POINT ( 'NONE',  ( 12.14591786802327356, -12.06949235617739191, 85.62609039468568994 ) ) ;
#20505 = CARTESIAN_POINT ( 'NONE',  ( -8.224510206698735004, -14.34966873604973081, 29.58442372801901854 ) ) ;
#20504 = CARTESIAN_POINT ( 'NONE',  ( 5.719274019375991003, -21.55341960407610458, 22.70724293864769194 ) ) ;
#20506 = CARTESIAN_POINT ( 'NONE',  ( -13.97604488694527625, -13.89961937509977652, 46.87390960531435979 ) ) ;
#20507 = CARTESIAN_POINT ( 'NONE',  ( 5.049401038298161559, -19.05341960407611168, 47.70724293864770260 ) ) ;
#20508 = CARTESIAN_POINT ( 'NONE',  ( 16.46253265017160672, -9.564922557960803928, 58.33224293864769550 ) ) ;
#20509 = CARTESIAN_POINT ( 'NONE',  ( -5.719274019375665041, -21.55341960407619695, 34.79275706135235424 ) ) ;
#20510 = CARTESIAN_POINT ( 'NONE',  ( 8.314922557961029526, -14.29746914071037800, 50.41775706135235424 ) ) ;
#20511 = CARTESIAN_POINT ( 'NONE',  ( 14.34966873604972726, -8.224510206698740333, 110.8344237280190043 ) ) ;
#20512 = CARTESIAN_POINT ( 'NONE',  ( -13.97604488694527625, -13.89961937509977652, 21.87390960531435979 ) ) ;
#20513 = CARTESIAN_POINT ( 'NONE',  ( -5.823673210054431948, 21.52544592524334988, 107.7094237280190328 ) ) ;
#20514 = CARTESIAN_POINT ( 'NONE',  ( 5.049401038297881783, 19.05341960407617563, 112.2927570613523471 ) ) ;
#20515 = CARTESIAN_POINT ( 'NONE',  ( 19.05341960407617918, -5.049401038297876454, 66.04275706135233293 ) ) ;
#20516 = CARTESIAN_POINT ( 'NONE',  ( -16.52544592524342804, 4.483927247898546575, 71.04057627198103830 ) ) ;
#20517 = CARTESIAN_POINT ( 'NONE',  ( 16.51473224551069308, 9.474510206698969483, 39.16557627198103120 ) ) ;
#20519 = CARTESIAN_POINT ( 'NONE',  ( 16.62475595723698163, 7.163666690055251252, 76.97286648189535185 ) ) ;
#20518 = CARTESIAN_POINT ( 'NONE',  ( -9.474510206698720793, -16.51473224551083518, 69.58442372801901854 ) ) ;
#20520 = CARTESIAN_POINT ( 'NONE',  ( -21.55341960407619339, 5.719274019375674811, 83.54275706135234714 ) ) ;
#20521 = CARTESIAN_POINT ( 'NONE',  ( 12.14591786802327356, -12.06949235617739191, 35.62609039468568994 ) ) ;
#20522 = CARTESIAN_POINT ( 'NONE',  ( 16.61371651742603461, 7.165104196376044676, 38.64584930007005426 ) ) ;
#20523 = CARTESIAN_POINT ( 'NONE',  ( 18.62759615963271287, -10.81492255796078972, 33.33224293864769550 ) ) ;
#20524 = CARTESIAN_POINT ( 'NONE',  ( 8.314922557961029526, -14.29746914071037800, 25.41775706135235779 ) ) ;
#20525 = CARTESIAN_POINT ( 'NONE',  ( -9.474510206698964154, 16.51473224551069663, 30.41557627198102054 ) ) ;
#20526 = CARTESIAN_POINT ( 'NONE',  ( -13.97604488694547697, 13.89961937509957934, 28.12609039468565797 ) ) ;
#20527 = CARTESIAN_POINT ( 'NONE',  ( 17.60769864724391098, -5.499999999999979572, 66.15024842019164453 ) ) ;
#20528 = CARTESIAN_POINT ( 'NONE',  ( -13.89961937509977652, 13.97604488694528158, 40.62390960531435979 ) ) ;
#20529 = FACE_OUTER_BOUND ( 'NONE', #10674, .T. ) ;
#20530 = CARTESIAN_POINT ( 'NONE',  ( -13.97604488694527625, -13.89961937509977652, 71.87390960531433848 ) ) ;
#20531 = CARTESIAN_POINT ( 'NONE',  ( -19.53091890409951858, -5.500000000000036415, 55.06097431831419442 ) ) ;
#20532 = CARTESIAN_POINT ( 'NONE',  ( 19.02544592524334988, 5.153800228976608722, 26.45942372801899722 ) ) ;
#20533 = CARTESIAN_POINT ( 'NONE',  ( 16.55341960407611168, 4.379528057220329451, 28.95724293864769905 ) ) ;
#20534 = CARTESIAN_POINT ( 'NONE',  ( 16.46253265017160672, -9.564922557960803928, 28.33224293864769550 ) ) ;
#20535 = CARTESIAN_POINT ( 'NONE',  ( -16.51473224551069308, -9.474510206698971260, 91.66557627198103830 ) ) ;
#20536 = CARTESIAN_POINT ( 'NONE',  ( -21.53943276465977519, -0.05219959533937600094, 68.75109039468568994 ) ) ;
#20537 = CARTESIAN_POINT ( 'NONE',  ( -0.05219959533909027116, -19.03943276465977164, 57.49890960531435979 ) ) ;
#20538 = CIRCLE ( 'NONE', #159380, 24.30000000000003268 ) ;
#20539 = CARTESIAN_POINT ( 'NONE',  ( 10.72451020669871369, 18.67979575497193778, 67.08442372801901854 ) ) ;
#20541 = CARTESIAN_POINT ( 'NONE',  ( 15.72974639402199770, -15.80617190586745480, 23.12390960531436335 ) ) ;
#20540 = CARTESIAN_POINT ( 'NONE',  ( -19.05341960407617563, 5.049401038297882671, 93.54275706135234714 ) ) ;
#20542 = CARTESIAN_POINT ( 'NONE',  ( 19.03943276465977164, -0.05219959533909143690, 33.74890960531435979 ) ) ;
#20543 = CARTESIAN_POINT ( 'NONE',  ( -21.52544592524343514, 5.823673210054127303, 116.0405762719810383 ) ) ;
#20544 = CARTESIAN_POINT ( 'NONE',  ( -5.153800228976607833, 19.02544592524334988, 32.70942372801899722 ) ) ;
#20545 = CARTESIAN_POINT ( 'NONE',  ( 12.14591786802309770, 12.06949235617756955, 104.3739096053143669 ) ) ;
#20546 = CARTESIAN_POINT ( 'NONE',  ( -5.153800228976328057, -19.02544592524343514, 62.29057627198100988 ) ) ;
#20547 = CARTESIAN_POINT ( 'NONE',  ( -19.05341960407617563, 5.049401038297882671, 108.5427570613523187 ) ) ;
#20548 = CARTESIAN_POINT ( 'NONE',  ( -16.52544592524342804, 4.483927247898546575, 76.04057627198102409 ) ) ;
#20549 = CARTESIAN_POINT ( 'NONE',  ( 5.823673210054125526, 21.52544592524343514, 29.79057627198102409 ) ) ;
#20550 = CARTESIAN_POINT ( 'NONE',  ( -19.05341960407617563, 5.049401038297882671, 83.54275706135233293 ) ) ;
#20551 = CARTESIAN_POINT ( 'NONE',  ( -0.05219959533907301413, -21.53943276465977519, 87.49890960531436690 ) ) ;
#20552 = CARTESIAN_POINT ( 'NONE',  ( -5.719274019375665041, -21.55341960407619695, 49.79275706135234714 ) ) ;
#20553 = CARTESIAN_POINT ( 'NONE',  ( -4.483927247898782831, 16.52544592524335698, 57.70942372801901143 ) ) ;
#20555 = CARTESIAN_POINT ( 'NONE',  ( 15.80617190586769283, -15.72974639402175789, 45.62609039468567573 ) ) ;
#20554 = CARTESIAN_POINT ( 'NONE',  ( 8.314922557961029526, -14.29746914071037800, 50.41775706135235424 ) ) ;
#20556 = CARTESIAN_POINT ( 'NONE',  ( 18.62759615963271287, -10.81492255796078972, 48.33224293864770260 ) ) ;
#20557 = CARTESIAN_POINT ( 'NONE',  ( -19.03943276465977164, 0.05219959533909376836, 51.24890960531436690 ) ) ;
#20558 = CARTESIAN_POINT ( 'NONE',  ( 11.74264578624799427, 36.14014761921585972, -6.349999994537625980 ) ) ;
#20559 = CARTESIAN_POINT ( 'NONE',  ( 12.06949235617739724, 12.14591786802326823, 81.87609039468568994 ) ) ;
#20560 = CARTESIAN_POINT ( 'NONE',  ( 15.72974639402199770, -15.80617190586745480, 103.1239096053143811 ) ) ;
#20561 = CARTESIAN_POINT ( 'NONE',  ( -12.14591786802309592, -12.06949235617757132, 51.87390960531437401 ) ) ;
#20562 = CARTESIAN_POINT ( 'NONE',  ( -14.34966873604972548, 8.224510206698743886, 58.33442372801901143 ) ) ;
#20563 = CARTESIAN_POINT ( 'NONE',  ( 16.51473224551083163, -9.474510206698727899, 100.8344237280190043 ) ) ;
#20564 = CARTESIAN_POINT ( 'NONE',  ( -21.52544592524343514, 5.823673210054127303, 96.04057627198102409 ) ) ;
#20565 = CARTESIAN_POINT ( 'NONE',  ( -16.52544592524342804, 4.483927247898546575, 41.04057627198103120 ) ) ;
#20566 = VERTEX_POINT ( 'NONE', #166652 ) ;
#20567 = CARTESIAN_POINT ( 'NONE',  ( 18.56453257813365809, -5.499999999999952038, 93.49000423690691264 ) ) ;
#20568 = CARTESIAN_POINT ( 'NONE',  ( -5.719274019375978568, 21.55341960407610458, 80.20724293864769550 ) ) ;
#20569 = CARTESIAN_POINT ( 'NONE',  ( -16.55341960407611168, -4.379528057220339221, 31.45724293864769550 ) ) ;
#20570 = VERTEX_POINT ( 'NONE', #197973 ) ;
#20571 = DIRECTION ( 'NONE',  ( 0.000000000000000000, 1.000000000000000000, 1.224646799147353207E-16 ) ) ;
#20572 = CARTESIAN_POINT ( 'NONE',  ( 10.81492255796078972, 18.62759615963270932, 104.5822429386477097 ) ) ;
#20573 = CARTESIAN_POINT ( 'NONE',  ( 21.52544592524344225, -5.823673210054117533, 113.5405762719810383 ) ) ;
#20574 = CARTESIAN_POINT ( 'NONE',  ( -14.29746914071049879, 8.314922557960819915, 40.83224293864769550 ) ) ;
#20575 = CARTESIAN_POINT ( 'NONE',  ( -4.379528057220086978, -16.55341960407618274, 54.79275706135235424 ) ) ;
#20577 = EDGE_CURVE ( 'NONE', #87119, #172465, #24387, .T. ) ;
#20576 = CARTESIAN_POINT ( 'NONE',  ( -16.46253265017160317, 9.564922557960807481, 45.83224293864769550 ) ) ;
#20578 = CARTESIAN_POINT ( 'NONE',  ( 5.049401038298161559, -19.05341960407611168, 62.70724293864769550 ) ) ;
#20579 = ORIENTED_EDGE ( 'NONE', *, *, #69149, .F. ) ;
#20580 = CARTESIAN_POINT ( 'NONE',  ( -15.72974639402197994, 15.80617190586746368, 30.62390960531436335 ) ) ;
#20581 = CARTESIAN_POINT ( 'NONE',  ( -26.32780677389376578, -26.67379781540345718, -18.43298970368158152 ) ) ;
#20582 = CARTESIAN_POINT ( 'NONE',  ( -16.53943276465976808, -0.05219959533934237506, 18.75109039468568639 ) ) ;
#20583 = CARTESIAN_POINT ( 'NONE',  ( -13.89961937509957401, -13.97604488694547875, 44.37609039468566863 ) ) ;
#20584 = CARTESIAN_POINT ( 'NONE',  ( -15.72974639402197994, 15.80617190586746368, 100.6239096053143811 ) ) ;
#20585 = CARTESIAN_POINT ( 'NONE',  ( 14.34966873604960469, 8.224510206698951720, 29.16557627198103120 ) ) ;
#20586 = CARTESIAN_POINT ( 'NONE',  ( -13.97604488694527625, -13.89961937509977652, 81.87390960531436690 ) ) ;
#20587 = CARTESIAN_POINT ( 'NONE',  ( -21.53943276465977519, 0.05219959533907696930, 51.24890960531436690 ) ) ;
#20589 = CARTESIAN_POINT ( 'NONE',  ( -0.05219959533934338120, 16.53943276465976808, 22.50109039468567573 ) ) ;
#20588 = CARTESIAN_POINT ( 'NONE',  ( 0.05219959533907565091, 21.53943276465977519, 79.99890960531435269 ) ) ;
#20590 = CARTESIAN_POINT ( 'NONE',  ( 21.55341960407610458, 5.719274019375980345, 23.95724293864769550 ) ) ;
#20591 = CARTESIAN_POINT ( 'NONE',  ( -21.52544592524334988, -5.823673210054445271, 73.95942372801901854 ) ) ;
#20592 = CARTESIAN_POINT ( 'NONE',  ( 19.05341960407611168, 5.049401038298154454, 68.95724293864769550 ) ) ;
#20593 = CARTESIAN_POINT ( 'NONE',  ( 13.89961937509977652, -13.97604488694527269, 33.12390960531434558 ) ) ;
#20594 = CARTESIAN_POINT ( 'NONE',  ( 13.97604488694527802, 13.89961937509977652, 89.37390960531436690 ) ) ;
#20595 = CARTESIAN_POINT ( 'NONE',  ( -16.53943276465976808, 0.05219959533911058130, 86.24890960531436690 ) ) ;
#20596 = ORIENTED_EDGE ( 'NONE', *, *, #2366, .T. ) ;
#20597 = CARTESIAN_POINT ( 'NONE',  ( 19.05341960407617918, -5.049401038297876454, 106.0427570613523471 ) ) ;
#20598 = DIRECTION ( 'NONE',  ( 1.000000000000000000, 0.000000000000000000, 0.000000000000000000 ) ) ;
#20599 = CARTESIAN_POINT ( 'NONE',  ( -5.049401038298153566, 19.05341960407611168, 80.20724293864769550 ) ) ;
#20601 = CARTESIAN_POINT ( 'NONE',  ( -5.153800228976328057, -19.02544592524343514, 112.2905762719810099 ) ) ;
#20600 = CARTESIAN_POINT ( 'NONE',  ( -5.823673210054431948, 21.52544592524334988, 82.70942372801900433 ) ) ;
#20602 = CARTESIAN_POINT ( 'NONE',  ( -12.06949235617739369, -12.14591786802326823, 79.37609039468567573 ) ) ;
#20603 = CARTESIAN_POINT ( 'NONE',  ( -16.38665767535051287, -7.295008042176176488, 74.73599135785458714 ) ) ;
#20604 = CARTESIAN_POINT ( 'NONE',  ( -5.049401038297874678, -19.05341960407617918, 54.79275706135234003 ) ) ;
#20605 = CARTESIAN_POINT ( 'NONE',  ( 21.53943276465977519, 0.05219959533937863772, 111.2510903946856899 ) ) ;
#20606 = DIRECTION ( 'NONE',  ( 0.000000000000000000, 0.000000000000000000, -1.000000000000000000 ) ) ;
#20607 = DIRECTION ( 'NONE',  ( 1.000000000000000000, 0.000000000000000000, -0.000000000000000000 ) ) ;
#20608 = CARTESIAN_POINT ( 'NONE',  ( -22.81625015709510507, 31.40387420917330275, -5.424999997268812990 ) ) ;
#20609 = CARTESIAN_POINT ( 'NONE',  ( -4.483927247898782831, 16.52544592524335698, 112.7094237280190328 ) ) ;
#20610 = EDGE_CURVE ( 'NONE', #35288, #152202, #4989, .T. ) ;
#20611 = CARTESIAN_POINT ( 'NONE',  ( 0.000000000000000000, -165.0000000000000000, -23.00000000000000000 ) ) ;
#20612 = CARTESIAN_POINT ( 'NONE',  ( -0.05219959533934338120, 16.53943276465976808, 107.5010903946856899 ) ) ;
#20613 = DIRECTION ( 'NONE',  ( -1.000000000000000000, 0.000000000000000000, 0.000000000000000000 ) ) ;
#20614 = CARTESIAN_POINT ( 'NONE',  ( -12.14591786802326823, 12.06949235617739902, 83.12609039468568994 ) ) ;
#20615 = CARTESIAN_POINT ( 'NONE',  ( 19.03943276465977164, -0.05219959533909143690, 23.74890960531435269 ) ) ;
#20616 = CARTESIAN_POINT ( 'NONE',  ( -18.67979575497193778, 10.72451020669871902, 88.33442372801901854 ) ) ;
#20617 = CARTESIAN_POINT ( 'NONE',  ( 9.474510206698729675, 16.51473224551082808, 102.0844237280190043 ) ) ;
#20618 = CARTESIAN_POINT ( 'NONE',  ( 10.72451020669871369, 18.67979575497193778, 67.08442372801901854 ) ) ;
#20619 = CARTESIAN_POINT ( 'NONE',  ( -19.02544592524334988, -5.153800228976617603, 43.95942372801899012 ) ) ;
#20620 = CARTESIAN_POINT ( 'NONE',  ( -9.474510206698964154, 16.51473224551069663, 80.41557627198103830 ) ) ;
#20621 = CARTESIAN_POINT ( 'NONE',  ( -19.05341960407611168, -5.049401038298163336, 76.45724293864769550 ) ) ;
#20622 = ADVANCED_FACE ( 'NONE', ( #74631 ), #158162, .T. ) ;
#20623 = CARTESIAN_POINT ( 'NONE',  ( -9.003469324749447722, -38.97944712463819883, -12.94545205561310119 ) ) ;
#20624 = CIRCLE ( 'NONE', #91768, 8.000000000000000000 ) ;
#20625 = CARTESIAN_POINT ( 'NONE',  ( -5.719274019375978568, 21.55341960407610458, 50.20724293864769550 ) ) ;
#20626 = CARTESIAN_POINT ( 'NONE',  ( -13.97604488694527625, -13.89961937509977652, 46.87390960531435979 ) ) ;
#20627 = CARTESIAN_POINT ( 'NONE',  ( 4.483927247898790824, -16.52544592524335698, 80.20942372801901854 ) ) ;
#20628 = ORIENTED_EDGE ( 'NONE', *, *, #156887, .F. ) ;
#20630 = CARTESIAN_POINT ( 'NONE',  ( 36.91746824999999887, 11.99521256947799053, -5.524999997268812635 ) ) ;
#20629 = CARTESIAN_POINT ( 'NONE',  ( 16.53943276465976808, -0.05219959533910856209, 78.74890960531436690 ) ) ;
#20631 = CARTESIAN_POINT ( 'NONE',  ( -4.379528057220086978, -16.55341960407618274, 44.79275706135234714 ) ) ;
#20632 = CARTESIAN_POINT ( 'NONE',  ( 8.314922557960818139, 14.29746914071049879, 109.5822429386476955 ) ) ;
#20633 = CARTESIAN_POINT ( 'NONE',  ( 13.89961937509957401, 13.97604488694547697, 51.87609039468566863 ) ) ;
#20634 = CARTESIAN_POINT ( 'NONE',  ( -8.314922557960811034, -14.29746914071050412, 72.08224293864769550 ) ) ;
#20635 = CARTESIAN_POINT ( 'NONE',  ( 15.72974639402176855, 15.80617190586768217, 26.87609039468567218 ) ) ;
#20637 = CARTESIAN_POINT ( 'NONE',  ( -15.80617190586745835, -15.72974639402198527, 86.87390960531438111 ) ) ;
#20636 = CARTESIAN_POINT ( 'NONE',  ( 13.89961937509977652, -13.97604488694527269, 23.12390960531436335 ) ) ;
#20638 = CARTESIAN_POINT ( 'NONE',  ( -5.049401038298153566, 19.05341960407611168, 105.2072429386476671 ) ) ;
#20639 = CARTESIAN_POINT ( 'NONE',  ( 16.55341960407611168, 4.379528057220329451, 68.95724293864769550 ) ) ;
#20640 = CARTESIAN_POINT ( 'NONE',  ( 21.50179914127970093, -34.93963825066541062, -18.44273973154308521 ) ) ;
#20641 = CARTESIAN_POINT ( 'NONE',  ( 22.81625015709510151, -31.40387420917324590, -5.924999997268812990 ) ) ;
#20642 = CARTESIAN_POINT ( 'NONE',  ( -16.51473224551082808, 9.474510206698731452, 83.33442372801899012 ) ) ;
#20643 = CARTESIAN_POINT ( 'NONE',  ( -10.72451020669870658, -18.67979575497194134, 24.58442372801901499 ) ) ;
#20644 = CARTESIAN_POINT ( 'NONE',  ( -16.51473224551069308, -9.474510206698971260, 71.66557627198102409 ) ) ;
#20645 = CARTESIAN_POINT ( 'NONE',  ( -19.03943276465977164, -0.05219959533935918106, 58.75109039468566863 ) ) ;
#20646 = CARTESIAN_POINT ( 'NONE',  ( 19.05341960407611168, 5.049401038298154454, 38.95724293864767418 ) ) ;
#20647 = CARTESIAN_POINT ( 'NONE',  ( 16.55341960407611168, 4.379528057220329451, 68.95724293864769550 ) ) ;
#20648 = CARTESIAN_POINT ( 'NONE',  ( 16.53943276465976808, -0.05219959533910856209, 58.74890960531436690 ) ) ;
#20649 = CARTESIAN_POINT ( 'NONE',  ( -0.05219959533909027116, -19.03943276465977164, 82.49890960531436690 ) ) ;
#20650 = CARTESIAN_POINT ( 'NONE',  ( -18.67979575497178146, -10.72451020669898902, 91.66557627198103830 ) ) ;
#20651 = CARTESIAN_POINT ( 'NONE',  ( 16.46253265017160672, -9.564922557960803928, 68.33224293864770971 ) ) ;
#20652 = CARTESIAN_POINT ( 'NONE',  ( 21.53943276465977519, -0.05219959533907433946, 83.74890960531435269 ) ) ;
#20653 = CARTESIAN_POINT ( 'NONE',  ( -10.81492255796105439, 18.62759615963255655, 112.9177570613523329 ) ) ;
#20656 = CARTESIAN_POINT ( 'NONE',  ( 4.379528057220339221, -16.55341960407611168, 92.70724293864770971 ) ) ;
#20655 = CARTESIAN_POINT ( 'NONE',  ( 4.379528057220092307, 16.55341960407617563, 112.2927570613523471 ) ) ;
#20654 = CARTESIAN_POINT ( 'NONE',  ( 13.89961937509977652, -13.97604488694527269, 28.12390960531435624 ) ) ;
#20657 = CARTESIAN_POINT ( 'NONE',  ( -5.049401038297874678, -19.05341960407617918, 99.79275706135234714 ) ) ;
#20658 = ORIENTED_EDGE ( 'NONE', *, *, #184816, .F. ) ;
#20659 = CARTESIAN_POINT ( 'NONE',  ( 5.719274019375991003, -21.55341960407610458, 112.7072429386476955 ) ) ;
#20660 = CARTESIAN_POINT ( 'NONE',  ( -19.05341960407617563, 5.049401038297882671, 58.54275706135234003 ) ) ;
#20661 = CARTESIAN_POINT ( 'NONE',  ( -4.483927247898539470, -16.52544592524342804, 27.29057627198103120 ) ) ;
#20662 = CARTESIAN_POINT ( 'NONE',  ( 9.474510206698729675, 16.51473224551082808, 42.08442372801900433 ) ) ;
#20663 = CARTESIAN_POINT ( 'NONE',  ( -13.89961937509977652, 13.97604488694528158, 105.6239096053143527 ) ) ;
#20664 = CARTESIAN_POINT ( 'NONE',  ( 16.52544592524342804, -4.483927247898539470, 53.54057627198103120 ) ) ;
#20665 = CARTESIAN_POINT ( 'NONE',  ( -26.00011078373267637, 10.07146799416499938, 166.7325096689061183 ) ) ;
#20666 = CARTESIAN_POINT ( 'NONE',  ( 9.474510206698971260, -16.51473224551069308, 32.91557627198102409 ) ) ;
#20667 = CARTESIAN_POINT ( 'NONE',  ( -10.72451020669870658, -18.67979575497194134, 104.5844237280190185 ) ) ;
#20668 = CARTESIAN_POINT ( 'NONE',  ( 12.06949235617739724, 12.14591786802326823, 86.87609039468568994 ) ) ;
#20669 = CARTESIAN_POINT ( 'NONE',  ( 5.823673210054444382, -21.52544592524334988, 40.20942372801901854 ) ) ;
#20670 = CARTESIAN_POINT ( 'NONE',  ( 0.05219959533934541429, -16.53943276465976808, 50.00109039468568994 ) ) ;
#20671 = CARTESIAN_POINT ( 'NONE',  ( -0.05219959533909027116, -19.03943276465977164, 102.4989096053143669 ) ) ;
#20672 = CARTESIAN_POINT ( 'NONE',  ( 16.46253265017160672, -9.564922557960803928, 48.33224293864769550 ) ) ;
#20673 = CARTESIAN_POINT ( 'NONE',  ( -0.05219959533909027116, -19.03943276465977164, 67.49890960531436690 ) ) ;
#20674 = CARTESIAN_POINT ( 'NONE',  ( 12.06949235617739724, 12.14591786802326823, 46.87609039468568994 ) ) ;
#20675 = CARTESIAN_POINT ( 'NONE',  ( -12.14591786802309592, -12.06949235617757132, 111.8739096053143669 ) ) ;
#20676 = CARTESIAN_POINT ( 'NONE',  ( 16.53943276465976808, 0.05219959533934440121, 111.2510903946856899 ) ) ;
#20677 = CARTESIAN_POINT ( 'NONE',  ( -38.00000000000000711, 2.893978650043524126E-14, -25.00000000000000000 ) ) ;
#20680 = CARTESIAN_POINT ( 'NONE',  ( 5.153800228976335163, 19.02544592524342804, 79.79057627198102409 ) ) ;
#20679 = CARTESIAN_POINT ( 'NONE',  ( 16.51473224551069308, 9.474510206698969483, 89.16557627198103830 ) ) ;
#20678 = CARTESIAN_POINT ( 'NONE',  ( 18.62759615963255655, 10.81492255796105972, 61.66775706135235424 ) ) ;
#20681 = CARTESIAN_POINT ( 'NONE',  ( -13.89961937509977652, 13.97604488694528158, 95.62390960531436690 ) ) ;
#20682 = CARTESIAN_POINT ( 'NONE',  ( 12.14591786802309770, 12.06949235617756955, 39.37390960531436690 ) ) ;
#20683 = CARTESIAN_POINT ( 'NONE',  ( 16.53943276465976808, -0.05219959533910856209, 23.74890960531435269 ) ) ;
#20684 = VECTOR ( 'NONE', #119233, 1000.000000000000000 ) ;
#20685 = CARTESIAN_POINT ( 'NONE',  ( -4.483927247898539470, -16.52544592524342804, 42.29057627198103120 ) ) ;
#20686 = ORIENTED_EDGE ( 'NONE', *, *, #10842, .T. ) ;
#20687 = FACE_OUTER_BOUND ( 'NONE', #166875, .T. ) ;
#20688 = CARTESIAN_POINT ( 'NONE',  ( 13.89961937509977652, -13.97604488694527269, 68.12390960531436690 ) ) ;
#20689 = CARTESIAN_POINT ( 'NONE',  ( -0.05219959533936034679, 19.03943276465977164, 52.50109039468566863 ) ) ;
#20690 = CARTESIAN_POINT ( 'NONE',  ( -11.40812507854755609, 35.11059874428196537, -1.024999997268813301 ) ) ;
#20691 = CARTESIAN_POINT ( 'NONE',  ( -0.05219959533909027116, -19.03943276465977164, 67.49890960531436690 ) ) ;
#20693 = CARTESIAN_POINT ( 'NONE',  ( -14.34966873604972548, 8.224510206698743886, 63.33442372801900433 ) ) ;
#20692 = CARTESIAN_POINT ( 'NONE',  ( 13.97604488694548053, -13.89961937509957401, 85.62609039468568994 ) ) ;
#20694 = CARTESIAN_POINT ( 'NONE',  ( -22.49873734152930282, -26.99873734152905058, 8.889087296526001936 ) ) ;
#20695 = CARTESIAN_POINT ( 'NONE',  ( -5.049401038298153566, 19.05341960407611168, 95.20724293864770971 ) ) ;
#20696 = CARTESIAN_POINT ( 'NONE',  ( -10.81492255796105439, 18.62759615963255655, 27.91775706135234358 ) ) ;
#20697 = CARTESIAN_POINT ( 'NONE',  ( 16.51473224551083163, -9.474510206698727899, 95.83442372801900433 ) ) ;
#20699 = CARTESIAN_POINT ( 'NONE',  ( 9.474510206698971260, -16.51473224551069308, 42.91557627198103120 ) ) ;
#20698 = CARTESIAN_POINT ( 'NONE',  ( 17.40805194822030444, 6.112264579159356614, 86.66628727489388950 ) ) ;
#20700 = CARTESIAN_POINT ( 'NONE',  ( 9.564922557960805705, 16.46253265017160317, 89.58224293864769550 ) ) ;
#20702 = CARTESIAN_POINT ( 'NONE',  ( -19.03943276465977164, 0.05219959533909376836, 56.24890960531435979 ) ) ;
#20701 = CARTESIAN_POINT ( 'NONE',  ( -4.483927247898539470, -16.52544592524342804, 52.29057627198102409 ) ) ;
#20703 = CARTESIAN_POINT ( 'NONE',  ( 0.05219959533936267826, -19.03943276465977164, 65.00109039468567573 ) ) ;
#20704 = ORIENTED_EDGE ( 'NONE', *, *, #172898, .F. ) ;
#20705 = CARTESIAN_POINT ( 'NONE',  ( 16.51473224551083163, -9.474510206698727899, 35.83442372801899722 ) ) ;
#20706 = CARTESIAN_POINT ( 'NONE',  ( -5.049401038298153566, 19.05341960407611168, 65.20724293864765286 ) ) ;
#20707 = VECTOR ( 'NONE', #52230, 1000.000000000000000 ) ;
#20708 = CARTESIAN_POINT ( 'NONE',  ( 10.72451020669898902, -18.67979575497178502, 57.91557627198103120 ) ) ;
#20710 = CARTESIAN_POINT ( 'NONE',  ( 19.02544592524334988, 5.153800228976608722, 26.45942372801899722 ) ) ;
#20709 = CARTESIAN_POINT ( 'NONE',  ( -12.14591786802309592, -12.06949235617757132, 66.87390960531436690 ) ) ;
#20711 = CARTESIAN_POINT ( 'NONE',  ( 16.51473224551069308, 9.474510206698969483, 109.1655762719810383 ) ) ;
#20712 = CARTESIAN_POINT ( 'NONE',  ( 18.67979575497178502, 10.72451020669898547, 29.16557627198103120 ) ) ;
#20713 = CARTESIAN_POINT ( 'NONE',  ( -0.05219959533909027116, -19.03943276465977164, 57.49890960531435979 ) ) ;
#20714 = CARTESIAN_POINT ( 'NONE',  ( -19.02544592524342804, 5.153800228976336051, 36.04057627198100988 ) ) ;
#20715 = CARTESIAN_POINT ( 'NONE',  ( 4.483927247898545687, 16.52544592524342804, 104.7905762719810241 ) ) ;
#20716 = CARTESIAN_POINT ( 'NONE',  ( -15.72974639402176322, -15.80617190586768395, 19.37609039468568639 ) ) ;
#20717 = CARTESIAN_POINT ( 'NONE',  ( -13.97604488694527625, -13.89961937509977652, 111.8739096053143243 ) ) ;
#20718 = CARTESIAN_POINT ( 'NONE',  ( 10.81492255796106328, -18.62759615963255655, 25.41775706135235779 ) ) ;
#20719 = CARTESIAN_POINT ( 'NONE',  ( -0.05219959533909027116, -19.03943276465977164, 107.4989096053143527 ) ) ;
#20720 = CARTESIAN_POINT ( 'NONE',  ( -8.224510206698948167, 14.34966873604960824, 115.4155762719810241 ) ) ;
#20721 = CARTESIAN_POINT ( 'NONE',  ( 5.719274019375673035, 21.55341960407619339, 72.29275706135236135 ) ) ;
#20722 = CARTESIAN_POINT ( 'NONE',  ( 18.67979575497178502, 10.72451020669898547, 94.16557627198103830 ) ) ;
#20723 = LINE ( 'NONE', #144068, #186001 ) ;
#20724 = CARTESIAN_POINT ( 'NONE',  ( 18.39635199886969730, -5.499999999999973355, 78.51967076359997577 ) ) ;
#20725 = CARTESIAN_POINT ( 'NONE',  ( -5.049401038298153566, 19.05341960407611168, 60.20724293864768129 ) ) ;
#20726 = CARTESIAN_POINT ( 'NONE',  ( -8.314922557961024197, 14.29746914071037800, 42.91775706135235424 ) ) ;
#20727 = CARTESIAN_POINT ( 'NONE',  ( 12.06949235617757843, -12.14591786802309237, 103.1239096053143811 ) ) ;
#20728 = CARTESIAN_POINT ( 'NONE',  ( 33.98208146068711244, -4.940236926081949420, 92.55634382532313964 ) ) ;
#20729 = CARTESIAN_POINT ( 'NONE',  ( -9.474510206698964154, 16.51473224551069663, 65.41557627198102409 ) ) ;
#20730 = CARTESIAN_POINT ( 'NONE',  ( 14.34966873604960469, 8.224510206698951720, 99.16557627198100988 ) ) ;
#20731 = CARTESIAN_POINT ( 'NONE',  ( -15.72974639402197994, 15.80617190586746368, 45.62390960531436690 ) ) ;
#20732 = CARTESIAN_POINT ( 'NONE',  ( 14.34966873604960469, 8.224510206698951720, 59.16557627198103120 ) ) ;
#20733 = CARTESIAN_POINT ( 'NONE',  ( -13.89961937509957401, -13.97604488694547875, 109.3760903946856331 ) ) ;
#20734 = CARTESIAN_POINT ( 'NONE',  ( 18.62759615963255655, 10.81492255796105972, 91.66775706135234714 ) ) ;
#20735 = CLOSED_SHELL ( 'NONE', ( #53954, #62013, #15330, #8758, #131099, #36061, #118478, #58975, #100272, #118076, #29180, #174575, #139677, #118804, #126981, #25179, #21859, #20987, #40707, #167499, #80645, #33166, #39556, #142192, #94239, #88055, #23155, #105774, #36457, #4267, #142831, #78668, #172386, #178138, #117993, #88662, #191817, #178327, #23384, #4997, #134178, #104476, #179718, #170147, #171155, #146080, #131794, #53484, #135466, #167295, #66940, #161317, #151556, #150985, #37984, #3115, #127113, #80812, #98642, #156677, #192253, #112604, #3634, #174610, #150382, #41490, #140471, #35819, #173686, #19722, #187715, #51167, #190456, #152031, #104135, #54195, #122206, #105509, #112590, #71917, #150746, #195963, #199055, #50148, #169454, #107904, #100461, #119850, #104879, #113246, #83445, #55872, #86379, #49614, #99315, #119326, #56930, #108877, #147415, #66633, #36976, #41657, #5652, #29559, #30297, #83247, #173443, #29760, #156805, #20441 ) ) ;
#20736 = CARTESIAN_POINT ( 'NONE',  ( 16.19135201231366139, -7.376712067591920885, 77.31319145947969673 ) ) ;
#20737 = CARTESIAN_POINT ( 'NONE',  ( 0.05219959533934541429, -16.53943276465976808, 95.00109039468568994 ) ) ;
#20738 = CARTESIAN_POINT ( 'NONE',  ( -16.53943276465976808, 0.05219959533911058130, 46.24890960531435979 ) ) ;
#20739 = CARTESIAN_POINT ( 'NONE',  ( -5.049401038298153566, 19.05341960407611168, 40.20724293864768839 ) ) ;
#20740 = CARTESIAN_POINT ( 'NONE',  ( 5.153800228976335163, 19.02544592524342804, 89.79057627198102409 ) ) ;
#20741 = CARTESIAN_POINT ( 'NONE',  ( -5.719274019375978568, 21.55341960407610458, 90.20724293864770971 ) ) ;
#20742 =( BOUNDED_SURFACE ( )  B_SPLINE_SURFACE ( 3, 2, ( 
 ( #43237, #178766, #25091, #86733, #193937, #150430, #181755, #148418, #104904, #133238, #165591, #101908, #163590, #102908, #194930, #118087, #27089, #26086, #88736, #164592, #28092, #87730, #149415, #72584, #134258, #195945, #119092, #178418, #148075, #177426, #37896, #130892, #128882, #83381, #191569, #97537, #147074, #190582, #159224, #176421, #36879, #99554, #20719, #192582, #82376, #161236, #70234, #22730, #144064, #55058, #174421, #38897, #52058, #5545, #127891, #146055, #6539, #84378, #113714, #98545, #7539, #193586, #54065, #116729, #100554, #145058, #69224, #115739, #162233, #68219, #39882, #86391, #101549, #67224, #23732, #175411, #160238, #66231, #189594, #85381, #8558, #51067, #53048, #21728, #129871, #112728, #35890, #131902, #114728, #163241, #24741, #149077, #198558, #117733, #121694, #166239, #87392, #44872, #41903, #90365, #10565, #72229, #13535, #75201, #165244, #103569, #106528, #12562, #151071, #168205, #197568, #73242, #179428, #28728, #40893, #74228, #194584, #134913, #102566, #167230, #133904, #196590, #60027, #164251, #59035, #150071, #195595, #181414, #26738, #135896, #56054, #183390, #58060, #120702, #57067, #104557, #29702, #132895, #105544, #25746, #42892, #136872, #91333, #9566, #118742, #180430, #27739, #71232, #11576, #88377, #119731, #43879, #89382, #182401, #152050, #104444, #28616, #105431, #165130, #14409, #29591, #91222, #199433, #90253, #89270, #182287, #180317, #134799, #42782, #148961, #198441, #41785, #10450, #27630, #88265, #150961, #72110, #43767, #133783, #12456, #121581, #74116, #195476, #106412, #25632, #151936, #103452, #56952, #179314, #197458, #57950, #135787, #26622, #149953, #58924, #44757, #167114, #168093, #13425, #196480, #120592, #75089, #136756, #119621, #152913, #137749, #76073, #118626, #59913, #11458, #73130, #117616, #40778, #183276, #102447, #164135, #166128, #181304, #87276, #95221, #61888, #15410, #33558, #31573, #122575, #107399, #123558, #81038, #124569, #48736, #94221, #3213, #45747, #77068, #153915, #96211, #79055, #110390, #169072, #125569, #30578, #186265, #142714, #188248, #92229, #187267, #156907, #46746, #184265, #185253, #126548, #138738, #47744, #172072, #18404, #108405, #157900, #173075, #34552, #60901, #80053, #32568, #141723, #170081, #78053, #109397, #219, #64887, #93224, #154909, #171077, #16407, #155901, #139722, #49722, #1211, #17398, #111389, #140728, #62889, #19389, #2217, #63899, #128533, #158876, #65872, #84029, #144705, #114363, #66870, #36526, #176068, #131546, #192230, #54704, #38547, #83031, #22378, #160887, #130532, #21373, #116376, #24391, #193230, #20365, #7189, #143709, #51706, #86040, #4194, #115388, #145707, #127546, #191226, #190228, #113369, #189246, #50724, #68873, #112382, #6191, #98180, #174074, #8202, #161884, #67871, #37535, #82013, #53711, #35543, #97190, #5189, #177076, #178065, #39533, #100203, #23379, #101191, #85025, #175060, #146705, #159884, #69877, #129526, #162882, #52700, #99199, #12223, #10214, #164897, #72893, #179074, #28388, #71874, #40544, #57718, #118389, #181071, #102214, #121351, #183044, #134561, #133543, #106183, #27387, #195234, #29366, #163903, #73886, #167866, #88030, #25399, #135556, #120359, #43535, #197228, #182052, #89033, #90026, #165890, #9215, #87041, #105200, #180083, #132550, #55704, #166887, #148726, #42546, #104209, #151709, #26391, #44527, #58690, #150724, #147728, #194238, #41552, #13202, #74865, #56717, #136527, #117377, #59679, #198208, #103215, #70882, #149718, #11217, #196249, #119388, #97691, #159382, #46504, #123325, #129036, #96709, #35054, #190737, #81527, #154677, #60667, #112883, #122340, #158397, #75841, #16172, #199199, #51222, #30344, #77826, #82535, #184031, #143214, #31340, #15176, #65389, #185019, #19886, #137518, #144217, #142227, #4695, #138506, #188756, #5701, #14172, #189750, #45513, #127050, #20877, #175565, #67378, #107168, #168839, #111897, #52211 ),
 ( #50241, #113868, #3712, #66386, #91985, #173585, #90997, #152683, #153680, #128048, #174577, #76835, #200188, #61657, #108164, #169846, #36042, #92991, #24898, #84530, #134062, #149232, #10723, #118901, #148229, #8718, #101711, #99708, #54219, #162385, #68373, #117894, #161392, #130025, #147227, #7695, #37041, #40038, #38052, #21884, #70387, #41056, #132055, #53206, #25900, #145213, #9723, #22884, #191724, #98701, #116881, #177580, #193744, #146207, #69377, #55212, #164408, #86545, #87545, #71387, #115890, #178573, #163402, #133051, #39047, #72387, #57227, #195753, #114884, #194741, #176578, #131047, #160395, #83534, #56213, #179584, #6695, #23888, #192737, #100705, #85540, #102719, #183544, #103723, #59187, #74381, #150236, #184531, #138023, #182556, #152204, #196746, #60182, #180585, #62158, #42059, #153181, #107666, #30852, #121852, #168361, #169343, #198715, #165403, #45030, #26896, #199706, #88539, #91494, #73399, #46011, #14684, #181567, #135070, #76346, #151226, #11732, #58213, #43045, #485, #44039, #29857, #13688, #122843, #119882, #104711, #166401, #15678, #106688, #61171, #27897, #136046, #12715, #77339, #92499, #154188, #139005, #89540, #105699, #197721, #120856, #167386, #28882, #90522, #75355, #137025, #81286, #63158, #48996, #112638, #16669, #173338, #64163, #48010, #95481, #156167, #126802, #108671, #174330, #172332, #188510, #171346, #18661, #35800, #47012, #19645, #78318, #157167, #189503, #5453, #50978, #139991, #93492, #141980, #82281, #125828, #79324, #159132, #158153, #124837, #20629, #31841, #80307, #187531, #3468, #143973, #155179, #142970, #65145, #123822, #110652, #97446, #170349, #111652, #49987, #1480, #94485, #4447, #34810, #185520, #186537, #96465, #109666, #32835, #17666, #140994, #2482, #33821, #66137, #127800, #146980, #114630, #148987, #160145, #193491, #25659, #7447, #144966, #131812, #39793, #163148, #116640, #101457, #8467, #147989, #85288, #128794, #83290, #24651, #37799, #51966, #175320, #86300, #6447, #100465, #162144, #9478, #145965, #102474, #54970, #23640, #67136, #113625, #161142, #178330, #71142, #68128, #55967, #36786, #179341, #70141, #129779, #164161, #99462, #132808, #191476, #52954, #194494, #117644, #69131, #177336, #176329, #22639, #38807, #40804, #87304, #190494, #98452, #130799, #21636, #84286, #192490, #53973, #115646, #30604, #137774, #26648, #13450, #149979, #57975, #92257, #10477, #121607, #167143, #133813, #197483, #73156, #119647, #72137, #56977, #75114, #195504, #89296, #104470, #180342, #14436, #168118, #12480, #182314, #88291, #90278, #118651, #41810, #103478, #183302, #199460, #60927, #151962, #198468, #122601, #28642, #165156, #136782, #11485, #29614, #134826, #44784, #196505, #76099, #106437, #181329, #42808, #91246, #166155, #27656, #150988, #74141, #135813, #58950, #59939, #43794, #152937, #120618, #105457, #184291, #45772, #107425, #169097, #61913, #18427, #123584, #79079, #174097, #81061, #185278, #80077, #126571, #139748, #15436, #154934, #19412, #170105, #140752, #64910, #141746, #1235, #50747, #65896, #127570, #35566, #188272, #125592, #3236, #16431, #171101, #2240, #46770, #34577, #78079, #108429, #63923, #124594, #153941, #156930, #62914, #138764, #187289, #157922, #48760, #31599, #142738, #93248, #49745, #186289, #47769, #77095, #33582, #111414, #109422, #110414, #4218, #245, #173100, #32594, #172096, #189271, #94246, #112405, #155927, #17422, #95245, #96234, #37561, #52724, #132577, #131573, #98205, #194265, #5214, #192256, #160911, #68899, #55732, #66895, #54731, #53738, #117406, #22404, #147756, #143735, #85052, #130558, #128558, #67896, #116403, #8229, #70909, #179103, #115412, #190253, #83056, #51730, #97214, #158900, #84055, #159909, #20391, #177101, #144730, #82038, #113393, #23404, #175083, #99224, #36551, #161910, #69907, #193257, #146733, #178092, #38572, #39562, #100228, #21398, #6217, #101220, #129549 ),
 ( #191249, #145733, #114389, #176091, #7214, #162909, #24417, #86066, #9242, #134590, #10242, #44554, #198235, #42573, #12250, #56747, #120385, #40572, #122368, #102242, #13228, #167893, #91023, #182079, #28416, #29393, #58716, #163930, #43562, #25427, #59706, #87068, #151735, #133573, #106209, #74891, #41579, #195263, #136554, #11247, #148753, #71901, #103243, #60692, #104236, #90053, #26418, #118418, #14200, #75868, #27415, #164925, #199227, #105227, #88058, #180111, #149745, #166915, #72921, #181099, #196276, #121379, #183071, #152709, #137544, #57745, #119415, #165919, #89061, #150752, #73912, #135582, #197254, #168865, #92014, #141521, #10, #17191, #78845, #18195, #62678, #19184, #171865, #140523, #65668, #30370, #77854, #33354, #95013, #123353, #172867, #153707, #96009, #2013, #61684, #80833, #16199, #64685, #185046, #46534, #188044, #49514, #139521, #1004, #142510, #187063, #125367, #3988, #156701, #47538, #15203, #3008, #76862, #48533, #138532, #109192, #108193, #126347, #169875, #170871, #34348, #31368, #79852, #124359, #93018, #155696, #186054, #110187, #154706, #157693, #32362, #111177, #94015, #63692, #184057, #107194, #45540, #20161, #160670, #193018, #9004, #54495, #81806, #96989, #145493, #85826, #67659, #82814, #162669, #161670, #128327, #24175, #35336, #22162, #191012, #98980, #147514, #158671, #84809, #83813, #127330, #52488, #177857, #173868, #115167, #6973, #143493, #97970, #146488, #38329, #100985, #189042, #68653, #4978, #23166, #190026, #50517, #66664, #130309, #114148, #192004, #112180, #51500, #7979, #53490, #113160, #175849, #39326, #174850, #176860, #99985, #36316, #159662, #69663, #131330, #21159, #144496, #116167, #5979, #129316, #37322, #44320, #105979, #57509, #133331, #29160, #150517, #118176, #152481, #163683, #197022, #90797, #11002, #148514, #135348, #43325, #166680, #120155, #104992, #12015, #151504, #88824, #132338, #86828, #28181, #41337, #55493, #178859, #89823, #10004, #104000, #165678, #12996, #149505, #167664, #58488, #27177, #70671, #117163, #164684, #181845, #74659, #71664, #59471, #40325, #182838, #73676, #195022, #194030, #102998, #136326, #56498, #179867, #198001, #121144, #26178, #87819, #102001, #25186, #72674, #134351, #196033, #119178, #180863, #42339, #45314, #78613, #198994, #77628, #122137, #171635, #153475, #139297, #2775, #106964, #63457, #154475, #138309, #185819, #46299, #16959, #60462, #64451, #62445, #140287, #61457, #108962, #126121, #137313, #109956, #168638, #47306, #79616, #95774, #141285, #30138, #183824, #32130, #172628, #15968, #169643, #49285, #170642, #110943, #775, #187816, #91781, #1778, #93788, #14971, #184813, #33124, #125133, #34116, #13968, #155468, #76631, #199990, #123128, #75635, #107956, #124119, #31139, #92787, #186831, #48299, #94781, #156462, #17961, #115936, #97737, #35101, #21929, #130071, #53253, #6740, #191770, #37087, #38099, #175611, #18954, #173631, #114931, #128092, #142275, #65434, #176624, #96753, #190780, #52255, #99754, #36087, #192781, #145259, #113912, #39094, #3757, #51267, #68418, #161438, #158443, #146254, #127095, #69426, #98746, #19931, #54264, #189796, #22930, #81572, #143258, #84576, #7740, #112927, #174622, #177626, #160439, #83580, #157460, #131093, #20922, #188804, #80599, #50287, #111944, #4742, #82580, #66431, #159426, #144261, #5748, #67424, #129080, #152975, #43830, #24945, #75151, #133096, #106476, #85587, #92295, #152000, #168155, #148276, #198506, #153979, #23932, #199498, #193789, #136822, #169137, #185314, #30642, #55258, #70433, #121644, #61952, #105494, #58987, #138802, #137814, #101760, #283, #8764, #59977, #167180, #183339, #123619, #132099, #60964, #100750, #28679, #178619, #29652, #76136, #122638, #14474, #184328, #44821, #45810, #91284, #162431, #116926, #107461, #71432, #147273, #40082, #15476, #163448, #77133, #86593, #9768, #182352, #197519, #120654, #90314, #13486 ),
 ( #186324, #47806, #50780, #112440, #154970, #174129, #16466, #19446, #35600, #97246, #126604, #34610, #158934, #64945, #128591, #188306, #108464, #4253, #170141, #157955, #139784, #20423, #81094, #109456, #1272, #142772, #17457, #31636, #93285, #171139, #66928, #110450, #96269, #80111, #189303, #78115, #62949, #124629, #82073, #49783, #65932, #32628, #111448, #94282, #172131, #46805, #143766, #155960, #173135, #127604, #79113, #140786, #2275, #5247, #63958, #33617, #125627, #187325, #48796, #95280, #156963, #18460, #141779, #3273, #161941, #54763, #52752, #7245, #115442, #21427, #70940, #114421, #83087, #100260, #160942, #71933, #193289, #191277, #175114, #23436, #194297, #85083, #6248, #179135, #98237, #101252, #176122, #116437, #148785, #130592, #67927, #178126, #162941, #86097, #39593, #24448, #69940, #132608, #8260, #51761, #129581, #147788, #22435, #36582, #159940, #9274, #37593, #146767, #131604, #55763, #68930, #25460, #117437, #40603, #190285, #144763, #84084, #102274, #163962, #99255, #87100, #145763, #10274, #113422, #192288, #53768, #177133, #38604, #72951, #134621, #137575, #184090, #199259, #196305, #57775, #136583, #74920, #30403, #121408, #197283, #103275, #152740, #164955, #198263, #118450, #58746, #41610, #91053, #119445, #120415, #122400, #26448, #183102, #73943, #181130, #105257, #165950, #59739, #180141, #45573, #182106, #44583, #42604, #28446, #107226, #56777, #29422, #88090, #166943, #60726, #15234, #168897, #149776, #11278, #151764, #92049, #135612, #89091, #153738, #167922, #104268, #133603, #27450, #90082, #43591, #13257, #195296, #150783, #14230, #106240, #12278, #75901, #127366, #123385, #64719, #110219, #185077, #47571, #96042, #188078, #50551, #112211, #171900, #46566, #62711, #31400, #173901, #35370, #63724, #139554, #97022, #156736, #124393, #158703, #169907, #1038, #186088, #76893, #108227, #79884, #42, #155727, #170902, #93051, #80868, #34382, #78877, #48566, #154738, #16234, #77886, #142544, #109223, #49549, #4022, #189078, #18229, #126381, #65700, #95047, #138564, #141554, #61717, #157729, #32394, #111212, #94049, #17225, #172904, #140556, #2044, #19218, #125399, #187096, #33388, #3043, #40361, #83845, #8014, #53523, #162705, #5014, #174884, #113195, #55527, #38364, #69697, #128360, #84845, #190056, #145527, #102036, #147548, #51532, #146523, #193053, #6015, #81838, #21194, #85859, #36350, #7006, #131364, #54530, #67694, #117201, #132373, #194066, #20192, #116203, #192042, #177892, #82850, #37356, #68688, #98003, #101020, #144529, #159697, #130343, #191047, #143526, #23202, #129352, #66696, #115201, #24210, #176893, #52520, #9036, #114181, #39362, #175885, #99014, #160705, #100019, #22196, #161706, #70705, #178893, #135383, #90828, #151538, #14000, #198034, #42370, #181877, #120187, #89855, #180895, #75667, #183859, #152512, #179903, #166711, #103035, #11034, #45346, #163719, #74693, #43356, #86863, #150548, #29194, #41369, #12047, #136358, #13027, #72710, #60493, #137344, #199024, #25221, #59502, #197053, #28215, #26212, #104033, #88855, #195056, #44352, #87851, #56534, #73711, #134382, #148547, #121177, #164717, #10038, #58521, #167697, #105027, #149539, #122169, #71698, #182871, #196068, #118212, #133365, #106011, #165712, #57541, #119210, #27209, #170676, #79651, #63492, #2809, #109990, #139330, #16994, #93821, #1813, #77661, #64487, #110979, #141320, #200023, #78648, #123161, #169675, #172664, #106998, #48335, #155501, #91815, #47340, #46333, #92821, #168671, #15004, #125167, #153507, #62482, #809, #138343, #126154, #156496, #124154, #140323, #184849, #76664, #61491, #187850, #107989, #171670, #49319, #30172, #31171, #154507, #16003, #185854, #108995, #32164, #186866, #33159, #17998, #94818, #180553, #91464, #121820, #88506, #42027, #60151, #58184, #149200, #134028, #150202, #107637, #151197, #75325, #120825, #29827, #72354, #103691, #165370, #122812 ),
 ( #11700, #184502, #14653, #26864, #57194, #105668, #45982, #27866, #43015, #169314, #183515, #73367, #87512, #195721, #182525, #12685, #59156, #10690, #118869, #44998, #44006, #135039, #74351, #137991, #196715, #136995, #167354, #119852, #181536, #106658, #198684, #61140, #104682, #28852, #166369, #89507, #136017, #197691, #90492, #152174, #13657, #168331, #153151, #76313, #199674, #123793, #157138, #189475, #171318, #108641, #95453, #3441, #126775, #80280, #65117, #110622, #111624, #48968, #92469, #46981, #188480, #1451, #15649, #138976, #49960, #170319, #64135, #125799, #173309, #109635, #66109, #18634, #187501, #112612, #77307, #124808, #141952, #34784, #31811, #19618, #454, #142941, #172304, #93462, #127775, #63129, #96439, #155148, #16641, #158126, #81260, #4423, #78288, #139962, #33793, #50953, #30821, #154158, #94457, #62129, #185491, #186508, #47982, #32805, #156138, #17636, #79296, #140965, #2453, #163121, #67108, #23615, #114602, #98421, #145939, #6420, #177309, #159106, #24624, #22611, #38781, #21605, #69104, #86272, #97420, #70114, #128766, #7420, #39766, #55939, #192462, #132781, #176299, #129753, #9450, #8441, #175292, #71115, #82252, #130770, #37771, #53945, #194468, #143943, #131785, #115621, #174304, #99434, #147963, #20600, #162118, #100437, #5424, #144938, #193465, #85262, #35773, #190465, #146953, #51938, #160118, #113598, #36758, #83264, #161115, #68101, #191450, #54942, #52927, #84257, #116614, #178302, #101430, #170621, #108940, #2754, #155448, #125111, #64430, #19910, #80579, #143238, #127075, #171616, #110923, #49265, #18934, #109934, #4721, #112907, #81552, #32110, #95754, #93767, #140265, #174601, #92765, #3737, #172609, #15947, #79595, #16938, #1757, #154455, #139277, #157439, #77606, #33104, #186809, #62425, #96733, #50266, #94760, #126100, #78592, #754, #124097, #158422, #185796, #65414, #66410, #128072, #34096, #142253, #189775, #188783, #47284, #111924, #63435, #173610, #48279, #35080, #156442, #51247, #17941, #141264, #187796, #8744, #6719, #97716, #82559, #37066, #56240, #99732, #23913, #69405, #178600, #20901, #190760, #129059, #71412, #54243, #85567, #144241, #100730, #5725, #161416, #159406, #67404, #98725, #117921, #22908, #147253, #131071, #40063, #52235, #113892, #175590, #133076, #115915, #70414, #160419, #162411, #21908, #84554, #36067, #163428, #83559, #132081, #193770, #145238, #68397, #130049, #101740, #191749, #146232, #55239, #116907, #53232, #194766, #148255, #9748, #114908, #24926, #7719, #86571, #176602, #38076, #192760, #177605, #39073, #103751, #72414, #89568, #150265, #61199, #182584, #180613, #164434, #12744, #183573, #74409, #195781, #168390, #87571, #90550, #165430, #44067, #119909, #57254, #118928, #151254, #42086, #11759, #136075, #106716, #167414, #29885, #13717, #58241, #197749, #59216, #105727, #196773, #91523, #199733, #153210, #26925, #28910, #88567, #73426, #179610, #41083, #152232, #120885, #102746, #166430, #135097, #181595, #25928, #149258, #75383, #10750, #43072, #104739, #134091, #45058, #137055, #27925, #198745, #60210, #121880, #14715, #76375, #138052, #95512, #50019, #173371, #2513, #110682, #111684, #141026, #4479, #64193, #184559, #80339, #46040, #33852, #15708, #126835, #157198, #123852, #77368, #18692, #93525, #172362, #156198, #65176, #107695, #139036, #516, #158186, #125860, #142011, #30882, #187560, #92529, #48041, #143001, #34841, #154218, #49027, #3500, #108701, #169374, #185550, #188541, #62188, #109697, #96496, #19676, #170380, #81318, #122871, #47044, #31871, #155210, #94516, #16699, #78349, #140023, #171379, #1512, #63189, #124869, #186568, #32866, #17698, #79355, #69164, #67167, #51009, #99494, #70175, #161174, #82313, #57758, #174362, #177367, #190523, #130831, #6479, #144003, #5484, #176361, #128824, #98484, #37834, #193526, #54005, #119428, #100496, #144998, #84318, #22671, #192522, #83321 ),
 ( #51997, #175350, #66169, #112670, #115679, #189537, #68159, #160177, #35832, #131843, #23673, #129811, #145997, #113656, #97478, #159164, #181112, #20659, #38838, #42586, #104249, #7480, #162175, #165932, #85321, #150765, #147013, #127831, #8498, #36818, #27430, #21667, #89074, #191510, #52987, #114665, #185060, #183085, #73926, #58729, #13241, #32376, #75883, #15217, #197267, #1019, #60706, #76876, #59723, #107209, #62692, #135595, #108210, #105240, #45555, #77868, #94029, #139535, #166928, #182092, #30384, #170885, #152724, #167907, #47552, #46548, #74904, #109205, #120399, #168879, #137558, #184071, #12262, #43576, #169889, #92031, #28429, #199241, #124374, #90066, #24, #153721, #151748, #44568, #31383, #123367, #186069, #136568, #138546, #198248, #121393, #106223, #29407, #91037, #122382, #14214, #61698, #93032, #154720, #16213, #48547, #20175, #19200, #191028, #112194, #81821, #128341, #143508, #141536, #82830, #4994, #5996, #190040, #34363, #173883, #35353, #66679, #172883, #67675, #175866, #144511, #171880, #158686, #95027, #3025, #37338, #155709, #51514, #97004, #78858, #142526, #18209, #64701, #17205, #2026, #113176, #140538, #96024, #49529, #125381, #159679, #174866, #157710, #127346, #33369, #63706, #187078, #21175, #110201, #36332, #129333, #52503, #97985, #114163, #156717, #79867, #126363, #188059, #111192, #80849, #4004, #65683, #189060, #50532, #133346, #100000, #53505, #71679, #69679, #160685, #145508, #115182, #87833, #6989, #10020, #23182, #102017, #39342, #176875, #38344, #161686, #84825, #86844, #146505, #26194, #148529, #149519, #195037, #177874, #117180, #55510, #25202, #116183, #11016, #119192, #72689, #7995, #163700, #131346, #193034, #180877, #98996, #56514, #178875, #22177, #85842, #54511, #101001, #83827, #68670, #118192, #130324, #162686, #24192, #192021, #103015, #179883, #147532, #70688, #9020, #132354, #194046, #164698, #40342, #41351, #134364, #196048, #57523, #30151, #31150, #60473, #124132, #183838, #104014, #200003, #165692, #153487, #135364, #46312, #76643, #43338, #197035, #14983, #13009, #27190, #88837, #105006, #62459, #105991, #91793, #75647, #184826, #150530, #58502, #120168, #77639, #122149, #138321, #12029, #106977, #73692, #167677, #42352, #169654, #181859, #168651, #61469, #28195, #166692, #89837, #107967, #151518, #29174, #123140, #92798, #74673, #139308, #154486, #15980, #136340, #787, #13981, #198015, #59484, #121158, #90810, #182851, #44334, #152493, #137325, #199006, #45327, #67434, #188814, #186843, #170654, #18965, #189806, #80611, #143269, #1791, #142288, #3768, #19942, #64465, #20932, #173643, #65445, #185831, #32142, #79628, #35112, #96764, #125144, #174632, #93799, #97749, #127107, #63469, #82590, #17974, #66441, #48312, #109967, #51278, #36097, #112939, #171646, #33136, #50297, #111954, #144271, #158453, #49296, #155479, #4752, #16971, #81583, #78625, #110955, #140300, #128102, #94794, #172639, #159437, #156473, #5758, #126132, #141296, #157472, #2786, #47318, #187827, #108973, #34127, #95786, #176634, #23943, #117952, #52265, #24956, #21940, #162442, #194796, #10780, #56269, #83590, #98756, #147284, #87600, #69436, #84586, #164463, #163458, #130083, #25957, #37097, #85597, #192792, #100760, #149286, #160449, #86603, #8774, #129091, #54274, #179643, #175623, #116937, #70443, #145270, #99764, #148286, #40093, #102776, #190791, #132109, #6751, #114941, #68430, #113923, #191782, #115947, #53264, #38109, #193802, #161449, #22940, #146266, #55268, #177637, #7752, #178630, #131104, #101771, #39104, #9780, #71442, #133107, #41112, #90584, #134122, #88599, #106749, #43104, #57283, #180643, #167446, #154252, #118957, #166460, #121915, #60244, #11791, #61234, #42118, #184594, #28943, #150295, #107729, #104772, #153247, #73455, #135128, #76410, #122906, #138086, #196802, #58270, #75418, #13750, #169411, #183608, #136107, #103780, #91559, #165460 ),
 ( #195811, #26956, #119939, #92564, #197783, #45092, #105760, #14749, #181624, #27957, #89598, #30916, #152265, #168424, #151286, #137092, #12775, #59249, #72447, #199767, #74440, #198778, #29919, #120918, #182617, #44102, #46075, #31906, #2549, #126871, #3535, #63225, #112706, #127868, #189572, #97514, #188578, #187596, #80376, #78383, #32901, #141063, #47077, #96531, #140059, #108738, #125896, #186603, #15743, #18728, #16735, #550, #49065, #19711, #110720, #93559, #4515, #123889, #50059, #1550, #142048, #156234, #155245, #124905, #48075, #109731, #65212, #171415, #143037, #111720, #66208, #173406, #94554, #33891, #172402, #34877, #17736, #51044, #35868, #174398, #79393, #158221, #64231, #95548, #77402, #157235, #81353, #139072, #170414, #62221, #185587, #194561, #115715, #190559, #70211, #114704, #5521, #131878, #38874, #39859, #177403, #20695, #175385, #193563, #129847, #144039, #67201, #116705, #36854, #192558, #54041, #55035, #37872, #56031, #147049, #100531, #40869, #128859, #53023, #8532, #178395, #98521, #148052, #52033, #71209, #162210, #160214, #117709, #191546, #101525, #21704, #83358, #163216, #9543, #24718, #145034, #6516, #23709, #85356, #179405, #86367, #22707, #113690, #132872, #68195, #159200, #176397, #84354, #99530, #82351, #161212, #146032, #7515, #69200, #130868, #42870, #26716, #74205, #134891, #105522, #87369, #91310, #151049, #167208, #150048, #197545, #153002, #25723, #198534, #195571, #135874, #168182, #184354, #29678, #57044, #72206, #120680, #60992, #104535, #58038, #137843, #136849, #103546, #199524, #10542, #59013, #166216, #182379, #122666, #133880, #60005, #43857, #102543, #27717, #14501, #149054, #90341, #28705, #118718, #73220, #121672, #13512, #76163, #164226, #152026, #180407, #88355, #41879, #165221, #11554, #89360, #196567, #119708, #181392, #12540, #75177, #183367, #44849, #106505, #96292, #125653, #33641, #34633, #63983, #127628, #187350, #107487, #3297, #169165, #156987, #138830, #49808, #80134, #46832, #310, #18485, #16494, #30669, #92322, #108492, #65957, #109485, #95303, #79141, #188329, #154007, #61978, #123644, #81116, #48820, #141804, #15503, #110473, #77160, #171168, #45836, #173158, #185341, #172155, #64969, #31664, #170171, #93314, #111473, #154998, #32655, #126628, #157979, #78143, #142796, #19471, #4277, #139811, #1299, #17484, #62977, #124657, #186353, #94309, #47833, #155987, #140812, #2302, #99280, #159966, #70966, #192313, #190311, #174155, #22461, #193315, #84109, #5275, #178153, #97271, #100287, #113447, #53793, #129606, #66957, #128618, #51787, #175140, #177157, #36607, #116464, #38630, #39618, #23461, #67952, #7270, #145788, #115468, #6274, #101277, #9300, #162967, #98264, #161965, #21453, #83114, #189328, #50805, #85108, #68954, #112463, #176148, #144791, #191302, #35626, #158959, #146794, #20449, #52778, #114447, #82100, #54789, #8287, #37618, #160967, #130617, #24473, #69965, #131631, #143792, #86123, #147814, #57800, #152766, #59766, #40628, #58772, #105281, #118476, #194322, #133631, #198288, #148811, #119471, #43617, #120440, #180167, #29447, #44610, #106265, #14256, #166969, #104293, #197308, #195323, #149801, #181154, #163987, #13281, #56803, #25484, #42629, #103301, #132634, #135638, #41636, #117461, #165974, #136608, #27476, #10301, #121434, #102298, #28471, #164980, #182133, #72977, #71958, #26475, #88117, #11307, #90106, #134646, #183127, #151790, #167949, #74945, #196332, #150807, #89119, #91079, #12303, #55790, #179160, #87126, #73969, #78900, #15260, #123409, #160490, #75927, #187117, #32416, #199285, #62735, #138589, #185102, #137602, #122425, #140578, #60752, #154760, #169932, #45599, #82628, #36136, #77909, #47592, #92076, #184117, #107252, #144310, #168923, #48589, #5800, #129132, #155750, #63747, #67473, #94071, #30429, #17248, #153765, #97788, #76918, #112978, #70, #190830, #174671, #61741, #46591, #159477 ) ),
 .UNSPECIFIED., .T., .F., .T. ) 
 B_SPLINE_SURFACE_WITH_KNOTS ( ( 4, 3, 4 ),
 ( 3, 2, 2, 2, 2, 2, 2, 2, 2, 2, 2, 2, 2, 2, 2, 2, 2, 2, 2, 2, 2, 2, 2, 2, 2, 2, 2, 2, 2, 2, 2, 2, 2, 2, 2, 2, 2, 2, 2, 2, 2, 2, 2, 2, 2, 2, 2, 2, 2, 2, 2, 2, 2, 2, 2, 2, 2, 2, 2, 2, 2, 2, 2, 2, 2, 2, 2, 2, 2, 2, 2, 2, 2, 2, 2, 2, 2, 2, 2, 2, 2, 2, 2, 2, 2, 2, 2, 2, 2, 2, 2, 2, 2, 2, 2, 2, 2, 2, 2, 2, 2, 2, 2, 2, 2, 2, 2, 2, 2, 2, 2, 2, 2, 2, 2, 2, 2, 2, 2, 2, 2, 2, 2, 2, 2, 2, 2, 2, 2, 2, 2, 2, 2, 2, 2, 2, 2, 2, 2, 2, 2, 2, 2, 2, 2, 2, 2, 2, 2, 2, 2, 2, 2, 2, 2, 2, 2, 2, 2, 2, 2, 2, 2, 2, 2, 2, 2, 2, 2, 2, 2, 2, 2, 2, 2, 2, 2, 2, 2, 2, 2, 2, 2, 2, 2, 2, 2, 2, 2, 2, 2, 2, 2, 2, 2, 2, 2, 2, 2, 2, 2, 2, 2, 2, 2, 2, 2, 2, 2, 2, 2, 2, 2, 2, 2, 2, 2, 2, 2, 2, 2, 2, 2, 2, 2, 2, 2, 2, 3 ),
 ( 0.000000000000000000, 0.5000000000000000000, 1.000000000000000000 ),
 ( 0.000000000000000000, 0.004385964912280701511, 0.008771929824561403022, 0.01315789473684210453, 0.01754385964912280604, 0.02192982456140350755, 0.02631578947368420907, 0.03070175438596491058, 0.03508771929824561209, 0.03947368421052631360, 0.04385964912280701511, 0.04824561403508771662, 0.05263157894736841813, 0.05701754385964911964, 0.06140350877192982115, 0.06578947368421052266, 0.07017543859649122417, 0.07456140350877192569, 0.07894736842105262720, 0.08333333333333332871, 0.08771929824561403022, 0.09210526315789473173, 0.09649122807017543324, 0.1008771929824561348, 0.1052631578947368363, 0.1096491228070175378, 0.1140350877192982393, 0.1184210526315789408, 0.1228070175438596423, 0.1271929824561403577, 0.1315789473684210453, 0.1359649122807017607, 0.1403508771929824483, 0.1447368421052631637, 0.1491228070175438514, 0.1535087719298245668, 0.1578947368421052544, 0.1622807017543859698, 0.1666666666666666574, 0.1710526315789473728, 0.1754385964912280604, 0.1798245614035087758, 0.1842105263157894635, 0.1885964912280701788, 0.1929824561403508665, 0.1973684210526315819, 0.2017543859649122695, 0.2061403508771929849, 0.2105263157894736725, 0.2149122807017543879, 0.2192982456140350755, 0.2236842105263157909, 0.2280701754385964786, 0.2324561403508771940, 0.2368421052631578816, 0.2412280701754385970, 0.2456140350877192846, 0.2500000000000000000, 0.2543859649122807154, 0.2587719298245614308, 0.2631578947368420907, 0.2675438596491228060, 0.2719298245614035214, 0.2763157894736842368, 0.2807017543859648967, 0.2850877192982456121, 0.2894736842105263275, 0.2938596491228070429, 0.2982456140350877027, 0.3026315789473684181, 0.3070175438596491335, 0.3114035087719298489, 0.3157894736842105088, 0.3201754385964912242, 0.3245614035087719396, 0.3289473684210526550, 0.3333333333333333148, 0.3377192982456140302, 0.3421052631578947456, 0.3464912280701754610, 0.3508771929824561209, 0.3552631578947368363, 0.3596491228070175517, 0.3640350877192982670, 0.3684210526315789269, 0.3728070175438596423, 0.3771929824561403577, 0.3815789473684210731, 0.3859649122807017330, 0.3903508771929824483, 0.3947368421052631637, 0.3991228070175438791, 0.4035087719298245390, 0.4078947368421052544, 0.4122807017543859698, 0.4166666666666666852, 0.4210526315789473450, 0.4254385964912280604, 0.4298245614035087758, 0.4342105263157894912, 0.4385964912280701511, 0.4429824561403508665, 0.4473684210526315819, 0.4517543859649122973, 0.4561403508771929571, 0.4605263157894736725, 0.4649122807017543879, 0.4692982456140351033, 0.4736842105263157632, 0.4780701754385964786, 0.4824561403508771940, 0.4868421052631579093, 0.4912280701754385692, 0.4956140350877192846, 0.5000000000000000000, 0.5043859649122807154, 0.5087719298245614308, 0.5131578947368421462, 0.5175438596491228616, 0.5219298245614034659, 0.5263157894736841813, 0.5307017543859648967, 0.5350877192982456121, 0.5394736842105263275, 0.5438596491228070429, 0.5482456140350877583, 0.5526315789473684736, 0.5570175438596490780, 0.5614035087719297934, 0.5657894736842105088, 0.5701754385964912242, 0.5745614035087719396, 0.5789473684210526550, 0.5833333333333333703, 0.5877192982456140857, 0.5921052631578946901, 0.5964912280701754055, 0.6008771929824561209, 0.6052631578947368363, 0.6096491228070175517, 0.6140350877192982670, 0.6184210526315789824, 0.6228070175438596978, 0.6271929824561403022, 0.6315789473684210176, 0.6359649122807017330, 0.6403508771929824483, 0.6447368421052631637, 0.6491228070175438791, 0.6535087719298245945, 0.6578947368421053099, 0.6622807017543859143, 0.6666666666666666297, 0.6710526315789473450, 0.6754385964912280604, 0.6798245614035087758, 0.6842105263157894912, 0.6885964912280702066, 0.6929824561403509220, 0.6973684210526315264, 0.7017543859649122417, 0.7061403508771929571, 0.7105263157894736725, 0.7149122807017543879, 0.7192982456140351033, 0.7236842105263158187, 0.7280701754385965341, 0.7324561403508771384, 0.7368421052631578538, 0.7412280701754385692, 0.7456140350877192846, 0.7500000000000000000, 0.7543859649122807154, 0.7587719298245614308, 0.7631578947368421462, 0.7675438596491228616, 0.7719298245614034659, 0.7763157894736841813, 0.7807017543859648967, 0.7850877192982456121, 0.7894736842105263275, 0.7938596491228070429, 0.7982456140350877583, 0.8026315789473684736, 0.8070175438596490780, 0.8114035087719297934, 0.8157894736842105088, 0.8201754385964912242, 0.8245614035087719396, 0.8289473684210526550, 0.8333333333333333703, 0.8377192982456140857, 0.8421052631578946901, 0.8464912280701754055, 0.8508771929824561209, 0.8552631578947368363, 0.8596491228070175517, 0.8640350877192982670, 0.8684210526315789824, 0.8728070175438596978, 0.8771929824561403022, 0.8815789473684210176, 0.8859649122807017330, 0.8903508771929824483, 0.8947368421052631637, 0.8991228070175438791, 0.9035087719298245945, 0.9078947368421053099, 0.9122807017543859143, 0.9166666666666666297, 0.9210526315789473450, 0.9254385964912280604, 0.9298245614035087758, 0.9342105263157894912, 0.9385964912280702066, 0.9429824561403509220, 0.9473684210526315264, 0.9517543859649122417, 0.9561403508771929571, 0.9605263157894736725, 0.9649122807017543879, 0.9692982456140351033, 0.9736842105263158187, 0.9780701754385965341, 0.9824561403508771384, 0.9868421052631578538, 0.9912280701754385692, 0.9956140350877192846, 1.000000000000000000 ),
 .UNSPECIFIED. ) 
 GEOMETRIC_REPRESENTATION_ITEM ( )  RATIONAL_B_SPLINE_SURFACE ( (
 ( 1.000000000000000000, 0.9659258262890683122, 1.000000000000000000, 0.9659258262890683122, 1.000000000000000000, 0.9659258262890683122, 1.000000000000000000, 0.9659258262890683122, 1.000000000000000000, 0.9659258262890683122, 1.000000000000000000, 0.9659258262890683122, 1.000000000000000000, 0.9659258262890683122, 1.000000000000000000, 0.9659258262890683122, 1.000000000000000000, 0.9659258262890683122, 1.000000000000000000, 0.9659258262890683122, 1.000000000000000000, 0.9659258262890683122, 1.000000000000000000, 0.9659258262890683122, 1.000000000000000000, 0.9659258262890683122, 1.000000000000000000, 0.9659258262890683122, 1.000000000000000000, 0.9659258262890683122, 1.000000000000000000, 0.9659258262890683122, 1.000000000000000000, 0.9659258262890683122, 1.000000000000000000, 0.9659258262890683122, 1.000000000000000000, 0.9659258262890683122, 1.000000000000000000, 0.9659258262890683122, 1.000000000000000000, 0.9659258262890683122, 1.000000000000000000, 0.9659258262890683122, 1.000000000000000000, 0.9659258262890683122, 1.000000000000000000, 0.9659258262890683122, 1.000000000000000000, 0.9659258262890683122, 1.000000000000000000, 0.9659258262890683122, 1.000000000000000000, 0.9659258262890683122, 1.000000000000000000, 0.9659258262890683122, 1.000000000000000000, 0.9659258262890683122, 1.000000000000000000, 0.9659258262890683122, 1.000000000000000000, 0.9659258262890683122, 1.000000000000000000, 0.9659258262890683122, 1.000000000000000000, 0.9659258262890683122, 1.000000000000000000, 0.9659258262890683122, 1.000000000000000000, 0.9659258262890683122, 1.000000000000000000, 0.9659258262890683122, 1.000000000000000000, 0.9659258262890683122, 1.000000000000000000, 0.9659258262890683122, 1.000000000000000000, 0.9659258262890683122, 1.000000000000000000, 0.9659258262890683122, 1.000000000000000000, 0.9659258262890683122, 1.000000000000000000, 0.9659258262890683122, 1.000000000000000000, 0.9659258262890683122, 1.000000000000000000, 0.9659258262890683122, 1.000000000000000000, 0.9659258262890683122, 1.000000000000000000, 0.9659258262890683122, 1.000000000000000000, 0.9659258262890683122, 1.000000000000000000, 0.9659258262890683122, 1.000000000000000000, 0.9659258262890683122, 1.000000000000000000, 0.9659258262890683122, 1.000000000000000000, 0.9659258262890683122, 1.000000000000000000, 0.9659258262890683122, 1.000000000000000000, 0.9659258262890683122, 1.000000000000000000, 0.9659258262890683122, 1.000000000000000000, 0.9659258262890683122, 1.000000000000000000, 0.9659258262890683122, 1.000000000000000000, 0.9659258262890683122, 1.000000000000000000, 0.9659258262890683122, 1.000000000000000000, 0.9659258262890683122, 1.000000000000000000, 0.9659258262890683122, 1.000000000000000000, 0.9659258262890683122, 1.000000000000000000, 0.9659258262890683122, 1.000000000000000000, 0.9659258262890683122, 1.000000000000000000, 0.9659258262890683122, 1.000000000000000000, 0.9659258262890683122, 1.000000000000000000, 0.9659258262890683122, 1.000000000000000000, 0.9659258262890683122, 1.000000000000000000, 0.9659258262890683122, 1.000000000000000000, 0.9659258262890683122, 1.000000000000000000, 0.9659258262890683122, 1.000000000000000000, 0.9659258262890683122, 1.000000000000000000, 0.9659258262890683122, 1.000000000000000000, 0.9659258262890683122, 1.000000000000000000, 0.9659258262890683122, 1.000000000000000000, 0.9659258262890683122, 1.000000000000000000, 0.9659258262890683122, 1.000000000000000000, 0.9659258262890683122, 1.000000000000000000, 0.9659258262890683122, 1.000000000000000000, 0.9659258262890683122, 1.000000000000000000, 0.9659258262890683122, 1.000000000000000000, 0.9659258262890683122, 1.000000000000000000, 0.9659258262890683122, 1.000000000000000000, 0.9659258262890683122, 1.000000000000000000, 0.9659258262890683122, 1.000000000000000000, 0.9659258262890683122, 1.000000000000000000, 0.9659258262890683122, 1.000000000000000000, 0.9659258262890683122, 1.000000000000000000, 0.9659258262890683122, 1.000000000000000000, 0.9659258262890683122, 1.000000000000000000, 0.9659258262890683122, 1.000000000000000000, 0.9659258262890683122, 1.000000000000000000, 0.9659258262890683122, 1.000000000000000000, 0.9659258262890683122, 1.000000000000000000, 0.9659258262890683122, 1.000000000000000000, 0.9659258262890683122, 1.000000000000000000, 0.9659258262890683122, 1.000000000000000000, 0.9659258262890683122, 1.000000000000000000, 0.9659258262890683122, 1.000000000000000000, 0.9659258262890683122, 1.000000000000000000, 0.9659258262890683122, 1.000000000000000000, 0.9659258262890683122, 1.000000000000000000, 0.9659258262890683122, 1.000000000000000000, 0.9659258262890683122, 1.000000000000000000, 0.9659258262890683122, 1.000000000000000000, 0.9659258262890683122, 1.000000000000000000, 0.9659258262890683122, 1.000000000000000000, 0.9659258262890683122, 1.000000000000000000, 0.9659258262890683122, 1.000000000000000000, 0.9659258262890683122, 1.000000000000000000, 0.9659258262890683122, 1.000000000000000000, 0.9659258262890683122, 1.000000000000000000, 0.9659258262890683122, 1.000000000000000000, 0.9659258262890683122, 1.000000000000000000, 0.9659258262890683122, 1.000000000000000000, 0.9659258262890683122, 1.000000000000000000, 0.9659258262890683122, 1.000000000000000000, 0.9659258262890683122, 1.000000000000000000, 0.9659258262890683122, 1.000000000000000000, 0.9659258262890683122, 1.000000000000000000, 0.9659258262890683122, 1.000000000000000000, 0.9659258262890683122, 1.000000000000000000, 0.9659258262890683122, 1.000000000000000000, 0.9659258262890683122, 1.000000000000000000, 0.9659258262890683122, 1.000000000000000000, 0.9659258262890683122, 1.000000000000000000, 0.9659258262890683122, 1.000000000000000000, 0.9659258262890683122, 1.000000000000000000, 0.9659258262890683122, 1.000000000000000000, 0.9659258262890683122, 1.000000000000000000, 0.9659258262890683122, 1.000000000000000000, 0.9659258262890683122, 1.000000000000000000, 0.9659258262890683122, 1.000000000000000000, 0.9659258262890683122, 1.000000000000000000, 0.9659258262890683122, 1.000000000000000000, 0.9659258262890683122, 1.000000000000000000, 0.9659258262890683122, 1.000000000000000000, 0.9659258262890683122, 1.000000000000000000, 0.9659258262890683122, 1.000000000000000000, 0.9659258262890683122, 1.000000000000000000, 0.9659258262890683122, 1.000000000000000000, 0.9659258262890683122, 1.000000000000000000, 0.9659258262890683122, 1.000000000000000000, 0.9659258262890683122, 1.000000000000000000, 0.9659258262890683122, 1.000000000000000000, 0.9659258262890683122, 1.000000000000000000, 0.9659258262890683122, 1.000000000000000000, 0.9659258262890683122, 1.000000000000000000, 0.9659258262890683122, 1.000000000000000000, 0.9659258262890683122, 1.000000000000000000, 0.9659258262890683122, 1.000000000000000000, 0.9659258262890683122, 1.000000000000000000, 0.9659258262890683122, 1.000000000000000000, 0.9659258262890683122, 1.000000000000000000, 0.9659258262890683122, 1.000000000000000000, 0.9659258262890683122, 1.000000000000000000, 0.9659258262890683122, 1.000000000000000000, 0.9659258262890683122, 1.000000000000000000, 0.9659258262890683122, 1.000000000000000000, 0.9659258262890683122, 1.000000000000000000, 0.9659258262890683122, 1.000000000000000000, 0.9659258262890683122, 1.000000000000000000, 0.9659258262890683122, 1.000000000000000000, 0.9659258262890683122, 1.000000000000000000, 0.9659258262890683122, 1.000000000000000000, 0.9659258262890683122, 1.000000000000000000, 0.9659258262890683122, 1.000000000000000000, 0.9659258262890683122, 1.000000000000000000, 0.9659258262890683122, 1.000000000000000000, 0.9659258262890683122, 1.000000000000000000, 0.9659258262890683122, 1.000000000000000000, 0.9659258262890683122, 1.000000000000000000, 0.9659258262890683122, 1.000000000000000000, 0.9659258262890683122, 1.000000000000000000, 0.9659258262890683122, 1.000000000000000000, 0.9659258262890683122, 1.000000000000000000, 0.9659258262890683122, 1.000000000000000000, 0.9659258262890683122, 1.000000000000000000, 0.9659258262890683122, 1.000000000000000000, 0.9659258262890683122, 1.000000000000000000, 0.9659258262890683122, 1.000000000000000000, 0.9659258262890683122, 1.000000000000000000, 0.9659258262890683122, 1.000000000000000000, 0.9659258262890683122, 1.000000000000000000, 0.9659258262890683122, 1.000000000000000000, 0.9659258262890683122, 1.000000000000000000, 0.9659258262890683122, 1.000000000000000000, 0.9659258262890683122, 1.000000000000000000, 0.9659258262890683122, 1.000000000000000000, 0.9659258262890683122, 1.000000000000000000, 0.9659258262890683122, 1.000000000000000000, 0.9659258262890683122, 1.000000000000000000, 0.9659258262890683122, 1.000000000000000000, 0.9659258262890683122, 1.000000000000000000, 0.9659258262890683122, 1.000000000000000000, 0.9659258262890683122, 1.000000000000000000, 0.9659258262890683122, 1.000000000000000000, 0.9659258262890683122, 1.000000000000000000, 0.9659258262890683122, 1.000000000000000000, 0.9659258262890683122, 1.000000000000000000, 0.9659258262890683122, 1.000000000000000000, 0.9659258262890683122, 1.000000000000000000, 0.9659258262890683122, 1.000000000000000000, 0.9659258262890683122, 1.000000000000000000, 0.9659258262890683122, 1.000000000000000000, 0.9659258262890683122, 1.000000000000000000, 0.9659258262890683122, 1.000000000000000000, 0.9659258262890683122, 1.000000000000000000, 0.9659258262890683122, 1.000000000000000000, 0.9659258262890683122, 1.000000000000000000, 0.9659258262890683122, 1.000000000000000000, 0.9659258262890683122, 1.000000000000000000, 0.9659258262890683122, 1.000000000000000000, 0.9659258262890683122, 1.000000000000000000, 0.9659258262890683122, 1.000000000000000000, 0.9659258262890683122, 1.000000000000000000, 0.9659258262890683122, 1.000000000000000000, 0.9659258262890683122, 1.000000000000000000, 0.9659258262890683122, 1.000000000000000000, 0.9659258262890683122, 1.000000000000000000, 0.9659258262890683122, 1.000000000000000000, 0.9659258262890683122, 1.000000000000000000, 0.9659258262890683122, 1.000000000000000000, 0.9659258262890683122, 1.000000000000000000, 0.9659258262890683122, 1.000000000000000000, 0.9659258262890683122, 1.000000000000000000, 0.9659258262890683122, 1.000000000000000000, 0.9659258262890683122, 1.000000000000000000, 0.9659258262890683122, 1.000000000000000000),
 ( 0.3333333333333333703, 0.3219752754296894559, 0.3333333333333333703, 0.3219752754296894559, 0.3333333333333333703, 0.3219752754296894559, 0.3333333333333333703, 0.3219752754296894559, 0.3333333333333333703, 0.3219752754296894559, 0.3333333333333333703, 0.3219752754296894559, 0.3333333333333333703, 0.3219752754296894559, 0.3333333333333333703, 0.3219752754296894559, 0.3333333333333333703, 0.3219752754296894559, 0.3333333333333333703, 0.3219752754296894559, 0.3333333333333333703, 0.3219752754296894559, 0.3333333333333333703, 0.3219752754296894559, 0.3333333333333333703, 0.3219752754296894559, 0.3333333333333333703, 0.3219752754296894559, 0.3333333333333333703, 0.3219752754296894559, 0.3333333333333333703, 0.3219752754296894559, 0.3333333333333333703, 0.3219752754296894559, 0.3333333333333333703, 0.3219752754296894559, 0.3333333333333333703, 0.3219752754296894559, 0.3333333333333333703, 0.3219752754296894559, 0.3333333333333333703, 0.3219752754296894559, 0.3333333333333333703, 0.3219752754296894559, 0.3333333333333333703, 0.3219752754296894559, 0.3333333333333333703, 0.3219752754296894559, 0.3333333333333333703, 0.3219752754296894559, 0.3333333333333333703, 0.3219752754296894559, 0.3333333333333333703, 0.3219752754296894559, 0.3333333333333333703, 0.3219752754296894559, 0.3333333333333333703, 0.3219752754296894559, 0.3333333333333333703, 0.3219752754296894559, 0.3333333333333333703, 0.3219752754296894559, 0.3333333333333333703, 0.3219752754296894559, 0.3333333333333333703, 0.3219752754296894559, 0.3333333333333333703, 0.3219752754296894559, 0.3333333333333333703, 0.3219752754296894559, 0.3333333333333333703, 0.3219752754296894559, 0.3333333333333333703, 0.3219752754296894559, 0.3333333333333333703, 0.3219752754296894559, 0.3333333333333333703, 0.3219752754296894559, 0.3333333333333333703, 0.3219752754296894559, 0.3333333333333333703, 0.3219752754296894559, 0.3333333333333333703, 0.3219752754296894559, 0.3333333333333333703, 0.3219752754296894559, 0.3333333333333333703, 0.3219752754296894559, 0.3333333333333333703, 0.3219752754296894559, 0.3333333333333333703, 0.3219752754296894559, 0.3333333333333333703, 0.3219752754296894559, 0.3333333333333333703, 0.3219752754296894559, 0.3333333333333333703, 0.3219752754296894559, 0.3333333333333333703, 0.3219752754296894559, 0.3333333333333333703, 0.3219752754296894559, 0.3333333333333333703, 0.3219752754296894559, 0.3333333333333333703, 0.3219752754296894559, 0.3333333333333333703, 0.3219752754296894559, 0.3333333333333333703, 0.3219752754296894559, 0.3333333333333333703, 0.3219752754296894559, 0.3333333333333333703, 0.3219752754296894559, 0.3333333333333333703, 0.3219752754296894559, 0.3333333333333333703, 0.3219752754296894559, 0.3333333333333333703, 0.3219752754296894559, 0.3333333333333333703, 0.3219752754296894559, 0.3333333333333333703, 0.3219752754296894559, 0.3333333333333333703, 0.3219752754296894559, 0.3333333333333333703, 0.3219752754296894559, 0.3333333333333333703, 0.3219752754296894559, 0.3333333333333333703, 0.3219752754296894559, 0.3333333333333333703, 0.3219752754296894559, 0.3333333333333333703, 0.3219752754296894559, 0.3333333333333333703, 0.3219752754296894559, 0.3333333333333333703, 0.3219752754296894559, 0.3333333333333333703, 0.3219752754296894559, 0.3333333333333333703, 0.3219752754296894559, 0.3333333333333333703, 0.3219752754296894559, 0.3333333333333333703, 0.3219752754296894559, 0.3333333333333333703, 0.3219752754296894559, 0.3333333333333333703, 0.3219752754296894559, 0.3333333333333333703, 0.3219752754296894559, 0.3333333333333333703, 0.3219752754296894559, 0.3333333333333333703, 0.3219752754296894559, 0.3333333333333333703, 0.3219752754296894559, 0.3333333333333333703, 0.3219752754296894559, 0.3333333333333333703, 0.3219752754296894559, 0.3333333333333333703, 0.3219752754296894559, 0.3333333333333333703, 0.3219752754296894559, 0.3333333333333333703, 0.3219752754296894559, 0.3333333333333333703, 0.3219752754296894559, 0.3333333333333333703, 0.3219752754296894559, 0.3333333333333333703, 0.3219752754296894559, 0.3333333333333333703, 0.3219752754296894559, 0.3333333333333333703, 0.3219752754296894559, 0.3333333333333333703, 0.3219752754296894559, 0.3333333333333333703, 0.3219752754296894559, 0.3333333333333333703, 0.3219752754296894559, 0.3333333333333333703, 0.3219752754296894559, 0.3333333333333333703, 0.3219752754296894559, 0.3333333333333333703, 0.3219752754296894559, 0.3333333333333333703, 0.3219752754296894559, 0.3333333333333333703, 0.3219752754296894559, 0.3333333333333333703, 0.3219752754296894559, 0.3333333333333333703, 0.3219752754296894559, 0.3333333333333333703, 0.3219752754296894559, 0.3333333333333333703, 0.3219752754296894559, 0.3333333333333333703, 0.3219752754296894559, 0.3333333333333333703, 0.3219752754296894559, 0.3333333333333333703, 0.3219752754296894559, 0.3333333333333333703, 0.3219752754296894559, 0.3333333333333333703, 0.3219752754296894559, 0.3333333333333333703, 0.3219752754296894559, 0.3333333333333333703, 0.3219752754296894559, 0.3333333333333333703, 0.3219752754296894559, 0.3333333333333333703, 0.3219752754296894559, 0.3333333333333333703, 0.3219752754296894559, 0.3333333333333333703, 0.3219752754296894559, 0.3333333333333333703, 0.3219752754296894559, 0.3333333333333333703, 0.3219752754296894559, 0.3333333333333333703, 0.3219752754296894559, 0.3333333333333333703, 0.3219752754296894559, 0.3333333333333333703, 0.3219752754296894559, 0.3333333333333333703, 0.3219752754296894559, 0.3333333333333333703, 0.3219752754296894559, 0.3333333333333333703, 0.3219752754296894559, 0.3333333333333333703, 0.3219752754296894559, 0.3333333333333333703, 0.3219752754296894559, 0.3333333333333333703, 0.3219752754296894559, 0.3333333333333333703, 0.3219752754296894559, 0.3333333333333333703, 0.3219752754296894559, 0.3333333333333333703, 0.3219752754296894559, 0.3333333333333333703, 0.3219752754296894559, 0.3333333333333333703, 0.3219752754296894559, 0.3333333333333333703, 0.3219752754296894559, 0.3333333333333333703, 0.3219752754296894559, 0.3333333333333333703, 0.3219752754296894559, 0.3333333333333333703, 0.3219752754296894559, 0.3333333333333333703, 0.3219752754296894559, 0.3333333333333333703, 0.3219752754296894559, 0.3333333333333333703, 0.3219752754296894559, 0.3333333333333333703, 0.3219752754296894559, 0.3333333333333333703, 0.3219752754296894559, 0.3333333333333333703, 0.3219752754296894559, 0.3333333333333333703, 0.3219752754296894559, 0.3333333333333333703, 0.3219752754296894559, 0.3333333333333333703, 0.3219752754296894559, 0.3333333333333333703, 0.3219752754296894559, 0.3333333333333333703, 0.3219752754296894559, 0.3333333333333333703, 0.3219752754296894559, 0.3333333333333333703, 0.3219752754296894559, 0.3333333333333333703, 0.3219752754296894559, 0.3333333333333333703, 0.3219752754296894559, 0.3333333333333333703, 0.3219752754296894559, 0.3333333333333333703, 0.3219752754296894559, 0.3333333333333333703, 0.3219752754296894559, 0.3333333333333333703, 0.3219752754296894559, 0.3333333333333333703, 0.3219752754296894559, 0.3333333333333333703, 0.3219752754296894559, 0.3333333333333333703, 0.3219752754296894559, 0.3333333333333333703, 0.3219752754296894559, 0.3333333333333333703, 0.3219752754296894559, 0.3333333333333333703, 0.3219752754296894559, 0.3333333333333333703, 0.3219752754296894559, 0.3333333333333333703, 0.3219752754296894559, 0.3333333333333333703, 0.3219752754296894559, 0.3333333333333333703, 0.3219752754296894559, 0.3333333333333333703, 0.3219752754296894559, 0.3333333333333333703, 0.3219752754296894559, 0.3333333333333333703, 0.3219752754296894559, 0.3333333333333333703, 0.3219752754296894559, 0.3333333333333333703, 0.3219752754296894559, 0.3333333333333333703, 0.3219752754296894559, 0.3333333333333333703, 0.3219752754296894559, 0.3333333333333333703, 0.3219752754296894559, 0.3333333333333333703, 0.3219752754296894559, 0.3333333333333333703, 0.3219752754296894559, 0.3333333333333333703, 0.3219752754296894559, 0.3333333333333333703, 0.3219752754296894559, 0.3333333333333333703, 0.3219752754296894559, 0.3333333333333333703, 0.3219752754296894559, 0.3333333333333333703, 0.3219752754296894559, 0.3333333333333333703, 0.3219752754296894559, 0.3333333333333333703, 0.3219752754296894559, 0.3333333333333333703, 0.3219752754296894559, 0.3333333333333333703, 0.3219752754296894559, 0.3333333333333333703, 0.3219752754296894559, 0.3333333333333333703, 0.3219752754296894559, 0.3333333333333333703, 0.3219752754296894559, 0.3333333333333333703, 0.3219752754296894559, 0.3333333333333333703, 0.3219752754296894559, 0.3333333333333333703, 0.3219752754296894559, 0.3333333333333333703, 0.3219752754296894559, 0.3333333333333333703, 0.3219752754296894559, 0.3333333333333333703, 0.3219752754296894559, 0.3333333333333333703, 0.3219752754296894559, 0.3333333333333333703, 0.3219752754296894559, 0.3333333333333333703, 0.3219752754296894559, 0.3333333333333333703, 0.3219752754296894559, 0.3333333333333333703, 0.3219752754296894559, 0.3333333333333333703, 0.3219752754296894559, 0.3333333333333333703, 0.3219752754296894559, 0.3333333333333333703, 0.3219752754296894559, 0.3333333333333333703, 0.3219752754296894559, 0.3333333333333333703, 0.3219752754296894559, 0.3333333333333333703, 0.3219752754296894559, 0.3333333333333333703, 0.3219752754296894559, 0.3333333333333333703, 0.3219752754296894559, 0.3333333333333333703, 0.3219752754296894559, 0.3333333333333333703, 0.3219752754296894559, 0.3333333333333333703, 0.3219752754296894559, 0.3333333333333333703, 0.3219752754296894559, 0.3333333333333333703, 0.3219752754296894559, 0.3333333333333333703, 0.3219752754296894559, 0.3333333333333333703, 0.3219752754296894559, 0.3333333333333333703, 0.3219752754296894559, 0.3333333333333333703, 0.3219752754296894559, 0.3333333333333333703, 0.3219752754296894559, 0.3333333333333333703, 0.3219752754296894559, 0.3333333333333333703, 0.3219752754296894559, 0.3333333333333333703, 0.3219752754296894559, 0.3333333333333333703, 0.3219752754296894559, 0.3333333333333333703, 0.3219752754296894559, 0.3333333333333333703, 0.3219752754296894559, 0.3333333333333333703, 0.3219752754296894559, 0.3333333333333333703, 0.3219752754296894559, 0.3333333333333333703, 0.3219752754296894559, 0.3333333333333333703, 0.3219752754296894559, 0.3333333333333333703, 0.3219752754296894559, 0.3333333333333333703, 0.3219752754296894559, 0.3333333333333333703, 0.3219752754296894559, 0.3333333333333333703, 0.3219752754296894559, 0.3333333333333333703, 0.3219752754296894559, 0.3333333333333333703),
 ( 0.3333333333333333703, 0.3219752754296894559, 0.3333333333333333703, 0.3219752754296894559, 0.3333333333333333703, 0.3219752754296894559, 0.3333333333333333703, 0.3219752754296894559, 0.3333333333333333703, 0.3219752754296894559, 0.3333333333333333703, 0.3219752754296894559, 0.3333333333333333703, 0.3219752754296894559, 0.3333333333333333703, 0.3219752754296894559, 0.3333333333333333703, 0.3219752754296894559, 0.3333333333333333703, 0.3219752754296894559, 0.3333333333333333703, 0.3219752754296894559, 0.3333333333333333703, 0.3219752754296894559, 0.3333333333333333703, 0.3219752754296894559, 0.3333333333333333703, 0.3219752754296894559, 0.3333333333333333703, 0.3219752754296894559, 0.3333333333333333703, 0.3219752754296894559, 0.3333333333333333703, 0.3219752754296894559, 0.3333333333333333703, 0.3219752754296894559, 0.3333333333333333703, 0.3219752754296894559, 0.3333333333333333703, 0.3219752754296894559, 0.3333333333333333703, 0.3219752754296894559, 0.3333333333333333703, 0.3219752754296894559, 0.3333333333333333703, 0.3219752754296894559, 0.3333333333333333703, 0.3219752754296894559, 0.3333333333333333703, 0.3219752754296894559, 0.3333333333333333703, 0.3219752754296894559, 0.3333333333333333703, 0.3219752754296894559, 0.3333333333333333703, 0.3219752754296894559, 0.3333333333333333703, 0.3219752754296894559, 0.3333333333333333703, 0.3219752754296894559, 0.3333333333333333703, 0.3219752754296894559, 0.3333333333333333703, 0.3219752754296894559, 0.3333333333333333703, 0.3219752754296894559, 0.3333333333333333703, 0.3219752754296894559, 0.3333333333333333703, 0.3219752754296894559, 0.3333333333333333703, 0.3219752754296894559, 0.3333333333333333703, 0.3219752754296894559, 0.3333333333333333703, 0.3219752754296894559, 0.3333333333333333703, 0.3219752754296894559, 0.3333333333333333703, 0.3219752754296894559, 0.3333333333333333703, 0.3219752754296894559, 0.3333333333333333703, 0.3219752754296894559, 0.3333333333333333703, 0.3219752754296894559, 0.3333333333333333703, 0.3219752754296894559, 0.3333333333333333703, 0.3219752754296894559, 0.3333333333333333703, 0.3219752754296894559, 0.3333333333333333703, 0.3219752754296894559, 0.3333333333333333703, 0.3219752754296894559, 0.3333333333333333703, 0.3219752754296894559, 0.3333333333333333703, 0.3219752754296894559, 0.3333333333333333703, 0.3219752754296894559, 0.3333333333333333703, 0.3219752754296894559, 0.3333333333333333703, 0.3219752754296894559, 0.3333333333333333703, 0.3219752754296894559, 0.3333333333333333703, 0.3219752754296894559, 0.3333333333333333703, 0.3219752754296894559, 0.3333333333333333703, 0.3219752754296894559, 0.3333333333333333703, 0.3219752754296894559, 0.3333333333333333703, 0.3219752754296894559, 0.3333333333333333703, 0.3219752754296894559, 0.3333333333333333703, 0.3219752754296894559, 0.3333333333333333703, 0.3219752754296894559, 0.3333333333333333703, 0.3219752754296894559, 0.3333333333333333703, 0.3219752754296894559, 0.3333333333333333703, 0.3219752754296894559, 0.3333333333333333703, 0.3219752754296894559, 0.3333333333333333703, 0.3219752754296894559, 0.3333333333333333703, 0.3219752754296894559, 0.3333333333333333703, 0.3219752754296894559, 0.3333333333333333703, 0.3219752754296894559, 0.3333333333333333703, 0.3219752754296894559, 0.3333333333333333703, 0.3219752754296894559, 0.3333333333333333703, 0.3219752754296894559, 0.3333333333333333703, 0.3219752754296894559, 0.3333333333333333703, 0.3219752754296894559, 0.3333333333333333703, 0.3219752754296894559, 0.3333333333333333703, 0.3219752754296894559, 0.3333333333333333703, 0.3219752754296894559, 0.3333333333333333703, 0.3219752754296894559, 0.3333333333333333703, 0.3219752754296894559, 0.3333333333333333703, 0.3219752754296894559, 0.3333333333333333703, 0.3219752754296894559, 0.3333333333333333703, 0.3219752754296894559, 0.3333333333333333703, 0.3219752754296894559, 0.3333333333333333703, 0.3219752754296894559, 0.3333333333333333703, 0.3219752754296894559, 0.3333333333333333703, 0.3219752754296894559, 0.3333333333333333703, 0.3219752754296894559, 0.3333333333333333703, 0.3219752754296894559, 0.3333333333333333703, 0.3219752754296894559, 0.3333333333333333703, 0.3219752754296894559, 0.3333333333333333703, 0.3219752754296894559, 0.3333333333333333703, 0.3219752754296894559, 0.3333333333333333703, 0.3219752754296894559, 0.3333333333333333703, 0.3219752754296894559, 0.3333333333333333703, 0.3219752754296894559, 0.3333333333333333703, 0.3219752754296894559, 0.3333333333333333703, 0.3219752754296894559, 0.3333333333333333703, 0.3219752754296894559, 0.3333333333333333703, 0.3219752754296894559, 0.3333333333333333703, 0.3219752754296894559, 0.3333333333333333703, 0.3219752754296894559, 0.3333333333333333703, 0.3219752754296894559, 0.3333333333333333703, 0.3219752754296894559, 0.3333333333333333703, 0.3219752754296894559, 0.3333333333333333703, 0.3219752754296894559, 0.3333333333333333703, 0.3219752754296894559, 0.3333333333333333703, 0.3219752754296894559, 0.3333333333333333703, 0.3219752754296894559, 0.3333333333333333703, 0.3219752754296894559, 0.3333333333333333703, 0.3219752754296894559, 0.3333333333333333703, 0.3219752754296894559, 0.3333333333333333703, 0.3219752754296894559, 0.3333333333333333703, 0.3219752754296894559, 0.3333333333333333703, 0.3219752754296894559, 0.3333333333333333703, 0.3219752754296894559, 0.3333333333333333703, 0.3219752754296894559, 0.3333333333333333703, 0.3219752754296894559, 0.3333333333333333703, 0.3219752754296894559, 0.3333333333333333703, 0.3219752754296894559, 0.3333333333333333703, 0.3219752754296894559, 0.3333333333333333703, 0.3219752754296894559, 0.3333333333333333703, 0.3219752754296894559, 0.3333333333333333703, 0.3219752754296894559, 0.3333333333333333703, 0.3219752754296894559, 0.3333333333333333703, 0.3219752754296894559, 0.3333333333333333703, 0.3219752754296894559, 0.3333333333333333703, 0.3219752754296894559, 0.3333333333333333703, 0.3219752754296894559, 0.3333333333333333703, 0.3219752754296894559, 0.3333333333333333703, 0.3219752754296894559, 0.3333333333333333703, 0.3219752754296894559, 0.3333333333333333703, 0.3219752754296894559, 0.3333333333333333703, 0.3219752754296894559, 0.3333333333333333703, 0.3219752754296894559, 0.3333333333333333703, 0.3219752754296894559, 0.3333333333333333703, 0.3219752754296894559, 0.3333333333333333703, 0.3219752754296894559, 0.3333333333333333703, 0.3219752754296894559, 0.3333333333333333703, 0.3219752754296894559, 0.3333333333333333703, 0.3219752754296894559, 0.3333333333333333703, 0.3219752754296894559, 0.3333333333333333703, 0.3219752754296894559, 0.3333333333333333703, 0.3219752754296894559, 0.3333333333333333703, 0.3219752754296894559, 0.3333333333333333703, 0.3219752754296894559, 0.3333333333333333703, 0.3219752754296894559, 0.3333333333333333703, 0.3219752754296894559, 0.3333333333333333703, 0.3219752754296894559, 0.3333333333333333703, 0.3219752754296894559, 0.3333333333333333703, 0.3219752754296894559, 0.3333333333333333703, 0.3219752754296894559, 0.3333333333333333703, 0.3219752754296894559, 0.3333333333333333703, 0.3219752754296894559, 0.3333333333333333703, 0.3219752754296894559, 0.3333333333333333703, 0.3219752754296894559, 0.3333333333333333703, 0.3219752754296894559, 0.3333333333333333703, 0.3219752754296894559, 0.3333333333333333703, 0.3219752754296894559, 0.3333333333333333703, 0.3219752754296894559, 0.3333333333333333703, 0.3219752754296894559, 0.3333333333333333703, 0.3219752754296894559, 0.3333333333333333703, 0.3219752754296894559, 0.3333333333333333703, 0.3219752754296894559, 0.3333333333333333703, 0.3219752754296894559, 0.3333333333333333703, 0.3219752754296894559, 0.3333333333333333703, 0.3219752754296894559, 0.3333333333333333703, 0.3219752754296894559, 0.3333333333333333703, 0.3219752754296894559, 0.3333333333333333703, 0.3219752754296894559, 0.3333333333333333703, 0.3219752754296894559, 0.3333333333333333703, 0.3219752754296894559, 0.3333333333333333703, 0.3219752754296894559, 0.3333333333333333703, 0.3219752754296894559, 0.3333333333333333703, 0.3219752754296894559, 0.3333333333333333703, 0.3219752754296894559, 0.3333333333333333703, 0.3219752754296894559, 0.3333333333333333703, 0.3219752754296894559, 0.3333333333333333703, 0.3219752754296894559, 0.3333333333333333703, 0.3219752754296894559, 0.3333333333333333703, 0.3219752754296894559, 0.3333333333333333703, 0.3219752754296894559, 0.3333333333333333703, 0.3219752754296894559, 0.3333333333333333703, 0.3219752754296894559, 0.3333333333333333703, 0.3219752754296894559, 0.3333333333333333703, 0.3219752754296894559, 0.3333333333333333703, 0.3219752754296894559, 0.3333333333333333703, 0.3219752754296894559, 0.3333333333333333703, 0.3219752754296894559, 0.3333333333333333703, 0.3219752754296894559, 0.3333333333333333703, 0.3219752754296894559, 0.3333333333333333703, 0.3219752754296894559, 0.3333333333333333703, 0.3219752754296894559, 0.3333333333333333703, 0.3219752754296894559, 0.3333333333333333703, 0.3219752754296894559, 0.3333333333333333703, 0.3219752754296894559, 0.3333333333333333703, 0.3219752754296894559, 0.3333333333333333703, 0.3219752754296894559, 0.3333333333333333703, 0.3219752754296894559, 0.3333333333333333703, 0.3219752754296894559, 0.3333333333333333703, 0.3219752754296894559, 0.3333333333333333703, 0.3219752754296894559, 0.3333333333333333703, 0.3219752754296894559, 0.3333333333333333703, 0.3219752754296894559, 0.3333333333333333703, 0.3219752754296894559, 0.3333333333333333703, 0.3219752754296894559, 0.3333333333333333703, 0.3219752754296894559, 0.3333333333333333703, 0.3219752754296894559, 0.3333333333333333703, 0.3219752754296894559, 0.3333333333333333703, 0.3219752754296894559, 0.3333333333333333703, 0.3219752754296894559, 0.3333333333333333703, 0.3219752754296894559, 0.3333333333333333703, 0.3219752754296894559, 0.3333333333333333703, 0.3219752754296894559, 0.3333333333333333703, 0.3219752754296894559, 0.3333333333333333703, 0.3219752754296894559, 0.3333333333333333703, 0.3219752754296894559, 0.3333333333333333703, 0.3219752754296894559, 0.3333333333333333703, 0.3219752754296894559, 0.3333333333333333703, 0.3219752754296894559, 0.3333333333333333703, 0.3219752754296894559, 0.3333333333333333703, 0.3219752754296894559, 0.3333333333333333703, 0.3219752754296894559, 0.3333333333333333703, 0.3219752754296894559, 0.3333333333333333703, 0.3219752754296894559, 0.3333333333333333703, 0.3219752754296894559, 0.3333333333333333703, 0.3219752754296894559, 0.3333333333333333703, 0.3219752754296894559, 0.3333333333333333703),
 ( 1.000000000000000000, 0.9659258262890683122, 1.000000000000000000, 0.9659258262890683122, 1.000000000000000000, 0.9659258262890683122, 1.000000000000000000, 0.9659258262890683122, 1.000000000000000000, 0.9659258262890683122, 1.000000000000000000, 0.9659258262890683122, 1.000000000000000000, 0.9659258262890683122, 1.000000000000000000, 0.9659258262890683122, 1.000000000000000000, 0.9659258262890683122, 1.000000000000000000, 0.9659258262890683122, 1.000000000000000000, 0.9659258262890683122, 1.000000000000000000, 0.9659258262890683122, 1.000000000000000000, 0.9659258262890683122, 1.000000000000000000, 0.9659258262890683122, 1.000000000000000000, 0.9659258262890683122, 1.000000000000000000, 0.9659258262890683122, 1.000000000000000000, 0.9659258262890683122, 1.000000000000000000, 0.9659258262890683122, 1.000000000000000000, 0.9659258262890683122, 1.000000000000000000, 0.9659258262890683122, 1.000000000000000000, 0.9659258262890683122, 1.000000000000000000, 0.9659258262890683122, 1.000000000000000000, 0.9659258262890683122, 1.000000000000000000, 0.9659258262890683122, 1.000000000000000000, 0.9659258262890683122, 1.000000000000000000, 0.9659258262890683122, 1.000000000000000000, 0.9659258262890683122, 1.000000000000000000, 0.9659258262890683122, 1.000000000000000000, 0.9659258262890683122, 1.000000000000000000, 0.9659258262890683122, 1.000000000000000000, 0.9659258262890683122, 1.000000000000000000, 0.9659258262890683122, 1.000000000000000000, 0.9659258262890683122, 1.000000000000000000, 0.9659258262890683122, 1.000000000000000000, 0.9659258262890683122, 1.000000000000000000, 0.9659258262890683122, 1.000000000000000000, 0.9659258262890683122, 1.000000000000000000, 0.9659258262890683122, 1.000000000000000000, 0.9659258262890683122, 1.000000000000000000, 0.9659258262890683122, 1.000000000000000000, 0.9659258262890683122, 1.000000000000000000, 0.9659258262890683122, 1.000000000000000000, 0.9659258262890683122, 1.000000000000000000, 0.9659258262890683122, 1.000000000000000000, 0.9659258262890683122, 1.000000000000000000, 0.9659258262890683122, 1.000000000000000000, 0.9659258262890683122, 1.000000000000000000, 0.9659258262890683122, 1.000000000000000000, 0.9659258262890683122, 1.000000000000000000, 0.9659258262890683122, 1.000000000000000000, 0.9659258262890683122, 1.000000000000000000, 0.9659258262890683122, 1.000000000000000000, 0.9659258262890683122, 1.000000000000000000, 0.9659258262890683122, 1.000000000000000000, 0.9659258262890683122, 1.000000000000000000, 0.9659258262890683122, 1.000000000000000000, 0.9659258262890683122, 1.000000000000000000, 0.9659258262890683122, 1.000000000000000000, 0.9659258262890683122, 1.000000000000000000, 0.9659258262890683122, 1.000000000000000000, 0.9659258262890683122, 1.000000000000000000, 0.9659258262890683122, 1.000000000000000000, 0.9659258262890683122, 1.000000000000000000, 0.9659258262890683122, 1.000000000000000000, 0.9659258262890683122, 1.000000000000000000, 0.9659258262890683122, 1.000000000000000000, 0.9659258262890683122, 1.000000000000000000, 0.9659258262890683122, 1.000000000000000000, 0.9659258262890683122, 1.000000000000000000, 0.9659258262890683122, 1.000000000000000000, 0.9659258262890683122, 1.000000000000000000, 0.9659258262890683122, 1.000000000000000000, 0.9659258262890683122, 1.000000000000000000, 0.9659258262890683122, 1.000000000000000000, 0.9659258262890683122, 1.000000000000000000, 0.9659258262890683122, 1.000000000000000000, 0.9659258262890683122, 1.000000000000000000, 0.9659258262890683122, 1.000000000000000000, 0.9659258262890683122, 1.000000000000000000, 0.9659258262890683122, 1.000000000000000000, 0.9659258262890683122, 1.000000000000000000, 0.9659258262890683122, 1.000000000000000000, 0.9659258262890683122, 1.000000000000000000, 0.9659258262890683122, 1.000000000000000000, 0.9659258262890683122, 1.000000000000000000, 0.9659258262890683122, 1.000000000000000000, 0.9659258262890683122, 1.000000000000000000, 0.9659258262890683122, 1.000000000000000000, 0.9659258262890683122, 1.000000000000000000, 0.9659258262890683122, 1.000000000000000000, 0.9659258262890683122, 1.000000000000000000, 0.9659258262890683122, 1.000000000000000000, 0.9659258262890683122, 1.000000000000000000, 0.9659258262890683122, 1.000000000000000000, 0.9659258262890683122, 1.000000000000000000, 0.9659258262890683122, 1.000000000000000000, 0.9659258262890683122, 1.000000000000000000, 0.9659258262890683122, 1.000000000000000000, 0.9659258262890683122, 1.000000000000000000, 0.9659258262890683122, 1.000000000000000000, 0.9659258262890683122, 1.000000000000000000, 0.9659258262890683122, 1.000000000000000000, 0.9659258262890683122, 1.000000000000000000, 0.9659258262890683122, 1.000000000000000000, 0.9659258262890683122, 1.000000000000000000, 0.9659258262890683122, 1.000000000000000000, 0.9659258262890683122, 1.000000000000000000, 0.9659258262890683122, 1.000000000000000000, 0.9659258262890683122, 1.000000000000000000, 0.9659258262890683122, 1.000000000000000000, 0.9659258262890683122, 1.000000000000000000, 0.9659258262890683122, 1.000000000000000000, 0.9659258262890683122, 1.000000000000000000, 0.9659258262890683122, 1.000000000000000000, 0.9659258262890683122, 1.000000000000000000, 0.9659258262890683122, 1.000000000000000000, 0.9659258262890683122, 1.000000000000000000, 0.9659258262890683122, 1.000000000000000000, 0.9659258262890683122, 1.000000000000000000, 0.9659258262890683122, 1.000000000000000000, 0.9659258262890683122, 1.000000000000000000, 0.9659258262890683122, 1.000000000000000000, 0.9659258262890683122, 1.000000000000000000, 0.9659258262890683122, 1.000000000000000000, 0.9659258262890683122, 1.000000000000000000, 0.9659258262890683122, 1.000000000000000000, 0.9659258262890683122, 1.000000000000000000, 0.9659258262890683122, 1.000000000000000000, 0.9659258262890683122, 1.000000000000000000, 0.9659258262890683122, 1.000000000000000000, 0.9659258262890683122, 1.000000000000000000, 0.9659258262890683122, 1.000000000000000000, 0.9659258262890683122, 1.000000000000000000, 0.9659258262890683122, 1.000000000000000000, 0.9659258262890683122, 1.000000000000000000, 0.9659258262890683122, 1.000000000000000000, 0.9659258262890683122, 1.000000000000000000, 0.9659258262890683122, 1.000000000000000000, 0.9659258262890683122, 1.000000000000000000, 0.9659258262890683122, 1.000000000000000000, 0.9659258262890683122, 1.000000000000000000, 0.9659258262890683122, 1.000000000000000000, 0.9659258262890683122, 1.000000000000000000, 0.9659258262890683122, 1.000000000000000000, 0.9659258262890683122, 1.000000000000000000, 0.9659258262890683122, 1.000000000000000000, 0.9659258262890683122, 1.000000000000000000, 0.9659258262890683122, 1.000000000000000000, 0.9659258262890683122, 1.000000000000000000, 0.9659258262890683122, 1.000000000000000000, 0.9659258262890683122, 1.000000000000000000, 0.9659258262890683122, 1.000000000000000000, 0.9659258262890683122, 1.000000000000000000, 0.9659258262890683122, 1.000000000000000000, 0.9659258262890683122, 1.000000000000000000, 0.9659258262890683122, 1.000000000000000000, 0.9659258262890683122, 1.000000000000000000, 0.9659258262890683122, 1.000000000000000000, 0.9659258262890683122, 1.000000000000000000, 0.9659258262890683122, 1.000000000000000000, 0.9659258262890683122, 1.000000000000000000, 0.9659258262890683122, 1.000000000000000000, 0.9659258262890683122, 1.000000000000000000, 0.9659258262890683122, 1.000000000000000000, 0.9659258262890683122, 1.000000000000000000, 0.9659258262890683122, 1.000000000000000000, 0.9659258262890683122, 1.000000000000000000, 0.9659258262890683122, 1.000000000000000000, 0.9659258262890683122, 1.000000000000000000, 0.9659258262890683122, 1.000000000000000000, 0.9659258262890683122, 1.000000000000000000, 0.9659258262890683122, 1.000000000000000000, 0.9659258262890683122, 1.000000000000000000, 0.9659258262890683122, 1.000000000000000000, 0.9659258262890683122, 1.000000000000000000, 0.9659258262890683122, 1.000000000000000000, 0.9659258262890683122, 1.000000000000000000, 0.9659258262890683122, 1.000000000000000000, 0.9659258262890683122, 1.000000000000000000, 0.9659258262890683122, 1.000000000000000000, 0.9659258262890683122, 1.000000000000000000, 0.9659258262890683122, 1.000000000000000000, 0.9659258262890683122, 1.000000000000000000, 0.9659258262890683122, 1.000000000000000000, 0.9659258262890683122, 1.000000000000000000, 0.9659258262890683122, 1.000000000000000000, 0.9659258262890683122, 1.000000000000000000, 0.9659258262890683122, 1.000000000000000000, 0.9659258262890683122, 1.000000000000000000, 0.9659258262890683122, 1.000000000000000000, 0.9659258262890683122, 1.000000000000000000, 0.9659258262890683122, 1.000000000000000000, 0.9659258262890683122, 1.000000000000000000, 0.9659258262890683122, 1.000000000000000000, 0.9659258262890683122, 1.000000000000000000, 0.9659258262890683122, 1.000000000000000000, 0.9659258262890683122, 1.000000000000000000, 0.9659258262890683122, 1.000000000000000000, 0.9659258262890683122, 1.000000000000000000, 0.9659258262890683122, 1.000000000000000000, 0.9659258262890683122, 1.000000000000000000, 0.9659258262890683122, 1.000000000000000000, 0.9659258262890683122, 1.000000000000000000, 0.9659258262890683122, 1.000000000000000000, 0.9659258262890683122, 1.000000000000000000, 0.9659258262890683122, 1.000000000000000000, 0.9659258262890683122, 1.000000000000000000, 0.9659258262890683122, 1.000000000000000000, 0.9659258262890683122, 1.000000000000000000, 0.9659258262890683122, 1.000000000000000000, 0.9659258262890683122, 1.000000000000000000, 0.9659258262890683122, 1.000000000000000000, 0.9659258262890683122, 1.000000000000000000, 0.9659258262890683122, 1.000000000000000000, 0.9659258262890683122, 1.000000000000000000, 0.9659258262890683122, 1.000000000000000000, 0.9659258262890683122, 1.000000000000000000, 0.9659258262890683122, 1.000000000000000000, 0.9659258262890683122, 1.000000000000000000, 0.9659258262890683122, 1.000000000000000000, 0.9659258262890683122, 1.000000000000000000, 0.9659258262890683122, 1.000000000000000000, 0.9659258262890683122, 1.000000000000000000, 0.9659258262890683122, 1.000000000000000000, 0.9659258262890683122, 1.000000000000000000, 0.9659258262890683122, 1.000000000000000000, 0.9659258262890683122, 1.000000000000000000, 0.9659258262890683122, 1.000000000000000000),
 ( 0.3333333333333333703, 0.3219752754296894559, 0.3333333333333333703, 0.3219752754296894559, 0.3333333333333333703, 0.3219752754296894559, 0.3333333333333333703, 0.3219752754296894559, 0.3333333333333333703, 0.3219752754296894559, 0.3333333333333333703, 0.3219752754296894559, 0.3333333333333333703, 0.3219752754296894559, 0.3333333333333333703, 0.3219752754296894559, 0.3333333333333333703, 0.3219752754296894559, 0.3333333333333333703, 0.3219752754296894559, 0.3333333333333333703, 0.3219752754296894559, 0.3333333333333333703, 0.3219752754296894559, 0.3333333333333333703, 0.3219752754296894559, 0.3333333333333333703, 0.3219752754296894559, 0.3333333333333333703, 0.3219752754296894559, 0.3333333333333333703, 0.3219752754296894559, 0.3333333333333333703, 0.3219752754296894559, 0.3333333333333333703, 0.3219752754296894559, 0.3333333333333333703, 0.3219752754296894559, 0.3333333333333333703, 0.3219752754296894559, 0.3333333333333333703, 0.3219752754296894559, 0.3333333333333333703, 0.3219752754296894559, 0.3333333333333333703, 0.3219752754296894559, 0.3333333333333333703, 0.3219752754296894559, 0.3333333333333333703, 0.3219752754296894559, 0.3333333333333333703, 0.3219752754296894559, 0.3333333333333333703, 0.3219752754296894559, 0.3333333333333333703, 0.3219752754296894559, 0.3333333333333333703, 0.3219752754296894559, 0.3333333333333333703, 0.3219752754296894559, 0.3333333333333333703, 0.3219752754296894559, 0.3333333333333333703, 0.3219752754296894559, 0.3333333333333333703, 0.3219752754296894559, 0.3333333333333333703, 0.3219752754296894559, 0.3333333333333333703, 0.3219752754296894559, 0.3333333333333333703, 0.3219752754296894559, 0.3333333333333333703, 0.3219752754296894559, 0.3333333333333333703, 0.3219752754296894559, 0.3333333333333333703, 0.3219752754296894559, 0.3333333333333333703, 0.3219752754296894559, 0.3333333333333333703, 0.3219752754296894559, 0.3333333333333333703, 0.3219752754296894559, 0.3333333333333333703, 0.3219752754296894559, 0.3333333333333333703, 0.3219752754296894559, 0.3333333333333333703, 0.3219752754296894559, 0.3333333333333333703, 0.3219752754296894559, 0.3333333333333333703, 0.3219752754296894559, 0.3333333333333333703, 0.3219752754296894559, 0.3333333333333333703, 0.3219752754296894559, 0.3333333333333333703, 0.3219752754296894559, 0.3333333333333333703, 0.3219752754296894559, 0.3333333333333333703, 0.3219752754296894559, 0.3333333333333333703, 0.3219752754296894559, 0.3333333333333333703, 0.3219752754296894559, 0.3333333333333333703, 0.3219752754296894559, 0.3333333333333333703, 0.3219752754296894559, 0.3333333333333333703, 0.3219752754296894559, 0.3333333333333333703, 0.3219752754296894559, 0.3333333333333333703, 0.3219752754296894559, 0.3333333333333333703, 0.3219752754296894559, 0.3333333333333333703, 0.3219752754296894559, 0.3333333333333333703, 0.3219752754296894559, 0.3333333333333333703, 0.3219752754296894559, 0.3333333333333333703, 0.3219752754296894559, 0.3333333333333333703, 0.3219752754296894559, 0.3333333333333333703, 0.3219752754296894559, 0.3333333333333333703, 0.3219752754296894559, 0.3333333333333333703, 0.3219752754296894559, 0.3333333333333333703, 0.3219752754296894559, 0.3333333333333333703, 0.3219752754296894559, 0.3333333333333333703, 0.3219752754296894559, 0.3333333333333333703, 0.3219752754296894559, 0.3333333333333333703, 0.3219752754296894559, 0.3333333333333333703, 0.3219752754296894559, 0.3333333333333333703, 0.3219752754296894559, 0.3333333333333333703, 0.3219752754296894559, 0.3333333333333333703, 0.3219752754296894559, 0.3333333333333333703, 0.3219752754296894559, 0.3333333333333333703, 0.3219752754296894559, 0.3333333333333333703, 0.3219752754296894559, 0.3333333333333333703, 0.3219752754296894559, 0.3333333333333333703, 0.3219752754296894559, 0.3333333333333333703, 0.3219752754296894559, 0.3333333333333333703, 0.3219752754296894559, 0.3333333333333333703, 0.3219752754296894559, 0.3333333333333333703, 0.3219752754296894559, 0.3333333333333333703, 0.3219752754296894559, 0.3333333333333333703, 0.3219752754296894559, 0.3333333333333333703, 0.3219752754296894559, 0.3333333333333333703, 0.3219752754296894559, 0.3333333333333333703, 0.3219752754296894559, 0.3333333333333333703, 0.3219752754296894559, 0.3333333333333333703, 0.3219752754296894559, 0.3333333333333333703, 0.3219752754296894559, 0.3333333333333333703, 0.3219752754296894559, 0.3333333333333333703, 0.3219752754296894559, 0.3333333333333333703, 0.3219752754296894559, 0.3333333333333333703, 0.3219752754296894559, 0.3333333333333333703, 0.3219752754296894559, 0.3333333333333333703, 0.3219752754296894559, 0.3333333333333333703, 0.3219752754296894559, 0.3333333333333333703, 0.3219752754296894559, 0.3333333333333333703, 0.3219752754296894559, 0.3333333333333333703, 0.3219752754296894559, 0.3333333333333333703, 0.3219752754296894559, 0.3333333333333333703, 0.3219752754296894559, 0.3333333333333333703, 0.3219752754296894559, 0.3333333333333333703, 0.3219752754296894559, 0.3333333333333333703, 0.3219752754296894559, 0.3333333333333333703, 0.3219752754296894559, 0.3333333333333333703, 0.3219752754296894559, 0.3333333333333333703, 0.3219752754296894559, 0.3333333333333333703, 0.3219752754296894559, 0.3333333333333333703, 0.3219752754296894559, 0.3333333333333333703, 0.3219752754296894559, 0.3333333333333333703, 0.3219752754296894559, 0.3333333333333333703, 0.3219752754296894559, 0.3333333333333333703, 0.3219752754296894559, 0.3333333333333333703, 0.3219752754296894559, 0.3333333333333333703, 0.3219752754296894559, 0.3333333333333333703, 0.3219752754296894559, 0.3333333333333333703, 0.3219752754296894559, 0.3333333333333333703, 0.3219752754296894559, 0.3333333333333333703, 0.3219752754296894559, 0.3333333333333333703, 0.3219752754296894559, 0.3333333333333333703, 0.3219752754296894559, 0.3333333333333333703, 0.3219752754296894559, 0.3333333333333333703, 0.3219752754296894559, 0.3333333333333333703, 0.3219752754296894559, 0.3333333333333333703, 0.3219752754296894559, 0.3333333333333333703, 0.3219752754296894559, 0.3333333333333333703, 0.3219752754296894559, 0.3333333333333333703, 0.3219752754296894559, 0.3333333333333333703, 0.3219752754296894559, 0.3333333333333333703, 0.3219752754296894559, 0.3333333333333333703, 0.3219752754296894559, 0.3333333333333333703, 0.3219752754296894559, 0.3333333333333333703, 0.3219752754296894559, 0.3333333333333333703, 0.3219752754296894559, 0.3333333333333333703, 0.3219752754296894559, 0.3333333333333333703, 0.3219752754296894559, 0.3333333333333333703, 0.3219752754296894559, 0.3333333333333333703, 0.3219752754296894559, 0.3333333333333333703, 0.3219752754296894559, 0.3333333333333333703, 0.3219752754296894559, 0.3333333333333333703, 0.3219752754296894559, 0.3333333333333333703, 0.3219752754296894559, 0.3333333333333333703, 0.3219752754296894559, 0.3333333333333333703, 0.3219752754296894559, 0.3333333333333333703, 0.3219752754296894559, 0.3333333333333333703, 0.3219752754296894559, 0.3333333333333333703, 0.3219752754296894559, 0.3333333333333333703, 0.3219752754296894559, 0.3333333333333333703, 0.3219752754296894559, 0.3333333333333333703, 0.3219752754296894559, 0.3333333333333333703, 0.3219752754296894559, 0.3333333333333333703, 0.3219752754296894559, 0.3333333333333333703, 0.3219752754296894559, 0.3333333333333333703, 0.3219752754296894559, 0.3333333333333333703, 0.3219752754296894559, 0.3333333333333333703, 0.3219752754296894559, 0.3333333333333333703, 0.3219752754296894559, 0.3333333333333333703, 0.3219752754296894559, 0.3333333333333333703, 0.3219752754296894559, 0.3333333333333333703, 0.3219752754296894559, 0.3333333333333333703, 0.3219752754296894559, 0.3333333333333333703, 0.3219752754296894559, 0.3333333333333333703, 0.3219752754296894559, 0.3333333333333333703, 0.3219752754296894559, 0.3333333333333333703, 0.3219752754296894559, 0.3333333333333333703, 0.3219752754296894559, 0.3333333333333333703, 0.3219752754296894559, 0.3333333333333333703, 0.3219752754296894559, 0.3333333333333333703, 0.3219752754296894559, 0.3333333333333333703, 0.3219752754296894559, 0.3333333333333333703, 0.3219752754296894559, 0.3333333333333333703, 0.3219752754296894559, 0.3333333333333333703, 0.3219752754296894559, 0.3333333333333333703, 0.3219752754296894559, 0.3333333333333333703, 0.3219752754296894559, 0.3333333333333333703, 0.3219752754296894559, 0.3333333333333333703, 0.3219752754296894559, 0.3333333333333333703, 0.3219752754296894559, 0.3333333333333333703, 0.3219752754296894559, 0.3333333333333333703, 0.3219752754296894559, 0.3333333333333333703, 0.3219752754296894559, 0.3333333333333333703, 0.3219752754296894559, 0.3333333333333333703, 0.3219752754296894559, 0.3333333333333333703, 0.3219752754296894559, 0.3333333333333333703, 0.3219752754296894559, 0.3333333333333333703, 0.3219752754296894559, 0.3333333333333333703, 0.3219752754296894559, 0.3333333333333333703, 0.3219752754296894559, 0.3333333333333333703, 0.3219752754296894559, 0.3333333333333333703, 0.3219752754296894559, 0.3333333333333333703, 0.3219752754296894559, 0.3333333333333333703, 0.3219752754296894559, 0.3333333333333333703, 0.3219752754296894559, 0.3333333333333333703, 0.3219752754296894559, 0.3333333333333333703, 0.3219752754296894559, 0.3333333333333333703, 0.3219752754296894559, 0.3333333333333333703, 0.3219752754296894559, 0.3333333333333333703, 0.3219752754296894559, 0.3333333333333333703, 0.3219752754296894559, 0.3333333333333333703, 0.3219752754296894559, 0.3333333333333333703, 0.3219752754296894559, 0.3333333333333333703, 0.3219752754296894559, 0.3333333333333333703, 0.3219752754296894559, 0.3333333333333333703, 0.3219752754296894559, 0.3333333333333333703, 0.3219752754296894559, 0.3333333333333333703, 0.3219752754296894559, 0.3333333333333333703, 0.3219752754296894559, 0.3333333333333333703, 0.3219752754296894559, 0.3333333333333333703, 0.3219752754296894559, 0.3333333333333333703, 0.3219752754296894559, 0.3333333333333333703, 0.3219752754296894559, 0.3333333333333333703, 0.3219752754296894559, 0.3333333333333333703, 0.3219752754296894559, 0.3333333333333333703, 0.3219752754296894559, 0.3333333333333333703, 0.3219752754296894559, 0.3333333333333333703, 0.3219752754296894559, 0.3333333333333333703, 0.3219752754296894559, 0.3333333333333333703, 0.3219752754296894559, 0.3333333333333333703, 0.3219752754296894559, 0.3333333333333333703, 0.3219752754296894559, 0.3333333333333333703, 0.3219752754296894559, 0.3333333333333333703, 0.3219752754296894559, 0.3333333333333333703, 0.3219752754296894559, 0.3333333333333333703),
 ( 0.3333333333333333703, 0.3219752754296894559, 0.3333333333333333703, 0.3219752754296894559, 0.3333333333333333703, 0.3219752754296894559, 0.3333333333333333703, 0.3219752754296894559, 0.3333333333333333703, 0.3219752754296894559, 0.3333333333333333703, 0.3219752754296894559, 0.3333333333333333703, 0.3219752754296894559, 0.3333333333333333703, 0.3219752754296894559, 0.3333333333333333703, 0.3219752754296894559, 0.3333333333333333703, 0.3219752754296894559, 0.3333333333333333703, 0.3219752754296894559, 0.3333333333333333703, 0.3219752754296894559, 0.3333333333333333703, 0.3219752754296894559, 0.3333333333333333703, 0.3219752754296894559, 0.3333333333333333703, 0.3219752754296894559, 0.3333333333333333703, 0.3219752754296894559, 0.3333333333333333703, 0.3219752754296894559, 0.3333333333333333703, 0.3219752754296894559, 0.3333333333333333703, 0.3219752754296894559, 0.3333333333333333703, 0.3219752754296894559, 0.3333333333333333703, 0.3219752754296894559, 0.3333333333333333703, 0.3219752754296894559, 0.3333333333333333703, 0.3219752754296894559, 0.3333333333333333703, 0.3219752754296894559, 0.3333333333333333703, 0.3219752754296894559, 0.3333333333333333703, 0.3219752754296894559, 0.3333333333333333703, 0.3219752754296894559, 0.3333333333333333703, 0.3219752754296894559, 0.3333333333333333703, 0.3219752754296894559, 0.3333333333333333703, 0.3219752754296894559, 0.3333333333333333703, 0.3219752754296894559, 0.3333333333333333703, 0.3219752754296894559, 0.3333333333333333703, 0.3219752754296894559, 0.3333333333333333703, 0.3219752754296894559, 0.3333333333333333703, 0.3219752754296894559, 0.3333333333333333703, 0.3219752754296894559, 0.3333333333333333703, 0.3219752754296894559, 0.3333333333333333703, 0.3219752754296894559, 0.3333333333333333703, 0.3219752754296894559, 0.3333333333333333703, 0.3219752754296894559, 0.3333333333333333703, 0.3219752754296894559, 0.3333333333333333703, 0.3219752754296894559, 0.3333333333333333703, 0.3219752754296894559, 0.3333333333333333703, 0.3219752754296894559, 0.3333333333333333703, 0.3219752754296894559, 0.3333333333333333703, 0.3219752754296894559, 0.3333333333333333703, 0.3219752754296894559, 0.3333333333333333703, 0.3219752754296894559, 0.3333333333333333703, 0.3219752754296894559, 0.3333333333333333703, 0.3219752754296894559, 0.3333333333333333703, 0.3219752754296894559, 0.3333333333333333703, 0.3219752754296894559, 0.3333333333333333703, 0.3219752754296894559, 0.3333333333333333703, 0.3219752754296894559, 0.3333333333333333703, 0.3219752754296894559, 0.3333333333333333703, 0.3219752754296894559, 0.3333333333333333703, 0.3219752754296894559, 0.3333333333333333703, 0.3219752754296894559, 0.3333333333333333703, 0.3219752754296894559, 0.3333333333333333703, 0.3219752754296894559, 0.3333333333333333703, 0.3219752754296894559, 0.3333333333333333703, 0.3219752754296894559, 0.3333333333333333703, 0.3219752754296894559, 0.3333333333333333703, 0.3219752754296894559, 0.3333333333333333703, 0.3219752754296894559, 0.3333333333333333703, 0.3219752754296894559, 0.3333333333333333703, 0.3219752754296894559, 0.3333333333333333703, 0.3219752754296894559, 0.3333333333333333703, 0.3219752754296894559, 0.3333333333333333703, 0.3219752754296894559, 0.3333333333333333703, 0.3219752754296894559, 0.3333333333333333703, 0.3219752754296894559, 0.3333333333333333703, 0.3219752754296894559, 0.3333333333333333703, 0.3219752754296894559, 0.3333333333333333703, 0.3219752754296894559, 0.3333333333333333703, 0.3219752754296894559, 0.3333333333333333703, 0.3219752754296894559, 0.3333333333333333703, 0.3219752754296894559, 0.3333333333333333703, 0.3219752754296894559, 0.3333333333333333703, 0.3219752754296894559, 0.3333333333333333703, 0.3219752754296894559, 0.3333333333333333703, 0.3219752754296894559, 0.3333333333333333703, 0.3219752754296894559, 0.3333333333333333703, 0.3219752754296894559, 0.3333333333333333703, 0.3219752754296894559, 0.3333333333333333703, 0.3219752754296894559, 0.3333333333333333703, 0.3219752754296894559, 0.3333333333333333703, 0.3219752754296894559, 0.3333333333333333703, 0.3219752754296894559, 0.3333333333333333703, 0.3219752754296894559, 0.3333333333333333703, 0.3219752754296894559, 0.3333333333333333703, 0.3219752754296894559, 0.3333333333333333703, 0.3219752754296894559, 0.3333333333333333703, 0.3219752754296894559, 0.3333333333333333703, 0.3219752754296894559, 0.3333333333333333703, 0.3219752754296894559, 0.3333333333333333703, 0.3219752754296894559, 0.3333333333333333703, 0.3219752754296894559, 0.3333333333333333703, 0.3219752754296894559, 0.3333333333333333703, 0.3219752754296894559, 0.3333333333333333703, 0.3219752754296894559, 0.3333333333333333703, 0.3219752754296894559, 0.3333333333333333703, 0.3219752754296894559, 0.3333333333333333703, 0.3219752754296894559, 0.3333333333333333703, 0.3219752754296894559, 0.3333333333333333703, 0.3219752754296894559, 0.3333333333333333703, 0.3219752754296894559, 0.3333333333333333703, 0.3219752754296894559, 0.3333333333333333703, 0.3219752754296894559, 0.3333333333333333703, 0.3219752754296894559, 0.3333333333333333703, 0.3219752754296894559, 0.3333333333333333703, 0.3219752754296894559, 0.3333333333333333703, 0.3219752754296894559, 0.3333333333333333703, 0.3219752754296894559, 0.3333333333333333703, 0.3219752754296894559, 0.3333333333333333703, 0.3219752754296894559, 0.3333333333333333703, 0.3219752754296894559, 0.3333333333333333703, 0.3219752754296894559, 0.3333333333333333703, 0.3219752754296894559, 0.3333333333333333703, 0.3219752754296894559, 0.3333333333333333703, 0.3219752754296894559, 0.3333333333333333703, 0.3219752754296894559, 0.3333333333333333703, 0.3219752754296894559, 0.3333333333333333703, 0.3219752754296894559, 0.3333333333333333703, 0.3219752754296894559, 0.3333333333333333703, 0.3219752754296894559, 0.3333333333333333703, 0.3219752754296894559, 0.3333333333333333703, 0.3219752754296894559, 0.3333333333333333703, 0.3219752754296894559, 0.3333333333333333703, 0.3219752754296894559, 0.3333333333333333703, 0.3219752754296894559, 0.3333333333333333703, 0.3219752754296894559, 0.3333333333333333703, 0.3219752754296894559, 0.3333333333333333703, 0.3219752754296894559, 0.3333333333333333703, 0.3219752754296894559, 0.3333333333333333703, 0.3219752754296894559, 0.3333333333333333703, 0.3219752754296894559, 0.3333333333333333703, 0.3219752754296894559, 0.3333333333333333703, 0.3219752754296894559, 0.3333333333333333703, 0.3219752754296894559, 0.3333333333333333703, 0.3219752754296894559, 0.3333333333333333703, 0.3219752754296894559, 0.3333333333333333703, 0.3219752754296894559, 0.3333333333333333703, 0.3219752754296894559, 0.3333333333333333703, 0.3219752754296894559, 0.3333333333333333703, 0.3219752754296894559, 0.3333333333333333703, 0.3219752754296894559, 0.3333333333333333703, 0.3219752754296894559, 0.3333333333333333703, 0.3219752754296894559, 0.3333333333333333703, 0.3219752754296894559, 0.3333333333333333703, 0.3219752754296894559, 0.3333333333333333703, 0.3219752754296894559, 0.3333333333333333703, 0.3219752754296894559, 0.3333333333333333703, 0.3219752754296894559, 0.3333333333333333703, 0.3219752754296894559, 0.3333333333333333703, 0.3219752754296894559, 0.3333333333333333703, 0.3219752754296894559, 0.3333333333333333703, 0.3219752754296894559, 0.3333333333333333703, 0.3219752754296894559, 0.3333333333333333703, 0.3219752754296894559, 0.3333333333333333703, 0.3219752754296894559, 0.3333333333333333703, 0.3219752754296894559, 0.3333333333333333703, 0.3219752754296894559, 0.3333333333333333703, 0.3219752754296894559, 0.3333333333333333703, 0.3219752754296894559, 0.3333333333333333703, 0.3219752754296894559, 0.3333333333333333703, 0.3219752754296894559, 0.3333333333333333703, 0.3219752754296894559, 0.3333333333333333703, 0.3219752754296894559, 0.3333333333333333703, 0.3219752754296894559, 0.3333333333333333703, 0.3219752754296894559, 0.3333333333333333703, 0.3219752754296894559, 0.3333333333333333703, 0.3219752754296894559, 0.3333333333333333703, 0.3219752754296894559, 0.3333333333333333703, 0.3219752754296894559, 0.3333333333333333703, 0.3219752754296894559, 0.3333333333333333703, 0.3219752754296894559, 0.3333333333333333703, 0.3219752754296894559, 0.3333333333333333703, 0.3219752754296894559, 0.3333333333333333703, 0.3219752754296894559, 0.3333333333333333703, 0.3219752754296894559, 0.3333333333333333703, 0.3219752754296894559, 0.3333333333333333703, 0.3219752754296894559, 0.3333333333333333703, 0.3219752754296894559, 0.3333333333333333703, 0.3219752754296894559, 0.3333333333333333703, 0.3219752754296894559, 0.3333333333333333703, 0.3219752754296894559, 0.3333333333333333703, 0.3219752754296894559, 0.3333333333333333703, 0.3219752754296894559, 0.3333333333333333703, 0.3219752754296894559, 0.3333333333333333703, 0.3219752754296894559, 0.3333333333333333703, 0.3219752754296894559, 0.3333333333333333703, 0.3219752754296894559, 0.3333333333333333703, 0.3219752754296894559, 0.3333333333333333703, 0.3219752754296894559, 0.3333333333333333703, 0.3219752754296894559, 0.3333333333333333703, 0.3219752754296894559, 0.3333333333333333703, 0.3219752754296894559, 0.3333333333333333703, 0.3219752754296894559, 0.3333333333333333703, 0.3219752754296894559, 0.3333333333333333703, 0.3219752754296894559, 0.3333333333333333703, 0.3219752754296894559, 0.3333333333333333703, 0.3219752754296894559, 0.3333333333333333703, 0.3219752754296894559, 0.3333333333333333703, 0.3219752754296894559, 0.3333333333333333703, 0.3219752754296894559, 0.3333333333333333703, 0.3219752754296894559, 0.3333333333333333703, 0.3219752754296894559, 0.3333333333333333703, 0.3219752754296894559, 0.3333333333333333703, 0.3219752754296894559, 0.3333333333333333703, 0.3219752754296894559, 0.3333333333333333703, 0.3219752754296894559, 0.3333333333333333703, 0.3219752754296894559, 0.3333333333333333703, 0.3219752754296894559, 0.3333333333333333703, 0.3219752754296894559, 0.3333333333333333703, 0.3219752754296894559, 0.3333333333333333703, 0.3219752754296894559, 0.3333333333333333703, 0.3219752754296894559, 0.3333333333333333703, 0.3219752754296894559, 0.3333333333333333703, 0.3219752754296894559, 0.3333333333333333703, 0.3219752754296894559, 0.3333333333333333703, 0.3219752754296894559, 0.3333333333333333703, 0.3219752754296894559, 0.3333333333333333703, 0.3219752754296894559, 0.3333333333333333703, 0.3219752754296894559, 0.3333333333333333703, 0.3219752754296894559, 0.3333333333333333703, 0.3219752754296894559, 0.3333333333333333703, 0.3219752754296894559, 0.3333333333333333703),
 ( 1.000000000000000000, 0.9659258262890683122, 1.000000000000000000, 0.9659258262890683122, 1.000000000000000000, 0.9659258262890683122, 1.000000000000000000, 0.9659258262890683122, 1.000000000000000000, 0.9659258262890683122, 1.000000000000000000, 0.9659258262890683122, 1.000000000000000000, 0.9659258262890683122, 1.000000000000000000, 0.9659258262890683122, 1.000000000000000000, 0.9659258262890683122, 1.000000000000000000, 0.9659258262890683122, 1.000000000000000000, 0.9659258262890683122, 1.000000000000000000, 0.9659258262890683122, 1.000000000000000000, 0.9659258262890683122, 1.000000000000000000, 0.9659258262890683122, 1.000000000000000000, 0.9659258262890683122, 1.000000000000000000, 0.9659258262890683122, 1.000000000000000000, 0.9659258262890683122, 1.000000000000000000, 0.9659258262890683122, 1.000000000000000000, 0.9659258262890683122, 1.000000000000000000, 0.9659258262890683122, 1.000000000000000000, 0.9659258262890683122, 1.000000000000000000, 0.9659258262890683122, 1.000000000000000000, 0.9659258262890683122, 1.000000000000000000, 0.9659258262890683122, 1.000000000000000000, 0.9659258262890683122, 1.000000000000000000, 0.9659258262890683122, 1.000000000000000000, 0.9659258262890683122, 1.000000000000000000, 0.9659258262890683122, 1.000000000000000000, 0.9659258262890683122, 1.000000000000000000, 0.9659258262890683122, 1.000000000000000000, 0.9659258262890683122, 1.000000000000000000, 0.9659258262890683122, 1.000000000000000000, 0.9659258262890683122, 1.000000000000000000, 0.9659258262890683122, 1.000000000000000000, 0.9659258262890683122, 1.000000000000000000, 0.9659258262890683122, 1.000000000000000000, 0.9659258262890683122, 1.000000000000000000, 0.9659258262890683122, 1.000000000000000000, 0.9659258262890683122, 1.000000000000000000, 0.9659258262890683122, 1.000000000000000000, 0.9659258262890683122, 1.000000000000000000, 0.9659258262890683122, 1.000000000000000000, 0.9659258262890683122, 1.000000000000000000, 0.9659258262890683122, 1.000000000000000000, 0.9659258262890683122, 1.000000000000000000, 0.9659258262890683122, 1.000000000000000000, 0.9659258262890683122, 1.000000000000000000, 0.9659258262890683122, 1.000000000000000000, 0.9659258262890683122, 1.000000000000000000, 0.9659258262890683122, 1.000000000000000000, 0.9659258262890683122, 1.000000000000000000, 0.9659258262890683122, 1.000000000000000000, 0.9659258262890683122, 1.000000000000000000, 0.9659258262890683122, 1.000000000000000000, 0.9659258262890683122, 1.000000000000000000, 0.9659258262890683122, 1.000000000000000000, 0.9659258262890683122, 1.000000000000000000, 0.9659258262890683122, 1.000000000000000000, 0.9659258262890683122, 1.000000000000000000, 0.9659258262890683122, 1.000000000000000000, 0.9659258262890683122, 1.000000000000000000, 0.9659258262890683122, 1.000000000000000000, 0.9659258262890683122, 1.000000000000000000, 0.9659258262890683122, 1.000000000000000000, 0.9659258262890683122, 1.000000000000000000, 0.9659258262890683122, 1.000000000000000000, 0.9659258262890683122, 1.000000000000000000, 0.9659258262890683122, 1.000000000000000000, 0.9659258262890683122, 1.000000000000000000, 0.9659258262890683122, 1.000000000000000000, 0.9659258262890683122, 1.000000000000000000, 0.9659258262890683122, 1.000000000000000000, 0.9659258262890683122, 1.000000000000000000, 0.9659258262890683122, 1.000000000000000000, 0.9659258262890683122, 1.000000000000000000, 0.9659258262890683122, 1.000000000000000000, 0.9659258262890683122, 1.000000000000000000, 0.9659258262890683122, 1.000000000000000000, 0.9659258262890683122, 1.000000000000000000, 0.9659258262890683122, 1.000000000000000000, 0.9659258262890683122, 1.000000000000000000, 0.9659258262890683122, 1.000000000000000000, 0.9659258262890683122, 1.000000000000000000, 0.9659258262890683122, 1.000000000000000000, 0.9659258262890683122, 1.000000000000000000, 0.9659258262890683122, 1.000000000000000000, 0.9659258262890683122, 1.000000000000000000, 0.9659258262890683122, 1.000000000000000000, 0.9659258262890683122, 1.000000000000000000, 0.9659258262890683122, 1.000000000000000000, 0.9659258262890683122, 1.000000000000000000, 0.9659258262890683122, 1.000000000000000000, 0.9659258262890683122, 1.000000000000000000, 0.9659258262890683122, 1.000000000000000000, 0.9659258262890683122, 1.000000000000000000, 0.9659258262890683122, 1.000000000000000000, 0.9659258262890683122, 1.000000000000000000, 0.9659258262890683122, 1.000000000000000000, 0.9659258262890683122, 1.000000000000000000, 0.9659258262890683122, 1.000000000000000000, 0.9659258262890683122, 1.000000000000000000, 0.9659258262890683122, 1.000000000000000000, 0.9659258262890683122, 1.000000000000000000, 0.9659258262890683122, 1.000000000000000000, 0.9659258262890683122, 1.000000000000000000, 0.9659258262890683122, 1.000000000000000000, 0.9659258262890683122, 1.000000000000000000, 0.9659258262890683122, 1.000000000000000000, 0.9659258262890683122, 1.000000000000000000, 0.9659258262890683122, 1.000000000000000000, 0.9659258262890683122, 1.000000000000000000, 0.9659258262890683122, 1.000000000000000000, 0.9659258262890683122, 1.000000000000000000, 0.9659258262890683122, 1.000000000000000000, 0.9659258262890683122, 1.000000000000000000, 0.9659258262890683122, 1.000000000000000000, 0.9659258262890683122, 1.000000000000000000, 0.9659258262890683122, 1.000000000000000000, 0.9659258262890683122, 1.000000000000000000, 0.9659258262890683122, 1.000000000000000000, 0.9659258262890683122, 1.000000000000000000, 0.9659258262890683122, 1.000000000000000000, 0.9659258262890683122, 1.000000000000000000, 0.9659258262890683122, 1.000000000000000000, 0.9659258262890683122, 1.000000000000000000, 0.9659258262890683122, 1.000000000000000000, 0.9659258262890683122, 1.000000000000000000, 0.9659258262890683122, 1.000000000000000000, 0.9659258262890683122, 1.000000000000000000, 0.9659258262890683122, 1.000000000000000000, 0.9659258262890683122, 1.000000000000000000, 0.9659258262890683122, 1.000000000000000000, 0.9659258262890683122, 1.000000000000000000, 0.9659258262890683122, 1.000000000000000000, 0.9659258262890683122, 1.000000000000000000, 0.9659258262890683122, 1.000000000000000000, 0.9659258262890683122, 1.000000000000000000, 0.9659258262890683122, 1.000000000000000000, 0.9659258262890683122, 1.000000000000000000, 0.9659258262890683122, 1.000000000000000000, 0.9659258262890683122, 1.000000000000000000, 0.9659258262890683122, 1.000000000000000000, 0.9659258262890683122, 1.000000000000000000, 0.9659258262890683122, 1.000000000000000000, 0.9659258262890683122, 1.000000000000000000, 0.9659258262890683122, 1.000000000000000000, 0.9659258262890683122, 1.000000000000000000, 0.9659258262890683122, 1.000000000000000000, 0.9659258262890683122, 1.000000000000000000, 0.9659258262890683122, 1.000000000000000000, 0.9659258262890683122, 1.000000000000000000, 0.9659258262890683122, 1.000000000000000000, 0.9659258262890683122, 1.000000000000000000, 0.9659258262890683122, 1.000000000000000000, 0.9659258262890683122, 1.000000000000000000, 0.9659258262890683122, 1.000000000000000000, 0.9659258262890683122, 1.000000000000000000, 0.9659258262890683122, 1.000000000000000000, 0.9659258262890683122, 1.000000000000000000, 0.9659258262890683122, 1.000000000000000000, 0.9659258262890683122, 1.000000000000000000, 0.9659258262890683122, 1.000000000000000000, 0.9659258262890683122, 1.000000000000000000, 0.9659258262890683122, 1.000000000000000000, 0.9659258262890683122, 1.000000000000000000, 0.9659258262890683122, 1.000000000000000000, 0.9659258262890683122, 1.000000000000000000, 0.9659258262890683122, 1.000000000000000000, 0.9659258262890683122, 1.000000000000000000, 0.9659258262890683122, 1.000000000000000000, 0.9659258262890683122, 1.000000000000000000, 0.9659258262890683122, 1.000000000000000000, 0.9659258262890683122, 1.000000000000000000, 0.9659258262890683122, 1.000000000000000000, 0.9659258262890683122, 1.000000000000000000, 0.9659258262890683122, 1.000000000000000000, 0.9659258262890683122, 1.000000000000000000, 0.9659258262890683122, 1.000000000000000000, 0.9659258262890683122, 1.000000000000000000, 0.9659258262890683122, 1.000000000000000000, 0.9659258262890683122, 1.000000000000000000, 0.9659258262890683122, 1.000000000000000000, 0.9659258262890683122, 1.000000000000000000, 0.9659258262890683122, 1.000000000000000000, 0.9659258262890683122, 1.000000000000000000, 0.9659258262890683122, 1.000000000000000000, 0.9659258262890683122, 1.000000000000000000, 0.9659258262890683122, 1.000000000000000000, 0.9659258262890683122, 1.000000000000000000, 0.9659258262890683122, 1.000000000000000000, 0.9659258262890683122, 1.000000000000000000, 0.9659258262890683122, 1.000000000000000000, 0.9659258262890683122, 1.000000000000000000, 0.9659258262890683122, 1.000000000000000000, 0.9659258262890683122, 1.000000000000000000, 0.9659258262890683122, 1.000000000000000000, 0.9659258262890683122, 1.000000000000000000, 0.9659258262890683122, 1.000000000000000000, 0.9659258262890683122, 1.000000000000000000, 0.9659258262890683122, 1.000000000000000000, 0.9659258262890683122, 1.000000000000000000, 0.9659258262890683122, 1.000000000000000000, 0.9659258262890683122, 1.000000000000000000, 0.9659258262890683122, 1.000000000000000000, 0.9659258262890683122, 1.000000000000000000, 0.9659258262890683122, 1.000000000000000000, 0.9659258262890683122, 1.000000000000000000, 0.9659258262890683122, 1.000000000000000000, 0.9659258262890683122, 1.000000000000000000, 0.9659258262890683122, 1.000000000000000000, 0.9659258262890683122, 1.000000000000000000, 0.9659258262890683122, 1.000000000000000000, 0.9659258262890683122, 1.000000000000000000, 0.9659258262890683122, 1.000000000000000000, 0.9659258262890683122, 1.000000000000000000, 0.9659258262890683122, 1.000000000000000000, 0.9659258262890683122, 1.000000000000000000, 0.9659258262890683122, 1.000000000000000000, 0.9659258262890683122, 1.000000000000000000, 0.9659258262890683122, 1.000000000000000000, 0.9659258262890683122, 1.000000000000000000, 0.9659258262890683122, 1.000000000000000000, 0.9659258262890683122, 1.000000000000000000, 0.9659258262890683122, 1.000000000000000000, 0.9659258262890683122, 1.000000000000000000, 0.9659258262890683122, 1.000000000000000000, 0.9659258262890683122, 1.000000000000000000, 0.9659258262890683122, 1.000000000000000000) ) ) 
 REPRESENTATION_ITEM ( '' )  SURFACE ( )  );
#20743 = CARTESIAN_POINT ( 'NONE',  ( -12.14591786802326823, 12.06949235617739902, 33.12609039468569705 ) ) ;
#20745 = CARTESIAN_POINT ( 'NONE',  ( -21.53943276465977519, -0.05219959533937600094, 83.75109039468568994 ) ) ;
#20744 = CARTESIAN_POINT ( 'NONE',  ( -4.379528057220328563, 16.55341960407611168, 65.20724293864768129 ) ) ;
#20746 = CARTESIAN_POINT ( 'NONE',  ( 14.34966873604972726, -8.224510206698740333, 105.8344237280190328 ) ) ;
#20747 = CARTESIAN_POINT ( 'NONE',  ( 17.26172910966779384, 6.454744622555870670, 26.69353091350777518 ) ) ;
#20748 = CARTESIAN_POINT ( 'NONE',  ( -18.87255363501903105, -5.499999999999950262, 66.32513748171827217 ) ) ;
#20749 = CARTESIAN_POINT ( 'NONE',  ( 14.34966873604960469, 8.224510206698951720, 24.16557627198103120 ) ) ;
#20750 = CARTESIAN_POINT ( 'NONE',  ( -8.314922557961024197, 14.29746914071037800, 72.91775706135234714 ) ) ;
#20751 = CARTESIAN_POINT ( 'NONE',  ( 16.51473224551069308, 9.474510206698969483, 84.16557627198102409 ) ) ;
#20752 = CARTESIAN_POINT ( 'NONE',  ( -5.153800228976328057, -19.02544592524343514, 97.29057627198099567 ) ) ;
#20753 = CARTESIAN_POINT ( 'NONE',  ( 5.719274019375673035, 21.55341960407619339, 92.29275706135236135 ) ) ;
#20754 = CARTESIAN_POINT ( 'NONE',  ( -0.05219959533934338120, 16.53943276465976808, 87.50109039468568994 ) ) ;
#20755 = CARTESIAN_POINT ( 'NONE',  ( -16.52544592524342804, 4.483927247898546575, 56.04057627198102409 ) ) ;
#20756 = CARTESIAN_POINT ( 'NONE',  ( -0.05219959533909027116, -19.03943276465977164, 72.49890960531435269 ) ) ;
#20757 = ORIENTED_EDGE ( 'NONE', *, *, #165015, .T. ) ;
#20758 = CARTESIAN_POINT ( 'NONE',  ( -9.564922557961040184, 16.46253265017147172, 107.9177570613523471 ) ) ;
#20759 = CARTESIAN_POINT ( 'NONE',  ( -16.51473224551069308, -9.474510206698971260, 21.66557627198102765 ) ) ;
#20760 = CARTESIAN_POINT ( 'NONE',  ( -16.46253265017160317, 9.564922557960807481, 80.83224293864769550 ) ) ;
#20762 = CARTESIAN_POINT ( 'NONE',  ( -36.91746825000001309, -11.99521256947794789, -6.524999997268810858 ) ) ;
#20761 = CARTESIAN_POINT ( 'NONE',  ( -5.049401038297874678, -19.05341960407617918, 109.7927570613523187 ) ) ;
#20763 = CARTESIAN_POINT ( 'NONE',  ( -19.05341960407617563, 5.049401038297882671, 23.54275706135233648 ) ) ;
#20764 = CARTESIAN_POINT ( 'NONE',  ( 4.379528057220092307, 16.55341960407617563, 82.29275706135234714 ) ) ;
#20765 = CARTESIAN_POINT ( 'NONE',  ( 19.03943276465977164, 0.05219959533936151252, 111.2510903946856757 ) ) ;
#20766 = CARTESIAN_POINT ( 'NONE',  ( 16.53943276465976808, -0.05219959533910856209, 113.7489096053143527 ) ) ;
#20767 = CARTESIAN_POINT ( 'NONE',  ( 4.483927247898790824, -16.52544592524335698, 60.20942372801902565 ) ) ;
#20768 = CARTESIAN_POINT ( 'NONE',  ( -12.14591786802326823, 12.06949235617739902, 48.12609039468568284 ) ) ;
#20769 = CARTESIAN_POINT ( 'NONE',  ( -9.474510206698964154, 16.51473224551069663, 25.41557627198103120 ) ) ;
#20770 = CARTESIAN_POINT ( 'NONE',  ( 9.564922557961047289, -16.46253265017146816, 70.41775706135233293 ) ) ;
#20771 = CARTESIAN_POINT ( 'NONE',  ( -5.719274019375665041, -21.55341960407619695, 109.7927570613523613 ) ) ;
#20772 = CARTESIAN_POINT ( 'NONE',  ( -9.474510206698964154, 16.51473224551069663, 40.41557627198103120 ) ) ;
#20773 = CARTESIAN_POINT ( 'NONE',  ( 19.05341960407611168, 5.049401038298154454, 78.95724293864769550 ) ) ;
#20774 = CARTESIAN_POINT ( 'NONE',  ( 14.29746914071049879, -8.314922557960816363, 73.33224293864769550 ) ) ;
#20775 = AXIS2_PLACEMENT_3D ( 'NONE', #17473, #52769, #3288 ) ;
#20776 = CARTESIAN_POINT ( 'NONE',  ( 13.97604488694548053, -13.89961937509957401, 35.62609039468567573 ) ) ;
#20777 = CARTESIAN_POINT ( 'NONE',  ( -15.72974639402197994, 15.80617190586746368, 40.62390960531435269 ) ) ;
#20778 = CARTESIAN_POINT ( 'NONE',  ( -15.80617190586768217, 15.72974639402176855, 108.1260903946856757 ) ) ;
#20779 = CARTESIAN_POINT ( 'NONE',  ( 13.89961937509977652, -13.97604488694527269, 88.12390960531438111 ) ) ;
#20780 = CARTESIAN_POINT ( 'NONE',  ( 21.53943276465977519, 0.05219959533937863772, 101.2510903946856757 ) ) ;
#20781 = CARTESIAN_POINT ( 'NONE',  ( -10.81492255796078084, -18.62759615963271287, 67.08224293864770971 ) ) ;
#20782 = CARTESIAN_POINT ( 'NONE',  ( -9.474510206698964154, 16.51473224551069663, 100.4155762719810241 ) ) ;
#20783 = CARTESIAN_POINT ( 'NONE',  ( -19.05341960407617563, 5.049401038297882671, 78.54275706135233293 ) ) ;
#20784 = CARTESIAN_POINT ( 'NONE',  ( -0.05219959533909027116, -19.03943276465977164, 97.49890960531436690 ) ) ;
#20785 = CARTESIAN_POINT ( 'NONE',  ( 16.51473224551083163, -9.474510206698727899, 95.83442372801900433 ) ) ;
#20786 = CARTESIAN_POINT ( 'NONE',  ( -12.14591786802326823, 12.06949235617739902, 53.12609039468568284 ) ) ;
#20787 = CARTESIAN_POINT ( 'NONE',  ( -19.03943276465977164, 0.05219959533909376836, 21.24890960531436335 ) ) ;
#20788 = CARTESIAN_POINT ( 'NONE',  ( 5.153800228976335163, 19.02544592524342804, 79.79057627198102409 ) ) ;
#20789 = CARTESIAN_POINT ( 'NONE',  ( 5.719274019375991003, -21.55341960407610458, 67.70724293864769550 ) ) ;
#20790 = CARTESIAN_POINT ( 'NONE',  ( -16.55341960407617563, 4.379528057220093196, 33.54275706135234714 ) ) ;
#20791 = CARTESIAN_POINT ( 'NONE',  ( -21.55341960407619339, 5.719274019375674811, 33.54275706135234714 ) ) ;
#20792 = CARTESIAN_POINT ( 'NONE',  ( 18.67979575497194134, -10.72451020669871369, 90.83442372801901854 ) ) ;
#20793 = CARTESIAN_POINT ( 'NONE',  ( -16.52544592524335698, -4.483927247898792601, 93.95942372801903275 ) ) ;
#20794 = CARTESIAN_POINT ( 'NONE',  ( 5.049401038298161559, -19.05341960407611168, 82.70724293864770971 ) ) ;
#20795 = CARTESIAN_POINT ( 'NONE',  ( -0.05219959533910754901, -16.53943276465976808, 77.49890960531433848 ) ) ;
#20796 = CARTESIAN_POINT ( 'NONE',  ( 14.34966873604960469, 8.224510206698951720, 24.16557627198103120 ) ) ;
#20797 = CARTESIAN_POINT ( 'NONE',  ( 5.153800228976615827, -19.02544592524334988, 70.20942372801899012 ) ) ;
#20798 = CARTESIAN_POINT ( 'NONE',  ( -5.719274019375665041, -21.55341960407619695, 49.79275706135234714 ) ) ;
#20799 = CARTESIAN_POINT ( 'NONE',  ( 16.53943276465976808, -0.05219959533910856209, 98.74890960531438111 ) ) ;
#20800 = CARTESIAN_POINT ( 'NONE',  ( 0.05219959533909260263, 19.03943276465977164, 109.9989096053143669 ) ) ;
#20801 = CARTESIAN_POINT ( 'NONE',  ( -8.314922557961024197, 14.29746914071037800, 107.9177570613523471 ) ) ;
#20802 = CARTESIAN_POINT ( 'NONE',  ( 21.53943276465977519, 0.05219959533937863772, 86.25109039468568994 ) ) ;
#20803 = CARTESIAN_POINT ( 'NONE',  ( 8.314922557961029526, -14.29746914071037800, 40.41775706135234714 ) ) ;
#20804 = CARTESIAN_POINT ( 'NONE',  ( -15.72974639402176322, -15.80617190586768395, 44.37609039468567573 ) ) ;
#20805 = ORIENTED_EDGE ( 'NONE', *, *, #93266, .F. ) ;
#20806 = CARTESIAN_POINT ( 'NONE',  ( -0.05219959533907301413, -21.53943276465977519, 112.4989096053143669 ) ) ;
#20807 = CARTESIAN_POINT ( 'NONE',  ( -4.483927247898539470, -16.52544592524342804, 97.29057627198105251 ) ) ;
#20808 = CARTESIAN_POINT ( 'NONE',  ( 17.50000000000005329, -4.049696124445820722, 26.68039670665946161 ) ) ;
#20809 = CARTESIAN_POINT ( 'NONE',  ( 0.05219959533910956823, 16.53943276465976808, 64.99890960531435269 ) ) ;
#20810 = CARTESIAN_POINT ( 'NONE',  ( -12.14591786802326823, 12.06949235617739902, 113.1260903946856899 ) ) ;
#20811 = CARTESIAN_POINT ( 'NONE',  ( -9.474510206698964154, 16.51473224551069663, 35.41557627198102409 ) ) ;
#20812 = CARTESIAN_POINT ( 'NONE',  ( -10.81492255796078084, -18.62759615963271287, 37.08224293864768129 ) ) ;
#20813 = CARTESIAN_POINT ( 'NONE',  ( 14.29746914071049879, -8.314922557960816363, 83.33224293864769550 ) ) ;
#20814 = CARTESIAN_POINT ( 'NONE',  ( -5.823673210054116645, -21.52544592524344225, 82.29057627198103830 ) ) ;
#20816 = EDGE_CURVE ( 'NONE', #189816, #194525, #82036, .T. ) ;
#20815 = CARTESIAN_POINT ( 'NONE',  ( -5.153800228976328057, -19.02544592524343514, 87.29057627198103830 ) ) ;
#20818 = CARTESIAN_POINT ( 'NONE',  ( -5.049401038297874678, -19.05341960407617918, 89.79275706135230450 ) ) ;
#20817 = CARTESIAN_POINT ( 'NONE',  ( 9.474510206698971260, -16.51473224551069308, 42.91557627198103120 ) ) ;
#20819 = CARTESIAN_POINT ( 'NONE',  ( 5.719274019375991003, -21.55341960407610458, 27.70724293864769905 ) ) ;
#20820 = CARTESIAN_POINT ( 'NONE',  ( -21.55341960407619339, 5.719274019375674811, 73.54275706135234714 ) ) ;
#20821 = CARTESIAN_POINT ( 'NONE',  ( 19.05341960407611168, 5.049401038298154454, 48.95724293864768129 ) ) ;
#20822 = CARTESIAN_POINT ( 'NONE',  ( -13.97604488694527625, -13.89961937509977652, 86.87390960531436690 ) ) ;
#20823 = ORIENTED_EDGE ( 'NONE', *, *, #158246, .T. ) ;
#20824 = CARTESIAN_POINT ( 'NONE',  ( 0.05219959533934541429, -16.53943276465976808, 60.00109039468568284 ) ) ;
#20825 = CARTESIAN_POINT ( 'NONE',  ( 0.05219959533937995610, -21.53943276465977519, 45.00109039468568284 ) ) ;
#20826 = AXIS2_PLACEMENT_3D ( 'NONE', #186359, #142800, #63988 ) ;
#20827 = CARTESIAN_POINT ( 'NONE',  ( 15.72974639402176855, 15.80617190586768217, 66.87609039468568994 ) ) ;
#20828 = CARTESIAN_POINT ( 'NONE',  ( 10.81492255796078972, 18.62759615963270932, 24.58224293864768839 ) ) ;
#20829 = CARTESIAN_POINT ( 'NONE',  ( 21.53943276465977519, -0.05219959533907433946, 98.74890960531438111 ) ) ;
#20831 = CARTESIAN_POINT ( 'NONE',  ( 0.05219959533934541429, -16.53943276465976808, 60.00109039468568284 ) ) ;
#20830 = CARTESIAN_POINT ( 'NONE',  ( -18.67979575497193778, 10.72451020669871902, 23.33442372801901499 ) ) ;
#20832 = CARTESIAN_POINT ( 'NONE',  ( -15.80617190586745835, -15.72974639402198527, 66.87390960531436690 ) ) ;
#20833 = CARTESIAN_POINT ( 'NONE',  ( 15.72974639402176855, 15.80617190586768217, 111.8760903946856615 ) ) ;
#20835 = CARTESIAN_POINT ( 'NONE',  ( -8.224510206698735004, -14.34966873604973081, 104.5844237280190185 ) ) ;
#20834 = CARTESIAN_POINT ( 'NONE',  ( -16.51473224551069308, -9.474510206698971260, 66.66557627198102409 ) ) ;
#20836 = CARTESIAN_POINT ( 'NONE',  ( -38.00000000000004263, -12.34694845685037023, -5.899999999999999467 ) ) ;
#20837 = CARTESIAN_POINT ( 'NONE',  ( -9.474510206698964154, 16.51473224551069663, 90.41557627198103830 ) ) ;
#20838 = CARTESIAN_POINT ( 'NONE',  ( -0.05219959533934338120, 16.53943276465976808, 42.50109039468567573 ) ) ;
#20839 = CARTESIAN_POINT ( 'NONE',  ( 20.25987216150956272, 20.63676584477893172, -49.65115959356506892 ) ) ;
#20840 = CARTESIAN_POINT ( 'NONE',  ( 9.474510206698729675, 16.51473224551082808, 82.08442372801899012 ) ) ;
#20841 = CARTESIAN_POINT ( 'NONE',  ( -18.62759615963270932, 10.81492255796079327, 60.83224293864769550 ) ) ;
#20842 = CARTESIAN_POINT ( 'NONE',  ( -4.379528057220328563, 16.55341960407611168, 25.20724293864769550 ) ) ;
#20843 = CARTESIAN_POINT ( 'NONE',  ( 16.51473224551083163, -9.474510206698727899, 100.8344237280190043 ) ) ;
#20844 = CARTESIAN_POINT ( 'NONE',  ( -17.49999999999999645, 5.499999999999997335, 120.0000000000000142 ) ) ;
#20845 = CARTESIAN_POINT ( 'NONE',  ( 0.05219959533936267826, -19.03943276465977164, 95.00109039468567573 ) ) ;
#20847 = CARTESIAN_POINT ( 'NONE',  ( -19.05341960407617563, 5.049401038297882671, 63.54275706135234003 ) ) ;
#20846 = CARTESIAN_POINT ( 'NONE',  ( -18.67979575497178146, -10.72451020669898902, 86.66557627198102409 ) ) ;
#20848 = CARTESIAN_POINT ( 'NONE',  ( 26.26083487095746349, -9.141127703660906434, 167.1337248662267712 ) ) ;
#20849 = CARTESIAN_POINT ( 'NONE',  ( 16.51473224551069308, 9.474510206698969483, 74.16557627198103830 ) ) ;
#20850 = CARTESIAN_POINT ( 'NONE',  ( 14.29746914071049879, -8.314922557960816363, 58.33224293864768839 ) ) ;
#20851 = EDGE_CURVE ( 'NONE', #66168, #27708, #136298, .T. ) ;
#20852 = AXIS2_PLACEMENT_3D ( 'NONE', #106884, #46212, #28098 ) ;
#20853 = CARTESIAN_POINT ( 'NONE',  ( 9.564922557960805705, 16.46253265017160317, 49.58224293864770260 ) ) ;
#20854 = CARTESIAN_POINT ( 'NONE',  ( 14.34966873604960469, 8.224510206698951720, 54.16557627198103120 ) ) ;
#20855 = CARTESIAN_POINT ( 'NONE',  ( 32.33375351741884174, -3.966103829525456259, 88.62974963220464986 ) ) ;
#20856 = CARTESIAN_POINT ( 'NONE',  ( 12.06949235617757843, -12.14591786802309237, 28.12390960531435979 ) ) ;
#20857 = CARTESIAN_POINT ( 'NONE',  ( -19.03943276465977164, 0.05219959533909376836, 66.24890960531436690 ) ) ;
#20858 = CARTESIAN_POINT ( 'NONE',  ( 3.181980515339539295, 6.791538853603031889, 1.110912703473986074 ) ) ;
#20859 = CARTESIAN_POINT ( 'NONE',  ( -9.564922557961040184, 16.46253265017147172, 32.91775706135233293 ) ) ;
#20860 = CARTESIAN_POINT ( 'NONE',  ( -4.379528057220086978, -16.55341960407618274, 49.79275706135234714 ) ) ;
#20861 = CARTESIAN_POINT ( 'NONE',  ( 10.72451020669898902, -18.67979575497178502, 52.91557627198103830 ) ) ;
#20862 = CARTESIAN_POINT ( 'NONE',  ( 18.62759615963255655, 10.81492255796105972, 111.6677570613523613 ) ) ;
#20863 = CARTESIAN_POINT ( 'NONE',  ( -5.153800228976328057, -19.02544592524343514, 72.29057627198102409 ) ) ;
#20864 = CARTESIAN_POINT ( 'NONE',  ( -16.46253265017160317, 9.564922557960807481, 115.8322429386477097 ) ) ;
#20865 = CARTESIAN_POINT ( 'NONE',  ( 19.02544592524343514, -5.153800228976328945, 108.5405762719810383 ) ) ;
#20866 = CARTESIAN_POINT ( 'NONE',  ( 3.556970738554034288E-15, -38.81732327939057114, -2.124999997268813168 ) ) ;
#20867 = CARTESIAN_POINT ( 'NONE',  ( -18.62759615963255300, -10.81492255796106328, 44.16775706135234714 ) ) ;
#20868 = CARTESIAN_POINT ( 'NONE',  ( 4.483927247898545687, 16.52544592524342804, 89.79057627198103830 ) ) ;
#20871 = CARTESIAN_POINT ( 'NONE',  ( 17.49999999999998579, -5.500000000000023981, 68.29690382534171533 ) ) ;
#20870 = CARTESIAN_POINT ( 'NONE',  ( 19.05341960407611168, 5.049401038298154454, 83.95724293864766707 ) ) ;
#20869 = CARTESIAN_POINT ( 'NONE',  ( 5.719274019375991003, -21.55341960407610458, 87.70724293864769550 ) ) ;
#20872 = CARTESIAN_POINT ( 'NONE',  ( 16.46253265017160672, -9.564922557960803928, 93.33224293864769550 ) ) ;
#20873 = CARTESIAN_POINT ( 'NONE',  ( -5.719274019375665041, -21.55341960407619695, 19.79275706135235069 ) ) ;
#20874 = ORIENTED_EDGE ( 'NONE', *, *, #64542, .T. ) ;
#20875 = CARTESIAN_POINT ( 'NONE',  ( -13.97604488694527625, -13.89961937509977652, 76.87390960531433848 ) ) ;
#20876 = CARTESIAN_POINT ( 'NONE',  ( 19.48894818550245489, -5.499999999999906741, 97.60307310435237582 ) ) ;
#20878 = CARTESIAN_POINT ( 'NONE',  ( -19.02544592524342804, 5.153800228976336051, 36.04057627198100988 ) ) ;
#20877 = CARTESIAN_POINT ( 'NONE',  ( -0.05219959533909027116, -19.03943276465977164, 22.49890960531436690 ) ) ;
#20879 = CARTESIAN_POINT ( 'NONE',  ( 5.153800228976615827, -19.02544592524334988, 110.2094237280189901 ) ) ;
#20880 = CARTESIAN_POINT ( 'NONE',  ( 22.81625015709510151, -31.40387420917324590, -10.42499999726881477 ) ) ;
#20881 = CARTESIAN_POINT ( 'NONE',  ( -16.55341960407611168, -4.379528057220339221, 111.4572429386476813 ) ) ;
#20882 = CARTESIAN_POINT ( 'NONE',  ( -21.52544592524334988, -5.823673210054445271, 73.95942372801901854 ) ) ;
#20884 = CARTESIAN_POINT ( 'NONE',  ( -10.72451020669870658, -18.67979575497194134, 39.58442372801901143 ) ) ;
#20883 = CARTESIAN_POINT ( 'NONE',  ( 13.89961937509977652, -13.97604488694527269, 58.12390960531436690 ) ) ;
#20885 = CARTESIAN_POINT ( 'NONE',  ( -21.53943276465977519, 0.05219959533907696930, 111.2489096053143669 ) ) ;
#20886 = CARTESIAN_POINT ( 'NONE',  ( -8.571926809382608425, 26.38167802310805854, 140.9750000027312069 ) ) ;
#20887 = CARTESIAN_POINT ( 'NONE',  ( -5.049401038298153566, 19.05341960407611168, 90.20724293864766707 ) ) ;
#20888 = CARTESIAN_POINT ( 'NONE',  ( 27.07824611089273148, 7.738748529345179428, 165.1039267699882771 ) ) ;
#20890 = CARTESIAN_POINT ( 'NONE',  ( 15.72974639402199770, -15.80617190586745480, 43.12390960531435269 ) ) ;
#20889 = CARTESIAN_POINT ( 'NONE',  ( 16.53943276465976808, 0.05219959533934440121, 31.25109039468568639 ) ) ;
#20891 = CARTESIAN_POINT ( 'NONE',  ( 15.72974639402176855, 15.80617190586768217, 56.87609039468568994 ) ) ;
#20892 = CARTESIAN_POINT ( 'NONE',  ( -16.46253265017160317, 9.564922557960807481, 115.8322429386477097 ) ) ;
#20893 = CARTESIAN_POINT ( 'NONE',  ( 19.03943276465977164, 0.05219959533936151252, 91.25109039468566152 ) ) ;
#20894 = CARTESIAN_POINT ( 'NONE',  ( 9.564922557960805705, 16.46253265017160317, 44.58224293864769550 ) ) ;
#20895 = CARTESIAN_POINT ( 'NONE',  ( 9.474510206698971260, -16.51473224551069308, 82.91557627198103830 ) ) ;
#20896 = CARTESIAN_POINT ( 'NONE',  ( -0.05219959533910754901, -16.53943276465976808, 97.49890960531436690 ) ) ;
#20897 = CARTESIAN_POINT ( 'NONE',  ( -14.34966873604960291, -8.224510206698953496, 96.66557627198102409 ) ) ;
#20898 = CARTESIAN_POINT ( 'NONE',  ( 5.153800228976335163, 19.02544592524342804, 109.7905762719810099 ) ) ;
#20900 = CARTESIAN_POINT ( 'NONE',  ( 9.474510206698971260, -16.51473224551069308, 47.91557627198102409 ) ) ;
#20899 = CARTESIAN_POINT ( 'NONE',  ( 0.05219959533910956823, 16.53943276465976808, 59.99890960531436690 ) ) ;
#20901 = CARTESIAN_POINT ( 'NONE',  ( 5.719274019375673035, 21.55341960407619339, 62.29275706135236845 ) ) ;
#20902 = CARTESIAN_POINT ( 'NONE',  ( 16.46253265017146816, 9.564922557961045513, 86.66775706135233293 ) ) ;
#20903 = CARTESIAN_POINT ( 'NONE',  ( 14.29746914071049879, -8.314922557960816363, 68.33224293864769550 ) ) ;
#20904 = CARTESIAN_POINT ( 'NONE',  ( 0.05219959533907565091, 21.53943276465977519, 114.9989096053143669 ) ) ;
#20905 = CARTESIAN_POINT ( 'NONE',  ( -18.62759615963270932, 10.81492255796079327, 40.83224293864769550 ) ) ;
#20906 = CARTESIAN_POINT ( 'NONE',  ( 13.97604488694527802, 13.89961937509977652, 109.3739096053143669 ) ) ;
#20907 = CARTESIAN_POINT ( 'NONE',  ( -23.31738231874055600, 16.94106989632528837, 142.0500000054623513 ) ) ;
#20908 = CARTESIAN_POINT ( 'NONE',  ( -13.89961937509977652, 13.97604488694528158, 55.62390960531434558 ) ) ;
#20909 = CARTESIAN_POINT ( 'NONE',  ( -16.53943276465976808, 0.05219959533911058130, 41.24890960531435269 ) ) ;
#20910 = AXIS2_PLACEMENT_3D ( 'NONE', #157148, #48977, #190475 ) ;
#20911 = CARTESIAN_POINT ( 'NONE',  ( -0.05219959533934338120, 16.53943276465976808, 107.5010903946856899 ) ) ;
#20912 = CARTESIAN_POINT ( 'NONE',  ( 14.29746914071037800, 8.314922557961029526, 81.66775706135236135 ) ) ;
#20913 = CARTESIAN_POINT ( 'NONE',  ( 16.51473224551083163, -9.474510206698727899, 35.83442372801899722 ) ) ;
#20914 = CARTESIAN_POINT ( 'NONE',  ( -17.48847506799968343, 5.747544572773791494, 70.82697437843283694 ) ) ;
#20915 = CARTESIAN_POINT ( 'NONE',  ( -5.153800228976328057, -19.02544592524343514, 97.29057627198099567 ) ) ;
#20916 = CARTESIAN_POINT ( 'NONE',  ( -9.474510206698964154, 16.51473224551069663, 50.41557627198102409 ) ) ;
#20917 = CARTESIAN_POINT ( 'NONE',  ( 12.14591786802309770, 12.06949235617756955, 59.37390960531436690 ) ) ;
#20919 = CARTESIAN_POINT ( 'NONE',  ( 0.05219959533907565091, 21.53943276465977519, 24.99890960531435624 ) ) ;
#20918 = CARTESIAN_POINT ( 'NONE',  ( 17.97161686094259991, -5.499999999999974243, 48.49637206859247840 ) ) ;
#20920 = CARTESIAN_POINT ( 'NONE',  ( 15.72974639402199770, -15.80617190586745480, 43.12390960531435269 ) ) ;
#20921 = CARTESIAN_POINT ( 'NONE',  ( 12.06949235617757843, -12.14591786802309237, 83.12390960531436690 ) ) ;
#20922 = CARTESIAN_POINT ( 'NONE',  ( -8.224510206698735004, -14.34966873604973081, 34.58442372801900433 ) ) ;
#20923 = CARTESIAN_POINT ( 'NONE',  ( 16.55341960407611168, 4.379528057220329451, 73.95724293864769550 ) ) ;
#20924 = CARTESIAN_POINT ( 'NONE',  ( -19.02130022317636815, 5.499999999999598543, 65.78188669246574705 ) ) ;
#20925 = CARTESIAN_POINT ( 'NONE',  ( -9.564922557961040184, 16.46253265017147172, 72.91775706135233293 ) ) ;
#20926 = CARTESIAN_POINT ( 'NONE',  ( 9.474510206698971260, -16.51473224551069308, 112.9155762719810383 ) ) ;
#20927 = CARTESIAN_POINT ( 'NONE',  ( 22.81625015709510151, -31.40387420917324590, -4.424999997268812990 ) ) ;
#20928 = CARTESIAN_POINT ( 'NONE',  ( -22.78074831271784362, 20.70421334297363458, -50.54281738342967856 ) ) ;
#20930 = CARTESIAN_POINT ( 'NONE',  ( -16.52544592524335698, -4.483927247898792601, 103.9594237280190185 ) ) ;
#20929 = CARTESIAN_POINT ( 'NONE',  ( 4.483927247898790824, -16.52544592524335698, 25.20942372801901854 ) ) ;
#20931 = CARTESIAN_POINT ( 'NONE',  ( 19.05341960407617918, -5.049401038297876454, 71.04275706135234714 ) ) ;
#20932 = CARTESIAN_POINT ( 'NONE',  ( 5.719274019375991003, -21.55341960407610458, 52.70724293864769550 ) ) ;
#20933 = CARTESIAN_POINT ( 'NONE',  ( -5.823673210054431948, 21.52544592524334988, 62.70942372801902565 ) ) ;
#20934 = CARTESIAN_POINT ( 'NONE',  ( 18.22780087662121673, 5.500000000000056843, 38.98459894673893444 ) ) ;
#20935 = CARTESIAN_POINT ( 'NONE',  ( 0.05219959533934541429, -16.53943276465976808, 35.00109039468568284 ) ) ;
#20937 = CARTESIAN_POINT ( 'NONE',  ( -16.51473224551069308, -9.474510206698971260, 91.66557627198103830 ) ) ;
#20936 = FACE_OUTER_BOUND ( 'NONE', #21633, .T. ) ;
#20938 = CARTESIAN_POINT ( 'NONE',  ( 13.89961937509977652, -13.97604488694527269, 23.12390960531436335 ) ) ;
#20939 = CARTESIAN_POINT ( 'NONE',  ( 0.05219959533910956823, 16.53943276465976808, 89.99890960531438111 ) ) ;
#20940 = APPLICATION_PROTOCOL_DEFINITION ( 'draft international standard', 'automotive_design', 1998, #164372 ) ;
#20941 = CARTESIAN_POINT ( 'NONE',  ( -16.46253265017160317, 9.564922557960807481, 105.8322429386476955 ) ) ;
#20942 = ORIENTED_EDGE ( 'NONE', *, *, #92116, .F. ) ;
#20943 = CARTESIAN_POINT ( 'NONE',  ( 9.474510206698729675, 16.51473224551082808, 102.0844237280190043 ) ) ;
#20944 = CARTESIAN_POINT ( 'NONE',  ( -10.72451020669898014, 18.67979575497178502, 80.41557627198103830 ) ) ;
#20945 = CARTESIAN_POINT ( 'NONE',  ( 13.97604488694527802, 13.89961937509977652, 44.37390960531435269 ) ) ;
#20947 = CARTESIAN_POINT ( 'NONE',  ( 15.80617190586746368, 15.72974639402197994, 114.3739096053143527 ) ) ;
#20946 = CARTESIAN_POINT ( 'NONE',  ( 9.564922557961047289, -16.46253265017146816, 65.41775706135233293 ) ) ;
#20948 = CARTESIAN_POINT ( 'NONE',  ( -16.51473224551069308, -9.474510206698971260, 71.66557627198102409 ) ) ;
#20949 = CARTESIAN_POINT ( 'NONE',  ( 19.05341960407611168, 5.049401038298154454, 103.9572429386476671 ) ) ;
#20950 = VERTEX_POINT ( 'NONE', #64172 ) ;
#20951 = CARTESIAN_POINT ( 'NONE',  ( 12.14591786802327356, -12.06949235617739191, 30.62609039468567929 ) ) ;
#20952 = CARTESIAN_POINT ( 'NONE',  ( -18.62759615963270932, 10.81492255796079327, 100.8322429386477097 ) ) ;
#20955 = CARTESIAN_POINT ( 'NONE',  ( 9.474510206698729675, 16.51473224551082808, 67.08442372801900433 ) ) ;
#20954 = CARTESIAN_POINT ( 'NONE',  ( -5.049401038298153566, 19.05341960407611168, 95.20724293864770971 ) ) ;
#20953 = CARTESIAN_POINT ( 'NONE',  ( 4.483927247898545687, 16.52544592524342804, 104.7905762719810241 ) ) ;
#20956 = CARTESIAN_POINT ( 'NONE',  ( 21.52544592524344225, -5.823673210054117533, 88.54057627198103830 ) ) ;
#20957 = CARTESIAN_POINT ( 'NONE',  ( -16.53943276465976808, 0.05219959533911058130, 41.24890960531435269 ) ) ;
#20958 = CARTESIAN_POINT ( 'NONE',  ( 21.52544592524334988, 5.823673210054432836, 111.4594237280190328 ) ) ;
#20959 = CARTESIAN_POINT ( 'NONE',  ( 16.55341960407618274, -4.379528057220086978, 61.04275706135234714 ) ) ;
#20960 = CARTESIAN_POINT ( 'NONE',  ( -0.05219959533909027116, -19.03943276465977164, 97.49890960531436690 ) ) ;
#20961 = CARTESIAN_POINT ( 'NONE',  ( -9.564922557960796823, -16.46253265017161027, 42.08224293864769550 ) ) ;
#20962 = CARTESIAN_POINT ( 'NONE',  ( 10.81492255796106328, -18.62759615963255655, 50.41775706135235424 ) ) ;
#20963 = CARTESIAN_POINT ( 'NONE',  ( 10.81492255796106328, -18.62759615963255655, 65.41775706135234714 ) ) ;
#20964 = CARTESIAN_POINT ( 'NONE',  ( 19.03943276465977164, -0.05219959533909143690, 63.74890960531435979 ) ) ;
#20965 = CARTESIAN_POINT ( 'NONE',  ( 10.72451020669871369, 18.67979575497193778, 32.08442372801901854 ) ) ;
#20966 = CARTESIAN_POINT ( 'NONE',  ( 0.05219959533936267826, -19.03943276465977164, 80.00109039468567573 ) ) ;
#20967 = CARTESIAN_POINT ( 'NONE',  ( 16.46253265017146816, 9.564922557961045513, 71.66775706135233293 ) ) ;
#20968 = CARTESIAN_POINT ( 'NONE',  ( -19.03943276465977164, 0.05219959533909376836, 41.24890960531435269 ) ) ;
#20969 = CARTESIAN_POINT ( 'NONE',  ( 14.29746914071037800, 8.314922557961029526, 91.66775706135234714 ) ) ;
#20970 = CARTESIAN_POINT ( 'NONE',  ( 5.153800228976335163, 19.02544592524342804, 54.79057627198103120 ) ) ;
#20971 = CARTESIAN_POINT ( 'NONE',  ( 21.98685479826776046, -13.98560643873834763, 165.5209445330007725 ) ) ;
#20972 = CARTESIAN_POINT ( 'NONE',  ( 16.51473224551069308, 9.474510206698969483, 99.16557627198102409 ) ) ;
#20973 = CARTESIAN_POINT ( 'NONE',  ( -5.049401038298153566, 19.05341960407611168, 45.20724293864769550 ) ) ;
#20974 = CARTESIAN_POINT ( 'NONE',  ( -18.67979575497178146, -10.72451020669898902, 91.66557627198103830 ) ) ;
#20975 = CARTESIAN_POINT ( 'NONE',  ( 4.379528057220092307, 16.55341960407617563, 57.29275706135234714 ) ) ;
#20976 = CARTESIAN_POINT ( 'NONE',  ( 16.46253265017146816, 9.564922557961045513, 26.66775706135234003 ) ) ;
#20977 = CARTESIAN_POINT ( 'NONE',  ( 19.05341960407611168, 5.049401038298154454, 48.95724293864768129 ) ) ;
#20978 = CARTESIAN_POINT ( 'NONE',  ( -12.06949235617756955, 12.14591786802309770, 40.62390960531435269 ) ) ;
#20979 = CARTESIAN_POINT ( 'NONE',  ( 4.483927247898545687, 16.52544592524342804, 74.79057627198105251 ) ) ;
#20980 = CARTESIAN_POINT ( 'NONE',  ( 16.46253265017160672, -9.564922557960803928, 98.33224293864769550 ) ) ;
#20981 = CARTESIAN_POINT ( 'NONE',  ( 13.89961937509977652, -13.97604488694527269, 78.12390960531433848 ) ) ;
#20982 = CARTESIAN_POINT ( 'NONE',  ( -18.62759615963255300, -10.81492255796106328, 34.16775706135234714 ) ) ;
#20984 = EDGE_CURVE ( 'NONE', #93070, #137808, #154116, .T. ) ;
#20983 = CARTESIAN_POINT ( 'NONE',  ( 19.03943276465977164, -0.05219959533909143690, 88.74890960531436690 ) ) ;
#20985 = CARTESIAN_POINT ( 'NONE',  ( -18.67979575497193778, 10.72451020669871902, 93.33442372801901854 ) ) ;
#20986 = CARTESIAN_POINT ( 'NONE',  ( 8.224510206698742110, 14.34966873604972548, 77.08442372801901854 ) ) ;
#20987 = ADVANCED_FACE ( 'NONE', ( #94494 ), #181639, .T. ) ;
#20988 = CARTESIAN_POINT ( 'NONE',  ( -15.80617190586768217, 15.72974639402176855, 23.12609039468567573 ) ) ;
#20989 = CARTESIAN_POINT ( 'NONE',  ( 5.719274019375991003, -21.55341960407610458, 92.70724293864770971 ) ) ;
#20990 = CARTESIAN_POINT ( 'NONE',  ( -12.14591786802309592, -12.06949235617757132, 46.87390960531435979 ) ) ;
#20992 = CARTESIAN_POINT ( 'NONE',  ( 0.05219959533909260263, 19.03943276465977164, 44.99890960531435979 ) ) ;
#20991 = VECTOR ( 'NONE', #68552, 1000.000000000000000 ) ;
#20993 = CARTESIAN_POINT ( 'NONE',  ( 14.34966873604960469, 8.224510206698951720, 69.16557627198102409 ) ) ;
#20994 = CARTESIAN_POINT ( 'NONE',  ( -5.823673210054116645, -21.52544592524344225, 27.29057627198103120 ) ) ;
#20995 = CARTESIAN_POINT ( 'NONE',  ( 19.02544592524334988, 5.153800228976608722, 31.45942372801900433 ) ) ;
#20996 = CARTESIAN_POINT ( 'NONE',  ( 0.05219959533910956823, 16.53943276465976808, 99.99890960531436690 ) ) ;
#20997 = ORIENTED_EDGE ( 'NONE', *, *, #134205, .T. ) ;
#20998 = CARTESIAN_POINT ( 'NONE',  ( -8.314922557961024197, 14.29746914071037800, 67.91775706135234714 ) ) ;
#20999 = CARTESIAN_POINT ( 'NONE',  ( 19.02544592524343514, -5.153800228976328945, 63.54057627198103830 ) ) ;
#21000 = CARTESIAN_POINT ( 'NONE',  ( -16.95034065685311830, -6.644554250676003804, 21.23116604354659032 ) ) ;
#21001 = CARTESIAN_POINT ( 'NONE',  ( -21.52544592524343514, 5.823673210054127303, 36.04057627198102409 ) ) ;
#21002 = CARTESIAN_POINT ( 'NONE',  ( -16.55341960407617563, 4.379528057220093196, 93.54275706135234714 ) ) ;
#21003 = CARTESIAN_POINT ( 'NONE',  ( -9.564922557961040184, 16.46253265017147172, 107.9177570613523471 ) ) ;
#21004 = CARTESIAN_POINT ( 'NONE',  ( -21.53943276465977519, -0.05219959533937600094, 83.75109039468568994 ) ) ;
#21005 = CARTESIAN_POINT ( 'NONE',  ( -16.46253265017160317, 9.564922557960807481, 70.83224293864770971 ) ) ;
#21006 = CARTESIAN_POINT ( 'NONE',  ( 0.05219959533907565091, 21.53943276465977519, 109.9989096053143527 ) ) ;
#21007 = CARTESIAN_POINT ( 'NONE',  ( -14.34966873604972548, 8.224510206698743886, 58.33442372801901143 ) ) ;
#21008 = CARTESIAN_POINT ( 'NONE',  ( -16.55341960407611168, -4.379528057220339221, 111.4572429386476813 ) ) ;
#21009 = CARTESIAN_POINT ( 'NONE',  ( 12.06949235617739724, 12.14591786802326823, 21.87609039468567573 ) ) ;
#21010 = CARTESIAN_POINT ( 'NONE',  ( 5.153800228976615827, -19.02544592524334988, 80.20942372801901854 ) ) ;
#21011 = CARTESIAN_POINT ( 'NONE',  ( 10.81492255796078972, 18.62759615963270932, 74.58224293864768129 ) ) ;
#21012 = CARTESIAN_POINT ( 'NONE',  ( -13.89961937509957401, -13.97604488694547875, 49.37609039468567573 ) ) ;
#21013 = LINE ( 'NONE', #82669, #44616 ) ;
#21014 = CARTESIAN_POINT ( 'NONE',  ( -10.72451020669898014, 18.67979575497178502, 110.4155762719810383 ) ) ;
#21015 = CARTESIAN_POINT ( 'NONE',  ( 28.82186960331496905, -9.364793116373544279, 148.8999999999999773 ) ) ;
#21016 = CARTESIAN_POINT ( 'NONE',  ( 9.474510206698971260, -16.51473224551069308, 82.91557627198103830 ) ) ;
#21017 = CIRCLE ( 'NONE', #79043, 12.50000000000000000 ) ;
#21018 = CARTESIAN_POINT ( 'NONE',  ( 11.74264578624800315, -36.14014761921581709, -11.14999999453762669 ) ) ;
#21019 = CARTESIAN_POINT ( 'NONE',  ( -4.483927247898782831, 16.52544592524335698, 32.70942372801900433 ) ) ;
#21020 = CARTESIAN_POINT ( 'NONE',  ( 37.11169547541890523, -4.770708601134445281, 42.23953901806349620 ) ) ;
#21022 = CARTESIAN_POINT ( 'NONE',  ( 16.52544592524342804, -4.483927247898539470, 63.54057627198103830 ) ) ;
#21021 = CARTESIAN_POINT ( 'NONE',  ( -5.719274019375978568, 21.55341960407610458, 100.2072429386476955 ) ) ;
#21023 = CARTESIAN_POINT ( 'NONE',  ( -9.564922557960796823, -16.46253265017161027, 72.08224293864770971 ) ) ;
#21024 = VECTOR ( 'NONE', #159887, 1000.000000000000114 ) ;
#21025 = CARTESIAN_POINT ( 'NONE',  ( 0.05219959533937995610, -21.53943276465977519, 90.00109039468567573 ) ) ;
#21026 = DIRECTION ( 'NONE',  ( -1.000000000000000000, 0.000000000000000000, 0.000000000000000000 ) ) ;
#21028 = CARTESIAN_POINT ( 'NONE',  ( -5.153800228976607833, 19.02544592524334988, 37.70942372801899722 ) ) ;
#21027 = CARTESIAN_POINT ( 'NONE',  ( 4.379528057220092307, 16.55341960407617563, 37.29275706135235424 ) ) ;
#21029 = CARTESIAN_POINT ( 'NONE',  ( 21.53943276465977519, 0.05219959533937863772, 46.25109039468567573 ) ) ;
#21030 = CARTESIAN_POINT ( 'NONE',  ( -0.05219959533907301413, -21.53943276465977519, 62.49890960531436690 ) ) ;
#21031 = CARTESIAN_POINT ( 'NONE',  ( -16.46253265017146816, -9.564922557961047289, 109.1677570613523471 ) ) ;
#21032 = CARTESIAN_POINT ( 'NONE',  ( -13.89961937509977652, 13.97604488694528158, 50.62390960531435979 ) ) ;
#21033 = CARTESIAN_POINT ( 'NONE',  ( 0.05219959533936267826, -19.03943276465977164, 65.00109039468567573 ) ) ;
#21034 = CARTESIAN_POINT ( 'NONE',  ( 0.05219959533937995610, -21.53943276465977519, 80.00109039468568994 ) ) ;
#21035 = CARTESIAN_POINT ( 'NONE',  ( 5.049401038297881783, 19.05341960407617563, 67.29275706135234714 ) ) ;
#21036 = CARTESIAN_POINT ( 'NONE',  ( -16.51473224551069308, -9.474510206698971260, 31.66557627198102054 ) ) ;
#21037 = CARTESIAN_POINT ( 'NONE',  ( -15.72974639402197994, 15.80617190586746368, 55.62390960531436690 ) ) ;
#21038 = CARTESIAN_POINT ( 'NONE',  ( -12.14591786802309592, -12.06949235617757132, 56.87390960531436690 ) ) ;
#21039 = DIRECTION ( 'NONE',  ( -0.000000000000000000, -0.000000000000000000, 1.000000000000000000 ) ) ;
#21040 = CARTESIAN_POINT ( 'NONE',  ( -19.05341960407617563, 5.049401038297882671, 28.54275706135232937 ) ) ;
#21041 = CARTESIAN_POINT ( 'NONE',  ( -16.52544592524335698, -4.483927247898792601, 83.95942372801900433 ) ) ;
#21042 = CARTESIAN_POINT ( 'NONE',  ( -14.29746914071049879, 8.314922557960819915, 50.83224293864770971 ) ) ;
#21043 = CARTESIAN_POINT ( 'NONE',  ( -5.719274019375665041, -21.55341960407619695, 84.79275706135234714 ) ) ;
#21044 = CARTESIAN_POINT ( 'NONE',  ( 18.62759615963255655, 10.81492255796105972, 76.66775706135234714 ) ) ;
#21045 = CARTESIAN_POINT ( 'NONE',  ( 21.53943276465977519, -0.05219959533907433946, 98.74890960531438111 ) ) ;
#21046 = CARTESIAN_POINT ( 'NONE',  ( 16.51473224551069308, 9.474510206698969483, 49.16557627198102409 ) ) ;
#21047 = CARTESIAN_POINT ( 'NONE',  ( 5.823673210054444382, -21.52544592524334988, 60.20942372801902565 ) ) ;
#21048 = CARTESIAN_POINT ( 'NONE',  ( -19.02544592524342804, 5.153800228976336051, 36.04057627198100988 ) ) ;
#21049 = CARTESIAN_POINT ( 'NONE',  ( -0.05219959533909027116, -19.03943276465977164, 52.49890960531436690 ) ) ;
#21050 = CARTESIAN_POINT ( 'NONE',  ( 16.52544592524342804, -4.483927247898539470, 103.5405762719810383 ) ) ;
#21051 = CARTESIAN_POINT ( 'NONE',  ( 0.05219959533909260263, 19.03943276465977164, 104.9989096053143669 ) ) ;
#21052 = CARTESIAN_POINT ( 'NONE',  ( -8.224510206698948167, 14.34966873604960824, 55.41557627198102409 ) ) ;
#21053 = CARTESIAN_POINT ( 'NONE',  ( 16.52544592524342804, -4.483927247898539470, 108.5405762719810241 ) ) ;
#21054 = VECTOR ( 'NONE', #112894, 1000.000000000000000 ) ;
#21055 = CARTESIAN_POINT ( 'NONE',  ( 21.55341960407610458, 5.719274019375980345, 78.95724293864769550 ) ) ;
#21056 = CARTESIAN_POINT ( 'NONE',  ( 15.72974639402176855, 15.80617190586768217, 41.87609039468568284 ) ) ;
#21057 = DIRECTION ( 'NONE',  ( 1.000000000000000000, 0.000000000000000000, 0.000000000000000000 ) ) ;
#21058 = EDGE_CURVE ( 'NONE', #31781, #51307, #153732, .T. ) ;
#21059 = CARTESIAN_POINT ( 'NONE',  ( 14.29746914071037800, 8.314922557961029526, 36.66775706135234714 ) ) ;
#21060 = ORIENTED_EDGE ( 'NONE', *, *, #135206, .T. ) ;
#21061 = CARTESIAN_POINT ( 'NONE',  ( 21.53943276465977519, -0.05219959533907433946, 88.74890960531436690 ) ) ;
#21062 = CARTESIAN_POINT ( 'NONE',  ( 15.80617190586769283, -15.72974639402175789, 110.6260903946857042 ) ) ;
#21063 = CARTESIAN_POINT ( 'NONE',  ( 19.03943276465977164, -0.05219959533909143690, 98.74890960531436690 ) ) ;
#21064 = CARTESIAN_POINT ( 'NONE',  ( -5.823673210054431948, 21.52544592524334988, 32.70942372801900433 ) ) ;
#21065 = CARTESIAN_POINT ( 'NONE',  ( -18.67979575497178146, -10.72451020669898902, 36.66557627198103120 ) ) ;
#21066 = CARTESIAN_POINT ( 'NONE',  ( -16.55341960407617563, 4.379528057220093196, 98.54275706135234714 ) ) ;
#21068 = CARTESIAN_POINT ( 'NONE',  ( -21.55341960407619339, 5.719274019375674811, 78.54275706135236135 ) ) ;
#21067 = CARTESIAN_POINT ( 'NONE',  ( -18.62759615963255300, -10.81492255796106328, 49.16775706135234003 ) ) ;
#21069 = CARTESIAN_POINT ( 'NONE',  ( -21.53943276465977519, -0.05219959533937600094, 108.7510903946857042 ) ) ;
#21070 = CARTESIAN_POINT ( 'NONE',  ( -14.34966873604972548, 8.224510206698743886, 73.33442372801901854 ) ) ;
#21071 = CARTESIAN_POINT ( 'NONE',  ( -21.55341960407619339, 5.719274019375674811, 43.54275706135235424 ) ) ;
#21072 = CARTESIAN_POINT ( 'NONE',  ( 0.05219959533909260263, 19.03943276465977164, 29.99890960531435979 ) ) ;
#21073 = CARTESIAN_POINT ( 'NONE',  ( -15.72974639402176322, -15.80617190586768395, 104.3760903946856899 ) ) ;
#21074 = CARTESIAN_POINT ( 'NONE',  ( -13.89961937509977652, 13.97604488694528158, 110.6239096053143243 ) ) ;
#21075 = CARTESIAN_POINT ( 'NONE',  ( 15.80617190586746368, 15.72974639402197994, 109.3739096053143811 ) ) ;
#21077 = CARTESIAN_POINT ( 'NONE',  ( 15.72974639402199770, -15.80617190586745480, 73.12390960531436690 ) ) ;
#21076 = CARTESIAN_POINT ( 'NONE',  ( -22.00000000000000000, -5.510910596163089556E-15, 47.50000000000000000 ) ) ;
#21079 = CARTESIAN_POINT ( 'NONE',  ( 16.52544592524342804, -4.483927247898539470, 48.54057627198103120 ) ) ;
#21078 = CARTESIAN_POINT ( 'NONE',  ( -16.53943276465976808, -0.05219959533934237506, 48.75109039468568284 ) ) ;
#21080 = DIRECTION ( 'NONE',  ( 1.000000000000000000, -0.000000000000000000, -0.000000000000000000 ) ) ;
#21081 = CARTESIAN_POINT ( 'NONE',  ( 9.474510206698729675, 16.51473224551082808, 87.08442372801900433 ) ) ;
#21082 = CARTESIAN_POINT ( 'NONE',  ( -16.20579543436678449, 7.371946100355082798, 104.4347916582812985 ) ) ;
#21083 = CARTESIAN_POINT ( 'NONE',  ( -8.314922557961024197, 14.29746914071037800, 32.91775706135234714 ) ) ;
#21084 = CARTESIAN_POINT ( 'NONE',  ( -18.62759615963270932, 10.81492255796079327, 95.83224293864770971 ) ) ;
#21085 = CARTESIAN_POINT ( 'NONE',  ( 18.62759615963271287, -10.81492255796078972, 73.33224293864769550 ) ) ;
#21086 = CARTESIAN_POINT ( 'NONE',  ( -9.564922557960796823, -16.46253265017161027, 112.0822429386476955 ) ) ;
#21087 = CARTESIAN_POINT ( 'NONE',  ( -4.379528057220086978, -16.55341960407618274, 39.79275706135235424 ) ) ;
#21088 = CARTESIAN_POINT ( 'NONE',  ( 5.049401038298161559, -19.05341960407611168, 57.70724293864769550 ) ) ;
#21090 = CARTESIAN_POINT ( 'NONE',  ( 9.474510206698729675, 16.51473224551082808, 102.0844237280190043 ) ) ;
#21089 = CARTESIAN_POINT ( 'NONE',  ( -5.719274019375665041, -21.55341960407619695, 24.79275706135235779 ) ) ;
#21091 = CARTESIAN_POINT ( 'NONE',  ( 16.51473224551069308, 9.474510206698969483, 104.1655762719810241 ) ) ;
#21092 = CARTESIAN_POINT ( 'NONE',  ( 19.03943276465977164, -0.05219959533909143690, 93.74890960531435269 ) ) ;
#21093 = CARTESIAN_POINT ( 'NONE',  ( 5.719274019375991003, -21.55341960407610458, 92.70724293864770971 ) ) ;
#21094 = CARTESIAN_POINT ( 'NONE',  ( 19.05341960407611168, 5.049401038298154454, 53.95724293864770260 ) ) ;
#21095 = CARTESIAN_POINT ( 'NONE',  ( -7.500000000000000000, 0.000000000000000000, 4.292893218813445877 ) ) ;
#21097 = B_SPLINE_CURVE_WITH_KNOTS ( 'NONE', 3,
 ( #172051, #96193, #18384, #51688, #158857, #141704, #84010, #66852, #188229, #21355, #143687, #145688 ),
 .UNSPECIFIED., .F., .F.,
 ( 4, 2, 2, 2, 2, 4 ),
 ( 1.967889508672852735E-07, 0.0003319461778748304345, 0.0006636955667987935086, 0.0009954449557227568537, 0.001327194344646719874, 0.002654191900342570219 ),
 .UNSPECIFIED. ) ;
#21096 = CARTESIAN_POINT ( 'NONE',  ( 4.483927247898545687, 16.52544592524342804, 69.79057627198102409 ) ) ;
#21098 = CARTESIAN_POINT ( 'NONE',  ( 9.564922557960805705, 16.46253265017160317, 109.5822429386476955 ) ) ;
#21099 = CARTESIAN_POINT ( 'NONE',  ( -17.60728821186567217, 5.500000000000031974, 60.86690927743003954 ) ) ;
#21100 = CARTESIAN_POINT ( 'NONE',  ( -19.05341960407617563, 5.049401038297882671, 83.54275706135233293 ) ) ;
#21101 = AXIS2_PLACEMENT_3D ( 'NONE', #122539, #10416, #184230 ) ;
#21102 = CARTESIAN_POINT ( 'NONE',  ( -10.72451020669898014, 18.67979575497178502, 95.41557627198102409 ) ) ;
#21103 = CARTESIAN_POINT ( 'NONE',  ( -16.51473224551082808, 9.474510206698731452, 48.33442372801900433 ) ) ;
#21104 = CARTESIAN_POINT ( 'NONE',  ( -5.719274019375978568, 21.55341960407610458, 25.20724293864769550 ) ) ;
#21105 = CARTESIAN_POINT ( 'NONE',  ( 11.30153831258469843, -180.0000000000000000, -4.999999999999999112 ) ) ;
#21106 = CARTESIAN_POINT ( 'NONE',  ( 5.719274019375991003, -21.55341960407610458, 57.70724293864770260 ) ) ;
#21107 = CARTESIAN_POINT ( 'NONE',  ( -16.51473224551069308, -9.474510206698971260, 81.66557627198103830 ) ) ;
#21108 = CARTESIAN_POINT ( 'NONE',  ( -15.80617190586768217, 15.72974639402176855, 78.12609039468570415 ) ) ;
#21109 = CARTESIAN_POINT ( 'NONE',  ( 19.05341960407611168, 5.049401038298154454, 38.95724293864767418 ) ) ;
#21110 = CARTESIAN_POINT ( 'NONE',  ( 0.05219959533910956823, 16.53943276465976808, 79.99890960531435269 ) ) ;
#21111 = CARTESIAN_POINT ( 'NONE',  ( 4.483927247898790824, -16.52544592524335698, 20.20942372801900788 ) ) ;
#21112 = CARTESIAN_POINT ( 'NONE',  ( -21.53943276465977519, -0.05219959533937600094, 63.75109039468568284 ) ) ;
#21113 = EDGE_LOOP ( 'NONE', ( #146922, #45592, #158394, #58948, #160275 ) ) ;
#21114 = CARTESIAN_POINT ( 'NONE',  ( -5.153800228976607833, 19.02544592524334988, 22.70942372801899012 ) ) ;
#21115 = CARTESIAN_POINT ( 'NONE',  ( -16.46253265017146816, -9.564922557961047289, 74.16775706135234714 ) ) ;
#21116 = CARTESIAN_POINT ( 'NONE',  ( -0.05219959533937732626, 21.53943276465977519, 27.50109039468567929 ) ) ;
#21117 = LINE ( 'NONE', #174809, #43151 ) ;
#21118 = CARTESIAN_POINT ( 'NONE',  ( -21.53943276465977519, -0.05219959533937600094, 113.7510903946856757 ) ) ;
#21119 = CARTESIAN_POINT ( 'NONE',  ( 19.02544592524343514, -5.153800228976328945, 53.54057627198102409 ) ) ;
#21120 = CARTESIAN_POINT ( 'NONE',  ( -19.03943276465977164, -0.05219959533935918106, 33.75109039468566863 ) ) ;
#21121 = CARTESIAN_POINT ( 'NONE',  ( -16.55341960407617563, 4.379528057220093196, 108.5427570613523756 ) ) ;
#21123 = CARTESIAN_POINT ( 'NONE',  ( 10.72451020669871369, 18.67979575497193778, 67.08442372801901854 ) ) ;
#21122 = CARTESIAN_POINT ( 'NONE',  ( -16.51473224551069308, -9.474510206698971260, 96.66557627198102409 ) ) ;
#21124 = CARTESIAN_POINT ( 'NONE',  ( -36.91746825000001309, 11.99521256947798342, -4.724999997268811924 ) ) ;
#21125 = CARTESIAN_POINT ( 'NONE',  ( -17.50000000000003197, -3.237210098469649466, 35.28763012620480310 ) ) ;
#21126 = B_SPLINE_CURVE_WITH_KNOTS ( 'NONE', 3,
 ( #18844, #129960, #100643, #115828, #85475, #114818, #191660, #193679, #175499, #176510, #54155, #36972, #83470, #145147, #97623, #177517, #130981, #35976, #20808, #192672, #38987, #70326 ),
 .UNSPECIFIED., .F., .F.,
 ( 4, 2, 2, 2, 2, 2, 2, 2, 2, 2, 4 ),
 ( 7.806255641895631925E-18, 0.001309639967555302834, 0.001964459951332950347, 0.002291869943221771719, 0.002455574939166182621, 0.002619279935110593090, 0.002782984931055003559, 0.002946689926999414462, 0.003274099918888229328, 0.003928919902665864265, 0.005238559870221130670 ),
 .UNSPECIFIED. ) ;
#21127 = CARTESIAN_POINT ( 'NONE',  ( -21.52544592524334988, -5.823673210054445271, 83.95942372801900433 ) ) ;
#21128 = CARTESIAN_POINT ( 'NONE',  ( 15.72974639402176855, 15.80617190586768217, 101.8760903946857042 ) ) ;
#21129 = DIRECTION ( 'NONE',  ( -0.000000000000000000, -0.000000000000000000, -1.000000000000000000 ) ) ;
#21130 = CARTESIAN_POINT ( 'NONE',  ( -13.89961937509977652, 13.97604488694528158, 100.6239096053143669 ) ) ;
#21131 = CARTESIAN_POINT ( 'NONE',  ( 19.03943276465977164, 0.05219959533936151252, 21.25109039468565797 ) ) ;
#21132 = CARTESIAN_POINT ( 'NONE',  ( 23.87356034986291320, -29.32389248808944160, -21.14071813158713908 ) ) ;
#21133 = CARTESIAN_POINT ( 'NONE',  ( 16.46253265017160672, -9.564922557960803928, 38.33224293864768839 ) ) ;
#21134 = CARTESIAN_POINT ( 'NONE',  ( -10.72451020669898014, 18.67979575497178502, 55.41557627198102409 ) ) ;
#21135 = CARTESIAN_POINT ( 'NONE',  ( -4.483927247898539470, -16.52544592524342804, 22.29057627198102765 ) ) ;
#21137 = CARTESIAN_POINT ( 'NONE',  ( -5.049401038298153566, 19.05341960407611168, 75.20724293864769550 ) ) ;
#21136 = CARTESIAN_POINT ( 'NONE',  ( 0.05219959533910956823, 16.53943276465976808, 94.99890960531436690 ) ) ;
#21138 = CARTESIAN_POINT ( 'NONE',  ( 21.55341960407619695, -5.719274019375665929, 106.0427570613523471 ) ) ;
#21139 = CARTESIAN_POINT ( 'NONE',  ( -9.564922557960796823, -16.46253265017161027, 37.08224293864768839 ) ) ;
#21140 = CARTESIAN_POINT ( 'NONE',  ( 14.29746914071049879, -8.314922557960816363, 108.3322429386477097 ) ) ;
#21141 = CARTESIAN_POINT ( 'NONE',  ( 5.823673210054444382, -21.52544592524334988, 60.20942372801902565 ) ) ;
#21142 = CARTESIAN_POINT ( 'NONE',  ( -10.81492255796078084, -18.62759615963271287, 87.08224293864769550 ) ) ;
#21143 = CARTESIAN_POINT ( 'NONE',  ( 13.89961937509957401, 13.97604488694547697, 51.87609039468566863 ) ) ;
#21144 = DIRECTION ( 'NONE',  ( 0.000000000000000000, 0.000000000000000000, -1.000000000000000000 ) ) ;
#21145 = CARTESIAN_POINT ( 'NONE',  ( -5.153800228976328057, -19.02544592524343514, 102.2905762719810383 ) ) ;
#21146 = CARTESIAN_POINT ( 'NONE',  ( -12.14591786802309592, -12.06949235617757132, 71.87390960531438111 ) ) ;
#21147 = VECTOR ( 'NONE', #98013, 1000.000000000000000 ) ;
#21148 = CARTESIAN_POINT ( 'NONE',  ( 19.02544592524334988, 5.153800228976608722, 51.45942372801900433 ) ) ;
#21149 = CARTESIAN_POINT ( 'NONE',  ( 13.89961937509977652, -13.97604488694527269, 68.12390960531436690 ) ) ;
#21150 = CARTESIAN_POINT ( 'NONE',  ( 8.314922557960818139, 14.29746914071049879, 54.58224293864769550 ) ) ;
#21151 = CARTESIAN_POINT ( 'NONE',  ( -13.89961937509957401, -13.97604488694547875, 74.37609039468566152 ) ) ;
#21152 = CARTESIAN_POINT ( 'NONE',  ( 17.59860650958994555, -7.585241751806880650, 90.92337014262493256 ) ) ;
#21153 = CARTESIAN_POINT ( 'NONE',  ( -5.719274019375978568, 21.55341960407610458, 35.20724293864768839 ) ) ;
#21154 = CARTESIAN_POINT ( 'NONE',  ( -0.05219959533910754901, -16.53943276465976808, 107.4989096053143669 ) ) ;
#21155 = CARTESIAN_POINT ( 'NONE',  ( 4.999999999999999112, 4.250000000000000000, 0.000000000000000000 ) ) ;
#21157 = CARTESIAN_POINT ( 'NONE',  ( -5.823673210054116645, -21.52544592524344225, 62.29057627198102409 ) ) ;
#21156 = CARTESIAN_POINT ( 'NONE',  ( 13.89961937509977652, -13.97604488694527269, 58.12390960531436690 ) ) ;
#21158 = CARTESIAN_POINT ( 'NONE',  ( 19.02544592524343514, -5.153800228976328945, 33.54057627198102409 ) ) ;
#21160 = CARTESIAN_POINT ( 'NONE',  ( -16.46253265017160317, 9.564922557960807481, 55.83224293864769550 ) ) ;
#21159 = CARTESIAN_POINT ( 'NONE',  ( -12.14591786802326823, 12.06949235617739902, 73.12609039468567573 ) ) ;
#21161 = CARTESIAN_POINT ( 'NONE',  ( 16.46253265017146816, 9.564922557961045513, 51.66775706135233293 ) ) ;
#21162 = CARTESIAN_POINT ( 'NONE',  ( -5.719274019375665041, -21.55341960407619695, 69.79275706135234714 ) ) ;
#21163 = CARTESIAN_POINT ( 'NONE',  ( 21.53943276465977519, -0.05219959533907433946, 53.74890960531437401 ) ) ;
#21164 = CARTESIAN_POINT ( 'NONE',  ( -13.97604488694527625, -13.89961937509977652, 21.87390960531435979 ) ) ;
#21165 = CARTESIAN_POINT ( 'NONE',  ( 14.29746914071037800, 8.314922557961029526, 86.66775706135234714 ) ) ;
#21166 = CARTESIAN_POINT ( 'NONE',  ( -9.474510206698720793, -16.51473224551083518, 99.58442372801900433 ) ) ;
#21167 = CARTESIAN_POINT ( 'NONE',  ( 27.32543223595550330, 4.845308524271299433, 167.4404622590899407 ) ) ;
#21169 = CARTESIAN_POINT ( 'NONE',  ( -10.81492255796078084, -18.62759615963271287, 57.08224293864769550 ) ) ;
#21168 = CARTESIAN_POINT ( 'NONE',  ( 16.79531203550650886, 7.028104445595489302, 53.75244988220445208 ) ) ;
#21170 = CARTESIAN_POINT ( 'NONE',  ( -10.72451020669870658, -18.67979575497194134, 94.58442372801901854 ) ) ;
#21171 = CIRCLE ( 'NONE', #11550, 1.000000000000000888 ) ;
#21172 = CARTESIAN_POINT ( 'NONE',  ( 0.05219959533910956823, 16.53943276465976808, 39.99890960531436690 ) ) ;
#21173 = CARTESIAN_POINT ( 'NONE',  ( 0.05219959533910956823, 16.53943276465976808, 54.99890960531435269 ) ) ;
#21174 = CARTESIAN_POINT ( 'NONE',  ( -21.55341960407610458, -5.719274019375992779, 86.45724293864770971 ) ) ;
#21175 = CARTESIAN_POINT ( 'NONE',  ( -15.72974639402197994, 15.80617190586746368, 85.62390960531436690 ) ) ;
#21176 = LINE ( 'NONE', #82831, #188792 ) ;
#21177 = CARTESIAN_POINT ( 'NONE',  ( 5.719274019375991003, -21.55341960407610458, 27.70724293864769905 ) ) ;
#21179 = CIRCLE ( 'NONE', #85400, 1.000000000000000888 ) ;
#21178 = CARTESIAN_POINT ( 'NONE',  ( -14.34966873604972548, 8.224510206698743886, 73.33442372801901854 ) ) ;
#21180 = CARTESIAN_POINT ( 'NONE',  ( -14.29746914071049879, 8.314922557960819915, 80.83224293864769550 ) ) ;
#21181 = CARTESIAN_POINT ( 'NONE',  ( 13.97604488694527802, 13.89961937509977652, 34.37390960531436690 ) ) ;
#21182 =( NAMED_UNIT ( * ) SI_UNIT ( $, .STERADIAN. ) SOLID_ANGLE_UNIT ( ) );
#21183 = DIRECTION ( 'NONE',  ( 0.000000000000000000, 0.000000000000000000, -1.000000000000000000 ) ) ;
#21184 = CARTESIAN_POINT ( 'NONE',  ( -4.379528057220086978, -16.55341960407618274, 99.79275706135234714 ) ) ;
#21185 = CARTESIAN_POINT ( 'NONE',  ( -18.62759615963255300, -10.81492255796106328, 24.16775706135235424 ) ) ;
#21186 = CARTESIAN_POINT ( 'NONE',  ( 13.89961937509977652, -13.97604488694527269, 83.12390960531436690 ) ) ;
#21187 = CARTESIAN_POINT ( 'NONE',  ( -21.52544592524334988, -5.823673210054445271, 48.95942372801902565 ) ) ;
#21188 = CARTESIAN_POINT ( 'NONE',  ( -13.89961937509977652, 13.97604488694528158, 110.6239096053143243 ) ) ;
#21189 = CARTESIAN_POINT ( 'NONE',  ( -12.04662589228467873, -37.70593178235914422, -30.82293284779907339 ) ) ;
#21190 = ORIENTED_EDGE ( 'NONE', *, *, #82044, .F. ) ;
#21191 = CARTESIAN_POINT ( 'NONE',  ( -10.81492255796105439, 18.62759615963255655, 42.91775706135235424 ) ) ;
#21193 = CARTESIAN_POINT ( 'NONE',  ( 9.564922557960805705, 16.46253265017160317, 99.58224293864770971 ) ) ;
#21192 = CARTESIAN_POINT ( 'NONE',  ( -16.46253265017160317, 9.564922557960807481, 35.83224293864768839 ) ) ;
#21194 = CARTESIAN_POINT ( 'NONE',  ( 16.51473224551083163, -9.474510206698727899, 55.83442372801899722 ) ) ;
#21195 = CARTESIAN_POINT ( 'NONE',  ( -15.72974639402176322, -15.80617190586768395, 29.37609039468568284 ) ) ;
#21196 = CARTESIAN_POINT ( 'NONE',  ( 13.89961937509957401, 13.97604488694547697, 56.87609039468564731 ) ) ;
#21197 = CARTESIAN_POINT ( 'NONE',  ( 13.89961937509977652, -13.97604488694527269, 23.12390960531436335 ) ) ;
#21198 = CARTESIAN_POINT ( 'NONE',  ( -0.05219959533934338120, 16.53943276465976808, 92.50109039468567573 ) ) ;
#21199 = CARTESIAN_POINT ( 'NONE',  ( -19.05341960407617563, 5.049401038297882671, 68.54275706135230450 ) ) ;
#21200 = CARTESIAN_POINT ( 'NONE',  ( -4.379528057220086978, -16.55341960407618274, 109.7927570613523613 ) ) ;
#21202 = ORIENTED_EDGE ( 'NONE', *, *, #144540, .F. ) ;
#21201 = FACE_OUTER_BOUND ( 'NONE', #139480, .T. ) ;
#21203 = CARTESIAN_POINT ( 'NONE',  ( -16.46253265017160317, 9.564922557960807481, 90.83224293864769550 ) ) ;
#21204 = CARTESIAN_POINT ( 'NONE',  ( 10.72451020669871369, 18.67979575497193778, 97.08442372801904696 ) ) ;
#21205 = CARTESIAN_POINT ( 'NONE',  ( -10.81492255796105439, 18.62759615963255655, 112.9177570613523329 ) ) ;
#21206 = CARTESIAN_POINT ( 'NONE',  ( 17.97058386085786097, 5.500000000000042633, 66.50390968646219392 ) ) ;
#21207 = CARTESIAN_POINT ( 'NONE',  ( 13.89961937509977652, -13.97604488694527269, 103.1239096053143527 ) ) ;
#21208 = CARTESIAN_POINT ( 'NONE',  ( -10.72451020669870658, -18.67979575497194134, 69.58442372801900433 ) ) ;
#21209 = CARTESIAN_POINT ( 'NONE',  ( 19.03943276465977164, 0.05219959533936151252, 111.2510903946856757 ) ) ;
#21210 = CARTESIAN_POINT ( 'NONE',  ( 9.564922557960805705, 16.46253265017160317, 79.58224293864769550 ) ) ;
#21211 = CARTESIAN_POINT ( 'NONE',  ( -21.52544592524343514, 5.823673210054127303, 26.04057627198103475 ) ) ;
#21212 = CARTESIAN_POINT ( 'NONE',  ( -16.46253265017160317, 9.564922557960807481, 95.83224293864769550 ) ) ;
#21213 = CARTESIAN_POINT ( 'NONE',  ( -23.48529157249599919, -32.32473071737749848, -9.449999994537623849 ) ) ;
#21214 = CARTESIAN_POINT ( 'NONE',  ( 0.05219959533909260263, 19.03943276465977164, 84.99890960531436690 ) ) ;
#21215 = CARTESIAN_POINT ( 'NONE',  ( 9.474510206698971260, -16.51473224551069308, 62.91557627198102409 ) ) ;
#21216 = CARTESIAN_POINT ( 'NONE',  ( -14.29746914071049879, 8.314922557960819915, 25.83224293864769194 ) ) ;
#21217 = CARTESIAN_POINT ( 'NONE',  ( -17.05116617787851752, 6.768360034955478000, 98.65675553259194430 ) ) ;
#21218 = CARTESIAN_POINT ( 'NONE',  ( 9.474510206698729675, 16.51473224551082808, 72.08442372801900433 ) ) ;
#21219 = B_SPLINE_CURVE_WITH_KNOTS ( 'NONE', 3,
 ( #81526, #143213, #139249, #3710, #112882, #188755, #34069, #109904, #50240, #79569, #32082, #124066, #49239, #725, #111896, #62397, #47255, #15919, #128047, #77577 ),
 .UNSPECIFIED., .F., .F.,
 ( 4, 2, 2, 2, 2, 2, 2, 2, 2, 4 ),
 ( 0.004000878361812005950, 0.004499404418916031455, 0.004997930476020056960, 0.005496456533124082465, 0.005994982590228108837, 0.006244245618780100773, 0.006493508647332092709, 0.006992034704436076581, 0.007490560761540060453, 0.007989086818644044324 ),
 .UNSPECIFIED. ) ;
#21220 = CARTESIAN_POINT ( 'NONE',  ( -5.153800228976328057, -19.02544592524343514, 92.29057627198099567 ) ) ;
#21221 = CARTESIAN_POINT ( 'NONE',  ( 16.53943276465976808, -0.05219959533910856209, 88.74890960531436690 ) ) ;
#21222 = CARTESIAN_POINT ( 'NONE',  ( -0.05219959533907301413, -21.53943276465977519, 47.49890960531435979 ) ) ;
#21223 = CARTESIAN_POINT ( 'NONE',  ( 10.72451020669898902, -18.67979575497178502, 27.91557627198103830 ) ) ;
#21224 = CARTESIAN_POINT ( 'NONE',  ( -16.53943276465976808, 0.05219959533911058130, 101.2489096053143669 ) ) ;
#21225 = CARTESIAN_POINT ( 'NONE',  ( -17.26058549869088665, 6.457015423128606990, 53.62254162523932166 ) ) ;
#21226 = CARTESIAN_POINT ( 'NONE',  ( 5.153800228976615827, -19.02544592524334988, 45.20942372801901143 ) ) ;
#21227 = CARTESIAN_POINT ( 'NONE',  ( -8.314922557960811034, -14.29746914071050412, 32.08224293864769550 ) ) ;
#21229 = EDGE_CURVE ( 'NONE', #71844, #46822, #122394, .T. ) ;
#21228 = CARTESIAN_POINT ( 'NONE',  ( -9.564922557960796823, -16.46253265017161027, 107.0822429386476955 ) ) ;
#21230 = CARTESIAN_POINT ( 'NONE',  ( 21.53943276465977519, 0.05219959533937863772, 61.25109039468567573 ) ) ;
#21231 = CARTESIAN_POINT ( 'NONE',  ( -0.05219959533907301413, -21.53943276465977519, 52.49890960531435979 ) ) ;
#21232 = CARTESIAN_POINT ( 'NONE',  ( -5.719274019375665041, -21.55341960407619695, 39.79275706135235424 ) ) ;
#21233 = CARTESIAN_POINT ( 'NONE',  ( 10.72451020669898902, -18.67979575497178502, 77.91557627198102409 ) ) ;
#21234 = CARTESIAN_POINT ( 'NONE',  ( 5.823673210054444382, -21.52544592524334988, 35.20942372801901854 ) ) ;
#21235 = CARTESIAN_POINT ( 'NONE',  ( 8.314922557960818139, 14.29746914071049879, 109.5822429386476955 ) ) ;
#21236 = CARTESIAN_POINT ( 'NONE',  ( 19.02544592524334988, 5.153800228976608722, 71.45942372801900433 ) ) ;
#21237 = CARTESIAN_POINT ( 'NONE',  ( -19.05341960407611168, -5.049401038298163336, 46.45724293864768129 ) ) ;
#21238 = CARTESIAN_POINT ( 'NONE',  ( 4.379528057220339221, -16.55341960407611168, 107.7072429386476955 ) ) ;
#21239 = CARTESIAN_POINT ( 'NONE',  ( -16.46253265017160317, 9.564922557960807481, 110.8322429386476955 ) ) ;
#21240 = AXIS2_PLACEMENT_3D ( 'NONE', #75249, #60075, #150124 ) ;
#21241 = CARTESIAN_POINT ( 'NONE',  ( 12.06949235617757843, -12.14591786802309237, 43.12390960531435269 ) ) ;
#21242 = CARTESIAN_POINT ( 'NONE',  ( 0.05219959533934541429, -16.53943276465976808, 100.0010903946857042 ) ) ;
#21243 = CARTESIAN_POINT ( 'NONE',  ( 13.89961937509977652, -13.97604488694527269, 48.12390960531435979 ) ) ;
#21244 = CARTESIAN_POINT ( 'NONE',  ( -0.05219959533909027116, -19.03943276465977164, 27.49890960531435624 ) ) ;
#21245 = CARTESIAN_POINT ( 'NONE',  ( -18.67979575497193778, 10.72451020669871902, 113.3344237280190328 ) ) ;
#21247 = CARTESIAN_POINT ( 'NONE',  ( 12.06949235617757843, -12.14591786802309237, 43.12390960531435269 ) ) ;
#21246 = CARTESIAN_POINT ( 'NONE',  ( -17.40861289039002813, -6.110651285853283099, 41.37232470827433417 ) ) ;
#21248 = CARTESIAN_POINT ( 'NONE',  ( -21.55341960407619339, 5.719274019375674811, 48.54275706135234714 ) ) ;
#21249 = DIRECTION ( 'NONE',  ( -0.1178549842436482503, 0.9930308165857338887, -1.226674847569999905E-16 ) ) ;
#21250 = CARTESIAN_POINT ( 'NONE',  ( -16.52544592524335698, -4.483927247898792601, 53.95942372801900433 ) ) ;
#21251 = CARTESIAN_POINT ( 'NONE',  ( -4.379528057220328563, 16.55341960407611168, 30.20724293864769550 ) ) ;
#21252 = CARTESIAN_POINT ( 'NONE',  ( 14.29746914071037800, 8.314922557961029526, 101.6677570613523613 ) ) ;
#21253 = CARTESIAN_POINT ( 'NONE',  ( -8.314922557961024197, 14.29746914071037800, 27.91775706135234358 ) ) ;
#21254 = CARTESIAN_POINT ( 'NONE',  ( 16.51473224551069308, 9.474510206698969483, 54.16557627198103120 ) ) ;
#21255 = CARTESIAN_POINT ( 'NONE',  ( 12.14591786802309770, 12.06949235617756955, 109.3739096053143811 ) ) ;
#21256 = CARTESIAN_POINT ( 'NONE',  ( 18.67979575497194134, -10.72451020669871369, 25.83442372801901499 ) ) ;
#21257 = CARTESIAN_POINT ( 'NONE',  ( -16.46253265017160317, 9.564922557960807481, 40.83224293864769550 ) ) ;
#21258 = CARTESIAN_POINT ( 'NONE',  ( 13.89961937509977652, -13.97604488694527269, 113.1239096053143527 ) ) ;
#21259 = CARTESIAN_POINT ( 'NONE',  ( -13.97604488694527625, -13.89961937509977652, 31.87390960531435979 ) ) ;
#21260 = CARTESIAN_POINT ( 'NONE',  ( 5.153800228976335163, 19.02544592524342804, 114.7905762719810241 ) ) ;
#21261 = CARTESIAN_POINT ( 'NONE',  ( -16.79531203550646978, -7.028104445595714900, 36.25244988220443787 ) ) ;
#21262 = CARTESIAN_POINT ( 'NONE',  ( 16.51473224551069308, 9.474510206698969483, 104.1655762719810241 ) ) ;
#21264 = CARTESIAN_POINT ( 'NONE',  ( -14.29746914071049879, 8.314922557960819915, 110.8322429386476955 ) ) ;
#21263 = CARTESIAN_POINT ( 'NONE',  ( -18.62759615963255300, -10.81492255796106328, 49.16775706135234003 ) ) ;
#21265 = CARTESIAN_POINT ( 'NONE',  ( -16.51473224551069308, -9.474510206698971260, 111.6655762719810383 ) ) ;
#21266 = CARTESIAN_POINT ( 'NONE',  ( -8.314922557961024197, 14.29746914071037800, 77.91775706135231871 ) ) ;
#21267 = CARTESIAN_POINT ( 'NONE',  ( -18.67979575497193778, 10.72451020669871902, 93.33442372801901854 ) ) ;
#21268 = CARTESIAN_POINT ( 'NONE',  ( -16.55341960407617563, 4.379528057220093196, 58.54275706135235424 ) ) ;
#21269 = CARTESIAN_POINT ( 'NONE',  ( -13.97604488694527625, -13.89961937509977652, 96.87390960531433848 ) ) ;
#21270 = CARTESIAN_POINT ( 'NONE',  ( 4.379528057220092307, 16.55341960407617563, 42.29275706135235424 ) ) ;
#21271 = CARTESIAN_POINT ( 'NONE',  ( 12.14591786802327356, -12.06949235617739191, 20.62609039468568639 ) ) ;
#21272 = CARTESIAN_POINT ( 'NONE',  ( -14.34966873604972548, 8.224510206698743886, 78.33442372801901854 ) ) ;
#21273 = CARTESIAN_POINT ( 'NONE',  ( -0.05219959533936034679, 19.03943276465977164, 102.5010903946856757 ) ) ;
#21274 = CARTESIAN_POINT ( 'NONE',  ( -9.474510206698964154, 16.51473224551069663, 80.41557627198103830 ) ) ;
#21275 = CARTESIAN_POINT ( 'NONE',  ( -0.05219959533907301413, -21.53943276465977519, 92.49890960531436690 ) ) ;
#21277 = CARTESIAN_POINT ( 'NONE',  ( -9.564922557961040184, 16.46253265017147172, 97.91775706135233293 ) ) ;
#21276 = CARTESIAN_POINT ( 'NONE',  ( 12.14591786802309770, 12.06949235617756955, 99.37390960531436690 ) ) ;
#21278 = CARTESIAN_POINT ( 'NONE',  ( -16.55341960407617563, 4.379528057220093196, 78.54275706135236135 ) ) ;
#21279 = CARTESIAN_POINT ( 'NONE',  ( 24.10180676228321062, 9.559744493757255768, 166.3058469464613154 ) ) ;
#21280 = CARTESIAN_POINT ( 'NONE',  ( 5.153800228976615827, -19.02544592524334988, 75.20942372801896170 ) ) ;
#21281 = CARTESIAN_POINT ( 'NONE',  ( 14.34966873604960469, 8.224510206698951720, 49.16557627198102409 ) ) ;
#21282 = CARTESIAN_POINT ( 'NONE',  ( 16.55341960407611168, 4.379528057220329451, 93.95724293864770971 ) ) ;
#21284 = CARTESIAN_POINT ( 'NONE',  ( -16.29526858892876007, 7.335722546920116827, 89.20329402199797642 ) ) ;
#21283 = CARTESIAN_POINT ( 'NONE',  ( 5.049401038297881783, 19.05341960407617563, 37.29275706135232582 ) ) ;
#21285 = CARTESIAN_POINT ( 'NONE',  ( 5.823673210054444382, -21.52544592524334988, 35.20942372801901854 ) ) ;
#21286 = CARTESIAN_POINT ( 'NONE',  ( -13.97604488694547697, 13.89961937509957934, 98.12609039468566152 ) ) ;
#21287 = CARTESIAN_POINT ( 'NONE',  ( -19.02544592524342804, 5.153800228976336051, 111.0405762719810099 ) ) ;
#21288 = CARTESIAN_POINT ( 'NONE',  ( 5.153800228976335163, 19.02544592524342804, 89.79057627198102409 ) ) ;
#21289 = CARTESIAN_POINT ( 'NONE',  ( -10.81492255796105439, 18.62759615963255655, 107.9177570613523471 ) ) ;
#21290 = CARTESIAN_POINT ( 'NONE',  ( -9.474510206698964154, 16.51473224551069663, 85.41557627198102409 ) ) ;
#21291 = CARTESIAN_POINT ( 'NONE',  ( 15.72974639402199770, -15.80617190586745480, 38.12390960531436690 ) ) ;
#21292 = CARTESIAN_POINT ( 'NONE',  ( 4.483927247898545687, 16.52544592524342804, 99.79057627198103830 ) ) ;
#21293 = CARTESIAN_POINT ( 'NONE',  ( -5.153800228976328057, -19.02544592524343514, 62.29057627198100988 ) ) ;
#21294 = CARTESIAN_POINT ( 'NONE',  ( -16.52544592524342804, 4.483927247898546575, 106.0405762719810525 ) ) ;
#21295 = CARTESIAN_POINT ( 'NONE',  ( -21.52544592524334988, -5.823673210054445271, 23.95942372801901143 ) ) ;
#21296 = CARTESIAN_POINT ( 'NONE',  ( 21.52544592524334988, 5.823673210054432836, 71.45942372801901854 ) ) ;
#21297 = CARTESIAN_POINT ( 'NONE',  ( 16.51473224551069308, 9.474510206698969483, 49.16557627198102409 ) ) ;
#21298 = ADVANCED_FACE ( 'NONE', ( #64712 ), #108221, .T. ) ;
#21299 = CARTESIAN_POINT ( 'NONE',  ( 8.314922557961029526, -14.29746914071037800, 80.41775706135234714 ) ) ;
#21300 = CARTESIAN_POINT ( 'NONE',  ( -15.80617190586768217, 15.72974639402176855, 23.12609039468567573 ) ) ;
#21301 = ORIENTED_EDGE ( 'NONE', *, *, #100282, .T. ) ;
#21302 = CARTESIAN_POINT ( 'NONE',  ( -0.05219959533937732626, 21.53943276465977519, 27.50109039468567929 ) ) ;
#21304 = CARTESIAN_POINT ( 'NONE',  ( 16.51473224551069308, 9.474510206698969483, 64.16557627198102409 ) ) ;
#21303 = CARTESIAN_POINT ( 'NONE',  ( 5.153800228976615827, -19.02544592524334988, 50.20942372801897591 ) ) ;
#21305 = CARTESIAN_POINT ( 'NONE',  ( 0.05219959533936267826, -19.03943276465977164, 30.00109039468566863 ) ) ;
#21306 = CARTESIAN_POINT ( 'NONE',  ( 10.72451020669871369, 18.67979575497193778, 77.08442372801901854 ) ) ;
#21307 = CARTESIAN_POINT ( 'NONE',  ( -0.05219959533907301413, -21.53943276465977519, 72.49890960531435269 ) ) ;
#21308 = CARTESIAN_POINT ( 'NONE',  ( -0.05219959533910754901, -16.53943276465976808, 47.49890960531435979 ) ) ;
#21310 = CARTESIAN_POINT ( 'NONE',  ( -9.564922557961040184, 16.46253265017147172, 32.91775706135233293 ) ) ;
#21309 = CARTESIAN_POINT ( 'NONE',  ( -18.62759615963255300, -10.81492255796106328, 89.16775706135236135 ) ) ;
#21311 = CARTESIAN_POINT ( 'NONE',  ( -8.314922557960811034, -14.29746914071050412, 72.08224293864769550 ) ) ;
#21312 = CARTESIAN_POINT ( 'NONE',  ( -16.52544592524342804, 4.483927247898546575, 116.0405762719810383 ) ) ;
#21313 = CARTESIAN_POINT ( 'NONE',  ( -5.153800228976607833, 19.02544592524334988, 52.70942372801900433 ) ) ;
#21314 = CARTESIAN_POINT ( 'NONE',  ( -14.34966873604960291, -8.224510206698953496, 21.66557627198102409 ) ) ;
#21315 = CARTESIAN_POINT ( 'NONE',  ( -10.81492255796105439, 18.62759615963255655, 77.91775706135231871 ) ) ;
#21316 = CARTESIAN_POINT ( 'NONE',  ( 9.474510206698971260, -16.51473224551069308, 82.91557627198103830 ) ) ;
#21317 = CARTESIAN_POINT ( 'NONE',  ( 19.05341960407617918, -5.049401038297876454, 51.04275706135231871 ) ) ;
#21318 = CARTESIAN_POINT ( 'NONE',  ( -18.67979575497178146, -10.72451020669898902, 51.66557627198102409 ) ) ;
#21319 = CARTESIAN_POINT ( 'NONE',  ( -18.67979575497193778, 10.72451020669871902, 43.33442372801901143 ) ) ;
#21320 = CARTESIAN_POINT ( 'NONE',  ( -15.80617190586745835, -15.72974639402198527, 106.8739096053143811 ) ) ;
#21321 = CARTESIAN_POINT ( 'NONE',  ( -16.46253265017146816, -9.564922557961047289, 94.16775706135233293 ) ) ;
#21322 = CARTESIAN_POINT ( 'NONE',  ( 4.483927247898790824, -16.52544592524335698, 60.20942372801902565 ) ) ;
#21324 = CARTESIAN_POINT ( 'NONE',  ( 18.67979575497178502, 10.72451020669898547, 109.1655762719810383 ) ) ;
#21323 = DIRECTION ( 'NONE',  ( -1.000000000000000000, 3.552713678800500929E-15, 0.000000000000000000 ) ) ;
#21325 = CARTESIAN_POINT ( 'NONE',  ( -16.55341960407611168, -4.379528057220339221, 91.45724293864769550 ) ) ;
#21326 = CARTESIAN_POINT ( 'NONE',  ( -36.91746825000001309, -11.99521256947794789, -11.02499999726881263 ) ) ;
#21327 = CARTESIAN_POINT ( 'NONE',  ( 14.34966873604972726, -8.224510206698740333, 40.83442372801901854 ) ) ;
#21328 = CARTESIAN_POINT ( 'NONE',  ( -10.81492255796078084, -18.62759615963271287, 47.08224293864770260 ) ) ;
#21329 = CARTESIAN_POINT ( 'NONE',  ( 8.224510206698742110, 14.34966873604972548, 87.08442372801901854 ) ) ;
#21330 = CARTESIAN_POINT ( 'NONE',  ( -5.153800228976328057, -19.02544592524343514, 32.29057627198102409 ) ) ;
#21331 = CARTESIAN_POINT ( 'NONE',  ( 4.483927247898790824, -16.52544592524335698, 60.20942372801902565 ) ) ;
#21332 = CARTESIAN_POINT ( 'NONE',  ( -21.52544592524334988, -5.823673210054445271, 38.95942372801901854 ) ) ;
#21333 = CARTESIAN_POINT ( 'NONE',  ( -5.823673210054116645, -21.52544592524344225, 52.29057627198102409 ) ) ;
#21334 = CARTESIAN_POINT ( 'NONE',  ( 12.06949235617739724, 12.14591786802326823, 86.87609039468568994 ) ) ;
#21335 = CARTESIAN_POINT ( 'NONE',  ( 5.823673210054444382, -21.52544592524334988, 70.20942372801904696 ) ) ;
#21336 = CARTESIAN_POINT ( 'NONE',  ( 21.52544592524344225, -5.823673210054117533, 53.54057627198103120 ) ) ;
#21337 = CARTESIAN_POINT ( 'NONE',  ( 5.823673210054125526, 21.52544592524343514, 39.79057627198103830 ) ) ;
#21338 = VERTEX_POINT ( 'NONE', #47563 ) ;
#21339 = CARTESIAN_POINT ( 'NONE',  ( 8.224510206698742110, 14.34966873604972548, 62.08442372801901143 ) ) ;
#21340 = CARTESIAN_POINT ( 'NONE',  ( 15.72974639402199770, -15.80617190586745480, 38.12390960531436690 ) ) ;
#21341 = EDGE_LOOP ( 'NONE', ( #181036, #99429, #128568, #179130 ) ) ;
#21342 = CARTESIAN_POINT ( 'NONE',  ( -9.474510206698964154, 16.51473224551069663, 95.41557627198102409 ) ) ;
#21343 = CARTESIAN_POINT ( 'NONE',  ( -16.55341960407611168, -4.379528057220339221, 21.45724293864769550 ) ) ;
#21344 = CARTESIAN_POINT ( 'NONE',  ( 17.50000000000000000, -5.499999999999992895, 38.29690382534171533 ) ) ;
#21345 = CARTESIAN_POINT ( 'NONE',  ( 14.29746914071049879, -8.314922557960816363, 113.3322429386476955 ) ) ;
#21346 = CARTESIAN_POINT ( 'NONE',  ( 21.55341960407610458, 5.719274019375980345, 63.95724293864770260 ) ) ;
#21347 = CARTESIAN_POINT ( 'NONE',  ( 9.564922557960805705, 16.46253265017160317, 39.58224293864768839 ) ) ;
#21348 = CARTESIAN_POINT ( 'NONE',  ( 14.29746914071037800, 8.314922557961029526, 91.66775706135234714 ) ) ;
#21349 = CARTESIAN_POINT ( 'NONE',  ( 18.67979575497194134, -10.72451020669871369, 30.83442372801902209 ) ) ;
#21350 = CARTESIAN_POINT ( 'NONE',  ( -9.564922557961040184, 16.46253265017147172, 87.91775706135233293 ) ) ;
#21351 = CARTESIAN_POINT ( 'NONE',  ( 4.483927247898545687, 16.52544592524342804, 104.7905762719810241 ) ) ;
#21352 = CARTESIAN_POINT ( 'NONE',  ( 5.049401038298161559, -19.05341960407611168, 47.70724293864770260 ) ) ;
#21353 = AXIS2_PLACEMENT_3D ( 'NONE', #190463, #159104, #20598 ) ;
#21354 = CARTESIAN_POINT ( 'NONE',  ( -19.05341960407611168, -5.049401038298163336, 21.45724293864768839 ) ) ;
#21355 = CARTESIAN_POINT ( 'NONE',  ( 1.376754478911074830, 23.51071581304989522, -54.82534132429363183 ) ) ;
#21356 = CARTESIAN_POINT ( 'NONE',  ( -9.564922557960796823, -16.46253265017161027, 77.08224293864769550 ) ) ;
#21357 = CARTESIAN_POINT ( 'NONE',  ( 16.55341960407618274, -4.379528057220086978, 56.04275706135235424 ) ) ;
#21358 = CARTESIAN_POINT ( 'NONE',  ( -10.81492255796105439, 18.62759615963255655, 107.9177570613523471 ) ) ;
#21359 = CARTESIAN_POINT ( 'NONE',  ( -15.72974639402197994, 15.80617190586746368, 45.62390960531436690 ) ) ;
#21360 = CARTESIAN_POINT ( 'NONE',  ( 14.34966873604972726, -8.224510206698740333, 70.83442372801901854 ) ) ;
#21361 = CARTESIAN_POINT ( 'NONE',  ( -16.51473224551082808, 9.474510206698731452, 68.33442372801900433 ) ) ;
#21362 = CARTESIAN_POINT ( 'NONE',  ( 21.53943276465977519, 0.05219959533937863772, 61.25109039468567573 ) ) ;
#21363 = CARTESIAN_POINT ( 'NONE',  ( 9.564922557960805705, 16.46253265017160317, 74.58224293864769550 ) ) ;
#21364 = CARTESIAN_POINT ( 'NONE',  ( 5.153800228976335163, 19.02544592524342804, 34.79057627198102409 ) ) ;
#21365 = CARTESIAN_POINT ( 'NONE',  ( 13.89961937509957401, 13.97604488694547697, 61.87609039468566863 ) ) ;
#21366 = CARTESIAN_POINT ( 'NONE',  ( -25.51209292918185056, 5.276535733812623974, 165.5596888358906540 ) ) ;
#21367 = CARTESIAN_POINT ( 'NONE',  ( -5.049401038298153566, 19.05341960407611168, 90.20724293864766707 ) ) ;
#21368 = CARTESIAN_POINT ( 'NONE',  ( 4.483927247898545687, 16.52544592524342804, 49.79057627198102409 ) ) ;
#21369 = CARTESIAN_POINT ( 'NONE',  ( -5.719274019375978568, 21.55341960407610458, 50.20724293864769550 ) ) ;
#21370 = CARTESIAN_POINT ( 'NONE',  ( -17.50000000000001776, 4.049696124445901546, 104.1803967066594794 ) ) ;
#21371 = CARTESIAN_POINT ( 'NONE',  ( -5.049401038297874678, -19.05341960407617918, 29.79275706135232227 ) ) ;
#21372 = DIRECTION ( 'NONE',  ( -1.000000000000000000, -0.000000000000000000, -0.000000000000000000 ) ) ;
#21373 = CARTESIAN_POINT ( 'NONE',  ( 19.03943276465977164, -0.05219959533909143690, 53.74890960531436690 ) ) ;
#21374 = CARTESIAN_POINT ( 'NONE',  ( -0.05219959533934338120, 16.53943276465976808, 32.50109039468568284 ) ) ;
#21375 = CARTESIAN_POINT ( 'NONE',  ( -33.67973855159211638, -4.949490125723493783, 97.42538428767439029 ) ) ;
#21376 = CARTESIAN_POINT ( 'NONE',  ( 14.34966873604972726, -8.224510206698740333, 75.83442372801900433 ) ) ;
#21377 = CARTESIAN_POINT ( 'NONE',  ( 0.05219959533907565091, 21.53943276465977519, 94.99890960531436690 ) ) ;
#21379 = DIRECTION ( 'NONE',  ( 0.000000000000000000, 0.8164965809277239250, 0.5773502691896288397 ) ) ;
#21378 = CARTESIAN_POINT ( 'NONE',  ( -5.049401038298153566, 19.05341960407611168, 45.20724293864769550 ) ) ;
#21380 = CARTESIAN_POINT ( 'NONE',  ( 15.80617190586769283, -15.72974639402175789, 45.62609039468567573 ) ) ;
#21381 = CARTESIAN_POINT ( 'NONE',  ( 16.51473224551083163, -9.474510206698727899, 45.83442372801900433 ) ) ;
#21382 = CARTESIAN_POINT ( 'NONE',  ( 5.049401038298161559, -19.05341960407611168, 52.70724293864767418 ) ) ;
#21383 = CARTESIAN_POINT ( 'NONE',  ( 15.72974639402176855, 15.80617190586768217, 96.87609039468568994 ) ) ;
#21384 = VECTOR ( 'NONE', #104477, 1000.000000000000000 ) ;
#21385 = CARTESIAN_POINT ( 'NONE',  ( 16.79531203550648044, 7.028104445595620753, 98.75244988220443076 ) ) ;
#21386 = CARTESIAN_POINT ( 'NONE',  ( 14.29746914071049879, -8.314922557960816363, 38.33224293864768839 ) ) ;
#21387 = CARTESIAN_POINT ( 'NONE',  ( 4.336808689942017736E-16, 0.000000000000000000, 0.000000000000000000 ) ) ;
#21388 = CARTESIAN_POINT ( 'NONE',  ( 21.53943276465977519, -0.05219959533907433946, 48.74890960531435979 ) ) ;
#21389 = CARTESIAN_POINT ( 'NONE',  ( 22.44159573604009594, -16.30477369853687364, 143.6750000027311671 ) ) ;
#21390 = CARTESIAN_POINT ( 'NONE',  ( -13.97604488694527625, -13.89961937509977652, 96.87390960531433848 ) ) ;
#21391 = CARTESIAN_POINT ( 'NONE',  ( 16.53943276465976808, -0.05219959533910856209, 98.74890960531438111 ) ) ;
#21392 = CARTESIAN_POINT ( 'NONE',  ( -4.379528057220086978, -16.55341960407618274, 24.79275706135235779 ) ) ;
#21393 = CARTESIAN_POINT ( 'NONE',  ( -8.224510206698735004, -14.34966873604973081, 104.5844237280190185 ) ) ;
#21394 = ORIENTED_EDGE ( 'NONE', *, *, #126396, .T. ) ;
#21395 = ADVANCED_FACE ( 'NONE', ( #80861 ), #48559, .F. ) ;
#21397 = CARTESIAN_POINT ( 'NONE',  ( 5.719274019375991003, -21.55341960407610458, 107.7072429386476955 ) ) ;
#21396 = CARTESIAN_POINT ( 'NONE',  ( 9.564922557960805705, 16.46253265017160317, 104.5822429386476955 ) ) ;
#21399 = CARTESIAN_POINT ( 'NONE',  ( 19.03943276465977164, -0.05219959533909143690, 98.74890960531436690 ) ) ;
#21398 = CARTESIAN_POINT ( 'NONE',  ( -12.14591786802309592, -12.06949235617757132, 21.87390960531436690 ) ) ;
#21400 = CARTESIAN_POINT ( 'NONE',  ( 19.03943276465977164, 0.05219959533936151252, 91.25109039468566152 ) ) ;
#21401 = CARTESIAN_POINT ( 'NONE',  ( -5.049401038297874678, -19.05341960407617918, 19.79275706135233293 ) ) ;
#21402 = CARTESIAN_POINT ( 'NONE',  ( 10.81492255796078972, 18.62759615963270932, 89.58224293864768129 ) ) ;
#21403 = CARTESIAN_POINT ( 'NONE',  ( -0.05219959533907301413, -21.53943276465977519, 57.49890960531435979 ) ) ;
#21404 = CARTESIAN_POINT ( 'NONE',  ( -16.51473224551069308, -9.474510206698971260, 66.66557627198102409 ) ) ;
#21405 = CARTESIAN_POINT ( 'NONE',  ( 14.34966873604960469, 8.224510206698951720, 29.16557627198103120 ) ) ;
#21406 = CARTESIAN_POINT ( 'NONE',  ( 0.05219959533909260263, 19.03943276465977164, 74.99890960531435269 ) ) ;
#21407 = EDGE_LOOP ( 'NONE', ( #199457, #55147, #162322, #160514, #189917, #90510 ) ) ;
#21408 = CARTESIAN_POINT ( 'NONE',  ( 19.36337904590688552, -5.500000000000142997, 62.91494137495619299 ) ) ;
#21409 = CARTESIAN_POINT ( 'NONE',  ( 5.049401038297881783, 19.05341960407617563, 37.29275706135232582 ) ) ;
#21410 = CARTESIAN_POINT ( 'NONE',  ( 21.53943276465977519, -0.05219959533907433946, 78.74890960531436690 ) ) ;
#21411 = CARTESIAN_POINT ( 'NONE',  ( -16.53943276465976808, 0.05219959533911058130, 81.24890960531436690 ) ) ;
#21412 = CARTESIAN_POINT ( 'NONE',  ( -15.72974639402176322, -15.80617190586768395, 34.37609039468568284 ) ) ;
#21413 = CARTESIAN_POINT ( 'NONE',  ( 1.784210473542230573E-15, -29.16686587814331588, 141.3750000027311557 ) ) ;
#21414 = CARTESIAN_POINT ( 'NONE',  ( -14.34966873604972548, 8.224510206698743886, 113.3344237280190328 ) ) ;
#21415 = CARTESIAN_POINT ( 'NONE',  ( 5.049401038298161559, -19.05341960407611168, 27.70724293864769550 ) ) ;
#21416 = CARTESIAN_POINT ( 'NONE',  ( 19.05341960407611168, 5.049401038298154454, 83.95724293864766707 ) ) ;
#21417 = CARTESIAN_POINT ( 'NONE',  ( 12.14591786802309770, 12.06949235617756955, 39.37390960531436690 ) ) ;
#21418 = CARTESIAN_POINT ( 'NONE',  ( -21.53943276465977519, -0.05219959533937600094, 63.75109039468568284 ) ) ;
#21419 = CARTESIAN_POINT ( 'NONE',  ( 26.12775673971824375, -26.86876869530867751, -18.42961048235288857 ) ) ;
#21420 = CARTESIAN_POINT ( 'NONE',  ( 0.05219959533909260263, 19.03943276465977164, 44.99890960531435979 ) ) ;
#21421 = CARTESIAN_POINT ( 'NONE',  ( 5.049401038298161559, -19.05341960407611168, 57.70724293864769550 ) ) ;
#21422 = ORIENTED_EDGE ( 'NONE', *, *, #98443, .T. ) ;
#21423 = CARTESIAN_POINT ( 'NONE',  ( 10.72451020669871369, 18.67979575497193778, 112.0844237280190185 ) ) ;
#21424 = CARTESIAN_POINT ( 'NONE',  ( 8.314922557961029526, -14.29746914071037800, 60.41775706135235424 ) ) ;
#21425 = CARTESIAN_POINT ( 'NONE',  ( -10.72451020669870658, -18.67979575497194134, 89.58442372801901854 ) ) ;
#21426 = CARTESIAN_POINT ( 'NONE',  ( -16.46253265017160317, 9.564922557960807481, 110.8322429386476955 ) ) ;
#21427 = CARTESIAN_POINT ( 'NONE',  ( -13.89961937509957401, -13.97604488694547875, 99.37609039468567573 ) ) ;
#21428 = CARTESIAN_POINT ( 'NONE',  ( 21.55341960407619695, -5.719274019375665929, 71.04275706135234714 ) ) ;
#21429 = CARTESIAN_POINT ( 'NONE',  ( -4.379528057220086978, -16.55341960407618274, 29.79275706135234358 ) ) ;
#21430 = CARTESIAN_POINT ( 'NONE',  ( 18.62759615963271287, -10.81492255796078972, 83.33224293864769550 ) ) ;
#21431 = CARTESIAN_POINT ( 'NONE',  ( -5.153800228976607833, 19.02544592524334988, 92.70942372801901854 ) ) ;
#21432 = CARTESIAN_POINT ( 'NONE',  ( -9.474510206698964154, 16.51473224551069663, 60.41557627198102409 ) ) ;
#21433 = CARTESIAN_POINT ( 'NONE',  ( -16.52544592524335698, -4.483927247898792601, 18.95942372801901143 ) ) ;
#21434 = CARTESIAN_POINT ( 'NONE',  ( -13.89961937509957401, -13.97604488694547875, 99.37609039468567573 ) ) ;
#21435 = CARTESIAN_POINT ( 'NONE',  ( 4.483927247898545687, 16.52544592524342804, 54.79057627198104541 ) ) ;
#21437 = ORIENTED_EDGE ( 'NONE', *, *, #117196, .F. ) ;
#21436 = CARTESIAN_POINT ( 'NONE',  ( -19.03943276465977164, -0.05219959533935918106, 83.75109039468567573 ) ) ;
#21438 = CARTESIAN_POINT ( 'NONE',  ( -4.379528057220086978, -16.55341960407618274, 59.79275706135234714 ) ) ;
#21440 = CARTESIAN_POINT ( 'NONE',  ( -19.03943276465977164, 0.05219959533909376836, 36.24890960531436690 ) ) ;
#21439 = CARTESIAN_POINT ( 'NONE',  ( -15.72974639402197994, 15.80617190586746368, 110.6239096053143669 ) ) ;
#21441 = CARTESIAN_POINT ( 'NONE',  ( -5.049401038298153566, 19.05341960407611168, 50.20724293864770260 ) ) ;
#21442 = CARTESIAN_POINT ( 'NONE',  ( -4.379528057220086978, -16.55341960407618274, 54.79275706135235424 ) ) ;
#21443 = CARTESIAN_POINT ( 'NONE',  ( 27.73933785331498214, 9.013057229001095294, 140.4750000027311785 ) ) ;
#21444 = CARTESIAN_POINT ( 'NONE',  ( -23.31738231874055600, 16.94106989632528837, 146.0500000054623797 ) ) ;
#21445 = CARTESIAN_POINT ( 'NONE',  ( -16.51473224551069308, -9.474510206698971260, 106.6655762719810383 ) ) ;
#21446 = DIRECTION ( 'NONE',  ( -6.948002486793210646E-15, 0.9991276842514723588, -0.04175967627138119781 ) ) ;
#21447 = VERTEX_POINT ( 'NONE', #110212 ) ;
#21448 = CARTESIAN_POINT ( 'NONE',  ( 12.14591786802327356, -12.06949235617739191, 20.62609039468568639 ) ) ;
#21449 = CARTESIAN_POINT ( 'NONE',  ( 18.62759615963271287, -10.81492255796078972, 43.33224293864769550 ) ) ;
#21451 = CARTESIAN_POINT ( 'NONE',  ( -14.34966873604972548, 8.224510206698743886, 33.33442372801900433 ) ) ;
#21450 = CARTESIAN_POINT ( 'NONE',  ( -19.02544592524334988, -5.153800228976617603, 43.95942372801899012 ) ) ;
#21452 = CARTESIAN_POINT ( 'NONE',  ( -9.474510206698964154, 16.51473224551069663, 25.41557627198103120 ) ) ;
#21453 = CARTESIAN_POINT ( 'NONE',  ( 5.153800228976335163, 19.02544592524342804, 49.79057627198100988 ) ) ;
#21454 = CARTESIAN_POINT ( 'NONE',  ( 21.53943276465977519, -0.05219959533907433946, 83.74890960531435269 ) ) ;
#21455 = CARTESIAN_POINT ( 'NONE',  ( -13.97604488694527625, -13.89961937509977652, 111.8739096053143243 ) ) ;
#21456 = CARTESIAN_POINT ( 'NONE',  ( 0.05219959533909260263, 19.03943276465977164, 49.99890960531435979 ) ) ;
#21457 = CARTESIAN_POINT ( 'NONE',  ( 8.571926809382597767, 26.38167802310806209, 142.7750000027311899 ) ) ;
#21458 = CARTESIAN_POINT ( 'NONE',  ( 16.51473224551083163, -9.474510206698727899, 90.83442372801900433 ) ) ;
#21459 = CARTESIAN_POINT ( 'NONE',  ( 8.224510206698953496, -14.34966873604960469, 62.91557627198102409 ) ) ;
#21460 = CARTESIAN_POINT ( 'NONE',  ( 0.05219959533937995610, -21.53943276465977519, 105.0010903946856757 ) ) ;
#21461 = CARTESIAN_POINT ( 'NONE',  ( -5.719274019375978568, 21.55341960407610458, 100.2072429386476955 ) ) ;
#21462 = CARTESIAN_POINT ( 'NONE',  ( 21.52544592524334988, 5.823673210054432836, 91.45942372801901854 ) ) ;
#21463 = CARTESIAN_POINT ( 'NONE',  ( 18.67979575497194134, -10.72451020669871369, 75.83442372801900433 ) ) ;
#21464 = CARTESIAN_POINT ( 'NONE',  ( 13.89961937509977652, -13.97604488694527269, 113.1239096053143527 ) ) ;
#21466 = CARTESIAN_POINT ( 'NONE',  ( -0.05219959533937732626, 21.53943276465977519, 77.50109039468567573 ) ) ;
#21465 = CARTESIAN_POINT ( 'NONE',  ( -4.379528057220086978, -16.55341960407618274, 99.79275706135234714 ) ) ;
#21467 = CARTESIAN_POINT ( 'NONE',  ( -13.97604488694527625, -13.89961937509977652, 61.87390960531435979 ) ) ;
#21468 = EDGE_CURVE ( 'NONE', #17663, #172412, #30396, .T. ) ;
#21469 = CARTESIAN_POINT ( 'NONE',  ( 15.80617190586769283, -15.72974639402175789, 40.62609039468567573 ) ) ;
#21470 = CARTESIAN_POINT ( 'NONE',  ( -9.474510206698964154, 16.51473224551069663, 80.41557627198103830 ) ) ;
#21471 = CARTESIAN_POINT ( 'NONE',  ( -8.314922557960811034, -14.29746914071050412, 82.08224293864768129 ) ) ;
#21472 = CARTESIAN_POINT ( 'NONE',  ( 0.05219959533910956823, 16.53943276465976808, 54.99890960531435269 ) ) ;
#21473 = CARTESIAN_POINT ( 'NONE',  ( 5.823673210054125526, 21.52544592524343514, 64.79057627198103830 ) ) ;
#21474 = CARTESIAN_POINT ( 'NONE',  ( 0.05219959533909260263, 19.03943276465977164, 64.99890960531436690 ) ) ;
#21475 = CARTESIAN_POINT ( 'NONE',  ( 5.719274019375991003, -21.55341960407610458, 72.70724293864769550 ) ) ;
#21476 = CARTESIAN_POINT ( 'NONE',  ( 5.049401038297881783, 19.05341960407617563, 62.29275706135234003 ) ) ;
#21479 = CARTESIAN_POINT ( 'NONE',  ( -12.06949235617756955, 12.14591786802309770, 80.62390960531438111 ) ) ;
#21478 = CARTESIAN_POINT ( 'NONE',  ( 19.03943276465977164, 0.05219959533936151252, 36.25109039468567573 ) ) ;
#21477 = VECTOR ( 'NONE', #81918, 1000.000000000000000 ) ;
#21480 = CARTESIAN_POINT ( 'NONE',  ( 10.81492255796078972, 18.62759615963270932, 54.58224293864769550 ) ) ;
#21481 = CARTESIAN_POINT ( 'NONE',  ( 17.50000000000000000, -5.499999999999992895, 96.21769037696437010 ) ) ;
#21483 = CARTESIAN_POINT ( 'NONE',  ( 22.44159573604009594, -16.30477369853687364, 142.1750000027311671 ) ) ;
#21482 = CARTESIAN_POINT ( 'NONE',  ( -14.34966873604972548, 8.224510206698743886, 98.33442372801901854 ) ) ;
#21484 = CARTESIAN_POINT ( 'NONE',  ( 5.153800228976615827, -19.02544592524334988, 100.2094237280190043 ) ) ;
#21485 = EDGE_CURVE ( 'NONE', #193461, #85102, #172879, .T. ) ;
#21486 = CARTESIAN_POINT ( 'NONE',  ( -16.55341960407611168, -4.379528057220339221, 66.45724293864768129 ) ) ;
#21487 = DIRECTION ( 'NONE',  ( 0.000000000000000000, 0.000000000000000000, 1.000000000000000000 ) ) ;
#21488 = CARTESIAN_POINT ( 'NONE',  ( 19.03943276465977164, -0.05219959533909143690, 63.74890960531435979 ) ) ;
#21489 = CARTESIAN_POINT ( 'NONE',  ( 0.05219959533910956823, 16.53943276465976808, 49.99890960531437401 ) ) ;
#21490 = CARTESIAN_POINT ( 'NONE',  ( -19.05341960407611168, -5.049401038298163336, 91.45724293864766707 ) ) ;
#21492 = CARTESIAN_POINT ( 'NONE',  ( -19.05341960407611168, -5.049401038298163336, 71.45724293864766707 ) ) ;
#21491 = CARTESIAN_POINT ( 'NONE',  ( 16.46253265017146816, 9.564922557961045513, 81.66775706135233293 ) ) ;
#21493 = CARTESIAN_POINT ( 'NONE',  ( 19.05341960407611168, 5.049401038298154454, 83.95724293864766707 ) ) ;
#21494 = CARTESIAN_POINT ( 'NONE',  ( 19.03943276465977164, -0.05219959533909143690, 68.74890960531436690 ) ) ;
#21495 = CARTESIAN_POINT ( 'NONE',  ( 15.80617190586746368, 15.72974639402197994, 69.37390960531436690 ) ) ;
#21496 = CARTESIAN_POINT ( 'NONE',  ( -16.52544592524335698, -4.483927247898792601, 58.95942372801902565 ) ) ;
#21497 = CARTESIAN_POINT ( 'NONE',  ( 21.98685479826775335, -13.98560643873835652, 165.5209445330007441 ) ) ;
#21498 = CARTESIAN_POINT ( 'NONE',  ( -0.05219959533909027116, -19.03943276465977164, 52.49890960531436690 ) ) ;
#21499 = CARTESIAN_POINT ( 'NONE',  ( 5.823673210054125526, 21.52544592524343514, 59.79057627198103120 ) ) ;
#21500 = CARTESIAN_POINT ( 'NONE',  ( -0.05219959533936034679, 19.03943276465977164, 87.50109039468567573 ) ) ;
#21501 = CARTESIAN_POINT ( 'NONE',  ( -12.14591786802309592, -12.06949235617757132, 21.87390960531436690 ) ) ;
#21502 = CARTESIAN_POINT ( 'NONE',  ( -16.51473224551082808, 9.474510206698731452, 43.33442372801900433 ) ) ;
#21504 = CARTESIAN_POINT ( 'NONE',  ( -14.34966873604972548, 8.224510206698743886, 93.33442372801901854 ) ) ;
#21503 = CARTESIAN_POINT ( 'NONE',  ( -4.379528057220086978, -16.55341960407618274, 64.79275706135234714 ) ) ;
#21505 = CARTESIAN_POINT ( 'NONE',  ( 19.02130022317639657, -5.499999999999599432, 43.28188669246573994 ) ) ;
#21506 = CARTESIAN_POINT ( 'NONE',  ( 12.06949235617739724, 12.14591786802326823, 86.87609039468568994 ) ) ;
#21508 = CARTESIAN_POINT ( 'NONE',  ( 16.52544592524335698, 4.483927247898782831, 36.45942372801901143 ) ) ;
#21507 = CARTESIAN_POINT ( 'NONE',  ( 5.719274019375991003, -21.55341960407610458, 27.70724293864769905 ) ) ;
#21509 = CARTESIAN_POINT ( 'NONE',  ( 13.89961937509977652, -13.97604488694527269, 43.12390960531434558 ) ) ;
#21510 = CARTESIAN_POINT ( 'NONE',  ( 19.03943276465977164, -0.05219959533909143690, 53.74890960531436690 ) ) ;
#21511 = CARTESIAN_POINT ( 'NONE',  ( 13.89961937509977652, -13.97604488694527269, 43.12390960531434558 ) ) ;
#21512 = CARTESIAN_POINT ( 'NONE',  ( -18.67979575497193778, 10.72451020669871902, 38.33442372801900433 ) ) ;
#21513 = CARTESIAN_POINT ( 'NONE',  ( -16.53943276465976808, -0.05219959533934237506, 53.75109039468568994 ) ) ;
#21514 = CARTESIAN_POINT ( 'NONE',  ( 8.314922557960818139, 14.29746914071049879, 24.58224293864768839 ) ) ;
#21515 = CARTESIAN_POINT ( 'NONE',  ( 9.474510206698971260, -16.51473224551069308, 32.91557627198102409 ) ) ;
#21516 = CARTESIAN_POINT ( 'NONE',  ( -16.46253265017146816, -9.564922557961047289, 24.16775706135233648 ) ) ;
#21517 = CARTESIAN_POINT ( 'NONE',  ( -12.06949235617739369, -12.14591786802326823, 19.37609039468568639 ) ) ;
#21518 = CARTESIAN_POINT ( 'NONE',  ( 19.02544592524334988, 5.153800228976608722, 66.45942372801899012 ) ) ;
#21519 = CARTESIAN_POINT ( 'NONE',  ( 16.55341960407611168, 4.379528057220329451, 68.95724293864769550 ) ) ;
#21520 = CARTESIAN_POINT ( 'NONE',  ( -19.05341960407611168, -5.049401038298163336, 41.45724293864769550 ) ) ;
#21522 = CARTESIAN_POINT ( 'NONE',  ( 16.19135201231366139, -7.376712067591919109, 92.31319145947965410 ) ) ;
#21521 = CARTESIAN_POINT ( 'NONE',  ( -9.564922557961040184, 16.46253265017147172, 72.91775706135233293 ) ) ;
#21523 = CARTESIAN_POINT ( 'NONE',  ( 18.62759615963255655, 10.81492255796105972, 76.66775706135234714 ) ) ;
#21524 = CARTESIAN_POINT ( 'NONE',  ( 16.55341960407618274, -4.379528057220086978, 36.04275706135234714 ) ) ;
#21525 = CYLINDRICAL_SURFACE ( 'NONE', #82564, 1.499999999999997780 ) ;
#21526 = CARTESIAN_POINT ( 'NONE',  ( 18.67979575497178502, 10.72451020669898547, 34.16557627198102409 ) ) ;
#21527 = CARTESIAN_POINT ( 'NONE',  ( 0.05219959533934541429, -16.53943276465976808, 30.00109039468568284 ) ) ;
#21528 = DIRECTION ( 'NONE',  ( 0.000000000000000000, 0.000000000000000000, 1.000000000000000000 ) ) ;
#21529 = CARTESIAN_POINT ( 'NONE',  ( -0.05219959533936034679, 19.03943276465977164, 22.50109039468566152 ) ) ;
#21530 = CARTESIAN_POINT ( 'NONE',  ( 17.97182807773875979, -5.499999999999868550, 66.03038844047287625 ) ) ;
#21531 = CARTESIAN_POINT ( 'NONE',  ( -5.153800228976328057, -19.02544592524343514, 37.29057627198102409 ) ) ;
#21532 = CARTESIAN_POINT ( 'NONE',  ( 1.988064558232696151E-15, -30.27659582821216588, 142.7656553485623760 ) ) ;
#21533 = CARTESIAN_POINT ( 'NONE',  ( 19.02544592524343514, -5.153800228976328945, 58.54057627198102409 ) ) ;
#21535 = CARTESIAN_POINT ( 'NONE',  ( 21.53943276465977519, 0.05219959533937863772, 71.25109039468568994 ) ) ;
#21534 = AXIS2_PLACEMENT_3D ( 'NONE', #28893, #63171, #78331 ) ;
#21536 = CARTESIAN_POINT ( 'NONE',  ( -19.03943276465977164, -0.05219959533935918106, 18.75109039468567218 ) ) ;
#21537 = CARTESIAN_POINT ( 'NONE',  ( 8.314922557960818139, 14.29746914071049879, 29.58224293864769905 ) ) ;
#21538 = CARTESIAN_POINT ( 'NONE',  ( -16.46253265017160317, 9.564922557960807481, 30.83224293864769550 ) ) ;
#21539 = CARTESIAN_POINT ( 'NONE',  ( 16.51473224551069308, 9.474510206698969483, 89.16557627198103830 ) ) ;
#21540 = CARTESIAN_POINT ( 'NONE',  ( -10.72451020669870658, -18.67979575497194134, 69.58442372801900433 ) ) ;
#21541 = CARTESIAN_POINT ( 'NONE',  ( -9.474510206698964154, 16.51473224551069663, 40.41557627198103120 ) ) ;
#21542 = CARTESIAN_POINT ( 'NONE',  ( -10.81492255796105439, 18.62759615963255655, 72.91775706135234714 ) ) ;
#21544 = CARTESIAN_POINT ( 'NONE',  ( 0.05219959533909260263, 19.03943276465977164, 99.99890960531436690 ) ) ;
#21543 = CARTESIAN_POINT ( 'NONE',  ( 19.02544592524334988, 5.153800228976608722, 96.45942372801897591 ) ) ;
#21545 = CARTESIAN_POINT ( 'NONE',  ( -19.03943276465977164, 0.05219959533909376836, 41.24890960531435269 ) ) ;
#21546 = CARTESIAN_POINT ( 'NONE',  ( 21.55341960407610458, 5.719274019375980345, 103.9572429386476813 ) ) ;
#21547 = CARTESIAN_POINT ( 'NONE',  ( 13.97604488694548053, -13.89961937509957401, 35.62609039468567573 ) ) ;
#21548 = CARTESIAN_POINT ( 'NONE',  ( 14.29746914071049879, -8.314922557960816363, 108.3322429386477097 ) ) ;
#21549 = CARTESIAN_POINT ( 'NONE',  ( 19.02544592524343514, -5.153800228976328945, 68.54057627198103830 ) ) ;
#21550 = CARTESIAN_POINT ( 'NONE',  ( -9.474510206698720793, -16.51473224551083518, 104.5844237280190043 ) ) ;
#21551 = CARTESIAN_POINT ( 'NONE',  ( -12.06949235617756955, 12.14591786802309770, 55.62390960531436690 ) ) ;
#21552 = CARTESIAN_POINT ( 'NONE',  ( 10.81492255796078972, 18.62759615963270932, 29.58224293864769905 ) ) ;
#21553 = CARTESIAN_POINT ( 'NONE',  ( 19.02544592524334988, 5.153800228976608722, 81.45942372801897591 ) ) ;
#21554 = CARTESIAN_POINT ( 'NONE',  ( -5.823673210054116645, -21.52544592524344225, 87.29057627198103830 ) ) ;
#21555 = CARTESIAN_POINT ( 'NONE',  ( 15.72974639402176855, 15.80617190586768217, 41.87609039468568284 ) ) ;
#21556 = CARTESIAN_POINT ( 'NONE',  ( 0.05219959533934541429, -16.53943276465976808, 40.00109039468567573 ) ) ;
#21558 = CARTESIAN_POINT ( 'NONE',  ( -10.81492255796105439, 18.62759615963255655, 47.91775706135234714 ) ) ;
#21557 = CARTESIAN_POINT ( 'NONE',  ( -8.224510206698735004, -14.34966873604973081, 39.58442372801901143 ) ) ;
#21559 = CARTESIAN_POINT ( 'NONE',  ( 5.823673210054125526, 21.52544592524343514, 54.79057627198104541 ) ) ;
#21560 = CARTESIAN_POINT ( 'NONE',  ( -19.02544592524342804, 5.153800228976336051, 31.04057627198102409 ) ) ;
#21561 = CARTESIAN_POINT ( 'NONE',  ( 38.00000000000000000, 12.34694845685046616, -2.649999994537626247 ) ) ;
#21562 = CARTESIAN_POINT ( 'NONE',  ( 16.55341960407618274, -4.379528057220086978, 71.04275706135234714 ) ) ;
#21563 = CARTESIAN_POINT ( 'NONE',  ( 21.53943276465977519, -0.05219959533907433946, 108.7489096053143669 ) ) ;
#21564 = CARTESIAN_POINT ( 'NONE',  ( 12.06949235617757843, -12.14591786802309237, 38.12390960531436690 ) ) ;
#21565 = CARTESIAN_POINT ( 'NONE',  ( -16.55341960407617563, 4.379528057220093196, 63.54275706135234003 ) ) ;
#21566 = CARTESIAN_POINT ( 'NONE',  ( 19.02544592524334988, 5.153800228976608722, 106.4594237280190185 ) ) ;
#21567 = CARTESIAN_POINT ( 'NONE',  ( 0.05219959533907565091, 21.53943276465977519, 94.99890960531436690 ) ) ;
#21568 = CARTESIAN_POINT ( 'NONE',  ( -14.29746914071049879, 8.314922557960819915, 35.83224293864768839 ) ) ;
#21569 = ORIENTED_EDGE ( 'NONE', *, *, #7520, .T. ) ;
#21570 = CARTESIAN_POINT ( 'NONE',  ( -14.29746914071037622, -8.314922557961029526, 79.16775706135234714 ) ) ;
#21571 = CARTESIAN_POINT ( 'NONE',  ( 18.39635199886970440, -5.499999999999975131, 93.51967076360001840 ) ) ;
#21572 =( BOUNDED_CURVE ( )  B_SPLINE_CURVE ( 2, ( #127101, #111950, #49291, #36093, #172634, #80605, #5754, #83586, #187822, #18960, #110949, #34122, #94787 ),
 .UNSPECIFIED., .F., .F. ) 
 B_SPLINE_CURVE_WITH_KNOTS ( ( 3, 2, 2, 2, 2, 2, 3 ),
 ( 0.7655883311638873590, 0.7675438596491228616, 0.7719298245614034659, 0.7763157894736841813, 0.7807017543859648967, 0.7850877192982456121, 0.7869975679613910868 ),
 .UNSPECIFIED. ) 
 CURVE ( )  GEOMETRIC_REPRESENTATION_ITEM ( )  RATIONAL_B_SPLINE_CURVE ( ( 0.9831626618144007068, 0.9848076720550096308, 1.000000000000000000, 0.9659258262890683122, 1.000000000000000000, 0.9659258262890683122, 1.000000000000000000, 0.9659258262890683122, 1.000000000000000000, 0.9659258262890683122, 1.000000000000000000, 0.9851625545550091179, 0.9832469066685282089 ) ) 
 REPRESENTATION_ITEM ( '' )  );
#21573 = CARTESIAN_POINT ( 'NONE',  ( -0.05219959533907301413, -21.53943276465977519, 72.49890960531435269 ) ) ;
#21574 = CARTESIAN_POINT ( 'NONE',  ( 12.14591786802327356, -12.06949235617739191, 105.6260903946856899 ) ) ;
#21575 = ORIENTED_EDGE ( 'NONE', *, *, #59660, .F. ) ;
#21576 = CARTESIAN_POINT ( 'NONE',  ( -16.62475595723696031, -7.163666690055266351, 54.47286648189535896 ) ) ;
#21577 = CARTESIAN_POINT ( 'NONE',  ( -0.05219959533907301413, -21.53943276465977519, 97.49890960531436690 ) ) ;
#21578 = CARTESIAN_POINT ( 'NONE',  ( 18.67979575497178502, 10.72451020669898547, 109.1655762719810383 ) ) ;
#21579 = CARTESIAN_POINT ( 'NONE',  ( 4.379528057220339221, -16.55341960407611168, 42.70724293864770260 ) ) ;
#21580 = CARTESIAN_POINT ( 'NONE',  ( 4.379528057220092307, 16.55341960407617563, 42.29275706135235424 ) ) ;
#21581 = CARTESIAN_POINT ( 'NONE',  ( -5.049401038298153566, 19.05341960407611168, 45.20724293864769550 ) ) ;
#21582 = CARTESIAN_POINT ( 'NONE',  ( -0.05219959533909027116, -19.03943276465977164, 62.49890960531435979 ) ) ;
#21583 = VERTEX_POINT ( 'NONE', #140549 ) ;
#21584 = CARTESIAN_POINT ( 'NONE',  ( 13.89961937509977652, -13.97604488694527269, 113.1239096053143527 ) ) ;
#21585 = CARTESIAN_POINT ( 'NONE',  ( -17.58332526062525858, 7.635886036038558977, 65.92334959558466778 ) ) ;
#21586 = CARTESIAN_POINT ( 'NONE',  ( 0.05219959533936267826, -19.03943276465977164, 110.0010903946856757 ) ) ;
#21587 = CARTESIAN_POINT ( 'NONE',  ( -9.564922557961040184, 16.46253265017147172, 47.91775706135233293 ) ) ;
#21588 = CARTESIAN_POINT ( 'NONE',  ( -18.67979575497178146, -10.72451020669898902, 86.66557627198102409 ) ) ;
#21589 = CARTESIAN_POINT ( 'NONE',  ( 16.55341960407611168, 4.379528057220329451, 23.95724293864769550 ) ) ;
#21590 = CARTESIAN_POINT ( 'NONE',  ( 13.89961937509977652, -13.97604488694527269, 73.12390960531436690 ) ) ;
#21591 = CARTESIAN_POINT ( 'NONE',  ( -18.67979575497178146, -10.72451020669898902, 46.66557627198102409 ) ) ;
#21593 = CARTESIAN_POINT ( 'NONE',  ( 16.53943276465976808, 0.05219959533934440121, 31.25109039468568639 ) ) ;
#21592 = CARTESIAN_POINT ( 'NONE',  ( 18.62759615963271287, -10.81492255796078972, 83.33224293864769550 ) ) ;
#21594 = ADVANCED_FACE ( 'NONE', ( #77879 ), #139546, .F. ) ;
#21595 = CARTESIAN_POINT ( 'NONE',  ( -21.53943276465977519, 0.05219959533907696930, 21.24890960531436690 ) ) ;
#21596 = CARTESIAN_POINT ( 'NONE',  ( 5.719274019375673035, 21.55341960407619339, 77.29275706135234714 ) ) ;
#21597 = CARTESIAN_POINT ( 'NONE',  ( -16.46253265017160317, 9.564922557960807481, 75.83224293864769550 ) ) ;
#21598 = CARTESIAN_POINT ( 'NONE',  ( -19.03943276465977164, 0.05219959533909376836, 21.24890960531436335 ) ) ;
#21599 = CARTESIAN_POINT ( 'NONE',  ( 9.474510206698971260, -16.51473224551069308, 72.91557627198102409 ) ) ;
#21600 = CARTESIAN_POINT ( 'NONE',  ( 16.53943276465976808, -0.05219959533910856209, 93.74890960531436690 ) ) ;
#21601 = VERTEX_POINT ( 'NONE', #124386 ) ;
#21602 = CARTESIAN_POINT ( 'NONE',  ( -19.03943276465977164, -0.05219959533935918106, 108.7510903946856615 ) ) ;
#21603 = CYLINDRICAL_SURFACE ( 'NONE', #24553, 214.0437394197456342 ) ;
#21604 = CARTESIAN_POINT ( 'NONE',  ( 0.05219959533909260263, 19.03943276465977164, 79.99890960531436690 ) ) ;
#21606 = CARTESIAN_POINT ( 'NONE',  ( 9.474510206698971260, -16.51473224551069308, 97.91557627198102409 ) ) ;
#21605 = CARTESIAN_POINT ( 'NONE',  ( -21.55341960407619339, 5.719274019375674811, 88.54275706135236135 ) ) ;
#21608 = EDGE_CURVE ( 'NONE', #17604, #49235, #69530, .T. ) ;
#21607 = CARTESIAN_POINT ( 'NONE',  ( -14.29746914071037622, -8.314922557961029526, 84.16775706135234714 ) ) ;
#21609 = CARTESIAN_POINT ( 'NONE',  ( -30.74964850363292257, 1.467638476639392398, -47.27948696604330081 ) ) ;
#21610 = CARTESIAN_POINT ( 'NONE',  ( 16.51473224551083163, -9.474510206698727899, 60.83442372801900433 ) ) ;
#21611 = CARTESIAN_POINT ( 'NONE',  ( 16.46253265017146816, 9.564922557961045513, 21.66775706135233648 ) ) ;
#21612 = CARTESIAN_POINT ( 'NONE',  ( 37.57676386873052365, 0.7175261378074928587, 39.53500980800842513 ) ) ;
#21613 = CARTESIAN_POINT ( 'NONE',  ( -30.74264578624800492, -22.33583958711396278, -7.549999994537627934 ) ) ;
#21614 = CARTESIAN_POINT ( 'NONE',  ( 11.40812507854755253, -35.11059874428192273, -6.524999997268813523 ) ) ;
#21615 = CARTESIAN_POINT ( 'NONE',  ( -12.14591786802326823, 12.06949235617739902, 113.1260903946856899 ) ) ;
#21616 = CARTESIAN_POINT ( 'NONE',  ( -22.00000000000000000, -5.510910596163089556E-15, 45.00000000000000000 ) ) ;
#21617 = CARTESIAN_POINT ( 'NONE',  ( -8.314922557961024197, 14.29746914071037800, 107.9177570613523471 ) ) ;
#21618 = CARTESIAN_POINT ( 'NONE',  ( 16.18388926212237422, 7.379444403734556346, 67.93953151366154941 ) ) ;
#21619 = CARTESIAN_POINT ( 'NONE',  ( -12.06949235617739369, -12.14591786802326823, 79.37609039468567573 ) ) ;
#21620 = CARTESIAN_POINT ( 'NONE',  ( -21.53943276465977519, -0.05219959533937600094, 78.75109039468568994 ) ) ;
#21621 = CARTESIAN_POINT ( 'NONE',  ( -19.05341960407617563, 5.049401038297882671, 108.5427570613523187 ) ) ;
#21622 = CARTESIAN_POINT ( 'NONE',  ( 21.52544592524334988, 5.823673210054432836, 61.45942372801901854 ) ) ;
#21623 = CARTESIAN_POINT ( 'NONE',  ( -9.474510206698720793, -16.51473224551083518, 44.58442372801900433 ) ) ;
#21624 = CARTESIAN_POINT ( 'NONE',  ( 0.05219959533909260263, 19.03943276465977164, 79.99890960531436690 ) ) ;
#21625 = CARTESIAN_POINT ( 'NONE',  ( 16.46253265017160672, -9.564922557960803928, 58.33224293864769550 ) ) ;
#21626 = FACE_OUTER_BOUND ( 'NONE', #29794, .T. ) ;
#21627 = CARTESIAN_POINT ( 'NONE',  ( -21.53943276465977519, 0.05219959533907696930, 96.24890960531435269 ) ) ;
#21628 = AXIS2_PLACEMENT_3D ( 'NONE', #11628, #163294, #150127 ) ;
#21629 = CARTESIAN_POINT ( 'NONE',  ( 15.72974639402199770, -15.80617190586745480, 48.12390960531436690 ) ) ;
#21630 = CARTESIAN_POINT ( 'NONE',  ( -9.564922557960796823, -16.46253265017161027, 52.08224293864768839 ) ) ;
#21631 = CARTESIAN_POINT ( 'NONE',  ( -14.34966873604972548, 8.224510206698743886, 68.33442372801900433 ) ) ;
#21632 = UNCERTAINTY_MEASURE_WITH_UNIT (LENGTH_MEASURE( 1.000000000000000082E-05 ), #176802, 'distance_accuracy_value', 'NONE');
#21633 = EDGE_LOOP ( 'NONE', ( #84606, #123613, #121849, #136515 ) ) ;
#21634 = ADVANCED_FACE ( 'NONE', ( #18222 ), #2037, .T. ) ;
#21635 = CARTESIAN_POINT ( 'NONE',  ( -18.67979575497193778, 10.72451020669871902, 38.33442372801900433 ) ) ;
#21637 = CARTESIAN_POINT ( 'NONE',  ( -29.86685920354755197, -21.69954338932560134, -4.424999997268812990 ) ) ;
#21636 = CARTESIAN_POINT ( 'NONE',  ( -4.379528057220328563, 16.55341960407611168, 60.20724293864768839 ) ) ;
#21638 = CARTESIAN_POINT ( 'NONE',  ( 0.05219959533934541429, -16.53943276465976808, 45.00109039468568284 ) ) ;
#21639 = CARTESIAN_POINT ( 'NONE',  ( -12.14591786802309592, -12.06949235617757132, 101.8739096053143811 ) ) ;
#21640 = CARTESIAN_POINT ( 'NONE',  ( 16.46253265017146816, 9.564922557961045513, 56.66775706135233293 ) ) ;
#21641 = AXIS2_PLACEMENT_3D ( 'NONE', #143178, #142191, #188721 ) ;
#21642 = CARTESIAN_POINT ( 'NONE',  ( -16.55341960407611168, -4.379528057220339221, 71.45724293864769550 ) ) ;
#21643 = CARTESIAN_POINT ( 'NONE',  ( 18.67979575497194134, -10.72451020669871369, 25.83442372801901499 ) ) ;
#21645 = CARTESIAN_POINT ( 'NONE',  ( -21.55341960407610458, -5.719274019375992779, 96.45724293864770971 ) ) ;
#21644 = CARTESIAN_POINT ( 'NONE',  ( -19.03943276465977164, 0.05219959533909376836, 21.24890960531436335 ) ) ;
#21646 = CARTESIAN_POINT ( 'NONE',  ( 5.049401038298161559, -19.05341960407611168, 107.7072429386476955 ) ) ;
#21647 = CARTESIAN_POINT ( 'NONE',  ( -8.224510206698948167, 14.34966873604960824, 80.41557627198103830 ) ) ;
#21648 = CARTESIAN_POINT ( 'NONE',  ( 31.83877234781633803, -24.10177343596294364, -22.51708424454470148 ) ) ;
#21649 = CARTESIAN_POINT ( 'NONE',  ( -36.91746825000000598, -11.99521256947794789, -2.524999997268813523 ) ) ;
#21650 = CARTESIAN_POINT ( 'NONE',  ( -13.89961937509957401, -13.97604488694547875, 84.37609039468567573 ) ) ;
#21651 = CARTESIAN_POINT ( 'NONE',  ( -15.72974639402197994, 15.80617190586746368, 115.6239096053143669 ) ) ;
#21652 = CARTESIAN_POINT ( 'NONE',  ( 5.049401038298161559, -19.05341960407611168, 72.70724293864768129 ) ) ;
#21653 = CARTESIAN_POINT ( 'NONE',  ( -9.474510206698720793, -16.51473224551083518, 54.58442372801899722 ) ) ;
#21654 = CARTESIAN_POINT ( 'NONE',  ( 16.51473224551069308, 9.474510206698969483, 34.16557627198102409 ) ) ;
#21655 = CARTESIAN_POINT ( 'NONE',  ( 8.314922557960818139, 14.29746914071049879, 69.58224293864769550 ) ) ;
#21656 = CARTESIAN_POINT ( 'NONE',  ( 12.06949235617757843, -12.14591786802309237, 53.12390960531436690 ) ) ;
#21657 = CARTESIAN_POINT ( 'NONE',  ( -19.03943276465977164, 0.05219959533909376836, 66.24890960531436690 ) ) ;
#21658 = CARTESIAN_POINT ( 'NONE',  ( 0.05219959533907565091, 21.53943276465977519, 89.99890960531438111 ) ) ;
#21659 = CARTESIAN_POINT ( 'NONE',  ( 5.049401038298161559, -19.05341960407611168, 57.70724293864769550 ) ) ;
#21660 = CARTESIAN_POINT ( 'NONE',  ( 21.52544592524344225, -5.823673210054117533, 78.54057627198103830 ) ) ;
#21661 = CARTESIAN_POINT ( 'NONE',  ( 18.62759615963255655, 10.81492255796105972, 106.6677570613523756 ) ) ;
#21664 = CARTESIAN_POINT ( 'NONE',  ( 4.483927247898545687, 16.52544592524342804, 94.79057627198105251 ) ) ;
#21663 = CARTESIAN_POINT ( 'NONE',  ( -12.06949235617739369, -12.14591786802326823, 109.3760903946857042 ) ) ;
#21662 = CARTESIAN_POINT ( 'NONE',  ( -19.05341960407611168, -5.049401038298163336, 26.45724293864769550 ) ) ;
#21665 = CARTESIAN_POINT ( 'NONE',  ( 16.51473224551083163, -9.474510206698727899, 85.83442372801900433 ) ) ;
#21666 = ORIENTED_EDGE ( 'NONE', *, *, #68776, .T. ) ;
#21667 = CARTESIAN_POINT ( 'NONE',  ( 5.823673210054125526, 21.52544592524343514, 109.7905762719810383 ) ) ;
#21668 = CARTESIAN_POINT ( 'NONE',  ( 5.049401038297881783, 19.05341960407617563, 47.29275706135231161 ) ) ;
#21669 = CARTESIAN_POINT ( 'NONE',  ( 14.34966873604972726, -8.224510206698740333, 105.8344237280190328 ) ) ;
#21670 = CARTESIAN_POINT ( 'NONE',  ( 16.51473224551083163, -9.474510206698727899, 25.83442372801900078 ) ) ;
#21671 = CARTESIAN_POINT ( 'NONE',  ( 9.564922557960805705, 16.46253265017160317, 99.58224293864770971 ) ) ;
#21672 = CARTESIAN_POINT ( 'NONE',  ( 15.72974639402199770, -15.80617190586745480, 68.12390960531436690 ) ) ;
#21673 = CARTESIAN_POINT ( 'NONE',  ( -4.500000000000001776, -140.0000000000000000, 12.99999999999998224 ) ) ;
#21674 = CARTESIAN_POINT ( 'NONE',  ( 0.05219959533909260263, 19.03943276465977164, 29.99890960531435979 ) ) ;
#21675 = CARTESIAN_POINT ( 'NONE',  ( -5.719274019375665041, -21.55341960407619695, 104.7927570613523898 ) ) ;
#21676 = CARTESIAN_POINT ( 'NONE',  ( -4.379528057220086978, -16.55341960407618274, 74.79275706135234714 ) ) ;
#21677 = CARTESIAN_POINT ( 'NONE',  ( 15.80617190586769283, -15.72974639402175789, 30.62609039468567929 ) ) ;
#21678 = CARTESIAN_POINT ( 'NONE',  ( -4.379528057220086978, -16.55341960407618274, 39.79275706135235424 ) ) ;
#21679 = CARTESIAN_POINT ( 'NONE',  ( -5.153800228976328057, -19.02544592524343514, 107.2905762719810383 ) ) ;
#21680 = CARTESIAN_POINT ( 'NONE',  ( -19.03943276465977164, 0.05219959533909376836, 56.24890960531435979 ) ) ;
#21681 = CARTESIAN_POINT ( 'NONE',  ( -19.05341960407611168, -5.049401038298163336, 61.45724293864769550 ) ) ;
#21682 = CIRCLE ( 'NONE', #192727, 1.000000000000000888 ) ;
#21683 = CARTESIAN_POINT ( 'NONE',  ( 16.52544592524335698, 4.483927247898782831, 41.45942372801901143 ) ) ;
#21684 = CARTESIAN_POINT ( 'NONE',  ( -0.05219959533910754901, -16.53943276465976808, 87.49890960531436690 ) ) ;
#21685 = CARTESIAN_POINT ( 'NONE',  ( -0.05219959533934338120, 16.53943276465976808, 107.5010903946856899 ) ) ;
#21686 = CARTESIAN_POINT ( 'NONE',  ( -16.46253265017160317, 9.564922557960807481, 50.83224293864770260 ) ) ;
#21689 = CARTESIAN_POINT ( 'NONE',  ( 19.05341960407611168, 5.049401038298154454, 63.95724293864769550 ) ) ;
#21688 = CARTESIAN_POINT ( 'NONE',  ( 16.51473224551069308, 9.474510206698969483, 79.16557627198103830 ) ) ;
#21687 = CARTESIAN_POINT ( 'NONE',  ( -18.62759615963255300, -10.81492255796106328, 59.16775706135234714 ) ) ;
#21690 = CARTESIAN_POINT ( 'NONE',  ( -5.049401038298153566, 19.05341960407611168, 90.20724293864766707 ) ) ;
#21691 = CARTESIAN_POINT ( 'NONE',  ( 12.14591786802309770, 12.06949235617756955, 44.37390960531435979 ) ) ;
#21692 = CARTESIAN_POINT ( 'NONE',  ( -12.06949235617756955, 12.14591786802309770, 25.62390960531435624 ) ) ;
#21693 = CARTESIAN_POINT ( 'NONE',  ( -8.224510206698948167, 14.34966873604960824, 45.41557627198103830 ) ) ;
#21694 = EDGE_LOOP ( 'NONE', ( #116199, #160088, #175349, #73679 ) ) ;
#21695 = CARTESIAN_POINT ( 'NONE',  ( -13.89961937509957401, -13.97604488694547875, 44.37609039468566863 ) ) ;
#21696 = CARTESIAN_POINT ( 'NONE',  ( -20.49784845693389101, -5.510910596163089556E-15, 45.00000000000000000 ) ) ;
#21697 = CARTESIAN_POINT ( 'NONE',  ( -16.46253265017160317, 9.564922557960807481, 60.83224293864769550 ) ) ;
#21698 = CARTESIAN_POINT ( 'NONE',  ( -0.05219959533936034679, 19.03943276465977164, 32.50109039468566863 ) ) ;
#21699 = CARTESIAN_POINT ( 'NONE',  ( 11.40812507854755253, -35.11059874428192273, -2.024999997268813079 ) ) ;
#21700 = LINE ( 'NONE', #98516, #128135 ) ;
#21702 = CARTESIAN_POINT ( 'NONE',  ( -16.55341960407617563, 4.379528057220093196, 63.54275706135234003 ) ) ;
#21701 = CARTESIAN_POINT ( 'NONE',  ( -16.51473224551082808, 9.474510206698731452, 78.33442372801900433 ) ) ;
#21703 = CARTESIAN_POINT ( 'NONE',  ( 16.88567814943162659, 6.947325034625703388, 93.79001122652590539 ) ) ;
#21704 = CARTESIAN_POINT ( 'NONE',  ( 16.51473224551069308, 9.474510206698969483, 89.16557627198103830 ) ) ;
#21705 = CARTESIAN_POINT ( 'NONE',  ( -21.55341960407619339, 5.719274019375674811, 23.54275706135235424 ) ) ;
#21706 = CARTESIAN_POINT ( 'NONE',  ( -19.03943276465977164, -0.05219959533935918106, 73.75109039468566152 ) ) ;
#21708 = CARTESIAN_POINT ( 'NONE',  ( 19.05341960407611168, 5.049401038298154454, 43.95724293864769550 ) ) ;
#21707 = CARTESIAN_POINT ( 'NONE',  ( 27.49873734152913229, -21.99873734152921045, 8.181980515339454030 ) ) ;
#21709 = CARTESIAN_POINT ( 'NONE',  ( 19.03943276465977164, -0.05219959533909143690, 83.74890960531436690 ) ) ;
#21711 = CARTESIAN_POINT ( 'NONE',  ( -19.05341960407611168, -5.049401038298163336, 56.45724293864768129 ) ) ;
#21710 = CARTESIAN_POINT ( 'NONE',  ( -16.55341960407611168, -4.379528057220339221, 46.45724293864769550 ) ) ;
#21712 = CARTESIAN_POINT ( 'NONE',  ( -16.51473224551082808, 9.474510206698731452, 53.33442372801900433 ) ) ;
#21713 = ORIENTED_EDGE ( 'NONE', *, *, #40967, .F. ) ;
#21714 = CARTESIAN_POINT ( 'NONE',  ( 4.379528057220339221, -16.55341960407611168, 87.70724293864769550 ) ) ;
#21715 = CARTESIAN_POINT ( 'NONE',  ( -13.97604488694547697, 13.89961937509957934, 28.12609039468565797 ) ) ;
#21716 = CARTESIAN_POINT ( 'NONE',  ( 0.05219959533909260263, 19.03943276465977164, 69.99890960531435269 ) ) ;
#21717 = CARTESIAN_POINT ( 'NONE',  ( 21.55341960407610458, 5.719274019375980345, 68.95724293864769550 ) ) ;
#21719 = CARTESIAN_POINT ( 'NONE',  ( 9.564922557961047289, -16.46253265017146816, 20.41775706135233293 ) ) ;
#21718 = CARTESIAN_POINT ( 'NONE',  ( -16.52544592524342804, 4.483927247898546575, 61.04057627198103120 ) ) ;
#21720 = CARTESIAN_POINT ( 'NONE',  ( -16.51473224551069308, -9.474510206698971260, 101.6655762719810241 ) ) ;
#21721 = CARTESIAN_POINT ( 'NONE',  ( -21.53943276465977519, 0.05219959533907696930, 26.24890960531435624 ) ) ;
#21722 = CARTESIAN_POINT ( 'NONE',  ( 9.474510206698971260, -16.51473224551069308, 57.91557627198103120 ) ) ;
#21723 = CARTESIAN_POINT ( 'NONE',  ( -19.03943276465977164, 0.05219959533909376836, 36.24890960531436690 ) ) ;
#21724 = CARTESIAN_POINT ( 'NONE',  ( 4.379528057220339221, -16.55341960407611168, 97.70724293864772392 ) ) ;
#21725 = CARTESIAN_POINT ( 'NONE',  ( 5.823673210054125526, 21.52544592524343514, 109.7905762719810383 ) ) ;
#21726 = CARTESIAN_POINT ( 'NONE',  ( 16.46253265017160672, -9.564922557960803928, 103.3322429386476955 ) ) ;
#21727 = CARTESIAN_POINT ( 'NONE',  ( -21.53943276465977519, 0.05219959533907696930, 116.2489096053143669 ) ) ;
#21728 = CARTESIAN_POINT ( 'NONE',  ( 19.05341960407611168, 5.049401038298154454, 98.95724293864766707 ) ) ;
#21729 = CARTESIAN_POINT ( 'NONE',  ( 16.53943276465976808, -0.05219959533910856209, 113.7489096053143527 ) ) ;
#21730 = CARTESIAN_POINT ( 'NONE',  ( 18.62759615963255655, 10.81492255796105972, 76.66775706135234714 ) ) ;
#21731 = CARTESIAN_POINT ( 'NONE',  ( 21.55341960407610458, 5.719274019375980345, 93.95724293864770971 ) ) ;
#21732 = FACE_OUTER_BOUND ( 'NONE', #93524, .T. ) ;
#21733 = FACE_OUTER_BOUND ( 'NONE', #88711, .T. ) ;
#21734 = CARTESIAN_POINT ( 'NONE',  ( 29.53952216915894269, -1.232294487434747010, -51.94279119241699760 ) ) ;
#21735 = CARTESIAN_POINT ( 'NONE',  ( -12.14591786802326823, 12.06949235617739902, 48.12609039468568284 ) ) ;
#21736 = ADVANCED_FACE ( 'NONE', ( #79878 ), #141547, .T. ) ;
#21737 = CARTESIAN_POINT ( 'NONE',  ( -12.06949235617756955, 12.14591786802309770, 110.6239096053143669 ) ) ;
#21738 = CARTESIAN_POINT ( 'NONE',  ( 11.30153831258473573, -180.0000000000000284, -15.00000000000000178 ) ) ;
#21739 = CARTESIAN_POINT ( 'NONE',  ( 19.05341960407611168, 5.049401038298154454, 63.95724293864769550 ) ) ;
#21740 = CARTESIAN_POINT ( 'NONE',  ( 8.224510206698953496, -14.34966873604960469, 97.91557627198103830 ) ) ;
#21741 = CARTESIAN_POINT ( 'NONE',  ( -18.67979575497178146, -10.72451020669898902, 46.66557627198102409 ) ) ;
#21742 = CARTESIAN_POINT ( 'NONE',  ( 14.29746914071049879, -8.314922557960816363, 63.33224293864770260 ) ) ;
#21743 = CARTESIAN_POINT ( 'NONE',  ( -8.314922557961024197, 14.29746914071037800, 22.91775706135235069 ) ) ;
#21744 = CARTESIAN_POINT ( 'NONE',  ( 15.80617190586769283, -15.72974639402175789, 70.62609039468567573 ) ) ;
#21745 = CARTESIAN_POINT ( 'NONE',  ( 16.38665767535050932, -7.295008042176168495, 77.76400864214544129 ) ) ;
#21746 = CARTESIAN_POINT ( 'NONE',  ( -16.53943276465976808, -0.05219959533934237506, 103.7510903946857042 ) ) ;
#21747 = CARTESIAN_POINT ( 'NONE',  ( 0.05219959533910956823, 16.53943276465976808, 39.99890960531436690 ) ) ;
#21748 = CARTESIAN_POINT ( 'NONE',  ( 19.03943276465977164, -0.05219959533909143690, 33.74890960531435979 ) ) ;
#21749 = CARTESIAN_POINT ( 'NONE',  ( -5.153800228976328057, -19.02544592524343514, 92.29057627198099567 ) ) ;
#21750 = CARTESIAN_POINT ( 'NONE',  ( -18.62759615963270932, 10.81492255796079327, 100.8322429386477097 ) ) ;
#21751 = CARTESIAN_POINT ( 'NONE',  ( 16.53943276465976808, 0.05219959533934440121, 31.25109039468568639 ) ) ;
#21753 = CARTESIAN_POINT ( 'NONE',  ( -18.67979575497193778, 10.72451020669871902, 78.33442372801901854 ) ) ;
#21752 = CARTESIAN_POINT ( 'NONE',  ( -16.52544592524342804, 4.483927247898546575, 71.04057627198103830 ) ) ;
#21754 = CARTESIAN_POINT ( 'NONE',  ( -16.52544592524335698, -4.483927247898792601, 103.9594237280190185 ) ) ;
#21755 = CARTESIAN_POINT ( 'NONE',  ( 17.48853670773249291, -5.747243402302948390, 46.16671299749997814 ) ) ;
#21756 = CARTESIAN_POINT ( 'NONE',  ( -19.53091890409951858, -5.500000000000037303, 65.06097431831420863 ) ) ;
#21757 = CARTESIAN_POINT ( 'NONE',  ( 12.06949235617757843, -12.14591786802309237, 23.12390960531436335 ) ) ;
#21758 = CARTESIAN_POINT ( 'NONE',  ( -4.483927247898782831, 16.52544592524335698, 77.70942372801900433 ) ) ;
#21759 = CARTESIAN_POINT ( 'NONE',  ( 16.46253265017160672, -9.564922557960803928, 88.33224293864769550 ) ) ;
#21760 = CARTESIAN_POINT ( 'NONE',  ( -9.564922557960796823, -16.46253265017161027, 102.0822429386477097 ) ) ;
#21761 = CARTESIAN_POINT ( 'NONE',  ( -18.67979575497193778, 10.72451020669871902, 88.33442372801901854 ) ) ;
#21762 = EDGE_CURVE ( 'NONE', #85102, #76043, #30864, .T. ) ;
#21763 = CARTESIAN_POINT ( 'NONE',  ( -8.224510206698735004, -14.34966873604973081, 89.58442372801901854 ) ) ;
#21764 = CARTESIAN_POINT ( 'NONE',  ( 14.34966873604960469, 8.224510206698951720, 59.16557627198103120 ) ) ;
#21765 = CARTESIAN_POINT ( 'NONE',  ( -16.46253265017160317, 9.564922557960807481, 65.83224293864769550 ) ) ;
#21766 = ORIENTED_EDGE ( 'NONE', *, *, #23834, .T. ) ;
#21767 = CARTESIAN_POINT ( 'NONE',  ( -4.379528057220086978, -16.55341960407618274, 19.79275706135235069 ) ) ;
#21768 = CARTESIAN_POINT ( 'NONE',  ( 12.14591786802309770, 12.06949235617756955, 104.3739096053143669 ) ) ;
#21769 = CARTESIAN_POINT ( 'NONE',  ( -19.03943276465977164, 0.05219959533909376836, 76.24890960531435269 ) ) ;
#21771 = CARTESIAN_POINT ( 'NONE',  ( -23.48529157249600985, 32.32473071737754111, -0.2999999999999999334 ) ) ;
#21770 = CARTESIAN_POINT ( 'NONE',  ( 14.29746914071037800, 8.314922557961029526, 21.66775706135235069 ) ) ;
#21772 = CARTESIAN_POINT ( 'NONE',  ( -5.823673210054431948, 21.52544592524334988, 112.7094237280190328 ) ) ;
#21773 = CARTESIAN_POINT ( 'NONE',  ( 0.05219959533934541429, -16.53943276465976808, 80.00109039468568994 ) ) ;
#21774 = CARTESIAN_POINT ( 'NONE',  ( -9.564922557961040184, 16.46253265017147172, 97.91775706135233293 ) ) ;
#21775 = CARTESIAN_POINT ( 'NONE',  ( -4.379528057220328563, 16.55341960407611168, 115.2072429386476955 ) ) ;
#21776 = CARTESIAN_POINT ( 'NONE',  ( -16.55341960407617563, 4.379528057220093196, 63.54275706135234003 ) ) ;
#21777 = CARTESIAN_POINT ( 'NONE',  ( -12.06949235617739369, -12.14591786802326823, 49.37609039468569705 ) ) ;
#21778 = DIRECTION ( 'NONE',  ( -1.000000000000000000, 0.000000000000000000, 0.000000000000000000 ) ) ;
#21779 = CARTESIAN_POINT ( 'NONE',  ( 16.46253265017146816, 9.564922557961045513, 71.66775706135233293 ) ) ;
#21780 = CARTESIAN_POINT ( 'NONE',  ( 15.72974639402176855, 15.80617190586768217, 96.87609039468568994 ) ) ;
#21781 = CARTESIAN_POINT ( 'NONE',  ( -16.46253265017160317, 9.564922557960807481, 35.83224293864768839 ) ) ;
#21782 = CARTESIAN_POINT ( 'NONE',  ( -19.05341960407611168, -5.049401038298163336, 76.45724293864769550 ) ) ;
#21783 = CARTESIAN_POINT ( 'NONE',  ( 16.53943276465976808, -0.05219959533910856209, 73.74890960531433848 ) ) ;
#21784 = CARTESIAN_POINT ( 'NONE',  ( -18.67979575497193778, 10.72451020669871902, 93.33442372801901854 ) ) ;
#21785 = CARTESIAN_POINT ( 'NONE',  ( 13.89961937509957401, 13.97604488694547697, 41.87609039468566152 ) ) ;
#21786 = CARTESIAN_POINT ( 'NONE',  ( -21.53943276465977519, 0.05219959533907696930, 36.24890960531435979 ) ) ;
#21787 = CARTESIAN_POINT ( 'NONE',  ( 10.72451020669871369, 18.67979575497193778, 112.0844237280190185 ) ) ;
#21788 = CARTESIAN_POINT ( 'NONE',  ( -19.05341960407611168, -5.049401038298163336, 76.45724293864769550 ) ) ;
#21789 = CARTESIAN_POINT ( 'NONE',  ( 21.55341960407619695, -5.719274019375665929, 111.0427570613523613 ) ) ;
#21790 = CARTESIAN_POINT ( 'NONE',  ( 21.55341960407610458, 5.719274019375980345, 68.95724293864769550 ) ) ;
#21791 = CARTESIAN_POINT ( 'NONE',  ( -9.564922557960796823, -16.46253265017161027, 97.08224293864769550 ) ) ;
#21792 = CARTESIAN_POINT ( 'NONE',  ( 9.564922557961047289, -16.46253265017146816, 70.41775706135233293 ) ) ;
#21793 = CARTESIAN_POINT ( 'NONE',  ( -19.05341960407611168, -5.049401038298163336, 96.45724293864769550 ) ) ;
#21794 = CARTESIAN_POINT ( 'NONE',  ( 19.05341960407617918, -5.049401038297876454, 96.04275706135231871 ) ) ;
#21795 = CARTESIAN_POINT ( 'NONE',  ( -12.06949235617739369, -12.14591786802326823, 44.37609039468567573 ) ) ;
#21796 = CARTESIAN_POINT ( 'NONE',  ( 8.314922557960818139, 14.29746914071049879, 114.5822429386477097 ) ) ;
#21797 = CARTESIAN_POINT ( 'NONE',  ( -5.049401038298153566, 19.05341960407611168, 80.20724293864769550 ) ) ;
#21798 = CARTESIAN_POINT ( 'NONE',  ( -15.80617190586745835, -15.72974639402198527, 56.87390960531436690 ) ) ;
#21799 = CARTESIAN_POINT ( 'NONE',  ( 12.06949235617739724, 12.14591786802326823, 26.87609039468567218 ) ) ;
#21800 = CARTESIAN_POINT ( 'NONE',  ( -18.62759615963255300, -10.81492255796106328, 39.16775706135235424 ) ) ;
#21801 = CARTESIAN_POINT ( 'NONE',  ( -18.62759615963255300, -10.81492255796106328, 79.16775706135234714 ) ) ;
#21802 = CARTESIAN_POINT ( 'NONE',  ( 4.379528057220092307, 16.55341960407617563, 87.29275706135236135 ) ) ;
#21803 = CARTESIAN_POINT ( 'NONE',  ( -9.474510206698964154, 16.51473224551069663, 90.41557627198103830 ) ) ;
#21804 = CARTESIAN_POINT ( 'NONE',  ( 0.05219959533910956823, 16.53943276465976808, 79.99890960531435269 ) ) ;
#21805 = CARTESIAN_POINT ( 'NONE',  ( 4.379528057220092307, 16.55341960407617563, 112.2927570613523471 ) ) ;
#21806 = CARTESIAN_POINT ( 'NONE',  ( 19.02544592524334988, 5.153800228976608722, 61.45942372801900433 ) ) ;
#21807 = AXIS2_PLACEMENT_3D ( 'NONE', #27386, #25398, #119387 ) ;
#21808 = CARTESIAN_POINT ( 'NONE',  ( 21.52544592524334988, 5.823673210054432836, 41.45942372801901143 ) ) ;
#21809 = CARTESIAN_POINT ( 'NONE',  ( 14.29746914071049879, -8.314922557960816363, 98.33224293864769550 ) ) ;
#21810 = CARTESIAN_POINT ( 'NONE',  ( -5.049401038298153566, 19.05341960407611168, 110.2072429386476671 ) ) ;
#21811 = CARTESIAN_POINT ( 'NONE',  ( -8.314922557961024197, 14.29746914071037800, 97.91775706135236135 ) ) ;
#21812 = CARTESIAN_POINT ( 'NONE',  ( -10.81492255796105439, 18.62759615963255655, 82.91775706135234714 ) ) ;
#21813 = CARTESIAN_POINT ( 'NONE',  ( -14.29746914071037622, -8.314922557961029526, 49.16775706135234003 ) ) ;
#21814 = CARTESIAN_POINT ( 'NONE',  ( 18.67979575497194134, -10.72451020669871369, 45.83442372801901854 ) ) ;
#21815 = VERTEX_POINT ( 'NONE', #19211 ) ;
#21816 = CARTESIAN_POINT ( 'NONE',  ( 18.62759615963271287, -10.81492255796078972, 108.3322429386477097 ) ) ;
#21817 = CARTESIAN_POINT ( 'NONE',  ( -12.06949235617756955, 12.14591786802309770, 95.62390960531436690 ) ) ;
#21818 = CARTESIAN_POINT ( 'NONE',  ( -19.53091890409952214, -5.500000000000036415, 50.06097431831421574 ) ) ;
#21819 = CARTESIAN_POINT ( 'NONE',  ( -0.05219959533910754901, -16.53943276465976808, 67.49890960531436690 ) ) ;
#21820 = CARTESIAN_POINT ( 'NONE',  ( -0.05219959533934338120, 16.53943276465976808, 97.50109039468567573 ) ) ;
#21821 = CARTESIAN_POINT ( 'NONE',  ( 0.05219959533909260263, 19.03943276465977164, 44.99890960531435979 ) ) ;
#21822 = CARTESIAN_POINT ( 'NONE',  ( -18.67979575497178146, -10.72451020669898902, 41.66557627198103120 ) ) ;
#21823 = CARTESIAN_POINT ( 'NONE',  ( 12.14591786802309770, 12.06949235617756955, 74.37390960531436690 ) ) ;
#21824 = CARTESIAN_POINT ( 'NONE',  ( 15.80617190586746368, 15.72974639402197994, 74.37390960531436690 ) ) ;
#21825 = CARTESIAN_POINT ( 'NONE',  ( -5.049401038298153566, 19.05341960407611168, 85.20724293864766707 ) ) ;
#21827 = CARTESIAN_POINT ( 'NONE',  ( -16.46253265017146816, -9.564922557961047289, 89.16775706135234714 ) ) ;
#21826 = CARTESIAN_POINT ( 'NONE',  ( 19.03943276465977164, -0.05219959533909143690, 38.74890960531436690 ) ) ;
#21828 = CARTESIAN_POINT ( 'NONE',  ( -15.72974639402197994, 15.80617190586746368, 35.62390960531437401 ) ) ;
#21829 = CARTESIAN_POINT ( 'NONE',  ( 21.55341960407619695, -5.719274019375665929, 56.04275706135235424 ) ) ;
#21830 = CARTESIAN_POINT ( 'NONE',  ( -9.564922557960796823, -16.46253265017161027, 57.08224293864769550 ) ) ;
#21831 = CARTESIAN_POINT ( 'NONE',  ( -5.049401038298153566, 19.05341960407611168, 85.20724293864766707 ) ) ;
#21832 = ORIENTED_EDGE ( 'NONE', *, *, #168639, .T. ) ;
#21833 = CARTESIAN_POINT ( 'NONE',  ( -4.379528057220086978, -16.55341960407618274, 54.79275706135235424 ) ) ;
#21834 = CARTESIAN_POINT ( 'NONE',  ( 21.53943276465977519, 0.05219959533937863772, 36.25109039468567573 ) ) ;
#21835 = CARTESIAN_POINT ( 'NONE',  ( -15.72974639402176322, -15.80617190586768395, 69.37609039468567573 ) ) ;
#21836 = CARTESIAN_POINT ( 'NONE',  ( -21.53943276465977519, 0.05219959533907696930, 26.24890960531435624 ) ) ;
#21837 = CARTESIAN_POINT ( 'NONE',  ( -5.823673210054116645, -21.52544592524344225, 87.29057627198103830 ) ) ;
#21839 = CARTESIAN_POINT ( 'NONE',  ( -16.55341960407617563, 4.379528057220093196, 63.54275706135234003 ) ) ;
#21838 = CARTESIAN_POINT ( 'NONE',  ( -21.55341960407619339, 5.719274019375674811, 28.54275706135234358 ) ) ;
#21840 = EDGE_CURVE ( 'NONE', #125859, #167341, #21171, .T. ) ;
#21841 = CARTESIAN_POINT ( 'NONE',  ( 21.52544592524344225, -5.823673210054117533, 63.54057627198103830 ) ) ;
#21842 = CARTESIAN_POINT ( 'NONE',  ( 13.89961937509957401, 13.97604488694547697, 21.87609039468566152 ) ) ;
#21844 = CARTESIAN_POINT ( 'NONE',  ( -16.55341960407617563, 4.379528057220093196, 103.5427570613523613 ) ) ;
#21843 = CARTESIAN_POINT ( 'NONE',  ( -0.05219959533909027116, -19.03943276465977164, 67.49890960531436690 ) ) ;
#21845 = CARTESIAN_POINT ( 'NONE',  ( -17.49999999999999645, -3.805241302050224039, 104.6264752721741331 ) ) ;
#21846 = CARTESIAN_POINT ( 'NONE',  ( 19.03943276465977164, -0.05219959533909143690, 83.74890960531436690 ) ) ;
#21847 = CARTESIAN_POINT ( 'NONE',  ( -0.05219959533936034679, 19.03943276465977164, 52.50109039468566863 ) ) ;
#21848 = CARTESIAN_POINT ( 'NONE',  ( -16.51473224551082808, 9.474510206698731452, 78.33442372801900433 ) ) ;
#21849 = CARTESIAN_POINT ( 'NONE',  ( -21.55341960407610458, -5.719274019375992779, 51.45724293864770260 ) ) ;
#21850 = CARTESIAN_POINT ( 'NONE',  ( 8.224510206698742110, 14.34966873604972548, 112.0844237280190185 ) ) ;
#21851 = CARTESIAN_POINT ( 'NONE',  ( 16.46253265017146816, 9.564922557961045513, 101.6677570613523329 ) ) ;
#21852 = CARTESIAN_POINT ( 'NONE',  ( -9.474510206698964154, 16.51473224551069663, 40.41557627198103120 ) ) ;
#21853 = CARTESIAN_POINT ( 'NONE',  ( 16.46253265017146816, 9.564922557961045513, 91.66775706135234714 ) ) ;
#21855 = CARTESIAN_POINT ( 'NONE',  ( -0.05219959533936034679, 19.03943276465977164, 52.50109039468566863 ) ) ;
#21854 = CARTESIAN_POINT ( 'NONE',  ( 21.52544592524344225, -5.823673210054117533, 88.54057627198103830 ) ) ;
#21856 = DIRECTION ( 'NONE',  ( 1.000000000000000000, -0.000000000000000000, -0.000000000000000000 ) ) ;
#21857 = CARTESIAN_POINT ( 'NONE',  ( 9.474510206698971260, -16.51473224551069308, 57.91557627198103120 ) ) ;
#21858 = CARTESIAN_POINT ( 'NONE',  ( 8.314922557960818139, 14.29746914071049879, 64.58224293864769550 ) ) ;
#21859 = ADVANCED_FACE ( 'NONE', ( #138558 ), #128447, .T. ) ;
#21860 = CARTESIAN_POINT ( 'NONE',  ( -13.97604488694527625, -13.89961937509977652, 51.87390960531436690 ) ) ;
#21861 = CARTESIAN_POINT ( 'NONE',  ( -12.14591786802309592, -12.06949235617757132, 56.87390960531436690 ) ) ;
#21862 = CARTESIAN_POINT ( 'NONE',  ( 17.97182807773875624, -5.499999999999865885, 56.03038844047289047 ) ) ;
#21863 = CARTESIAN_POINT ( 'NONE',  ( 0.9208130691986635696, 8.788201535090163219, -61.95848299590669939 ) ) ;
#21864 = CARTESIAN_POINT ( 'NONE',  ( -12.06949235617756955, 12.14591786802309770, 30.62390960531436335 ) ) ;
#21865 = CARTESIAN_POINT ( 'NONE',  ( -9.474510206698964154, 16.51473224551069663, 65.41557627198102409 ) ) ;
#21866 = CARTESIAN_POINT ( 'NONE',  ( -36.91746825000000598, 2.428612866367529932E-14, -10.87499999726881228 ) ) ;
#21867 = CARTESIAN_POINT ( 'NONE',  ( 19.03943276465977164, 0.05219959533936151252, 41.25109039468566152 ) ) ;
#21868 = CARTESIAN_POINT ( 'NONE',  ( 16.52544592524335698, 4.483927247898782831, 46.45942372801901854 ) ) ;
#21869 = CARTESIAN_POINT ( 'NONE',  ( 15.80617190586746368, 15.72974639402197994, 44.37390960531435979 ) ) ;
#21870 = CARTESIAN_POINT ( 'NONE',  ( 15.72974639402176855, 15.80617190586768217, 101.8760903946857042 ) ) ;
#21871 = CARTESIAN_POINT ( 'NONE',  ( -19.05341960407611168, -5.049401038298163336, 66.45724293864769550 ) ) ;
#21872 = DIRECTION ( 'NONE',  ( 1.000000000000000000, 0.000000000000000000, 0.000000000000000000 ) ) ;
#21873 = CARTESIAN_POINT ( 'NONE',  ( -19.03943276465977164, 0.05219959533909376836, 101.2489096053143669 ) ) ;
#21874 = CARTESIAN_POINT ( 'NONE',  ( 29.86685920354754487, 21.69954338932564752, -5.424999997268813878 ) ) ;
#21875 = CARTESIAN_POINT ( 'NONE',  ( -18.62759615963255300, -10.81492255796106328, 29.16775706135234003 ) ) ;
#21876 = CARTESIAN_POINT ( 'NONE',  ( 8.224510206698953496, -14.34966873604960469, 97.91557627198103830 ) ) ;
#21878 = CARTESIAN_POINT ( 'NONE',  ( -16.51473224551069308, -9.474510206698971260, 86.66557627198102409 ) ) ;
#21877 = CARTESIAN_POINT ( 'NONE',  ( 21.55341960407610458, 5.719274019375980345, 88.95724293864769550 ) ) ;
#21879 = CARTESIAN_POINT ( 'NONE',  ( -13.97604488694527625, -13.89961937509977652, 86.87390960531436690 ) ) ;
#21880 = CARTESIAN_POINT ( 'NONE',  ( -15.72974639402197994, 15.80617190586746368, 105.6239096053143669 ) ) ;
#21881 = ORIENTED_EDGE ( 'NONE', *, *, #82288, .T. ) ;
#21882 = CARTESIAN_POINT ( 'NONE',  ( -13.97604488694527625, -13.89961937509977652, 71.87390960531433848 ) ) ;
#21883 = CARTESIAN_POINT ( 'NONE',  ( -31.88446454451164414, -20.67411064994756487, -24.22501891791619855 ) ) ;
#21885 = CARTESIAN_POINT ( 'NONE',  ( 9.564922557960805705, 16.46253265017160317, 29.58224293864769550 ) ) ;
#21884 = CARTESIAN_POINT ( 'NONE',  ( 12.06949235617757843, -12.14591786802309237, 108.1239096053143811 ) ) ;
#21886 = CARTESIAN_POINT ( 'NONE',  ( -16.51473224551082808, 9.474510206698731452, 98.33442372801900433 ) ) ;
#21887 = CARTESIAN_POINT ( 'NONE',  ( -16.53943276465976808, 0.05219959533911058130, 111.2489096053143669 ) ) ;
#21888 = CARTESIAN_POINT ( 'NONE',  ( 10.72451020669871369, 18.67979575497193778, 67.08442372801901854 ) ) ;
#21890 = CARTESIAN_POINT ( 'NONE',  ( -5.823673210054431948, 21.52544592524334988, 32.70942372801900433 ) ) ;
#21889 = CARTESIAN_POINT ( 'NONE',  ( 5.153800228976335163, 19.02544592524342804, 59.79057627198100988 ) ) ;
#21891 = CARTESIAN_POINT ( 'NONE',  ( -10.81492255796078084, -18.62759615963271287, 107.0822429386476955 ) ) ;
#21892 = CARTESIAN_POINT ( 'NONE',  ( 17.81289503416610742, 24.51734667627700404, 145.2999999999999829 ) ) ;
#21893 = CARTESIAN_POINT ( 'NONE',  ( 19.02544592524343514, -5.153800228976328945, 78.54057627198099567 ) ) ;
#21894 = DIRECTION ( 'NONE',  ( 0.000000000000000000, 1.224646799147353207E-16, -1.000000000000000000 ) ) ;
#21896 = CARTESIAN_POINT ( 'NONE',  ( -18.62759615963270932, 10.81492255796079327, 35.83224293864768839 ) ) ;
#21895 = CARTESIAN_POINT ( 'NONE',  ( 4.379528057220092307, 16.55341960407617563, 27.29275706135234358 ) ) ;
#21897 = CARTESIAN_POINT ( 'NONE',  ( 21.53943276465977519, 0.05219959533937863772, 61.25109039468567573 ) ) ;
#21898 = CARTESIAN_POINT ( 'NONE',  ( 19.03943276465977164, -0.05219959533909143690, 113.7489096053143669 ) ) ;
#21899 = CARTESIAN_POINT ( 'NONE',  ( -19.05341960407617563, 5.049401038297882671, 98.54275706135233293 ) ) ;
#21900 = CARTESIAN_POINT ( 'NONE',  ( 16.46253265017160672, -9.564922557960803928, 53.33224293864768839 ) ) ;
#21901 = CARTESIAN_POINT ( 'NONE',  ( -9.474510206698964154, 16.51473224551069663, 70.41557627198102409 ) ) ;
#21902 = CARTESIAN_POINT ( 'NONE',  ( 8.224510206698953496, -14.34966873604960469, 97.91557627198103830 ) ) ;
#21903 = CARTESIAN_POINT ( 'NONE',  ( -16.51473224551069308, -9.474510206698971260, 111.6655762719810383 ) ) ;
#21904 = CARTESIAN_POINT ( 'NONE',  ( 4.379528057220339221, -16.55341960407611168, 97.70724293864772392 ) ) ;
#21905 = CARTESIAN_POINT ( 'NONE',  ( -0.05219959533907301413, -21.53943276465977519, 22.49890960531436335 ) ) ;
#21907 = CARTESIAN_POINT ( 'NONE',  ( 5.049401038298161559, -19.05341960407611168, 42.70724293864767418 ) ) ;
#21906 = CARTESIAN_POINT ( 'NONE',  ( -16.55341960407611168, -4.379528057220339221, 61.45724293864770260 ) ) ;
#21908 = CARTESIAN_POINT ( 'NONE',  ( 15.72974639402176855, 15.80617190586768217, 56.87609039468568994 ) ) ;
#21909 = CARTESIAN_POINT ( 'NONE',  ( -9.564922557961040184, 16.46253265017147172, 97.91775706135233293 ) ) ;
#21910 = CARTESIAN_POINT ( 'NONE',  ( -8.314922557960811034, -14.29746914071050412, 52.08224293864768839 ) ) ;
#21911 = CARTESIAN_POINT ( 'NONE',  ( -5.719274019375665041, -21.55341960407619695, 19.79275706135235069 ) ) ;
#21912 = CARTESIAN_POINT ( 'NONE',  ( -10.81492255796078084, -18.62759615963271287, 47.08224293864770260 ) ) ;
#21913 = CARTESIAN_POINT ( 'NONE',  ( 19.03943276465977164, -0.05219959533909143690, 113.7489096053143669 ) ) ;
#21914 = CARTESIAN_POINT ( 'NONE',  ( 28.82186960331498327, 2.781578969918950771E-14, 141.2500000054623683 ) ) ;
#21915 = CARTESIAN_POINT ( 'NONE',  ( -19.05341960407611168, -5.049401038298163336, 61.45724293864769550 ) ) ;
#21916 = CARTESIAN_POINT ( 'NONE',  ( 16.55341960407618274, -4.379528057220086978, 111.0427570613523613 ) ) ;
#21917 = VECTOR ( 'NONE', #49537, 999.9999999999997726 ) ;
#21918 = CARTESIAN_POINT ( 'NONE',  ( 12.14591786802327356, -12.06949235617739191, 105.6260903946856899 ) ) ;
#21919 = CARTESIAN_POINT ( 'NONE',  ( -14.34966873604972548, 8.224510206698743886, 88.33442372801901854 ) ) ;
#21920 = CARTESIAN_POINT ( 'NONE',  ( 9.564922557961047289, -16.46253265017146816, 45.41775706135232582 ) ) ;
#21921 = DIRECTION ( 'NONE',  ( 0.000000000000000000, 0.000000000000000000, -1.000000000000000000 ) ) ;
#21922 = CARTESIAN_POINT ( 'NONE',  ( -0.05219959533909027116, -19.03943276465977164, 87.49890960531436690 ) ) ;
#21923 = CARTESIAN_POINT ( 'NONE',  ( 0.05219959533909260263, 19.03943276465977164, 49.99890960531435979 ) ) ;
#21924 = CARTESIAN_POINT ( 'NONE',  ( -4.483927247898539470, -16.52544592524342804, 67.29057627198103830 ) ) ;
#21926 = CARTESIAN_POINT ( 'NONE',  ( 9.474510206698971260, -16.51473224551069308, 107.9155762719810383 ) ) ;
#21925 = CARTESIAN_POINT ( 'NONE',  ( 17.48853670773245383, -5.747243402303093163, 101.1667129974999426 ) ) ;
#21927 = CARTESIAN_POINT ( 'NONE',  ( 10.81492255796078972, 18.62759615963270932, 39.58224293864769550 ) ) ;
#21928 = CARTESIAN_POINT ( 'NONE',  ( 0.05219959533910956823, 16.53943276465976808, 89.99890960531438111 ) ) ;
#21929 = CARTESIAN_POINT ( 'NONE',  ( -8.224510206698735004, -14.34966873604973081, 44.58442372801901854 ) ) ;
#21930 = CARTESIAN_POINT ( 'NONE',  ( -12.06949235617756955, 12.14591786802309770, 80.62390960531438111 ) ) ;
#21931 = DIRECTION ( 'NONE',  ( -0.000000000000000000, -0.000000000000000000, 1.000000000000000000 ) ) ;
#21932 = CARTESIAN_POINT ( 'NONE',  ( 13.89961937509957401, 13.97604488694547697, 76.87609039468566152 ) ) ;
#21933 = CARTESIAN_POINT ( 'NONE',  ( -5.153800228976328057, -19.02544592524343514, 97.29057627198099567 ) ) ;
#21934 = CARTESIAN_POINT ( 'NONE',  ( 5.049401038297881783, 19.05341960407617563, 77.29275706135231871 ) ) ;
#21935 = CARTESIAN_POINT ( 'NONE',  ( -22.84806810306151093, 22.15679140170787065, -49.22928680315004613 ) ) ;
#21937 = CARTESIAN_POINT ( 'NONE',  ( 4.379528057220092307, 16.55341960407617563, 107.2927570613523471 ) ) ;
#21936 = CARTESIAN_POINT ( 'NONE',  ( 0.05219959533934541429, -16.53943276465976808, 35.00109039468568284 ) ) ;
#21938 = CARTESIAN_POINT ( 'NONE',  ( 16.51473224551083163, -9.474510206698727899, 75.83442372801900433 ) ) ;
#21939 =( BOUNDED_SURFACE ( )  B_SPLINE_SURFACE ( 3, 2, ( 
 ( #70636, #71628, #133294, #118140, #119143, #88786, #10963, #162632, #7946, #194984, #131295, #100948, #191970, #53456, #164646, #56462, #176824, #178821, #54462, #24139, #150479, #40291, #72637, #42302, #132302, #85791, #23130, #195998, #134312, #193994, #163646, #69629, #179830, #84775, #192984, #116132, #26141, #180824, #103963, #87783, #57471, #165641, #27139, #177821, #11974, #147477, #8967, #117127, #101965, #185779, #124078, #91742, #136287, #89783, #107917, #105941, #196983, #181808, #197963, #155431, #198958, #123090, #168602, #77589, #120117, #151468, #28143, #170603, #153437, #184776, #43286, #199954, #104955, #60425, #16921, #62408, #166641, #61419, #169602, #121106, #58449, #59433, #736, #12957, #182800, #154436, #108923, #44283, #32093, #47266, #93750, #135310, #46262, #106929, #31100, #167626, #152444, #122098, #74621, #15930, #29123, #90761, #45276, #13930, #30102, #75597, #76595, #137276, #92748, #183789, #14935, #138271, #139260, #35064, #79579, #33087, #51232, #49249, #140248, #125093, #141248, #98710, #142237, #66396, #111907, #20887, #63418, #94743, #171599, #113877, #96719, #128058, #186791, #143224, #48262, #3722, #160404, #5711, #109915, #4706, #112893, #64414, #1740, #2737, #144227, #156423, #126083, #97701, #52220, #187779, #175574, #190746, #37051, #78574, #189760, #50251, #174587, #110907, #95737, #65399, #17924, #159392, #172593, #34079, #188767, #157423, #173595, #18917, #36052, #80562, #158407, #82545, #19896, #127060, #67388, #81537, #129045, #146216, #191733, #10733, #25911, #21893, #133061, #149242, #7704, #40048, #72397, #9733, #134073, #56223, #100714, #101722, #178583, #148239, #195763, #118911, #179594, #192745, #38061, #24908, #161401, #69387, #103733, #83543, #194751, #163412, #145222, #8728, #84539, #131056, #180595, #70397, #41066, #57237, #162394, #115899, #53215, #87555, #102729, #23897, #193754, #99717, #86555, #6704, #68382, #130034, #117905, #42069, #114893, #71397, #164418, #176587, #22893, #54228, #177589, #39056, #85549, #147236, #132065, #55222, #116891, #30863, #181577, #151236, #184541, #139017, #12725, #62169, #77350, #497, #47023, #76357, #137035, #29867, #27907, #182566, #90532, #196756, #46021, #89550, #58223, #75365, #136056, #198725, #119892, #91504, #43055, #60192, #169354, #121862, #104721, #154199, #73409, #138034, #74391, #135080, #15689, #92510, #165413, #199715, #123833, #197731, #183554, #185531, #153191, #26906, #61181, #44049, #45040, #106698, #14694, #88549, #150247, #122853, #59197, #166412, #168371, #120866, #105709, #11742, #167396, #107677, #28892, #152214, #13698, #171359, #17678, #69904, #95493, #127812, #159144, #187542, #2494, #78330, #112650, #66149, #110664, #80319, #124849, #188522, #108682, #193254, #170360, #81298, #35812, #23401, #49999, #96477, #97458, #126816, #31852, #111664, #93505, #189517, #155191, #16681, #85048, #146729, #65157, #109678, #63170, #142982, #79336, #140003, #1492, #32847, #131570, #172344, #158165, #141992, #50990, #186549, #48021, #94497, #8226, #173351, #19657, #156179, #34822, #141006, #33833, #174342, #64175, #125840, #49009, #157179, #4460, #18673, #3480, #119412, #24414, #180108, #74888, #182075, #162905, #181096, #27412, #40569, #116400, #55729, #120382, #70906, #102239, #73909, #28413, #163927, #151732, #166912, #90050, #136551, #165914, #26415, #42570, #117402, #71898, #41576, #86063, #135579, #179100, #147753, #164921, #25424, #88054, #9239, #104233, #132573, #149742, #58713, #11243, #194262, #43558, #87065, #89058, #148750, #10238, #105224, #13225, #54727, #150749, #178089, #133569, #72918, #39559, #12247, #101216, #197251, #195260, #134587, #196273, #56744, #118415, #103240, #57742, #168861, #14196, #1000, #137541, #45536, #79848, #198231, #109188, #154700, #121375, #185042, #60689, #107190, #156697, #46529, #17187, #48529, #76857, #92010, #167890, #2009, #155692, #6, #169871 ),
 ( #62674, #183068, #61680, #106206, #170867, #199223, #138528, #63688, #91020, #47534, #123349, #122364, #31364, #30366, #124355, #44551, #187059, #108189, #186050, #78841, #93014, #33350, #16195, #110183, #29389, #32358, #77850, #152706, #153703, #140519, #94011, #171862, #95009, #139517, #125363, #18191, #75865, #184053, #59703, #15198, #3983, #99980, #21154, #189037, #23161, #34343, #81801, #191007, #97965, #114143, #126342, #65663, #173863, #113155, #68648, #129311, #191999, #175844, #20156, #159657, #82809, #67654, #130304, #38324, #98975, #112175, #157688, #144491, #80828, #50512, #141517, #3004, #52483, #5974, #64680, #128322, #127325, #35331, #161665, #190021, #160665, #53485, #143488, #96984, #111172, #145488, #22157, #4973, #174845, #19179, #37317, #188039, #49509, #172862, #83808, #115162, #176855, #6968, #96004, #142505, #158666, #66659, #51495, #36311, #42333, #7974, #84804, #135342, #73670, #41331, #85821, #39321, #57503, #55487, #146483, #131325, #147509, #104986, #148508, #72668, #118170, #27171, #69658, #100980, #177852, #120149, #102992, #134345, #193013, #149499, #54490, #9998, #166673, #12009, #116162, #10996, #119172, #70666, #162664, #8999, #150511, #24170, #132333, #103993, #58482, #194024, #181839, #88818, #117157, #178853, #40319, #43319, #164678, #196028, #101995, #180857, #163677, #71658, #25180, #197016, #86822, #165672, #133325, #195016, #56492, #179861, #26172, #87813, #13962, #47299, #1772, #75629, #125127, #140280, #63450, #109949, #139291, #199984, #92780, #90791, #45308, #153469, #59465, #108956, #152475, #121138, #138303, #198988, #61451, #182832, #154469, #44314, #123121, #32124, #184806, #105973, #16952, #136320, #768, #137307, #197995, #78606, #93781, #28175, #46292, #60456, #122131, #107949, #155462, #15961, #186824, #62438, #106958, #169636, #31132, #77621, #48293, #89817, #185812, #183818, #167658, #124112, #29154, #168632, #151498, #12990, #170635, #74653, #30132, #14965, #91775, #76625, #130066, #158438, #190775, #21924, #50281, #65428, #141279, #175606, #129074, #173626, #143253, #187810, #51262, #171630, #53249, #33118, #144256, #98741, #83575, #112922, #159421, #160434, #189791, #94775, #174617, #156457, #52250, #17956, #79609, #145254, #6735, #128087, #172623, #126115, #5743, #142269, #2769, #64445, #34111, #191765, #35096, #20917, #4737, #36082, #49279, #95768, #68413, #19926, #157454, #110937, #97732, #18948, #80594, #3751, #111939, #82575, #67419, #113907, #37082, #127089, #188798, #96748, #81567, #66426, #195797, #133091, #176619, #131088, #149273, #85582, #73440, #41098, #42101, #72429, #148271, #9763, #10765, #193784, #150279, #102762, #71427, #196787, #161433, #8759, #164450, #25943, #134107, #147268, #23927, #26939, #194781, #192776, #11776, #70429, #57269, #54260, #115931, #118943, #180628, #132095, #55253, #135111, #117937, #56255, #114926, #87586, #178614, #84571, #103765, #146249, #179626, #99749, #40077, #22925, #165444, #177621, #116921, #88581, #7735, #38094, #101755, #39089, #86588, #163443, #69421, #100745, #162426, #24940, #122886, #105742, #153226, #47059, #181609, #154233, #151268, #91538, #123867, #140038, #185565, #12758, #27940, #76391, #16714, #198760, #13732, #93540, #92545, #59230, #155225, #166444, #77383, #15723, #75399, #104754, #89582, #139051, #14730, #78364, #121895, #108718, #74423, #46055, #138067, #136089, #28925, #531, #169389, #31886, #58255, #199748, #60226, #184574, #197764, #183588, #119924, #170395, #120899, #107710, #30898, #44084, #43087, #182599, #167429, #90565, #152247, #62203, #137070, #45073, #106731, #168405, #29900, #61214, #112687, #173388, #66187, #64211, #18710, #126853, #32883, #82331, #125877, #94533, #111702, #172380, #34858, #156215, #127849, #17715, #96513, #5502, #158203, #79373, #190540, #109713, #174379, #187577, #171396, #52014, #67184, #1527, #19693, #49045, #33871, #81335, #128841 ),
 ( #141044, #110700, #83338, #63206, #35849, #143018, #124886, #188559, #95530, #157217, #160195, #50038, #20676, #113673, #80357, #142030, #2530, #175367, #159181, #3518, #4496, #65194, #189554, #186585, #48057, #51026, #97495, #36835, #98501, #144021, #21685, #133862, #163197, #26698, #86350, #6496, #102526, #68176, #145015, #195553, #57027, #101507, #146014, #99511, #117692, #115696, #129828, #191527, #7497, #165203, #8515, #132855, #178377, #87351, #53004, #161192, #37852, #180391, #24701, #194543, #114683, #72188, #164209, #39841, #148036, #179389, #23690, #41862, #56014, #9525, #176378, #22688, #38856, #40852, #25706, #149037, #177385, #54023, #118700, #71191, #84335, #103528, #100513, #10525, #69182, #130848, #192540, #162192, #85338, #147031, #70193, #131860, #193544, #55017, #116687, #152010, #58023, #107471, #119693, #152985, #73204, #13496, #196552, #60974, #27701, #28689, #153989, #181376, #137825, #90325, #12525, #59987, #120664, #91294, #134875, #77143, #136833, #14484, #135859, #183349, #138813, #11535, #184338, #42854, #121655, #15486, #170153, #293, #104519, #166200, #106487, #46815, #75161, #43840, #123629, #122649, #89343, #185325, #151035, #169148, #45820, #105505, #74190, #197530, #30652, #44831, #108475, #198516, #61962, #58998, #76146, #168165, #182362, #167191, #92306, #199508, #88338, #150029, #29662, #172140, #96278, #16476, #32638, #66939, #18470, #94292, #190295, #111458, #79124, #113432, #124640, #33626, #81103, #188315, #4262, #157964, #65942, #127613, #142781, #189312, #173144, #112449, #49793, #93295, #47817, #50790, #2286, #51772, #19456, #174138, #34619, #35610, #97255, #158943, #20432, #82083, #143776, #5257, #128602, #31646, #154981, #109466, #78125, #63968, #139794, #1283, #62959, #186335, #64954, #126613, #171150, #110459, #155970, #17468, #140797, #125638, #187335, #48805, #95289, #156973, #80120, #141789, #3283, #87109, #131615, #52763, #10285, #7255, #55772, #114432, #176133, #179145, #40613, #130604, #68940, #71943, #178136, #116448, #133613, #162952, #38614, #144773, #194306, #6258, #39603, #159950, #100271, #83098, #147799, #37603, #115453, #102283, #67938, #24458, #177143, #99266, #146778, #192299, #101262, #21438, #163972, #23446, #86108, #22445, #69950, #25469, #98248, #70949, #129591, #8272, #148795, #56788, #195307, #191287, #160952, #193299, #175125, #161951, #53778, #36592, #9284, #84095, #145774, #85093, #117446, #132619, #54774, #164965, #88101, #78643, #13267, #156491, #182116, #171665, #26458, #106250, #151774, #149786, #89102, #140318, #29432, #94813, #17993, #74930, #58756, #183112, #103285, #119456, #79646, #105267, #181140, #141315, #198273, #165960, #2804, #11289, #120425, #41621, #118460, #33154, #109985, #136593, #42614, #72962, #91063, #150793, #180152, #134631, #104278, #196316, #43602, #167932, #59750, #63486, #57785, #27461, #12289, #73954, #121420, #152750, #135622, #44594, #197293, #166953, #28456, #48330, #90092, #14240, #1808, #125162, #186861, #142307, #37115, #157491, #65464, #190810, #83610, #127127, #145288, #21959, #6771, #130104, #144289, #128123, #159455, #3787, #35132, #143287, #172659, #52284, #188833, #95805, #66460, #50318, #189825, #34146, #97768, #18984, #51297, #175641, #112958, #80630, #160468, #110974, #5779, #111973, #173665, #98774, #68450, #64482, #174651, #96784, #158473, #36116, #126149, #67453, #187845, #113942, #81603, #20951, #82608, #129111, #49314, #19961, #4773, #15646, #61137, #47980, #184499, #92466, #126772, #42268, #156135, #1449, #168328, #31809, #107633, #154154, #3438, #93460, #64132, #95450, #123790, #138974, #14650, #48965, #2450, #46979, #16639, #122809, #124806, #106655, #29824, #91460, #17634, #172301, #157135, #186504, #32803, #33790, #63127, #153148, #109633, #76310, #125797, #77305, #141948, #18630, #80277, #137988, #79294, #78286, #171316, #169311, #62127, #170316, #199671 ),
 ( #94455, #452, #45979, #30817, #185489, #140963, #187499, #110619, #65114, #108638, #155146, #139959, #161112, #68098, #69100, #6417, #49957, #4419, #22608, #159103, #146950, #114599, #115617, #145935, #21602, #83260, #84254, #67104, #23612, #176296, #144935, #70111, #34780, #82249, #37768, #99430, #7417, #20597, #97416, #100434, #129750, #66106, #85258, #143940, #130767, #127772, #189472, #192459, #53942, #5421, #128763, #8439, #191447, #52923, #188476, #177306, #51935, #158123, #38778, #19614, #162115, #173306, #113595, #96436, #111621, #50950, #190462, #81257, #142938, #112609, #175289, #174301, #160114, #36754, #35770, #98418, #120588, #180313, #196476, #179310, #26618, #182282, #54939, #27626, #24621, #165126, #197454, #13421, #58920, #86269, #101426, #149948, #90249, #72106, #87273, #167110, #166124, #132777, #28611, #39763, #150957, #89265, #148957, #194464, #151932, #163118, #12451, #74113, #10446, #178299, #147959, #135783, #88261, #131780, #195472, #43763, #9446, #119617, #11454, #71111, #102443, #105427, #42778, #193462, #116611, #73126, #133779, #57946, #55935, #117610, #40774, #118622, #164130, #25628, #134795, #56948, #41781, #103447, #181300, #104440, #32678, #93335, #63001, #15524, #185362, #124678, #80155, #140834, #3319, #187373, #31686, #171189, #109507, #79164, #61015, #110496, #169186, #186375, #47854, #48842, #155020, #188353, #2323, #94331, #34656, #199545, #46854, #64005, #125675, #172178, #108513, #61999, #64992, #156009, #30693, #49831, #170192, #33663, #92343, #154029, #157009, #18507, #16516, #78164, #111495, #17506, #95325, #173180, #141826, #139832, #122687, #126650, #184376, #153025, #137865, #1321, #45857, #14525, #77181, #76185, #107510, #138851, #331, #123665, #20473, #67975, #128640, #99305, #81138, #85134, #144813, #160990, #143816, #191324, #146818, #19493, #192337, #189350, #129629, #161989, #178177, #23485, #50828, #65981, #114469, #54813, #36631, #51811, #131657, #130643, #158001, #142819, #97295, #116488, #159990, #84132, #52802, #38654, #4299, #112485, #174178, #193339, #176172, #145811, #127651, #22484, #35648, #21476, #96315, #8313, #158981, #7294, #68978, #82123, #5297, #66980, #69989, #190334, #113470, #115493, #175165, #98288, #83137, #6296, #37641, #53818, #177181, #100311, #104315, #102321, #56825, #165003, #70990, #120463, #164011, #132658, #149823, #10324, #73000, #194346, #165998, #55814, #134668, #43639, #196354, #117486, #28492, #147839, #150829, #25507, #179184, #101303, #119494, #180190, #11329, #87151, #71980, #57822, #166989, #27499, #90126, #73991, #118499, #181176, #42653, #89141, #41660, #151810, #59788, #13301, #40652, #12326, #148834, #133654, #121456, #39642, #135660, #197332, #162992, #26497, #195345, #103323, #198309, #88139, #58795, #74966, #182154, #105302, #9325, #136628, #24497, #86148, #154782, #199308, #62759, #183148, #64764, #44633, #155773, #110264, #33434, #124440, #170948, #171945, #1084, #106285, #186136, #167970, #140601, #29469, #91102, #95093, #156782, #139598, #184139, #137624, #17271, #153786, #14281, #16279, #187140, #77931, #60775, #18275, #152790, #94094, #107273, #122447, #75950, #47615, #123430, #93098, #45621, #15281, #109269, #79928, #32440, #141601, #78924, #61762, #2091, #63771, #125444, #92, #3088, #168944, #30451, #92098, #48612, #76941, #138610, #185123, #46613, #108275, #169953, #31444, #113242, #189125, #35415, #84894, #174933, #145578, #176944, #5061, #20238, #96087, #130395, #83895, #128406, #98050, #142590, #6064, #126427, #8067, #188124, #99066, #53575, #38414, #67742, #114231, #115252, #144577, #49595, #129400, #111258, #7055, #172950, #34428, #100071, #161756, #82899, #127415, #80913, #160754, #97067, #157776, #19267, #50597, #146573, #190103, #175936, #159749, #68737, #4070, #65747, #112256, #23251, #191096, #37408, #173948, #52571, #158749, #51578, #81886, #143578, #66746, #22246 ),
 ( #36396, #192092, #21245, #134431, #132420, #86910, #195103, #101066, #150597, #194112, #162751, #179950, #40411, #103083, #24259, #196117, #27256, #85910, #164764, #26259, #104080, #148593, #105075, #57587, #87900, #151584, #116247, #163767, #119257, #180941, #88906, #102083, #178941, #181924, #149586, #147597, #166761, #25267, #12095, #9082, #70752, #73758, #135430, #10085, #71743, #28263, #72760, #11084, #89901, #42417, #133414, #39406, #197101, #55575, #165762, #54575, #56585, #177939, #58568, #117249, #118260, #120233, #41417, #43405, #69744, #131413, #193100, #45391, #16048, #198081, #1859, #61536, #77707, #60539, #108036, #63541, #136403, #109042, #106056, #46377, #78695, #94866, #140372, #167742, #182917, #31215, #171718, #153553, #168716, #48382, #47387, #14046, #110039, #121226, #32212, #170720, #30218, #59548, #44402, #93868, #169722, #33207, #76711, #125215, #29240, #855, #92866, #90873, #183906, #155547, #124202, #186911, #13073, #154553, #15050, #139373, #152557, #75712, #74740, #200068, #137390, #199070, #62529, #122215, #107044, #91860, #185902, #138386, #123205, #184895, #17041, #129164, #52338, #5831, #190861, #36167, #37167, #174703, #18046, #172714, #113994, #127178, #141370, #64535, #21004, #19036, #173718, #81656, #187897, #98826, #80683, #49364, #66514, #188888, #189875, #111028, #82659, #34197, #51350, #160520, #113010, #95859, #145341, #126201, #67507, #142359, #157542, #79699, #97819, #96840, #128176, #3839, #50369, #159508, #83663, #144343, #6823, #175692, #35186, #22011, #68501, #130156, #158525, #191853, #176707, #53334, #65518, #115013, #112029, #20013, #38181, #156547, #2857, #143339, #4826, #86672, #162514, #8846, #61049, #148355, #121730, #153060, #178704, #193873, #69510, #106563, #60062, #101842, #71510, #116016, #179713, #99837, #184411, #161521, #75236, #29736, #14562, #41185, #87671, #91369, #118023, #23013, #102848, #84659, #183422, #146337, #7825, #76220, #137899, #56341, #100831, #54345, #136907, #70514, #131176, #192866, #24016, #122721, #163528, #152084, #133178, #44906, #177706, #39173, #85671, #199581, #164533, #13569, #147358, #26026, #132182, #25028, #55339, #117009, #40166, #198594, #168240, #9851, #194868, #46889, #111531, #62036, #31721, #65028, #19527, #93369, #142854, #158036, #81172, #127685, #157046, #17541, #30730, #34692, #94365, #110533, #155056, #140871, #96349, #169221, #141862, #138885, #79202, #173216, #45892, #4333, #365, #15558, #64041, #66017, #186412, #1357, #107545, #80190, #108549, #92377, #154063, #126684, #3353, #63036, #77216, #123700, #188388, #2360, #185398, #109542, #170228, #16551, #33698, #125711, #78198, #139868, #49865, #18543, #124714, #47889, #187410, #171224, #172214, #32713, #156044, #48878, #95361, #51847, #147872, #69011, #36666, #71023, #82157, #115528, #9358, #129662, #67016, #53854, #162024, #85166, #38689, #23520, #130677, #70022, #7327, #50862, #5332, #146854, #160025, #174214, #97330, #8347, #128675, #22518, #84165, #131691, #68010, #24531, #177216, #145845, #189385, #35682, #83173, #100345, #193372, #54848, #21512, #98325, #101336, #192371, #190372, #86182, #144847, #116522, #113506, #175201, #178210, #39674, #6330, #191358, #112520, #163025, #159016, #20509, #143853, #52836, #114505, #176207, #37676, #99341, #161024, #196387, #40684, #105334, #72015, #73032, #198344, #25542, #182187, #134704, #56859, #104348, #165036, #135692, #27532, #14316, #179218, #26529, #43672, #120496, #151842, #88173, #41693, #44664, #89173, #10358, #168003, #149857, #13332, #133688, #195381, #136662, #59818, #11362, #57856, #29499, #197364, #74022, #91132, #167022, #119528, #102354, #74997, #164043, #58829, #117520, #181211, #87186, #28523, #118534, #42687, #121488, #148867, #90159, #166032, #180223, #150865, #12359, #183182, #103358, #106317, #152822, #132691, #194379, #55846, #64796, #199341, #171978, #168975, #109301, #141631 ),
 ( #92131, #61793, #95124, #49628, #123463, #172980, #188155, #111291, #157805, #187173, #47650, #140632, #138643, #93128, #1116, #107303, #156814, #124, #30480, #186168, #46645, #170980, #153818, #2122, #15313, #32473, #79962, #94126, #76972, #126457, #184170, #48644, #185155, #108305, #137654, #155805, #16311, #17303, #169985, #31476, #78957, #3121, #63804, #34458, #110296, #154813, #125477, #33466, #18306, #77961, #96117, #75981, #60806, #139628, #122479, #62790, #124471, #45652, #101096, #4098, #20268, #54604, #6095, #81914, #177968, #99098, #66774, #19296, #112286, #145610, #39436, #159780, #97096, #83929, #192127, #115284, #68770, #53608, #160790, #100102, #37438, #80944, #35444, #176977, #190132, #65777, #127446, #38447, #158780, #52603, #114265, #161786, #98082, #116278, #7089, #175969, #142619, #189152, #113271, #130428, #23281, #84925, #51607, #128435, #131444, #22278, #143607, #50625, #174963, #146605, #5091, #36427, #8098, #69776, #21275, #82932, #173976, #193131, #144610, #67774, #129431, #191129, #132451, #181955, #194142, #27291, #147628, #26292, #70783, #135461, #102114, #103116, #28293, #55606, #12125, #164797, #86943, #134463, #195137, #165794, #9116, #151614, #11118, #88938, #10117, #57620, #13106, #85939, #58597, #117280, #196148, #89933, #44432, #74771, #178974, #40441, #180971, #121255, #87933, #118292, #198114, #197130, #163799, #59581, #25301, #43437, #120263, #179983, #148627, #71777, #105106, #119288, #182949, #149620, #136433, #133447, #150629, #42448, #56618, #41451, #166792, #73789, #162782, #24290, #104112, #72793, #170750, #91890, #167772, #107072, #171748, #122244, #153581, #125243, #79729, #15079, #2886, #18074, #141398, #187925, #17070, #77735, #32239, #168743, #123232, #31245, #137421, #186941, #30247, #199101, #16077, #76740, #139401, #60568, #93897, #183934, #883, #110068, #62558, #45419, #94895, #14078, #78724, #138415, #200095, #29270, #185930, #46407, #124234, #61563, #184923, #47415, #33237, #155575, #156579, #140400, #108066, #109071, #1888, #63569, #169750, #64565, #126230, #106086, #92895, #48412, #154581, #90901, #152587, #75744, #160553, #5861, #172745, #36196, #112058, #158552, #7856, #157571, #161551, #67537, #127206, #84689, #81685, #130188, #188920, #50398, #53368, #115046, #4859, #143367, #146369, #52369, #190893, #69543, #37202, #113041, #19064, #68533, #80711, #114026, #34226, #174733, #142389, #22043, #173746, #189905, #176738, #3868, #98858, #51380, #35215, #21037, #66544, #175723, #95888, #38211, #97850, #83694, #96868, #144374, #99867, #65547, #145372, #20042, #82690, #23044, #131207, #49394, #128208, #159539, #129195, #111057, #6854, #191884, #180742, #43204, #27056, #71540, #10879, #149383, #119060, #9880, #104871, #12876, #120036, #8877, #195912, #132213, #40196, #74541, #192898, #103879, #72549, #116047, #179744, #55368, #101876, #54375, #39205, #57387, #177736, #133206, #86701, #162543, #196902, #150398, #194897, #164560, #70545, #134227, #100861, #24047, #85703, #165559, #181722, #166560, #42218, #88702, #28059, #11894, #147389, #73557, #193904, #135230, #117038, #178733, #89700, #151386, #58369, #163558, #25058, #148386, #56371, #118054, #41214, #102875, #26054, #87698, #123991, #169514, #78490, #121018, #90682, #29042, #171517, #154352, #185689, #44201, #651, #105860, #61336, #156340, #63333, #167547, #62321, #108838, #122018, #197881, #137190, #1655, #152364, #183709, #155350, #109834, #45195, #33006, #48178, #94661, #17840, #47179, #107830, #170519, #198877, #153349, #123007, #13849, #16840, #60344, #75516, #46177, #106849, #31014, #168524, #32008, #30022, #92664, #140163, #15845, #91660, #125011, #14851, #93665, #76513, #138189, #59350, #77504, #199872, #139175, #184693, #186707, #136206, #182716, #175491, #172511, #112808, #145139, #161319, #6622, #33996, #49168, #97615, #37979, #19813, #34983, #114810, #113796, #80480 ),
 ( #67304, #174501, #187698, #50164, #98625, #190663, #53131, #176502, #35968, #81454, #144143, #64333, #142154, #99636, #66311, #3638, #79498, #159305, #126975, #141167, #95652, #5627, #2656, #143140, #157340, #128963, #52139, #36964, #160319, #21810, #20800, #83462, #82455, #126001, #18835, #68301, #111822, #110827, #65316, #129952, #188684, #191652, #173510, #96636, #158324, #4620, #127972, #189675, #51147, #69306, #116812, #72316, #10653, #162316, #11663, #130972, #135001, #179515, #100635, #58148, #55141, #103655, #23817, #85467, #26825, #88466, #178503, #39969, #119816, #25832, #164337, #181501, #133992, #86476, #192663, #41989, #54146, #87476, #7622, #148161, #115819, #195683, #147156, #163330, #150163, #177509, #57154, #24826, #8644, #194672, #101639, #149163, #38979, #73329, #71318, #118833, #70318, #117822, #196679, #146136, #165333, #131985, #193670, #42979, #104644, #9652, #132981, #22812, #180516, #84458, #56141, #40983, #102652, #135983, #185450, #197654, #30781, #151161, #29788, #74316, #138934, #105629, #106618, #31771, #59120, #15608, #168292, #90454, #137950, #198648, #169275, #12649, #155106, #14615, #92428, #13621, #61100, #16599, #89470, #62088, #120786, #199633, #93419, #47943, #78247, #182486, #43967, #184463, #124767, #91424, #121782, #1409, #414, #167318, #63088, #28814, #46940, #123751, #183476, #152138, #75288, #108600, #122773, #186465, #153111, #139920, #136959, #154114, #45942, #60114, #44960, #170277, #77265, #166331, #27829, #107597, #76272, #177017, #94417, #110582, #147668, #96400, #172263, #70822, #192168, #157097, #194180, #2412, #38486, #132491, #49917, #187460, #100143, #84963, #8139, #161824, #146645, #53648, #193170, #130471, #171277, #125760, #69816, #80241, #156097, #17595, #131483, #48928, #142903, #7129, #54642, #188438, #9156, #23319, #68812, #109594, #79254, #3402, #116317, #178006, #33753, #101134, #140926, #24329, #115326, #95412, #32765, #141911, #39473, #111582, #64092, #162820, #85979, #18593, #65077, #126735, #173267, #34741, #158087, #19579, #81222, #167807, #12163, #133484, #90937, #87972, #136469, #195176, #56657, #59619, #121292, #11158, #149660, #152624, #58634, #197169, #14114, #43475, #119327, #25340, #74807, #86981, #120300, #40481, #181013, #163839, #28330, #118330, #196188, #182985, #148668, #105143, #57660, #180023, #27329, #72832, #181993, #102153, #44469, #104150, #166829, #103155, #150665, #106123, #179013, #151649, #10156, #88975, #29307, #137459, #75781, #71816, #41491, #73828, #55644, #42487, #134502, #117317, #89969, #164836, #26332, #165832, #198149, #13144, #135498, #45455, #168779, #156615, #93932, #34263, #62592, #49431, #107109, #186977, #32275, #30282, #169786, #18110, #110104, #172782, #95922, #155611, #139436, #63604, #183968, #200129, #157607, #185966, #61598, #19098, #78758, #46442, #80747, #91927, #125280, #199138, #918, #76776, #48447, #171783, #94930, #33271, #79764, #140435, #141435, #17106, #60605, #15115, #2922, #31279, #153619, #138448, #64600, #123267, #1925, #126264, #184958, #187961, #108102, #124270, #122280, #111092, #92930, #154617, #16111, #77769, #47450, #109106, #170785, #158587, #128241, #161583, #116079, #189938, #39236, #54407, #177767, #24080, #53401, #114062, #6887, #4894, #159575, #67571, #173783, #23077, #66576, #35250, #52403, #113073, #175760, #96903, #68565, #20076, #37236, #146400, #98892, #81720, #131241, #50434, #115079, #51413, #143406, #3904, #22075, #82728, #160586, #174765, #36231, #83726, #69575, #130222, #192929, #176771, #21072, #145405, #191918, #38243, #144409, #100892, #162576, #142425, #97883, #99898, #5895, #129229, #65584, #127244, #84722, #7890, #188957, #190926, #112093, #9913, #85735, #132245, #180774, #8909, #179777, #56406, #55400, #58401, #73589, #41246, #10911, #40232, #57419, #147422, #70577, #117070, #135261, #166592, #89731, #103910, #11925, #151417, #42249 ) ),
 .UNSPECIFIED., .T., .F., .F. ) 
 B_SPLINE_SURFACE_WITH_KNOTS ( ( 4, 3, 4 ),
 ( 3, 2, 2, 2, 2, 2, 2, 2, 2, 2, 2, 2, 2, 2, 2, 2, 2, 2, 2, 2, 2, 2, 2, 2, 2, 2, 2, 2, 2, 2, 2, 2, 2, 2, 2, 2, 2, 2, 2, 2, 2, 2, 2, 2, 2, 2, 2, 2, 2, 2, 2, 2, 2, 2, 2, 2, 2, 2, 2, 2, 2, 2, 2, 2, 2, 2, 2, 2, 2, 2, 2, 2, 2, 2, 2, 2, 2, 2, 2, 2, 2, 2, 2, 2, 2, 2, 2, 2, 2, 2, 2, 2, 2, 2, 2, 2, 2, 2, 2, 2, 2, 2, 2, 2, 2, 2, 2, 2, 2, 2, 2, 2, 2, 2, 2, 2, 2, 2, 2, 2, 2, 2, 2, 2, 2, 2, 2, 2, 2, 2, 2, 2, 2, 2, 2, 2, 2, 2, 2, 2, 2, 2, 2, 2, 2, 2, 2, 2, 2, 2, 2, 2, 2, 2, 2, 2, 2, 2, 2, 2, 2, 2, 2, 2, 2, 2, 2, 2, 2, 2, 2, 2, 2, 2, 2, 2, 2, 2, 2, 2, 2, 2, 2, 2, 2, 2, 2, 2, 2, 2, 2, 2, 2, 2, 2, 2, 2, 2, 2, 2, 2, 2, 2, 2, 2, 2, 2, 2, 2, 2, 2, 2, 2, 2, 2, 2, 2, 2, 2, 2, 2, 2, 2, 2, 2, 2, 2, 2, 3 ),
 ( 0.000000000000000000, 0.5000000000000000000, 1.000000000000000000 ),
 ( 0.000000000000000000, 0.004385964912280701511, 0.008771929824561403022, 0.01315789473684210453, 0.01754385964912280604, 0.02192982456140350755, 0.02631578947368420907, 0.03070175438596491058, 0.03508771929824561209, 0.03947368421052631360, 0.04385964912280701511, 0.04824561403508771662, 0.05263157894736841813, 0.05701754385964911964, 0.06140350877192982115, 0.06578947368421052266, 0.07017543859649122417, 0.07456140350877192569, 0.07894736842105262720, 0.08333333333333332871, 0.08771929824561403022, 0.09210526315789473173, 0.09649122807017543324, 0.1008771929824561348, 0.1052631578947368363, 0.1096491228070175378, 0.1140350877192982393, 0.1184210526315789408, 0.1228070175438596423, 0.1271929824561403577, 0.1315789473684210453, 0.1359649122807017607, 0.1403508771929824483, 0.1447368421052631637, 0.1491228070175438514, 0.1535087719298245668, 0.1578947368421052544, 0.1622807017543859698, 0.1666666666666666574, 0.1710526315789473728, 0.1754385964912280604, 0.1798245614035087758, 0.1842105263157894635, 0.1885964912280701788, 0.1929824561403508665, 0.1973684210526315819, 0.2017543859649122695, 0.2061403508771929849, 0.2105263157894736725, 0.2149122807017543879, 0.2192982456140350755, 0.2236842105263157909, 0.2280701754385964786, 0.2324561403508771940, 0.2368421052631578816, 0.2412280701754385970, 0.2456140350877192846, 0.2500000000000000000, 0.2543859649122807154, 0.2587719298245614308, 0.2631578947368420907, 0.2675438596491228060, 0.2719298245614035214, 0.2763157894736842368, 0.2807017543859648967, 0.2850877192982456121, 0.2894736842105263275, 0.2938596491228070429, 0.2982456140350877027, 0.3026315789473684181, 0.3070175438596491335, 0.3114035087719298489, 0.3157894736842105088, 0.3201754385964912242, 0.3245614035087719396, 0.3289473684210526550, 0.3333333333333333148, 0.3377192982456140302, 0.3421052631578947456, 0.3464912280701754610, 0.3508771929824561209, 0.3552631578947368363, 0.3596491228070175517, 0.3640350877192982670, 0.3684210526315789269, 0.3728070175438596423, 0.3771929824561403577, 0.3815789473684210731, 0.3859649122807017330, 0.3903508771929824483, 0.3947368421052631637, 0.3991228070175438791, 0.4035087719298245390, 0.4078947368421052544, 0.4122807017543859698, 0.4166666666666666852, 0.4210526315789473450, 0.4254385964912280604, 0.4298245614035087758, 0.4342105263157894912, 0.4385964912280701511, 0.4429824561403508665, 0.4473684210526315819, 0.4517543859649122973, 0.4561403508771929571, 0.4605263157894736725, 0.4649122807017543879, 0.4692982456140351033, 0.4736842105263157632, 0.4780701754385964786, 0.4824561403508771940, 0.4868421052631579093, 0.4912280701754385692, 0.4956140350877192846, 0.5000000000000000000, 0.5043859649122807154, 0.5087719298245614308, 0.5131578947368421462, 0.5175438596491228616, 0.5219298245614034659, 0.5263157894736841813, 0.5307017543859648967, 0.5350877192982456121, 0.5394736842105263275, 0.5438596491228070429, 0.5482456140350877583, 0.5526315789473684736, 0.5570175438596490780, 0.5614035087719297934, 0.5657894736842105088, 0.5701754385964912242, 0.5745614035087719396, 0.5789473684210526550, 0.5833333333333333703, 0.5877192982456140857, 0.5921052631578946901, 0.5964912280701754055, 0.6008771929824561209, 0.6052631578947368363, 0.6096491228070175517, 0.6140350877192982670, 0.6184210526315789824, 0.6228070175438596978, 0.6271929824561403022, 0.6315789473684210176, 0.6359649122807017330, 0.6403508771929824483, 0.6447368421052631637, 0.6491228070175438791, 0.6535087719298245945, 0.6578947368421053099, 0.6622807017543859143, 0.6666666666666666297, 0.6710526315789473450, 0.6754385964912280604, 0.6798245614035087758, 0.6842105263157894912, 0.6885964912280702066, 0.6929824561403509220, 0.6973684210526315264, 0.7017543859649122417, 0.7061403508771929571, 0.7105263157894736725, 0.7149122807017543879, 0.7192982456140351033, 0.7236842105263158187, 0.7280701754385965341, 0.7324561403508771384, 0.7368421052631578538, 0.7412280701754385692, 0.7456140350877192846, 0.7500000000000000000, 0.7543859649122807154, 0.7587719298245614308, 0.7631578947368421462, 0.7675438596491228616, 0.7719298245614034659, 0.7763157894736841813, 0.7807017543859648967, 0.7850877192982456121, 0.7894736842105263275, 0.7938596491228070429, 0.7982456140350877583, 0.8026315789473684736, 0.8070175438596490780, 0.8114035087719297934, 0.8157894736842105088, 0.8201754385964912242, 0.8245614035087719396, 0.8289473684210526550, 0.8333333333333333703, 0.8377192982456140857, 0.8421052631578946901, 0.8464912280701754055, 0.8508771929824561209, 0.8552631578947368363, 0.8596491228070175517, 0.8640350877192982670, 0.8684210526315789824, 0.8728070175438596978, 0.8771929824561403022, 0.8815789473684210176, 0.8859649122807017330, 0.8903508771929824483, 0.8947368421052631637, 0.8991228070175438791, 0.9035087719298245945, 0.9078947368421053099, 0.9122807017543859143, 0.9166666666666666297, 0.9210526315789473450, 0.9254385964912280604, 0.9298245614035087758, 0.9342105263157894912, 0.9385964912280702066, 0.9429824561403509220, 0.9473684210526315264, 0.9517543859649122417, 0.9561403508771929571, 0.9605263157894736725, 0.9649122807017543879, 0.9692982456140351033, 0.9736842105263158187, 0.9780701754385965341, 0.9824561403508771384, 0.9868421052631578538, 0.9912280701754385692, 0.9956140350877192846, 1.000000000000000000 ),
 .UNSPECIFIED. ) 
 GEOMETRIC_REPRESENTATION_ITEM ( )  RATIONAL_B_SPLINE_SURFACE ( (
 ( 1.000000000000000000, 0.9659258262890683122, 1.000000000000000000, 0.9659258262890683122, 1.000000000000000000, 0.9659258262890683122, 1.000000000000000000, 0.9659258262890683122, 1.000000000000000000, 0.9659258262890683122, 1.000000000000000000, 0.9659258262890683122, 1.000000000000000000, 0.9659258262890683122, 1.000000000000000000, 0.9659258262890683122, 1.000000000000000000, 0.9659258262890683122, 1.000000000000000000, 0.9659258262890683122, 1.000000000000000000, 0.9659258262890683122, 1.000000000000000000, 0.9659258262890683122, 1.000000000000000000, 0.9659258262890683122, 1.000000000000000000, 0.9659258262890683122, 1.000000000000000000, 0.9659258262890683122, 1.000000000000000000, 0.9659258262890683122, 1.000000000000000000, 0.9659258262890683122, 1.000000000000000000, 0.9659258262890683122, 1.000000000000000000, 0.9659258262890683122, 1.000000000000000000, 0.9659258262890683122, 1.000000000000000000, 0.9659258262890683122, 1.000000000000000000, 0.9659258262890683122, 1.000000000000000000, 0.9659258262890683122, 1.000000000000000000, 0.9659258262890683122, 1.000000000000000000, 0.9659258262890683122, 1.000000000000000000, 0.9659258262890683122, 1.000000000000000000, 0.9659258262890683122, 1.000000000000000000, 0.9659258262890683122, 1.000000000000000000, 0.9659258262890683122, 1.000000000000000000, 0.9659258262890683122, 1.000000000000000000, 0.9659258262890683122, 1.000000000000000000, 0.9659258262890683122, 1.000000000000000000, 0.9659258262890683122, 1.000000000000000000, 0.9659258262890683122, 1.000000000000000000, 0.9659258262890683122, 1.000000000000000000, 0.9659258262890683122, 1.000000000000000000, 0.9659258262890683122, 1.000000000000000000, 0.9659258262890683122, 1.000000000000000000, 0.9659258262890683122, 1.000000000000000000, 0.9659258262890683122, 1.000000000000000000, 0.9659258262890683122, 1.000000000000000000, 0.9659258262890683122, 1.000000000000000000, 0.9659258262890683122, 1.000000000000000000, 0.9659258262890683122, 1.000000000000000000, 0.9659258262890683122, 1.000000000000000000, 0.9659258262890683122, 1.000000000000000000, 0.9659258262890683122, 1.000000000000000000, 0.9659258262890683122, 1.000000000000000000, 0.9659258262890683122, 1.000000000000000000, 0.9659258262890683122, 1.000000000000000000, 0.9659258262890683122, 1.000000000000000000, 0.9659258262890683122, 1.000000000000000000, 0.9659258262890683122, 1.000000000000000000, 0.9659258262890683122, 1.000000000000000000, 0.9659258262890683122, 1.000000000000000000, 0.9659258262890683122, 1.000000000000000000, 0.9659258262890683122, 1.000000000000000000, 0.9659258262890683122, 1.000000000000000000, 0.9659258262890683122, 1.000000000000000000, 0.9659258262890683122, 1.000000000000000000, 0.9659258262890683122, 1.000000000000000000, 0.9659258262890683122, 1.000000000000000000, 0.9659258262890683122, 1.000000000000000000, 0.9659258262890683122, 1.000000000000000000, 0.9659258262890683122, 1.000000000000000000, 0.9659258262890683122, 1.000000000000000000, 0.9659258262890683122, 1.000000000000000000, 0.9659258262890683122, 1.000000000000000000, 0.9659258262890683122, 1.000000000000000000, 0.9659258262890683122, 1.000000000000000000, 0.9659258262890683122, 1.000000000000000000, 0.9659258262890683122, 1.000000000000000000, 0.9659258262890683122, 1.000000000000000000, 0.9659258262890683122, 1.000000000000000000, 0.9659258262890683122, 1.000000000000000000, 0.9659258262890683122, 1.000000000000000000, 0.9659258262890683122, 1.000000000000000000, 0.9659258262890683122, 1.000000000000000000, 0.9659258262890683122, 1.000000000000000000, 0.9659258262890683122, 1.000000000000000000, 0.9659258262890683122, 1.000000000000000000, 0.9659258262890683122, 1.000000000000000000, 0.9659258262890683122, 1.000000000000000000, 0.9659258262890683122, 1.000000000000000000, 0.9659258262890683122, 1.000000000000000000, 0.9659258262890683122, 1.000000000000000000, 0.9659258262890683122, 1.000000000000000000, 0.9659258262890683122, 1.000000000000000000, 0.9659258262890683122, 1.000000000000000000, 0.9659258262890683122, 1.000000000000000000, 0.9659258262890683122, 1.000000000000000000, 0.9659258262890683122, 1.000000000000000000, 0.9659258262890683122, 1.000000000000000000, 0.9659258262890683122, 1.000000000000000000, 0.9659258262890683122, 1.000000000000000000, 0.9659258262890683122, 1.000000000000000000, 0.9659258262890683122, 1.000000000000000000, 0.9659258262890683122, 1.000000000000000000, 0.9659258262890683122, 1.000000000000000000, 0.9659258262890683122, 1.000000000000000000, 0.9659258262890683122, 1.000000000000000000, 0.9659258262890683122, 1.000000000000000000, 0.9659258262890683122, 1.000000000000000000, 0.9659258262890683122, 1.000000000000000000, 0.9659258262890683122, 1.000000000000000000, 0.9659258262890683122, 1.000000000000000000, 0.9659258262890683122, 1.000000000000000000, 0.9659258262890683122, 1.000000000000000000, 0.9659258262890683122, 1.000000000000000000, 0.9659258262890683122, 1.000000000000000000, 0.9659258262890683122, 1.000000000000000000, 0.9659258262890683122, 1.000000000000000000, 0.9659258262890683122, 1.000000000000000000, 0.9659258262890683122, 1.000000000000000000, 0.9659258262890683122, 1.000000000000000000, 0.9659258262890683122, 1.000000000000000000, 0.9659258262890683122, 1.000000000000000000, 0.9659258262890683122, 1.000000000000000000, 0.9659258262890683122, 1.000000000000000000, 0.9659258262890683122, 1.000000000000000000, 0.9659258262890683122, 1.000000000000000000, 0.9659258262890683122, 1.000000000000000000, 0.9659258262890683122, 1.000000000000000000, 0.9659258262890683122, 1.000000000000000000, 0.9659258262890683122, 1.000000000000000000, 0.9659258262890683122, 1.000000000000000000, 0.9659258262890683122, 1.000000000000000000, 0.9659258262890683122, 1.000000000000000000, 0.9659258262890683122, 1.000000000000000000, 0.9659258262890683122, 1.000000000000000000, 0.9659258262890683122, 1.000000000000000000, 0.9659258262890683122, 1.000000000000000000, 0.9659258262890683122, 1.000000000000000000, 0.9659258262890683122, 1.000000000000000000, 0.9659258262890683122, 1.000000000000000000, 0.9659258262890683122, 1.000000000000000000, 0.9659258262890683122, 1.000000000000000000, 0.9659258262890683122, 1.000000000000000000, 0.9659258262890683122, 1.000000000000000000, 0.9659258262890683122, 1.000000000000000000, 0.9659258262890683122, 1.000000000000000000, 0.9659258262890683122, 1.000000000000000000, 0.9659258262890683122, 1.000000000000000000, 0.9659258262890683122, 1.000000000000000000, 0.9659258262890683122, 1.000000000000000000, 0.9659258262890683122, 1.000000000000000000, 0.9659258262890683122, 1.000000000000000000, 0.9659258262890683122, 1.000000000000000000, 0.9659258262890683122, 1.000000000000000000, 0.9659258262890683122, 1.000000000000000000, 0.9659258262890683122, 1.000000000000000000, 0.9659258262890683122, 1.000000000000000000, 0.9659258262890683122, 1.000000000000000000, 0.9659258262890683122, 1.000000000000000000, 0.9659258262890683122, 1.000000000000000000, 0.9659258262890683122, 1.000000000000000000, 0.9659258262890683122, 1.000000000000000000, 0.9659258262890683122, 1.000000000000000000, 0.9659258262890683122, 1.000000000000000000, 0.9659258262890683122, 1.000000000000000000, 0.9659258262890683122, 1.000000000000000000, 0.9659258262890683122, 1.000000000000000000, 0.9659258262890683122, 1.000000000000000000, 0.9659258262890683122, 1.000000000000000000, 0.9659258262890683122, 1.000000000000000000, 0.9659258262890683122, 1.000000000000000000, 0.9659258262890683122, 1.000000000000000000, 0.9659258262890683122, 1.000000000000000000, 0.9659258262890683122, 1.000000000000000000, 0.9659258262890683122, 1.000000000000000000, 0.9659258262890683122, 1.000000000000000000, 0.9659258262890683122, 1.000000000000000000, 0.9659258262890683122, 1.000000000000000000, 0.9659258262890683122, 1.000000000000000000, 0.9659258262890683122, 1.000000000000000000, 0.9659258262890683122, 1.000000000000000000, 0.9659258262890683122, 1.000000000000000000, 0.9659258262890683122, 1.000000000000000000, 0.9659258262890683122, 1.000000000000000000, 0.9659258262890683122, 1.000000000000000000, 0.9659258262890683122, 1.000000000000000000, 0.9659258262890683122, 1.000000000000000000, 0.9659258262890683122, 1.000000000000000000, 0.9659258262890683122, 1.000000000000000000, 0.9659258262890683122, 1.000000000000000000, 0.9659258262890683122, 1.000000000000000000, 0.9659258262890683122, 1.000000000000000000, 0.9659258262890683122, 1.000000000000000000, 0.9659258262890683122, 1.000000000000000000, 0.9659258262890683122, 1.000000000000000000, 0.9659258262890683122, 1.000000000000000000, 0.9659258262890683122, 1.000000000000000000, 0.9659258262890683122, 1.000000000000000000, 0.9659258262890683122, 1.000000000000000000, 0.9659258262890683122, 1.000000000000000000, 0.9659258262890683122, 1.000000000000000000, 0.9659258262890683122, 1.000000000000000000, 0.9659258262890683122, 1.000000000000000000, 0.9659258262890683122, 1.000000000000000000, 0.9659258262890683122, 1.000000000000000000, 0.9659258262890683122, 1.000000000000000000, 0.9659258262890683122, 1.000000000000000000, 0.9659258262890683122, 1.000000000000000000, 0.9659258262890683122, 1.000000000000000000, 0.9659258262890683122, 1.000000000000000000, 0.9659258262890683122, 1.000000000000000000, 0.9659258262890683122, 1.000000000000000000, 0.9659258262890683122, 1.000000000000000000, 0.9659258262890683122, 1.000000000000000000, 0.9659258262890683122, 1.000000000000000000, 0.9659258262890683122, 1.000000000000000000, 0.9659258262890683122, 1.000000000000000000, 0.9659258262890683122, 1.000000000000000000, 0.9659258262890683122, 1.000000000000000000, 0.9659258262890683122, 1.000000000000000000, 0.9659258262890683122, 1.000000000000000000, 0.9659258262890683122, 1.000000000000000000, 0.9659258262890683122, 1.000000000000000000, 0.9659258262890683122, 1.000000000000000000, 0.9659258262890683122, 1.000000000000000000, 0.9659258262890683122, 1.000000000000000000, 0.9659258262890683122, 1.000000000000000000, 0.9659258262890683122, 1.000000000000000000, 0.9659258262890683122, 1.000000000000000000, 0.9659258262890683122, 1.000000000000000000, 0.9659258262890683122, 1.000000000000000000, 0.9659258262890683122, 1.000000000000000000, 0.9659258262890683122, 1.000000000000000000),
 ( 0.3333333333333333703, 0.3219752754296894559, 0.3333333333333333703, 0.3219752754296894559, 0.3333333333333333703, 0.3219752754296894559, 0.3333333333333333703, 0.3219752754296894559, 0.3333333333333333703, 0.3219752754296894559, 0.3333333333333333703, 0.3219752754296894559, 0.3333333333333333703, 0.3219752754296894559, 0.3333333333333333703, 0.3219752754296894559, 0.3333333333333333703, 0.3219752754296894559, 0.3333333333333333703, 0.3219752754296894559, 0.3333333333333333703, 0.3219752754296894559, 0.3333333333333333703, 0.3219752754296894559, 0.3333333333333333703, 0.3219752754296894559, 0.3333333333333333703, 0.3219752754296894559, 0.3333333333333333703, 0.3219752754296894559, 0.3333333333333333703, 0.3219752754296894559, 0.3333333333333333703, 0.3219752754296894559, 0.3333333333333333703, 0.3219752754296894559, 0.3333333333333333703, 0.3219752754296894559, 0.3333333333333333703, 0.3219752754296894559, 0.3333333333333333703, 0.3219752754296894559, 0.3333333333333333703, 0.3219752754296894559, 0.3333333333333333703, 0.3219752754296894559, 0.3333333333333333703, 0.3219752754296894559, 0.3333333333333333703, 0.3219752754296894559, 0.3333333333333333703, 0.3219752754296894559, 0.3333333333333333703, 0.3219752754296894559, 0.3333333333333333703, 0.3219752754296894559, 0.3333333333333333703, 0.3219752754296894559, 0.3333333333333333703, 0.3219752754296894559, 0.3333333333333333703, 0.3219752754296894559, 0.3333333333333333703, 0.3219752754296894559, 0.3333333333333333703, 0.3219752754296894559, 0.3333333333333333703, 0.3219752754296894559, 0.3333333333333333703, 0.3219752754296894559, 0.3333333333333333703, 0.3219752754296894559, 0.3333333333333333703, 0.3219752754296894559, 0.3333333333333333703, 0.3219752754296894559, 0.3333333333333333703, 0.3219752754296894559, 0.3333333333333333703, 0.3219752754296894559, 0.3333333333333333703, 0.3219752754296894559, 0.3333333333333333703, 0.3219752754296894559, 0.3333333333333333703, 0.3219752754296894559, 0.3333333333333333703, 0.3219752754296894559, 0.3333333333333333703, 0.3219752754296894559, 0.3333333333333333703, 0.3219752754296894559, 0.3333333333333333703, 0.3219752754296894559, 0.3333333333333333703, 0.3219752754296894559, 0.3333333333333333703, 0.3219752754296894559, 0.3333333333333333703, 0.3219752754296894559, 0.3333333333333333703, 0.3219752754296894559, 0.3333333333333333703, 0.3219752754296894559, 0.3333333333333333703, 0.3219752754296894559, 0.3333333333333333703, 0.3219752754296894559, 0.3333333333333333703, 0.3219752754296894559, 0.3333333333333333703, 0.3219752754296894559, 0.3333333333333333703, 0.3219752754296894559, 0.3333333333333333703, 0.3219752754296894559, 0.3333333333333333703, 0.3219752754296894559, 0.3333333333333333703, 0.3219752754296894559, 0.3333333333333333703, 0.3219752754296894559, 0.3333333333333333703, 0.3219752754296894559, 0.3333333333333333703, 0.3219752754296894559, 0.3333333333333333703, 0.3219752754296894559, 0.3333333333333333703, 0.3219752754296894559, 0.3333333333333333703, 0.3219752754296894559, 0.3333333333333333703, 0.3219752754296894559, 0.3333333333333333703, 0.3219752754296894559, 0.3333333333333333703, 0.3219752754296894559, 0.3333333333333333703, 0.3219752754296894559, 0.3333333333333333703, 0.3219752754296894559, 0.3333333333333333703, 0.3219752754296894559, 0.3333333333333333703, 0.3219752754296894559, 0.3333333333333333703, 0.3219752754296894559, 0.3333333333333333703, 0.3219752754296894559, 0.3333333333333333703, 0.3219752754296894559, 0.3333333333333333703, 0.3219752754296894559, 0.3333333333333333703, 0.3219752754296894559, 0.3333333333333333703, 0.3219752754296894559, 0.3333333333333333703, 0.3219752754296894559, 0.3333333333333333703, 0.3219752754296894559, 0.3333333333333333703, 0.3219752754296894559, 0.3333333333333333703, 0.3219752754296894559, 0.3333333333333333703, 0.3219752754296894559, 0.3333333333333333703, 0.3219752754296894559, 0.3333333333333333703, 0.3219752754296894559, 0.3333333333333333703, 0.3219752754296894559, 0.3333333333333333703, 0.3219752754296894559, 0.3333333333333333703, 0.3219752754296894559, 0.3333333333333333703, 0.3219752754296894559, 0.3333333333333333703, 0.3219752754296894559, 0.3333333333333333703, 0.3219752754296894559, 0.3333333333333333703, 0.3219752754296894559, 0.3333333333333333703, 0.3219752754296894559, 0.3333333333333333703, 0.3219752754296894559, 0.3333333333333333703, 0.3219752754296894559, 0.3333333333333333703, 0.3219752754296894559, 0.3333333333333333703, 0.3219752754296894559, 0.3333333333333333703, 0.3219752754296894559, 0.3333333333333333703, 0.3219752754296894559, 0.3333333333333333703, 0.3219752754296894559, 0.3333333333333333703, 0.3219752754296894559, 0.3333333333333333703, 0.3219752754296894559, 0.3333333333333333703, 0.3219752754296894559, 0.3333333333333333703, 0.3219752754296894559, 0.3333333333333333703, 0.3219752754296894559, 0.3333333333333333703, 0.3219752754296894559, 0.3333333333333333703, 0.3219752754296894559, 0.3333333333333333703, 0.3219752754296894559, 0.3333333333333333703, 0.3219752754296894559, 0.3333333333333333703, 0.3219752754296894559, 0.3333333333333333703, 0.3219752754296894559, 0.3333333333333333703, 0.3219752754296894559, 0.3333333333333333703, 0.3219752754296894559, 0.3333333333333333703, 0.3219752754296894559, 0.3333333333333333703, 0.3219752754296894559, 0.3333333333333333703, 0.3219752754296894559, 0.3333333333333333703, 0.3219752754296894559, 0.3333333333333333703, 0.3219752754296894559, 0.3333333333333333703, 0.3219752754296894559, 0.3333333333333333703, 0.3219752754296894559, 0.3333333333333333703, 0.3219752754296894559, 0.3333333333333333703, 0.3219752754296894559, 0.3333333333333333703, 0.3219752754296894559, 0.3333333333333333703, 0.3219752754296894559, 0.3333333333333333703, 0.3219752754296894559, 0.3333333333333333703, 0.3219752754296894559, 0.3333333333333333703, 0.3219752754296894559, 0.3333333333333333703, 0.3219752754296894559, 0.3333333333333333703, 0.3219752754296894559, 0.3333333333333333703, 0.3219752754296894559, 0.3333333333333333703, 0.3219752754296894559, 0.3333333333333333703, 0.3219752754296894559, 0.3333333333333333703, 0.3219752754296894559, 0.3333333333333333703, 0.3219752754296894559, 0.3333333333333333703, 0.3219752754296894559, 0.3333333333333333703, 0.3219752754296894559, 0.3333333333333333703, 0.3219752754296894559, 0.3333333333333333703, 0.3219752754296894559, 0.3333333333333333703, 0.3219752754296894559, 0.3333333333333333703, 0.3219752754296894559, 0.3333333333333333703, 0.3219752754296894559, 0.3333333333333333703, 0.3219752754296894559, 0.3333333333333333703, 0.3219752754296894559, 0.3333333333333333703, 0.3219752754296894559, 0.3333333333333333703, 0.3219752754296894559, 0.3333333333333333703, 0.3219752754296894559, 0.3333333333333333703, 0.3219752754296894559, 0.3333333333333333703, 0.3219752754296894559, 0.3333333333333333703, 0.3219752754296894559, 0.3333333333333333703, 0.3219752754296894559, 0.3333333333333333703, 0.3219752754296894559, 0.3333333333333333703, 0.3219752754296894559, 0.3333333333333333703, 0.3219752754296894559, 0.3333333333333333703, 0.3219752754296894559, 0.3333333333333333703, 0.3219752754296894559, 0.3333333333333333703, 0.3219752754296894559, 0.3333333333333333703, 0.3219752754296894559, 0.3333333333333333703, 0.3219752754296894559, 0.3333333333333333703, 0.3219752754296894559, 0.3333333333333333703, 0.3219752754296894559, 0.3333333333333333703, 0.3219752754296894559, 0.3333333333333333703, 0.3219752754296894559, 0.3333333333333333703, 0.3219752754296894559, 0.3333333333333333703, 0.3219752754296894559, 0.3333333333333333703, 0.3219752754296894559, 0.3333333333333333703, 0.3219752754296894559, 0.3333333333333333703, 0.3219752754296894559, 0.3333333333333333703, 0.3219752754296894559, 0.3333333333333333703, 0.3219752754296894559, 0.3333333333333333703, 0.3219752754296894559, 0.3333333333333333703, 0.3219752754296894559, 0.3333333333333333703, 0.3219752754296894559, 0.3333333333333333703, 0.3219752754296894559, 0.3333333333333333703, 0.3219752754296894559, 0.3333333333333333703, 0.3219752754296894559, 0.3333333333333333703, 0.3219752754296894559, 0.3333333333333333703, 0.3219752754296894559, 0.3333333333333333703, 0.3219752754296894559, 0.3333333333333333703, 0.3219752754296894559, 0.3333333333333333703, 0.3219752754296894559, 0.3333333333333333703, 0.3219752754296894559, 0.3333333333333333703, 0.3219752754296894559, 0.3333333333333333703, 0.3219752754296894559, 0.3333333333333333703, 0.3219752754296894559, 0.3333333333333333703, 0.3219752754296894559, 0.3333333333333333703, 0.3219752754296894559, 0.3333333333333333703, 0.3219752754296894559, 0.3333333333333333703, 0.3219752754296894559, 0.3333333333333333703, 0.3219752754296894559, 0.3333333333333333703, 0.3219752754296894559, 0.3333333333333333703, 0.3219752754296894559, 0.3333333333333333703, 0.3219752754296894559, 0.3333333333333333703, 0.3219752754296894559, 0.3333333333333333703, 0.3219752754296894559, 0.3333333333333333703, 0.3219752754296894559, 0.3333333333333333703, 0.3219752754296894559, 0.3333333333333333703, 0.3219752754296894559, 0.3333333333333333703, 0.3219752754296894559, 0.3333333333333333703, 0.3219752754296894559, 0.3333333333333333703, 0.3219752754296894559, 0.3333333333333333703, 0.3219752754296894559, 0.3333333333333333703, 0.3219752754296894559, 0.3333333333333333703, 0.3219752754296894559, 0.3333333333333333703, 0.3219752754296894559, 0.3333333333333333703, 0.3219752754296894559, 0.3333333333333333703, 0.3219752754296894559, 0.3333333333333333703, 0.3219752754296894559, 0.3333333333333333703, 0.3219752754296894559, 0.3333333333333333703, 0.3219752754296894559, 0.3333333333333333703, 0.3219752754296894559, 0.3333333333333333703, 0.3219752754296894559, 0.3333333333333333703, 0.3219752754296894559, 0.3333333333333333703, 0.3219752754296894559, 0.3333333333333333703, 0.3219752754296894559, 0.3333333333333333703, 0.3219752754296894559, 0.3333333333333333703, 0.3219752754296894559, 0.3333333333333333703, 0.3219752754296894559, 0.3333333333333333703, 0.3219752754296894559, 0.3333333333333333703, 0.3219752754296894559, 0.3333333333333333703, 0.3219752754296894559, 0.3333333333333333703, 0.3219752754296894559, 0.3333333333333333703, 0.3219752754296894559, 0.3333333333333333703, 0.3219752754296894559, 0.3333333333333333703, 0.3219752754296894559, 0.3333333333333333703, 0.3219752754296894559, 0.3333333333333333703, 0.3219752754296894559, 0.3333333333333333703, 0.3219752754296894559, 0.3333333333333333703),
 ( 0.3333333333333333703, 0.3219752754296894559, 0.3333333333333333703, 0.3219752754296894559, 0.3333333333333333703, 0.3219752754296894559, 0.3333333333333333703, 0.3219752754296894559, 0.3333333333333333703, 0.3219752754296894559, 0.3333333333333333703, 0.3219752754296894559, 0.3333333333333333703, 0.3219752754296894559, 0.3333333333333333703, 0.3219752754296894559, 0.3333333333333333703, 0.3219752754296894559, 0.3333333333333333703, 0.3219752754296894559, 0.3333333333333333703, 0.3219752754296894559, 0.3333333333333333703, 0.3219752754296894559, 0.3333333333333333703, 0.3219752754296894559, 0.3333333333333333703, 0.3219752754296894559, 0.3333333333333333703, 0.3219752754296894559, 0.3333333333333333703, 0.3219752754296894559, 0.3333333333333333703, 0.3219752754296894559, 0.3333333333333333703, 0.3219752754296894559, 0.3333333333333333703, 0.3219752754296894559, 0.3333333333333333703, 0.3219752754296894559, 0.3333333333333333703, 0.3219752754296894559, 0.3333333333333333703, 0.3219752754296894559, 0.3333333333333333703, 0.3219752754296894559, 0.3333333333333333703, 0.3219752754296894559, 0.3333333333333333703, 0.3219752754296894559, 0.3333333333333333703, 0.3219752754296894559, 0.3333333333333333703, 0.3219752754296894559, 0.3333333333333333703, 0.3219752754296894559, 0.3333333333333333703, 0.3219752754296894559, 0.3333333333333333703, 0.3219752754296894559, 0.3333333333333333703, 0.3219752754296894559, 0.3333333333333333703, 0.3219752754296894559, 0.3333333333333333703, 0.3219752754296894559, 0.3333333333333333703, 0.3219752754296894559, 0.3333333333333333703, 0.3219752754296894559, 0.3333333333333333703, 0.3219752754296894559, 0.3333333333333333703, 0.3219752754296894559, 0.3333333333333333703, 0.3219752754296894559, 0.3333333333333333703, 0.3219752754296894559, 0.3333333333333333703, 0.3219752754296894559, 0.3333333333333333703, 0.3219752754296894559, 0.3333333333333333703, 0.3219752754296894559, 0.3333333333333333703, 0.3219752754296894559, 0.3333333333333333703, 0.3219752754296894559, 0.3333333333333333703, 0.3219752754296894559, 0.3333333333333333703, 0.3219752754296894559, 0.3333333333333333703, 0.3219752754296894559, 0.3333333333333333703, 0.3219752754296894559, 0.3333333333333333703, 0.3219752754296894559, 0.3333333333333333703, 0.3219752754296894559, 0.3333333333333333703, 0.3219752754296894559, 0.3333333333333333703, 0.3219752754296894559, 0.3333333333333333703, 0.3219752754296894559, 0.3333333333333333703, 0.3219752754296894559, 0.3333333333333333703, 0.3219752754296894559, 0.3333333333333333703, 0.3219752754296894559, 0.3333333333333333703, 0.3219752754296894559, 0.3333333333333333703, 0.3219752754296894559, 0.3333333333333333703, 0.3219752754296894559, 0.3333333333333333703, 0.3219752754296894559, 0.3333333333333333703, 0.3219752754296894559, 0.3333333333333333703, 0.3219752754296894559, 0.3333333333333333703, 0.3219752754296894559, 0.3333333333333333703, 0.3219752754296894559, 0.3333333333333333703, 0.3219752754296894559, 0.3333333333333333703, 0.3219752754296894559, 0.3333333333333333703, 0.3219752754296894559, 0.3333333333333333703, 0.3219752754296894559, 0.3333333333333333703, 0.3219752754296894559, 0.3333333333333333703, 0.3219752754296894559, 0.3333333333333333703, 0.3219752754296894559, 0.3333333333333333703, 0.3219752754296894559, 0.3333333333333333703, 0.3219752754296894559, 0.3333333333333333703, 0.3219752754296894559, 0.3333333333333333703, 0.3219752754296894559, 0.3333333333333333703, 0.3219752754296894559, 0.3333333333333333703, 0.3219752754296894559, 0.3333333333333333703, 0.3219752754296894559, 0.3333333333333333703, 0.3219752754296894559, 0.3333333333333333703, 0.3219752754296894559, 0.3333333333333333703, 0.3219752754296894559, 0.3333333333333333703, 0.3219752754296894559, 0.3333333333333333703, 0.3219752754296894559, 0.3333333333333333703, 0.3219752754296894559, 0.3333333333333333703, 0.3219752754296894559, 0.3333333333333333703, 0.3219752754296894559, 0.3333333333333333703, 0.3219752754296894559, 0.3333333333333333703, 0.3219752754296894559, 0.3333333333333333703, 0.3219752754296894559, 0.3333333333333333703, 0.3219752754296894559, 0.3333333333333333703, 0.3219752754296894559, 0.3333333333333333703, 0.3219752754296894559, 0.3333333333333333703, 0.3219752754296894559, 0.3333333333333333703, 0.3219752754296894559, 0.3333333333333333703, 0.3219752754296894559, 0.3333333333333333703, 0.3219752754296894559, 0.3333333333333333703, 0.3219752754296894559, 0.3333333333333333703, 0.3219752754296894559, 0.3333333333333333703, 0.3219752754296894559, 0.3333333333333333703, 0.3219752754296894559, 0.3333333333333333703, 0.3219752754296894559, 0.3333333333333333703, 0.3219752754296894559, 0.3333333333333333703, 0.3219752754296894559, 0.3333333333333333703, 0.3219752754296894559, 0.3333333333333333703, 0.3219752754296894559, 0.3333333333333333703, 0.3219752754296894559, 0.3333333333333333703, 0.3219752754296894559, 0.3333333333333333703, 0.3219752754296894559, 0.3333333333333333703, 0.3219752754296894559, 0.3333333333333333703, 0.3219752754296894559, 0.3333333333333333703, 0.3219752754296894559, 0.3333333333333333703, 0.3219752754296894559, 0.3333333333333333703, 0.3219752754296894559, 0.3333333333333333703, 0.3219752754296894559, 0.3333333333333333703, 0.3219752754296894559, 0.3333333333333333703, 0.3219752754296894559, 0.3333333333333333703, 0.3219752754296894559, 0.3333333333333333703, 0.3219752754296894559, 0.3333333333333333703, 0.3219752754296894559, 0.3333333333333333703, 0.3219752754296894559, 0.3333333333333333703, 0.3219752754296894559, 0.3333333333333333703, 0.3219752754296894559, 0.3333333333333333703, 0.3219752754296894559, 0.3333333333333333703, 0.3219752754296894559, 0.3333333333333333703, 0.3219752754296894559, 0.3333333333333333703, 0.3219752754296894559, 0.3333333333333333703, 0.3219752754296894559, 0.3333333333333333703, 0.3219752754296894559, 0.3333333333333333703, 0.3219752754296894559, 0.3333333333333333703, 0.3219752754296894559, 0.3333333333333333703, 0.3219752754296894559, 0.3333333333333333703, 0.3219752754296894559, 0.3333333333333333703, 0.3219752754296894559, 0.3333333333333333703, 0.3219752754296894559, 0.3333333333333333703, 0.3219752754296894559, 0.3333333333333333703, 0.3219752754296894559, 0.3333333333333333703, 0.3219752754296894559, 0.3333333333333333703, 0.3219752754296894559, 0.3333333333333333703, 0.3219752754296894559, 0.3333333333333333703, 0.3219752754296894559, 0.3333333333333333703, 0.3219752754296894559, 0.3333333333333333703, 0.3219752754296894559, 0.3333333333333333703, 0.3219752754296894559, 0.3333333333333333703, 0.3219752754296894559, 0.3333333333333333703, 0.3219752754296894559, 0.3333333333333333703, 0.3219752754296894559, 0.3333333333333333703, 0.3219752754296894559, 0.3333333333333333703, 0.3219752754296894559, 0.3333333333333333703, 0.3219752754296894559, 0.3333333333333333703, 0.3219752754296894559, 0.3333333333333333703, 0.3219752754296894559, 0.3333333333333333703, 0.3219752754296894559, 0.3333333333333333703, 0.3219752754296894559, 0.3333333333333333703, 0.3219752754296894559, 0.3333333333333333703, 0.3219752754296894559, 0.3333333333333333703, 0.3219752754296894559, 0.3333333333333333703, 0.3219752754296894559, 0.3333333333333333703, 0.3219752754296894559, 0.3333333333333333703, 0.3219752754296894559, 0.3333333333333333703, 0.3219752754296894559, 0.3333333333333333703, 0.3219752754296894559, 0.3333333333333333703, 0.3219752754296894559, 0.3333333333333333703, 0.3219752754296894559, 0.3333333333333333703, 0.3219752754296894559, 0.3333333333333333703, 0.3219752754296894559, 0.3333333333333333703, 0.3219752754296894559, 0.3333333333333333703, 0.3219752754296894559, 0.3333333333333333703, 0.3219752754296894559, 0.3333333333333333703, 0.3219752754296894559, 0.3333333333333333703, 0.3219752754296894559, 0.3333333333333333703, 0.3219752754296894559, 0.3333333333333333703, 0.3219752754296894559, 0.3333333333333333703, 0.3219752754296894559, 0.3333333333333333703, 0.3219752754296894559, 0.3333333333333333703, 0.3219752754296894559, 0.3333333333333333703, 0.3219752754296894559, 0.3333333333333333703, 0.3219752754296894559, 0.3333333333333333703, 0.3219752754296894559, 0.3333333333333333703, 0.3219752754296894559, 0.3333333333333333703, 0.3219752754296894559, 0.3333333333333333703, 0.3219752754296894559, 0.3333333333333333703, 0.3219752754296894559, 0.3333333333333333703, 0.3219752754296894559, 0.3333333333333333703, 0.3219752754296894559, 0.3333333333333333703, 0.3219752754296894559, 0.3333333333333333703, 0.3219752754296894559, 0.3333333333333333703, 0.3219752754296894559, 0.3333333333333333703, 0.3219752754296894559, 0.3333333333333333703, 0.3219752754296894559, 0.3333333333333333703, 0.3219752754296894559, 0.3333333333333333703, 0.3219752754296894559, 0.3333333333333333703, 0.3219752754296894559, 0.3333333333333333703, 0.3219752754296894559, 0.3333333333333333703, 0.3219752754296894559, 0.3333333333333333703, 0.3219752754296894559, 0.3333333333333333703, 0.3219752754296894559, 0.3333333333333333703, 0.3219752754296894559, 0.3333333333333333703, 0.3219752754296894559, 0.3333333333333333703, 0.3219752754296894559, 0.3333333333333333703, 0.3219752754296894559, 0.3333333333333333703, 0.3219752754296894559, 0.3333333333333333703, 0.3219752754296894559, 0.3333333333333333703, 0.3219752754296894559, 0.3333333333333333703, 0.3219752754296894559, 0.3333333333333333703, 0.3219752754296894559, 0.3333333333333333703, 0.3219752754296894559, 0.3333333333333333703, 0.3219752754296894559, 0.3333333333333333703, 0.3219752754296894559, 0.3333333333333333703, 0.3219752754296894559, 0.3333333333333333703, 0.3219752754296894559, 0.3333333333333333703, 0.3219752754296894559, 0.3333333333333333703, 0.3219752754296894559, 0.3333333333333333703, 0.3219752754296894559, 0.3333333333333333703, 0.3219752754296894559, 0.3333333333333333703, 0.3219752754296894559, 0.3333333333333333703, 0.3219752754296894559, 0.3333333333333333703, 0.3219752754296894559, 0.3333333333333333703, 0.3219752754296894559, 0.3333333333333333703, 0.3219752754296894559, 0.3333333333333333703, 0.3219752754296894559, 0.3333333333333333703, 0.3219752754296894559, 0.3333333333333333703, 0.3219752754296894559, 0.3333333333333333703, 0.3219752754296894559, 0.3333333333333333703, 0.3219752754296894559, 0.3333333333333333703, 0.3219752754296894559, 0.3333333333333333703, 0.3219752754296894559, 0.3333333333333333703, 0.3219752754296894559, 0.3333333333333333703, 0.3219752754296894559, 0.3333333333333333703),
 ( 1.000000000000000000, 0.9659258262890683122, 1.000000000000000000, 0.9659258262890683122, 1.000000000000000000, 0.9659258262890683122, 1.000000000000000000, 0.9659258262890683122, 1.000000000000000000, 0.9659258262890683122, 1.000000000000000000, 0.9659258262890683122, 1.000000000000000000, 0.9659258262890683122, 1.000000000000000000, 0.9659258262890683122, 1.000000000000000000, 0.9659258262890683122, 1.000000000000000000, 0.9659258262890683122, 1.000000000000000000, 0.9659258262890683122, 1.000000000000000000, 0.9659258262890683122, 1.000000000000000000, 0.9659258262890683122, 1.000000000000000000, 0.9659258262890683122, 1.000000000000000000, 0.9659258262890683122, 1.000000000000000000, 0.9659258262890683122, 1.000000000000000000, 0.9659258262890683122, 1.000000000000000000, 0.9659258262890683122, 1.000000000000000000, 0.9659258262890683122, 1.000000000000000000, 0.9659258262890683122, 1.000000000000000000, 0.9659258262890683122, 1.000000000000000000, 0.9659258262890683122, 1.000000000000000000, 0.9659258262890683122, 1.000000000000000000, 0.9659258262890683122, 1.000000000000000000, 0.9659258262890683122, 1.000000000000000000, 0.9659258262890683122, 1.000000000000000000, 0.9659258262890683122, 1.000000000000000000, 0.9659258262890683122, 1.000000000000000000, 0.9659258262890683122, 1.000000000000000000, 0.9659258262890683122, 1.000000000000000000, 0.9659258262890683122, 1.000000000000000000, 0.9659258262890683122, 1.000000000000000000, 0.9659258262890683122, 1.000000000000000000, 0.9659258262890683122, 1.000000000000000000, 0.9659258262890683122, 1.000000000000000000, 0.9659258262890683122, 1.000000000000000000, 0.9659258262890683122, 1.000000000000000000, 0.9659258262890683122, 1.000000000000000000, 0.9659258262890683122, 1.000000000000000000, 0.9659258262890683122, 1.000000000000000000, 0.9659258262890683122, 1.000000000000000000, 0.9659258262890683122, 1.000000000000000000, 0.9659258262890683122, 1.000000000000000000, 0.9659258262890683122, 1.000000000000000000, 0.9659258262890683122, 1.000000000000000000, 0.9659258262890683122, 1.000000000000000000, 0.9659258262890683122, 1.000000000000000000, 0.9659258262890683122, 1.000000000000000000, 0.9659258262890683122, 1.000000000000000000, 0.9659258262890683122, 1.000000000000000000, 0.9659258262890683122, 1.000000000000000000, 0.9659258262890683122, 1.000000000000000000, 0.9659258262890683122, 1.000000000000000000, 0.9659258262890683122, 1.000000000000000000, 0.9659258262890683122, 1.000000000000000000, 0.9659258262890683122, 1.000000000000000000, 0.9659258262890683122, 1.000000000000000000, 0.9659258262890683122, 1.000000000000000000, 0.9659258262890683122, 1.000000000000000000, 0.9659258262890683122, 1.000000000000000000, 0.9659258262890683122, 1.000000000000000000, 0.9659258262890683122, 1.000000000000000000, 0.9659258262890683122, 1.000000000000000000, 0.9659258262890683122, 1.000000000000000000, 0.9659258262890683122, 1.000000000000000000, 0.9659258262890683122, 1.000000000000000000, 0.9659258262890683122, 1.000000000000000000, 0.9659258262890683122, 1.000000000000000000, 0.9659258262890683122, 1.000000000000000000, 0.9659258262890683122, 1.000000000000000000, 0.9659258262890683122, 1.000000000000000000, 0.9659258262890683122, 1.000000000000000000, 0.9659258262890683122, 1.000000000000000000, 0.9659258262890683122, 1.000000000000000000, 0.9659258262890683122, 1.000000000000000000, 0.9659258262890683122, 1.000000000000000000, 0.9659258262890683122, 1.000000000000000000, 0.9659258262890683122, 1.000000000000000000, 0.9659258262890683122, 1.000000000000000000, 0.9659258262890683122, 1.000000000000000000, 0.9659258262890683122, 1.000000000000000000, 0.9659258262890683122, 1.000000000000000000, 0.9659258262890683122, 1.000000000000000000, 0.9659258262890683122, 1.000000000000000000, 0.9659258262890683122, 1.000000000000000000, 0.9659258262890683122, 1.000000000000000000, 0.9659258262890683122, 1.000000000000000000, 0.9659258262890683122, 1.000000000000000000, 0.9659258262890683122, 1.000000000000000000, 0.9659258262890683122, 1.000000000000000000, 0.9659258262890683122, 1.000000000000000000, 0.9659258262890683122, 1.000000000000000000, 0.9659258262890683122, 1.000000000000000000, 0.9659258262890683122, 1.000000000000000000, 0.9659258262890683122, 1.000000000000000000, 0.9659258262890683122, 1.000000000000000000, 0.9659258262890683122, 1.000000000000000000, 0.9659258262890683122, 1.000000000000000000, 0.9659258262890683122, 1.000000000000000000, 0.9659258262890683122, 1.000000000000000000, 0.9659258262890683122, 1.000000000000000000, 0.9659258262890683122, 1.000000000000000000, 0.9659258262890683122, 1.000000000000000000, 0.9659258262890683122, 1.000000000000000000, 0.9659258262890683122, 1.000000000000000000, 0.9659258262890683122, 1.000000000000000000, 0.9659258262890683122, 1.000000000000000000, 0.9659258262890683122, 1.000000000000000000, 0.9659258262890683122, 1.000000000000000000, 0.9659258262890683122, 1.000000000000000000, 0.9659258262890683122, 1.000000000000000000, 0.9659258262890683122, 1.000000000000000000, 0.9659258262890683122, 1.000000000000000000, 0.9659258262890683122, 1.000000000000000000, 0.9659258262890683122, 1.000000000000000000, 0.9659258262890683122, 1.000000000000000000, 0.9659258262890683122, 1.000000000000000000, 0.9659258262890683122, 1.000000000000000000, 0.9659258262890683122, 1.000000000000000000, 0.9659258262890683122, 1.000000000000000000, 0.9659258262890683122, 1.000000000000000000, 0.9659258262890683122, 1.000000000000000000, 0.9659258262890683122, 1.000000000000000000, 0.9659258262890683122, 1.000000000000000000, 0.9659258262890683122, 1.000000000000000000, 0.9659258262890683122, 1.000000000000000000, 0.9659258262890683122, 1.000000000000000000, 0.9659258262890683122, 1.000000000000000000, 0.9659258262890683122, 1.000000000000000000, 0.9659258262890683122, 1.000000000000000000, 0.9659258262890683122, 1.000000000000000000, 0.9659258262890683122, 1.000000000000000000, 0.9659258262890683122, 1.000000000000000000, 0.9659258262890683122, 1.000000000000000000, 0.9659258262890683122, 1.000000000000000000, 0.9659258262890683122, 1.000000000000000000, 0.9659258262890683122, 1.000000000000000000, 0.9659258262890683122, 1.000000000000000000, 0.9659258262890683122, 1.000000000000000000, 0.9659258262890683122, 1.000000000000000000, 0.9659258262890683122, 1.000000000000000000, 0.9659258262890683122, 1.000000000000000000, 0.9659258262890683122, 1.000000000000000000, 0.9659258262890683122, 1.000000000000000000, 0.9659258262890683122, 1.000000000000000000, 0.9659258262890683122, 1.000000000000000000, 0.9659258262890683122, 1.000000000000000000, 0.9659258262890683122, 1.000000000000000000, 0.9659258262890683122, 1.000000000000000000, 0.9659258262890683122, 1.000000000000000000, 0.9659258262890683122, 1.000000000000000000, 0.9659258262890683122, 1.000000000000000000, 0.9659258262890683122, 1.000000000000000000, 0.9659258262890683122, 1.000000000000000000, 0.9659258262890683122, 1.000000000000000000, 0.9659258262890683122, 1.000000000000000000, 0.9659258262890683122, 1.000000000000000000, 0.9659258262890683122, 1.000000000000000000, 0.9659258262890683122, 1.000000000000000000, 0.9659258262890683122, 1.000000000000000000, 0.9659258262890683122, 1.000000000000000000, 0.9659258262890683122, 1.000000000000000000, 0.9659258262890683122, 1.000000000000000000, 0.9659258262890683122, 1.000000000000000000, 0.9659258262890683122, 1.000000000000000000, 0.9659258262890683122, 1.000000000000000000, 0.9659258262890683122, 1.000000000000000000, 0.9659258262890683122, 1.000000000000000000, 0.9659258262890683122, 1.000000000000000000, 0.9659258262890683122, 1.000000000000000000, 0.9659258262890683122, 1.000000000000000000, 0.9659258262890683122, 1.000000000000000000, 0.9659258262890683122, 1.000000000000000000, 0.9659258262890683122, 1.000000000000000000, 0.9659258262890683122, 1.000000000000000000, 0.9659258262890683122, 1.000000000000000000, 0.9659258262890683122, 1.000000000000000000, 0.9659258262890683122, 1.000000000000000000, 0.9659258262890683122, 1.000000000000000000, 0.9659258262890683122, 1.000000000000000000, 0.9659258262890683122, 1.000000000000000000, 0.9659258262890683122, 1.000000000000000000, 0.9659258262890683122, 1.000000000000000000, 0.9659258262890683122, 1.000000000000000000, 0.9659258262890683122, 1.000000000000000000, 0.9659258262890683122, 1.000000000000000000, 0.9659258262890683122, 1.000000000000000000, 0.9659258262890683122, 1.000000000000000000, 0.9659258262890683122, 1.000000000000000000, 0.9659258262890683122, 1.000000000000000000, 0.9659258262890683122, 1.000000000000000000, 0.9659258262890683122, 1.000000000000000000, 0.9659258262890683122, 1.000000000000000000, 0.9659258262890683122, 1.000000000000000000, 0.9659258262890683122, 1.000000000000000000, 0.9659258262890683122, 1.000000000000000000, 0.9659258262890683122, 1.000000000000000000, 0.9659258262890683122, 1.000000000000000000, 0.9659258262890683122, 1.000000000000000000, 0.9659258262890683122, 1.000000000000000000, 0.9659258262890683122, 1.000000000000000000, 0.9659258262890683122, 1.000000000000000000, 0.9659258262890683122, 1.000000000000000000, 0.9659258262890683122, 1.000000000000000000, 0.9659258262890683122, 1.000000000000000000, 0.9659258262890683122, 1.000000000000000000, 0.9659258262890683122, 1.000000000000000000, 0.9659258262890683122, 1.000000000000000000, 0.9659258262890683122, 1.000000000000000000, 0.9659258262890683122, 1.000000000000000000, 0.9659258262890683122, 1.000000000000000000, 0.9659258262890683122, 1.000000000000000000, 0.9659258262890683122, 1.000000000000000000, 0.9659258262890683122, 1.000000000000000000, 0.9659258262890683122, 1.000000000000000000, 0.9659258262890683122, 1.000000000000000000, 0.9659258262890683122, 1.000000000000000000, 0.9659258262890683122, 1.000000000000000000, 0.9659258262890683122, 1.000000000000000000, 0.9659258262890683122, 1.000000000000000000, 0.9659258262890683122, 1.000000000000000000, 0.9659258262890683122, 1.000000000000000000, 0.9659258262890683122, 1.000000000000000000, 0.9659258262890683122, 1.000000000000000000, 0.9659258262890683122, 1.000000000000000000, 0.9659258262890683122, 1.000000000000000000, 0.9659258262890683122, 1.000000000000000000, 0.9659258262890683122, 1.000000000000000000),
 ( 0.3333333333333333703, 0.3219752754296894559, 0.3333333333333333703, 0.3219752754296894559, 0.3333333333333333703, 0.3219752754296894559, 0.3333333333333333703, 0.3219752754296894559, 0.3333333333333333703, 0.3219752754296894559, 0.3333333333333333703, 0.3219752754296894559, 0.3333333333333333703, 0.3219752754296894559, 0.3333333333333333703, 0.3219752754296894559, 0.3333333333333333703, 0.3219752754296894559, 0.3333333333333333703, 0.3219752754296894559, 0.3333333333333333703, 0.3219752754296894559, 0.3333333333333333703, 0.3219752754296894559, 0.3333333333333333703, 0.3219752754296894559, 0.3333333333333333703, 0.3219752754296894559, 0.3333333333333333703, 0.3219752754296894559, 0.3333333333333333703, 0.3219752754296894559, 0.3333333333333333703, 0.3219752754296894559, 0.3333333333333333703, 0.3219752754296894559, 0.3333333333333333703, 0.3219752754296894559, 0.3333333333333333703, 0.3219752754296894559, 0.3333333333333333703, 0.3219752754296894559, 0.3333333333333333703, 0.3219752754296894559, 0.3333333333333333703, 0.3219752754296894559, 0.3333333333333333703, 0.3219752754296894559, 0.3333333333333333703, 0.3219752754296894559, 0.3333333333333333703, 0.3219752754296894559, 0.3333333333333333703, 0.3219752754296894559, 0.3333333333333333703, 0.3219752754296894559, 0.3333333333333333703, 0.3219752754296894559, 0.3333333333333333703, 0.3219752754296894559, 0.3333333333333333703, 0.3219752754296894559, 0.3333333333333333703, 0.3219752754296894559, 0.3333333333333333703, 0.3219752754296894559, 0.3333333333333333703, 0.3219752754296894559, 0.3333333333333333703, 0.3219752754296894559, 0.3333333333333333703, 0.3219752754296894559, 0.3333333333333333703, 0.3219752754296894559, 0.3333333333333333703, 0.3219752754296894559, 0.3333333333333333703, 0.3219752754296894559, 0.3333333333333333703, 0.3219752754296894559, 0.3333333333333333703, 0.3219752754296894559, 0.3333333333333333703, 0.3219752754296894559, 0.3333333333333333703, 0.3219752754296894559, 0.3333333333333333703, 0.3219752754296894559, 0.3333333333333333703, 0.3219752754296894559, 0.3333333333333333703, 0.3219752754296894559, 0.3333333333333333703, 0.3219752754296894559, 0.3333333333333333703, 0.3219752754296894559, 0.3333333333333333703, 0.3219752754296894559, 0.3333333333333333703, 0.3219752754296894559, 0.3333333333333333703, 0.3219752754296894559, 0.3333333333333333703, 0.3219752754296894559, 0.3333333333333333703, 0.3219752754296894559, 0.3333333333333333703, 0.3219752754296894559, 0.3333333333333333703, 0.3219752754296894559, 0.3333333333333333703, 0.3219752754296894559, 0.3333333333333333703, 0.3219752754296894559, 0.3333333333333333703, 0.3219752754296894559, 0.3333333333333333703, 0.3219752754296894559, 0.3333333333333333703, 0.3219752754296894559, 0.3333333333333333703, 0.3219752754296894559, 0.3333333333333333703, 0.3219752754296894559, 0.3333333333333333703, 0.3219752754296894559, 0.3333333333333333703, 0.3219752754296894559, 0.3333333333333333703, 0.3219752754296894559, 0.3333333333333333703, 0.3219752754296894559, 0.3333333333333333703, 0.3219752754296894559, 0.3333333333333333703, 0.3219752754296894559, 0.3333333333333333703, 0.3219752754296894559, 0.3333333333333333703, 0.3219752754296894559, 0.3333333333333333703, 0.3219752754296894559, 0.3333333333333333703, 0.3219752754296894559, 0.3333333333333333703, 0.3219752754296894559, 0.3333333333333333703, 0.3219752754296894559, 0.3333333333333333703, 0.3219752754296894559, 0.3333333333333333703, 0.3219752754296894559, 0.3333333333333333703, 0.3219752754296894559, 0.3333333333333333703, 0.3219752754296894559, 0.3333333333333333703, 0.3219752754296894559, 0.3333333333333333703, 0.3219752754296894559, 0.3333333333333333703, 0.3219752754296894559, 0.3333333333333333703, 0.3219752754296894559, 0.3333333333333333703, 0.3219752754296894559, 0.3333333333333333703, 0.3219752754296894559, 0.3333333333333333703, 0.3219752754296894559, 0.3333333333333333703, 0.3219752754296894559, 0.3333333333333333703, 0.3219752754296894559, 0.3333333333333333703, 0.3219752754296894559, 0.3333333333333333703, 0.3219752754296894559, 0.3333333333333333703, 0.3219752754296894559, 0.3333333333333333703, 0.3219752754296894559, 0.3333333333333333703, 0.3219752754296894559, 0.3333333333333333703, 0.3219752754296894559, 0.3333333333333333703, 0.3219752754296894559, 0.3333333333333333703, 0.3219752754296894559, 0.3333333333333333703, 0.3219752754296894559, 0.3333333333333333703, 0.3219752754296894559, 0.3333333333333333703, 0.3219752754296894559, 0.3333333333333333703, 0.3219752754296894559, 0.3333333333333333703, 0.3219752754296894559, 0.3333333333333333703, 0.3219752754296894559, 0.3333333333333333703, 0.3219752754296894559, 0.3333333333333333703, 0.3219752754296894559, 0.3333333333333333703, 0.3219752754296894559, 0.3333333333333333703, 0.3219752754296894559, 0.3333333333333333703, 0.3219752754296894559, 0.3333333333333333703, 0.3219752754296894559, 0.3333333333333333703, 0.3219752754296894559, 0.3333333333333333703, 0.3219752754296894559, 0.3333333333333333703, 0.3219752754296894559, 0.3333333333333333703, 0.3219752754296894559, 0.3333333333333333703, 0.3219752754296894559, 0.3333333333333333703, 0.3219752754296894559, 0.3333333333333333703, 0.3219752754296894559, 0.3333333333333333703, 0.3219752754296894559, 0.3333333333333333703, 0.3219752754296894559, 0.3333333333333333703, 0.3219752754296894559, 0.3333333333333333703, 0.3219752754296894559, 0.3333333333333333703, 0.3219752754296894559, 0.3333333333333333703, 0.3219752754296894559, 0.3333333333333333703, 0.3219752754296894559, 0.3333333333333333703, 0.3219752754296894559, 0.3333333333333333703, 0.3219752754296894559, 0.3333333333333333703, 0.3219752754296894559, 0.3333333333333333703, 0.3219752754296894559, 0.3333333333333333703, 0.3219752754296894559, 0.3333333333333333703, 0.3219752754296894559, 0.3333333333333333703, 0.3219752754296894559, 0.3333333333333333703, 0.3219752754296894559, 0.3333333333333333703, 0.3219752754296894559, 0.3333333333333333703, 0.3219752754296894559, 0.3333333333333333703, 0.3219752754296894559, 0.3333333333333333703, 0.3219752754296894559, 0.3333333333333333703, 0.3219752754296894559, 0.3333333333333333703, 0.3219752754296894559, 0.3333333333333333703, 0.3219752754296894559, 0.3333333333333333703, 0.3219752754296894559, 0.3333333333333333703, 0.3219752754296894559, 0.3333333333333333703, 0.3219752754296894559, 0.3333333333333333703, 0.3219752754296894559, 0.3333333333333333703, 0.3219752754296894559, 0.3333333333333333703, 0.3219752754296894559, 0.3333333333333333703, 0.3219752754296894559, 0.3333333333333333703, 0.3219752754296894559, 0.3333333333333333703, 0.3219752754296894559, 0.3333333333333333703, 0.3219752754296894559, 0.3333333333333333703, 0.3219752754296894559, 0.3333333333333333703, 0.3219752754296894559, 0.3333333333333333703, 0.3219752754296894559, 0.3333333333333333703, 0.3219752754296894559, 0.3333333333333333703, 0.3219752754296894559, 0.3333333333333333703, 0.3219752754296894559, 0.3333333333333333703, 0.3219752754296894559, 0.3333333333333333703, 0.3219752754296894559, 0.3333333333333333703, 0.3219752754296894559, 0.3333333333333333703, 0.3219752754296894559, 0.3333333333333333703, 0.3219752754296894559, 0.3333333333333333703, 0.3219752754296894559, 0.3333333333333333703, 0.3219752754296894559, 0.3333333333333333703, 0.3219752754296894559, 0.3333333333333333703, 0.3219752754296894559, 0.3333333333333333703, 0.3219752754296894559, 0.3333333333333333703, 0.3219752754296894559, 0.3333333333333333703, 0.3219752754296894559, 0.3333333333333333703, 0.3219752754296894559, 0.3333333333333333703, 0.3219752754296894559, 0.3333333333333333703, 0.3219752754296894559, 0.3333333333333333703, 0.3219752754296894559, 0.3333333333333333703, 0.3219752754296894559, 0.3333333333333333703, 0.3219752754296894559, 0.3333333333333333703, 0.3219752754296894559, 0.3333333333333333703, 0.3219752754296894559, 0.3333333333333333703, 0.3219752754296894559, 0.3333333333333333703, 0.3219752754296894559, 0.3333333333333333703, 0.3219752754296894559, 0.3333333333333333703, 0.3219752754296894559, 0.3333333333333333703, 0.3219752754296894559, 0.3333333333333333703, 0.3219752754296894559, 0.3333333333333333703, 0.3219752754296894559, 0.3333333333333333703, 0.3219752754296894559, 0.3333333333333333703, 0.3219752754296894559, 0.3333333333333333703, 0.3219752754296894559, 0.3333333333333333703, 0.3219752754296894559, 0.3333333333333333703, 0.3219752754296894559, 0.3333333333333333703, 0.3219752754296894559, 0.3333333333333333703, 0.3219752754296894559, 0.3333333333333333703, 0.3219752754296894559, 0.3333333333333333703, 0.3219752754296894559, 0.3333333333333333703, 0.3219752754296894559, 0.3333333333333333703, 0.3219752754296894559, 0.3333333333333333703, 0.3219752754296894559, 0.3333333333333333703, 0.3219752754296894559, 0.3333333333333333703, 0.3219752754296894559, 0.3333333333333333703, 0.3219752754296894559, 0.3333333333333333703, 0.3219752754296894559, 0.3333333333333333703, 0.3219752754296894559, 0.3333333333333333703, 0.3219752754296894559, 0.3333333333333333703, 0.3219752754296894559, 0.3333333333333333703, 0.3219752754296894559, 0.3333333333333333703, 0.3219752754296894559, 0.3333333333333333703, 0.3219752754296894559, 0.3333333333333333703, 0.3219752754296894559, 0.3333333333333333703, 0.3219752754296894559, 0.3333333333333333703, 0.3219752754296894559, 0.3333333333333333703, 0.3219752754296894559, 0.3333333333333333703, 0.3219752754296894559, 0.3333333333333333703, 0.3219752754296894559, 0.3333333333333333703, 0.3219752754296894559, 0.3333333333333333703, 0.3219752754296894559, 0.3333333333333333703, 0.3219752754296894559, 0.3333333333333333703, 0.3219752754296894559, 0.3333333333333333703, 0.3219752754296894559, 0.3333333333333333703, 0.3219752754296894559, 0.3333333333333333703, 0.3219752754296894559, 0.3333333333333333703, 0.3219752754296894559, 0.3333333333333333703, 0.3219752754296894559, 0.3333333333333333703, 0.3219752754296894559, 0.3333333333333333703, 0.3219752754296894559, 0.3333333333333333703, 0.3219752754296894559, 0.3333333333333333703, 0.3219752754296894559, 0.3333333333333333703, 0.3219752754296894559, 0.3333333333333333703, 0.3219752754296894559, 0.3333333333333333703, 0.3219752754296894559, 0.3333333333333333703, 0.3219752754296894559, 0.3333333333333333703, 0.3219752754296894559, 0.3333333333333333703, 0.3219752754296894559, 0.3333333333333333703, 0.3219752754296894559, 0.3333333333333333703, 0.3219752754296894559, 0.3333333333333333703),
 ( 0.3333333333333333703, 0.3219752754296894559, 0.3333333333333333703, 0.3219752754296894559, 0.3333333333333333703, 0.3219752754296894559, 0.3333333333333333703, 0.3219752754296894559, 0.3333333333333333703, 0.3219752754296894559, 0.3333333333333333703, 0.3219752754296894559, 0.3333333333333333703, 0.3219752754296894559, 0.3333333333333333703, 0.3219752754296894559, 0.3333333333333333703, 0.3219752754296894559, 0.3333333333333333703, 0.3219752754296894559, 0.3333333333333333703, 0.3219752754296894559, 0.3333333333333333703, 0.3219752754296894559, 0.3333333333333333703, 0.3219752754296894559, 0.3333333333333333703, 0.3219752754296894559, 0.3333333333333333703, 0.3219752754296894559, 0.3333333333333333703, 0.3219752754296894559, 0.3333333333333333703, 0.3219752754296894559, 0.3333333333333333703, 0.3219752754296894559, 0.3333333333333333703, 0.3219752754296894559, 0.3333333333333333703, 0.3219752754296894559, 0.3333333333333333703, 0.3219752754296894559, 0.3333333333333333703, 0.3219752754296894559, 0.3333333333333333703, 0.3219752754296894559, 0.3333333333333333703, 0.3219752754296894559, 0.3333333333333333703, 0.3219752754296894559, 0.3333333333333333703, 0.3219752754296894559, 0.3333333333333333703, 0.3219752754296894559, 0.3333333333333333703, 0.3219752754296894559, 0.3333333333333333703, 0.3219752754296894559, 0.3333333333333333703, 0.3219752754296894559, 0.3333333333333333703, 0.3219752754296894559, 0.3333333333333333703, 0.3219752754296894559, 0.3333333333333333703, 0.3219752754296894559, 0.3333333333333333703, 0.3219752754296894559, 0.3333333333333333703, 0.3219752754296894559, 0.3333333333333333703, 0.3219752754296894559, 0.3333333333333333703, 0.3219752754296894559, 0.3333333333333333703, 0.3219752754296894559, 0.3333333333333333703, 0.3219752754296894559, 0.3333333333333333703, 0.3219752754296894559, 0.3333333333333333703, 0.3219752754296894559, 0.3333333333333333703, 0.3219752754296894559, 0.3333333333333333703, 0.3219752754296894559, 0.3333333333333333703, 0.3219752754296894559, 0.3333333333333333703, 0.3219752754296894559, 0.3333333333333333703, 0.3219752754296894559, 0.3333333333333333703, 0.3219752754296894559, 0.3333333333333333703, 0.3219752754296894559, 0.3333333333333333703, 0.3219752754296894559, 0.3333333333333333703, 0.3219752754296894559, 0.3333333333333333703, 0.3219752754296894559, 0.3333333333333333703, 0.3219752754296894559, 0.3333333333333333703, 0.3219752754296894559, 0.3333333333333333703, 0.3219752754296894559, 0.3333333333333333703, 0.3219752754296894559, 0.3333333333333333703, 0.3219752754296894559, 0.3333333333333333703, 0.3219752754296894559, 0.3333333333333333703, 0.3219752754296894559, 0.3333333333333333703, 0.3219752754296894559, 0.3333333333333333703, 0.3219752754296894559, 0.3333333333333333703, 0.3219752754296894559, 0.3333333333333333703, 0.3219752754296894559, 0.3333333333333333703, 0.3219752754296894559, 0.3333333333333333703, 0.3219752754296894559, 0.3333333333333333703, 0.3219752754296894559, 0.3333333333333333703, 0.3219752754296894559, 0.3333333333333333703, 0.3219752754296894559, 0.3333333333333333703, 0.3219752754296894559, 0.3333333333333333703, 0.3219752754296894559, 0.3333333333333333703, 0.3219752754296894559, 0.3333333333333333703, 0.3219752754296894559, 0.3333333333333333703, 0.3219752754296894559, 0.3333333333333333703, 0.3219752754296894559, 0.3333333333333333703, 0.3219752754296894559, 0.3333333333333333703, 0.3219752754296894559, 0.3333333333333333703, 0.3219752754296894559, 0.3333333333333333703, 0.3219752754296894559, 0.3333333333333333703, 0.3219752754296894559, 0.3333333333333333703, 0.3219752754296894559, 0.3333333333333333703, 0.3219752754296894559, 0.3333333333333333703, 0.3219752754296894559, 0.3333333333333333703, 0.3219752754296894559, 0.3333333333333333703, 0.3219752754296894559, 0.3333333333333333703, 0.3219752754296894559, 0.3333333333333333703, 0.3219752754296894559, 0.3333333333333333703, 0.3219752754296894559, 0.3333333333333333703, 0.3219752754296894559, 0.3333333333333333703, 0.3219752754296894559, 0.3333333333333333703, 0.3219752754296894559, 0.3333333333333333703, 0.3219752754296894559, 0.3333333333333333703, 0.3219752754296894559, 0.3333333333333333703, 0.3219752754296894559, 0.3333333333333333703, 0.3219752754296894559, 0.3333333333333333703, 0.3219752754296894559, 0.3333333333333333703, 0.3219752754296894559, 0.3333333333333333703, 0.3219752754296894559, 0.3333333333333333703, 0.3219752754296894559, 0.3333333333333333703, 0.3219752754296894559, 0.3333333333333333703, 0.3219752754296894559, 0.3333333333333333703, 0.3219752754296894559, 0.3333333333333333703, 0.3219752754296894559, 0.3333333333333333703, 0.3219752754296894559, 0.3333333333333333703, 0.3219752754296894559, 0.3333333333333333703, 0.3219752754296894559, 0.3333333333333333703, 0.3219752754296894559, 0.3333333333333333703, 0.3219752754296894559, 0.3333333333333333703, 0.3219752754296894559, 0.3333333333333333703, 0.3219752754296894559, 0.3333333333333333703, 0.3219752754296894559, 0.3333333333333333703, 0.3219752754296894559, 0.3333333333333333703, 0.3219752754296894559, 0.3333333333333333703, 0.3219752754296894559, 0.3333333333333333703, 0.3219752754296894559, 0.3333333333333333703, 0.3219752754296894559, 0.3333333333333333703, 0.3219752754296894559, 0.3333333333333333703, 0.3219752754296894559, 0.3333333333333333703, 0.3219752754296894559, 0.3333333333333333703, 0.3219752754296894559, 0.3333333333333333703, 0.3219752754296894559, 0.3333333333333333703, 0.3219752754296894559, 0.3333333333333333703, 0.3219752754296894559, 0.3333333333333333703, 0.3219752754296894559, 0.3333333333333333703, 0.3219752754296894559, 0.3333333333333333703, 0.3219752754296894559, 0.3333333333333333703, 0.3219752754296894559, 0.3333333333333333703, 0.3219752754296894559, 0.3333333333333333703, 0.3219752754296894559, 0.3333333333333333703, 0.3219752754296894559, 0.3333333333333333703, 0.3219752754296894559, 0.3333333333333333703, 0.3219752754296894559, 0.3333333333333333703, 0.3219752754296894559, 0.3333333333333333703, 0.3219752754296894559, 0.3333333333333333703, 0.3219752754296894559, 0.3333333333333333703, 0.3219752754296894559, 0.3333333333333333703, 0.3219752754296894559, 0.3333333333333333703, 0.3219752754296894559, 0.3333333333333333703, 0.3219752754296894559, 0.3333333333333333703, 0.3219752754296894559, 0.3333333333333333703, 0.3219752754296894559, 0.3333333333333333703, 0.3219752754296894559, 0.3333333333333333703, 0.3219752754296894559, 0.3333333333333333703, 0.3219752754296894559, 0.3333333333333333703, 0.3219752754296894559, 0.3333333333333333703, 0.3219752754296894559, 0.3333333333333333703, 0.3219752754296894559, 0.3333333333333333703, 0.3219752754296894559, 0.3333333333333333703, 0.3219752754296894559, 0.3333333333333333703, 0.3219752754296894559, 0.3333333333333333703, 0.3219752754296894559, 0.3333333333333333703, 0.3219752754296894559, 0.3333333333333333703, 0.3219752754296894559, 0.3333333333333333703, 0.3219752754296894559, 0.3333333333333333703, 0.3219752754296894559, 0.3333333333333333703, 0.3219752754296894559, 0.3333333333333333703, 0.3219752754296894559, 0.3333333333333333703, 0.3219752754296894559, 0.3333333333333333703, 0.3219752754296894559, 0.3333333333333333703, 0.3219752754296894559, 0.3333333333333333703, 0.3219752754296894559, 0.3333333333333333703, 0.3219752754296894559, 0.3333333333333333703, 0.3219752754296894559, 0.3333333333333333703, 0.3219752754296894559, 0.3333333333333333703, 0.3219752754296894559, 0.3333333333333333703, 0.3219752754296894559, 0.3333333333333333703, 0.3219752754296894559, 0.3333333333333333703, 0.3219752754296894559, 0.3333333333333333703, 0.3219752754296894559, 0.3333333333333333703, 0.3219752754296894559, 0.3333333333333333703, 0.3219752754296894559, 0.3333333333333333703, 0.3219752754296894559, 0.3333333333333333703, 0.3219752754296894559, 0.3333333333333333703, 0.3219752754296894559, 0.3333333333333333703, 0.3219752754296894559, 0.3333333333333333703, 0.3219752754296894559, 0.3333333333333333703, 0.3219752754296894559, 0.3333333333333333703, 0.3219752754296894559, 0.3333333333333333703, 0.3219752754296894559, 0.3333333333333333703, 0.3219752754296894559, 0.3333333333333333703, 0.3219752754296894559, 0.3333333333333333703, 0.3219752754296894559, 0.3333333333333333703, 0.3219752754296894559, 0.3333333333333333703, 0.3219752754296894559, 0.3333333333333333703, 0.3219752754296894559, 0.3333333333333333703, 0.3219752754296894559, 0.3333333333333333703, 0.3219752754296894559, 0.3333333333333333703, 0.3219752754296894559, 0.3333333333333333703, 0.3219752754296894559, 0.3333333333333333703, 0.3219752754296894559, 0.3333333333333333703, 0.3219752754296894559, 0.3333333333333333703, 0.3219752754296894559, 0.3333333333333333703, 0.3219752754296894559, 0.3333333333333333703, 0.3219752754296894559, 0.3333333333333333703, 0.3219752754296894559, 0.3333333333333333703, 0.3219752754296894559, 0.3333333333333333703, 0.3219752754296894559, 0.3333333333333333703, 0.3219752754296894559, 0.3333333333333333703, 0.3219752754296894559, 0.3333333333333333703, 0.3219752754296894559, 0.3333333333333333703, 0.3219752754296894559, 0.3333333333333333703, 0.3219752754296894559, 0.3333333333333333703, 0.3219752754296894559, 0.3333333333333333703, 0.3219752754296894559, 0.3333333333333333703, 0.3219752754296894559, 0.3333333333333333703, 0.3219752754296894559, 0.3333333333333333703, 0.3219752754296894559, 0.3333333333333333703, 0.3219752754296894559, 0.3333333333333333703, 0.3219752754296894559, 0.3333333333333333703, 0.3219752754296894559, 0.3333333333333333703, 0.3219752754296894559, 0.3333333333333333703, 0.3219752754296894559, 0.3333333333333333703, 0.3219752754296894559, 0.3333333333333333703, 0.3219752754296894559, 0.3333333333333333703, 0.3219752754296894559, 0.3333333333333333703, 0.3219752754296894559, 0.3333333333333333703, 0.3219752754296894559, 0.3333333333333333703, 0.3219752754296894559, 0.3333333333333333703, 0.3219752754296894559, 0.3333333333333333703, 0.3219752754296894559, 0.3333333333333333703, 0.3219752754296894559, 0.3333333333333333703, 0.3219752754296894559, 0.3333333333333333703, 0.3219752754296894559, 0.3333333333333333703, 0.3219752754296894559, 0.3333333333333333703, 0.3219752754296894559, 0.3333333333333333703, 0.3219752754296894559, 0.3333333333333333703, 0.3219752754296894559, 0.3333333333333333703, 0.3219752754296894559, 0.3333333333333333703, 0.3219752754296894559, 0.3333333333333333703, 0.3219752754296894559, 0.3333333333333333703),
 ( 1.000000000000000000, 0.9659258262890683122, 1.000000000000000000, 0.9659258262890683122, 1.000000000000000000, 0.9659258262890683122, 1.000000000000000000, 0.9659258262890683122, 1.000000000000000000, 0.9659258262890683122, 1.000000000000000000, 0.9659258262890683122, 1.000000000000000000, 0.9659258262890683122, 1.000000000000000000, 0.9659258262890683122, 1.000000000000000000, 0.9659258262890683122, 1.000000000000000000, 0.9659258262890683122, 1.000000000000000000, 0.9659258262890683122, 1.000000000000000000, 0.9659258262890683122, 1.000000000000000000, 0.9659258262890683122, 1.000000000000000000, 0.9659258262890683122, 1.000000000000000000, 0.9659258262890683122, 1.000000000000000000, 0.9659258262890683122, 1.000000000000000000, 0.9659258262890683122, 1.000000000000000000, 0.9659258262890683122, 1.000000000000000000, 0.9659258262890683122, 1.000000000000000000, 0.9659258262890683122, 1.000000000000000000, 0.9659258262890683122, 1.000000000000000000, 0.9659258262890683122, 1.000000000000000000, 0.9659258262890683122, 1.000000000000000000, 0.9659258262890683122, 1.000000000000000000, 0.9659258262890683122, 1.000000000000000000, 0.9659258262890683122, 1.000000000000000000, 0.9659258262890683122, 1.000000000000000000, 0.9659258262890683122, 1.000000000000000000, 0.9659258262890683122, 1.000000000000000000, 0.9659258262890683122, 1.000000000000000000, 0.9659258262890683122, 1.000000000000000000, 0.9659258262890683122, 1.000000000000000000, 0.9659258262890683122, 1.000000000000000000, 0.9659258262890683122, 1.000000000000000000, 0.9659258262890683122, 1.000000000000000000, 0.9659258262890683122, 1.000000000000000000, 0.9659258262890683122, 1.000000000000000000, 0.9659258262890683122, 1.000000000000000000, 0.9659258262890683122, 1.000000000000000000, 0.9659258262890683122, 1.000000000000000000, 0.9659258262890683122, 1.000000000000000000, 0.9659258262890683122, 1.000000000000000000, 0.9659258262890683122, 1.000000000000000000, 0.9659258262890683122, 1.000000000000000000, 0.9659258262890683122, 1.000000000000000000, 0.9659258262890683122, 1.000000000000000000, 0.9659258262890683122, 1.000000000000000000, 0.9659258262890683122, 1.000000000000000000, 0.9659258262890683122, 1.000000000000000000, 0.9659258262890683122, 1.000000000000000000, 0.9659258262890683122, 1.000000000000000000, 0.9659258262890683122, 1.000000000000000000, 0.9659258262890683122, 1.000000000000000000, 0.9659258262890683122, 1.000000000000000000, 0.9659258262890683122, 1.000000000000000000, 0.9659258262890683122, 1.000000000000000000, 0.9659258262890683122, 1.000000000000000000, 0.9659258262890683122, 1.000000000000000000, 0.9659258262890683122, 1.000000000000000000, 0.9659258262890683122, 1.000000000000000000, 0.9659258262890683122, 1.000000000000000000, 0.9659258262890683122, 1.000000000000000000, 0.9659258262890683122, 1.000000000000000000, 0.9659258262890683122, 1.000000000000000000, 0.9659258262890683122, 1.000000000000000000, 0.9659258262890683122, 1.000000000000000000, 0.9659258262890683122, 1.000000000000000000, 0.9659258262890683122, 1.000000000000000000, 0.9659258262890683122, 1.000000000000000000, 0.9659258262890683122, 1.000000000000000000, 0.9659258262890683122, 1.000000000000000000, 0.9659258262890683122, 1.000000000000000000, 0.9659258262890683122, 1.000000000000000000, 0.9659258262890683122, 1.000000000000000000, 0.9659258262890683122, 1.000000000000000000, 0.9659258262890683122, 1.000000000000000000, 0.9659258262890683122, 1.000000000000000000, 0.9659258262890683122, 1.000000000000000000, 0.9659258262890683122, 1.000000000000000000, 0.9659258262890683122, 1.000000000000000000, 0.9659258262890683122, 1.000000000000000000, 0.9659258262890683122, 1.000000000000000000, 0.9659258262890683122, 1.000000000000000000, 0.9659258262890683122, 1.000000000000000000, 0.9659258262890683122, 1.000000000000000000, 0.9659258262890683122, 1.000000000000000000, 0.9659258262890683122, 1.000000000000000000, 0.9659258262890683122, 1.000000000000000000, 0.9659258262890683122, 1.000000000000000000, 0.9659258262890683122, 1.000000000000000000, 0.9659258262890683122, 1.000000000000000000, 0.9659258262890683122, 1.000000000000000000, 0.9659258262890683122, 1.000000000000000000, 0.9659258262890683122, 1.000000000000000000, 0.9659258262890683122, 1.000000000000000000, 0.9659258262890683122, 1.000000000000000000, 0.9659258262890683122, 1.000000000000000000, 0.9659258262890683122, 1.000000000000000000, 0.9659258262890683122, 1.000000000000000000, 0.9659258262890683122, 1.000000000000000000, 0.9659258262890683122, 1.000000000000000000, 0.9659258262890683122, 1.000000000000000000, 0.9659258262890683122, 1.000000000000000000, 0.9659258262890683122, 1.000000000000000000, 0.9659258262890683122, 1.000000000000000000, 0.9659258262890683122, 1.000000000000000000, 0.9659258262890683122, 1.000000000000000000, 0.9659258262890683122, 1.000000000000000000, 0.9659258262890683122, 1.000000000000000000, 0.9659258262890683122, 1.000000000000000000, 0.9659258262890683122, 1.000000000000000000, 0.9659258262890683122, 1.000000000000000000, 0.9659258262890683122, 1.000000000000000000, 0.9659258262890683122, 1.000000000000000000, 0.9659258262890683122, 1.000000000000000000, 0.9659258262890683122, 1.000000000000000000, 0.9659258262890683122, 1.000000000000000000, 0.9659258262890683122, 1.000000000000000000, 0.9659258262890683122, 1.000000000000000000, 0.9659258262890683122, 1.000000000000000000, 0.9659258262890683122, 1.000000000000000000, 0.9659258262890683122, 1.000000000000000000, 0.9659258262890683122, 1.000000000000000000, 0.9659258262890683122, 1.000000000000000000, 0.9659258262890683122, 1.000000000000000000, 0.9659258262890683122, 1.000000000000000000, 0.9659258262890683122, 1.000000000000000000, 0.9659258262890683122, 1.000000000000000000, 0.9659258262890683122, 1.000000000000000000, 0.9659258262890683122, 1.000000000000000000, 0.9659258262890683122, 1.000000000000000000, 0.9659258262890683122, 1.000000000000000000, 0.9659258262890683122, 1.000000000000000000, 0.9659258262890683122, 1.000000000000000000, 0.9659258262890683122, 1.000000000000000000, 0.9659258262890683122, 1.000000000000000000, 0.9659258262890683122, 1.000000000000000000, 0.9659258262890683122, 1.000000000000000000, 0.9659258262890683122, 1.000000000000000000, 0.9659258262890683122, 1.000000000000000000, 0.9659258262890683122, 1.000000000000000000, 0.9659258262890683122, 1.000000000000000000, 0.9659258262890683122, 1.000000000000000000, 0.9659258262890683122, 1.000000000000000000, 0.9659258262890683122, 1.000000000000000000, 0.9659258262890683122, 1.000000000000000000, 0.9659258262890683122, 1.000000000000000000, 0.9659258262890683122, 1.000000000000000000, 0.9659258262890683122, 1.000000000000000000, 0.9659258262890683122, 1.000000000000000000, 0.9659258262890683122, 1.000000000000000000, 0.9659258262890683122, 1.000000000000000000, 0.9659258262890683122, 1.000000000000000000, 0.9659258262890683122, 1.000000000000000000, 0.9659258262890683122, 1.000000000000000000, 0.9659258262890683122, 1.000000000000000000, 0.9659258262890683122, 1.000000000000000000, 0.9659258262890683122, 1.000000000000000000, 0.9659258262890683122, 1.000000000000000000, 0.9659258262890683122, 1.000000000000000000, 0.9659258262890683122, 1.000000000000000000, 0.9659258262890683122, 1.000000000000000000, 0.9659258262890683122, 1.000000000000000000, 0.9659258262890683122, 1.000000000000000000, 0.9659258262890683122, 1.000000000000000000, 0.9659258262890683122, 1.000000000000000000, 0.9659258262890683122, 1.000000000000000000, 0.9659258262890683122, 1.000000000000000000, 0.9659258262890683122, 1.000000000000000000, 0.9659258262890683122, 1.000000000000000000, 0.9659258262890683122, 1.000000000000000000, 0.9659258262890683122, 1.000000000000000000, 0.9659258262890683122, 1.000000000000000000, 0.9659258262890683122, 1.000000000000000000, 0.9659258262890683122, 1.000000000000000000, 0.9659258262890683122, 1.000000000000000000, 0.9659258262890683122, 1.000000000000000000, 0.9659258262890683122, 1.000000000000000000, 0.9659258262890683122, 1.000000000000000000, 0.9659258262890683122, 1.000000000000000000, 0.9659258262890683122, 1.000000000000000000, 0.9659258262890683122, 1.000000000000000000, 0.9659258262890683122, 1.000000000000000000, 0.9659258262890683122, 1.000000000000000000, 0.9659258262890683122, 1.000000000000000000, 0.9659258262890683122, 1.000000000000000000, 0.9659258262890683122, 1.000000000000000000, 0.9659258262890683122, 1.000000000000000000, 0.9659258262890683122, 1.000000000000000000, 0.9659258262890683122, 1.000000000000000000, 0.9659258262890683122, 1.000000000000000000, 0.9659258262890683122, 1.000000000000000000, 0.9659258262890683122, 1.000000000000000000, 0.9659258262890683122, 1.000000000000000000, 0.9659258262890683122, 1.000000000000000000, 0.9659258262890683122, 1.000000000000000000, 0.9659258262890683122, 1.000000000000000000, 0.9659258262890683122, 1.000000000000000000, 0.9659258262890683122, 1.000000000000000000, 0.9659258262890683122, 1.000000000000000000, 0.9659258262890683122, 1.000000000000000000, 0.9659258262890683122, 1.000000000000000000, 0.9659258262890683122, 1.000000000000000000, 0.9659258262890683122, 1.000000000000000000, 0.9659258262890683122, 1.000000000000000000, 0.9659258262890683122, 1.000000000000000000, 0.9659258262890683122, 1.000000000000000000, 0.9659258262890683122, 1.000000000000000000, 0.9659258262890683122, 1.000000000000000000, 0.9659258262890683122, 1.000000000000000000, 0.9659258262890683122, 1.000000000000000000, 0.9659258262890683122, 1.000000000000000000, 0.9659258262890683122, 1.000000000000000000, 0.9659258262890683122, 1.000000000000000000, 0.9659258262890683122, 1.000000000000000000, 0.9659258262890683122, 1.000000000000000000, 0.9659258262890683122, 1.000000000000000000, 0.9659258262890683122, 1.000000000000000000, 0.9659258262890683122, 1.000000000000000000, 0.9659258262890683122, 1.000000000000000000, 0.9659258262890683122, 1.000000000000000000, 0.9659258262890683122, 1.000000000000000000, 0.9659258262890683122, 1.000000000000000000, 0.9659258262890683122, 1.000000000000000000, 0.9659258262890683122, 1.000000000000000000, 0.9659258262890683122, 1.000000000000000000, 0.9659258262890683122, 1.000000000000000000, 0.9659258262890683122, 1.000000000000000000) ) ) 
 REPRESENTATION_ITEM ( '' )  SURFACE ( )  );
#21940 = CARTESIAN_POINT ( 'NONE',  ( -21.52544592524343514, 5.823673210054127303, 41.04057627198103120 ) ) ;
#21941 = CARTESIAN_POINT ( 'NONE',  ( 15.72974639402176855, 15.80617190586768217, 66.87609039468568994 ) ) ;
#21942 = CARTESIAN_POINT ( 'NONE',  ( -23.75112013235312602, -10.51683317207933044, 166.0021274478077942 ) ) ;
#21943 = CARTESIAN_POINT ( 'NONE',  ( 16.55341960407618274, -4.379528057220086978, 36.04275706135234714 ) ) ;
#21945 = CARTESIAN_POINT ( 'NONE',  ( -9.474510206698964154, 16.51473224551069663, 90.41557627198103830 ) ) ;
#21944 = CARTESIAN_POINT ( 'NONE',  ( 8.673617379884035472E-16, -1.899999999999999689, -3.490243377569955075E-16 ) ) ;
#21946 = AXIS2_PLACEMENT_3D ( 'NONE', #139266, #63424, #47272 ) ;
#21947 = CARTESIAN_POINT ( 'NONE',  ( -19.03943276465977164, 0.05219959533909376836, 26.24890960531435624 ) ) ;
#21948 = CARTESIAN_POINT ( 'NONE',  ( -8.314922557960811034, -14.29746914071050412, 82.08224293864768129 ) ) ;
#21949 = APPLICATION_PROTOCOL_DEFINITION ( 'draft international standard', 'automotive_design', 1998, #161685 ) ;
#21950 = CARTESIAN_POINT ( 'NONE',  ( -0.05219959533909027116, -19.03943276465977164, 82.49890960531436690 ) ) ;
#21951 = CARTESIAN_POINT ( 'NONE',  ( -9.564922557961040184, 16.46253265017147172, 107.9177570613523471 ) ) ;
#21952 = CARTESIAN_POINT ( 'NONE',  ( 18.67979575497178502, 10.72451020669898547, 79.16557627198103830 ) ) ;
#21953 = CARTESIAN_POINT ( 'NONE',  ( -13.97604488694527625, -13.89961937509977652, 46.87390960531435979 ) ) ;
#21955 = CARTESIAN_POINT ( 'NONE',  ( -18.62759615963255300, -10.81492255796106328, 19.16775706135234714 ) ) ;
#21954 = CARTESIAN_POINT ( 'NONE',  ( 9.564922557961047289, -16.46253265017146816, 75.41775706135234714 ) ) ;
#21956 = CARTESIAN_POINT ( 'NONE',  ( 5.049401038298161559, -19.05341960407611168, 72.70724293864768129 ) ) ;
#21957 = CARTESIAN_POINT ( 'NONE',  ( 16.46253265017160672, -9.564922557960803928, 103.3322429386476955 ) ) ;
#21958 = EDGE_LOOP ( 'NONE', ( #92255, #31727, #20171, #184052, #194551, #101490, #20874, #110591 ) ) ;
#21959 = CARTESIAN_POINT ( 'NONE',  ( -16.52544592524335698, -4.483927247898792601, 38.95942372801901854 ) ) ;
#21960 = CARTESIAN_POINT ( 'NONE',  ( 5.823673210054125526, 21.52544592524343514, 104.7905762719810241 ) ) ;
#21963 = CARTESIAN_POINT ( 'NONE',  ( 9.474510206698729675, 16.51473224551082808, 57.08442372801900433 ) ) ;
#21962 = CARTESIAN_POINT ( 'NONE',  ( 13.97604488694527802, 13.89961937509977652, 89.37390960531436690 ) ) ;
#21961 = CARTESIAN_POINT ( 'NONE',  ( -4.483927247898539470, -16.52544592524342804, 102.2905762719810383 ) ) ;
#21964 = CARTESIAN_POINT ( 'NONE',  ( 21.53943276465977519, -0.05219959533907433946, 93.74890960531436690 ) ) ;
#21965 = CARTESIAN_POINT ( 'NONE',  ( 5.719274019375991003, -21.55341960407610458, 72.70724293864769550 ) ) ;
#21966 = CARTESIAN_POINT ( 'NONE',  ( 8.314922557960818139, 14.29746914071049879, 44.58224293864769550 ) ) ;
#21967 = CARTESIAN_POINT ( 'NONE',  ( 13.97604488694548053, -13.89961937509957401, 20.62609039468567573 ) ) ;
#21968 = CARTESIAN_POINT ( 'NONE',  ( 0.05219959533934541429, -16.53943276465976808, 65.00109039468568994 ) ) ;
#21969 = CARTESIAN_POINT ( 'NONE',  ( -19.05341960407611168, -5.049401038298163336, 86.45724293864769550 ) ) ;
#21970 = CARTESIAN_POINT ( 'NONE',  ( 5.049401038298161559, -19.05341960407611168, 42.70724293864767418 ) ) ;
#21971 = CARTESIAN_POINT ( 'NONE',  ( -18.67979575497193778, 10.72451020669871902, 48.33442372801902565 ) ) ;
#21972 = CARTESIAN_POINT ( 'NONE',  ( -21.53943276465977519, -0.05219959533937600094, 63.75109039468568284 ) ) ;
#21973 = CARTESIAN_POINT ( 'NONE',  ( 5.049401038298161559, -19.05341960407611168, 57.70724293864769550 ) ) ;
#21974 = CARTESIAN_POINT ( 'NONE',  ( 15.72974639402176855, 15.80617190586768217, 41.87609039468568284 ) ) ;
#21975 = CARTESIAN_POINT ( 'NONE',  ( -19.03943276465977164, -0.05219959533935918106, 78.75109039468567573 ) ) ;
#21976 = CARTESIAN_POINT ( 'NONE',  ( 9.564922557961047289, -16.46253265017146816, 70.41775706135233293 ) ) ;
#21977 = CARTESIAN_POINT ( 'NONE',  ( 13.89961937509977652, -13.97604488694527269, 33.12390960531434558 ) ) ;
#21978 = CARTESIAN_POINT ( 'NONE',  ( 12.06949235617739724, 12.14591786802326823, 91.87609039468568994 ) ) ;
#21979 = CARTESIAN_POINT ( 'NONE',  ( 0.05219959533909260263, 19.03943276465977164, 49.99890960531435979 ) ) ;
#21980 = CARTESIAN_POINT ( 'NONE',  ( 24.57691432906898044, -7.727872488963283715, 167.2019946024468595 ) ) ;
#21981 = CARTESIAN_POINT ( 'NONE',  ( -5.049401038298153566, 19.05341960407611168, 105.2072429386476671 ) ) ;
#21982 = CARTESIAN_POINT ( 'NONE',  ( -19.03943276465977164, 0.05219959533909376836, 36.24890960531436690 ) ) ;
#21983 = CARTESIAN_POINT ( 'NONE',  ( -10.81492255796078084, -18.62759615963271287, 82.08224293864768129 ) ) ;
#21984 = CARTESIAN_POINT ( 'NONE',  ( -4.379528057220086978, -16.55341960407618274, 54.79275706135235424 ) ) ;
#21985 = CARTESIAN_POINT ( 'NONE',  ( 9.564922557961047289, -16.46253265017146816, 20.41775706135233293 ) ) ;
#21986 = CARTESIAN_POINT ( 'NONE',  ( 9.474510206698971260, -16.51473224551069308, 57.91557627198103120 ) ) ;
#21987 = CARTESIAN_POINT ( 'NONE',  ( -12.06949235617756955, 12.14591786802309770, 50.62390960531435979 ) ) ;
#21988 = CARTESIAN_POINT ( 'NONE',  ( -12.06949235617756955, 12.14591786802309770, 80.62390960531438111 ) ) ;
#21989 = CARTESIAN_POINT ( 'NONE',  ( 16.46253265017160672, -9.564922557960803928, 73.33224293864769550 ) ) ;
#21990 = CARTESIAN_POINT ( 'NONE',  ( -0.05219959533937732626, 21.53943276465977519, 37.50109039468568284 ) ) ;
#21991 = CARTESIAN_POINT ( 'NONE',  ( -19.03943276465977164, 0.05219959533909376836, 86.24890960531436690 ) ) ;
#21992 = CARTESIAN_POINT ( 'NONE',  ( 21.52544592524334988, 5.823673210054432836, 96.45942372801901854 ) ) ;
#21993 = CARTESIAN_POINT ( 'NONE',  ( 8.314922557961029526, -14.29746914071037800, 80.41775706135234714 ) ) ;
#21994 = CARTESIAN_POINT ( 'NONE',  ( 21.52544592524334988, 5.823673210054432836, 31.45942372801901854 ) ) ;
#21995 = CARTESIAN_POINT ( 'NONE',  ( 19.03943276465977164, -0.05219959533909143690, 113.7489096053143669 ) ) ;
#21996 = CARTESIAN_POINT ( 'NONE',  ( -15.72974639402197994, 15.80617190586746368, 85.62390960531436690 ) ) ;
#21997 = CARTESIAN_POINT ( 'NONE',  ( -14.34966873604960291, -8.224510206698953496, 41.66557627198103120 ) ) ;
#21998 = CARTESIAN_POINT ( 'NONE',  ( -9.564922557960796823, -16.46253265017161027, 37.08224293864768839 ) ) ;
#21999 = CARTESIAN_POINT ( 'NONE',  ( 16.55341960407611168, 4.379528057220329451, 63.95724293864770260 ) ) ;
#22000 = CARTESIAN_POINT ( 'NONE',  ( 15.72974639402199770, -15.80617190586745480, 28.12390960531435979 ) ) ;
#22001 = CARTESIAN_POINT ( 'NONE',  ( 5.153800228976615827, -19.02544592524334988, 30.20942372801900433 ) ) ;
#22002 = EDGE_CURVE ( 'NONE', #55198, #133171, #122580, .T. ) ;
#22003 = CARTESIAN_POINT ( 'NONE',  ( 12.14591786802309770, 12.06949235617756955, 94.37390960531436690 ) ) ;
#22004 = CARTESIAN_POINT ( 'NONE',  ( -19.03943276465977164, 0.05219959533909376836, 106.2489096053143669 ) ) ;
#22005 = VERTEX_POINT ( 'NONE', #28190 ) ;
#22006 = CARTESIAN_POINT ( 'NONE',  ( -0.05219959533934338120, 16.53943276465976808, 47.50109039468568994 ) ) ;
#22007 = CARTESIAN_POINT ( 'NONE',  ( -13.89961937509977652, 13.97604488694528158, 55.62390960531434558 ) ) ;
#22008 = LINE ( 'NONE', #162510, #85543 ) ;
#22009 = CARTESIAN_POINT ( 'NONE',  ( -4.379528057220086978, -16.55341960407618274, 89.79275706135236135 ) ) ;
#22010 = CARTESIAN_POINT ( 'NONE',  ( 13.97604488694548053, -13.89961937509957401, 110.6260903946856615 ) ) ;
#22011 = CARTESIAN_POINT ( 'NONE',  ( 21.52544592524334988, 5.823673210054432836, 76.45942372801901854 ) ) ;
#22012 = CARTESIAN_POINT ( 'NONE',  ( -13.97604488694527625, -13.89961937509977652, 76.87390960531433848 ) ) ;
#22013 = CARTESIAN_POINT ( 'NONE',  ( -15.72974639402197994, 15.80617190586746368, 105.6239096053143669 ) ) ;
#22014 = CARTESIAN_POINT ( 'NONE',  ( 0.05219959533934541429, -16.53943276465976808, 60.00109039468568284 ) ) ;
#22015 = CARTESIAN_POINT ( 'NONE',  ( 12.06949235617757843, -12.14591786802309237, 113.1239096053143953 ) ) ;
#22016 = CARTESIAN_POINT ( 'NONE',  ( -16.53943276465976808, -0.05219959533934237506, 18.75109039468568639 ) ) ;
#22017 = CARTESIAN_POINT ( 'NONE',  ( -5.049401038297874678, -19.05341960407617918, 84.79275706135233293 ) ) ;
#22018 = CARTESIAN_POINT ( 'NONE',  ( 10.72451020669898902, -18.67979575497178502, 77.91557627198102409 ) ) ;
#22019 = CARTESIAN_POINT ( 'NONE',  ( -19.03943276465977164, -0.05219959533935918106, 48.75109039468566863 ) ) ;
#22020 = CARTESIAN_POINT ( 'NONE',  ( 2.500000000000000000, -2.357898499370432610, 3.252606517456513302E-15 ) ) ;
#22021 = CARTESIAN_POINT ( 'NONE',  ( 18.67979575497178502, 10.72451020669898547, 109.1655762719810383 ) ) ;
#22022 = CARTESIAN_POINT ( 'NONE',  ( 17.50000000000147793, 3.254303733634570595, 27.47604106928601553 ) ) ;
#22023 = CARTESIAN_POINT ( 'NONE',  ( -5.153800228976328057, -19.02544592524343514, 67.29057627198102409 ) ) ;
#22024 = DIRECTION ( 'NONE',  ( 1.000000000000000000, 0.000000000000000000, 0.000000000000000000 ) ) ;
#22025 = CARTESIAN_POINT ( 'NONE',  ( 14.34966873604972726, -8.224510206698740333, 20.83442372801901143 ) ) ;
#22026 = CARTESIAN_POINT ( 'NONE',  ( 9.003517414636718286, -38.97943997941770533, -12.94545749024833547 ) ) ;
#22027 = CARTESIAN_POINT ( 'NONE',  ( 5.823673210054444382, -21.52544592524334988, 50.20942372801901854 ) ) ;
#22029 = CARTESIAN_POINT ( 'NONE',  ( 14.34966873604960469, 8.224510206698951720, 59.16557627198103120 ) ) ;
#22028 = CARTESIAN_POINT ( 'NONE',  ( -5.823673210054116645, -21.52544592524344225, 97.29057627198105251 ) ) ;
#22030 = CARTESIAN_POINT ( 'NONE',  ( 13.89961937509977652, -13.97604488694527269, 68.12390960531436690 ) ) ;
#22031 = CARTESIAN_POINT ( 'NONE',  ( -18.67979575497193778, 10.72451020669871902, 78.33442372801901854 ) ) ;
#22033 = CARTESIAN_POINT ( 'NONE',  ( -5.153800228976607833, 19.02544592524334988, 32.70942372801899722 ) ) ;
#22032 = CARTESIAN_POINT ( 'NONE',  ( 16.53943276465976808, 0.05219959533934440121, 26.25109039468567573 ) ) ;
#22034 = CARTESIAN_POINT ( 'NONE',  ( 18.67979575497194134, -10.72451020669871369, 50.83442372801901143 ) ) ;
#22035 = CARTESIAN_POINT ( 'NONE',  ( 21.52544592524334988, 5.823673210054432836, 21.45942372801901499 ) ) ;
#22036 = CARTESIAN_POINT ( 'NONE',  ( 21.52544592524344225, -5.823673210054117533, 63.54057627198103830 ) ) ;
#22038 = CARTESIAN_POINT ( 'NONE',  ( -5.049401038297874678, -19.05341960407617918, 99.79275706135234714 ) ) ;
#22037 = B_SPLINE_CURVE_WITH_KNOTS ( 'NONE', 3,
 ( #46387, #14057, #863, #170728, #136413, #108045 ),
 .UNSPECIFIED., .F., .F.,
 ( 4, 2, 4 ),
 ( 0.003989672132298100089, 0.004372778065220536345, 0.004755883998142971733 ),
 .UNSPECIFIED. ) ;
#22039 = CARTESIAN_POINT ( 'NONE',  ( -13.89961937509957401, -13.97604488694547875, 64.37609039468567573 ) ) ;
#22040 = CARTESIAN_POINT ( 'NONE',  ( 15.72974639402176855, 15.80617190586768217, 86.87609039468568994 ) ) ;
#22041 = CARTESIAN_POINT ( 'NONE',  ( -0.05219959533936034679, 19.03943276465977164, 47.50109039468566863 ) ) ;
#22042 = CARTESIAN_POINT ( 'NONE',  ( -5.049401038298153566, 19.05341960407611168, 35.20724293864768839 ) ) ;
#22043 = CARTESIAN_POINT ( 'NONE',  ( -5.823673210054116645, -21.52544592524344225, 57.29057627198103120 ) ) ;
#22044 = CARTESIAN_POINT ( 'NONE',  ( 4.483927247898545687, 16.52544592524342804, 54.79057627198104541 ) ) ;
#22045 = CARTESIAN_POINT ( 'NONE',  ( -17.26058549869091152, -6.457015423128557252, 26.37745837476068900 ) ) ;
#22046 = CARTESIAN_POINT ( 'NONE',  ( -5.049401038297874678, -19.05341960407617918, 29.79275706135232227 ) ) ;
#22047 = CARTESIAN_POINT ( 'NONE',  ( 4.483927247898790824, -16.52544592524335698, 85.20942372801901854 ) ) ;
#22048 = CARTESIAN_POINT ( 'NONE',  ( 0.05219959533910956823, 16.53943276465976808, 54.99890960531435269 ) ) ;
#22049 = CARTESIAN_POINT ( 'NONE',  ( -15.80617190586768217, 15.72974639402176855, 88.12609039468570415 ) ) ;
#22050 = CARTESIAN_POINT ( 'NONE',  ( 21.53943276465977519, 0.05219959533937863772, 81.25109039468568994 ) ) ;
#22051 = CARTESIAN_POINT ( 'NONE',  ( -21.52544592524343514, 5.823673210054127303, 81.04057627198102409 ) ) ;
#22052 = CARTESIAN_POINT ( 'NONE',  ( 0.05219959533909260263, 19.03943276465977164, 39.99890960531436690 ) ) ;
#22053 = CARTESIAN_POINT ( 'NONE',  ( 15.72974639402176855, 15.80617190586768217, 51.87609039468568284 ) ) ;
#22054 = CARTESIAN_POINT ( 'NONE',  ( -5.153800228976328057, -19.02544592524343514, 37.29057627198102409 ) ) ;
#22055 = CARTESIAN_POINT ( 'NONE',  ( 0.05219959533909260263, 19.03943276465977164, 49.99890960531435979 ) ) ;
#22056 = CARTESIAN_POINT ( 'NONE',  ( 4.379528057220339221, -16.55341960407611168, 102.7072429386476955 ) ) ;
#22057 = CARTESIAN_POINT ( 'NONE',  ( -16.46253265017160317, 9.564922557960807481, 95.83224293864769550 ) ) ;
#22058 = CARTESIAN_POINT ( 'NONE',  ( 12.06949235617757843, -12.14591786802309237, 48.12390960531436690 ) ) ;
#22059 = CARTESIAN_POINT ( 'NONE',  ( -16.52544592524342804, 4.483927247898546575, 106.0405762719810525 ) ) ;
#22060 = CARTESIAN_POINT ( 'NONE',  ( 18.67979575497178502, 10.72451020669898547, 84.16557627198103830 ) ) ;
#22061 = CARTESIAN_POINT ( 'NONE',  ( 21.52544592524334988, 5.823673210054432836, 21.45942372801901499 ) ) ;
#22062 = DIRECTION ( 'NONE',  ( 0.000000000000000000, -0.4999999999999993894, 0.8660254037844389297 ) ) ;
#22063 = CARTESIAN_POINT ( 'NONE',  ( -0.05219959533934338120, 16.53943276465976808, 37.50109039468568284 ) ) ;
#22064 = ORIENTED_EDGE ( 'NONE', *, *, #48766, .T. ) ;
#22065 = CARTESIAN_POINT ( 'NONE',  ( -18.67979575497178146, -10.72451020669898902, 66.66557627198102409 ) ) ;
#22066 = CARTESIAN_POINT ( 'NONE',  ( -21.52544592524334988, -5.823673210054445271, 88.95942372801901854 ) ) ;
#22067 = CARTESIAN_POINT ( 'NONE',  ( -19.03943276465977164, 0.05219959533909376836, 91.24890960531436690 ) ) ;
#22068 = CARTESIAN_POINT ( 'NONE',  ( 21.55341960407619695, -5.719274019375665929, 26.04275706135235779 ) ) ;
#22069 = CARTESIAN_POINT ( 'NONE',  ( -15.80617190586745835, -15.72974639402198527, 26.87390960531435979 ) ) ;
#22070 = CARTESIAN_POINT ( 'NONE',  ( -12.14591786802326823, 12.06949235617739902, 88.12609039468570415 ) ) ;
#22071 = CARTESIAN_POINT ( 'NONE',  ( 18.62759615963255655, 10.81492255796105972, 81.66775706135236135 ) ) ;
#22072 = CARTESIAN_POINT ( 'NONE',  ( 5.049401038297881783, 19.05341960407617563, 22.29275706135233648 ) ) ;
#22073 = CARTESIAN_POINT ( 'NONE',  ( -16.53943276465976808, -0.05219959533934237506, 73.75109039468567573 ) ) ;
#22074 = CARTESIAN_POINT ( 'NONE',  ( -15.80617190586768217, 15.72974639402176855, 28.12609039468568284 ) ) ;
#22075 = CARTESIAN_POINT ( 'NONE',  ( -9.564922557960796823, -16.46253265017161027, 32.08224293864769550 ) ) ;
#22076 = CARTESIAN_POINT ( 'NONE',  ( -5.719274019375665041, -21.55341960407619695, 109.7927570613523613 ) ) ;
#22077 = CARTESIAN_POINT ( 'NONE',  ( 13.89961937509977652, -13.97604488694527269, 103.1239096053143527 ) ) ;
#22078 = CARTESIAN_POINT ( 'NONE',  ( 0.05219959533907565091, 21.53943276465977519, 99.99890960531436690 ) ) ;
#22080 = CARTESIAN_POINT ( 'NONE',  ( -0.05219959533907301413, -21.53943276465977519, 62.49890960531436690 ) ) ;
#22079 = CARTESIAN_POINT ( 'NONE',  ( 17.50000000001358202, -5.500000000000038192, 88.29690382535061133 ) ) ;
#22082 = CARTESIAN_POINT ( 'NONE',  ( 16.52544592524342804, -4.483927247898539470, 53.54057627198103120 ) ) ;
#22081 = CARTESIAN_POINT ( 'NONE',  ( -12.06949235617739369, -12.14591786802326823, 49.37609039468569705 ) ) ;
#22083 = CARTESIAN_POINT ( 'NONE',  ( -6.412877669190335972, 3.889087296526014814, 1.818019484660534424 ) ) ;
#22084 = CARTESIAN_POINT ( 'NONE',  ( 9.474510206698729675, 16.51473224551082808, 72.08442372801900433 ) ) ;
#22085 = AXIS2_PLACEMENT_3D ( 'NONE', #187246, #127524, #5169 ) ;
#22086 = DIRECTION ( 'NONE',  ( 0.000000000000000000, 1.000000000000000000, -1.224646799147353207E-16 ) ) ;
#22087 = CARTESIAN_POINT ( 'NONE',  ( -0.05219959533934338120, 16.53943276465976808, 22.50109039468567573 ) ) ;
#22088 = CARTESIAN_POINT ( 'NONE',  ( -21.52544592524343514, 5.823673210054127303, 96.04057627198102409 ) ) ;
#22089 = CARTESIAN_POINT ( 'NONE',  ( 14.29746914071049879, -8.314922557960816363, 68.33224293864769550 ) ) ;
#22090 = CARTESIAN_POINT ( 'NONE',  ( 16.51473224551069308, 9.474510206698969483, 104.1655762719810241 ) ) ;
#22091 = CARTESIAN_POINT ( 'NONE',  ( -8.314922557961024197, 14.29746914071037800, 37.91775706135235424 ) ) ;
#22092 = CARTESIAN_POINT ( 'NONE',  ( 0.05219959533909260263, 19.03943276465977164, 59.99890960531436690 ) ) ;
#22094 = CARTESIAN_POINT ( 'NONE',  ( 19.02544592524334988, 5.153800228976608722, 96.45942372801897591 ) ) ;
#22093 = CARTESIAN_POINT ( 'NONE',  ( 10.81492255796106328, -18.62759615963255655, 35.41775706135234003 ) ) ;
#22095 = CARTESIAN_POINT ( 'NONE',  ( 19.03943276465977164, -0.05219959533909143690, 98.74890960531436690 ) ) ;
#22096 = CARTESIAN_POINT ( 'NONE',  ( -5.049401038298153566, 19.05341960407611168, 90.20724293864766707 ) ) ;
#22097 = CARTESIAN_POINT ( 'NONE',  ( 21.52544592524344225, -5.823673210054117533, 88.54057627198103830 ) ) ;
#22098 = CARTESIAN_POINT ( 'NONE',  ( -19.05341960407611168, -5.049401038298163336, 46.45724293864768129 ) ) ;
#22099 = CARTESIAN_POINT ( 'NONE',  ( 30.74264578624799782, 22.33583958711400541, -0.7999999999999999334 ) ) ;
#22100 = CARTESIAN_POINT ( 'NONE',  ( -4.379528057220328563, 16.55341960407611168, 70.20724293864769550 ) ) ;
#22101 = CARTESIAN_POINT ( 'NONE',  ( 13.97604488694527802, 13.89961937509977652, 99.37390960531436690 ) ) ;
#22102 = CARTESIAN_POINT ( 'NONE',  ( -17.97161686093721400, 5.500000000000142997, 60.99637206859166838 ) ) ;
#22103 = CARTESIAN_POINT ( 'NONE',  ( -19.02544592524334988, -5.153800228976617603, 83.95942372801901854 ) ) ;
#22104 = CARTESIAN_POINT ( 'NONE',  ( 15.72974639402199770, -15.80617190586745480, 88.12390960531436690 ) ) ;
#22105 = CARTESIAN_POINT ( 'NONE',  ( 16.46253265017146816, 9.564922557961045513, 46.66775706135233293 ) ) ;
#22106 = CARTESIAN_POINT ( 'NONE',  ( -18.62759615963270932, 10.81492255796079327, 25.83224293864769194 ) ) ;
#22107 = DIRECTION ( 'NONE',  ( 1.000000000000000000, 0.000000000000000000, 0.000000000000000000 ) ) ;
#22108 = CARTESIAN_POINT ( 'NONE',  ( 5.823673210054125526, 21.52544592524343514, 44.79057627198103120 ) ) ;
#22109 = CARTESIAN_POINT ( 'NONE',  ( 5.049401038298161559, -19.05341960407611168, 87.70724293864769550 ) ) ;
#22110 = CARTESIAN_POINT ( 'NONE',  ( 15.72974639402176855, 15.80617190586768217, 61.87609039468568284 ) ) ;
#22111 = CARTESIAN_POINT ( 'NONE',  ( -19.03943276465977164, 0.05219959533909376836, 36.24890960531436690 ) ) ;
#22112 = CARTESIAN_POINT ( 'NONE',  ( -4.483927247898539470, -16.52544592524342804, 67.29057627198103830 ) ) ;
#22113 = CARTESIAN_POINT ( 'NONE',  ( 16.52544592524335698, 4.483927247898782831, 21.45942372801901499 ) ) ;
#22114 = CARTESIAN_POINT ( 'NONE',  ( 5.719274019375673035, 21.55341960407619339, 47.29275706135234003 ) ) ;
#22115 = ORIENTED_EDGE ( 'NONE', *, *, #199224, .F. ) ;
#22116 = CARTESIAN_POINT ( 'NONE',  ( 0.05219959533909260263, 19.03943276465977164, 114.9989096053143669 ) ) ;
#22117 = CARTESIAN_POINT ( 'NONE',  ( 0.05219959533936267826, -19.03943276465977164, 80.00109039468567573 ) ) ;
#22118 = CARTESIAN_POINT ( 'NONE',  ( 11.30153831258470731, -188.0000000000000000, -4.999999999999999112 ) ) ;
#22119 = CARTESIAN_POINT ( 'NONE',  ( 5.719274019375673035, 21.55341960407619339, 22.29275706135235069 ) ) ;
#22120 = CARTESIAN_POINT ( 'NONE',  ( 2.802625768539491968, -39.09149893265183806, -33.00000000000000000 ) ) ;
#22121 = CARTESIAN_POINT ( 'NONE',  ( -15.80617190586768217, 15.72974639402176855, 113.1260903946856899 ) ) ;
#22122 = CARTESIAN_POINT ( 'NONE',  ( 5.153800228976335163, 19.02544592524342804, 54.79057627198103120 ) ) ;
#22123 = CARTESIAN_POINT ( 'NONE',  ( -5.153800228976607833, 19.02544592524334988, 22.70942372801899012 ) ) ;
#22124 = CARTESIAN_POINT ( 'NONE',  ( -16.55341960407617563, 4.379528057220093196, 103.5427570613523613 ) ) ;
#22126 = CARTESIAN_POINT ( 'NONE',  ( -18.67979575497193778, 10.72451020669871902, 78.33442372801901854 ) ) ;
#22125 = CARTESIAN_POINT ( 'NONE',  ( 0.05219959533909260263, 19.03943276465977164, 104.9989096053143669 ) ) ;
#22127 = CARTESIAN_POINT ( 'NONE',  ( -36.91746825000001309, -11.99521256947794789, -6.524999997268810858 ) ) ;
#22128 = CARTESIAN_POINT ( 'NONE',  ( -17.50000000000002487, -4.049696124445982370, 35.81960329334061299 ) ) ;
#22129 = CARTESIAN_POINT ( 'NONE',  ( 30.00000000000000000, 5.499999999999992895, 102.5000000000000142 ) ) ;
#22130 = CARTESIAN_POINT ( 'NONE',  ( -21.53943276465977519, -0.05219959533937600094, 73.75109039468567573 ) ) ;
#22131 = CARTESIAN_POINT ( 'NONE',  ( -18.62759615963255300, -10.81492255796106328, 99.16775706135234714 ) ) ;
#22132 = CARTESIAN_POINT ( 'NONE',  ( 0.000000000000000000, 0.000000000000000000, -64.92279855667830191 ) ) ;
#22133 = CARTESIAN_POINT ( 'NONE',  ( -5.153800228976328057, -19.02544592524343514, 87.29057627198103830 ) ) ;
#22134 = ADVANCED_FACE ( 'NONE', ( #151512 ), #12024, .T. ) ;
#22135 = CARTESIAN_POINT ( 'NONE',  ( 9.474510206698729675, 16.51473224551082808, 22.08442372801899722 ) ) ;
#22136 = CARTESIAN_POINT ( 'NONE',  ( 30.51643230682437036, -22.56685799121280311, -22.94790682118908975 ) ) ;
#22137 = CARTESIAN_POINT ( 'NONE',  ( -19.02544592524342804, 5.153800228976336051, 41.04057627198103120 ) ) ;
#22138 = CARTESIAN_POINT ( 'NONE',  ( -18.67979575497178146, -10.72451020669898902, 51.66557627198102409 ) ) ;
#22139 = CARTESIAN_POINT ( 'NONE',  ( -12.06949235617739369, -12.14591786802326823, 104.3760903946856899 ) ) ;
#22141 = CARTESIAN_POINT ( 'NONE',  ( 0.05219959533909260263, 19.03943276465977164, 84.99890960531436690 ) ) ;
#22140 = CARTESIAN_POINT ( 'NONE',  ( -12.14591786802309592, -12.06949235617757132, 96.87390960531436690 ) ) ;
#22142 = CARTESIAN_POINT ( 'NONE',  ( -0.05219959533937732626, 21.53943276465977519, 97.50109039468567573 ) ) ;
#22143 = CARTESIAN_POINT ( 'NONE',  ( -0.05219959533909027116, -19.03943276465977164, 42.49890960531435269 ) ) ;
#22144 = CARTESIAN_POINT ( 'NONE',  ( 4.379528057220339221, -16.55341960407611168, 92.70724293864770971 ) ) ;
#22145 = CARTESIAN_POINT ( 'NONE',  ( 21.52544592524334988, 5.823673210054432836, 56.45942372801902565 ) ) ;
#22146 = CARTESIAN_POINT ( 'NONE',  ( 21.52544592524344225, -5.823673210054117533, 83.54057627198102409 ) ) ;
#22147 = CARTESIAN_POINT ( 'NONE',  ( -19.05341960407617563, 5.049401038297882671, 53.54275706135231871 ) ) ;
#22148 = CARTESIAN_POINT ( 'NONE',  ( -5.153800228976328057, -19.02544592524343514, 47.29057627198102409 ) ) ;
#22149 = CARTESIAN_POINT ( 'NONE',  ( 9.474510206698971260, -16.51473224551069308, 97.91557627198102409 ) ) ;
#22150 = CARTESIAN_POINT ( 'NONE',  ( 8.224510206698953496, -14.34966873604960469, 72.91557627198103830 ) ) ;
#22151 = CARTESIAN_POINT ( 'NONE',  ( -13.97604488694547697, 13.89961937509957934, 43.12609039468566152 ) ) ;
#22152 = CARTESIAN_POINT ( 'NONE',  ( 19.02544592524343514, -5.153800228976328945, 68.54057627198103830 ) ) ;
#22153 = CARTESIAN_POINT ( 'NONE',  ( 16.52544592524342804, -4.483927247898539470, 43.54057627198103830 ) ) ;
#22154 = CARTESIAN_POINT ( 'NONE',  ( -5.049401038297874678, -19.05341960407617918, 79.79275706135233293 ) ) ;
#22155 = CARTESIAN_POINT ( 'NONE',  ( -19.53037848336980886, 5.499999999999899636, 84.85532783611448338 ) ) ;
#22156 = CARTESIAN_POINT ( 'NONE',  ( -21.55341960407610458, -5.719274019375992779, 31.45724293864769550 ) ) ;
#22157 = CARTESIAN_POINT ( 'NONE',  ( 14.29746914071049879, -8.314922557960816363, 98.33224293864769550 ) ) ;
#22158 = CARTESIAN_POINT ( 'NONE',  ( -17.50000000000001421, -3.305555262949453788, 25.37482847843392264 ) ) ;
#22160 = CARTESIAN_POINT ( 'NONE',  ( 15.72974639402199770, -15.80617190586745480, 58.12390960531435979 ) ) ;
#22159 = CARTESIAN_POINT ( 'NONE',  ( -16.46253265017160317, 9.564922557960807481, 60.83224293864769550 ) ) ;
#22161 = CARTESIAN_POINT ( 'NONE',  ( 19.03943276465977164, -0.05219959533909143690, 33.74890960531435979 ) ) ;
#22163 = CARTESIAN_POINT ( 'NONE',  ( 9.564922557960805705, 16.46253265017160317, 54.58224293864769550 ) ) ;
#22162 = CARTESIAN_POINT ( 'NONE',  ( 12.06949235617739724, 12.14591786802326823, 81.87609039468568994 ) ) ;
#22164 = CARTESIAN_POINT ( 'NONE',  ( 19.03943276465977164, 0.05219959533936151252, 41.25109039468566152 ) ) ;
#22165 = CARTESIAN_POINT ( 'NONE',  ( -5.719274019375665041, -21.55341960407619695, 74.79275706135234714 ) ) ;
#22166 = CARTESIAN_POINT ( 'NONE',  ( 5.823673210054125526, 21.52544592524343514, 54.79057627198104541 ) ) ;
#22167 = CARTESIAN_POINT ( 'NONE',  ( -13.97604488694527625, -13.89961937509977652, 26.87390960531434558 ) ) ;
#22168 = CARTESIAN_POINT ( 'NONE',  ( -8.314922557961024197, 14.29746914071037800, 82.91775706135234714 ) ) ;
#22169 = CARTESIAN_POINT ( 'NONE',  ( -19.02544592524334988, -5.153800228976617603, 103.9594237280190043 ) ) ;
#22170 = CARTESIAN_POINT ( 'NONE',  ( 30.00000000000000000, 5.499999999999992895, 37.50000000000000000 ) ) ;
#22172 = CARTESIAN_POINT ( 'NONE',  ( 5.823673210054125526, 21.52544592524343514, 44.79057627198103120 ) ) ;
#22171 = CARTESIAN_POINT ( 'NONE',  ( -0.7207009035786708928, -24.11964846217544789, -56.90195918390939767 ) ) ;
#22173 = CARTESIAN_POINT ( 'NONE',  ( -21.53943276465977519, -0.05219959533937600094, 78.75109039468568994 ) ) ;
#22174 = CARTESIAN_POINT ( 'NONE',  ( -16.55341960407611168, -4.379528057220339221, 51.45724293864770260 ) ) ;
#22175 = CARTESIAN_POINT ( 'NONE',  ( 16.55341960407611168, 4.379528057220329451, 58.95724293864770971 ) ) ;
#22176 = CARTESIAN_POINT ( 'NONE',  ( -21.52544592524343514, 5.823673210054127303, 81.04057627198102409 ) ) ;
#22177 = CARTESIAN_POINT ( 'NONE',  ( 21.53943276465977519, -0.05219959533907433946, 73.74890960531433848 ) ) ;
#22178 = FACE_OUTER_BOUND ( 'NONE', #67549, .T. ) ;
#22179 = CARTESIAN_POINT ( 'NONE',  ( -10.72451020669898014, 18.67979575497178502, 30.41557627198101699 ) ) ;
#22180 = CARTESIAN_POINT ( 'NONE',  ( -14.29746914071037622, -8.314922557961029526, 59.16775706135234714 ) ) ;
#22181 = CARTESIAN_POINT ( 'NONE',  ( 14.29746914071049879, -8.314922557960816363, 83.33224293864769550 ) ) ;
#22182 = CARTESIAN_POINT ( 'NONE',  ( 16.46253265017160672, -9.564922557960803928, 28.33224293864769550 ) ) ;
#22183 = PRESENTATION_STYLE_ASSIGNMENT (( #192028 ) ) ;
#22184 = CARTESIAN_POINT ( 'NONE',  ( 17.60779699588838199, 5.500000000000005329, 48.84981316670106111 ) ) ;
#22185 = VERTEX_POINT ( 'NONE', #15973 ) ;
#22186 = CARTESIAN_POINT ( 'NONE',  ( 4.483927247898790824, -16.52544592524335698, 85.20942372801901854 ) ) ;
#22187 = CARTESIAN_POINT ( 'NONE',  ( 10.72451020669898902, -18.67979575497178502, 112.9155762719810383 ) ) ;
#22188 = CARTESIAN_POINT ( 'NONE',  ( -13.97604488694527625, -13.89961937509977652, 81.87390960531436690 ) ) ;
#22189 = CARTESIAN_POINT ( 'NONE',  ( -21.53943276465977519, -0.05219959533937600094, 58.75109039468568994 ) ) ;
#22190 = CARTESIAN_POINT ( 'NONE',  ( -9.564922557960796823, -16.46253265017161027, 107.0822429386476955 ) ) ;
#22191 = CARTESIAN_POINT ( 'NONE',  ( -16.25089620724270745, -36.76456463896731464, -23.32760966624081078 ) ) ;
#22192 = ORIENTED_EDGE ( 'NONE', *, *, #13320, .T. ) ;
#22193 = CARTESIAN_POINT ( 'NONE',  ( -21.55341960407619339, 5.719274019375674811, 48.54275706135234714 ) ) ;
#22195 = CARTESIAN_POINT ( 'NONE',  ( 19.03943276465977164, -0.05219959533909143690, 108.7489096053143527 ) ) ;
#22194 = CARTESIAN_POINT ( 'NONE',  ( -5.049401038298153566, 19.05341960407611168, 35.20724293864768839 ) ) ;
#22196 = CARTESIAN_POINT ( 'NONE',  ( -9.564922557961040184, 16.46253265017147172, 47.91775706135233293 ) ) ;
#22197 = CARTESIAN_POINT ( 'NONE',  ( 5.823673210054444382, -21.52544592524334988, 30.20942372801902565 ) ) ;
#22198 = CARTESIAN_POINT ( 'NONE',  ( 19.05341960407617918, -5.049401038297876454, 51.04275706135231871 ) ) ;
#22199 = CARTESIAN_POINT ( 'NONE',  ( 13.89961937509977652, -13.97604488694527269, 28.12390960531435624 ) ) ;
#22200 = CARTESIAN_POINT ( 'NONE',  ( 16.55341960407618274, -4.379528057220086978, 91.04275706135236135 ) ) ;
#22201 = CARTESIAN_POINT ( 'NONE',  ( -13.89961937509957401, -13.97604488694547875, 59.37609039468566863 ) ) ;
#22202 = CARTESIAN_POINT ( 'NONE',  ( -4.379528057220086978, -16.55341960407618274, 104.7927570613523898 ) ) ;
#22203 = LINE ( 'NONE', #131369, #28078 ) ;
#22204 = CARTESIAN_POINT ( 'NONE',  ( -5.153800228976328057, -19.02544592524343514, 87.29057627198103830 ) ) ;
#22205 = CARTESIAN_POINT ( 'NONE',  ( 15.72974639402176855, 15.80617190586768217, 91.87609039468568994 ) ) ;
#22207 = ADVANCED_FACE ( 'NONE', ( #120163 ), #33228, .F. ) ;
#22206 = CARTESIAN_POINT ( 'NONE',  ( 5.719274019375673035, 21.55341960407619339, 102.2927570613523613 ) ) ;
#22208 = DIRECTION ( 'NONE',  ( 0.000000000000000000, 0.000000000000000000, 1.000000000000000000 ) ) ;
#22209 = CARTESIAN_POINT ( 'NONE',  ( 19.03943276465977164, -0.05219959533909143690, 98.74890960531436690 ) ) ;
#22210 = CARTESIAN_POINT ( 'NONE',  ( -10.81492255796105439, 18.62759615963255655, 77.91775706135231871 ) ) ;
#22211 = CARTESIAN_POINT ( 'NONE',  ( 14.29746914071037800, 8.314922557961029526, 21.66775706135235069 ) ) ;
#22212 = CARTESIAN_POINT ( 'NONE',  ( -9.474510206698964154, 16.51473224551069663, 85.41557627198102409 ) ) ;
#22213 = CARTESIAN_POINT ( 'NONE',  ( -21.53943276465977519, 0.05219959533907696930, 26.24890960531435624 ) ) ;
#22214 = CARTESIAN_POINT ( 'NONE',  ( -13.89961937509977652, 13.97604488694528158, 90.62390960531432427 ) ) ;
#22215 = CARTESIAN_POINT ( 'NONE',  ( -16.20579543436679160, -7.371946100355096121, 90.56520834171878676 ) ) ;
#22216 = CARTESIAN_POINT ( 'NONE',  ( -5.049401038298153566, 19.05341960407611168, 75.20724293864769550 ) ) ;
#22217 = CARTESIAN_POINT ( 'NONE',  ( -19.02544592524342804, 5.153800228976336051, 61.04057627198103120 ) ) ;
#22218 = CARTESIAN_POINT ( 'NONE',  ( 4.483927247898790824, -16.52544592524335698, 95.20942372801903275 ) ) ;
#22219 = PLANE ( 'NONE',  #26466 ) ;
#22220 = CARTESIAN_POINT ( 'NONE',  ( 13.89961937509957401, 13.97604488694547697, 66.87609039468567573 ) ) ;
#22221 = CARTESIAN_POINT ( 'NONE',  ( -16.51473224551069308, -9.474510206698971260, 86.66557627198102409 ) ) ;
#22222 = CARTESIAN_POINT ( 'NONE',  ( -14.34966873604960291, -8.224510206698953496, 86.66557627198102409 ) ) ;
#22223 = CARTESIAN_POINT ( 'NONE',  ( -5.823673210054116645, -21.52544592524344225, 32.29057627198102409 ) ) ;
#22224 = CARTESIAN_POINT ( 'NONE',  ( -5.719274019375978568, 21.55341960407610458, 25.20724293864769550 ) ) ;
#22225 = CARTESIAN_POINT ( 'NONE',  ( -16.53943276465976808, 0.05219959533911058130, 111.2489096053143669 ) ) ;
#22226 = DIRECTION ( 'NONE',  ( 1.000000000000000000, -0.000000000000000000, -0.000000000000000000 ) ) ;
#22227 = CARTESIAN_POINT ( 'NONE',  ( -13.89961937509957401, -13.97604488694547875, 44.37609039468566863 ) ) ;
#22228 = CARTESIAN_POINT ( 'NONE',  ( -8.314922557960811034, -14.29746914071050412, 27.08224293864769550 ) ) ;
#22229 = CARTESIAN_POINT ( 'NONE',  ( -5.153800228976328057, -19.02544592524343514, 107.2905762719810383 ) ) ;
#22230 = CARTESIAN_POINT ( 'NONE',  ( -21.53943276465977519, -0.05219959533937600094, 68.75109039468568994 ) ) ;
#22231 = CARTESIAN_POINT ( 'NONE',  ( 5.719274019375991003, -21.55341960407610458, 62.70724293864769550 ) ) ;
#22232 = CARTESIAN_POINT ( 'NONE',  ( 0.05219959533937995610, -21.53943276465977519, 35.00109039468568284 ) ) ;
#22233 = CARTESIAN_POINT ( 'NONE',  ( -5.823673210054116645, -21.52544592524344225, 77.29057627198102409 ) ) ;
#22234 = CARTESIAN_POINT ( 'NONE',  ( -15.80617190586768217, 15.72974639402176855, 43.12609039468568284 ) ) ;
#22235 = CARTESIAN_POINT ( 'NONE',  ( 0.05219959533910956823, 16.53943276465976808, 104.9989096053143669 ) ) ;
#22236 = CARTESIAN_POINT ( 'NONE',  ( 5.049401038297881783, 19.05341960407617563, 72.29275706135234714 ) ) ;
#22237 = CARTESIAN_POINT ( 'NONE',  ( -5.049401038298153566, 19.05341960407611168, 40.20724293864768839 ) ) ;
#22239 = CARTESIAN_POINT ( 'NONE',  ( 9.564922557960805705, 16.46253265017160317, 94.58224293864769550 ) ) ;
#22238 = CARTESIAN_POINT ( 'NONE',  ( 16.55341960407611168, 4.379528057220329451, 88.95724293864769550 ) ) ;
#22240 = CARTESIAN_POINT ( 'NONE',  ( 9.564922557960805705, 16.46253265017160317, 94.58224293864769550 ) ) ;
#22241 = CARTESIAN_POINT ( 'NONE',  ( 16.55341960407611168, 4.379528057220329451, 108.9572429386476955 ) ) ;
#22242 = CARTESIAN_POINT ( 'NONE',  ( -14.34966873604960291, -8.224510206698953496, 41.66557627198103120 ) ) ;
#22243 = CARTESIAN_POINT ( 'NONE',  ( 8.314922557961029526, -14.29746914071037800, 95.41775706135234714 ) ) ;
#22244 = CARTESIAN_POINT ( 'NONE',  ( 19.05341960407611168, 5.049401038298154454, 48.95724293864768129 ) ) ;
#22245 = CARTESIAN_POINT ( 'NONE',  ( 16.51473224551069308, 9.474510206698969483, 24.16557627198102765 ) ) ;
#22246 = CARTESIAN_POINT ( 'NONE',  ( -19.03943276465977164, -0.05219959533935918106, 18.75109039468567218 ) ) ;
#22248 = CARTESIAN_POINT ( 'NONE',  ( 4.379528057220092307, 16.55341960407617563, 112.2927570613523471 ) ) ;
#22247 = FACE_OUTER_BOUND ( 'NONE', #164526, .T. ) ;
#22249 = CARTESIAN_POINT ( 'NONE',  ( -15.80617190586768217, 15.72974639402176855, 43.12609039468568284 ) ) ;
#22250 = DIRECTION ( 'NONE',  ( 0.000000000000000000, 0.000000000000000000, 1.000000000000000000 ) ) ;
#22251 = CARTESIAN_POINT ( 'NONE',  ( -16.52544592524335698, -4.483927247898792601, 48.95942372801902565 ) ) ;
#22252 = CARTESIAN_POINT ( 'NONE',  ( 14.34966873604960469, 8.224510206698951720, 34.16557627198102409 ) ) ;
#22253 = CARTESIAN_POINT ( 'NONE',  ( -9.564922557960796823, -16.46253265017161027, 52.08224293864768839 ) ) ;
#22254 = CARTESIAN_POINT ( 'NONE',  ( -16.55341960407617563, 4.379528057220093196, 103.5427570613523613 ) ) ;
#22255 = CARTESIAN_POINT ( 'NONE',  ( 12.14591786802327356, -12.06949235617739191, 20.62609039468568639 ) ) ;
#22256 = CARTESIAN_POINT ( 'NONE',  ( -5.153800228976328057, -19.02544592524343514, 52.29057627198100988 ) ) ;
#22257 = CARTESIAN_POINT ( 'NONE',  ( 16.53943276465976808, -0.05219959533910856209, 113.7489096053143527 ) ) ;
#22258 = CARTESIAN_POINT ( 'NONE',  ( 21.53943276465977519, -0.05219959533907433946, 113.7489096053143527 ) ) ;
#22259 = CARTESIAN_POINT ( 'NONE',  ( 16.51473224551069308, 9.474510206698969483, 44.16557627198103120 ) ) ;
#22260 = CARTESIAN_POINT ( 'NONE',  ( -13.97604488694527625, -13.89961937509977652, 106.8739096053143669 ) ) ;
#22261 = CARTESIAN_POINT ( 'NONE',  ( -19.03943276465977164, 0.05219959533909376836, 26.24890960531435624 ) ) ;
#22262 = CARTESIAN_POINT ( 'NONE',  ( -19.03943276465977164, 0.05219959533909376836, 111.2489096053143669 ) ) ;
#22263 = DIRECTION ( 'NONE',  ( -1.000000000000000000, -0.000000000000000000, -0.000000000000000000 ) ) ;
#22264 = CARTESIAN_POINT ( 'NONE',  ( 16.51473224551069308, 9.474510206698969483, 99.16557627198102409 ) ) ;
#22266 = CARTESIAN_POINT ( 'NONE',  ( 14.34966873604960469, 8.224510206698951720, 99.16557627198100988 ) ) ;
#22265 = CARTESIAN_POINT ( 'NONE',  ( 18.67979575497194134, -10.72451020669871369, 40.83442372801901854 ) ) ;
#22267 = CARTESIAN_POINT ( 'NONE',  ( 0.05219959533909260263, 19.03943276465977164, 109.9989096053143669 ) ) ;
#22268 = CARTESIAN_POINT ( 'NONE',  ( -5.049401038297874678, -19.05341960407618274, 69.79275706135233293 ) ) ;
#22269 = CARTESIAN_POINT ( 'NONE',  ( 14.29746914071037800, 8.314922557961029526, 61.66775706135235424 ) ) ;
#22270 = CARTESIAN_POINT ( 'NONE',  ( -10.81492255796105439, 18.62759615963255655, 97.91775706135236135 ) ) ;
#22271 = CARTESIAN_POINT ( 'NONE',  ( -16.52544592524335698, -4.483927247898792601, 58.95942372801902565 ) ) ;
#22272 = CARTESIAN_POINT ( 'NONE',  ( 9.474510206698971260, -16.51473224551069308, 82.91557627198103830 ) ) ;
#22273 = CARTESIAN_POINT ( 'NONE',  ( -16.53943276465976808, -0.05219959533934237506, 38.75109039468567573 ) ) ;
#22274 = CARTESIAN_POINT ( 'NONE',  ( -0.05219959533936034679, 19.03943276465977164, 107.5010903946856615 ) ) ;
#22275 = CARTESIAN_POINT ( 'NONE',  ( -16.53943276465976808, -0.05219959533934237506, 83.75109039468568994 ) ) ;
#22276 = CARTESIAN_POINT ( 'NONE',  ( -19.05341960407617563, 5.049401038297882671, 93.54275706135234714 ) ) ;
#22277 = CARTESIAN_POINT ( 'NONE',  ( 19.05341960407611168, 5.049401038298154454, 78.95724293864769550 ) ) ;
#22278 = CARTESIAN_POINT ( 'NONE',  ( 15.80617190586746368, 15.72974639402197994, 94.37390960531436690 ) ) ;
#22280 = CARTESIAN_POINT ( 'NONE',  ( -16.46253265017146816, -9.564922557961047289, 104.1677570613523329 ) ) ;
#22279 = CARTESIAN_POINT ( 'NONE',  ( 4.483927247898545687, 16.52544592524342804, 94.79057627198105251 ) ) ;
#22281 = CARTESIAN_POINT ( 'NONE',  ( 14.34966873604972726, -8.224510206698740333, 70.83442372801901854 ) ) ;
#22282 = CARTESIAN_POINT ( 'NONE',  ( 19.49401214000076976, 12.39993551617566681, 167.9999999999999716 ) ) ;
#22283 = CARTESIAN_POINT ( 'NONE',  ( 19.02544592524334988, 5.153800228976608722, 71.45942372801900433 ) ) ;
#22284 = CARTESIAN_POINT ( 'NONE',  ( -16.53943276465976808, 0.05219959533911058130, 31.24890960531435979 ) ) ;
#22285 = CARTESIAN_POINT ( 'NONE',  ( -14.29746914071049879, 8.314922557960819915, 90.83224293864769550 ) ) ;
#22287 = CARTESIAN_POINT ( 'NONE',  ( -17.26172910966779739, 6.454744622555856459, 90.80646908649227100 ) ) ;
#22286 = CARTESIAN_POINT ( 'NONE',  ( 9.564922557961047289, -16.46253265017146816, 35.41775706135233293 ) ) ;
#22288 = CARTESIAN_POINT ( 'NONE',  ( 0.05219959533937995610, -21.53943276465977519, 30.00109039468568284 ) ) ;
#22289 = CARTESIAN_POINT ( 'NONE',  ( -9.474510206698720793, -16.51473224551083518, 99.58442372801900433 ) ) ;
#22290 = CARTESIAN_POINT ( 'NONE',  ( -16.46253265017160317, 9.564922557960807481, 110.8322429386476955 ) ) ;
#22291 = CARTESIAN_POINT ( 'NONE',  ( -19.03943276465977164, 0.05219959533909376836, 96.24890960531436690 ) ) ;
#22292 = CARTESIAN_POINT ( 'NONE',  ( 5.719274019375673035, 21.55341960407619339, 97.29275706135234714 ) ) ;
#22293 = CARTESIAN_POINT ( 'NONE',  ( 5.153800228976335163, 19.02544592524342804, 79.79057627198102409 ) ) ;
#22294 = CARTESIAN_POINT ( 'NONE',  ( -5.719274019375978568, 21.55341960407610458, 45.20724293864769550 ) ) ;
#22295 = CARTESIAN_POINT ( 'NONE',  ( -16.55341960407611168, -4.379528057220339221, 96.45724293864770971 ) ) ;
#22296 = CARTESIAN_POINT ( 'NONE',  ( -5.049401038298153566, 19.05341960407611168, 60.20724293864768129 ) ) ;
#22297 = CARTESIAN_POINT ( 'NONE',  ( -16.51473224551069308, -9.474510206698971260, 21.66557627198102765 ) ) ;
#22298 = CARTESIAN_POINT ( 'NONE',  ( 18.67979575497194134, -10.72451020669871369, 30.83442372801902209 ) ) ;
#22299 = CARTESIAN_POINT ( 'NONE',  ( -21.52544592524334988, -5.823673210054445271, 58.95942372801902565 ) ) ;
#22300 = CARTESIAN_POINT ( 'NONE',  ( -16.46253265017160317, 9.564922557960807481, 50.83224293864770260 ) ) ;
#22301 = CARTESIAN_POINT ( 'NONE',  ( 14.29746914071037800, 8.314922557961029526, 81.66775706135236135 ) ) ;
#22302 = CARTESIAN_POINT ( 'NONE',  ( 21.52544592524344225, -5.823673210054117533, 108.5405762719810241 ) ) ;
#22303 = ORIENTED_EDGE ( 'NONE', *, *, #38861, .T. ) ;
#22304 = CARTESIAN_POINT ( 'NONE',  ( -15.72974639402197994, 15.80617190586746368, 110.6239096053143669 ) ) ;
#22306 = CARTESIAN_POINT ( 'NONE',  ( 5.153800228976335163, 19.02544592524342804, 64.79057627198100988 ) ) ;
#22305 = CARTESIAN_POINT ( 'NONE',  ( -13.97604488694547697, 13.89961937509957934, 53.12609039468565442 ) ) ;
#22307 = CARTESIAN_POINT ( 'NONE',  ( -5.049401038297874678, -19.05341960407617918, 34.79275706135233293 ) ) ;
#22308 = CARTESIAN_POINT ( 'NONE',  ( -5.719274019375665041, -21.55341960407619695, 64.79275706135234714 ) ) ;
#22309 = CARTESIAN_POINT ( 'NONE',  ( -18.62759615963270932, 10.81492255796079327, 70.83224293864770971 ) ) ;
#22310 = CARTESIAN_POINT ( 'NONE',  ( -8.314922557960811034, -14.29746914071050412, 52.08224293864768839 ) ) ;
#22312 = CARTESIAN_POINT ( 'NONE',  ( -9.474510206698720793, -16.51473224551083518, 24.58442372801900078 ) ) ;
#22311 = CARTESIAN_POINT ( 'NONE',  ( 5.823673210054444382, -21.52544592524334988, 90.20942372801903275 ) ) ;
#22313 = CARTESIAN_POINT ( 'NONE',  ( -14.29746914071049879, 8.314922557960819915, 65.83224293864769550 ) ) ;
#22314 = CARTESIAN_POINT ( 'NONE',  ( 16.53943276465976808, -0.05219959533910856209, 113.7489096053143527 ) ) ;
#22315 = CARTESIAN_POINT ( 'NONE',  ( 9.474510206698729675, 16.51473224551082808, 62.08442372801899722 ) ) ;
#22316 = CARTESIAN_POINT ( 'NONE',  ( -8.224510206698735004, -14.34966873604973081, 109.5844237280190328 ) ) ;
#22317 = CARTESIAN_POINT ( 'NONE',  ( 10.81492255796106328, -18.62759615963255655, 80.41775706135234714 ) ) ;
#22318 = CARTESIAN_POINT ( 'NONE',  ( -13.89961937509957401, -13.97604488694547875, 49.37609039468567573 ) ) ;
#22319 = CARTESIAN_POINT ( 'NONE',  ( 21.53943276465977519, -0.05219959533907433946, 53.74890960531437401 ) ) ;
#22320 = CARTESIAN_POINT ( 'NONE',  ( 5.823673210054444382, -21.52544592524334988, 50.20942372801901854 ) ) ;
#22321 = AXIS2_PLACEMENT_3D ( 'NONE', #9968, #86790, #55456 ) ;
#22322 = CARTESIAN_POINT ( 'NONE',  ( -21.55341960407610458, -5.719274019375992779, 106.4572429386477097 ) ) ;
#22323 = CARTESIAN_POINT ( 'NONE',  ( 5.049401038297881783, 19.05341960407617563, 102.2927570613523045 ) ) ;
#22324 = CARTESIAN_POINT ( 'NONE',  ( 4.379528057220092307, 16.55341960407617563, 62.29275706135236845 ) ) ;
#22326 = CARTESIAN_POINT ( 'NONE',  ( -21.53943276465977519, 0.05219959533907696930, 111.2489096053143669 ) ) ;
#22325 = CARTESIAN_POINT ( 'NONE',  ( -30.00000000000000000, -1.163414459189985801E-14, 95.00000000000000000 ) ) ;
#22327 = CARTESIAN_POINT ( 'NONE',  ( -14.29746914071049879, 8.314922557960819915, 95.83224293864770971 ) ) ;
#22328 = CARTESIAN_POINT ( 'NONE',  ( -16.81555441253552985, -7.025013491695489165, 99.36314554665746357 ) ) ;
#22329 = CARTESIAN_POINT ( 'NONE',  ( 12.06949235617739724, 12.14591786802326823, 26.87609039468567218 ) ) ;
#22330 = CARTESIAN_POINT ( 'NONE',  ( -10.72451020669898014, 18.67979575497178502, 55.41557627198102409 ) ) ;
#22331 = CARTESIAN_POINT ( 'NONE',  ( -0.05219959533934338120, 16.53943276465976808, 92.50109039468567573 ) ) ;
#22332 = DIRECTION ( 'NONE',  ( 1.000000000000000000, 0.000000000000000000, 0.000000000000000000 ) ) ;
#22333 = CARTESIAN_POINT ( 'NONE',  ( -12.06949235617739369, -12.14591786802326823, 64.37609039468568994 ) ) ;
#22334 = CARTESIAN_POINT ( 'NONE',  ( -18.67979575497193778, 10.72451020669871902, 38.33442372801900433 ) ) ;
#22335 = CARTESIAN_POINT ( 'NONE',  ( -15.72974639402197994, 15.80617190586746368, 60.62390960531437401 ) ) ;
#22336 = CARTESIAN_POINT ( 'NONE',  ( 16.55341960407618274, -4.379528057220086978, 81.04275706135236135 ) ) ;
#22337 = CARTESIAN_POINT ( 'NONE',  ( 5.153800228976335163, 19.02544592524342804, 99.79057627198102409 ) ) ;
#22338 = CARTESIAN_POINT ( 'NONE',  ( -5.823673210054431948, 21.52544592524334988, 67.70942372801901854 ) ) ;
#22339 = CARTESIAN_POINT ( 'NONE',  ( 5.719274019375991003, -21.55341960407610458, 47.70724293864770260 ) ) ;
#22340 = CARTESIAN_POINT ( 'NONE',  ( 18.62759615963271287, -10.81492255796078972, 33.33224293864769550 ) ) ;
#22341 = VERTEX_POINT ( 'NONE', #185824 ) ;
#22342 = CARTESIAN_POINT ( 'NONE',  ( 19.02544592524334988, 5.153800228976608722, 51.45942372801900433 ) ) ;
#22343 = CARTESIAN_POINT ( 'NONE',  ( -8.224510206698735004, -14.34966873604973081, 59.58442372801901854 ) ) ;
#22344 = CARTESIAN_POINT ( 'NONE',  ( 21.55341960407610458, 5.719274019375980345, 38.95724293864768839 ) ) ;
#22345 = ORIENTED_EDGE ( 'NONE', *, *, #44596, .F. ) ;
#22346 = CARTESIAN_POINT ( 'NONE',  ( -19.02544592524342804, 5.153800228976336051, 101.0405762719810241 ) ) ;
#22347 = CARTESIAN_POINT ( 'NONE',  ( 14.34966873604972726, -8.224510206698740333, 110.8344237280190043 ) ) ;
#22348 = DIRECTION ( 'NONE',  ( 1.000000000000000000, 0.000000000000000000, 0.000000000000000000 ) ) ;
#22349 = CARTESIAN_POINT ( 'NONE',  ( 14.29746914071049879, -8.314922557960816363, 108.3322429386477097 ) ) ;
#22350 = CARTESIAN_POINT ( 'NONE',  ( 18.67979575497178502, 10.72451020669898547, 54.16557627198103120 ) ) ;
#22351 = CARTESIAN_POINT ( 'NONE',  ( 13.97604488694527802, 13.89961937509977652, 39.37390960531435269 ) ) ;
#22352 = CARTESIAN_POINT ( 'NONE',  ( -4.379528057220086978, -16.55341960407618274, 89.79275706135236135 ) ) ;
#22353 = CARTESIAN_POINT ( 'NONE',  ( 10.81492255796106328, -18.62759615963255655, 30.41775706135234358 ) ) ;
#22354 = CARTESIAN_POINT ( 'NONE',  ( -19.02544592524334988, -5.153800228976617603, 83.95942372801901854 ) ) ;
#22355 = CARTESIAN_POINT ( 'NONE',  ( -8.314922557960811034, -14.29746914071050412, 107.0822429386476955 ) ) ;
#22356 = CARTESIAN_POINT ( 'NONE',  ( 5.049401038298161559, -19.05341960407611168, 52.70724293864767418 ) ) ;
#22357 = CARTESIAN_POINT ( 'NONE',  ( -13.89961937509977652, 13.97604488694528158, 30.62390960531435269 ) ) ;
#22358 = CARTESIAN_POINT ( 'NONE',  ( -3.573655867282028392E-15, 2.428612866367529932E-14, 139.9999999999999716 ) ) ;
#22359 = CARTESIAN_POINT ( 'NONE',  ( -5.153800228976328057, -19.02544592524343514, 72.29057627198102409 ) ) ;
#22360 = CARTESIAN_POINT ( 'NONE',  ( -12.14591786802326823, 12.06949235617739902, 68.12609039468567573 ) ) ;
#22361 = CARTESIAN_POINT ( 'NONE',  ( 10.81492255796106328, -18.62759615963255655, 110.4177570613523756 ) ) ;
#22362 = CARTESIAN_POINT ( 'NONE',  ( 0.05219959533907565091, 21.53943276465977519, 44.99890960531435979 ) ) ;
#22363 = CARTESIAN_POINT ( 'NONE',  ( 14.29746914071037800, 8.314922557961029526, 71.66775706135234714 ) ) ;
#22364 = CARTESIAN_POINT ( 'NONE',  ( 13.89961937509957401, 13.97604488694547697, 46.87609039468565442 ) ) ;
#22365 = CARTESIAN_POINT ( 'NONE',  ( -9.564922557961040184, 16.46253265017147172, 72.91775706135233293 ) ) ;
#22366 = ORIENTED_EDGE ( 'NONE', *, *, #158172, .F. ) ;
#22367 = CARTESIAN_POINT ( 'NONE',  ( 5.719274019375673035, 21.55341960407619339, 57.29275706135234714 ) ) ;
#22368 = CARTESIAN_POINT ( 'NONE',  ( -19.03943276465977164, 0.05219959533909376836, 61.24890960531436690 ) ) ;
#22369 = CARTESIAN_POINT ( 'NONE',  ( 9.474510206698971260, -16.51473224551069308, 37.91557627198102409 ) ) ;
#22370 = CARTESIAN_POINT ( 'NONE',  ( -13.89961937509957401, -13.97604488694547875, 59.37609039468566863 ) ) ;
#22371 = CARTESIAN_POINT ( 'NONE',  ( -9.474510206698964154, 16.51473224551069663, 115.4155762719810241 ) ) ;
#22372 = CARTESIAN_POINT ( 'NONE',  ( -13.89961937509977652, 13.97604488694528158, 95.62390960531436690 ) ) ;
#22373 = CARTESIAN_POINT ( 'NONE',  ( -4.483927247898539470, -16.52544592524342804, 57.29057627198103120 ) ) ;
#22374 = CARTESIAN_POINT ( 'NONE',  ( -15.80617190586745835, -15.72974639402198527, 51.87390960531437401 ) ) ;
#22375 = CARTESIAN_POINT ( 'NONE',  ( 4.500000000000000888, -139.2199041982123617, 21.73825240834792893 ) ) ;
#22376 = CARTESIAN_POINT ( 'NONE',  ( 5.719274019375673035, 21.55341960407619339, 112.2927570613523471 ) ) ;
#22377 =( NAMED_UNIT ( * ) PLANE_ANGLE_UNIT ( ) SI_UNIT ( $, .RADIAN. ) );
#22378 = CARTESIAN_POINT ( 'NONE',  ( 13.97604488694527802, 13.89961937509977652, 54.37390960531435979 ) ) ;
#22379 = ADVANCED_FACE ( 'NONE', ( #45321 ), #74667, .T. ) ;
#22380 = CARTESIAN_POINT ( 'NONE',  ( -33.71409597518589152, -4.151718627496499892, 98.62556914322647117 ) ) ;
#22381 = CARTESIAN_POINT ( 'NONE',  ( -69.65682714487590488, -71.74905178543390605, -15.00000000000000000 ) ) ;
#22382 = CARTESIAN_POINT ( 'NONE',  ( -12.14591786802326823, 12.06949235617739902, 73.12609039468567573 ) ) ;
#22383 = CARTESIAN_POINT ( 'NONE',  ( -21.55341960407610458, -5.719274019375992779, 96.45724293864770971 ) ) ;
#22384 = CARTESIAN_POINT ( 'NONE',  ( -12.06949235617756955, 12.14591786802309770, 55.62390960531436690 ) ) ;
#22386 = CARTESIAN_POINT ( 'NONE',  ( 30.74264578624800137, -22.33583958711395212, -4.949999994537626513 ) ) ;
#22385 = CARTESIAN_POINT ( 'NONE',  ( 16.46253265017160672, -9.564922557960803928, 38.33224293864768839 ) ) ;
#22387 = CARTESIAN_POINT ( 'NONE',  ( 15.80617190586769283, -15.72974639402175789, 35.62609039468568994 ) ) ;
#22388 = CARTESIAN_POINT ( 'NONE',  ( 0.05219959533936267826, -19.03943276465977164, 55.00109039468566863 ) ) ;
#22389 = CARTESIAN_POINT ( 'NONE',  ( 19.03943276465977164, -0.05219959533909143690, 43.74890960531435979 ) ) ;
#22390 = CARTESIAN_POINT ( 'NONE',  ( 18.67979575497194134, -10.72451020669871369, 90.83442372801901854 ) ) ;
#22391 = CARTESIAN_POINT ( 'NONE',  ( 17.31747979337949062, 6.344076630961054342, 98.87944868065186199 ) ) ;
#22392 = ORIENTED_EDGE ( 'NONE', *, *, #193896, .T. ) ;
#22393 = CARTESIAN_POINT ( 'NONE',  ( -12.06949235617756955, 12.14591786802309770, 40.62390960531435269 ) ) ;
#22394 = CARTESIAN_POINT ( 'NONE',  ( -14.46985881644522642, 1.324169127979245797, -60.11284999819415020 ) ) ;
#22395 = CARTESIAN_POINT ( 'NONE',  ( -21.53943276465977519, 0.05219959533907696930, 36.24890960531435979 ) ) ;
#22396 = DIRECTION ( 'NONE',  ( 0.000000000000000000, 0.000000000000000000, 1.000000000000000000 ) ) ;
#22397 = CARTESIAN_POINT ( 'NONE',  ( 0.05219959533909260263, 19.03943276465977164, 99.99890960531436690 ) ) ;
#22398 = CARTESIAN_POINT ( 'NONE',  ( -8.314922557960811034, -14.29746914071050412, 87.08224293864769550 ) ) ;
#22399 = CARTESIAN_POINT ( 'NONE',  ( -4.483927247898782831, 16.52544592524335698, 27.70942372801901854 ) ) ;
#22400 = CARTESIAN_POINT ( 'NONE',  ( 4.379528057220092307, 16.55341960407617563, 112.2927570613523471 ) ) ;
#22401 = ORIENTED_EDGE ( 'NONE', *, *, #129491, .F. ) ;
#22403 = CARTESIAN_POINT ( 'NONE',  ( -15.80617190586745835, -15.72974639402198527, 101.8739096053143811 ) ) ;
#22402 = CARTESIAN_POINT ( 'NONE',  ( -16.46253265017160317, 9.564922557960807481, 100.8322429386477097 ) ) ;
#22405 = CARTESIAN_POINT ( 'NONE',  ( -19.05341960407611168, -5.049401038298163336, 101.4572429386476955 ) ) ;
#22404 = CARTESIAN_POINT ( 'NONE',  ( 12.14591786802309770, 12.06949235617756955, 29.37390960531435269 ) ) ;
#22406 = CARTESIAN_POINT ( 'NONE',  ( -0.05219959533936034679, 19.03943276465977164, 97.50109039468567573 ) ) ;
#22407 = CARTESIAN_POINT ( 'NONE',  ( -13.89961937509957401, -13.97604488694547875, 19.37609039468566507 ) ) ;
#22408 = CARTESIAN_POINT ( 'NONE',  ( 0.05219959533907565091, 21.53943276465977519, 89.99890960531438111 ) ) ;
#22409 = CARTESIAN_POINT ( 'NONE',  ( 10.72451020669898902, -18.67979575497178502, 47.91557627198102409 ) ) ;
#22410 = CARTESIAN_POINT ( 'NONE',  ( -5.153800228976328057, -19.02544592524343514, 57.29057627198103120 ) ) ;
#22411 = CARTESIAN_POINT ( 'NONE',  ( 12.06949235617757843, -12.14591786802309237, 33.12390960531435979 ) ) ;
#22412 = CARTESIAN_POINT ( 'NONE',  ( -13.89961937509977652, 13.97604488694528158, 80.62390960531436690 ) ) ;
#22413 = VERTEX_POINT ( 'NONE', #44328 ) ;
#22414 = CARTESIAN_POINT ( 'NONE',  ( -31.40318257579882655, -7.397807925419286335, 93.74221852110633790 ) ) ;
#22415 = CARTESIAN_POINT ( 'NONE',  ( -16.46253265017146816, -9.564922557961047289, 24.16775706135233648 ) ) ;
#22416 = CARTESIAN_POINT ( 'NONE',  ( 12.06949235617757843, -12.14591786802309237, 93.12390960531436690 ) ) ;
#22417 = CARTESIAN_POINT ( 'NONE',  ( 21.52544592524334988, 5.823673210054432836, 21.45942372801901499 ) ) ;
#22418 = CARTESIAN_POINT ( 'NONE',  ( 22.44159573604009239, 16.30477369853692693, 144.5750000027311728 ) ) ;
#22419 = CARTESIAN_POINT ( 'NONE',  ( 8.224510206698742110, 14.34966873604972548, 102.0844237280190185 ) ) ;
#22420 = CARTESIAN_POINT ( 'NONE',  ( 16.46253265017160672, -9.564922557960803928, 23.33224293864769194 ) ) ;
#22421 = CARTESIAN_POINT ( 'NONE',  ( 19.05341960407611168, 5.049401038298154454, 73.95724293864768129 ) ) ;
#22422 = CARTESIAN_POINT ( 'NONE',  ( 16.46253265017146816, 9.564922557961045513, 91.66775706135234714 ) ) ;
#22423 = CARTESIAN_POINT ( 'NONE',  ( 14.29746914071049879, -8.314922557960816363, 43.33224293864769550 ) ) ;
#22424 = CARTESIAN_POINT ( 'NONE',  ( -21.52544592524334988, -5.823673210054445271, 53.95942372801900433 ) ) ;
#22425 = CARTESIAN_POINT ( 'NONE',  ( 3.181980515339446924, -6.791538853603077186, 8.889087296526001936 ) ) ;
#22426 = CARTESIAN_POINT ( 'NONE',  ( -10.72451020669870658, -18.67979575497194134, 89.58442372801901854 ) ) ;
#22427 = CARTESIAN_POINT ( 'NONE',  ( -0.05219959533909027116, -19.03943276465977164, 42.49890960531435269 ) ) ;
#22428 = CARTESIAN_POINT ( 'NONE',  ( 9.474510206698971260, -16.51473224551069308, 57.91557627198103120 ) ) ;
#22429 = ORIENTED_EDGE ( 'NONE', *, *, #37807, .F. ) ;
#22430 = CARTESIAN_POINT ( 'NONE',  ( -5.719274019375665041, -21.55341960407619695, 89.79275706135236135 ) ) ;
#22431 = CARTESIAN_POINT ( 'NONE',  ( 4.379528057220092307, 16.55341960407617563, 57.29275706135234714 ) ) ;
#22432 = CARTESIAN_POINT ( 'NONE',  ( 5.719274019375673035, 21.55341960407619339, 87.29275706135236135 ) ) ;
#22433 = CARTESIAN_POINT ( 'NONE',  ( 5.719274019375991003, -21.55341960407610458, 22.70724293864769194 ) ) ;
#22434 = ORIENTED_EDGE ( 'NONE', *, *, #91774, .F. ) ;
#22435 = CARTESIAN_POINT ( 'NONE',  ( -0.05219959533936034679, 19.03943276465977164, 92.50109039468566152 ) ) ;
#22436 = CARTESIAN_POINT ( 'NONE',  ( -18.67979575497193778, 10.72451020669871902, 68.33442372801900433 ) ) ;
#22437 = CARTESIAN_POINT ( 'NONE',  ( -0.05219959533934338120, 16.53943276465976808, 42.50109039468567573 ) ) ;
#22438 = CARTESIAN_POINT ( 'NONE',  ( 0.05219959533907565091, 21.53943276465977519, 89.99890960531438111 ) ) ;
#22439 = CARTESIAN_POINT ( 'NONE',  ( 19.03943276465977164, 0.05219959533936151252, 81.25109039468567573 ) ) ;
#22440 = CARTESIAN_POINT ( 'NONE',  ( -19.05341960407611168, -5.049401038298163336, 71.45724293864766707 ) ) ;
#22441 = CARTESIAN_POINT ( 'NONE',  ( -13.97604488694547697, 13.89961937509957934, 98.12609039468566152 ) ) ;
#22442 = CARTESIAN_POINT ( 'NONE',  ( -16.46253265017146816, -9.564922557961047289, 109.1677570613523471 ) ) ;
#22443 = CARTESIAN_POINT ( 'NONE',  ( -16.53943276465976808, 0.05219959533911058130, 46.24890960531435979 ) ) ;
#22444 = CARTESIAN_POINT ( 'NONE',  ( 16.51473224551083163, -9.474510206698727899, 70.83442372801900433 ) ) ;
#22445 = CARTESIAN_POINT ( 'NONE',  ( -16.52544592524335698, -4.483927247898792601, 58.95942372801902565 ) ) ;
#22446 = EDGE_CURVE ( 'NONE', #197949, #150223, #139302, .T. ) ;
#22447 = CARTESIAN_POINT ( 'NONE',  ( 9.474510206698971260, -16.51473224551069308, 37.91557627198102409 ) ) ;
#22448 = CARTESIAN_POINT ( 'NONE',  ( 19.03943276465977164, -0.05219959533909143690, 58.74890960531435979 ) ) ;
#22449 = CARTESIAN_POINT ( 'NONE',  ( -4.379528057220086978, -16.55341960407618274, 64.79275706135234714 ) ) ;
#22450 = CARTESIAN_POINT ( 'NONE',  ( 11.30153831258470731, -190.0000000000000000, 0.000000000000000000 ) ) ;
#22451 = CARTESIAN_POINT ( 'NONE',  ( 8.906447517083057264, -27.41122689804191026, 138.8500000054623911 ) ) ;
#22452 = CARTESIAN_POINT ( 'NONE',  ( -19.02544592524342804, 5.153800228976336051, 101.0405762719810241 ) ) ;
#22453 = CARTESIAN_POINT ( 'NONE',  ( -5.153800228976328057, -19.02544592524343514, 22.29057627198102765 ) ) ;
#22454 = ORIENTED_EDGE ( 'NONE', *, *, #193877, .F. ) ;
#22455 = CARTESIAN_POINT ( 'NONE',  ( -0.05219959533934338120, 16.53943276465976808, 22.50109039468567573 ) ) ;
#22457 = CARTESIAN_POINT ( 'NONE',  ( -5.823673210054116645, -21.52544592524344225, 37.29057627198102409 ) ) ;
#22456 = AXIS2_PLACEMENT_3D ( 'NONE', #131667, #193349, #21487 ) ;
#22459 = CARTESIAN_POINT ( 'NONE',  ( 16.52544592524335698, 4.483927247898782831, 26.45942372801901854 ) ) ;
#22458 = CARTESIAN_POINT ( 'NONE',  ( 9.564922557961047289, -16.46253265017146816, 25.41775706135234003 ) ) ;
#22460 = CARTESIAN_POINT ( 'NONE',  ( 13.89961937509977652, -13.97604488694527269, 33.12390960531434558 ) ) ;
#22461 = CARTESIAN_POINT ( 'NONE',  ( -19.02544592524342804, 5.153800228976336051, 56.04057627198100988 ) ) ;
#22462 = CARTESIAN_POINT ( 'NONE',  ( -0.05219959533907301413, -21.53943276465977519, 82.49890960531436690 ) ) ;
#22463 = CARTESIAN_POINT ( 'NONE',  ( -9.474510206698964154, 16.51473224551069663, 100.4155762719810241 ) ) ;
#22464 = CARTESIAN_POINT ( 'NONE',  ( 5.153800228976335163, 19.02544592524342804, 54.79057627198103120 ) ) ;
#22465 = CARTESIAN_POINT ( 'NONE',  ( -17.14385361876520975, 23.59649016807275856, 141.0750000027311728 ) ) ;
#22466 = CARTESIAN_POINT ( 'NONE',  ( -5.153800228976607833, 19.02544592524334988, 77.70942372801900433 ) ) ;
#22467 = CARTESIAN_POINT ( 'NONE',  ( -8.314922557960811034, -14.29746914071050412, 67.08224293864770971 ) ) ;
#22468 = CARTESIAN_POINT ( 'NONE',  ( 5.719274019375991003, -21.55341960407610458, 42.70724293864770260 ) ) ;
#22469 = CARTESIAN_POINT ( 'NONE',  ( 18.62759615963255655, 10.81492255796105972, 111.6677570613523613 ) ) ;
#22470 = CARTESIAN_POINT ( 'NONE',  ( 21.55341960407610458, 5.719274019375980345, 103.9572429386476813 ) ) ;
#22471 = CARTESIAN_POINT ( 'NONE',  ( 18.62759615963255655, 10.81492255796105972, 76.66775706135234714 ) ) ;
#22472 = CARTESIAN_POINT ( 'NONE',  ( 21.53943276465977519, 0.05219959533937863772, 71.25109039468568994 ) ) ;
#22473 = CARTESIAN_POINT ( 'NONE',  ( -16.46253265017160317, 9.564922557960807481, 105.8322429386476955 ) ) ;
#22475 = CARTESIAN_POINT ( 'NONE',  ( 21.52544592524334988, 5.823673210054432836, 81.45942372801900433 ) ) ;
#22474 = CARTESIAN_POINT ( 'NONE',  ( 14.34966873604972726, -8.224510206698740333, 105.8344237280190328 ) ) ;
#22476 = CARTESIAN_POINT ( 'NONE',  ( 0.05219959533909260263, 19.03943276465977164, 59.99890960531436690 ) ) ;
#22477 = CARTESIAN_POINT ( 'NONE',  ( 0.05219959533937995610, -21.53943276465977519, 25.00109039468567218 ) ) ;
#22478 = CARTESIAN_POINT ( 'NONE',  ( -16.51473224551069308, -9.474510206698971260, 66.66557627198102409 ) ) ;
#22479 = CARTESIAN_POINT ( 'NONE',  ( 0.05219959533910956823, 16.53943276465976808, 74.99890960531435269 ) ) ;
#22480 = CARTESIAN_POINT ( 'NONE',  ( -14.34966873604960291, -8.224510206698953496, 46.66557627198102409 ) ) ;
#22481 = CARTESIAN_POINT ( 'NONE',  ( 5.823673210054125526, 21.52544592524343514, 54.79057627198104541 ) ) ;
#22482 = CARTESIAN_POINT ( 'NONE',  ( -16.51473224551069308, -9.474510206698971260, 66.66557627198102409 ) ) ;
#22483 = CARTESIAN_POINT ( 'NONE',  ( -21.52544592524343514, 5.823673210054127303, 66.04057627198103830 ) ) ;
#22484 = CARTESIAN_POINT ( 'NONE',  ( -5.153800228976607833, 19.02544592524334988, 62.70942372801899722 ) ) ;
#22486 = CARTESIAN_POINT ( 'NONE',  ( -16.55341960407611168, -4.379528057220339221, 66.45724293864768129 ) ) ;
#22485 = CARTESIAN_POINT ( 'NONE',  ( -19.03943276465977164, -0.05219959533935918106, 23.75109039468566152 ) ) ;
#22488 = AXIS2_PLACEMENT_3D ( 'NONE', #169792, #19103, #171788 ) ;
#22487 = CARTESIAN_POINT ( 'NONE',  ( -5.823673210054116645, -21.52544592524344225, 57.29057627198103120 ) ) ;
#22489 = ORIENTED_EDGE ( 'NONE', *, *, #137048, .F. ) ;
#22490 = LINE ( 'NONE', #84137, #185093 ) ;
#22492 = CARTESIAN_POINT ( 'NONE',  ( 27.73933785331498569, 2.768321779492822058E-14, 144.3750000027311842 ) ) ;
#22491 = CARTESIAN_POINT ( 'NONE',  ( -12.14591786802326823, 12.06949235617739902, 93.12609039468568994 ) ) ;
#22493 = CARTESIAN_POINT ( 'NONE',  ( 5.153800228976615827, -19.02544592524334988, 85.20942372801900433 ) ) ;
#22494 = CARTESIAN_POINT ( 'NONE',  ( -8.314922557960811034, -14.29746914071050412, 72.08224293864769550 ) ) ;
#22495 = CARTESIAN_POINT ( 'NONE',  ( -18.87255363501902394, -5.499999999999947597, 61.32513748171826506 ) ) ;
#22496 = CARTESIAN_POINT ( 'NONE',  ( -5.153800228976328057, -19.02544592524343514, 62.29057627198100988 ) ) ;
#22497 = CARTESIAN_POINT ( 'NONE',  ( 4.483927247898545687, 16.52544592524342804, 54.79057627198104541 ) ) ;
#22498 = CARTESIAN_POINT ( 'NONE',  ( 19.03943276465977164, -0.05219959533909143690, 83.74890960531436690 ) ) ;
#22500 = CARTESIAN_POINT ( 'NONE',  ( 5.049401038298161559, -19.05341960407611168, 57.70724293864769550 ) ) ;
#22499 = CARTESIAN_POINT ( 'NONE',  ( 16.51473224551083163, -9.474510206698727899, 80.83442372801899012 ) ) ;
#22501 = CARTESIAN_POINT ( 'NONE',  ( -9.564922557960796823, -16.46253265017161027, 82.08224293864768129 ) ) ;
#22502 = CARTESIAN_POINT ( 'NONE',  ( -9.474510206698964154, 16.51473224551069663, 70.41557627198102409 ) ) ;
#22503 = CARTESIAN_POINT ( 'NONE',  ( 15.80617190586746368, 15.72974639402197994, 59.37390960531436690 ) ) ;
#22504 = CARTESIAN_POINT ( 'NONE',  ( 2.500000000000000000, 2.357898499370431722, -2.818925648462311528E-15 ) ) ;
#22505 = CARTESIAN_POINT ( 'NONE',  ( 13.89961937509977652, -13.97604488694527269, 48.12390960531435979 ) ) ;
#22506 = CARTESIAN_POINT ( 'NONE',  ( -18.62759615963270932, 10.81492255796079327, 60.83224293864769550 ) ) ;
#22507 = CARTESIAN_POINT ( 'NONE',  ( 0.05219959533936267826, -19.03943276465977164, 85.00109039468567573 ) ) ;
#22508 = CARTESIAN_POINT ( 'NONE',  ( 8.224510206698742110, 14.34966873604972548, 112.0844237280190185 ) ) ;
#22509 = CARTESIAN_POINT ( 'NONE',  ( -19.02544592524334988, -5.153800228976617603, 33.95942372801897591 ) ) ;
#22511 = CARTESIAN_POINT ( 'NONE',  ( -4.379528057220086978, -16.55341960407618274, 99.79275706135234714 ) ) ;
#22510 = CARTESIAN_POINT ( 'NONE',  ( 4.483927247898790824, -16.52544592524335698, 60.20942372801902565 ) ) ;
#22512 = CARTESIAN_POINT ( 'NONE',  ( 19.48894818550243002, -5.500000000000108358, 42.60307310435238293 ) ) ;
#22513 = CARTESIAN_POINT ( 'NONE',  ( -4.379528057220086978, -16.55341960407618274, 79.79275706135236135 ) ) ;
#22514 = CARTESIAN_POINT ( 'NONE',  ( -16.46253265017160317, 9.564922557960807481, 115.8322429386477097 ) ) ;
#22515 = CARTESIAN_POINT ( 'NONE',  ( 9.564922557960805705, 16.46253265017160317, 34.58224293864770260 ) ) ;
#22516 = CARTESIAN_POINT ( 'NONE',  ( 8.224510206698742110, 14.34966873604972548, 42.08442372801901854 ) ) ;
#22517 = CARTESIAN_POINT ( 'NONE',  ( -13.97604488694527625, -13.89961937509977652, 46.87390960531435979 ) ) ;
#22518 = CARTESIAN_POINT ( 'NONE',  ( 21.55341960407619695, -5.719274019375665929, 41.04275706135236135 ) ) ;
#22519 = CARTESIAN_POINT ( 'NONE',  ( -16.52544592524335698, -4.483927247898792601, 48.95942372801902565 ) ) ;
#22520 = CARTESIAN_POINT ( 'NONE',  ( 4.379528057220092307, 16.55341960407617563, 112.2927570613523471 ) ) ;
#22521 = CARTESIAN_POINT ( 'NONE',  ( 9.564922557960805705, 16.46253265017160317, 34.58224293864770260 ) ) ;
#22522 = CARTESIAN_POINT ( 'NONE',  ( -19.05341960407617563, 5.049401038297882671, 23.54275706135233648 ) ) ;
#22523 = CARTESIAN_POINT ( 'NONE',  ( -4.379528057220086978, -16.55341960407618274, 19.79275706135235069 ) ) ;
#22524 = CARTESIAN_POINT ( 'NONE',  ( 19.05341960407617918, -5.049401038297876454, 71.04275706135234714 ) ) ;
#22525 = CARTESIAN_POINT ( 'NONE',  ( -0.05219959533910754901, -16.53943276465976808, 72.49890960531435269 ) ) ;
#22526 = CARTESIAN_POINT ( 'NONE',  ( 13.89961937509977652, -13.97604488694527269, 38.12390960531436690 ) ) ;
#22528 = CARTESIAN_POINT ( 'NONE',  ( 16.36317988757060604, -7.306389748694920527, 91.59789608363225000 ) ) ;
#22527 = CARTESIAN_POINT ( 'NONE',  ( -13.97604488694547697, 13.89961937509957934, 78.12609039468567573 ) ) ;
#22529 = CARTESIAN_POINT ( 'NONE',  ( 21.55341960407619695, -5.719274019375665929, 81.04275706135236135 ) ) ;
#22530 = CARTESIAN_POINT ( 'NONE',  ( -16.52544592524335698, -4.483927247898792601, 38.95942372801901854 ) ) ;
#22531 = CARTESIAN_POINT ( 'NONE',  ( 19.26498983726237668, -5.499999999999590550, 58.05319577422003618 ) ) ;
#22532 = CARTESIAN_POINT ( 'NONE',  ( 10.72451020669898902, -18.67979575497178502, 32.91557627198102409 ) ) ;
#22533 = CARTESIAN_POINT ( 'NONE',  ( -14.34966873604972548, 8.224510206698743886, 23.33442372801901499 ) ) ;
#22534 = CARTESIAN_POINT ( 'NONE',  ( -16.46253265017160317, 9.564922557960807481, 115.8322429386477097 ) ) ;
#22535 = CARTESIAN_POINT ( 'NONE',  ( 11.30153831258469843, -180.0000000000000000, -15.00000000000000178 ) ) ;
#22536 = CARTESIAN_POINT ( 'NONE',  ( -19.02544592524342804, 5.153800228976336051, 36.04057627198100988 ) ) ;
#22537 = CARTESIAN_POINT ( 'NONE',  ( -3.573655867282028392E-15, 2.428612866367529932E-14, 2.000000000000000000 ) ) ;
#22538 = CARTESIAN_POINT ( 'NONE',  ( 16.51473224551069308, 9.474510206698969483, 59.16557627198102409 ) ) ;
#22539 = CARTESIAN_POINT ( 'NONE',  ( -15.80617190586768217, 15.72974639402176855, 63.12609039468568994 ) ) ;
#22540 = CARTESIAN_POINT ( 'NONE',  ( 10.72451020669871369, 18.67979575497193778, 107.0844237280190043 ) ) ;
#22541 = CARTESIAN_POINT ( 'NONE',  ( 4.379528057220339221, -16.55341960407611168, 22.70724293864769194 ) ) ;
#22542 = CARTESIAN_POINT ( 'NONE',  ( -19.02544592524342804, 5.153800228976336051, 31.04057627198102409 ) ) ;
#22543 = CARTESIAN_POINT ( 'NONE',  ( -16.46253265017160317, 9.564922557960807481, 95.83224293864769550 ) ) ;
#22544 = CARTESIAN_POINT ( 'NONE',  ( 18.62759615963255655, 10.81492255796105972, 61.66775706135235424 ) ) ;
#22545 = CARTESIAN_POINT ( 'NONE',  ( 5.049401038298161559, -19.05341960407611168, 32.70724293864768129 ) ) ;
#22546 = ADVANCED_FACE ( 'NONE', ( #106971 ), #154480, .T. ) ;
#22547 = CARTESIAN_POINT ( 'NONE',  ( 15.80617190586769283, -15.72974639402175789, 65.62609039468568994 ) ) ;
#22549 = CARTESIAN_POINT ( 'NONE',  ( -16.51473224551069308, -9.474510206698971260, 111.6655762719810383 ) ) ;
#22548 = CARTESIAN_POINT ( 'NONE',  ( -9.474510206698720793, -16.51473224551083518, 99.58442372801900433 ) ) ;
#22550 = CARTESIAN_POINT ( 'NONE',  ( 4.379528057220339221, -16.55341960407611168, 112.7072429386476955 ) ) ;
#22551 = CARTESIAN_POINT ( 'NONE',  ( -21.55341960407610458, -5.719274019375992779, 111.4572429386476813 ) ) ;
#22552 = CARTESIAN_POINT ( 'NONE',  ( -0.05219959533936034679, 19.03943276465977164, 32.50109039468566863 ) ) ;
#22553 = CARTESIAN_POINT ( 'NONE',  ( -16.55341960407611168, -4.379528057220339221, 106.4572429386477097 ) ) ;
#22554 = CARTESIAN_POINT ( 'NONE',  ( 9.474510206698971260, -16.51473224551069308, 62.91557627198102409 ) ) ;
#22555 = CARTESIAN_POINT ( 'NONE',  ( 9.474510206698729675, 16.51473224551082808, 97.08442372801900433 ) ) ;
#22556 = CARTESIAN_POINT ( 'NONE',  ( 16.53943276465976808, -0.05219959533910856209, 63.74890960531435979 ) ) ;
#22557 = CARTESIAN_POINT ( 'NONE',  ( 19.02544592524334988, 5.153800228976608722, 21.45942372801899012 ) ) ;
#22558 = CARTESIAN_POINT ( 'NONE',  ( 5.153800228976335163, 19.02544592524342804, 114.7905762719810241 ) ) ;
#22559 = CARTESIAN_POINT ( 'NONE',  ( 9.474510206698729675, 16.51473224551082808, 87.08442372801900433 ) ) ;
#22560 = CARTESIAN_POINT ( 'NONE',  ( -5.719274019375978568, 21.55341960407610458, 85.20724293864770971 ) ) ;
#22561 = CARTESIAN_POINT ( 'NONE',  ( 5.719274019375673035, 21.55341960407619339, 47.29275706135234003 ) ) ;
#22562 = CARTESIAN_POINT ( 'NONE',  ( -12.06949235617739369, -12.14591786802326823, 39.37609039468567573 ) ) ;
#22563 = CARTESIAN_POINT ( 'NONE',  ( -12.06949235617739369, -12.14591786802326823, 104.3760903946856899 ) ) ;
#22565 = CARTESIAN_POINT ( 'NONE',  ( -21.53943276465977519, -0.05219959533937600094, 43.75109039468568284 ) ) ;
#22564 = CARTESIAN_POINT ( 'NONE',  ( 16.55341960407618274, -4.379528057220086978, 36.04275706135234714 ) ) ;
#22566 = CARTESIAN_POINT ( 'NONE',  ( -0.05219959533907301413, -21.53943276465977519, 52.49890960531435979 ) ) ;
#22567 = CARTESIAN_POINT ( 'NONE',  ( 16.46253265017160672, -9.564922557960803928, 38.33224293864768839 ) ) ;
#22568 = CARTESIAN_POINT ( 'NONE',  ( -38.00000000000001421, 12.34694845685046438, -3.849999994537626868 ) ) ;
#22569 = CARTESIAN_POINT ( 'NONE',  ( -8.314922557961024197, 14.29746914071037800, 77.91775706135231871 ) ) ;
#22570 = CARTESIAN_POINT ( 'NONE',  ( 0.05219959533907565091, 21.53943276465977519, 94.99890960531436690 ) ) ;
#22571 = CARTESIAN_POINT ( 'NONE',  ( 16.53943276465976808, -0.05219959533910856209, 33.74890960531436690 ) ) ;
#22572 = CARTESIAN_POINT ( 'NONE',  ( -12.14591786802326823, 12.06949235617739902, 58.12609039468568994 ) ) ;
#22573 = CARTESIAN_POINT ( 'NONE',  ( 13.97604488694548053, -13.89961937509957401, 105.6260903946856757 ) ) ;
#22574 = CARTESIAN_POINT ( 'NONE',  ( 18.62759615963271287, -10.81492255796078972, 103.3322429386476955 ) ) ;
#22575 = CARTESIAN_POINT ( 'NONE',  ( -4.379528057220328563, 16.55341960407611168, 25.20724293864769550 ) ) ;
#22576 = VERTEX_POINT ( 'NONE', #138315 ) ;
#22577 = CARTESIAN_POINT ( 'NONE',  ( 8.224510206698742110, 14.34966873604972548, 77.08442372801901854 ) ) ;
#22578 = CARTESIAN_POINT ( 'NONE',  ( 26.57611637973579732, 7.696099174151423306, 167.9177021574031983 ) ) ;
#22579 = CARTESIAN_POINT ( 'NONE',  ( -10.72451020669898014, 18.67979575497178502, 80.41557627198103830 ) ) ;
#22580 = CARTESIAN_POINT ( 'NONE',  ( 8.314922557961029526, -14.29746914071037800, 105.4177570613523613 ) ) ;
#22581 = ORIENTED_EDGE ( 'NONE', *, *, #23142, .F. ) ;
#22582 = CARTESIAN_POINT ( 'NONE',  ( 19.25918095147778786, 5.499999999999572786, 86.95284276293935477 ) ) ;
#22583 = CARTESIAN_POINT ( 'NONE',  ( 21.52544592524344225, -5.823673210054117533, 88.54057627198103830 ) ) ;
#22584 = CARTESIAN_POINT ( 'NONE',  ( 15.80617190586746368, 15.72974639402197994, 104.3739096053143669 ) ) ;
#22585 = CARTESIAN_POINT ( 'NONE',  ( 8.314922557960818139, 14.29746914071049879, 39.58224293864769550 ) ) ;
#22586 = CARTESIAN_POINT ( 'NONE',  ( 8.314922557961029526, -14.29746914071037800, 30.41775706135234358 ) ) ;
#22587 = CARTESIAN_POINT ( 'NONE',  ( -0.05219959533909027116, -19.03943276465977164, 52.49890960531436690 ) ) ;
#22588 = CARTESIAN_POINT ( 'NONE',  ( 16.46253265017160672, -9.564922557960803928, 73.33224293864769550 ) ) ;
#22589 = ORIENTED_EDGE ( 'NONE', *, *, #123102, .F. ) ;
#22590 = CARTESIAN_POINT ( 'NONE',  ( 19.03943276465977164, -0.05219959533909143690, 113.7489096053143669 ) ) ;
#22591 = CARTESIAN_POINT ( 'NONE',  ( -19.02544592524342804, 5.153800228976336051, 116.0405762719810383 ) ) ;
#22592 = CARTESIAN_POINT ( 'NONE',  ( -5.049401038297874678, -19.05341960407617918, 99.79275706135234714 ) ) ;
#22593 = CARTESIAN_POINT ( 'NONE',  ( 16.46253265017146816, 9.564922557961045513, 46.66775706135233293 ) ) ;
#22594 = CARTESIAN_POINT ( 'NONE',  ( -0.05219959533907301413, -21.53943276465977519, 92.49890960531436690 ) ) ;
#22596 = B_SPLINE_CURVE_WITH_KNOTS ( 'NONE', 3,
 ( #129312, #173864, #98976, #6969, #4974, #96985, #114144, #159658, #24171, #161666, #176856, #23162, #112176, #22158, #175845, #160666, #20157, #67655, #177853, #65664, #145489, #99981 ),
 .UNSPECIFIED., .F., .F.,
 ( 4, 2, 2, 2, 2, 2, 2, 2, 2, 2, 4 ),
 ( 2.776912483567713316E-17, 0.001309639967555188992, 0.001964459951332769502, 0.002291869943221559649, 0.002455574939165955373, 0.002619279935110351096, 0.002782984931054747254, 0.002946689926999142544, 0.003274099918887933124, 0.003928919902665513851, 0.005238559870220677039 ),
 .UNSPECIFIED. ) ;
#22595 = CARTESIAN_POINT ( 'NONE',  ( -16.55341960407611168, -4.379528057220339221, 26.45724293864768839 ) ) ;
#22597 = CARTESIAN_POINT ( 'NONE',  ( 18.67979575497178502, 10.72451020669898547, 49.16557627198102409 ) ) ;
#22599 = CARTESIAN_POINT ( 'NONE',  ( -13.89961937509957401, -13.97604488694547875, 104.3760903946856757 ) ) ;
#22598 = CARTESIAN_POINT ( 'NONE',  ( -15.80617190586745835, -15.72974639402198527, 86.87390960531438111 ) ) ;
#22600 = CARTESIAN_POINT ( 'NONE',  ( 19.05341960407611168, 5.049401038298154454, 98.95724293864766707 ) ) ;
#22601 = CARTESIAN_POINT ( 'NONE',  ( 21.53943276465977519, 0.05219959533937863772, 71.25109039468568994 ) ) ;
#22602 = CARTESIAN_POINT ( 'NONE',  ( 0.05219959533909260263, 19.03943276465977164, 69.99890960531435269 ) ) ;
#22603 = VECTOR ( 'NONE', #78540, 1000.000000000000114 ) ;
#22604 = CARTESIAN_POINT ( 'NONE',  ( 31.72709406046299918, -1.071565338629617092E-14, 102.5000000000000142 ) ) ;
#22605 = CARTESIAN_POINT ( 'NONE',  ( -13.97604488694527625, -13.89961937509977652, 66.87390960531436690 ) ) ;
#22606 = CARTESIAN_POINT ( 'NONE',  ( 0.05219959533910956823, 16.53943276465976808, 94.99890960531436690 ) ) ;
#22607 = ORIENTED_EDGE ( 'NONE', *, *, #187510, .T. ) ;
#22608 = CARTESIAN_POINT ( 'NONE',  ( 0.05219959533936267826, -19.03943276465977164, 110.0010903946856757 ) ) ;
#22609 = CARTESIAN_POINT ( 'NONE',  ( 16.81555441253553340, -7.025013491695478507, 83.13685445334260748 ) ) ;
#22610 = CARTESIAN_POINT ( 'NONE',  ( -16.46253265017160317, 9.564922557960807481, 70.83224293864770971 ) ) ;
#22612 = CARTESIAN_POINT ( 'NONE',  ( 19.05341960407611168, 5.049401038298154454, 93.95724293864769550 ) ) ;
#22611 = CARTESIAN_POINT ( 'NONE',  ( -21.52544592524334988, -5.823673210054445271, 88.95942372801901854 ) ) ;
#22613 = EDGE_CURVE ( 'NONE', #169869, #120001, #43333, .T. ) ;
#22614 = CARTESIAN_POINT ( 'NONE',  ( 8.314922557961029526, -14.29746914071037800, 75.41775706135233293 ) ) ;
#22615 = CARTESIAN_POINT ( 'NONE',  ( -31.05479031690789427, 1.359215367441364730, -46.85916094508149143 ) ) ;
#22616 = CARTESIAN_POINT ( 'NONE',  ( -9.564922557961040184, 16.46253265017147172, 57.91775706135233293 ) ) ;
#22617 = CARTESIAN_POINT ( 'NONE',  ( -21.53943276465977519, -0.05219959533937600094, 108.7510903946857042 ) ) ;
#22618 = CYLINDRICAL_SURFACE ( 'NONE', #188909, 2.500000000000000000 ) ;
#22619 = PLANE ( 'NONE',  #91802 ) ;
#22620 = CARTESIAN_POINT ( 'NONE',  ( 14.34966873604972726, -8.224510206698740333, 110.8344237280190043 ) ) ;
#22621 = CARTESIAN_POINT ( 'NONE',  ( -34.87614885797844977, -6.488895056989333554, 41.23117619273099876 ) ) ;
#22622 = CARTESIAN_POINT ( 'NONE',  ( -4.483927247898782831, 16.52544592524335698, 92.70942372801901854 ) ) ;
#22623 = CARTESIAN_POINT ( 'NONE',  ( 33.50392338572245166, -21.85172282306471203, -24.09813222787957443 ) ) ;
#22624 = CARTESIAN_POINT ( 'NONE',  ( -16.53943276465976808, -0.05219959533934237506, 73.75109039468567573 ) ) ;
#22625 = CARTESIAN_POINT ( 'NONE',  ( 5.823673210054444382, -21.52544592524334988, 75.20942372801901854 ) ) ;
#22626 = CARTESIAN_POINT ( 'NONE',  ( -16.46253265017146816, -9.564922557961047289, 94.16775706135233293 ) ) ;
#22627 = CARTESIAN_POINT ( 'NONE',  ( -16.51473224551082808, 9.474510206698731452, 38.33442372801899722 ) ) ;
#22628 = CARTESIAN_POINT ( 'NONE',  ( -19.05341960407611168, -5.049401038298163336, 76.45724293864769550 ) ) ;
#22629 = CARTESIAN_POINT ( 'NONE',  ( 16.46253265017160672, -9.564922557960803928, 63.33224293864769550 ) ) ;
#22630 = CARTESIAN_POINT ( 'NONE',  ( 17.72696623605161292, -5.499999999999851674, 41.09811031808418136 ) ) ;
#22631 = CARTESIAN_POINT ( 'NONE',  ( -5.823673210054116645, -21.52544592524344225, 82.29057627198103830 ) ) ;
#22632 = AXIS2_PLACEMENT_3D ( 'NONE', #76957, #61778, #151828 ) ;
#22633 = CARTESIAN_POINT ( 'NONE',  ( 21.55341960407610458, 5.719274019375980345, 43.95724293864769550 ) ) ;
#22634 = CARTESIAN_POINT ( 'NONE',  ( 16.51473224551069308, 9.474510206698969483, 34.16557627198102409 ) ) ;
#22635 = CARTESIAN_POINT ( 'NONE',  ( -12.14591786802326823, 12.06949235617739902, 68.12609039468567573 ) ) ;
#22636 = EDGE_CURVE ( 'NONE', #198944, #186287, #155898, .T. ) ;
#22637 = VERTEX_POINT ( 'NONE', #30144 ) ;
#22638 = CARTESIAN_POINT ( 'NONE',  ( -5.719274019375665041, -21.55341960407619695, 49.79275706135234714 ) ) ;
#22640 = CARTESIAN_POINT ( 'NONE',  ( 11.40812507854754365, 35.11059874428196537, -9.224999997268813701 ) ) ;
#22639 = CARTESIAN_POINT ( 'NONE',  ( -14.34966873604960291, -8.224510206698953496, 61.66557627198103120 ) ) ;
#22641 = CARTESIAN_POINT ( 'NONE',  ( -12.06949235617739369, -12.14591786802326823, 39.37609039468567573 ) ) ;
#22642 = CARTESIAN_POINT ( 'NONE',  ( -8.224510206698948167, 14.34966873604960824, 105.4155762719810383 ) ) ;
#22643 = CARTESIAN_POINT ( 'NONE',  ( -13.97604488694547697, 13.89961937509957934, 58.12609039468566863 ) ) ;
#22644 = CARTESIAN_POINT ( 'NONE',  ( -16.55341960407611168, -4.379528057220339221, 56.45724293864768839 ) ) ;
#22645 = CARTESIAN_POINT ( 'NONE',  ( -10.81492255796105439, 18.62759615963255655, 27.91775706135234358 ) ) ;
#22647 = CARTESIAN_POINT ( 'NONE',  ( -18.67979575497178146, -10.72451020669898902, 91.66557627198103830 ) ) ;
#22646 = CARTESIAN_POINT ( 'NONE',  ( -13.97604488694527625, -13.89961937509977652, 26.87390960531434558 ) ) ;
#22648 = CARTESIAN_POINT ( 'NONE',  ( 16.46253265017160672, -9.564922557960803928, 98.33224293864769550 ) ) ;
#22649 = CARTESIAN_POINT ( 'NONE',  ( 14.34966873604960469, 8.224510206698951720, 74.16557627198102409 ) ) ;
#22650 = CARTESIAN_POINT ( 'NONE',  ( -16.51473224551069308, -9.474510206698971260, 111.6655762719810383 ) ) ;
#22651 = CARTESIAN_POINT ( 'NONE',  ( -36.91746825000000598, 2.428612866367529932E-14, -6.624999997268814056 ) ) ;
#22652 = CARTESIAN_POINT ( 'NONE',  ( -9.564922557961040184, 16.46253265017147172, 82.91775706135233293 ) ) ;
#22653 = CARTESIAN_POINT ( 'NONE',  ( -5.719274019375665041, -21.55341960407619695, 19.79275706135235069 ) ) ;
#22654 = CARTESIAN_POINT ( 'NONE',  ( 19.05341960407611168, 5.049401038298154454, 63.95724293864769550 ) ) ;
#22655 = CARTESIAN_POINT ( 'NONE',  ( 13.89961937509957401, 13.97604488694547697, 51.87609039468566863 ) ) ;
#22656 = CARTESIAN_POINT ( 'NONE',  ( -5.049401038298153566, 19.05341960407611168, 30.20724293864768839 ) ) ;
#22657 = CARTESIAN_POINT ( 'NONE',  ( -18.67979575497193778, 10.72451020669871902, 63.33442372801900433 ) ) ;
#22658 = FACE_OUTER_BOUND ( 'NONE', #101157, .T. ) ;
#22659 = CARTESIAN_POINT ( 'NONE',  ( 8.224510206698953496, -14.34966873604960469, 52.91557627198103830 ) ) ;
#22660 = CARTESIAN_POINT ( 'NONE',  ( -9.474510206698964154, 16.51473224551069663, 60.41557627198102409 ) ) ;
#22661 = CARTESIAN_POINT ( 'NONE',  ( 18.62759615963271287, -10.81492255796078972, 88.33224293864769550 ) ) ;
#22662 = CARTESIAN_POINT ( 'NONE',  ( 0.05219959533909260263, 19.03943276465977164, 54.99890960531435979 ) ) ;
#22663 = ORIENTED_EDGE ( 'NONE', *, *, #120340, .F. ) ;
#22664 = CARTESIAN_POINT ( 'NONE',  ( 15.80617190586746368, 15.72974639402197994, 79.37390960531436690 ) ) ;
#22665 = CARTESIAN_POINT ( 'NONE',  ( -18.62759615963255300, -10.81492255796106328, 94.16775706135237556 ) ) ;
#22668 = CARTESIAN_POINT ( 'NONE',  ( -16.55341960407611168, -4.379528057220339221, 96.45724293864770971 ) ) ;
#22667 = CARTESIAN_POINT ( 'NONE',  ( -12.14591786802326823, 12.06949235617739902, 93.12609039468568994 ) ) ;
#22666 = CARTESIAN_POINT ( 'NONE',  ( 19.02544592524343514, -5.153800228976328945, 23.54057627198102054 ) ) ;
#22669 = CARTESIAN_POINT ( 'NONE',  ( -16.51473224551082808, 9.474510206698731452, 88.33442372801900433 ) ) ;
#22670 = EDGE_LOOP ( 'NONE', ( #127996, #170160, #88143, #37570 ) ) ;
#22671 = CARTESIAN_POINT ( 'NONE',  ( -18.62759615963255300, -10.81492255796106328, 19.16775706135234714 ) ) ;
#22672 = CARTESIAN_POINT ( 'NONE',  ( 0.05219959533936267826, -19.03943276465977164, 35.00109039468566863 ) ) ;
#22673 = CARTESIAN_POINT ( 'NONE',  ( 16.52544592524335698, 4.483927247898782831, 106.4594237280190328 ) ) ;
#22674 = CARTESIAN_POINT ( 'NONE',  ( 5.153800228976615827, -19.02544592524334988, 25.20942372801900433 ) ) ;
#22675 = CARTESIAN_POINT ( 'NONE',  ( -16.46253265017160317, 9.564922557960807481, 100.8322429386477097 ) ) ;
#22676 = CARTESIAN_POINT ( 'NONE',  ( 18.67979575497178502, 10.72451020669898547, 59.16557627198103120 ) ) ;
#22677 = CARTESIAN_POINT ( 'NONE',  ( -16.51473224551069308, -9.474510206698971260, 21.66557627198102765 ) ) ;
#22678 = CARTESIAN_POINT ( 'NONE',  ( 16.51473224551069308, 9.474510206698969483, 24.16557627198102765 ) ) ;
#22679 = CARTESIAN_POINT ( 'NONE',  ( 10.72451020669871369, 18.67979575497193778, 107.0844237280190043 ) ) ;
#22680 = CARTESIAN_POINT ( 'NONE',  ( -4.483927247898782831, 16.52544592524335698, 77.70942372801900433 ) ) ;
#22681 = CARTESIAN_POINT ( 'NONE',  ( 21.53943276465977519, 0.05219959533937863772, 31.25109039468568639 ) ) ;
#22682 = CARTESIAN_POINT ( 'NONE',  ( -16.53943276465976808, -0.05219959533934237506, 38.75109039468567573 ) ) ;
#22683 = CARTESIAN_POINT ( 'NONE',  ( -19.05341960407611168, -5.049401038298163336, 101.4572429386476955 ) ) ;
#22684 = CARTESIAN_POINT ( 'NONE',  ( -19.02544592524342804, 5.153800228976336051, 41.04057627198103120 ) ) ;
#22685 = CARTESIAN_POINT ( 'NONE',  ( -19.02544592524342804, 5.153800228976336051, 71.04057627198099567 ) ) ;
#22686 = CARTESIAN_POINT ( 'NONE',  ( 0.05219959533934541429, -16.53943276465976808, 50.00109039468568994 ) ) ;
#22687 = CARTESIAN_POINT ( 'NONE',  ( 16.53943276465976808, -0.05219959533910856209, 88.74890960531436690 ) ) ;
#22688 = CARTESIAN_POINT ( 'NONE',  ( -16.52544592524335698, -4.483927247898792601, 98.95942372801903275 ) ) ;
#22689 = CARTESIAN_POINT ( 'NONE',  ( 9.564922557960805705, 16.46253265017160317, 49.58224293864770260 ) ) ;
#22692 = CARTESIAN_POINT ( 'NONE',  ( 19.03943276465977164, -0.05219959533909143690, 63.74890960531435979 ) ) ;
#22691 = CARTESIAN_POINT ( 'NONE',  ( 9.564922557960805705, 16.46253265017160317, 74.58224293864769550 ) ) ;
#22690 = CARTESIAN_POINT ( 'NONE',  ( -18.67979575497193778, 10.72451020669871902, 63.33442372801900433 ) ) ;
#22693 = CARTESIAN_POINT ( 'NONE',  ( -19.03943276465977164, 0.05219959533909376836, 101.2489096053143669 ) ) ;
#22694 = CARTESIAN_POINT ( 'NONE',  ( -8.314922557960811034, -14.29746914071050412, 47.08224293864770260 ) ) ;
#22695 = CARTESIAN_POINT ( 'NONE',  ( 4.379528057220092307, 16.55341960407617563, 102.2927570613523613 ) ) ;
#22696 = CARTESIAN_POINT ( 'NONE',  ( 12.14591786802309770, 12.06949235617756955, 29.37390960531435269 ) ) ;
#22697 = ORIENTED_EDGE ( 'NONE', *, *, #25125, .T. ) ;
#22698 = CARTESIAN_POINT ( 'NONE',  ( 5.049401038297881783, 19.05341960407617563, 42.29275706135234003 ) ) ;
#22699 = CARTESIAN_POINT ( 'NONE',  ( -13.89961937509977652, 13.97604488694528158, 110.6239096053143243 ) ) ;
#22700 = CARTESIAN_POINT ( 'NONE',  ( 13.97604488694527802, 13.89961937509977652, 64.37390960531436690 ) ) ;
#22701 = CARTESIAN_POINT ( 'NONE',  ( 13.89961937509957401, 13.97604488694547697, 36.87609039468565442 ) ) ;
#22702 = CARTESIAN_POINT ( 'NONE',  ( 29.86685920354754842, -21.69954338932559068, -3.824999997268813345 ) ) ;
#22703 = CARTESIAN_POINT ( 'NONE',  ( 17.49999999999999645, 3.242565516156353134, 37.49999999998637179 ) ) ;
#22705 = CARTESIAN_POINT ( 'NONE',  ( 16.53943276465976808, 0.05219959533934440121, 66.25109039468567573 ) ) ;
#22704 = CARTESIAN_POINT ( 'NONE',  ( 5.049401038297881783, 19.05341960407617563, 87.29275706135234714 ) ) ;
#22706 = CARTESIAN_POINT ( 'NONE',  ( 17.26058549869090797, 6.457015423128543929, 93.87745837476069255 ) ) ;
#22707 = CARTESIAN_POINT ( 'NONE',  ( -13.97604488694527625, -13.89961937509977652, 86.87390960531436690 ) ) ;
#22708 = CARTESIAN_POINT ( 'NONE',  ( -0.05219959533937732626, 21.53943276465977519, 32.50109039468568284 ) ) ;
#22709 = CARTESIAN_POINT ( 'NONE',  ( 9.564922557961047289, -16.46253265017146816, 70.41775706135233293 ) ) ;
#22711 = CARTESIAN_POINT ( 'NONE',  ( -13.97604488694527625, -13.89961937509977652, 31.87390960531435979 ) ) ;
#22710 = CARTESIAN_POINT ( 'NONE',  ( -16.46253265017160317, 9.564922557960807481, 115.8322429386477097 ) ) ;
#22712 = CARTESIAN_POINT ( 'NONE',  ( -0.05219959533909027116, -19.03943276465977164, 87.49890960531436690 ) ) ;
#22714 = CARTESIAN_POINT ( 'NONE',  ( -13.97604488694527625, -13.89961937509977652, 41.87390960531435979 ) ) ;
#22713 = CARTESIAN_POINT ( 'NONE',  ( -16.53943276465976808, 0.05219959533911058130, 46.24890960531435979 ) ) ;
#22715 = CARTESIAN_POINT ( 'NONE',  ( -19.03943276465977164, -0.05219959533935918106, 48.75109039468566863 ) ) ;
#22716 = CARTESIAN_POINT ( 'NONE',  ( 16.53943276465976808, -0.05219959533910856209, 88.74890960531436690 ) ) ;
#22717 = CARTESIAN_POINT ( 'NONE',  ( -0.05219959533936034679, 19.03943276465977164, 32.50109039468566863 ) ) ;
#22718 = CARTESIAN_POINT ( 'NONE',  ( 19.05341960407611168, 5.049401038298154454, 58.95724293864768129 ) ) ;
#22719 = CARTESIAN_POINT ( 'NONE',  ( -18.62759615963270932, 10.81492255796079327, 60.83224293864769550 ) ) ;
#22721 = CARTESIAN_POINT ( 'NONE',  ( -0.05219959533936034679, 19.03943276465977164, 27.50109039468566507 ) ) ;
#22720 = CARTESIAN_POINT ( 'NONE',  ( 14.34966873604960469, 8.224510206698951720, 59.16557627198103120 ) ) ;
#22722 = CARTESIAN_POINT ( 'NONE',  ( 19.05341960407611168, 5.049401038298154454, 108.9572429386477097 ) ) ;
#22723 = CARTESIAN_POINT ( 'NONE',  ( -10.81492255796078084, -18.62759615963271287, 22.08224293864769194 ) ) ;
#22724 = CARTESIAN_POINT ( 'NONE',  ( 16.51473224551069308, 9.474510206698969483, 54.16557627198103120 ) ) ;
#22725 = CARTESIAN_POINT ( 'NONE',  ( -9.474510206698964154, 16.51473224551069663, 25.41557627198103120 ) ) ;
#22726 = CARTESIAN_POINT ( 'NONE',  ( -12.14591786802309592, -12.06949235617757132, 91.87390960531436690 ) ) ;
#22727 = CARTESIAN_POINT ( 'NONE',  ( -18.62759615963270932, 10.81492255796079327, 100.8322429386477097 ) ) ;
#22728 = CARTESIAN_POINT ( 'NONE',  ( 16.51473224551069308, 9.474510206698969483, 99.16557627198102409 ) ) ;
#22729 = CARTESIAN_POINT ( 'NONE',  ( -15.72974639402197994, 15.80617190586746368, 105.6239096053143669 ) ) ;
#22730 = CARTESIAN_POINT ( 'NONE',  ( -19.05341960407611168, -5.049401038298163336, 106.4572429386476955 ) ) ;
#22731 = CARTESIAN_POINT ( 'NONE',  ( -9.564922557960796823, -16.46253265017161027, 27.08224293864769550 ) ) ;
#22732 = CARTESIAN_POINT ( 'NONE',  ( 0.05219959533937995610, -21.53943276465977519, 75.00109039468568994 ) ) ;
#22733 = CARTESIAN_POINT ( 'NONE',  ( -21.53943276465977519, 0.05219959533907696930, 96.24890960531435269 ) ) ;
#22734 = CARTESIAN_POINT ( 'NONE',  ( 16.20579543436677739, -7.371946100355110332, 106.9347916582812559 ) ) ;
#22735 = CARTESIAN_POINT ( 'NONE',  ( 19.36337904590693881, -5.499999999999943157, 77.91494137495617167 ) ) ;
#22736 = CARTESIAN_POINT ( 'NONE',  ( 31.78116016545943268, -0.5954834035867749842, -49.28208245900466977 ) ) ;
#22737 = CARTESIAN_POINT ( 'NONE',  ( 12.14591786802327356, -12.06949235617739191, 35.62609039468568994 ) ) ;
#22738 = CARTESIAN_POINT ( 'NONE',  ( -8.314922557960811034, -14.29746914071050412, 107.0822429386476955 ) ) ;
#22739 = CARTESIAN_POINT ( 'NONE',  ( -17.50000000000000355, -3.345213924137315331, 110.4123137690565102 ) ) ;
#22740 = CARTESIAN_POINT ( 'NONE',  ( -13.89961937509977652, 13.97604488694528158, 55.62390960531434558 ) ) ;
#22741 = CARTESIAN_POINT ( 'NONE',  ( 12.14591786802309770, 12.06949235617756955, 94.37390960531436690 ) ) ;
#22742 = CARTESIAN_POINT ( 'NONE',  ( 10.72451020669898902, -18.67979575497178502, 37.91557627198102409 ) ) ;
#22743 = CARTESIAN_POINT ( 'NONE',  ( -16.55341960407611168, -4.379528057220339221, 61.45724293864770260 ) ) ;
#22744 = CARTESIAN_POINT ( 'NONE',  ( 0.05219959533934541429, -16.53943276465976808, 25.00109039468567218 ) ) ;
#22745 = CARTESIAN_POINT ( 'NONE',  ( -5.719274019375665041, -21.55341960407619695, 69.79275706135234714 ) ) ;
#22746 = CARTESIAN_POINT ( 'NONE',  ( 17.40805194822031154, -6.112264579159332634, 78.33371272510611050 ) ) ;
#22747 = CARTESIAN_POINT ( 'NONE',  ( -19.03943276465977164, 0.05219959533909376836, 116.2489096053143669 ) ) ;
#22748 = CARTESIAN_POINT ( 'NONE',  ( 12.06949235617739724, 12.14591786802326823, 96.87609039468568994 ) ) ;
#22749 = CARTESIAN_POINT ( 'NONE',  ( -5.049401038298153566, 19.05341960407611168, 45.20724293864769550 ) ) ;
#22750 = CARTESIAN_POINT ( 'NONE',  ( -9.474510206698964154, 16.51473224551069663, 95.41557627198102409 ) ) ;
#22751 = CARTESIAN_POINT ( 'NONE',  ( -21.52544592524343514, 5.823673210054127303, 96.04057627198102409 ) ) ;
#22752 = CARTESIAN_POINT ( 'NONE',  ( -14.29746914071037622, -8.314922557961029526, 24.16775706135235424 ) ) ;
#22754 = CARTESIAN_POINT ( 'NONE',  ( 21.55341960407619695, -5.719274019375665929, 71.04275706135234714 ) ) ;
#22753 = CARTESIAN_POINT ( 'NONE',  ( 4.379528057220339221, -16.55341960407611168, 67.70724293864769550 ) ) ;
#22755 = CARTESIAN_POINT ( 'NONE',  ( 8.314922557961029526, -14.29746914071037800, 105.4177570613523613 ) ) ;
#22756 = CARTESIAN_POINT ( 'NONE',  ( 17.48847506799950224, -5.747544572775292515, 48.32697437843292931 ) ) ;
#22757 = LINE ( 'NONE', #84406, #129264 ) ;
#22758 = CARTESIAN_POINT ( 'NONE',  ( -16.55341960407611168, -4.379528057220339221, 26.45724293864768839 ) ) ;
#22759 = CARTESIAN_POINT ( 'NONE',  ( 12.06949235617739724, 12.14591786802326823, 71.87609039468568994 ) ) ;
#22760 = CARTESIAN_POINT ( 'NONE',  ( 5.153800228976335163, 19.02544592524342804, 79.79057627198102409 ) ) ;
#22761 = CARTESIAN_POINT ( 'NONE',  ( 19.03943276465977164, -0.05219959533909143690, 88.74890960531436690 ) ) ;
#22762 = CARTESIAN_POINT ( 'NONE',  ( 21.52544592524334988, 5.823673210054432836, 86.45942372801901854 ) ) ;
#22763 = CARTESIAN_POINT ( 'NONE',  ( -12.06949235617739369, -12.14591786802326823, 84.37609039468570415 ) ) ;
#22764 = CARTESIAN_POINT ( 'NONE',  ( 4.379528057220339221, -16.55341960407611168, 62.70724293864769550 ) ) ;
#22765 = CARTESIAN_POINT ( 'NONE',  ( 5.049401038298161559, -19.05341960407611168, 62.70724293864769550 ) ) ;
#22766 = VERTEX_POINT ( 'NONE', #150525 ) ;
#22768 = CARTESIAN_POINT ( 'NONE',  ( -19.02544592524334988, -5.153800228976617603, 103.9594237280190043 ) ) ;
#22767 =( BOUNDED_CURVE ( )  B_SPLINE_CURVE ( 2, ( #29210, #46347, #169690, #150566, #183877, #90844, #152529, #108004, #199040, #196087, #60510, #57557, #119227 ),
 .UNSPECIFIED., .F., .T. ) 
 B_SPLINE_CURVE_WITH_KNOTS ( ( 3, 2, 2, 2, 2, 2, 3 ),
 ( 0.3971672785323083210, 0.3991228070175438791, 0.4035087719298245390, 0.4078947368421052544, 0.4122807017543859698, 0.4166666666666666852, 0.4185765153298121599 ),
 .UNSPECIFIED. ) 
 CURVE ( )  GEOMETRIC_REPRESENTATION_ITEM ( )  RATIONAL_B_SPLINE_CURVE ( ( 0.9831626618144004848, 0.9848076720550091867, 1.000000000000000000, 0.9659258262890683122, 1.000000000000000000, 0.9659258262890683122, 1.000000000000000000, 0.9659258262890683122, 1.000000000000000000, 0.9659258262890683122, 1.000000000000000000, 0.9851625545550088958, 0.9832469066685279868 ) ) 
 REPRESENTATION_ITEM ( '' )  );
#22769 = CARTESIAN_POINT ( 'NONE',  ( 8.314922557960818139, 14.29746914071049879, 114.5822429386477097 ) ) ;
#22770 = CARTESIAN_POINT ( 'NONE',  ( -13.89961937509977652, 13.97604488694528158, 80.62390960531436690 ) ) ;
#22772 = CARTESIAN_POINT ( 'NONE',  ( 37.99999999999999289, 2.893978650043524126E-14, -1.000000000000000000 ) ) ;
#22771 = CARTESIAN_POINT ( 'NONE',  ( -19.05341960407617563, 5.049401038297882671, 108.5427570613523187 ) ) ;
#22773 = CARTESIAN_POINT ( 'NONE',  ( -5.049401038297874678, -19.05341960407617918, 24.79275706135233648 ) ) ;
#22774 = CARTESIAN_POINT ( 'NONE',  ( 8.314922557961029526, -14.29746914071037800, 85.41775706135236135 ) ) ;
#22775 = CARTESIAN_POINT ( 'NONE',  ( 5.153800228976615827, -19.02544592524334988, 90.20942372801900433 ) ) ;
#22776 = CARTESIAN_POINT ( 'NONE',  ( -16.52544592524342804, 4.483927247898546575, 111.0405762719810525 ) ) ;
#22777 = CARTESIAN_POINT ( 'NONE',  ( -16.53943276465976808, -0.05219959533934237506, 68.75109039468568994 ) ) ;
#22778 = CARTESIAN_POINT ( 'NONE',  ( 12.99999999999999822, 0.000000000000000000, 2.055000000000000160 ) ) ;
#22779 = CARTESIAN_POINT ( 'NONE',  ( 13.89961937509957401, 13.97604488694547697, 61.87609039468566863 ) ) ;
#22780 = CARTESIAN_POINT ( 'NONE',  ( 21.53943276465977519, 0.05219959533937863772, 101.2510903946856757 ) ) ;
#22781 = CARTESIAN_POINT ( 'NONE',  ( 19.03943276465977164, -0.05219959533909143690, 38.74890960531436690 ) ) ;
#22782 = CARTESIAN_POINT ( 'NONE',  ( -5.049401038298153566, 19.05341960407611168, 80.20724293864769550 ) ) ;
#22783 = CARTESIAN_POINT ( 'NONE',  ( -8.224510206698948167, 14.34966873604960824, 75.41557627198102409 ) ) ;
#22784 = VECTOR ( 'NONE', #55026, 1000.000000000000000 ) ;
#22785 = CARTESIAN_POINT ( 'NONE',  ( 18.62759615963255655, 10.81492255796105972, 91.66775706135234714 ) ) ;
#22786 = CARTESIAN_POINT ( 'NONE',  ( 13.89961937509957401, 13.97604488694547697, 61.87609039468566863 ) ) ;
#22787 = CARTESIAN_POINT ( 'NONE',  ( -5.049401038297874678, -19.05341960407617918, 44.79275706135232582 ) ) ;
#22788 = CARTESIAN_POINT ( 'NONE',  ( 18.62759615963271287, -10.81492255796078972, 33.33224293864769550 ) ) ;
#22789 = CARTESIAN_POINT ( 'NONE',  ( 21.55341960407619695, -5.719274019375665929, 101.0427570613523756 ) ) ;
#22790 = CARTESIAN_POINT ( 'NONE',  ( 16.51473224551069308, 9.474510206698969483, 84.16557627198102409 ) ) ;
#22791 = EDGE_CURVE ( 'NONE', #48134, #137596, #13885, .T. ) ;
#22792 = CARTESIAN_POINT ( 'NONE',  ( 18.67979575497194134, -10.72451020669871369, 100.8344237280190185 ) ) ;
#22793 = CARTESIAN_POINT ( 'NONE',  ( -18.67979575497178146, -10.72451020669898902, 51.66557627198102409 ) ) ;
#22794 = CARTESIAN_POINT ( 'NONE',  ( 16.51473224551069308, 9.474510206698969483, 94.16557627198103830 ) ) ;
#22795 = CARTESIAN_POINT ( 'NONE',  ( -19.03943276465977164, -0.05219959533935918106, 73.75109039468566152 ) ) ;
#22796 = CARTESIAN_POINT ( 'NONE',  ( -19.02544592524342804, 5.153800228976336051, 106.0405762719810241 ) ) ;
#22797 = CARTESIAN_POINT ( 'NONE',  ( 13.89961937509957401, 13.97604488694547697, 96.87609039468566152 ) ) ;
#22798 = CARTESIAN_POINT ( 'NONE',  ( -8.314922557961024197, 14.29746914071037800, 37.91775706135235424 ) ) ;
#22799 = CARTESIAN_POINT ( 'NONE',  ( -16.55341960407611168, -4.379528057220339221, 101.4572429386476955 ) ) ;
#22800 = CARTESIAN_POINT ( 'NONE',  ( -16.46253265017160317, 9.564922557960807481, 85.83224293864769550 ) ) ;
#22801 = CARTESIAN_POINT ( 'NONE',  ( 18.67979575497178502, 10.72451020669898547, 59.16557627198103120 ) ) ;
#22802 = CARTESIAN_POINT ( 'NONE',  ( -12.06949235617739369, -12.14591786802326823, 34.37609039468568284 ) ) ;
#22803 = CARTESIAN_POINT ( 'NONE',  ( 18.62759615963255655, 10.81492255796105972, 31.66775706135234358 ) ) ;
#22804 = CARTESIAN_POINT ( 'NONE',  ( 10.81492255796106328, -18.62759615963255655, 85.41775706135236135 ) ) ;
#22805 = CARTESIAN_POINT ( 'NONE',  ( 16.52544592524335698, 4.483927247898782831, 76.45942372801901854 ) ) ;
#22806 = CARTESIAN_POINT ( 'NONE',  ( -9.474510206698964154, 16.51473224551069663, 80.41557627198103830 ) ) ;
#22807 = CARTESIAN_POINT ( 'NONE',  ( 14.34966873604960469, 8.224510206698951720, 84.16557627198103830 ) ) ;
#22808 = CARTESIAN_POINT ( 'NONE',  ( 14.29746914071037800, 8.314922557961029526, 111.6677570613523613 ) ) ;
#22809 = CARTESIAN_POINT ( 'NONE',  ( -5.153800228976607833, 19.02544592524334988, 52.70942372801900433 ) ) ;
#22810 = CARTESIAN_POINT ( 'NONE',  ( -10.81492255796105439, 18.62759615963255655, 32.91775706135234714 ) ) ;
#22811 = CARTESIAN_POINT ( 'NONE',  ( 4.483927247898545687, 16.52544592524342804, 74.79057627198105251 ) ) ;
#22812 = CARTESIAN_POINT ( 'NONE',  ( 19.05341960407611168, 5.049401038298154454, 93.95724293864769550 ) ) ;
#22813 = CARTESIAN_POINT ( 'NONE',  ( -12.14591786802326823, 12.06949235617739902, 108.1260903946856757 ) ) ;
#22814 = CARTESIAN_POINT ( 'NONE',  ( -21.53943276465977519, -0.05219959533937600094, 68.75109039468568994 ) ) ;
#22815 = CARTESIAN_POINT ( 'NONE',  ( 4.379528057220092307, 16.55341960407617563, 47.29275706135234003 ) ) ;
#22816 = CARTESIAN_POINT ( 'NONE',  ( 21.55341960407619695, -5.719274019375665929, 41.04275706135236135 ) ) ;
#22817 = ORIENTED_EDGE ( 'NONE', *, *, #167117, .F. ) ;
#22818 = CARTESIAN_POINT ( 'NONE',  ( 10.81492255796078972, 18.62759615963270932, 109.5822429386476955 ) ) ;
#22819 = CARTESIAN_POINT ( 'NONE',  ( -8.224510206698948167, 14.34966873604960824, 85.41557627198102409 ) ) ;
#22820 = CARTESIAN_POINT ( 'NONE',  ( -19.19724070472091526, -5.500000000000167866, 51.06193348274386778 ) ) ;
#22821 = CARTESIAN_POINT ( 'NONE',  ( -14.34966873604960291, -8.224510206698953496, 46.66557627198102409 ) ) ;
#22822 = CARTESIAN_POINT ( 'NONE',  ( -0.05219959533909027116, -19.03943276465977164, 22.49890960531436690 ) ) ;
#22823 = CARTESIAN_POINT ( 'NONE',  ( 18.62759615963271287, -10.81492255796078972, 48.33224293864770260 ) ) ;
#22824 = CARTESIAN_POINT ( 'NONE',  ( -14.29746914071049879, 8.314922557960819915, 75.83224293864769550 ) ) ;
#22825 = CARTESIAN_POINT ( 'NONE',  ( -21.52544592524343514, 5.823673210054127303, 86.04057627198102409 ) ) ;
#22826 = CARTESIAN_POINT ( 'NONE',  ( -19.03943276465977164, 0.05219959533909376836, 86.24890960531436690 ) ) ;
#22828 = CARTESIAN_POINT ( 'NONE',  ( 19.02544592524334988, 5.153800228976608722, 76.45942372801897591 ) ) ;
#22827 = CARTESIAN_POINT ( 'NONE',  ( -9.564922557960796823, -16.46253265017161027, 42.08224293864769550 ) ) ;
#22829 = CARTESIAN_POINT ( 'NONE',  ( -21.53943276465977519, 0.05219959533907696930, 26.24890960531435624 ) ) ;
#22831 = CARTESIAN_POINT ( 'NONE',  ( 18.67979575497178502, 10.72451020669898547, 64.16557627198102409 ) ) ;
#22830 = CARTESIAN_POINT ( 'NONE',  ( -21.53943276465977519, -0.05219959533937600094, 58.75109039468568994 ) ) ;
#22832 = CARTESIAN_POINT ( 'NONE',  ( -16.46253265017160317, 9.564922557960807481, 35.83224293864768839 ) ) ;
#22833 = CARTESIAN_POINT ( 'NONE',  ( 13.97604488694527802, 13.89961937509977652, 69.37390960531436690 ) ) ;
#22834 = VERTEX_POINT ( 'NONE', #61463 ) ;
#22835 = CARTESIAN_POINT ( 'NONE',  ( 8.224510206698742110, 14.34966873604972548, 52.08442372801901854 ) ) ;
#22836 = CARTESIAN_POINT ( 'NONE',  ( -10.72451020669870658, -18.67979575497194134, 24.58442372801901499 ) ) ;
#22837 = CARTESIAN_POINT ( 'NONE',  ( 10.81492255796106328, -18.62759615963255655, 70.41775706135236135 ) ) ;
#22838 = CARTESIAN_POINT ( 'NONE',  ( -10.72451020669898014, 18.67979575497178502, 25.41557627198103120 ) ) ;
#22839 = CARTESIAN_POINT ( 'NONE',  ( -10.81492255796078084, -18.62759615963271287, 82.08224293864768129 ) ) ;
#22841 = CARTESIAN_POINT ( 'NONE',  ( 16.55341960407618274, -4.379528057220086978, 51.04275706135234714 ) ) ;
#22840 = CARTESIAN_POINT ( 'NONE',  ( -10.72451020669870658, -18.67979575497194134, 29.58442372801901854 ) ) ;
#22842 = CARTESIAN_POINT ( 'NONE',  ( -5.823673210054116645, -21.52544592524344225, 67.29057627198103830 ) ) ;
#22843 = CARTESIAN_POINT ( 'NONE',  ( -9.564922557961040184, 16.46253265017147172, 22.91775706135233648 ) ) ;
#22844 = CARTESIAN_POINT ( 'NONE',  ( 13.89961937509977652, -13.97604488694527269, 58.12390960531436690 ) ) ;
#22845 = CARTESIAN_POINT ( 'NONE',  ( -13.97604488694527625, -13.89961937509977652, 111.8739096053143243 ) ) ;
#22846 = CARTESIAN_POINT ( 'NONE',  ( -13.89961937509977652, 13.97604488694528158, 90.62390960531432427 ) ) ;
#22847 = CARTESIAN_POINT ( 'NONE',  ( 17.50000000000001421, 5.047551163040773226, 103.6653608652058836 ) ) ;
#22848 = CARTESIAN_POINT ( 'NONE',  ( -19.02544592524334988, -5.153800228976617603, 63.95942372801899012 ) ) ;
#22849 = CARTESIAN_POINT ( 'NONE',  ( -15.80617190586745835, -15.72974639402198527, 46.87390960531435979 ) ) ;
#22850 = CARTESIAN_POINT ( 'NONE',  ( 14.29746914071049879, -8.314922557960816363, 28.33224293864769550 ) ) ;
#22851 = CARTESIAN_POINT ( 'NONE',  ( 9.474510206698729675, 16.51473224551082808, 102.0844237280190043 ) ) ;
#22852 = CARTESIAN_POINT ( 'NONE',  ( 17.97182807773873492, -5.500000000000077272, 51.03038844047286204 ) ) ;
#22853 = CARTESIAN_POINT ( 'NONE',  ( 19.03943276465977164, 0.05219959533936151252, 26.25109039468566507 ) ) ;
#22854 = CARTESIAN_POINT ( 'NONE',  ( -9.474510206698720793, -16.51473224551083518, 94.58442372801900433 ) ) ;
#22856 = CARTESIAN_POINT ( 'NONE',  ( -16.46253265017146816, -9.564922557961047289, 59.16775706135233293 ) ) ;
#22855 = CARTESIAN_POINT ( 'NONE',  ( -15.72974639402197994, 15.80617190586746368, 85.62390960531436690 ) ) ;
#22857 = CARTESIAN_POINT ( 'NONE',  ( 26.47577687012304182, -8.223210953690971436, 167.6032987643051513 ) ) ;
#22858 = CARTESIAN_POINT ( 'NONE',  ( 16.51473224551069308, 9.474510206698969483, 54.16557627198103120 ) ) ;
#22859 = CARTESIAN_POINT ( 'NONE',  ( 16.52544592524342804, -4.483927247898539470, 63.54057627198103830 ) ) ;
#22860 = CARTESIAN_POINT ( 'NONE',  ( 19.03943276465977164, -0.05219959533909143690, 53.74890960531436690 ) ) ;
#22861 = CARTESIAN_POINT ( 'NONE',  ( 12.06949235617757843, -12.14591786802309237, 58.12390960531435979 ) ) ;
#22862 = CARTESIAN_POINT ( 'NONE',  ( -22.49873734152892624, 26.99873734152936677, 1.110912703473986074 ) ) ;
#22863 = CARTESIAN_POINT ( 'NONE',  ( -4.379528057220328563, 16.55341960407611168, 25.20724293864769550 ) ) ;
#22864 = CARTESIAN_POINT ( 'NONE',  ( 13.97604488694527802, 13.89961937509977652, 64.37390960531436690 ) ) ;
#22865 = CARTESIAN_POINT ( 'NONE',  ( -19.05341960407617563, 5.049401038297882671, 28.54275706135232937 ) ) ;
#22866 = CARTESIAN_POINT ( 'NONE',  ( 16.52544592524335698, 4.483927247898782831, 31.45942372801901854 ) ) ;
#22867 = CARTESIAN_POINT ( 'NONE',  ( -21.52544592524343514, 5.823673210054127303, 56.04057627198102409 ) ) ;
#22869 = ORIENTED_EDGE ( 'NONE', *, *, #178067, .F. ) ;
#22868 = CARTESIAN_POINT ( 'NONE',  ( 18.67979575497194134, -10.72451020669871369, 110.8344237280190043 ) ) ;
#22870 = CARTESIAN_POINT ( 'NONE',  ( 13.97604488694527802, 13.89961937509977652, 59.37390960531434558 ) ) ;
#22871 = DIRECTION ( 'NONE',  ( -0.5000000000000037748, -0.4999999999999950595, -0.7071067811865484609 ) ) ;
#22872 = CARTESIAN_POINT ( 'NONE',  ( 5.153800228976335163, 19.02544592524342804, 94.79057627198103830 ) ) ;
#22873 = CARTESIAN_POINT ( 'NONE',  ( -17.72560187377284890, -5.500000000000053291, 44.07814504131320632 ) ) ;
#22874 = CARTESIAN_POINT ( 'NONE',  ( -15.72974639402176322, -15.80617190586768395, 24.37609039468567573 ) ) ;
#22875 = CARTESIAN_POINT ( 'NONE',  ( -12.14591786802309592, -12.06949235617757132, 96.87390960531436690 ) ) ;
#22877 = CARTESIAN_POINT ( 'NONE',  ( -9.564922557960796823, -16.46253265017161027, 67.08224293864769550 ) ) ;
#22876 = CARTESIAN_POINT ( 'NONE',  ( 18.62759615963271287, -10.81492255796078972, 93.33224293864769550 ) ) ;
#22878 = CARTESIAN_POINT ( 'NONE',  ( 5.049401038298161559, -19.05341960407611168, 87.70724293864769550 ) ) ;
#22879 = CARTESIAN_POINT ( 'NONE',  ( -21.52544592524343514, 5.823673210054127303, 111.0405762719810525 ) ) ;
#22880 = EDGE_CURVE ( 'NONE', #44580, #196699, #122143, .T. ) ;
#22881 = ORIENTED_EDGE ( 'NONE', *, *, #199123, .F. ) ;
#22882 = CARTESIAN_POINT ( 'NONE',  ( -19.05341960407611168, -5.049401038298163336, 76.45724293864769550 ) ) ;
#22883 = CARTESIAN_POINT ( 'NONE',  ( 18.39443945427639093, -5.500000000000021316, 96.01745347608654413 ) ) ;
#22885 = CARTESIAN_POINT ( 'NONE',  ( 2.500000000000000000, 0.000000000000000000, 0.000000000000000000 ) ) ;
#22884 = CARTESIAN_POINT ( 'NONE',  ( -16.55341960407611168, -4.379528057220339221, 106.4572429386477097 ) ) ;
#22886 = CARTESIAN_POINT ( 'NONE',  ( -19.05341960407617563, 5.049401038297882671, 93.54275706135234714 ) ) ;
#22887 = CARTESIAN_POINT ( 'NONE',  ( -4.379528057220328563, 16.55341960407611168, 95.20724293864769550 ) ) ;
#22888 = CARTESIAN_POINT ( 'NONE',  ( -18.67979575497193778, 10.72451020669871902, 73.33442372801901854 ) ) ;
#22890 = CARTESIAN_POINT ( 'NONE',  ( 10.72451020669871369, 18.67979575497193778, 32.08442372801901854 ) ) ;
#22889 = CARTESIAN_POINT ( 'NONE',  ( -5.153800228976328057, -19.02544592524343514, 67.29057627198102409 ) ) ;
#22891 = CARTESIAN_POINT ( 'NONE',  ( -18.62759615963270932, 10.81492255796079327, 115.8322429386477097 ) ) ;
#22892 = CARTESIAN_POINT ( 'NONE',  ( 28.82186960331498327, 2.781578969918950771E-14, 141.0000000000000000 ) ) ;
#22893 = CARTESIAN_POINT ( 'NONE',  ( 9.474510206698971260, -16.51473224551069308, 67.91557627198102409 ) ) ;
#22894 = CARTESIAN_POINT ( 'NONE',  ( 27.91695578976620951, 6.846979738060676723, 161.8037495850574032 ) ) ;
#22896 = CARTESIAN_POINT ( 'NONE',  ( -21.53943276465977519, 0.05219959533907696930, 31.24890960531435979 ) ) ;
#22895 = CARTESIAN_POINT ( 'NONE',  ( 8.224510206698742110, 14.34966873604972548, 32.08442372801901854 ) ) ;
#22897 = CARTESIAN_POINT ( 'NONE',  ( -21.53943276465977519, -0.05219959533937600094, 68.75109039468568994 ) ) ;
#22898 = CARTESIAN_POINT ( 'NONE',  ( -5.153800228976328057, -19.02544592524343514, 107.2905762719810383 ) ) ;
#22899 = CARTESIAN_POINT ( 'NONE',  ( -5.049401038297874678, -19.05341960407617918, 99.79275706135234714 ) ) ;
#22900 = CARTESIAN_POINT ( 'NONE',  ( -19.05341960407611168, -5.049401038298163336, 46.45724293864768129 ) ) ;
#22901 = CARTESIAN_POINT ( 'NONE',  ( 9.474510206698971260, -16.51473224551069308, 67.91557627198102409 ) ) ;
#22902 = CARTESIAN_POINT ( 'NONE',  ( 12.14591786802309770, 12.06949235617756955, 89.37390960531435269 ) ) ;
#22903 = CARTESIAN_POINT ( 'NONE',  ( 0.05219959533909260263, 19.03943276465977164, 99.99890960531436690 ) ) ;
#22904 = CARTESIAN_POINT ( 'NONE',  ( -12.14591786802309592, -12.06949235617757132, 96.87390960531436690 ) ) ;
#22905 = CARTESIAN_POINT ( 'NONE',  ( 19.03943276465977164, -0.05219959533909143690, 93.74890960531435269 ) ) ;
#22907 = CARTESIAN_POINT ( 'NONE',  ( -5.153800228976328057, -19.02544592524343514, 47.29057627198102409 ) ) ;
#22906 = CARTESIAN_POINT ( 'NONE',  ( 8.224510206698953496, -14.34966873604960469, 47.91557627198102409 ) ) ;
#22908 = CARTESIAN_POINT ( 'NONE',  ( -15.72974639402176322, -15.80617190586768395, 59.37609039468568284 ) ) ;
#22909 = CARTESIAN_POINT ( 'NONE',  ( -16.51473224551082808, 9.474510206698731452, 93.33442372801900433 ) ) ;
#22910 = CARTESIAN_POINT ( 'NONE',  ( -4.379528057220328563, 16.55341960407611168, 50.20724293864769550 ) ) ;
#22911 = CARTESIAN_POINT ( 'NONE',  ( 15.72974639402199770, -15.80617190586745480, 103.1239096053143811 ) ) ;
#22912 = CARTESIAN_POINT ( 'NONE',  ( -10.81492255796078084, -18.62759615963271287, 52.08224293864768839 ) ) ;
#22914 = CARTESIAN_POINT ( 'NONE',  ( 12.14591786802309770, 12.06949235617756955, 84.37390960531438111 ) ) ;
#22913 = CARTESIAN_POINT ( 'NONE',  ( 18.89770734986045397, 5.500000000000087930, 71.60214472496640781 ) ) ;
#22915 = CARTESIAN_POINT ( 'NONE',  ( -8.571926809382601320, -26.38167802310801591, 143.2750000027311899 ) ) ;
#22916 = CARTESIAN_POINT ( 'NONE',  ( 19.02544592524343514, -5.153800228976328945, 53.54057627198102409 ) ) ;
#22917 = CARTESIAN_POINT ( 'NONE',  ( 14.29746914071037800, 8.314922557961029526, 111.6677570613523613 ) ) ;
#22918 = CARTESIAN_POINT ( 'NONE',  ( -8.314922557961024197, 14.29746914071037800, 107.9177570613523471 ) ) ;
#22919 = CARTESIAN_POINT ( 'NONE',  ( -14.29746914071037622, -8.314922557961029526, 89.16775706135236135 ) ) ;
#22920 = CARTESIAN_POINT ( 'NONE',  ( -16.51473224551082808, 9.474510206698731452, 38.33442372801899722 ) ) ;
#22922 = CARTESIAN_POINT ( 'NONE',  ( -9.474510206698964154, 16.51473224551069663, 110.4155762719810383 ) ) ;
#22921 = CARTESIAN_POINT ( 'NONE',  ( 30.00000000000000000, 5.499999999999992895, 37.50000000000000000 ) ) ;
#22923 = CARTESIAN_POINT ( 'NONE',  ( -0.05219959533909027116, -19.03943276465977164, 82.49890960531436690 ) ) ;
#22924 = CARTESIAN_POINT ( 'NONE',  ( 16.51473224551069308, 9.474510206698969483, 39.16557627198103120 ) ) ;
#22925 = CARTESIAN_POINT ( 'NONE',  ( 12.14591786802309770, 12.06949235617756955, 44.37390960531435979 ) ) ;
#22927 = CARTESIAN_POINT ( 'NONE',  ( 9.564922557960805705, 16.46253265017160317, 109.5822429386476955 ) ) ;
#22926 = LINE ( 'NONE', #162427, #85530 ) ;
#22928 = CARTESIAN_POINT ( 'NONE',  ( -0.05219959533907301413, -21.53943276465977519, 42.49890960531435979 ) ) ;
#22929 = CARTESIAN_POINT ( 'NONE',  ( 12.14591786802309770, 12.06949235617756955, 89.37390960531435269 ) ) ;
#22930 = CARTESIAN_POINT ( 'NONE',  ( 8.224510206698742110, 14.34966873604972548, 37.08442372801901143 ) ) ;
#22931 = CARTESIAN_POINT ( 'NONE',  ( 8.224510206698953496, -14.34966873604960469, 62.91557627198102409 ) ) ;
#22932 = CARTESIAN_POINT ( 'NONE',  ( 29.03295818733085198, -0.6278704076485333019, -49.50940399778504286 ) ) ;
#22933 = CARTESIAN_POINT ( 'NONE',  ( 13.97604488694548053, -13.89961937509957401, 65.62609039468567573 ) ) ;
#22934 = CARTESIAN_POINT ( 'NONE',  ( -19.03943276465977164, 0.05219959533909376836, 96.24890960531436690 ) ) ;
#22935 = CARTESIAN_POINT ( 'NONE',  ( -13.89961937509957401, -13.97604488694547875, 79.37609039468567573 ) ) ;
#22936 = CARTESIAN_POINT ( 'NONE',  ( 9.564922557961047289, -16.46253265017146816, 40.41775706135234003 ) ) ;
#22938 = CARTESIAN_POINT ( 'NONE',  ( 14.29746914071037800, 8.314922557961029526, 106.6677570613523756 ) ) ;
#22937 = CARTESIAN_POINT ( 'NONE',  ( -16.53943276465976808, -0.05219959533934237506, 33.75109039468568284 ) ) ;
#22939 = CARTESIAN_POINT ( 'NONE',  ( -19.05341960407617563, 5.049401038297882671, 73.54275706135233293 ) ) ;
#22940 = CARTESIAN_POINT ( 'NONE',  ( -21.55341960407610458, -5.719274019375992779, 31.45724293864769550 ) ) ;
#22941 = CARTESIAN_POINT ( 'NONE',  ( 5.719274019375673035, 21.55341960407619339, 72.29275706135236135 ) ) ;
#22942 = CARTESIAN_POINT ( 'NONE',  ( -23.14613071126279209, -10.96668486446954560, 168.1016194467971445 ) ) ;
#22943 = CARTESIAN_POINT ( 'NONE',  ( 16.53943276465976808, 0.05219959533934440121, 21.25109039468567218 ) ) ;
#22945 = CARTESIAN_POINT ( 'NONE',  ( -19.03943276465977164, 0.05219959533909376836, 86.24890960531436690 ) ) ;
#22944 = CARTESIAN_POINT ( 'NONE',  ( -16.51473224551069308, -9.474510206698971260, 21.66557627198102765 ) ) ;
#22946 = CARTESIAN_POINT ( 'NONE',  ( 9.474510206698971260, -16.51473224551069308, 22.91557627198102765 ) ) ;
#22948 = CARTESIAN_POINT ( 'NONE',  ( -5.153800228976328057, -19.02544592524343514, 82.29057627198103830 ) ) ;
#22947 = CARTESIAN_POINT ( 'NONE',  ( -16.55341960407611168, -4.379528057220339221, 91.45724293864769550 ) ) ;
#22949 = CARTESIAN_POINT ( 'NONE',  ( 16.51473224551069308, 9.474510206698969483, 84.16557627198102409 ) ) ;
#22950 = EDGE_LOOP ( 'NONE', ( #136347, #41835 ) ) ;
#22951 = CARTESIAN_POINT ( 'NONE',  ( 13.89961937509957401, 13.97604488694547697, 96.87609039468566152 ) ) ;
#22952 = CARTESIAN_POINT ( 'NONE',  ( 10.72451020669898902, -18.67979575497178502, 82.91557627198103830 ) ) ;
#22953 = CARTESIAN_POINT ( 'NONE',  ( 13.97604488694527802, 13.89961937509977652, 29.37390960531435979 ) ) ;
#22955 = CARTESIAN_POINT ( 'NONE',  ( 5.823673210054125526, 21.52544592524343514, 109.7905762719810383 ) ) ;
#22954 = CARTESIAN_POINT ( 'NONE',  ( 5.049401038297881783, 19.05341960407617563, 67.29275706135234714 ) ) ;
#22956 = CARTESIAN_POINT ( 'NONE',  ( -9.564922557960796823, -16.46253265017161027, 67.08224293864769550 ) ) ;
#22957 = CARTESIAN_POINT ( 'NONE',  ( 5.049401038298161559, -19.05341960407611168, 107.7072429386476955 ) ) ;
#22958 = VERTEX_POINT ( 'NONE', #105987 ) ;
#22959 = CARTESIAN_POINT ( 'NONE',  ( -10.72451020669898014, 18.67979575497178502, 100.4155762719810241 ) ) ;
#22962 = CARTESIAN_POINT ( 'NONE',  ( -0.05219959533936034679, 19.03943276465977164, 67.50109039468566152 ) ) ;
#22961 = CARTESIAN_POINT ( 'NONE',  ( 9.564922557960805705, 16.46253265017160317, 84.58224293864769550 ) ) ;
#22960 = CARTESIAN_POINT ( 'NONE',  ( 8.314922557960818139, 14.29746914071049879, 89.58224293864768129 ) ) ;
#22963 = CARTESIAN_POINT ( 'NONE',  ( 15.80617190586746368, 15.72974639402197994, 89.37390960531435269 ) ) ;
#22964 = CARTESIAN_POINT ( 'NONE',  ( 15.72974639402199770, -15.80617190586745480, 68.12390960531436690 ) ) ;
#22965 = CARTESIAN_POINT ( 'NONE',  ( -16.52544592524342804, 4.483927247898546575, 41.04057627198103120 ) ) ;
#22966 = CARTESIAN_POINT ( 'NONE',  ( -18.62759615963255300, -10.81492255796106328, 99.16775706135234714 ) ) ;
#22967 = CARTESIAN_POINT ( 'NONE',  ( -16.53943276465976808, -0.05219959533934237506, 63.75109039468568284 ) ) ;
#22968 = CARTESIAN_POINT ( 'NONE',  ( -0.05219959533909027116, -19.03943276465977164, 92.49890960531436690 ) ) ;
#22969 = CARTESIAN_POINT ( 'NONE',  ( 5.153800228976335163, 19.02544592524342804, 39.79057627198100988 ) ) ;
#22970 = CARTESIAN_POINT ( 'NONE',  ( 21.52544592524334988, 5.823673210054432836, 46.45942372801901854 ) ) ;
#22971 = CARTESIAN_POINT ( 'NONE',  ( -15.80617190586768217, 15.72974639402176855, 48.12609039468568284 ) ) ;
#22972 = CARTESIAN_POINT ( 'NONE',  ( 19.03943276465977164, -0.05219959533909143690, 58.74890960531435979 ) ) ;
#22973 = CARTESIAN_POINT ( 'NONE',  ( -10.72451020669870658, -18.67979575497194134, 39.58442372801901143 ) ) ;
#22974 = CARTESIAN_POINT ( 'NONE',  ( 16.46253265017146816, 9.564922557961045513, 71.66775706135233293 ) ) ;
#22975 = CARTESIAN_POINT ( 'NONE',  ( -16.46253265017146816, -9.564922557961047289, 79.16775706135234714 ) ) ;
#22976 = CARTESIAN_POINT ( 'NONE',  ( -19.02544592524342804, 5.153800228976336051, 36.04057627198100988 ) ) ;
#22977 = CARTESIAN_POINT ( 'NONE',  ( 8.314922557961029526, -14.29746914071037800, 80.41775706135234714 ) ) ;
#22978 = CARTESIAN_POINT ( 'NONE',  ( -13.89961937509977652, 13.97604488694528158, 50.62390960531435979 ) ) ;
#22979 = CARTESIAN_POINT ( 'NONE',  ( 21.93180397000137205, -7.641141194974085948, 169.8616410530775909 ) ) ;
#22980 = CARTESIAN_POINT ( 'NONE',  ( 19.05341960407611168, 5.049401038298154454, 93.95724293864769550 ) ) ;
#22981 = CARTESIAN_POINT ( 'NONE',  ( 19.03943276465977164, -0.05219959533909143690, 33.74890960531435979 ) ) ;
#22982 = CARTESIAN_POINT ( 'NONE',  ( -5.823673210054116645, -21.52544592524344225, 77.29057627198102409 ) ) ;
#22983 = CARTESIAN_POINT ( 'NONE',  ( 16.53943276465976808, 0.05219959533934440121, 61.25109039468567573 ) ) ;
#22984 = CARTESIAN_POINT ( 'NONE',  ( -19.05341960407617563, 5.049401038297882671, 23.54275706135233648 ) ) ;
#22985 = EDGE_CURVE ( 'NONE', #154964, #58211, #94556, .T. ) ;
#22986 = ADVANCED_BREP_SHAPE_REPRESENTATION ( '', ( #11768, #82054 ), #85555 ) ;
#22987 = CARTESIAN_POINT ( 'NONE',  ( -9.564922557960796823, -16.46253265017161027, 52.08224293864768839 ) ) ;
#22988 = CARTESIAN_POINT ( 'NONE',  ( 12.06949235617757843, -12.14591786802309237, 43.12390960531435269 ) ) ;
#22989 = CARTESIAN_POINT ( 'NONE',  ( -14.29746914071049879, 8.314922557960819915, 80.83224293864769550 ) ) ;
#22990 = CARTESIAN_POINT ( 'NONE',  ( 9.474510206698971260, -16.51473224551069308, 82.91557627198103830 ) ) ;
#22991 = CARTESIAN_POINT ( 'NONE',  ( 15.80617190586769283, -15.72974639402175789, 30.62609039468567929 ) ) ;
#22992 = CARTESIAN_POINT ( 'NONE',  ( -19.02544592524342804, 5.153800228976336051, 96.04057627198103830 ) ) ;
#22993 = CARTESIAN_POINT ( 'NONE',  ( 5.719274019375673035, 21.55341960407619339, 97.29275706135234714 ) ) ;
#22994 = CARTESIAN_POINT ( 'NONE',  ( 8.314922557961029526, -14.29746914071037800, 65.41775706135234714 ) ) ;
#22995 = CARTESIAN_POINT ( 'NONE',  ( 18.62759615963255655, 10.81492255796105972, 31.66775706135234358 ) ) ;
#22996 = CARTESIAN_POINT ( 'NONE',  ( -13.89961937509977652, 13.97604488694528158, 105.6239096053143527 ) ) ;
#22997 = B_SPLINE_CURVE_WITH_KNOTS ( 'NONE', 3,
 ( #66011, #189379, #50856, #68004, #114499, #112514 ),
 .UNSPECIFIED., .F., .F.,
 ( 4, 2, 4 ),
 ( 0.003239945802372208323, 0.003620412082092060516, 0.004000878361811913142 ),
 .UNSPECIFIED. ) ;
#22998 = EDGE_CURVE ( 'NONE', #88472, #5512, #16601, .T. ) ;
#22999 = CARTESIAN_POINT ( 'NONE',  ( 21.52544592524344225, -5.823673210054117533, 83.54057627198102409 ) ) ;
#23000 = CARTESIAN_POINT ( 'NONE',  ( -12.06949235617756955, 12.14591786802309770, 45.62390960531436690 ) ) ;
#23001 = CARTESIAN_POINT ( 'NONE',  ( -13.97604488694527625, -13.89961937509977652, 46.87390960531435979 ) ) ;
#23002 = CARTESIAN_POINT ( 'NONE',  ( -14.34966873604960291, -8.224510206698953496, 71.66557627198100988 ) ) ;
#23003 = CARTESIAN_POINT ( 'NONE',  ( -10.81492255796078084, -18.62759615963271287, 32.08224293864769550 ) ) ;
#23004 = CARTESIAN_POINT ( 'NONE',  ( 16.51473224551083163, -9.474510206698727899, 30.83442372801900433 ) ) ;
#23005 = CARTESIAN_POINT ( 'NONE',  ( 14.34966873604960469, 8.224510206698951720, 99.16557627198100988 ) ) ;
#23006 = CARTESIAN_POINT ( 'NONE',  ( -19.02544592524342804, 5.153800228976336051, 111.0405762719810099 ) ) ;
#23007 = EDGE_LOOP ( 'NONE', ( #10202, #34067, #25210, #125161, #73095 ) ) ;
#23008 = CARTESIAN_POINT ( 'NONE',  ( 0.05219959533934541429, -16.53943276465976808, 60.00109039468568284 ) ) ;
#23009 = CARTESIAN_POINT ( 'NONE',  ( 9.564922557960805705, 16.46253265017160317, 49.58224293864770260 ) ) ;
#23010 = CARTESIAN_POINT ( 'NONE',  ( -22.44159573604010305, 16.30477369853692338, 140.6750000027311671 ) ) ;
#23011 = CARTESIAN_POINT ( 'NONE',  ( -0.05219959533934338120, 16.53943276465976808, 97.50109039468567573 ) ) ;
#23012 = CARTESIAN_POINT ( 'NONE',  ( -0.05219959533936034679, 19.03943276465977164, 102.5010903946856757 ) ) ;
#23013 = CARTESIAN_POINT ( 'NONE',  ( -5.823673210054431948, 21.52544592524334988, 67.70942372801901854 ) ) ;
#23014 = CARTESIAN_POINT ( 'NONE',  ( 16.51473224551069308, 9.474510206698969483, 74.16557627198103830 ) ) ;
#23015 = CARTESIAN_POINT ( 'NONE',  ( -5.823673210054116645, -21.52544592524344225, 87.29057627198103830 ) ) ;
#23016 = CARTESIAN_POINT ( 'NONE',  ( -4.483927247898782831, 16.52544592524335698, 37.70942372801900433 ) ) ;
#23017 = CARTESIAN_POINT ( 'NONE',  ( 19.03943276465977164, -0.05219959533909143690, 23.74890960531435269 ) ) ;
#23018 = CARTESIAN_POINT ( 'NONE',  ( 16.51473224551083163, -9.474510206698727899, 80.83442372801899012 ) ) ;
#23019 = CARTESIAN_POINT ( 'NONE',  ( 5.823673210054125526, 21.52544592524343514, 74.79057627198105251 ) ) ;
#23020 = CARTESIAN_POINT ( 'NONE',  ( 9.564922557961047289, -16.46253265017146816, 45.41775706135232582 ) ) ;
#23021 = CARTESIAN_POINT ( 'NONE',  ( -16.46253265017160317, 9.564922557960807481, 115.8322429386477097 ) ) ;
#23022 = ADVANCED_FACE ( 'NONE', ( #108966 ), #163337, .F. ) ;
#23023 = CARTESIAN_POINT ( 'NONE',  ( -10.72451020669898014, 18.67979575497178502, 95.41557627198102409 ) ) ;
#23024 = CARTESIAN_POINT ( 'NONE',  ( -8.906447517083053711, -27.41122689804191026, 148.4000000000000057 ) ) ;
#23025 = CARTESIAN_POINT ( 'NONE',  ( -13.89961937509977652, 13.97604488694528158, 65.62390960531436690 ) ) ;
#23026 = CARTESIAN_POINT ( 'NONE',  ( -22.55670631985092456, 22.55670631985084995, -65.00100000000003320 ) ) ;
#23027 = CARTESIAN_POINT ( 'NONE',  ( -19.05341960407617563, 5.049401038297882671, 108.5427570613523187 ) ) ;
#23028 = CARTESIAN_POINT ( 'NONE',  ( 10.31991442469048614, -38.65177141104609149, -12.74737010625873523 ) ) ;
#23029 = CARTESIAN_POINT ( 'NONE',  ( -19.02544592524342804, 5.153800228976336051, 41.04057627198103120 ) ) ;
#23031 = CARTESIAN_POINT ( 'NONE',  ( -4.483927247898539470, -16.52544592524342804, 57.29057627198103120 ) ) ;
#23030 = CARTESIAN_POINT ( 'NONE',  ( -18.62759615963270932, 10.81492255796079327, 100.8322429386477097 ) ) ;
#23032 = CARTESIAN_POINT ( 'NONE',  ( -19.05341960407611168, -5.049401038298163336, 56.45724293864768129 ) ) ;
#23033 = CARTESIAN_POINT ( 'NONE',  ( 21.52544592524334988, 5.823673210054432836, 76.45942372801901854 ) ) ;
#23035 = CARTESIAN_POINT ( 'NONE',  ( 5.049401038297881783, 19.05341960407617563, 27.29275706135232937 ) ) ;
#23034 = CARTESIAN_POINT ( 'NONE',  ( 0.05219959533934541429, -16.53943276465976808, 20.00109039468568639 ) ) ;
#23036 = CARTESIAN_POINT ( 'NONE',  ( 15.72974639402176855, 15.80617190586768217, 36.87609039468568994 ) ) ;
#23037 = CARTESIAN_POINT ( 'NONE',  ( -5.823673210054116645, -21.52544592524344225, 107.2905762719810525 ) ) ;
#23038 = CARTESIAN_POINT ( 'NONE',  ( 10.81492255796078972, 18.62759615963270932, 54.58224293864769550 ) ) ;
#23039 = CARTESIAN_POINT ( 'NONE',  ( 5.049401038297881783, 19.05341960407617563, 102.2927570613523045 ) ) ;
#23040 = CARTESIAN_POINT ( 'NONE',  ( -13.89961937509957401, -13.97604488694547875, 74.37609039468566152 ) ) ;
#23041 = CARTESIAN_POINT ( 'NONE',  ( 21.52544592524334988, 5.823673210054432836, 81.45942372801900433 ) ) ;
#23042 = CARTESIAN_POINT ( 'NONE',  ( 19.05341960407617918, -5.049401038297876454, 51.04275706135231871 ) ) ;
#23043 = CARTESIAN_POINT ( 'NONE',  ( -9.564922557960796823, -16.46253265017161027, 22.08224293864768839 ) ) ;
#23044 = CARTESIAN_POINT ( 'NONE',  ( 5.719274019375991003, -21.55341960407610458, 52.70724293864769550 ) ) ;
#23045 = CARTESIAN_POINT ( 'NONE',  ( 16.53943276465976808, -0.05219959533910856209, 43.74890960531435979 ) ) ;
#23046 = CARTESIAN_POINT ( 'NONE',  ( -16.29526858892873875, -7.335722546920240283, 25.79670597800208753 ) ) ;
#23047 = CARTESIAN_POINT ( 'NONE',  ( -21.53943276465977519, -0.05219959533937600094, 113.7510903946856757 ) ) ;
#23048 = CARTESIAN_POINT ( 'NONE',  ( -14.29746914071037622, -8.314922557961029526, 89.16775706135236135 ) ) ;
#23049 = CARTESIAN_POINT ( 'NONE',  ( 0.05219959533910956823, 16.53943276465976808, 44.99890960531435979 ) ) ;
#23050 = CARTESIAN_POINT ( 'NONE',  ( -21.52544592524334988, -5.823673210054445271, 73.95942372801901854 ) ) ;
#23051 = CARTESIAN_POINT ( 'NONE',  ( -0.05219959533937732626, 21.53943276465977519, 82.50109039468568994 ) ) ;
#23052 = CARTESIAN_POINT ( 'NONE',  ( -21.55341960407610458, -5.719274019375992779, 76.45724293864769550 ) ) ;
#23053 = CARTESIAN_POINT ( 'NONE',  ( 16.51473224551069308, 9.474510206698969483, 39.16557627198103120 ) ) ;
#23054 = CARTESIAN_POINT ( 'NONE',  ( 5.823673210054444382, -21.52544592524334988, 50.20942372801901854 ) ) ;
#23055 = CARTESIAN_POINT ( 'NONE',  ( -5.049401038298153566, 19.05341960407611168, 30.20724293864768839 ) ) ;
#23056 = VERTEX_POINT ( 'NONE', #1292 ) ;
#23057 = CARTESIAN_POINT ( 'NONE',  ( -13.97604488694527625, -13.89961937509977652, 51.87390960531436690 ) ) ;
#23058 = CARTESIAN_POINT ( 'NONE',  ( 12.14591786802309770, 12.06949235617756955, 94.37390960531436690 ) ) ;
#23059 = CARTESIAN_POINT ( 'NONE',  ( 19.02544592524343514, -5.153800228976328945, 98.54057627198100988 ) ) ;
#23060 = CARTESIAN_POINT ( 'NONE',  ( 14.34966873604960469, 8.224510206698951720, 39.16557627198102409 ) ) ;
#23061 = CARTESIAN_POINT ( 'NONE',  ( -14.29746914071049879, 8.314922557960819915, 115.8322429386477097 ) ) ;
#23062 = CARTESIAN_POINT ( 'NONE',  ( -15.72974639402197994, 15.80617190586746368, 85.62390960531436690 ) ) ;
#23063 = CARTESIAN_POINT ( 'NONE',  ( 18.62759615963255655, 10.81492255796105972, 21.66775706135235069 ) ) ;
#23064 = CARTESIAN_POINT ( 'NONE',  ( 6.100000000000006750, -2.167155344068307965E-14, -64.92279855667830191 ) ) ;
#23065 = CARTESIAN_POINT ( 'NONE',  ( -16.55341960407617563, 4.379528057220093196, 43.54275706135235424 ) ) ;
#23066 = CARTESIAN_POINT ( 'NONE',  ( -0.05219959533907301413, -21.53943276465977519, 67.49890960531436690 ) ) ;
#23067 = CARTESIAN_POINT ( 'NONE',  ( 18.67979575497194134, -10.72451020669871369, 100.8344237280190185 ) ) ;
#23068 = CARTESIAN_POINT ( 'NONE',  ( -5.049401038298153566, 19.05341960407611168, 90.20724293864766707 ) ) ;
#23069 = CARTESIAN_POINT ( 'NONE',  ( 5.823673210054444382, -21.52544592524334988, 25.20942372801901854 ) ) ;
#23070 = CARTESIAN_POINT ( 'NONE',  ( 15.80617190586746368, 15.72974639402197994, 29.37390960531435269 ) ) ;
#23071 = CARTESIAN_POINT ( 'NONE',  ( 12.06949235617739724, 12.14591786802326823, 86.87609039468568994 ) ) ;
#23072 = CARTESIAN_POINT ( 'NONE',  ( -15.72974639402176322, -15.80617190586768395, 74.37609039468568994 ) ) ;
#23073 = B_SPLINE_CURVE_WITH_KNOTS ( 'NONE', 3,
 ( #20934, #191784, #189808, #83592, #114943, #177639, #132111, #116939, #84588, #178632, #54276, #192794 ),
 .UNSPECIFIED., .F., .F.,
 ( 4, 2, 2, 2, 2, 4 ),
 ( 0.002244533994399181866, 0.002800305961463223602, 0.003078191944995248373, 0.003356077928527273144, 0.003911849895591323553, 0.004467621862655373095 ),
 .UNSPECIFIED. ) ;
#23074 = CARTESIAN_POINT ( 'NONE',  ( -21.55341960407619339, 5.719274019375674811, 108.5427570613523756 ) ) ;
#23075 = CARTESIAN_POINT ( 'NONE',  ( 12.14591786802327356, -12.06949235617739191, 80.62609039468567573 ) ) ;
#23076 = CARTESIAN_POINT ( 'NONE',  ( -21.55341960407619339, 5.719274019375674811, 33.54275706135234714 ) ) ;
#23077 = CARTESIAN_POINT ( 'NONE',  ( -19.02544592524342804, 5.153800228976336051, 36.04057627198100988 ) ) ;
#23078 = CARTESIAN_POINT ( 'NONE',  ( 21.55341960407619695, -5.719274019375665929, 91.04275706135236135 ) ) ;
#23079 = CARTESIAN_POINT ( 'NONE',  ( 9.474510206698971260, -16.51473224551069308, 107.9155762719810383 ) ) ;
#23080 = CARTESIAN_POINT ( 'NONE',  ( -5.823673210054116645, -21.52544592524344225, 107.2905762719810525 ) ) ;
#23082 = CARTESIAN_POINT ( 'NONE',  ( -10.72451020669898014, 18.67979575497178502, 55.41557627198102409 ) ) ;
#23081 = CARTESIAN_POINT ( 'NONE',  ( 18.22780087662121673, 5.500000000000056843, 83.98459894673892734 ) ) ;
#23084 = CARTESIAN_POINT ( 'NONE',  ( -8.314922557960811034, -14.29746914071050412, 47.08224293864770260 ) ) ;
#23083 = CARTESIAN_POINT ( 'NONE',  ( -16.46253265017160317, 9.564922557960807481, 95.83224293864769550 ) ) ;
#23085 = CARTESIAN_POINT ( 'NONE',  ( 12.24802307403562907, -10.59837847217739082, -61.57437130795283053 ) ) ;
#23086 = CARTESIAN_POINT ( 'NONE',  ( -19.05341960407617563, 5.049401038297882671, 78.54275706135233293 ) ) ;
#23087 = CARTESIAN_POINT ( 'NONE',  ( -16.62475595723699229, 7.163666690055301878, 105.5271335181047476 ) ) ;
#23088 = CARTESIAN_POINT ( 'NONE',  ( 16.46253265017146816, 9.564922557961045513, 111.6677570613523329 ) ) ;
#23089 = CARTESIAN_POINT ( 'NONE',  ( -18.62759615963270932, 10.81492255796079327, 90.83224293864769550 ) ) ;
#23090 = CARTESIAN_POINT ( 'NONE',  ( -0.05219959533910754901, -16.53943276465976808, 62.49890960531436690 ) ) ;
#23091 = CARTESIAN_POINT ( 'NONE',  ( -16.46253265017160317, 9.564922557960807481, 105.8322429386476955 ) ) ;
#23092 = CARTESIAN_POINT ( 'NONE',  ( -14.34966873604972548, 8.224510206698743886, 48.33442372801902565 ) ) ;
#23093 = CARTESIAN_POINT ( 'NONE',  ( 9.474510206698971260, -16.51473224551069308, 52.91557627198102409 ) ) ;
#23095 = CARTESIAN_POINT ( 'NONE',  ( 16.46253265017146816, 9.564922557961045513, 91.66775706135234714 ) ) ;
#23094 = CARTESIAN_POINT ( 'NONE',  ( -10.81492255796105439, 18.62759615963255655, 27.91775706135234358 ) ) ;
#23096 = CARTESIAN_POINT ( 'NONE',  ( 13.97604488694527802, 13.89961937509977652, 94.37390960531436690 ) ) ;
#23097 = CARTESIAN_POINT ( 'NONE',  ( 19.05341960407611168, 5.049401038298154454, 88.95724293864769550 ) ) ;
#23098 = CARTESIAN_POINT ( 'NONE',  ( 5.823673210054125526, 21.52544592524343514, 94.79057627198105251 ) ) ;
#23099 = CARTESIAN_POINT ( 'NONE',  ( -19.02544592524342804, 5.153800228976336051, 51.04057627198103120 ) ) ;
#23100 = CARTESIAN_POINT ( 'NONE',  ( -16.88567814943164791, -6.947325034625601248, 61.29001122652586986 ) ) ;
#23101 = CARTESIAN_POINT ( 'NONE',  ( 12.14591786802309770, 12.06949235617756955, 74.37390960531436690 ) ) ;
#23102 = CARTESIAN_POINT ( 'NONE',  ( -0.05219959533909027116, -19.03943276465977164, 102.4989096053143669 ) ) ;
#23103 = CARTESIAN_POINT ( 'NONE',  ( 17.62203461105334767, -15.97121552610937911, -54.63804455921930270 ) ) ;
#23104 = CARTESIAN_POINT ( 'NONE',  ( 19.05341960407617918, -5.049401038297876454, 61.04275706135232582 ) ) ;
#23105 = CARTESIAN_POINT ( 'NONE',  ( 5.823673210054125526, 21.52544592524343514, 84.79057627198102409 ) ) ;
#23106 = CARTESIAN_POINT ( 'NONE',  ( -19.03943276465977164, -0.05219959533935918106, 53.75109039468566863 ) ) ;
#23107 = CARTESIAN_POINT ( 'NONE',  ( 16.46253265017160672, -9.564922557960803928, 98.33224293864769550 ) ) ;
#23108 = CARTESIAN_POINT ( 'NONE',  ( 17.60691670004650433, 5.500000000000060396, 76.63333313366442212 ) ) ;
#23109 = CARTESIAN_POINT ( 'NONE',  ( 10.81492255796078972, 18.62759615963270932, 39.58224293864769550 ) ) ;
#23110 = CARTESIAN_POINT ( 'NONE',  ( 13.97604488694527802, 13.89961937509977652, 89.37390960531436690 ) ) ;
#23111 = EDGE_CURVE ( 'NONE', #14026, #142736, #166211, .T. ) ;
#23112 = CARTESIAN_POINT ( 'NONE',  ( 10.72451020669871369, 18.67979575497193778, 62.08442372801901143 ) ) ;
#23113 = CARTESIAN_POINT ( 'NONE',  ( 16.46253265017160672, -9.564922557960803928, 33.33224293864770260 ) ) ;
#23114 = CARTESIAN_POINT ( 'NONE',  ( 12.06949235617757843, -12.14591786802309237, 78.12390960531436690 ) ) ;
#23115 = CARTESIAN_POINT ( 'NONE',  ( 8.314922557961029526, -14.29746914071037800, 25.41775706135235779 ) ) ;
#23116 = CARTESIAN_POINT ( 'NONE',  ( 5.823673210054444382, -21.52544592524334988, 55.20942372801902565 ) ) ;
#23117 = VERTEX_POINT ( 'NONE', #198529 ) ;
#23118 = DIRECTION ( 'NONE',  ( 0.000000000000000000, 0.000000000000000000, -1.000000000000000000 ) ) ;
#23119 = CARTESIAN_POINT ( 'NONE',  ( -13.89961937509957401, -13.97604488694547875, 69.37609039468564731 ) ) ;
#23120 = CARTESIAN_POINT ( 'NONE',  ( -17.49999999999999645, 5.499999999999997335, 120.0000000000000142 ) ) ;
#23121 = CARTESIAN_POINT ( 'NONE',  ( -18.62759615963255300, -10.81492255796106328, 24.16775706135235424 ) ) ;
#23122 = CARTESIAN_POINT ( 'NONE',  ( -38.00000000000001421, -12.34694845685042708, -5.649999994537625803 ) ) ;
#23123 = CARTESIAN_POINT ( 'NONE',  ( -13.89961937509957401, -13.97604488694547875, 19.37609039468566507 ) ) ;
#23124 = CARTESIAN_POINT ( 'NONE',  ( -19.03943276465977164, 0.05219959533909376836, 56.24890960531435979 ) ) ;
#23125 = CARTESIAN_POINT ( 'NONE',  ( 21.52544592524334988, 5.823673210054432836, 111.4594237280190328 ) ) ;
#23126 = CARTESIAN_POINT ( 'NONE',  ( 14.29746914071037800, 8.314922557961029526, 106.6677570613523756 ) ) ;
#23128 = CARTESIAN_POINT ( 'NONE',  ( -15.72974639402176322, -15.80617190586768395, 74.37609039468568994 ) ) ;
#23127 = CARTESIAN_POINT ( 'NONE',  ( -0.05219959533909027116, -19.03943276465977164, 107.4989096053143527 ) ) ;
#23129 = FACE_OUTER_BOUND ( 'NONE', #118201, .T. ) ;
#23130 = CARTESIAN_POINT ( 'NONE',  ( -16.46253265017160317, 9.564922557960807481, 110.8322429386476955 ) ) ;
#23131 = DIRECTION ( 'NONE',  ( -0.06104853953485701173, -7.476289853398329258E-18, -0.9981347984218670311 ) ) ;
#23133 = CARTESIAN_POINT ( 'NONE',  ( 21.55341960407619695, -5.719274019375665929, 76.04275706135237556 ) ) ;
#23132 = CARTESIAN_POINT ( 'NONE',  ( 16.53943276465976808, 0.05219959533934440121, 66.25109039468567573 ) ) ;
#23134 = CARTESIAN_POINT ( 'NONE',  ( 21.52544592524334988, 5.823673210054432836, 106.4594237280190328 ) ) ;
#23135 = CARTESIAN_POINT ( 'NONE',  ( 17.50000000000000711, -5.499999999999978684, 41.21769037696436300 ) ) ;
#23136 = CARTESIAN_POINT ( 'NONE',  ( 16.46253265017160672, -9.564922557960803928, 83.33224293864768129 ) ) ;
#23137 = CARTESIAN_POINT ( 'NONE',  ( 16.46253265017160672, -9.564922557960803928, 108.3322429386476955 ) ) ;
#23138 = ORIENTED_EDGE ( 'NONE', *, *, #80326, .F. ) ;
#23139 = CARTESIAN_POINT ( 'NONE',  ( -0.1280799071097934450, -28.90000000000004476, -52.65483682830182488 ) ) ;
#23140 = CARTESIAN_POINT ( 'NONE',  ( 16.51473224551069308, 9.474510206698969483, 44.16557627198103120 ) ) ;
#23142 = EDGE_CURVE ( 'NONE', #15137, #42057, #175583, .T. ) ;
#23141 = CARTESIAN_POINT ( 'NONE',  ( 5.719274019375991003, -21.55341960407610458, 37.70724293864769550 ) ) ;
#23143 = CARTESIAN_POINT ( 'NONE',  ( 4.379528057220092307, 16.55341960407617563, 102.2927570613523613 ) ) ;
#23145 = CARTESIAN_POINT ( 'NONE',  ( -9.564922557960796823, -16.46253265017161027, 87.08224293864769550 ) ) ;
#23144 = CARTESIAN_POINT ( 'NONE',  ( -12.06949235617756955, 12.14591786802309770, 95.62390960531436690 ) ) ;
#23146 = CARTESIAN_POINT ( 'NONE',  ( 15.72974639402176855, 15.80617190586768217, 106.8760903946856899 ) ) ;
#23147 = CARTESIAN_POINT ( 'NONE',  ( 16.51473224551069308, 9.474510206698969483, 39.16557627198103120 ) ) ;
#23148 = CARTESIAN_POINT ( 'NONE',  ( -8.314922557960811034, -14.29746914071050412, 92.08224293864769550 ) ) ;
#23149 = CARTESIAN_POINT ( 'NONE',  ( 5.719274019375673035, 21.55341960407619339, 52.29275706135236135 ) ) ;
#23150 = CARTESIAN_POINT ( 'NONE',  ( 15.72974639402199770, -15.80617190586745480, 88.12390960531436690 ) ) ;
#23151 = CARTESIAN_POINT ( 'NONE',  ( 16.51473224551083163, -9.474510206698727899, 55.83442372801899722 ) ) ;
#23152 = CARTESIAN_POINT ( 'NONE',  ( -26.21509334545639192, -30.21538139615938334, -6.441305576064758398 ) ) ;
#23153 = CARTESIAN_POINT ( 'NONE',  ( -9.474510206698964154, 16.51473224551069663, 90.41557627198103830 ) ) ;
#23154 = CARTESIAN_POINT ( 'NONE',  ( -16.52544592524342804, 4.483927247898546575, 66.04057627198103830 ) ) ;
#23155 = ADVANCED_FACE ( 'NONE', ( #62970 ), #175108, .T. ) ;
#23156 = CARTESIAN_POINT ( 'NONE',  ( -9.474510206698720793, -16.51473224551083518, 49.58442372801899722 ) ) ;
#23157 = CARTESIAN_POINT ( 'NONE',  ( -4.483927247898539470, -16.52544592524342804, 42.29057627198103120 ) ) ;
#23158 = CARTESIAN_POINT ( 'NONE',  ( 16.46253265017146816, 9.564922557961045513, 76.66775706135234714 ) ) ;
#23159 = CARTESIAN_POINT ( 'NONE',  ( -18.39443945427639093, 5.500000000000031086, 83.51745347608650150 ) ) ;
#23160 = CARTESIAN_POINT ( 'NONE',  ( 15.80617190586746368, 15.72974639402197994, 34.37390960531435979 ) ) ;
#23161 = CARTESIAN_POINT ( 'NONE',  ( -8.314922557960811034, -14.29746914071050412, 107.0822429386476955 ) ) ;
#23162 = CARTESIAN_POINT ( 'NONE',  ( -17.49999999999996803, -3.209263204892610855, 25.23803174393711402 ) ) ;
#23164 = CARTESIAN_POINT ( 'NONE',  ( 5.719274019375991003, -21.55341960407610458, 47.70724293864770260 ) ) ;
#23163 = CARTESIAN_POINT ( 'NONE',  ( 16.51473224551069308, 9.474510206698969483, 44.16557627198103120 ) ) ;
#23165 = CARTESIAN_POINT ( 'NONE',  ( -19.05341960407611168, -5.049401038298163336, 26.45724293864769550 ) ) ;
#23167 = CARTESIAN_POINT ( 'NONE',  ( 16.46253265017160672, -9.564922557960803928, 63.33224293864769550 ) ) ;
#23166 = CARTESIAN_POINT ( 'NONE',  ( -0.05219959533934338120, 16.53943276465976808, 77.50109039468567573 ) ) ;
#23168 = CARTESIAN_POINT ( 'NONE',  ( 13.97604488694548053, -13.89961937509957401, 35.62609039468567573 ) ) ;
#23169 = CARTESIAN_POINT ( 'NONE',  ( 10.81492255796106328, -18.62759615963255655, 70.41775706135236135 ) ) ;
#23170 = CARTESIAN_POINT ( 'NONE',  ( 21.52544592524344225, -5.823673210054117533, 53.54057627198103120 ) ) ;
#23171 = CARTESIAN_POINT ( 'NONE',  ( -0.05219959533909027116, -19.03943276465977164, 22.49890960531436690 ) ) ;
#23172 = CARTESIAN_POINT ( 'NONE',  ( 16.51473224551083163, -9.474510206698727899, 110.8344237280190043 ) ) ;
#23173 = CARTESIAN_POINT ( 'NONE',  ( 27.74069374691240242, 6.311165852663350506, 163.4895129000348390 ) ) ;
#23175 = CARTESIAN_POINT ( 'NONE',  ( 15.72974639402199770, -15.80617190586745480, 43.12390960531435269 ) ) ;
#23174 = PLANE ( 'NONE',  #160525 ) ;
#23176 = CARTESIAN_POINT ( 'NONE',  ( 17.49999999999998579, -5.500000000000023981, 68.29690382534171533 ) ) ;
#23177 = CARTESIAN_POINT ( 'NONE',  ( 21.52544592524334988, 5.823673210054432836, 81.45942372801900433 ) ) ;
#23178 = ORIENTED_EDGE ( 'NONE', *, *, #77338, .T. ) ;
#23179 = CARTESIAN_POINT ( 'NONE',  ( -12.14591786802309592, -12.06949235617757132, 41.87390960531435979 ) ) ;
#23180 = CARTESIAN_POINT ( 'NONE',  ( 16.53943276465976808, -0.05219959533910856209, 58.74890960531436690 ) ) ;
#23181 = CARTESIAN_POINT ( 'NONE',  ( 15.80617190586746368, 15.72974639402197994, 84.37390960531438111 ) ) ;
#23182 = CARTESIAN_POINT ( 'NONE',  ( 5.823673210054125526, 21.52544592524343514, 79.79057627198102409 ) ) ;
#23183 = CARTESIAN_POINT ( 'NONE',  ( -69.65682714487590488, -71.74905178543390605, -15.00000000000000178 ) ) ;
#23184 = CARTESIAN_POINT ( 'NONE',  ( 5.719274019375991003, -21.55341960407610458, 37.70724293864769550 ) ) ;
#23185 = CARTESIAN_POINT ( 'NONE',  ( 14.29746914071037800, 8.314922557961029526, 51.66775706135234714 ) ) ;
#23186 = CARTESIAN_POINT ( 'NONE',  ( -12.14591786802309592, -12.06949235617757132, 81.87390960531435269 ) ) ;
#23187 = CARTESIAN_POINT ( 'NONE',  ( -19.03943276465977164, 0.05219959533909376836, 56.24890960531435979 ) ) ;
#23188 = CARTESIAN_POINT ( 'NONE',  ( 13.89961937509977652, -13.97604488694527269, 33.12390960531434558 ) ) ;
#23189 =( NAMED_UNIT ( * ) SI_UNIT ( $, .STERADIAN. ) SOLID_ANGLE_UNIT ( ) );
#23190 = CARTESIAN_POINT ( 'NONE',  ( -17.49999999999999645, 5.499999999999997335, 30.79690382534172599 ) ) ;
#23191 = EDGE_LOOP ( 'NONE', ( #102945, #168389, #1725, #52952, #125256 ) ) ;
#23192 = CARTESIAN_POINT ( 'NONE',  ( -4.379528057220086978, -16.55341960407618274, 84.79275706135234714 ) ) ;
#23193 = CARTESIAN_POINT ( 'NONE',  ( 18.67979575497178502, 10.72451020669898547, 114.1655762719810383 ) ) ;
#23194 = CARTESIAN_POINT ( 'NONE',  ( 5.153800228976335163, 19.02544592524342804, 64.79057627198100988 ) ) ;
#23195 = CARTESIAN_POINT ( 'NONE',  ( 5.823673210054444382, -21.52544592524334988, 60.20942372801902565 ) ) ;
#23196 = CARTESIAN_POINT ( 'NONE',  ( 9.564922557960805705, 16.46253265017160317, 104.5822429386476955 ) ) ;
#23197 = CARTESIAN_POINT ( 'NONE',  ( -18.40487137061491296, -35.48337831123046726, -26.72115582344491358 ) ) ;
#23198 = EDGE_LOOP ( 'NONE', ( #178889, #79567, #165701, #74174 ) ) ;
#23199 = CARTESIAN_POINT ( 'NONE',  ( 21.55341960407619695, -5.719274019375665929, 51.04275706135234714 ) ) ;
#23201 = CARTESIAN_POINT ( 'NONE',  ( 13.89961937509977652, -13.97604488694527269, 103.1239096053143527 ) ) ;
#23200 = CARTESIAN_POINT ( 'NONE',  ( 16.46253265017160672, -9.564922557960803928, 23.33224293864769194 ) ) ;
#23202 = CARTESIAN_POINT ( 'NONE',  ( 16.51473224551083163, -9.474510206698727899, 50.83442372801899722 ) ) ;
#23203 = CARTESIAN_POINT ( 'NONE',  ( -18.62759615963270932, 10.81492255796079327, 115.8322429386477097 ) ) ;
#23204 = CARTESIAN_POINT ( 'NONE',  ( 19.02544592524334988, 5.153800228976608722, 41.45942372801900433 ) ) ;
#23205 = CARTESIAN_POINT ( 'NONE',  ( -13.97604488694527625, -13.89961937509977652, 26.87390960531434558 ) ) ;
#23206 = CARTESIAN_POINT ( 'NONE',  ( 16.53943276465976808, 0.05219959533934440121, 91.25109039468568994 ) ) ;
#23207 = CARTESIAN_POINT ( 'NONE',  ( 5.049401038297881783, 19.05341960407617563, 62.29275706135234003 ) ) ;
#23208 = CARTESIAN_POINT ( 'NONE',  ( 12.06949235617739724, 12.14591786802326823, 111.8760903946856615 ) ) ;
#23209 = DIRECTION ( 'NONE',  ( 0.000000000000000000, 0.000000000000000000, 1.000000000000000000 ) ) ;
#23210 = CARTESIAN_POINT ( 'NONE',  ( 16.51473224551069308, 9.474510206698969483, 89.16557627198103830 ) ) ;
#23211 = CARTESIAN_POINT ( 'NONE',  ( 0.05219959533937995610, -21.53943276465977519, 90.00109039468567573 ) ) ;
#23212 = CARTESIAN_POINT ( 'NONE',  ( 0.05219959533937995610, -21.53943276465977519, 100.0010903946857042 ) ) ;
#23213 = CARTESIAN_POINT ( 'NONE',  ( -11.30153831258471975, -180.0000000000000000, -4.999999999999999112 ) ) ;
#23214 = CARTESIAN_POINT ( 'NONE',  ( -19.03943276465977164, 0.05219959533909376836, 106.2489096053143669 ) ) ;
#23215 = CARTESIAN_POINT ( 'NONE',  ( 15.72974639402176855, 15.80617190586768217, 76.87609039468567573 ) ) ;
#23216 = CARTESIAN_POINT ( 'NONE',  ( 16.55341960407618274, -4.379528057220086978, 21.04275706135234714 ) ) ;
#23217 = CARTESIAN_POINT ( 'NONE',  ( 16.51473224551069308, 9.474510206698969483, 79.16557627198103830 ) ) ;
#23218 = CARTESIAN_POINT ( 'NONE',  ( -10.72451020669898014, 18.67979575497178502, 30.41557627198101699 ) ) ;
#23219 = CARTESIAN_POINT ( 'NONE',  ( -0.05219959533909027116, -19.03943276465977164, 97.49890960531436690 ) ) ;
#23220 = CARTESIAN_POINT ( 'NONE',  ( -16.31925111598456724, -7.325300261831609205, 89.83575461032749843 ) ) ;
#23221 = CARTESIAN_POINT ( 'NONE',  ( -9.564922557960796823, -16.46253265017161027, 82.08224293864768129 ) ) ;
#23222 = CARTESIAN_POINT ( 'NONE',  ( -16.51473224551069308, -9.474510206698971260, 71.66557627198102409 ) ) ;
#23223 = CARTESIAN_POINT ( 'NONE',  ( 12.14591786802327356, -12.06949235617739191, 100.6260903946857184 ) ) ;
#23224 = FACE_OUTER_BOUND ( 'NONE', #117136, .T. ) ;
#23225 = CARTESIAN_POINT ( 'NONE',  ( -16.51473224551082808, 9.474510206698731452, 53.33442372801900433 ) ) ;
#23226 = CARTESIAN_POINT ( 'NONE',  ( -0.05219959533909027116, -19.03943276465977164, 92.49890960531436690 ) ) ;
#23227 = CARTESIAN_POINT ( 'NONE',  ( -16.53943276465976808, 0.05219959533911058130, 91.24890960531436690 ) ) ;
#23228 = CARTESIAN_POINT ( 'NONE',  ( -15.80617190586745835, -15.72974639402198527, 36.87390960531435979 ) ) ;
#23229 = CARTESIAN_POINT ( 'NONE',  ( 5.719274019375991003, -21.55341960407610458, 22.70724293864769194 ) ) ;
#23230 = CARTESIAN_POINT ( 'NONE',  ( -12.14591786802309592, -12.06949235617757132, 86.87390960531438111 ) ) ;
#23231 = CARTESIAN_POINT ( 'NONE',  ( -16.18388926212242396, 7.379444403734377822, 54.56046848633847191 ) ) ;
#23232 = CARTESIAN_POINT ( 'NONE',  ( 0.05219959533936267826, -19.03943276465977164, 45.00109039468566863 ) ) ;
#23233 = CARTESIAN_POINT ( 'NONE',  ( -8.224510206698735004, -14.34966873604973081, 99.58442372801900433 ) ) ;
#23234 = CARTESIAN_POINT ( 'NONE',  ( -9.564922557960796823, -16.46253265017161027, 102.0822429386477097 ) ) ;
#23235 = CARTESIAN_POINT ( 'NONE',  ( -5.719274019375665041, -21.55341960407619695, 64.79275706135234714 ) ) ;
#23236 = CARTESIAN_POINT ( 'NONE',  ( 21.55341960407610458, 5.719274019375980345, 58.95724293864770971 ) ) ;
#23237 = CARTESIAN_POINT ( 'NONE',  ( -10.81492255796105439, 18.62759615963255655, 27.91775706135234358 ) ) ;
#23238 = CARTESIAN_POINT ( 'NONE',  ( 5.823673210054125526, 21.52544592524343514, 89.79057627198103830 ) ) ;
#23239 = CARTESIAN_POINT ( 'NONE',  ( -10.72451020669870658, -18.67979575497194134, 34.58442372801900433 ) ) ;
#23240 = CARTESIAN_POINT ( 'NONE',  ( 14.34966873604960469, 8.224510206698951720, 109.1655762719810383 ) ) ;
#23241 = CARTESIAN_POINT ( 'NONE',  ( 19.02544592524334988, 5.153800228976608722, 66.45942372801899012 ) ) ;
#23242 = CARTESIAN_POINT ( 'NONE',  ( -16.46253265017160317, 9.564922557960807481, 45.83224293864769550 ) ) ;
#23244 = CARTESIAN_POINT ( 'NONE',  ( -0.05219959533909027116, -19.03943276465977164, 102.4989096053143669 ) ) ;
#23243 = CARTESIAN_POINT ( 'NONE',  ( -8.314922557960811034, -14.29746914071050412, 97.08224293864770971 ) ) ;
#23245 = CARTESIAN_POINT ( 'NONE',  ( 9.564922557960805705, 16.46253265017160317, 99.58224293864770971 ) ) ;
#23246 = CARTESIAN_POINT ( 'NONE',  ( -4.379528057220328563, 16.55341960407611168, 115.2072429386476955 ) ) ;
#23247 = CARTESIAN_POINT ( 'NONE',  ( 8.314922557960818139, 14.29746914071049879, 34.58224293864770260 ) ) ;
#23248 = CARTESIAN_POINT ( 'NONE',  ( -12.06949235617739369, -12.14591786802326823, 104.3760903946856899 ) ) ;
#23249 = CARTESIAN_POINT ( 'NONE',  ( -9.474510206698964154, 16.51473224551069663, 50.41557627198102409 ) ) ;
#23250 = CARTESIAN_POINT ( 'NONE',  ( 0.05219959533909260263, 19.03943276465977164, 24.99890960531435269 ) ) ;
#23251 = CARTESIAN_POINT ( 'NONE',  ( 16.51473224551083163, -9.474510206698727899, 20.83442372801899722 ) ) ;
#23253 = CARTESIAN_POINT ( 'NONE',  ( 14.34966873604960469, 8.224510206698951720, 29.16557627198103120 ) ) ;
#23252 = CARTESIAN_POINT ( 'NONE',  ( -5.153800228976328057, -19.02544592524343514, 112.2905762719810099 ) ) ;
#23254 = CARTESIAN_POINT ( 'NONE',  ( -15.80617190586768217, 15.72974639402176855, 33.12609039468569705 ) ) ;
#23255 = CARTESIAN_POINT ( 'NONE',  ( 16.51473224551069308, 9.474510206698969483, 99.16557627198102409 ) ) ;
#23256 = CARTESIAN_POINT ( 'NONE',  ( 16.55341960407618274, -4.379528057220086978, 51.04275706135234714 ) ) ;
#23257 = CARTESIAN_POINT ( 'NONE',  ( -16.53943276465976808, -0.05219959533934237506, 113.7510903946856757 ) ) ;
#23258 = CARTESIAN_POINT ( 'NONE',  ( -0.05219959533934338120, 16.53943276465976808, 87.50109039468568994 ) ) ;
#23259 = CARTESIAN_POINT ( 'NONE',  ( -8.224510206698735004, -14.34966873604973081, 29.58442372801901854 ) ) ;
#23260 = CARTESIAN_POINT ( 'NONE',  ( -0.05219959533909027116, -19.03943276465977164, 52.49890960531436690 ) ) ;
#23261 = CARTESIAN_POINT ( 'NONE',  ( -8.224510206698948167, 14.34966873604960824, 105.4155762719810383 ) ) ;
#23262 = CARTESIAN_POINT ( 'NONE',  ( 0.05219959533907565091, 21.53943276465977519, 114.9989096053143669 ) ) ;
#23263 = CARTESIAN_POINT ( 'NONE',  ( 19.02544592524343514, -5.153800228976328945, 38.54057627198103120 ) ) ;
#23264 = CARTESIAN_POINT ( 'NONE',  ( -19.02544592524342804, 5.153800228976336051, 111.0405762719810099 ) ) ;
#23265 = CARTESIAN_POINT ( 'NONE',  ( -19.03943276465977164, 0.05219959533909376836, 31.24890960531435979 ) ) ;
#23266 = CARTESIAN_POINT ( 'NONE',  ( 13.97604488694527802, 13.89961937509977652, 99.37390960531436690 ) ) ;
#23267 = DIRECTION ( 'NONE',  ( -0.000000000000000000, -0.000000000000000000, 1.000000000000000000 ) ) ;
#23268 = CARTESIAN_POINT ( 'NONE',  ( -16.51473224551069308, -9.474510206698971260, 101.6655762719810241 ) ) ;
#23270 = CARTESIAN_POINT ( 'NONE',  ( -12.14591786802309592, -12.06949235617757132, 101.8739096053143811 ) ) ;
#23269 = CARTESIAN_POINT ( 'NONE',  ( -15.72974639402176322, -15.80617190586768395, 44.37609039468567573 ) ) ;
#23271 = CARTESIAN_POINT ( 'NONE',  ( -19.05341960407611168, -5.049401038298163336, 111.4572429386476671 ) ) ;
#23272 = CARTESIAN_POINT ( 'NONE',  ( -13.89961937509957401, -13.97604488694547697, 69.37609039468566152 ) ) ;
#23273 = CARTESIAN_POINT ( 'NONE',  ( -14.34966873604972548, 8.224510206698743886, 58.33442372801901143 ) ) ;
#23274 = CARTESIAN_POINT ( 'NONE',  ( 18.67979575497194134, -10.72451020669871369, 80.83442372801901854 ) ) ;
#23275 = CARTESIAN_POINT ( 'NONE',  ( 8.224510206698742110, 14.34966873604972548, 47.08442372801901854 ) ) ;
#23276 = CARTESIAN_POINT ( 'NONE',  ( -13.89961937509977652, 13.97604488694528158, 75.62390960531438111 ) ) ;
#23277 = CARTESIAN_POINT ( 'NONE',  ( 13.97604488694548053, -13.89961937509957401, 110.6260903946856615 ) ) ;
#23278 = CARTESIAN_POINT ( 'NONE',  ( 8.314922557961029526, -14.29746914071037800, 85.41775706135236135 ) ) ;
#23279 = CARTESIAN_POINT ( 'NONE',  ( -9.474510206698720793, -16.51473224551083518, 99.58442372801900433 ) ) ;
#23280 = CARTESIAN_POINT ( 'NONE',  ( 16.51473224551069308, 9.474510206698969483, 69.16557627198102409 ) ) ;
#23281 = CARTESIAN_POINT ( 'NONE',  ( -10.72451020669898014, 18.67979575497178502, 95.41557627198102409 ) ) ;
#23283 = CARTESIAN_POINT ( 'NONE',  ( -5.049401038297874678, -19.05341960407617918, 84.79275706135233293 ) ) ;
#23282 = CARTESIAN_POINT ( 'NONE',  ( -12.06949235617756955, 12.14591786802309770, 85.62390960531436690 ) ) ;
#23284 = CARTESIAN_POINT ( 'NONE',  ( -8.314922557961024197, 14.29746914071037800, 62.91775706135236135 ) ) ;
#23285 = CARTESIAN_POINT ( 'NONE',  ( 24.79447686064953871, 6.332871904612077607, 168.1804317516251501 ) ) ;
#23286 = CARTESIAN_POINT ( 'NONE',  ( -19.02544592524334988, -5.153800228976617603, 68.95942372801896170 ) ) ;
#23287 = CARTESIAN_POINT ( 'NONE',  ( -14.34966873604960291, -8.224510206698953496, 31.66557627198102054 ) ) ;
#23288 = CARTESIAN_POINT ( 'NONE',  ( 4.483927247898545687, 16.52544592524342804, 74.79057627198105251 ) ) ;
#23290 = CARTESIAN_POINT ( 'NONE',  ( -16.81555441253465943, 7.025013491696270762, 40.63685445334211011 ) ) ;
#23289 = CARTESIAN_POINT ( 'NONE',  ( -9.564922557961040184, 16.46253265017147172, 22.91775706135233648 ) ) ;
#23291 = CARTESIAN_POINT ( 'NONE',  ( -18.67979575497193778, 10.72451020669871902, 28.33442372801902209 ) ) ;
#23292 = CARTESIAN_POINT ( 'NONE',  ( 19.03943276465977164, -0.05219959533909143690, 108.7489096053143527 ) ) ;
#23293 = CARTESIAN_POINT ( 'NONE',  ( 0.05219959533909260263, 19.03943276465977164, 79.99890960531436690 ) ) ;
#23294 = CARTESIAN_POINT ( 'NONE',  ( 10.72451020669871369, 18.67979575497193778, 97.08442372801904696 ) ) ;
#23295 = CARTESIAN_POINT ( 'NONE',  ( 9.474510206698971260, -16.51473224551069308, 82.91557627198103830 ) ) ;
#23296 = CARTESIAN_POINT ( 'NONE',  ( 5.823673210054125526, 21.52544592524343514, 44.79057627198103120 ) ) ;
#23297 = CARTESIAN_POINT ( 'NONE',  ( -16.52544592524342804, 4.483927247898546575, 86.04057627198102409 ) ) ;
#23298 = CARTESIAN_POINT ( 'NONE',  ( 13.89961937509977652, -13.97604488694527269, 63.12390960531435979 ) ) ;
#23299 = CARTESIAN_POINT ( 'NONE',  ( 14.34966873604960469, 8.224510206698951720, 114.1655762719810383 ) ) ;
#23300 = CARTESIAN_POINT ( 'NONE',  ( 18.62759615963255655, 10.81492255796105972, 31.66775706135234358 ) ) ;
#23301 = CARTESIAN_POINT ( 'NONE',  ( 10.72451020669871369, 18.67979575497193778, 57.08442372801901854 ) ) ;
#23302 = CARTESIAN_POINT ( 'NONE',  ( -9.474510206698964154, 16.51473224551069663, 50.41557627198102409 ) ) ;
#23303 = CARTESIAN_POINT ( 'NONE',  ( -4.483927247898782831, 16.52544592524335698, 72.70942372801901854 ) ) ;
#23304 = CARTESIAN_POINT ( 'NONE',  ( 21.55341960407610458, 5.719274019375980345, 108.9572429386476955 ) ) ;
#23305 = CARTESIAN_POINT ( 'NONE',  ( -21.55341960407610458, -5.719274019375992779, 106.4572429386477097 ) ) ;
#23307 = CARTESIAN_POINT ( 'NONE',  ( -19.05341960407611168, -5.049401038298163336, 66.45724293864769550 ) ) ;
#23306 = CARTESIAN_POINT ( 'NONE',  ( 9.474510206698729675, 16.51473224551082808, 37.08442372801899722 ) ) ;
#23308 = CARTESIAN_POINT ( 'NONE',  ( -9.564922557961040184, 16.46253265017147172, 37.91775706135233293 ) ) ;
#23309 = CARTESIAN_POINT ( 'NONE',  ( -10.72451020669870658, -18.67979575497194134, 69.58442372801900433 ) ) ;
#23310 = CARTESIAN_POINT ( 'NONE',  ( 21.53943276465977519, -0.05219959533907433946, 63.74890960531435979 ) ) ;
#23311 = CARTESIAN_POINT ( 'NONE',  ( 16.53943276465976808, -0.05219959533910856209, 43.74890960531435979 ) ) ;
#23313 = CARTESIAN_POINT ( 'NONE',  ( -21.52544592524334988, -5.823673210054445271, 108.9594237280190185 ) ) ;
#23312 = CARTESIAN_POINT ( 'NONE',  ( 5.719274019375673035, 21.55341960407619339, 92.29275706135236135 ) ) ;
#23314 = CARTESIAN_POINT ( 'NONE',  ( -14.29746914071049879, 8.314922557960819915, 60.83224293864769550 ) ) ;
#23315 = CARTESIAN_POINT ( 'NONE',  ( -12.14591786802309592, -12.06949235617757132, 101.8739096053143811 ) ) ;
#23316 = CARTESIAN_POINT ( 'NONE',  ( 9.564922557961047289, -16.46253265017146816, 55.41775706135234003 ) ) ;
#23317 = CARTESIAN_POINT ( 'NONE',  ( 4.483927247898545687, 16.52544592524342804, 24.79057627198103120 ) ) ;
#23318 = CARTESIAN_POINT ( 'NONE',  ( -15.80617190586768217, 15.72974639402176855, 68.12609039468567573 ) ) ;
#23319 = CARTESIAN_POINT ( 'NONE',  ( -13.97604488694527625, -13.89961937509977652, 71.87390960531433848 ) ) ;
#23320 = CARTESIAN_POINT ( 'NONE',  ( -13.89961937509957401, -13.97604488694547875, 54.37609039468565442 ) ) ;
#23321 = CARTESIAN_POINT ( 'NONE',  ( -15.72974639402197994, 15.80617190586746368, 55.62390960531436690 ) ) ;
#23322 = CARTESIAN_POINT ( 'NONE',  ( 15.80617190586769283, -15.72974639402175789, 45.62609039468567573 ) ) ;
#23323 = CARTESIAN_POINT ( 'NONE',  ( -18.62759615963270932, 10.81492255796079327, 100.8322429386477097 ) ) ;
#23324 = CARTESIAN_POINT ( 'NONE',  ( 13.89961937509957401, 13.97604488694547697, 96.87609039468566152 ) ) ;
#23325 = CARTESIAN_POINT ( 'NONE',  ( -8.314922557961024197, 14.29746914071037800, 62.91775706135236135 ) ) ;
#23327 = CARTESIAN_POINT ( 'NONE',  ( -18.67979575497178146, -10.72451020669898902, 111.6655762719810525 ) ) ;
#23326 = CARTESIAN_POINT ( 'NONE',  ( -11.74149087413294623, -36.13659316521243881, -5.602157773949822506 ) ) ;
#23328 = CARTESIAN_POINT ( 'NONE',  ( 16.53943276465976808, -0.05219959533910856209, 93.74890960531436690 ) ) ;
#23329 = CARTESIAN_POINT ( 'NONE',  ( -17.49999999999997868, -5.076555817581236418, 31.17951492049776263 ) ) ;
#23330 = CARTESIAN_POINT ( 'NONE',  ( -19.03943276465977164, -0.05219959533935918106, 113.7510903946856757 ) ) ;
#23331 = CARTESIAN_POINT ( 'NONE',  ( -15.72974639402197994, 15.80617190586746368, 50.62390960531435979 ) ) ;
#23332 = CARTESIAN_POINT ( 'NONE',  ( 4.379528057220092307, 16.55341960407617563, 87.29275706135236135 ) ) ;
#23333 = CARTESIAN_POINT ( 'NONE',  ( 36.62451201681301427, 4.795837538146646928, -8.000000000000001776 ) ) ;
#23334 = CARTESIAN_POINT ( 'NONE',  ( 12.06949235617739724, 12.14591786802326823, 66.87609039468568994 ) ) ;
#23335 = CARTESIAN_POINT ( 'NONE',  ( -15.80617190586768217, 15.72974639402176855, 23.12609039468567573 ) ) ;
#23336 = CARTESIAN_POINT ( 'NONE',  ( -5.719274019375978568, 21.55341960407610458, 45.20724293864769550 ) ) ;
#23337 = CARTESIAN_POINT ( 'NONE',  ( 12.14591786802327356, -12.06949235617739191, 85.62609039468568994 ) ) ;
#23338 = CARTESIAN_POINT ( 'NONE',  ( -5.153800228976328057, -19.02544592524343514, 102.2905762719810383 ) ) ;
#23339 = CARTESIAN_POINT ( 'NONE',  ( -10.72451020669870658, -18.67979575497194134, 64.58442372801900433 ) ) ;
#23340 = CARTESIAN_POINT ( 'NONE',  ( -21.55341960407610458, -5.719274019375992779, 46.45724293864769550 ) ) ;
#23341 = CARTESIAN_POINT ( 'NONE',  ( -18.67979575497178146, -10.72451020669898902, 31.66557627198102054 ) ) ;
#23342 = ORIENTED_EDGE ( 'NONE', *, *, #21058, .T. ) ;
#23343 = CARTESIAN_POINT ( 'NONE',  ( 16.51473224551083163, -9.474510206698727899, 55.83442372801899722 ) ) ;
#23344 = CARTESIAN_POINT ( 'NONE',  ( 16.55341960407618274, -4.379528057220086978, 66.04275706135236135 ) ) ;
#23345 = CARTESIAN_POINT ( 'NONE',  ( 21.55341960407610458, 5.719274019375980345, 28.95724293864769905 ) ) ;
#23346 = VERTEX_POINT ( 'NONE', #102034 ) ;
#23347 = CARTESIAN_POINT ( 'NONE',  ( 13.97604488694527802, 13.89961937509977652, 84.37390960531433848 ) ) ;
#23348 = CARTESIAN_POINT ( 'NONE',  ( 12.14591786802309770, 12.06949235617756955, 24.37390960531435979 ) ) ;
#23349 = CARTESIAN_POINT ( 'NONE',  ( -17.60728821186566151, 5.500000000000029310, 85.86690927743002533 ) ) ;
#23350 = CARTESIAN_POINT ( 'NONE',  ( -16.53943276465976808, 0.05219959533911058130, 106.2489096053143811 ) ) ;
#23351 = CARTESIAN_POINT ( 'NONE',  ( 21.55341960407610458, 5.719274019375980345, 43.95724293864769550 ) ) ;
#23352 = CARTESIAN_POINT ( 'NONE',  ( -9.564922557960796823, -16.46253265017161027, 47.08224293864769550 ) ) ;
#23353 = CARTESIAN_POINT ( 'NONE',  ( 4.483927247898790824, -16.52544592524335698, 75.20942372801901854 ) ) ;
#23354 = CARTESIAN_POINT ( 'NONE',  ( -21.52544592524334988, -5.823673210054445271, 38.95942372801901854 ) ) ;
#23355 = CARTESIAN_POINT ( 'NONE',  ( 19.03943276465977164, 0.05219959533936151252, 91.25109039468566152 ) ) ;
#23356 = CARTESIAN_POINT ( 'NONE',  ( -4.379528057220328563, 16.55341960407611168, 85.20724293864770971 ) ) ;
#23357 = CARTESIAN_POINT ( 'NONE',  ( 13.97604488694527802, 13.89961937509977652, 54.37390960531435979 ) ) ;
#23358 = CARTESIAN_POINT ( 'NONE',  ( -13.97604488694527625, -13.89961937509977652, 26.87390960531434558 ) ) ;
#23359 = CARTESIAN_POINT ( 'NONE',  ( -15.72974639402176322, -15.80617190586768395, 109.3760903946857042 ) ) ;
#23360 = CARTESIAN_POINT ( 'NONE',  ( 16.51473224551069308, 9.474510206698969483, 79.16557627198103830 ) ) ;
#23361 = CARTESIAN_POINT ( 'NONE',  ( -12.14591786802326823, 12.06949235617739902, 63.12609039468568994 ) ) ;
#23362 = CARTESIAN_POINT ( 'NONE',  ( 0.05219959533937995610, -21.53943276465977519, 90.00109039468567573 ) ) ;
#23363 = CARTESIAN_POINT ( 'NONE',  ( 5.823673210054125526, 21.52544592524343514, 49.79057627198102409 ) ) ;
#23364 = CARTESIAN_POINT ( 'NONE',  ( -14.29746914071037622, -8.314922557961029526, 79.16775706135234714 ) ) ;
#23365 = CARTESIAN_POINT ( 'NONE',  ( -9.474510206698720793, -16.51473224551083518, 49.58442372801899722 ) ) ;
#23366 = CARTESIAN_POINT ( 'NONE',  ( -13.89961937509957401, -13.97604488694547875, 69.37609039468564731 ) ) ;
#23367 = ORIENTED_EDGE ( 'NONE', *, *, #829, .T. ) ;
#23368 = CARTESIAN_POINT ( 'NONE',  ( 18.67979575497194134, -10.72451020669871369, 65.83442372801900433 ) ) ;
#23369 = CARTESIAN_POINT ( 'NONE',  ( -16.51473224551069308, -9.474510206698971260, 71.66557627198102409 ) ) ;
#23370 = CARTESIAN_POINT ( 'NONE',  ( 19.03943276465977164, -0.05219959533909143690, 33.74890960531435979 ) ) ;
#23371 = CARTESIAN_POINT ( 'NONE',  ( -5.153800228976607833, 19.02544592524334988, 62.70942372801899722 ) ) ;
#23372 = CARTESIAN_POINT ( 'NONE',  ( -9.564922557960796823, -16.46253265017161027, 107.0822429386476955 ) ) ;
#23373 = CARTESIAN_POINT ( 'NONE',  ( -9.474510206698964154, 16.51473224551069663, 90.41557627198103830 ) ) ;
#23374 = CARTESIAN_POINT ( 'NONE',  ( 12.06949235617757843, -12.14591786802309237, 48.12390960531436690 ) ) ;
#23375 = CARTESIAN_POINT ( 'NONE',  ( 10.72451020669898902, -18.67979575497178502, 52.91557627198103830 ) ) ;
#23376 = CARTESIAN_POINT ( 'NONE',  ( 22.15679140170794881, 22.84806810306143632, -49.22928680315006034 ) ) ;
#23377 = CARTESIAN_POINT ( 'NONE',  ( -15.72974639402176322, -15.80617190586768395, 109.3760903946857042 ) ) ;
#23378 = CARTESIAN_POINT ( 'NONE',  ( -16.88567814943162659, -6.947325034625696283, 81.29001122652589117 ) ) ;
#23379 = CARTESIAN_POINT ( 'NONE',  ( -19.03943276465977164, 0.05219959533909376836, 46.24890960531435979 ) ) ;
#23380 = CARTESIAN_POINT ( 'NONE',  ( -11.74264578624800670, 36.14014761921585972, -4.400000000000000355 ) ) ;
#23381 = CYLINDRICAL_SURFACE ( 'NONE', #59719, 61.99999999999998579 ) ;
#23382 = CARTESIAN_POINT ( 'NONE',  ( -14.34966873604972548, 8.224510206698743886, 68.33442372801900433 ) ) ;
#23384 = ADVANCED_FACE ( 'NONE', ( #84843 ), #87142, .T. ) ;
#23383 = CARTESIAN_POINT ( 'NONE',  ( -10.81492255796078084, -18.62759615963271287, 77.08224293864769550 ) ) ;
#23385 = CARTESIAN_POINT ( 'NONE',  ( -12.14591786802309592, -12.06949235617757132, 46.87390960531435979 ) ) ;
#23387 = CARTESIAN_POINT ( 'NONE',  ( -7.500000000000000000, 0.000000000000000000, 5.707106781186540800 ) ) ;
#23386 = CARTESIAN_POINT ( 'NONE',  ( -13.97604488694527625, -13.89961937509977652, 41.87390960531435979 ) ) ;
#23388 = CARTESIAN_POINT ( 'NONE',  ( -18.62759615963255300, -10.81492255796106328, 39.16775706135235424 ) ) ;
#23389 = CARTESIAN_POINT ( 'NONE',  ( -5.153800228976607833, 19.02544592524334988, 52.70942372801900433 ) ) ;
#23390 = CARTESIAN_POINT ( 'NONE',  ( 19.05341960407611168, 5.049401038298154454, 33.95724293864769550 ) ) ;
#23391 = CARTESIAN_POINT ( 'NONE',  ( 10.81492255796106328, -18.62759615963255655, 100.4177570613523471 ) ) ;
#23392 = DIRECTION ( 'NONE',  ( -6.938893903907234689E-15, -0.000000000000000000, -1.000000000000000000 ) ) ;
#23393 = CARTESIAN_POINT ( 'NONE',  ( -4.483927247898539470, -16.52544592524342804, 37.29057627198102409 ) ) ;
#23394 = CARTESIAN_POINT ( 'NONE',  ( -16.16661445520354334, 1.151164073136760946, -59.37042179516131313 ) ) ;
#23395 = CARTESIAN_POINT ( 'NONE',  ( 0.05219959533907565091, 21.53943276465977519, 34.99890960531435979 ) ) ;
#23396 = CARTESIAN_POINT ( 'NONE',  ( 19.03943276465977164, -0.05219959533909143690, 83.74890960531436690 ) ) ;
#23397 = CARTESIAN_POINT ( 'NONE',  ( 14.29746914071049879, -8.314922557960816363, 83.33224293864769550 ) ) ;
#23398 = CARTESIAN_POINT ( 'NONE',  ( -0.05219959533934338120, 16.53943276465976808, 22.50109039468567573 ) ) ;
#23399 = CARTESIAN_POINT ( 'NONE',  ( 14.34966873604972726, -8.224510206698740333, 110.8344237280190043 ) ) ;
#23400 = ORIENTED_EDGE ( 'NONE', *, *, #157314, .T. ) ;
#23401 = CARTESIAN_POINT ( 'NONE',  ( 19.02544592524343514, -5.153800228976328945, 48.54057627198103120 ) ) ;
#23403 = CARTESIAN_POINT ( 'NONE',  ( 0.05219959533907565091, 21.53943276465977519, 84.99890960531436690 ) ) ;
#23402 = CARTESIAN_POINT ( 'NONE',  ( 16.46253265017160672, -9.564922557960803928, 98.33224293864769550 ) ) ;
#23405 = CARTESIAN_POINT ( 'NONE',  ( 13.97604488694527802, 13.89961937509977652, 104.3739096053143385 ) ) ;
#23404 = CARTESIAN_POINT ( 'NONE',  ( 12.14591786802309770, 12.06949235617756955, 24.37390960531435979 ) ) ;
#23406 = CARTESIAN_POINT ( 'NONE',  ( 13.97604488694548053, -13.89961937509957401, 75.62609039468564731 ) ) ;
#23407 = CARTESIAN_POINT ( 'NONE',  ( 10.81492255796106328, -18.62759615963255655, 105.4177570613523613 ) ) ;
#23408 = CARTESIAN_POINT ( 'NONE',  ( 18.67979575497178502, 10.72451020669898547, 89.16557627198102409 ) ) ;
#23409 = CARTESIAN_POINT ( 'NONE',  ( 0.05219959533907565091, 21.53943276465977519, 34.99890960531435979 ) ) ;
#23410 = CARTESIAN_POINT ( 'NONE',  ( -5.153800228976328057, -19.02544592524343514, 62.29057627198100988 ) ) ;
#23411 = CARTESIAN_POINT ( 'NONE',  ( -4.379528057220328563, 16.55341960407611168, 35.20724293864768839 ) ) ;
#23412 = CARTESIAN_POINT ( 'NONE',  ( 19.05341960407611168, 5.049401038298154454, 83.95724293864766707 ) ) ;
#23413 = ORIENTED_EDGE ( 'NONE', *, *, #182035, .T. ) ;
#23414 = CARTESIAN_POINT ( 'NONE',  ( -32.45678934495599322, -3.100610132747052550, 88.16656412605021842 ) ) ;
#23415 = CARTESIAN_POINT ( 'NONE',  ( -5.153800228976607833, 19.02544592524334988, 22.70942372801899012 ) ) ;
#23416 = CARTESIAN_POINT ( 'NONE',  ( 16.53943276465976808, -0.05219959533910856209, 83.74890960531435269 ) ) ;
#23417 = CARTESIAN_POINT ( 'NONE',  ( 18.67979575497194134, -10.72451020669871369, 25.83442372801901499 ) ) ;
#23418 = CARTESIAN_POINT ( 'NONE',  ( -27.73933785331498925, 9.013057229001089965, 147.2750000027311614 ) ) ;
#23419 = CARTESIAN_POINT ( 'NONE',  ( 15.80617190586746368, 15.72974639402197994, 69.37390960531436690 ) ) ;
#23420 = CARTESIAN_POINT ( 'NONE',  ( -12.06949235617739369, -12.14591786802326823, 89.37609039468568994 ) ) ;
#23421 = CARTESIAN_POINT ( 'NONE',  ( 19.05341960407611168, 5.049401038298154454, 23.95724293864769194 ) ) ;
#23422 = CARTESIAN_POINT ( 'NONE',  ( -0.05219959533909027116, -19.03943276465977164, 67.49890960531436690 ) ) ;
#23423 = DIRECTION ( 'NONE',  ( -0.000000000000000000, -0.000000000000000000, -1.000000000000000000 ) ) ;
#23424 = CARTESIAN_POINT ( 'NONE',  ( 13.89961937509977652, -13.97604488694527269, 23.12390960531436335 ) ) ;
#23425 = CARTESIAN_POINT ( 'NONE',  ( -8.224510206698948167, 14.34966873604960824, 35.41557627198102409 ) ) ;
#23426 = CARTESIAN_POINT ( 'NONE',  ( -21.55341960407619339, 5.719274019375674811, 58.54275706135235424 ) ) ;
#23427 = CARTESIAN_POINT ( 'NONE',  ( 0.000000000000000000, 0.000000000000000000, -18.00000000000000000 ) ) ;
#23428 = CARTESIAN_POINT ( 'NONE',  ( -10.81492255796105439, 18.62759615963255655, 92.91775706135236135 ) ) ;
#23429 = CARTESIAN_POINT ( 'NONE',  ( -9.564922557960796823, -16.46253265017161027, 42.08224293864769550 ) ) ;
#23430 = CARTESIAN_POINT ( 'NONE',  ( 19.05341960407611168, 5.049401038298154454, 48.95724293864768129 ) ) ;
#23431 = ORIENTED_EDGE ( 'NONE', *, *, #100813, .F. ) ;
#23432 = CARTESIAN_POINT ( 'NONE',  ( -21.55341960407619339, 5.719274019375674811, 88.54275706135236135 ) ) ;
#23433 = CARTESIAN_POINT ( 'NONE',  ( 8.224510206698742110, 14.34966873604972548, 62.08442372801901143 ) ) ;
#23434 = CARTESIAN_POINT ( 'NONE',  ( -5.719274019375665041, -21.55341960407619695, 79.79275706135236135 ) ) ;
#23435 = CARTESIAN_POINT ( 'NONE',  ( 5.719274019375991003, -21.55341960407610458, 27.70724293864769905 ) ) ;
#23436 = CARTESIAN_POINT ( 'NONE',  ( 5.049401038297881783, 19.05341960407617563, 97.29275706135233293 ) ) ;
#23437 = CARTESIAN_POINT ( 'NONE',  ( -15.80617190586768217, 15.72974639402176855, 58.12609039468568994 ) ) ;
#23438 = CARTESIAN_POINT ( 'NONE',  ( -4.379528057220086978, -16.55341960407618274, 34.79275706135235424 ) ) ;
#23439 = CARTESIAN_POINT ( 'NONE',  ( 10.72451020669898902, -18.67979575497178502, 87.91557627198103830 ) ) ;
#23440 = CARTESIAN_POINT ( 'NONE',  ( -16.46253265017146816, -9.564922557961047289, 84.16775706135233293 ) ) ;
#23441 = CARTESIAN_POINT ( 'NONE',  ( 16.51473224551069308, 9.474510206698969483, 69.16557627198102409 ) ) ;
#23442 = CARTESIAN_POINT ( 'NONE',  ( -9.474510206698720793, -16.51473224551083518, 99.58442372801900433 ) ) ;
#23443 = CARTESIAN_POINT ( 'NONE',  ( -13.97604488694547697, 13.89961937509957934, 108.1260903946856331 ) ) ;
#23444 = CARTESIAN_POINT ( 'NONE',  ( -12.14591786802309592, -12.06949235617757132, 46.87390960531435979 ) ) ;
#23445 = CARTESIAN_POINT ( 'NONE',  ( -0.05219959533936034679, 19.03943276465977164, 72.50109039468566152 ) ) ;
#23446 = CARTESIAN_POINT ( 'NONE',  ( -12.06949235617739369, -12.14591786802326823, 59.37609039468568284 ) ) ;
#23447 = CARTESIAN_POINT ( 'NONE',  ( 19.02544592524334988, 5.153800228976608722, 41.45942372801900433 ) ) ;
#23448 = CARTESIAN_POINT ( 'NONE',  ( 19.05341960407611168, 5.049401038298154454, 43.95724293864769550 ) ) ;
#23449 = CARTESIAN_POINT ( 'NONE',  ( 16.51473224551069308, 9.474510206698969483, 59.16557627198102409 ) ) ;
#23450 = CARTESIAN_POINT ( 'NONE',  ( -4.379528057220086978, -16.55341960407618274, 59.79275706135234714 ) ) ;
#23451 = CARTESIAN_POINT ( 'NONE',  ( 17.14385361876520264, -23.59649016807271238, 142.0750000027311444 ) ) ;
#23452 = CARTESIAN_POINT ( 'NONE',  ( -23.31738231874055245, -16.94106989632524574, 138.4500000054623570 ) ) ;
#23453 = CARTESIAN_POINT ( 'NONE',  ( 19.05341960407611168, 5.049401038298154454, 103.9572429386476671 ) ) ;
#23454 = DIRECTION ( 'NONE',  ( -1.000000000000000000, 0.000000000000000000, 0.000000000000000000 ) ) ;
#23455 = ORIENTED_EDGE ( 'NONE', *, *, #67374, .T. ) ;
#23456 = CARTESIAN_POINT ( 'NONE',  ( -0.05219959533936034679, 19.03943276465977164, 102.5010903946856757 ) ) ;
#23457 = CARTESIAN_POINT ( 'NONE',  ( 18.62759615963271287, -10.81492255796078972, 33.33224293864769550 ) ) ;
#23459 = CARTESIAN_POINT ( 'NONE',  ( -8.224510206698735004, -14.34966873604973081, 19.58442372801901143 ) ) ;
#23458 = CARTESIAN_POINT ( 'NONE',  ( -16.46253265017146816, -9.564922557961047289, 34.16775706135233293 ) ) ;
#23460 = CARTESIAN_POINT ( 'NONE',  ( 5.153800228976335163, 19.02544592524342804, 24.79057627198102765 ) ) ;
#23461 = CARTESIAN_POINT ( 'NONE',  ( -9.564922557960796823, -16.46253265017161027, 52.08224293864768839 ) ) ;
#23462 = CARTESIAN_POINT ( 'NONE',  ( 10.72451020669898902, -18.67979575497178502, 67.91557627198102409 ) ) ;
#23463 = CARTESIAN_POINT ( 'NONE',  ( 5.153800228976335163, 19.02544592524342804, 104.7905762719809957 ) ) ;
#23464 = CARTESIAN_POINT ( 'NONE',  ( 5.153800228976335163, 19.02544592524342804, 34.79057627198102409 ) ) ;
#23465 = CARTESIAN_POINT ( 'NONE',  ( -27.73933785331498925, -9.013057229001049109, 143.4750000027312069 ) ) ;
#23466 = CARTESIAN_POINT ( 'NONE',  ( 16.46253265017146816, 9.564922557961045513, 86.66775706135233293 ) ) ;
#23467 = CARTESIAN_POINT ( 'NONE',  ( 16.52544592524342804, -4.483927247898539470, 63.54057627198103830 ) ) ;
#23468 = CARTESIAN_POINT ( 'NONE',  ( 18.62759615963271287, -10.81492255796078972, 48.33224293864770260 ) ) ;
#23469 = CARTESIAN_POINT ( 'NONE',  ( 5.719274019375673035, 21.55341960407619339, 107.2927570613523471 ) ) ;
#23470 = CARTESIAN_POINT ( 'NONE',  ( 10.72451020669898902, -18.67979575497178502, 102.9155762719810383 ) ) ;
#23471 = CARTESIAN_POINT ( 'NONE',  ( -0.05219959533937732626, 21.53943276465977519, 67.50109039468568994 ) ) ;
#23472 = CARTESIAN_POINT ( 'NONE',  ( -15.80617190586768217, 15.72974639402176855, 83.12609039468568994 ) ) ;
#23473 = CARTESIAN_POINT ( 'NONE',  ( 5.049401038298161559, -19.05341960407611168, 107.7072429386476955 ) ) ;
#23475 = CARTESIAN_POINT ( 'NONE',  ( -15.72974639402176322, -15.80617190586768395, 74.37609039468568994 ) ) ;
#23474 = CARTESIAN_POINT ( 'NONE',  ( 4.379528057220092307, 16.55341960407617563, 107.2927570613523471 ) ) ;
#23476 = CARTESIAN_POINT ( 'NONE',  ( -19.05341960407611168, -5.049401038298163336, 71.45724293864766707 ) ) ;
#23477 = CARTESIAN_POINT ( 'NONE',  ( 19.05341960407617918, -5.049401038297876454, 31.04275706135232227 ) ) ;
#23478 = CARTESIAN_POINT ( 'NONE',  ( 18.62759615963255655, 10.81492255796105972, 26.66775706135235424 ) ) ;
#23479 = CARTESIAN_POINT ( 'NONE',  ( 5.153800228976335163, 19.02544592524342804, 69.79057627198103830 ) ) ;
#23480 = CARTESIAN_POINT ( 'NONE',  ( -16.52544592524342804, 4.483927247898546575, 81.04057627198102409 ) ) ;
#23481 = CARTESIAN_POINT ( 'NONE',  ( 8.314922557960818139, 14.29746914071049879, 44.58224293864769550 ) ) ;
#23482 = CARTESIAN_POINT ( 'NONE',  ( 18.62759615963271287, -10.81492255796078972, 53.33224293864769550 ) ) ;
#23483 = CARTESIAN_POINT ( 'NONE',  ( 16.46253265017160672, -9.564922557960803928, 63.33224293864769550 ) ) ;
#23484 = CARTESIAN_POINT ( 'NONE',  ( 10.81492255796078972, 18.62759615963270932, 69.58224293864769550 ) ) ;
#23485 = CARTESIAN_POINT ( 'NONE',  ( -5.153800228976607833, 19.02544592524334988, 67.70942372801900433 ) ) ;
#23487 = CARTESIAN_POINT ( 'NONE',  ( -8.314922557960811034, -14.29746914071050412, 62.08224293864769550 ) ) ;
#23486 = CARTESIAN_POINT ( 'NONE',  ( 69.65682714487590488, -71.74905178543389184, -25.00000000000000000 ) ) ;
#23488 = CARTESIAN_POINT ( 'NONE',  ( 5.719274019375991003, -21.55341960407610458, 42.70724293864770260 ) ) ;
#23489 = ORIENTED_EDGE ( 'NONE', *, *, #168230, .T. ) ;
#23490 = CARTESIAN_POINT ( 'NONE',  ( 17.50000000000000000, 5.622605283950862010, 103.8120731059611046 ) ) ;
#23492 = DIRECTION ( 'NONE',  ( -0.5000000000000037748, -0.4999999999999950595, -0.7071067811865484609 ) ) ;
#23491 = CARTESIAN_POINT ( 'NONE',  ( 8.314922557961029526, -14.29746914071037800, 90.41775706135236135 ) ) ;
#23493 = CARTESIAN_POINT ( 'NONE',  ( -9.564922557961040184, 16.46253265017147172, 82.91775706135233293 ) ) ;
#23494 = CARTESIAN_POINT ( 'NONE',  ( -8.224510206698948167, 14.34966873604960824, 50.41557627198103120 ) ) ;
#23495 = LINE ( 'NONE', #9335, #9642 ) ;
#23496 = CARTESIAN_POINT ( 'NONE',  ( -0.05219959533909027116, -19.03943276465977164, 52.49890960531436690 ) ) ;
#23497 = CARTESIAN_POINT ( 'NONE',  ( 8.314922557960818139, 14.29746914071049879, 34.58224293864770260 ) ) ;
#23498 = CARTESIAN_POINT ( 'NONE',  ( -16.51473224551069308, -9.474510206698971260, 81.66557627198103830 ) ) ;
#23500 = CARTESIAN_POINT ( 'NONE',  ( 13.89961937509977652, -13.97604488694527269, 53.12390960531434558 ) ) ;
#23499 = CARTESIAN_POINT ( 'NONE',  ( -13.97604488694547697, 13.89961937509957934, 78.12609039468567573 ) ) ;
#23501 = CARTESIAN_POINT ( 'NONE',  ( 5.719274019375673035, 21.55341960407619339, 62.29275706135236845 ) ) ;
#23502 = CARTESIAN_POINT ( 'NONE',  ( -19.05341960407611168, -5.049401038298163336, 71.45724293864766707 ) ) ;
#23503 = CARTESIAN_POINT ( 'NONE',  ( -19.05341960407611168, -5.049401038298163336, 21.45724293864768839 ) ) ;
#23504 = CARTESIAN_POINT ( 'NONE',  ( 16.51473224551069308, 9.474510206698969483, 79.16557627198103830 ) ) ;
#23505 = CARTESIAN_POINT ( 'NONE',  ( 21.55341960407610458, 5.719274019375980345, 53.95724293864770260 ) ) ;
#23506 = CARTESIAN_POINT ( 'NONE',  ( -13.89961937509977652, 13.97604488694528158, 45.62390960531433848 ) ) ;
#23507 = CARTESIAN_POINT ( 'NONE',  ( -21.53943276465977519, 0.05219959533907696930, 56.24890960531436690 ) ) ;
#23508 = CARTESIAN_POINT ( 'NONE',  ( 13.89961937509957401, 13.97604488694547697, 86.87609039468567573 ) ) ;
#23509 = CARTESIAN_POINT ( 'NONE',  ( 4.483927247898790824, -16.52544592524335698, 100.2094237280190043 ) ) ;
#23510 = EDGE_CURVE ( 'NONE', #101588, #4163, #39723, .T. ) ;
#23511 = CARTESIAN_POINT ( 'NONE',  ( 19.05341960407617918, -5.049401038297876454, 41.04275706135233293 ) ) ;
#23513 = CARTESIAN_POINT ( 'NONE',  ( 8.314922557961029526, -14.29746914071037800, 80.41775706135234714 ) ) ;
#23512 = CARTESIAN_POINT ( 'NONE',  ( 0.05219959533934541429, -16.53943276465976808, 55.00109039468568284 ) ) ;
#23514 = DIRECTION ( 'NONE',  ( 1.000000000000000000, 0.000000000000000000, 0.000000000000000000 ) ) ;
#23515 = CARTESIAN_POINT ( 'NONE',  ( 12.14591786802327356, -12.06949235617739191, 70.62609039468567573 ) ) ;
#23516 = CARTESIAN_POINT ( 'NONE',  ( -15.80617190586745835, -15.72974639402198527, 21.87390960531436690 ) ) ;
#23517 = CARTESIAN_POINT ( 'NONE',  ( -0.05219959533909027116, -19.03943276465977164, 37.49890960531436690 ) ) ;
#23518 = CARTESIAN_POINT ( 'NONE',  ( 16.52544592524335698, 4.483927247898782831, 31.45942372801901854 ) ) ;
#23519 = CARTESIAN_POINT ( 'NONE',  ( 16.46253265017160672, -9.564922557960803928, 53.33224293864768839 ) ) ;
#23520 = CARTESIAN_POINT ( 'NONE',  ( -21.55341960407619339, 5.719274019375674811, 43.54275706135235424 ) ) ;
#23521 = CARTESIAN_POINT ( 'NONE',  ( 12.14591786802327356, -12.06949235617739191, 35.62609039468568994 ) ) ;
#23522 = CARTESIAN_POINT ( 'NONE',  ( -16.55341960407611168, -4.379528057220339221, 21.45724293864769550 ) ) ;
#23523 = CARTESIAN_POINT ( 'NONE',  ( -25.51181203389340268, -5.285008086477787081, 165.5623613760384387 ) ) ;
#23524 = CARTESIAN_POINT ( 'NONE',  ( 0.05219959533936267826, -19.03943276465977164, 20.00109039468567218 ) ) ;
#23525 = CARTESIAN_POINT ( 'NONE',  ( 19.02544592524334988, 5.153800228976608722, 111.4594237280190043 ) ) ;
#23526 = CARTESIAN_POINT ( 'NONE',  ( 16.46253265017146816, 9.564922557961045513, 66.66775706135233293 ) ) ;
#23527 = CARTESIAN_POINT ( 'NONE',  ( 4.379528057220339221, -16.55341960407611168, 72.70724293864769550 ) ) ;
#23528 = CARTESIAN_POINT ( 'NONE',  ( -16.46253265017160317, 9.564922557960807481, 35.83224293864768839 ) ) ;
#23530 = CARTESIAN_POINT ( 'NONE',  ( 16.31925111598407696, -7.325300261831841020, 57.66424538967171998 ) ) ;
#23529 = CARTESIAN_POINT ( 'NONE',  ( -5.153800228976607833, 19.02544592524334988, 72.70942372801900433 ) ) ;
#23531 = CARTESIAN_POINT ( 'NONE',  ( -5.823673210054431948, 21.52544592524334988, 67.70942372801901854 ) ) ;
#23532 = CARTESIAN_POINT ( 'NONE',  ( -0.05219959533934338120, 16.53943276465976808, 42.50109039468567573 ) ) ;
#23533 = DIRECTION ( 'NONE',  ( 0.000000000000000000, 0.000000000000000000, 1.000000000000000000 ) ) ;
#23534 = CARTESIAN_POINT ( 'NONE',  ( -16.51473224551069308, -9.474510206698971260, 111.6655762719810383 ) ) ;
#23535 = CARTESIAN_POINT ( 'NONE',  ( 14.34966873604972726, -8.224510206698740333, 20.83442372801901143 ) ) ;
#23536 = CARTESIAN_POINT ( 'NONE',  ( 9.474510206698971260, -16.51473224551069308, 112.9155762719810383 ) ) ;
#23537 = CARTESIAN_POINT ( 'NONE',  ( 11.80868324581537543, 11.80868324581533990, -59.13370768023891344 ) ) ;
#23538 = CARTESIAN_POINT ( 'NONE',  ( -9.474510206698964154, 16.51473224551069663, 30.41557627198102054 ) ) ;
#23539 = CARTESIAN_POINT ( 'NONE',  ( 5.719274019375673035, 21.55341960407619339, 107.2927570613523471 ) ) ;
#23540 = CARTESIAN_POINT ( 'NONE',  ( 5.049401038298161559, -19.05341960407611168, 62.70724293864769550 ) ) ;
#23541 = CARTESIAN_POINT ( 'NONE',  ( 21.55341960407619695, -5.719274019375665929, 71.04275706135234714 ) ) ;
#23542 = CARTESIAN_POINT ( 'NONE',  ( 21.55341960407619695, -5.719274019375665929, 101.0427570613523756 ) ) ;
#23543 = CARTESIAN_POINT ( 'NONE',  ( 14.29746914071037800, 8.314922557961029526, 111.6677570613523613 ) ) ;
#23544 = CARTESIAN_POINT ( 'NONE',  ( -16.51473224551069308, -9.474510206698971260, 26.66557627198103120 ) ) ;
#23545 = CARTESIAN_POINT ( 'NONE',  ( 13.89961937509977652, -13.97604488694527269, 98.12390960531433848 ) ) ;
#23546 = CARTESIAN_POINT ( 'NONE',  ( -5.823673210054431948, 21.52544592524334988, 62.70942372801902565 ) ) ;
#23547 = CARTESIAN_POINT ( 'NONE',  ( -19.02544592524342804, 5.153800228976336051, 31.04057627198102409 ) ) ;
#23548 = CARTESIAN_POINT ( 'NONE',  ( -0.05219959533937732626, 21.53943276465977519, 52.50109039468567573 ) ) ;
#23550 = CARTESIAN_POINT ( 'NONE',  ( -19.05341960407611168, -5.049401038298163336, 106.4572429386476955 ) ) ;
#23549 = CARTESIAN_POINT ( 'NONE',  ( 0.05219959533936267826, -19.03943276465977164, 85.00109039468567573 ) ) ;
#23551 = CARTESIAN_POINT ( 'NONE',  ( 5.049401038298161559, -19.05341960407611168, 27.70724293864769550 ) ) ;
#23552 = CARTESIAN_POINT ( 'NONE',  ( 15.72974639402199770, -15.80617190586745480, 108.1239096053143811 ) ) ;
#23553 = CARTESIAN_POINT ( 'NONE',  ( 13.89961937509957401, 13.97604488694547697, 36.87609039468565442 ) ) ;
#23554 = CARTESIAN_POINT ( 'NONE',  ( -8.314922557960811034, -14.29746914071050412, 107.0822429386476955 ) ) ;
#23555 = CARTESIAN_POINT ( 'NONE',  ( -0.05219959533909027116, -19.03943276465977164, 52.49890960531436690 ) ) ;
#23556 = CARTESIAN_POINT ( 'NONE',  ( 19.03943276465977164, 0.05219959533936151252, 101.2510903946856757 ) ) ;
#23557 = CARTESIAN_POINT ( 'NONE',  ( -14.34966873604960291, -8.224510206698953496, 56.66557627198103830 ) ) ;
#23558 = CARTESIAN_POINT ( 'NONE',  ( 21.53943276465977519, 0.05219959533937863772, 106.2510903946856757 ) ) ;
#23559 = CARTESIAN_POINT ( 'NONE',  ( 19.05341960407611168, 5.049401038298154454, 113.9572429386477097 ) ) ;
#23560 = CARTESIAN_POINT ( 'NONE',  ( -9.474510206698720793, -16.51473224551083518, 84.58442372801900433 ) ) ;
#23561 = CARTESIAN_POINT ( 'NONE',  ( 5.719274019375991003, -21.55341960407610458, 92.70724293864770971 ) ) ;
#23562 = CARTESIAN_POINT ( 'NONE',  ( 18.67979575497194134, -10.72451020669871369, 45.83442372801901854 ) ) ;
#23563 = CARTESIAN_POINT ( 'NONE',  ( -8.224510206698735004, -14.34966873604973081, 39.58442372801901143 ) ) ;
#23564 = CARTESIAN_POINT ( 'NONE',  ( 16.53943276465976808, 0.05219959533934440121, 101.2510903946856757 ) ) ;
#23566 = CARTESIAN_POINT ( 'NONE',  ( -18.67979575497193778, 10.72451020669871902, 53.33442372801901854 ) ) ;
#23565 = CARTESIAN_POINT ( 'NONE',  ( -4.483927247898782831, 16.52544592524335698, 47.70942372801902565 ) ) ;
#23567 = CARTESIAN_POINT ( 'NONE',  ( -21.55341960407610458, -5.719274019375992779, 41.45724293864769550 ) ) ;
#23568 = CARTESIAN_POINT ( 'NONE',  ( -5.049401038298153566, 19.05341960407611168, 35.20724293864768839 ) ) ;
#23569 = CARTESIAN_POINT ( 'NONE',  ( -11.74264578624799782, -36.14014761921581709, -7.349999994537626868 ) ) ;
#23570 = CARTESIAN_POINT ( 'NONE',  ( -16.52544592524335698, -4.483927247898792601, 68.95942372801901854 ) ) ;
#23571 = CARTESIAN_POINT ( 'NONE',  ( -21.53943276465977519, 0.05219959533907696930, 91.24890960531436690 ) ) ;
#23572 = CARTESIAN_POINT ( 'NONE',  ( -0.05219959533910754901, -16.53943276465976808, 37.49890960531436690 ) ) ;
#23573 = CARTESIAN_POINT ( 'NONE',  ( -0.05219959533934338120, 16.53943276465976808, 67.50109039468568994 ) ) ;
#23574 = CARTESIAN_POINT ( 'NONE',  ( -9.564922557960796823, -16.46253265017161027, 52.08224293864768839 ) ) ;
#23575 = CARTESIAN_POINT ( 'NONE',  ( 19.05341960407617918, -5.049401038297876454, 106.0427570613523471 ) ) ;
#23576 = CARTESIAN_POINT ( 'NONE',  ( 18.62759615963271287, -10.81492255796078972, 83.33224293864769550 ) ) ;
#23577 = CARTESIAN_POINT ( 'NONE',  ( -4.379528057220328563, 16.55341960407611168, 35.20724293864768839 ) ) ;
#23578 = ORIENTED_EDGE ( 'NONE', *, *, #173336, .T. ) ;
#23579 = CARTESIAN_POINT ( 'NONE',  ( 12.14591786802327356, -12.06949235617739191, 80.62609039468567573 ) ) ;
#23580 = CARTESIAN_POINT ( 'NONE',  ( 24.54404792736140095, 12.06373989673628877, 169.8487138613017180 ) ) ;
#23581 = CARTESIAN_POINT ( 'NONE',  ( 21.55341960407610458, 5.719274019375980345, 68.95724293864769550 ) ) ;
#23582 = ORIENTED_EDGE ( 'NONE', *, *, #188483, .T. ) ;
#23583 = CARTESIAN_POINT ( 'NONE',  ( 14.29746914071037800, 8.314922557961029526, 106.6677570613523756 ) ) ;
#23584 = ORIENTED_EDGE ( 'NONE', *, *, #45012, .T. ) ;
#23585 = DIRECTION ( 'NONE',  ( -0.000000000000000000, 0.000000000000000000, 1.000000000000000000 ) ) ;
#23586 = CARTESIAN_POINT ( 'NONE',  ( 10.72451020669898902, -18.67979575497178502, 82.91557627198103830 ) ) ;
#23587 = CARTESIAN_POINT ( 'NONE',  ( 21.53943276465977519, -0.05219959533907433946, 113.7489096053143527 ) ) ;
#23588 = CARTESIAN_POINT ( 'NONE',  ( 16.55341960407611168, 4.379528057220329451, 33.95724293864769550 ) ) ;
#23589 = CARTESIAN_POINT ( 'NONE',  ( 14.34966873604972726, -8.224510206698740333, 30.83442372801902209 ) ) ;
#23590 = CARTESIAN_POINT ( 'NONE',  ( 9.474510206698971260, -16.51473224551069308, 37.91557627198102409 ) ) ;
#23591 = CARTESIAN_POINT ( 'NONE',  ( -13.89961937509977652, 13.97604488694528158, 70.62390960531432427 ) ) ;
#23592 = EDGE_CURVE ( 'NONE', #192734, #116714, #88935, .T. ) ;
#23593 = CARTESIAN_POINT ( 'NONE',  ( 8.571926809382603096, -26.38167802310801235, 139.9750000027311785 ) ) ;
#23594 = CARTESIAN_POINT ( 'NONE',  ( -5.049401038298153566, 19.05341960407611168, 115.2072429386477097 ) ) ;
#23595 = CARTESIAN_POINT ( 'NONE',  ( 1.274273735257150042, 29.60376251271834747, -51.87022419674244844 ) ) ;
#23596 = CARTESIAN_POINT ( 'NONE',  ( -16.46253265017146816, -9.564922557961047289, 104.1677570613523329 ) ) ;
#23597 = CARTESIAN_POINT ( 'NONE',  ( -0.05219959533936034679, 19.03943276465977164, 42.50109039468566152 ) ) ;
#23598 = CARTESIAN_POINT ( 'NONE',  ( -5.823673210054116645, -21.52544592524344225, 92.29057627198103830 ) ) ;
#23599 = CARTESIAN_POINT ( 'NONE',  ( 14.29746914071049879, -8.314922557960816363, 23.33224293864769194 ) ) ;
#23600 = VECTOR ( 'NONE', #193587, 1000.000000000000000 ) ;
#23601 = CARTESIAN_POINT ( 'NONE',  ( -10.72451020669898014, 18.67979575497178502, 40.41557627198103120 ) ) ;
#23603 = CARTESIAN_POINT ( 'NONE',  ( -0.05219959533936034679, 19.03943276465977164, 112.5010903946856757 ) ) ;
#23602 = CARTESIAN_POINT ( 'NONE',  ( 21.52544592524344225, -5.823673210054117533, 88.54057627198103830 ) ) ;
#23604 = CARTESIAN_POINT ( 'NONE',  ( 9.564922557960805705, 16.46253265017160317, 99.58224293864770971 ) ) ;
#23605 = CARTESIAN_POINT ( 'NONE',  ( -5.719274019375665041, -21.55341960407619695, 79.79275706135236135 ) ) ;
#23606 = CARTESIAN_POINT ( 'NONE',  ( -0.05219959533909027116, -19.03943276465977164, 72.49890960531435269 ) ) ;
#23607 = CARTESIAN_POINT ( 'NONE',  ( 12.14591786802309770, 12.06949235617756955, 104.3739096053143669 ) ) ;
#23608 = CARTESIAN_POINT ( 'NONE',  ( 31.64990063023044442, 6.823060802858333496, 91.87658598274001065 ) ) ;
#23609 = CARTESIAN_POINT ( 'NONE',  ( -19.02544592524342804, 5.153800228976336051, 71.04057627198099567 ) ) ;
#23610 = CARTESIAN_POINT ( 'NONE',  ( -12.14591786802309592, -12.06949235617757132, 91.87390960531436690 ) ) ;
#23611 = VERTEX_POINT ( 'NONE', #176579 ) ;
#23612 = CARTESIAN_POINT ( 'NONE',  ( -9.564922557961040184, 16.46253265017147172, 107.9177570613523471 ) ) ;
#23613 = FACE_OUTER_BOUND ( 'NONE', #7153, .T. ) ;
#23614 = CARTESIAN_POINT ( 'NONE',  ( 5.153800228976335163, 19.02544592524342804, 54.79057627198103120 ) ) ;
#23616 = CARTESIAN_POINT ( 'NONE',  ( -0.05219959533909027116, -19.03943276465977164, 102.4989096053143669 ) ) ;
#23615 = CARTESIAN_POINT ( 'NONE',  ( 15.80617190586769283, -15.72974639402175789, 90.62609039468567573 ) ) ;
#23617 = CARTESIAN_POINT ( 'NONE',  ( 14.29746914071037800, 8.314922557961029526, 81.66775706135236135 ) ) ;
#23618 = CARTESIAN_POINT ( 'NONE',  ( -16.62475595723696742, -7.163666690055377373, 74.47286648189532343 ) ) ;
#23619 = CARTESIAN_POINT ( 'NONE',  ( 9.474510206698729675, 16.51473224551082808, 62.08442372801899722 ) ) ;
#23620 = CARTESIAN_POINT ( 'NONE',  ( 0.05219959533937995610, -21.53943276465977519, 105.0010903946856757 ) ) ;
#23621 = CARTESIAN_POINT ( 'NONE',  ( 37.55508611250748174, 1.249935417488353906, 39.64085810587564396 ) ) ;
#23622 = CARTESIAN_POINT ( 'NONE',  ( -4.483927247898539470, -16.52544592524342804, 22.29057627198102765 ) ) ;
#23623 = DIRECTION ( 'NONE',  ( 1.000000000000000000, 0.000000000000000000, 0.000000000000000000 ) ) ;
#23624 = CARTESIAN_POINT ( 'NONE',  ( -16.52544592524335698, -4.483927247898792601, 88.95942372801901854 ) ) ;
#23625 = CARTESIAN_POINT ( 'NONE',  ( 33.56007109372392705, -21.76539027157619088, -24.27853470289443294 ) ) ;
#23626 = CARTESIAN_POINT ( 'NONE',  ( -16.52544592524335698, -4.483927247898792601, 63.95942372801901854 ) ) ;
#23627 = CARTESIAN_POINT ( 'NONE',  ( 18.62759615963255655, 10.81492255796105972, 81.66775706135236135 ) ) ;
#23628 = CARTESIAN_POINT ( 'NONE',  ( 9.564922557961047289, -16.46253265017146816, 95.41775706135233293 ) ) ;
#23629 = CARTESIAN_POINT ( 'NONE',  ( 19.02544592524334988, 5.153800228976608722, 41.45942372801900433 ) ) ;
#23630 = CARTESIAN_POINT ( 'NONE',  ( -16.46253265017160317, 9.564922557960807481, 70.83224293864770971 ) ) ;
#23631 = CARTESIAN_POINT ( 'NONE',  ( -16.46253265017160317, 9.564922557960807481, 60.83224293864769550 ) ) ;
#23632 = CARTESIAN_POINT ( 'NONE',  ( -7.052343178074620411, 2.552343178074692354, 8.889087296526001936 ) ) ;
#23633 = CARTESIAN_POINT ( 'NONE',  ( -0.05219959533907301413, -21.53943276465977519, 77.49890960531433848 ) ) ;
#23634 = CARTESIAN_POINT ( 'NONE',  ( -21.55341960407610458, -5.719274019375992779, 51.45724293864770260 ) ) ;
#23635 = CARTESIAN_POINT ( 'NONE',  ( -0.05219959533909027116, -19.03943276465977164, 32.49890960531435979 ) ) ;
#23636 = CARTESIAN_POINT ( 'NONE',  ( -16.53943276465976808, -0.05219959533934237506, 68.75109039468568994 ) ) ;
#23637 = UNCERTAINTY_MEASURE_WITH_UNIT (LENGTH_MEASURE( 1.000000000000000082E-05 ), #54703, 'distance_accuracy_value', 'NONE');
#23638 = ORIENTED_EDGE ( 'NONE', *, *, #148455, .T. ) ;
#23639 = CARTESIAN_POINT ( 'NONE',  ( -21.52544592524334988, -5.823673210054445271, 48.95942372801902565 ) ) ;
#23641 = CARTESIAN_POINT ( 'NONE',  ( 23.48529157249600630, -32.32473071737749137, -1.299999999999999822 ) ) ;
#23640 = CARTESIAN_POINT ( 'NONE',  ( -16.53943276465976808, 0.05219959533911058130, 66.24890960531436690 ) ) ;
#23642 = CARTESIAN_POINT ( 'NONE',  ( 14.34966873604972726, -8.224510206698740333, 25.83442372801901499 ) ) ;
#23643 = CARTESIAN_POINT ( 'NONE',  ( -0.05219959533936034679, 19.03943276465977164, 57.50109039468566863 ) ) ;
#23644 = CARTESIAN_POINT ( 'NONE',  ( -4.379528057220328563, 16.55341960407611168, 55.20724293864770260 ) ) ;
#23645 = CARTESIAN_POINT ( 'NONE',  ( 5.719274019375673035, 21.55341960407619339, 37.29275706135235424 ) ) ;
#23647 = CARTESIAN_POINT ( 'NONE',  ( -15.80617190586745835, -15.72974639402198527, 71.87390960531438111 ) ) ;
#23646 = CARTESIAN_POINT ( 'NONE',  ( 1.456047670377071501, 15.57251747167111056, -59.63216870564059491 ) ) ;
#23648 = CARTESIAN_POINT ( 'NONE',  ( -0.05219959533909027116, -19.03943276465977164, 102.4989096053143669 ) ) ;
#23649 = CARTESIAN_POINT ( 'NONE',  ( 4.379528057220339221, -16.55341960407611168, 72.70724293864769550 ) ) ;
#23650 = CARTESIAN_POINT ( 'NONE',  ( 5.153800228976335163, 19.02544592524342804, 114.7905762719810241 ) ) ;
#23651 = CARTESIAN_POINT ( 'NONE',  ( 17.97214573761829470, 5.500000000000074607, 43.96970049038656470 ) ) ;
#23652 = CARTESIAN_POINT ( 'NONE',  ( -19.05341960407617563, 5.049401038297882671, 73.54275706135233293 ) ) ;
#23653 = CARTESIAN_POINT ( 'NONE',  ( 15.80617190586769283, -15.72974639402175789, 25.62609039468567929 ) ) ;
#23654 = CARTESIAN_POINT ( 'NONE',  ( -13.89961937509977652, 13.97604488694528158, 55.62390960531434558 ) ) ;
#23655 = CARTESIAN_POINT ( 'NONE',  ( -19.03943276465977164, -0.05219959533935918106, 43.75109039468566863 ) ) ;
#23656 = CARTESIAN_POINT ( 'NONE',  ( -19.05341960407611168, -5.049401038298163336, 26.45724293864769550 ) ) ;
#23657 = AXIS2_PLACEMENT_3D ( 'NONE', #65046, #189403, #80209 ) ;
#23658 = CARTESIAN_POINT ( 'NONE',  ( -10.72451020669870658, -18.67979575497194134, 69.58442372801900433 ) ) ;
#23659 = CARTESIAN_POINT ( 'NONE',  ( 18.22780087662114212, -5.499999999999987566, 41.01540105326107977 ) ) ;
#23660 = CARTESIAN_POINT ( 'NONE',  ( -4.483927247898539470, -16.52544592524342804, 42.29057627198103120 ) ) ;
#23661 = CARTESIAN_POINT ( 'NONE',  ( 9.474510206698971260, -16.51473224551069308, 57.91557627198103120 ) ) ;
#23662 = CARTESIAN_POINT ( 'NONE',  ( -5.823673210054116645, -21.52544592524344225, 92.29057627198103830 ) ) ;
#23663 = CARTESIAN_POINT ( 'NONE',  ( 9.564922557960805705, 16.46253265017160317, 64.58224293864769550 ) ) ;
#23664 = ORIENTED_EDGE ( 'NONE', *, *, #67401, .F. ) ;
#23665 = CARTESIAN_POINT ( 'NONE',  ( 18.67979575497178502, 10.72451020669898547, 64.16557627198102409 ) ) ;
#23666 = ORIENTED_EDGE ( 'NONE', *, *, #45131, .T. ) ;
#23667 = CARTESIAN_POINT ( 'NONE',  ( 18.67979575497194134, -10.72451020669871369, 105.8344237280190328 ) ) ;
#23670 = CARTESIAN_POINT ( 'NONE',  ( -16.52544592524342804, 4.483927247898546575, 86.04057627198102409 ) ) ;
#23669 = CARTESIAN_POINT ( 'NONE',  ( -0.05219959533934338120, 16.53943276465976808, 92.50109039468567573 ) ) ;
#23668 = DIRECTION ( 'NONE',  ( 0.000000000000000000, 0.000000000000000000, -1.000000000000000000 ) ) ;
#23671 = CARTESIAN_POINT ( 'NONE',  ( 5.049401038297881783, 19.05341960407617563, 97.29275706135233293 ) ) ;
#23672 = ORIENTED_EDGE ( 'NONE', *, *, #141950, .F. ) ;
#23673 = CARTESIAN_POINT ( 'NONE',  ( 18.67979575497178502, 10.72451020669898547, 114.1655762719810383 ) ) ;
#23674 = CARTESIAN_POINT ( 'NONE',  ( -5.049401038297874678, -19.05341960407617918, 34.79275706135233293 ) ) ;
#23675 = CARTESIAN_POINT ( 'NONE',  ( -4.483927247898782831, 16.52544592524335698, 97.70942372801904696 ) ) ;
#23676 = CARTESIAN_POINT ( 'NONE',  ( -19.02544592524334988, -5.153800228976617603, 23.95942372801900078 ) ) ;
#23677 = CARTESIAN_POINT ( 'NONE',  ( -9.474510206698964154, 16.51473224551069663, 95.41557627198102409 ) ) ;
#23678 = CARTESIAN_POINT ( 'NONE',  ( -21.53943276465977519, 0.05219959533907696930, 61.24890960531435979 ) ) ;
#23679 = DIRECTION ( 'NONE',  ( -0.3041824702427711191, -0.9526137857479313187, 0.000000000000000000 ) ) ;
#23680 = CARTESIAN_POINT ( 'NONE',  ( 19.02544592524343514, -5.153800228976328945, 23.54057627198102054 ) ) ;
#23681 = CARTESIAN_POINT ( 'NONE',  ( 0.05219959533937995610, -21.53943276465977519, 110.0010903946856757 ) ) ;
#23682 = CARTESIAN_POINT ( 'NONE',  ( 14.29746914071037800, 8.314922557961029526, 76.66775706135234714 ) ) ;
#23683 = CARTESIAN_POINT ( 'NONE',  ( -15.72974639402176322, -15.80617190586768395, 29.37609039468568284 ) ) ;
#23684 = CARTESIAN_POINT ( 'NONE',  ( -0.05219959533934338120, 16.53943276465976808, 27.50109039468567929 ) ) ;
#23685 = CARTESIAN_POINT ( 'NONE',  ( -19.03943276465977164, 0.05219959533909376836, 101.2489096053143669 ) ) ;
#23686 = CARTESIAN_POINT ( 'NONE',  ( -19.03943276465977164, 0.05219959533909376836, 36.24890960531436690 ) ) ;
#23687 = CARTESIAN_POINT ( 'NONE',  ( 0.05219959533909260263, 19.03943276465977164, 64.99890960531436690 ) ) ;
#23688 = CARTESIAN_POINT ( 'NONE',  ( 14.29746914071037800, 8.314922557961029526, 51.66775706135234714 ) ) ;
#23689 = CARTESIAN_POINT ( 'NONE',  ( -16.52544592524342804, 4.483927247898546575, 86.04057627198102409 ) ) ;
#23690 = CARTESIAN_POINT ( 'NONE',  ( 0.05219959533934541429, -16.53943276465976808, 100.0010903946857042 ) ) ;
#23693 = CARTESIAN_POINT ( 'NONE',  ( 19.03943276465977164, -0.05219959533909143690, 68.74890960531436690 ) ) ;
#23692 = CARTESIAN_POINT ( 'NONE',  ( 13.89961937509977652, -13.97604488694527269, 73.12390960531436690 ) ) ;
#23691 = CARTESIAN_POINT ( 'NONE',  ( -18.62759615963255300, -10.81492255796106328, 49.16775706135234003 ) ) ;
#23694 = CARTESIAN_POINT ( 'NONE',  ( 13.97604488694527802, 13.89961937509977652, 94.37390960531436690 ) ) ;
#23695 = CARTESIAN_POINT ( 'NONE',  ( 8.224510206698953496, -14.34966873604960469, 32.91557627198102409 ) ) ;
#23696 = CARTESIAN_POINT ( 'NONE',  ( -4.483927247898782831, 16.52544592524335698, 97.70942372801904696 ) ) ;
#23697 = ORIENTED_EDGE ( 'NONE', *, *, #45727, .T. ) ;
#23698 = CARTESIAN_POINT ( 'NONE',  ( 16.46253265017146816, 9.564922557961045513, 46.66775706135233293 ) ) ;
#23699 = CARTESIAN_POINT ( 'NONE',  ( 0.05219959533909260263, 19.03943276465977164, 114.9989096053143669 ) ) ;
#23700 = CARTESIAN_POINT ( 'NONE',  ( -19.02544592524342804, 5.153800228976336051, 61.04057627198103120 ) ) ;
#23701 = CARTESIAN_POINT ( 'NONE',  ( 5.049401038297881783, 19.05341960407617563, 42.29275706135234003 ) ) ;
#23702 = CARTESIAN_POINT ( 'NONE',  ( 29.86685920354754842, -21.69954338932559068, -9.824999997268813345 ) ) ;
#23703 = CARTESIAN_POINT ( 'NONE',  ( 19.35633801406911303, -5.499999999999579892, 71.63373818172765084 ) ) ;
#23704 = CARTESIAN_POINT ( 'NONE',  ( 12.14591786802327356, -12.06949235617739191, 60.62609039468567573 ) ) ;
#23706 = CARTESIAN_POINT ( 'NONE',  ( -4.379528057220086978, -16.55341960407618274, 64.79275706135234714 ) ) ;
#23705 = CARTESIAN_POINT ( 'NONE',  ( 16.51473224551083163, -9.474510206698727899, 70.83442372801900433 ) ) ;
#23707 = CARTESIAN_POINT ( 'NONE',  ( 4.419688410474993390, -4.207014320000904917, -64.53213882399992940 ) ) ;
#23708 =( BOUNDED_CURVE ( )  B_SPLINE_CURVE ( 2, ( #89808, #149491, #85813, #101988, #150502, #87805, #11999, #73662, #7967, #147499, #163669, #72660, #135334 ),
 .UNSPECIFIED., .F., .T. ) 
 B_SPLINE_CURVE_WITH_KNOTS ( ( 3, 2, 2, 2, 2, 2, 3 ),
 ( 0.7392725416902030666, 0.7412280701754385692, 0.7456140350877192846, 0.7500000000000000000, 0.7543859649122807154, 0.7587719298245614308, 0.7606817784877069055 ),
 .UNSPECIFIED. ) 
 CURVE ( )  GEOMETRIC_REPRESENTATION_ITEM ( )  RATIONAL_B_SPLINE_CURVE ( ( 0.9831626618144007068, 0.9848076720550096308, 1.000000000000000000, 0.9659258262890683122, 1.000000000000000000, 0.9659258262890683122, 1.000000000000000000, 0.9659258262890683122, 1.000000000000000000, 0.9659258262890683122, 1.000000000000000000, 0.9851625545550091179, 0.9832469066685282089 ) ) 
 REPRESENTATION_ITEM ( '' )  );
#23709 = CARTESIAN_POINT ( 'NONE',  ( 5.049401038298161559, -19.05341960407611168, 87.70724293864769550 ) ) ;
#23710 = CARTESIAN_POINT ( 'NONE',  ( -21.53943276465977519, 0.05219959533907696930, 116.2489096053143669 ) ) ;
#23711 = CARTESIAN_POINT ( 'NONE',  ( 19.02544592524334988, 5.153800228976608722, 81.45942372801897591 ) ) ;
#23713 = CARTESIAN_POINT ( 'NONE',  ( -19.05341960407611168, -5.049401038298163336, 31.45724293864769550 ) ) ;
#23712 = CARTESIAN_POINT ( 'NONE',  ( 19.03943276465977164, -0.05219959533909143690, 108.7489096053143527 ) ) ;
#23714 = CARTESIAN_POINT ( 'NONE',  ( -9.474510206698964154, 16.51473224551069663, 75.41557627198103830 ) ) ;
#23716 = CARTESIAN_POINT ( 'NONE',  ( 0.05219959533909260263, 19.03943276465977164, 34.99890960531435979 ) ) ;
#23715 = CARTESIAN_POINT ( 'NONE',  ( -4.483927247898539470, -16.52544592524342804, 42.29057627198103120 ) ) ;
#23717 = CARTESIAN_POINT ( 'NONE',  ( 13.89961937509957401, 13.97604488694547697, 51.87609039468566863 ) ) ;
#23718 = CARTESIAN_POINT ( 'NONE',  ( -16.53943276465976808, 0.05219959533911058130, 81.24890960531436690 ) ) ;
#23719 = CARTESIAN_POINT ( 'NONE',  ( -21.52544592524334988, -5.823673210054445271, 108.9594237280190185 ) ) ;
#23720 = CARTESIAN_POINT ( 'NONE',  ( 16.51473224551069308, 9.474510206698969483, 59.16557627198102409 ) ) ;
#23721 = CARTESIAN_POINT ( 'NONE',  ( -15.72974639402197994, 15.80617190586746368, 55.62390960531436690 ) ) ;
#23723 = CARTESIAN_POINT ( 'NONE',  ( 19.02544592524334988, 5.153800228976608722, 21.45942372801899012 ) ) ;
#23722 = CARTESIAN_POINT ( 'NONE',  ( 8.224510206698953496, -14.34966873604960469, 47.91557627198102409 ) ) ;
#23724 = CARTESIAN_POINT ( 'NONE',  ( -9.474510206698964154, 16.51473224551069663, 110.4155762719810383 ) ) ;
#23725 = CARTESIAN_POINT ( 'NONE',  ( 19.03943276465977164, -0.05219959533909143690, 103.7489096053143669 ) ) ;
#23726 = CARTESIAN_POINT ( 'NONE',  ( -19.03943276465977164, 0.05219959533909376836, 36.24890960531436690 ) ) ;
#23727 = CARTESIAN_POINT ( 'NONE',  ( 13.89961937509977652, -13.97604488694527269, 23.12390960531436335 ) ) ;
#23728 = CARTESIAN_POINT ( 'NONE',  ( -4.379528057220328563, 16.55341960407611168, 85.20724293864770971 ) ) ;
#23729 = CARTESIAN_POINT ( 'NONE',  ( -18.67979575497178146, -10.72451020669898902, 101.6655762719810383 ) ) ;
#23730 = CARTESIAN_POINT ( 'NONE',  ( -0.05219959533909027116, -19.03943276465977164, 107.4989096053143527 ) ) ;
#23731 = CARTESIAN_POINT ( 'NONE',  ( 21.53943276465977519, -0.05219959533907433946, 113.7489096053143527 ) ) ;
#23732 = CARTESIAN_POINT ( 'NONE',  ( -16.46253265017160317, 9.564922557960807481, 100.8322429386477097 ) ) ;
#23734 = CARTESIAN_POINT ( 'NONE',  ( 16.53943276465976808, -0.05219959533910856209, 108.7489096053143669 ) ) ;
#23733 = CARTESIAN_POINT ( 'NONE',  ( 69.65682714487590488, -71.74905178543389184, -15.00000000000000178 ) ) ;
#23735 = CARTESIAN_POINT ( 'NONE',  ( -0.05219959533937732626, 21.53943276465977519, 77.50109039468567573 ) ) ;
#23736 = CARTESIAN_POINT ( 'NONE',  ( 15.80617190586746368, 15.72974639402197994, 84.37390960531438111 ) ) ;
#23737 = CARTESIAN_POINT ( 'NONE',  ( 17.13100169013301510, -6.664070546373136672, 108.2678983569985434 ) ) ;
#23738 = CARTESIAN_POINT ( 'NONE',  ( 19.52217212775661892, -5.499999999999912070, 77.43993709005262360 ) ) ;
#23740 = CARTESIAN_POINT ( 'NONE',  ( 3.660253528765689435, 6.551653823223101192, 1.589185716900141543 ) ) ;
#23739 = CARTESIAN_POINT ( 'NONE',  ( 5.823673210054125526, 21.52544592524343514, 34.79057627198103120 ) ) ;
#23741 = CARTESIAN_POINT ( 'NONE',  ( -0.05219959533934338120, 16.53943276465976808, 27.50109039468567929 ) ) ;
#23742 = CARTESIAN_POINT ( 'NONE',  ( -8.314922557960811034, -14.29746914071050412, 112.0822429386477097 ) ) ;
#23743 = CARTESIAN_POINT ( 'NONE',  ( -17.50000000000000711, -3.305555262949610107, 110.3748284784340399 ) ) ;
#23744 = CARTESIAN_POINT ( 'NONE',  ( 13.97604488694527802, 13.89961937509977652, 54.37390960531435979 ) ) ;
#23745 = CARTESIAN_POINT ( 'NONE',  ( 4.483927247898545687, 16.52544592524342804, 84.79057627198102409 ) ) ;
#23746 = CIRCLE ( 'NONE', #39898, 0.5000000000000004441 ) ;
#23747 = CARTESIAN_POINT ( 'NONE',  ( -21.53943276465977519, 0.05219959533907696930, 31.24890960531435979 ) ) ;
#23748 = CARTESIAN_POINT ( 'NONE',  ( -4.379528057220328563, 16.55341960407611168, 70.20724293864769550 ) ) ;
#23749 = CARTESIAN_POINT ( 'NONE',  ( -4.379528057220086978, -16.55341960407618274, 19.79275706135235069 ) ) ;
#23750 = CARTESIAN_POINT ( 'NONE',  ( -21.52544592524334988, -5.823673210054445271, 73.95942372801901854 ) ) ;
#23751 = CARTESIAN_POINT ( 'NONE',  ( 16.61371651742601685, -7.165104196376138823, 76.35415069992995996 ) ) ;
#23752 = CARTESIAN_POINT ( 'NONE',  ( -21.53943276465977519, 0.05219959533907696930, 21.24890960531436690 ) ) ;
#23753 = CARTESIAN_POINT ( 'NONE',  ( -12.06949235617739369, -12.14591786802326823, 89.37609039468568994 ) ) ;
#23754 = CARTESIAN_POINT ( 'NONE',  ( 9.474510206698971260, -16.51473224551069308, 37.91557627198102409 ) ) ;
#23755 = CARTESIAN_POINT ( 'NONE',  ( -5.049401038298153566, 19.05341960407611168, 90.20724293864766707 ) ) ;
#23756 = CARTESIAN_POINT ( 'NONE',  ( -21.52544592524343514, 5.823673210054127303, 91.04057627198103830 ) ) ;
#23757 = CARTESIAN_POINT ( 'NONE',  ( -4.483927247898782831, 16.52544592524335698, 32.70942372801900433 ) ) ;
#23759 = CARTESIAN_POINT ( 'NONE',  ( -5.823673210054431948, 21.52544592524334988, 77.70942372801900433 ) ) ;
#23758 = CARTESIAN_POINT ( 'NONE',  ( -12.06949235617756955, 12.14591786802309770, 55.62390960531436690 ) ) ;
#23760 = EDGE_CURVE ( 'NONE', #121632, #74887, #117230, .T. ) ;
#23761 = CARTESIAN_POINT ( 'NONE',  ( 4.483927247898790824, -16.52544592524335698, 95.20942372801903275 ) ) ;
#23762 = CARTESIAN_POINT ( 'NONE',  ( 24.37439536253439343, 13.84063584238319322, 165.9041067986157998 ) ) ;
#23763 = FACE_OUTER_BOUND ( 'NONE', #185221, .T. ) ;
#23764 = CARTESIAN_POINT ( 'NONE',  ( -0.05219959533910754901, -16.53943276465976808, 22.49890960531436335 ) ) ;
#23765 = CARTESIAN_POINT ( 'NONE',  ( 12.14591786802327356, -12.06949235617739191, 60.62609039468567573 ) ) ;
#23766 = CARTESIAN_POINT ( 'NONE',  ( 19.02544592524343514, -5.153800228976328945, 68.54057627198103830 ) ) ;
#23767 = CARTESIAN_POINT ( 'NONE',  ( 0.05219959533909260263, 19.03943276465977164, 89.99890960531436690 ) ) ;
#23768 = CARTESIAN_POINT ( 'NONE',  ( 21.52544592524334988, 5.823673210054432836, 71.45942372801901854 ) ) ;
#23769 = CARTESIAN_POINT ( 'NONE',  ( 16.52544592524335698, 4.483927247898782831, 91.45942372801901854 ) ) ;
#23770 = CARTESIAN_POINT ( 'NONE',  ( 16.53943276465976808, -0.05219959533910856209, 53.74890960531437401 ) ) ;
#23771 = CARTESIAN_POINT ( 'NONE',  ( 19.03943276465977164, -0.05219959533909143690, 68.74890960531436690 ) ) ;
#23772 = ORIENTED_EDGE ( 'NONE', *, *, #8686, .T. ) ;
#23773 = CARTESIAN_POINT ( 'NONE',  ( -13.97604488694547697, 13.89961937509957934, 108.1260903946856331 ) ) ;
#23774 = CARTESIAN_POINT ( 'NONE',  ( -16.53943276465976808, 0.05219959533911058130, 106.2489096053143811 ) ) ;
#23775 = CARTESIAN_POINT ( 'NONE',  ( -5.049401038298153566, 19.05341960407611168, 80.20724293864769550 ) ) ;
#23777 = CARTESIAN_POINT ( 'NONE',  ( 36.91746824999999177, 2.880721459617395097E-14, -7.624999997268813168 ) ) ;
#23776 = CARTESIAN_POINT ( 'NONE',  ( -0.05219959533936034679, 19.03943276465977164, 107.5010903946856615 ) ) ;
#23778 = CARTESIAN_POINT ( 'NONE',  ( -10.72451020669870658, -18.67979575497194134, 104.5844237280190185 ) ) ;
#23779 = CARTESIAN_POINT ( 'NONE',  ( 8.224510206698742110, 14.34966873604972548, 82.08442372801901854 ) ) ;
#23780 = CARTESIAN_POINT ( 'NONE',  ( -5.153800228976607833, 19.02544592524334988, 92.70942372801901854 ) ) ;
#23781 = CARTESIAN_POINT ( 'NONE',  ( 16.55341960407611168, 4.379528057220329451, 108.9572429386476955 ) ) ;
#23782 = CARTESIAN_POINT ( 'NONE',  ( 12.06949235617739724, 12.14591786802326823, 61.87609039468568284 ) ) ;
#23783 = FACE_OUTER_BOUND ( 'NONE', #28695, .T. ) ;
#23784 = CARTESIAN_POINT ( 'NONE',  ( -16.46253265017146816, -9.564922557961047289, 54.16775706135234003 ) ) ;
#23785 = CARTESIAN_POINT ( 'NONE',  ( -15.80617190586768217, 15.72974639402176855, 98.12609039468570415 ) ) ;
#23786 = CARTESIAN_POINT ( 'NONE',  ( 19.02544592524343514, -5.153800228976328945, 38.54057627198103120 ) ) ;
#23787 = CARTESIAN_POINT ( 'NONE',  ( -13.89961937509977652, 13.97604488694528158, 75.62390960531438111 ) ) ;
#23788 = CARTESIAN_POINT ( 'NONE',  ( 16.55341960407611168, 4.379528057220329451, 73.95724293864769550 ) ) ;
#23789 = CARTESIAN_POINT ( 'NONE',  ( -21.53943276465977519, -0.05219959533937600094, 93.75109039468567573 ) ) ;
#23790 = EDGE_CURVE ( 'NONE', #122541, #40748, #25901, .T. ) ;
#23791 = CARTESIAN_POINT ( 'NONE',  ( 16.51473224551083163, -9.474510206698727899, 45.83442372801900433 ) ) ;
#23792 = CARTESIAN_POINT ( 'NONE',  ( 13.89961937509957401, 13.97604488694547697, 36.87609039468565442 ) ) ;
#23793 = CARTESIAN_POINT ( 'NONE',  ( 18.62759615963271287, -10.81492255796078972, 38.33224293864768839 ) ) ;
#23794 = CARTESIAN_POINT ( 'NONE',  ( 15.72974639402176855, 15.80617190586768217, 91.87609039468568994 ) ) ;
#23795 = CARTESIAN_POINT ( 'NONE',  ( -5.153800228976328057, -19.02544592524343514, 77.29057627198099567 ) ) ;
#23796 = CARTESIAN_POINT ( 'NONE',  ( 10.72451020669871369, 18.67979575497193778, 87.08442372801901854 ) ) ;
#23797 = CARTESIAN_POINT ( 'NONE',  ( 15.80617190586746368, 15.72974639402197994, 54.37390960531435979 ) ) ;
#23798 = CARTESIAN_POINT ( 'NONE',  ( 16.51473224551069308, 9.474510206698969483, 84.16557627198102409 ) ) ;
#23799 = CARTESIAN_POINT ( 'NONE',  ( -19.05341960407617563, 5.049401038297882671, 68.54275706135230450 ) ) ;
#23800 = CARTESIAN_POINT ( 'NONE',  ( 13.97604488694527802, 13.89961937509977652, 84.37390960531433848 ) ) ;
#23801 = CARTESIAN_POINT ( 'NONE',  ( 19.02544592524334988, 5.153800228976608722, 101.4594237280189759 ) ) ;
#23802 = CARTESIAN_POINT ( 'NONE',  ( -14.29746914071037622, -8.314922557961029526, 39.16775706135235424 ) ) ;
#23803 = CARTESIAN_POINT ( 'NONE',  ( -4.483927247898539470, -16.52544592524342804, 97.29057627198105251 ) ) ;
#23804 = CARTESIAN_POINT ( 'NONE',  ( 9.474510206698971260, -16.51473224551069308, 72.91557627198102409 ) ) ;
#23805 = CARTESIAN_POINT ( 'NONE',  ( 18.67979575497178502, 10.72451020669898547, 69.16557627198102409 ) ) ;
#23806 = CARTESIAN_POINT ( 'NONE',  ( -16.52544592524335698, -4.483927247898792601, 33.95942372801901143 ) ) ;
#23807 = CARTESIAN_POINT ( 'NONE',  ( -21.55341960407619339, 5.719274019375674811, 38.54275706135234714 ) ) ;
#23808 = CARTESIAN_POINT ( 'NONE',  ( 15.72974639402176855, 15.80617190586768217, 81.87609039468568994 ) ) ;
#23809 = CARTESIAN_POINT ( 'NONE',  ( 16.55341960407618274, -4.379528057220086978, 86.04275706135236135 ) ) ;
#23810 = AXIS2_PLACEMENT_3D ( 'NONE', #124828, #140985, #171338 ) ;
#23811 = CARTESIAN_POINT ( 'NONE',  ( 19.05341960407611168, 5.049401038298154454, 68.95724293864769550 ) ) ;
#23812 = CARTESIAN_POINT ( 'NONE',  ( -0.05219959533910754901, -16.53943276465976808, 82.49890960531436690 ) ) ;
#23813 = CARTESIAN_POINT ( 'NONE',  ( -12.14591786802326823, 12.06949235617739902, 103.1260903946856757 ) ) ;
#23814 = CARTESIAN_POINT ( 'NONE',  ( 5.153800228976615827, -19.02544592524334988, 50.20942372801897591 ) ) ;
#23815 = CARTESIAN_POINT ( 'NONE',  ( 10.72451020669871369, 18.67979575497193778, 32.08442372801901854 ) ) ;
#23816 = CARTESIAN_POINT ( 'NONE',  ( -14.29746914071049879, 8.314922557960819915, 75.83224293864769550 ) ) ;
#23817 = CARTESIAN_POINT ( 'NONE',  ( 16.46253265017160672, -9.564922557960803928, 103.3322429386476955 ) ) ;
#23818 = CARTESIAN_POINT ( 'NONE',  ( 16.53943276465976808, 0.05219959533934440121, 106.2510903946856757 ) ) ;
#23819 = CARTESIAN_POINT ( 'NONE',  ( -18.62759615963255300, -10.81492255796106328, 69.16775706135234714 ) ) ;
#23820 = CARTESIAN_POINT ( 'NONE',  ( 16.55341960407618274, -4.379528057220086978, 51.04275706135234714 ) ) ;
#23821 = CARTESIAN_POINT ( 'NONE',  ( -10.72451020669870658, -18.67979575497194134, 39.58442372801901143 ) ) ;
#23822 = CARTESIAN_POINT ( 'NONE',  ( 16.52544592524342804, -4.483927247898539470, 73.54057627198102409 ) ) ;
#23823 = ORIENTED_EDGE ( 'NONE', *, *, #61085, .F. ) ;
#23824 = CARTESIAN_POINT ( 'NONE',  ( 21.53943276465977519, 0.05219959533937863772, 21.25109039468567218 ) ) ;
#23825 = DIRECTION ( 'NONE',  ( 0.000000000000000000, 0.000000000000000000, -1.000000000000000000 ) ) ;
#23826 = CARTESIAN_POINT ( 'NONE',  ( -16.55341960407611168, -4.379528057220339221, 51.45724293864770260 ) ) ;
#23827 = DIRECTION ( 'NONE',  ( -1.000000000000000000, -0.000000000000000000, -0.000000000000000000 ) ) ;
#23828 = CARTESIAN_POINT ( 'NONE',  ( -21.52544592524343514, 5.823673210054127303, 41.04057627198103120 ) ) ;
#23829 = CARTESIAN_POINT ( 'NONE',  ( 0.05219959533910956823, 16.53943276465976808, 79.99890960531435269 ) ) ;
#23830 = CARTESIAN_POINT ( 'NONE',  ( -5.719274019375978568, 21.55341960407610458, 80.20724293864769550 ) ) ;
#23831 = CARTESIAN_POINT ( 'NONE',  ( 19.02544592524343514, -5.153800228976328945, 93.54057627198102409 ) ) ;
#23833 = CARTESIAN_POINT ( 'NONE',  ( -0.05219959533936034679, 19.03943276465977164, 77.50109039468566152 ) ) ;
#23832 = CARTESIAN_POINT ( 'NONE',  ( 0.05219959533909260263, 19.03943276465977164, 34.99890960531435979 ) ) ;
#23834 = EDGE_CURVE ( 'NONE', #41521, #36107, #20363, .T. ) ;
#23836 = CARTESIAN_POINT ( 'NONE',  ( -21.53943276465977519, 0.05219959533907696930, 66.24890960531436690 ) ) ;
#23835 = CARTESIAN_POINT ( 'NONE',  ( 15.80617190586769283, -15.72974639402175789, 55.62609039468568284 ) ) ;
#23837 = CARTESIAN_POINT ( 'NONE',  ( 19.05341960407611168, 5.049401038298154454, 33.95724293864769550 ) ) ;
#23838 = CARTESIAN_POINT ( 'NONE',  ( 0.05219959533909260263, 19.03943276465977164, 69.99890960531435269 ) ) ;
#23839 = ORIENTED_EDGE ( 'NONE', *, *, #16988, .T. ) ;
#23840 = CARTESIAN_POINT ( 'NONE',  ( 16.53943276465976808, 0.05219959533934440121, 56.25109039468568284 ) ) ;
#23841 = CARTESIAN_POINT ( 'NONE',  ( -5.719274019375665041, -21.55341960407619695, 29.79275706135234358 ) ) ;
#23842 = CARTESIAN_POINT ( 'NONE',  ( 5.719274019375673035, 21.55341960407619339, 62.29275706135236845 ) ) ;
#23843 = CARTESIAN_POINT ( 'NONE',  ( -5.153800228976328057, -19.02544592524343514, 107.2905762719810383 ) ) ;
#23844 = CARTESIAN_POINT ( 'NONE',  ( 0.05219959533907565091, 21.53943276465977519, 79.99890960531435269 ) ) ;
#23846 = CARTESIAN_POINT ( 'NONE',  ( 16.53943276465976808, 0.05219959533934440121, 46.25109039468567573 ) ) ;
#23845 = CARTESIAN_POINT ( 'NONE',  ( 21.52544592524334988, 5.823673210054432836, 26.45942372801901854 ) ) ;
#23847 = CARTESIAN_POINT ( 'NONE',  ( -18.67979575497178146, -10.72451020669898902, 51.66557627198102409 ) ) ;
#23848 = CARTESIAN_POINT ( 'NONE',  ( -21.52544592524334988, -5.823673210054445271, 108.9594237280190185 ) ) ;
#23849 = CARTESIAN_POINT ( 'NONE',  ( -19.03943276465977164, 0.05219959533909376836, 56.24890960531435979 ) ) ;
#23850 = DIRECTION ( 'NONE',  ( -1.000000000000000000, 0.000000000000000000, 0.000000000000000000 ) ) ;
#23851 = CARTESIAN_POINT ( 'NONE',  ( 9.564922557960805705, 16.46253265017160317, 89.58224293864769550 ) ) ;
#23852 = DIRECTION ( 'NONE',  ( -0.000000000000000000, 0.7071067811865466846, -0.7071067811865484609 ) ) ;
#23853 = CARTESIAN_POINT ( 'NONE',  ( -19.02544592524334988, -5.153800228976617603, 73.95942372801900433 ) ) ;
#23854 = CARTESIAN_POINT ( 'NONE',  ( -0.05219959533907301413, -21.53943276465977519, 42.49890960531435979 ) ) ;
#23855 = CARTESIAN_POINT ( 'NONE',  ( -14.34966873604960291, -8.224510206698953496, 21.66557627198102409 ) ) ;
#23856 = CARTESIAN_POINT ( 'NONE',  ( -0.05219959533936034679, 19.03943276465977164, 97.50109039468567573 ) ) ;
#23857 = CARTESIAN_POINT ( 'NONE',  ( -9.248023074035629065, -10.74802307403544077, -62.40259441833023857 ) ) ;
#23858 = CARTESIAN_POINT ( 'NONE',  ( 13.89961937509957401, 13.97604488694547697, 26.87609039468566507 ) ) ;
#23859 = CARTESIAN_POINT ( 'NONE',  ( 0.05219959533936267826, -19.03943276465977164, 100.0010903946856757 ) ) ;
#23860 = CARTESIAN_POINT ( 'NONE',  ( -0.05219959533936034679, 19.03943276465977164, 42.50109039468566152 ) ) ;
#23861 = CARTESIAN_POINT ( 'NONE',  ( 16.19135201231367915, 7.376712067591916444, 107.6868085405203743 ) ) ;
#23862 = CARTESIAN_POINT ( 'NONE',  ( -5.049401038298153566, 19.05341960407611168, 55.20724293864769550 ) ) ;
#23863 = CARTESIAN_POINT ( 'NONE',  ( 8.314922557960818139, 14.29746914071049879, 59.58224293864770260 ) ) ;
#23864 = CARTESIAN_POINT ( 'NONE',  ( -9.564922557960796823, -16.46253265017161027, 32.08224293864769550 ) ) ;
#23865 = CARTESIAN_POINT ( 'NONE',  ( -12.06949235617756955, 12.14591786802309770, 45.62390960531436690 ) ) ;
#23866 = CARTESIAN_POINT ( 'NONE',  ( -2.577820198429831642E-15, -9.100000000000001421, -64.92279855667830191 ) ) ;
#23867 = CARTESIAN_POINT ( 'NONE',  ( -12.06949235617739369, -12.14591786802326823, 104.3760903946856899 ) ) ;
#23868 = CARTESIAN_POINT ( 'NONE',  ( -5.153800228976328057, -19.02544592524343514, 62.29057627198100988 ) ) ;
#23869 = CARTESIAN_POINT ( 'NONE',  ( 13.97604488694548053, -13.89961937509957401, 20.62609039468567573 ) ) ;
#23870 = CARTESIAN_POINT ( 'NONE',  ( -14.34966873604972548, 8.224510206698743886, 28.33442372801902209 ) ) ;
#23871 = CARTESIAN_POINT ( 'NONE',  ( -5.719274019375978568, 21.55341960407610458, 50.20724293864769550 ) ) ;
#23873 = ORIENTED_EDGE ( 'NONE', *, *, #59341, .F. ) ;
#23872 = CARTESIAN_POINT ( 'NONE',  ( 21.55341960407619695, -5.719274019375665929, 111.0427570613523613 ) ) ;
#23874 = CARTESIAN_POINT ( 'NONE',  ( 9.564922557960805705, 16.46253265017160317, 59.58224293864769550 ) ) ;
#23875 = CARTESIAN_POINT ( 'NONE',  ( 5.049401038298161559, -19.05341960407611168, 107.7072429386476955 ) ) ;
#23876 = CARTESIAN_POINT ( 'NONE',  ( 0.05219959533909260263, 19.03943276465977164, 94.99890960531436690 ) ) ;
#23877 = CARTESIAN_POINT ( 'NONE',  ( 22.81625015709509441, 31.40387420917330275, -3.324999997268812901 ) ) ;
#23878 = CARTESIAN_POINT ( 'NONE',  ( -21.53943276465977519, -0.05219959533937600094, 28.75109039468567929 ) ) ;
#23879 = CARTESIAN_POINT ( 'NONE',  ( -12.06949235617756955, 12.14591786802309770, 90.62390960531436690 ) ) ;
#23881 = CARTESIAN_POINT ( 'NONE',  ( 5.049401038298161559, -19.05341960407611168, 62.70724293864769550 ) ) ;
#23880 = CARTESIAN_POINT ( 'NONE',  ( 21.53943276465977519, -0.05219959533907433946, 83.74890960531435269 ) ) ;
#23882 = CARTESIAN_POINT ( 'NONE',  ( -9.564922557960796823, -16.46253265017161027, 72.08224293864770971 ) ) ;
#23883 = CARTESIAN_POINT ( 'NONE',  ( -15.72974639402197994, 15.80617190586746368, 110.6239096053143669 ) ) ;
#23884 = VERTEX_POINT ( 'NONE', #147228 ) ;
#23885 = CARTESIAN_POINT ( 'NONE',  ( 9.474510206698971260, -16.51473224551069308, 77.91557627198103830 ) ) ;
#23886 = AXIS2_PLACEMENT_3D ( 'NONE', #181840, #166675, #55488 ) ;
#23887 = CARTESIAN_POINT ( 'NONE',  ( 30.00000000000000000, -5.499999999999992895, 102.5000000000000142 ) ) ;
#23889 = CARTESIAN_POINT ( 'NONE',  ( 0.05219959533909260263, 19.03943276465977164, 24.99890960531435269 ) ) ;
#23888 = CARTESIAN_POINT ( 'NONE',  ( -4.379528057220328563, 16.55341960407611168, 100.2072429386476955 ) ) ;
#23890 = CARTESIAN_POINT ( 'NONE',  ( 13.89961937509957401, 13.97604488694547697, 96.87609039468566152 ) ) ;
#23891 = CARTESIAN_POINT ( 'NONE',  ( -4.483927247898539470, -16.52544592524342804, 102.2905762719810383 ) ) ;
#23892 = CARTESIAN_POINT ( 'NONE',  ( 21.53943276465977519, 0.05219959533937863772, 76.25109039468568994 ) ) ;
#23894 = CARTESIAN_POINT ( 'NONE',  ( -10.81492255796105439, 18.62759615963255655, 27.91775706135234358 ) ) ;
#23893 = CARTESIAN_POINT ( 'NONE',  ( -19.05341960407611168, -5.049401038298163336, 66.45724293864769550 ) ) ;
#23895 = CARTESIAN_POINT ( 'NONE',  ( 18.67979575497178502, 10.72451020669898547, 109.1655762719810383 ) ) ;
#23896 = CARTESIAN_POINT ( 'NONE',  ( -23.31738231874055600, 16.94106989632528837, 141.7999999999999829 ) ) ;
#23897 = CARTESIAN_POINT ( 'NONE',  ( -13.89961937509977652, 13.97604488694528158, 70.62390960531432427 ) ) ;
#23898 = DIRECTION ( 'NONE',  ( -1.000000000000000000, 0.000000000000000000, -0.000000000000000000 ) ) ;
#23900 = CARTESIAN_POINT ( 'NONE',  ( 21.55341960407610458, 5.719274019375980345, 23.95724293864769550 ) ) ;
#23899 = CARTESIAN_POINT ( 'NONE',  ( -14.29746914071037622, -8.314922557961029526, 19.16775706135234714 ) ) ;
#23901 = CARTESIAN_POINT ( 'NONE',  ( 15.80617190586769283, -15.72974639402175789, 60.62609039468567573 ) ) ;
#23902 = CARTESIAN_POINT ( 'NONE',  ( -9.564922557960796823, -16.46253265017161027, 102.0822429386477097 ) ) ;
#23903 = CARTESIAN_POINT ( 'NONE',  ( 0.05219959533936267826, -19.03943276465977164, 80.00109039468567573 ) ) ;
#23904 = CARTESIAN_POINT ( 'NONE',  ( -5.049401038298153566, 19.05341960407611168, 50.20724293864770260 ) ) ;
#23905 = CARTESIAN_POINT ( 'NONE',  ( 5.049401038298161559, -19.05341960407611168, 67.70724293864769550 ) ) ;
#23906 = CARTESIAN_POINT ( 'NONE',  ( 12.06949235617757843, -12.14591786802309237, 93.12390960531436690 ) ) ;
#23907 = CARTESIAN_POINT ( 'NONE',  ( 13.89961937509977652, -13.97604488694527269, 103.1239096053143527 ) ) ;
#23908 = CARTESIAN_POINT ( 'NONE',  ( -8.314922557960811034, -14.29746914071050412, 97.08224293864770971 ) ) ;
#23909 = CARTESIAN_POINT ( 'NONE',  ( -0.05219959533909027116, -19.03943276465977164, 97.49890960531436690 ) ) ;
#23911 = CARTESIAN_POINT ( 'NONE',  ( 19.03943276465977164, -0.05219959533909143690, 33.74890960531435979 ) ) ;
#23910 = CARTESIAN_POINT ( 'NONE',  ( 4.483927247898545687, 16.52544592524342804, 39.79057627198103830 ) ) ;
#23912 = ORIENTED_EDGE ( 'NONE', *, *, #106542, .F. ) ;
#23913 = CARTESIAN_POINT ( 'NONE',  ( -10.81492255796105439, 18.62759615963255655, 62.91775706135236135 ) ) ;
#23914 = CARTESIAN_POINT ( 'NONE',  ( 5.153800228976615827, -19.02544592524334988, 75.20942372801896170 ) ) ;
#23915 = CARTESIAN_POINT ( 'NONE',  ( -8.224510206698948167, 14.34966873604960824, 45.41557627198103830 ) ) ;
#23916 = CARTESIAN_POINT ( 'NONE',  ( -15.72974639402197994, 15.80617190586746368, 95.62390960531436690 ) ) ;
#23917 = CARTESIAN_POINT ( 'NONE',  ( 15.72974639402199770, -15.80617190586745480, 38.12390960531436690 ) ) ;
#23918 = CARTESIAN_POINT ( 'NONE',  ( -0.05219959533910754901, -16.53943276465976808, 77.49890960531433848 ) ) ;
#23919 = CARTESIAN_POINT ( 'NONE',  ( 5.153800228976335163, 19.02544592524342804, 54.79057627198103120 ) ) ;
#23920 = CARTESIAN_POINT ( 'NONE',  ( -4.379528057220328563, 16.55341960407611168, 25.20724293864769550 ) ) ;
#23921 = CARTESIAN_POINT ( 'NONE',  ( -16.55341960407617563, 4.379528057220093196, 103.5427570613523613 ) ) ;
#23922 = CARTESIAN_POINT ( 'NONE',  ( -4.379528057220086978, -16.55341960407618274, 74.79275706135234714 ) ) ;
#23923 = CARTESIAN_POINT ( 'NONE',  ( 19.03943276465977164, 0.05219959533936151252, 31.25109039468566863 ) ) ;
#23924 = CARTESIAN_POINT ( 'NONE',  ( -19.05341960407611168, -5.049401038298163336, 111.4572429386476671 ) ) ;
#23925 = CARTESIAN_POINT ( 'NONE',  ( 9.564922557960805705, 16.46253265017160317, 84.58224293864769550 ) ) ;
#23926 = CARTESIAN_POINT ( 'NONE',  ( -19.05341960407611168, -5.049401038298163336, 41.45724293864769550 ) ) ;
#23927 = CARTESIAN_POINT ( 'NONE',  ( 8.314922557960818139, 14.29746914071049879, 49.58224293864769550 ) ) ;
#23929 = CARTESIAN_POINT ( 'NONE',  ( 16.51473224551069308, 9.474510206698969483, 104.1655762719810241 ) ) ;
#23928 = CARTESIAN_POINT ( 'NONE',  ( 30.00000000000000000, 5.499999999999992895, 37.50000000000000000 ) ) ;
#23930 = CARTESIAN_POINT ( 'NONE',  ( -15.72974639402197994, 15.80617190586746368, 45.62390960531436690 ) ) ;
#23931 = CARTESIAN_POINT ( 'NONE',  ( 12.14591786802309770, 12.06949235617756955, 79.37390960531436690 ) ) ;
#23932 = CARTESIAN_POINT ( 'NONE',  ( -14.29746914071037622, -8.314922557961029526, 29.16775706135234003 ) ) ;
#23933 = EDGE_CURVE ( 'NONE', #130647, #131569, #146223, .T. ) ;
#23934 = CARTESIAN_POINT ( 'NONE',  ( -14.34966873604960291, -8.224510206698953496, 71.66557627198100988 ) ) ;
#23935 = DIRECTION ( 'NONE',  ( -0.000000000000000000, -0.000000000000000000, 1.000000000000000000 ) ) ;
#23936 = CARTESIAN_POINT ( 'NONE',  ( -5.049401038297874678, -19.05341960407617918, 59.79275706135231871 ) ) ;
#23937 = CARTESIAN_POINT ( 'NONE',  ( -0.05219959533909027116, -19.03943276465977164, 107.4989096053143527 ) ) ;
#23938 = CARTESIAN_POINT ( 'NONE',  ( 13.89961937509957401, 13.97604488694547697, 76.87609039468566152 ) ) ;
#23939 = CARTESIAN_POINT ( 'NONE',  ( -16.46253265017146816, -9.564922557961047289, 94.16775706135233293 ) ) ;
#23941 = CARTESIAN_POINT ( 'NONE',  ( -8.224510206698735004, -14.34966873604973081, 109.5844237280190328 ) ) ;
#23940 = CARTESIAN_POINT ( 'NONE',  ( -8.314922557961024197, 14.29746914071037800, 22.91775706135235069 ) ) ;
#23942 = CARTESIAN_POINT ( 'NONE',  ( -9.474510206698720793, -16.51473224551083518, 74.58442372801900433 ) ) ;
#23943 = CARTESIAN_POINT ( 'NONE',  ( -15.80617190586745835, -15.72974639402198527, 41.87390960531435979 ) ) ;
#23944 = CARTESIAN_POINT ( 'NONE',  ( -21.55341960407619339, 5.719274019375674811, 63.54275706135234003 ) ) ;
#23945 = CARTESIAN_POINT ( 'NONE',  ( -23.63516320021014749, -9.722623904421999086, 168.4908852323012241 ) ) ;
#23946 = CARTESIAN_POINT ( 'NONE',  ( 19.03943276465977164, 0.05219959533936151252, 111.2510903946856757 ) ) ;
#23948 = CARTESIAN_POINT ( 'NONE',  ( 9.474510206698971260, -16.51473224551069308, 77.91557627198103830 ) ) ;
#23947 = CARTESIAN_POINT ( 'NONE',  ( 17.49999999999997868, 3.373831961294261106, 22.36044703459066341 ) ) ;
#23949 = CARTESIAN_POINT ( 'NONE',  ( -13.97604488694527625, -13.89961937509977652, 26.87390960531434558 ) ) ;
#23951 = CARTESIAN_POINT ( 'NONE',  ( -13.97604488694527625, -13.89961937509977652, 81.87390960531436690 ) ) ;
#23950 = CARTESIAN_POINT ( 'NONE',  ( -0.05219959533910754901, -16.53943276465976808, 92.49890960531436690 ) ) ;
#23952 = CARTESIAN_POINT ( 'NONE',  ( 13.97604488694527802, 13.89961937509977652, 84.37390960531433848 ) ) ;
#23953 = VERTEX_POINT ( 'NONE', #55213 ) ;
#23954 = CARTESIAN_POINT ( 'NONE',  ( 19.02544592524334988, 5.153800228976608722, 86.45942372801900433 ) ) ;
#23955 = CARTESIAN_POINT ( 'NONE',  ( 21.52544592524344225, -5.823673210054117533, 73.54057627198102409 ) ) ;
#23956 = CARTESIAN_POINT ( 'NONE',  ( 13.97604488694527802, 13.89961937509977652, 34.37390960531436690 ) ) ;
#23957 = CARTESIAN_POINT ( 'NONE',  ( -9.474510206698720793, -16.51473224551083518, 54.58442372801899722 ) ) ;
#23958 = CARTESIAN_POINT ( 'NONE',  ( -16.46253265017160317, 9.564922557960807481, 55.83224293864769550 ) ) ;
#23959 = CARTESIAN_POINT ( 'NONE',  ( -0.05219959533909027116, -19.03943276465977164, 87.49890960531436690 ) ) ;
#23960 = ORIENTED_EDGE ( 'NONE', *, *, #159956, .T. ) ;
#23961 = CARTESIAN_POINT ( 'NONE',  ( 0.05219959533907565091, 21.53943276465977519, 104.9989096053143669 ) ) ;
#23964 = CARTESIAN_POINT ( 'NONE',  ( 19.02544592524334988, 5.153800228976608722, 61.45942372801900433 ) ) ;
#23963 = CARTESIAN_POINT ( 'NONE',  ( -13.97604488694527625, -13.89961937509977652, 86.87390960531436690 ) ) ;
#23962 = CARTESIAN_POINT ( 'NONE',  ( -4.483927247898539470, -16.52544592524342804, 87.29057627198103830 ) ) ;
#23965 = CARTESIAN_POINT ( 'NONE',  ( 15.72974639402199770, -15.80617190586745480, 93.12390960531436690 ) ) ;
#23966 = CARTESIAN_POINT ( 'NONE',  ( -10.81492255796078084, -18.62759615963271287, 72.08224293864769550 ) ) ;
#23967 = CARTESIAN_POINT ( 'NONE',  ( -8.224510206698948167, 14.34966873604960824, 35.41557627198102409 ) ) ;
#23968 = CARTESIAN_POINT ( 'NONE',  ( -5.719274019375665041, -21.55341960407619695, 99.79275706135234714 ) ) ;
#23969 = CARTESIAN_POINT ( 'NONE',  ( 8.314922557961029526, -14.29746914071037800, 60.41775706135235424 ) ) ;
#23970 = CARTESIAN_POINT ( 'NONE',  ( 9.474510206698971260, -16.51473224551069308, 97.91557627198102409 ) ) ;
#23971 = CARTESIAN_POINT ( 'NONE',  ( 16.46253265017160672, -9.564922557960803928, 33.33224293864770260 ) ) ;
#23972 = CIRCLE ( 'NONE', #30321, 206.0437394197456911 ) ;
#23973 = CARTESIAN_POINT ( 'NONE',  ( -0.05219959533937732626, 21.53943276465977519, 42.50109039468567573 ) ) ;
#23974 = CARTESIAN_POINT ( 'NONE',  ( 0.05219959533937995610, -21.53943276465977519, 60.00109039468568284 ) ) ;
#23975 = CARTESIAN_POINT ( 'NONE',  ( 13.97604488694527802, 13.89961937509977652, 44.37390960531435269 ) ) ;
#23976 = CARTESIAN_POINT ( 'NONE',  ( 21.55341960407619695, -5.719274019375665929, 41.04275706135236135 ) ) ;
#23977 = CARTESIAN_POINT ( 'NONE',  ( 16.46253265017146816, 9.564922557961045513, 76.66775706135234714 ) ) ;
#23978 = CARTESIAN_POINT ( 'NONE',  ( 19.03943276465977164, 0.05219959533936151252, 76.25109039468566152 ) ) ;
#23979 = CARTESIAN_POINT ( 'NONE',  ( 19.03943276465977164, -0.05219959533909143690, 23.74890960531435269 ) ) ;
#23980 = CARTESIAN_POINT ( 'NONE',  ( -0.05219959533934338120, 16.53943276465976808, 77.50109039468567573 ) ) ;
#23981 = CARTESIAN_POINT ( 'NONE',  ( 5.049401038298161559, -19.05341960407611168, 57.70724293864769550 ) ) ;
#23982 = CARTESIAN_POINT ( 'NONE',  ( 21.56952297831669441, -5.557039098534934496, 173.4609804364286276 ) ) ;
#23983 = CARTESIAN_POINT ( 'NONE',  ( 9.474510206698971260, -16.51473224551069308, 102.9155762719810241 ) ) ;
#23984 = CARTESIAN_POINT ( 'NONE',  ( -13.89961937509977652, 13.97604488694528158, 40.62390960531435979 ) ) ;
#23985 = CARTESIAN_POINT ( 'NONE',  ( 5.719274019375991003, -21.55341960407610458, 67.70724293864769550 ) ) ;
#23986 = CARTESIAN_POINT ( 'NONE',  ( 8.314922557961029526, -14.29746914071037800, 65.41775706135234714 ) ) ;
#23987 = CARTESIAN_POINT ( 'NONE',  ( 0.05219959533937995610, -21.53943276465977519, 110.0010903946856757 ) ) ;
#23988 = CARTESIAN_POINT ( 'NONE',  ( 0.05219959533909260263, 19.03943276465977164, 49.99890960531435979 ) ) ;
#23989 = CARTESIAN_POINT ( 'NONE',  ( -12.06949235617756955, 12.14591786802309770, 45.62390960531436690 ) ) ;
#23990 = CARTESIAN_POINT ( 'NONE',  ( 16.55341960407611168, 4.379528057220329451, 83.95724293864770971 ) ) ;
#23991 = CARTESIAN_POINT ( 'NONE',  ( -19.03943276465977164, 0.05219959533909376836, 81.24890960531436690 ) ) ;
#23992 = CARTESIAN_POINT ( 'NONE',  ( -21.53943276465977519, -0.05219959533937600094, 38.75109039468567573 ) ) ;
#23993 = CARTESIAN_POINT ( 'NONE',  ( 9.474510206698971260, -16.51473224551069308, 92.91557627198103830 ) ) ;
#23994 = CARTESIAN_POINT ( 'NONE',  ( -10.72451020669870658, -18.67979575497194134, 99.58442372801900433 ) ) ;
#23995 = CARTESIAN_POINT ( 'NONE',  ( -4.483927247898782831, 16.52544592524335698, 67.70942372801901854 ) ) ;
#23996 = CARTESIAN_POINT ( 'NONE',  ( -13.97604488694527625, -13.89961937509977652, 101.8739096053143811 ) ) ;
#23997 = CARTESIAN_POINT ( 'NONE',  ( -18.62759615963270932, 10.81492255796079327, 85.83224293864768129 ) ) ;
#23998 = VECTOR ( 'NONE', #40008, 1000.000000000000000 ) ;
#23999 = CARTESIAN_POINT ( 'NONE',  ( -8.314922557960811034, -14.29746914071050412, 47.08224293864770260 ) ) ;
#24000 = CARTESIAN_POINT ( 'NONE',  ( 13.89961937509977652, -13.97604488694527269, 48.12390960531435979 ) ) ;
#24001 = CARTESIAN_POINT ( 'NONE',  ( 12.06949235617739724, 12.14591786802326823, 51.87609039468568284 ) ) ;
#24002 = CARTESIAN_POINT ( 'NONE',  ( -8.314922557960811034, -14.29746914071050412, 67.08224293864770971 ) ) ;
#24003 = CARTESIAN_POINT ( 'NONE',  ( 16.46253265017160672, -9.564922557960803928, 108.3322429386476955 ) ) ;
#24004 = CARTESIAN_POINT ( 'NONE',  ( 5.823673210054125526, 21.52544592524343514, 29.79057627198102409 ) ) ;
#24005 = CARTESIAN_POINT ( 'NONE',  ( -16.46253265017146816, -9.564922557961047289, 29.16775706135232937 ) ) ;
#24006 = CARTESIAN_POINT ( 'NONE',  ( -16.53943276465976808, 0.05219959533911058130, 101.2489096053143669 ) ) ;
#24007 = CARTESIAN_POINT ( 'NONE',  ( 5.049401038298161559, -19.05341960407611168, 107.7072429386476955 ) ) ;
#24008 = ORIENTED_EDGE ( 'NONE', *, *, #133545, .T. ) ;
#24009 = CARTESIAN_POINT ( 'NONE',  ( -16.55341960407617563, 4.379528057220093196, 58.54275706135235424 ) ) ;
#24010 = CARTESIAN_POINT ( 'NONE',  ( 19.05341960407611168, 5.049401038298154454, 58.95724293864768129 ) ) ;
#24011 = DIRECTION ( 'NONE',  ( -5.690990215841557531E-14, -0.9396926207859042091, 0.3420201433256805368 ) ) ;
#24012 = CARTESIAN_POINT ( 'NONE',  ( 5.049401038297881783, 19.05341960407617563, 57.29275706135231871 ) ) ;
#24013 = ADVANCED_FACE ( 'NONE', ( #100706, #8719 ), #194742, .T. ) ;
#24014 = CARTESIAN_POINT ( 'NONE',  ( 0.05219959533934541429, -16.53943276465976808, 95.00109039468568994 ) ) ;
#24015 = CARTESIAN_POINT ( 'NONE',  ( 9.474510206698729675, 16.51473224551082808, 92.08442372801900433 ) ) ;
#24016 = CARTESIAN_POINT ( 'NONE',  ( -10.72451020669870658, -18.67979575497194134, 64.58442372801900433 ) ) ;
#24017 = CARTESIAN_POINT ( 'NONE',  ( -13.97604488694527625, -13.89961937509977652, 71.87390960531433848 ) ) ;
#24018 = CARTESIAN_POINT ( 'NONE',  ( -5.719274019375978568, 21.55341960407610458, 90.20724293864770971 ) ) ;
#24019 = CARTESIAN_POINT ( 'NONE',  ( -4.483927247898539470, -16.52544592524342804, 107.2905762719810525 ) ) ;
#24020 = ADVANCED_FACE ( 'NONE', ( #132056, #149233 ), #10724, .F. ) ;
#24021 = CARTESIAN_POINT ( 'NONE',  ( 19.02544592524334988, 5.153800228976608722, 81.45942372801897591 ) ) ;
#24022 = CARTESIAN_POINT ( 'NONE',  ( -18.67979575497178146, -10.72451020669898902, 81.66557627198103830 ) ) ;
#24023 = CARTESIAN_POINT ( 'NONE',  ( -9.474510206698720793, -16.51473224551083518, 44.58442372801900433 ) ) ;
#24024 = CARTESIAN_POINT ( 'NONE',  ( 19.49671883438227837, 5.500000000000021316, 97.39279849105680853 ) ) ;
#24025 = CARTESIAN_POINT ( 'NONE',  ( 21.55341960407610458, 5.719274019375980345, 93.95724293864770971 ) ) ;
#24026 = CARTESIAN_POINT ( 'NONE',  ( -6.856101608890825108E-16, -71.74905178543389184, -12.99263613531267936 ) ) ;
#24027 = CARTESIAN_POINT ( 'NONE',  ( 5.049401038298161559, -19.05341960407611168, 67.70724293864769550 ) ) ;
#24028 = CARTESIAN_POINT ( 'NONE',  ( 30.00000000000000000, 5.499999999999992895, 102.5000000000000142 ) ) ;
#24029 = CARTESIAN_POINT ( 'NONE',  ( -16.51473224551082808, 9.474510206698731452, 113.3344237280190043 ) ) ;
#24030 = CARTESIAN_POINT ( 'NONE',  ( 36.77186724307695442, -4.769522647520276770, 47.74487706083471039 ) ) ;
#24031 = CARTESIAN_POINT ( 'NONE',  ( -16.51473224551069308, -9.474510206698971260, 51.66557627198102409 ) ) ;
#24032 = CARTESIAN_POINT ( 'NONE',  ( 16.51473224551069308, 9.474510206698969483, 114.1655762719810241 ) ) ;
#24034 = CARTESIAN_POINT ( 'NONE',  ( -12.14591786802309592, -12.06949235617757132, 46.87390960531435979 ) ) ;
#24033 = CARTESIAN_POINT ( 'NONE',  ( 5.823673210054125526, 21.52544592524343514, 99.79057627198103830 ) ) ;
#24035 = CARTESIAN_POINT ( 'NONE',  ( -0.05219959533937732626, 21.53943276465977519, 77.50109039468567573 ) ) ;
#24037 = CARTESIAN_POINT ( 'NONE',  ( -5.049401038297874678, -19.05341960407617918, 24.79275706135233648 ) ) ;
#24036 = CARTESIAN_POINT ( 'NONE',  ( 4.483927247898790824, -16.52544592524335698, 30.20942372801902565 ) ) ;
#24038 = CARTESIAN_POINT ( 'NONE',  ( 16.55341960407611168, 4.379528057220329451, 23.95724293864769550 ) ) ;
#24039 = CARTESIAN_POINT ( 'NONE',  ( -21.53943276465977519, -0.05219959533937600094, 38.75109039468567573 ) ) ;
#24040 = CARTESIAN_POINT ( 'NONE',  ( 18.67979575497178502, 10.72451020669898547, 114.1655762719810383 ) ) ;
#24041 = CARTESIAN_POINT ( 'NONE',  ( -5.719274019375978568, 21.55341960407610458, 60.20724293864768839 ) ) ;
#24042 = CARTESIAN_POINT ( 'NONE',  ( -16.46253265017146816, -9.564922557961047289, 89.16775706135234714 ) ) ;
#24043 = CARTESIAN_POINT ( 'NONE',  ( -0.05219959533936034679, 19.03943276465977164, 72.50109039468566152 ) ) ;
#24044 = CARTESIAN_POINT ( 'NONE',  ( -10.72451020669870658, -18.67979575497194134, 74.58442372801901854 ) ) ;
#24045 = CARTESIAN_POINT ( 'NONE',  ( -19.02544592524334988, -5.153800228976617603, 53.95942372801898301 ) ) ;
#24046 = CARTESIAN_POINT ( 'NONE',  ( 12.14591786802309770, 12.06949235617756955, 114.3739096053143527 ) ) ;
#24047 = CARTESIAN_POINT ( 'NONE',  ( 15.72974639402199770, -15.80617190586745480, 43.12390960531435269 ) ) ;
#24048 = CARTESIAN_POINT ( 'NONE',  ( -12.06949235617756955, 12.14591786802309770, 45.62390960531436690 ) ) ;
#24049 = CARTESIAN_POINT ( 'NONE',  ( -18.39443945427638383, 5.500000000000031086, 93.51745347608651571 ) ) ;
#24050 = CARTESIAN_POINT ( 'NONE',  ( 15.80617190586769283, -15.72974639402175789, 110.6260903946857042 ) ) ;
#24051 = CARTESIAN_POINT ( 'NONE',  ( 16.55341960407618274, -4.379528057220086978, 81.04275706135236135 ) ) ;
#24052 = CARTESIAN_POINT ( 'NONE',  ( -4.483927247898539470, -16.52544592524342804, 37.29057627198102409 ) ) ;
#24053 = CARTESIAN_POINT ( 'NONE',  ( 18.62759615963255655, 10.81492255796105972, 71.66775706135234714 ) ) ;
#24054 = CARTESIAN_POINT ( 'NONE',  ( -21.53943276465977519, -0.05219959533937600094, 78.75109039468568994 ) ) ;
#24055 = CARTESIAN_POINT ( 'NONE',  ( 0.05219959533907565091, 21.53943276465977519, 84.99890960531436690 ) ) ;
#24056 = VECTOR ( 'NONE', #152570, 1000.000000000000000 ) ;
#24057 = CARTESIAN_POINT ( 'NONE',  ( -9.564922557960796823, -16.46253265017161027, 32.08224293864769550 ) ) ;
#24058 = CARTESIAN_POINT ( 'NONE',  ( -21.52544592524334988, -5.823673210054445271, 58.95942372801902565 ) ) ;
#24059 = CARTESIAN_POINT ( 'NONE',  ( 19.05341960407611168, 5.049401038298154454, 38.95724293864767418 ) ) ;
#24060 = CARTESIAN_POINT ( 'NONE',  ( 9.564922557960805705, 16.46253265017160317, 49.58224293864770260 ) ) ;
#24061 = CARTESIAN_POINT ( 'NONE',  ( -4.379528057220328563, 16.55341960407611168, 95.20724293864769550 ) ) ;
#24062 = CARTESIAN_POINT ( 'NONE',  ( 13.97604488694527802, 13.89961937509977652, 104.3739096053143385 ) ) ;
#24063 = CARTESIAN_POINT ( 'NONE',  ( 4.483927247898545687, 16.52544592524342804, 39.79057627198103830 ) ) ;
#24064 = CARTESIAN_POINT ( 'NONE',  ( -16.51473224551069308, -9.474510206698971260, 21.66557627198102765 ) ) ;
#24065 = CARTESIAN_POINT ( 'NONE',  ( -5.823673210054116645, -21.52544592524344225, 82.29057627198103830 ) ) ;
#24066 = CARTESIAN_POINT ( 'NONE',  ( -10.81492255796105439, 18.62759615963255655, 22.91775706135235069 ) ) ;
#24067 = CARTESIAN_POINT ( 'NONE',  ( -15.20000000000001883, 1.574768255752702759E-13, -64.92279855667830191 ) ) ;
#24068 = CARTESIAN_POINT ( 'NONE',  ( -16.55341960407617563, 4.379528057220093196, 28.54275706135234358 ) ) ;
#24069 = CARTESIAN_POINT ( 'NONE',  ( -0.05219959533907301413, -21.53943276465977519, 72.49890960531435269 ) ) ;
#24070 = CARTESIAN_POINT ( 'NONE',  ( 5.719274019375673035, 21.55341960407619339, 97.29275706135234714 ) ) ;
#24071 = CARTESIAN_POINT ( 'NONE',  ( 13.89961937509977652, -13.97604488694527269, 78.12390960531433848 ) ) ;
#24072 = CARTESIAN_POINT ( 'NONE',  ( 21.52544592524334988, 5.823673210054432836, 31.45942372801901854 ) ) ;
#24073 = CARTESIAN_POINT ( 'NONE',  ( 9.564922557960805705, 16.46253265017160317, 109.5822429386476955 ) ) ;
#24074 = CARTESIAN_POINT ( 'NONE',  ( 12.14591786802327356, -12.06949235617739191, 90.62609039468567573 ) ) ;
#24075 = CARTESIAN_POINT ( 'NONE',  ( -21.53943276465977519, -0.05219959533937600094, 68.75109039468568994 ) ) ;
#24076 = CARTESIAN_POINT ( 'NONE',  ( 18.62759615963255655, 10.81492255796105972, 111.6677570613523613 ) ) ;
#24077 = CARTESIAN_POINT ( 'NONE',  ( -0.05219959533934338120, 16.53943276465976808, 77.50109039468567573 ) ) ;
#24078 = CARTESIAN_POINT ( 'NONE',  ( -15.80617190586768217, 15.72974639402176855, 33.12609039468569705 ) ) ;
#24079 = VECTOR ( 'NONE', #11583, 1000.000000000000000 ) ;
#24080 = CARTESIAN_POINT ( 'NONE',  ( 5.049401038298161559, -19.05341960407611168, 37.70724293864768839 ) ) ;
#24081 = CARTESIAN_POINT ( 'NONE',  ( 18.67979575497194134, -10.72451020669871369, 95.83442372801903275 ) ) ;
#24082 = CARTESIAN_POINT ( 'NONE',  ( -16.46253265017160317, 9.564922557960807481, 90.83224293864769550 ) ) ;
#24083 = CARTESIAN_POINT ( 'NONE',  ( -21.55341960407610458, -5.719274019375992779, 86.45724293864770971 ) ) ;
#24084 = CARTESIAN_POINT ( 'NONE',  ( -19.02544592524334988, -5.153800228976617603, 53.95942372801898301 ) ) ;
#24086 = CARTESIAN_POINT ( 'NONE',  ( 0.05219959533907565091, 21.53943276465977519, 54.99890960531435269 ) ) ;
#24085 = LINE ( 'NONE', #114066, #138666 ) ;
#24088 = CARTESIAN_POINT ( 'NONE',  ( 8.314922557960818139, 14.29746914071049879, 44.58224293864769550 ) ) ;
#24087 = CARTESIAN_POINT ( 'NONE',  ( -13.89961937509977652, 13.97604488694528158, 90.62390960531432427 ) ) ;
#24089 = CARTESIAN_POINT ( 'NONE',  ( 17.81289503416610742, 24.51734667627700404, 145.2999999999999829 ) ) ;
#24090 = CARTESIAN_POINT ( 'NONE',  ( 19.05341960407617918, -5.049401038297876454, 76.04275706135230450 ) ) ;
#24091 =( GEOMETRIC_REPRESENTATION_CONTEXT ( 3 ) GLOBAL_UNCERTAINTY_ASSIGNED_CONTEXT ( ( #114627 ) ) GLOBAL_UNIT_ASSIGNED_CONTEXT ( ( #101239, #86084, #176109 ) ) REPRESENTATION_CONTEXT ( 'NONE', 'WORKASPACE' ) );
#24092 = CARTESIAN_POINT ( 'NONE',  ( -17.50000000000000000, 5.622605283950888655, 103.6879268940388954 ) ) ;
#24093 = CARTESIAN_POINT ( 'NONE',  ( -13.97604488694547697, 13.89961937509957934, 103.1260903946856473 ) ) ;
#24094 = CARTESIAN_POINT ( 'NONE',  ( 5.823673210054125526, 21.52544592524343514, 84.79057627198102409 ) ) ;
#24095 = CARTESIAN_POINT ( 'NONE',  ( 16.52544592524342804, -4.483927247898539470, 63.54057627198103830 ) ) ;
#24096 = CARTESIAN_POINT ( 'NONE',  ( -5.049401038298153566, 19.05341960407611168, 105.2072429386476671 ) ) ;
#24097 = CARTESIAN_POINT ( 'NONE',  ( -16.55341960407617563, 4.379528057220093196, 43.54275706135235424 ) ) ;
#24098 = CARTESIAN_POINT ( 'NONE',  ( 19.02544592524343514, -5.153800228976328945, 53.54057627198102409 ) ) ;
#24100 = CARTESIAN_POINT ( 'NONE',  ( 19.03943276465977164, 0.05219959533936151252, 101.2510903946856757 ) ) ;
#24099 = CARTESIAN_POINT ( 'NONE',  ( -18.62759615963270932, 10.81492255796079327, 115.8322429386477097 ) ) ;
#24101 = CARTESIAN_POINT ( 'NONE',  ( 13.89961937509977652, -13.97604488694527269, 98.12390960531433848 ) ) ;
#24102 = CARTESIAN_POINT ( 'NONE',  ( 19.03943276465977164, -0.05219959533909143690, 78.74890960531436690 ) ) ;
#24103 = CARTESIAN_POINT ( 'NONE',  ( -18.67979575497178146, -10.72451020669898902, 71.66557627198100988 ) ) ;
#24104 = CARTESIAN_POINT ( 'NONE',  ( -13.97604488694527625, -13.89961937509977652, 51.87390960531436690 ) ) ;
#24105 = CARTESIAN_POINT ( 'NONE',  ( 21.10861677039925866, 30.68312529381453757, -8.000000000000003553 ) ) ;
#24106 = CARTESIAN_POINT ( 'NONE',  ( 16.55341960407611168, 4.379528057220329451, 53.95724293864770260 ) ) ;
#24107 = CARTESIAN_POINT ( 'NONE',  ( -16.46253265017160317, 9.564922557960807481, 100.8322429386477097 ) ) ;
#24108 = DIRECTION ( 'NONE',  ( 0.000000000000000000, 0.000000000000000000, -1.000000000000000000 ) ) ;
#24109 = CARTESIAN_POINT ( 'NONE',  ( 9.564922557961047289, -16.46253265017146816, 70.41775706135233293 ) ) ;
#24110 = CARTESIAN_POINT ( 'NONE',  ( 10.81492255796078972, 18.62759615963270932, 94.58224293864769550 ) ) ;
#24111 = CARTESIAN_POINT ( 'NONE',  ( 16.46253265017146816, 9.564922557961045513, 51.66775706135233293 ) ) ;
#24112 = CARTESIAN_POINT ( 'NONE',  ( -13.89961937509977652, 13.97604488694528158, 95.62390960531436690 ) ) ;
#24113 = SURFACE_STYLE_FILL_AREA ( #7922 ) ;
#24114 = CARTESIAN_POINT ( 'NONE',  ( -18.67979575497178146, -10.72451020669898902, 36.66557627198103120 ) ) ;
#24115 = AXIS2_PLACEMENT_3D ( 'NONE', #59003, #135864, #120669 ) ;
#24116 = CARTESIAN_POINT ( 'NONE',  ( 9.564922557960805705, 16.46253265017160317, 69.58224293864770971 ) ) ;
#24117 = CARTESIAN_POINT ( 'NONE',  ( 15.80617190586769283, -15.72974639402175789, 65.62609039468568994 ) ) ;
#24118 = CARTESIAN_POINT ( 'NONE',  ( 9.474510206698971260, -16.51473224551069308, 42.91557627198103120 ) ) ;
#24120 = EDGE_LOOP ( 'NONE', ( #125826, #149302, #22429, #55672 ) ) ;
#24119 = CARTESIAN_POINT ( 'NONE',  ( 14.29746914071049879, -8.314922557960816363, 78.33224293864770971 ) ) ;
#24122 = B_SPLINE_CURVE_WITH_KNOTS ( 'NONE', 3,
 ( #37000, #158360, #142189, #127011, #21845, #36003, #159339, #81489, #82493, #19848, #63368, #17877, #144176, #157377, #79531, #18870, #129000, #143176, #190698, #112844, #52173, #2690 ),
 .UNSPECIFIED., .F., .F.,
 ( 4, 2, 2, 2, 2, 2, 2, 2, 2, 2, 4 ),
 ( 8.673617379884035472E-19, 0.001309639967555459826, 0.001964459951333189305, 0.002291869943222054045, 0.002455574939166472754, 0.002619279935110891463, 0.002782984931055310605, 0.002946689926999729314, 0.003274099918888538976, 0.003928919902666159168, 0.005238559870221396950 ),
 .UNSPECIFIED. ) ;
#24121 = CARTESIAN_POINT ( 'NONE',  ( 12.06949235617739724, 12.14591786802326823, 21.87609039468567573 ) ) ;
#24123 = CARTESIAN_POINT ( 'NONE',  ( 21.53943276465977519, 0.05219959533937863772, 46.25109039468567573 ) ) ;
#24124 = VERTEX_POINT ( 'NONE', #168362 ) ;
#24125 = CARTESIAN_POINT ( 'NONE',  ( -19.05341960407611168, -5.049401038298163336, 111.4572429386476671 ) ) ;
#24126 = CARTESIAN_POINT ( 'NONE',  ( 16.46253265017146816, 9.564922557961045513, 66.66775706135233293 ) ) ;
#24127 = CARTESIAN_POINT ( 'NONE',  ( 25.13006352617149375, -30.86725525062045605, -20.93759803324961055 ) ) ;
#24128 = CARTESIAN_POINT ( 'NONE',  ( 21.52544592524334988, 5.823673210054432836, 21.45942372801901499 ) ) ;
#24129 = CARTESIAN_POINT ( 'NONE',  ( 5.153800228976335163, 19.02544592524342804, 54.79057627198103120 ) ) ;
#24130 = EDGE_CURVE ( 'NONE', #177464, #45827, #93493, .T. ) ;
#24131 = CARTESIAN_POINT ( 'NONE',  ( -30.74264578624800492, -22.33583958711396278, -5.549999994537627046 ) ) ;
#24132 = CARTESIAN_POINT ( 'NONE',  ( 0.05219959533936267826, -19.03943276465977164, 25.00109039468566152 ) ) ;
#24133 = CARTESIAN_POINT ( 'NONE',  ( 5.049401038298161559, -19.05341960407611168, 42.70724293864767418 ) ) ;
#24134 = CARTESIAN_POINT ( 'NONE',  ( 5.153800228976615827, -19.02544592524334988, 20.20942372801899722 ) ) ;
#24135 = CARTESIAN_POINT ( 'NONE',  ( 8.314922557961029526, -14.29746914071037800, 85.41775706135236135 ) ) ;
#24137 = CARTESIAN_POINT ( 'NONE',  ( -10.72451020669870658, -18.67979575497194134, 69.58442372801900433 ) ) ;
#24136 = CARTESIAN_POINT ( 'NONE',  ( -19.03943276465977164, 0.05219959533909376836, 106.2489096053143669 ) ) ;
#24138 = CARTESIAN_POINT ( 'NONE',  ( -17.14385361876520264, -23.59649016807271593, 147.6750000027311671 ) ) ;
#24139 = CARTESIAN_POINT ( 'NONE',  ( -5.153800228976328057, -19.02544592524343514, 112.2905762719810099 ) ) ;
#24140 = FACE_OUTER_BOUND ( 'NONE', #196057, .T. ) ;
#24142 = CARTESIAN_POINT ( 'NONE',  ( -5.719274019375665041, -21.55341960407619695, 69.79275706135234714 ) ) ;
#24141 = CARTESIAN_POINT ( 'NONE',  ( -4.483927247898782831, 16.52544592524335698, 67.70942372801901854 ) ) ;
#24143 = CARTESIAN_POINT ( 'NONE',  ( 18.62759615963255655, 10.81492255796105972, 106.6677570613523756 ) ) ;
#24144 = LINE ( 'NONE', #177826, #141302 ) ;
#24145 = CARTESIAN_POINT ( 'NONE',  ( 12.14591786802327356, -12.06949235617739191, 45.62609039468567573 ) ) ;
#24146 = CARTESIAN_POINT ( 'NONE',  ( 13.89961937509977652, -13.97604488694527269, 88.12390960531438111 ) ) ;
#24147 = CARTESIAN_POINT ( 'NONE',  ( -9.474510206698964154, 16.51473224551069663, 115.4155762719810241 ) ) ;
#24148 = ORIENTED_EDGE ( 'NONE', *, *, #198087, .F. ) ;
#24149 = EDGE_CURVE ( 'NONE', #100314, #159084, #92500, .T. ) ;
#24150 = CARTESIAN_POINT ( 'NONE',  ( -0.2552802045322777325, -28.91687668646900988, -52.63629878241253834 ) ) ;
#24151 = CARTESIAN_POINT ( 'NONE',  ( 5.153800228976335163, 19.02544592524342804, 39.79057627198100988 ) ) ;
#24152 = CARTESIAN_POINT ( 'NONE',  ( 15.72974639402199770, -15.80617190586745480, 43.12390960531435269 ) ) ;
#24153 = CARTESIAN_POINT ( 'NONE',  ( -4.483927247898782831, 16.52544592524335698, 112.7094237280190328 ) ) ;
#24155 = CARTESIAN_POINT ( 'NONE',  ( 9.564922557960805705, 16.46253265017160317, 84.58224293864769550 ) ) ;
#24154 = CARTESIAN_POINT ( 'NONE',  ( -8.224510206698948167, 14.34966873604960824, 85.41557627198102409 ) ) ;
#24156 = CARTESIAN_POINT ( 'NONE',  ( 15.72974639402176855, 15.80617190586768217, 101.8760903946857042 ) ) ;
#24157 = CARTESIAN_POINT ( 'NONE',  ( 8.314922557961029526, -14.29746914071037800, 30.41775706135234358 ) ) ;
#24158 = CARTESIAN_POINT ( 'NONE',  ( 8.224510206698953496, -14.34966873604960469, 82.91557627198103830 ) ) ;
#24159 = CARTESIAN_POINT ( 'NONE',  ( 5.719274019375673035, 21.55341960407619339, 42.29275706135235424 ) ) ;
#24160 = CARTESIAN_POINT ( 'NONE',  ( -0.05219959533907301413, -21.53943276465977519, 82.49890960531436690 ) ) ;
#24161 = CARTESIAN_POINT ( 'NONE',  ( -19.02544592524334988, -5.153800228976617603, 53.95942372801898301 ) ) ;
#24162 = CARTESIAN_POINT ( 'NONE',  ( 16.12203461105333702, -16.12203461105326951, -64.92279855667830191 ) ) ;
#24163 = CARTESIAN_POINT ( 'NONE',  ( 0.05219959533909260263, 19.03943276465977164, 94.99890960531436690 ) ) ;
#24164 = CARTESIAN_POINT ( 'NONE',  ( -14.34966873604960291, -8.224510206698953496, 66.66557627198102409 ) ) ;
#24165 = CARTESIAN_POINT ( 'NONE',  ( 16.52544592524342804, -4.483927247898539470, 48.54057627198103120 ) ) ;
#24166 = CARTESIAN_POINT ( 'NONE',  ( 14.29746914071049879, -8.314922557960816363, 28.33224293864769550 ) ) ;
#24167 = CARTESIAN_POINT ( 'NONE',  ( 19.05341960407617918, -5.049401038297876454, 76.04275706135230450 ) ) ;
#24168 = DIRECTION ( 'NONE',  ( 0.000000000000000000, 0.000000000000000000, 1.000000000000000000 ) ) ;
#24169 = CARTESIAN_POINT ( 'NONE',  ( 19.03943276465977164, -0.05219959533909143690, 113.7489096053143669 ) ) ;
#24170 = CARTESIAN_POINT ( 'NONE',  ( -12.14591786802309592, -12.06949235617757132, 86.87390960531438111 ) ) ;
#24171 = CARTESIAN_POINT ( 'NONE',  ( -17.50000000000147438, -3.254303733634695384, 24.97604106928582013 ) ) ;
#24173 = CARTESIAN_POINT ( 'NONE',  ( 10.72451020669898902, -18.67979575497178502, 42.91557627198103120 ) ) ;
#24172 = CARTESIAN_POINT ( 'NONE',  ( 19.03943276465977164, -0.05219959533909143690, 43.74890960531435979 ) ) ;
#24174 = CARTESIAN_POINT ( 'NONE',  ( 13.97604488694527802, 13.89961937509977652, 29.37390960531435979 ) ) ;
#24176 = CARTESIAN_POINT ( 'NONE',  ( 13.97604488694527802, 13.89961937509977652, 59.37390960531434558 ) ) ;
#24175 = CARTESIAN_POINT ( 'NONE',  ( 4.379528057220092307, 16.55341960407617563, 82.29275706135234714 ) ) ;
#24178 = EDGE_CURVE ( 'NONE', #105726, #189536, #182557, .T. ) ;
#24177 = CARTESIAN_POINT ( 'NONE',  ( -16.51473224551082808, 9.474510206698731452, 38.33442372801899722 ) ) ;
#24179 = CARTESIAN_POINT ( 'NONE',  ( -21.52544592524334988, -5.823673210054445271, 53.95942372801900433 ) ) ;
#24180 = CARTESIAN_POINT ( 'NONE',  ( 15.72974639402199770, -15.80617190586745480, 33.12390960531435979 ) ) ;
#24181 = CARTESIAN_POINT ( 'NONE',  ( -4.483927247898539470, -16.52544592524342804, 107.2905762719810525 ) ) ;
#24182 = CARTESIAN_POINT ( 'NONE',  ( 19.02544592524334988, 5.153800228976608722, 91.45942372801900433 ) ) ;
#24183 = CARTESIAN_POINT ( 'NONE',  ( 22.81625015709509441, 31.40387420917330275, -5.824999997268813345 ) ) ;
#24185 = CARTESIAN_POINT ( 'NONE',  ( -10.81492255796078084, -18.62759615963271287, 52.08224293864768839 ) ) ;
#24184 = CARTESIAN_POINT ( 'NONE',  ( 17.50000000000004263, 3.926509638708173711, 37.08294989138502729 ) ) ;
#24186 = CARTESIAN_POINT ( 'NONE',  ( 17.26172910966779739, -6.454744622555849354, 68.30646908649225679 ) ) ;
#24187 = CARTESIAN_POINT ( 'NONE',  ( 21.53943276465977519, 0.05219959533937863772, 86.25109039468568994 ) ) ;
#24188 = CARTESIAN_POINT ( 'NONE',  ( 16.53943276465976808, -0.05219959533910856209, 43.74890960531435979 ) ) ;
#24190 = CARTESIAN_POINT ( 'NONE',  ( -4.483927247898539470, -16.52544592524342804, 57.29057627198103120 ) ) ;
#24189 = CARTESIAN_POINT ( 'NONE',  ( -14.29746914071037622, -8.314922557961029526, 54.16775706135235424 ) ) ;
#24191 = CARTESIAN_POINT ( 'NONE',  ( -15.80617190586745835, -15.72974639402198527, 81.87390960531435269 ) ) ;
#24192 = CARTESIAN_POINT ( 'NONE',  ( -15.80617190586745835, -15.72974639402198527, 71.87390960531438111 ) ) ;
#24193 = DIRECTION ( 'NONE',  ( 1.000000000000000000, 0.000000000000000000, 0.000000000000000000 ) ) ;
#24194 = CARTESIAN_POINT ( 'NONE',  ( 19.03943276465977164, -0.05219959533909143690, 108.7489096053143527 ) ) ;
#24195 = CARTESIAN_POINT ( 'NONE',  ( -16.51473224551069308, -9.474510206698971260, 56.66557627198103120 ) ) ;
#24196 = CARTESIAN_POINT ( 'NONE',  ( 13.97604488694527802, 13.89961937509977652, 29.37390960531435979 ) ) ;
#24197 = CARTESIAN_POINT ( 'NONE',  ( 37.99999999999999289, 2.428612866367529932E-14, -15.00000000000000000 ) ) ;
#24198 = ORIENTED_EDGE ( 'NONE', *, *, #114298, .F. ) ;
#24200 = CARTESIAN_POINT ( 'NONE',  ( 12.06949235617739724, 12.14591786802326823, 86.87609039468568994 ) ) ;
#24199 = CIRCLE ( 'NONE', #8003, 2.000000000000000000 ) ;
#24201 = CARTESIAN_POINT ( 'NONE',  ( 5.823673210054444382, -21.52544592524334988, 20.20942372801900788 ) ) ;
#24202 = CARTESIAN_POINT ( 'NONE',  ( 13.97604488694527802, 13.89961937509977652, 69.37390960531436690 ) ) ;
#24203 = CARTESIAN_POINT ( 'NONE',  ( 15.72974639402176855, 15.80617190586768217, 56.87609039468568994 ) ) ;
#24204 = CARTESIAN_POINT ( 'NONE',  ( 9.564922557960805705, 16.46253265017160317, 114.5822429386476955 ) ) ;
#24205 = CARTESIAN_POINT ( 'NONE',  ( -24.03200911576545096, -31.81637637394599238, -21.77892875005238693 ) ) ;
#24206 = ORIENTED_EDGE ( 'NONE', *, *, #48766, .F. ) ;
#24207 = CARTESIAN_POINT ( 'NONE',  ( 15.80617190586769283, -15.72974639402175789, 50.62609039468568994 ) ) ;
#24209 = CARTESIAN_POINT ( 'NONE',  ( -19.02544592524342804, 5.153800228976336051, 106.0405762719810241 ) ) ;
#24208 = CARTESIAN_POINT ( 'NONE',  ( 19.05341960407611168, 5.049401038298154454, 113.9572429386477097 ) ) ;
#24210 = CARTESIAN_POINT ( 'NONE',  ( 0.05219959533936267826, -19.03943276465977164, 50.00109039468566863 ) ) ;
#24211 = CARTESIAN_POINT ( 'NONE',  ( -5.823673210054116645, -21.52544592524344225, 107.2905762719810525 ) ) ;
#24212 = CARTESIAN_POINT ( 'NONE',  ( 19.02544592524334988, 5.153800228976608722, 51.45942372801900433 ) ) ;
#24213 = CARTESIAN_POINT ( 'NONE',  ( -9.474510206698720793, -16.51473224551083518, 54.58442372801899722 ) ) ;
#24215 = ORIENTED_EDGE ( 'NONE', *, *, #28979, .F. ) ;
#24214 = CARTESIAN_POINT ( 'NONE',  ( 16.55341960407618274, -4.379528057220086978, 111.0427570613523613 ) ) ;
#24216 = CARTESIAN_POINT ( 'NONE',  ( 11.11254985580166910, 12.21717160642876543, -61.43205129781978258 ) ) ;
#24217 = CARTESIAN_POINT ( 'NONE',  ( 16.46253265017160672, -9.564922557960803928, 73.33224293864769550 ) ) ;
#24218 = AXIS2_PLACEMENT_3D ( 'NONE', #145200, #176565, #6683 ) ;
#24219 = CARTESIAN_POINT ( 'NONE',  ( -21.53943276465977519, -0.05219959533937600094, 78.75109039468568994 ) ) ;
#24220 = CARTESIAN_POINT ( 'NONE',  ( -5.823673210054431948, 21.52544592524334988, 87.70942372801901854 ) ) ;
#24221 = CARTESIAN_POINT ( 'NONE',  ( 27.05641397906351386, 2.428612866367529932E-14, 169.9999999999999716 ) ) ;
#24222 = CARTESIAN_POINT ( 'NONE',  ( -16.51473224551069308, -9.474510206698971260, 106.6655762719810383 ) ) ;
#24223 = CARTESIAN_POINT ( 'NONE',  ( 18.62759615963255655, 10.81492255796105972, 76.66775706135234714 ) ) ;
#24224 = CARTESIAN_POINT ( 'NONE',  ( -14.34966873604972548, 8.224510206698743886, 23.33442372801901499 ) ) ;
#24225 = CARTESIAN_POINT ( 'NONE',  ( 13.89961937509977652, -13.97604488694527269, 83.12390960531436690 ) ) ;
#24226 = CARTESIAN_POINT ( 'NONE',  ( -19.03943276465977164, 0.05219959533909376836, 116.2489096053143669 ) ) ;
#24227 = CARTESIAN_POINT ( 'NONE',  ( 9.564922557960805705, 16.46253265017160317, 89.58224293864769550 ) ) ;
#24228 = CARTESIAN_POINT ( 'NONE',  ( -17.59860650958993844, 7.585241751806885979, 88.42337014262494677 ) ) ;
#24229 = CARTESIAN_POINT ( 'NONE',  ( -13.89961937509977652, 13.97604488694528158, 80.62390960531436690 ) ) ;
#24230 = CARTESIAN_POINT ( 'NONE',  ( -16.51473224551069308, -9.474510206698971260, 61.66557627198103120 ) ) ;
#24231 = CARTESIAN_POINT ( 'NONE',  ( 21.53943276465977519, -0.05219959533907433946, 113.7489096053143527 ) ) ;
#24232 = CARTESIAN_POINT ( 'NONE',  ( -14.34966873604972548, 8.224510206698743886, 103.3344237280190043 ) ) ;
#24233 = DIRECTION ( 'NONE',  ( 0.9974398506828144884, 0.07151044867601406840, -0.000000000000000000 ) ) ;
#24234 = VECTOR ( 'NONE', #7822, 1000.000000000000000 ) ;
#24235 = CARTESIAN_POINT ( 'NONE',  ( -19.05341960407617563, 5.049401038297882671, 53.54275706135231871 ) ) ;
#24236 = CARTESIAN_POINT ( 'NONE',  ( -9.564922557960796823, -16.46253265017161027, 92.08224293864769550 ) ) ;
#24237 = CARTESIAN_POINT ( 'NONE',  ( -12.06949235617756955, 12.14591786802309770, 85.62390960531436690 ) ) ;
#24238 = CARTESIAN_POINT ( 'NONE',  ( -5.049401038298153566, 19.05341960407611168, 30.20724293864768839 ) ) ;
#24239 = CONICAL_SURFACE ( 'NONE', #169549, 2.500000000000002220, 1.029744260000000189 ) ;
#24240 = CARTESIAN_POINT ( 'NONE',  ( 0.05219959533907565091, 21.53943276465977519, 34.99890960531435979 ) ) ;
#24241 = CARTESIAN_POINT ( 'NONE',  ( 0.05219959533907565091, 21.53943276465977519, 29.99890960531435979 ) ) ;
#24242 = CARTESIAN_POINT ( 'NONE',  ( -12.14591786802309592, -12.06949235617757132, 96.87390960531436690 ) ) ;
#24243 = DIRECTION ( 'NONE',  ( 0.000000000000000000, 0.000000000000000000, -1.000000000000000000 ) ) ;
#24244 = CARTESIAN_POINT ( 'NONE',  ( -13.89961937509957401, -13.97604488694547875, 49.37609039468567573 ) ) ;
#24245 = CARTESIAN_POINT ( 'NONE',  ( -14.34966873604972548, 8.224510206698743886, 108.3344237280190185 ) ) ;
#24246 = CARTESIAN_POINT ( 'NONE',  ( 19.02544592524343514, -5.153800228976328945, 83.54057627198100988 ) ) ;
#24247 = CARTESIAN_POINT ( 'NONE',  ( -18.62759615963255300, -10.81492255796106328, 64.16775706135234714 ) ) ;
#24248 = CARTESIAN_POINT ( 'NONE',  ( -10.81492255796078084, -18.62759615963271287, 57.08224293864769550 ) ) ;
#24249 = CARTESIAN_POINT ( 'NONE',  ( -21.52544592524334988, -5.823673210054445271, 28.95942372801902209 ) ) ;
#24250 = CARTESIAN_POINT ( 'NONE',  ( 10.81492255796078972, 18.62759615963270932, 84.58224293864769550 ) ) ;
#24251 = CARTESIAN_POINT ( 'NONE',  ( -4.379528057220328563, 16.55341960407611168, 110.2072429386477239 ) ) ;
#24252 = CARTESIAN_POINT ( 'NONE',  ( -19.02544592524334988, -5.153800228976617603, 73.95942372801900433 ) ) ;
#24253 = CARTESIAN_POINT ( 'NONE',  ( -19.02544592524342804, 5.153800228976336051, 51.04057627198103120 ) ) ;
#24254 = CARTESIAN_POINT ( 'NONE',  ( 13.89961937509977652, -13.97604488694527269, 93.12390960531436690 ) ) ;
#24255 = CARTESIAN_POINT ( 'NONE',  ( 19.02544592524343514, -5.153800228976328945, 88.54057627198102409 ) ) ;
#24256 = CARTESIAN_POINT ( 'NONE',  ( 16.51473224551069308, 9.474510206698969483, 24.16557627198102765 ) ) ;
#24257 = CARTESIAN_POINT ( 'NONE',  ( -0.05219959533910754901, -16.53943276465976808, 47.49890960531435979 ) ) ;
#24258 = CARTESIAN_POINT ( 'NONE',  ( 12.14591786802327356, -12.06949235617739191, 40.62609039468567573 ) ) ;
#24260 = VECTOR ( 'NONE', #39292, 1000.000000000000000 ) ;
#24259 = CARTESIAN_POINT ( 'NONE',  ( 18.67979575497194134, -10.72451020669871369, 110.8344237280190043 ) ) ;
#24262 = CARTESIAN_POINT ( 'NONE',  ( 16.53943276465976808, -0.05219959533910856209, 28.74890960531435624 ) ) ;
#24261 = CARTESIAN_POINT ( 'NONE',  ( 0.05219959533909260263, 19.03943276465977164, 114.9989096053143669 ) ) ;
#24263 = CARTESIAN_POINT ( 'NONE',  ( -10.81492255796105439, 18.62759615963255655, 27.91775706135234358 ) ) ;
#24264 = CARTESIAN_POINT ( 'NONE',  ( 19.03943276465977164, -0.05219959533909143690, 108.7489096053143527 ) ) ;
#24265 = CARTESIAN_POINT ( 'NONE',  ( -8.224510206698735004, -14.34966873604973081, 109.5844237280190328 ) ) ;
#24266 = CARTESIAN_POINT ( 'NONE',  ( 16.55341960407618274, -4.379528057220086978, 96.04275706135236135 ) ) ;
#24267 = CARTESIAN_POINT ( 'NONE',  ( 8.314922557961029526, -14.29746914071037800, 25.41775706135235779 ) ) ;
#24268 = CARTESIAN_POINT ( 'NONE',  ( 5.153800228976335163, 19.02544592524342804, 44.79057627198103830 ) ) ;
#24269 = CARTESIAN_POINT ( 'NONE',  ( 14.34966873604960469, 8.224510206698951720, 114.1655762719810383 ) ) ;
#24270 = CARTESIAN_POINT ( 'NONE',  ( -15.72974639402176322, -15.80617190586768395, 24.37609039468567573 ) ) ;
#24271 = CARTESIAN_POINT ( 'NONE',  ( -5.153800228976328057, -19.02544592524343514, 37.29057627198102409 ) ) ;
#24272 = CARTESIAN_POINT ( 'NONE',  ( 19.05341960407611168, 5.049401038298154454, 103.9572429386476671 ) ) ;
#24273 = CARTESIAN_POINT ( 'NONE',  ( 5.823673210054444382, -21.52544592524334988, 35.20942372801901854 ) ) ;
#24274 = CARTESIAN_POINT ( 'NONE',  ( 0.05219959533909260263, 19.03943276465977164, 29.99890960531435979 ) ) ;
#24275 = CARTESIAN_POINT ( 'NONE',  ( 16.46253265017160672, -9.564922557960803928, 108.3322429386476955 ) ) ;
#24276 = FACE_OUTER_BOUND ( 'NONE', #146520, .T. ) ;
#24277 = CARTESIAN_POINT ( 'NONE',  ( 9.474510206698971260, -16.51473224551069308, 102.9155762719810241 ) ) ;
#24279 = CARTESIAN_POINT ( 'NONE',  ( -0.05219959533910754901, -16.53943276465976808, 97.49890960531436690 ) ) ;
#24278 = CARTESIAN_POINT ( 'NONE',  ( 15.80617190586769283, -15.72974639402175789, 45.62609039468567573 ) ) ;
#24280 = CARTESIAN_POINT ( 'NONE',  ( 13.97604488694527802, 13.89961937509977652, 99.37390960531436690 ) ) ;
#24281 = CARTESIAN_POINT ( 'NONE',  ( -27.86188877290821964, -7.554847477551930091, 161.1024127393599201 ) ) ;
#24282 = CARTESIAN_POINT ( 'NONE',  ( -12.06949235617739369, -12.14591786802326823, 69.37609039468567573 ) ) ;
#24283 = CARTESIAN_POINT ( 'NONE',  ( 21.52544592524334988, 5.823673210054432836, 81.45942372801900433 ) ) ;
#24284 = CARTESIAN_POINT ( 'NONE',  ( -16.53943276465976808, -0.05219959533934237506, 38.75109039468567573 ) ) ;
#24285 = CARTESIAN_POINT ( 'NONE',  ( 19.05341960407611168, 5.049401038298154454, 78.95724293864769550 ) ) ;
#24286 = CARTESIAN_POINT ( 'NONE',  ( -9.564922557961040184, 16.46253265017147172, 107.9177570613523471 ) ) ;
#24287 = CARTESIAN_POINT ( 'NONE',  ( 0.05219959533934541429, -16.53943276465976808, 80.00109039468568994 ) ) ;
#24288 = CARTESIAN_POINT ( 'NONE',  ( -9.564922557961040184, 16.46253265017147172, 92.91775706135233293 ) ) ;
#24289 = CARTESIAN_POINT ( 'NONE',  ( -19.02544592524342804, 5.153800228976336051, 61.04057627198103120 ) ) ;
#24290 = CARTESIAN_POINT ( 'NONE',  ( 15.72974639402199770, -15.80617190586745480, 78.12390960531436690 ) ) ;
#24292 = CARTESIAN_POINT ( 'NONE',  ( 0.05219959533936267826, -19.03943276465977164, 90.00109039468567573 ) ) ;
#24291 = CARTESIAN_POINT ( 'NONE',  ( -16.53943276465976808, 0.05219959533911058130, 86.24890960531436690 ) ) ;
#24293 = CARTESIAN_POINT ( 'NONE',  ( 4.483927247898790824, -16.52544592524335698, 55.20942372801902565 ) ) ;
#24294 = CARTESIAN_POINT ( 'NONE',  ( 17.50000000000002132, -5.624438216177543914, 63.31670344914647330 ) ) ;
#24296 = ADVANCED_FACE ( 'NONE', ( #123823 ), #59188, .F. ) ;
#24295 = CARTESIAN_POINT ( 'NONE',  ( 13.97604488694548053, -13.89961937509957401, 55.62609039468566863 ) ) ;
#24297 = CARTESIAN_POINT ( 'NONE',  ( -0.05219959533910754901, -16.53943276465976808, 37.49890960531436690 ) ) ;
#24298 = CARTESIAN_POINT ( 'NONE',  ( -8.224510206698948167, 14.34966873604960824, 85.41557627198102409 ) ) ;
#24300 = CARTESIAN_POINT ( 'NONE',  ( -16.21995358207276539, 7.366697692864364377, 39.93551001512066989 ) ) ;
#24299 = CARTESIAN_POINT ( 'NONE',  ( 15.80617190586769283, -15.72974639402175789, 110.6260903946857042 ) ) ;
#24301 = CARTESIAN_POINT ( 'NONE',  ( -5.719274019375665041, -21.55341960407619695, 24.79275706135235779 ) ) ;
#24302 = CARTESIAN_POINT ( 'NONE',  ( 9.564922557960805705, 16.46253265017160317, 109.5822429386476955 ) ) ;
#24303 = CARTESIAN_POINT ( 'NONE',  ( 16.46253265017160672, -9.564922557960803928, 83.33224293864768129 ) ) ;
#24304 = CARTESIAN_POINT ( 'NONE',  ( -21.53943276465977519, -0.05219959533937600094, 98.75109039468568994 ) ) ;
#24305 = CARTESIAN_POINT ( 'NONE',  ( -0.05219959533909027116, -19.03943276465977164, 77.49890960531435269 ) ) ;
#24306 = CARTESIAN_POINT ( 'NONE',  ( -0.05219959533907301413, -21.53943276465977519, 42.49890960531435979 ) ) ;
#24307 = CARTESIAN_POINT ( 'NONE',  ( 14.29746914071049879, -8.314922557960816363, 83.33224293864769550 ) ) ;
#24308 = CARTESIAN_POINT ( 'NONE',  ( 19.02544592524343514, -5.153800228976328945, 63.54057627198103830 ) ) ;
#24309 = CARTESIAN_POINT ( 'NONE',  ( 16.52544592524342804, -4.483927247898539470, 113.5405762719810383 ) ) ;
#24310 = CARTESIAN_POINT ( 'NONE',  ( 21.53943276465977519, 0.05219959533937863772, 26.25109039468567573 ) ) ;
#24311 = CARTESIAN_POINT ( 'NONE',  ( 5.719274019375673035, 21.55341960407619339, 67.29275706135234714 ) ) ;
#24312 = CARTESIAN_POINT ( 'NONE',  ( 19.05341960407611168, 5.049401038298154454, 43.95724293864769550 ) ) ;
#24313 = CARTESIAN_POINT ( 'NONE',  ( -12.14591786802326823, 12.06949235617739902, 58.12609039468568994 ) ) ;
#24314 = CARTESIAN_POINT ( 'NONE',  ( -0.05219959533937732626, 21.53943276465977519, 22.50109039468567573 ) ) ;
#24315 = CARTESIAN_POINT ( 'NONE',  ( 21.52544592524344225, -5.823673210054117533, 113.5405762719810383 ) ) ;
#24317 = CARTESIAN_POINT ( 'NONE',  ( 5.153800228976335163, 19.02544592524342804, 69.79057627198103830 ) ) ;
#24316 = CARTESIAN_POINT ( 'NONE',  ( -16.51473224551082808, 9.474510206698731452, 33.33442372801899722 ) ) ;
#24318 = DIRECTION ( 'NONE',  ( -1.000000000000000000, 0.000000000000000000, 0.000000000000000000 ) ) ;
#24319 = CARTESIAN_POINT ( 'NONE',  ( 10.72451020669871369, 18.67979575497193778, 67.08442372801901854 ) ) ;
#24320 = CARTESIAN_POINT ( 'NONE',  ( 21.55341960407610458, 5.719274019375980345, 58.95724293864770971 ) ) ;
#24321 = CARTESIAN_POINT ( 'NONE',  ( -12.14591786802309592, -12.06949235617757132, 41.87390960531435979 ) ) ;
#24323 = CARTESIAN_POINT ( 'NONE',  ( -10.72451020669870658, -18.67979575497194134, 104.5844237280190185 ) ) ;
#24322 = CARTESIAN_POINT ( 'NONE',  ( -15.72974639402176322, -15.80617190586768395, 74.37609039468568994 ) ) ;
#24324 = CARTESIAN_POINT ( 'NONE',  ( -12.06949235617756955, 12.14591786802309770, 55.62390960531436690 ) ) ;
#24325 = CARTESIAN_POINT ( 'NONE',  ( 4.483927247898545687, 16.52544592524342804, 99.79057627198103830 ) ) ;
#24326 = CARTESIAN_POINT ( 'NONE',  ( 19.02544592524334988, 5.153800228976608722, 56.45942372801898301 ) ) ;
#24327 = CARTESIAN_POINT ( 'NONE',  ( -12.06949235617756955, 12.14591786802309770, 25.62390960531435624 ) ) ;
#24328 = CARTESIAN_POINT ( 'NONE',  ( -0.05219959533937732626, 21.53943276465977519, 62.50109039468568284 ) ) ;
#24329 = CARTESIAN_POINT ( 'NONE',  ( 5.153800228976335163, 19.02544592524342804, 69.79057627198103830 ) ) ;
#24330 = CARTESIAN_POINT ( 'NONE',  ( -16.46253265017146816, -9.564922557961047289, 29.16775706135232937 ) ) ;
#24331 = CARTESIAN_POINT ( 'NONE',  ( 10.72451020669898902, -18.67979575497178502, 32.91557627198102409 ) ) ;
#24332 = CARTESIAN_POINT ( 'NONE',  ( -5.719274019375665041, -21.55341960407619695, 49.79275706135234714 ) ) ;
#24333 = CARTESIAN_POINT ( 'NONE',  ( 5.719274019375991003, -21.55341960407610458, 97.70724293864772392 ) ) ;
#24334 = CARTESIAN_POINT ( 'NONE',  ( -16.51473224551082808, 9.474510206698731452, 103.3344237280190043 ) ) ;
#24335 = CARTESIAN_POINT ( 'NONE',  ( -16.53943276465976808, -0.05219959533934237506, 58.75109039468568994 ) ) ;
#24337 = CARTESIAN_POINT ( 'NONE',  ( -18.67979575497178146, -10.72451020669898902, 91.66557627198103830 ) ) ;
#24336 = CARTESIAN_POINT ( 'NONE',  ( -18.09805431107246676, 5.500000000000103029, 56.01606229291885342 ) ) ;
#24338 = CARTESIAN_POINT ( 'NONE',  ( 4.483927247898545687, 16.52544592524342804, 89.79057627198103830 ) ) ;
#24339 = CARTESIAN_POINT ( 'NONE',  ( 18.22780087662126647, 5.499999999999818812, 41.48236817873107185 ) ) ;
#24340 = CARTESIAN_POINT ( 'NONE',  ( -4.379528057220086978, -16.55341960407618274, 24.79275706135235779 ) ) ;
#24341 = CARTESIAN_POINT ( 'NONE',  ( 5.823673210054125526, 21.52544592524343514, 54.79057627198104541 ) ) ;
#24342 = CARTESIAN_POINT ( 'NONE',  ( -16.55341960407617563, 4.379528057220093196, 93.54275706135234714 ) ) ;
#24343 = CARTESIAN_POINT ( 'NONE',  ( 9.474510206698971260, -16.51473224551069308, 22.91557627198102765 ) ) ;
#24344 = CARTESIAN_POINT ( 'NONE',  ( -12.14591786802326823, 12.06949235617739902, 53.12609039468568284 ) ) ;
#24345 = CARTESIAN_POINT ( 'NONE',  ( -18.67979575497193778, 10.72451020669871902, 28.33442372801902209 ) ) ;
#24346 = CARTESIAN_POINT ( 'NONE',  ( 10.81492255796078972, 18.62759615963270932, 44.58224293864769550 ) ) ;
#24347 = CARTESIAN_POINT ( 'NONE',  ( -16.53943276465976808, -0.05219959533934237506, 78.75109039468568994 ) ) ;
#24348 = CARTESIAN_POINT ( 'NONE',  ( -9.564922557960796823, -16.46253265017161027, 102.0822429386477097 ) ) ;
#24349 = CARTESIAN_POINT ( 'NONE',  ( 15.80617190586769283, -15.72974639402175789, 75.62609039468567573 ) ) ;
#24350 = CARTESIAN_POINT ( 'NONE',  ( 5.719274019375991003, -21.55341960407610458, 42.70724293864770260 ) ) ;
#24351 = CARTESIAN_POINT ( 'NONE',  ( 19.05341960407611168, 5.049401038298154454, 113.9572429386477097 ) ) ;
#24352 = ORIENTED_EDGE ( 'NONE', *, *, #42529, .T. ) ;
#24353 = CARTESIAN_POINT ( 'NONE',  ( -19.03943276465977164, -0.05219959533935918106, 48.75109039468566863 ) ) ;
#24354 = CARTESIAN_POINT ( 'NONE',  ( 12.14591786802327356, -12.06949235617739191, 65.62609039468568994 ) ) ;
#24355 = CARTESIAN_POINT ( 'NONE',  ( -15.80617190586745835, -15.72974639402198527, 36.87390960531435979 ) ) ;
#24356 = ORIENTED_EDGE ( 'NONE', *, *, #146444, .T. ) ;
#24357 = CARTESIAN_POINT ( 'NONE',  ( -9.564922557960796823, -16.46253265017161027, 92.08224293864769550 ) ) ;
#24358 = CARTESIAN_POINT ( 'NONE',  ( 4.483927247898790824, -16.52544592524335698, 110.2094237280190185 ) ) ;
#24359 = FACE_OUTER_BOUND ( 'NONE', #107478, .T. ) ;
#24360 = CARTESIAN_POINT ( 'NONE',  ( -4.483927247898539470, -16.52544592524342804, 107.2905762719810525 ) ) ;
#24361 = CARTESIAN_POINT ( 'NONE',  ( -21.55341960407610458, -5.719274019375992779, 51.45724293864770260 ) ) ;
#24362 = CARTESIAN_POINT ( 'NONE',  ( 5.049401038298161559, -19.05341960407611168, 42.70724293864767418 ) ) ;
#24363 = CARTESIAN_POINT ( 'NONE',  ( 4.379528057220092307, 16.55341960407617563, 82.29275706135234714 ) ) ;
#24364 = CARTESIAN_POINT ( 'NONE',  ( 15.72974639402176855, 15.80617190586768217, 36.87609039468568994 ) ) ;
#24365 = CARTESIAN_POINT ( 'NONE',  ( 16.46253265017146816, 9.564922557961045513, 91.66775706135234714 ) ) ;
#24366 = CARTESIAN_POINT ( 'NONE',  ( 14.29746914071049879, -8.314922557960816363, 83.33224293864769550 ) ) ;
#24367 = CARTESIAN_POINT ( 'NONE',  ( -5.049401038298153566, 19.05341960407611168, 50.20724293864770260 ) ) ;
#24368 = AXIS2_PLACEMENT_3D ( 'NONE', #112720, #4530, #198044 ) ;
#24369 = CARTESIAN_POINT ( 'NONE',  ( -5.049401038298153566, 19.05341960407611168, 30.20724293864768839 ) ) ;
#24370 = CARTESIAN_POINT ( 'NONE',  ( 18.67979575497194134, -10.72451020669871369, 110.8344237280190043 ) ) ;
#24371 = CARTESIAN_POINT ( 'NONE',  ( -19.03943276465977164, 0.05219959533909376836, 76.24890960531435269 ) ) ;
#24372 = CARTESIAN_POINT ( 'NONE',  ( -16.55341960407617563, 4.379528057220093196, 63.54275706135234003 ) ) ;
#24373 = CARTESIAN_POINT ( 'NONE',  ( -0.05219959533937732626, 21.53943276465977519, 97.50109039468567573 ) ) ;
#24374 = CARTESIAN_POINT ( 'NONE',  ( 10.72451020669898902, -18.67979575497178502, 52.91557627198103830 ) ) ;
#24375 = CARTESIAN_POINT ( 'NONE',  ( 14.34966873604972726, -8.224510206698740333, 75.83442372801900433 ) ) ;
#24376 = CARTESIAN_POINT ( 'NONE',  ( 19.03943276465977164, 0.05219959533936151252, 56.25109039468566863 ) ) ;
#24377 = CARTESIAN_POINT ( 'NONE',  ( 5.049401038297881783, 19.05341960407617563, 67.29275706135234714 ) ) ;
#24378 = ORIENTED_EDGE ( 'NONE', *, *, #107016, .T. ) ;
#24379 = CARTESIAN_POINT ( 'NONE',  ( 18.62759615963255655, 10.81492255796105972, 66.66775706135234714 ) ) ;
#24380 = CARTESIAN_POINT ( 'NONE',  ( 9.564922557960805705, 16.46253265017160317, 69.58224293864770971 ) ) ;
#24381 = CARTESIAN_POINT ( 'NONE',  ( 16.46253265017160672, -9.564922557960803928, 23.33224293864769194 ) ) ;
#24382 = CARTESIAN_POINT ( 'NONE',  ( 19.05341960407617918, -5.049401038297876454, 66.04275706135233293 ) ) ;
#24383 = CARTESIAN_POINT ( 'NONE',  ( 16.46253265017160672, -9.564922557960803928, 113.3322429386476955 ) ) ;
#24384 = CARTESIAN_POINT ( 'NONE',  ( -13.97604488694527625, -13.89961937509977652, 81.87390960531436690 ) ) ;
#24385 = CARTESIAN_POINT ( 'NONE',  ( -4.483927247898539470, -16.52544592524342804, 32.29057627198102409 ) ) ;
#24386 = CARTESIAN_POINT ( 'NONE',  ( 18.62759615963271287, -10.81492255796078972, 48.33224293864770260 ) ) ;
#24387 = CIRCLE ( 'NONE', #169250, 1.899999999999999689 ) ;
#24388 = CARTESIAN_POINT ( 'NONE',  ( -3.573655867282028392E-15, -180.0000000000000000, -23.00000000000000000 ) ) ;
#24389 = CARTESIAN_POINT ( 'NONE',  ( -0.05219959533937732626, 21.53943276465977519, 107.5010903946856899 ) ) ;
#24390 = SURFACE_SIDE_STYLE ('',( #39532 ) ) ;
#24391 = CARTESIAN_POINT ( 'NONE',  ( 16.46253265017160672, -9.564922557960803928, 53.33224293864768839 ) ) ;
#24392 = CARTESIAN_POINT ( 'NONE',  ( -13.97604488694527625, -13.89961937509977652, 26.87390960531434558 ) ) ;
#24393 = CIRCLE ( 'NONE', #14703, 37.87393738558669298 ) ;
#24394 = DIRECTION ( 'NONE',  ( 0.000000000000000000, -0.7071067811865485719, 0.7071067811865465735 ) ) ;
#24395 = CARTESIAN_POINT ( 'NONE',  ( -8.314922557961024197, 14.29746914071037800, 57.91775706135234714 ) ) ;
#24396 = CARTESIAN_POINT ( 'NONE',  ( -18.67979575497178146, -10.72451020669898902, 76.66557627198103830 ) ) ;
#24397 = CARTESIAN_POINT ( 'NONE',  ( 0.05219959533910956823, 16.53943276465976808, 59.99890960531436690 ) ) ;
#24399 = CARTESIAN_POINT ( 'NONE',  ( -26.99873734152928506, -22.49873734152901861, 1.110912703473986074 ) ) ;
#24398 = CARTESIAN_POINT ( 'NONE',  ( 0.05219959533909260263, 19.03943276465977164, 24.99890960531435269 ) ) ;
#24400 = CARTESIAN_POINT ( 'NONE',  ( 21.53943276465977519, 0.05219959533937863772, 41.25109039468568284 ) ) ;
#24401 = CARTESIAN_POINT ( 'NONE',  ( -5.049401038297874678, -19.05341960407617918, 49.79275706135231871 ) ) ;
#24402 = CARTESIAN_POINT ( 'NONE',  ( 16.51473224551069308, 9.474510206698969483, 29.16557627198103475 ) ) ;
#24403 = CARTESIAN_POINT ( 'NONE',  ( -15.80617190586768217, 15.72974639402176855, 83.12609039468568994 ) ) ;
#24404 = CARTESIAN_POINT ( 'NONE',  ( 16.19135201231366850, 7.376712067591940425, 97.68680854052031748 ) ) ;
#24405 = CARTESIAN_POINT ( 'NONE',  ( -16.55341960407611168, -4.379528057220339221, 41.45724293864769550 ) ) ;
#24406 = CARTESIAN_POINT ( 'NONE',  ( -36.91746825000000598, 11.99521256947798520, -1.224999997268813257 ) ) ;
#24407 = CARTESIAN_POINT ( 'NONE',  ( 0.05219959533907565091, 21.53943276465977519, 44.99890960531435979 ) ) ;
#24408 = CARTESIAN_POINT ( 'NONE',  ( -17.14385361876520975, 23.59649016807275856, 142.5750000027311728 ) ) ;
#24409 = CARTESIAN_POINT ( 'NONE',  ( 13.89961937509977652, -13.97604488694527269, 88.12390960531438111 ) ) ;
#24410 = CARTESIAN_POINT ( 'NONE',  ( 0.05219959533910956823, 16.53943276465976808, 89.99890960531438111 ) ) ;
#24411 = CARTESIAN_POINT ( 'NONE',  ( -12.14591786802326823, 12.06949235617739902, 23.12609039468567573 ) ) ;
#24412 = CARTESIAN_POINT ( 'NONE',  ( 15.72974639402199770, -15.80617190586745480, 63.12390960531435979 ) ) ;
#24413 = ORIENTED_EDGE ( 'NONE', *, *, #109644, .T. ) ;
#24414 = CARTESIAN_POINT ( 'NONE',  ( 16.51473224551069308, 9.474510206698969483, 39.16557627198103120 ) ) ;
#24416 = CARTESIAN_POINT ( 'NONE',  ( 15.80617190586746368, 15.72974639402197994, 94.37390960531436690 ) ) ;
#24415 = CARTESIAN_POINT ( 'NONE',  ( -13.97604488694527625, -13.89961937509977652, 81.87390960531436690 ) ) ;
#24418 = CARTESIAN_POINT ( 'NONE',  ( 13.89961937509977652, -13.97604488694527269, 98.12390960531433848 ) ) ;
#24417 = CARTESIAN_POINT ( 'NONE',  ( -0.05219959533934338120, 16.53943276465976808, 112.5010903946857042 ) ) ;
#24419 = CARTESIAN_POINT ( 'NONE',  ( -13.89961937509957401, -13.97604488694547875, 74.37609039468566152 ) ) ;
#24420 = CARTESIAN_POINT ( 'NONE',  ( -18.67979575497193778, 10.72451020669871902, 103.3344237280190043 ) ) ;
#24421 = CARTESIAN_POINT ( 'NONE',  ( -21.53943276465977519, 0.05219959533907696930, 71.24890960531435269 ) ) ;
#24422 = CARTESIAN_POINT ( 'NONE',  ( 21.55341960407610458, 5.719274019375980345, 43.95724293864769550 ) ) ;
#24423 = CARTESIAN_POINT ( 'NONE',  ( 19.03943276465977164, -0.05219959533909143690, 48.74890960531435979 ) ) ;
#24424 = CARTESIAN_POINT ( 'NONE',  ( -14.34966873604960291, -8.224510206698953496, 26.66557627198103475 ) ) ;
#24425 = CARTESIAN_POINT ( 'NONE',  ( 13.97604488694527802, 13.89961937509977652, 74.37390960531436690 ) ) ;
#24426 = ORIENTED_EDGE ( 'NONE', *, *, #8545, .F. ) ;
#24427 = CARTESIAN_POINT ( 'NONE',  ( -31.25074303019346189, -7.456059982492099891, 95.94898436327792979 ) ) ;
#24428 = CARTESIAN_POINT ( 'NONE',  ( -5.153800228976607833, 19.02544592524334988, 32.70942372801899722 ) ) ;
#24429 = CARTESIAN_POINT ( 'NONE',  ( -16.55341960407611168, -4.379528057220339221, 86.45724293864770971 ) ) ;
#24430 = CARTESIAN_POINT ( 'NONE',  ( -21.55341960407619339, 5.719274019375674811, 23.54275706135235424 ) ) ;
#24431 = CARTESIAN_POINT ( 'NONE',  ( -27.73933785331498925, -9.013057229001049109, 143.4750000027311785 ) ) ;
#24432 = CARTESIAN_POINT ( 'NONE',  ( 18.67979575497178502, 10.72451020669898547, 69.16557627198102409 ) ) ;
#24433 = CARTESIAN_POINT ( 'NONE',  ( 16.53943276465976808, 0.05219959533934440121, 96.25109039468568994 ) ) ;
#24434 = CARTESIAN_POINT ( 'NONE',  ( -19.03943276465977164, 0.05219959533909376836, 21.24890960531436335 ) ) ;
#24435 = CARTESIAN_POINT ( 'NONE',  ( 16.51473224551069308, 9.474510206698969483, 74.16557627198103830 ) ) ;
#24436 = CARTESIAN_POINT ( 'NONE',  ( -19.05341960407611168, -5.049401038298163336, 21.45724293864768839 ) ) ;
#24437 = CARTESIAN_POINT ( 'NONE',  ( 16.53943276465976808, -0.05219959533910856209, 23.74890960531435269 ) ) ;
#24438 = CARTESIAN_POINT ( 'NONE',  ( -5.719274019375665041, -21.55341960407619695, 59.79275706135234714 ) ) ;
#24439 = CARTESIAN_POINT ( 'NONE',  ( 13.89961937509977652, -13.97604488694527269, 113.1239096053143527 ) ) ;
#24440 = CARTESIAN_POINT ( 'NONE',  ( -15.72974639402176322, -15.80617190586768395, 89.37609039468568994 ) ) ;
#24441 = CARTESIAN_POINT ( 'NONE',  ( 16.51473224551069308, 9.474510206698969483, 49.16557627198102409 ) ) ;
#24442 = CARTESIAN_POINT ( 'NONE',  ( 5.049401038298161559, -19.05341960407611168, 52.70724293864767418 ) ) ;
#24443 = EDGE_LOOP ( 'NONE', ( #191036, #51219, #183121 ) ) ;
#24444 = CARTESIAN_POINT ( 'NONE',  ( -10.72451020669870658, -18.67979575497194134, 89.58442372801901854 ) ) ;
#24445 = CARTESIAN_POINT ( 'NONE',  ( 4.483927247898790824, -16.52544592524335698, 65.20942372801901854 ) ) ;
#24446 = CARTESIAN_POINT ( 'NONE',  ( -10.72451020669870658, -18.67979575497194134, 84.58442372801903275 ) ) ;
#24447 = CARTESIAN_POINT ( 'NONE',  ( -19.03943276465977164, 0.05219959533909376836, 116.2489096053143669 ) ) ;
#24448 = CARTESIAN_POINT ( 'NONE',  ( -19.02544592524334988, -5.153800228976617603, 93.95942372801900433 ) ) ;
#24449 = CARTESIAN_POINT ( 'NONE',  ( -18.62759615963255300, -10.81492255796106328, 59.16775706135234714 ) ) ;
#24450 = CARTESIAN_POINT ( 'NONE',  ( -8.224510206698735004, -14.34966873604973081, 39.58442372801901143 ) ) ;
#24451 = CARTESIAN_POINT ( 'NONE',  ( -10.72451020669898014, 18.67979575497178502, 85.41557627198102409 ) ) ;
#24452 = CARTESIAN_POINT ( 'NONE',  ( 13.97604488694548053, -13.89961937509957401, 85.62609039468568994 ) ) ;
#24453 = CARTESIAN_POINT ( 'NONE',  ( 19.03943276465977164, -0.05219959533909143690, 68.74890960531436690 ) ) ;
#24454 = CARTESIAN_POINT ( 'NONE',  ( 16.46253265017146816, 9.564922557961045513, 91.66775706135234714 ) ) ;
#24455 = CARTESIAN_POINT ( 'NONE',  ( -9.474510206698720793, -16.51473224551083518, 89.58442372801900433 ) ) ;
#24456 = CARTESIAN_POINT ( 'NONE',  ( -16.53943276465976808, 0.05219959533911058130, 51.24890960531436690 ) ) ;
#24457 = CARTESIAN_POINT ( 'NONE',  ( 19.02544592524334988, 5.153800228976608722, 81.45942372801897591 ) ) ;
#24458 = CARTESIAN_POINT ( 'NONE',  ( 16.55341960407618274, -4.379528057220086978, 61.04275706135234714 ) ) ;
#24459 = CARTESIAN_POINT ( 'NONE',  ( 19.03943276465977164, 0.05219959533936151252, 36.25109039468567573 ) ) ;
#24460 = CARTESIAN_POINT ( 'NONE',  ( -5.049401038298153566, 19.05341960407611168, 35.20724293864768839 ) ) ;
#24461 = CARTESIAN_POINT ( 'NONE',  ( 19.02544592524343514, -5.153800228976328945, 43.54057627198103120 ) ) ;
#24462 = CARTESIAN_POINT ( 'NONE',  ( -16.55341960407617563, 4.379528057220093196, 53.54275706135234714 ) ) ;
#24463 = CARTESIAN_POINT ( 'NONE',  ( -5.359611314223446995E-15, 29.16686587814335496, 140.8750000027311842 ) ) ;
#24464 = CARTESIAN_POINT ( 'NONE',  ( -28.82186960331499037, 2.428612866367529932E-14, 138.2500000054623683 ) ) ;
#24465 = CARTESIAN_POINT ( 'NONE',  ( -5.153800228976328057, -19.02544592524343514, 107.2905762719810383 ) ) ;
#24466 = CARTESIAN_POINT ( 'NONE',  ( 16.46253265017160672, -9.564922557960803928, 28.33224293864769550 ) ) ;
#24467 = ORIENTED_EDGE ( 'NONE', *, *, #177460, .T. ) ;
#24468 = CARTESIAN_POINT ( 'NONE',  ( 19.03943276465977164, 0.05219959533936151252, 96.25109039468567573 ) ) ;
#24469 = CARTESIAN_POINT ( 'NONE',  ( 21.55341960407610458, 5.719274019375980345, 43.95724293864769550 ) ) ;
#24471 = CARTESIAN_POINT ( 'NONE',  ( -16.51473224551082808, 9.474510206698731452, 108.3344237280190043 ) ) ;
#24470 = CARTESIAN_POINT ( 'NONE',  ( -5.049401038297874678, -19.05341960407617918, 29.79275706135232227 ) ) ;
#24472 = CARTESIAN_POINT ( 'NONE',  ( -19.03943276465977164, 0.05219959533909376836, 26.24890960531435624 ) ) ;
#24473 = CARTESIAN_POINT ( 'NONE',  ( -5.049401038298153566, 19.05341960407611168, 45.20724293864769550 ) ) ;
#24474 = CARTESIAN_POINT ( 'NONE',  ( -21.55341960407610458, -5.719274019375992779, 66.45724293864768129 ) ) ;
#24475 = CARTESIAN_POINT ( 'NONE',  ( 19.02544592524343514, -5.153800228976328945, 98.54057627198100988 ) ) ;
#24476 = CARTESIAN_POINT ( 'NONE',  ( -5.153800228976328057, -19.02544592524343514, 32.29057627198102409 ) ) ;
#24477 = CARTESIAN_POINT ( 'NONE',  ( -17.14385361876520264, -23.59649016807271238, 143.6750000027311671 ) ) ;
#24478 = CARTESIAN_POINT ( 'NONE',  ( -19.05341960407617563, 5.049401038297882671, 83.54275706135233293 ) ) ;
#24479 = CARTESIAN_POINT ( 'NONE',  ( -12.06949235617756955, 12.14591786802309770, 55.62390960531436690 ) ) ;
#24480 = CARTESIAN_POINT ( 'NONE',  ( -21.53943276465977519, 0.05219959533907696930, 36.24890960531435979 ) ) ;
#24481 = CARTESIAN_POINT ( 'NONE',  ( 15.80617190586769283, -15.72974639402175789, 105.6260903946856899 ) ) ;
#24482 = CARTESIAN_POINT ( 'NONE',  ( 10.72451020669898902, -18.67979575497178502, 92.91557627198103830 ) ) ;
#24483 = CARTESIAN_POINT ( 'NONE',  ( 10.81492255796106328, -18.62759615963255655, 75.41775706135233293 ) ) ;
#24484 = CARTESIAN_POINT ( 'NONE',  ( -10.81492255796105439, 18.62759615963255655, 72.91775706135234714 ) ) ;
#24485 = CARTESIAN_POINT ( 'NONE',  ( 13.97604488694527802, 13.89961937509977652, 114.3739096053143669 ) ) ;
#24487 = CARTESIAN_POINT ( 'NONE',  ( -10.81492255796105439, 18.62759615963255655, 57.91775706135234714 ) ) ;
#24486 = CARTESIAN_POINT ( 'NONE',  ( 16.55341960407618274, -4.379528057220086978, 106.0427570613523471 ) ) ;
#24488 = CARTESIAN_POINT ( 'NONE',  ( 16.51473224551069308, 9.474510206698969483, 64.16557627198102409 ) ) ;
#24489 = CARTESIAN_POINT ( 'NONE',  ( -5.153800228976607833, 19.02544592524334988, 37.70942372801899722 ) ) ;
#24490 = CARTESIAN_POINT ( 'NONE',  ( 15.72974639402176855, 15.80617190586768217, 36.87609039468568994 ) ) ;
#24491 = CARTESIAN_POINT ( 'NONE',  ( -19.05341960407611168, -5.049401038298163336, 71.45724293864766707 ) ) ;
#24492 = CARTESIAN_POINT ( 'NONE',  ( -12.14591786802309592, -12.06949235617757132, 81.87390960531435269 ) ) ;
#24493 = CARTESIAN_POINT ( 'NONE',  ( -16.55341960407611168, -4.379528057220339221, 41.45724293864769550 ) ) ;
#24494 = CARTESIAN_POINT ( 'NONE',  ( -15.72974639402197994, 15.80617190586746368, 60.62390960531437401 ) ) ;
#24495 = CARTESIAN_POINT ( 'NONE',  ( -5.153800228976328057, -19.02544592524343514, 57.29057627198103120 ) ) ;
#24496 = CARTESIAN_POINT ( 'NONE',  ( -21.53943276465977519, 0.05219959533907696930, 71.24890960531435269 ) ) ;
#24497 = CARTESIAN_POINT ( 'NONE',  ( 0.05219959533936267826, -19.03943276465977164, 45.00109039468566863 ) ) ;
#24499 = CARTESIAN_POINT ( 'NONE',  ( 12.06949235617757843, -12.14591786802309237, 63.12390960531435979 ) ) ;
#24498 = CARTESIAN_POINT ( 'NONE',  ( -9.564922557961040184, 16.46253265017147172, 22.91775706135233648 ) ) ;
#24500 = CARTESIAN_POINT ( 'NONE',  ( 10.81492255796078972, 18.62759615963270932, 39.58224293864769550 ) ) ;
#24501 = VERTEX_POINT ( 'NONE', #58214 ) ;
#24502 = ADVANCED_FACE ( 'NONE', ( #154189 ), #136047, .F. ) ;
#24503 = CARTESIAN_POINT ( 'NONE',  ( 0.000000000000000000, 0.000000000000000000, -33.00000000000000000 ) ) ;
#24505 = CARTESIAN_POINT ( 'NONE',  ( -5.359611314223446995E-15, 29.16686587814335851, 148.3750000027311842 ) ) ;
#24504 = CARTESIAN_POINT ( 'NONE',  ( -12.06949235617739369, -12.14591786802326823, 89.37609039468568994 ) ) ;
#24506 = CARTESIAN_POINT ( 'NONE',  ( -16.51473224551082808, 9.474510206698731452, 93.33442372801900433 ) ) ;
#24507 = CARTESIAN_POINT ( 'NONE',  ( -16.53943276465976808, 0.05219959533911058130, 61.24890960531435979 ) ) ;
#24508 = B_SPLINE_CURVE_WITH_KNOTS ( 'NONE', 3,
 ( #31117, #13947, #135328, #134329, #182818, #76611, #44300, #165658, #184792, #180841, #106945, #197001, #168618, #151484, #27156, #58467, #181825, #43304, #30118, #104972, #169620, #91759, #29140, #10981 ),
 .UNSPECIFIED., .F., .F.,
 ( 4, 2, 2, 2, 2, 2, 2, 2, 2, 2, 2, 4 ),
 ( 1.968491853871462031E-07, 0.0003260565056758917544, 0.0006519161621663963025, 0.0009777758186569011217, 0.001303635475147405616, 0.001955354788128404846, 0.002607074101109404726, 0.003258793414090403739, 0.003910512727071403620, 0.004562232040052403501, 0.004888091696542901272, 0.005213951353033399044 ),
 .UNSPECIFIED. ) ;
#24509 = DIRECTION ( 'NONE',  ( -1.000000000000000000, 0.000000000000000000, 0.000000000000000000 ) ) ;
#24510 = CARTESIAN_POINT ( 'NONE',  ( 5.153800228976335163, 19.02544592524342804, 44.79057627198103830 ) ) ;
#24511 = CARTESIAN_POINT ( 'NONE',  ( 14.34966873604960469, 8.224510206698951720, 34.16557627198102409 ) ) ;
#24512 = CARTESIAN_POINT ( 'NONE',  ( -9.564922557960796823, -16.46253265017161027, 92.08224293864769550 ) ) ;
#24513 = CARTESIAN_POINT ( 'NONE',  ( 19.03943276465977164, -0.05219959533909143690, 53.74890960531436690 ) ) ;
#24514 = CARTESIAN_POINT ( 'NONE',  ( -5.823673210054431948, 21.52544592524334988, 62.70942372801902565 ) ) ;
#24515 = CARTESIAN_POINT ( 'NONE',  ( 0.05219959533909260263, 19.03943276465977164, 74.99890960531435269 ) ) ;
#24516 = CARTESIAN_POINT ( 'NONE',  ( -5.049401038298153566, 19.05341960407611168, 30.20724293864768839 ) ) ;
#24517 = CARTESIAN_POINT ( 'NONE',  ( -19.05341960407611168, -5.049401038298163336, 76.45724293864769550 ) ) ;
#24518 = CARTESIAN_POINT ( 'NONE',  ( 0.05219959533907565091, 21.53943276465977519, 44.99890960531435979 ) ) ;
#24519 = CARTESIAN_POINT ( 'NONE',  ( 5.153800228976335163, 19.02544592524342804, 39.79057627198100988 ) ) ;
#24520 = CARTESIAN_POINT ( 'NONE',  ( -21.52544592524343514, 5.823673210054127303, 41.04057627198103120 ) ) ;
#24521 = CARTESIAN_POINT ( 'NONE',  ( 12.06949235617739724, 12.14591786802326823, 106.8760903946856899 ) ) ;
#24522 = CARTESIAN_POINT ( 'NONE',  ( -19.02544592524334988, -5.153800228976617603, 28.95942372801900433 ) ) ;
#24524 = CARTESIAN_POINT ( 'NONE',  ( -14.29746914071037622, -8.314922557961029526, 74.16775706135231871 ) ) ;
#24523 = CARTESIAN_POINT ( 'NONE',  ( 16.52544592524335698, 4.483927247898782831, 46.45942372801901854 ) ) ;
#24525 = DIRECTION ( 'NONE',  ( -1.000000000000000000, 0.000000000000000000, -0.000000000000000000 ) ) ;
#24526 = CARTESIAN_POINT ( 'NONE',  ( -14.34966873604972548, 8.224510206698743886, 63.33442372801900433 ) ) ;
#24527 = CARTESIAN_POINT ( 'NONE',  ( 21.53943276465977519, -0.05219959533907433946, 28.74890960531435624 ) ) ;
#24528 = CARTESIAN_POINT ( 'NONE',  ( -16.51473224551069308, -9.474510206698971260, 31.66557627198102054 ) ) ;
#24529 = CARTESIAN_POINT ( 'NONE',  ( 8.314922557961029526, -14.29746914071037800, 40.41775706135234714 ) ) ;
#24530 = CARTESIAN_POINT ( 'NONE',  ( 19.03943276465977164, -0.05219959533909143690, 53.74890960531436690 ) ) ;
#24531 = CARTESIAN_POINT ( 'NONE',  ( 5.823673210054444382, -21.52544592524334988, 40.20942372801901854 ) ) ;
#24532 = CARTESIAN_POINT ( 'NONE',  ( 8.314922557961029526, -14.29746914071037800, 40.41775706135234714 ) ) ;
#24533 = CARTESIAN_POINT ( 'NONE',  ( 4.379528057220092307, 16.55341960407617563, 97.29275706135234714 ) ) ;
#24534 = CARTESIAN_POINT ( 'NONE',  ( -26.03370437638690049, -6.875205692009850544, 160.5968874236872637 ) ) ;
#24535 = CARTESIAN_POINT ( 'NONE',  ( 21.53943276465977519, 0.05219959533937863772, 96.25109039468568994 ) ) ;
#24537 = EDGE_CURVE ( 'NONE', #74939, #108968, #153182, .T. ) ;
#24536 = CARTESIAN_POINT ( 'NONE',  ( -0.05219959533936034679, 19.03943276465977164, 97.50109039468567573 ) ) ;
#24538 = CARTESIAN_POINT ( 'NONE',  ( -19.03943276465977164, -0.05219959533935918106, 73.75109039468566152 ) ) ;
#24539 = CARTESIAN_POINT ( 'NONE',  ( -12.14591786802309592, -12.06949235617757132, 66.87390960531436690 ) ) ;
#24540 = CARTESIAN_POINT ( 'NONE',  ( -13.97604488694527625, -13.89961937509977652, 21.87390960531435979 ) ) ;
#24542 = CARTESIAN_POINT ( 'NONE',  ( 17.44270441346520428, 5.991230190322989202, 78.86335079264232206 ) ) ;
#24541 = CARTESIAN_POINT ( 'NONE',  ( 16.46253265017146816, 9.564922557961045513, 56.66775706135233293 ) ) ;
#24543 = CARTESIAN_POINT ( 'NONE',  ( -15.80617190586768217, 15.72974639402176855, 63.12609039468568994 ) ) ;
#24544 = CARTESIAN_POINT ( 'NONE',  ( -14.29746914071037622, -8.314922557961029526, 24.16775706135235424 ) ) ;
#24545 = CARTESIAN_POINT ( 'NONE',  ( -18.22780087662123805, 5.499999999999981348, 91.01763182126894947 ) ) ;
#24546 = CARTESIAN_POINT ( 'NONE',  ( 21.52544592524344225, -5.823673210054117533, 28.54057627198103120 ) ) ;
#24547 = CARTESIAN_POINT ( 'NONE',  ( -16.51473224551082808, 9.474510206698731452, 103.3344237280190043 ) ) ;
#24548 = CARTESIAN_POINT ( 'NONE',  ( 19.03943276465977164, -0.05219959533909143690, 113.7489096053143669 ) ) ;
#24549 = CARTESIAN_POINT ( 'NONE',  ( -24.95262708931866769, 12.69764001896744432, 166.0532406165024497 ) ) ;
#24550 = CARTESIAN_POINT ( 'NONE',  ( -16.53943276465976808, 0.05219959533911058130, 116.2489096053143669 ) ) ;
#24551 = CARTESIAN_POINT ( 'NONE',  ( -19.03943276465977164, -0.05219959533935918106, 18.75109039468567218 ) ) ;
#24552 = CARTESIAN_POINT ( 'NONE',  ( 5.049401038298161559, -19.05341960407611168, 57.70724293864769550 ) ) ;
#24553 = AXIS2_PLACEMENT_3D ( 'NONE', #178300, #5422, #4421 ) ;
#24554 = CARTESIAN_POINT ( 'NONE',  ( -21.55341960407619339, 5.719274019375674811, 68.54275706135234714 ) ) ;
#24555 = CARTESIAN_POINT ( 'NONE',  ( -15.80617190586768217, 15.72974639402176855, 98.12609039468570415 ) ) ;
#24556 = CARTESIAN_POINT ( 'NONE',  ( 14.34966873604960469, 8.224510206698951720, 29.16557627198103120 ) ) ;
#24557 = CARTESIAN_POINT ( 'NONE',  ( 5.049401038298161559, -19.05341960407611168, 82.70724293864770971 ) ) ;
#24558 = CARTESIAN_POINT ( 'NONE',  ( 18.67979575497194134, -10.72451020669871369, 60.83442372801901854 ) ) ;
#24559 = CARTESIAN_POINT ( 'NONE',  ( -10.72451020669870658, -18.67979575497194134, 49.58442372801901143 ) ) ;
#24561 = CARTESIAN_POINT ( 'NONE',  ( 16.46253265017160672, -9.564922557960803928, 108.3322429386476955 ) ) ;
#24560 = CARTESIAN_POINT ( 'NONE',  ( 19.05341960407617918, -5.049401038297876454, 86.04275706135233293 ) ) ;
#24562 = CARTESIAN_POINT ( 'NONE',  ( -0.05219959533909027116, -19.03943276465977164, 22.49890960531436690 ) ) ;
#24563 = CARTESIAN_POINT ( 'NONE',  ( -5.719274019375978568, 21.55341960407610458, 90.20724293864770971 ) ) ;
#24564 = CARTESIAN_POINT ( 'NONE',  ( -13.97604488694547697, 13.89961937509957934, 33.12609039468566863 ) ) ;
#24565 = CARTESIAN_POINT ( 'NONE',  ( -16.53943276465976808, 0.05219959533911058130, 96.24890960531435269 ) ) ;
#24566 = CARTESIAN_POINT ( 'NONE',  ( -13.97604488694527625, -13.89961937509977652, 51.87390960531436690 ) ) ;
#24567 = CARTESIAN_POINT ( 'NONE',  ( 19.02544592524334988, 5.153800228976608722, 96.45942372801897591 ) ) ;
#24568 = CARTESIAN_POINT ( 'NONE',  ( -16.55341960407611168, -4.379528057220339221, 56.45724293864768839 ) ) ;
#24569 = CARTESIAN_POINT ( 'NONE',  ( -21.52544592524334988, -5.823673210054445271, 108.9594237280190185 ) ) ;
#24570 = CARTESIAN_POINT ( 'NONE',  ( 9.564922557960805705, 16.46253265017160317, 99.58224293864770971 ) ) ;
#24571 = CARTESIAN_POINT ( 'NONE',  ( 16.46253265017146816, 9.564922557961045513, 71.66775706135233293 ) ) ;
#24572 = CARTESIAN_POINT ( 'NONE',  ( 21.52544592524344225, -5.823673210054117533, 93.54057627198103830 ) ) ;
#24573 = CARTESIAN_POINT ( 'NONE',  ( -10.81492255796105439, 18.62759615963255655, 47.91775706135234714 ) ) ;
#24574 = CARTESIAN_POINT ( 'NONE',  ( -4.379528057220086978, -16.55341960407618274, 39.79275706135235424 ) ) ;
#24575 = CARTESIAN_POINT ( 'NONE',  ( -16.53943276465976808, -0.05219959533934237506, 93.75109039468567573 ) ) ;
#24577 = CARTESIAN_POINT ( 'NONE',  ( 10.72451020669871369, 18.67979575497193778, 37.08442372801901143 ) ) ;
#24576 = CARTESIAN_POINT ( 'NONE',  ( 14.29746914071037800, 8.314922557961029526, 41.66775706135235424 ) ) ;
#24578 = CARTESIAN_POINT ( 'NONE',  ( -10.72451020669898014, 18.67979575497178502, 40.41557627198103120 ) ) ;
#24579 = CARTESIAN_POINT ( 'NONE',  ( -5.153800228976328057, -19.02544592524343514, 37.29057627198102409 ) ) ;
#24580 = CARTESIAN_POINT ( 'NONE',  ( -6.020228577223754586E-15, 39.95556452105416412, -8.249999994537628112 ) ) ;
#24581 = CARTESIAN_POINT ( 'NONE',  ( -14.29746914071037622, -8.314922557961029526, 59.16775706135234714 ) ) ;
#24582 = B_SPLINE_CURVE_WITH_KNOTS ( 'NONE', 3,
 ( #73885, #74864, #89032, #136526, #152682, #87040, #102213, #163902, #148725, #150723, #12222, #133542, #195233, #198207, #135555, #180082, #59678, #121350, #164896, #56716, #183043, #41551, #118388, #197227, #26390, #58689, #44526, #106182 ),
 .UNSPECIFIED., .F., .F.,
 ( 4, 2, 2, 2, 2, 2, 2, 2, 2, 2, 2, 2, 2, 4 ),
 ( 1.734723475976807094E-18, 0.0005512667261461052853, 0.001102533452292208836, 0.001240350133828699080, 0.001378166815365189542, 0.001447075156133453963, 0.001515983496901718384, 0.001653800178438247226, 0.001929433541511376684, 0.002205066904584506143, 0.003307600356876775477, 0.004410133809169045245, 0.006615200713753665446, 0.008820267618338286514 ),
 .UNSPECIFIED. ) ;
#24583 = CARTESIAN_POINT ( 'NONE',  ( -18.67979575497178146, -10.72451020669898902, 86.66557627198102409 ) ) ;
#24584 = CARTESIAN_POINT ( 'NONE',  ( -12.06949235617756955, 12.14591786802309770, 35.62390960531437401 ) ) ;
#24585 = CARTESIAN_POINT ( 'NONE',  ( -16.52544592524335698, -4.483927247898792601, 63.95942372801901854 ) ) ;
#24586 = CARTESIAN_POINT ( 'NONE',  ( -19.05341960407611168, -5.049401038298163336, 61.45724293864769550 ) ) ;
#24587 = CARTESIAN_POINT ( 'NONE',  ( 5.049401038297881783, 19.05341960407617563, 87.29275706135234714 ) ) ;
#24588 = CARTESIAN_POINT ( 'NONE',  ( -10.72451020669898014, 18.67979575497178502, 80.41557627198103830 ) ) ;
#24589 = CARTESIAN_POINT ( 'NONE',  ( 8.314922557960818139, 14.29746914071049879, 34.58224293864770260 ) ) ;
#24590 = ORIENTED_EDGE ( 'NONE', *, *, #123454, .T. ) ;
#24591 = CARTESIAN_POINT ( 'NONE',  ( 25.52568752982265110, 9.519068727185217682, 170.8917780290381927 ) ) ;
#24592 = CARTESIAN_POINT ( 'NONE',  ( 15.80617190586746368, 15.72974639402197994, 59.37390960531436690 ) ) ;
#24593 = ORIENTED_EDGE ( 'NONE', *, *, #170916, .F. ) ;
#24594 = CARTESIAN_POINT ( 'NONE',  ( -16.53943276465976808, -0.05219959533934237506, 103.7510903946857042 ) ) ;
#24595 = ORIENTED_EDGE ( 'NONE', *, *, #145326, .F. ) ;
#24596 = CYLINDRICAL_SURFACE ( 'NONE', #111451, 1.500000000000001332 ) ;
#24597 = CARTESIAN_POINT ( 'NONE',  ( 18.62759615963271287, -10.81492255796078972, 93.33224293864769550 ) ) ;
#24598 = AXIS2_PLACEMENT_3D ( 'NONE', #73668, #196026, #165670 ) ;
#24599 = CARTESIAN_POINT ( 'NONE',  ( -8.314922557960811034, -14.29746914071050412, 22.08224293864769194 ) ) ;
#24600 = CARTESIAN_POINT ( 'NONE',  ( 16.55341960407618274, -4.379528057220086978, 31.04275706135234714 ) ) ;
#24601 = CARTESIAN_POINT ( 'NONE',  ( -5.049401038298153566, 19.05341960407611168, 30.20724293864768839 ) ) ;
#24602 = CARTESIAN_POINT ( 'NONE',  ( -13.97604488694527625, -13.89961937509977652, 66.87390960531436690 ) ) ;
#24603 = CARTESIAN_POINT ( 'NONE',  ( -28.82186960331499392, 9.364793116373565596, 145.8999999999999773 ) ) ;
#24604 = CARTESIAN_POINT ( 'NONE',  ( 21.53943276465977519, -0.05219959533907433946, 23.74890960531435269 ) ) ;
#24605 = CARTESIAN_POINT ( 'NONE',  ( 5.153800228976335163, 19.02544592524342804, 114.7905762719810241 ) ) ;
#24606 = CARTESIAN_POINT ( 'NONE',  ( 19.02544592524334988, 5.153800228976608722, 111.4594237280190043 ) ) ;
#24607 = CARTESIAN_POINT ( 'NONE',  ( -16.51473224551082808, 9.474510206698731452, 33.33442372801899722 ) ) ;
#24608 = CARTESIAN_POINT ( 'NONE',  ( 21.53943276465977519, -0.05219959533907433946, 83.74890960531435269 ) ) ;
#24609 = CARTESIAN_POINT ( 'NONE',  ( 0.05219959533910956823, 16.53943276465976808, 24.99890960531435624 ) ) ;
#24610 = CARTESIAN_POINT ( 'NONE',  ( 5.719274019375991003, -21.55341960407610458, 47.70724293864770260 ) ) ;
#24612 = CARTESIAN_POINT ( 'NONE',  ( 5.153800228976615827, -19.02544592524334988, 110.2094237280189901 ) ) ;
#24611 = CARTESIAN_POINT ( 'NONE',  ( 21.52544592524344225, -5.823673210054117533, 83.54057627198102409 ) ) ;
#24613 = CARTESIAN_POINT ( 'NONE',  ( 19.03943276465977164, -0.05219959533909143690, 108.7489096053143527 ) ) ;
#24614 = CARTESIAN_POINT ( 'NONE',  ( -0.05219959533937732626, 21.53943276465977519, 77.50109039468567573 ) ) ;
#24615 = CARTESIAN_POINT ( 'NONE',  ( -5.049401038298153566, 19.05341960407611168, 55.20724293864769550 ) ) ;
#24616 = CARTESIAN_POINT ( 'NONE',  ( -0.05219959533910754901, -16.53943276465976808, 102.4989096053143811 ) ) ;
#24617 = CARTESIAN_POINT ( 'NONE',  ( 31.99745974829802719, 5.643669518723337220, 90.03617080843918075 ) ) ;
#24618 = CARTESIAN_POINT ( 'NONE',  ( -5.153800228976328057, -19.02544592524343514, 72.29057627198102409 ) ) ;
#24619 = CARTESIAN_POINT ( 'NONE',  ( -4.379528057220328563, 16.55341960407611168, 95.20724293864769550 ) ) ;
#24620 = ORIENTED_EDGE ( 'NONE', *, *, #59575, .F. ) ;
#24621 = CARTESIAN_POINT ( 'NONE',  ( 19.03943276465977164, 0.05219959533936151252, 96.25109039468567573 ) ) ;
#24622 = CARTESIAN_POINT ( 'NONE',  ( 19.35543954521081034, 5.499999999999526601, 92.08901960356452321 ) ) ;
#24623 = CARTESIAN_POINT ( 'NONE',  ( -9.474510206698964154, 16.51473224551069663, 65.41557627198102409 ) ) ;
#24625 = CARTESIAN_POINT ( 'NONE',  ( -0.05219959533909027116, -19.03943276465977164, 97.49890960531436690 ) ) ;
#24624 = CARTESIAN_POINT ( 'NONE',  ( -18.62759615963255300, -10.81492255796106328, 89.16775706135236135 ) ) ;
#24626 = CARTESIAN_POINT ( 'NONE',  ( 4.483927247898790824, -16.52544592524335698, 75.20942372801901854 ) ) ;
#24627 = CARTESIAN_POINT ( 'NONE',  ( 21.99873734152949822, 27.49873734152890137, 8.181980515339454030 ) ) ;
#24628 = CARTESIAN_POINT ( 'NONE',  ( 0.05219959533936267826, -19.03943276465977164, 50.00109039468566863 ) ) ;
#24629 = CARTESIAN_POINT ( 'NONE',  ( 15.80617190586769283, -15.72974639402175789, 105.6260903946856899 ) ) ;
#24630 = CARTESIAN_POINT ( 'NONE',  ( 36.82860559483758323, 3.362349505172660624, 49.36759404993755851 ) ) ;
#24631 = DIRECTION ( 'NONE',  ( -0.000000000000000000, -0.000000000000000000, 1.000000000000000000 ) ) ;
#24632 = CARTESIAN_POINT ( 'NONE',  ( 0.05219959533934541429, -16.53943276465976808, 100.0010903946857042 ) ) ;
#24633 = CARTESIAN_POINT ( 'NONE',  ( 16.37811251030165849, -0.9487569900773658027, -59.27680374464309665 ) ) ;
#24634 = CARTESIAN_POINT ( 'NONE',  ( -4.483927247898782831, 16.52544592524335698, 87.70942372801901854 ) ) ;
#24635 = CARTESIAN_POINT ( 'NONE',  ( 17.44270441346519718, 5.991230190322989202, 68.86335079264230785 ) ) ;
#24636 = CARTESIAN_POINT ( 'NONE',  ( 8.314922557961029526, -14.29746914071037800, 70.41775706135236135 ) ) ;
#24637 = VERTEX_POINT ( 'NONE', #120857 ) ;
#24639 = EDGE_CURVE ( 'NONE', #179364, #113699, #76347, .T. ) ;
#24638 = CARTESIAN_POINT ( 'NONE',  ( 10.81492255796106328, -18.62759615963255655, 75.41775706135233293 ) ) ;
#24640 = CARTESIAN_POINT ( 'NONE',  ( -19.03943276465977164, -0.05219959533935918106, 83.75109039468567573 ) ) ;
#24641 = CARTESIAN_POINT ( 'NONE',  ( 9.564922557961047289, -16.46253265017146816, 20.41775706135233293 ) ) ;
#24642 = CARTESIAN_POINT ( 'NONE',  ( 16.46253265017160672, -9.564922557960803928, 63.33224293864769550 ) ) ;
#24643 = CARTESIAN_POINT ( 'NONE',  ( 19.02544592524343514, -5.153800228976328945, 53.54057627198102409 ) ) ;
#24644 = DIRECTION ( 'NONE',  ( 0.000000000000000000, 0.000000000000000000, -1.000000000000000000 ) ) ;
#24645 = CARTESIAN_POINT ( 'NONE',  ( -18.62759615963270932, 10.81492255796079327, 85.83224293864768129 ) ) ;
#24646 = CARTESIAN_POINT ( 'NONE',  ( 18.62759615963271287, -10.81492255796078972, 33.33224293864769550 ) ) ;
#24647 = CARTESIAN_POINT ( 'NONE',  ( -5.049401038298153566, 19.05341960407611168, 35.20724293864768839 ) ) ;
#24648 = CARTESIAN_POINT ( 'NONE',  ( -12.06949235617739369, -12.14591786802326823, 69.37609039468567573 ) ) ;
#24649 = ORIENTED_EDGE ( 'NONE', *, *, #61842, .T. ) ;
#24650 = CARTESIAN_POINT ( 'NONE',  ( 21.53943276465977519, 0.05219959533937863772, 26.25109039468567573 ) ) ;
#24652 = CARTESIAN_POINT ( 'NONE',  ( -11.74264578624799782, -36.14014761921581709, -1.599999999999999867 ) ) ;
#24651 = CARTESIAN_POINT ( 'NONE',  ( 16.53943276465976808, -0.05219959533910856209, 68.74890960531435269 ) ) ;
#24653 = CARTESIAN_POINT ( 'NONE',  ( 16.53943276465976808, 0.05219959533934440121, 21.25109039468567218 ) ) ;
#24654 = CARTESIAN_POINT ( 'NONE',  ( -19.02544592524334988, -5.153800228976617603, 48.95942372801900433 ) ) ;
#24655 = CARTESIAN_POINT ( 'NONE',  ( -16.53943276465976808, 0.05219959533911058130, 56.24890960531436690 ) ) ;
#24656 = CARTESIAN_POINT ( 'NONE',  ( -15.72974639402176322, -15.80617190586768395, 34.37609039468568284 ) ) ;
#24658 = CARTESIAN_POINT ( 'NONE',  ( 21.53943276465977519, -0.05219959533907433946, 78.74890960531436690 ) ) ;
#24657 = CARTESIAN_POINT ( 'NONE',  ( 24.95432927374998400, -4.974562764236790002, 189.9999999999999716 ) ) ;
#24659 = CARTESIAN_POINT ( 'NONE',  ( 9.564922557960805705, 16.46253265017160317, 99.58224293864770971 ) ) ;
#24660 = CARTESIAN_POINT ( 'NONE',  ( -14.34966873604960291, -8.224510206698953496, 66.66557627198102409 ) ) ;
#24661 = CARTESIAN_POINT ( 'NONE',  ( 31.47347929072392247, -24.22385046035867262, -19.66336643903433767 ) ) ;
#24662 = CARTESIAN_POINT ( 'NONE',  ( -26.46959431505283789, -27.26463967846487435, -25.00000000000000000 ) ) ;
#24663 = CARTESIAN_POINT ( 'NONE',  ( -19.02544592524334988, -5.153800228976617603, 63.95942372801899012 ) ) ;
#24664 = CARTESIAN_POINT ( 'NONE',  ( 5.823673210054125526, 21.52544592524343514, 109.7905762719810383 ) ) ;
#24665 = CARTESIAN_POINT ( 'NONE',  ( 13.89961937509977652, -13.97604488694527269, 58.12390960531436690 ) ) ;
#24666 = CARTESIAN_POINT ( 'NONE',  ( -0.05219959533936034679, 19.03943276465977164, 42.50109039468566152 ) ) ;
#24667 = CARTESIAN_POINT ( 'NONE',  ( 5.153800228976335163, 19.02544592524342804, 34.79057627198102409 ) ) ;
#24668 = EDGE_CURVE ( 'NONE', #19818, #122419, #104712, .T. ) ;
#24669 = CARTESIAN_POINT ( 'NONE',  ( -21.53943276465977519, -0.05219959533937600094, 63.75109039468568284 ) ) ;
#24670 = CARTESIAN_POINT ( 'NONE',  ( -17.44279575226823908, -5.990770900252440079, 69.16442432485682446 ) ) ;
#24671 = CARTESIAN_POINT ( 'NONE',  ( 12.06949235617757843, -12.14591786802309237, 38.12390960531436690 ) ) ;
#24672 = CARTESIAN_POINT ( 'NONE',  ( -19.02544592524342804, 5.153800228976336051, 66.04057627198103830 ) ) ;
#24673 = CARTESIAN_POINT ( 'NONE',  ( -0.05219959533907301413, -21.53943276465977519, 72.49890960531435269 ) ) ;
#24674 = CARTESIAN_POINT ( 'NONE',  ( -19.05341960407611168, -5.049401038298163336, 61.45724293864769550 ) ) ;
#24675 = ORIENTED_EDGE ( 'NONE', *, *, #182212, .F. ) ;
#24676 = CARTESIAN_POINT ( 'NONE',  ( 21.52544592524344225, -5.823673210054117533, 63.54057627198103830 ) ) ;
#24677 = ORIENTED_EDGE ( 'NONE', *, *, #121976, .T. ) ;
#24678 = CARTESIAN_POINT ( 'NONE',  ( -5.719274019375665041, -21.55341960407619695, 99.79275706135234714 ) ) ;
#24681 = CARTESIAN_POINT ( 'NONE',  ( -8.224510206698948167, 14.34966873604960824, 80.41557627198103830 ) ) ;
#24680 = CARTESIAN_POINT ( 'NONE',  ( -14.29746914071037622, -8.314922557961029526, 99.16775706135234714 ) ) ;
#24679 = CYLINDRICAL_SURFACE ( 'NONE', #186623, 5.000000000000002665 ) ;
#24682 = CARTESIAN_POINT ( 'NONE',  ( 19.02544592524334988, 5.153800228976608722, 96.45942372801897591 ) ) ;
#24683 = EDGE_LOOP ( 'NONE', ( #195751, #105223, #94010 ) ) ;
#24684 = CARTESIAN_POINT ( 'NONE',  ( -19.05341960407617563, 5.049401038297882671, 38.54275706135233293 ) ) ;
#24685 = CARTESIAN_POINT ( 'NONE',  ( 0.05219959533934541429, -16.53943276465976808, 105.0010903946856757 ) ) ;
#24686 = CARTESIAN_POINT ( 'NONE',  ( -9.474510206698720793, -16.51473224551083518, 29.58442372801900433 ) ) ;
#24687 = CARTESIAN_POINT ( 'NONE',  ( 19.03943276465977164, -0.05219959533909143690, 83.74890960531436690 ) ) ;
#24688 = CARTESIAN_POINT ( 'NONE',  ( -18.67979575497178146, -10.72451020669898902, 66.66557627198102409 ) ) ;
#24689 = CARTESIAN_POINT ( 'NONE',  ( -29.64655366937558867, -26.74020568361526529, -17.07338589137929574 ) ) ;
#24690 = CARTESIAN_POINT ( 'NONE',  ( -8.314922557960811034, -14.29746914071050412, 112.0822429386477097 ) ) ;
#24691 = CARTESIAN_POINT ( 'NONE',  ( 10.72451020669871369, 18.67979575497193778, 92.08442372801901854 ) ) ;
#24692 = CARTESIAN_POINT ( 'NONE',  ( -12.06949235617739369, -12.14591786802326823, 74.37609039468568994 ) ) ;
#24693 = CARTESIAN_POINT ( 'NONE',  ( 21.55341960407619695, -5.719274019375665929, 31.04275706135234714 ) ) ;
#24694 = CARTESIAN_POINT ( 'NONE',  ( -16.55341960407617563, 4.379528057220093196, 33.54275706135234714 ) ) ;
#24695 = CARTESIAN_POINT ( 'NONE',  ( -16.51473224551069308, -9.474510206698971260, 111.6655762719810383 ) ) ;
#24696 = CARTESIAN_POINT ( 'NONE',  ( -19.02544592524342804, 5.153800228976336051, 36.04057627198100988 ) ) ;
#24697 = CARTESIAN_POINT ( 'NONE',  ( -19.05341960407611168, -5.049401038298163336, 46.45724293864768129 ) ) ;
#24698 = AXIS2_PLACEMENT_3D ( 'NONE', #120499, #73035, #193375 ) ;
#24699 = CARTESIAN_POINT ( 'NONE',  ( 8.314922557961029526, -14.29746914071037800, 50.41775706135235424 ) ) ;
#24700 = CARTESIAN_POINT ( 'NONE',  ( -16.55341960407611168, -4.379528057220339221, 91.45724293864769550 ) ) ;
#24701 = CARTESIAN_POINT ( 'NONE',  ( 14.29746914071037800, 8.314922557961029526, 101.6677570613523613 ) ) ;
#24704 = CARTESIAN_POINT ( 'NONE',  ( 13.89961937509977652, -13.97604488694527269, 68.12390960531436690 ) ) ;
#24703 = CARTESIAN_POINT ( 'NONE',  ( -0.05219959533909027116, -19.03943276465977164, 77.49890960531435269 ) ) ;
#24702 = CARTESIAN_POINT ( 'NONE',  ( -18.62759615963255300, -10.81492255796106328, 39.16775706135235424 ) ) ;
#24705 = CARTESIAN_POINT ( 'NONE',  ( -9.474510206698964154, 16.51473224551069663, 100.4155762719810241 ) ) ;
#24706 = CARTESIAN_POINT ( 'NONE',  ( 16.52544592524342804, -4.483927247898539470, 28.54057627198103120 ) ) ;
#24707 = CARTESIAN_POINT ( 'NONE',  ( 12.06949235617739724, 12.14591786802326823, 96.87609039468568994 ) ) ;
#24708 = VERTEX_POINT ( 'NONE', #151227 ) ;
#24709 = CARTESIAN_POINT ( 'NONE',  ( 0.05219959533936267826, -19.03943276465977164, 40.00109039468566152 ) ) ;
#24710 = CARTESIAN_POINT ( 'NONE',  ( 9.474510206698971260, -16.51473224551069308, 107.9155762719810383 ) ) ;
#24711 = CARTESIAN_POINT ( 'NONE',  ( -13.97604488694527625, -13.89961937509977652, 56.87390960531434558 ) ) ;
#24712 = CARTESIAN_POINT ( 'NONE',  ( -16.46253265017146816, -9.564922557961047289, 34.16775706135233293 ) ) ;
#24713 = CARTESIAN_POINT ( 'NONE',  ( -22.81625015709510507, 31.40387420917330275, -4.924999997268813878 ) ) ;
#24714 = CARTESIAN_POINT ( 'NONE',  ( 16.52544592524335698, 4.483927247898782831, 46.45942372801901854 ) ) ;
#24716 = CARTESIAN_POINT ( 'NONE',  ( 8.224510206698742110, 14.34966873604972548, 52.08442372801901854 ) ) ;
#24715 = CARTESIAN_POINT ( 'NONE',  ( -13.97604488694547697, 13.89961937509957934, 78.12609039468567573 ) ) ;
#24717 = DIRECTION ( 'NONE',  ( 4.336808689942017120E-17, 1.000000000000000000, 0.000000000000000000 ) ) ;
#24718 = CARTESIAN_POINT ( 'NONE',  ( 16.46253265017160672, -9.564922557960803928, 88.33224293864769550 ) ) ;
#24719 = CARTESIAN_POINT ( 'NONE',  ( 15.80617190586746368, 15.72974639402197994, 114.3739096053143527 ) ) ;
#24720 = CARTESIAN_POINT ( 'NONE',  ( -5.049401038297874678, -19.05341960407617918, 79.79275706135233293 ) ) ;
#24722 = CARTESIAN_POINT ( 'NONE',  ( -19.03943276465977164, 0.05219959533909376836, 36.24890960531436690 ) ) ;
#24721 = CARTESIAN_POINT ( 'NONE',  ( 5.153800228976335163, 19.02544592524342804, 109.7905762719810099 ) ) ;
#24723 = CARTESIAN_POINT ( 'NONE',  ( -19.05341960407611168, -5.049401038298163336, 71.45724293864766707 ) ) ;
#24725 = CARTESIAN_POINT ( 'NONE',  ( -13.97604488694527625, -13.89961937509977652, 31.87390960531435979 ) ) ;
#24724 = CARTESIAN_POINT ( 'NONE',  ( -8.224510206698948167, 14.34966873604960824, 40.41557627198103120 ) ) ;
#24726 = CARTESIAN_POINT ( 'NONE',  ( 16.51473224551083163, -9.474510206698727899, 50.83442372801899722 ) ) ;
#24727 = CARTESIAN_POINT ( 'NONE',  ( 14.29746914071049879, -8.314922557960816363, 83.33224293864769550 ) ) ;
#24728 = CARTESIAN_POINT ( 'NONE',  ( 13.89961937509957401, 13.97604488694547697, 21.87609039468566152 ) ) ;
#24729 = CARTESIAN_POINT ( 'NONE',  ( -0.05219959533909027116, -19.03943276465977164, 47.49890960531435979 ) ) ;
#24730 = CARTESIAN_POINT ( 'NONE',  ( 10.81492255796078972, 18.62759615963270932, 49.58224293864769550 ) ) ;
#24732 = CARTESIAN_POINT ( 'NONE',  ( -5.823673210054431948, 21.52544592524334988, 97.70942372801904696 ) ) ;
#24731 = CARTESIAN_POINT ( 'NONE',  ( -12.06949235617756955, 12.14591786802309770, 55.62390960531436690 ) ) ;
#24733 = CARTESIAN_POINT ( 'NONE',  ( 9.474510206698971260, -16.51473224551069308, 107.9155762719810383 ) ) ;
#24734 = CARTESIAN_POINT ( 'NONE',  ( 5.049401038298161559, -19.05341960407611168, 112.7072429386476813 ) ) ;
#24735 = CARTESIAN_POINT ( 'NONE',  ( 13.89961937509977652, -13.97604488694527269, 38.12390960531436690 ) ) ;
#24736 = CARTESIAN_POINT ( 'NONE',  ( 16.46253265017160672, -9.564922557960803928, 23.33224293864769194 ) ) ;
#24737 = CARTESIAN_POINT ( 'NONE',  ( 14.29746914071049879, -8.314922557960816363, 93.33224293864769550 ) ) ;
#24738 = CARTESIAN_POINT ( 'NONE',  ( 10.81492255796078972, 18.62759615963270932, 94.58224293864769550 ) ) ;
#24739 = CARTESIAN_POINT ( 'NONE',  ( -13.97604488694527625, -13.89961937509977652, 96.87390960531433848 ) ) ;
#24740 = CARTESIAN_POINT ( 'NONE',  ( -15.80617190586745835, -15.72974639402198527, 111.8739096053143669 ) ) ;
#24741 = CARTESIAN_POINT ( 'NONE',  ( -0.05219959533909027116, -19.03943276465977164, 97.49890960531436690 ) ) ;
#24743 = CARTESIAN_POINT ( 'NONE',  ( 12.06949235617757843, -12.14591786802309237, 103.1239096053143811 ) ) ;
#24742 = CARTESIAN_POINT ( 'NONE',  ( 13.97604488694548053, -13.89961937509957401, 65.62609039468567573 ) ) ;
#24745 = CARTESIAN_POINT ( 'NONE',  ( -13.89961937509977652, 13.97604488694528158, 75.62390960531438111 ) ) ;
#24744 = CIRCLE ( 'NONE', #147407, 5.500000000000032863 ) ;
#24746 = CARTESIAN_POINT ( 'NONE',  ( -5.823673210054116645, -21.52544592524344225, 82.29057627198103830 ) ) ;
#24747 = EDGE_CURVE ( 'NONE', #105726, #186058, #62031, .T. ) ;
#24748 = CYLINDRICAL_SURFACE ( 'NONE', #43981, 1.499999999999994449 ) ;
#24749 = CARTESIAN_POINT ( 'NONE',  ( -3.573655867282028392E-15, 2.428612866367529932E-14, 169.9999999999999716 ) ) ;
#24751 = DIRECTION ( 'NONE',  ( 0.000000000000000000, -0.8660254037844385966, 0.5000000000000001110 ) ) ;
#24750 = CARTESIAN_POINT ( 'NONE',  ( 5.823673210054125526, 21.52544592524343514, 29.79057627198102409 ) ) ;
#24752 = CARTESIAN_POINT ( 'NONE',  ( 8.224510206698742110, 14.34966873604972548, 32.08442372801901854 ) ) ;
#24753 = CARTESIAN_POINT ( 'NONE',  ( -16.55341960407611168, -4.379528057220339221, 96.45724293864770971 ) ) ;
#24754 = CARTESIAN_POINT ( 'NONE',  ( 19.53037848336977689, -5.500000000000094147, 52.35532783611441943 ) ) ;
#24755 = CARTESIAN_POINT ( 'NONE',  ( -19.03943276465977164, 0.05219959533909376836, 91.24890960531436690 ) ) ;
#24756 = CARTESIAN_POINT ( 'NONE',  ( -0.05219959533909027116, -19.03943276465977164, 57.49890960531435979 ) ) ;
#24757 = CARTESIAN_POINT ( 'NONE',  ( 14.34966873604960469, 8.224510206698951720, 79.16557627198103830 ) ) ;
#24758 = CARTESIAN_POINT ( 'NONE',  ( 21.55341960407610458, 5.719274019375980345, 33.95724293864769550 ) ) ;
#24759 = CARTESIAN_POINT ( 'NONE',  ( 14.29746914071049879, -8.314922557960816363, 53.33224293864769550 ) ) ;
#24760 = CARTESIAN_POINT ( 'NONE',  ( 16.52544592524335698, 4.483927247898782831, 26.45942372801901854 ) ) ;
#24761 = CARTESIAN_POINT ( 'NONE',  ( 5.823673210054444382, -21.52544592524334988, 75.20942372801901854 ) ) ;
#24762 = CARTESIAN_POINT ( 'NONE',  ( 8.571926809382603096, -26.38167802310801235, 147.4750000027311785 ) ) ;
#24763 = CARTESIAN_POINT ( 'NONE',  ( 10.72451020669898902, -18.67979575497178502, 22.91557627198102765 ) ) ;
#24764 = CARTESIAN_POINT ( 'NONE',  ( 0.05219959533934541429, -16.53943276465976808, 90.00109039468567573 ) ) ;
#24765 = CARTESIAN_POINT ( 'NONE',  ( 0.05219959533909260263, 19.03943276465977164, 29.99890960531435979 ) ) ;
#24766 = CARTESIAN_POINT ( 'NONE',  ( -19.02544592524342804, 5.153800228976336051, 91.04057627198100988 ) ) ;
#24767 = CARTESIAN_POINT ( 'NONE',  ( -15.72974639402197994, 15.80617190586746368, 100.6239096053143811 ) ) ;
#24768 = CARTESIAN_POINT ( 'NONE',  ( -12.06949235617739369, -12.14591786802326823, 29.37609039468568284 ) ) ;
#24770 = CARTESIAN_POINT ( 'NONE',  ( 18.62759615963255655, 10.81492255796105972, 76.66775706135234714 ) ) ;
#24769 = CARTESIAN_POINT ( 'NONE',  ( -16.53943276465976808, 0.05219959533911058130, 56.24890960531436690 ) ) ;
#24772 = CARTESIAN_POINT ( 'NONE',  ( -5.719274019375978568, 21.55341960407610458, 25.20724293864769550 ) ) ;
#24771 = CARTESIAN_POINT ( 'NONE',  ( 14.29746914071037800, 8.314922557961029526, 91.66775706135234714 ) ) ;
#24773 = CARTESIAN_POINT ( 'NONE',  ( 17.31747979337949417, 6.344076630961017926, 28.87944868065185489 ) ) ;
#24774 = CARTESIAN_POINT ( 'NONE',  ( -17.13100169013300444, 6.664070546373148218, 80.76789835699848652 ) ) ;
#24775 = CARTESIAN_POINT ( 'NONE',  ( -16.52544592524335698, -4.483927247898792601, 103.9594237280190185 ) ) ;
#24776 = CARTESIAN_POINT ( 'NONE',  ( 12.06949235617739724, 12.14591786802326823, 66.87609039468568994 ) ) ;
#24777 = CARTESIAN_POINT ( 'NONE',  ( 19.03943276465977164, -0.05219959533909143690, 78.74890960531436690 ) ) ;
#24778 = CARTESIAN_POINT ( 'NONE',  ( -0.05219959533909027116, -19.03943276465977164, 87.49890960531436690 ) ) ;
#24779 = CARTESIAN_POINT ( 'NONE',  ( 18.62759615963255655, 10.81492255796105972, 66.66775706135234714 ) ) ;
#24780 = CARTESIAN_POINT ( 'NONE',  ( 12.06949235617739724, 12.14591786802326823, 81.87609039468568994 ) ) ;
#24781 = CARTESIAN_POINT ( 'NONE',  ( 14.34966873604960469, 8.224510206698951720, 49.16557627198102409 ) ) ;
#24782 = CARTESIAN_POINT ( 'NONE',  ( -5.049401038298153566, 19.05341960407611168, 60.20724293864768129 ) ) ;
#24783 = EDGE_LOOP ( 'NONE', ( #9417, #54938, #40276, #29561 ) ) ;
#24784 = CARTESIAN_POINT ( 'NONE',  ( 9.474510206698729675, 16.51473224551082808, 112.0844237280190043 ) ) ;
#24785 = CARTESIAN_POINT ( 'NONE',  ( -14.34966873604960291, -8.224510206698953496, 111.6655762719810525 ) ) ;
#24786 = CARTESIAN_POINT ( 'NONE',  ( -19.03943276465977164, 0.05219959533909376836, 71.24890960531435269 ) ) ;
#24788 = CARTESIAN_POINT ( 'NONE',  ( -11.74264578624800670, 36.14014761921585972, -6.400000000000000355 ) ) ;
#24787 = CARTESIAN_POINT ( 'NONE',  ( 13.97604488694548053, -13.89961937509957401, 95.62609039468563310 ) ) ;
#24789 = CARTESIAN_POINT ( 'NONE',  ( -18.67979575497193778, 10.72451020669871902, 98.33442372801901854 ) ) ;
#24790 = CARTESIAN_POINT ( 'NONE',  ( -16.53943276465976808, -0.05219959533934237506, 68.75109039468568994 ) ) ;
#24791 = CARTESIAN_POINT ( 'NONE',  ( 5.049401038297881783, 19.05341960407617563, 97.29275706135233293 ) ) ;
#24792 = CARTESIAN_POINT ( 'NONE',  ( -21.53943276465977519, 0.05219959533907696930, 66.24890960531436690 ) ) ;
#24793 = CARTESIAN_POINT ( 'NONE',  ( 14.29746914071037800, 8.314922557961029526, 51.66775706135234714 ) ) ;
#24794 = PLANE ( 'NONE',  #192677 ) ;
#24795 = CARTESIAN_POINT ( 'NONE',  ( -19.02544592524334988, -5.153800228976617603, 58.95942372801900433 ) ) ;
#24796 = CARTESIAN_POINT ( 'NONE',  ( -5.823673210054431948, 21.52544592524334988, 97.70942372801904696 ) ) ;
#24797 = CARTESIAN_POINT ( 'NONE',  ( -5.153800228976328057, -19.02544592524343514, 37.29057627198102409 ) ) ;
#24798 = CARTESIAN_POINT ( 'NONE',  ( 16.51473224551069308, 9.474510206698969483, 69.16557627198102409 ) ) ;
#24799 = CARTESIAN_POINT ( 'NONE',  ( -14.29746914071049879, 8.314922557960819915, 60.83224293864769550 ) ) ;
#24800 = CARTESIAN_POINT ( 'NONE',  ( 21.53943276465977519, 0.05219959533937863772, 86.25109039468568994 ) ) ;
#24801 = CARTESIAN_POINT ( 'NONE',  ( 16.51473224551083163, -9.474510206698727899, 50.83442372801899722 ) ) ;
#24802 = CARTESIAN_POINT ( 'NONE',  ( 5.049401038297881783, 19.05341960407617563, 32.29275706135233293 ) ) ;
#24803 = CARTESIAN_POINT ( 'NONE',  ( 13.89961937509977652, -13.97604488694527269, 113.1239096053143527 ) ) ;
#24804 = CARTESIAN_POINT ( 'NONE',  ( 21.52544592524334988, 5.823673210054432836, 101.4594237280190185 ) ) ;
#24805 = CARTESIAN_POINT ( 'NONE',  ( -13.89961937509977652, 13.97604488694528158, 80.62390960531436690 ) ) ;
#24806 = CARTESIAN_POINT ( 'NONE',  ( -5.719274019375665041, -21.55341960407619695, 94.79275706135234714 ) ) ;
#24807 = CARTESIAN_POINT ( 'NONE',  ( 21.52544592524344225, -5.823673210054117533, 53.54057627198103120 ) ) ;
#24808 = CARTESIAN_POINT ( 'NONE',  ( -19.03943276465977164, 0.05219959533909376836, 81.24890960531436690 ) ) ;
#24809 = CARTESIAN_POINT ( 'NONE',  ( 19.05341960407617918, -5.049401038297876454, 71.04275706135234714 ) ) ;
#24810 = CARTESIAN_POINT ( 'NONE',  ( 16.51473224551069308, 9.474510206698969483, 44.16557627198103120 ) ) ;
#24811 = CARTESIAN_POINT ( 'NONE',  ( -9.474510206698964154, 16.51473224551069663, 85.41557627198102409 ) ) ;
#24812 = CARTESIAN_POINT ( 'NONE',  ( 19.03943276465977164, 0.05219959533936151252, 86.25109039468567573 ) ) ;
#24813 = CARTESIAN_POINT ( 'NONE',  ( -14.29746914071037622, -8.314922557961029526, 44.16775706135234714 ) ) ;
#24814 = CARTESIAN_POINT ( 'NONE',  ( -16.53943276465976808, 0.05219959533911058130, 101.2489096053143669 ) ) ;
#24815 = CARTESIAN_POINT ( 'NONE',  ( -16.51473224551069308, -9.474510206698971260, 71.66557627198102409 ) ) ;
#24816 = CARTESIAN_POINT ( 'NONE',  ( 21.52544592524344225, -5.823673210054117533, 48.54057627198103120 ) ) ;
#24817 = CARTESIAN_POINT ( 'NONE',  ( -16.53943276465976808, -0.05219959533934237506, 33.75109039468568284 ) ) ;
#24818 = CARTESIAN_POINT ( 'NONE',  ( -18.67979575497193778, 10.72451020669871902, 38.33442372801900433 ) ) ;
#24819 = CARTESIAN_POINT ( 'NONE',  ( -0.05219959533937732626, 21.53943276465977519, 77.50109039468567573 ) ) ;
#24820 = CARTESIAN_POINT ( 'NONE',  ( 12.06949235617739724, 12.14591786802326823, 86.87609039468568994 ) ) ;
#24821 = CARTESIAN_POINT ( 'NONE',  ( -13.97604488694527625, -13.89961937509977652, 76.87390960531433848 ) ) ;
#24822 = CARTESIAN_POINT ( 'NONE',  ( -4.483927247898782831, 16.52544592524335698, 102.7094237280190185 ) ) ;
#24823 = CARTESIAN_POINT ( 'NONE',  ( 19.05341960407617918, -5.049401038297876454, 56.04275706135234714 ) ) ;
#24824 = CARTESIAN_POINT ( 'NONE',  ( 5.719274019375673035, 21.55341960407619339, 27.29275706135234358 ) ) ;
#24825 = CARTESIAN_POINT ( 'NONE',  ( -4.379528057220328563, 16.55341960407611168, 80.20724293864769550 ) ) ;
#24826 = CARTESIAN_POINT ( 'NONE',  ( 13.89961937509977652, -13.97604488694527269, 98.12390960531433848 ) ) ;
#24827 = CARTESIAN_POINT ( 'NONE',  ( 4.379528057220092307, 16.55341960407617563, 102.2927570613523613 ) ) ;
#24828 = CARTESIAN_POINT ( 'NONE',  ( 5.823673210054444382, -21.52544592524334988, 75.20942372801901854 ) ) ;
#24829 = CARTESIAN_POINT ( 'NONE',  ( -12.06949235617739369, -12.14591786802326823, 44.37609039468567573 ) ) ;
#24830 = CARTESIAN_POINT ( 'NONE',  ( 21.52544592524334988, 5.823673210054432836, 31.45942372801901854 ) ) ;
#24831 = CARTESIAN_POINT ( 'NONE',  ( -12.06949235617756955, 12.14591786802309770, 70.62390960531436690 ) ) ;
#24832 = ORIENTED_EDGE ( 'NONE', *, *, #149135, .T. ) ;
#24833 = CARTESIAN_POINT ( 'NONE',  ( 21.52544592524344225, -5.823673210054117533, 108.5405762719810241 ) ) ;
#24834 = CARTESIAN_POINT ( 'NONE',  ( -16.52544592524342804, 4.483927247898546575, 56.04057627198102409 ) ) ;
#24835 = CARTESIAN_POINT ( 'NONE',  ( 9.474510206698971260, -16.51473224551069308, 27.91557627198103120 ) ) ;
#24836 = CARTESIAN_POINT ( 'NONE',  ( -21.55341960407610458, -5.719274019375992779, 31.45724293864769550 ) ) ;
#24837 = CARTESIAN_POINT ( 'NONE',  ( 15.80617190586769283, -15.72974639402175789, 50.62609039468568994 ) ) ;
#24838 = CARTESIAN_POINT ( 'NONE',  ( 8.314922557960818139, 14.29746914071049879, 69.58224293864769550 ) ) ;
#24839 = VECTOR ( 'NONE', #7343, 1000.000000000000000 ) ;
#24840 = CARTESIAN_POINT ( 'NONE',  ( 0.05219959533907565091, 21.53943276465977519, 74.99890960531435269 ) ) ;
#24841 = CARTESIAN_POINT ( 'NONE',  ( -19.03943276465977164, 0.05219959533909376836, 71.24890960531435269 ) ) ;
#24843 = CARTESIAN_POINT ( 'NONE',  ( 13.89961937509957401, 13.97604488694547697, 76.87609039468566152 ) ) ;
#24842 = CARTESIAN_POINT ( 'NONE',  ( 19.02544592524343514, -5.153800228976328945, 43.54057627198103120 ) ) ;
#24845 = CARTESIAN_POINT ( 'NONE',  ( -21.52544592524343514, 5.823673210054127303, 66.04057627198103830 ) ) ;
#24844 = CARTESIAN_POINT ( 'NONE',  ( 5.719274019375673035, 21.55341960407619339, 52.29275706135236135 ) ) ;
#24846 = CARTESIAN_POINT ( 'NONE',  ( 16.51473224551069308, 9.474510206698969483, 44.16557627198103120 ) ) ;
#24847 = CARTESIAN_POINT ( 'NONE',  ( -5.153800228976328057, -19.02544592524343514, 67.29057627198102409 ) ) ;
#24848 = EDGE_LOOP ( 'NONE', ( #145730, #192513, #149528, #70905, #9465 ) ) ;
#24849 = CARTESIAN_POINT ( 'NONE',  ( 16.53943276465976808, 0.05219959533934440121, 46.25109039468567573 ) ) ;
#24850 = CARTESIAN_POINT ( 'NONE',  ( -21.52544592524334988, -5.823673210054445271, 28.95942372801902209 ) ) ;
#24851 = CARTESIAN_POINT ( 'NONE',  ( 21.53943276465977519, 0.05219959533937863772, 56.25109039468568284 ) ) ;
#24852 = CARTESIAN_POINT ( 'NONE',  ( 9.564922557960805705, 16.46253265017160317, 104.5822429386476955 ) ) ;
#24853 = CARTESIAN_POINT ( 'NONE',  ( 5.823673210054125526, 21.52544592524343514, 79.79057627198102409 ) ) ;
#24855 = CARTESIAN_POINT ( 'NONE',  ( -14.34966873604972548, 8.224510206698743886, 53.33442372801901854 ) ) ;
#24854 = CARTESIAN_POINT ( 'NONE',  ( -21.53943276465977519, -0.05219959533937600094, 28.75109039468567929 ) ) ;
#24856 = CARTESIAN_POINT ( 'NONE',  ( 18.62759615963271287, -10.81492255796078972, 43.33224293864769550 ) ) ;
#24857 = CARTESIAN_POINT ( 'NONE',  ( -15.80617190586768217, 15.72974639402176855, 113.1260903946856899 ) ) ;
#24858 = CARTESIAN_POINT ( 'NONE',  ( -19.05341960407611168, -5.049401038298163336, 56.45724293864768129 ) ) ;
#24859 = CARTESIAN_POINT ( 'NONE',  ( -19.03943276465977164, 0.05219959533909376836, 106.2489096053143669 ) ) ;
#24860 = CARTESIAN_POINT ( 'NONE',  ( 13.97604488694527802, 13.89961937509977652, 84.37390960531433848 ) ) ;
#24861 = CARTESIAN_POINT ( 'NONE',  ( 0.000000000000000000, 0.000000000000000000, -65.00100000000003320 ) ) ;
#24862 = CARTESIAN_POINT ( 'NONE',  ( 19.03943276465977164, 0.05219959533936151252, 66.25109039468567573 ) ) ;
#24863 = CARTESIAN_POINT ( 'NONE',  ( 5.719274019375991003, -21.55341960407610458, 47.70724293864770260 ) ) ;
#24864 = EDGE_CURVE ( 'NONE', #86852, #56947, #90523, .T. ) ;
#24865 = CARTESIAN_POINT ( 'NONE',  ( -0.05219959533910754901, -16.53943276465976808, 27.49890960531435269 ) ) ;
#24866 = CARTESIAN_POINT ( 'NONE',  ( 16.51473224551083163, -9.474510206698727899, 80.83442372801899012 ) ) ;
#24867 = CARTESIAN_POINT ( 'NONE',  ( -16.36317988757059538, 7.306389748694926745, 59.09789608363227842 ) ) ;
#24868 = CARTESIAN_POINT ( 'NONE',  ( 21.53943276465977519, 0.05219959533937863772, 111.2510903946856899 ) ) ;
#24869 = CARTESIAN_POINT ( 'NONE',  ( -0.05219959533936034679, 19.03943276465977164, 97.50109039468567573 ) ) ;
#24870 = CARTESIAN_POINT ( 'NONE',  ( -9.564922557961040184, 16.46253265017147172, 47.91775706135233293 ) ) ;
#24871 = CARTESIAN_POINT ( 'NONE',  ( 2.649999999999999911, -165.0000000000000000, -13.00000000000000000 ) ) ;
#24872 = CARTESIAN_POINT ( 'NONE',  ( -19.02544592524342804, 5.153800228976336051, 51.04057627198103120 ) ) ;
#24873 = CARTESIAN_POINT ( 'NONE',  ( -8.224510206698948167, 14.34966873604960824, 50.41557627198103120 ) ) ;
#24874 = CARTESIAN_POINT ( 'NONE',  ( -13.97604488694527625, -13.89961937509977652, 31.87390960531435979 ) ) ;
#24875 = CARTESIAN_POINT ( 'NONE',  ( 14.34966873604960469, 8.224510206698951720, 44.16557627198103120 ) ) ;
#24876 = CARTESIAN_POINT ( 'NONE',  ( -19.49401214000077331, 12.39993551617566681, 167.9999999999999716 ) ) ;
#24877 = CARTESIAN_POINT ( 'NONE',  ( 16.55341960407618274, -4.379528057220086978, 111.0427570613523613 ) ) ;
#24878 = CARTESIAN_POINT ( 'NONE',  ( 5.153800228976335163, 19.02544592524342804, 64.79057627198100988 ) ) ;
#24879 = CARTESIAN_POINT ( 'NONE',  ( 16.46253265017146816, 9.564922557961045513, 21.66775706135233648 ) ) ;
#24880 = CARTESIAN_POINT ( 'NONE',  ( 0.05219959533934541429, -16.53943276465976808, 40.00109039468567573 ) ) ;
#24881 = CARTESIAN_POINT ( 'NONE',  ( 5.823673210054125526, 21.52544592524343514, 34.79057627198103120 ) ) ;
#24883 = EDGE_LOOP ( 'NONE', ( #143497, #39612 ) ) ;
#24882 = CARTESIAN_POINT ( 'NONE',  ( 15.80617190586769283, -15.72974639402175789, 90.62609039468567573 ) ) ;
#24884 = CARTESIAN_POINT ( 'NONE',  ( -16.51473224551069308, -9.474510206698971260, 66.66557627198102409 ) ) ;
#24885 = CARTESIAN_POINT ( 'NONE',  ( 5.153800228976335163, 19.02544592524342804, 104.7905762719809957 ) ) ;
#24886 = CARTESIAN_POINT ( 'NONE',  ( 0.05219959533909260263, 19.03943276465977164, 99.99890960531436690 ) ) ;
#24887 = DIRECTION ( 'NONE',  ( 1.000000000000000000, 0.000000000000000000, 0.000000000000000000 ) ) ;
#24888 = CARTESIAN_POINT ( 'NONE',  ( -5.719274019375665041, -21.55341960407619695, 29.79275706135234358 ) ) ;
#24889 = AXIS2_PLACEMENT_3D ( 'NONE', #89830, #120161, #154234 ) ;
#24890 = CARTESIAN_POINT ( 'NONE',  ( 8.314922557960818139, 14.29746914071049879, 79.58224293864769550 ) ) ;
#24892 = CARTESIAN_POINT ( 'NONE',  ( 16.51473224551069308, 9.474510206698969483, 69.16557627198102409 ) ) ;
#24891 = CARTESIAN_POINT ( 'NONE',  ( -10.72451020669898014, 18.67979575497178502, 80.41557627198103830 ) ) ;
#24893 = CARTESIAN_POINT ( 'NONE',  ( 19.02544592524343514, -5.153800228976328945, 73.54057627198103830 ) ) ;
#24894 = CARTESIAN_POINT ( 'NONE',  ( -15.72974639402176322, -15.80617190586768395, 19.37609039468568639 ) ) ;
#24895 = VERTEX_POINT ( 'NONE', #75356 ) ;
#24896 = CARTESIAN_POINT ( 'NONE',  ( -13.89961937509977652, 13.97604488694528158, 75.62390960531438111 ) ) ;
#24897 = CARTESIAN_POINT ( 'NONE',  ( 0.000000000000000000, -105.0000000000000000, 12.00000000000000355 ) ) ;
#24899 = CARTESIAN_POINT ( 'NONE',  ( 9.564922557960805705, 16.46253265017160317, 24.58224293864769194 ) ) ;
#24898 = CARTESIAN_POINT ( 'NONE',  ( -0.05219959533910754901, -16.53943276465976808, 112.4989096053143669 ) ) ;
#24900 = CARTESIAN_POINT ( 'NONE',  ( 19.03943276465977164, -0.05219959533909143690, 68.74890960531436690 ) ) ;
#24901 = CARTESIAN_POINT ( 'NONE',  ( 5.153800228976615827, -19.02544592524334988, 95.20942372801897591 ) ) ;
#24902 = CARTESIAN_POINT ( 'NONE',  ( -12.14591786802309592, -12.06949235617757132, 96.87390960531436690 ) ) ;
#24903 = CARTESIAN_POINT ( 'NONE',  ( 18.67979575497194134, -10.72451020669871369, 65.83442372801900433 ) ) ;
#24905 = CARTESIAN_POINT ( 'NONE',  ( -5.823673210054116645, -21.52544592524344225, 112.2905762719810241 ) ) ;
#24904 = CARTESIAN_POINT ( 'NONE',  ( -9.564922557960796823, -16.46253265017161027, 52.08224293864768839 ) ) ;
#24906 = CARTESIAN_POINT ( 'NONE',  ( -21.53943276465977519, 0.05219959533907696930, 106.2489096053143811 ) ) ;
#24907 = CARTESIAN_POINT ( 'NONE',  ( 8.906447517083057264, -27.41122689804191026, 144.5999999999999943 ) ) ;
#24908 = CARTESIAN_POINT ( 'NONE',  ( 5.153800228976335163, 19.02544592524342804, 74.79057627198103830 ) ) ;
#24909 = CARTESIAN_POINT ( 'NONE',  ( 16.81555441253555117, 7.025013491695454526, 111.8631455466574636 ) ) ;
#24911 = CARTESIAN_POINT ( 'NONE',  ( -10.72451020669898014, 18.67979575497178502, 35.41557627198102409 ) ) ;
#24910 = CARTESIAN_POINT ( 'NONE',  ( -13.89961937509957401, -13.97604488694547875, 104.3760903946856757 ) ) ;
#24912 = CARTESIAN_POINT ( 'NONE',  ( -5.823673210054431948, 21.52544592524334988, 52.70942372801902565 ) ) ;
#24913 = CARTESIAN_POINT ( 'NONE',  ( -19.03943276465977164, 0.05219959533909376836, 96.24890960531436690 ) ) ;
#24914 =( BOUNDED_CURVE ( )  B_SPLINE_CURVE ( 2, ( #39108, #80615, #142292, #197786, #71445, #195814, #12778, #103783, #43107, #181627, #180646, #165463, #134125 ),
 .UNSPECIFIED., .F., .F. ) 
 B_SPLINE_CURVE_WITH_KNOTS ( ( 3, 2, 2, 2, 2, 2, 3 ),
 ( 0.6077392741438721879, 0.6096491228070175517, 0.6140350877192982670, 0.6184210526315789824, 0.6228070175438596978, 0.6271929824561403022, 0.6291485109413760268 ),
 .UNSPECIFIED. ) 
 CURVE ( )  GEOMETRIC_REPRESENTATION_ITEM ( )  RATIONAL_B_SPLINE_CURVE ( ( 0.9832469066685285419, 0.9851625545550100060, 1.000000000000000000, 0.9659258262890683122, 1.000000000000000000, 0.9659258262890683122, 1.000000000000000000, 0.9659258262890683122, 1.000000000000000000, 0.9659258262890683122, 1.000000000000000000, 0.9848076720550078544, 0.9831626618144001517 ) ) 
 REPRESENTATION_ITEM ( '' )  );
#24915 = CARTESIAN_POINT ( 'NONE',  ( -19.03943276465977164, -0.05219959533935918106, 78.75109039468567573 ) ) ;
#24916 = CARTESIAN_POINT ( 'NONE',  ( -19.03943276465977164, 0.05219959533909376836, 51.24890960531436690 ) ) ;
#24917 = CARTESIAN_POINT ( 'NONE',  ( 5.049401038298161559, -19.05341960407611168, 77.70724293864765286 ) ) ;
#24918 = EDGE_CURVE ( 'NONE', #135939, #11685, #137026, .T. ) ;
#24919 = CARTESIAN_POINT ( 'NONE',  ( -16.53943276465976808, 0.05219959533911058130, 81.24890960531436690 ) ) ;
#24920 = CARTESIAN_POINT ( 'NONE',  ( -13.89961937509977652, 13.97604488694528158, 105.6239096053143527 ) ) ;
#24921 = CARTESIAN_POINT ( 'NONE',  ( -12.06949235617756955, 12.14591786802309770, 90.62390960531436690 ) ) ;
#24922 = CARTESIAN_POINT ( 'NONE',  ( 5.153800228976335163, 19.02544592524342804, 94.79057627198103830 ) ) ;
#24924 = CARTESIAN_POINT ( 'NONE',  ( -13.97604488694527625, -13.89961937509977652, 26.87390960531434558 ) ) ;
#24923 = CARTESIAN_POINT ( 'NONE',  ( -8.314922557960811034, -14.29746914071050412, 37.08224293864768129 ) ) ;
#24925 = ORIENTED_EDGE ( 'NONE', *, *, #54327, .F. ) ;
#24926 = CARTESIAN_POINT ( 'NONE',  ( -5.823673210054431948, 21.52544592524334988, 52.70942372801902565 ) ) ;
#24927 = CARTESIAN_POINT ( 'NONE',  ( -16.51473224551082808, 9.474510206698731452, 73.33442372801900433 ) ) ;
#24928 = CARTESIAN_POINT ( 'NONE',  ( 4.379528057220339221, -16.55341960407611168, 42.70724293864770260 ) ) ;
#24929 = CARTESIAN_POINT ( 'NONE',  ( 18.67979575497178502, 10.72451020669898547, 99.16557627198100988 ) ) ;
#24930 = CARTESIAN_POINT ( 'NONE',  ( -5.823673210054116645, -21.52544592524344225, 37.29057627198102409 ) ) ;
#24931 = CARTESIAN_POINT ( 'NONE',  ( 16.53943276465976808, -0.05219959533910856209, 88.74890960531436690 ) ) ;
#24932 = CARTESIAN_POINT ( 'NONE',  ( -19.02544592524342804, 5.153800228976336051, 51.04057627198103120 ) ) ;
#24933 = CARTESIAN_POINT ( 'NONE',  ( 8.224510206698953496, -14.34966873604960469, 22.91557627198102765 ) ) ;
#24934 = CARTESIAN_POINT ( 'NONE',  ( 16.55341960407618274, -4.379528057220086978, 101.0427570613523756 ) ) ;
#24935 = CARTESIAN_POINT ( 'NONE',  ( -0.05219959533934338120, 16.53943276465976808, 67.50109039468568994 ) ) ;
#24936 = CARTESIAN_POINT ( 'NONE',  ( 13.97604488694548053, -13.89961937509957401, 25.62609039468566507 ) ) ;
#24937 = CARTESIAN_POINT ( 'NONE',  ( -13.89961937509977652, 13.97604488694528158, 105.6239096053143527 ) ) ;
#24938 = CARTESIAN_POINT ( 'NONE',  ( -9.474510206698964154, 16.51473224551069663, 80.41557627198103830 ) ) ;
#24939 = CARTESIAN_POINT ( 'NONE',  ( 19.02544592524343514, -5.153800228976328945, 38.54057627198103120 ) ) ;
#24940 = CARTESIAN_POINT ( 'NONE',  ( -16.55341960407611168, -4.379528057220339221, 41.45724293864769550 ) ) ;
#24942 = CARTESIAN_POINT ( 'NONE',  ( -16.46253265017160317, 9.564922557960807481, 110.8322429386476955 ) ) ;
#24941 = LINE ( 'NONE', #23928, #111366 ) ;
#24943 = CARTESIAN_POINT ( 'NONE',  ( -21.53943276465977519, 0.05219959533907696930, 36.24890960531435979 ) ) ;
#24944 = CARTESIAN_POINT ( 'NONE',  ( -8.314922557960811034, -14.29746914071050412, 77.08224293864769550 ) ) ;
#24945 = CARTESIAN_POINT ( 'NONE',  ( 16.52544592524335698, 4.483927247898782831, 31.45942372801901854 ) ) ;
#24946 = ORIENTED_EDGE ( 'NONE', *, *, #2987, .F. ) ;
#24947 = CARTESIAN_POINT ( 'NONE',  ( 16.55341960407611168, 4.379528057220329451, 68.95724293864769550 ) ) ;
#24948 = CARTESIAN_POINT ( 'NONE',  ( 17.50000000000000000, -3.512728167237040289, 32.72809995181130915 ) ) ;
#24949 = CARTESIAN_POINT ( 'NONE',  ( 0.05219959533936267826, -19.03943276465977164, 70.00109039468566152 ) ) ;
#24950 = CARTESIAN_POINT ( 'NONE',  ( 0.05219959533909260263, 19.03943276465977164, 104.9989096053143669 ) ) ;
#24951 = CARTESIAN_POINT ( 'NONE',  ( 19.03943276465977164, 0.05219959533936151252, 76.25109039468566152 ) ) ;
#24952 = CARTESIAN_POINT ( 'NONE',  ( -16.46253265017146816, -9.564922557961047289, 39.16775706135234003 ) ) ;
#24954 = CARTESIAN_POINT ( 'NONE',  ( 12.06949235617739724, 12.14591786802326823, 91.87609039468568994 ) ) ;
#24953 = CARTESIAN_POINT ( 'NONE',  ( -13.89961937509957401, -13.97604488694547875, 109.3760903946856331 ) ) ;
#24955 = CARTESIAN_POINT ( 'NONE',  ( 9.474510206698971260, -16.51473224551069308, 37.91557627198102409 ) ) ;
#24956 = CARTESIAN_POINT ( 'NONE',  ( -21.53943276465977519, 0.05219959533907696930, 41.24890960531435269 ) ) ;
#24957 = CARTESIAN_POINT ( 'NONE',  ( 21.53943276465977519, 0.05219959533937863772, 56.25109039468568284 ) ) ;
#24958 = CARTESIAN_POINT ( 'NONE',  ( -23.31738231874055245, -16.94106989632524574, 146.4500000054623854 ) ) ;
#24959 = CARTESIAN_POINT ( 'NONE',  ( 0.05219959533934541429, -16.53943276465976808, 20.00109039468568639 ) ) ;
#24961 = CARTESIAN_POINT ( 'NONE',  ( 19.02544592524343514, -5.153800228976328945, 68.54057627198103830 ) ) ;
#24960 = CARTESIAN_POINT ( 'NONE',  ( -9.327895405754907554E-15, -64.84118668444966715, -25.00000000000000000 ) ) ;
#24962 = CARTESIAN_POINT ( 'NONE',  ( -36.91746825000000598, 2.428612866367529932E-14, -1.124999997268813390 ) ) ;
#24964 = CARTESIAN_POINT ( 'NONE',  ( -0.05219959533909027116, -19.03943276465977164, 82.49890960531436690 ) ) ;
#24963 = CARTESIAN_POINT ( 'NONE',  ( 12.06949235617757843, -12.14591786802309237, 93.12390960531436690 ) ) ;
#24965 = CARTESIAN_POINT ( 'NONE',  ( -19.03943276465977164, 0.05219959533909376836, 81.24890960531436690 ) ) ;
#24966 = VERTEX_POINT ( 'NONE', #121853 ) ;
#24967 = CARTESIAN_POINT ( 'NONE',  ( 9.474510206698729675, 16.51473224551082808, 92.08442372801900433 ) ) ;
#24968 = CARTESIAN_POINT ( 'NONE',  ( -15.72974639402197994, 15.80617190586746368, 60.62390960531437401 ) ) ;
#24969 = CARTESIAN_POINT ( 'NONE',  ( -19.05341960407611168, -5.049401038298163336, 26.45724293864769550 ) ) ;
#24970 = CARTESIAN_POINT ( 'NONE',  ( 13.97604488694548053, -13.89961937509957401, 50.62609039468566152 ) ) ;
#24971 = CARTESIAN_POINT ( 'NONE',  ( -13.97604488694527625, -13.89961937509977652, 56.87390960531434558 ) ) ;
#24972 = CARTESIAN_POINT ( 'NONE',  ( -9.564922557960796823, -16.46253265017161027, 92.08224293864769550 ) ) ;
#24973 = ORIENTED_EDGE ( 'NONE', *, *, #198449, .F. ) ;
#24974 = CARTESIAN_POINT ( 'NONE',  ( -15.72974639402197994, 15.80617190586746368, 90.62390960531436690 ) ) ;
#24976 = CARTESIAN_POINT ( 'NONE',  ( -19.02544592524334988, -5.153800228976617603, 58.95942372801900433 ) ) ;
#24975 = CARTESIAN_POINT ( 'NONE',  ( 4.379528057220339221, -16.55341960407611168, 92.70724293864770971 ) ) ;
#24977 = CARTESIAN_POINT ( 'NONE',  ( -21.53943276465977519, 0.05219959533907696930, 96.24890960531435269 ) ) ;
#24978 = CARTESIAN_POINT ( 'NONE',  ( 21.55341960407610458, 5.719274019375980345, 78.95724293864769550 ) ) ;
#24979 = CARTESIAN_POINT ( 'NONE',  ( 0.05219959533910956823, 16.53943276465976808, 34.99890960531435979 ) ) ;
#24980 = CARTESIAN_POINT ( 'NONE',  ( -0.05219959533937732626, 21.53943276465977519, 102.5010903946856899 ) ) ;
#24981 = CARTESIAN_POINT ( 'NONE',  ( 8.224510206698742110, 14.34966873604972548, 57.08442372801901854 ) ) ;
#24982 = CARTESIAN_POINT ( 'NONE',  ( -0.05219959533909027116, -19.03943276465977164, 82.49890960531436690 ) ) ;
#24983 = CARTESIAN_POINT ( 'NONE',  ( -13.89961937509977652, 13.97604488694528158, 35.62390960531435269 ) ) ;
#24984 = CIRCLE ( 'NONE', #2429, 27.29906736325805028 ) ;
#24985 = CARTESIAN_POINT ( 'NONE',  ( -21.52544592524334988, -5.823673210054445271, 43.95942372801902565 ) ) ;
#24986 = CARTESIAN_POINT ( 'NONE',  ( -10.72451020669870658, -18.67979575497194134, 59.58442372801901854 ) ) ;
#24987 = CARTESIAN_POINT ( 'NONE',  ( 16.46253265017160672, -9.564922557960803928, 48.33224293864769550 ) ) ;
#24988 = CARTESIAN_POINT ( 'NONE',  ( 21.55341960407619695, -5.719274019375665929, 21.04275706135234714 ) ) ;
#24989 = ADVANCED_FACE ( 'NONE', ( #111653 ), #79454, .F. ) ;
#24990 = CARTESIAN_POINT ( 'NONE',  ( -16.51473224551082808, 9.474510206698731452, 58.33442372801900433 ) ) ;
#24991 = CARTESIAN_POINT ( 'NONE',  ( 16.51473224551083163, -9.474510206698727899, 75.83442372801900433 ) ) ;
#24992 = CARTESIAN_POINT ( 'NONE',  ( 4.483927247898790824, -16.52544592524335698, 30.20942372801902565 ) ) ;
#24993 = CARTESIAN_POINT ( 'NONE',  ( -5.153800228976328057, -19.02544592524343514, 32.29057627198102409 ) ) ;
#24994 = CARTESIAN_POINT ( 'NONE',  ( 16.53943276465976808, 0.05219959533934440121, 76.25109039468568994 ) ) ;
#24995 = CARTESIAN_POINT ( 'NONE',  ( -5.049401038298153566, 19.05341960407611168, 45.20724293864769550 ) ) ;
#24996 = CARTESIAN_POINT ( 'NONE',  ( 24.14511064691487263, -7.743397529684092007, 169.7652520481140073 ) ) ;
#24997 = CARTESIAN_POINT ( 'NONE',  ( 5.049401038298161559, -19.05341960407611168, 102.7072429386476955 ) ) ;
#24998 = CARTESIAN_POINT ( 'NONE',  ( -16.46253265017160317, 9.564922557960807481, 30.83224293864769550 ) ) ;
#24999 = CARTESIAN_POINT ( 'NONE',  ( 15.80617190586746368, 15.72974639402197994, 74.37390960531436690 ) ) ;
#25000 = CARTESIAN_POINT ( 'NONE',  ( 14.29746914071037800, 8.314922557961029526, 61.66775706135235424 ) ) ;
#25001 = CARTESIAN_POINT ( 'NONE',  ( -19.02544592524334988, -5.153800228976617603, 23.95942372801900078 ) ) ;
#25002 = CARTESIAN_POINT ( 'NONE',  ( 9.474510206698971260, -16.51473224551069308, 37.91557627198102409 ) ) ;
#25003 = CARTESIAN_POINT ( 'NONE',  ( -14.34966873604960291, -8.224510206698953496, 31.66557627198102054 ) ) ;
#25004 = CARTESIAN_POINT ( 'NONE',  ( -8.314922557960811034, -14.29746914071050412, 72.08224293864769550 ) ) ;
#25005 = CARTESIAN_POINT ( 'NONE',  ( -19.03943276465977164, 0.05219959533909376836, 71.24890960531435269 ) ) ;
#25006 = CARTESIAN_POINT ( 'NONE',  ( -18.67979575497193778, 10.72451020669871902, 33.33442372801900433 ) ) ;
#25007 = CARTESIAN_POINT ( 'NONE',  ( 13.97604488694527802, 13.89961937509977652, 79.37390960531435269 ) ) ;
#25008 = CARTESIAN_POINT ( 'NONE',  ( 10.72451020669871369, 18.67979575497193778, 92.08442372801901854 ) ) ;
#25009 = CARTESIAN_POINT ( 'NONE',  ( 0.05219959533934541429, -16.53943276465976808, 60.00109039468568284 ) ) ;
#25010 = CARTESIAN_POINT ( 'NONE',  ( -9.474510206698964154, 16.51473224551069663, 110.4155762719810383 ) ) ;
#25011 = AXIS2_PLACEMENT_3D ( 'NONE', #126547, #96210, #189245 ) ;
#25012 = CARTESIAN_POINT ( 'NONE',  ( -0.05219959533910754901, -16.53943276465976808, 42.49890960531435979 ) ) ;
#25013 = CARTESIAN_POINT ( 'NONE',  ( -19.02544592524342804, 5.153800228976336051, 31.04057627198102409 ) ) ;
#25014 = CARTESIAN_POINT ( 'NONE',  ( -16.52544592524335698, -4.483927247898792601, 58.95942372801902565 ) ) ;
#25015 = CARTESIAN_POINT ( 'NONE',  ( -16.53943276465976808, 0.05219959533911058130, 51.24890960531436690 ) ) ;
#25016 = CARTESIAN_POINT ( 'NONE',  ( -5.153800228976328057, -19.02544592524343514, 107.2905762719810383 ) ) ;
#25017 = CARTESIAN_POINT ( 'NONE',  ( -0.05219959533907301413, -21.53943276465977519, 32.49890960531435979 ) ) ;
#25018 = CARTESIAN_POINT ( 'NONE',  ( -5.719274019375665041, -21.55341960407619695, 109.7927570613523613 ) ) ;
#25019 = CARTESIAN_POINT ( 'NONE',  ( 12.14591786802309770, 12.06949235617756955, 104.3739096053143669 ) ) ;
#25020 = CARTESIAN_POINT ( 'NONE',  ( 16.46253265017160672, -9.564922557960803928, 98.33224293864769550 ) ) ;
#25021 = ORIENTED_EDGE ( 'NONE', *, *, #3260, .T. ) ;
#25022 = CARTESIAN_POINT ( 'NONE',  ( -8.314922557961024197, 14.29746914071037800, 47.91775706135234714 ) ) ;
#25023 = CARTESIAN_POINT ( 'NONE',  ( -5.049401038298153566, 19.05341960407611168, 60.20724293864768129 ) ) ;
#25024 = CARTESIAN_POINT ( 'NONE',  ( 1.300000000000000044, -0.7216878364870318308, 1.249999999999999778 ) ) ;
#25025 = CARTESIAN_POINT ( 'NONE',  ( -13.97604488694547697, 13.89961937509957934, 48.12609039468566863 ) ) ;
#25026 = CARTESIAN_POINT ( 'NONE',  ( 8.224510206698742110, 14.34966873604972548, 77.08442372801901854 ) ) ;
#25027 = CARTESIAN_POINT ( 'NONE',  ( 19.03943276465977164, 0.05219959533936151252, 96.25109039468567573 ) ) ;
#25028 = CARTESIAN_POINT ( 'NONE',  ( 21.52544592524334988, 5.823673210054432836, 61.45942372801901854 ) ) ;
#25029 = CARTESIAN_POINT ( 'NONE',  ( 13.97604488694527802, 13.89961937509977652, 79.37390960531435269 ) ) ;
#25030 = CARTESIAN_POINT ( 'NONE',  ( -18.67979575497178146, -10.72451020669898902, 96.66557627198102409 ) ) ;
#25031 = CARTESIAN_POINT ( 'NONE',  ( 16.46253265017160672, -9.564922557960803928, 23.33224293864769194 ) ) ;
#25032 = AXIS2_PLACEMENT_3D ( 'NONE', #79551, #186762, #171571 ) ;
#25033 = CARTESIAN_POINT ( 'NONE',  ( 0.05219959533936267826, -19.03943276465977164, 85.00109039468567573 ) ) ;
#25034 = CARTESIAN_POINT ( 'NONE',  ( -21.55341960407610458, -5.719274019375992779, 71.45724293864769550 ) ) ;
#25035 = CARTESIAN_POINT ( 'NONE',  ( 19.03943276465977164, 0.05219959533936151252, 36.25109039468567573 ) ) ;
#25036 = FACE_BOUND ( 'NONE', #33199, .T. ) ;
#25037 = CARTESIAN_POINT ( 'NONE',  ( 21.52544592524344225, -5.823673210054117533, 88.54057627198103830 ) ) ;
#25038 = CARTESIAN_POINT ( 'NONE',  ( -37.99626262588762415, 12.34573411038923219, -7.847842220587805784 ) ) ;
#25039 = CARTESIAN_POINT ( 'NONE',  ( -16.46253265017160317, 9.564922557960807481, 60.83224293864769550 ) ) ;
#25040 = CARTESIAN_POINT ( 'NONE',  ( 13.89961937509978007, -13.97604488694527269, 93.12390960531435269 ) ) ;
#25041 = CARTESIAN_POINT ( 'NONE',  ( -16.53943276465976808, -0.05219959533934237506, 18.75109039468568639 ) ) ;
#25042 = LINE ( 'NONE', #182700, #28874 ) ;
#25043 = CARTESIAN_POINT ( 'NONE',  ( -19.05341960407611168, -5.049401038298163336, 46.45724293864768129 ) ) ;
#25044 = CARTESIAN_POINT ( 'NONE',  ( -19.02544592524342804, 5.153800228976336051, 106.0405762719810241 ) ) ;
#25046 = CARTESIAN_POINT ( 'NONE',  ( 4.483927247898545687, 16.52544592524342804, 49.79057627198102409 ) ) ;
#25045 = CARTESIAN_POINT ( 'NONE',  ( 10.81492255796078972, 18.62759615963270932, 99.58224293864770971 ) ) ;
#25047 = CARTESIAN_POINT ( 'NONE',  ( -15.80617190586768217, 15.72974639402176855, 73.12609039468567573 ) ) ;
#25049 = CARTESIAN_POINT ( 'NONE',  ( 5.153800228976615827, -19.02544592524334988, 35.20942372801899722 ) ) ;
#25048 = CARTESIAN_POINT ( 'NONE',  ( 8.314922557961029526, -14.29746914071037800, 30.41775706135234358 ) ) ;
#25050 = CARTESIAN_POINT ( 'NONE',  ( -12.06949235617756955, 12.14591786802309770, 35.62390960531437401 ) ) ;
#25051 = CARTESIAN_POINT ( 'NONE',  ( -18.62759615963270932, 10.81492255796079327, 110.8322429386476955 ) ) ;
#25052 = CARTESIAN_POINT ( 'NONE',  ( 16.55341960407611168, 4.379528057220329451, 48.95724293864770971 ) ) ;
#25053 = CARTESIAN_POINT ( 'NONE',  ( -13.97604488694547697, 13.89961937509957934, 93.12609039468566152 ) ) ;
#25054 = CARTESIAN_POINT ( 'NONE',  ( -0.05219959533936034679, 19.03943276465977164, 67.50109039468566152 ) ) ;
#25055 = CARTESIAN_POINT ( 'NONE',  ( -15.80617190586768217, 15.72974639402176855, 73.12609039468567573 ) ) ;
#25056 = CARTESIAN_POINT ( 'NONE',  ( -9.474510206698720793, -16.51473224551083518, 49.58442372801899722 ) ) ;
#25057 = CARTESIAN_POINT ( 'NONE',  ( 9.564922557960805705, 16.46253265017160317, 24.58224293864769194 ) ) ;
#25058 = CARTESIAN_POINT ( 'NONE',  ( 18.67979575497178502, 10.72451020669898547, 39.16557627198102409 ) ) ;
#25059 = CARTESIAN_POINT ( 'NONE',  ( -12.14591786802309592, -12.06949235617757132, 46.87390960531435979 ) ) ;
#25060 = CARTESIAN_POINT ( 'NONE',  ( -19.26498983726236602, 5.499999999999802824, 95.55319577422001487 ) ) ;
#25061 = CARTESIAN_POINT ( 'NONE',  ( 9.474510206698729675, 16.51473224551082808, 22.08442372801899722 ) ) ;
#25062 = CARTESIAN_POINT ( 'NONE',  ( -16.52544592524335698, -4.483927247898792601, 78.95942372801901854 ) ) ;
#25063 = CARTESIAN_POINT ( 'NONE',  ( 8.314922557960818139, 14.29746914071049879, 39.58224293864769550 ) ) ;
#25064 = CARTESIAN_POINT ( 'NONE',  ( 18.62759615963255655, 10.81492255796105972, 76.66775706135234714 ) ) ;
#25065 = CARTESIAN_POINT ( 'NONE',  ( -18.67979575497193778, 10.72451020669871902, 68.33442372801900433 ) ) ;
#25066 = CARTESIAN_POINT ( 'NONE',  ( 5.823673210054125526, 21.52544592524343514, 79.79057627198102409 ) ) ;
#25067 = CARTESIAN_POINT ( 'NONE',  ( -9.474510206698964154, 16.51473224551069663, 40.41557627198103120 ) ) ;
#25068 = CARTESIAN_POINT ( 'NONE',  ( -18.62759615963255300, -10.81492255796106328, 54.16775706135235424 ) ) ;
#25069 = CARTESIAN_POINT ( 'NONE',  ( -16.46253265017160317, 9.564922557960807481, 35.83224293864768839 ) ) ;
#25070 = CARTESIAN_POINT ( 'NONE',  ( 5.049401038298161559, -19.05341960407611168, 47.70724293864770260 ) ) ;
#25071 = CARTESIAN_POINT ( 'NONE',  ( 12.14591786802309770, 12.06949235617756955, 99.37390960531436690 ) ) ;
#25072 = CARTESIAN_POINT ( 'NONE',  ( 16.46253265017160672, -9.564922557960803928, 93.33224293864769550 ) ) ;
#25073 = CARTESIAN_POINT ( 'NONE',  ( -16.52544592524342804, 4.483927247898546575, 46.04057627198103830 ) ) ;
#25074 = CARTESIAN_POINT ( 'NONE',  ( -16.53943276465976808, 0.05219959533911058130, 96.24890960531435269 ) ) ;
#25075 = CARTESIAN_POINT ( 'NONE',  ( -15.72974639402197994, 15.80617190586746368, 75.62390960531439532 ) ) ;
#25076 = CARTESIAN_POINT ( 'NONE',  ( -15.72974639402176322, -15.80617190586768395, 19.37609039468568639 ) ) ;
#25077 = CARTESIAN_POINT ( 'NONE',  ( -17.60909914540868115, 15.84704938773722560, -54.71262039249372577 ) ) ;
#25079 = CARTESIAN_POINT ( 'NONE',  ( -4.379528057220086978, -16.55341960407618274, 19.79275706135235069 ) ) ;
#25078 = CARTESIAN_POINT ( 'NONE',  ( 19.05341960407611168, 5.049401038298154454, 83.95724293864766707 ) ) ;
#25080 = CARTESIAN_POINT ( 'NONE',  ( -21.53943276465977519, 0.05219959533907696930, 66.24890960531436690 ) ) ;
#25081 = CARTESIAN_POINT ( 'NONE',  ( -18.67979575497193778, 10.72451020669871902, 93.33442372801901854 ) ) ;
#25082 = CARTESIAN_POINT ( 'NONE',  ( 5.153800228976335163, 19.02544592524342804, 74.79057627198103830 ) ) ;
#25083 = CARTESIAN_POINT ( 'NONE',  ( -15.80617190586768217, 15.72974639402176855, 28.12609039468568284 ) ) ;
#25084 = EDGE_CURVE ( 'NONE', #182160, #27470, #78080, .T. ) ;
#25085 = CARTESIAN_POINT ( 'NONE',  ( -19.03943276465977164, 0.05219959533909376836, 116.2489096053143669 ) ) ;
#25086 = CARTESIAN_POINT ( 'NONE',  ( 16.53943276465976808, 0.05219959533934440121, 86.25109039468568994 ) ) ;
#25087 = CARTESIAN_POINT ( 'NONE',  ( -0.05219959533937732626, 21.53943276465977519, 72.50109039468568994 ) ) ;
#25088 = CARTESIAN_POINT ( 'NONE',  ( 0.05219959533937995610, -21.53943276465977519, 105.0010903946856757 ) ) ;
#25089 = CARTESIAN_POINT ( 'NONE',  ( 14.34966873604972726, -8.224510206698740333, 65.83442372801900433 ) ) ;
#25090 = CARTESIAN_POINT ( 'NONE',  ( -0.05219959533937732626, 21.53943276465977519, 22.50109039468567573 ) ) ;
#25091 = CARTESIAN_POINT ( 'NONE',  ( -16.46253265017160317, 9.564922557960807481, 115.8322429386477097 ) ) ;
#25092 = CARTESIAN_POINT ( 'NONE',  ( 0.05219959533937995610, -21.53943276465977519, 90.00109039468567573 ) ) ;
#25093 = CARTESIAN_POINT ( 'NONE',  ( -13.97604488694527625, -13.89961937509977652, 96.87390960531433848 ) ) ;
#25094 = CARTESIAN_POINT ( 'NONE',  ( 18.62759615963271287, -10.81492255796078972, 83.33224293864769550 ) ) ;
#25095 = CARTESIAN_POINT ( 'NONE',  ( 16.46253265017146816, 9.564922557961045513, 56.66775706135233293 ) ) ;
#25097 = CARTESIAN_POINT ( 'NONE',  ( -10.81492255796078084, -18.62759615963271287, 57.08224293864769550 ) ) ;
#25096 = CARTESIAN_POINT ( 'NONE',  ( -16.29108346408469288, -34.51247628902108033, -22.00899094814154822 ) ) ;
#25099 = CARTESIAN_POINT ( 'NONE',  ( 8.224510206698953496, -14.34966873604960469, 37.91557627198102409 ) ) ;
#25098 = CARTESIAN_POINT ( 'NONE',  ( -9.564922557960796823, -16.46253265017161027, 97.08224293864769550 ) ) ;
#25100 = CARTESIAN_POINT ( 'NONE',  ( 10.19682395672834119, -9.344414726942043004, -62.53306532695916786 ) ) ;
#25101 = CARTESIAN_POINT ( 'NONE',  ( -0.05219959533936034679, 19.03943276465977164, 77.50109039468566152 ) ) ;
#25102 = CARTESIAN_POINT ( 'NONE',  ( -17.05587630539787014, 6.762274262135693270, 105.7418030903731534 ) ) ;
#25103 = CARTESIAN_POINT ( 'NONE',  ( -16.53943276465976808, -0.05219959533934237506, 18.75109039468568639 ) ) ;
#25104 = CARTESIAN_POINT ( 'NONE',  ( -5.823673210054116645, -21.52544592524344225, 87.29057627198103830 ) ) ;
#25105 = CARTESIAN_POINT ( 'NONE',  ( -16.53943276465976808, 0.05219959533911058130, 61.24890960531435979 ) ) ;
#25106 = CARTESIAN_POINT ( 'NONE',  ( 5.049401038298161559, -19.05341960407611168, 102.7072429386476955 ) ) ;
#25107 = CARTESIAN_POINT ( 'NONE',  ( -14.34966873604972548, 8.224510206698743886, 33.33442372801900433 ) ) ;
#25108 = CARTESIAN_POINT ( 'NONE',  ( -0.05219959533909027116, -19.03943276465977164, 57.49890960531435979 ) ) ;
#25110 = CARTESIAN_POINT ( 'NONE',  ( 16.51473224551083163, -9.474510206698727899, 80.83442372801899012 ) ) ;
#25109 = CARTESIAN_POINT ( 'NONE',  ( 21.53943276465977519, 0.05219959533937863772, 21.25109039468567218 ) ) ;
#25111 = CARTESIAN_POINT ( 'NONE',  ( 5.153800228976335163, 19.02544592524342804, 94.79057627198103830 ) ) ;
#25112 = CARTESIAN_POINT ( 'NONE',  ( -13.89961937509977652, 13.97604488694528158, 70.62390960531432427 ) ) ;
#25113 = CARTESIAN_POINT ( 'NONE',  ( -21.53943276465977519, 0.05219959533907696930, 76.24890960531435269 ) ) ;
#25114 = CARTESIAN_POINT ( 'NONE',  ( 16.51473224551069308, 9.474510206698969483, 49.16557627198102409 ) ) ;
#25115 = DIRECTION ( 'NONE',  ( 0.000000000000000000, 0.000000000000000000, 1.000000000000000000 ) ) ;
#25116 = CARTESIAN_POINT ( 'NONE',  ( 4.379528057220339221, -16.55341960407611168, 57.70724293864770260 ) ) ;
#25117 = CARTESIAN_POINT ( 'NONE',  ( 5.153800228976335163, 19.02544592524342804, 104.7905762719809957 ) ) ;
#25118 = CARTESIAN_POINT ( 'NONE',  ( -17.81289503416611097, -24.51734667627696496, 140.5500000054623513 ) ) ;
#25119 = CARTESIAN_POINT ( 'NONE',  ( -16.51473224551082808, 9.474510206698731452, 63.33442372801900433 ) ) ;
#25120 = CARTESIAN_POINT ( 'NONE',  ( 21.53943276465977519, -0.05219959533907433946, 83.74890960531435269 ) ) ;
#25121 = CARTESIAN_POINT ( 'NONE',  ( -0.05219959533936034679, 19.03943276465977164, 52.50109039468566863 ) ) ;
#25122 = CARTESIAN_POINT ( 'NONE',  ( -16.51473224551069308, -9.474510206698971260, 106.6655762719810383 ) ) ;
#25123 = CARTESIAN_POINT ( 'NONE',  ( -17.97058386085787873, -5.499999999999975131, 74.00390968646215129 ) ) ;
#25125 = EDGE_CURVE ( 'NONE', #125859, #133361, #62915, .T. ) ;
#25124 = CARTESIAN_POINT ( 'NONE',  ( 21.52544592524344225, -5.823673210054117533, 48.54057627198103120 ) ) ;
#25126 = AXIS2_PLACEMENT_3D ( 'NONE', #120644, #182342, #163175 ) ;
#25127 = CARTESIAN_POINT ( 'NONE',  ( 16.46253265017160672, -9.564922557960803928, 68.33224293864770971 ) ) ;
#25128 = CARTESIAN_POINT ( 'NONE',  ( 21.55341960407619695, -5.719274019375665929, 71.04275706135234714 ) ) ;
#25129 = CARTESIAN_POINT ( 'NONE',  ( 13.89961937509977652, -13.97604488694527269, 38.12390960531436690 ) ) ;
#25131 = ORIENTED_EDGE ( 'NONE', *, *, #52643, .F. ) ;
#25130 = CARTESIAN_POINT ( 'NONE',  ( -8.224510206698948167, 14.34966873604960824, 80.41557627198103830 ) ) ;
#25132 = CARTESIAN_POINT ( 'NONE',  ( 5.719274019375673035, 21.55341960407619339, 57.29275706135234714 ) ) ;
#25133 = VERTEX_POINT ( 'NONE', #111415 ) ;
#25134 = CARTESIAN_POINT ( 'NONE',  ( 16.46253265017160672, -9.564922557960803928, 108.3322429386476955 ) ) ;
#25135 = CARTESIAN_POINT ( 'NONE',  ( -9.564922557961040184, 16.46253265017147172, 72.91775706135233293 ) ) ;
#25136 = CARTESIAN_POINT ( 'NONE',  ( 26.05560406886092295, -30.01072603040624998, -20.45417971608936725 ) ) ;
#25137 = CARTESIAN_POINT ( 'NONE',  ( 5.719274019375673035, 21.55341960407619339, 27.29275706135234358 ) ) ;
#25138 = CARTESIAN_POINT ( 'NONE',  ( 5.153800228976335163, 19.02544592524342804, 64.79057627198100988 ) ) ;
#25139 = CARTESIAN_POINT ( 'NONE',  ( 16.53943276465976808, 0.05219959533934440121, 41.25109039468568284 ) ) ;
#25140 = CARTESIAN_POINT ( 'NONE',  ( -6.020228577223754586E-15, 39.95556452105416412, -4.249999994537627224 ) ) ;
#25141 = CARTESIAN_POINT ( 'NONE',  ( 9.564922557961047289, -16.46253265017146816, 20.41775706135233293 ) ) ;
#25142 = CARTESIAN_POINT ( 'NONE',  ( 19.05341960407611168, 5.049401038298154454, 38.95724293864767418 ) ) ;
#25143 = CARTESIAN_POINT ( 'NONE',  ( -10.81492255796105439, 18.62759615963255655, 112.9177570613523329 ) ) ;
#25144 = CARTESIAN_POINT ( 'NONE',  ( 16.53943276465976808, 0.05219959533934440121, 86.25109039468568994 ) ) ;
#25146 = CARTESIAN_POINT ( 'NONE',  ( -5.823673210054431948, 21.52544592524334988, 62.70942372801902565 ) ) ;
#25145 = CARTESIAN_POINT ( 'NONE',  ( -13.89961937509977652, 13.97604488694528158, 85.62390960531433848 ) ) ;
#25147 = CARTESIAN_POINT ( 'NONE',  ( 36.91746825000000598, -11.99521256947793546, -9.724999997268813701 ) ) ;
#25148 = FACE_OUTER_BOUND ( 'NONE', #147177, .T. ) ;
#25149 = CARTESIAN_POINT ( 'NONE',  ( 5.000000000000001776, -120.0000000000000142, -15.00000000000000000 ) ) ;
#25151 = CARTESIAN_POINT ( 'NONE',  ( -5.719274019375665041, -21.55341960407619695, 74.79275706135234714 ) ) ;
#25150 = CARTESIAN_POINT ( 'NONE',  ( -14.29746914071037622, -8.314922557961029526, 49.16775706135234003 ) ) ;
#25152 = CARTESIAN_POINT ( 'NONE',  ( -0.05219959533937732626, 21.53943276465977519, 107.5010903946856899 ) ) ;
#25153 = CARTESIAN_POINT ( 'NONE',  ( 26.12113310390727250, -7.698689789033765329, 169.4288210027979460 ) ) ;
#25154 = CARTESIAN_POINT ( 'NONE',  ( 12.14591786802327356, -12.06949235617739191, 30.62609039468567929 ) ) ;
#25155 = CARTESIAN_POINT ( 'NONE',  ( 5.049401038298161559, -19.05341960407611168, 92.70724293864769550 ) ) ;
#25156 = CARTESIAN_POINT ( 'NONE',  ( 19.05341960407611168, 5.049401038298154454, 113.9572429386477097 ) ) ;
#25157 = EDGE_LOOP ( 'NONE', ( #86325, #134189, #138051, #172711, #183482 ) ) ;
#25158 = AXIS2_PLACEMENT_3D ( 'NONE', #53461, #38301, #99955 ) ;
#25159 = LINE ( 'NONE', #161644, #82490 ) ;
#25160 = CARTESIAN_POINT ( 'NONE',  ( -19.03943276465977164, 0.05219959533909376836, 26.24890960531435624 ) ) ;
#25161 = CARTESIAN_POINT ( 'NONE',  ( -0.05219959533907301413, -21.53943276465977519, 42.49890960531435979 ) ) ;
#25162 = CARTESIAN_POINT ( 'NONE',  ( 4.483927247898790824, -16.52544592524335698, 105.2094237280190328 ) ) ;
#25164 = CARTESIAN_POINT ( 'NONE',  ( -16.51473224551069308, -9.474510206698971260, 71.66557627198102409 ) ) ;
#25163 = CARTESIAN_POINT ( 'NONE',  ( 16.52544592524342804, -4.483927247898539470, 78.54057627198103830 ) ) ;
#25165 = CARTESIAN_POINT ( 'NONE',  ( 15.80617190586769283, -15.72974639402175789, 110.6260903946857042 ) ) ;
#25166 = CARTESIAN_POINT ( 'NONE',  ( 14.29746914071037800, 8.314922557961029526, 21.66775706135235069 ) ) ;
#25167 = CARTESIAN_POINT ( 'NONE',  ( -12.06949235617756955, 12.14591786802309770, 90.62390960531436690 ) ) ;
#25168 = CARTESIAN_POINT ( 'NONE',  ( -0.05219959533937732626, 21.53943276465977519, 47.50109039468568994 ) ) ;
#25169 = CARTESIAN_POINT ( 'NONE',  ( 15.80617190586746368, 15.72974639402197994, 79.37390960531436690 ) ) ;
#25170 = CARTESIAN_POINT ( 'NONE',  ( -0.05219959533936034679, 19.03943276465977164, 52.50109039468566863 ) ) ;
#25171 = CARTESIAN_POINT ( 'NONE',  ( -34.74703179323500279, 1.946018278951686442, 52.24735473369669592 ) ) ;
#25172 = CARTESIAN_POINT ( 'NONE',  ( 9.564922557960805705, 16.46253265017160317, 94.58224293864769550 ) ) ;
#25173 = CARTESIAN_POINT ( 'NONE',  ( 8.314922557960818139, 14.29746914071049879, 69.58224293864769550 ) ) ;
#25174 = CARTESIAN_POINT ( 'NONE',  ( 14.34966873604960469, 8.224510206698951720, 49.16557627198102409 ) ) ;
#25175 = CARTESIAN_POINT ( 'NONE',  ( -0.05219959533910754901, -16.53943276465976808, 22.49890960531436335 ) ) ;
#25176 = CARTESIAN_POINT ( 'NONE',  ( 16.51473224551083163, -9.474510206698727899, 65.83442372801900433 ) ) ;
#25177 = CARTESIAN_POINT ( 'NONE',  ( 13.97604488694548053, -13.89961937509957401, 90.62609039468566152 ) ) ;
#25178 = CARTESIAN_POINT ( 'NONE',  ( -19.02544592524342804, 5.153800228976336051, 116.0405762719810383 ) ) ;
#25179 = ADVANCED_FACE ( 'NONE', ( #19413 ), #183994, .T. ) ;
#25180 = CARTESIAN_POINT ( 'NONE',  ( 14.29746914071049879, -8.314922557960816363, 83.33224293864769550 ) ) ;
#25181 = CARTESIAN_POINT ( 'NONE',  ( -3.573655867281984216E-15, 2.428612866367529932E-14, -13.00000000000000000 ) ) ;
#25183 = CARTESIAN_POINT ( 'NONE',  ( 10.72451020669898902, -18.67979575497178502, 52.91557627198103830 ) ) ;
#25182 = CARTESIAN_POINT ( 'NONE',  ( -5.153800228976328057, -19.02544592524343514, 47.29057627198102409 ) ) ;
#25184 = CARTESIAN_POINT ( 'NONE',  ( 10.81492255796078972, 18.62759615963270932, 74.58224293864768129 ) ) ;
#25185 = CARTESIAN_POINT ( 'NONE',  ( 16.53943276465976808, -0.05219959533910856209, 113.7489096053143527 ) ) ;
#25187 = CARTESIAN_POINT ( 'NONE',  ( -5.153800228976328057, -19.02544592524343514, 57.29057627198103120 ) ) ;
#25186 = CARTESIAN_POINT ( 'NONE',  ( 0.05219959533934541429, -16.53943276465976808, 60.00109039468568284 ) ) ;
#25188 = CARTESIAN_POINT ( 'NONE',  ( -9.564922557961040184, 16.46253265017147172, 37.91775706135233293 ) ) ;
#25189 = CARTESIAN_POINT ( 'NONE',  ( -21.55341960407619339, 5.719274019375674811, 48.54275706135234714 ) ) ;
#25190 = CARTESIAN_POINT ( 'NONE',  ( 4.483927247898545687, 16.52544592524342804, 109.7905762719810383 ) ) ;
#25191 = CARTESIAN_POINT ( 'NONE',  ( 16.46253265017146816, 9.564922557961045513, 96.66775706135233293 ) ) ;
#25192 = CARTESIAN_POINT ( 'NONE',  ( -29.86685920354755552, 21.69954338932564397, -5.324999997268814234 ) ) ;
#25194 = CARTESIAN_POINT ( 'NONE',  ( -15.80617190586745835, -15.72974639402198527, 51.87390960531437401 ) ) ;
#25193 = DIRECTION ( 'NONE',  ( 0.000000000000000000, 0.000000000000000000, 1.000000000000000000 ) ) ;
#25195 = CARTESIAN_POINT ( 'NONE',  ( 16.20579543436674541, -7.371946100355224019, 66.93479165828121324 ) ) ;
#25196 = CARTESIAN_POINT ( 'NONE',  ( 21.53943276465977519, 0.05219959533937863772, 81.25109039468568994 ) ) ;
#25197 = CARTESIAN_POINT ( 'NONE',  ( 12.14591786802309770, 12.06949235617756955, 39.37390960531436690 ) ) ;
#25199 = CARTESIAN_POINT ( 'NONE',  ( 12.06949235617757843, -12.14591786802309237, 38.12390960531436690 ) ) ;
#25198 = CARTESIAN_POINT ( 'NONE',  ( -0.05219959533934338120, 16.53943276465976808, 57.50109039468568994 ) ) ;
#25200 = CARTESIAN_POINT ( 'NONE',  ( 15.80617190586746368, 15.72974639402197994, 79.37390960531436690 ) ) ;
#25202 = CARTESIAN_POINT ( 'NONE',  ( -21.55341960407610458, -5.719274019375992779, 76.45724293864769550 ) ) ;
#25201 = PRODUCT_DEFINITION ( 'UNKNOWN', '', #127543, #36219 ) ;
#25203 = CARTESIAN_POINT ( 'NONE',  ( 20.96320343559668942, 21.46320343559617427, 4.646446609406718942 ) ) ;
#25205 = CARTESIAN_POINT ( 'NONE',  ( 9.564922557960805705, 16.46253265017160317, 114.5822429386476955 ) ) ;
#25204 = CARTESIAN_POINT ( 'NONE',  ( -19.05341960407617563, 5.049401038297882671, 78.54275706135233293 ) ) ;
#25206 = CARTESIAN_POINT ( 'NONE',  ( -0.05219959533909027116, -19.03943276465977164, 47.49890960531435979 ) ) ;
#25207 = CARTESIAN_POINT ( 'NONE',  ( -19.05341960407611168, -5.049401038298163336, 36.45724293864766707 ) ) ;
#25208 = SHAPE_REPRESENTATION_RELATIONSHIP ( 'NONE' , 'NONE' ,  #71529, #51975 ) ;
#25209 = LINE ( 'NONE', #145514, #196311 ) ;
#25210 = ORIENTED_EDGE ( 'NONE', *, *, #10139, .F. ) ;
#25211 = CARTESIAN_POINT ( 'NONE',  ( 14.29746914071037800, 8.314922557961029526, 81.66775706135236135 ) ) ;
#25212 = CARTESIAN_POINT ( 'NONE',  ( 15.72974639402199770, -15.80617190586745480, 108.1239096053143811 ) ) ;
#25213 = CARTESIAN_POINT ( 'NONE',  ( 16.51473224551069308, 9.474510206698969483, 69.16557627198102409 ) ) ;
#25214 = CARTESIAN_POINT ( 'NONE',  ( 0.05219959533937995610, -21.53943276465977519, 40.00109039468567573 ) ) ;
#25215 = CARTESIAN_POINT ( 'NONE',  ( 0.05219959533909260263, 19.03943276465977164, 89.99890960531436690 ) ) ;
#25216 = CARTESIAN_POINT ( 'NONE',  ( -27.99776551637687305, -28.30561827218003046, -16.93438536460645949 ) ) ;
#25217 = VERTEX_POINT ( 'NONE', #143785 ) ;
#25218 = CARTESIAN_POINT ( 'NONE',  ( -18.67979575497193778, 10.72451020669871902, 33.33442372801900433 ) ) ;
#25220 = CARTESIAN_POINT ( 'NONE',  ( -5.049401038298153566, 19.05341960407611168, 110.2072429386476671 ) ) ;
#25219 = CARTESIAN_POINT ( 'NONE',  ( 13.89961937509977652, -13.97604488694527269, 28.12390960531435624 ) ) ;
#25221 = CARTESIAN_POINT ( 'NONE',  ( 9.564922557961047289, -16.46253265017146816, 40.41775706135234003 ) ) ;
#25222 = CARTESIAN_POINT ( 'NONE',  ( -15.72974639402176322, -15.80617190586768395, 19.37609039468568639 ) ) ;
#25223 = CARTESIAN_POINT ( 'NONE',  ( -0.05219959533936034679, 19.03943276465977164, 42.50109039468566152 ) ) ;
#25224 = CARTESIAN_POINT ( 'NONE',  ( -19.02544592524334988, -5.153800228976617603, 48.95942372801900433 ) ) ;
#25225 = CARTESIAN_POINT ( 'NONE',  ( 12.14591786802327356, -12.06949235617739191, 85.62609039468568994 ) ) ;
#25227 = ORIENTED_EDGE ( 'NONE', *, *, #106983, .T. ) ;
#25226 = CARTESIAN_POINT ( 'NONE',  ( -19.03943276465977164, 0.05219959533909376836, 116.2489096053143669 ) ) ;
#25228 = CARTESIAN_POINT ( 'NONE',  ( 0.05219959533909260263, 19.03943276465977164, 74.99890960531435269 ) ) ;
#25229 = CARTESIAN_POINT ( 'NONE',  ( 21.55341960407619695, -5.719274019375665929, 81.04275706135236135 ) ) ;
#25230 = CARTESIAN_POINT ( 'NONE',  ( 21.55341960407619695, -5.719274019375665929, 96.04275706135236135 ) ) ;
#25231 = LINE ( 'NONE', #24221, #11077 ) ;
#25232 = CARTESIAN_POINT ( 'NONE',  ( -16.46253265017160317, 9.564922557960807481, 90.83224293864769550 ) ) ;
#25233 = CARTESIAN_POINT ( 'NONE',  ( -10.81492255796105439, 18.62759615963255655, 57.91775706135234714 ) ) ;
#25234 = CARTESIAN_POINT ( 'NONE',  ( -13.97604488694547697, 13.89961937509957934, 108.1260903946856331 ) ) ;
#25235 = CARTESIAN_POINT ( 'NONE',  ( -13.97604488694527625, -13.89961937509977652, 71.87390960531433848 ) ) ;
#25236 = CARTESIAN_POINT ( 'NONE',  ( 0.05219959533909260263, 19.03943276465977164, 109.9989096053143669 ) ) ;
#25237 = CARTESIAN_POINT ( 'NONE',  ( -19.05341960407611168, -5.049401038298163336, 86.45724293864769550 ) ) ;
#25238 = PLANE ( 'NONE',  #78925 ) ;
#25239 = CARTESIAN_POINT ( 'NONE',  ( -16.51473224551069308, -9.474510206698971260, 66.66557627198102409 ) ) ;
#25240 = CARTESIAN_POINT ( 'NONE',  ( 19.02544592524343514, -5.153800228976328945, 53.54057627198102409 ) ) ;
#25241 = CARTESIAN_POINT ( 'NONE',  ( 21.55341960407619695, -5.719274019375665929, 21.04275706135234714 ) ) ;
#25242 = CARTESIAN_POINT ( 'NONE',  ( -8.224510206698735004, -14.34966873604973081, 104.5844237280190185 ) ) ;
#25243 = CYLINDRICAL_SURFACE ( 'NONE', #166356, 24.30000000000003268 ) ;
#25244 = CARTESIAN_POINT ( 'NONE',  ( -19.05341960407617563, 5.049401038297882671, 58.54275706135234003 ) ) ;
#25245 = CARTESIAN_POINT ( 'NONE',  ( -16.46253265017160317, 9.564922557960807481, 90.83224293864769550 ) ) ;
#25246 = CARTESIAN_POINT ( 'NONE',  ( -16.53943276465976808, 0.05219959533911058130, 76.24890960531435269 ) ) ;
#25247 = CARTESIAN_POINT ( 'NONE',  ( -14.34966873604960291, -8.224510206698953496, 111.6655762719810525 ) ) ;
#25248 = CARTESIAN_POINT ( 'NONE',  ( 0.05219959533907565091, 21.53943276465977519, 29.99890960531435979 ) ) ;
#25249 = CARTESIAN_POINT ( 'NONE',  ( -15.80617190586745835, -15.72974639402198527, 21.87390960531436690 ) ) ;
#25250 = CARTESIAN_POINT ( 'NONE',  ( -4.483927247898539470, -16.52544592524342804, 92.29057627198103830 ) ) ;
#25251 = CARTESIAN_POINT ( 'NONE',  ( -16.88567814943165502, 6.947325034625572826, 53.70998877347415146 ) ) ;
#25252 = CARTESIAN_POINT ( 'NONE',  ( -16.51473224551082808, 9.474510206698731452, 48.33442372801900433 ) ) ;
#25253 = CARTESIAN_POINT ( 'NONE',  ( -12.06949235617739369, -12.14591786802326823, 109.3760903946857042 ) ) ;
#25254 = CARTESIAN_POINT ( 'NONE',  ( -5.049401038298153566, 19.05341960407611168, 85.20724293864766707 ) ) ;
#25255 = CARTESIAN_POINT ( 'NONE',  ( -15.72974639402176322, -15.80617190586768395, 49.37609039468569705 ) ) ;
#25256 = CARTESIAN_POINT ( 'NONE',  ( -5.823673210054116645, -21.52544592524344225, 47.29057627198103120 ) ) ;
#25257 = CARTESIAN_POINT ( 'NONE',  ( 0.05219959533937995610, -21.53943276465977519, 30.00109039468568284 ) ) ;
#25258 = CARTESIAN_POINT ( 'NONE',  ( -21.53943276465977519, 0.05219959533907696930, 86.24890960531436690 ) ) ;
#25259 = CARTESIAN_POINT ( 'NONE',  ( -4.483927247898539470, -16.52544592524342804, 102.2905762719810383 ) ) ;
#25260 = CARTESIAN_POINT ( 'NONE',  ( -19.03943276465977164, -0.05219959533935918106, 63.75109039468566863 ) ) ;
#25261 = CARTESIAN_POINT ( 'NONE',  ( 5.049401038298161559, -19.05341960407611168, 42.70724293864767418 ) ) ;
#25262 = CARTESIAN_POINT ( 'NONE',  ( -5.049401038298153566, 19.05341960407611168, 95.20724293864770971 ) ) ;
#25263 = CARTESIAN_POINT ( 'NONE',  ( 0.05219959533909260263, 19.03943276465977164, 99.99890960531436690 ) ) ;
#25264 = CARTESIAN_POINT ( 'NONE',  ( -19.03943276465977164, 0.05219959533909376836, 21.24890960531436335 ) ) ;
#25265 = CARTESIAN_POINT ( 'NONE',  ( 4.483927247898545687, 16.52544592524342804, 44.79057627198103120 ) ) ;
#25266 = CARTESIAN_POINT ( 'NONE',  ( 4.379528057220092307, 16.55341960407617563, 37.29275706135235424 ) ) ;
#25267 = CARTESIAN_POINT ( 'NONE',  ( 21.55341960407619695, -5.719274019375665929, 106.0427570613523471 ) ) ;
#25270 = CARTESIAN_POINT ( 'NONE',  ( 12.06949235617739724, 12.14591786802326823, 111.8760903946856615 ) ) ;
#25269 = CARTESIAN_POINT ( 'NONE',  ( 16.46253265017160672, -9.564922557960803928, 113.3322429386476955 ) ) ;
#25268 = CIRCLE ( 'NONE', #147520, 31.90000000000003411 ) ;
#25271 = CARTESIAN_POINT ( 'NONE',  ( 21.53943276465977519, 0.05219959533937863772, 36.25109039468567573 ) ) ;
#25272 = CARTESIAN_POINT ( 'NONE',  ( -19.03943276465977164, 0.05219959533909376836, 106.2489096053143669 ) ) ;
#25273 = CARTESIAN_POINT ( 'NONE',  ( -14.34966873604972548, 8.224510206698743886, 53.33442372801901854 ) ) ;
#25274 = CARTESIAN_POINT ( 'NONE',  ( 14.29746914071037800, 8.314922557961029526, 101.6677570613523613 ) ) ;
#25275 = CARTESIAN_POINT ( 'NONE',  ( 0.05219959533934541429, -16.53943276465976808, 95.00109039468568994 ) ) ;
#25276 = CARTESIAN_POINT ( 'NONE',  ( 8.224510206698742110, 14.34966873604972548, 32.08442372801901854 ) ) ;
#25277 = CARTESIAN_POINT ( 'NONE',  ( 16.46253265017160672, -9.564922557960803928, 48.33224293864769550 ) ) ;
#25278 = CARTESIAN_POINT ( 'NONE',  ( 16.55341960407611168, 4.379528057220329451, 103.9572429386476813 ) ) ;
#25279 = CARTESIAN_POINT ( 'NONE',  ( -15.80617190586768217, 15.72974639402176855, 23.12609039468567573 ) ) ;
#25280 = CARTESIAN_POINT ( 'NONE',  ( 13.89961937509977652, -13.97604488694527269, 38.12390960531436690 ) ) ;
#25281 = CARTESIAN_POINT ( 'NONE',  ( -16.46253265017160317, 9.564922557960807481, 110.8322429386476955 ) ) ;
#25282 = CARTESIAN_POINT ( 'NONE',  ( 10.81492255796106328, -18.62759615963255655, 30.41775706135234358 ) ) ;
#25283 = CARTESIAN_POINT ( 'NONE',  ( 16.46253265017160672, -9.564922557960803928, 23.33224293864769194 ) ) ;
#25284 = CARTESIAN_POINT ( 'NONE',  ( 5.049401038298161559, -19.05341960407611168, 107.7072429386476955 ) ) ;
#25285 = CARTESIAN_POINT ( 'NONE',  ( 28.79475375365512946, -9.355982642740189092, 142.8843446568999980 ) ) ;
#25286 = CARTESIAN_POINT ( 'NONE',  ( -5.153800228976328057, -19.02544592524343514, 97.29057627198099567 ) ) ;
#25288 = CARTESIAN_POINT ( 'NONE',  ( 8.314922557960818139, 14.29746914071049879, 89.58224293864768129 ) ) ;
#25287 = CARTESIAN_POINT ( 'NONE',  ( 15.80617190586769283, -15.72974639402175789, 50.62609039468568994 ) ) ;
#25289 = CARTESIAN_POINT ( 'NONE',  ( 13.89961937509977652, -13.97604488694527269, 103.1239096053143527 ) ) ;
#25290 = CARTESIAN_POINT ( 'NONE',  ( 9.564922557961047289, -16.46253265017146816, 70.41775706135233293 ) ) ;
#25291 = CARTESIAN_POINT ( 'NONE',  ( 16.55341960407618274, -4.379528057220086978, 66.04275706135236135 ) ) ;
#25292 = CARTESIAN_POINT ( 'NONE',  ( 21.55341960407619695, -5.719274019375665929, 76.04275706135237556 ) ) ;
#25293 = VECTOR ( 'NONE', #35104, 1000.000000000000000 ) ;
#25294 = CARTESIAN_POINT ( 'NONE',  ( -4.379528057220086978, -16.55341960407618274, 34.79275706135235424 ) ) ;
#25295 = CARTESIAN_POINT ( 'NONE',  ( 16.51473224551069308, 9.474510206698969483, 79.16557627198103830 ) ) ;
#25296 = CARTESIAN_POINT ( 'NONE',  ( -16.46253265017146816, -9.564922557961047289, 104.1677570613523329 ) ) ;
#25297 = CARTESIAN_POINT ( 'NONE',  ( 12.14591786802327356, -12.06949235617739191, 75.62609039468567573 ) ) ;
#25298 = CARTESIAN_POINT ( 'NONE',  ( -10.81492255796105439, 18.62759615963255655, 112.9177570613523329 ) ) ;
#25299 = CARTESIAN_POINT ( 'NONE',  ( -13.89961937509957401, -13.97604488694547875, 94.37609039468566152 ) ) ;
#25300 = CARTESIAN_POINT ( 'NONE',  ( 9.564922557960805705, 16.46253265017160317, 59.58224293864769550 ) ) ;
#25301 = CARTESIAN_POINT ( 'NONE',  ( -10.81492255796078084, -18.62759615963271287, 82.08224293864768129 ) ) ;
#25303 = CARTESIAN_POINT ( 'NONE',  ( 9.474510206698729675, 16.51473224551082808, 92.08442372801900433 ) ) ;
#25302 = CARTESIAN_POINT ( 'NONE',  ( 12.14591786802309770, 12.06949235617756955, 94.37390960531436690 ) ) ;
#25304 = CARTESIAN_POINT ( 'NONE',  ( 0.05219959533934541429, -16.53943276465976808, 65.00109039468568994 ) ) ;
#25305 = CARTESIAN_POINT ( 'NONE',  ( -19.49149378614660577, 5.499999999999577227, 79.43757513605360998 ) ) ;
#25306 = CARTESIAN_POINT ( 'NONE',  ( 13.89961937509957401, 13.97604488694547697, 51.87609039468566863 ) ) ;
#25307 = CARTESIAN_POINT ( 'NONE',  ( 14.29746914071049879, -8.314922557960816363, 28.33224293864769550 ) ) ;
#25308 = CARTESIAN_POINT ( 'NONE',  ( 0.05219959533910956823, 16.53943276465976808, 84.99890960531436690 ) ) ;
#25310 = CARTESIAN_POINT ( 'NONE',  ( -17.26172910966715790, 6.454744622556963130, 40.80646908649207205 ) ) ;
#25309 = CARTESIAN_POINT ( 'NONE',  ( 18.62759615963255655, 10.81492255796105972, 111.6677570613523613 ) ) ;
#25311 = CARTESIAN_POINT ( 'NONE',  ( 10.72451020669871369, 18.67979575497193778, 22.08442372801901143 ) ) ;
#25312 = CARTESIAN_POINT ( 'NONE',  ( 16.46253265017160672, -9.564922557960803928, 98.33224293864769550 ) ) ;
#25313 = CARTESIAN_POINT ( 'NONE',  ( 13.97604488694527802, 13.89961937509977652, 79.37390960531435269 ) ) ;
#25314 = CARTESIAN_POINT ( 'NONE',  ( -15.80617190586768217, 15.72974639402176855, 98.12609039468570415 ) ) ;
#25315 = CARTESIAN_POINT ( 'NONE',  ( 9.564922557960805705, 16.46253265017160317, 79.58224293864769550 ) ) ;
#25316 = CARTESIAN_POINT ( 'NONE',  ( 15.72974639402199770, -15.80617190586745480, 48.12390960531436690 ) ) ;
#25317 = CARTESIAN_POINT ( 'NONE',  ( -8.314922557960811034, -14.29746914071050412, 87.08224293864769550 ) ) ;
#25318 = CARTESIAN_POINT ( 'NONE',  ( -0.05219959533909027116, -19.03943276465977164, 57.49890960531435979 ) ) ;
#25319 = CARTESIAN_POINT ( 'NONE',  ( 4.483927247898545687, 16.52544592524342804, 99.79057627198103830 ) ) ;
#25320 = CARTESIAN_POINT ( 'NONE',  ( -10.72451020669870658, -18.67979575497194134, 29.58442372801901854 ) ) ;
#25321 = CARTESIAN_POINT ( 'NONE',  ( 10.72451020669871369, 18.67979575497193778, 67.08442372801901854 ) ) ;
#25322 = CARTESIAN_POINT ( 'NONE',  ( 9.564922557960805705, 16.46253265017160317, 49.58224293864770260 ) ) ;
#25323 = CARTESIAN_POINT ( 'NONE',  ( -16.55341960407617563, 4.379528057220093196, 58.54275706135235424 ) ) ;
#25324 = CARTESIAN_POINT ( 'NONE',  ( -10.72451020669898014, 18.67979575497178502, 110.4155762719810383 ) ) ;
#25325 = CARTESIAN_POINT ( 'NONE',  ( -10.72451020669898014, 18.67979575497178502, 110.4155762719810383 ) ) ;
#25327 = CARTESIAN_POINT ( 'NONE',  ( -16.51473224551069308, -9.474510206698971260, 71.66557627198102409 ) ) ;
#25326 = CARTESIAN_POINT ( 'NONE',  ( -0.05219959533936034679, 19.03943276465977164, 42.50109039468566152 ) ) ;
#25328 = DIRECTION ( 'NONE',  ( 0.000000000000000000, 0.000000000000000000, 1.000000000000000000 ) ) ;
#25329 = CARTESIAN_POINT ( 'NONE',  ( 15.72974639402176855, 15.80617190586768217, 71.87609039468568994 ) ) ;
#25330 = ADVANCED_FACE ( 'NONE', ( #5267 ), #6266, .F. ) ;
#25331 = CARTESIAN_POINT ( 'NONE',  ( -21.52544592524343514, 5.823673210054127303, 56.04057627198102409 ) ) ;
#25332 = CARTESIAN_POINT ( 'NONE',  ( 4.379528057220339221, -16.55341960407611168, 37.70724293864769550 ) ) ;
#25334 = CARTESIAN_POINT ( 'NONE',  ( 9.564922557961047289, -16.46253265017146816, 20.41775706135233293 ) ) ;
#25333 = CARTESIAN_POINT ( 'NONE',  ( 15.80617190586769283, -15.72974639402175789, 70.62609039468567573 ) ) ;
#25335 = CARTESIAN_POINT ( 'NONE',  ( -0.05219959533910754901, -16.53943276465976808, 57.49890960531435979 ) ) ;
#25336 = CARTESIAN_POINT ( 'NONE',  ( -4.379528057220328563, 16.55341960407611168, 100.2072429386476955 ) ) ;
#25337 = CARTESIAN_POINT ( 'NONE',  ( -16.46253265017146816, -9.564922557961047289, 49.16775706135233293 ) ) ;
#25338 = CARTESIAN_POINT ( 'NONE',  ( -16.53943276465976808, 0.05219959533911058130, 21.24890960531436690 ) ) ;
#25339 = CARTESIAN_POINT ( 'NONE',  ( 15.80617190586769283, -15.72974639402175789, 70.62609039468567573 ) ) ;
#25340 = CARTESIAN_POINT ( 'NONE',  ( -5.153800228976328057, -19.02544592524343514, 62.29057627198100988 ) ) ;
#25341 = CARTESIAN_POINT ( 'NONE',  ( -9.474510206698720793, -16.51473224551083518, 34.58442372801899722 ) ) ;
#25342 = CARTESIAN_POINT ( 'NONE',  ( 10.81492255796078972, 18.62759615963270932, 44.58224293864769550 ) ) ;
#25343 = CARTESIAN_POINT ( 'NONE',  ( 0.05219959533937995610, -21.53943276465977519, 35.00109039468568284 ) ) ;
#25344 = CARTESIAN_POINT ( 'NONE',  ( -21.55341960407610458, -5.719274019375992779, 86.45724293864770971 ) ) ;
#25345 = CARTESIAN_POINT ( 'NONE',  ( 9.564922557961047289, -16.46253265017146816, 90.41775706135234714 ) ) ;
#25346 = CARTESIAN_POINT ( 'NONE',  ( 16.52544592524335698, 4.483927247898782831, 46.45942372801901854 ) ) ;
#25348 = CARTESIAN_POINT ( 'NONE',  ( 15.72974639402199770, -15.80617190586745480, 88.12390960531436690 ) ) ;
#25347 = CARTESIAN_POINT ( 'NONE',  ( -17.72517630440430025, 5.500000000000144773, 55.92175719257211597 ) ) ;
#25349 = CARTESIAN_POINT ( 'NONE',  ( -8.314922557960811034, -14.29746914071050412, 92.08224293864769550 ) ) ;
#25350 = CARTESIAN_POINT ( 'NONE',  ( 18.09867054820433907, 5.499999999999817923, 41.48393025253587751 ) ) ;
#25351 = CARTESIAN_POINT ( 'NONE',  ( -16.55341960407617563, 4.379528057220093196, 23.54275706135235424 ) ) ;
#25352 = CARTESIAN_POINT ( 'NONE',  ( 5.719274019375991003, -21.55341960407610458, 52.70724293864769550 ) ) ;
#25353 = CARTESIAN_POINT ( 'NONE',  ( -14.34966873604972548, 8.224510206698743886, 88.33442372801901854 ) ) ;
#25354 = CARTESIAN_POINT ( 'NONE',  ( 16.51473224551069308, 9.474510206698969483, 24.16557627198102765 ) ) ;
#25355 = CARTESIAN_POINT ( 'NONE',  ( -12.14591786802326823, 12.06949235617739902, 58.12609039468568994 ) ) ;
#25356 = CARTESIAN_POINT ( 'NONE',  ( 21.55341960407619695, -5.719274019375665929, 26.04275706135235779 ) ) ;
#25357 = CARTESIAN_POINT ( 'NONE',  ( -0.05219959533907301413, -21.53943276465977519, 47.49890960531435979 ) ) ;
#25358 = CARTESIAN_POINT ( 'NONE',  ( -8.314922557961024197, 14.29746914071037800, 77.91775706135231871 ) ) ;
#25359 = CARTESIAN_POINT ( 'NONE',  ( -16.51473224551069308, -9.474510206698971260, 96.66557627198102409 ) ) ;
#25361 = CARTESIAN_POINT ( 'NONE',  ( -19.03943276465977164, 0.05219959533909376836, 26.24890960531435624 ) ) ;
#25360 = CARTESIAN_POINT ( 'NONE',  ( -0.05219959533937732626, 21.53943276465977519, 57.50109039468568994 ) ) ;
#25362 = CARTESIAN_POINT ( 'NONE',  ( -18.67979575497178146, -10.72451020669898902, 41.66557627198103120 ) ) ;
#25363 = CARTESIAN_POINT ( 'NONE',  ( 5.153800228976335163, 19.02544592524342804, 109.7905762719810099 ) ) ;
#25364 = VERTEX_POINT ( 'NONE', #159959 ) ;
#25365 = CARTESIAN_POINT ( 'NONE',  ( 9.474510206698729675, 16.51473224551082808, 42.08442372801900433 ) ) ;
#25366 = CARTESIAN_POINT ( 'NONE',  ( 8.314922557961029526, -14.29746914071037800, 60.41775706135235424 ) ) ;
#25367 = CARTESIAN_POINT ( 'NONE',  ( 19.05341960407611168, 5.049401038298154454, 113.9572429386477097 ) ) ;
#25368 = EDGE_LOOP ( 'NONE', ( #119199, #156979, #46328, #191792, #150172, #57214 ) ) ;
#25369 = CARTESIAN_POINT ( 'NONE',  ( -13.97604488694527625, -13.89961937509977652, 86.87390960531436690 ) ) ;
#25370 = CARTESIAN_POINT ( 'NONE',  ( -14.29746914071037622, -8.314922557961029526, 99.16775706135234714 ) ) ;
#25371 = CARTESIAN_POINT ( 'NONE',  ( 17.49999999999999645, 5.500000000000007994, 73.78230962303568674 ) ) ;
#25372 = CARTESIAN_POINT ( 'NONE',  ( -8.314922557960811034, -14.29746914071050412, 97.08224293864770971 ) ) ;
#25373 = CARTESIAN_POINT ( 'NONE',  ( 18.62759615963271287, -10.81492255796078972, 53.33224293864769550 ) ) ;
#25374 = CARTESIAN_POINT ( 'NONE',  ( 5.049401038298161559, -19.05341960407611168, 37.70724293864768839 ) ) ;
#25375 = CARTESIAN_POINT ( 'NONE',  ( -0.05219959533934338120, 16.53943276465976808, 77.50109039468567573 ) ) ;
#25376 = CARTESIAN_POINT ( 'NONE',  ( -21.52544592524334988, -5.823673210054445271, 33.95942372801901143 ) ) ;
#25377 = CARTESIAN_POINT ( 'NONE',  ( -19.02544592524334988, -5.153800228976617603, 93.95942372801900433 ) ) ;
#25378 = CARTESIAN_POINT ( 'NONE',  ( -16.46253265017160317, 9.564922557960807481, 40.83224293864769550 ) ) ;
#25379 = CARTESIAN_POINT ( 'NONE',  ( -19.03943276465977164, 0.05219959533909376836, 116.2489096053143669 ) ) ;
#25380 = CARTESIAN_POINT ( 'NONE',  ( 21.55341960407619695, -5.719274019375665929, 101.0427570613523756 ) ) ;
#25381 = CARTESIAN_POINT ( 'NONE',  ( 16.51473224551069308, 9.474510206698969483, 84.16557627198102409 ) ) ;
#25382 = CARTESIAN_POINT ( 'NONE',  ( -14.34966873604972548, 8.224510206698743886, 58.33442372801901143 ) ) ;
#25383 = CARTESIAN_POINT ( 'NONE',  ( -21.55341960407619339, 5.719274019375674811, 93.54275706135234714 ) ) ;
#25384 = CARTESIAN_POINT ( 'NONE',  ( 0.05219959533934541429, -16.53943276465976808, 60.00109039468568284 ) ) ;
#25385 = CARTESIAN_POINT ( 'NONE',  ( 16.51473224551083163, -9.474510206698727899, 50.83442372801899722 ) ) ;
#25386 = CARTESIAN_POINT ( 'NONE',  ( 19.02544592524334988, 5.153800228976608722, 66.45942372801899012 ) ) ;
#25387 = VERTEX_POINT ( 'NONE', #7262 ) ;
#25388 = CARTESIAN_POINT ( 'NONE',  ( -10.81492255796105439, 18.62759615963255655, 57.91775706135234714 ) ) ;
#25389 = CARTESIAN_POINT ( 'NONE',  ( -9.564922557960796823, -16.46253265017161027, 67.08224293864769550 ) ) ;
#25390 = CARTESIAN_POINT ( 'NONE',  ( 19.05341960407611168, 5.049401038298154454, 23.95724293864769194 ) ) ;
#25391 = CARTESIAN_POINT ( 'NONE',  ( 9.564922557961047289, -16.46253265017146816, 55.41775706135234003 ) ) ;
#25392 = CARTESIAN_POINT ( 'NONE',  ( -13.89961937509977652, 13.97604488694528158, 110.6239096053143243 ) ) ;
#25393 = CARTESIAN_POINT ( 'NONE',  ( -19.05341960407611168, -5.049401038298163336, 81.45724293864769550 ) ) ;
#25394 = CARTESIAN_POINT ( 'NONE',  ( 8.224510206698953496, -14.34966873604960469, 32.91557627198102409 ) ) ;
#25395 = CARTESIAN_POINT ( 'NONE',  ( -0.05219959533907301413, -21.53943276465977519, 52.49890960531435979 ) ) ;
#25396 = CARTESIAN_POINT ( 'NONE',  ( 0.000000000000000000, 0.000000000000000000, -63.95112321872120731 ) ) ;
#25397 = CARTESIAN_POINT ( 'NONE',  ( -19.03943276465977164, -0.05219959533935918106, 18.75109039468567218 ) ) ;
#25398 = DIRECTION ( 'NONE',  ( -0.000000000000000000, -0.000000000000000000, 1.000000000000000000 ) ) ;
#25399 = CARTESIAN_POINT ( 'NONE',  ( 19.05341960407611168, 5.049401038298154454, 38.95724293864767418 ) ) ;
#25400 = CARTESIAN_POINT ( 'NONE',  ( -5.049401038298153566, 19.05341960407611168, 25.20724293864768484 ) ) ;
#25401 = CARTESIAN_POINT ( 'NONE',  ( -33.79565148458098633, -5.463178417057487302, 94.26852713616584367 ) ) ;
#25402 = CARTESIAN_POINT ( 'NONE',  ( -18.67979575497193778, 10.72451020669871902, 68.33442372801900433 ) ) ;
#25403 = CARTESIAN_POINT ( 'NONE',  ( -22.19900124254457907, -30.24112288620522904, -8.000000000000000000 ) ) ;
#25404 = CARTESIAN_POINT ( 'NONE',  ( -16.52544592524335698, -4.483927247898792601, 68.95942372801901854 ) ) ;
#25405 = CARTESIAN_POINT ( 'NONE',  ( 10.72451020669898902, -18.67979575497178502, 77.91557627198102409 ) ) ;
#25406 = CARTESIAN_POINT ( 'NONE',  ( -16.55341960407611168, -4.379528057220339221, 51.45724293864770260 ) ) ;
#25408 = CARTESIAN_POINT ( 'NONE',  ( -19.02544592524342804, 5.153800228976336051, 111.0405762719810099 ) ) ;
#25407 = CARTESIAN_POINT ( 'NONE',  ( -9.564922557960796823, -16.46253265017161027, 32.08224293864769550 ) ) ;
#25409 = CARTESIAN_POINT ( 'NONE',  ( -5.823673210054431948, 21.52544592524334988, 37.70942372801900433 ) ) ;
#25410 = CARTESIAN_POINT ( 'NONE',  ( 19.02544592524334988, 5.153800228976608722, 51.45942372801900433 ) ) ;
#25411 = CARTESIAN_POINT ( 'NONE',  ( 5.049401038298161559, -19.05341960407611168, 27.70724293864769550 ) ) ;
#25412 = CARTESIAN_POINT ( 'NONE',  ( -5.719274019375665041, -21.55341960407619695, 84.79275706135234714 ) ) ;
#25413 = CARTESIAN_POINT ( 'NONE',  ( 16.88567814943165857, -6.947325034625568385, 31.20998877347416212 ) ) ;
#25414 = CARTESIAN_POINT ( 'NONE',  ( 16.52544592524342804, -4.483927247898539470, 33.54057627198102409 ) ) ;
#25415 = CARTESIAN_POINT ( 'NONE',  ( -29.86685920354755197, -21.69954338932560134, -2.924999997268813878 ) ) ;
#25416 = CARTESIAN_POINT ( 'NONE',  ( -5.823673210054116645, -21.52544592524344225, 37.29057627198102409 ) ) ;
#25417 = PLANE ( 'NONE',  #165918 ) ;
#25418 = CARTESIAN_POINT ( 'NONE',  ( 19.03943276465977164, -0.05219959533909143690, 88.74890960531436690 ) ) ;
#25419 = CARTESIAN_POINT ( 'NONE',  ( -4.379528057220328563, 16.55341960407611168, 90.20724293864770971 ) ) ;
#25420 = CARTESIAN_POINT ( 'NONE',  ( 13.89961937509957401, 13.97604488694547697, 101.8760903946856331 ) ) ;
#25421 = CARTESIAN_POINT ( 'NONE',  ( -15.80617190586745835, -15.72974639402198527, 56.87390960531436690 ) ) ;
#25422 = ORIENTED_EDGE ( 'NONE', *, *, #30838, .T. ) ;
#25423 = EDGE_CURVE ( 'NONE', #71084, #197513, #67946, .T. ) ;
#25424 = CARTESIAN_POINT ( 'NONE',  ( 5.049401038298161559, -19.05341960407611168, 32.70724293864768129 ) ) ;
#25426 = CARTESIAN_POINT ( 'NONE',  ( 10.72451020669898902, -18.67979575497178502, 82.91557627198103830 ) ) ;
#25425 = CARTESIAN_POINT ( 'NONE',  ( -5.153800228976328057, -19.02544592524343514, 92.29057627198099567 ) ) ;
#25428 = CARTESIAN_POINT ( 'NONE',  ( 19.02544592524343514, -5.153800228976328945, 103.5405762719809957 ) ) ;
#25427 = CARTESIAN_POINT ( 'NONE',  ( -4.483927247898782831, 16.52544592524335698, 107.7094237280190328 ) ) ;
#25429 = CARTESIAN_POINT ( 'NONE',  ( -9.474510206698720793, -16.51473224551083518, 79.58442372801899012 ) ) ;
#25430 = CARTESIAN_POINT ( 'NONE',  ( 15.80617190586769283, -15.72974639402175789, 95.62609039468568994 ) ) ;
#25431 = CARTESIAN_POINT ( 'NONE',  ( 15.80617190586746368, 15.72974639402197994, 74.37390960531436690 ) ) ;
#25432 = CARTESIAN_POINT ( 'NONE',  ( -21.52544592524343514, 5.823673210054127303, 41.04057627198103120 ) ) ;
#25433 = CARTESIAN_POINT ( 'NONE',  ( 16.51473224551069308, 9.474510206698969483, 44.16557627198103120 ) ) ;
#25434 = CARTESIAN_POINT ( 'NONE',  ( 8.314922557961029526, -14.29746914071037800, 110.4177570613523756 ) ) ;
#25435 = CARTESIAN_POINT ( 'NONE',  ( -5.049401038298153566, 19.05341960407611168, 70.20724293864769550 ) ) ;
#25436 = ORIENTED_EDGE ( 'NONE', *, *, #98879, .T. ) ;
#25437 = CARTESIAN_POINT ( 'NONE',  ( 17.50000000000000000, 5.499999999999992895, 38.78230962303566542 ) ) ;
#25438 = CARTESIAN_POINT ( 'NONE',  ( -19.03943276465977164, -0.05219959533935918106, 28.75109039468566507 ) ) ;
#25439 = CARTESIAN_POINT ( 'NONE',  ( -0.05219959533910754901, -16.53943276465976808, 72.49890960531435269 ) ) ;
#25440 = CARTESIAN_POINT ( 'NONE',  ( -15.80617190586768217, 15.72974639402176855, 28.12609039468568284 ) ) ;
#25441 = VECTOR ( 'NONE', #187587, 1000.000000000000000 ) ;
#25442 = CARTESIAN_POINT ( 'NONE',  ( -17.14385361876520264, -23.59649016807271593, 143.6750000027311671 ) ) ;
#25443 = CARTESIAN_POINT ( 'NONE',  ( -0.05219959533907301413, -21.53943276465977519, 62.49890960531436690 ) ) ;
#25444 = CARTESIAN_POINT ( 'NONE',  ( -8.314922557961024197, 14.29746914071037800, 97.91775706135236135 ) ) ;
#25445 = CARTESIAN_POINT ( 'NONE',  ( 9.474510206698971260, -16.51473224551069308, 22.91557627198102765 ) ) ;
#25446 = CARTESIAN_POINT ( 'NONE',  ( 19.05341960407611168, 5.049401038298154454, 78.95724293864769550 ) ) ;
#25447 = CARTESIAN_POINT ( 'NONE',  ( 16.46253265017160672, -9.564922557960803928, 23.33224293864769194 ) ) ;
#25448 = CARTESIAN_POINT ( 'NONE',  ( -4.379528057220328563, 16.55341960407611168, 25.20724293864769550 ) ) ;
#25449 = EDGE_CURVE ( 'NONE', #144525, #33153, #188245, .T. ) ;
#25450 = CARTESIAN_POINT ( 'NONE',  ( 0.05219959533937995610, -21.53943276465977519, 60.00109039468568284 ) ) ;
#25451 = CARTESIAN_POINT ( 'NONE',  ( 16.51473224551069308, 9.474510206698969483, 114.1655762719810241 ) ) ;
#25452 = CARTESIAN_POINT ( 'NONE',  ( -18.67979575497193778, 10.72451020669871902, 93.33442372801901854 ) ) ;
#25453 = CARTESIAN_POINT ( 'NONE',  ( -13.97604488694527625, -13.89961937509977652, 31.87390960531435979 ) ) ;
#25454 = CARTESIAN_POINT ( 'NONE',  ( 0.05219959533909260263, 19.03943276465977164, 44.99890960531435979 ) ) ;
#25455 = ORIENTED_EDGE ( 'NONE', *, *, #183353, .T. ) ;
#25456 = CARTESIAN_POINT ( 'NONE',  ( -21.53943276465977519, -0.05219959533937600094, 93.75109039468567573 ) ) ;
#25457 = CARTESIAN_POINT ( 'NONE',  ( -14.34966873604972548, 8.224510206698743886, 48.33442372801902565 ) ) ;
#25458 = CARTESIAN_POINT ( 'NONE',  ( -18.67979575497193778, 10.72451020669871902, 83.33442372801903275 ) ) ;
#25459 = CARTESIAN_POINT ( 'NONE',  ( -5.823673210054116645, -21.52544592524344225, 22.29057627198102765 ) ) ;
#25460 = CARTESIAN_POINT ( 'NONE',  ( 13.97604488694548053, -13.89961937509957401, 90.62609039468567573 ) ) ;
#25461 = CARTESIAN_POINT ( 'NONE',  ( -0.05219959533937732626, 21.53943276465977519, 52.50109039468567573 ) ) ;
#25462 = CARTESIAN_POINT ( 'NONE',  ( -9.564922557961040184, 16.46253265017147172, 112.9177570613523329 ) ) ;
#25463 = CARTESIAN_POINT ( 'NONE',  ( -19.05341960407617563, 5.049401038297882671, 88.54275706135230450 ) ) ;
#25464 = CARTESIAN_POINT ( 'NONE',  ( -5.049401038298153566, 19.05341960407611168, 50.20724293864770260 ) ) ;
#25465 = CARTESIAN_POINT ( 'NONE',  ( 0.05219959533936267826, -19.03943276465977164, 95.00109039468567573 ) ) ;
#25466 = CARTESIAN_POINT ( 'NONE',  ( 13.97604488694548053, -13.89961937509957401, 85.62609039468568994 ) ) ;
#25467 = CARTESIAN_POINT ( 'NONE',  ( -8.224510206698948167, 14.34966873604960824, 50.41557627198103120 ) ) ;
#25468 = CARTESIAN_POINT ( 'NONE',  ( 13.97604488694548053, -13.89961937509957401, 75.62609039468564731 ) ) ;
#25469 = CARTESIAN_POINT ( 'NONE',  ( -16.55341960407617563, 4.379528057220093196, 58.54275706135235424 ) ) ;
#25470 = CARTESIAN_POINT ( 'NONE',  ( 16.46253265017146816, 9.564922557961045513, 26.66775706135234003 ) ) ;
#25471 = CARTESIAN_POINT ( 'NONE',  ( 9.564922557960805705, 16.46253265017160317, 44.58224293864769550 ) ) ;
#25472 = CARTESIAN_POINT ( 'NONE',  ( -19.05341960407611168, -5.049401038298163336, 41.45724293864769550 ) ) ;
#25473 = CARTESIAN_POINT ( 'NONE',  ( -12.14591786802326823, 12.06949235617739902, 58.12609039468568994 ) ) ;
#25474 = CARTESIAN_POINT ( 'NONE',  ( 0.000000000000000000, 0.000000000000000000, 0.000000000000000000 ) ) ;
#25475 = CARTESIAN_POINT ( 'NONE',  ( 17.14385361876520264, 23.59649016807275856, 148.1750000027311955 ) ) ;
#25476 = CARTESIAN_POINT ( 'NONE',  ( -9.564922557960796823, -16.46253265017161027, 102.0822429386477097 ) ) ;
#25477 = CARTESIAN_POINT ( 'NONE',  ( 2.500000000000000000, 2.357898499370431722, -2.818925648462311528E-15 ) ) ;
#25478 = EDGE_LOOP ( 'NONE', ( #158929, #120044, #87890, #82703 ) ) ;
#25479 = CARTESIAN_POINT ( 'NONE',  ( -0.05219959533936034679, 19.03943276465977164, 97.50109039468567573 ) ) ;
#25480 = CARTESIAN_POINT ( 'NONE',  ( -10.72451020669898014, 18.67979575497178502, 35.41557627198102409 ) ) ;
#25482 = CARTESIAN_POINT ( 'NONE',  ( -9.564922557961040184, 16.46253265017147172, 112.9177570613523329 ) ) ;
#25481 = CARTESIAN_POINT ( 'NONE',  ( 5.153800228976615827, -19.02544592524334988, 30.20942372801900433 ) ) ;
#25483 = CARTESIAN_POINT ( 'NONE',  ( -0.05219959533909027116, -19.03943276465977164, 27.49890960531435624 ) ) ;
#25484 = CARTESIAN_POINT ( 'NONE',  ( 13.89961937509977652, -13.97604488694527269, 38.12390960531436690 ) ) ;
#25485 = CARTESIAN_POINT ( 'NONE',  ( 18.67979575497178502, 10.72451020669898547, 79.16557627198103830 ) ) ;
#25486 = CARTESIAN_POINT ( 'NONE',  ( 5.049401038298161559, -19.05341960407611168, 37.70724293864768839 ) ) ;
#25487 = CARTESIAN_POINT ( 'NONE',  ( 27.73933785331498569, 9.013057229001093518, 144.4750000027311785 ) ) ;
#25488 = CARTESIAN_POINT ( 'NONE',  ( -19.03943276465977164, -0.05219959533935918106, 83.75109039468567573 ) ) ;
#25489 = CARTESIAN_POINT ( 'NONE',  ( 8.314922557960818139, 14.29746914071049879, 54.58224293864769550 ) ) ;
#25490 = CARTESIAN_POINT ( 'NONE',  ( 0.05219959533907565091, 21.53943276465977519, 29.99890960531435979 ) ) ;
#25491 = CARTESIAN_POINT ( 'NONE',  ( -5.823673210054431948, 21.52544592524334988, 102.7094237280190185 ) ) ;
#25492 = CARTESIAN_POINT ( 'NONE',  ( 21.52544592524344225, -5.823673210054117533, 88.54057627198103830 ) ) ;
#25493 = CARTESIAN_POINT ( 'NONE',  ( 0.05219959533937995610, -21.53943276465977519, 70.00109039468568994 ) ) ;
#25494 = CARTESIAN_POINT ( 'NONE',  ( 15.80617190586769283, -15.72974639402175789, 60.62609039468567573 ) ) ;
#25495 = CARTESIAN_POINT ( 'NONE',  ( -5.153800228976328057, -19.02544592524343514, 107.2905762719810383 ) ) ;
#25497 = CARTESIAN_POINT ( 'NONE',  ( -18.67979575497193778, 10.72451020669871902, 68.33442372801900433 ) ) ;
#25496 = CARTESIAN_POINT ( 'NONE',  ( 14.29746914071037800, 8.314922557961029526, 111.6677570613523613 ) ) ;
#25498 = CARTESIAN_POINT ( 'NONE',  ( 5.049401038298161559, -19.05341960407611168, 57.70724293864769550 ) ) ;
#25499 = CARTESIAN_POINT ( 'NONE',  ( 0.05219959533936267826, -19.03943276465977164, 35.00109039468566863 ) ) ;
#25500 = CARTESIAN_POINT ( 'NONE',  ( 5.823673210054444382, -21.52544592524334988, 35.20942372801901854 ) ) ;
#25501 = CARTESIAN_POINT ( 'NONE',  ( 13.89961937509977652, -13.97604488694527269, 68.12390960531436690 ) ) ;
#25502 = CARTESIAN_POINT ( 'NONE',  ( 16.55341960407611168, 4.379528057220329451, 83.95724293864770971 ) ) ;
#25503 = CARTESIAN_POINT ( 'NONE',  ( 4.379528057220339221, -16.55341960407611168, 47.70724293864770260 ) ) ;
#25504 = CARTESIAN_POINT ( 'NONE',  ( 18.62759615963271287, -10.81492255796078972, 63.33224293864770260 ) ) ;
#25505 = CARTESIAN_POINT ( 'NONE',  ( 19.03943276465977164, -0.05219959533909143690, 48.74890960531435979 ) ) ;
#25506 = CARTESIAN_POINT ( 'NONE',  ( -10.81492255796078084, -18.62759615963271287, 67.08224293864770971 ) ) ;
#25507 = CARTESIAN_POINT ( 'NONE',  ( -19.05341960407617563, 5.049401038297882671, 53.54275706135231871 ) ) ;
#25509 = CARTESIAN_POINT ( 'NONE',  ( 16.52544592524342804, -4.483927247898539470, 63.54057627198103830 ) ) ;
#25508 = DIRECTION ( 'NONE',  ( -1.000000000000000000, 0.000000000000000000, 0.000000000000000000 ) ) ;
#25510 = CARTESIAN_POINT ( 'NONE',  ( -0.05219959533907301413, -21.53943276465977519, 42.49890960531435979 ) ) ;
#25511 = ORIENTED_EDGE ( 'NONE', *, *, #129609, .F. ) ;
#25512 = CARTESIAN_POINT ( 'NONE',  ( 16.61371651742599909, 7.165104196376152146, 103.6458493000700543 ) ) ;
#25514 = CARTESIAN_POINT ( 'NONE',  ( -17.14385361876520264, -23.59649016807271238, 147.1750000027311671 ) ) ;
#25513 = CARTESIAN_POINT ( 'NONE',  ( 16.52544592524335698, 4.483927247898782831, 81.45942372801900433 ) ) ;
#25515 = CARTESIAN_POINT ( 'NONE',  ( -13.97604488694547697, 13.89961937509957934, 93.12609039468566152 ) ) ;
#25516 = CARTESIAN_POINT ( 'NONE',  ( -14.29746914071049879, 8.314922557960819915, 50.83224293864770971 ) ) ;
#25517 = CARTESIAN_POINT ( 'NONE',  ( -3.573655867282028392E-15, 2.428612866367529932E-14, 167.9999999999999716 ) ) ;
#25518 = CARTESIAN_POINT ( 'NONE',  ( 16.51473224551069308, 9.474510206698969483, 54.16557627198103120 ) ) ;
#25519 = CARTESIAN_POINT ( 'NONE',  ( 12.06949235617757843, -12.14591786802309237, 43.12390960531435269 ) ) ;
#25520 = CARTESIAN_POINT ( 'NONE',  ( -5.049401038298153566, 19.05341960407611168, 90.20724293864766707 ) ) ;
#25521 = CARTESIAN_POINT ( 'NONE',  ( -5.049401038298153566, 19.05341960407611168, 50.20724293864770260 ) ) ;
#25522 = CARTESIAN_POINT ( 'NONE',  ( -5.719274019375665041, -21.55341960407619695, 64.79275706135234714 ) ) ;
#25523 = CARTESIAN_POINT ( 'NONE',  ( -13.89961937509977652, 13.97604488694528158, 65.62390960531436690 ) ) ;
#25524 = CARTESIAN_POINT ( 'NONE',  ( 19.02544592524343514, -5.153800228976328945, 33.54057627198102409 ) ) ;
#25525 = CARTESIAN_POINT ( 'NONE',  ( -13.89961937509977652, 13.97604488694528158, 75.62390960531438111 ) ) ;
#25526 = EDGE_CURVE ( 'NONE', #22766, #45079, #71615, .T. ) ;
#25527 = CARTESIAN_POINT ( 'NONE',  ( -10.72451020669898014, 18.67979575497178502, 50.41557627198103120 ) ) ;
#25528 = AXIS2_PLACEMENT_3D ( 'NONE', #137746, #95218, #199430 ) ;
#25529 = CARTESIAN_POINT ( 'NONE',  ( -19.02544592524342804, 5.153800228976336051, 31.04057627198102409 ) ) ;
#25530 = CARTESIAN_POINT ( 'NONE',  ( -15.80617190586745835, -15.72974639402198527, 46.87390960531435979 ) ) ;
#25531 = CARTESIAN_POINT ( 'NONE',  ( 0.05219959533934541429, -16.53943276465976808, 105.0010903946856757 ) ) ;
#25532 = CARTESIAN_POINT ( 'NONE',  ( -0.05219959533936034679, 19.03943276465977164, 27.50109039468566507 ) ) ;
#25534 = CARTESIAN_POINT ( 'NONE',  ( 4.483927247898790824, -16.52544592524335698, 85.20942372801901854 ) ) ;
#25533 = CARTESIAN_POINT ( 'NONE',  ( -4.483927247898782831, 16.52544592524335698, 42.70942372801901854 ) ) ;
#25535 = CARTESIAN_POINT ( 'NONE',  ( 2.552343178074723884, 7.052343178074616858, 8.889087296526001936 ) ) ;
#25536 = CARTESIAN_POINT ( 'NONE',  ( 4.379528057220092307, 16.55341960407617563, 67.29275706135234714 ) ) ;
#25537 = CARTESIAN_POINT ( 'NONE',  ( 8.224510206698742110, 14.34966873604972548, 52.08442372801901854 ) ) ;
#25538 = CARTESIAN_POINT ( 'NONE',  ( 5.049401038298161559, -19.05341960407611168, 102.7072429386476955 ) ) ;
#25539 = CARTESIAN_POINT ( 'NONE',  ( 13.97604488694527802, 13.89961937509977652, 34.37390960531436690 ) ) ;
#25540 = CARTESIAN_POINT ( 'NONE',  ( 8.224510206698742110, 14.34966873604972548, 37.08442372801901143 ) ) ;
#25541 = CARTESIAN_POINT ( 'NONE',  ( -9.564922557960796823, -16.46253265017161027, 42.08224293864769550 ) ) ;
#25542 = CARTESIAN_POINT ( 'NONE',  ( 15.72974639402176855, 15.80617190586768217, 31.87609039468567929 ) ) ;
#25543 = CARTESIAN_POINT ( 'NONE',  ( 12.06949235617739724, 12.14591786802326823, 31.87609039468567929 ) ) ;
#25544 = CARTESIAN_POINT ( 'NONE',  ( -16.55341960407617563, 4.379528057220093196, 93.54275706135234714 ) ) ;
#25545 = CYLINDRICAL_SURFACE ( 'NONE', #57024, 6.100000000000006750 ) ;
#25546 = CARTESIAN_POINT ( 'NONE',  ( -15.72974639402176322, -15.80617190586768395, 94.37609039468568994 ) ) ;
#25547 = CARTESIAN_POINT ( 'NONE',  ( -5.153800228976607833, 19.02544592524334988, 92.70942372801901854 ) ) ;
#25548 = CARTESIAN_POINT ( 'NONE',  ( -13.89961937509957401, -13.97604488694547875, 54.37609039468565442 ) ) ;
#25549 = CARTESIAN_POINT ( 'NONE',  ( 8.314922557960818139, 14.29746914071049879, 54.58224293864769550 ) ) ;
#25550 = CARTESIAN_POINT ( 'NONE',  ( -19.03943276465977164, 0.05219959533909376836, 31.24890960531435979 ) ) ;
#25552 = CARTESIAN_POINT ( 'NONE',  ( -38.00000000000000711, 2.428612866367529932E-14, -2.000000000000000000 ) ) ;
#25551 = CARTESIAN_POINT ( 'NONE',  ( 13.89961937509957401, 13.97604488694547697, 56.87609039468564731 ) ) ;
#25553 = CARTESIAN_POINT ( 'NONE',  ( -15.72974639402176322, -15.80617190586768395, 64.37609039468568994 ) ) ;
#25554 = CARTESIAN_POINT ( 'NONE',  ( -16.55341960407617563, 4.379528057220093196, 33.54275706135234714 ) ) ;
#25555 = CARTESIAN_POINT ( 'NONE',  ( 19.01533133064926773, -5.499999999999448441, 56.26586590595741200 ) ) ;
#25556 = CARTESIAN_POINT ( 'NONE',  ( -5.823673210054116645, -21.52544592524344225, 27.29057627198103120 ) ) ;
#25557 = CARTESIAN_POINT ( 'NONE',  ( 9.474510206698729675, 16.51473224551082808, 102.0844237280190043 ) ) ;
#25558 = CARTESIAN_POINT ( 'NONE',  ( -5.049401038298153566, 19.05341960407611168, 110.2072429386476671 ) ) ;
#25559 = CARTESIAN_POINT ( 'NONE',  ( -21.88033147701377601, 9.239123595177357373, 171.1226046679828983 ) ) ;
#25560 = CARTESIAN_POINT ( 'NONE',  ( 16.46253265017160672, -9.564922557960803928, 28.33224293864769550 ) ) ;
#25561 = CARTESIAN_POINT ( 'NONE',  ( -0.05219959533937732626, 21.53943276465977519, 112.5010903946857042 ) ) ;
#25562 = CARTESIAN_POINT ( 'NONE',  ( 9.474510206698971260, -16.51473224551069308, 42.91557627198103120 ) ) ;
#25563 = CARTESIAN_POINT ( 'NONE',  ( -0.05219959533937732626, 21.53943276465977519, 62.50109039468568284 ) ) ;
#25564 = CARTESIAN_POINT ( 'NONE',  ( 10.81492255796106328, -18.62759615963255655, 105.4177570613523613 ) ) ;
#25565 = CARTESIAN_POINT ( 'NONE',  ( 12.14591786802327356, -12.06949235617739191, 105.6260903946856899 ) ) ;
#25566 = CARTESIAN_POINT ( 'NONE',  ( 16.51473224551069308, 9.474510206698969483, 74.16557627198103830 ) ) ;
#25567 = CARTESIAN_POINT ( 'NONE',  ( 0.05219959533937995610, -21.53943276465977519, 60.00109039468568284 ) ) ;
#25568 = CARTESIAN_POINT ( 'NONE',  ( -10.81492255796105439, 18.62759615963255655, 47.91775706135234714 ) ) ;
#25570 = CARTESIAN_POINT ( 'NONE',  ( 9.474510206698971260, -16.51473224551069308, 107.9155762719810383 ) ) ;
#25569 = CARTESIAN_POINT ( 'NONE',  ( -19.02544592524334988, -5.153800228976617603, 78.95942372801900433 ) ) ;
#25571 = CARTESIAN_POINT ( 'NONE',  ( -14.34966873604960291, -8.224510206698953496, 111.6655762719810525 ) ) ;
#25572 = CARTESIAN_POINT ( 'NONE',  ( -5.823673210054116645, -21.52544592524344225, 92.29057627198103830 ) ) ;
#25573 = CARTESIAN_POINT ( 'NONE',  ( -5.049401038297874678, -19.05341960407617918, 19.79275706135233293 ) ) ;
#25574 = CARTESIAN_POINT ( 'NONE',  ( 0.05219959533910956823, 16.53943276465976808, 94.99890960531436690 ) ) ;
#25575 = CARTESIAN_POINT ( 'NONE',  ( 13.89961937509977652, -13.97604488694527269, 53.12390960531434558 ) ) ;
#25576 = CARTESIAN_POINT ( 'NONE',  ( 16.46253265017146816, 9.564922557961045513, 101.6677570613523329 ) ) ;
#25577 = CARTESIAN_POINT ( 'NONE',  ( -12.14591786802309592, -12.06949235617757132, 61.87390960531436690 ) ) ;
#25578 = CARTESIAN_POINT ( 'NONE',  ( -21.53943276465977519, -0.05219959533937600094, 103.7510903946857042 ) ) ;
#25579 = CARTESIAN_POINT ( 'NONE',  ( -9.564922557960796823, -16.46253265017161027, 102.0822429386477097 ) ) ;
#25580 = CARTESIAN_POINT ( 'NONE',  ( 9.474510206698729675, 16.51473224551082808, 72.08442372801900433 ) ) ;
#25581 = CARTESIAN_POINT ( 'NONE',  ( -18.62759615963270932, 10.81492255796079327, 80.83224293864769550 ) ) ;
#25582 = CARTESIAN_POINT ( 'NONE',  ( 10.72451020669871369, 18.67979575497193778, 32.08442372801901854 ) ) ;
#25583 = CARTESIAN_POINT ( 'NONE',  ( 4.379528057220092307, 16.55341960407617563, 37.29275706135235424 ) ) ;
#25584 = CARTESIAN_POINT ( 'NONE',  ( 8.314922557961029526, -14.29746914071037800, 90.41775706135236135 ) ) ;
#25586 = CARTESIAN_POINT ( 'NONE',  ( -15.72974639402176322, -15.80617190586768395, 39.37609039468567573 ) ) ;
#25585 = CARTESIAN_POINT ( 'NONE',  ( 0.05219959533934541429, -16.53943276465976808, 45.00109039468568284 ) ) ;
#25587 = CARTESIAN_POINT ( 'NONE',  ( -10.72451020669898014, 18.67979575497178502, 45.41557627198103830 ) ) ;
#25588 = CARTESIAN_POINT ( 'NONE',  ( -13.97604488694527625, -13.89961937509977652, 36.87390960531436690 ) ) ;
#25589 = CARTESIAN_POINT ( 'NONE',  ( 22.81625015709509441, 31.40387420917330275, -1.824999997268813567 ) ) ;
#25590 = CARTESIAN_POINT ( 'NONE',  ( -16.52544592524335698, -4.483927247898792601, 58.95942372801902565 ) ) ;
#25591 = CARTESIAN_POINT ( 'NONE',  ( 10.81492255796078972, 18.62759615963270932, 89.58224293864768129 ) ) ;
#25592 = CARTESIAN_POINT ( 'NONE',  ( 14.29746914071049879, -8.314922557960816363, 43.33224293864769550 ) ) ;
#25593 = CARTESIAN_POINT ( 'NONE',  ( -16.53943276465976808, -0.05219959533934237506, 43.75109039468568284 ) ) ;
#25594 = CARTESIAN_POINT ( 'NONE',  ( -5.049401038298153566, 19.05341960407611168, 65.20724293864765286 ) ) ;
#25595 = CARTESIAN_POINT ( 'NONE',  ( -14.29746914071037622, -8.314922557961029526, 89.16775706135236135 ) ) ;
#25596 = CARTESIAN_POINT ( 'NONE',  ( -19.05341960407617563, 5.049401038297882671, 88.54275706135230450 ) ) ;
#25597 = CARTESIAN_POINT ( 'NONE',  ( -21.55341960407610458, -5.719274019375992779, 91.45724293864769550 ) ) ;
#25598 = CARTESIAN_POINT ( 'NONE',  ( 16.52544592524342804, -4.483927247898539470, 33.54057627198102409 ) ) ;
#25599 = ORIENTED_EDGE ( 'NONE', *, *, #143390, .F. ) ;
#25600 = CARTESIAN_POINT ( 'NONE',  ( -32.00000000000000000, -5.510910596163089556E-15, 47.64999999999999147 ) ) ;
#25601 = CARTESIAN_POINT ( 'NONE',  ( 21.53943276465977519, -0.05219959533907433946, 63.74890960531435979 ) ) ;
#25602 = CARTESIAN_POINT ( 'NONE',  ( -0.05219959533934338120, 16.53943276465976808, 107.5010903946856899 ) ) ;
#25603 = ORIENTED_EDGE ( 'NONE', *, *, #41891, .F. ) ;
#25604 = CARTESIAN_POINT ( 'NONE',  ( 19.01529144963336648, 5.499999999999968914, 88.73431955728439391 ) ) ;
#25605 = CARTESIAN_POINT ( 'NONE',  ( 21.55341960407610458, 5.719274019375980345, 83.95724293864770971 ) ) ;
#25606 = CARTESIAN_POINT ( 'NONE',  ( -8.314922557960811034, -14.29746914071050412, 27.08224293864769550 ) ) ;
#25607 = CARTESIAN_POINT ( 'NONE',  ( 16.52544592524335698, 4.483927247898782831, 41.45942372801901143 ) ) ;
#25608 = CARTESIAN_POINT ( 'NONE',  ( -19.05341960407611168, -5.049401038298163336, 36.45724293864766707 ) ) ;
#25609 = CARTESIAN_POINT ( 'NONE',  ( -16.51473224551069308, -9.474510206698971260, 51.66557627198102409 ) ) ;
#25610 = CARTESIAN_POINT ( 'NONE',  ( 27.73933785331498569, 2.768321779492822058E-14, 140.3750000027311842 ) ) ;
#25611 = CARTESIAN_POINT ( 'NONE',  ( -13.89961937509977652, 13.97604488694528158, 115.6239096053143669 ) ) ;
#25612 = CARTESIAN_POINT ( 'NONE',  ( 0.05219959533909260263, 19.03943276465977164, 114.9989096053143669 ) ) ;
#25613 = CARTESIAN_POINT ( 'NONE',  ( -14.29746914071037622, -8.314922557961029526, 109.1677570613523613 ) ) ;
#25614 = CARTESIAN_POINT ( 'NONE',  ( -19.02544592524334988, -5.153800228976617603, 88.95942372801897591 ) ) ;
#25615 = CARTESIAN_POINT ( 'NONE',  ( -5.049401038297874678, -19.05341960407617918, 39.79275706135232582 ) ) ;
#25616 = CARTESIAN_POINT ( 'NONE',  ( 5.719274019375991003, -21.55341960407610458, 92.70724293864770971 ) ) ;
#25617 = CARTESIAN_POINT ( 'NONE',  ( 8.314922557961029526, -14.29746914071037800, 110.4177570613523756 ) ) ;
#25618 = CARTESIAN_POINT ( 'NONE',  ( 18.67979575497178502, 10.72451020669898547, 39.16557627198102409 ) ) ;
#25619 = CARTESIAN_POINT ( 'NONE',  ( -19.05341960407617563, 5.049401038297882671, 103.5427570613523329 ) ) ;
#25620 = CARTESIAN_POINT ( 'NONE',  ( -9.474510206698964154, 16.51473224551069663, 110.4155762719810383 ) ) ;
#25621 = CARTESIAN_POINT ( 'NONE',  ( -21.53943276465977519, -0.05219959533937600094, 68.75109039468568994 ) ) ;
#25622 = CARTESIAN_POINT ( 'NONE',  ( -5.049401038298153566, 19.05341960407611168, 65.20724293864765286 ) ) ;
#25623 = CARTESIAN_POINT ( 'NONE',  ( -12.14591786802309592, -12.06949235617757132, 101.8739096053143811 ) ) ;
#25624 = FACE_OUTER_BOUND ( 'NONE', #84344, .T. ) ;
#25625 = CARTESIAN_POINT ( 'NONE',  ( -19.05341960407611168, -5.049401038298163336, 71.45724293864766707 ) ) ;
#25626 = CARTESIAN_POINT ( 'NONE',  ( -0.05219959533910754901, -16.53943276465976808, 72.49890960531435269 ) ) ;
#25627 = VERTEX_POINT ( 'NONE', #112457 ) ;
#25628 = CARTESIAN_POINT ( 'NONE',  ( 19.05341960407617918, -5.049401038297876454, 86.04275706135233293 ) ) ;
#25629 = CARTESIAN_POINT ( 'NONE',  ( 19.53091890409952924, 5.499999999999984901, 92.56097431831422284 ) ) ;
#25630 = CARTESIAN_POINT ( 'NONE',  ( -9.474510206698964154, 16.51473224551069663, 60.41557627198102409 ) ) ;
#25631 = CARTESIAN_POINT ( 'NONE',  ( 0.7573736981518488509, 8.898500934826572006, -61.93579448831083312 ) ) ;
#25633 = CARTESIAN_POINT ( 'NONE',  ( 13.97604488694527802, 13.89961937509977652, 99.37390960531436690 ) ) ;
#25632 = CARTESIAN_POINT ( 'NONE',  ( 9.474510206698971260, -16.51473224551069308, 77.91557627198103830 ) ) ;
#25634 = CARTESIAN_POINT ( 'NONE',  ( -12.06949235617739369, -12.14591786802326823, 59.37609039468568284 ) ) ;
#25635 = CYLINDRICAL_SURFACE ( 'NONE', #199637, 1.500000000000001332 ) ;
#25636 = CARTESIAN_POINT ( 'NONE',  ( 19.02544592524334988, 5.153800228976608722, 41.45942372801900433 ) ) ;
#25637 = CARTESIAN_POINT ( 'NONE',  ( 5.823673210054444382, -21.52544592524334988, 95.20942372801903275 ) ) ;
#25638 = LINE ( 'NONE', #119626, #182422 ) ;
#25639 = CARTESIAN_POINT ( 'NONE',  ( 16.46253265017160672, -9.564922557960803928, 108.3322429386476955 ) ) ;
#25640 = CARTESIAN_POINT ( 'NONE',  ( 12.14591786802327356, -12.06949235617739191, 100.6260903946857184 ) ) ;
#25641 = CARTESIAN_POINT ( 'NONE',  ( 18.22780087662122384, -5.500000000000022204, 76.01540105326107266 ) ) ;
#25642 = CARTESIAN_POINT ( 'NONE',  ( -8.224510206698735004, -14.34966873604973081, 94.58442372801901854 ) ) ;
#25643 = CARTESIAN_POINT ( 'NONE',  ( -16.79531203550651242, 7.028104445595467986, 28.74755011779559055 ) ) ;
#25644 = CARTESIAN_POINT ( 'NONE',  ( -16.53943276465976808, -0.05219959533934237506, 63.75109039468568284 ) ) ;
#25645 = ORIENTED_EDGE ( 'NONE', *, *, #191495, .T. ) ;
#25646 = CARTESIAN_POINT ( 'NONE',  ( 0.05219959533937995610, -21.53943276465977519, 85.00109039468568994 ) ) ;
#25647 = CARTESIAN_POINT ( 'NONE',  ( -19.02544592524334988, -5.153800228976617603, 83.95942372801901854 ) ) ;
#25648 = CARTESIAN_POINT ( 'NONE',  ( 5.153800228976615827, -19.02544592524334988, 25.20942372801900433 ) ) ;
#25649 = CARTESIAN_POINT ( 'NONE',  ( -5.153800228976328057, -19.02544592524343514, 62.29057627198100988 ) ) ;
#25650 = CARTESIAN_POINT ( 'NONE',  ( 13.97604488694527802, 13.89961937509977652, 44.37390960531435269 ) ) ;
#25651 = CYLINDRICAL_SURFACE ( 'NONE', #1250, 5.500000000001017852 ) ;
#25652 = CARTESIAN_POINT ( 'NONE',  ( 5.823673210054125526, 21.52544592524343514, 79.79057627198102409 ) ) ;
#25653 = ADVANCED_FACE ( 'NONE', ( #65950 ), #101270, .T. ) ;
#25654 = CARTESIAN_POINT ( 'NONE',  ( 21.52544592524344225, -5.823673210054117533, 38.54057627198103120 ) ) ;
#25655 = CARTESIAN_POINT ( 'NONE',  ( -19.05341960407611168, -5.049401038298163336, 36.45724293864766707 ) ) ;
#25656 = CARTESIAN_POINT ( 'NONE',  ( 14.29746914071037800, 8.314922557961029526, 56.66775706135235424 ) ) ;
#25657 = ORIENTED_EDGE ( 'NONE', *, *, #24864, .F. ) ;
#25658 = CARTESIAN_POINT ( 'NONE',  ( 10.72451020669871369, 18.67979575497193778, 37.08442372801901143 ) ) ;
#25660 = CARTESIAN_POINT ( 'NONE',  ( -22.81625015709510507, 31.40387420917330275, -8.924999997268814766 ) ) ;
#25659 = CARTESIAN_POINT ( 'NONE',  ( -16.55341960407611168, -4.379528057220339221, 71.45724293864769550 ) ) ;
#25661 = CARTESIAN_POINT ( 'NONE',  ( -8.224510206698735004, -14.34966873604973081, 19.58442372801901143 ) ) ;
#25662 = CARTESIAN_POINT ( 'NONE',  ( 9.474510206698729675, 16.51473224551082808, 37.08442372801899722 ) ) ;
#25663 = CARTESIAN_POINT ( 'NONE',  ( 4.483927247898545687, 16.52544592524342804, 59.79057627198103120 ) ) ;
#25664 = CARTESIAN_POINT ( 'NONE',  ( 21.53943276465977519, 0.05219959533937863772, 21.25109039468567218 ) ) ;
#25666 = CARTESIAN_POINT ( 'NONE',  ( 21.53943276465977519, -0.05219959533907433946, 83.74890960531435269 ) ) ;
#25665 = CARTESIAN_POINT ( 'NONE',  ( 22.96528548301342809, -5.795830589372932273, 190.0000000000000000 ) ) ;
#25667 = CARTESIAN_POINT ( 'NONE',  ( 19.03943276465977164, -0.05219959533909143690, 93.74890960531435269 ) ) ;
#25668 = CARTESIAN_POINT ( 'NONE',  ( -0.05219959533910754901, -16.53943276465976808, 57.49890960531435979 ) ) ;
#25669 = CARTESIAN_POINT ( 'NONE',  ( 37.24154831888315442, -19.83237144080993275, -19.76300508100036524 ) ) ;
#25670 = CARTESIAN_POINT ( 'NONE',  ( 18.22780087662121673, 5.500000000000056843, 43.98459894673892734 ) ) ;
#25671 = CARTESIAN_POINT ( 'NONE',  ( -9.474510206698720793, -16.51473224551083518, 69.58442372801901854 ) ) ;
#25672 = CARTESIAN_POINT ( 'NONE',  ( 15.72974639402199770, -15.80617190586745480, 113.1239096053143953 ) ) ;
#25673 = CARTESIAN_POINT ( 'NONE',  ( -9.474510206698964154, 16.51473224551069663, 50.41557627198102409 ) ) ;
#25674 = CARTESIAN_POINT ( 'NONE',  ( 16.46253265017146816, 9.564922557961045513, 46.66775706135233293 ) ) ;
#25675 = CARTESIAN_POINT ( 'NONE',  ( -9.474510206698964154, 16.51473224551069663, 25.41557627198103120 ) ) ;
#25676 = CARTESIAN_POINT ( 'NONE',  ( 21.53943276465977519, 0.05219959533937863772, 66.25109039468567573 ) ) ;
#25677 = CARTESIAN_POINT ( 'NONE',  ( -17.48847506799969054, -5.747544572773760407, 69.17302562156721990 ) ) ;
#25678 = CARTESIAN_POINT ( 'NONE',  ( -16.53943276465976808, 0.05219959533911058130, 46.24890960531435979 ) ) ;
#25679 = CARTESIAN_POINT ( 'NONE',  ( 0.05219959533909260263, 19.03943276465977164, 64.99890960531436690 ) ) ;
#25680 = CARTESIAN_POINT ( 'NONE',  ( 18.67979575497178502, 10.72451020669898547, 69.16557627198102409 ) ) ;
#25681 = CARTESIAN_POINT ( 'NONE',  ( 19.03943276465977164, -0.05219959533909143690, 53.74890960531436690 ) ) ;
#25682 = CARTESIAN_POINT ( 'NONE',  ( 10.81492255796078972, 18.62759615963270932, 64.58224293864769550 ) ) ;
#25683 = ADVANCED_FACE ( 'NONE', ( #127621 ), #118468, .F. ) ;
#25684 = CARTESIAN_POINT ( 'NONE',  ( -10.72451020669870658, -18.67979575497194134, 94.58442372801901854 ) ) ;
#25687 = CARTESIAN_POINT ( 'NONE',  ( 14.34966873604960469, 8.224510206698951720, 89.16557627198102409 ) ) ;
#25686 = CARTESIAN_POINT ( 'NONE',  ( -12.14591786802326823, 12.06949235617739902, 98.12609039468570415 ) ) ;
#25685 = CARTESIAN_POINT ( 'NONE',  ( 4.595912276381225681, -38.76652190273247811, -23.69787631203871214 ) ) ;
#25688 = CARTESIAN_POINT ( 'NONE',  ( 13.89961937509957401, 13.97604488694547697, 86.87609039468567573 ) ) ;
#25689 = ORIENTED_EDGE ( 'NONE', *, *, #120968, .F. ) ;
#25690 = CARTESIAN_POINT ( 'NONE',  ( -5.153800228976607833, 19.02544592524334988, 42.70942372801901143 ) ) ;
#25691 = CARTESIAN_POINT ( 'NONE',  ( -16.53943276465976808, -0.05219959533934237506, 83.75109039468568994 ) ) ;
#25692 = CARTESIAN_POINT ( 'NONE',  ( 9.474510206698729675, 16.51473224551082808, 32.08442372801900433 ) ) ;
#25693 = CARTESIAN_POINT ( 'NONE',  ( -19.02544592524342804, 5.153800228976336051, 86.04057627198103830 ) ) ;
#25694 = CARTESIAN_POINT ( 'NONE',  ( -10.72451020669898014, 18.67979575497178502, 55.41557627198102409 ) ) ;
#25695 = CARTESIAN_POINT ( 'NONE',  ( -27.44803035730395635, -28.83687526680896340, -16.92468093647912752 ) ) ;
#25696 = CARTESIAN_POINT ( 'NONE',  ( -5.049401038298153566, 19.05341960407611168, 25.20724293864768484 ) ) ;
#25697 = CARTESIAN_POINT ( 'NONE',  ( -21.53943276465977519, -0.05219959533937600094, 98.75109039468568994 ) ) ;
#25698 = CARTESIAN_POINT ( 'NONE',  ( 4.483927247898790824, -16.52544592524335698, 75.20942372801901854 ) ) ;
#25699 = CARTESIAN_POINT ( 'NONE',  ( -5.719274019375665041, -21.55341960407619695, 24.79275706135235779 ) ) ;
#25700 = CARTESIAN_POINT ( 'NONE',  ( 8.314922557961029526, -14.29746914071037800, 30.41775706135234358 ) ) ;
#25701 = CARTESIAN_POINT ( 'NONE',  ( -19.05341960407611168, -5.049401038298163336, 91.45724293864766707 ) ) ;
#25702 = CARTESIAN_POINT ( 'NONE',  ( 16.51473224551069308, 9.474510206698969483, 39.16557627198103120 ) ) ;
#25703 = CARTESIAN_POINT ( 'NONE',  ( -19.03943276465977164, 0.05219959533909376836, 46.24890960531435979 ) ) ;
#25704 = CARTESIAN_POINT ( 'NONE',  ( 4.483927247898790824, -16.52544592524335698, 40.20942372801901854 ) ) ;
#25705 = CARTESIAN_POINT ( 'NONE',  ( -4.379528057220328563, 16.55341960407611168, 90.20724293864770971 ) ) ;
#25706 = CARTESIAN_POINT ( 'NONE',  ( -14.34966873604972548, 8.224510206698743886, 98.33442372801901854 ) ) ;
#25709 = CARTESIAN_POINT ( 'NONE',  ( 5.153800228976335163, 19.02544592524342804, 59.79057627198100988 ) ) ;
#25708 = CARTESIAN_POINT ( 'NONE',  ( -19.02544592524342804, 5.153800228976336051, 81.04057627198103830 ) ) ;
#25707 = CARTESIAN_POINT ( 'NONE',  ( 15.72974639402176855, 15.80617190586768217, 36.87609039468568994 ) ) ;
#25710 = CARTESIAN_POINT ( 'NONE',  ( -13.89961937509977652, 13.97604488694528158, 80.62390960531436690 ) ) ;
#25711 = CARTESIAN_POINT ( 'NONE',  ( 8.224510206698953496, -14.34966873604960469, 37.91557627198102409 ) ) ;
#25712 = CARTESIAN_POINT ( 'NONE',  ( 0.05219959533934541429, -16.53943276465976808, 100.0010903946857042 ) ) ;
#25713 = ORIENTED_EDGE ( 'NONE', *, *, #162842, .T. ) ;
#25714 = CARTESIAN_POINT ( 'NONE',  ( -19.05341960407617563, 5.049401038297882671, 48.54275706135233293 ) ) ;
#25715 = CARTESIAN_POINT ( 'NONE',  ( -17.18269478283316332, 17.18269478283309226, -65.00100000000003320 ) ) ;
#25716 = CARTESIAN_POINT ( 'NONE',  ( 0.05219959533909260263, 19.03943276465977164, 49.99890960531435979 ) ) ;
#25717 = CARTESIAN_POINT ( 'NONE',  ( 13.97604488694548053, -13.89961937509957401, 45.62609039468566863 ) ) ;
#25718 = CARTESIAN_POINT ( 'NONE',  ( 11.40812507854754365, 35.11059874428196537, -5.224999997268813701 ) ) ;
#25719 = CARTESIAN_POINT ( 'NONE',  ( -14.34966873604972548, 8.224510206698743886, 38.33442372801900433 ) ) ;
#25721 = CARTESIAN_POINT ( 'NONE',  ( 4.379528057220092307, 16.55341960407617563, 57.29275706135234714 ) ) ;
#25720 = CARTESIAN_POINT ( 'NONE',  ( 16.51473224551083163, -9.474510206698727899, 75.83442372801900433 ) ) ;
#25722 = DIRECTION ( 'NONE',  ( -0.000000000000000000, 1.000000000000000000, 0.000000000000000000 ) ) ;
#25723 = CARTESIAN_POINT ( 'NONE',  ( -19.05341960407611168, -5.049401038298163336, 81.45724293864769550 ) ) ;
#25724 = CARTESIAN_POINT ( 'NONE',  ( 21.52544592524344225, -5.823673210054117533, 113.5405762719810383 ) ) ;
#25725 = CARTESIAN_POINT ( 'NONE',  ( -16.51473224551082808, 9.474510206698731452, 73.33442372801900433 ) ) ;
#25727 = CARTESIAN_POINT ( 'NONE',  ( -13.89961937509977652, 13.97604488694528158, 30.62390960531435269 ) ) ;
#25726 = CARTESIAN_POINT ( 'NONE',  ( -16.46253265017160317, 9.564922557960807481, 105.8322429386476955 ) ) ;
#25728 = CARTESIAN_POINT ( 'NONE',  ( -13.97604488694527625, -13.89961937509977652, 76.87390960531433848 ) ) ;
#25730 = CARTESIAN_POINT ( 'NONE',  ( -16.46253265017160317, 9.564922557960807481, 30.83224293864769550 ) ) ;
#25729 = CARTESIAN_POINT ( 'NONE',  ( 0.05219959533910956823, 16.53943276465976808, 39.99890960531436690 ) ) ;
#25731 = CARTESIAN_POINT ( 'NONE',  ( 5.153800228976615827, -19.02544592524334988, 55.20942372801899722 ) ) ;
#25732 = CARTESIAN_POINT ( 'NONE',  ( 8.224510206698953496, -14.34966873604960469, 67.91557627198102409 ) ) ;
#25733 = CARTESIAN_POINT ( 'NONE',  ( 19.02544592524334988, 5.153800228976608722, 21.45942372801899012 ) ) ;
#25734 = CARTESIAN_POINT ( 'NONE',  ( 16.46253265017160672, -9.564922557960803928, 48.33224293864769550 ) ) ;
#25735 = CARTESIAN_POINT ( 'NONE',  ( -18.62759615963270932, 10.81492255796079327, 50.83224293864770971 ) ) ;
#25737 = CARTESIAN_POINT ( 'NONE',  ( 10.72451020669871369, 18.67979575497193778, 102.0844237280190185 ) ) ;
#25736 = CARTESIAN_POINT ( 'NONE',  ( 4.379528057220339221, -16.55341960407611168, 57.70724293864770260 ) ) ;
#25738 = CARTESIAN_POINT ( 'NONE',  ( -13.97604488694527625, -13.89961937509977652, 96.87390960531433848 ) ) ;
#25739 = CARTESIAN_POINT ( 'NONE',  ( -19.02544592524342804, 5.153800228976336051, 106.0405762719810241 ) ) ;
#25740 = CARTESIAN_POINT ( 'NONE',  ( 19.03943276465977164, -0.05219959533909143690, 38.74890960531436690 ) ) ;
#25741 = CARTESIAN_POINT ( 'NONE',  ( -5.153800228976328057, -19.02544592524343514, 32.29057627198102409 ) ) ;
#25742 = CARTESIAN_POINT ( 'NONE',  ( -4.483927247898539470, -16.52544592524342804, 92.29057627198103830 ) ) ;
#25743 = CARTESIAN_POINT ( 'NONE',  ( 10.72451020669898902, -18.67979575497178502, 97.91557627198103830 ) ) ;
#25744 = CARTESIAN_POINT ( 'NONE',  ( -19.03943276465977164, 0.05219959533909376836, 101.2489096053143669 ) ) ;
#25745 = CARTESIAN_POINT ( 'NONE',  ( -21.52544592524343514, 5.823673210054127303, 116.0405762719810383 ) ) ;
#25746 = CARTESIAN_POINT ( 'NONE',  ( -5.153800228976328057, -19.02544592524343514, 87.29057627198103830 ) ) ;
#25748 = CARTESIAN_POINT ( 'NONE',  ( -12.06949235617756955, 12.14591786802309770, 100.6239096053143811 ) ) ;
#25747 = CARTESIAN_POINT ( 'NONE',  ( -21.47377332591982224, 5.474134792251751591, 173.8918256800988900 ) ) ;
#25749 = CARTESIAN_POINT ( 'NONE',  ( -13.97604488694527625, -13.89961937509977652, 71.87390960531433848 ) ) ;
#25750 = CARTESIAN_POINT ( 'NONE',  ( -15.80617190586745835, -15.72974639402198527, 81.87390960531435269 ) ) ;
#25751 = CARTESIAN_POINT ( 'NONE',  ( -31.34393194264162830, 5.972569355670991342, 99.56318414118020144 ) ) ;
#25752 = DIRECTION ( 'NONE',  ( -1.000000000000000000, 0.000000000000000000, 0.000000000000000000 ) ) ;
#25754 = CARTESIAN_POINT ( 'NONE',  ( 6.551653823223139383, -3.660253528765621045, 1.589185716900141543 ) ) ;
#25753 = CARTESIAN_POINT ( 'NONE',  ( -10.72451020669898014, 18.67979575497178502, 25.41557627198103120 ) ) ;
#25755 = CARTESIAN_POINT ( 'NONE',  ( 14.34966873604972726, -8.224510206698740333, 35.83442372801901143 ) ) ;
#25756 = CARTESIAN_POINT ( 'NONE',  ( 16.52544592524342804, -4.483927247898539470, 88.54057627198103830 ) ) ;
#25757 = CARTESIAN_POINT ( 'NONE',  ( -17.50000000000014211, -3.417042746626972605, 109.8261960376752597 ) ) ;
#25758 = CARTESIAN_POINT ( 'NONE',  ( 9.564922557960805705, 16.46253265017160317, 84.58224293864769550 ) ) ;
#25759 = CARTESIAN_POINT ( 'NONE',  ( 13.89961937509977652, -13.97604488694527269, 43.12390960531434558 ) ) ;
#25760 = CARTESIAN_POINT ( 'NONE',  ( -8.224510206698948167, 14.34966873604960824, 80.41557627198103830 ) ) ;
#25761 = CARTESIAN_POINT ( 'NONE',  ( -10.81492255796078084, -18.62759615963271287, 27.08224293864769550 ) ) ;
#25762 = CARTESIAN_POINT ( 'NONE',  ( 16.53943276465976808, -0.05219959533910856209, 48.74890960531435979 ) ) ;
#25763 = CARTESIAN_POINT ( 'NONE',  ( 16.46253265017146816, 9.564922557961045513, 101.6677570613523329 ) ) ;
#25764 = CARTESIAN_POINT ( 'NONE',  ( 18.62759615963255655, 10.81492255796105972, 76.66775706135234714 ) ) ;
#25765 = CARTESIAN_POINT ( 'NONE',  ( 8.571926809382597767, 26.38167802310806209, 148.2750000027311899 ) ) ;
#25766 = CARTESIAN_POINT ( 'NONE',  ( -5.049401038298153566, 19.05341960407611168, 110.2072429386476671 ) ) ;
#25767 = CARTESIAN_POINT ( 'NONE',  ( 16.52544592524335698, 4.483927247898782831, 86.45942372801901854 ) ) ;
#25768 = CARTESIAN_POINT ( 'NONE',  ( -5.153800228976328057, -19.02544592524343514, 27.29057627198103120 ) ) ;
#25769 = CARTESIAN_POINT ( 'NONE',  ( 19.03943276465977164, -0.05219959533909143690, 78.74890960531436690 ) ) ;
#25770 = CARTESIAN_POINT ( 'NONE',  ( -5.719274019375978568, 21.55341960407610458, 85.20724293864770971 ) ) ;
#25771 = CARTESIAN_POINT ( 'NONE',  ( -12.06949235617739369, -12.14591786802326823, 24.37609039468567573 ) ) ;
#25773 = CARTESIAN_POINT ( 'NONE',  ( -21.53943276465977519, -0.05219959533937600094, 73.75109039468567573 ) ) ;
#25772 = CARTESIAN_POINT ( 'NONE',  ( -4.483927247898539470, -16.52544592524342804, 57.29057627198103120 ) ) ;
#25775 = CARTESIAN_POINT ( 'NONE',  ( -10.72451020669898014, 18.67979575497178502, 25.41557627198103120 ) ) ;
#25774 = CARTESIAN_POINT ( 'NONE',  ( 16.55341960407618274, -4.379528057220086978, 91.04275706135236135 ) ) ;
#25776 = CARTESIAN_POINT ( 'NONE',  ( 5.153800228976335163, 19.02544592524342804, 109.7905762719810241 ) ) ;
#25777 = CARTESIAN_POINT ( 'NONE',  ( 0.000000000000000000, 0.000000000000000000, -18.00000000000000000 ) ) ;
#25778 = CARTESIAN_POINT ( 'NONE',  ( -16.53943276465976808, 0.05219959533911058130, 21.24890960531436690 ) ) ;
#25779 = CARTESIAN_POINT ( 'NONE',  ( -8.314922557961024197, 14.29746914071037800, 57.91775706135234714 ) ) ;
#25780 = CARTESIAN_POINT ( 'NONE',  ( 13.89961937509977652, -13.97604488694527269, 68.12390960531436690 ) ) ;
#25781 = CARTESIAN_POINT ( 'NONE',  ( -5.153800228976328057, -19.02544592524343514, 87.29057627198103830 ) ) ;
#25782 = CARTESIAN_POINT ( 'NONE',  ( 21.52544592524334988, 5.823673210054432836, 76.45942372801901854 ) ) ;
#25783 = CARTESIAN_POINT ( 'NONE',  ( 8.224510206698742110, 14.34966873604972548, 72.08442372801899012 ) ) ;
#25784 = CARTESIAN_POINT ( 'NONE',  ( -12.06949235617756955, 12.14591786802309770, 40.62390960531435269 ) ) ;
#25785 = CARTESIAN_POINT ( 'NONE',  ( -9.564922557960796823, -16.46253265017161027, 57.08224293864769550 ) ) ;
#25786 = CARTESIAN_POINT ( 'NONE',  ( -19.05341960407611168, -5.049401038298163336, 46.45724293864768129 ) ) ;
#25787 = ORIENTED_EDGE ( 'NONE', *, *, #128552, .F. ) ;
#25788 = CARTESIAN_POINT ( 'NONE',  ( -19.05341960407617563, 5.049401038297882671, 93.54275706135234714 ) ) ;
#25789 = CARTESIAN_POINT ( 'NONE',  ( 12.06949235617757843, -12.14591786802309237, 93.12390960531436690 ) ) ;
#25790 = CARTESIAN_POINT ( 'NONE',  ( -19.05341960407611168, -5.049401038298163336, 61.45724293864769550 ) ) ;
#25792 = CARTESIAN_POINT ( 'NONE',  ( 30.74264578624800137, -22.33583958711395212, -5.200000000000001066 ) ) ;
#25791 = CARTESIAN_POINT ( 'NONE',  ( -19.05341960407617563, 5.049401038297882671, 103.5427570613523329 ) ) ;
#25793 = CARTESIAN_POINT ( 'NONE',  ( 18.67979575497194134, -10.72451020669871369, 100.8344237280190185 ) ) ;
#25794 = CARTESIAN_POINT ( 'NONE',  ( -4.483927247898782831, 16.52544592524335698, 67.70942372801901854 ) ) ;
#25795 = CARTESIAN_POINT ( 'NONE',  ( -16.51473224551082808, 9.474510206698731452, 88.33442372801900433 ) ) ;
#25796 = CARTESIAN_POINT ( 'NONE',  ( -5.823673210054116645, -21.52544592524344225, 67.29057627198103830 ) ) ;
#25797 = CARTESIAN_POINT ( 'NONE',  ( 14.29746914071037800, 8.314922557961029526, 46.66775706135234714 ) ) ;
#25798 = CARTESIAN_POINT ( 'NONE',  ( 9.720660689315817393, -38.81505388558687031, -14.89813180556192407 ) ) ;
#25799 = CARTESIAN_POINT ( 'NONE',  ( -13.89961937509957401, -13.97604488694547875, 54.37609039468565442 ) ) ;
#25800 = CARTESIAN_POINT ( 'NONE',  ( -15.72974639402176322, -15.80617190586768395, 94.37609039468568994 ) ) ;
#25801 = CARTESIAN_POINT ( 'NONE',  ( 9.474510206698971260, -16.51473224551069308, 27.91557627198103120 ) ) ;
#25802 = CARTESIAN_POINT ( 'NONE',  ( -13.97604488694527625, -13.89961937509977652, 61.87390960531435979 ) ) ;
#25803 = CARTESIAN_POINT ( 'NONE',  ( 12.14591786802309770, 12.06949235617756955, 54.37390960531435979 ) ) ;
#25804 = CARTESIAN_POINT ( 'NONE',  ( 21.53943276465977519, 0.05219959533937863772, 91.25109039468568994 ) ) ;
#25805 = CARTESIAN_POINT ( 'NONE',  ( 5.049401038297881783, 19.05341960407617563, 42.29275706135234003 ) ) ;
#25806 = CARTESIAN_POINT ( 'NONE',  ( 5.153800228976615827, -19.02544592524334988, 25.20942372801900433 ) ) ;
#25807 = CARTESIAN_POINT ( 'NONE',  ( 5.049401038298161559, -19.05341960407611168, 112.7072429386476813 ) ) ;
#25808 = CARTESIAN_POINT ( 'NONE',  ( 5.719274019375673035, 21.55341960407619339, 92.29275706135236135 ) ) ;
#25809 = CARTESIAN_POINT ( 'NONE',  ( -16.51473224551069308, -9.474510206698971260, 71.66557627198102409 ) ) ;
#25810 = CARTESIAN_POINT ( 'NONE',  ( -10.81492255796105439, 18.62759615963255655, 87.91775706135234714 ) ) ;
#25811 = CARTESIAN_POINT ( 'NONE',  ( 15.72974639402199770, -15.80617190586745480, 48.12390960531436690 ) ) ;
#25812 = CARTESIAN_POINT ( 'NONE',  ( -0.05219959533909027116, -19.03943276465977164, 82.49890960531436690 ) ) ;
#25813 = CARTESIAN_POINT ( 'NONE',  ( 5.049401038297881783, 19.05341960407617563, 67.29275706135234714 ) ) ;
#25814 = CARTESIAN_POINT ( 'NONE',  ( -9.564922557960796823, -16.46253265017161027, 47.08224293864769550 ) ) ;
#25815 = CARTESIAN_POINT ( 'NONE',  ( 9.474510206698971260, -16.51473224551069308, 92.91557627198103830 ) ) ;
#25816 = CARTESIAN_POINT ( 'NONE',  ( 5.153800228976615827, -19.02544592524334988, 85.20942372801900433 ) ) ;
#25817 = CARTESIAN_POINT ( 'NONE',  ( 4.483927247898790824, -16.52544592524335698, 45.20942372801901854 ) ) ;
#25818 = CARTESIAN_POINT ( 'NONE',  ( -8.314922557960811034, -14.29746914071050412, 107.0822429386476955 ) ) ;
#25819 = CARTESIAN_POINT ( 'NONE',  ( -16.51473224551069308, -9.474510206698971260, 76.66557627198103830 ) ) ;
#25820 = CARTESIAN_POINT ( 'NONE',  ( 10.72451020669898902, -18.67979575497178502, 47.91557627198102409 ) ) ;
#25821 = CIRCLE ( 'NONE', #190601, 2.649999999999999911 ) ;
#25822 = CARTESIAN_POINT ( 'NONE',  ( -4.379528057220086978, -16.55341960407618274, 19.79275706135235069 ) ) ;
#25823 = CARTESIAN_POINT ( 'NONE',  ( 10.81492255796106328, -18.62759615963255655, 25.41775706135235779 ) ) ;
#25824 = CARTESIAN_POINT ( 'NONE',  ( -15.72974639402176322, -15.80617190586768395, 89.37609039468568994 ) ) ;
#25825 = CARTESIAN_POINT ( 'NONE',  ( -16.55341960407617563, 4.379528057220093196, 78.54275706135236135 ) ) ;
#25826 = CARTESIAN_POINT ( 'NONE',  ( 19.05341960407611168, 5.049401038298154454, 78.95724293864769550 ) ) ;
#25827 = CARTESIAN_POINT ( 'NONE',  ( 16.53943276465976808, 0.05219959533934440121, 106.2510903946856757 ) ) ;
#25828 = CARTESIAN_POINT ( 'NONE',  ( -9.564922557961040184, 16.46253265017147172, 57.91775706135233293 ) ) ;
#25829 = ADVANCED_FACE ( 'NONE', ( #55782 ), #134639, .F. ) ;
#25830 = CARTESIAN_POINT ( 'NONE',  ( -10.81492255796105439, 18.62759615963255655, 27.91775706135234358 ) ) ;
#25831 = CARTESIAN_POINT ( 'NONE',  ( -8.314922557960811034, -14.29746914071050412, 77.08224293864769550 ) ) ;
#25832 = CARTESIAN_POINT ( 'NONE',  ( -13.97604488694527625, -13.89961937509977652, 101.8739096053143811 ) ) ;
#25833 = CARTESIAN_POINT ( 'NONE',  ( -14.34966873604972548, 8.224510206698743886, 88.33442372801901854 ) ) ;
#25834 = CARTESIAN_POINT ( 'NONE',  ( 0.05219959533937995610, -21.53943276465977519, 70.00109039468568994 ) ) ;
#25835 = CARTESIAN_POINT ( 'NONE',  ( 4.379528057220092307, 16.55341960407617563, 32.29275706135235424 ) ) ;
#25836 = CARTESIAN_POINT ( 'NONE',  ( 10.72451020669871369, 18.67979575497193778, 32.08442372801901854 ) ) ;
#25837 = CARTESIAN_POINT ( 'NONE',  ( 0.05219959533910956823, 16.53943276465976808, 64.99890960531435269 ) ) ;
#25838 = ORIENTED_EDGE ( 'NONE', *, *, #63994, .T. ) ;
#25839 = CARTESIAN_POINT ( 'NONE',  ( -0.05219959533907301413, -21.53943276465977519, 97.49890960531436690 ) ) ;
#25840 = CARTESIAN_POINT ( 'NONE',  ( 8.224510206698953496, -14.34966873604960469, 57.91557627198103120 ) ) ;
#25841 = ORIENTED_EDGE ( 'NONE', *, *, #52789, .T. ) ;
#25842 = CARTESIAN_POINT ( 'NONE',  ( -19.05341960407611168, -5.049401038298163336, 31.45724293864769550 ) ) ;
#25843 = CARTESIAN_POINT ( 'NONE',  ( -10.81492255796078084, -18.62759615963271287, 27.08224293864769550 ) ) ;
#25844 = CARTESIAN_POINT ( 'NONE',  ( -21.53943276465977519, -0.05219959533937600094, 53.75109039468568994 ) ) ;
#25845 = CARTESIAN_POINT ( 'NONE',  ( 14.29746914071049879, -8.314922557960816363, 58.33224293864768839 ) ) ;
#25846 = VECTOR ( 'NONE', #45626, 1000.000000000000000 ) ;
#25847 = CARTESIAN_POINT ( 'NONE',  ( -18.67979575497178146, -10.72451020669898902, 61.66557627198103120 ) ) ;
#25848 = CARTESIAN_POINT ( 'NONE',  ( 16.46253265017160672, -9.564922557960803928, 68.33224293864770971 ) ) ;
#25850 = CARTESIAN_POINT ( 'NONE',  ( -16.51473224551082808, 9.474510206698731452, 78.33442372801900433 ) ) ;
#25849 = CARTESIAN_POINT ( 'NONE',  ( 9.564922557960805705, 16.46253265017160317, 29.58224293864769550 ) ) ;
#25851 = CARTESIAN_POINT ( 'NONE',  ( 18.62759615963271287, -10.81492255796078972, 63.33224293864770260 ) ) ;
#25852 = CARTESIAN_POINT ( 'NONE',  ( -19.02544592524342804, 5.153800228976336051, 41.04057627198103120 ) ) ;
#25853 = CARTESIAN_POINT ( 'NONE',  ( -9.564922557960796823, -16.46253265017161027, 77.08224293864769550 ) ) ;
#25854 = CARTESIAN_POINT ( 'NONE',  ( -0.05219959533934338120, 16.53943276465976808, 52.50109039468567573 ) ) ;
#25855 = CARTESIAN_POINT ( 'NONE',  ( 21.55341960407619695, -5.719274019375665929, 26.04275706135235779 ) ) ;
#25856 = CARTESIAN_POINT ( 'NONE',  ( 5.823673210054444382, -21.52544592524334988, 65.20942372801901854 ) ) ;
#25857 = CARTESIAN_POINT ( 'NONE',  ( -16.51473224551069308, -9.474510206698971260, 101.6655762719810241 ) ) ;
#25858 = CARTESIAN_POINT ( 'NONE',  ( 15.80617190586746368, 15.72974639402197994, 89.37390960531435269 ) ) ;
#25860 = CARTESIAN_POINT ( 'NONE',  ( 16.52544592524335698, 4.483927247898782831, 51.45942372801901854 ) ) ;
#25859 = CARTESIAN_POINT ( 'NONE',  ( 10.72451020669898902, -18.67979575497178502, 102.9155762719810383 ) ) ;
#25861 = CARTESIAN_POINT ( 'NONE',  ( -0.05219959533907301413, -21.53943276465977519, 52.49890960531435979 ) ) ;
#25862 = CARTESIAN_POINT ( 'NONE',  ( 21.52544592524334988, 5.823673210054432836, 101.4594237280190185 ) ) ;
#25863 = CARTESIAN_POINT ( 'NONE',  ( -13.89961937509977652, 13.97604488694528158, 50.62390960531435979 ) ) ;
#25864 = CARTESIAN_POINT ( 'NONE',  ( -16.46253265017160317, 9.564922557960807481, 115.8322429386477097 ) ) ;
#25865 = CARTESIAN_POINT ( 'NONE',  ( -13.89961937509977652, 13.97604488694528158, 80.62390960531436690 ) ) ;
#25866 = EDGE_CURVE ( 'NONE', #192458, #121091, #57793, .T. ) ;
#25867 = CARTESIAN_POINT ( 'NONE',  ( 16.36317988757097908, -7.306389748694713582, 86.59789608363178104 ) ) ;
#25868 = CARTESIAN_POINT ( 'NONE',  ( -19.05341960407617563, 5.049401038297882671, 73.54275706135233293 ) ) ;
#25869 = CARTESIAN_POINT ( 'NONE',  ( 21.52544592524344225, -5.823673210054117533, 43.54057627198103830 ) ) ;
#25870 = CARTESIAN_POINT ( 'NONE',  ( 16.53943276465976808, 0.05219959533934440121, 111.2510903946856899 ) ) ;
#25871 = CARTESIAN_POINT ( 'NONE',  ( -19.03943276465977164, -0.05219959533935918106, 88.75109039468567573 ) ) ;
#25872 = CARTESIAN_POINT ( 'NONE',  ( -16.19135201231370047, 7.376712067591781441, 59.81319145947970384 ) ) ;
#25873 = CARTESIAN_POINT ( 'NONE',  ( 16.51473224551083163, -9.474510206698727899, 20.83442372801899722 ) ) ;
#25874 = CARTESIAN_POINT ( 'NONE',  ( -9.564922557961040184, 16.46253265017147172, 87.91775706135233293 ) ) ;
#25875 = CARTESIAN_POINT ( 'NONE',  ( -16.51473224551082808, 9.474510206698731452, 38.33442372801899722 ) ) ;
#25876 = CARTESIAN_POINT ( 'NONE',  ( -14.62203461105304036, -16.12203461105356794, -56.14925526931841659 ) ) ;
#25877 = CARTESIAN_POINT ( 'NONE',  ( -9.564922557960796823, -16.46253265017161027, 52.08224293864768839 ) ) ;
#25878 = CARTESIAN_POINT ( 'NONE',  ( -16.53943276465976808, 0.05219959533911058130, 46.24890960531435979 ) ) ;
#25879 = CARTESIAN_POINT ( 'NONE',  ( -9.564922557960796823, -16.46253265017161027, 37.08224293864768839 ) ) ;
#25880 = CARTESIAN_POINT ( 'NONE',  ( -8.224510206698948167, 14.34966873604960824, 40.41557627198103120 ) ) ;
#25881 = CARTESIAN_POINT ( 'NONE',  ( -28.92784451463922579, -27.23096741515445629, -20.32502560054414076 ) ) ;
#25882 = CARTESIAN_POINT ( 'NONE',  ( -4.483927247898782831, 16.52544592524335698, 107.7094237280190328 ) ) ;
#25883 = CARTESIAN_POINT ( 'NONE',  ( -16.51473224551069308, -9.474510206698971260, 51.66557627198102409 ) ) ;
#25884 = CARTESIAN_POINT ( 'NONE',  ( 19.02544592524334988, 5.153800228976608722, 21.45942372801899012 ) ) ;
#25885 = CARTESIAN_POINT ( 'NONE',  ( 0.05219959533934541429, -16.53943276465976808, 35.00109039468568284 ) ) ;
#25886 = CARTESIAN_POINT ( 'NONE',  ( -0.05219959533907301413, -21.53943276465977519, 42.49890960531435979 ) ) ;
#25888 = ORIENTED_EDGE ( 'NONE', *, *, #28343, .F. ) ;
#25887 = CARTESIAN_POINT ( 'NONE',  ( -18.67979575497193778, 10.72451020669871902, 88.33442372801901854 ) ) ;
#25889 = CARTESIAN_POINT ( 'NONE',  ( -5.153800228976328057, -19.02544592524343514, 102.2905762719810383 ) ) ;
#25890 = CARTESIAN_POINT ( 'NONE',  ( 9.474510206698971260, -16.51473224551069308, 92.91557627198103830 ) ) ;
#25891 = CARTESIAN_POINT ( 'NONE',  ( 29.86685920354754842, -21.69954338932559068, -5.824999997268813345 ) ) ;
#25892 = CARTESIAN_POINT ( 'NONE',  ( -10.72451020669870658, -18.67979575497194134, 19.58442372801901143 ) ) ;
#25893 = CARTESIAN_POINT ( 'NONE',  ( 12.14591786802309770, 12.06949235617756955, 74.37390960531436690 ) ) ;
#25895 = CARTESIAN_POINT ( 'NONE',  ( 16.51473224551069308, 9.474510206698969483, 74.16557627198103830 ) ) ;
#25894 = CARTESIAN_POINT ( 'NONE',  ( -15.72974639402197994, 15.80617190586746368, 80.62390960531438111 ) ) ;
#25896 = CARTESIAN_POINT ( 'NONE',  ( 13.97604488694527802, 13.89961937509977652, 74.37390960531436690 ) ) ;
#25897 = CARTESIAN_POINT ( 'NONE',  ( 21.53943276465977519, -0.05219959533907433946, 108.7489096053143669 ) ) ;
#25898 = ORIENTED_EDGE ( 'NONE', *, *, #118723, .F. ) ;
#25899 = CARTESIAN_POINT ( 'NONE',  ( 16.46253265017160672, -9.564922557960803928, 63.33224293864769550 ) ) ;
#25901 = LINE ( 'NONE', #180586, #110722 ) ;
#25900 = CARTESIAN_POINT ( 'NONE',  ( -8.314922557960811034, -14.29746914071050412, 107.0822429386476955 ) ) ;
#25902 = CARTESIAN_POINT ( 'NONE',  ( -9.474510206698964154, 16.51473224551069663, 60.41557627198102409 ) ) ;
#25903 = CARTESIAN_POINT ( 'NONE',  ( 9.474510206698729675, 16.51473224551082808, 87.08442372801900433 ) ) ;
#25904 = CARTESIAN_POINT ( 'NONE',  ( -0.05219959533910754901, -16.53943276465976808, 102.4989096053143811 ) ) ;
#25905 = CARTESIAN_POINT ( 'NONE',  ( 0.05219959533937995610, -21.53943276465977519, 65.00109039468568994 ) ) ;
#25907 = CARTESIAN_POINT ( 'NONE',  ( -0.05219959533907301413, -21.53943276465977519, 112.4989096053143669 ) ) ;
#25906 = CARTESIAN_POINT ( 'NONE',  ( 9.474510206698971260, -16.51473224551069308, 42.91557627198103120 ) ) ;
#25908 = B_SPLINE_CURVE_WITH_KNOTS ( 'NONE', 3,
 ( #475, #46002, #17656, #77328, #107657, #138996, #79316, #62149, #123813, #185511, #108661, #37790, #52946, #191468, #143964, #98444, #51958, #163141, #7439, #146972 ),
 .UNSPECIFIED., .F., .F.,
 ( 4, 2, 2, 2, 2, 2, 2, 2, 2, 4 ),
 ( 0.004000878361811907070, 0.004499404418915900483, 0.004997930476019893896, 0.005496456533123887309, 0.005994982590227879854, 0.006244245618779876994, 0.006493508647331874134, 0.006992034704435890098, 0.007490560761539906062, 0.007989086818643922894 ),
 .UNSPECIFIED. ) ;
#25909 = CARTESIAN_POINT ( 'NONE',  ( 12.14591786802309770, 12.06949235617756955, 99.37390960531436690 ) ) ;
#25910 = CARTESIAN_POINT ( 'NONE',  ( 8.906447517083050158, 27.41122689804195645, 141.4000000000000057 ) ) ;
#25911 = CARTESIAN_POINT ( 'NONE',  ( 19.03943276465977164, -0.05219959533909143690, 78.74890960531436690 ) ) ;
#25912 = CARTESIAN_POINT ( 'NONE',  ( 8.906447517083057264, -27.41122689804191026, 138.8500000054623911 ) ) ;
#25914 = CARTESIAN_POINT ( 'NONE',  ( 18.62759615963271287, -10.81492255796078972, 28.33224293864769550 ) ) ;
#25913 = CARTESIAN_POINT ( 'NONE',  ( -16.51473224551082808, 9.474510206698731452, 108.3344237280190043 ) ) ;
#25915 = CARTESIAN_POINT ( 'NONE',  ( -0.05219959533937732626, 21.53943276465977519, 47.50109039468568994 ) ) ;
#25916 = CARTESIAN_POINT ( 'NONE',  ( -16.46253265017160317, 9.564922557960807481, 100.8322429386477097 ) ) ;
#25917 = CARTESIAN_POINT ( 'NONE',  ( 16.46253265017146816, 9.564922557961045513, 76.66775706135234714 ) ) ;
#25918 = CARTESIAN_POINT ( 'NONE',  ( -16.51473224551069308, -9.474510206698971260, 66.66557627198102409 ) ) ;
#25919 = CARTESIAN_POINT ( 'NONE',  ( -4.483927247898539470, -16.52544592524342804, 87.29057627198103830 ) ) ;
#25920 = CARTESIAN_POINT ( 'NONE',  ( -13.97604488694527625, -13.89961937509977652, 96.87390960531433848 ) ) ;
#25921 = CARTESIAN_POINT ( 'NONE',  ( -14.29746914071049879, 8.314922557960819915, 80.83224293864769550 ) ) ;
#25922 = CARTESIAN_POINT ( 'NONE',  ( 13.89961937509977652, -13.97604488694527269, 93.12390960531436690 ) ) ;
#25923 = EDGE_CURVE ( 'NONE', #53380, #83853, #150801, .T. ) ;
#25926 = CARTESIAN_POINT ( 'NONE',  ( 0.05219959533909260263, 19.03943276465977164, 29.99890960531435979 ) ) ;
#25925 = CARTESIAN_POINT ( 'NONE',  ( 8.314922557960818139, 14.29746914071049879, 44.58224293864769550 ) ) ;
#25924 = CARTESIAN_POINT ( 'NONE',  ( 13.89961937509977652, -13.97604488694527269, 48.12390960531435979 ) ) ;
#25927 = EDGE_LOOP ( 'NONE', ( #72413, #118591, #153995, #166852 ) ) ;
#25928 = CARTESIAN_POINT ( 'NONE',  ( 21.55341960407619695, -5.719274019375665929, 41.04275706135236135 ) ) ;
#25929 = CARTESIAN_POINT ( 'NONE',  ( -19.02544592524334988, -5.153800228976617603, 78.95942372801900433 ) ) ;
#25930 = CARTESIAN_POINT ( 'NONE',  ( -12.06949235617756955, 12.14591786802309770, 45.62390960531436690 ) ) ;
#25931 = CARTESIAN_POINT ( 'NONE',  ( -21.52544592524343514, 5.823673210054127303, 96.04057627198102409 ) ) ;
#25932 = CARTESIAN_POINT ( 'NONE',  ( 21.55341960407610458, 5.719274019375980345, 28.95724293864769905 ) ) ;
#25933 = CARTESIAN_POINT ( 'NONE',  ( -8.224510206698948167, 14.34966873604960824, 80.41557627198103830 ) ) ;
#25934 = CARTESIAN_POINT ( 'NONE',  ( -19.02544592524342804, 5.153800228976336051, 41.04057627198103120 ) ) ;
#25935 = CARTESIAN_POINT ( 'NONE',  ( -16.55341960407611168, -4.379528057220339221, 26.45724293864768839 ) ) ;
#25936 = CARTESIAN_POINT ( 'NONE',  ( 8.224510206698742110, 14.34966873604972548, 92.08442372801901854 ) ) ;
#25937 = CARTESIAN_POINT ( 'NONE',  ( 16.53943276465976808, 0.05219959533934440121, 66.25109039468567573 ) ) ;
#25938 = CARTESIAN_POINT ( 'NONE',  ( -9.564922557961040184, 16.46253265017147172, 27.91775706135232582 ) ) ;
#25939 = CARTESIAN_POINT ( 'NONE',  ( -0.05219959533909027116, -19.03943276465977164, 87.49890960531436690 ) ) ;
#25940 = CARTESIAN_POINT ( 'NONE',  ( -16.46253265017160317, 9.564922557960807481, 75.83224293864769550 ) ) ;
#25941 = CARTESIAN_POINT ( 'NONE',  ( 14.34966873604972726, -8.224510206698740333, 75.83442372801900433 ) ) ;
#25942 = CARTESIAN_POINT ( 'NONE',  ( -9.564922557960796823, -16.46253265017161027, 42.08224293864769550 ) ) ;
#25943 = CARTESIAN_POINT ( 'NONE',  ( -4.379528057220328563, 16.55341960407611168, 50.20724293864769550 ) ) ;
#25945 = CARTESIAN_POINT ( 'NONE',  ( 0.05219959533909260263, 19.03943276465977164, 104.9989096053143669 ) ) ;
#25944 = CARTESIAN_POINT ( 'NONE',  ( -6.100000000000006750, 6.426762577456935076E-14, -64.92279855667830191 ) ) ;
#25946 = CARTESIAN_POINT ( 'NONE',  ( 18.67979575497178502, 10.72451020669898547, 29.16557627198103120 ) ) ;
#25947 = CARTESIAN_POINT ( 'NONE',  ( -8.224510206698948167, 14.34966873604960824, 70.41557627198102409 ) ) ;
#25948 = CARTESIAN_POINT ( 'NONE',  ( -16.55341960407611168, -4.379528057220339221, 71.45724293864769550 ) ) ;
#25949 = CARTESIAN_POINT ( 'NONE',  ( 17.50000000000150280, -3.202012800152198135, 32.42822416027275523 ) ) ;
#25950 = CARTESIAN_POINT ( 'NONE',  ( -9.564922557961040184, 16.46253265017147172, 62.91775706135233293 ) ) ;
#25951 = CARTESIAN_POINT ( 'NONE',  ( 13.89961937509977652, -13.97604488694527269, 98.12390960531433848 ) ) ;
#25952 = CARTESIAN_POINT ( 'NONE',  ( -19.05341960407617563, 5.049401038297882671, 83.54275706135233293 ) ) ;
#25953 = CARTESIAN_POINT ( 'NONE',  ( 17.14385361876520264, 23.59649016807275856, 146.6750000027311671 ) ) ;
#25955 = CARTESIAN_POINT ( 'NONE',  ( -14.34966873604972548, 8.224510206698743886, 98.33442372801901854 ) ) ;
#25954 = CARTESIAN_POINT ( 'NONE',  ( 9.564922557961047289, -16.46253265017146816, 105.4177570613523471 ) ) ;
#25956 = CARTESIAN_POINT ( 'NONE',  ( 9.474510206698971260, -16.51473224551069308, 42.91557627198103120 ) ) ;
#25957 = CARTESIAN_POINT ( 'NONE',  ( 15.72974639402199770, -15.80617190586745480, 38.12390960531436690 ) ) ;
#25958 = CARTESIAN_POINT ( 'NONE',  ( 21.53943276465977519, 0.05219959533937863772, 51.25109039468568994 ) ) ;
#25959 = CARTESIAN_POINT ( 'NONE',  ( 16.52544592524335698, 4.483927247898782831, 26.45942372801901854 ) ) ;
#25961 = CARTESIAN_POINT ( 'NONE',  ( -16.46253265017160317, 9.564922557960807481, 80.83224293864769550 ) ) ;
#25960 = CARTESIAN_POINT ( 'NONE',  ( 1.508955259217861487E-14, -71.74905152827281540, -24.99410988490251029 ) ) ;
#25962 = CARTESIAN_POINT ( 'NONE',  ( 5.049401038298161559, -19.05341960407611168, 112.7072429386476813 ) ) ;
#25964 = CARTESIAN_POINT ( 'NONE',  ( 16.51473224551069308, 9.474510206698969483, 79.16557627198103830 ) ) ;
#25963 = CARTESIAN_POINT ( 'NONE',  ( 12.14591786802309770, 12.06949235617756955, 69.37390960531436690 ) ) ;
#25965 = CARTESIAN_POINT ( 'NONE',  ( 5.153800228976335163, 19.02544592524342804, 89.79057627198102409 ) ) ;
#25966 = ORIENTED_EDGE ( 'NONE', *, *, #191573, .F. ) ;
#25967 = CARTESIAN_POINT ( 'NONE',  ( 19.03943276465977164, 0.05219959533936151252, 96.25109039468567573 ) ) ;
#25968 = CARTESIAN_POINT ( 'NONE',  ( 18.62759615963271287, -10.81492255796078972, 58.33224293864768839 ) ) ;
#25969 = CARTESIAN_POINT ( 'NONE',  ( -16.51473224551069308, -9.474510206698971260, 26.66557627198103120 ) ) ;
#25970 = CARTESIAN_POINT ( 'NONE',  ( 0.05219959533936267826, -19.03943276465977164, 60.00109039468566863 ) ) ;
#25971 = CARTESIAN_POINT ( 'NONE',  ( 13.97604488694527802, 13.89961937509977652, 59.37390960531434558 ) ) ;
#25972 = CARTESIAN_POINT ( 'NONE',  ( -13.97604488694527625, -13.89961937509977652, 96.87390960531433848 ) ) ;
#25973 = EDGE_LOOP ( 'NONE', ( #153117, #171378, #73335, #185218, #84762 ) ) ;
#25974 = CARTESIAN_POINT ( 'NONE',  ( 21.55341960407610458, 5.719274019375980345, 88.95724293864769550 ) ) ;
#25976 = CARTESIAN_POINT ( 'NONE',  ( 9.474510206698729675, 16.51473224551082808, 47.08442372801900433 ) ) ;
#25975 = CARTESIAN_POINT ( 'NONE',  ( 14.29746914071049879, -8.314922557960816363, 93.33224293864769550 ) ) ;
#25977 = CARTESIAN_POINT ( 'NONE',  ( 10.81492255796078972, 18.62759615963270932, 94.58224293864769550 ) ) ;
#25978 = CARTESIAN_POINT ( 'NONE',  ( -15.80617190586745835, -15.72974639402198527, 76.87390960531439532 ) ) ;
#25979 = CARTESIAN_POINT ( 'NONE',  ( -8.314922557960811034, -14.29746914071050412, 37.08224293864768129 ) ) ;
#25980 = CARTESIAN_POINT ( 'NONE',  ( 15.72974639402176855, 15.80617190586768217, 101.8760903946857042 ) ) ;
#25981 = CARTESIAN_POINT ( 'NONE',  ( -19.03943276465977164, 0.05219959533909376836, 81.24890960531436690 ) ) ;
#25982 = CARTESIAN_POINT ( 'NONE',  ( -19.02544592524342804, 5.153800228976336051, 31.04057627198102409 ) ) ;
#25983 = CARTESIAN_POINT ( 'NONE',  ( -5.719274019375665041, -21.55341960407619695, 39.79275706135235424 ) ) ;
#25984 = CARTESIAN_POINT ( 'NONE',  ( 5.823673210054444382, -21.52544592524334988, 55.20942372801902565 ) ) ;
#25985 = CARTESIAN_POINT ( 'NONE',  ( -19.02544592524342804, 5.153800228976336051, 51.04057627198103120 ) ) ;
#25986 = CARTESIAN_POINT ( 'NONE',  ( 15.80617190586746368, 15.72974639402197994, 114.3739096053143527 ) ) ;
#25987 = CARTESIAN_POINT ( 'NONE',  ( -5.049401038297874678, -19.05341960407617918, 64.79275706135233293 ) ) ;
#25988 = CARTESIAN_POINT ( 'NONE',  ( 13.89961937509977652, -13.97604488694527269, 38.12390960531436690 ) ) ;
#25989 = CARTESIAN_POINT ( 'NONE',  ( -8.224510206698735004, -14.34966873604973081, 24.58442372801901499 ) ) ;
#25990 = CARTESIAN_POINT ( 'NONE',  ( 19.02544592524343514, -5.153800228976328945, 23.54057627198102054 ) ) ;
#25991 = CARTESIAN_POINT ( 'NONE',  ( 8.224510206698742110, 14.34966873604972548, 77.08442372801901854 ) ) ;
#25992 = CARTESIAN_POINT ( 'NONE',  ( -19.03943276465977164, 0.05219959533909376836, 36.24890960531436690 ) ) ;
#25993 = CARTESIAN_POINT ( 'NONE',  ( 24.17640770809924078, -7.553848413212526758, 169.9412368235734618 ) ) ;
#25994 = CARTESIAN_POINT ( 'NONE',  ( 19.03943276465977164, -0.05219959533909143690, 83.74890960531436690 ) ) ;
#25995 = CARTESIAN_POINT ( 'NONE',  ( 8.314922557960818139, 14.29746914071049879, 114.5822429386477097 ) ) ;
#25997 = B_SPLINE_CURVE_WITH_KNOTS ( 'NONE', 3,
 ( #131347, #147533, #102018, #86845 ),
 .UNSPECIFIED., .F., .F.,
 ( 4, 4 ),
 ( 0.000000000000000000, 0.003358941478145230711 ),
 .UNSPECIFIED. ) ;
#25996 = CARTESIAN_POINT ( 'NONE',  ( 21.55341960407610458, 5.719274019375980345, 73.95724293864769550 ) ) ;
#25998 = CARTESIAN_POINT ( 'NONE',  ( 16.52544592524335698, 4.483927247898782831, 41.45942372801901143 ) ) ;
#25999 = CARTESIAN_POINT ( 'NONE',  ( 18.62759615963255655, 10.81492255796105972, 111.6677570613523613 ) ) ;
#26000 = CARTESIAN_POINT ( 'NONE',  ( 0.05219959533909260263, 19.03943276465977164, 34.99890960531435979 ) ) ;
#26001 = CARTESIAN_POINT ( 'NONE',  ( 8.224510206698953496, -14.34966873604960469, 27.91557627198103830 ) ) ;
#26002 = CARTESIAN_POINT ( 'NONE',  ( -14.34966873604960291, -8.224510206698953496, 71.66557627198100988 ) ) ;
#26003 = CARTESIAN_POINT ( 'NONE',  ( 5.153800228976335163, 19.02544592524342804, 64.79057627198100988 ) ) ;
#26004 = CARTESIAN_POINT ( 'NONE',  ( -16.46253265017146816, -9.564922557961047289, 19.16775706135233293 ) ) ;
#26005 = CARTESIAN_POINT ( 'NONE',  ( -18.67979575497193778, 10.72451020669871902, 23.33442372801901499 ) ) ;
#26006 = CARTESIAN_POINT ( 'NONE',  ( 9.474510206698971260, -16.51473224551069308, 77.91557627198103830 ) ) ;
#26007 = CARTESIAN_POINT ( 'NONE',  ( 18.67979575497194134, -10.72451020669871369, 80.83442372801901854 ) ) ;
#26008 = CARTESIAN_POINT ( 'NONE',  ( -0.05219959533934338120, 16.53943276465976808, 67.50109039468568994 ) ) ;
#26009 = CARTESIAN_POINT ( 'NONE',  ( -9.564922557960796823, -16.46253265017161027, 112.0822429386476955 ) ) ;
#26010 = CARTESIAN_POINT ( 'NONE',  ( 14.34966873604960469, 8.224510206698951720, 39.16557627198102409 ) ) ;
#26011 = CARTESIAN_POINT ( 'NONE',  ( 19.02544592524343514, -5.153800228976328945, 33.54057627198102409 ) ) ;
#26012 = CARTESIAN_POINT ( 'NONE',  ( 16.52544592524335698, 4.483927247898782831, 51.45942372801901854 ) ) ;
#26013 = CARTESIAN_POINT ( 'NONE',  ( -8.314922557960811034, -14.29746914071050412, 52.08224293864768839 ) ) ;
#26014 = CARTESIAN_POINT ( 'NONE',  ( -16.46253265017160317, 9.564922557960807481, 105.8322429386476955 ) ) ;
#26015 = CARTESIAN_POINT ( 'NONE',  ( 10.81492255796078972, 18.62759615963270932, 34.58224293864770260 ) ) ;
#26016 = CARTESIAN_POINT ( 'NONE',  ( 9.474510206698729675, 16.51473224551082808, 22.08442372801899722 ) ) ;
#26017 = CARTESIAN_POINT ( 'NONE',  ( -8.314922557960811034, -14.29746914071050412, 87.08224293864769550 ) ) ;
#26018 = CARTESIAN_POINT ( 'NONE',  ( -16.46253265017160317, 9.564922557960807481, 90.83224293864769550 ) ) ;
#26019 = ORIENTED_EDGE ( 'NONE', *, *, #129249, .F. ) ;
#26020 = CARTESIAN_POINT ( 'NONE',  ( -16.52544592524335698, -4.483927247898792601, 43.95942372801902565 ) ) ;
#26021 = CARTESIAN_POINT ( 'NONE',  ( 0.05219959533909260263, 19.03943276465977164, 59.99890960531436690 ) ) ;
#26022 = CARTESIAN_POINT ( 'NONE',  ( 5.049401038297881783, 19.05341960407617563, 47.29275706135231161 ) ) ;
#26023 = CARTESIAN_POINT ( 'NONE',  ( -19.03943276465977164, 0.05219959533909376836, 51.24890960531436690 ) ) ;
#26024 = CARTESIAN_POINT ( 'NONE',  ( -14.29746914071037622, -8.314922557961029526, 79.16775706135234714 ) ) ;
#26025 = CARTESIAN_POINT ( 'NONE',  ( -13.97604488694547697, 13.89961937509957934, 93.12609039468566152 ) ) ;
#26026 = CARTESIAN_POINT ( 'NONE',  ( 15.72974639402176855, 15.80617190586768217, 61.87609039468568284 ) ) ;
#26027 = CARTESIAN_POINT ( 'NONE',  ( 16.51473224551069308, 9.474510206698969483, 64.16557627198102409 ) ) ;
#26028 = CARTESIAN_POINT ( 'NONE',  ( -10.81492255796078084, -18.62759615963271287, 92.08224293864769550 ) ) ;
#26029 = CARTESIAN_POINT ( 'NONE',  ( -12.14591786802309592, -12.06949235617757132, 96.87390960531436690 ) ) ;
#26030 = CARTESIAN_POINT ( 'NONE',  ( -5.153800228976607833, 19.02544592524334988, 67.70942372801900433 ) ) ;
#26031 = CARTESIAN_POINT ( 'NONE',  ( -0.05219959533907301413, -21.53943276465977519, 67.49890960531436690 ) ) ;
#26032 = CARTESIAN_POINT ( 'NONE',  ( 16.51473224551083163, -9.474510206698727899, 45.83442372801900433 ) ) ;
#26033 = CARTESIAN_POINT ( 'NONE',  ( 16.51473224551069308, 9.474510206698969483, 114.1655762719810241 ) ) ;
#26034 = CARTESIAN_POINT ( 'NONE',  ( 15.80617190586746368, 15.72974639402197994, 94.37390960531436690 ) ) ;
#26035 = CARTESIAN_POINT ( 'NONE',  ( -18.87580814761071935, 5.500000000000041744, 55.87172394265761000 ) ) ;
#26036 = CARTESIAN_POINT ( 'NONE',  ( -4.483927247898782831, 16.52544592524335698, 22.70942372801901499 ) ) ;
#26037 = CARTESIAN_POINT ( 'NONE',  ( -19.36337904590691039, 5.499999999999949374, 60.41494137495623562 ) ) ;
#26038 = CARTESIAN_POINT ( 'NONE',  ( -16.53943276465976808, -0.05219959533934237506, 28.75109039468567929 ) ) ;
#26039 = CARTESIAN_POINT ( 'NONE',  ( -9.474510206698964154, 16.51473224551069663, 40.41557627198103120 ) ) ;
#26040 = CARTESIAN_POINT ( 'NONE',  ( 9.564922557960805705, 16.46253265017160317, 104.5822429386476955 ) ) ;
#26041 = CARTESIAN_POINT ( 'NONE',  ( 15.80617190586746368, 15.72974639402197994, 84.37390960531438111 ) ) ;
#26042 = CARTESIAN_POINT ( 'NONE',  ( -15.72974639402176322, -15.80617190586768395, 69.37609039468567573 ) ) ;
#26044 = CARTESIAN_POINT ( 'NONE',  ( -19.03943276465977164, -0.05219959533935918106, 33.75109039468566863 ) ) ;
#26043 = CARTESIAN_POINT ( 'NONE',  ( 0.05219959533934541429, -16.53943276465976808, 30.00109039468568284 ) ) ;
#26045 = CARTESIAN_POINT ( 'NONE',  ( -0.05219959533910754901, -16.53943276465976808, 27.49890960531435269 ) ) ;
#26046 = CARTESIAN_POINT ( 'NONE',  ( -18.67979575497178146, -10.72451020669898902, 111.6655762719810525 ) ) ;
#26047 = CARTESIAN_POINT ( 'NONE',  ( -14.34966873604960291, -8.224510206698953496, 51.66557627198102409 ) ) ;
#26048 = CARTESIAN_POINT ( 'NONE',  ( 19.05341960407617918, -5.049401038297876454, 101.0427570613523045 ) ) ;
#26049 = EDGE_CURVE ( 'NONE', #119129, #151905, #42620, .T. ) ;
#26050 = CARTESIAN_POINT ( 'NONE',  ( 5.153800228976615827, -19.02544592524334988, 55.20942372801899722 ) ) ;
#26051 = CARTESIAN_POINT ( 'NONE',  ( 21.55341960407619695, -5.719274019375665929, 66.04275706135236135 ) ) ;
#26052 = CARTESIAN_POINT ( 'NONE',  ( 19.02544592524334988, 5.153800228976608722, 41.45942372801900433 ) ) ;
#26053 = CARTESIAN_POINT ( 'NONE',  ( -13.89961937509977652, 13.97604488694528158, 25.62390960531434558 ) ) ;
#26054 = CARTESIAN_POINT ( 'NONE',  ( 10.72451020669898902, -18.67979575497178502, 37.91557627198102409 ) ) ;
#26055 = CARTESIAN_POINT ( 'NONE',  ( -16.53943276465976808, 0.05219959533911058130, 46.24890960531435979 ) ) ;
#26056 = CARTESIAN_POINT ( 'NONE',  ( -18.22780087662121673, -5.500000000000063061, 51.48459894673893444 ) ) ;
#26057 = CARTESIAN_POINT ( 'NONE',  ( -9.564922557961040184, 16.46253265017147172, 22.91775706135233648 ) ) ;
#26058 = CARTESIAN_POINT ( 'NONE',  ( 8.224510206698742110, 14.34966873604972548, 77.08442372801901854 ) ) ;
#26059 = CARTESIAN_POINT ( 'NONE',  ( -16.53943276465976808, 0.05219959533911058130, 41.24890960531435269 ) ) ;
#26060 = CARTESIAN_POINT ( 'NONE',  ( -21.53943276465977519, -0.05219959533937600094, 73.75109039468567573 ) ) ;
#26061 = CARTESIAN_POINT ( 'NONE',  ( -10.72451020669870658, -18.67979575497194134, 64.58442372801900433 ) ) ;
#26062 = CARTESIAN_POINT ( 'NONE',  ( 5.719274019375991003, -21.55341960407610458, 82.70724293864770971 ) ) ;
#26063 = CARTESIAN_POINT ( 'NONE',  ( -16.46253265017160317, 9.564922557960807481, 40.83224293864769550 ) ) ;
#26064 = CARTESIAN_POINT ( 'NONE',  ( -0.05219959533937732626, 21.53943276465977519, 42.50109039468567573 ) ) ;
#26065 = CARTESIAN_POINT ( 'NONE',  ( 13.97604488694527802, 13.89961937509977652, 29.37390960531435979 ) ) ;
#26066 = CARTESIAN_POINT ( 'NONE',  ( 9.564922557960805705, 16.46253265017160317, 34.58224293864770260 ) ) ;
#26067 = CARTESIAN_POINT ( 'NONE',  ( -4.379528057220328563, 16.55341960407611168, 90.20724293864770971 ) ) ;
#26068 = CARTESIAN_POINT ( 'NONE',  ( 9.474510206698971260, -16.51473224551069308, 87.91557627198102409 ) ) ;
#26069 = CARTESIAN_POINT ( 'NONE',  ( -0.05219959533910754901, -16.53943276465976808, 37.49890960531436690 ) ) ;
#26070 = CARTESIAN_POINT ( 'NONE',  ( -14.34966873604960291, -8.224510206698953496, 96.66557627198102409 ) ) ;
#26071 = CARTESIAN_POINT ( 'NONE',  ( -5.823673210054116645, -21.52544592524344225, 72.29057627198102409 ) ) ;
#26072 = CARTESIAN_POINT ( 'NONE',  ( 15.80617190586746368, 15.72974639402197994, 109.3739096053143811 ) ) ;
#26073 = CARTESIAN_POINT ( 'NONE',  ( 9.564922557960805705, 16.46253265017160317, 109.5822429386476955 ) ) ;
#26075 = CARTESIAN_POINT ( 'NONE',  ( -0.05219959533934338120, 16.53943276465976808, 22.50109039468567573 ) ) ;
#26074 = CARTESIAN_POINT ( 'NONE',  ( -9.564922557960796823, -16.46253265017161027, 67.08224293864769550 ) ) ;
#26076 = CARTESIAN_POINT ( 'NONE',  ( 21.53943276465977519, -0.05219959533907433946, 68.74890960531435269 ) ) ;
#26077 = CARTESIAN_POINT ( 'NONE',  ( 10.72451020669871369, 18.67979575497193778, 92.08442372801901854 ) ) ;
#26078 = CARTESIAN_POINT ( 'NONE',  ( 9.474510206698971260, -16.51473224551069308, 82.91557627198103830 ) ) ;
#26079 = CARTESIAN_POINT ( 'NONE',  ( 21.53943276465977519, -0.05219959533907433946, 108.7489096053143669 ) ) ;
#26080 = CARTESIAN_POINT ( 'NONE',  ( -21.55341960407610458, -5.719274019375992779, 21.45724293864769550 ) ) ;
#26081 = CARTESIAN_POINT ( 'NONE',  ( -16.52544592524335698, -4.483927247898792601, 83.95942372801900433 ) ) ;
#26082 = CARTESIAN_POINT ( 'NONE',  ( 10.81492255796106328, -18.62759615963255655, 70.41775706135236135 ) ) ;
#26083 = CARTESIAN_POINT ( 'NONE',  ( 15.72974639402176855, 15.80617190586768217, 101.8760903946857042 ) ) ;
#26084 = CARTESIAN_POINT ( 'NONE',  ( -12.14591786802326823, 12.06949235617739902, 63.12609039468568994 ) ) ;
#26085 = CARTESIAN_POINT ( 'NONE',  ( 15.80617190586769283, -15.72974639402175789, 25.62609039468567929 ) ) ;
#26086 = CARTESIAN_POINT ( 'NONE',  ( 5.049401038298161559, -19.05341960407611168, 112.7072429386476813 ) ) ;
#26087 = CARTESIAN_POINT ( 'NONE',  ( -0.05219959533937732626, 21.53943276465977519, 87.50109039468568994 ) ) ;
#26088 = CARTESIAN_POINT ( 'NONE',  ( 19.02544592524343514, -5.153800228976328945, 93.54057627198102409 ) ) ;
#26089 = CARTESIAN_POINT ( 'NONE',  ( -18.62759615963270932, 10.81492255796079327, 90.83224293864769550 ) ) ;
#26090 = CARTESIAN_POINT ( 'NONE',  ( 0.05219959533936267826, -19.03943276465977164, 55.00109039468566863 ) ) ;
#26091 = CARTESIAN_POINT ( 'NONE',  ( -21.53943276465977519, 0.05219959533907696930, 51.24890960531436690 ) ) ;
#26093 = CARTESIAN_POINT ( 'NONE',  ( 12.14591786802309770, 12.06949235617756955, 34.37390960531435979 ) ) ;
#26092 = CARTESIAN_POINT ( 'NONE',  ( -9.474510206698964154, 16.51473224551069663, 100.4155762719810241 ) ) ;
#26094 = CARTESIAN_POINT ( 'NONE',  ( 12.24802307403557933, -10.74802307403627921, -61.53034260416801260 ) ) ;
#26095 = CARTESIAN_POINT ( 'NONE',  ( 9.474510206698729675, 16.51473224551082808, 82.08442372801899012 ) ) ;
#26096 =( BOUNDED_CURVE ( )  B_SPLINE_CURVE ( 3, ( #116778, #194637, #103622, #42945 ),
 .UNSPECIFIED., .F., .T. ) 
 B_SPLINE_CURVE_WITH_KNOTS ( ( 4, 4 ),
 ( 1.132647296210726795, 2.115944711806982514 ),
 .UNSPECIFIED. ) 
 CURVE ( )  GEOMETRIC_REPRESENTATION_ITEM ( )  RATIONAL_B_SPLINE_CURVE ( ( 1.000000000000000000, 0.9210371567966664230, 0.9210371567966664230, 1.000000000000000000 ) ) 
 REPRESENTATION_ITEM ( '' )  );
#26097 = CARTESIAN_POINT ( 'NONE',  ( -19.39056639909675894, -5.499999999999968914, 80.78948781074343799 ) ) ;
#26098 = CARTESIAN_POINT ( 'NONE',  ( 19.05341960407617918, -5.049401038297876454, 106.0427570613523471 ) ) ;
#26099 = CARTESIAN_POINT ( 'NONE',  ( 15.80617190586746368, 15.72974639402197994, 84.37390960531438111 ) ) ;
#26100 = CARTESIAN_POINT ( 'NONE',  ( 8.314922557960818139, 14.29746914071049879, 69.58224293864769550 ) ) ;
#26101 = CARTESIAN_POINT ( 'NONE',  ( 12.06949235617739724, 12.14591786802326823, 31.87609039468567929 ) ) ;
#26102 = CARTESIAN_POINT ( 'NONE',  ( -5.153800228976328057, -19.02544592524343514, 42.29057627198101699 ) ) ;
#26104 = CARTESIAN_POINT ( 'NONE',  ( 5.049401038297881783, 19.05341960407617563, 82.29275706135229029 ) ) ;
#26103 = CARTESIAN_POINT ( 'NONE',  ( 15.72974639402176855, 15.80617190586768217, 21.87609039468567573 ) ) ;
#26105 = CARTESIAN_POINT ( 'NONE',  ( -19.05341960407611168, -5.049401038298163336, 91.45724293864766707 ) ) ;
#26106 = CARTESIAN_POINT ( 'NONE',  ( -16.51473224551069308, -9.474510206698971260, 76.66557627198103830 ) ) ;
#26107 = CARTESIAN_POINT ( 'NONE',  ( 18.62759615963271287, -10.81492255796078972, 78.33224293864770971 ) ) ;
#26108 = CARTESIAN_POINT ( 'NONE',  ( -19.05341960407611168, -5.049401038298163336, 51.45724293864770260 ) ) ;
#26109 = CARTESIAN_POINT ( 'NONE',  ( 17.23098935283880095, 33.12085103290880284, -7.999999999999992895 ) ) ;
#26110 = CARTESIAN_POINT ( 'NONE',  ( -14.29746914071049879, 8.314922557960819915, 60.83224293864769550 ) ) ;
#26111 = CARTESIAN_POINT ( 'NONE',  ( 9.474510206698971260, -16.51473224551069308, 87.91557627198102409 ) ) ;
#26112 = DIRECTION ( 'NONE',  ( 1.000000000000000000, 8.881784197001252323E-16, 0.000000000000000000 ) ) ;
#26113 = CARTESIAN_POINT ( 'NONE',  ( 5.049401038297881783, 19.05341960407617563, 67.29275706135234714 ) ) ;
#26114 = CARTESIAN_POINT ( 'NONE',  ( 21.52544592524344225, -5.823673210054117533, 73.54057627198102409 ) ) ;
#26115 = CARTESIAN_POINT ( 'NONE',  ( -19.02544592524334988, -5.153800228976617603, 38.95942372801900433 ) ) ;
#26116 = CARTESIAN_POINT ( 'NONE',  ( 13.97604488694527802, 13.89961937509977652, 104.3739096053143385 ) ) ;
#26117 = CARTESIAN_POINT ( 'NONE',  ( -17.50000000000000355, 3.237210098469587738, 114.7123698737954101 ) ) ;
#26118 = CARTESIAN_POINT ( 'NONE',  ( 21.55341960407610458, 5.719274019375980345, 38.95724293864768839 ) ) ;
#26119 = CARTESIAN_POINT ( 'NONE',  ( -16.51473224551069308, -9.474510206698971260, 71.66557627198102409 ) ) ;
#26120 = CARTESIAN_POINT ( 'NONE',  ( -5.719274019375665041, -21.55341960407619695, 64.79275706135234714 ) ) ;
#26121 = CARTESIAN_POINT ( 'NONE',  ( -9.564922557960796823, -16.46253265017161027, 27.08224293864769550 ) ) ;
#26122 = EDGE_CURVE ( 'NONE', #25627, #5010, #132627, .T. ) ;
#26124 = ORIENTED_EDGE ( 'NONE', *, *, #154768, .T. ) ;
#26123 = CARTESIAN_POINT ( 'NONE',  ( 0.05219959533907565091, 21.53943276465977519, 114.9989096053143669 ) ) ;
#26125 = CARTESIAN_POINT ( 'NONE',  ( -21.55341960407619339, 5.719274019375674811, 48.54275706135234714 ) ) ;
#26126 = VERTEX_POINT ( 'NONE', #40621 ) ;
#26127 = CARTESIAN_POINT ( 'NONE',  ( -28.09353542562696404, -5.934688857626441383, 140.0000000000000000 ) ) ;
#26128 = CARTESIAN_POINT ( 'NONE',  ( -16.51473224551082808, 9.474510206698731452, 63.33442372801900433 ) ) ;
#26129 = CARTESIAN_POINT ( 'NONE',  ( 24.54195369798078374, -31.38977029645258909, -21.36864394644164733 ) ) ;
#26130 = CARTESIAN_POINT ( 'NONE',  ( 15.80617190586746368, 15.72974639402197994, 109.3739096053143811 ) ) ;
#26131 = CARTESIAN_POINT ( 'NONE',  ( -16.46253265017160317, 9.564922557960807481, 65.83224293864769550 ) ) ;
#26132 = CARTESIAN_POINT ( 'NONE',  ( 0.05219959533934541429, -16.53943276465976808, 35.00109039468568284 ) ) ;
#26133 = CARTESIAN_POINT ( 'NONE',  ( -38.00000000000001421, 12.34694845685046438, -9.849999994537625980 ) ) ;
#26134 = CARTESIAN_POINT ( 'NONE',  ( 21.53943276465977519, 0.05219959533937863772, 101.2510903946856757 ) ) ;
#26135 = CARTESIAN_POINT ( 'NONE',  ( 5.153800228976335163, 19.02544592524342804, 44.79057627198103830 ) ) ;
#26136 = CARTESIAN_POINT ( 'NONE',  ( -10.81492255796105439, 18.62759615963255655, 107.9177570613523471 ) ) ;
#26137 = ADVANCED_FACE ( 'NONE', ( #12297 ), #104287, .T. ) ;
#26139 = CARTESIAN_POINT ( 'NONE',  ( -10.72451020669870658, -18.67979575497194134, 54.58442372801901143 ) ) ;
#26138 = CARTESIAN_POINT ( 'NONE',  ( 19.02544592524343514, -5.153800228976328945, 83.54057627198100988 ) ) ;
#26140 = CARTESIAN_POINT ( 'NONE',  ( -8.571926809382608425, 26.38167802310805854, 148.9750000027311785 ) ) ;
#26141 = CARTESIAN_POINT ( 'NONE',  ( 19.03943276465977164, -0.05219959533909143690, 108.7489096053143527 ) ) ;
#26142 = CARTESIAN_POINT ( 'NONE',  ( -20.34036572606774484, 20.41983568886641365, 139.9999999999999716 ) ) ;
#26144 = CARTESIAN_POINT ( 'NONE',  ( -21.53943276465977519, -0.05219959533937600094, 68.75109039468568994 ) ) ;
#26143 = CARTESIAN_POINT ( 'NONE',  ( 8.224510206698742110, 14.34966873604972548, 52.08442372801901854 ) ) ;
#26145 = CARTESIAN_POINT ( 'NONE',  ( -21.52544592524334988, -5.823673210054445271, 88.95942372801901854 ) ) ;
#26146 = CARTESIAN_POINT ( 'NONE',  ( 24.93942350307310107, -7.769968609432603479, 171.2173313942149377 ) ) ;
#26147 = CARTESIAN_POINT ( 'NONE',  ( -8.314922557961024197, 14.29746914071037800, 22.91775706135235069 ) ) ;
#26148 = CARTESIAN_POINT ( 'NONE',  ( -5.049401038298153566, 19.05341960407611168, 85.20724293864766707 ) ) ;
#26149 = CARTESIAN_POINT ( 'NONE',  ( -19.05341960407611168, -5.049401038298163336, 106.4572429386476955 ) ) ;
#26150 = ORIENTED_EDGE ( 'NONE', *, *, #3493, .F. ) ;
#26151 = CARTESIAN_POINT ( 'NONE',  ( 17.49999999999999289, 5.500000000000063061, 41.70309617465829177 ) ) ;
#26152 = CARTESIAN_POINT ( 'NONE',  ( -19.03943276465977164, 0.05219959533909376836, 21.24890960531436335 ) ) ;
#26153 = CARTESIAN_POINT ( 'NONE',  ( 18.67979575497178502, 10.72451020669898547, 44.16557627198103120 ) ) ;
#26154 = CARTESIAN_POINT ( 'NONE',  ( -8.224510206698735004, -14.34966873604973081, 94.58442372801901854 ) ) ;
#26156 = CARTESIAN_POINT ( 'NONE',  ( 5.049401038298161559, -19.05341960407611168, 72.70724293864768129 ) ) ;
#26155 = CARTESIAN_POINT ( 'NONE',  ( -12.14591786802309592, -12.06949235617757132, 86.87390960531438111 ) ) ;
#26157 = CARTESIAN_POINT ( 'NONE',  ( 10.81492255796106328, -18.62759615963255655, 90.41775706135236135 ) ) ;
#26158 = B_SPLINE_CURVE_WITH_KNOTS ( 'NONE', 3,
 ( #100845, #83678, #145356, #131190, #129179, #37184, #161535, #192880, #68517, #70527, #96855, #130171, #191868, #112045 ),
 .UNSPECIFIED., .F., .F.,
 ( 4, 2, 2, 2, 2, 2, 4 ),
 ( 3.469446951953614189E-18, 0.002289927113134818983, 0.003434890669702226739, 0.004579854226269634496, 0.006869781339404426590, 0.008014744895971800953, 0.009159708452539173582 ),
 .UNSPECIFIED. ) ;
#26159 = CARTESIAN_POINT ( 'NONE',  ( 4.483927247898790824, -16.52544592524335698, 20.20942372801900788 ) ) ;
#26160 = CARTESIAN_POINT ( 'NONE',  ( 8.314922557960818139, 14.29746914071049879, 89.58224293864768129 ) ) ;
#26161 = CARTESIAN_POINT ( 'NONE',  ( 21.52544592524334988, 5.823673210054432836, 41.45942372801901143 ) ) ;
#26162 = CARTESIAN_POINT ( 'NONE',  ( -18.62759615963270932, 10.81492255796079327, 75.83224293864769550 ) ) ;
#26163 = CARTESIAN_POINT ( 'NONE',  ( 19.02544592524334988, 5.153800228976608722, 41.45942372801900433 ) ) ;
#26164 = CARTESIAN_POINT ( 'NONE',  ( -34.98624150382332232, 6.090157606732317319, 40.61607269374898266 ) ) ;
#26165 = CARTESIAN_POINT ( 'NONE',  ( 13.97604488694527802, 13.89961937509977652, 89.37390960531436690 ) ) ;
#26166 = CARTESIAN_POINT ( 'NONE',  ( -4.379528057220328563, 16.55341960407611168, 65.20724293864768129 ) ) ;
#26167 = CARTESIAN_POINT ( 'NONE',  ( 16.52544592524342804, -4.483927247898539470, 38.54057627198103120 ) ) ;
#26168 = CARTESIAN_POINT ( 'NONE',  ( 8.224510206698953496, -14.34966873604960469, 22.91557627198102765 ) ) ;
#26169 = CARTESIAN_POINT ( 'NONE',  ( 5.049401038297881783, 19.05341960407617563, 67.29275706135234714 ) ) ;
#26170 = DIRECTION ( 'NONE',  ( -1.000000000000000000, -0.000000000000000000, -0.000000000000000000 ) ) ;
#26171 = CARTESIAN_POINT ( 'NONE',  ( -13.97604488694527625, -13.89961937509977652, 111.8739096053143243 ) ) ;
#26172 = CARTESIAN_POINT ( 'NONE',  ( -14.34966873604960291, -8.224510206698953496, 81.66557627198103830 ) ) ;
#26173 = CARTESIAN_POINT ( 'NONE',  ( 19.27311148717739897, -5.499999999999809930, 38.03971402910765676 ) ) ;
#26175 = CARTESIAN_POINT ( 'NONE',  ( -18.67979575497178146, -10.72451020669898902, 51.66557627198102409 ) ) ;
#26174 = CARTESIAN_POINT ( 'NONE',  ( 13.89961937509977652, -13.97604488694527269, 43.12390960531434558 ) ) ;
#26176 = CARTESIAN_POINT ( 'NONE',  ( 18.62759615963271287, -10.81492255796078972, 73.33224293864769550 ) ) ;
#26177 = CARTESIAN_POINT ( 'NONE',  ( -0.05219959533910754901, -16.53943276465976808, 107.4989096053143669 ) ) ;
#26179 = CARTESIAN_POINT ( 'NONE',  ( 13.97604488694527802, 13.89961937509977652, 44.37390960531435269 ) ) ;
#26178 = CARTESIAN_POINT ( 'NONE',  ( 12.14591786802327356, -12.06949235617739191, 60.62609039468567573 ) ) ;
#26180 = CARTESIAN_POINT ( 'NONE',  ( 5.823673210054444382, -21.52544592524334988, 60.20942372801902565 ) ) ;
#26181 = ORIENTED_EDGE ( 'NONE', *, *, #24918, .T. ) ;
#26182 = CARTESIAN_POINT ( 'NONE',  ( -8.224510206698948167, 14.34966873604960824, 100.4155762719810241 ) ) ;
#26183 = CARTESIAN_POINT ( 'NONE',  ( 13.97604488694548053, -13.89961937509957401, 95.62609039468563310 ) ) ;
#26184 = CARTESIAN_POINT ( 'NONE',  ( -5.950531402560715689E-15, 38.81732327939063509, -5.624999997268813168 ) ) ;
#26186 = CARTESIAN_POINT ( 'NONE',  ( 21.53943276465977519, -0.05219959533907433946, 43.74890960531435979 ) ) ;
#26185 = FACE_OUTER_BOUND ( 'NONE', #151731, .T. ) ;
#26187 = CARTESIAN_POINT ( 'NONE',  ( 19.05341960407611168, 5.049401038298154454, 28.95724293864769550 ) ) ;
#26188 = CARTESIAN_POINT ( 'NONE',  ( 18.67979575497194134, -10.72451020669871369, 85.83442372801901854 ) ) ;
#26189 = CARTESIAN_POINT ( 'NONE',  ( 8.314922557960818139, 14.29746914071049879, 39.58224293864769550 ) ) ;
#26191 = CARTESIAN_POINT ( 'NONE',  ( 14.29746914071049879, -8.314922557960816363, 43.33224293864769550 ) ) ;
#26190 = CARTESIAN_POINT ( 'NONE',  ( 16.55341960407618274, -4.379528057220086978, 51.04275706135234714 ) ) ;
#26192 = CARTESIAN_POINT ( 'NONE',  ( -0.05219959533907301413, -21.53943276465977519, 72.49890960531435269 ) ) ;
#26193 =( REPRESENTATION_RELATIONSHIP ('NONE','NONE', #154205, #112845 ) REPRESENTATION_RELATIONSHIP_WITH_TRANSFORMATION ( #69445 )SHAPE_REPRESENTATION_RELATIONSHIP( ) );
#26194 = CARTESIAN_POINT ( 'NONE',  ( 10.72451020669898902, -18.67979575497178502, 77.91557627198102409 ) ) ;
#26195 = CARTESIAN_POINT ( 'NONE',  ( -21.96405779611666631, 8.831116573701658368, 171.4809137887048962 ) ) ;
#26197 = CARTESIAN_POINT ( 'NONE',  ( -0.05219959533907301413, -21.53943276465977519, 22.49890960531436335 ) ) ;
#26196 = CARTESIAN_POINT ( 'NONE',  ( -13.89961937509957401, -13.97604488694547875, 89.37609039468563310 ) ) ;
#26198 = CARTESIAN_POINT ( 'NONE',  ( -5.153800228976328057, -19.02544592524343514, 47.29057627198102409 ) ) ;
#26199 = CARTESIAN_POINT ( 'NONE',  ( 13.89961937509977652, -13.97604488694527269, 23.12390960531436335 ) ) ;
#26200 = CARTESIAN_POINT ( 'NONE',  ( -4.647474457565486646E-15, 28.90000000000004476, -52.65483682830183199 ) ) ;
#26201 = ORIENTED_EDGE ( 'NONE', *, *, #108101, .F. ) ;
#26202 = CARTESIAN_POINT ( 'NONE',  ( 4.483927247898790824, -16.52544592524335698, 80.20942372801901854 ) ) ;
#26203 = CARTESIAN_POINT ( 'NONE',  ( -18.62759615963270932, 10.81492255796079327, 110.8322429386476955 ) ) ;
#26204 = CARTESIAN_POINT ( 'NONE',  ( 13.89961937509977652, -13.97604488694527269, 73.12390960531436690 ) ) ;
#26205 = CARTESIAN_POINT ( 'NONE',  ( -10.72451020669870658, -18.67979575497194134, 39.58442372801901143 ) ) ;
#26206 = CARTESIAN_POINT ( 'NONE',  ( -16.51473224551069308, -9.474510206698971260, 101.6655762719810241 ) ) ;
#26207 = CARTESIAN_POINT ( 'NONE',  ( -25.49187754477127399, -30.53313611124044158, -20.74730905735241393 ) ) ;
#26208 = VERTEX_POINT ( 'NONE', #182126 ) ;
#26209 = CARTESIAN_POINT ( 'NONE',  ( 15.72974639402176855, 15.80617190586768217, 26.87609039468567218 ) ) ;
#26211 = CARTESIAN_POINT ( 'NONE',  ( -13.97604488694547697, 13.89961937509957934, 88.12609039468563310 ) ) ;
#26210 = CARTESIAN_POINT ( 'NONE',  ( 19.03943276465977164, -0.05219959533909143690, 23.74890960531435269 ) ) ;
#26212 = CARTESIAN_POINT ( 'NONE',  ( -9.474510206698720793, -16.51473224551083518, 39.58442372801899722 ) ) ;
#26213 = CARTESIAN_POINT ( 'NONE',  ( -0.05219959533907301413, -21.53943276465977519, 107.4989096053143669 ) ) ;
#26214 = CARTESIAN_POINT ( 'NONE',  ( -9.474510206698720793, -16.51473224551083518, 39.58442372801899722 ) ) ;
#26215 = CARTESIAN_POINT ( 'NONE',  ( 13.89961937509957401, 13.97604488694547697, 51.87609039468566863 ) ) ;
#26216 = CARTESIAN_POINT ( 'NONE',  ( 4.379528057220092307, 16.55341960407617563, 92.29275706135236135 ) ) ;
#26217 = CARTESIAN_POINT ( 'NONE',  ( 18.22780087662122384, -5.500000000000022204, 56.01540105326107977 ) ) ;
#26218 = CARTESIAN_POINT ( 'NONE',  ( 16.51473224551069308, 9.474510206698969483, 69.16557627198102409 ) ) ;
#26219 = CARTESIAN_POINT ( 'NONE',  ( 21.55341960407619695, -5.719274019375665929, 86.04275706135236135 ) ) ;
#26220 = CARTESIAN_POINT ( 'NONE',  ( -10.72451020669870658, -18.67979575497194134, 94.58442372801901854 ) ) ;
#26221 = CARTESIAN_POINT ( 'NONE',  ( 22.45286902209802804, -1.470710558936461521, -55.62279185774873014 ) ) ;
#26222 = CARTESIAN_POINT ( 'NONE',  ( -19.05341960407611168, -5.049401038298163336, 86.45724293864769550 ) ) ;
#26223 = CARTESIAN_POINT ( 'NONE',  ( -18.67979575497193778, 10.72451020669871902, 63.33442372801900433 ) ) ;
#26224 = CARTESIAN_POINT ( 'NONE',  ( 16.46253265017146816, 9.564922557961045513, 106.6677570613523471 ) ) ;
#26225 = CARTESIAN_POINT ( 'NONE',  ( 19.05341960407611168, 5.049401038298154454, 63.95724293864769550 ) ) ;
#26227 = EDGE_CURVE ( 'NONE', #70081, #30365, #194315, .T. ) ;
#26226 = CARTESIAN_POINT ( 'NONE',  ( -5.049401038298153566, 19.05341960407611168, 110.2072429386476671 ) ) ;
#26228 = CARTESIAN_POINT ( 'NONE',  ( -19.05341960407611168, -5.049401038298163336, 81.45724293864769550 ) ) ;
#26229 = CARTESIAN_POINT ( 'NONE',  ( -17.26172910966779739, -6.454744622555839584, 89.19353091350777163 ) ) ;
#26230 = CARTESIAN_POINT ( 'NONE',  ( 5.049401038298161559, -19.05341960407611168, 67.70724293864769550 ) ) ;
#26231 = CARTESIAN_POINT ( 'NONE',  ( 5.049401038298161559, -19.05341960407611168, 47.70724293864770260 ) ) ;
#26232 = CARTESIAN_POINT ( 'NONE',  ( -18.62759615963255300, -10.81492255796106328, 19.16775706135234714 ) ) ;
#26233 = CARTESIAN_POINT ( 'NONE',  ( -8.224510206698735004, -14.34966873604973081, 99.58442372801900433 ) ) ;
#26234 = CARTESIAN_POINT ( 'NONE',  ( 3.503282210674389052, -48.86437366581480291, -35.00000000000000000 ) ) ;
#26235 = SPHERICAL_SURFACE ( 'NONE', #78701, 2.000000000000000000 ) ;
#26236 = CARTESIAN_POINT ( 'NONE',  ( -13.89961937509957401, -13.97604488694547875, 54.37609039468565442 ) ) ;
#26237 = CARTESIAN_POINT ( 'NONE',  ( -19.05341960407611168, -5.049401038298163336, 81.45724293864769550 ) ) ;
#26238 = CARTESIAN_POINT ( 'NONE',  ( -4.483927247898539470, -16.52544592524342804, 77.29057627198102409 ) ) ;
#26239 = CARTESIAN_POINT ( 'NONE',  ( -8.314922557960811034, -14.29746914071050412, 107.0822429386476955 ) ) ;
#26240 = CARTESIAN_POINT ( 'NONE',  ( 5.823673210054125526, 21.52544592524343514, 34.79057627198103120 ) ) ;
#26241 = CARTESIAN_POINT ( 'NONE',  ( 19.02544592524343514, -5.153800228976328945, 108.5405762719810383 ) ) ;
#26242 = CARTESIAN_POINT ( 'NONE',  ( 14.34966873604960469, 8.224510206698951720, 89.16557627198102409 ) ) ;
#26243 = CARTESIAN_POINT ( 'NONE',  ( 37.99626262588773074, -12.34573411038900126, -3.102157773949822062 ) ) ;
#26244 = CARTESIAN_POINT ( 'NONE',  ( 13.97604488694548053, -13.89961937509957401, 35.62609039468567573 ) ) ;
#26245 = CARTESIAN_POINT ( 'NONE',  ( 12.06949235617739724, 12.14591786802326823, 111.8760903946856615 ) ) ;
#26246 = CARTESIAN_POINT ( 'NONE',  ( -9.474510206698964154, 16.51473224551069663, 90.41557627198103830 ) ) ;
#26247 = CARTESIAN_POINT ( 'NONE',  ( 10.72451020669871369, 18.67979575497193778, 52.08442372801901854 ) ) ;
#26248 = CARTESIAN_POINT ( 'NONE',  ( 21.52544592524344225, -5.823673210054117533, 38.54057627198103120 ) ) ;
#26249 = CARTESIAN_POINT ( 'NONE',  ( -21.53943276465977519, -0.05219959533937600094, 28.75109039468567929 ) ) ;
#26250 = CARTESIAN_POINT ( 'NONE',  ( -0.05219959533907301413, -21.53943276465977519, 67.49890960531436690 ) ) ;
#26251 = CARTESIAN_POINT ( 'NONE',  ( -16.55341960407611168, -4.379528057220339221, 101.4572429386476955 ) ) ;
#26252 = CARTESIAN_POINT ( 'NONE',  ( 5.153800228976615827, -19.02544592524334988, 55.20942372801899722 ) ) ;
#26253 = CARTESIAN_POINT ( 'NONE',  ( 19.03943276465977164, -0.05219959533909143690, 33.74890960531435979 ) ) ;
#26254 = CARTESIAN_POINT ( 'NONE',  ( 9.474510206698971260, -16.51473224551069308, 102.9155762719810241 ) ) ;
#26255 = CARTESIAN_POINT ( 'NONE',  ( -19.02544592524342804, 5.153800228976336051, 96.04057627198103830 ) ) ;
#26256 = CARTESIAN_POINT ( 'NONE',  ( -5.049401038298153566, 19.05341960407611168, 25.20724293864768484 ) ) ;
#26257 = CARTESIAN_POINT ( 'NONE',  ( 14.29746914071049879, -8.314922557960816363, 33.33224293864769550 ) ) ;
#26258 = CARTESIAN_POINT ( 'NONE',  ( 0.05219959533934541429, -16.53943276465976808, 35.00109039468568284 ) ) ;
#26259 = CARTESIAN_POINT ( 'NONE',  ( -5.719274019375665041, -21.55341960407619695, 109.7927570613523613 ) ) ;
#26261 = CARTESIAN_POINT ( 'NONE',  ( -16.55341960407611168, -4.379528057220339221, 26.45724293864768839 ) ) ;
#26260 = CARTESIAN_POINT ( 'NONE',  ( -13.97604488694527625, -13.89961937509977652, 96.87390960531433848 ) ) ;
#26262 = CARTESIAN_POINT ( 'NONE',  ( -10.72451020669870658, -18.67979575497194134, 34.58442372801900433 ) ) ;
#26263 = CARTESIAN_POINT ( 'NONE',  ( 0.05219959533909260263, 19.03943276465977164, 39.99890960531436690 ) ) ;
#26264 = CARTESIAN_POINT ( 'NONE',  ( 12.06949235617739724, 12.14591786802326823, 41.87609039468568284 ) ) ;
#26265 = CARTESIAN_POINT ( 'NONE',  ( 4.483927247898790824, -16.52544592524335698, 105.2094237280190328 ) ) ;
#26266 = CARTESIAN_POINT ( 'NONE',  ( 4.379528057220092307, 16.55341960407617563, 92.29275706135236135 ) ) ;
#26267 = CARTESIAN_POINT ( 'NONE',  ( 5.153800228976615827, -19.02544592524334988, 110.2094237280189901 ) ) ;
#26268 = CARTESIAN_POINT ( 'NONE',  ( 13.97604488694527802, 13.89961937509977652, 39.37390960531435269 ) ) ;
#26269 = CARTESIAN_POINT ( 'NONE',  ( 8.314922557960818139, 14.29746914071049879, 94.58224293864769550 ) ) ;
#26270 = CARTESIAN_POINT ( 'NONE',  ( 5.719274019375991003, -21.55341960407610458, 97.70724293864772392 ) ) ;
#26271 = CARTESIAN_POINT ( 'NONE',  ( -13.97604488694527625, -13.89961937509977652, 36.87390960531436690 ) ) ;
#26272 = CARTESIAN_POINT ( 'NONE',  ( -9.474510206698964154, 16.51473224551069663, 110.4155762719810383 ) ) ;
#26273 = CARTESIAN_POINT ( 'NONE',  ( -21.52544592524334988, -5.823673210054445271, 28.95942372801902209 ) ) ;
#26274 = CARTESIAN_POINT ( 'NONE',  ( 3.889087296525912674, -30.00000000000002132, 8.181980515339454030 ) ) ;
#26275 = CARTESIAN_POINT ( 'NONE',  ( 5.049401038298161559, -19.05341960407611168, 102.7072429386476955 ) ) ;
#26276 = DIRECTION ( 'NONE',  ( -0.000000000000000000, -1.000000000000000000, -0.000000000000000000 ) ) ;
#26277 = CARTESIAN_POINT ( 'NONE',  ( -9.564922557960796823, -16.46253265017161027, 82.08224293864768129 ) ) ;
#26279 = CARTESIAN_POINT ( 'NONE',  ( -4.379528057220328563, 16.55341960407611168, 95.20724293864769550 ) ) ;
#26278 = CARTESIAN_POINT ( 'NONE',  ( 18.67979575497194134, -10.72451020669871369, 35.83442372801901143 ) ) ;
#26280 = CARTESIAN_POINT ( 'NONE',  ( -16.51473224551069308, -9.474510206698971260, 96.66557627198102409 ) ) ;
#26281 = CARTESIAN_POINT ( 'NONE',  ( 19.05341960407617918, -5.049401038297876454, 21.04275706135232582 ) ) ;
#26282 = CARTESIAN_POINT ( 'NONE',  ( 0.05219959533934541429, -16.53943276465976808, 60.00109039468568284 ) ) ;
#26283 = CARTESIAN_POINT ( 'NONE',  ( 15.80617190586769283, -15.72974639402175789, 85.62609039468568994 ) ) ;
#26284 = CARTESIAN_POINT ( 'NONE',  ( -0.05219959533934338120, 16.53943276465976808, 37.50109039468568284 ) ) ;
#26286 = EDGE_CURVE ( 'NONE', #41521, #11425, #45774, .T. ) ;
#26285 = CARTESIAN_POINT ( 'NONE',  ( -16.51473224551069308, -9.474510206698971260, 86.66557627198102409 ) ) ;
#26287 = CARTESIAN_POINT ( 'NONE',  ( -16.53943276465976808, -0.05219959533934237506, 18.75109039468568639 ) ) ;
#26288 = CARTESIAN_POINT ( 'NONE',  ( -16.55341960407617563, 4.379528057220093196, 63.54275706135234003 ) ) ;
#26289 = CARTESIAN_POINT ( 'NONE',  ( -13.89961937509957401, -13.97604488694547875, 19.37609039468566507 ) ) ;
#26290 = CARTESIAN_POINT ( 'NONE',  ( 9.474510206698729675, 16.51473224551082808, 87.08442372801900433 ) ) ;
#26291 = CARTESIAN_POINT ( 'NONE',  ( -13.97604488694527625, -13.89961937509977652, 61.87390960531435979 ) ) ;
#26292 = CARTESIAN_POINT ( 'NONE',  ( 5.823673210054125526, 21.52544592524343514, 89.79057627198103830 ) ) ;
#26294 = CARTESIAN_POINT ( 'NONE',  ( -19.03943276465977164, -0.05219959533935918106, 88.75109039468567573 ) ) ;
#26293 = CARTESIAN_POINT ( 'NONE',  ( 4.483927247898545687, 16.52544592524342804, 89.79057627198103830 ) ) ;
#26295 = CARTESIAN_POINT ( 'NONE',  ( -14.29746914071037622, -8.314922557961029526, 59.16775706135234714 ) ) ;
#26296 = CARTESIAN_POINT ( 'NONE',  ( -19.26498983726236602, 5.499999999999801048, 80.55319577422004329 ) ) ;
#26297 = CARTESIAN_POINT ( 'NONE',  ( -16.46253265017146816, -9.564922557961047289, 59.16775706135233293 ) ) ;
#26298 = CARTESIAN_POINT ( 'NONE',  ( -16.53943276465976808, 0.05219959533911058130, 36.24890960531435979 ) ) ;
#26299 = CARTESIAN_POINT ( 'NONE',  ( -16.55341960407611168, -4.379528057220339221, 86.45724293864770971 ) ) ;
#26301 = FACE_OUTER_BOUND ( 'NONE', #135865, .T. ) ;
#26300 = CARTESIAN_POINT ( 'NONE',  ( -18.67979575497193778, 10.72451020669871902, 113.3344237280190328 ) ) ;
#26302 = CARTESIAN_POINT ( 'NONE',  ( -5.823673210054431948, 21.52544592524334988, 27.70942372801901854 ) ) ;
#26303 = CARTESIAN_POINT ( 'NONE',  ( 5.153800228976335163, 19.02544592524342804, 94.79057627198103830 ) ) ;
#26304 = CARTESIAN_POINT ( 'NONE',  ( 16.46253265017160672, -9.564922557960803928, 73.33224293864769550 ) ) ;
#26305 = CARTESIAN_POINT ( 'NONE',  ( -0.05219959533937732626, 21.53943276465977519, 102.5010903946856899 ) ) ;
#26306 = CARTESIAN_POINT ( 'NONE',  ( -0.05219959533909027116, -19.03943276465977164, 62.49890960531435979 ) ) ;
#26307 = ORIENTED_EDGE ( 'NONE', *, *, #120448, .F. ) ;
#26308 = CARTESIAN_POINT ( 'NONE',  ( -10.72451020669898014, 18.67979575497178502, 30.41557627198101699 ) ) ;
#26309 = CARTESIAN_POINT ( 'NONE',  ( 4.483927247898545687, 16.52544592524342804, 84.79057627198102409 ) ) ;
#26310 = CARTESIAN_POINT ( 'NONE',  ( 19.05341960407611168, 5.049401038298154454, 43.95724293864769550 ) ) ;
#26311 = CARTESIAN_POINT ( 'NONE',  ( -14.29746914071049879, 8.314922557960819915, 95.83224293864770971 ) ) ;
#26312 = CARTESIAN_POINT ( 'NONE',  ( -21.52544592524343514, 5.823673210054127303, 116.0405762719810383 ) ) ;
#26313 = CARTESIAN_POINT ( 'NONE',  ( 21.52544592524334988, 5.823673210054432836, 61.45942372801901854 ) ) ;
#26314 = CARTESIAN_POINT ( 'NONE',  ( -0.05219959533909027116, -19.03943276465977164, 37.49890960531436690 ) ) ;
#26315 = CARTESIAN_POINT ( 'NONE',  ( -4.379528057220086978, -16.55341960407618274, 64.79275706135234714 ) ) ;
#26316 = EDGE_CURVE ( 'NONE', #14227, #109472, #42623, .T. ) ;
#26317 = CARTESIAN_POINT ( 'NONE',  ( 15.72974639402199770, -15.80617190586745480, 103.1239096053143811 ) ) ;
#26318 = CARTESIAN_POINT ( 'NONE',  ( -21.53943276465977519, 0.05219959533907696930, 111.2489096053143669 ) ) ;
#26320 = CARTESIAN_POINT ( 'NONE',  ( 5.049401038298161559, -19.05341960407611168, 57.70724293864769550 ) ) ;
#26319 = CARTESIAN_POINT ( 'NONE',  ( -19.03943276465977164, -0.05219959533935918106, 38.75109039468566152 ) ) ;
#26321 = CARTESIAN_POINT ( 'NONE',  ( -16.46253265017160317, 9.564922557960807481, 115.8322429386477097 ) ) ;
#26322 = CARTESIAN_POINT ( 'NONE',  ( 5.719274019375673035, 21.55341960407619339, 62.29275706135236845 ) ) ;
#26323 = CARTESIAN_POINT ( 'NONE',  ( 5.719274019375991003, -21.55341960407610458, 57.70724293864770260 ) ) ;
#26324 = CARTESIAN_POINT ( 'NONE',  ( -4.483927247898539470, -16.52544592524342804, 37.29057627198102409 ) ) ;
#26326 = CARTESIAN_POINT ( 'NONE',  ( 15.80617190586769283, -15.72974639402175789, 105.6260903946856899 ) ) ;
#26325 = CARTESIAN_POINT ( 'NONE',  ( 21.55341960407619695, -5.719274019375665929, 71.04275706135234714 ) ) ;
#26327 = CARTESIAN_POINT ( 'NONE',  ( -8.224510206698948167, 14.34966873604960824, 60.41557627198102409 ) ) ;
#26328 = CARTESIAN_POINT ( 'NONE',  ( -16.52544592524342804, 4.483927247898546575, 111.0405762719810525 ) ) ;
#26329 = CARTESIAN_POINT ( 'NONE',  ( 0.05219959533936267826, -19.03943276465977164, 45.00109039468566863 ) ) ;
#26330 = CARTESIAN_POINT ( 'NONE',  ( -8.224510206698735004, -14.34966873604973081, 99.58442372801900433 ) ) ;
#26331 = CARTESIAN_POINT ( 'NONE',  ( -5.719274019375665041, -21.55341960407619695, 69.79275706135234714 ) ) ;
#26332 = CARTESIAN_POINT ( 'NONE',  ( 19.03943276465977164, -0.05219959533909143690, 53.74890960531436690 ) ) ;
#26333 = CARTESIAN_POINT ( 'NONE',  ( 19.03943276465977164, 0.05219959533936151252, 31.25109039468566863 ) ) ;
#26334 = CARTESIAN_POINT ( 'NONE',  ( 10.72451020669898902, -18.67979575497178502, 37.91557627198102409 ) ) ;
#26335 = CARTESIAN_POINT ( 'NONE',  ( 15.80617190586769283, -15.72974639402175789, 25.62609039468567929 ) ) ;
#26336 = CARTESIAN_POINT ( 'NONE',  ( 15.80617190586746368, 15.72974639402197994, 89.37390960531435269 ) ) ;
#26337 = CARTESIAN_POINT ( 'NONE',  ( -0.05219959533936034679, 19.03943276465977164, 87.50109039468567573 ) ) ;
#26338 = CARTESIAN_POINT ( 'NONE',  ( 12.06949235617739724, 12.14591786802326823, 46.87609039468568994 ) ) ;
#26340 = CARTESIAN_POINT ( 'NONE',  ( 5.719274019375991003, -21.55341960407610458, 92.70724293864770971 ) ) ;
#26339 = CARTESIAN_POINT ( 'NONE',  ( -5.284191517680379313, 3.873512393789712238, -62.43104308550747561 ) ) ;
#26341 = CARTESIAN_POINT ( 'NONE',  ( 8.314922557960818139, 14.29746914071049879, 79.58224293864769550 ) ) ;
#26342 = CARTESIAN_POINT ( 'NONE',  ( 0.9209418409973284536, 31.60467972784392643, -46.08008370242323792 ) ) ;
#26343 = CARTESIAN_POINT ( 'NONE',  ( -19.05341960407617563, 5.049401038297882671, 113.5427570613523471 ) ) ;
#26344 = CARTESIAN_POINT ( 'NONE',  ( -21.52544592524343514, 5.823673210054127303, 41.04057627198103120 ) ) ;
#26345 = CARTESIAN_POINT ( 'NONE',  ( -0.05219959533934338120, 16.53943276465976808, 82.50109039468568994 ) ) ;
#26346 = CARTESIAN_POINT ( 'NONE',  ( -15.49999999999999822, -5.500000000000000888, 22.00000000000000711 ) ) ;
#26347 = CARTESIAN_POINT ( 'NONE',  ( 14.29746914071037800, 8.314922557961029526, 51.66775706135234714 ) ) ;
#26348 = CARTESIAN_POINT ( 'NONE',  ( 10.72451020669871369, 18.67979575497193778, 22.08442372801901143 ) ) ;
#26349 = CARTESIAN_POINT ( 'NONE',  ( 5.823673210054125526, 21.52544592524343514, 44.79057627198103120 ) ) ;
#26350 = CARTESIAN_POINT ( 'NONE',  ( 12.06949235617739724, 12.14591786802326823, 71.87609039468568994 ) ) ;
#26351 = CARTESIAN_POINT ( 'NONE',  ( -19.05341960407611168, -5.049401038298163336, 81.45724293864769550 ) ) ;
#26353 = CARTESIAN_POINT ( 'NONE',  ( -13.97604488694527625, -13.89961937509977652, 26.87390960531434558 ) ) ;
#26352 = CARTESIAN_POINT ( 'NONE',  ( -18.62759615963255300, -10.81492255796106328, 54.16775706135235424 ) ) ;
#26354 = CARTESIAN_POINT ( 'NONE',  ( 15.80617190586746368, 15.72974639402197994, 44.37390960531435979 ) ) ;
#26355 = CARTESIAN_POINT ( 'NONE',  ( 21.55341960407610458, 5.719274019375980345, 23.95724293864769550 ) ) ;
#26356 = VERTEX_POINT ( 'NONE', #56796 ) ;
#26357 = CARTESIAN_POINT ( 'NONE',  ( -9.474510206698720793, -16.51473224551083518, 44.58442372801900433 ) ) ;
#26358 = CARTESIAN_POINT ( 'NONE',  ( -14.34966873604972548, 8.224510206698743886, 48.33442372801902565 ) ) ;
#26359 = CARTESIAN_POINT ( 'NONE',  ( 19.03943276465977164, -0.05219959533909143690, 108.7489096053143527 ) ) ;
#26360 = ORIENTED_EDGE ( 'NONE', *, *, #29949, .F. ) ;
#26361 = CARTESIAN_POINT ( 'NONE',  ( 5.153800228976335163, 19.02544592524342804, 89.79057627198102409 ) ) ;
#26362 = CARTESIAN_POINT ( 'NONE',  ( -8.314922557961024197, 14.29746914071037800, 102.9177570613523756 ) ) ;
#26363 = FACE_OUTER_BOUND ( 'NONE', #86357, .T. ) ;
#26364 = CARTESIAN_POINT ( 'NONE',  ( 14.34966873604960469, 8.224510206698951720, 89.16557627198102409 ) ) ;
#26365 = CARTESIAN_POINT ( 'NONE',  ( 15.80617190586746368, 15.72974639402197994, 44.37390960531435979 ) ) ;
#26366 = CARTESIAN_POINT ( 'NONE',  ( -9.564922557960796823, -16.46253265017161027, 32.08224293864769550 ) ) ;
#26367 = CARTESIAN_POINT ( 'NONE',  ( -0.05219959533934338120, 16.53943276465976808, 72.50109039468568994 ) ) ;
#26368 = CARTESIAN_POINT ( 'NONE',  ( -10.81492255796105439, 18.62759615963255655, 22.91775706135235069 ) ) ;
#26369 = CARTESIAN_POINT ( 'NONE',  ( -5.153800228976607833, 19.02544592524334988, 77.70942372801900433 ) ) ;
#26370 = CARTESIAN_POINT ( 'NONE',  ( -9.474510206698964154, 16.51473224551069663, 35.41557627198102409 ) ) ;
#26371 = CARTESIAN_POINT ( 'NONE',  ( 9.564922557960805705, 16.46253265017160317, 114.5822429386476955 ) ) ;
#26372 = CARTESIAN_POINT ( 'NONE',  ( 18.62759615963255655, 10.81492255796105972, 111.6677570613523613 ) ) ;
#26373 = CARTESIAN_POINT ( 'NONE',  ( -19.03943276465977164, 0.05219959533909376836, 71.24890960531435269 ) ) ;
#26374 = EDGE_CURVE ( 'NONE', #133811, #144727, #93622, .T. ) ;
#26375 = CARTESIAN_POINT ( 'NONE',  ( -16.53943276465976808, -0.05219959533934237506, 53.75109039468568994 ) ) ;
#26376 = CARTESIAN_POINT ( 'NONE',  ( 18.67979575497194134, -10.72451020669871369, 95.83442372801903275 ) ) ;
#26377 = CARTESIAN_POINT ( 'NONE',  ( -13.97604488694547697, 13.89961937509957934, 48.12609039468566863 ) ) ;
#26378 = CARTESIAN_POINT ( 'NONE',  ( 19.02544592524334988, 5.153800228976608722, 51.45942372801900433 ) ) ;
#26379 = ORIENTED_EDGE ( 'NONE', *, *, #82917, .F. ) ;
#26380 = CARTESIAN_POINT ( 'NONE',  ( -18.67979575497193778, 10.72451020669871902, 48.33442372801902565 ) ) ;
#26381 = CARTESIAN_POINT ( 'NONE',  ( 37.66961640367472341, -4.999999999999976019, -25.00000000000000000 ) ) ;
#26382 = CARTESIAN_POINT ( 'NONE',  ( 16.51473224551083163, -9.474510206698727899, 45.83442372801900433 ) ) ;
#26383 = CARTESIAN_POINT ( 'NONE',  ( 5.049401038298161559, -19.05341960407611168, 97.70724293864766707 ) ) ;
#26384 = CARTESIAN_POINT ( 'NONE',  ( 0.05219959533909260263, 19.03943276465977164, 79.99890960531436690 ) ) ;
#26385 = CARTESIAN_POINT ( 'NONE',  ( 8.224510206698953496, -14.34966873604960469, 42.91557627198103120 ) ) ;
#26386 = CARTESIAN_POINT ( 'NONE',  ( -5.823673210054116645, -21.52544592524344225, 32.29057627198102409 ) ) ;
#26387 = CARTESIAN_POINT ( 'NONE',  ( -22.81625015709510507, 31.40387420917330275, -1.424999997268813212 ) ) ;
#26388 = CARTESIAN_POINT ( 'NONE',  ( -28.90000000000004476, 2.980639576201346218E-13, -49.67367017693150189 ) ) ;
#26389 = CARTESIAN_POINT ( 'NONE',  ( -18.62759615963255300, -10.81492255796106328, 109.1677570613523613 ) ) ;
#26390 = CARTESIAN_POINT ( 'NONE',  ( -27.07812102864229686, 7.738729533396094595, 165.1046384229469766 ) ) ;
#26391 = CARTESIAN_POINT ( 'NONE',  ( 5.153800228976335163, 19.02544592524342804, 34.79057627198102409 ) ) ;
#26392 = CARTESIAN_POINT ( 'NONE',  ( 9.474510206698971260, -16.51473224551069308, 22.91557627198102765 ) ) ;
#26393 = CARTESIAN_POINT ( 'NONE',  ( 23.48529157249599564, 32.32473071737754111, -4.699999999999999289 ) ) ;
#26394 = CARTESIAN_POINT ( 'NONE',  ( -16.24461471443676430, -33.67505824103404422, -7.999999999999998224 ) ) ;
#26395 = CARTESIAN_POINT ( 'NONE',  ( -16.52544592524335698, -4.483927247898792601, 63.95942372801901854 ) ) ;
#26396 = CARTESIAN_POINT ( 'NONE',  ( 21.53943276465977519, -0.05219959533907433946, 83.74890960531435269 ) ) ;
#26397 = CARTESIAN_POINT ( 'NONE',  ( 14.34966873604960469, 8.224510206698951720, 54.16557627198103120 ) ) ;
#26399 = CARTESIAN_POINT ( 'NONE',  ( -13.97604488694527625, -13.89961937509977652, 101.8739096053143811 ) ) ;
#26398 = CARTESIAN_POINT ( 'NONE',  ( 9.474510206698971260, -16.51473224551069308, 32.91557627198102409 ) ) ;
#26400 = CARTESIAN_POINT ( 'NONE',  ( -21.52544592524334988, -5.823673210054445271, 23.95942372801901143 ) ) ;
#26401 = CARTESIAN_POINT ( 'NONE',  ( 5.049401038297881783, 19.05341960407617563, 37.29275706135232582 ) ) ;
#26402 = CARTESIAN_POINT ( 'NONE',  ( -5.153800228976328057, -19.02544592524343514, 27.29057627198103120 ) ) ;
#26403 = CARTESIAN_POINT ( 'NONE',  ( 10.72451020669871369, 18.67979575497193778, 82.08442372801901854 ) ) ;
#26404 = CARTESIAN_POINT ( 'NONE',  ( 67.00000000000000000, -1.230770033143102596E-14, 100.5000000000010232 ) ) ;
#26405 = CARTESIAN_POINT ( 'NONE',  ( -0.05219959533910754901, -16.53943276465976808, 22.49890960531436335 ) ) ;
#26406 = CARTESIAN_POINT ( 'NONE',  ( -29.86685920354755552, 21.69954338932564397, -3.324999997268813345 ) ) ;
#26407 = CARTESIAN_POINT ( 'NONE',  ( 21.53943276465977519, -0.05219959533907433946, 43.74890960531435979 ) ) ;
#26408 = CARTESIAN_POINT ( 'NONE',  ( 4.379528057220339221, -16.55341960407611168, 102.7072429386476955 ) ) ;
#26409 = DIRECTION ( 'NONE',  ( 0.000000000000000000, 0.000000000000000000, -1.000000000000000000 ) ) ;
#26410 = CARTESIAN_POINT ( 'NONE',  ( -5.153800228976328057, -19.02544592524343514, 92.29057627198099567 ) ) ;
#26411 = CARTESIAN_POINT ( 'NONE',  ( 16.53943276465976808, -0.05219959533910856209, 93.74890960531436690 ) ) ;
#26412 = CARTESIAN_POINT ( 'NONE',  ( 16.51473224551083163, -9.474510206698727899, 110.8344237280190043 ) ) ;
#26413 = CARTESIAN_POINT ( 'NONE',  ( 21.55341960407610458, 5.719274019375980345, 58.95724293864770971 ) ) ;
#26414 = ORIENTED_EDGE ( 'NONE', *, *, #118990, .T. ) ;
#26415 = CARTESIAN_POINT ( 'NONE',  ( 5.153800228976335163, 19.02544592524342804, 34.79057627198102409 ) ) ;
#26417 = CARTESIAN_POINT ( 'NONE',  ( -21.55341960407610458, -5.719274019375992779, 91.45724293864769550 ) ) ;
#26416 = CARTESIAN_POINT ( 'NONE',  ( 5.153800228976335163, 19.02544592524342804, 89.79057627198102409 ) ) ;
#26419 = CARTESIAN_POINT ( 'NONE',  ( -19.03943276465977164, 0.05219959533909376836, 81.24890960531436690 ) ) ;
#26418 = CARTESIAN_POINT ( 'NONE',  ( -14.29746914071037622, -8.314922557961029526, 104.1677570613523471 ) ) ;
#26420 = CARTESIAN_POINT ( 'NONE',  ( 19.03943276465977164, 0.05219959533936151252, 86.25109039468567573 ) ) ;
#26421 = CARTESIAN_POINT ( 'NONE',  ( 5.719274019375673035, 21.55341960407619339, 97.29275706135234714 ) ) ;
#26422 = CARTESIAN_POINT ( 'NONE',  ( 10.81492255796078972, 18.62759615963270932, 74.58224293864768129 ) ) ;
#26423 = CARTESIAN_POINT ( 'NONE',  ( 18.67979575497178502, 10.72451020669898547, 44.16557627198103120 ) ) ;
#26424 = CARTESIAN_POINT ( 'NONE',  ( -19.05341960407611168, -5.049401038298163336, 46.45724293864768129 ) ) ;
#26425 = CARTESIAN_POINT ( 'NONE',  ( -8.314922557960811034, -14.29746914071050412, 22.08224293864769194 ) ) ;
#26426 = CARTESIAN_POINT ( 'NONE',  ( 19.02544592524343514, -5.153800228976328945, 68.54057627198103830 ) ) ;
#26427 = ORIENTED_EDGE ( 'NONE', *, *, #148652, .T. ) ;
#26428 = CARTESIAN_POINT ( 'NONE',  ( -31.37893600750393830, -5.659358439387607298, 99.94586368981258317 ) ) ;
#26429 = CARTESIAN_POINT ( 'NONE',  ( 19.03943276465977164, 0.05219959533936151252, 26.25109039468566507 ) ) ;
#26430 = CARTESIAN_POINT ( 'NONE',  ( -4.379528057220328563, 16.55341960407611168, 75.20724293864769550 ) ) ;
#26431 = CARTESIAN_POINT ( 'NONE',  ( -10.81492255796105439, 18.62759615963255655, 22.91775706135235069 ) ) ;
#26432 = CARTESIAN_POINT ( 'NONE',  ( 8.571926809382603096, -26.38167802310801235, 145.9750000027311785 ) ) ;
#26433 = CARTESIAN_POINT ( 'NONE',  ( 21.52544592524344225, -5.823673210054117533, 53.54057627198103120 ) ) ;
#26434 = CARTESIAN_POINT ( 'NONE',  ( -0.05219959533934338120, 16.53943276465976808, 92.50109039468567573 ) ) ;
#26435 = CARTESIAN_POINT ( 'NONE',  ( -8.314922557960811034, -14.29746914071050412, 102.0822429386476955 ) ) ;
#26436 = CARTESIAN_POINT ( 'NONE',  ( 13.89961937509977652, -13.97604488694527269, 68.12390960531436690 ) ) ;
#26437 = CARTESIAN_POINT ( 'NONE',  ( -4.483927247898539470, -16.52544592524342804, 27.29057627198103120 ) ) ;
#26438 = CARTESIAN_POINT ( 'NONE',  ( 21.52544592524334988, 5.823673210054432836, 51.45942372801901854 ) ) ;
#26439 = CARTESIAN_POINT ( 'NONE',  ( 5.049401038298161559, -19.05341960407611168, 107.7072429386476955 ) ) ;
#26440 = CARTESIAN_POINT ( 'NONE',  ( 10.81492255796106328, -18.62759615963255655, 75.41775706135233293 ) ) ;
#26441 = CARTESIAN_POINT ( 'NONE',  ( -5.049401038298153566, 19.05341960407611168, 35.20724293864768839 ) ) ;
#26442 = CARTESIAN_POINT ( 'NONE',  ( -16.46253265017160317, 9.564922557960807481, 40.83224293864769550 ) ) ;
#26443 = ORIENTED_EDGE ( 'NONE', *, *, #196667, .F. ) ;
#26444 = CARTESIAN_POINT ( 'NONE',  ( 21.53943276465977519, 0.05219959533937863772, 101.2510903946856757 ) ) ;
#26445 = CARTESIAN_POINT ( 'NONE',  ( 4.483927247898790824, -16.52544592524335698, 45.20942372801901854 ) ) ;
#26446 = CARTESIAN_POINT ( 'NONE',  ( 5.719274019375673035, 21.55341960407619339, 77.29275706135234714 ) ) ;
#26447 = CARTESIAN_POINT ( 'NONE',  ( -19.03943276465977164, 0.05219959533909376836, 101.2489096053143669 ) ) ;
#26448 = CARTESIAN_POINT ( 'NONE',  ( 5.049401038297881783, 19.05341960407617563, 82.29275706135229029 ) ) ;
#26449 = CARTESIAN_POINT ( 'NONE',  ( 10.81492255796106328, -18.62759615963255655, 55.41775706135234714 ) ) ;
#26450 = CARTESIAN_POINT ( 'NONE',  ( 13.89961937509957401, 13.97604488694547697, 111.8760903946856757 ) ) ;
#26451 = CARTESIAN_POINT ( 'NONE',  ( -16.51473224551082808, 9.474510206698731452, 88.33442372801900433 ) ) ;
#26452 = CARTESIAN_POINT ( 'NONE',  ( -16.51473224551069308, -9.474510206698971260, 56.66557627198103120 ) ) ;
#26453 = CARTESIAN_POINT ( 'NONE',  ( 19.03943276465977164, 0.05219959533936151252, 91.25109039468566152 ) ) ;
#26454 = CARTESIAN_POINT ( 'NONE',  ( -4.379528057220328563, 16.55341960407611168, 25.20724293864769550 ) ) ;
#26455 = CARTESIAN_POINT ( 'NONE',  ( -9.564922557961040184, 16.46253265017147172, 82.91775706135233293 ) ) ;
#26456 = CARTESIAN_POINT ( 'NONE',  ( 4.379528057220339221, -16.55341960407611168, 42.70724293864770260 ) ) ;
#26457 = CARTESIAN_POINT ( 'NONE',  ( -19.02544592524334988, -5.153800228976617603, 63.95942372801899012 ) ) ;
#26458 = CARTESIAN_POINT ( 'NONE',  ( -0.05219959533934338120, 16.53943276465976808, 52.50109039468567573 ) ) ;
#26459 = CARTESIAN_POINT ( 'NONE',  ( -5.049401038297874678, -19.05341960407617918, 24.79275706135233648 ) ) ;
#26460 = CARTESIAN_POINT ( 'NONE',  ( -19.03943276465977164, 0.05219959533909376836, 31.24890960531435979 ) ) ;
#26461 = CARTESIAN_POINT ( 'NONE',  ( -16.46253265017160317, 9.564922557960807481, 45.83224293864769550 ) ) ;
#26462 = CARTESIAN_POINT ( 'NONE',  ( 12.14591786802327356, -12.06949235617739191, 40.62609039468567573 ) ) ;
#26463 = DIRECTION ( 'NONE',  ( 1.000000000000000000, 0.000000000000000000, 3.469446951953612217E-15 ) ) ;
#26464 = EDGE_CURVE ( 'NONE', #78021, #111651, #28434, .T. ) ;
#26466 = AXIS2_PLACEMENT_3D ( 'NONE', #82874, #100043, #34401 ) ;
#26465 = CARTESIAN_POINT ( 'NONE',  ( 8.906447517083050158, 27.41122689804195645, 141.6500000054623740 ) ) ;
#26467 = CARTESIAN_POINT ( 'NONE',  ( -19.05341960407611168, -5.049401038298163336, 96.45724293864769550 ) ) ;
#26468 = CARTESIAN_POINT ( 'NONE',  ( 17.78954161113924926, -0.5375896797866550614, 102.5000000000000284 ) ) ;
#26469 = ORIENTED_EDGE ( 'NONE', *, *, #135545, .F. ) ;
#26470 = CARTESIAN_POINT ( 'NONE',  ( -19.02544592524334988, -5.153800228976617603, 93.95942372801900433 ) ) ;
#26471 = CARTESIAN_POINT ( 'NONE',  ( 10.81492255796078972, 18.62759615963270932, 29.58224293864769905 ) ) ;
#26473 = CARTESIAN_POINT ( 'NONE',  ( -13.97604488694547697, 13.89961937509957934, 108.1260903946856331 ) ) ;
#26472 = CARTESIAN_POINT ( 'NONE',  ( -0.05219959533936034679, 19.03943276465977164, 32.50109039468566863 ) ) ;
#26474 = CARTESIAN_POINT ( 'NONE',  ( -8.224510206698948167, 14.34966873604960824, 105.4155762719810383 ) ) ;
#26475 = CARTESIAN_POINT ( 'NONE',  ( 13.97604488694527802, 13.89961937509977652, 34.37390960531436690 ) ) ;
#26476 = CARTESIAN_POINT ( 'NONE',  ( 18.67979575497178502, 10.72451020669898547, 74.16557627198102409 ) ) ;
#26477 = CARTESIAN_POINT ( 'NONE',  ( -13.97604488694527625, -13.89961937509977652, 41.87390960531435979 ) ) ;
#26478 = DIRECTION ( 'NONE',  ( -0.000000000000000000, -0.000000000000000000, 1.000000000000000000 ) ) ;
#26479 = CARTESIAN_POINT ( 'NONE',  ( 9.564922557961047289, -16.46253265017146816, 75.41775706135234714 ) ) ;
#26480 = CARTESIAN_POINT ( 'NONE',  ( -0.05219959533910754901, -16.53943276465976808, 52.49890960531435979 ) ) ;
#26481 = CARTESIAN_POINT ( 'NONE',  ( 15.72974639402199770, -15.80617190586745480, 38.12390960531436690 ) ) ;
#26482 = CARTESIAN_POINT ( 'NONE',  ( -10.81492255796105439, 18.62759615963255655, 92.91775706135236135 ) ) ;
#26483 = CARTESIAN_POINT ( 'NONE',  ( 10.81492255796078972, 18.62759615963270932, 89.58224293864768129 ) ) ;
#26484 = CARTESIAN_POINT ( 'NONE',  ( -5.823673210054431948, 21.52544592524334988, 77.70942372801900433 ) ) ;
#26485 = CARTESIAN_POINT ( 'NONE',  ( 21.55341960407619695, -5.719274019375665929, 66.04275706135236135 ) ) ;
#26486 = CARTESIAN_POINT ( 'NONE',  ( 16.51473224551069308, 9.474510206698969483, 99.16557627198102409 ) ) ;
#26488 = CARTESIAN_POINT ( 'NONE',  ( 18.67979575497194134, -10.72451020669871369, 65.83442372801900433 ) ) ;
#26487 = CARTESIAN_POINT ( 'NONE',  ( 14.29746914071037800, 8.314922557961029526, 96.66775706135234714 ) ) ;
#26489 = CARTESIAN_POINT ( 'NONE',  ( -19.02544592524342804, 5.153800228976336051, 56.04057627198100988 ) ) ;
#26490 = CARTESIAN_POINT ( 'NONE',  ( -18.62759615963255300, -10.81492255796106328, 34.16775706135234714 ) ) ;
#26491 = CARTESIAN_POINT ( 'NONE',  ( 0.05219959533909260263, 19.03943276465977164, 64.99890960531436690 ) ) ;
#26492 = CARTESIAN_POINT ( 'NONE',  ( 14.34966873604960469, 8.224510206698951720, 69.16557627198102409 ) ) ;
#26493 = CARTESIAN_POINT ( 'NONE',  ( 12.14591786802309770, 12.06949235617756955, 49.37390960531436690 ) ) ;
#26494 = CARTESIAN_POINT ( 'NONE',  ( -10.81492255796078084, -18.62759615963271287, 62.08224293864769550 ) ) ;
#26495 = CARTESIAN_POINT ( 'NONE',  ( 16.46253265017160672, -9.564922557960803928, 48.33224293864769550 ) ) ;
#26496 = CARTESIAN_POINT ( 'NONE',  ( 15.80617190586746368, 15.72974639402197994, 54.37390960531435979 ) ) ;
#26497 = CARTESIAN_POINT ( 'NONE',  ( 5.049401038297881783, 19.05341960407617563, 47.29275706135231161 ) ) ;
#26499 = CARTESIAN_POINT ( 'NONE',  ( -14.29746914071049879, 8.314922557960819915, 65.83224293864769550 ) ) ;
#26498 = DIRECTION ( 'NONE',  ( 0.000000000000000000, 0.000000000000000000, 1.000000000000000000 ) ) ;
#26500 = CARTESIAN_POINT ( 'NONE',  ( 18.67979575497178502, 10.72451020669898547, 34.16557627198102409 ) ) ;
#26501 = EDGE_LOOP ( 'NONE', ( #164706, #72706, #61298, #54216, #97504, #26469, #19584, #54993 ) ) ;
#26502 = CARTESIAN_POINT ( 'NONE',  ( 17.31747979337948351, 6.344076630961057894, 103.8794486806518478 ) ) ;
#26503 = CARTESIAN_POINT ( 'NONE',  ( 16.53943276465976808, 0.05219959533934440121, 91.25109039468568994 ) ) ;
#26504 = CARTESIAN_POINT ( 'NONE',  ( -19.03943276465977164, -0.05219959533935918106, 83.75109039468567573 ) ) ;
#26505 = CARTESIAN_POINT ( 'NONE',  ( 14.29746914071049879, -8.314922557960816363, 53.33224293864769550 ) ) ;
#26506 = DIRECTION ( 'NONE',  ( 0.8437662581494456138, -0.5367108174878562066, 0.000000000000000000 ) ) ;
#26507 = CARTESIAN_POINT ( 'NONE',  ( -19.03943276465977164, 0.05219959533909376836, 46.24890960531435979 ) ) ;
#26508 = CARTESIAN_POINT ( 'NONE',  ( 14.34966873604960469, 8.224510206698951720, 39.16557627198102409 ) ) ;
#26509 = CARTESIAN_POINT ( 'NONE',  ( 9.474510206698971260, -16.51473224551069308, 72.91557627198102409 ) ) ;
#26510 = CARTESIAN_POINT ( 'NONE',  ( -19.03943276465977164, 0.05219959533909376836, 46.24890960531435979 ) ) ;
#26511 = CARTESIAN_POINT ( 'NONE',  ( 21.55341960407619695, -5.719274019375665929, 61.04275706135234714 ) ) ;
#26512 = CARTESIAN_POINT ( 'NONE',  ( -16.51473224551069308, -9.474510206698971260, 76.66557627198103830 ) ) ;
#26513 = CARTESIAN_POINT ( 'NONE',  ( 5.049401038298161559, -19.05341960407611168, 32.70724293864768129 ) ) ;
#26514 = CARTESIAN_POINT ( 'NONE',  ( 5.049401038298161559, -19.05341960407611168, 57.70724293864769550 ) ) ;
#26515 = CARTESIAN_POINT ( 'NONE',  ( -10.72451020669898014, 18.67979575497178502, 55.41557627198102409 ) ) ;
#26516 = CARTESIAN_POINT ( 'NONE',  ( -19.03943276465977164, 0.05219959533909376836, 41.24890960531435269 ) ) ;
#26517 = CARTESIAN_POINT ( 'NONE',  ( 21.52544592524344225, -5.823673210054117533, 38.54057627198103120 ) ) ;
#26518 = CARTESIAN_POINT ( 'NONE',  ( 14.34966873604972726, -8.224510206698740333, 105.8344237280190328 ) ) ;
#26519 = CARTESIAN_POINT ( 'NONE',  ( -0.05219959533937732626, 21.53943276465977519, 112.5010903946857042 ) ) ;
#26521 = CARTESIAN_POINT ( 'NONE',  ( 0.05219959533934541429, -16.53943276465976808, 85.00109039468568994 ) ) ;
#26520 = CARTESIAN_POINT ( 'NONE',  ( 12.06949235617739724, 12.14591786802326823, 46.87609039468568994 ) ) ;
#26522 = CARTESIAN_POINT ( 'NONE',  ( 30.00000000000000000, -5.510910596163089556E-15, 45.00000000000000000 ) ) ;
#26523 = CARTESIAN_POINT ( 'NONE',  ( -16.52544592524335698, -4.483927247898792601, 73.95942372801901854 ) ) ;
#26524 = CARTESIAN_POINT ( 'NONE',  ( -12.14591786802326823, 12.06949235617739902, 58.12609039468568994 ) ) ;
#26525 = CARTESIAN_POINT ( 'NONE',  ( -19.03943276465977164, 0.05219959533909376836, 111.2489096053143669 ) ) ;
#26526 = CARTESIAN_POINT ( 'NONE',  ( 16.51473224551069308, 9.474510206698969483, 29.16557627198103475 ) ) ;
#26527 = CARTESIAN_POINT ( 'NONE',  ( -12.06949235617739369, -12.14591786802326823, 44.37609039468567573 ) ) ;
#26528 = CARTESIAN_POINT ( 'NONE',  ( -16.46253265017160317, 9.564922557960807481, 35.83224293864768839 ) ) ;
#26529 = CARTESIAN_POINT ( 'NONE',  ( -5.719274019375665041, -21.55341960407619695, 29.79275706135234358 ) ) ;
#26530 = CARTESIAN_POINT ( 'NONE',  ( 12.06949235617739724, 12.14591786802326823, 36.87609039468568994 ) ) ;
#26531 = CARTESIAN_POINT ( 'NONE',  ( 4.483927247898790824, -16.52544592524335698, 95.20942372801903275 ) ) ;
#26532 = DIRECTION ( 'NONE',  ( -0.000000000000000000, -0.000000000000000000, 1.000000000000000000 ) ) ;
#26533 = CARTESIAN_POINT ( 'NONE',  ( 10.72451020669871369, 18.67979575497193778, 107.0844237280190043 ) ) ;
#26534 = CARTESIAN_POINT ( 'NONE',  ( -13.97604488694547697, 13.89961937509957934, 98.12609039468566152 ) ) ;
#26535 = CARTESIAN_POINT ( 'NONE',  ( 4.483927247898545687, 16.52544592524342804, 54.79057627198104541 ) ) ;
#26536 = CARTESIAN_POINT ( 'NONE',  ( -13.97604488694527625, -13.89961937509977652, 26.87390960531434558 ) ) ;
#26538 = CARTESIAN_POINT ( 'NONE',  ( 16.88567814943162304, 6.947325034625711382, 78.79001122652589117 ) ) ;
#26537 = CARTESIAN_POINT ( 'NONE',  ( -16.46253265017146816, -9.564922557961047289, 64.16775706135233293 ) ) ;
#26539 = CARTESIAN_POINT ( 'NONE',  ( 10.72451020669871369, 18.67979575497193778, 67.08442372801901854 ) ) ;
#26540 = CARTESIAN_POINT ( 'NONE',  ( -0.05219959533934338120, 16.53943276465976808, 22.50109039468567573 ) ) ;
#26541 = CARTESIAN_POINT ( 'NONE',  ( 16.29526858892874230, 7.335722546920140807, 83.29670597800203780 ) ) ;
#26542 = CARTESIAN_POINT ( 'NONE',  ( 9.564922557960805705, 16.46253265017160317, 114.5822429386476955 ) ) ;
#26543 = CARTESIAN_POINT ( 'NONE',  ( 5.049401038297881783, 19.05341960407617563, 107.2927570613523187 ) ) ;
#26544 = CARTESIAN_POINT ( 'NONE',  ( 28.82186960331507208, 9.364793116373459014, 147.1000000000000227 ) ) ;
#26545 = CARTESIAN_POINT ( 'NONE',  ( -25.76143648877210524, 7.343476467573863076, 174.8772314887147843 ) ) ;
#26546 = CARTESIAN_POINT ( 'NONE',  ( 13.97604488694527802, 13.89961937509977652, 29.37390960531435979 ) ) ;
#26547 = CARTESIAN_POINT ( 'NONE',  ( 21.53943276465977519, 0.05219959533937863772, 101.2510903946856757 ) ) ;
#26548 = CARTESIAN_POINT ( 'NONE',  ( 9.474510206698971260, -16.51473224551069308, 47.91557627198102409 ) ) ;
#26549 = CARTESIAN_POINT ( 'NONE',  ( -10.81492255796105439, 18.62759615963255655, 52.91775706135235424 ) ) ;
#26550 = CARTESIAN_POINT ( 'NONE',  ( -10.72451020669870658, -18.67979575497194134, 99.58442372801900433 ) ) ;
#26551 = CARTESIAN_POINT ( 'NONE',  ( -0.05219959533934338120, 16.53943276465976808, 97.50109039468567573 ) ) ;
#26552 = EDGE_CURVE ( 'NONE', #26208, #112608, #131887, .T. ) ;
#26553 = CARTESIAN_POINT ( 'NONE',  ( 13.89961937509977652, -13.97604488694527269, 78.12390960531433848 ) ) ;
#26554 = CARTESIAN_POINT ( 'NONE',  ( 21.53943276465977519, 0.05219959533937863772, 41.25109039468568284 ) ) ;
#26555 = CARTESIAN_POINT ( 'NONE',  ( -10.81492255796105439, 18.62759615963255655, 52.91775706135235424 ) ) ;
#26557 = CARTESIAN_POINT ( 'NONE',  ( 19.05341960407611168, 5.049401038298154454, 93.95724293864769550 ) ) ;
#26556 = CARTESIAN_POINT ( 'NONE',  ( 5.049401038297881783, 19.05341960407617563, 82.29275706135229029 ) ) ;
#26558 = CARTESIAN_POINT ( 'NONE',  ( 19.02544592524343514, -5.153800228976328945, 23.54057627198102054 ) ) ;
#26559 = CARTESIAN_POINT ( 'NONE',  ( 5.823673210054125526, 21.52544592524343514, 99.79057627198103830 ) ) ;
#26560 = CARTESIAN_POINT ( 'NONE',  ( 19.03943276465977164, 0.05219959533936151252, 26.25109039468566507 ) ) ;
#26561 = CARTESIAN_POINT ( 'NONE',  ( 8.224510206698953496, -14.34966873604960469, 102.9155762719810383 ) ) ;
#26562 = CARTESIAN_POINT ( 'NONE',  ( 9.474510206698971260, -16.51473224551069308, 47.91557627198102409 ) ) ;
#26563 = CARTESIAN_POINT ( 'NONE',  ( -16.51473224551082808, 9.474510206698731452, 78.33442372801900433 ) ) ;
#26564 = CARTESIAN_POINT ( 'NONE',  ( -12.06949235617756955, 12.14591786802309770, 45.62390960531436690 ) ) ;
#26565 = CARTESIAN_POINT ( 'NONE',  ( -15.72974639402176322, -15.80617190586768395, 104.3760903946856899 ) ) ;
#26566 = CARTESIAN_POINT ( 'NONE',  ( 13.89961937509977652, -13.97604488694527269, 103.1239096053143527 ) ) ;
#26567 = CARTESIAN_POINT ( 'NONE',  ( -5.049401038297874678, -19.05341960407617918, 69.79275706135233293 ) ) ;
#26568 = CARTESIAN_POINT ( 'NONE',  ( -0.05219959533907301413, -21.53943276465977519, 72.49890960531435269 ) ) ;
#26569 = CARTESIAN_POINT ( 'NONE',  ( 10.81492255796106328, -18.62759615963255655, 30.41775706135234358 ) ) ;
#26570 = CARTESIAN_POINT ( 'NONE',  ( 14.34966873604972726, -8.224510206698740333, 35.83442372801901143 ) ) ;
#26571 = CARTESIAN_POINT ( 'NONE',  ( -16.55341960407617563, 4.379528057220093196, 98.54275706135234714 ) ) ;
#26573 = CARTESIAN_POINT ( 'NONE',  ( 5.719274019375673035, 21.55341960407619339, 37.29275706135235424 ) ) ;
#26572 = CARTESIAN_POINT ( 'NONE',  ( -13.97604488694527625, -13.89961937509977652, 26.87390960531434558 ) ) ;
#26574 = CARTESIAN_POINT ( 'NONE',  ( 21.53943276465977519, -0.05219959533907433946, 38.74890960531435979 ) ) ;
#26575 = CARTESIAN_POINT ( 'NONE',  ( 13.89961937509977652, -13.97604488694527269, 23.12390960531436335 ) ) ;
#26576 = CARTESIAN_POINT ( 'NONE',  ( 3.766062262543149401E-15, -39.95556452105413570, -9.249999994537628112 ) ) ;
#26577 = CARTESIAN_POINT ( 'NONE',  ( 14.34966873604972726, -8.224510206698740333, 60.83442372801901854 ) ) ;
#26578 = CARTESIAN_POINT ( 'NONE',  ( 4.483927247898545687, 16.52544592524342804, 94.79057627198105251 ) ) ;
#26579 = CARTESIAN_POINT ( 'NONE',  ( 10.81492255796078972, 18.62759615963270932, 84.58224293864769550 ) ) ;
#26580 = CARTESIAN_POINT ( 'NONE',  ( -0.05219959533934338120, 16.53943276465976808, 112.5010903946857042 ) ) ;
#26581 = CARTESIAN_POINT ( 'NONE',  ( -14.29746914071037622, -8.314922557961029526, 49.16775706135234003 ) ) ;
#26582 = CARTESIAN_POINT ( 'NONE',  ( -9.474510206698964154, 16.51473224551069663, 60.41557627198102409 ) ) ;
#26583 = CARTESIAN_POINT ( 'NONE',  ( -0.05219959533934338120, 16.53943276465976808, 87.50109039468568994 ) ) ;
#26584 = CARTESIAN_POINT ( 'NONE',  ( 19.02544592524334988, 5.153800228976608722, 91.45942372801900433 ) ) ;
#26585 = CARTESIAN_POINT ( 'NONE',  ( 5.719274019375991003, -21.55341960407610458, 82.70724293864770971 ) ) ;
#26586 = CARTESIAN_POINT ( 'NONE',  ( -8.314922557960811034, -14.29746914071050412, 22.08224293864769194 ) ) ;
#26587 = VERTEX_POINT ( 'NONE', #153758 ) ;
#26588 = CARTESIAN_POINT ( 'NONE',  ( -19.03943276465977164, 0.05219959533909376836, 116.2489096053143669 ) ) ;
#26589 = CARTESIAN_POINT ( 'NONE',  ( -21.53943276465977519, 0.05219959533907696930, 61.24890960531435979 ) ) ;
#26590 = CARTESIAN_POINT ( 'NONE',  ( 16.53943276465976808, 0.05219959533934440121, 91.25109039468568994 ) ) ;
#26591 = ORIENTED_EDGE ( 'NONE', *, *, #57096, .F. ) ;
#26592 = CARTESIAN_POINT ( 'NONE',  ( 18.67979575497178502, 10.72451020669898547, 29.16557627198103120 ) ) ;
#26593 = CARTESIAN_POINT ( 'NONE',  ( -28.28060372831499336, 2.428612866367529932E-14, 139.6875000013656063 ) ) ;
#26594 = CARTESIAN_POINT ( 'NONE',  ( 15.72974639402199770, -15.80617190586745480, 88.12390960531436690 ) ) ;
#26595 = CARTESIAN_POINT ( 'NONE',  ( -16.55341960407611168, -4.379528057220339221, 26.45724293864768839 ) ) ;
#26596 = CARTESIAN_POINT ( 'NONE',  ( 16.53943276465976808, 0.05219959533934440121, 41.25109039468568284 ) ) ;
#26597 = CARTESIAN_POINT ( 'NONE',  ( 19.02544592524343514, -5.153800228976328945, 38.54057627198103120 ) ) ;
#26598 = CARTESIAN_POINT ( 'NONE',  ( 4.483927247898790824, -16.52544592524335698, 30.20942372801902565 ) ) ;
#26599 = CARTESIAN_POINT ( 'NONE',  ( 16.46253265017160672, -9.564922557960803928, 48.33224293864769550 ) ) ;
#26600 = CARTESIAN_POINT ( 'NONE',  ( 1.784210473542230573E-15, -29.16686587814331588, 139.8750000027311842 ) ) ;
#26601 = CARTESIAN_POINT ( 'NONE',  ( 19.05341960407611168, 5.049401038298154454, 108.9572429386477097 ) ) ;
#26602 = CARTESIAN_POINT ( 'NONE',  ( 1.105192082801339515, 29.38149524799785084, -52.12050502002018959 ) ) ;
#26603 = CARTESIAN_POINT ( 'NONE',  ( -14.34966873604972548, 8.224510206698743886, 103.3344237280190043 ) ) ;
#26604 = CARTESIAN_POINT ( 'NONE',  ( 9.474510206698729675, 16.51473224551082808, 92.08442372801900433 ) ) ;
#26605 = CARTESIAN_POINT ( 'NONE',  ( -9.474510206698720793, -16.51473224551083518, 39.58442372801899722 ) ) ;
#26606 = CARTESIAN_POINT ( 'NONE',  ( -21.52544592524343514, 5.823673210054127303, 76.04057627198102409 ) ) ;
#26607 = CARTESIAN_POINT ( 'NONE',  ( -8.314922557961024197, 14.29746914071037800, 102.9177570613523756 ) ) ;
#26608 = CARTESIAN_POINT ( 'NONE',  ( 21.53943276465977519, -0.05219959533907433946, 38.74890960531435979 ) ) ;
#26609 = CARTESIAN_POINT ( 'NONE',  ( -13.97604488694547697, 13.89961937509957934, 113.1260903946856757 ) ) ;
#26610 = CARTESIAN_POINT ( 'NONE',  ( 13.89961937509977652, -13.97604488694527269, 108.1239096053143669 ) ) ;
#26611 = CARTESIAN_POINT ( 'NONE',  ( 5.719274019375673035, 21.55341960407619339, 57.29275706135234714 ) ) ;
#26612 = CARTESIAN_POINT ( 'NONE',  ( -9.474510206698964154, 16.51473224551069663, 60.41557627198102409 ) ) ;
#26613 = CARTESIAN_POINT ( 'NONE',  ( 4.483927247898545687, 16.52544592524342804, 94.79057627198105251 ) ) ;
#26614 = CARTESIAN_POINT ( 'NONE',  ( -17.44279575226824264, -5.990770900252441855, 84.16442432485685288 ) ) ;
#26615 = CARTESIAN_POINT ( 'NONE',  ( 8.224510206698953496, -14.34966873604960469, 72.91557627198103830 ) ) ;
#26616 = CARTESIAN_POINT ( 'NONE',  ( 0.05219959533907565091, 21.53943276465977519, 74.99890960531435269 ) ) ;
#26617 = VERTEX_POINT ( 'NONE', #188095 ) ;
#26618 = CARTESIAN_POINT ( 'NONE',  ( 9.474510206698729675, 16.51473224551082808, 97.08442372801900433 ) ) ;
#26619 = CARTESIAN_POINT ( 'NONE',  ( 10.20000000000000107, 0.000000000000000000, 0.000000000000000000 ) ) ;
#26620 = CARTESIAN_POINT ( 'NONE',  ( 0.05219959533909260263, 19.03943276465977164, 59.99890960531436690 ) ) ;
#26621 = CARTESIAN_POINT ( 'NONE',  ( 17.05116617787848554, -6.768360034955527738, 71.15675553259190167 ) ) ;
#26623 = CARTESIAN_POINT ( 'NONE',  ( 0.05219959533909260263, 19.03943276465977164, 89.99890960531436690 ) ) ;
#26622 = CARTESIAN_POINT ( 'NONE',  ( -19.03943276465977164, 0.05219959533909376836, 76.24890960531435269 ) ) ;
#26624 = CARTESIAN_POINT ( 'NONE',  ( -8.224510206698735004, -14.34966873604973081, 69.58442372801900433 ) ) ;
#26625 = CARTESIAN_POINT ( 'NONE',  ( -22.54345066063601166, 5.578190839439332471, 172.9373910537578638 ) ) ;
#26626 = CARTESIAN_POINT ( 'NONE',  ( -16.51473224551082808, 9.474510206698731452, 43.33442372801900433 ) ) ;
#26627 = CARTESIAN_POINT ( 'NONE',  ( 36.77885060843719600, 5.319724886534320518, 46.40826345025691069 ) ) ;
#26628 = CARTESIAN_POINT ( 'NONE',  ( -16.51473224551069308, -9.474510206698971260, 111.6655762719810383 ) ) ;
#26629 = CARTESIAN_POINT ( 'NONE',  ( 16.53943276465976808, 0.05219959533934440121, 106.2510903946856757 ) ) ;
#26630 = CARTESIAN_POINT ( 'NONE',  ( -34.64437015671237674, -3.766696895669992884, 51.50405731776596951 ) ) ;
#26631 = CARTESIAN_POINT ( 'NONE',  ( -16.55341960407617563, 4.379528057220093196, 93.54275706135234714 ) ) ;
#26632 = CARTESIAN_POINT ( 'NONE',  ( -16.36317988757059894, 7.306389748694930297, 29.09789608363226066 ) ) ;
#26633 = CARTESIAN_POINT ( 'NONE',  ( 16.53943276465976808, 0.05219959533934440121, 66.25109039468567573 ) ) ;
#26634 = LINE ( 'NONE', #198454, #82046 ) ;
#26635 = CARTESIAN_POINT ( 'NONE',  ( 10.81492255796106328, -18.62759615963255655, 65.41775706135234714 ) ) ;
#26636 = CARTESIAN_POINT ( 'NONE',  ( 9.474510206698729675, 16.51473224551082808, 72.08442372801900433 ) ) ;
#26637 = CARTESIAN_POINT ( 'NONE',  ( 9.564922557961047289, -16.46253265017146816, 30.41775706135232937 ) ) ;
#26638 = CARTESIAN_POINT ( 'NONE',  ( -13.97604488694527625, -13.89961937509977652, 66.87390960531436690 ) ) ;
#26639 = CARTESIAN_POINT ( 'NONE',  ( -16.51473224551069308, -9.474510206698971260, 41.66557627198103120 ) ) ;
#26640 = CARTESIAN_POINT ( 'NONE',  ( 16.17801625226016782, -7.381721853229580965, 22.13251340186824478 ) ) ;
#26641 = CARTESIAN_POINT ( 'NONE',  ( 0.05219959533907565091, 21.53943276465977519, 84.99890960531436690 ) ) ;
#26642 = CARTESIAN_POINT ( 'NONE',  ( 21.53943276465977519, -0.05219959533907433946, 38.74890960531435979 ) ) ;
#26643 = CARTESIAN_POINT ( 'NONE',  ( -13.97604488694527625, -13.89961937509977652, 36.87390960531436690 ) ) ;
#26644 = CARTESIAN_POINT ( 'NONE',  ( 8.314922557961029526, -14.29746914071037800, 50.41775706135235424 ) ) ;
#26646 = ORIENTED_EDGE ( 'NONE', *, *, #153757, .T. ) ;
#26645 = B_SPLINE_CURVE_WITH_KNOTS ( 'NONE', 3,
 ( #37488, #20317, #158829, #173028, #68822, #126504, #67825, #81965, #96165, #19345, #80993, #130481, #4147, #65826, #189200, #82984, #53659, #129480, #192178, #159831, #23329, #127495 ),
 .UNSPECIFIED., .F., .F.,
 ( 4, 2, 2, 2, 2, 2, 2, 2, 2, 2, 4 ),
 ( 2.024876365526581719E-17, 0.001309639967555213495, 0.001964459951332811569, 0.002291869943221612558, 0.002455574939166013486, 0.002619279935110414414, 0.002782984931054815342, 0.002946689926999216270, 0.003274099918888017692, 0.003928919902665620537, 0.005238559870220827960 ),
 .UNSPECIFIED. ) ;
#26647 = CARTESIAN_POINT ( 'NONE',  ( 18.62759615963255655, 10.81492255796105972, 36.66775706135234714 ) ) ;
#26649 = CARTESIAN_POINT ( 'NONE',  ( 3.766062262543149401E-15, -39.95556452105413570, -5.500000000000000000 ) ) ;
#26648 = CARTESIAN_POINT ( 'NONE',  ( 16.53943276465976808, -0.05219959533910856209, 58.74890960531436690 ) ) ;
#26650 = CARTESIAN_POINT ( 'NONE',  ( 12.14591786802327356, -12.06949235617739191, 30.62609039468567929 ) ) ;
#26651 = CARTESIAN_POINT ( 'NONE',  ( 16.51473224551083163, -9.474510206698727899, 45.83442372801900433 ) ) ;
#26652 = CARTESIAN_POINT ( 'NONE',  ( 16.55341960407611168, 4.379528057220329451, 63.95724293864770260 ) ) ;
#26654 = EDGE_CURVE ( 'NONE', #89236, #140310, #145923, .T. ) ;
#26653 = CARTESIAN_POINT ( 'NONE',  ( -21.55341960407610458, -5.719274019375992779, 111.4572429386476813 ) ) ;
#26656 = CARTESIAN_POINT ( 'NONE',  ( -10.72451020669898014, 18.67979575497178502, 80.41557627198103830 ) ) ;
#26655 = CARTESIAN_POINT ( 'NONE',  ( 0.2056090276421982943, 16.68933881255749085, -59.13845611041300288 ) ) ;
#26657 = CARTESIAN_POINT ( 'NONE',  ( 5.153800228976335163, 19.02544592524342804, 84.79057627198099567 ) ) ;
#26658 = CARTESIAN_POINT ( 'NONE',  ( 4.483927247898545687, 16.52544592524342804, 54.79057627198104541 ) ) ;
#26659 = CARTESIAN_POINT ( 'NONE',  ( -19.02544592524342804, 5.153800228976336051, 101.0405762719810241 ) ) ;
#26660 = CARTESIAN_POINT ( 'NONE',  ( -3.181980515339104532, 35.00000000000003553, 8.889087296526001936 ) ) ;
#26661 = CARTESIAN_POINT ( 'NONE',  ( 16.46253265017146816, 9.564922557961045513, 61.66775706135234003 ) ) ;
#26662 = CARTESIAN_POINT ( 'NONE',  ( 15.80617190586746368, 15.72974639402197994, 104.3739096053143669 ) ) ;
#26663 = CARTESIAN_POINT ( 'NONE',  ( -19.02544592524342804, 5.153800228976336051, 51.04057627198103120 ) ) ;
#26664 = CARTESIAN_POINT ( 'NONE',  ( -9.564922557961040184, 16.46253265017147172, 47.91775706135233293 ) ) ;
#26665 = CARTESIAN_POINT ( 'NONE',  ( -16.55341960407611168, -4.379528057220339221, 111.4572429386476813 ) ) ;
#26666 = CARTESIAN_POINT ( 'NONE',  ( -18.62759615963255300, -10.81492255796106328, 59.16775706135234714 ) ) ;
#26667 = LINE ( 'NONE', #86320, #52948 ) ;
#26668 = ADVANCED_FACE ( 'NONE', ( #32411 ), #94248, .T. ) ;
#26669 = CARTESIAN_POINT ( 'NONE',  ( -0.05219959533910754901, -16.53943276465976808, 47.49890960531435979 ) ) ;
#26670 = CARTESIAN_POINT ( 'NONE',  ( 13.89961937509977652, -13.97604488694527269, 53.12390960531434558 ) ) ;
#26671 = CARTESIAN_POINT ( 'NONE',  ( 13.89961937509977652, -13.97604488694527269, 113.1239096053143527 ) ) ;
#26672 = CARTESIAN_POINT ( 'NONE',  ( 21.53943276465977519, -0.05219959533907433946, 78.74890960531436690 ) ) ;
#26673 = CARTESIAN_POINT ( 'NONE',  ( 8.571926809382603096, -26.38167802310801235, 147.4750000027311785 ) ) ;
#26674 = CARTESIAN_POINT ( 'NONE',  ( 19.05341960407611168, 5.049401038298154454, 38.95724293864767418 ) ) ;
#26675 = EDGE_LOOP ( 'NONE', ( #852, #62453, #94412, #14434 ) ) ;
#26676 = CARTESIAN_POINT ( 'NONE',  ( -15.80617190586745835, -15.72974639402198527, 71.87390960531438111 ) ) ;
#26677 = CARTESIAN_POINT ( 'NONE',  ( -21.55341960407619339, 5.719274019375674811, 83.54275706135234714 ) ) ;
#26680 = CARTESIAN_POINT ( 'NONE',  ( -8.314922557960811034, -14.29746914071050412, 82.08224293864768129 ) ) ;
#26679 = CARTESIAN_POINT ( 'NONE',  ( 4.483927247898790824, -16.52544592524335698, 95.20942372801903275 ) ) ;
#26678 = CARTESIAN_POINT ( 'NONE',  ( 8.377002814025898303, -36.45346134345118827, -31.71922177526206710 ) ) ;
#26681 = CARTESIAN_POINT ( 'NONE',  ( -13.97604488694527625, -13.89961937509977652, 76.87390960531433848 ) ) ;
#26682 = ORIENTED_EDGE ( 'NONE', *, *, #129852, .F. ) ;
#26683 = CARTESIAN_POINT ( 'NONE',  ( -19.02544592524334988, -5.153800228976617603, 38.95942372801900433 ) ) ;
#26684 = CARTESIAN_POINT ( 'NONE',  ( 16.53943276465976808, 0.05219959533934440121, 86.25109039468568994 ) ) ;
#26685 = CARTESIAN_POINT ( 'NONE',  ( 16.51473224551083163, -9.474510206698727899, 20.83442372801899722 ) ) ;
#26686 = CARTESIAN_POINT ( 'NONE',  ( -9.564922557960796823, -16.46253265017161027, 87.08224293864769550 ) ) ;
#26687 = CARTESIAN_POINT ( 'NONE',  ( 10.72451020669898902, -18.67979575497178502, 47.91557627198102409 ) ) ;
#26688 = DIRECTION ( 'NONE',  ( 1.000000000000000000, 0.000000000000000000, 0.000000000000000000 ) ) ;
#26689 = CARTESIAN_POINT ( 'NONE',  ( 18.67979575497194134, -10.72451020669871369, 90.83442372801901854 ) ) ;
#26690 = CARTESIAN_POINT ( 'NONE',  ( -8.224510206698735004, -14.34966873604973081, 59.58442372801901854 ) ) ;
#26691 = CARTESIAN_POINT ( 'NONE',  ( 15.72974639402199770, -15.80617190586745480, 113.1239096053143953 ) ) ;
#26692 = CARTESIAN_POINT ( 'NONE',  ( 14.34966873604972726, -8.224510206698740333, 25.83442372801901499 ) ) ;
#26693 = CARTESIAN_POINT ( 'NONE',  ( -13.89961937509977652, 13.97604488694528158, 90.62390960531432427 ) ) ;
#26694 = CARTESIAN_POINT ( 'NONE',  ( -5.049401038298153566, 19.05341960407611168, 35.20724293864768839 ) ) ;
#26695 = CARTESIAN_POINT ( 'NONE',  ( 19.03943276465977164, -0.05219959533909143690, 48.74890960531435979 ) ) ;
#26696 = CARTESIAN_POINT ( 'NONE',  ( -16.53943276465976808, -0.05219959533934237506, 38.75109039468567573 ) ) ;
#26697 = CARTESIAN_POINT ( 'NONE',  ( 8.224510206698953496, -14.34966873604960469, 77.91557627198102409 ) ) ;
#26698 = CARTESIAN_POINT ( 'NONE',  ( 12.06949235617739724, 12.14591786802326823, 106.8760903946856899 ) ) ;
#26701 = CARTESIAN_POINT ( 'NONE',  ( -16.46253265017160317, 9.564922557960807481, 50.83224293864770260 ) ) ;
#26700 = CARTESIAN_POINT ( 'NONE',  ( 19.02544592524343514, -5.153800228976328945, 63.54057627198103830 ) ) ;
#26699 = CARTESIAN_POINT ( 'NONE',  ( 18.62759615963255655, 10.81492255796105972, 46.66775706135234714 ) ) ;
#26702 = CARTESIAN_POINT ( 'NONE',  ( -5.153800228976328057, -19.02544592524343514, 77.29057627198099567 ) ) ;
#26703 = CARTESIAN_POINT ( 'NONE',  ( 4.379528057220339221, -16.55341960407611168, 32.70724293864770260 ) ) ;
#26704 = CARTESIAN_POINT ( 'NONE',  ( -4.483927247898782831, 16.52544592524335698, 87.70942372801901854 ) ) ;
#26705 = EDGE_CURVE ( 'NONE', #105638, #107603, #61915, .T. ) ;
#26706 = ORIENTED_EDGE ( 'NONE', *, *, #63306, .F. ) ;
#26707 = CARTESIAN_POINT ( 'NONE',  ( -9.474510206698720793, -16.51473224551083518, 34.58442372801899722 ) ) ;
#26708 = DIRECTION ( 'NONE',  ( 0.9974398506828147104, -0.07151044867601312471, 6.797078445321206297E-16 ) ) ;
#26709 = CARTESIAN_POINT ( 'NONE',  ( 5.153800228976335163, 19.02544592524342804, 44.79057627198103830 ) ) ;
#26710 = CARTESIAN_POINT ( 'NONE',  ( 19.02544592524334988, 5.153800228976608722, 21.45942372801899012 ) ) ;
#26711 = CARTESIAN_POINT ( 'NONE',  ( 36.91746824999999177, 2.880721459617395097E-14, -5.624999997268813168 ) ) ;
#26712 = CARTESIAN_POINT ( 'NONE',  ( -4.483927247898782831, 16.52544592524335698, 42.70942372801901854 ) ) ;
#26714 = CARTESIAN_POINT ( 'NONE',  ( 12.14591786802327356, -12.06949235617739191, 60.62609039468567573 ) ) ;
#26713 = CARTESIAN_POINT ( 'NONE',  ( -5.153800228976607833, 19.02544592524334988, 67.70942372801900433 ) ) ;
#26715 = CARTESIAN_POINT ( 'NONE',  ( 6.767090645865133425, -4.798697441033914934, -64.13056706087778025 ) ) ;
#26716 = CARTESIAN_POINT ( 'NONE',  ( 19.03943276465977164, -0.05219959533909143690, 83.74890960531436690 ) ) ;
#26717 = CARTESIAN_POINT ( 'NONE',  ( 18.62759615963271287, -10.81492255796078972, 113.3322429386476955 ) ) ;
#26718 = CARTESIAN_POINT ( 'NONE',  ( -13.89961937509957401, -13.97604488694547875, 64.37609039468567573 ) ) ;
#26720 = CARTESIAN_POINT ( 'NONE',  ( -0.05219959533909027116, -19.03943276465977164, 37.49890960531436690 ) ) ;
#26719 = CARTESIAN_POINT ( 'NONE',  ( -9.564922557960796823, -16.46253265017161027, 102.0822429386477097 ) ) ;
#26721 = CARTESIAN_POINT ( 'NONE',  ( -13.89961937509977652, 13.97604488694528158, 80.62390960531436690 ) ) ;
#26723 = CARTESIAN_POINT ( 'NONE',  ( -19.03943276465977164, 0.05219959533909376836, 41.24890960531435269 ) ) ;
#26722 = CARTESIAN_POINT ( 'NONE',  ( 4.379528057220339221, -16.55341960407611168, 32.70724293864770260 ) ) ;
#26724 = CARTESIAN_POINT ( 'NONE',  ( -19.03943276465977164, -0.05219959533935918106, 33.75109039468566863 ) ) ;
#26725 = CARTESIAN_POINT ( 'NONE',  ( 4.483927247898545687, 16.52544592524342804, 79.79057627198102409 ) ) ;
#26726 = CARTESIAN_POINT ( 'NONE',  ( 21.53943276465977519, 0.05219959533937863772, 111.2510903946856899 ) ) ;
#26727 = CARTESIAN_POINT ( 'NONE',  ( 16.46253265017160672, -9.564922557960803928, 58.33224293864769550 ) ) ;
#26729 = CARTESIAN_POINT ( 'NONE',  ( 18.67979575497194134, -10.72451020669871369, 105.8344237280190328 ) ) ;
#26728 = CARTESIAN_POINT ( 'NONE',  ( -14.34966873604960291, -8.224510206698953496, 56.66557627198103830 ) ) ;
#26730 = CARTESIAN_POINT ( 'NONE',  ( 0.05219959533909260263, 19.03943276465977164, 94.99890960531436690 ) ) ;
#26731 = CARTESIAN_POINT ( 'NONE',  ( 13.89961937509977652, -13.97604488694527269, 108.1239096053143669 ) ) ;
#26732 = CARTESIAN_POINT ( 'NONE',  ( -9.474510206698964154, 16.51473224551069663, 40.41557627198103120 ) ) ;
#26733 = CARTESIAN_POINT ( 'NONE',  ( 19.02544592524343514, -5.153800228976328945, 23.54057627198102054 ) ) ;
#26734 = CARTESIAN_POINT ( 'NONE',  ( -16.55341960407611168, -4.379528057220339221, 86.45724293864770971 ) ) ;
#26735 = CARTESIAN_POINT ( 'NONE',  ( -21.53943276465977519, 0.05219959533907696930, 96.24890960531435269 ) ) ;
#26736 = CARTESIAN_POINT ( 'NONE',  ( -16.51473224551069308, -9.474510206698971260, 81.66557627198103830 ) ) ;
#26737 = CARTESIAN_POINT ( 'NONE',  ( 21.55341960407610458, 5.719274019375980345, 103.9572429386476813 ) ) ;
#26738 = CARTESIAN_POINT ( 'NONE',  ( 9.564922557960805705, 16.46253265017160317, 89.58224293864769550 ) ) ;
#26740 = CARTESIAN_POINT ( 'NONE',  ( -0.05219959533910754901, -16.53943276465976808, 102.4989096053143811 ) ) ;
#26739 = CARTESIAN_POINT ( 'NONE',  ( -3.573655867282028392E-15, 2.428612866367529932E-14, 0.000000000000000000 ) ) ;
#26741 = CARTESIAN_POINT ( 'NONE',  ( 13.89961937509977652, -13.97604488694527269, 73.12390960531436690 ) ) ;
#26742 = CARTESIAN_POINT ( 'NONE',  ( -10.72451020669898014, 18.67979575497178502, 85.41557627198102409 ) ) ;
#26743 = CARTESIAN_POINT ( 'NONE',  ( -31.69373074887817765, 1.710217150889093984, 102.3065243757511098 ) ) ;
#26744 = FACE_OUTER_BOUND ( 'NONE', #180367, .T. ) ;
#26746 = CARTESIAN_POINT ( 'NONE',  ( -30.00000000000000355, -3.181980515339470905, 8.889087296526001936 ) ) ;
#26745 = CARTESIAN_POINT ( 'NONE',  ( -21.53943276465977519, 0.05219959533907696930, 31.24890960531435979 ) ) ;
#26747 = CARTESIAN_POINT ( 'NONE',  ( -8.224510206698735004, -14.34966873604973081, 29.58442372801901854 ) ) ;
#26748 = CARTESIAN_POINT ( 'NONE',  ( -16.53943276465976808, 0.05219959533911058130, 91.24890960531436690 ) ) ;
#26749 = CARTESIAN_POINT ( 'NONE',  ( -17.31728774477273447, -6.344390552232393787, 94.18093348310682700 ) ) ;
#26750 = CARTESIAN_POINT ( 'NONE',  ( -19.05341960407611168, -5.049401038298163336, 91.45724293864766707 ) ) ;
#26751 = CARTESIAN_POINT ( 'NONE',  ( -5.049401038298153566, 19.05341960407611168, 40.20724293864768839 ) ) ;
#26752 = CARTESIAN_POINT ( 'NONE',  ( 8.314922557960818139, 14.29746914071049879, 79.58224293864769550 ) ) ;
#26753 = CARTESIAN_POINT ( 'NONE',  ( 5.719274019375991003, -21.55341960407610458, 37.70724293864769550 ) ) ;
#26754 = CARTESIAN_POINT ( 'NONE',  ( 12.06949235617757843, -12.14591786802309237, 48.12390960531436690 ) ) ;
#26755 = CARTESIAN_POINT ( 'NONE',  ( -19.02544592524334988, -5.153800228976617603, 103.9594237280190043 ) ) ;
#26756 = CARTESIAN_POINT ( 'NONE',  ( -18.62759615963255300, -10.81492255796106328, 64.16775706135234714 ) ) ;
#26757 = CARTESIAN_POINT ( 'NONE',  ( -5.359611314223446995E-15, 29.16686587814335851, 146.3750000027311842 ) ) ;
#26758 = CARTESIAN_POINT ( 'NONE',  ( 19.05341960407611168, 5.049401038298154454, 98.95724293864766707 ) ) ;
#26759 = CARTESIAN_POINT ( 'NONE',  ( 14.34966873604972726, -8.224510206698740333, 85.83442372801901854 ) ) ;
#26760 = CARTESIAN_POINT ( 'NONE',  ( 13.97604488694527802, 13.89961937509977652, 29.37390960531435979 ) ) ;
#26761 = CARTESIAN_POINT ( 'NONE',  ( 19.03943276465977164, -0.05219959533909143690, 73.74890960531435269 ) ) ;
#26762 = CARTESIAN_POINT ( 'NONE',  ( 5.823673210054125526, 21.52544592524343514, 74.79057627198105251 ) ) ;
#26763 = CARTESIAN_POINT ( 'NONE',  ( -19.03943276465977164, -0.05219959533935918106, 113.7510903946856757 ) ) ;
#26765 = CARTESIAN_POINT ( 'NONE',  ( -21.55341960407619339, 5.719274019375674811, 63.54275706135234003 ) ) ;
#26764 = CARTESIAN_POINT ( 'NONE',  ( 12.06949235617757843, -12.14591786802309237, 58.12390960531435979 ) ) ;
#26767 = CARTESIAN_POINT ( 'NONE',  ( 5.719274019375991003, -21.55341960407610458, 22.70724293864769194 ) ) ;
#26766 = CARTESIAN_POINT ( 'NONE',  ( 16.53943276465976808, 0.05219959533934440121, 81.25109039468568994 ) ) ;
#26768 = CARTESIAN_POINT ( 'NONE',  ( 26.58496454516999563, 7.626754437231445749, 167.9682100371138915 ) ) ;
#26769 = PLANE ( 'NONE',  #119641 ) ;
#26770 = CARTESIAN_POINT ( 'NONE',  ( -16.55341960407617563, 4.379528057220093196, 113.5427570613523756 ) ) ;
#26771 = CARTESIAN_POINT ( 'NONE',  ( 8.224510206698742110, 14.34966873604972548, 62.08442372801901143 ) ) ;
#26772 = CARTESIAN_POINT ( 'NONE',  ( -9.564922557960796823, -16.46253265017161027, 77.08224293864769550 ) ) ;
#26773 = CARTESIAN_POINT ( 'NONE',  ( 16.51473224551069308, 9.474510206698969483, 89.16557627198103830 ) ) ;
#26774 = CARTESIAN_POINT ( 'NONE',  ( -18.62759615963255300, -10.81492255796106328, 69.16775706135234714 ) ) ;
#26775 = CARTESIAN_POINT ( 'NONE',  ( 16.55341960407618274, -4.379528057220086978, 81.04275706135236135 ) ) ;
#26776 = CARTESIAN_POINT ( 'NONE',  ( -8.224510206698948167, 14.34966873604960824, 50.41557627198103120 ) ) ;
#26777 = CARTESIAN_POINT ( 'NONE',  ( -19.02544592524342804, 5.153800228976336051, 51.04057627198103120 ) ) ;
#26778 = CARTESIAN_POINT ( 'NONE',  ( -13.97604488694527625, -13.89961937509977652, 51.87390960531436690 ) ) ;
#26780 = ORIENTED_EDGE ( 'NONE', *, *, #128791, .F. ) ;
#26779 = CARTESIAN_POINT ( 'NONE',  ( -16.55341960407617563, 4.379528057220093196, 38.54275706135234714 ) ) ;
#26781 = CARTESIAN_POINT ( 'NONE',  ( 19.03943276465977164, 0.05219959533936151252, 101.2510903946856757 ) ) ;
#26782 = CARTESIAN_POINT ( 'NONE',  ( -4.483927247898539470, -16.52544592524342804, 102.2905762719810383 ) ) ;
#26783 = CARTESIAN_POINT ( 'NONE',  ( -16.46253265017160317, 9.564922557960807481, 65.83224293864769550 ) ) ;
#26785 = CARTESIAN_POINT ( 'NONE',  ( -11.74264578624800670, 36.14014761921585972, -2.400000000000000355 ) ) ;
#26784 = CARTESIAN_POINT ( 'NONE',  ( -16.51473224551082808, 9.474510206698731452, 98.33442372801900433 ) ) ;
#26786 = CARTESIAN_POINT ( 'NONE',  ( -15.80617190586768217, 15.72974639402176855, 103.1260903946856757 ) ) ;
#26787 = CARTESIAN_POINT ( 'NONE',  ( 14.29746914071037800, 8.314922557961029526, 71.66775706135234714 ) ) ;
#26788 = FACE_OUTER_BOUND ( 'NONE', #168802, .T. ) ;
#26789 = CARTESIAN_POINT ( 'NONE',  ( 15.72974639402199770, -15.80617190586745480, 63.12390960531435979 ) ) ;
#26790 = CARTESIAN_POINT ( 'NONE',  ( 16.52544592524335698, 4.483927247898782831, 51.45942372801901854 ) ) ;
#26791 = CARTESIAN_POINT ( 'NONE',  ( 3.889087296526381632, 34.99999999999996447, 1.818019484660534424 ) ) ;
#26792 = CARTESIAN_POINT ( 'NONE',  ( -5.153800228976607833, 19.02544592524334988, 57.70942372801899012 ) ) ;
#26793 = CARTESIAN_POINT ( 'NONE',  ( -13.97604488694527625, -13.89961937509977652, 96.87390960531433848 ) ) ;
#26794 = CARTESIAN_POINT ( 'NONE',  ( 5.049401038298161559, -19.05341960407611168, 27.70724293864769550 ) ) ;
#26795 = CARTESIAN_POINT ( 'NONE',  ( 13.97604488694527802, 13.89961937509977652, 59.37390960531434558 ) ) ;
#26796 = CARTESIAN_POINT ( 'NONE',  ( 4.379528057220339221, -16.55341960407611168, 52.70724293864769550 ) ) ;
#26797 = EDGE_CURVE ( 'NONE', #94779, #9238, #76911, .T. ) ;
#26798 = CARTESIAN_POINT ( 'NONE',  ( -18.62759615963255300, -10.81492255796106328, 79.16775706135234714 ) ) ;
#26799 = CARTESIAN_POINT ( 'NONE',  ( 16.46253265017146816, 9.564922557961045513, 41.66775706135234003 ) ) ;
#26800 = CARTESIAN_POINT ( 'NONE',  ( 16.46253265017146816, 9.564922557961045513, 31.66775706135232937 ) ) ;
#26801 = CARTESIAN_POINT ( 'NONE',  ( -5.153800228976328057, -19.02544592524343514, 52.29057627198100988 ) ) ;
#26802 = CARTESIAN_POINT ( 'NONE',  ( -16.46253265017160317, 9.564922557960807481, 115.8322429386477097 ) ) ;
#26803 = CARTESIAN_POINT ( 'NONE',  ( -10.81492255796105439, 18.62759615963255655, 92.91775706135236135 ) ) ;
#26804 = CARTESIAN_POINT ( 'NONE',  ( 19.03943276465977164, -0.05219959533909143690, 68.74890960531436690 ) ) ;
#26805 = AXIS2_PLACEMENT_3D ( 'NONE', #91589, #92593, #153279 ) ;
#26806 = CARTESIAN_POINT ( 'NONE',  ( -5.719274019375665041, -21.55341960407619695, 89.79275706135236135 ) ) ;
#26807 = CARTESIAN_POINT ( 'NONE',  ( 15.72974639402199770, -15.80617190586745480, 43.12390960531435269 ) ) ;
#26808 = CARTESIAN_POINT ( 'NONE',  ( 19.05341960407611168, 5.049401038298154454, 78.95724293864769550 ) ) ;
#26809 = CARTESIAN_POINT ( 'NONE',  ( 19.03943276465977164, 0.05219959533936151252, 56.25109039468566863 ) ) ;
#26810 = CARTESIAN_POINT ( 'NONE',  ( -9.474510206698964154, 16.51473224551069663, 40.41557627198103120 ) ) ;
#26811 = CARTESIAN_POINT ( 'NONE',  ( -9.564922557960796823, -16.46253265017161027, 92.08224293864769550 ) ) ;
#26812 = CARTESIAN_POINT ( 'NONE',  ( 4.483927247898790824, -16.52544592524335698, 35.20942372801901854 ) ) ;
#26813 = CARTESIAN_POINT ( 'NONE',  ( -14.29746914071049879, 8.314922557960819915, 100.8322429386477097 ) ) ;
#26814 = CARTESIAN_POINT ( 'NONE',  ( -13.97604488694527625, -13.89961937509977652, 76.87390960531433848 ) ) ;
#26815 = CARTESIAN_POINT ( 'NONE',  ( 10.81492255796078972, 18.62759615963270932, 49.58224293864769550 ) ) ;
#26816 = CARTESIAN_POINT ( 'NONE',  ( 0.05219959533936267826, -19.03943276465977164, 110.0010903946856757 ) ) ;
#26817 = CARTESIAN_POINT ( 'NONE',  ( 18.62759615963271287, -10.81492255796078972, 113.3322429386476955 ) ) ;
#26818 = CARTESIAN_POINT ( 'NONE',  ( -5.719274019375665041, -21.55341960407619695, 64.79275706135234714 ) ) ;
#26819 = CARTESIAN_POINT ( 'NONE',  ( 4.483927247898790824, -16.52544592524335698, 65.20942372801901854 ) ) ;
#26820 = CARTESIAN_POINT ( 'NONE',  ( 9.474510206698971260, -16.51473224551069308, 77.91557627198103830 ) ) ;
#26821 = CARTESIAN_POINT ( 'NONE',  ( -16.55341960407617563, 4.379528057220093196, 103.5427570613523613 ) ) ;
#26822 = CARTESIAN_POINT ( 'NONE',  ( -19.05341960407617563, 5.049401038297882671, 38.54275706135233293 ) ) ;
#26823 = CARTESIAN_POINT ( 'NONE',  ( 0.05219959533937995610, -21.53943276465977519, 35.00109039468568284 ) ) ;
#26824 = CARTESIAN_POINT ( 'NONE',  ( 0.05219959533910956823, 16.53943276465976808, 64.99890960531435269 ) ) ;
#26825 = CARTESIAN_POINT ( 'NONE',  ( 9.474510206698971260, -16.51473224551069308, 102.9155762719810241 ) ) ;
#26826 = CARTESIAN_POINT ( 'NONE',  ( 14.34966873604972726, -8.224510206698740333, 95.83442372801903275 ) ) ;
#26827 = CARTESIAN_POINT ( 'NONE',  ( -18.62759615963255300, -10.81492255796106328, 74.16775706135231871 ) ) ;
#26828 = CARTESIAN_POINT ( 'NONE',  ( 8.224510206698742110, 14.34966873604972548, 27.08442372801901854 ) ) ;
#26829 = CARTESIAN_POINT ( 'NONE',  ( -10.81492255796105439, 18.62759615963255655, 32.91775706135234714 ) ) ;
#26830 = CARTESIAN_POINT ( 'NONE',  ( 12.14591786802309770, 12.06949235617756955, 69.37390960531436690 ) ) ;
#26831 = EDGE_CURVE ( 'NONE', #69916, #33580, #79901, .T. ) ;
#26832 = ORIENTED_EDGE ( 'NONE', *, *, #147658, .F. ) ;
#26833 = CARTESIAN_POINT ( 'NONE',  ( -15.72974639402197994, 15.80617190586746368, 100.6239096053143811 ) ) ;
#26834 = CARTESIAN_POINT ( 'NONE',  ( 8.224510206698953496, -14.34966873604960469, 47.91557627198102409 ) ) ;
#26835 = EDGE_LOOP ( 'NONE', ( #16484, #11512, #112832, #116767 ) ) ;
#26836 = CARTESIAN_POINT ( 'NONE',  ( -0.05219959533909027116, -19.03943276465977164, 27.49890960531435624 ) ) ;
#26837 = CARTESIAN_POINT ( 'NONE',  ( 21.52544592524344225, -5.823673210054117533, 33.54057627198102409 ) ) ;
#26838 = CARTESIAN_POINT ( 'NONE',  ( -5.823673210054431948, 21.52544592524334988, 42.70942372801901854 ) ) ;
#26839 = CARTESIAN_POINT ( 'NONE',  ( 16.53943276465976808, -0.05219959533910856209, 68.74890960531435269 ) ) ;
#26840 = EDGE_CURVE ( 'NONE', #191474, #188707, #78894, .T. ) ;
#26841 = CARTESIAN_POINT ( 'NONE',  ( -5.823673210054116645, -21.52544592524344225, 72.29057627198102409 ) ) ;
#26842 = CARTESIAN_POINT ( 'NONE',  ( -16.46253265017160317, 9.564922557960807481, 75.83224293864769550 ) ) ;
#26844 = CARTESIAN_POINT ( 'NONE',  ( 0.05219959533936267826, -19.03943276465977164, 80.00109039468567573 ) ) ;
#26843 = CARTESIAN_POINT ( 'NONE',  ( -19.03943276465977164, 0.05219959533909376836, 26.24890960531435624 ) ) ;
#26845 = CARTESIAN_POINT ( 'NONE',  ( -18.67979575497178146, -10.72451020669898902, 51.66557627198102409 ) ) ;
#26846 = CARTESIAN_POINT ( 'NONE',  ( 9.474510206698971260, -16.51473224551069308, 42.91557627198103120 ) ) ;
#26847 = CARTESIAN_POINT ( 'NONE',  ( -16.46253265017160317, 9.564922557960807481, 75.83224293864769550 ) ) ;
#26848 = ORIENTED_EDGE ( 'NONE', *, *, #33627, .F. ) ;
#26849 = CARTESIAN_POINT ( 'NONE',  ( -16.55341960407617563, 4.379528057220093196, 38.54275706135234714 ) ) ;
#26850 = CARTESIAN_POINT ( 'NONE',  ( 21.53943276465977519, -0.05219959533907433946, 113.7489096053143527 ) ) ;
#26851 = CARTESIAN_POINT ( 'NONE',  ( 16.52544592524342804, -4.483927247898539470, 43.54057627198103830 ) ) ;
#26852 = CARTESIAN_POINT ( 'NONE',  ( 21.55341960407619695, -5.719274019375665929, 61.04275706135234714 ) ) ;
#26853 = CARTESIAN_POINT ( 'NONE',  ( -5.049401038298153566, 19.05341960407611168, 105.2072429386476671 ) ) ;
#26854 = CARTESIAN_POINT ( 'NONE',  ( 5.823673210054125526, 21.52544592524343514, 69.79057627198102409 ) ) ;
#26856 = CARTESIAN_POINT ( 'NONE',  ( -14.29746914071037622, -8.314922557961029526, 49.16775706135234003 ) ) ;
#26855 = CARTESIAN_POINT ( 'NONE',  ( 21.52544592524344225, -5.823673210054117533, 108.5405762719810241 ) ) ;
#26857 = CARTESIAN_POINT ( 'NONE',  ( 10.72451020669898902, -18.67979575497178502, 47.91557627198102409 ) ) ;
#26858 = CARTESIAN_POINT ( 'NONE',  ( -5.719274019375665041, -21.55341960407619695, 104.7927570613523898 ) ) ;
#26859 = CARTESIAN_POINT ( 'NONE',  ( -19.03943276465977164, 0.05219959533909376836, 51.24890960531436690 ) ) ;
#26860 = CARTESIAN_POINT ( 'NONE',  ( 5.153800228976335163, 19.02544592524342804, 114.7905762719810241 ) ) ;
#26861 = CARTESIAN_POINT ( 'NONE',  ( -13.89961937509977652, 13.97604488694528158, 70.62390960531432427 ) ) ;
#26862 = DIRECTION ( 'NONE',  ( -0.000000000000000000, -0.000000000000000000, 1.000000000000000000 ) ) ;
#26863 = CARTESIAN_POINT ( 'NONE',  ( -19.03943276465977164, -0.05219959533935918106, 63.75109039468566863 ) ) ;
#26865 = CARTESIAN_POINT ( 'NONE',  ( -21.55341960407610458, -5.719274019375992779, 26.45724293864768839 ) ) ;
#26864 = CARTESIAN_POINT ( 'NONE',  ( -15.80617190586768217, 15.72974639402176855, 113.1260903946856899 ) ) ;
#26866 = CARTESIAN_POINT ( 'NONE',  ( -16.55341960407617563, 4.379528057220093196, 108.5427570613523756 ) ) ;
#26867 = CARTESIAN_POINT ( 'NONE',  ( 5.153800228976615827, -19.02544592524334988, 90.20942372801900433 ) ) ;
#26868 = CARTESIAN_POINT ( 'NONE',  ( -17.48847506799968698, 5.747544572773787053, 60.82697437843280142 ) ) ;
#26869 = CARTESIAN_POINT ( 'NONE',  ( -21.55341960407619339, 5.719274019375674811, 113.5427570613523756 ) ) ;
#26870 = CARTESIAN_POINT ( 'NONE',  ( -19.05341960407617563, 5.049401038297882671, 83.54275706135233293 ) ) ;
#26871 = CARTESIAN_POINT ( 'NONE',  ( -19.03943276465977164, -0.05219959533935918106, 48.75109039468566863 ) ) ;
#26872 = CARTESIAN_POINT ( 'NONE',  ( 17.48853670773245028, 5.747243402303108262, 108.8332870025001142 ) ) ;
#26873 = CARTESIAN_POINT ( 'NONE',  ( -19.05341960407611168, -5.049401038298163336, 41.45724293864769550 ) ) ;
#26874 = CARTESIAN_POINT ( 'NONE',  ( 16.55341960407611168, 4.379528057220329451, 48.95724293864770971 ) ) ;
#26875 = CARTESIAN_POINT ( 'NONE',  ( -9.474510206698964154, 16.51473224551069663, 30.41557627198102054 ) ) ;
#26876 = CARTESIAN_POINT ( 'NONE',  ( 8.224510206698953496, -14.34966873604960469, 42.91557627198103120 ) ) ;
#26877 = CARTESIAN_POINT ( 'NONE',  ( -4.500000000000000000, 5.510910596163088569E-16, -20.00000000000000000 ) ) ;
#26878 = CARTESIAN_POINT ( 'NONE',  ( -14.34966873604972548, 8.224510206698743886, 113.3344237280190328 ) ) ;
#26879 = CARTESIAN_POINT ( 'NONE',  ( 9.564922557960805705, 16.46253265017160317, 54.58224293864769550 ) ) ;
#26880 = CARTESIAN_POINT ( 'NONE',  ( 19.05341960407617918, -5.049401038297876454, 26.04275706135233293 ) ) ;
#26881 = CARTESIAN_POINT ( 'NONE',  ( -8.224510206698735004, -14.34966873604973081, 29.58442372801901854 ) ) ;
#26882 = CARTESIAN_POINT ( 'NONE',  ( 5.719274019375991003, -21.55341960407610458, 42.70724293864770260 ) ) ;
#26884 = ORIENTED_EDGE ( 'NONE', *, *, #197067, .F. ) ;
#26883 = CARTESIAN_POINT ( 'NONE',  ( -21.55341960407619339, 5.719274019375674811, 88.54275706135236135 ) ) ;
#26885 = CARTESIAN_POINT ( 'NONE',  ( -13.97604488694527625, -13.89961937509977652, 101.8739096053143811 ) ) ;
#26886 = CARTESIAN_POINT ( 'NONE',  ( -5.153800228976328057, -19.02544592524343514, 82.29057627198103830 ) ) ;
#26887 = CARTESIAN_POINT ( 'NONE',  ( -31.05874284564964682, -25.21260394624121304, -18.17714894250296709 ) ) ;
#26888 = CARTESIAN_POINT ( 'NONE',  ( -21.53943276465977519, 0.05219959533907696930, 116.2489096053143669 ) ) ;
#26889 = CARTESIAN_POINT ( 'NONE',  ( 14.29746914071049879, -8.314922557960816363, 83.33224293864769550 ) ) ;
#26891 = CARTESIAN_POINT ( 'NONE',  ( 0.05219959533909260263, 19.03943276465977164, 74.99890960531435269 ) ) ;
#26890 = CARTESIAN_POINT ( 'NONE',  ( -18.62759615963270932, 10.81492255796079327, 70.83224293864770971 ) ) ;
#26892 = CARTESIAN_POINT ( 'NONE',  ( 19.02544592524343514, -5.153800228976328945, 78.54057627198099567 ) ) ;
#26893 = CARTESIAN_POINT ( 'NONE',  ( -15.80617190586745835, -15.72974639402198527, 96.87390960531436690 ) ) ;
#26894 = VERTEX_POINT ( 'NONE', #49568 ) ;
#26895 = CARTESIAN_POINT ( 'NONE',  ( 13.97604488694527802, 13.89961937509977652, 54.37390960531435979 ) ) ;
#26897 = CARTESIAN_POINT ( 'NONE',  ( -5.153800228976328057, -19.02544592524343514, 22.29057627198102765 ) ) ;
#26896 = CARTESIAN_POINT ( 'NONE',  ( 12.14591786802309770, 12.06949235617756955, 94.37390960531436690 ) ) ;
#26898 = CARTESIAN_POINT ( 'NONE',  ( 16.46253265017160672, -9.564922557960803928, 58.33224293864769550 ) ) ;
#26899 = CARTESIAN_POINT ( 'NONE',  ( 5.049401038297881783, 19.05341960407617563, 77.29275706135231871 ) ) ;
#26900 = CARTESIAN_POINT ( 'NONE',  ( -14.34966873604960291, -8.224510206698953496, 101.6655762719810383 ) ) ;
#26901 = CARTESIAN_POINT ( 'NONE',  ( -5.823673210054431948, 21.52544592524334988, 52.70942372801902565 ) ) ;
#26903 = CARTESIAN_POINT ( 'NONE',  ( 15.80617190586769283, -15.72974639402175789, 20.62609039468568639 ) ) ;
#26902 = CARTESIAN_POINT ( 'NONE',  ( 16.51473224551069308, 9.474510206698969483, 49.16557627198102409 ) ) ;
#26904 = CARTESIAN_POINT ( 'NONE',  ( 4.379528057220339221, -16.55341960407611168, 102.7072429386476955 ) ) ;
#26905 = LINE ( 'NONE', #138032, #75540 ) ;
#26906 = CARTESIAN_POINT ( 'NONE',  ( -13.97604488694527625, -13.89961937509977652, 56.87390960531434558 ) ) ;
#26907 = CARTESIAN_POINT ( 'NONE',  ( 28.82186960331511827, 9.364793116373395065, 143.3500000054623911 ) ) ;
#26909 = CARTESIAN_POINT ( 'NONE',  ( 19.02544592524343514, -5.153800228976328945, 113.5405762719810241 ) ) ;
#26908 = CARTESIAN_POINT ( 'NONE',  ( -19.03943276465977164, -0.05219959533935918106, 108.7510903946856615 ) ) ;
#26910 = CARTESIAN_POINT ( 'NONE',  ( 0.05219959533937995610, -21.53943276465977519, 55.00109039468568284 ) ) ;
#26911 = CARTESIAN_POINT ( 'NONE',  ( 5.049401038298161559, -19.05341960407611168, 97.70724293864766707 ) ) ;
#26912 = CARTESIAN_POINT ( 'NONE',  ( 19.02544592524334988, 5.153800228976608722, 81.45942372801897591 ) ) ;
#26913 = VECTOR ( 'NONE', #29672, 1000.000000000000000 ) ;
#26914 = CARTESIAN_POINT ( 'NONE',  ( 13.97604488694527802, 13.89961937509977652, 59.37390960531434558 ) ) ;
#26915 = CARTESIAN_POINT ( 'NONE',  ( -8.224510206698948167, 14.34966873604960824, 75.41557627198102409 ) ) ;
#26916 = CARTESIAN_POINT ( 'NONE',  ( -0.05219959533909027116, -19.03943276465977164, 107.4989096053143527 ) ) ;
#26917 = CARTESIAN_POINT ( 'NONE',  ( 14.29746914071049879, -8.314922557960816363, 78.33224293864770971 ) ) ;
#26918 = CARTESIAN_POINT ( 'NONE',  ( 19.02544592524343514, -5.153800228976328945, 78.54057627198099567 ) ) ;
#26919 = CARTESIAN_POINT ( 'NONE',  ( 16.51473224551083163, -9.474510206698727899, 45.83442372801900433 ) ) ;
#26923 = CARTESIAN_POINT ( 'NONE',  ( -16.46253265017160317, 9.564922557960807481, 30.83224293864769550 ) ) ;
#26922 =( BOUNDED_CURVE ( )  B_SPLINE_CURVE ( 2, ( #39883, #101550, #163242, #24742, #198559, #46855, #105545, #167231, #170193, #122688, #92345, #60029, #43881 ),
 .UNSPECIFIED., .F., .F. ) 
 B_SPLINE_CURVE_WITH_KNOTS ( ( 3, 2, 2, 2, 2, 2, 3 ),
 ( 0.5024761162491353517, 0.5043859649122807154, 0.5087719298245614308, 0.5131578947368421462, 0.5175438596491228616, 0.5219298245614034659, 0.5238853530466391906 ),
 .UNSPECIFIED. ) 
 CURVE ( )  GEOMETRIC_REPRESENTATION_ITEM ( )  RATIONAL_B_SPLINE_CURVE ( ( 0.9832469066685285419, 0.9851625545550100060, 1.000000000000000000, 0.9659258262890683122, 1.000000000000000000, 0.9659258262890683122, 1.000000000000000000, 0.9659258262890683122, 1.000000000000000000, 0.9659258262890683122, 1.000000000000000000, 0.9848076720550078544, 0.9831626618144001517 ) ) 
 REPRESENTATION_ITEM ( '' )  );
#26921 = CARTESIAN_POINT ( 'NONE',  ( -16.53943276465976808, 0.05219959533911058130, 46.24890960531435979 ) ) ;
#26920 = CARTESIAN_POINT ( 'NONE',  ( -13.89961937509977652, 13.97604488694528158, 55.62390960531434558 ) ) ;
#26924 = ORIENTED_EDGE ( 'NONE', *, *, #107568, .F. ) ;
#26925 = CARTESIAN_POINT ( 'NONE',  ( -21.55341960407619339, 5.719274019375674811, 43.54275706135235424 ) ) ;
#26926 = CARTESIAN_POINT ( 'NONE',  ( 19.03943276465977164, 0.05219959533936151252, 81.25109039468567573 ) ) ;
#26927 = CARTESIAN_POINT ( 'NONE',  ( 8.314922557960818139, 14.29746914071049879, 39.58224293864769550 ) ) ;
#26928 = CARTESIAN_POINT ( 'NONE',  ( -0.05219959533907301413, -21.53943276465977519, 97.49890960531436690 ) ) ;
#26929 = CARTESIAN_POINT ( 'NONE',  ( 18.62759615963271287, -10.81492255796078972, 38.33224293864768839 ) ) ;
#26930 = CARTESIAN_POINT ( 'NONE',  ( 4.483927247898545687, 16.52544592524342804, 69.79057627198102409 ) ) ;
#26931 = CARTESIAN_POINT ( 'NONE',  ( -16.51473224551069308, -9.474510206698971260, 36.66557627198102409 ) ) ;
#26932 = CARTESIAN_POINT ( 'NONE',  ( -14.34966873604972548, 8.224510206698743886, 103.3344237280190043 ) ) ;
#26933 = CARTESIAN_POINT ( 'NONE',  ( -8.314922557961024197, 14.29746914071037800, 67.91775706135234714 ) ) ;
#26934 = CARTESIAN_POINT ( 'NONE',  ( -13.97604488694547697, 13.89961937509957934, 28.12609039468565797 ) ) ;
#26935 = CARTESIAN_POINT ( 'NONE',  ( -16.46253265017160317, 9.564922557960807481, 95.83224293864769550 ) ) ;
#26936 = CARTESIAN_POINT ( 'NONE',  ( 19.03943276465977164, -0.05219959533909143690, 83.74890960531436690 ) ) ;
#26937 = CARTESIAN_POINT ( 'NONE',  ( -16.52544592524335698, -4.483927247898792601, 68.95942372801901854 ) ) ;
#26938 = CARTESIAN_POINT ( 'NONE',  ( -16.46253265017160317, 9.564922557960807481, 30.83224293864769550 ) ) ;
#26939 = CARTESIAN_POINT ( 'NONE',  ( 12.14591786802309770, 12.06949235617756955, 49.37390960531436690 ) ) ;
#26941 = CARTESIAN_POINT ( 'NONE',  ( -16.51473224551069308, -9.474510206698971260, 91.66557627198103830 ) ) ;
#26940 = CARTESIAN_POINT ( 'NONE',  ( 5.000000000000000000, -139.6710100716628631, 12.88025745871188477 ) ) ;
#26942 = CARTESIAN_POINT ( 'NONE',  ( 5.719274019375991003, -21.55341960407610458, 32.70724293864770260 ) ) ;
#26943 = CARTESIAN_POINT ( 'NONE',  ( -0.05219959533910754901, -16.53943276465976808, 72.49890960531435269 ) ) ;
#26944 = VECTOR ( 'NONE', #55819, 1000.000000000000000 ) ;
#26945 = EDGE_LOOP ( 'NONE', ( #611, #153759, #65082, #146158 ) ) ;
#26946 = CARTESIAN_POINT ( 'NONE',  ( -16.52544592524342804, 4.483927247898546575, 61.04057627198103120 ) ) ;
#26948 = CARTESIAN_POINT ( 'NONE',  ( 17.50000000000001066, -3.209263204892516264, 32.26196825606286467 ) ) ;
#26947 = CARTESIAN_POINT ( 'NONE',  ( -8.224510206698735004, -14.34966873604973081, 54.58442372801901143 ) ) ;
#26949 = CARTESIAN_POINT ( 'NONE',  ( 16.51473224551083163, -9.474510206698727899, 65.83442372801900433 ) ) ;
#26950 = CARTESIAN_POINT ( 'NONE',  ( 0.05219959533909260263, 19.03943276465977164, 89.99890960531436690 ) ) ;
#26951 = CARTESIAN_POINT ( 'NONE',  ( -19.03943276465977164, -0.05219959533935918106, 63.75109039468566863 ) ) ;
#26952 = CARTESIAN_POINT ( 'NONE',  ( 17.59860650958994555, -7.585241751806880650, 95.92337014262491834 ) ) ;
#26954 = CARTESIAN_POINT ( 'NONE',  ( 12.06949235617739724, 12.14591786802326823, 101.8760903946857042 ) ) ;
#26953 = CARTESIAN_POINT ( 'NONE',  ( 12.06949235617739724, 12.14591786802326823, 21.87609039468567573 ) ) ;
#26955 = CARTESIAN_POINT ( 'NONE',  ( -5.049401038298153566, 19.05341960407611168, 40.20724293864768839 ) ) ;
#26956 = CARTESIAN_POINT ( 'NONE',  ( -19.02544592524342804, 5.153800228976336051, 116.0405762719810383 ) ) ;
#26957 = CARTESIAN_POINT ( 'NONE',  ( -18.67979575497193778, 10.72451020669871902, 58.33442372801901143 ) ) ;
#26958 = CARTESIAN_POINT ( 'NONE',  ( -8.314922557961024197, 14.29746914071037800, 27.91775706135234358 ) ) ;
#26960 = CARTESIAN_POINT ( 'NONE',  ( 19.02544592524343514, -5.153800228976328945, 73.54057627198103830 ) ) ;
#26959 = CARTESIAN_POINT ( 'NONE',  ( -1.371772415827590191E-14, -64.85621347262016911, -24.99999966871768819 ) ) ;
#26961 = CARTESIAN_POINT ( 'NONE',  ( 16.51473224551069308, 9.474510206698969483, 114.1655762719810241 ) ) ;
#26963 = CARTESIAN_POINT ( 'NONE',  ( 9.474510206698971260, -16.51473224551069308, 77.91557627198103830 ) ) ;
#26962 = CARTESIAN_POINT ( 'NONE',  ( 0.05219959533910956823, 16.53943276465976808, 79.99890960531435269 ) ) ;
#26964 = CARTESIAN_POINT ( 'NONE',  ( -19.03943276465977164, 0.05219959533909376836, 76.24890960531435269 ) ) ;
#26965 = CARTESIAN_POINT ( 'NONE',  ( 0.05219959533936267826, -19.03943276465977164, 90.00109039468567573 ) ) ;
#26966 = CARTESIAN_POINT ( 'NONE',  ( 15.80617190586746368, 15.72974639402197994, 64.37390960531435269 ) ) ;
#26967 = CARTESIAN_POINT ( 'NONE',  ( -13.97604488694527625, -13.89961937509977652, 31.87390960531435979 ) ) ;
#26968 = CARTESIAN_POINT ( 'NONE',  ( 16.51473224551083163, -9.474510206698727899, 55.83442372801899722 ) ) ;
#26969 = CARTESIAN_POINT ( 'NONE',  ( 9.474510206698971260, -16.51473224551069308, 52.91557627198102409 ) ) ;
#26970 = CARTESIAN_POINT ( 'NONE',  ( -13.89961937509977652, 13.97604488694528158, 90.62390960531432427 ) ) ;
#26971 = ORIENTED_EDGE ( 'NONE', *, *, #93425, .F. ) ;
#26972 = CARTESIAN_POINT ( 'NONE',  ( 10.81492255796078972, 18.62759615963270932, 94.58224293864769550 ) ) ;
#26974 = CARTESIAN_POINT ( 'NONE',  ( -19.05341960407617563, 5.049401038297882671, 43.54275706135232582 ) ) ;
#26973 = CARTESIAN_POINT ( 'NONE',  ( -14.29746914071049879, 8.314922557960819915, 90.83224293864769550 ) ) ;
#26975 = CARTESIAN_POINT ( 'NONE',  ( 0.05219959533907565091, 21.53943276465977519, 79.99890960531435269 ) ) ;
#26976 = CARTESIAN_POINT ( 'NONE',  ( 10.81492255796078972, 18.62759615963270932, 64.58224293864769550 ) ) ;
#26977 = CARTESIAN_POINT ( 'NONE',  ( 16.55341960407611168, 4.379528057220329451, 28.95724293864769905 ) ) ;
#26978 = CARTESIAN_POINT ( 'NONE',  ( -21.52544592524334988, -5.823673210054445271, 103.9594237280190185 ) ) ;
#26979 = CARTESIAN_POINT ( 'NONE',  ( 5.153800228976335163, 19.02544592524342804, 79.79057627198102409 ) ) ;
#26980 = CARTESIAN_POINT ( 'NONE',  ( 9.474510206698971260, -16.51473224551069308, 37.91557627198102409 ) ) ;
#26981 = CARTESIAN_POINT ( 'NONE',  ( -5.719274019375665041, -21.55341960407619695, 34.79275706135235424 ) ) ;
#26982 = CARTESIAN_POINT ( 'NONE',  ( -18.62759615963255300, -10.81492255796106328, 49.16775706135234003 ) ) ;
#26983 = CARTESIAN_POINT ( 'NONE',  ( 9.474510206698971260, -16.51473224551069308, 52.91557627198102409 ) ) ;
#26984 = CARTESIAN_POINT ( 'NONE',  ( -18.67979575497193778, 10.72451020669871902, 28.33442372801902209 ) ) ;
#26985 = CARTESIAN_POINT ( 'NONE',  ( -16.51473224551082808, 9.474510206698731452, 63.33442372801900433 ) ) ;
#26986 = CARTESIAN_POINT ( 'NONE',  ( -5.153800228976328057, -19.02544592524343514, 32.29057627198102409 ) ) ;
#26987 = CARTESIAN_POINT ( 'NONE',  ( 8.314922557961029526, -14.29746914071037800, 30.41775706135234358 ) ) ;
#26988 = CARTESIAN_POINT ( 'NONE',  ( -5.153800228976328057, -19.02544592524343514, 27.29057627198103120 ) ) ;
#26989 = CARTESIAN_POINT ( 'NONE',  ( -16.52544592524335698, -4.483927247898792601, 78.95942372801901854 ) ) ;
#26990 = CARTESIAN_POINT ( 'NONE',  ( 9.474510206698971260, -16.51473224551069308, 42.91557627198103120 ) ) ;
#26991 = CARTESIAN_POINT ( 'NONE',  ( -23.64729612845568596, -13.72274676820315342, 169.8070494178799663 ) ) ;
#26992 = CARTESIAN_POINT ( 'NONE',  ( 5.049401038298161559, -19.05341960407611168, 82.70724293864770971 ) ) ;
#26993 = CARTESIAN_POINT ( 'NONE',  ( -9.474510206698964154, 16.51473224551069663, 25.41557627198103120 ) ) ;
#26994 = CARTESIAN_POINT ( 'NONE',  ( -10.72451020669898014, 18.67979575497178502, 70.41557627198102409 ) ) ;
#26995 = CARTESIAN_POINT ( 'NONE',  ( 16.52544592524335698, 4.483927247898782831, 46.45942372801901854 ) ) ;
#26996 = CARTESIAN_POINT ( 'NONE',  ( 0.05219959533937995610, -21.53943276465977519, 105.0010903946856757 ) ) ;
#26997 = CARTESIAN_POINT ( 'NONE',  ( -13.89961937509977652, 13.97604488694528158, 45.62390960531433848 ) ) ;
#26998 = CARTESIAN_POINT ( 'NONE',  ( 16.53943276465976808, -0.05219959533910856209, 33.74890960531436690 ) ) ;
#26999 = CARTESIAN_POINT ( 'NONE',  ( -8.314922557960811034, -14.29746914071050412, 67.08224293864770971 ) ) ;
#27000 = CARTESIAN_POINT ( 'NONE',  ( 13.89961937509977652, -13.97604488694527269, 68.12390960531436690 ) ) ;
#27001 = CARTESIAN_POINT ( 'NONE',  ( 0.05219959533937995610, -21.53943276465977519, 105.0010903946856757 ) ) ;
#27002 = CARTESIAN_POINT ( 'NONE',  ( -21.53943276465977519, -0.05219959533937600094, 23.75109039468567929 ) ) ;
#27003 = CARTESIAN_POINT ( 'NONE',  ( 16.46253265017160672, -9.564922557960803928, 83.33224293864768129 ) ) ;
#27004 = VECTOR ( 'NONE', #88775, 1000.000000000000000 ) ;
#27005 = CARTESIAN_POINT ( 'NONE',  ( -0.05219959533937732626, 21.53943276465977519, 82.50109039468568994 ) ) ;
#27006 = CARTESIAN_POINT ( 'NONE',  ( -8.224510206698735004, -14.34966873604973081, 59.58442372801901854 ) ) ;
#27007 = CARTESIAN_POINT ( 'NONE',  ( 16.55341960407618274, -4.379528057220086978, 26.04275706135235779 ) ) ;
#27009 = CARTESIAN_POINT ( 'NONE',  ( 18.62759615963255655, 10.81492255796105972, 96.66775706135234714 ) ) ;
#27008 = CARTESIAN_POINT ( 'NONE',  ( -12.14591786802309592, -12.06949235617757132, 96.87390960531436690 ) ) ;
#27010 = CARTESIAN_POINT ( 'NONE',  ( -16.52544592524342804, 4.483927247898546575, 31.04057627198102409 ) ) ;
#27011 = CARTESIAN_POINT ( 'NONE',  ( 16.51473224551069308, 9.474510206698969483, 34.16557627198102409 ) ) ;
#27012 = CARTESIAN_POINT ( 'NONE',  ( -0.05219959533934338120, 16.53943276465976808, 47.50109039468568994 ) ) ;
#27013 = CARTESIAN_POINT ( 'NONE',  ( 4.379528057220339221, -16.55341960407611168, 52.70724293864769550 ) ) ;
#27014 = CARTESIAN_POINT ( 'NONE',  ( -4.379528057220086978, -16.55341960407618274, 99.79275706135234714 ) ) ;
#27015 = CARTESIAN_POINT ( 'NONE',  ( -18.67979575497178146, -10.72451020669898902, 21.66557627198102409 ) ) ;
#27016 = CARTESIAN_POINT ( 'NONE',  ( -18.67979575497178146, -10.72451020669898902, 26.66557627198103475 ) ) ;
#27017 = CARTESIAN_POINT ( 'NONE',  ( 5.049401038297881783, 19.05341960407617563, 22.29275706135233648 ) ) ;
#27018 = CARTESIAN_POINT ( 'NONE',  ( 16.53943276465976808, -0.05219959533910856209, 88.74890960531436690 ) ) ;
#27019 = CARTESIAN_POINT ( 'NONE',  ( 19.02544592524343514, -5.153800228976328945, 88.54057627198102409 ) ) ;
#27020 = ORIENTED_EDGE ( 'NONE', *, *, #119343, .T. ) ;
#27021 = CARTESIAN_POINT ( 'NONE',  ( -0.05219959533934338120, 16.53943276465976808, 42.50109039468567573 ) ) ;
#27022 = CARTESIAN_POINT ( 'NONE',  ( -13.97604488694527625, -13.89961937509977652, 41.87390960531435979 ) ) ;
#27024 = DIRECTION ( 'NONE',  ( 1.000000000000000000, 0.000000000000000000, 0.000000000000000000 ) ) ;
#27023 = CARTESIAN_POINT ( 'NONE',  ( -14.29746914071037622, -8.314922557961029526, 39.16775706135235424 ) ) ;
#27025 = CARTESIAN_POINT ( 'NONE',  ( 0.05219959533936267826, -19.03943276465977164, 55.00109039468566863 ) ) ;
#27026 = CARTESIAN_POINT ( 'NONE',  ( 19.05341960407611168, 5.049401038298154454, 43.95724293864769550 ) ) ;
#27027 = CARTESIAN_POINT ( 'NONE',  ( -16.55341960407617563, 4.379528057220093196, 83.54275706135234714 ) ) ;
#27028 = CARTESIAN_POINT ( 'NONE',  ( 19.03943276465977164, 0.05219959533936151252, 101.2510903946856757 ) ) ;
#27029 = CARTESIAN_POINT ( 'NONE',  ( -19.03943276465977164, -0.05219959533935918106, 33.75109039468566863 ) ) ;
#27030 = CARTESIAN_POINT ( 'NONE',  ( -9.564922557960796823, -16.46253265017161027, 67.08224293864769550 ) ) ;
#27031 = CARTESIAN_POINT ( 'NONE',  ( 16.55341960407611168, 4.379528057220329451, 93.95724293864770971 ) ) ;
#27032 = B_SPLINE_CURVE_WITH_KNOTS ( 'NONE', 3,
 ( #129363, #142556, #21206, #191059, #37368, #84856 ),
 .UNSPECIFIED., .F., .F.,
 ( 4, 2, 4 ),
 ( 0.003989672132298176417, 0.004372778065220590121, 0.004755883998143003825 ),
 .UNSPECIFIED. ) ;
#27033 = CARTESIAN_POINT ( 'NONE',  ( -9.474510206698720793, -16.51473224551083518, 69.58442372801901854 ) ) ;
#27034 = CARTESIAN_POINT ( 'NONE',  ( 15.80617190586746368, 15.72974639402197994, 64.37390960531435269 ) ) ;
#27035 = CARTESIAN_POINT ( 'NONE',  ( 19.03943276465977164, 0.05219959533936151252, 46.25109039468566863 ) ) ;
#27036 = CARTESIAN_POINT ( 'NONE',  ( -19.05341960407611168, -5.049401038298163336, 106.4572429386476955 ) ) ;
#27037 = CARTESIAN_POINT ( 'NONE',  ( -21.55341960407610458, -5.719274019375992779, 91.45724293864769550 ) ) ;
#27038 = CARTESIAN_POINT ( 'NONE',  ( -16.21995358207302829, 7.366697692864236480, 84.93551001512155096 ) ) ;
#27039 = CARTESIAN_POINT ( 'NONE',  ( -19.02544592524334988, -5.153800228976617603, 98.95942372801900433 ) ) ;
#27040 = CARTESIAN_POINT ( 'NONE',  ( 11.30153831258469843, -180.0000000000000000, -23.00000000000000000 ) ) ;
#27041 = CARTESIAN_POINT ( 'NONE',  ( -4.483927247898782831, 16.52544592524335698, 32.70942372801900433 ) ) ;
#27042 = CARTESIAN_POINT ( 'NONE',  ( 13.97604488694527802, 13.89961937509977652, 49.37390960531434558 ) ) ;
#27043 = CARTESIAN_POINT ( 'NONE',  ( -16.51473224551069308, -9.474510206698971260, 106.6655762719810383 ) ) ;
#27044 = CARTESIAN_POINT ( 'NONE',  ( -15.72974639402197994, 15.80617190586746368, 95.62390960531436690 ) ) ;
#27045 = CARTESIAN_POINT ( 'NONE',  ( 15.80617190586769283, -15.72974639402175789, 60.62609039468567573 ) ) ;
#27047 = CARTESIAN_POINT ( 'NONE',  ( -15.72974639402176322, -15.80617190586768395, 109.3760903946857042 ) ) ;
#27046 = CARTESIAN_POINT ( 'NONE',  ( 16.46253265017146816, 9.564922557961045513, 106.6677570613523471 ) ) ;
#27048 = CARTESIAN_POINT ( 'NONE',  ( 8.224510206698953496, -14.34966873604960469, 22.91557627198102765 ) ) ;
#27049 = CARTESIAN_POINT ( 'NONE',  ( -5.823673210054116645, -21.52544592524344225, 97.29057627198105251 ) ) ;
#27050 = CARTESIAN_POINT ( 'NONE',  ( -16.52544592524342804, 4.483927247898546575, 56.04057627198102409 ) ) ;
#27051 = CARTESIAN_POINT ( 'NONE',  ( 9.474510206698729675, 16.51473224551082808, 87.08442372801900433 ) ) ;
#27052 = CARTESIAN_POINT ( 'NONE',  ( -5.049401038297874678, -19.05341960407617918, 59.79275706135231871 ) ) ;
#27053 = CARTESIAN_POINT ( 'NONE',  ( 15.80617190586769283, -15.72974639402175789, 70.62609039468567573 ) ) ;
#27054 = CARTESIAN_POINT ( 'NONE',  ( 19.03943276465977164, 0.05219959533936151252, 36.25109039468567573 ) ) ;
#27055 = CARTESIAN_POINT ( 'NONE',  ( 13.97604488694527802, 13.89961937509977652, 24.37390960531435624 ) ) ;
#27056 = CARTESIAN_POINT ( 'NONE',  ( -10.72451020669898014, 18.67979575497178502, 50.41557627198103120 ) ) ;
#27057 = CARTESIAN_POINT ( 'NONE',  ( 16.52544592524342804, -4.483927247898539470, 33.54057627198102409 ) ) ;
#27058 = CARTESIAN_POINT ( 'NONE',  ( 18.62759615963255655, 10.81492255796105972, 111.6677570613523613 ) ) ;
#27059 = CARTESIAN_POINT ( 'NONE',  ( -12.14591786802326823, 12.06949235617739902, 68.12609039468567573 ) ) ;
#27060 = CARTESIAN_POINT ( 'NONE',  ( -0.05219959533910754901, -16.53943276465976808, 42.49890960531435979 ) ) ;
#27061 = CARTESIAN_POINT ( 'NONE',  ( -18.67979575497193778, 10.72451020669871902, 78.33442372801901854 ) ) ;
#27062 = CARTESIAN_POINT ( 'NONE',  ( 10.81492255796106328, -18.62759615963255655, 65.41775706135234714 ) ) ;
#27063 = CARTESIAN_POINT ( 'NONE',  ( 21.52544592524344225, -5.823673210054117533, 73.54057627198102409 ) ) ;
#27064 = EDGE_CURVE ( 'NONE', #92863, #63341, #105389, .T. ) ;
#27065 = ORIENTED_EDGE ( 'NONE', *, *, #193126, .F. ) ;
#27066 = CARTESIAN_POINT ( 'NONE',  ( -13.97604488694527625, -13.89961937509977830, 61.87390960531435269 ) ) ;
#27067 = CARTESIAN_POINT ( 'NONE',  ( -0.05219959533937732626, 21.53943276465977519, 37.50109039468568284 ) ) ;
#27068 = CARTESIAN_POINT ( 'NONE',  ( 8.314922557960818139, 14.29746914071049879, 114.5822429386477097 ) ) ;
#27069 = CARTESIAN_POINT ( 'NONE',  ( -5.049401038298153566, 19.05341960407611168, 40.20724293864768839 ) ) ;
#27070 = CARTESIAN_POINT ( 'NONE',  ( -8.314922557960811034, -14.29746914071050412, 97.08224293864770971 ) ) ;
#27071 = CARTESIAN_POINT ( 'NONE',  ( 19.02544592524343514, -5.153800228976328945, 88.54057627198102409 ) ) ;
#27072 = CARTESIAN_POINT ( 'NONE',  ( -0.05219959533910754901, -16.53943276465976808, 22.49890960531436335 ) ) ;
#27073 = CARTESIAN_POINT ( 'NONE',  ( -4.379528057220328563, 16.55341960407611168, 100.2072429386476955 ) ) ;
#27074 = CARTESIAN_POINT ( 'NONE',  ( -18.62759615963270932, 10.81492255796079327, 75.83224293864769550 ) ) ;
#27075 = CARTESIAN_POINT ( 'NONE',  ( -18.62759615963270932, 10.81492255796079327, 100.8322429386477097 ) ) ;
#27076 = CARTESIAN_POINT ( 'NONE',  ( 16.51473224551069308, 9.474510206698969483, 109.1655762719810383 ) ) ;
#27078 = CARTESIAN_POINT ( 'NONE',  ( 8.314922557961029526, -14.29746914071037800, 20.41775706135234714 ) ) ;
#27077 = CARTESIAN_POINT ( 'NONE',  ( 16.51473224551069308, 9.474510206698969483, 59.16557627198102409 ) ) ;
#27079 = CARTESIAN_POINT ( 'NONE',  ( -15.72974639402197994, 15.80617190586746368, 55.62390960531436690 ) ) ;
#27080 = CARTESIAN_POINT ( 'NONE',  ( -10.72451020669870658, -18.67979575497194134, 84.58442372801903275 ) ) ;
#27081 = CARTESIAN_POINT ( 'NONE',  ( -13.89961937509977652, 13.97604488694528158, 80.62390960531436690 ) ) ;
#27082 = AXIS2_PLACEMENT_3D ( 'NONE', #20694, #84353, #19710 ) ;
#27083 = CARTESIAN_POINT ( 'NONE',  ( -19.05341960407611168, -5.049401038298163336, 106.4572429386476955 ) ) ;
#27084 = CARTESIAN_POINT ( 'NONE',  ( 0.05219959533934541429, -16.53943276465976808, 75.00109039468568994 ) ) ;
#27085 = CARTESIAN_POINT ( 'NONE',  ( -5.719274019375665041, -21.55341960407619695, 69.79275706135234714 ) ) ;
#27086 = CARTESIAN_POINT ( 'NONE',  ( -18.62759615963255300, -10.81492255796106328, 104.1677570613523471 ) ) ;
#27087 = CARTESIAN_POINT ( 'NONE',  ( 8.224510206698742110, 14.34966873604972548, 67.08442372801901854 ) ) ;
#27088 = CARTESIAN_POINT ( 'NONE',  ( 10.81492255796078972, 18.62759615963270932, 114.5822429386477097 ) ) ;
#27089 = CARTESIAN_POINT ( 'NONE',  ( 9.474510206698971260, -16.51473224551069308, 112.9155762719810383 ) ) ;
#27090 = CARTESIAN_POINT ( 'NONE',  ( 21.53943276465977519, 0.05219959533937863772, 91.25109039468568994 ) ) ;
#27091 = CARTESIAN_POINT ( 'NONE',  ( 15.80617190586746368, 15.72974639402197994, 94.37390960531436690 ) ) ;
#27092 = CARTESIAN_POINT ( 'NONE',  ( -13.97604488694547697, 13.89961937509957934, 53.12609039468565442 ) ) ;
#27093 = CARTESIAN_POINT ( 'NONE',  ( 21.55341960407610458, 5.719274019375980345, 48.95724293864770971 ) ) ;
#27095 = CARTESIAN_POINT ( 'NONE',  ( -4.483927247898539470, -16.52544592524342804, 37.29057627198102409 ) ) ;
#27094 = CARTESIAN_POINT ( 'NONE',  ( 5.153800228976335163, 19.02544592524342804, 94.79057627198103830 ) ) ;
#27096 = CARTESIAN_POINT ( 'NONE',  ( -17.49999999999999289, 5.500000000000036415, 65.79690382534171533 ) ) ;
#27098 = B_SPLINE_CURVE_WITH_KNOTS ( 'NONE', 3,
 ( #64626, #199167, #944, #62619, #30312, #107138, #77795, #75809, #169815, #124297, #63632, #18136, #141463, #170812, #126288, #140463, #78786, #152652, #185994, #123295, #1953, #60634, #171809, #168808, #91955, #125308, #153648, #172806, #187004, #156640, #47477, #187985 ),
 .UNSPECIFIED., .F., .F.,
 ( 4, 2, 2, 2, 2, 2, 2, 2, 2, 2, 2, 2, 2, 2, 2, 4 ),
 ( 1.262897753262582698E-17, 0.0003712461730036966984, 0.0007424923460073807116, 0.001113738519011064779, 0.001484984692014748846, 0.002227477038022110042, 0.002598723211025783918, 0.002969969384029457361, 0.003341215557033131237, 0.003712461730036805546, 0.004083707903040478988, 0.004454954076044153298, 0.004826200249047825873, 0.005197446422051500182, 0.005568692595055173625, 0.005939938768058847067 ),
 .UNSPECIFIED. ) ;
#27097 = CARTESIAN_POINT ( 'NONE',  ( 18.09867054820430710, 5.500000000000001776, 81.48393025253585620 ) ) ;
#27099 = CARTESIAN_POINT ( 'NONE',  ( -14.29746914071037622, -8.314922557961029526, 19.16775706135234714 ) ) ;
#27100 = CARTESIAN_POINT ( 'NONE',  ( -18.67979575497178146, -10.72451020669898902, 86.66557627198102409 ) ) ;
#27101 = CARTESIAN_POINT ( 'NONE',  ( -14.29746914071049879, 8.314922557960819915, 45.83224293864769550 ) ) ;
#27102 = CARTESIAN_POINT ( 'NONE',  ( 8.224510206698742110, 14.34966873604972548, 32.08442372801901854 ) ) ;
#27103 = CARTESIAN_POINT ( 'NONE',  ( 19.02544592524343514, -5.153800228976328945, 38.54057627198103120 ) ) ;
#27105 = CARTESIAN_POINT ( 'NONE',  ( -9.564922557961040184, 16.46253265017147172, 87.91775706135233293 ) ) ;
#27104 = CARTESIAN_POINT ( 'NONE',  ( 18.67979575497178502, 10.72451020669898547, 109.1655762719810383 ) ) ;
#27106 = CARTESIAN_POINT ( 'NONE',  ( 5.049401038298161559, -19.05341960407611168, 82.70724293864770971 ) ) ;
#27107 = CARTESIAN_POINT ( 'NONE',  ( -0.05219959533909027116, -19.03943276465977164, 77.49890960531435269 ) ) ;
#27108 = CARTESIAN_POINT ( 'NONE',  ( 21.55341960407610458, 5.719274019375980345, 73.95724293864769550 ) ) ;
#27109 = CARTESIAN_POINT ( 'NONE',  ( -19.05341960407611168, -5.049401038298163336, 36.45724293864766707 ) ) ;
#27110 = CARTESIAN_POINT ( 'NONE',  ( 3.444780402933648400, 37.36484951828411738, -8.000000000000003553 ) ) ;
#27111 = CARTESIAN_POINT ( 'NONE',  ( 12.14591786802309770, 12.06949235617756955, 54.37390960531435979 ) ) ;
#27112 = CARTESIAN_POINT ( 'NONE',  ( 13.97604488694527802, 13.89961937509977652, 84.37390960531433848 ) ) ;
#27113 = CARTESIAN_POINT ( 'NONE',  ( -3.573655867282028392E-15, 2.428612866367529932E-14, 139.9999999999999716 ) ) ;
#27114 = CARTESIAN_POINT ( 'NONE',  ( 9.474510206698729675, 16.51473224551082808, 72.08442372801900433 ) ) ;
#27115 = CARTESIAN_POINT ( 'NONE',  ( -5.823673210054116645, -21.52544592524344225, 77.29057627198102409 ) ) ;
#27116 = CARTESIAN_POINT ( 'NONE',  ( -5.049401038297874678, -19.05341960407617918, 34.79275706135233293 ) ) ;
#27117 = CARTESIAN_POINT ( 'NONE',  ( -19.05341960407611168, -5.049401038298163336, 106.4572429386476955 ) ) ;
#27118 = CARTESIAN_POINT ( 'NONE',  ( -17.49999999999999645, 3.189878218039174040, 114.8705143742876089 ) ) ;
#27119 = CARTESIAN_POINT ( 'NONE',  ( -15.72974639402197994, 15.80617190586746368, 25.62390960531435624 ) ) ;
#27120 = CARTESIAN_POINT ( 'NONE',  ( 16.51473224551069308, 9.474510206698969483, 74.16557627198103830 ) ) ;
#27121 = CARTESIAN_POINT ( 'NONE',  ( 15.80617190586769283, -15.72974639402175789, 50.62609039468568994 ) ) ;
#27122 = CARTESIAN_POINT ( 'NONE',  ( -16.46253265017160317, 9.564922557960807481, 25.83224293864769194 ) ) ;
#27124 = ORIENTED_EDGE ( 'NONE', *, *, #38220, .T. ) ;
#27123 = CARTESIAN_POINT ( 'NONE',  ( -5.719274019375978568, 21.55341960407610458, 115.2072429386476955 ) ) ;
#27125 = CARTESIAN_POINT ( 'NONE',  ( 21.52544592524334988, 5.823673210054432836, 36.45942372801901143 ) ) ;
#27126 = ORIENTED_EDGE ( 'NONE', *, *, #107016, .F. ) ;
#27127 = CARTESIAN_POINT ( 'NONE',  ( -13.97604488694527625, -13.89961937509977652, 106.8739096053143669 ) ) ;
#27128 = CARTESIAN_POINT ( 'NONE',  ( -21.58577566615619503, 5.573877917343206256, 173.3856758005497340 ) ) ;
#27129 = CARTESIAN_POINT ( 'NONE',  ( 0.05219959533907565091, 21.53943276465977519, 109.9989096053143527 ) ) ;
#27130 = CARTESIAN_POINT ( 'NONE',  ( 9.564922557960805705, 16.46253265017160317, 59.58224293864769550 ) ) ;
#27131 = CARTESIAN_POINT ( 'NONE',  ( -14.34966873604972548, 8.224510206698743886, 23.33442372801901499 ) ) ;
#27132 = CARTESIAN_POINT ( 'NONE',  ( 37.99999999999999289, 2.893978650043524126E-14, -4.749999994537627224 ) ) ;
#27133 = CARTESIAN_POINT ( 'NONE',  ( -21.55341960407619339, 5.719274019375674811, 103.5427570613523613 ) ) ;
#27134 = CARTESIAN_POINT ( 'NONE',  ( -9.564922557960796823, -16.46253265017161027, 47.08224293864769550 ) ) ;
#27135 = CARTESIAN_POINT ( 'NONE',  ( -21.52544592524334988, -5.823673210054445271, 98.95942372801903275 ) ) ;
#27137 = CARTESIAN_POINT ( 'NONE',  ( -18.67979575497193778, 10.72451020669871902, 63.33442372801900433 ) ) ;
#27136 = CARTESIAN_POINT ( 'NONE',  ( 19.03943276465977164, -0.05219959533909143690, 88.74890960531436690 ) ) ;
#27138 = DIRECTION ( 'NONE',  ( 1.000000000000000000, -3.552713678800500929E-15, 0.000000000000000000 ) ) ;
#27139 = CARTESIAN_POINT ( 'NONE',  ( -0.05219959533909027116, -19.03943276465977164, 107.4989096053143527 ) ) ;
#27140 = CARTESIAN_POINT ( 'NONE',  ( -17.50000000000001421, 3.189878218039132296, 29.87051437428767287 ) ) ;
#27143 = CARTESIAN_POINT ( 'NONE',  ( 5.719274019375673035, 21.55341960407619339, 52.29275706135236135 ) ) ;
#27142 = CARTESIAN_POINT ( 'NONE',  ( 16.55341960407618274, -4.379528057220086978, 66.04275706135236135 ) ) ;
#27141 = CARTESIAN_POINT ( 'NONE',  ( -0.05219959533934338120, 16.53943276465976808, 47.50109039468568994 ) ) ;
#27144 = CARTESIAN_POINT ( 'NONE',  ( 21.53943276465977519, 0.05219959533937863772, 96.25109039468568994 ) ) ;
#27145 = CARTESIAN_POINT ( 'NONE',  ( -193.3062444957834884, -155.7167183371838064, -13.00000000000000000 ) ) ;
#27146 = CARTESIAN_POINT ( 'NONE',  ( -14.34966873604972548, 8.224510206698743886, 28.33442372801902209 ) ) ;
#27147 = CARTESIAN_POINT ( 'NONE',  ( 16.51473224551069308, 9.474510206698969483, 69.16557627198102409 ) ) ;
#27148 = CARTESIAN_POINT ( 'NONE',  ( 0.05219959533909260263, 19.03943276465977164, 109.9989096053143669 ) ) ;
#27149 = CARTESIAN_POINT ( 'NONE',  ( 17.13100169013298668, 6.664070546373162429, 41.73210164300153480 ) ) ;
#27150 = CARTESIAN_POINT ( 'NONE',  ( -13.89961937509977652, 13.97604488694528158, 25.62390960531434558 ) ) ;
#27151 = CARTESIAN_POINT ( 'NONE',  ( 10.72451020669898902, -18.67979575497178502, 47.91557627198102409 ) ) ;
#27152 = CARTESIAN_POINT ( 'NONE',  ( 12.06949235617739724, 12.14591786802326823, 91.87609039468568994 ) ) ;
#27154 = CARTESIAN_POINT ( 'NONE',  ( -9.564922557960796823, -16.46253265017161027, 62.08224293864769550 ) ) ;
#27153 = CARTESIAN_POINT ( 'NONE',  ( -0.05219959533910754901, -16.53943276465976808, 77.49890960531433848 ) ) ;
#27155 = CARTESIAN_POINT ( 'NONE',  ( -21.53943276465977519, -0.05219959533937600094, 93.75109039468567573 ) ) ;
#27156 = CARTESIAN_POINT ( 'NONE',  ( -22.44763431097441142, 1.469699867062036480, -58.07555020237587939 ) ) ;
#27157 = CARTESIAN_POINT ( 'NONE',  ( -16.52544592524335698, -4.483927247898792601, 23.95942372801901143 ) ) ;
#27158 = CARTESIAN_POINT ( 'NONE',  ( -16.52544592524342804, 4.483927247898546575, 71.04057627198103830 ) ) ;
#27159 = CARTESIAN_POINT ( 'NONE',  ( 15.80617190586769283, -15.72974639402175789, 40.62609039468567573 ) ) ;
#27160 = CARTESIAN_POINT ( 'NONE',  ( -10.81492255796078084, -18.62759615963271287, 72.08224293864769550 ) ) ;
#27161 = CARTESIAN_POINT ( 'NONE',  ( -9.564922557961040184, 16.46253265017147172, 37.91775706135233293 ) ) ;
#27162 = CYLINDRICAL_SURFACE ( 'NONE', #127105, 1.500000000000001332 ) ;
#27163 = CARTESIAN_POINT ( 'NONE',  ( -0.05219959533909027116, -19.03943276465977164, 77.49890960531435269 ) ) ;
#27164 = CARTESIAN_POINT ( 'NONE',  ( -12.14591786802309592, -12.06949235617757132, 51.87390960531437401 ) ) ;
#27165 = AXIS2_PLACEMENT_3D ( 'NONE', #192508, #117662, #179359 ) ;
#27166 = CARTESIAN_POINT ( 'NONE',  ( -4.379528057220328563, 16.55341960407611168, 30.20724293864769550 ) ) ;
#27167 = CARTESIAN_POINT ( 'NONE',  ( -14.34966873604972548, 8.224510206698743886, 108.3344237280190185 ) ) ;
#27168 = CARTESIAN_POINT ( 'NONE',  ( -16.46253265017146816, -9.564922557961047289, 69.16775706135233293 ) ) ;
#27169 = CARTESIAN_POINT ( 'NONE',  ( 19.97888994334919843, -34.65319547504301312, 0.000000000000000000 ) ) ;
#27170 = CARTESIAN_POINT ( 'NONE',  ( 15.72974639402199770, -15.80617190586745480, 28.12390960531435979 ) ) ;
#27171 = CARTESIAN_POINT ( 'NONE',  ( -16.52544592524342804, 4.483927247898546575, 91.04057627198103830 ) ) ;
#27172 = CARTESIAN_POINT ( 'NONE',  ( -18.10062525802553424, 5.500000000000031086, 58.51383468041921532 ) ) ;
#27174 = CARTESIAN_POINT ( 'NONE',  ( 18.67979575497178502, 10.72451020669898547, 44.16557627198103120 ) ) ;
#27173 = CARTESIAN_POINT ( 'NONE',  ( 0.05219959533909260263, 19.03943276465977164, 39.99890960531436690 ) ) ;
#27175 = CARTESIAN_POINT ( 'NONE',  ( 21.52544592524344225, -5.823673210054117533, 63.54057627198103830 ) ) ;
#27176 = CARTESIAN_POINT ( 'NONE',  ( 16.55341960407611168, 4.379528057220329451, 108.9572429386476955 ) ) ;
#27178 = CARTESIAN_POINT ( 'NONE',  ( -5.153800228976328057, -19.02544592524343514, 42.29057627198101699 ) ) ;
#27177 = CARTESIAN_POINT ( 'NONE',  ( -8.224510206698735004, -14.34966873604973081, 64.58442372801900433 ) ) ;
#27179 = CARTESIAN_POINT ( 'NONE',  ( 15.80617190586769283, -15.72974639402175789, 60.62609039468567573 ) ) ;
#27180 = CARTESIAN_POINT ( 'NONE',  ( 8.314922557960818139, 14.29746914071049879, 104.5822429386477097 ) ) ;
#27181 = CARTESIAN_POINT ( 'NONE',  ( -16.51473224551082808, 9.474510206698731452, 93.33442372801900433 ) ) ;
#27182 = CARTESIAN_POINT ( 'NONE',  ( 36.91746824999999177, 2.880721459617395097E-14, -2.124999997268813168 ) ) ;
#27184 = CARTESIAN_POINT ( 'NONE',  ( -5.823673210054116645, -21.52544592524344225, 37.29057627198102409 ) ) ;
#27183 = DIRECTION ( 'NONE',  ( 1.000000000000000000, -0.000000000000000000, 6.982962677686266711E-15 ) ) ;
#27185 = CARTESIAN_POINT ( 'NONE',  ( 17.48847506799968343, -5.747544572773780835, 68.32697437843283694 ) ) ;
#27186 = CARTESIAN_POINT ( 'NONE',  ( -18.67979575497193778, 10.72451020669871902, 73.33442372801901854 ) ) ;
#27188 = CARTESIAN_POINT ( 'NONE',  ( 4.483927247898545687, 16.52544592524342804, 49.79057627198102409 ) ) ;
#27187 = CARTESIAN_POINT ( 'NONE',  ( 16.52544592524335698, 4.483927247898782831, 56.45942372801902565 ) ) ;
#27189 = CARTESIAN_POINT ( 'NONE',  ( 10.72451020669898902, -18.67979575497178502, 62.91557627198102409 ) ) ;
#27190 = CARTESIAN_POINT ( 'NONE',  ( -10.72451020669898014, 18.67979575497178502, 65.41557627198102409 ) ) ;
#27191 = CARTESIAN_POINT ( 'NONE',  ( -21.96329795405619123, -8.386426352705242948, 172.0132153625897899 ) ) ;
#27194 = EDGE_CURVE ( 'NONE', #17663, #130010, #45803, .T. ) ;
#27193 = CARTESIAN_POINT ( 'NONE',  ( 13.89961937509977652, -13.97604488694527269, 108.1239096053143669 ) ) ;
#27192 = CARTESIAN_POINT ( 'NONE',  ( 19.03943276465977164, 0.05219959533936151252, 81.25109039468567573 ) ) ;
#27195 = CARTESIAN_POINT ( 'NONE',  ( 19.03943276465977164, -0.05219959533909143690, 43.74890960531435979 ) ) ;
#27196 = CARTESIAN_POINT ( 'NONE',  ( 0.05219959533910956823, 16.53943276465976808, 109.9989096053143527 ) ) ;
#27197 = CARTESIAN_POINT ( 'NONE',  ( 19.02544592524343514, -5.153800228976328945, 113.5405762719810241 ) ) ;
#27198 = ORIENTED_EDGE ( 'NONE', *, *, #43624, .T. ) ;
#27199 = CARTESIAN_POINT ( 'NONE',  ( -12.06949235617739369, -12.14591786802326823, 74.37609039468568994 ) ) ;
#27200 = CARTESIAN_POINT ( 'NONE',  ( -18.62759615963270932, 10.81492255796079327, 105.8322429386476955 ) ) ;
#27201 = CARTESIAN_POINT ( 'NONE',  ( 16.51473224551069308, 9.474510206698969483, 74.16557627198103830 ) ) ;
#27202 = CARTESIAN_POINT ( 'NONE',  ( 15.72974639402176855, 15.80617190586768217, 36.87609039468568994 ) ) ;
#27203 = CARTESIAN_POINT ( 'NONE',  ( 19.05341960407611168, 5.049401038298154454, 98.95724293864766707 ) ) ;
#27204 = CARTESIAN_POINT ( 'NONE',  ( -30.11221142034060350, -26.30828378221708519, -17.15571736053662377 ) ) ;
#27205 = VERTEX_POINT ( 'NONE', #110236 ) ;
#27206 = CARTESIAN_POINT ( 'NONE',  ( -21.55341960407619339, 5.719274019375674811, 33.54275706135234714 ) ) ;
#27208 = CARTESIAN_POINT ( 'NONE',  ( -9.474510206698720793, -16.51473224551083518, 84.58442372801900433 ) ) ;
#27207 = CARTESIAN_POINT ( 'NONE',  ( 9.474510206698971260, -16.51473224551069308, 27.91557627198103120 ) ) ;
#27209 = CARTESIAN_POINT ( 'NONE',  ( -19.02544592524334988, -5.153800228976617603, 33.95942372801897591 ) ) ;
#27210 = CARTESIAN_POINT ( 'NONE',  ( -10.72451020669898014, 18.67979575497178502, 110.4155762719810383 ) ) ;
#27211 = CARTESIAN_POINT ( 'NONE',  ( 16.46253265017146816, 9.564922557961045513, 36.66775706135233293 ) ) ;
#27212 = CARTESIAN_POINT ( 'NONE',  ( 5.049401038297881783, 19.05341960407617563, 47.29275706135231161 ) ) ;
#27213 = CARTESIAN_POINT ( 'NONE',  ( -12.06949235617739369, -12.14591786802326823, 94.37609039468568994 ) ) ;
#27214 = DIRECTION ( 'NONE',  ( -1.000000000000000000, -0.000000000000000000, -3.709348145883536076E-20 ) ) ;
#27215 = CARTESIAN_POINT ( 'NONE',  ( -0.05219959533909027116, -19.03943276465977164, 67.49890960531436690 ) ) ;
#27216 = CARTESIAN_POINT ( 'NONE',  ( 21.52544592524334988, 5.823673210054432836, 81.45942372801900433 ) ) ;
#27217 = CARTESIAN_POINT ( 'NONE',  ( -18.62759615963255300, -10.81492255796106328, 94.16775706135237556 ) ) ;
#27218 = CARTESIAN_POINT ( 'NONE',  ( 22.10945809693574304, -1.344113590474677267, -55.87741762761908859 ) ) ;
#27219 = CARTESIAN_POINT ( 'NONE',  ( -19.05341960407611168, -5.049401038298163336, 81.45724293864769550 ) ) ;
#27220 = CARTESIAN_POINT ( 'NONE',  ( -21.52544592524334988, -5.823673210054445271, 58.95942372801902565 ) ) ;
#27221 = CARTESIAN_POINT ( 'NONE',  ( 19.02544592524334988, 5.153800228976608722, 101.4594237280189759 ) ) ;
#27222 = CARTESIAN_POINT ( 'NONE',  ( 19.02544592524343514, -5.153800228976328945, 68.54057627198103830 ) ) ;
#27223 = CARTESIAN_POINT ( 'NONE',  ( -0.05219959533907301413, -21.53943276465977519, 22.49890960531436335 ) ) ;
#27224 = CARTESIAN_POINT ( 'NONE',  ( 5.049401038298161559, -19.05341960407611168, 82.70724293864770971 ) ) ;
#27225 = CARTESIAN_POINT ( 'NONE',  ( 10.59477242850415024, -90.60836494048558620, -25.00000000000000000 ) ) ;
#27226 = CARTESIAN_POINT ( 'NONE',  ( 13.89961937509977652, -13.97604488694527269, 63.12390960531435979 ) ) ;
#27227 = CARTESIAN_POINT ( 'NONE',  ( 19.03943276465977164, -0.05219959533909143690, 48.74890960531435979 ) ) ;
#27228 = CARTESIAN_POINT ( 'NONE',  ( -15.80617190586745835, -15.72974639402198527, 111.8739096053143669 ) ) ;
#27229 = CARTESIAN_POINT ( 'NONE',  ( 14.34966873604972726, -8.224510206698740333, 90.83442372801901854 ) ) ;
#27230 = CYLINDRICAL_SURFACE ( 'NONE', #169200, 2.500000000000000444 ) ;
#27231 = CARTESIAN_POINT ( 'NONE',  ( -19.03943276465977164, -0.05219959533935918106, 58.75109039468566863 ) ) ;
#27232 = CARTESIAN_POINT ( 'NONE',  ( 16.46253265017160672, -9.564922557960803928, 73.33224293864769550 ) ) ;
#27233 = CARTESIAN_POINT ( 'NONE',  ( -4.483927247898539470, -16.52544592524342804, 72.29057627198102409 ) ) ;
#27234 = CARTESIAN_POINT ( 'NONE',  ( -14.34966873604960291, -8.224510206698953496, 101.6655762719810383 ) ) ;
#27235 = CARTESIAN_POINT ( 'NONE',  ( -5.049401038298153566, 19.05341960407611168, 115.2072429386477097 ) ) ;
#27236 = CARTESIAN_POINT ( 'NONE',  ( 19.03943276465977164, -0.05219959533909143690, 98.74890960531436690 ) ) ;
#27237 = CARTESIAN_POINT ( 'NONE',  ( -8.314922557960811034, -14.29746914071050412, 77.08224293864769550 ) ) ;
#27238 = CARTESIAN_POINT ( 'NONE',  ( -5.049401038298153566, 19.05341960407611168, 115.2072429386477097 ) ) ;
#27239 = CARTESIAN_POINT ( 'NONE',  ( 16.51473224551083163, -9.474510206698727899, 30.83442372801900433 ) ) ;
#27240 = CARTESIAN_POINT ( 'NONE',  ( -4.379528057220086978, -16.55341960407618274, 109.7927570613523613 ) ) ;
#27241 = CARTESIAN_POINT ( 'NONE',  ( -13.89961937509977652, 13.97604488694528158, 90.62390960531432427 ) ) ;
#27242 = CARTESIAN_POINT ( 'NONE',  ( -18.62759615963255300, -10.81492255796106328, 54.16775706135235424 ) ) ;
#27243 = CARTESIAN_POINT ( 'NONE',  ( 18.67979575497178502, 10.72451020669898547, 44.16557627198103120 ) ) ;
#27244 = CARTESIAN_POINT ( 'NONE',  ( 21.52544592524344225, -5.823673210054117533, 113.5405762719810383 ) ) ;
#27245 = CARTESIAN_POINT ( 'NONE',  ( 15.80617190586746368, 15.72974639402197994, 64.37390960531435269 ) ) ;
#27246 = CARTESIAN_POINT ( 'NONE',  ( 16.53943276465976808, -0.05219959533910856209, 88.74890960531436690 ) ) ;
#27247 = CARTESIAN_POINT ( 'NONE',  ( -16.46253265017146816, -9.564922557961047289, 54.16775706135234003 ) ) ;
#27248 = AXIS2_PLACEMENT_3D ( 'NONE', #90715, #185727, #152398 ) ;
#27249 = CARTESIAN_POINT ( 'NONE',  ( -19.05341960407611168, -5.049401038298163336, 26.45724293864769550 ) ) ;
#27250 = CARTESIAN_POINT ( 'NONE',  ( 19.02544592524343514, -5.153800228976328945, 88.54057627198102409 ) ) ;
#27251 = CARTESIAN_POINT ( 'NONE',  ( -19.05341960407611168, -5.049401038298163336, 81.45724293864769550 ) ) ;
#27252 = CARTESIAN_POINT ( 'NONE',  ( -12.06949235617756955, 12.14591786802309770, 100.6239096053143811 ) ) ;
#27253 = EDGE_LOOP ( 'NONE', ( #10796, #34522, #184016, #2962, #187341 ) ) ;
#27254 = CARTESIAN_POINT ( 'NONE',  ( -16.55341960407611168, -4.379528057220339221, 26.45724293864768839 ) ) ;
#27255 = CARTESIAN_POINT ( 'NONE',  ( 8.224510206698742110, 14.34966873604972548, 47.08442372801901854 ) ) ;
#27256 = CARTESIAN_POINT ( 'NONE',  ( 10.81492255796106328, -18.62759615963255655, 110.4177570613523756 ) ) ;
#27257 = CARTESIAN_POINT ( 'NONE',  ( 5.049401038298161559, -19.05341960407611168, 97.70724293864766707 ) ) ;
#27258 = CARTESIAN_POINT ( 'NONE',  ( -0.05219959533937732626, 21.53943276465977519, 27.50109039468567929 ) ) ;
#27259 = CARTESIAN_POINT ( 'NONE',  ( -5.153800228976328057, -19.02544592524343514, 47.29057627198102409 ) ) ;
#27260 = EDGE_CURVE ( 'NONE', #90645, #95772, #139430, .T. ) ;
#27261 = CARTESIAN_POINT ( 'NONE',  ( 16.53943276465976808, 0.05219959533934440121, 41.25109039468568284 ) ) ;
#27262 = CARTESIAN_POINT ( 'NONE',  ( -14.29746914071037622, -8.314922557961029526, 84.16775706135234714 ) ) ;
#27263 = CARTESIAN_POINT ( 'NONE',  ( -9.564922557961040184, 16.46253265017147172, 107.9177570613523471 ) ) ;
#27264 = CARTESIAN_POINT ( 'NONE',  ( -5.049401038298153566, 19.05341960407611168, 35.20724293864768839 ) ) ;
#27265 = CARTESIAN_POINT ( 'NONE',  ( 16.53943276465976808, -0.05219959533910856209, 93.74890960531436690 ) ) ;
#27266 = CARTESIAN_POINT ( 'NONE',  ( -0.05219959533907301413, -21.53943276465977519, 97.49890960531436690 ) ) ;
#27267 = CARTESIAN_POINT ( 'NONE',  ( 16.46253265017146816, 9.564922557961045513, 76.66775706135234714 ) ) ;
#27268 = CARTESIAN_POINT ( 'NONE',  ( -16.46253265017160317, 9.564922557960807481, 25.83224293864769194 ) ) ;
#27269 = CARTESIAN_POINT ( 'NONE',  ( 13.97604488694527802, 13.89961937509977652, 89.37390960531436690 ) ) ;
#27270 = CARTESIAN_POINT ( 'NONE',  ( -5.719274019375665041, -21.55341960407619695, 34.79275706135235424 ) ) ;
#27271 = CARTESIAN_POINT ( 'NONE',  ( -37.99626262588765968, 12.34573411038917179, -2.102157773949823394 ) ) ;
#27272 = CARTESIAN_POINT ( 'NONE',  ( -19.02544592524342804, 5.153800228976336051, 96.04057627198103830 ) ) ;
#27273 = VECTOR ( 'NONE', #87400, 1000.000000000000000 ) ;
#27274 = LINE ( 'NONE', #197115, #168112 ) ;
#27275 = CARTESIAN_POINT ( 'NONE',  ( 19.02544592524343514, -5.153800228976328945, 88.54057627198102409 ) ) ;
#27277 = CARTESIAN_POINT ( 'NONE',  ( -14.29746914071049879, 8.314922557960819915, 85.83224293864768129 ) ) ;
#27276 = CARTESIAN_POINT ( 'NONE',  ( 21.52544592524334988, 5.823673210054432836, 36.45942372801901143 ) ) ;
#27278 = CARTESIAN_POINT ( 'NONE',  ( -5.049401038298153566, 19.05341960407611168, 100.2072429386476955 ) ) ;
#27279 = CARTESIAN_POINT ( 'NONE',  ( 16.46253265017146816, 9.564922557961045513, 21.66775706135233648 ) ) ;
#27280 = MECHANICAL_DESIGN_GEOMETRIC_PRESENTATION_REPRESENTATION (  '', ( #7900 ), #130572 ) ;
#27282 =( BOUNDED_CURVE ( )  B_SPLINE_CURVE ( 2, ( #146964, #132792, #190477, #70125, #179325, #6431, #40789, #8452, #51950, #113610, #175304 ),
 .UNSPECIFIED., .F., .F. ) 
 B_SPLINE_CURVE_WITH_KNOTS ( ( 3, 2, 2, 2, 2, 3 ),
 ( 0.2000000000000029532, 0.2200000000000029710, 0.2400000000000029887, 0.2600000000000030065, 0.2800000000000030798, 0.3000000000000030420 ),
 .UNSPECIFIED. ) 
 CURVE ( )  GEOMETRIC_REPRESENTATION_ITEM ( )  RATIONAL_B_SPLINE_CURVE ( ( 0.9999999999999927836, 0.9510565162951607476, 1.000000000000000000, 0.9510565162951535312, 1.000000000000000000, 0.9510565162951535312, 1.000000000000000000, 0.9510565162951535312, 1.000000000000000000, 0.9510565162951460927, 1.000000000000007550 ) ) 
 REPRESENTATION_ITEM ( '' )  );
#27281 = CARTESIAN_POINT ( 'NONE',  ( -8.224510206698735004, -14.34966873604973081, 54.58442372801901143 ) ) ;
#27283 = CARTESIAN_POINT ( 'NONE',  ( 5.823673210054444382, -21.52544592524334988, 75.20942372801901854 ) ) ;
#27284 = CARTESIAN_POINT ( 'NONE',  ( -4.483927247898782831, 16.52544592524335698, 42.70942372801901854 ) ) ;
#27285 = CARTESIAN_POINT ( 'NONE',  ( 13.89961937509977652, -13.97604488694527269, 68.12390960531436690 ) ) ;
#27286 = CARTESIAN_POINT ( 'NONE',  ( -19.02544592524334988, -5.153800228976617603, 93.95942372801900433 ) ) ;
#27287 = CARTESIAN_POINT ( 'NONE',  ( 16.55341960407618274, -4.379528057220086978, 71.04275706135234714 ) ) ;
#27288 = CARTESIAN_POINT ( 'NONE',  ( -21.52544592524334988, -5.823673210054445271, 108.9594237280190185 ) ) ;
#27289 = CARTESIAN_POINT ( 'NONE',  ( -9.474510206698720793, -16.51473224551083518, 74.58442372801900433 ) ) ;
#27290 = CARTESIAN_POINT ( 'NONE',  ( -19.03943276465977164, 0.05219959533909376836, 61.24890960531436690 ) ) ;
#27291 = CARTESIAN_POINT ( 'NONE',  ( -5.719274019375978568, 21.55341960407610458, 90.20724293864770971 ) ) ;
#27293 = CARTESIAN_POINT ( 'NONE',  ( -19.02544592524334988, -5.153800228976617603, 93.95942372801900433 ) ) ;
#27292 = CARTESIAN_POINT ( 'NONE',  ( 12.06949235617757843, -12.14591786802309237, 83.12390960531436690 ) ) ;
#27294 = CARTESIAN_POINT ( 'NONE',  ( -19.35633801406908816, 5.499999999999577227, 79.13373818172760821 ) ) ;
#27295 = CARTESIAN_POINT ( 'NONE',  ( 19.03943276465977164, 0.05219959533936151252, 56.25109039468566863 ) ) ;
#27296 = CARTESIAN_POINT ( 'NONE',  ( 12.06949235617739724, 12.14591786802326823, 111.8760903946856615 ) ) ;
#27297 = CARTESIAN_POINT ( 'NONE',  ( -12.14591786802309592, -12.06949235617757132, 76.87390960531439532 ) ) ;
#27299 = CARTESIAN_POINT ( 'NONE',  ( -16.31925111598407341, 7.325300261831847237, 40.16424538967169866 ) ) ;
#27298 = CARTESIAN_POINT ( 'NONE',  ( 5.153800228976615827, -19.02544592524334988, 20.20942372801899722 ) ) ;
#27300 = CARTESIAN_POINT ( 'NONE',  ( -21.52544592524343514, 5.823673210054127303, 106.0405762719810525 ) ) ;
#27301 = CARTESIAN_POINT ( 'NONE',  ( -5.153800228976328057, -19.02544592524343514, 102.2905762719810383 ) ) ;
#27302 = CARTESIAN_POINT ( 'NONE',  ( 19.02544592524343514, -5.153800228976328945, 83.54057627198100988 ) ) ;
#27303 = CARTESIAN_POINT ( 'NONE',  ( 18.62759615963255655, 10.81492255796105972, 81.66775706135236135 ) ) ;
#27304 = CARTESIAN_POINT ( 'NONE',  ( 5.153800228976335163, 19.02544592524342804, 64.79057627198100988 ) ) ;
#27305 = CARTESIAN_POINT ( 'NONE',  ( -16.51473224551069308, -9.474510206698971260, 41.66557627198103120 ) ) ;
#27306 = CARTESIAN_POINT ( 'NONE',  ( -21.52544592524343514, 5.823673210054127303, 26.04057627198103475 ) ) ;
#27307 = CARTESIAN_POINT ( 'NONE',  ( -16.53943276465976808, 0.05219959533911058130, 86.24890960531436690 ) ) ;
#27308 = CARTESIAN_POINT ( 'NONE',  ( 0.05219959533909260263, 19.03943276465977164, 49.99890960531435979 ) ) ;
#27309 = CARTESIAN_POINT ( 'NONE',  ( 8.314922557960818139, 14.29746914071049879, 99.58224293864770971 ) ) ;
#27310 = CIRCLE ( 'NONE', #30597, 2.649999999999999467 ) ;
#27311 = CARTESIAN_POINT ( 'NONE',  ( 18.62759615963271287, -10.81492255796078972, 103.3322429386476955 ) ) ;
#27312 = CARTESIAN_POINT ( 'NONE',  ( 15.72974639402176855, 15.80617190586768217, 46.87609039468568994 ) ) ;
#27313 = CARTESIAN_POINT ( 'NONE',  ( 19.03943276465977164, -0.05219959533909143690, 33.74890960531435979 ) ) ;
#27314 = CARTESIAN_POINT ( 'NONE',  ( -14.34966873604972548, 8.224510206698743886, 58.33442372801901143 ) ) ;
#27315 = CARTESIAN_POINT ( 'NONE',  ( 21.53943276465977519, -0.05219959533907433946, 98.74890960531438111 ) ) ;
#27316 = CARTESIAN_POINT ( 'NONE',  ( -5.823673210054116645, -21.52544592524344225, 102.2905762719810383 ) ) ;
#27318 = CARTESIAN_POINT ( 'NONE',  ( -9.564922557960796823, -16.46253265017161027, 47.08224293864769550 ) ) ;
#27317 = CARTESIAN_POINT ( 'NONE',  ( -13.89961937509957401, -13.97604488694547875, 34.37609039468566863 ) ) ;
#27319 = CARTESIAN_POINT ( 'NONE',  ( -5.049401038298153566, 19.05341960407611168, 115.2072429386477097 ) ) ;
#27320 = CARTESIAN_POINT ( 'NONE',  ( 18.67979575497194134, -10.72451020669871369, 50.83442372801901143 ) ) ;
#27321 = CARTESIAN_POINT ( 'NONE',  ( -5.823673210054116645, -21.52544592524344225, 52.29057627198102409 ) ) ;
#27322 = CARTESIAN_POINT ( 'NONE',  ( -14.34966873604960291, -8.224510206698953496, 41.66557627198103120 ) ) ;
#27324 = CARTESIAN_POINT ( 'NONE',  ( -18.67979575497193778, 10.72451020669871902, 113.3344237280190328 ) ) ;
#27323 = CARTESIAN_POINT ( 'NONE',  ( -10.81492255796105439, 18.62759615963255655, 77.91775706135231871 ) ) ;
#27325 = CARTESIAN_POINT ( 'NONE',  ( 0.05219959533910956823, 16.53943276465976808, 84.99890960531436690 ) ) ;
#27326 = CARTESIAN_POINT ( 'NONE',  ( -19.02544592524334988, -5.153800228976617603, 43.95942372801899012 ) ) ;
#27327 = CARTESIAN_POINT ( 'NONE',  ( -14.34966873604972548, 8.224510206698743886, 103.3344237280190043 ) ) ;
#27328 = CARTESIAN_POINT ( 'NONE',  ( -10.81492255796105439, 18.62759615963255655, 72.91775706135234714 ) ) ;
#27329 = CARTESIAN_POINT ( 'NONE',  ( 16.51473224551069308, 9.474510206698969483, 59.16557627198102409 ) ) ;
#27330 = CARTESIAN_POINT ( 'NONE',  ( 13.97604488694548053, -13.89961937509957401, 40.62609039468564731 ) ) ;
#27331 = CARTESIAN_POINT ( 'NONE',  ( -18.62759615963270932, 10.81492255796079327, 35.83224293864768839 ) ) ;
#27332 = CARTESIAN_POINT ( 'NONE',  ( 21.55341960407619695, -5.719274019375665929, 31.04275706135234714 ) ) ;
#27333 = CARTESIAN_POINT ( 'NONE',  ( -10.81492255796078084, -18.62759615963271287, 87.08224293864769550 ) ) ;
#27334 = CARTESIAN_POINT ( 'NONE',  ( 16.51473224551083163, -9.474510206698727899, 90.83442372801900433 ) ) ;
#27335 = CARTESIAN_POINT ( 'NONE',  ( 12.06949235617739724, 12.14591786802326823, 51.87609039468568284 ) ) ;
#27337 = CARTESIAN_POINT ( 'NONE',  ( -0.05219959533907301413, -21.53943276465977519, 87.49890960531436690 ) ) ;
#27336 = CARTESIAN_POINT ( 'NONE',  ( 30.74264578624799782, 22.33583958711400541, -6.800000000000000711 ) ) ;
#27339 = CARTESIAN_POINT ( 'NONE',  ( -16.55341960407611168, -4.379528057220339221, 76.45724293864769550 ) ) ;
#27338 = CARTESIAN_POINT ( 'NONE',  ( -8.224510206698735004, -14.34966873604973081, 74.58442372801901854 ) ) ;
#27340 = CARTESIAN_POINT ( 'NONE',  ( -20.53360937444638168, -31.96911244174559386, -23.96531494639239313 ) ) ;
#27341 = CARTESIAN_POINT ( 'NONE',  ( 5.153800228976615827, -19.02544592524334988, 100.2094237280190043 ) ) ;
#27342 = CARTESIAN_POINT ( 'NONE',  ( -21.52544592524343514, 5.823673210054127303, 31.04057627198102409 ) ) ;
#27343 = CARTESIAN_POINT ( 'NONE',  ( 18.54787882382429487, -32.01089502393746500, -8.000000000000000000 ) ) ;
#27344 = CARTESIAN_POINT ( 'NONE',  ( -12.06949235617739369, -12.14591786802326823, 54.37609039468568994 ) ) ;
#27345 = CARTESIAN_POINT ( 'NONE',  ( 10.72451020669871369, 18.67979575497193778, 27.08442372801901854 ) ) ;
#27346 = CARTESIAN_POINT ( 'NONE',  ( -15.72974639402197994, 15.80617190586746368, 40.62390960531435269 ) ) ;
#27347 = CARTESIAN_POINT ( 'NONE',  ( -12.14591786802326823, 12.06949235617739902, 68.12609039468567573 ) ) ;
#27348 = CARTESIAN_POINT ( 'NONE',  ( -5.049401038298153566, 19.05341960407611168, 85.20724293864766707 ) ) ;
#27350 = CARTESIAN_POINT ( 'NONE',  ( -16.51473224551069308, -9.474510206698971260, 21.66557627198102765 ) ) ;
#27349 = CARTESIAN_POINT ( 'NONE',  ( -15.80617190586768217, 15.72974639402176855, 53.12609039468568284 ) ) ;
#27351 = CARTESIAN_POINT ( 'NONE',  ( -5.719274019375978568, 21.55341960407610458, 40.20724293864769550 ) ) ;
#27352 = VERTEX_POINT ( 'NONE', #184110 ) ;
#27353 = CARTESIAN_POINT ( 'NONE',  ( 19.05341960407617918, -5.049401038297876454, 41.04275706135233293 ) ) ;
#27354 = CARTESIAN_POINT ( 'NONE',  ( -14.34966873604972548, 8.224510206698743886, 58.33442372801901143 ) ) ;
#27355 = CARTESIAN_POINT ( 'NONE',  ( -19.03943276465977164, 0.05219959533909376836, 116.2489096053143669 ) ) ;
#27356 = ORIENTED_EDGE ( 'NONE', *, *, #79706, .F. ) ;
#27357 = CARTESIAN_POINT ( 'NONE',  ( -0.05219959533909027116, -19.03943276465977164, 92.49890960531436690 ) ) ;
#27358 = CARTESIAN_POINT ( 'NONE',  ( 4.379528057220092307, 16.55341960407617563, 102.2927570613523613 ) ) ;
#27359 = CARTESIAN_POINT ( 'NONE',  ( 17.79613651744293534, 24.49428055684532524, 141.5656553485623590 ) ) ;
#27360 = CARTESIAN_POINT ( 'NONE',  ( -14.34966873604960291, -8.224510206698953496, 101.6655762719810383 ) ) ;
#27361 = CARTESIAN_POINT ( 'NONE',  ( 15.80617190586746368, 15.72974639402197994, 39.37390960531436690 ) ) ;
#27362 = CARTESIAN_POINT ( 'NONE',  ( -16.46253265017160317, 9.564922557960807481, 35.83224293864768839 ) ) ;
#27363 = CARTESIAN_POINT ( 'NONE',  ( 12.06949235617739724, 12.14591786802326823, 81.87609039468568994 ) ) ;
#27364 = CARTESIAN_POINT ( 'NONE',  ( -21.53943276465977519, 0.05219959533907696930, 111.2489096053143669 ) ) ;
#27365 = CARTESIAN_POINT ( 'NONE',  ( 13.97604488694548053, -13.89961937509957401, 70.62609039468567573 ) ) ;
#27366 = CARTESIAN_POINT ( 'NONE',  ( 16.46253265017160672, -9.564922557960803928, 43.33224293864769550 ) ) ;
#27367 = FACE_OUTER_BOUND ( 'NONE', #29474, .T. ) ;
#27368 = CARTESIAN_POINT ( 'NONE',  ( 21.55341960407619695, -5.719274019375665929, 111.0427570613523613 ) ) ;
#27369 = CARTESIAN_POINT ( 'NONE',  ( 9.564922557960805705, 16.46253265017160317, 59.58224293864769550 ) ) ;
#27370 = CARTESIAN_POINT ( 'NONE',  ( 8.314922557961029526, -14.29746914071037800, 55.41775706135234714 ) ) ;
#27371 = CARTESIAN_POINT ( 'NONE',  ( -5.823673210054431948, 21.52544592524334988, 97.70942372801904696 ) ) ;
#27372 = CARTESIAN_POINT ( 'NONE',  ( 16.46253265017146816, 9.564922557961045513, 36.66775706135233293 ) ) ;
#27373 = CIRCLE ( 'NONE', #46676, 16.70000000000002061 ) ;
#27374 = CARTESIAN_POINT ( 'NONE',  ( 5.049401038297881783, 19.05341960407617563, 47.29275706135231161 ) ) ;
#27375 = ORIENTED_EDGE ( 'NONE', *, *, #136231, .F. ) ;
#27376 = CARTESIAN_POINT ( 'NONE',  ( -5.719274019375665041, -21.55341960407619695, 44.79275706135234714 ) ) ;
#27377 = CARTESIAN_POINT ( 'NONE',  ( -0.05219959533909027116, -19.03943276465977164, 22.49890960531436690 ) ) ;
#27378 = CARTESIAN_POINT ( 'NONE',  ( 19.02544592524334988, 5.153800228976608722, 46.45942372801899012 ) ) ;
#27379 = CARTESIAN_POINT ( 'NONE',  ( 9.564922557960805705, 16.46253265017160317, 104.5822429386476955 ) ) ;
#27380 = CARTESIAN_POINT ( 'NONE',  ( -5.049401038298153566, 19.05341960407611168, 80.20724293864769550 ) ) ;
#27381 = CARTESIAN_POINT ( 'NONE',  ( 16.55341960407611168, 4.379528057220329451, 38.95724293864768839 ) ) ;
#27382 = CARTESIAN_POINT ( 'NONE',  ( -0.05219959533907301413, -21.53943276465977519, 27.49890960531435269 ) ) ;
#27383 = CARTESIAN_POINT ( 'NONE',  ( -22.81625015709509441, -31.40387420917324590, -2.824999997268812901 ) ) ;
#27384 = CARTESIAN_POINT ( 'NONE',  ( 15.50000000000000178, 5.499999999999998224, 22.00000000000000711 ) ) ;
#27385 = CARTESIAN_POINT ( 'NONE',  ( 15.72974639402176855, 15.80617190586768217, 101.8760903946857042 ) ) ;
#27386 = CARTESIAN_POINT ( 'NONE',  ( 0.000000000000000000, -165.0000000000000000, 12.00000000000000355 ) ) ;
#27387 = CARTESIAN_POINT ( 'NONE',  ( -9.474510206698964154, 16.51473224551069663, 40.41557627198103120 ) ) ;
#27388 = FACE_OUTER_BOUND ( 'NONE', #124646, .T. ) ;
#27389 = LINE ( 'NONE', #181073, #94965 ) ;
#27390 = DIRECTION ( 'NONE',  ( 0.000000000000000000, 0.000000000000000000, -1.000000000000000000 ) ) ;
#27391 = CARTESIAN_POINT ( 'NONE',  ( -16.55341960407617563, 4.379528057220093196, 63.54275706135234003 ) ) ;
#27392 = CARTESIAN_POINT ( 'NONE',  ( -10.81492255796078084, -18.62759615963271287, 87.08224293864769550 ) ) ;
#27393 = AXIS2_PLACEMENT_3D ( 'NONE', #34112, #145255, #133092 ) ;
#27394 = CARTESIAN_POINT ( 'NONE',  ( 16.53943276465976808, -0.05219959533910856209, 38.74890960531435979 ) ) ;
#27396 = CARTESIAN_POINT ( 'NONE',  ( -5.049401038298153566, 19.05341960407611168, 110.2072429386476671 ) ) ;
#27395 = CARTESIAN_POINT ( 'NONE',  ( -0.05219959533909027116, -19.03943276465977164, 32.49890960531435979 ) ) ;
#27397 = CARTESIAN_POINT ( 'NONE',  ( -15.72974639402176322, -15.80617190586768395, 24.37609039468567573 ) ) ;
#27398 = CARTESIAN_POINT ( 'NONE',  ( -16.51473224551082808, 9.474510206698731452, 38.33442372801899722 ) ) ;
#27399 = CARTESIAN_POINT ( 'NONE',  ( 19.02544592524343514, -5.153800228976328945, 28.54057627198102409 ) ) ;
#27400 = CARTESIAN_POINT ( 'NONE',  ( 18.62759615963255655, 10.81492255796105972, 76.66775706135234714 ) ) ;
#27401 = CARTESIAN_POINT ( 'NONE',  ( 0.000000000000000000, 0.000000000000000000, -62.58071313852362039 ) ) ;
#27402 = CARTESIAN_POINT ( 'NONE',  ( -16.55341960407611168, -4.379528057220339221, 26.45724293864768839 ) ) ;
#27403 = CARTESIAN_POINT ( 'NONE',  ( -11.40812507854754720, -35.11059874428192273, -2.724999997268813257 ) ) ;
#27404 = CARTESIAN_POINT ( 'NONE',  ( 18.67979575497178502, 10.72451020669898547, 24.16557627198103120 ) ) ;
#27405 = CARTESIAN_POINT ( 'NONE',  ( 16.55341960407611168, 4.379528057220329451, 98.95724293864770971 ) ) ;
#27406 = CARTESIAN_POINT ( 'NONE',  ( -17.72560187377285246, -5.500000000000055955, 39.07814504131320632 ) ) ;
#27407 = CARTESIAN_POINT ( 'NONE',  ( -5.049401038298153566, 19.05341960407611168, 90.20724293864766707 ) ) ;
#27408 = CARTESIAN_POINT ( 'NONE',  ( 14.29746914071049879, -8.314922557960816363, 73.33224293864769550 ) ) ;
#27409 = CARTESIAN_POINT ( 'NONE',  ( 9.564922557961047289, -16.46253265017146816, 110.4177570613523471 ) ) ;
#27410 = CARTESIAN_POINT ( 'NONE',  ( 0.05219959533907565091, 21.53943276465977519, 64.99890960531435269 ) ) ;
#27411 = VERTEX_POINT ( 'NONE', #93069 ) ;
#27412 = CARTESIAN_POINT ( 'NONE',  ( 9.474510206698971260, -16.51473224551069308, 37.91557627198102409 ) ) ;
#27414 = CARTESIAN_POINT ( 'NONE',  ( 21.52544592524344225, -5.823673210054117533, 93.54057627198103830 ) ) ;
#27413 = CARTESIAN_POINT ( 'NONE',  ( 19.02544592524343514, -5.153800228976328945, 88.54057627198102409 ) ) ;
#27416 = CARTESIAN_POINT ( 'NONE',  ( 9.564922557960805705, 16.46253265017160317, 89.58224293864769550 ) ) ;
#27415 = CARTESIAN_POINT ( 'NONE',  ( -14.34966873604972548, 8.224510206698743886, 103.3344237280190043 ) ) ;
#27417 = CARTESIAN_POINT ( 'NONE',  ( 16.46253265017146816, 9.564922557961045513, 86.66775706135233293 ) ) ;
#27418 = CARTESIAN_POINT ( 'NONE',  ( -18.62759615963255300, -10.81492255796106328, 94.16775706135237556 ) ) ;
#27419 = CARTESIAN_POINT ( 'NONE',  ( 21.53943276465977519, -0.05219959533907433946, 78.74890960531436690 ) ) ;
#27420 = CARTESIAN_POINT ( 'NONE',  ( -21.53943276465977519, 0.05219959533907696930, 31.24890960531435979 ) ) ;
#27421 = CIRCLE ( 'NONE', #4840, 27.29906736325805028 ) ;
#27422 = CARTESIAN_POINT ( 'NONE',  ( 16.51473224551069308, 9.474510206698969483, 54.16557627198103120 ) ) ;
#27423 = CARTESIAN_POINT ( 'NONE',  ( -16.55341960407611168, -4.379528057220339221, 21.45724293864769550 ) ) ;
#27424 = CARTESIAN_POINT ( 'NONE',  ( 9.564922557960805705, 16.46253265017160317, 69.58224293864770971 ) ) ;
#27425 = DIRECTION ( 'NONE',  ( 0.000000000000000000, 0.000000000000000000, -1.000000000000000000 ) ) ;
#27426 = CARTESIAN_POINT ( 'NONE',  ( -21.55341960407619339, 5.719274019375674811, 113.5427570613523756 ) ) ;
#27427 = CARTESIAN_POINT ( 'NONE',  ( 4.483927247898545687, 16.52544592524342804, 69.79057627198102409 ) ) ;
#27428 = MECHANICAL_DESIGN_GEOMETRIC_PRESENTATION_REPRESENTATION (  '', ( #79052 ), #111386 ) ;
#27429 = CARTESIAN_POINT ( 'NONE',  ( -10.81492255796078084, -18.62759615963271287, 107.0822429386476955 ) ) ;
#27430 = CARTESIAN_POINT ( 'NONE',  ( 0.05219959533907565091, 21.53943276465977519, 109.9989096053143527 ) ) ;
#27431 = DIRECTION ( 'NONE',  ( 1.000000000000000000, 0.000000000000000000, 0.000000000000000000 ) ) ;
#27433 = EDGE_CURVE ( 'NONE', #96037, #182127, #14248, .T. ) ;
#27432 = CARTESIAN_POINT ( 'NONE',  ( 10.81492255796078972, 18.62759615963270932, 59.58224293864770260 ) ) ;
#27434 = CARTESIAN_POINT ( 'NONE',  ( -4.379528057220086978, -16.55341960407618274, 94.79275706135234714 ) ) ;
#27435 = CARTESIAN_POINT ( 'NONE',  ( 8.314922557960818139, 14.29746914071049879, 109.5822429386476955 ) ) ;
#27436 = CARTESIAN_POINT ( 'NONE',  ( 5.049401038298161559, -19.05341960407611168, 62.70724293864769550 ) ) ;
#27437 = SURFACE_SIDE_STYLE ('',( #88078 ) ) ;
#27438 = CARTESIAN_POINT ( 'NONE',  ( 4.483927247898545687, 16.52544592524342804, 29.79057627198102409 ) ) ;
#27439 = EDGE_LOOP ( 'NONE', ( #5, #177531, #143908, #11617 ) ) ;
#27440 = CARTESIAN_POINT ( 'NONE',  ( 15.72974639402176855, 15.80617190586768217, 41.87609039468568284 ) ) ;
#27441 = CARTESIAN_POINT ( 'NONE',  ( 19.03943276465977164, -0.05219959533909143690, 103.7489096053143669 ) ) ;
#27442 = CARTESIAN_POINT ( 'NONE',  ( 5.823673210054444382, -21.52544592524334988, 75.20942372801901854 ) ) ;
#27443 = CARTESIAN_POINT ( 'NONE',  ( -19.02544592524342804, 5.153800228976336051, 26.04057627198103120 ) ) ;
#27444 = CARTESIAN_POINT ( 'NONE',  ( 9.564922557960805705, 16.46253265017160317, 39.58224293864768839 ) ) ;
#27445 = ORIENTED_EDGE ( 'NONE', *, *, #61925, .F. ) ;
#27446 = CARTESIAN_POINT ( 'NONE',  ( -5.719274019375665041, -21.55341960407619695, 79.79275706135236135 ) ) ;
#27447 = CARTESIAN_POINT ( 'NONE',  ( -16.53943276465976808, -0.05219959533934237506, 43.75109039468568284 ) ) ;
#27448 = CARTESIAN_POINT ( 'NONE',  ( -10.81492255796105439, 18.62759615963255655, 67.91775706135234714 ) ) ;
#27449 = CARTESIAN_POINT ( 'NONE',  ( 16.51473224551069308, 9.474510206698969483, 99.16557627198102409 ) ) ;
#27450 = CARTESIAN_POINT ( 'NONE',  ( 16.51473224551083163, -9.474510206698727899, 75.83442372801900433 ) ) ;
#27451 = CARTESIAN_POINT ( 'NONE',  ( -21.52544592524334988, -5.823673210054445271, 53.95942372801900433 ) ) ;
#27452 = CARTESIAN_POINT ( 'NONE',  ( 0.05219959533934541429, -16.53943276465976808, 25.00109039468567218 ) ) ;
#27453 = CARTESIAN_POINT ( 'NONE',  ( -9.474510206698720793, -16.51473224551083518, 74.58442372801900433 ) ) ;
#27454 = CARTESIAN_POINT ( 'NONE',  ( -5.153800228976328057, -19.02544592524343514, 57.29057627198103120 ) ) ;
#27455 = CARTESIAN_POINT ( 'NONE',  ( -13.97604488694547697, 13.89961937509957934, 83.12609039468564731 ) ) ;
#27456 = AXIS2_PLACEMENT_3D ( 'NONE', #158408, #21894, #160405 ) ;
#27457 = CARTESIAN_POINT ( 'NONE',  ( -16.53943276465976808, 0.05219959533911058130, 26.24890960531435624 ) ) ;
#27458 = CARTESIAN_POINT ( 'NONE',  ( -13.97604488694547697, 13.89961937509957934, 93.12609039468566152 ) ) ;
#27459 = CARTESIAN_POINT ( 'NONE',  ( 8.224510206698953496, -14.34966873604960469, 37.91557627198102409 ) ) ;
#27460 = CARTESIAN_POINT ( 'NONE',  ( 9.564922557961047289, -16.46253265017146816, 60.41775706135233293 ) ) ;
#27461 = CARTESIAN_POINT ( 'NONE',  ( -16.52544592524335698, -4.483927247898792601, 43.95942372801902565 ) ) ;
#27462 = CARTESIAN_POINT ( 'NONE',  ( -19.02544592524334988, -5.153800228976617603, 28.95942372801900433 ) ) ;
#27463 = CARTESIAN_POINT ( 'NONE',  ( 16.46253265017160672, -9.564922557960803928, 43.33224293864769550 ) ) ;
#27464 = CARTESIAN_POINT ( 'NONE',  ( 18.87580814761075132, -5.500000000000047073, 73.37172394265759579 ) ) ;
#27465 = CARTESIAN_POINT ( 'NONE',  ( -0.05219959533934338120, 16.53943276465976808, 47.50109039468568994 ) ) ;
#27466 = CARTESIAN_POINT ( 'NONE',  ( 28.79475375365586132, 2.781246896534039337E-14, 155.0000000000000000 ) ) ;
#27467 = CARTESIAN_POINT ( 'NONE',  ( -22.44159573604010305, 16.30477369853692338, 146.6750000027311671 ) ) ;
#27468 = CARTESIAN_POINT ( 'NONE',  ( 19.02544592524343514, -5.153800228976328945, 98.54057627198100988 ) ) ;
#27469 = CARTESIAN_POINT ( 'NONE',  ( -16.46253265017146816, -9.564922557961047289, 84.16775706135233293 ) ) ;
#27470 = VERTEX_POINT ( 'NONE', #137595 ) ;
#27471 = CARTESIAN_POINT ( 'NONE',  ( 5.153800228976615827, -19.02544592524334988, 100.2094237280190043 ) ) ;
#27472 = CARTESIAN_POINT ( 'NONE',  ( 21.53943276465977519, -0.05219959533907433946, 28.74890960531435624 ) ) ;
#27474 = CARTESIAN_POINT ( 'NONE',  ( 19.05341960407617918, -5.049401038297876454, 106.0427570613523471 ) ) ;
#27473 = CARTESIAN_POINT ( 'NONE',  ( -5.823673210054431948, 21.52544592524334988, 107.7094237280190328 ) ) ;
#27475 = CARTESIAN_POINT ( 'NONE',  ( -16.53943276465976808, 0.05219959533911058130, 111.2489096053143669 ) ) ;
#27476 = CARTESIAN_POINT ( 'NONE',  ( -19.03943276465977164, 0.05219959533909376836, 36.24890960531436690 ) ) ;
#27477 = CARTESIAN_POINT ( 'NONE',  ( -18.67979575497178146, -10.72451020669898902, 71.66557627198100988 ) ) ;
#27478 = CARTESIAN_POINT ( 'NONE',  ( 9.474510206698971260, -16.51473224551069308, 37.91557627198102409 ) ) ;
#27479 = CARTESIAN_POINT ( 'NONE',  ( 5.049401038297881783, 19.05341960407617918, 47.29275706135232582 ) ) ;
#27480 = CARTESIAN_POINT ( 'NONE',  ( 16.51473224551083163, -9.474510206698727899, 70.83442372801900433 ) ) ;
#27481 = CARTESIAN_POINT ( 'NONE',  ( -0.05219959533910754901, -16.53943276465976808, 47.49890960531435979 ) ) ;
#27482 = CARTESIAN_POINT ( 'NONE',  ( 5.719274019375991003, -21.55341960407610458, 32.70724293864770260 ) ) ;
#27483 = CARTESIAN_POINT ( 'NONE',  ( 18.62759615963255655, 10.81492255796105972, 86.66775706135234714 ) ) ;
#27484 = CARTESIAN_POINT ( 'NONE',  ( -10.72451020669898014, 18.67979575497178502, 85.41557627198102409 ) ) ;
#27485 = CARTESIAN_POINT ( 'NONE',  ( 21.52544592524334988, 5.823673210054432836, 56.45942372801902565 ) ) ;
#27486 = CARTESIAN_POINT ( 'NONE',  ( -10.81492255796105439, 18.62759615963255655, 57.91775706135234714 ) ) ;
#27487 = CARTESIAN_POINT ( 'NONE',  ( -19.05341960407611168, -5.049401038298163336, 96.45724293864769550 ) ) ;
#27489 = CARTESIAN_POINT ( 'NONE',  ( 10.81492255796106328, -18.62759615963255655, 60.41775706135235424 ) ) ;
#27488 = CARTESIAN_POINT ( 'NONE',  ( -16.55341960407617563, 4.379528057220093196, 93.54275706135234714 ) ) ;
#27490 = CARTESIAN_POINT ( 'NONE',  ( -16.46253265017160317, 9.564922557960807481, 55.83224293864769550 ) ) ;
#27491 = CARTESIAN_POINT ( 'NONE',  ( 9.474510206698971260, -16.51473224551069308, 27.91557627198103120 ) ) ;
#27492 = CARTESIAN_POINT ( 'NONE',  ( -16.51473224551069308, -9.474510206698971260, 51.66557627198102409 ) ) ;
#27493 = AXIS2_PLACEMENT_3D ( 'NONE', #111358, #20336, #63870 ) ;
#27494 = CARTESIAN_POINT ( 'NONE',  ( 16.52544592524342804, -4.483927247898539470, 63.54057627198103830 ) ) ;
#27495 = CARTESIAN_POINT ( 'NONE',  ( 12.14591786802309770, 12.06949235617756955, 34.37390960531435979 ) ) ;
#27496 = CARTESIAN_POINT ( 'NONE',  ( 5.719274019375991003, -21.55341960407610458, 42.70724293864770260 ) ) ;
#27497 = CARTESIAN_POINT ( 'NONE',  ( 19.03943276465977164, -0.05219959533909143690, 53.74890960531436690 ) ) ;
#27498 = CARTESIAN_POINT ( 'NONE',  ( 15.80617190586746368, 15.72974639402197994, 64.37390960531435269 ) ) ;
#27499 = CARTESIAN_POINT ( 'NONE',  ( 19.02544592524334988, 5.153800228976608722, 51.45942372801900433 ) ) ;
#27501 = CARTESIAN_POINT ( 'NONE',  ( 12.14591786802309770, 12.06949235617756955, 49.37390960531436690 ) ) ;
#27500 = DIRECTION ( 'NONE',  ( -1.000000000000000000, -0.000000000000000000, -0.000000000000000000 ) ) ;
#27502 = CARTESIAN_POINT ( 'NONE',  ( 21.52544592524344225, -5.823673210054117533, 33.54057627198102409 ) ) ;
#27503 = EDGE_LOOP ( 'NONE', ( #118449, #100255, #111070, #174329, #1293, #112415, #32832, #37106 ) ) ;
#27504 = ORIENTED_EDGE ( 'NONE', *, *, #125615, .F. ) ;
#27505 = CARTESIAN_POINT ( 'NONE',  ( 16.81555441253553340, 7.025013491695490941, 101.8631455466574494 ) ) ;
#27506 = CARTESIAN_POINT ( 'NONE',  ( 14.29746914071037800, 8.314922557961029526, 91.66775706135234714 ) ) ;
#27507 = EDGE_CURVE ( 'NONE', #155869, #16989, #146558, .T. ) ;
#27508 = CARTESIAN_POINT ( 'NONE',  ( -13.89961937509957401, -13.97604488694547875, 69.37609039468564731 ) ) ;
#27509 = CARTESIAN_POINT ( 'NONE',  ( 16.55341960407611168, 4.379528057220329451, 48.95724293864770971 ) ) ;
#27510 = CARTESIAN_POINT ( 'NONE',  ( 17.44279575226827816, -5.990770900252369913, 53.33557567514319686 ) ) ;
#27511 = CARTESIAN_POINT ( 'NONE',  ( -12.14591786802309592, -12.06949235617757132, 36.87390960531435979 ) ) ;
#27512 = CARTESIAN_POINT ( 'NONE',  ( 13.97604488694527802, 13.89961937509977652, 49.37390960531434558 ) ) ;
#27513 = CARTESIAN_POINT ( 'NONE',  ( 19.05341960407611168, 5.049401038298154454, 68.95724293864769550 ) ) ;
#27514 = CARTESIAN_POINT ( 'NONE',  ( -19.02544592524342804, 5.153800228976336051, 36.04057627198100988 ) ) ;
#27515 = CARTESIAN_POINT ( 'NONE',  ( -21.53943276465977519, -0.05219959533937600094, 48.75109039468568284 ) ) ;
#27516 = CARTESIAN_POINT ( 'NONE',  ( -0.05219959533909027116, -19.03943276465977164, 72.49890960531435269 ) ) ;
#27517 = CARTESIAN_POINT ( 'NONE',  ( 9.474510206698971260, -16.51473224551069308, 22.91557627198102765 ) ) ;
#27518 = CARTESIAN_POINT ( 'NONE',  ( 19.05341960407611168, 5.049401038298154454, 53.95724293864770260 ) ) ;
#27519 = CARTESIAN_POINT ( 'NONE',  ( -21.55341960407610458, -5.719274019375992779, 46.45724293864769550 ) ) ;
#27520 = CARTESIAN_POINT ( 'NONE',  ( -9.564922557960796823, -16.46253265017161027, 37.08224293864768839 ) ) ;
#27521 = CARTESIAN_POINT ( 'NONE',  ( -0.05219959533907301413, -21.53943276465977519, 37.49890960531436690 ) ) ;
#27522 = CARTESIAN_POINT ( 'NONE',  ( 16.52544592524335698, 4.483927247898782831, 106.4594237280190328 ) ) ;
#27523 = CARTESIAN_POINT ( 'NONE',  ( -18.67979575497193778, 10.72451020669871902, 113.3344237280190328 ) ) ;
#27525 = CARTESIAN_POINT ( 'NONE',  ( -8.224510206698735004, -14.34966873604973081, 74.58442372801901854 ) ) ;
#27524 = CARTESIAN_POINT ( 'NONE',  ( -14.34966873604972548, 8.224510206698743886, 48.33442372801902565 ) ) ;
#27526 = DIRECTION ( 'NONE',  ( 0.000000000000000000, 0.1045284632676537068, 0.9945218953682734009 ) ) ;
#27527 = CARTESIAN_POINT ( 'NONE',  ( -12.14591786802326823, 12.06949235617739902, 63.12609039468568994 ) ) ;
#27528 = CARTESIAN_POINT ( 'NONE',  ( -4.483927247898782831, 16.52544592524335698, 37.70942372801900433 ) ) ;
#27529 = CARTESIAN_POINT ( 'NONE',  ( 16.46253265017160672, -9.564922557960803928, 103.3322429386476955 ) ) ;
#27530 = CARTESIAN_POINT ( 'NONE',  ( -16.53943276465976808, -0.05219959533934237506, 28.75109039468567929 ) ) ;
#27531 = CARTESIAN_POINT ( 'NONE',  ( 13.97604488694527802, 13.89961937509977652, 29.37390960531435979 ) ) ;
#27532 = CARTESIAN_POINT ( 'NONE',  ( 10.81492255796106328, -18.62759615963255655, 30.41775706135234358 ) ) ;
#27533 = CARTESIAN_POINT ( 'NONE',  ( -16.52544592524335698, -4.483927247898792601, 33.95942372801901143 ) ) ;
#27534 = CARTESIAN_POINT ( 'NONE',  ( 14.34966873604972726, -8.224510206698740333, 95.83442372801903275 ) ) ;
#27535 = DIRECTION ( 'NONE',  ( 0.000000000000000000, 0.000000000000000000, -1.000000000000000000 ) ) ;
#27536 = CARTESIAN_POINT ( 'NONE',  ( -15.72974639402176322, -15.80617190586768395, 99.37609039468568994 ) ) ;
#27537 = CARTESIAN_POINT ( 'NONE',  ( -19.03943276465977164, -0.05219959533935918106, 93.75109039468566152 ) ) ;
#27538 = CARTESIAN_POINT ( 'NONE',  ( 12.06949235617757843, -12.14591786802309237, 63.12390960531435979 ) ) ;
#27539 = CARTESIAN_POINT ( 'NONE',  ( 5.049401038298161559, -19.05341960407611168, 22.70724293864769194 ) ) ;
#27541 = CARTESIAN_POINT ( 'NONE',  ( 16.79531203550645913, 7.028104445595632299, 78.75244988220443076 ) ) ;
#27540 = CARTESIAN_POINT ( 'NONE',  ( 13.89961937509957401, 13.97604488694547697, 61.87609039468566863 ) ) ;
#27542 = CARTESIAN_POINT ( 'NONE',  ( -18.62759615963255300, -10.81492255796106328, 69.16775706135234714 ) ) ;
#27543 = CARTESIAN_POINT ( 'NONE',  ( 8.314922557961029526, -14.29746914071037800, 25.41775706135235779 ) ) ;
#27544 = DIRECTION ( 'NONE',  ( 1.000000000000000000, 0.000000000000000000, 3.709348145883536076E-20 ) ) ;
#27545 = CARTESIAN_POINT ( 'NONE',  ( 21.53943276465977519, -0.05219959533907433946, 28.74890960531435624 ) ) ;
#27546 = CARTESIAN_POINT ( 'NONE',  ( -10.81492255796078084, -18.62759615963271287, 72.08224293864769550 ) ) ;
#27547 = CARTESIAN_POINT ( 'NONE',  ( -19.03943276465977164, -0.05219959533935918106, 103.7510903946856757 ) ) ;
#27548 = CARTESIAN_POINT ( 'NONE',  ( 19.05341960407611168, 5.049401038298154454, 103.9572429386476671 ) ) ;
#27549 = CARTESIAN_POINT ( 'NONE',  ( -25.85392304583292855, 7.514126903508655531, 173.7688241862488212 ) ) ;
#27550 = CARTESIAN_POINT ( 'NONE',  ( 19.02544592524343514, -5.153800228976328945, 28.54057627198102409 ) ) ;
#27551 = CARTESIAN_POINT ( 'NONE',  ( -5.823673210054431948, 21.52544592524334988, 107.7094237280190328 ) ) ;
#27552 = CARTESIAN_POINT ( 'NONE',  ( -13.97604488694527625, -13.89961937509977652, 46.87390960531435979 ) ) ;
#27553 = COLOUR_RGB ( '', 0.66274510, 0.83137255, 0.94901961) ;
#27554 = CARTESIAN_POINT ( 'NONE',  ( 0.05219959533937995610, -21.53943276465977519, 50.00109039468568994 ) ) ;
#27555 = CARTESIAN_POINT ( 'NONE',  ( 21.52544592524334988, 5.823673210054432836, 91.45942372801901854 ) ) ;
#27556 = CARTESIAN_POINT ( 'NONE',  ( -12.14591786802326823, 12.06949235617739902, 103.1260903946856757 ) ) ;
#27557 = CARTESIAN_POINT ( 'NONE',  ( 0.05219959533909260263, 19.03943276465977164, 79.99890960531436690 ) ) ;
#27558 = CARTESIAN_POINT ( 'NONE',  ( 15.80617190586769283, -15.72974639402175789, 40.62609039468567573 ) ) ;
#27559 = CARTESIAN_POINT ( 'NONE',  ( -10.72451020669870658, -18.67979575497194134, 54.58442372801901143 ) ) ;
#27561 = CARTESIAN_POINT ( 'NONE',  ( 19.05341960407611168, 5.049401038298154454, 98.95724293864766707 ) ) ;
#27560 = CARTESIAN_POINT ( 'NONE',  ( -5.049401038297874678, -19.05341960407617918, 74.79275706135231871 ) ) ;
#27562 = CARTESIAN_POINT ( 'NONE',  ( -14.29746914071049879, 8.314922557960819915, 100.8322429386477097 ) ) ;
#27563 = CARTESIAN_POINT ( 'NONE',  ( -15.72974639402197994, 15.80617190586746368, 100.6239096053143811 ) ) ;
#27564 = CARTESIAN_POINT ( 'NONE',  ( -16.53943276465976808, 0.05219959533911058130, 71.24890960531435269 ) ) ;
#27565 = CARTESIAN_POINT ( 'NONE',  ( 5.153800228976615827, -19.02544592524334988, 25.20942372801900433 ) ) ;
#27566 = CARTESIAN_POINT ( 'NONE',  ( -14.29746914071049879, 8.314922557960819915, 100.8322429386477097 ) ) ;
#27567 = CARTESIAN_POINT ( 'NONE',  ( 9.564922557960805705, 16.46253265017160317, 49.58224293864770260 ) ) ;
#27569 = AXIS2_PLACEMENT_3D ( 'NONE', #47660, #140643, #199350 ) ;
#27568 = CARTESIAN_POINT ( 'NONE',  ( 5.153800228976615827, -19.02544592524334988, 90.20942372801900433 ) ) ;
#27570 = CARTESIAN_POINT ( 'NONE',  ( 8.224510206698953496, -14.34966873604960469, 47.91557627198102409 ) ) ;
#27571 = CARTESIAN_POINT ( 'NONE',  ( -9.474510206698720793, -16.51473224551083518, 19.58442372801899722 ) ) ;
#27572 = CARTESIAN_POINT ( 'NONE',  ( 5.049401038298161559, -19.05341960407611168, 102.7072429386476955 ) ) ;
#27573 = CARTESIAN_POINT ( 'NONE',  ( -19.05341960407617563, 5.049401038297882671, 73.54275706135233293 ) ) ;
#27574 = CARTESIAN_POINT ( 'NONE',  ( 21.53943276465977519, -0.05219959533907433946, 78.74890960531436690 ) ) ;
#27575 = VECTOR ( 'NONE', #139496, 999.9999999999998863 ) ;
#27576 = CARTESIAN_POINT ( 'NONE',  ( 0.05219959533937995610, -21.53943276465977519, 35.00109039468568284 ) ) ;
#27577 = CARTESIAN_POINT ( 'NONE',  ( 16.55341960407618274, -4.379528057220086978, 26.04275706135235779 ) ) ;
#27578 = CARTESIAN_POINT ( 'NONE',  ( -14.34966873604972548, 8.224510206698743886, 93.33442372801901854 ) ) ;
#27580 = CARTESIAN_POINT ( 'NONE',  ( 21.55341960407619695, -5.719274019375665929, 31.04275706135234714 ) ) ;
#27579 = CARTESIAN_POINT ( 'NONE',  ( 17.13100169013300089, 6.664070546373172199, 61.73210164300152059 ) ) ;
#27581 = CARTESIAN_POINT ( 'NONE',  ( 14.29746914071049879, -8.314922557960816363, 113.3322429386476955 ) ) ;
#27582 = CARTESIAN_POINT ( 'NONE',  ( -23.48529157249600985, 32.32473071737754111, -10.04999999453762705 ) ) ;
#27583 = CARTESIAN_POINT ( 'NONE',  ( -14.34966873604972548, 8.224510206698743886, 68.33442372801900433 ) ) ;
#27584 = CARTESIAN_POINT ( 'NONE',  ( 8.314922557960818139, 14.29746914071049879, 94.58224293864769550 ) ) ;
#27585 = CARTESIAN_POINT ( 'NONE',  ( 21.52544592524344225, -5.823673210054117533, 78.54057627198103830 ) ) ;
#27586 = CARTESIAN_POINT ( 'NONE',  ( 16.52544592524342804, -4.483927247898539470, 23.54057627198102765 ) ) ;
#27587 = CARTESIAN_POINT ( 'NONE',  ( -8.224510206698735004, -14.34966873604973081, 54.58442372801901143 ) ) ;
#27588 = CARTESIAN_POINT ( 'NONE',  ( -16.51473224551069308, -9.474510206698971260, 51.66557627198102409 ) ) ;
#27589 = CARTESIAN_POINT ( 'NONE',  ( 16.53943276465976808, 0.05219959533934440121, 91.25109039468568994 ) ) ;
#27590 = CARTESIAN_POINT ( 'NONE',  ( -19.02544592524334988, -5.153800228976617603, 88.95942372801897591 ) ) ;
#27591 = CARTESIAN_POINT ( 'NONE',  ( -15.80617190586745835, -15.72974639402198527, 91.87390960531436690 ) ) ;
#27592 = CARTESIAN_POINT ( 'NONE',  ( -14.29746914071037622, -8.314922557961029526, 109.1677570613523613 ) ) ;
#27593 = ORIENTED_EDGE ( 'NONE', *, *, #6630, .F. ) ;
#27594 = CARTESIAN_POINT ( 'NONE',  ( 26.77293948118378353, 6.014770499723010033, 169.2063755025576199 ) ) ;
#27595 = CARTESIAN_POINT ( 'NONE',  ( 5.719274019375991003, -21.55341960407610458, 57.70724293864770260 ) ) ;
#27596 = ORIENTED_EDGE ( 'NONE', *, *, #126710, .F. ) ;
#27597 = CARTESIAN_POINT ( 'NONE',  ( -12.14591786802326823, 12.06949235617739902, 88.12609039468570415 ) ) ;
#27598 = EDGE_LOOP ( 'NONE', ( #27020, #125207, #145675, #94863 ) ) ;
#27599 = CARTESIAN_POINT ( 'NONE',  ( 15.80617190586746368, 15.72974639402197994, 24.37390960531435979 ) ) ;
#27600 = CARTESIAN_POINT ( 'NONE',  ( 17.50000000000000711, 5.068104630630374530, 106.7718159465997303 ) ) ;
#27601 = CARTESIAN_POINT ( 'NONE',  ( 0.05219959533907565091, 21.53943276465977519, 79.99890960531435269 ) ) ;
#27602 = CARTESIAN_POINT ( 'NONE',  ( 16.53943276465976808, -0.05219959533910856209, 28.74890960531435624 ) ) ;
#27603 = CARTESIAN_POINT ( 'NONE',  ( 16.55341960407618274, -4.379528057220086978, 26.04275706135235779 ) ) ;
#27604 = CARTESIAN_POINT ( 'NONE',  ( -9.474510206698964154, 16.51473224551069663, 40.41557627198103120 ) ) ;
#27605 = CARTESIAN_POINT ( 'NONE',  ( -8.224510206698735004, -14.34966873604973081, 29.58442372801901854 ) ) ;
#27606 = CARTESIAN_POINT ( 'NONE',  ( 9.474510206698971260, -16.51473224551069308, 57.91557627198103120 ) ) ;
#27607 = CARTESIAN_POINT ( 'NONE',  ( 28.82186960331498327, 9.364793116373570925, 147.0999999999999943 ) ) ;
#27608 = CARTESIAN_POINT ( 'NONE',  ( -9.474510206698964154, 16.51473224551069663, 105.4155762719810383 ) ) ;
#27609 = CARTESIAN_POINT ( 'NONE',  ( 5.049401038298161559, -19.05341960407611168, 107.7072429386476955 ) ) ;
#27610 = CARTESIAN_POINT ( 'NONE',  ( 8.224510206698742110, 14.34966873604972548, 87.08442372801901854 ) ) ;
#27611 = CARTESIAN_POINT ( 'NONE',  ( -9.474510206698720793, -16.51473224551083518, 89.58442372801900433 ) ) ;
#27612 = CARTESIAN_POINT ( 'NONE',  ( 0.05219959533936267826, -19.03943276465977164, 35.00109039468566863 ) ) ;
#27613 = CARTESIAN_POINT ( 'NONE',  ( -15.72974639402197994, 15.80617190586746368, 70.62390960531436690 ) ) ;
#27614 = ADVANCED_FACE ( 'NONE', ( #7028 ), #58763, .T. ) ;
#27615 = CARTESIAN_POINT ( 'NONE',  ( 8.224510206698742110, 14.34966873604972548, 97.08442372801904696 ) ) ;
#27616 = CARTESIAN_POINT ( 'NONE',  ( 15.80617190586746368, 15.72974639402197994, 39.37390960531436690 ) ) ;
#27617 = CARTESIAN_POINT ( 'NONE',  ( 13.89961937509957401, 13.97604488694547697, 86.87609039468567573 ) ) ;
#27618 = CARTESIAN_POINT ( 'NONE',  ( -19.02544592524342804, 5.153800228976336051, 46.04057627198101699 ) ) ;
#27619 = CARTESIAN_POINT ( 'NONE',  ( 19.03943276465977164, -0.05219959533909143690, 88.74890960531436690 ) ) ;
#27620 = CARTESIAN_POINT ( 'NONE',  ( -10.72451020669870658, -18.67979575497194134, 64.58442372801900433 ) ) ;
#27621 = CARTESIAN_POINT ( 'NONE',  ( -19.03943276465977164, 0.05219959533909376836, 56.24890960531435979 ) ) ;
#27622 = CARTESIAN_POINT ( 'NONE',  ( 8.224510206698953496, -14.34966873604960469, 97.91557627198103830 ) ) ;
#27623 = CARTESIAN_POINT ( 'NONE',  ( -17.05587630539786659, -6.762274262135685277, 84.25819690962686082 ) ) ;
#27624 = CARTESIAN_POINT ( 'NONE',  ( 16.55341960407611168, 4.379528057220329451, 73.95724293864769550 ) ) ;
#27625 = CARTESIAN_POINT ( 'NONE',  ( 5.719274019375991003, -21.55341960407610458, 67.70724293864769550 ) ) ;
#27626 = CARTESIAN_POINT ( 'NONE',  ( 19.02544592524334988, 5.153800228976608722, 96.45942372801897591 ) ) ;
#27627 = DIRECTION ( 'NONE',  ( 1.000000000000000000, 0.000000000000000000, 0.000000000000000000 ) ) ;
#27628 = CARTESIAN_POINT ( 'NONE',  ( -13.97604488694527625, -13.89961937509977652, 61.87390960531435979 ) ) ;
#27629 = DIRECTION ( 'NONE',  ( 0.000000000000000000, -0.5601916035752871892, -0.8283630648959117160 ) ) ;
#27631 = CARTESIAN_POINT ( 'NONE',  ( -19.03943276465977164, 0.05219959533909376836, 81.24890960531436690 ) ) ;
#27630 = CARTESIAN_POINT ( 'NONE',  ( -5.049401038298153566, 19.05341960407611168, 80.20724293864769550 ) ) ;
#27632 = CARTESIAN_POINT ( 'NONE',  ( -4.379528057220086978, -16.55341960407618274, 69.79275706135234714 ) ) ;
#27633 = CARTESIAN_POINT ( 'NONE',  ( -16.88567814943163725, -6.947325034625594142, 51.29001122652586986 ) ) ;
#27634 = CARTESIAN_POINT ( 'NONE',  ( 9.564922557961047289, -16.46253265017146816, 45.41775706135232582 ) ) ;
#27635 = CARTESIAN_POINT ( 'NONE',  ( 36.86305638906669202, 5.498848518248650841, 44.61989603102466617 ) ) ;
#27636 = CARTESIAN_POINT ( 'NONE',  ( 5.153800228976335163, 19.02544592524342804, 109.7905762719810099 ) ) ;
#27637 = CARTESIAN_POINT ( 'NONE',  ( -14.34966873604972548, 8.224510206698743886, 108.3344237280190185 ) ) ;
#27638 = CARTESIAN_POINT ( 'NONE',  ( -0.1121107154831215841, -24.30000000000003624, -54.21489346206830362 ) ) ;
#27639 = CARTESIAN_POINT ( 'NONE',  ( -14.29746914071037622, -8.314922557961029526, 84.16775706135234714 ) ) ;
#27640 = DIRECTION ( 'NONE',  ( -0.000000000000000000, -0.000000000000000000, 1.000000000000000000 ) ) ;
#27641 = CARTESIAN_POINT ( 'NONE',  ( 0.05219959533934541429, -16.53943276465976808, 50.00109039468568994 ) ) ;
#27642 = DIRECTION ( 'NONE',  ( -0.000000000000000000, 1.000000000000000000, -0.000000000000000000 ) ) ;
#27643 = CARTESIAN_POINT ( 'NONE',  ( -21.52544592524334988, -5.823673210054445271, 63.95942372801901854 ) ) ;
#27644 = CARTESIAN_POINT ( 'NONE',  ( -0.05219959533936034679, 19.03943276465977164, 77.50109039468566152 ) ) ;
#27645 = CARTESIAN_POINT ( 'NONE',  ( 19.03943276465977164, 0.05219959533936151252, 31.25109039468566863 ) ) ;
#27646 = CIRCLE ( 'NONE', #30934, 26.79475375365586487 ) ;
#27647 = CARTESIAN_POINT ( 'NONE',  ( 0.05219959533909260263, 19.03943276465977164, 69.99890960531435269 ) ) ;
#27648 = CARTESIAN_POINT ( 'NONE',  ( 16.46253265017160672, -9.564922557960803928, 48.33224293864769550 ) ) ;
#27649 = CARTESIAN_POINT ( 'NONE',  ( 17.08558671903228188, -6.726026106045698505, 23.25235570636825955 ) ) ;
#27650 = CARTESIAN_POINT ( 'NONE',  ( 5.719274019375991003, -21.55341960407610458, 67.70724293864769550 ) ) ;
#27651 = CARTESIAN_POINT ( 'NONE',  ( 5.719274019375991003, -21.55341960407610458, 37.70724293864769550 ) ) ;
#27652 = CARTESIAN_POINT ( 'NONE',  ( 16.53943276465976808, -0.05219959533910856209, 108.7489096053143669 ) ) ;
#27653 = CARTESIAN_POINT ( 'NONE',  ( 14.29746914071037800, 8.314922557961029526, 46.66775706135234714 ) ) ;
#27654 = EDGE_LOOP ( 'NONE', ( #126119, #152794, #178102, #51671 ) ) ;
#27655 = CARTESIAN_POINT ( 'NONE',  ( -5.823673210054431948, 21.52544592524334988, 37.70942372801900433 ) ) ;
#27657 = CARTESIAN_POINT ( 'NONE',  ( 30.74264578624799782, 22.33583958711400541, -8.800000000000000711 ) ) ;
#27656 = CARTESIAN_POINT ( 'NONE',  ( 16.53943276465976808, -0.05219959533910856209, 48.74890960531435979 ) ) ;
#27658 = CARTESIAN_POINT ( 'NONE',  ( 14.29746914071037800, 8.314922557961029526, 31.66775706135234358 ) ) ;
#27659 = CARTESIAN_POINT ( 'NONE',  ( -0.05219959533936034679, 19.03943276465977164, 37.50109039468567573 ) ) ;
#27660 = CARTESIAN_POINT ( 'NONE',  ( 4.483927247898545687, 16.52544592524342804, 44.79057627198103120 ) ) ;
#27661 = CARTESIAN_POINT ( 'NONE',  ( -15.72974639402176322, -15.80617190586768395, 24.37609039468567573 ) ) ;
#27663 = CARTESIAN_POINT ( 'NONE',  ( 0.05219959533907565091, 21.53943276465977519, 79.99890960531435269 ) ) ;
#27662 = CARTESIAN_POINT ( 'NONE',  ( -16.46253265017160317, 9.564922557960807481, 100.8322429386477097 ) ) ;
#27664 = CARTESIAN_POINT ( 'NONE',  ( -16.46253265017160317, 9.564922557960807481, 90.83224293864769550 ) ) ;
#27665 = CARTESIAN_POINT ( 'NONE',  ( -14.29746914071049879, 8.314922557960819915, 60.83224293864769550 ) ) ;
#27666 = CARTESIAN_POINT ( 'NONE',  ( -0.05219959533909027116, -19.03943276465977164, 97.49890960531436690 ) ) ;
#27667 = CARTESIAN_POINT ( 'NONE',  ( 40.00000000000001421, 2.428612866367529932E-14, 0.000000000000000000 ) ) ;
#27668 = CARTESIAN_POINT ( 'NONE',  ( -16.51473224551082808, 9.474510206698731452, 73.33442372801900433 ) ) ;
#27669 = CARTESIAN_POINT ( 'NONE',  ( -21.52544592524343514, 5.823673210054127303, 101.0405762719810383 ) ) ;
#27670 = CARTESIAN_POINT ( 'NONE',  ( 5.049401038298161559, -19.05341960407611168, 62.70724293864769550 ) ) ;
#27671 = CARTESIAN_POINT ( 'NONE',  ( 0.05219959533910956823, 16.53943276465976808, 114.9989096053143669 ) ) ;
#27672 = CARTESIAN_POINT ( 'NONE',  ( -15.80617190586768217, 15.72974639402176855, 53.12609039468568284 ) ) ;
#27673 = CARTESIAN_POINT ( 'NONE',  ( -8.571926809382601320, -26.38167802310801591, 145.2750000027311899 ) ) ;
#27674 = CARTESIAN_POINT ( 'NONE',  ( -4.379528057220328563, 16.55341960407611168, 40.20724293864769550 ) ) ;
#27675 = CARTESIAN_POINT ( 'NONE',  ( 0.05219959533909260263, 19.03943276465977164, 44.99890960531435979 ) ) ;
#27676 = CARTESIAN_POINT ( 'NONE',  ( 9.564922557960805705, 16.46253265017160317, 99.58224293864770971 ) ) ;
#27677 = CARTESIAN_POINT ( 'NONE',  ( -15.80617190586745835, -15.72974639402198527, 76.87390960531439532 ) ) ;
#27678 = CARTESIAN_POINT ( 'NONE',  ( -8.571926809382608425, 26.38167802310805854, 144.4750000027312069 ) ) ;
#27679 = CARTESIAN_POINT ( 'NONE',  ( 16.46253265017160672, -9.564922557960803928, 38.33224293864768839 ) ) ;
#27680 = CARTESIAN_POINT ( 'NONE',  ( -21.53943276465977519, 0.05219959533907696930, 61.24890960531435979 ) ) ;
#27681 = CARTESIAN_POINT ( 'NONE',  ( 18.62759615963255655, 10.81492255796105972, 91.66775706135234714 ) ) ;
#27684 = CARTESIAN_POINT ( 'NONE',  ( -4.379528057220328563, 16.55341960407611168, 85.20724293864770971 ) ) ;
#27683 = CARTESIAN_POINT ( 'NONE',  ( 8.314922557961029526, -14.29746914071037800, 85.41775706135236135 ) ) ;
#27682 = CARTESIAN_POINT ( 'NONE',  ( 21.46320343559668231, 20.96320343559617072, 5.353553390593268624 ) ) ;
#27685 = CARTESIAN_POINT ( 'NONE',  ( 13.89961937509977652, -13.97604488694527269, 68.12390960531436690 ) ) ;
#27686 = ORIENTED_EDGE ( 'NONE', *, *, #95255, .F. ) ;
#27687 = CARTESIAN_POINT ( 'NONE',  ( 19.03943276465977164, 0.05219959533936151252, 21.25109039468565797 ) ) ;
#27688 = CARTESIAN_POINT ( 'NONE',  ( -16.55341960407617563, 4.379528057220093196, 93.54275706135234714 ) ) ;
#27689 = CARTESIAN_POINT ( 'NONE',  ( 15.72974639402176855, 15.80617190586768217, 106.8760903946856899 ) ) ;
#27690 = CARTESIAN_POINT ( 'NONE',  ( 19.02544592524343514, -5.153800228976328945, 88.54057627198102409 ) ) ;
#27691 = CARTESIAN_POINT ( 'NONE',  ( -18.62759615963270932, 10.81492255796079327, 50.83224293864770971 ) ) ;
#27692 = CARTESIAN_POINT ( 'NONE',  ( 21.52544592524334988, 5.823673210054432836, 91.45942372801901854 ) ) ;
#27693 = CARTESIAN_POINT ( 'NONE',  ( 8.224510206698742110, 14.34966873604972548, 57.08442372801901854 ) ) ;
#27694 = CARTESIAN_POINT ( 'NONE',  ( 21.55341960407619695, -5.719274019375665929, 21.04275706135234714 ) ) ;
#27695 = CARTESIAN_POINT ( 'NONE',  ( -8.224510206698735004, -14.34966873604973081, 29.58442372801901854 ) ) ;
#27696 = CARTESIAN_POINT ( 'NONE',  ( -5.049401038298153566, 19.05341960407611168, 95.20724293864770971 ) ) ;
#27697 = CARTESIAN_POINT ( 'NONE',  ( -8.224510206698735004, -14.34966873604973081, 34.58442372801900433 ) ) ;
#27698 = CARTESIAN_POINT ( 'NONE',  ( -13.97604488694527625, -13.89961937509977652, 46.87390960531435979 ) ) ;
#27699 = CARTESIAN_POINT ( 'NONE',  ( -0.05219959533934338120, 16.53943276465976808, 27.50109039468567929 ) ) ;
#27700 = CARTESIAN_POINT ( 'NONE',  ( 16.52544592524342804, -4.483927247898539470, 83.54057627198102409 ) ) ;
#27701 = CARTESIAN_POINT ( 'NONE',  ( 8.224510206698742110, 14.34966873604972548, 92.08442372801901854 ) ) ;
#27703 = CARTESIAN_POINT ( 'NONE',  ( 13.97604488694527802, 13.89961937509977652, 64.37390960531436690 ) ) ;
#27702 = CARTESIAN_POINT ( 'NONE',  ( 10.81492255796106328, -18.62759615963255655, 45.41775706135234003 ) ) ;
#27705 = ADVANCED_FACE ( 'NONE', ( #131387 ), #130367, .T. ) ;
#27704 = CARTESIAN_POINT ( 'NONE',  ( -5.153800228976328057, -19.02544592524343514, 82.29057627198103830 ) ) ;
#27706 = CARTESIAN_POINT ( 'NONE',  ( 16.53943276465976808, -0.05219959533910856209, 28.74890960531435624 ) ) ;
#27707 = CARTESIAN_POINT ( 'NONE',  ( -8.224510206698735004, -14.34966873604973081, 79.58442372801903275 ) ) ;
#27708 = VERTEX_POINT ( 'NONE', #37380 ) ;
#27709 = CARTESIAN_POINT ( 'NONE',  ( -5.153800228976607833, 19.02544592524334988, 32.70942372801899722 ) ) ;
#27710 = CARTESIAN_POINT ( 'NONE',  ( 19.05341960407611168, 5.049401038298154454, 98.95724293864766707 ) ) ;
#27711 = CARTESIAN_POINT ( 'NONE',  ( 5.153800228976335163, 19.02544592524342804, 54.79057627198103120 ) ) ;
#27712 = CARTESIAN_POINT ( 'NONE',  ( -36.91746825000001309, -11.99521256947794789, -10.52499999726881441 ) ) ;
#27713 = CARTESIAN_POINT ( 'NONE',  ( -16.52544592524335698, -4.483927247898792601, 43.95942372801902565 ) ) ;
#27715 = CARTESIAN_POINT ( 'NONE',  ( 8.314922557961029526, -14.29746914071037800, 60.41775706135235424 ) ) ;
#27714 = CARTESIAN_POINT ( 'NONE',  ( -13.89961937509957401, -13.97604488694547875, 64.37609039468567573 ) ) ;
#27716 = CARTESIAN_POINT ( 'NONE',  ( 23.64874990377911246, -15.04272038711346937, 165.8682408883346397 ) ) ;
#27717 = CARTESIAN_POINT ( 'NONE',  ( -19.02544592524342804, 5.153800228976336051, 76.04057627198102409 ) ) ;
#27718 = CARTESIAN_POINT ( 'NONE',  ( 21.55341960407610458, 5.719274019375980345, 108.9572429386476955 ) ) ;
#27719 = CARTESIAN_POINT ( 'NONE',  ( -0.05219959533936034679, 19.03943276465977164, 62.50109039468566863 ) ) ;
#27721 = CARTESIAN_POINT ( 'NONE',  ( -13.89961937509977652, 13.97604488694528158, 25.62390960531434558 ) ) ;
#27720 = CARTESIAN_POINT ( 'NONE',  ( -13.89961937509977652, 13.97604488694528158, 100.6239096053143669 ) ) ;
#27722 = CARTESIAN_POINT ( 'NONE',  ( 0.05219959533909260263, 19.03943276465977164, 79.99890960531436690 ) ) ;
#27724 = CARTESIAN_POINT ( 'NONE',  ( 22.00000000000000000, -1.163414459189985801E-14, 95.00000000000000000 ) ) ;
#27723 = CARTESIAN_POINT ( 'NONE',  ( -4.483927247898539470, -16.52544592524342804, 32.29057627198102409 ) ) ;
#27725 = CARTESIAN_POINT ( 'NONE',  ( 16.46253265017146816, 9.564922557961045513, 31.66775706135232937 ) ) ;
#27726 = CARTESIAN_POINT ( 'NONE',  ( -4.379528057220328563, 16.55341960407611168, 70.20724293864769550 ) ) ;
#27727 = CARTESIAN_POINT ( 'NONE',  ( -18.67979575497193778, 10.72451020669871902, 113.3344237280190328 ) ) ;
#27728 = CARTESIAN_POINT ( 'NONE',  ( 19.05341960407611168, 5.049401038298154454, 33.95724293864769550 ) ) ;
#27730 = CARTESIAN_POINT ( 'NONE',  ( -18.62759615963255300, -10.81492255796106328, 109.1677570613523613 ) ) ;
#27729 = CARTESIAN_POINT ( 'NONE',  ( 16.55341960407611168, 4.379528057220329451, 43.95724293864769550 ) ) ;
#27731 = CARTESIAN_POINT ( 'NONE',  ( 9.474510206698971260, -16.51473224551069308, 87.91557627198102409 ) ) ;
#27732 = CARTESIAN_POINT ( 'NONE',  ( -13.89961937509977652, 13.97604488694528158, 110.6239096053143243 ) ) ;
#27733 = CARTESIAN_POINT ( 'NONE',  ( 0.05219959533909260263, 19.03943276465977164, 39.99890960531436690 ) ) ;
#27734 = CARTESIAN_POINT ( 'NONE',  ( 16.53943276465976808, -0.05219959533910856209, 113.7489096053143527 ) ) ;
#27735 = CARTESIAN_POINT ( 'NONE',  ( -8.224510206698948167, 14.34966873604960824, 70.41557627198102409 ) ) ;
#27736 = CARTESIAN_POINT ( 'NONE',  ( 10.81492255796078972, 18.62759615963270932, 84.58224293864769550 ) ) ;
#27737 = CARTESIAN_POINT ( 'NONE',  ( -5.153800228976328057, -19.02544592524343514, 92.29057627198099567 ) ) ;
#27738 = CARTESIAN_POINT ( 'NONE',  ( 10.72451020669898902, -18.67979575497178502, 92.91557627198103830 ) ) ;
#27739 = CARTESIAN_POINT ( 'NONE',  ( -16.46253265017160317, 9.564922557960807481, 85.83224293864769550 ) ) ;
#27742 = CARTESIAN_POINT ( 'NONE',  ( -4.483927247898539470, -16.52544592524342804, 102.2905762719810383 ) ) ;
#27741 = CARTESIAN_POINT ( 'NONE',  ( -18.39639308325438805, -5.499999999999988454, 91.48252246182197212 ) ) ;
#27740 = AXIS2_PLACEMENT_3D ( 'NONE', #191960, #177810, #114103 ) ;
#27743 = CARTESIAN_POINT ( 'NONE',  ( 16.46253265017160672, -9.564922557960803928, 68.33224293864770971 ) ) ;
#27744 = CARTESIAN_POINT ( 'NONE',  ( 10.72451020669898902, -18.67979575497178502, 82.91557627198103830 ) ) ;
#27745 = CARTESIAN_POINT ( 'NONE',  ( -21.58591991293347689, -5.574009794464002354, 173.3850233475172615 ) ) ;
#27747 = DIRECTION ( 'NONE',  ( 1.000000000000000000, -0.000000000000000000, -0.000000000000000000 ) ) ;
#27746 = CARTESIAN_POINT ( 'NONE',  ( 10.81492255796078972, 18.62759615963270932, 29.58224293864769905 ) ) ;
#27748 = CARTESIAN_POINT ( 'NONE',  ( -4.483927247898782831, 16.52544592524335698, 22.70942372801901499 ) ) ;
#27749 = CARTESIAN_POINT ( 'NONE',  ( -0.05219959533910754901, -16.53943276465976808, 92.49890960531436690 ) ) ;
#27750 = CARTESIAN_POINT ( 'NONE',  ( -16.19135201231365784, -7.376712067591944866, 95.18680854052031748 ) ) ;
#27751 = CARTESIAN_POINT ( 'NONE',  ( -13.97604488694527625, -13.89961937509977652, 81.87390960531436690 ) ) ;
#27752 = CARTESIAN_POINT ( 'NONE',  ( -19.03943276465977164, 0.05219959533909376836, 46.24890960531435979 ) ) ;
#27753 = CARTESIAN_POINT ( 'NONE',  ( -12.14591786802309592, -12.06949235617757132, 86.87390960531438111 ) ) ;
#27754 = CARTESIAN_POINT ( 'NONE',  ( 18.62759615963271287, -10.81492255796078972, 23.33224293864769194 ) ) ;
#27755 = CARTESIAN_POINT ( 'NONE',  ( -12.06949235617756955, 12.14591786802309770, 50.62390960531435979 ) ) ;
#27756 = CARTESIAN_POINT ( 'NONE',  ( 19.05341960407617918, -5.049401038297876454, 96.04275706135231871 ) ) ;
#27757 = CARTESIAN_POINT ( 'NONE',  ( 21.55341960407619695, -5.719274019375665929, 66.04275706135236135 ) ) ;
#27758 = CARTESIAN_POINT ( 'NONE',  ( -22.44159573604009950, -16.30477369853688430, 147.0750000027312012 ) ) ;
#27759 = CARTESIAN_POINT ( 'NONE',  ( 13.97604488694527802, 13.89961937509977652, 94.37390960531436690 ) ) ;
#27760 = CARTESIAN_POINT ( 'NONE',  ( 10.81492255796078972, 18.62759615963270932, 89.58224293864768129 ) ) ;
#27761 = CARTESIAN_POINT ( 'NONE',  ( -14.34966873604972548, 8.224510206698743886, 88.33442372801901854 ) ) ;
#27762 = CARTESIAN_POINT ( 'NONE',  ( 19.03943276465977164, -0.05219959533909143690, 28.74890960531435624 ) ) ;
#27763 = CARTESIAN_POINT ( 'NONE',  ( -5.153800228976328057, -19.02544592524343514, 82.29057627198103830 ) ) ;
#27764 = CARTESIAN_POINT ( 'NONE',  ( 10.81492255796078972, 18.62759615963270932, 84.58224293864769550 ) ) ;
#27765 = CARTESIAN_POINT ( 'NONE',  ( -9.474510206698720793, -16.51473224551083518, 104.5844237280190043 ) ) ;
#27767 = CARTESIAN_POINT ( 'NONE',  ( -5.719274019375665041, -21.55341960407619695, 59.79275706135234714 ) ) ;
#27766 = CARTESIAN_POINT ( 'NONE',  ( -14.34966873604960291, -8.224510206698953496, 51.66557627198102409 ) ) ;
#27769 = CARTESIAN_POINT ( 'NONE',  ( -15.80617190586745835, -15.72974639402198527, 21.87390960531436690 ) ) ;
#27768 = CARTESIAN_POINT ( 'NONE',  ( 12.14591786802327356, -12.06949235617739191, 85.62609039468568994 ) ) ;
#27770 = CARTESIAN_POINT ( 'NONE',  ( 17.49999999999999289, 5.622605283950886879, 28.81207310596113302 ) ) ;
#27771 = CARTESIAN_POINT ( 'NONE',  ( -16.38665767535054840, 7.295008042176047702, 80.26400864214549813 ) ) ;
#27772 = CARTESIAN_POINT ( 'NONE',  ( 16.53943276465976808, 0.05219959533934440121, 106.2510903946856757 ) ) ;
#27773 = CARTESIAN_POINT ( 'NONE',  ( 12.06949235617739724, 12.14591786802326823, 56.87609039468568994 ) ) ;
#27774 = CARTESIAN_POINT ( 'NONE',  ( 9.474510206698971260, -16.51473224551069308, 77.91557627198103830 ) ) ;
#27775 = CARTESIAN_POINT ( 'NONE',  ( 19.02544592524343514, -5.153800228976328945, 78.54057627198099567 ) ) ;
#27776 = CARTESIAN_POINT ( 'NONE',  ( -15.80617190586768217, 15.72974639402176855, 78.12609039468570415 ) ) ;
#27777 = CARTESIAN_POINT ( 'NONE',  ( 16.53943276465976808, 0.05219959533934440121, 81.25109039468568994 ) ) ;
#27778 = CARTESIAN_POINT ( 'NONE',  ( -14.34966873604960291, -8.224510206698953496, 46.66557627198102409 ) ) ;
#27779 = CARTESIAN_POINT ( 'NONE',  ( 9.474510206698971260, -16.51473224551069308, 52.91557627198102409 ) ) ;
#27780 = CARTESIAN_POINT ( 'NONE',  ( 9.564922557960805705, 16.46253265017160317, 49.58224293864770260 ) ) ;
#27782 = ORIENTED_EDGE ( 'NONE', *, *, #35307, .F. ) ;
#27781 = CARTESIAN_POINT ( 'NONE',  ( -16.53943276465976808, -0.05219959533934237506, 43.75109039468568284 ) ) ;
#27783 = CARTESIAN_POINT ( 'NONE',  ( -13.97604488694547697, 13.89961937509957934, 98.12609039468566152 ) ) ;
#27784 = CARTESIAN_POINT ( 'NONE',  ( 12.06949235617757843, -12.14591786802309237, 98.12390960531436690 ) ) ;
#27785 = CARTESIAN_POINT ( 'NONE',  ( 19.02544592524343514, -5.153800228976328945, 63.54057627198103830 ) ) ;
#27787 = CARTESIAN_POINT ( 'NONE',  ( -6.020228577223754586E-15, 39.95556452105416412, -4.500000000000000888 ) ) ;
#27786 = CARTESIAN_POINT ( 'NONE',  ( 0.05219959533936267826, -19.03943276465977164, 95.00109039468567573 ) ) ;
#27788 = CARTESIAN_POINT ( 'NONE',  ( -18.62759615963255300, -10.81492255796106328, 99.16775706135234714 ) ) ;
#27789 = CARTESIAN_POINT ( 'NONE',  ( 4.483927247898790824, -16.52544592524335698, 70.20942372801904696 ) ) ;
#27790 = LINE ( 'NONE', #154077, #127747 ) ;
#27791 = CARTESIAN_POINT ( 'NONE',  ( -21.52544592524343514, 5.823673210054127303, 61.04057627198103120 ) ) ;
#27792 = CARTESIAN_POINT ( 'NONE',  ( -8.224510206698735004, -14.34966873604973081, 54.58442372801901143 ) ) ;
#27793 = CARTESIAN_POINT ( 'NONE',  ( 19.05341960407611168, 5.049401038298154454, 33.95724293864770260 ) ) ;
#27794 = CARTESIAN_POINT ( 'NONE',  ( -5.049401038297874678, -19.05341960407617918, 39.79275706135232582 ) ) ;
#27795 = AXIS2_PLACEMENT_3D ( 'NONE', #188401, #187423, #48891 ) ;
#27796 = CARTESIAN_POINT ( 'NONE',  ( -19.02544592524342804, 5.153800228976336051, 96.04057627198103830 ) ) ;
#27797 = CARTESIAN_POINT ( 'NONE',  ( 12.14591786802309770, 12.06949235617756955, 114.3739096053143527 ) ) ;
#27798 = CARTESIAN_POINT ( 'NONE',  ( 5.153800228976335163, 19.02544592524342804, 69.79057627198103830 ) ) ;
#27799 = CARTESIAN_POINT ( 'NONE',  ( 5.823673210054444382, -21.52544592524334988, 70.20942372801904696 ) ) ;
#27800 = CARTESIAN_POINT ( 'NONE',  ( 16.51473224551083163, -9.474510206698727899, 40.83442372801900433 ) ) ;
#27801 = CARTESIAN_POINT ( 'NONE',  ( 13.89961937509957401, 13.97604488694547697, 26.87609039468566507 ) ) ;
#27802 = CARTESIAN_POINT ( 'NONE',  ( -13.97604488694527625, -13.89961937509977652, 61.87390960531435979 ) ) ;
#27804 = B_SPLINE_CURVE_WITH_KNOTS ( 'NONE', 3,
 ( #138856, #336, #62004, #185367, #46859, #170198 ),
 .UNSPECIFIED., .F., .F.,
 ( 4, 2, 4 ),
 ( 0.003989672132298080140, 0.004372778065220498181, 0.004755883998142916222 ),
 .UNSPECIFIED. ) ;
#27803 = CARTESIAN_POINT ( 'NONE',  ( 16.51473224551069308, 9.474510206698969483, 114.1655762719810241 ) ) ;
#27805 = CARTESIAN_POINT ( 'NONE',  ( -0.05219959533937732626, 21.53943276465977519, 87.50109039468568994 ) ) ;
#27806 = CARTESIAN_POINT ( 'NONE',  ( 13.89961937509977652, -13.97604488694527269, 63.12390960531435979 ) ) ;
#27807 = CARTESIAN_POINT ( 'NONE',  ( -21.52544592524334988, -5.823673210054445271, 93.95942372801903275 ) ) ;
#27808 = CARTESIAN_POINT ( 'NONE',  ( 10.72451020669898902, -18.67979575497178502, 32.91557627198102409 ) ) ;
#27809 = CARTESIAN_POINT ( 'NONE',  ( 16.46253265017160672, -9.564922557960803928, 88.33224293864769550 ) ) ;
#27810 = CARTESIAN_POINT ( 'NONE',  ( 15.80617190586769283, -15.72974639402175789, 45.62609039468567573 ) ) ;
#27811 = CARTESIAN_POINT ( 'NONE',  ( -0.05219959533936034679, 19.03943276465977164, 62.50109039468566863 ) ) ;
#27812 = CARTESIAN_POINT ( 'NONE',  ( -13.89961937509977652, 13.97604488694528158, 40.62390960531435979 ) ) ;
#27813 = CARTESIAN_POINT ( 'NONE',  ( -5.153800228976328057, -19.02544592524343514, 87.29057627198103830 ) ) ;
#27814 = CARTESIAN_POINT ( 'NONE',  ( -8.224510206698735004, -14.34966873604973081, 24.58442372801901499 ) ) ;
#27815 = CARTESIAN_POINT ( 'NONE',  ( 14.34966873604960469, 8.224510206698951720, 84.16557627198103830 ) ) ;
#27816 = CARTESIAN_POINT ( 'NONE',  ( 19.05341960407611168, 5.049401038298154454, 68.95724293864769550 ) ) ;
#27817 = CARTESIAN_POINT ( 'NONE',  ( -5.719274019375978568, 21.55341960407610458, 45.20724293864769550 ) ) ;
#27818 = CARTESIAN_POINT ( 'NONE',  ( 8.224510206698742110, 14.34966873604972548, 22.08442372801901143 ) ) ;
#27819 = CARTESIAN_POINT ( 'NONE',  ( -5.719274019375665041, -21.55341960407619695, 24.79275706135235779 ) ) ;
#27820 = CARTESIAN_POINT ( 'NONE',  ( -5.823673210054431948, 21.52544592524334988, 72.70942372801901854 ) ) ;
#27821 = CARTESIAN_POINT ( 'NONE',  ( -12.06949235617739369, -12.14591786802326823, 64.37609039468568994 ) ) ;
#27822 = CARTESIAN_POINT ( 'NONE',  ( 14.29746914071037800, 8.314922557961029526, 66.66775706135234714 ) ) ;
#27823 = CARTESIAN_POINT ( 'NONE',  ( -9.564922557960796823, -16.46253265017161027, 62.08224293864769550 ) ) ;
#27824 = CARTESIAN_POINT ( 'NONE',  ( -14.29746914071037622, -8.314922557961029526, 104.1677570613523471 ) ) ;
#27825 = CARTESIAN_POINT ( 'NONE',  ( 19.05341960407617918, -5.049401038297876454, 46.04275706135233293 ) ) ;
#27826 = CARTESIAN_POINT ( 'NONE',  ( 15.80617190586746368, 15.72974639402197994, 114.3739096053143527 ) ) ;
#27827 = EDGE_CURVE ( 'NONE', #66087, #104760, #87771, .T. ) ;
#27828 = CARTESIAN_POINT ( 'NONE',  ( -12.06949235617756955, 12.14591786802309770, 70.62390960531436690 ) ) ;
#27829 = CARTESIAN_POINT ( 'NONE',  ( 0.05219959533909260263, 19.03943276465977164, 79.99890960531436690 ) ) ;
#27830 = CARTESIAN_POINT ( 'NONE',  ( -12.14591786802326823, 12.06949235617739902, 83.12609039468568994 ) ) ;
#27831 = CARTESIAN_POINT ( 'NONE',  ( 10.81492255796106328, -18.62759615963255655, 60.41775706135235424 ) ) ;
#27832 = CARTESIAN_POINT ( 'NONE',  ( 8.224510206698742110, 14.34966873604972548, 37.08442372801901143 ) ) ;
#27833 = CARTESIAN_POINT ( 'NONE',  ( 21.53943276465977519, 0.05219959533937863772, 21.25109039468567218 ) ) ;
#27834 = CARTESIAN_POINT ( 'NONE',  ( 4.483927247898545687, 16.52544592524342804, 64.79057627198103830 ) ) ;
#27835 = ORIENTED_EDGE ( 'NONE', *, *, #22636, .T. ) ;
#27836 = CARTESIAN_POINT ( 'NONE',  ( -5.823673210054116645, -21.52544592524344225, 107.2905762719810525 ) ) ;
#27837 = CARTESIAN_POINT ( 'NONE',  ( -12.06949235617756955, 12.14591786802309770, 45.62390960531436690 ) ) ;
#27838 = VERTEX_POINT ( 'NONE', #54551 ) ;
#27839 = CARTESIAN_POINT ( 'NONE',  ( 35.02332884957463932, 5.945191563609818708, 40.42135061281683761 ) ) ;
#27840 = CARTESIAN_POINT ( 'NONE',  ( 10.72451020669898902, -18.67979575497178502, 32.91557627198102409 ) ) ;
#27841 = CARTESIAN_POINT ( 'NONE',  ( 21.55341960407619695, -5.719274019375665929, 41.04275706135236135 ) ) ;
#27842 = CARTESIAN_POINT ( 'NONE',  ( -14.29746914071049879, 8.314922557960819915, 70.83224293864770971 ) ) ;
#27843 = CIRCLE ( 'NONE', #53626, 25.62086810090349331 ) ;
#27844 = CARTESIAN_POINT ( 'NONE',  ( 21.53943276465977519, -0.05219959533907433946, 68.74890960531435269 ) ) ;
#27845 = CARTESIAN_POINT ( 'NONE',  ( -5.049401038298153566, 19.05341960407611168, 75.20724293864769550 ) ) ;
#27847 = CARTESIAN_POINT ( 'NONE',  ( -19.05341960407617563, 5.049401038297882671, 63.54275706135234003 ) ) ;
#27846 = CARTESIAN_POINT ( 'NONE',  ( 19.05341960407611168, 5.049401038298154454, 28.95724293864769550 ) ) ;
#27848 = CARTESIAN_POINT ( 'NONE',  ( 5.719274019375991003, -21.55341960407610458, 52.70724293864769550 ) ) ;
#27849 = CARTESIAN_POINT ( 'NONE',  ( 13.97604488694527802, 13.89961937509977652, 64.37390960531436690 ) ) ;
#27850 = VERTEX_POINT ( 'NONE', #66720 ) ;
#27851 = CARTESIAN_POINT ( 'NONE',  ( -8.314922557961024197, 14.29746914071037800, 32.91775706135234714 ) ) ;
#27852 = CARTESIAN_POINT ( 'NONE',  ( -21.55341960407619339, 5.719274019375674811, 23.54275706135235424 ) ) ;
#27853 = ADVANCED_FACE ( 'NONE', ( #142563, #160727 ), #22219, .T. ) ;
#27854 = CARTESIAN_POINT ( 'NONE',  ( -16.53943276465976808, 0.05219959533911058130, 41.24890960531435269 ) ) ;
#27855 = CARTESIAN_POINT ( 'NONE',  ( 19.05341960407611168, 5.049401038298154454, 98.95724293864766707 ) ) ;
#27856 = CARTESIAN_POINT ( 'NONE',  ( -21.55341960407610458, -5.719274019375992779, 71.45724293864769550 ) ) ;
#27858 = CARTESIAN_POINT ( 'NONE',  ( 16.55341960407618274, -4.379528057220086978, 41.04275706135236135 ) ) ;
#27857 = CARTESIAN_POINT ( 'NONE',  ( 18.67979575497178502, 10.72451020669898547, 114.1655762719810383 ) ) ;
#27859 = CARTESIAN_POINT ( 'NONE',  ( -21.53943276465977519, 0.05219959533907696930, 56.24890960531436690 ) ) ;
#27860 = CARTESIAN_POINT ( 'NONE',  ( -18.67979575497193778, 10.72451020669871902, 108.3344237280190185 ) ) ;
#27861 = CARTESIAN_POINT ( 'NONE',  ( 5.153800228976335163, 19.02544592524342804, 39.79057627198100988 ) ) ;
#27862 = CARTESIAN_POINT ( 'NONE',  ( -5.049401038298153566, 19.05341960407611168, 100.2072429386476955 ) ) ;
#27863 = CARTESIAN_POINT ( 'NONE',  ( -19.05341960407611168, -5.049401038298163336, 81.45724293864769550 ) ) ;
#27864 = CARTESIAN_POINT ( 'NONE',  ( 16.20579543436696213, -7.371946100355082798, 86.93479165828053112 ) ) ;
#27865 = CARTESIAN_POINT ( 'NONE',  ( 19.03943276465977164, 0.05219959533936151252, 56.25109039468566863 ) ) ;
#27867 = CARTESIAN_POINT ( 'NONE',  ( -21.55341960407610458, -5.719274019375992779, 31.45724293864769550 ) ) ;
#27866 = CARTESIAN_POINT ( 'NONE',  ( 5.719274019375673035, 21.55341960407619339, 112.2927570613523471 ) ) ;
#27868 = CARTESIAN_POINT ( 'NONE',  ( -4.379528057220086978, -16.55341960407618274, 109.7927570613523613 ) ) ;
#27869 = CARTESIAN_POINT ( 'NONE',  ( 0.05219959533936267826, -19.03943276465977164, 80.00109039468567573 ) ) ;
#27870 = CARTESIAN_POINT ( 'NONE',  ( -14.62203461105279700, -15.93801742227414486, -58.64843802457497901 ) ) ;
#27871 = CARTESIAN_POINT ( 'NONE',  ( 19.03943276465977164, 0.05219959533936151252, 86.25109039468567573 ) ) ;
#27872 = CARTESIAN_POINT ( 'NONE',  ( 19.03943276465977164, 0.05219959533936151252, 41.25109039468566152 ) ) ;
#27873 = DIRECTION ( 'NONE',  ( 0.000000000000000000, 0.000000000000000000, -1.000000000000000000 ) ) ;
#27874 = CARTESIAN_POINT ( 'NONE',  ( 13.89961937509977652, -13.97604488694527269, 43.12390960531434558 ) ) ;
#27875 = CARTESIAN_POINT ( 'NONE',  ( -12.14591786802309592, -12.06949235617757132, 46.87390960531435979 ) ) ;
#27876 = CARTESIAN_POINT ( 'NONE',  ( -9.474510206698964154, 16.51473224551069663, 40.41557627198103120 ) ) ;
#27877 = CARTESIAN_POINT ( 'NONE',  ( 12.14591786802309770, 12.06949235617756955, 44.37390960531435979 ) ) ;
#27878 = CARTESIAN_POINT ( 'NONE',  ( 0.000000000000000000, -1.178949249685214307, 2.042000000000002036 ) ) ;
#27879 = CARTESIAN_POINT ( 'NONE',  ( -4.379528057220086978, -16.55341960407618274, 104.7927570613523898 ) ) ;
#27880 = CARTESIAN_POINT ( 'NONE',  ( 13.89961937509977652, -13.97604488694527269, 48.12390960531435979 ) ) ;
#27881 = CARTESIAN_POINT ( 'NONE',  ( -10.81492255796105439, 18.62759615963255655, 112.9177570613523329 ) ) ;
#27882 = CARTESIAN_POINT ( 'NONE',  ( 16.51473224551083163, -9.474510206698727899, 110.8344237280190043 ) ) ;
#27883 = CARTESIAN_POINT ( 'NONE',  ( -18.62759615963270932, 10.81492255796079327, 35.83224293864768839 ) ) ;
#27885 = ORIENTED_EDGE ( 'NONE', *, *, #73810, .F. ) ;
#27884 = CARTESIAN_POINT ( 'NONE',  ( 0.05219959533937995610, -21.53943276465977519, 95.00109039468568994 ) ) ;
#27886 = CARTESIAN_POINT ( 'NONE',  ( -13.89961937509977652, 13.97604488694528158, 110.6239096053143243 ) ) ;
#27887 = CARTESIAN_POINT ( 'NONE',  ( -13.89961937509977652, 13.97604488694528158, 85.62390960531433848 ) ) ;
#27888 = CARTESIAN_POINT ( 'NONE',  ( -32.05804330925093382, -23.92378017333652451, -20.06701077757416840 ) ) ;
#27889 = CARTESIAN_POINT ( 'NONE',  ( -5.823673210054116645, -21.52544592524344225, 107.2905762719810525 ) ) ;
#27890 = VECTOR ( 'NONE', #27535, 1000.000000000000000 ) ;
#27891 = CARTESIAN_POINT ( 'NONE',  ( -14.29746914071049879, 8.314922557960819915, 75.83224293864769550 ) ) ;
#27892 = CARTESIAN_POINT ( 'NONE',  ( 21.55341960407610458, 5.719274019375980345, 73.95724293864769550 ) ) ;
#27893 = CARTESIAN_POINT ( 'NONE',  ( -16.51473224551069308, -9.474510206698971260, 56.66557627198103120 ) ) ;
#27894 = CARTESIAN_POINT ( 'NONE',  ( -21.52544592524343514, 5.823673210054127303, 96.04057627198102409 ) ) ;
#27895 = ORIENTED_EDGE ( 'NONE', *, *, #15250, .T. ) ;
#27896 = CARTESIAN_POINT ( 'NONE',  ( -16.46253265017160317, 9.564922557960807481, 60.83224293864769550 ) ) ;
#27898 = CARTESIAN_POINT ( 'NONE',  ( 21.97154029300583389, -7.270820338085814072, 170.2141396987978226 ) ) ;
#27897 = CARTESIAN_POINT ( 'NONE',  ( 14.34966873604960469, 8.224510206698951720, 89.16557627198102409 ) ) ;
#27899 = CARTESIAN_POINT ( 'NONE',  ( 16.46253265017160672, -9.564922557960803928, 68.33224293864770971 ) ) ;
#27900 = CARTESIAN_POINT ( 'NONE',  ( -5.049401038297874678, -19.05341960407617918, 79.79275706135233293 ) ) ;
#27901 = CARTESIAN_POINT ( 'NONE',  ( 14.29746914071049879, -8.314922557960816363, 88.33224293864769550 ) ) ;
#27902 = CARTESIAN_POINT ( 'NONE',  ( -21.53943276465977519, -0.05219959533937600094, 53.75109039468568994 ) ) ;
#27904 = CARTESIAN_POINT ( 'NONE',  ( -21.52544592524334988, -5.823673210054445271, 23.95942372801901143 ) ) ;
#27903 = CARTESIAN_POINT ( 'NONE',  ( -13.89961937509977652, 13.97604488694528158, 45.62390960531433848 ) ) ;
#27905 = CARTESIAN_POINT ( 'NONE',  ( -0.05219959533910754901, -16.53943276465976808, 102.4989096053143811 ) ) ;
#27906 = CARTESIAN_POINT ( 'NONE',  ( 2.802625768539491968, -39.09149893265183806, -33.00000000000000000 ) ) ;
#27907 = CARTESIAN_POINT ( 'NONE',  ( 16.46253265017160672, -9.564922557960803928, 63.33224293864769550 ) ) ;
#27908 = CARTESIAN_POINT ( 'NONE',  ( 16.29526858892874230, 7.335722546920135478, 113.2967059780020946 ) ) ;
#27910 = CARTESIAN_POINT ( 'NONE',  ( -13.89961937509977652, 13.97604488694528158, 115.6239096053143669 ) ) ;
#27909 = CARTESIAN_POINT ( 'NONE',  ( -9.564922557961040184, 16.46253265017147172, 112.9177570613523329 ) ) ;
#27911 = CARTESIAN_POINT ( 'NONE',  ( 5.823673210054444382, -21.52544592524334988, 55.20942372801902565 ) ) ;
#27912 = CARTESIAN_POINT ( 'NONE',  ( 9.474510206698971260, -16.51473224551069308, 97.91557627198102409 ) ) ;
#27913 = CARTESIAN_POINT ( 'NONE',  ( -13.89961937509957401, -13.97604488694547875, 84.37609039468567573 ) ) ;
#27914 = CARTESIAN_POINT ( 'NONE',  ( 5.049401038298161559, -19.05341960407611168, 52.70724293864767418 ) ) ;
#27915 = CARTESIAN_POINT ( 'NONE',  ( -14.29746914071049879, 8.314922557960819915, 80.83224293864769550 ) ) ;
#27916 = CARTESIAN_POINT ( 'NONE',  ( -12.14591786802309592, -12.06949235617757132, 81.87390960531435269 ) ) ;
#27917 = CARTESIAN_POINT ( 'NONE',  ( 9.474510206698971260, -16.51473224551069308, 92.91557627198103830 ) ) ;
#27918 = CARTESIAN_POINT ( 'NONE',  ( 8.314922557960818139, 14.29746914071049879, 79.58224293864769550 ) ) ;
#27919 = CARTESIAN_POINT ( 'NONE',  ( 16.51473224551069308, 9.474510206698969483, 84.16557627198102409 ) ) ;
#27920 = CARTESIAN_POINT ( 'NONE',  ( -19.03943276465977164, -0.05219959533935918106, 33.75109039468566863 ) ) ;
#27923 = CARTESIAN_POINT ( 'NONE',  ( 13.89961937509977652, -13.97604488694527269, 28.12390960531435624 ) ) ;
#27922 = CARTESIAN_POINT ( 'NONE',  ( -16.52544592524342804, 4.483927247898546575, 26.04057627198103475 ) ) ;
#27921 = CARTESIAN_POINT ( 'NONE',  ( -5.153800228976328057, -19.02544592524343514, 52.29057627198100988 ) ) ;
#27924 = VERTEX_POINT ( 'NONE', #157747 ) ;
#27925 = CARTESIAN_POINT ( 'NONE',  ( -18.62759615963255300, -10.81492255796106328, 39.16775706135235424 ) ) ;
#27926 = CARTESIAN_POINT ( 'NONE',  ( 5.153800228976615827, -19.02544592524334988, 80.20942372801901854 ) ) ;
#27927 = CARTESIAN_POINT ( 'NONE',  ( 16.55341960407611168, 4.379528057220329451, 38.95724293864768839 ) ) ;
#27928 = CARTESIAN_POINT ( 'NONE',  ( 15.80617190586746368, 15.72974639402197994, 84.37390960531438111 ) ) ;
#27929 = CARTESIAN_POINT ( 'NONE',  ( 0.05219959533907565091, 21.53943276465977519, 29.99890960531435979 ) ) ;
#27930 = CARTESIAN_POINT ( 'NONE',  ( 16.55341960407611168, 4.379528057220329451, 63.95724293864770260 ) ) ;
#27931 = CARTESIAN_POINT ( 'NONE',  ( -5.153800228976328057, -19.02544592524343514, 42.29057627198101699 ) ) ;
#27932 = CARTESIAN_POINT ( 'NONE',  ( 4.483927247898790824, -16.52544592524335698, 100.2094237280190043 ) ) ;
#27933 = CARTESIAN_POINT ( 'NONE',  ( 12.06949235617739724, 12.14591786802326823, 66.87609039468568994 ) ) ;
#27934 = CARTESIAN_POINT ( 'NONE',  ( 21.52544592524344225, -5.823673210054117533, 33.54057627198102409 ) ) ;
#27935 = CARTESIAN_POINT ( 'NONE',  ( 19.02544592524334988, 5.153800228976608722, 21.45942372801899012 ) ) ;
#27936 = CARTESIAN_POINT ( 'NONE',  ( 16.46253265017160672, -9.564922557960803928, 93.33224293864769550 ) ) ;
#27937 = CIRCLE ( 'NONE', #150601, 13.70000000000001528 ) ;
#27938 = CARTESIAN_POINT ( 'NONE',  ( 16.52544592524335698, 4.483927247898782831, 71.45942372801901854 ) ) ;
#27939 = CARTESIAN_POINT ( 'NONE',  ( -0.05219959533909027116, -19.03943276465977164, 27.49890960531435624 ) ) ;
#27940 = CARTESIAN_POINT ( 'NONE',  ( 16.53943276465976808, -0.05219959533910856209, 38.74890960531435979 ) ) ;
#27942 = CARTESIAN_POINT ( 'NONE',  ( -19.05341960407611168, -5.049401038298163336, 96.45724293864769550 ) ) ;
#27941 = CARTESIAN_POINT ( 'NONE',  ( 5.153800228976335163, 19.02544592524342804, 104.7905762719809957 ) ) ;
#27944 = ADVANCED_FACE ( 'NONE', ( #23224 ), #84867, .T. ) ;
#27943 = CARTESIAN_POINT ( 'NONE',  ( -15.80617190586745835, -15.72974639402198527, 21.87390960531436690 ) ) ;
#27945 = CARTESIAN_POINT ( 'NONE',  ( 14.29746914071049879, -8.314922557960816363, 78.33224293864770971 ) ) ;
#27946 = CARTESIAN_POINT ( 'NONE',  ( -4.483927247898539470, -16.52544592524342804, 47.29057627198103120 ) ) ;
#27947 = VERTEX_POINT ( 'NONE', #144552 ) ;
#27949 = CARTESIAN_POINT ( 'NONE',  ( -11.30153831258470731, -180.0000000000000000, -25.00000000000000000 ) ) ;
#27948 = CARTESIAN_POINT ( 'NONE',  ( -14.29746914071037622, -8.314922557961029526, 49.16775706135234003 ) ) ;
#27950 = CARTESIAN_POINT ( 'NONE',  ( -5.153800228976607833, 19.02544592524334988, 52.70942372801900433 ) ) ;
#27951 = CARTESIAN_POINT ( 'NONE',  ( -19.05341960407611168, -5.049401038298163336, 86.45724293864769550 ) ) ;
#27952 = CARTESIAN_POINT ( 'NONE',  ( 5.153800228976615827, -19.02544592524334988, 65.20942372801900433 ) ) ;
#27953 = CARTESIAN_POINT ( 'NONE',  ( 17.14385361876520264, -23.59649016807271238, 142.0750000027311444 ) ) ;
#27955 = CARTESIAN_POINT ( 'NONE',  ( 14.29746914071037800, 8.314922557961029526, 91.66775706135234714 ) ) ;
#27954 = CARTESIAN_POINT ( 'NONE',  ( -16.52544592524335698, -4.483927247898792601, 18.95942372801901143 ) ) ;
#27956 = CARTESIAN_POINT ( 'NONE',  ( 5.153800228976335163, 19.02544592524342804, 34.79057627198102409 ) ) ;
#27957 = CARTESIAN_POINT ( 'NONE',  ( 13.97604488694527802, 13.89961937509977652, 114.3739096053143669 ) ) ;
#27958 = CARTESIAN_POINT ( 'NONE',  ( -18.62759615963255300, -10.81492255796106328, 49.16775706135234003 ) ) ;
#27959 = CARTESIAN_POINT ( 'NONE',  ( 9.564922557961047289, -16.46253265017146816, 100.4177570613523329 ) ) ;
#27961 = CARTESIAN_POINT ( 'NONE',  ( -9.564922557960796823, -16.46253265017161027, 72.08224293864770971 ) ) ;
#27960 = CARTESIAN_POINT ( 'NONE',  ( -30.00000000000000000, -1.163414459189985801E-14, 95.00000000000000000 ) ) ;
#27962 = CARTESIAN_POINT ( 'NONE',  ( 17.18269478283314911, 17.18269478283310647, -56.77278709839600879 ) ) ;
#27964 = CARTESIAN_POINT ( 'NONE',  ( 9.474510206698971260, -16.51473224551069308, 67.91557627198102409 ) ) ;
#27963 = CARTESIAN_POINT ( 'NONE',  ( 16.52544592524342804, -4.483927247898539470, 78.54057627198103830 ) ) ;
#27965 = CONTEXT_DEPENDENT_SHAPE_REPRESENTATION ( #98470, #63060 ) ;
#27966 = CARTESIAN_POINT ( 'NONE',  ( -5.049401038298153566, 19.05341960407611168, 75.20724293864769550 ) ) ;
#27967 = CARTESIAN_POINT ( 'NONE',  ( -9.564922557961040184, 16.46253265017147172, 72.91775706135233293 ) ) ;
#27968 = CARTESIAN_POINT ( 'NONE',  ( 21.55341960407610458, 5.719274019375980345, 68.95724293864769550 ) ) ;
#27969 = CARTESIAN_POINT ( 'NONE',  ( -0.05219959533910754901, -16.53943276465976808, 112.4989096053143669 ) ) ;
#27970 = CARTESIAN_POINT ( 'NONE',  ( -0.05219959533936034679, 19.03943276465977164, 62.50109039468566863 ) ) ;
#27971 = CARTESIAN_POINT ( 'NONE',  ( -5.153800228976328057, -19.02544592524343514, 62.29057627198100988 ) ) ;
#27973 = EDGE_CURVE ( 'NONE', #138021, #60866, #16219, .T. ) ;
#27972 = CARTESIAN_POINT ( 'NONE',  ( -19.05341960407611168, -5.049401038298163336, 96.45724293864769550 ) ) ;
#27974 = CARTESIAN_POINT ( 'NONE',  ( -15.72974639402197994, 15.80617190586746368, 95.62390960531436690 ) ) ;
#27976 = CARTESIAN_POINT ( 'NONE',  ( -5.153800228976607833, 19.02544592524334988, 42.70942372801901143 ) ) ;
#27975 = CARTESIAN_POINT ( 'NONE',  ( -8.314922557960811034, -14.29746914071050412, 77.08224293864769550 ) ) ;
#27977 = CARTESIAN_POINT ( 'NONE',  ( 0.05219959533907565091, 21.53943276465977519, 74.99890960531435269 ) ) ;
#27978 = CARTESIAN_POINT ( 'NONE',  ( -0.05219959533907301413, -21.53943276465977519, 62.49890960531436690 ) ) ;
#27979 = CARTESIAN_POINT ( 'NONE',  ( 8.224510206698953496, -14.34966873604960469, 27.91557627198103830 ) ) ;
#27980 = CARTESIAN_POINT ( 'NONE',  ( 18.67979575497194134, -10.72451020669871369, 95.83442372801903275 ) ) ;
#27981 = CARTESIAN_POINT ( 'NONE',  ( 13.97604488694527802, 13.89961937509977652, 79.37390960531435269 ) ) ;
#27982 = CARTESIAN_POINT ( 'NONE',  ( -16.51473224551069308, -9.474510206698971260, 36.66557627198102409 ) ) ;
#27983 = CARTESIAN_POINT ( 'NONE',  ( 21.55341960407619695, -5.719274019375665929, 46.04275706135234714 ) ) ;
#27985 = CARTESIAN_POINT ( 'NONE',  ( 10.72451020669871369, 18.67979575497193778, 37.08442372801901143 ) ) ;
#27984 = B_SPLINE_CURVE_WITH_KNOTS ( 'NONE', 3,
 ( #148521, #146497, #176868, #55502, #194038, #22171, #10011, #195029, #83821, #7988, #116175, #145501, #6982, #131338, #54503, #179875, #68662, #181852, #197028, #109714, #88830, #196041, #141045, #150523 ),
 .UNSPECIFIED., .F., .F.,
 ( 4, 2, 2, 2, 2, 2, 2, 2, 2, 2, 2, 4 ),
 ( 1.968491853561852430E-07, 0.0003260565056758578189, 0.0006519161621663594397, 0.0009777758186568610062, 0.001303635475147362681, 0.001955354788128363646, 0.002607074101109364394, 0.003258793414090365576, 0.003910512727071366323, 0.004562232040052367071, 0.004888091696542867445, 0.005213951353033367819 ),
 .UNSPECIFIED. ) ;
#27986 = CARTESIAN_POINT ( 'NONE',  ( 19.03943276465977164, -0.05219959533909143690, 43.74890960531435979 ) ) ;
#27987 = CARTESIAN_POINT ( 'NONE',  ( -15.72974639402176322, -15.80617190586768395, 19.37609039468568639 ) ) ;
#27988 = CARTESIAN_POINT ( 'NONE',  ( 19.02544592524334988, 5.153800228976608722, 56.45942372801898301 ) ) ;
#27989 = CARTESIAN_POINT ( 'NONE',  ( 13.89961937509977652, -13.97604488694527269, 43.12390960531434558 ) ) ;
#27990 = CARTESIAN_POINT ( 'NONE',  ( -0.05219959533934338120, 16.53943276465976808, 27.50109039468567929 ) ) ;
#27991 = CARTESIAN_POINT ( 'NONE',  ( -16.51473224551069308, -9.474510206698971260, 26.66557627198103120 ) ) ;
#27992 = CARTESIAN_POINT ( 'NONE',  ( -8.224510206698735004, -14.34966873604973081, 69.58442372801900433 ) ) ;
#27993 = CARTESIAN_POINT ( 'NONE',  ( -5.049401038298153566, 19.05341960407611168, 40.20724293864768839 ) ) ;
#27994 = CARTESIAN_POINT ( 'NONE',  ( -26.13941622279033794, -9.616497135380848604, 166.9083969906205027 ) ) ;
#27995 = CARTESIAN_POINT ( 'NONE',  ( -13.89961937509977652, 13.97604488694528158, 85.62390960531433848 ) ) ;
#27996 = CARTESIAN_POINT ( 'NONE',  ( -14.29746914071049879, 8.314922557960819915, 115.8322429386477097 ) ) ;
#27997 = CARTESIAN_POINT ( 'NONE',  ( -18.67979575497178146, -10.72451020669898902, 61.66557627198103120 ) ) ;
#27998 = CARTESIAN_POINT ( 'NONE',  ( -0.05219959533934338120, 16.53943276465976808, 42.50109039468567573 ) ) ;
#27999 = CARTESIAN_POINT ( 'NONE',  ( 18.62759615963255655, 10.81492255796105972, 96.66775706135234714 ) ) ;
#28000 = CARTESIAN_POINT ( 'NONE',  ( -19.02544592524342804, 5.153800228976336051, 46.04057627198101699 ) ) ;
#28001 = CARTESIAN_POINT ( 'NONE',  ( -12.14591786802309592, -12.06949235617757132, 36.87390960531435979 ) ) ;
#28002 = CARTESIAN_POINT ( 'NONE',  ( 4.483927247898545687, 16.52544592524342804, 64.79057627198103830 ) ) ;
#28003 = CARTESIAN_POINT ( 'NONE',  ( -5.153800228976328057, -19.02544592524343514, 67.29057627198102409 ) ) ;
#28004 = CARTESIAN_POINT ( 'NONE',  ( -5.049401038297874678, -19.05341960407617918, 19.79275706135233293 ) ) ;
#28005 = CARTESIAN_POINT ( 'NONE',  ( 18.67979575497194134, -10.72451020669871369, 20.83442372801901143 ) ) ;
#28006 = CARTESIAN_POINT ( 'NONE',  ( 0.05219959533909260263, 19.03943276465977164, 74.99890960531435269 ) ) ;
#28007 = CARTESIAN_POINT ( 'NONE',  ( -5.823673210054431948, 21.52544592524334988, 87.70942372801901854 ) ) ;
#28008 = CARTESIAN_POINT ( 'NONE',  ( -16.53943276465976808, -0.05219959533934237506, 58.75109039468568994 ) ) ;
#28009 = CARTESIAN_POINT ( 'NONE',  ( 12.06949235617739724, 12.14591786802326823, 26.87609039468567218 ) ) ;
#28011 = CARTESIAN_POINT ( 'NONE',  ( 5.719274019375673035, 21.55341960407619339, 97.29275706135234714 ) ) ;
#28010 = CARTESIAN_POINT ( 'NONE',  ( -8.314922557960811034, -14.29746914071050412, 87.08224293864769550 ) ) ;
#28012 = CARTESIAN_POINT ( 'NONE',  ( 16.55341960407611168, 4.379528057220329451, 33.95724293864769550 ) ) ;
#28013 = CARTESIAN_POINT ( 'NONE',  ( -5.153800228976328057, -19.02544592524343514, 32.29057627198102409 ) ) ;
#28014 = CARTESIAN_POINT ( 'NONE',  ( 16.53943276465976808, 0.05219959533934440121, 56.25109039468568284 ) ) ;
#28015 = CARTESIAN_POINT ( 'NONE',  ( 16.53943276465976808, -0.05219959533910856209, 58.74890960531436690 ) ) ;
#28016 = CARTESIAN_POINT ( 'NONE',  ( -0.05219959533934338120, 16.53943276465976808, 102.5010903946856899 ) ) ;
#28017 = CARTESIAN_POINT ( 'NONE',  ( 5.153800228976335163, 19.02544592524342804, 109.7905762719810099 ) ) ;
#28018 = CARTESIAN_POINT ( 'NONE',  ( 5.049401038298161559, -19.05341960407611168, 112.7072429386476813 ) ) ;
#28019 = CARTESIAN_POINT ( 'NONE',  ( -21.53943276465977519, -0.05219959533937600094, 113.7510903946856757 ) ) ;
#28020 = CARTESIAN_POINT ( 'NONE',  ( 14.29746914071049879, -8.314922557960816363, 83.33224293864769550 ) ) ;
#28021 = CARTESIAN_POINT ( 'NONE',  ( -13.89961937509977652, 13.97604488694528158, 95.62390960531436690 ) ) ;
#28022 = ORIENTED_EDGE ( 'NONE', *, *, #98879, .F. ) ;
#28023 = CARTESIAN_POINT ( 'NONE',  ( 0.05219959533934541429, -16.53943276465976808, 35.00109039468568284 ) ) ;
#28024 = CARTESIAN_POINT ( 'NONE',  ( 13.97604488694527802, 13.89961937509977652, 44.37390960531435269 ) ) ;
#28026 =( LENGTH_UNIT ( ) NAMED_UNIT ( * ) SI_UNIT ( .MILLI., .METRE. ) );
#28025 = CARTESIAN_POINT ( 'NONE',  ( 4.379528057220092307, 16.55341960407617563, 47.29275706135234003 ) ) ;
#28027 = CARTESIAN_POINT ( 'NONE',  ( 19.05341960407617918, -5.049401038297876454, 51.04275706135231871 ) ) ;
#28028 = CARTESIAN_POINT ( 'NONE',  ( 13.97604488694527802, 13.89961937509977652, 49.37390960531434558 ) ) ;
#28029 = CARTESIAN_POINT ( 'NONE',  ( 4.379528057220092307, 16.55341960407617563, 82.29275706135234714 ) ) ;
#28030 = CARTESIAN_POINT ( 'NONE',  ( 13.89961937509957401, 13.97604488694547697, 76.87609039468566152 ) ) ;
#28031 = CARTESIAN_POINT ( 'NONE',  ( -13.89961937509957401, -13.97604488694547875, 24.37609039468565442 ) ) ;
#28032 = CARTESIAN_POINT ( 'NONE',  ( -16.51473224551069308, -9.474510206698971260, 61.66557627198103120 ) ) ;
#28033 = CARTESIAN_POINT ( 'NONE',  ( -16.52544592524342804, 4.483927247898546575, 101.0405762719810383 ) ) ;
#28034 = VECTOR ( 'NONE', #197159, 1000.000000000000000 ) ;
#28035 = CARTESIAN_POINT ( 'NONE',  ( -19.03943276465977164, -0.05219959533935918106, 73.75109039468566152 ) ) ;
#28036 = CARTESIAN_POINT ( 'NONE',  ( -5.719274019375978568, 21.55341960407610458, 65.20724293864768129 ) ) ;
#28037 = CARTESIAN_POINT ( 'NONE',  ( -13.97604488694547697, 13.89961937509957934, 33.12609039468566863 ) ) ;
#28038 = CARTESIAN_POINT ( 'NONE',  ( 13.97604488694527802, 13.89961937509977652, 99.37390960531436690 ) ) ;
#28039 = CARTESIAN_POINT ( 'NONE',  ( 5.719274019375991003, -21.55341960407610458, 82.70724293864770971 ) ) ;
#28040 = CARTESIAN_POINT ( 'NONE',  ( -17.44270441346519007, 5.991230190322971438, 83.63664920735773478 ) ) ;
#28041 = CARTESIAN_POINT ( 'NONE',  ( -19.03943276465977164, -0.05219959533935918106, 103.7510903946856757 ) ) ;
#28042 = CARTESIAN_POINT ( 'NONE',  ( 37.52651979737520094, -1.772832052285338689, 39.78107084225509027 ) ) ;
#28043 = EDGE_CURVE ( 'NONE', #60651, #37524, #38130, .T. ) ;
#28044 = CARTESIAN_POINT ( 'NONE',  ( 12.06949235617739724, 12.14591786802326823, 21.87609039468567573 ) ) ;
#28045 = CARTESIAN_POINT ( 'NONE',  ( -16.51473224551069308, -9.474510206698971260, 36.66557627198102409 ) ) ;
#28046 = CARTESIAN_POINT ( 'NONE',  ( 9.474510206698971260, -16.51473224551069308, 107.9155762719810383 ) ) ;
#28047 = CARTESIAN_POINT ( 'NONE',  ( -18.67979575497178146, -10.72451020669898902, 91.66557627198103830 ) ) ;
#28048 = CARTESIAN_POINT ( 'NONE',  ( -5.719274019375665041, -21.55341960407619695, 54.79275706135235424 ) ) ;
#28050 = CARTESIAN_POINT ( 'NONE',  ( -18.67979575497193778, 10.72451020669871902, 113.3344237280190328 ) ) ;
#28049 = CARTESIAN_POINT ( 'NONE',  ( 5.153800228976615827, -19.02544592524334988, 105.2094237280190185 ) ) ;
#28051 = CARTESIAN_POINT ( 'NONE',  ( -16.53943276465976808, -0.05219959533934237506, 103.7510903946857042 ) ) ;
#28052 = CARTESIAN_POINT ( 'NONE',  ( 0.05219959533907565091, 21.53943276465977519, 99.99890960531436690 ) ) ;
#28053 = CARTESIAN_POINT ( 'NONE',  ( -16.55341960407611168, -4.379528057220339221, 51.45724293864770260 ) ) ;
#28054 = CARTESIAN_POINT ( 'NONE',  ( -13.89961937509957401, -13.97604488694547875, 84.37609039468567573 ) ) ;
#28055 = CARTESIAN_POINT ( 'NONE',  ( -13.97604488694547697, 13.89961937509957934, 58.12609039468566863 ) ) ;
#28056 = CARTESIAN_POINT ( 'NONE',  ( -18.67979575497193778, 10.72451020669871902, 68.33442372801900433 ) ) ;
#28057 = CARTESIAN_POINT ( 'NONE',  ( -9.474510206698720793, -16.51473224551083518, 44.58442372801900433 ) ) ;
#28058 = CARTESIAN_POINT ( 'NONE',  ( 0.05219959533910956823, 16.53943276465976808, 104.9989096053143669 ) ) ;
#28059 = CARTESIAN_POINT ( 'NONE',  ( -18.67979575497178146, -10.72451020669898902, 41.66557627198103120 ) ) ;
#28060 = CARTESIAN_POINT ( 'NONE',  ( -14.29746914071049879, 8.314922557960819915, 30.83224293864770260 ) ) ;
#28061 = CARTESIAN_POINT ( 'NONE',  ( -15.72974639402176322, -15.80617190586768395, 94.37609039468568994 ) ) ;
#28062 = CARTESIAN_POINT ( 'NONE',  ( -12.06949235617739369, -12.14591786802326823, 69.37609039468567573 ) ) ;
#28063 = CARTESIAN_POINT ( 'NONE',  ( -14.29746914071049879, 8.314922557960819915, 25.83224293864769194 ) ) ;
#28064 = CARTESIAN_POINT ( 'NONE',  ( -21.52544592524334988, -5.823673210054445271, 58.95942372801902565 ) ) ;
#28066 = EDGE_CURVE ( 'NONE', #48561, #28823, #172825, .T. ) ;
#28065 = CARTESIAN_POINT ( 'NONE',  ( -0.05219959533937732626, 21.53943276465977519, 67.50109039468568994 ) ) ;
#28067 = CARTESIAN_POINT ( 'NONE',  ( -21.52544592524343514, 5.823673210054127303, 66.04057627198103830 ) ) ;
#28068 = ORIENTED_EDGE ( 'NONE', *, *, #134694, .F. ) ;
#28069 = CARTESIAN_POINT ( 'NONE',  ( -13.89961937509977652, 13.97604488694528158, 25.62390960531434558 ) ) ;
#28070 = CARTESIAN_POINT ( 'NONE',  ( -21.55341960407619339, 5.719274019375674811, 43.54275706135235424 ) ) ;
#28071 = CARTESIAN_POINT ( 'NONE',  ( -5.049401038298153566, 19.05341960407611168, 25.20724293864768484 ) ) ;
#28072 = CARTESIAN_POINT ( 'NONE',  ( -0.05219959533909027116, -19.03943276465977164, 37.49890960531436690 ) ) ;
#28073 = CARTESIAN_POINT ( 'NONE',  ( 16.53943276465976808, -0.05219959533910856209, 73.74890960531433848 ) ) ;
#28074 = CARTESIAN_POINT ( 'NONE',  ( 16.51473224551069308, 9.474510206698969483, 84.16557627198102409 ) ) ;
#28075 = CARTESIAN_POINT ( 'NONE',  ( -14.34966873604960291, -8.224510206698953496, 21.66557627198102409 ) ) ;
#28076 = CARTESIAN_POINT ( 'NONE',  ( 14.29746914071049879, -8.314922557960816363, 103.3322429386476955 ) ) ;
#28077 = CARTESIAN_POINT ( 'NONE',  ( 21.53943276465977519, -0.05219959533907433946, 73.74890960531433848 ) ) ;
#28078 = VECTOR ( 'NONE', #39367, 1000.000000000000000 ) ;
#28079 = CARTESIAN_POINT ( 'NONE',  ( 10.81492255796078972, 18.62759615963270932, 104.5822429386477097 ) ) ;
#28080 = CARTESIAN_POINT ( 'NONE',  ( -17.60430054815012113, 16.43460366218429414, -54.39459263522237364 ) ) ;
#28082 = CARTESIAN_POINT ( 'NONE',  ( -12.06949235617739369, -12.14591786802326823, 19.37609039468568639 ) ) ;
#28081 = CARTESIAN_POINT ( 'NONE',  ( 19.03943276465977164, -0.05219959533909143690, 68.74890960531436690 ) ) ;
#28083 = CARTESIAN_POINT ( 'NONE',  ( -10.81492255796078084, -18.62759615963271287, 52.08224293864768839 ) ) ;
#28084 = CARTESIAN_POINT ( 'NONE',  ( -5.823673210054431948, 21.52544592524334988, 77.70942372801900433 ) ) ;
#28085 = CARTESIAN_POINT ( 'NONE',  ( 16.51473224551069308, 9.474510206698969483, 79.16557627198103830 ) ) ;
#28086 = CARTESIAN_POINT ( 'NONE',  ( 5.153800228976335163, 19.02544592524342804, 99.79057627198102409 ) ) ;
#28087 = CARTESIAN_POINT ( 'NONE',  ( -4.379528057220086978, -16.55341960407618274, 74.79275706135234714 ) ) ;
#28088 = CARTESIAN_POINT ( 'NONE',  ( 5.719274019375673035, 21.55341960407619339, 57.29275706135234714 ) ) ;
#28089 = CARTESIAN_POINT ( 'NONE',  ( 10.81492255796106328, -18.62759615963255655, 100.4177570613523471 ) ) ;
#28090 = CARTESIAN_POINT ( 'NONE',  ( 16.52544592524335698, 4.483927247898782831, 66.45942372801903275 ) ) ;
#28091 = CARTESIAN_POINT ( 'NONE',  ( -5.823673210054116645, -21.52544592524344225, 107.2905762719810525 ) ) ;
#28092 = CARTESIAN_POINT ( 'NONE',  ( -9.564922557960796823, -16.46253265017161027, 112.0822429386476955 ) ) ;
#28093 = CARTESIAN_POINT ( 'NONE',  ( -10.72451020669898014, 18.67979575497178502, 85.41557627198102409 ) ) ;
#28094 = CARTESIAN_POINT ( 'NONE',  ( 9.474510206698729675, 16.51473224551082808, 42.08442372801900433 ) ) ;
#28095 = CARTESIAN_POINT ( 'NONE',  ( 21.52544592524344225, -5.823673210054117533, 38.54057627198103120 ) ) ;
#28097 = CARTESIAN_POINT ( 'NONE',  ( 4.483927247898545687, 16.52544592524342804, 34.79057627198103120 ) ) ;
#28096 = CARTESIAN_POINT ( 'NONE',  ( 9.564922557960805705, 16.46253265017160317, 79.58224293864769550 ) ) ;
#28098 = DIRECTION ( 'NONE',  ( -1.000000000000000000, 0.000000000000000000, 0.000000000000000000 ) ) ;
#28099 = CARTESIAN_POINT ( 'NONE',  ( -18.87255363501902750, -5.500000000000066613, 81.32513748171831480 ) ) ;
#28100 = CARTESIAN_POINT ( 'NONE',  ( -19.02544592524334988, -5.153800228976617603, 93.95942372801900433 ) ) ;
#28101 = CARTESIAN_POINT ( 'NONE',  ( -5.823673210054116645, -21.52544592524344225, 67.29057627198103830 ) ) ;
#28102 = CARTESIAN_POINT ( 'NONE',  ( 16.52544592524342804, -4.483927247898539470, 48.54057627198103120 ) ) ;
#28103 = CARTESIAN_POINT ( 'NONE',  ( -8.224510206698735004, -14.34966873604973081, 29.58442372801901854 ) ) ;
#28104 = CARTESIAN_POINT ( 'NONE',  ( -5.049401038298153566, 19.05341960407611168, 45.20724293864769550 ) ) ;
#28106 = CARTESIAN_POINT ( 'NONE',  ( -9.474510206698720793, -16.51473224551083518, 89.58442372801900433 ) ) ;
#28105 = CARTESIAN_POINT ( 'NONE',  ( 5.719274019375991003, -21.55341960407610458, 112.7072429386476955 ) ) ;
#28107 = CARTESIAN_POINT ( 'NONE',  ( -16.51473224551069308, -9.474510206698971260, 76.66557627198103830 ) ) ;
#28108 = CARTESIAN_POINT ( 'NONE',  ( -0.05219959533910754901, -16.53943276465976808, 87.49890960531436690 ) ) ;
#28109 =( BOUNDED_CURVE ( )  B_SPLINE_CURVE ( 2, ( #42276, #72609, #40262, #74591, #55427, #120090, #103934, #25118, #28116, #12927, #73612 ),
 .UNSPECIFIED., .F., .F. ) 
 B_SPLINE_CURVE_WITH_KNOTS ( ( 3, 2, 2, 2, 2, 3 ),
 ( 0.7000000000000006217, 0.7200000000000006395, 0.7400000000000006573, 0.7600000000000006750, 0.7800000000000006928, 0.8000000000000007105 ),
 .UNSPECIFIED. ) 
 CURVE ( )  GEOMETRIC_REPRESENTATION_ITEM ( )  RATIONAL_B_SPLINE_CURVE ( ( 0.9999999999999983347, 0.9510565162951551965, 1.000000000000000000, 0.9510565162951535312, 1.000000000000000000, 0.9510565162951535312, 1.000000000000000000, 0.9510565162951535312, 1.000000000000000000, 0.9510565162951518658, 1.000000000000001554 ) ) 
 REPRESENTATION_ITEM ( '' )  );
#28110 = CARTESIAN_POINT ( 'NONE',  ( 19.03943276465977164, -0.05219959533909143690, 68.74890960531436690 ) ) ;
#28111 = CARTESIAN_POINT ( 'NONE',  ( -5.823673210054116645, -21.52544592524344225, 77.29057627198102409 ) ) ;
#28112 = CARTESIAN_POINT ( 'NONE',  ( 16.46253265017160672, -9.564922557960803928, 33.33224293864770260 ) ) ;
#28113 = DIRECTION ( 'NONE',  ( -1.000000000000000000, 0.000000000000000000, -4.336808689942016750E-16 ) ) ;
#28114 = CARTESIAN_POINT ( 'NONE',  ( -16.53943276465976808, 0.05219959533911058130, 56.24890960531436690 ) ) ;
#28115 = CARTESIAN_POINT ( 'NONE',  ( -19.03943276465977164, 0.05219959533909376836, 91.24890960531436690 ) ) ;
#28116 = CARTESIAN_POINT ( 'NONE',  ( -23.31738231874055245, -16.94106989632524574, 140.4500000054623854 ) ) ;
#28117 = CARTESIAN_POINT ( 'NONE',  ( -5.049401038297874678, -19.05341960407617918, 49.79275706135231871 ) ) ;
#28118 = CARTESIAN_POINT ( 'NONE',  ( -15.80617190586745835, -15.72974639402198527, 71.87390960531438111 ) ) ;
#28119 = CARTESIAN_POINT ( 'NONE',  ( -13.89961937509957401, -13.97604488694547875, 34.37609039468566863 ) ) ;
#28120 = CARTESIAN_POINT ( 'NONE',  ( 19.05341960407611168, 5.049401038298154454, 83.95724293864766707 ) ) ;
#28121 = CARTESIAN_POINT ( 'NONE',  ( -19.03943276465977164, -1.327063459122257427E-13, 20.00000000000001776 ) ) ;
#28122 = CARTESIAN_POINT ( 'NONE',  ( -21.53943276465977519, 0.05219959533907696930, 31.24890960531435979 ) ) ;
#28123 = CARTESIAN_POINT ( 'NONE',  ( 19.03943276465977164, -0.05219959533909143690, 73.74890960531435269 ) ) ;
#28124 = CARTESIAN_POINT ( 'NONE',  ( -18.67979575497193778, 10.72451020669871902, 53.33442372801901854 ) ) ;
#28125 = CARTESIAN_POINT ( 'NONE',  ( 14.34966873604960469, 8.224510206698951720, 114.1655762719810383 ) ) ;
#28128 = ORIENTED_EDGE ( 'NONE', *, *, #4069, .T. ) ;
#28127 = CARTESIAN_POINT ( 'NONE',  ( 19.05341960407611168, 5.049401038298154454, 93.95724293864769550 ) ) ;
#28126 = CARTESIAN_POINT ( 'NONE',  ( -21.53943276465977519, 0.05219959533907696930, 116.2489096053143669 ) ) ;
#28129 = CARTESIAN_POINT ( 'NONE',  ( -18.62759615963255300, -10.81492255796106328, 44.16775706135234714 ) ) ;
#28130 = EDGE_LOOP ( 'NONE', ( #185336, #131114, #86532, #183362 ) ) ;
#28131 = CARTESIAN_POINT ( 'NONE',  ( 0.05219959533909260263, 19.03943276465977164, 104.9989096053143669 ) ) ;
#28132 = CARTESIAN_POINT ( 'NONE',  ( 5.000000000000000000, -130.0000000000000000, 15.00000000000000000 ) ) ;
#28133 = CARTESIAN_POINT ( 'NONE',  ( 5.823673210054125526, 21.52544592524343514, 104.7905762719810241 ) ) ;
#28134 = CARTESIAN_POINT ( 'NONE',  ( 9.474510206698971260, -16.51473224551069308, 42.91557627198103120 ) ) ;
#28135 = CARTESIAN_POINT ( 'NONE',  ( 0.05219959533934541429, -16.53943276465976808, 30.00109039468568284 ) ) ;
#28136 = CARTESIAN_POINT ( 'NONE',  ( 29.86685920354754842, -21.69954338932559068, -2.324999997268813345 ) ) ;
#28137 = CARTESIAN_POINT ( 'NONE',  ( 15.72974639402176855, 15.80617190586768217, 106.8760903946856899 ) ) ;
#28138 = CARTESIAN_POINT ( 'NONE',  ( 19.03943276465977164, -0.05219959533909143690, 43.74890960531435979 ) ) ;
#28139 = CARTESIAN_POINT ( 'NONE',  ( -21.53943276465977519, -0.05219959533937600094, 93.75109039468567573 ) ) ;
#28141 = CARTESIAN_POINT ( 'NONE',  ( 10.72451020669871369, 18.67979575497193778, 57.08442372801901854 ) ) ;
#28140 = CARTESIAN_POINT ( 'NONE',  ( 19.02544592524343514, -5.153800228976328945, 88.54057627198102409 ) ) ;
#28142 = CARTESIAN_POINT ( 'NONE',  ( -8.571926809382601320, -26.38167802310801591, 141.7750000027311899 ) ) ;
#28143 = CARTESIAN_POINT ( 'NONE',  ( -0.05219959533909027116, -19.03943276465977164, 102.4989096053143669 ) ) ;
#28144 = CARTESIAN_POINT ( 'NONE',  ( -17.50000000000002487, 4.658240926743135724, 28.94470417816804186 ) ) ;
#28147 = CARTESIAN_POINT ( 'NONE',  ( -15.72974639402176322, -15.80617190586768395, 59.37609039468568284 ) ) ;
#28146 = CARTESIAN_POINT ( 'NONE',  ( -14.34966873604972548, 8.224510206698743886, 63.33442372801900433 ) ) ;
#28145 = CARTESIAN_POINT ( 'NONE',  ( -0.05219959533934338120, 16.53943276465976808, 57.50109039468568994 ) ) ;
#28148 = CARTESIAN_POINT ( 'NONE',  ( 21.52544592524334988, 5.823673210054432836, 86.45942372801901854 ) ) ;
#28149 = CARTESIAN_POINT ( 'NONE',  ( 25.66098555633790923, -7.783268508282407794, 170.2231668181882185 ) ) ;
#28150 = CARTESIAN_POINT ( 'NONE',  ( 4.379528057220092307, 16.55341960407617563, 27.29275706135234358 ) ) ;
#28151 = CARTESIAN_POINT ( 'NONE',  ( -0.05219959533909027116, -19.03943276465977164, 67.49890960531436690 ) ) ;
#28152 = CARTESIAN_POINT ( 'NONE',  ( -5.153800228976328057, -19.02544592524343514, 97.29057627198099567 ) ) ;
#28153 = CARTESIAN_POINT ( 'NONE',  ( 5.153800228976335163, 19.02544592524342804, 114.7905762719810241 ) ) ;
#28154 = CARTESIAN_POINT ( 'NONE',  ( -5.049401038298153566, 19.05341960407611168, 25.20724293864768484 ) ) ;
#28155 = CARTESIAN_POINT ( 'NONE',  ( 10.72451020669898902, -18.67979575497178502, 27.91557627198103830 ) ) ;
#28156 = CARTESIAN_POINT ( 'NONE',  ( 8.224510206698742110, 14.34966873604972548, 87.08442372801901854 ) ) ;
#28158 = CARTESIAN_POINT ( 'NONE',  ( -0.05219959533909027116, -19.03943276465977164, 62.49890960531435979 ) ) ;
#28157 = CARTESIAN_POINT ( 'NONE',  ( -16.53943276465976808, 0.05219959533911058130, 81.24890960531436690 ) ) ;
#28159 = CARTESIAN_POINT ( 'NONE',  ( 5.719274019375673035, 21.55341960407619339, 92.29275706135236135 ) ) ;
#28160 = CARTESIAN_POINT ( 'NONE',  ( 17.48941328179922294, 5.058624476862394026, 21.78938172987509247 ) ) ;
#28161 = CARTESIAN_POINT ( 'NONE',  ( 12.06949235617739724, 12.14591786802326823, 21.87609039468567573 ) ) ;
#28162 = CARTESIAN_POINT ( 'NONE',  ( 0.05219959533910956823, 16.53943276465976808, 69.99890960531435269 ) ) ;
#28163 = CARTESIAN_POINT ( 'NONE',  ( 18.62759615963255655, 10.81492255796105972, 31.66775706135234358 ) ) ;
#28164 = CARTESIAN_POINT ( 'NONE',  ( -0.05219959533907301413, -21.53943276465977519, 67.49890960531436690 ) ) ;
#28165 = CARTESIAN_POINT ( 'NONE',  ( -5.153800228976607833, 19.02544592524334988, 37.70942372801899722 ) ) ;
#28166 = CARTESIAN_POINT ( 'NONE',  ( -35.02332884957466064, 5.945191563609817820, 40.42135061281684472 ) ) ;
#28167 = CARTESIAN_POINT ( 'NONE',  ( 19.05341960407611168, 5.049401038298154454, 83.95724293864766707 ) ) ;
#28168 = CARTESIAN_POINT ( 'NONE',  ( 8.314922557960818139, 14.29746914071049879, 44.58224293864769550 ) ) ;
#28169 = CIRCLE ( 'NONE', #166867, 61.99999999999998579 ) ;
#28170 = CARTESIAN_POINT ( 'NONE',  ( 16.53943276465976808, -0.05219959533910856209, 33.74890960531436690 ) ) ;
#28171 = CARTESIAN_POINT ( 'NONE',  ( 0.05219959533934541429, -16.53943276465976808, 105.0010903946856757 ) ) ;
#28172 = CARTESIAN_POINT ( 'NONE',  ( 16.51473224551083163, -9.474510206698727899, 70.83442372801900433 ) ) ;
#28173 = CARTESIAN_POINT ( 'NONE',  ( 19.53091890409952214, 5.500000000000025757, 52.56097431831423705 ) ) ;
#28174 = CARTESIAN_POINT ( 'NONE',  ( -10.81492255796078084, -18.62759615963271287, 22.08224293864769194 ) ) ;
#28175 = CARTESIAN_POINT ( 'NONE',  ( 16.55341960407611168, 4.379528057220329451, 73.95724293864769550 ) ) ;
#28176 = DIRECTION ( 'NONE',  ( 0.000000000000000000, 0.000000000000000000, -1.000000000000000000 ) ) ;
#28178 = CARTESIAN_POINT ( 'NONE',  ( 0.05219959533907565091, 21.53943276465977519, 29.99890960531435979 ) ) ;
#28177 = CARTESIAN_POINT ( 'NONE',  ( 16.46253265017160672, -9.564922557960803928, 28.33224293864769550 ) ) ;
#28179 = CARTESIAN_POINT ( 'NONE',  ( -10.81492255796078084, -18.62759615963271287, 62.08224293864769550 ) ) ;
#28180 = CARTESIAN_POINT ( 'NONE',  ( -19.05341960407611168, -5.049401038298163336, 21.45724293864768839 ) ) ;
#28182 = CARTESIAN_POINT ( 'NONE',  ( -5.153800228976328057, -19.02544592524343514, 52.29057627198100988 ) ) ;
#28181 = CARTESIAN_POINT ( 'NONE',  ( 8.224510206698742110, 14.34966873604972548, 67.08442372801901854 ) ) ;
#28183 = CARTESIAN_POINT ( 'NONE',  ( -5.823673210054431948, 21.52544592524334988, 57.70942372801901143 ) ) ;
#28184 = TOROIDAL_SURFACE ( 'NONE', #53977, 69.99999999999998579, 10.00000000000000000 ) ;
#28185 = CARTESIAN_POINT ( 'NONE',  ( -14.34966873604960291, -8.224510206698953496, 101.6655762719810383 ) ) ;
#28186 = CARTESIAN_POINT ( 'NONE',  ( -5.153800228976607833, 19.02544592524334988, 87.70942372801897591 ) ) ;
#28187 = CARTESIAN_POINT ( 'NONE',  ( -17.31747979337948706, 6.344076630960993057, 48.62055131934816643 ) ) ;
#28189 = CARTESIAN_POINT ( 'NONE',  ( 10.81492255796078972, 18.62759615963270932, 39.58224293864769550 ) ) ;
#28188 = DIRECTION ( 'NONE',  ( 0.000000000000000000, 0.000000000000000000, -1.000000000000000000 ) ) ;
#28190 = CARTESIAN_POINT ( 'NONE',  ( -17.49999999999999645, 5.500000000000000888, 108.7176903769643559 ) ) ;
#28191 = CARTESIAN_POINT ( 'NONE',  ( 21.52544592524334988, 5.823673210054432836, 71.45942372801901854 ) ) ;
#28193 = CARTESIAN_POINT ( 'NONE',  ( 8.224510206698953496, -14.34966873604960469, 42.91557627198103120 ) ) ;
#28192 = CARTESIAN_POINT ( 'NONE',  ( 4.483927247898790824, -16.52544592524335698, 55.20942372801902565 ) ) ;
#28194 = CARTESIAN_POINT ( 'NONE',  ( 0.05219959533907565091, 21.53943276465977519, 74.99890960531435269 ) ) ;
#28195 = CARTESIAN_POINT ( 'NONE',  ( -15.72974639402197994, 15.80617190586746368, 60.62390960531437401 ) ) ;
#28196 = CARTESIAN_POINT ( 'NONE',  ( -19.49401214000077331, 12.39993551617566681, 169.9999999999999716 ) ) ;
#28198 = CARTESIAN_POINT ( 'NONE',  ( 0.05219959533909260263, 19.03943276465977164, 109.9989096053143669 ) ) ;
#28197 = CARTESIAN_POINT ( 'NONE',  ( 13.97604488694548053, -13.89961937509957401, 85.62609039468568994 ) ) ;
#28199 = CARTESIAN_POINT ( 'NONE',  ( -9.564922557960796823, -16.46253265017161027, 52.08224293864768839 ) ) ;
#28200 = CARTESIAN_POINT ( 'NONE',  ( -12.06949235617756955, 12.14591786802309770, 110.6239096053143669 ) ) ;
#28201 = SURFACE_STYLE_USAGE ( .BOTH. , #58508 ) ;
#28202 = FACE_OUTER_BOUND ( 'NONE', #78803, .T. ) ;
#28203 = ORIENTED_EDGE ( 'NONE', *, *, #79617, .T. ) ;
#28204 = CARTESIAN_POINT ( 'NONE',  ( -4.379528057220086978, -16.55341960407618274, 64.79275706135234714 ) ) ;
#28205 = CARTESIAN_POINT ( 'NONE',  ( 15.72974639402199770, -15.80617190586745480, 103.1239096053143811 ) ) ;
#28206 = CARTESIAN_POINT ( 'NONE',  ( -19.05341960407611168, -5.049401038298163336, 51.45724293864770260 ) ) ;
#28207 = CARTESIAN_POINT ( 'NONE',  ( 15.72974639402176855, 15.80617190586768217, 46.87609039468568994 ) ) ;
#28208 = CARTESIAN_POINT ( 'NONE',  ( 19.05341960407611168, 5.049401038298154454, 93.95724293864769550 ) ) ;
#28210 = ADVANCED_FACE ( 'NONE', ( #138111 ), #87873, .F. ) ;
#28209 = CARTESIAN_POINT ( 'NONE',  ( -27.67003201002285806, -28.46598819372283984, -20.09023003179696332 ) ) ;
#28211 = VERTEX_POINT ( 'NONE', #132395 ) ;
#28212 = CARTESIAN_POINT ( 'NONE',  ( 10.81492255796106328, -18.62759615963255655, 35.41775706135234003 ) ) ;
#28214 = CARTESIAN_POINT ( 'NONE',  ( 13.97604488694548053, -13.89961937509957401, 85.62609039468568994 ) ) ;
#28213 = CARTESIAN_POINT ( 'NONE',  ( -16.51473224551069308, -9.474510206698971260, 101.6655762719810241 ) ) ;
#28215 = CARTESIAN_POINT ( 'NONE',  ( -5.049401038297874678, -19.05341960407617918, 39.79275706135232582 ) ) ;
#28216 = CARTESIAN_POINT ( 'NONE',  ( 5.823673210054125526, 21.52544592524343514, 94.79057627198105251 ) ) ;
#28217 = CARTESIAN_POINT ( 'NONE',  ( -19.05341960407617563, 5.049401038297882671, 38.54275706135233293 ) ) ;
#28218 = CARTESIAN_POINT ( 'NONE',  ( -9.474510206698720793, -16.51473224551083518, 44.58442372801900433 ) ) ;
#28219 = CARTESIAN_POINT ( 'NONE',  ( -16.55341960407617563, 4.379528057220093196, 93.54275706135234714 ) ) ;
#28220 = CARTESIAN_POINT ( 'NONE',  ( 0.05219959533909260263, 19.03943276465977164, 114.9989096053143669 ) ) ;
#28221 = CARTESIAN_POINT ( 'NONE',  ( -13.97604488694527625, -13.89961937509977652, 71.87390960531433848 ) ) ;
#28222 = CIRCLE ( 'NONE', #112169, 30.82560697742735556 ) ;
#28223 = CARTESIAN_POINT ( 'NONE',  ( 21.53943276465977519, 0.05219959533937863772, 76.25109039468568994 ) ) ;
#28224 = CARTESIAN_POINT ( 'NONE',  ( -21.53943276465977519, -0.05219959533937600094, 78.75109039468568994 ) ) ;
#28225 = CARTESIAN_POINT ( 'NONE',  ( 24.30000000000003624, -0.1121107154831149089, -54.21489346206828230 ) ) ;
#28226 = CARTESIAN_POINT ( 'NONE',  ( 19.05341960407611168, 5.049401038298154454, 93.95724293864769550 ) ) ;
#28227 = CARTESIAN_POINT ( 'NONE',  ( -15.72974639402176322, -15.80617190586768395, 59.37609039468568284 ) ) ;
#28228 = CARTESIAN_POINT ( 'NONE',  ( -19.02544592524334988, -5.153800228976617603, 98.95942372801900433 ) ) ;
#28229 = CARTESIAN_POINT ( 'NONE',  ( 19.03943276465977164, -0.05219959533909143690, 68.74890960531436690 ) ) ;
#28230 = CARTESIAN_POINT ( 'NONE',  ( 13.89961937509977652, -13.97604488694527269, 108.1239096053143669 ) ) ;
#28231 = CARTESIAN_POINT ( 'NONE',  ( 13.89961937509977652, -13.97604488694527269, 78.12390960531433848 ) ) ;
#28232 = CARTESIAN_POINT ( 'NONE',  ( 17.50000000000002487, -3.194745095267013557, 22.41015012971208265 ) ) ;
#28233 = CARTESIAN_POINT ( 'NONE',  ( 16.46253265017160672, -9.564922557960803928, 63.33224293864769550 ) ) ;
#28234 = CARTESIAN_POINT ( 'NONE',  ( -19.03943276465977164, 0.05219959533909376836, 56.24890960531435979 ) ) ;
#28235 = CARTESIAN_POINT ( 'NONE',  ( 5.823673210054125526, 21.52544592524343514, 109.7905762719810383 ) ) ;
#28236 = CARTESIAN_POINT ( 'NONE',  ( 16.53943276465976808, 0.05219959533934440121, 81.25109039468568994 ) ) ;
#28237 = CARTESIAN_POINT ( 'NONE',  ( -21.61802400803986757, 13.75099706318440340, 167.9999999999999432 ) ) ;
#28238 = CARTESIAN_POINT ( 'NONE',  ( -19.05341960407617563, 5.049401038297882671, 48.54275706135233293 ) ) ;
#28239 = CARTESIAN_POINT ( 'NONE',  ( -13.89961937509977652, 13.97604488694528158, 80.62390960531436690 ) ) ;
#28240 = CARTESIAN_POINT ( 'NONE',  ( -14.34966873604960291, -8.224510206698953496, 71.66557627198100988 ) ) ;
#28241 = CARTESIAN_POINT ( 'NONE',  ( -16.55341960407611168, -4.379528057220339221, 111.4572429386476813 ) ) ;
#28242 = CARTESIAN_POINT ( 'NONE',  ( 5.153800228976335163, 19.02544592524342804, 109.7905762719810099 ) ) ;
#28243 = CARTESIAN_POINT ( 'NONE',  ( -16.46253265017160317, 9.564922557960807481, 105.8322429386476955 ) ) ;
#28244 = CARTESIAN_POINT ( 'NONE',  ( 8.224510206698953496, -14.34966873604960469, 72.91557627198103830 ) ) ;
#28245 = DIRECTION ( 'NONE',  ( 1.000000000000000000, 0.000000000000000000, 3.469446951953612217E-15 ) ) ;
#28246 = CARTESIAN_POINT ( 'NONE',  ( -9.474510206698720793, -16.51473224551083518, 34.58442372801899722 ) ) ;
#28247 = CARTESIAN_POINT ( 'NONE',  ( -14.34966873604972548, 8.224510206698743886, 98.33442372801901854 ) ) ;
#28248 = CARTESIAN_POINT ( 'NONE',  ( -19.02544592524342804, 5.153800228976336051, 76.04057627198102409 ) ) ;
#28249 = CARTESIAN_POINT ( 'NONE',  ( -21.52544592524334988, -5.823673210054445271, 53.95942372801900433 ) ) ;
#28250 = CARTESIAN_POINT ( 'NONE',  ( -5.719274019375978568, 21.55341960407610458, 40.20724293864769550 ) ) ;
#28252 = ORIENTED_EDGE ( 'NONE', *, *, #58814, .T. ) ;
#28251 = CARTESIAN_POINT ( 'NONE',  ( -21.52544592524334988, -5.823673210054445271, 18.95942372801901143 ) ) ;
#28253 = CARTESIAN_POINT ( 'NONE',  ( -18.62759615963270932, 10.81492255796079327, 75.83224293864769550 ) ) ;
#28254 = CARTESIAN_POINT ( 'NONE',  ( -12.14591786802309592, -12.06949235617757132, 96.87390960531436690 ) ) ;
#28255 = CARTESIAN_POINT ( 'NONE',  ( -16.46253265017146816, -9.564922557961047289, 59.16775706135233293 ) ) ;
#28256 = CARTESIAN_POINT ( 'NONE',  ( 13.97604488694527802, 13.89961937509977652, 34.37390960531436690 ) ) ;
#28257 = CARTESIAN_POINT ( 'NONE',  ( 5.049401038298161559, -19.05341960407611168, 82.70724293864770971 ) ) ;
#28258 = CARTESIAN_POINT ( 'NONE',  ( 9.474510206698971260, -16.51473224551069308, 87.91557627198102409 ) ) ;
#28259 = CARTESIAN_POINT ( 'NONE',  ( 14.34966873604960469, 8.224510206698951720, 104.1655762719810241 ) ) ;
#28260 = ORIENTED_EDGE ( 'NONE', *, *, #60978, .T. ) ;
#28261 = CARTESIAN_POINT ( 'NONE',  ( 4.483927247898545687, 16.52544592524342804, 29.79057627198102409 ) ) ;
#28262 = CARTESIAN_POINT ( 'NONE',  ( 4.483927247898790824, -16.52544592524335698, 35.20942372801901854 ) ) ;
#28263 = CARTESIAN_POINT ( 'NONE',  ( -15.72974639402176322, -15.80617190586768395, 104.3760903946856899 ) ) ;
#28264 = CARTESIAN_POINT ( 'NONE',  ( -19.03943276465977164, 0.05219959533909376836, 106.2489096053143669 ) ) ;
#28265 = CARTESIAN_POINT ( 'NONE',  ( -15.80617190586768217, 15.72974639402176855, 23.12609039468567573 ) ) ;
#28266 = CARTESIAN_POINT ( 'NONE',  ( -5.049401038298153566, 19.05341960407611168, 40.20724293864768839 ) ) ;
#28267 = CARTESIAN_POINT ( 'NONE',  ( -4.483927247898782831, 16.52544592524335698, 47.70942372801902565 ) ) ;
#28268 = CARTESIAN_POINT ( 'NONE',  ( 13.89961937509957401, 13.97604488694547697, 101.8760903946856331 ) ) ;
#28269 = CARTESIAN_POINT ( 'NONE',  ( -16.46253265017160317, 9.564922557960807481, 35.83224293864768839 ) ) ;
#28270 = CARTESIAN_POINT ( 'NONE',  ( -4.483927247898539470, -16.52544592524342804, 97.29057627198105251 ) ) ;
#28271 = CARTESIAN_POINT ( 'NONE',  ( -5.719274019375978568, 21.55341960407610458, 110.2072429386477239 ) ) ;
#28272 = CARTESIAN_POINT ( 'NONE',  ( 0.05219959533936267826, -19.03943276465977164, 80.00109039468567573 ) ) ;
#28273 = CARTESIAN_POINT ( 'NONE',  ( 9.564922557960805705, 16.46253265017160317, 24.58224293864769194 ) ) ;
#28274 = CARTESIAN_POINT ( 'NONE',  ( 5.153800228976335163, 19.02544592524342804, 89.79057627198102409 ) ) ;
#28275 = CARTESIAN_POINT ( 'NONE',  ( 18.67979575497194134, -10.72451020669871369, 20.83442372801901143 ) ) ;
#28276 = CARTESIAN_POINT ( 'NONE',  ( 13.89961937509977652, -13.97604488694527269, 23.12390960531436335 ) ) ;
#28277 = CARTESIAN_POINT ( 'NONE',  ( 5.049401038298161559, -19.05341960407611168, 87.70724293864769550 ) ) ;
#28278 = DIRECTION ( 'NONE',  ( 0.000000000000000000, 0.000000000000000000, -1.000000000000000000 ) ) ;
#28279 = CARTESIAN_POINT ( 'NONE',  ( -16.46253265017160317, 9.564922557960807481, 85.83224293864769550 ) ) ;
#28281 = CARTESIAN_POINT ( 'NONE',  ( 4.483927247898545687, 16.52544592524342804, 89.79057627198103830 ) ) ;
#28280 = CARTESIAN_POINT ( 'NONE',  ( -21.52544592524334988, -5.823673210054445271, 28.95942372801902209 ) ) ;
#28282 = CARTESIAN_POINT ( 'NONE',  ( 9.474510206698971260, -16.51473224551069308, 92.91557627198103830 ) ) ;
#28283 = CARTESIAN_POINT ( 'NONE',  ( -9.474510206698720793, -16.51473224551083518, 29.58442372801900433 ) ) ;
#28284 = CARTESIAN_POINT ( 'NONE',  ( 12.14591786802327356, -12.06949235617739191, 45.62609039468567573 ) ) ;
#28285 = CARTESIAN_POINT ( 'NONE',  ( -21.53943276465977519, -0.05219959533937600094, 63.75109039468568284 ) ) ;
#28286 = CARTESIAN_POINT ( 'NONE',  ( 12.14591786802327356, -12.06949235617739191, 25.62609039468567929 ) ) ;
#28287 = CARTESIAN_POINT ( 'NONE',  ( -9.474510206698964154, 16.51473224551069663, 75.41557627198103830 ) ) ;
#28288 = CARTESIAN_POINT ( 'NONE',  ( 16.46253265017146816, 9.564922557961045513, 96.66775706135233293 ) ) ;
#28289 = CARTESIAN_POINT ( 'NONE',  ( -14.34966873604972548, 8.224510206698743886, 68.33442372801900433 ) ) ;
#28290 = CARTESIAN_POINT ( 'NONE',  ( 15.72974639402176855, 15.80617190586768217, 111.8760903946856615 ) ) ;
#28291 = CARTESIAN_POINT ( 'NONE',  ( -13.89961937509957401, -13.97604488694547875, 84.37609039468567573 ) ) ;
#28292 = CARTESIAN_POINT ( 'NONE',  ( 16.51473224551069308, 9.474510206698969483, 54.16557627198103120 ) ) ;
#28293 = CARTESIAN_POINT ( 'NONE',  ( 21.53943276465977519, -0.05219959533907433946, 88.74890960531436690 ) ) ;
#28295 = CARTESIAN_POINT ( 'NONE',  ( -16.51473224551082808, 9.474510206698731452, 73.33442372801900433 ) ) ;
#28294 = CARTESIAN_POINT ( 'NONE',  ( 8.314922557960818139, 14.29746914071049879, 79.58224293864769550 ) ) ;
#28296 = DIRECTION ( 'NONE',  ( -1.000000000000000000, 0.000000000000000000, 5.421010862427522170E-16 ) ) ;
#28297 = CARTESIAN_POINT ( 'NONE',  ( 5.049401038297881783, 19.05341960407617563, 62.29275706135234003 ) ) ;
#28298 = CARTESIAN_POINT ( 'NONE',  ( -12.14591786802309592, -12.06949235617757132, 21.87390960531436690 ) ) ;
#28299 = CARTESIAN_POINT ( 'NONE',  ( -8.314922557960811034, -14.29746914071050412, 67.08224293864770971 ) ) ;
#28301 = CARTESIAN_POINT ( 'NONE',  ( 8.571926809382603096, -26.38167802310801235, 143.4750000027312069 ) ) ;
#28300 = CARTESIAN_POINT ( 'NONE',  ( 15.80617190586769283, -15.72974639402175789, 100.6260903946857184 ) ) ;
#28302 = CARTESIAN_POINT ( 'NONE',  ( 21.53943276465977519, -0.05219959533907433946, 103.7489096053143669 ) ) ;
#28303 = CARTESIAN_POINT ( 'NONE',  ( 9.474510206698971260, -16.51473224551069308, 62.91557627198102409 ) ) ;
#28304 = CARTESIAN_POINT ( 'NONE',  ( -15.80617190586768217, 15.72974639402176855, 88.12609039468570415 ) ) ;
#28305 = CARTESIAN_POINT ( 'NONE',  ( 16.51473224551069308, 9.474510206698969483, 69.16557627198102409 ) ) ;
#28306 = VERTEX_POINT ( 'NONE', #162728 ) ;
#28307 = CARTESIAN_POINT ( 'NONE',  ( 14.34966873604960469, 8.224510206698951720, 114.1655762719810383 ) ) ;
#28308 = CARTESIAN_POINT ( 'NONE',  ( -18.62759615963270932, 10.81492255796079327, 30.83224293864770260 ) ) ;
#28309 = CARTESIAN_POINT ( 'NONE',  ( -14.29746914071049879, 8.314922557960819915, 65.83224293864769550 ) ) ;
#28310 = CARTESIAN_POINT ( 'NONE',  ( 13.89961937509977652, -13.97604488694527269, 48.12390960531435979 ) ) ;
#28311 = CARTESIAN_POINT ( 'NONE',  ( -16.53943276465976808, 0.05219959533911058130, 96.24890960531435269 ) ) ;
#28312 = AXIS2_PLACEMENT_3D ( 'NONE', #41777, #70107, #193458 ) ;
#28313 = CARTESIAN_POINT ( 'NONE',  ( 5.719274019375991003, -21.55341960407610458, 112.7072429386476955 ) ) ;
#28314 = CARTESIAN_POINT ( 'NONE',  ( -18.62759615963255300, -10.81492255796106328, 49.16775706135234003 ) ) ;
#28315 = CARTESIAN_POINT ( 'NONE',  ( -13.97604488694527625, -13.89961937509977652, 26.87390960531434558 ) ) ;
#28316 = CARTESIAN_POINT ( 'NONE',  ( 4.483927247898790824, -16.52544592524335698, 65.20942372801901854 ) ) ;
#28317 = CARTESIAN_POINT ( 'NONE',  ( -0.05219959533907301413, -21.53943276465977519, 102.4989096053143811 ) ) ;
#28318 = CARTESIAN_POINT ( 'NONE',  ( 18.62759615963271287, -10.81492255796078972, 93.33224293864769550 ) ) ;
#28320 = CARTESIAN_POINT ( 'NONE',  ( 16.46253265017160672, -9.564922557960803928, 53.33224293864768839 ) ) ;
#28319 = CARTESIAN_POINT ( 'NONE',  ( 5.153800228976615827, -19.02544592524334988, 30.20942372801900433 ) ) ;
#28321 = CARTESIAN_POINT ( 'NONE',  ( 35.00000000000000000, -0.3535533905932707888, 5.353553390593270400 ) ) ;
#28322 = CARTESIAN_POINT ( 'NONE',  ( -0.05219959533937732626, 21.53943276465977519, 57.50109039468568994 ) ) ;
#28323 = CARTESIAN_POINT ( 'NONE',  ( 21.53943276465977519, -0.05219959533907433946, 53.74890960531437401 ) ) ;
#28324 = CARTESIAN_POINT ( 'NONE',  ( -12.06949235617756955, 12.14591786802309770, 30.62390960531436335 ) ) ;
#28326 = CARTESIAN_POINT ( 'NONE',  ( 21.52544592524334988, 5.823673210054432836, 101.4594237280190185 ) ) ;
#28325 = CARTESIAN_POINT ( 'NONE',  ( -21.52544592524334988, -5.823673210054445271, 78.95942372801901854 ) ) ;
#28327 = CARTESIAN_POINT ( 'NONE',  ( 9.564922557961047289, -16.46253265017146816, 50.41775706135233293 ) ) ;
#28328 = CARTESIAN_POINT ( 'NONE',  ( 8.224510206698742110, 14.34966873604972548, 107.0844237280190043 ) ) ;
#28329 = CARTESIAN_POINT ( 'NONE',  ( 21.53943276465977519, 0.05219959533937863772, 61.25109039468567573 ) ) ;
#28330 = CARTESIAN_POINT ( 'NONE',  ( -16.46253265017160317, 9.564922557960807481, 60.83224293864769550 ) ) ;
#28331 = CARTESIAN_POINT ( 'NONE',  ( -5.049401038297874678, -19.05341960407617918, 34.79275706135233293 ) ) ;
#28332 = CARTESIAN_POINT ( 'NONE',  ( -15.80617190586745835, -15.72974639402198527, 41.87390960531435979 ) ) ;
#28333 = CARTESIAN_POINT ( 'NONE',  ( -21.55341960407619339, 5.719274019375674811, 28.54275706135234358 ) ) ;
#28334 = CARTESIAN_POINT ( 'NONE',  ( 0.05219959533907565091, 21.53943276465977519, 84.99890960531436690 ) ) ;
#28335 = CARTESIAN_POINT ( 'NONE',  ( -5.049401038297874678, -19.05341960407617918, 89.79275706135230450 ) ) ;
#28336 = CARTESIAN_POINT ( 'NONE',  ( 16.55341960407618274, -4.379528057220086978, 56.04275706135235424 ) ) ;
#28338 = CARTESIAN_POINT ( 'NONE',  ( 21.52544592524344225, -5.823673210054117533, 98.54057627198105251 ) ) ;
#28337 = CARTESIAN_POINT ( 'NONE',  ( 17.50000000000001066, -5.272787497354020303, 36.27284815830161335 ) ) ;
#28340 = CARTESIAN_POINT ( 'NONE',  ( -4.379528057220328563, 16.55341960407611168, 75.20724293864769550 ) ) ;
#28339 = CARTESIAN_POINT ( 'NONE',  ( 12.06949235617739724, 12.14591786802326823, 76.87609039468567573 ) ) ;
#28341 = CARTESIAN_POINT ( 'NONE',  ( -22.96834507599308139, 21.15706064682967380, -46.65423976109394744 ) ) ;
#28342 = CARTESIAN_POINT ( 'NONE',  ( 16.46253265017146816, 9.564922557961045513, 106.6677570613523471 ) ) ;
#28343 = EDGE_CURVE ( 'NONE', #37524, #123075, #155634, .T. ) ;
#28344 = CARTESIAN_POINT ( 'NONE',  ( 10.72451020669898902, -18.67979575497178502, 32.91557627198102409 ) ) ;
#28345 = CYLINDRICAL_SURFACE ( 'NONE', #138251, 16.70000000000002061 ) ;
#28346 = CARTESIAN_POINT ( 'NONE',  ( 0.05219959533934541429, -16.53943276465976808, 55.00109039468568284 ) ) ;
#28347 = CARTESIAN_POINT ( 'NONE',  ( 21.55341960407610458, 5.719274019375980345, 108.9572429386476955 ) ) ;
#28348 = CARTESIAN_POINT ( 'NONE',  ( -15.72974639402197994, 15.80617190586746368, 30.62390960531436335 ) ) ;
#28349 = CARTESIAN_POINT ( 'NONE',  ( 16.53943276465976808, 0.05219959533934440121, 76.25109039468568994 ) ) ;
#28350 = CARTESIAN_POINT ( 'NONE',  ( -13.97604488694527625, -13.89961937509977652, 86.87390960531436690 ) ) ;
#28352 = CARTESIAN_POINT ( 'NONE',  ( 16.46253265017160672, -9.564922557960803928, 33.33224293864770260 ) ) ;
#28351 = CARTESIAN_POINT ( 'NONE',  ( 18.67979575497194134, -10.72451020669871369, 55.83442372801901854 ) ) ;
#28353 = CARTESIAN_POINT ( 'NONE',  ( 15.72974639402199770, -15.80617190586745480, 23.12390960531436335 ) ) ;
#28354 = ORIENTED_EDGE ( 'NONE', *, *, #57463, .F. ) ;
#28355 = CARTESIAN_POINT ( 'NONE',  ( 9.564922557961047289, -16.46253265017146816, 40.41775706135234003 ) ) ;
#28356 = CARTESIAN_POINT ( 'NONE',  ( -4.483927247898782831, 16.52544592524335698, 57.70942372801901143 ) ) ;
#28357 = CARTESIAN_POINT ( 'NONE',  ( -19.05341960407611168, -5.049401038298163336, 111.4572429386476671 ) ) ;
#28358 = CARTESIAN_POINT ( 'NONE',  ( -19.05341960407611168, -5.049401038298163336, 76.45724293864769550 ) ) ;
#28359 = CARTESIAN_POINT ( 'NONE',  ( -8.224510206698735004, -14.34966873604973081, 104.5844237280190185 ) ) ;
#28360 = DIRECTION ( 'NONE',  ( 1.000000000000000000, 0.000000000000000000, 0.000000000000000000 ) ) ;
#28361 = CARTESIAN_POINT ( 'NONE',  ( 16.52544592524342804, -4.483927247898539470, 93.54057627198103830 ) ) ;
#28362 = CARTESIAN_POINT ( 'NONE',  ( 5.823673210054125526, 21.52544592524343514, 39.79057627198103830 ) ) ;
#28363 = CARTESIAN_POINT ( 'NONE',  ( 5.153800228976335163, 19.02544592524342804, 34.79057627198102409 ) ) ;
#28364 = CARTESIAN_POINT ( 'NONE',  ( 14.34966873604972726, -8.224510206698740333, 70.83442372801901854 ) ) ;
#28365 = CARTESIAN_POINT ( 'NONE',  ( -21.52544592524334988, -5.823673210054445271, 23.95942372801901143 ) ) ;
#28366 = CARTESIAN_POINT ( 'NONE',  ( 5.153800228976615827, -19.02544592524334988, 70.20942372801899012 ) ) ;
#28367 = CARTESIAN_POINT ( 'NONE',  ( -16.46253265017160317, 9.564922557960807481, 45.83224293864769550 ) ) ;
#28368 = CARTESIAN_POINT ( 'NONE',  ( 5.823673210054125526, 21.52544592524343514, 74.79057627198105251 ) ) ;
#28369 = AXIS2_PLACEMENT_3D ( 'NONE', #56430, #118110, #135280 ) ;
#28370 = CARTESIAN_POINT ( 'NONE',  ( -15.72974639402176322, -15.80617190586768395, 89.37609039468568994 ) ) ;
#28371 = CARTESIAN_POINT ( 'NONE',  ( 16.46253265017160672, -9.564922557960803928, 63.33224293864769550 ) ) ;
#28372 = CARTESIAN_POINT ( 'NONE',  ( 14.34966873604972726, -8.224510206698740333, 50.83442372801901143 ) ) ;
#28373 = CARTESIAN_POINT ( 'NONE',  ( -15.80617190586768217, 15.72974639402176855, 73.12609039468567573 ) ) ;
#28374 = CARTESIAN_POINT ( 'NONE',  ( -5.153800228976607833, 19.02544592524334988, 37.70942372801899722 ) ) ;
#28375 = CARTESIAN_POINT ( 'NONE',  ( -5.049401038297874678, -19.05341960407617918, 54.79275706135234003 ) ) ;
#28376 = ORIENTED_EDGE ( 'NONE', *, *, #181949, .F. ) ;
#28377 = CARTESIAN_POINT ( 'NONE',  ( -21.53943276465977519, -0.05219959533937600094, 43.75109039468568284 ) ) ;
#28378 = CARTESIAN_POINT ( 'NONE',  ( -8.788389965099090873, 0.9205664139721330130, -61.95844424577442311 ) ) ;
#28379 = CARTESIAN_POINT ( 'NONE',  ( -5.049401038297874678, -19.05341960407617918, 44.79275706135232582 ) ) ;
#28380 = CARTESIAN_POINT ( 'NONE',  ( -16.46253265017160317, 9.564922557960807481, 105.8322429386476955 ) ) ;
#28381 = CARTESIAN_POINT ( 'NONE',  ( -13.97604488694527625, -13.89961937509977652, 76.87390960531433848 ) ) ;
#28382 = CARTESIAN_POINT ( 'NONE',  ( -12.06949235617756955, 12.14591786802309770, 40.62390960531435269 ) ) ;
#28383 = CARTESIAN_POINT ( 'NONE',  ( -5.823673210054116645, -21.52544592524344225, 37.29057627198102409 ) ) ;
#28384 = CARTESIAN_POINT ( 'NONE',  ( 29.86685920354754487, 21.69954338932564752, -9.924999997268812990 ) ) ;
#28385 = CARTESIAN_POINT ( 'NONE',  ( 17.40861289039004234, 6.110651285853276882, 58.87232470827434838 ) ) ;
#28386 = CARTESIAN_POINT ( 'NONE',  ( 15.80617190586769283, -15.72974639402175789, 100.6260903946857184 ) ) ;
#28387 = CARTESIAN_POINT ( 'NONE',  ( 2.500000000000000000, -1.178949249685214307, 2.042000000000002036 ) ) ;
#28388 = CARTESIAN_POINT ( 'NONE',  ( 9.474510206698971260, -16.51473224551069308, 42.91557627198103120 ) ) ;
#28389 = DIRECTION ( 'NONE',  ( 1.000000000000000000, 0.000000000000000000, 0.000000000000000000 ) ) ;
#28390 = CARTESIAN_POINT ( 'NONE',  ( 30.73962218707677962, -22.33364281372841376, -1.202157773949823039 ) ) ;
#28391 = CARTESIAN_POINT ( 'NONE',  ( 8.224510206698742110, 14.34966873604972548, 47.08442372801901854 ) ) ;
#28392 = CARTESIAN_POINT ( 'NONE',  ( 15.72974639402199770, -15.80617190586745480, 63.12390960531435979 ) ) ;
#28393 = CARTESIAN_POINT ( 'NONE',  ( 14.34966873604960469, 8.224510206698951720, 34.16557627198102409 ) ) ;
#28395 = CARTESIAN_POINT ( 'NONE',  ( 0.05219959533909260263, 19.03943276465977164, 104.9989096053143669 ) ) ;
#28394 = CARTESIAN_POINT ( 'NONE',  ( -19.03943276465977164, 0.05219959533909376836, 26.24890960531435624 ) ) ;
#28396 = CARTESIAN_POINT ( 'NONE',  ( 21.53943276465977519, 0.05219959533937863772, 31.25109039468568639 ) ) ;
#28397 = CARTESIAN_POINT ( 'NONE',  ( -13.89961937509957401, -13.97604488694547875, 29.37609039468565797 ) ) ;
#28398 = CARTESIAN_POINT ( 'NONE',  ( -12.06949235617756955, 12.14591786802309770, 115.6239096053143669 ) ) ;
#28399 = CARTESIAN_POINT ( 'NONE',  ( -10.81492255796105439, 18.62759615963255655, 82.91775706135234714 ) ) ;
#28400 = DIRECTION ( 'NONE',  ( -0.000000000000000000, -0.000000000000000000, 1.000000000000000000 ) ) ;
#28401 = CARTESIAN_POINT ( 'NONE',  ( -0.05219959533910754901, -16.53943276465976808, 32.49890960531435979 ) ) ;
#28402 = CARTESIAN_POINT ( 'NONE',  ( 12.55500000000001748, 0.000000000000000000, 0.000000000000000000 ) ) ;
#28403 = CARTESIAN_POINT ( 'NONE',  ( 15.72974639402199770, -15.80617190586745480, 28.12390960531435979 ) ) ;
#28404 = CARTESIAN_POINT ( 'NONE',  ( 4.483927247898545687, 16.52544592524342804, 84.79057627198102409 ) ) ;
#28405 = CARTESIAN_POINT ( 'NONE',  ( -3.874011537017815421, -5.374011537017721274, -64.44758591613756948 ) ) ;
#28406 = CARTESIAN_POINT ( 'NONE',  ( 13.97604488694527802, 13.89961937509977652, 79.37390960531435269 ) ) ;
#28407 = CARTESIAN_POINT ( 'NONE',  ( -12.14591786802309592, -12.06949235617757132, 71.87390960531438111 ) ) ;
#28409 = EDGE_CURVE ( 'NONE', #196359, #111207, #196092, .T. ) ;
#28408 = CARTESIAN_POINT ( 'NONE',  ( 16.46253265017146816, 9.564922557961045513, 101.6677570613523329 ) ) ;
#28410 = EDGE_CURVE ( 'NONE', #170763, #111352, #40193, .T. ) ;
#28411 = CARTESIAN_POINT ( 'NONE',  ( 21.55341960407610458, 5.719274019375980345, 63.95724293864770260 ) ) ;
#28412 = EDGE_LOOP ( 'NONE', ( #68441, #200151, #170272 ) ) ;
#28413 = CARTESIAN_POINT ( 'NONE',  ( -19.03943276465977164, 0.05219959533909376836, 36.24890960531436690 ) ) ;
#28415 = CARTESIAN_POINT ( 'NONE',  ( -15.72974639402197994, 15.80617190586746368, 70.62390960531436690 ) ) ;
#28414 = CARTESIAN_POINT ( 'NONE',  ( -13.89961937509977652, 13.97604488694528158, 70.62390960531432427 ) ) ;
#28417 = CARTESIAN_POINT ( 'NONE',  ( 16.51473224551069308, 9.474510206698969483, 89.16557627198103830 ) ) ;
#28416 = CARTESIAN_POINT ( 'NONE',  ( -16.53943276465976808, -0.05219959533934237506, 108.7510903946857042 ) ) ;
#28418 = CARTESIAN_POINT ( 'NONE',  ( 16.46253265017146816, 9.564922557961045513, 71.66775706135233293 ) ) ;
#28419 = CARTESIAN_POINT ( 'NONE',  ( 21.55341960407619695, -5.719274019375665929, 96.04275706135236135 ) ) ;
#28420 = CARTESIAN_POINT ( 'NONE',  ( 21.55341960407610458, 5.719274019375980345, 78.95724293864769550 ) ) ;
#28421 = CARTESIAN_POINT ( 'NONE',  ( 19.02544592524343514, -5.153800228976328945, 113.5405762719810241 ) ) ;
#28422 = CARTESIAN_POINT ( 'NONE',  ( 5.153800228976335163, 19.02544592524342804, 44.79057627198103830 ) ) ;
#28423 = CARTESIAN_POINT ( 'NONE',  ( 16.53943276465976808, 0.05219959533934440121, 111.2510903946856899 ) ) ;
#28424 = CARTESIAN_POINT ( 'NONE',  ( 9.474510206698971260, -16.51473224551069308, 67.91557627198102409 ) ) ;
#28425 = CARTESIAN_POINT ( 'NONE',  ( -17.59860650958993844, 7.585241751806885979, 83.42337014262491834 ) ) ;
#28426 = CARTESIAN_POINT ( 'NONE',  ( 18.62759615963255655, 10.81492255796105972, 106.6677570613523756 ) ) ;
#28427 = CARTESIAN_POINT ( 'NONE',  ( -0.05219959533910754901, -16.53943276465976808, 67.49890960531436690 ) ) ;
#28428 = CARTESIAN_POINT ( 'NONE',  ( 0.05219959533907565091, 21.53943276465977519, 114.9989096053143669 ) ) ;
#28429 = CARTESIAN_POINT ( 'NONE',  ( -10.72451020669898014, 18.67979575497178502, 100.4155762719810241 ) ) ;
#28430 = CARTESIAN_POINT ( 'NONE',  ( -6.873473828371201577, 5.267258167721591278, -64.05152134952703591 ) ) ;
#28431 = CARTESIAN_POINT ( 'NONE',  ( -21.52544592524343514, 5.823673210054127303, 56.04057627198102409 ) ) ;
#28432 = CARTESIAN_POINT ( 'NONE',  ( 16.52544592524335698, 4.483927247898782831, 81.45942372801900433 ) ) ;
#28433 = CARTESIAN_POINT ( 'NONE',  ( -8.224510206698948167, 14.34966873604960824, 105.4155762719810383 ) ) ;
#28434 = B_SPLINE_CURVE_WITH_KNOTS ( 'NONE', 3,
 ( #136601, #197301, #164974, #59759, #121427, #179153 ),
 .UNSPECIFIED., .F., .F.,
 ( 4, 2, 4 ),
 ( 0.003989672132298133916, 0.004372778065220557162, 0.004755883998142979539 ),
 .UNSPECIFIED. ) ;
#28435 = CARTESIAN_POINT ( 'NONE',  ( 9.474510206698971260, -16.51473224551069308, 52.91557627198102409 ) ) ;
#28436 = CARTESIAN_POINT ( 'NONE',  ( 8.224510206698742110, 14.34966873604972548, 112.0844237280190185 ) ) ;
#28437 = VERTEX_POINT ( 'NONE', #85884 ) ;
#28438 = CARTESIAN_POINT ( 'NONE',  ( 10.81492255796106328, -18.62759615963255655, 45.41775706135234003 ) ) ;
#28439 = CARTESIAN_POINT ( 'NONE',  ( -5.049401038298153566, 19.05341960407611168, 110.2072429386476671 ) ) ;
#28440 = CARTESIAN_POINT ( 'NONE',  ( -10.81492255796105439, 18.62759615963255655, 77.91775706135231871 ) ) ;
#28441 = CARTESIAN_POINT ( 'NONE',  ( 13.89961937509977652, -13.97604488694527269, 33.12390960531434558 ) ) ;
#28442 = CARTESIAN_POINT ( 'NONE',  ( -5.049401038298153566, 19.05341960407611168, 35.20724293864768839 ) ) ;
#28443 = ORIENTED_EDGE ( 'NONE', *, *, #54823, .F. ) ;
#28444 = CARTESIAN_POINT ( 'NONE',  ( 0.05219959533937995610, -21.53943276465977519, 70.00109039468568994 ) ) ;
#28445 = CARTESIAN_POINT ( 'NONE',  ( 16.51473224551069308, 9.474510206698969483, 109.1655762719810383 ) ) ;
#28446 = CARTESIAN_POINT ( 'NONE',  ( -5.049401038297874678, -19.05341960407617918, 79.79275706135233293 ) ) ;
#28447 = CARTESIAN_POINT ( 'NONE',  ( 21.52544592524334988, 5.823673210054432836, 41.45942372801901143 ) ) ;
#28448 = CARTESIAN_POINT ( 'NONE',  ( 8.314922557961029526, -14.29746914071037800, 25.41775706135235779 ) ) ;
#28449 = CARTESIAN_POINT ( 'NONE',  ( 13.97604488694548053, -13.89961937509957401, 70.62609039468567573 ) ) ;
#28450 = CARTESIAN_POINT ( 'NONE',  ( -0.05219959533909027116, -19.03943276465977164, 47.49890960531435979 ) ) ;
#28451 = CARTESIAN_POINT ( 'NONE',  ( -5.153800228976607833, 19.02544592524334988, 87.70942372801897591 ) ) ;
#28452 = CARTESIAN_POINT ( 'NONE',  ( 14.29746914071049879, -8.314922557960816363, 28.33224293864769550 ) ) ;
#28453 = CARTESIAN_POINT ( 'NONE',  ( -16.51473224551082808, 9.474510206698731452, 93.33442372801900433 ) ) ;
#28454 = CARTESIAN_POINT ( 'NONE',  ( -16.53943276465976808, 0.05219959533911058130, 41.24890960531435269 ) ) ;
#28455 = CARTESIAN_POINT ( 'NONE',  ( -9.564922557961040184, 16.46253265017147172, 62.91775706135233293 ) ) ;
#28456 = CARTESIAN_POINT ( 'NONE',  ( 8.224510206698742110, 14.34966873604972548, 42.08442372801901854 ) ) ;
#28457 = CARTESIAN_POINT ( 'NONE',  ( 9.564922557961047289, -16.46253265017146816, 25.41775706135234003 ) ) ;
#28458 = CARTESIAN_POINT ( 'NONE',  ( 19.02544592524343514, -5.153800228976328945, 48.54057627198103120 ) ) ;
#28459 = CARTESIAN_POINT ( 'NONE',  ( -18.22780087662121673, -5.500000000000062172, 66.48459894673892734 ) ) ;
#28460 = CARTESIAN_POINT ( 'NONE',  ( 12.06949235617739724, 12.14591786802326823, 46.87609039468568994 ) ) ;
#28461 = DIRECTION ( 'NONE',  ( 1.000000000000000000, 0.000000000000000000, 0.000000000000000000 ) ) ;
#28462 = CARTESIAN_POINT ( 'NONE',  ( 27.73933785331498214, 9.013057229001095294, 143.9750000027312069 ) ) ;
#28463 = CARTESIAN_POINT ( 'NONE',  ( -16.51473224551069308, -9.474510206698971260, 91.66557627198103830 ) ) ;
#28464 = CARTESIAN_POINT ( 'NONE',  ( 0.05219959533936267826, -19.03943276465977164, 85.00109039468567573 ) ) ;
#28465 = EDGE_LOOP ( 'NONE', ( #148974, #121662, #36817, #23839 ) ) ;
#28466 = CARTESIAN_POINT ( 'NONE',  ( -5.153800228976607833, 19.02544592524334988, 87.70942372801897591 ) ) ;
#28467 = CARTESIAN_POINT ( 'NONE',  ( 18.62759615963271287, -10.81492255796078972, 28.33224293864769550 ) ) ;
#28469 = CARTESIAN_POINT ( 'NONE',  ( -16.51473224551082808, 9.474510206698731452, 98.33442372801900433 ) ) ;
#28468 = CARTESIAN_POINT ( 'NONE',  ( -5.153800228976607833, 19.02544592524334988, 22.70942372801899012 ) ) ;
#28470 = CARTESIAN_POINT ( 'NONE',  ( 0.05219959533910956823, 16.53943276465976808, 109.9989096053143527 ) ) ;
#28471 = CARTESIAN_POINT ( 'NONE',  ( -9.474510206698964154, 16.51473224551069663, 35.41557627198102409 ) ) ;
#28472 = CARTESIAN_POINT ( 'NONE',  ( 21.52544592524344225, -5.823673210054117533, 58.54057627198103120 ) ) ;
#28473 =( BOUNDED_SURFACE ( )  B_SPLINE_SURFACE ( 3, 2, ( 
 ( #138517, #94998, #141505, #123337, #30355, #40392, #64668, #61668, #156684, #126330, #113887, #140507, #79835, #175585, #17175, #83553, #1996, #60678, #2990, #122353, #160414, #46517, #21903, #108176, #169857, #77838, #988, #170855, #47520, #125350, #109176, #32346, #93999, #9742, #192755, #40057, #134083, #68392, #41075, #38071, #178594, #10742, #26916, #72406, #99727, #114903, #163422, #103742, #85561, #100724, #180605, #24920, #148248, #84549, #147247, #54238, #8738, #86565, #6714, #101734, #165422, #87564, #130044, #23907, #118920, #145232, #179603, #71406, #53227, #115909, #164427, #56232, #42078, #191744, #133070, #176597, #131066, #161411, #22903, #146227, #132075, #7714, #69399, #194760, #177599, #39067, #162405, #117914, #70407, #193764, #102739, #55232, #116901, #25920, #149251, #195773, #57246, #169365, #91515, #89560, #73418, #121872, #92520, #183565, #104730, #77360, #196765, #199725, #12735, #153201, #28902, #166422, #27917, #135089, #138044, #181586, #151246, #15699, #76367, #139028, #122863, #167406, #106708, #45050, #14706, #105719, #507, #108692, #62179, #170370, #60202, #58233, #119901, #47035, #152224, #107687, #61191, #11751, #75375, #74401, #197741, #136067, #44059, #182576, #184551, #90542, #13709, #43064, #154210, #59207, #46032, #30874, #120876, #137045, #198737, #123843, #168382, #185541, #88558, #150257, #29877, #19666, #20649, #50008, #113646, #173361, #93515, #189527, #155201, #142991, #124860, #35822, #66158, #34831, #4469, #31862, #140014, #16690, #78340, #32857, #51987, #95502, #81307, #65166, #174351, #1502, #186559, #48031, #67157, #111674, #127821, #63180, #96486, #109688, #157188, #171369, #159153, #94507, #158175, #50999, #17688, #112660, #156189, #97468, #82303, #188531, #143993, #5474, #128814, #190513, #126825, #79346, #80329, #110673, #141017, #2504, #18682, #49018, #142001, #64184, #125850, #187551, #172353, #3489, #33842, #56997, #176350, #160167, #8487, #179361, #70163, #191499, #164181, #83310, #86322, #99483, #178350, #115668, #52975, #114652, #21657, #24672, #68149, #37823, #102496, #163168, #25679, #9499, #53994, #193514, #131832, #101478, #192510, #87324, #195524, #149009, #175340, #147001, #144987, #6468, #133833, #38827, #194514, #39813, #98473, #162164, #161164, #84307, #22660, #130819, #69153, #71163, #177357, #100485, #129800, #40824, #145986, #148009, #117664, #7469, #23661, #85309, #10497, #54990, #132828, #72158, #36807, #116659, #55988, #107444, #136803, #265, #59960, #180363, #76118, #41831, #29633, #11505, #122621, #152957, #121626, #91266, #118672, #26670, #103498, #165176, #119666, #138784, #182335, #106458, #151981, #60946, #88311, #73176, #134847, #153960, #198487, #168137, #149999, #183322, #196525, #43813, #57996, #45792, #181348, #44803, #14455, #104492, #137796, #42827, #199480, #184311, #75133, #169118, #30623, #92276, #15458, #13470, #77114, #167163, #197502, #166174, #27675, #105476, #135833, #28662, #89315, #151008, #12499, #74161, #90297, #58969, #120637, #64928, #49767, #50766, #80095, #143752, #3255, #123602, #19430, #185297, #173119, #154953, #65916, #96252, #126588, #34594, #61933, #170123, #46788, #108447, #62932, #82058, #125609, #111432, #95264, #4236, #31618, #16449, #78098, #97231, #141763, #157939, #93268, #188290, #139767, #187308, #1255, #189288, #124612, #81077, #142756, #47788, #127589, #186307, #112424, #174115, #18444, #35585, #158919, #20409, #109439, #156947, #171122, #110433, #140769, #32611, #94265, #48779, #79096, #172115, #155944, #17440, #2258, #63941, #33601, #176107, #87085, #8246, #6234, #190271, #38590, #9260, #100245, #21415, #194283, #113409, #116422, #129566, #69924, #145749, #83073, #144749, #51748, #54748, #98223, #67913, #132593, #193275, #55749, #39578, #84070, #23421, #161927, #131590, #22420, #117423, #25445, #179121, #5232, #177119, #175100, #36568, #163947, #68915, #24434 ),
 ( #37577, #85069, #40589, #102260, #70926, #191264, #52739, #178110, #146751, #66913, #101237, #130577, #128577, #159926, #114406, #162926, #99240, #7230, #160929, #192272, #86082, #147773, #53754, #115428, #57762, #150769, #166932, #10259, #43580, #168883, #91041, #133590, #27435, #122386, #30388, #183090, #182096, #56763, #119432, #167911, #59727, #184075, #45559, #105245, #195281, #134606, #103260, #107213, #148770, #135599, #11265, #71919, #28433, #196292, #118435, #41596, #13245, #12266, #180128, #90070, #89078, #73930, #164942, #44572, #121397, #151752, #29411, #74908, #26435, #88076, #106227, #181116, #149762, #72937, #152728, #42590, #14218, #136572, #198252, #197271, #75887, #137562, #199245, #104253, #165936, #58733, #60712, #120403, #111196, #189065, #185064, #171885, #48551, #169893, #127351, #124378, #79871, #186073, #110205, #19204, #142530, #157714, #154724, #31387, #95031, #33373, #50536, #141540, #155713, #61702, #172888, #123371, #156721, #76880, #17209, #28, #49534, #93036, #78862, #80853, #3029, #140542, #62696, #47556, #63710, #109209, #18213, #138551, #4008, #2030, #64705, #139539, #187082, #65687, #15221, #188063, #46552, #125385, #112198, #173888, #92035, #153725, #126367, #108214, #77872, #16218, #1023, #170888, #34367, #32380, #94034, #96028, #97989, #101004, #5000, #68674, #191032, #116188, #22181, #129337, #52507, #39345, #38349, #115186, #145512, #23186, #83831, #97008, #128345, #100004, #21180, #158690, #81825, #161691, #190044, #84829, #130328, #160690, #114167, #6993, #192025, #131350, #144515, #143512, #6000, #53509, #176879, #146509, #177877, #66683, #7999, #69683, #51518, #35357, #67679, #193038, #175870, #54515, #20179, #113180, #174870, #37342, #99000, #36336, #159683, #82835, #38636, #114453, #115474, #144797, #8293, #67958, #188336, #84115, #49814, #37624, #19476, #130623, #160973, #129613, #99286, #126634, #34639, #111479, #173164, #127634, #146800, #190317, #176154, #159972, #68961, #96299, #81122, #142802, #161971, #6280, #22467, #157985, #191308, #4283, #51794, #65963, #53799, #189334, #52784, #145794, #112469, #7277, #50811, #192319, #177163, #83120, #100293, #23467, #85116, #174162, #21459, #35632, #175146, #5281, #97277, #158965, #113453, #143798, #36614, #20456, #82106, #66963, #98270, #128624, #119476, #118482, #40634, #102303, #41641, #163992, #72982, #54795, #58777, #180172, #134651, #117468, #164985, #120445, #193321, #165980, #162974, #103306, #135643, #151795, #197313, #24479, #39624, #88122, #28477, #10306, #25489, #105286, #149806, #196337, #9306, #71963, #179166, #133637, #11312, #131637, #26480, #90111, #12308, #116470, #148816, #43622, #69971, #104298, #57805, #178159, #87131, #89124, #181159, #166974, #101284, #42635, #86129, #55796, #147820, #70972, #132640, #56808, #194328, #195328, #27481, #150812, #73974, #182139, #77915, #76924, #48595, #169938, #153771, #138595, #33417, #47598, #186118, #93082, #94077, #31429, #74950, #29453, #109251, #184123, #198294, #121439, #170931, #91085, #32422, #139582, #46598, #15266, #154766, #16264, #63753, #168929, #59771, #107258, #62742, #1067, #155756, #110246, #106269, #124422, #17254, #152772, #171928, #45605, #78907, #30435, #140584, #2074, #125427, #187123, #75933, #14264, #92082, #108258, #95076, #123415, #77, #183132, #13286, #44615, #136613, #167954, #61747, #137608, #199291, #60758, #122431, #185108, #127398, #141582, #64747, #114213, #172932, #175918, #21227, #190086, #97050, #36380, #159731, #7037, #112240, #3070, #50580, #6047, #144561, #37389, #53555, #49578, #98034, #113226, #34411, #192074, #189107, #67725, #173930, #174916, #83877, #68719, #22228, #19249, #96069, #35399, #51562, #129383, #66730, #20222, #126409, #99046, #188105, #82883, #111241, #81870, #157758, #160736, #80896, #143561, #145559, #191079, #5044, #158732, #128390, #52552, #130376, #115234, #142573, #176925, #38396 ),
 ( #156764, #18258, #4052, #79911, #65729, #85894, #118245, #100052, #87884, #26245, #56571, #180927, #165746, #164750, #196103, #133399, #88889, #148579, #178927, #27240, #84877, #25253, #117234, #86895, #131397, #42402, #24245, #193085, #10069, #70738, #181909, #103068, #101052, #146554, #195088, #104065, #179936, #116233, #150581, #8050, #11068, #147582, #149572, #40397, #177924, #39392, #69729, #72746, #54560, #162737, #12080, #134417, #73743, #57573, #9068, #132405, #71729, #194098, #161738, #119243, #55560, #102068, #41403, #135415, #197086, #163753, #58553, #120219, #23233, #167726, #46360, #183890, #121210, #59532, #28247, #92849, #136389, #182901, #170703, #31198, #93850, #77689, #122198, #61520, #200051, #169704, #60523, #155528, #63522, #32192, #125197, #15034, #151570, #13059, #1840, #107028, #62511, #108018, #166744, #30202, #106040, #152542, #29224, #199053, #137375, #139357, #45375, #168700, #74725, #47369, #89887, #154534, #91843, #198066, #44385, #90857, #109024, #14030, #75695, #153537, #123189, #17023, #16031, #78676, #184878, #43388, #838, #105060, #124183, #185884, #76694, #138371, #140352, #36151, #35167, #157524, #19018, #158507, #80664, #189859, #171699, #175676, #96822, #51333, #34179, #81638, #37150, #110019, #82642, #79680, #19994, #52320, #68484, #113978, #141351, #156528, #4807, #145323, #127160, #142340, #21993, #66496, #112993, #126183, #188868, #95840, #50351, #128159, #48364, #143320, #6806, #129147, #33188, #65498, #160503, #186893, #20986, #174687, #94847, #3820, #5814, #97803, #2838, #98809, #18027, #159492, #111008, #144325, #112010, #64516, #187878, #49346, #67489, #172694, #173699, #83646, #190844, #180693, #164515, #8826, #148337, #86653, #56322, #147339, #42169, #150346, #57334, #11842, #101823, #38164, #99819, #88650, #193854, #149336, #133158, #53317, #116990, #192846, #39155, #54326, #85652, #23995, #26008, #70495, #132162, #161504, #134174, #114995, #118005, #55319, #84642, #176689, #22994, #195862, #146319, #7808, #177687, #9832, #103829, #179694, #119010, #71492, #130139, #69492, #163511, #131157, #10831, #41166, #115998, #165509, #87650, #194850, #102829, #191836, #100811, #162495, #178684, #40146, #25009, #72500, #27006, #106797, #15789, #58319, #28008, #166510, #108783, #91608, #122953, #181673, #138134, #43153, #198825, #93607, #596, #104821, #199815, #46122, #59298, #153296, #73507, #61283, #184641, #29969, #154299, #139120, #107776, #169461, #168471, #62267, #121963, #152313, #123935, #119987, #60290, #90631, #183656, #89648, #77449, #197832, #151336, #45140, #44149, #155292, #76457, #74491, #12825, #14797, #185633, #136157, #92609, #120966, #182665, #105808, #30962, #47125, #170461, #167495, #31952, #135179, #196853, #28991, #13799, #75465, #137138, #49112, #19757, #1597, #5567, #65259, #81398, #64276, #111766, #67246, #140106, #112750, #109777, #50106, #82398, #98567, #144086, #171460, #186649, #34924, #175434, #157280, #172451, #52081, #96579, #143084, #156282, #18776, #125943, #80423, #158268, #78431, #173455, #36904, #159247, #63273, #95596, #190605, #16782, #51090, #4563, #124953, #187641, #35913, #127915, #113737, #48120, #66255, #32948, #2597, #94603, #17783, #79438, #3581, #141109, #110769, #189617, #33938, #142096, #126919, #174444, #188626, #97559, #20743, #128905, #23757, #180456, #194608, #132921, #39910, #40919, #178443, #21751, #176444, #56080, #130914, #145080, #68240, #117761, #37917, #179453, #24768, #193610, #100576, #101577, #163266, #10592, #115761, #6563, #54087, #9592, #148100, #102592, #57093, #53072, #86415, #116752, #99576, #195621, #192605, #71257, #177449, #164277, #87417, #72253, #25771, #22752, #161258, #38919, #55082, #149102, #70258, #85407, #133931, #84401, #146077, #162258, #118767, #41928, #131926, #147099, #129893, #160261, #191593, #114750, #7562, #83402, #69248, #8584, #42916, #28752, #92365, #153048 ),
 ( #26763, #199568, #196615, #136896, #169209, #185386, #30718, #58085, #73268, #121719, #62023, #43904, #59059, #138873, #183411, #106551, #104582, #105567, #12588, #167253, #44894, #165269, #198583, #123687, #45879, #88403, #182426, #77204, #103594, #137887, #60051, #11600, #74253, #122709, #14550, #353, #150099, #168227, #134937, #89408, #119755, #181438, #166267, #90388, #27765, #151097, #29724, #135923, #197593, #120726, #91356, #152073, #13558, #76208, #75224, #61037, #184399, #107533, #154051, #15546, #127673, #65016, #108537, #63025, #81160, #17529, #31709, #155044, #4321, #124703, #66004, #111518, #80178, #187397, #126672, #49853, #97317, #2347, #93358, #140858, #96337, #34679, #189373, #143840, #139855, #188376, #3341, #186400, #82144, #79188, #158024, #64028, #173203, #174201, #159003, #19515, #142842, #20496, #125698, #16539, #48865, #50850, #112507, #35669, #5319, #1344, #67003, #128662, #47877, #46877, #110520, #170216, #172201, #78186, #109530, #171212, #32702, #94353, #156032, #33686, #141850, #95349, #157033, #18531, #160012, #12104, #21500, #83161, #144835, #23508, #42428, #150608, #129651, #115517, #181934, #104090, #38678, #161013, #22507, #162012, #84154, #193361, #175188, #43415, #100334, #54837, #37665, #85156, #105085, #113493, #88916, #6319, #146842, #58577, #74749, #120243, #67998, #191347, #8336, #151593, #130666, #145833, #28272, #70011, #116511, #52825, #192360, #99330, #53843, #131680, #51834, #178199, #13084, #135440, #36654, #69000, #166771, #190357, #27267, #165773, #98312, #7315, #73767, #197110, #89911, #114494, #176196, #177205, #122223, #90883, #110047, #171727, #123212, #199080, #94875, #16056, #183914, #18055, #29249, #862, #200075, #33215, #92873, #76718, #61543, #156555, #170727, #109050, #77714, #17048, #154560, #198092, #152567, #32219, #107052, #121235, #44411, #93876, #14056, #155554, #62537, #169729, #138394, #124211, #78703, #45399, #139380, #136412, #185909, #47395, #140380, #1867, #63548, #125222, #186920, #31224, #48390, #184902, #15058, #59557, #182928, #46386, #153561, #108044, #167751, #106065, #60548, #75723, #137399, #168725, #30226, #91868, #80691, #64544, #113019, #83671, #174711, #95868, #68510, #187905, #190870, #3847, #82668, #20022, #157551, #19044, #126209, #129172, #172723, #142368, #6831, #67515, #130164, #114002, #158533, #97828, #36175, #5839, #96848, #191861, #99844, #53343, #161528, #51358, #49374, #111037, #38188, #143347, #98835, #144352, #2866, #66522, #65526, #188897, #127186, #35195, #173726, #175700, #81664, #4835, #34205, #145349, #50378, #52346, #128185, #112038, #189883, #159516, #115022, #21012, #37176, #160530, #22019, #176715, #79709, #141378, #41192, #104849, #39180, #194874, #177712, #42196, #134203, #116023, #27035, #57366, #26032, #195891, #23020, #131183, #84666, #69518, #24023, #43181, #86678, #10858, #56347, #165538, #7832, #100837, #162520, #58347, #102854, #72527, #192873, #87677, #54351, #148362, #146345, #150376, #85677, #101851, #196881, #147364, #119039, #118030, #8853, #193880, #103857, #180721, #120015, #181700, #179721, #70520, #132189, #55345, #117015, #178710, #9857, #40172, #163535, #164540, #25035, #71516, #133184, #149362, #88680, #11872, #73536, #135209, #30001, #186684, #628, #139151, #46155, #47157, #184672, #28037, #182695, #62299, #137167, #151364, #74520, #123969, #44180, #185666, #30992, #199849, #106828, #107810, #169492, #16815, #121997, #12855, #60322, #15821, #154331, #108816, #63309, #59327, #92641, #122985, #105838, #1632, #198856, #77482, #183687, #170495, #93642, #78465, #31985, #29021, #167525, #45173, #61315, #155327, #76491, #91639, #136185, #140140, #197860, #120996, #90661, #124988, #48154, #166539, #152343, #153327, #89678, #13828, #14829, #168503, #138168, #75494, #142131, #112786, #94637, #98603, #158303, #174480, #157317, #4598, #160297, #32984, #5602, #2634, #143118 ),
 ( #97593, #35947, #66290, #190641, #175469, #159281, #67281, #127949, #21787, #19791, #128940, #189652, #83438, #81432, #188662, #36941, #156317, #34962, #126953, #96614, #141144, #52117, #33973, #64310, #51126, #80457, #191629, #20778, #110804, #17818, #82433, #113773, #144121, #125978, #145115, #79476, #6600, #95630, #68279, #50141, #187676, #49146, #172486, #129930, #18813, #3615, #109812, #171495, #65294, #111800, #173489, #71296, #9629, #179493, #70294, #103633, #73307, #180494, #134978, #24804, #161294, #22789, #11640, #116788, #72291, #56117, #176480, #39946, #115796, #162294, #177486, #8622, #147134, #87454, #131962, #193647, #84436, #57132, #37956, #40958, #55119, #7598, #99614, #146114, #118808, #69284, #130950, #100611, #132959, #165310, #102630, #41966, #194647, #53109, #192640, #86453, #54123, #133969, #164315, #38955, #26803, #149140, #117800, #25808, #114787, #23794, #85444, #178479, #101617, #163306, #148138, #10630, #195661, #88444, #150139, #151135, #89445, #31750, #14593, #45920, #104619, #61077, #166308, #121759, #16579, #123730, #27805, #122749, #169252, #182463, #76249, #196655, #184440, #107574, #153089, #77244, #62065, #30759, #183452, #12626, #138912, #120762, #74291, #106593, #167293, #78226, #199611, #197630, #181477, #29766, #392, #91400, #135960, #185429, #59096, #92406, #43944, #154092, #136936, #105606, #28790, #42955, #15586, #90429, #152115, #46919, #108579, #170256, #93399, #75265, #137927, #155085, #58124, #13598, #119793, #198625, #60091, #44936, #168269, #47918, #109572, #98354, #3380, #159043, #142880, #63067, #126712, #2389, #48906, #64068, #95389, #33727, #174242, #18571, #157075, #171255, #143879, #124746, #66045, #80218, #94394, #186442, #32742, #5360, #156073, #17571, #187438, #19555, #51875, #127712, #128702, #158064, #21540, #79232, #111559, #140903, #20536, #50889, #125738, #67043, #35710, #4361, #112547, #139897, #110560, #1386, #172241, #141889, #160053, #65055, #189413, #188415, #34719, #190399, #49893, #97357, #173244, #96377, #113534, #81199, #175228, #82186, #36693, #101361, #41718, #23546, #38714, #118558, #163051, #86207, #22544, #85193, #192398, #146882, #24558, #144874, #178236, #103382, #25567, #68037, #162050, #56884, #165060, #117545, #116548, #179245, #39699, #72040, #131717, #8374, #148893, #129689, #70049, #100371, #193399, #114534, #164068, #7354, #176234, #54874, #53880, #83200, #147897, #84191, #191386, #9383, #87211, #71049, #99367, #133713, #52862, #194403, #69038, #132715, #55871, #161050, #145871, #37705, #40711, #130703, #115555, #10383, #102380, #195406, #180248, #6357, #177242, #183208, #152846, #43698, #76997, #46671, #153843, #108331, #198369, #134729, #196411, #185181, #90185, #45677, #29524, #149881, #13358, #89198, #135718, #150891, #182214, #120521, #60830, #105360, #167047, #57881, #30505, #11387, #14340, #28548, #181236, #73057, #119553, #92156, #42712, #104374, #74047, #106343, #138669, #76006, #15341, #44689, #26554, #166057, #59846, #27558, #107328, #137681, #12385, #149, #122505, #91157, #199366, #88197, #197389, #58854, #151868, #75022, #136687, #121513, #168027, #184195, #169001, #61818, #123488, #62815, #5115, #188179, #19321, #77986, #34483, #139653, #95147, #190156, #97120, #1141, #96141, #142644, #155830, #49651, #170011, #157830, #80968, #126481, #50649, #35471, #4123, #140657, #141654, #2149, #173004, #154840, #3145, #63827, #65802, #124499, #64819, #158803, #93155, #127470, #186194, #111315, #20292, #51632, #81940, #47675, #109326, #189176, #128460, #110320, #125499, #66797, #112310, #174000, #171008, #172001, #78982, #33489, #143631, #31502, #16337, #32499, #94151, #17327, #48668, #187197, #156836, #18331, #79986, #21300, #83953, #132476, #24314, #86966, #148653, #146630, #159805, #99124, #67800, #10141, #71801, #100127, #175993, #133470, #193155, #160814, #195161, #6117, #177991, #177001, #113296 ),
 ( #98108, #82957, #70807, #129455, #194165, #39458, #8122, #53632, #54627, #116302, #163823, #68795, #144634, #7113, #162805, #101119, #55629, #174987, #191154, #85963, #69800, #52628, #36451, #145633, #147652, #130454, #131468, #40466, #25324, #178998, #37463, #114291, #192151, #9140, #117302, #23304, #38470, #22302, #102138, #115309, #161809, #84948, #181980, #74793, #121279, #72817, #73815, #90924, #136455, #197155, #42473, #119311, #166816, #14100, #198136, #152610, #105130, #122267, #149645, #120287, #11143, #182972, #59606, #26317, #167794, #44456, #28317, #106110, #56642, #164821, #180008, #103139, #134486, #118315, #88962, #151636, #43462, #89956, #87957, #196173, #57645, #41475, #29294, #199125, #27315, #75768, #150652, #137446, #180997, #104136, #12150, #60592, #165818, #135485, #58620, #13131, #24977, #163480, #193824, #117972, #102797, #101792, #133127, #70466, #25977, #85620, #115969, #164483, #21964, #162464, #54297, #23965, #68455, #179663, #161474, #130109, #147307, #7777, #118979, #40114, #38135, #83615, #132131, #41133, #55289, #53286, #87620, #145293, #148306, #22963, #86623, #177657, #114965, #176658, #6776, #9800, #191805, #99788, #149306, #71462, #10800, #194817, #39126, #116961, #178652, #56290, #100781, #72469, #57302, #134142, #37120, #8796, #84611, #146290, #195831, #98779, #160473, #69460, #131127, #192815, #43122, #89616, #104790, #136125, #74459, #14766, #59267, #197801, #150315, #187357, #165479, #106766, #120936, #135148, #26975, #88618, #48827, #11811, #58288, #76427, #13767, #172163, #28960, #182635, #110480, #73475, #105778, #44119, #167465, #196821, #61252, #166478, #119957, #90601, #151305, #64975, #183627, #181643, #27977, #75435, #33648, #137109, #12794, #95309, #152283, #91576, #198795, #45109, #60261, #121932, #168441, #29937, #153265, #138103, #199784, #156993, #125660, #18492, #80140, #141810, #3303, #180662, #42138, #103799, #197618, #88431, #151121, #196642, #165296, #72279, #11626, #134964, #182449, #87442, #178467, #25796, #181465, #119781, #12614, #28775, #24792, #73294, #150125, #9617, #167277, #164303, #42943, #149127, #58111, #59083, #43929, #120750, #194635, #71282, #102617, #26789, #104607, #41954, #195647, #101603, #74278, #163291, #86440, #148126, #166295, #27791, #89433, #132947, #57120, #105591, #135948, #180483, #10618, #133956, #103620, #118794, #90414, #116776, #152099, #13583, #131950, #56105, #193634, #55106, #39934, #117786, #179480, #40945, #140885, #157060, #2375, #29750, #44921, #93384, #33713, #15572, #30743, #110547, #155070, #78212, #14576, #77230, #184426, #138899, #16565, #136921, #170242, #32727, #76234, #379, #64055, #124729, #123716, #45906, #107559, #46904, #169237, #139882, #60076, #108564, #92391, #171238, #106577, #31736, #125725, #198608, #94379, #168254, #1371, #187424, #75250, #48892, #91385, #153074, #63050, #95375, #62051, #154078, #172228, #186427, #47903, #137914, #185413, #109557, #156059, #17556, #121744, #79216, #183436, #199596, #61063, #122735, #192385, #100359, #52849, #51861, #126698, #189399, #37690, #129675, #53868, #115542, #113521, #65042, #4347, #173230, #177230, #38702, #5346, #81186, #18557, #98340, #66032, #80205, #111545, #83187, #82171, #141876, #175215, #159030, #143867, #3367, #114520, #191373, #160039, #99355, #36680, #188402, #34706, #176221, #50876, #96363, #174228, #84179, #21526, #161038, #144861, #6344, #20523, #68024, #22532, #69026, #35697, #49880, #112534, #145859, #7341, #130691, #158051, #19541, #142868, #127699, #97344, #67030, #128689, #190386, #194393, #180237, #89186, #12372, #27545, #24546, #101350, #132704, #56872, #134717, #72029, #25556, #131705, #181224, #193386, #54862, #116536, #195394, #11375, #165049, #85180, #148881, #86196, #71037, #147886, #117534, #55860, #196400, #40698, #179232, #178224, #166045, #146869, #88186, #102368, #39688, #8361, #70036, #150878, #163039, #9372 ),
 ( #87200, #74035, #73045, #10372, #164057, #133702, #118547, #41706, #26542, #103371, #149870, #57869, #119541, #42700, #104361, #135706, #197377, #58842, #120509, #182200, #43685, #162038, #23534, #59831, #75010, #123477, #63817, #45666, #60819, #140647, #185169, #108319, #44677, #107317, #14329, #168990, #46660, #167034, #138, #125490, #47663, #90172, #184184, #78972, #187187, #139642, #138657, #13346, #75994, #124486, #16325, #2137, #105347, #61807, #151855, #91146, #121501, #28536, #136675, #92145, #168016, #198357, #169999, #152835, #183195, #106330, #31490, #30494, #29512, #93142, #153831, #15327, #137667, #1130, #77975, #154827, #186182, #62804, #199354, #122493, #109315, #76986, #170994, #32487, #94140, #155819, #17317, #113285, #81928, #189166, #128449, #51620, #99111, #191143, #33480, #127460, #22291, #130440, #82945, #143620, #156827, #19310, #67787, #159793, #83942, #145622, #5104, #95138, #34472, #3135, #7101, #68783, #35459, #111305, #48658, #190144, #96131, #110310, #141645, #174976, #112300, #171992, #66785, #50638, #173990, #18320, #144623, #21288, #36440, #129444, #98095, #79977, #64810, #6106, #80958, #126471, #4112, #114279, #52616, #175982, #37450, #160803, #97110, #188169, #49642, #172994, #65791, #157820, #142634, #158793, #20282, #11130, #88949, #84937, #71790, #148639, #69788, #27302, #24303, #179996, #85952, #10129, #119300, #42459, #57634, #54615, #131456, #162794, #86955, #164809, #102127, #55618, #161798, #72805, #23293, #146618, #8110, #25313, #41463, #149632, #193143, #117291, #180983, #103128, #40453, #147640, #9129, #163811, #70795, #195149, #176989, #133459, #132463, #87944, #116290, #56630, #104123, #115296, #134475, #177980, #118304, #165805, #73800, #150640, #39447, #101108, #26304, #12136, #194154, #178986, #192139, #196160, #53620, #38459, #100115, #44442, #137431, #153591, #197141, #30257, #155585, #185940, #169760, #14088, #15090, #91900, #61573, #75754, #106096, #17080, #152597, #135473, #107082, #43449, #105117, #93907, #199111, #154591, #138425, #58608, #122254, #198124, #167782, #59591, #90912, #29281, #31255, #60578, #183944, #166803, #139411, #120274, #123242, #45429, #89943, #181966, #28303, #894, #151624, #13117, #182959, #76750, #47425, #184933, #124245, #200105, #74781, #136443, #168754, #121265, #16087, #46418, #108076, #62568, #92905, #77745, #109081, #170760, #32249, #140410, #125253, #79739, #98867, #111067, #158562, #127218, #35225, #63579, #33247, #171758, #114035, #96878, #128217, #186952, #143377, #48422, #3879, #160563, #5870, #110078, #4869, #51389, #64575, #20051, #78734, #66553, #189914, #81694, #159549, #144384, #113050, #174742, #112069, #67546, #188931, #157581, #129204, #94905, #65558, #95898, #50409, #156589, #21046, #2896, #18084, #173757, #49404, #1899, #36205, #141408, #126240, #97859, #82700, #190902, #52378, #187935, #172756, #34236, #175733, #142400, #37211, #19074, #80722, #85712, #42226, #56381, #194906, #101885, #102884, #69552, #163567, #134235, #9889, #10887, #40206, #103887, #38221, #193914, #176747, #41223, #133215, #115055, #26063, #118063, #25067, #179753, #22052, #130198, #83703, #68542, #23053, #145381, #54384, #86710, #70554, #178742, #6863, #99876, #161560, #57396, #148395, #71550, #191893, #164569, #53377, #147398, #84698, #149392, #146378, #87706, #72560, #7866, #195920, #131216, #119068, #180750, #192907, #116057, #177745, #39214, #100870, #55377, #162552, #132221, #24057, #8886, #117047, #90690, #182726, #152373, #196911, #46185, #89710, #58378, #75525, #136215, #47186, #168531, #166569, #150407, #120045, #61344, #169522, #30029, #154360, #73566, #76521, #151395, #91667, #105869, #43213, #181732, #11902, #14860, #104881, #28069, #92672, #153358, #15854, #199880, #44210, #183717, #122027, #138198, #167556, #197890, #185697, #29050, #165567, #137200, #135239, #12885, #123999, #13858, #184700, #123015, #88712 ) ),
 .UNSPECIFIED., .T., .F., .F. ) 
 B_SPLINE_SURFACE_WITH_KNOTS ( ( 4, 3, 4 ),
 ( 3, 2, 2, 2, 2, 2, 2, 2, 2, 2, 2, 2, 2, 2, 2, 2, 2, 2, 2, 2, 2, 2, 2, 2, 2, 2, 2, 2, 2, 2, 2, 2, 2, 2, 2, 2, 2, 2, 2, 2, 2, 2, 2, 2, 2, 2, 2, 2, 2, 2, 2, 2, 2, 2, 2, 2, 2, 2, 2, 2, 2, 2, 2, 2, 2, 2, 2, 2, 2, 2, 2, 2, 2, 2, 2, 2, 2, 2, 2, 2, 2, 2, 2, 2, 2, 2, 2, 2, 2, 2, 2, 2, 2, 2, 2, 2, 2, 2, 2, 2, 2, 2, 2, 2, 2, 2, 2, 2, 2, 2, 2, 2, 2, 2, 2, 2, 2, 2, 2, 2, 2, 2, 2, 2, 2, 2, 2, 2, 2, 2, 2, 2, 2, 2, 2, 2, 2, 2, 2, 2, 2, 2, 2, 2, 2, 2, 2, 2, 2, 2, 2, 2, 2, 2, 2, 2, 2, 2, 2, 2, 2, 2, 2, 2, 2, 2, 2, 2, 2, 2, 2, 2, 2, 2, 2, 2, 2, 2, 2, 2, 2, 2, 2, 2, 2, 2, 2, 2, 2, 2, 2, 2, 2, 2, 2, 2, 2, 2, 2, 2, 2, 2, 2, 2, 2, 2, 2, 2, 2, 2, 2, 2, 2, 2, 2, 2, 2, 2, 2, 2, 2, 2, 2, 2, 2, 2, 2, 2, 3 ),
 ( 0.000000000000000000, 0.5000000000000000000, 1.000000000000000000 ),
 ( 0.000000000000000000, 0.004385964912280701511, 0.008771929824561403022, 0.01315789473684210453, 0.01754385964912280604, 0.02192982456140350755, 0.02631578947368420907, 0.03070175438596491058, 0.03508771929824561209, 0.03947368421052631360, 0.04385964912280701511, 0.04824561403508771662, 0.05263157894736841813, 0.05701754385964911964, 0.06140350877192982115, 0.06578947368421052266, 0.07017543859649122417, 0.07456140350877192569, 0.07894736842105262720, 0.08333333333333332871, 0.08771929824561403022, 0.09210526315789473173, 0.09649122807017543324, 0.1008771929824561348, 0.1052631578947368363, 0.1096491228070175378, 0.1140350877192982393, 0.1184210526315789408, 0.1228070175438596423, 0.1271929824561403577, 0.1315789473684210453, 0.1359649122807017607, 0.1403508771929824483, 0.1447368421052631637, 0.1491228070175438514, 0.1535087719298245668, 0.1578947368421052544, 0.1622807017543859698, 0.1666666666666666574, 0.1710526315789473728, 0.1754385964912280604, 0.1798245614035087758, 0.1842105263157894635, 0.1885964912280701788, 0.1929824561403508665, 0.1973684210526315819, 0.2017543859649122695, 0.2061403508771929849, 0.2105263157894736725, 0.2149122807017543879, 0.2192982456140350755, 0.2236842105263157909, 0.2280701754385964786, 0.2324561403508771940, 0.2368421052631578816, 0.2412280701754385970, 0.2456140350877192846, 0.2500000000000000000, 0.2543859649122807154, 0.2587719298245614308, 0.2631578947368420907, 0.2675438596491228060, 0.2719298245614035214, 0.2763157894736842368, 0.2807017543859648967, 0.2850877192982456121, 0.2894736842105263275, 0.2938596491228070429, 0.2982456140350877027, 0.3026315789473684181, 0.3070175438596491335, 0.3114035087719298489, 0.3157894736842105088, 0.3201754385964912242, 0.3245614035087719396, 0.3289473684210526550, 0.3333333333333333148, 0.3377192982456140302, 0.3421052631578947456, 0.3464912280701754610, 0.3508771929824561209, 0.3552631578947368363, 0.3596491228070175517, 0.3640350877192982670, 0.3684210526315789269, 0.3728070175438596423, 0.3771929824561403577, 0.3815789473684210731, 0.3859649122807017330, 0.3903508771929824483, 0.3947368421052631637, 0.3991228070175438791, 0.4035087719298245390, 0.4078947368421052544, 0.4122807017543859698, 0.4166666666666666852, 0.4210526315789473450, 0.4254385964912280604, 0.4298245614035087758, 0.4342105263157894912, 0.4385964912280701511, 0.4429824561403508665, 0.4473684210526315819, 0.4517543859649122973, 0.4561403508771929571, 0.4605263157894736725, 0.4649122807017543879, 0.4692982456140351033, 0.4736842105263157632, 0.4780701754385964786, 0.4824561403508771940, 0.4868421052631579093, 0.4912280701754385692, 0.4956140350877192846, 0.5000000000000000000, 0.5043859649122807154, 0.5087719298245614308, 0.5131578947368421462, 0.5175438596491228616, 0.5219298245614034659, 0.5263157894736841813, 0.5307017543859648967, 0.5350877192982456121, 0.5394736842105263275, 0.5438596491228070429, 0.5482456140350877583, 0.5526315789473684736, 0.5570175438596490780, 0.5614035087719297934, 0.5657894736842105088, 0.5701754385964912242, 0.5745614035087719396, 0.5789473684210526550, 0.5833333333333333703, 0.5877192982456140857, 0.5921052631578946901, 0.5964912280701754055, 0.6008771929824561209, 0.6052631578947368363, 0.6096491228070175517, 0.6140350877192982670, 0.6184210526315789824, 0.6228070175438596978, 0.6271929824561403022, 0.6315789473684210176, 0.6359649122807017330, 0.6403508771929824483, 0.6447368421052631637, 0.6491228070175438791, 0.6535087719298245945, 0.6578947368421053099, 0.6622807017543859143, 0.6666666666666666297, 0.6710526315789473450, 0.6754385964912280604, 0.6798245614035087758, 0.6842105263157894912, 0.6885964912280702066, 0.6929824561403509220, 0.6973684210526315264, 0.7017543859649122417, 0.7061403508771929571, 0.7105263157894736725, 0.7149122807017543879, 0.7192982456140351033, 0.7236842105263158187, 0.7280701754385965341, 0.7324561403508771384, 0.7368421052631578538, 0.7412280701754385692, 0.7456140350877192846, 0.7500000000000000000, 0.7543859649122807154, 0.7587719298245614308, 0.7631578947368421462, 0.7675438596491228616, 0.7719298245614034659, 0.7763157894736841813, 0.7807017543859648967, 0.7850877192982456121, 0.7894736842105263275, 0.7938596491228070429, 0.7982456140350877583, 0.8026315789473684736, 0.8070175438596490780, 0.8114035087719297934, 0.8157894736842105088, 0.8201754385964912242, 0.8245614035087719396, 0.8289473684210526550, 0.8333333333333333703, 0.8377192982456140857, 0.8421052631578946901, 0.8464912280701754055, 0.8508771929824561209, 0.8552631578947368363, 0.8596491228070175517, 0.8640350877192982670, 0.8684210526315789824, 0.8728070175438596978, 0.8771929824561403022, 0.8815789473684210176, 0.8859649122807017330, 0.8903508771929824483, 0.8947368421052631637, 0.8991228070175438791, 0.9035087719298245945, 0.9078947368421053099, 0.9122807017543859143, 0.9166666666666666297, 0.9210526315789473450, 0.9254385964912280604, 0.9298245614035087758, 0.9342105263157894912, 0.9385964912280702066, 0.9429824561403509220, 0.9473684210526315264, 0.9517543859649122417, 0.9561403508771929571, 0.9605263157894736725, 0.9649122807017543879, 0.9692982456140351033, 0.9736842105263158187, 0.9780701754385965341, 0.9824561403508771384, 0.9868421052631578538, 0.9912280701754385692, 0.9956140350877192846, 1.000000000000000000 ),
 .UNSPECIFIED. ) 
 GEOMETRIC_REPRESENTATION_ITEM ( )  RATIONAL_B_SPLINE_SURFACE ( (
 ( 1.000000000000000000, 0.9659258262890683122, 1.000000000000000000, 0.9659258262890683122, 1.000000000000000000, 0.9659258262890683122, 1.000000000000000000, 0.9659258262890683122, 1.000000000000000000, 0.9659258262890683122, 1.000000000000000000, 0.9659258262890683122, 1.000000000000000000, 0.9659258262890683122, 1.000000000000000000, 0.9659258262890683122, 1.000000000000000000, 0.9659258262890683122, 1.000000000000000000, 0.9659258262890683122, 1.000000000000000000, 0.9659258262890683122, 1.000000000000000000, 0.9659258262890683122, 1.000000000000000000, 0.9659258262890683122, 1.000000000000000000, 0.9659258262890683122, 1.000000000000000000, 0.9659258262890683122, 1.000000000000000000, 0.9659258262890683122, 1.000000000000000000, 0.9659258262890683122, 1.000000000000000000, 0.9659258262890683122, 1.000000000000000000, 0.9659258262890683122, 1.000000000000000000, 0.9659258262890683122, 1.000000000000000000, 0.9659258262890683122, 1.000000000000000000, 0.9659258262890683122, 1.000000000000000000, 0.9659258262890683122, 1.000000000000000000, 0.9659258262890683122, 1.000000000000000000, 0.9659258262890683122, 1.000000000000000000, 0.9659258262890683122, 1.000000000000000000, 0.9659258262890683122, 1.000000000000000000, 0.9659258262890683122, 1.000000000000000000, 0.9659258262890683122, 1.000000000000000000, 0.9659258262890683122, 1.000000000000000000, 0.9659258262890683122, 1.000000000000000000, 0.9659258262890683122, 1.000000000000000000, 0.9659258262890683122, 1.000000000000000000, 0.9659258262890683122, 1.000000000000000000, 0.9659258262890683122, 1.000000000000000000, 0.9659258262890683122, 1.000000000000000000, 0.9659258262890683122, 1.000000000000000000, 0.9659258262890683122, 1.000000000000000000, 0.9659258262890683122, 1.000000000000000000, 0.9659258262890683122, 1.000000000000000000, 0.9659258262890683122, 1.000000000000000000, 0.9659258262890683122, 1.000000000000000000, 0.9659258262890683122, 1.000000000000000000, 0.9659258262890683122, 1.000000000000000000, 0.9659258262890683122, 1.000000000000000000, 0.9659258262890683122, 1.000000000000000000, 0.9659258262890683122, 1.000000000000000000, 0.9659258262890683122, 1.000000000000000000, 0.9659258262890683122, 1.000000000000000000, 0.9659258262890683122, 1.000000000000000000, 0.9659258262890683122, 1.000000000000000000, 0.9659258262890683122, 1.000000000000000000, 0.9659258262890683122, 1.000000000000000000, 0.9659258262890683122, 1.000000000000000000, 0.9659258262890683122, 1.000000000000000000, 0.9659258262890683122, 1.000000000000000000, 0.9659258262890683122, 1.000000000000000000, 0.9659258262890683122, 1.000000000000000000, 0.9659258262890683122, 1.000000000000000000, 0.9659258262890683122, 1.000000000000000000, 0.9659258262890683122, 1.000000000000000000, 0.9659258262890683122, 1.000000000000000000, 0.9659258262890683122, 1.000000000000000000, 0.9659258262890683122, 1.000000000000000000, 0.9659258262890683122, 1.000000000000000000, 0.9659258262890683122, 1.000000000000000000, 0.9659258262890683122, 1.000000000000000000, 0.9659258262890683122, 1.000000000000000000, 0.9659258262890683122, 1.000000000000000000, 0.9659258262890683122, 1.000000000000000000, 0.9659258262890683122, 1.000000000000000000, 0.9659258262890683122, 1.000000000000000000, 0.9659258262890683122, 1.000000000000000000, 0.9659258262890683122, 1.000000000000000000, 0.9659258262890683122, 1.000000000000000000, 0.9659258262890683122, 1.000000000000000000, 0.9659258262890683122, 1.000000000000000000, 0.9659258262890683122, 1.000000000000000000, 0.9659258262890683122, 1.000000000000000000, 0.9659258262890683122, 1.000000000000000000, 0.9659258262890683122, 1.000000000000000000, 0.9659258262890683122, 1.000000000000000000, 0.9659258262890683122, 1.000000000000000000, 0.9659258262890683122, 1.000000000000000000, 0.9659258262890683122, 1.000000000000000000, 0.9659258262890683122, 1.000000000000000000, 0.9659258262890683122, 1.000000000000000000, 0.9659258262890683122, 1.000000000000000000, 0.9659258262890683122, 1.000000000000000000, 0.9659258262890683122, 1.000000000000000000, 0.9659258262890683122, 1.000000000000000000, 0.9659258262890683122, 1.000000000000000000, 0.9659258262890683122, 1.000000000000000000, 0.9659258262890683122, 1.000000000000000000, 0.9659258262890683122, 1.000000000000000000, 0.9659258262890683122, 1.000000000000000000, 0.9659258262890683122, 1.000000000000000000, 0.9659258262890683122, 1.000000000000000000, 0.9659258262890683122, 1.000000000000000000, 0.9659258262890683122, 1.000000000000000000, 0.9659258262890683122, 1.000000000000000000, 0.9659258262890683122, 1.000000000000000000, 0.9659258262890683122, 1.000000000000000000, 0.9659258262890683122, 1.000000000000000000, 0.9659258262890683122, 1.000000000000000000, 0.9659258262890683122, 1.000000000000000000, 0.9659258262890683122, 1.000000000000000000, 0.9659258262890683122, 1.000000000000000000, 0.9659258262890683122, 1.000000000000000000, 0.9659258262890683122, 1.000000000000000000, 0.9659258262890683122, 1.000000000000000000, 0.9659258262890683122, 1.000000000000000000, 0.9659258262890683122, 1.000000000000000000, 0.9659258262890683122, 1.000000000000000000, 0.9659258262890683122, 1.000000000000000000, 0.9659258262890683122, 1.000000000000000000, 0.9659258262890683122, 1.000000000000000000, 0.9659258262890683122, 1.000000000000000000, 0.9659258262890683122, 1.000000000000000000, 0.9659258262890683122, 1.000000000000000000, 0.9659258262890683122, 1.000000000000000000, 0.9659258262890683122, 1.000000000000000000, 0.9659258262890683122, 1.000000000000000000, 0.9659258262890683122, 1.000000000000000000, 0.9659258262890683122, 1.000000000000000000, 0.9659258262890683122, 1.000000000000000000, 0.9659258262890683122, 1.000000000000000000, 0.9659258262890683122, 1.000000000000000000, 0.9659258262890683122, 1.000000000000000000, 0.9659258262890683122, 1.000000000000000000, 0.9659258262890683122, 1.000000000000000000, 0.9659258262890683122, 1.000000000000000000, 0.9659258262890683122, 1.000000000000000000, 0.9659258262890683122, 1.000000000000000000, 0.9659258262890683122, 1.000000000000000000, 0.9659258262890683122, 1.000000000000000000, 0.9659258262890683122, 1.000000000000000000, 0.9659258262890683122, 1.000000000000000000, 0.9659258262890683122, 1.000000000000000000, 0.9659258262890683122, 1.000000000000000000, 0.9659258262890683122, 1.000000000000000000, 0.9659258262890683122, 1.000000000000000000, 0.9659258262890683122, 1.000000000000000000, 0.9659258262890683122, 1.000000000000000000, 0.9659258262890683122, 1.000000000000000000, 0.9659258262890683122, 1.000000000000000000, 0.9659258262890683122, 1.000000000000000000, 0.9659258262890683122, 1.000000000000000000, 0.9659258262890683122, 1.000000000000000000, 0.9659258262890683122, 1.000000000000000000, 0.9659258262890683122, 1.000000000000000000, 0.9659258262890683122, 1.000000000000000000, 0.9659258262890683122, 1.000000000000000000, 0.9659258262890683122, 1.000000000000000000, 0.9659258262890683122, 1.000000000000000000, 0.9659258262890683122, 1.000000000000000000, 0.9659258262890683122, 1.000000000000000000, 0.9659258262890683122, 1.000000000000000000, 0.9659258262890683122, 1.000000000000000000, 0.9659258262890683122, 1.000000000000000000, 0.9659258262890683122, 1.000000000000000000, 0.9659258262890683122, 1.000000000000000000, 0.9659258262890683122, 1.000000000000000000, 0.9659258262890683122, 1.000000000000000000, 0.9659258262890683122, 1.000000000000000000, 0.9659258262890683122, 1.000000000000000000, 0.9659258262890683122, 1.000000000000000000, 0.9659258262890683122, 1.000000000000000000, 0.9659258262890683122, 1.000000000000000000, 0.9659258262890683122, 1.000000000000000000, 0.9659258262890683122, 1.000000000000000000, 0.9659258262890683122, 1.000000000000000000, 0.9659258262890683122, 1.000000000000000000, 0.9659258262890683122, 1.000000000000000000, 0.9659258262890683122, 1.000000000000000000, 0.9659258262890683122, 1.000000000000000000, 0.9659258262890683122, 1.000000000000000000, 0.9659258262890683122, 1.000000000000000000, 0.9659258262890683122, 1.000000000000000000, 0.9659258262890683122, 1.000000000000000000, 0.9659258262890683122, 1.000000000000000000, 0.9659258262890683122, 1.000000000000000000, 0.9659258262890683122, 1.000000000000000000, 0.9659258262890683122, 1.000000000000000000, 0.9659258262890683122, 1.000000000000000000, 0.9659258262890683122, 1.000000000000000000, 0.9659258262890683122, 1.000000000000000000, 0.9659258262890683122, 1.000000000000000000, 0.9659258262890683122, 1.000000000000000000, 0.9659258262890683122, 1.000000000000000000, 0.9659258262890683122, 1.000000000000000000, 0.9659258262890683122, 1.000000000000000000, 0.9659258262890683122, 1.000000000000000000, 0.9659258262890683122, 1.000000000000000000, 0.9659258262890683122, 1.000000000000000000, 0.9659258262890683122, 1.000000000000000000, 0.9659258262890683122, 1.000000000000000000, 0.9659258262890683122, 1.000000000000000000, 0.9659258262890683122, 1.000000000000000000, 0.9659258262890683122, 1.000000000000000000, 0.9659258262890683122, 1.000000000000000000, 0.9659258262890683122, 1.000000000000000000, 0.9659258262890683122, 1.000000000000000000, 0.9659258262890683122, 1.000000000000000000, 0.9659258262890683122, 1.000000000000000000, 0.9659258262890683122, 1.000000000000000000, 0.9659258262890683122, 1.000000000000000000, 0.9659258262890683122, 1.000000000000000000, 0.9659258262890683122, 1.000000000000000000, 0.9659258262890683122, 1.000000000000000000, 0.9659258262890683122, 1.000000000000000000, 0.9659258262890683122, 1.000000000000000000, 0.9659258262890683122, 1.000000000000000000, 0.9659258262890683122, 1.000000000000000000, 0.9659258262890683122, 1.000000000000000000, 0.9659258262890683122, 1.000000000000000000, 0.9659258262890683122, 1.000000000000000000, 0.9659258262890683122, 1.000000000000000000, 0.9659258262890683122, 1.000000000000000000, 0.9659258262890683122, 1.000000000000000000, 0.9659258262890683122, 1.000000000000000000, 0.9659258262890683122, 1.000000000000000000, 0.9659258262890683122, 1.000000000000000000, 0.9659258262890683122, 1.000000000000000000, 0.9659258262890683122, 1.000000000000000000, 0.9659258262890683122, 1.000000000000000000, 0.9659258262890683122, 1.000000000000000000, 0.9659258262890683122, 1.000000000000000000),
 ( 0.3333333333333333703, 0.3219752754296894559, 0.3333333333333333703, 0.3219752754296894559, 0.3333333333333333703, 0.3219752754296894559, 0.3333333333333333703, 0.3219752754296894559, 0.3333333333333333703, 0.3219752754296894559, 0.3333333333333333703, 0.3219752754296894559, 0.3333333333333333703, 0.3219752754296894559, 0.3333333333333333703, 0.3219752754296894559, 0.3333333333333333703, 0.3219752754296894559, 0.3333333333333333703, 0.3219752754296894559, 0.3333333333333333703, 0.3219752754296894559, 0.3333333333333333703, 0.3219752754296894559, 0.3333333333333333703, 0.3219752754296894559, 0.3333333333333333703, 0.3219752754296894559, 0.3333333333333333703, 0.3219752754296894559, 0.3333333333333333703, 0.3219752754296894559, 0.3333333333333333703, 0.3219752754296894559, 0.3333333333333333703, 0.3219752754296894559, 0.3333333333333333703, 0.3219752754296894559, 0.3333333333333333703, 0.3219752754296894559, 0.3333333333333333703, 0.3219752754296894559, 0.3333333333333333703, 0.3219752754296894559, 0.3333333333333333703, 0.3219752754296894559, 0.3333333333333333703, 0.3219752754296894559, 0.3333333333333333703, 0.3219752754296894559, 0.3333333333333333703, 0.3219752754296894559, 0.3333333333333333703, 0.3219752754296894559, 0.3333333333333333703, 0.3219752754296894559, 0.3333333333333333703, 0.3219752754296894559, 0.3333333333333333703, 0.3219752754296894559, 0.3333333333333333703, 0.3219752754296894559, 0.3333333333333333703, 0.3219752754296894559, 0.3333333333333333703, 0.3219752754296894559, 0.3333333333333333703, 0.3219752754296894559, 0.3333333333333333703, 0.3219752754296894559, 0.3333333333333333703, 0.3219752754296894559, 0.3333333333333333703, 0.3219752754296894559, 0.3333333333333333703, 0.3219752754296894559, 0.3333333333333333703, 0.3219752754296894559, 0.3333333333333333703, 0.3219752754296894559, 0.3333333333333333703, 0.3219752754296894559, 0.3333333333333333703, 0.3219752754296894559, 0.3333333333333333703, 0.3219752754296894559, 0.3333333333333333703, 0.3219752754296894559, 0.3333333333333333703, 0.3219752754296894559, 0.3333333333333333703, 0.3219752754296894559, 0.3333333333333333703, 0.3219752754296894559, 0.3333333333333333703, 0.3219752754296894559, 0.3333333333333333703, 0.3219752754296894559, 0.3333333333333333703, 0.3219752754296894559, 0.3333333333333333703, 0.3219752754296894559, 0.3333333333333333703, 0.3219752754296894559, 0.3333333333333333703, 0.3219752754296894559, 0.3333333333333333703, 0.3219752754296894559, 0.3333333333333333703, 0.3219752754296894559, 0.3333333333333333703, 0.3219752754296894559, 0.3333333333333333703, 0.3219752754296894559, 0.3333333333333333703, 0.3219752754296894559, 0.3333333333333333703, 0.3219752754296894559, 0.3333333333333333703, 0.3219752754296894559, 0.3333333333333333703, 0.3219752754296894559, 0.3333333333333333703, 0.3219752754296894559, 0.3333333333333333703, 0.3219752754296894559, 0.3333333333333333703, 0.3219752754296894559, 0.3333333333333333703, 0.3219752754296894559, 0.3333333333333333703, 0.3219752754296894559, 0.3333333333333333703, 0.3219752754296894559, 0.3333333333333333703, 0.3219752754296894559, 0.3333333333333333703, 0.3219752754296894559, 0.3333333333333333703, 0.3219752754296894559, 0.3333333333333333703, 0.3219752754296894559, 0.3333333333333333703, 0.3219752754296894559, 0.3333333333333333703, 0.3219752754296894559, 0.3333333333333333703, 0.3219752754296894559, 0.3333333333333333703, 0.3219752754296894559, 0.3333333333333333703, 0.3219752754296894559, 0.3333333333333333703, 0.3219752754296894559, 0.3333333333333333703, 0.3219752754296894559, 0.3333333333333333703, 0.3219752754296894559, 0.3333333333333333703, 0.3219752754296894559, 0.3333333333333333703, 0.3219752754296894559, 0.3333333333333333703, 0.3219752754296894559, 0.3333333333333333703, 0.3219752754296894559, 0.3333333333333333703, 0.3219752754296894559, 0.3333333333333333703, 0.3219752754296894559, 0.3333333333333333703, 0.3219752754296894559, 0.3333333333333333703, 0.3219752754296894559, 0.3333333333333333703, 0.3219752754296894559, 0.3333333333333333703, 0.3219752754296894559, 0.3333333333333333703, 0.3219752754296894559, 0.3333333333333333703, 0.3219752754296894559, 0.3333333333333333703, 0.3219752754296894559, 0.3333333333333333703, 0.3219752754296894559, 0.3333333333333333703, 0.3219752754296894559, 0.3333333333333333703, 0.3219752754296894559, 0.3333333333333333703, 0.3219752754296894559, 0.3333333333333333703, 0.3219752754296894559, 0.3333333333333333703, 0.3219752754296894559, 0.3333333333333333703, 0.3219752754296894559, 0.3333333333333333703, 0.3219752754296894559, 0.3333333333333333703, 0.3219752754296894559, 0.3333333333333333703, 0.3219752754296894559, 0.3333333333333333703, 0.3219752754296894559, 0.3333333333333333703, 0.3219752754296894559, 0.3333333333333333703, 0.3219752754296894559, 0.3333333333333333703, 0.3219752754296894559, 0.3333333333333333703, 0.3219752754296894559, 0.3333333333333333703, 0.3219752754296894559, 0.3333333333333333703, 0.3219752754296894559, 0.3333333333333333703, 0.3219752754296894559, 0.3333333333333333703, 0.3219752754296894559, 0.3333333333333333703, 0.3219752754296894559, 0.3333333333333333703, 0.3219752754296894559, 0.3333333333333333703, 0.3219752754296894559, 0.3333333333333333703, 0.3219752754296894559, 0.3333333333333333703, 0.3219752754296894559, 0.3333333333333333703, 0.3219752754296894559, 0.3333333333333333703, 0.3219752754296894559, 0.3333333333333333703, 0.3219752754296894559, 0.3333333333333333703, 0.3219752754296894559, 0.3333333333333333703, 0.3219752754296894559, 0.3333333333333333703, 0.3219752754296894559, 0.3333333333333333703, 0.3219752754296894559, 0.3333333333333333703, 0.3219752754296894559, 0.3333333333333333703, 0.3219752754296894559, 0.3333333333333333703, 0.3219752754296894559, 0.3333333333333333703, 0.3219752754296894559, 0.3333333333333333703, 0.3219752754296894559, 0.3333333333333333703, 0.3219752754296894559, 0.3333333333333333703, 0.3219752754296894559, 0.3333333333333333703, 0.3219752754296894559, 0.3333333333333333703, 0.3219752754296894559, 0.3333333333333333703, 0.3219752754296894559, 0.3333333333333333703, 0.3219752754296894559, 0.3333333333333333703, 0.3219752754296894559, 0.3333333333333333703, 0.3219752754296894559, 0.3333333333333333703, 0.3219752754296894559, 0.3333333333333333703, 0.3219752754296894559, 0.3333333333333333703, 0.3219752754296894559, 0.3333333333333333703, 0.3219752754296894559, 0.3333333333333333703, 0.3219752754296894559, 0.3333333333333333703, 0.3219752754296894559, 0.3333333333333333703, 0.3219752754296894559, 0.3333333333333333703, 0.3219752754296894559, 0.3333333333333333703, 0.3219752754296894559, 0.3333333333333333703, 0.3219752754296894559, 0.3333333333333333703, 0.3219752754296894559, 0.3333333333333333703, 0.3219752754296894559, 0.3333333333333333703, 0.3219752754296894559, 0.3333333333333333703, 0.3219752754296894559, 0.3333333333333333703, 0.3219752754296894559, 0.3333333333333333703, 0.3219752754296894559, 0.3333333333333333703, 0.3219752754296894559, 0.3333333333333333703, 0.3219752754296894559, 0.3333333333333333703, 0.3219752754296894559, 0.3333333333333333703, 0.3219752754296894559, 0.3333333333333333703, 0.3219752754296894559, 0.3333333333333333703, 0.3219752754296894559, 0.3333333333333333703, 0.3219752754296894559, 0.3333333333333333703, 0.3219752754296894559, 0.3333333333333333703, 0.3219752754296894559, 0.3333333333333333703, 0.3219752754296894559, 0.3333333333333333703, 0.3219752754296894559, 0.3333333333333333703, 0.3219752754296894559, 0.3333333333333333703, 0.3219752754296894559, 0.3333333333333333703, 0.3219752754296894559, 0.3333333333333333703, 0.3219752754296894559, 0.3333333333333333703, 0.3219752754296894559, 0.3333333333333333703, 0.3219752754296894559, 0.3333333333333333703, 0.3219752754296894559, 0.3333333333333333703, 0.3219752754296894559, 0.3333333333333333703, 0.3219752754296894559, 0.3333333333333333703, 0.3219752754296894559, 0.3333333333333333703, 0.3219752754296894559, 0.3333333333333333703, 0.3219752754296894559, 0.3333333333333333703, 0.3219752754296894559, 0.3333333333333333703, 0.3219752754296894559, 0.3333333333333333703, 0.3219752754296894559, 0.3333333333333333703, 0.3219752754296894559, 0.3333333333333333703, 0.3219752754296894559, 0.3333333333333333703, 0.3219752754296894559, 0.3333333333333333703, 0.3219752754296894559, 0.3333333333333333703, 0.3219752754296894559, 0.3333333333333333703, 0.3219752754296894559, 0.3333333333333333703, 0.3219752754296894559, 0.3333333333333333703, 0.3219752754296894559, 0.3333333333333333703, 0.3219752754296894559, 0.3333333333333333703, 0.3219752754296894559, 0.3333333333333333703, 0.3219752754296894559, 0.3333333333333333703, 0.3219752754296894559, 0.3333333333333333703, 0.3219752754296894559, 0.3333333333333333703, 0.3219752754296894559, 0.3333333333333333703, 0.3219752754296894559, 0.3333333333333333703, 0.3219752754296894559, 0.3333333333333333703, 0.3219752754296894559, 0.3333333333333333703, 0.3219752754296894559, 0.3333333333333333703, 0.3219752754296894559, 0.3333333333333333703, 0.3219752754296894559, 0.3333333333333333703, 0.3219752754296894559, 0.3333333333333333703, 0.3219752754296894559, 0.3333333333333333703, 0.3219752754296894559, 0.3333333333333333703, 0.3219752754296894559, 0.3333333333333333703, 0.3219752754296894559, 0.3333333333333333703, 0.3219752754296894559, 0.3333333333333333703, 0.3219752754296894559, 0.3333333333333333703, 0.3219752754296894559, 0.3333333333333333703, 0.3219752754296894559, 0.3333333333333333703, 0.3219752754296894559, 0.3333333333333333703, 0.3219752754296894559, 0.3333333333333333703, 0.3219752754296894559, 0.3333333333333333703, 0.3219752754296894559, 0.3333333333333333703, 0.3219752754296894559, 0.3333333333333333703, 0.3219752754296894559, 0.3333333333333333703, 0.3219752754296894559, 0.3333333333333333703, 0.3219752754296894559, 0.3333333333333333703, 0.3219752754296894559, 0.3333333333333333703, 0.3219752754296894559, 0.3333333333333333703, 0.3219752754296894559, 0.3333333333333333703, 0.3219752754296894559, 0.3333333333333333703, 0.3219752754296894559, 0.3333333333333333703, 0.3219752754296894559, 0.3333333333333333703, 0.3219752754296894559, 0.3333333333333333703, 0.3219752754296894559, 0.3333333333333333703, 0.3219752754296894559, 0.3333333333333333703, 0.3219752754296894559, 0.3333333333333333703, 0.3219752754296894559, 0.3333333333333333703, 0.3219752754296894559, 0.3333333333333333703, 0.3219752754296894559, 0.3333333333333333703),
 ( 0.3333333333333333703, 0.3219752754296894559, 0.3333333333333333703, 0.3219752754296894559, 0.3333333333333333703, 0.3219752754296894559, 0.3333333333333333703, 0.3219752754296894559, 0.3333333333333333703, 0.3219752754296894559, 0.3333333333333333703, 0.3219752754296894559, 0.3333333333333333703, 0.3219752754296894559, 0.3333333333333333703, 0.3219752754296894559, 0.3333333333333333703, 0.3219752754296894559, 0.3333333333333333703, 0.3219752754296894559, 0.3333333333333333703, 0.3219752754296894559, 0.3333333333333333703, 0.3219752754296894559, 0.3333333333333333703, 0.3219752754296894559, 0.3333333333333333703, 0.3219752754296894559, 0.3333333333333333703, 0.3219752754296894559, 0.3333333333333333703, 0.3219752754296894559, 0.3333333333333333703, 0.3219752754296894559, 0.3333333333333333703, 0.3219752754296894559, 0.3333333333333333703, 0.3219752754296894559, 0.3333333333333333703, 0.3219752754296894559, 0.3333333333333333703, 0.3219752754296894559, 0.3333333333333333703, 0.3219752754296894559, 0.3333333333333333703, 0.3219752754296894559, 0.3333333333333333703, 0.3219752754296894559, 0.3333333333333333703, 0.3219752754296894559, 0.3333333333333333703, 0.3219752754296894559, 0.3333333333333333703, 0.3219752754296894559, 0.3333333333333333703, 0.3219752754296894559, 0.3333333333333333703, 0.3219752754296894559, 0.3333333333333333703, 0.3219752754296894559, 0.3333333333333333703, 0.3219752754296894559, 0.3333333333333333703, 0.3219752754296894559, 0.3333333333333333703, 0.3219752754296894559, 0.3333333333333333703, 0.3219752754296894559, 0.3333333333333333703, 0.3219752754296894559, 0.3333333333333333703, 0.3219752754296894559, 0.3333333333333333703, 0.3219752754296894559, 0.3333333333333333703, 0.3219752754296894559, 0.3333333333333333703, 0.3219752754296894559, 0.3333333333333333703, 0.3219752754296894559, 0.3333333333333333703, 0.3219752754296894559, 0.3333333333333333703, 0.3219752754296894559, 0.3333333333333333703, 0.3219752754296894559, 0.3333333333333333703, 0.3219752754296894559, 0.3333333333333333703, 0.3219752754296894559, 0.3333333333333333703, 0.3219752754296894559, 0.3333333333333333703, 0.3219752754296894559, 0.3333333333333333703, 0.3219752754296894559, 0.3333333333333333703, 0.3219752754296894559, 0.3333333333333333703, 0.3219752754296894559, 0.3333333333333333703, 0.3219752754296894559, 0.3333333333333333703, 0.3219752754296894559, 0.3333333333333333703, 0.3219752754296894559, 0.3333333333333333703, 0.3219752754296894559, 0.3333333333333333703, 0.3219752754296894559, 0.3333333333333333703, 0.3219752754296894559, 0.3333333333333333703, 0.3219752754296894559, 0.3333333333333333703, 0.3219752754296894559, 0.3333333333333333703, 0.3219752754296894559, 0.3333333333333333703, 0.3219752754296894559, 0.3333333333333333703, 0.3219752754296894559, 0.3333333333333333703, 0.3219752754296894559, 0.3333333333333333703, 0.3219752754296894559, 0.3333333333333333703, 0.3219752754296894559, 0.3333333333333333703, 0.3219752754296894559, 0.3333333333333333703, 0.3219752754296894559, 0.3333333333333333703, 0.3219752754296894559, 0.3333333333333333703, 0.3219752754296894559, 0.3333333333333333703, 0.3219752754296894559, 0.3333333333333333703, 0.3219752754296894559, 0.3333333333333333703, 0.3219752754296894559, 0.3333333333333333703, 0.3219752754296894559, 0.3333333333333333703, 0.3219752754296894559, 0.3333333333333333703, 0.3219752754296894559, 0.3333333333333333703, 0.3219752754296894559, 0.3333333333333333703, 0.3219752754296894559, 0.3333333333333333703, 0.3219752754296894559, 0.3333333333333333703, 0.3219752754296894559, 0.3333333333333333703, 0.3219752754296894559, 0.3333333333333333703, 0.3219752754296894559, 0.3333333333333333703, 0.3219752754296894559, 0.3333333333333333703, 0.3219752754296894559, 0.3333333333333333703, 0.3219752754296894559, 0.3333333333333333703, 0.3219752754296894559, 0.3333333333333333703, 0.3219752754296894559, 0.3333333333333333703, 0.3219752754296894559, 0.3333333333333333703, 0.3219752754296894559, 0.3333333333333333703, 0.3219752754296894559, 0.3333333333333333703, 0.3219752754296894559, 0.3333333333333333703, 0.3219752754296894559, 0.3333333333333333703, 0.3219752754296894559, 0.3333333333333333703, 0.3219752754296894559, 0.3333333333333333703, 0.3219752754296894559, 0.3333333333333333703, 0.3219752754296894559, 0.3333333333333333703, 0.3219752754296894559, 0.3333333333333333703, 0.3219752754296894559, 0.3333333333333333703, 0.3219752754296894559, 0.3333333333333333703, 0.3219752754296894559, 0.3333333333333333703, 0.3219752754296894559, 0.3333333333333333703, 0.3219752754296894559, 0.3333333333333333703, 0.3219752754296894559, 0.3333333333333333703, 0.3219752754296894559, 0.3333333333333333703, 0.3219752754296894559, 0.3333333333333333703, 0.3219752754296894559, 0.3333333333333333703, 0.3219752754296894559, 0.3333333333333333703, 0.3219752754296894559, 0.3333333333333333703, 0.3219752754296894559, 0.3333333333333333703, 0.3219752754296894559, 0.3333333333333333703, 0.3219752754296894559, 0.3333333333333333703, 0.3219752754296894559, 0.3333333333333333703, 0.3219752754296894559, 0.3333333333333333703, 0.3219752754296894559, 0.3333333333333333703, 0.3219752754296894559, 0.3333333333333333703, 0.3219752754296894559, 0.3333333333333333703, 0.3219752754296894559, 0.3333333333333333703, 0.3219752754296894559, 0.3333333333333333703, 0.3219752754296894559, 0.3333333333333333703, 0.3219752754296894559, 0.3333333333333333703, 0.3219752754296894559, 0.3333333333333333703, 0.3219752754296894559, 0.3333333333333333703, 0.3219752754296894559, 0.3333333333333333703, 0.3219752754296894559, 0.3333333333333333703, 0.3219752754296894559, 0.3333333333333333703, 0.3219752754296894559, 0.3333333333333333703, 0.3219752754296894559, 0.3333333333333333703, 0.3219752754296894559, 0.3333333333333333703, 0.3219752754296894559, 0.3333333333333333703, 0.3219752754296894559, 0.3333333333333333703, 0.3219752754296894559, 0.3333333333333333703, 0.3219752754296894559, 0.3333333333333333703, 0.3219752754296894559, 0.3333333333333333703, 0.3219752754296894559, 0.3333333333333333703, 0.3219752754296894559, 0.3333333333333333703, 0.3219752754296894559, 0.3333333333333333703, 0.3219752754296894559, 0.3333333333333333703, 0.3219752754296894559, 0.3333333333333333703, 0.3219752754296894559, 0.3333333333333333703, 0.3219752754296894559, 0.3333333333333333703, 0.3219752754296894559, 0.3333333333333333703, 0.3219752754296894559, 0.3333333333333333703, 0.3219752754296894559, 0.3333333333333333703, 0.3219752754296894559, 0.3333333333333333703, 0.3219752754296894559, 0.3333333333333333703, 0.3219752754296894559, 0.3333333333333333703, 0.3219752754296894559, 0.3333333333333333703, 0.3219752754296894559, 0.3333333333333333703, 0.3219752754296894559, 0.3333333333333333703, 0.3219752754296894559, 0.3333333333333333703, 0.3219752754296894559, 0.3333333333333333703, 0.3219752754296894559, 0.3333333333333333703, 0.3219752754296894559, 0.3333333333333333703, 0.3219752754296894559, 0.3333333333333333703, 0.3219752754296894559, 0.3333333333333333703, 0.3219752754296894559, 0.3333333333333333703, 0.3219752754296894559, 0.3333333333333333703, 0.3219752754296894559, 0.3333333333333333703, 0.3219752754296894559, 0.3333333333333333703, 0.3219752754296894559, 0.3333333333333333703, 0.3219752754296894559, 0.3333333333333333703, 0.3219752754296894559, 0.3333333333333333703, 0.3219752754296894559, 0.3333333333333333703, 0.3219752754296894559, 0.3333333333333333703, 0.3219752754296894559, 0.3333333333333333703, 0.3219752754296894559, 0.3333333333333333703, 0.3219752754296894559, 0.3333333333333333703, 0.3219752754296894559, 0.3333333333333333703, 0.3219752754296894559, 0.3333333333333333703, 0.3219752754296894559, 0.3333333333333333703, 0.3219752754296894559, 0.3333333333333333703, 0.3219752754296894559, 0.3333333333333333703, 0.3219752754296894559, 0.3333333333333333703, 0.3219752754296894559, 0.3333333333333333703, 0.3219752754296894559, 0.3333333333333333703, 0.3219752754296894559, 0.3333333333333333703, 0.3219752754296894559, 0.3333333333333333703, 0.3219752754296894559, 0.3333333333333333703, 0.3219752754296894559, 0.3333333333333333703, 0.3219752754296894559, 0.3333333333333333703, 0.3219752754296894559, 0.3333333333333333703, 0.3219752754296894559, 0.3333333333333333703, 0.3219752754296894559, 0.3333333333333333703, 0.3219752754296894559, 0.3333333333333333703, 0.3219752754296894559, 0.3333333333333333703, 0.3219752754296894559, 0.3333333333333333703, 0.3219752754296894559, 0.3333333333333333703, 0.3219752754296894559, 0.3333333333333333703, 0.3219752754296894559, 0.3333333333333333703, 0.3219752754296894559, 0.3333333333333333703, 0.3219752754296894559, 0.3333333333333333703, 0.3219752754296894559, 0.3333333333333333703, 0.3219752754296894559, 0.3333333333333333703, 0.3219752754296894559, 0.3333333333333333703, 0.3219752754296894559, 0.3333333333333333703, 0.3219752754296894559, 0.3333333333333333703, 0.3219752754296894559, 0.3333333333333333703, 0.3219752754296894559, 0.3333333333333333703, 0.3219752754296894559, 0.3333333333333333703, 0.3219752754296894559, 0.3333333333333333703, 0.3219752754296894559, 0.3333333333333333703, 0.3219752754296894559, 0.3333333333333333703, 0.3219752754296894559, 0.3333333333333333703, 0.3219752754296894559, 0.3333333333333333703, 0.3219752754296894559, 0.3333333333333333703, 0.3219752754296894559, 0.3333333333333333703, 0.3219752754296894559, 0.3333333333333333703, 0.3219752754296894559, 0.3333333333333333703, 0.3219752754296894559, 0.3333333333333333703, 0.3219752754296894559, 0.3333333333333333703, 0.3219752754296894559, 0.3333333333333333703, 0.3219752754296894559, 0.3333333333333333703, 0.3219752754296894559, 0.3333333333333333703, 0.3219752754296894559, 0.3333333333333333703, 0.3219752754296894559, 0.3333333333333333703, 0.3219752754296894559, 0.3333333333333333703, 0.3219752754296894559, 0.3333333333333333703, 0.3219752754296894559, 0.3333333333333333703, 0.3219752754296894559, 0.3333333333333333703, 0.3219752754296894559, 0.3333333333333333703, 0.3219752754296894559, 0.3333333333333333703, 0.3219752754296894559, 0.3333333333333333703, 0.3219752754296894559, 0.3333333333333333703, 0.3219752754296894559, 0.3333333333333333703, 0.3219752754296894559, 0.3333333333333333703, 0.3219752754296894559, 0.3333333333333333703, 0.3219752754296894559, 0.3333333333333333703, 0.3219752754296894559, 0.3333333333333333703, 0.3219752754296894559, 0.3333333333333333703, 0.3219752754296894559, 0.3333333333333333703),
 ( 1.000000000000000000, 0.9659258262890683122, 1.000000000000000000, 0.9659258262890683122, 1.000000000000000000, 0.9659258262890683122, 1.000000000000000000, 0.9659258262890683122, 1.000000000000000000, 0.9659258262890683122, 1.000000000000000000, 0.9659258262890683122, 1.000000000000000000, 0.9659258262890683122, 1.000000000000000000, 0.9659258262890683122, 1.000000000000000000, 0.9659258262890683122, 1.000000000000000000, 0.9659258262890683122, 1.000000000000000000, 0.9659258262890683122, 1.000000000000000000, 0.9659258262890683122, 1.000000000000000000, 0.9659258262890683122, 1.000000000000000000, 0.9659258262890683122, 1.000000000000000000, 0.9659258262890683122, 1.000000000000000000, 0.9659258262890683122, 1.000000000000000000, 0.9659258262890683122, 1.000000000000000000, 0.9659258262890683122, 1.000000000000000000, 0.9659258262890683122, 1.000000000000000000, 0.9659258262890683122, 1.000000000000000000, 0.9659258262890683122, 1.000000000000000000, 0.9659258262890683122, 1.000000000000000000, 0.9659258262890683122, 1.000000000000000000, 0.9659258262890683122, 1.000000000000000000, 0.9659258262890683122, 1.000000000000000000, 0.9659258262890683122, 1.000000000000000000, 0.9659258262890683122, 1.000000000000000000, 0.9659258262890683122, 1.000000000000000000, 0.9659258262890683122, 1.000000000000000000, 0.9659258262890683122, 1.000000000000000000, 0.9659258262890683122, 1.000000000000000000, 0.9659258262890683122, 1.000000000000000000, 0.9659258262890683122, 1.000000000000000000, 0.9659258262890683122, 1.000000000000000000, 0.9659258262890683122, 1.000000000000000000, 0.9659258262890683122, 1.000000000000000000, 0.9659258262890683122, 1.000000000000000000, 0.9659258262890683122, 1.000000000000000000, 0.9659258262890683122, 1.000000000000000000, 0.9659258262890683122, 1.000000000000000000, 0.9659258262890683122, 1.000000000000000000, 0.9659258262890683122, 1.000000000000000000, 0.9659258262890683122, 1.000000000000000000, 0.9659258262890683122, 1.000000000000000000, 0.9659258262890683122, 1.000000000000000000, 0.9659258262890683122, 1.000000000000000000, 0.9659258262890683122, 1.000000000000000000, 0.9659258262890683122, 1.000000000000000000, 0.9659258262890683122, 1.000000000000000000, 0.9659258262890683122, 1.000000000000000000, 0.9659258262890683122, 1.000000000000000000, 0.9659258262890683122, 1.000000000000000000, 0.9659258262890683122, 1.000000000000000000, 0.9659258262890683122, 1.000000000000000000, 0.9659258262890683122, 1.000000000000000000, 0.9659258262890683122, 1.000000000000000000, 0.9659258262890683122, 1.000000000000000000, 0.9659258262890683122, 1.000000000000000000, 0.9659258262890683122, 1.000000000000000000, 0.9659258262890683122, 1.000000000000000000, 0.9659258262890683122, 1.000000000000000000, 0.9659258262890683122, 1.000000000000000000, 0.9659258262890683122, 1.000000000000000000, 0.9659258262890683122, 1.000000000000000000, 0.9659258262890683122, 1.000000000000000000, 0.9659258262890683122, 1.000000000000000000, 0.9659258262890683122, 1.000000000000000000, 0.9659258262890683122, 1.000000000000000000, 0.9659258262890683122, 1.000000000000000000, 0.9659258262890683122, 1.000000000000000000, 0.9659258262890683122, 1.000000000000000000, 0.9659258262890683122, 1.000000000000000000, 0.9659258262890683122, 1.000000000000000000, 0.9659258262890683122, 1.000000000000000000, 0.9659258262890683122, 1.000000000000000000, 0.9659258262890683122, 1.000000000000000000, 0.9659258262890683122, 1.000000000000000000, 0.9659258262890683122, 1.000000000000000000, 0.9659258262890683122, 1.000000000000000000, 0.9659258262890683122, 1.000000000000000000, 0.9659258262890683122, 1.000000000000000000, 0.9659258262890683122, 1.000000000000000000, 0.9659258262890683122, 1.000000000000000000, 0.9659258262890683122, 1.000000000000000000, 0.9659258262890683122, 1.000000000000000000, 0.9659258262890683122, 1.000000000000000000, 0.9659258262890683122, 1.000000000000000000, 0.9659258262890683122, 1.000000000000000000, 0.9659258262890683122, 1.000000000000000000, 0.9659258262890683122, 1.000000000000000000, 0.9659258262890683122, 1.000000000000000000, 0.9659258262890683122, 1.000000000000000000, 0.9659258262890683122, 1.000000000000000000, 0.9659258262890683122, 1.000000000000000000, 0.9659258262890683122, 1.000000000000000000, 0.9659258262890683122, 1.000000000000000000, 0.9659258262890683122, 1.000000000000000000, 0.9659258262890683122, 1.000000000000000000, 0.9659258262890683122, 1.000000000000000000, 0.9659258262890683122, 1.000000000000000000, 0.9659258262890683122, 1.000000000000000000, 0.9659258262890683122, 1.000000000000000000, 0.9659258262890683122, 1.000000000000000000, 0.9659258262890683122, 1.000000000000000000, 0.9659258262890683122, 1.000000000000000000, 0.9659258262890683122, 1.000000000000000000, 0.9659258262890683122, 1.000000000000000000, 0.9659258262890683122, 1.000000000000000000, 0.9659258262890683122, 1.000000000000000000, 0.9659258262890683122, 1.000000000000000000, 0.9659258262890683122, 1.000000000000000000, 0.9659258262890683122, 1.000000000000000000, 0.9659258262890683122, 1.000000000000000000, 0.9659258262890683122, 1.000000000000000000, 0.9659258262890683122, 1.000000000000000000, 0.9659258262890683122, 1.000000000000000000, 0.9659258262890683122, 1.000000000000000000, 0.9659258262890683122, 1.000000000000000000, 0.9659258262890683122, 1.000000000000000000, 0.9659258262890683122, 1.000000000000000000, 0.9659258262890683122, 1.000000000000000000, 0.9659258262890683122, 1.000000000000000000, 0.9659258262890683122, 1.000000000000000000, 0.9659258262890683122, 1.000000000000000000, 0.9659258262890683122, 1.000000000000000000, 0.9659258262890683122, 1.000000000000000000, 0.9659258262890683122, 1.000000000000000000, 0.9659258262890683122, 1.000000000000000000, 0.9659258262890683122, 1.000000000000000000, 0.9659258262890683122, 1.000000000000000000, 0.9659258262890683122, 1.000000000000000000, 0.9659258262890683122, 1.000000000000000000, 0.9659258262890683122, 1.000000000000000000, 0.9659258262890683122, 1.000000000000000000, 0.9659258262890683122, 1.000000000000000000, 0.9659258262890683122, 1.000000000000000000, 0.9659258262890683122, 1.000000000000000000, 0.9659258262890683122, 1.000000000000000000, 0.9659258262890683122, 1.000000000000000000, 0.9659258262890683122, 1.000000000000000000, 0.9659258262890683122, 1.000000000000000000, 0.9659258262890683122, 1.000000000000000000, 0.9659258262890683122, 1.000000000000000000, 0.9659258262890683122, 1.000000000000000000, 0.9659258262890683122, 1.000000000000000000, 0.9659258262890683122, 1.000000000000000000, 0.9659258262890683122, 1.000000000000000000, 0.9659258262890683122, 1.000000000000000000, 0.9659258262890683122, 1.000000000000000000, 0.9659258262890683122, 1.000000000000000000, 0.9659258262890683122, 1.000000000000000000, 0.9659258262890683122, 1.000000000000000000, 0.9659258262890683122, 1.000000000000000000, 0.9659258262890683122, 1.000000000000000000, 0.9659258262890683122, 1.000000000000000000, 0.9659258262890683122, 1.000000000000000000, 0.9659258262890683122, 1.000000000000000000, 0.9659258262890683122, 1.000000000000000000, 0.9659258262890683122, 1.000000000000000000, 0.9659258262890683122, 1.000000000000000000, 0.9659258262890683122, 1.000000000000000000, 0.9659258262890683122, 1.000000000000000000, 0.9659258262890683122, 1.000000000000000000, 0.9659258262890683122, 1.000000000000000000, 0.9659258262890683122, 1.000000000000000000, 0.9659258262890683122, 1.000000000000000000, 0.9659258262890683122, 1.000000000000000000, 0.9659258262890683122, 1.000000000000000000, 0.9659258262890683122, 1.000000000000000000, 0.9659258262890683122, 1.000000000000000000, 0.9659258262890683122, 1.000000000000000000, 0.9659258262890683122, 1.000000000000000000, 0.9659258262890683122, 1.000000000000000000, 0.9659258262890683122, 1.000000000000000000, 0.9659258262890683122, 1.000000000000000000, 0.9659258262890683122, 1.000000000000000000, 0.9659258262890683122, 1.000000000000000000, 0.9659258262890683122, 1.000000000000000000, 0.9659258262890683122, 1.000000000000000000, 0.9659258262890683122, 1.000000000000000000, 0.9659258262890683122, 1.000000000000000000, 0.9659258262890683122, 1.000000000000000000, 0.9659258262890683122, 1.000000000000000000, 0.9659258262890683122, 1.000000000000000000, 0.9659258262890683122, 1.000000000000000000, 0.9659258262890683122, 1.000000000000000000, 0.9659258262890683122, 1.000000000000000000, 0.9659258262890683122, 1.000000000000000000, 0.9659258262890683122, 1.000000000000000000, 0.9659258262890683122, 1.000000000000000000, 0.9659258262890683122, 1.000000000000000000, 0.9659258262890683122, 1.000000000000000000, 0.9659258262890683122, 1.000000000000000000, 0.9659258262890683122, 1.000000000000000000, 0.9659258262890683122, 1.000000000000000000, 0.9659258262890683122, 1.000000000000000000, 0.9659258262890683122, 1.000000000000000000, 0.9659258262890683122, 1.000000000000000000, 0.9659258262890683122, 1.000000000000000000, 0.9659258262890683122, 1.000000000000000000, 0.9659258262890683122, 1.000000000000000000, 0.9659258262890683122, 1.000000000000000000, 0.9659258262890683122, 1.000000000000000000, 0.9659258262890683122, 1.000000000000000000, 0.9659258262890683122, 1.000000000000000000, 0.9659258262890683122, 1.000000000000000000, 0.9659258262890683122, 1.000000000000000000, 0.9659258262890683122, 1.000000000000000000, 0.9659258262890683122, 1.000000000000000000, 0.9659258262890683122, 1.000000000000000000, 0.9659258262890683122, 1.000000000000000000, 0.9659258262890683122, 1.000000000000000000, 0.9659258262890683122, 1.000000000000000000, 0.9659258262890683122, 1.000000000000000000, 0.9659258262890683122, 1.000000000000000000, 0.9659258262890683122, 1.000000000000000000, 0.9659258262890683122, 1.000000000000000000, 0.9659258262890683122, 1.000000000000000000, 0.9659258262890683122, 1.000000000000000000, 0.9659258262890683122, 1.000000000000000000, 0.9659258262890683122, 1.000000000000000000, 0.9659258262890683122, 1.000000000000000000, 0.9659258262890683122, 1.000000000000000000, 0.9659258262890683122, 1.000000000000000000, 0.9659258262890683122, 1.000000000000000000, 0.9659258262890683122, 1.000000000000000000, 0.9659258262890683122, 1.000000000000000000, 0.9659258262890683122, 1.000000000000000000),
 ( 0.3333333333333333703, 0.3219752754296894559, 0.3333333333333333703, 0.3219752754296894559, 0.3333333333333333703, 0.3219752754296894559, 0.3333333333333333703, 0.3219752754296894559, 0.3333333333333333703, 0.3219752754296894559, 0.3333333333333333703, 0.3219752754296894559, 0.3333333333333333703, 0.3219752754296894559, 0.3333333333333333703, 0.3219752754296894559, 0.3333333333333333703, 0.3219752754296894559, 0.3333333333333333703, 0.3219752754296894559, 0.3333333333333333703, 0.3219752754296894559, 0.3333333333333333703, 0.3219752754296894559, 0.3333333333333333703, 0.3219752754296894559, 0.3333333333333333703, 0.3219752754296894559, 0.3333333333333333703, 0.3219752754296894559, 0.3333333333333333703, 0.3219752754296894559, 0.3333333333333333703, 0.3219752754296894559, 0.3333333333333333703, 0.3219752754296894559, 0.3333333333333333703, 0.3219752754296894559, 0.3333333333333333703, 0.3219752754296894559, 0.3333333333333333703, 0.3219752754296894559, 0.3333333333333333703, 0.3219752754296894559, 0.3333333333333333703, 0.3219752754296894559, 0.3333333333333333703, 0.3219752754296894559, 0.3333333333333333703, 0.3219752754296894559, 0.3333333333333333703, 0.3219752754296894559, 0.3333333333333333703, 0.3219752754296894559, 0.3333333333333333703, 0.3219752754296894559, 0.3333333333333333703, 0.3219752754296894559, 0.3333333333333333703, 0.3219752754296894559, 0.3333333333333333703, 0.3219752754296894559, 0.3333333333333333703, 0.3219752754296894559, 0.3333333333333333703, 0.3219752754296894559, 0.3333333333333333703, 0.3219752754296894559, 0.3333333333333333703, 0.3219752754296894559, 0.3333333333333333703, 0.3219752754296894559, 0.3333333333333333703, 0.3219752754296894559, 0.3333333333333333703, 0.3219752754296894559, 0.3333333333333333703, 0.3219752754296894559, 0.3333333333333333703, 0.3219752754296894559, 0.3333333333333333703, 0.3219752754296894559, 0.3333333333333333703, 0.3219752754296894559, 0.3333333333333333703, 0.3219752754296894559, 0.3333333333333333703, 0.3219752754296894559, 0.3333333333333333703, 0.3219752754296894559, 0.3333333333333333703, 0.3219752754296894559, 0.3333333333333333703, 0.3219752754296894559, 0.3333333333333333703, 0.3219752754296894559, 0.3333333333333333703, 0.3219752754296894559, 0.3333333333333333703, 0.3219752754296894559, 0.3333333333333333703, 0.3219752754296894559, 0.3333333333333333703, 0.3219752754296894559, 0.3333333333333333703, 0.3219752754296894559, 0.3333333333333333703, 0.3219752754296894559, 0.3333333333333333703, 0.3219752754296894559, 0.3333333333333333703, 0.3219752754296894559, 0.3333333333333333703, 0.3219752754296894559, 0.3333333333333333703, 0.3219752754296894559, 0.3333333333333333703, 0.3219752754296894559, 0.3333333333333333703, 0.3219752754296894559, 0.3333333333333333703, 0.3219752754296894559, 0.3333333333333333703, 0.3219752754296894559, 0.3333333333333333703, 0.3219752754296894559, 0.3333333333333333703, 0.3219752754296894559, 0.3333333333333333703, 0.3219752754296894559, 0.3333333333333333703, 0.3219752754296894559, 0.3333333333333333703, 0.3219752754296894559, 0.3333333333333333703, 0.3219752754296894559, 0.3333333333333333703, 0.3219752754296894559, 0.3333333333333333703, 0.3219752754296894559, 0.3333333333333333703, 0.3219752754296894559, 0.3333333333333333703, 0.3219752754296894559, 0.3333333333333333703, 0.3219752754296894559, 0.3333333333333333703, 0.3219752754296894559, 0.3333333333333333703, 0.3219752754296894559, 0.3333333333333333703, 0.3219752754296894559, 0.3333333333333333703, 0.3219752754296894559, 0.3333333333333333703, 0.3219752754296894559, 0.3333333333333333703, 0.3219752754296894559, 0.3333333333333333703, 0.3219752754296894559, 0.3333333333333333703, 0.3219752754296894559, 0.3333333333333333703, 0.3219752754296894559, 0.3333333333333333703, 0.3219752754296894559, 0.3333333333333333703, 0.3219752754296894559, 0.3333333333333333703, 0.3219752754296894559, 0.3333333333333333703, 0.3219752754296894559, 0.3333333333333333703, 0.3219752754296894559, 0.3333333333333333703, 0.3219752754296894559, 0.3333333333333333703, 0.3219752754296894559, 0.3333333333333333703, 0.3219752754296894559, 0.3333333333333333703, 0.3219752754296894559, 0.3333333333333333703, 0.3219752754296894559, 0.3333333333333333703, 0.3219752754296894559, 0.3333333333333333703, 0.3219752754296894559, 0.3333333333333333703, 0.3219752754296894559, 0.3333333333333333703, 0.3219752754296894559, 0.3333333333333333703, 0.3219752754296894559, 0.3333333333333333703, 0.3219752754296894559, 0.3333333333333333703, 0.3219752754296894559, 0.3333333333333333703, 0.3219752754296894559, 0.3333333333333333703, 0.3219752754296894559, 0.3333333333333333703, 0.3219752754296894559, 0.3333333333333333703, 0.3219752754296894559, 0.3333333333333333703, 0.3219752754296894559, 0.3333333333333333703, 0.3219752754296894559, 0.3333333333333333703, 0.3219752754296894559, 0.3333333333333333703, 0.3219752754296894559, 0.3333333333333333703, 0.3219752754296894559, 0.3333333333333333703, 0.3219752754296894559, 0.3333333333333333703, 0.3219752754296894559, 0.3333333333333333703, 0.3219752754296894559, 0.3333333333333333703, 0.3219752754296894559, 0.3333333333333333703, 0.3219752754296894559, 0.3333333333333333703, 0.3219752754296894559, 0.3333333333333333703, 0.3219752754296894559, 0.3333333333333333703, 0.3219752754296894559, 0.3333333333333333703, 0.3219752754296894559, 0.3333333333333333703, 0.3219752754296894559, 0.3333333333333333703, 0.3219752754296894559, 0.3333333333333333703, 0.3219752754296894559, 0.3333333333333333703, 0.3219752754296894559, 0.3333333333333333703, 0.3219752754296894559, 0.3333333333333333703, 0.3219752754296894559, 0.3333333333333333703, 0.3219752754296894559, 0.3333333333333333703, 0.3219752754296894559, 0.3333333333333333703, 0.3219752754296894559, 0.3333333333333333703, 0.3219752754296894559, 0.3333333333333333703, 0.3219752754296894559, 0.3333333333333333703, 0.3219752754296894559, 0.3333333333333333703, 0.3219752754296894559, 0.3333333333333333703, 0.3219752754296894559, 0.3333333333333333703, 0.3219752754296894559, 0.3333333333333333703, 0.3219752754296894559, 0.3333333333333333703, 0.3219752754296894559, 0.3333333333333333703, 0.3219752754296894559, 0.3333333333333333703, 0.3219752754296894559, 0.3333333333333333703, 0.3219752754296894559, 0.3333333333333333703, 0.3219752754296894559, 0.3333333333333333703, 0.3219752754296894559, 0.3333333333333333703, 0.3219752754296894559, 0.3333333333333333703, 0.3219752754296894559, 0.3333333333333333703, 0.3219752754296894559, 0.3333333333333333703, 0.3219752754296894559, 0.3333333333333333703, 0.3219752754296894559, 0.3333333333333333703, 0.3219752754296894559, 0.3333333333333333703, 0.3219752754296894559, 0.3333333333333333703, 0.3219752754296894559, 0.3333333333333333703, 0.3219752754296894559, 0.3333333333333333703, 0.3219752754296894559, 0.3333333333333333703, 0.3219752754296894559, 0.3333333333333333703, 0.3219752754296894559, 0.3333333333333333703, 0.3219752754296894559, 0.3333333333333333703, 0.3219752754296894559, 0.3333333333333333703, 0.3219752754296894559, 0.3333333333333333703, 0.3219752754296894559, 0.3333333333333333703, 0.3219752754296894559, 0.3333333333333333703, 0.3219752754296894559, 0.3333333333333333703, 0.3219752754296894559, 0.3333333333333333703, 0.3219752754296894559, 0.3333333333333333703, 0.3219752754296894559, 0.3333333333333333703, 0.3219752754296894559, 0.3333333333333333703, 0.3219752754296894559, 0.3333333333333333703, 0.3219752754296894559, 0.3333333333333333703, 0.3219752754296894559, 0.3333333333333333703, 0.3219752754296894559, 0.3333333333333333703, 0.3219752754296894559, 0.3333333333333333703, 0.3219752754296894559, 0.3333333333333333703, 0.3219752754296894559, 0.3333333333333333703, 0.3219752754296894559, 0.3333333333333333703, 0.3219752754296894559, 0.3333333333333333703, 0.3219752754296894559, 0.3333333333333333703, 0.3219752754296894559, 0.3333333333333333703, 0.3219752754296894559, 0.3333333333333333703, 0.3219752754296894559, 0.3333333333333333703, 0.3219752754296894559, 0.3333333333333333703, 0.3219752754296894559, 0.3333333333333333703, 0.3219752754296894559, 0.3333333333333333703, 0.3219752754296894559, 0.3333333333333333703, 0.3219752754296894559, 0.3333333333333333703, 0.3219752754296894559, 0.3333333333333333703, 0.3219752754296894559, 0.3333333333333333703, 0.3219752754296894559, 0.3333333333333333703, 0.3219752754296894559, 0.3333333333333333703, 0.3219752754296894559, 0.3333333333333333703, 0.3219752754296894559, 0.3333333333333333703, 0.3219752754296894559, 0.3333333333333333703, 0.3219752754296894559, 0.3333333333333333703, 0.3219752754296894559, 0.3333333333333333703, 0.3219752754296894559, 0.3333333333333333703, 0.3219752754296894559, 0.3333333333333333703, 0.3219752754296894559, 0.3333333333333333703, 0.3219752754296894559, 0.3333333333333333703, 0.3219752754296894559, 0.3333333333333333703, 0.3219752754296894559, 0.3333333333333333703, 0.3219752754296894559, 0.3333333333333333703, 0.3219752754296894559, 0.3333333333333333703, 0.3219752754296894559, 0.3333333333333333703, 0.3219752754296894559, 0.3333333333333333703, 0.3219752754296894559, 0.3333333333333333703, 0.3219752754296894559, 0.3333333333333333703, 0.3219752754296894559, 0.3333333333333333703, 0.3219752754296894559, 0.3333333333333333703, 0.3219752754296894559, 0.3333333333333333703, 0.3219752754296894559, 0.3333333333333333703, 0.3219752754296894559, 0.3333333333333333703, 0.3219752754296894559, 0.3333333333333333703, 0.3219752754296894559, 0.3333333333333333703, 0.3219752754296894559, 0.3333333333333333703, 0.3219752754296894559, 0.3333333333333333703, 0.3219752754296894559, 0.3333333333333333703, 0.3219752754296894559, 0.3333333333333333703, 0.3219752754296894559, 0.3333333333333333703, 0.3219752754296894559, 0.3333333333333333703, 0.3219752754296894559, 0.3333333333333333703, 0.3219752754296894559, 0.3333333333333333703, 0.3219752754296894559, 0.3333333333333333703, 0.3219752754296894559, 0.3333333333333333703, 0.3219752754296894559, 0.3333333333333333703, 0.3219752754296894559, 0.3333333333333333703, 0.3219752754296894559, 0.3333333333333333703, 0.3219752754296894559, 0.3333333333333333703, 0.3219752754296894559, 0.3333333333333333703, 0.3219752754296894559, 0.3333333333333333703, 0.3219752754296894559, 0.3333333333333333703, 0.3219752754296894559, 0.3333333333333333703, 0.3219752754296894559, 0.3333333333333333703, 0.3219752754296894559, 0.3333333333333333703, 0.3219752754296894559, 0.3333333333333333703),
 ( 0.3333333333333333703, 0.3219752754296894559, 0.3333333333333333703, 0.3219752754296894559, 0.3333333333333333703, 0.3219752754296894559, 0.3333333333333333703, 0.3219752754296894559, 0.3333333333333333703, 0.3219752754296894559, 0.3333333333333333703, 0.3219752754296894559, 0.3333333333333333703, 0.3219752754296894559, 0.3333333333333333703, 0.3219752754296894559, 0.3333333333333333703, 0.3219752754296894559, 0.3333333333333333703, 0.3219752754296894559, 0.3333333333333333703, 0.3219752754296894559, 0.3333333333333333703, 0.3219752754296894559, 0.3333333333333333703, 0.3219752754296894559, 0.3333333333333333703, 0.3219752754296894559, 0.3333333333333333703, 0.3219752754296894559, 0.3333333333333333703, 0.3219752754296894559, 0.3333333333333333703, 0.3219752754296894559, 0.3333333333333333703, 0.3219752754296894559, 0.3333333333333333703, 0.3219752754296894559, 0.3333333333333333703, 0.3219752754296894559, 0.3333333333333333703, 0.3219752754296894559, 0.3333333333333333703, 0.3219752754296894559, 0.3333333333333333703, 0.3219752754296894559, 0.3333333333333333703, 0.3219752754296894559, 0.3333333333333333703, 0.3219752754296894559, 0.3333333333333333703, 0.3219752754296894559, 0.3333333333333333703, 0.3219752754296894559, 0.3333333333333333703, 0.3219752754296894559, 0.3333333333333333703, 0.3219752754296894559, 0.3333333333333333703, 0.3219752754296894559, 0.3333333333333333703, 0.3219752754296894559, 0.3333333333333333703, 0.3219752754296894559, 0.3333333333333333703, 0.3219752754296894559, 0.3333333333333333703, 0.3219752754296894559, 0.3333333333333333703, 0.3219752754296894559, 0.3333333333333333703, 0.3219752754296894559, 0.3333333333333333703, 0.3219752754296894559, 0.3333333333333333703, 0.3219752754296894559, 0.3333333333333333703, 0.3219752754296894559, 0.3333333333333333703, 0.3219752754296894559, 0.3333333333333333703, 0.3219752754296894559, 0.3333333333333333703, 0.3219752754296894559, 0.3333333333333333703, 0.3219752754296894559, 0.3333333333333333703, 0.3219752754296894559, 0.3333333333333333703, 0.3219752754296894559, 0.3333333333333333703, 0.3219752754296894559, 0.3333333333333333703, 0.3219752754296894559, 0.3333333333333333703, 0.3219752754296894559, 0.3333333333333333703, 0.3219752754296894559, 0.3333333333333333703, 0.3219752754296894559, 0.3333333333333333703, 0.3219752754296894559, 0.3333333333333333703, 0.3219752754296894559, 0.3333333333333333703, 0.3219752754296894559, 0.3333333333333333703, 0.3219752754296894559, 0.3333333333333333703, 0.3219752754296894559, 0.3333333333333333703, 0.3219752754296894559, 0.3333333333333333703, 0.3219752754296894559, 0.3333333333333333703, 0.3219752754296894559, 0.3333333333333333703, 0.3219752754296894559, 0.3333333333333333703, 0.3219752754296894559, 0.3333333333333333703, 0.3219752754296894559, 0.3333333333333333703, 0.3219752754296894559, 0.3333333333333333703, 0.3219752754296894559, 0.3333333333333333703, 0.3219752754296894559, 0.3333333333333333703, 0.3219752754296894559, 0.3333333333333333703, 0.3219752754296894559, 0.3333333333333333703, 0.3219752754296894559, 0.3333333333333333703, 0.3219752754296894559, 0.3333333333333333703, 0.3219752754296894559, 0.3333333333333333703, 0.3219752754296894559, 0.3333333333333333703, 0.3219752754296894559, 0.3333333333333333703, 0.3219752754296894559, 0.3333333333333333703, 0.3219752754296894559, 0.3333333333333333703, 0.3219752754296894559, 0.3333333333333333703, 0.3219752754296894559, 0.3333333333333333703, 0.3219752754296894559, 0.3333333333333333703, 0.3219752754296894559, 0.3333333333333333703, 0.3219752754296894559, 0.3333333333333333703, 0.3219752754296894559, 0.3333333333333333703, 0.3219752754296894559, 0.3333333333333333703, 0.3219752754296894559, 0.3333333333333333703, 0.3219752754296894559, 0.3333333333333333703, 0.3219752754296894559, 0.3333333333333333703, 0.3219752754296894559, 0.3333333333333333703, 0.3219752754296894559, 0.3333333333333333703, 0.3219752754296894559, 0.3333333333333333703, 0.3219752754296894559, 0.3333333333333333703, 0.3219752754296894559, 0.3333333333333333703, 0.3219752754296894559, 0.3333333333333333703, 0.3219752754296894559, 0.3333333333333333703, 0.3219752754296894559, 0.3333333333333333703, 0.3219752754296894559, 0.3333333333333333703, 0.3219752754296894559, 0.3333333333333333703, 0.3219752754296894559, 0.3333333333333333703, 0.3219752754296894559, 0.3333333333333333703, 0.3219752754296894559, 0.3333333333333333703, 0.3219752754296894559, 0.3333333333333333703, 0.3219752754296894559, 0.3333333333333333703, 0.3219752754296894559, 0.3333333333333333703, 0.3219752754296894559, 0.3333333333333333703, 0.3219752754296894559, 0.3333333333333333703, 0.3219752754296894559, 0.3333333333333333703, 0.3219752754296894559, 0.3333333333333333703, 0.3219752754296894559, 0.3333333333333333703, 0.3219752754296894559, 0.3333333333333333703, 0.3219752754296894559, 0.3333333333333333703, 0.3219752754296894559, 0.3333333333333333703, 0.3219752754296894559, 0.3333333333333333703, 0.3219752754296894559, 0.3333333333333333703, 0.3219752754296894559, 0.3333333333333333703, 0.3219752754296894559, 0.3333333333333333703, 0.3219752754296894559, 0.3333333333333333703, 0.3219752754296894559, 0.3333333333333333703, 0.3219752754296894559, 0.3333333333333333703, 0.3219752754296894559, 0.3333333333333333703, 0.3219752754296894559, 0.3333333333333333703, 0.3219752754296894559, 0.3333333333333333703, 0.3219752754296894559, 0.3333333333333333703, 0.3219752754296894559, 0.3333333333333333703, 0.3219752754296894559, 0.3333333333333333703, 0.3219752754296894559, 0.3333333333333333703, 0.3219752754296894559, 0.3333333333333333703, 0.3219752754296894559, 0.3333333333333333703, 0.3219752754296894559, 0.3333333333333333703, 0.3219752754296894559, 0.3333333333333333703, 0.3219752754296894559, 0.3333333333333333703, 0.3219752754296894559, 0.3333333333333333703, 0.3219752754296894559, 0.3333333333333333703, 0.3219752754296894559, 0.3333333333333333703, 0.3219752754296894559, 0.3333333333333333703, 0.3219752754296894559, 0.3333333333333333703, 0.3219752754296894559, 0.3333333333333333703, 0.3219752754296894559, 0.3333333333333333703, 0.3219752754296894559, 0.3333333333333333703, 0.3219752754296894559, 0.3333333333333333703, 0.3219752754296894559, 0.3333333333333333703, 0.3219752754296894559, 0.3333333333333333703, 0.3219752754296894559, 0.3333333333333333703, 0.3219752754296894559, 0.3333333333333333703, 0.3219752754296894559, 0.3333333333333333703, 0.3219752754296894559, 0.3333333333333333703, 0.3219752754296894559, 0.3333333333333333703, 0.3219752754296894559, 0.3333333333333333703, 0.3219752754296894559, 0.3333333333333333703, 0.3219752754296894559, 0.3333333333333333703, 0.3219752754296894559, 0.3333333333333333703, 0.3219752754296894559, 0.3333333333333333703, 0.3219752754296894559, 0.3333333333333333703, 0.3219752754296894559, 0.3333333333333333703, 0.3219752754296894559, 0.3333333333333333703, 0.3219752754296894559, 0.3333333333333333703, 0.3219752754296894559, 0.3333333333333333703, 0.3219752754296894559, 0.3333333333333333703, 0.3219752754296894559, 0.3333333333333333703, 0.3219752754296894559, 0.3333333333333333703, 0.3219752754296894559, 0.3333333333333333703, 0.3219752754296894559, 0.3333333333333333703, 0.3219752754296894559, 0.3333333333333333703, 0.3219752754296894559, 0.3333333333333333703, 0.3219752754296894559, 0.3333333333333333703, 0.3219752754296894559, 0.3333333333333333703, 0.3219752754296894559, 0.3333333333333333703, 0.3219752754296894559, 0.3333333333333333703, 0.3219752754296894559, 0.3333333333333333703, 0.3219752754296894559, 0.3333333333333333703, 0.3219752754296894559, 0.3333333333333333703, 0.3219752754296894559, 0.3333333333333333703, 0.3219752754296894559, 0.3333333333333333703, 0.3219752754296894559, 0.3333333333333333703, 0.3219752754296894559, 0.3333333333333333703, 0.3219752754296894559, 0.3333333333333333703, 0.3219752754296894559, 0.3333333333333333703, 0.3219752754296894559, 0.3333333333333333703, 0.3219752754296894559, 0.3333333333333333703, 0.3219752754296894559, 0.3333333333333333703, 0.3219752754296894559, 0.3333333333333333703, 0.3219752754296894559, 0.3333333333333333703, 0.3219752754296894559, 0.3333333333333333703, 0.3219752754296894559, 0.3333333333333333703, 0.3219752754296894559, 0.3333333333333333703, 0.3219752754296894559, 0.3333333333333333703, 0.3219752754296894559, 0.3333333333333333703, 0.3219752754296894559, 0.3333333333333333703, 0.3219752754296894559, 0.3333333333333333703, 0.3219752754296894559, 0.3333333333333333703, 0.3219752754296894559, 0.3333333333333333703, 0.3219752754296894559, 0.3333333333333333703, 0.3219752754296894559, 0.3333333333333333703, 0.3219752754296894559, 0.3333333333333333703, 0.3219752754296894559, 0.3333333333333333703, 0.3219752754296894559, 0.3333333333333333703, 0.3219752754296894559, 0.3333333333333333703, 0.3219752754296894559, 0.3333333333333333703, 0.3219752754296894559, 0.3333333333333333703, 0.3219752754296894559, 0.3333333333333333703, 0.3219752754296894559, 0.3333333333333333703, 0.3219752754296894559, 0.3333333333333333703, 0.3219752754296894559, 0.3333333333333333703, 0.3219752754296894559, 0.3333333333333333703, 0.3219752754296894559, 0.3333333333333333703, 0.3219752754296894559, 0.3333333333333333703, 0.3219752754296894559, 0.3333333333333333703, 0.3219752754296894559, 0.3333333333333333703, 0.3219752754296894559, 0.3333333333333333703, 0.3219752754296894559, 0.3333333333333333703, 0.3219752754296894559, 0.3333333333333333703, 0.3219752754296894559, 0.3333333333333333703, 0.3219752754296894559, 0.3333333333333333703, 0.3219752754296894559, 0.3333333333333333703, 0.3219752754296894559, 0.3333333333333333703, 0.3219752754296894559, 0.3333333333333333703, 0.3219752754296894559, 0.3333333333333333703, 0.3219752754296894559, 0.3333333333333333703, 0.3219752754296894559, 0.3333333333333333703, 0.3219752754296894559, 0.3333333333333333703, 0.3219752754296894559, 0.3333333333333333703, 0.3219752754296894559, 0.3333333333333333703, 0.3219752754296894559, 0.3333333333333333703, 0.3219752754296894559, 0.3333333333333333703, 0.3219752754296894559, 0.3333333333333333703, 0.3219752754296894559, 0.3333333333333333703, 0.3219752754296894559, 0.3333333333333333703, 0.3219752754296894559, 0.3333333333333333703, 0.3219752754296894559, 0.3333333333333333703, 0.3219752754296894559, 0.3333333333333333703, 0.3219752754296894559, 0.3333333333333333703, 0.3219752754296894559, 0.3333333333333333703, 0.3219752754296894559, 0.3333333333333333703),
 ( 1.000000000000000000, 0.9659258262890683122, 1.000000000000000000, 0.9659258262890683122, 1.000000000000000000, 0.9659258262890683122, 1.000000000000000000, 0.9659258262890683122, 1.000000000000000000, 0.9659258262890683122, 1.000000000000000000, 0.9659258262890683122, 1.000000000000000000, 0.9659258262890683122, 1.000000000000000000, 0.9659258262890683122, 1.000000000000000000, 0.9659258262890683122, 1.000000000000000000, 0.9659258262890683122, 1.000000000000000000, 0.9659258262890683122, 1.000000000000000000, 0.9659258262890683122, 1.000000000000000000, 0.9659258262890683122, 1.000000000000000000, 0.9659258262890683122, 1.000000000000000000, 0.9659258262890683122, 1.000000000000000000, 0.9659258262890683122, 1.000000000000000000, 0.9659258262890683122, 1.000000000000000000, 0.9659258262890683122, 1.000000000000000000, 0.9659258262890683122, 1.000000000000000000, 0.9659258262890683122, 1.000000000000000000, 0.9659258262890683122, 1.000000000000000000, 0.9659258262890683122, 1.000000000000000000, 0.9659258262890683122, 1.000000000000000000, 0.9659258262890683122, 1.000000000000000000, 0.9659258262890683122, 1.000000000000000000, 0.9659258262890683122, 1.000000000000000000, 0.9659258262890683122, 1.000000000000000000, 0.9659258262890683122, 1.000000000000000000, 0.9659258262890683122, 1.000000000000000000, 0.9659258262890683122, 1.000000000000000000, 0.9659258262890683122, 1.000000000000000000, 0.9659258262890683122, 1.000000000000000000, 0.9659258262890683122, 1.000000000000000000, 0.9659258262890683122, 1.000000000000000000, 0.9659258262890683122, 1.000000000000000000, 0.9659258262890683122, 1.000000000000000000, 0.9659258262890683122, 1.000000000000000000, 0.9659258262890683122, 1.000000000000000000, 0.9659258262890683122, 1.000000000000000000, 0.9659258262890683122, 1.000000000000000000, 0.9659258262890683122, 1.000000000000000000, 0.9659258262890683122, 1.000000000000000000, 0.9659258262890683122, 1.000000000000000000, 0.9659258262890683122, 1.000000000000000000, 0.9659258262890683122, 1.000000000000000000, 0.9659258262890683122, 1.000000000000000000, 0.9659258262890683122, 1.000000000000000000, 0.9659258262890683122, 1.000000000000000000, 0.9659258262890683122, 1.000000000000000000, 0.9659258262890683122, 1.000000000000000000, 0.9659258262890683122, 1.000000000000000000, 0.9659258262890683122, 1.000000000000000000, 0.9659258262890683122, 1.000000000000000000, 0.9659258262890683122, 1.000000000000000000, 0.9659258262890683122, 1.000000000000000000, 0.9659258262890683122, 1.000000000000000000, 0.9659258262890683122, 1.000000000000000000, 0.9659258262890683122, 1.000000000000000000, 0.9659258262890683122, 1.000000000000000000, 0.9659258262890683122, 1.000000000000000000, 0.9659258262890683122, 1.000000000000000000, 0.9659258262890683122, 1.000000000000000000, 0.9659258262890683122, 1.000000000000000000, 0.9659258262890683122, 1.000000000000000000, 0.9659258262890683122, 1.000000000000000000, 0.9659258262890683122, 1.000000000000000000, 0.9659258262890683122, 1.000000000000000000, 0.9659258262890683122, 1.000000000000000000, 0.9659258262890683122, 1.000000000000000000, 0.9659258262890683122, 1.000000000000000000, 0.9659258262890683122, 1.000000000000000000, 0.9659258262890683122, 1.000000000000000000, 0.9659258262890683122, 1.000000000000000000, 0.9659258262890683122, 1.000000000000000000, 0.9659258262890683122, 1.000000000000000000, 0.9659258262890683122, 1.000000000000000000, 0.9659258262890683122, 1.000000000000000000, 0.9659258262890683122, 1.000000000000000000, 0.9659258262890683122, 1.000000000000000000, 0.9659258262890683122, 1.000000000000000000, 0.9659258262890683122, 1.000000000000000000, 0.9659258262890683122, 1.000000000000000000, 0.9659258262890683122, 1.000000000000000000, 0.9659258262890683122, 1.000000000000000000, 0.9659258262890683122, 1.000000000000000000, 0.9659258262890683122, 1.000000000000000000, 0.9659258262890683122, 1.000000000000000000, 0.9659258262890683122, 1.000000000000000000, 0.9659258262890683122, 1.000000000000000000, 0.9659258262890683122, 1.000000000000000000, 0.9659258262890683122, 1.000000000000000000, 0.9659258262890683122, 1.000000000000000000, 0.9659258262890683122, 1.000000000000000000, 0.9659258262890683122, 1.000000000000000000, 0.9659258262890683122, 1.000000000000000000, 0.9659258262890683122, 1.000000000000000000, 0.9659258262890683122, 1.000000000000000000, 0.9659258262890683122, 1.000000000000000000, 0.9659258262890683122, 1.000000000000000000, 0.9659258262890683122, 1.000000000000000000, 0.9659258262890683122, 1.000000000000000000, 0.9659258262890683122, 1.000000000000000000, 0.9659258262890683122, 1.000000000000000000, 0.9659258262890683122, 1.000000000000000000, 0.9659258262890683122, 1.000000000000000000, 0.9659258262890683122, 1.000000000000000000, 0.9659258262890683122, 1.000000000000000000, 0.9659258262890683122, 1.000000000000000000, 0.9659258262890683122, 1.000000000000000000, 0.9659258262890683122, 1.000000000000000000, 0.9659258262890683122, 1.000000000000000000, 0.9659258262890683122, 1.000000000000000000, 0.9659258262890683122, 1.000000000000000000, 0.9659258262890683122, 1.000000000000000000, 0.9659258262890683122, 1.000000000000000000, 0.9659258262890683122, 1.000000000000000000, 0.9659258262890683122, 1.000000000000000000, 0.9659258262890683122, 1.000000000000000000, 0.9659258262890683122, 1.000000000000000000, 0.9659258262890683122, 1.000000000000000000, 0.9659258262890683122, 1.000000000000000000, 0.9659258262890683122, 1.000000000000000000, 0.9659258262890683122, 1.000000000000000000, 0.9659258262890683122, 1.000000000000000000, 0.9659258262890683122, 1.000000000000000000, 0.9659258262890683122, 1.000000000000000000, 0.9659258262890683122, 1.000000000000000000, 0.9659258262890683122, 1.000000000000000000, 0.9659258262890683122, 1.000000000000000000, 0.9659258262890683122, 1.000000000000000000, 0.9659258262890683122, 1.000000000000000000, 0.9659258262890683122, 1.000000000000000000, 0.9659258262890683122, 1.000000000000000000, 0.9659258262890683122, 1.000000000000000000, 0.9659258262890683122, 1.000000000000000000, 0.9659258262890683122, 1.000000000000000000, 0.9659258262890683122, 1.000000000000000000, 0.9659258262890683122, 1.000000000000000000, 0.9659258262890683122, 1.000000000000000000, 0.9659258262890683122, 1.000000000000000000, 0.9659258262890683122, 1.000000000000000000, 0.9659258262890683122, 1.000000000000000000, 0.9659258262890683122, 1.000000000000000000, 0.9659258262890683122, 1.000000000000000000, 0.9659258262890683122, 1.000000000000000000, 0.9659258262890683122, 1.000000000000000000, 0.9659258262890683122, 1.000000000000000000, 0.9659258262890683122, 1.000000000000000000, 0.9659258262890683122, 1.000000000000000000, 0.9659258262890683122, 1.000000000000000000, 0.9659258262890683122, 1.000000000000000000, 0.9659258262890683122, 1.000000000000000000, 0.9659258262890683122, 1.000000000000000000, 0.9659258262890683122, 1.000000000000000000, 0.9659258262890683122, 1.000000000000000000, 0.9659258262890683122, 1.000000000000000000, 0.9659258262890683122, 1.000000000000000000, 0.9659258262890683122, 1.000000000000000000, 0.9659258262890683122, 1.000000000000000000, 0.9659258262890683122, 1.000000000000000000, 0.9659258262890683122, 1.000000000000000000, 0.9659258262890683122, 1.000000000000000000, 0.9659258262890683122, 1.000000000000000000, 0.9659258262890683122, 1.000000000000000000, 0.9659258262890683122, 1.000000000000000000, 0.9659258262890683122, 1.000000000000000000, 0.9659258262890683122, 1.000000000000000000, 0.9659258262890683122, 1.000000000000000000, 0.9659258262890683122, 1.000000000000000000, 0.9659258262890683122, 1.000000000000000000, 0.9659258262890683122, 1.000000000000000000, 0.9659258262890683122, 1.000000000000000000, 0.9659258262890683122, 1.000000000000000000, 0.9659258262890683122, 1.000000000000000000, 0.9659258262890683122, 1.000000000000000000, 0.9659258262890683122, 1.000000000000000000, 0.9659258262890683122, 1.000000000000000000, 0.9659258262890683122, 1.000000000000000000, 0.9659258262890683122, 1.000000000000000000, 0.9659258262890683122, 1.000000000000000000, 0.9659258262890683122, 1.000000000000000000, 0.9659258262890683122, 1.000000000000000000, 0.9659258262890683122, 1.000000000000000000, 0.9659258262890683122, 1.000000000000000000, 0.9659258262890683122, 1.000000000000000000, 0.9659258262890683122, 1.000000000000000000, 0.9659258262890683122, 1.000000000000000000, 0.9659258262890683122, 1.000000000000000000, 0.9659258262890683122, 1.000000000000000000, 0.9659258262890683122, 1.000000000000000000, 0.9659258262890683122, 1.000000000000000000, 0.9659258262890683122, 1.000000000000000000, 0.9659258262890683122, 1.000000000000000000, 0.9659258262890683122, 1.000000000000000000, 0.9659258262890683122, 1.000000000000000000, 0.9659258262890683122, 1.000000000000000000, 0.9659258262890683122, 1.000000000000000000, 0.9659258262890683122, 1.000000000000000000, 0.9659258262890683122, 1.000000000000000000, 0.9659258262890683122, 1.000000000000000000, 0.9659258262890683122, 1.000000000000000000, 0.9659258262890683122, 1.000000000000000000, 0.9659258262890683122, 1.000000000000000000, 0.9659258262890683122, 1.000000000000000000, 0.9659258262890683122, 1.000000000000000000, 0.9659258262890683122, 1.000000000000000000, 0.9659258262890683122, 1.000000000000000000, 0.9659258262890683122, 1.000000000000000000, 0.9659258262890683122, 1.000000000000000000, 0.9659258262890683122, 1.000000000000000000, 0.9659258262890683122, 1.000000000000000000, 0.9659258262890683122, 1.000000000000000000, 0.9659258262890683122, 1.000000000000000000, 0.9659258262890683122, 1.000000000000000000, 0.9659258262890683122, 1.000000000000000000, 0.9659258262890683122, 1.000000000000000000, 0.9659258262890683122, 1.000000000000000000, 0.9659258262890683122, 1.000000000000000000, 0.9659258262890683122, 1.000000000000000000, 0.9659258262890683122, 1.000000000000000000, 0.9659258262890683122, 1.000000000000000000, 0.9659258262890683122, 1.000000000000000000, 0.9659258262890683122, 1.000000000000000000, 0.9659258262890683122, 1.000000000000000000, 0.9659258262890683122, 1.000000000000000000, 0.9659258262890683122, 1.000000000000000000, 0.9659258262890683122, 1.000000000000000000, 0.9659258262890683122, 1.000000000000000000) ) ) 
 REPRESENTATION_ITEM ( '' )  SURFACE ( )  );
#28474 = CARTESIAN_POINT ( 'NONE',  ( 5.049401038298161559, -19.05341960407611168, 22.70724293864769194 ) ) ;
#28475 = DIRECTION ( 'NONE',  ( -1.000000000000000000, 0.000000000000000000, 0.000000000000000000 ) ) ;
#28476 = CARTESIAN_POINT ( 'NONE',  ( -16.51473224551082808, 9.474510206698731452, 68.33442372801900433 ) ) ;
#28477 = CARTESIAN_POINT ( 'NONE',  ( 0.05219959533910956823, 16.53943276465976808, 54.99890960531435269 ) ) ;
#28478 = CARTESIAN_POINT ( 'NONE',  ( -21.52544592524343514, 5.823673210054127303, 31.04057627198102409 ) ) ;
#28479 = CARTESIAN_POINT ( 'NONE',  ( 10.72451020669871369, 18.67979575497193778, 92.08442372801901854 ) ) ;
#28480 = CARTESIAN_POINT ( 'NONE',  ( -10.72451020669898014, 18.67979575497178502, 90.41557627198103830 ) ) ;
#28481 = CARTESIAN_POINT ( 'NONE',  ( 10.81492255796106328, -18.62759615963255655, 60.41775706135235424 ) ) ;
#28482 = CARTESIAN_POINT ( 'NONE',  ( -0.05219959533937732626, 21.53943276465977519, 67.50109039468568994 ) ) ;
#28483 = CARTESIAN_POINT ( 'NONE',  ( -13.89961937509977652, 13.97604488694528158, 100.6239096053143669 ) ) ;
#28485 = CARTESIAN_POINT ( 'NONE',  ( -21.55341960407619339, 5.719274019375674811, 63.54275706135234003 ) ) ;
#28484 = CARTESIAN_POINT ( 'NONE',  ( -4.379528057220086978, -16.55341960407618274, 94.79275706135234714 ) ) ;
#28486 = CARTESIAN_POINT ( 'NONE',  ( -16.52544592524342804, 4.483927247898546575, 116.0405762719810383 ) ) ;
#28487 = CARTESIAN_POINT ( 'NONE',  ( 14.29746914071049879, -8.314922557960816363, 68.33224293864769550 ) ) ;
#28488 = CARTESIAN_POINT ( 'NONE',  ( -16.52544592524342804, 4.483927247898546575, 36.04057627198102409 ) ) ;
#28489 = CARTESIAN_POINT ( 'NONE',  ( 10.81492255796078972, 18.62759615963270932, 49.58224293864769550 ) ) ;
#28490 = CARTESIAN_POINT ( 'NONE',  ( 9.564922557960805705, 16.46253265017160317, 44.58224293864769550 ) ) ;
#28491 = CARTESIAN_POINT ( 'NONE',  ( 10.81492255796078972, 18.62759615963270932, 64.58224293864769550 ) ) ;
#28492 = CARTESIAN_POINT ( 'NONE',  ( -16.46253265017146816, -9.564922557961047289, 54.16775706135234003 ) ) ;
#28494 = CARTESIAN_POINT ( 'NONE',  ( 16.55341960407611168, 4.379528057220329451, 43.95724293864769550 ) ) ;
#28493 = CYLINDRICAL_SURFACE ( 'NONE', #17098, 5.500000000001017852 ) ;
#28495 = CARTESIAN_POINT ( 'NONE',  ( 0.05219959533907565091, 21.53943276465977519, 24.99890960531435624 ) ) ;
#28496 = ORIENTED_EDGE ( 'NONE', *, *, #167527, .T. ) ;
#28497 = ORIENTED_EDGE ( 'NONE', *, *, #128725, .F. ) ;
#28498 = CARTESIAN_POINT ( 'NONE',  ( 1.988064558232696151E-15, -30.27659582821216588, 140.4843446568999923 ) ) ;
#28499 = CARTESIAN_POINT ( 'NONE',  ( 14.29746914071037800, 8.314922557961029526, 76.66775706135234714 ) ) ;
#28500 = CARTESIAN_POINT ( 'NONE',  ( 13.89961937509957401, 13.97604488694547697, 81.87609039468564731 ) ) ;
#28501 = CARTESIAN_POINT ( 'NONE',  ( -14.29746914071049879, 8.314922557960819915, 45.83224293864769550 ) ) ;
#28502 = CARTESIAN_POINT ( 'NONE',  ( 17.50000000000002487, -5.499999999999880984, 53.29690382534172244 ) ) ;
#28503 = CARTESIAN_POINT ( 'NONE',  ( -4.483927247898539470, -16.52544592524342804, 27.29057627198103120 ) ) ;
#28504 = CARTESIAN_POINT ( 'NONE',  ( -19.05341960407611168, -5.049401038298163336, 46.45724293864768129 ) ) ;
#28505 = CARTESIAN_POINT ( 'NONE',  ( -16.46253265017160317, 9.564922557960807481, 70.83224293864770971 ) ) ;
#28506 = CARTESIAN_POINT ( 'NONE',  ( -5.049401038298153566, 19.05341960407611168, 45.20724293864769550 ) ) ;
#28507 = CARTESIAN_POINT ( 'NONE',  ( -15.80617190586768217, 15.72974639402176855, 48.12609039468568284 ) ) ;
#28508 = CARTESIAN_POINT ( 'NONE',  ( -9.474510206698964154, 16.51473224551069663, 60.41557627198102409 ) ) ;
#28509 = CYLINDRICAL_SURFACE ( 'NONE', #190488, 7.500000000000000000 ) ;
#28510 = CARTESIAN_POINT ( 'NONE',  ( -19.03943276465977164, 0.05219959533909376836, 61.24890960531436690 ) ) ;
#28511 = CARTESIAN_POINT ( 'NONE',  ( -18.67979575497178146, -10.72451020669898902, 36.66557627198103120 ) ) ;
#28512 = CARTESIAN_POINT ( 'NONE',  ( -19.05341960407611168, -5.049401038298163336, 36.45724293864766707 ) ) ;
#28513 = CARTESIAN_POINT ( 'NONE',  ( 18.67979575497178502, 10.72451020669898547, 39.16557627198102409 ) ) ;
#28514 = CARTESIAN_POINT ( 'NONE',  ( -8.224510206698735004, -14.34966873604973081, 89.58442372801901854 ) ) ;
#28515 = CARTESIAN_POINT ( 'NONE',  ( -16.51473224551082808, 9.474510206698731452, 23.33442372801900078 ) ) ;
#28516 = CARTESIAN_POINT ( 'NONE',  ( -16.52544592524335698, -4.483927247898792601, 68.95942372801901854 ) ) ;
#28517 = CARTESIAN_POINT ( 'NONE',  ( 5.049401038298161559, -19.05341960407611168, 102.7072429386476955 ) ) ;
#28518 = CARTESIAN_POINT ( 'NONE',  ( -14.34966873604972548, 8.224510206698743886, 58.33442372801901143 ) ) ;
#28519 = CARTESIAN_POINT ( 'NONE',  ( -4.379528057220086978, -16.55341960407618274, 34.79275706135235424 ) ) ;
#28520 = CARTESIAN_POINT ( 'NONE',  ( 19.03943276465977164, -0.05219959533909143690, 103.7489096053143669 ) ) ;
#28521 = CARTESIAN_POINT ( 'NONE',  ( 16.52544592524335698, 4.483927247898782831, 21.45942372801901499 ) ) ;
#28522 = CARTESIAN_POINT ( 'NONE',  ( 19.02544592524343514, -5.153800228976328945, 33.54057627198102409 ) ) ;
#28523 = CARTESIAN_POINT ( 'NONE',  ( -18.67979575497193778, 10.72451020669871902, 23.33442372801901499 ) ) ;
#28524 = CARTESIAN_POINT ( 'NONE',  ( 12.06949235617739724, 12.14591786802326823, 26.87609039468567218 ) ) ;
#28525 = CARTESIAN_POINT ( 'NONE',  ( 16.55341960407618274, -4.379528057220086978, 106.0427570613523471 ) ) ;
#28526 = DIRECTION ( 'NONE',  ( -0.000000000000000000, 0.5000000000000001110, 0.8660254037844385966 ) ) ;
#28527 = CARTESIAN_POINT ( 'NONE',  ( -15.72974639402176322, -15.80617190586768395, 104.3760903946856899 ) ) ;
#28528 = CARTESIAN_POINT ( 'NONE',  ( 19.02544592524334988, 5.153800228976608722, 91.45942372801900433 ) ) ;
#28529 = CARTESIAN_POINT ( 'NONE',  ( 12.14591786802309770, 12.06949235617756955, 54.37390960531435979 ) ) ;
#28530 = CARTESIAN_POINT ( 'NONE',  ( -12.06949235617756955, 12.14591786802309770, 115.6239096053143669 ) ) ;
#28532 = CARTESIAN_POINT ( 'NONE',  ( -7.503727747132419523, 1.500047742438238352, -64.26135111332263250 ) ) ;
#28531 = CARTESIAN_POINT ( 'NONE',  ( -13.89961937509957401, -13.97604488694547875, 49.37609039468567573 ) ) ;
#28533 = CARTESIAN_POINT ( 'NONE',  ( 21.53943276465977519, 0.05219959533937863772, 46.25109039468567573 ) ) ;
#28534 = CARTESIAN_POINT ( 'NONE',  ( -16.53943276465976808, -0.05219959533934237506, 23.75109039468567929 ) ) ;
#28535 = CARTESIAN_POINT ( 'NONE',  ( 17.49999999999999645, 5.624438216177598981, 81.68329655085356933 ) ) ;
#28536 = CARTESIAN_POINT ( 'NONE',  ( 13.97604488694527802, 13.89961937509977652, 104.3739096053143385 ) ) ;
#28537 = CARTESIAN_POINT ( 'NONE',  ( -18.62759615963270932, 10.81492255796079327, 75.83224293864769550 ) ) ;
#28538 = CARTESIAN_POINT ( 'NONE',  ( -13.89961937509957401, -13.97604488694547875, 104.3760903946856757 ) ) ;
#28539 = CARTESIAN_POINT ( 'NONE',  ( -19.03943276465977164, 0.05219959533909376836, 101.2489096053143669 ) ) ;
#28540 = CARTESIAN_POINT ( 'NONE',  ( -20.19161698411414463, -19.96942110459088582, 140.0000000000000000 ) ) ;
#28541 = CARTESIAN_POINT ( 'NONE',  ( -16.52544592524342804, 4.483927247898546575, 111.0405762719810525 ) ) ;
#28542 = CARTESIAN_POINT ( 'NONE',  ( -15.80617190586768217, 15.72974639402176855, 98.12609039468570415 ) ) ;
#28543 = CARTESIAN_POINT ( 'NONE',  ( -9.474510206698964154, 16.51473224551069663, 40.41557627198103120 ) ) ;
#28544 = CARTESIAN_POINT ( 'NONE',  ( 5.719274019375673035, 21.55341960407619339, 52.29275706135236135 ) ) ;
#28545 = CARTESIAN_POINT ( 'NONE',  ( -21.52544592524334988, -5.823673210054445271, 88.95942372801901854 ) ) ;
#28546 = CARTESIAN_POINT ( 'NONE',  ( -16.55341960407617563, 4.379528057220093196, 103.5427570613523613 ) ) ;
#28547 = CARTESIAN_POINT ( 'NONE',  ( -19.03943276465977164, 0.05219959533909376836, 76.24890960531435269 ) ) ;
#28548 = CARTESIAN_POINT ( 'NONE',  ( -21.52544592524334988, -5.823673210054445271, 43.95942372801902565 ) ) ;
#28549 = CARTESIAN_POINT ( 'NONE',  ( -5.719274019375665041, -21.55341960407619695, 44.79275706135234714 ) ) ;
#28551 = CARTESIAN_POINT ( 'NONE',  ( -19.02544592524342804, 5.153800228976336051, 86.04057627198103830 ) ) ;
#28550 = CARTESIAN_POINT ( 'NONE',  ( -13.89961937509957401, -13.97604488694547875, 64.37609039468567573 ) ) ;
#28552 = CARTESIAN_POINT ( 'NONE',  ( -12.14591786802309592, -12.06949235617757132, 101.8739096053143811 ) ) ;
#28553 = CARTESIAN_POINT ( 'NONE',  ( -0.05219959533907301413, -21.53943276465977519, 92.49890960531436690 ) ) ;
#28554 = CARTESIAN_POINT ( 'NONE',  ( -0.05219959533910754901, -16.53943276465976808, 67.49890960531436690 ) ) ;
#28555 = CARTESIAN_POINT ( 'NONE',  ( -16.46253265017146816, -9.564922557961047289, 24.16775706135233648 ) ) ;
#28556 = CARTESIAN_POINT ( 'NONE',  ( -4.379528057220328563, 16.55341960407611168, 90.20724293864770971 ) ) ;
#28557 = CARTESIAN_POINT ( 'NONE',  ( -0.05219959533909027116, -19.03943276465977164, 37.49890960531436690 ) ) ;
#28558 = CARTESIAN_POINT ( 'NONE',  ( 16.51473224551083163, -9.474510206698727899, 85.83442372801900433 ) ) ;
#28559 = CARTESIAN_POINT ( 'NONE',  ( -4.379528057220328563, 16.55341960407611168, 55.20724293864770260 ) ) ;
#28560 = CARTESIAN_POINT ( 'NONE',  ( 10.72451020669871369, 18.67979575497193778, 97.08442372801904696 ) ) ;
#28561 = CARTESIAN_POINT ( 'NONE',  ( -19.03943276465977164, 0.05219959533909376836, 101.2489096053143669 ) ) ;
#28562 = CARTESIAN_POINT ( 'NONE',  ( -13.97604488694547697, 13.89961937509957934, 78.12609039468567573 ) ) ;
#28563 = CARTESIAN_POINT ( 'NONE',  ( -21.52544592524343514, 5.823673210054127303, 81.04057627198102409 ) ) ;
#28564 = CARTESIAN_POINT ( 'NONE',  ( 5.823673210054444382, -21.52544592524334988, 30.20942372801902565 ) ) ;
#28565 = CARTESIAN_POINT ( 'NONE',  ( -4.483927247898782831, 16.52544592524335698, 32.70942372801900433 ) ) ;
#28566 = CARTESIAN_POINT ( 'NONE',  ( 0.05219959533934541429, -16.53943276465976808, 90.00109039468567573 ) ) ;
#28568 = CARTESIAN_POINT ( 'NONE',  ( 21.55341960407619695, -5.719274019375665929, 36.04275706135234714 ) ) ;
#28567 = CARTESIAN_POINT ( 'NONE',  ( -19.03943276465977164, 0.05219959533909376836, 26.24890960531435624 ) ) ;
#28569 = CARTESIAN_POINT ( 'NONE',  ( -16.52544592524342804, 4.483927247898546575, 116.0405762719810383 ) ) ;
#28570 = CARTESIAN_POINT ( 'NONE',  ( -29.86685920354755197, -21.69954338932560134, -2.924999997268813878 ) ) ;
#28571 = CARTESIAN_POINT ( 'NONE',  ( 14.29746914071037800, 8.314922557961029526, 46.66775706135234714 ) ) ;
#28572 = ADVANCED_FACE ( 'NONE', ( #133387 ), #25243, .F. ) ;
#28573 = CARTESIAN_POINT ( 'NONE',  ( -16.53943276465976808, 0.05219959533911058130, 76.24890960531435269 ) ) ;
#28574 = CARTESIAN_POINT ( 'NONE',  ( -10.72451020669898014, 18.67979575497178502, 70.41557627198102409 ) ) ;
#28575 = CARTESIAN_POINT ( 'NONE',  ( 4.379528057220339221, -16.55341960407611168, 27.70724293864769905 ) ) ;
#28576 = CARTESIAN_POINT ( 'NONE',  ( 14.34966873604972726, -8.224510206698740333, 55.83442372801901854 ) ) ;
#28577 = CARTESIAN_POINT ( 'NONE',  ( 5.153800228976335163, 19.02544592524342804, 49.79057627198100988 ) ) ;
#28578 = CARTESIAN_POINT ( 'NONE',  ( -16.52544592524335698, -4.483927247898792601, 88.95942372801901854 ) ) ;
#28579 = CARTESIAN_POINT ( 'NONE',  ( 19.02544592524334988, 5.153800228976608722, 86.45942372801900433 ) ) ;
#28580 = CARTESIAN_POINT ( 'NONE',  ( 5.823673210054125526, 21.52544592524343514, 74.79057627198105251 ) ) ;
#28581 = CARTESIAN_POINT ( 'NONE',  ( -4.483927247898782831, 16.52544592524335698, 112.7094237280190328 ) ) ;
#28582 = ORIENTED_EDGE ( 'NONE', *, *, #49370, .F. ) ;
#28583 = CARTESIAN_POINT ( 'NONE',  ( 25.70602947687971707, 7.354137148287277270, 175.2376750527030538 ) ) ;
#28584 = CARTESIAN_POINT ( 'NONE',  ( -15.72974639402197994, 15.80617190586746368, 65.62390960531436690 ) ) ;
#28585 = ORIENTED_EDGE ( 'NONE', *, *, #96802, .T. ) ;
#28586 = CARTESIAN_POINT ( 'NONE',  ( -4.379528057220086978, -16.55341960407618274, 94.79275706135234714 ) ) ;
#28587 = ORIENTED_EDGE ( 'NONE', *, *, #116598, .T. ) ;
#28588 = CARTESIAN_POINT ( 'NONE',  ( -16.46253265017160317, 9.564922557960807481, 110.8322429386476955 ) ) ;
#28589 = CARTESIAN_POINT ( 'NONE',  ( 5.823673210054125526, 21.52544592524343514, 74.79057627198105251 ) ) ;
#28590 = CARTESIAN_POINT ( 'NONE',  ( 14.34966873604960469, 8.224510206698951720, 24.16557627198103120 ) ) ;
#28591 = CARTESIAN_POINT ( 'NONE',  ( -16.53943276465976808, -0.05219959533934237506, 23.75109039468567929 ) ) ;
#28592 = CARTESIAN_POINT ( 'NONE',  ( -19.05341960407611168, -5.049401038298163336, 21.45724293864768839 ) ) ;
#28593 = CARTESIAN_POINT ( 'NONE',  ( -16.53943276465976808, -0.05219959533934237506, 33.75109039468568284 ) ) ;
#28594 = CARTESIAN_POINT ( 'NONE',  ( -13.89961937509977652, 13.97604488694528158, 55.62390960531434558 ) ) ;
#28595 = CARTESIAN_POINT ( 'NONE',  ( 8.906447517083050158, 27.41122689804195645, 143.4000000000000057 ) ) ;
#28596 = CARTESIAN_POINT ( 'NONE',  ( -5.049401038298153566, 19.05341960407611168, 100.2072429386476955 ) ) ;
#28597 = CARTESIAN_POINT ( 'NONE',  ( 0.05219959533934541429, -16.53943276465976808, 95.00109039468568994 ) ) ;
#28598 = CARTESIAN_POINT ( 'NONE',  ( 19.02544592524334988, 5.153800228976608722, 91.45942372801900433 ) ) ;
#28599 = CARTESIAN_POINT ( 'NONE',  ( -13.97604488694547697, 13.89961937509957934, 28.12609039468565797 ) ) ;
#28600 = CARTESIAN_POINT ( 'NONE',  ( -18.67979575497178146, -10.72451020669898902, 81.66557627198103830 ) ) ;
#28601 = CARTESIAN_POINT ( 'NONE',  ( -14.29746914071037622, -8.314922557961029526, 94.16775706135237556 ) ) ;
#28602 = CARTESIAN_POINT ( 'NONE',  ( 5.049401038297881783, 19.05341960407617563, 92.29275706135234714 ) ) ;
#28603 = CARTESIAN_POINT ( 'NONE',  ( -13.89961937509977652, 13.97604488694528158, 55.62390960531434558 ) ) ;
#28604 = CARTESIAN_POINT ( 'NONE',  ( -19.03943276465977164, 0.05219959533909376836, 91.24890960531436690 ) ) ;
#28605 = CARTESIAN_POINT ( 'NONE',  ( 10.72451020669871369, 18.67979575497193778, 57.08442372801901854 ) ) ;
#28606 = CARTESIAN_POINT ( 'NONE',  ( -19.05341960407611168, -5.049401038298163336, 61.45724293864769550 ) ) ;
#28607 = CARTESIAN_POINT ( 'NONE',  ( -16.53943276465976808, 0.05219959533911058130, 86.24890960531436690 ) ) ;
#28608 = CARTESIAN_POINT ( 'NONE',  ( -17.31747979337950838, -6.344076630960981511, 86.37944868065183357 ) ) ;
#28609 = CARTESIAN_POINT ( 'NONE',  ( 8.224510206698953496, -14.34966873604960469, 77.91557627198102409 ) ) ;
#28610 = CARTESIAN_POINT ( 'NONE',  ( 21.53943276465977519, -0.05219959533907433946, 73.74890960531433848 ) ) ;
#28611 = CARTESIAN_POINT ( 'NONE',  ( -16.51473224551082808, 9.474510206698731452, 93.33442372801900433 ) ) ;
#28612 = CARTESIAN_POINT ( 'NONE',  ( 16.79531203550648044, -7.028104445595602989, 81.24755011779561187 ) ) ;
#28613 = CARTESIAN_POINT ( 'NONE',  ( 16.46253265017146816, 9.564922557961045513, 41.66775706135234003 ) ) ;
#28614 = DIRECTION ( 'NONE',  ( -1.000000000000000000, 0.000000000000000000, 0.000000000000000000 ) ) ;
#28615 = CIRCLE ( 'NONE', #73781, 1.000000000000000888 ) ;
#28617 = CARTESIAN_POINT ( 'NONE',  ( 13.89961937509977652, -13.97604488694527269, 93.12390960531436690 ) ) ;
#28616 = CARTESIAN_POINT ( 'NONE',  ( 19.03943276465977164, -0.05219959533909143690, 83.74890960531436690 ) ) ;
#28618 = CARTESIAN_POINT ( 'NONE',  ( -16.53943276465976808, -0.05219959533934237506, 63.75109039468568284 ) ) ;
#28619 = CARTESIAN_POINT ( 'NONE',  ( -21.50819313649950359, 5.452397343345392500, 174.1340046013915241 ) ) ;
#28620 = CARTESIAN_POINT ( 'NONE',  ( 19.05341960407617918, -5.049401038297876454, 46.04275706135233293 ) ) ;
#28621 = CARTESIAN_POINT ( 'NONE',  ( 15.06137443927351249, -15.06137443927345210, -58.85720012050613548 ) ) ;
#28622 = CARTESIAN_POINT ( 'NONE',  ( 0.05219959533909260263, 19.03943276465977164, 109.9989096053143669 ) ) ;
#28623 = CARTESIAN_POINT ( 'NONE',  ( -16.53943276465976808, -0.05219959533934237506, 108.7510903946857042 ) ) ;
#28624 = CARTESIAN_POINT ( 'NONE',  ( -3.921794856358155723, -4.985877495913942248, -64.49392664332130209 ) ) ;
#28625 = CARTESIAN_POINT ( 'NONE',  ( -8.224510206698735004, -14.34966873604973081, 74.58442372801901854 ) ) ;
#28626 = CARTESIAN_POINT ( 'NONE',  ( -16.20579543436675252, 7.371946100355233789, 29.43479165828123101 ) ) ;
#28627 = CARTESIAN_POINT ( 'NONE',  ( 16.55341960407618274, -4.379528057220086978, 51.04275706135234714 ) ) ;
#28628 = CARTESIAN_POINT ( 'NONE',  ( 0.05219959533909260263, 19.03943276465977164, 74.99890960531435269 ) ) ;
#28629 = CARTESIAN_POINT ( 'NONE',  ( 21.53943276465977519, 0.05219959533937863772, 66.25109039468567573 ) ) ;
#28630 = CARTESIAN_POINT ( 'NONE',  ( -16.46253265017146816, -9.564922557961047289, 69.16775706135233293 ) ) ;
#28631 = CARTESIAN_POINT ( 'NONE',  ( 19.05341960407617918, -5.049401038297876454, 26.04275706135233293 ) ) ;
#28632 = CARTESIAN_POINT ( 'NONE',  ( -13.97604488694527625, -13.89961937509977652, 56.87390960531434558 ) ) ;
#28633 = CARTESIAN_POINT ( 'NONE',  ( 19.03943276465977164, -0.05219959533909143690, 48.74890960531435979 ) ) ;
#28634 = CARTESIAN_POINT ( 'NONE',  ( -17.82155712959115590, -35.81153309740783897, -9.011975243048143014 ) ) ;
#28635 = CARTESIAN_POINT ( 'NONE',  ( -18.62759615963270932, 10.81492255796079327, 65.83224293864769550 ) ) ;
#28636 = CARTESIAN_POINT ( 'NONE',  ( -0.05219959533907301413, -21.53943276465977519, 32.49890960531435979 ) ) ;
#28637 = CARTESIAN_POINT ( 'NONE',  ( -8.224510206698948167, 14.34966873604960824, 115.4155762719810241 ) ) ;
#28638 = CARTESIAN_POINT ( 'NONE',  ( -14.34966873604972548, 8.224510206698743886, 48.33442372801902565 ) ) ;
#28639 = EDGE_CURVE ( 'NONE', #138825, #39558, #39383, .T. ) ;
#28640 = ORIENTED_EDGE ( 'NONE', *, *, #42025, .T. ) ;
#28641 = CARTESIAN_POINT ( 'NONE',  ( 21.52544592524344225, -5.823673210054117533, 113.5405762719810383 ) ) ;
#28643 = CARTESIAN_POINT ( 'NONE',  ( -11.74264578624800670, 36.14014761921585972, -6.400000000000000355 ) ) ;
#28642 = CARTESIAN_POINT ( 'NONE',  ( -14.34966873604960291, -8.224510206698953496, 51.66557627198102409 ) ) ;
#28644 = CARTESIAN_POINT ( 'NONE',  ( -5.153800228976607833, 19.02544592524334988, 112.7094237280190043 ) ) ;
#28645 = CARTESIAN_POINT ( 'NONE',  ( 19.03943276465977164, 0.05219959533936151252, 46.25109039468566863 ) ) ;
#28646 = CARTESIAN_POINT ( 'NONE',  ( -8.314922557960811034, -14.29746914071050412, 42.08224293864769550 ) ) ;
#28647 = CARTESIAN_POINT ( 'NONE',  ( 18.67979575497194134, -10.72451020669871369, 20.83442372801901143 ) ) ;
#28649 = CARTESIAN_POINT ( 'NONE',  ( -15.72974639402197994, 15.80617190586746368, 70.62390960531436690 ) ) ;
#28648 = DIRECTION ( 'NONE',  ( 1.000000000000000000, 0.000000000000000000, 0.000000000000000000 ) ) ;
#28650 = CARTESIAN_POINT ( 'NONE',  ( -19.02544592524342804, 5.153800228976336051, 91.04057627198100988 ) ) ;
#28651 = CARTESIAN_POINT ( 'NONE',  ( -8.224510206698948167, 14.34966873604960824, 65.41557627198102409 ) ) ;
#28652 = CARTESIAN_POINT ( 'NONE',  ( 19.02544592524343514, -5.153800228976328945, 108.5405762719810383 ) ) ;
#28653 = EDGE_CURVE ( 'NONE', #91449, #137808, #101042, .T. ) ;
#28654 = CARTESIAN_POINT ( 'NONE',  ( -16.46253265017160317, 9.564922557960807481, 80.83224293864769550 ) ) ;
#28655 = CARTESIAN_POINT ( 'NONE',  ( -13.89961937509957401, -13.97604488694547875, 49.37609039468567573 ) ) ;
#28656 = CARTESIAN_POINT ( 'NONE',  ( 18.62759615963271287, -10.81492255796078972, 113.3322429386476955 ) ) ;
#28657 = CARTESIAN_POINT ( 'NONE',  ( 5.153800228976335163, 19.02544592524342804, 39.79057627198100988 ) ) ;
#28658 = CARTESIAN_POINT ( 'NONE',  ( -0.05219959533910754901, -16.53943276465976808, 112.4989096053143669 ) ) ;
#28659 = CARTESIAN_POINT ( 'NONE',  ( -15.80617190586768217, 15.72974639402176855, 48.12609039468568284 ) ) ;
#28660 = CARTESIAN_POINT ( 'NONE',  ( -22.44159573604009950, -16.30477369853688430, 147.0750000027312012 ) ) ;
#28661 = CARTESIAN_POINT ( 'NONE',  ( 8.224510206698953496, -14.34966873604960469, 22.91557627198102765 ) ) ;
#28662 = CARTESIAN_POINT ( 'NONE',  ( 13.97604488694527802, 13.89961937509977652, 44.37390960531435269 ) ) ;
#28663 = CARTESIAN_POINT ( 'NONE',  ( 9.564922557960805705, 16.46253265017160317, 94.58224293864769550 ) ) ;
#28664 = CARTESIAN_POINT ( 'NONE',  ( 0.05219959533907565091, 21.53943276465977519, 74.99890960531435269 ) ) ;
#28665 = CARTESIAN_POINT ( 'NONE',  ( 27.73933785331498214, 9.013057229001095294, 141.9750000027311501 ) ) ;
#28666 = CARTESIAN_POINT ( 'NONE',  ( 16.51473224551069308, 9.474510206698969483, 49.16557627198102409 ) ) ;
#28667 = CARTESIAN_POINT ( 'NONE',  ( -21.52544592524343514, 5.823673210054127303, 56.04057627198102409 ) ) ;
#28668 = CARTESIAN_POINT ( 'NONE',  ( 15.72974639402176855, 15.80617190586768217, 81.87609039468568994 ) ) ;
#28671 = CARTESIAN_POINT ( 'NONE',  ( 14.34966873604960469, 8.224510206698951720, 64.16557627198102409 ) ) ;
#28670 = CARTESIAN_POINT ( 'NONE',  ( -0.05219959533934338120, 16.53943276465976808, 82.50109039468568994 ) ) ;
#28669 = CARTESIAN_POINT ( 'NONE',  ( 17.97214573761831957, 5.500000000000083489, 53.96970049038659312 ) ) ;
#28672 = CARTESIAN_POINT ( 'NONE',  ( -19.02544592524342804, 5.153800228976336051, 76.04057627198102409 ) ) ;
#28673 = VERTEX_POINT ( 'NONE', #165734 ) ;
#28674 = CARTESIAN_POINT ( 'NONE',  ( 5.049401038297881783, 19.05341960407617563, 27.29275706135232937 ) ) ;
#28675 = CARTESIAN_POINT ( 'NONE',  ( 12.06949235617739724, 12.14591786802326823, 91.87609039468568994 ) ) ;
#28676 = CARTESIAN_POINT ( 'NONE',  ( -9.564922557961040184, 16.46253265017147172, 22.91775706135233648 ) ) ;
#28677 = CARTESIAN_POINT ( 'NONE',  ( -13.89961937509977652, 13.97604488694528158, 80.62390960531436690 ) ) ;
#28678 = CARTESIAN_POINT ( 'NONE',  ( -5.823673210054116645, -21.52544592524344225, 42.29057627198103120 ) ) ;
#28679 = CARTESIAN_POINT ( 'NONE',  ( -16.52544592524335698, -4.483927247898792601, 23.95942372801901143 ) ) ;
#28680 = CARTESIAN_POINT ( 'NONE',  ( 18.62759615963255655, 10.81492255796105972, 96.66775706135234714 ) ) ;
#28681 = CARTESIAN_POINT ( 'NONE',  ( 16.53943276465976808, 0.05219959533934440121, 66.25109039468567573 ) ) ;
#28682 = CARTESIAN_POINT ( 'NONE',  ( -10.72451020669898014, 18.67979575497178502, 110.4155762719810383 ) ) ;
#28683 = CARTESIAN_POINT ( 'NONE',  ( -14.29746914071037622, -8.314922557961029526, 19.16775706135234714 ) ) ;
#28684 = CARTESIAN_POINT ( 'NONE',  ( -16.46253265017160317, 9.564922557960807481, 90.83224293864769550 ) ) ;
#28685 = CARTESIAN_POINT ( 'NONE',  ( -0.05219959533934338120, 16.53943276465976808, 22.50109039468567573 ) ) ;
#28686 = CARTESIAN_POINT ( 'NONE',  ( 19.02544592524343514, -5.153800228976328945, 48.54057627198103120 ) ) ;
#28687 = CARTESIAN_POINT ( 'NONE',  ( -4.379528057220086978, -16.55341960407618274, 34.79275706135235424 ) ) ;
#28688 = CARTESIAN_POINT ( 'NONE',  ( 16.53943276465976808, -0.05219959533910856209, 78.74890960531436690 ) ) ;
#28689 = CARTESIAN_POINT ( 'NONE',  ( 12.06949235617739724, 12.14591786802326823, 91.87609039468568994 ) ) ;
#28691 = CARTESIAN_POINT ( 'NONE',  ( 9.474510206698971260, -16.51473224551069308, 67.91557627198102409 ) ) ;
#28690 = CARTESIAN_POINT ( 'NONE',  ( 21.53943276465977519, 0.05219959533937863772, 31.25109039468568639 ) ) ;
#28692 = CARTESIAN_POINT ( 'NONE',  ( -9.474510206698964154, 16.51473224551069663, 80.41557627198103830 ) ) ;
#28693 = CARTESIAN_POINT ( 'NONE',  ( 16.52544592524335698, 4.483927247898782831, 81.45942372801900433 ) ) ;
#28695 = EDGE_LOOP ( 'NONE', ( #73188, #180107, #173277 ) ) ;
#28694 = CARTESIAN_POINT ( 'NONE',  ( -24.57691432906831963, -7.727872488968206888, 167.2019946024424257 ) ) ;
#28696 = ORIENTED_EDGE ( 'NONE', *, *, #136135, .F. ) ;
#28697 = CARTESIAN_POINT ( 'NONE',  ( -5.049401038297874678, -19.05341960407617918, 34.79275706135233293 ) ) ;
#28698 = CARTESIAN_POINT ( 'NONE',  ( 16.51473224551069308, 9.474510206698969483, 104.1655762719810241 ) ) ;
#28699 = CARTESIAN_POINT ( 'NONE',  ( -9.564922557960796823, -16.46253265017161027, 47.08224293864769550 ) ) ;
#28700 = CARTESIAN_POINT ( 'NONE',  ( 0.7811817504636909826, 13.90344567069866599, -62.49835084440437072 ) ) ;
#28701 = CARTESIAN_POINT ( 'NONE',  ( 14.29746914071037800, 8.314922557961029526, 36.66775706135234714 ) ) ;
#28703 = CARTESIAN_POINT ( 'NONE',  ( -8.314922557961024197, 14.29746914071037800, 47.91775706135234714 ) ) ;
#28702 = CARTESIAN_POINT ( 'NONE',  ( 5.049401038297881783, 19.05341960407617563, 57.29275706135231871 ) ) ;
#28704 = CARTESIAN_POINT ( 'NONE',  ( 19.02544592524343514, -5.153800228976328945, 103.5405762719809957 ) ) ;
#28705 = CARTESIAN_POINT ( 'NONE',  ( -5.049401038298153566, 19.05341960407611168, 75.20724293864769550 ) ) ;
#28706 = CARTESIAN_POINT ( 'NONE',  ( -0.05219959533907301413, -21.53943276465977519, 97.49890960531436690 ) ) ;
#28707 = CARTESIAN_POINT ( 'NONE',  ( 19.03943276465977164, 0.05219959533936151252, 66.25109039468567573 ) ) ;
#28709 = CARTESIAN_POINT ( 'NONE',  ( 17.43360820948602097, -4.799606864746338353, 21.47765276293580428 ) ) ;
#28708 = CARTESIAN_POINT ( 'NONE',  ( -5.153800228976328057, -19.02544592524343514, 87.29057627198103830 ) ) ;
#28710 = CARTESIAN_POINT ( 'NONE',  ( 13.89961937509977652, -13.97604488694527269, 63.12390960531435979 ) ) ;
#28712 = CARTESIAN_POINT ( 'NONE',  ( -9.474510206698964154, 16.51473224551069663, 70.41557627198102409 ) ) ;
#28711 = CARTESIAN_POINT ( 'NONE',  ( -16.52544592524342804, 4.483927247898546575, 36.04057627198102409 ) ) ;
#28713 = CARTESIAN_POINT ( 'NONE',  ( 13.97604488694548053, -13.89961937509957401, 40.62609039468564731 ) ) ;
#28714 = CARTESIAN_POINT ( 'NONE',  ( 4.379528057220339221, -16.55341960407611168, 77.70724293864770971 ) ) ;
#28715 = CARTESIAN_POINT ( 'NONE',  ( -15.80617190586768217, 15.72974639402176855, 103.1260903946856757 ) ) ;
#28716 = CARTESIAN_POINT ( 'NONE',  ( -16.46253265017160317, 9.564922557960807481, 35.83224293864768839 ) ) ;
#28717 = CARTESIAN_POINT ( 'NONE',  ( 12.14591786802327356, -12.06949235617739191, 55.62609039468568284 ) ) ;
#28719 = CARTESIAN_POINT ( 'NONE',  ( -10.81492255796105439, 18.62759615963255655, 107.9177570613523471 ) ) ;
#28718 = CARTESIAN_POINT ( 'NONE',  ( 16.53943276465976808, -0.05219959533910856209, 33.74890960531436690 ) ) ;
#28720 = CARTESIAN_POINT ( 'NONE',  ( -5.049401038298153566, 19.05341960407611168, 90.20724293864766707 ) ) ;
#28721 = CARTESIAN_POINT ( 'NONE',  ( 9.564922557960805705, 16.46253265017160317, 94.58224293864769550 ) ) ;
#28722 = CARTESIAN_POINT ( 'NONE',  ( 9.474510206698971260, -16.51473224551069308, 22.91557627198102765 ) ) ;
#28723 = CARTESIAN_POINT ( 'NONE',  ( -16.55341960407611168, -4.379528057220339221, 111.4572429386476813 ) ) ;
#28724 = CARTESIAN_POINT ( 'NONE',  ( -4.483927247898539470, -16.52544592524342804, 77.29057627198102409 ) ) ;
#28725 = CARTESIAN_POINT ( 'NONE',  ( -10.72451020669898014, 18.67979575497178502, 85.41557627198102409 ) ) ;
#28726 = CARTESIAN_POINT ( 'NONE',  ( 16.46253265017160672, -9.564922557960803928, 88.33224293864769550 ) ) ;
#28727 = CARTESIAN_POINT ( 'NONE',  ( -21.55341960407610458, -5.719274019375992779, 101.4572429386476955 ) ) ;
#28728 = CARTESIAN_POINT ( 'NONE',  ( 5.049401038298161559, -19.05341960407611168, 92.70724293864769550 ) ) ;
#28730 = CARTESIAN_POINT ( 'NONE',  ( -8.224510206698948167, 14.34966873604960824, 95.41557627198102409 ) ) ;
#28729 = CARTESIAN_POINT ( 'NONE',  ( 18.22780087662122384, -5.500000000000022204, 46.01540105326107266 ) ) ;
#28731 = CARTESIAN_POINT ( 'NONE',  ( 16.46253265017160672, -9.564922557960803928, 58.33224293864769550 ) ) ;
#28732 = CARTESIAN_POINT ( 'NONE',  ( -18.62759615963270932, 10.81492255796079327, 60.83224293864769550 ) ) ;
#28733 = DIRECTION ( 'NONE',  ( -0.5000000000000004441, -0.4999999999999987232, 0.7071067811865482389 ) ) ;
#28735 = DIRECTION ( 'NONE',  ( -1.000000000000000000, -0.000000000000000000, -0.000000000000000000 ) ) ;
#28734 = CARTESIAN_POINT ( 'NONE',  ( 16.52544592524335698, 4.483927247898782831, 111.4594237280190328 ) ) ;
#28736 = CARTESIAN_POINT ( 'NONE',  ( -8.314922557961024197, 14.29746914071037800, 22.91775706135235069 ) ) ;
#28737 = CARTESIAN_POINT ( 'NONE',  ( 4.379528057220339221, -16.55341960407611168, 92.70724293864770971 ) ) ;
#28738 = CARTESIAN_POINT ( 'NONE',  ( 19.26498983726236247, -5.499999999999801936, 53.05319577422001487 ) ) ;
#28739 = CARTESIAN_POINT ( 'NONE',  ( 9.474510206698971260, -16.51473224551069308, 82.91557627198103830 ) ) ;
#28740 = CARTESIAN_POINT ( 'NONE',  ( 9.474510206698971260, -16.51473224551069308, 47.91557627198102409 ) ) ;
#28742 = EDGE_CURVE ( 'NONE', #178146, #15137, #54903, .T. ) ;
#28741 = CARTESIAN_POINT ( 'NONE',  ( -16.55341960407611168, -4.379528057220339221, 61.45724293864770260 ) ) ;
#28743 = CARTESIAN_POINT ( 'NONE',  ( 19.02544592524343514, -5.153800228976328945, 108.5405762719810383 ) ) ;
#28744 = CARTESIAN_POINT ( 'NONE',  ( -9.564922557961040184, 16.46253265017147172, 102.9177570613523329 ) ) ;
#28745 = CARTESIAN_POINT ( 'NONE',  ( 5.823673210054444382, -21.52544592524334988, 60.20942372801902565 ) ) ;
#28746 = CARTESIAN_POINT ( 'NONE',  ( 16.46253265017160672, -9.564922557960803928, 103.3322429386476955 ) ) ;
#28747 = CARTESIAN_POINT ( 'NONE',  ( 18.62759615963271287, -10.81492255796078972, 78.33224293864770971 ) ) ;
#28748 = CARTESIAN_POINT ( 'NONE',  ( -4.379528057220086978, -16.55341960407618274, 64.79275706135234714 ) ) ;
#28749 = CARTESIAN_POINT ( 'NONE',  ( -5.049401038298153566, 19.05341960407611168, 30.20724293864768839 ) ) ;
#28750 = CARTESIAN_POINT ( 'NONE',  ( 19.02544592524343514, -5.153800228976328945, 78.54057627198099567 ) ) ;
#28751 = CARTESIAN_POINT ( 'NONE',  ( -18.67979575497178146, -10.72451020669898902, 76.66557627198103830 ) ) ;
#28752 = CARTESIAN_POINT ( 'NONE',  ( -14.29746914071037622, -8.314922557961029526, 19.16775706135234714 ) ) ;
#28754 = CARTESIAN_POINT ( 'NONE',  ( -0.05219959533937732626, 21.53943276465977519, 57.50109039468568994 ) ) ;
#28753 = CARTESIAN_POINT ( 'NONE',  ( 12.06949235617757843, -12.14591786802309237, 38.12390960531436690 ) ) ;
#28756 = CARTESIAN_POINT ( 'NONE',  ( 0.05219959533907565091, 21.53943276465977519, 24.99890960531435624 ) ) ;
#28755 = CARTESIAN_POINT ( 'NONE',  ( -16.55341960407617563, 4.379528057220093196, 88.54275706135236135 ) ) ;
#28757 = CARTESIAN_POINT ( 'NONE',  ( -19.02544592524342804, 5.153800228976336939, 106.0405762719810383 ) ) ;
#28758 = CARTESIAN_POINT ( 'NONE',  ( 1.473582404419343517, 30.72737312094908901, -50.56799658405696363 ) ) ;
#28759 = CARTESIAN_POINT ( 'NONE',  ( -12.14591786802326823, 12.06949235617739902, 113.1260903946856899 ) ) ;
#28760 = CARTESIAN_POINT ( 'NONE',  ( -12.14591786802326823, 12.06949235617739902, 43.12609039468568284 ) ) ;
#28761 = CARTESIAN_POINT ( 'NONE',  ( 13.97604488694527802, 13.89961937509977652, 59.37390960531434558 ) ) ;
#28762 = CARTESIAN_POINT ( 'NONE',  ( 9.474510206698971260, -16.51473224551069308, 67.91557627198102409 ) ) ;
#28763 = CARTESIAN_POINT ( 'NONE',  ( 12.06949235617739724, 12.14591786802326823, 56.87609039468568994 ) ) ;
#28764 = CARTESIAN_POINT ( 'NONE',  ( -14.34966873604960291, -8.224510206698953496, 51.66557627198102409 ) ) ;
#28765 = CARTESIAN_POINT ( 'NONE',  ( 19.03943276465977164, -0.05219959533909143690, 53.74890960531436690 ) ) ;
#28766 = CARTESIAN_POINT ( 'NONE',  ( -19.03943276465977164, 0.05219959533909376836, 46.24890960531435979 ) ) ;
#28767 = CARTESIAN_POINT ( 'NONE',  ( 8.224510206698742110, 14.34966873604972548, 47.08442372801901854 ) ) ;
#28768 = CARTESIAN_POINT ( 'NONE',  ( 19.05341960407617918, -5.049401038297876454, 96.04275706135231871 ) ) ;
#28769 = CARTESIAN_POINT ( 'NONE',  ( 4.483927247898545687, 16.52544592524342804, 94.79057627198105251 ) ) ;
#28770 = CARTESIAN_POINT ( 'NONE',  ( 0.05219959533909260263, 19.03943276465977164, 69.99890960531435269 ) ) ;
#28772 = CARTESIAN_POINT ( 'NONE',  ( 38.00000000000000711, -12.34694845685040754, -1.099999999999999645 ) ) ;
#28771 = CARTESIAN_POINT ( 'NONE',  ( -19.02544592524334988, -5.153800228976617603, 98.95942372801900433 ) ) ;
#28773 = CARTESIAN_POINT ( 'NONE',  ( 18.62759615963255655, 10.81492255796105972, 91.66775706135234714 ) ) ;
#28774 = CARTESIAN_POINT ( 'NONE',  ( -16.52544592524335698, -4.483927247898792601, 73.95942372801901854 ) ) ;
#28775 = CARTESIAN_POINT ( 'NONE',  ( -21.55341960407610458, -5.719274019375992779, 66.45724293864768129 ) ) ;
#28776 = CARTESIAN_POINT ( 'NONE',  ( 4.483927247898790824, -16.52544592524335698, 50.20942372801901854 ) ) ;
#28777 = CARTESIAN_POINT ( 'NONE',  ( 5.049401038298163336, -19.05341960407611168, 32.70724293864768839 ) ) ;
#28778 = CARTESIAN_POINT ( 'NONE',  ( -16.51473224551082808, 9.474510206698731452, 43.33442372801900433 ) ) ;
#28779 = CARTESIAN_POINT ( 'NONE',  ( 0.05219959533909260263, 19.03943276465977164, 94.99890960531436690 ) ) ;
#28780 = CARTESIAN_POINT ( 'NONE',  ( -0.05219959533910754901, -16.53943276465976808, 112.4989096053143669 ) ) ;
#28781 = CARTESIAN_POINT ( 'NONE',  ( 13.89961937509977652, -13.97604488694527269, 63.12390960531435979 ) ) ;
#28782 = CARTESIAN_POINT ( 'NONE',  ( 26.97479053218977185, 7.816291847812730786, 151.6430507545553894 ) ) ;
#28783 = CARTESIAN_POINT ( 'NONE',  ( 18.67979575497194134, -10.72451020669871369, 80.83442372801901854 ) ) ;
#28784 = DIRECTION ( 'NONE',  ( 1.000000000000000000, 0.000000000000000000, 0.000000000000000000 ) ) ;
#28785 = CARTESIAN_POINT ( 'NONE',  ( 13.97604488694548053, -13.89961937509957401, 30.62609039468566863 ) ) ;
#28786 = CARTESIAN_POINT ( 'NONE',  ( 19.05341960407617918, -5.049401038297876454, 31.04275706135232227 ) ) ;
#28787 = CARTESIAN_POINT ( 'NONE',  ( -14.34966873604960291, -8.224510206698953496, 56.66557627198103830 ) ) ;
#28788 = CARTESIAN_POINT ( 'NONE',  ( 9.474510206698971260, -16.51473224551069308, 62.91557627198102409 ) ) ;
#28789 = CARTESIAN_POINT ( 'NONE',  ( 15.80617190586746368, 15.72974639402197994, 29.37390960531435269 ) ) ;
#28790 = CARTESIAN_POINT ( 'NONE',  ( 10.81492255796106328, -18.62759615963255655, 80.41775706135234714 ) ) ;
#28791 = CARTESIAN_POINT ( 'NONE',  ( 19.05341960407611168, 5.049401038298154454, 63.95724293864769550 ) ) ;
#28792 = CARTESIAN_POINT ( 'NONE',  ( -5.719274019375665041, -21.55341960407619695, 79.79275706135236135 ) ) ;
#28793 = CARTESIAN_POINT ( 'NONE',  ( -21.55341960407610458, -5.719274019375992779, 31.45724293864769550 ) ) ;
#28794 = CARTESIAN_POINT ( 'NONE',  ( 13.89961937509977652, -13.97604488694527269, 73.12390960531436690 ) ) ;
#28795 = CARTESIAN_POINT ( 'NONE',  ( -18.62759615963255300, -10.81492255796106328, 44.16775706135234714 ) ) ;
#28796 = CARTESIAN_POINT ( 'NONE',  ( -16.51473224551082808, 9.474510206698731452, 58.33442372801900433 ) ) ;
#28797 = CARTESIAN_POINT ( 'NONE',  ( 9.474510206698971260, -16.51473224551069308, 37.91557627198102409 ) ) ;
#28798 = CARTESIAN_POINT ( 'NONE',  ( 9.564922557960805705, 16.46253265017160317, 79.58224293864769550 ) ) ;
#28799 = CARTESIAN_POINT ( 'NONE',  ( -12.06949235617739369, -12.14591786802326823, 29.37609039468568284 ) ) ;
#28800 = CARTESIAN_POINT ( 'NONE',  ( -8.224510206698948167, 14.34966873604960824, 85.41557627198102409 ) ) ;
#28801 = CARTESIAN_POINT ( 'NONE',  ( 19.03943276465977164, -0.05219959533909143690, 53.74890960531436690 ) ) ;
#28802 = CARTESIAN_POINT ( 'NONE',  ( -21.53943276465977519, 0.05219959533907696930, 51.24890960531436690 ) ) ;
#28803 = CARTESIAN_POINT ( 'NONE',  ( 12.14591786802327356, -12.06949235617739191, 25.62609039468567929 ) ) ;
#28804 = CARTESIAN_POINT ( 'NONE',  ( -18.62759615963255300, -10.81492255796106328, 24.16775706135235424 ) ) ;
#28805 = CARTESIAN_POINT ( 'NONE',  ( -18.62759615963255300, -10.81492255796106328, 64.16775706135234714 ) ) ;
#28806 = CARTESIAN_POINT ( 'NONE',  ( -14.29746914071037622, -8.314922557961029526, 69.16775706135234714 ) ) ;
#28807 = CARTESIAN_POINT ( 'NONE',  ( 14.29746914071037800, 8.314922557961029526, 71.66775706135234714 ) ) ;
#28808 = CARTESIAN_POINT ( 'NONE',  ( -9.474510206698964154, 16.51473224551069663, 55.41557627198103120 ) ) ;
#28809 = CARTESIAN_POINT ( 'NONE',  ( 12.06949235617739724, 12.14591786802326823, 91.87609039468568994 ) ) ;
#28810 = CARTESIAN_POINT ( 'NONE',  ( -5.049401038297874678, -19.05341960407617918, 44.79275706135232582 ) ) ;
#28811 = EDGE_CURVE ( 'NONE', #189747, #83417, #46820, .T. ) ;
#28812 = CARTESIAN_POINT ( 'NONE',  ( 15.80617190586746368, 15.72974639402197994, 109.3739096053143811 ) ) ;
#28813 = CARTESIAN_POINT ( 'NONE',  ( 14.34966873604960469, 8.224510206698951720, 69.16557627198102409 ) ) ;
#28814 = CARTESIAN_POINT ( 'NONE',  ( 19.05341960407611168, 5.049401038298154454, 83.95724293864766707 ) ) ;
#28815 = CARTESIAN_POINT ( 'NONE',  ( -8.314922557961024197, 14.29746914071037800, 87.91775706135234714 ) ) ;
#28816 = CARTESIAN_POINT ( 'NONE',  ( -18.62759615963255300, -10.81492255796106328, 64.16775706135234714 ) ) ;
#28817 = CARTESIAN_POINT ( 'NONE',  ( 16.52544592524335698, 4.483927247898782831, 31.45942372801901854 ) ) ;
#28818 = CARTESIAN_POINT ( 'NONE',  ( -0.05219959533937732626, 21.53943276465977519, 22.50109039468567573 ) ) ;
#28819 = CARTESIAN_POINT ( 'NONE',  ( -12.06949235617756955, 12.14591786802309770, 55.62390960531436690 ) ) ;
#28820 = ORIENTED_EDGE ( 'NONE', *, *, #170016, .T. ) ;
#28821 = CARTESIAN_POINT ( 'NONE',  ( 10.81492255796078972, 18.62759615963270932, 99.58224293864770971 ) ) ;
#28822 = CARTESIAN_POINT ( 'NONE',  ( -0.05219959533910754901, -16.53943276465976808, 37.49890960531436690 ) ) ;
#28823 = VERTEX_POINT ( 'NONE', #187617 ) ;
#28824 = CARTESIAN_POINT ( 'NONE',  ( 34.40742850069380410, 7.501893140248843572, 45.46088305597103130 ) ) ;
#28825 = CARTESIAN_POINT ( 'NONE',  ( 15.80617190586746368, 15.72974639402197994, 34.37390960531435979 ) ) ;
#28826 = CARTESIAN_POINT ( 'NONE',  ( -5.719274019375665041, -21.55341960407619695, 34.79275706135235424 ) ) ;
#28827 = CARTESIAN_POINT ( 'NONE',  ( 16.52544592524342804, -4.483927247898539470, 68.54057627198103830 ) ) ;
#28828 = CARTESIAN_POINT ( 'NONE',  ( 16.46253265017160672, -9.564922557960803928, 78.33224293864769550 ) ) ;
#28830 = CARTESIAN_POINT ( 'NONE',  ( 5.153800228976615827, -19.02544592524334988, 65.20942372801900433 ) ) ;
#28829 = CARTESIAN_POINT ( 'NONE',  ( 19.03943276465977164, -0.05219959533909143690, 23.74890960531435269 ) ) ;
#28831 = EDGE_CURVE ( 'NONE', #193677, #173655, #150189, .T. ) ;
#28832 = CARTESIAN_POINT ( 'NONE',  ( 21.52544592524344225, -5.823673210054117533, 48.54057627198103120 ) ) ;
#28833 = CARTESIAN_POINT ( 'NONE',  ( -23.76806875053281942, -29.07479876791513362, -18.77372378131338948 ) ) ;
#28834 = CARTESIAN_POINT ( 'NONE',  ( -5.049401038298153566, 19.05341960407611168, 55.20724293864769550 ) ) ;
#28835 = CARTESIAN_POINT ( 'NONE',  ( 14.29746914071037800, 8.314922557961029526, 41.66775706135235424 ) ) ;
#28836 = CARTESIAN_POINT ( 'NONE',  ( -5.823673210054116645, -21.52544592524344225, 112.2905762719810241 ) ) ;
#28837 = CARTESIAN_POINT ( 'NONE',  ( 12.14591786802309770, 12.06949235617756955, 49.37390960531436690 ) ) ;
#28838 = ORIENTED_EDGE ( 'NONE', *, *, #121940, .F. ) ;
#28839 = CARTESIAN_POINT ( 'NONE',  ( -9.474510206698964154, 16.51473224551069663, 95.41557627198102409 ) ) ;
#28840 = CARTESIAN_POINT ( 'NONE',  ( -21.55341960407610458, -5.719274019375992779, 76.45724293864769550 ) ) ;
#28842 = CARTESIAN_POINT ( 'NONE',  ( 14.29746914071037800, 8.314922557961029526, 31.66775706135234358 ) ) ;
#28841 = CARTESIAN_POINT ( 'NONE',  ( 18.62759615963271287, -10.81492255796078972, 113.3322429386476955 ) ) ;
#28843 = CARTESIAN_POINT ( 'NONE',  ( 5.719274019375991003, -21.55341960407610458, 32.70724293864770260 ) ) ;
#28844 = CARTESIAN_POINT ( 'NONE',  ( -0.05219959533937732626, 21.53943276465977519, 107.5010903946856899 ) ) ;
#28845 = CARTESIAN_POINT ( 'NONE',  ( 0.05219959533909260263, 19.03943276465977164, 99.99890960531436690 ) ) ;
#28846 = VECTOR ( 'NONE', #56608, 1000.000000000000000 ) ;
#28847 = CARTESIAN_POINT ( 'NONE',  ( -13.89961937509977652, 13.97604488694528158, 35.62390960531435269 ) ) ;
#28848 = CARTESIAN_POINT ( 'NONE',  ( -9.564922557960796823, -16.46253265017161027, 97.08224293864769550 ) ) ;
#28849 = CARTESIAN_POINT ( 'NONE',  ( 19.03943276465977164, -0.05219959533909143690, 73.74890960531435269 ) ) ;
#28850 = CARTESIAN_POINT ( 'NONE',  ( -3.503282210674349528, -48.86437366581481001, -23.00000000000000000 ) ) ;
#28851 = CARTESIAN_POINT ( 'NONE',  ( 5.153800228976615827, -19.02544592524334988, 60.20942372801899012 ) ) ;
#28853 = CARTESIAN_POINT ( 'NONE',  ( 21.52544592524344225, -5.823673210054117533, 33.54057627198102409 ) ) ;
#28852 = CARTESIAN_POINT ( 'NONE',  ( 15.72974639402176855, 15.80617190586768217, 106.8760903946856899 ) ) ;
#28854 = CARTESIAN_POINT ( 'NONE',  ( -14.29746914071037622, -8.314922557961029526, 104.1677570613523471 ) ) ;
#28855 = CARTESIAN_POINT ( 'NONE',  ( 9.474510206698729675, 16.51473224551082808, 87.08442372801900433 ) ) ;
#28856 = CARTESIAN_POINT ( 'NONE',  ( -31.74999999999995737, 0.000000000000000000, 0.000000000000000000 ) ) ;
#28857 = CARTESIAN_POINT ( 'NONE',  ( -16.51473224551082808, 9.474510206698731452, 78.33442372801900433 ) ) ;
#28858 = CARTESIAN_POINT ( 'NONE',  ( 19.03943276465977164, 0.05219959533936151252, 31.25109039468566863 ) ) ;
#28859 = CARTESIAN_POINT ( 'NONE',  ( -16.20579543436681291, -7.371946100354976217, 45.56520834171876544 ) ) ;
#28860 = CARTESIAN_POINT ( 'NONE',  ( 13.89961937509977652, -13.97604488694527269, 48.12390960531435979 ) ) ;
#28861 = CARTESIAN_POINT ( 'NONE',  ( 16.55341960407611168, 4.379528057220329451, 53.95724293864770260 ) ) ;
#28862 = CARTESIAN_POINT ( 'NONE',  ( -16.36317988757057762, -7.306389748694935626, 110.9021039163677784 ) ) ;
#28863 = CARTESIAN_POINT ( 'NONE',  ( -12.14591786802309592, -12.06949235617757132, 21.87390960531436690 ) ) ;
#28864 = LINE ( 'NONE', #76325, #174296 ) ;
#28865 = CARTESIAN_POINT ( 'NONE',  ( -14.29746914071037622, -8.314922557961029526, 89.16775706135236135 ) ) ;
#28866 = CARTESIAN_POINT ( 'NONE',  ( -9.474510206698964154, 16.51473224551069663, 45.41557627198103120 ) ) ;
#28867 = CARTESIAN_POINT ( 'NONE',  ( 10.81492255796106328, -18.62759615963255655, 110.4177570613523756 ) ) ;
#28868 = CARTESIAN_POINT ( 'NONE',  ( -9.564922557961040184, 16.46253265017147172, 112.9177570613523329 ) ) ;
#28869 = CARTESIAN_POINT ( 'NONE',  ( -10.81492255796105439, 18.62759615963255655, 92.91775706135236135 ) ) ;
#28870 = CARTESIAN_POINT ( 'NONE',  ( -19.05341960407611168, -5.049401038298163336, 86.45724293864769550 ) ) ;
#28871 = CARTESIAN_POINT ( 'NONE',  ( 16.51473224551069308, 9.474510206698969483, 89.16557627198103830 ) ) ;
#28872 = CARTESIAN_POINT ( 'NONE',  ( 36.91746824999999177, 11.99521256947799230, -7.524999997268813523 ) ) ;
#28873 = CARTESIAN_POINT ( 'NONE',  ( -21.52544592524343514, 5.823673210054127303, 116.0405762719810383 ) ) ;
#28874 = VECTOR ( 'NONE', #149367, 1000.000000000000000 ) ;
#28875 = CARTESIAN_POINT ( 'NONE',  ( -16.52544592524342804, 4.483927247898546575, 86.04057627198102409 ) ) ;
#28876 = CARTESIAN_POINT ( 'NONE',  ( 10.81492255796078972, 18.62759615963270932, 69.58224293864769550 ) ) ;
#28877 = CARTESIAN_POINT ( 'NONE',  ( -16.46253265017160317, 9.564922557960807481, 55.83224293864769550 ) ) ;
#28879 = CARTESIAN_POINT ( 'NONE',  ( 14.34966873604972726, -8.224510206698740333, 95.83442372801903275 ) ) ;
#28878 = CARTESIAN_POINT ( 'NONE',  ( 18.62759615963271287, -10.81492255796078972, 103.3322429386476955 ) ) ;
#28880 = ORIENTED_EDGE ( 'NONE', *, *, #99957, .F. ) ;
#28881 = CARTESIAN_POINT ( 'NONE',  ( -16.51473224551069308, -9.474510206698971260, 61.66557627198103120 ) ) ;
#28883 = CARTESIAN_POINT ( 'NONE',  ( 21.82762259161258811, -6.010869995788711506, 172.1044450858201742 ) ) ;
#28882 = CARTESIAN_POINT ( 'NONE',  ( -14.34966873604960291, -8.224510206698953496, 86.66557627198102409 ) ) ;
#28884 = CARTESIAN_POINT ( 'NONE',  ( 9.474510206698971260, -16.51473224551069308, 62.91557627198102409 ) ) ;
#28885 = CARTESIAN_POINT ( 'NONE',  ( 9.564922557961047289, -16.46253265017146816, 80.41775706135234714 ) ) ;
#28886 = CARTESIAN_POINT ( 'NONE',  ( -12.06949235617756955, 12.14591786802309770, 85.62390960531436690 ) ) ;
#28887 = CARTESIAN_POINT ( 'NONE',  ( -10.72451020669870658, -18.67979575497194134, 59.58442372801901854 ) ) ;
#28889 = CARTESIAN_POINT ( 'NONE',  ( 18.67979575497178502, 10.72451020669898547, 114.1655762719810383 ) ) ;
#28888 = CARTESIAN_POINT ( 'NONE',  ( -13.97604488694527625, -13.89961937509977652, 51.87390960531436690 ) ) ;
#28890 = CARTESIAN_POINT ( 'NONE',  ( -0.05219959533910754901, -16.53943276465976808, 107.4989096053143669 ) ) ;
#28891 = CARTESIAN_POINT ( 'NONE',  ( 3.503282210674364627, -48.86437366581479580, -25.00000000000000000 ) ) ;
#28892 = CARTESIAN_POINT ( 'NONE',  ( 16.46253265017160672, -9.564922557960803928, 53.33224293864768839 ) ) ;
#28893 = CARTESIAN_POINT ( 'NONE',  ( 30.00000000000000000, -1.163414459189985801E-14, 95.00000000000000000 ) ) ;
#28895 = CARTESIAN_POINT ( 'NONE',  ( -16.51473224551069308, -9.474510206698971260, 111.6655762719810383 ) ) ;
#28894 = CARTESIAN_POINT ( 'NONE',  ( -19.05341960407617563, 5.049401038297882671, 98.54275706135233293 ) ) ;
#28896 = CARTESIAN_POINT ( 'NONE',  ( 18.67979575497194134, -10.72451020669871369, 45.83442372801901854 ) ) ;
#28897 = CARTESIAN_POINT ( 'NONE',  ( -5.049401038298153566, 19.05341960407611168, 85.20724293864766707 ) ) ;
#28898 = CARTESIAN_POINT ( 'NONE',  ( 9.564922557961047289, -16.46253265017146816, 75.41775706135234714 ) ) ;
#28899 = CARTESIAN_POINT ( 'NONE',  ( -16.46253265017160317, 9.564922557960807481, 60.83224293864769550 ) ) ;
#28900 = CARTESIAN_POINT ( 'NONE',  ( 12.06949235617757843, -12.14591786802309237, 78.12390960531436690 ) ) ;
#28901 = CARTESIAN_POINT ( 'NONE',  ( 8.314922557960818139, 14.29746914071049879, 74.58224293864768129 ) ) ;
#28902 = CARTESIAN_POINT ( 'NONE',  ( 16.46253265017160672, -9.564922557960803928, 93.33224293864769550 ) ) ;
#28903 = CARTESIAN_POINT ( 'NONE',  ( 16.53943276465976808, -0.05219959533910856209, 83.74890960531435269 ) ) ;
#28904 = CARTESIAN_POINT ( 'NONE',  ( -9.564922557960796823, -16.46253265017161027, 82.08224293864768129 ) ) ;
#28905 = CARTESIAN_POINT ( 'NONE',  ( -13.97604488694547697, 13.89961937509957934, 38.12609039468566152 ) ) ;
#28908 = CARTESIAN_POINT ( 'NONE',  ( -14.29746914071049879, 8.314922557960819915, 110.8322429386476955 ) ) ;
#28907 = CARTESIAN_POINT ( 'NONE',  ( 14.34966873604960469, 8.224510206698951720, 34.16557627198102409 ) ) ;
#28906 = CARTESIAN_POINT ( 'NONE',  ( 19.02544592524343514, -5.153800228976328945, 53.54057627198102409 ) ) ;
#28909 = ORIENTED_EDGE ( 'NONE', *, *, #116672, .F. ) ;
#28910 = CARTESIAN_POINT ( 'NONE',  ( -18.67979575497193778, 10.72451020669871902, 43.33442372801901143 ) ) ;
#28911 = CARTESIAN_POINT ( 'NONE',  ( -16.46253265017146816, -9.564922557961047289, 64.16775706135233293 ) ) ;
#28912 = CARTESIAN_POINT ( 'NONE',  ( 4.379528057220339221, -16.55341960407611168, 37.70724293864769550 ) ) ;
#28913 = CARTESIAN_POINT ( 'NONE',  ( -21.52544592524343514, 5.823673210054127303, 81.04057627198102409 ) ) ;
#28914 = CARTESIAN_POINT ( 'NONE',  ( -19.05341960407611168, -5.049401038298163336, 111.4572429386476671 ) ) ;
#28915 = CARTESIAN_POINT ( 'NONE',  ( 8.224510206698953496, -14.34966873604960469, 72.91557627198103830 ) ) ;
#28916 = CARTESIAN_POINT ( 'NONE',  ( -13.89961937509977652, 13.97604488694528158, 40.62390960531435979 ) ) ;
#28917 = CARTESIAN_POINT ( 'NONE',  ( -19.05341960407617563, 5.049401038297882671, 43.54275706135232582 ) ) ;
#28918 = CARTESIAN_POINT ( 'NONE',  ( -12.06949235617739369, -12.14591786802326823, 99.37609039468568994 ) ) ;
#28919 = CARTESIAN_POINT ( 'NONE',  ( -14.34966873604972548, 8.224510206698743886, 53.33442372801901854 ) ) ;
#28920 = CARTESIAN_POINT ( 'NONE',  ( 21.53943276465977519, -0.05219959533907433946, 33.74890960531436690 ) ) ;
#28921 = CARTESIAN_POINT ( 'NONE',  ( 10.81492255796106328, -18.62759615963255655, 105.4177570613523613 ) ) ;
#28922 = CARTESIAN_POINT ( 'NONE',  ( 9.474510206698971260, -16.51473224551069308, 87.91557627198102409 ) ) ;
#28923 = CARTESIAN_POINT ( 'NONE',  ( 16.55341960407618274, -4.379528057220086978, 71.04275706135234714 ) ) ;
#28924 = CARTESIAN_POINT ( 'NONE',  ( -9.474510206698964154, 16.51473224551069663, 25.41557627198103120 ) ) ;
#28925 = CARTESIAN_POINT ( 'NONE',  ( 16.53943276465976808, -0.05219959533910856209, 33.74890960531436690 ) ) ;
#28927 = CARTESIAN_POINT ( 'NONE',  ( 9.564922557960805705, 16.46253265017160317, 94.58224293864769550 ) ) ;
#28926 = CARTESIAN_POINT ( 'NONE',  ( 19.02544592524343514, -5.153800228976328945, 108.5405762719810383 ) ) ;
#28928 = CARTESIAN_POINT ( 'NONE',  ( 10.72451020669898902, -18.67979575497178502, 32.91557627198102409 ) ) ;
#28929 = CARTESIAN_POINT ( 'NONE',  ( 4.379528057220339221, -16.55341960407611168, 67.70724293864769550 ) ) ;
#28930 = CARTESIAN_POINT ( 'NONE',  ( -16.55341960407611168, -4.379528057220339221, 46.45724293864769550 ) ) ;
#28931 = ORIENTED_EDGE ( 'NONE', *, *, #142282, .F. ) ;
#28933 = DIRECTION ( 'NONE',  ( 0.000000000000000000, 0.000000000000000000, -1.000000000000000000 ) ) ;
#28932 = CARTESIAN_POINT ( 'NONE',  ( 12.06949235617739724, 12.14591786802326823, 56.87609039468568994 ) ) ;
#28934 = CARTESIAN_POINT ( 'NONE',  ( -19.03943276465977164, -0.05219959533935918106, 53.75109039468566863 ) ) ;
#28935 = CARTESIAN_POINT ( 'NONE',  ( 16.46253265017160672, -9.564922557960803928, 83.33224293864768129 ) ) ;
#28936 = CARTESIAN_POINT ( 'NONE',  ( -19.02544592524334988, -5.153800228976617603, 63.95942372801899012 ) ) ;
#28937 = CARTESIAN_POINT ( 'NONE',  ( -8.571926809382608425, 26.38167802310805854, 142.9750000027312069 ) ) ;
#28938 = CARTESIAN_POINT ( 'NONE',  ( 13.89961937509957401, 13.97604488694547697, 51.87609039468566863 ) ) ;
#28940 = CARTESIAN_POINT ( 'NONE',  ( -0.05219959533934338120, 16.53943276465976808, 102.5010903946856899 ) ) ;
#28939 = CARTESIAN_POINT ( 'NONE',  ( 19.02544592524334988, 5.153800228976608722, 101.4594237280189759 ) ) ;
#28941 = CARTESIAN_POINT ( 'NONE',  ( 22.44159573604009239, 16.30477369853692693, 146.5750000027312012 ) ) ;
#28942 = CARTESIAN_POINT ( 'NONE',  ( 19.02544592524343514, -5.153800228976328945, 43.54057627198103120 ) ) ;
#28943 = CARTESIAN_POINT ( 'NONE',  ( -5.719274019375978568, 21.55341960407610458, 25.20724293864769550 ) ) ;
#28944 = CARTESIAN_POINT ( 'NONE',  ( -18.67979575497193778, 10.72451020669871902, 48.33442372801902565 ) ) ;
#28945 = CARTESIAN_POINT ( 'NONE',  ( 19.05341960407617918, -5.049401038297876454, 101.0427570613523045 ) ) ;
#28947 = CARTESIAN_POINT ( 'NONE',  ( -16.51473224551069308, -9.474510206698971260, 66.66557627198102409 ) ) ;
#28946 = FACE_OUTER_BOUND ( 'NONE', #55332, .T. ) ;
#28948 = CARTESIAN_POINT ( 'NONE',  ( 30.73962218707677607, 22.33364281372847060, -0.8021577739498229054 ) ) ;
#28950 = CARTESIAN_POINT ( 'NONE',  ( 19.03943276465977164, -0.05219959533909143690, 58.74890960531435979 ) ) ;
#28949 = CARTESIAN_POINT ( 'NONE',  ( -16.55341960407611168, -4.379528057220339221, 71.45724293864769550 ) ) ;
#28951 = CARTESIAN_POINT ( 'NONE',  ( 19.05341960407611168, 5.049401038298154454, 73.95724293864768129 ) ) ;
#28952 = CARTESIAN_POINT ( 'NONE',  ( 9.474510206698729675, 16.51473224551082808, 82.08442372801899012 ) ) ;
#28953 = CARTESIAN_POINT ( 'NONE',  ( 18.67979575497178502, 10.72451020669898547, 64.16557627198102409 ) ) ;
#28954 = CARTESIAN_POINT ( 'NONE',  ( 16.53943276465976808, -0.05219959533910856209, 113.7489096053143527 ) ) ;
#28955 = CARTESIAN_POINT ( 'NONE',  ( 0.05219959533936267826, -19.03943276465977164, 45.00109039468566863 ) ) ;
#28956 = CARTESIAN_POINT ( 'NONE',  ( 19.02544592524343514, -5.153800228976328945, 78.54057627198099567 ) ) ;
#28957 = CARTESIAN_POINT ( 'NONE',  ( 5.823673210054125526, 21.52544592524343514, 84.79057627198102409 ) ) ;
#28959 = CARTESIAN_POINT ( 'NONE',  ( 19.03943276465977164, 0.05219959533936151252, 51.25109039468567573 ) ) ;
#28958 = CARTESIAN_POINT ( 'NONE',  ( 16.53943276465976808, -0.05219959533910856209, 73.74890960531433848 ) ) ;
#28960 = CARTESIAN_POINT ( 'NONE',  ( 18.62759615963271287, -10.81492255796078972, 78.33224293864770971 ) ) ;
#28961 = CARTESIAN_POINT ( 'NONE',  ( -15.72974639402197994, 15.80617190586746368, 60.62390960531437401 ) ) ;
#28962 = CARTESIAN_POINT ( 'NONE',  ( 21.53943276465977519, -0.05219959533907433946, 38.74890960531435979 ) ) ;
#28963 = CARTESIAN_POINT ( 'NONE',  ( -10.81492255796105439, 18.62759615963255655, 87.91775706135234714 ) ) ;
#28964 = CARTESIAN_POINT ( 'NONE',  ( 16.51473224551069308, 9.474510206698969483, 79.16557627198103830 ) ) ;
#28965 = CARTESIAN_POINT ( 'NONE',  ( 13.89961937509977652, -13.97604488694527269, 23.12390960531436335 ) ) ;
#28966 = CARTESIAN_POINT ( 'NONE',  ( -5.823673210054431948, 21.52544592524334988, 32.70942372801900433 ) ) ;
#28967 = CARTESIAN_POINT ( 'NONE',  ( -0.05219959533937732626, 21.53943276465977519, 47.50109039468568994 ) ) ;
#28968 = CARTESIAN_POINT ( 'NONE',  ( -5.049401038298153566, 19.05341960407611168, 40.20724293864768839 ) ) ;
#28969 = CARTESIAN_POINT ( 'NONE',  ( -21.55341960407619339, 5.719274019375674811, 28.54275706135234358 ) ) ;
#28970 = CARTESIAN_POINT ( 'NONE',  ( 19.02544592524334988, 5.153800228976608722, 61.45942372801900433 ) ) ;
#28971 = CARTESIAN_POINT ( 'NONE',  ( 0.05219959533909260263, 19.03943276465977164, 34.99890960531435979 ) ) ;
#28972 = CARTESIAN_POINT ( 'NONE',  ( -16.52544592524335698, -4.483927247898792601, 33.95942372801901143 ) ) ;
#28973 = CARTESIAN_POINT ( 'NONE',  ( 21.30000000000002913, -7.567280135845077329E-14, -64.92279855667830191 ) ) ;
#28974 = CARTESIAN_POINT ( 'NONE',  ( 16.52544592524335698, 4.483927247898782831, 61.45942372801901854 ) ) ;
#28975 = CARTESIAN_POINT ( 'NONE',  ( 13.89961937509977652, -13.97604488694527269, 38.12390960531436690 ) ) ;
#28976 = CARTESIAN_POINT ( 'NONE',  ( -25.86526910843991445, -7.630673861715466799, 173.3900163844746203 ) ) ;
#28977 = CARTESIAN_POINT ( 'NONE',  ( 5.153800228976335163, 19.02544592524342804, 84.79057627198099567 ) ) ;
#28979 = EDGE_CURVE ( 'NONE', #86852, #122599, #199576, .T. ) ;
#28978 = CARTESIAN_POINT ( 'NONE',  ( 0.05219959533909260263, 19.03943276465977164, 24.99890960531435269 ) ) ;
#28980 = CARTESIAN_POINT ( 'NONE',  ( -18.62759615963270932, 10.81492255796079327, 55.83224293864770260 ) ) ;
#28981 = CARTESIAN_POINT ( 'NONE',  ( -12.14591786802326823, 12.06949235617739902, 53.12609039468568284 ) ) ;
#28982 = CARTESIAN_POINT ( 'NONE',  ( -21.52544592524334988, -5.823673210054445271, 103.9594237280190185 ) ) ;
#28983 = CARTESIAN_POINT ( 'NONE',  ( -13.89961937509977652, 13.97604488694528158, 40.62390960531435979 ) ) ;
#28984 = CARTESIAN_POINT ( 'NONE',  ( -0.05219959533910754901, -16.53943276465976808, 27.49890960531435269 ) ) ;
#28985 = CARTESIAN_POINT ( 'NONE',  ( -8.224510206698948167, 14.34966873604960824, 60.41557627198102409 ) ) ;
#28986 = AXIS2_PLACEMENT_3D ( 'NONE', #113724, #84387, #86401 ) ;
#28987 = CARTESIAN_POINT ( 'NONE',  ( 16.51473224551069308, 9.474510206698969483, 59.16557627198102409 ) ) ;
#28988 = CARTESIAN_POINT ( 'NONE',  ( 21.52544592524334988, 5.823673210054432836, 106.4594237280190328 ) ) ;
#28989 = CARTESIAN_POINT ( 'NONE',  ( -5.719274019375665041, -21.55341960407619695, 19.79275706135235069 ) ) ;
#28990 = CARTESIAN_POINT ( 'NONE',  ( -0.05219959533937732626, 21.53943276465977519, 87.50109039468568994 ) ) ;
#28991 = CARTESIAN_POINT ( 'NONE',  ( 12.06949235617739724, 12.14591786802326823, 46.87609039468568994 ) ) ;
#28992 = CARTESIAN_POINT ( 'NONE',  ( 4.483927247898790824, -16.52544592524335698, 30.20942372801902565 ) ) ;
#28994 = CARTESIAN_POINT ( 'NONE',  ( -21.53943276465977519, -0.05219959533937600094, 103.7510903946857042 ) ) ;
#28993 = CARTESIAN_POINT ( 'NONE',  ( -8.224510206698948167, 14.34966873604960824, 95.41557627198102409 ) ) ;
#28995 = CARTESIAN_POINT ( 'NONE',  ( -16.53943276465976808, 0.05219959533911058130, 31.24890960531435979 ) ) ;
#28996 = CARTESIAN_POINT ( 'NONE',  ( -5.049401038298153566, 19.05341960407611168, 25.20724293864768484 ) ) ;
#28997 = CARTESIAN_POINT ( 'NONE',  ( -8.224510206698735004, -14.34966873604973081, 44.58442372801901854 ) ) ;
#28998 = CARTESIAN_POINT ( 'NONE',  ( -16.55341960407611168, -4.379528057220339221, 56.45724293864768839 ) ) ;
#28999 = CARTESIAN_POINT ( 'NONE',  ( 8.224510206698742110, 14.34966873604972548, 92.08442372801901854 ) ) ;
#29000 = CARTESIAN_POINT ( 'NONE',  ( 9.564922557960805705, 16.46253265017160317, 94.58224293864769550 ) ) ;
#29001 = CARTESIAN_POINT ( 'NONE',  ( -21.55341960407610458, -5.719274019375992779, 21.45724293864769550 ) ) ;
#29002 = CARTESIAN_POINT ( 'NONE',  ( -15.80617190586768217, 15.72974639402176855, 108.1260903946856757 ) ) ;
#29003 = CARTESIAN_POINT ( 'NONE',  ( 16.55341960407611168, 4.379528057220329451, 88.95724293864769550 ) ) ;
#29004 = CARTESIAN_POINT ( 'NONE',  ( -5.049401038298153566, 19.05341960407611168, 100.2072429386476955 ) ) ;
#29005 = EDGE_LOOP ( 'NONE', ( #150930, #57009 ) ) ;
#29006 = VERTEX_POINT ( 'NONE', #79415 ) ;
#29007 = CARTESIAN_POINT ( 'NONE',  ( 8.224510206698742110, 14.34966873604972548, 42.08442372801901854 ) ) ;
#29008 = CARTESIAN_POINT ( 'NONE',  ( 0.05219959533909260263, 19.03943276465977164, 44.99890960531435979 ) ) ;
#29009 = CARTESIAN_POINT ( 'NONE',  ( 5.153800228976335163, 19.02544592524342804, 109.7905762719810099 ) ) ;
#29010 = CARTESIAN_POINT ( 'NONE',  ( 14.29746914071037800, 8.314922557961029526, 46.66775706135234714 ) ) ;
#29011 = CARTESIAN_POINT ( 'NONE',  ( -16.46253265017146816, -9.564922557961047289, 29.16775706135232937 ) ) ;
#29012 = CARTESIAN_POINT ( 'NONE',  ( 19.02544592524343514, -5.153800228976328945, 43.54057627198103120 ) ) ;
#29013 = CARTESIAN_POINT ( 'NONE',  ( 14.29746914071037800, 8.314922557961029526, 76.66775706135234714 ) ) ;
#29014 = CARTESIAN_POINT ( 'NONE',  ( 19.05341960407617918, -5.049401038297876454, 81.04275706135231871 ) ) ;
#29015 = CARTESIAN_POINT ( 'NONE',  ( -16.46253265017146816, -9.564922557961047289, 24.16775706135233648 ) ) ;
#29016 = CARTESIAN_POINT ( 'NONE',  ( -13.97604488694527625, -13.89961937509977652, 56.87390960531434558 ) ) ;
#29017 = CARTESIAN_POINT ( 'NONE',  ( 16.55341960407611168, 4.379528057220329451, 103.9572429386476813 ) ) ;
#29018 = CIRCLE ( 'NONE', #100123, 61.99999999999998579 ) ;
#29019 = CARTESIAN_POINT ( 'NONE',  ( -16.46253265017146816, -9.564922557961047289, 74.16775706135234714 ) ) ;
#29020 = CARTESIAN_POINT ( 'NONE',  ( -10.81492255796078084, -18.62759615963271287, 62.08224293864769550 ) ) ;
#29021 = CARTESIAN_POINT ( 'NONE',  ( 19.05341960407617918, -5.049401038297876454, 26.04275706135233293 ) ) ;
#29022 = CARTESIAN_POINT ( 'NONE',  ( 9.564922557960805705, 16.46253265017160317, 99.58224293864770971 ) ) ;
#29023 = CARTESIAN_POINT ( 'NONE',  ( -21.55341960407610458, -5.719274019375992779, 76.45724293864769550 ) ) ;
#29024 = CARTESIAN_POINT ( 'NONE',  ( -18.39443945427639093, 5.500000000000031974, 53.51745347608652992 ) ) ;
#29025 = CARTESIAN_POINT ( 'NONE',  ( 19.05341960407617918, -5.049401038297876454, 96.04275706135231871 ) ) ;
#29026 = CARTESIAN_POINT ( 'NONE',  ( -19.49149378614658445, 5.499999999999785949, 59.43757513605363840 ) ) ;
#29027 = CARTESIAN_POINT ( 'NONE',  ( -16.55341960407617563, 4.379528057220093196, 23.54275706135235424 ) ) ;
#29028 = CARTESIAN_POINT ( 'NONE',  ( 16.51473224551069308, 9.474510206698969483, 34.16557627198102409 ) ) ;
#29029 = CARTESIAN_POINT ( 'NONE',  ( 19.02544592524343514, -5.153800228976328945, 103.5405762719809957 ) ) ;
#29030 = CARTESIAN_POINT ( 'NONE',  ( 5.823673210054125526, 21.52544592524343514, 89.79057627198103830 ) ) ;
#29031 = CARTESIAN_POINT ( 'NONE',  ( 18.67979575497194134, -10.72451020669871369, 65.83442372801900433 ) ) ;
#29033 = CARTESIAN_POINT ( 'NONE',  ( -15.72974639402176322, -15.80617190586768395, 104.3760903946856899 ) ) ;
#29032 = CARTESIAN_POINT ( 'NONE',  ( -19.05341960407617563, 5.049401038297882671, 103.5427570613523329 ) ) ;
#29034 = CARTESIAN_POINT ( 'NONE',  ( -8.224510206698735004, -14.34966873604973081, 109.5844237280190328 ) ) ;
#29035 = CARTESIAN_POINT ( 'NONE',  ( 15.80617190586746368, 15.72974639402197994, 104.3739096053143669 ) ) ;
#29036 = CARTESIAN_POINT ( 'NONE',  ( -4.379528057220328563, 16.55341960407611168, 50.20724293864769550 ) ) ;
#29037 = CARTESIAN_POINT ( 'NONE',  ( 16.51473224551083163, -9.474510206698727899, 85.83442372801900433 ) ) ;
#29038 = CARTESIAN_POINT ( 'NONE',  ( 5.153800228976615827, -19.02544592524334988, 60.20942372801899012 ) ) ;
#29039 = CARTESIAN_POINT ( 'NONE',  ( -5.823673210054431948, 21.52544592524334988, 57.70942372801901143 ) ) ;
#29040 = CARTESIAN_POINT ( 'NONE',  ( -19.05341960407617563, 5.049401038297882671, 43.54275706135232582 ) ) ;
#29041 = CARTESIAN_POINT ( 'NONE',  ( 12.14591786802309770, 12.06949235617756955, 109.3739096053143811 ) ) ;
#29042 = CARTESIAN_POINT ( 'NONE',  ( -21.55341960407610458, -5.719274019375992779, 36.45724293864768839 ) ) ;
#29043 = CARTESIAN_POINT ( 'NONE',  ( 0.05219959533910956823, 16.53943276465976808, 34.99890960531435979 ) ) ;
#29044 = CARTESIAN_POINT ( 'NONE',  ( -21.55341960407619339, 5.719274019375674811, 93.54275706135234714 ) ) ;
#29045 = CARTESIAN_POINT ( 'NONE',  ( 14.29746914071037800, 8.314922557961029526, 76.66775706135234714 ) ) ;
#29046 = CARTESIAN_POINT ( 'NONE',  ( 12.14591786802309770, 12.06949235617756955, 29.37390960531435269 ) ) ;
#29047 = CARTESIAN_POINT ( 'NONE',  ( -18.62759615963255300, -10.81492255796106328, 59.16775706135234714 ) ) ;
#29048 = CARTESIAN_POINT ( 'NONE',  ( 21.53943276465977519, 0.05219959533937863772, 61.25109039468567573 ) ) ;
#29049 = CARTESIAN_POINT ( 'NONE',  ( -21.53943276465977519, 0.05219959533907696930, 71.24890960531435269 ) ) ;
#29050 = CARTESIAN_POINT ( 'NONE',  ( 13.89961937509977652, -13.97604488694527269, 23.12390960531436335 ) ) ;
#29051 = CARTESIAN_POINT ( 'NONE',  ( 10.72451020669871369, 18.67979575497193778, 42.08442372801901854 ) ) ;
#29052 = CARTESIAN_POINT ( 'NONE',  ( 19.05341960407611168, 5.049401038298154454, 23.95724293864769194 ) ) ;
#29053 = CARTESIAN_POINT ( 'NONE',  ( -13.89961937509977652, 13.97604488694528158, 40.62390960531435979 ) ) ;
#29054 = CARTESIAN_POINT ( 'NONE',  ( -16.52544592524342804, 4.483927247898546575, 86.04057627198102409 ) ) ;
#29055 = CARTESIAN_POINT ( 'NONE',  ( 9.474510206698971260, -16.51473224551069308, 82.91557627198103830 ) ) ;
#29056 = CARTESIAN_POINT ( 'NONE',  ( 12.06949235617757843, -12.14591786802309237, 33.12390960531435979 ) ) ;
#29057 = CARTESIAN_POINT ( 'NONE',  ( -10.72451020669898014, 18.67979575497178502, 65.41557627198102409 ) ) ;
#29058 = CARTESIAN_POINT ( 'NONE',  ( 15.72974639402199770, -15.80617190586745480, 108.1239096053143811 ) ) ;
#29059 = CARTESIAN_POINT ( 'NONE',  ( 5.049401038298161559, -19.05341960407611168, 112.7072429386476813 ) ) ;
#29061 = CARTESIAN_POINT ( 'NONE',  ( 9.474510206698729675, 16.51473224551082808, 107.0844237280190043 ) ) ;
#29060 = CARTESIAN_POINT ( 'NONE',  ( -16.51473224551069308, -9.474510206698971260, 71.66557627198102409 ) ) ;
#29062 = ADVANCED_FACE ( 'NONE', ( #126894 ), #63248, .T. ) ;
#29063 = CARTESIAN_POINT ( 'NONE',  ( -10.72451020669898014, 18.67979575497178502, 60.41557627198102409 ) ) ;
#29064 = CARTESIAN_POINT ( 'NONE',  ( -21.55341960407619339, 5.719274019375674811, 78.54275706135236135 ) ) ;
#29065 = CARTESIAN_POINT ( 'NONE',  ( 16.46253265017160672, -9.564922557960803928, 73.33224293864769550 ) ) ;
#29066 = CARTESIAN_POINT ( 'NONE',  ( 5.049401038298161559, -19.05341960407611168, 97.70724293864766707 ) ) ;
#29067 = CARTESIAN_POINT ( 'NONE',  ( -16.52544592524335698, -4.483927247898792601, 73.95942372801901854 ) ) ;
#29068 = CARTESIAN_POINT ( 'NONE',  ( 0.05219959533937995610, -21.53943276465977519, 55.00109039468568284 ) ) ;
#29069 = CARTESIAN_POINT ( 'NONE',  ( 15.72974639402176855, 15.80617190586768217, 96.87609039468568994 ) ) ;
#29070 = CARTESIAN_POINT ( 'NONE',  ( 18.67979575497178502, 10.72451020669898547, 109.1655762719810383 ) ) ;
#29071 = CARTESIAN_POINT ( 'NONE',  ( -5.823673210054116645, -21.52544592524344225, 77.29057627198102409 ) ) ;
#29072 = CARTESIAN_POINT ( 'NONE',  ( 16.46253265017146816, 9.564922557961045513, 41.66775706135234003 ) ) ;
#29073 = CARTESIAN_POINT ( 'NONE',  ( 21.53943276465977519, -0.05219959533907433946, 38.74890960531435979 ) ) ;
#29075 = CARTESIAN_POINT ( 'NONE',  ( 16.53943276465976808, -0.05219959533910856209, 33.74890960531436690 ) ) ;
#29074 = CARTESIAN_POINT ( 'NONE',  ( -5.049401038298153566, 19.05341960407611168, 75.20724293864769550 ) ) ;
#29076 = CARTESIAN_POINT ( 'NONE',  ( -17.26172910966778673, 6.454744622555848466, 65.80646908649227100 ) ) ;
#29077 = LINE ( 'NONE', #152399, #192837 ) ;
#29078 = CARTESIAN_POINT ( 'NONE',  ( 13.97604488694548053, -13.89961937509957401, 90.62609039468567573 ) ) ;
#29079 = CARTESIAN_POINT ( 'NONE',  ( 18.67979575497178502, 10.72451020669898547, 74.16557627198102409 ) ) ;
#29080 = CARTESIAN_POINT ( 'NONE',  ( -8.224510206698948167, 14.34966873604960824, 50.41557627198103120 ) ) ;
#29081 = CARTESIAN_POINT ( 'NONE',  ( 4.379528057220092307, 16.55341960407617563, 27.29275706135234358 ) ) ;
#29082 = CARTESIAN_POINT ( 'NONE',  ( -19.05341960407611168, -5.049401038298163336, 41.45724293864769550 ) ) ;
#29084 = CARTESIAN_POINT ( 'NONE',  ( -19.05341960407617563, 5.049401038297882671, 88.54275706135230450 ) ) ;
#29083 = CARTESIAN_POINT ( 'NONE',  ( 18.62759615963271287, -10.81492255796078972, 103.3322429386476955 ) ) ;
#29085 = CARTESIAN_POINT ( 'NONE',  ( 16.46253265017160672, -9.564922557960803928, 83.33224293864768129 ) ) ;
#29086 = CARTESIAN_POINT ( 'NONE',  ( -16.55341960407611168, -4.379528057220339221, 96.45724293864770971 ) ) ;
#29087 = CARTESIAN_POINT ( 'NONE',  ( -13.89961937509977652, 13.97604488694528158, 65.62390960531436690 ) ) ;
#29088 = CARTESIAN_POINT ( 'NONE',  ( -4.379528057220328563, 16.55341960407611168, 65.20724293864768129 ) ) ;
#29089 = CARTESIAN_POINT ( 'NONE',  ( 9.564922557960805705, 16.46253265017160317, 34.58224293864770260 ) ) ;
#29090 = CARTESIAN_POINT ( 'NONE',  ( -37.47059448506522727, -2.437326220201143201, 40.06626038917661248 ) ) ;
#29091 = CARTESIAN_POINT ( 'NONE',  ( -16.55341960407611168, -4.379528057220339221, 36.45724293864768839 ) ) ;
#29092 = CARTESIAN_POINT ( 'NONE',  ( 13.89961937509977652, -13.97604488694527269, 88.12390960531438111 ) ) ;
#29093 = CARTESIAN_POINT ( 'NONE',  ( -1.220661533321835801, -14.30620887846973055, -60.18359034246772410 ) ) ;
#29094 = CARTESIAN_POINT ( 'NONE',  ( -9.474510206698720793, -16.51473224551083518, 54.58442372801899722 ) ) ;
#29095 = CARTESIAN_POINT ( 'NONE',  ( -4.379528057220086978, -16.55341960407618274, 54.79275706135235424 ) ) ;
#29096 = CARTESIAN_POINT ( 'NONE',  ( -0.05219959533907301413, -21.53943276465977519, 82.49890960531436690 ) ) ;
#29097 = CARTESIAN_POINT ( 'NONE',  ( 19.02544592524334988, 5.153800228976608722, 36.45942372801900433 ) ) ;
#29098 = CARTESIAN_POINT ( 'NONE',  ( 16.51473224551069308, 9.474510206698969483, 89.16557627198103830 ) ) ;
#29099 = CARTESIAN_POINT ( 'NONE',  ( -17.50000000000002487, 4.049696124445873124, 114.1803967066594652 ) ) ;
#29100 = CARTESIAN_POINT ( 'NONE',  ( -5.823673210054116645, -21.52544592524344225, 32.29057627198102409 ) ) ;
#29101 = CARTESIAN_POINT ( 'NONE',  ( -5.049401038298153566, 19.05341960407611168, 55.20724293864769550 ) ) ;
#29102 = CARTESIAN_POINT ( 'NONE',  ( -15.80617190586768217, 15.72974639402176855, 48.12609039468568284 ) ) ;
#29104 = CARTESIAN_POINT ( 'NONE',  ( -9.564922557960796823, -16.46253265017161027, 22.08224293864768839 ) ) ;
#29103 = PRODUCT ( 'Front Concentrator Nozzle', 'Front Concentrator Nozzle', '', ( #84596 ) ) ;
#29107 = ORIENTED_EDGE ( 'NONE', *, *, #68319, .T. ) ;
#29106 = CARTESIAN_POINT ( 'NONE',  ( 0.05219959533909260263, 19.03943276465977164, 89.99890960531436690 ) ) ;
#29105 = CARTESIAN_POINT ( 'NONE',  ( 15.72974639402176855, 15.80617190586768217, 21.87609039468567573 ) ) ;
#29108 = CARTESIAN_POINT ( 'NONE',  ( 10.72451020669871369, 18.67979575497193778, 42.08442372801901854 ) ) ;
#29109 = ORIENTED_EDGE ( 'NONE', *, *, #155151, .T. ) ;
#29110 = CARTESIAN_POINT ( 'NONE',  ( -19.03943276465977164, 0.05219959533909376836, 96.24890960531436690 ) ) ;
#29111 = CARTESIAN_POINT ( 'NONE',  ( -69.65682714487590488, -71.74905178543390605, -13.00000000000000000 ) ) ;
#29112 = CARTESIAN_POINT ( 'NONE',  ( -21.53943276465977519, 0.05219959533907696930, 111.2489096053143669 ) ) ;
#29113 = CARTESIAN_POINT ( 'NONE',  ( 19.03943276465977164, -0.05219959533909143690, 43.74890960531435979 ) ) ;
#29114 = CARTESIAN_POINT ( 'NONE',  ( -14.29746914071037622, -8.314922557961029526, 24.16775706135235424 ) ) ;
#29115 = CARTESIAN_POINT ( 'NONE',  ( 36.91746824999999177, 2.880721459617395097E-14, -6.124999997268813168 ) ) ;
#29116 = CARTESIAN_POINT ( 'NONE',  ( -21.55341960407619339, 5.719274019375674811, 98.54275706135234714 ) ) ;
#29117 = CARTESIAN_POINT ( 'NONE',  ( 19.05341960407611168, 5.049401038298154454, 28.95724293864769550 ) ) ;
#29118 = CARTESIAN_POINT ( 'NONE',  ( -18.67979575497193778, 10.72451020669871902, 98.33442372801901854 ) ) ;
#29120 = CARTESIAN_POINT ( 'NONE',  ( 5.719274019375673035, 21.55341960407619339, 57.29275706135234714 ) ) ;
#29119 = CARTESIAN_POINT ( 'NONE',  ( -0.05219959533909027116, -19.03943276465977164, 87.49890960531436690 ) ) ;
#29121 = AXIS2_PLACEMENT_3D ( 'NONE', #119864, #43028, #90504 ) ;
#29122 = CARTESIAN_POINT ( 'NONE',  ( -8.571926809382601320, -26.38167802310801591, 145.7750000027311899 ) ) ;
#29123 = CARTESIAN_POINT ( 'NONE',  ( -9.474510206698964154, 16.51473224551069663, 95.41557627198102409 ) ) ;
#29124 = CARTESIAN_POINT ( 'NONE',  ( -17.49999999999999645, 3.237210098469573083, 29.71236987379550598 ) ) ;
#29127 = CARTESIAN_POINT ( 'NONE',  ( 15.80617190586769283, -15.72974639402175789, 60.62609039468567573 ) ) ;
#29126 = CARTESIAN_POINT ( 'NONE',  ( -0.05219959533934338120, 16.53943276465976808, 67.50109039468568994 ) ) ;
#29125 = CARTESIAN_POINT ( 'NONE',  ( 16.52544592524335698, 4.483927247898782831, 51.45942372801901854 ) ) ;
#29128 = CARTESIAN_POINT ( 'NONE',  ( 18.67979575497194134, -10.72451020669871369, 85.83442372801901854 ) ) ;
#29129 = DIRECTION ( 'NONE',  ( 0.000000000000000000, 0.7660444431189601389, -0.6427876096865606792 ) ) ;
#29130 = CARTESIAN_POINT ( 'NONE',  ( -8.314922557961024197, 14.29746914071037800, 27.91775706135234358 ) ) ;
#29131 = CARTESIAN_POINT ( 'NONE',  ( 0.05219959533909260263, 19.03943276465977164, 74.99890960531435269 ) ) ;
#29132 = CARTESIAN_POINT ( 'NONE',  ( -13.89961937509977652, 13.97604488694528158, 95.62390960531436690 ) ) ;
#29133 = CARTESIAN_POINT ( 'NONE',  ( 18.22780087662123805, 5.499999999999960032, 91.48236817873106475 ) ) ;
#29134 = CARTESIAN_POINT ( 'NONE',  ( 19.05341960407611168, 5.049401038298154454, 28.95724293864769550 ) ) ;
#29135 = CARTESIAN_POINT ( 'NONE',  ( 15.72974639402199770, -15.80617190586745480, 28.12390960531435979 ) ) ;
#29136 = CARTESIAN_POINT ( 'NONE',  ( -16.53943276465976808, -0.05219959533934237506, 98.75109039468568994 ) ) ;
#29138 = CARTESIAN_POINT ( 'NONE',  ( -19.03943276465977164, 0.05219959533909376836, 71.24890960531435269 ) ) ;
#29137 = CARTESIAN_POINT ( 'NONE',  ( 16.52544592524342804, -4.483927247898539470, 73.54057627198102409 ) ) ;
#29139 = CARTESIAN_POINT ( 'NONE',  ( 21.55341960407619695, -5.719274019375665929, 91.04275706135236135 ) ) ;
#29140 = CARTESIAN_POINT ( 'NONE',  ( -21.30000000000002913, 0.1105695005020707194, -58.85720012050614258 ) ) ;
#29141 = CARTESIAN_POINT ( 'NONE',  ( -13.89961937509957401, -13.97604488694547875, 104.3760903946856757 ) ) ;
#29142 = CARTESIAN_POINT ( 'NONE',  ( -8.314922557960811034, -14.29746914071050412, 82.08224293864768129 ) ) ;
#29143 = CARTESIAN_POINT ( 'NONE',  ( -5.823673210054431948, 21.52544592524334988, 27.70942372801901854 ) ) ;
#29144 = CARTESIAN_POINT ( 'NONE',  ( 0.05219959533907565091, 21.53943276465977519, 74.99890960531435269 ) ) ;
#29145 = CARTESIAN_POINT ( 'NONE',  ( -19.02544592524334988, -5.153800228976617603, 43.95942372801899012 ) ) ;
#29146 = CARTESIAN_POINT ( 'NONE',  ( -28.82186960331499037, 2.428612866367529932E-14, 146.2500000054623683 ) ) ;
#29147 = CARTESIAN_POINT ( 'NONE',  ( 19.03943276465977164, -0.05219959533909143690, 78.74890960531436690 ) ) ;
#29148 = CARTESIAN_POINT ( 'NONE',  ( 8.314922557960818139, 14.29746914071049879, 54.58224293864769550 ) ) ;
#29149 = CARTESIAN_POINT ( 'NONE',  ( 14.34966873604960469, 8.224510206698951720, 29.16557627198103120 ) ) ;
#29150 = CARTESIAN_POINT ( 'NONE',  ( 12.14591786802327356, -12.06949235617739191, 95.62609039468568994 ) ) ;
#29151 = CARTESIAN_POINT ( 'NONE',  ( 13.97604488694548053, -13.89961937509957401, 50.62609039468566152 ) ) ;
#29152 = CARTESIAN_POINT ( 'NONE',  ( 5.049401038297881783, 19.05341960407617918, 77.29275706135233293 ) ) ;
#29153 = CARTESIAN_POINT ( 'NONE',  ( -16.46253265017160317, 9.564922557960807481, 105.8322429386476955 ) ) ;
#29154 = CARTESIAN_POINT ( 'NONE',  ( 0.05219959533910956823, 16.53943276465976808, 69.99890960531435269 ) ) ;
#29155 = DIRECTION ( 'NONE',  ( -0.000000000000000000, -0.000000000000000000, 1.000000000000000000 ) ) ;
#29157 = CARTESIAN_POINT ( 'NONE',  ( 5.823673210054125526, 21.52544592524343514, 29.79057627198102409 ) ) ;
#29156 = CARTESIAN_POINT ( 'NONE',  ( -9.564922557960796823, -16.46253265017161027, 37.08224293864768839 ) ) ;
#29158 = CARTESIAN_POINT ( 'NONE',  ( 18.67979575497178502, 10.72451020669898547, 64.16557627198102409 ) ) ;
#29159 = CARTESIAN_POINT ( 'NONE',  ( 4.379528057220339221, -16.55341960407611168, 107.7072429386476955 ) ) ;
#29161 = CARTESIAN_POINT ( 'NONE',  ( -9.474510206698964154, 16.51473224551069663, 45.41557627198103120 ) ) ;
#29160 = CARTESIAN_POINT ( 'NONE',  ( 16.55341960407618274, -4.379528057220086978, 71.04275706135234714 ) ) ;
#29162 = CARTESIAN_POINT ( 'NONE',  ( 21.55341960407619695, -5.719274019375665929, 36.04275706135234714 ) ) ;
#29163 = EDGE_LOOP ( 'NONE', ( #53823, #165475, #199587 ) ) ;
#29164 = CARTESIAN_POINT ( 'NONE',  ( -8.314922557960811034, -14.29746914071050412, 87.08224293864769550 ) ) ;
#29165 = EDGE_CURVE ( 'NONE', #49313, #196867, #156659, .T. ) ;
#29166 = CARTESIAN_POINT ( 'NONE',  ( -30.00000000000000000, -5.186379194389042044E-15, 42.35000000000000853 ) ) ;
#29167 = CARTESIAN_POINT ( 'NONE',  ( 36.91746824999999177, 2.880721459617395097E-14, -10.12499999726881583 ) ) ;
#29168 = CARTESIAN_POINT ( 'NONE',  ( -21.52544592524343514, 5.823673210054127303, 36.04057627198102409 ) ) ;
#29169 = CARTESIAN_POINT ( 'NONE',  ( 17.50000000000000711, -5.622605283950866450, 66.18792689403889540 ) ) ;
#29170 = DIRECTION ( 'NONE',  ( -1.000000000000000000, -4.336808689942018352E-17, 3.574525976782710181E-31 ) ) ;
#29172 = CARTESIAN_POINT ( 'NONE',  ( -0.05219959533910754901, -16.53943276465976808, 47.49890960531435979 ) ) ;
#29171 = CARTESIAN_POINT ( 'NONE',  ( 8.314922557961029526, -14.29746914071037800, 40.41775706135234714 ) ) ;
#29173 = CARTESIAN_POINT ( 'NONE',  ( 21.52544592524344225, -5.823673210054117533, 73.54057627198102409 ) ) ;
#29174 = CARTESIAN_POINT ( 'NONE',  ( 10.81492255796078972, 18.62759615963270932, 59.58224293864770260 ) ) ;
#29175 = CYLINDRICAL_SURFACE ( 'NONE', #69279, 3.799999999999999378 ) ;
#29177 = CARTESIAN_POINT ( 'NONE',  ( 19.05341960407611168, 5.049401038298154454, 98.95724293864766707 ) ) ;
#29176 = CARTESIAN_POINT ( 'NONE',  ( -9.474510206698720793, -16.51473224551083518, 79.58442372801899012 ) ) ;
#29178 = CARTESIAN_POINT ( 'NONE',  ( 13.97604488694527802, 13.89961937509977652, 44.37390960531435269 ) ) ;
#29180 = ADVANCED_FACE ( 'NONE', ( #127889 ), #58787, .T. ) ;
#29179 = CARTESIAN_POINT ( 'NONE',  ( 16.52544592524342804, -4.483927247898539470, 113.5405762719810383 ) ) ;
#29181 =( NAMED_UNIT ( * ) SI_UNIT ( $, .STERADIAN. ) SOLID_ANGLE_UNIT ( ) );
#29182 = FACE_BOUND ( 'NONE', #8465, .T. ) ;
#29183 = ORIENTED_EDGE ( 'NONE', *, *, #92116, .T. ) ;
#29184 = CARTESIAN_POINT ( 'NONE',  ( 14.34966873604972726, -8.224510206698740333, 70.83442372801901854 ) ) ;
#29185 = CARTESIAN_POINT ( 'NONE',  ( -21.52544592524343514, 5.823673210054127303, 101.0405762719810383 ) ) ;
#29186 = CARTESIAN_POINT ( 'NONE',  ( -5.049401038298153566, 19.05341960407611168, 50.20724293864770260 ) ) ;
#29187 = CARTESIAN_POINT ( 'NONE',  ( -21.52544592524334988, -5.823673210054445271, 38.95942372801901854 ) ) ;
#29188 = CARTESIAN_POINT ( 'NONE',  ( -9.474510206698964154, 16.51473224551069663, 90.41557627198103830 ) ) ;
#29189 = CARTESIAN_POINT ( 'NONE',  ( -35.06017246933182463, -19.40171014085577283, -22.29041292151830334 ) ) ;
#29190 = ORIENTED_EDGE ( 'NONE', *, *, #125853, .F. ) ;
#29191 = CARTESIAN_POINT ( 'NONE',  ( -21.55341960407619339, 5.719274019375674811, 28.54275706135234358 ) ) ;
#29193 = CARTESIAN_POINT ( 'NONE',  ( 5.153800228976615827, -19.02544592524334988, 90.20942372801900433 ) ) ;
#29192 = CARTESIAN_POINT ( 'NONE',  ( 16.46253265017160672, -9.564922557960803928, 108.3322429386476955 ) ) ;
#29194 = CARTESIAN_POINT ( 'NONE',  ( 5.049401038297881783, 19.05341960407617563, 42.29275706135234003 ) ) ;
#29195 = CARTESIAN_POINT ( 'NONE',  ( -21.53943276465977519, 0.05219959533907696930, 106.2489096053143811 ) ) ;
#29196 = CARTESIAN_POINT ( 'NONE',  ( 0.05219959533936267826, -19.03943276465977164, 35.00109039468566863 ) ) ;
#29197 = CARTESIAN_POINT ( 'NONE',  ( 19.05341960407617918, -5.049401038297876454, 36.04275706135234003 ) ) ;
#29198 = CARTESIAN_POINT ( 'NONE',  ( -4.483927247898782831, 16.52544592524335698, 92.70942372801901854 ) ) ;
#29199 = DIRECTION ( 'NONE',  ( 0.000000000000000000, 0.000000000000000000, -1.000000000000000000 ) ) ;
#29200 = CARTESIAN_POINT ( 'NONE',  ( -16.51473224551069308, -9.474510206698971260, 56.66557627198103120 ) ) ;
#29201 = CARTESIAN_POINT ( 'NONE',  ( -15.72974639402176322, -15.80617190586768395, 69.37609039468567573 ) ) ;
#29202 = CARTESIAN_POINT ( 'NONE',  ( 18.67979575497194134, -10.72451020669871369, 80.83442372801901854 ) ) ;
#29203 = CARTESIAN_POINT ( 'NONE',  ( 35.00000000000000000, -3.181980515339468241, 1.110912703473986074 ) ) ;
#29204 = CARTESIAN_POINT ( 'NONE',  ( 13.97604488694527802, 13.89961937509977652, 84.37390960531433848 ) ) ;
#29205 = CARTESIAN_POINT ( 'NONE',  ( -0.05219959533937732626, 21.53943276465977519, 67.50109039468568994 ) ) ;
#29206 = CARTESIAN_POINT ( 'NONE',  ( 5.153800228976615827, -19.02544592524334988, 100.2094237280190043 ) ) ;
#29207 = CARTESIAN_POINT ( 'NONE',  ( -5.153800228976328057, -19.02544592524343514, 72.29057627198102409 ) ) ;
#29208 = CARTESIAN_POINT ( 'NONE',  ( -0.05219959533909027116, -19.03943276465977164, 97.49890960531436690 ) ) ;
#29209 = CARTESIAN_POINT ( 'NONE',  ( 5.153800228976335163, 19.02544592524342804, 74.79057627198103830 ) ) ;
#29210 = CARTESIAN_POINT ( 'NONE',  ( 18.22780087662123805, -5.499999999999976019, 78.51763182126894947 ) ) ;
#29212 = EDGE_CURVE ( 'NONE', #105512, #73939, #66461, .T. ) ;
#29211 = CARTESIAN_POINT ( 'NONE',  ( -9.564922557960796823, -16.46253265017161027, 62.08224293864769550 ) ) ;
#29213 = CARTESIAN_POINT ( 'NONE',  ( 10.81492255796078972, 18.62759615963270932, 99.58224293864770971 ) ) ;
#29214 = CARTESIAN_POINT ( 'NONE',  ( 14.29746914071037800, 8.314922557961029526, 91.66775706135234714 ) ) ;
#29215 = CARTESIAN_POINT ( 'NONE',  ( 12.99999999999999822, 0.000000000000000000, 0.000000000000000000 ) ) ;
#29216 = CARTESIAN_POINT ( 'NONE',  ( -19.02544592524334988, -5.153800228976617603, 43.95942372801899012 ) ) ;
#29217 = CARTESIAN_POINT ( 'NONE',  ( 19.02544592524343514, -5.153800228976328945, 78.54057627198099567 ) ) ;
#29218 = CARTESIAN_POINT ( 'NONE',  ( -8.224510206698948167, 14.34966873604960824, 70.41557627198102409 ) ) ;
#29219 = CARTESIAN_POINT ( 'NONE',  ( 12.06949235617757843, -12.14591786802309237, 108.1239096053143811 ) ) ;
#29220 = CARTESIAN_POINT ( 'NONE',  ( 19.02544592524343514, -5.153800228976328945, 113.5405762719810241 ) ) ;
#29221 = CARTESIAN_POINT ( 'NONE',  ( 0.05219959533909260263, 19.03943276465977164, 109.9989096053143669 ) ) ;
#29222 = CARTESIAN_POINT ( 'NONE',  ( -0.05219959533909027116, -19.03943276465977164, 82.49890960531436690 ) ) ;
#29223 = CARTESIAN_POINT ( 'NONE',  ( -19.05341960407617563, 5.049401038297882671, 28.54275706135232937 ) ) ;
#29224 = CARTESIAN_POINT ( 'NONE',  ( -0.05219959533934338120, 16.53943276465976808, 92.50109039468567573 ) ) ;
#29225 = CARTESIAN_POINT ( 'NONE',  ( -19.03943276465977164, 0.05219959533909376836, 76.24890960531435269 ) ) ;
#29226 = CARTESIAN_POINT ( 'NONE',  ( 21.53943276465977519, 0.05219959533937863772, 56.25109039468568284 ) ) ;
#29227 = CARTESIAN_POINT ( 'NONE',  ( 21.55341960407610458, 5.719274019375980345, 28.95724293864769905 ) ) ;
#29228 = CARTESIAN_POINT ( 'NONE',  ( -5.719274019375978568, 21.55341960407610458, 115.2072429386476955 ) ) ;
#29229 = CARTESIAN_POINT ( 'NONE',  ( -15.80617190586745835, -15.72974639402198527, 66.87390960531436690 ) ) ;
#29230 = CARTESIAN_POINT ( 'NONE',  ( -14.29746914071049879, 8.314922557960819915, 90.83224293864769550 ) ) ;
#29231 = CARTESIAN_POINT ( 'NONE',  ( -9.564922557961040184, 16.46253265017147172, 57.91775706135233293 ) ) ;
#29232 = CARTESIAN_POINT ( 'NONE',  ( 19.03943276465977164, -0.05219959533909143690, 28.74890960531435624 ) ) ;
#29233 = CARTESIAN_POINT ( 'NONE',  ( -0.05219959533909027116, -19.03943276465977164, 82.49890960531436690 ) ) ;
#29234 = CARTESIAN_POINT ( 'NONE',  ( -19.03943276465977164, 0.05219959533909376836, 81.24890960531436690 ) ) ;
#29235 = CARTESIAN_POINT ( 'NONE',  ( -17.14385361876520264, -23.59649016807271238, 141.6750000027311387 ) ) ;
#29236 = CARTESIAN_POINT ( 'NONE',  ( 14.29746914071049879, -8.314922557960816363, 103.3322429386476955 ) ) ;
#29237 = ORIENTED_EDGE ( 'NONE', *, *, #129082, .F. ) ;
#29238 = CARTESIAN_POINT ( 'NONE',  ( 14.29746914071049879, -8.314922557960816363, 23.33224293864769194 ) ) ;
#29239 = CARTESIAN_POINT ( 'NONE',  ( -16.55341960407617563, 4.379528057220093196, 28.54275706135234358 ) ) ;
#29240 = CARTESIAN_POINT ( 'NONE',  ( 10.72451020669871369, 18.67979575497193778, 92.08442372801901854 ) ) ;
#29241 = CARTESIAN_POINT ( 'NONE',  ( -5.153800228976328057, -19.02544592524343514, 107.2905762719810383 ) ) ;
#29242 = CARTESIAN_POINT ( 'NONE',  ( -21.53943276465977519, -0.05219959533937600094, 18.75109039468568639 ) ) ;
#29243 = CARTESIAN_POINT ( 'NONE',  ( 19.05341960407611168, 5.049401038298154454, 38.95724293864767418 ) ) ;
#29244 = CARTESIAN_POINT ( 'NONE',  ( -14.34966873604972548, 8.224510206698743886, 43.33442372801901143 ) ) ;
#29245 = CARTESIAN_POINT ( 'NONE',  ( 9.474510206698729675, 16.51473224551082808, 112.0844237280190043 ) ) ;
#29246 = CARTESIAN_POINT ( 'NONE',  ( -9.564922557960796823, -16.46253265017161027, 32.08224293864769550 ) ) ;
#29247 = CARTESIAN_POINT ( 'NONE',  ( 12.06949235617757843, -12.14591786802309237, 93.12390960531436690 ) ) ;
#29248 = CARTESIAN_POINT ( 'NONE',  ( 21.52544592524344225, -5.823673210054117533, 98.54057627198105251 ) ) ;
#29249 = CARTESIAN_POINT ( 'NONE',  ( -0.05219959533936034679, 19.03943276465977164, 72.50109039468566152 ) ) ;
#29250 = CARTESIAN_POINT ( 'NONE',  ( -32.00000000000000000, -1.163414459189985801E-14, 95.00000000000000000 ) ) ;
#29251 = CARTESIAN_POINT ( 'NONE',  ( -0.05219959533937732626, 21.53943276465977519, 22.50109039468567573 ) ) ;
#29252 = CARTESIAN_POINT ( 'NONE',  ( -9.564922557960796823, -16.46253265017161027, 22.08224293864768839 ) ) ;
#29253 = CARTESIAN_POINT ( 'NONE',  ( -0.05219959533909027116, -19.03943276465977164, 92.49890960531436690 ) ) ;
#29254 = CARTESIAN_POINT ( 'NONE',  ( 17.31747979337949772, -6.344076630961069441, 111.1205513193481949 ) ) ;
#29255 = CARTESIAN_POINT ( 'NONE',  ( 13.97604488694527802, 13.89961937509977652, 84.37390960531433848 ) ) ;
#29257 = CARTESIAN_POINT ( 'NONE',  ( -12.14591786802309592, -12.06949235617757132, 81.87390960531435269 ) ) ;
#29256 = CARTESIAN_POINT ( 'NONE',  ( -5.823673210054431948, 21.52544592524334988, 27.70942372801901854 ) ) ;
#29258 = CARTESIAN_POINT ( 'NONE',  ( -5.153800228976328057, -19.02544592524343514, 77.29057627198099567 ) ) ;
#29259 = CARTESIAN_POINT ( 'NONE',  ( 13.97604488694548053, -13.89961937509957401, 30.62609039468566863 ) ) ;
#29261 = CARTESIAN_POINT ( 'NONE',  ( 5.049401038297881783, 19.05341960407617563, 52.29275706135234003 ) ) ;
#29260 = CARTESIAN_POINT ( 'NONE',  ( -16.52544592524335698, -4.483927247898792601, 48.95942372801902565 ) ) ;
#29262 = CARTESIAN_POINT ( 'NONE',  ( 21.52544592524334988, 5.823673210054432836, 71.45942372801901854 ) ) ;
#29263 = CARTESIAN_POINT ( 'NONE',  ( -4.483927247898782831, 16.52544592524335698, 32.70942372801900433 ) ) ;
#29264 = CARTESIAN_POINT ( 'NONE',  ( -0.05219959533909027116, -19.03943276465977164, 62.49890960531435979 ) ) ;
#29265 = CARTESIAN_POINT ( 'NONE',  ( 16.51473224551083163, -9.474510206698727899, 95.83442372801900433 ) ) ;
#29266 = CARTESIAN_POINT ( 'NONE',  ( 16.55341960407618274, -4.379528057220086978, 66.04275706135236135 ) ) ;
#29267 = CARTESIAN_POINT ( 'NONE',  ( -15.80617190586768217, 15.72974639402176855, 93.12609039468568994 ) ) ;
#29268 = CARTESIAN_POINT ( 'NONE',  ( 16.51473224551083163, -9.474510206698727899, 85.83442372801900433 ) ) ;
#29269 = CARTESIAN_POINT ( 'NONE',  ( -5.153800228976328057, -19.02544592524343514, 52.29057627198100988 ) ) ;
#29270 = CARTESIAN_POINT ( 'NONE',  ( 15.80617190586746368, 15.72974639402197994, 69.37390960531436690 ) ) ;
#29272 = CARTESIAN_POINT ( 'NONE',  ( 5.153800228976615827, -19.02544592524334988, 80.20942372801901854 ) ) ;
#29271 = CARTESIAN_POINT ( 'NONE',  ( -16.55341960407611168, -4.379528057220339221, 76.45724293864769550 ) ) ;
#29273 = CARTESIAN_POINT ( 'NONE',  ( 17.50000000000000000, -5.499999999999992895, 61.21769037696436300 ) ) ;
#29274 = CARTESIAN_POINT ( 'NONE',  ( 5.049401038297881783, 19.05341960407617563, 47.29275706135231161 ) ) ;
#29275 = CARTESIAN_POINT ( 'NONE',  ( -8.224510206698735004, -14.34966873604973081, 109.5844237280190328 ) ) ;
#29276 = CARTESIAN_POINT ( 'NONE',  ( 16.53943276465976808, -0.05219959533910856209, 68.74890960531435269 ) ) ;
#29278 = CARTESIAN_POINT ( 'NONE',  ( 27.73933785331498569, 2.768321779492822058E-14, 147.8750000027311842 ) ) ;
#29277 = CARTESIAN_POINT ( 'NONE',  ( -21.52544592524334988, -5.823673210054445271, 108.9594237280190185 ) ) ;
#29279 = CARTESIAN_POINT ( 'NONE',  ( 10.72451020669898902, -18.67979575497178502, 112.9155762719810383 ) ) ;
#29280 =( BOUNDED_SURFACE ( )  B_SPLINE_SURFACE ( 3, 2, ( 
 ( #178204, #132685, #55840, #117514, #122473, #90153, #43666, #77955, #109295, #106311, #107297, #121482, #108299, #91126, #16305, #14308, #61787, #168969, #76966, #137648, #118, #32467, #29493, #153812, #31470, #199335, #139622, #198336, #1110, #184164, #47643, #17297, #15307, #167997, #183176, #59812, #44658, #152816, #94120, #93122, #62784, #138637, #151836, #124465, #155799, #186162, #45646, #182181, #60800, #75975, #74991, #123457, #170974, #167016, #154807, #135686, #30474, #197358, #92124, #185149, #46639, #169978, #58822, #120490, #105328, #28517, #13326, #136655, #129425, #37432, #50620, #140626, #2116, #160784, #143602, #156808, #158774, #4093, #18300, #99092, #78951, #36420, #190126, #63798, #175963, #189147, #6089, #65772, #67768, #191123, #66768, #35439, #82926, #21269, #81909, #49622, #19291, #97091, #51601, #112281, #159774, #111284, #110290, #113265, #127441, #5086, #173971, #141625, #95118, #172974, #144604, #125470, #3114, #52597, #114258, #174957, #20263, #48638, #34453, #171972, #128429, #33460, #98076, #96112, #187167, #79956, #64790, #157800, #80938, #126451, #188149, #142614, #103110, #54599, #53602, #195131, #147623, #86937, #117275, #84920, #38441, #116273, #26285, #42442, #146600, #72787, #57614, #118286, #194137, #192120, #177963, #115278, #148620, #176972, #71771, #193125, #7083, #55601, #104105, #180965, #22272, #163793, #83923, #145604, #9111, #100097, #130422, #164791, #196142, #39431, #178969, #8093, #56612, #101091, #87927, #162777, #10111, #40436, #25295, #24285, #133441, #119282, #85934, #102108, #179977, #70777, #149614, #69771, #11112, #132446, #134457, #68764, #41445, #161781, #131439, #23276, #28287, #89927, #124228, #123226, #31239, #45413, #181948, #92888, #62552, #154575, #14071, #12119, #167766, #13100, #105100, #168737, #16071, #197124, #184917, #77729, #44426, #165788, #137414, #121249, #91884, #75738, #107066, #88931, #139395, #152581, #74765, #108060, #877, #185924, #199095, #27285, #150623, #47409, #30241, #43431, #153575, #90895, #166786, #73783, #135455, #46401, #76733, #58591, #120257, #60562, #151608, #122238, #136427, #198108, #15072, #183928, #169744, #59574, #182943, #106080, #138409, #200089, #29264, #61557, #97845, #155569, #93891, #17064, #157566, #143362, #113036, #50393, #129190, #95883, #142384, #66539, #1882, #79724, #170743, #78718, #65542, #141393, #32233, #127201, #158547, #33231, #19059, #140394, #112053, #188915, #80706, #3862, #48405, #125237, #173741, #189900, #94890, #110062, #63563, #156574, #35210, #96863, #67532, #171742, #186935, #81679, #20037, #18069, #2881, #144369, #4854, #128203, #51375, #109065, #174728, #36191, #159533, #5856, #64560, #21032, #82685, #190888, #126224, #187920, #49389, #111052, #34221, #172740, #90436, #196662, #114021, #181485, #152122, #175718, #89453, #39952, #25814, #40964, #86459, #165317, #197638, #101623, #13604, #87460, #9635, #75272, #120769, #57138, #150145, #136942, #24810, #180500, #149147, #134984, #182470, #58131, #11647, #164321, #43951, #10637, #72297, #166315, #52364, #71302, #195667, #163312, #119800, #27812, #26810, #148144, #42963, #104626, #151142, #132965, #41972, #105613, #73313, #167301, #12633, #194654, #28797, #88450, #56124, #117806, #133976, #179499, #102636, #118814, #103639, #74298, #135967, #59104, #60097, #16585, #47925, #122756, #46925, #44944, #1393, #78233, #108585, #170262, #137933, #14599, #185435, #79239, #184446, #199617, #121765, #45926, #139904, #155091, #157082, #61083, #183458, #171262, #109579, #106599, #168275, #33735, #93405, #31756, #156082, #198631, #63074, #32750, #94401, #95396, #91407, #124753, #186449, #17578, #140910, #2396, #64075, #172248, #123736, #125745, #18578, #187445, #29772, #48913, #80225, #153095, #110567, #76255, #169258, #107581, #30765, #92412, #154098, #15592, #77250, #138918, #399, #62071, #7362, #143887, #36701, #100380, #111567 ),
 ( #82194, #49900, #83208, #52871, #113542, #141896, #144883, #191394, #37713, #177250, #67052, #69047, #160061, #130712, #68045, #188423, #192406, #175236, #173251, #34726, #159051, #96384, #112555, #19562, #114542, #98362, #35718, #142887, #53888, #158071, #126719, #81206, #190407, #176242, #145879, #6365, #162058, #128710, #21548, #99375, #161058, #174250, #4369, #129697, #23554, #3387, #65062, #22553, #66052, #127720, #51883, #189422, #50897, #84199, #115563, #97365, #38722, #20545, #5368, #40718, #166065, #164075, #11394, #118565, #26561, #87218, #149888, #182222, #179252, #103389, #181243, #148900, #89206, #147904, #27566, #72047, #197397, #167055, #165067, #55880, #71056, #9390, #132722, #194410, #43706, #42720, #150899, #88204, #101369, #12393, #105368, #74055, #133721, #131725, #10390, #117553, #24565, #73064, #135726, #116556, #104382, #58863, #25574, #85202, #56891, #102387, #134736, #195413, #196418, #8382, #120529, #180255, #146890, #70057, #193407, #41725, #57888, #119560, #54882, #39706, #178245, #163058, #86214, #139661, #157, #28556, #31510, #77994, #124507, #63835, #153851, #94159, #46680, #17335, #154848, #75030, #155838, #61826, #59854, #121521, #45685, #136696, #199374, #106351, #1149, #123496, #122513, #29532, #78991, #198377, #13366, #183216, #77005, #62824, #32507, #170020, #48676, #15349, #185189, #186202, #44697, #60838, #90193, #168035, #108339, #184203, #151876, #47684, #93163, #91165, #16345, #109334, #171016, #125508, #138677, #140665, #2157, #187205, #110328, #152854, #14349, #76014, #137689, #107336, #169009, #30513, #92165, #49660, #82968, #5125, #65812, #173014, #160825, #18340, #156845, #79995, #20302, #6128, #176005, #113306, #192163, #158814, #66807, #129466, #64828, #142654, #33498, #141663, #128470, #4133, #95157, #190166, #21311, #96151, #81950, #3155, #174997, #51642, #143642, #36462, #111324, #188188, #98119, #52638, #157840, #34493, #126490, #19331, #159816, #144645, #130465, #80979, #127481, #67811, #191165, #189186, #50659, #7124, #114303, #37474, #99135, #172009, #22313, #83964, #145644, #68806, #112320, #53643, #174010, #35481, #97130, #103150, #164831, #134496, #132486, #55639, #196183, #86976, #177012, #10151, #57655, #38481, #56652, #100138, #101129, #116312, #23314, #117312, #26327, #161819, #119321, #162815, #8133, #181008, #87967, #70817, #102148, #115320, #193165, #163833, #194175, #195171, #25335, #180018, #149655, #146640, #84958, #179008, #40476, #11153, #69811, #24324, #148663, #178001, #72827, #131478, #54637, #39468, #85973, #147663, #9150, #71811, #133479, #118325, #41485, #161476, #67459, #127133, #188839, #112964, #142313, #66467, #173671, #6778, #129117, #189831, #96790, #84613, #3793, #80636, #65470, #144295, #130111, #99790, #37122, #115971, #82614, #190816, #53289, #50324, #128129, #157497, #111979, #52291, #51303, #18990, #113948, #145295, #19967, #5785, #35138, #98781, #175647, #160475, #21966, #158479, #81609, #83617, #176660, #143293, #4779, #174657, #36122, #68457, #191807, #54299, #97774, #159461, #114967, #38137, #20957, #22965, #131129, #146292, #7779, #69463, #95811, #192817, #177659, #73477, #74461, #132134, #134145, #195833, #57305, #72471, #119959, #43124, #12796, #164485, #25979, #136127, #180664, #100783, #165481, #197803, #162466, #135150, #23967, #9802, #24979, #70468, #149308, #181645, #85623, #59269, #71464, #193826, #120938, #104792, #41135, #118981, #39128, #8798, #87622, #133129, #42140, #10802, #103801, #196823, #147309, #166481, #148308, #194820, #150318, #55291, #116963, #179665, #178654, #26977, #11813, #88620, #40116, #58290, #27979, #89618, #151307, #101795, #163482, #86625, #56292, #117975, #102799, #29708, #45863, #62005, #78170, #77187, #186382, #137872, #136878, #139838, #30699, #170199, #337, #168211, #121701, #199551, #109513, #125680, #91340, #156015, #140841, #1327, #138857, #75207, #61021 ),
 ( #183396, #92350, #47860, #153031, #44878, #167236, #14531, #46860, #123671, #64011, #106534, #28734, #63007, #155026, #90371, #13542, #2330, #185368, #154036, #124686, #105551, #15530, #16522, #171195, #187378, #198564, #108520, #31692, #93341, #32684, #94337, #17512, #79170, #152056, #60034, #76192, #122693, #184382, #107516, #169192, #110501, #83143, #33668, #19498, #34662, #80160, #158986, #191330, #172183, #84138, #81143, #3324, #145817, #114475, #50833, #143821, #7300, #18513, #174184, #142824, #128645, #35652, #113476, #6302, #95330, #176178, #158007, #4304, #159995, #48847, #64997, #189356, #157015, #190340, #21482, #20478, #141832, #51816, #98293, #144818, #68985, #126655, #188358, #130649, #5302, #97300, #67980, #49836, #82128, #129634, #52808, #111500, #173186, #66986, #175170, #36636, #37648, #99312, #160996, #22491, #96320, #65986, #127656, #112490, #53825, #118506, #27506, #115500, #26503, #177187, #162998, #178183, #23491, #102327, #134675, #38660, #89148, #24504, #146825, #150837, #57829, #194352, #87158, #12333, #161995, #117493, #86155, #71986, #179190, #56831, #149830, #100316, #119502, #101309, #147845, #103330, #192343, #8319, #132664, #85140, #133661, #165009, #164017, #69995, #195351, #41666, #88145, #73997, #40658, #181183, #10330, #42660, #180196, #131663, #104322, #25513, #9331, #70997, #55820, #148840, #11335, #193345, #73006, #196361, #166006, #54820, #116494, #39648, #120470, #182162, #184146, #169958, #139603, #76946, #155780, #122453, #168950, #93103, #28499, #106292, #197339, #105309, #92104, #167978, #58802, #153792, #185128, #59794, #45627, #43646, #138615, #15287, #107279, #30456, #74973, #151818, #98, #16285, #121463, #136635, #166997, #183155, #61767, #123435, #94100, #198317, #90133, #108280, #46619, #31450, #77936, #13307, #170954, #29476, #44640, #32447, #1089, #137630, #154787, #17277, #91107, #60781, #152796, #62765, #124446, #186142, #47621, #14288, #109275, #75956, #199315, #135667, #78931, #33440, #19272, #187146, #20243, #190108, #50602, #140607, #81891, #128412, #174938, #114236, #4075, #144583, #97073, #67747, #5066, #125450, #6069, #112261, #34433, #49600, #111264, #96093, #172955, #156788, #51583, #173953, #157782, #79936, #129405, #48619, #63778, #110270, #127421, #113248, #82904, #143584, #99071, #65752, #35420, #36401, #171951, #80919, #2097, #95099, #158754, #142595, #18281, #66751, #98055, #3093, #189130, #141606, #159755, #21250, #191102, #52576, #64770, #126432, #175942, #37412, #188129, #160760, #83900, #69749, #166528, #181690, #183675, #23256, #145583, #197849, #74508, #7061, #130400, #60309, #120004, #11860, #182683, #22251, #73525, #136174, #59316, #121985, #115257, #43171, #104838, #28025, #58336, #105827, #29010, #198845, #150364, #135196, #45160, #89667, #68742, #151353, #106816, #192098, #120985, #53580, #195879, #8073, #176950, #38419, #100076, #165527, #161761, #12842, #44168, #196870, #84899, #167514, #90649, #152331, #146578, #13817, #75483, #137156, #131418, #57352, #119027, #180710, #42186, #103846, #27023, #88668, #185651, #139138, #46141, #79458, #1615, #62285, #169479, #157299, #14816, #153315, #76477, #16800, #2617, #172469, #109795, #188645, #155311, #63291, #125961, #61302, #615, #29988, #138154, #124971, #123953, #91627, #186668, #17801, #92627, #78450, #199835, #171478, #48138, #140124, #32967, #107795, #184659, #94621, #49130, #154318, #30980, #122972, #15807, #156300, #141127, #126937, #77468, #47143, #64294, #187659, #108801, #170480, #3599, #110788, #33956, #95614, #168490, #18796, #80441, #142114, #65278, #31970, #50124, #93626, #68260, #145098, #192623, #115779, #85426, #36923, #98585, #147117, #53090, #173472, #37935, #8604, #34945, #146096, #96597, #82416, #97577, #143102, #21770, #54105, #158286, #70277, #144105, #66274, #131945, #177468, #113756, #6581, #193629, #81416, #160279, #5585, #191611 ),
 ( #35931, #162276, #111784, #7580, #83421, #4581, #67265, #127933, #176462, #189635, #161276, #128923, #19775, #129911, #51110, #112769, #174462, #114768, #159265, #20761, #99596, #190624, #52099, #38937, #175452, #22771, #84419, #69266, #130932, #100594, #23776, #133951, #181460, #88426, #196637, #57115, #119776, #152094, #149122, #73289, #151117, #118789, #59078, #117781, #135943, #41949, #167272, #136916, #134959, #25791, #40940, #179475, #102612, #164298, #13578, #12609, #120745, #58106, #71277, #182444, #75245, #43924, #103615, #101598, #180478, #87437, #194630, #42938, #105586, #86435, #74273, #28771, #195642, #55101, #26784, #10613, #104602, #165291, #166290, #178462, #132942, #116771, #39929, #150120, #90409, #163286, #11621, #24787, #148121, #9612, #27786, #56100, #89428, #197613, #72274, #157055, #198603, #156054, #109552, #18552, #95370, #108559, #125720, #185408, #187419, #48887, #186422, #155065, #80200, #60071, #46899, #122730, #138894, #16560, #171233, #170237, #79211, #30739, #29745, #32722, #123711, #63045, #93379, #110542, #91380, #17551, #172223, #77225, #121739, #31731, #154073, #124724, #78207, #139877, #183431, #76229, #44916, #106572, #374, #33708, #168249, #1366, #153069, #14571, #137909, #47898, #199591, #94374, #140880, #61058, #184421, #45901, #2370, #64050, #107554, #169232, #92386, #15567, #62046, #130686, #192380, #129671, #98335, #38698, #3362, #190381, #66027, #82166, #160034, #114515, #113516, #22527, #174223, #173225, #176216, #67025, #6339, #36675, #4342, #158046, #35692, #145854, #162033, #127694, #53863, #177225, #37685, #175210, #111540, #97339, #34701, #68019, #96358, #191368, #112529, #126693, #21521, #23529, #100354, #141871, #83182, #65037, #188397, #128684, #19536, #49875, #84174, #115537, #159025, #144856, #189394, #99350, #20518, #7336, #143862, #81181, #52845, #142863, #161033, #69021, #51856, #50871, #5341, #133697, #196395, #119536, #120504, #178219, #180232, #41701, #103366, #118542, #166040, #89181, #58837, #10367, #72024, #182195, #26537, #146864, #11370, #43680, #8356, #181219, #70031, #55855, #71032, #116531, #195389, #27540, #131700, #117529, #179227, #102363, #40693, #163034, #57864, #165044, #164052, #86191, #74030, #193381, #54857, #39683, #56867, #42695, #150873, #88181, #105342, #149865, #73040, #104356, #101345, #25551, #24541, #147881, #134712, #87195, #9367, #12367, #135701, #132699, #197372, #194388, #167029, #85175, #148876, #138652, #168011, #44672, #15322, #109310, #152830, #29507, #90167, #75989, #169994, #185164, #187182, #91141, #151850, #1125, #63813, #139637, #110305, #46655, #123472, #76981, #186177, #28531, #133, #62799, #124481, #125486, #121496, #108314, #31485, #93137, #61802, #170989, #32482, #2132, #153827, #154822, #48653, #16320, #13341, #77970, #75005, #136670, #47659, #198352, #199349, #14324, #59826, #94135, #155814, #183190, #106325, #60814, #137662, #122488, #17312, #30489, #78967, #184179, #45661, #140642, #107312, #168985, #92140, #36435, #129439, #95133, #37446, #80953, #65786, #82940, #171987, #126466, #112295, #79972, #113280, #144618, #143615, #33475, #174971, #21283, #67782, #7097, #97105, #99106, #190140, #160798, #98090, #18315, #22286, #5099, #127455, #158789, #111300, #130436, #156823, #191138, #6102, #192135, #68779, #81923, #83937, #20277, #145618, #53616, #159788, #128443, #141640, #3130, #66782, #96126, #173985, #51615, #52611, #114273, #175977, #4107, #64805, #188164, #49637, #172989, #34467, #157815, #19305, #189161, #142628, #50634, #35454, #165801, #150636, #11126, #86951, #84933, #70791, #8106, #179992, #69784, #164805, #85947, #100110, #148635, #197137, #73796, #115292, #56626, #176985, #38455, #102123, #131452, #23289, #57629, #88945, #147636, #10125, #101104, #87941, #132459, #196156, #194150, #118300, #161794, #134471, #27298, #41459, #12132, #9125, #133455, #72801, #117288, #119296 ),
 ( #103124, #146614, #26300, #135469, #193139, #149628, #54612, #55614, #162790, #116286, #25309, #180979, #177976, #39444, #178982, #24299, #40449, #42455, #163807, #71785, #195145, #104119, #183941, #29277, #138422, #45426, #123239, #16084, #181962, #124242, #167779, #152594, #169757, #58604, #13114, #199108, #166799, #105113, #61570, #76747, #107079, #168751, #198121, #74778, #30254, #139408, #182956, #59588, #120270, #106093, #200102, #15086, #17077, #121262, #43444, #31252, #93904, #92902, #140407, #184930, #153588, #91897, #77742, #28300, #46415, #154588, #890, #155582, #151621, #108073, #62565, #185937, #47422, #109078, #170757, #32246, #78731, #89940, #136440, #44439, #90909, #14085, #75751, #137428, #60575, #122251, #172752, #187932, #33244, #112065, #144380, #63576, #37208, #34233, #156586, #98864, #67543, #3875, #96874, #160559, #171755, #127213, #95895, #81691, #188927, #66550, #159545, #125250, #129201, #111064, #157578, #113047, #1896, #18081, #142396, #110075, #143373, #174739, #173753, #186948, #4865, #51386, #97856, #22049, #50405, #190899, #20048, #52375, #128214, #48419, #114032, #35221, #19071, #80718, #65554, #158558, #189911, #79736, #36202, #21043, #82696, #2893, #175729, #94902, #141405, #64572, #5867, #83700, #126237, #49401, #165564, #132218, #178739, #102881, #38217, #116053, #6860, #115052, #101882, #177742, #68539, #163564, #194903, #69549, #193910, #191890, #55374, #179750, #149388, #86707, #27061, #117044, #40202, #164566, #99873, #39211, #130194, #176744, #25064, #100867, #53374, #148392, #56377, #131213, #9886, #161557, #71546, #133212, #118060, #41220, #84695, #23050, #26060, #87703, #192904, #146375, #7862, #54381, #10884, #72554, #103884, #162549, #24053, #134232, #180747, #195917, #145378, #57392, #119065, #42223, #85709, #147395, #8883, #70551, #123012, #123996, #181728, #183714, #45200, #106854, #122023, #169519, #92669, #62326, #13854, #75521, #185694, #30027, #150403, #14857, #47184, #11899, #184698, #73562, #59355, #74546, #120041, #198882, #31019, #135235, #108843, #121024, #43209, #170524, #154357, #90687, #168529, #88707, #58374, #137196, #182721, #91665, #60349, #153355, #46182, #196907, #15850, #197886, #44206, #199877, #104876, #166565, #29047, #28064, #76518, #61341, #138194, #89705, #107835, #77509, #139180, #151391, #656, #12881, #136211, #105865, #167552, #152369, #100392, #6375, #190417, #5378, #67062, #51893, #128720, #112565, #145891, #68055, #113552, #35728, #23566, #78495, #16845, #115575, #175246, #63339, #7374, #160071, #99387, #129709, #97375, #50907, #36711, #38734, #54894, #159061, #85214, #70069, #130726, #191405, #1661, #98373, #125016, #161070, #186712, #84211, #21558, #140168, #52882, #116568, #193419, #32013, #176254, #93670, #155355, #83218, #174260, #20555, #177262, #8394, #144893, #114556, #82205, #69059, #37725, #162070, #22565, #192418, #143897, #53900, #146904, #131737, #75042, #72059, #196430, #74067, #180267, #182234, #40730, #58875, #165079, #90205, #59866, #57900, #148912, #164087, #102400, #25586, #87230, #136708, #135738, #43719, #119572, #194422, #105380, #198389, #167067, #26573, #24577, #41737, #10402, #117565, #181255, #28568, #9402, #197409, #151888, #56903, #178257, #149900, #133733, #104394, #88216, #42732, #101381, #55892, #39718, #163072, #118577, #13378, #86226, #11407, #147916, #71068, #132734, #166077, #179265, #27580, #103401, #195426, #73076, #134748, #120541, #89218, #150911, #12405, #31522, #48687, #108353, #110340, #172021, #109346, #78006, #18352, #183228, #170032, #45697, #61838, #139673, #94171, #93175, #95169, #92178, #154860, #107348, #155850, #77017, #2169, #170, #62836, #121533, #140677, #33510, #186215, #80007, #15361, #1161, #17347, #123508, #125520, #184215, #63848, #16358, #156857, #3167, #124520, #153863, #169021, #30526, #138689, #185201, #141676, #79003, #187217, #47696, #137701, #44709 ),
 ( #106363, #171028, #46692, #32519, #168047, #29544, #91177, #199386, #152866, #14361, #76026, #60850, #122525, #36475, #126502, #188200, #146653, #129478, #142666, #144658, #190180, #4145, #23327, #64840, #22326, #176017, #84970, #161832, #175011, #192176, #51655, #53657, #115334, #52651, #21324, #49672, #111336, #113319, #189198, #5139, #82982, #37486, #98132, #145656, #97144, #96163, #99148, #159829, #191177, #6141, #127493, #80991, #158827, #68820, #173026, #50673, #177025, #100151, #160837, #67823, #34505, #20315, #157852, #114315, #19343, #83976, #35494, #65824, #7137, #112333, #174023, #81963, #130479, #143655, #66821, #38495, #128484, #116325, #150673, #131491, #85987, #166837, #193178, #86989, #58642, #28338, #180031, #69824, #54651, #89977, #72840, #147676, #87980, #133492, #9164, #8147, #178014, #165840, #119335, #39481, #105151, #118338, #135507, #195184, #197177, #120308, #196196, #164844, #101142, #162828, #56665, #132499, #148676, #26340, #181021, #41500, #88983, #40489, #24337, #42495, #103164, #134510, #149668, #70831, #194188, #102161, #12171, #55653, #117325, #182001, #43484, #104159, #11166, #179021, #163847, #25348, #57668, #10164, #27337, #71824, #73836, #123274, #33277, #110111, #151658, #92937, #13152, #74815, #138455, #106131, #59627, #93939, #125286, #122287, #184965, #137466, #124277, #107116, #32284, #30289, #154625, #136477, #170792, #63611, #16119, #48454, #45462, #169793, #47457, #153626, #155618, #14121, #17114, #200136, #186983, #198157, #31286, #183976, #199146, #75788, #60612, #168787, #171789, #109113, #78765, #77775, #167815, #140442, #121301, #1932, #61605, #182993, #15122, #91934, #90944, #139443, #44476, #29314, #152631, #76784, #46449, #108109, #925, #62599, #185973, #4899, #36236, #21077, #141441, #160591, #66581, #50439, #65590, #127250, #112098, #188963, #172788, #5900, #128246, #173788, #95928, #83731, #2928, #79771, #64607, #143411, #129235, #98897, #97888, #115084, #81726, #189943, #52408, #187967, #35255, #156621, #126270, #51418, #96909, #18116, #113078, #144414, #19104, #174770, #49437, #159580, #82733, #67577, #190931, #34269, #111098, #114067, #175765, #80754, #157613, #142431, #3910, #37241, #22080, #53406, #158592, #20081, #145410, #130227, #6892, #176776, #68570, #191922, #94936, #195950, #38248, #86739, #149420, #72589, #73592, #131246, #133244, #194936, #56412, #71578, #119096, #42253, #11928, #163596, #25097, #135265, #179782, #99903, #164597, #196936, #161588, #134263, #23082, #8915, #24086, #69580, #148424, #180778, #84727, #58404, #70583, #192935, #120070, #103915, #40238, #118092, #146405, #7895, #9919, #132252, #41251, #102913, #26091, #57423, #54412, #165595, #147428, #193943, #116084, #177772, #87735, #39242, #10916, #27093, #100898, #162582, #85741, #88739, #150433, #55406, #117076, #178772, #101914, #60377, #15879, #136239, #91693, #198909, #197913, #124025, #181758, #107863, #123039, #185723, #47213, #45227, #77537, #122049, #139209, #684, #61368, #153384, #43240, #104907, #106881, #167579, #183740, #14885, #169548, #30052, #154384, #13881, #59383, #31047, #168554, #199904, #76546, #44235, #121056, #75548, #62355, #166595, #29073, #28095, #89734, #151420, #138222, #182751, #184725, #105892, #92696, #90712, #12907, #46209, #152395, #74571, #137223, #120708, #43886, #103576, #162239, #23739, #149084, #116736, #70241, #104563, #135903, #132902, #133911, #148082, #134919, #117740, #42898, #40901, #165251, #85388, #181420, #74234, #26745, #59041, #56061, #180438, #58067, #164258, #166245, #24750, #27746, #10572, #197574, #147082, #41910, #194591, #9573, #86397, #71239, #179435, #182407, #119737, #89389, #88383, #178425, #151077, #8566, #12568, #72235, #131909, #25753, #102574, #101556, #150077, #193593, #55064, #39889, #163248, #87399, #195602, #57075, #118749, #11582, #73249, #196596, #117024, #149370, #88689, #181708, #147373, #55354 ),
 ( #194883, #71525, #85686, #105847, #150385, #101860, #103865, #10866, #163544, #182703, #24032, #43189, #135217, #44188, #121005, #134212, #151372, #72536, #12863, #74528, #11881, #180729, #8862, #70529, #195899, #148371, #164547, #42205, #196889, #57374, #104858, #56357, #178719, #58356, #119047, #73544, #165546, #86687, #40181, #118039, #28046, #132198, #9866, #136193, #59335, #120023, #27043, #193889, #179730, #25044, #166547, #133192, #89687, #41200, #102862, #197868, #26040, #87685, #49155, #108824, #167534, #29029, #154338, #122005, #75502, #109821, #141154, #138176, #139160, #153336, #140149, #122994, #48163, #46163, #170503, #90669, #186693, #79485, #31993, #64319, #61323, #185675, #63318, #169501, #171504, #30009, #32993, #15830, #2643, #152351, #47165, #199857, #14837, #91647, #76500, #184680, #125987, #124998, #94647, #93651, #183696, #156327, #187685, #17827, #77490, #13836, #31000, #107817, #106836, #155336, #137176, #198864, #60331, #45182, #92649, #168511, #637, #62307, #123977, #16825, #78476, #1641, #192650, #190651, #81441, #96623, #34971, #173498, #158312, #69294, #68289, #176490, #52127, #126962, #37966, #7608, #99624, #159291, #157327, #112795, #19800, #50151, #113783, #161305, #142140, #129940, #22800, #189662, #110813, #82443, #66299, #143127, #144131, #51135, #175479, #188671, #130960, #33983, #174489, #65303, #36951, #4607, #127959, #172496, #95639, #98613, #111810, #160307, #35956, #97603, #18822, #80466, #191639, #21797, #3624, #20788, #5613, #84446, #67292, #146124, #128950, #83449, #145126, #6610, #53119, #114797, #178490, #194660, #10642, #26814, #25819, #134988, #86464, #85454, #88454, #179504, #118819, #149152, #116799, #70304, #148149, #58135, #74302, #39957, #104630, #89457, #150150, #87465, #23804, #9640, #147144, #180505, #8632, #103644, #24815, #38966, #72303, #135971, #12637, #54133, #195672, #115806, #177496, #40970, #131973, #162304, #196666, #27816, #71307, #133981, #101628, #11651, #132970, #119804, #56129, #57143, #100622, #73317, #166319, #41977, #151146, #117811, #165322, #181489, #102641, #42967, #163317, #193657, #55129, #164326, #197642, #184450, #152126, #105617, #142642, #173998, #168279, #169263, #183462, #173002, #153099, #80966, #76259, #138922, #59108, #19319, #112308, #62075, #97118, #91411, #15596, #96139, #199621, #4120, #60101, #65799, #45930, #35469, #81937, #77254, #29776, #44948, #121769, #106603, #14603, #158801, #157828, #127468, #403, #13608, #189174, #20290, #50647, #107585, #43955, #61088, #137937, #136946, #123740, #120773, #28801, #182474, #167305, #122760, #90440, #30769, #92416, #154102, #185439, #46929, #111313, #75276, #198635, #34481, #22300, #98106, #23302, #114289, #191152, #5113, #25322, #8120, #21297, #84946, #68793, #82955, #102136, #143628, #101117, #54624, #163821, #40464, #53630, #70804, #130451, #132473, #194163, #131466, #100125, #66795, #128458, #192149, #67798, #83951, #161807, #116300, #115306, #24312, #175991, #174985, #177989, #176998, #69798, #38468, #6115, #159802, #37460, #147650, #190154, #129453, #55627, #178996, #39456, #146628, #113294, #99121, #36449, #193152, #144632, #162803, #160812, #51630, #85961, #52626, #145631, #7111, #9138, #117300, #26314, #45441, #86964, #44454, #198134, #107094, #183954, #197153, #14098, #73813, #75766, #137443, #74791, #43459, #168764, #148650, #135483, #11141, #27313, #105128, #59603, #58618, #167792, #119309, #118313, #121276, #12148, #151634, #181977, #149643, #103137, #180994, #90922, #10138, #72815, #199122, #122265, #182970, #120285, #56640, #42471, #180006, #13129, #41473, #136453, #57643, #71799, #166814, #133468, #195159, #164819, #28315, #87954, #134484, #89954, #196171, #104133, #29292, #60590, #165815, #106107, #88960, #152608, #150650, #111079, #109093, #171769, #30267, #49417, #142412, #94916, #127229, #124257, #48434, #126251, #32261, #34249, #92917, #172769 ) ),
 .UNSPECIFIED., .T., .F., .F. ) 
 B_SPLINE_SURFACE_WITH_KNOTS ( ( 4, 3, 4 ),
 ( 3, 2, 2, 2, 2, 2, 2, 2, 2, 2, 2, 2, 2, 2, 2, 2, 2, 2, 2, 2, 2, 2, 2, 2, 2, 2, 2, 2, 2, 2, 2, 2, 2, 2, 2, 2, 2, 2, 2, 2, 2, 2, 2, 2, 2, 2, 2, 2, 2, 2, 2, 2, 2, 2, 2, 2, 2, 2, 2, 2, 2, 2, 2, 2, 2, 2, 2, 2, 2, 2, 2, 2, 2, 2, 2, 2, 2, 2, 2, 2, 2, 2, 2, 2, 2, 2, 2, 2, 2, 2, 2, 2, 2, 2, 2, 2, 2, 2, 2, 2, 2, 2, 2, 2, 2, 2, 2, 2, 2, 2, 2, 2, 2, 2, 2, 2, 2, 2, 2, 2, 2, 2, 2, 2, 2, 2, 2, 2, 2, 2, 2, 2, 2, 2, 2, 2, 2, 2, 2, 2, 2, 2, 2, 2, 2, 2, 2, 2, 2, 2, 2, 2, 2, 2, 2, 2, 2, 2, 2, 2, 2, 2, 2, 2, 2, 2, 2, 2, 2, 2, 2, 2, 2, 2, 2, 2, 2, 2, 2, 2, 2, 2, 2, 2, 2, 2, 2, 2, 2, 2, 2, 2, 2, 2, 2, 2, 2, 2, 2, 2, 2, 2, 2, 2, 2, 2, 2, 2, 2, 2, 2, 2, 2, 2, 2, 2, 2, 2, 2, 2, 2, 2, 2, 2, 2, 2, 2, 2, 3 ),
 ( 0.000000000000000000, 0.5000000000000000000, 1.000000000000000000 ),
 ( 0.000000000000000000, 0.004385964912280701511, 0.008771929824561403022, 0.01315789473684210453, 0.01754385964912280604, 0.02192982456140350755, 0.02631578947368420907, 0.03070175438596491058, 0.03508771929824561209, 0.03947368421052631360, 0.04385964912280701511, 0.04824561403508771662, 0.05263157894736841813, 0.05701754385964911964, 0.06140350877192982115, 0.06578947368421052266, 0.07017543859649122417, 0.07456140350877192569, 0.07894736842105262720, 0.08333333333333332871, 0.08771929824561403022, 0.09210526315789473173, 0.09649122807017543324, 0.1008771929824561348, 0.1052631578947368363, 0.1096491228070175378, 0.1140350877192982393, 0.1184210526315789408, 0.1228070175438596423, 0.1271929824561403577, 0.1315789473684210453, 0.1359649122807017607, 0.1403508771929824483, 0.1447368421052631637, 0.1491228070175438514, 0.1535087719298245668, 0.1578947368421052544, 0.1622807017543859698, 0.1666666666666666574, 0.1710526315789473728, 0.1754385964912280604, 0.1798245614035087758, 0.1842105263157894635, 0.1885964912280701788, 0.1929824561403508665, 0.1973684210526315819, 0.2017543859649122695, 0.2061403508771929849, 0.2105263157894736725, 0.2149122807017543879, 0.2192982456140350755, 0.2236842105263157909, 0.2280701754385964786, 0.2324561403508771940, 0.2368421052631578816, 0.2412280701754385970, 0.2456140350877192846, 0.2500000000000000000, 0.2543859649122807154, 0.2587719298245614308, 0.2631578947368420907, 0.2675438596491228060, 0.2719298245614035214, 0.2763157894736842368, 0.2807017543859648967, 0.2850877192982456121, 0.2894736842105263275, 0.2938596491228070429, 0.2982456140350877027, 0.3026315789473684181, 0.3070175438596491335, 0.3114035087719298489, 0.3157894736842105088, 0.3201754385964912242, 0.3245614035087719396, 0.3289473684210526550, 0.3333333333333333148, 0.3377192982456140302, 0.3421052631578947456, 0.3464912280701754610, 0.3508771929824561209, 0.3552631578947368363, 0.3596491228070175517, 0.3640350877192982670, 0.3684210526315789269, 0.3728070175438596423, 0.3771929824561403577, 0.3815789473684210731, 0.3859649122807017330, 0.3903508771929824483, 0.3947368421052631637, 0.3991228070175438791, 0.4035087719298245390, 0.4078947368421052544, 0.4122807017543859698, 0.4166666666666666852, 0.4210526315789473450, 0.4254385964912280604, 0.4298245614035087758, 0.4342105263157894912, 0.4385964912280701511, 0.4429824561403508665, 0.4473684210526315819, 0.4517543859649122973, 0.4561403508771929571, 0.4605263157894736725, 0.4649122807017543879, 0.4692982456140351033, 0.4736842105263157632, 0.4780701754385964786, 0.4824561403508771940, 0.4868421052631579093, 0.4912280701754385692, 0.4956140350877192846, 0.5000000000000000000, 0.5043859649122807154, 0.5087719298245614308, 0.5131578947368421462, 0.5175438596491228616, 0.5219298245614034659, 0.5263157894736841813, 0.5307017543859648967, 0.5350877192982456121, 0.5394736842105263275, 0.5438596491228070429, 0.5482456140350877583, 0.5526315789473684736, 0.5570175438596490780, 0.5614035087719297934, 0.5657894736842105088, 0.5701754385964912242, 0.5745614035087719396, 0.5789473684210526550, 0.5833333333333333703, 0.5877192982456140857, 0.5921052631578946901, 0.5964912280701754055, 0.6008771929824561209, 0.6052631578947368363, 0.6096491228070175517, 0.6140350877192982670, 0.6184210526315789824, 0.6228070175438596978, 0.6271929824561403022, 0.6315789473684210176, 0.6359649122807017330, 0.6403508771929824483, 0.6447368421052631637, 0.6491228070175438791, 0.6535087719298245945, 0.6578947368421053099, 0.6622807017543859143, 0.6666666666666666297, 0.6710526315789473450, 0.6754385964912280604, 0.6798245614035087758, 0.6842105263157894912, 0.6885964912280702066, 0.6929824561403509220, 0.6973684210526315264, 0.7017543859649122417, 0.7061403508771929571, 0.7105263157894736725, 0.7149122807017543879, 0.7192982456140351033, 0.7236842105263158187, 0.7280701754385965341, 0.7324561403508771384, 0.7368421052631578538, 0.7412280701754385692, 0.7456140350877192846, 0.7500000000000000000, 0.7543859649122807154, 0.7587719298245614308, 0.7631578947368421462, 0.7675438596491228616, 0.7719298245614034659, 0.7763157894736841813, 0.7807017543859648967, 0.7850877192982456121, 0.7894736842105263275, 0.7938596491228070429, 0.7982456140350877583, 0.8026315789473684736, 0.8070175438596490780, 0.8114035087719297934, 0.8157894736842105088, 0.8201754385964912242, 0.8245614035087719396, 0.8289473684210526550, 0.8333333333333333703, 0.8377192982456140857, 0.8421052631578946901, 0.8464912280701754055, 0.8508771929824561209, 0.8552631578947368363, 0.8596491228070175517, 0.8640350877192982670, 0.8684210526315789824, 0.8728070175438596978, 0.8771929824561403022, 0.8815789473684210176, 0.8859649122807017330, 0.8903508771929824483, 0.8947368421052631637, 0.8991228070175438791, 0.9035087719298245945, 0.9078947368421053099, 0.9122807017543859143, 0.9166666666666666297, 0.9210526315789473450, 0.9254385964912280604, 0.9298245614035087758, 0.9342105263157894912, 0.9385964912280702066, 0.9429824561403509220, 0.9473684210526315264, 0.9517543859649122417, 0.9561403508771929571, 0.9605263157894736725, 0.9649122807017543879, 0.9692982456140351033, 0.9736842105263158187, 0.9780701754385965341, 0.9824561403508771384, 0.9868421052631578538, 0.9912280701754385692, 0.9956140350877192846, 1.000000000000000000 ),
 .UNSPECIFIED. ) 
 GEOMETRIC_REPRESENTATION_ITEM ( )  RATIONAL_B_SPLINE_SURFACE ( (
 ( 1.000000000000000000, 0.9659258262890683122, 1.000000000000000000, 0.9659258262890683122, 1.000000000000000000, 0.9659258262890683122, 1.000000000000000000, 0.9659258262890683122, 1.000000000000000000, 0.9659258262890683122, 1.000000000000000000, 0.9659258262890683122, 1.000000000000000000, 0.9659258262890683122, 1.000000000000000000, 0.9659258262890683122, 1.000000000000000000, 0.9659258262890683122, 1.000000000000000000, 0.9659258262890683122, 1.000000000000000000, 0.9659258262890683122, 1.000000000000000000, 0.9659258262890683122, 1.000000000000000000, 0.9659258262890683122, 1.000000000000000000, 0.9659258262890683122, 1.000000000000000000, 0.9659258262890683122, 1.000000000000000000, 0.9659258262890683122, 1.000000000000000000, 0.9659258262890683122, 1.000000000000000000, 0.9659258262890683122, 1.000000000000000000, 0.9659258262890683122, 1.000000000000000000, 0.9659258262890683122, 1.000000000000000000, 0.9659258262890683122, 1.000000000000000000, 0.9659258262890683122, 1.000000000000000000, 0.9659258262890683122, 1.000000000000000000, 0.9659258262890683122, 1.000000000000000000, 0.9659258262890683122, 1.000000000000000000, 0.9659258262890683122, 1.000000000000000000, 0.9659258262890683122, 1.000000000000000000, 0.9659258262890683122, 1.000000000000000000, 0.9659258262890683122, 1.000000000000000000, 0.9659258262890683122, 1.000000000000000000, 0.9659258262890683122, 1.000000000000000000, 0.9659258262890683122, 1.000000000000000000, 0.9659258262890683122, 1.000000000000000000, 0.9659258262890683122, 1.000000000000000000, 0.9659258262890683122, 1.000000000000000000, 0.9659258262890683122, 1.000000000000000000, 0.9659258262890683122, 1.000000000000000000, 0.9659258262890683122, 1.000000000000000000, 0.9659258262890683122, 1.000000000000000000, 0.9659258262890683122, 1.000000000000000000, 0.9659258262890683122, 1.000000000000000000, 0.9659258262890683122, 1.000000000000000000, 0.9659258262890683122, 1.000000000000000000, 0.9659258262890683122, 1.000000000000000000, 0.9659258262890683122, 1.000000000000000000, 0.9659258262890683122, 1.000000000000000000, 0.9659258262890683122, 1.000000000000000000, 0.9659258262890683122, 1.000000000000000000, 0.9659258262890683122, 1.000000000000000000, 0.9659258262890683122, 1.000000000000000000, 0.9659258262890683122, 1.000000000000000000, 0.9659258262890683122, 1.000000000000000000, 0.9659258262890683122, 1.000000000000000000, 0.9659258262890683122, 1.000000000000000000, 0.9659258262890683122, 1.000000000000000000, 0.9659258262890683122, 1.000000000000000000, 0.9659258262890683122, 1.000000000000000000, 0.9659258262890683122, 1.000000000000000000, 0.9659258262890683122, 1.000000000000000000, 0.9659258262890683122, 1.000000000000000000, 0.9659258262890683122, 1.000000000000000000, 0.9659258262890683122, 1.000000000000000000, 0.9659258262890683122, 1.000000000000000000, 0.9659258262890683122, 1.000000000000000000, 0.9659258262890683122, 1.000000000000000000, 0.9659258262890683122, 1.000000000000000000, 0.9659258262890683122, 1.000000000000000000, 0.9659258262890683122, 1.000000000000000000, 0.9659258262890683122, 1.000000000000000000, 0.9659258262890683122, 1.000000000000000000, 0.9659258262890683122, 1.000000000000000000, 0.9659258262890683122, 1.000000000000000000, 0.9659258262890683122, 1.000000000000000000, 0.9659258262890683122, 1.000000000000000000, 0.9659258262890683122, 1.000000000000000000, 0.9659258262890683122, 1.000000000000000000, 0.9659258262890683122, 1.000000000000000000, 0.9659258262890683122, 1.000000000000000000, 0.9659258262890683122, 1.000000000000000000, 0.9659258262890683122, 1.000000000000000000, 0.9659258262890683122, 1.000000000000000000, 0.9659258262890683122, 1.000000000000000000, 0.9659258262890683122, 1.000000000000000000, 0.9659258262890683122, 1.000000000000000000, 0.9659258262890683122, 1.000000000000000000, 0.9659258262890683122, 1.000000000000000000, 0.9659258262890683122, 1.000000000000000000, 0.9659258262890683122, 1.000000000000000000, 0.9659258262890683122, 1.000000000000000000, 0.9659258262890683122, 1.000000000000000000, 0.9659258262890683122, 1.000000000000000000, 0.9659258262890683122, 1.000000000000000000, 0.9659258262890683122, 1.000000000000000000, 0.9659258262890683122, 1.000000000000000000, 0.9659258262890683122, 1.000000000000000000, 0.9659258262890683122, 1.000000000000000000, 0.9659258262890683122, 1.000000000000000000, 0.9659258262890683122, 1.000000000000000000, 0.9659258262890683122, 1.000000000000000000, 0.9659258262890683122, 1.000000000000000000, 0.9659258262890683122, 1.000000000000000000, 0.9659258262890683122, 1.000000000000000000, 0.9659258262890683122, 1.000000000000000000, 0.9659258262890683122, 1.000000000000000000, 0.9659258262890683122, 1.000000000000000000, 0.9659258262890683122, 1.000000000000000000, 0.9659258262890683122, 1.000000000000000000, 0.9659258262890683122, 1.000000000000000000, 0.9659258262890683122, 1.000000000000000000, 0.9659258262890683122, 1.000000000000000000, 0.9659258262890683122, 1.000000000000000000, 0.9659258262890683122, 1.000000000000000000, 0.9659258262890683122, 1.000000000000000000, 0.9659258262890683122, 1.000000000000000000, 0.9659258262890683122, 1.000000000000000000, 0.9659258262890683122, 1.000000000000000000, 0.9659258262890683122, 1.000000000000000000, 0.9659258262890683122, 1.000000000000000000, 0.9659258262890683122, 1.000000000000000000, 0.9659258262890683122, 1.000000000000000000, 0.9659258262890683122, 1.000000000000000000, 0.9659258262890683122, 1.000000000000000000, 0.9659258262890683122, 1.000000000000000000, 0.9659258262890683122, 1.000000000000000000, 0.9659258262890683122, 1.000000000000000000, 0.9659258262890683122, 1.000000000000000000, 0.9659258262890683122, 1.000000000000000000, 0.9659258262890683122, 1.000000000000000000, 0.9659258262890683122, 1.000000000000000000, 0.9659258262890683122, 1.000000000000000000, 0.9659258262890683122, 1.000000000000000000, 0.9659258262890683122, 1.000000000000000000, 0.9659258262890683122, 1.000000000000000000, 0.9659258262890683122, 1.000000000000000000, 0.9659258262890683122, 1.000000000000000000, 0.9659258262890683122, 1.000000000000000000, 0.9659258262890683122, 1.000000000000000000, 0.9659258262890683122, 1.000000000000000000, 0.9659258262890683122, 1.000000000000000000, 0.9659258262890683122, 1.000000000000000000, 0.9659258262890683122, 1.000000000000000000, 0.9659258262890683122, 1.000000000000000000, 0.9659258262890683122, 1.000000000000000000, 0.9659258262890683122, 1.000000000000000000, 0.9659258262890683122, 1.000000000000000000, 0.9659258262890683122, 1.000000000000000000, 0.9659258262890683122, 1.000000000000000000, 0.9659258262890683122, 1.000000000000000000, 0.9659258262890683122, 1.000000000000000000, 0.9659258262890683122, 1.000000000000000000, 0.9659258262890683122, 1.000000000000000000, 0.9659258262890683122, 1.000000000000000000, 0.9659258262890683122, 1.000000000000000000, 0.9659258262890683122, 1.000000000000000000, 0.9659258262890683122, 1.000000000000000000, 0.9659258262890683122, 1.000000000000000000, 0.9659258262890683122, 1.000000000000000000, 0.9659258262890683122, 1.000000000000000000, 0.9659258262890683122, 1.000000000000000000, 0.9659258262890683122, 1.000000000000000000, 0.9659258262890683122, 1.000000000000000000, 0.9659258262890683122, 1.000000000000000000, 0.9659258262890683122, 1.000000000000000000, 0.9659258262890683122, 1.000000000000000000, 0.9659258262890683122, 1.000000000000000000, 0.9659258262890683122, 1.000000000000000000, 0.9659258262890683122, 1.000000000000000000, 0.9659258262890683122, 1.000000000000000000, 0.9659258262890683122, 1.000000000000000000, 0.9659258262890683122, 1.000000000000000000, 0.9659258262890683122, 1.000000000000000000, 0.9659258262890683122, 1.000000000000000000, 0.9659258262890683122, 1.000000000000000000, 0.9659258262890683122, 1.000000000000000000, 0.9659258262890683122, 1.000000000000000000, 0.9659258262890683122, 1.000000000000000000, 0.9659258262890683122, 1.000000000000000000, 0.9659258262890683122, 1.000000000000000000, 0.9659258262890683122, 1.000000000000000000, 0.9659258262890683122, 1.000000000000000000, 0.9659258262890683122, 1.000000000000000000, 0.9659258262890683122, 1.000000000000000000, 0.9659258262890683122, 1.000000000000000000, 0.9659258262890683122, 1.000000000000000000, 0.9659258262890683122, 1.000000000000000000, 0.9659258262890683122, 1.000000000000000000, 0.9659258262890683122, 1.000000000000000000, 0.9659258262890683122, 1.000000000000000000, 0.9659258262890683122, 1.000000000000000000, 0.9659258262890683122, 1.000000000000000000, 0.9659258262890683122, 1.000000000000000000, 0.9659258262890683122, 1.000000000000000000, 0.9659258262890683122, 1.000000000000000000, 0.9659258262890683122, 1.000000000000000000, 0.9659258262890683122, 1.000000000000000000, 0.9659258262890683122, 1.000000000000000000, 0.9659258262890683122, 1.000000000000000000, 0.9659258262890683122, 1.000000000000000000, 0.9659258262890683122, 1.000000000000000000, 0.9659258262890683122, 1.000000000000000000, 0.9659258262890683122, 1.000000000000000000, 0.9659258262890683122, 1.000000000000000000, 0.9659258262890683122, 1.000000000000000000, 0.9659258262890683122, 1.000000000000000000, 0.9659258262890683122, 1.000000000000000000, 0.9659258262890683122, 1.000000000000000000, 0.9659258262890683122, 1.000000000000000000, 0.9659258262890683122, 1.000000000000000000, 0.9659258262890683122, 1.000000000000000000, 0.9659258262890683122, 1.000000000000000000, 0.9659258262890683122, 1.000000000000000000, 0.9659258262890683122, 1.000000000000000000, 0.9659258262890683122, 1.000000000000000000, 0.9659258262890683122, 1.000000000000000000, 0.9659258262890683122, 1.000000000000000000, 0.9659258262890683122, 1.000000000000000000, 0.9659258262890683122, 1.000000000000000000, 0.9659258262890683122, 1.000000000000000000, 0.9659258262890683122, 1.000000000000000000, 0.9659258262890683122, 1.000000000000000000, 0.9659258262890683122, 1.000000000000000000, 0.9659258262890683122, 1.000000000000000000, 0.9659258262890683122, 1.000000000000000000, 0.9659258262890683122, 1.000000000000000000, 0.9659258262890683122, 1.000000000000000000, 0.9659258262890683122, 1.000000000000000000, 0.9659258262890683122, 1.000000000000000000, 0.9659258262890683122, 1.000000000000000000),
 ( 0.3333333333333333703, 0.3219752754296894559, 0.3333333333333333703, 0.3219752754296894559, 0.3333333333333333703, 0.3219752754296894559, 0.3333333333333333703, 0.3219752754296894559, 0.3333333333333333703, 0.3219752754296894559, 0.3333333333333333703, 0.3219752754296894559, 0.3333333333333333703, 0.3219752754296894559, 0.3333333333333333703, 0.3219752754296894559, 0.3333333333333333703, 0.3219752754296894559, 0.3333333333333333703, 0.3219752754296894559, 0.3333333333333333703, 0.3219752754296894559, 0.3333333333333333703, 0.3219752754296894559, 0.3333333333333333703, 0.3219752754296894559, 0.3333333333333333703, 0.3219752754296894559, 0.3333333333333333703, 0.3219752754296894559, 0.3333333333333333703, 0.3219752754296894559, 0.3333333333333333703, 0.3219752754296894559, 0.3333333333333333703, 0.3219752754296894559, 0.3333333333333333703, 0.3219752754296894559, 0.3333333333333333703, 0.3219752754296894559, 0.3333333333333333703, 0.3219752754296894559, 0.3333333333333333703, 0.3219752754296894559, 0.3333333333333333703, 0.3219752754296894559, 0.3333333333333333703, 0.3219752754296894559, 0.3333333333333333703, 0.3219752754296894559, 0.3333333333333333703, 0.3219752754296894559, 0.3333333333333333703, 0.3219752754296894559, 0.3333333333333333703, 0.3219752754296894559, 0.3333333333333333703, 0.3219752754296894559, 0.3333333333333333703, 0.3219752754296894559, 0.3333333333333333703, 0.3219752754296894559, 0.3333333333333333703, 0.3219752754296894559, 0.3333333333333333703, 0.3219752754296894559, 0.3333333333333333703, 0.3219752754296894559, 0.3333333333333333703, 0.3219752754296894559, 0.3333333333333333703, 0.3219752754296894559, 0.3333333333333333703, 0.3219752754296894559, 0.3333333333333333703, 0.3219752754296894559, 0.3333333333333333703, 0.3219752754296894559, 0.3333333333333333703, 0.3219752754296894559, 0.3333333333333333703, 0.3219752754296894559, 0.3333333333333333703, 0.3219752754296894559, 0.3333333333333333703, 0.3219752754296894559, 0.3333333333333333703, 0.3219752754296894559, 0.3333333333333333703, 0.3219752754296894559, 0.3333333333333333703, 0.3219752754296894559, 0.3333333333333333703, 0.3219752754296894559, 0.3333333333333333703, 0.3219752754296894559, 0.3333333333333333703, 0.3219752754296894559, 0.3333333333333333703, 0.3219752754296894559, 0.3333333333333333703, 0.3219752754296894559, 0.3333333333333333703, 0.3219752754296894559, 0.3333333333333333703, 0.3219752754296894559, 0.3333333333333333703, 0.3219752754296894559, 0.3333333333333333703, 0.3219752754296894559, 0.3333333333333333703, 0.3219752754296894559, 0.3333333333333333703, 0.3219752754296894559, 0.3333333333333333703, 0.3219752754296894559, 0.3333333333333333703, 0.3219752754296894559, 0.3333333333333333703, 0.3219752754296894559, 0.3333333333333333703, 0.3219752754296894559, 0.3333333333333333703, 0.3219752754296894559, 0.3333333333333333703, 0.3219752754296894559, 0.3333333333333333703, 0.3219752754296894559, 0.3333333333333333703, 0.3219752754296894559, 0.3333333333333333703, 0.3219752754296894559, 0.3333333333333333703, 0.3219752754296894559, 0.3333333333333333703, 0.3219752754296894559, 0.3333333333333333703, 0.3219752754296894559, 0.3333333333333333703, 0.3219752754296894559, 0.3333333333333333703, 0.3219752754296894559, 0.3333333333333333703, 0.3219752754296894559, 0.3333333333333333703, 0.3219752754296894559, 0.3333333333333333703, 0.3219752754296894559, 0.3333333333333333703, 0.3219752754296894559, 0.3333333333333333703, 0.3219752754296894559, 0.3333333333333333703, 0.3219752754296894559, 0.3333333333333333703, 0.3219752754296894559, 0.3333333333333333703, 0.3219752754296894559, 0.3333333333333333703, 0.3219752754296894559, 0.3333333333333333703, 0.3219752754296894559, 0.3333333333333333703, 0.3219752754296894559, 0.3333333333333333703, 0.3219752754296894559, 0.3333333333333333703, 0.3219752754296894559, 0.3333333333333333703, 0.3219752754296894559, 0.3333333333333333703, 0.3219752754296894559, 0.3333333333333333703, 0.3219752754296894559, 0.3333333333333333703, 0.3219752754296894559, 0.3333333333333333703, 0.3219752754296894559, 0.3333333333333333703, 0.3219752754296894559, 0.3333333333333333703, 0.3219752754296894559, 0.3333333333333333703, 0.3219752754296894559, 0.3333333333333333703, 0.3219752754296894559, 0.3333333333333333703, 0.3219752754296894559, 0.3333333333333333703, 0.3219752754296894559, 0.3333333333333333703, 0.3219752754296894559, 0.3333333333333333703, 0.3219752754296894559, 0.3333333333333333703, 0.3219752754296894559, 0.3333333333333333703, 0.3219752754296894559, 0.3333333333333333703, 0.3219752754296894559, 0.3333333333333333703, 0.3219752754296894559, 0.3333333333333333703, 0.3219752754296894559, 0.3333333333333333703, 0.3219752754296894559, 0.3333333333333333703, 0.3219752754296894559, 0.3333333333333333703, 0.3219752754296894559, 0.3333333333333333703, 0.3219752754296894559, 0.3333333333333333703, 0.3219752754296894559, 0.3333333333333333703, 0.3219752754296894559, 0.3333333333333333703, 0.3219752754296894559, 0.3333333333333333703, 0.3219752754296894559, 0.3333333333333333703, 0.3219752754296894559, 0.3333333333333333703, 0.3219752754296894559, 0.3333333333333333703, 0.3219752754296894559, 0.3333333333333333703, 0.3219752754296894559, 0.3333333333333333703, 0.3219752754296894559, 0.3333333333333333703, 0.3219752754296894559, 0.3333333333333333703, 0.3219752754296894559, 0.3333333333333333703, 0.3219752754296894559, 0.3333333333333333703, 0.3219752754296894559, 0.3333333333333333703, 0.3219752754296894559, 0.3333333333333333703, 0.3219752754296894559, 0.3333333333333333703, 0.3219752754296894559, 0.3333333333333333703, 0.3219752754296894559, 0.3333333333333333703, 0.3219752754296894559, 0.3333333333333333703, 0.3219752754296894559, 0.3333333333333333703, 0.3219752754296894559, 0.3333333333333333703, 0.3219752754296894559, 0.3333333333333333703, 0.3219752754296894559, 0.3333333333333333703, 0.3219752754296894559, 0.3333333333333333703, 0.3219752754296894559, 0.3333333333333333703, 0.3219752754296894559, 0.3333333333333333703, 0.3219752754296894559, 0.3333333333333333703, 0.3219752754296894559, 0.3333333333333333703, 0.3219752754296894559, 0.3333333333333333703, 0.3219752754296894559, 0.3333333333333333703, 0.3219752754296894559, 0.3333333333333333703, 0.3219752754296894559, 0.3333333333333333703, 0.3219752754296894559, 0.3333333333333333703, 0.3219752754296894559, 0.3333333333333333703, 0.3219752754296894559, 0.3333333333333333703, 0.3219752754296894559, 0.3333333333333333703, 0.3219752754296894559, 0.3333333333333333703, 0.3219752754296894559, 0.3333333333333333703, 0.3219752754296894559, 0.3333333333333333703, 0.3219752754296894559, 0.3333333333333333703, 0.3219752754296894559, 0.3333333333333333703, 0.3219752754296894559, 0.3333333333333333703, 0.3219752754296894559, 0.3333333333333333703, 0.3219752754296894559, 0.3333333333333333703, 0.3219752754296894559, 0.3333333333333333703, 0.3219752754296894559, 0.3333333333333333703, 0.3219752754296894559, 0.3333333333333333703, 0.3219752754296894559, 0.3333333333333333703, 0.3219752754296894559, 0.3333333333333333703, 0.3219752754296894559, 0.3333333333333333703, 0.3219752754296894559, 0.3333333333333333703, 0.3219752754296894559, 0.3333333333333333703, 0.3219752754296894559, 0.3333333333333333703, 0.3219752754296894559, 0.3333333333333333703, 0.3219752754296894559, 0.3333333333333333703, 0.3219752754296894559, 0.3333333333333333703, 0.3219752754296894559, 0.3333333333333333703, 0.3219752754296894559, 0.3333333333333333703, 0.3219752754296894559, 0.3333333333333333703, 0.3219752754296894559, 0.3333333333333333703, 0.3219752754296894559, 0.3333333333333333703, 0.3219752754296894559, 0.3333333333333333703, 0.3219752754296894559, 0.3333333333333333703, 0.3219752754296894559, 0.3333333333333333703, 0.3219752754296894559, 0.3333333333333333703, 0.3219752754296894559, 0.3333333333333333703, 0.3219752754296894559, 0.3333333333333333703, 0.3219752754296894559, 0.3333333333333333703, 0.3219752754296894559, 0.3333333333333333703, 0.3219752754296894559, 0.3333333333333333703, 0.3219752754296894559, 0.3333333333333333703, 0.3219752754296894559, 0.3333333333333333703, 0.3219752754296894559, 0.3333333333333333703, 0.3219752754296894559, 0.3333333333333333703, 0.3219752754296894559, 0.3333333333333333703, 0.3219752754296894559, 0.3333333333333333703, 0.3219752754296894559, 0.3333333333333333703, 0.3219752754296894559, 0.3333333333333333703, 0.3219752754296894559, 0.3333333333333333703, 0.3219752754296894559, 0.3333333333333333703, 0.3219752754296894559, 0.3333333333333333703, 0.3219752754296894559, 0.3333333333333333703, 0.3219752754296894559, 0.3333333333333333703, 0.3219752754296894559, 0.3333333333333333703, 0.3219752754296894559, 0.3333333333333333703, 0.3219752754296894559, 0.3333333333333333703, 0.3219752754296894559, 0.3333333333333333703, 0.3219752754296894559, 0.3333333333333333703, 0.3219752754296894559, 0.3333333333333333703, 0.3219752754296894559, 0.3333333333333333703, 0.3219752754296894559, 0.3333333333333333703, 0.3219752754296894559, 0.3333333333333333703, 0.3219752754296894559, 0.3333333333333333703, 0.3219752754296894559, 0.3333333333333333703, 0.3219752754296894559, 0.3333333333333333703, 0.3219752754296894559, 0.3333333333333333703, 0.3219752754296894559, 0.3333333333333333703, 0.3219752754296894559, 0.3333333333333333703, 0.3219752754296894559, 0.3333333333333333703, 0.3219752754296894559, 0.3333333333333333703, 0.3219752754296894559, 0.3333333333333333703, 0.3219752754296894559, 0.3333333333333333703, 0.3219752754296894559, 0.3333333333333333703, 0.3219752754296894559, 0.3333333333333333703, 0.3219752754296894559, 0.3333333333333333703, 0.3219752754296894559, 0.3333333333333333703, 0.3219752754296894559, 0.3333333333333333703, 0.3219752754296894559, 0.3333333333333333703, 0.3219752754296894559, 0.3333333333333333703, 0.3219752754296894559, 0.3333333333333333703, 0.3219752754296894559, 0.3333333333333333703, 0.3219752754296894559, 0.3333333333333333703, 0.3219752754296894559, 0.3333333333333333703, 0.3219752754296894559, 0.3333333333333333703, 0.3219752754296894559, 0.3333333333333333703, 0.3219752754296894559, 0.3333333333333333703, 0.3219752754296894559, 0.3333333333333333703, 0.3219752754296894559, 0.3333333333333333703, 0.3219752754296894559, 0.3333333333333333703, 0.3219752754296894559, 0.3333333333333333703, 0.3219752754296894559, 0.3333333333333333703, 0.3219752754296894559, 0.3333333333333333703, 0.3219752754296894559, 0.3333333333333333703),
 ( 0.3333333333333333703, 0.3219752754296894559, 0.3333333333333333703, 0.3219752754296894559, 0.3333333333333333703, 0.3219752754296894559, 0.3333333333333333703, 0.3219752754296894559, 0.3333333333333333703, 0.3219752754296894559, 0.3333333333333333703, 0.3219752754296894559, 0.3333333333333333703, 0.3219752754296894559, 0.3333333333333333703, 0.3219752754296894559, 0.3333333333333333703, 0.3219752754296894559, 0.3333333333333333703, 0.3219752754296894559, 0.3333333333333333703, 0.3219752754296894559, 0.3333333333333333703, 0.3219752754296894559, 0.3333333333333333703, 0.3219752754296894559, 0.3333333333333333703, 0.3219752754296894559, 0.3333333333333333703, 0.3219752754296894559, 0.3333333333333333703, 0.3219752754296894559, 0.3333333333333333703, 0.3219752754296894559, 0.3333333333333333703, 0.3219752754296894559, 0.3333333333333333703, 0.3219752754296894559, 0.3333333333333333703, 0.3219752754296894559, 0.3333333333333333703, 0.3219752754296894559, 0.3333333333333333703, 0.3219752754296894559, 0.3333333333333333703, 0.3219752754296894559, 0.3333333333333333703, 0.3219752754296894559, 0.3333333333333333703, 0.3219752754296894559, 0.3333333333333333703, 0.3219752754296894559, 0.3333333333333333703, 0.3219752754296894559, 0.3333333333333333703, 0.3219752754296894559, 0.3333333333333333703, 0.3219752754296894559, 0.3333333333333333703, 0.3219752754296894559, 0.3333333333333333703, 0.3219752754296894559, 0.3333333333333333703, 0.3219752754296894559, 0.3333333333333333703, 0.3219752754296894559, 0.3333333333333333703, 0.3219752754296894559, 0.3333333333333333703, 0.3219752754296894559, 0.3333333333333333703, 0.3219752754296894559, 0.3333333333333333703, 0.3219752754296894559, 0.3333333333333333703, 0.3219752754296894559, 0.3333333333333333703, 0.3219752754296894559, 0.3333333333333333703, 0.3219752754296894559, 0.3333333333333333703, 0.3219752754296894559, 0.3333333333333333703, 0.3219752754296894559, 0.3333333333333333703, 0.3219752754296894559, 0.3333333333333333703, 0.3219752754296894559, 0.3333333333333333703, 0.3219752754296894559, 0.3333333333333333703, 0.3219752754296894559, 0.3333333333333333703, 0.3219752754296894559, 0.3333333333333333703, 0.3219752754296894559, 0.3333333333333333703, 0.3219752754296894559, 0.3333333333333333703, 0.3219752754296894559, 0.3333333333333333703, 0.3219752754296894559, 0.3333333333333333703, 0.3219752754296894559, 0.3333333333333333703, 0.3219752754296894559, 0.3333333333333333703, 0.3219752754296894559, 0.3333333333333333703, 0.3219752754296894559, 0.3333333333333333703, 0.3219752754296894559, 0.3333333333333333703, 0.3219752754296894559, 0.3333333333333333703, 0.3219752754296894559, 0.3333333333333333703, 0.3219752754296894559, 0.3333333333333333703, 0.3219752754296894559, 0.3333333333333333703, 0.3219752754296894559, 0.3333333333333333703, 0.3219752754296894559, 0.3333333333333333703, 0.3219752754296894559, 0.3333333333333333703, 0.3219752754296894559, 0.3333333333333333703, 0.3219752754296894559, 0.3333333333333333703, 0.3219752754296894559, 0.3333333333333333703, 0.3219752754296894559, 0.3333333333333333703, 0.3219752754296894559, 0.3333333333333333703, 0.3219752754296894559, 0.3333333333333333703, 0.3219752754296894559, 0.3333333333333333703, 0.3219752754296894559, 0.3333333333333333703, 0.3219752754296894559, 0.3333333333333333703, 0.3219752754296894559, 0.3333333333333333703, 0.3219752754296894559, 0.3333333333333333703, 0.3219752754296894559, 0.3333333333333333703, 0.3219752754296894559, 0.3333333333333333703, 0.3219752754296894559, 0.3333333333333333703, 0.3219752754296894559, 0.3333333333333333703, 0.3219752754296894559, 0.3333333333333333703, 0.3219752754296894559, 0.3333333333333333703, 0.3219752754296894559, 0.3333333333333333703, 0.3219752754296894559, 0.3333333333333333703, 0.3219752754296894559, 0.3333333333333333703, 0.3219752754296894559, 0.3333333333333333703, 0.3219752754296894559, 0.3333333333333333703, 0.3219752754296894559, 0.3333333333333333703, 0.3219752754296894559, 0.3333333333333333703, 0.3219752754296894559, 0.3333333333333333703, 0.3219752754296894559, 0.3333333333333333703, 0.3219752754296894559, 0.3333333333333333703, 0.3219752754296894559, 0.3333333333333333703, 0.3219752754296894559, 0.3333333333333333703, 0.3219752754296894559, 0.3333333333333333703, 0.3219752754296894559, 0.3333333333333333703, 0.3219752754296894559, 0.3333333333333333703, 0.3219752754296894559, 0.3333333333333333703, 0.3219752754296894559, 0.3333333333333333703, 0.3219752754296894559, 0.3333333333333333703, 0.3219752754296894559, 0.3333333333333333703, 0.3219752754296894559, 0.3333333333333333703, 0.3219752754296894559, 0.3333333333333333703, 0.3219752754296894559, 0.3333333333333333703, 0.3219752754296894559, 0.3333333333333333703, 0.3219752754296894559, 0.3333333333333333703, 0.3219752754296894559, 0.3333333333333333703, 0.3219752754296894559, 0.3333333333333333703, 0.3219752754296894559, 0.3333333333333333703, 0.3219752754296894559, 0.3333333333333333703, 0.3219752754296894559, 0.3333333333333333703, 0.3219752754296894559, 0.3333333333333333703, 0.3219752754296894559, 0.3333333333333333703, 0.3219752754296894559, 0.3333333333333333703, 0.3219752754296894559, 0.3333333333333333703, 0.3219752754296894559, 0.3333333333333333703, 0.3219752754296894559, 0.3333333333333333703, 0.3219752754296894559, 0.3333333333333333703, 0.3219752754296894559, 0.3333333333333333703, 0.3219752754296894559, 0.3333333333333333703, 0.3219752754296894559, 0.3333333333333333703, 0.3219752754296894559, 0.3333333333333333703, 0.3219752754296894559, 0.3333333333333333703, 0.3219752754296894559, 0.3333333333333333703, 0.3219752754296894559, 0.3333333333333333703, 0.3219752754296894559, 0.3333333333333333703, 0.3219752754296894559, 0.3333333333333333703, 0.3219752754296894559, 0.3333333333333333703, 0.3219752754296894559, 0.3333333333333333703, 0.3219752754296894559, 0.3333333333333333703, 0.3219752754296894559, 0.3333333333333333703, 0.3219752754296894559, 0.3333333333333333703, 0.3219752754296894559, 0.3333333333333333703, 0.3219752754296894559, 0.3333333333333333703, 0.3219752754296894559, 0.3333333333333333703, 0.3219752754296894559, 0.3333333333333333703, 0.3219752754296894559, 0.3333333333333333703, 0.3219752754296894559, 0.3333333333333333703, 0.3219752754296894559, 0.3333333333333333703, 0.3219752754296894559, 0.3333333333333333703, 0.3219752754296894559, 0.3333333333333333703, 0.3219752754296894559, 0.3333333333333333703, 0.3219752754296894559, 0.3333333333333333703, 0.3219752754296894559, 0.3333333333333333703, 0.3219752754296894559, 0.3333333333333333703, 0.3219752754296894559, 0.3333333333333333703, 0.3219752754296894559, 0.3333333333333333703, 0.3219752754296894559, 0.3333333333333333703, 0.3219752754296894559, 0.3333333333333333703, 0.3219752754296894559, 0.3333333333333333703, 0.3219752754296894559, 0.3333333333333333703, 0.3219752754296894559, 0.3333333333333333703, 0.3219752754296894559, 0.3333333333333333703, 0.3219752754296894559, 0.3333333333333333703, 0.3219752754296894559, 0.3333333333333333703, 0.3219752754296894559, 0.3333333333333333703, 0.3219752754296894559, 0.3333333333333333703, 0.3219752754296894559, 0.3333333333333333703, 0.3219752754296894559, 0.3333333333333333703, 0.3219752754296894559, 0.3333333333333333703, 0.3219752754296894559, 0.3333333333333333703, 0.3219752754296894559, 0.3333333333333333703, 0.3219752754296894559, 0.3333333333333333703, 0.3219752754296894559, 0.3333333333333333703, 0.3219752754296894559, 0.3333333333333333703, 0.3219752754296894559, 0.3333333333333333703, 0.3219752754296894559, 0.3333333333333333703, 0.3219752754296894559, 0.3333333333333333703, 0.3219752754296894559, 0.3333333333333333703, 0.3219752754296894559, 0.3333333333333333703, 0.3219752754296894559, 0.3333333333333333703, 0.3219752754296894559, 0.3333333333333333703, 0.3219752754296894559, 0.3333333333333333703, 0.3219752754296894559, 0.3333333333333333703, 0.3219752754296894559, 0.3333333333333333703, 0.3219752754296894559, 0.3333333333333333703, 0.3219752754296894559, 0.3333333333333333703, 0.3219752754296894559, 0.3333333333333333703, 0.3219752754296894559, 0.3333333333333333703, 0.3219752754296894559, 0.3333333333333333703, 0.3219752754296894559, 0.3333333333333333703, 0.3219752754296894559, 0.3333333333333333703, 0.3219752754296894559, 0.3333333333333333703, 0.3219752754296894559, 0.3333333333333333703, 0.3219752754296894559, 0.3333333333333333703, 0.3219752754296894559, 0.3333333333333333703, 0.3219752754296894559, 0.3333333333333333703, 0.3219752754296894559, 0.3333333333333333703, 0.3219752754296894559, 0.3333333333333333703, 0.3219752754296894559, 0.3333333333333333703, 0.3219752754296894559, 0.3333333333333333703, 0.3219752754296894559, 0.3333333333333333703, 0.3219752754296894559, 0.3333333333333333703, 0.3219752754296894559, 0.3333333333333333703, 0.3219752754296894559, 0.3333333333333333703, 0.3219752754296894559, 0.3333333333333333703, 0.3219752754296894559, 0.3333333333333333703, 0.3219752754296894559, 0.3333333333333333703, 0.3219752754296894559, 0.3333333333333333703, 0.3219752754296894559, 0.3333333333333333703, 0.3219752754296894559, 0.3333333333333333703, 0.3219752754296894559, 0.3333333333333333703, 0.3219752754296894559, 0.3333333333333333703, 0.3219752754296894559, 0.3333333333333333703, 0.3219752754296894559, 0.3333333333333333703, 0.3219752754296894559, 0.3333333333333333703, 0.3219752754296894559, 0.3333333333333333703, 0.3219752754296894559, 0.3333333333333333703, 0.3219752754296894559, 0.3333333333333333703, 0.3219752754296894559, 0.3333333333333333703, 0.3219752754296894559, 0.3333333333333333703, 0.3219752754296894559, 0.3333333333333333703, 0.3219752754296894559, 0.3333333333333333703, 0.3219752754296894559, 0.3333333333333333703, 0.3219752754296894559, 0.3333333333333333703, 0.3219752754296894559, 0.3333333333333333703, 0.3219752754296894559, 0.3333333333333333703, 0.3219752754296894559, 0.3333333333333333703, 0.3219752754296894559, 0.3333333333333333703, 0.3219752754296894559, 0.3333333333333333703, 0.3219752754296894559, 0.3333333333333333703, 0.3219752754296894559, 0.3333333333333333703, 0.3219752754296894559, 0.3333333333333333703, 0.3219752754296894559, 0.3333333333333333703, 0.3219752754296894559, 0.3333333333333333703, 0.3219752754296894559, 0.3333333333333333703, 0.3219752754296894559, 0.3333333333333333703, 0.3219752754296894559, 0.3333333333333333703, 0.3219752754296894559, 0.3333333333333333703, 0.3219752754296894559, 0.3333333333333333703),
 ( 1.000000000000000000, 0.9659258262890683122, 1.000000000000000000, 0.9659258262890683122, 1.000000000000000000, 0.9659258262890683122, 1.000000000000000000, 0.9659258262890683122, 1.000000000000000000, 0.9659258262890683122, 1.000000000000000000, 0.9659258262890683122, 1.000000000000000000, 0.9659258262890683122, 1.000000000000000000, 0.9659258262890683122, 1.000000000000000000, 0.9659258262890683122, 1.000000000000000000, 0.9659258262890683122, 1.000000000000000000, 0.9659258262890683122, 1.000000000000000000, 0.9659258262890683122, 1.000000000000000000, 0.9659258262890683122, 1.000000000000000000, 0.9659258262890683122, 1.000000000000000000, 0.9659258262890683122, 1.000000000000000000, 0.9659258262890683122, 1.000000000000000000, 0.9659258262890683122, 1.000000000000000000, 0.9659258262890683122, 1.000000000000000000, 0.9659258262890683122, 1.000000000000000000, 0.9659258262890683122, 1.000000000000000000, 0.9659258262890683122, 1.000000000000000000, 0.9659258262890683122, 1.000000000000000000, 0.9659258262890683122, 1.000000000000000000, 0.9659258262890683122, 1.000000000000000000, 0.9659258262890683122, 1.000000000000000000, 0.9659258262890683122, 1.000000000000000000, 0.9659258262890683122, 1.000000000000000000, 0.9659258262890683122, 1.000000000000000000, 0.9659258262890683122, 1.000000000000000000, 0.9659258262890683122, 1.000000000000000000, 0.9659258262890683122, 1.000000000000000000, 0.9659258262890683122, 1.000000000000000000, 0.9659258262890683122, 1.000000000000000000, 0.9659258262890683122, 1.000000000000000000, 0.9659258262890683122, 1.000000000000000000, 0.9659258262890683122, 1.000000000000000000, 0.9659258262890683122, 1.000000000000000000, 0.9659258262890683122, 1.000000000000000000, 0.9659258262890683122, 1.000000000000000000, 0.9659258262890683122, 1.000000000000000000, 0.9659258262890683122, 1.000000000000000000, 0.9659258262890683122, 1.000000000000000000, 0.9659258262890683122, 1.000000000000000000, 0.9659258262890683122, 1.000000000000000000, 0.9659258262890683122, 1.000000000000000000, 0.9659258262890683122, 1.000000000000000000, 0.9659258262890683122, 1.000000000000000000, 0.9659258262890683122, 1.000000000000000000, 0.9659258262890683122, 1.000000000000000000, 0.9659258262890683122, 1.000000000000000000, 0.9659258262890683122, 1.000000000000000000, 0.9659258262890683122, 1.000000000000000000, 0.9659258262890683122, 1.000000000000000000, 0.9659258262890683122, 1.000000000000000000, 0.9659258262890683122, 1.000000000000000000, 0.9659258262890683122, 1.000000000000000000, 0.9659258262890683122, 1.000000000000000000, 0.9659258262890683122, 1.000000000000000000, 0.9659258262890683122, 1.000000000000000000, 0.9659258262890683122, 1.000000000000000000, 0.9659258262890683122, 1.000000000000000000, 0.9659258262890683122, 1.000000000000000000, 0.9659258262890683122, 1.000000000000000000, 0.9659258262890683122, 1.000000000000000000, 0.9659258262890683122, 1.000000000000000000, 0.9659258262890683122, 1.000000000000000000, 0.9659258262890683122, 1.000000000000000000, 0.9659258262890683122, 1.000000000000000000, 0.9659258262890683122, 1.000000000000000000, 0.9659258262890683122, 1.000000000000000000, 0.9659258262890683122, 1.000000000000000000, 0.9659258262890683122, 1.000000000000000000, 0.9659258262890683122, 1.000000000000000000, 0.9659258262890683122, 1.000000000000000000, 0.9659258262890683122, 1.000000000000000000, 0.9659258262890683122, 1.000000000000000000, 0.9659258262890683122, 1.000000000000000000, 0.9659258262890683122, 1.000000000000000000, 0.9659258262890683122, 1.000000000000000000, 0.9659258262890683122, 1.000000000000000000, 0.9659258262890683122, 1.000000000000000000, 0.9659258262890683122, 1.000000000000000000, 0.9659258262890683122, 1.000000000000000000, 0.9659258262890683122, 1.000000000000000000, 0.9659258262890683122, 1.000000000000000000, 0.9659258262890683122, 1.000000000000000000, 0.9659258262890683122, 1.000000000000000000, 0.9659258262890683122, 1.000000000000000000, 0.9659258262890683122, 1.000000000000000000, 0.9659258262890683122, 1.000000000000000000, 0.9659258262890683122, 1.000000000000000000, 0.9659258262890683122, 1.000000000000000000, 0.9659258262890683122, 1.000000000000000000, 0.9659258262890683122, 1.000000000000000000, 0.9659258262890683122, 1.000000000000000000, 0.9659258262890683122, 1.000000000000000000, 0.9659258262890683122, 1.000000000000000000, 0.9659258262890683122, 1.000000000000000000, 0.9659258262890683122, 1.000000000000000000, 0.9659258262890683122, 1.000000000000000000, 0.9659258262890683122, 1.000000000000000000, 0.9659258262890683122, 1.000000000000000000, 0.9659258262890683122, 1.000000000000000000, 0.9659258262890683122, 1.000000000000000000, 0.9659258262890683122, 1.000000000000000000, 0.9659258262890683122, 1.000000000000000000, 0.9659258262890683122, 1.000000000000000000, 0.9659258262890683122, 1.000000000000000000, 0.9659258262890683122, 1.000000000000000000, 0.9659258262890683122, 1.000000000000000000, 0.9659258262890683122, 1.000000000000000000, 0.9659258262890683122, 1.000000000000000000, 0.9659258262890683122, 1.000000000000000000, 0.9659258262890683122, 1.000000000000000000, 0.9659258262890683122, 1.000000000000000000, 0.9659258262890683122, 1.000000000000000000, 0.9659258262890683122, 1.000000000000000000, 0.9659258262890683122, 1.000000000000000000, 0.9659258262890683122, 1.000000000000000000, 0.9659258262890683122, 1.000000000000000000, 0.9659258262890683122, 1.000000000000000000, 0.9659258262890683122, 1.000000000000000000, 0.9659258262890683122, 1.000000000000000000, 0.9659258262890683122, 1.000000000000000000, 0.9659258262890683122, 1.000000000000000000, 0.9659258262890683122, 1.000000000000000000, 0.9659258262890683122, 1.000000000000000000, 0.9659258262890683122, 1.000000000000000000, 0.9659258262890683122, 1.000000000000000000, 0.9659258262890683122, 1.000000000000000000, 0.9659258262890683122, 1.000000000000000000, 0.9659258262890683122, 1.000000000000000000, 0.9659258262890683122, 1.000000000000000000, 0.9659258262890683122, 1.000000000000000000, 0.9659258262890683122, 1.000000000000000000, 0.9659258262890683122, 1.000000000000000000, 0.9659258262890683122, 1.000000000000000000, 0.9659258262890683122, 1.000000000000000000, 0.9659258262890683122, 1.000000000000000000, 0.9659258262890683122, 1.000000000000000000, 0.9659258262890683122, 1.000000000000000000, 0.9659258262890683122, 1.000000000000000000, 0.9659258262890683122, 1.000000000000000000, 0.9659258262890683122, 1.000000000000000000, 0.9659258262890683122, 1.000000000000000000, 0.9659258262890683122, 1.000000000000000000, 0.9659258262890683122, 1.000000000000000000, 0.9659258262890683122, 1.000000000000000000, 0.9659258262890683122, 1.000000000000000000, 0.9659258262890683122, 1.000000000000000000, 0.9659258262890683122, 1.000000000000000000, 0.9659258262890683122, 1.000000000000000000, 0.9659258262890683122, 1.000000000000000000, 0.9659258262890683122, 1.000000000000000000, 0.9659258262890683122, 1.000000000000000000, 0.9659258262890683122, 1.000000000000000000, 0.9659258262890683122, 1.000000000000000000, 0.9659258262890683122, 1.000000000000000000, 0.9659258262890683122, 1.000000000000000000, 0.9659258262890683122, 1.000000000000000000, 0.9659258262890683122, 1.000000000000000000, 0.9659258262890683122, 1.000000000000000000, 0.9659258262890683122, 1.000000000000000000, 0.9659258262890683122, 1.000000000000000000, 0.9659258262890683122, 1.000000000000000000, 0.9659258262890683122, 1.000000000000000000, 0.9659258262890683122, 1.000000000000000000, 0.9659258262890683122, 1.000000000000000000, 0.9659258262890683122, 1.000000000000000000, 0.9659258262890683122, 1.000000000000000000, 0.9659258262890683122, 1.000000000000000000, 0.9659258262890683122, 1.000000000000000000, 0.9659258262890683122, 1.000000000000000000, 0.9659258262890683122, 1.000000000000000000, 0.9659258262890683122, 1.000000000000000000, 0.9659258262890683122, 1.000000000000000000, 0.9659258262890683122, 1.000000000000000000, 0.9659258262890683122, 1.000000000000000000, 0.9659258262890683122, 1.000000000000000000, 0.9659258262890683122, 1.000000000000000000, 0.9659258262890683122, 1.000000000000000000, 0.9659258262890683122, 1.000000000000000000, 0.9659258262890683122, 1.000000000000000000, 0.9659258262890683122, 1.000000000000000000, 0.9659258262890683122, 1.000000000000000000, 0.9659258262890683122, 1.000000000000000000, 0.9659258262890683122, 1.000000000000000000, 0.9659258262890683122, 1.000000000000000000, 0.9659258262890683122, 1.000000000000000000, 0.9659258262890683122, 1.000000000000000000, 0.9659258262890683122, 1.000000000000000000, 0.9659258262890683122, 1.000000000000000000, 0.9659258262890683122, 1.000000000000000000, 0.9659258262890683122, 1.000000000000000000, 0.9659258262890683122, 1.000000000000000000, 0.9659258262890683122, 1.000000000000000000, 0.9659258262890683122, 1.000000000000000000, 0.9659258262890683122, 1.000000000000000000, 0.9659258262890683122, 1.000000000000000000, 0.9659258262890683122, 1.000000000000000000, 0.9659258262890683122, 1.000000000000000000, 0.9659258262890683122, 1.000000000000000000, 0.9659258262890683122, 1.000000000000000000, 0.9659258262890683122, 1.000000000000000000, 0.9659258262890683122, 1.000000000000000000, 0.9659258262890683122, 1.000000000000000000, 0.9659258262890683122, 1.000000000000000000, 0.9659258262890683122, 1.000000000000000000, 0.9659258262890683122, 1.000000000000000000, 0.9659258262890683122, 1.000000000000000000, 0.9659258262890683122, 1.000000000000000000, 0.9659258262890683122, 1.000000000000000000, 0.9659258262890683122, 1.000000000000000000, 0.9659258262890683122, 1.000000000000000000, 0.9659258262890683122, 1.000000000000000000, 0.9659258262890683122, 1.000000000000000000, 0.9659258262890683122, 1.000000000000000000, 0.9659258262890683122, 1.000000000000000000, 0.9659258262890683122, 1.000000000000000000, 0.9659258262890683122, 1.000000000000000000, 0.9659258262890683122, 1.000000000000000000, 0.9659258262890683122, 1.000000000000000000, 0.9659258262890683122, 1.000000000000000000, 0.9659258262890683122, 1.000000000000000000, 0.9659258262890683122, 1.000000000000000000, 0.9659258262890683122, 1.000000000000000000, 0.9659258262890683122, 1.000000000000000000, 0.9659258262890683122, 1.000000000000000000),
 ( 0.3333333333333333703, 0.3219752754296894559, 0.3333333333333333703, 0.3219752754296894559, 0.3333333333333333703, 0.3219752754296894559, 0.3333333333333333703, 0.3219752754296894559, 0.3333333333333333703, 0.3219752754296894559, 0.3333333333333333703, 0.3219752754296894559, 0.3333333333333333703, 0.3219752754296894559, 0.3333333333333333703, 0.3219752754296894559, 0.3333333333333333703, 0.3219752754296894559, 0.3333333333333333703, 0.3219752754296894559, 0.3333333333333333703, 0.3219752754296894559, 0.3333333333333333703, 0.3219752754296894559, 0.3333333333333333703, 0.3219752754296894559, 0.3333333333333333703, 0.3219752754296894559, 0.3333333333333333703, 0.3219752754296894559, 0.3333333333333333703, 0.3219752754296894559, 0.3333333333333333703, 0.3219752754296894559, 0.3333333333333333703, 0.3219752754296894559, 0.3333333333333333703, 0.3219752754296894559, 0.3333333333333333703, 0.3219752754296894559, 0.3333333333333333703, 0.3219752754296894559, 0.3333333333333333703, 0.3219752754296894559, 0.3333333333333333703, 0.3219752754296894559, 0.3333333333333333703, 0.3219752754296894559, 0.3333333333333333703, 0.3219752754296894559, 0.3333333333333333703, 0.3219752754296894559, 0.3333333333333333703, 0.3219752754296894559, 0.3333333333333333703, 0.3219752754296894559, 0.3333333333333333703, 0.3219752754296894559, 0.3333333333333333703, 0.3219752754296894559, 0.3333333333333333703, 0.3219752754296894559, 0.3333333333333333703, 0.3219752754296894559, 0.3333333333333333703, 0.3219752754296894559, 0.3333333333333333703, 0.3219752754296894559, 0.3333333333333333703, 0.3219752754296894559, 0.3333333333333333703, 0.3219752754296894559, 0.3333333333333333703, 0.3219752754296894559, 0.3333333333333333703, 0.3219752754296894559, 0.3333333333333333703, 0.3219752754296894559, 0.3333333333333333703, 0.3219752754296894559, 0.3333333333333333703, 0.3219752754296894559, 0.3333333333333333703, 0.3219752754296894559, 0.3333333333333333703, 0.3219752754296894559, 0.3333333333333333703, 0.3219752754296894559, 0.3333333333333333703, 0.3219752754296894559, 0.3333333333333333703, 0.3219752754296894559, 0.3333333333333333703, 0.3219752754296894559, 0.3333333333333333703, 0.3219752754296894559, 0.3333333333333333703, 0.3219752754296894559, 0.3333333333333333703, 0.3219752754296894559, 0.3333333333333333703, 0.3219752754296894559, 0.3333333333333333703, 0.3219752754296894559, 0.3333333333333333703, 0.3219752754296894559, 0.3333333333333333703, 0.3219752754296894559, 0.3333333333333333703, 0.3219752754296894559, 0.3333333333333333703, 0.3219752754296894559, 0.3333333333333333703, 0.3219752754296894559, 0.3333333333333333703, 0.3219752754296894559, 0.3333333333333333703, 0.3219752754296894559, 0.3333333333333333703, 0.3219752754296894559, 0.3333333333333333703, 0.3219752754296894559, 0.3333333333333333703, 0.3219752754296894559, 0.3333333333333333703, 0.3219752754296894559, 0.3333333333333333703, 0.3219752754296894559, 0.3333333333333333703, 0.3219752754296894559, 0.3333333333333333703, 0.3219752754296894559, 0.3333333333333333703, 0.3219752754296894559, 0.3333333333333333703, 0.3219752754296894559, 0.3333333333333333703, 0.3219752754296894559, 0.3333333333333333703, 0.3219752754296894559, 0.3333333333333333703, 0.3219752754296894559, 0.3333333333333333703, 0.3219752754296894559, 0.3333333333333333703, 0.3219752754296894559, 0.3333333333333333703, 0.3219752754296894559, 0.3333333333333333703, 0.3219752754296894559, 0.3333333333333333703, 0.3219752754296894559, 0.3333333333333333703, 0.3219752754296894559, 0.3333333333333333703, 0.3219752754296894559, 0.3333333333333333703, 0.3219752754296894559, 0.3333333333333333703, 0.3219752754296894559, 0.3333333333333333703, 0.3219752754296894559, 0.3333333333333333703, 0.3219752754296894559, 0.3333333333333333703, 0.3219752754296894559, 0.3333333333333333703, 0.3219752754296894559, 0.3333333333333333703, 0.3219752754296894559, 0.3333333333333333703, 0.3219752754296894559, 0.3333333333333333703, 0.3219752754296894559, 0.3333333333333333703, 0.3219752754296894559, 0.3333333333333333703, 0.3219752754296894559, 0.3333333333333333703, 0.3219752754296894559, 0.3333333333333333703, 0.3219752754296894559, 0.3333333333333333703, 0.3219752754296894559, 0.3333333333333333703, 0.3219752754296894559, 0.3333333333333333703, 0.3219752754296894559, 0.3333333333333333703, 0.3219752754296894559, 0.3333333333333333703, 0.3219752754296894559, 0.3333333333333333703, 0.3219752754296894559, 0.3333333333333333703, 0.3219752754296894559, 0.3333333333333333703, 0.3219752754296894559, 0.3333333333333333703, 0.3219752754296894559, 0.3333333333333333703, 0.3219752754296894559, 0.3333333333333333703, 0.3219752754296894559, 0.3333333333333333703, 0.3219752754296894559, 0.3333333333333333703, 0.3219752754296894559, 0.3333333333333333703, 0.3219752754296894559, 0.3333333333333333703, 0.3219752754296894559, 0.3333333333333333703, 0.3219752754296894559, 0.3333333333333333703, 0.3219752754296894559, 0.3333333333333333703, 0.3219752754296894559, 0.3333333333333333703, 0.3219752754296894559, 0.3333333333333333703, 0.3219752754296894559, 0.3333333333333333703, 0.3219752754296894559, 0.3333333333333333703, 0.3219752754296894559, 0.3333333333333333703, 0.3219752754296894559, 0.3333333333333333703, 0.3219752754296894559, 0.3333333333333333703, 0.3219752754296894559, 0.3333333333333333703, 0.3219752754296894559, 0.3333333333333333703, 0.3219752754296894559, 0.3333333333333333703, 0.3219752754296894559, 0.3333333333333333703, 0.3219752754296894559, 0.3333333333333333703, 0.3219752754296894559, 0.3333333333333333703, 0.3219752754296894559, 0.3333333333333333703, 0.3219752754296894559, 0.3333333333333333703, 0.3219752754296894559, 0.3333333333333333703, 0.3219752754296894559, 0.3333333333333333703, 0.3219752754296894559, 0.3333333333333333703, 0.3219752754296894559, 0.3333333333333333703, 0.3219752754296894559, 0.3333333333333333703, 0.3219752754296894559, 0.3333333333333333703, 0.3219752754296894559, 0.3333333333333333703, 0.3219752754296894559, 0.3333333333333333703, 0.3219752754296894559, 0.3333333333333333703, 0.3219752754296894559, 0.3333333333333333703, 0.3219752754296894559, 0.3333333333333333703, 0.3219752754296894559, 0.3333333333333333703, 0.3219752754296894559, 0.3333333333333333703, 0.3219752754296894559, 0.3333333333333333703, 0.3219752754296894559, 0.3333333333333333703, 0.3219752754296894559, 0.3333333333333333703, 0.3219752754296894559, 0.3333333333333333703, 0.3219752754296894559, 0.3333333333333333703, 0.3219752754296894559, 0.3333333333333333703, 0.3219752754296894559, 0.3333333333333333703, 0.3219752754296894559, 0.3333333333333333703, 0.3219752754296894559, 0.3333333333333333703, 0.3219752754296894559, 0.3333333333333333703, 0.3219752754296894559, 0.3333333333333333703, 0.3219752754296894559, 0.3333333333333333703, 0.3219752754296894559, 0.3333333333333333703, 0.3219752754296894559, 0.3333333333333333703, 0.3219752754296894559, 0.3333333333333333703, 0.3219752754296894559, 0.3333333333333333703, 0.3219752754296894559, 0.3333333333333333703, 0.3219752754296894559, 0.3333333333333333703, 0.3219752754296894559, 0.3333333333333333703, 0.3219752754296894559, 0.3333333333333333703, 0.3219752754296894559, 0.3333333333333333703, 0.3219752754296894559, 0.3333333333333333703, 0.3219752754296894559, 0.3333333333333333703, 0.3219752754296894559, 0.3333333333333333703, 0.3219752754296894559, 0.3333333333333333703, 0.3219752754296894559, 0.3333333333333333703, 0.3219752754296894559, 0.3333333333333333703, 0.3219752754296894559, 0.3333333333333333703, 0.3219752754296894559, 0.3333333333333333703, 0.3219752754296894559, 0.3333333333333333703, 0.3219752754296894559, 0.3333333333333333703, 0.3219752754296894559, 0.3333333333333333703, 0.3219752754296894559, 0.3333333333333333703, 0.3219752754296894559, 0.3333333333333333703, 0.3219752754296894559, 0.3333333333333333703, 0.3219752754296894559, 0.3333333333333333703, 0.3219752754296894559, 0.3333333333333333703, 0.3219752754296894559, 0.3333333333333333703, 0.3219752754296894559, 0.3333333333333333703, 0.3219752754296894559, 0.3333333333333333703, 0.3219752754296894559, 0.3333333333333333703, 0.3219752754296894559, 0.3333333333333333703, 0.3219752754296894559, 0.3333333333333333703, 0.3219752754296894559, 0.3333333333333333703, 0.3219752754296894559, 0.3333333333333333703, 0.3219752754296894559, 0.3333333333333333703, 0.3219752754296894559, 0.3333333333333333703, 0.3219752754296894559, 0.3333333333333333703, 0.3219752754296894559, 0.3333333333333333703, 0.3219752754296894559, 0.3333333333333333703, 0.3219752754296894559, 0.3333333333333333703, 0.3219752754296894559, 0.3333333333333333703, 0.3219752754296894559, 0.3333333333333333703, 0.3219752754296894559, 0.3333333333333333703, 0.3219752754296894559, 0.3333333333333333703, 0.3219752754296894559, 0.3333333333333333703, 0.3219752754296894559, 0.3333333333333333703, 0.3219752754296894559, 0.3333333333333333703, 0.3219752754296894559, 0.3333333333333333703, 0.3219752754296894559, 0.3333333333333333703, 0.3219752754296894559, 0.3333333333333333703, 0.3219752754296894559, 0.3333333333333333703, 0.3219752754296894559, 0.3333333333333333703, 0.3219752754296894559, 0.3333333333333333703, 0.3219752754296894559, 0.3333333333333333703, 0.3219752754296894559, 0.3333333333333333703, 0.3219752754296894559, 0.3333333333333333703, 0.3219752754296894559, 0.3333333333333333703, 0.3219752754296894559, 0.3333333333333333703, 0.3219752754296894559, 0.3333333333333333703, 0.3219752754296894559, 0.3333333333333333703, 0.3219752754296894559, 0.3333333333333333703, 0.3219752754296894559, 0.3333333333333333703, 0.3219752754296894559, 0.3333333333333333703, 0.3219752754296894559, 0.3333333333333333703, 0.3219752754296894559, 0.3333333333333333703, 0.3219752754296894559, 0.3333333333333333703, 0.3219752754296894559, 0.3333333333333333703, 0.3219752754296894559, 0.3333333333333333703, 0.3219752754296894559, 0.3333333333333333703, 0.3219752754296894559, 0.3333333333333333703, 0.3219752754296894559, 0.3333333333333333703, 0.3219752754296894559, 0.3333333333333333703, 0.3219752754296894559, 0.3333333333333333703, 0.3219752754296894559, 0.3333333333333333703, 0.3219752754296894559, 0.3333333333333333703, 0.3219752754296894559, 0.3333333333333333703, 0.3219752754296894559, 0.3333333333333333703, 0.3219752754296894559, 0.3333333333333333703, 0.3219752754296894559, 0.3333333333333333703, 0.3219752754296894559, 0.3333333333333333703, 0.3219752754296894559, 0.3333333333333333703),
 ( 0.3333333333333333703, 0.3219752754296894559, 0.3333333333333333703, 0.3219752754296894559, 0.3333333333333333703, 0.3219752754296894559, 0.3333333333333333703, 0.3219752754296894559, 0.3333333333333333703, 0.3219752754296894559, 0.3333333333333333703, 0.3219752754296894559, 0.3333333333333333703, 0.3219752754296894559, 0.3333333333333333703, 0.3219752754296894559, 0.3333333333333333703, 0.3219752754296894559, 0.3333333333333333703, 0.3219752754296894559, 0.3333333333333333703, 0.3219752754296894559, 0.3333333333333333703, 0.3219752754296894559, 0.3333333333333333703, 0.3219752754296894559, 0.3333333333333333703, 0.3219752754296894559, 0.3333333333333333703, 0.3219752754296894559, 0.3333333333333333703, 0.3219752754296894559, 0.3333333333333333703, 0.3219752754296894559, 0.3333333333333333703, 0.3219752754296894559, 0.3333333333333333703, 0.3219752754296894559, 0.3333333333333333703, 0.3219752754296894559, 0.3333333333333333703, 0.3219752754296894559, 0.3333333333333333703, 0.3219752754296894559, 0.3333333333333333703, 0.3219752754296894559, 0.3333333333333333703, 0.3219752754296894559, 0.3333333333333333703, 0.3219752754296894559, 0.3333333333333333703, 0.3219752754296894559, 0.3333333333333333703, 0.3219752754296894559, 0.3333333333333333703, 0.3219752754296894559, 0.3333333333333333703, 0.3219752754296894559, 0.3333333333333333703, 0.3219752754296894559, 0.3333333333333333703, 0.3219752754296894559, 0.3333333333333333703, 0.3219752754296894559, 0.3333333333333333703, 0.3219752754296894559, 0.3333333333333333703, 0.3219752754296894559, 0.3333333333333333703, 0.3219752754296894559, 0.3333333333333333703, 0.3219752754296894559, 0.3333333333333333703, 0.3219752754296894559, 0.3333333333333333703, 0.3219752754296894559, 0.3333333333333333703, 0.3219752754296894559, 0.3333333333333333703, 0.3219752754296894559, 0.3333333333333333703, 0.3219752754296894559, 0.3333333333333333703, 0.3219752754296894559, 0.3333333333333333703, 0.3219752754296894559, 0.3333333333333333703, 0.3219752754296894559, 0.3333333333333333703, 0.3219752754296894559, 0.3333333333333333703, 0.3219752754296894559, 0.3333333333333333703, 0.3219752754296894559, 0.3333333333333333703, 0.3219752754296894559, 0.3333333333333333703, 0.3219752754296894559, 0.3333333333333333703, 0.3219752754296894559, 0.3333333333333333703, 0.3219752754296894559, 0.3333333333333333703, 0.3219752754296894559, 0.3333333333333333703, 0.3219752754296894559, 0.3333333333333333703, 0.3219752754296894559, 0.3333333333333333703, 0.3219752754296894559, 0.3333333333333333703, 0.3219752754296894559, 0.3333333333333333703, 0.3219752754296894559, 0.3333333333333333703, 0.3219752754296894559, 0.3333333333333333703, 0.3219752754296894559, 0.3333333333333333703, 0.3219752754296894559, 0.3333333333333333703, 0.3219752754296894559, 0.3333333333333333703, 0.3219752754296894559, 0.3333333333333333703, 0.3219752754296894559, 0.3333333333333333703, 0.3219752754296894559, 0.3333333333333333703, 0.3219752754296894559, 0.3333333333333333703, 0.3219752754296894559, 0.3333333333333333703, 0.3219752754296894559, 0.3333333333333333703, 0.3219752754296894559, 0.3333333333333333703, 0.3219752754296894559, 0.3333333333333333703, 0.3219752754296894559, 0.3333333333333333703, 0.3219752754296894559, 0.3333333333333333703, 0.3219752754296894559, 0.3333333333333333703, 0.3219752754296894559, 0.3333333333333333703, 0.3219752754296894559, 0.3333333333333333703, 0.3219752754296894559, 0.3333333333333333703, 0.3219752754296894559, 0.3333333333333333703, 0.3219752754296894559, 0.3333333333333333703, 0.3219752754296894559, 0.3333333333333333703, 0.3219752754296894559, 0.3333333333333333703, 0.3219752754296894559, 0.3333333333333333703, 0.3219752754296894559, 0.3333333333333333703, 0.3219752754296894559, 0.3333333333333333703, 0.3219752754296894559, 0.3333333333333333703, 0.3219752754296894559, 0.3333333333333333703, 0.3219752754296894559, 0.3333333333333333703, 0.3219752754296894559, 0.3333333333333333703, 0.3219752754296894559, 0.3333333333333333703, 0.3219752754296894559, 0.3333333333333333703, 0.3219752754296894559, 0.3333333333333333703, 0.3219752754296894559, 0.3333333333333333703, 0.3219752754296894559, 0.3333333333333333703, 0.3219752754296894559, 0.3333333333333333703, 0.3219752754296894559, 0.3333333333333333703, 0.3219752754296894559, 0.3333333333333333703, 0.3219752754296894559, 0.3333333333333333703, 0.3219752754296894559, 0.3333333333333333703, 0.3219752754296894559, 0.3333333333333333703, 0.3219752754296894559, 0.3333333333333333703, 0.3219752754296894559, 0.3333333333333333703, 0.3219752754296894559, 0.3333333333333333703, 0.3219752754296894559, 0.3333333333333333703, 0.3219752754296894559, 0.3333333333333333703, 0.3219752754296894559, 0.3333333333333333703, 0.3219752754296894559, 0.3333333333333333703, 0.3219752754296894559, 0.3333333333333333703, 0.3219752754296894559, 0.3333333333333333703, 0.3219752754296894559, 0.3333333333333333703, 0.3219752754296894559, 0.3333333333333333703, 0.3219752754296894559, 0.3333333333333333703, 0.3219752754296894559, 0.3333333333333333703, 0.3219752754296894559, 0.3333333333333333703, 0.3219752754296894559, 0.3333333333333333703, 0.3219752754296894559, 0.3333333333333333703, 0.3219752754296894559, 0.3333333333333333703, 0.3219752754296894559, 0.3333333333333333703, 0.3219752754296894559, 0.3333333333333333703, 0.3219752754296894559, 0.3333333333333333703, 0.3219752754296894559, 0.3333333333333333703, 0.3219752754296894559, 0.3333333333333333703, 0.3219752754296894559, 0.3333333333333333703, 0.3219752754296894559, 0.3333333333333333703, 0.3219752754296894559, 0.3333333333333333703, 0.3219752754296894559, 0.3333333333333333703, 0.3219752754296894559, 0.3333333333333333703, 0.3219752754296894559, 0.3333333333333333703, 0.3219752754296894559, 0.3333333333333333703, 0.3219752754296894559, 0.3333333333333333703, 0.3219752754296894559, 0.3333333333333333703, 0.3219752754296894559, 0.3333333333333333703, 0.3219752754296894559, 0.3333333333333333703, 0.3219752754296894559, 0.3333333333333333703, 0.3219752754296894559, 0.3333333333333333703, 0.3219752754296894559, 0.3333333333333333703, 0.3219752754296894559, 0.3333333333333333703, 0.3219752754296894559, 0.3333333333333333703, 0.3219752754296894559, 0.3333333333333333703, 0.3219752754296894559, 0.3333333333333333703, 0.3219752754296894559, 0.3333333333333333703, 0.3219752754296894559, 0.3333333333333333703, 0.3219752754296894559, 0.3333333333333333703, 0.3219752754296894559, 0.3333333333333333703, 0.3219752754296894559, 0.3333333333333333703, 0.3219752754296894559, 0.3333333333333333703, 0.3219752754296894559, 0.3333333333333333703, 0.3219752754296894559, 0.3333333333333333703, 0.3219752754296894559, 0.3333333333333333703, 0.3219752754296894559, 0.3333333333333333703, 0.3219752754296894559, 0.3333333333333333703, 0.3219752754296894559, 0.3333333333333333703, 0.3219752754296894559, 0.3333333333333333703, 0.3219752754296894559, 0.3333333333333333703, 0.3219752754296894559, 0.3333333333333333703, 0.3219752754296894559, 0.3333333333333333703, 0.3219752754296894559, 0.3333333333333333703, 0.3219752754296894559, 0.3333333333333333703, 0.3219752754296894559, 0.3333333333333333703, 0.3219752754296894559, 0.3333333333333333703, 0.3219752754296894559, 0.3333333333333333703, 0.3219752754296894559, 0.3333333333333333703, 0.3219752754296894559, 0.3333333333333333703, 0.3219752754296894559, 0.3333333333333333703, 0.3219752754296894559, 0.3333333333333333703, 0.3219752754296894559, 0.3333333333333333703, 0.3219752754296894559, 0.3333333333333333703, 0.3219752754296894559, 0.3333333333333333703, 0.3219752754296894559, 0.3333333333333333703, 0.3219752754296894559, 0.3333333333333333703, 0.3219752754296894559, 0.3333333333333333703, 0.3219752754296894559, 0.3333333333333333703, 0.3219752754296894559, 0.3333333333333333703, 0.3219752754296894559, 0.3333333333333333703, 0.3219752754296894559, 0.3333333333333333703, 0.3219752754296894559, 0.3333333333333333703, 0.3219752754296894559, 0.3333333333333333703, 0.3219752754296894559, 0.3333333333333333703, 0.3219752754296894559, 0.3333333333333333703, 0.3219752754296894559, 0.3333333333333333703, 0.3219752754296894559, 0.3333333333333333703, 0.3219752754296894559, 0.3333333333333333703, 0.3219752754296894559, 0.3333333333333333703, 0.3219752754296894559, 0.3333333333333333703, 0.3219752754296894559, 0.3333333333333333703, 0.3219752754296894559, 0.3333333333333333703, 0.3219752754296894559, 0.3333333333333333703, 0.3219752754296894559, 0.3333333333333333703, 0.3219752754296894559, 0.3333333333333333703, 0.3219752754296894559, 0.3333333333333333703, 0.3219752754296894559, 0.3333333333333333703, 0.3219752754296894559, 0.3333333333333333703, 0.3219752754296894559, 0.3333333333333333703, 0.3219752754296894559, 0.3333333333333333703, 0.3219752754296894559, 0.3333333333333333703, 0.3219752754296894559, 0.3333333333333333703, 0.3219752754296894559, 0.3333333333333333703, 0.3219752754296894559, 0.3333333333333333703, 0.3219752754296894559, 0.3333333333333333703, 0.3219752754296894559, 0.3333333333333333703, 0.3219752754296894559, 0.3333333333333333703, 0.3219752754296894559, 0.3333333333333333703, 0.3219752754296894559, 0.3333333333333333703, 0.3219752754296894559, 0.3333333333333333703, 0.3219752754296894559, 0.3333333333333333703, 0.3219752754296894559, 0.3333333333333333703, 0.3219752754296894559, 0.3333333333333333703, 0.3219752754296894559, 0.3333333333333333703, 0.3219752754296894559, 0.3333333333333333703, 0.3219752754296894559, 0.3333333333333333703, 0.3219752754296894559, 0.3333333333333333703, 0.3219752754296894559, 0.3333333333333333703, 0.3219752754296894559, 0.3333333333333333703, 0.3219752754296894559, 0.3333333333333333703, 0.3219752754296894559, 0.3333333333333333703, 0.3219752754296894559, 0.3333333333333333703, 0.3219752754296894559, 0.3333333333333333703, 0.3219752754296894559, 0.3333333333333333703, 0.3219752754296894559, 0.3333333333333333703, 0.3219752754296894559, 0.3333333333333333703, 0.3219752754296894559, 0.3333333333333333703, 0.3219752754296894559, 0.3333333333333333703, 0.3219752754296894559, 0.3333333333333333703, 0.3219752754296894559, 0.3333333333333333703, 0.3219752754296894559, 0.3333333333333333703, 0.3219752754296894559, 0.3333333333333333703, 0.3219752754296894559, 0.3333333333333333703, 0.3219752754296894559, 0.3333333333333333703, 0.3219752754296894559, 0.3333333333333333703, 0.3219752754296894559, 0.3333333333333333703, 0.3219752754296894559, 0.3333333333333333703),
 ( 1.000000000000000000, 0.9659258262890683122, 1.000000000000000000, 0.9659258262890683122, 1.000000000000000000, 0.9659258262890683122, 1.000000000000000000, 0.9659258262890683122, 1.000000000000000000, 0.9659258262890683122, 1.000000000000000000, 0.9659258262890683122, 1.000000000000000000, 0.9659258262890683122, 1.000000000000000000, 0.9659258262890683122, 1.000000000000000000, 0.9659258262890683122, 1.000000000000000000, 0.9659258262890683122, 1.000000000000000000, 0.9659258262890683122, 1.000000000000000000, 0.9659258262890683122, 1.000000000000000000, 0.9659258262890683122, 1.000000000000000000, 0.9659258262890683122, 1.000000000000000000, 0.9659258262890683122, 1.000000000000000000, 0.9659258262890683122, 1.000000000000000000, 0.9659258262890683122, 1.000000000000000000, 0.9659258262890683122, 1.000000000000000000, 0.9659258262890683122, 1.000000000000000000, 0.9659258262890683122, 1.000000000000000000, 0.9659258262890683122, 1.000000000000000000, 0.9659258262890683122, 1.000000000000000000, 0.9659258262890683122, 1.000000000000000000, 0.9659258262890683122, 1.000000000000000000, 0.9659258262890683122, 1.000000000000000000, 0.9659258262890683122, 1.000000000000000000, 0.9659258262890683122, 1.000000000000000000, 0.9659258262890683122, 1.000000000000000000, 0.9659258262890683122, 1.000000000000000000, 0.9659258262890683122, 1.000000000000000000, 0.9659258262890683122, 1.000000000000000000, 0.9659258262890683122, 1.000000000000000000, 0.9659258262890683122, 1.000000000000000000, 0.9659258262890683122, 1.000000000000000000, 0.9659258262890683122, 1.000000000000000000, 0.9659258262890683122, 1.000000000000000000, 0.9659258262890683122, 1.000000000000000000, 0.9659258262890683122, 1.000000000000000000, 0.9659258262890683122, 1.000000000000000000, 0.9659258262890683122, 1.000000000000000000, 0.9659258262890683122, 1.000000000000000000, 0.9659258262890683122, 1.000000000000000000, 0.9659258262890683122, 1.000000000000000000, 0.9659258262890683122, 1.000000000000000000, 0.9659258262890683122, 1.000000000000000000, 0.9659258262890683122, 1.000000000000000000, 0.9659258262890683122, 1.000000000000000000, 0.9659258262890683122, 1.000000000000000000, 0.9659258262890683122, 1.000000000000000000, 0.9659258262890683122, 1.000000000000000000, 0.9659258262890683122, 1.000000000000000000, 0.9659258262890683122, 1.000000000000000000, 0.9659258262890683122, 1.000000000000000000, 0.9659258262890683122, 1.000000000000000000, 0.9659258262890683122, 1.000000000000000000, 0.9659258262890683122, 1.000000000000000000, 0.9659258262890683122, 1.000000000000000000, 0.9659258262890683122, 1.000000000000000000, 0.9659258262890683122, 1.000000000000000000, 0.9659258262890683122, 1.000000000000000000, 0.9659258262890683122, 1.000000000000000000, 0.9659258262890683122, 1.000000000000000000, 0.9659258262890683122, 1.000000000000000000, 0.9659258262890683122, 1.000000000000000000, 0.9659258262890683122, 1.000000000000000000, 0.9659258262890683122, 1.000000000000000000, 0.9659258262890683122, 1.000000000000000000, 0.9659258262890683122, 1.000000000000000000, 0.9659258262890683122, 1.000000000000000000, 0.9659258262890683122, 1.000000000000000000, 0.9659258262890683122, 1.000000000000000000, 0.9659258262890683122, 1.000000000000000000, 0.9659258262890683122, 1.000000000000000000, 0.9659258262890683122, 1.000000000000000000, 0.9659258262890683122, 1.000000000000000000, 0.9659258262890683122, 1.000000000000000000, 0.9659258262890683122, 1.000000000000000000, 0.9659258262890683122, 1.000000000000000000, 0.9659258262890683122, 1.000000000000000000, 0.9659258262890683122, 1.000000000000000000, 0.9659258262890683122, 1.000000000000000000, 0.9659258262890683122, 1.000000000000000000, 0.9659258262890683122, 1.000000000000000000, 0.9659258262890683122, 1.000000000000000000, 0.9659258262890683122, 1.000000000000000000, 0.9659258262890683122, 1.000000000000000000, 0.9659258262890683122, 1.000000000000000000, 0.9659258262890683122, 1.000000000000000000, 0.9659258262890683122, 1.000000000000000000, 0.9659258262890683122, 1.000000000000000000, 0.9659258262890683122, 1.000000000000000000, 0.9659258262890683122, 1.000000000000000000, 0.9659258262890683122, 1.000000000000000000, 0.9659258262890683122, 1.000000000000000000, 0.9659258262890683122, 1.000000000000000000, 0.9659258262890683122, 1.000000000000000000, 0.9659258262890683122, 1.000000000000000000, 0.9659258262890683122, 1.000000000000000000, 0.9659258262890683122, 1.000000000000000000, 0.9659258262890683122, 1.000000000000000000, 0.9659258262890683122, 1.000000000000000000, 0.9659258262890683122, 1.000000000000000000, 0.9659258262890683122, 1.000000000000000000, 0.9659258262890683122, 1.000000000000000000, 0.9659258262890683122, 1.000000000000000000, 0.9659258262890683122, 1.000000000000000000, 0.9659258262890683122, 1.000000000000000000, 0.9659258262890683122, 1.000000000000000000, 0.9659258262890683122, 1.000000000000000000, 0.9659258262890683122, 1.000000000000000000, 0.9659258262890683122, 1.000000000000000000, 0.9659258262890683122, 1.000000000000000000, 0.9659258262890683122, 1.000000000000000000, 0.9659258262890683122, 1.000000000000000000, 0.9659258262890683122, 1.000000000000000000, 0.9659258262890683122, 1.000000000000000000, 0.9659258262890683122, 1.000000000000000000, 0.9659258262890683122, 1.000000000000000000, 0.9659258262890683122, 1.000000000000000000, 0.9659258262890683122, 1.000000000000000000, 0.9659258262890683122, 1.000000000000000000, 0.9659258262890683122, 1.000000000000000000, 0.9659258262890683122, 1.000000000000000000, 0.9659258262890683122, 1.000000000000000000, 0.9659258262890683122, 1.000000000000000000, 0.9659258262890683122, 1.000000000000000000, 0.9659258262890683122, 1.000000000000000000, 0.9659258262890683122, 1.000000000000000000, 0.9659258262890683122, 1.000000000000000000, 0.9659258262890683122, 1.000000000000000000, 0.9659258262890683122, 1.000000000000000000, 0.9659258262890683122, 1.000000000000000000, 0.9659258262890683122, 1.000000000000000000, 0.9659258262890683122, 1.000000000000000000, 0.9659258262890683122, 1.000000000000000000, 0.9659258262890683122, 1.000000000000000000, 0.9659258262890683122, 1.000000000000000000, 0.9659258262890683122, 1.000000000000000000, 0.9659258262890683122, 1.000000000000000000, 0.9659258262890683122, 1.000000000000000000, 0.9659258262890683122, 1.000000000000000000, 0.9659258262890683122, 1.000000000000000000, 0.9659258262890683122, 1.000000000000000000, 0.9659258262890683122, 1.000000000000000000, 0.9659258262890683122, 1.000000000000000000, 0.9659258262890683122, 1.000000000000000000, 0.9659258262890683122, 1.000000000000000000, 0.9659258262890683122, 1.000000000000000000, 0.9659258262890683122, 1.000000000000000000, 0.9659258262890683122, 1.000000000000000000, 0.9659258262890683122, 1.000000000000000000, 0.9659258262890683122, 1.000000000000000000, 0.9659258262890683122, 1.000000000000000000, 0.9659258262890683122, 1.000000000000000000, 0.9659258262890683122, 1.000000000000000000, 0.9659258262890683122, 1.000000000000000000, 0.9659258262890683122, 1.000000000000000000, 0.9659258262890683122, 1.000000000000000000, 0.9659258262890683122, 1.000000000000000000, 0.9659258262890683122, 1.000000000000000000, 0.9659258262890683122, 1.000000000000000000, 0.9659258262890683122, 1.000000000000000000, 0.9659258262890683122, 1.000000000000000000, 0.9659258262890683122, 1.000000000000000000, 0.9659258262890683122, 1.000000000000000000, 0.9659258262890683122, 1.000000000000000000, 0.9659258262890683122, 1.000000000000000000, 0.9659258262890683122, 1.000000000000000000, 0.9659258262890683122, 1.000000000000000000, 0.9659258262890683122, 1.000000000000000000, 0.9659258262890683122, 1.000000000000000000, 0.9659258262890683122, 1.000000000000000000, 0.9659258262890683122, 1.000000000000000000, 0.9659258262890683122, 1.000000000000000000, 0.9659258262890683122, 1.000000000000000000, 0.9659258262890683122, 1.000000000000000000, 0.9659258262890683122, 1.000000000000000000, 0.9659258262890683122, 1.000000000000000000, 0.9659258262890683122, 1.000000000000000000, 0.9659258262890683122, 1.000000000000000000, 0.9659258262890683122, 1.000000000000000000, 0.9659258262890683122, 1.000000000000000000, 0.9659258262890683122, 1.000000000000000000, 0.9659258262890683122, 1.000000000000000000, 0.9659258262890683122, 1.000000000000000000, 0.9659258262890683122, 1.000000000000000000, 0.9659258262890683122, 1.000000000000000000, 0.9659258262890683122, 1.000000000000000000, 0.9659258262890683122, 1.000000000000000000, 0.9659258262890683122, 1.000000000000000000, 0.9659258262890683122, 1.000000000000000000, 0.9659258262890683122, 1.000000000000000000, 0.9659258262890683122, 1.000000000000000000, 0.9659258262890683122, 1.000000000000000000, 0.9659258262890683122, 1.000000000000000000, 0.9659258262890683122, 1.000000000000000000, 0.9659258262890683122, 1.000000000000000000, 0.9659258262890683122, 1.000000000000000000, 0.9659258262890683122, 1.000000000000000000, 0.9659258262890683122, 1.000000000000000000, 0.9659258262890683122, 1.000000000000000000, 0.9659258262890683122, 1.000000000000000000, 0.9659258262890683122, 1.000000000000000000, 0.9659258262890683122, 1.000000000000000000, 0.9659258262890683122, 1.000000000000000000, 0.9659258262890683122, 1.000000000000000000, 0.9659258262890683122, 1.000000000000000000, 0.9659258262890683122, 1.000000000000000000, 0.9659258262890683122, 1.000000000000000000, 0.9659258262890683122, 1.000000000000000000, 0.9659258262890683122, 1.000000000000000000, 0.9659258262890683122, 1.000000000000000000, 0.9659258262890683122, 1.000000000000000000, 0.9659258262890683122, 1.000000000000000000, 0.9659258262890683122, 1.000000000000000000, 0.9659258262890683122, 1.000000000000000000, 0.9659258262890683122, 1.000000000000000000, 0.9659258262890683122, 1.000000000000000000, 0.9659258262890683122, 1.000000000000000000, 0.9659258262890683122, 1.000000000000000000, 0.9659258262890683122, 1.000000000000000000, 0.9659258262890683122, 1.000000000000000000, 0.9659258262890683122, 1.000000000000000000, 0.9659258262890683122, 1.000000000000000000, 0.9659258262890683122, 1.000000000000000000, 0.9659258262890683122, 1.000000000000000000, 0.9659258262890683122, 1.000000000000000000, 0.9659258262890683122, 1.000000000000000000) ) ) 
 REPRESENTATION_ITEM ( '' )  SURFACE ( )  );
#29281 = CARTESIAN_POINT ( 'NONE',  ( -5.049401038298153566, 19.05341960407611168, 65.20724293864765286 ) ) ;
#29282 = CARTESIAN_POINT ( 'NONE',  ( 15.72974639402176855, 15.80617190586768217, 76.87609039468567573 ) ) ;
#29283 = CARTESIAN_POINT ( 'NONE',  ( -16.46253265017160317, 9.564922557960807481, 60.83224293864769550 ) ) ;
#29284 = CARTESIAN_POINT ( 'NONE',  ( 16.46253265017160672, -9.564922557960803928, 23.33224293864769194 ) ) ;
#29285 = CARTESIAN_POINT ( 'NONE',  ( -5.823673210054116645, -21.52544592524344225, 32.29057627198102409 ) ) ;
#29286 = CARTESIAN_POINT ( 'NONE',  ( 12.06949235617757843, -12.14591786802309237, 63.12390960531435979 ) ) ;
#29287 = CARTESIAN_POINT ( 'NONE',  ( 16.46253265017160672, -9.564922557960803928, 43.33224293864769550 ) ) ;
#29288 = CARTESIAN_POINT ( 'NONE',  ( 12.06949235617757843, -12.14591786802309237, 98.12390960531436690 ) ) ;
#29289 = CARTESIAN_POINT ( 'NONE',  ( -10.81492255796078084, -18.62759615963271287, 107.0822429386476955 ) ) ;
#29290 = VECTOR ( 'NONE', #123695, 1000.000000000000000 ) ;
#29291 = CARTESIAN_POINT ( 'NONE',  ( 0.05219959533937995610, -21.53943276465977519, 50.00109039468568994 ) ) ;
#29292 = CARTESIAN_POINT ( 'NONE',  ( -13.89961937509977652, 13.97604488694528158, 25.62390960531434558 ) ) ;
#29293 = CARTESIAN_POINT ( 'NONE',  ( 14.29746914071037800, 8.314922557961029526, 51.66775706135234714 ) ) ;
#29294 = CARTESIAN_POINT ( 'NONE',  ( 18.67979575497178502, 10.72451020669898547, 99.16557627198100988 ) ) ;
#29295 = CARTESIAN_POINT ( 'NONE',  ( -21.53943276465977519, 0.05219959533907696930, 91.24890960531436690 ) ) ;
#29297 = CARTESIAN_POINT ( 'NONE',  ( 5.049401038298161559, -19.05341960407611168, 52.70724293864767418 ) ) ;
#29296 = CARTESIAN_POINT ( 'NONE',  ( 0.05219959533936267826, -19.03943276465977164, 25.00109039468566152 ) ) ;
#29298 = CARTESIAN_POINT ( 'NONE',  ( -13.97604488694527625, -13.89961937509977652, 106.8739096053143669 ) ) ;
#29299 = CARTESIAN_POINT ( 'NONE',  ( -10.81492255796105439, 18.62759615963255655, 62.91775706135236135 ) ) ;
#29300 = CARTESIAN_POINT ( 'NONE',  ( -21.55341960407610458, -5.719274019375992779, 46.45724293864769550 ) ) ;
#29301 = CARTESIAN_POINT ( 'NONE',  ( 8.224510206698742110, 14.34966873604972548, 112.0844237280190185 ) ) ;
#29303 = CARTESIAN_POINT ( 'NONE',  ( 5.823673210054444382, -21.52544592524334988, 95.20942372801903275 ) ) ;
#29302 = CARTESIAN_POINT ( 'NONE',  ( 10.81492255796106328, -18.62759615963255655, 65.41775706135234714 ) ) ;
#29304 = CARTESIAN_POINT ( 'NONE',  ( 9.474510206698729675, 16.51473224551082808, 47.08442372801900433 ) ) ;
#29305 = CARTESIAN_POINT ( 'NONE',  ( 14.34966873604972726, -8.224510206698740333, 105.8344237280190328 ) ) ;
#29306 = CARTESIAN_POINT ( 'NONE',  ( -21.53943276465977519, -0.05219959533937600094, 48.75109039468568284 ) ) ;
#29307 = CARTESIAN_POINT ( 'NONE',  ( -19.03943276465977164, 0.05219959533909376836, 56.24890960531435979 ) ) ;
#29308 = CARTESIAN_POINT ( 'NONE',  ( 15.80617190586769283, -15.72974639402175789, 110.6260903946857042 ) ) ;
#29309 = CARTESIAN_POINT ( 'NONE',  ( -13.89961937509977652, 13.97604488694528158, 115.6239096053143669 ) ) ;
#29310 = CARTESIAN_POINT ( 'NONE',  ( -0.05219959533907301413, -21.53943276465977519, 112.4989096053143669 ) ) ;
#29311 = CARTESIAN_POINT ( 'NONE',  ( -5.823673210054116645, -21.52544592524344225, 82.29057627198103830 ) ) ;
#29312 = CARTESIAN_POINT ( 'NONE',  ( -0.05219959533934338120, 16.53943276465976808, 37.50109039468568284 ) ) ;
#29314 = CARTESIAN_POINT ( 'NONE',  ( -5.719274019375978568, 21.55341960407610458, 75.20724293864769550 ) ) ;
#29313 = CARTESIAN_POINT ( 'NONE',  ( -4.384162112346980500, 4.242540618128916918, -62.50719930893271226 ) ) ;
#29316 = CARTESIAN_POINT ( 'NONE',  ( 8.314922557960818139, 14.29746914071049879, 74.58224293864768129 ) ) ;
#29315 = CARTESIAN_POINT ( 'NONE',  ( -16.52544592524335698, -4.483927247898792601, 58.95942372801902565 ) ) ;
#29317 = CARTESIAN_POINT ( 'NONE',  ( -21.88112277201193123, 20.03432139805442702, -48.74685162679677575 ) ) ;
#29318 = CARTESIAN_POINT ( 'NONE',  ( 19.02544592524334988, 5.153800228976608722, 106.4594237280190185 ) ) ;
#29319 = CARTESIAN_POINT ( 'NONE',  ( -15.80617190586745835, -15.72974639402198527, 31.87390960531435979 ) ) ;
#29320 = DIRECTION ( 'NONE',  ( 1.000000000000000000, 0.000000000000000000, 0.000000000000000000 ) ) ;
#29321 = CARTESIAN_POINT ( 'NONE',  ( 16.53943276465976808, 0.05219959533934440121, 36.25109039468567573 ) ) ;
#29322 = CARTESIAN_POINT ( 'NONE',  ( -18.62759615963270932, 10.81492255796079327, 105.8322429386476955 ) ) ;
#29323 = CARTESIAN_POINT ( 'NONE',  ( -21.53943276465977519, 0.05219959533907696930, 31.24890960531435979 ) ) ;
#29324 = CARTESIAN_POINT ( 'NONE',  ( 14.29746914071037800, 8.314922557961029526, 66.66775706135234714 ) ) ;
#29325 = B_SPLINE_CURVE_WITH_KNOTS ( 'NONE', 3,
 ( #194899, #102877, #161553, #162545, #71542, #26056 ),
 .UNSPECIFIED., .F., .F.,
 ( 4, 2, 4 ),
 ( 0.007228050697041544029, 0.007608510107495010041, 0.007988969517948476054 ),
 .UNSPECIFIED. ) ;
#29326 = CARTESIAN_POINT ( 'NONE',  ( -16.51473224551069308, -9.474510206698971260, 86.66557627198102409 ) ) ;
#29328 = CARTESIAN_POINT ( 'NONE',  ( 13.97604488694527802, 13.89961937509977652, 24.37390960531435624 ) ) ;
#29327 = CARTESIAN_POINT ( 'NONE',  ( 21.55341960407619695, -5.719274019375665929, 61.04275706135234714 ) ) ;
#29329 = EDGE_CURVE ( 'NONE', #183247, #158096, #119715, .T. ) ;
#29330 = CARTESIAN_POINT ( 'NONE',  ( 10.72451020669898902, -18.67979575497178502, 22.91557627198102765 ) ) ;
#29331 = ORIENTED_EDGE ( 'NONE', *, *, #187522, .T. ) ;
#29332 = CARTESIAN_POINT ( 'NONE',  ( 0.05219959533936267826, -19.03943276465977164, 35.00109039468566863 ) ) ;
#29333 = CARTESIAN_POINT ( 'NONE',  ( -16.55341960407617563, 4.379528057220093196, 58.54275706135235424 ) ) ;
#29334 = CARTESIAN_POINT ( 'NONE',  ( 19.05341960407611168, 5.049401038298154454, 108.9572429386477097 ) ) ;
#29335 = CARTESIAN_POINT ( 'NONE',  ( 19.03943276465977164, -0.05219959533909143690, 73.74890960531435269 ) ) ;
#29336 = CARTESIAN_POINT ( 'NONE',  ( -16.53943276465976808, -0.05219959533934237506, 93.75109039468567573 ) ) ;
#29337 = DIRECTION ( 'NONE',  ( -1.000000000000000000, 0.000000000000000000, 5.421010862427522170E-16 ) ) ;
#29338 = CARTESIAN_POINT ( 'NONE',  ( -14.34966873604960291, -8.224510206698953496, 91.66557627198103830 ) ) ;
#29339 = CARTESIAN_POINT ( 'NONE',  ( -15.80617190586745835, -15.72974639402198527, 31.87390960531435979 ) ) ;
#29340 = CARTESIAN_POINT ( 'NONE',  ( 19.03943276465977164, -0.05219959533909143690, 33.74890960531435979 ) ) ;
#29341 = CARTESIAN_POINT ( 'NONE',  ( -8.314922557961024197, 14.29746914071037800, 67.91775706135234714 ) ) ;
#29342 = CARTESIAN_POINT ( 'NONE',  ( -18.67979575497193778, 10.72451020669871902, 23.33442372801901499 ) ) ;
#29343 = CARTESIAN_POINT ( 'NONE',  ( 0.05219959533936267826, -19.03943276465977164, 75.00109039468566152 ) ) ;
#29344 = CARTESIAN_POINT ( 'NONE',  ( 9.474510206698971260, -16.51473224551069308, 37.91557627198102409 ) ) ;
#29345 = CARTESIAN_POINT ( 'NONE',  ( 15.72974639402199770, -15.80617190586745480, 73.12390960531436690 ) ) ;
#29346 = CARTESIAN_POINT ( 'NONE',  ( 5.153800228976335163, 19.02544592524342804, 109.7905762719810099 ) ) ;
#29347 = CARTESIAN_POINT ( 'NONE',  ( 18.62759615963255655, 10.81492255796105972, 86.66775706135234714 ) ) ;
#29348 = CARTESIAN_POINT ( 'NONE',  ( -16.51473224551069308, -9.474510206698971260, 61.66557627198103120 ) ) ;
#29349 = CARTESIAN_POINT ( 'NONE',  ( -4.379528057220086978, -16.55341960407618274, 44.79275706135234714 ) ) ;
#29350 = CARTESIAN_POINT ( 'NONE',  ( 16.51473224551069308, 9.474510206698969483, 54.16557627198103120 ) ) ;
#29351 = CARTESIAN_POINT ( 'NONE',  ( 10.72451020669871369, 18.67979575497193778, 82.08442372801901854 ) ) ;
#29352 = CARTESIAN_POINT ( 'NONE',  ( -0.05219959533936034679, 19.03943276465977164, 37.50109039468567573 ) ) ;
#29353 = CARTESIAN_POINT ( 'NONE',  ( -13.97604488694547697, 13.89961937509957934, 48.12609039468566863 ) ) ;
#29354 = CARTESIAN_POINT ( 'NONE',  ( 21.53943276465977519, 0.05219959533937863772, 51.25109039468568994 ) ) ;
#29355 = CARTESIAN_POINT ( 'NONE',  ( 23.29544513554940011, 16.92513159979228021, 143.1843446569000093 ) ) ;
#29356 = CARTESIAN_POINT ( 'NONE',  ( -19.05341960407617563, 5.049401038297882671, 48.54275706135233293 ) ) ;
#29357 = CARTESIAN_POINT ( 'NONE',  ( 5.153800228976335163, 19.02544592524342804, 104.7905762719809957 ) ) ;
#29358 = CARTESIAN_POINT ( 'NONE',  ( -19.05341960407611168, -5.049401038298163336, 66.45724293864769550 ) ) ;
#29359 = CARTESIAN_POINT ( 'NONE',  ( -16.55341960407611168, -4.379528057220339221, 26.45724293864768839 ) ) ;
#29361 = CARTESIAN_POINT ( 'NONE',  ( -18.62759615963255300, -10.81492255796106328, 99.16775706135234714 ) ) ;
#29360 = CARTESIAN_POINT ( 'NONE',  ( 5.719274019375991003, -21.55341960407610458, 32.70724293864770260 ) ) ;
#29362 = CARTESIAN_POINT ( 'NONE',  ( -22.81625015709509441, -31.40387420917324590, -2.324999997268813789 ) ) ;
#29363 = CARTESIAN_POINT ( 'NONE',  ( -34.46456012332993168, 1.775814316247263713, 89.78225565739067804 ) ) ;
#29364 = CARTESIAN_POINT ( 'NONE',  ( 15.72974639402176855, 15.80617190586768217, 91.87609039468568994 ) ) ;
#29365 = CARTESIAN_POINT ( 'NONE',  ( -38.00000000000000711, 2.893978650043524126E-14, -25.00000000000000000 ) ) ;
#29366 = CARTESIAN_POINT ( 'NONE',  ( 0.05219959533909260263, 19.03943276465977164, 39.99890960531436690 ) ) ;
#29367 = CARTESIAN_POINT ( 'NONE',  ( 19.02544592524343514, -5.153800228976328945, 108.5405762719810383 ) ) ;
#29368 = CARTESIAN_POINT ( 'NONE',  ( 33.83483822987808765, 1.427510505796701690, 100.3145928531378672 ) ) ;
#29369 = CARTESIAN_POINT ( 'NONE',  ( 16.53943276465976808, 0.05219959533934440121, 46.25109039468567573 ) ) ;
#29370 = CARTESIAN_POINT ( 'NONE',  ( -21.53943276465977519, 0.05219959533907696930, 66.24890960531436690 ) ) ;
#29371 = CARTESIAN_POINT ( 'NONE',  ( -14.34966873604960291, -8.224510206698953496, 46.66557627198102409 ) ) ;
#29373 = CARTESIAN_POINT ( 'NONE',  ( 0.05219959533909260263, 19.03943276465977164, 109.9989096053143669 ) ) ;
#29372 = CARTESIAN_POINT ( 'NONE',  ( -4.483927247898539470, -16.52544592524342804, 107.2905762719810525 ) ) ;
#29374 = CARTESIAN_POINT ( 'NONE',  ( -10.81492255796105439, 18.62759615963255655, 27.91775706135234358 ) ) ;
#29375 = CARTESIAN_POINT ( 'NONE',  ( -16.46253265017146816, -9.564922557961047289, 39.16775706135234003 ) ) ;
#29376 = CARTESIAN_POINT ( 'NONE',  ( -9.564922557960796823, -16.46253265017161027, 27.08224293864769550 ) ) ;
#29377 = CARTESIAN_POINT ( 'NONE',  ( -21.53943276465977519, -0.05219959533937600094, 68.75109039468568994 ) ) ;
#29378 = CARTESIAN_POINT ( 'NONE',  ( 17.50000000000000355, -5.622605283950867339, 31.18792689403888829 ) ) ;
#29379 = CARTESIAN_POINT ( 'NONE',  ( -14.34966873604960291, -8.224510206698953496, 31.66557627198102054 ) ) ;
#29380 = CARTESIAN_POINT ( 'NONE',  ( -36.91746825000000598, 11.99521256947798520, -5.224999997268812812 ) ) ;
#29381 = CARTESIAN_POINT ( 'NONE',  ( -21.55341960407610458, -5.719274019375992779, 21.45724293864769550 ) ) ;
#29382 = CARTESIAN_POINT ( 'NONE',  ( -16.53943276465976808, 0.05219959533911058130, 86.24890960531436690 ) ) ;
#29383 = CARTESIAN_POINT ( 'NONE',  ( 9.100000000000001421, 0.000000000000000000, -63.95112321872120731 ) ) ;
#29384 = CARTESIAN_POINT ( 'NONE',  ( 9.564922557960805705, 16.46253265017160317, 79.58224293864769550 ) ) ;
#29385 = CARTESIAN_POINT ( 'NONE',  ( -8.224510206698948167, 14.34966873604960824, 75.41557627198102409 ) ) ;
#29386 = CARTESIAN_POINT ( 'NONE',  ( -13.97604488694547697, 13.89961937509957934, 108.1260903946856331 ) ) ;
#29387 = CARTESIAN_POINT ( 'NONE',  ( 15.80617190586746368, 15.72974639402197994, 54.37390960531435979 ) ) ;
#29388 = ORIENTED_EDGE ( 'NONE', *, *, #195257, .F. ) ;
#29389 = CARTESIAN_POINT ( 'NONE',  ( -16.53943276465976808, 0.05219959533911058130, 111.2489096053143669 ) ) ;
#29392 = CARTESIAN_POINT ( 'NONE',  ( 0.05219959533907565091, 21.53943276465977519, 79.99890960531435269 ) ) ;
#29391 = B_SPLINE_CURVE_WITH_KNOTS ( 'NONE', 3,
 ( #74814, #198156, #42494, #180030, #167814, #136476 ),
 .UNSPECIFIED., .F., .F.,
 ( 4, 2, 4 ),
 ( 0.007228050697041449486, 0.007608510107494925040, 0.007988969517948399726 ),
 .UNSPECIFIED. ) ;
#29390 = CARTESIAN_POINT ( 'NONE',  ( -19.05341960407611168, -5.049401038298163336, 66.45724293864769550 ) ) ;
#29394 = CARTESIAN_POINT ( 'NONE',  ( 0.05219959533909260263, 19.03943276465977164, 84.99890960531436690 ) ) ;
#29393 = CARTESIAN_POINT ( 'NONE',  ( -16.55341960407617563, 4.379528057220093196, 108.5427570613523756 ) ) ;
#29395 = CARTESIAN_POINT ( 'NONE',  ( -9.564922557961040184, 16.46253265017147172, 67.91775706135233293 ) ) ;
#29396 = CARTESIAN_POINT ( 'NONE',  ( -0.05219959533937732626, 21.53943276465977519, 97.50109039468567573 ) ) ;
#29397 = CARTESIAN_POINT ( 'NONE',  ( -21.53943276465977519, 0.05219959533907696930, 66.24890960531436690 ) ) ;
#29398 = CARTESIAN_POINT ( 'NONE',  ( -10.81492255796078084, -18.62759615963271287, 27.08224293864769550 ) ) ;
#29399 = CARTESIAN_POINT ( 'NONE',  ( -5.153800228976328057, -19.02544592524343514, 32.29057627198102409 ) ) ;
#29400 = CARTESIAN_POINT ( 'NONE',  ( 16.52544592524335698, 4.483927247898782831, 101.4594237280190185 ) ) ;
#29401 = CARTESIAN_POINT ( 'NONE',  ( -9.474510206698964154, 16.51473224551069663, 60.41557627198102409 ) ) ;
#29402 = CARTESIAN_POINT ( 'NONE',  ( 0.05219959533934541429, -16.53943276465976808, 20.00109039468568639 ) ) ;
#29403 = CARTESIAN_POINT ( 'NONE',  ( 16.31925111598457079, 7.325300261831481308, 52.33575461032751974 ) ) ;
#29404 = CARTESIAN_POINT ( 'NONE',  ( 10.81492255796106328, -18.62759615963255655, 110.4177570613523756 ) ) ;
#29405 = CARTESIAN_POINT ( 'NONE',  ( 12.14591786802309770, 12.06949235617756955, 74.37390960531436690 ) ) ;
#29406 = CARTESIAN_POINT ( 'NONE',  ( -21.53943276465977519, 0.05219959533907696930, 106.2489096053143811 ) ) ;
#29407 = CARTESIAN_POINT ( 'NONE',  ( -10.81492255796078084, -18.62759615963271287, 97.08224293864770971 ) ) ;
#29408 = CARTESIAN_POINT ( 'NONE',  ( -6.719938155502488186, 4.704672000039124669, -64.14994679864909699 ) ) ;
#29409 = CARTESIAN_POINT ( 'NONE',  ( -5.823673210054116645, -21.52544592524344225, 62.29057627198102409 ) ) ;
#29410 = CARTESIAN_POINT ( 'NONE',  ( -12.06949235617739369, -12.14591786802326823, 84.37609039468570415 ) ) ;
#29411 = CARTESIAN_POINT ( 'NONE',  ( -0.05219959533910754901, -16.53943276465976808, 102.4989096053143811 ) ) ;
#29412 = CARTESIAN_POINT ( 'NONE',  ( 9.474510206698971260, -16.51473224551069308, 57.91557627198103120 ) ) ;
#29413 = CARTESIAN_POINT ( 'NONE',  ( 12.06949235617739724, 12.14591786802326823, 106.8760903946856899 ) ) ;
#29414 = CARTESIAN_POINT ( 'NONE',  ( 15.72974639402176855, 15.80617190586768217, 46.87609039468568994 ) ) ;
#29415 = CARTESIAN_POINT ( 'NONE',  ( 9.474510206698971260, -16.51473224551069308, 97.91557627198102409 ) ) ;
#29416 = CARTESIAN_POINT ( 'NONE',  ( -21.55341960407619339, 5.719274019375674811, 78.54275706135236135 ) ) ;
#29417 = CARTESIAN_POINT ( 'NONE',  ( 16.46253265017160672, -9.564922557960803928, 28.33224293864769550 ) ) ;
#29418 = CARTESIAN_POINT ( 'NONE',  ( 19.05341960407611168, 5.049401038298154454, 38.95724293864767418 ) ) ;
#29419 = ORIENTED_EDGE ( 'NONE', *, *, #160927, .F. ) ;
#29420 = CARTESIAN_POINT ( 'NONE',  ( -21.52544592524334988, -5.823673210054445271, 78.95942372801901854 ) ) ;
#29421 = CARTESIAN_POINT ( 'NONE',  ( -13.97604488694527625, -13.89961937509977652, 106.8739096053143669 ) ) ;
#29422 = CARTESIAN_POINT ( 'NONE',  ( -16.46253265017146816, -9.564922557961047289, 79.16775706135234714 ) ) ;
#29423 = CARTESIAN_POINT ( 'NONE',  ( -5.823673210054431948, 21.52544592524334988, 37.70942372801900433 ) ) ;
#29424 = CARTESIAN_POINT ( 'NONE',  ( -4.483927247898782831, 16.52544592524335698, 27.70942372801901854 ) ) ;
#29425 = CARTESIAN_POINT ( 'NONE',  ( 9.474510206698729675, 16.51473224551082808, 67.08442372801900433 ) ) ;
#29426 = CARTESIAN_POINT ( 'NONE',  ( 19.03943276465977164, -0.05219959533909143690, 48.74890960531435979 ) ) ;
#29427 = CARTESIAN_POINT ( 'NONE',  ( -13.89961937509957401, -13.97604488694547875, 79.37609039468567573 ) ) ;
#29428 = CARTESIAN_POINT ( 'NONE',  ( 14.29746914071049879, -8.314922557960816363, 23.33224293864769194 ) ) ;
#29429 = CARTESIAN_POINT ( 'NONE',  ( 19.03943276465977164, 0.05219959533936151252, 81.25109039468567573 ) ) ;
#29430 = CARTESIAN_POINT ( 'NONE',  ( -8.224510206698948167, 14.34966873604960824, 40.41557627198103120 ) ) ;
#29431 = CARTESIAN_POINT ( 'NONE',  ( -16.51473224551082808, 9.474510206698731452, 63.33442372801900433 ) ) ;
#29432 = CARTESIAN_POINT ( 'NONE',  ( 16.53943276465976808, 0.05219959533934440121, 51.25109039468568994 ) ) ;
#29433 = CARTESIAN_POINT ( 'NONE',  ( -16.46253265017146816, -9.564922557961047289, 29.16775706135232937 ) ) ;
#29434 = CARTESIAN_POINT ( 'NONE',  ( 9.564922557960805705, 16.46253265017160317, 34.58224293864770260 ) ) ;
#29435 = CARTESIAN_POINT ( 'NONE',  ( -17.48847506799969054, -5.747544572773811034, 64.17302562156720569 ) ) ;
#29436 = CARTESIAN_POINT ( 'NONE',  ( -16.55341960407617563, 4.379528057220093196, 48.54275706135234714 ) ) ;
#29437 = DIRECTION ( 'NONE',  ( 0.000000000000000000, 0.000000000000000000, -1.000000000000000000 ) ) ;
#29438 = CARTESIAN_POINT ( 'NONE',  ( -5.359611314223446995E-15, 29.16686587814335496, 146.3750000027311842 ) ) ;
#29439 = CARTESIAN_POINT ( 'NONE',  ( 19.03943276465977164, -0.05219959533909143690, 93.74890960531435269 ) ) ;
#29440 = DIRECTION ( 'NONE',  ( 1.000000000000000000, 6.391086490440868450E-16, 0.000000000000000000 ) ) ;
#29441 = EDGE_LOOP ( 'NONE', ( #71166, #121903, #199643, #195876, #16796, #178830 ) ) ;
#29442 = CARTESIAN_POINT ( 'NONE',  ( -9.474510206698720793, -16.51473224551083518, 84.58442372801900433 ) ) ;
#29443 = CARTESIAN_POINT ( 'NONE',  ( -5.823673210054116645, -21.52544592524344225, 22.29057627198102765 ) ) ;
#29445 = CARTESIAN_POINT ( 'NONE',  ( -16.46253265017146816, -9.564922557961047289, 104.1677570613523329 ) ) ;
#29444 = CARTESIAN_POINT ( 'NONE',  ( -16.46253265017146816, -9.564922557961047289, 19.16775706135233293 ) ) ;
#29446 = CARTESIAN_POINT ( 'NONE',  ( 4.379528057220339221, -16.55341960407611168, 107.7072429386476955 ) ) ;
#29447 = CARTESIAN_POINT ( 'NONE',  ( -16.46253265017160317, 9.564922557960807481, 40.83224293864769550 ) ) ;
#29448 = CARTESIAN_POINT ( 'NONE',  ( 15.72974639402199770, -15.80617190586745480, 53.12390960531436690 ) ) ;
#29449 = CARTESIAN_POINT ( 'NONE',  ( -21.53943276465977519, 0.05219959533907696930, 56.24890960531436690 ) ) ;
#29450 = CARTESIAN_POINT ( 'NONE',  ( -9.564922557960796823, -16.46253265017161027, 27.08224293864769550 ) ) ;
#29451 = FACE_OUTER_BOUND ( 'NONE', #110681, .T. ) ;
#29452 = CARTESIAN_POINT ( 'NONE',  ( 19.03943276465977164, 0.05219959533936151252, 66.25109039468567573 ) ) ;
#29453 = CARTESIAN_POINT ( 'NONE',  ( 16.55341960407611168, 4.379528057220329451, 43.95724293864769550 ) ) ;
#29454 = CARTESIAN_POINT ( 'NONE',  ( -18.62759615963270932, 10.81492255796079327, 25.83224293864769194 ) ) ;
#29455 = CARTESIAN_POINT ( 'NONE',  ( -18.62759615963255300, -10.81492255796106328, 99.16775706135234714 ) ) ;
#29456 = CARTESIAN_POINT ( 'NONE',  ( -5.719274019375978568, 21.55341960407610458, 90.20724293864770971 ) ) ;
#29457 = CARTESIAN_POINT ( 'NONE',  ( -5.823673210054431948, 21.52544592524334988, 57.70942372801901143 ) ) ;
#29458 = CARTESIAN_POINT ( 'NONE',  ( 21.55341960407619695, -5.719274019375665929, 71.04275706135234714 ) ) ;
#29459 = CARTESIAN_POINT ( 'NONE',  ( -19.05341960407611168, -5.049401038298163336, 91.45724293864766707 ) ) ;
#29461 = CARTESIAN_POINT ( 'NONE',  ( -0.05219959533937732626, 21.53943276465977519, 47.50109039468568994 ) ) ;
#29460 = CARTESIAN_POINT ( 'NONE',  ( -8.314922557961024197, 14.29746914071037800, 92.91775706135236135 ) ) ;
#29462 = CARTESIAN_POINT ( 'NONE',  ( -4.483927247898539470, -16.52544592524342804, 112.2905762719810241 ) ) ;
#29463 = CARTESIAN_POINT ( 'NONE',  ( 12.14591786802309770, 12.06949235617756955, 69.37390960531436690 ) ) ;
#29464 = CARTESIAN_POINT ( 'NONE',  ( -8.224510206698948167, 14.34966873604960824, 30.41557627198101699 ) ) ;
#29465 = CARTESIAN_POINT ( 'NONE',  ( -21.53943276465977519, 0.05219959533907696930, 41.24890960531435269 ) ) ;
#29466 = CARTESIAN_POINT ( 'NONE',  ( -16.46253265017160317, 9.564922557960807481, 70.83224293864770971 ) ) ;
#29467 = CARTESIAN_POINT ( 'NONE',  ( -5.153800228976328057, -19.02544592524343514, 52.29057627198100988 ) ) ;
#29468 = CARTESIAN_POINT ( 'NONE',  ( -5.823673210054116645, -21.52544592524344225, 62.29057627198102409 ) ) ;
#29469 = CARTESIAN_POINT ( 'NONE',  ( 19.05341960407617918, -5.049401038297876454, 41.04275706135233293 ) ) ;
#29471 = CARTESIAN_POINT ( 'NONE',  ( -16.55341960407611168, -4.379528057220339221, 46.45724293864769550 ) ) ;
#29470 = CARTESIAN_POINT ( 'NONE',  ( 22.99604614807110181, -21.49604614807104142, -49.67998909148434450 ) ) ;
#29472 = CARTESIAN_POINT ( 'NONE',  ( -15.72974639402197994, 15.80617190586746368, 25.62390960531435624 ) ) ;
#29473 = ORIENTED_EDGE ( 'NONE', *, *, #36295, .F. ) ;
#29474 = EDGE_LOOP ( 'NONE', ( #122212, #62042, #7298, #67452, #164950, #5265, #111171, #42746 ) ) ;
#29475 = CARTESIAN_POINT ( 'NONE',  ( 2.577820198429831642E-15, 9.100000000000001421, -61.89430850415821794 ) ) ;
#29476 = CARTESIAN_POINT ( 'NONE',  ( -12.06949235617739369, -12.14591786802326823, 69.37609039468567573 ) ) ;
#29477 = CARTESIAN_POINT ( 'NONE',  ( -19.05341960407617563, 5.049401038297882671, 73.54275706135233293 ) ) ;
#29478 = CARTESIAN_POINT ( 'NONE',  ( 0.05219959533910956823, 16.53943276465976808, 34.99890960531435979 ) ) ;
#29479 = FACE_OUTER_BOUND ( 'NONE', #30544, .T. ) ;
#29480 = CARTESIAN_POINT ( 'NONE',  ( -16.55341960407611168, -4.379528057220339221, 21.45724293864769550 ) ) ;
#29481 = CARTESIAN_POINT ( 'NONE',  ( -5.049401038298153566, 19.05341960407611168, 45.20724293864769550 ) ) ;
#29482 = CARTESIAN_POINT ( 'NONE',  ( 19.03943276465977164, -0.05219959533909143690, 78.74890960531436690 ) ) ;
#29483 = CARTESIAN_POINT ( 'NONE',  ( 13.97604488694527802, 13.89961937509977652, 44.37390960531435269 ) ) ;
#29484 = CARTESIAN_POINT ( 'NONE',  ( 5.719274019375673035, 21.55341960407619339, 52.29275706135236135 ) ) ;
#29485 = CARTESIAN_POINT ( 'NONE',  ( -5.153800228976328057, -19.02544592524343514, 52.29057627198100988 ) ) ;
#29486 = CARTESIAN_POINT ( 'NONE',  ( -0.05219959533909027116, -19.03943276465977164, 57.49890960531435979 ) ) ;
#29487 = CARTESIAN_POINT ( 'NONE',  ( -15.72974639402197994, 15.80617190586746368, 30.62390960531436335 ) ) ;
#29488 = CARTESIAN_POINT ( 'NONE',  ( -5.049401038298153566, 19.05341960407611168, 25.20724293864768484 ) ) ;
#29489 = CARTESIAN_POINT ( 'NONE',  ( -18.67979575497178146, -10.72451020669898902, 31.66557627198102054 ) ) ;
#29490 = CARTESIAN_POINT ( 'NONE',  ( 14.34966873604972726, -8.224510206698740333, 85.83442372801901854 ) ) ;
#29491 = CARTESIAN_POINT ( 'NONE',  ( 10.81492255796106328, -18.62759615963255655, 105.4177570613523613 ) ) ;
#29492 = CARTESIAN_POINT ( 'NONE',  ( -8.224510206698735004, -14.34966873604973081, 64.58442372801900433 ) ) ;
#29493 = CARTESIAN_POINT ( 'NONE',  ( -16.51473224551069308, -9.474510206698971260, 111.6655762719810383 ) ) ;
#29494 = CARTESIAN_POINT ( 'NONE',  ( -4.483927247898782831, 16.52544592524335698, 57.70942372801901143 ) ) ;
#29495 = CARTESIAN_POINT ( 'NONE',  ( -14.29746914071037622, -8.314922557961029526, 44.16775706135234714 ) ) ;
#29496 = CARTESIAN_POINT ( 'NONE',  ( 0.05219959533909260263, 19.03943276465977164, 109.9989096053143669 ) ) ;
#29497 = CARTESIAN_POINT ( 'NONE',  ( -19.05341960407617563, 5.049401038297882671, 113.5427570613523471 ) ) ;
#29498 = CARTESIAN_POINT ( 'NONE',  ( -19.02544592524342804, 5.153800228976336051, 36.04057627198100988 ) ) ;
#29499 = CARTESIAN_POINT ( 'NONE',  ( 21.55341960407619695, -5.719274019375665929, 26.04275706135235779 ) ) ;
#29500 = CARTESIAN_POINT ( 'NONE',  ( -4.483927247898782831, 16.52544592524335698, 22.70942372801901499 ) ) ;
#29501 = CARTESIAN_POINT ( 'NONE',  ( 14.29746914071037800, 8.314922557961029526, 91.66775706135234714 ) ) ;
#29502 = CARTESIAN_POINT ( 'NONE',  ( 10.74802307403555623, 10.74802307403551360, -64.92279855667830191 ) ) ;
#29503 = CARTESIAN_POINT ( 'NONE',  ( -10.81492255796105439, 18.62759615963255655, 87.91775706135234714 ) ) ;
#29504 = CARTESIAN_POINT ( 'NONE',  ( -0.05219959533936034679, 19.03943276465977164, 87.50109039468567573 ) ) ;
#29505 = CARTESIAN_POINT ( 'NONE',  ( -8.314922557960811034, -14.29746914071050412, 52.08224293864768839 ) ) ;
#29506 = CARTESIAN_POINT ( 'NONE',  ( -0.05219959533910754901, -16.53943276465976808, 107.4989096053143669 ) ) ;
#29508 = CARTESIAN_POINT ( 'NONE',  ( -6.139823915386823927, 0.3964520562364309830, -64.52448473163053677 ) ) ;
#29507 = CARTESIAN_POINT ( 'NONE',  ( -5.153800228976607833, 19.02544592524334988, 52.70942372801900433 ) ) ;
#29509 = CARTESIAN_POINT ( 'NONE',  ( -21.55341960407619339, 5.719274019375674811, 48.54275706135234714 ) ) ;
#29510 = CARTESIAN_POINT ( 'NONE',  ( 5.049401038297881783, 19.05341960407617563, 107.2927570613523187 ) ) ;
#29511 = CARTESIAN_POINT ( 'NONE',  ( 16.61371651742599553, 7.165104196376154810, 83.64584930007004004 ) ) ;
#29512 = CARTESIAN_POINT ( 'NONE',  ( -9.564922557960796823, -16.46253265017161027, 102.0822429386477097 ) ) ;
#29513 = CARTESIAN_POINT ( 'NONE',  ( 15.72974639402199770, -15.80617190586745480, 73.12390960531436690 ) ) ;
#29514 = CARTESIAN_POINT ( 'NONE',  ( 19.02544592524334988, 5.153800228976608722, 91.45942372801900433 ) ) ;
#29515 = CARTESIAN_POINT ( 'NONE',  ( 0.05219959533909260263, 19.03943276465977164, 99.99890960531436690 ) ) ;
#29516 = CARTESIAN_POINT ( 'NONE',  ( -11.82020350747949955, -25.60187801590574352, 139.9999999999999716 ) ) ;
#29517 = CARTESIAN_POINT ( 'NONE',  ( 16.55341960407611168, 4.379528057220329451, 103.9572429386476813 ) ) ;
#29518 = CARTESIAN_POINT ( 'NONE',  ( -15.72974639402176322, -15.80617190586768395, 99.37609039468568994 ) ) ;
#29519 = CARTESIAN_POINT ( 'NONE',  ( 16.51473224551069308, 9.474510206698969483, 39.16557627198103120 ) ) ;
#29520 = CARTESIAN_POINT ( 'NONE',  ( -0.05219959533937732626, 21.53943276465977519, 57.50109039468568994 ) ) ;
#29521 = CARTESIAN_POINT ( 'NONE',  ( -0.05219959533937732626, 21.53943276465977519, 82.50109039468568994 ) ) ;
#29522 = CARTESIAN_POINT ( 'NONE',  ( -12.06949235617739369, -12.14591786802326823, 99.37609039468568994 ) ) ;
#29523 = B_SPLINE_CURVE_WITH_KNOTS ( 'NONE', 3,
 ( #194076, #28225, #39371, #11044, #10047, #181887, #103045, #177903, #57550, #102046, #193063, #119219, #26221, #27218, #164727, #8026, #162715, #180904, #117211, #131375, #54539, #166721 ),
 .UNSPECIFIED., .F., .F.,
 ( 4, 2, 2, 2, 2, 2, 2, 2, 2, 2, 4 ),
 ( 1.967889507820273575E-07, 0.0003311341139580519974, 0.0006620714389653219612, 0.0009930087639725918708, 0.001323946088979861780, 0.002647695389008961585, 0.003309570039023516149, 0.003971444689038069846, 0.004633319339052623977, 0.004964256664059899307, 0.005295193989067173770 ),
 .UNSPECIFIED. ) ;
#29524 = CARTESIAN_POINT ( 'NONE',  ( 10.72451020669871369, 18.67979575497193778, 47.08442372801901854 ) ) ;
#29525 = CARTESIAN_POINT ( 'NONE',  ( -5.719274019375665041, -21.55341960407619695, 34.79275706135235424 ) ) ;
#29527 = CARTESIAN_POINT ( 'NONE',  ( 16.51473224551069308, 9.474510206698969483, 94.16557627198103830 ) ) ;
#29526 = CARTESIAN_POINT ( 'NONE',  ( -19.02544592524334988, -5.153800228976617603, 63.95942372801899012 ) ) ;
#29528 = CARTESIAN_POINT ( 'NONE',  ( -16.53943276465976808, 0.05219959533911058130, 106.2489096053143811 ) ) ;
#29529 = CARTESIAN_POINT ( 'NONE',  ( 15.72974639402199770, -15.80617190586745480, 88.12390960531436690 ) ) ;
#29530 = CARTESIAN_POINT ( 'NONE',  ( -16.52544592524342804, 4.483927247898546575, 61.04057627198103120 ) ) ;
#29531 = CARTESIAN_POINT ( 'NONE',  ( -19.02544592524334988, -5.153800228976617603, 18.95942372801899722 ) ) ;
#29532 = CARTESIAN_POINT ( 'NONE',  ( -12.06949235617756955, 12.14591786802309770, 85.62390960531436690 ) ) ;
#29533 = CARTESIAN_POINT ( 'NONE',  ( 16.51473224551069308, 9.474510206698969483, 39.16557627198103120 ) ) ;
#29534 = CARTESIAN_POINT ( 'NONE',  ( -19.03943276465977164, -0.05219959533935918106, 83.75109039468567573 ) ) ;
#29535 = CARTESIAN_POINT ( 'NONE',  ( -4.379528057220328563, 16.55341960407611168, 45.20724293864769550 ) ) ;
#29536 = CARTESIAN_POINT ( 'NONE',  ( 18.67979575497194134, -10.72451020669871369, 95.83442372801903275 ) ) ;
#29537 = CARTESIAN_POINT ( 'NONE',  ( -0.05219959533909027116, -19.03943276465977164, 87.49890960531436690 ) ) ;
#29538 = CARTESIAN_POINT ( 'NONE',  ( 13.89961937509957401, 13.97604488694547697, 61.87609039468566863 ) ) ;
#29539 = CARTESIAN_POINT ( 'NONE',  ( 18.62759615963271287, -10.81492255796078972, 73.33224293864769550 ) ) ;
#29540 = CARTESIAN_POINT ( 'NONE',  ( -18.62759615963255300, -10.81492255796106328, 34.16775706135234714 ) ) ;
#29541 = CARTESIAN_POINT ( 'NONE',  ( 12.14591786802327356, -12.06949235617739191, 30.62609039468567929 ) ) ;
#29542 = CARTESIAN_POINT ( 'NONE',  ( -4.379528057220086978, -16.55341960407618274, 84.79275706135234714 ) ) ;
#29544 = CARTESIAN_POINT ( 'NONE',  ( -5.719274019375978568, 21.55341960407610458, 115.2072429386476955 ) ) ;
#29543 = CARTESIAN_POINT ( 'NONE',  ( -13.97604488694527625, -13.89961937509977652, 21.87390960531435979 ) ) ;
#29545 = CARTESIAN_POINT ( 'NONE',  ( 16.52544592524342804, -4.483927247898539470, 113.5405762719810383 ) ) ;
#29546 = CARTESIAN_POINT ( 'NONE',  ( -22.81625015709509441, -31.40387420917324590, -8.824999997268811569 ) ) ;
#29547 = CARTESIAN_POINT ( 'NONE',  ( -4.379528057220086978, -16.55341960407618274, 44.79275706135234714 ) ) ;
#29548 = CARTESIAN_POINT ( 'NONE',  ( 14.34966873604960469, 8.224510206698951720, 74.16557627198102409 ) ) ;
#29549 = CARTESIAN_POINT ( 'NONE',  ( -10.81492255796078084, -18.62759615963271287, 72.08224293864769550 ) ) ;
#29550 = CARTESIAN_POINT ( 'NONE',  ( 8.314922557960818139, 14.29746914071049879, 24.58224293864768839 ) ) ;
#29551 = CARTESIAN_POINT ( 'NONE',  ( -12.14591786802326823, 12.06949235617739902, 53.12609039468568284 ) ) ;
#29552 = CARTESIAN_POINT ( 'NONE',  ( 13.89961937509977652, -13.97604488694527269, 43.12390960531434558 ) ) ;
#29553 = CARTESIAN_POINT ( 'NONE',  ( -14.34966873604972548, 8.224510206698743886, 78.33442372801901854 ) ) ;
#29554 = CARTESIAN_POINT ( 'NONE',  ( 13.89961937509957401, 13.97604488694547697, 71.87609039468567573 ) ) ;
#29555 = CARTESIAN_POINT ( 'NONE',  ( 15.72974639402199770, -15.80617190586745480, 73.12390960531436690 ) ) ;
#29556 = CARTESIAN_POINT ( 'NONE',  ( -12.14591786802326823, 12.06949235617739902, 108.1260903946856757 ) ) ;
#29557 = VERTEX_POINT ( 'NONE', #181399 ) ;
#29558 = CARTESIAN_POINT ( 'NONE',  ( -13.89961937509977652, 13.97604488694528158, 115.6239096053143669 ) ) ;
#29559 = ADVANCED_FACE ( 'NONE', ( #42877 ), #130798, .F. ) ;
#29560 = CARTESIAN_POINT ( 'NONE',  ( -10.81492255796078084, -18.62759615963271287, 52.08224293864768839 ) ) ;
#29561 = ORIENTED_EDGE ( 'NONE', *, *, #22985, .T. ) ;
#29562 = CARTESIAN_POINT ( 'NONE',  ( -16.55341960407617563, 4.379528057220093196, 88.54275706135236135 ) ) ;
#29563 = ORIENTED_EDGE ( 'NONE', *, *, #80974, .T. ) ;
#29564 = CARTESIAN_POINT ( 'NONE',  ( -9.564922557960796823, -16.46253265017161027, 107.0822429386476955 ) ) ;
#29565 = CARTESIAN_POINT ( 'NONE',  ( -18.39635199886969730, 5.499999999999980460, 76.01967076360001840 ) ) ;
#29566 = CARTESIAN_POINT ( 'NONE',  ( 15.80617190586746368, 15.72974639402197994, 69.37390960531436690 ) ) ;
#29567 = CARTESIAN_POINT ( 'NONE',  ( -16.55341960407617563, 4.379528057220093196, 103.5427570613523613 ) ) ;
#29568 = CARTESIAN_POINT ( 'NONE',  ( 13.89961937509957401, 13.97604488694547697, 111.8760903946856757 ) ) ;
#29569 = CARTESIAN_POINT ( 'NONE',  ( -16.52544592524342804, 4.483927247898546575, 111.0405762719810525 ) ) ;
#29570 = CARTESIAN_POINT ( 'NONE',  ( 0.05219959533934541429, -16.53943276465976808, 30.00109039468568284 ) ) ;
#29571 = CARTESIAN_POINT ( 'NONE',  ( -16.51473224551069308, -9.474510206698971260, 56.66557627198103120 ) ) ;
#29572 = CARTESIAN_POINT ( 'NONE',  ( 16.68945015508927554, -0.2045547421925976994, -61.35148950497489295 ) ) ;
#29573 = CARTESIAN_POINT ( 'NONE',  ( 19.02544592524343514, -5.153800228976328945, 98.54057627198100988 ) ) ;
#29574 = CARTESIAN_POINT ( 'NONE',  ( -4.483927247898782831, 16.52544592524335698, 92.70942372801901854 ) ) ;
#29575 = CARTESIAN_POINT ( 'NONE',  ( 13.97604488694548053, -13.89961937509957401, 85.62609039468568994 ) ) ;
#29576 = CARTESIAN_POINT ( 'NONE',  ( 0.05219959533936267826, -19.03943276465977164, 30.00109039468566863 ) ) ;
#29577 = CARTESIAN_POINT ( 'NONE',  ( -5.823673210054116645, -21.52544592524344225, 77.29057627198102409 ) ) ;
#29578 = CARTESIAN_POINT ( 'NONE',  ( 12.14591786802327356, -12.06949235617739191, 105.6260903946856899 ) ) ;
#29579 = CARTESIAN_POINT ( 'NONE',  ( -13.97604488694547697, 13.89961937509957934, 98.12609039468566152 ) ) ;
#29580 = CARTESIAN_POINT ( 'NONE',  ( -5.153800228976328057, -19.02544592524343514, 52.29057627198100988 ) ) ;
#29581 = CARTESIAN_POINT ( 'NONE',  ( 19.02544592524343514, -5.153800228976328945, 93.54057627198102409 ) ) ;
#29582 = CARTESIAN_POINT ( 'NONE',  ( 15.72974639402176855, 15.80617190586768217, 61.87609039468568284 ) ) ;
#29583 = CARTESIAN_POINT ( 'NONE',  ( -13.89961937509977652, 13.97604488694528158, 50.62390960531435979 ) ) ;
#29584 = CARTESIAN_POINT ( 'NONE',  ( -6.791538853603066528, -3.181980515339470905, 8.889087296526001936 ) ) ;
#29585 = CARTESIAN_POINT ( 'NONE',  ( 16.53943276465976808, -0.05219959533910856209, 73.74890960531433848 ) ) ;
#29586 = CARTESIAN_POINT ( 'NONE',  ( -21.53943276465977519, 0.05219959533907696930, 76.24890960531435269 ) ) ;
#29587 = CARTESIAN_POINT ( 'NONE',  ( -24.30000000000003268, 2.668083032619853614E-13, -54.21489346206828230 ) ) ;
#29588 = DIRECTION ( 'NONE',  ( -1.000000000000000000, -0.000000000000000000, -0.000000000000000000 ) ) ;
#29589 = CARTESIAN_POINT ( 'NONE',  ( -16.51473224551082808, 9.474510206698731452, 38.33442372801899722 ) ) ;
#29590 = CARTESIAN_POINT ( 'NONE',  ( 17.40861289039006365, -6.110651285853166748, 71.12767529172569425 ) ) ;
#29592 = CARTESIAN_POINT ( 'NONE',  ( 5.049401038298161559, -19.05341960407611168, 82.70724293864770971 ) ) ;
#29591 = CARTESIAN_POINT ( 'NONE',  ( 9.474510206698971260, -16.51473224551069308, 82.91557627198103830 ) ) ;
#29593 = CARTESIAN_POINT ( 'NONE',  ( -4.483927247898782831, 16.52544592524335698, 62.70942372801902565 ) ) ;
#29594 = CARTESIAN_POINT ( 'NONE',  ( 10.65638358537376362, -44.90791467878717924, -23.56120423312990297 ) ) ;
#29595 = CARTESIAN_POINT ( 'NONE',  ( -0.05219959533936034679, 19.03943276465977164, 32.50109039468566863 ) ) ;
#29596 = CARTESIAN_POINT ( 'NONE',  ( 30.00000000000000711, -5.510910596163089556E-15, 37.50000000000000000 ) ) ;
#29597 = CARTESIAN_POINT ( 'NONE',  ( -4.379528057220086978, -16.55341960407618274, 89.79275706135236135 ) ) ;
#29598 = CARTESIAN_POINT ( 'NONE',  ( -1.500606516337470886, -22.62812085840269560, -55.49205433527804132 ) ) ;
#29599 = CARTESIAN_POINT ( 'NONE',  ( -16.55341960407617563, 4.379528057220093196, 83.54275706135234714 ) ) ;
#29600 = CARTESIAN_POINT ( 'NONE',  ( -16.55341960407617563, 4.379528057220093196, 53.54275706135234714 ) ) ;
#29601 = CARTESIAN_POINT ( 'NONE',  ( -17.97058386085787163, -5.500000000000058620, 59.00390968646216550 ) ) ;
#29602 = CARTESIAN_POINT ( 'NONE',  ( 18.67979575497194134, -10.72451020669871369, 65.83442372801900433 ) ) ;
#29603 = CARTESIAN_POINT ( 'NONE',  ( -5.153800228976607833, 19.02544592524334988, 77.70942372801900433 ) ) ;
#29604 = CARTESIAN_POINT ( 'NONE',  ( -18.62759615963255300, -10.81492255796106328, 104.1677570613523471 ) ) ;
#29605 = CARTESIAN_POINT ( 'NONE',  ( -19.02544592524342804, 5.153800228976336051, 51.04057627198103120 ) ) ;
#29606 = CARTESIAN_POINT ( 'NONE',  ( 19.02544592524343514, -5.153800228976328945, 38.54057627198103120 ) ) ;
#29607 = CARTESIAN_POINT ( 'NONE',  ( -19.91688362670921464, -34.68888220807522060, -5.694635852519195574 ) ) ;
#29608 = CARTESIAN_POINT ( 'NONE',  ( -5.823673210054116645, -21.52544592524344225, 62.29057627198102409 ) ) ;
#29609 = CARTESIAN_POINT ( 'NONE',  ( 21.55341960407610458, 5.719274019375980345, 23.95724293864769550 ) ) ;
#29610 = CARTESIAN_POINT ( 'NONE',  ( -16.52544592524342804, 4.483927247898546575, 111.0405762719810525 ) ) ;
#29611 = CARTESIAN_POINT ( 'NONE',  ( -16.53943276465976808, -0.05219959533934237506, 53.75109039468568994 ) ) ;
#29612 = VERTEX_POINT ( 'NONE', #187355 ) ;
#29613 = CARTESIAN_POINT ( 'NONE',  ( -0.05219959533907301413, -21.53943276465977519, 112.4989096053143669 ) ) ;
#29615 = CARTESIAN_POINT ( 'NONE',  ( 37.99999999999999289, 2.893978650043524126E-14, -3.000000000000000000 ) ) ;
#29614 = CARTESIAN_POINT ( 'NONE',  ( -14.29746914071049879, 8.314922557960819915, 50.83224293864770971 ) ) ;
#29616 = CARTESIAN_POINT ( 'NONE',  ( -5.049401038297874678, -19.05341960407617918, 104.7927570613523471 ) ) ;
#29617 = CARTESIAN_POINT ( 'NONE',  ( 0.05219959533936267826, -19.03943276465977164, 40.00109039468566152 ) ) ;
#29618 = CARTESIAN_POINT ( 'NONE',  ( -12.14591786802309592, -12.06949235617757132, 46.87390960531435979 ) ) ;
#29619 = CARTESIAN_POINT ( 'NONE',  ( -15.80617190586768217, 15.72974639402176855, 23.12609039468567573 ) ) ;
#29621 = CARTESIAN_POINT ( 'NONE',  ( -18.62759615963270932, 10.81492255796079327, 70.83224293864770971 ) ) ;
#29620 = CARTESIAN_POINT ( 'NONE',  ( 0.000000000000000000, 0.000000000000000000, -64.92279855667830191 ) ) ;
#29622 = CARTESIAN_POINT ( 'NONE',  ( 5.049401038298161559, -19.05341960407611168, 87.70724293864769550 ) ) ;
#29623 = CARTESIAN_POINT ( 'NONE',  ( 16.55341960407611168, 4.379528057220329451, 48.95724293864770971 ) ) ;
#29624 = CARTESIAN_POINT ( 'NONE',  ( -16.46253265017160317, 9.564922557960807481, 100.8322429386477097 ) ) ;
#29625 = CARTESIAN_POINT ( 'NONE',  ( -36.77100073307799022, 4.779104515855422619, 47.74589100149062659 ) ) ;
#29626 = CARTESIAN_POINT ( 'NONE',  ( -19.03943276465977164, -0.05219959533935918106, 53.75109039468566863 ) ) ;
#29627 = CARTESIAN_POINT ( 'NONE',  ( -5.719274019375978568, 21.55341960407610458, 100.2072429386476955 ) ) ;
#29628 = CARTESIAN_POINT ( 'NONE',  ( 13.97604488694527802, 13.89961937509977652, 39.37390960531435269 ) ) ;
#29629 = CARTESIAN_POINT ( 'NONE',  ( 19.02544592524343514, -5.153800228976328945, 23.54057627198102054 ) ) ;
#29630 = CARTESIAN_POINT ( 'NONE',  ( -0.05219959533937732626, 21.53943276465977519, 47.50109039468568994 ) ) ;
#29631 = CARTESIAN_POINT ( 'NONE',  ( 22.44159573604009594, -16.30477369853687364, 145.6750000027311671 ) ) ;
#29632 = CARTESIAN_POINT ( 'NONE',  ( -4.483927247898539470, -16.52544592524342804, 22.29057627198102765 ) ) ;
#29633 = CARTESIAN_POINT ( 'NONE',  ( 9.564922557960805705, 16.46253265017160317, 54.58224293864769550 ) ) ;
#29634 = CARTESIAN_POINT ( 'NONE',  ( 0.05219959533909260263, 19.03943276465977164, 99.99890960531436690 ) ) ;
#29635 = CARTESIAN_POINT ( 'NONE',  ( -10.72451020669898014, 18.67979575497178502, 65.41557627198102409 ) ) ;
#29636 = CARTESIAN_POINT ( 'NONE',  ( 27.73933785331498214, 9.013057229001095294, 145.9750000027311785 ) ) ;
#29637 = CARTESIAN_POINT ( 'NONE',  ( 16.46253265017160672, -9.564922557960803928, 43.33224293864769550 ) ) ;
#29638 = CARTESIAN_POINT ( 'NONE',  ( 5.823673210054125526, 21.52544592524343514, 49.79057627198102409 ) ) ;
#29639 = EDGE_LOOP ( 'NONE', ( #1419, #158329 ) ) ;
#29640 = CARTESIAN_POINT ( 'NONE',  ( 5.823673210054444382, -21.52544592524334988, 85.20942372801901854 ) ) ;
#29643 = CARTESIAN_POINT ( 'NONE',  ( 12.14591786802309770, 12.06949235617756955, 74.37390960531436690 ) ) ;
#29642 = CARTESIAN_POINT ( 'NONE',  ( -4.483927247898782831, 16.52544592524335698, 87.70942372801901854 ) ) ;
#29641 = CARTESIAN_POINT ( 'NONE',  ( 18.67464278970748381, -33.09908666442214553, -25.63618526508991380 ) ) ;
#29644 = CARTESIAN_POINT ( 'NONE',  ( -12.06949235617739369, -12.14591786802326823, 94.37609039468568994 ) ) ;
#29645 = CARTESIAN_POINT ( 'NONE',  ( -19.03943276465977164, 0.05219959533909376836, 76.24890960531435269 ) ) ;
#29646 = VERTEX_POINT ( 'NONE', #93320 ) ;
#29647 = CARTESIAN_POINT ( 'NONE',  ( -16.46253265017146816, -9.564922557961047289, 29.16775706135232937 ) ) ;
#29648 = CARTESIAN_POINT ( 'NONE',  ( -12.06949235617739369, -12.14591786802326823, 84.37609039468570415 ) ) ;
#29649 = CARTESIAN_POINT ( 'NONE',  ( 5.719274019375673035, 21.55341960407619339, 112.2927570613523471 ) ) ;
#29650 = CARTESIAN_POINT ( 'NONE',  ( -9.564922557960796823, -16.46253265017161027, 77.08224293864769550 ) ) ;
#29651 = CARTESIAN_POINT ( 'NONE',  ( -15.80617190586745835, -15.72974639402198527, 41.87390960531435979 ) ) ;
#29652 = CARTESIAN_POINT ( 'NONE',  ( -16.55341960407617563, 4.379528057220093196, 23.54275706135235424 ) ) ;
#29653 = CARTESIAN_POINT ( 'NONE',  ( 15.72974639402176855, 15.80617190586768217, 86.87609039468568994 ) ) ;
#29654 = CARTESIAN_POINT ( 'NONE',  ( -12.06949235617739369, -12.14591786802326823, 64.37609039468568994 ) ) ;
#29655 = CARTESIAN_POINT ( 'NONE',  ( 21.55341960407610458, 5.719274019375980345, 113.9572429386477239 ) ) ;
#29656 = CARTESIAN_POINT ( 'NONE',  ( -13.97604488694547697, 13.89961937509957934, 113.1260903946856757 ) ) ;
#29657 = CARTESIAN_POINT ( 'NONE',  ( 5.153800228976335163, 19.02544592524342804, 94.79057627198103830 ) ) ;
#29658 = CARTESIAN_POINT ( 'NONE',  ( 16.52544592524335698, 4.483927247898782831, 26.45942372801901854 ) ) ;
#29659 = CARTESIAN_POINT ( 'NONE',  ( 19.05341960407611168, 5.049401038298154454, 38.95724293864767418 ) ) ;
#29660 = CARTESIAN_POINT ( 'NONE',  ( 8.314922557961029526, -14.29746914071037800, 40.41775706135234714 ) ) ;
#29661 = CARTESIAN_POINT ( 'NONE',  ( -8.224510206698948167, 14.34966873604960824, 85.41557627198102409 ) ) ;
#29662 = CARTESIAN_POINT ( 'NONE',  ( 14.34966873604972726, -8.224510206698740333, 80.83442372801901854 ) ) ;
#29664 = CARTESIAN_POINT ( 'NONE',  ( 19.03943276465977164, -0.05219959533909143690, 63.74890960531435979 ) ) ;
#29663 = CARTESIAN_POINT ( 'NONE',  ( -18.62759615963255300, -10.81492255796106328, 24.16775706135235424 ) ) ;
#29665 = CARTESIAN_POINT ( 'NONE',  ( -16.46253265017160317, 9.564922557960807481, 75.83224293864769550 ) ) ;
#29666 = CARTESIAN_POINT ( 'NONE',  ( -0.05219959533934338120, 16.53943276465976808, 92.50109039468567573 ) ) ;
#29668 = ORIENTED_EDGE ( 'NONE', *, *, #148562, .F. ) ;
#29667 = CARTESIAN_POINT ( 'NONE',  ( -32.00000000000000000, -1.163414459189985801E-14, 89.49999999999897682 ) ) ;
#29669 = EDGE_LOOP ( 'NONE', ( #85230, #152997, #142160, #142681 ) ) ;
#29670 = CARTESIAN_POINT ( 'NONE',  ( 9.474510206698729675, 16.51473224551082808, 32.08442372801900433 ) ) ;
#29671 = CARTESIAN_POINT ( 'NONE',  ( 13.89961937509977652, -13.97604488694527269, 53.12390960531434558 ) ) ;
#29673 = ORIENTED_EDGE ( 'NONE', *, *, #139182, .T. ) ;
#29672 = DIRECTION ( 'NONE',  ( 0.000000000000000000, 0.000000000000000000, -1.000000000000000000 ) ) ;
#29674 = CARTESIAN_POINT ( 'NONE',  ( -16.52544592524335698, -4.483927247898792601, 23.95942372801901143 ) ) ;
#29676 = CARTESIAN_POINT ( 'NONE',  ( 12.14591786802327356, -12.06949235617739191, 45.62609039468567573 ) ) ;
#29675 = CARTESIAN_POINT ( 'NONE',  ( -13.97604488694547697, 13.89961937509957934, 53.12609039468565442 ) ) ;
#29677 = CARTESIAN_POINT ( 'NONE',  ( -19.03943276465977164, 0.05219959533909376836, 101.2489096053143669 ) ) ;
#29678 = CARTESIAN_POINT ( 'NONE',  ( -5.049401038298153566, 19.05341960407611168, 80.20724293864769550 ) ) ;
#29679 = CARTESIAN_POINT ( 'NONE',  ( 18.62759615963271287, -10.81492255796078972, 93.33224293864769550 ) ) ;
#29680 = CARTESIAN_POINT ( 'NONE',  ( 16.51473224551083163, -9.474510206698727899, 65.83442372801900433 ) ) ;
#29682 = CARTESIAN_POINT ( 'NONE',  ( 17.40593841890343896, -5.148608847476693562, 21.38766112942987974 ) ) ;
#29681 = CARTESIAN_POINT ( 'NONE',  ( 16.46253265017160672, -9.564922557960803928, 98.33224293864769550 ) ) ;
#29683 = EDGE_CURVE ( 'NONE', #154069, #83417, #19474, .T. ) ;
#29684 = CARTESIAN_POINT ( 'NONE',  ( 9.474510206698971260, -16.51473224551069308, 57.91557627198103120 ) ) ;
#29686 = CARTESIAN_POINT ( 'NONE',  ( 13.97604488694527802, 13.89961937509977652, 24.37390960531435624 ) ) ;
#29685 = CARTESIAN_POINT ( 'NONE',  ( -8.224510206698735004, -14.34966873604973081, 109.5844237280190328 ) ) ;
#29687 = CARTESIAN_POINT ( 'NONE',  ( 5.049401038297881783, 19.05341960407617563, 37.29275706135232582 ) ) ;
#29688 = EDGE_CURVE ( 'NONE', #166995, #120001, #127476, .T. ) ;
#29689 = CARTESIAN_POINT ( 'NONE',  ( -14.29746914071049879, 8.314922557960819915, 80.83224293864769550 ) ) ;
#29690 = CARTESIAN_POINT ( 'NONE',  ( 10.81492255796106328, -18.62759615963255655, 95.41775706135234714 ) ) ;
#29691 = CARTESIAN_POINT ( 'NONE',  ( -19.02544592524342804, 5.153800228976336051, 41.04057627198103120 ) ) ;
#29692 = CARTESIAN_POINT ( 'NONE',  ( 4.483927247898790824, -16.52544592524335698, 55.20942372801902565 ) ) ;
#29694 = CARTESIAN_POINT ( 'NONE',  ( 10.81492255796106328, -18.62759615963255655, 90.41775706135236135 ) ) ;
#29693 = CARTESIAN_POINT ( 'NONE',  ( -0.05219959533910754901, -16.53943276465976808, 42.49890960531435979 ) ) ;
#29695 = CARTESIAN_POINT ( 'NONE',  ( -16.51473224551069308, -9.474510206698971260, 86.66557627198102409 ) ) ;
#29696 = CARTESIAN_POINT ( 'NONE',  ( -13.89961937509977652, 13.97604488694528158, 95.62390960531436690 ) ) ;
#29697 = CARTESIAN_POINT ( 'NONE',  ( 16.53943276465976808, -0.05219959533910856209, 108.7489096053143669 ) ) ;
#29698 = CARTESIAN_POINT ( 'NONE',  ( 16.52544592524342804, -4.483927247898539470, 73.54057627198102409 ) ) ;
#29699 = CARTESIAN_POINT ( 'NONE',  ( 5.719274019375991003, -21.55341960407610458, 87.70724293864769550 ) ) ;
#29700 = CARTESIAN_POINT ( 'NONE',  ( 13.89961937509977652, -13.97604488694527269, 83.12390960531436690 ) ) ;
#29701 = CARTESIAN_POINT ( 'NONE',  ( 0.05219959533907565091, 21.53943276465977519, 99.99890960531436690 ) ) ;
#29702 = CARTESIAN_POINT ( 'NONE',  ( 9.474510206698971260, -16.51473224551069308, 87.91557627198102409 ) ) ;
#29704 = CARTESIAN_POINT ( 'NONE',  ( -4.379528057220328563, 16.55341960407611168, 90.20724293864770971 ) ) ;
#29703 = CARTESIAN_POINT ( 'NONE',  ( 19.25663599770063072, -5.499999999999451106, 46.49419308057203182 ) ) ;
#29705 = CARTESIAN_POINT ( 'NONE',  ( 16.51473224551069308, 9.474510206698969483, 54.16557627198103120 ) ) ;
#29706 = CARTESIAN_POINT ( 'NONE',  ( -21.53943276465977519, 0.05219959533907696930, 66.24890960531436690 ) ) ;
#29707 = DIRECTION ( 'NONE',  ( -0.000000000000000000, -0.7071067811865467956, 0.7071067811865483499 ) ) ;
#29709 = DIRECTION ( 'NONE',  ( 0.000000000000000000, 0.000000000000000000, -1.000000000000000000 ) ) ;
#29708 = CARTESIAN_POINT ( 'NONE',  ( -16.52544592524342804, 4.483927247898546575, 26.04057627198103475 ) ) ;
#29710 = CARTESIAN_POINT ( 'NONE',  ( 19.05341960407617918, -5.049401038297876454, 111.0427570613523329 ) ) ;
#29711 = CARTESIAN_POINT ( 'NONE',  ( -12.14591786802309592, -12.06949235617757132, 76.87390960531439532 ) ) ;
#29712 = CARTESIAN_POINT ( 'NONE',  ( -16.29526858892875296, -7.335722546920131926, 95.79670597800208043 ) ) ;
#29713 = CARTESIAN_POINT ( 'NONE',  ( 9.474510206698971260, -16.51473224551069308, 72.91557627198102409 ) ) ;
#29714 = CARTESIAN_POINT ( 'NONE',  ( 13.97604488694527802, 13.89961937509977652, 49.37390960531434558 ) ) ;
#29715 = CARTESIAN_POINT ( 'NONE',  ( -16.55341960407611168, -4.379528057220339221, 71.45724293864769550 ) ) ;
#29716 = CARTESIAN_POINT ( 'NONE',  ( -19.02544592524342804, 5.153800228976336051, 116.0405762719810383 ) ) ;
#29717 = CARTESIAN_POINT ( 'NONE',  ( 19.05341960407617918, -5.049401038297876454, 101.0427570613523045 ) ) ;
#29718 = CARTESIAN_POINT ( 'NONE',  ( -19.03943276465977164, 0.05219959533909376836, 101.2489096053143669 ) ) ;
#29719 = CARTESIAN_POINT ( 'NONE',  ( 21.52544592524344225, -5.823673210054117533, 73.54057627198102409 ) ) ;
#29720 = CARTESIAN_POINT ( 'NONE',  ( 4.379528057220092307, 16.55341960407617563, 67.29275706135234714 ) ) ;
#29721 = CARTESIAN_POINT ( 'NONE',  ( -16.38665767534994089, 7.295008042176404750, 95.26400864214467390 ) ) ;
#29722 = CARTESIAN_POINT ( 'NONE',  ( 13.97604488694527802, 13.89961937509977652, 74.37390960531436690 ) ) ;
#29723 = CARTESIAN_POINT ( 'NONE',  ( -21.55341960407610458, -5.719274019375992779, 81.45724293864769550 ) ) ;
#29724 = CARTESIAN_POINT ( 'NONE',  ( -16.46253265017146816, -9.564922557961047289, 104.1677570613523329 ) ) ;
#29726 = CARTESIAN_POINT ( 'NONE',  ( -15.80617190586768217, 15.72974639402176855, 53.12609039468568284 ) ) ;
#29725 = CARTESIAN_POINT ( 'NONE',  ( -12.06949235617756955, 12.14591786802309770, 40.62390960531435269 ) ) ;
#29727 = DIRECTION ( 'NONE',  ( -1.000000000000000000, -1.249000902703301424E-14, 0.000000000000000000 ) ) ;
#29729 = CARTESIAN_POINT ( 'NONE',  ( -19.03943276465977164, 0.05219959533909376836, 106.2489096053143669 ) ) ;
#29728 = CARTESIAN_POINT ( 'NONE',  ( -14.29746914071037622, -8.314922557961029526, 69.16775706135234714 ) ) ;
#29730 = LINE ( 'NONE', #153054, #85508 ) ;
#29731 = CARTESIAN_POINT ( 'NONE',  ( -17.05116617787825106, 6.768360034955815507, 78.65675553259198693 ) ) ;
#29732 = CARTESIAN_POINT ( 'NONE',  ( 16.53943276465976808, 0.05219959533934440121, 96.25109039468568994 ) ) ;
#29733 = CARTESIAN_POINT ( 'NONE',  ( -0.05219959533934338120, 16.53943276465976808, 52.50109039468567573 ) ) ;
#29734 = CARTESIAN_POINT ( 'NONE',  ( 13.97604488694527802, 13.89961937509977652, 54.37390960531435979 ) ) ;
#29735 = CARTESIAN_POINT ( 'NONE',  ( 0.05219959533909260263, 19.03943276465977164, 74.99890960531435269 ) ) ;
#29736 = CARTESIAN_POINT ( 'NONE',  ( -21.52544592524334988, -5.823673210054445271, 68.95942372801901854 ) ) ;
#29737 = CARTESIAN_POINT ( 'NONE',  ( -4.483927247898782831, 16.52544592524335698, 57.70942372801901143 ) ) ;
#29738 = CARTESIAN_POINT ( 'NONE',  ( -14.29746914071049879, 8.314922557960819915, 35.83224293864768839 ) ) ;
#29739 = CARTESIAN_POINT ( 'NONE',  ( -19.05341960407611168, -5.049401038298163336, 41.45724293864769550 ) ) ;
#29740 = CARTESIAN_POINT ( 'NONE',  ( 16.46253265017160672, -9.564922557960803928, 38.33224293864768839 ) ) ;
#29741 = CARTESIAN_POINT ( 'NONE',  ( 4.483927247898790824, -16.52544592524335698, 35.20942372801901854 ) ) ;
#29742 = CARTESIAN_POINT ( 'NONE',  ( -16.46253265017146816, -9.564922557961047289, 89.16775706135234714 ) ) ;
#29743 = CARTESIAN_POINT ( 'NONE',  ( 8.314922557960818139, 14.29746914071049879, 99.58224293864770971 ) ) ;
#29744 = CARTESIAN_POINT ( 'NONE',  ( 13.89961937509977652, -13.97604488694527269, 53.12390960531434558 ) ) ;
#29746 = CARTESIAN_POINT ( 'NONE',  ( 23.48529157249599919, 32.32473071737754111, -8.700000000000002842 ) ) ;
#29745 = CARTESIAN_POINT ( 'NONE',  ( -16.46253265017146816, -9.564922557961047289, 89.16775706135234714 ) ) ;
#29747 = CARTESIAN_POINT ( 'NONE',  ( -10.81492255796105439, 18.62759615963255655, 92.91775706135236135 ) ) ;
#29748 = CARTESIAN_POINT ( 'NONE',  ( 4.379528057220092307, 16.55341960407617563, 57.29275706135234714 ) ) ;
#29749 = CARTESIAN_POINT ( 'NONE',  ( 11.30153831258470731, -188.0000000000000000, -25.00000000000000000 ) ) ;
#29750 = CARTESIAN_POINT ( 'NONE',  ( -15.72974639402197994, 15.80617190586746368, 55.62390960531436690 ) ) ;
#29751 = CARTESIAN_POINT ( 'NONE',  ( 0.05219959533934541429, -16.53943276465976808, 45.00109039468568284 ) ) ;
#29752 = CARTESIAN_POINT ( 'NONE',  ( -19.48894818550245844, 5.499999999999919176, 70.10307310435241845 ) ) ;
#29753 = CARTESIAN_POINT ( 'NONE',  ( 19.02544592524334988, 5.153800228976608722, 41.45942372801900433 ) ) ;
#29754 = CARTESIAN_POINT ( 'NONE',  ( 0.05219959533909260263, 19.03943276465977164, 89.99890960531436690 ) ) ;
#29755 = CARTESIAN_POINT ( 'NONE',  ( -8.314922557960811034, -14.29746914071050412, 102.0822429386476955 ) ) ;
#29756 = CARTESIAN_POINT ( 'NONE',  ( 5.153800228976335163, 19.02544592524342804, 54.79057627198103120 ) ) ;
#29757 = CARTESIAN_POINT ( 'NONE',  ( -22.41419083229811804, -22.69922180740366358, -49.13275782002544645 ) ) ;
#29758 = CARTESIAN_POINT ( 'NONE',  ( -5.719274019375665041, -21.55341960407619695, 79.79275706135236135 ) ) ;
#29759 = CARTESIAN_POINT ( 'NONE',  ( -18.22780087662124160, -5.499999999999927169, 88.98236817873107896 ) ) ;
#29760 = ADVANCED_FACE ( 'NONE', ( #33646 ), #137169, .F. ) ;
#29761 = CARTESIAN_POINT ( 'NONE',  ( 5.049401038297881783, 19.05341960407617563, 32.29275706135233293 ) ) ;
#29762 = CARTESIAN_POINT ( 'NONE',  ( -21.53943276465977519, -0.05219959533937600094, 113.7510903946856757 ) ) ;
#29763 = CARTESIAN_POINT ( 'NONE',  ( -16.55341960407611168, -4.379528057220339221, 56.45724293864768839 ) ) ;
#29764 = CARTESIAN_POINT ( 'NONE',  ( 16.46253265017160672, -9.564922557960803928, 58.33224293864769550 ) ) ;
#29765 = CARTESIAN_POINT ( 'NONE',  ( -19.02544592524342804, 5.153800228976336051, 106.0405762719810241 ) ) ;
#29766 = CARTESIAN_POINT ( 'NONE',  ( -5.823673210054431948, 21.52544592524334988, 82.70942372801900433 ) ) ;
#29767 = CARTESIAN_POINT ( 'NONE',  ( 13.97604488694527802, 13.89961937509977652, 69.37390960531436690 ) ) ;
#29768 = CARTESIAN_POINT ( 'NONE',  ( -21.55341960407619339, 5.719274019375674811, 73.54275706135234714 ) ) ;
#29769 = CARTESIAN_POINT ( 'NONE',  ( -21.52544592524343514, 5.823673210054127303, 36.04057627198102409 ) ) ;
#29770 = CARTESIAN_POINT ( 'NONE',  ( 15.80617190586769283, -15.72974639402175789, 35.62609039468568994 ) ) ;
#29771 = CARTESIAN_POINT ( 'NONE',  ( 13.89961937509957401, 13.97604488694547697, 56.87609039468564731 ) ) ;
#29772 = CARTESIAN_POINT ( 'NONE',  ( -9.474510206698964154, 16.51473224551069663, 25.41557627198103120 ) ) ;
#29773 = CARTESIAN_POINT ( 'NONE',  ( 16.46253265017160672, -9.564922557960803928, 73.33224293864769550 ) ) ;
#29774 = CARTESIAN_POINT ( 'NONE',  ( -16.53943276465976808, -0.05219959533934237506, 28.75109039468567929 ) ) ;
#29775 = CARTESIAN_POINT ( 'NONE',  ( -0.05219959533910754901, -16.53943276465976808, 92.49890960531436690 ) ) ;
#29776 = CARTESIAN_POINT ( 'NONE',  ( 9.474510206698971260, -16.51473224551069308, 57.91557627198103120 ) ) ;
#29777 = CARTESIAN_POINT ( 'NONE',  ( -10.72451020669898014, 18.67979575497178502, 30.41557627198101699 ) ) ;
#29778 = CARTESIAN_POINT ( 'NONE',  ( -16.52544592524335698, -4.483927247898792601, 18.95942372801901143 ) ) ;
#29779 = CARTESIAN_POINT ( 'NONE',  ( 15.80617190586769283, -15.72974639402175789, 20.62609039468568639 ) ) ;
#29780 = CARTESIAN_POINT ( 'NONE',  ( 15.80617190586769283, -15.72974639402175789, 65.62609039468568994 ) ) ;
#29781 = CARTESIAN_POINT ( 'NONE',  ( -0.05219959533934338120, 16.53943276465976808, 72.50109039468568994 ) ) ;
#29782 = CARTESIAN_POINT ( 'NONE',  ( -4.483927247898782831, 16.52544592524335698, 72.70942372801901854 ) ) ;
#29783 = CARTESIAN_POINT ( 'NONE',  ( 13.89961937509977652, -13.97604488694527269, 63.12390960531435979 ) ) ;
#29784 = CARTESIAN_POINT ( 'NONE',  ( -16.55341960407617563, 4.379528057220093196, 88.54275706135236135 ) ) ;
#29785 = CARTESIAN_POINT ( 'NONE',  ( 19.05341960407617918, -5.049401038297876454, 36.04275706135234003 ) ) ;
#29786 = CARTESIAN_POINT ( 'NONE',  ( 15.80617190586769283, -15.72974639402175789, 20.62609039468568639 ) ) ;
#29787 = CARTESIAN_POINT ( 'NONE',  ( 14.34966873604960469, 8.224510206698951720, 64.16557627198102409 ) ) ;
#29788 = CARTESIAN_POINT ( 'NONE',  ( -16.51473224551069308, -9.474510206698971260, 91.66557627198103830 ) ) ;
#29789 = CARTESIAN_POINT ( 'NONE',  ( 16.52544592524335698, 4.483927247898782831, 91.45942372801901854 ) ) ;
#29790 = CARTESIAN_POINT ( 'NONE',  ( 21.55341960407619695, -5.719274019375665929, 61.04275706135234714 ) ) ;
#29791 = CARTESIAN_POINT ( 'NONE',  ( -16.55341960407617563, 4.379528057220093196, 33.54275706135234714 ) ) ;
#29792 = CARTESIAN_POINT ( 'NONE',  ( -21.52544592524343514, 5.823673210054127303, 116.0405762719810383 ) ) ;
#29793 = CARTESIAN_POINT ( 'NONE',  ( -12.06949235617756955, 12.14591786802309770, 60.62390960531437401 ) ) ;
#29794 = EDGE_LOOP ( 'NONE', ( #87485, #63464, #136171, #43735 ) ) ;
#29795 = CARTESIAN_POINT ( 'NONE',  ( -21.53943276465977519, 0.05219959533907696930, 106.2489096053143811 ) ) ;
#29796 = CARTESIAN_POINT ( 'NONE',  ( 8.314922557960818139, 14.29746914071049879, 44.58224293864769550 ) ) ;
#29797 = ORIENTED_EDGE ( 'NONE', *, *, #84815, .T. ) ;
#29798 = CARTESIAN_POINT ( 'NONE',  ( 35.31606782002515388, 4.574060259307362486, 39.03637847775443248 ) ) ;
#29799 = CARTESIAN_POINT ( 'NONE',  ( 18.62759615963271287, -10.81492255796078972, 113.3322429386476955 ) ) ;
#29800 = CARTESIAN_POINT ( 'NONE',  ( 9.564922557960805705, 16.46253265017160317, 109.5822429386476955 ) ) ;
#29801 = CARTESIAN_POINT ( 'NONE',  ( 21.55341960407619695, -5.719274019375665929, 36.04275706135234714 ) ) ;
#29802 = CARTESIAN_POINT ( 'NONE',  ( 0.05219959533910956823, 16.53943276465976808, 49.99890960531437401 ) ) ;
#29803 = CARTESIAN_POINT ( 'NONE',  ( 5.049401038298161559, -19.05341960407611168, 67.70724293864769550 ) ) ;
#29804 = CARTESIAN_POINT ( 'NONE',  ( 5.049401038297881783, 19.05341960407617563, 72.29275706135234714 ) ) ;
#29805 = CARTESIAN_POINT ( 'NONE',  ( 16.51473224551069308, 9.474510206698969483, 99.16557627198102409 ) ) ;
#29806 = CARTESIAN_POINT ( 'NONE',  ( -10.81492255796078084, -18.62759615963271287, 47.08224293864770260 ) ) ;
#29807 = CARTESIAN_POINT ( 'NONE',  ( -12.38288446667173837, -41.98357824128019899, -20.85955585120584033 ) ) ;
#29808 = CARTESIAN_POINT ( 'NONE',  ( 19.02544592524343514, -5.153800228976328945, 53.54057627198102409 ) ) ;
#29809 = CARTESIAN_POINT ( 'NONE',  ( 12.14591786802327356, -12.06949235617739191, 35.62609039468568994 ) ) ;
#29810 = CARTESIAN_POINT ( 'NONE',  ( -13.97604488694547697, 13.89961937509957934, 63.12609039468566152 ) ) ;
#29811 = CARTESIAN_POINT ( 'NONE',  ( -21.53943276465977519, 0.05219959533907696930, 116.2489096053143669 ) ) ;
#29812 = CARTESIAN_POINT ( 'NONE',  ( -16.52544592524342804, 4.483927247898546575, 46.04057627198103830 ) ) ;
#29813 = ORIENTED_EDGE ( 'NONE', *, *, #165696, .T. ) ;
#29814 = CARTESIAN_POINT ( 'NONE',  ( -16.51473224551069308, -9.474510206698971260, 86.66557627198102409 ) ) ;
#29815 = CARTESIAN_POINT ( 'NONE',  ( -5.823673210054116645, -21.52544592524344225, 77.29057627198102409 ) ) ;
#29817 = CARTESIAN_POINT ( 'NONE',  ( 14.29746914071037800, 8.314922557961029526, 36.66775706135234714 ) ) ;
#29816 = CARTESIAN_POINT ( 'NONE',  ( 21.53943276465977519, -0.05219959533907433946, 113.7489096053143527 ) ) ;
#29818 = CARTESIAN_POINT ( 'NONE',  ( 21.52544592524344225, -5.823673210054117533, 33.54057627198102409 ) ) ;
#29819 = CARTESIAN_POINT ( 'NONE',  ( -10.81492255796105439, 18.62759615963255655, 107.9177570613523471 ) ) ;
#29820 = CARTESIAN_POINT ( 'NONE',  ( 16.46253265017160672, -9.564922557960803928, 88.33224293864769550 ) ) ;
#29821 = CARTESIAN_POINT ( 'NONE',  ( -16.46253265017160317, 9.564922557960807481, 40.83224293864769550 ) ) ;
#29822 = CARTESIAN_POINT ( 'NONE',  ( 5.049401038298161559, -19.05341960407611168, 97.70724293864766707 ) ) ;
#29823 = CARTESIAN_POINT ( 'NONE',  ( 13.89961937509977652, -13.97604488694527269, 73.12390960531436690 ) ) ;
#29824 = CARTESIAN_POINT ( 'NONE',  ( -16.53943276465976808, -0.05219959533934237506, 23.75109039468567929 ) ) ;
#29825 = CARTESIAN_POINT ( 'NONE',  ( 16.52216118717250382, -7.221426719304220754, 86.42400978952974810 ) ) ;
#29826 = CARTESIAN_POINT ( 'NONE',  ( -5.153800228976607833, 19.02544592524334988, 57.70942372801899012 ) ) ;
#29828 = CARTESIAN_POINT ( 'NONE',  ( -15.72974639402197994, 15.80617190586746368, 35.62390960531437401 ) ) ;
#29827 = CARTESIAN_POINT ( 'NONE',  ( -9.474510206698720793, -16.51473224551083518, 19.58442372801899722 ) ) ;
#29829 = CARTESIAN_POINT ( 'NONE',  ( 14.34966873604972726, -8.224510206698740333, 100.8344237280190185 ) ) ;
#29830 = CARTESIAN_POINT ( 'NONE',  ( 1.500000000004064082, 7.599999999999568878, -62.20201607440122871 ) ) ;
#29831 = CARTESIAN_POINT ( 'NONE',  ( -9.474510206698720793, -16.51473224551083518, 69.58442372801901854 ) ) ;
#29832 = CARTESIAN_POINT ( 'NONE',  ( -0.05219959533936034679, 19.03943276465977164, 27.50109039468566507 ) ) ;
#29833 = CARTESIAN_POINT ( 'NONE',  ( 1.500000000000005329, 15.20000000000001883, -61.96904110198155280 ) ) ;
#29834 = CARTESIAN_POINT ( 'NONE',  ( -19.02544592524342804, 5.153800228976336051, 36.04057627198100988 ) ) ;
#29835 = CARTESIAN_POINT ( 'NONE',  ( -8.224510206698948167, 14.34966873604960824, 40.41557627198103120 ) ) ;
#29836 = CARTESIAN_POINT ( 'NONE',  ( -19.02544592524342804, 5.153800228976336051, 26.04057627198103120 ) ) ;
#29837 = CARTESIAN_POINT ( 'NONE',  ( -12.14591786802326823, 12.06949235617739902, 113.1260903946856899 ) ) ;
#29838 = CARTESIAN_POINT ( 'NONE',  ( 26.46959431505287341, -27.26463967846483527, -11.00411086000093519 ) ) ;
#29839 = CARTESIAN_POINT ( 'NONE',  ( 14.29746914071037800, 8.314922557961029526, 96.66775706135234714 ) ) ;
#29840 = CARTESIAN_POINT ( 'NONE',  ( 19.03943276465977164, -0.05219959533909143690, 53.74890960531436690 ) ) ;
#29841 = CARTESIAN_POINT ( 'NONE',  ( 0.05219959533937995610, -21.53943276465977519, 110.0010903946856757 ) ) ;
#29842 = CARTESIAN_POINT ( 'NONE',  ( 14.29746914071037800, 8.314922557961029526, 26.66775706135235424 ) ) ;
#29844 = ORIENTED_EDGE ( 'NONE', *, *, #125821, .T. ) ;
#29843 = CARTESIAN_POINT ( 'NONE',  ( -21.55341960407619339, 5.719274019375674811, 83.54275706135234714 ) ) ;
#29845 = CARTESIAN_POINT ( 'NONE',  ( 19.05341960407617918, -5.049401038297876454, 61.04275706135232582 ) ) ;
#29846 = CARTESIAN_POINT ( 'NONE',  ( -19.02544592524342804, 5.153800228976336051, 86.04057627198103830 ) ) ;
#29847 = CARTESIAN_POINT ( 'NONE',  ( -9.564922557960796823, -16.46253265017161027, 82.08224293864768129 ) ) ;
#29848 = CARTESIAN_POINT ( 'NONE',  ( -11.40812507854755609, 35.11059874428196537, -9.024999997268814411 ) ) ;
#29849 = CARTESIAN_POINT ( 'NONE',  ( -18.67979575497178146, -10.72451020669898902, 111.6655762719810525 ) ) ;
#29850 = CARTESIAN_POINT ( 'NONE',  ( -4.379528057220328563, 16.55341960407611168, 70.20724293864769550 ) ) ;
#29851 = CARTESIAN_POINT ( 'NONE',  ( -18.62759615963270932, 10.81492255796079327, 65.83224293864769550 ) ) ;
#29852 = CARTESIAN_POINT ( 'NONE',  ( 19.03943276465977164, -0.05219959533909143690, 53.74890960531436690 ) ) ;
#29854 = CARTESIAN_POINT ( 'NONE',  ( -4.483927247898782831, 16.52544592524335698, 92.70942372801901854 ) ) ;
#29853 = CARTESIAN_POINT ( 'NONE',  ( -0.05219959533907301413, -21.53943276465977519, 92.49890960531436690 ) ) ;
#29855 = ORIENTED_EDGE ( 'NONE', *, *, #111391, .F. ) ;
#29856 = CARTESIAN_POINT ( 'NONE',  ( -9.564922557960796823, -16.46253265017161027, 57.08224293864769550 ) ) ;
#29858 = CARTESIAN_POINT ( 'NONE',  ( 5.374011537017778117, -5.374011537017756801, -64.92279855667830191 ) ) ;
#29857 = CARTESIAN_POINT ( 'NONE',  ( -16.52544592524342804, 4.483927247898546575, 91.04057627198103830 ) ) ;
#29859 = CARTESIAN_POINT ( 'NONE',  ( 5.153800228976335163, 19.02544592524342804, 49.79057627198100988 ) ) ;
#29860 = CARTESIAN_POINT ( 'NONE',  ( -19.05341960407617563, 5.049401038297882671, 78.54275706135233293 ) ) ;
#29861 = CARTESIAN_POINT ( 'NONE',  ( -4.379528057220328563, 16.55341960407611168, 85.20724293864770971 ) ) ;
#29862 = CARTESIAN_POINT ( 'NONE',  ( -15.80617190586768217, 15.72974639402176855, 63.12609039468568994 ) ) ;
#29864 = CARTESIAN_POINT ( 'NONE',  ( 0.05219959533907565091, 21.53943276465977519, 109.9989096053143527 ) ) ;
#29863 = CARTESIAN_POINT ( 'NONE',  ( 19.02544592524343514, -5.153800228976328945, 38.54057627198103120 ) ) ;
#29865 = CARTESIAN_POINT ( 'NONE',  ( 8.224510206698953496, -14.34966873604960469, 97.91557627198103830 ) ) ;
#29866 = CARTESIAN_POINT ( 'NONE',  ( 28.82186960331498327, 2.781578969918950771E-14, 147.2500000054623683 ) ) ;
#29867 = CARTESIAN_POINT ( 'NONE',  ( 19.02544592524343514, -5.153800228976328945, 63.54057627198103830 ) ) ;
#29868 = DIRECTION ( 'NONE',  ( 0.8437662581494463909, 0.5367108174878553184, 0.000000000000000000 ) ) ;
#29870 = CARTESIAN_POINT ( 'NONE',  ( 16.51473224551069308, 9.474510206698969483, 114.1655762719810241 ) ) ;
#29869 = CARTESIAN_POINT ( 'NONE',  ( -16.51473224551082808, 9.474510206698731452, 88.33442372801900433 ) ) ;
#29871 = CARTESIAN_POINT ( 'NONE',  ( -21.52544592524334988, -5.823673210054445271, 38.95942372801901854 ) ) ;
#29872 = CARTESIAN_POINT ( 'NONE',  ( -16.51473224551069308, -9.474510206698971260, 81.66557627198103830 ) ) ;
#29873 = CARTESIAN_POINT ( 'NONE',  ( 19.03943276465977164, 0.05219959533936151252, 66.25109039468567573 ) ) ;
#29874 = CARTESIAN_POINT ( 'NONE',  ( 5.153800228976335163, 19.02544592524342804, 59.79057627198100988 ) ) ;
#29875 = CARTESIAN_POINT ( 'NONE',  ( 8.224510206698953496, -14.34966873604960469, 82.91557627198103830 ) ) ;
#29876 = CARTESIAN_POINT ( 'NONE',  ( -4.379528057220328563, 16.55341960407611168, 65.20724293864768129 ) ) ;
#29877 = CARTESIAN_POINT ( 'NONE',  ( 9.474510206698971260, -16.51473224551069308, 82.91557627198103830 ) ) ;
#29878 = CARTESIAN_POINT ( 'NONE',  ( 8.224510206698953496, -14.34966873604960469, 82.91557627198103830 ) ) ;
#29879 = CARTESIAN_POINT ( 'NONE',  ( -16.46253265017160317, 9.564922557960807481, 90.83224293864769550 ) ) ;
#29880 = CARTESIAN_POINT ( 'NONE',  ( 16.46253265017146816, 9.564922557961045513, 36.66775706135233293 ) ) ;
#29883 = CARTESIAN_POINT ( 'NONE',  ( -16.52544592524342804, 4.483927247898546575, 106.0405762719810525 ) ) ;
#29882 = CARTESIAN_POINT ( 'NONE',  ( 16.55341960407611168, 4.379528057220329451, 28.95724293864769905 ) ) ;
#29881 = CARTESIAN_POINT ( 'NONE',  ( 16.46253265017160672, -9.564922557960803928, 48.33224293864769550 ) ) ;
#29884 = ORIENTED_EDGE ( 'NONE', *, *, #12228, .T. ) ;
#29885 = CARTESIAN_POINT ( 'NONE',  ( 15.80617190586769283, -15.72974639402175789, 45.62609039468567573 ) ) ;
#29886 = CARTESIAN_POINT ( 'NONE',  ( -19.03943276465977164, -0.05219959533935918106, 63.75109039468566863 ) ) ;
#29887 = CARTESIAN_POINT ( 'NONE',  ( 14.34966873604960469, 8.224510206698951720, 39.16557627198102409 ) ) ;
#29888 = CARTESIAN_POINT ( 'NONE',  ( -10.72451020669898014, 18.67979575497178502, 90.41557627198103830 ) ) ;
#29889 = CARTESIAN_POINT ( 'NONE',  ( -19.02544592524342804, 5.153800228976336051, 111.0405762719810099 ) ) ;
#29890 = CARTESIAN_POINT ( 'NONE',  ( -16.53943276465976808, 0.05219959533911058130, 71.24890960531435269 ) ) ;
#29891 = CARTESIAN_POINT ( 'NONE',  ( 19.02544592524343514, -5.153800228976328945, 48.54057627198103120 ) ) ;
#29892 = CARTESIAN_POINT ( 'NONE',  ( -19.03943276465977164, -0.05219959533935918106, 28.75109039468566507 ) ) ;
#29893 = CARTESIAN_POINT ( 'NONE',  ( 12.14591786802327356, -12.06949235617739191, 105.6260903946856899 ) ) ;
#29894 = CARTESIAN_POINT ( 'NONE',  ( -4.379528057220086978, -16.55341960407618274, 54.79275706135235424 ) ) ;
#29895 = CARTESIAN_POINT ( 'NONE',  ( 0.05219959533907565091, 21.53943276465977519, 39.99890960531436690 ) ) ;
#29896 = CARTESIAN_POINT ( 'NONE',  ( -19.03943276465977164, -0.05219959533935918106, 18.75109039468567218 ) ) ;
#29897 = CARTESIAN_POINT ( 'NONE',  ( -19.02544592524342804, 5.153800228976336051, 86.04057627198103830 ) ) ;
#29898 = CARTESIAN_POINT ( 'NONE',  ( -12.06949235617739369, -12.14591786802326823, 69.37609039468567573 ) ) ;
#29899 = CARTESIAN_POINT ( 'NONE',  ( -16.46253265017160317, 9.564922557960807481, 25.83224293864769194 ) ) ;
#29900 = CARTESIAN_POINT ( 'NONE',  ( 14.29746914071049879, -8.314922557960816363, 28.33224293864769550 ) ) ;
#29902 = CARTESIAN_POINT ( 'NONE',  ( 13.97604488694527802, 13.89961937509977652, 94.37390960531436690 ) ) ;
#29901 = CARTESIAN_POINT ( 'NONE',  ( 0.05219959533909260263, 19.03943276465977164, 99.99890960531436690 ) ) ;
#29903 = CARTESIAN_POINT ( 'NONE',  ( -10.72451020669898014, 18.67979575497178502, 25.41557627198103120 ) ) ;
#29904 = CARTESIAN_POINT ( 'NONE',  ( -0.05219959533910754901, -16.53943276465976808, 57.49890960531435979 ) ) ;
#29905 = CARTESIAN_POINT ( 'NONE',  ( 12.06949235617757843, -12.14591786802309237, 38.12390960531436690 ) ) ;
#29906 = ORIENTED_EDGE ( 'NONE', *, *, #99562, .F. ) ;
#29907 = CARTESIAN_POINT ( 'NONE',  ( -14.29746914071049879, 8.314922557960819915, 45.83224293864769550 ) ) ;
#29909 = CARTESIAN_POINT ( 'NONE',  ( 17.50000000000001776, -4.049696124445805623, 31.68039670665950780 ) ) ;
#29908 = CARTESIAN_POINT ( 'NONE',  ( 16.53943276465976808, 0.05219959533934440121, 41.25109039468568284 ) ) ;
#29910 = CARTESIAN_POINT ( 'NONE',  ( -13.97604488694547697, 13.89961937509957934, 53.12609039468565442 ) ) ;
#29911 = CARTESIAN_POINT ( 'NONE',  ( -13.89961937509977652, 13.97604488694528158, 95.62390960531436690 ) ) ;
#29912 = CARTESIAN_POINT ( 'NONE',  ( -0.05219959533936034679, 19.03943276465977164, 62.50109039468566863 ) ) ;
#29913 = CARTESIAN_POINT ( 'NONE',  ( -27.73933785331498925, 2.428612866367529932E-14, 141.3750000027311842 ) ) ;
#29914 = CARTESIAN_POINT ( 'NONE',  ( 5.153800228976615827, -19.02544592524334988, 55.20942372801899722 ) ) ;
#29916 = CARTESIAN_POINT ( 'NONE',  ( 12.06949235617739724, 12.14591786802326823, 81.87609039468568994 ) ) ;
#29915 = CARTESIAN_POINT ( 'NONE',  ( -19.03943276465977164, -0.05219959533935918106, 98.75109039468567573 ) ) ;
#29917 = CARTESIAN_POINT ( 'NONE',  ( 17.14385361876520264, 23.59649016807275856, 148.6750000027311387 ) ) ;
#29918 = CARTESIAN_POINT ( 'NONE',  ( 9.474510206698971260, -16.51473224551069308, 22.91557627198102765 ) ) ;
#29919 = CARTESIAN_POINT ( 'NONE',  ( -16.51473224551069308, -9.474510206698971260, 111.6655762719810383 ) ) ;
#29920 = CARTESIAN_POINT ( 'NONE',  ( -18.62759615963255300, -10.81492255796106328, 39.16775706135235424 ) ) ;
#29921 = CARTESIAN_POINT ( 'NONE',  ( 13.97604488694548053, -13.89961937509957401, 100.6260903946856615 ) ) ;
#29923 = CARTESIAN_POINT ( 'NONE',  ( 0.05219959533909260263, 19.03943276465977164, 64.99890960531436690 ) ) ;
#29922 = CARTESIAN_POINT ( 'NONE',  ( 17.50000000000000000, -5.500000000000000888, 108.2969038253417153 ) ) ;
#29924 = EDGE_CURVE ( 'NONE', #168590, #83320, #173162, .T. ) ;
#29925 = CARTESIAN_POINT ( 'NONE',  ( 16.51473224551069308, 9.474510206698969483, 104.1655762719810241 ) ) ;
#29927 = CARTESIAN_POINT ( 'NONE',  ( 16.46253265017160672, -9.564922557960803928, 58.33224293864769550 ) ) ;
#29926 = CARTESIAN_POINT ( 'NONE',  ( 8.314922557960818139, 14.29746914071049879, 69.58224293864769550 ) ) ;
#29928 = CARTESIAN_POINT ( 'NONE',  ( -9.474510206698964154, 16.51473224551069663, 70.41557627198102409 ) ) ;
#29929 = CARTESIAN_POINT ( 'NONE',  ( -9.564922557961040184, 16.46253265017147172, 82.91775706135233293 ) ) ;
#29930 = CARTESIAN_POINT ( 'NONE',  ( -10.81492255796078084, -18.62759615963271287, 52.08224293864768839 ) ) ;
#29931 = CARTESIAN_POINT ( 'NONE',  ( -5.153800228976328057, -19.02544592524343514, 22.29057627198102765 ) ) ;
#29932 = CARTESIAN_POINT ( 'NONE',  ( 9.474510206698729675, 16.51473224551082808, 37.08442372801899722 ) ) ;
#29933 = CARTESIAN_POINT ( 'NONE',  ( 13.97604488694527802, 13.89961937509977652, 74.37390960531436690 ) ) ;
#29934 = CARTESIAN_POINT ( 'NONE',  ( -21.55341960407610458, -5.719274019375992779, 71.45724293864769550 ) ) ;
#29936 = CARTESIAN_POINT ( 'NONE',  ( -5.153800228976607833, 19.02544592524334988, 47.70942372801900433 ) ) ;
#29935 = CARTESIAN_POINT ( 'NONE',  ( -16.52544592524342804, 4.483927247898546575, 81.04057627198102409 ) ) ;
#29937 = CARTESIAN_POINT ( 'NONE',  ( -5.823673210054116645, -21.52544592524344225, 72.29057627198102409 ) ) ;
#29938 = CARTESIAN_POINT ( 'NONE',  ( -10.72451020669898014, 18.67979575497178502, 60.41557627198102409 ) ) ;
#29939 = CARTESIAN_POINT ( 'NONE',  ( 15.72974639402199770, -15.80617190586745480, 33.12390960531435979 ) ) ;
#29940 = CARTESIAN_POINT ( 'NONE',  ( -18.67979575497193778, 10.72451020669871902, 93.33442372801901854 ) ) ;
#29941 = CARTESIAN_POINT ( 'NONE',  ( 19.02544592524343514, -5.153800228976328945, 63.54057627198103830 ) ) ;
#29942 = CARTESIAN_POINT ( 'NONE',  ( 9.564922557960805705, 16.46253265017160317, 24.58224293864769194 ) ) ;
#29943 = CARTESIAN_POINT ( 'NONE',  ( -15.80617190586768217, 15.72974639402176855, 28.12609039468568284 ) ) ;
#29944 = CARTESIAN_POINT ( 'NONE',  ( 1.022580077288041090E-15, 16.70000000000002061, -61.34707691135562868 ) ) ;
#29945 = CARTESIAN_POINT ( 'NONE',  ( 21.53943276465977519, 0.05219959533937863772, 46.25109039468567573 ) ) ;
#29946 = CARTESIAN_POINT ( 'NONE',  ( -13.89961937509977652, 13.97604488694528158, 35.62390960531435269 ) ) ;
#29947 = CARTESIAN_POINT ( 'NONE',  ( -18.67979575497178146, -10.72451020669898902, 106.6655762719810383 ) ) ;
#29948 = CARTESIAN_POINT ( 'NONE',  ( -13.89961937509957401, -13.97604488694547875, 54.37609039468565442 ) ) ;
#29949 = EDGE_CURVE ( 'NONE', #11857, #161202, #199201, .T. ) ;
#29950 = CARTESIAN_POINT ( 'NONE',  ( 13.89961937509977652, -13.97604488694527269, 33.12390960531434558 ) ) ;
#29951 = CARTESIAN_POINT ( 'NONE',  ( 13.97604488694527802, 13.89961937509977652, 29.37390960531435979 ) ) ;
#29952 = CARTESIAN_POINT ( 'NONE',  ( 11.80868324581537543, 11.80868324581533990, -64.92279855667830191 ) ) ;
#29953 = CARTESIAN_POINT ( 'NONE',  ( -16.52544592524335698, -4.483927247898792601, 63.95942372801901854 ) ) ;
#29954 = CARTESIAN_POINT ( 'NONE',  ( 9.474510206698971260, -16.51473224551069308, 22.91557627198102765 ) ) ;
#29955 = CARTESIAN_POINT ( 'NONE',  ( -25.62062145120300372, -9.171473787273981770, 171.1688781158170798 ) ) ;
#29956 = CARTESIAN_POINT ( 'NONE',  ( 5.049401038298161559, -19.05341960407611168, 87.70724293864769550 ) ) ;
#29957 = CARTESIAN_POINT ( 'NONE',  ( -8.224510206698948167, 14.34966873604960824, 110.4155762719810383 ) ) ;
#29958 = AXIS2_PLACEMENT_3D ( 'NONE', #118743, #9567, #194585 ) ;
#29959 = CARTESIAN_POINT ( 'NONE',  ( 21.53943276465977519, -0.05219959533907433946, 53.74890960531437401 ) ) ;
#29960 = CARTESIAN_POINT ( 'NONE',  ( -8.314922557961024197, 14.29746914071037800, 42.91775706135235424 ) ) ;
#29961 = CARTESIAN_POINT ( 'NONE',  ( -15.80617190586768217, 15.72974639402176855, 98.12609039468570415 ) ) ;
#29962 = CARTESIAN_POINT ( 'NONE',  ( 16.46253265017160672, -9.564922557960803928, 23.33224293864769194 ) ) ;
#29963 = CARTESIAN_POINT ( 'NONE',  ( 8.314922557961029526, -14.29746914071037800, 105.4177570613523613 ) ) ;
#29964 = CARTESIAN_POINT ( 'NONE',  ( 8.224510206698953496, -14.34966873604960469, 52.91557627198103830 ) ) ;
#29965 = CARTESIAN_POINT ( 'NONE',  ( 16.46253265017160672, -9.564922557960803928, 58.33224293864769550 ) ) ;
#29966 = CARTESIAN_POINT ( 'NONE',  ( -10.81492255796105439, 18.62759615963255655, 112.9177570613523329 ) ) ;
#29967 = CARTESIAN_POINT ( 'NONE',  ( 10.81492255796106328, -18.62759615963255655, 25.41775706135235779 ) ) ;
#29968 = CARTESIAN_POINT ( 'NONE',  ( -10.81492255796105439, 18.62759615963255655, 72.91775706135234714 ) ) ;
#29969 = CARTESIAN_POINT ( 'NONE',  ( -4.379528057220086978, -16.55341960407618274, 54.79275706135235424 ) ) ;
#29970 = CARTESIAN_POINT ( 'NONE',  ( -4.483927247898782831, 16.52544592524335698, 32.70942372801900433 ) ) ;
#29972 = CARTESIAN_POINT ( 'NONE',  ( 18.67979575497194134, -10.72451020669871369, 100.8344237280190185 ) ) ;
#29971 = CARTESIAN_POINT ( 'NONE',  ( 8.224510206698953496, -14.34966873604960469, 72.91557627198103830 ) ) ;
#29973 = CARTESIAN_POINT ( 'NONE',  ( 16.53943276465976808, -0.05219959533910856209, 28.74890960531435624 ) ) ;
#29974 = CARTESIAN_POINT ( 'NONE',  ( -17.31747979337947285, 6.344076630961062335, 113.6205513193481522 ) ) ;
#29975 = CARTESIAN_POINT ( 'NONE',  ( -12.06949235617739369, -12.14591786802326823, 44.37609039468567573 ) ) ;
#29976 = CARTESIAN_POINT ( 'NONE',  ( 12.14591786802309770, 12.06949235617756955, 44.37390960531435979 ) ) ;
#29977 = CARTESIAN_POINT ( 'NONE',  ( 8.314922557961029526, -14.29746914071037800, 85.41775706135236135 ) ) ;
#29978 = CARTESIAN_POINT ( 'NONE',  ( 9.474510206698971260, -16.51473224551069308, 92.91557627198103830 ) ) ;
#29979 = CARTESIAN_POINT ( 'NONE',  ( 21.52544592524344225, -5.823673210054117533, 23.54057627198102765 ) ) ;
#29980 = CARTESIAN_POINT ( 'NONE',  ( 10.81492255796106328, -18.62759615963255655, 100.4177570613523471 ) ) ;
#29981 = CARTESIAN_POINT ( 'NONE',  ( -12.14591786802326823, 12.06949235617739902, 98.12609039468570415 ) ) ;
#29982 = CARTESIAN_POINT ( 'NONE',  ( -16.52544592524342804, 4.483927247898546575, 91.04057627198103830 ) ) ;
#29983 = CARTESIAN_POINT ( 'NONE',  ( 5.049401038298161559, -19.05341960407611168, 87.70724293864769550 ) ) ;
#29984 = VERTEX_POINT ( 'NONE', #189332 ) ;
#29985 = CARTESIAN_POINT ( 'NONE',  ( 16.52544592524335698, 4.483927247898782831, 36.45942372801901143 ) ) ;
#29986 = CARTESIAN_POINT ( 'NONE',  ( 13.89961937509977652, -13.97604488694527269, 43.12390960531434558 ) ) ;
#29987 = CARTESIAN_POINT ( 'NONE',  ( -9.474510206698964154, 16.51473224551069663, 110.4155762719810383 ) ) ;
#29989 = CARTESIAN_POINT ( 'NONE',  ( 3.556970738554033499E-15, -38.81732327939057825, -2.124999997268813612 ) ) ;
#29988 = CARTESIAN_POINT ( 'NONE',  ( -12.06949235617739369, -12.14591786802326823, 34.37609039468568284 ) ) ;
#29990 = CARTESIAN_POINT ( 'NONE',  ( -16.51473224551082808, 9.474510206698731452, 38.33442372801899722 ) ) ;
#29991 = CARTESIAN_POINT ( 'NONE',  ( -16.53943276465976808, -0.05219959533934237506, 108.7510903946857042 ) ) ;
#29992 = CARTESIAN_POINT ( 'NONE',  ( -13.97604488694527625, -13.89961937509977652, 36.87390960531436690 ) ) ;
#29993 = CARTESIAN_POINT ( 'NONE',  ( -4.483927247898782831, 16.52544592524335698, 72.70942372801901854 ) ) ;
#29994 = CARTESIAN_POINT ( 'NONE',  ( 19.05341960407617918, -5.049401038297876454, 76.04275706135230450 ) ) ;
#29995 = CARTESIAN_POINT ( 'NONE',  ( 16.51473224551083163, -9.474510206698727899, 30.83442372801900433 ) ) ;
#29996 = CARTESIAN_POINT ( 'NONE',  ( 9.474510206698971260, -16.51473224551069308, 62.91557627198102409 ) ) ;
#29997 = CARTESIAN_POINT ( 'NONE',  ( -12.14591786802309592, -12.06949235617757132, 81.87390960531435269 ) ) ;
#29998 = EDGE_CURVE ( 'NONE', #64402, #12092, #51792, .T. ) ;
#29999 = CARTESIAN_POINT ( 'NONE',  ( 5.049401038297881783, 19.05341960407617563, 62.29275706135234003 ) ) ;
#30000 = CARTESIAN_POINT ( 'NONE',  ( 21.53943276465977519, -0.05219959533907433946, 58.74890960531436690 ) ) ;
#30001 = CARTESIAN_POINT ( 'NONE',  ( -9.474510206698720793, -16.51473224551083518, 34.58442372801899722 ) ) ;
#30002 = CARTESIAN_POINT ( 'NONE',  ( 5.153800228976335163, 19.02544592524342804, 109.7905762719810099 ) ) ;
#30003 = CARTESIAN_POINT ( 'NONE',  ( 5.719274019375991003, -21.55341960407610458, 77.70724293864770971 ) ) ;
#30004 = CARTESIAN_POINT ( 'NONE',  ( -9.474510206698964154, 16.51473224551069663, 105.4155762719810383 ) ) ;
#30005 = CARTESIAN_POINT ( 'NONE',  ( -16.46253265017146816, -9.564922557961047289, 104.1677570613523329 ) ) ;
#30006 = CARTESIAN_POINT ( 'NONE',  ( -17.50000000000000355, 5.076555817581250629, 108.8204850795023049 ) ) ;
#30007 = CARTESIAN_POINT ( 'NONE',  ( 12.06949235617739724, 12.14591786802326823, 31.87609039468567929 ) ) ;
#30008 = CARTESIAN_POINT ( 'NONE',  ( 19.03943276465977164, -0.05219959533909143690, 38.74890960531436690 ) ) ;
#30009 = CARTESIAN_POINT ( 'NONE',  ( 19.02544592524343514, -5.153800228976328945, 98.54057627198100988 ) ) ;
#30010 = CARTESIAN_POINT ( 'NONE',  ( -15.80617190586745835, -15.72974639402198527, 81.87390960531435269 ) ) ;
#30011 = CARTESIAN_POINT ( 'NONE',  ( 14.34966873604972726, -8.224510206698740333, 55.83442372801901854 ) ) ;
#30012 = CARTESIAN_POINT ( 'NONE',  ( -10.72451020669870658, -18.67979575497194134, 59.58442372801901854 ) ) ;
#30014 = CARTESIAN_POINT ( 'NONE',  ( 21.53943276465977519, 0.05219959533937863772, 106.2510903946856757 ) ) ;
#30013 = CARTESIAN_POINT ( 'NONE',  ( -16.46253265017146816, -9.564922557961047289, 109.1677570613523471 ) ) ;
#30015 = CARTESIAN_POINT ( 'NONE',  ( -16.53943276465976808, 0.05219959533911058130, 21.24890960531436690 ) ) ;
#30016 = CARTESIAN_POINT ( 'NONE',  ( 10.81492255796078972, 18.62759615963270932, 94.58224293864769550 ) ) ;
#30017 = CARTESIAN_POINT ( 'NONE',  ( -16.55341960407611168, -4.379528057220339221, 41.45724293864769550 ) ) ;
#30018 = CARTESIAN_POINT ( 'NONE',  ( 16.46253265017146816, 9.564922557961045513, 81.66775706135233293 ) ) ;
#30019 = CARTESIAN_POINT ( 'NONE',  ( -15.80617190586768217, 15.72974639402176855, 53.12609039468568284 ) ) ;
#30020 = CARTESIAN_POINT ( 'NONE',  ( -19.02544592524334988, -5.153800228976617603, 43.95942372801899012 ) ) ;
#30021 = CARTESIAN_POINT ( 'NONE',  ( -16.53943276465976808, 0.05219959533911058130, 106.2489096053143811 ) ) ;
#30022 = CARTESIAN_POINT ( 'NONE',  ( 10.72451020669898902, -18.67979575497178502, 27.91557627198103830 ) ) ;
#30023 = CARTESIAN_POINT ( 'NONE',  ( 14.34966873604960469, 8.224510206698951720, 34.16557627198102409 ) ) ;
#30024 = CARTESIAN_POINT ( 'NONE',  ( 18.67979575497194134, -10.72451020669871369, 95.83442372801903275 ) ) ;
#30025 = CARTESIAN_POINT ( 'NONE',  ( -0.05219959533934338120, 16.53943276465976808, 77.50109039468567573 ) ) ;
#30026 = CARTESIAN_POINT ( 'NONE',  ( -4.483927247898539470, -16.52544592524342804, 27.29057627198103120 ) ) ;
#30027 = CARTESIAN_POINT ( 'NONE',  ( 21.52544592524334988, 5.823673210054432836, 66.45942372801903275 ) ) ;
#30028 = CARTESIAN_POINT ( 'NONE',  ( 5.719274019375673035, 21.55341960407619339, 52.29275706135236135 ) ) ;
#30029 = CARTESIAN_POINT ( 'NONE',  ( 13.89961937509977652, -13.97604488694527269, 28.12390960531435624 ) ) ;
#30030 = CARTESIAN_POINT ( 'NONE',  ( -5.719274019375665041, -21.55341960407619695, 39.79275706135235424 ) ) ;
#30031 = CARTESIAN_POINT ( 'NONE',  ( 8.224510206698953496, -14.34966873604960469, 112.9155762719810383 ) ) ;
#30032 = CARTESIAN_POINT ( 'NONE',  ( 5.153800228976335163, 19.02544592524342804, 39.79057627198100988 ) ) ;
#30033 = CARTESIAN_POINT ( 'NONE',  ( 16.55341960407611168, 4.379528057220329451, 78.95724293864769550 ) ) ;
#30034 = CARTESIAN_POINT ( 'NONE',  ( -5.153800228976328057, -19.02544592524343514, 77.29057627198099567 ) ) ;
#30035 = CARTESIAN_POINT ( 'NONE',  ( -8.314922557960811034, -14.29746914071050412, 32.08224293864769550 ) ) ;
#30036 = CARTESIAN_POINT ( 'NONE',  ( -0.05219959533907301413, -21.53943276465977519, 62.49890960531436690 ) ) ;
#30037 = CARTESIAN_POINT ( 'NONE',  ( -15.72974639402197994, 15.80617190586746368, 110.6239096053143669 ) ) ;
#30038 = CARTESIAN_POINT ( 'NONE',  ( 16.51473224551069308, 9.474510206698969483, 99.16557627198102409 ) ) ;
#30040 = CARTESIAN_POINT ( 'NONE',  ( -13.89961937509957401, -13.97604488694547875, 99.37609039468567573 ) ) ;
#30039 = CARTESIAN_POINT ( 'NONE',  ( -0.05219959533909027116, -19.03943276465977164, 62.49890960531435979 ) ) ;
#30041 = CARTESIAN_POINT ( 'NONE',  ( 15.72974639402199770, -15.80617190586745480, 58.12390960531435979 ) ) ;
#30042 = CARTESIAN_POINT ( 'NONE',  ( 15.72974639402176855, 15.80617190586768217, 81.87609039468568994 ) ) ;
#30043 = CARTESIAN_POINT ( 'NONE',  ( 16.46253265017160672, -9.564922557960803928, 68.33224293864770971 ) ) ;
#30044 = CARTESIAN_POINT ( 'NONE',  ( -13.89961937509977652, 13.97604488694528158, 100.6239096053143669 ) ) ;
#30045 = CARTESIAN_POINT ( 'NONE',  ( -12.14591786802326823, 12.06949235617739902, 78.12609039468570415 ) ) ;
#30046 = CARTESIAN_POINT ( 'NONE',  ( -15.72974639402176322, -15.80617190586768395, 54.37609039468568994 ) ) ;
#30047 = CARTESIAN_POINT ( 'NONE',  ( -10.81492255796105439, 18.62759615963255655, 87.91775706135234714 ) ) ;
#30048 = CARTESIAN_POINT ( 'NONE',  ( 5.719274019375991003, -21.55341960407610458, 112.7072429386476955 ) ) ;
#30049 = CARTESIAN_POINT ( 'NONE',  ( -16.55341960407617563, 4.379528057220093196, 83.54275706135234714 ) ) ;
#30050 = CARTESIAN_POINT ( 'NONE',  ( 5.719274019375991003, -21.55341960407610458, 72.70724293864769550 ) ) ;
#30051 = CARTESIAN_POINT ( 'NONE',  ( 13.89961937509957401, 13.97604488694547697, 46.87609039468565442 ) ) ;
#30052 = CARTESIAN_POINT ( 'NONE',  ( -21.55341960407610458, -5.719274019375992779, 41.45724293864769550 ) ) ;
#30054 = CARTESIAN_POINT ( 'NONE',  ( 4.483927247898545687, 16.52544592524342804, 29.79057627198102409 ) ) ;
#30053 = CARTESIAN_POINT ( 'NONE',  ( 16.51473224551069308, 9.474510206698969483, 84.16557627198102409 ) ) ;
#30056 = VECTOR ( 'NONE', #139006, 1000.000000000000000 ) ;
#30055 = CARTESIAN_POINT ( 'NONE',  ( 5.719274019375991003, -21.55341960407610458, 27.70724293864769905 ) ) ;
#30057 = CARTESIAN_POINT ( 'NONE',  ( 0.2076433133274071252, 13.70000000000001528, -60.44446360152740993 ) ) ;
#30058 = CARTESIAN_POINT ( 'NONE',  ( -9.564922557961040184, 16.46253265017147172, 92.91775706135233293 ) ) ;
#30059 = CARTESIAN_POINT ( 'NONE',  ( -18.62759615963270932, 10.81492255796079327, 70.83224293864770971 ) ) ;
#30060 = CARTESIAN_POINT ( 'NONE',  ( 16.55341960407611168, 4.379528057220329451, 48.95724293864770971 ) ) ;
#30061 = CARTESIAN_POINT ( 'NONE',  ( 16.46253265017146816, 9.564922557961045513, 106.6677570613523471 ) ) ;
#30062 = CARTESIAN_POINT ( 'NONE',  ( 16.51473224551069308, 9.474510206698969483, 39.16557627198103120 ) ) ;
#30064 = CARTESIAN_POINT ( 'NONE',  ( 19.03943276465977164, 0.05219959533936151252, 71.25109039468566152 ) ) ;
#30063 = CARTESIAN_POINT ( 'NONE',  ( 21.55341960407610458, 5.719274019375980345, 98.95724293864770971 ) ) ;
#30065 = CARTESIAN_POINT ( 'NONE',  ( 16.46253265017160672, -9.564922557960803928, 88.33224293864769550 ) ) ;
#30066 = CARTESIAN_POINT ( 'NONE',  ( -16.53943276465976808, 0.05219959533911058130, 91.24890960531436690 ) ) ;
#30067 = CARTESIAN_POINT ( 'NONE',  ( -19.05341960407611168, -5.049401038298163336, 61.45724293864769550 ) ) ;
#30068 = CARTESIAN_POINT ( 'NONE',  ( -8.314922557960811034, -14.29746914071050412, 67.08224293864770971 ) ) ;
#30069 = CARTESIAN_POINT ( 'NONE',  ( -9.564922557960796823, -16.46253265017161027, 37.08224293864768839 ) ) ;
#30070 = CARTESIAN_POINT ( 'NONE',  ( 17.57923699280061314, -16.49001817116781865, -54.37788754106805555 ) ) ;
#30071 = CARTESIAN_POINT ( 'NONE',  ( 16.55341960407611168, 4.379528057220329451, 43.95724293864769550 ) ) ;
#30072 = CARTESIAN_POINT ( 'NONE',  ( -19.02544592524342804, 5.153800228976336051, 86.04057627198103830 ) ) ;
#30073 = CARTESIAN_POINT ( 'NONE',  ( -0.7820921006973207135, -16.49581645235993221, -59.22453004090982631 ) ) ;
#30074 = CARTESIAN_POINT ( 'NONE',  ( -9.564922557961040184, 16.46253265017147172, 57.91775706135233293 ) ) ;
#30075 = CARTESIAN_POINT ( 'NONE',  ( 8.314922557961029526, -14.29746914071037800, 65.41775706135234714 ) ) ;
#30076 = CARTESIAN_POINT ( 'NONE',  ( 10.72451020669898902, -18.67979575497178502, 67.91557627198102409 ) ) ;
#30077 = CARTESIAN_POINT ( 'NONE',  ( -16.51473224551082808, 9.474510206698731452, 33.33442372801899722 ) ) ;
#30078 = CARTESIAN_POINT ( 'NONE',  ( -19.02544592524342804, 5.153800228976336051, 91.04057627198100988 ) ) ;
#30079 = CARTESIAN_POINT ( 'NONE',  ( -20.37894794865908921, -22.50499723050164746, -47.85318311809130165 ) ) ;
#30080 = CARTESIAN_POINT ( 'NONE',  ( -18.62759615963270932, 10.81492255796079327, 25.83224293864769194 ) ) ;
#30081 = CARTESIAN_POINT ( 'NONE',  ( -9.474510206698964154, 16.51473224551069663, 60.41557627198102409 ) ) ;
#30082 = CARTESIAN_POINT ( 'NONE',  ( 18.67979575497194134, -10.72451020669871369, 45.83442372801901854 ) ) ;
#30083 = CARTESIAN_POINT ( 'NONE',  ( 19.05341960407611168, 5.049401038298154454, 28.95724293864769550 ) ) ;
#30086 = ORIENTED_EDGE ( 'NONE', *, *, #85875, .T. ) ;
#30085 = CARTESIAN_POINT ( 'NONE',  ( 19.05341960407611168, 5.049401038298154454, 88.95724293864769550 ) ) ;
#30084 = CARTESIAN_POINT ( 'NONE',  ( -18.67979575497178146, -10.72451020669898902, 101.6655762719810383 ) ) ;
#30087 = CARTESIAN_POINT ( 'NONE',  ( 15.72974639402176855, 15.80617190586768217, 41.87609039468568284 ) ) ;
#30088 = VERTEX_POINT ( 'NONE', #48825 ) ;
#30089 = CARTESIAN_POINT ( 'NONE',  ( -13.89961937509977652, 13.97604488694528158, 100.6239096053143669 ) ) ;
#30090 = EDGE_CURVE ( 'NONE', #164159, #164433, #169494, .T. ) ;
#30091 = VECTOR ( 'NONE', #145579, 1000.000000000000114 ) ;
#30092 = CARTESIAN_POINT ( 'NONE',  ( -17.49999999999999645, -5.500000000000000888, 109.2030961746582847 ) ) ;
#30093 = CARTESIAN_POINT ( 'NONE',  ( -0.05219959533907301413, -21.53943276465977519, 112.4989096053143669 ) ) ;
#30094 = CARTESIAN_POINT ( 'NONE',  ( -13.97604488694527625, -13.89961937509977652, 41.87390960531435979 ) ) ;
#30095 = CARTESIAN_POINT ( 'NONE',  ( -16.52544592524335698, -4.483927247898792601, 23.95942372801901143 ) ) ;
#30096 = CARTESIAN_POINT ( 'NONE',  ( 29.86685920354754842, -21.69954338932559068, -4.324999997268814234 ) ) ;
#30097 = CARTESIAN_POINT ( 'NONE',  ( 13.97604488694527802, 13.89961937509977652, 34.37390960531436690 ) ) ;
#30098 = CARTESIAN_POINT ( 'NONE',  ( -21.55341960407619339, 5.719274019375674811, 98.54275706135234714 ) ) ;
#30100 = CARTESIAN_POINT ( 'NONE',  ( -21.52544592524334988, -5.823673210054445271, 43.95942372801902565 ) ) ;
#30099 = CARTESIAN_POINT ( 'NONE',  ( -5.153800228976328057, -19.02544592524343514, 77.29057627198099567 ) ) ;
#30101 = CARTESIAN_POINT ( 'NONE',  ( 27.73933785331498925, -9.013057229001033122, 146.2750000027311899 ) ) ;
#30102 = CARTESIAN_POINT ( 'NONE',  ( 9.564922557960805705, 16.46253265017160317, 94.58224293864769550 ) ) ;
#30103 = CARTESIAN_POINT ( 'NONE',  ( 19.49190055781010145, 5.500000000000047962, 63.06116087098784107 ) ) ;
#30106 = CARTESIAN_POINT ( 'NONE',  ( -0.05219959533937732626, 21.53943276465977519, 57.50109039468568994 ) ) ;
#30105 = CARTESIAN_POINT ( 'NONE',  ( -16.53943276465976808, -0.05219959533934237506, 73.75109039468567573 ) ) ;
#30104 = CARTESIAN_POINT ( 'NONE',  ( 14.34966873604972726, -8.224510206698740333, 45.83442372801901854 ) ) ;
#30107 = CARTESIAN_POINT ( 'NONE',  ( 15.72974639402176855, 15.80617190586768217, 91.87609039468568994 ) ) ;
#30108 = CARTESIAN_POINT ( 'NONE',  ( 5.169469635059304125, 6.863180944108024484, -62.01598399707661002 ) ) ;
#30109 = CARTESIAN_POINT ( 'NONE',  ( -5.049401038297874678, -19.05341960407617918, 104.7927570613523471 ) ) ;
#30110 = CARTESIAN_POINT ( 'NONE',  ( -9.564922557960796823, -16.46253265017161027, 72.08224293864770971 ) ) ;
#30111 = CARTESIAN_POINT ( 'NONE',  ( 19.03943276465977164, -0.05219959533909143690, 98.74890960531436690 ) ) ;
#30112 = CARTESIAN_POINT ( 'NONE',  ( -16.55341960407611168, -4.379528057220339221, 111.4572429386476813 ) ) ;
#30113 = CARTESIAN_POINT ( 'NONE',  ( 21.55341960407610458, 5.719274019375980345, 28.95724293864769905 ) ) ;
#30114 = CARTESIAN_POINT ( 'NONE',  ( 16.52544592524335698, 4.483927247898782831, 91.45942372801901854 ) ) ;
#30116 = CARTESIAN_POINT ( 'NONE',  ( 19.05341960407611168, 5.049401038298154454, 53.95724293864770260 ) ) ;
#30115 = CARTESIAN_POINT ( 'NONE',  ( -12.06949235617756955, 12.14591786802309770, 75.62390960531439532 ) ) ;
#30117 = CARTESIAN_POINT ( 'NONE',  ( 10.81492255796106328, -18.62759615963255655, 75.41775706135233293 ) ) ;
#30118 = CARTESIAN_POINT ( 'NONE',  ( -21.52594032250404865, 0.8193109935769098406, -58.70475745007092883 ) ) ;
#30119 = CARTESIAN_POINT ( 'NONE',  ( 16.46253265017146816, 9.564922557961045513, 101.6677570613523329 ) ) ;
#30120 = CARTESIAN_POINT ( 'NONE',  ( -12.14591786802309592, -12.06949235617757132, 76.87390960531439532 ) ) ;
#30121 = CARTESIAN_POINT ( 'NONE',  ( 15.72974639402176855, 15.80617190586768217, 31.87609039468567929 ) ) ;
#30122 = CARTESIAN_POINT ( 'NONE',  ( 5.719274019375991003, -21.55341960407610458, 57.70724293864770260 ) ) ;
#30123 = CARTESIAN_POINT ( 'NONE',  ( -13.97604488694547697, 13.89961937509957934, 33.12609039468566863 ) ) ;
#30124 = CARTESIAN_POINT ( 'NONE',  ( 23.31738231874054534, 16.94106989632529192, 145.4500000054623854 ) ) ;
#30125 = CARTESIAN_POINT ( 'NONE',  ( 13.89961937509977652, -13.97604488694527269, 88.12390960531438111 ) ) ;
#30126 = CARTESIAN_POINT ( 'NONE',  ( -16.53943276465976808, 0.05219959533911058130, 51.24890960531436690 ) ) ;
#30127 = CARTESIAN_POINT ( 'NONE',  ( 0.05219959533910956823, 16.53943276465976808, 39.99890960531436690 ) ) ;
#30128 = CARTESIAN_POINT ( 'NONE',  ( -14.29746914071037622, -8.314922557961029526, 94.16775706135237556 ) ) ;
#30129 = CARTESIAN_POINT ( 'NONE',  ( -0.05219959533936034679, 19.03943276465977164, 47.50109039468566863 ) ) ;
#30130 = CARTESIAN_POINT ( 'NONE',  ( 9.474510206698729675, 16.51473224551082808, 77.08442372801900433 ) ) ;
#30131 = CARTESIAN_POINT ( 'NONE',  ( 19.05341960407611168, 5.049401038298154454, 98.95724293864766707 ) ) ;
#30132 = CARTESIAN_POINT ( 'NONE',  ( 16.53943276465976808, -0.05219959533910856209, 68.74890960531435269 ) ) ;
#30133 = CARTESIAN_POINT ( 'NONE',  ( -16.46253265017146816, -9.564922557961047289, 49.16775706135233293 ) ) ;
#30135 = CARTESIAN_POINT ( 'NONE',  ( -21.53943276465977519, 0.05219959533907696930, 36.24890960531435979 ) ) ;
#30134 = CARTESIAN_POINT ( 'NONE',  ( 19.05341960407611168, 5.049401038298154454, 28.95724293864769550 ) ) ;
#30136 = CARTESIAN_POINT ( 'NONE',  ( -5.823673210054116645, -21.52544592524344225, 62.29057627198102409 ) ) ;
#30137 = CARTESIAN_POINT ( 'NONE',  ( 14.29746914071049879, -8.314922557960816363, 98.33224293864769550 ) ) ;
#30138 = CARTESIAN_POINT ( 'NONE',  ( 4.379528057220092307, 16.55341960407617563, 52.29275706135236135 ) ) ;
#30139 = CARTESIAN_POINT ( 'NONE',  ( 5.823673210054444382, -21.52544592524334988, 35.20942372801901854 ) ) ;
#30140 = CARTESIAN_POINT ( 'NONE',  ( -12.06949235617756955, 12.14591786802309770, 85.62390960531436690 ) ) ;
#30141 = DIRECTION ( 'NONE',  ( 1.000000000000000000, 0.000000000000000000, 0.000000000000000000 ) ) ;
#30142 = CARTESIAN_POINT ( 'NONE',  ( 22.81625015709510151, -31.40387420917324590, -10.42499999726881299 ) ) ;
#30143 = CARTESIAN_POINT ( 'NONE',  ( 18.62759615963271287, -10.81492255796078972, 38.33224293864768839 ) ) ;
#30144 = CARTESIAN_POINT ( 'NONE',  ( -7.656827144875921753, -71.74905178543390605, 8.936314941956774358E-29 ) ) ;
#30145 = CARTESIAN_POINT ( 'NONE',  ( 1.046079508147533810, 23.87944126242780740, -57.07319907805452175 ) ) ;
#30147 = CARTESIAN_POINT ( 'NONE',  ( 8.314922557960818139, 14.29746914071049879, 29.58224293864769905 ) ) ;
#30146 = CARTESIAN_POINT ( 'NONE',  ( -14.29746914071037622, -8.314922557961029526, 39.16775706135235424 ) ) ;
#30148 = CARTESIAN_POINT ( 'NONE',  ( 21.55341960407610458, 5.719274019375980345, 68.95724293864769550 ) ) ;
#30150 = CARTESIAN_POINT ( 'NONE',  ( 13.97604488694548053, -13.89961937509957401, 90.62609039468567573 ) ) ;
#30149 = VECTOR ( 'NONE', #51221, 1000.000000000000000 ) ;
#30151 = CARTESIAN_POINT ( 'NONE',  ( 21.53943276465977519, -0.05219959533907433946, 68.74890960531435269 ) ) ;
#30152 = CARTESIAN_POINT ( 'NONE',  ( -21.49230439284897543, -7.461675232480832420, 174.1505469413571063 ) ) ;
#30154 = CARTESIAN_POINT ( 'NONE',  ( -19.02544592524342804, 5.153800228976336051, 96.04057627198103830 ) ) ;
#30153 = CARTESIAN_POINT ( 'NONE',  ( -0.05219959533909027116, -19.03943276465977164, 42.49890960531435269 ) ) ;
#30155 = CARTESIAN_POINT ( 'NONE',  ( -13.97604488694527625, -13.89961937509977652, 41.87390960531435979 ) ) ;
#30156 = CARTESIAN_POINT ( 'NONE',  ( 9.474510206698971260, -16.51473224551069308, 22.91557627198102765 ) ) ;
#30157 = DIRECTION ( 'NONE',  ( 0.000000000000000000, 0.000000000000000000, 1.000000000000000000 ) ) ;
#30158 = CARTESIAN_POINT ( 'NONE',  ( 0.05219959533909260263, 19.03943276465977164, 109.9989096053143669 ) ) ;
#30159 = VERTEX_POINT ( 'NONE', #4281 ) ;
#30160 = CARTESIAN_POINT ( 'NONE',  ( -16.55341960407617563, 4.379528057220093196, 68.54275706135234714 ) ) ;
#30161 = CARTESIAN_POINT ( 'NONE',  ( 5.823673210054125526, 21.52544592524343514, 94.79057627198105251 ) ) ;
#30162 = CARTESIAN_POINT ( 'NONE',  ( -5.049401038298153566, 19.05341960407611168, 60.20724293864768129 ) ) ;
#30163 = CARTESIAN_POINT ( 'NONE',  ( 0.05219959533937995610, -21.53943276465977519, 30.00109039468568284 ) ) ;
#30164 = CARTESIAN_POINT ( 'NONE',  ( -19.02544592524342804, 5.153800228976336051, 81.04057627198103830 ) ) ;
#30165 = CARTESIAN_POINT ( 'NONE',  ( -13.89961937509977652, 13.97604488694528158, 115.6239096053143669 ) ) ;
#30166 = VERTEX_POINT ( 'NONE', #158963 ) ;
#30167 = CARTESIAN_POINT ( 'NONE',  ( 5.823673210054444382, -21.52544592524334988, 20.20942372801900788 ) ) ;
#30170 = CARTESIAN_POINT ( 'NONE',  ( 0.05219959533936267826, -19.03943276465977164, 90.00109039468567573 ) ) ;
#30169 = CARTESIAN_POINT ( 'NONE',  ( -13.89961937509977652, 13.97604488694528158, 100.6239096053143669 ) ) ;
#30168 = CARTESIAN_POINT ( 'NONE',  ( -19.05341960407611168, -5.049401038298163336, 21.45724293864768839 ) ) ;
#30171 = ADVANCED_FACE ( 'NONE', ( #143796 ), #78149, .F. ) ;
#30172 = CARTESIAN_POINT ( 'NONE',  ( -5.049401038297874678, -19.05341960407617918, 24.79275706135233648 ) ) ;
#30173 = CARTESIAN_POINT ( 'NONE',  ( -5.719274019375978568, 21.55341960407610458, 95.20724293864769550 ) ) ;
#30174 = CARTESIAN_POINT ( 'NONE',  ( 19.02544592524334988, 5.153800228976608722, 31.45942372801900433 ) ) ;
#30175 = CARTESIAN_POINT ( 'NONE',  ( -8.224510206698735004, -14.34966873604973081, 84.58442372801903275 ) ) ;
#30176 = CARTESIAN_POINT ( 'NONE',  ( 5.153800228976335163, 19.02544592524342804, 104.7905762719809957 ) ) ;
#30177 = CARTESIAN_POINT ( 'NONE',  ( -0.05219959533909027116, -19.03943276465977164, 57.49890960531435979 ) ) ;
#30178 = CARTESIAN_POINT ( 'NONE',  ( 5.823673210054444382, -21.52544592524334988, 65.20942372801901854 ) ) ;
#30179 = CARTESIAN_POINT ( 'NONE',  ( -18.67979575497193778, 10.72451020669871902, 78.33442372801901854 ) ) ;
#30180 = CARTESIAN_POINT ( 'NONE',  ( 26.46959431505287341, -27.26463967846483527, -11.00411086000093519 ) ) ;
#30181 = CARTESIAN_POINT ( 'NONE',  ( 13.89961937509977652, -13.97604488694527269, 78.12390960531433848 ) ) ;
#30182 = CARTESIAN_POINT ( 'NONE',  ( -18.62759615963255300, -10.81492255796106328, 54.16775706135235424 ) ) ;
#30183 = CARTESIAN_POINT ( 'NONE',  ( 13.89961937509957401, 13.97604488694547697, 81.87609039468564731 ) ) ;
#30184 = EDGE_CURVE ( 'NONE', #31781, #144449, #3266, .T. ) ;
#30185 = CARTESIAN_POINT ( 'NONE',  ( -13.89961937509977652, 13.97604488694528158, 55.62390960531434558 ) ) ;
#30186 = CARTESIAN_POINT ( 'NONE',  ( 9.474510206698971260, -16.51473224551069308, 102.9155762719810241 ) ) ;
#30187 = CARTESIAN_POINT ( 'NONE',  ( -5.153800228976328057, -19.02544592524343514, 77.29057627198099567 ) ) ;
#30188 = CARTESIAN_POINT ( 'NONE',  ( 17.49999999999999645, -5.249764055310042643, 23.25708826289255882 ) ) ;
#30189 = CARTESIAN_POINT ( 'NONE',  ( -13.97604488694527625, -13.89961937509977652, 51.87390960531436690 ) ) ;
#30190 = CARTESIAN_POINT ( 'NONE',  ( 18.62759615963271287, -10.81492255796078972, 93.33224293864769550 ) ) ;
#30191 = CARTESIAN_POINT ( 'NONE',  ( 16.55341960407618274, -4.379528057220086978, 91.04275706135236135 ) ) ;
#30192 = DIRECTION ( 'NONE',  ( 1.000000000000000000, 0.000000000000000000, -0.000000000000000000 ) ) ;
#30193 = CARTESIAN_POINT ( 'NONE',  ( -19.03943276465977164, -0.05219959533935918106, 43.75109039468566863 ) ) ;
#30194 = CARTESIAN_POINT ( 'NONE',  ( 0.05219959533909260263, 19.03943276465977164, 84.99890960531436690 ) ) ;
#30195 = CARTESIAN_POINT ( 'NONE',  ( -14.34966873604960291, -8.224510206698953496, 56.66557627198103830 ) ) ;
#30196 = CARTESIAN_POINT ( 'NONE',  ( -14.34966873604960291, -8.224510206698953496, 96.66557627198102409 ) ) ;
#30197 = CARTESIAN_POINT ( 'NONE',  ( -21.53943276465977519, 0.05219959533907696930, 21.24890960531436690 ) ) ;
#30198 =( BOUNDED_CURVE ( )  B_SPLINE_CURVE ( 2, ( #119378, #150714, #12213, #197218, #58680, #198198, #187026, #77815, #186017, #32326, #15165, #48497, #45502 ),
 .UNSPECIFIED., .F., .F. ) 
 B_SPLINE_CURVE_WITH_KNOTS ( ( 3, 2, 2, 2, 2, 2, 3 ),
 ( 0.6340093837954662304, 0.6359649122807017330, 0.6403508771929824483, 0.6447368421052631637, 0.6491228070175438791, 0.6535087719298245945, 0.6554186205929700693 ),
 .UNSPECIFIED. ) 
 CURVE ( )  GEOMETRIC_REPRESENTATION_ITEM ( )  RATIONAL_B_SPLINE_CURVE ( ( 0.9831626618144007068, 0.9848076720550096308, 1.000000000000000000, 0.9659258262890683122, 1.000000000000000000, 0.9659258262890683122, 1.000000000000000000, 0.9659258262890683122, 1.000000000000000000, 0.9659258262890683122, 1.000000000000000000, 0.9851625545550091179, 0.9832469066685282089 ) ) 
 REPRESENTATION_ITEM ( '' )  );
#30199 = CARTESIAN_POINT ( 'NONE',  ( -0.05219959533909027116, -19.03943276465977164, 107.4989096053143527 ) ) ;
#30200 = CARTESIAN_POINT ( 'NONE',  ( -9.474510206698964154, 16.51473224551069663, 115.4155762719810241 ) ) ;
#30201 = CARTESIAN_POINT ( 'NONE',  ( 16.46253265017146816, 9.564922557961045513, 21.66775706135233648 ) ) ;
#30202 = CARTESIAN_POINT ( 'NONE',  ( -12.14591786802326823, 12.06949235617739902, 93.12609039468568994 ) ) ;
#30203 = CARTESIAN_POINT ( 'NONE',  ( 13.97604488694527802, 13.89961937509977652, 79.37390960531435269 ) ) ;
#30204 = CARTESIAN_POINT ( 'NONE',  ( -15.72974639402176322, -15.80617190586768395, 44.37609039468567573 ) ) ;
#30205 = CARTESIAN_POINT ( 'NONE',  ( 5.823673210054125526, 21.52544592524343514, 34.79057627198103120 ) ) ;
#30206 = CARTESIAN_POINT ( 'NONE',  ( 5.719274019375991003, -21.55341960407610458, 112.7072429386476955 ) ) ;
#30207 = CARTESIAN_POINT ( 'NONE',  ( -21.52544592524343514, 5.823673210054127303, 66.04057627198103830 ) ) ;
#30208 = CARTESIAN_POINT ( 'NONE',  ( 14.29746914071049879, -8.314922557960816363, 93.33224293864769550 ) ) ;
#30209 = CARTESIAN_POINT ( 'NONE',  ( -13.97604488694547697, 13.89961937509957934, 38.12609039468566152 ) ) ;
#30210 = CARTESIAN_POINT ( 'NONE',  ( 5.049401038298161559, -19.05341960407611168, 27.70724293864769550 ) ) ;
#30211 = CARTESIAN_POINT ( 'NONE',  ( -16.46253265017160317, 9.564922557960807481, 85.83224293864769550 ) ) ;
#30212 = CARTESIAN_POINT ( 'NONE',  ( -13.89961937509977652, 13.97604488694528158, 80.62390960531436690 ) ) ;
#30213 = CARTESIAN_POINT ( 'NONE',  ( 27.73933785331498569, 9.013057229001093518, 143.9750000027312069 ) ) ;
#30214 = CARTESIAN_POINT ( 'NONE',  ( -16.55341960407611168, -4.379528057220339221, 106.4572429386477097 ) ) ;
#30215 = ORIENTED_EDGE ( 'NONE', *, *, #187746, .F. ) ;
#30216 = CARTESIAN_POINT ( 'NONE',  ( -4.483927247898539470, -16.52544592524342804, 22.29057627198102765 ) ) ;
#30217 = CARTESIAN_POINT ( 'NONE',  ( -0.05219959533934338120, 16.53943276465976808, 32.50109039468568284 ) ) ;
#30218 = CARTESIAN_POINT ( 'NONE',  ( -21.53943276465977519, -0.05219959533937600094, 93.75109039468567573 ) ) ;
#30219 = CARTESIAN_POINT ( 'NONE',  ( -19.05341960407611168, -5.049401038298163336, 106.4572429386476955 ) ) ;
#30220 = CARTESIAN_POINT ( 'NONE',  ( -21.52544592524343514, 5.823673210054127303, 111.0405762719810525 ) ) ;
#30221 = CARTESIAN_POINT ( 'NONE',  ( 5.153800228976335163, 19.02544592524342804, 49.79057627198100988 ) ) ;
#30222 = CARTESIAN_POINT ( 'NONE',  ( -4.379528057220086978, -16.55341960407618274, 49.79275706135234714 ) ) ;
#30223 = CARTESIAN_POINT ( 'NONE',  ( -19.05341960407617563, 5.049401038297882671, 108.5427570613523187 ) ) ;
#30224 = VECTOR ( 'NONE', #12332, 1000.000000000000000 ) ;
#30225 = CARTESIAN_POINT ( 'NONE',  ( -21.53943276465977519, 0.05219959533907696930, 101.2489096053143669 ) ) ;
#30226 = CARTESIAN_POINT ( 'NONE',  ( 16.46253265017146816, 9.564922557961045513, 61.66775706135234003 ) ) ;
#30227 = DIRECTION ( 'NONE',  ( 0.000000000000000000, -0.9396926207859095381, 0.3420201433256656043 ) ) ;
#30228 = B_SPLINE_CURVE_WITH_KNOTS ( 'NONE', 3,
 ( #2223, #173081, #171083, #64893, #98948, #161637 ),
 .UNSPECIFIED., .F., .F.,
 ( 4, 2, 4 ),
 ( 0.003239945802372284651, 0.003620412082092146384, 0.004000878361812008552 ),
 .UNSPECIFIED. ) ;
#30229 = CARTESIAN_POINT ( 'NONE',  ( -21.55341960407610458, -5.719274019375992779, 111.4572429386476813 ) ) ;
#30230 = DIRECTION ( 'NONE',  ( 0.000000000000000000, 0.000000000000000000, 1.000000000000000000 ) ) ;
#30231 = CARTESIAN_POINT ( 'NONE',  ( 9.564922557960805705, 16.46253265017160317, 89.58224293864769550 ) ) ;
#30232 = CARTESIAN_POINT ( 'NONE',  ( 18.22780087662123805, 5.499999999999960032, 91.48236817873106475 ) ) ;
#30233 = CARTESIAN_POINT ( 'NONE',  ( -13.97604488694527625, -13.89961937509977652, 86.87390960531436690 ) ) ;
#30235 = CARTESIAN_POINT ( 'NONE',  ( -4.379528057220328563, 16.55341960407611168, 80.20724293864769550 ) ) ;
#30234 = CARTESIAN_POINT ( 'NONE',  ( 10.72451020669871369, 18.67979575497193778, 27.08442372801901854 ) ) ;
#30236 = CARTESIAN_POINT ( 'NONE',  ( -13.89961937509977652, 13.97604488694528158, 80.62390960531436690 ) ) ;
#30238 = CARTESIAN_POINT ( 'NONE',  ( 13.89961937509957401, 13.97604488694547697, 61.87609039468566863 ) ) ;
#30237 = CARTESIAN_POINT ( 'NONE',  ( 14.29746914071037800, 8.314922557961029526, 56.66775706135235424 ) ) ;
#30239 = CARTESIAN_POINT ( 'NONE',  ( -15.72974639402176322, -15.80617190586768395, 69.37609039468567573 ) ) ;
#30240 = CARTESIAN_POINT ( 'NONE',  ( -14.29746914071037622, -8.314922557961029526, 24.16775706135235424 ) ) ;
#30241 = CARTESIAN_POINT ( 'NONE',  ( -0.05219959533909027116, -19.03943276465977164, 67.49890960531436690 ) ) ;
#30242 = CARTESIAN_POINT ( 'NONE',  ( 5.049401038297881783, 19.05341960407617563, 92.29275706135234714 ) ) ;
#30243 = CARTESIAN_POINT ( 'NONE',  ( 14.29746914071037800, 8.314922557961029526, 56.66775706135235424 ) ) ;
#30244 = CARTESIAN_POINT ( 'NONE',  ( 21.52544592524334988, 5.823673210054432836, 96.45942372801901854 ) ) ;
#30245 = CARTESIAN_POINT ( 'NONE',  ( 16.46253265017146816, 9.564922557961045513, 76.66775706135234714 ) ) ;
#30246 = CARTESIAN_POINT ( 'NONE',  ( 9.564922557960805705, 16.46253265017160317, 44.58224293864769550 ) ) ;
#30247 = CARTESIAN_POINT ( 'NONE',  ( 10.72451020669898902, -18.67979575497178502, 72.91557627198103830 ) ) ;
#30249 = CARTESIAN_POINT ( 'NONE',  ( -0.05219959533936034679, 19.03943276465977164, 77.50109039468566152 ) ) ;
#30248 = CARTESIAN_POINT ( 'NONE',  ( 16.52544592524342804, -4.483927247898539470, 78.54057627198103830 ) ) ;
#30250 = DIRECTION ( 'NONE',  ( 0.000000000000000000, 0.000000000000000000, -1.000000000000000000 ) ) ;
#30251 = CARTESIAN_POINT ( 'NONE',  ( 5.153800228976615827, -19.02544592524334988, 45.20942372801901143 ) ) ;
#30252 = CARTESIAN_POINT ( 'NONE',  ( 0.05219959533934541429, -16.53943276465976808, 110.0010903946856757 ) ) ;
#30253 = CARTESIAN_POINT ( 'NONE',  ( -16.55341960407611168, -4.379528057220339221, 66.45724293864768129 ) ) ;
#30255 = CARTESIAN_POINT ( 'NONE',  ( -27.73933785331498925, 2.428612866367529932E-14, 142.8750000027311842 ) ) ;
#30254 = CARTESIAN_POINT ( 'NONE',  ( -10.72451020669870658, -18.67979575497194134, 104.5844237280190185 ) ) ;
#30256 = CARTESIAN_POINT ( 'NONE',  ( -15.72974639402197994, 15.80617190586746368, 105.6239096053143669 ) ) ;
#30257 = CARTESIAN_POINT ( 'NONE',  ( -13.89961937509977652, 13.97604488694528158, 70.62390960531432427 ) ) ;
#30258 = CARTESIAN_POINT ( 'NONE',  ( -21.53943276465977519, -0.05219959533937600094, 88.75109039468567573 ) ) ;
#30259 = CARTESIAN_POINT ( 'NONE',  ( 0.05219959533909260263, 19.03943276465977164, 64.99890960531436690 ) ) ;
#30260 = CARTESIAN_POINT ( 'NONE',  ( -19.03943276465977164, 0.05219959533909376836, 26.24890960531435624 ) ) ;
#30261 = CARTESIAN_POINT ( 'NONE',  ( -18.67979575497178146, -10.72451020669898902, 26.66557627198103475 ) ) ;
#30262 = CARTESIAN_POINT ( 'NONE',  ( -16.53943276465976808, 0.05219959533911058130, 61.24890960531435979 ) ) ;
#30263 = CARTESIAN_POINT ( 'NONE',  ( -19.05341960407611168, -5.049401038298163336, 41.45724293864769550 ) ) ;
#30264 = CARTESIAN_POINT ( 'NONE',  ( 12.14591786802309770, 12.06949235617756955, 89.37390960531435269 ) ) ;
#30265 = CARTESIAN_POINT ( 'NONE',  ( 21.53943276465977519, -0.05219959533907433946, 108.7489096053143669 ) ) ;
#30266 = CARTESIAN_POINT ( 'NONE',  ( 21.52544592524334988, 5.823673210054432836, 46.45942372801901854 ) ) ;
#30267 = CARTESIAN_POINT ( 'NONE',  ( 19.02544592524343514, -5.153800228976328945, 23.54057627198102054 ) ) ;
#30268 = CARTESIAN_POINT ( 'NONE',  ( 12.14591786802327356, -12.06949235617739191, 45.62609039468567573 ) ) ;
#30269 = CARTESIAN_POINT ( 'NONE',  ( 21.53943276465977519, -0.05219959533907433946, 98.74890960531438111 ) ) ;
#30271 = CARTESIAN_POINT ( 'NONE',  ( 5.049401038298161559, -19.05341960407611168, 37.70724293864768839 ) ) ;
#30270 = CARTESIAN_POINT ( 'NONE',  ( 13.89961937509957401, 13.97604488694547697, 26.87609039468566507 ) ) ;
#30272 = CARTESIAN_POINT ( 'NONE',  ( -9.474510206698964154, 16.51473224551069663, 105.4155762719810383 ) ) ;
#30273 = CARTESIAN_POINT ( 'NONE',  ( 18.62759615963255655, 10.81492255796105972, 56.66775706135235424 ) ) ;
#30274 = CARTESIAN_POINT ( 'NONE',  ( -18.67979575497178146, -10.72451020669898902, 41.66557627198103120 ) ) ;
#30275 = CARTESIAN_POINT ( 'NONE',  ( -4.483927247898539470, -16.52544592524342804, 22.29057627198102765 ) ) ;
#30277 = CARTESIAN_POINT ( 'NONE',  ( -15.80617190586768217, 15.72974639402176855, 93.12609039468568994 ) ) ;
#30276 = CARTESIAN_POINT ( 'NONE',  ( -21.52544592524334988, -5.823673210054445271, 68.95942372801901854 ) ) ;
#30278 = CARTESIAN_POINT ( 'NONE',  ( -5.153800228976607833, 19.02544592524334988, 37.70942372801899722 ) ) ;
#30279 = CARTESIAN_POINT ( 'NONE',  ( -4.483927247898782831, 16.52544592524335698, 97.70942372801904696 ) ) ;
#30281 = ADVANCED_FACE ( 'NONE', ( #76922 ), #45603, .T. ) ;
#30280 = CARTESIAN_POINT ( 'NONE',  ( -10.72451020669870658, -18.67979575497194134, 59.58442372801901854 ) ) ;
#30282 = CARTESIAN_POINT ( 'NONE',  ( -13.89961937509977652, 13.97604488694528158, 50.62390960531435979 ) ) ;
#30283 = CARTESIAN_POINT ( 'NONE',  ( 5.049401038297881783, 19.05341960407617563, 27.29275706135232937 ) ) ;
#30284 = CARTESIAN_POINT ( 'NONE',  ( 13.97604488694527802, 13.89961937509977652, 114.3739096053143669 ) ) ;
#30285 = CARTESIAN_POINT ( 'NONE',  ( 10.72451020669871369, 18.67979575497193778, 22.08442372801901143 ) ) ;
#30286 = CARTESIAN_POINT ( 'NONE',  ( -15.72974639402197994, 15.80617190586746368, 80.62390960531438111 ) ) ;
#30287 = CARTESIAN_POINT ( 'NONE',  ( 8.314922557961029526, -14.29746914071037800, 35.41775706135234003 ) ) ;
#30289 = CARTESIAN_POINT ( 'NONE',  ( 15.72974639402199770, -15.80617190586745480, 83.12390960531436690 ) ) ;
#30288 = DIRECTION ( 'NONE',  ( 0.000000000000000000, 0.000000000000000000, -1.000000000000000000 ) ) ;
#30291 = CARTESIAN_POINT ( 'NONE',  ( -4.379528057220328563, 16.55341960407611168, 70.20724293864769550 ) ) ;
#30290 = CARTESIAN_POINT ( 'NONE',  ( 14.29746914071037800, 8.314922557961029526, 66.66775706135234714 ) ) ;
#30292 = CARTESIAN_POINT ( 'NONE',  ( -32.09281931051391012, -20.34824190692417289, -24.99999999999999289 ) ) ;
#30293 = CARTESIAN_POINT ( 'NONE',  ( 19.05341960407617918, -5.049401038297876454, 101.0427570613523045 ) ) ;
#30294 = AXIS2_PLACEMENT_3D ( 'NONE', #32584, #2232, #63914 ) ;
#30295 = CARTESIAN_POINT ( 'NONE',  ( -15.72974639402197994, 15.80617190586746368, 35.62390960531437401 ) ) ;
#30296 = CARTESIAN_POINT ( 'NONE',  ( 17.59860650958990647, 7.585241751807016541, 94.07662985737508166 ) ) ;
#30297 = ADVANCED_FACE ( 'NONE', ( #29451 ), #74948, .F. ) ;
#30298 = CARTESIAN_POINT ( 'NONE',  ( 4.379528057220092307, 16.55341960407617563, 37.29275706135235424 ) ) ;
#30299 = CARTESIAN_POINT ( 'NONE',  ( -21.52544592524334988, -5.823673210054445271, 18.95942372801901143 ) ) ;
#30300 = CARTESIAN_POINT ( 'NONE',  ( 18.67979575497178502, 10.72451020669898547, 34.16557627198102409 ) ) ;
#30301 = CARTESIAN_POINT ( 'NONE',  ( -12.06949235617739369, -12.14591786802326823, 69.37609039468567573 ) ) ;
#30302 = CARTESIAN_POINT ( 'NONE',  ( -13.89961937509977652, 13.97604488694528158, 90.62390960531432427 ) ) ;
#30304 = CARTESIAN_POINT ( 'NONE',  ( -16.53943276465976808, -0.05219959533934237506, 18.75109039468568639 ) ) ;
#30303 = CARTESIAN_POINT ( 'NONE',  ( 21.55341960407619695, -5.719274019375665929, 46.04275706135234714 ) ) ;
#30305 = CARTESIAN_POINT ( 'NONE',  ( -5.719274019375978568, 21.55341960407610458, 30.20724293864769550 ) ) ;
#30306 = ORIENTED_EDGE ( 'NONE', *, *, #193551, .F. ) ;
#30307 = CARTESIAN_POINT ( 'NONE',  ( 13.97604488694548053, -13.89961937509957401, 30.62609039468566863 ) ) ;
#30308 = CARTESIAN_POINT ( 'NONE',  ( -16.53943276465976808, -0.05219959533934237506, 48.75109039468568284 ) ) ;
#30309 = CARTESIAN_POINT ( 'NONE',  ( -0.05219959533909027116, -19.03943276465977164, 102.4989096053143669 ) ) ;
#30310 = CARTESIAN_POINT ( 'NONE',  ( 21.52544592524344225, -5.823673210054117533, 103.5405762719810383 ) ) ;
#30311 = CARTESIAN_POINT ( 'NONE',  ( 13.89961937509977652, -13.97604488694527269, 68.12390960531436690 ) ) ;
#30312 = CARTESIAN_POINT ( 'NONE',  ( -17.40805194822030089, 6.112264579159337963, 25.83371272510612116 ) ) ;
#30313 = CARTESIAN_POINT ( 'NONE',  ( -8.314922557960811034, -14.29746914071050412, 82.08224293864768129 ) ) ;
#30314 = CARTESIAN_POINT ( 'NONE',  ( 21.53943276465977519, -0.05219959533907433946, 33.74890960531436690 ) ) ;
#30315 = CARTESIAN_POINT ( 'NONE',  ( -9.564922557960796823, -16.46253265017161027, 22.08224293864768839 ) ) ;
#30316 = CARTESIAN_POINT ( 'NONE',  ( 4.379528057220092307, 16.55341960407617563, 67.29275706135234714 ) ) ;
#30317 = CARTESIAN_POINT ( 'NONE',  ( 18.62759615963271287, -10.81492255796078972, 113.3322429386476955 ) ) ;
#30318 = CARTESIAN_POINT ( 'NONE',  ( -16.51473224551082808, 9.474510206698731452, 73.33442372801900433 ) ) ;
#30319 = CARTESIAN_POINT ( 'NONE',  ( 5.049401038298161559, -19.05341960407611168, 32.70724293864768129 ) ) ;
#30320 = CARTESIAN_POINT ( 'NONE',  ( -10.72451020669898014, 18.67979575497178502, 65.41557627198102409 ) ) ;
#30321 = AXIS2_PLACEMENT_3D ( 'NONE', #83033, #51708, #157903 ) ;
#30322 = CARTESIAN_POINT ( 'NONE',  ( 16.51473224551069308, 9.474510206698969483, 104.1655762719810241 ) ) ;
#30323 = CARTESIAN_POINT ( 'NONE',  ( -21.52544592524334988, -5.823673210054445271, 88.95942372801901854 ) ) ;
#30324 = CARTESIAN_POINT ( 'NONE',  ( -16.46253265017160317, 9.564922557960807481, 65.83224293864769550 ) ) ;
#30325 = CARTESIAN_POINT ( 'NONE',  ( -16.53943276465976808, -0.05219959533934237506, 43.75109039468568284 ) ) ;
#30326 = CARTESIAN_POINT ( 'NONE',  ( -19.05341960407611168, -5.049401038298163336, 56.45724293864768129 ) ) ;
#30327 = CARTESIAN_POINT ( 'NONE',  ( -15.80617190586768217, 15.72974639402176855, 83.12609039468568994 ) ) ;
#30328 = ORIENTED_EDGE ( 'NONE', *, *, #100701, .F. ) ;
#30329 = CARTESIAN_POINT ( 'NONE',  ( -19.02544592524334988, -5.153800228976617603, 33.95942372801897591 ) ) ;
#30330 = ADVANCED_FACE ( 'NONE', ( #60756 ), #184121, .T. ) ;
#30331 = CARTESIAN_POINT ( 'NONE',  ( 19.02544592524334988, 5.153800228976608722, 56.45942372801898301 ) ) ;
#30332 = CARTESIAN_POINT ( 'NONE',  ( 5.719274019375673035, 21.55341960407619339, 52.29275706135236135 ) ) ;
#30333 = CARTESIAN_POINT ( 'NONE',  ( -7.503800738396974701, 1.500046863536517172, -62.22166870076607381 ) ) ;
#30334 = CARTESIAN_POINT ( 'NONE',  ( 13.97604488694548053, -13.89961937509957401, 50.62609039468566152 ) ) ;
#30335 = CARTESIAN_POINT ( 'NONE',  ( -13.97604488694527625, -13.89961937509977652, 101.8739096053143811 ) ) ;
#30336 = CARTESIAN_POINT ( 'NONE',  ( -0.05219959533909027116, -19.03943276465977164, 67.49890960531436690 ) ) ;
#30337 = CARTESIAN_POINT ( 'NONE',  ( 14.34966873604960469, 8.224510206698951720, 29.16557627198103120 ) ) ;
#30339 = CARTESIAN_POINT ( 'NONE',  ( -10.72451020669870658, -18.67979575497194134, 94.58442372801901854 ) ) ;
#30338 = CARTESIAN_POINT ( 'NONE',  ( 13.97604488694527802, 13.89961937509977652, 114.3739096053143669 ) ) ;
#30340 = CARTESIAN_POINT ( 'NONE',  ( -11.40812507854755609, 35.11059874428196537, -7.524999997268813523 ) ) ;
#30341 = CARTESIAN_POINT ( 'NONE',  ( -34.11680238834244960, 4.370175642590067966, 91.64155955192003944 ) ) ;
#30342 = CARTESIAN_POINT ( 'NONE',  ( -10.72451020669870658, -18.67979575497194134, 99.58442372801900433 ) ) ;
#30343 = CARTESIAN_POINT ( 'NONE',  ( 37.99626262588767389, -12.34573411038910251, -2.847842220587804007 ) ) ;
#30344 = CARTESIAN_POINT ( 'NONE',  ( -13.97604488694527625, -13.89961937509977652, 26.87390960531434558 ) ) ;
#30345 = CARTESIAN_POINT ( 'NONE',  ( 0.000000000000000000, 0.000000000000000000, -56.46919128290398504 ) ) ;
#30346 = CARTESIAN_POINT ( 'NONE',  ( 33.85315667487626712, 0.3602237081833412069, 100.5000000000009948 ) ) ;
#30347 = CARTESIAN_POINT ( 'NONE',  ( 16.52544592524335698, 4.483927247898782831, 51.45942372801901854 ) ) ;
#30348 = CARTESIAN_POINT ( 'NONE',  ( 5.823673210054125526, 21.52544592524343514, 69.79057627198102409 ) ) ;
#30349 = CARTESIAN_POINT ( 'NONE',  ( -16.55341960407611168, -4.379528057220339221, 46.45724293864769550 ) ) ;
#30351 = CARTESIAN_POINT ( 'NONE',  ( -13.97604488694527625, -13.89961937509977652, 96.87390960531433848 ) ) ;
#30350 = CARTESIAN_POINT ( 'NONE',  ( -12.06949235617756955, 12.14591786802309770, 105.6239096053143669 ) ) ;
#30352 = CARTESIAN_POINT ( 'NONE',  ( -19.02544592524334988, -5.153800228976617603, 38.95942372801900433 ) ) ;
#30353 = CARTESIAN_POINT ( 'NONE',  ( 0.05219959533910956823, 16.53943276465976808, 114.9989096053143669 ) ) ;
#30354 = CARTESIAN_POINT ( 'NONE',  ( 18.67979575497194134, -10.72451020669871369, 70.83442372801901854 ) ) ;
#30355 = CARTESIAN_POINT ( 'NONE',  ( -9.474510206698964154, 16.51473224551069663, 115.4155762719810241 ) ) ;
#30356 = CARTESIAN_POINT ( 'NONE',  ( -14.34966873604972548, 8.224510206698743886, 103.3344237280190043 ) ) ;
#30357 = CARTESIAN_POINT ( 'NONE',  ( 5.000000000000000000, 0.000000000000000000, -18.00000000000000000 ) ) ;
#30358 = CARTESIAN_POINT ( 'NONE',  ( 5.823673210054125526, 21.52544592524343514, 24.79057627198103120 ) ) ;
#30359 = CARTESIAN_POINT ( 'NONE',  ( -14.34966873604960291, -8.224510206698953496, 96.66557627198102409 ) ) ;
#30360 = CARTESIAN_POINT ( 'NONE',  ( -9.564922557961040184, 16.46253265017147172, 62.91775706135233293 ) ) ;
#30361 = CARTESIAN_POINT ( 'NONE',  ( -5.153800228976328057, -19.02544592524343514, 82.29057627198103830 ) ) ;
#30362 = CARTESIAN_POINT ( 'NONE',  ( 4.483927247898545687, 16.52544592524342804, 74.79057627198105251 ) ) ;
#30363 = CARTESIAN_POINT ( 'NONE',  ( 19.02544592524334988, 5.153800228976608722, 86.45942372801900433 ) ) ;
#30364 = CARTESIAN_POINT ( 'NONE',  ( -21.55341960407610458, -5.719274019375992779, 46.45724293864769550 ) ) ;
#30365 = VERTEX_POINT ( 'NONE', #90109 ) ;
#30366 = CARTESIAN_POINT ( 'NONE',  ( 16.52544592524342804, -4.483927247898539470, 113.5405762719810383 ) ) ;
#30367 = CARTESIAN_POINT ( 'NONE',  ( -16.62475595723695676, -7.163666690055260133, 29.47286648189535896 ) ) ;
#30369 = CARTESIAN_POINT ( 'NONE',  ( -0.05219959533907301413, -21.53943276465977519, 82.49890960531436690 ) ) ;
#30368 = CARTESIAN_POINT ( 'NONE',  ( 16.46253265017160672, -9.564922557960803928, 78.33224293864769550 ) ) ;
#30371 = CARTESIAN_POINT ( 'NONE',  ( -13.97604488694527625, -13.89961937509977652, 86.87390960531436690 ) ) ;
#30370 = CARTESIAN_POINT ( 'NONE',  ( 16.55341960407618274, -4.379528057220086978, 96.04275706135236135 ) ) ;
#30372 = CARTESIAN_POINT ( 'NONE',  ( 16.51473224551083163, -9.474510206698727899, 70.83442372801900433 ) ) ;
#30373 = CARTESIAN_POINT ( 'NONE',  ( -21.53943276465977519, -0.05219959533937600094, 78.75109039468568994 ) ) ;
#30374 = CARTESIAN_POINT ( 'NONE',  ( 18.62759615963271287, -10.81492255796078972, 58.33224293864768839 ) ) ;
#30375 = CARTESIAN_POINT ( 'NONE',  ( -16.46253265017160317, 9.564922557960807481, 115.8322429386477097 ) ) ;
#30376 = CARTESIAN_POINT ( 'NONE',  ( 19.05341960407611168, 5.049401038298154454, 38.95724293864767418 ) ) ;
#30377 = CARTESIAN_POINT ( 'NONE',  ( -14.34966873604972548, 8.224510206698743886, 103.3344237280190043 ) ) ;
#30378 = CARTESIAN_POINT ( 'NONE',  ( 16.46253265017160672, -9.564922557960803928, 53.33224293864768839 ) ) ;
#30379 = CARTESIAN_POINT ( 'NONE',  ( 19.03943276465977164, 0.05219959533936151252, 111.2510903946856757 ) ) ;
#30380 = CARTESIAN_POINT ( 'NONE',  ( -31.72709406046301339, 2.040068635034919209E-14, 102.5000000000000142 ) ) ;
#30381 = CARTESIAN_POINT ( 'NONE',  ( 5.153800228976615827, -19.02544592524334988, 20.20942372801899722 ) ) ;
#30382 = CARTESIAN_POINT ( 'NONE',  ( -16.55341960407611168, -4.379528057220339221, 61.45724293864770260 ) ) ;
#30383 = CARTESIAN_POINT ( 'NONE',  ( -5.719274019375978568, 21.55341960407610458, 105.2072429386477097 ) ) ;
#30384 = CARTESIAN_POINT ( 'NONE',  ( 21.53943276465977519, -0.05219959533907433946, 103.7489096053143669 ) ) ;
#30385 = CARTESIAN_POINT ( 'NONE',  ( 17.48847506799968698, -5.747544572773782612, 98.32697437843285115 ) ) ;
#30386 = CARTESIAN_POINT ( 'NONE',  ( 21.55341960407610458, 5.719274019375980345, 48.95724293864770971 ) ) ;
#30387 = CARTESIAN_POINT ( 'NONE',  ( 8.314922557961029526, -14.29746914071037800, 75.41775706135233293 ) ) ;
#30388 = CARTESIAN_POINT ( 'NONE',  ( 14.34966873604960469, 8.224510206698951720, 109.1655762719810383 ) ) ;
#30389 = CARTESIAN_POINT ( 'NONE',  ( 9.564922557960805705, 16.46253265017160317, 64.58224293864769550 ) ) ;
#30390 = FILL_AREA_STYLE_COLOUR ( '', #36903 ) ;
#30391 = CARTESIAN_POINT ( 'NONE',  ( -10.06251177737617120, -45.32665049860681705, -23.77652626631511978 ) ) ;
#30392 = CARTESIAN_POINT ( 'NONE',  ( -12.14591786802326823, 12.06949235617739902, 108.1260903946856757 ) ) ;
#30393 = CARTESIAN_POINT ( 'NONE',  ( -18.62759615963255300, -10.81492255796106328, 49.16775706135234003 ) ) ;
#30394 = CARTESIAN_POINT ( 'NONE',  ( 19.03943276465977164, -0.05219959533909143690, 93.74890960531435269 ) ) ;
#30395 = CARTESIAN_POINT ( 'NONE',  ( 18.62759615963255655, 10.81492255796105972, 81.66775706135236135 ) ) ;
#30396 = LINE ( 'NONE', #94042, #134214 ) ;
#30397 = CARTESIAN_POINT ( 'NONE',  ( -9.474510206698964154, 16.51473224551069663, 30.41557627198102054 ) ) ;
#30398 = AXIS2_PLACEMENT_3D ( 'NONE', #128371, #143538, #51543 ) ;
#30399 = ORIENTED_EDGE ( 'NONE', *, *, #52038, .F. ) ;
#30400 = CARTESIAN_POINT ( 'NONE',  ( -21.55341960407619339, 5.719274019375674811, 78.54275706135236135 ) ) ;
#30401 = CARTESIAN_POINT ( 'NONE',  ( 9.474510206698971260, -16.51473224551069308, 52.91557627198102409 ) ) ;
#30402 = CARTESIAN_POINT ( 'NONE',  ( -9.474510206698964154, 16.51473224551069663, 85.41557627198102409 ) ) ;
#30403 = CARTESIAN_POINT ( 'NONE',  ( 5.153800228976615827, -19.02544592524334988, 85.20942372801900433 ) ) ;
#30404 = CARTESIAN_POINT ( 'NONE',  ( -15.72974639402176322, -15.80617190586768395, 44.37609039468567573 ) ) ;
#30405 = CARTESIAN_POINT ( 'NONE',  ( -13.89961937509957401, -13.97604488694547875, 109.3760903946856331 ) ) ;
#30406 = CARTESIAN_POINT ( 'NONE',  ( -9.564922557961040184, 16.46253265017147172, 77.91775706135234714 ) ) ;
#30407 = CARTESIAN_POINT ( 'NONE',  ( 9.474510206698971260, -16.51473224551069308, 37.91557627198102409 ) ) ;
#30408 = CARTESIAN_POINT ( 'NONE',  ( -0.05219959533936034679, 19.03943276465977164, 82.50109039468567573 ) ) ;
#30409 = CARTESIAN_POINT ( 'NONE',  ( 14.34966873604972726, -8.224510206698740333, 110.8344237280190043 ) ) ;
#30410 = CARTESIAN_POINT ( 'NONE',  ( 9.564922557961047289, -16.46253265017146816, 80.41775706135234714 ) ) ;
#30411 = CARTESIAN_POINT ( 'NONE',  ( -0.05219959533910754901, -16.53943276465976808, 42.49890960531435979 ) ) ;
#30412 = CARTESIAN_POINT ( 'NONE',  ( 5.049401038297881783, 19.05341960407617563, 47.29275706135231161 ) ) ;
#30413 = CARTESIAN_POINT ( 'NONE',  ( -5.719274019375665041, -21.55341960407619695, 109.7927570613523613 ) ) ;
#30414 = CARTESIAN_POINT ( 'NONE',  ( -19.02544592524334988, -5.153800228976617603, 23.95942372801900078 ) ) ;
#30415 = CARTESIAN_POINT ( 'NONE',  ( 19.02544592524343514, -5.153800228976328945, 28.54057627198102409 ) ) ;
#30416 = CARTESIAN_POINT ( 'NONE',  ( 10.72451020669871369, 18.67979575497193778, 87.08442372801901854 ) ) ;
#30417 = CARTESIAN_POINT ( 'NONE',  ( 4.379528057220092307, 16.55341960407617563, 52.29275706135236135 ) ) ;
#30418 = CARTESIAN_POINT ( 'NONE',  ( 9.564922557960805705, 16.46253265017160317, 94.58224293864769550 ) ) ;
#30419 = CARTESIAN_POINT ( 'NONE',  ( -27.73933785331498925, 2.428612866367529932E-14, 142.8750000027311842 ) ) ;
#30420 = CARTESIAN_POINT ( 'NONE',  ( -19.03943276465977164, 0.05219959533909376836, 91.24890960531436690 ) ) ;
#30421 = CARTESIAN_POINT ( 'NONE',  ( -17.26172910966711882, 6.454744622557081257, 100.8064690864920863 ) ) ;
#30422 = CLOSED_SHELL ( 'NONE', ( #154540, #106869, #89797, #21298, #65004, #129684, #197689, #91262, #49601, #185178, #189850, #186823, #58481, #71549, #36411, #60710, #65126, #6760, #116252, #152511, #62467, #63405, #110107, #107491, #169227, #194656, #141333 ) ) ;
#30423 = ORIENTED_EDGE ( 'NONE', *, *, #138817, .F. ) ;
#30424 = CARTESIAN_POINT ( 'NONE',  ( 19.05341960407617918, -5.049401038297876454, 86.04275706135233293 ) ) ;
#30425 = CARTESIAN_POINT ( 'NONE',  ( 10.72451020669898902, -18.67979575497178502, 22.91557627198102765 ) ) ;
#30427 = CARTESIAN_POINT ( 'NONE',  ( -13.89961937509957401, -13.97604488694547875, 99.37609039468567573 ) ) ;
#30426 = CARTESIAN_POINT ( 'NONE',  ( 15.80617190586769283, -15.72974639402175789, 110.6260903946857042 ) ) ;
#30428 = CARTESIAN_POINT ( 'NONE',  ( -12.06949235617756955, 12.14591786802309770, 115.6239096053143669 ) ) ;
#30429 = CARTESIAN_POINT ( 'NONE',  ( 19.02544592524343514, -5.153800228976328945, 23.54057627198102054 ) ) ;
#30430 = CARTESIAN_POINT ( 'NONE',  ( -15.72974639402197994, 15.80617190586746368, 60.62390960531437401 ) ) ;
#30431 = CARTESIAN_POINT ( 'NONE',  ( 21.52544592524344225, -5.823673210054117533, 43.54057627198103830 ) ) ;
#30432 = CARTESIAN_POINT ( 'NONE',  ( 19.05341960407611168, 5.049401038298154454, 23.95724293864769194 ) ) ;
#30433 = CARTESIAN_POINT ( 'NONE',  ( 28.82186960331498327, 2.781578969918950771E-14, 143.2500000054623683 ) ) ;
#30434 = CARTESIAN_POINT ( 'NONE',  ( 19.03943276465977164, 0.05219959533936151252, 76.25109039468566152 ) ) ;
#30435 = CARTESIAN_POINT ( 'NONE',  ( 12.06949235617757843, -12.14591786802309237, 38.12390960531436690 ) ) ;
#30436 = CARTESIAN_POINT ( 'NONE',  ( 21.55341960407610458, 5.719274019375980345, 23.95724293864769550 ) ) ;
#30437 = CARTESIAN_POINT ( 'NONE',  ( -18.62759615963255300, -10.81492255796106328, 89.16775706135236135 ) ) ;
#30438 = CARTESIAN_POINT ( 'NONE',  ( -10.72451020669898014, 18.67979575497178502, 70.41557627198102409 ) ) ;
#30439 = CARTESIAN_POINT ( 'NONE',  ( -21.52544592524334988, -5.823673210054445271, 63.95942372801901854 ) ) ;
#30440 = CARTESIAN_POINT ( 'NONE',  ( 21.52544592524334988, 5.823673210054432836, 46.45942372801901854 ) ) ;
#30441 = EDGE_CURVE ( 'NONE', #193525, #80788, #75931, .T. ) ;
#30442 = CARTESIAN_POINT ( 'NONE',  ( -5.153800228976328057, -19.02544592524343514, 92.29057627198099567 ) ) ;
#30443 = CARTESIAN_POINT ( 'NONE',  ( 16.53943276465976808, 0.05219959533934440121, 91.25109039468568994 ) ) ;
#30444 = CARTESIAN_POINT ( 'NONE',  ( 5.153800228976335163, 19.02544592524342804, 29.79057627198102409 ) ) ;
#30445 = CARTESIAN_POINT ( 'NONE',  ( -32.33351994418283937, 3.967450966133711177, 88.63067128610950363 ) ) ;
#30446 = CARTESIAN_POINT ( 'NONE',  ( -16.53943276465976808, 0.05219959533911058130, 66.24890960531436690 ) ) ;
#30447 = CARTESIAN_POINT ( 'NONE',  ( -4.483927247898539470, -16.52544592524342804, 32.29057627198102409 ) ) ;
#30448 = CARTESIAN_POINT ( 'NONE',  ( 16.46253265017160672, -9.564922557960803928, 63.33224293864769550 ) ) ;
#30449 = CARTESIAN_POINT ( 'NONE',  ( 5.153800228976335163, 19.02544592524342804, 39.79057627198100988 ) ) ;
#30450 = CARTESIAN_POINT ( 'NONE',  ( -18.62759615963270932, 10.81492255796079327, 60.83224293864769550 ) ) ;
#30451 = CARTESIAN_POINT ( 'NONE',  ( -16.51473224551082808, 9.474510206698731452, 33.33442372801899722 ) ) ;
#30453 = CARTESIAN_POINT ( 'NONE',  ( -12.14591786802309592, -12.06949235617757132, 51.87390960531437401 ) ) ;
#30452 = CARTESIAN_POINT ( 'NONE',  ( 22.55670631985092456, -22.55670631985084995, -49.13275782002545355 ) ) ;
#30454 = CARTESIAN_POINT ( 'NONE',  ( -18.67979575497178146, -10.72451020669898902, 31.66557627198102054 ) ) ;
#30455 = CARTESIAN_POINT ( 'NONE',  ( -23.29544513554940721, -16.92513159979223403, 140.1843446569000093 ) ) ;
#30456 = CARTESIAN_POINT ( 'NONE',  ( -16.55341960407617563, 4.379528057220093196, 73.54275706135234714 ) ) ;
#30457 = CARTESIAN_POINT ( 'NONE',  ( 19.03943276465977164, 0.05219959533936151252, 71.25109039468566152 ) ) ;
#30458 = CARTESIAN_POINT ( 'NONE',  ( 4.379528057220339221, -16.55341960407611168, 37.70724293864769550 ) ) ;
#30459 = DIRECTION ( 'NONE',  ( 0.000000000000000000, 0.000000000000000000, -1.000000000000000000 ) ) ;
#30460 = CARTESIAN_POINT ( 'NONE',  ( -4.483927247898539470, -16.52544592524342804, 32.29057627198102409 ) ) ;
#30461 = CARTESIAN_POINT ( 'NONE',  ( 19.02544592524343514, -5.153800228976328945, 53.54057627198102409 ) ) ;
#30462 = CARTESIAN_POINT ( 'NONE',  ( 9.564922557960805705, 16.46253265017160317, 74.58224293864769550 ) ) ;
#30463 = CARTESIAN_POINT ( 'NONE',  ( 9.564922557960805705, 16.46253265017160317, 34.58224293864770260 ) ) ;
#30464 = CARTESIAN_POINT ( 'NONE',  ( -21.55341960407619339, 5.719274019375674811, 48.54275706135234714 ) ) ;
#30465 = CARTESIAN_POINT ( 'NONE',  ( -13.97604488694527625, -13.89961937509977652, 61.87390960531435979 ) ) ;
#30466 = CARTESIAN_POINT ( 'NONE',  ( 0.000000000000000000, 0.000000000000000000, -35.00000000000000000 ) ) ;
#30467 = CARTESIAN_POINT ( 'NONE',  ( 13.89961937509977652, -13.97604488694527269, 63.12390960531435979 ) ) ;
#30468 = CARTESIAN_POINT ( 'NONE',  ( 0.05219959533907565091, 21.53943276465977519, 29.99890960531435979 ) ) ;
#30469 = CARTESIAN_POINT ( 'NONE',  ( 16.52544592524342804, -4.483927247898539470, 113.5405762719810383 ) ) ;
#30470 = CARTESIAN_POINT ( 'NONE',  ( 21.55341960407610458, 5.719274019375980345, 33.95724293864769550 ) ) ;
#30471 = CARTESIAN_POINT ( 'NONE',  ( -4.379528057220086978, -16.55341960407618274, 94.79275706135234714 ) ) ;
#30472 = CARTESIAN_POINT ( 'NONE',  ( -5.823673210054431948, 21.52544592524334988, 102.7094237280190185 ) ) ;
#30473 = CARTESIAN_POINT ( 'NONE',  ( -14.29746914071037622, -8.314922557961029526, 69.16775706135234714 ) ) ;
#30474 = CARTESIAN_POINT ( 'NONE',  ( 9.564922557960805705, 16.46253265017160317, 104.5822429386476955 ) ) ;
#30475 = CARTESIAN_POINT ( 'NONE',  ( -12.06949235617739369, -12.14591786802326823, 59.37609039468568284 ) ) ;
#30476 = CARTESIAN_POINT ( 'NONE',  ( 8.224510206698742110, 14.34966873604972548, 42.08442372801901854 ) ) ;
#30477 = CARTESIAN_POINT ( 'NONE',  ( 16.53943276465976808, 0.05219959533934440121, 96.25109039468568994 ) ) ;
#30478 = CARTESIAN_POINT ( 'NONE',  ( -14.34966873604972548, 8.224510206698743886, 28.33442372801902209 ) ) ;
#30479 = CARTESIAN_POINT ( 'NONE',  ( 19.03943276465977164, -0.05219959533909143690, 33.74890960531435979 ) ) ;
#30480 = CARTESIAN_POINT ( 'NONE',  ( -0.05219959533907301413, -21.53943276465977519, 112.4989096053143669 ) ) ;
#30481 = CARTESIAN_POINT ( 'NONE',  ( -16.53943276465976808, -0.05219959533934237506, 23.75109039468567929 ) ) ;
#30482 = CARTESIAN_POINT ( 'NONE',  ( 16.52544592524335698, 4.483927247898782831, 81.45942372801900433 ) ) ;
#30483 = CARTESIAN_POINT ( 'NONE',  ( -17.05587630539706723, 6.762274262136762637, 45.74180309037284786 ) ) ;
#30484 = CARTESIAN_POINT ( 'NONE',  ( -18.67979575497193778, 10.72451020669871902, 83.33442372801903275 ) ) ;
#30485 = CARTESIAN_POINT ( 'NONE',  ( -0.05219959533936034679, 19.03943276465977164, 77.50109039468566152 ) ) ;
#30486 = CARTESIAN_POINT ( 'NONE',  ( -12.06949235617756955, 12.14591786802309770, 65.62390960531436690 ) ) ;
#30487 = CARTESIAN_POINT ( 'NONE',  ( -14.29746914071049879, 8.314922557960819915, 40.83224293864769550 ) ) ;
#30488 = CARTESIAN_POINT ( 'NONE',  ( 4.483927247898545687, 16.52544592524342804, 104.7905762719810241 ) ) ;
#30490 = CARTESIAN_POINT ( 'NONE',  ( -6.100000000000009415, 0.2000799437545254522, -64.53213882399991519 ) ) ;
#30489 = CARTESIAN_POINT ( 'NONE',  ( 5.049401038297881783, 19.05341960407617563, 42.29275706135234003 ) ) ;
#30491 = CARTESIAN_POINT ( 'NONE',  ( -15.72974639402176322, -15.80617190586768395, 54.37609039468568994 ) ) ;
#30492 = CARTESIAN_POINT ( 'NONE',  ( 12.14591786802327356, -12.06949235617739191, 20.62609039468568639 ) ) ;
#30493 = CARTESIAN_POINT ( 'NONE',  ( 16.81555441253551564, 7.025013491695493606, 81.86314554665740673 ) ) ;
#30494 = CARTESIAN_POINT ( 'NONE',  ( -5.153800228976328057, -19.02544592524343514, 102.2905762719810383 ) ) ;
#30495 = CARTESIAN_POINT ( 'NONE',  ( -21.55341960407610458, -5.719274019375992779, 71.45724293864769550 ) ) ;
#30496 = CARTESIAN_POINT ( 'NONE',  ( 0.05219959533936267826, -19.03943276465977164, 95.00109039468567573 ) ) ;
#30497 = CARTESIAN_POINT ( 'NONE',  ( -0.05219959533909027116, -19.03943276465977164, 107.4989096053143527 ) ) ;
#30498 = CARTESIAN_POINT ( 'NONE',  ( -25.70602947687972417, 7.354137148287277270, 175.2376750527030538 ) ) ;
#30499 = CARTESIAN_POINT ( 'NONE',  ( 8.314922557960818139, 14.29746914071049879, 109.5822429386476955 ) ) ;
#30500 = CARTESIAN_POINT ( 'NONE',  ( 5.719274019375673035, 21.55341960407619339, 97.29275706135234714 ) ) ;
#30501 = CARTESIAN_POINT ( 'NONE',  ( -9.564922557960796823, -16.46253265017161027, 27.08224293864769550 ) ) ;
#30502 = CARTESIAN_POINT ( 'NONE',  ( -15.80617190586768217, 15.72974639402176855, 53.12609039468568284 ) ) ;
#30503 = CARTESIAN_POINT ( 'NONE',  ( 10.81492255796106328, -18.62759615963255655, 85.41775706135236135 ) ) ;
#30504 = CARTESIAN_POINT ( 'NONE',  ( -8.224510206698735004, -14.34966873604973081, 94.58442372801901854 ) ) ;
#30505 = CARTESIAN_POINT ( 'NONE',  ( -10.72451020669870658, -18.67979575497194134, 44.58442372801901854 ) ) ;
#30506 = CARTESIAN_POINT ( 'NONE',  ( 5.823673210054444382, -21.52544592524334988, 40.20942372801901854 ) ) ;
#30508 = CARTESIAN_POINT ( 'NONE',  ( -16.51473224551069308, -9.474510206698971260, 91.66557627198103830 ) ) ;
#30507 = CARTESIAN_POINT ( 'NONE',  ( 13.89961937509957401, 13.97604488694547697, 61.87609039468566863 ) ) ;
#30509 = CARTESIAN_POINT ( 'NONE',  ( 12.06949235617757843, -12.14591786802309237, 103.1239096053143811 ) ) ;
#30510 = CARTESIAN_POINT ( 'NONE',  ( -15.72974639402197994, 15.80617190586746368, 85.62390960531436690 ) ) ;
#30511 = CARTESIAN_POINT ( 'NONE',  ( -4.379528057220328563, 16.55341960407611168, 65.20724293864768129 ) ) ;
#30512 = CARTESIAN_POINT ( 'NONE',  ( 21.55341960407619695, -5.719274019375665929, 101.0427570613523756 ) ) ;
#30513 = CARTESIAN_POINT ( 'NONE',  ( 4.379528057220339221, -16.55341960407611168, 77.70724293864770971 ) ) ;
#30514 = CARTESIAN_POINT ( 'NONE',  ( 5.153800228976335163, 19.02544592524342804, 34.79057627198102409 ) ) ;
#30515 = CARTESIAN_POINT ( 'NONE',  ( -13.97604488694547697, 13.89961937509957934, 83.12609039468564731 ) ) ;
#30516 = CARTESIAN_POINT ( 'NONE',  ( -4.379528057220328563, 16.55341960407611168, 50.20724293864769550 ) ) ;
#30517 = CARTESIAN_POINT ( 'NONE',  ( 18.67979575497194134, -10.72451020669871369, 100.8344237280190185 ) ) ;
#30518 = CARTESIAN_POINT ( 'NONE',  ( -5.049401038298153566, 19.05341960407611168, 90.20724293864766707 ) ) ;
#30519 = B_SPLINE_CURVE_WITH_KNOTS ( 'NONE', 3,
 ( #136774, #195496, #118643, #168110, #14426, #95236, #110405, #141738, #186281, #199450, #126563, #49737, #185270, #31590, #80068, #184281, #30595, #155918, #237, #122593 ),
 .UNSPECIFIED., .F., .F.,
 ( 4, 2, 2, 2, 2, 2, 2, 2, 2, 4 ),
 ( 4.982613841084487634E-18, 0.0002490660040300066245, 0.0004981320080600082616, 0.0009962640161200063318, 0.001494396024180004402, 0.001992528032240002255, 0.002490660040300000759, 0.002988792048359998395, 0.003486924056419996899, 0.003985056064479994969 ),
 .UNSPECIFIED. ) ;
#30520 = CARTESIAN_POINT ( 'NONE',  ( 5.049401038297881783, 19.05341960407617563, 67.29275706135234714 ) ) ;
#30521 = CARTESIAN_POINT ( 'NONE',  ( -5.719274019375978568, 21.55341960407610458, 65.20724293864768129 ) ) ;
#30522 = CARTESIAN_POINT ( 'NONE',  ( -18.67979575497193778, 10.72451020669871902, 23.33442372801901499 ) ) ;
#30523 = CARTESIAN_POINT ( 'NONE',  ( 19.02544592524334988, 5.153800228976608722, 111.4594237280190043 ) ) ;
#30524 = CARTESIAN_POINT ( 'NONE',  ( -14.34966873604972548, 8.224510206698743886, 78.33442372801901854 ) ) ;
#30526 = CARTESIAN_POINT ( 'NONE',  ( 10.81492255796106328, -18.62759615963255655, 20.41775706135234714 ) ) ;
#30525 = CARTESIAN_POINT ( 'NONE',  ( -13.89961937509977652, 13.97604488694528158, 25.62390960531434558 ) ) ;
#30527 = CARTESIAN_POINT ( 'NONE',  ( -4.483927247898539470, -16.52544592524342804, 112.2905762719810241 ) ) ;
#30528 = CARTESIAN_POINT ( 'NONE',  ( -11.40812507854754720, -35.11059874428192273, -6.724999997268813701 ) ) ;
#30529 = CARTESIAN_POINT ( 'NONE',  ( -0.05219959533934338120, 16.53943276465976808, 52.50109039468567573 ) ) ;
#30530 = CARTESIAN_POINT ( 'NONE',  ( -14.34966873604960291, -8.224510206698953496, 76.66557627198103830 ) ) ;
#30531 = CARTESIAN_POINT ( 'NONE',  ( 5.823673210054125526, 21.52544592524343514, 79.79057627198102409 ) ) ;
#30532 = CARTESIAN_POINT ( 'NONE',  ( -8.224510206698948167, 14.34966873604960824, 25.41557627198103120 ) ) ;
#30533 = CARTESIAN_POINT ( 'NONE',  ( -4.379528057220086978, -16.55341960407618274, 34.79275706135235424 ) ) ;
#30534 = CARTESIAN_POINT ( 'NONE',  ( 5.153800228976335163, 19.02544592524342804, 39.79057627198100988 ) ) ;
#30535 = B_SPLINE_CURVE_WITH_KNOTS ( 'NONE', 3,
 ( #20502, #130671, #7321, #48871, #51840, #110526, #172207, #35675, #3347, #157040, #191352, #22512, #19521, #82150, #34686, #21505, #4327, #52830, #127679, #175194 ),
 .UNSPECIFIED., .F., .F.,
 ( 4, 2, 2, 2, 2, 2, 2, 2, 2, 4 ),
 ( 0.004000878361811823804, 0.004499404418915833696, 0.004997930476019843589, 0.005496456533123854349, 0.005994982590227864241, 0.006244245618779868320, 0.006493508647331874134, 0.006992034704435884027, 0.007490560761539893919, 0.007989086818643903812 ),
 .UNSPECIFIED. ) ;
#30536 = CARTESIAN_POINT ( 'NONE',  ( 12.14591786802327356, -12.06949235617739191, 75.62609039468567573 ) ) ;
#30537 = CARTESIAN_POINT ( 'NONE',  ( -13.89961937509957401, -13.97604488694547875, 74.37609039468566152 ) ) ;
#30538 = CARTESIAN_POINT ( 'NONE',  ( -10.81492255796078084, -18.62759615963271287, 77.08224293864769550 ) ) ;
#30539 = CARTESIAN_POINT ( 'NONE',  ( 16.52544592524342804, -4.483927247898539470, 23.54057627198102765 ) ) ;
#30540 = ORIENTED_EDGE ( 'NONE', *, *, #100204, .T. ) ;
#30541 = CARTESIAN_POINT ( 'NONE',  ( -21.55341960407619339, 5.719274019375674811, 78.54275706135236135 ) ) ;
#30542 = AXIS2_PLACEMENT_3D ( 'NONE', #147678, #10166, #58645 ) ;
#30543 = CARTESIAN_POINT ( 'NONE',  ( 5.719274019375991003, -21.55341960407610458, 42.70724293864770260 ) ) ;
#30544 = EDGE_LOOP ( 'NONE', ( #24925, #25021, #101661, #82248 ) ) ;
#30545 = CARTESIAN_POINT ( 'NONE',  ( -16.55341960407617563, 4.379528057220093196, 98.54275706135234714 ) ) ;
#30546 = CARTESIAN_POINT ( 'NONE',  ( 5.823673210054125526, 21.52544592524343514, 39.79057627198103830 ) ) ;
#30547 = EDGE_LOOP ( 'NONE', ( #174696, #51288, #88771 ) ) ;
#30548 = CARTESIAN_POINT ( 'NONE',  ( 16.51473224551069308, 9.474510206698969483, 109.1655762719810383 ) ) ;
#30549 = CARTESIAN_POINT ( 'NONE',  ( 17.49999999999999289, 3.189878218039149615, 107.6294856257125048 ) ) ;
#30550 = CARTESIAN_POINT ( 'NONE',  ( -12.06949235617756955, 12.14591786802309770, 115.6239096053143669 ) ) ;
#30551 = CARTESIAN_POINT ( 'NONE',  ( 10.81492255796078972, 18.62759615963270932, 69.58224293864769550 ) ) ;
#30552 = CARTESIAN_POINT ( 'NONE',  ( -12.14591786802326823, 12.06949235617739902, 103.1260903946856757 ) ) ;
#30553 = CARTESIAN_POINT ( 'NONE',  ( 10.72451020669871369, 18.67979575497193778, 57.08442372801901854 ) ) ;
#30554 = CARTESIAN_POINT ( 'NONE',  ( 16.53943276465976808, 0.05219959533934440121, 21.25109039468567218 ) ) ;
#30555 = CARTESIAN_POINT ( 'NONE',  ( 16.52544592524342804, -4.483927247898539470, 113.5405762719810383 ) ) ;
#30556 = CARTESIAN_POINT ( 'NONE',  ( -16.55341960407617563, 4.379528057220093196, 28.54275706135234358 ) ) ;
#30557 = CARTESIAN_POINT ( 'NONE',  ( 16.51473224551069308, 9.474510206698969483, 39.16557627198103120 ) ) ;
#30558 = CARTESIAN_POINT ( 'NONE',  ( -28.82186960331499392, 9.364793116373565596, 143.9000000000000057 ) ) ;
#30559 = CARTESIAN_POINT ( 'NONE',  ( 13.97604488694527802, 13.89961937509977652, 109.3739096053143669 ) ) ;
#30560 = AXIS2_PLACEMENT_3D ( 'NONE', #197298, #198278, #199274 ) ;
#30561 = CARTESIAN_POINT ( 'NONE',  ( 8.314922557961029526, -14.29746914071037800, 85.41775706135236135 ) ) ;
#30562 = CARTESIAN_POINT ( 'NONE',  ( 19.05341960407617918, -5.049401038297876454, 81.04275706135231871 ) ) ;
#30563 = CARTESIAN_POINT ( 'NONE',  ( -16.51473224551082808, 9.474510206698731452, 28.33442372801900433 ) ) ;
#30564 = CARTESIAN_POINT ( 'NONE',  ( 0.05219959533907565091, 21.53943276465977519, 74.99890960531435269 ) ) ;
#30565 = CARTESIAN_POINT ( 'NONE',  ( -4.379528057220086978, -16.55341960407618274, 94.79275706135234714 ) ) ;
#30566 = CARTESIAN_POINT ( 'NONE',  ( -19.03943276465977164, -0.05219959533935918106, 93.75109039468566152 ) ) ;
#30567 = CARTESIAN_POINT ( 'NONE',  ( 19.02544592524343514, -5.153800228976328945, 53.54057627198102409 ) ) ;
#30568 = CARTESIAN_POINT ( 'NONE',  ( 9.474510206698971260, -16.51473224551069308, 87.91557627198102409 ) ) ;
#30569 = CARTESIAN_POINT ( 'NONE',  ( 21.55341960407619695, -5.719274019375665929, 51.04275706135234714 ) ) ;
#30570 = CARTESIAN_POINT ( 'NONE',  ( -0.05219959533909027116, -19.03943276465977164, 42.49890960531435269 ) ) ;
#30571 = CARTESIAN_POINT ( 'NONE',  ( 23.64874990377911246, -15.04272038711346937, 165.8682408883346397 ) ) ;
#30572 = CARTESIAN_POINT ( 'NONE',  ( 9.474510206698971260, -16.51473224551069308, 107.9155762719810383 ) ) ;
#30573 = CARTESIAN_POINT ( 'NONE',  ( 16.53943276465976808, -0.05219959533910856209, 63.74890960531435979 ) ) ;
#30574 = CARTESIAN_POINT ( 'NONE',  ( -5.719274019375978568, 21.55341960407610458, 75.20724293864769550 ) ) ;
#30575 = CARTESIAN_POINT ( 'NONE',  ( 0.000000000000000000, 0.000000000000000000, -64.92279855667830191 ) ) ;
#30576 = CARTESIAN_POINT ( 'NONE',  ( -5.049401038297874678, -19.05341960407617918, 44.79275706135232582 ) ) ;
#30577 = CARTESIAN_POINT ( 'NONE',  ( 16.21995358207278670, -7.366697692864217828, 72.43551001512068410 ) ) ;
#30579 = CARTESIAN_POINT ( 'NONE',  ( -0.05219959533909027116, -19.03943276465977164, 92.49890960531436690 ) ) ;
#30578 = CARTESIAN_POINT ( 'NONE',  ( -19.03943276465977164, 0.05219959533909376836, 66.24890960531436690 ) ) ;
#30580 = CARTESIAN_POINT ( 'NONE',  ( 8.224510206698742110, 14.34966873604972548, 47.08442372801901854 ) ) ;
#30581 = CARTESIAN_POINT ( 'NONE',  ( -17.58332526062526213, -7.635886036038624702, 79.07665040441536064 ) ) ;
#30582 = CARTESIAN_POINT ( 'NONE',  ( 19.02544592524334988, 5.153800228976608722, 36.45942372801900433 ) ) ;
#30583 = CARTESIAN_POINT ( 'NONE',  ( -17.49999999999999645, 5.499999999999992006, 28.71769037696435234 ) ) ;
#30584 = CARTESIAN_POINT ( 'NONE',  ( 16.53943276465976808, 0.05219959533934440121, 86.25109039468568994 ) ) ;
#30585 = CARTESIAN_POINT ( 'NONE',  ( -0.5392447798056579922, -21.39623730026199411, -56.39940532337661949 ) ) ;
#30586 = CARTESIAN_POINT ( 'NONE',  ( -8.314922557961024197, 14.29746914071037800, 82.91775706135234714 ) ) ;
#30587 = CARTESIAN_POINT ( 'NONE',  ( -12.14591786802326823, 12.06949235617739902, 53.12609039468568284 ) ) ;
#30588 = CARTESIAN_POINT ( 'NONE',  ( -21.53943276465977519, -0.05219959533937600094, 113.7510903946856757 ) ) ;
#30590 = CARTESIAN_POINT ( 'NONE',  ( 11.30153831258470731, -190.0000000000000000, -25.00000000000000000 ) ) ;
#30589 = CARTESIAN_POINT ( 'NONE',  ( 13.97604488694527802, 13.89961937509977652, 54.37390960531435979 ) ) ;
#30591 = CARTESIAN_POINT ( 'NONE',  ( -0.05219959533937732626, 21.53943276465977519, 67.50109039468568994 ) ) ;
#30592 = CARTESIAN_POINT ( 'NONE',  ( 9.564922557961047289, -16.46253265017146816, 80.41775706135234714 ) ) ;
#30593 = CARTESIAN_POINT ( 'NONE',  ( 15.80617190586769283, -15.72974639402175789, 105.6260903946856899 ) ) ;
#30594 = CARTESIAN_POINT ( 'NONE',  ( 9.564922557960805705, 16.46253265017160317, 24.58224293864769194 ) ) ;
#30595 = CARTESIAN_POINT ( 'NONE',  ( 17.39952324805926409, 6.147335277187066183, 23.87583945527051910 ) ) ;
#30596 = CARTESIAN_POINT ( 'NONE',  ( -15.80617190586745835, -15.72974639402198527, 66.87390960531436690 ) ) ;
#30597 = AXIS2_PLACEMENT_3D ( 'NONE', #53506, #132355, #55511 ) ;
#30598 = CARTESIAN_POINT ( 'NONE',  ( 10.81492255796078972, 18.62759615963270932, 24.58224293864768839 ) ) ;
#30599 = CARTESIAN_POINT ( 'NONE',  ( 16.51473224551069308, 9.474510206698969483, 24.16557627198102765 ) ) ;
#30600 = CARTESIAN_POINT ( 'NONE',  ( -16.52544592524335698, -4.483927247898792601, 38.95942372801901854 ) ) ;
#30601 = CARTESIAN_POINT ( 'NONE',  ( -8.224510206698948167, 14.34966873604960824, 35.41557627198102409 ) ) ;
#30602 = EDGE_LOOP ( 'NONE', ( #35051, #142222, #192547, #91547 ) ) ;
#30603 = CARTESIAN_POINT ( 'NONE',  ( 10.72451020669871369, 18.67979575497193778, 22.08442372801901143 ) ) ;
#30605 = CARTESIAN_POINT ( 'NONE',  ( 30.74264578624799782, 22.33583958711400541, -6.800000000000000711 ) ) ;
#30604 = CARTESIAN_POINT ( 'NONE',  ( 14.34966873604960469, 8.224510206698951720, 59.16557627198103120 ) ) ;
#30606 = CARTESIAN_POINT ( 'NONE',  ( 9.474510206698729675, 16.51473224551082808, 112.0844237280190043 ) ) ;
#30607 = CARTESIAN_POINT ( 'NONE',  ( 5.049401038297881783, 19.05341960407617563, 32.29275706135233293 ) ) ;
#30608 = CARTESIAN_POINT ( 'NONE',  ( 14.34966873604960469, 8.224510206698951720, 49.16557627198102409 ) ) ;
#30609 = CARTESIAN_POINT ( 'NONE',  ( 15.80617190586746368, 15.72974639402197994, 109.3739096053143811 ) ) ;
#30611 = CARTESIAN_POINT ( 'NONE',  ( 5.719274019375991003, -21.55341960407610458, 67.70724293864769550 ) ) ;
#30610 = CYLINDRICAL_SURFACE ( 'NONE', #50415, 5.000000000000000000 ) ;
#30612 = CARTESIAN_POINT ( 'NONE',  ( 19.02544592524343514, -5.153800228976328945, 83.54057627198100988 ) ) ;
#30613 = CARTESIAN_POINT ( 'NONE',  ( -8.314922557960811034, -14.29746914071050412, 47.08224293864770260 ) ) ;
#30614 = CARTESIAN_POINT ( 'NONE',  ( 19.03943276465977164, -0.05219959533909143690, 98.74890960531436690 ) ) ;
#30615 = CARTESIAN_POINT ( 'NONE',  ( -4.622231866529366047E-30, -105.0000000000000000, -15.00000000000000000 ) ) ;
#30616 = CARTESIAN_POINT ( 'NONE',  ( 16.51473224551083163, -9.474510206698727899, 60.83442372801900433 ) ) ;
#30617 = CARTESIAN_POINT ( 'NONE',  ( 21.55341960407610458, 5.719274019375980345, 93.95724293864770971 ) ) ;
#30618 = CARTESIAN_POINT ( 'NONE',  ( -9.474510206698964154, 16.51473224551069663, 40.41557627198103120 ) ) ;
#30619 = CARTESIAN_POINT ( 'NONE',  ( -4.379528057220328563, 16.55341960407611168, 115.2072429386476955 ) ) ;
#30620 = CARTESIAN_POINT ( 'NONE',  ( -10.81492255796105439, 18.62759615963255655, 52.91775706135235424 ) ) ;
#30621 = CARTESIAN_POINT ( 'NONE',  ( -27.73933785331498925, -9.013057229001049109, 144.9750000027312069 ) ) ;
#30622 = CARTESIAN_POINT ( 'NONE',  ( -14.29746914071049879, 8.314922557960819915, 30.83224293864770260 ) ) ;
#30623 = CARTESIAN_POINT ( 'NONE',  ( -16.51473224551069308, -9.474510206698971260, 46.66557627198102409 ) ) ;
#30624 = CARTESIAN_POINT ( 'NONE',  ( -19.02544592524342804, 5.153800228976336051, 106.0405762719810241 ) ) ;
#30625 = CARTESIAN_POINT ( 'NONE',  ( -15.72974639402197994, 15.80617190586746368, 55.62390960531436690 ) ) ;
#30626 = DIRECTION ( 'NONE',  ( -0.3041824702427683436, -0.9526137857479322069, 2.960637879548173518E-15 ) ) ;
#30627 = CARTESIAN_POINT ( 'NONE',  ( -5.049401038298153566, 19.05341960407611168, 45.20724293864769550 ) ) ;
#30628 = CARTESIAN_POINT ( 'NONE',  ( 5.719274019375991003, -21.55341960407610458, 47.70724293864770260 ) ) ;
#30629 = ORIENTED_EDGE ( 'NONE', *, *, #162141, .T. ) ;
#30630 = CARTESIAN_POINT ( 'NONE',  ( -5.823673210054431948, 21.52544592524334988, 92.70942372801901854 ) ) ;
#30632 = CARTESIAN_POINT ( 'NONE',  ( -8.224510206698735004, -14.34966873604973081, 84.58442372801903275 ) ) ;
#30631 = CARTESIAN_POINT ( 'NONE',  ( 10.75775780537444959, -37.01749054246350568, -23.73535027651007567 ) ) ;
#30633 = CARTESIAN_POINT ( 'NONE',  ( -16.55341960407617563, 4.379528057220093196, 93.54275706135234714 ) ) ;
#30634 = CARTESIAN_POINT ( 'NONE',  ( 9.474510206698971260, -16.51473224551069308, 52.91557627198102409 ) ) ;
#30635 = CARTESIAN_POINT ( 'NONE',  ( 16.46253265017160672, -9.564922557960803928, 68.33224293864770971 ) ) ;
#30636 = VERTEX_POINT ( 'NONE', #44613 ) ;
#30637 = CARTESIAN_POINT ( 'NONE',  ( -5.049401038297874678, -19.05341960407617918, 29.79275706135232227 ) ) ;
#30638 = CARTESIAN_POINT ( 'NONE',  ( -16.53943276465976808, -0.05219959533934237506, 73.75109039468567573 ) ) ;
#30639 = CARTESIAN_POINT ( 'NONE',  ( 16.46253265017146816, 9.564922557961045513, 21.66775706135233648 ) ) ;
#30640 = CARTESIAN_POINT ( 'NONE',  ( -16.46253265017160317, 9.564922557960807481, 75.83224293864769550 ) ) ;
#30641 = CARTESIAN_POINT ( 'NONE',  ( 15.72974639402199770, -15.80617190586745480, 53.12390960531436690 ) ) ;
#30642 = CARTESIAN_POINT ( 'NONE',  ( -8.314922557961024197, 14.29746914071037800, 27.91775706135234358 ) ) ;
#30643 = CARTESIAN_POINT ( 'NONE',  ( -21.52544592524334988, -5.823673210054445271, 78.95942372801901854 ) ) ;
#30644 = CARTESIAN_POINT ( 'NONE',  ( 12.14591786802327356, -12.06949235617739191, 50.62609039468568994 ) ) ;
#30645 = CARTESIAN_POINT ( 'NONE',  ( 15.72974639402199770, -15.80617190586745480, 108.1239096053143811 ) ) ;
#30646 = CARTESIAN_POINT ( 'NONE',  ( -16.53943276465976808, -0.05219959533934237506, 18.75109039468568639 ) ) ;
#30647 = CARTESIAN_POINT ( 'NONE',  ( -19.05341960407611168, -5.049401038298163336, 76.45724293864769550 ) ) ;
#30648 = CARTESIAN_POINT ( 'NONE',  ( 4.379528057220092307, 16.55341960407617563, 32.29275706135235424 ) ) ;
#30649 = CARTESIAN_POINT ( 'NONE',  ( 9.474510206698971260, -16.51473224551069308, 37.91557627198102409 ) ) ;
#30650 = CARTESIAN_POINT ( 'NONE',  ( -16.55341960407617563, 4.379528057220093196, 23.54275706135235424 ) ) ;
#30651 = CARTESIAN_POINT ( 'NONE',  ( -16.53943276465976808, 0.05219959533911058130, 76.24890960531435269 ) ) ;
#30652 = CARTESIAN_POINT ( 'NONE',  ( -16.53943276465976808, -0.05219959533934237506, 83.75109039468568994 ) ) ;
#30654 = CARTESIAN_POINT ( 'NONE',  ( -5.049401038298153566, 19.05341960407611168, 60.20724293864768129 ) ) ;
#30653 = CARTESIAN_POINT ( 'NONE',  ( 5.823673210054444382, -21.52544592524334988, 30.20942372801902565 ) ) ;
#30655 = CARTESIAN_POINT ( 'NONE',  ( -19.05341960407611168, -5.049401038298163336, 71.45724293864766707 ) ) ;
#30656 = CARTESIAN_POINT ( 'NONE',  ( -14.34966873604972548, 8.224510206698743886, 88.33442372801901854 ) ) ;
#30657 = AXIS2_PLACEMENT_3D ( 'NONE', #199289, #134649, #150810 ) ;
#30659 = VERTEX_POINT ( 'NONE', #182137 ) ;
#30658 = CARTESIAN_POINT ( 'NONE',  ( -24.30454888808800362, -2.781629622375087152, 174.5654150192188183 ) ) ;
#30660 = ORIENTED_EDGE ( 'NONE', *, *, #23111, .T. ) ;
#30661 = CARTESIAN_POINT ( 'NONE',  ( 13.89961937509957401, 13.97604488694547697, 36.87609039468565442 ) ) ;
#30662 = CARTESIAN_POINT ( 'NONE',  ( 19.03943276465977164, -0.05219959533909143690, 38.74890960531436690 ) ) ;
#30664 = ORIENTED_EDGE ( 'NONE', *, *, #41288, .F. ) ;
#30663 = CARTESIAN_POINT ( 'NONE',  ( -5.049401038298153566, 19.05341960407611168, 115.2072429386477097 ) ) ;
#30665 = CARTESIAN_POINT ( 'NONE',  ( -14.29746914071037622, -8.314922557961029526, 24.16775706135235424 ) ) ;
#30667 = CARTESIAN_POINT ( 'NONE',  ( 16.52544592524335698, 4.483927247898782831, 41.45942372801901143 ) ) ;
#30666 = CARTESIAN_POINT ( 'NONE',  ( -5.153800228976607833, 19.02544592524334988, 57.70942372801899012 ) ) ;
#30668 = CARTESIAN_POINT ( 'NONE',  ( -16.46253265017160317, 9.564922557960807481, 110.8322429386476955 ) ) ;
#30669 = CARTESIAN_POINT ( 'NONE',  ( -13.97604488694527625, -13.89961937509977652, 66.87390960531436690 ) ) ;
#30670 = CARTESIAN_POINT ( 'NONE',  ( 10.81492255796078972, 18.62759615963270932, 104.5822429386477097 ) ) ;
#30672 = CARTESIAN_POINT ( 'NONE',  ( 0.05219959533909260263, 19.03943276465977164, 24.99890960531435269 ) ) ;
#30671 = CARTESIAN_POINT ( 'NONE',  ( -5.153800228976328057, -19.02544592524343514, 92.29057627198099567 ) ) ;
#30673 = CARTESIAN_POINT ( 'NONE',  ( -19.02544592524342804, 5.153800228976336051, 66.04057627198103830 ) ) ;
#30675 = CARTESIAN_POINT ( 'NONE',  ( 17.59860650958989936, 7.585241751807028088, 69.07662985737508166 ) ) ;
#30674 = CARTESIAN_POINT ( 'NONE',  ( -4.483927247898539470, -16.52544592524342804, 27.29057627198103120 ) ) ;
#30676 = CARTESIAN_POINT ( 'NONE',  ( -5.153800228976607833, 19.02544592524334988, 42.70942372801901143 ) ) ;
#30677 = VECTOR ( 'NONE', #79195, 1000.000000000000000 ) ;
#30678 = CARTESIAN_POINT ( 'NONE',  ( 14.29746914071049879, -8.314922557960816363, 58.33224293864768839 ) ) ;
#30679 = CARTESIAN_POINT ( 'NONE',  ( -5.719274019375665041, -21.55341960407619695, 94.79275706135234714 ) ) ;
#30680 = CARTESIAN_POINT ( 'NONE',  ( -9.474510206698964154, 16.51473224551069663, 35.41557627198102409 ) ) ;
#30681 = CARTESIAN_POINT ( 'NONE',  ( -4.379528057220086978, -16.55341960407618274, 54.79275706135235424 ) ) ;
#30682 = EDGE_CURVE ( 'NONE', #164148, #135024, #143637, .T. ) ;
#30684 = CARTESIAN_POINT ( 'NONE',  ( -21.53943276465977519, -0.05219959533937600094, 88.75109039468567573 ) ) ;
#30683 = CARTESIAN_POINT ( 'NONE',  ( -12.14591786802309592, -12.06949235617757132, 36.87390960531435979 ) ) ;
#30685 = CARTESIAN_POINT ( 'NONE',  ( 16.51473224551069308, 9.474510206698969483, 84.16557627198102409 ) ) ;
#30686 = CARTESIAN_POINT ( 'NONE',  ( 19.02544592524343514, -5.153800228976328945, 98.54057627198100988 ) ) ;
#30687 = CARTESIAN_POINT ( 'NONE',  ( -8.224510206698948167, 14.34966873604960824, 105.4155762719810383 ) ) ;
#30688 = CARTESIAN_POINT ( 'NONE',  ( 0.05219959533910956823, 16.53943276465976808, 74.99890960531435269 ) ) ;
#30689 = CARTESIAN_POINT ( 'NONE',  ( 18.62759615963271287, -10.81492255796078972, 83.33224293864769550 ) ) ;
#30690 = CARTESIAN_POINT ( 'NONE',  ( -0.05219959533909027116, -19.03943276465977164, 92.49890960531436690 ) ) ;
#30691 = CARTESIAN_POINT ( 'NONE',  ( -10.81492255796078084, -18.62759615963271287, 102.0822429386476955 ) ) ;
#30692 = AXIS2_PLACEMENT_3D ( 'NONE', #160382, #158386, #112871 ) ;
#30693 = CARTESIAN_POINT ( 'NONE',  ( -0.05219959533936034679, 19.03943276465977164, 77.50109039468566152 ) ) ;
#30695 = CARTESIAN_POINT ( 'NONE',  ( 16.55341960407611168, 4.379528057220329451, 83.95724293864770971 ) ) ;
#30694 = DIRECTION ( 'NONE',  ( 0.000000000000000000, -0.7071067811865467956, 0.7071067811865483499 ) ) ;
#30696 = CARTESIAN_POINT ( 'NONE',  ( -19.02544592524342804, 5.153800228976336051, 56.04057627198100988 ) ) ;
#30697 = CARTESIAN_POINT ( 'NONE',  ( -15.80617190586745835, -15.72974639402198527, 71.87390960531438111 ) ) ;
#30698 = CARTESIAN_POINT ( 'NONE',  ( 17.48853670773243252, -5.747243402303153559, 26.16671299749992130 ) ) ;
#30700 = CARTESIAN_POINT ( 'NONE',  ( 193.3062444957835453, -155.7167183371837496, -25.00000000000000000 ) ) ;
#30699 = CARTESIAN_POINT ( 'NONE',  ( 14.34966873604960469, 8.224510206698951720, 24.16557627198103120 ) ) ;
#30701 = CARTESIAN_POINT ( 'NONE',  ( 16.55341960407618274, -4.379528057220086978, 21.04275706135234714 ) ) ;
#30702 = CARTESIAN_POINT ( 'NONE',  ( -8.314922557960811034, -14.29746914071050412, 82.08224293864768129 ) ) ;
#30703 = CARTESIAN_POINT ( 'NONE',  ( 24.49873734152946625, 24.99873734152886939, 4.646446609406719830 ) ) ;
#30704 = CARTESIAN_POINT ( 'NONE',  ( -13.89961937509977652, 13.97604488694528158, 80.62390960531436690 ) ) ;
#30705 = CARTESIAN_POINT ( 'NONE',  ( 13.97604488694527802, 13.89961937509977652, 34.37390960531436690 ) ) ;
#30706 = CARTESIAN_POINT ( 'NONE',  ( 14.29746914071049879, -8.314922557960816363, 63.33224293864770260 ) ) ;
#30707 = CARTESIAN_POINT ( 'NONE',  ( -13.89961937509977652, 13.97604488694528158, 110.6239096053143243 ) ) ;
#30708 = CARTESIAN_POINT ( 'NONE',  ( -19.02544592524334988, -5.153800228976617603, 93.95942372801900433 ) ) ;
#30709 = CIRCLE ( 'NONE', #1684, 9.100000000000001421 ) ;
#30710 = CARTESIAN_POINT ( 'NONE',  ( 19.03943276465977164, -0.05219959533909143690, 98.74890960531436690 ) ) ;
#30711 = CARTESIAN_POINT ( 'NONE',  ( 21.53943276465977519, -0.05219959533907433946, 73.74890960531433848 ) ) ;
#30712 = CARTESIAN_POINT ( 'NONE',  ( 12.06949235617739724, 12.14591786802326823, 76.87609039468567573 ) ) ;
#30713 = AXIS2_PLACEMENT_3D ( 'NONE', #154163, #62135, #123799 ) ;
#30714 = CARTESIAN_POINT ( 'NONE',  ( 5.153800228976617603, -19.02544592524335343, 110.2094237280189901 ) ) ;
#30715 = CARTESIAN_POINT ( 'NONE',  ( 13.97604488694527802, 13.89961937509977652, 59.37390960531434558 ) ) ;
#30716 = CARTESIAN_POINT ( 'NONE',  ( 10.81492255796078972, 18.62759615963270932, 69.58224293864769550 ) ) ;
#30717 = CARTESIAN_POINT ( 'NONE',  ( 4.379528057220092307, 16.55341960407617563, 107.2927570613523471 ) ) ;
#30718 = CARTESIAN_POINT ( 'NONE',  ( -0.05219959533936034679, 19.03943276465977164, 112.5010903946856757 ) ) ;
#30720 = CARTESIAN_POINT ( 'NONE',  ( -18.67979575497193778, 10.72451020669871902, 63.33442372801900433 ) ) ;
#30719 = CARTESIAN_POINT ( 'NONE',  ( 4.379528057220339221, -16.55341960407611168, 32.70724293864770260 ) ) ;
#30721 = CARTESIAN_POINT ( 'NONE',  ( -8.906447517083053711, -27.41122689804191026, 144.6500000054623740 ) ) ;
#30723 = CARTESIAN_POINT ( 'NONE',  ( 16.51473224551069308, 9.474510206698969483, 104.1655762719810241 ) ) ;
#30722 = CARTESIAN_POINT ( 'NONE',  ( -16.53943276465976808, -0.05219959533934237506, 73.75109039468567573 ) ) ;
#30724 = CARTESIAN_POINT ( 'NONE',  ( 19.05341960407611168, 5.049401038298154454, 103.9572429386476813 ) ) ;
#30725 = CARTESIAN_POINT ( 'NONE',  ( -17.44270441346519007, 5.991230190322968774, 78.63664920735773478 ) ) ;
#30726 = CARTESIAN_POINT ( 'NONE',  ( -8.314922557961024197, 14.29746914071037800, 97.91775706135236135 ) ) ;
#30727 = CARTESIAN_POINT ( 'NONE',  ( 14.34966873604972726, -8.224510206698740333, 45.83442372801901854 ) ) ;
#30728 = CARTESIAN_POINT ( 'NONE',  ( 13.89961937509977652, -13.97604488694527269, 53.12390960531434558 ) ) ;
#30729 = CARTESIAN_POINT ( 'NONE',  ( -16.46253265017160317, 9.564922557960807481, 75.83224293864769550 ) ) ;
#30730 = CARTESIAN_POINT ( 'NONE',  ( 10.72451020669871369, 18.67979575497193778, 57.08442372801901854 ) ) ;
#30731 = CARTESIAN_POINT ( 'NONE',  ( 16.53943276465976808, 0.05219959533934440121, 56.25109039468568284 ) ) ;
#30732 = CARTESIAN_POINT ( 'NONE',  ( 14.29746914071049879, -8.314922557960816363, 28.33224293864769550 ) ) ;
#30733 = CARTESIAN_POINT ( 'NONE',  ( -13.97604488694527625, -13.89961937509977652, 36.87390960531436690 ) ) ;
#30734 = CARTESIAN_POINT ( 'NONE',  ( -5.153800228976328057, -19.02544592524343514, 32.29057627198102409 ) ) ;
#30735 = CARTESIAN_POINT ( 'NONE',  ( -16.55341960407617563, 4.379528057220093196, 33.54275706135234714 ) ) ;
#30736 = CARTESIAN_POINT ( 'NONE',  ( -19.03943276465977164, -0.05219959533935918106, 83.75109039468567573 ) ) ;
#30737 = CARTESIAN_POINT ( 'NONE',  ( 12.14591786802309770, 12.06949235617756955, 79.37390960531436690 ) ) ;
#30738 = CARTESIAN_POINT ( 'NONE',  ( 5.049401038298161559, -19.05341960407611168, 47.70724293864770260 ) ) ;
#30739 = CARTESIAN_POINT ( 'NONE',  ( -13.89961937509957401, -13.97604488694547875, 89.37609039468563310 ) ) ;
#30740 = CARTESIAN_POINT ( 'NONE',  ( -18.67979575497193778, 10.72451020669871902, 93.33442372801901854 ) ) ;
#30741 = CARTESIAN_POINT ( 'NONE',  ( -8.224510206698735004, -14.34966873604973081, 54.58442372801901143 ) ) ;
#30742 = CARTESIAN_POINT ( 'NONE',  ( -17.50000000000000000, 5.068104630630428709, 25.72818405340030523 ) ) ;
#30743 = CARTESIAN_POINT ( 'NONE',  ( 10.81492255796078972, 18.62759615963270932, 54.58224293864769550 ) ) ;
#30744 = CARTESIAN_POINT ( 'NONE',  ( -16.55341960407617563, 4.379528057220093196, 38.54275706135234714 ) ) ;
#30745 = CARTESIAN_POINT ( 'NONE',  ( 18.22780087662119897, -5.500000000000146549, 38.51763182126893525 ) ) ;
#30746 = CARTESIAN_POINT ( 'NONE',  ( 5.049401038297881783, 19.05341960407617563, 37.29275706135232582 ) ) ;
#30747 = CARTESIAN_POINT ( 'NONE',  ( -9.474510206698964154, 16.51473224551069663, 95.41557627198102409 ) ) ;
#30748 = CARTESIAN_POINT ( 'NONE',  ( 16.46253265017160672, -9.564922557960803928, 48.33224293864769550 ) ) ;
#30749 = CONICAL_SURFACE ( 'NONE', #143726, 2.500000000000000000, 1.029744258676656976 ) ;
#30750 = FACE_OUTER_BOUND ( 'NONE', #102793, .T. ) ;
#30751 = CARTESIAN_POINT ( 'NONE',  ( 15.72974639402176855, 15.80617190586768217, 76.87609039468567573 ) ) ;
#30752 = CARTESIAN_POINT ( 'NONE',  ( -17.49999999999999645, 5.500000000000037303, 50.79690382534172244 ) ) ;
#30753 = PRODUCT_DEFINITION_SHAPE ( 'NONE', 'NONE',  #200196 ) ;
#30754 = CARTESIAN_POINT ( 'NONE',  ( -9.564922557961040184, 16.46253265017147172, 32.91775706135233293 ) ) ;
#30755 = CARTESIAN_POINT ( 'NONE',  ( -10.72451020669870658, -18.67979575497194134, 104.5844237280190185 ) ) ;
#30756 = CARTESIAN_POINT ( 'NONE',  ( -0.05219959533910754901, -16.53943276465976808, 32.49890960531435979 ) ) ;
#30757 = CARTESIAN_POINT ( 'NONE',  ( -19.05341960407611168, -5.049401038298163336, 46.45724293864768129 ) ) ;
#30758 = CARTESIAN_POINT ( 'NONE',  ( -19.03943276465977164, 0.05219959533909376836, 101.2489096053143669 ) ) ;
#30759 = CARTESIAN_POINT ( 'NONE',  ( 5.823673210054444382, -21.52544592524334988, 85.20942372801901854 ) ) ;
#30760 = CARTESIAN_POINT ( 'NONE',  ( -5.049401038298153566, 19.05341960407611168, 60.20724293864768129 ) ) ;
#30761 = CARTESIAN_POINT ( 'NONE',  ( 15.72974639402176855, 15.80617190586768217, 81.87609039468568994 ) ) ;
#30762 = CARTESIAN_POINT ( 'NONE',  ( -18.67979575497178146, -10.72451020669898902, 36.66557627198103120 ) ) ;
#30763 = CARTESIAN_POINT ( 'NONE',  ( -5.823673210054431948, 21.52544592524334988, 27.70942372801901854 ) ) ;
#30764 = CARTESIAN_POINT ( 'NONE',  ( 13.89961937509957401, 13.97604488694547697, 41.87609039468566152 ) ) ;
#30765 = CARTESIAN_POINT ( 'NONE',  ( 19.03943276465977164, -0.05219959533909143690, 23.74890960531435269 ) ) ;
#30766 = CARTESIAN_POINT ( 'NONE',  ( 16.51473224551069308, 9.474510206698969483, 74.16557627198103830 ) ) ;
#30767 = CARTESIAN_POINT ( 'NONE',  ( -4.379528057220086978, -16.55341960407618274, 29.79275706135234358 ) ) ;
#30768 = CARTESIAN_POINT ( 'NONE',  ( 16.53943276465976808, -0.05219959533910856209, 83.74890960531435269 ) ) ;
#30769 = CARTESIAN_POINT ( 'NONE',  ( 5.049401038298161559, -19.05341960407611168, 52.70724293864767418 ) ) ;
#30770 = CARTESIAN_POINT ( 'NONE',  ( -21.52544592524343514, 5.823673210054127303, 31.04057627198102409 ) ) ;
#30771 = CARTESIAN_POINT ( 'NONE',  ( 13.89961937509957401, 13.97604488694547697, 101.8760903946856331 ) ) ;
#30772 = CARTESIAN_POINT ( 'NONE',  ( -5.823673210054116645, -21.52544592524344225, 107.2905762719810525 ) ) ;
#30773 = CARTESIAN_POINT ( 'NONE',  ( 5.719274019375673035, 21.55341960407619339, 72.29275706135236135 ) ) ;
#30774 = CARTESIAN_POINT ( 'NONE',  ( 12.06949235617739724, 12.14591786802326823, 66.87609039468568994 ) ) ;
#30775 = CARTESIAN_POINT ( 'NONE',  ( 8.314922557961029526, -14.29746914071037800, 65.41775706135234714 ) ) ;
#30776 = VERTEX_POINT ( 'NONE', #136611 ) ;
#30777 = CARTESIAN_POINT ( 'NONE',  ( 13.97604488694527802, 13.89961937509977652, 59.37390960531434558 ) ) ;
#30778 = CARTESIAN_POINT ( 'NONE',  ( -16.55341960407617563, 4.379528057220093196, 93.54275706135234714 ) ) ;
#30779 = CARTESIAN_POINT ( 'NONE',  ( -15.72974639402176322, -15.80617190586768395, 19.37609039468568639 ) ) ;
#30780 = CARTESIAN_POINT ( 'NONE',  ( -4.379528057220328563, 16.55341960407611168, 65.20724293864768129 ) ) ;
#30781 = CARTESIAN_POINT ( 'NONE',  ( -9.564922557960796823, -16.46253265017161027, 92.08224293864769550 ) ) ;
#30782 = CARTESIAN_POINT ( 'NONE',  ( 12.06949235617739724, 12.14591786802326823, 81.87609039468568994 ) ) ;
#30783 = CARTESIAN_POINT ( 'NONE',  ( 5.823673210054444382, -21.52544592524334988, 55.20942372801902565 ) ) ;
#30784 = CARTESIAN_POINT ( 'NONE',  ( 19.02544592524334988, 5.153800228976608722, 111.4594237280190043 ) ) ;
#30785 = CARTESIAN_POINT ( 'NONE',  ( 18.67979575497178502, 10.72451020669898547, 114.1655762719810383 ) ) ;
#30786 = CARTESIAN_POINT ( 'NONE',  ( -0.05219959533910754901, -16.53943276465976808, 62.49890960531436690 ) ) ;
#30787 = ORIENTED_EDGE ( 'NONE', *, *, #94101, .F. ) ;
#30788 = CARTESIAN_POINT ( 'NONE',  ( -0.05219959533907301413, -21.53943276465977519, 87.49890960531436690 ) ) ;
#30789 = CARTESIAN_POINT ( 'NONE',  ( 16.53943276465976808, -0.05219959533910856209, 38.74890960531435979 ) ) ;
#30790 = ORIENTED_EDGE ( 'NONE', *, *, #131008, .F. ) ;
#30791 = CARTESIAN_POINT ( 'NONE',  ( 35.13534055906293929, 5.469967203781499698, 39.86293573631996878 ) ) ;
#30792 = CARTESIAN_POINT ( 'NONE',  ( 5.823673210054444382, -21.52544592524334988, 20.20942372801900788 ) ) ;
#30793 = CARTESIAN_POINT ( 'NONE',  ( 19.03943276465977164, -0.05219959533909143690, 113.7489096053143669 ) ) ;
#30794 = CARTESIAN_POINT ( 'NONE',  ( 5.823673210054444382, -21.52544592524334988, 35.20942372801901854 ) ) ;
#30795 = CARTESIAN_POINT ( 'NONE',  ( -4.379528057220328563, 16.55341960407611168, 45.20724293864769550 ) ) ;
#30796 = CARTESIAN_POINT ( 'NONE',  ( -16.51473224551069308, -9.474510206698971260, 66.66557627198102409 ) ) ;
#30797 = CARTESIAN_POINT ( 'NONE',  ( 19.05341960407617918, -5.049401038297876454, 61.04275706135232582 ) ) ;
#30798 = CARTESIAN_POINT ( 'NONE',  ( -0.05219959533909027116, -19.03943276465977164, 92.49890960531436690 ) ) ;
#30799 = CARTESIAN_POINT ( 'NONE',  ( 18.67979575497178502, 10.72451020669898547, 49.16557627198102409 ) ) ;
#30800 = CARTESIAN_POINT ( 'NONE',  ( -12.88217944815594684, -35.43691452638693562, -29.79217952741210951 ) ) ;
#30801 = CARTESIAN_POINT ( 'NONE',  ( -0.05219959533909027116, -19.03943276465977164, 52.49890960531436690 ) ) ;
#30802 = CARTESIAN_POINT ( 'NONE',  ( 12.06949235617739724, 12.14591786802326823, 36.87609039468568994 ) ) ;
#30803 = CARTESIAN_POINT ( 'NONE',  ( -19.05341960407617563, 5.049401038297882671, 58.54275706135234003 ) ) ;
#30804 = CARTESIAN_POINT ( 'NONE',  ( -5.823673210054431948, 21.52544592524334988, 22.70942372801901499 ) ) ;
#30805 = CARTESIAN_POINT ( 'NONE',  ( 16.53943276465976808, -0.05219959533910856209, 43.74890960531435979 ) ) ;
#30806 = CARTESIAN_POINT ( 'NONE',  ( 9.564922557960805705, 16.46253265017160317, 84.58224293864769550 ) ) ;
#30807 = CARTESIAN_POINT ( 'NONE',  ( -18.67979575497178146, -10.72451020669898902, 76.66557627198103830 ) ) ;
#30809 = CARTESIAN_POINT ( 'NONE',  ( -16.55341960407617563, 4.379528057220093196, 43.54275706135235424 ) ) ;
#30808 = CARTESIAN_POINT ( 'NONE',  ( -18.67979575497178146, -10.72451020669898902, 96.66557627198102409 ) ) ;
#30810 = CARTESIAN_POINT ( 'NONE',  ( -21.53943276465977519, 0.05219959533907696930, 31.24890960531435979 ) ) ;
#30811 = CARTESIAN_POINT ( 'NONE',  ( 18.62759615963255655, 10.81492255796105972, 91.66775706135234714 ) ) ;
#30812 = CARTESIAN_POINT ( 'NONE',  ( -9.474510206698964154, 16.51473224551069663, 90.41557627198103830 ) ) ;
#30813 = CARTESIAN_POINT ( 'NONE',  ( -19.05341960407611168, -5.049401038298163336, 41.45724293864769550 ) ) ;
#30814 = CARTESIAN_POINT ( 'NONE',  ( -13.97604488694527625, -13.89961937509977652, 91.87390960531432427 ) ) ;
#30815 = CARTESIAN_POINT ( 'NONE',  ( -14.34966873604960291, -8.224510206698953496, 101.6655762719810383 ) ) ;
#30816 = CARTESIAN_POINT ( 'NONE',  ( 13.97604488694527802, 13.89961937509977652, 59.37390960531434558 ) ) ;
#30817 = CARTESIAN_POINT ( 'NONE',  ( -13.97604488694547697, 13.89961937509957934, 113.1260903946856757 ) ) ;
#30818 = CARTESIAN_POINT ( 'NONE',  ( 17.44270441346519007, -5.991230190322930582, 86.13664920735777741 ) ) ;
#30819 = EDGE_CURVE ( 'NONE', #128112, #172412, #141459, .T. ) ;
#30820 = CARTESIAN_POINT ( 'NONE',  ( 0.05219959533936267826, -19.03943276465977164, 60.00109039468566863 ) ) ;
#30822 = CARTESIAN_POINT ( 'NONE',  ( -21.53943276465977519, 0.05219959533907696930, 36.24890960531435979 ) ) ;
#30821 = CARTESIAN_POINT ( 'NONE',  ( -21.53943276465977519, -0.05219959533937600094, 93.75109039468567573 ) ) ;
#30823 = CARTESIAN_POINT ( 'NONE',  ( 0.05219959533934541429, -16.53943276465976808, 90.00109039468567573 ) ) ;
#30824 = DIRECTION ( 'NONE',  ( -0.000000000000000000, -0.000000000000000000, 1.000000000000000000 ) ) ;
#30825 = CARTESIAN_POINT ( 'NONE',  ( 16.46253265017146816, 9.564922557961045513, 76.66775706135234714 ) ) ;
#30826 = CARTESIAN_POINT ( 'NONE',  ( -5.049401038297874678, -19.05341960407617918, 34.79275706135233293 ) ) ;
#30827 = DIRECTION ( 'NONE',  ( 0.000000000000000000, 0.000000000000000000, 1.000000000000000000 ) ) ;
#30828 = CARTESIAN_POINT ( 'NONE',  ( 16.46253265017160672, -9.564922557960803928, 48.33224293864769550 ) ) ;
#30829 = CARTESIAN_POINT ( 'NONE',  ( 4.379528057220339221, -16.55341960407611168, 32.70724293864770260 ) ) ;
#30830 = CARTESIAN_POINT ( 'NONE',  ( -16.81555441253553340, -7.025013491695469625, 109.3631455466574209 ) ) ;
#30831 = CARTESIAN_POINT ( 'NONE',  ( 12.06949235617757843, -12.14591786802309237, 23.12390960531436335 ) ) ;
#30832 = DIRECTION ( 'NONE',  ( 0.000000000000000000, 0.000000000000000000, -1.000000000000000000 ) ) ;
#30833 = CARTESIAN_POINT ( 'NONE',  ( -4.483927247898782831, 16.52544592524335698, 97.70942372801904696 ) ) ;
#30834 = CARTESIAN_POINT ( 'NONE',  ( -0.05219959533909027116, -19.03943276465977164, 32.49890960531435979 ) ) ;
#30835 = CARTESIAN_POINT ( 'NONE',  ( -21.55341960407619339, 5.719274019375674811, 108.5427570613523756 ) ) ;
#30836 = CARTESIAN_POINT ( 'NONE',  ( 14.34966873604972726, -8.224510206698740333, 20.83442372801901143 ) ) ;
#30837 = CARTESIAN_POINT ( 'NONE',  ( -21.52544592524334988, -5.823673210054445271, 78.95942372801901854 ) ) ;
#30838 = EDGE_CURVE ( 'NONE', #177278, #34604, #192007, .T. ) ;
#30839 = CARTESIAN_POINT ( 'NONE',  ( -5.049401038297874678, -19.05341960407617918, 54.79275706135234003 ) ) ;
#30840 = CARTESIAN_POINT ( 'NONE',  ( 19.02544592524343514, -5.153800228976328945, 88.54057627198102409 ) ) ;
#30841 = CARTESIAN_POINT ( 'NONE',  ( -16.46253265017160317, 9.564922557960807481, 85.83224293864769550 ) ) ;
#30842 = CARTESIAN_POINT ( 'NONE',  ( 16.20579543436676673, 7.371946100355104114, 73.06520834171871570 ) ) ;
#30843 = CARTESIAN_POINT ( 'NONE',  ( 18.62759615963271287, -10.81492255796078972, 113.3322429386476955 ) ) ;
#30844 = CIRCLE ( 'NONE', #56696, 5.000000000000001776 ) ;
#30845 = CARTESIAN_POINT ( 'NONE',  ( -12.14591786802309592, -12.06949235617757132, 61.87390960531436690 ) ) ;
#30846 = CARTESIAN_POINT ( 'NONE',  ( -21.55341960407610458, -5.719274019375992779, 66.45724293864768129 ) ) ;
#30847 = CARTESIAN_POINT ( 'NONE',  ( -16.46253265017160317, 9.564922557960807481, 60.83224293864769550 ) ) ;
#30849 = CARTESIAN_POINT ( 'NONE',  ( 16.55341960407618274, -4.379528057220086978, 96.04275706135236135 ) ) ;
#30848 = CARTESIAN_POINT ( 'NONE',  ( -15.80617190586745835, -15.72974639402198527, 91.87390960531436690 ) ) ;
#30850 = ORIENTED_EDGE ( 'NONE', *, *, #99562, .T. ) ;
#30851 = CARTESIAN_POINT ( 'NONE',  ( 13.97604488694527802, 13.89961937509977652, 49.37390960531434558 ) ) ;
#30853 = CARTESIAN_POINT ( 'NONE',  ( -9.100000000000001421, 9.789526074884739315E-14, -64.92279855667830191 ) ) ;
#30852 = CARTESIAN_POINT ( 'NONE',  ( -14.29746914071049879, 8.314922557960819915, 95.83224293864770971 ) ) ;
#30854 = CARTESIAN_POINT ( 'NONE',  ( -19.02544592524342804, 5.153800228976336051, 51.04057627198103120 ) ) ;
#30855 = CARTESIAN_POINT ( 'NONE',  ( -8.224510206698948167, 14.34966873604960824, 115.4155762719810241 ) ) ;
#30856 = CARTESIAN_POINT ( 'NONE',  ( -5.153800228976607833, 19.02544592524334988, 77.70942372801900433 ) ) ;
#30857 = CARTESIAN_POINT ( 'NONE',  ( -4.483927247898539470, -16.52544592524342804, 82.29057627198103830 ) ) ;
#30858 = CARTESIAN_POINT ( 'NONE',  ( 21.55341960407619695, -5.719274019375665929, 46.04275706135234714 ) ) ;
#30860 = CARTESIAN_POINT ( 'NONE',  ( 5.823673210054125526, 21.52544592524343514, 109.7905762719810383 ) ) ;
#30859 = CARTESIAN_POINT ( 'NONE',  ( -9.564922557960796823, -16.46253265017161027, 32.08224293864769550 ) ) ;
#30861 = CARTESIAN_POINT ( 'NONE',  ( -8.224510206698948167, 14.34966873604960824, 85.41557627198102409 ) ) ;
#30862 = CARTESIAN_POINT ( 'NONE',  ( 3.964304649043745243, -40.57928608015685512, -25.32305239479493508 ) ) ;
#30863 = CARTESIAN_POINT ( 'NONE',  ( -19.02544592524342804, 5.153800228976336051, 66.04057627198103830 ) ) ;
#30864 = CIRCLE ( 'NONE', #137370, 69.99999999999998579 ) ;
#30865 = DIRECTION ( 'NONE',  ( 1.000000000000000000, 0.000000000000000000, -0.000000000000000000 ) ) ;
#30867 = CARTESIAN_POINT ( 'NONE',  ( 5.049401038298161559, -19.05341960407611168, 107.7072429386476955 ) ) ;
#30866 = CARTESIAN_POINT ( 'NONE',  ( 13.97604488694548053, -13.89961937509957401, 90.62609039468567573 ) ) ;
#30868 = CARTESIAN_POINT ( 'NONE',  ( 21.53943276465977519, 0.05219959533937863772, 41.25109039468568284 ) ) ;
#30869 = CARTESIAN_POINT ( 'NONE',  ( 13.89961937509977652, -13.97604488694527269, 83.12390960531436690 ) ) ;
#30870 = CARTESIAN_POINT ( 'NONE',  ( 16.46253265017146816, 9.564922557961045513, 71.66775706135233293 ) ) ;
#30871 = CARTESIAN_POINT ( 'NONE',  ( 19.05341960407611168, 5.049401038298154454, 53.95724293864770260 ) ) ;
#30872 = CARTESIAN_POINT ( 'NONE',  ( -8.314922557960811034, -14.29746914071050412, 82.08224293864768129 ) ) ;
#30873 = CARTESIAN_POINT ( 'NONE',  ( -16.53943276465976808, 0.05219959533911058130, 66.24890960531436690 ) ) ;
#30874 = CARTESIAN_POINT ( 'NONE',  ( 5.153800228976335163, 19.02544592524342804, 84.79057627198099567 ) ) ;
#30875 = CARTESIAN_POINT ( 'NONE',  ( -15.72974639402197994, 15.80617190586746368, 95.62390960531436690 ) ) ;
#30876 = CARTESIAN_POINT ( 'NONE',  ( -9.474510206698964154, 16.51473224551069663, 90.41557627198103830 ) ) ;
#30877 = CARTESIAN_POINT ( 'NONE',  ( 5.153800228976615827, -19.02544592524334988, 35.20942372801899722 ) ) ;
#30880 = CARTESIAN_POINT ( 'NONE',  ( -12.06949235617756955, 12.14591786802309770, 115.6239096053143669 ) ) ;
#30879 = CARTESIAN_POINT ( 'NONE',  ( -4.483927247898539470, -16.52544592524342804, 32.29057627198102409 ) ) ;
#30878 = CARTESIAN_POINT ( 'NONE',  ( -9.564922557960796823, -16.46253265017161027, 42.08224293864769550 ) ) ;
#30881 = ORIENTED_EDGE ( 'NONE', *, *, #48487, .T. ) ;
#30882 = CARTESIAN_POINT ( 'NONE',  ( 18.62759615963255655, 10.81492255796105972, 31.66775706135234358 ) ) ;
#30883 = CARTESIAN_POINT ( 'NONE',  ( -19.05341960407617563, 5.049401038297882671, 63.54275706135234003 ) ) ;
#30884 = CARTESIAN_POINT ( 'NONE',  ( -16.53943276465976808, 0.05219959533911058130, 31.24890960531435979 ) ) ;
#30885 = CARTESIAN_POINT ( 'NONE',  ( -0.05219959533907301413, -21.53943276465977519, 87.49890960531436690 ) ) ;
#30886 = CARTESIAN_POINT ( 'NONE',  ( 5.153800228976335163, 19.02544592524342804, 114.7905762719810241 ) ) ;
#30887 = CARTESIAN_POINT ( 'NONE',  ( -14.34966873604960291, -8.224510206698953496, 66.66557627198102409 ) ) ;
#30888 = CARTESIAN_POINT ( 'NONE',  ( 0.05219959533909260263, 19.03943276465977164, 24.99890960531435269 ) ) ;
#30889 = CARTESIAN_POINT ( 'NONE',  ( 5.049401038297881783, 19.05341960407617563, 22.29275706135233648 ) ) ;
#30890 = CARTESIAN_POINT ( 'NONE',  ( -0.05219959533934338120, 16.53943276465976808, 102.5010903946856899 ) ) ;
#30891 = CARTESIAN_POINT ( 'NONE',  ( -8.224510206698735004, -14.34966873604973081, 54.58442372801901143 ) ) ;
#30892 = CARTESIAN_POINT ( 'NONE',  ( -18.67979575497178146, -10.72451020669898902, 41.66557627198103120 ) ) ;
#30893 = CARTESIAN_POINT ( 'NONE',  ( 18.62759615963255655, 10.81492255796105972, 111.6677570613523613 ) ) ;
#30894 = CARTESIAN_POINT ( 'NONE',  ( 9.474510206698971260, -16.51473224551069308, 82.91557627198103830 ) ) ;
#30895 = CARTESIAN_POINT ( 'NONE',  ( 12.06949235617739724, 12.14591786802326823, 56.87609039468568994 ) ) ;
#30896 = CARTESIAN_POINT ( 'NONE',  ( 0.05219959533910956823, 16.53943276465976808, 114.9989096053143669 ) ) ;
#30897 = EDGE_CURVE ( 'NONE', #45388, #139989, #56501, .T. ) ;
#30898 = CARTESIAN_POINT ( 'NONE',  ( -14.29746914071049879, 8.314922557960819915, 30.83224293864770260 ) ) ;
#30900 = CARTESIAN_POINT ( 'NONE',  ( 0.05219959533909260263, 19.03943276465977164, 89.99890960531436690 ) ) ;
#30899 = CARTESIAN_POINT ( 'NONE',  ( 9.564922557960805705, 16.46253265017160317, 104.5822429386476955 ) ) ;
#30901 = CARTESIAN_POINT ( 'NONE',  ( -13.89961937509977652, 13.97604488694528158, 115.6239096053143669 ) ) ;
#30902 = CARTESIAN_POINT ( 'NONE',  ( 14.29746914071049879, -8.314922557960816363, 63.33224293864770260 ) ) ;
#30903 = CARTESIAN_POINT ( 'NONE',  ( 4.379528057220339221, -16.55341960407611168, 37.70724293864769550 ) ) ;
#30904 = CARTESIAN_POINT ( 'NONE',  ( -16.55341960407611168, -4.379528057220339221, 56.45724293864768839 ) ) ;
#30906 = CARTESIAN_POINT ( 'NONE',  ( -5.049401038297874678, -19.05341960407618274, 59.79275706135232582 ) ) ;
#30905 = CARTESIAN_POINT ( 'NONE',  ( 4.483927247898790824, -16.52544592524335698, 45.20942372801901854 ) ) ;
#30907 = CARTESIAN_POINT ( 'NONE',  ( -13.89961937509957401, -13.97604488694547875, 49.37609039468567573 ) ) ;
#30908 = CARTESIAN_POINT ( 'NONE',  ( -19.02544592524342804, 5.153800228976336051, 71.04057627198099567 ) ) ;
#30909 = CARTESIAN_POINT ( 'NONE',  ( 19.05341960407617918, -5.049401038297876454, 71.04275706135234714 ) ) ;
#30910 = CARTESIAN_POINT ( 'NONE',  ( -17.14385361876520619, 23.59649016807275856, 145.0750000027311728 ) ) ;
#30911 = CARTESIAN_POINT ( 'NONE',  ( -9.474510206698720793, -16.51473224551083518, 54.58442372801899722 ) ) ;
#30913 = CARTESIAN_POINT ( 'NONE',  ( 12.06949235617739724, 12.14591786802326823, 76.87609039468567573 ) ) ;
#30912 = CARTESIAN_POINT ( 'NONE',  ( -0.05219959533936034679, 19.03943276465977164, 102.5010903946856757 ) ) ;
#30914 = CARTESIAN_POINT ( 'NONE',  ( -17.14385361876520264, -23.59649016807271593, 147.6750000027311671 ) ) ;
#30915 = FACE_OUTER_BOUND ( 'NONE', #76581, .T. ) ;
#30916 = CARTESIAN_POINT ( 'NONE',  ( 19.05341960407611168, 5.049401038298154454, 113.9572429386477097 ) ) ;
#30917 = CARTESIAN_POINT ( 'NONE',  ( 15.80617190586769283, -15.72974639402175789, 35.62609039468568994 ) ) ;
#30918 = CARTESIAN_POINT ( 'NONE',  ( -5.049401038297874678, -19.05341960407617918, 109.7927570613523187 ) ) ;
#30920 = CARTESIAN_POINT ( 'NONE',  ( -13.89961937509977652, 13.97604488694528158, 65.62390960531436690 ) ) ;
#30919 = DIRECTION ( 'NONE',  ( -1.000000000000000000, 8.673617379884036458E-16, -0.000000000000000000 ) ) ;
#30921 = CARTESIAN_POINT ( 'NONE',  ( -19.05341960407611168, -5.049401038298163336, 101.4572429386476955 ) ) ;
#30923 = CARTESIAN_POINT ( 'NONE',  ( 5.049401038298161559, -19.05341960407611168, 57.70724293864769550 ) ) ;
#30922 = CARTESIAN_POINT ( 'NONE',  ( 4.483927247898545687, 16.52544592524342804, 64.79057627198103830 ) ) ;
#30924 = CARTESIAN_POINT ( 'NONE',  ( 9.564922557960805705, 16.46253265017160317, 59.58224293864769550 ) ) ;
#30925 = CARTESIAN_POINT ( 'NONE',  ( 0.05219959533936267826, -19.03943276465977164, 75.00109039468566152 ) ) ;
#30926 = CARTESIAN_POINT ( 'NONE',  ( 10.81492255796078972, 18.62759615963270932, 49.58224293864769550 ) ) ;
#30927 = CARTESIAN_POINT ( 'NONE',  ( 0.05219959533910956823, 16.53943276465976808, 114.9989096053143669 ) ) ;
#30928 = CARTESIAN_POINT ( 'NONE',  ( -13.89961937509957401, -13.97604488694547875, 39.37609039468566152 ) ) ;
#30929 = CARTESIAN_POINT ( 'NONE',  ( -0.05219959533909027116, -19.03943276465977164, 77.49890960531435269 ) ) ;
#30930 = CARTESIAN_POINT ( 'NONE',  ( 18.62759615963271287, -10.81492255796078972, 73.33224293864769550 ) ) ;
#30932 = CARTESIAN_POINT ( 'NONE',  ( -19.05341960407617563, 5.049401038297882671, 28.54275706135232937 ) ) ;
#30931 = CARTESIAN_POINT ( 'NONE',  ( 4.379528057220339221, -16.55341960407611168, 82.70724293864770971 ) ) ;
#30933 = CARTESIAN_POINT ( 'NONE',  ( -5.719274019375978568, 21.55341960407610458, 55.20724293864770260 ) ) ;
#30934 = AXIS2_PLACEMENT_3D ( 'NONE', #67312, #82464, #99644 ) ;
#30935 = CARTESIAN_POINT ( 'NONE',  ( -5.719274019375978568, 21.55341960407610458, 35.20724293864768839 ) ) ;
#30936 = CARTESIAN_POINT ( 'NONE',  ( -5.719274019375665041, -21.55341960407619695, 89.79275706135236135 ) ) ;
#30937 = CARTESIAN_POINT ( 'NONE',  ( 5.153800228976335163, 19.02544592524342804, 69.79057627198103830 ) ) ;
#30938 = CARTESIAN_POINT ( 'NONE',  ( 14.34966873604960469, 8.224510206698951720, 109.1655762719810383 ) ) ;
#30939 = CARTESIAN_POINT ( 'NONE',  ( -0.05219959533937732626, 21.53943276465977519, 22.50109039468567573 ) ) ;
#30940 = CARTESIAN_POINT ( 'NONE',  ( 7.143419655154867876, -2.300691058039452397, 8.646741581399133736 ) ) ;
#30941 = CARTESIAN_POINT ( 'NONE',  ( -0.05219959533937732626, 21.53943276465977519, 42.50109039468567573 ) ) ;
#30942 = CARTESIAN_POINT ( 'NONE',  ( -9.564922557960796823, -16.46253265017161027, 32.08224293864769550 ) ) ;
#30943 = CARTESIAN_POINT ( 'NONE',  ( -0.05219959533907301413, -21.53943276465977519, 107.4989096053143669 ) ) ;
#30944 = CARTESIAN_POINT ( 'NONE',  ( -16.46253265017146816, -9.564922557961047289, 54.16775706135234003 ) ) ;
#30945 = CARTESIAN_POINT ( 'NONE',  ( 13.97604488694527802, 13.89961937509977652, 29.37390960531435979 ) ) ;
#30946 = CARTESIAN_POINT ( 'NONE',  ( -0.05219959533909027116, -19.03943276465977164, 27.49890960531435624 ) ) ;
#30947 = CARTESIAN_POINT ( 'NONE',  ( 16.52544592524335698, 4.483927247898782831, 56.45942372801902565 ) ) ;
#30948 = CARTESIAN_POINT ( 'NONE',  ( 16.51473224551069308, 9.474510206698969483, 29.16557627198103475 ) ) ;
#30949 = CARTESIAN_POINT ( 'NONE',  ( -26.45594755429640799, -8.318738267476385673, 167.5492909577823752 ) ) ;
#30950 = CARTESIAN_POINT ( 'NONE',  ( -19.03943276465977164, 0.05219959533909376836, 71.24890960531435269 ) ) ;
#30951 = CARTESIAN_POINT ( 'NONE',  ( -16.55341960407611168, -4.379528057220339221, 111.4572429386476813 ) ) ;
#30952 = CARTESIAN_POINT ( 'NONE',  ( 10.81492255796078972, 18.62759615963270932, 64.58224293864769550 ) ) ;
#30953 = CARTESIAN_POINT ( 'NONE',  ( -16.53943276465976808, -0.05219959533934237506, 38.75109039468567573 ) ) ;
#30954 = CARTESIAN_POINT ( 'NONE',  ( 10.72451020669871369, 18.67979575497193778, 102.0844237280190185 ) ) ;
#30955 = CARTESIAN_POINT ( 'NONE',  ( -9.564922557960796823, -16.46253265017161027, 22.08224293864768839 ) ) ;
#30956 = CARTESIAN_POINT ( 'NONE',  ( -16.53943276465976808, -0.05219959533934237506, 108.7510903946857042 ) ) ;
#30957 = CARTESIAN_POINT ( 'NONE',  ( 8.314922557960818139, 14.29746914071049879, 49.58224293864769550 ) ) ;
#30958 = CARTESIAN_POINT ( 'NONE',  ( -19.03943276465977164, 0.05219959533909376836, 46.24890960531435979 ) ) ;
#30959 = CARTESIAN_POINT ( 'NONE',  ( 0.05219959533937995610, -21.53943276465977519, 100.0010903946857042 ) ) ;
#30960 = CARTESIAN_POINT ( 'NONE',  ( -0.05219959533907301413, -21.53943276465977519, 107.4989096053143669 ) ) ;
#30961 = CARTESIAN_POINT ( 'NONE',  ( -18.67979575497193778, 10.72451020669871902, 68.33442372801900433 ) ) ;
#30962 = CARTESIAN_POINT ( 'NONE',  ( -14.34966873604972548, 8.224510206698743886, 48.33442372801902565 ) ) ;
#30964 = CARTESIAN_POINT ( 'NONE',  ( 5.823673210054444382, -21.52544592524334988, 100.2094237280190043 ) ) ;
#30963 = CARTESIAN_POINT ( 'NONE',  ( 0.05219959533910956823, 16.53943276465976808, 74.99890960531435269 ) ) ;
#30965 = CARTESIAN_POINT ( 'NONE',  ( 16.55341960407611168, 4.379528057220329451, 23.95724293864769550 ) ) ;
#30966 = FACE_OUTER_BOUND ( 'NONE', #4390, .T. ) ;
#30967 = CARTESIAN_POINT ( 'NONE',  ( -16.53943276465976808, -0.05219959533934237506, 33.75109039468568284 ) ) ;
#30968 = CARTESIAN_POINT ( 'NONE',  ( 16.53943276465976808, -0.05219959533910856209, 43.74890960531435979 ) ) ;
#30969 = CARTESIAN_POINT ( 'NONE',  ( 16.52544592524335698, 4.483927247898782831, 86.45942372801901854 ) ) ;
#30970 = CARTESIAN_POINT ( 'NONE',  ( 13.89961937509977652, -13.97604488694527269, 103.1239096053143527 ) ) ;
#30971 = CARTESIAN_POINT ( 'NONE',  ( 18.62759615963271287, -10.81492255796078972, 23.33224293864769194 ) ) ;
#30972 = CARTESIAN_POINT ( 'NONE',  ( 5.823673210054444382, -21.52544592524334988, 95.20942372801903275 ) ) ;
#30973 = CARTESIAN_POINT ( 'NONE',  ( 14.29746914071037800, 8.314922557961029526, 96.66775706135234714 ) ) ;
#30974 = CARTESIAN_POINT ( 'NONE',  ( -4.483927247898539470, -16.52544592524342804, 77.29057627198102409 ) ) ;
#30975 = CARTESIAN_POINT ( 'NONE',  ( 16.46253265017160672, -9.564922557960803928, 78.33224293864769550 ) ) ;
#30976 = ORIENTED_EDGE ( 'NONE', *, *, #101847, .F. ) ;
#30977 = CARTESIAN_POINT ( 'NONE',  ( 12.06949235617739724, 12.14591786802326823, 26.87609039468567218 ) ) ;
#30978 = CARTESIAN_POINT ( 'NONE',  ( 9.474510206698971260, -16.51473224551069308, 47.91557627198102409 ) ) ;
#30979 = CARTESIAN_POINT ( 'NONE',  ( -16.46253265017160317, 9.564922557960807481, 90.83224293864769550 ) ) ;
#30980 = CARTESIAN_POINT ( 'NONE',  ( 8.314922557961029526, -14.29746914071037800, 30.41775706135234358 ) ) ;
#30981 = CARTESIAN_POINT ( 'NONE',  ( -19.05341960407617563, 5.049401038297882671, 38.54275706135233293 ) ) ;
#30982 = CARTESIAN_POINT ( 'NONE',  ( -8.224510206698735004, -14.34966873604973081, 89.58442372801901854 ) ) ;
#30983 = CARTESIAN_POINT ( 'NONE',  ( -5.049401038298153566, 19.05341960407611168, 35.20724293864768839 ) ) ;
#30984 = CARTESIAN_POINT ( 'NONE',  ( -16.55341960407617563, 4.379528057220093196, 83.54275706135234714 ) ) ;
#30985 = CARTESIAN_POINT ( 'NONE',  ( 4.379528057220092307, 16.55341960407617563, 62.29275706135236845 ) ) ;
#30986 = CARTESIAN_POINT ( 'NONE',  ( -19.03943276465977164, -0.05219959533935918106, 78.75109039468567573 ) ) ;
#30987 = CARTESIAN_POINT ( 'NONE',  ( 5.049401038297881783, 19.05341960407617563, 22.29275706135233648 ) ) ;
#30988 = CARTESIAN_POINT ( 'NONE',  ( -13.89961937509977652, 13.97604488694528158, 50.62390960531435979 ) ) ;
#30989 = CARTESIAN_POINT ( 'NONE',  ( 12.06949235617757843, -12.14591786802309237, 88.12390960531436690 ) ) ;
#30990 = CARTESIAN_POINT ( 'NONE',  ( -5.153800228976607833, 19.02544592524334988, 52.70942372801900433 ) ) ;
#30991 = CARTESIAN_POINT ( 'NONE',  ( 0.05219959533907565091, 21.53943276465977519, 54.99890960531435269 ) ) ;
#30992 = CARTESIAN_POINT ( 'NONE',  ( 19.03943276465977164, 0.05219959533936151252, 31.25109039468566863 ) ) ;
#30993 = CARTESIAN_POINT ( 'NONE',  ( -19.03943276465977164, 0.05219959533909376836, 106.2489096053143669 ) ) ;
#30994 = CARTESIAN_POINT ( 'NONE',  ( -10.81492255796078084, -18.62759615963271287, 82.08224293864768129 ) ) ;
#30995 = CARTESIAN_POINT ( 'NONE',  ( -13.89961937509977652, 13.97604488694528158, 110.6239096053143243 ) ) ;
#30996 = CARTESIAN_POINT ( 'NONE',  ( 19.02544592524334988, 5.153800228976608722, 91.45942372801900433 ) ) ;
#30997 = CARTESIAN_POINT ( 'NONE',  ( -19.03943276465977164, 0.05219959533909376836, 111.2489096053143669 ) ) ;
#30998 = CARTESIAN_POINT ( 'NONE',  ( 14.34966873604972726, -8.224510206698740333, 20.83442372801901143 ) ) ;
#30999 = CARTESIAN_POINT ( 'NONE',  ( -5.153800228976328057, -19.02544592524343514, 37.29057627198102409 ) ) ;
#31000 = CARTESIAN_POINT ( 'NONE',  ( 16.51473224551069308, 9.474510206698969483, 94.16557627198103830 ) ) ;
#31001 = CARTESIAN_POINT ( 'NONE',  ( 15.72974639402199770, -15.80617190586745480, 83.12390960531436690 ) ) ;
#31002 = CARTESIAN_POINT ( 'NONE',  ( 16.53943276465976808, 0.05219959533934440121, 51.25109039468568994 ) ) ;
#31003 = CARTESIAN_POINT ( 'NONE',  ( -5.823673210054431948, 21.52544592524334988, 57.70942372801901143 ) ) ;
#31005 = CARTESIAN_POINT ( 'NONE',  ( -0.05219959533937732626, 21.53943276465977519, 112.5010903946857042 ) ) ;
#31004 = CARTESIAN_POINT ( 'NONE',  ( -5.153800228976607833, 19.02544592524334988, 112.7094237280190043 ) ) ;
#31006 = CARTESIAN_POINT ( 'NONE',  ( 14.29746914071037800, 8.314922557961029526, 106.6677570613523756 ) ) ;
#31007 = CARTESIAN_POINT ( 'NONE',  ( 19.05341960407611168, 5.049401038298154454, 103.9572429386476671 ) ) ;
#31008 = CARTESIAN_POINT ( 'NONE',  ( 18.67979575497178502, 10.72451020669898547, 99.16557627198100988 ) ) ;
#31009 = CARTESIAN_POINT ( 'NONE',  ( -8.314922557960811034, -14.29746914071050412, 32.08224293864769550 ) ) ;
#31010 = CARTESIAN_POINT ( 'NONE',  ( 16.46253265017146816, 9.564922557961045513, 76.66775706135234714 ) ) ;
#31011 = CARTESIAN_POINT ( 'NONE',  ( 15.72974639402176855, 15.80617190586768217, 61.87609039468568284 ) ) ;
#31012 = CARTESIAN_POINT ( 'NONE',  ( 5.049401038297881783, 19.05341960407617563, 32.29275706135233293 ) ) ;
#31013 = CARTESIAN_POINT ( 'NONE',  ( -14.29746914071049879, 8.314922557960819915, 105.8322429386476955 ) ) ;
#31014 = CARTESIAN_POINT ( 'NONE',  ( 21.52544592524344225, -5.823673210054117533, 28.54057627198103120 ) ) ;
#31015 = CARTESIAN_POINT ( 'NONE',  ( -14.34966873604960291, -8.224510206698953496, 31.66557627198102054 ) ) ;
#31016 = CARTESIAN_POINT ( 'NONE',  ( -0.05219959533937732626, 21.53943276465977519, 102.5010903946856899 ) ) ;
#31017 = CARTESIAN_POINT ( 'NONE',  ( -16.53943276465976808, -0.05219959533934237506, 58.75109039468568994 ) ) ;
#31018 = CARTESIAN_POINT ( 'NONE',  ( -12.14591786802326823, 12.06949235617739902, 113.1260903946856899 ) ) ;
#31019 = CARTESIAN_POINT ( 'NONE',  ( -18.62759615963255300, -10.81492255796106328, 64.16775706135234714 ) ) ;
#31020 = CARTESIAN_POINT ( 'NONE',  ( -10.72451020669870658, -18.67979575497194134, 54.58442372801901143 ) ) ;
#31021 = ORIENTED_EDGE ( 'NONE', *, *, #105010, .F. ) ;
#31022 = CARTESIAN_POINT ( 'NONE',  ( -0.05219959533909027116, -19.03943276465977164, 62.49890960531435979 ) ) ;
#31023 = CARTESIAN_POINT ( 'NONE',  ( -21.52544592524334988, -5.823673210054445271, 33.95942372801901143 ) ) ;
#31024 = CARTESIAN_POINT ( 'NONE',  ( 4.379528057220339221, -16.55341960407611168, 107.7072429386476955 ) ) ;
#31025 = CARTESIAN_POINT ( 'NONE',  ( -19.03943276465977164, 0.05219959533909376836, 31.24890960531435979 ) ) ;
#31026 = CARTESIAN_POINT ( 'NONE',  ( -8.224510206698948167, 14.34966873604960824, 75.41557627198102409 ) ) ;
#31027 = CARTESIAN_POINT ( 'NONE',  ( 9.474510206698971260, -16.51473224551069308, 72.91557627198102409 ) ) ;
#31028 = CARTESIAN_POINT ( 'NONE',  ( -16.53943276465976808, 0.05219959533911058130, 31.24890960531435979 ) ) ;
#31029 = CARTESIAN_POINT ( 'NONE',  ( -5.823673210054116645, -21.52544592524344225, 52.29057627198102409 ) ) ;
#31030 = CARTESIAN_POINT ( 'NONE',  ( -8.314922557960811034, -14.29746914071050412, 92.08224293864769550 ) ) ;
#31031 = AXIS2_PLACEMENT_3D ( 'NONE', #198438, #165127, #58921 ) ;
#31032 = CARTESIAN_POINT ( 'NONE',  ( 5.823673210054125526, 21.52544592524343514, 94.79057627198105251 ) ) ;
#31033 = CARTESIAN_POINT ( 'NONE',  ( -9.564922557960796823, -16.46253265017161027, 102.0822429386477097 ) ) ;
#31035 = CARTESIAN_POINT ( 'NONE',  ( -9.474510206698720793, -16.51473224551083518, 104.5844237280190043 ) ) ;
#31034 = CARTESIAN_POINT ( 'NONE',  ( 5.049401038298161559, -19.05341960407611168, 57.70724293864769550 ) ) ;
#31036 = CARTESIAN_POINT ( 'NONE',  ( 5.823673210054125526, 21.52544592524343514, 59.79057627198103120 ) ) ;
#31037 = CARTESIAN_POINT ( 'NONE',  ( 10.81492255796106328, -18.62759615963255655, 80.41775706135234714 ) ) ;
#31038 = CARTESIAN_POINT ( 'NONE',  ( -19.02544592524342804, 5.153800228976336051, 71.04057627198099567 ) ) ;
#31039 = CARTESIAN_POINT ( 'NONE',  ( 19.02544592524343514, -5.153800228976328945, 98.54057627198100988 ) ) ;
#31040 = CARTESIAN_POINT ( 'NONE',  ( 14.29746914071037800, 8.314922557961029526, 76.66775706135234714 ) ) ;
#31041 = CARTESIAN_POINT ( 'NONE',  ( 21.55341960407619695, -5.719274019375665929, 56.04275706135235424 ) ) ;
#31042 = CARTESIAN_POINT ( 'NONE',  ( 21.55341960407619695, -5.719274019375665929, 81.04275706135236135 ) ) ;
#31043 = CARTESIAN_POINT ( 'NONE',  ( -15.80617190586745835, -15.72974639402198527, 111.8739096053143669 ) ) ;
#31044 = CARTESIAN_POINT ( 'NONE',  ( 12.06949235617739724, 12.14591786802326823, 81.87609039468568994 ) ) ;
#31045 = CARTESIAN_POINT ( 'NONE',  ( 18.67979575497178502, 10.72451020669898547, 74.16557627198102409 ) ) ;
#31046 = CARTESIAN_POINT ( 'NONE',  ( 9.564922557961047289, -16.46253265017146816, 40.41775706135234003 ) ) ;
#31047 = CARTESIAN_POINT ( 'NONE',  ( -15.72974639402197994, 15.80617190586746368, 40.62390960531435269 ) ) ;
#31049 = CARTESIAN_POINT ( 'NONE',  ( 4.379528057220092307, 16.55341960407617563, 112.2927570613523471 ) ) ;
#31048 = CARTESIAN_POINT ( 'NONE',  ( -9.564922557960796823, -16.46253265017161027, 82.08224293864768129 ) ) ;
#31050 = CARTESIAN_POINT ( 'NONE',  ( -17.31747979337949772, 6.344076630960997498, 63.62055131934819485 ) ) ;
#31051 = CARTESIAN_POINT ( 'NONE',  ( -16.46253265017160317, 9.564922557960807481, 115.8322429386477097 ) ) ;
#31052 = DIRECTION ( 'NONE',  ( 0.000000000000000000, 0.000000000000000000, 1.000000000000000000 ) ) ;
#31053 = EDGE_CURVE ( 'NONE', #182127, #147958, #17665, .T. ) ;
#31054 = CARTESIAN_POINT ( 'NONE',  ( 0.05219959533936267826, -19.03943276465977164, 95.00109039468567573 ) ) ;
#31055 = CARTESIAN_POINT ( 'NONE',  ( -0.05219959533907301413, -21.53943276465977519, 72.49890960531435269 ) ) ;
#31056 = CARTESIAN_POINT ( 'NONE',  ( -8.314922557960811034, -14.29746914071050412, 47.08224293864770260 ) ) ;
#31057 = CARTESIAN_POINT ( 'NONE',  ( 16.52544592524335698, 4.483927247898782831, 21.45942372801901499 ) ) ;
#31058 = CARTESIAN_POINT ( 'NONE',  ( -13.89961937509977652, 13.97604488694528158, 25.62390960531434558 ) ) ;
#31059 = CARTESIAN_POINT ( 'NONE',  ( -5.049401038297874678, -19.05341960407617918, 104.7927570613523471 ) ) ;
#31061 = CARTESIAN_POINT ( 'NONE',  ( 13.89961937509957401, 13.97604488694547697, 76.87609039468566152 ) ) ;
#31060 = CARTESIAN_POINT ( 'NONE',  ( 5.719274019375991003, -21.55341960407610458, 102.7072429386476955 ) ) ;
#31062 = CARTESIAN_POINT ( 'NONE',  ( 14.34966873604972726, -8.224510206698740333, 80.83442372801901854 ) ) ;
#31063 = CARTESIAN_POINT ( 'NONE',  ( 16.51473224551069308, 9.474510206698969483, 79.16557627198103830 ) ) ;
#31064 = CARTESIAN_POINT ( 'NONE',  ( -4.483927247898539470, -16.52544592524342804, 72.29057627198102409 ) ) ;
#31065 = CARTESIAN_POINT ( 'NONE',  ( 19.02544592524343514, -5.153800228976328945, 58.54057627198102409 ) ) ;
#31066 = CARTESIAN_POINT ( 'NONE',  ( -4.379528057220328563, 16.55341960407611168, 70.20724293864769550 ) ) ;
#31067 = CARTESIAN_POINT ( 'NONE',  ( 13.97604488694527802, 13.89961937509977652, 39.37390960531435269 ) ) ;
#31068 = CARTESIAN_POINT ( 'NONE',  ( -36.80065496640119704, -5.465942522010068139, 45.70922642070194541 ) ) ;
#31069 = CARTESIAN_POINT ( 'NONE',  ( 16.52544592524342804, -4.483927247898539470, 38.54057627198103120 ) ) ;
#31070 = CARTESIAN_POINT ( 'NONE',  ( 5.153800228976335163, 19.02544592524342804, 74.79057627198103830 ) ) ;
#31071 = CARTESIAN_POINT ( 'NONE',  ( -1.211883243535121890, -16.08916976210839067, -59.40465844715060229 ) ) ;
#31072 = CARTESIAN_POINT ( 'NONE',  ( -9.564922557961040184, 16.46253265017147172, 52.91775706135233293 ) ) ;
#31073 = CARTESIAN_POINT ( 'NONE',  ( -0.05219959533934338120, 16.53943276465976808, 62.50109039468568284 ) ) ;
#31074 = VECTOR ( 'NONE', #167212, 1000.000000000000000 ) ;
#31075 = CARTESIAN_POINT ( 'NONE',  ( -21.52544592524343514, 5.823673210054127303, 61.04057627198103120 ) ) ;
#31076 = CARTESIAN_POINT ( 'NONE',  ( -5.049401038297874678, -19.05341960407617918, 29.79275706135232227 ) ) ;
#31077 = CARTESIAN_POINT ( 'NONE',  ( -9.474510206698964154, 16.51473224551069663, 85.41557627198102409 ) ) ;
#31078 = CARTESIAN_POINT ( 'NONE',  ( -20.88951479300308733, -22.87381821414430405, -47.01046684957792365 ) ) ;
#31079 = CARTESIAN_POINT ( 'NONE',  ( 10.72451020669898902, -18.67979575497178502, 27.91557627198103830 ) ) ;
#31080 = CARTESIAN_POINT ( 'NONE',  ( -19.02544592524342804, 5.153800228976336051, 66.04057627198103830 ) ) ;
#31081 = CARTESIAN_POINT ( 'NONE',  ( 10.72451020669871369, 18.67979575497193778, 52.08442372801901854 ) ) ;
#31082 = CARTESIAN_POINT ( 'NONE',  ( 4.483927247898545687, 16.52544592524342804, 109.7905762719810383 ) ) ;
#31085 = ORIENTED_EDGE ( 'NONE', *, *, #135350, .F. ) ;
#31084 = CARTESIAN_POINT ( 'NONE',  ( -5.049401038298153566, 19.05341960407611168, 95.20724293864770971 ) ) ;
#31083 = CARTESIAN_POINT ( 'NONE',  ( -21.52544592524343514, 5.823673210054127303, 101.0405762719810383 ) ) ;
#31086 = CARTESIAN_POINT ( 'NONE',  ( 18.67979575497194134, -10.72451020669871369, 45.83442372801901854 ) ) ;
#31087 = VERTEX_POINT ( 'NONE', #88120 ) ;
#31088 = CARTESIAN_POINT ( 'NONE',  ( -13.97604488694527625, -13.89961937509977652, 101.8739096053143811 ) ) ;
#31089 = CARTESIAN_POINT ( 'NONE',  ( 17.59860650958989936, 7.585241751807028088, 89.07662985737509587 ) ) ;
#31090 = CARTESIAN_POINT ( 'NONE',  ( 15.80617190586746368, 15.72974639402197994, 94.37390960531436690 ) ) ;
#31091 = CARTESIAN_POINT ( 'NONE',  ( -9.564922557960796823, -16.46253265017161027, 52.08224293864768839 ) ) ;
#31092 = CARTESIAN_POINT ( 'NONE',  ( -12.14591786802326823, 12.06949235617739902, 23.12609039468567573 ) ) ;
#31093 = CARTESIAN_POINT ( 'NONE',  ( -29.86685920354755552, 21.69954338932564397, -5.324999997268814234 ) ) ;
#31094 = CARTESIAN_POINT ( 'NONE',  ( 0.05219959533909260263, 19.03943276465977164, 34.99890960531435979 ) ) ;
#31095 = CARTESIAN_POINT ( 'NONE',  ( 5.719274019375673035, 21.55341960407619339, 102.2927570613523613 ) ) ;
#31097 = CARTESIAN_POINT ( 'NONE',  ( 15.80617190586769283, -15.72974639402175789, 45.62609039468567573 ) ) ;
#31096 = CARTESIAN_POINT ( 'NONE',  ( 19.02544592524343514, -5.153800228976328945, 78.54057627198099567 ) ) ;
#31098 = CARTESIAN_POINT ( 'NONE',  ( 10.81492255796106328, -18.62759615963255655, 25.41775706135235779 ) ) ;
#31099 = CARTESIAN_POINT ( 'NONE',  ( -22.44159573604009950, -16.30477369853688430, 145.5750000027311728 ) ) ;
#31100 = CARTESIAN_POINT ( 'NONE',  ( -16.51473224551069308, -9.474510206698971260, 96.66557627198102409 ) ) ;
#31101 = CARTESIAN_POINT ( 'NONE',  ( 17.07321893155272363, 22.25586454244016110, 139.9999999999999432 ) ) ;
#31104 = CARTESIAN_POINT ( 'NONE',  ( 18.67979575497194134, -10.72451020669871369, 60.83442372801901854 ) ) ;
#31103 = CARTESIAN_POINT ( 'NONE',  ( -16.52544592524335698, -4.483927247898792601, 73.95942372801901854 ) ) ;
#31102 = CARTESIAN_POINT ( 'NONE',  ( -0.05219959533934338120, 16.53943276465976808, 37.50109039468568284 ) ) ;
#31105 = CARTESIAN_POINT ( 'NONE',  ( 15.72974639402176855, 15.80617190586768217, 81.87609039468568994 ) ) ;
#31106 = DIRECTION ( 'NONE',  ( 0.000000000000000000, 0.000000000000000000, -1.000000000000000000 ) ) ;
#31107 = CARTESIAN_POINT ( 'NONE',  ( -5.153800228976607833, 19.02544592524334988, 112.7094237280190043 ) ) ;
#31108 = CARTESIAN_POINT ( 'NONE',  ( -9.564922557960796823, -16.46253265017161027, 77.08224293864769550 ) ) ;
#31109 = CARTESIAN_POINT ( 'NONE',  ( -16.51473224551069308, -9.474510206698971260, 101.6655762719810241 ) ) ;
#31110 = CARTESIAN_POINT ( 'NONE',  ( 16.55341960407611168, 4.379528057220329451, 103.9572429386476813 ) ) ;
#31111 = CARTESIAN_POINT ( 'NONE',  ( 16.52544592524342804, -4.483927247898539470, 108.5405762719810241 ) ) ;
#31112 = CARTESIAN_POINT ( 'NONE',  ( 5.719274019375991003, -21.55341960407610458, 27.70724293864769905 ) ) ;
#31113 = CARTESIAN_POINT ( 'NONE',  ( 4.483927247898790824, -16.52544592524335698, 80.20942372801901854 ) ) ;
#31115 = CARTESIAN_POINT ( 'NONE',  ( -19.02544592524342804, 5.153800228976336051, 61.04057627198103120 ) ) ;
#31114 = CARTESIAN_POINT ( 'NONE',  ( 16.53943276465976808, -0.05219959533910856209, 68.74890960531435269 ) ) ;
#31116 = CARTESIAN_POINT ( 'NONE',  ( -21.52544592524334988, -5.823673210054445271, 78.95942372801901854 ) ) ;
#31117 = CARTESIAN_POINT ( 'NONE',  ( -24.30000000000003268, 2.668083032619853614E-13, -56.77278709839600879 ) ) ;
#31118 = CARTESIAN_POINT ( 'NONE',  ( 9.474510206698729675, 16.51473224551082808, 112.0844237280190043 ) ) ;
#31119 = CARTESIAN_POINT ( 'NONE',  ( 14.29746914071049879, -8.314922557960816363, 73.33224293864769550 ) ) ;
#31120 = CARTESIAN_POINT ( 'NONE',  ( 5.823673210054444382, -21.52544592524334988, 25.20942372801901854 ) ) ;
#31121 = CARTESIAN_POINT ( 'NONE',  ( 18.67979575497178502, 10.72451020669898547, 64.16557627198102409 ) ) ;
#31122 = DIRECTION ( 'NONE',  ( -0.000000000000000000, -0.6427876096865403621, -0.7660444431189770143 ) ) ;
#31123 = CARTESIAN_POINT ( 'NONE',  ( -28.82186960331499392, -9.364793116373526516, 144.3500000054623627 ) ) ;
#31124 = CARTESIAN_POINT ( 'NONE',  ( -16.46253265017160317, 9.564922557960807481, 75.83224293864769550 ) ) ;
#31125 = CARTESIAN_POINT ( 'NONE',  ( -14.34966873604960291, -8.224510206698953496, 46.66557627198102409 ) ) ;
#31126 = CARTESIAN_POINT ( 'NONE',  ( -14.34966873604960291, -8.224510206698953496, 26.66557627198103475 ) ) ;
#31127 = CARTESIAN_POINT ( 'NONE',  ( 16.52544592524335698, 4.483927247898782831, 91.45942372801901854 ) ) ;
#31128 = CARTESIAN_POINT ( 'NONE',  ( -13.97604488694547697, 13.89961937509957934, 58.12609039468566863 ) ) ;
#31129 = CARTESIAN_POINT ( 'NONE',  ( 17.50000000000001421, 5.622605283950889543, 48.81207310596114013 ) ) ;
#31130 = CARTESIAN_POINT ( 'NONE',  ( -19.02544592524342804, 5.153800228976336051, 111.0405762719810099 ) ) ;
#31131 = EDGE_CURVE ( 'NONE', #59793, #74699, #44625, .T. ) ;
#31132 = CARTESIAN_POINT ( 'NONE',  ( -14.34966873604960291, -8.224510206698953496, 71.66557627198100988 ) ) ;
#31133 = CARTESIAN_POINT ( 'NONE',  ( -9.474510206698720793, -16.51473224551083518, 44.58442372801900433 ) ) ;
#31135 = CARTESIAN_POINT ( 'NONE',  ( -5.823673210054116645, -21.52544592524344225, 37.29057627198102409 ) ) ;
#31134 = CARTESIAN_POINT ( 'NONE',  ( -5.049401038298153566, 19.05341960407611168, 30.20724293864768839 ) ) ;
#31137 = ORIENTED_EDGE ( 'NONE', *, *, #28343, .T. ) ;
#31136 = CARTESIAN_POINT ( 'NONE',  ( 21.52544592524344225, -5.823673210054117533, 48.54057627198103120 ) ) ;
#31138 = CARTESIAN_POINT ( 'NONE',  ( -4.379528057220328563, 16.55341960407611168, 105.2072429386477097 ) ) ;
#31139 = CARTESIAN_POINT ( 'NONE',  ( 14.29746914071037800, 8.314922557961029526, 46.66775706135234714 ) ) ;
#31140 = CARTESIAN_POINT ( 'NONE',  ( -12.06949235617756955, 12.14591786802309770, 95.62390960531436690 ) ) ;
#31141 = CARTESIAN_POINT ( 'NONE',  ( 16.21995358207306026, -7.366697692864082825, 37.43551001512158649 ) ) ;
#31142 = CARTESIAN_POINT ( 'NONE',  ( -29.86685920354755552, 21.69954338932564397, -9.324999997268813345 ) ) ;
#31143 = CARTESIAN_POINT ( 'NONE',  ( -21.55341960407610458, -5.719274019375992779, 36.45724293864768839 ) ) ;
#31144 = CARTESIAN_POINT ( 'NONE',  ( 18.22780087662123805, -5.499999999999976019, 78.51763182126894947 ) ) ;
#31145 = CARTESIAN_POINT ( 'NONE',  ( -37.99626262588769521, -12.34573411038907764, -7.647842220587804718 ) ) ;
#31147 = CARTESIAN_POINT ( 'NONE',  ( 16.55341960407611168, 4.379528057220329451, 28.95724293864769905 ) ) ;
#31146 = CARTESIAN_POINT ( 'NONE',  ( 14.29746914071037800, 8.314922557961029526, 36.66775706135234714 ) ) ;
#31148 = CARTESIAN_POINT ( 'NONE',  ( -21.55341960407610458, -5.719274019375992779, 56.45724293864768839 ) ) ;
#31149 = CARTESIAN_POINT ( 'NONE',  ( -19.03943276465977164, -0.05219959533935918106, 78.75109039468567573 ) ) ;
#31150 = CARTESIAN_POINT ( 'NONE',  ( 21.52544592524344225, -5.823673210054117533, 68.54057627198103830 ) ) ;
#31151 = CARTESIAN_POINT ( 'NONE',  ( 21.55341960407619695, -5.719274019375665929, 81.04275706135236135 ) ) ;
#31152 = CARTESIAN_POINT ( 'NONE',  ( 2.500000000000000000, 2.357898499370431722, -2.818925648462311528E-15 ) ) ;
#31153 = CARTESIAN_POINT ( 'NONE',  ( -8.314922557961024197, 14.29746914071037800, 42.91775706135235424 ) ) ;
#31155 = CARTESIAN_POINT ( 'NONE',  ( -9.564922557960796823, -16.46253265017161027, 102.0822429386477097 ) ) ;
#31154 = CARTESIAN_POINT ( 'NONE',  ( 16.51473224551069308, 9.474510206698969483, 34.16557627198102409 ) ) ;
#31156 = CARTESIAN_POINT ( 'NONE',  ( -9.564922557960796823, -16.46253265017161027, 32.08224293864769550 ) ) ;
#31157 = CARTESIAN_POINT ( 'NONE',  ( 14.29746914071049879, -8.314922557960816363, 103.3322429386476955 ) ) ;
#31158 = CARTESIAN_POINT ( 'NONE',  ( -16.46253265017160317, 9.564922557960807481, 110.8322429386476955 ) ) ;
#31159 = EDGE_LOOP ( 'NONE', ( #100520, #49126, #110587, #197677 ) ) ;
#31160 = CARTESIAN_POINT ( 'NONE',  ( 16.52544592524335698, 4.483927247898782831, 71.45942372801901854 ) ) ;
#31161 = CARTESIAN_POINT ( 'NONE',  ( -15.72974639402197994, 15.80617190586746368, 85.62390960531436690 ) ) ;
#31162 = CARTESIAN_POINT ( 'NONE',  ( 5.153800228976335163, 19.02544592524342804, 54.79057627198103120 ) ) ;
#31163 = CARTESIAN_POINT ( 'NONE',  ( -21.55341960407619339, 5.719274019375674811, 23.54275706135235424 ) ) ;
#31164 = CARTESIAN_POINT ( 'NONE',  ( 9.564922557960805705, 16.46253265017160317, 84.58224293864769550 ) ) ;
#31165 = DIRECTION ( 'NONE',  ( 0.000000000000000000, 0.000000000000000000, 1.000000000000000000 ) ) ;
#31166 = ORIENTED_EDGE ( 'NONE', *, *, #95942, .T. ) ;
#31167 = CARTESIAN_POINT ( 'NONE',  ( -5.719274019375978568, 21.55341960407610458, 115.2072429386476955 ) ) ;
#31170 = CARTESIAN_POINT ( 'NONE',  ( -13.97604488694547697, 13.89961937509957934, 73.12609039468568994 ) ) ;
#31169 = CARTESIAN_POINT ( 'NONE',  ( 19.03943276465977164, -0.05219959533909143690, 108.7489096053143527 ) ) ;
#31168 = CARTESIAN_POINT ( 'NONE',  ( -16.51473224551069308, -9.474510206698971260, 31.66557627198102054 ) ) ;
#31171 = CARTESIAN_POINT ( 'NONE',  ( -9.474510206698720793, -16.51473224551083518, 24.58442372801900078 ) ) ;
#31172 = CARTESIAN_POINT ( 'NONE',  ( -21.55341960407610458, -5.719274019375992779, 96.45724293864770971 ) ) ;
#31173 = CARTESIAN_POINT ( 'NONE',  ( 19.02544592524334988, 5.153800228976608722, 36.45942372801900433 ) ) ;
#31174 = CARTESIAN_POINT ( 'NONE',  ( -16.55341960407617563, 4.379528057220093196, 83.54275706135234714 ) ) ;
#31175 = CARTESIAN_POINT ( 'NONE',  ( -5.049401038298153566, 19.05341960407611168, 110.2072429386476671 ) ) ;
#31176 = CARTESIAN_POINT ( 'NONE',  ( -9.474510206698964154, 16.51473224551069663, 65.41557627198102409 ) ) ;
#31177 = CARTESIAN_POINT ( 'NONE',  ( 5.823673210054444382, -21.52544592524334988, 60.20942372801902565 ) ) ;
#31178 = CARTESIAN_POINT ( 'NONE',  ( -5.823673210054431948, 21.52544592524334988, 77.70942372801900433 ) ) ;
#31179 = CARTESIAN_POINT ( 'NONE',  ( 13.97604488694527802, 13.89961937509977652, 69.37390960531436690 ) ) ;
#31180 = CARTESIAN_POINT ( 'NONE',  ( -5.823673210054431948, 21.52544592524334988, 42.70942372801901854 ) ) ;
#31181 = CARTESIAN_POINT ( 'NONE',  ( 0.05219959533936267826, -19.03943276465977164, 85.00109039468567573 ) ) ;
#31182 = CARTESIAN_POINT ( 'NONE',  ( 19.02544592524343514, -5.153800228976328945, 48.54057627198103120 ) ) ;
#31183 = CARTESIAN_POINT ( 'NONE',  ( 5.049401038298161559, -19.05341960407611168, 92.70724293864769550 ) ) ;
#31184 = CARTESIAN_POINT ( 'NONE',  ( 9.564922557960805705, 16.46253265017160317, 69.58224293864770971 ) ) ;
#31185 = CARTESIAN_POINT ( 'NONE',  ( 9.564922557960805705, 16.46253265017160317, 54.58224293864769550 ) ) ;
#31186 = CARTESIAN_POINT ( 'NONE',  ( 18.67979575497178502, 10.72451020669898547, 104.1655762719810241 ) ) ;
#31187 = CARTESIAN_POINT ( 'NONE',  ( -8.314922557961024197, 14.29746914071037800, 87.91775706135234714 ) ) ;
#31188 = CARTESIAN_POINT ( 'NONE',  ( -21.96844466259092243, 7.174710485416647465, 170.3366942299255413 ) ) ;
#31189 = CARTESIAN_POINT ( 'NONE',  ( -16.46253265017146816, -9.564922557961047289, 39.16775706135234003 ) ) ;
#31190 = CARTESIAN_POINT ( 'NONE',  ( 16.46253265017160672, -9.564922557960803928, 63.33224293864769550 ) ) ;
#31191 = CARTESIAN_POINT ( 'NONE',  ( 14.29746914071049879, -8.314922557960816363, 53.33224293864769550 ) ) ;
#31192 = CARTESIAN_POINT ( 'NONE',  ( -4.483927247898539470, -16.52544592524342804, 97.29057627198105251 ) ) ;
#31193 = CARTESIAN_POINT ( 'NONE',  ( -13.89961937509977652, 13.97604488694528158, 110.6239096053143243 ) ) ;
#31194 = B_SPLINE_CURVE_WITH_KNOTS ( 'NONE', 3,
 ( #137251, #32071, #92725, #46239, #62385, #75575, #30079, #94721, #154414, #31078, #140225, #185754, #107893, #198937, #138249, #168581, #126062, #199933, #63394, #110887 ),
 .UNSPECIFIED., .F., .F.,
 ( 4, 2, 2, 2, 2, 2, 2, 2, 2, 4 ),
 ( 0.001320702335622901420, 0.001953861884282702497, 0.002587021432942503141, 0.003220180981602304218, 0.003853340530262105296, 0.004486500078921906373, 0.005119659627581707451, 0.005752819176241508528, 0.006069398950571413404, 0.006385978724901320014 ),
 .UNSPECIFIED. ) ;
#31195 = CARTESIAN_POINT ( 'NONE',  ( 19.03943276465977164, -0.05219959533909143690, 88.74890960531436690 ) ) ;
#31196 = CARTESIAN_POINT ( 'NONE',  ( -9.474510206698964154, 16.51473224551069663, 100.4155762719810241 ) ) ;
#31197 = CARTESIAN_POINT ( 'NONE',  ( 19.05341960407617918, -5.049401038297876454, 21.04275706135232582 ) ) ;
#31198 = CARTESIAN_POINT ( 'NONE',  ( 4.379528057220092307, 16.55341960407617563, 97.29275706135234714 ) ) ;
#31199 = CARTESIAN_POINT ( 'NONE',  ( -9.564922557960796823, -16.46253265017161027, 77.08224293864769550 ) ) ;
#31200 = CARTESIAN_POINT ( 'NONE',  ( 21.52544592524334988, 5.823673210054432836, 41.45942372801901143 ) ) ;
#31201 = CARTESIAN_POINT ( 'NONE',  ( -15.72974639402197994, 15.80617190586746368, 25.62390960531435624 ) ) ;
#31202 = CARTESIAN_POINT ( 'NONE',  ( -18.62759615963270932, 10.81492255796079327, 115.8322429386477097 ) ) ;
#31203 = CARTESIAN_POINT ( 'NONE',  ( 8.224510206698953496, -14.34966873604960469, 62.91557627198102409 ) ) ;
#31204 = CARTESIAN_POINT ( 'NONE',  ( 13.97604488694527802, 13.89961937509977652, 59.37390960531434558 ) ) ;
#31205 = CARTESIAN_POINT ( 'NONE',  ( 14.34966873604960469, 8.224510206698951720, 84.16557627198103830 ) ) ;
#31206 = CARTESIAN_POINT ( 'NONE',  ( 9.564922557961047289, -16.46253265017146816, 45.41775706135232582 ) ) ;
#31207 = CARTESIAN_POINT ( 'NONE',  ( 12.06949235617757843, -12.14591786802309237, 113.1239096053143953 ) ) ;
#31208 = CARTESIAN_POINT ( 'NONE',  ( 16.51473224551069308, 9.474510206698969483, 84.16557627198102409 ) ) ;
#31209 = CARTESIAN_POINT ( 'NONE',  ( -19.03943276465977164, 0.05219959533909376836, 86.24890960531436690 ) ) ;
#31210 = CARTESIAN_POINT ( 'NONE',  ( -27.73933785331498925, 9.013057229001088189, 140.7750000027311899 ) ) ;
#31211 = CARTESIAN_POINT ( 'NONE',  ( -16.55341960407611168, -4.379528057220339221, 101.4572429386476955 ) ) ;
#31212 = ORIENTED_EDGE ( 'NONE', *, *, #27827, .T. ) ;
#31213 = CARTESIAN_POINT ( 'NONE',  ( 16.52544592524335698, 4.483927247898782831, 101.4594237280190185 ) ) ;
#31214 = CARTESIAN_POINT ( 'NONE',  ( 8.314922557961029526, -14.29746914071037800, 30.41775706135234358 ) ) ;
#31215 = CARTESIAN_POINT ( 'NONE',  ( 21.55341960407619695, -5.719274019375665929, 96.04275706135236135 ) ) ;
#31216 = CARTESIAN_POINT ( 'NONE',  ( 5.153800228976335163, 19.02544592524342804, 84.79057627198099567 ) ) ;
#31217 = CARTESIAN_POINT ( 'NONE',  ( 21.53943276465977519, 0.05219959533937863772, 21.25109039468567218 ) ) ;
#31218 = CARTESIAN_POINT ( 'NONE',  ( 5.153800228976335163, 19.02544592524342804, 24.79057627198102765 ) ) ;
#31219 = VECTOR ( 'NONE', #15448, 1000.000000000000000 ) ;
#31220 = CARTESIAN_POINT ( 'NONE',  ( -12.14591786802326823, 12.06949235617739902, 33.12609039468569705 ) ) ;
#31221 = CARTESIAN_POINT ( 'NONE',  ( 9.564922557961047289, -16.46253265017146816, 95.41775706135233293 ) ) ;
#31222 = EDGE_CURVE ( 'NONE', #176653, #179099, #110244, .T. ) ;
#31223 = CARTESIAN_POINT ( 'NONE',  ( -21.52544592524343514, 5.823673210054127303, 96.04057627198102409 ) ) ;
#31224 = CARTESIAN_POINT ( 'NONE',  ( -5.049401038297874678, -19.05341960407617918, 64.79275706135233293 ) ) ;
#31225 = CARTESIAN_POINT ( 'NONE',  ( -19.03943276465977164, 0.05219959533909376836, 21.24890960531436335 ) ) ;
#31226 = CARTESIAN_POINT ( 'NONE',  ( 0.05219959533937995610, -21.53943276465977519, 20.00109039468568639 ) ) ;
#31227 = CARTESIAN_POINT ( 'NONE',  ( 37.99626262588765258, 2.893932880411085066E-14, -4.747842220587804363 ) ) ;
#31228 = CARTESIAN_POINT ( 'NONE',  ( 19.03943276465977164, -0.05219959533909143690, 93.74890960531435269 ) ) ;
#31229 = CARTESIAN_POINT ( 'NONE',  ( 4.379528057220092307, 16.55341960407617563, 42.29275706135235424 ) ) ;
#31230 = CARTESIAN_POINT ( 'NONE',  ( -17.60728821187777271, 5.499999999999950262, 100.8669092774361076 ) ) ;
#31231 = CARTESIAN_POINT ( 'NONE',  ( -9.474510206698720793, -16.51473224551083518, 54.58442372801899722 ) ) ;
#31233 = CARTESIAN_POINT ( 'NONE',  ( -14.29746914071049879, 8.314922557960819915, 80.83224293864769550 ) ) ;
#31232 = CARTESIAN_POINT ( 'NONE',  ( 10.81492255796106328, -18.62759615963255655, 25.41775706135235779 ) ) ;
#31234 = CARTESIAN_POINT ( 'NONE',  ( 9.564922557960805705, 16.46253265017160317, 84.58224293864769550 ) ) ;
#31236 = CARTESIAN_POINT ( 'NONE',  ( 9.474510206698729675, 16.51473224551082808, 62.08442372801899722 ) ) ;
#31235 = CARTESIAN_POINT ( 'NONE',  ( -4.483927247898782831, 16.52544592524335698, 57.70942372801901143 ) ) ;
#31237 = CARTESIAN_POINT ( 'NONE',  ( 5.719274019375673035, 21.55341960407619339, 72.29275706135236135 ) ) ;
#31238 = CARTESIAN_POINT ( 'NONE',  ( 12.14591786802327356, -12.06949235617739191, 30.62609039468567929 ) ) ;
#31239 = CARTESIAN_POINT ( 'NONE',  ( 9.564922557960805705, 16.46253265017160317, 74.58224293864769550 ) ) ;
#31240 = CARTESIAN_POINT ( 'NONE',  ( 5.049401038297881783, 19.05341960407617563, 87.29275706135234714 ) ) ;
#31241 = CARTESIAN_POINT ( 'NONE',  ( 12.14591786802327356, -12.06949235617739191, 60.62609039468567573 ) ) ;
#31242 = CARTESIAN_POINT ( 'NONE',  ( -18.67979575497193778, 10.72451020669871902, 103.3344237280190043 ) ) ;
#31243 = CARTESIAN_POINT ( 'NONE',  ( -16.46253265017146816, -9.564922557961047289, 79.16775706135234714 ) ) ;
#31244 = CARTESIAN_POINT ( 'NONE',  ( -9.564922557960796823, -16.46253265017161027, 52.08224293864768839 ) ) ;
#31245 = CARTESIAN_POINT ( 'NONE',  ( 21.52544592524344225, -5.823673210054117533, 73.54057627198102409 ) ) ;
#31247 = CARTESIAN_POINT ( 'NONE',  ( 9.564922557961047289, -16.46253265017146816, 75.41775706135234714 ) ) ;
#31246 = CARTESIAN_POINT ( 'NONE',  ( -16.55341960407611168, -4.379528057220339221, 71.45724293864769550 ) ) ;
#31248 = CARTESIAN_POINT ( 'NONE',  ( 16.52216118717208815, -7.221426719304427699, 61.42400978953011759 ) ) ;
#31249 = CARTESIAN_POINT ( 'NONE',  ( 13.97604488694548053, -13.89961937509957401, 45.62609039468566863 ) ) ;
#31250 = CARTESIAN_POINT ( 'NONE',  ( -16.55341960407617563, 4.379528057220093196, 108.5427570613523756 ) ) ;
#31251 = CARTESIAN_POINT ( 'NONE',  ( 14.34966873604960469, 8.224510206698951720, 69.16557627198102409 ) ) ;
#31253 = CARTESIAN_POINT ( 'NONE',  ( -22.44159573604010305, 16.30477369853692338, 142.6750000027311671 ) ) ;
#31252 = CARTESIAN_POINT ( 'NONE',  ( 5.719274019375673035, 21.55341960407619339, 102.2927570613523613 ) ) ;
#31254 = CARTESIAN_POINT ( 'NONE',  ( 15.80617190586746368, 15.72974639402197994, 104.3739096053143669 ) ) ;
#31255 = CARTESIAN_POINT ( 'NONE',  ( 0.05219959533909260263, 19.03943276465977164, 64.99890960531436690 ) ) ;
#31256 = CARTESIAN_POINT ( 'NONE',  ( -5.823673210054431948, 21.52544592524334988, 82.70942372801900433 ) ) ;
#31257 = CARTESIAN_POINT ( 'NONE',  ( 16.46253265017160672, -9.564922557960803928, 53.33224293864768839 ) ) ;
#31258 = CARTESIAN_POINT ( 'NONE',  ( -16.46253265017160317, 9.564922557960807481, 30.83224293864769550 ) ) ;
#31259 = CARTESIAN_POINT ( 'NONE',  ( -9.474510206698964154, 16.51473224551069663, 115.4155762719810241 ) ) ;
#31260 = CARTESIAN_POINT ( 'NONE',  ( 16.52544592524342804, -4.483927247898539470, 73.54057627198102409 ) ) ;
#31261 = CARTESIAN_POINT ( 'NONE',  ( -13.97604488694527625, -13.89961937509977652, 26.87390960531434558 ) ) ;
#31262 = CARTESIAN_POINT ( 'NONE',  ( -0.05219959533910754901, -16.53943276465976808, 87.49890960531436690 ) ) ;
#31263 = ADVANCED_FACE ( 'NONE', ( #64745 ), #186116, .F. ) ;
#31264 = CARTESIAN_POINT ( 'NONE',  ( 21.53943276465977519, -0.05219959533907433946, 98.74890960531438111 ) ) ;
#31265 = CARTESIAN_POINT ( 'NONE',  ( 21.52544592524334988, 5.823673210054432836, 51.45942372801901854 ) ) ;
#31266 = CARTESIAN_POINT ( 'NONE',  ( 27.96892006433830247, -7.184979517970438323, 161.0508495487522680 ) ) ;
#31267 = CARTESIAN_POINT ( 'NONE',  ( -12.06949235617739369, -12.14591786802326823, 49.37609039468569705 ) ) ;
#31268 = CARTESIAN_POINT ( 'NONE',  ( -5.719274019375978568, 21.55341960407610458, 95.20724293864769550 ) ) ;
#31269 = CARTESIAN_POINT ( 'NONE',  ( -16.46253265017146816, -9.564922557961047289, 24.16775706135233648 ) ) ;
#31270 = CARTESIAN_POINT ( 'NONE',  ( -13.89961937509977652, 13.97604488694528158, 100.6239096053143669 ) ) ;
#31271 = CARTESIAN_POINT ( 'NONE',  ( 10.81492255796106328, -18.62759615963255655, 40.41775706135234714 ) ) ;
#31272 = CARTESIAN_POINT ( 'NONE',  ( -21.52544592524343514, 5.823673210054127303, 46.04057627198103830 ) ) ;
#31273 = CARTESIAN_POINT ( 'NONE',  ( -8.314922557961024197, 14.29746914071037800, 112.9177570613523329 ) ) ;
#31275 = CARTESIAN_POINT ( 'NONE',  ( -5.719274019375665041, -21.55341960407619695, 99.79275706135234714 ) ) ;
#31274 = CARTESIAN_POINT ( 'NONE',  ( 0.05219959533937995610, -21.53943276465977519, 70.00109039468568994 ) ) ;
#31276 = CARTESIAN_POINT ( 'NONE',  ( 16.46253265017146816, 9.564922557961045513, 26.66775706135234003 ) ) ;
#31277 = CARTESIAN_POINT ( 'NONE',  ( -0.05219959533934338120, 16.53943276465976808, 82.50109039468568994 ) ) ;
#31278 = CARTESIAN_POINT ( 'NONE',  ( -15.80617190586768217, 15.72974639402176855, 53.12609039468568284 ) ) ;
#31279 = CARTESIAN_POINT ( 'NONE',  ( 19.02544592524343514, -5.153800228976328945, 43.54057627198103120 ) ) ;
#31280 = CARTESIAN_POINT ( 'NONE',  ( 9.564922557961047289, -16.46253265017146816, 25.41775706135234003 ) ) ;
#31281 = CARTESIAN_POINT ( 'NONE',  ( 21.55341960407610458, 5.719274019375980345, 28.95724293864769905 ) ) ;
#31282 = CARTESIAN_POINT ( 'NONE',  ( -5.823673210054431948, 21.52544592524334988, 22.70942372801901499 ) ) ;
#31283 = CARTESIAN_POINT ( 'NONE',  ( 5.719274019375991003, -21.55341960407610458, 72.70724293864769550 ) ) ;
#31284 = CARTESIAN_POINT ( 'NONE',  ( 16.55341960407618274, -4.379528057220086978, 46.04275706135234714 ) ) ;
#31286 = CARTESIAN_POINT ( 'NONE',  ( 10.81492255796078972, 18.62759615963270932, 79.58224293864769550 ) ) ;
#31285 = PLANE ( 'NONE',  #48341 ) ;
#31288 = CARTESIAN_POINT ( 'NONE',  ( -4.483927247898539470, -16.52544592524342804, 62.29057627198102409 ) ) ;
#31287 = CARTESIAN_POINT ( 'NONE',  ( 8.314922557961029526, -14.29746914071037800, 60.41775706135235424 ) ) ;
#31289 = CARTESIAN_POINT ( 'NONE',  ( 2.500000000000000000, 0.000000000000000000, 0.000000000000000000 ) ) ;
#31290 = CARTESIAN_POINT ( 'NONE',  ( -13.89961937509957401, -13.97604488694547875, 104.3760903946856757 ) ) ;
#31291 = CARTESIAN_POINT ( 'NONE',  ( 21.55341960407610458, 5.719274019375980345, 23.95724293864769550 ) ) ;
#31292 = CARTESIAN_POINT ( 'NONE',  ( -4.500000000000000888, -126.1226662136678272, 8.481152457036388981 ) ) ;
#31293 = CARTESIAN_POINT ( 'NONE',  ( -12.06949235617739369, -12.14591786802326823, 44.37609039468567573 ) ) ;
#31294 = CARTESIAN_POINT ( 'NONE',  ( 15.72974639402199770, -15.80617190586745480, 108.1239096053143811 ) ) ;
#31295 = CARTESIAN_POINT ( 'NONE',  ( -18.62759615963270932, 10.81492255796079327, 25.83224293864769194 ) ) ;
#31296 = CARTESIAN_POINT ( 'NONE',  ( 12.06949235617739724, 12.14591786802326823, 51.87609039468568284 ) ) ;
#31297 = CARTESIAN_POINT ( 'NONE',  ( -5.153800228976328057, -19.02544592524343514, 67.29057627198102409 ) ) ;
#31299 = CARTESIAN_POINT ( 'NONE',  ( 0.05219959533934541429, -16.53943276465976808, 20.00109039468568639 ) ) ;
#31298 = CARTESIAN_POINT ( 'NONE',  ( -18.62759615963255300, -10.81492255796106328, 44.16775706135234714 ) ) ;
#31300 = CARTESIAN_POINT ( 'NONE',  ( 10.72451020669898902, -18.67979575497178502, 27.91557627198103830 ) ) ;
#31301 = CARTESIAN_POINT ( 'NONE',  ( -16.51473224551082808, 9.474510206698731452, 28.33442372801900433 ) ) ;
#31302 = CARTESIAN_POINT ( 'NONE',  ( 12.06949235617739724, 12.14591786802326823, 41.87609039468568284 ) ) ;
#31303 = CARTESIAN_POINT ( 'NONE',  ( -16.46253265017160317, 9.564922557960807481, 105.8322429386476955 ) ) ;
#31304 = CARTESIAN_POINT ( 'NONE',  ( 18.67979575497178502, 10.72451020669898547, 104.1655762719810241 ) ) ;
#31305 = CARTESIAN_POINT ( 'NONE',  ( -19.02544592524342804, 5.153800228976336051, 76.04057627198102409 ) ) ;
#31306 = DIRECTION ( 'NONE',  ( -0.5000000000000044409, 1.060575238724903587E-16, -0.8660254037844360431 ) ) ;
#31307 = CARTESIAN_POINT ( 'NONE',  ( 14.34966873604960469, 8.224510206698951720, 84.16557627198103830 ) ) ;
#31308 = CARTESIAN_POINT ( 'NONE',  ( 18.67979575497178502, 10.72451020669898547, 39.16557627198102409 ) ) ;
#31309 = CARTESIAN_POINT ( 'NONE',  ( -16.21995358207306737, 7.366697692864094371, 34.93551001512157939 ) ) ;
#31310 = CARTESIAN_POINT ( 'NONE',  ( -16.53943276465976808, -0.05219959533934237506, 68.75109039468568994 ) ) ;
#31311 = CARTESIAN_POINT ( 'NONE',  ( -5.719274019375978568, 21.55341960407610458, 110.2072429386477239 ) ) ;
#31312 = CARTESIAN_POINT ( 'NONE',  ( -9.474510206698720793, -16.51473224551083518, 59.58442372801900433 ) ) ;
#31313 = CARTESIAN_POINT ( 'NONE',  ( -21.55341960407610458, -5.719274019375992779, 31.45724293864769550 ) ) ;
#31314 = CARTESIAN_POINT ( 'NONE',  ( -16.51473224551069308, -9.474510206698971260, 21.66557627198102765 ) ) ;
#31315 = CARTESIAN_POINT ( 'NONE',  ( 0.05219959533907565091, 21.53943276465977519, 74.99890960531435269 ) ) ;
#31316 = VECTOR ( 'NONE', #88433, 1000.000000000000000 ) ;
#31317 = CARTESIAN_POINT ( 'NONE',  ( 16.51473224551069308, 9.474510206698969483, 94.16557627198103830 ) ) ;
#31318 = CARTESIAN_POINT ( 'NONE',  ( 21.55341960407619695, -5.719274019375665929, 96.04275706135236135 ) ) ;
#31319 = CARTESIAN_POINT ( 'NONE',  ( -19.03943276465977164, 0.05219959533909376836, 51.24890960531436690 ) ) ;
#31320 = EDGE_CURVE ( 'NONE', #12839, #85226, #27373, .T. ) ;
#31321 = CARTESIAN_POINT ( 'NONE',  ( 4.379528057220092307, 16.55341960407617563, 32.29275706135235424 ) ) ;
#31322 = CARTESIAN_POINT ( 'NONE',  ( -19.05341960407611168, -5.049401038298163336, 61.45724293864769550 ) ) ;
#31323 = CARTESIAN_POINT ( 'NONE',  ( 0.05219959533937995610, -21.53943276465977519, 85.00109039468568994 ) ) ;
#31324 = ORIENTED_EDGE ( 'NONE', *, *, #9833, .T. ) ;
#31325 = CARTESIAN_POINT ( 'NONE',  ( -5.049401038297874678, -19.05341960407617918, 44.79275706135232582 ) ) ;
#31326 = CARTESIAN_POINT ( 'NONE',  ( 9.474510206698729675, 16.51473224551082808, 42.08442372801900433 ) ) ;
#31327 = CARTESIAN_POINT ( 'NONE',  ( 10.81492255796106328, -18.62759615963255655, 35.41775706135234003 ) ) ;
#31328 = AXIS2_PLACEMENT_3D ( 'NONE', #49205, #110863, #157379 ) ;
#31329 = CARTESIAN_POINT ( 'NONE',  ( -9.100000000000001421, 9.789526074884739315E-14, -61.89430850415821794 ) ) ;
#31330 = CARTESIAN_POINT ( 'NONE',  ( 13.97604488694548053, -13.89961937509957401, 35.62609039468567573 ) ) ;
#31331 = CARTESIAN_POINT ( 'NONE',  ( -16.46253265017160317, 9.564922557960807481, 90.83224293864769550 ) ) ;
#31332 = CARTESIAN_POINT ( 'NONE',  ( 13.97604488694527802, 13.89961937509977652, 69.37390960531436690 ) ) ;
#31333 = CARTESIAN_POINT ( 'NONE',  ( 14.34966873604972726, -8.224510206698740333, 110.8344237280190043 ) ) ;
#31335 = CARTESIAN_POINT ( 'NONE',  ( 5.719274019375673035, 21.55341960407619339, 92.29275706135236135 ) ) ;
#31334 = CARTESIAN_POINT ( 'NONE',  ( 15.72974639402199770, -15.80617190586745480, 23.12390960531436335 ) ) ;
#31336 = CARTESIAN_POINT ( 'NONE',  ( -29.86685920354755552, 21.69954338932564397, -0.8249999972688133454 ) ) ;
#31337 = CARTESIAN_POINT ( 'NONE',  ( -34.16333257229422316, 4.138830072290156536, 91.36021987110632381 ) ) ;
#31338 = CARTESIAN_POINT ( 'NONE',  ( 5.719274019375673035, 21.55341960407619339, 97.29275706135234714 ) ) ;
#31339 = CARTESIAN_POINT ( 'NONE',  ( -23.48298174826589602, -32.32155151706771790, -3.447842220587803652 ) ) ;
#31340 = CARTESIAN_POINT ( 'NONE',  ( -16.46253265017160317, 9.564922557960807481, 25.83224293864769194 ) ) ;
#31341 = CARTESIAN_POINT ( 'NONE',  ( -13.89961937509977652, 13.97604488694528158, 115.6239096053143669 ) ) ;
#31342 = CARTESIAN_POINT ( 'NONE',  ( 33.70206089117255743, 4.379927107397421082, 98.34612363080974262 ) ) ;
#31343 = CARTESIAN_POINT ( 'NONE',  ( -16.55341960407617563, 4.379528057220093196, 48.54275706135234714 ) ) ;
#31344 = CARTESIAN_POINT ( 'NONE',  ( -5.719274019375978568, 21.55341960407610458, 75.20724293864769550 ) ) ;
#31345 = CARTESIAN_POINT ( 'NONE',  ( -16.53943276465976808, 0.05219959533911058130, 36.24890960531435979 ) ) ;
#31347 = CARTESIAN_POINT ( 'NONE',  ( 0.05219959533909260263, 19.03943276465977164, 89.99890960531436690 ) ) ;
#31346 = CARTESIAN_POINT ( 'NONE',  ( 16.53943276465976808, -0.05219959533910856209, 103.7489096053143669 ) ) ;
#31348 = CARTESIAN_POINT ( 'NONE',  ( -9.474510206698720793, -16.51473224551083518, 19.58442372801899722 ) ) ;
#31349 = CARTESIAN_POINT ( 'NONE',  ( 16.46253265017160672, -9.564922557960803928, 23.33224293864769194 ) ) ;
#31350 = CARTESIAN_POINT ( 'NONE',  ( -5.719274019375665041, -21.55341960407619695, 69.79275706135234714 ) ) ;
#31351 = CARTESIAN_POINT ( 'NONE',  ( -17.59860650958990647, -7.585241751807021870, 96.57662985737508166 ) ) ;
#31352 = CARTESIAN_POINT ( 'NONE',  ( 14.34966873604972726, -8.224510206698740333, 100.8344237280190185 ) ) ;
#31353 = CARTESIAN_POINT ( 'NONE',  ( -16.46253265017146816, -9.564922557961047289, 59.16775706135233293 ) ) ;
#31354 = CARTESIAN_POINT ( 'NONE',  ( 36.91746824999999177, 11.99521256947799230, -4.024999997268814411 ) ) ;
#31355 = CARTESIAN_POINT ( 'NONE',  ( -0.05219959533907301413, -21.53943276465977519, 32.49890960531435979 ) ) ;
#31356 = CARTESIAN_POINT ( 'NONE',  ( -12.06949235617756955, 12.14591786802309770, 95.62390960531436690 ) ) ;
#31357 = CARTESIAN_POINT ( 'NONE',  ( -0.05219959533936034679, 19.03943276465977164, 52.50109039468566863 ) ) ;
#31358 = AXIS2_PLACEMENT_3D ( 'NONE', #125878, #27183, #63207 ) ;
#31359 = CARTESIAN_POINT ( 'NONE',  ( 19.02544592524343514, -5.153800228976328945, 73.54057627198103830 ) ) ;
#31360 = CARTESIAN_POINT ( 'NONE',  ( 12.06949235617757843, -12.14591786802309237, 63.12390960531435979 ) ) ;
#31361 = CARTESIAN_POINT ( 'NONE',  ( -13.97604488694547697, 13.89961937509957934, 88.12609039468563310 ) ) ;
#31362 = CARTESIAN_POINT ( 'NONE',  ( 21.52544592524344225, -5.823673210054117533, 48.54057627198103120 ) ) ;
#31363 = VERTEX_POINT ( 'NONE', #189105 ) ;
#31364 = CARTESIAN_POINT ( 'NONE',  ( 16.53943276465976808, -0.05219959533910856209, 113.7489096053143527 ) ) ;
#31365 = DIRECTION ( 'NONE',  ( -0.7071067811865483499, 2.468850131082268499E-15, -0.7071067811865467956 ) ) ;
#31367 = CARTESIAN_POINT ( 'NONE',  ( 15.72974639402199770, -15.80617190586745480, 73.12390960531436690 ) ) ;
#31366 = CARTESIAN_POINT ( 'NONE',  ( -9.474510206698964154, 16.51473224551069663, 70.41557627198102409 ) ) ;
#31369 = CARTESIAN_POINT ( 'NONE',  ( 16.51473224551069308, 9.474510206698969483, 69.16557627198102409 ) ) ;
#31368 = CARTESIAN_POINT ( 'NONE',  ( -16.55341960407617563, 4.379528057220093196, 88.54275706135236135 ) ) ;
#31370 = CARTESIAN_POINT ( 'NONE',  ( -16.46253265017146816, -9.564922557961047289, 64.16775706135233293 ) ) ;
#31371 = CARTESIAN_POINT ( 'NONE',  ( 18.67979575497194134, -10.72451020669871369, 75.83442372801900433 ) ) ;
#31372 = CARTESIAN_POINT ( 'NONE',  ( -18.67979575497178146, -10.72451020669898902, 66.66557627198102409 ) ) ;
#31373 = CARTESIAN_POINT ( 'NONE',  ( 0.05219959533909260263, 19.03943276465977164, 114.9989096053143669 ) ) ;
#31374 = CARTESIAN_POINT ( 'NONE',  ( -16.51473224551069308, -9.474510206698971260, 31.66557627198102054 ) ) ;
#31375 = CARTESIAN_POINT ( 'NONE',  ( -8.224510206698735004, -14.34966873604973081, 104.5844237280190185 ) ) ;
#31376 = CARTESIAN_POINT ( 'NONE',  ( 16.51473224551069308, 9.474510206698969483, 54.16557627198103120 ) ) ;
#31377 = CARTESIAN_POINT ( 'NONE',  ( 14.29746914071037800, 8.314922557961029526, 21.66775706135235069 ) ) ;
#31378 = FACE_OUTER_BOUND ( 'NONE', #112348, .T. ) ;
#31379 = CARTESIAN_POINT ( 'NONE',  ( -10.81492255796105439, 18.62759615963255655, 112.9177570613523329 ) ) ;
#31380 = CARTESIAN_POINT ( 'NONE',  ( 8.224510206698953496, -14.34966873604960469, 57.91557627198103120 ) ) ;
#31381 = SHAPE_REPRESENTATION ( 'Front Concentrator Nozzle', ( #82054 ), #62737 ) ;
#31382 = CARTESIAN_POINT ( 'NONE',  ( 18.62759615963271287, -10.81492255796078972, 113.3322429386476955 ) ) ;
#31383 = CARTESIAN_POINT ( 'NONE',  ( 21.53943276465977519, -0.05219959533907433946, 98.74890960531438111 ) ) ;
#31384 = CARTESIAN_POINT ( 'NONE',  ( 16.38665767535052709, -7.295008042176097440, 97.76400864214549813 ) ) ;
#31385 = CARTESIAN_POINT ( 'NONE',  ( 10.81492255796078972, 18.62759615963270932, 49.58224293864769550 ) ) ;
#31386 = CARTESIAN_POINT ( 'NONE',  ( -16.52544592524335698, -4.483927247898792601, 78.95942372801901854 ) ) ;
#31387 = CARTESIAN_POINT ( 'NONE',  ( 4.483927247898545687, 16.52544592524342804, 94.79057627198105251 ) ) ;
#31388 = CARTESIAN_POINT ( 'NONE',  ( -13.97604488694527625, -13.89961937509977652, 56.87390960531434558 ) ) ;
#31389 = CARTESIAN_POINT ( 'NONE',  ( -8.207766490800743497, -46.52841682978064597, -24.35011552987000272 ) ) ;
#31390 = CARTESIAN_POINT ( 'NONE',  ( 14.29746914071037800, 8.314922557961029526, 111.6677570613523613 ) ) ;
#31391 = CARTESIAN_POINT ( 'NONE',  ( -10.81492255796105439, 18.62759615963255655, 37.91775706135235424 ) ) ;
#31392 = CARTESIAN_POINT ( 'NONE',  ( -13.89961937509977652, 13.97604488694528158, 90.62390960531432427 ) ) ;
#31393 = CARTESIAN_POINT ( 'NONE',  ( -21.55341960407619339, 5.719274019375674811, 73.54275706135234714 ) ) ;
#31394 = CARTESIAN_POINT ( 'NONE',  ( -5.153800228976328057, -19.02544592524343514, 22.29057627198102765 ) ) ;
#31395 = CARTESIAN_POINT ( 'NONE',  ( 12.50000000000001066, -90.00000000000005684, -15.00000000000000000 ) ) ;
#31396 = ORIENTED_EDGE ( 'NONE', *, *, #43889, .T. ) ;
#31397 = CARTESIAN_POINT ( 'NONE',  ( 5.719274019375673035, 21.55341960407619339, 62.29275706135236845 ) ) ;
#31398 = CARTESIAN_POINT ( 'NONE',  ( -19.05341960407611168, -5.049401038298163336, 56.45724293864768129 ) ) ;
#31399 = CARTESIAN_POINT ( 'NONE',  ( 19.02544592524343514, -5.153800228976328945, 83.54057627198100988 ) ) ;
#31400 = CARTESIAN_POINT ( 'NONE',  ( 19.05341960407617918, -5.049401038297876454, 71.04275706135234714 ) ) ;
#31401 = CARTESIAN_POINT ( 'NONE',  ( -21.55341960407619339, 5.719274019375674811, 43.54275706135235424 ) ) ;
#31402 = CARTESIAN_POINT ( 'NONE',  ( 16.46253265017146816, 9.564922557961045513, 101.6677570613523329 ) ) ;
#31403 = CARTESIAN_POINT ( 'NONE',  ( -13.89961937509957401, -13.97604488694547875, 69.37609039468564731 ) ) ;
#31404 = CARTESIAN_POINT ( 'NONE',  ( 5.153800228976335163, 19.02544592524342804, 34.79057627198102409 ) ) ;
#31405 = CARTESIAN_POINT ( 'NONE',  ( 14.29746914071037800, 8.314922557961029526, 106.6677570613523756 ) ) ;
#31406 = CARTESIAN_POINT ( 'NONE',  ( 19.05341960407617918, -5.049401038297876454, 71.04275706135234714 ) ) ;
#31407 = CARTESIAN_POINT ( 'NONE',  ( 4.483927247898545687, 16.52544592524342804, 24.79057627198103120 ) ) ;
#31408 = CARTESIAN_POINT ( 'NONE',  ( 13.97604488694548053, -13.89961937509957401, 45.62609039468566863 ) ) ;
#31409 = CARTESIAN_POINT ( 'NONE',  ( -5.719274019375665041, -21.55341960407619695, 99.79275706135234714 ) ) ;
#31410 = CARTESIAN_POINT ( 'NONE',  ( -5.153800228976607833, 19.02544592524334988, 27.70942372801899722 ) ) ;
#31411 = CARTESIAN_POINT ( 'NONE',  ( 13.89961937509977652, -13.97604488694527269, 23.12390960531436335 ) ) ;
#31412 = CARTESIAN_POINT ( 'NONE',  ( 0.05219959533937995610, -21.53943276465977519, 85.00109039468568994 ) ) ;
#31413 = CARTESIAN_POINT ( 'NONE',  ( -4.483927247898782831, 16.52544592524335698, 27.70942372801901854 ) ) ;
#31414 = CARTESIAN_POINT ( 'NONE',  ( 19.03943276465977164, -0.05219959533909143690, 93.74890960531435269 ) ) ;
#31415 = CARTESIAN_POINT ( 'NONE',  ( -17.14385361876520264, -23.59649016807271593, 143.1750000027311671 ) ) ;
#31416 = CARTESIAN_POINT ( 'NONE',  ( -5.153800228976328057, -19.02544592524343514, 82.29057627198103830 ) ) ;
#31417 = DIRECTION ( 'NONE',  ( -0.000000000000000000, -0.000000000000000000, 1.000000000000000000 ) ) ;
#31418 = ORIENTED_EDGE ( 'NONE', *, *, #78315, .T. ) ;
#31419 = CARTESIAN_POINT ( 'NONE',  ( -13.97604488694547697, 13.89961937509957934, 83.12609039468564731 ) ) ;
#31420 = CARTESIAN_POINT ( 'NONE',  ( -0.05219959533909027116, -19.03943276465977164, 112.4989096053143669 ) ) ;
#31421 = CARTESIAN_POINT ( 'NONE',  ( -21.53943276465977519, -0.05219959533937600094, 113.7510903946856757 ) ) ;
#31422 = CARTESIAN_POINT ( 'NONE',  ( -0.05219959533910754901, -16.53943276465976808, 92.49890960531436690 ) ) ;
#31423 = CARTESIAN_POINT ( 'NONE',  ( 22.72581825106559350, -12.75361973299573926, 165.5645137041833550 ) ) ;
#31424 = CARTESIAN_POINT ( 'NONE',  ( 15.80617190586746368, 15.72974639402197994, 54.37390960531435979 ) ) ;
#31425 = CARTESIAN_POINT ( 'NONE',  ( -15.80617190586745835, -15.72974639402198527, 41.87390960531435979 ) ) ;
#31426 = CARTESIAN_POINT ( 'NONE',  ( 19.02544592524343514, -5.153800228976328945, 23.54057627198102054 ) ) ;
#31427 = CARTESIAN_POINT ( 'NONE',  ( -15.93273212980863462, 1.322671946311657187, -61.66661032175890256 ) ) ;
#31428 = CARTESIAN_POINT ( 'NONE',  ( -13.97604488694547697, 13.89961937509957934, 58.12609039468566863 ) ) ;
#31429 = CARTESIAN_POINT ( 'NONE',  ( 12.14591786802309770, 12.06949235617756955, 44.37390960531435979 ) ) ;
#31430 = CARTESIAN_POINT ( 'NONE',  ( 18.67979575497178502, 10.72451020669898547, 24.16557627198103120 ) ) ;
#31431 = CARTESIAN_POINT ( 'NONE',  ( 18.67979575497194134, -10.72451020669871369, 85.83442372801901854 ) ) ;
#31432 = CARTESIAN_POINT ( 'NONE',  ( 21.53943276465977519, -0.05219959533907433946, 73.74890960531433848 ) ) ;
#31433 = CARTESIAN_POINT ( 'NONE',  ( -15.72974639402176322, -15.80617190586768395, 59.37609039468568284 ) ) ;
#31434 = CARTESIAN_POINT ( 'NONE',  ( -5.823673210054431948, 21.52544592524334988, 47.70942372801902565 ) ) ;
#31435 = CARTESIAN_POINT ( 'NONE',  ( 9.474510206698971260, -16.51473224551069308, 87.91557627198102409 ) ) ;
#31436 = CARTESIAN_POINT ( 'NONE',  ( 14.29746914071037800, 8.314922557961029526, 76.66775706135234714 ) ) ;
#31437 = CARTESIAN_POINT ( 'NONE',  ( 19.05341960407611168, 5.049401038298154454, 28.95724293864769550 ) ) ;
#31438 = CARTESIAN_POINT ( 'NONE',  ( -32.64453336272028139, 0.4913919212617717247, 87.50000000000000000 ) ) ;
#31439 = CARTESIAN_POINT ( 'NONE',  ( -8.224510206698948167, 14.34966873604960824, 55.41557627198102409 ) ) ;
#31440 = CARTESIAN_POINT ( 'NONE',  ( 16.52544592524342804, -4.483927247898539470, 28.54057627198103120 ) ) ;
#31441 = CARTESIAN_POINT ( 'NONE',  ( 16.46253265017160672, -9.564922557960803928, 68.33224293864770971 ) ) ;
#31442 = CARTESIAN_POINT ( 'NONE',  ( 5.049401038298161559, -19.05341960407611168, 32.70724293864768129 ) ) ;
#31443 = CARTESIAN_POINT ( 'NONE',  ( 18.67979575497178502, 10.72451020669898547, 39.16557627198102409 ) ) ;
#31444 = CARTESIAN_POINT ( 'NONE',  ( 19.02544592524334988, 5.153800228976608722, 31.45942372801900433 ) ) ;
#31447 = CARTESIAN_POINT ( 'NONE',  ( -16.52544592524342804, 4.483927247898546575, 56.04057627198102409 ) ) ;
#31446 = LINE ( 'NONE', #169954, #194649 ) ;
#31445 = CIRCLE ( 'NONE', #57309, 8.000000000000001776 ) ;
#31448 = CARTESIAN_POINT ( 'NONE',  ( -21.55341960407610458, -5.719274019375992779, 21.45724293864769550 ) ) ;
#31449 = CARTESIAN_POINT ( 'NONE',  ( -12.73749492396214578, -155.7167183371837496, -25.00000000000000000 ) ) ;
#31450 = CARTESIAN_POINT ( 'NONE',  ( 4.483927247898790824, -16.52544592524335698, 70.20942372801904696 ) ) ;
#31451 = CARTESIAN_POINT ( 'NONE',  ( -9.474510206698720793, -16.51473224551083518, 69.58442372801901854 ) ) ;
#31452 = CARTESIAN_POINT ( 'NONE',  ( -8.224510206698948167, 14.34966873604960824, 40.41557627198103120 ) ) ;
#31453 = CARTESIAN_POINT ( 'NONE',  ( 17.44270441346517941, -5.991230190323000748, 51.13664920735774899 ) ) ;
#31454 = CARTESIAN_POINT ( 'NONE',  ( 8.224510206698953496, -14.34966873604960469, 27.91557627198103830 ) ) ;
#31455 = CARTESIAN_POINT ( 'NONE',  ( -13.97604488694527625, -13.89961937509977652, 31.87390960531435979 ) ) ;
#31456 = EDGE_CURVE ( 'NONE', #199067, #20570, #94075, .T. ) ;
#31457 = CARTESIAN_POINT ( 'NONE',  ( 9.474510206698971260, -16.51473224551069308, 62.91557627198102409 ) ) ;
#31458 = CARTESIAN_POINT ( 'NONE',  ( -19.02544592524342804, 5.153800228976336051, 46.04057627198101699 ) ) ;
#31459 = CARTESIAN_POINT ( 'NONE',  ( 15.80617190586769283, -15.72974639402175789, 45.62609039468567573 ) ) ;
#31460 = CARTESIAN_POINT ( 'NONE',  ( -16.46253265017160317, 9.564922557960807481, 60.83224293864769550 ) ) ;
#31461 = DIRECTION ( 'NONE',  ( -0.000000000000000000, -0.000000000000000000, -1.000000000000000000 ) ) ;
#31462 = CARTESIAN_POINT ( 'NONE',  ( 9.564922557960805705, 16.46253265017160317, 39.58224293864768839 ) ) ;
#31463 = CARTESIAN_POINT ( 'NONE',  ( -10.81492255796078084, -18.62759615963271287, 37.08224293864768129 ) ) ;
#31465 = CARTESIAN_POINT ( 'NONE',  ( -19.03943276465977164, 0.05219959533909376836, 21.24890960531436335 ) ) ;
#31464 = CARTESIAN_POINT ( 'NONE',  ( 5.823673210054444382, -21.52544592524334988, 60.20942372801902565 ) ) ;
#31466 = CARTESIAN_POINT ( 'NONE',  ( -5.823673210054116645, -21.52544592524344225, 22.29057627198102765 ) ) ;
#31467 = CARTESIAN_POINT ( 'NONE',  ( 16.55341960407618274, -4.379528057220086978, 96.04275706135236135 ) ) ;
#31468 = CARTESIAN_POINT ( 'NONE',  ( 18.67979575497194134, -10.72451020669871369, 105.8344237280190328 ) ) ;
#31469 = CARTESIAN_POINT ( 'NONE',  ( -16.55341960407617563, 4.379528057220093196, 68.54275706135234714 ) ) ;
#31470 = CARTESIAN_POINT ( 'NONE',  ( -19.03943276465977164, 0.05219959533909376836, 111.2489096053143669 ) ) ;
#31471 = CARTESIAN_POINT ( 'NONE',  ( 8.224510206698742110, 14.34966873604972548, 52.08442372801901854 ) ) ;
#31472 = CARTESIAN_POINT ( 'NONE',  ( 12.06949235617739724, 12.14591786802326823, 41.87609039468568284 ) ) ;
#31473 = CARTESIAN_POINT ( 'NONE',  ( 14.29746914071037800, 8.314922557961029526, 96.66775706135234714 ) ) ;
#31474 = CARTESIAN_POINT ( 'NONE',  ( 15.80617190586769283, -15.72974639402175789, 55.62609039468568284 ) ) ;
#31475 = CARTESIAN_POINT ( 'NONE',  ( -19.03943276465977164, -0.05219959533935918106, 113.7510903946856757 ) ) ;
#31476 = CARTESIAN_POINT ( 'NONE',  ( 15.72974639402199770, -15.80617190586745480, 108.1239096053143811 ) ) ;
#31477 = CARTESIAN_POINT ( 'NONE',  ( 12.14591786802327356, -12.06949235617739191, 25.62609039468567929 ) ) ;
#31478 = CARTESIAN_POINT ( 'NONE',  ( -8.224510206698735004, -14.34966873604973081, 84.58442372801903275 ) ) ;
#31479 = PLANE ( 'NONE',  #192537 ) ;
#31480 = CARTESIAN_POINT ( 'NONE',  ( 18.67979575497194134, -10.72451020669871369, 80.83442372801901854 ) ) ;
#31481 = CARTESIAN_POINT ( 'NONE',  ( -19.05341960407617563, 5.049401038297882671, 83.54275706135233293 ) ) ;
#31482 = CARTESIAN_POINT ( 'NONE',  ( 8.224510206698953496, -14.34966873604960469, 52.91557627198103830 ) ) ;
#31483 = CARTESIAN_POINT ( 'NONE',  ( 16.53943276465976808, -0.05219959533910856209, 43.74890960531435979 ) ) ;
#31484 = CARTESIAN_POINT ( 'NONE',  ( -16.53943276465976808, 0.05219959533911058130, 106.2489096053143811 ) ) ;
#31486 = FILL_AREA_STYLE ('',( #46656 ) ) ;
#31485 = CARTESIAN_POINT ( 'NONE',  ( -9.564922557961040184, 16.46253265017147172, 47.91775706135233293 ) ) ;
#31487 = CARTESIAN_POINT ( 'NONE',  ( -21.53943276465977519, -0.05219959533937600094, 53.75109039468568994 ) ) ;
#31488 = CARTESIAN_POINT ( 'NONE',  ( -16.51473224551082808, 9.474510206698731452, 108.3344237280190043 ) ) ;
#31489 = CARTESIAN_POINT ( 'NONE',  ( -11.78083973539056473, -37.76997396076110647, -30.94638762609308458 ) ) ;
#31490 = CARTESIAN_POINT ( 'NONE',  ( -0.05219959533909027116, -19.03943276465977164, 102.4989096053143669 ) ) ;
#31491 = CARTESIAN_POINT ( 'NONE',  ( 21.53943276465977519, -0.05219959533907433946, 68.74890960531435269 ) ) ;
#31492 = CARTESIAN_POINT ( 'NONE',  ( 19.03943276465977164, 0.05219959533936151252, 101.2510903946856757 ) ) ;
#31493 = CARTESIAN_POINT ( 'NONE',  ( 16.51473224551069308, 9.474510206698969483, 99.16557627198102409 ) ) ;
#31494 = CARTESIAN_POINT ( 'NONE',  ( 15.72974639402199770, -15.80617190586745480, 58.12390960531435979 ) ) ;
#31495 = CARTESIAN_POINT ( 'NONE',  ( 16.53943276465976808, -0.05219959533910856209, 103.7489096053143669 ) ) ;
#31496 = CARTESIAN_POINT ( 'NONE',  ( 10.81492255796106328, -18.62759615963255655, 90.41775706135236135 ) ) ;
#31497 = CARTESIAN_POINT ( 'NONE',  ( 16.51473224551069308, 9.474510206698969483, 24.16557627198102765 ) ) ;
#31499 = CARTESIAN_POINT ( 'NONE',  ( 10.72451020669871369, 18.67979575497193778, 37.08442372801901143 ) ) ;
#31498 = AXIS2_PLACEMENT_3D ( 'NONE', #158380, #145193, #187753 ) ;
#31500 = CARTESIAN_POINT ( 'NONE',  ( -18.62759615963255300, -10.81492255796106328, 84.16775706135234714 ) ) ;
#31501 = CARTESIAN_POINT ( 'NONE',  ( 4.379528057220092307, 16.55341960407617563, 92.29275706135236135 ) ) ;
#31502 = CARTESIAN_POINT ( 'NONE',  ( 5.823673210054444382, -21.52544592524334988, 25.20942372801901854 ) ) ;
#31503 = CARTESIAN_POINT ( 'NONE',  ( -18.67979575497193778, 10.72451020669871902, 33.33442372801900433 ) ) ;
#31505 = CARTESIAN_POINT ( 'NONE',  ( -19.05341960407611168, -5.049401038298163336, 81.45724293864769550 ) ) ;
#31504 = CARTESIAN_POINT ( 'NONE',  ( 19.05341960407617918, -5.049401038297876454, 71.04275706135234714 ) ) ;
#31506 = CARTESIAN_POINT ( 'NONE',  ( -0.05219959533937732626, 21.53943276465977519, 82.50109039468568994 ) ) ;
#31507 = CARTESIAN_POINT ( 'NONE',  ( -15.80617190586745835, -15.72974639402198527, 76.87390960531439532 ) ) ;
#31508 = CARTESIAN_POINT ( 'NONE',  ( 4.483927247898545687, 16.52544592524342804, 59.79057627198103120 ) ) ;
#31509 = CARTESIAN_POINT ( 'NONE',  ( 15.80617190586769283, -15.72974639402175789, 105.6260903946856899 ) ) ;
#31510 = CARTESIAN_POINT ( 'NONE',  ( 0.05219959533910956823, 16.53943276465976808, 89.99890960531438111 ) ) ;
#31511 = CARTESIAN_POINT ( 'NONE',  ( 19.05341960407611168, 5.049401038298154454, 38.95724293864767418 ) ) ;
#31512 = CARTESIAN_POINT ( 'NONE',  ( 5.153800228976615827, -19.02544592524334988, 75.20942372801896170 ) ) ;
#31513 = CARTESIAN_POINT ( 'NONE',  ( -14.29746914071049879, 8.314922557960819915, 30.83224293864770260 ) ) ;
#31514 = CARTESIAN_POINT ( 'NONE',  ( 21.55341960407619695, -5.719274019375665929, 101.0427570613523756 ) ) ;
#31515 = CARTESIAN_POINT ( 'NONE',  ( 5.049401038298161559, -19.05341960407611168, 92.70724293864769550 ) ) ;
#31516 = CARTESIAN_POINT ( 'NONE',  ( 13.89961937509957401, 13.97604488694547697, 66.87609039468567573 ) ) ;
#31517 = CARTESIAN_POINT ( 'NONE',  ( -18.67979575497178146, -10.72451020669898902, 66.66557627198102409 ) ) ;
#31518 = CARTESIAN_POINT ( 'NONE',  ( -21.53943276465977519, 0.05219959533907696930, 111.2489096053143669 ) ) ;
#31519 = CARTESIAN_POINT ( 'NONE',  ( 9.564922557961047289, -16.46253265017146816, 110.4177570613523471 ) ) ;
#31520 = CARTESIAN_POINT ( 'NONE',  ( 8.314922557961029526, -14.29746914071037800, 75.41775706135233293 ) ) ;
#31522 = CARTESIAN_POINT ( 'NONE',  ( -18.62759615963255300, -10.81492255796106328, 29.16775706135234003 ) ) ;
#31521 = CARTESIAN_POINT ( 'NONE',  ( 16.81555441253551209, 7.025013491695494494, 61.86314554665744936 ) ) ;
#31523 = CARTESIAN_POINT ( 'NONE',  ( -12.06949235617756955, 12.14591786802309770, 100.6239096053143811 ) ) ;
#31524 = CARTESIAN_POINT ( 'NONE',  ( 29.86685920354754487, 21.69954338932564752, -3.924999997268812990 ) ) ;
#31525 = CARTESIAN_POINT ( 'NONE',  ( -8.224510206698735004, -14.34966873604973081, 44.58442372801901854 ) ) ;
#31526 = CARTESIAN_POINT ( 'NONE',  ( -16.55341960407611168, -4.379528057220339221, 76.45724293864769550 ) ) ;
#31527 = CARTESIAN_POINT ( 'NONE',  ( 21.55341960407610458, 5.719274019375980345, 68.95724293864769550 ) ) ;
#31528 = CARTESIAN_POINT ( 'NONE',  ( 12.06949235617739724, 12.14591786802326823, 106.8760903946856899 ) ) ;
#31529 = CARTESIAN_POINT ( 'NONE',  ( 8.224510206698742110, 14.34966873604972548, 42.08442372801901854 ) ) ;
#31530 = CARTESIAN_POINT ( 'NONE',  ( 5.049401038298161559, -19.05341960407611168, 42.70724293864767418 ) ) ;
#31531 = CARTESIAN_POINT ( 'NONE',  ( 4.379528057220092307, 16.55341960407617563, 77.29275706135234714 ) ) ;
#31532 = CARTESIAN_POINT ( 'NONE',  ( -5.153800228976607833, 19.02544592524334988, 67.70942372801900433 ) ) ;
#31533 = CARTESIAN_POINT ( 'NONE',  ( 18.67979575497178502, 10.72451020669898547, 74.16557627198102409 ) ) ;
#31534 = CARTESIAN_POINT ( 'NONE',  ( -16.55341960407617563, 4.379528057220093196, 93.54275706135234714 ) ) ;
#31535 = CARTESIAN_POINT ( 'NONE',  ( -10.72451020669870658, -18.67979575497194134, 84.58442372801903275 ) ) ;
#31536 = CARTESIAN_POINT ( 'NONE',  ( 10.72451020669898902, -18.67979575497178502, 67.91557627198102409 ) ) ;
#31537 = CARTESIAN_POINT ( 'NONE',  ( 15.72974639402199770, -15.80617190586745480, 53.12390960531436690 ) ) ;
#31538 = ORIENTED_EDGE ( 'NONE', *, *, #128894, .F. ) ;
#31539 = ORIENTED_EDGE ( 'NONE', *, *, #141448, .T. ) ;
#31540 = CARTESIAN_POINT ( 'NONE',  ( -4.379528057220086978, -16.55341960407618274, 74.79275706135234714 ) ) ;
#31541 = CARTESIAN_POINT ( 'NONE',  ( 5.823673210054125526, 21.52544592524343514, 44.79057627198103120 ) ) ;
#31542 = VERTEX_POINT ( 'NONE', #171926 ) ;
#31543 = CARTESIAN_POINT ( 'NONE',  ( -9.564922557960796823, -16.46253265017161027, 112.0822429386476955 ) ) ;
#31544 = CARTESIAN_POINT ( 'NONE',  ( -19.35633801406909171, 5.499999999999578115, 74.13373818172760821 ) ) ;
#31545 = CARTESIAN_POINT ( 'NONE',  ( -9.564922557960796823, -16.46253265017161027, 27.08224293864769550 ) ) ;
#31546 = CARTESIAN_POINT ( 'NONE',  ( 18.62759615963271287, -10.81492255796078972, 73.33224293864769550 ) ) ;
#31547 = CARTESIAN_POINT ( 'NONE',  ( 16.52544592524335698, 4.483927247898782831, 106.4594237280190328 ) ) ;
#31548 = CARTESIAN_POINT ( 'NONE',  ( 10.81492255796106328, -18.62759615963255655, 45.41775706135234003 ) ) ;
#31549 = CARTESIAN_POINT ( 'NONE',  ( 16.55341960407618274, -4.379528057220086978, 21.04275706135234714 ) ) ;
#31550 = CARTESIAN_POINT ( 'NONE',  ( 0.05219959533910956823, 16.53943276465976808, 114.9989096053143669 ) ) ;
#31551 = CARTESIAN_POINT ( 'NONE',  ( -0.05219959533936034679, 19.03943276465977164, 107.5010903946856615 ) ) ;
#31552 = CARTESIAN_POINT ( 'NONE',  ( -19.05341960407611168, -5.049401038298163336, 41.45724293864769550 ) ) ;
#31553 = CARTESIAN_POINT ( 'NONE',  ( 8.906447517083050158, 27.41122689804195645, 141.4000000000000057 ) ) ;
#31554 = CARTESIAN_POINT ( 'NONE',  ( 19.05341960407611168, 5.049401038298154454, 108.9572429386477097 ) ) ;
#31555 = ADVANCED_FACE ( 'NONE', ( #172930 ), #2072, .F. ) ;
#31556 = CARTESIAN_POINT ( 'NONE',  ( -4.483927247898782831, 16.52544592524335698, 87.70942372801901854 ) ) ;
#31557 = CARTESIAN_POINT ( 'NONE',  ( -13.89961937509957401, -13.97604488694547875, 74.37609039468566152 ) ) ;
#31558 = CARTESIAN_POINT ( 'NONE',  ( 19.03943276465977164, 0.05219959533936151252, 26.25109039468566507 ) ) ;
#31559 = CARTESIAN_POINT ( 'NONE',  ( 18.62759615963271287, -10.81492255796078972, 63.33224293864770260 ) ) ;
#31560 = CARTESIAN_POINT ( 'NONE',  ( -4.379528057220086978, -16.55341960407618274, 89.79275706135236135 ) ) ;
#31561 = CARTESIAN_POINT ( 'NONE',  ( -13.97604488694547697, 13.89961937509957934, 88.12609039468563310 ) ) ;
#31562 = CARTESIAN_POINT ( 'NONE',  ( 16.46253265017160672, -9.564922557960803928, 48.33224293864769550 ) ) ;
#31563 = CARTESIAN_POINT ( 'NONE',  ( -5.049401038298153566, 19.05341960407611168, 95.20724293864770971 ) ) ;
#31564 = CARTESIAN_POINT ( 'NONE',  ( 18.67979575497194134, -10.72451020669871369, 45.83442372801901854 ) ) ;
#31565 = CARTESIAN_POINT ( 'NONE',  ( -19.03943276465977164, 0.05219959533909376836, 41.24890960531435269 ) ) ;
#31566 = CARTESIAN_POINT ( 'NONE',  ( 21.93180397000137205, -9.000796715316949914, 171.3297436093415058 ) ) ;
#31567 = CARTESIAN_POINT ( 'NONE',  ( -16.46253265017160317, 9.564922557960807481, 105.8322429386476955 ) ) ;
#31568 = CARTESIAN_POINT ( 'NONE',  ( -16.52544592524342804, 4.483927247898546575, 66.04057627198103830 ) ) ;
#31569 = CARTESIAN_POINT ( 'NONE',  ( 21.55341960407610458, 5.719274019375980345, 63.95724293864770260 ) ) ;
#31570 = CARTESIAN_POINT ( 'NONE',  ( 8.898068258721465895, 27.38543819252877398, 143.6656553485623817 ) ) ;
#31571 = CARTESIAN_POINT ( 'NONE',  ( -9.564922557961040184, 16.46253265017147172, 42.91775706135234003 ) ) ;
#31572 = FILL_AREA_STYLE ('',( #81037 ) ) ;
#31574 = CARTESIAN_POINT ( 'NONE',  ( -16.46253265017160317, 9.564922557960807481, 75.83224293864769550 ) ) ;
#31573 = CARTESIAN_POINT ( 'NONE',  ( 5.153800228976335163, 19.02544592524342804, 69.79057627198103830 ) ) ;
#31575 = CARTESIAN_POINT ( 'NONE',  ( 14.34966873604972726, -8.224510206698740333, 50.83442372801901143 ) ) ;
#31576 = CARTESIAN_POINT ( 'NONE',  ( -24.81835880841865816, 6.052260367207988878, 168.4265213779230521 ) ) ;
#31577 = CARTESIAN_POINT ( 'NONE',  ( -17.31728774477274868, 6.344390552232366254, 110.8190665168931872 ) ) ;
#31578 = CARTESIAN_POINT ( 'NONE',  ( -16.53943276465976808, -0.05219959533934237506, 93.75109039468567573 ) ) ;
#31579 = EDGE_CURVE ( 'NONE', #53136, #190734, #117184, .T. ) ;
#31580 = CARTESIAN_POINT ( 'NONE',  ( 15.01195240492206473, -1.500078752102888879, -59.87740586969341905 ) ) ;
#31581 = CARTESIAN_POINT ( 'NONE',  ( 14.34966873604972726, -8.224510206698740333, 85.83442372801901854 ) ) ;
#31582 = CARTESIAN_POINT ( 'NONE',  ( 4.483927247898790824, -16.52544592524335698, 55.20942372801902565 ) ) ;
#31583 = CARTESIAN_POINT ( 'NONE',  ( -0.05219959533937732626, 21.53943276465977519, 112.5010903946857042 ) ) ;
#31585 = LINE ( 'NONE', #79065, #34035 ) ;
#31584 = CARTESIAN_POINT ( 'NONE',  ( 9.564922557960805705, 16.46253265017160317, 49.58224293864770260 ) ) ;
#31586 = CARTESIAN_POINT ( 'NONE',  ( -18.67979575497193778, 10.72451020669871902, 48.33442372801902565 ) ) ;
#31587 = CARTESIAN_POINT ( 'NONE',  ( -5.153800228976607833, 19.02544592524334988, 57.70942372801899012 ) ) ;
#31588 = CARTESIAN_POINT ( 'NONE',  ( 21.55341960407619695, -5.719274019375665929, 111.0427570613523613 ) ) ;
#31589 = CARTESIAN_POINT ( 'NONE',  ( -19.02544592524342804, 5.153800228976336051, 31.04057627198102409 ) ) ;
#31590 = CARTESIAN_POINT ( 'NONE',  ( 17.08218171090884141, 6.734076229372654154, 23.85283434757613819 ) ) ;
#31591 = CARTESIAN_POINT ( 'NONE',  ( -21.55341960407610458, -5.719274019375992779, 66.45724293864768129 ) ) ;
#31592 = AXIS2_PLACEMENT_3D ( 'NONE', #83833, #192029, #161694 ) ;
#31593 = CARTESIAN_POINT ( 'NONE',  ( 16.46253265017160672, -9.564922557960803928, 113.3322429386476955 ) ) ;
#31594 = CARTESIAN_POINT ( 'NONE',  ( 16.53943276465976808, -0.05219959533910856209, 113.7489096053143527 ) ) ;
#31595 = CARTESIAN_POINT ( 'NONE',  ( -8.314922557961024197, 14.29746914071037800, 32.91775706135234714 ) ) ;
#31596 = CARTESIAN_POINT ( 'NONE',  ( -14.29746914071049879, 8.314922557960819915, 25.83224293864769194 ) ) ;
#31597 = ORIENTED_EDGE ( 'NONE', *, *, #23790, .F. ) ;
#31598 = CARTESIAN_POINT ( 'NONE',  ( -0.05219959533937732626, 21.53943276465977519, 22.50109039468567573 ) ) ;
#31600 = CARTESIAN_POINT ( 'NONE',  ( -19.03943276465977164, 0.05219959533909376836, 111.2489096053143669 ) ) ;
#31599 = CARTESIAN_POINT ( 'NONE',  ( -4.483927247898539470, -16.52544592524342804, 37.29057627198102409 ) ) ;
#31601 = CARTESIAN_POINT ( 'NONE',  ( 19.02544592524334988, 5.153800228976608722, 111.4594237280190043 ) ) ;
#31602 = CARTESIAN_POINT ( 'NONE',  ( -13.97604488694547697, 13.89961937509957934, 33.12609039468566863 ) ) ;
#31603 = CARTESIAN_POINT ( 'NONE',  ( -14.29746914071049879, 8.314922557960819915, 45.83224293864769550 ) ) ;
#31604 = CARTESIAN_POINT ( 'NONE',  ( -5.823673210054116645, -21.52544592524344225, 97.29057627198105251 ) ) ;
#31606 = CARTESIAN_POINT ( 'NONE',  ( 5.719274019375991003, -21.55341960407610458, 62.70724293864769550 ) ) ;
#31605 = CYLINDRICAL_SURFACE ( 'NONE', #160230, 5.000000000000004441 ) ;
#31607 = CARTESIAN_POINT ( 'NONE',  ( 19.03943276465977164, -0.05219959533909143690, 73.74890960531435269 ) ) ;
#31608 = CARTESIAN_POINT ( 'NONE',  ( 4.379528057220339221, -16.55341960407611168, 42.70724293864770260 ) ) ;
#31609 = CARTESIAN_POINT ( 'NONE',  ( -16.51473224551069308, -9.474510206698971260, 91.66557627198103830 ) ) ;
#31610 = CARTESIAN_POINT ( 'NONE',  ( -36.87151287952131185, 2.273789158011777722, 50.01119746921813913 ) ) ;
#31611 = CARTESIAN_POINT ( 'NONE',  ( 19.05341960407617918, -5.049401038297876454, 56.04275706135234714 ) ) ;
#31612 = CARTESIAN_POINT ( 'NONE',  ( 5.719274019375991003, -21.55341960407610458, 87.70724293864769550 ) ) ;
#31613 = CARTESIAN_POINT ( 'NONE',  ( -4.379528057220328563, 16.55341960407611168, 95.20724293864769550 ) ) ;
#31614 = CARTESIAN_POINT ( 'NONE',  ( -18.62759615963255300, -10.81492255796106328, 49.16775706135234003 ) ) ;
#31615 = VECTOR ( 'NONE', #95742, 1000.000000000000000 ) ;
#31616 = CARTESIAN_POINT ( 'NONE',  ( -5.359611314223446995E-15, 29.16686587814335496, 144.3750000027311842 ) ) ;
#31617 = CARTESIAN_POINT ( 'NONE',  ( 4.483927247898545687, 16.52544592524342804, 29.79057627198102409 ) ) ;
#31618 = CARTESIAN_POINT ( 'NONE',  ( -0.05219959533909027116, -19.03943276465977164, 37.49890960531436690 ) ) ;
#31619 = CARTESIAN_POINT ( 'NONE',  ( 19.02544592524343514, -5.153800228976328945, 103.5405762719809957 ) ) ;
#31620 = CARTESIAN_POINT ( 'NONE',  ( -18.67979575497178146, -10.72451020669898902, 56.66557627198103830 ) ) ;
#31621 = CARTESIAN_POINT ( 'NONE',  ( -17.59860650958993844, 7.585241751806885979, 93.42337014262493256 ) ) ;
#31622 = CARTESIAN_POINT ( 'NONE',  ( -19.03943276465977164, 0.05219959533909376836, 31.24890960531435979 ) ) ;
#31623 = CARTESIAN_POINT ( 'NONE',  ( 15.72974639402199770, -15.80617190586745480, 53.12390960531436690 ) ) ;
#31624 = CARTESIAN_POINT ( 'NONE',  ( -21.55341960407619339, 5.719274019375674811, 68.54275706135234714 ) ) ;
#31626 = CARTESIAN_POINT ( 'NONE',  ( 4.379528057220092307, 16.55341960407617563, 87.29275706135236135 ) ) ;
#31625 = CARTESIAN_POINT ( 'NONE',  ( 20.74701606029799450, -32.99105665080598015, -17.50853973932387930 ) ) ;
#31627 = CARTESIAN_POINT ( 'NONE',  ( -13.97604488694527625, -13.89961937509977652, 61.87390960531435979 ) ) ;
#31628 = CARTESIAN_POINT ( 'NONE',  ( -19.02544592524342804, 5.153800228976336051, 66.04057627198103830 ) ) ;
#31629 =( BOUNDED_CURVE ( )  B_SPLINE_CURVE ( 2, ( #190588, #96562, #158250, #97543, #159230, #20725, #52064, #6545, #68224, #129877, #191576, #53054, #37902 ),
 .UNSPECIFIED., .F., .T. ) 
 B_SPLINE_CURVE_WITH_KNOTS ( ( 3, 2, 2, 2, 2, 2, 3 ),
 ( 0.5813778048480978677, 0.5833333333333333703, 0.5877192982456140857, 0.5921052631578946901, 0.5964912280701754055, 0.6008771929824561209, 0.6027870416456015956 ),
 .UNSPECIFIED. ) 
 CURVE ( )  GEOMETRIC_REPRESENTATION_ITEM ( )  RATIONAL_B_SPLINE_CURVE ( ( 0.9831626618144007068, 0.9848076720550096308, 1.000000000000000000, 0.9659258262890683122, 1.000000000000000000, 0.9659258262890683122, 1.000000000000000000, 0.9659258262890683122, 1.000000000000000000, 0.9659258262890683122, 1.000000000000000000, 0.9851625545550091179, 0.9832469066685282089 ) ) 
 REPRESENTATION_ITEM ( '' )  );
#31630 = EDGE_LOOP ( 'NONE', ( #177392, #24946 ) ) ;
#31631 = CARTESIAN_POINT ( 'NONE',  ( 19.03943276465977164, 0.05219959533936151252, 31.25109039468566863 ) ) ;
#31632 = CARTESIAN_POINT ( 'NONE',  ( 16.53943276465976808, 0.05219959533934440121, 71.25109039468568994 ) ) ;
#31633 = CARTESIAN_POINT ( 'NONE',  ( -10.72451020669870658, -18.67979575497194134, 104.5844237280190185 ) ) ;
#31634 = CARTESIAN_POINT ( 'NONE',  ( -5.049401038298153566, 19.05341960407611168, 70.20724293864769550 ) ) ;
#31635 = CARTESIAN_POINT ( 'NONE',  ( -10.81492255796078084, -18.62759615963271287, 32.08224293864769550 ) ) ;
#31636 = CARTESIAN_POINT ( 'NONE',  ( -13.97604488694547697, 13.89961937509957934, 108.1260903946856331 ) ) ;
#31637 = CARTESIAN_POINT ( 'NONE',  ( 15.72974639402176855, 15.80617190586768217, 76.87609039468567573 ) ) ;
#31638 = CARTESIAN_POINT ( 'NONE',  ( 14.34966873604972726, -8.224510206698740333, 45.83442372801901854 ) ) ;
#31639 = CARTESIAN_POINT ( 'NONE',  ( -5.719274019375978568, 21.55341960407610458, 95.20724293864769550 ) ) ;
#31640 = CARTESIAN_POINT ( 'NONE',  ( 16.51473224551083163, -9.474510206698727899, 105.8344237280190043 ) ) ;
#31641 = CARTESIAN_POINT ( 'NONE',  ( -13.89961937509977652, 13.97604488694528158, 75.62390960531438111 ) ) ;
#31642 = CARTESIAN_POINT ( 'NONE',  ( -14.34966873604972548, 8.224510206698743886, 23.33442372801901499 ) ) ;
#31643 = CARTESIAN_POINT ( 'NONE',  ( -5.153800228976328057, -19.02544592524343514, 42.29057627198101699 ) ) ;
#31644 = CARTESIAN_POINT ( 'NONE',  ( 9.564922557961047289, -16.46253265017146816, 110.4177570613523471 ) ) ;
#31645 = CARTESIAN_POINT ( 'NONE',  ( -16.55341960407611168, -4.379528057220339221, 66.45724293864768129 ) ) ;
#31646 = CARTESIAN_POINT ( 'NONE',  ( 4.379528057220092307, 16.55341960407617563, 72.29275706135236135 ) ) ;
#31648 = CARTESIAN_POINT ( 'NONE',  ( 13.97604488694527802, 13.89961937509977652, 49.37390960531434558 ) ) ;
#31647 = CARTESIAN_POINT ( 'NONE',  ( -5.823673210054431948, 21.52544592524334988, 27.70942372801901854 ) ) ;
#31649 = CARTESIAN_POINT ( 'NONE',  ( -9.564922557960796823, -16.46253265017161027, 67.08224293864769550 ) ) ;
#31650 = CARTESIAN_POINT ( 'NONE',  ( -14.34966873604972548, 8.224510206698743886, 78.33442372801901854 ) ) ;
#31652 = ORIENTED_EDGE ( 'NONE', *, *, #83840, .F. ) ;
#31651 = CARTESIAN_POINT ( 'NONE',  ( -24.85114155361886290, -5.582993631595906336, 168.8590791472331034 ) ) ;
#31653 = ORIENTED_EDGE ( 'NONE', *, *, #145117, .F. ) ;
#31654 = CARTESIAN_POINT ( 'NONE',  ( -15.80617190586768217, 15.72974639402176855, 108.1260903946856757 ) ) ;
#31655 = EDGE_CURVE ( 'NONE', #127799, #156928, #80998, .T. ) ;
#31656 = CARTESIAN_POINT ( 'NONE',  ( -16.51473224551069308, -9.474510206698971260, 41.66557627198103120 ) ) ;
#31658 = ORIENTED_EDGE ( 'NONE', *, *, #4625, .T. ) ;
#31657 = CARTESIAN_POINT ( 'NONE',  ( 19.05341960407611168, 5.049401038298154454, 108.9572429386477097 ) ) ;
#31659 = CARTESIAN_POINT ( 'NONE',  ( -12.06949235617739369, -12.14591786802326823, 34.37609039468568284 ) ) ;
#31661 = CARTESIAN_POINT ( 'NONE',  ( -14.34966873604972548, 8.224510206698743886, 38.33442372801900433 ) ) ;
#31660 = CARTESIAN_POINT ( 'NONE',  ( 16.46253265017146816, 9.564922557961045513, 61.66775706135234003 ) ) ;
#31662 = CARTESIAN_POINT ( 'NONE',  ( -9.564922557960796823, -16.46253265017161027, 42.08224293864769550 ) ) ;
#31663 = CARTESIAN_POINT ( 'NONE',  ( 19.03943276465977164, -0.05219959533909143690, 103.7489096053143669 ) ) ;
#31664 = CARTESIAN_POINT ( 'NONE',  ( -9.564922557960796823, -16.46253265017161027, 62.08224293864769550 ) ) ;
#31665 = CARTESIAN_POINT ( 'NONE',  ( 21.53943276465977519, -0.05219959533907433946, 98.74890960531438111 ) ) ;
#31667 = CARTESIAN_POINT ( 'NONE',  ( -5.153800228976328057, -19.02544592524343514, 22.29057627198102765 ) ) ;
#31666 = CARTESIAN_POINT ( 'NONE',  ( 5.049401038298161559, -19.05341960407611168, 92.70724293864769550 ) ) ;
#31668 = CARTESIAN_POINT ( 'NONE',  ( -13.89961937509977652, 13.97604488694528158, 65.62390960531436690 ) ) ;
#31670 = CARTESIAN_POINT ( 'NONE',  ( 5.153800228976335163, 19.02544592524342804, 24.79057627198102765 ) ) ;
#31669 = CARTESIAN_POINT ( 'NONE',  ( -16.52544592524335698, -4.483927247898792601, 108.9594237280190185 ) ) ;
#31671 = CARTESIAN_POINT ( 'NONE',  ( -16.46253265017146816, -9.564922557961047289, 104.1677570613523329 ) ) ;
#31672 = CARTESIAN_POINT ( 'NONE',  ( -18.67979575497193778, 10.72451020669871902, 113.3344237280190328 ) ) ;
#31673 = EDGE_CURVE ( 'NONE', #122542, #87433, #43521, .T. ) ;
#31674 = CARTESIAN_POINT ( 'NONE',  ( -16.55341960407611168, -4.379528057220339221, 56.45724293864768839 ) ) ;
#31675 = CARTESIAN_POINT ( 'NONE',  ( -18.67979575497193778, 10.72451020669871902, 98.33442372801901854 ) ) ;
#31676 = CARTESIAN_POINT ( 'NONE',  ( 9.474510206698971260, -16.51473224551069308, 37.91557627198102409 ) ) ;
#31678 = CARTESIAN_POINT ( 'NONE',  ( -5.719274019375665041, -21.55341960407619695, 84.79275706135234714 ) ) ;
#31677 = CARTESIAN_POINT ( 'NONE',  ( 8.224510206698953496, -14.34966873604960469, 42.91557627198103120 ) ) ;
#31679 = CARTESIAN_POINT ( 'NONE',  ( -5.153800228976328057, -19.02544592524343514, 77.29057627198099567 ) ) ;
#31680 = CARTESIAN_POINT ( 'NONE',  ( -9.564922557960796823, -16.46253265017161027, 92.08224293864769550 ) ) ;
#31681 = CARTESIAN_POINT ( 'NONE',  ( 16.55341960407611168, 4.379528057220329451, 113.9572429386477239 ) ) ;
#31682 = CARTESIAN_POINT ( 'NONE',  ( 8.314922557960818139, 14.29746914071049879, 79.58224293864769550 ) ) ;
#31683 = CARTESIAN_POINT ( 'NONE',  ( -5.823673210054116645, -21.52544592524344225, 82.29057627198103830 ) ) ;
#31684 = CARTESIAN_POINT ( 'NONE',  ( 19.03943276465977164, -0.05219959533909143690, 68.74890960531436690 ) ) ;
#31685 = CARTESIAN_POINT ( 'NONE',  ( -15.72974639402197994, 15.80617190586746368, 85.62390960531436690 ) ) ;
#31686 = CARTESIAN_POINT ( 'NONE',  ( -0.05219959533936034679, 19.03943276465977164, 82.50109039468567573 ) ) ;
#31688 = CARTESIAN_POINT ( 'NONE',  ( 16.55341960407611168, 4.379528057220329451, 88.95724293864769550 ) ) ;
#31687 = CARTESIAN_POINT ( 'NONE',  ( 0.3535533905935877019, 30.00000000000000000, 5.353553390593268624 ) ) ;
#31689 = CARTESIAN_POINT ( 'NONE',  ( 19.03943276465977164, -0.05219959533909143690, 58.74890960531435979 ) ) ;
#31690 = CARTESIAN_POINT ( 'NONE',  ( 21.55341960407610458, 5.719274019375980345, 63.95724293864770260 ) ) ;
#31691 = CARTESIAN_POINT ( 'NONE',  ( 7.500000000000000000, 9.184850993605147944E-16, 5.707106781186540800 ) ) ;
#31693 = LINE ( 'NONE', #14532, #114545 ) ;
#31692 = CARTESIAN_POINT ( 'NONE',  ( -12.14591786802326823, 12.06949235617739902, 108.1260903946856757 ) ) ;
#31694 = CARTESIAN_POINT ( 'NONE',  ( -5.153800228976607833, 19.02544592524334988, 112.7094237280190043 ) ) ;
#31695 = CARTESIAN_POINT ( 'NONE',  ( 16.53943276465976808, -0.05219959533910856209, 83.74890960531435269 ) ) ;
#31696 = CARTESIAN_POINT ( 'NONE',  ( 8.788389965099115742, -0.9205664139720534100, -61.95844424577443021 ) ) ;
#31697 = CARTESIAN_POINT ( 'NONE',  ( 9.564922557960805705, 16.46253265017160317, 79.58224293864769550 ) ) ;
#31698 = CARTESIAN_POINT ( 'NONE',  ( 0.05219959533909260263, 19.03943276465977164, 29.99890960531435979 ) ) ;
#31699 = CARTESIAN_POINT ( 'NONE',  ( -16.52544592524342804, 4.483927247898546575, 71.04057627198103830 ) ) ;
#31700 = CARTESIAN_POINT ( 'NONE',  ( -16.46253265017160317, 9.564922557960807481, 115.8322429386477097 ) ) ;
#31702 = CARTESIAN_POINT ( 'NONE',  ( 5.153800228976335163, 19.02544592524342804, 74.79057627198103830 ) ) ;
#31701 = CARTESIAN_POINT ( 'NONE',  ( 19.05341960407617918, -5.049401038297876454, 86.04275706135233293 ) ) ;
#31703 = CARTESIAN_POINT ( 'NONE',  ( -9.474510206698964154, 16.51473224551069663, 90.41557627198103830 ) ) ;
#31704 = CARTESIAN_POINT ( 'NONE',  ( 15.80617190586746368, 15.72974639402197994, 74.37390960531436690 ) ) ;
#31705 = CARTESIAN_POINT ( 'NONE',  ( -8.314922557961024197, 14.29746914071037800, 67.91775706135234714 ) ) ;
#31706 = CARTESIAN_POINT ( 'NONE',  ( -17.31747979337959009, 6.344076630960794994, 93.62055131934819485 ) ) ;
#31707 = CARTESIAN_POINT ( 'NONE',  ( 0.05219959533909260263, 19.03943276465977164, 59.99890960531436690 ) ) ;
#31708 = CARTESIAN_POINT ( 'NONE',  ( -21.53943276465977519, 0.05219959533907696930, 71.24890960531435269 ) ) ;
#31709 = CARTESIAN_POINT ( 'NONE',  ( 0.05219959533936267826, -19.03943276465977164, 100.0010903946856757 ) ) ;
#31711 = CARTESIAN_POINT ( 'NONE',  ( -18.62759615963255300, -10.81492255796106328, 44.16775706135234714 ) ) ;
#31710 = CARTESIAN_POINT ( 'NONE',  ( 16.52544592524342804, -4.483927247898539470, 33.54057627198102409 ) ) ;
#31712 = CARTESIAN_POINT ( 'NONE',  ( -17.81289503416611097, -24.51734667627696496, 144.5500000054623513 ) ) ;
#31714 = CARTESIAN_POINT ( 'NONE',  ( 5.153800228976335163, 19.02544592524342804, 99.79057627198102409 ) ) ;
#31713 = CARTESIAN_POINT ( 'NONE',  ( 12.14591786802327356, -12.06949235617739191, 70.62609039468567573 ) ) ;
#31715 = DIRECTION ( 'NONE',  ( -0.000000000000000000, -0.000000000000000000, 1.000000000000000000 ) ) ;
#31716 = CARTESIAN_POINT ( 'NONE',  ( 1.038764921308847677, 31.48673128579449099, -49.64798258954322563 ) ) ;
#31717 = CARTESIAN_POINT ( 'NONE',  ( -16.55341960407617563, 4.379528057220093196, 93.54275706135234714 ) ) ;
#31718 = CARTESIAN_POINT ( 'NONE',  ( 14.34966873604972726, -8.224510206698740333, 50.83442372801901143 ) ) ;
#31719 = CARTESIAN_POINT ( 'NONE',  ( 9.474510206698971260, -16.51473224551069308, 57.91557627198103120 ) ) ;
#31720 = CARTESIAN_POINT ( 'NONE',  ( 19.05341960407611168, 5.049401038298154454, 68.95724293864769550 ) ) ;
#31721 = CARTESIAN_POINT ( 'NONE',  ( -18.62759615963255300, -10.81492255796106328, 59.16775706135234714 ) ) ;
#31722 = CARTESIAN_POINT ( 'NONE',  ( -14.34966873604972548, 8.224510206698743886, 63.33442372801900433 ) ) ;
#31723 = CARTESIAN_POINT ( 'NONE',  ( 14.29746914071049879, -8.314922557960816363, 38.33224293864768839 ) ) ;
#31724 = CARTESIAN_POINT ( 'NONE',  ( -16.46253265017160317, 9.564922557960807481, 45.83224293864769550 ) ) ;
#31725 = CARTESIAN_POINT ( 'NONE',  ( 16.51473224551069308, 9.474510206698969483, 29.16557627198103475 ) ) ;
#31727 = ORIENTED_EDGE ( 'NONE', *, *, #198449, .T. ) ;
#31726 = CARTESIAN_POINT ( 'NONE',  ( -8.224510206698735004, -14.34966873604973081, 24.58442372801901499 ) ) ;
#31728 = CARTESIAN_POINT ( 'NONE',  ( 0.05219959533936267826, -19.03943276465977164, 85.00109039468567573 ) ) ;
#31729 = CARTESIAN_POINT ( 'NONE',  ( -14.29746914071049879, 8.314922557960819915, 85.83224293864768129 ) ) ;
#31730 = CARTESIAN_POINT ( 'NONE',  ( 9.474510206698971260, -16.51473224551069308, 47.91557627198102409 ) ) ;
#31732 = CARTESIAN_POINT ( 'NONE',  ( -18.22780087662119541, 5.500000000000102141, 56.01763182126894947 ) ) ;
#31731 = CARTESIAN_POINT ( 'NONE',  ( 13.89961937509957401, 13.97604488694547697, 86.87609039468567573 ) ) ;
#31733 = CARTESIAN_POINT ( 'NONE',  ( 5.719274019375673035, 21.55341960407619339, 87.29275706135236135 ) ) ;
#31734 = CARTESIAN_POINT ( 'NONE',  ( -0.05219959533934338120, 16.53943276465976808, 47.50109039468568994 ) ) ;
#31735 = CARTESIAN_POINT ( 'NONE',  ( -17.50000000000013145, 3.292511757969945663, 25.06520270210549839 ) ) ;
#31736 = CARTESIAN_POINT ( 'NONE',  ( 21.55341960407610458, 5.719274019375980345, 48.95724293864770971 ) ) ;
#31737 = CARTESIAN_POINT ( 'NONE',  ( -16.55341960407617563, 4.379528057220093196, 43.54275706135235424 ) ) ;
#31738 = CARTESIAN_POINT ( 'NONE',  ( 9.474510206698971260, -16.51473224551069308, 32.91557627198102409 ) ) ;
#31739 = CARTESIAN_POINT ( 'NONE',  ( -19.02544592524334988, -5.153800228976617603, 43.95942372801899012 ) ) ;
#31740 = CARTESIAN_POINT ( 'NONE',  ( -5.153800228976328057, -19.02544592524343514, 82.29057627198103830 ) ) ;
#31741 = CARTESIAN_POINT ( 'NONE',  ( 19.03943276465977164, -0.05219959533909143690, 53.74890960531436690 ) ) ;
#31742 = CARTESIAN_POINT ( 'NONE',  ( 20.49784845243110709, -5.510910596163089556E-15, 45.00000000000000000 ) ) ;
#31743 = CARTESIAN_POINT ( 'NONE',  ( 19.02544592524343514, -5.153800228976328945, 63.54057627198103830 ) ) ;
#31744 = CARTESIAN_POINT ( 'NONE',  ( -0.05219959533909027116, -19.03943276465977164, 92.49890960531436690 ) ) ;
#31745 = CARTESIAN_POINT ( 'NONE',  ( 19.05341960407617918, -5.049401038297876454, 31.04275706135232227 ) ) ;
#31746 = CARTESIAN_POINT ( 'NONE',  ( 5.153800228976615827, -19.02544592524334988, 20.20942372801899722 ) ) ;
#31747 = CARTESIAN_POINT ( 'NONE',  ( -16.55341960407611168, -4.379528057220339221, 36.45724293864768839 ) ) ;
#31748 = CARTESIAN_POINT ( 'NONE',  ( 19.05341960407611168, 5.049401038298154454, 48.95724293864768129 ) ) ;
#31749 = CARTESIAN_POINT ( 'NONE',  ( -9.564922557960796823, -16.46253265017161027, 102.0822429386477097 ) ) ;
#31750 = CARTESIAN_POINT ( 'NONE',  ( -15.72974639402176322, -15.80617190586768395, 89.37609039468568994 ) ) ;
#31751 = CARTESIAN_POINT ( 'NONE',  ( 16.46253265017160672, -9.564922557960803928, 48.33224293864769550 ) ) ;
#31752 = CARTESIAN_POINT ( 'NONE',  ( -21.55341960407619339, 5.719274019375674811, 83.54275706135234714 ) ) ;
#31753 = CARTESIAN_POINT ( 'NONE',  ( -5.823673210054116645, -21.52544592524344225, 27.29057627198103120 ) ) ;
#31754 = CARTESIAN_POINT ( 'NONE',  ( -10.72451020669870658, -18.67979575497194134, 19.58442372801901143 ) ) ;
#31755 = CARTESIAN_POINT ( 'NONE',  ( 5.153800228976615827, -19.02544592524334988, 45.20942372801901143 ) ) ;
#31756 = CARTESIAN_POINT ( 'NONE',  ( 13.97604488694527802, 13.89961937509977652, 29.37390960531435979 ) ) ;
#31757 = CARTESIAN_POINT ( 'NONE',  ( -19.03943276465977164, 0.05219959533909376836, 76.24890960531435269 ) ) ;
#31758 = CARTESIAN_POINT ( 'NONE',  ( 8.224510206698742110, 14.34966873604972548, 22.08442372801901143 ) ) ;
#31759 = CARTESIAN_POINT ( 'NONE',  ( 12.14591786802309770, 12.06949235617756955, 89.37390960531435269 ) ) ;
#31760 = CARTESIAN_POINT ( 'NONE',  ( 10.72451020669898902, -18.67979575497178502, 42.91557627198103120 ) ) ;
#31761 = CARTESIAN_POINT ( 'NONE',  ( 13.97604488694548053, -13.89961937509957401, 95.62609039468563310 ) ) ;
#31762 = CARTESIAN_POINT ( 'NONE',  ( 21.52544592524344225, -5.823673210054117533, 103.5405762719810383 ) ) ;
#31763 = CARTESIAN_POINT ( 'NONE',  ( -10.81492255796105439, 18.62759615963255655, 62.91775706135236135 ) ) ;
#31764 = CARTESIAN_POINT ( 'NONE',  ( 8.224510206698742110, 14.34966873604972548, 52.08442372801901854 ) ) ;
#31765 = CARTESIAN_POINT ( 'NONE',  ( -14.29746914071037622, -8.314922557961029526, 69.16775706135234714 ) ) ;
#31766 = CARTESIAN_POINT ( 'NONE',  ( -19.05341960407611168, -5.049401038298163336, 56.45724293864768129 ) ) ;
#31767 = CARTESIAN_POINT ( 'NONE',  ( 12.06949235617739724, 12.14591786802326823, 86.87609039468568994 ) ) ;
#31768 = AXIS2_PLACEMENT_3D ( 'NONE', #16962, #78615, #140290 ) ;
#31769 = CARTESIAN_POINT ( 'NONE',  ( -10.81492255796105439, 18.62759615963255655, 22.91775706135235069 ) ) ;
#31770 = CARTESIAN_POINT ( 'NONE',  ( -8.224510206698948167, 14.34966873604960824, 55.41557627198102409 ) ) ;
#31771 = CARTESIAN_POINT ( 'NONE',  ( -13.89961937509977652, 13.97604488694528158, 90.62390960531432427 ) ) ;
#31772 = CARTESIAN_POINT ( 'NONE',  ( 4.483927247898790824, -16.52544592524335698, 70.20942372801904696 ) ) ;
#31773 = CARTESIAN_POINT ( 'NONE',  ( -15.72974639402176322, -15.80617190586768395, 64.37609039468568994 ) ) ;
#31774 = CARTESIAN_POINT ( 'NONE',  ( -16.51473224551082808, 9.474510206698731452, 108.3344237280190043 ) ) ;
#31775 = CARTESIAN_POINT ( 'NONE',  ( -21.55341960407610458, -5.719274019375992779, 106.4572429386477097 ) ) ;
#31776 = CARTESIAN_POINT ( 'NONE',  ( 16.53943276465976808, -0.05219959533910856209, 48.74890960531435979 ) ) ;
#31777 = ORIENTED_EDGE ( 'NONE', *, *, #169612, .T. ) ;
#31778 = CARTESIAN_POINT ( 'NONE',  ( -17.05587630539787014, 6.762274262135696823, 75.74180309037312497 ) ) ;
#31779 = CARTESIAN_POINT ( 'NONE',  ( 5.823673210054125526, 21.52544592524343514, 89.79057627198103830 ) ) ;
#31780 = CARTESIAN_POINT ( 'NONE',  ( -16.53943276465976808, 0.05219959533911058130, 21.24890960531436690 ) ) ;
#31781 = VERTEX_POINT ( 'NONE', #194096 ) ;
#31782 = LINE ( 'NONE', #90464, #172810 ) ;
#31783 = CARTESIAN_POINT ( 'NONE',  ( -21.53943276465977519, 0.05219959533907696930, 116.2489096053143669 ) ) ;
#31784 = CARTESIAN_POINT ( 'NONE',  ( -13.97604488694527625, -13.89961937509977652, 111.8739096053143243 ) ) ;
#31785 = CARTESIAN_POINT ( 'NONE',  ( 5.823673210054444382, -21.52544592524334988, 30.20942372801902565 ) ) ;
#31786 = CARTESIAN_POINT ( 'NONE',  ( -16.52544592524342804, 4.483927247898546575, 51.04057627198103120 ) ) ;
#31787 = CARTESIAN_POINT ( 'NONE',  ( 12.14591786802327356, -12.06949235617739191, 65.62609039468568994 ) ) ;
#31788 = CARTESIAN_POINT ( 'NONE',  ( -19.03943276465977164, 0.05219959533909376836, 66.24890960531436690 ) ) ;
#31789 = CARTESIAN_POINT ( 'NONE',  ( -5.153800228976607833, 19.02544592524334988, 62.70942372801899722 ) ) ;
#31790 = CARTESIAN_POINT ( 'NONE',  ( -19.02544592524342804, 5.153800228976336051, 86.04057627198103830 ) ) ;
#31791 = CARTESIAN_POINT ( 'NONE',  ( 18.62759615963271287, -10.81492255796078972, 33.33224293864769550 ) ) ;
#31792 = CARTESIAN_POINT ( 'NONE',  ( -14.90098780495876696, -35.24605353402532160, -22.56189394118115743 ) ) ;
#31793 = CARTESIAN_POINT ( 'NONE',  ( -9.474510206698964154, 16.51473224551069663, 55.41557627198103120 ) ) ;
#31794 = CARTESIAN_POINT ( 'NONE',  ( 0.05219959533934541429, -16.53943276465976808, 30.00109039468568284 ) ) ;
#31795 = CARTESIAN_POINT ( 'NONE',  ( 16.51473224551083163, -9.474510206698727899, 60.83442372801900433 ) ) ;
#31796 = CARTESIAN_POINT ( 'NONE',  ( 0.05219959533907565091, 21.53943276465977519, 99.99890960531436690 ) ) ;
#31797 = CARTESIAN_POINT ( 'NONE',  ( 16.55341960407611168, 4.379528057220329451, 28.95724293864769905 ) ) ;
#31798 = CARTESIAN_POINT ( 'NONE',  ( 9.564922557960805705, 16.46253265017160317, 94.58224293864769550 ) ) ;
#31799 = CARTESIAN_POINT ( 'NONE',  ( 0.05219959533907565091, 21.53943276465977519, 59.99890960531436690 ) ) ;
#31801 = CARTESIAN_POINT ( 'NONE',  ( 8.314922557961029526, -14.29746914071037800, 35.41775706135234003 ) ) ;
#31800 = CARTESIAN_POINT ( 'NONE',  ( 21.53943276465977519, -0.05219959533907433946, 93.74890960531436690 ) ) ;
#31802 = CARTESIAN_POINT ( 'NONE',  ( 21.53943276465977519, -0.05219959533907433946, 33.74890960531436690 ) ) ;
#31803 = CARTESIAN_POINT ( 'NONE',  ( -5.719274019375665041, -21.55341960407619695, 94.79275706135234714 ) ) ;
#31804 = CARTESIAN_POINT ( 'NONE',  ( -13.97604488694527625, -13.89961937509977652, 91.87390960531432427 ) ) ;
#31805 = CARTESIAN_POINT ( 'NONE',  ( 9.564922557960805705, 16.46253265017160317, 39.58224293864768839 ) ) ;
#31806 = CARTESIAN_POINT ( 'NONE',  ( -16.51473224551069308, -9.474510206698971260, 86.66557627198102409 ) ) ;
#31807 = CARTESIAN_POINT ( 'NONE',  ( -12.14591786802309592, -12.06949235617757132, 101.8739096053143811 ) ) ;
#31808 = CARTESIAN_POINT ( 'NONE',  ( 19.02544592524343514, -5.153800228976328945, 58.54057627198102409 ) ) ;
#31809 = CARTESIAN_POINT ( 'NONE',  ( 4.379528057220092307, 16.55341960407617563, 27.29275706135234358 ) ) ;
#31810 = CARTESIAN_POINT ( 'NONE',  ( -16.51473224551082808, 9.474510206698731452, 43.33442372801900433 ) ) ;
#31812 = CARTESIAN_POINT ( 'NONE',  ( 16.51473224551069308, 9.474510206698969483, 109.1655762719810383 ) ) ;
#31811 = CARTESIAN_POINT ( 'NONE',  ( -0.05219959533937732626, 21.53943276465977519, 97.50109039468567573 ) ) ;
#31813 = CARTESIAN_POINT ( 'NONE',  ( 12.14591786802327356, -12.06949235617739191, 95.62609039468568994 ) ) ;
#31814 = CARTESIAN_POINT ( 'NONE',  ( 22.99604614807110181, -21.49604614807103786, -46.28618945597792589 ) ) ;
#31815 = CARTESIAN_POINT ( 'NONE',  ( -13.89961937509957401, -13.97604488694547875, 74.37609039468566152 ) ) ;
#31816 = CARTESIAN_POINT ( 'NONE',  ( 16.51473224551083163, -9.474510206698727899, 30.83442372801900433 ) ) ;
#31817 = CARTESIAN_POINT ( 'NONE',  ( 4.064918688780018385, 6.131632772416324428, -64.31816925299779086 ) ) ;
#31818 = CARTESIAN_POINT ( 'NONE',  ( -9.474510206698964154, 16.51473224551069663, 25.41557627198103120 ) ) ;
#31819 = CARTESIAN_POINT ( 'NONE',  ( 16.55341960407611168, 4.379528057220329451, 38.95724293864768839 ) ) ;
#31820 = EDGE_CURVE ( 'NONE', #6681, #171715, #66728, .T. ) ;
#31821 = CARTESIAN_POINT ( 'NONE',  ( -16.31925111598457434, -7.325300261831539039, 109.8357546103274700 ) ) ;
#31822 = CARTESIAN_POINT ( 'NONE',  ( 12.06949235617757843, -12.14591786802309237, 28.12390960531435979 ) ) ;
#31823 = CARTESIAN_POINT ( 'NONE',  ( 21.98965532995689642, -20.07258295882801491, -51.71301205850239313 ) ) ;
#31824 = CARTESIAN_POINT ( 'NONE',  ( -16.55341960407617563, 4.379528057220093196, 98.54275706135234714 ) ) ;
#31825 = CARTESIAN_POINT ( 'NONE',  ( 19.03943276465977164, -0.05219959533909143690, 38.74890960531436690 ) ) ;
#31826 = CARTESIAN_POINT ( 'NONE',  ( -5.823673210054431948, 21.52544592524334988, 92.70942372801901854 ) ) ;
#31827 = CARTESIAN_POINT ( 'NONE',  ( -13.97604488694547697, 13.89961937509957934, 113.1260903946856757 ) ) ;
#31828 = CARTESIAN_POINT ( 'NONE',  ( -10.72451020669870658, -18.67979575497194134, 74.58442372801901854 ) ) ;
#31829 = CARTESIAN_POINT ( 'NONE',  ( -19.05341960407617563, 5.049401038297882671, 48.54275706135233293 ) ) ;
#31830 = CARTESIAN_POINT ( 'NONE',  ( -5.049401038298153566, 19.05341960407611168, 90.20724293864766707 ) ) ;
#31831 = CARTESIAN_POINT ( 'NONE',  ( -9.564922557960796823, -16.46253265017161027, 77.08224293864769550 ) ) ;
#31832 = LINE ( 'NONE', #3461, #7749 ) ;
#31833 = CARTESIAN_POINT ( 'NONE',  ( -21.52544592524343514, 5.823673210054127303, 91.04057627198103830 ) ) ;
#31834 = CARTESIAN_POINT ( 'NONE',  ( -4.379528057220328563, 16.55341960407611168, 60.20724293864768839 ) ) ;
#31835 = CARTESIAN_POINT ( 'NONE',  ( -5.823673210054116645, -21.52544592524344225, 62.29057627198102409 ) ) ;
#31836 = CARTESIAN_POINT ( 'NONE',  ( 13.89961937509977652, -13.97604488694527269, 63.12390960531435979 ) ) ;
#31838 = CARTESIAN_POINT ( 'NONE',  ( 16.53943276465976808, 0.05219959533934440121, 81.25109039468568994 ) ) ;
#31837 = CARTESIAN_POINT ( 'NONE',  ( -5.823673210054116645, -21.52544592524344225, 87.29057627198103830 ) ) ;
#31839 = ORIENTED_EDGE ( 'NONE', *, *, #87024, .F. ) ;
#31840 = CARTESIAN_POINT ( 'NONE',  ( -16.46253265017160317, 9.564922557960807481, 40.83224293864769550 ) ) ;
#31842 = DIRECTION ( 'NONE',  ( -1.000000000000000000, -0.000000000000000000, 0.000000000000000000 ) ) ;
#31841 = CARTESIAN_POINT ( 'NONE',  ( 16.52544592524342804, -4.483927247898539470, 78.54057627198103830 ) ) ;
#31843 = CARTESIAN_POINT ( 'NONE',  ( -13.89961937509977652, 13.97604488694528158, 50.62390960531435979 ) ) ;
#31844 = CARTESIAN_POINT ( 'NONE',  ( -4.483927247898539470, -16.52544592524342804, 112.2905762719810241 ) ) ;
#31845 = CARTESIAN_POINT ( 'NONE',  ( 9.564922557961047289, -16.46253265017146816, 60.41775706135233293 ) ) ;
#31846 = CARTESIAN_POINT ( 'NONE',  ( -12.06949235617756955, 12.14591786802309770, 90.62390960531436690 ) ) ;
#31847 = CARTESIAN_POINT ( 'NONE',  ( 10.72451020669871369, 18.67979575497193778, 42.08442372801901854 ) ) ;
#31849 = CARTESIAN_POINT ( 'NONE',  ( 0.05219959533907565091, 21.53943276465977519, 99.99890960531436690 ) ) ;
#31848 = CARTESIAN_POINT ( 'NONE',  ( -19.03943276465977164, 0.05219959533909376836, 36.24890960531436690 ) ) ;
#31850 = CARTESIAN_POINT ( 'NONE',  ( -16.55341960407611168, -4.379528057220339221, 86.45724293864770971 ) ) ;
#31851 = CARTESIAN_POINT ( 'NONE',  ( 25.79201298823733879, -30.25621121864868357, -20.58051720723745248 ) ) ;
#31852 = CARTESIAN_POINT ( 'NONE',  ( -0.05219959533909027116, -19.03943276465977164, 47.49890960531435979 ) ) ;
#31853 = CARTESIAN_POINT ( 'NONE',  ( 17.49999999999998224, 5.622605283950877109, 113.8120731059611188 ) ) ;
#31855 = CARTESIAN_POINT ( 'NONE',  ( -5.153800228976328057, -19.02544592524343514, 97.29057627198099567 ) ) ;
#31854 = CARTESIAN_POINT ( 'NONE',  ( 16.46253265017146816, 9.564922557961045513, 91.66775706135234714 ) ) ;
#31856 = CARTESIAN_POINT ( 'NONE',  ( 5.719274019375673035, 21.55341960407619339, 42.29275706135235424 ) ) ;
#31857 = CARTESIAN_POINT ( 'NONE',  ( -5.153800228976328057, -19.02544592524343514, 87.29057627198103830 ) ) ;
#31858 = CARTESIAN_POINT ( 'NONE',  ( -5.153800228976607833, 19.02544592524334988, 67.70942372801900433 ) ) ;
#31859 = CARTESIAN_POINT ( 'NONE',  ( 9.564922557960805705, 16.46253265017160317, 49.58224293864770260 ) ) ;
#31860 = CARTESIAN_POINT ( 'NONE',  ( -14.29746914071049879, 8.314922557960819915, 75.83224293864769550 ) ) ;
#31861 = CARTESIAN_POINT ( 'NONE',  ( -4.379528057220328563, 16.55341960407611168, 70.20724293864769550 ) ) ;
#31862 = CARTESIAN_POINT ( 'NONE',  ( 5.153800228976335163, 19.02544592524342804, 79.79057627198102409 ) ) ;
#31863 = CARTESIAN_POINT ( 'NONE',  ( 5.823673210054125526, 21.52544592524343514, 94.79057627198105251 ) ) ;
#31864 = CARTESIAN_POINT ( 'NONE',  ( 19.05341960407611168, 5.049401038298154454, 68.95724293864769550 ) ) ;
#31865 = CARTESIAN_POINT ( 'NONE',  ( 13.97604488694548053, -13.89961937509957401, 35.62609039468567573 ) ) ;
#31868 = CARTESIAN_POINT ( 'NONE',  ( -16.52544592524342804, 4.483927247898546575, 111.0405762719810525 ) ) ;
#31867 = CARTESIAN_POINT ( 'NONE',  ( 14.29746914071049879, -8.314922557960816363, 33.33224293864769550 ) ) ;
#31866 = CARTESIAN_POINT ( 'NONE',  ( 5.049401038298161559, -19.05341960407611168, 32.70724293864768129 ) ) ;
#31869 = CARTESIAN_POINT ( 'NONE',  ( -16.46253265017146816, -9.564922557961047289, 104.1677570613523329 ) ) ;
#31870 = ORIENTED_EDGE ( 'NONE', *, *, #16216, .T. ) ;
#31871 = CARTESIAN_POINT ( 'NONE',  ( 5.719274019375673035, 21.55341960407619339, 27.29275706135234358 ) ) ;
#31872 = CARTESIAN_POINT ( 'NONE',  ( 16.46253265017146816, 9.564922557961045513, 66.66775706135233293 ) ) ;
#31873 = CARTESIAN_POINT ( 'NONE',  ( -4.483927247898539470, -16.52544592524342804, 22.29057627198102765 ) ) ;
#31874 = CARTESIAN_POINT ( 'NONE',  ( -5.823673210054116645, -21.52544592524344225, 82.29057627198103830 ) ) ;
#31875 = CARTESIAN_POINT ( 'NONE',  ( -21.55341960407610458, -5.719274019375992779, 26.45724293864768839 ) ) ;
#31876 = CARTESIAN_POINT ( 'NONE',  ( 12.14591786802309770, 12.06949235617756955, 59.37390960531436690 ) ) ;
#31877 = CARTESIAN_POINT ( 'NONE',  ( -9.474510206698964154, 16.51473224551069663, 35.41557627198102409 ) ) ;
#31878 = CARTESIAN_POINT ( 'NONE',  ( 19.05341960407617918, -5.049401038297876454, 31.04275706135232227 ) ) ;
#31879 = CARTESIAN_POINT ( 'NONE',  ( -12.06949235617739369, -12.14591786802326823, 84.37609039468570415 ) ) ;
#31880 = CARTESIAN_POINT ( 'NONE',  ( 12.14591786802327356, -12.06949235617739191, 55.62609039468568284 ) ) ;
#31881 = CARTESIAN_POINT ( 'NONE',  ( -18.67979575497178146, -10.72451020669898902, 26.66557627198103475 ) ) ;
#31882 = CARTESIAN_POINT ( 'NONE',  ( 18.62759615963255655, 10.81492255796105972, 106.6677570613523756 ) ) ;
#31883 = CARTESIAN_POINT ( 'NONE',  ( 0.05219959533909260263, 19.03943276465977164, 84.99890960531436690 ) ) ;
#31884 = CARTESIAN_POINT ( 'NONE',  ( -8.224510206698735004, -14.34966873604973081, 54.58442372801901143 ) ) ;
#31885 = CARTESIAN_POINT ( 'NONE',  ( 0.05219959533909260263, 19.03943276465977164, 24.99890960531435269 ) ) ;
#31886 = CARTESIAN_POINT ( 'NONE',  ( 12.06949235617757843, -12.14591786802309237, 33.12390960531435979 ) ) ;
#31887 = DIRECTION ( 'NONE',  ( 0.7071067811865483499, 0.000000000000000000, 0.7071067811865465735 ) ) ;
#31890 = CARTESIAN_POINT ( 'NONE',  ( 9.564922557960805705, 16.46253265017160317, 74.58224293864769550 ) ) ;
#31889 = CARTESIAN_POINT ( 'NONE',  ( -19.02544592524342804, 5.153800228976336051, 96.04057627198103830 ) ) ;
#31888 = CARTESIAN_POINT ( 'NONE',  ( -5.719274019375665041, -21.55341960407619695, 69.79275706135234714 ) ) ;
#31891 = CARTESIAN_POINT ( 'NONE',  ( -13.89961937509977652, 13.97604488694528158, 105.6239096053143527 ) ) ;
#31892 = CARTESIAN_POINT ( 'NONE',  ( -4.483927247898539470, -16.52544592524342804, 52.29057627198102409 ) ) ;
#31893 = CARTESIAN_POINT ( 'NONE',  ( -12.14591786802309592, -12.06949235617757132, 31.87390960531435979 ) ) ;
#31894 = ORIENTED_EDGE ( 'NONE', *, *, #189089, .F. ) ;
#31895 = CARTESIAN_POINT ( 'NONE',  ( -16.53943276465976808, 0.05219959533911058130, 51.24890960531436690 ) ) ;
#31897 = CARTESIAN_POINT ( 'NONE',  ( 5.199999999999996625, 0.000000000000000000, 0.000000000000000000 ) ) ;
#31896 = CARTESIAN_POINT ( 'NONE',  ( 8.224510206698742110, 14.34966873604972548, 37.08442372801901143 ) ) ;
#31898 = CARTESIAN_POINT ( 'NONE',  ( 9.564922557961047289, -16.46253265017146816, 45.41775706135232582 ) ) ;
#31899 = CARTESIAN_POINT ( 'NONE',  ( -5.049401038298153566, 19.05341960407611168, 70.20724293864769550 ) ) ;
#31900 = CARTESIAN_POINT ( 'NONE',  ( 5.049401038297881783, 19.05341960407617563, 47.29275706135231161 ) ) ;
#31901 = CARTESIAN_POINT ( 'NONE',  ( 19.02544592524334988, 5.153800228976608722, 51.45942372801900433 ) ) ;
#31903 = CARTESIAN_POINT ( 'NONE',  ( 14.29746914071037800, 8.314922557961029526, 86.66775706135234714 ) ) ;
#31902 = CARTESIAN_POINT ( 'NONE',  ( 16.46253265017146816, 9.564922557961045513, 91.66775706135234714 ) ) ;
#31904 = CARTESIAN_POINT ( 'NONE',  ( -22.44159573604010305, 16.30477369853692338, 143.1750000027311671 ) ) ;
#31905 = CARTESIAN_POINT ( 'NONE',  ( 13.89961937509977652, -13.97604488694527269, 28.12390960531435624 ) ) ;
#31906 = CARTESIAN_POINT ( 'NONE',  ( -13.89961937509977652, 13.97604488694528158, 110.6239096053143243 ) ) ;
#31907 = CARTESIAN_POINT ( 'NONE',  ( -18.67979575497193778, 10.72451020669871902, 38.33442372801900433 ) ) ;
#31908 = CARTESIAN_POINT ( 'NONE',  ( 19.05341960407617918, -5.049401038297876454, 86.04275706135233293 ) ) ;
#31910 = CARTESIAN_POINT ( 'NONE',  ( -0.05219959533909027116, -19.03943276465977164, 67.49890960531436690 ) ) ;
#31909 = CARTESIAN_POINT ( 'NONE',  ( 30.74264578624799782, 22.33583958711400541, -2.799999999999999822 ) ) ;
#31911 = CARTESIAN_POINT ( 'NONE',  ( 19.02544592524343514, -5.153800228976328945, 103.5405762719809957 ) ) ;
#31913 = CARTESIAN_POINT ( 'NONE',  ( -19.03943276465977164, 0.05219959533909376836, 61.24890960531436690 ) ) ;
#31912 = CARTESIAN_POINT ( 'NONE',  ( -8.314922557960811034, -14.29746914071050412, 62.08224293864769550 ) ) ;
#31914 = CARTESIAN_POINT ( 'NONE',  ( 19.03943276465977164, -0.05219959533909143690, 58.74890960531435979 ) ) ;
#31915 = CARTESIAN_POINT ( 'NONE',  ( 16.46253265017146816, 9.564922557961045513, 81.66775706135233293 ) ) ;
#31916 = CARTESIAN_POINT ( 'NONE',  ( -18.67979575497178146, -10.72451020669898902, 46.66557627198102409 ) ) ;
#31917 = CARTESIAN_POINT ( 'NONE',  ( -19.03943276465977164, -0.05219959533935918106, 48.75109039468566863 ) ) ;
#31918 = CARTESIAN_POINT ( 'NONE',  ( -9.564922557960796823, -16.46253265017161027, 77.08224293864769550 ) ) ;
#31919 = CARTESIAN_POINT ( 'NONE',  ( 10.72451020669898902, -18.67979575497178502, 82.91557627198103830 ) ) ;
#31921 = CARTESIAN_POINT ( 'NONE',  ( 16.51473224551083163, -9.474510206698727899, 35.83442372801899722 ) ) ;
#31920 = CARTESIAN_POINT ( 'NONE',  ( -14.29746914071049879, 8.314922557960819915, 80.83224293864769550 ) ) ;
#31922 = CARTESIAN_POINT ( 'NONE',  ( -18.67979575497178146, -10.72451020669898902, 41.66557627198103120 ) ) ;
#31923 = CARTESIAN_POINT ( 'NONE',  ( -10.72451020669898014, 18.67979575497178502, 40.41557627198103120 ) ) ;
#31924 = CARTESIAN_POINT ( 'NONE',  ( 16.46253265017160672, -9.564922557960803928, 68.33224293864770971 ) ) ;
#31925 = CARTESIAN_POINT ( 'NONE',  ( 5.153800228976335163, 19.02544592524342804, 54.79057627198103120 ) ) ;
#31926 = CARTESIAN_POINT ( 'NONE',  ( 16.55341960407611168, 4.379528057220329451, 108.9572429386476955 ) ) ;
#31927 = CARTESIAN_POINT ( 'NONE',  ( 10.81492255796106328, -18.62759615963255655, 30.41775706135234358 ) ) ;
#31928 = CARTESIAN_POINT ( 'NONE',  ( -16.46253265017160317, 9.564922557960807481, 110.8322429386476955 ) ) ;
#31929 = CARTESIAN_POINT ( 'NONE',  ( 18.62759615963255655, 10.81492255796105972, 36.66775706135234714 ) ) ;
#31930 = CARTESIAN_POINT ( 'NONE',  ( 16.51473224551069308, 9.474510206698969483, 34.16557627198102409 ) ) ;
#31931 = CARTESIAN_POINT ( 'NONE',  ( -21.52544592524343514, 5.823673210054127303, 111.0405762719810525 ) ) ;
#31932 = CARTESIAN_POINT ( 'NONE',  ( -9.564922557961040184, 16.46253265017147172, 52.91775706135233293 ) ) ;
#31933 = CARTESIAN_POINT ( 'NONE',  ( 17.97182807773871360, -5.500000000000043521, 76.03038844047287625 ) ) ;
#31934 = CARTESIAN_POINT ( 'NONE',  ( -3.573655867282028392E-15, 2.428612866367529932E-14, -25.00000000000000000 ) ) ;
#31935 = LINE ( 'NONE', #28973, #127387 ) ;
#31936 = CARTESIAN_POINT ( 'NONE',  ( -16.52544592524335698, -4.483927247898792601, 53.95942372801900433 ) ) ;
#31937 = CARTESIAN_POINT ( 'NONE',  ( -0.05219959533909027116, -19.03943276465977164, 32.49890960531435979 ) ) ;
#31938 = CARTESIAN_POINT ( 'NONE',  ( -26.26139018963107929, -3.005588016160666953, 174.9127113745526572 ) ) ;
#31939 = CARTESIAN_POINT ( 'NONE',  ( -9.564922557960796823, -16.46253265017161027, 67.08224293864769550 ) ) ;
#31940 = CARTESIAN_POINT ( 'NONE',  ( 14.29746914071049879, -8.314922557960816363, 108.3322429386477097 ) ) ;
#31941 = CARTESIAN_POINT ( 'NONE',  ( -15.72974639402197994, 15.80617190586746368, 65.62390960531436690 ) ) ;
#31942 = CARTESIAN_POINT ( 'NONE',  ( -16.53943276465976808, 0.05219959533911058130, 81.24890960531436690 ) ) ;
#31943 = CARTESIAN_POINT ( 'NONE',  ( 16.53943276465976808, 0.05219959533934440121, 31.25109039468568639 ) ) ;
#31944 = CARTESIAN_POINT ( 'NONE',  ( 15.80617190586769283, -15.72974639402175789, 85.62609039468568994 ) ) ;
#31945 = CARTESIAN_POINT ( 'NONE',  ( -16.51473224551069308, -9.474510206698971260, 31.66557627198102054 ) ) ;
#31946 = CARTESIAN_POINT ( 'NONE',  ( -8.314922557960811034, -14.29746914071050412, 22.08224293864769194 ) ) ;
#31947 = CARTESIAN_POINT ( 'NONE',  ( -4.483927247898539470, -16.52544592524342804, 52.29057627198102409 ) ) ;
#31948 = CARTESIAN_POINT ( 'NONE',  ( -19.05341960407611168, -5.049401038298163336, 56.45724293864768129 ) ) ;
#31949 = CARTESIAN_POINT ( 'NONE',  ( 10.81492255796106328, -18.62759615963255655, 95.41775706135234714 ) ) ;
#31950 = CARTESIAN_POINT ( 'NONE',  ( 10.72451020669898902, -18.67979575497178502, 102.9155762719810383 ) ) ;
#31951 = CARTESIAN_POINT ( 'NONE',  ( -15.72974639402176322, -15.80617190586768395, 79.37609039468567573 ) ) ;
#31952 = CARTESIAN_POINT ( 'NONE',  ( -0.05219959533934338120, 16.53943276465976808, 47.50109039468568994 ) ) ;
#31954 = CARTESIAN_POINT ( 'NONE',  ( -10.72451020669870658, -18.67979575497194134, 79.58442372801903275 ) ) ;
#31953 = CARTESIAN_POINT ( 'NONE',  ( -4.483927247898539470, -16.52544592524342804, 72.29057627198102409 ) ) ;
#31955 = CARTESIAN_POINT ( 'NONE',  ( -4.379528057220328563, 16.55341960407611168, 25.20724293864769550 ) ) ;
#31956 = CARTESIAN_POINT ( 'NONE',  ( -17.49999999999999645, 5.499999999999996447, 113.7176903769643417 ) ) ;
#31957 = CARTESIAN_POINT ( 'NONE',  ( -16.55341960407617563, 4.379528057220093196, 43.54275706135235424 ) ) ;
#31958 = CARTESIAN_POINT ( 'NONE',  ( -14.34966873604960291, -8.224510206698953496, 41.66557627198103120 ) ) ;
#31959 = CARTESIAN_POINT ( 'NONE',  ( -0.05219959533934338120, 16.53943276465976808, 92.50109039468567573 ) ) ;
#31960 = CARTESIAN_POINT ( 'NONE',  ( 5.153800228976335163, 19.02544592524342804, 104.7905762719809957 ) ) ;
#31961 = CARTESIAN_POINT ( 'NONE',  ( 16.51473224551069308, 9.474510206698969483, 109.1655762719810383 ) ) ;
#31962 = CARTESIAN_POINT ( 'NONE',  ( -21.52544592524334988, -5.823673210054445271, 103.9594237280190185 ) ) ;
#31963 = CARTESIAN_POINT ( 'NONE',  ( -14.34966873604972548, 8.224510206698743886, 98.33442372801901854 ) ) ;
#31964 = CARTESIAN_POINT ( 'NONE',  ( 4.483927247898545687, 16.52544592524342804, 74.79057627198105251 ) ) ;
#31965 = CARTESIAN_POINT ( 'NONE',  ( -9.474510206698964154, 16.51473224551069663, 75.41557627198103830 ) ) ;
#31966 = VERTEX_POINT ( 'NONE', #51560 ) ;
#31967 = CARTESIAN_POINT ( 'NONE',  ( 4.379528057220092307, 16.55341960407617563, 22.29275706135235069 ) ) ;
#31968 = CARTESIAN_POINT ( 'NONE',  ( 19.05341960407611168, 5.049401038298154454, 23.95724293864769194 ) ) ;
#31969 = CARTESIAN_POINT ( 'NONE',  ( -13.89961937509977652, 13.97604488694528158, 85.62390960531433848 ) ) ;
#31971 = CARTESIAN_POINT ( 'NONE',  ( 22.81625015709509441, 31.40387420917330275, -1.324999997268813123 ) ) ;
#31970 = CARTESIAN_POINT ( 'NONE',  ( 16.55341960407618274, -4.379528057220086978, 26.04275706135235779 ) ) ;
#31972 = CARTESIAN_POINT ( 'NONE',  ( 19.03943276465977164, 0.05219959533936151252, 31.25109039468566863 ) ) ;
#31973 = CARTESIAN_POINT ( 'NONE',  ( 16.52544592524335698, 4.483927247898782831, 91.45942372801901854 ) ) ;
#31974 = CARTESIAN_POINT ( 'NONE',  ( -16.51473224551082808, 9.474510206698731452, 103.3344237280190043 ) ) ;
#31975 = CARTESIAN_POINT ( 'NONE',  ( 19.05341960407611168, 5.049401038298154454, 28.95724293864769550 ) ) ;
#31976 = CARTESIAN_POINT ( 'NONE',  ( 12.06949235617739724, 12.14591786802326823, 76.87609039468567573 ) ) ;
#31977 = CARTESIAN_POINT ( 'NONE',  ( -12.06949235617739369, -12.14591786802326823, 64.37609039468568994 ) ) ;
#31978 = CARTESIAN_POINT ( 'NONE',  ( 9.474510206698729675, 16.51473224551082808, 82.08442372801899012 ) ) ;
#31979 = CARTESIAN_POINT ( 'NONE',  ( -21.55341960407619339, 5.719274019375674811, 113.5427570613523756 ) ) ;
#31980 = CARTESIAN_POINT ( 'NONE',  ( -19.03943276465977164, 0.05219959533909376836, 46.24890960531435979 ) ) ;
#31981 = CARTESIAN_POINT ( 'NONE',  ( 0.05219959533909260263, 19.03943276465977164, 89.99890960531436690 ) ) ;
#31982 = CARTESIAN_POINT ( 'NONE',  ( 16.52544592524342804, -4.483927247898539470, 83.54057627198102409 ) ) ;
#31983 = CARTESIAN_POINT ( 'NONE',  ( -13.89961937509957401, -13.97604488694547875, 49.37609039468567573 ) ) ;
#31984 = CARTESIAN_POINT ( 'NONE',  ( 15.80617190586746368, 15.72974639402197994, 44.37390960531435979 ) ) ;
#31985 = CARTESIAN_POINT ( 'NONE',  ( 19.03943276465977164, 0.05219959533936151252, 26.25109039468566507 ) ) ;
#31986 = CARTESIAN_POINT ( 'NONE',  ( 13.89961937509977652, -13.97604488694527269, 93.12390960531436690 ) ) ;
#31987 = CARTESIAN_POINT ( 'NONE',  ( 18.67979575497178502, 10.72451020669898547, 74.16557627198102409 ) ) ;
#31988 = CARTESIAN_POINT ( 'NONE',  ( 9.564922557960805705, 16.46253265017160317, 109.5822429386476955 ) ) ;
#31989 = CARTESIAN_POINT ( 'NONE',  ( -9.564922557961040184, 16.46253265017147172, 87.91775706135233293 ) ) ;
#31990 = CARTESIAN_POINT ( 'NONE',  ( 16.51473224551069308, 9.474510206698969483, 114.1655762719810241 ) ) ;
#31991 = CARTESIAN_POINT ( 'NONE',  ( 13.89961937509957401, 13.97604488694547697, 106.8760903946856757 ) ) ;
#31992 = CARTESIAN_POINT ( 'NONE',  ( 19.05341960407611168, 5.049401038298154454, 28.95724293864769550 ) ) ;
#31993 = CARTESIAN_POINT ( 'NONE',  ( 0.05219959533909260263, 19.03943276465977164, 99.99890960531436690 ) ) ;
#31994 = CARTESIAN_POINT ( 'NONE',  ( -10.72451020669898014, 18.67979575497178502, 70.41557627198102409 ) ) ;
#31995 = VECTOR ( 'NONE', #149468, 1000.000000000000114 ) ;
#31996 = CARTESIAN_POINT ( 'NONE',  ( 0.05219959533934541429, -16.53943276465976808, 45.00109039468568284 ) ) ;
#31997 = CARTESIAN_POINT ( 'NONE',  ( 10.72451020669871369, 18.67979575497193778, 52.08442372801901854 ) ) ;
#31999 = CARTESIAN_POINT ( 'NONE',  ( 15.72974639402176855, 15.80617190586768217, 96.87609039468568994 ) ) ;
#31998 = CARTESIAN_POINT ( 'NONE',  ( -0.05219959533936034679, 19.03943276465977164, 87.50109039468567573 ) ) ;
#32000 = CARTESIAN_POINT ( 'NONE',  ( 4.379528057220092307, 16.55341960407617563, 102.2927570613523613 ) ) ;
#32001 = CARTESIAN_POINT ( 'NONE',  ( -9.564922557960796823, -16.46253265017161027, 102.0822429386477097 ) ) ;
#32002 = CARTESIAN_POINT ( 'NONE',  ( 0.05219959533910956823, 16.53943276465976808, 89.99890960531438111 ) ) ;
#32003 = CARTESIAN_POINT ( 'NONE',  ( -12.14591786802309592, -12.06949235617757132, 36.87390960531435979 ) ) ;
#32004 = CARTESIAN_POINT ( 'NONE',  ( -13.97604488694547697, 13.89961937509957934, 68.12609039468563310 ) ) ;
#32005 = CARTESIAN_POINT ( 'NONE',  ( -15.80617190586768217, 15.72974639402176855, 63.12609039468568994 ) ) ;
#32006 = CARTESIAN_POINT ( 'NONE',  ( -9.564922557961040184, 16.46253265017147172, 22.91775706135233648 ) ) ;
#32007 = CARTESIAN_POINT ( 'NONE',  ( -0.05219959533910754901, -16.53943276465976808, 102.4989096053143811 ) ) ;
#32008 = CARTESIAN_POINT ( 'NONE',  ( 15.72974639402199770, -15.80617190586745480, 28.12390960531435979 ) ) ;
#32009 = CARTESIAN_POINT ( 'NONE',  ( -12.14591786802309592, -12.06949235617757132, 21.87390960531436690 ) ) ;
#32010 = CARTESIAN_POINT ( 'NONE',  ( -15.72974639402176322, -15.80617190586768395, 99.37609039468568994 ) ) ;
#32011 = CARTESIAN_POINT ( 'NONE',  ( -16.52544592524335698, -4.483927247898792601, 53.95942372801900433 ) ) ;
#32012 = CARTESIAN_POINT ( 'NONE',  ( 16.52544592524342804, -4.483927247898539470, 33.54057627198102409 ) ) ;
#32013 = CARTESIAN_POINT ( 'NONE',  ( 15.72974639402176855, 15.80617190586768217, 46.87609039468568994 ) ) ;
#32014 = CARTESIAN_POINT ( 'NONE',  ( -15.72974639402176322, -15.80617190586768395, 54.37609039468568994 ) ) ;
#32015 = ORIENTED_EDGE ( 'NONE', *, *, #106786, .T. ) ;
#32016 = CARTESIAN_POINT ( 'NONE',  ( 38.00000000000000711, -12.34694845685040754, -6.849999994537626868 ) ) ;
#32017 = CARTESIAN_POINT ( 'NONE',  ( -21.53943276465977519, -0.05219959533937600094, 23.75109039468567929 ) ) ;
#32018 = CARTESIAN_POINT ( 'NONE',  ( 14.29746914071049879, -8.314922557960816363, 108.3322429386477097 ) ) ;
#32019 = CARTESIAN_POINT ( 'NONE',  ( 19.96322699617727636, 3.697860406115289322, 37.49999999999999289 ) ) ;
#32020 = CARTESIAN_POINT ( 'NONE',  ( 12.14591786802309770, 12.06949235617756955, 79.37390960531436690 ) ) ;
#32021 = CARTESIAN_POINT ( 'NONE',  ( -16.51473224551069308, -9.474510206698971260, 66.66557627198102409 ) ) ;
#32022 = CARTESIAN_POINT ( 'NONE',  ( 8.314922557961029526, -14.29746914071037800, 105.4177570613523613 ) ) ;
#32023 = CARTESIAN_POINT ( 'NONE',  ( -15.80617190586745835, -15.72974639402198527, 61.87390960531436690 ) ) ;
#32024 = CARTESIAN_POINT ( 'NONE',  ( 14.29746914071049879, -8.314922557960816363, 88.33224293864769550 ) ) ;
#32025 = CARTESIAN_POINT ( 'NONE',  ( 21.52544592524344225, -5.823673210054117533, 93.54057627198103830 ) ) ;
#32026 = CARTESIAN_POINT ( 'NONE',  ( 9.564922557960805705, 16.46253265017160317, 104.5822429386476955 ) ) ;
#32028 = CARTESIAN_POINT ( 'NONE',  ( 0.05219959533936267826, -19.03943276465977164, 105.0010903946856615 ) ) ;
#32027 = CARTESIAN_POINT ( 'NONE',  ( 19.05341960407611168, 5.049401038298154454, 53.95724293864770260 ) ) ;
#32029 = CARTESIAN_POINT ( 'NONE',  ( 0.05219959533907565091, 21.53943276465977519, 49.99890960531437401 ) ) ;
#32030 = CARTESIAN_POINT ( 'NONE',  ( -21.52544592524334988, -5.823673210054445271, 63.95942372801901854 ) ) ;
#32031 = B_SPLINE_CURVE_WITH_KNOTS ( 'NONE', 3,
 ( #9577, #147086, #87403, #177436, #54074, #83390, #25757, #69235, #38906, #6548, #132907, #37905, #68227, #23743, #22739, #133916, #55069, #53058, #36889, #85393, #56065, #72239 ),
 .UNSPECIFIED., .F., .F.,
 ( 4, 2, 2, 2, 2, 2, 2, 2, 2, 2, 4 ),
 ( 0.000000000000000000, 0.001309639967555296328, 0.001964459951332936903, 0.002291869943221747433, 0.002455574939166153131, 0.002619279935110557962, 0.002782984931054963227, 0.002946689926999368058, 0.003274099918888177720, 0.003928919902665816560, 0.005238559870221097710 ),
 .UNSPECIFIED. ) ;
#32032 = CARTESIAN_POINT ( 'NONE',  ( -0.05219959533909027116, -19.03943276465977164, 62.49890960531435979 ) ) ;
#32033 = CARTESIAN_POINT ( 'NONE',  ( -9.474510206698964154, 16.51473224551069663, 95.41557627198102409 ) ) ;
#32034 = CARTESIAN_POINT ( 'NONE',  ( -12.14591786802326823, 12.06949235617739902, 63.12609039468568994 ) ) ;
#32035 = CARTESIAN_POINT ( 'NONE',  ( -10.81492255796105439, 18.62759615963255655, 52.91775706135235424 ) ) ;
#32036 = CARTESIAN_POINT ( 'NONE',  ( 5.719274019375673035, 21.55341960407619339, 87.29275706135236135 ) ) ;
#32037 = CARTESIAN_POINT ( 'NONE',  ( 5.823673210054125526, 21.52544592524343514, 94.79057627198105251 ) ) ;
#32039 = CARTESIAN_POINT ( 'NONE',  ( -4.379528057220086978, -16.55341960407618274, 84.79275706135234714 ) ) ;
#32038 = CARTESIAN_POINT ( 'NONE',  ( 5.719274019375673035, 21.55341960407619339, 37.29275706135235424 ) ) ;
#32040 = CARTESIAN_POINT ( 'NONE',  ( -18.62759615963270932, 10.81492255796079327, 80.83224293864769550 ) ) ;
#32041 = CARTESIAN_POINT ( 'NONE',  ( -13.89961937509957401, -13.97604488694547875, 39.37609039468566152 ) ) ;
#32043 = CARTESIAN_POINT ( 'NONE',  ( 14.29746914071049879, -8.314922557960816363, 28.33224293864769550 ) ) ;
#32042 = CARTESIAN_POINT ( 'NONE',  ( 13.89961937509977652, -13.97604488694527269, 83.12390960531436690 ) ) ;
#32044 = LINE ( 'NONE', #124028, #88561 ) ;
#32045 = CARTESIAN_POINT ( 'NONE',  ( -5.153800228976328057, -19.02544592524343514, 107.2905762719810383 ) ) ;
#32046 = FACE_OUTER_BOUND ( 'NONE', #54152, .T. ) ;
#32047 = CARTESIAN_POINT ( 'NONE',  ( 19.02544592524334988, 5.153800228976608722, 91.45942372801900433 ) ) ;
#32048 = CARTESIAN_POINT ( 'NONE',  ( 0.05219959533907565091, 21.53943276465977519, 74.99890960531435269 ) ) ;
#32049 = CARTESIAN_POINT ( 'NONE',  ( -4.483927247898539470, -16.52544592524342804, 42.29057627198103120 ) ) ;
#32050 = CARTESIAN_POINT ( 'NONE',  ( 5.049401038297881783, 19.05341960407617563, 107.2927570613523187 ) ) ;
#32051 = CARTESIAN_POINT ( 'NONE',  ( -16.46253265017160317, 9.564922557960807481, 30.83224293864769550 ) ) ;
#32052 = CARTESIAN_POINT ( 'NONE',  ( -5.153800228976607833, 19.02544592524334988, 107.7094237280189759 ) ) ;
#32054 = CARTESIAN_POINT ( 'NONE',  ( 5.153800228976615827, -19.02544592524334988, 75.20942372801896170 ) ) ;
#32053 = CARTESIAN_POINT ( 'NONE',  ( 10.81492255796078972, 18.62759615963270932, 104.5822429386477097 ) ) ;
#32055 = CARTESIAN_POINT ( 'NONE',  ( -14.29746914071037622, -8.314922557961029526, 84.16775706135234714 ) ) ;
#32056 = CARTESIAN_POINT ( 'NONE',  ( -9.564922557960796823, -16.46253265017161027, 67.08224293864769550 ) ) ;
#32057 = CARTESIAN_POINT ( 'NONE',  ( 8.224510206698953496, -14.34966873604960469, 77.91557627198102409 ) ) ;
#32058 = EDGE_CURVE ( 'NONE', #162084, #199519, #53553, .T. ) ;
#32059 = CARTESIAN_POINT ( 'NONE',  ( 19.05341960407611168, 5.049401038298154454, 58.95724293864768129 ) ) ;
#32060 = CARTESIAN_POINT ( 'NONE',  ( -12.06949235617756955, 12.14591786802309770, 70.62390960531436690 ) ) ;
#32061 = DIRECTION ( 'NONE',  ( 0.000000000000000000, 0.000000000000000000, 1.000000000000000000 ) ) ;
#32062 = CARTESIAN_POINT ( 'NONE',  ( -36.99122028029232467, -5.215067209438918105, 43.21662174228439568 ) ) ;
#32063 = CARTESIAN_POINT ( 'NONE',  ( 4.379528057220339221, -16.55341960407611168, 37.70724293864769550 ) ) ;
#32064 = CARTESIAN_POINT ( 'NONE',  ( -19.05341960407611168, -5.049401038298163336, 71.45724293864766707 ) ) ;
#32065 = FACE_BOUND ( 'NONE', #198523, .T. ) ;
#32066 = CARTESIAN_POINT ( 'NONE',  ( 16.51473224551083163, -9.474510206698727899, 55.83442372801899722 ) ) ;
#32067 = CARTESIAN_POINT ( 'NONE',  ( 16.55341960407618274, -4.379528057220086978, 56.04275706135235424 ) ) ;
#32068 = CARTESIAN_POINT ( 'NONE',  ( -0.05219959533907301413, -21.53943276465977519, 62.49890960531436690 ) ) ;
#32069 = CARTESIAN_POINT ( 'NONE',  ( -16.46253265017146816, -9.564922557961047289, 29.16775706135232937 ) ) ;
#32070 = CARTESIAN_POINT ( 'NONE',  ( -19.02544592524342804, 5.153800228976336051, 86.04057627198103830 ) ) ;
#32071 = CARTESIAN_POINT ( 'NONE',  ( -19.99604614807109826, -21.65519653700129155, -48.98449577164771540 ) ) ;
#32072 = CARTESIAN_POINT ( 'NONE',  ( 9.474510206698971260, -16.51473224551069308, 112.9155762719810383 ) ) ;
#32073 = CARTESIAN_POINT ( 'NONE',  ( 13.97604488694527802, 13.89961937509977652, 64.37390960531436690 ) ) ;
#32074 = CARTESIAN_POINT ( 'NONE',  ( 18.62759615963255655, 10.81492255796105972, 36.66775706135234714 ) ) ;
#32075 = CARTESIAN_POINT ( 'NONE',  ( -4.483927247898539470, -16.52544592524342804, 107.2905762719810525 ) ) ;
#32078 = ORIENTED_EDGE ( 'NONE', *, *, #80571, .T. ) ;
#32077 = CARTESIAN_POINT ( 'NONE',  ( -19.02544592524342804, 5.153800228976336051, 101.0405762719810241 ) ) ;
#32076 = CARTESIAN_POINT ( 'NONE',  ( 10.81492255796078972, 18.62759615963270932, 99.58224293864770971 ) ) ;
#32079 = CARTESIAN_POINT ( 'NONE',  ( -18.67979575497193778, 10.72451020669871902, 23.33442372801901499 ) ) ;
#32080 = ORIENTED_EDGE ( 'NONE', *, *, #150187, .T. ) ;
#32081 = CARTESIAN_POINT ( 'NONE',  ( 5.049401038298161559, -19.05341960407611168, 92.70724293864769550 ) ) ;
#32082 = CARTESIAN_POINT ( 'NONE',  ( 19.52217212775662247, -5.499999999999912959, 82.43993709005258097 ) ) ;
#32083 = CARTESIAN_POINT ( 'NONE',  ( 5.719274019375991003, -21.55341960407610458, 92.70724293864770971 ) ) ;
#32084 = CARTESIAN_POINT ( 'NONE',  ( -9.564922557960796823, -16.46253265017161027, 47.08224293864769550 ) ) ;
#32085 = CARTESIAN_POINT ( 'NONE',  ( -13.97604488694547697, 13.89961937509957934, 108.1260903946856331 ) ) ;
#32086 = CARTESIAN_POINT ( 'NONE',  ( -29.86685920354755197, -21.69954338932560134, -4.924999997268813878 ) ) ;
#32087 = CARTESIAN_POINT ( 'NONE',  ( 0.05219959533909260263, 19.03943276465977164, 24.99890960531435269 ) ) ;
#32088 = CARTESIAN_POINT ( 'NONE',  ( 0.05219959533937995610, -21.53943276465977519, 90.00109039468567573 ) ) ;
#32090 = CARTESIAN_POINT ( 'NONE',  ( -5.823673210054431948, 21.52544592524334988, 47.70942372801902565 ) ) ;
#32089 = CARTESIAN_POINT ( 'NONE',  ( 16.46253265017160672, -9.564922557960803928, 73.33224293864769550 ) ) ;
#32091 = CARTESIAN_POINT ( 'NONE',  ( -10.72451020669870658, -18.67979575497194134, 29.58442372801901854 ) ) ;
#32092 = CARTESIAN_POINT ( 'NONE',  ( 17.14385361876520264, -23.59649016807271238, 142.0750000027311444 ) ) ;
#32093 = CARTESIAN_POINT ( 'NONE',  ( 9.474510206698971260, -16.51473224551069308, 97.91557627198102409 ) ) ;
#32094 = CARTESIAN_POINT ( 'NONE',  ( -18.87309089550571883, 21.74014469927720228, 140.0000000000000284 ) ) ;
#32097 = CARTESIAN_POINT ( 'NONE',  ( 21.53943276465977519, 0.05219959533937863772, 41.25109039468568284 ) ) ;
#32096 = CARTESIAN_POINT ( 'NONE',  ( -10.72451020669898014, 18.67979575497178502, 40.41557627198103120 ) ) ;
#32095 = CARTESIAN_POINT ( 'NONE',  ( 16.53943276465976808, 0.05219959533934440121, 41.25109039468568284 ) ) ;
#32098 = CARTESIAN_POINT ( 'NONE',  ( 21.52544592524334988, 5.823673210054432836, 71.45942372801901854 ) ) ;
#32099 = CARTESIAN_POINT ( 'NONE',  ( 17.97035753253448576, -5.500000000000063949, 38.49602986858894127 ) ) ;
#32100 = CARTESIAN_POINT ( 'NONE',  ( -13.89961937509957401, -13.97604488694547875, 109.3760903946856331 ) ) ;
#32101 = CARTESIAN_POINT ( 'NONE',  ( -0.05219959533909027116, -19.03943276465977164, 57.49890960531435979 ) ) ;
#32102 = CARTESIAN_POINT ( 'NONE',  ( 13.97604488694527802, 13.89961937509977652, 94.37390960531436690 ) ) ;
#32103 = CARTESIAN_POINT ( 'NONE',  ( -8.224510206698948167, 14.34966873604960824, 105.4155762719810383 ) ) ;
#32104 = CARTESIAN_POINT ( 'NONE',  ( -16.53943276465976808, 0.05219959533911058130, 111.2489096053143669 ) ) ;
#32105 = CARTESIAN_POINT ( 'NONE',  ( 21.53943276465977519, -0.05219959533907433946, 33.74890960531436690 ) ) ;
#32106 = CARTESIAN_POINT ( 'NONE',  ( -16.53943276465976808, -0.05219959533934237506, 83.75109039468568994 ) ) ;
#32108 = CARTESIAN_POINT ( 'NONE',  ( -9.474510206698964154, 16.51473224551069663, 50.41557627198102409 ) ) ;
#32107 = CARTESIAN_POINT ( 'NONE',  ( -14.29746914071049879, 8.314922557960819915, 65.83224293864769550 ) ) ;
#32109 = CARTESIAN_POINT ( 'NONE',  ( 21.52544592524334988, 5.823673210054432836, 71.45942372801901854 ) ) ;
#32110 = CARTESIAN_POINT ( 'NONE',  ( -21.52544592524334988, -5.823673210054445271, 73.95942372801901854 ) ) ;
#32111 = CARTESIAN_POINT ( 'NONE',  ( 5.049401038297881783, 19.05341960407617563, 102.2927570613523045 ) ) ;
#32112 = CARTESIAN_POINT ( 'NONE',  ( -12.14591786802309592, -12.06949235617757132, 56.87390960531436690 ) ) ;
#32113 = CARTESIAN_POINT ( 'NONE',  ( -18.67979575497193778, 10.72451020669871902, 33.33442372801900433 ) ) ;
#32114 = CARTESIAN_POINT ( 'NONE',  ( 5.823673210054125526, 21.52544592524343514, 54.79057627198104541 ) ) ;
#32115 = CARTESIAN_POINT ( 'NONE',  ( 17.81289503416611453, -24.51734667627695785, 140.6999999999999602 ) ) ;
#32116 = CARTESIAN_POINT ( 'NONE',  ( 17.81289503416610742, 24.51734667627700404, 143.5500000054623513 ) ) ;
#32117 = CARTESIAN_POINT ( 'NONE',  ( 9.564922557960805705, 16.46253265017160317, 64.58224293864769550 ) ) ;
#32118 = CARTESIAN_POINT ( 'NONE',  ( -12.14591786802309592, -12.06949235617757132, 31.87390960531435979 ) ) ;
#32119 = CARTESIAN_POINT ( 'NONE',  ( -14.29746914071049879, 8.314922557960819915, 25.83224293864769194 ) ) ;
#32120 = CARTESIAN_POINT ( 'NONE',  ( 8.314922557961029526, -14.29746914071037800, 95.41775706135234714 ) ) ;
#32121 = CARTESIAN_POINT ( 'NONE',  ( 19.02544592524334988, 5.153800228976608722, 51.45942372801900433 ) ) ;
#32122 = CARTESIAN_POINT ( 'NONE',  ( 17.05116617787827238, 6.768360034955707150, 48.84324446740802728 ) ) ;
#32123 = CARTESIAN_POINT ( 'NONE',  ( -16.51473224551069308, -9.474510206698971260, 106.6655762719810383 ) ) ;
#32124 = CARTESIAN_POINT ( 'NONE',  ( -16.52544592524342804, 4.483927247898546575, 76.04057627198102409 ) ) ;
#32125 = CARTESIAN_POINT ( 'NONE',  ( 9.564922557961047289, -16.46253265017146816, 40.41775706135234003 ) ) ;
#32127 = CARTESIAN_POINT ( 'NONE',  ( 18.67979575497178502, 10.72451020669898547, 24.16557627198103120 ) ) ;
#32126 = CARTESIAN_POINT ( 'NONE',  ( 9.564922557960805705, 16.46253265017160317, 29.58224293864769550 ) ) ;
#32128 = CARTESIAN_POINT ( 'NONE',  ( -21.55341960407610458, -5.719274019375992779, 56.45724293864768839 ) ) ;
#32129 = CARTESIAN_POINT ( 'NONE',  ( 16.55341960407611168, 4.379528057220329451, 98.95724293864770971 ) ) ;
#32130 = CARTESIAN_POINT ( 'NONE',  ( 12.06949235617739724, 12.14591786802326823, 51.87609039468568284 ) ) ;
#32131 = CARTESIAN_POINT ( 'NONE',  ( -0.05219959533910754901, -16.53943276465976808, 92.49890960531436690 ) ) ;
#32132 = CARTESIAN_POINT ( 'NONE',  ( 16.81555441253552274, -7.025013491695476731, 38.13685445334257906 ) ) ;
#32133 = CARTESIAN_POINT ( 'NONE',  ( -36.91746825000000598, 2.428612866367529932E-14, -11.12499999726881228 ) ) ;
#32134 = CARTESIAN_POINT ( 'NONE',  ( 9.564922557960805705, 16.46253265017160317, 114.5822429386476955 ) ) ;
#32135 = CARTESIAN_POINT ( 'NONE',  ( 22.81625015709509441, 31.40387420917330275, -5.824999997268813345 ) ) ;
#32136 = CARTESIAN_POINT ( 'NONE',  ( 1.500000000000323519, 7.794094698433090329, -64.20511667583481596 ) ) ;
#32137 = AXIS2_PLACEMENT_3D ( 'NONE', #14292, #135670, #151821 ) ;
#32139 = CARTESIAN_POINT ( 'NONE',  ( 12.06949235617757843, -12.14591786802309237, 33.12390960531435979 ) ) ;
#32138 = CARTESIAN_POINT ( 'NONE',  ( 14.29746914071037800, 8.314922557961029526, 41.66775706135235424 ) ) ;
#32140 = CARTESIAN_POINT ( 'NONE',  ( 5.823673210054125526, 21.52544592524343514, 59.79057627198103120 ) ) ;
#32141 = CARTESIAN_POINT ( 'NONE',  ( 5.049401038297881783, 19.05341960407617563, 87.29275706135234714 ) ) ;
#32142 = CARTESIAN_POINT ( 'NONE',  ( -15.80617190586745835, -15.72974639402198527, 51.87390960531437401 ) ) ;
#32143 = CARTESIAN_POINT ( 'NONE',  ( -18.67979575497193778, 10.72451020669871902, 83.33442372801903275 ) ) ;
#32144 = CARTESIAN_POINT ( 'NONE',  ( -11.67072985713514299, 9.561620553927742350, -62.04564570087489983 ) ) ;
#32145 = CARTESIAN_POINT ( 'NONE',  ( 4.379528057220092307, 16.55341960407617563, 52.29275706135236135 ) ) ;
#32147 = CARTESIAN_POINT ( 'NONE',  ( 19.05341960407611168, 5.049401038298154454, 103.9572429386476671 ) ) ;
#32146 = CARTESIAN_POINT ( 'NONE',  ( -9.564922557960796823, -16.46253265017161027, 32.08224293864769550 ) ) ;
#32148 = CARTESIAN_POINT ( 'NONE',  ( 16.51473224551069308, 9.474510206698969483, 29.16557627198103475 ) ) ;
#32149 = CARTESIAN_POINT ( 'NONE',  ( -4.379528057220328563, 16.55341960407611168, 95.20724293864769550 ) ) ;
#32150 = DIRECTION ( 'NONE',  ( 1.000000000000000000, 0.000000000000000000, 0.000000000000000000 ) ) ;
#32151 = CARTESIAN_POINT ( 'NONE',  ( 16.46253265017160672, -9.564922557960803928, 98.33224293864769550 ) ) ;
#32152 = ORIENTED_EDGE ( 'NONE', *, *, #146342, .T. ) ;
#32153 = CARTESIAN_POINT ( 'NONE',  ( -0.05219959533934338120, 16.53943276465976808, 62.50109039468568284 ) ) ;
#32154 = CARTESIAN_POINT ( 'NONE',  ( -18.67979575497178146, -10.72451020669898902, 96.66557627198102409 ) ) ;
#32155 = CARTESIAN_POINT ( 'NONE',  ( 9.564922557960805705, 16.46253265017160317, 54.58224293864769550 ) ) ;
#32156 = CARTESIAN_POINT ( 'NONE',  ( 15.72974639402176855, 15.80617190586768217, 21.87609039468567573 ) ) ;
#32157 = CARTESIAN_POINT ( 'NONE',  ( -19.05341960407611168, -5.049401038298163336, 86.45724293864769550 ) ) ;
#32158 = CARTESIAN_POINT ( 'NONE',  ( 2.552343178074723884, 7.052343178074616858, 8.889087296526001936 ) ) ;
#32159 = ORIENTED_EDGE ( 'NONE', *, *, #140691, .F. ) ;
#32160 = CARTESIAN_POINT ( 'NONE',  ( -21.52544592524334988, -5.823673210054445271, 23.95942372801901143 ) ) ;
#32163 = CARTESIAN_POINT ( 'NONE',  ( 13.97604488694548053, -13.89961937509957401, 70.62609039468567573 ) ) ;
#32162 = CARTESIAN_POINT ( 'NONE',  ( 16.51473224551069308, 9.474510206698969483, 109.1655762719810383 ) ) ;
#32161 = CARTESIAN_POINT ( 'NONE',  ( -19.05341960407611168, -5.049401038298163336, 26.45724293864769550 ) ) ;
#32164 = CARTESIAN_POINT ( 'NONE',  ( -19.05341960407617563, 5.049401038297882671, 23.54275706135233648 ) ) ;
#32165 = CARTESIAN_POINT ( 'NONE',  ( -5.823673210054116645, -21.52544592524344225, 97.29057627198105251 ) ) ;
#32166 = CARTESIAN_POINT ( 'NONE',  ( -19.03943276465977164, -0.05219959533935918106, 38.75109039468566152 ) ) ;
#32167 = CARTESIAN_POINT ( 'NONE',  ( 0.05219959533934541429, -16.53943276465976808, 85.00109039468568994 ) ) ;
#32168 = CARTESIAN_POINT ( 'NONE',  ( -19.05341960407611168, -5.049401038298163336, 101.4572429386476955 ) ) ;
#32169 = CARTESIAN_POINT ( 'NONE',  ( -5.049401038298153566, 19.05341960407611168, 55.20724293864769550 ) ) ;
#32170 = CIRCLE ( 'NONE', #64493, 10.00000000000000178 ) ;
#32171 = CARTESIAN_POINT ( 'NONE',  ( 5.823673210054444382, -21.52544592524334988, 70.20942372801904696 ) ) ;
#32172 = CARTESIAN_POINT ( 'NONE',  ( 0.05219959533937995610, -21.53943276465977519, 85.00109039468568994 ) ) ;
#32173 = CARTESIAN_POINT ( 'NONE',  ( -5.049401038298153566, 19.05341960407611168, 80.20724293864769550 ) ) ;
#32174 = CARTESIAN_POINT ( 'NONE',  ( -21.55341960407619339, 5.719274019375674811, 48.54275706135234714 ) ) ;
#32175 = CARTESIAN_POINT ( 'NONE',  ( -0.05219959533936034679, 19.03943276465977164, 82.50109039468567573 ) ) ;
#32176 = CARTESIAN_POINT ( 'NONE',  ( -19.03943276465977164, 0.05219959533909376836, 56.24890960531435979 ) ) ;
#32177 = CARTESIAN_POINT ( 'NONE',  ( 19.03943276465977164, -0.05219959533909143690, 103.7489096053143669 ) ) ;
#32178 = CARTESIAN_POINT ( 'NONE',  ( 0.05219959533909260263, 19.03943276465977164, 64.99890960531436690 ) ) ;
#32179 = CARTESIAN_POINT ( 'NONE',  ( -37.99626262588765968, 12.34573411038917179, -1.847842220587803341 ) ) ;
#32180 = CARTESIAN_POINT ( 'NONE',  ( 5.153800228976335163, 19.02544592524342804, 54.79057627198103120 ) ) ;
#32181 = CARTESIAN_POINT ( 'NONE',  ( -5.823673210054116645, -21.52544592524344225, 97.29057627198105251 ) ) ;
#32182 = CARTESIAN_POINT ( 'NONE',  ( 8.314922557961029526, -14.29746914071037800, 80.41775706135234714 ) ) ;
#32183 = CARTESIAN_POINT ( 'NONE',  ( -22.24685556490158689, 12.75834802357609910, 167.9013491530738520 ) ) ;
#32184 = CARTESIAN_POINT ( 'NONE',  ( -5.049401038297874678, -19.05341960407617918, 49.79275706135231871 ) ) ;
#32185 = CARTESIAN_POINT ( 'NONE',  ( -19.05341960407611168, -5.049401038298163336, 66.45724293864769550 ) ) ;
#32186 = CARTESIAN_POINT ( 'NONE',  ( 16.53943276465976808, -0.05219959533910856209, 58.74890960531436690 ) ) ;
#32187 = CARTESIAN_POINT ( 'NONE',  ( 14.29746914071049879, -8.314922557960816363, 88.33224293864769550 ) ) ;
#32188 = CARTESIAN_POINT ( 'NONE',  ( 13.97604488694527802, 13.89961937509977652, 99.37390960531436690 ) ) ;
#32189 = CARTESIAN_POINT ( 'NONE',  ( -19.03943276465977164, 0.05219959533909376836, 91.24890960531436690 ) ) ;
#32190 = CARTESIAN_POINT ( 'NONE',  ( -13.89961937509977652, 13.97604488694528158, 100.6239096053143669 ) ) ;
#32191 = CARTESIAN_POINT ( 'NONE',  ( -19.03943276465977164, -0.05219959533935918106, 23.75109039468566152 ) ) ;
#32192 = CARTESIAN_POINT ( 'NONE',  ( 4.483927247898790824, -16.52544592524335698, 95.20942372801903275 ) ) ;
#32194 = EDGE_CURVE ( 'NONE', #45716, #149545, #78987, .T. ) ;
#32193 = CARTESIAN_POINT ( 'NONE',  ( 16.51473224551069308, 9.474510206698969483, 74.16557627198103830 ) ) ;
#32195 = CARTESIAN_POINT ( 'NONE',  ( -10.72451020669870658, -18.67979575497194134, 44.58442372801901854 ) ) ;
#32196 = CARTESIAN_POINT ( 'NONE',  ( 0.05219959533907565091, 21.53943276465977519, 34.99890960531435979 ) ) ;
#32197 = CARTESIAN_POINT ( 'NONE',  ( 15.72974639402199770, -15.80617190586745480, 108.1239096053143811 ) ) ;
#32198 = CARTESIAN_POINT ( 'NONE',  ( 8.224510206698953496, -14.34966873604960469, 57.91557627198103120 ) ) ;
#32199 = CARTESIAN_POINT ( 'NONE',  ( -9.474510206698964154, 16.51473224551069663, 60.41557627198102409 ) ) ;
#32200 = CARTESIAN_POINT ( 'NONE',  ( 8.224510206698953496, -14.34966873604960469, 87.91557627198103830 ) ) ;
#32201 = B_SPLINE_CURVE_WITH_KNOTS ( 'NONE', 3,
 ( #179284, #70086, #131755, #116585, #40749, #102418, #178274, #164105, #87248, #148932, #10422, #44730 ),
 .UNSPECIFIED., .F., .F.,
 ( 4, 2, 2, 2, 2, 4 ),
 ( 7.806255641895631925E-18, 0.001213821615221375490, 0.001820732422832063453, 0.002124187826637407434, 0.002275915528540080075, 0.002427643230442752716 ),
 .UNSPECIFIED. ) ;
#32202 = CARTESIAN_POINT ( 'NONE',  ( -5.049401038297874678, -19.05341960407617918, 39.79275706135232582 ) ) ;
#32203 = CARTESIAN_POINT ( 'NONE',  ( 9.564922557960805705, 16.46253265017160317, 24.58224293864769194 ) ) ;
#32204 = CARTESIAN_POINT ( 'NONE',  ( -12.06949235617739369, -12.14591786802326823, 69.37609039468567573 ) ) ;
#32205 = CARTESIAN_POINT ( 'NONE',  ( -13.89961937509977652, 13.97604488694528158, 70.62390960531432427 ) ) ;
#32206 = CARTESIAN_POINT ( 'NONE',  ( 27.73933785331498569, 9.013057229001093518, 145.9750000027311785 ) ) ;
#32207 = CARTESIAN_POINT ( 'NONE',  ( -12.06949235617756955, 12.14591786802309770, 90.62390960531436690 ) ) ;
#32208 = CARTESIAN_POINT ( 'NONE',  ( 21.55341960407610458, 5.719274019375980345, 43.95724293864769550 ) ) ;
#32209 = ORIENTED_EDGE ( 'NONE', *, *, #126426, .T. ) ;
#32210 = CARTESIAN_POINT ( 'NONE',  ( -16.53943276465976808, -0.05219959533934237506, 108.7510903946857042 ) ) ;
#32211 = CARTESIAN_POINT ( 'NONE',  ( 8.224510206698742110, 14.34966873604972548, 27.08442372801901854 ) ) ;
#32212 = CARTESIAN_POINT ( 'NONE',  ( -18.62759615963255300, -10.81492255796106328, 94.16775706135237556 ) ) ;
#32213 = CARTESIAN_POINT ( 'NONE',  ( -5.049401038298153566, 19.05341960407611168, 90.20724293864766707 ) ) ;
#32214 = CARTESIAN_POINT ( 'NONE',  ( -21.52544592524334988, -5.823673210054445271, 23.95942372801901143 ) ) ;
#32215 = CARTESIAN_POINT ( 'NONE',  ( -5.049401038298153566, 19.05341960407611168, 35.20724293864768839 ) ) ;
#32216 = CARTESIAN_POINT ( 'NONE',  ( 0.05219959533934541429, -16.53943276465976808, 25.00109039468567218 ) ) ;
#32217 = CARTESIAN_POINT ( 'NONE',  ( -5.153800228976607833, 19.02544592524334988, 92.70942372801901854 ) ) ;
#32218 = CARTESIAN_POINT ( 'NONE',  ( 15.80617190586746368, 15.72974639402197994, 84.37390960531438111 ) ) ;
#32219 = CARTESIAN_POINT ( 'NONE',  ( -13.89961937509957401, -13.97604488694547875, 69.37609039468564731 ) ) ;
#32220 = CARTESIAN_POINT ( 'NONE',  ( -21.52544592524334988, -5.823673210054445271, 18.95942372801901143 ) ) ;
#32221 = FACE_OUTER_BOUND ( 'NONE', #159072, .T. ) ;
#32222 = CARTESIAN_POINT ( 'NONE',  ( -13.97604488694527625, -13.89961937509977652, 76.87390960531433848 ) ) ;
#32223 = CARTESIAN_POINT ( 'NONE',  ( 0.05219959533934541429, -16.53943276465976808, 35.00109039468568284 ) ) ;
#32224 = FACE_OUTER_BOUND ( 'NONE', #179278, .T. ) ;
#32225 = CARTESIAN_POINT ( 'NONE',  ( 19.05341960407617918, -5.049401038297876454, 61.04275706135232582 ) ) ;
#32227 = CARTESIAN_POINT ( 'NONE',  ( 4.379528057220339221, -16.55341960407611168, 82.70724293864770971 ) ) ;
#32226 = CARTESIAN_POINT ( 'NONE',  ( -21.55341960407619339, 5.719274019375674811, 23.54275706135235424 ) ) ;
#32228 = CARTESIAN_POINT ( 'NONE',  ( 13.89961937509977652, -13.97604488694527269, 88.12390960531438111 ) ) ;
#32230 = CARTESIAN_POINT ( 'NONE',  ( -19.02544592524334988, -5.153800228976617603, 38.95942372801900433 ) ) ;
#32229 = CARTESIAN_POINT ( 'NONE',  ( -12.06949235617739369, -12.14591786802326823, 39.37609039468567573 ) ) ;
#32231 = CARTESIAN_POINT ( 'NONE',  ( -0.05219959533937732626, 21.53943276465977519, 62.50109039468568284 ) ) ;
#32232 = CARTESIAN_POINT ( 'NONE',  ( -16.53943276465976808, -0.05219959533934237506, 33.75109039468568284 ) ) ;
#32233 = CARTESIAN_POINT ( 'NONE',  ( 16.46253265017160672, -9.564922557960803928, 58.33224293864769550 ) ) ;
#32234 = CARTESIAN_POINT ( 'NONE',  ( -9.564922557961040184, 16.46253265017147172, 77.91775706135234714 ) ) ;
#32235 = CARTESIAN_POINT ( 'NONE',  ( 8.224510206698742110, 14.34966873604972548, 52.08442372801901854 ) ) ;
#32236 = CARTESIAN_POINT ( 'NONE',  ( 15.72974639402176855, 15.80617190586768217, 101.8760903946857042 ) ) ;
#32237 = CARTESIAN_POINT ( 'NONE',  ( -19.05341960407617563, 5.049401038297882671, 63.54275706135234003 ) ) ;
#32238 = CARTESIAN_POINT ( 'NONE',  ( -9.564922557960796823, -16.46253265017161027, 47.08224293864769550 ) ) ;
#32239 = CARTESIAN_POINT ( 'NONE',  ( 18.67979575497178502, 10.72451020669898547, 74.16557627198102409 ) ) ;
#32241 = CARTESIAN_POINT ( 'NONE',  ( 9.474510206698729675, 16.51473224551082808, 67.08442372801900433 ) ) ;
#32240 = CARTESIAN_POINT ( 'NONE',  ( -12.06949235617756955, 12.14591786802309770, 65.62390960531436690 ) ) ;
#32242 = CARTESIAN_POINT ( 'NONE',  ( 16.21995358207300697, -7.366697692864327074, 62.43551001512160781 ) ) ;
#32243 = CARTESIAN_POINT ( 'NONE',  ( 9.564922557961047289, -16.46253265017146816, 45.41775706135232582 ) ) ;
#32244 = CARTESIAN_POINT ( 'NONE',  ( 12.06949235617739724, 12.14591786802326823, 96.87609039468568994 ) ) ;
#32245 = CARTESIAN_POINT ( 'NONE',  ( 4.379528057220339221, -16.55341960407611168, 67.70724293864769550 ) ) ;
#32247 = CARTESIAN_POINT ( 'NONE',  ( -22.44159573604010305, 16.30477369853692338, 146.6750000027311671 ) ) ;
#32246 = CARTESIAN_POINT ( 'NONE',  ( -15.80617190586768217, 15.72974639402176855, 98.12609039468570415 ) ) ;
#32248 = CARTESIAN_POINT ( 'NONE',  ( -0.05219959533907301413, -21.53943276465977519, 97.49890960531436690 ) ) ;
#32249 = CARTESIAN_POINT ( 'NONE',  ( 16.46253265017160672, -9.564922557960803928, 58.33224293864769550 ) ) ;
#32250 = CARTESIAN_POINT ( 'NONE',  ( -15.80617190586768217, 15.72974639402176855, 68.12609039468567573 ) ) ;
#32251 = CARTESIAN_POINT ( 'NONE',  ( -19.03943276465977164, 0.05219959533909376836, 46.24890960531435979 ) ) ;
#32252 = ORIENTED_EDGE ( 'NONE', *, *, #73850, .T. ) ;
#32253 = CARTESIAN_POINT ( 'NONE',  ( -19.05341960407611168, -5.049401038298163336, 71.45724293864766707 ) ) ;
#32254 = CARTESIAN_POINT ( 'NONE',  ( -4.379528057220328563, 16.55341960407611168, 115.2072429386476955 ) ) ;
#32255 = CARTESIAN_POINT ( 'NONE',  ( -0.05219959533909027116, -19.03943276465977164, 107.4989096053143527 ) ) ;
#32256 = CARTESIAN_POINT ( 'NONE',  ( 0.05219959533910956823, 16.53943276465976808, 64.99890960531435269 ) ) ;
#32257 = CARTESIAN_POINT ( 'NONE',  ( 13.89961937509977652, -13.97604488694527269, 33.12390960531434558 ) ) ;
#32258 = CARTESIAN_POINT ( 'NONE',  ( 4.379528057220339221, -16.55341960407611168, 87.70724293864769550 ) ) ;
#32259 = CARTESIAN_POINT ( 'NONE',  ( 0.05219959533907565091, 21.53943276465977519, 89.99890960531438111 ) ) ;
#32260 = CARTESIAN_POINT ( 'NONE',  ( -5.719274019375665041, -21.55341960407619695, 39.79275706135235424 ) ) ;
#32261 = CARTESIAN_POINT ( 'NONE',  ( -13.97604488694527625, -13.89961937509977652, 21.87390960531435979 ) ) ;
#32262 = ADVANCED_FACE ( 'NONE', ( #192072, #38394 ), #52550, .F. ) ;
#32263 = CARTESIAN_POINT ( 'NONE',  ( -14.34966873604972548, 8.224510206698743886, 53.33442372801901854 ) ) ;
#32264 = CARTESIAN_POINT ( 'NONE',  ( -0.05219959533907301413, -21.53943276465977519, 87.49890960531436690 ) ) ;
#32265 = CARTESIAN_POINT ( 'NONE',  ( 0.05219959533936267826, -19.03943276465977164, 30.00109039468566863 ) ) ;
#32266 = CARTESIAN_POINT ( 'NONE',  ( 16.51473224551069308, 9.474510206698969483, 109.1655762719810383 ) ) ;
#32267 = CARTESIAN_POINT ( 'NONE',  ( -21.53943276465977519, -0.05219959533937600094, 48.75109039468568284 ) ) ;
#32268 = CARTESIAN_POINT ( 'NONE',  ( -10.81492255796078084, -18.62759615963271287, 47.08224293864770260 ) ) ;
#32269 = CARTESIAN_POINT ( 'NONE',  ( -14.34966873604960291, -8.224510206698953496, 21.66557627198102409 ) ) ;
#32271 = CARTESIAN_POINT ( 'NONE',  ( -5.823673210054431948, 21.52544592524334988, 92.70942372801901854 ) ) ;
#32270 = CARTESIAN_POINT ( 'NONE',  ( 10.81492255796106328, -18.62759615963255655, 60.41775706135235424 ) ) ;
#32272 = CARTESIAN_POINT ( 'NONE',  ( -13.97604488694547697, 13.89961937509957934, 28.12609039468565797 ) ) ;
#32273 = CARTESIAN_POINT ( 'NONE',  ( 8.314922557961029526, -14.29746914071037800, 90.41775706135236135 ) ) ;
#32274 = CARTESIAN_POINT ( 'NONE',  ( 18.62759615963255655, 10.81492255796105972, 46.66775706135234714 ) ) ;
#32275 = CARTESIAN_POINT ( 'NONE',  ( -16.46253265017160317, 9.564922557960807481, 50.83224293864770260 ) ) ;
#32276 = CARTESIAN_POINT ( 'NONE',  ( 5.719274019375673035, 21.55341960407619339, 112.2927570613523471 ) ) ;
#32277 = CARTESIAN_POINT ( 'NONE',  ( -18.62759615963270932, 10.81492255796079327, 25.83224293864769194 ) ) ;
#32278 = EDGE_CURVE ( 'NONE', #165187, #194003, #54516, .T. ) ;
#32279 = CARTESIAN_POINT ( 'NONE',  ( 5.719274019375673035, 21.55341960407619339, 22.29275706135235069 ) ) ;
#32280 = AXIS2_PLACEMENT_3D ( 'NONE', #5065, #97072, #22250 ) ;
#32281 = CARTESIAN_POINT ( 'NONE',  ( 5.823673210054125526, 21.52544592524343514, 69.79057627198102409 ) ) ;
#32282 = CARTESIAN_POINT ( 'NONE',  ( 8.224510206698742110, 14.34966873604972548, 42.08442372801901854 ) ) ;
#32284 = CARTESIAN_POINT ( 'NONE',  ( 18.62759615963271287, -10.81492255796078972, 83.33224293864769550 ) ) ;
#32283 = CARTESIAN_POINT ( 'NONE',  ( 27.49873734152943427, 21.99873734152882676, 1.818019484660534424 ) ) ;
#32286 = CARTESIAN_POINT ( 'NONE',  ( 0.05219959533910956823, 16.53943276465976808, 64.99890960531435269 ) ) ;
#32285 = CARTESIAN_POINT ( 'NONE',  ( -14.29746914071037622, -8.314922557961029526, 69.16775706135234714 ) ) ;
#32287 = DIRECTION ( 'NONE',  ( -1.000000000000000000, 0.000000000000000000, -0.000000000000000000 ) ) ;
#32288 = CARTESIAN_POINT ( 'NONE',  ( -9.474510206698720793, -16.51473224551083518, 89.58442372801900433 ) ) ;
#32289 = CARTESIAN_POINT ( 'NONE',  ( -24.23981148858510792, 0.4346045811325345842, -54.26183423998841704 ) ) ;
#32290 = CARTESIAN_POINT ( 'NONE',  ( -8.224510206698735004, -14.34966873604973081, 34.58442372801900433 ) ) ;
#32291 = CARTESIAN_POINT ( 'NONE',  ( 15.72974639402199770, -15.80617190586745480, 113.1239096053143953 ) ) ;
#32292 = CARTESIAN_POINT ( 'NONE',  ( -18.67979575497178146, -10.72451020669898902, 76.66557627198103830 ) ) ;
#32293 = CARTESIAN_POINT ( 'NONE',  ( -5.719274019375978568, 21.55341960407610458, 35.20724293864768839 ) ) ;
#32294 = CARTESIAN_POINT ( 'NONE',  ( -4.483927247898782831, 16.52544592524335698, 62.70942372801902565 ) ) ;
#32295 = CARTESIAN_POINT ( 'NONE',  ( 16.51473224551069308, 9.474510206698969483, 74.16557627198103830 ) ) ;
#32297 = CARTESIAN_POINT ( 'NONE',  ( 16.53943276465976808, 0.05219959533934440121, 21.25109039468567218 ) ) ;
#32296 = CARTESIAN_POINT ( 'NONE',  ( -15.72974639402176322, -15.80617190586768395, 49.37609039468569705 ) ) ;
#32298 = CARTESIAN_POINT ( 'NONE',  ( 16.51473224551069308, 9.474510206698969483, 109.1655762719810383 ) ) ;
#32299 = ORIENTED_EDGE ( 'NONE', *, *, #185673, .F. ) ;
#32300 = CARTESIAN_POINT ( 'NONE',  ( -9.564922557961040184, 16.46253265017147172, 22.91775706135233648 ) ) ;
#32301 = CARTESIAN_POINT ( 'NONE',  ( -4.379528057220086978, -16.55341960407618274, 39.79275706135235424 ) ) ;
#32302 = CARTESIAN_POINT ( 'NONE',  ( 5.153800228976335163, 19.02544592524342804, 104.7905762719809957 ) ) ;
#32303 = CARTESIAN_POINT ( 'NONE',  ( 5.719274019375991003, -21.55341960407610458, 107.7072429386476955 ) ) ;
#32304 = CARTESIAN_POINT ( 'NONE',  ( 9.474510206698971260, -16.51473224551069308, 67.91557627198102409 ) ) ;
#32305 = FACE_OUTER_BOUND ( 'NONE', #74325, .T. ) ;
#32306 = CARTESIAN_POINT ( 'NONE',  ( -16.55341960407611168, -4.379528057220339221, 86.45724293864770971 ) ) ;
#32307 = CARTESIAN_POINT ( 'NONE',  ( 5.719274019375991003, -21.55341960407610458, 22.70724293864769194 ) ) ;
#32308 = CARTESIAN_POINT ( 'NONE',  ( -16.61371651742598132, 7.165104196376278267, 33.85415069992996706 ) ) ;
#32309 = CARTESIAN_POINT ( 'NONE',  ( 5.719274019375991003, -21.55341960407610458, 102.7072429386476955 ) ) ;
#32310 = CARTESIAN_POINT ( 'NONE',  ( 5.153800228976615827, -19.02544592524334988, 60.20942372801899012 ) ) ;
#32311 = CARTESIAN_POINT ( 'NONE',  ( 18.62759615963271287, -10.81492255796078972, 33.33224293864769550 ) ) ;
#32312 = CARTESIAN_POINT ( 'NONE',  ( 5.049401038298161559, -19.05341960407611168, 22.70724293864769194 ) ) ;
#32313 = CARTESIAN_POINT ( 'NONE',  ( -15.72974639402197994, 15.80617190586746368, 65.62390960531436690 ) ) ;
#32314 = AXIS2_PLACEMENT_3D ( 'NONE', #108190, #31365, #3984 ) ;
#32315 = CARTESIAN_POINT ( 'NONE',  ( -16.46253265017160317, 9.564922557960807481, 105.8322429386476955 ) ) ;
#32316 = CARTESIAN_POINT ( 'NONE',  ( 10.81492255796106328, -18.62759615963255655, 90.41775706135236135 ) ) ;
#32317 = CARTESIAN_POINT ( 'NONE',  ( -16.46253265017160317, 9.564922557960807481, 45.83224293864769550 ) ) ;
#32318 = CARTESIAN_POINT ( 'NONE',  ( 8.224510206698953496, -14.34966873604960469, 82.91557627198103830 ) ) ;
#32319 = CARTESIAN_POINT ( 'NONE',  ( 16.55341960407618274, -4.379528057220086978, 31.04275706135234714 ) ) ;
#32320 = CARTESIAN_POINT ( 'NONE',  ( 13.97604488694527802, 13.89961937509977652, 59.37390960531434558 ) ) ;
#32321 = CARTESIAN_POINT ( 'NONE',  ( -18.67979575497193778, 10.72451020669871902, 73.33442372801901854 ) ) ;
#32322 = ORIENTED_EDGE ( 'NONE', *, *, #96372, .F. ) ;
#32323 = CARTESIAN_POINT ( 'NONE',  ( -5.049401038297874678, -19.05341960407617918, 29.79275706135232227 ) ) ;
#32324 = CARTESIAN_POINT ( 'NONE',  ( -19.02544592524334988, -5.153800228976617603, 43.95942372801899012 ) ) ;
#32325 = CARTESIAN_POINT ( 'NONE',  ( 10.81492255796106328, -18.62759615963255655, 30.41775706135234358 ) ) ;
#32326 = CARTESIAN_POINT ( 'NONE',  ( 13.97604488694527802, 13.89961937509977830, 54.37390960531435979 ) ) ;
#32327 = CARTESIAN_POINT ( 'NONE',  ( -13.89961937509957401, -13.97604488694547875, 29.37609039468565797 ) ) ;
#32328 = CARTESIAN_POINT ( 'NONE',  ( -13.89961937509977652, 13.97604488694528158, 85.62390960531433848 ) ) ;
#32329 = CARTESIAN_POINT ( 'NONE',  ( 16.46253265017160672, -9.564922557960803928, 63.33224293864769550 ) ) ;
#32330 = CARTESIAN_POINT ( 'NONE',  ( 14.34966873604960469, 8.224510206698951720, 24.16557627198103120 ) ) ;
#32332 = CARTESIAN_POINT ( 'NONE',  ( 10.81492255796106328, -18.62759615963255655, 85.41775706135236135 ) ) ;
#32331 = CARTESIAN_POINT ( 'NONE',  ( -19.02544592524342804, 5.153800228976336051, 111.0405762719810099 ) ) ;
#32333 = CARTESIAN_POINT ( 'NONE',  ( -29.86685920354755552, 21.69954338932564397, -7.324999997268814234 ) ) ;
#32334 = CARTESIAN_POINT ( 'NONE',  ( 17.48853670773242186, 5.747243402303175763, 58.83328700250011423 ) ) ;
#32335 = CARTESIAN_POINT ( 'NONE',  ( -21.52544592524334988, -5.823673210054445271, 78.95942372801901854 ) ) ;
#32336 = CARTESIAN_POINT ( 'NONE',  ( 21.35939100396078771, -0.4315818942738698927, -58.81718527612542147 ) ) ;
#32337 = CARTESIAN_POINT ( 'NONE',  ( -19.05341960407611168, -5.049401038298163336, 96.45724293864769550 ) ) ;
#32338 = DIRECTION ( 'NONE',  ( 0.000000000000000000, 0.000000000000000000, 1.000000000000000000 ) ) ;
#32339 = CARTESIAN_POINT ( 'NONE',  ( 21.55341960407610458, 5.719274019375980345, 68.95724293864769550 ) ) ;
#32340 = CARTESIAN_POINT ( 'NONE',  ( -8.224510206698948167, 14.34966873604960824, 30.41557627198101699 ) ) ;
#32342 = CARTESIAN_POINT ( 'NONE',  ( -5.049401038298153566, 19.05341960407611168, 95.20724293864770971 ) ) ;
#32341 = CARTESIAN_POINT ( 'NONE',  ( 12.06949235617757843, -12.14591786802309237, 113.1239096053143953 ) ) ;
#32343 = CARTESIAN_POINT ( 'NONE',  ( -5.823673210054431948, 21.52544592524334988, 112.7094237280190328 ) ) ;
#32344 = CARTESIAN_POINT ( 'NONE',  ( 19.03943276465977164, -0.05219959533909143690, 23.74890960531435269 ) ) ;
#32345 = CARTESIAN_POINT ( 'NONE',  ( -0.05219959533937732626, 21.53943276465977519, 62.50109039468568284 ) ) ;
#32346 = CARTESIAN_POINT ( 'NONE',  ( 5.153800228976335163, 19.02544592524342804, 109.7905762719810099 ) ) ;
#32347 = CARTESIAN_POINT ( 'NONE',  ( 14.29746914071037800, 8.314922557961029526, 106.6677570613523756 ) ) ;
#32348 = CARTESIAN_POINT ( 'NONE',  ( 16.51473224551083163, -9.474510206698727899, 70.83442372801900433 ) ) ;
#32349 = CARTESIAN_POINT ( 'NONE',  ( 13.89961937509957579, 13.97604488694547520, 66.87609039468567573 ) ) ;
#32350 = CARTESIAN_POINT ( 'NONE',  ( 19.05341960407611168, 5.049401038298154454, 103.9572429386476671 ) ) ;
#32351 = CARTESIAN_POINT ( 'NONE',  ( -12.06949235617756955, 12.14591786802309770, 90.62390960531436690 ) ) ;
#32352 = CARTESIAN_POINT ( 'NONE',  ( 9.564922557961047289, -16.46253265017146816, 55.41775706135234003 ) ) ;
#32353 = CARTESIAN_POINT ( 'NONE',  ( 19.02544592524343514, -5.153800228976328945, 78.54057627198099567 ) ) ;
#32354 = CARTESIAN_POINT ( 'NONE',  ( -14.34966873604960291, -8.224510206698953496, 66.66557627198102409 ) ) ;
#32355 = CARTESIAN_POINT ( 'NONE',  ( -16.51473224551082808, 9.474510206698731452, 93.33442372801900433 ) ) ;
#32356 = CARTESIAN_POINT ( 'NONE',  ( 10.72451020669898902, -18.67979575497178502, 47.91557627198102409 ) ) ;
#32357 = ORIENTED_EDGE ( 'NONE', *, *, #181589, .F. ) ;
#32358 = CARTESIAN_POINT ( 'NONE',  ( -16.52544592524342804, 4.483927247898546575, 111.0405762719810525 ) ) ;
#32359 = LINE ( 'NONE', #138529, #51628 ) ;
#32361 = CARTESIAN_POINT ( 'NONE',  ( -5.719274019375978568, 21.55341960407610458, 80.20724293864769550 ) ) ;
#32360 = CARTESIAN_POINT ( 'NONE',  ( -19.05341960407611168, -5.049401038298163336, 71.45724293864766707 ) ) ;
#32363 = CARTESIAN_POINT ( 'NONE',  ( -0.05219959533909027116, -19.03943276465977164, 67.49890960531436690 ) ) ;
#32362 = CARTESIAN_POINT ( 'NONE',  ( 14.29746914071037800, 8.314922557961029526, 86.66775706135234714 ) ) ;
#32364 = CARTESIAN_POINT ( 'NONE',  ( -5.153800228976607833, 19.02544592524334988, 62.70942372801899722 ) ) ;
#32365 = CARTESIAN_POINT ( 'NONE',  ( -21.52544592524334988, -5.823673210054445271, 83.95942372801900433 ) ) ;
#32366 = CARTESIAN_POINT ( 'NONE',  ( 15.80617190586746368, 15.72974639402197994, 64.37390960531435269 ) ) ;
#32367 = CARTESIAN_POINT ( 'NONE',  ( -21.55341960407610458, -5.719274019375992779, 21.45724293864769550 ) ) ;
#32368 = CARTESIAN_POINT ( 'NONE',  ( -16.46253265017160317, 9.564922557960807481, 30.83224293864769550 ) ) ;
#32369 = CARTESIAN_POINT ( 'NONE',  ( 8.224510206698742110, 14.34966873604972548, 102.0844237280190185 ) ) ;
#32370 = CARTESIAN_POINT ( 'NONE',  ( 14.34966873604972726, -8.224510206698740333, 25.83442372801901499 ) ) ;
#32371 = CARTESIAN_POINT ( 'NONE',  ( 18.22780087662122739, 5.500000000000000888, 76.48236817873106475 ) ) ;
#32372 = CARTESIAN_POINT ( 'NONE',  ( 21.55341960407619695, -5.719274019375665929, 91.04275706135236135 ) ) ;
#32373 = ORIENTED_EDGE ( 'NONE', *, *, #61610, .T. ) ;
#32374 = CARTESIAN_POINT ( 'NONE',  ( 14.29746914071049879, -8.314922557960816363, 53.33224293864769550 ) ) ;
#32375 = CARTESIAN_POINT ( 'NONE',  ( -18.62759615963270932, 10.81492255796079327, 90.83224293864769550 ) ) ;
#32376 = CARTESIAN_POINT ( 'NONE',  ( 5.719274019375991003, -21.55341960407610458, 107.7072429386476955 ) ) ;
#32377 = CARTESIAN_POINT ( 'NONE',  ( -28.79475375365586842, 9.355982642739222754, 149.8843446568999980 ) ) ;
#32378 = CARTESIAN_POINT ( 'NONE',  ( -21.55341960407610458, -5.719274019375992779, 41.45724293864769550 ) ) ;
#32379 = CARTESIAN_POINT ( 'NONE',  ( -16.52544592524335698, -4.483927247898792601, 73.95942372801901854 ) ) ;
#32380 = CARTESIAN_POINT ( 'NONE',  ( -4.379528057220328563, 16.55341960407611168, 85.20724293864770971 ) ) ;
#32381 = CARTESIAN_POINT ( 'NONE',  ( -5.049401038298153566, 19.05341960407611168, 45.20724293864769550 ) ) ;
#32382 = CARTESIAN_POINT ( 'NONE',  ( 34.67490716095262826, -3.335491994402099092, 51.73554620185606012 ) ) ;
#32383 = CARTESIAN_POINT ( 'NONE',  ( 12.06949235617757843, -12.14591786802309237, 23.12390960531436335 ) ) ;
#32384 = CARTESIAN_POINT ( 'NONE',  ( -5.719274019375665041, -21.55341960407619695, 29.79275706135234358 ) ) ;
#32385 = CARTESIAN_POINT ( 'NONE',  ( -5.049401038298153566, 19.05341960407611168, 90.20724293864766707 ) ) ;
#32386 = CARTESIAN_POINT ( 'NONE',  ( 18.62759615963255655, 10.81492255796105972, 61.66775706135235424 ) ) ;
#32387 = DIRECTION ( 'NONE',  ( 1.000000000000000000, 0.000000000000000000, 0.000000000000000000 ) ) ;
#32388 = CARTESIAN_POINT ( 'NONE',  ( 19.02544592524343514, -5.153800228976328945, 28.54057627198102409 ) ) ;
#32389 = EDGE_LOOP ( 'NONE', ( #162936, #185817, #77336, #138820, #96284, #163282, #32536, #177807, #21713, #188073, #165154, #129216, #80845, #178640, #143786, #2039, #107041, #13813, #23638, #96495 ) ) ;
#32390 = CARTESIAN_POINT ( 'NONE',  ( -5.823673210054431948, 21.52544592524334988, 57.70942372801901143 ) ) ;
#32392 = CARTESIAN_POINT ( 'NONE',  ( 5.153800228976335163, 19.02544592524342804, 24.79057627198102765 ) ) ;
#32391 = CARTESIAN_POINT ( 'NONE',  ( -13.89961937509977652, 13.97604488694528158, 55.62390960531434558 ) ) ;
#32393 = CARTESIAN_POINT ( 'NONE',  ( 16.51473224551069308, 9.474510206698969483, 89.16557627198103830 ) ) ;
#32394 = CARTESIAN_POINT ( 'NONE',  ( -9.564922557961040184, 16.46253265017147172, 62.91775706135233293 ) ) ;
#32395 = CARTESIAN_POINT ( 'NONE',  ( -21.53943276465977519, -0.05219959533937600094, 43.75109039468568284 ) ) ;
#32396 = CARTESIAN_POINT ( 'NONE',  ( -5.153800228976607833, 19.02544592524334988, 62.70942372801899722 ) ) ;
#32397 = CARTESIAN_POINT ( 'NONE',  ( -19.02544592524342804, 5.153800228976336051, 36.04057627198100988 ) ) ;
#32398 = CARTESIAN_POINT ( 'NONE',  ( 16.55341960407618274, -4.379528057220086978, 101.0427570613523756 ) ) ;
#32399 = CARTESIAN_POINT ( 'NONE',  ( -19.05341960407617563, 5.049401038297882671, 78.54275706135233293 ) ) ;
#32400 = CARTESIAN_POINT ( 'NONE',  ( 14.29746914071049879, -8.314922557960816363, 28.33224293864769550 ) ) ;
#32401 = CARTESIAN_POINT ( 'NONE',  ( -19.02544592524334988, -5.153800228976617603, 43.95942372801899012 ) ) ;
#32402 = CARTESIAN_POINT ( 'NONE',  ( 13.89961937509977652, -13.97604488694527269, 103.1239096053143527 ) ) ;
#32403 = CARTESIAN_POINT ( 'NONE',  ( 5.719274019375673035, 21.55341960407619339, 112.2927570613523471 ) ) ;
#32404 = CARTESIAN_POINT ( 'NONE',  ( 16.51473224551083163, -9.474510206698727899, 25.83442372801900078 ) ) ;
#32405 = CARTESIAN_POINT ( 'NONE',  ( -0.05219959533909027116, -19.03943276465977164, 32.49890960531435979 ) ) ;
#32406 = CARTESIAN_POINT ( 'NONE',  ( -15.80617190586768217, 15.72974639402176855, 93.12609039468568994 ) ) ;
#32407 = CARTESIAN_POINT ( 'NONE',  ( 12.14591786802327356, -12.06949235617739191, 30.62609039468567929 ) ) ;
#32408 = CARTESIAN_POINT ( 'NONE',  ( -19.03943276465977164, 0.05219959533909376836, 86.24890960531436690 ) ) ;
#32409 = CARTESIAN_POINT ( 'NONE',  ( 22.44159573604009239, 16.30477369853692693, 140.0750000027311728 ) ) ;
#32410 = CARTESIAN_POINT ( 'NONE',  ( 19.02544592524343514, -5.153800228976328945, 78.54057627198099567 ) ) ;
#32411 = FACE_OUTER_BOUND ( 'NONE', #25157, .T. ) ;
#32412 = CARTESIAN_POINT ( 'NONE',  ( -13.97604488694547697, 13.89961937509957934, 78.12609039468567573 ) ) ;
#32413 = CARTESIAN_POINT ( 'NONE',  ( 13.97604488694527802, 13.89961937509977652, 104.3739096053143385 ) ) ;
#32414 = CARTESIAN_POINT ( 'NONE',  ( -18.62759615963255300, -10.81492255796106328, 104.1677570613523471 ) ) ;
#32415 = CARTESIAN_POINT ( 'NONE',  ( 14.29746914071049879, -8.314922557960816363, 98.33224293864769550 ) ) ;
#32416 = CARTESIAN_POINT ( 'NONE',  ( 13.97604488694527802, 13.89961937509977652, 29.37390960531435979 ) ) ;
#32417 = CARTESIAN_POINT ( 'NONE',  ( 0.05219959533907565091, 21.53943276465977519, 39.99890960531436690 ) ) ;
#32418 = CARTESIAN_POINT ( 'NONE',  ( -18.67979575497178146, -10.72451020669898902, 31.66557627198102054 ) ) ;
#32419 = CARTESIAN_POINT ( 'NONE',  ( -4.379528057220328563, 16.55341960407611168, 115.2072429386476955 ) ) ;
#32420 = CARTESIAN_POINT ( 'NONE',  ( -0.9974278668897548217, -8.724588103088160906, -61.97156292062778249 ) ) ;
#32421 = CARTESIAN_POINT ( 'NONE',  ( 9.474510206698729675, 16.51473224551082808, 62.08442372801899722 ) ) ;
#32422 = CARTESIAN_POINT ( 'NONE',  ( -0.05219959533910754901, -16.53943276465976808, 42.49890960531435979 ) ) ;
#32424 = EDGE_CURVE ( 'NONE', #172658, #119499, #182368, .T. ) ;
#32423 = CARTESIAN_POINT ( 'NONE',  ( 16.46253265017160672, -9.564922557960803928, 113.3322429386476955 ) ) ;
#32425 = CARTESIAN_POINT ( 'NONE',  ( -21.53943276465977519, -0.05219959533937600094, 73.75109039468567573 ) ) ;
#32426 = CARTESIAN_POINT ( 'NONE',  ( -5.823673210054116645, -21.52544592524344225, 77.29057627198102409 ) ) ;
#32427 = CARTESIAN_POINT ( 'NONE',  ( 5.823673210054444382, -21.52544592524334988, 50.20942372801901854 ) ) ;
#32428 = CARTESIAN_POINT ( 'NONE',  ( 21.52544592524344225, -5.823673210054117533, 93.54057627198103830 ) ) ;
#32429 = CARTESIAN_POINT ( 'NONE',  ( 15.72974639402176855, 15.80617190586768217, 56.87609039468568994 ) ) ;
#32430 = CARTESIAN_POINT ( 'NONE',  ( -16.46253265017160317, 9.564922557960807481, 30.83224293864769550 ) ) ;
#32431 = CARTESIAN_POINT ( 'NONE',  ( 0.05219959533909260263, 19.03943276465977164, 79.99890960531436690 ) ) ;
#32432 = CARTESIAN_POINT ( 'NONE',  ( 14.34966873604972726, -8.224510206698740333, 75.83442372801900433 ) ) ;
#32433 = CARTESIAN_POINT ( 'NONE',  ( -4.379528057220328563, 16.55341960407611168, 105.2072429386477097 ) ) ;
#32434 = CARTESIAN_POINT ( 'NONE',  ( -31.49214409296861916, 4.585214664522601069, 100.9553921309669562 ) ) ;
#32435 = CARTESIAN_POINT ( 'NONE',  ( 12.06949235617757843, -12.14591786802309237, 48.12390960531436690 ) ) ;
#32436 = CARTESIAN_POINT ( 'NONE',  ( -16.53943276465976808, 0.05219959533911058130, 21.24890960531436690 ) ) ;
#32437 = CARTESIAN_POINT ( 'NONE',  ( -5.153800228976328057, -19.02544592524343514, 62.29057627198100988 ) ) ;
#32438 = CARTESIAN_POINT ( 'NONE',  ( -19.02544592524342804, 5.153800228976336051, 36.04057627198100988 ) ) ;
#32439 = CARTESIAN_POINT ( 'NONE',  ( 15.72974639402199770, -15.80617190586745480, 48.12390960531436690 ) ) ;
#32440 = CARTESIAN_POINT ( 'NONE',  ( 9.564922557961047289, -16.46253265017146816, 35.41775706135233293 ) ) ;
#32442 = CARTESIAN_POINT ( 'NONE',  ( -14.34966873604960291, -8.224510206698953496, 41.66557627198103120 ) ) ;
#32441 = CARTESIAN_POINT ( 'NONE',  ( -17.12812012977023812, -6.668231424566066323, 41.35948759323144230 ) ) ;
#32444 = AXIS2_PLACEMENT_3D ( 'NONE', #54590, #84911, #162767 ) ;
#32443 = CARTESIAN_POINT ( 'NONE',  ( -15.80617190586745835, -15.72974639402198527, 31.87390960531435979 ) ) ;
#32445 = CARTESIAN_POINT ( 'NONE',  ( -15.80617190586768217, 15.72974639402176855, 58.12609039468568994 ) ) ;
#32446 = DIRECTION ( 'NONE',  ( -1.000000000000000000, 1.154084784954514691E-14, 0.000000000000000000 ) ) ;
#32447 = CARTESIAN_POINT ( 'NONE',  ( -16.52544592524335698, -4.483927247898792601, 68.95942372801901854 ) ) ;
#32448 = CARTESIAN_POINT ( 'NONE',  ( -9.564922557961040184, 16.46253265017147172, 67.91775706135233293 ) ) ;
#32449 = EDGE_CURVE ( 'NONE', #158096, #89826, #62820, .T. ) ;
#32450 = CARTESIAN_POINT ( 'NONE',  ( 14.29746914071049879, -8.314922557960816363, 43.33224293864769550 ) ) ;
#32451 = CARTESIAN_POINT ( 'NONE',  ( -19.35543954521082455, -5.499999999999491074, 74.58901960356450900 ) ) ;
#32452 = CARTESIAN_POINT ( 'NONE',  ( -12.14591786802309592, -12.06949235617757132, 31.87390960531435979 ) ) ;
#32453 = CARTESIAN_POINT ( 'NONE',  ( 16.51473224551069308, 9.474510206698969483, 44.16557627198103120 ) ) ;
#32454 = CARTESIAN_POINT ( 'NONE',  ( 16.46253265017160672, -9.564922557960803928, 58.33224293864769550 ) ) ;
#32455 = CARTESIAN_POINT ( 'NONE',  ( 9.474510206698971260, -16.51473224551069308, 27.91557627198103120 ) ) ;
#32456 = CARTESIAN_POINT ( 'NONE',  ( -21.55341960407619339, 5.719274019375674811, 28.54275706135234358 ) ) ;
#32457 = CARTESIAN_POINT ( 'NONE',  ( 5.153800228976335163, 19.02544592524342804, 54.79057627198103120 ) ) ;
#32458 = DIRECTION ( 'NONE',  ( 1.000000000000000000, 0.000000000000000000, 0.000000000000000000 ) ) ;
#32459 = CARTESIAN_POINT ( 'NONE',  ( 19.05341960407611168, 5.049401038298154454, 48.95724293864768129 ) ) ;
#32460 = CARTESIAN_POINT ( 'NONE',  ( 15.72974639402199770, -15.80617190586745480, 33.12390960531435979 ) ) ;
#32462 = CARTESIAN_POINT ( 'NONE',  ( 0.05219959533910956823, 16.53943276465976808, 114.9989096053143669 ) ) ;
#32461 = CARTESIAN_POINT ( 'NONE',  ( -5.719274019375665041, -21.55341960407619695, 54.79275706135235424 ) ) ;
#32463 = CARTESIAN_POINT ( 'NONE',  ( 15.72974639402199770, -15.80617190586745480, 23.12390960531436335 ) ) ;
#32464 = CARTESIAN_POINT ( 'NONE',  ( 14.34966873604972726, -8.224510206698740333, 90.83442372801901854 ) ) ;
#32465 = CARTESIAN_POINT ( 'NONE',  ( 15.72974639402176855, 15.80617190586768217, 106.8760903946856899 ) ) ;
#32466 = CARTESIAN_POINT ( 'NONE',  ( 12.14591786802327356, -12.06949235617739191, 60.62609039468567573 ) ) ;
#32467 = CARTESIAN_POINT ( 'NONE',  ( -13.97604488694527625, -13.89961937509977652, 111.8739096053143243 ) ) ;
#32468 = CARTESIAN_POINT ( 'NONE',  ( 14.29746914071037800, 8.314922557961029526, 56.66775706135235424 ) ) ;
#32469 = CARTESIAN_POINT ( 'NONE',  ( 16.53943276465976808, 0.05219959533934440121, 31.25109039468568639 ) ) ;
#32470 = CARTESIAN_POINT ( 'NONE',  ( -4.379528057220086978, -16.55341960407618274, 89.79275706135236135 ) ) ;
#32471 = CARTESIAN_POINT ( 'NONE',  ( -0.05219959533937732626, 21.53943276465977519, 47.50109039468568994 ) ) ;
#32472 = CARTESIAN_POINT ( 'NONE',  ( 13.89961937509957401, 13.97604488694547697, 111.8760903946856757 ) ) ;
#32473 = CARTESIAN_POINT ( 'NONE',  ( -21.52544592524343514, 5.823673210054127303, 111.0405762719810525 ) ) ;
#32474 = CARTESIAN_POINT ( 'NONE',  ( 14.34966873604972726, -8.224510206698740333, 20.83442372801901143 ) ) ;
#32475 = CARTESIAN_POINT ( 'NONE',  ( 4.379528057220092307, 16.55341960407617563, 87.29275706135236135 ) ) ;
#32476 = CARTESIAN_POINT ( 'NONE',  ( 37.99626262588765258, 2.893932880411085066E-14, -4.747842220587804363 ) ) ;
#32477 = CARTESIAN_POINT ( 'NONE',  ( 5.823673210054444382, -21.52544592524334988, 90.20942372801903275 ) ) ;
#32478 = CARTESIAN_POINT ( 'NONE',  ( 9.474510206698729675, 16.51473224551082808, 82.08442372801899012 ) ) ;
#32479 = CARTESIAN_POINT ( 'NONE',  ( 12.14591786802309770, 12.06949235617756955, 49.37390960531436690 ) ) ;
#32480 = CARTESIAN_POINT ( 'NONE',  ( -16.53943276465976808, 0.05219959533911058130, 41.24890960531435269 ) ) ;
#32481 = CARTESIAN_POINT ( 'NONE',  ( 0.05219959533910956823, 16.53943276465976808, 104.9989096053143669 ) ) ;
#32483 = CARTESIAN_POINT ( 'NONE',  ( -8.945614359730852172, 0.6701480022147746629, -63.98123544873404711 ) ) ;
#32482 = CARTESIAN_POINT ( 'NONE',  ( 9.474510206698729675, 16.51473224551082808, 47.08442372801900433 ) ) ;
#32484 = CARTESIAN_POINT ( 'NONE',  ( 21.53943276465977519, 0.05219959533937863772, 31.25109039468568639 ) ) ;
#32485 = CARTESIAN_POINT ( 'NONE',  ( -14.29746914071037622, -8.314922557961029526, 19.16775706135234714 ) ) ;
#32486 = CARTESIAN_POINT ( 'NONE',  ( 17.50000000000000000, -5.500000000000000888, 120.0000000000000142 ) ) ;
#32487 = CARTESIAN_POINT ( 'NONE',  ( 19.05341960407611168, 5.049401038298154454, 98.95724293864766707 ) ) ;
#32488 = CARTESIAN_POINT ( 'NONE',  ( -5.719274019375978568, 21.55341960407610458, 55.20724293864770260 ) ) ;
#32489 = CARTESIAN_POINT ( 'NONE',  ( 5.049401038297881783, 19.05341960407617563, 92.29275706135234714 ) ) ;
#32490 = CARTESIAN_POINT ( 'NONE',  ( 9.474510206698971260, -16.51473224551069308, 87.91557627198102409 ) ) ;
#32491 = CARTESIAN_POINT ( 'NONE',  ( 15.80617190586746368, 15.72974639402197994, 59.37390960531436690 ) ) ;
#32492 = CARTESIAN_POINT ( 'NONE',  ( 14.29746914071049879, -8.314922557960816363, 103.3322429386476955 ) ) ;
#32493 = CARTESIAN_POINT ( 'NONE',  ( 19.05341960407611168, 5.049401038298154454, 63.95724293864769550 ) ) ;
#32494 = CARTESIAN_POINT ( 'NONE',  ( -9.474510206698964154, 16.51473224551069663, 35.41557627198102409 ) ) ;
#32495 = CARTESIAN_POINT ( 'NONE',  ( -21.55341960407619339, 5.719274019375674811, 33.54275706135234714 ) ) ;
#32496 = CARTESIAN_POINT ( 'NONE',  ( 10.81492255796106328, -18.62759615963255655, 80.41775706135234714 ) ) ;
#32497 = EDGE_CURVE ( 'NONE', #17723, #55000, #88682, .T. ) ;
#32498 = CARTESIAN_POINT ( 'NONE',  ( 12.06949235617739724, 12.14591786802326823, 96.87609039468568994 ) ) ;
#32499 = CARTESIAN_POINT ( 'NONE',  ( -5.719274019375665041, -21.55341960407619695, 24.79275706135235779 ) ) ;
#32500 = CARTESIAN_POINT ( 'NONE',  ( 15.72974639402176855, 15.80617190586768217, 26.87609039468567218 ) ) ;
#32502 = CARTESIAN_POINT ( 'NONE',  ( 19.03943276465977164, -0.05219959533909143690, 83.74890960531436690 ) ) ;
#32501 = CARTESIAN_POINT ( 'NONE',  ( -19.05341960407617563, 5.049401038297882671, 68.54275706135230450 ) ) ;
#32503 = CARTESIAN_POINT ( 'NONE',  ( -18.67979575497193778, 10.72451020669871902, 78.33442372801901854 ) ) ;
#32504 = CARTESIAN_POINT ( 'NONE',  ( 0.05219959533907565091, 21.53943276465977519, 79.99890960531435269 ) ) ;
#32505 = CARTESIAN_POINT ( 'NONE',  ( -8.314922557960811034, -14.29746914071050412, 67.08224293864770971 ) ) ;
#32506 = CARTESIAN_POINT ( 'NONE',  ( 5.823673210054444382, -21.52544592524334988, 105.2094237280190328 ) ) ;
#32507 = CARTESIAN_POINT ( 'NONE',  ( 14.34966873604960469, 8.224510206698951720, 84.16557627198103830 ) ) ;
#32508 = CARTESIAN_POINT ( 'NONE',  ( -19.03943276465977164, 0.05219959533909376836, 31.24890960531435979 ) ) ;
#32509 = CARTESIAN_POINT ( 'NONE',  ( 19.02544592524334988, 5.153800228976608722, 76.45942372801897591 ) ) ;
#32510 = CARTESIAN_POINT ( 'NONE',  ( 8.224510206698953496, -14.34966873604960469, 37.91557627198102409 ) ) ;
#32511 = CARTESIAN_POINT ( 'NONE',  ( -21.53943276465977519, -0.05219959533937600094, 88.75109039468567573 ) ) ;
#32512 = CARTESIAN_POINT ( 'NONE',  ( -19.05341960407611168, -5.049401038298163336, 96.45724293864769550 ) ) ;
#32513 = CARTESIAN_POINT ( 'NONE',  ( -9.474510206698720793, -16.51473224551083518, 59.58442372801900433 ) ) ;
#32514 = CARTESIAN_POINT ( 'NONE',  ( 21.55341960407610458, 5.719274019375980345, 68.95724293864769550 ) ) ;
#32515 = CARTESIAN_POINT ( 'NONE',  ( 15.72974639402199770, -15.80617190586745480, 113.1239096053143953 ) ) ;
#32516 = CARTESIAN_POINT ( 'NONE',  ( 16.46253265017146816, 9.564922557961045513, 106.6677570613523471 ) ) ;
#32517 = CARTESIAN_POINT ( 'NONE',  ( 16.55341960407618274, -4.379528057220086978, 86.04275706135236135 ) ) ;
#32519 = CARTESIAN_POINT ( 'NONE',  ( -15.72974639402197994, 15.80617190586746368, 115.6239096053143669 ) ) ;
#32518 = CARTESIAN_POINT ( 'NONE',  ( 5.035744501201078851E-13, -76.33743099897125717, -12.99988689144064402 ) ) ;
#32520 = CARTESIAN_POINT ( 'NONE',  ( -4.483927247898539470, -16.52544592524342804, 97.29057627198105251 ) ) ;
#32521 = CARTESIAN_POINT ( 'NONE',  ( 29.86685920354754487, 21.69954338932564752, -5.924999997268813878 ) ) ;
#32522 = CARTESIAN_POINT ( 'NONE',  ( -12.06949235617739369, -12.14591786802326823, 49.37609039468569705 ) ) ;
#32523 = CARTESIAN_POINT ( 'NONE',  ( 15.80617190586746368, 15.72974639402197994, 64.37390960531435269 ) ) ;
#32524 = CARTESIAN_POINT ( 'NONE',  ( 16.52544592524335698, 4.483927247898782831, 111.4594237280190328 ) ) ;
#32525 = CARTESIAN_POINT ( 'NONE',  ( -16.55341960407617563, 4.379528057220093196, 38.54275706135234714 ) ) ;
#32526 = CARTESIAN_POINT ( 'NONE',  ( 19.05341960407611168, 5.049401038298154454, 33.95724293864769550 ) ) ;
#32527 = CARTESIAN_POINT ( 'NONE',  ( -14.34966873604972548, 8.224510206698743886, 83.33442372801903275 ) ) ;
#32528 = CARTESIAN_POINT ( 'NONE',  ( -16.46253265017146816, -9.564922557961047289, 79.16775706135234714 ) ) ;
#32529 = CARTESIAN_POINT ( 'NONE',  ( 18.62759615963271287, -10.81492255796078972, 68.33224293864769550 ) ) ;
#32530 = CARTESIAN_POINT ( 'NONE',  ( -4.483927247898782831, 16.52544592524335698, 102.7094237280190185 ) ) ;
#32531 = CARTESIAN_POINT ( 'NONE',  ( 0.05219959533937995610, -21.53943276465977519, 80.00109039468568994 ) ) ;
#32532 = CARTESIAN_POINT ( 'NONE',  ( -10.81492255796078084, -18.62759615963271287, 62.08224293864769550 ) ) ;
#32533 = CARTESIAN_POINT ( 'NONE',  ( 10.72451020669898902, -18.67979575497178502, 47.91557627198102409 ) ) ;
#32534 = CARTESIAN_POINT ( 'NONE',  ( -16.52544592524335698, -4.483927247898792601, 78.95942372801901854 ) ) ;
#32535 = CARTESIAN_POINT ( 'NONE',  ( 15.72974639402199770, -15.80617190586745480, 48.12390960531436690 ) ) ;
#32536 = ORIENTED_EDGE ( 'NONE', *, *, #25084, .F. ) ;
#32537 = CARTESIAN_POINT ( 'NONE',  ( 9.564922557960805705, 16.46253265017160317, 109.5822429386476955 ) ) ;
#32538 = CARTESIAN_POINT ( 'NONE',  ( -23.58953014017658489, -7.613468834709958166, 172.7063272879299234 ) ) ;
#32539 = CARTESIAN_POINT ( 'NONE',  ( 5.049401038298161559, -19.05341960407611168, 22.70724293864769194 ) ) ;
#32540 = CARTESIAN_POINT ( 'NONE',  ( -15.80617190586745835, -15.72974639402198527, 56.87390960531436690 ) ) ;
#32541 = CARTESIAN_POINT ( 'NONE',  ( 12.06949235617739724, 12.14591786802326823, 106.8760903946856899 ) ) ;
#32542 = CARTESIAN_POINT ( 'NONE',  ( 15.80617190586769283, -15.72974639402175789, 50.62609039468568994 ) ) ;
#32543 = CARTESIAN_POINT ( 'NONE',  ( -19.02544592524334988, -5.153800228976617603, 98.95942372801900433 ) ) ;
#32544 = CARTESIAN_POINT ( 'NONE',  ( -14.34966873604960291, -8.224510206698953496, 111.6655762719810525 ) ) ;
#32545 = CARTESIAN_POINT ( 'NONE',  ( -5.049401038297874678, -19.05341960407617918, 109.7927570613523187 ) ) ;
#32546 = CARTESIAN_POINT ( 'NONE',  ( 19.02544592524343514, -5.153800228976328945, 43.54057627198103120 ) ) ;
#32547 = CARTESIAN_POINT ( 'NONE',  ( 1.993301997531345292E-15, -30.30510711980685912, 140.5000000000000000 ) ) ;
#32548 = CARTESIAN_POINT ( 'NONE',  ( 19.05341960407611168, 5.049401038298154454, 88.95724293864769550 ) ) ;
#32549 = CARTESIAN_POINT ( 'NONE',  ( 14.34966873604972726, -8.224510206698740333, 75.83442372801900433 ) ) ;
#32550 = CARTESIAN_POINT ( 'NONE',  ( -13.97604488694547697, 13.89961937509957934, 73.12609039468568994 ) ) ;
#32551 = CARTESIAN_POINT ( 'NONE',  ( -19.03943276465977164, -0.05219959533935918106, 18.75109039468567218 ) ) ;
#32552 = CARTESIAN_POINT ( 'NONE',  ( -21.52544592524343514, 5.823673210054127303, 61.04057627198103120 ) ) ;
#32553 = CARTESIAN_POINT ( 'NONE',  ( 16.53943276465976808, 0.05219959533934440121, 81.25109039468568994 ) ) ;
#32554 = CARTESIAN_POINT ( 'NONE',  ( -9.564922557961040184, 16.46253265017147172, 77.91775706135234714 ) ) ;
#32555 = CARTESIAN_POINT ( 'NONE',  ( 5.049401038298161559, -19.05341960407611168, 37.70724293864768839 ) ) ;
#32556 = CARTESIAN_POINT ( 'NONE',  ( -0.05219959533909027116, -19.03943276465977164, 72.49890960531435269 ) ) ;
#32557 = CARTESIAN_POINT ( 'NONE',  ( -10.81492255796105439, 18.62759615963255655, 47.91775706135234714 ) ) ;
#32558 = CARTESIAN_POINT ( 'NONE',  ( -13.89961937509977652, 13.97604488694528158, 40.62390960531435979 ) ) ;
#32559 = CARTESIAN_POINT ( 'NONE',  ( 9.474510206698729675, 16.51473224551082808, 72.08442372801900433 ) ) ;
#32560 = CARTESIAN_POINT ( 'NONE',  ( 21.36928693577338478, -7.422813773936193016, 174.5222352431090087 ) ) ;
#32561 = CARTESIAN_POINT ( 'NONE',  ( 16.51473224551069308, 9.474510206698969483, 104.1655762719810241 ) ) ;
#32562 = CARTESIAN_POINT ( 'NONE',  ( 4.483927247898545687, 16.52544592524342804, 69.79057627198102409 ) ) ;
#32563 = CARTESIAN_POINT ( 'NONE',  ( -21.53943276465977519, 0.05219959533907696930, 61.24890960531435979 ) ) ;
#32564 = CARTESIAN_POINT ( 'NONE',  ( -28.79475375365497314, 9.355982642740462651, 144.1656553485623533 ) ) ;
#32565 =( BOUNDED_CURVE ( )  B_SPLINE_CURVE ( 2, ( #90162, #139631, #108308, #152825, #154816, #75000, #186171, #168978, #121491, #151845, #140636 ),
 .UNSPECIFIED., .F., .F. ) 
 B_SPLINE_CURVE_WITH_KNOTS ( ( 3, 2, 2, 2, 2, 3 ),
 ( 0.2000000000000000111, 0.2200000000000000011, 0.2400000000000000189, 0.2600000000000000644, 0.2800000000000000822, 0.3000000000000000444 ),
 .UNSPECIFIED. ) 
 CURVE ( )  GEOMETRIC_REPRESENTATION_ITEM ( )  RATIONAL_B_SPLINE_CURVE ( ( 1.000000000000000000, 0.9510565162951535312, 1.000000000000000000, 0.9510565162951535312, 1.000000000000000000, 0.9510565162951535312, 1.000000000000000000, 0.9510565162951535312, 1.000000000000000000, 0.9510565162951534202, 1.000000000000000222 ) ) 
 REPRESENTATION_ITEM ( '' )  );
#32566 = CARTESIAN_POINT ( 'NONE',  ( -16.46253265017146816, -9.564922557961047289, 44.16775706135232582 ) ) ;
#32567 = DIRECTION ( 'NONE',  ( -0.000000000000000000, -0.000000000000000000, 1.000000000000000000 ) ) ;
#32569 = CARTESIAN_POINT ( 'NONE',  ( -5.049401038298153566, 19.05341960407611168, 70.20724293864769550 ) ) ;
#32568 = CARTESIAN_POINT ( 'NONE',  ( -13.97604488694527625, -13.89961937509977652, 61.87390960531435979 ) ) ;
#32570 = CARTESIAN_POINT ( 'NONE',  ( 16.53943276465976808, 0.05219959533934440121, 56.25109039468568284 ) ) ;
#32571 = DIRECTION ( 'NONE',  ( -0.000000000000000000, -0.000000000000000000, 1.000000000000000000 ) ) ;
#32572 = CARTESIAN_POINT ( 'NONE',  ( -28.82186960331494419, 9.364793116373629545, 146.1500000054623456 ) ) ;
#32573 = CARTESIAN_POINT ( 'NONE',  ( -4.379528057220086978, -16.55341960407618274, 94.79275706135234714 ) ) ;
#32574 = LINE ( 'NONE', #83780, #150133 ) ;
#32575 = CARTESIAN_POINT ( 'NONE',  ( 14.29746914071037800, 8.314922557961029526, 71.66775706135234714 ) ) ;
#32576 = CARTESIAN_POINT ( 'NONE',  ( -4.483927247898782831, 16.52544592524335698, 37.70942372801900433 ) ) ;
#32577 = CARTESIAN_POINT ( 'NONE',  ( -16.51473224551082808, 9.474510206698731452, 28.33442372801900433 ) ) ;
#32579 = FACE_BOUND ( 'NONE', #71168, .T. ) ;
#32578 = CARTESIAN_POINT ( 'NONE',  ( -19.02544592524342804, 5.153800228976336051, 61.04057627198103120 ) ) ;
#32580 = CARTESIAN_POINT ( 'NONE',  ( -18.67979575497193778, 10.72451020669871902, 58.33442372801901143 ) ) ;
#32581 = CARTESIAN_POINT ( 'NONE',  ( 19.02544592524334988, 5.153800228976608722, 61.45942372801900433 ) ) ;
#32582 = CARTESIAN_POINT ( 'NONE',  ( -21.55341960407619339, 5.719274019375674811, 108.5427570613523756 ) ) ;
#32583 = CARTESIAN_POINT ( 'NONE',  ( -9.564922557960796823, -16.46253265017161027, 32.08224293864769550 ) ) ;
#32584 = CARTESIAN_POINT ( 'NONE',  ( -3.573655867282028392E-15, 2.428612866367529932E-14, -25.00000000000000000 ) ) ;
#32585 = CARTESIAN_POINT ( 'NONE',  ( 15.80617190586746368, 15.72974639402197994, 54.37390960531435979 ) ) ;
#32586 = B_SPLINE_CURVE_WITH_KNOTS ( 'NONE', 3,
 ( #155226, #165685, #156216, #95531, #12022, #78365 ),
 .UNSPECIFIED., .F., .F.,
 ( 4, 2, 4 ),
 ( 0.003239945802372214394, 0.003620412082092060516, 0.004000878361811907070 ),
 .UNSPECIFIED. ) ;
#32587 = CARTESIAN_POINT ( 'NONE',  ( 19.02544592524343514, -5.153800228976328945, 113.5405762719810241 ) ) ;
#32588 = CARTESIAN_POINT ( 'NONE',  ( -12.14591786802309592, -12.06949235617757132, 96.87390960531436690 ) ) ;
#32589 = CARTESIAN_POINT ( 'NONE',  ( 12.14591786802327356, -12.06949235617739191, 40.62609039468567573 ) ) ;
#32590 = CARTESIAN_POINT ( 'NONE',  ( 4.483927247898545687, 16.52544592524342804, 29.79057627198102409 ) ) ;
#32591 = EDGE_LOOP ( 'NONE', ( #2848, #92953, #23342, #132518, #55758, #177128, #84991, #51494, #34137, #91301, #50189, #138708, #21437 ) ) ;
#32592 = EDGE_CURVE ( 'NONE', #23346, #56239, #53157, .T. ) ;
#32593 = CARTESIAN_POINT ( 'NONE',  ( -21.55341960407619339, 5.719274019375674811, 23.54275706135235424 ) ) ;
#32595 = CARTESIAN_POINT ( 'NONE',  ( 19.03943276465977164, -0.05219959533909143690, 108.7489096053143527 ) ) ;
#32594 = CARTESIAN_POINT ( 'NONE',  ( 12.14591786802309770, 12.06949235617756955, 34.37390960531435979 ) ) ;
#32596 = CARTESIAN_POINT ( 'NONE',  ( -9.564922557961040184, 16.46253265017147172, 102.9177570613523329 ) ) ;
#32597 = CARTESIAN_POINT ( 'NONE',  ( -5.049401038297874678, -19.05341960407617918, 29.79275706135232227 ) ) ;
#32598 = CARTESIAN_POINT ( 'NONE',  ( -12.14591786802309592, -12.06949235617757132, 26.87390960531435979 ) ) ;
#32599 = CARTESIAN_POINT ( 'NONE',  ( 18.62759615963271287, -10.81492255796078972, 103.3322429386476955 ) ) ;
#32600 = CARTESIAN_POINT ( 'NONE',  ( -18.67979575497178146, -10.72451020669898902, 61.66557627198103120 ) ) ;
#32601 = CARTESIAN_POINT ( 'NONE',  ( 19.05341960407611168, 5.049401038298154454, 73.95724293864768129 ) ) ;
#32602 = CARTESIAN_POINT ( 'NONE',  ( -16.55341960407611168, -4.379528057220339221, 46.45724293864769550 ) ) ;
#32603 = CARTESIAN_POINT ( 'NONE',  ( -19.05341960407611168, -5.049401038298163336, 96.45724293864769550 ) ) ;
#32604 = CARTESIAN_POINT ( 'NONE',  ( -36.76795047837064345, 4.947931209100015160, 47.42876213711301858 ) ) ;
#32605 = CARTESIAN_POINT ( 'NONE',  ( -5.153800228976607833, 19.02544592524334988, 52.70942372801900433 ) ) ;
#32606 = CARTESIAN_POINT ( 'NONE',  ( -0.05219959533907301413, -21.53943276465977519, 92.49890960531436690 ) ) ;
#32607 = CARTESIAN_POINT ( 'NONE',  ( -12.06949235617756955, 12.14591786802309770, 100.6239096053143811 ) ) ;
#32608 = CARTESIAN_POINT ( 'NONE',  ( 15.72974639402176855, 15.80617190586768217, 41.87609039468568284 ) ) ;
#32609 = CARTESIAN_POINT ( 'NONE',  ( -27.73933785331498925, 2.428612866367529932E-14, 142.8750000027311842 ) ) ;
#32610 = CARTESIAN_POINT ( 'NONE',  ( 14.34966873604960469, 8.224510206698951720, 34.16557627198102409 ) ) ;
#32611 = CARTESIAN_POINT ( 'NONE',  ( -19.05341960407611168, -5.049401038298163336, 31.45724293864769550 ) ) ;
#32612 = CARTESIAN_POINT ( 'NONE',  ( 9.564922557960805705, 16.46253265017160317, 79.58224293864769550 ) ) ;
#32613 = CARTESIAN_POINT ( 'NONE',  ( -21.52544592524343514, 5.823673210054127303, 61.04057627198103120 ) ) ;
#32614 = CARTESIAN_POINT ( 'NONE',  ( -16.51473224551082808, 9.474510206698731452, 93.33442372801900433 ) ) ;
#32615 = CARTESIAN_POINT ( 'NONE',  ( -9.474510206698964154, 16.51473224551069663, 25.41557627198103120 ) ) ;
#32616 = CARTESIAN_POINT ( 'NONE',  ( -21.52544592524343514, 5.823673210054127303, 51.04057627198103120 ) ) ;
#32617 = CARTESIAN_POINT ( 'NONE',  ( -21.53943276465977519, -0.05219959533937600094, 73.75109039468567573 ) ) ;
#32619 = CARTESIAN_POINT ( 'NONE',  ( 4.379528057220092307, 16.55341960407617563, 67.29275706135234714 ) ) ;
#32618 = CARTESIAN_POINT ( 'NONE',  ( 23.37981185087573976, -29.75599608462244561, -21.51565039292758286 ) ) ;
#32620 = CARTESIAN_POINT ( 'NONE',  ( 13.89961937509977652, -13.97604488694527269, 53.12390960531434558 ) ) ;
#32621 = CARTESIAN_POINT ( 'NONE',  ( -13.97604488694527625, -13.89961937509977652, 66.87390960531436690 ) ) ;
#32622 = ORIENTED_EDGE ( 'NONE', *, *, #91774, .T. ) ;
#32623 = CARTESIAN_POINT ( 'NONE',  ( 18.62759615963255655, 10.81492255796105972, 106.6677570613523756 ) ) ;
#32624 = CARTESIAN_POINT ( 'NONE',  ( 14.34966873604972726, -8.224510206698740333, 75.83442372801900433 ) ) ;
#32625 = CARTESIAN_POINT ( 'NONE',  ( -10.81492255796105439, 18.62759615963255655, 92.91775706135236135 ) ) ;
#32626 = CARTESIAN_POINT ( 'NONE',  ( 19.05341960407611168, 5.049401038298154454, 78.95724293864769550 ) ) ;
#32627 = CARTESIAN_POINT ( 'NONE',  ( -21.52544592524343514, 5.823673210054127303, 31.04057627198102409 ) ) ;
#32628 = CARTESIAN_POINT ( 'NONE',  ( 5.153800228976615827, -19.02544592524334988, 105.2094237280190185 ) ) ;
#32629 = CARTESIAN_POINT ( 'NONE',  ( 10.81492255796106328, -18.62759615963255655, 85.41775706135236135 ) ) ;
#32630 = CARTESIAN_POINT ( 'NONE',  ( -16.55341960407617563, 4.379528057220093196, 48.54275706135234714 ) ) ;
#32631 = CARTESIAN_POINT ( 'NONE',  ( -0.05219959533907301413, -21.53943276465977519, 102.4989096053143811 ) ) ;
#32632 = CARTESIAN_POINT ( 'NONE',  ( 13.97604488694548053, -13.89961937509957401, 100.6260903946856615 ) ) ;
#32633 = CARTESIAN_POINT ( 'NONE',  ( -5.153800228976328057, -19.02544592524343514, 72.29057627198102409 ) ) ;
#32634 = CARTESIAN_POINT ( 'NONE',  ( 19.02544592524334988, 5.153800228976608722, 111.4594237280190043 ) ) ;
#32635 = CARTESIAN_POINT ( 'NONE',  ( -9.564922557960796823, -16.46253265017161027, 37.08224293864768839 ) ) ;
#32636 = CARTESIAN_POINT ( 'NONE',  ( 4.379528057220092307, 16.55341960407617563, 27.29275706135234358 ) ) ;
#32637 = CARTESIAN_POINT ( 'NONE',  ( 4.483927247898545687, 16.52544592524342804, 64.79057627198103830 ) ) ;
#32638 = CARTESIAN_POINT ( 'NONE',  ( 0.05219959533934541429, -16.53943276465976808, 80.00109039468568994 ) ) ;
#32640 = CARTESIAN_POINT ( 'NONE',  ( 5.049401038298161559, -19.05341960407611168, 57.70724293864769550 ) ) ;
#32639 = CARTESIAN_POINT ( 'NONE',  ( 5.823673210054444382, -21.52544592524334988, 25.20942372801901854 ) ) ;
#32641 = CARTESIAN_POINT ( 'NONE',  ( 16.51473224551069308, 9.474510206698969483, 74.16557627198103830 ) ) ;
#32642 = CARTESIAN_POINT ( 'NONE',  ( -0.05219959533934338120, 16.53943276465976808, 67.50109039468568994 ) ) ;
#32643 = CARTESIAN_POINT ( 'NONE',  ( -24.14511064691488329, -7.743397529681040226, 169.7652520481184126 ) ) ;
#32644 = EDGE_LOOP ( 'NONE', ( #38049, #100008, #36115, #193625 ) ) ;
#32645 = CARTESIAN_POINT ( 'NONE',  ( -0.05219959533937732626, 21.53943276465977519, 107.5010903946856899 ) ) ;
#32646 = CARTESIAN_POINT ( 'NONE',  ( -16.51473224551069308, -9.474510206698971260, 31.66557627198102054 ) ) ;
#32647 = B_SPLINE_CURVE_WITH_KNOTS ( 'NONE', 3,
 ( #81791, #36301, #161656, #159648, #50501, #66648, #190010, #145478 ),
 .UNSPECIFIED., .F., .F.,
 ( 4, 2, 2, 4 ),
 ( 2.775519118949223281E-07, 0.0006604899437673964792, 0.0009905961396951489494, 0.001320702335622901420 ),
 .UNSPECIFIED. ) ;
#32649 = ORIENTED_EDGE ( 'NONE', *, *, #62981, .T. ) ;
#32648 = CARTESIAN_POINT ( 'NONE',  ( 19.03943276465977164, -0.05219959533909143690, 103.7489096053143669 ) ) ;
#32650 = CARTESIAN_POINT ( 'NONE',  ( 12.06949235617739724, 12.14591786802326823, 26.87609039468567218 ) ) ;
#32652 = CARTESIAN_POINT ( 'NONE',  ( 14.29746914071037800, 8.314922557961029526, 36.66775706135234714 ) ) ;
#32651 = CARTESIAN_POINT ( 'NONE',  ( 9.564922557961047289, -16.46253265017146816, 45.41775706135232582 ) ) ;
#32653 = CARTESIAN_POINT ( 'NONE',  ( -16.51473224551069308, -9.474510206698971260, 36.66557627198102409 ) ) ;
#32654 = CARTESIAN_POINT ( 'NONE',  ( 5.153800228976335163, 19.02544592524342804, 109.7905762719810099 ) ) ;
#32655 = CARTESIAN_POINT ( 'NONE',  ( -19.02544592524342804, 5.153800228976336051, 61.04057627198103120 ) ) ;
#32656 = CARTESIAN_POINT ( 'NONE',  ( -21.52544592524343514, 5.823673210054127303, 106.0405762719810525 ) ) ;
#32658 = CARTESIAN_POINT ( 'NONE',  ( -19.02544592524342804, 5.153800228976336051, 116.0405762719810383 ) ) ;
#32657 = CARTESIAN_POINT ( 'NONE',  ( -9.564922557960796823, -16.46253265017161027, 97.08224293864769550 ) ) ;
#32659 = CARTESIAN_POINT ( 'NONE',  ( 5.153800228976335163, 19.02544592524342804, 69.79057627198103830 ) ) ;
#32661 = CARTESIAN_POINT ( 'NONE',  ( 22.44159573604009594, -16.30477369853687364, 148.1750000027311671 ) ) ;
#32660 = CARTESIAN_POINT ( 'NONE',  ( -14.34966873604960291, -8.224510206698953496, 21.66557627198102409 ) ) ;
#32662 = CARTESIAN_POINT ( 'NONE',  ( 9.474510206698729675, 16.51473224551082808, 97.08442372801900433 ) ) ;
#32663 = CARTESIAN_POINT ( 'NONE',  ( 16.51473224551083163, -9.474510206698727899, 25.83442372801900078 ) ) ;
#32664 = B_SPLINE_CURVE_WITH_KNOTS ( 'NONE', 3,
 ( #176201, #145839, #87179, #179211, #149851, #192365 ),
 .UNSPECIFIED., .F., .F.,
 ( 4, 2, 4 ),
 ( 0.003989672132298143457, 0.004372778065220561498, 0.004755883998142979539 ),
 .UNSPECIFIED. ) ;
#32665 = CARTESIAN_POINT ( 'NONE',  ( 12.14591786802309770, 12.06949235617756955, 54.37390960531435979 ) ) ;
#32666 = CARTESIAN_POINT ( 'NONE',  ( -15.72974639402176322, -15.80617190586768395, 104.3760903946856899 ) ) ;
#32667 = CARTESIAN_POINT ( 'NONE',  ( 16.51473224551069308, 9.474510206698969483, 29.16557627198103475 ) ) ;
#32669 = CARTESIAN_POINT ( 'NONE',  ( 18.62759615963255655, 10.81492255796105972, 96.66775706135234714 ) ) ;
#32668 = CARTESIAN_POINT ( 'NONE',  ( 14.34966873604960469, 8.224510206698951720, 29.16557627198103120 ) ) ;
#32670 = CARTESIAN_POINT ( 'NONE',  ( -19.05341960407611168, -5.049401038298163336, 86.45724293864769550 ) ) ;
#32671 = CARTESIAN_POINT ( 'NONE',  ( -15.72974639402176322, -15.80617190586768395, 49.37609039468569705 ) ) ;
#32672 = CARTESIAN_POINT ( 'NONE',  ( 16.51473224551069308, 9.474510206698969483, 94.16557627198103830 ) ) ;
#32673 = CARTESIAN_POINT ( 'NONE',  ( 12.14591786802309770, 12.06949235617756955, 94.37390960531436690 ) ) ;
#32674 = CARTESIAN_POINT ( 'NONE',  ( -16.53943276465976808, 0.05219959533911058130, 66.24890960531436690 ) ) ;
#32675 = CARTESIAN_POINT ( 'NONE',  ( -10.72451020669898014, 18.67979575497178502, 75.41557627198102409 ) ) ;
#32676 = CARTESIAN_POINT ( 'NONE',  ( -5.049401038298153566, 19.05341960407611168, 70.20724293864769550 ) ) ;
#32677 = CARTESIAN_POINT ( 'NONE',  ( 18.67979575497178502, 10.72451020669898547, 84.16557627198103830 ) ) ;
#32678 = CARTESIAN_POINT ( 'NONE',  ( -9.474510206698720793, -16.51473224551083518, 84.58442372801900433 ) ) ;
#32680 = CARTESIAN_POINT ( 'NONE',  ( -8.224510206698948167, 14.34966873604960824, 85.41557627198102409 ) ) ;
#32679 = CARTESIAN_POINT ( 'NONE',  ( 5.049401038297881783, 19.05341960407617918, 32.29275706135233293 ) ) ;
#32681 = CARTESIAN_POINT ( 'NONE',  ( -16.46253265017160317, 9.564922557960807481, 60.83224293864769550 ) ) ;
#32682 = CARTESIAN_POINT ( 'NONE',  ( 21.52544592524344225, -5.823673210054117533, 68.54057627198103830 ) ) ;
#32683 = CARTESIAN_POINT ( 'NONE',  ( 16.36317988757059183, -7.306389748694916975, 26.59789608363226421 ) ) ;
#32685 = CARTESIAN_POINT ( 'NONE',  ( -4.500000000000000888, -120.9970989573719038, 14.58956564881029827 ) ) ;
#32684 = CARTESIAN_POINT ( 'NONE',  ( -4.483927247898782831, 16.52544592524335698, 107.7094237280190328 ) ) ;
#32686 = CARTESIAN_POINT ( 'NONE',  ( -5.049401038297874678, -19.05341960407617918, 104.7927570613523471 ) ) ;
#32687 = EDGE_CURVE ( 'NONE', #167889, #46374, #65274, .T. ) ;
#32688 = CARTESIAN_POINT ( 'NONE',  ( 0.05219959533910956823, 16.53943276465976808, 84.99890960531436690 ) ) ;
#32689 = CARTESIAN_POINT ( 'NONE',  ( 6.293264767923585801, -0.7627558185761198484, -62.46802126132829613 ) ) ;
#32690 = CARTESIAN_POINT ( 'NONE',  ( 9.564922557960805705, 16.46253265017160317, 74.58224293864769550 ) ) ;
#32691 = CARTESIAN_POINT ( 'NONE',  ( 16.46253265017160672, -9.564922557960803928, 33.33224293864770260 ) ) ;
#32692 = CARTESIAN_POINT ( 'NONE',  ( 4.379528057220339221, -16.55341960407611168, 62.70724293864769550 ) ) ;
#32693 = CARTESIAN_POINT ( 'NONE',  ( 9.474510206698971260, -16.51473224551069308, 97.91557627198102409 ) ) ;
#32695 = CARTESIAN_POINT ( 'NONE',  ( -19.05341960407611168, -5.049401038298163336, 66.45724293864769550 ) ) ;
#32694 = CARTESIAN_POINT ( 'NONE',  ( -0.05219959533936034679, 19.03943276465977164, 92.50109039468566152 ) ) ;
#32696 = CARTESIAN_POINT ( 'NONE',  ( 13.89961937509977652, -13.97604488694527269, 88.12390960531438111 ) ) ;
#32697 = CARTESIAN_POINT ( 'NONE',  ( 21.55341960407610458, 5.719274019375980345, 73.95724293864769550 ) ) ;
#32698 = CARTESIAN_POINT ( 'NONE',  ( 12.06949235617739724, 12.14591786802326823, 71.87609039468568994 ) ) ;
#32699 = CARTESIAN_POINT ( 'NONE',  ( -17.05587630539708854, 6.762274262136623193, 95.74180309037286918 ) ) ;
#32700 = CARTESIAN_POINT ( 'NONE',  ( -5.153800228976328057, -19.02544592524343514, 62.29057627198100988 ) ) ;
#32701 = CARTESIAN_POINT ( 'NONE',  ( 0.05219959533907565091, 21.53943276465977519, 64.99890960531435269 ) ) ;
#32702 = CARTESIAN_POINT ( 'NONE',  ( -9.474510206698720793, -16.51473224551083518, 89.58442372801900433 ) ) ;
#32704 = CARTESIAN_POINT ( 'NONE',  ( -0.05219959533937732626, 21.53943276465977519, 47.50109039468568994 ) ) ;
#32703 = CARTESIAN_POINT ( 'NONE',  ( 12.14591786802309770, 12.06949235617756955, 44.37390960531435979 ) ) ;
#32706 = CARTESIAN_POINT ( 'NONE',  ( 9.474510206698971260, -16.51473224551069308, 107.9155762719810383 ) ) ;
#32705 = CARTESIAN_POINT ( 'NONE',  ( 14.34966873604972726, -8.224510206698740333, 75.83442372801900433 ) ) ;
#32707 = CARTESIAN_POINT ( 'NONE',  ( 0.05219959533909260263, 19.03943276465977164, 104.9989096053143669 ) ) ;
#32708 = DIRECTION ( 'NONE',  ( 0.000000000000000000, 0.000000000000000000, -1.000000000000000000 ) ) ;
#32709 = CARTESIAN_POINT ( 'NONE',  ( -4.379528057220086978, -16.55341960407618274, 89.79275706135236135 ) ) ;
#32710 = CARTESIAN_POINT ( 'NONE',  ( 14.29746914071037800, 8.314922557961029526, 51.66775706135234714 ) ) ;
#32711 = CARTESIAN_POINT ( 'NONE',  ( 9.564922557960805705, 16.46253265017160317, 64.58224293864769550 ) ) ;
#32712 = CARTESIAN_POINT ( 'NONE',  ( 19.02544592524343514, -5.153800228976328945, 58.54057627198102409 ) ) ;
#32713 = CARTESIAN_POINT ( 'NONE',  ( 5.719274019375673035, 21.55341960407619339, 47.29275706135234003 ) ) ;
#32714 = CARTESIAN_POINT ( 'NONE',  ( -16.55341960407617563, 4.379528057220093196, 68.54275706135234714 ) ) ;
#32715 = CARTESIAN_POINT ( 'NONE',  ( -4.379528057220328563, 16.55341960407611168, 30.20724293864769550 ) ) ;
#32716 = CARTESIAN_POINT ( 'NONE',  ( 19.03943276465977164, -0.05219959533909143690, 43.74890960531435979 ) ) ;
#32717 = CARTESIAN_POINT ( 'NONE',  ( -19.05341960407611168, -5.049401038298163336, 41.45724293864769550 ) ) ;
#32718 = CARTESIAN_POINT ( 'NONE',  ( 0.05219959533934541429, -16.53943276465976808, 30.00109039468568284 ) ) ;
#32719 = CARTESIAN_POINT ( 'NONE',  ( -0.05219959533936034679, 19.03943276465977164, 82.50109039468567573 ) ) ;
#32720 = CARTESIAN_POINT ( 'NONE',  ( 12.06949235617757843, -12.14591786802309237, 83.12390960531436690 ) ) ;
#32721 = CARTESIAN_POINT ( 'NONE',  ( 9.564922557960805705, 16.46253265017160317, 54.58224293864769550 ) ) ;
#32723 = CARTESIAN_POINT ( 'NONE',  ( -23.48529157249599919, -32.32473071737750558, -9.699999999999999289 ) ) ;
#32722 = CARTESIAN_POINT ( 'NONE',  ( -19.02544592524334988, -5.153800228976617603, 88.95942372801897591 ) ) ;
#32724 = CARTESIAN_POINT ( 'NONE',  ( 5.823673210054444382, -21.52544592524334988, 90.20942372801903275 ) ) ;
#32725 = CARTESIAN_POINT ( 'NONE',  ( 16.52544592524335698, 4.483927247898782831, 56.45942372801902565 ) ) ;
#32726 = CARTESIAN_POINT ( 'NONE',  ( 17.05116617787827593, 6.768360034955705373, 38.84324446740802017 ) ) ;
#32727 = CARTESIAN_POINT ( 'NONE',  ( -5.823673210054116645, -21.52544592524344225, 52.29057627198102409 ) ) ;
#32728 = CARTESIAN_POINT ( 'NONE',  ( 14.29746914071037800, 8.314922557961029526, 41.66775706135235424 ) ) ;
#32729 = CARTESIAN_POINT ( 'NONE',  ( 17.60779699588838909, 5.500000000000005329, 88.84981316670105400 ) ) ;
#32730 = CARTESIAN_POINT ( 'NONE',  ( 5.153800228976615827, -19.02544592524334988, 25.20942372801900433 ) ) ;
#32731 = CARTESIAN_POINT ( 'NONE',  ( -5.049401038298153566, 19.05341960407611168, 80.20724293864769550 ) ) ;
#32732 = FACE_OUTER_BOUND ( 'NONE', #161272, .T. ) ;
#32733 = CARTESIAN_POINT ( 'NONE',  ( -19.03943276465977164, 0.05219959533909376836, 56.24890960531435979 ) ) ;
#32734 = CARTESIAN_POINT ( 'NONE',  ( -20.29917818118329720, -22.40963075479333355, -51.18760544280081604 ) ) ;
#32735 = CARTESIAN_POINT ( 'NONE',  ( 9.474510206698971260, -16.51473224551069308, 72.91557627198102409 ) ) ;
#32736 = CARTESIAN_POINT ( 'NONE',  ( -19.52851543214742236, -5.500000000000035527, 55.39357721762581122 ) ) ;
#32737 = CARTESIAN_POINT ( 'NONE',  ( -0.05219959533936034679, 19.03943276465977164, 37.50109039468567573 ) ) ;
#32738 = CARTESIAN_POINT ( 'NONE',  ( 5.719274019375673035, 21.55341960407619339, 107.2927570613523471 ) ) ;
#32739 = CARTESIAN_POINT ( 'NONE',  ( -14.34966873604960291, -8.224510206698953496, 36.66557627198103120 ) ) ;
#32740 = CARTESIAN_POINT ( 'NONE',  ( 5.049401038298161559, -19.05341960407611168, 42.70724293864767418 ) ) ;
#32741 = CARTESIAN_POINT ( 'NONE',  ( 9.564922557960805705, 16.46253265017160317, 109.5822429386476955 ) ) ;
#32742 = CARTESIAN_POINT ( 'NONE',  ( 18.62759615963255655, 10.81492255796105972, 71.66775706135234714 ) ) ;
#32743 = CARTESIAN_POINT ( 'NONE',  ( -19.03943276465977164, 0.05219959533909376836, 56.24890960531435979 ) ) ;
#32744 = CARTESIAN_POINT ( 'NONE',  ( -21.55341960407619339, 5.719274019375674811, 78.54275706135236135 ) ) ;
#32745 = CARTESIAN_POINT ( 'NONE',  ( 13.97604488694527802, 13.89961937509977652, 114.3739096053143669 ) ) ;
#32746 = CARTESIAN_POINT ( 'NONE',  ( -9.564922557960796823, -16.46253265017161027, 42.08224293864769550 ) ) ;
#32747 = B_SPLINE_CURVE_WITH_KNOTS ( 'NONE', 3,
 ( #191459, #159116, #172313, #83274, #52937, #188490, #112621, #111633, #173318, #19627, #81269, #174313, #41793, #161125, #22621, #195485, #72120, #69114, #165139, #101439, #194477, #116623, #56960, #102456, #71124, #177319, #57958, #84268, #178312, #88273, #148970, #38790, #119629, #55949, #26630, #73138, #40787, #85271, #11467, #134808, #99445, #39775, #164144 ),
 .UNSPECIFIED., .F., .F.,
 ( 4, 2, 2, 2, 2, 2, 2, 2, 2, 2, 2, 2, 2, 1, 2, 2, 2, 2, 2, 2, 2, 4 ),
 ( 0.04122229388621103524, 0.04269295678691728546, 0.04416361968762353568, 0.04489895113797665732, 0.04563428258832977896, 0.04710494548903602918, 0.04857560838974227940, 0.04931093984009541492, 0.05004627129044855044, 0.05151693419115481454, 0.05298759709186107864, 0.05445825999256734273, 0.05519359144292046437, 0.05592892289327358601, 0.05666425434362670766, 0.05739958579397982930, 0.05887024869468609339, 0.06034091159539235749, 0.06181157449609861465, 0.06254690594645175017, 0.06328223739680488569, 0.06475290029751114285 ),
 .UNSPECIFIED. ) ;
#32748 = CARTESIAN_POINT ( 'NONE',  ( -5.719274019375665041, -21.55341960407619695, 19.79275706135235069 ) ) ;
#32749 = CARTESIAN_POINT ( 'NONE',  ( 19.02544592524334988, 5.153800228976608722, 46.45942372801899012 ) ) ;
#32750 = CARTESIAN_POINT ( 'NONE',  ( 19.02544592524343514, -5.153800228976328945, 28.54057627198102409 ) ) ;
#32751 = CARTESIAN_POINT ( 'NONE',  ( 19.03943276465977164, -0.05219959533909143690, 73.74890960531435269 ) ) ;
#32752 = CARTESIAN_POINT ( 'NONE',  ( -0.05219959533936034679, 19.03943276465977164, 107.5010903946856615 ) ) ;
#32753 = CARTESIAN_POINT ( 'NONE',  ( -8.314922557960811034, -14.29746914071050412, 72.08224293864769550 ) ) ;
#32754 = CARTESIAN_POINT ( 'NONE',  ( -21.53943276465977519, 0.05219959533907696930, 41.24890960531435269 ) ) ;
#32755 = CARTESIAN_POINT ( 'NONE',  ( -19.05341960407617563, 5.049401038297882671, 98.54275706135233293 ) ) ;
#32756 = CARTESIAN_POINT ( 'NONE',  ( 10.81492255796078972, 18.62759615963270932, 104.5822429386477097 ) ) ;
#32757 = CARTESIAN_POINT ( 'NONE',  ( -5.823673210054431948, 21.52544592524334988, 57.70942372801901143 ) ) ;
#32758 = CARTESIAN_POINT ( 'NONE',  ( 14.34966873604972726, -8.224510206698740333, 50.83442372801901143 ) ) ;
#32759 = CARTESIAN_POINT ( 'NONE',  ( 14.29746914071037800, 8.314922557961029526, 51.66775706135234714 ) ) ;
#32760 = CARTESIAN_POINT ( 'NONE',  ( 15.72974639402199770, -15.80617190586745480, 73.12390960531436690 ) ) ;
#32761 = CARTESIAN_POINT ( 'NONE',  ( 16.46253265017160672, -9.564922557960803928, 48.33224293864769550 ) ) ;
#32762 = CARTESIAN_POINT ( 'NONE',  ( 4.483927247898790824, -16.52544592524335698, 85.20942372801901854 ) ) ;
#32763 = CARTESIAN_POINT ( 'NONE',  ( 21.52544592524344225, -5.823673210054117533, 108.5405762719810241 ) ) ;
#32764 = CARTESIAN_POINT ( 'NONE',  ( 8.224510206698953496, -14.34966873604960469, 57.91557627198103120 ) ) ;
#32765 = CARTESIAN_POINT ( 'NONE',  ( 16.51473224551069308, 9.474510206698969483, 69.16557627198102409 ) ) ;
#32766 = CARTESIAN_POINT ( 'NONE',  ( 16.53943276465976808, 0.05219959533934440121, 76.25109039468568994 ) ) ;
#32767 = CARTESIAN_POINT ( 'NONE',  ( -4.483927247898782831, 16.52544592524335698, 22.70942372801901499 ) ) ;
#32768 = CARTESIAN_POINT ( 'NONE',  ( 5.823673210054125526, 21.52544592524343514, 109.7905762719810383 ) ) ;
#32769 = CARTESIAN_POINT ( 'NONE',  ( 12.06949235617757843, -12.14591786802309237, 48.12390960531436690 ) ) ;
#32770 = ORIENTED_EDGE ( 'NONE', *, *, #183088, .F. ) ;
#32771 = CARTESIAN_POINT ( 'NONE',  ( -17.26172910966778673, 6.454744622555849354, 75.80646908649225679 ) ) ;
#32772 = CARTESIAN_POINT ( 'NONE',  ( 10.72451020669898902, -18.67979575497178502, 92.91557627198103830 ) ) ;
#32773 = CARTESIAN_POINT ( 'NONE',  ( -4.483927247898539470, -16.52544592524342804, 32.29057627198102409 ) ) ;
#32774 = ORIENTED_EDGE ( 'NONE', *, *, #4359, .T. ) ;
#32775 = CARTESIAN_POINT ( 'NONE',  ( -16.61371651742604172, -7.165104196376049117, 56.14584930007003294 ) ) ;
#32776 = CARTESIAN_POINT ( 'NONE',  ( 5.719274019375991003, -21.55341960407610458, 112.7072429386476955 ) ) ;
#32777 = CARTESIAN_POINT ( 'NONE',  ( -5.153800228976328057, -19.02544592524343514, 107.2905762719810383 ) ) ;
#32778 = CARTESIAN_POINT ( 'NONE',  ( 18.62759615963255655, 10.81492255796105972, 21.66775706135235069 ) ) ;
#32779 = CARTESIAN_POINT ( 'NONE',  ( -16.53943276465976808, 0.05219959533911058130, 51.24890960531436690 ) ) ;
#32780 = CARTESIAN_POINT ( 'NONE',  ( 12.06949235617739724, 12.14591786802326823, 51.87609039468568284 ) ) ;
#32781 = CARTESIAN_POINT ( 'NONE',  ( -16.46253265017160317, 9.564922557960807481, 55.83224293864769550 ) ) ;
#32782 = CARTESIAN_POINT ( 'NONE',  ( 5.049401038297881783, 19.05341960407617563, 57.29275706135231871 ) ) ;
#32783 = CARTESIAN_POINT ( 'NONE',  ( 16.51473224551069308, 9.474510206698969483, 84.16557627198102409 ) ) ;
#32784 = CARTESIAN_POINT ( 'NONE',  ( 21.53943276465977519, -0.05219959533907433946, 33.74890960531436690 ) ) ;
#32785 = CARTESIAN_POINT ( 'NONE',  ( -24.54856932377555268, -28.36614238946897970, -18.58410241722922862 ) ) ;
#32786 = CARTESIAN_POINT ( 'NONE',  ( 19.03943276465977164, -0.05219959533909143690, 48.74890960531435979 ) ) ;
#32787 = CARTESIAN_POINT ( 'NONE',  ( 0.05219959533934541429, -16.53943276465976808, 20.00109039468568639 ) ) ;
#32788 = CARTESIAN_POINT ( 'NONE',  ( -9.564922557961040184, 16.46253265017147172, 57.91775706135233293 ) ) ;
#32789 = CARTESIAN_POINT ( 'NONE',  ( -0.05219959533907301413, -21.53943276465977519, 97.49890960531436690 ) ) ;
#32790 = CARTESIAN_POINT ( 'NONE',  ( 8.224510206698953496, -14.34966873604960469, 27.91557627198103830 ) ) ;
#32791 = CARTESIAN_POINT ( 'NONE',  ( 5.153800228976335163, 19.02544592524342804, 89.79057627198102409 ) ) ;
#32792 = CARTESIAN_POINT ( 'NONE',  ( 15.72974639402199770, -15.80617190586745480, 63.12390960531435979 ) ) ;
#32794 = CARTESIAN_POINT ( 'NONE',  ( 4.483927247898790824, -16.52544592524335698, 30.20942372801902565 ) ) ;
#32793 = CARTESIAN_POINT ( 'NONE',  ( 10.72451020669898902, -18.67979575497178502, 92.91557627198103830 ) ) ;
#32795 = EDGE_CURVE ( 'NONE', #41468, #92045, #152540, .T. ) ;
#32796 = CARTESIAN_POINT ( 'NONE',  ( -18.67979575497178146, -10.72451020669898902, 21.66557627198102409 ) ) ;
#32797 = CARTESIAN_POINT ( 'NONE',  ( 21.55341960407619695, -5.719274019375665929, 91.04275706135236135 ) ) ;
#32798 = CARTESIAN_POINT ( 'NONE',  ( -16.51473224551069308, -9.474510206698971260, 81.66557627198103830 ) ) ;
#32799 = CARTESIAN_POINT ( 'NONE',  ( 5.153800228976335163, 19.02544592524342804, 29.79057627198102409 ) ) ;
#32800 = CARTESIAN_POINT ( 'NONE',  ( -16.46253265017160317, 9.564922557960807481, 85.83224293864769550 ) ) ;
#32801 = CARTESIAN_POINT ( 'NONE',  ( -8.314922557960811034, -14.29746914071050412, 107.0822429386476955 ) ) ;
#32802 = CARTESIAN_POINT ( 'NONE',  ( 16.51473224551069308, 9.474510206698969483, 64.16557627198102409 ) ) ;
#32803 = CARTESIAN_POINT ( 'NONE',  ( -0.05219959533934338120, 16.53943276465976808, 22.50109039468567573 ) ) ;
#32804 = FACE_OUTER_BOUND ( 'NONE', #112589, .T. ) ;
#32806 = CARTESIAN_POINT ( 'NONE',  ( 9.564922557960805705, 16.46253265017160317, 109.5822429386476955 ) ) ;
#32805 = CARTESIAN_POINT ( 'NONE',  ( 5.719274019375673035, 21.55341960407619339, 92.29275706135236135 ) ) ;
#32808 = EDGE_CURVE ( 'NONE', #36107, #119352, #95152, .T. ) ;
#32807 = CARTESIAN_POINT ( 'NONE',  ( -16.53943276465976808, -0.05219959533934237506, 93.75109039468567573 ) ) ;
#32809 = CARTESIAN_POINT ( 'NONE',  ( 38.00000000000000000, -12.34694845685040754, -9.099999999999999645 ) ) ;
#32810 = CARTESIAN_POINT ( 'NONE',  ( -16.46253265017146816, -9.564922557961047289, 69.16775706135233293 ) ) ;
#32811 = CARTESIAN_POINT ( 'NONE',  ( 9.474510206698729675, 16.51473224551082808, 37.08442372801899722 ) ) ;
#32812 = CARTESIAN_POINT ( 'NONE',  ( 27.73881904903412021, -0.9222476559034787913, 140.0000000000000000 ) ) ;
#32813 = CARTESIAN_POINT ( 'NONE',  ( 5.153800228976335163, 19.02544592524342804, 34.79057627198102409 ) ) ;
#32814 = CARTESIAN_POINT ( 'NONE',  ( -16.52544592524342804, 4.483927247898546575, 41.04057627198103120 ) ) ;
#32815 = CARTESIAN_POINT ( 'NONE',  ( 19.03943276465977164, -0.05219959533909143690, 23.74890960531435269 ) ) ;
#32816 = CARTESIAN_POINT ( 'NONE',  ( 0.05219959533910956823, 16.53943276465976808, 24.99890960531435624 ) ) ;
#32817 = CARTESIAN_POINT ( 'NONE',  ( 17.13100169013299734, 6.664070546373170423, 66.73210164300152769 ) ) ;
#32818 = CARTESIAN_POINT ( 'NONE',  ( -8.314922557961024197, 14.29746914071037800, 92.91775706135236135 ) ) ;
#32819 = CARTESIAN_POINT ( 'NONE',  ( -9.474510206698964154, 16.51473224551069663, 30.41557627198102054 ) ) ;
#32820 = CARTESIAN_POINT ( 'NONE',  ( -21.52544592524334988, -5.823673210054445271, 88.95942372801901854 ) ) ;
#32821 = CARTESIAN_POINT ( 'NONE',  ( 19.05341960407617918, -5.049401038297876454, 106.0427570613523471 ) ) ;
#32822 = CARTESIAN_POINT ( 'NONE',  ( 18.62759615963255655, 10.81492255796105972, 81.66775706135236135 ) ) ;
#32823 = CARTESIAN_POINT ( 'NONE',  ( 13.89961937509957401, 13.97604488694547697, 46.87609039468565442 ) ) ;
#32824 = CARTESIAN_POINT ( 'NONE',  ( 9.564922557960805705, 16.46253265017160317, 89.58224293864769550 ) ) ;
#32825 = CARTESIAN_POINT ( 'NONE',  ( -16.51473224551069308, -9.474510206698971260, 66.66557627198102409 ) ) ;
#32826 = LINE ( 'NONE', #141972, #136799 ) ;
#32827 = CARTESIAN_POINT ( 'NONE',  ( 16.55341960407611168, 4.379528057220329451, 68.95724293864769550 ) ) ;
#32828 = CARTESIAN_POINT ( 'NONE',  ( -18.62759615963270932, 10.81492255796079327, 55.83224293864770260 ) ) ;
#32829 = CARTESIAN_POINT ( 'NONE',  ( 19.05341960407611168, 5.049401038298154454, 43.95724293864769550 ) ) ;
#32831 = CARTESIAN_POINT ( 'NONE',  ( 4.483927247898790824, -16.52544592524335698, 75.20942372801901854 ) ) ;
#32830 = CARTESIAN_POINT ( 'NONE',  ( 10.72451020669898902, -18.67979575497178502, 87.91557627198103830 ) ) ;
#32832 = ORIENTED_EDGE ( 'NONE', *, *, #1535, .T. ) ;
#32833 = CARTESIAN_POINT ( 'NONE',  ( -13.89961937509977652, 13.97604488694528158, 50.62390960531435979 ) ) ;
#32834 = EDGE_CURVE ( 'NONE', #141234, #72646, #42269, .T. ) ;
#32836 = CARTESIAN_POINT ( 'NONE',  ( 36.91746825000000598, -11.99521256947793546, -5.724999997268813701 ) ) ;
#32835 = CARTESIAN_POINT ( 'NONE',  ( 16.55341960407611168, 4.379528057220329451, 73.95724293864769550 ) ) ;
#32837 = CARTESIAN_POINT ( 'NONE',  ( 16.46253265017160672, -9.564922557960803928, 53.33224293864768839 ) ) ;
#32838 = CARTESIAN_POINT ( 'NONE',  ( 9.474510206698971260, -16.51473224551069308, 27.91557627198103120 ) ) ;
#32839 = CARTESIAN_POINT ( 'NONE',  ( -0.05219959533936034679, 19.03943276465977164, 67.50109039468566152 ) ) ;
#32840 = CARTESIAN_POINT ( 'NONE',  ( -16.53943276465976808, 0.05219959533911058130, 71.24890960531435269 ) ) ;
#32841 = CARTESIAN_POINT ( 'NONE',  ( -21.52544592524334988, -5.823673210054445271, 43.95942372801902565 ) ) ;
#32843 = CARTESIAN_POINT ( 'NONE',  ( 21.52544592524344225, -5.823673210054117533, 103.5405762719810383 ) ) ;
#32842 = CARTESIAN_POINT ( 'NONE',  ( -19.03943276465977164, 0.05219959533909376836, 41.24890960531435269 ) ) ;
#32844 = DIRECTION ( 'NONE',  ( 0.000000000000000000, 0.000000000000000000, 1.000000000000000000 ) ) ;
#32845 = CARTESIAN_POINT ( 'NONE',  ( -8.314922557960811034, -14.29746914071050412, 92.08224293864769550 ) ) ;
#32846 = CARTESIAN_POINT ( 'NONE',  ( 18.08554851550187337, -38.44972689946076372, -20.08432885666353229 ) ) ;
#32847 = CARTESIAN_POINT ( 'NONE',  ( 13.97604488694527802, 13.89961937509977652, 44.37390960531435269 ) ) ;
#32848 = CARTESIAN_POINT ( 'NONE',  ( 19.49671883438229258, 5.499999999999973355, 47.39279849105685827 ) ) ;
#32850 = CARTESIAN_POINT ( 'NONE',  ( -16.51473224551069308, -9.474510206698971260, 101.6655762719810241 ) ) ;
#32849 = CARTESIAN_POINT ( 'NONE',  ( -0.05219959533936034679, 19.03943276465977164, 92.50109039468566152 ) ) ;
#32851 = CARTESIAN_POINT ( 'NONE',  ( 10.81492255796106328, -18.62759615963255655, 35.41775706135234003 ) ) ;
#32852 = CARTESIAN_POINT ( 'NONE',  ( 5.153800228976335163, 19.02544592524342804, 79.79057627198102409 ) ) ;
#32853 = CARTESIAN_POINT ( 'NONE',  ( -13.97604488694547697, 13.89961937509957934, 68.12609039468563310 ) ) ;
#32854 = CARTESIAN_POINT ( 'NONE',  ( -19.03943276465977164, 0.05219959533909376836, 51.24890960531436690 ) ) ;
#32855 = CARTESIAN_POINT ( 'NONE',  ( 16.52544592524342804, -4.483927247898539470, 68.54057627198103830 ) ) ;
#32856 = CARTESIAN_POINT ( 'NONE',  ( -8.314922557960811034, -14.29746914071050412, 72.08224293864769550 ) ) ;
#32857 = CARTESIAN_POINT ( 'NONE',  ( 19.05341960407611168, 5.049401038298154454, 78.95724293864769550 ) ) ;
#32858 = CARTESIAN_POINT ( 'NONE',  ( 21.52544592524344225, -5.823673210054117533, 103.5405762719810383 ) ) ;
#32859 = CARTESIAN_POINT ( 'NONE',  ( -13.89961937509977652, 13.97604488694528158, 65.62390960531436690 ) ) ;
#32860 = CARTESIAN_POINT ( 'NONE',  ( 15.80617190586769283, -15.72974639402175789, 110.6260903946857042 ) ) ;
#32863 = CARTESIAN_POINT ( 'NONE',  ( -14.29746914071049879, 8.314922557960819915, 115.8322429386477097 ) ) ;
#32862 = CARTESIAN_POINT ( 'NONE',  ( 8.314922557961029526, -14.29746914071037800, 105.4177570613523613 ) ) ;
#32861 = CARTESIAN_POINT ( 'NONE',  ( -16.51473224551069308, -9.474510206698971260, 41.66557627198103120 ) ) ;
#32864 = CARTESIAN_POINT ( 'NONE',  ( -0.05219959533936034679, 19.03943276465977164, 107.5010903946856615 ) ) ;
#32865 = EDGE_LOOP ( 'NONE', ( #20596, #55441, #88903, #13254 ) ) ;
#32866 = CARTESIAN_POINT ( 'NONE',  ( 0.05219959533937995610, -21.53943276465977519, 25.00109039468567218 ) ) ;
#32867 = CARTESIAN_POINT ( 'NONE',  ( 5.049401038297881783, 19.05341960407617563, 67.29275706135234714 ) ) ;
#32868 = CARTESIAN_POINT ( 'NONE',  ( 16.53943276465976808, -0.05219959533910856209, 23.74890960531435269 ) ) ;
#32869 = CARTESIAN_POINT ( 'NONE',  ( -15.80617190586745835, -15.72974639402198527, 76.87390960531439532 ) ) ;
#32870 = CARTESIAN_POINT ( 'NONE',  ( -5.049401038298153566, 19.05341960407611168, 115.2072429386477097 ) ) ;
#32871 = CARTESIAN_POINT ( 'NONE',  ( -16.52544592524342804, 4.483927247898546575, 51.04057627198103120 ) ) ;
#32872 = CARTESIAN_POINT ( 'NONE',  ( 13.97604488694527802, 13.89961937509977652, 24.37390960531435624 ) ) ;
#32873 = CARTESIAN_POINT ( 'NONE',  ( 19.05341960407611168, 5.049401038298154454, 28.95724293864769550 ) ) ;
#32874 = CARTESIAN_POINT ( 'NONE',  ( -19.05341960407617563, 5.049401038297882671, 28.54275706135232937 ) ) ;
#32875 = CARTESIAN_POINT ( 'NONE',  ( -8.314922557961024197, 14.29746914071037800, 82.91775706135234714 ) ) ;
#32876 = CARTESIAN_POINT ( 'NONE',  ( 4.379528057220092307, 16.55341960407617563, 57.29275706135234714 ) ) ;
#32877 = CARTESIAN_POINT ( 'NONE',  ( -9.564922557960796823, -16.46253265017161027, 112.0822429386476955 ) ) ;
#32879 = CARTESIAN_POINT ( 'NONE',  ( -5.719274019375665041, -21.55341960407619695, 109.7927570613523613 ) ) ;
#32878 = CARTESIAN_POINT ( 'NONE',  ( -5.049401038298153566, 19.05341960407611168, 55.20724293864769550 ) ) ;
#32880 = CARTESIAN_POINT ( 'NONE',  ( 19.03943276465977164, -0.05219959533909143690, 83.74890960531436690 ) ) ;
#32881 = CARTESIAN_POINT ( 'NONE',  ( 16.52544592524335698, 4.483927247898782831, 56.45942372801902565 ) ) ;
#32882 = CARTESIAN_POINT ( 'NONE',  ( -16.53943276465976808, 0.05219959533911058130, 111.2489096053143669 ) ) ;
#32883 = CARTESIAN_POINT ( 'NONE',  ( -14.34966873604960291, -8.224510206698953496, 26.66557627198103475 ) ) ;
#32884 = FACE_OUTER_BOUND ( 'NONE', #143534, .T. ) ;
#32887 = CARTESIAN_POINT ( 'NONE',  ( -9.564922557960796823, -16.46253265017161027, 82.08224293864768129 ) ) ;
#32886 = CARTESIAN_POINT ( 'NONE',  ( 19.02544592524343514, -5.153800228976328945, 93.54057627198102409 ) ) ;
#32885 = CARTESIAN_POINT ( 'NONE',  ( -21.55341960407619339, 5.719274019375674811, 63.54275706135234003 ) ) ;
#32888 = CARTESIAN_POINT ( 'NONE',  ( 19.02544592524343514, -5.153800228976328945, 113.5405762719810241 ) ) ;
#32889 = CARTESIAN_POINT ( 'NONE',  ( -8.314922557960811034, -14.29746914071050412, 52.08224293864768839 ) ) ;
#32890 = CARTESIAN_POINT ( 'NONE',  ( -4.379528057220328563, 16.55341960407611168, 25.20724293864769550 ) ) ;
#32891 = CARTESIAN_POINT ( 'NONE',  ( 14.34966873604960469, 8.224510206698951720, 34.16557627198102409 ) ) ;
#32893 = CARTESIAN_POINT ( 'NONE',  ( -16.46419947420532282, -17.59054176770899147, -54.38591257391895795 ) ) ;
#32892 = CARTESIAN_POINT ( 'NONE',  ( -8.224510206698735004, -14.34966873604973081, 44.58442372801901854 ) ) ;
#32894 = CARTESIAN_POINT ( 'NONE',  ( -13.97604488694547697, 13.89961937509957934, 38.12609039468566152 ) ) ;
#32895 = CARTESIAN_POINT ( 'NONE',  ( 13.97604488694527802, 13.89961937509977652, 79.37390960531435269 ) ) ;
#32896 = CARTESIAN_POINT ( 'NONE',  ( -9.564922557961040184, 16.46253265017147172, 57.91775706135233293 ) ) ;
#32897 = CARTESIAN_POINT ( 'NONE',  ( 9.474510206698729675, 16.51473224551082808, 62.08442372801899722 ) ) ;
#32899 = CARTESIAN_POINT ( 'NONE',  ( -16.53943276465976808, -0.05219959533934237506, 88.75109039468567573 ) ) ;
#32898 = CARTESIAN_POINT ( 'NONE',  ( 13.89961937509957401, 13.97604488694547697, 96.87609039468566152 ) ) ;
#32900 = CARTESIAN_POINT ( 'NONE',  ( -5.153800228976328057, -19.02544592524343514, 32.29057627198102409 ) ) ;
#32901 = CARTESIAN_POINT ( 'NONE',  ( 9.474510206698971260, -16.51473224551069308, 107.9155762719810383 ) ) ;
#32902 = CARTESIAN_POINT ( 'NONE',  ( 5.823673210054444382, -21.52544592524334988, 35.20942372801901854 ) ) ;
#32903 = CARTESIAN_POINT ( 'NONE',  ( 9.564922557961047289, -16.46253265017146816, 85.41775706135233293 ) ) ;
#32905 = CARTESIAN_POINT ( 'NONE',  ( 0.05219959533909260263, 19.03943276465977164, 59.99890960531436690 ) ) ;
#32904 = CARTESIAN_POINT ( 'NONE',  ( 17.50000000000003197, 3.964703510696900413, 23.28111287675285368 ) ) ;
#32906 = CARTESIAN_POINT ( 'NONE',  ( 0.05219959533909260263, 19.03943276465977164, 104.9989096053143669 ) ) ;
#32908 = CARTESIAN_POINT ( 'NONE',  ( -19.05341960407611168, -5.049401038298163336, 46.45724293864768129 ) ) ;
#32907 = CARTESIAN_POINT ( 'NONE',  ( 8.224510206698953496, -14.34966873604960469, 67.91557627198102409 ) ) ;
#32909 = CARTESIAN_POINT ( 'NONE',  ( -9.564922557960796823, -16.46253265017161027, 67.08224293864769550 ) ) ;
#32910 = CARTESIAN_POINT ( 'NONE',  ( -9.564922557961040184, 16.46253265017147172, 67.91775706135233293 ) ) ;
#32911 = CARTESIAN_POINT ( 'NONE',  ( 13.97604488694548053, -13.89961937509957401, 30.62609039468566863 ) ) ;
#32912 = CARTESIAN_POINT ( 'NONE',  ( -9.474510206698720793, -16.51473224551083518, 44.58442372801900433 ) ) ;
#32913 = CARTESIAN_POINT ( 'NONE',  ( 16.46253265017160672, -9.564922557960803928, 78.33224293864769550 ) ) ;
#32914 = CARTESIAN_POINT ( 'NONE',  ( 5.719274019375991003, -21.55341960407610458, 77.70724293864770971 ) ) ;
#32916 = CARTESIAN_POINT ( 'NONE',  ( 19.05341960407617918, -5.049401038297876454, 31.04275706135232227 ) ) ;
#32915 = CARTESIAN_POINT ( 'NONE',  ( -4.379528057220328563, 16.55341960407611168, 65.20724293864768129 ) ) ;
#32917 = CARTESIAN_POINT ( 'NONE',  ( -5.719274019375978568, 21.55341960407610458, 40.20724293864769550 ) ) ;
#32918 = CARTESIAN_POINT ( 'NONE',  ( 10.81492255796078972, 18.62759615963270932, 39.58224293864769550 ) ) ;
#32919 = CARTESIAN_POINT ( 'NONE',  ( -16.51473224551069308, -9.474510206698971260, 61.66557627198103120 ) ) ;
#32920 = CARTESIAN_POINT ( 'NONE',  ( -16.46253265017160317, 9.564922557960807481, 40.83224293864769550 ) ) ;
#32921 = CARTESIAN_POINT ( 'NONE',  ( -13.97604488694527625, -13.89961937509977652, 21.87390960531435979 ) ) ;
#32922 = CARTESIAN_POINT ( 'NONE',  ( -10.72451020669870658, -18.67979575497194134, 24.58442372801901499 ) ) ;
#32923 = CARTESIAN_POINT ( 'NONE',  ( 19.05341960407611168, 5.049401038298154454, 113.9572429386477097 ) ) ;
#32924 = CARTESIAN_POINT ( 'NONE',  ( -15.80617190586768217, 15.72974639402176855, 33.12609039468569705 ) ) ;
#32925 = CARTESIAN_POINT ( 'NONE',  ( 19.05341960407611168, 5.049401038298154454, 33.95724293864769550 ) ) ;
#32926 = CARTESIAN_POINT ( 'NONE',  ( 18.67979575497178502, 10.72451020669898547, 104.1655762719810241 ) ) ;
#32927 = CARTESIAN_POINT ( 'NONE',  ( 5.049401038297881783, 19.05341960407617563, 52.29275706135234003 ) ) ;
#32928 = CARTESIAN_POINT ( 'NONE',  ( 9.564922557960805705, 16.46253265017160317, 24.58224293864769194 ) ) ;
#32929 = CARTESIAN_POINT ( 'NONE',  ( 0.05219959533909260263, 19.03943276465977164, 24.99890960531435269 ) ) ;
#32930 = LINE ( 'NONE', #29952, #40231 ) ;
#32931 = CARTESIAN_POINT ( 'NONE',  ( -4.379528057220086978, -16.55341960407618274, 59.79275706135234714 ) ) ;
#32932 = CARTESIAN_POINT ( 'NONE',  ( -16.51473224551069308, -9.474510206698971260, 31.66557627198102054 ) ) ;
#32933 = CARTESIAN_POINT ( 'NONE',  ( 34.16298174666832921, -4.140866818352566092, 91.36220571553955949 ) ) ;
#32934 = CARTESIAN_POINT ( 'NONE',  ( 19.03943276465977164, -0.05219959533909143690, 78.74890960531436690 ) ) ;
#32935 = CARTESIAN_POINT ( 'NONE',  ( -16.53943276465976808, 0.05219959533911058130, 106.2489096053143811 ) ) ;
#32936 = VECTOR ( 'NONE', #3060, 1000.000000000000000 ) ;
#32937 = CARTESIAN_POINT ( 'NONE',  ( -18.67979575497178146, -10.72451020669898902, 41.66557627198103120 ) ) ;
#32938 = CARTESIAN_POINT ( 'NONE',  ( 8.224510206698953496, -14.34966873604960469, 77.91557627198102409 ) ) ;
#32939 = CARTESIAN_POINT ( 'NONE',  ( -0.05219959533934338120, 16.53943276465976808, 37.50109039468568284 ) ) ;
#32940 = CARTESIAN_POINT ( 'NONE',  ( 21.52544592524334988, 5.823673210054432836, 81.45942372801900433 ) ) ;
#32941 = CARTESIAN_POINT ( 'NONE',  ( 5.049401038298161559, -19.05341960407611168, 22.70724293864769194 ) ) ;
#32942 = CARTESIAN_POINT ( 'NONE',  ( 14.34966873604972726, -8.224510206698740333, 110.8344237280190043 ) ) ;
#32943 = CARTESIAN_POINT ( 'NONE',  ( -14.34966873604960291, -8.224510206698953496, 51.66557627198102409 ) ) ;
#32944 = CARTESIAN_POINT ( 'NONE',  ( -13.97604488694527625, -13.89961937509977652, 56.87390960531434558 ) ) ;
#32945 = CARTESIAN_POINT ( 'NONE',  ( -10.81492255796105439, 18.62759615963255655, 92.91775706135236135 ) ) ;
#32946 = CARTESIAN_POINT ( 'NONE',  ( 5.823673210054125526, 21.52544592524343514, 109.7905762719810383 ) ) ;
#32947 = CARTESIAN_POINT ( 'NONE',  ( 21.52544592524334988, 5.823673210054432836, 76.45942372801901854 ) ) ;
#32948 = CARTESIAN_POINT ( 'NONE',  ( 16.53943276465976808, 0.05219959533934440121, 36.25109039468567573 ) ) ;
#32950 = CARTESIAN_POINT ( 'NONE',  ( 21.53943276465977519, 0.05219959533937863772, 86.25109039468568994 ) ) ;
#32949 = CARTESIAN_POINT ( 'NONE',  ( -12.14591786802309592, -12.06949235617757132, 71.87390960531438111 ) ) ;
#32951 = CARTESIAN_POINT ( 'NONE',  ( -16.52544592524335698, -4.483927247898792601, 108.9594237280190185 ) ) ;
#32952 = CARTESIAN_POINT ( 'NONE',  ( -19.03943276465977164, 0.05219959533909376836, 21.24890960531436335 ) ) ;
#32953 = CARTESIAN_POINT ( 'NONE',  ( -4.483927247898782831, 16.52544592524335698, 37.70942372801900433 ) ) ;
#32954 = CARTESIAN_POINT ( 'NONE',  ( 14.29746914071049879, -8.314922557960816363, 43.33224293864769550 ) ) ;
#32955 = CARTESIAN_POINT ( 'NONE',  ( 14.29746914071037800, 8.314922557961029526, 86.66775706135234714 ) ) ;
#32956 = CARTESIAN_POINT ( 'NONE',  ( 9.564922557960805705, 16.46253265017160317, 104.5822429386476955 ) ) ;
#32957 = CARTESIAN_POINT ( 'NONE',  ( 16.46253265017160672, -9.564922557960803928, 103.3322429386476955 ) ) ;
#32958 = CARTESIAN_POINT ( 'NONE',  ( -15.72974639402176322, -15.80617190586768395, 94.37609039468568994 ) ) ;
#32959 = EDGE_CURVE ( 'NONE', #141549, #94189, #180925, .T. ) ;
#32960 = CARTESIAN_POINT ( 'NONE',  ( 4.379528057220092307, 16.55341960407617563, 107.2927570613523471 ) ) ;
#32961 = CARTESIAN_POINT ( 'NONE',  ( 8.314922557960818139, 14.29746914071049879, 74.58224293864768129 ) ) ;
#32962 = CARTESIAN_POINT ( 'NONE',  ( -16.46253265017160317, 9.564922557960807481, 75.83224293864769550 ) ) ;
#32963 = ORIENTED_EDGE ( 'NONE', *, *, #43025, .F. ) ;
#32964 = CARTESIAN_POINT ( 'NONE',  ( 8.314922557961029526, -14.29746914071037800, 20.41775706135234714 ) ) ;
#32965 = CARTESIAN_POINT ( 'NONE',  ( 13.89961937509977652, -13.97604488694527269, 28.12390960531435624 ) ) ;
#32966 = CARTESIAN_POINT ( 'NONE',  ( -13.89961937509977652, 13.97604488694528158, 95.62390960531436690 ) ) ;
#32968 = CARTESIAN_POINT ( 'NONE',  ( 29.86685920354754487, 21.69954338932564752, -1.424999997268813212 ) ) ;
#32967 = CARTESIAN_POINT ( 'NONE',  ( 14.29746914071037800, 8.314922557961029526, 31.66775706135234358 ) ) ;
#32969 = CARTESIAN_POINT ( 'NONE',  ( -16.46253265017146816, -9.564922557961047289, 34.16775706135233293 ) ) ;
#32970 = CARTESIAN_POINT ( 'NONE',  ( -12.06949235617739369, -12.14591786802326823, 99.37609039468568994 ) ) ;
#32971 = CARTESIAN_POINT ( 'NONE',  ( -9.564922557961040184, 16.46253265017147172, 107.9177570613523471 ) ) ;
#32972 = CARTESIAN_POINT ( 'NONE',  ( 13.89961937509977652, -13.97604488694527269, 33.12390960531434558 ) ) ;
#32973 = CARTESIAN_POINT ( 'NONE',  ( 12.14591786802327356, -12.06949235617739191, 80.62609039468567573 ) ) ;
#32974 = CARTESIAN_POINT ( 'NONE',  ( -12.14591786802326823, 12.06949235617739902, 63.12609039468568994 ) ) ;
#32975 = CARTESIAN_POINT ( 'NONE',  ( 16.46253265017160672, -9.564922557960803928, 33.33224293864770260 ) ) ;
#32976 = CARTESIAN_POINT ( 'NONE',  ( 19.03943276465977164, 0.05219959533936151252, 71.25109039468566152 ) ) ;
#32977 = CARTESIAN_POINT ( 'NONE',  ( 15.80617190586769283, -15.72974639402175789, 110.6260903946857042 ) ) ;
#32978 = CARTESIAN_POINT ( 'NONE',  ( 16.46253265017160672, -9.564922557960803928, 43.33224293864769550 ) ) ;
#32979 = CARTESIAN_POINT ( 'NONE',  ( -13.97604488694527625, -13.89961937509977652, 91.87390960531432427 ) ) ;
#32980 = CARTESIAN_POINT ( 'NONE',  ( 14.29746914071049879, -8.314922557960816363, 88.33224293864769550 ) ) ;
#32981 = B_SPLINE_CURVE_WITH_KNOTS ( 'NONE', 3,
 ( #157932, #50759, #51741, #6227, #129559, #158911, #191258, #128569, #190264, #140762, #34587, #111425, #173111, #96244, #110426, #112416, #83065, #113402, #79089, #97224 ),
 .UNSPECIFIED., .F., .F.,
 ( 4, 2, 2, 2, 2, 2, 2, 2, 2, 4 ),
 ( 0.000000000000000000, 0.0004987090165372478744, 0.0009974180330744957489, 0.001246772541343130420, 0.001496127049611765090, 0.001994836066149034866, 0.002493545082686304207, 0.002742899590954927386, 0.002992254099223550130, 0.003989672132298028098 ),
 .UNSPECIFIED. ) ;
#32982 = CARTESIAN_POINT ( 'NONE',  ( -16.51473224551082808, 9.474510206698731452, 48.33442372801900433 ) ) ;
#32983 = CARTESIAN_POINT ( 'NONE',  ( -21.55341960407610458, -5.719274019375992779, 51.45724293864770260 ) ) ;
#32984 = CARTESIAN_POINT ( 'NONE',  ( -13.89961937509957401, -13.97604488694547875, 19.37609039468566507 ) ) ;
#32985 = CARTESIAN_POINT ( 'NONE',  ( 13.97604488694527802, 13.89961937509977652, 84.37390960531433848 ) ) ;
#32986 = CARTESIAN_POINT ( 'NONE',  ( -5.049401038297874678, -19.05341960407617918, 29.79275706135232227 ) ) ;
#32987 = CARTESIAN_POINT ( 'NONE',  ( 15.72974639402199770, -15.80617190586745480, 68.12390960531436690 ) ) ;
#32988 = CARTESIAN_POINT ( 'NONE',  ( -16.46253265017160317, 9.564922557960807481, 105.8322429386476955 ) ) ;
#32989 = CARTESIAN_POINT ( 'NONE',  ( -5.153800228976607833, 19.02544592524334988, 87.70942372801897591 ) ) ;
#32990 = CARTESIAN_POINT ( 'NONE',  ( -5.049401038298153566, 19.05341960407611168, 110.2072429386476671 ) ) ;
#32991 = CARTESIAN_POINT ( 'NONE',  ( 5.049401038297881783, 19.05341960407617563, 107.2927570613523187 ) ) ;
#32992 = CARTESIAN_POINT ( 'NONE',  ( 14.29746914071049879, -8.314922557960816363, 113.3322429386476955 ) ) ;
#32993 = CARTESIAN_POINT ( 'NONE',  ( 16.46253265017160672, -9.564922557960803928, 98.33224293864769550 ) ) ;
#32994 = CARTESIAN_POINT ( 'NONE',  ( -5.719274019375978568, 21.55341960407610458, 80.20724293864769550 ) ) ;
#32995 = CARTESIAN_POINT ( 'NONE',  ( -16.52544592524335698, -4.483927247898792601, 43.95942372801902565 ) ) ;
#32996 = CARTESIAN_POINT ( 'NONE',  ( -5.823673210054431948, 21.52544592524334988, 52.70942372801902565 ) ) ;
#32997 = CARTESIAN_POINT ( 'NONE',  ( 18.62759615963255655, 10.81492255796105972, 101.6677570613523613 ) ) ;
#32998 = CARTESIAN_POINT ( 'NONE',  ( 4.379528057220092307, 16.55341960407617563, 97.29275706135234714 ) ) ;
#32999 = CARTESIAN_POINT ( 'NONE',  ( -19.05341960407611168, -5.049401038298163336, 86.45724293864769550 ) ) ;
#33000 = CARTESIAN_POINT ( 'NONE',  ( -8.314922557960811034, -14.29746914071050412, 97.08224293864770971 ) ) ;
#33001 = CARTESIAN_POINT ( 'NONE',  ( 16.52544592524342804, -4.483927247898539470, 33.54057627198102409 ) ) ;
#33002 = CARTESIAN_POINT ( 'NONE',  ( 13.97604488694548053, -13.89961937509957401, 75.62609039468564731 ) ) ;
#33003 = CARTESIAN_POINT ( 'NONE',  ( 10.81492255796106328, -18.62759615963255655, 60.41775706135235424 ) ) ;
#33004 = CARTESIAN_POINT ( 'NONE',  ( 5.153800228976615827, -19.02544592524334988, 20.20942372801899722 ) ) ;
#33005 = CARTESIAN_POINT ( 'NONE',  ( -4.483927247898539470, -16.52544592524342804, 92.29057627198103830 ) ) ;
#33006 = CARTESIAN_POINT ( 'NONE',  ( -15.80617190586745835, -15.72974639402198527, 31.87390960531435979 ) ) ;
#33007 = CARTESIAN_POINT ( 'NONE',  ( 8.314922557960818139, 14.29746914071049879, 24.58224293864768839 ) ) ;
#33008 = CARTESIAN_POINT ( 'NONE',  ( -5.823673210054431948, 21.52544592524334988, 82.70942372801900433 ) ) ;
#33009 = CARTESIAN_POINT ( 'NONE',  ( -16.55341960407617563, 4.379528057220093196, 53.54275706135234714 ) ) ;
#33010 = CARTESIAN_POINT ( 'NONE',  ( -8.314922557961024197, 14.29746914071037800, 107.9177570613523471 ) ) ;
#33011 = CARTESIAN_POINT ( 'NONE',  ( 18.67979575497194134, -10.72451020669871369, 50.83442372801901143 ) ) ;
#33012 = ORIENTED_EDGE ( 'NONE', *, *, #73347, .F. ) ;
#33013 = CARTESIAN_POINT ( 'NONE',  ( -18.67979575497193778, 10.72451020669871902, 33.33442372801900433 ) ) ;
#33014 = CARTESIAN_POINT ( 'NONE',  ( 14.29746914071049879, -8.314922557960816363, 98.33224293864769550 ) ) ;
#33015 = CARTESIAN_POINT ( 'NONE',  ( 5.049401038298161559, -19.05341960407611168, 22.70724293864769194 ) ) ;
#33016 = CARTESIAN_POINT ( 'NONE',  ( 8.224510206698953496, -14.34966873604960469, 62.91557627198102409 ) ) ;
#33017 = CARTESIAN_POINT ( 'NONE',  ( -9.474510206698964154, 16.51473224551069663, 65.41557627198102409 ) ) ;
#33018 = CARTESIAN_POINT ( 'NONE',  ( 12.14591786802327356, -12.06949235617739191, 105.6260903946856899 ) ) ;
#33019 = CARTESIAN_POINT ( 'NONE',  ( 5.823673210054125526, 21.52544592524343514, 59.79057627198103120 ) ) ;
#33020 = CARTESIAN_POINT ( 'NONE',  ( -16.52544592524342804, 4.483927247898546575, 86.04057627198102409 ) ) ;
#33021 = CARTESIAN_POINT ( 'NONE',  ( -18.62759615963270932, 10.81492255796079327, 95.83224293864770971 ) ) ;
#33022 = CARTESIAN_POINT ( 'NONE',  ( -19.03943276465977164, 0.05219959533909376836, 96.24890960531436690 ) ) ;
#33024 = CARTESIAN_POINT ( 'NONE',  ( 19.03943276465977164, 0.05219959533936151252, 101.2510903946856757 ) ) ;
#33023 = CARTESIAN_POINT ( 'NONE',  ( -16.51473224551069308, -9.474510206698971260, 56.66557627198103120 ) ) ;
#33025 = CARTESIAN_POINT ( 'NONE',  ( 5.719274019375991003, -21.55341960407610458, 37.70724293864769550 ) ) ;
#33026 = CARTESIAN_POINT ( 'NONE',  ( -5.823673210054431948, 21.52544592524334988, 62.70942372801902565 ) ) ;
#33027 = CARTESIAN_POINT ( 'NONE',  ( 19.03943276465977164, -0.05219959533909143690, 48.74890960531435979 ) ) ;
#33028 = CARTESIAN_POINT ( 'NONE',  ( 19.03943276465977164, -0.05219959533909143690, 88.74890960531436690 ) ) ;
#33029 = CARTESIAN_POINT ( 'NONE',  ( 8.314922557961029526, -14.29746914071037800, 60.41775706135235424 ) ) ;
#33030 = CARTESIAN_POINT ( 'NONE',  ( 21.55341960407619695, -5.719274019375665929, 46.04275706135234714 ) ) ;
#33031 = CARTESIAN_POINT ( 'NONE',  ( -18.62759615963255300, -10.81492255796106328, 89.16775706135236135 ) ) ;
#33032 = CARTESIAN_POINT ( 'NONE',  ( 5.823673210054125526, 21.52544592524343514, 104.7905762719810241 ) ) ;
#33034 = CARTESIAN_POINT ( 'NONE',  ( 16.53943276465976808, 0.05219959533934440121, 61.25109039468567573 ) ) ;
#33033 = CARTESIAN_POINT ( 'NONE',  ( -0.05219959533937732626, 21.53943276465977519, 32.50109039468568284 ) ) ;
#33036 = CARTESIAN_POINT ( 'NONE',  ( 21.53943276465977519, -0.05219959533907433946, 73.74890960531433848 ) ) ;
#33035 = B_SPLINE_CURVE_WITH_KNOTS ( 'NONE', 3,
 ( #6438, #129772, #22630, #144957, #160138, #114621 ),
 .UNSPECIFIED., .F., .F.,
 ( 4, 2, 4 ),
 ( 0.003239945802372206588, 0.003620412082092015413, 0.004000878361811823804 ),
 .UNSPECIFIED. ) ;
#33037 = CARTESIAN_POINT ( 'NONE',  ( 16.46253265017146816, 9.564922557961045513, 36.66775706135233293 ) ) ;
#33039 = CARTESIAN_POINT ( 'NONE',  ( 4.379528057220339221, -16.55341960407611168, 22.70724293864769194 ) ) ;
#33038 = CARTESIAN_POINT ( 'NONE',  ( -5.049401038298153566, 19.05341960407611168, 65.20724293864765286 ) ) ;
#33040 = CARTESIAN_POINT ( 'NONE',  ( -38.00000000000000711, 2.428612866367529932E-14, -6.000000000000000000 ) ) ;
#33041 = CARTESIAN_POINT ( 'NONE',  ( -9.564922557960796823, -16.46253265017161027, 97.08224293864769550 ) ) ;
#33042 = CARTESIAN_POINT ( 'NONE',  ( 69.65682714487590488, -71.74905178543389184, -4.999999999999999112 ) ) ;
#33043 = CARTESIAN_POINT ( 'NONE',  ( 5.049401038297881783, 19.05341960407617563, 87.29275706135234714 ) ) ;
#33044 = CARTESIAN_POINT ( 'NONE',  ( -18.67979575497178146, -10.72451020669898902, 56.66557627198103830 ) ) ;
#33045 = CARTESIAN_POINT ( 'NONE',  ( 12.14591786802309770, 12.06949235617756955, 44.37390960531435979 ) ) ;
#33046 = CARTESIAN_POINT ( 'NONE',  ( 19.03943276465977164, 0.05219959533936151252, 111.2510903946856757 ) ) ;
#33047 = CARTESIAN_POINT ( 'NONE',  ( 19.05341960407611168, 5.049401038298154454, 33.95724293864769550 ) ) ;
#33048 = CARTESIAN_POINT ( 'NONE',  ( 12.14591786802327356, -12.06949235617739191, 20.62609039468568639 ) ) ;
#33050 = CARTESIAN_POINT ( 'NONE',  ( 13.89961937509957401, 13.97604488694547697, 71.87609039468567573 ) ) ;
#33049 = CARTESIAN_POINT ( 'NONE',  ( -18.62759615963270932, 10.81492255796079327, 95.83224293864770971 ) ) ;
#33051 = CARTESIAN_POINT ( 'NONE',  ( 12.06949235617739724, 12.14591786802326823, 76.87609039468567573 ) ) ;
#33052 = CARTESIAN_POINT ( 'NONE',  ( 5.049401038298161559, -19.05341960407611168, 67.70724293864769550 ) ) ;
#33053 = CARTESIAN_POINT ( 'NONE',  ( 12.14591786802309770, 12.06949235617756955, 74.37390960531436690 ) ) ;
#33054 = CARTESIAN_POINT ( 'NONE',  ( -5.049401038298153566, 19.05341960407611168, 55.20724293864769550 ) ) ;
#33055 = CARTESIAN_POINT ( 'NONE',  ( 8.224510206698953496, -14.34966873604960469, 72.91557627198103830 ) ) ;
#33056 = FACE_BOUND ( 'NONE', #183865, .T. ) ;
#33057 = CARTESIAN_POINT ( 'NONE',  ( -37.42090987696013116, -2.907880681671515255, 40.32815749938560401 ) ) ;
#33058 = CARTESIAN_POINT ( 'NONE',  ( 4.379528057220339221, -16.55341960407611168, 47.70724293864770260 ) ) ;
#33059 = CARTESIAN_POINT ( 'NONE',  ( 9.564922557960805705, 16.46253265017160317, 74.58224293864769550 ) ) ;
#33060 = FACE_BOUND ( 'NONE', #127771, .T. ) ;
#33061 = CARTESIAN_POINT ( 'NONE',  ( 5.049401038297881783, 19.05341960407617563, 32.29275706135233293 ) ) ;
#33062 = CARTESIAN_POINT ( 'NONE',  ( 16.53943276465976808, 0.05219959533934440121, 46.25109039468567573 ) ) ;
#33063 = CARTESIAN_POINT ( 'NONE',  ( -21.53943276465977519, 0.05219959533907696930, 66.24890960531436690 ) ) ;
#33064 = CARTESIAN_POINT ( 'NONE',  ( -19.03943276465977164, -0.05219959533935918106, 23.75109039468566152 ) ) ;
#33065 = CARTESIAN_POINT ( 'NONE',  ( -13.89961937509977652, 13.97604488694528158, 70.62390960531432427 ) ) ;
#33066 = CARTESIAN_POINT ( 'NONE',  ( 10.65970682939788716, -25.60940286011448919, 139.9999999999999716 ) ) ;
#33067 = CARTESIAN_POINT ( 'NONE',  ( -9.564922557960796823, -16.46253265017161027, 112.0822429386476955 ) ) ;
#33068 = CARTESIAN_POINT ( 'NONE',  ( -5.823673210054431948, 21.52544592524334988, 32.70942372801900433 ) ) ;
#33069 = CARTESIAN_POINT ( 'NONE',  ( -0.05219959533910754901, -16.53943276465976808, 102.4989096053143811 ) ) ;
#33072 = VERTEX_POINT ( 'NONE', #199051 ) ;
#33071 = CARTESIAN_POINT ( 'NONE',  ( -9.474510206698964154, 16.51473224551069663, 85.41557627198102409 ) ) ;
#33070 = CARTESIAN_POINT ( 'NONE',  ( -21.55341960407610458, -5.719274019375992779, 106.4572429386477097 ) ) ;
#33073 = CARTESIAN_POINT ( 'NONE',  ( -15.72974639402176322, -15.80617190586768395, 29.37609039468568284 ) ) ;
#33074 = ORIENTED_EDGE ( 'NONE', *, *, #173264, .T. ) ;
#33075 = CARTESIAN_POINT ( 'NONE',  ( 9.474510206698971260, -16.51473224551069308, 87.91557627198102409 ) ) ;
#33076 = DIRECTION ( 'NONE',  ( 0.000000000000000000, -1.000000000000000000, 0.000000000000000000 ) ) ;
#33077 = CARTESIAN_POINT ( 'NONE',  ( 15.80617190586746368, 15.72974639402197994, 99.37390960531436690 ) ) ;
#33078 = CARTESIAN_POINT ( 'NONE',  ( -5.153800228976328057, -19.02544592524343514, 32.29057627198102409 ) ) ;
#33079 = CARTESIAN_POINT ( 'NONE',  ( -5.153800228976607833, 19.02544592524334988, 107.7094237280189759 ) ) ;
#33080 = CARTESIAN_POINT ( 'NONE',  ( 29.86685920354754487, 21.69954338932564752, -7.924999997268814766 ) ) ;
#33081 = CARTESIAN_POINT ( 'NONE',  ( -0.05219959533909027116, -19.03943276465977164, 32.49890960531435979 ) ) ;
#33082 = CARTESIAN_POINT ( 'NONE',  ( 15.80617190586769283, -15.72974639402175789, 85.62609039468568994 ) ) ;
#33084 = CARTESIAN_POINT ( 'NONE',  ( 21.53943276465977519, 0.05219959533937863772, 46.25109039468567573 ) ) ;
#33083 = CARTESIAN_POINT ( 'NONE',  ( -13.97604488694527625, -13.89961937509977652, 76.87390960531433848 ) ) ;
#33085 = CARTESIAN_POINT ( 'NONE',  ( 15.72974639402176855, 15.80617190586768217, 21.87609039468567573 ) ) ;
#33086 = CARTESIAN_POINT ( 'NONE',  ( -28.82186960331499037, 2.428612866367529932E-14, 146.0000000000000000 ) ) ;
#33087 = CARTESIAN_POINT ( 'NONE',  ( -5.153800228976328057, -19.02544592524343514, 92.29057627198099567 ) ) ;
#33088 = LINE ( 'NONE', #154437, #169434 ) ;
#33091 = CARTESIAN_POINT ( 'NONE',  ( 15.80617190586769283, -15.72974639402175789, 40.62609039468567573 ) ) ;
#33090 = CARTESIAN_POINT ( 'NONE',  ( 10.72451020669898902, -18.67979575497178502, 47.91557627198102409 ) ) ;
#33089 = CARTESIAN_POINT ( 'NONE',  ( 8.314922557961029526, -14.29746914071037800, 45.41775706135234003 ) ) ;
#33092 = CARTESIAN_POINT ( 'NONE',  ( 0.05219959533937995610, -21.53943276465977519, 70.00109039468568994 ) ) ;
#33093 = FACE_OUTER_BOUND ( 'NONE', #180286, .T. ) ;
#33094 = CARTESIAN_POINT ( 'NONE',  ( 19.03943276465977164, 0.05219959533936151252, 111.2510903946856757 ) ) ;
#33095 = CARTESIAN_POINT ( 'NONE',  ( 16.51473224551069308, 9.474510206698969483, 64.16557627198102409 ) ) ;
#33096 = CARTESIAN_POINT ( 'NONE',  ( 16.51473224551069308, 9.474510206698969483, 89.16557627198103830 ) ) ;
#33097 = CARTESIAN_POINT ( 'NONE',  ( 0.05219959533910956823, 16.53943276465976808, 109.9989096053143527 ) ) ;
#33098 = CARTESIAN_POINT ( 'NONE',  ( -12.14591786802309592, -12.06949235617757132, 101.8739096053143811 ) ) ;
#33099 = CARTESIAN_POINT ( 'NONE',  ( 13.97604488694527802, 13.89961937509977652, 114.3739096053143669 ) ) ;
#33100 = CARTESIAN_POINT ( 'NONE',  ( 4.379528057220092307, 16.55341960407617563, 77.29275706135234714 ) ) ;
#33102 = CARTESIAN_POINT ( 'NONE',  ( 19.03943276465977164, -0.05219959533909143690, 48.74890960531435979 ) ) ;
#33101 = CARTESIAN_POINT ( 'NONE',  ( 16.52544592524342804, -4.483927247898539470, 68.54057627198103830 ) ) ;
#33103 = CARTESIAN_POINT ( 'NONE',  ( -18.62759615963255300, -10.81492255796106328, 79.16775706135234714 ) ) ;
#33104 = CARTESIAN_POINT ( 'NONE',  ( 15.80617190586769283, -15.72974639402175789, 70.62609039468567573 ) ) ;
#33105 = CARTESIAN_POINT ( 'NONE',  ( -16.46253265017146816, -9.564922557961047289, 109.1677570613523471 ) ) ;
#33106 = CARTESIAN_POINT ( 'NONE',  ( 8.314922557960818139, 14.29746914071049879, 59.58224293864770260 ) ) ;
#33107 = CARTESIAN_POINT ( 'NONE',  ( 21.52544592524334988, 5.823673210054432836, 21.45942372801901499 ) ) ;
#33108 = CARTESIAN_POINT ( 'NONE',  ( 21.53943276465977519, -0.05219959533907433946, 58.74890960531436690 ) ) ;
#33109 = CARTESIAN_POINT ( 'NONE',  ( -16.21995358207304605, -7.366697692864190294, 105.0644899848784490 ) ) ;
#33110 = CARTESIAN_POINT ( 'NONE',  ( -35.31606782002515388, 4.574060259307354492, 39.03637847775443248 ) ) ;
#33111 = CARTESIAN_POINT ( 'NONE',  ( 16.46253265017160672, -9.564922557960803928, 73.33224293864769550 ) ) ;
#33112 = CARTESIAN_POINT ( 'NONE',  ( 16.53943276465976808, -0.05219959533910856209, 33.74890960531436690 ) ) ;
#33113 = CARTESIAN_POINT ( 'NONE',  ( -12.14591786802326823, 12.06949235617739902, 113.1260903946856899 ) ) ;
#33114 = CARTESIAN_POINT ( 'NONE',  ( 14.29746914071037800, 8.314922557961029526, 91.66775706135234714 ) ) ;
#33115 = CARTESIAN_POINT ( 'NONE',  ( 0.05219959533936267826, -19.03943276465977164, 50.00109039468566863 ) ) ;
#33116 = CARTESIAN_POINT ( 'NONE',  ( 16.21995358207306381, 7.366697692864114799, 47.56448998487843483 ) ) ;
#33117 = CARTESIAN_POINT ( 'NONE',  ( 5.153800228976335163, 19.02544592524342804, 104.7905762719809957 ) ) ;
#33118 = CARTESIAN_POINT ( 'NONE',  ( 4.483927247898545687, 16.52544592524342804, 64.79057627198103830 ) ) ;
#33120 = CARTESIAN_POINT ( 'NONE',  ( -5.153800228976328057, -19.02544592524343514, 112.2905762719810099 ) ) ;
#33119 = CARTESIAN_POINT ( 'NONE',  ( 16.46253265017160672, -9.564922557960803928, 23.33224293864769194 ) ) ;
#33122 = VERTEX_POINT ( 'NONE', #10067 ) ;
#33121 = CARTESIAN_POINT ( 'NONE',  ( -0.05219959533907301413, -21.53943276465977519, 57.49890960531435979 ) ) ;
#33123 = CARTESIAN_POINT ( 'NONE',  ( -14.34966873604960291, -8.224510206698953496, 101.6655762719810383 ) ) ;
#33124 = CARTESIAN_POINT ( 'NONE',  ( -16.52544592524335698, -4.483927247898792601, 48.95942372801902565 ) ) ;
#33125 = B_SPLINE_CURVE_WITH_KNOTS ( 'NONE', 3,
 ( #132826, #164179, #25677, #24670, #7467, #85307, #53992, #87322, #148007, #54988, #115665, #165174, #69151, #130817, #177355, #9497, #149006, #118670, #10495, #134845, #72156, #88309, #11503, #133831, #73174, #38825, #56995, #180361, #100483, #41829, #162162, #116657 ),
 .UNSPECIFIED., .F., .F.,
 ( 4, 2, 2, 2, 2, 2, 2, 2, 2, 2, 2, 2, 2, 2, 2, 4 ),
 ( 5.204170427930422054E-18, 0.0003712461730036866695, 0.0007424923460073681349, 0.001113738519011049600, 0.001484984692014731066, 0.002227477038022093996, 0.002598723211025772209, 0.002969969384029450422, 0.003341215557033128634, 0.003712461730036806414, 0.004083707903040484193, 0.004454954076044162839, 0.004826200249047841485, 0.005197446422051519264, 0.005568692595055197911, 0.005939938768058875690 ),
 .UNSPECIFIED. ) ;
#33126 = CARTESIAN_POINT ( 'NONE',  ( -0.05219959533910754901, -16.53943276465976808, 87.49890960531436690 ) ) ;
#33127 = CARTESIAN_POINT ( 'NONE',  ( -19.01533133064925352, 5.499999999999452882, 63.76586590595741200 ) ) ;
#33128 = CARTESIAN_POINT ( 'NONE',  ( 5.153800228976615827, -19.02544592524334988, 80.20942372801901854 ) ) ;
#33129 = CARTESIAN_POINT ( 'NONE',  ( -9.474510206698964154, 16.51473224551069663, 110.4155762719810383 ) ) ;
#33130 = CARTESIAN_POINT ( 'NONE',  ( 11.40812507854755253, -35.11059874428192273, -2.524999997268813523 ) ) ;
#33131 = CARTESIAN_POINT ( 'NONE',  ( -22.68575836265095447, 20.56805782000746063, -50.73663675503804882 ) ) ;
#33133 = CARTESIAN_POINT ( 'NONE',  ( 0.05219959533910956823, 16.53943276465976808, 34.99890960531435979 ) ) ;
#33132 = CARTESIAN_POINT ( 'NONE',  ( -4.379528057220086978, -16.55341960407618274, 44.79275706135234714 ) ) ;
#33134 = CARTESIAN_POINT ( 'NONE',  ( -0.05219959533907301413, -21.53943276465977519, 57.49890960531435979 ) ) ;
#33135 = CARTESIAN_POINT ( 'NONE',  ( 9.474510206698729675, 16.51473224551082808, 87.08442372801900433 ) ) ;
#33136 = CARTESIAN_POINT ( 'NONE',  ( 10.72451020669898902, -18.67979575497178502, 47.91557627198102409 ) ) ;
#33137 = CARTESIAN_POINT ( 'NONE',  ( -5.823673210054431948, 21.52544592524334988, 87.70942372801901854 ) ) ;
#33138 = CARTESIAN_POINT ( 'NONE',  ( -21.49230329115315996, 7.461674882483885440, 174.1505502713556837 ) ) ;
#33139 = CARTESIAN_POINT ( 'NONE',  ( -14.34966873604972548, 8.224510206698743886, 33.33442372801900433 ) ) ;
#33141 = CARTESIAN_POINT ( 'NONE',  ( -16.46253265017160317, 9.564922557960807481, 100.8322429386477097 ) ) ;
#33140 = CARTESIAN_POINT ( 'NONE',  ( -9.564922557960796823, -16.46253265017161027, 42.08224293864769550 ) ) ;
#33142 = CARTESIAN_POINT ( 'NONE',  ( 16.46253265017160672, -9.564922557960803928, 33.33224293864770260 ) ) ;
#33143 = CARTESIAN_POINT ( 'NONE',  ( -12.06949235617756955, 12.14591786802309770, 95.62390960531436690 ) ) ;
#33144 = DIRECTION ( 'NONE',  ( -1.000000000000000000, -7.216449660063515541E-16, -5.551115123125781470E-17 ) ) ;
#33145 = CARTESIAN_POINT ( 'NONE',  ( 19.03943276465977164, -0.05219959533909143690, 98.74890960531436690 ) ) ;
#33146 = ORIENTED_EDGE ( 'NONE', *, *, #177829, .F. ) ;
#33147 = CARTESIAN_POINT ( 'NONE',  ( -16.55341960407617563, 4.379528057220093196, 53.54275706135234714 ) ) ;
#33148 = CARTESIAN_POINT ( 'NONE',  ( -21.53943276465977519, 0.05219959533907696930, 86.24890960531436690 ) ) ;
#33149 = CARTESIAN_POINT ( 'NONE',  ( 19.05341960407611168, 5.049401038298154454, 48.95724293864768129 ) ) ;
#33150 = CARTESIAN_POINT ( 'NONE',  ( 21.52544592524334988, 5.823673210054432836, 21.45942372801901499 ) ) ;
#33151 = CARTESIAN_POINT ( 'NONE',  ( -9.564922557960796823, -16.46253265017161027, 82.08224293864768129 ) ) ;
#33152 = CARTESIAN_POINT ( 'NONE',  ( 0.05219959533909260263, 19.03943276465977164, 114.9989096053143669 ) ) ;
#33153 = VERTEX_POINT ( 'NONE', #133397 ) ;
#33154 = CARTESIAN_POINT ( 'NONE',  ( 4.379528057220092307, 16.55341960407617563, 47.29275706135234003 ) ) ;
#33155 = CARTESIAN_POINT ( 'NONE',  ( -0.05219959533937732626, 21.53943276465977519, 22.50109039468567573 ) ) ;
#33158 = CARTESIAN_POINT ( 'NONE',  ( -13.89961937509957401, -13.97604488694547875, 69.37609039468564731 ) ) ;
#33157 = CARTESIAN_POINT ( 'NONE',  ( 19.05341960407611168, 5.049401038298154454, 98.95724293864766707 ) ) ;
#33156 = CARTESIAN_POINT ( 'NONE',  ( -9.474510206698964154, 16.51473224551069663, 25.41557627198103120 ) ) ;
#33159 = CARTESIAN_POINT ( 'NONE',  ( -13.97604488694547697, 13.89961937509957934, 23.12609039468565442 ) ) ;
#33160 = CARTESIAN_POINT ( 'NONE',  ( 21.55341960407610458, 5.719274019375980345, 83.95724293864770971 ) ) ;
#33161 = CARTESIAN_POINT ( 'NONE',  ( 19.05341960407617918, -5.049401038297876454, 31.04275706135232227 ) ) ;
#33162 = CARTESIAN_POINT ( 'NONE',  ( -4.483927247898782831, 16.52544592524335698, 82.70942372801900433 ) ) ;
#33163 = CARTESIAN_POINT ( 'NONE',  ( 16.46253265017160672, -9.564922557960803928, 108.3322429386476955 ) ) ;
#33164 = CARTESIAN_POINT ( 'NONE',  ( 16.46253265017160672, -9.564922557960803928, 63.33224293864769550 ) ) ;
#33165 = CARTESIAN_POINT ( 'NONE',  ( -18.62759615963255300, -10.81492255796106328, 64.16775706135234714 ) ) ;
#33166 = ADVANCED_FACE ( 'NONE', ( #88887 ), #158561, .T. ) ;
#33167 = CARTESIAN_POINT ( 'NONE',  ( -18.67979575497193778, 10.72451020669871902, 68.33442372801900433 ) ) ;
#33168 = CARTESIAN_POINT ( 'NONE',  ( -5.049401038298153566, 19.05341960407611168, 75.20724293864769550 ) ) ;
#33169 = CARTESIAN_POINT ( 'NONE',  ( -15.72974639402176322, -15.80617190586768395, 44.37609039468567573 ) ) ;
#33170 = CARTESIAN_POINT ( 'NONE',  ( -5.153800228976607833, 19.02544592524334988, 82.70942372801897591 ) ) ;
#33171 = CARTESIAN_POINT ( 'NONE',  ( 13.97604488694527802, 13.89961937509977652, 54.37390960531435979 ) ) ;
#33172 = CARTESIAN_POINT ( 'NONE',  ( 9.564922557960805705, 16.46253265017160317, 104.5822429386476955 ) ) ;
#33173 = CARTESIAN_POINT ( 'NONE',  ( 9.474510206698971260, -16.51473224551069308, 67.91557627198102409 ) ) ;
#33174 = CARTESIAN_POINT ( 'NONE',  ( 13.89961937509977652, -13.97604488694527269, 113.1239096053143527 ) ) ;
#33175 = CARTESIAN_POINT ( 'NONE',  ( -13.89961937509977652, 13.97604488694528158, 50.62390960531435979 ) ) ;
#33176 = CARTESIAN_POINT ( 'NONE',  ( -18.67979575497178146, -10.72451020669898902, 96.66557627198102409 ) ) ;
#33177 = CARTESIAN_POINT ( 'NONE',  ( 14.34966873604972726, -8.224510206698740333, 70.83442372801901854 ) ) ;
#33178 = CARTESIAN_POINT ( 'NONE',  ( -23.34492853952160019, 11.48509598731696890, 165.7658222004386914 ) ) ;
#33179 = CARTESIAN_POINT ( 'NONE',  ( 9.474510206698729675, 16.51473224551082808, 37.08442372801899722 ) ) ;
#33180 = CARTESIAN_POINT ( 'NONE',  ( -16.51473224551069308, -9.474510206698971260, 71.66557627198102409 ) ) ;
#33181 = CARTESIAN_POINT ( 'NONE',  ( 4.483927247898545687, 16.52544592524342804, 64.79057627198103830 ) ) ;
#33182 = CARTESIAN_POINT ( 'NONE',  ( 14.29746914071049879, -8.314922557960816363, 98.33224293864769550 ) ) ;
#33183 = CARTESIAN_POINT ( 'NONE',  ( -13.89961937509977652, 13.97604488694528158, 105.6239096053143527 ) ) ;
#33184 = CARTESIAN_POINT ( 'NONE',  ( -0.05219959533909027116, -19.03943276465977164, 92.49890960531436690 ) ) ;
#33185 = CARTESIAN_POINT ( 'NONE',  ( 10.72451020669871369, 18.67979575497193778, 47.08442372801901854 ) ) ;
#33186 = CARTESIAN_POINT ( 'NONE',  ( -5.049401038298153566, 19.05341960407611168, 105.2072429386476671 ) ) ;
#33187 = CARTESIAN_POINT ( 'NONE',  ( -21.55341960407619339, 5.719274019375674811, 108.5427570613523756 ) ) ;
#33188 = CARTESIAN_POINT ( 'NONE',  ( -8.314922557961024197, 14.29746914071037800, 77.91775706135231871 ) ) ;
#33189 = CARTESIAN_POINT ( 'NONE',  ( -15.80617190586768217, 15.72974639402176855, 38.12609039468567573 ) ) ;
#33190 = CARTESIAN_POINT ( 'NONE',  ( 21.55341960407610458, 5.719274019375980345, 33.95724293864769550 ) ) ;
#33191 = CARTESIAN_POINT ( 'NONE',  ( 21.55341960407610458, 5.719274019375980345, 103.9572429386476813 ) ) ;
#33192 = CARTESIAN_POINT ( 'NONE',  ( -8.314922557960811034, -14.29746914071050412, 57.08224293864769550 ) ) ;
#33193 = CARTESIAN_POINT ( 'NONE',  ( -19.02544592524342804, 5.153800228976336051, 51.04057627198103120 ) ) ;
#33194 = CARTESIAN_POINT ( 'NONE',  ( -4.483927247898539470, -16.52544592524342804, 87.29057627198103830 ) ) ;
#33195 = CARTESIAN_POINT ( 'NONE',  ( -15.72974639402197994, 15.80617190586746368, 45.62390960531436690 ) ) ;
#33196 = CARTESIAN_POINT ( 'NONE',  ( -16.46253265017146816, -9.564922557961047289, 49.16775706135233293 ) ) ;
#33197 = EDGE_CURVE ( 'NONE', #26356, #60581, #7982, .T. ) ;
#33198 = CARTESIAN_POINT ( 'NONE',  ( -0.05219959533910754901, -16.53943276465976808, 112.4989096053143669 ) ) ;
#33199 = EDGE_LOOP ( 'NONE', ( #80621, #173709 ) ) ;
#33200 = CARTESIAN_POINT ( 'NONE',  ( -12.06949235617739369, -12.14591786802326823, 64.37609039468568994 ) ) ;
#33201 = CARTESIAN_POINT ( 'NONE',  ( -19.05341960407611168, -5.049401038298163336, 66.45724293864769550 ) ) ;
#33202 = CARTESIAN_POINT ( 'NONE',  ( 27.73933785331498925, -9.013057229001034898, 145.7750000027311899 ) ) ;
#33203 = CARTESIAN_POINT ( 'NONE',  ( 8.314922557960818139, 14.29746914071049879, 84.58224293864769550 ) ) ;
#33204 = CARTESIAN_POINT ( 'NONE',  ( -21.53943276465977519, 0.05219959533907696930, 41.24890960531435269 ) ) ;
#33205 = CARTESIAN_POINT ( 'NONE',  ( -12.06949235617739369, -12.14591786802326823, 104.3760903946856899 ) ) ;
#33206 = CARTESIAN_POINT ( 'NONE',  ( -16.46253265017146816, -9.564922557961047289, 109.1677570613523471 ) ) ;
#33207 = CARTESIAN_POINT ( 'NONE',  ( -5.823673210054431948, 21.52544592524334988, 92.70942372801901854 ) ) ;
#33208 = CARTESIAN_POINT ( 'NONE',  ( -9.474510206698964154, 16.51473224551069663, 90.41557627198103830 ) ) ;
#33209 = CARTESIAN_POINT ( 'NONE',  ( 21.55341960407610458, 5.719274019375980345, 103.9572429386476813 ) ) ;
#33210 = CARTESIAN_POINT ( 'NONE',  ( -12.06949235617739369, -12.14591786802326823, 54.37609039468568994 ) ) ;
#33211 = CARTESIAN_POINT ( 'NONE',  ( 5.049401038298161559, -19.05341960407611168, 32.70724293864768129 ) ) ;
#33212 = CARTESIAN_POINT ( 'NONE',  ( 4.483927247898790824, -16.52544592524335698, 35.20942372801901854 ) ) ;
#33213 = CARTESIAN_POINT ( 'NONE',  ( 5.153800228976615827, -19.02544592524334988, 90.20942372801900433 ) ) ;
#33214 = CARTESIAN_POINT ( 'NONE',  ( -18.67979575497178146, -10.72451020669898902, 96.66557627198102409 ) ) ;
#33215 = CARTESIAN_POINT ( 'NONE',  ( 13.89961937509957401, 13.97604488694547697, 71.87609039468567573 ) ) ;
#33216 = CARTESIAN_POINT ( 'NONE',  ( 19.25663599770061296, -5.499999999999443112, 86.49419308057204603 ) ) ;
#33217 = CARTESIAN_POINT ( 'NONE',  ( 10.72451020669898902, -18.67979575497178502, 102.9155762719810383 ) ) ;
#33218 = LINE ( 'NONE', #126212, #150060 ) ;
#33219 = CARTESIAN_POINT ( 'NONE',  ( -13.89961937509977652, 13.97604488694528158, 75.62390960531438111 ) ) ;
#33220 = CARTESIAN_POINT ( 'NONE',  ( -12.06949235617739369, -12.14591786802326823, 34.37609039468568284 ) ) ;
#33221 = CARTESIAN_POINT ( 'NONE',  ( -18.22780087662123805, 5.499999999999981348, 101.0176318212689495 ) ) ;
#33222 = CARTESIAN_POINT ( 'NONE',  ( 9.474510206698729675, 16.51473224551082808, 62.08442372801899722 ) ) ;
#33224 = CARTESIAN_POINT ( 'NONE',  ( -12.14591786802309592, -12.06949235617757132, 76.87390960531439532 ) ) ;
#33223 = CARTESIAN_POINT ( 'NONE',  ( -21.53943276465977519, -0.05219959533937600094, 23.75109039468567929 ) ) ;
#33225 = CARTESIAN_POINT ( 'NONE',  ( 16.51473224551069308, 9.474510206698969483, 84.16557627198102409 ) ) ;
#33227 = CARTESIAN_POINT ( 'NONE',  ( 19.05341960407617918, -5.049401038297876454, 46.04275706135233293 ) ) ;
#33226 = CARTESIAN_POINT ( 'NONE',  ( -0.05219959533934338120, 16.53943276465976808, 32.50109039468568284 ) ) ;
#33228 = CONICAL_SURFACE ( 'NONE', #65539, 28.85599147140294107, 0.1745329251994333364 ) ;
#33229 = CARTESIAN_POINT ( 'NONE',  ( 5.823673210054444382, -21.52544592524334988, 50.20942372801901854 ) ) ;
#33230 = CARTESIAN_POINT ( 'NONE',  ( -5.153800228976607833, 19.02544592524334988, 107.7094237280189759 ) ) ;
#33231 = CARTESIAN_POINT ( 'NONE',  ( 5.049401038298161559, -19.05341960407611168, 57.70724293864769550 ) ) ;
#33232 = CARTESIAN_POINT ( 'NONE',  ( 5.049401038297881783, 19.05341960407617563, 77.29275706135231871 ) ) ;
#33233 = CARTESIAN_POINT ( 'NONE',  ( 12.06949235617739724, 12.14591786802326823, 51.87609039468568284 ) ) ;
#33234 = CARTESIAN_POINT ( 'NONE',  ( 5.823673210054444382, -21.52544592524334988, 95.20942372801903275 ) ) ;
#33235 = CARTESIAN_POINT ( 'NONE',  ( 16.46253265017146816, 9.564922557961045513, 61.66775706135234003 ) ) ;
#33236 = CARTESIAN_POINT ( 'NONE',  ( 13.89961937509977652, -13.97604488694527269, 43.12390960531434558 ) ) ;
#33237 = CARTESIAN_POINT ( 'NONE',  ( 10.72451020669898902, -18.67979575497178502, 67.91557627198102409 ) ) ;
#33239 = CARTESIAN_POINT ( 'NONE',  ( 0.05219959533936267826, -19.03943276465977164, 70.00109039468566152 ) ) ;
#33238 = CARTESIAN_POINT ( 'NONE',  ( -4.483927247898539470, -16.52544592524342804, 62.29057627198102409 ) ) ;
#33240 = CARTESIAN_POINT ( 'NONE',  ( -17.60779699588839620, -5.499999999999975131, 101.3498131667010256 ) ) ;
#33241 = CARTESIAN_POINT ( 'NONE',  ( -13.97604488694547697, 13.89961937509957934, 38.12609039468566152 ) ) ;
#33242 = CARTESIAN_POINT ( 'NONE',  ( 14.34966873604972726, -8.224510206698740333, 95.83442372801903275 ) ) ;
#33243 = CARTESIAN_POINT ( 'NONE',  ( 16.55341960407611168, 4.379528057220329451, 53.95724293864770260 ) ) ;
#33245 = CARTESIAN_POINT ( 'NONE',  ( -17.14385361876520264, -23.59649016807271593, 139.1750000027311955 ) ) ;
#33244 = CARTESIAN_POINT ( 'NONE',  ( 10.81492255796106328, -18.62759615963255655, 95.41775706135234714 ) ) ;
#33246 = CARTESIAN_POINT ( 'NONE',  ( 21.55341960407610458, 5.719274019375980345, 88.95724293864769550 ) ) ;
#33247 = CARTESIAN_POINT ( 'NONE',  ( -19.03943276465977164, 0.05219959533909376836, 56.24890960531435979 ) ) ;
#33248 = CARTESIAN_POINT ( 'NONE',  ( 5.823673210054444382, -21.52544592524334988, 70.20942372801904696 ) ) ;
#33249 = CARTESIAN_POINT ( 'NONE',  ( 9.564922557960805705, 16.46253265017160317, 54.58224293864769550 ) ) ;
#33250 = CARTESIAN_POINT ( 'NONE',  ( -5.153800228976328057, -19.02544592524343514, 72.29057627198102409 ) ) ;
#33251 = CARTESIAN_POINT ( 'NONE',  ( 14.29746914071049879, -8.314922557960816363, 108.3322429386477097 ) ) ;
#33252 = CARTESIAN_POINT ( 'NONE',  ( -19.02544592524342804, 5.153800228976336051, 106.0405762719810241 ) ) ;
#33253 = CARTESIAN_POINT ( 'NONE',  ( 16.52544592524342804, -4.483927247898539470, 58.54057627198103120 ) ) ;
#33254 = CARTESIAN_POINT ( 'NONE',  ( -5.049401038298153566, 19.05341960407611168, 35.20724293864768839 ) ) ;
#33255 = CARTESIAN_POINT ( 'NONE',  ( 4.483927247898545687, 16.52544592524342804, 79.79057627198102409 ) ) ;
#33256 = CARTESIAN_POINT ( 'NONE',  ( -18.67979575497178146, -10.72451020669898902, 91.66557627198103830 ) ) ;
#33257 = CARTESIAN_POINT ( 'NONE',  ( -5.719274019375665041, -21.55341960407619695, 29.79275706135234358 ) ) ;
#33258 = CARTESIAN_POINT ( 'NONE',  ( 0.9274610294345855266, 6.404617898468148773, -62.44543528848620895 ) ) ;
#33259 = CARTESIAN_POINT ( 'NONE',  ( -16.55341960407617563, 4.379528057220093196, 48.54275706135234714 ) ) ;
#33260 = CARTESIAN_POINT ( 'NONE',  ( 15.72974639402199770, -15.80617190586745480, 83.12390960531436690 ) ) ;
#33261 = CARTESIAN_POINT ( 'NONE',  ( 5.823673210054444382, -21.52544592524334988, 110.2094237280190185 ) ) ;
#33262 = CARTESIAN_POINT ( 'NONE',  ( 9.474510206698971260, -16.51473224551069308, 107.9155762719810383 ) ) ;
#33263 = CARTESIAN_POINT ( 'NONE',  ( -10.72451020669870658, -18.67979575497194134, 49.58442372801901143 ) ) ;
#33264 = CARTESIAN_POINT ( 'NONE',  ( 5.719274019375991003, -21.55341960407610458, 37.70724293864769550 ) ) ;
#33265 = CARTESIAN_POINT ( 'NONE',  ( -0.05219959533934338120, 16.53943276465976808, 107.5010903946856899 ) ) ;
#33267 = CARTESIAN_POINT ( 'NONE',  ( -21.53943276465977519, -0.05219959533937600094, 83.75109039468568994 ) ) ;
#33266 = CARTESIAN_POINT ( 'NONE',  ( -10.81492255796105439, 18.62759615963255655, 57.91775706135234714 ) ) ;
#33268 = CARTESIAN_POINT ( 'NONE',  ( -19.02544592524334988, -5.153800228976617603, 28.95942372801900433 ) ) ;
#33269 = CARTESIAN_POINT ( 'NONE',  ( -12.06949235617739369, -12.14591786802326823, 94.37609039468568994 ) ) ;
#33270 = CARTESIAN_POINT ( 'NONE',  ( 21.55341960407619695, -5.719274019375665929, 36.04275706135234714 ) ) ;
#33271 = CARTESIAN_POINT ( 'NONE',  ( -5.049401038298153566, 19.05341960407611168, 45.20724293864769550 ) ) ;
#33272 = CARTESIAN_POINT ( 'NONE',  ( 19.02544592524334988, 5.153800228976608722, 26.45942372801899722 ) ) ;
#33273 = CARTESIAN_POINT ( 'NONE',  ( 5.719274019375991003, -21.55341960407610458, 27.70724293864769905 ) ) ;
#33274 = CARTESIAN_POINT ( 'NONE',  ( 0.05219959533937995610, -21.53943276465977519, 25.00109039468567218 ) ) ;
#33275 = CARTESIAN_POINT ( 'NONE',  ( -21.55341960407610458, -5.719274019375992779, 76.45724293864769550 ) ) ;
#33277 = CARTESIAN_POINT ( 'NONE',  ( -18.67979575497178146, -10.72451020669898902, 86.66557627198102409 ) ) ;
#33276 = CARTESIAN_POINT ( 'NONE',  ( 37.99626262588765258, 2.893932880411085066E-14, -7.002157773949822861 ) ) ;
#33279 = CARTESIAN_POINT ( 'NONE',  ( 12.14591786802309770, 12.06949235617756955, 69.37390960531436690 ) ) ;
#33278 = CARTESIAN_POINT ( 'NONE',  ( 8.314922557961029526, -14.29746914071037800, 65.41775706135234714 ) ) ;
#33280 = CARTESIAN_POINT ( 'NONE',  ( 23.29544513554940366, -16.92513159979222337, 147.0656553485623590 ) ) ;
#33281 = CARTESIAN_POINT ( 'NONE',  ( 19.03943276465977164, 0.05219959533936151252, 91.25109039468566152 ) ) ;
#33282 = CARTESIAN_POINT ( 'NONE',  ( -24.30000000000003268, 2.668083032619853614E-13, -54.21489346206828230 ) ) ;
#33283 = CARTESIAN_POINT ( 'NONE',  ( 16.53943276465976808, 0.05219959533934440121, 21.25109039468567218 ) ) ;
#33284 = CARTESIAN_POINT ( 'NONE',  ( -5.823673210054116645, -21.52544592524344225, 97.29057627198105251 ) ) ;
#33285 = CARTESIAN_POINT ( 'NONE',  ( 5.823673210054125526, 21.52544592524343514, 74.79057627198105251 ) ) ;
#33286 = CARTESIAN_POINT ( 'NONE',  ( -19.02544592524342804, 5.153800228976336051, 111.0405762719810099 ) ) ;
#33287 = CARTESIAN_POINT ( 'NONE',  ( 14.29746914071037800, 8.314922557961029526, 56.66775706135235424 ) ) ;
#33288 = CARTESIAN_POINT ( 'NONE',  ( -16.46253265017160317, 9.564922557960807481, 75.83224293864769550 ) ) ;
#33290 = CARTESIAN_POINT ( 'NONE',  ( 5.049401038297881783, 19.05341960407617563, 107.2927570613523187 ) ) ;
#33289 = CARTESIAN_POINT ( 'NONE',  ( 5.719274019375673035, 21.55341960407619339, 47.29275706135234003 ) ) ;
#33291 = CARTESIAN_POINT ( 'NONE',  ( 9.564922557960805705, 16.46253265017160317, 104.5822429386476955 ) ) ;
#33292 = CARTESIAN_POINT ( 'NONE',  ( -5.153800228976607833, 19.02544592524334988, 22.70942372801899012 ) ) ;
#33293 = CARTESIAN_POINT ( 'NONE',  ( -16.52544592524335698, -4.483927247898792601, 43.95942372801902565 ) ) ;
#33294 = CARTESIAN_POINT ( 'NONE',  ( -0.05219959533909027116, -19.03943276465977164, 107.4989096053143527 ) ) ;
#33295 = CARTESIAN_POINT ( 'NONE',  ( 5.719274019375991003, -21.55341960407610458, 102.7072429386476955 ) ) ;
#33296 = CARTESIAN_POINT ( 'NONE',  ( -13.89961937509977652, 13.97604488694528158, 60.62390960531436690 ) ) ;
#33297 = CARTESIAN_POINT ( 'NONE',  ( 0.000000000000000000, 0.000000000000000000, -65.00100000000003320 ) ) ;
#33298 = CARTESIAN_POINT ( 'NONE',  ( -12.14591786802309592, -12.06949235617757132, 76.87390960531439532 ) ) ;
#33299 = CARTESIAN_POINT ( 'NONE',  ( 21.55341960407610458, 5.719274019375980345, 23.95724293864769550 ) ) ;
#33300 = CARTESIAN_POINT ( 'NONE',  ( -17.31728774477272381, 6.344390552232388458, 35.81906651689320142 ) ) ;
#33301 = CARTESIAN_POINT ( 'NONE',  ( -15.80617190586745835, -15.72974639402198527, 106.8739096053143811 ) ) ;
#33302 = CARTESIAN_POINT ( 'NONE',  ( 13.89961937509957401, 13.97604488694547697, 56.87609039468564731 ) ) ;
#33303 = CARTESIAN_POINT ( 'NONE',  ( -0.05219959533909027116, -19.03943276465977164, 112.4989096053143669 ) ) ;
#33304 = CARTESIAN_POINT ( 'NONE',  ( -0.05219959533909027116, -19.03943276465977164, 32.49890960531435979 ) ) ;
#33305 = CARTESIAN_POINT ( 'NONE',  ( 10.72451020669898902, -18.67979575497178502, 52.91557627198103830 ) ) ;
#33306 = CARTESIAN_POINT ( 'NONE',  ( -19.03943276465977164, 0.05219959533909376836, 96.24890960531436690 ) ) ;
#33307 = CARTESIAN_POINT ( 'NONE',  ( -0.05219959533937732626, 21.53943276465977519, 82.50109039468568994 ) ) ;
#33308 = CARTESIAN_POINT ( 'NONE',  ( -19.02544592524342804, 5.153800228976336051, 46.04057627198101699 ) ) ;
#33309 = CARTESIAN_POINT ( 'NONE',  ( 0.05219959533910956823, 16.53943276465976808, 84.99890960531436690 ) ) ;
#33310 = CARTESIAN_POINT ( 'NONE',  ( 4.379528057220092307, 16.55341960407617563, 37.29275706135235424 ) ) ;
#33311 = CARTESIAN_POINT ( 'NONE',  ( -10.72451020669870658, -18.67979575497194134, 69.58442372801900433 ) ) ;
#33312 = VERTEX_POINT ( 'NONE', #31956 ) ;
#33313 = CARTESIAN_POINT ( 'NONE',  ( 16.51473224551083163, -9.474510206698727899, 30.83442372801900433 ) ) ;
#33314 = CARTESIAN_POINT ( 'NONE',  ( -9.474510206698720793, -16.51473224551083518, 74.58442372801900433 ) ) ;
#33315 = CARTESIAN_POINT ( 'NONE',  ( -13.89961937509957401, -13.97604488694547875, 39.37609039468566152 ) ) ;
#33316 = CARTESIAN_POINT ( 'NONE',  ( 10.72451020669871369, 18.67979575497193778, 37.08442372801901143 ) ) ;
#33317 = CARTESIAN_POINT ( 'NONE',  ( -38.00000000000000711, 2.428612866367529932E-14, -1.749999994537626558 ) ) ;
#33318 = CARTESIAN_POINT ( 'NONE',  ( -13.97604488694547697, 13.89961937509957934, 28.12609039468565797 ) ) ;
#33319 = CARTESIAN_POINT ( 'NONE',  ( 9.474510206698971260, -16.51473224551069308, 62.91557627198102409 ) ) ;
#33320 = CARTESIAN_POINT ( 'NONE',  ( -16.55341960407611168, -4.379528057220339221, 21.45724293864769550 ) ) ;
#33322 = CARTESIAN_POINT ( 'NONE',  ( 0.05219959533937995610, -21.53943276465977519, 90.00109039468567573 ) ) ;
#33321 = CARTESIAN_POINT ( 'NONE',  ( 5.049401038298161559, -19.05341960407611168, 112.7072429386476813 ) ) ;
#33323 = CARTESIAN_POINT ( 'NONE',  ( -22.81625015709510507, 31.40387420917330275, -4.924999997268813878 ) ) ;
#33324 = CARTESIAN_POINT ( 'NONE',  ( -18.22780087662122028, 5.500000000000031086, 98.51540105326105845 ) ) ;
#33325 = CARTESIAN_POINT ( 'NONE',  ( -15.80617190586768217, 15.72974639402176855, 83.12609039468568994 ) ) ;
#33326 = CARTESIAN_POINT ( 'NONE',  ( 16.81555441253550143, -7.025013491695467849, 43.13685445334256485 ) ) ;
#33327 = CARTESIAN_POINT ( 'NONE',  ( 19.02544592524343514, -5.153800228976328945, 98.54057627198100988 ) ) ;
#33328 = EDGE_CURVE ( 'NONE', #115197, #33312, #44858, .T. ) ;
#33329 = CARTESIAN_POINT ( 'NONE',  ( -26.33867313280595468, -8.832717389288097465, 167.2809140985657450 ) ) ;
#33330 = CARTESIAN_POINT ( 'NONE',  ( 9.474510206698971260, -16.51473224551069308, 52.91557627198102409 ) ) ;
#33331 = CARTESIAN_POINT ( 'NONE',  ( -21.53943276465977519, 0.05219959533907696930, 61.24890960531435979 ) ) ;
#33332 = CARTESIAN_POINT ( 'NONE',  ( -8.314922557960811034, -14.29746914071050412, 32.08224293864769550 ) ) ;
#33334 = CARTESIAN_POINT ( 'NONE',  ( -16.46253265017160317, 9.564922557960807481, 95.83224293864769550 ) ) ;
#33333 = CARTESIAN_POINT ( 'NONE',  ( -4.379528057220328563, 16.55341960407611168, 115.2072429386476955 ) ) ;
#33335 = CARTESIAN_POINT ( 'NONE',  ( -5.153800228976607833, 19.02544592524334988, 27.70942372801899722 ) ) ;
#33336 = CARTESIAN_POINT ( 'NONE',  ( 16.53943276465976808, -0.05219959533910856209, 103.7489096053143669 ) ) ;
#33337 = CARTESIAN_POINT ( 'NONE',  ( -10.72451020669870658, -18.67979575497194134, 69.58442372801900433 ) ) ;
#33338 = DIRECTION ( 'NONE',  ( -0.4999999999999932832, 0.5000000000000055511, -0.7071067811865483499 ) ) ;
#33339 = CARTESIAN_POINT ( 'NONE',  ( -4.483927247898782831, 16.52544592524335698, 112.7094237280190328 ) ) ;
#33340 = CARTESIAN_POINT ( 'NONE',  ( -5.049401038297874678, -19.05341960407617918, 59.79275706135231871 ) ) ;
#33341 = CARTESIAN_POINT ( 'NONE',  ( 34.12434206616184440, 14.08647367304311260, -8.000000000000001776 ) ) ;
#33342 = CARTESIAN_POINT ( 'NONE',  ( -5.049401038298153566, 19.05341960407611168, 110.2072429386476671 ) ) ;
#33343 = CARTESIAN_POINT ( 'NONE',  ( -0.05219959533910754901, -16.53943276465976808, 82.49890960531436690 ) ) ;
#33344 = CARTESIAN_POINT ( 'NONE',  ( 0.05219959533936267826, -19.03943276465977164, 55.00109039468566863 ) ) ;
#33345 = CARTESIAN_POINT ( 'NONE',  ( 16.46253265017160672, -9.564922557960803928, 63.33224293864769550 ) ) ;
#33346 = CARTESIAN_POINT ( 'NONE',  ( -14.29746914071049879, 8.314922557960819915, 65.83224293864769550 ) ) ;
#33347 = CARTESIAN_POINT ( 'NONE',  ( 19.03943276465977164, 0.05219959533936151252, 96.25109039468567573 ) ) ;
#33348 = CARTESIAN_POINT ( 'NONE',  ( 10.72451020669898902, -18.67979575497178502, 52.91557627198103830 ) ) ;
#33349 = EDGE_LOOP ( 'NONE', ( #103795, #87497, #161848, #120277 ) ) ;
#33350 = CARTESIAN_POINT ( 'NONE',  ( -12.14591786802309592, -12.06949235617757132, 111.8739096053143669 ) ) ;
#33351 = CARTESIAN_POINT ( 'NONE',  ( 5.153800228976617603, -19.02544592524335343, 100.2094237280190043 ) ) ;
#33353 = CARTESIAN_POINT ( 'NONE',  ( -5.719274019375978568, 21.55341960407610458, 60.20724293864768839 ) ) ;
#33352 = CARTESIAN_POINT ( 'NONE',  ( -16.46253265017160317, 9.564922557960807481, 55.83224293864769550 ) ) ;
#33355 = CARTESIAN_POINT ( 'NONE',  ( 9.474510206698971260, -16.51473224551069308, 72.91557627198102409 ) ) ;
#33354 = CARTESIAN_POINT ( 'NONE',  ( 12.14591786802327356, -12.06949235617739191, 95.62609039468568994 ) ) ;
#33356 = CARTESIAN_POINT ( 'NONE',  ( -9.474510206698720793, -16.51473224551083518, 49.58442372801899722 ) ) ;
#33357 = CARTESIAN_POINT ( 'NONE',  ( -21.52544592524334988, -5.823673210054445271, 78.95942372801901854 ) ) ;
#33358 = CARTESIAN_POINT ( 'NONE',  ( 5.823673210054125526, 21.52544592524343514, 69.79057627198102409 ) ) ;
#33359 = CARTESIAN_POINT ( 'NONE',  ( -19.02544592524342804, 5.153800228976336051, 111.0405762719810099 ) ) ;
#33360 = CARTESIAN_POINT ( 'NONE',  ( -9.474510206698964154, 16.51473224551069663, 40.41557627198103120 ) ) ;
#33361 = CARTESIAN_POINT ( 'NONE',  ( 14.34966873604972726, -8.224510206698740333, 95.83442372801903275 ) ) ;
#33362 = CARTESIAN_POINT ( 'NONE',  ( -9.564922557961040184, 16.46253265017147172, 112.9177570613523329 ) ) ;
#33363 = CARTESIAN_POINT ( 'NONE',  ( 17.12812012977023812, 6.668231424566061882, 53.85948759323142809 ) ) ;
#33364 = CARTESIAN_POINT ( 'NONE',  ( -21.52544592524334988, -5.823673210054445271, 98.95942372801903275 ) ) ;
#33365 = ORIENTED_EDGE ( 'NONE', *, *, #13191, .F. ) ;
#33366 = CARTESIAN_POINT ( 'NONE',  ( 16.55341960407611168, 4.379528057220329451, 63.95724293864770260 ) ) ;
#33367 = CARTESIAN_POINT ( 'NONE',  ( 14.29746914071049879, -8.314922557960816363, 73.33224293864769550 ) ) ;
#33368 = CARTESIAN_POINT ( 'NONE',  ( -5.719274019375978568, 21.55341960407610458, 90.20724293864770971 ) ) ;
#33369 = CARTESIAN_POINT ( 'NONE',  ( -21.53943276465977519, 0.05219959533907696930, 86.24890960531436690 ) ) ;
#33370 = CARTESIAN_POINT ( 'NONE',  ( 16.52216118717208460, -7.221426719304491648, 96.42400978953010338 ) ) ;
#33371 = CARTESIAN_POINT ( 'NONE',  ( -21.55341960407610458, -5.719274019375992779, 46.45724293864769550 ) ) ;
#33372 = CARTESIAN_POINT ( 'NONE',  ( 16.52544592524335698, 4.483927247898782831, 66.45942372801903275 ) ) ;
#33373 = CARTESIAN_POINT ( 'NONE',  ( 12.14591786802309770, 12.06949235617756955, 94.37390960531436690 ) ) ;
#33374 = CARTESIAN_POINT ( 'NONE',  ( -16.46253265017160317, 9.564922557960807481, 40.83224293864769550 ) ) ;
#33375 = CARTESIAN_POINT ( 'NONE',  ( 30.00000000000000711, -5.510910596163089556E-15, 45.00000000000000000 ) ) ;
#33376 = CARTESIAN_POINT ( 'NONE',  ( 4.483927247898790824, -16.52544592524335698, 95.20942372801903275 ) ) ;
#33377 = CARTESIAN_POINT ( 'NONE',  ( -18.67979575497193778, 10.72451020669871902, 28.33442372801902209 ) ) ;
#33378 = CARTESIAN_POINT ( 'NONE',  ( 19.02544592524343514, -5.153800228976328945, 98.54057627198100988 ) ) ;
#33379 = CARTESIAN_POINT ( 'NONE',  ( -15.80617190586768217, 15.72974639402176855, 68.12609039468567573 ) ) ;
#33380 = CARTESIAN_POINT ( 'NONE',  ( 5.049401038298161559, -19.05341960407611168, 22.70724293864769194 ) ) ;
#33381 = CARTESIAN_POINT ( 'NONE',  ( 19.05341960407611168, 5.049401038298154454, 28.95724293864769550 ) ) ;
#33382 =( BOUNDED_CURVE ( )  B_SPLINE_CURVE ( 2, ( #75955, #61766, #30455, #92103, #184145, #28498, #13306, #93102, #170953, #121462, #16284 ),
 .UNSPECIFIED., .F., .T. ) 
 B_SPLINE_CURVE_WITH_KNOTS ( ( 3, 2, 2, 2, 2, 3 ),
 ( 0.001627243422692786377, 0.02000000000000003858, 0.04000000000000008410, 0.06000000000000012268, 0.08000000000000004330, 0.1000000000000000888 ),
 .UNSPECIFIED. ) 
 CURVE ( )  GEOMETRIC_REPRESENTATION_ITEM ( )  RATIONAL_B_SPLINE_CURVE ( ( 0.9926836962356841987, 0.9550386643922726959, 1.000000000000000000, 0.9510565162951535312, 1.000000000000000000, 0.9510565162951535312, 1.000000000000000000, 0.9510565162951535312, 1.000000000000000000, 0.9510565162951533091, 1.000000000000000222 ) ) 
 REPRESENTATION_ITEM ( '' )  );
#33383 = VERTEX_POINT ( 'NONE', #187645 ) ;
#33384 = CARTESIAN_POINT ( 'NONE',  ( -0.05219959533937732626, 21.53943276465977519, 52.50109039468567573 ) ) ;
#33386 = CARTESIAN_POINT ( 'NONE',  ( 18.09805431107521301, -5.500000000000095923, 58.51606229291888894 ) ) ;
#33385 = CARTESIAN_POINT ( 'NONE',  ( 9.564922557960805705, 16.46253265017160317, 44.58224293864769550 ) ) ;
#33387 = CARTESIAN_POINT ( 'NONE',  ( 5.049401038298161559, -19.05341960407611168, 92.70724293864769550 ) ) ;
#33388 = CARTESIAN_POINT ( 'NONE',  ( 16.51473224551083163, -9.474510206698727899, 60.83442372801900433 ) ) ;
#33389 = CARTESIAN_POINT ( 'NONE',  ( 5.823673210054444382, -21.52544592524334988, 25.20942372801901854 ) ) ;
#33390 = CARTESIAN_POINT ( 'NONE',  ( 0.05219959533936267826, -19.03943276465977164, 60.00109039468566863 ) ) ;
#33391 = CARTESIAN_POINT ( 'NONE',  ( 9.564922557960805705, 16.46253265017160317, 34.58224293864770260 ) ) ;
#33392 = CARTESIAN_POINT ( 'NONE',  ( 12.06949235617739724, 12.14591786802326823, 101.8760903946857042 ) ) ;
#33393 = CARTESIAN_POINT ( 'NONE',  ( 0.05219959533936267826, -19.03943276465977164, 70.00109039468566152 ) ) ;
#33394 = CARTESIAN_POINT ( 'NONE',  ( -14.34966873604960291, -8.224510206698953496, 31.66557627198102054 ) ) ;
#33395 = CARTESIAN_POINT ( 'NONE',  ( 13.89961937509957401, 13.97604488694547697, 56.87609039468564731 ) ) ;
#33396 = CARTESIAN_POINT ( 'NONE',  ( -16.46253265017160317, 9.564922557960807481, 100.8322429386477097 ) ) ;
#33397 = CARTESIAN_POINT ( 'NONE',  ( 10.72451020669871369, 18.67979575497193778, 102.0844237280190185 ) ) ;
#33399 = ADVANCED_FACE ( 'NONE', ( #199820 ), #188873, .F. ) ;
#33398 = CARTESIAN_POINT ( 'NONE',  ( 5.153800228976615827, -19.02544592524334988, 20.20942372801899722 ) ) ;
#33400 = CARTESIAN_POINT ( 'NONE',  ( -13.97604488694527625, -13.89961937509977652, 26.87390960531434558 ) ) ;
#33401 = CARTESIAN_POINT ( 'NONE',  ( 15.80617190586769283, -15.72974639402175789, 90.62609039468567573 ) ) ;
#33402 = CARTESIAN_POINT ( 'NONE',  ( -14.34966873604972548, 8.224510206698743886, 33.33442372801900433 ) ) ;
#33403 = CARTESIAN_POINT ( 'NONE',  ( 5.049401038298161559, -19.05341960407611168, 97.70724293864766707 ) ) ;
#33404 = AXIS2_PLACEMENT_3D ( 'NONE', #193592, #195601, #116735 ) ;
#33405 = CARTESIAN_POINT ( 'NONE',  ( 30.00000000000000000, -1.132798289211302014E-14, 97.50000000000000000 ) ) ;
#33406 = CARTESIAN_POINT ( 'NONE',  ( -9.564922557960796823, -16.46253265017161027, 77.08224293864769550 ) ) ;
#33407 = CARTESIAN_POINT ( 'NONE',  ( 23.31738231874054534, 16.94106989632529192, 141.1999999999999886 ) ) ;
#33408 = CARTESIAN_POINT ( 'NONE',  ( 9.474510206698729675, 16.51473224551082808, 77.08442372801900433 ) ) ;
#33409 = CARTESIAN_POINT ( 'NONE',  ( -5.049401038298153566, 19.05341960407611168, 110.2072429386476671 ) ) ;
#33410 = CARTESIAN_POINT ( 'NONE',  ( 21.53943276465977519, 0.05219959533937863772, 96.25109039468568994 ) ) ;
#33411 = CARTESIAN_POINT ( 'NONE',  ( 16.52544592524342804, -4.483927247898539470, 93.54057627198103830 ) ) ;
#33412 = CARTESIAN_POINT ( 'NONE',  ( 10.81492255796078972, 18.62759615963270932, 39.58224293864769550 ) ) ;
#33413 = CARTESIAN_POINT ( 'NONE',  ( 18.62759615963271287, -10.81492255796078972, 33.33224293864769550 ) ) ;
#33414 = CARTESIAN_POINT ( 'NONE',  ( 12.14591786802309770, 12.06949235617756955, 104.3739096053143669 ) ) ;
#33415 = CARTESIAN_POINT ( 'NONE',  ( -16.38029848613151174, 0.9460486868806974314, -61.48057501744757758 ) ) ;
#33416 = CARTESIAN_POINT ( 'NONE',  ( 9.564922557961047289, -16.46253265017146816, 60.41775706135233293 ) ) ;
#33417 = CARTESIAN_POINT ( 'NONE',  ( -8.224510206698948167, 14.34966873604960824, 45.41557627198103830 ) ) ;
#33418 = CARTESIAN_POINT ( 'NONE',  ( -13.89961937509977652, 13.97604488694528158, 110.6239096053143243 ) ) ;
#33419 = CARTESIAN_POINT ( 'NONE',  ( 5.823673210054444382, -21.52544592524334988, 80.20942372801901854 ) ) ;
#33420 = CARTESIAN_POINT ( 'NONE',  ( -5.823673210054116645, -21.52544592524344225, 72.29057627198102409 ) ) ;
#33421 = CARTESIAN_POINT ( 'NONE',  ( 18.67979575497194134, -10.72451020669871369, 40.83442372801901854 ) ) ;
#33422 = CARTESIAN_POINT ( 'NONE',  ( -0.05219959533907301413, -21.53943276465977519, 102.4989096053143811 ) ) ;
#33423 = CARTESIAN_POINT ( 'NONE',  ( -15.72974639402176322, -15.80617190586768395, 54.37609039468568994 ) ) ;
#33424 = CARTESIAN_POINT ( 'NONE',  ( -19.03943276465977164, 0.05219959533909376836, 31.24890960531435979 ) ) ;
#33425 = CARTESIAN_POINT ( 'NONE',  ( -19.05341960407611168, -5.049401038298163336, 81.45724293864769550 ) ) ;
#33426 = CARTESIAN_POINT ( 'NONE',  ( 16.52544592524335698, 4.483927247898782831, 81.45942372801900433 ) ) ;
#33427 = CARTESIAN_POINT ( 'NONE',  ( 14.34966873604960469, 8.224510206698951720, 99.16557627198100988 ) ) ;
#33428 = CARTESIAN_POINT ( 'NONE',  ( 16.46253265017160672, -9.564922557960803928, 113.3322429386476955 ) ) ;
#33429 = CARTESIAN_POINT ( 'NONE',  ( -14.29746914071049879, 8.314922557960819915, 50.83224293864770971 ) ) ;
#33430 = CARTESIAN_POINT ( 'NONE',  ( -8.314922557960811034, -14.29746914071050412, 27.08224293864769550 ) ) ;
#33431 = CARTESIAN_POINT ( 'NONE',  ( 13.89961937509977652, -13.97604488694527269, 68.12390960531436690 ) ) ;
#33432 = CARTESIAN_POINT ( 'NONE',  ( -19.03943276465977164, 0.05219959533909376836, 41.24890960531435269 ) ) ;
#33433 = CARTESIAN_POINT ( 'NONE',  ( -5.823673210054116645, -21.52544592524344225, 47.29057627198103120 ) ) ;
#33434 = CARTESIAN_POINT ( 'NONE',  ( -9.564922557961040184, 16.46253265017147172, 42.91775706135234003 ) ) ;
#33436 = CARTESIAN_POINT ( 'NONE',  ( -16.52544592524342804, 4.483927247898546575, 31.04057627198102409 ) ) ;
#33435 = CARTESIAN_POINT ( 'NONE',  ( 11.30153831258471797, -180.0000000000000000, -15.00000000000000178 ) ) ;
#33437 = CARTESIAN_POINT ( 'NONE',  ( -9.564922557960796823, -16.46253265017161027, 107.0822429386476955 ) ) ;
#33438 = CARTESIAN_POINT ( 'NONE',  ( -18.62759615963255300, -10.81492255796106328, 54.16775706135235424 ) ) ;
#33439 = CARTESIAN_POINT ( 'NONE',  ( 23.14225647005876851, -5.657937718899350266, 172.1775255543084882 ) ) ;
#33440 = CARTESIAN_POINT ( 'NONE',  ( 4.483927247898790824, -16.52544592524335698, 65.20942372801901854 ) ) ;
#33441 = CARTESIAN_POINT ( 'NONE',  ( 19.05341960407617918, -5.049401038297876454, 56.04275706135234714 ) ) ;
#33442 = CARTESIAN_POINT ( 'NONE',  ( 4.379528057220339221, -16.55341960407611168, 27.70724293864769905 ) ) ;
#33443 = CARTESIAN_POINT ( 'NONE',  ( -18.89770734986047884, -5.500000000000005329, 74.10214472496639360 ) ) ;
#33444 = CARTESIAN_POINT ( 'NONE',  ( -4.483927247898782831, 16.52544592524335698, 107.7094237280190328 ) ) ;
#33445 = CARTESIAN_POINT ( 'NONE',  ( -9.474510206698964154, 16.51473224551069663, 40.41557627198103120 ) ) ;
#33446 = CARTESIAN_POINT ( 'NONE',  ( -19.05341960407611168, -5.049401038298163336, 61.45724293864769550 ) ) ;
#33447 = CARTESIAN_POINT ( 'NONE',  ( 9.474510206698971260, -16.51473224551069308, 22.91557627198102765 ) ) ;
#33448 = CARTESIAN_POINT ( 'NONE',  ( 10.72451020669871369, 18.67979575497193778, 37.08442372801901143 ) ) ;
#33449 = CARTESIAN_POINT ( 'NONE',  ( 9.564922557960805705, 16.46253265017160317, 44.58224293864769550 ) ) ;
#33450 = CARTESIAN_POINT ( 'NONE',  ( -6.328208617727321794, -6.541134799867854177, -61.89430850415823215 ) ) ;
#33451 = CARTESIAN_POINT ( 'NONE',  ( 19.03943276465977164, -0.05219959533909143690, 48.74890960531435979 ) ) ;
#33452 = CARTESIAN_POINT ( 'NONE',  ( -15.80617190586745835, -15.72974639402198527, 21.87390960531436690 ) ) ;
#33454 = CARTESIAN_POINT ( 'NONE',  ( -8.314922557960811034, -14.29746914071050412, 112.0822429386477097 ) ) ;
#33453 = CARTESIAN_POINT ( 'NONE',  ( 15.72974639402176855, 15.80617190586768217, 61.87609039468568284 ) ) ;
#33455 = CARTESIAN_POINT ( 'NONE',  ( 15.80617190586746368, 15.72974639402197994, 34.37390960531435979 ) ) ;
#33456 = CIRCLE ( 'NONE', #59153, 16.70000000000002061 ) ;
#33457 = CARTESIAN_POINT ( 'NONE',  ( 4.379528057220092307, 16.55341960407617563, 82.29275706135234714 ) ) ;
#33458 = CARTESIAN_POINT ( 'NONE',  ( 18.67979575497194134, -10.72451020669871369, 100.8344237280190185 ) ) ;
#33459 = CARTESIAN_POINT ( 'NONE',  ( -8.314922557961024197, 14.29746914071037800, 52.91775706135235424 ) ) ;
#33460 = CARTESIAN_POINT ( 'NONE',  ( -19.02544592524342804, 5.153800228976336051, 91.04057627198100988 ) ) ;
#33461 = CARTESIAN_POINT ( 'NONE',  ( 14.29746914071037800, 8.314922557961029526, 36.66775706135234714 ) ) ;
#33462 = CARTESIAN_POINT ( 'NONE',  ( 8.314922557961029526, -14.29746914071037800, 30.41775706135234358 ) ) ;
#33463 = CARTESIAN_POINT ( 'NONE',  ( -4.379528057220086978, -16.55341960407618274, 99.79275706135234714 ) ) ;
#33464 = CARTESIAN_POINT ( 'NONE',  ( -5.719274019375665041, -21.55341960407619695, 49.79275706135234714 ) ) ;
#33465 = CARTESIAN_POINT ( 'NONE',  ( 13.89961937509957401, 13.97604488694547697, 101.8760903946856331 ) ) ;
#33466 = CARTESIAN_POINT ( 'NONE',  ( -21.55341960407610458, -5.719274019375992779, 106.4572429386477097 ) ) ;
#33468 = CARTESIAN_POINT ( 'NONE',  ( 19.05341960407617918, -5.049401038297876454, 101.0427570613523045 ) ) ;
#33467 = CARTESIAN_POINT ( 'NONE',  ( -0.05219959533910754901, -16.53943276465976808, 102.4989096053143811 ) ) ;
#33469 = CARTESIAN_POINT ( 'NONE',  ( 14.29746914071037800, 8.314922557961029526, 86.66775706135234714 ) ) ;
#33470 = CARTESIAN_POINT ( 'NONE',  ( -17.31747979337961851, 6.344076630960740815, 43.62055131934818064 ) ) ;
#33471 = CARTESIAN_POINT ( 'NONE',  ( -5.153800228976607833, 19.02544592524334988, 77.70942372801900433 ) ) ;
#33472 = CARTESIAN_POINT ( 'NONE',  ( -8.224510206698948167, 14.34966873604960824, 40.41557627198103120 ) ) ;
#33473 = CARTESIAN_POINT ( 'NONE',  ( -12.14591786802309592, -12.06949235617757132, 41.87390960531435979 ) ) ;
#33474 = CARTESIAN_POINT ( 'NONE',  ( -16.52544592524342804, 4.483927247898546575, 106.0405762719810525 ) ) ;
#33476 = CARTESIAN_POINT ( 'NONE',  ( -18.22780087662122028, 5.500000000000031086, 88.51540105326107266 ) ) ;
#33475 = CARTESIAN_POINT ( 'NONE',  ( -5.153800228976607833, 19.02544592524334988, 37.70942372801899722 ) ) ;
#33477 = CARTESIAN_POINT ( 'NONE',  ( -21.55341960407619339, 5.719274019375674811, 33.54275706135234714 ) ) ;
#33478 = CARTESIAN_POINT ( 'NONE',  ( 4.483927247898790824, -16.52544592524335698, 20.20942372801900788 ) ) ;
#33479 = CARTESIAN_POINT ( 'NONE',  ( -9.441188956457237325, -38.26011958722978079, -31.87100816096939582 ) ) ;
#33480 = CARTESIAN_POINT ( 'NONE',  ( -16.51473224551069308, -9.474510206698971260, 96.66557627198102409 ) ) ;
#33481 = CARTESIAN_POINT ( 'NONE',  ( 13.89961937509977652, -13.97604488694527269, 83.12390960531436690 ) ) ;
#33482 = CARTESIAN_POINT ( 'NONE',  ( -5.719274019375978568, 21.55341960407610458, 55.20724293864770260 ) ) ;
#33483 = CARTESIAN_POINT ( 'NONE',  ( -4.379528057220328563, 16.55341960407611168, 100.2072429386476955 ) ) ;
#33484 = CARTESIAN_POINT ( 'NONE',  ( -9.474510206698964154, 16.51473224551069663, 65.41557627198102409 ) ) ;
#33485 = CARTESIAN_POINT ( 'NONE',  ( 9.474510206698971260, -16.51473224551069308, 32.91557627198102409 ) ) ;
#33486 = CARTESIAN_POINT ( 'NONE',  ( 0.05219959533937995610, -21.53943276465977519, 40.00109039468567573 ) ) ;
#33487 = CARTESIAN_POINT ( 'NONE',  ( 21.55341960407619695, -5.719274019375665929, 71.04275706135234714 ) ) ;
#33488 = CARTESIAN_POINT ( 'NONE',  ( 14.29746914071037800, 8.314922557961029526, 91.66775706135234714 ) ) ;
#33489 = CARTESIAN_POINT ( 'NONE',  ( 15.80617190586769283, -15.72974639402175789, 25.62609039468567929 ) ) ;
#33490 = CARTESIAN_POINT ( 'NONE',  ( -21.55341960407619339, 5.719274019375674811, 28.54275706135234358 ) ) ;
#33492 = CARTESIAN_POINT ( 'NONE',  ( -5.049401038298153566, 19.05341960407611168, 85.20724293864766707 ) ) ;
#33491 = CARTESIAN_POINT ( 'NONE',  ( 5.049401038297881783, 19.05341960407617563, 57.29275706135231871 ) ) ;
#33493 = CARTESIAN_POINT ( 'NONE',  ( 5.719274019375673035, 21.55341960407619339, 82.29275706135234714 ) ) ;
#33494 = CARTESIAN_POINT ( 'NONE',  ( -21.53943276465977519, 0.05219959533907696930, 81.24890960531436690 ) ) ;
#33495 = CARTESIAN_POINT ( 'NONE',  ( 16.52544592524342804, -4.483927247898539470, 48.54057627198103120 ) ) ;
#33497 = CARTESIAN_POINT ( 'NONE',  ( 5.049401038297881783, 19.05341960407617563, 37.29275706135232582 ) ) ;
#33496 = CARTESIAN_POINT ( 'NONE',  ( 5.823673210054444382, -21.52544592524334988, 100.2094237280190043 ) ) ;
#33498 = CARTESIAN_POINT ( 'NONE',  ( 14.29746914071049879, -8.314922557960816363, 73.33224293864769550 ) ) ;
#33499 = CARTESIAN_POINT ( 'NONE',  ( 14.29746914071049879, -8.314922557960816363, 113.3322429386476955 ) ) ;
#33500 = CARTESIAN_POINT ( 'NONE',  ( 19.05341960407617918, -5.049401038297876454, 76.04275706135230450 ) ) ;
#33501 = CARTESIAN_POINT ( 'NONE',  ( 8.314922557960818139, 14.29746914071049879, 29.58224293864769905 ) ) ;
#33502 = CARTESIAN_POINT ( 'NONE',  ( 21.52544592524334988, 5.823673210054432836, 81.45942372801900433 ) ) ;
#33503 = CARTESIAN_POINT ( 'NONE',  ( 19.03943276465977164, -0.05219959533909143690, 83.74890960531436690 ) ) ;
#33504 = CARTESIAN_POINT ( 'NONE',  ( -9.564922557961040184, 16.46253265017147172, 57.91775706135233293 ) ) ;
#33505 = CARTESIAN_POINT ( 'NONE',  ( -21.52544592524343514, 5.823673210054127303, 61.04057627198103120 ) ) ;
#33506 = CARTESIAN_POINT ( 'NONE',  ( -10.72451020669898014, 18.67979575497178502, 110.4155762719810383 ) ) ;
#33507 = CARTESIAN_POINT ( 'NONE',  ( -19.05341960407617563, 5.049401038297882671, 113.5427570613523471 ) ) ;
#33508 = CARTESIAN_POINT ( 'NONE',  ( 14.34966873604972726, -8.224510206698740333, 75.83442372801900433 ) ) ;
#33510 = CARTESIAN_POINT ( 'NONE',  ( -21.53943276465977519, -0.05219959533937600094, 23.75109039468567929 ) ) ;
#33509 = CARTESIAN_POINT ( 'NONE',  ( -37.99626262588762415, -12.34573411038919311, -5.902157773949822328 ) ) ;
#33511 = CARTESIAN_POINT ( 'NONE',  ( 16.55341960407611168, 4.379528057220329451, 103.9572429386476813 ) ) ;
#33512 = CARTESIAN_POINT ( 'NONE',  ( 22.81625015709509441, 31.40387420917330275, -3.824999997268813345 ) ) ;
#33513 = CARTESIAN_POINT ( 'NONE',  ( 16.55341960407618274, -4.379528057220086978, 41.04275706135236135 ) ) ;
#33514 = CARTESIAN_POINT ( 'NONE',  ( 5.823673210054125526, 21.52544592524343514, 59.79057627198103120 ) ) ;
#33515 = CARTESIAN_POINT ( 'NONE',  ( 12.14591786802327356, -12.06949235617739191, 105.6260903946856899 ) ) ;
#33516 = CARTESIAN_POINT ( 'NONE',  ( 4.483927247898790824, -16.52544592524335698, 40.20942372801901854 ) ) ;
#33517 = CARTESIAN_POINT ( 'NONE',  ( 5.153800228976335163, 19.02544592524342804, 29.79057627198102409 ) ) ;
#33518 = CARTESIAN_POINT ( 'NONE',  ( 12.06949235617739724, 12.14591786802326823, 76.87609039468567573 ) ) ;
#33519 = CARTESIAN_POINT ( 'NONE',  ( -19.02544592524334988, -5.153800228976617603, 78.95942372801900433 ) ) ;
#33520 = CARTESIAN_POINT ( 'NONE',  ( -5.719274019375978568, 21.55341960407610458, 60.20724293864768839 ) ) ;
#33521 = CARTESIAN_POINT ( 'NONE',  ( -12.06949235617739369, -12.14591786802326823, 94.37609039468568994 ) ) ;
#33522 = CARTESIAN_POINT ( 'NONE',  ( 18.62759615963255655, 10.81492255796105972, 76.66775706135234714 ) ) ;
#33523 = CARTESIAN_POINT ( 'NONE',  ( 18.67979575497178502, 10.72451020669898547, 54.16557627198103120 ) ) ;
#33524 = CARTESIAN_POINT ( 'NONE',  ( 5.823673210054125526, 21.52544592524343514, 44.79057627198103120 ) ) ;
#33525 = CARTESIAN_POINT ( 'NONE',  ( 16.53943276465976808, 0.05219959533934440121, 81.25109039468568994 ) ) ;
#33526 = CARTESIAN_POINT ( 'NONE',  ( -10.72451020669898014, 18.67979575497178502, 45.41557627198103830 ) ) ;
#33527 = ORIENTED_EDGE ( 'NONE', *, *, #132358, .F. ) ;
#33528 = CARTESIAN_POINT ( 'NONE',  ( 19.02544592524343514, -5.153800228976328945, 98.54057627198100988 ) ) ;
#33529 = CARTESIAN_POINT ( 'NONE',  ( -24.69864206457980771, -7.736332803992566731, 171.5373547058827626 ) ) ;
#33530 = CARTESIAN_POINT ( 'NONE',  ( 13.89961937509977652, -13.97604488694527269, 23.12390960531436335 ) ) ;
#33531 = CARTESIAN_POINT ( 'NONE',  ( 21.52544592524344225, -5.823673210054117533, 63.54057627198103830 ) ) ;
#33532 = CARTESIAN_POINT ( 'NONE',  ( 16.55341960407618274, -4.379528057220086978, 86.04275706135236135 ) ) ;
#33533 = CARTESIAN_POINT ( 'NONE',  ( -10.72451020669870658, -18.67979575497194134, 49.58442372801901143 ) ) ;
#33534 = CARTESIAN_POINT ( 'NONE',  ( 13.97604488694548053, -13.89961937509957401, 105.6260903946856757 ) ) ;
#33535 = CARTESIAN_POINT ( 'NONE',  ( 8.224510206698953496, -14.34966873604960469, 102.9155762719810383 ) ) ;
#33536 = CARTESIAN_POINT ( 'NONE',  ( -9.474510206698720793, -16.51473224551083518, 104.5844237280190043 ) ) ;
#33537 = CARTESIAN_POINT ( 'NONE',  ( -16.46253265017160317, 9.564922557960807481, 40.83224293864769550 ) ) ;
#33538 = DIRECTION ( 'NONE',  ( -1.000000000000000000, -4.336808689942018352E-17, 3.574525976782710619E-31 ) ) ;
#33539 = CARTESIAN_POINT ( 'NONE',  ( -16.46253265017160317, 9.564922557960807481, 95.83224293864769550 ) ) ;
#33540 = CARTESIAN_POINT ( 'NONE',  ( -14.29746914071037622, -8.314922557961029526, 79.16775706135234714 ) ) ;
#33541 = CARTESIAN_POINT ( 'NONE',  ( -19.02544592524334988, -5.153800228976617603, 73.95942372801900433 ) ) ;
#33542 = CARTESIAN_POINT ( 'NONE',  ( -5.719274019375665041, -21.55341960407619695, 109.7927570613523613 ) ) ;
#33543 = CARTESIAN_POINT ( 'NONE',  ( -5.719274019375978568, 21.55341960407610458, 60.20724293864768839 ) ) ;
#33544 = CARTESIAN_POINT ( 'NONE',  ( 4.483927247898790824, -16.52544592524335698, 90.20942372801903275 ) ) ;
#33545 = CIRCLE ( 'NONE', #136886, 31.90000000000003411 ) ;
#33546 = CARTESIAN_POINT ( 'NONE',  ( 19.03943276465977164, 0.05219959533936151252, 86.25109039468567573 ) ) ;
#33547 = CARTESIAN_POINT ( 'NONE',  ( -16.51473224551069308, -9.474510206698971260, 36.66557627198102409 ) ) ;
#33548 = CARTESIAN_POINT ( 'NONE',  ( -19.05341960407611168, -5.049401038298163336, 81.45724293864769550 ) ) ;
#33549 = CARTESIAN_POINT ( 'NONE',  ( 15.80617190586769283, -15.72974639402175789, 45.62609039468567573 ) ) ;
#33550 = CARTESIAN_POINT ( 'NONE',  ( -5.153800228976328057, -19.02544592524343514, 42.29057627198101699 ) ) ;
#33551 = CARTESIAN_POINT ( 'NONE',  ( 19.05341960407617918, -5.049401038297876454, 71.04275706135234714 ) ) ;
#33552 = CARTESIAN_POINT ( 'NONE',  ( 25.47140278216198439, -9.703455644538477642, 170.7619267275323409 ) ) ;
#33553 = CARTESIAN_POINT ( 'NONE',  ( -9.564922557960796823, -16.46253265017161027, 112.0822429386476955 ) ) ;
#33554 = CARTESIAN_POINT ( 'NONE',  ( 16.52544592524342804, -4.483927247898539470, 68.54057627198103830 ) ) ;
#33555 = CARTESIAN_POINT ( 'NONE',  ( 10.81492255796078972, 18.62759615963270932, 64.58224293864769550 ) ) ;
#33556 = DIRECTION ( 'NONE',  ( 0.000000000000000000, 0.4999999999999991118, -0.8660254037844391517 ) ) ;
#33557 = CARTESIAN_POINT ( 'NONE',  ( -19.05341960407617563, 5.049401038297882671, 23.54275706135233648 ) ) ;
#33559 = CARTESIAN_POINT ( 'NONE',  ( 0.05219959533909260263, 19.03943276465977164, 79.99890960531436690 ) ) ;
#33558 = CARTESIAN_POINT ( 'NONE',  ( 0.05219959533909260263, 19.03943276465977164, 69.99890960531435269 ) ) ;
#33560 = ADVANCED_FACE ( 'NONE', ( #30966 ), #63277, .T. ) ;
#33561 = CARTESIAN_POINT ( 'NONE',  ( -12.14591786802326823, 12.06949235617739902, 53.12609039468568284 ) ) ;
#33562 = CARTESIAN_POINT ( 'NONE',  ( 4.215739103160468737, -48.58376198229545651, -25.00000000000000711 ) ) ;
#33563 = CARTESIAN_POINT ( 'NONE',  ( -17.49999999999999645, 5.499999999999997335, 110.7969038253417295 ) ) ;
#33564 = CARTESIAN_POINT ( 'NONE',  ( -12.06949235617739369, -12.14591786802326823, 89.37609039468568994 ) ) ;
#33565 = CARTESIAN_POINT ( 'NONE',  ( 17.72560187377285956, 5.500000000000005329, 96.57814504131322053 ) ) ;
#33566 = CARTESIAN_POINT ( 'NONE',  ( -8.314922557961024197, 14.29746914071037800, 72.91775706135234714 ) ) ;
#33567 = CARTESIAN_POINT ( 'NONE',  ( 16.52544592524335698, 4.483927247898782831, 36.45942372801901143 ) ) ;
#33569 = LINE ( 'NONE', #123570, #163225 ) ;
#33568 = CARTESIAN_POINT ( 'NONE',  ( -13.97604488694527625, -13.89961937509977652, 56.87390960531434558 ) ) ;
#33570 = CARTESIAN_POINT ( 'NONE',  ( -15.80617190586768217, 15.72974639402176855, 58.12609039468568994 ) ) ;
#33571 = CARTESIAN_POINT ( 'NONE',  ( -16.51473224551082808, 9.474510206698731452, 58.33442372801900433 ) ) ;
#33572 = CARTESIAN_POINT ( 'NONE',  ( 5.719274019375673035, 21.55341960407619339, 102.2927570613523613 ) ) ;
#33573 = CARTESIAN_POINT ( 'NONE',  ( -19.03943276465977164, 0.05219959533909376836, 36.24890960531436690 ) ) ;
#33574 = CARTESIAN_POINT ( 'NONE',  ( 37.99626262588765258, 2.893932880411085066E-14, -7.002157773949822861 ) ) ;
#33575 = CARTESIAN_POINT ( 'NONE',  ( 15.72974639402199770, -15.80617190586745480, 48.12390960531436690 ) ) ;
#33576 = CARTESIAN_POINT ( 'NONE',  ( -0.05219959533909027116, -19.03943276465977164, 107.4989096053143527 ) ) ;
#33577 = CARTESIAN_POINT ( 'NONE',  ( -8.224510206698948167, 14.34966873604960824, 95.41557627198102409 ) ) ;
#33578 = CARTESIAN_POINT ( 'NONE',  ( 4.483927247898790824, -16.52544592524335698, 35.20942372801901854 ) ) ;
#33579 = CARTESIAN_POINT ( 'NONE',  ( 0.05219959533910956823, 16.53943276465976808, 29.99890960531435979 ) ) ;
#33580 = VERTEX_POINT ( 'NONE', #92613 ) ;
#33581 = CARTESIAN_POINT ( 'NONE',  ( -18.67979575497178146, -10.72451020669898902, 106.6655762719810383 ) ) ;
#33583 = CARTESIAN_POINT ( 'NONE',  ( 9.474510206698971260, -16.51473224551069308, 107.9155762719810383 ) ) ;
#33582 = CARTESIAN_POINT ( 'NONE',  ( -14.29746914071049879, 8.314922557960819915, 35.83224293864768839 ) ) ;
#33584 = CARTESIAN_POINT ( 'NONE',  ( 19.05341960407617918, -5.049401038297876454, 96.04275706135231871 ) ) ;
#33585 = CARTESIAN_POINT ( 'NONE',  ( -9.564922557961040184, 16.46253265017147172, 32.91775706135233293 ) ) ;
#33586 = CARTESIAN_POINT ( 'NONE',  ( 8.314922557960818139, 14.29746914071049879, 29.58224293864769905 ) ) ;
#33587 = CARTESIAN_POINT ( 'NONE',  ( 21.53943276465977519, -0.05219959533907433946, 108.7489096053143669 ) ) ;
#33588 = CARTESIAN_POINT ( 'NONE',  ( 0.05219959533907565091, 21.53943276465977519, 54.99890960531435269 ) ) ;
#33589 = CARTESIAN_POINT ( 'NONE',  ( -19.05341960407611168, -5.049401038298163336, 76.45724293864769550 ) ) ;
#33590 = CARTESIAN_POINT ( 'NONE',  ( -12.14591786802309592, -12.06949235617757132, 41.87390960531435979 ) ) ;
#33591 = CARTESIAN_POINT ( 'NONE',  ( 9.564922557960805705, 16.46253265017160317, 94.58224293864769550 ) ) ;
#33592 = ORIENTED_EDGE ( 'NONE', *, *, #152340, .F. ) ;
#33593 = DIRECTION ( 'NONE',  ( 0.000000000000000000, 0.000000000000000000, 1.000000000000000000 ) ) ;
#33594 = CARTESIAN_POINT ( 'NONE',  ( 9.564922557961047289, -16.46253265017146816, 45.41775706135232582 ) ) ;
#33595 = CARTESIAN_POINT ( 'NONE',  ( -10.81492255796078084, -18.62759615963271287, 92.08224293864769550 ) ) ;
#33596 = CARTESIAN_POINT ( 'NONE',  ( -4.379528057220328563, 16.55341960407611168, 105.2072429386477097 ) ) ;
#33597 = VECTOR ( 'NONE', #53965, 1000.000000000000000 ) ;
#33598 = CARTESIAN_POINT ( 'NONE',  ( 5.719274019375673035, 21.55341960407619339, 37.29275706135235424 ) ) ;
#33599 = CARTESIAN_POINT ( 'NONE',  ( -27.73933785331498925, 2.428612866367529932E-14, 140.8750000027311842 ) ) ;
#33600 = CARTESIAN_POINT ( 'NONE',  ( 4.379528057220092307, 16.55341960407617563, 107.2927570613523471 ) ) ;
#33601 = CARTESIAN_POINT ( 'NONE',  ( 9.564922557960805705, 16.46253265017160317, 29.58224293864769550 ) ) ;
#33602 = CARTESIAN_POINT ( 'NONE',  ( 13.89961937509977652, -13.97604488694527269, 83.12390960531436690 ) ) ;
#33603 = CARTESIAN_POINT ( 'NONE',  ( -8.571926809382608425, 26.38167802310805854, 140.4750000027312069 ) ) ;
#33604 = CARTESIAN_POINT ( 'NONE',  ( -5.049401038298153566, 19.05341960407611168, 30.20724293864768839 ) ) ;
#33605 = CARTESIAN_POINT ( 'NONE',  ( -12.06949235617756955, 12.14591786802309770, 40.62390960531435269 ) ) ;
#33606 = CARTESIAN_POINT ( 'NONE',  ( 15.80617190586769283, -15.72974639402175789, 70.62609039468567573 ) ) ;
#33608 = CARTESIAN_POINT ( 'NONE',  ( 12.14591786802327356, -12.06949235617739191, 70.62609039468567573 ) ) ;
#33607 = CARTESIAN_POINT ( 'NONE',  ( 19.06840828308530433, -32.80151167437067983, -20.74459427420917379 ) ) ;
#33609 = CARTESIAN_POINT ( 'NONE',  ( 19.02544592524343514, -5.153800228976328945, 53.54057627198102409 ) ) ;
#33610 = CARTESIAN_POINT ( 'NONE',  ( 13.97604488694527802, 13.89961937509977652, 64.37390960531436690 ) ) ;
#33611 = ORIENTED_EDGE ( 'NONE', *, *, #158579, .T. ) ;
#33612 = CARTESIAN_POINT ( 'NONE',  ( -16.46253265017146816, -9.564922557961047289, 19.16775706135233293 ) ) ;
#33613 = CARTESIAN_POINT ( 'NONE',  ( 8.224510206698742110, 14.34966873604972548, 77.08442372801901854 ) ) ;
#33614 = CARTESIAN_POINT ( 'NONE',  ( -21.52544592524334988, -5.823673210054445271, 103.9594237280190185 ) ) ;
#33615 = CARTESIAN_POINT ( 'NONE',  ( -5.153800228976328057, -19.02544592524343514, 67.29057627198102409 ) ) ;
#33616 = CARTESIAN_POINT ( 'NONE',  ( 18.67979575497178502, 10.72451020669898547, 34.16557627198102409 ) ) ;
#33617 = CARTESIAN_POINT ( 'NONE',  ( 5.049401038297881783, 19.05341960407617563, 102.2927570613523045 ) ) ;
#33618 = CARTESIAN_POINT ( 'NONE',  ( 18.67979575497194134, -10.72451020669871369, 85.83442372801901854 ) ) ;
#33619 = CARTESIAN_POINT ( 'NONE',  ( -14.34966873604972548, 8.224510206698743886, 48.33442372801902565 ) ) ;
#33620 = CARTESIAN_POINT ( 'NONE',  ( -5.823673210054116645, -21.52544592524344225, 102.2905762719810383 ) ) ;
#33621 = CARTESIAN_POINT ( 'NONE',  ( 19.03943276465977164, 0.05219959533936151252, 96.25109039468567573 ) ) ;
#33622 = CARTESIAN_POINT ( 'NONE',  ( 13.97604488694527802, 13.89961937509977652, 84.37390960531433848 ) ) ;
#33623 = CARTESIAN_POINT ( 'NONE',  ( 19.03943276465977164, 0.05219959533936151252, 111.2510903946856757 ) ) ;
#33624 = CARTESIAN_POINT ( 'NONE',  ( 16.55341960407618274, -4.379528057220086978, 26.04275706135235779 ) ) ;
#33625 = CARTESIAN_POINT ( 'NONE',  ( -8.224510206698948167, 14.34966873604960824, 60.41557627198102409 ) ) ;
#33626 = CARTESIAN_POINT ( 'NONE',  ( -12.14591786802326823, 12.06949235617739902, 78.12609039468570415 ) ) ;
#33627 = EDGE_CURVE ( 'NONE', #192458, #83484, #139026, .T. ) ;
#33629 = CARTESIAN_POINT ( 'NONE',  ( -0.05219959533909027116, -19.03943276465977164, 52.49890960531436690 ) ) ;
#33628 = CARTESIAN_POINT ( 'NONE',  ( 18.62759615963255655, 10.81492255796105972, 21.66775706135235069 ) ) ;
#33630 = CARTESIAN_POINT ( 'NONE',  ( -5.049401038298153566, 19.05341960407611168, 75.20724293864769550 ) ) ;
#33631 = CARTESIAN_POINT ( 'NONE',  ( 8.224510206698742110, 14.34966873604972548, 77.08442372801901854 ) ) ;
#33632 = CARTESIAN_POINT ( 'NONE',  ( 15.50000000000000355, 5.499999999999998224, 120.0000000000000142 ) ) ;
#33633 = ORIENTED_EDGE ( 'NONE', *, *, #142366, .F. ) ;
#33634 = CARTESIAN_POINT ( 'NONE',  ( -5.049401038297874678, -19.05341960407617918, 19.79275706135233293 ) ) ;
#33635 = CARTESIAN_POINT ( 'NONE',  ( 5.153800228976335163, 19.02544592524342804, 34.79057627198102409 ) ) ;
#33636 = ORIENTED_EDGE ( 'NONE', *, *, #6795, .T. ) ;
#33637 = CARTESIAN_POINT ( 'NONE',  ( -14.29746914071037622, -8.314922557961029526, 29.16775706135234003 ) ) ;
#33639 = CARTESIAN_POINT ( 'NONE',  ( 16.53943276465976808, 0.05219959533934440121, 31.25109039468568639 ) ) ;
#33638 = CARTESIAN_POINT ( 'NONE',  ( 13.97604488694548053, -13.89961937509957401, 40.62609039468564731 ) ) ;
#33640 = CARTESIAN_POINT ( 'NONE',  ( 0.05219959533909260263, 19.03943276465977164, 39.99890960531436690 ) ) ;
#33641 = CARTESIAN_POINT ( 'NONE',  ( -5.049401038298153566, 19.05341960407611168, 70.20724293864769550 ) ) ;
#33642 = CARTESIAN_POINT ( 'NONE',  ( -10.72451020669898014, 18.67979575497178502, 80.41557627198103830 ) ) ;
#33644 = DIRECTION ( 'NONE',  ( -1.000000000000000000, -1.071875439572228152E-15, -5.204170427930421283E-16 ) ) ;
#33643 = CARTESIAN_POINT ( 'NONE',  ( -16.46253265017160317, 9.564922557960807481, 75.83224293864769550 ) ) ;
#33645 = CARTESIAN_POINT ( 'NONE',  ( -19.05341960407611168, -5.049401038298163336, 51.45724293864770260 ) ) ;
#33646 = FACE_OUTER_BOUND ( 'NONE', #187559, .T. ) ;
#33647 = CARTESIAN_POINT ( 'NONE',  ( -5.153800228976607833, 19.02544592524334988, 102.7094237280189759 ) ) ;
#33648 = CARTESIAN_POINT ( 'NONE',  ( 10.81492255796078972, 18.62759615963270932, 74.58224293864768129 ) ) ;
#33649 = CARTESIAN_POINT ( 'NONE',  ( 19.02544592524334988, 5.153800228976608722, 21.45942372801899012 ) ) ;
#33650 = CARTESIAN_POINT ( 'NONE',  ( -16.52544592524342804, 4.483927247898546575, 61.04057627198103120 ) ) ;
#33651 = CARTESIAN_POINT ( 'NONE',  ( 18.62759615963255655, 10.81492255796105972, 86.66775706135234714 ) ) ;
#33652 = CARTESIAN_POINT ( 'NONE',  ( -5.153800228976328057, -19.02544592524343514, 22.29057627198102765 ) ) ;
#33654 = CARTESIAN_POINT ( 'NONE',  ( -21.52544592524334988, -5.823673210054445271, 93.95942372801903275 ) ) ;
#33653 = CARTESIAN_POINT ( 'NONE',  ( 16.52544592524342804, -4.483927247898539470, 28.54057627198103120 ) ) ;
#33655 = CARTESIAN_POINT ( 'NONE',  ( 19.05341960407611168, 5.049401038298154454, 83.95724293864766707 ) ) ;
#33656 = CARTESIAN_POINT ( 'NONE',  ( -21.53943276465977519, -0.05219959533937600094, 48.75109039468568284 ) ) ;
#33657 = CARTESIAN_POINT ( 'NONE',  ( 5.049401038298161559, -19.05341960407611168, 87.70724293864769550 ) ) ;
#33658 = CARTESIAN_POINT ( 'NONE',  ( 16.55341960407611168, 4.379528057220329451, 93.95724293864770971 ) ) ;
#33659 = CARTESIAN_POINT ( 'NONE',  ( -8.224510206698948167, 14.34966873604960824, 65.41557627198102409 ) ) ;
#33660 = CARTESIAN_POINT ( 'NONE',  ( -21.55341960407610458, -5.719274019375992779, 76.45724293864769550 ) ) ;
#33661 = CARTESIAN_POINT ( 'NONE',  ( 13.89961937509977652, -13.97604488694527269, 68.12390960531436690 ) ) ;
#33662 = CARTESIAN_POINT ( 'NONE',  ( -18.67979575497178146, -10.72451020669898902, 81.66557627198103830 ) ) ;
#33663 = CARTESIAN_POINT ( 'NONE',  ( 13.89961937509957401, 13.97604488694547697, 76.87609039468566152 ) ) ;
#33665 = CARTESIAN_POINT ( 'NONE',  ( -8.224510206698948167, 14.34966873604960824, 70.41557627198102409 ) ) ;
#33664 = CARTESIAN_POINT ( 'NONE',  ( 5.153800228976617603, -19.02544592524335343, 30.20942372801900433 ) ) ;
#33666 = CARTESIAN_POINT ( 'NONE',  ( 5.823673210054125526, 21.52544592524343514, 54.79057627198104541 ) ) ;
#33667 = CARTESIAN_POINT ( 'NONE',  ( 16.21995358207307092, -7.366697692864084601, 27.43551001512161136 ) ) ;
#33669 = CARTESIAN_POINT ( 'NONE',  ( -8.571926809382608425, 26.38167802310805854, 146.9750000027311785 ) ) ;
#33668 = CARTESIAN_POINT ( 'NONE',  ( 0.05219959533934541429, -16.53943276465976808, 105.0010903946856757 ) ) ;
#33670 = CARTESIAN_POINT ( 'NONE',  ( 19.05341960407617918, -5.049401038297876454, 101.0427570613523045 ) ) ;
#33671 = CARTESIAN_POINT ( 'NONE',  ( -16.52544592524342804, 4.483927247898546575, 76.04057627198102409 ) ) ;
#33672 = CARTESIAN_POINT ( 'NONE',  ( 9.021779378622690970, -0.4881926659581901640, -61.91041879129569026 ) ) ;
#33673 = CARTESIAN_POINT ( 'NONE',  ( -13.89961937509977652, 13.97604488694528158, 70.62390960531432427 ) ) ;
#33674 = CARTESIAN_POINT ( 'NONE',  ( -13.89961937509977652, 13.97604488694528158, 35.62390960531435269 ) ) ;
#33675 = CARTESIAN_POINT ( 'NONE',  ( 12.14591786802309770, 12.06949235617756955, 49.37390960531436690 ) ) ;
#33676 = CARTESIAN_POINT ( 'NONE',  ( 9.474510206698971260, -16.51473224551069308, 107.9155762719810383 ) ) ;
#33678 = CARTESIAN_POINT ( 'NONE',  ( 0.05219959533909260263, 19.03943276465977164, 59.99890960531436690 ) ) ;
#33677 = CARTESIAN_POINT ( 'NONE',  ( 16.51473224551083163, -9.474510206698727899, 85.83442372801900433 ) ) ;
#33679 = CARTESIAN_POINT ( 'NONE',  ( -16.55341960407617563, 4.379528057220093196, 23.54275706135235424 ) ) ;
#33680 = CARTESIAN_POINT ( 'NONE',  ( 19.02544592524343514, -5.153800228976328945, 88.54057627198102409 ) ) ;
#33681 = CARTESIAN_POINT ( 'NONE',  ( -0.05219959533907301413, -21.53943276465977519, 62.49890960531436690 ) ) ;
#33682 = CARTESIAN_POINT ( 'NONE',  ( -12.06949235617739369, -12.14591786802326823, 59.37609039468568284 ) ) ;
#33683 = CARTESIAN_POINT ( 'NONE',  ( -16.51473224551082808, 9.474510206698731452, 108.3344237280190043 ) ) ;
#33684 = CARTESIAN_POINT ( 'NONE',  ( -5.049401038298153566, 19.05341960407611168, 65.20724293864765286 ) ) ;
#33685 = CARTESIAN_POINT ( 'NONE',  ( 21.52544592524344225, -5.823673210054117533, 63.54057627198103830 ) ) ;
#33686 = CARTESIAN_POINT ( 'NONE',  ( -19.02544592524334988, -5.153800228976617603, 88.95942372801897591 ) ) ;
#33688 = CARTESIAN_POINT ( 'NONE',  ( 18.67979575497194134, -10.72451020669871369, 50.83442372801901143 ) ) ;
#33687 = CARTESIAN_POINT ( 'NONE',  ( 12.06949235617757843, -12.14591786802309237, 23.12390960531436335 ) ) ;
#33689 = DIRECTION ( 'NONE',  ( 0.000000000000000000, 0.9945218953682734009, 0.1045284632676537068 ) ) ;
#33691 = CARTESIAN_POINT ( 'NONE',  ( -9.564922557960796823, -16.46253265017161027, 107.0822429386476955 ) ) ;
#33690 = CARTESIAN_POINT ( 'NONE',  ( -14.34966873604972548, 8.224510206698743886, 68.33442372801900433 ) ) ;
#33692 = CARTESIAN_POINT ( 'NONE',  ( -17.97182807773872071, 5.500000000000055955, 73.53038844047289047 ) ) ;
#33693 = CARTESIAN_POINT ( 'NONE',  ( -14.29746914071037622, -8.314922557961029526, 94.16775706135237556 ) ) ;
#33694 = CARTESIAN_POINT ( 'NONE',  ( -4.483927247898782831, 16.52544592524335698, 32.70942372801900433 ) ) ;
#33695 = CARTESIAN_POINT ( 'NONE',  ( -9.564922557960796823, -16.46253265017161027, 47.08224293864769550 ) ) ;
#33696 = CARTESIAN_POINT ( 'NONE',  ( 13.97604488694527802, 13.89961937509977652, 49.37390960531434558 ) ) ;
#33697 = CARTESIAN_POINT ( 'NONE',  ( 5.153800228976335163, 19.02544592524342804, 64.79057627198100988 ) ) ;
#33698 = CARTESIAN_POINT ( 'NONE',  ( -10.72451020669870658, -18.67979575497194134, 49.58442372801901143 ) ) ;
#33699 = CARTESIAN_POINT ( 'NONE',  ( 4.483927247898790824, -16.52544592524335698, 45.20942372801901854 ) ) ;
#33700 = CARTESIAN_POINT ( 'NONE',  ( -4.379528057220328563, 16.55341960407611168, 35.20724293864768839 ) ) ;
#33701 = CARTESIAN_POINT ( 'NONE',  ( 5.153800228976335163, 19.02544592524342804, 39.79057627198100988 ) ) ;
#33702 = CARTESIAN_POINT ( 'NONE',  ( -5.049401038298153566, 19.05341960407611168, 40.20724293864768839 ) ) ;
#33703 = CARTESIAN_POINT ( 'NONE',  ( 8.224510206698742110, 14.34966873604972548, 32.08442372801901854 ) ) ;
#33704 = VECTOR ( 'NONE', #33338, 1000.000000000000114 ) ;
#33705 = CARTESIAN_POINT ( 'NONE',  ( -13.89961937509957401, -13.97604488694547875, 84.37609039468567573 ) ) ;
#33706 = CARTESIAN_POINT ( 'NONE',  ( -0.05219959533910754901, -16.53943276465976808, 82.49890960531436690 ) ) ;
#33707 = CARTESIAN_POINT ( 'NONE',  ( -9.474510206698964154, 16.51473224551069663, 55.41557627198103120 ) ) ;
#33709 = CARTESIAN_POINT ( 'NONE',  ( 16.31925111598456013, -7.325300261831516835, 92.66424538967251578 ) ) ;
#33708 = CARTESIAN_POINT ( 'NONE',  ( -5.049401038297874678, -19.05341960407617918, 84.79275706135233293 ) ) ;
#33710 = CARTESIAN_POINT ( 'NONE',  ( 21.55341960407619695, -5.719274019375665929, 76.04275706135237556 ) ) ;
#33711 = CARTESIAN_POINT ( 'NONE',  ( -14.29746914071037622, -8.314922557961029526, 59.16775706135234714 ) ) ;
#33712 = DIRECTION ( 'NONE',  ( 0.1039620511844979445, -0.1039620511844979445, -0.9891328443778539814 ) ) ;
#33713 = CARTESIAN_POINT ( 'NONE',  ( 0.05219959533907565091, 21.53943276465977519, 54.99890960531435269 ) ) ;
#33714 = CARTESIAN_POINT ( 'NONE',  ( 4.379528057220092307, 16.55341960407617563, 37.29275706135235424 ) ) ;
#33715 = CARTESIAN_POINT ( 'NONE',  ( -17.81289503416611808, 24.51734667627700404, 147.6999999999999886 ) ) ;
#33716 = CARTESIAN_POINT ( 'NONE',  ( -19.02544592524334988, -5.153800228976617603, 28.95942372801900433 ) ) ;
#33717 = DIRECTION ( 'NONE',  ( -1.000000000000000000, 0.000000000000000000, -3.709348145883536076E-20 ) ) ;
#33718 = CARTESIAN_POINT ( 'NONE',  ( -16.51473224551069308, -9.474510206698971260, 46.66557627198102409 ) ) ;
#33719 = CARTESIAN_POINT ( 'NONE',  ( -17.59860650958993844, 7.585241751806885979, 58.42337014262493256 ) ) ;
#33720 = CARTESIAN_POINT ( 'NONE',  ( -16.51473224551069308, -9.474510206698971260, 71.66557627198102409 ) ) ;
#33721 = CARTESIAN_POINT ( 'NONE',  ( -19.01529144963332740, -5.500000000000168754, 56.23431955728440101 ) ) ;
#33722 = CARTESIAN_POINT ( 'NONE',  ( 21.53943276465977519, 0.05219959533937863772, 111.2510903946856899 ) ) ;
#33723 = CARTESIAN_POINT ( 'NONE',  ( -4.483927247898539470, -16.52544592524342804, 32.29057627198102409 ) ) ;
#33724 = CARTESIAN_POINT ( 'NONE',  ( 19.02544592524343514, -5.153800228976328945, 43.54057627198103120 ) ) ;
#33725 = AXIS2_PLACEMENT_3D ( 'NONE', #53782, #193304, #175130 ) ;
#33726 = CARTESIAN_POINT ( 'NONE',  ( 13.97604488694527802, 13.89961937509977652, 99.37390960531436690 ) ) ;
#33727 = CARTESIAN_POINT ( 'NONE',  ( -21.52544592524334988, -5.823673210054445271, 73.95942372801901854 ) ) ;
#33728 = CARTESIAN_POINT ( 'NONE',  ( 0.05219959533909260263, 19.03943276465977164, 44.99890960531435979 ) ) ;
#33729 = EDGE_CURVE ( 'NONE', #31966, #101974, #82363, .T. ) ;
#33730 = CARTESIAN_POINT ( 'NONE',  ( -21.55341960407619339, 5.719274019375674811, 63.54275706135234003 ) ) ;
#33731 = CARTESIAN_POINT ( 'NONE',  ( -21.53943276465977519, 0.05219959533907696930, 26.24890960531435624 ) ) ;
#33732 = CARTESIAN_POINT ( 'NONE',  ( -19.05341960407611168, -5.049401038298163336, 36.45724293864766707 ) ) ;
#33733 = CARTESIAN_POINT ( 'NONE',  ( 21.53943276465977519, 0.05219959533937863772, 31.25109039468568639 ) ) ;
#33734 = CARTESIAN_POINT ( 'NONE',  ( -16.51473224551082808, 9.474510206698731452, 43.33442372801900433 ) ) ;
#33735 = CARTESIAN_POINT ( 'NONE',  ( 5.153800228976335163, 19.02544592524342804, 29.79057627198102409 ) ) ;
#33736 = CARTESIAN_POINT ( 'NONE',  ( -9.474510206698964154, 16.51473224551069663, 60.41557627198102409 ) ) ;
#33738 = AXIS2_PLACEMENT_3D ( 'NONE', #72236, #24751, #162240 ) ;
#33737 = CARTESIAN_POINT ( 'NONE',  ( 8.314922557961029526, -14.29746914071037800, 20.41775706135234714 ) ) ;
#33739 = CARTESIAN_POINT ( 'NONE',  ( 16.55341960407611168, 4.379528057220329451, 68.95724293864769550 ) ) ;
#33740 = CARTESIAN_POINT ( 'NONE',  ( 5.823673210054125526, 21.52544592524343514, 34.79057627198103120 ) ) ;
#33741 = CARTESIAN_POINT ( 'NONE',  ( -13.97604488694547697, 13.89961937509957934, 103.1260903946856473 ) ) ;
#33742 = CARTESIAN_POINT ( 'NONE',  ( 10.81492255796078972, 18.62759615963270932, 109.5822429386476955 ) ) ;
#33743 = CARTESIAN_POINT ( 'NONE',  ( -5.719274019375665041, -21.55341960407619695, 54.79275706135235424 ) ) ;
#33744 = CARTESIAN_POINT ( 'NONE',  ( -16.55341960407617563, 4.379528057220093196, 53.54275706135234714 ) ) ;
#33745 = CARTESIAN_POINT ( 'NONE',  ( 12.14591786802327356, -12.06949235617739191, 60.62609039468567573 ) ) ;
#33746 = CARTESIAN_POINT ( 'NONE',  ( -5.823673210054116645, -21.52544592524344225, 62.29057627198102409 ) ) ;
#33747 = PRESENTATION_LAYER_ASSIGNMENT (  '', '', ( #124084 ) ) ;
#33748 =( BOUNDED_SURFACE ( )  B_SPLINE_SURFACE ( 3, 2, ( 
 ( #26588, #168061, #198403, #29558, #59881, #88231, #149915, #57915, #90219, #11422, #196445, #181270, #42747, #104409, #166091, #74081, #135752, #151902, #13392, #55781, #68946, #145780, #115460, #113439, #54781, #7261, #83106, #99272, #84101, #130609, #177149, #69957, #114439, #117453, #40620, #116456, #179152, #146786, #10293, #86115, #192305, #53784, #193307, #24465, #38621, #178144, #21445, #8279, #102290, #85100, #161957, #160959, #51779, #131622, #100278, #159958, #6265, #147806, #163979, #23453, #39610, #144782, #101269, #162959, #9291, #70957, #132626, #194314, #25476, #87116, #148803, #175132, #128610, #22452, #36599, #190302, #98255, #67945, #129598, #191294, #52770, #176140, #37610, #199277, #196324, #27468, #165966, #106257, #60744, #12296, #89110, #58764, #56795, #198280, #150800, #26467, #42621, #73961, #135629, #120433, #13274, #57792, #122417, #184109, #59758, #45590, #90099, #153756, #29439, #197300, #182125, #136600, #167940, #43609, #121426, #164972, #151781, #107244, #28463, #168915, #30420, #105274, #92068, #44602, #104286, #74937, #166961, #183119, #118467, #88109, #149793, #71950, #91071, #152758, #180159, #14247, #75919, #137594, #41628, #133621, #195314, #103292, #72969, #11298, #134638, #119462, #181146, #156753, #109239, #3059, #18247, #80885, #15252, #142562, #157746, #1055, #19237, #34400, #65718, #110235, #35388, #186105, #140572, #31416, #155744, #4041, #108245, #154754, #46583, #97039, #76910, #16251, #170918, #138581, #61, #169924, #62728, #127385, #96058, #93068, #124411, #32410, #171916, #126398, #189096, #188094, #50569, #112229, #33406, #95064, #173919, #61734, #123402, #17242, #94065, #77903, #48583, #47586, #111229, #139570, #79900, #185095, #78893, #172921, #2062, #141571, #63741, #125415, #187112, #64736, #49567, #174905, #191068, #52541, #23222, #113215, #145548, #178914, #175906, #68708, #144550, #130365, #40381, #190075, #129372, #161727, #54548, #193073, #176914, #99035, #114202, #192062, #147569, #100041, #128379, #146543, #67714, #51551, #7026, #131384, #116221, #37378, #98023, #84865, #82872, #36369, #117220, #8036, #177912, #38385, #39380, #69717, #101039, #132392, #70725, #158720, #21215, #160725, #159718, #162725, #6035, #53544, #24230, #85881, #20210, #22217, #9054, #83866, #115222, #81858, #194085, #55547, #143546, #5032, #66718, #186621, #196089, #166730, #182889, #63245, #140078, #13046, #93579, #102055, #121196, #1569, #195075, #181896, #28234, #11054, #74713, #71716, #89874, #134402, #120206, #31925, #16754, #57559, #58540, #163740, #133384, #25240, #78402, #86881, #165731, #56554, #43374, #155264, #124924, #104051, #148566, #136376, #119229, #105046, #150568, #151557, #10056, #118231, #179922, #41389, #198053, #59519, #103054, #44372, #27227, #88875, #164736, #108757, #170433, #26231, #87870, #149558, #72729, #180913, #42388, #12067, #73729, #135402, #197073, #113709, #48093, #175406, #190577, #33910, #52053, #67219, #98539, #143054, #68214, #18748, #173426, #64249, #188597, #36874, #141082, #187614, #79412, #129866, #109749, #49084, #3553, #171433, #32920, #2567, #95568, #160233, #81370, #80395, #94575, #127886, #50078, #125916, #110741, #5540, #83376, #19729, #159219, #172422, #158238, #4533, #126891, #66225, #189589, #174416, #21723, #20714, #145053, #156253, #6534, #142067, #17755, #157254, #51061, #65231, #112723, #111739, #34895, #96551, #35885, #97532, #82370, #144059, #128877, #25741, #118737, #131897, #8553, #178413, #176416, #117728, #70229, #146050, #162228, #147069, #193581, #39877, #132890, #177421, #180425, #103564, #179423, #41898, #9561, #73237, #149072, #55053, #116724, #56049, #87387, #101544, #40888, #84373, #71227, #165239, #7534, #130887, #22725, #191564, #53043, #192577, #163236, #114723, #37891, #69219, #38892, #26733, #24736, #23727, #99549, #194579, #86386, #54060, #115734, #10560, #88372, #148070, #102561 ),
 ( #161231, #100549, #85376, #164246, #72224, #150066, #11571, #133899, #195590, #57062, #154024, #31681, #27734, #14519, #199540, #43874, #45852, #104552, #122682, #167225, #153020, #61994, #46848, #28723, #91328, #196585, #166234, #134908, #108508, #16511, #198552, #89377, #15519, #151066, #105539, #90360, #29697, #107505, #77176, #169181, #138846, #123660, #76180, #137860, #93330, #185357, #170187, #75196, #152045, #135891, #168200, #13530, #30687, #12557, #61010, #155015, #58055, #92338, #74223, #184371, #326, #119726, #136867, #44867, #181409, #197563, #60022, #121689, #42887, #59030, #183385, #120697, #106523, #182396, #64000, #188348, #98283, #109502, #48837, #81133, #174173, #112480, #96310, #18502, #172173, #49826, #66975, #19488, #47849, #65976, #187368, #171184, #126645, #186370, #142814, #3314, #64987, #124673, #20468, #35643, #139827, #79158, #94326, #113465, #128635, #32673, #4294, #33658, #127645, #189345, #143810, #78159, #5292, #82118, #125670, #190329, #97289, #51806, #173175, #159984, #110491, #111490, #156004, #80150, #175159, #17501, #140829, #2318, #1316, #62995, #95319, #157004, #141821, #34651, #157996, #50823, #36626, #158976, #53813, #144808, #101298, #161984, #52796, #99300, #179179, #56820, #193334, #132653, #37636, #131652, #178172, #100306, #39637, #162987, #147834, #25502, #194341, #133649, #6291, #195340, #115488, #67970, #87146, #54808, #21471, #24492, #177176, #83132, #10319, #23480, #148829, #145806, #38649, #85129, #55809, #71975, #146813, #8307, #69984, #129624, #9320, #116483, #176166, #192332, #86143, #70985, #117481, #40647, #7289, #118494, #180185, #102316, #41654, #164006, #103318, #191319, #114464, #160985, #22479, #84127, #68973, #130637, #57817, #183142, #92093, #121450, #153781, #15276, #166984, #123425, #137619, #197326, #44627, #13296, #106279, #149818, #119489, #181171, #87, #167964, #14275, #60770, #134663, #198304, #184134, #29463, #26492, #42648, #199303, #135655, #28487, #46608, #45616, #122442, #168939, #107268, #164998, #88134, #58790, #91096, #30446, #185118, #61757, #75945, #76936, #11324, #138605, #72994, #104310, #152784, #196349, #73986, #165993, #27494, #89136, #120458, #150824, #12321, #182149, #43634, #105296, #90121, #151805, #74961, #136623, #59782, #171940, #77926, #127410, #139593, #17266, #2086, #3083, #19262, #189120, #80908, #50592, #97062, #64759, #126421, #5056, #158744, #20233, #48607, #63766, #109264, #141596, #78919, #4064, #1079, #188119, #81881, #31439, #65742, #62754, #49590, #173943, #190099, #187135, #18270, #154777, #124435, #140596, #125439, #172945, #186131, #95088, #128402, #110259, #79923, #94089, #111253, #108270, #47610, #33429, #34423, #112251, #142585, #96082, #156777, #157771, #35410, #143573, #66741, #170943, #169948, #93093, #32435, #16274, #155768, #24257, #160750, #191092, #54573, #175932, #144573, #10083, #39404, #70750, #131410, #9080, #69741, #101064, #25265, #163765, #71741, #114227, #68733, #82895, #6060, #147595, #21241, #84891, #132418, #193097, #113238, #67738, #85908, #22242, #53571, #133412, #194110, #55573, #117247, #178939, #51574, #174929, #145574, #116245, #40409, #36392, #86908, #162749, #102081, #98046, #148591, #159744, #129396, #177937, #52567, #83891, #37404, #99062, #7051, #130391, #192088, #115248, #176940, #38410, #8064, #100067, #161752, #23247, #146570, #76709, #58566, #164762, #14044, #26257, #104078, #88904, #89899, #106054, #75710, #167740, #137388, #183904, #151582, #13071, #91858, #45389, #107042, #135428, #150595, #196115, #28261, #165760, #90871, #87898, #74738, #168714, #118258, #152555, #149584, #136401, #60537, #195101, #73756, #105073, #41415, #11082, #27254, #12093, #59546, #72758, #181922, #15048, #197099, #166759, #180939, #198079, #56583, #134429, #120231, #121224, #199068, #29238, #182915, #43403, #44400, #122213, #30216, #153551, #57585, #179948, #103081, #119255 ),
 ( #42415, #187895, #112027, #50367, #158523, #853, #155545, #16046, #95857, #173716, #110037, #49362, #154551, #48380, #94864, #17039, #156545, #18044, #64533, #142357, #111026, #35184, #123203, #96838, #32210, #184893, #3837, #171716, #138384, #79697, #93866, #200066, #127176, #78693, #65516, #62527, #140370, #1857, #172712, #188886, #63539, #125213, #186909, #46375, #126199, #33205, #92864, #109040, #141368, #2855, #34195, #157540, #124200, #20011, #61534, #19034, #108034, #80681, #169720, #31213, #77705, #139371, #185900, #47385, #170718, #131174, #174701, #99835, #8844, #38179, #70512, #132180, #83661, #40164, #54343, #113992, #161519, #130154, #23011, #66512, #36165, #97817, #117007, #84657, #192864, #189873, #146335, #6821, #68499, #128174, #24014, #39171, #143337, #82657, #159506, #178702, #193871, #21002, #7823, #175690, #69508, #116014, #147356, #81654, #55337, #85669, #67505, #101840, #100829, #163526, #176705, #4824, #52336, #191851, #144341, #22009, #51348, #5829, #129162, #113008, #190859, #37165, #98824, #160518, #145339, #53332, #115011, #177704, #162512, #58340, #57357, #148353, #104841, #165531, #56339, #89670, #120989, #135201, #74512, #118021, #43174, #152335, #181693, #13821, #75487, #27027, #183680, #197853, #119031, #166532, #73529, #28029, #9849, #179711, #41183, #60313, #151357, #136178, #133176, #12846, #150368, #11864, #71508, #167518, #182687, #86670, #26024, #102846, #121989, #137160, #164531, #59320, #180714, #44172, #105831, #90653, #25026, #198849, #29013, #10851, #45165, #106821, #194866, #120008, #87669, #195883, #196873, #149354, #88672, #72520, #134195, #42190, #103850, #50131, #168495, #169485, #123959, #29993, #153320, #199841, #15813, #80448, #1622, #621, #91632, #48145, #108807, #61308, #46147, #125968, #3606, #140131, #79465, #184665, #78457, #124978, #47149, #186675, #109802, #94628, #172476, #141134, #142121, #14822, #65285, #62292, #76483, #33963, #63298, #138160, #171485, #185657, #122978, #157306, #170486, #95621, #92633, #31977, #93633, #2624, #18803, #155318, #16807, #32974, #107801, #156307, #17808, #30985, #139144, #64301, #187667, #49137, #110795, #154324, #126944, #188652, #77474, #103353, #129918, #196383, #72010, #175459, #190631, #191618, #41688, #68267, #165031, #26524, #113763, #73028, #87181, #144112, #53097, #160286, #114775, #96604, #66281, #4588, #149853, #176469, #161283, #19782, #37943, #36930, #98592, #158293, #56854, #133683, #173479, #112776, #127940, #11357, #88169, #189642, #99603, #5592, #25537, #148862, #180218, #111791, #134700, #118529, #97584, #34952, #195375, #81423, #6588, #143109, #82423, #21777, #51117, #52106, #174469, #35938, #159272, #20768, #67272, #128930, #83428, #145105, #10353, #42683, #89169, #105330, #169981, #91128, #90155, #181207, #137650, #198338, #150861, #135688, #15309, #93124, #29495, #168971, #74018, #167999, #14311, #136658, #75977, #199337, #184166, #61789, #30476, #31472, #123459, #153814, #57852, #139624, #151838, #122475, #138639, #16307, #154809, #92127, #46641, #119524, #76968, #77957, #12355, #60802, #45648, #167018, #120, #27528, #107299, #13328, #185151, #108301, #104344, #74993, #166028, #197360, #58825, #120492, #182183, #43668, #121484, #28519, #59814, #183178, #44660, #106313, #152818, #112283, #81911, #173973, #143604, #190128, #82928, #1112, #2118, #156810, #62786, #186164, #32469, #48640, #113267, #34455, #33462, #124467, #80941, #141627, #94122, #78953, #158777, #36423, #172976, #35441, #17299, #111286, #157802, #79958, #19293, #142616, #127443, #63800, #4095, #18302, #155801, #174959, #95120, #47646, #66770, #96114, #109297, #65774, #3117, #170976, #51603, #64792, #128431, #125473, #126453, #188151, #97093, #98078, #49624, #189149, #50622, #140628, #20265, #5088, #187169, #171974, #159776, #21271, #110292, #85935, #130424, #71772, #56613, #132447, #133442, #162778, #26287 ),
 ( #84921, #100098, #145606, #177964, #115280, #40437, #175965, #39432, #195132, #67770, #102109, #37434, #101092, #10112, #144606, #23277, #54600, #191125, #160786, #176973, #38442, #9112, #99094, #131440, #164792, #161782, #116274, #192123, #24286, #6091, #22274, #146601, #147624, #163794, #178970, #70779, #8094, #69772, #194138, #118287, #55602, #114261, #117276, #53604, #83925, #193127, #25296, #86938, #148622, #179978, #41446, #103111, #7085, #129427, #52599, #68766, #183929, #180966, #121250, #153576, #169745, #166787, #198109, #134458, #104107, #120258, #181950, #152582, #42443, #74766, #108061, #105101, #59576, #73784, #182944, #87928, #119283, #58592, #90896, #45414, #122239, #106081, #28288, #43432, #44427, #76734, #29265, #57615, #75739, #197125, #165789, #136428, #60563, #107067, #89928, #27286, #14072, #12120, #88932, #46402, #137416, #168738, #167767, #30242, #199096, #91885, #61558, #200090, #149615, #150624, #151609, #135456, #15074, #13101, #138410, #123227, #184918, #11113, #72788, #196143, #1883, #34222, #79725, #47410, #81681, #35211, #127202, #31240, #113037, #125238, #95884, #112054, #189901, #66540, #142385, #20038, #92890, #50394, #128204, #124229, #111053, #157567, #140395, #3864, #878, #19060, #63564, #49390, #158548, #143363, #186936, #187921, #154576, #62553, #16072, #4855, #77730, #94891, #185925, #173742, #109066, #48407, #110063, #126226, #65543, #96864, #188916, #51376, #139396, #172741, #80707, #170745, #32234, #93892, #171743, #33232, #155570, #17065, #78719, #156575, #18070, #141394, #2882, #64561, #116043, #144370, #162539, #83690, #5857, #23040, #147385, #8873, #145368, #114022, #177732, #98854, #67533, #133202, #24043, #193900, #54371, #132209, #192894, #85698, #148382, #86697, #194893, #37198, #191880, #129191, #70541, #190889, #7852, #55364, #39201, #36192, #52365, #117034, #6850, #100857, #84685, #175719, #25054, #178729, #40191, #174729, #56367, #68529, #101871, #163554, #97846, #9876, #71536, #159535, #21033, #82686, #160549, #22039, #130184, #53364, #115042, #176734, #38207, #99863, #161547, #146365, #69539, #131203, #165555, #166556, #179740, #87694, #118050, #198873, #41210, #120032, #10875, #29038, #72545, #27052, #11890, #89696, #182712, #90678, #44197, #152360, #60340, #28055, #151382, #183705, #122014, #137186, #196898, #73553, #180738, #12872, #88698, #167543, #134222, #74537, #102871, #26050, #13845, #195908, #136202, #75512, #164556, #181718, #197877, #57383, #103875, #58365, #43200, #105856, #42214, #59346, #149379, #121014, #119056, #150394, #135226, #104867, #129838, #69190, #101515, #149045, #53014, #39849, #192548, #86358, #163205, #164217, #98510, #25714, #40860, #84345, #102534, #117700, #10533, #193553, #118708, #130856, #23698, #114693, #38865, #87359, #191537, #37862, #176388, #180398, #160205, #99521, #54031, #21695, #83349, #161203, #146023, #72197, #131868, #115705, #145025, #178385, #100521, #22698, #7506, #56022, #133871, #70201, #9533, #177393, #8523, #55025, #162200, #116696, #24709, #148043, #85346, #71200, #147039, #132863, #195561, #194552, #6506, #57035, #179397, #68186, #121663, #135866, #103536, #30661, #120671, #169157, #166208, #197537, #59005, #76154, #92314, #182371, #43848, #28697, #26707, #168173, #105514, #196559, #12532, #167199, #90333, #152018, #183358, #27709, #153997, #15495, #29670, #77151, #59996, #123636, #199516, #13504, #75169, #106496, #137834, #136841, #91302, #134883, #44840, #138822, #198525, #302, #61970, #152993, #41870, #14493, #74197, #60983, #122658, #184346, #88346, #58030, #119700, #165211, #45828, #107479, #150039, #11544, #73212, #181383, #42861, #104527, #89352, #151042, #186343, #1290, #20440, #3290, #34626, #158951, #97263, #5266, #47824, #2293, #16485, #81109, #154989, #18477, #4270, #64961, #46823, #62968, #19464, #155978, #188322, #33634, #124648, #35618, #189320, #142788, #185333 ),
 ( #49801, #94300, #96285, #78134, #173151, #17475, #126621, #112456, #82092, #79132, #141796, #108483, #139802, #170161, #143784, #66948, #48813, #109474, #65949, #171159, #140804, #63975, #80127, #157971, #127620, #50797, #174146, #31654, #111466, #93304, #32645, #125645, #187342, #110466, #172148, #95296, #156980, #137141, #45143, #139122, #88653, #58322, #196856, #598, #121966, #153299, #11845, #168474, #28994, #90634, #150349, #46124, #61286, #165513, #104824, #119990, #62269, #154302, #181676, #106800, #197835, #91611, #29972, #169463, #103832, #30964, #107778, #89651, #92611, #122955, #15791, #198829, #123937, #74494, #152316, #43157, #44152, #77451, #166513, #28011, #135182, #185635, #27009, #151339, #59301, #73510, #12828, #136160, #120970, #182668, #184643, #105811, #167498, #13802, #60293, #14800, #75468, #76461, #183659, #138137, #199818, #3583, #144088, #97561, #35915, #187643, #2599, #48122, #155294, #66257, #108785, #16784, #142098, #159249, #170463, #143086, #140108, #80425, #112752, #128907, #125945, #157282, #93609, #63275, #79440, #141111, #111768, #1599, #33940, #67248, #64278, #18778, #32950, #65261, #47127, #78433, #17785, #50108, #4565, #81400, #126921, #49114, #110771, #188628, #20745, #173457, #124955, #34926, #156284, #186651, #95598, #19759, #127917, #172453, #109779, #96581, #171462, #94605, #5569, #158270, #189619, #51092, #174446, #82400, #31954, #164279, #102594, #10594, #53074, #7564, #21753, #86417, #160263, #23759, #9594, #8586, #52083, #6565, #24770, #161260, #193612, #38921, #68242, #40921, #194610, #148102, #190607, #72255, #84403, #55084, #71259, #149104, #25773, #101579, #179455, #113739, #132923, #87419, #83404, #70260, #116754, #99578, #163268, #145082, #178445, #22754, #131928, #117763, #175436, #146079, #147101, #36906, #129895, #98569, #191595, #114752, #54089, #176446, #37919, #56082, #115763, #69250, #39912, #130916, #100578, #192607, #177451, #162260, #85409, #90390, #61039, #122711, #135925, #92367, #106553, #73270, #167255, #75227, #169211, #118769, #88405, #26765, #30720, #152075, #183413, #41930, #198585, #59061, #120728, #180458, #76210, #91359, #195623, #134939, #150101, #154053, #184401, #11602, #136898, #27767, #121721, #60053, #199570, #133933, #45881, #137889, #119757, #107535, #153050, #15548, #28754, #57095, #104584, #182428, #196617, #74255, #103596, #58087, #181440, #165271, #42919, #166269, #89410, #151099, #12590, #197595, #43906, #105569, #13560, #44896, #168229, #29726, #14552, #17531, #108539, #155046, #34681, #112509, #48867, #188378, #93360, #187399, #33688, #156034, #95351, #157035, #3343, #139858, #18533, #94355, #170218, #189375, #171214, #62025, #142844, #110522, #77206, #80180, #32704, #138875, #66007, #79190, #4323, #1346, #140860, #2349, #111520, #127675, #64030, #125700, #172203, #123689, #65018, #141852, #31711, #47879, #126674, #49855, #173206, #96339, #63027, #50852, #174203, #158026, #35671, #19517, #81162, #109532, #97319, #159005, #355, #185388, #46879, #16541, #78188, #124705, #186402, #105088, #86925, #190359, #42431, #51836, #132433, #117263, #118274, #134445, #104093, #196130, #165776, #12107, #179965, #41431, #120245, #73770, #135443, #163781, #178955, #24273, #128664, #27270, #82146, #113495, #103097, #197112, #143842, #119270, #175190, #56600, #88919, #20498, #102096, #133429, #67005, #36656, #55588, #40425, #87915, #98314, #10099, #43418, #25282, #195117, #9098, #164779, #5321, #160014, #194125, #26273, #180953, #57601, #149602, #148607, #71759, #11099, #58579, #72775, #85922, #150611, #181936, #147610, #70765, #139382, #864, #75725, #106067, #169731, #90884, #59560, #125224, #154562, #185911, #46388, #124213, #184904, #16058, #140382, #78705, #186922, #29251, #183916, #198095, #62539, #136415, #200077, #47396, #108046, #28275, #182930, #109052, #137401, #31226, #15060, #44413, #17050, #170729, #32220, #166774 ),
 ( #93878, #155556, #107054, #45401, #153563, #199082, #92875, #76720, #167753, #1869, #63550, #48392, #89914, #151596, #60550, #77716, #13087, #74752, #121236, #152569, #14058, #122225, #168726, #30229, #91870, #138396, #61545, #123214, #21014, #79711, #97830, #142370, #128187, #37178, #22021, #3849, #66524, #171729, #141380, #110049, #83673, #191863, #173728, #2868, #129174, #64546, #19046, #65528, #4837, #82670, #190872, #144354, #52348, #98837, #189885, #51360, #6833, #160532, #145351, #50380, #127188, #111039, #18057, #114004, #33217, #126211, #113021, #68512, #94877, #5841, #187907, #143349, #175702, #156557, #188899, #20024, #49376, #172725, #112040, #35197, #174713, #34207, #96850, #130166, #158535, #81666, #95870, #36177, #157553, #80693, #159518, #67517, #149364, #87679, #71518, #193882, #147366, #163537, #42198, #194876, #23023, #41194, #162522, #84668, #101853, #26034, #10860, #24025, #192875, #56350, #177714, #146347, #11875, #102856, #72529, #133185, #134206, #118032, #164542, #27037, #165540, #73538, #116025, #70522, #7834, #195893, #69520, #86680, #57368, #179723, #115024, #131185, #119041, #25037, #99846, #54353, #85679, #8855, #180723, #39182, #40174, #135211, #132191, #148364, #100840, #9859, #53345, #55347, #117017, #103859, #88683, #150378, #176717, #178713, #38190, #161530, #185668, #138170, #166541, #184674, #105840, #28039, #45176, #169495, #30994, #167528, #136187, #199851, #120999, #89681, #155330, #46157, #15823, #76493, #154333, #14831, #107812, #170497, #108818, #16818, #59329, #13830, #151366, #92643, #12857, #30003, #77484, #61317, #58349, #74522, #139153, #29023, #122988, #106830, #197862, #47159, #631, #62301, #196883, #78469, #90663, #123971, #31987, #120017, #93645, #181702, #43183, #104852, #182697, #44182, #152345, #75496, #137170, #198858, #60324, #121999, #183689, #168505, #91641, #153330, #52120, #172489, #96617, #1635, #171498, #140143, #113776, #21790, #3618, #109815, #159284, #32987, #49149, #33977, #34965, #51129, #20781, #112789, #82436, #128943, #158306, #19794, #36944, #190644, #175472, #80460, #95633, #141147, #48157, #144124, #63312, #94640, #81435, #98606, #124991, #35950, #156321, #173492, #5605, #186687, #18816, #142134, #157320, #2637, #17821, #67285, #79479, #64313, #143121, #160300, #125981, #97596, #187679, #4601, #110807, #65297, #126956, #50144, #188665, #111804, #66293, #127952, #189656, #174483, #70297, #103636, #100615, #193650, #69287, #55122, #165313, #114790, #54126, #86456, #179496, #117803, #101620, #23797, #177489, #116791, #72294, #24807, #53112, #71299, #192643, #176483, #131965, #56121, #40961, #115799, #22793, #148141, #7601, #37959, #41969, #132962, #102633, #163309, #164318, #9632, #194651, #57135, #195664, #83441, #146117, #162297, #99617, #25811, #161297, #178483, #87457, #149143, #145119, #84439, #10634, #38958, #133973, #39949, #130953, #118811, #180497, #6603, #68282, #129933, #85447, #191632, #147137, #8625, #62068, #137930, #15589, #26807, #45923, #123733, #119796, #106596, #91404, #135963, #199614, #196658, #14596, #59100, #44940, #154095, #138915, #120765, #183455, #88447, #58127, #150142, #396, #108582, #90432, #181480, #107577, #42959, #197633, #182466, #121762, #61080, #169255, #122753, #30762, #77247, #168272, #29769, #185432, #46922, #11644, #60094, #92409, #153092, #73310, #104622, #184443, #43947, #76252, #75269, #166311, #134981, #27808, #89449, #151138, #12629, #105609, #74294, #167297, #28793, #152118, #13601, #136939, #198628, #189418, #67048, #63070, #49896, #34722, #79235, #81202, #139901, #158067, #2392, #188419, #97361, #82190, #64071, #126715, #31753, #1389, #170259, #143883, #51879, #33731, #124749, #50893, #186445, #140906, #125741, #65058, #142883, #112551, #4365, #174246, #159047, #111563, #173247, #128706, #20541, #5364, #110563, #187441, #171258, #78230, #35714, #93402, #47921, #96380 ),
 ( #19558, #109575, #157078, #190403, #48909, #80221, #156078, #141892, #155088, #32745, #172244, #66048, #127716, #16582, #94397, #95392, #18574, #3383, #17574, #54878, #83204, #101365, #22549, #144879, #162054, #86210, #147900, #84195, #52867, #116552, #37709, #6361, #72043, #163054, #132718, #193403, #71052, #131721, #24561, #87214, #25570, #133717, #176238, #130708, #68041, #9386, #129693, #23550, #102383, #178241, #191390, #194406, #145875, #114538, #85198, #55876, #117549, #7358, #99371, #39702, #161054, #69043, #195409, #179248, #40714, #164071, #148896, #10386, #113538, #175232, #36697, #98358, #192402, #53884, #115559, #160057, #177246, #146886, #21544, #38718, #100376, #8378, #70053, #27561, #59849, #105363, #73060, #107331, #60833, #152849, #56887, #138672, #150894, #121516, #137684, #15344, #92159, #168030, #45680, #118561, #76009, #153846, #149884, #136690, #183211, #166060, #29527, #26557, #44692, #89201, #75025, #184198, #169004, #12388, #13361, #180251, #88200, #41721, #30508, #103385, #120524, #11390, #199369, #134732, #74050, #135721, #151871, #91160, #122508, #14343, #77000, #165063, #198372, #106346, #196414, #57884, #119556, #197392, #58857, #181239, #42715, #104377, #182217, #43701, #167050, #28551, #90188, #96144, #93158, #33492, #65805, #81943, #78985, #110323, #46674, #16340, #32502, #94154, #64822, #154843, #187200, #20295, #17330, #172004, #186197, #95150, #152, #31505, #171011, #3148, #157833, #34486, #18334, #140660, #155833, #61821, #77989, #19324, #2152, #126484, #48671, #139656, #50652, #4126, #80971, #123491, #185184, #63830, #188182, #142647, #158806, #35474, #111318, #189179, #108334, #127473, #97123, #1144, #79989, #49654, #109329, #173007, #170014, #112313, #125502, #141657, #174003, #62818, #156839, #124502, #47678, #174990, #143634, #55632, #25327, #7117, #113299, #162808, #36454, #52631, #37467, #38474, #54630, #24317, #116305, #85966, #132479, #100131, #161812, #40469, #194168, #117305, #83957, #99128, #144638, #51635, #147655, #5118, #98112, #23307, #179001, #66800, #39461, #159809, #177005, #9143, #128463, #22306, #53636, #190159, #21304, #175997, #160818, #8125, #82961, #130458, #163826, #145637, #115313, #129459, #84951, #6121, #67804, #114295, #146633, #101122, #177994, #69803, #68799, #192155, #131471, #102141, #193158, #191158, #70810, #196176, #56645, #135488, #59609, #121282, #57648, #26320, #89959, #11146, #180011, #45445, #74796, #106113, #166819, #44459, #105133, #136458, #60595, #199128, #107098, #149648, #104139, #118318, #182975, #41478, #120290, #167797, #28320, #181000, #151639, #29297, #168768, #122270, #198139, #75771, #86969, #90927, #183958, #103142, #13134, #152613, #119314, #14103, #164824, #137449, #42476, #148656, #10144, #71804, #165821, #43465, #133473, #87960, #195164, #72820, #134489, #150655, #27318, #88965, #12153, #73818, #197158, #181983, #58623, #113807, #144153, #175502, #21821, #127984, #189687, #129963, #83473, #145150, #173523, #188696, #34009, #141179, #52150, #91916, #2669, #51160, #6634, #153609, #128975, #126015, #66323, #98636, #114821, #111834, #143152, #76766, #49182, #65329, #126989, #97627, #187710, #19825, #53142, #50177, #4633, #18848, #112820, #30271, #64346, #3651, #35980, #190674, #67315, #174513, #34994, #96648, #159316, #68312, #20811, #110840, #82467, #142167, #172524, #81466, #5638, #36975, #158336, #95666, #160331, #157353, #80493, #191663, #15105, #195693, #56150, #134002, #194681, #25842, #150173, #88476, #196689, #38989, #193681, #7633, #72326, #146146, #9661, #57164, #117832, #37990, #192674, #10663, #147166, #179525, #24835, #54157, #26836, #180526, #118843, #176513, #58158, #69317, #99646, #11673, #161329, #39978, #130983, #41999, #115830, #85477, #70328, #71328, #87486, #103665, #149174, #165343, #73339, #132990, #40994, #135012, #22822, #84468, #116821, #131995, #177519, #100645, #162326 ) ),
 .UNSPECIFIED., .T., .F., .F. ) 
 B_SPLINE_SURFACE_WITH_KNOTS ( ( 4, 3, 4 ),
 ( 3, 2, 2, 2, 2, 2, 2, 2, 2, 2, 2, 2, 2, 2, 2, 2, 2, 2, 2, 2, 2, 2, 2, 2, 2, 2, 2, 2, 2, 2, 2, 2, 2, 2, 2, 2, 2, 2, 2, 2, 2, 2, 2, 2, 2, 2, 2, 2, 2, 2, 2, 2, 2, 2, 2, 2, 2, 2, 2, 2, 2, 2, 2, 2, 2, 2, 2, 2, 2, 2, 2, 2, 2, 2, 2, 2, 2, 2, 2, 2, 2, 2, 2, 2, 2, 2, 2, 2, 2, 2, 2, 2, 2, 2, 2, 2, 2, 2, 2, 2, 2, 2, 2, 2, 2, 2, 2, 2, 2, 2, 2, 2, 2, 2, 2, 2, 2, 2, 2, 2, 2, 2, 2, 2, 2, 2, 2, 2, 2, 2, 2, 2, 2, 2, 2, 2, 2, 2, 2, 2, 2, 2, 2, 2, 2, 2, 2, 2, 2, 2, 2, 2, 2, 2, 2, 2, 2, 2, 2, 2, 2, 2, 2, 2, 2, 2, 2, 2, 2, 2, 2, 2, 2, 2, 2, 2, 2, 2, 2, 2, 2, 2, 2, 2, 2, 2, 2, 2, 2, 2, 2, 2, 2, 2, 2, 2, 2, 2, 2, 2, 2, 2, 2, 2, 2, 2, 2, 2, 2, 2, 2, 2, 2, 2, 2, 2, 2, 2, 2, 2, 2, 2, 2, 2, 2, 2, 2, 2, 3 ),
 ( 0.000000000000000000, 0.5000000000000000000, 1.000000000000000000 ),
 ( 0.000000000000000000, 0.004385964912280701511, 0.008771929824561403022, 0.01315789473684210453, 0.01754385964912280604, 0.02192982456140350755, 0.02631578947368420907, 0.03070175438596491058, 0.03508771929824561209, 0.03947368421052631360, 0.04385964912280701511, 0.04824561403508771662, 0.05263157894736841813, 0.05701754385964911964, 0.06140350877192982115, 0.06578947368421052266, 0.07017543859649122417, 0.07456140350877192569, 0.07894736842105262720, 0.08333333333333332871, 0.08771929824561403022, 0.09210526315789473173, 0.09649122807017543324, 0.1008771929824561348, 0.1052631578947368363, 0.1096491228070175378, 0.1140350877192982393, 0.1184210526315789408, 0.1228070175438596423, 0.1271929824561403577, 0.1315789473684210453, 0.1359649122807017607, 0.1403508771929824483, 0.1447368421052631637, 0.1491228070175438514, 0.1535087719298245668, 0.1578947368421052544, 0.1622807017543859698, 0.1666666666666666574, 0.1710526315789473728, 0.1754385964912280604, 0.1798245614035087758, 0.1842105263157894635, 0.1885964912280701788, 0.1929824561403508665, 0.1973684210526315819, 0.2017543859649122695, 0.2061403508771929849, 0.2105263157894736725, 0.2149122807017543879, 0.2192982456140350755, 0.2236842105263157909, 0.2280701754385964786, 0.2324561403508771940, 0.2368421052631578816, 0.2412280701754385970, 0.2456140350877192846, 0.2500000000000000000, 0.2543859649122807154, 0.2587719298245614308, 0.2631578947368420907, 0.2675438596491228060, 0.2719298245614035214, 0.2763157894736842368, 0.2807017543859648967, 0.2850877192982456121, 0.2894736842105263275, 0.2938596491228070429, 0.2982456140350877027, 0.3026315789473684181, 0.3070175438596491335, 0.3114035087719298489, 0.3157894736842105088, 0.3201754385964912242, 0.3245614035087719396, 0.3289473684210526550, 0.3333333333333333148, 0.3377192982456140302, 0.3421052631578947456, 0.3464912280701754610, 0.3508771929824561209, 0.3552631578947368363, 0.3596491228070175517, 0.3640350877192982670, 0.3684210526315789269, 0.3728070175438596423, 0.3771929824561403577, 0.3815789473684210731, 0.3859649122807017330, 0.3903508771929824483, 0.3947368421052631637, 0.3991228070175438791, 0.4035087719298245390, 0.4078947368421052544, 0.4122807017543859698, 0.4166666666666666852, 0.4210526315789473450, 0.4254385964912280604, 0.4298245614035087758, 0.4342105263157894912, 0.4385964912280701511, 0.4429824561403508665, 0.4473684210526315819, 0.4517543859649122973, 0.4561403508771929571, 0.4605263157894736725, 0.4649122807017543879, 0.4692982456140351033, 0.4736842105263157632, 0.4780701754385964786, 0.4824561403508771940, 0.4868421052631579093, 0.4912280701754385692, 0.4956140350877192846, 0.5000000000000000000, 0.5043859649122807154, 0.5087719298245614308, 0.5131578947368421462, 0.5175438596491228616, 0.5219298245614034659, 0.5263157894736841813, 0.5307017543859648967, 0.5350877192982456121, 0.5394736842105263275, 0.5438596491228070429, 0.5482456140350877583, 0.5526315789473684736, 0.5570175438596490780, 0.5614035087719297934, 0.5657894736842105088, 0.5701754385964912242, 0.5745614035087719396, 0.5789473684210526550, 0.5833333333333333703, 0.5877192982456140857, 0.5921052631578946901, 0.5964912280701754055, 0.6008771929824561209, 0.6052631578947368363, 0.6096491228070175517, 0.6140350877192982670, 0.6184210526315789824, 0.6228070175438596978, 0.6271929824561403022, 0.6315789473684210176, 0.6359649122807017330, 0.6403508771929824483, 0.6447368421052631637, 0.6491228070175438791, 0.6535087719298245945, 0.6578947368421053099, 0.6622807017543859143, 0.6666666666666666297, 0.6710526315789473450, 0.6754385964912280604, 0.6798245614035087758, 0.6842105263157894912, 0.6885964912280702066, 0.6929824561403509220, 0.6973684210526315264, 0.7017543859649122417, 0.7061403508771929571, 0.7105263157894736725, 0.7149122807017543879, 0.7192982456140351033, 0.7236842105263158187, 0.7280701754385965341, 0.7324561403508771384, 0.7368421052631578538, 0.7412280701754385692, 0.7456140350877192846, 0.7500000000000000000, 0.7543859649122807154, 0.7587719298245614308, 0.7631578947368421462, 0.7675438596491228616, 0.7719298245614034659, 0.7763157894736841813, 0.7807017543859648967, 0.7850877192982456121, 0.7894736842105263275, 0.7938596491228070429, 0.7982456140350877583, 0.8026315789473684736, 0.8070175438596490780, 0.8114035087719297934, 0.8157894736842105088, 0.8201754385964912242, 0.8245614035087719396, 0.8289473684210526550, 0.8333333333333333703, 0.8377192982456140857, 0.8421052631578946901, 0.8464912280701754055, 0.8508771929824561209, 0.8552631578947368363, 0.8596491228070175517, 0.8640350877192982670, 0.8684210526315789824, 0.8728070175438596978, 0.8771929824561403022, 0.8815789473684210176, 0.8859649122807017330, 0.8903508771929824483, 0.8947368421052631637, 0.8991228070175438791, 0.9035087719298245945, 0.9078947368421053099, 0.9122807017543859143, 0.9166666666666666297, 0.9210526315789473450, 0.9254385964912280604, 0.9298245614035087758, 0.9342105263157894912, 0.9385964912280702066, 0.9429824561403509220, 0.9473684210526315264, 0.9517543859649122417, 0.9561403508771929571, 0.9605263157894736725, 0.9649122807017543879, 0.9692982456140351033, 0.9736842105263158187, 0.9780701754385965341, 0.9824561403508771384, 0.9868421052631578538, 0.9912280701754385692, 0.9956140350877192846, 1.000000000000000000 ),
 .UNSPECIFIED. ) 
 GEOMETRIC_REPRESENTATION_ITEM ( )  RATIONAL_B_SPLINE_SURFACE ( (
 ( 1.000000000000000000, 0.9659258262890683122, 1.000000000000000000, 0.9659258262890683122, 1.000000000000000000, 0.9659258262890683122, 1.000000000000000000, 0.9659258262890683122, 1.000000000000000000, 0.9659258262890683122, 1.000000000000000000, 0.9659258262890683122, 1.000000000000000000, 0.9659258262890683122, 1.000000000000000000, 0.9659258262890683122, 1.000000000000000000, 0.9659258262890683122, 1.000000000000000000, 0.9659258262890683122, 1.000000000000000000, 0.9659258262890683122, 1.000000000000000000, 0.9659258262890683122, 1.000000000000000000, 0.9659258262890683122, 1.000000000000000000, 0.9659258262890683122, 1.000000000000000000, 0.9659258262890683122, 1.000000000000000000, 0.9659258262890683122, 1.000000000000000000, 0.9659258262890683122, 1.000000000000000000, 0.9659258262890683122, 1.000000000000000000, 0.9659258262890683122, 1.000000000000000000, 0.9659258262890683122, 1.000000000000000000, 0.9659258262890683122, 1.000000000000000000, 0.9659258262890683122, 1.000000000000000000, 0.9659258262890683122, 1.000000000000000000, 0.9659258262890683122, 1.000000000000000000, 0.9659258262890683122, 1.000000000000000000, 0.9659258262890683122, 1.000000000000000000, 0.9659258262890683122, 1.000000000000000000, 0.9659258262890683122, 1.000000000000000000, 0.9659258262890683122, 1.000000000000000000, 0.9659258262890683122, 1.000000000000000000, 0.9659258262890683122, 1.000000000000000000, 0.9659258262890683122, 1.000000000000000000, 0.9659258262890683122, 1.000000000000000000, 0.9659258262890683122, 1.000000000000000000, 0.9659258262890683122, 1.000000000000000000, 0.9659258262890683122, 1.000000000000000000, 0.9659258262890683122, 1.000000000000000000, 0.9659258262890683122, 1.000000000000000000, 0.9659258262890683122, 1.000000000000000000, 0.9659258262890683122, 1.000000000000000000, 0.9659258262890683122, 1.000000000000000000, 0.9659258262890683122, 1.000000000000000000, 0.9659258262890683122, 1.000000000000000000, 0.9659258262890683122, 1.000000000000000000, 0.9659258262890683122, 1.000000000000000000, 0.9659258262890683122, 1.000000000000000000, 0.9659258262890683122, 1.000000000000000000, 0.9659258262890683122, 1.000000000000000000, 0.9659258262890683122, 1.000000000000000000, 0.9659258262890683122, 1.000000000000000000, 0.9659258262890683122, 1.000000000000000000, 0.9659258262890683122, 1.000000000000000000, 0.9659258262890683122, 1.000000000000000000, 0.9659258262890683122, 1.000000000000000000, 0.9659258262890683122, 1.000000000000000000, 0.9659258262890683122, 1.000000000000000000, 0.9659258262890683122, 1.000000000000000000, 0.9659258262890683122, 1.000000000000000000, 0.9659258262890683122, 1.000000000000000000, 0.9659258262890683122, 1.000000000000000000, 0.9659258262890683122, 1.000000000000000000, 0.9659258262890683122, 1.000000000000000000, 0.9659258262890683122, 1.000000000000000000, 0.9659258262890683122, 1.000000000000000000, 0.9659258262890683122, 1.000000000000000000, 0.9659258262890683122, 1.000000000000000000, 0.9659258262890683122, 1.000000000000000000, 0.9659258262890683122, 1.000000000000000000, 0.9659258262890683122, 1.000000000000000000, 0.9659258262890683122, 1.000000000000000000, 0.9659258262890683122, 1.000000000000000000, 0.9659258262890683122, 1.000000000000000000, 0.9659258262890683122, 1.000000000000000000, 0.9659258262890683122, 1.000000000000000000, 0.9659258262890683122, 1.000000000000000000, 0.9659258262890683122, 1.000000000000000000, 0.9659258262890683122, 1.000000000000000000, 0.9659258262890683122, 1.000000000000000000, 0.9659258262890683122, 1.000000000000000000, 0.9659258262890683122, 1.000000000000000000, 0.9659258262890683122, 1.000000000000000000, 0.9659258262890683122, 1.000000000000000000, 0.9659258262890683122, 1.000000000000000000, 0.9659258262890683122, 1.000000000000000000, 0.9659258262890683122, 1.000000000000000000, 0.9659258262890683122, 1.000000000000000000, 0.9659258262890683122, 1.000000000000000000, 0.9659258262890683122, 1.000000000000000000, 0.9659258262890683122, 1.000000000000000000, 0.9659258262890683122, 1.000000000000000000, 0.9659258262890683122, 1.000000000000000000, 0.9659258262890683122, 1.000000000000000000, 0.9659258262890683122, 1.000000000000000000, 0.9659258262890683122, 1.000000000000000000, 0.9659258262890683122, 1.000000000000000000, 0.9659258262890683122, 1.000000000000000000, 0.9659258262890683122, 1.000000000000000000, 0.9659258262890683122, 1.000000000000000000, 0.9659258262890683122, 1.000000000000000000, 0.9659258262890683122, 1.000000000000000000, 0.9659258262890683122, 1.000000000000000000, 0.9659258262890683122, 1.000000000000000000, 0.9659258262890683122, 1.000000000000000000, 0.9659258262890683122, 1.000000000000000000, 0.9659258262890683122, 1.000000000000000000, 0.9659258262890683122, 1.000000000000000000, 0.9659258262890683122, 1.000000000000000000, 0.9659258262890683122, 1.000000000000000000, 0.9659258262890683122, 1.000000000000000000, 0.9659258262890683122, 1.000000000000000000, 0.9659258262890683122, 1.000000000000000000, 0.9659258262890683122, 1.000000000000000000, 0.9659258262890683122, 1.000000000000000000, 0.9659258262890683122, 1.000000000000000000, 0.9659258262890683122, 1.000000000000000000, 0.9659258262890683122, 1.000000000000000000, 0.9659258262890683122, 1.000000000000000000, 0.9659258262890683122, 1.000000000000000000, 0.9659258262890683122, 1.000000000000000000, 0.9659258262890683122, 1.000000000000000000, 0.9659258262890683122, 1.000000000000000000, 0.9659258262890683122, 1.000000000000000000, 0.9659258262890683122, 1.000000000000000000, 0.9659258262890683122, 1.000000000000000000, 0.9659258262890683122, 1.000000000000000000, 0.9659258262890683122, 1.000000000000000000, 0.9659258262890683122, 1.000000000000000000, 0.9659258262890683122, 1.000000000000000000, 0.9659258262890683122, 1.000000000000000000, 0.9659258262890683122, 1.000000000000000000, 0.9659258262890683122, 1.000000000000000000, 0.9659258262890683122, 1.000000000000000000, 0.9659258262890683122, 1.000000000000000000, 0.9659258262890683122, 1.000000000000000000, 0.9659258262890683122, 1.000000000000000000, 0.9659258262890683122, 1.000000000000000000, 0.9659258262890683122, 1.000000000000000000, 0.9659258262890683122, 1.000000000000000000, 0.9659258262890683122, 1.000000000000000000, 0.9659258262890683122, 1.000000000000000000, 0.9659258262890683122, 1.000000000000000000, 0.9659258262890683122, 1.000000000000000000, 0.9659258262890683122, 1.000000000000000000, 0.9659258262890683122, 1.000000000000000000, 0.9659258262890683122, 1.000000000000000000, 0.9659258262890683122, 1.000000000000000000, 0.9659258262890683122, 1.000000000000000000, 0.9659258262890683122, 1.000000000000000000, 0.9659258262890683122, 1.000000000000000000, 0.9659258262890683122, 1.000000000000000000, 0.9659258262890683122, 1.000000000000000000, 0.9659258262890683122, 1.000000000000000000, 0.9659258262890683122, 1.000000000000000000, 0.9659258262890683122, 1.000000000000000000, 0.9659258262890683122, 1.000000000000000000, 0.9659258262890683122, 1.000000000000000000, 0.9659258262890683122, 1.000000000000000000, 0.9659258262890683122, 1.000000000000000000, 0.9659258262890683122, 1.000000000000000000, 0.9659258262890683122, 1.000000000000000000, 0.9659258262890683122, 1.000000000000000000, 0.9659258262890683122, 1.000000000000000000, 0.9659258262890683122, 1.000000000000000000, 0.9659258262890683122, 1.000000000000000000, 0.9659258262890683122, 1.000000000000000000, 0.9659258262890683122, 1.000000000000000000, 0.9659258262890683122, 1.000000000000000000, 0.9659258262890683122, 1.000000000000000000, 0.9659258262890683122, 1.000000000000000000, 0.9659258262890683122, 1.000000000000000000, 0.9659258262890683122, 1.000000000000000000, 0.9659258262890683122, 1.000000000000000000, 0.9659258262890683122, 1.000000000000000000, 0.9659258262890683122, 1.000000000000000000, 0.9659258262890683122, 1.000000000000000000, 0.9659258262890683122, 1.000000000000000000, 0.9659258262890683122, 1.000000000000000000, 0.9659258262890683122, 1.000000000000000000, 0.9659258262890683122, 1.000000000000000000, 0.9659258262890683122, 1.000000000000000000, 0.9659258262890683122, 1.000000000000000000, 0.9659258262890683122, 1.000000000000000000, 0.9659258262890683122, 1.000000000000000000, 0.9659258262890683122, 1.000000000000000000, 0.9659258262890683122, 1.000000000000000000, 0.9659258262890683122, 1.000000000000000000, 0.9659258262890683122, 1.000000000000000000, 0.9659258262890683122, 1.000000000000000000, 0.9659258262890683122, 1.000000000000000000, 0.9659258262890683122, 1.000000000000000000, 0.9659258262890683122, 1.000000000000000000, 0.9659258262890683122, 1.000000000000000000, 0.9659258262890683122, 1.000000000000000000, 0.9659258262890683122, 1.000000000000000000, 0.9659258262890683122, 1.000000000000000000, 0.9659258262890683122, 1.000000000000000000, 0.9659258262890683122, 1.000000000000000000, 0.9659258262890683122, 1.000000000000000000, 0.9659258262890683122, 1.000000000000000000, 0.9659258262890683122, 1.000000000000000000, 0.9659258262890683122, 1.000000000000000000, 0.9659258262890683122, 1.000000000000000000, 0.9659258262890683122, 1.000000000000000000, 0.9659258262890683122, 1.000000000000000000, 0.9659258262890683122, 1.000000000000000000, 0.9659258262890683122, 1.000000000000000000, 0.9659258262890683122, 1.000000000000000000, 0.9659258262890683122, 1.000000000000000000, 0.9659258262890683122, 1.000000000000000000, 0.9659258262890683122, 1.000000000000000000, 0.9659258262890683122, 1.000000000000000000, 0.9659258262890683122, 1.000000000000000000, 0.9659258262890683122, 1.000000000000000000, 0.9659258262890683122, 1.000000000000000000, 0.9659258262890683122, 1.000000000000000000, 0.9659258262890683122, 1.000000000000000000, 0.9659258262890683122, 1.000000000000000000, 0.9659258262890683122, 1.000000000000000000, 0.9659258262890683122, 1.000000000000000000, 0.9659258262890683122, 1.000000000000000000, 0.9659258262890683122, 1.000000000000000000, 0.9659258262890683122, 1.000000000000000000, 0.9659258262890683122, 1.000000000000000000, 0.9659258262890683122, 1.000000000000000000, 0.9659258262890683122, 1.000000000000000000, 0.9659258262890683122, 1.000000000000000000, 0.9659258262890683122, 1.000000000000000000, 0.9659258262890683122, 1.000000000000000000),
 ( 0.3333333333333333703, 0.3219752754296894559, 0.3333333333333333703, 0.3219752754296894559, 0.3333333333333333703, 0.3219752754296894559, 0.3333333333333333703, 0.3219752754296894559, 0.3333333333333333703, 0.3219752754296894559, 0.3333333333333333703, 0.3219752754296894559, 0.3333333333333333703, 0.3219752754296894559, 0.3333333333333333703, 0.3219752754296894559, 0.3333333333333333703, 0.3219752754296894559, 0.3333333333333333703, 0.3219752754296894559, 0.3333333333333333703, 0.3219752754296894559, 0.3333333333333333703, 0.3219752754296894559, 0.3333333333333333703, 0.3219752754296894559, 0.3333333333333333703, 0.3219752754296894559, 0.3333333333333333703, 0.3219752754296894559, 0.3333333333333333703, 0.3219752754296894559, 0.3333333333333333703, 0.3219752754296894559, 0.3333333333333333703, 0.3219752754296894559, 0.3333333333333333703, 0.3219752754296894559, 0.3333333333333333703, 0.3219752754296894559, 0.3333333333333333703, 0.3219752754296894559, 0.3333333333333333703, 0.3219752754296894559, 0.3333333333333333703, 0.3219752754296894559, 0.3333333333333333703, 0.3219752754296894559, 0.3333333333333333703, 0.3219752754296894559, 0.3333333333333333703, 0.3219752754296894559, 0.3333333333333333703, 0.3219752754296894559, 0.3333333333333333703, 0.3219752754296894559, 0.3333333333333333703, 0.3219752754296894559, 0.3333333333333333703, 0.3219752754296894559, 0.3333333333333333703, 0.3219752754296894559, 0.3333333333333333703, 0.3219752754296894559, 0.3333333333333333703, 0.3219752754296894559, 0.3333333333333333703, 0.3219752754296894559, 0.3333333333333333703, 0.3219752754296894559, 0.3333333333333333703, 0.3219752754296894559, 0.3333333333333333703, 0.3219752754296894559, 0.3333333333333333703, 0.3219752754296894559, 0.3333333333333333703, 0.3219752754296894559, 0.3333333333333333703, 0.3219752754296894559, 0.3333333333333333703, 0.3219752754296894559, 0.3333333333333333703, 0.3219752754296894559, 0.3333333333333333703, 0.3219752754296894559, 0.3333333333333333703, 0.3219752754296894559, 0.3333333333333333703, 0.3219752754296894559, 0.3333333333333333703, 0.3219752754296894559, 0.3333333333333333703, 0.3219752754296894559, 0.3333333333333333703, 0.3219752754296894559, 0.3333333333333333703, 0.3219752754296894559, 0.3333333333333333703, 0.3219752754296894559, 0.3333333333333333703, 0.3219752754296894559, 0.3333333333333333703, 0.3219752754296894559, 0.3333333333333333703, 0.3219752754296894559, 0.3333333333333333703, 0.3219752754296894559, 0.3333333333333333703, 0.3219752754296894559, 0.3333333333333333703, 0.3219752754296894559, 0.3333333333333333703, 0.3219752754296894559, 0.3333333333333333703, 0.3219752754296894559, 0.3333333333333333703, 0.3219752754296894559, 0.3333333333333333703, 0.3219752754296894559, 0.3333333333333333703, 0.3219752754296894559, 0.3333333333333333703, 0.3219752754296894559, 0.3333333333333333703, 0.3219752754296894559, 0.3333333333333333703, 0.3219752754296894559, 0.3333333333333333703, 0.3219752754296894559, 0.3333333333333333703, 0.3219752754296894559, 0.3333333333333333703, 0.3219752754296894559, 0.3333333333333333703, 0.3219752754296894559, 0.3333333333333333703, 0.3219752754296894559, 0.3333333333333333703, 0.3219752754296894559, 0.3333333333333333703, 0.3219752754296894559, 0.3333333333333333703, 0.3219752754296894559, 0.3333333333333333703, 0.3219752754296894559, 0.3333333333333333703, 0.3219752754296894559, 0.3333333333333333703, 0.3219752754296894559, 0.3333333333333333703, 0.3219752754296894559, 0.3333333333333333703, 0.3219752754296894559, 0.3333333333333333703, 0.3219752754296894559, 0.3333333333333333703, 0.3219752754296894559, 0.3333333333333333703, 0.3219752754296894559, 0.3333333333333333703, 0.3219752754296894559, 0.3333333333333333703, 0.3219752754296894559, 0.3333333333333333703, 0.3219752754296894559, 0.3333333333333333703, 0.3219752754296894559, 0.3333333333333333703, 0.3219752754296894559, 0.3333333333333333703, 0.3219752754296894559, 0.3333333333333333703, 0.3219752754296894559, 0.3333333333333333703, 0.3219752754296894559, 0.3333333333333333703, 0.3219752754296894559, 0.3333333333333333703, 0.3219752754296894559, 0.3333333333333333703, 0.3219752754296894559, 0.3333333333333333703, 0.3219752754296894559, 0.3333333333333333703, 0.3219752754296894559, 0.3333333333333333703, 0.3219752754296894559, 0.3333333333333333703, 0.3219752754296894559, 0.3333333333333333703, 0.3219752754296894559, 0.3333333333333333703, 0.3219752754296894559, 0.3333333333333333703, 0.3219752754296894559, 0.3333333333333333703, 0.3219752754296894559, 0.3333333333333333703, 0.3219752754296894559, 0.3333333333333333703, 0.3219752754296894559, 0.3333333333333333703, 0.3219752754296894559, 0.3333333333333333703, 0.3219752754296894559, 0.3333333333333333703, 0.3219752754296894559, 0.3333333333333333703, 0.3219752754296894559, 0.3333333333333333703, 0.3219752754296894559, 0.3333333333333333703, 0.3219752754296894559, 0.3333333333333333703, 0.3219752754296894559, 0.3333333333333333703, 0.3219752754296894559, 0.3333333333333333703, 0.3219752754296894559, 0.3333333333333333703, 0.3219752754296894559, 0.3333333333333333703, 0.3219752754296894559, 0.3333333333333333703, 0.3219752754296894559, 0.3333333333333333703, 0.3219752754296894559, 0.3333333333333333703, 0.3219752754296894559, 0.3333333333333333703, 0.3219752754296894559, 0.3333333333333333703, 0.3219752754296894559, 0.3333333333333333703, 0.3219752754296894559, 0.3333333333333333703, 0.3219752754296894559, 0.3333333333333333703, 0.3219752754296894559, 0.3333333333333333703, 0.3219752754296894559, 0.3333333333333333703, 0.3219752754296894559, 0.3333333333333333703, 0.3219752754296894559, 0.3333333333333333703, 0.3219752754296894559, 0.3333333333333333703, 0.3219752754296894559, 0.3333333333333333703, 0.3219752754296894559, 0.3333333333333333703, 0.3219752754296894559, 0.3333333333333333703, 0.3219752754296894559, 0.3333333333333333703, 0.3219752754296894559, 0.3333333333333333703, 0.3219752754296894559, 0.3333333333333333703, 0.3219752754296894559, 0.3333333333333333703, 0.3219752754296894559, 0.3333333333333333703, 0.3219752754296894559, 0.3333333333333333703, 0.3219752754296894559, 0.3333333333333333703, 0.3219752754296894559, 0.3333333333333333703, 0.3219752754296894559, 0.3333333333333333703, 0.3219752754296894559, 0.3333333333333333703, 0.3219752754296894559, 0.3333333333333333703, 0.3219752754296894559, 0.3333333333333333703, 0.3219752754296894559, 0.3333333333333333703, 0.3219752754296894559, 0.3333333333333333703, 0.3219752754296894559, 0.3333333333333333703, 0.3219752754296894559, 0.3333333333333333703, 0.3219752754296894559, 0.3333333333333333703, 0.3219752754296894559, 0.3333333333333333703, 0.3219752754296894559, 0.3333333333333333703, 0.3219752754296894559, 0.3333333333333333703, 0.3219752754296894559, 0.3333333333333333703, 0.3219752754296894559, 0.3333333333333333703, 0.3219752754296894559, 0.3333333333333333703, 0.3219752754296894559, 0.3333333333333333703, 0.3219752754296894559, 0.3333333333333333703, 0.3219752754296894559, 0.3333333333333333703, 0.3219752754296894559, 0.3333333333333333703, 0.3219752754296894559, 0.3333333333333333703, 0.3219752754296894559, 0.3333333333333333703, 0.3219752754296894559, 0.3333333333333333703, 0.3219752754296894559, 0.3333333333333333703, 0.3219752754296894559, 0.3333333333333333703, 0.3219752754296894559, 0.3333333333333333703, 0.3219752754296894559, 0.3333333333333333703, 0.3219752754296894559, 0.3333333333333333703, 0.3219752754296894559, 0.3333333333333333703, 0.3219752754296894559, 0.3333333333333333703, 0.3219752754296894559, 0.3333333333333333703, 0.3219752754296894559, 0.3333333333333333703, 0.3219752754296894559, 0.3333333333333333703, 0.3219752754296894559, 0.3333333333333333703, 0.3219752754296894559, 0.3333333333333333703, 0.3219752754296894559, 0.3333333333333333703, 0.3219752754296894559, 0.3333333333333333703, 0.3219752754296894559, 0.3333333333333333703, 0.3219752754296894559, 0.3333333333333333703, 0.3219752754296894559, 0.3333333333333333703, 0.3219752754296894559, 0.3333333333333333703, 0.3219752754296894559, 0.3333333333333333703, 0.3219752754296894559, 0.3333333333333333703, 0.3219752754296894559, 0.3333333333333333703, 0.3219752754296894559, 0.3333333333333333703, 0.3219752754296894559, 0.3333333333333333703, 0.3219752754296894559, 0.3333333333333333703, 0.3219752754296894559, 0.3333333333333333703, 0.3219752754296894559, 0.3333333333333333703, 0.3219752754296894559, 0.3333333333333333703, 0.3219752754296894559, 0.3333333333333333703, 0.3219752754296894559, 0.3333333333333333703, 0.3219752754296894559, 0.3333333333333333703, 0.3219752754296894559, 0.3333333333333333703, 0.3219752754296894559, 0.3333333333333333703, 0.3219752754296894559, 0.3333333333333333703, 0.3219752754296894559, 0.3333333333333333703, 0.3219752754296894559, 0.3333333333333333703, 0.3219752754296894559, 0.3333333333333333703, 0.3219752754296894559, 0.3333333333333333703, 0.3219752754296894559, 0.3333333333333333703, 0.3219752754296894559, 0.3333333333333333703, 0.3219752754296894559, 0.3333333333333333703, 0.3219752754296894559, 0.3333333333333333703, 0.3219752754296894559, 0.3333333333333333703, 0.3219752754296894559, 0.3333333333333333703, 0.3219752754296894559, 0.3333333333333333703, 0.3219752754296894559, 0.3333333333333333703, 0.3219752754296894559, 0.3333333333333333703, 0.3219752754296894559, 0.3333333333333333703, 0.3219752754296894559, 0.3333333333333333703, 0.3219752754296894559, 0.3333333333333333703, 0.3219752754296894559, 0.3333333333333333703, 0.3219752754296894559, 0.3333333333333333703, 0.3219752754296894559, 0.3333333333333333703, 0.3219752754296894559, 0.3333333333333333703, 0.3219752754296894559, 0.3333333333333333703, 0.3219752754296894559, 0.3333333333333333703, 0.3219752754296894559, 0.3333333333333333703, 0.3219752754296894559, 0.3333333333333333703, 0.3219752754296894559, 0.3333333333333333703, 0.3219752754296894559, 0.3333333333333333703, 0.3219752754296894559, 0.3333333333333333703, 0.3219752754296894559, 0.3333333333333333703, 0.3219752754296894559, 0.3333333333333333703, 0.3219752754296894559, 0.3333333333333333703, 0.3219752754296894559, 0.3333333333333333703, 0.3219752754296894559, 0.3333333333333333703, 0.3219752754296894559, 0.3333333333333333703, 0.3219752754296894559, 0.3333333333333333703, 0.3219752754296894559, 0.3333333333333333703, 0.3219752754296894559, 0.3333333333333333703, 0.3219752754296894559, 0.3333333333333333703, 0.3219752754296894559, 0.3333333333333333703),
 ( 0.3333333333333333703, 0.3219752754296894559, 0.3333333333333333703, 0.3219752754296894559, 0.3333333333333333703, 0.3219752754296894559, 0.3333333333333333703, 0.3219752754296894559, 0.3333333333333333703, 0.3219752754296894559, 0.3333333333333333703, 0.3219752754296894559, 0.3333333333333333703, 0.3219752754296894559, 0.3333333333333333703, 0.3219752754296894559, 0.3333333333333333703, 0.3219752754296894559, 0.3333333333333333703, 0.3219752754296894559, 0.3333333333333333703, 0.3219752754296894559, 0.3333333333333333703, 0.3219752754296894559, 0.3333333333333333703, 0.3219752754296894559, 0.3333333333333333703, 0.3219752754296894559, 0.3333333333333333703, 0.3219752754296894559, 0.3333333333333333703, 0.3219752754296894559, 0.3333333333333333703, 0.3219752754296894559, 0.3333333333333333703, 0.3219752754296894559, 0.3333333333333333703, 0.3219752754296894559, 0.3333333333333333703, 0.3219752754296894559, 0.3333333333333333703, 0.3219752754296894559, 0.3333333333333333703, 0.3219752754296894559, 0.3333333333333333703, 0.3219752754296894559, 0.3333333333333333703, 0.3219752754296894559, 0.3333333333333333703, 0.3219752754296894559, 0.3333333333333333703, 0.3219752754296894559, 0.3333333333333333703, 0.3219752754296894559, 0.3333333333333333703, 0.3219752754296894559, 0.3333333333333333703, 0.3219752754296894559, 0.3333333333333333703, 0.3219752754296894559, 0.3333333333333333703, 0.3219752754296894559, 0.3333333333333333703, 0.3219752754296894559, 0.3333333333333333703, 0.3219752754296894559, 0.3333333333333333703, 0.3219752754296894559, 0.3333333333333333703, 0.3219752754296894559, 0.3333333333333333703, 0.3219752754296894559, 0.3333333333333333703, 0.3219752754296894559, 0.3333333333333333703, 0.3219752754296894559, 0.3333333333333333703, 0.3219752754296894559, 0.3333333333333333703, 0.3219752754296894559, 0.3333333333333333703, 0.3219752754296894559, 0.3333333333333333703, 0.3219752754296894559, 0.3333333333333333703, 0.3219752754296894559, 0.3333333333333333703, 0.3219752754296894559, 0.3333333333333333703, 0.3219752754296894559, 0.3333333333333333703, 0.3219752754296894559, 0.3333333333333333703, 0.3219752754296894559, 0.3333333333333333703, 0.3219752754296894559, 0.3333333333333333703, 0.3219752754296894559, 0.3333333333333333703, 0.3219752754296894559, 0.3333333333333333703, 0.3219752754296894559, 0.3333333333333333703, 0.3219752754296894559, 0.3333333333333333703, 0.3219752754296894559, 0.3333333333333333703, 0.3219752754296894559, 0.3333333333333333703, 0.3219752754296894559, 0.3333333333333333703, 0.3219752754296894559, 0.3333333333333333703, 0.3219752754296894559, 0.3333333333333333703, 0.3219752754296894559, 0.3333333333333333703, 0.3219752754296894559, 0.3333333333333333703, 0.3219752754296894559, 0.3333333333333333703, 0.3219752754296894559, 0.3333333333333333703, 0.3219752754296894559, 0.3333333333333333703, 0.3219752754296894559, 0.3333333333333333703, 0.3219752754296894559, 0.3333333333333333703, 0.3219752754296894559, 0.3333333333333333703, 0.3219752754296894559, 0.3333333333333333703, 0.3219752754296894559, 0.3333333333333333703, 0.3219752754296894559, 0.3333333333333333703, 0.3219752754296894559, 0.3333333333333333703, 0.3219752754296894559, 0.3333333333333333703, 0.3219752754296894559, 0.3333333333333333703, 0.3219752754296894559, 0.3333333333333333703, 0.3219752754296894559, 0.3333333333333333703, 0.3219752754296894559, 0.3333333333333333703, 0.3219752754296894559, 0.3333333333333333703, 0.3219752754296894559, 0.3333333333333333703, 0.3219752754296894559, 0.3333333333333333703, 0.3219752754296894559, 0.3333333333333333703, 0.3219752754296894559, 0.3333333333333333703, 0.3219752754296894559, 0.3333333333333333703, 0.3219752754296894559, 0.3333333333333333703, 0.3219752754296894559, 0.3333333333333333703, 0.3219752754296894559, 0.3333333333333333703, 0.3219752754296894559, 0.3333333333333333703, 0.3219752754296894559, 0.3333333333333333703, 0.3219752754296894559, 0.3333333333333333703, 0.3219752754296894559, 0.3333333333333333703, 0.3219752754296894559, 0.3333333333333333703, 0.3219752754296894559, 0.3333333333333333703, 0.3219752754296894559, 0.3333333333333333703, 0.3219752754296894559, 0.3333333333333333703, 0.3219752754296894559, 0.3333333333333333703, 0.3219752754296894559, 0.3333333333333333703, 0.3219752754296894559, 0.3333333333333333703, 0.3219752754296894559, 0.3333333333333333703, 0.3219752754296894559, 0.3333333333333333703, 0.3219752754296894559, 0.3333333333333333703, 0.3219752754296894559, 0.3333333333333333703, 0.3219752754296894559, 0.3333333333333333703, 0.3219752754296894559, 0.3333333333333333703, 0.3219752754296894559, 0.3333333333333333703, 0.3219752754296894559, 0.3333333333333333703, 0.3219752754296894559, 0.3333333333333333703, 0.3219752754296894559, 0.3333333333333333703, 0.3219752754296894559, 0.3333333333333333703, 0.3219752754296894559, 0.3333333333333333703, 0.3219752754296894559, 0.3333333333333333703, 0.3219752754296894559, 0.3333333333333333703, 0.3219752754296894559, 0.3333333333333333703, 0.3219752754296894559, 0.3333333333333333703, 0.3219752754296894559, 0.3333333333333333703, 0.3219752754296894559, 0.3333333333333333703, 0.3219752754296894559, 0.3333333333333333703, 0.3219752754296894559, 0.3333333333333333703, 0.3219752754296894559, 0.3333333333333333703, 0.3219752754296894559, 0.3333333333333333703, 0.3219752754296894559, 0.3333333333333333703, 0.3219752754296894559, 0.3333333333333333703, 0.3219752754296894559, 0.3333333333333333703, 0.3219752754296894559, 0.3333333333333333703, 0.3219752754296894559, 0.3333333333333333703, 0.3219752754296894559, 0.3333333333333333703, 0.3219752754296894559, 0.3333333333333333703, 0.3219752754296894559, 0.3333333333333333703, 0.3219752754296894559, 0.3333333333333333703, 0.3219752754296894559, 0.3333333333333333703, 0.3219752754296894559, 0.3333333333333333703, 0.3219752754296894559, 0.3333333333333333703, 0.3219752754296894559, 0.3333333333333333703, 0.3219752754296894559, 0.3333333333333333703, 0.3219752754296894559, 0.3333333333333333703, 0.3219752754296894559, 0.3333333333333333703, 0.3219752754296894559, 0.3333333333333333703, 0.3219752754296894559, 0.3333333333333333703, 0.3219752754296894559, 0.3333333333333333703, 0.3219752754296894559, 0.3333333333333333703, 0.3219752754296894559, 0.3333333333333333703, 0.3219752754296894559, 0.3333333333333333703, 0.3219752754296894559, 0.3333333333333333703, 0.3219752754296894559, 0.3333333333333333703, 0.3219752754296894559, 0.3333333333333333703, 0.3219752754296894559, 0.3333333333333333703, 0.3219752754296894559, 0.3333333333333333703, 0.3219752754296894559, 0.3333333333333333703, 0.3219752754296894559, 0.3333333333333333703, 0.3219752754296894559, 0.3333333333333333703, 0.3219752754296894559, 0.3333333333333333703, 0.3219752754296894559, 0.3333333333333333703, 0.3219752754296894559, 0.3333333333333333703, 0.3219752754296894559, 0.3333333333333333703, 0.3219752754296894559, 0.3333333333333333703, 0.3219752754296894559, 0.3333333333333333703, 0.3219752754296894559, 0.3333333333333333703, 0.3219752754296894559, 0.3333333333333333703, 0.3219752754296894559, 0.3333333333333333703, 0.3219752754296894559, 0.3333333333333333703, 0.3219752754296894559, 0.3333333333333333703, 0.3219752754296894559, 0.3333333333333333703, 0.3219752754296894559, 0.3333333333333333703, 0.3219752754296894559, 0.3333333333333333703, 0.3219752754296894559, 0.3333333333333333703, 0.3219752754296894559, 0.3333333333333333703, 0.3219752754296894559, 0.3333333333333333703, 0.3219752754296894559, 0.3333333333333333703, 0.3219752754296894559, 0.3333333333333333703, 0.3219752754296894559, 0.3333333333333333703, 0.3219752754296894559, 0.3333333333333333703, 0.3219752754296894559, 0.3333333333333333703, 0.3219752754296894559, 0.3333333333333333703, 0.3219752754296894559, 0.3333333333333333703, 0.3219752754296894559, 0.3333333333333333703, 0.3219752754296894559, 0.3333333333333333703, 0.3219752754296894559, 0.3333333333333333703, 0.3219752754296894559, 0.3333333333333333703, 0.3219752754296894559, 0.3333333333333333703, 0.3219752754296894559, 0.3333333333333333703, 0.3219752754296894559, 0.3333333333333333703, 0.3219752754296894559, 0.3333333333333333703, 0.3219752754296894559, 0.3333333333333333703, 0.3219752754296894559, 0.3333333333333333703, 0.3219752754296894559, 0.3333333333333333703, 0.3219752754296894559, 0.3333333333333333703, 0.3219752754296894559, 0.3333333333333333703, 0.3219752754296894559, 0.3333333333333333703, 0.3219752754296894559, 0.3333333333333333703, 0.3219752754296894559, 0.3333333333333333703, 0.3219752754296894559, 0.3333333333333333703, 0.3219752754296894559, 0.3333333333333333703, 0.3219752754296894559, 0.3333333333333333703, 0.3219752754296894559, 0.3333333333333333703, 0.3219752754296894559, 0.3333333333333333703, 0.3219752754296894559, 0.3333333333333333703, 0.3219752754296894559, 0.3333333333333333703, 0.3219752754296894559, 0.3333333333333333703, 0.3219752754296894559, 0.3333333333333333703, 0.3219752754296894559, 0.3333333333333333703, 0.3219752754296894559, 0.3333333333333333703, 0.3219752754296894559, 0.3333333333333333703, 0.3219752754296894559, 0.3333333333333333703, 0.3219752754296894559, 0.3333333333333333703, 0.3219752754296894559, 0.3333333333333333703, 0.3219752754296894559, 0.3333333333333333703, 0.3219752754296894559, 0.3333333333333333703, 0.3219752754296894559, 0.3333333333333333703, 0.3219752754296894559, 0.3333333333333333703, 0.3219752754296894559, 0.3333333333333333703, 0.3219752754296894559, 0.3333333333333333703, 0.3219752754296894559, 0.3333333333333333703, 0.3219752754296894559, 0.3333333333333333703, 0.3219752754296894559, 0.3333333333333333703, 0.3219752754296894559, 0.3333333333333333703, 0.3219752754296894559, 0.3333333333333333703, 0.3219752754296894559, 0.3333333333333333703, 0.3219752754296894559, 0.3333333333333333703, 0.3219752754296894559, 0.3333333333333333703, 0.3219752754296894559, 0.3333333333333333703, 0.3219752754296894559, 0.3333333333333333703, 0.3219752754296894559, 0.3333333333333333703, 0.3219752754296894559, 0.3333333333333333703, 0.3219752754296894559, 0.3333333333333333703, 0.3219752754296894559, 0.3333333333333333703, 0.3219752754296894559, 0.3333333333333333703, 0.3219752754296894559, 0.3333333333333333703, 0.3219752754296894559, 0.3333333333333333703, 0.3219752754296894559, 0.3333333333333333703, 0.3219752754296894559, 0.3333333333333333703, 0.3219752754296894559, 0.3333333333333333703, 0.3219752754296894559, 0.3333333333333333703),
 ( 1.000000000000000000, 0.9659258262890683122, 1.000000000000000000, 0.9659258262890683122, 1.000000000000000000, 0.9659258262890683122, 1.000000000000000000, 0.9659258262890683122, 1.000000000000000000, 0.9659258262890683122, 1.000000000000000000, 0.9659258262890683122, 1.000000000000000000, 0.9659258262890683122, 1.000000000000000000, 0.9659258262890683122, 1.000000000000000000, 0.9659258262890683122, 1.000000000000000000, 0.9659258262890683122, 1.000000000000000000, 0.9659258262890683122, 1.000000000000000000, 0.9659258262890683122, 1.000000000000000000, 0.9659258262890683122, 1.000000000000000000, 0.9659258262890683122, 1.000000000000000000, 0.9659258262890683122, 1.000000000000000000, 0.9659258262890683122, 1.000000000000000000, 0.9659258262890683122, 1.000000000000000000, 0.9659258262890683122, 1.000000000000000000, 0.9659258262890683122, 1.000000000000000000, 0.9659258262890683122, 1.000000000000000000, 0.9659258262890683122, 1.000000000000000000, 0.9659258262890683122, 1.000000000000000000, 0.9659258262890683122, 1.000000000000000000, 0.9659258262890683122, 1.000000000000000000, 0.9659258262890683122, 1.000000000000000000, 0.9659258262890683122, 1.000000000000000000, 0.9659258262890683122, 1.000000000000000000, 0.9659258262890683122, 1.000000000000000000, 0.9659258262890683122, 1.000000000000000000, 0.9659258262890683122, 1.000000000000000000, 0.9659258262890683122, 1.000000000000000000, 0.9659258262890683122, 1.000000000000000000, 0.9659258262890683122, 1.000000000000000000, 0.9659258262890683122, 1.000000000000000000, 0.9659258262890683122, 1.000000000000000000, 0.9659258262890683122, 1.000000000000000000, 0.9659258262890683122, 1.000000000000000000, 0.9659258262890683122, 1.000000000000000000, 0.9659258262890683122, 1.000000000000000000, 0.9659258262890683122, 1.000000000000000000, 0.9659258262890683122, 1.000000000000000000, 0.9659258262890683122, 1.000000000000000000, 0.9659258262890683122, 1.000000000000000000, 0.9659258262890683122, 1.000000000000000000, 0.9659258262890683122, 1.000000000000000000, 0.9659258262890683122, 1.000000000000000000, 0.9659258262890683122, 1.000000000000000000, 0.9659258262890683122, 1.000000000000000000, 0.9659258262890683122, 1.000000000000000000, 0.9659258262890683122, 1.000000000000000000, 0.9659258262890683122, 1.000000000000000000, 0.9659258262890683122, 1.000000000000000000, 0.9659258262890683122, 1.000000000000000000, 0.9659258262890683122, 1.000000000000000000, 0.9659258262890683122, 1.000000000000000000, 0.9659258262890683122, 1.000000000000000000, 0.9659258262890683122, 1.000000000000000000, 0.9659258262890683122, 1.000000000000000000, 0.9659258262890683122, 1.000000000000000000, 0.9659258262890683122, 1.000000000000000000, 0.9659258262890683122, 1.000000000000000000, 0.9659258262890683122, 1.000000000000000000, 0.9659258262890683122, 1.000000000000000000, 0.9659258262890683122, 1.000000000000000000, 0.9659258262890683122, 1.000000000000000000, 0.9659258262890683122, 1.000000000000000000, 0.9659258262890683122, 1.000000000000000000, 0.9659258262890683122, 1.000000000000000000, 0.9659258262890683122, 1.000000000000000000, 0.9659258262890683122, 1.000000000000000000, 0.9659258262890683122, 1.000000000000000000, 0.9659258262890683122, 1.000000000000000000, 0.9659258262890683122, 1.000000000000000000, 0.9659258262890683122, 1.000000000000000000, 0.9659258262890683122, 1.000000000000000000, 0.9659258262890683122, 1.000000000000000000, 0.9659258262890683122, 1.000000000000000000, 0.9659258262890683122, 1.000000000000000000, 0.9659258262890683122, 1.000000000000000000, 0.9659258262890683122, 1.000000000000000000, 0.9659258262890683122, 1.000000000000000000, 0.9659258262890683122, 1.000000000000000000, 0.9659258262890683122, 1.000000000000000000, 0.9659258262890683122, 1.000000000000000000, 0.9659258262890683122, 1.000000000000000000, 0.9659258262890683122, 1.000000000000000000, 0.9659258262890683122, 1.000000000000000000, 0.9659258262890683122, 1.000000000000000000, 0.9659258262890683122, 1.000000000000000000, 0.9659258262890683122, 1.000000000000000000, 0.9659258262890683122, 1.000000000000000000, 0.9659258262890683122, 1.000000000000000000, 0.9659258262890683122, 1.000000000000000000, 0.9659258262890683122, 1.000000000000000000, 0.9659258262890683122, 1.000000000000000000, 0.9659258262890683122, 1.000000000000000000, 0.9659258262890683122, 1.000000000000000000, 0.9659258262890683122, 1.000000000000000000, 0.9659258262890683122, 1.000000000000000000, 0.9659258262890683122, 1.000000000000000000, 0.9659258262890683122, 1.000000000000000000, 0.9659258262890683122, 1.000000000000000000, 0.9659258262890683122, 1.000000000000000000, 0.9659258262890683122, 1.000000000000000000, 0.9659258262890683122, 1.000000000000000000, 0.9659258262890683122, 1.000000000000000000, 0.9659258262890683122, 1.000000000000000000, 0.9659258262890683122, 1.000000000000000000, 0.9659258262890683122, 1.000000000000000000, 0.9659258262890683122, 1.000000000000000000, 0.9659258262890683122, 1.000000000000000000, 0.9659258262890683122, 1.000000000000000000, 0.9659258262890683122, 1.000000000000000000, 0.9659258262890683122, 1.000000000000000000, 0.9659258262890683122, 1.000000000000000000, 0.9659258262890683122, 1.000000000000000000, 0.9659258262890683122, 1.000000000000000000, 0.9659258262890683122, 1.000000000000000000, 0.9659258262890683122, 1.000000000000000000, 0.9659258262890683122, 1.000000000000000000, 0.9659258262890683122, 1.000000000000000000, 0.9659258262890683122, 1.000000000000000000, 0.9659258262890683122, 1.000000000000000000, 0.9659258262890683122, 1.000000000000000000, 0.9659258262890683122, 1.000000000000000000, 0.9659258262890683122, 1.000000000000000000, 0.9659258262890683122, 1.000000000000000000, 0.9659258262890683122, 1.000000000000000000, 0.9659258262890683122, 1.000000000000000000, 0.9659258262890683122, 1.000000000000000000, 0.9659258262890683122, 1.000000000000000000, 0.9659258262890683122, 1.000000000000000000, 0.9659258262890683122, 1.000000000000000000, 0.9659258262890683122, 1.000000000000000000, 0.9659258262890683122, 1.000000000000000000, 0.9659258262890683122, 1.000000000000000000, 0.9659258262890683122, 1.000000000000000000, 0.9659258262890683122, 1.000000000000000000, 0.9659258262890683122, 1.000000000000000000, 0.9659258262890683122, 1.000000000000000000, 0.9659258262890683122, 1.000000000000000000, 0.9659258262890683122, 1.000000000000000000, 0.9659258262890683122, 1.000000000000000000, 0.9659258262890683122, 1.000000000000000000, 0.9659258262890683122, 1.000000000000000000, 0.9659258262890683122, 1.000000000000000000, 0.9659258262890683122, 1.000000000000000000, 0.9659258262890683122, 1.000000000000000000, 0.9659258262890683122, 1.000000000000000000, 0.9659258262890683122, 1.000000000000000000, 0.9659258262890683122, 1.000000000000000000, 0.9659258262890683122, 1.000000000000000000, 0.9659258262890683122, 1.000000000000000000, 0.9659258262890683122, 1.000000000000000000, 0.9659258262890683122, 1.000000000000000000, 0.9659258262890683122, 1.000000000000000000, 0.9659258262890683122, 1.000000000000000000, 0.9659258262890683122, 1.000000000000000000, 0.9659258262890683122, 1.000000000000000000, 0.9659258262890683122, 1.000000000000000000, 0.9659258262890683122, 1.000000000000000000, 0.9659258262890683122, 1.000000000000000000, 0.9659258262890683122, 1.000000000000000000, 0.9659258262890683122, 1.000000000000000000, 0.9659258262890683122, 1.000000000000000000, 0.9659258262890683122, 1.000000000000000000, 0.9659258262890683122, 1.000000000000000000, 0.9659258262890683122, 1.000000000000000000, 0.9659258262890683122, 1.000000000000000000, 0.9659258262890683122, 1.000000000000000000, 0.9659258262890683122, 1.000000000000000000, 0.9659258262890683122, 1.000000000000000000, 0.9659258262890683122, 1.000000000000000000, 0.9659258262890683122, 1.000000000000000000, 0.9659258262890683122, 1.000000000000000000, 0.9659258262890683122, 1.000000000000000000, 0.9659258262890683122, 1.000000000000000000, 0.9659258262890683122, 1.000000000000000000, 0.9659258262890683122, 1.000000000000000000, 0.9659258262890683122, 1.000000000000000000, 0.9659258262890683122, 1.000000000000000000, 0.9659258262890683122, 1.000000000000000000, 0.9659258262890683122, 1.000000000000000000, 0.9659258262890683122, 1.000000000000000000, 0.9659258262890683122, 1.000000000000000000, 0.9659258262890683122, 1.000000000000000000, 0.9659258262890683122, 1.000000000000000000, 0.9659258262890683122, 1.000000000000000000, 0.9659258262890683122, 1.000000000000000000, 0.9659258262890683122, 1.000000000000000000, 0.9659258262890683122, 1.000000000000000000, 0.9659258262890683122, 1.000000000000000000, 0.9659258262890683122, 1.000000000000000000, 0.9659258262890683122, 1.000000000000000000, 0.9659258262890683122, 1.000000000000000000, 0.9659258262890683122, 1.000000000000000000, 0.9659258262890683122, 1.000000000000000000, 0.9659258262890683122, 1.000000000000000000, 0.9659258262890683122, 1.000000000000000000, 0.9659258262890683122, 1.000000000000000000, 0.9659258262890683122, 1.000000000000000000, 0.9659258262890683122, 1.000000000000000000, 0.9659258262890683122, 1.000000000000000000, 0.9659258262890683122, 1.000000000000000000, 0.9659258262890683122, 1.000000000000000000, 0.9659258262890683122, 1.000000000000000000, 0.9659258262890683122, 1.000000000000000000, 0.9659258262890683122, 1.000000000000000000, 0.9659258262890683122, 1.000000000000000000, 0.9659258262890683122, 1.000000000000000000, 0.9659258262890683122, 1.000000000000000000, 0.9659258262890683122, 1.000000000000000000, 0.9659258262890683122, 1.000000000000000000, 0.9659258262890683122, 1.000000000000000000, 0.9659258262890683122, 1.000000000000000000, 0.9659258262890683122, 1.000000000000000000, 0.9659258262890683122, 1.000000000000000000, 0.9659258262890683122, 1.000000000000000000, 0.9659258262890683122, 1.000000000000000000, 0.9659258262890683122, 1.000000000000000000, 0.9659258262890683122, 1.000000000000000000, 0.9659258262890683122, 1.000000000000000000, 0.9659258262890683122, 1.000000000000000000, 0.9659258262890683122, 1.000000000000000000, 0.9659258262890683122, 1.000000000000000000, 0.9659258262890683122, 1.000000000000000000, 0.9659258262890683122, 1.000000000000000000, 0.9659258262890683122, 1.000000000000000000),
 ( 0.3333333333333333703, 0.3219752754296894559, 0.3333333333333333703, 0.3219752754296894559, 0.3333333333333333703, 0.3219752754296894559, 0.3333333333333333703, 0.3219752754296894559, 0.3333333333333333703, 0.3219752754296894559, 0.3333333333333333703, 0.3219752754296894559, 0.3333333333333333703, 0.3219752754296894559, 0.3333333333333333703, 0.3219752754296894559, 0.3333333333333333703, 0.3219752754296894559, 0.3333333333333333703, 0.3219752754296894559, 0.3333333333333333703, 0.3219752754296894559, 0.3333333333333333703, 0.3219752754296894559, 0.3333333333333333703, 0.3219752754296894559, 0.3333333333333333703, 0.3219752754296894559, 0.3333333333333333703, 0.3219752754296894559, 0.3333333333333333703, 0.3219752754296894559, 0.3333333333333333703, 0.3219752754296894559, 0.3333333333333333703, 0.3219752754296894559, 0.3333333333333333703, 0.3219752754296894559, 0.3333333333333333703, 0.3219752754296894559, 0.3333333333333333703, 0.3219752754296894559, 0.3333333333333333703, 0.3219752754296894559, 0.3333333333333333703, 0.3219752754296894559, 0.3333333333333333703, 0.3219752754296894559, 0.3333333333333333703, 0.3219752754296894559, 0.3333333333333333703, 0.3219752754296894559, 0.3333333333333333703, 0.3219752754296894559, 0.3333333333333333703, 0.3219752754296894559, 0.3333333333333333703, 0.3219752754296894559, 0.3333333333333333703, 0.3219752754296894559, 0.3333333333333333703, 0.3219752754296894559, 0.3333333333333333703, 0.3219752754296894559, 0.3333333333333333703, 0.3219752754296894559, 0.3333333333333333703, 0.3219752754296894559, 0.3333333333333333703, 0.3219752754296894559, 0.3333333333333333703, 0.3219752754296894559, 0.3333333333333333703, 0.3219752754296894559, 0.3333333333333333703, 0.3219752754296894559, 0.3333333333333333703, 0.3219752754296894559, 0.3333333333333333703, 0.3219752754296894559, 0.3333333333333333703, 0.3219752754296894559, 0.3333333333333333703, 0.3219752754296894559, 0.3333333333333333703, 0.3219752754296894559, 0.3333333333333333703, 0.3219752754296894559, 0.3333333333333333703, 0.3219752754296894559, 0.3333333333333333703, 0.3219752754296894559, 0.3333333333333333703, 0.3219752754296894559, 0.3333333333333333703, 0.3219752754296894559, 0.3333333333333333703, 0.3219752754296894559, 0.3333333333333333703, 0.3219752754296894559, 0.3333333333333333703, 0.3219752754296894559, 0.3333333333333333703, 0.3219752754296894559, 0.3333333333333333703, 0.3219752754296894559, 0.3333333333333333703, 0.3219752754296894559, 0.3333333333333333703, 0.3219752754296894559, 0.3333333333333333703, 0.3219752754296894559, 0.3333333333333333703, 0.3219752754296894559, 0.3333333333333333703, 0.3219752754296894559, 0.3333333333333333703, 0.3219752754296894559, 0.3333333333333333703, 0.3219752754296894559, 0.3333333333333333703, 0.3219752754296894559, 0.3333333333333333703, 0.3219752754296894559, 0.3333333333333333703, 0.3219752754296894559, 0.3333333333333333703, 0.3219752754296894559, 0.3333333333333333703, 0.3219752754296894559, 0.3333333333333333703, 0.3219752754296894559, 0.3333333333333333703, 0.3219752754296894559, 0.3333333333333333703, 0.3219752754296894559, 0.3333333333333333703, 0.3219752754296894559, 0.3333333333333333703, 0.3219752754296894559, 0.3333333333333333703, 0.3219752754296894559, 0.3333333333333333703, 0.3219752754296894559, 0.3333333333333333703, 0.3219752754296894559, 0.3333333333333333703, 0.3219752754296894559, 0.3333333333333333703, 0.3219752754296894559, 0.3333333333333333703, 0.3219752754296894559, 0.3333333333333333703, 0.3219752754296894559, 0.3333333333333333703, 0.3219752754296894559, 0.3333333333333333703, 0.3219752754296894559, 0.3333333333333333703, 0.3219752754296894559, 0.3333333333333333703, 0.3219752754296894559, 0.3333333333333333703, 0.3219752754296894559, 0.3333333333333333703, 0.3219752754296894559, 0.3333333333333333703, 0.3219752754296894559, 0.3333333333333333703, 0.3219752754296894559, 0.3333333333333333703, 0.3219752754296894559, 0.3333333333333333703, 0.3219752754296894559, 0.3333333333333333703, 0.3219752754296894559, 0.3333333333333333703, 0.3219752754296894559, 0.3333333333333333703, 0.3219752754296894559, 0.3333333333333333703, 0.3219752754296894559, 0.3333333333333333703, 0.3219752754296894559, 0.3333333333333333703, 0.3219752754296894559, 0.3333333333333333703, 0.3219752754296894559, 0.3333333333333333703, 0.3219752754296894559, 0.3333333333333333703, 0.3219752754296894559, 0.3333333333333333703, 0.3219752754296894559, 0.3333333333333333703, 0.3219752754296894559, 0.3333333333333333703, 0.3219752754296894559, 0.3333333333333333703, 0.3219752754296894559, 0.3333333333333333703, 0.3219752754296894559, 0.3333333333333333703, 0.3219752754296894559, 0.3333333333333333703, 0.3219752754296894559, 0.3333333333333333703, 0.3219752754296894559, 0.3333333333333333703, 0.3219752754296894559, 0.3333333333333333703, 0.3219752754296894559, 0.3333333333333333703, 0.3219752754296894559, 0.3333333333333333703, 0.3219752754296894559, 0.3333333333333333703, 0.3219752754296894559, 0.3333333333333333703, 0.3219752754296894559, 0.3333333333333333703, 0.3219752754296894559, 0.3333333333333333703, 0.3219752754296894559, 0.3333333333333333703, 0.3219752754296894559, 0.3333333333333333703, 0.3219752754296894559, 0.3333333333333333703, 0.3219752754296894559, 0.3333333333333333703, 0.3219752754296894559, 0.3333333333333333703, 0.3219752754296894559, 0.3333333333333333703, 0.3219752754296894559, 0.3333333333333333703, 0.3219752754296894559, 0.3333333333333333703, 0.3219752754296894559, 0.3333333333333333703, 0.3219752754296894559, 0.3333333333333333703, 0.3219752754296894559, 0.3333333333333333703, 0.3219752754296894559, 0.3333333333333333703, 0.3219752754296894559, 0.3333333333333333703, 0.3219752754296894559, 0.3333333333333333703, 0.3219752754296894559, 0.3333333333333333703, 0.3219752754296894559, 0.3333333333333333703, 0.3219752754296894559, 0.3333333333333333703, 0.3219752754296894559, 0.3333333333333333703, 0.3219752754296894559, 0.3333333333333333703, 0.3219752754296894559, 0.3333333333333333703, 0.3219752754296894559, 0.3333333333333333703, 0.3219752754296894559, 0.3333333333333333703, 0.3219752754296894559, 0.3333333333333333703, 0.3219752754296894559, 0.3333333333333333703, 0.3219752754296894559, 0.3333333333333333703, 0.3219752754296894559, 0.3333333333333333703, 0.3219752754296894559, 0.3333333333333333703, 0.3219752754296894559, 0.3333333333333333703, 0.3219752754296894559, 0.3333333333333333703, 0.3219752754296894559, 0.3333333333333333703, 0.3219752754296894559, 0.3333333333333333703, 0.3219752754296894559, 0.3333333333333333703, 0.3219752754296894559, 0.3333333333333333703, 0.3219752754296894559, 0.3333333333333333703, 0.3219752754296894559, 0.3333333333333333703, 0.3219752754296894559, 0.3333333333333333703, 0.3219752754296894559, 0.3333333333333333703, 0.3219752754296894559, 0.3333333333333333703, 0.3219752754296894559, 0.3333333333333333703, 0.3219752754296894559, 0.3333333333333333703, 0.3219752754296894559, 0.3333333333333333703, 0.3219752754296894559, 0.3333333333333333703, 0.3219752754296894559, 0.3333333333333333703, 0.3219752754296894559, 0.3333333333333333703, 0.3219752754296894559, 0.3333333333333333703, 0.3219752754296894559, 0.3333333333333333703, 0.3219752754296894559, 0.3333333333333333703, 0.3219752754296894559, 0.3333333333333333703, 0.3219752754296894559, 0.3333333333333333703, 0.3219752754296894559, 0.3333333333333333703, 0.3219752754296894559, 0.3333333333333333703, 0.3219752754296894559, 0.3333333333333333703, 0.3219752754296894559, 0.3333333333333333703, 0.3219752754296894559, 0.3333333333333333703, 0.3219752754296894559, 0.3333333333333333703, 0.3219752754296894559, 0.3333333333333333703, 0.3219752754296894559, 0.3333333333333333703, 0.3219752754296894559, 0.3333333333333333703, 0.3219752754296894559, 0.3333333333333333703, 0.3219752754296894559, 0.3333333333333333703, 0.3219752754296894559, 0.3333333333333333703, 0.3219752754296894559, 0.3333333333333333703, 0.3219752754296894559, 0.3333333333333333703, 0.3219752754296894559, 0.3333333333333333703, 0.3219752754296894559, 0.3333333333333333703, 0.3219752754296894559, 0.3333333333333333703, 0.3219752754296894559, 0.3333333333333333703, 0.3219752754296894559, 0.3333333333333333703, 0.3219752754296894559, 0.3333333333333333703, 0.3219752754296894559, 0.3333333333333333703, 0.3219752754296894559, 0.3333333333333333703, 0.3219752754296894559, 0.3333333333333333703, 0.3219752754296894559, 0.3333333333333333703, 0.3219752754296894559, 0.3333333333333333703, 0.3219752754296894559, 0.3333333333333333703, 0.3219752754296894559, 0.3333333333333333703, 0.3219752754296894559, 0.3333333333333333703, 0.3219752754296894559, 0.3333333333333333703, 0.3219752754296894559, 0.3333333333333333703, 0.3219752754296894559, 0.3333333333333333703, 0.3219752754296894559, 0.3333333333333333703, 0.3219752754296894559, 0.3333333333333333703, 0.3219752754296894559, 0.3333333333333333703, 0.3219752754296894559, 0.3333333333333333703, 0.3219752754296894559, 0.3333333333333333703, 0.3219752754296894559, 0.3333333333333333703, 0.3219752754296894559, 0.3333333333333333703, 0.3219752754296894559, 0.3333333333333333703, 0.3219752754296894559, 0.3333333333333333703, 0.3219752754296894559, 0.3333333333333333703, 0.3219752754296894559, 0.3333333333333333703, 0.3219752754296894559, 0.3333333333333333703, 0.3219752754296894559, 0.3333333333333333703, 0.3219752754296894559, 0.3333333333333333703, 0.3219752754296894559, 0.3333333333333333703, 0.3219752754296894559, 0.3333333333333333703, 0.3219752754296894559, 0.3333333333333333703, 0.3219752754296894559, 0.3333333333333333703, 0.3219752754296894559, 0.3333333333333333703, 0.3219752754296894559, 0.3333333333333333703, 0.3219752754296894559, 0.3333333333333333703, 0.3219752754296894559, 0.3333333333333333703, 0.3219752754296894559, 0.3333333333333333703, 0.3219752754296894559, 0.3333333333333333703, 0.3219752754296894559, 0.3333333333333333703, 0.3219752754296894559, 0.3333333333333333703, 0.3219752754296894559, 0.3333333333333333703, 0.3219752754296894559, 0.3333333333333333703, 0.3219752754296894559, 0.3333333333333333703, 0.3219752754296894559, 0.3333333333333333703, 0.3219752754296894559, 0.3333333333333333703, 0.3219752754296894559, 0.3333333333333333703, 0.3219752754296894559, 0.3333333333333333703, 0.3219752754296894559, 0.3333333333333333703, 0.3219752754296894559, 0.3333333333333333703, 0.3219752754296894559, 0.3333333333333333703, 0.3219752754296894559, 0.3333333333333333703),
 ( 0.3333333333333333703, 0.3219752754296894559, 0.3333333333333333703, 0.3219752754296894559, 0.3333333333333333703, 0.3219752754296894559, 0.3333333333333333703, 0.3219752754296894559, 0.3333333333333333703, 0.3219752754296894559, 0.3333333333333333703, 0.3219752754296894559, 0.3333333333333333703, 0.3219752754296894559, 0.3333333333333333703, 0.3219752754296894559, 0.3333333333333333703, 0.3219752754296894559, 0.3333333333333333703, 0.3219752754296894559, 0.3333333333333333703, 0.3219752754296894559, 0.3333333333333333703, 0.3219752754296894559, 0.3333333333333333703, 0.3219752754296894559, 0.3333333333333333703, 0.3219752754296894559, 0.3333333333333333703, 0.3219752754296894559, 0.3333333333333333703, 0.3219752754296894559, 0.3333333333333333703, 0.3219752754296894559, 0.3333333333333333703, 0.3219752754296894559, 0.3333333333333333703, 0.3219752754296894559, 0.3333333333333333703, 0.3219752754296894559, 0.3333333333333333703, 0.3219752754296894559, 0.3333333333333333703, 0.3219752754296894559, 0.3333333333333333703, 0.3219752754296894559, 0.3333333333333333703, 0.3219752754296894559, 0.3333333333333333703, 0.3219752754296894559, 0.3333333333333333703, 0.3219752754296894559, 0.3333333333333333703, 0.3219752754296894559, 0.3333333333333333703, 0.3219752754296894559, 0.3333333333333333703, 0.3219752754296894559, 0.3333333333333333703, 0.3219752754296894559, 0.3333333333333333703, 0.3219752754296894559, 0.3333333333333333703, 0.3219752754296894559, 0.3333333333333333703, 0.3219752754296894559, 0.3333333333333333703, 0.3219752754296894559, 0.3333333333333333703, 0.3219752754296894559, 0.3333333333333333703, 0.3219752754296894559, 0.3333333333333333703, 0.3219752754296894559, 0.3333333333333333703, 0.3219752754296894559, 0.3333333333333333703, 0.3219752754296894559, 0.3333333333333333703, 0.3219752754296894559, 0.3333333333333333703, 0.3219752754296894559, 0.3333333333333333703, 0.3219752754296894559, 0.3333333333333333703, 0.3219752754296894559, 0.3333333333333333703, 0.3219752754296894559, 0.3333333333333333703, 0.3219752754296894559, 0.3333333333333333703, 0.3219752754296894559, 0.3333333333333333703, 0.3219752754296894559, 0.3333333333333333703, 0.3219752754296894559, 0.3333333333333333703, 0.3219752754296894559, 0.3333333333333333703, 0.3219752754296894559, 0.3333333333333333703, 0.3219752754296894559, 0.3333333333333333703, 0.3219752754296894559, 0.3333333333333333703, 0.3219752754296894559, 0.3333333333333333703, 0.3219752754296894559, 0.3333333333333333703, 0.3219752754296894559, 0.3333333333333333703, 0.3219752754296894559, 0.3333333333333333703, 0.3219752754296894559, 0.3333333333333333703, 0.3219752754296894559, 0.3333333333333333703, 0.3219752754296894559, 0.3333333333333333703, 0.3219752754296894559, 0.3333333333333333703, 0.3219752754296894559, 0.3333333333333333703, 0.3219752754296894559, 0.3333333333333333703, 0.3219752754296894559, 0.3333333333333333703, 0.3219752754296894559, 0.3333333333333333703, 0.3219752754296894559, 0.3333333333333333703, 0.3219752754296894559, 0.3333333333333333703, 0.3219752754296894559, 0.3333333333333333703, 0.3219752754296894559, 0.3333333333333333703, 0.3219752754296894559, 0.3333333333333333703, 0.3219752754296894559, 0.3333333333333333703, 0.3219752754296894559, 0.3333333333333333703, 0.3219752754296894559, 0.3333333333333333703, 0.3219752754296894559, 0.3333333333333333703, 0.3219752754296894559, 0.3333333333333333703, 0.3219752754296894559, 0.3333333333333333703, 0.3219752754296894559, 0.3333333333333333703, 0.3219752754296894559, 0.3333333333333333703, 0.3219752754296894559, 0.3333333333333333703, 0.3219752754296894559, 0.3333333333333333703, 0.3219752754296894559, 0.3333333333333333703, 0.3219752754296894559, 0.3333333333333333703, 0.3219752754296894559, 0.3333333333333333703, 0.3219752754296894559, 0.3333333333333333703, 0.3219752754296894559, 0.3333333333333333703, 0.3219752754296894559, 0.3333333333333333703, 0.3219752754296894559, 0.3333333333333333703, 0.3219752754296894559, 0.3333333333333333703, 0.3219752754296894559, 0.3333333333333333703, 0.3219752754296894559, 0.3333333333333333703, 0.3219752754296894559, 0.3333333333333333703, 0.3219752754296894559, 0.3333333333333333703, 0.3219752754296894559, 0.3333333333333333703, 0.3219752754296894559, 0.3333333333333333703, 0.3219752754296894559, 0.3333333333333333703, 0.3219752754296894559, 0.3333333333333333703, 0.3219752754296894559, 0.3333333333333333703, 0.3219752754296894559, 0.3333333333333333703, 0.3219752754296894559, 0.3333333333333333703, 0.3219752754296894559, 0.3333333333333333703, 0.3219752754296894559, 0.3333333333333333703, 0.3219752754296894559, 0.3333333333333333703, 0.3219752754296894559, 0.3333333333333333703, 0.3219752754296894559, 0.3333333333333333703, 0.3219752754296894559, 0.3333333333333333703, 0.3219752754296894559, 0.3333333333333333703, 0.3219752754296894559, 0.3333333333333333703, 0.3219752754296894559, 0.3333333333333333703, 0.3219752754296894559, 0.3333333333333333703, 0.3219752754296894559, 0.3333333333333333703, 0.3219752754296894559, 0.3333333333333333703, 0.3219752754296894559, 0.3333333333333333703, 0.3219752754296894559, 0.3333333333333333703, 0.3219752754296894559, 0.3333333333333333703, 0.3219752754296894559, 0.3333333333333333703, 0.3219752754296894559, 0.3333333333333333703, 0.3219752754296894559, 0.3333333333333333703, 0.3219752754296894559, 0.3333333333333333703, 0.3219752754296894559, 0.3333333333333333703, 0.3219752754296894559, 0.3333333333333333703, 0.3219752754296894559, 0.3333333333333333703, 0.3219752754296894559, 0.3333333333333333703, 0.3219752754296894559, 0.3333333333333333703, 0.3219752754296894559, 0.3333333333333333703, 0.3219752754296894559, 0.3333333333333333703, 0.3219752754296894559, 0.3333333333333333703, 0.3219752754296894559, 0.3333333333333333703, 0.3219752754296894559, 0.3333333333333333703, 0.3219752754296894559, 0.3333333333333333703, 0.3219752754296894559, 0.3333333333333333703, 0.3219752754296894559, 0.3333333333333333703, 0.3219752754296894559, 0.3333333333333333703, 0.3219752754296894559, 0.3333333333333333703, 0.3219752754296894559, 0.3333333333333333703, 0.3219752754296894559, 0.3333333333333333703, 0.3219752754296894559, 0.3333333333333333703, 0.3219752754296894559, 0.3333333333333333703, 0.3219752754296894559, 0.3333333333333333703, 0.3219752754296894559, 0.3333333333333333703, 0.3219752754296894559, 0.3333333333333333703, 0.3219752754296894559, 0.3333333333333333703, 0.3219752754296894559, 0.3333333333333333703, 0.3219752754296894559, 0.3333333333333333703, 0.3219752754296894559, 0.3333333333333333703, 0.3219752754296894559, 0.3333333333333333703, 0.3219752754296894559, 0.3333333333333333703, 0.3219752754296894559, 0.3333333333333333703, 0.3219752754296894559, 0.3333333333333333703, 0.3219752754296894559, 0.3333333333333333703, 0.3219752754296894559, 0.3333333333333333703, 0.3219752754296894559, 0.3333333333333333703, 0.3219752754296894559, 0.3333333333333333703, 0.3219752754296894559, 0.3333333333333333703, 0.3219752754296894559, 0.3333333333333333703, 0.3219752754296894559, 0.3333333333333333703, 0.3219752754296894559, 0.3333333333333333703, 0.3219752754296894559, 0.3333333333333333703, 0.3219752754296894559, 0.3333333333333333703, 0.3219752754296894559, 0.3333333333333333703, 0.3219752754296894559, 0.3333333333333333703, 0.3219752754296894559, 0.3333333333333333703, 0.3219752754296894559, 0.3333333333333333703, 0.3219752754296894559, 0.3333333333333333703, 0.3219752754296894559, 0.3333333333333333703, 0.3219752754296894559, 0.3333333333333333703, 0.3219752754296894559, 0.3333333333333333703, 0.3219752754296894559, 0.3333333333333333703, 0.3219752754296894559, 0.3333333333333333703, 0.3219752754296894559, 0.3333333333333333703, 0.3219752754296894559, 0.3333333333333333703, 0.3219752754296894559, 0.3333333333333333703, 0.3219752754296894559, 0.3333333333333333703, 0.3219752754296894559, 0.3333333333333333703, 0.3219752754296894559, 0.3333333333333333703, 0.3219752754296894559, 0.3333333333333333703, 0.3219752754296894559, 0.3333333333333333703, 0.3219752754296894559, 0.3333333333333333703, 0.3219752754296894559, 0.3333333333333333703, 0.3219752754296894559, 0.3333333333333333703, 0.3219752754296894559, 0.3333333333333333703, 0.3219752754296894559, 0.3333333333333333703, 0.3219752754296894559, 0.3333333333333333703, 0.3219752754296894559, 0.3333333333333333703, 0.3219752754296894559, 0.3333333333333333703, 0.3219752754296894559, 0.3333333333333333703, 0.3219752754296894559, 0.3333333333333333703, 0.3219752754296894559, 0.3333333333333333703, 0.3219752754296894559, 0.3333333333333333703, 0.3219752754296894559, 0.3333333333333333703, 0.3219752754296894559, 0.3333333333333333703, 0.3219752754296894559, 0.3333333333333333703, 0.3219752754296894559, 0.3333333333333333703, 0.3219752754296894559, 0.3333333333333333703, 0.3219752754296894559, 0.3333333333333333703, 0.3219752754296894559, 0.3333333333333333703, 0.3219752754296894559, 0.3333333333333333703, 0.3219752754296894559, 0.3333333333333333703, 0.3219752754296894559, 0.3333333333333333703, 0.3219752754296894559, 0.3333333333333333703, 0.3219752754296894559, 0.3333333333333333703, 0.3219752754296894559, 0.3333333333333333703, 0.3219752754296894559, 0.3333333333333333703, 0.3219752754296894559, 0.3333333333333333703, 0.3219752754296894559, 0.3333333333333333703, 0.3219752754296894559, 0.3333333333333333703, 0.3219752754296894559, 0.3333333333333333703, 0.3219752754296894559, 0.3333333333333333703, 0.3219752754296894559, 0.3333333333333333703, 0.3219752754296894559, 0.3333333333333333703, 0.3219752754296894559, 0.3333333333333333703, 0.3219752754296894559, 0.3333333333333333703, 0.3219752754296894559, 0.3333333333333333703, 0.3219752754296894559, 0.3333333333333333703, 0.3219752754296894559, 0.3333333333333333703, 0.3219752754296894559, 0.3333333333333333703, 0.3219752754296894559, 0.3333333333333333703, 0.3219752754296894559, 0.3333333333333333703, 0.3219752754296894559, 0.3333333333333333703, 0.3219752754296894559, 0.3333333333333333703, 0.3219752754296894559, 0.3333333333333333703, 0.3219752754296894559, 0.3333333333333333703, 0.3219752754296894559, 0.3333333333333333703, 0.3219752754296894559, 0.3333333333333333703, 0.3219752754296894559, 0.3333333333333333703, 0.3219752754296894559, 0.3333333333333333703, 0.3219752754296894559, 0.3333333333333333703, 0.3219752754296894559, 0.3333333333333333703, 0.3219752754296894559, 0.3333333333333333703, 0.3219752754296894559, 0.3333333333333333703),
 ( 1.000000000000000000, 0.9659258262890683122, 1.000000000000000000, 0.9659258262890683122, 1.000000000000000000, 0.9659258262890683122, 1.000000000000000000, 0.9659258262890683122, 1.000000000000000000, 0.9659258262890683122, 1.000000000000000000, 0.9659258262890683122, 1.000000000000000000, 0.9659258262890683122, 1.000000000000000000, 0.9659258262890683122, 1.000000000000000000, 0.9659258262890683122, 1.000000000000000000, 0.9659258262890683122, 1.000000000000000000, 0.9659258262890683122, 1.000000000000000000, 0.9659258262890683122, 1.000000000000000000, 0.9659258262890683122, 1.000000000000000000, 0.9659258262890683122, 1.000000000000000000, 0.9659258262890683122, 1.000000000000000000, 0.9659258262890683122, 1.000000000000000000, 0.9659258262890683122, 1.000000000000000000, 0.9659258262890683122, 1.000000000000000000, 0.9659258262890683122, 1.000000000000000000, 0.9659258262890683122, 1.000000000000000000, 0.9659258262890683122, 1.000000000000000000, 0.9659258262890683122, 1.000000000000000000, 0.9659258262890683122, 1.000000000000000000, 0.9659258262890683122, 1.000000000000000000, 0.9659258262890683122, 1.000000000000000000, 0.9659258262890683122, 1.000000000000000000, 0.9659258262890683122, 1.000000000000000000, 0.9659258262890683122, 1.000000000000000000, 0.9659258262890683122, 1.000000000000000000, 0.9659258262890683122, 1.000000000000000000, 0.9659258262890683122, 1.000000000000000000, 0.9659258262890683122, 1.000000000000000000, 0.9659258262890683122, 1.000000000000000000, 0.9659258262890683122, 1.000000000000000000, 0.9659258262890683122, 1.000000000000000000, 0.9659258262890683122, 1.000000000000000000, 0.9659258262890683122, 1.000000000000000000, 0.9659258262890683122, 1.000000000000000000, 0.9659258262890683122, 1.000000000000000000, 0.9659258262890683122, 1.000000000000000000, 0.9659258262890683122, 1.000000000000000000, 0.9659258262890683122, 1.000000000000000000, 0.9659258262890683122, 1.000000000000000000, 0.9659258262890683122, 1.000000000000000000, 0.9659258262890683122, 1.000000000000000000, 0.9659258262890683122, 1.000000000000000000, 0.9659258262890683122, 1.000000000000000000, 0.9659258262890683122, 1.000000000000000000, 0.9659258262890683122, 1.000000000000000000, 0.9659258262890683122, 1.000000000000000000, 0.9659258262890683122, 1.000000000000000000, 0.9659258262890683122, 1.000000000000000000, 0.9659258262890683122, 1.000000000000000000, 0.9659258262890683122, 1.000000000000000000, 0.9659258262890683122, 1.000000000000000000, 0.9659258262890683122, 1.000000000000000000, 0.9659258262890683122, 1.000000000000000000, 0.9659258262890683122, 1.000000000000000000, 0.9659258262890683122, 1.000000000000000000, 0.9659258262890683122, 1.000000000000000000, 0.9659258262890683122, 1.000000000000000000, 0.9659258262890683122, 1.000000000000000000, 0.9659258262890683122, 1.000000000000000000, 0.9659258262890683122, 1.000000000000000000, 0.9659258262890683122, 1.000000000000000000, 0.9659258262890683122, 1.000000000000000000, 0.9659258262890683122, 1.000000000000000000, 0.9659258262890683122, 1.000000000000000000, 0.9659258262890683122, 1.000000000000000000, 0.9659258262890683122, 1.000000000000000000, 0.9659258262890683122, 1.000000000000000000, 0.9659258262890683122, 1.000000000000000000, 0.9659258262890683122, 1.000000000000000000, 0.9659258262890683122, 1.000000000000000000, 0.9659258262890683122, 1.000000000000000000, 0.9659258262890683122, 1.000000000000000000, 0.9659258262890683122, 1.000000000000000000, 0.9659258262890683122, 1.000000000000000000, 0.9659258262890683122, 1.000000000000000000, 0.9659258262890683122, 1.000000000000000000, 0.9659258262890683122, 1.000000000000000000, 0.9659258262890683122, 1.000000000000000000, 0.9659258262890683122, 1.000000000000000000, 0.9659258262890683122, 1.000000000000000000, 0.9659258262890683122, 1.000000000000000000, 0.9659258262890683122, 1.000000000000000000, 0.9659258262890683122, 1.000000000000000000, 0.9659258262890683122, 1.000000000000000000, 0.9659258262890683122, 1.000000000000000000, 0.9659258262890683122, 1.000000000000000000, 0.9659258262890683122, 1.000000000000000000, 0.9659258262890683122, 1.000000000000000000, 0.9659258262890683122, 1.000000000000000000, 0.9659258262890683122, 1.000000000000000000, 0.9659258262890683122, 1.000000000000000000, 0.9659258262890683122, 1.000000000000000000, 0.9659258262890683122, 1.000000000000000000, 0.9659258262890683122, 1.000000000000000000, 0.9659258262890683122, 1.000000000000000000, 0.9659258262890683122, 1.000000000000000000, 0.9659258262890683122, 1.000000000000000000, 0.9659258262890683122, 1.000000000000000000, 0.9659258262890683122, 1.000000000000000000, 0.9659258262890683122, 1.000000000000000000, 0.9659258262890683122, 1.000000000000000000, 0.9659258262890683122, 1.000000000000000000, 0.9659258262890683122, 1.000000000000000000, 0.9659258262890683122, 1.000000000000000000, 0.9659258262890683122, 1.000000000000000000, 0.9659258262890683122, 1.000000000000000000, 0.9659258262890683122, 1.000000000000000000, 0.9659258262890683122, 1.000000000000000000, 0.9659258262890683122, 1.000000000000000000, 0.9659258262890683122, 1.000000000000000000, 0.9659258262890683122, 1.000000000000000000, 0.9659258262890683122, 1.000000000000000000, 0.9659258262890683122, 1.000000000000000000, 0.9659258262890683122, 1.000000000000000000, 0.9659258262890683122, 1.000000000000000000, 0.9659258262890683122, 1.000000000000000000, 0.9659258262890683122, 1.000000000000000000, 0.9659258262890683122, 1.000000000000000000, 0.9659258262890683122, 1.000000000000000000, 0.9659258262890683122, 1.000000000000000000, 0.9659258262890683122, 1.000000000000000000, 0.9659258262890683122, 1.000000000000000000, 0.9659258262890683122, 1.000000000000000000, 0.9659258262890683122, 1.000000000000000000, 0.9659258262890683122, 1.000000000000000000, 0.9659258262890683122, 1.000000000000000000, 0.9659258262890683122, 1.000000000000000000, 0.9659258262890683122, 1.000000000000000000, 0.9659258262890683122, 1.000000000000000000, 0.9659258262890683122, 1.000000000000000000, 0.9659258262890683122, 1.000000000000000000, 0.9659258262890683122, 1.000000000000000000, 0.9659258262890683122, 1.000000000000000000, 0.9659258262890683122, 1.000000000000000000, 0.9659258262890683122, 1.000000000000000000, 0.9659258262890683122, 1.000000000000000000, 0.9659258262890683122, 1.000000000000000000, 0.9659258262890683122, 1.000000000000000000, 0.9659258262890683122, 1.000000000000000000, 0.9659258262890683122, 1.000000000000000000, 0.9659258262890683122, 1.000000000000000000, 0.9659258262890683122, 1.000000000000000000, 0.9659258262890683122, 1.000000000000000000, 0.9659258262890683122, 1.000000000000000000, 0.9659258262890683122, 1.000000000000000000, 0.9659258262890683122, 1.000000000000000000, 0.9659258262890683122, 1.000000000000000000, 0.9659258262890683122, 1.000000000000000000, 0.9659258262890683122, 1.000000000000000000, 0.9659258262890683122, 1.000000000000000000, 0.9659258262890683122, 1.000000000000000000, 0.9659258262890683122, 1.000000000000000000, 0.9659258262890683122, 1.000000000000000000, 0.9659258262890683122, 1.000000000000000000, 0.9659258262890683122, 1.000000000000000000, 0.9659258262890683122, 1.000000000000000000, 0.9659258262890683122, 1.000000000000000000, 0.9659258262890683122, 1.000000000000000000, 0.9659258262890683122, 1.000000000000000000, 0.9659258262890683122, 1.000000000000000000, 0.9659258262890683122, 1.000000000000000000, 0.9659258262890683122, 1.000000000000000000, 0.9659258262890683122, 1.000000000000000000, 0.9659258262890683122, 1.000000000000000000, 0.9659258262890683122, 1.000000000000000000, 0.9659258262890683122, 1.000000000000000000, 0.9659258262890683122, 1.000000000000000000, 0.9659258262890683122, 1.000000000000000000, 0.9659258262890683122, 1.000000000000000000, 0.9659258262890683122, 1.000000000000000000, 0.9659258262890683122, 1.000000000000000000, 0.9659258262890683122, 1.000000000000000000, 0.9659258262890683122, 1.000000000000000000, 0.9659258262890683122, 1.000000000000000000, 0.9659258262890683122, 1.000000000000000000, 0.9659258262890683122, 1.000000000000000000, 0.9659258262890683122, 1.000000000000000000, 0.9659258262890683122, 1.000000000000000000, 0.9659258262890683122, 1.000000000000000000, 0.9659258262890683122, 1.000000000000000000, 0.9659258262890683122, 1.000000000000000000, 0.9659258262890683122, 1.000000000000000000, 0.9659258262890683122, 1.000000000000000000, 0.9659258262890683122, 1.000000000000000000, 0.9659258262890683122, 1.000000000000000000, 0.9659258262890683122, 1.000000000000000000, 0.9659258262890683122, 1.000000000000000000, 0.9659258262890683122, 1.000000000000000000, 0.9659258262890683122, 1.000000000000000000, 0.9659258262890683122, 1.000000000000000000, 0.9659258262890683122, 1.000000000000000000, 0.9659258262890683122, 1.000000000000000000, 0.9659258262890683122, 1.000000000000000000, 0.9659258262890683122, 1.000000000000000000, 0.9659258262890683122, 1.000000000000000000, 0.9659258262890683122, 1.000000000000000000, 0.9659258262890683122, 1.000000000000000000, 0.9659258262890683122, 1.000000000000000000, 0.9659258262890683122, 1.000000000000000000, 0.9659258262890683122, 1.000000000000000000, 0.9659258262890683122, 1.000000000000000000, 0.9659258262890683122, 1.000000000000000000, 0.9659258262890683122, 1.000000000000000000, 0.9659258262890683122, 1.000000000000000000, 0.9659258262890683122, 1.000000000000000000, 0.9659258262890683122, 1.000000000000000000, 0.9659258262890683122, 1.000000000000000000, 0.9659258262890683122, 1.000000000000000000, 0.9659258262890683122, 1.000000000000000000, 0.9659258262890683122, 1.000000000000000000, 0.9659258262890683122, 1.000000000000000000, 0.9659258262890683122, 1.000000000000000000, 0.9659258262890683122, 1.000000000000000000, 0.9659258262890683122, 1.000000000000000000, 0.9659258262890683122, 1.000000000000000000, 0.9659258262890683122, 1.000000000000000000, 0.9659258262890683122, 1.000000000000000000, 0.9659258262890683122, 1.000000000000000000, 0.9659258262890683122, 1.000000000000000000, 0.9659258262890683122, 1.000000000000000000, 0.9659258262890683122, 1.000000000000000000, 0.9659258262890683122, 1.000000000000000000, 0.9659258262890683122, 1.000000000000000000, 0.9659258262890683122, 1.000000000000000000) ) ) 
 REPRESENTATION_ITEM ( '' )  SURFACE ( )  );
#33749 = CARTESIAN_POINT ( 'NONE',  ( -0.05219959533909027116, -19.03943276465977164, 42.49890960531435269 ) ) ;
#33750 = CARTESIAN_POINT ( 'NONE',  ( 4.379528057220092307, 16.55341960407617563, 82.29275706135234714 ) ) ;
#33751 = CARTESIAN_POINT ( 'NONE',  ( 5.823673210054125526, 21.52544592524343514, 104.7905762719810241 ) ) ;
#33752 = CARTESIAN_POINT ( 'NONE',  ( -14.34966873604960291, -8.224510206698953496, 51.66557627198102409 ) ) ;
#33753 = CARTESIAN_POINT ( 'NONE',  ( -9.474510206698964154, 16.51473224551069663, 70.41557627198102409 ) ) ;
#33754 = CARTESIAN_POINT ( 'NONE',  ( -8.224510206698735004, -14.34966873604973081, 74.58442372801901854 ) ) ;
#33755 = CARTESIAN_POINT ( 'NONE',  ( -4.379528057220086978, -16.55341960407618274, 19.79275706135235069 ) ) ;
#33756 = CARTESIAN_POINT ( 'NONE',  ( -21.52544592524343514, 5.823673210054127303, 111.0405762719810525 ) ) ;
#33757 = CARTESIAN_POINT ( 'NONE',  ( -16.55341960407611168, -4.379528057220339221, 41.45724293864769550 ) ) ;
#33758 = VERTEX_POINT ( 'NONE', #174448 ) ;
#33759 = CARTESIAN_POINT ( 'NONE',  ( -17.12812012977028431, 6.668231424565926879, 73.64051240676856480 ) ) ;
#33760 = CARTESIAN_POINT ( 'NONE',  ( -5.823673210054116645, -21.52544592524344225, 87.29057627198103830 ) ) ;
#33761 = CARTESIAN_POINT ( 'NONE',  ( 4.379528057220339221, -16.55341960407611168, 27.70724293864769905 ) ) ;
#33762 = ORIENTED_EDGE ( 'NONE', *, *, #94686, .F. ) ;
#33763 = FACE_OUTER_BOUND ( 'NONE', #130824, .T. ) ;
#33764 = CARTESIAN_POINT ( 'NONE',  ( -21.52544592524343514, 5.823673210054127303, 106.0405762719810525 ) ) ;
#33765 = CARTESIAN_POINT ( 'NONE',  ( 5.153800228976335163, 19.02544592524342804, 114.7905762719810241 ) ) ;
#33766 = CARTESIAN_POINT ( 'NONE',  ( 21.52544592524334988, 5.823673210054432836, 26.45942372801901854 ) ) ;
#33767 = CARTESIAN_POINT ( 'NONE',  ( -0.05219959533910754901, -16.53943276465976808, 47.49890960531435979 ) ) ;
#33768 = CARTESIAN_POINT ( 'NONE',  ( 8.224510206698742110, 14.34966873604972548, 52.08442372801901854 ) ) ;
#33769 = CARTESIAN_POINT ( 'NONE',  ( -9.564922557960796823, -16.46253265017161027, 52.08224293864768839 ) ) ;
#33770 = CARTESIAN_POINT ( 'NONE',  ( -19.05341960407617563, 5.049401038297882671, 48.54275706135233293 ) ) ;
#33771 = CARTESIAN_POINT ( 'NONE',  ( -5.049401038298153566, 19.05341960407611168, 85.20724293864766707 ) ) ;
#33772 = ORIENTED_EDGE ( 'NONE', *, *, #175018, .T. ) ;
#33773 = CARTESIAN_POINT ( 'NONE',  ( -0.05219959533907301413, -21.53943276465977519, 37.49890960531436690 ) ) ;
#33774 = CARTESIAN_POINT ( 'NONE',  ( -31.47295357026017726, -21.29310327862334518, -24.13113353489229596 ) ) ;
#33775 = CARTESIAN_POINT ( 'NONE',  ( -13.97604488694547697, 13.89961937509957934, 113.1260903946856757 ) ) ;
#33776 = CARTESIAN_POINT ( 'NONE',  ( -16.46253265017146816, -9.564922557961047289, 69.16775706135233293 ) ) ;
#33777 = CARTESIAN_POINT ( 'NONE',  ( 5.823673210054125526, 21.52544592524343514, 99.79057627198103830 ) ) ;
#33778 = CARTESIAN_POINT ( 'NONE',  ( -14.34966873604960291, -8.224510206698953496, 31.66557627198102054 ) ) ;
#33779 = CARTESIAN_POINT ( 'NONE',  ( -0.05219959533909027116, -19.03943276465977164, 77.49890960531435269 ) ) ;
#33780 = CARTESIAN_POINT ( 'NONE',  ( 5.823673210054125526, 21.52544592524343514, 59.79057627198103120 ) ) ;
#33782 = CARTESIAN_POINT ( 'NONE',  ( 12.14591786802327356, -12.06949235617739191, 20.62609039468568639 ) ) ;
#33781 = CARTESIAN_POINT ( 'NONE',  ( 18.67979575497178502, 10.72451020669898547, 94.16557627198103830 ) ) ;
#33783 = CARTESIAN_POINT ( 'NONE',  ( -19.03943276465977164, 0.05219959533909376836, 116.2489096053143669 ) ) ;
#33784 = CARTESIAN_POINT ( 'NONE',  ( -18.62759615963255300, -10.81492255796106328, 94.16775706135237556 ) ) ;
#33785 = CARTESIAN_POINT ( 'NONE',  ( 5.049401038298161559, -19.05341960407611168, 92.70724293864769550 ) ) ;
#33786 = CARTESIAN_POINT ( 'NONE',  ( 9.474510206698971260, -16.51473224551069308, 27.91557627198103120 ) ) ;
#33787 = CARTESIAN_POINT ( 'NONE',  ( 5.049401038298161559, -19.05341960407611168, 77.70724293864765286 ) ) ;
#33788 = CARTESIAN_POINT ( 'NONE',  ( 0.05219959533910956823, 16.53943276465976808, 99.99890960531436690 ) ) ;
#33789 = CARTESIAN_POINT ( 'NONE',  ( -16.46253265017160317, 9.564922557960807481, 60.83224293864769550 ) ) ;
#33790 = CARTESIAN_POINT ( 'NONE',  ( 4.379528057220092307, 16.55341960407617563, 22.29275706135235069 ) ) ;
#33791 = CARTESIAN_POINT ( 'NONE',  ( 17.50000000000000000, -5.499999999999992895, 86.21769037696435589 ) ) ;
#33792 = CARTESIAN_POINT ( 'NONE',  ( -9.474510206698964154, 16.51473224551069663, 70.41557627198102409 ) ) ;
#33794 = CARTESIAN_POINT ( 'NONE',  ( -0.05219959533907301413, -21.53943276465977519, 22.49890960531436335 ) ) ;
#33793 = CARTESIAN_POINT ( 'NONE',  ( -18.62759615963255300, -10.81492255796106328, 94.16775706135237556 ) ) ;
#33795 = CARTESIAN_POINT ( 'NONE',  ( 8.314922557961029526, -14.29746914071037800, 95.41775706135234714 ) ) ;
#33796 = CARTESIAN_POINT ( 'NONE',  ( -11.74264578624799782, -36.14014761921581709, -9.600000000000001421 ) ) ;
#33797 = CARTESIAN_POINT ( 'NONE',  ( 16.46253265017146816, 9.564922557961045513, 66.66775706135233293 ) ) ;
#33798 = CARTESIAN_POINT ( 'NONE',  ( -19.03943276465977164, -0.05219959533935918106, 18.75109039468567218 ) ) ;
#33799 = CARTESIAN_POINT ( 'NONE',  ( -16.52216118717206328, -7.221426719304521846, 46.07599021046992505 ) ) ;
#33800 = CARTESIAN_POINT ( 'NONE',  ( 9.474510206698971260, -16.51473224551069308, 27.91557627198103120 ) ) ;
#33801 = CARTESIAN_POINT ( 'NONE',  ( 8.224510206698953496, -14.34966873604960469, 42.91557627198103120 ) ) ;
#33802 = CARTESIAN_POINT ( 'NONE',  ( 1.820000000000000062, 0.000000000000000000, 0.000000000000000000 ) ) ;
#33803 = CARTESIAN_POINT ( 'NONE',  ( 4.483927247898790824, -16.52544592524335698, 105.2094237280190328 ) ) ;
#33804 = CARTESIAN_POINT ( 'NONE',  ( 21.56593590501845981, -19.98930001671141454, -52.11784087944676003 ) ) ;
#33805 = CARTESIAN_POINT ( 'NONE',  ( 14.34966873604972726, -8.224510206698740333, 80.83442372801901854 ) ) ;
#33806 = CARTESIAN_POINT ( 'NONE',  ( 5.049401038298161559, -19.05341960407611168, 32.70724293864768129 ) ) ;
#33807 = CARTESIAN_POINT ( 'NONE',  ( 10.81492255796106328, -18.62759615963255655, 95.41775706135234714 ) ) ;
#33808 = CARTESIAN_POINT ( 'NONE',  ( -19.05341960407617563, 5.049401038297882671, 98.54275706135233293 ) ) ;
#33809 = CARTESIAN_POINT ( 'NONE',  ( 21.52544592524334988, 5.823673210054432836, 76.45942372801901854 ) ) ;
#33810 = CARTESIAN_POINT ( 'NONE',  ( 9.564922557961047289, -16.46253265017146816, 55.41775706135234003 ) ) ;
#33811 = CARTESIAN_POINT ( 'NONE',  ( -0.05219959533909027116, -19.03943276465977164, 77.49890960531435269 ) ) ;
#33812 = CARTESIAN_POINT ( 'NONE',  ( 9.474510206698971260, -16.51473224551069308, 72.91557627198102409 ) ) ;
#33813 = CARTESIAN_POINT ( 'NONE',  ( 16.88567814943160883, 6.947325034625710494, 73.79001122652587696 ) ) ;
#33814 = CARTESIAN_POINT ( 'NONE',  ( 16.55341960407611168, 4.379528057220329451, 63.95724293864770260 ) ) ;
#33815 = CARTESIAN_POINT ( 'NONE',  ( -21.55341960407610458, -5.719274019375992779, 61.45724293864770260 ) ) ;
#33816 = CARTESIAN_POINT ( 'NONE',  ( 9.474510206698971260, -16.51473224551069308, 42.91557627198103120 ) ) ;
#33818 = CARTESIAN_POINT ( 'NONE',  ( -4.483927247898782831, 16.52544592524335698, 77.70942372801900433 ) ) ;
#33817 = CARTESIAN_POINT ( 'NONE',  ( -21.53943276465977519, 0.05219959533907696930, 86.24890960531436690 ) ) ;
#33819 = EDGE_CURVE ( 'NONE', #190522, #188457, #179887, .T. ) ;
#33820 = ORIENTED_EDGE ( 'NONE', *, *, #148013, .T. ) ;
#33822 = CARTESIAN_POINT ( 'NONE',  ( -36.91746825000001309, -11.99521256947794789, -6.524999997268810858 ) ) ;
#33821 = CARTESIAN_POINT ( 'NONE',  ( 12.06949235617757843, -12.14591786802309237, 73.12390960531436690 ) ) ;
#33823 = CARTESIAN_POINT ( 'NONE',  ( -13.97604488694527625, -13.89961937509977652, 46.87390960531435979 ) ) ;
#33824 = CARTESIAN_POINT ( 'NONE',  ( -12.14591786802309592, -12.06949235617757132, 111.8739096053143669 ) ) ;
#33825 = CARTESIAN_POINT ( 'NONE',  ( 0.05219959533936267826, -19.03943276465977164, 70.00109039468566152 ) ) ;
#33826 = CARTESIAN_POINT ( 'NONE',  ( 16.52544592524342804, -4.483927247898539470, 73.54057627198102409 ) ) ;
#33827 = CARTESIAN_POINT ( 'NONE',  ( 5.823673210054444382, -21.52544592524334988, 40.20942372801901854 ) ) ;
#33829 = CARTESIAN_POINT ( 'NONE',  ( 21.53943276465977519, -0.05219959533907433946, 98.74890960531438111 ) ) ;
#33828 = CARTESIAN_POINT ( 'NONE',  ( -19.05341960407611168, -5.049401038298163336, 21.45724293864768839 ) ) ;
#33830 = CARTESIAN_POINT ( 'NONE',  ( 16.51473224551069308, 9.474510206698969483, 114.1655762719810241 ) ) ;
#33831 = CARTESIAN_POINT ( 'NONE',  ( -4.379528057220328563, 16.55341960407611168, 85.20724293864770971 ) ) ;
#33832 = CARTESIAN_POINT ( 'NONE',  ( 14.22875182907821490, -42.06737590809383676, -22.02417070750506412 ) ) ;
#33833 = CARTESIAN_POINT ( 'NONE',  ( -19.03943276465977164, 0.05219959533909376836, 41.24890960531435269 ) ) ;
#33834 = CARTESIAN_POINT ( 'NONE',  ( -11.40812507854755609, 35.11059874428196537, -5.024999997268813523 ) ) ;
#33835 = CARTESIAN_POINT ( 'NONE',  ( 19.05341960407617918, -5.049401038297876454, 86.04275706135233293 ) ) ;
#33836 = CARTESIAN_POINT ( 'NONE',  ( -5.823673210054431948, 21.52544592524334988, 37.70942372801900433 ) ) ;
#33837 = CARTESIAN_POINT ( 'NONE',  ( 5.153800228976335163, 19.02544592524342804, 69.79057627198103830 ) ) ;
#33838 = CARTESIAN_POINT ( 'NONE',  ( 5.049401038297881783, 19.05341960407617563, 57.29275706135231871 ) ) ;
#33839 = CARTESIAN_POINT ( 'NONE',  ( 5.049401038298161559, -19.05341960407611168, 47.70724293864770260 ) ) ;
#33840 = CARTESIAN_POINT ( 'NONE',  ( 14.34966873604960469, 8.224510206698951720, 59.16557627198103120 ) ) ;
#33841 = CARTESIAN_POINT ( 'NONE',  ( -16.53943276465976808, 0.05219959533911058130, 61.24890960531435979 ) ) ;
#33842 = CARTESIAN_POINT ( 'NONE',  ( 9.564922557960805705, 16.46253265017160317, 69.58224293864770971 ) ) ;
#33843 = CARTESIAN_POINT ( 'NONE',  ( -18.62759615963270932, 10.81492255796079327, 100.8322429386477097 ) ) ;
#33844 = CARTESIAN_POINT ( 'NONE',  ( -19.02544592524342804, 5.153800228976336051, 76.04057627198102409 ) ) ;
#33845 = CARTESIAN_POINT ( 'NONE',  ( -10.72451020669898014, 18.67979575497178502, 85.41557627198102409 ) ) ;
#33846 = CARTESIAN_POINT ( 'NONE',  ( -13.89961937509957401, -13.97604488694547875, 19.37609039468566507 ) ) ;
#33849 = CARTESIAN_POINT ( 'NONE',  ( -0.05219959533910754901, -16.53943276465976808, 102.4989096053143811 ) ) ;
#33848 = CARTESIAN_POINT ( 'NONE',  ( 14.34966873604972726, -8.224510206698740333, 105.8344237280190328 ) ) ;
#33847 = CARTESIAN_POINT ( 'NONE',  ( -13.97604488694527625, -13.89961937509977652, 36.87390960531436690 ) ) ;
#33850 = CARTESIAN_POINT ( 'NONE',  ( -19.02544592524334988, -5.153800228976617603, 103.9594237280190043 ) ) ;
#33851 = ORIENTED_EDGE ( 'NONE', *, *, #198419, .F. ) ;
#33852 = CARTESIAN_POINT ( 'NONE',  ( 5.823673210054444382, -21.52544592524334988, 35.20942372801901854 ) ) ;
#33853 = CARTESIAN_POINT ( 'NONE',  ( -19.05341960407617563, 5.049401038297882671, 48.54275706135233293 ) ) ;
#33854 = CARTESIAN_POINT ( 'NONE',  ( 0.05219959533910956823, 16.53943276465976808, 24.99890960531435624 ) ) ;
#33855 = CARTESIAN_POINT ( 'NONE',  ( -5.719274019375978568, 21.55341960407610458, 75.20724293864769550 ) ) ;
#33856 = CARTESIAN_POINT ( 'NONE',  ( 9.474510206698971260, -16.51473224551069308, 97.91557627198102409 ) ) ;
#33857 = CARTESIAN_POINT ( 'NONE',  ( -4.379528057220328563, 16.55341960407611168, 50.20724293864769550 ) ) ;
#33858 = CARTESIAN_POINT ( 'NONE',  ( -19.02544592524342804, 5.153800228976336051, 26.04057627198103120 ) ) ;
#33859 = CARTESIAN_POINT ( 'NONE',  ( 19.02544592524343514, -5.153800228976328945, 28.54057627198102409 ) ) ;
#33860 = CARTESIAN_POINT ( 'NONE',  ( -9.474510206698720793, -16.51473224551083518, 29.58442372801900433 ) ) ;
#33861 = CARTESIAN_POINT ( 'NONE',  ( -8.314922557961024197, 14.29746914071037800, 92.91775706135236135 ) ) ;
#33862 = CARTESIAN_POINT ( 'NONE',  ( 15.72974639402176855, 15.80617190586768217, 36.87609039468568994 ) ) ;
#33863 = CARTESIAN_POINT ( 'NONE',  ( 12.14591786802327356, -12.06949235617739191, 45.62609039468567573 ) ) ;
#33864 = CARTESIAN_POINT ( 'NONE',  ( 15.80617190586746368, 15.72974639402197994, 29.37390960531435269 ) ) ;
#33866 = CARTESIAN_POINT ( 'NONE',  ( 10.72451020669871369, 18.67979575497193778, 92.08442372801901854 ) ) ;
#33865 = CARTESIAN_POINT ( 'NONE',  ( -0.05219959533909027116, -19.03943276465977164, 52.49890960531436690 ) ) ;
#33867 = CARTESIAN_POINT ( 'NONE',  ( -19.02544592524342804, 5.153800228976336051, 76.04057627198102409 ) ) ;
#33868 = AXIS2_PLACEMENT_3D ( 'NONE', #28121, #73617, #42281 ) ;
#33869 = CARTESIAN_POINT ( 'NONE',  ( 4.483927247898790824, -16.52544592524335698, 65.20942372801901854 ) ) ;
#33870 = CARTESIAN_POINT ( 'NONE',  ( 4.483927247898545687, 16.52544592524342804, 109.7905762719810383 ) ) ;
#33871 = CARTESIAN_POINT ( 'NONE',  ( -14.34966873604960291, -8.224510206698953496, 21.66557627198102409 ) ) ;
#33872 = FACE_OUTER_BOUND ( 'NONE', #199222, .T. ) ;
#33875 = CARTESIAN_POINT ( 'NONE',  ( 16.46253265017160672, -9.564922557960803928, 78.33224293864769550 ) ) ;
#33874 = CARTESIAN_POINT ( 'NONE',  ( -9.474510206698964154, 16.51473224551069663, 95.41557627198102409 ) ) ;
#33873 = CARTESIAN_POINT ( 'NONE',  ( -18.67979575497193778, 10.72451020669871902, 68.33442372801900433 ) ) ;
#33876 = CARTESIAN_POINT ( 'NONE',  ( 9.564922557960805705, 16.46253265017160317, 109.5822429386476955 ) ) ;
#33877 = CARTESIAN_POINT ( 'NONE',  ( 14.34966873604960469, 8.224510206698951720, 59.16557627198103120 ) ) ;
#33878 = CARTESIAN_POINT ( 'NONE',  ( 0.05219959533910956823, 16.53943276465976808, 24.99890960531435624 ) ) ;
#33879 = CARTESIAN_POINT ( 'NONE',  ( 12.14591786802309770, 12.06949235617756955, 44.37390960531435979 ) ) ;
#33882 =( GEOMETRIC_REPRESENTATION_CONTEXT ( 3 ) GLOBAL_UNCERTAINTY_ASSIGNED_CONTEXT ( ( #19643 ) ) GLOBAL_UNIT_ASSIGNED_CONTEXT ( ( #1328, #108521, #121702 ) ) REPRESENTATION_CONTEXT ( 'NONE', 'WORKASPACE' ) );
#33881 = CARTESIAN_POINT ( 'NONE',  ( -27.49873734152897953, 21.99873734152939875, 8.181980515339454030 ) ) ;
#33880 = CARTESIAN_POINT ( 'NONE',  ( 16.55341960407618274, -4.379528057220086978, 46.04275706135234714 ) ) ;
#33883 = CARTESIAN_POINT ( 'NONE',  ( 16.46253265017146816, 9.564922557961045513, 36.66775706135233293 ) ) ;
#33884 = CARTESIAN_POINT ( 'NONE',  ( 19.03943276465977164, -0.05219959533909143690, 73.74890960531435269 ) ) ;
#33885 = CARTESIAN_POINT ( 'NONE',  ( 19.03943276465977164, 0.05219959533936151252, 56.25109039468566863 ) ) ;
#33886 = CARTESIAN_POINT ( 'NONE',  ( -22.81625015709509441, -31.40387420917324590, -8.824999997268811569 ) ) ;
#33887 = CARTESIAN_POINT ( 'NONE',  ( 11.30153831258469843, -180.0000000000000000, -13.00000000000000000 ) ) ;
#33888 = VECTOR ( 'NONE', #60906, 1000.000000000000000 ) ;
#33890 = CARTESIAN_POINT ( 'NONE',  ( 16.53943276465976808, 0.05219959533934440121, 86.25109039468568994 ) ) ;
#33889 = CARTESIAN_POINT ( 'NONE',  ( -19.03943276465977164, -0.05219959533935918106, 88.75109039468567573 ) ) ;
#33891 = CARTESIAN_POINT ( 'NONE',  ( -19.02544592524342804, 5.153800228976336051, 101.0405762719810241 ) ) ;
#33892 = CARTESIAN_POINT ( 'NONE',  ( -21.53943276465977519, -0.05219959533937600094, 23.75109039468567929 ) ) ;
#33893 = CARTESIAN_POINT ( 'NONE',  ( 0.05219959533936267826, -19.03943276465977164, 95.00109039468567573 ) ) ;
#33895 = CARTESIAN_POINT ( 'NONE',  ( -19.02544592524342804, 5.153800228976336051, 51.04057627198103120 ) ) ;
#33894 = CARTESIAN_POINT ( 'NONE',  ( -17.49999999999999645, 5.499999999999997335, 35.79690382534171533 ) ) ;
#33896 = CARTESIAN_POINT ( 'NONE',  ( -9.474510206698964154, 16.51473224551069663, 100.4155762719810241 ) ) ;
#33898 = CARTESIAN_POINT ( 'NONE',  ( -13.89961937509977652, 13.97604488694528158, 50.62390960531435979 ) ) ;
#33897 = CARTESIAN_POINT ( 'NONE',  ( 12.14591786802309770, 12.06949235617756955, 64.37390960531435269 ) ) ;
#33899 = CARTESIAN_POINT ( 'NONE',  ( 9.474510206698971260, -16.51473224551069308, 62.91557627198102409 ) ) ;
#33900 = CARTESIAN_POINT ( 'NONE',  ( -19.03943276465977164, -0.05219959533935918106, 68.75109039468566152 ) ) ;
#33901 = CARTESIAN_POINT ( 'NONE',  ( -19.05341960407617563, 5.049401038297882671, 33.54275706135231871 ) ) ;
#33902 = CARTESIAN_POINT ( 'NONE',  ( -16.51473224551069308, -9.474510206698971260, 66.66557627198102409 ) ) ;
#33903 = CARTESIAN_POINT ( 'NONE',  ( 10.72451020669898902, -18.67979575497178502, 72.91557627198103830 ) ) ;
#33905 = CARTESIAN_POINT ( 'NONE',  ( -19.03943276465977164, -0.05219959533935918106, 38.75109039468566152 ) ) ;
#33904 = CARTESIAN_POINT ( 'NONE',  ( 16.55341960407611168, 4.379528057220329451, 68.95724293864769550 ) ) ;
#33906 = DIRECTION ( 'NONE',  ( 0.000000000000000000, 0.000000000000000000, -1.000000000000000000 ) ) ;
#33907 = CARTESIAN_POINT ( 'NONE',  ( 5.823673210054125526, 21.52544592524343514, 49.79057627198102409 ) ) ;
#33908 = CARTESIAN_POINT ( 'NONE',  ( 5.719274019375991003, -21.55341960407610458, 27.70724293864769905 ) ) ;
#33909 = CARTESIAN_POINT ( 'NONE',  ( -9.564922557960796823, -16.46253265017161027, 57.08224293864769550 ) ) ;
#33910 = CARTESIAN_POINT ( 'NONE',  ( 5.153800228976335163, 19.02544592524342804, 44.79057627198103830 ) ) ;
#33911 = CARTESIAN_POINT ( 'NONE',  ( 0.05219959533910956823, 16.53943276465976808, 104.9989096053143669 ) ) ;
#33912 = AXIS2_PLACEMENT_3D ( 'NONE', #137756, #62894, #167124 ) ;
#33913 = CARTESIAN_POINT ( 'NONE',  ( -10.72451020669898014, 18.67979575497178502, 115.4155762719810241 ) ) ;
#33914 = DIRECTION ( 'NONE',  ( 1.000000000000000000, 0.000000000000000000, 0.000000000000000000 ) ) ;
#33915 = CARTESIAN_POINT ( 'NONE',  ( 0.05219959533937995610, -21.53943276465977519, 25.00109039468567218 ) ) ;
#33916 = CARTESIAN_POINT ( 'NONE',  ( 5.153800228976335163, 19.02544592524342804, 24.79057627198102765 ) ) ;
#33917 = CARTESIAN_POINT ( 'NONE',  ( -10.81492255796078084, -18.62759615963271287, 97.08224293864770971 ) ) ;
#33918 = CARTESIAN_POINT ( 'NONE',  ( -5.153800228976607833, 19.02544592524334988, 42.70942372801901143 ) ) ;
#33919 = CARTESIAN_POINT ( 'NONE',  ( 18.22780087662122384, -5.500000000000022204, 76.01540105326107266 ) ) ;
#33920 = CARTESIAN_POINT ( 'NONE',  ( 19.25663599770060586, -5.499999999999438671, 76.49419308057197497 ) ) ;
#33921 = DIRECTION ( 'NONE',  ( -1.000000000000000000, 0.000000000000000000, 0.000000000000000000 ) ) ;
#33922 = CARTESIAN_POINT ( 'NONE',  ( -4.483927247898782831, 16.52544592524335698, 42.70942372801901854 ) ) ;
#33923 = CARTESIAN_POINT ( 'NONE',  ( -12.06949235617756955, 12.14591786802309770, 115.6239096053143669 ) ) ;
#33924 = LINE ( 'NONE', #95581, #106449 ) ;
#33925 = CARTESIAN_POINT ( 'NONE',  ( 19.03943276465977164, -0.05219959533909143690, 68.74890960531436690 ) ) ;
#33926 = CARTESIAN_POINT ( 'NONE',  ( 16.55341960407611168, 4.379528057220329451, 103.9572429386476813 ) ) ;
#33927 = CARTESIAN_POINT ( 'NONE',  ( -5.719274019375978568, 21.55341960407610458, 40.20724293864769550 ) ) ;
#33928 = CARTESIAN_POINT ( 'NONE',  ( -4.483927247898539470, -16.52544592524342804, 77.29057627198102409 ) ) ;
#33929 = CARTESIAN_POINT ( 'NONE',  ( -0.05219959533934338120, 16.53943276465976808, 32.50109039468568284 ) ) ;
#33930 = CARTESIAN_POINT ( 'NONE',  ( -0.05219959533937732626, 21.53943276465977519, 92.50109039468567573 ) ) ;
#33931 = CARTESIAN_POINT ( 'NONE',  ( -19.05341960407611168, -5.049401038298163336, 21.45724293864768839 ) ) ;
#33932 = CARTESIAN_POINT ( 'NONE',  ( 16.52544592524335698, 4.483927247898782831, 106.4594237280190328 ) ) ;
#33933 = CARTESIAN_POINT ( 'NONE',  ( -16.52544592524342804, 4.483927247898546575, 46.04057627198103830 ) ) ;
#33934 = CARTESIAN_POINT ( 'NONE',  ( -13.97604488694527625, -13.89961937509977652, 51.87390960531436690 ) ) ;
#33935 = CARTESIAN_POINT ( 'NONE',  ( -18.67979575497193778, 10.72451020669871902, 98.33442372801901854 ) ) ;
#33936 = CARTESIAN_POINT ( 'NONE',  ( -21.55341960407610458, -5.719274019375992779, 106.4572429386477097 ) ) ;
#33937 = CARTESIAN_POINT ( 'NONE',  ( -5.823673210054431948, 21.52544592524334988, 67.70942372801901854 ) ) ;
#33938 = CARTESIAN_POINT ( 'NONE',  ( -12.06949235617739369, -12.14591786802326823, 34.37609039468568284 ) ) ;
#33940 = CARTESIAN_POINT ( 'NONE',  ( 10.72451020669871369, 18.67979575497193778, 87.08442372801901854 ) ) ;
#33939 = CARTESIAN_POINT ( 'NONE',  ( 0.05219959533910956823, 16.53943276465976808, 79.99890960531435269 ) ) ;
#33941 = CARTESIAN_POINT ( 'NONE',  ( -12.14591786802326823, 12.06949235617739902, 108.1260903946856757 ) ) ;
#33942 = CARTESIAN_POINT ( 'NONE',  ( -19.05341960407611168, -5.049401038298163336, 21.45724293864768839 ) ) ;
#33943 = DIRECTION ( 'NONE',  ( 0.7071067811865485719, -2.775557561562891351E-15, 0.7071067811865465735 ) ) ;
#33944 = CARTESIAN_POINT ( 'NONE',  ( -8.314922557960811034, -14.29746914071050412, 37.08224293864768129 ) ) ;
#33945 = CARTESIAN_POINT ( 'NONE',  ( -14.34966873604972548, 8.224510206698743886, 73.33442372801901854 ) ) ;
#33946 = CARTESIAN_POINT ( 'NONE',  ( 5.153800228976335163, 19.02544592524342804, 84.79057627198099567 ) ) ;
#33947 = CARTESIAN_POINT ( 'NONE',  ( 19.05341960407611168, 5.049401038298154454, 93.95724293864769550 ) ) ;
#33948 = CARTESIAN_POINT ( 'NONE',  ( -15.72974639402176322, -15.80617190586768395, 104.3760903946856899 ) ) ;
#33949 = CARTESIAN_POINT ( 'NONE',  ( -8.224510206698735004, -14.34966873604973081, 104.5844237280190185 ) ) ;
#33950 = CARTESIAN_POINT ( 'NONE',  ( -0.05219959533910754901, -16.53943276465976808, 67.49890960531436690 ) ) ;
#33951 = CARTESIAN_POINT ( 'NONE',  ( -19.05341960407611168, -5.049401038298163336, 81.45724293864769550 ) ) ;
#33952 = ORIENTED_EDGE ( 'NONE', *, *, #183981, .F. ) ;
#33953 = CARTESIAN_POINT ( 'NONE',  ( 4.379528057220092307, 16.55341960407617563, 32.29275706135235424 ) ) ;
#33954 = CARTESIAN_POINT ( 'NONE',  ( -16.46253265017160317, 9.564922557960807481, 30.83224293864769550 ) ) ;
#33955 = CARTESIAN_POINT ( 'NONE',  ( 19.03943276465977164, -0.05219959533909143690, 93.74890960531435269 ) ) ;
#33957 = CARTESIAN_POINT ( 'NONE',  ( 11.40812507854754365, 35.11059874428196537, -5.224999997268813701 ) ) ;
#33956 = CARTESIAN_POINT ( 'NONE',  ( -0.05219959533934338120, 16.53943276465976808, 27.50109039468567929 ) ) ;
#33958 = CARTESIAN_POINT ( 'NONE',  ( -19.02544592524334988, -5.153800228976617603, 23.95942372801900078 ) ) ;
#33959 = CARTESIAN_POINT ( 'NONE',  ( 16.55341960407618274, -4.379528057220086978, 91.04275706135236135 ) ) ;
#33960 = CARTESIAN_POINT ( 'NONE',  ( -19.05341960407617563, 5.049401038297882671, 108.5427570613523187 ) ) ;
#33961 = CARTESIAN_POINT ( 'NONE',  ( -16.46253265017160317, 9.564922557960807481, 35.83224293864768839 ) ) ;
#33962 = CARTESIAN_POINT ( 'NONE',  ( -14.29746914071037622, -8.314922557961029526, 79.16775706135234714 ) ) ;
#33963 = CARTESIAN_POINT ( 'NONE',  ( 16.52544592524335698, 4.483927247898782831, 66.45942372801903275 ) ) ;
#33964 = CARTESIAN_POINT ( 'NONE',  ( 5.153800228976335163, 19.02544592524342804, 24.79057627198102765 ) ) ;
#33965 = CARTESIAN_POINT ( 'NONE',  ( -5.153800228976607833, 19.02544592524334988, 62.70942372801899722 ) ) ;
#33966 = VECTOR ( 'NONE', #8413, 1000.000000000000000 ) ;
#33967 = CARTESIAN_POINT ( 'NONE',  ( 19.02544592524334988, 5.153800228976608722, 21.45942372801899012 ) ) ;
#33968 = CARTESIAN_POINT ( 'NONE',  ( 19.02544592524343514, -5.153800228976328945, 48.54057627198103120 ) ) ;
#33969 = CARTESIAN_POINT ( 'NONE',  ( 5.049401038298161559, -19.05341960407611168, 97.70724293864766707 ) ) ;
#33970 = CARTESIAN_POINT ( 'NONE',  ( -0.05219959533910754901, -16.53943276465976808, 87.49890960531436690 ) ) ;
#33971 = CARTESIAN_POINT ( 'NONE',  ( -9.564922557961040184, 16.46253265017147172, 57.91775706135233293 ) ) ;
#33972 = CARTESIAN_POINT ( 'NONE',  ( 10.72451020669898902, -18.67979575497178502, 47.91557627198102409 ) ) ;
#33973 = CARTESIAN_POINT ( 'NONE',  ( -18.62759615963255300, -10.81492255796106328, 109.1677570613523613 ) ) ;
#33974 = CARTESIAN_POINT ( 'NONE',  ( 0.05219959533909260263, 19.03943276465977164, 94.99890960531436690 ) ) ;
#33975 = ADVANCED_FACE ( 'NONE', ( #68246 ), #36908, .T. ) ;
#33976 = CARTESIAN_POINT ( 'NONE',  ( -21.53943276465977519, -0.05219959533937600094, 108.7510903946857042 ) ) ;
#33977 = CARTESIAN_POINT ( 'NONE',  ( 5.719274019375991003, -21.55341960407610458, 67.70724293864769550 ) ) ;
#33978 = CARTESIAN_POINT ( 'NONE',  ( -19.03943276465977164, 0.05219959533909376836, 116.2489096053143669 ) ) ;
#33979 = CARTESIAN_POINT ( 'NONE',  ( -0.05219959533936034679, 19.03943276465977164, 82.50109039468567573 ) ) ;
#33980 = CARTESIAN_POINT ( 'NONE',  ( -13.97604488694527625, -13.89961937509977652, 111.8739096053143243 ) ) ;
#33981 = CARTESIAN_POINT ( 'NONE',  ( -16.53943276465976808, -0.05219959533934237506, 18.75109039468568639 ) ) ;
#33982 = CARTESIAN_POINT ( 'NONE',  ( -16.53943276465976808, 0.05219959533911058130, 116.2489096053143669 ) ) ;
#33983 = CARTESIAN_POINT ( 'NONE',  ( 19.02544592524343514, -5.153800228976328945, 83.54057627198100988 ) ) ;
#33984 = CARTESIAN_POINT ( 'NONE',  ( 21.53943276465977519, -0.05219959533907433946, 78.74890960531436690 ) ) ;
#33985 = CARTESIAN_POINT ( 'NONE',  ( -14.29746914071037622, -8.314922557961029526, 49.16775706135234003 ) ) ;
#33986 = CARTESIAN_POINT ( 'NONE',  ( 18.62759615963255655, 10.81492255796105972, 46.66775706135234714 ) ) ;
#33987 = CARTESIAN_POINT ( 'NONE',  ( 0.05219959533937995610, -21.53943276465977519, 100.0010903946857042 ) ) ;
#33988 = CARTESIAN_POINT ( 'NONE',  ( -12.14591786802326823, 12.06949235617739902, 93.12609039468568994 ) ) ;
#33989 = CARTESIAN_POINT ( 'NONE',  ( -0.05219959533909027116, -19.03943276465977164, 92.49890960531436690 ) ) ;
#33990 = CARTESIAN_POINT ( 'NONE',  ( -16.52544592524342804, 4.483927247898546575, 91.04057627198103830 ) ) ;
#33991 = CARTESIAN_POINT ( 'NONE',  ( 0.05219959533934541429, -16.53943276465976808, 110.0010903946856757 ) ) ;
#33992 = CARTESIAN_POINT ( 'NONE',  ( 9.474510206698729675, 16.51473224551082808, 67.08442372801900433 ) ) ;
#33993 = CARTESIAN_POINT ( 'NONE',  ( 21.52544592524334988, 5.823673210054432836, 46.45942372801901854 ) ) ;
#33994 = CARTESIAN_POINT ( 'NONE',  ( 16.51473224551083163, -9.474510206698727899, 25.83442372801900078 ) ) ;
#33995 = CARTESIAN_POINT ( 'NONE',  ( -14.34966873604960291, -8.224510206698953496, 91.66557627198103830 ) ) ;
#33996 = CARTESIAN_POINT ( 'NONE',  ( 10.72451020669898902, -18.67979575497178502, 22.91557627198102765 ) ) ;
#33997 = CARTESIAN_POINT ( 'NONE',  ( -16.52544592524342804, 4.483927247898546575, 26.04057627198103475 ) ) ;
#33998 = CARTESIAN_POINT ( 'NONE',  ( -5.719274019375665041, -21.55341960407619695, 79.79275706135236135 ) ) ;
#33999 = CARTESIAN_POINT ( 'NONE',  ( -12.14591786802326823, 12.06949235617739902, 58.12609039468568994 ) ) ;
#34000 = CARTESIAN_POINT ( 'NONE',  ( 4.483927247898790824, -16.52544592524335698, 105.2094237280190328 ) ) ;
#34001 = CARTESIAN_POINT ( 'NONE',  ( 21.52544592524334988, 5.823673210054432836, 56.45942372801902565 ) ) ;
#34002 = ORIENTED_EDGE ( 'NONE', *, *, #16626, .F. ) ;
#34003 = CARTESIAN_POINT ( 'NONE',  ( -21.55341960407619339, 5.719274019375674811, 28.54275706135234358 ) ) ;
#34004 = CARTESIAN_POINT ( 'NONE',  ( 12.14591786802309770, 12.06949235617756955, 109.3739096053143811 ) ) ;
#34005 = CARTESIAN_POINT ( 'NONE',  ( -19.02544592524342804, 5.153800228976336051, 31.04057627198102409 ) ) ;
#34006 = CARTESIAN_POINT ( 'NONE',  ( -14.29746914071049879, 8.314922557960819915, 70.83224293864770971 ) ) ;
#34007 = CARTESIAN_POINT ( 'NONE',  ( -9.474510206698964154, 16.51473224551069663, 70.41557627198102409 ) ) ;
#34008 = CARTESIAN_POINT ( 'NONE',  ( -14.34966873604972548, 8.224510206698743886, 108.3344237280190185 ) ) ;
#34009 = CARTESIAN_POINT ( 'NONE',  ( 16.46253265017160672, -9.564922557960803928, 43.33224293864769550 ) ) ;
#34010 = CARTESIAN_POINT ( 'NONE',  ( -10.72451020669898014, 18.67979575497178502, 55.41557627198102409 ) ) ;
#34011 = CARTESIAN_POINT ( 'NONE',  ( -16.52544592524342804, 4.483927247898546575, 91.04057627198103830 ) ) ;
#34012 = AXIS2_PLACEMENT_3D ( 'NONE', #35382, #22208, #49560 ) ;
#34013 = CARTESIAN_POINT ( 'NONE',  ( 15.80617190586746368, 15.72974639402197994, 94.37390960531436690 ) ) ;
#34014 = CARTESIAN_POINT ( 'NONE',  ( 16.46253265017160672, -9.564922557960803928, 98.33224293864769550 ) ) ;
#34016 = CARTESIAN_POINT ( 'NONE',  ( 19.02544592524334988, 5.153800228976608722, 96.45942372801897591 ) ) ;
#34015 = CARTESIAN_POINT ( 'NONE',  ( 16.46253265017160672, -9.564922557960803928, 48.33224293864769550 ) ) ;
#34017 = CARTESIAN_POINT ( 'NONE',  ( -10.72451020669898014, 18.67979575497178502, 45.41557627198103830 ) ) ;
#34018 = CARTESIAN_POINT ( 'NONE',  ( 18.67979575497194134, -10.72451020669871369, 65.83442372801900433 ) ) ;
#34019 = CARTESIAN_POINT ( 'NONE',  ( 5.049401038298161559, -19.05341960407611168, 52.70724293864767418 ) ) ;
#34020 = CARTESIAN_POINT ( 'NONE',  ( -19.05341960407611168, -5.049401038298163336, 86.45724293864769550 ) ) ;
#34021 = CARTESIAN_POINT ( 'NONE',  ( 4.379528057220092307, 16.55341960407617563, 62.29275706135236845 ) ) ;
#34022 = CARTESIAN_POINT ( 'NONE',  ( 21.53943276465977519, 0.05219959533937863772, 46.25109039468567573 ) ) ;
#34023 = CARTESIAN_POINT ( 'NONE',  ( 0.05219959533937995610, -21.53943276465977519, 85.00109039468568994 ) ) ;
#34024 = CARTESIAN_POINT ( 'NONE',  ( 10.81492255796078972, 18.62759615963270932, 104.5822429386477097 ) ) ;
#34026 = CARTESIAN_POINT ( 'NONE',  ( -14.29746914071037622, -8.314922557961029526, 64.16775706135234714 ) ) ;
#34025 = CARTESIAN_POINT ( 'NONE',  ( -0.05219959533937732626, 21.53943276465977519, 37.50109039468568284 ) ) ;
#34027 = CARTESIAN_POINT ( 'NONE',  ( 15.80617190586746368, 15.72974639402197994, 64.37390960531435269 ) ) ;
#34028 = CARTESIAN_POINT ( 'NONE',  ( 5.049401038297881783, 19.05341960407617563, 37.29275706135232582 ) ) ;
#34030 = CARTESIAN_POINT ( 'NONE',  ( 4.483927247898790824, -16.52544592524335698, 110.2094237280190185 ) ) ;
#34029 = CARTESIAN_POINT ( 'NONE',  ( 9.474510206698971260, -16.51473224551069308, 67.91557627198102409 ) ) ;
#34031 = CARTESIAN_POINT ( 'NONE',  ( 17.72517630440434644, -5.499999999999968026, 83.42175719257211597 ) ) ;
#34032 = CARTESIAN_POINT ( 'NONE',  ( 19.02544592524343514, -5.153800228976328945, 108.5405762719810383 ) ) ;
#34033 = CARTESIAN_POINT ( 'NONE',  ( -3.889087296525950421, 6.412877669190374164, 8.181980515339454030 ) ) ;
#34034 = CARTESIAN_POINT ( 'NONE',  ( -13.89961937509957401, -13.97604488694547875, 79.37609039468567573 ) ) ;
#34035 = VECTOR ( 'NONE', #63909, 1000.000000000000000 ) ;
#34036 = CARTESIAN_POINT ( 'NONE',  ( -15.80617190586745835, -15.72974639402198527, 56.87390960531436690 ) ) ;
#34037 = CARTESIAN_POINT ( 'NONE',  ( -16.52544592524342804, 4.483927247898546575, 36.04057627198102409 ) ) ;
#34038 = CARTESIAN_POINT ( 'NONE',  ( -4.379528057220086978, -16.55341960407618274, 19.79275706135235069 ) ) ;
#34039 = CARTESIAN_POINT ( 'NONE',  ( 19.03943276465977164, -0.05219959533909143690, 33.74890960531435979 ) ) ;
#34040 = CARTESIAN_POINT ( 'NONE',  ( 19.03943276465977164, 0.05219959533936151252, 111.2510903946856757 ) ) ;
#34042 = CARTESIAN_POINT ( 'NONE',  ( 5.049401038297881783, 19.05341960407617563, 77.29275706135231871 ) ) ;
#34041 = CARTESIAN_POINT ( 'NONE',  ( 18.62759615963271287, -10.81492255796078972, 88.33224293864769550 ) ) ;
#34043 = CARTESIAN_POINT ( 'NONE',  ( -12.14591786802326823, 12.06949235617739902, 83.12609039468568994 ) ) ;
#34044 = CARTESIAN_POINT ( 'NONE',  ( 5.049401038298161559, -19.05341960407611168, 72.70724293864768129 ) ) ;
#34045 = CARTESIAN_POINT ( 'NONE',  ( 12.06949235617757843, -12.14591786802309237, 78.12390960531436690 ) ) ;
#34046 = CARTESIAN_POINT ( 'NONE',  ( -13.89961937509977652, 13.97604488694528158, 45.62390960531433848 ) ) ;
#34047 = CARTESIAN_POINT ( 'NONE',  ( -12.06949235617756955, 12.14591786802309770, 55.62390960531436690 ) ) ;
#34048 = CARTESIAN_POINT ( 'NONE',  ( -11.74149087413295511, 36.13659316521247433, -6.147842220587803830 ) ) ;
#34049 = CARTESIAN_POINT ( 'NONE',  ( 1.500000000000347500, 7.793921569590667175, -62.16239983623972165 ) ) ;
#34050 = CARTESIAN_POINT ( 'NONE',  ( 14.29746914071049879, -8.314922557960816363, 23.33224293864769194 ) ) ;
#34051 = CARTESIAN_POINT ( 'NONE',  ( -16.51473224551069308, -9.474510206698971260, 81.66557627198103830 ) ) ;
#34052 = CYLINDRICAL_SURFACE ( 'NONE', #54020, 1.499999999999997780 ) ;
#34053 = CARTESIAN_POINT ( 'NONE',  ( -5.049401038297874678, -19.05341960407617918, 44.79275706135232582 ) ) ;
#34054 = CARTESIAN_POINT ( 'NONE',  ( 16.55341960407618274, -4.379528057220086978, 41.04275706135236135 ) ) ;
#34055 = CARTESIAN_POINT ( 'NONE',  ( 10.81492255796078972, 18.62759615963270932, 69.58224293864769550 ) ) ;
#34056 = CARTESIAN_POINT ( 'NONE',  ( 16.51473224551083163, -9.474510206698727899, 25.83442372801900078 ) ) ;
#34057 = CARTESIAN_POINT ( 'NONE',  ( -19.02544592524342804, 5.153800228976336051, 81.04057627198103830 ) ) ;
#34058 = DIRECTION ( 'NONE',  ( 1.000000000000000000, 0.000000000000000000, 0.000000000000000000 ) ) ;
#34059 = CARTESIAN_POINT ( 'NONE',  ( 5.153800228976335163, 19.02544592524342804, 104.7905762719809957 ) ) ;
#34060 = CARTESIAN_POINT ( 'NONE',  ( -5.823673210054431948, 21.52544592524334988, 37.70942372801900433 ) ) ;
#34061 = CARTESIAN_POINT ( 'NONE',  ( -16.53943276465976808, 0.05219959533911058130, 106.2489096053143811 ) ) ;
#34064 = FACE_OUTER_BOUND ( 'NONE', #131281, .T. ) ;
#34063 = CARTESIAN_POINT ( 'NONE',  ( -9.564922557960796823, -16.46253265017161027, 77.08224293864769550 ) ) ;
#34062 = CARTESIAN_POINT ( 'NONE',  ( 10.72451020669898902, -18.67979575497178502, 102.9155762719810383 ) ) ;
#34065 = CARTESIAN_POINT ( 'NONE',  ( 21.55341960407619695, -5.719274019375665929, 31.04275706135234714 ) ) ;
#34066 = EDGE_CURVE ( 'NONE', #133123, #126008, #143663, .T. ) ;
#34067 = ORIENTED_EDGE ( 'NONE', *, *, #182492, .F. ) ;
#34068 = CARTESIAN_POINT ( 'NONE',  ( -19.02544592524342804, 5.153800228976336051, 86.04057627198103830 ) ) ;
#34069 = CARTESIAN_POINT ( 'NONE',  ( 19.35633801406909882, -5.499999999999572786, 81.63373818172763663 ) ) ;
#34070 = CARTESIAN_POINT ( 'NONE',  ( 0.05219959533909260263, 19.03943276465977164, 39.99890960531436690 ) ) ;
#34071 = CARTESIAN_POINT ( 'NONE',  ( -13.97604488694547697, 13.89961937509957934, 113.1260903946856757 ) ) ;
#34072 = CARTESIAN_POINT ( 'NONE',  ( -22.81625015709509441, -31.40387420917324590, -8.824999997268811569 ) ) ;
#34073 = CARTESIAN_POINT ( 'NONE',  ( 16.53943276465976808, -0.05219959533910856209, 113.7489096053143527 ) ) ;
#34074 = CARTESIAN_POINT ( 'NONE',  ( -18.67979575497193778, 10.72451020669871902, 88.33442372801901854 ) ) ;
#34076 = CARTESIAN_POINT ( 'NONE',  ( -18.67979575497193778, 10.72451020669871902, 48.33442372801902565 ) ) ;
#34075 = CARTESIAN_POINT ( 'NONE',  ( 13.89961937509977652, -13.97604488694527269, 73.12390960531436690 ) ) ;
#34077 = CARTESIAN_POINT ( 'NONE',  ( 21.53943276465977519, 0.05219959533937863772, 26.25109039468567573 ) ) ;
#34078 = CARTESIAN_POINT ( 'NONE',  ( 22.44159573604009239, 16.30477369853692693, 140.5750000027311728 ) ) ;
#34079 = CARTESIAN_POINT ( 'NONE',  ( -5.153800228976328057, -19.02544592524343514, 82.29057627198103830 ) ) ;
#34080 = CARTESIAN_POINT ( 'NONE',  ( -17.07606455188742345, 23.12338299651413820, 140.0000000000000284 ) ) ;
#34082 = CARTESIAN_POINT ( 'NONE',  ( -0.05219959533907301413, -21.53943276465977519, 37.49890960531436690 ) ) ;
#34081 = CARTESIAN_POINT ( 'NONE',  ( -14.34966873604972548, 8.224510206698743886, 43.33442372801901143 ) ) ;
#34083 = CARTESIAN_POINT ( 'NONE',  ( 10.81492255796106328, -18.62759615963255655, 75.41775706135233293 ) ) ;
#34084 = CARTESIAN_POINT ( 'NONE',  ( 6.434671708797586653, 6.434671708797580436, -61.89430850415821794 ) ) ;
#34085 = CARTESIAN_POINT ( 'NONE',  ( -5.153800228976607833, 19.02544592524334988, 107.7094237280189759 ) ) ;
#34086 = CARTESIAN_POINT ( 'NONE',  ( 16.51473224551069308, 9.474510206698969483, 54.16557627198103120 ) ) ;
#34087 = CARTESIAN_POINT ( 'NONE',  ( 13.89961937509977652, -13.97604488694527269, 78.12390960531433848 ) ) ;
#34088 = CARTESIAN_POINT ( 'NONE',  ( 16.53943276465976808, -0.05219959533910856209, 108.7489096053143669 ) ) ;
#34089 = CARTESIAN_POINT ( 'NONE',  ( -12.14591786802309592, -12.06949235617757132, 106.8739096053143811 ) ) ;
#34091 = EDGE_CURVE ( 'NONE', #88085, #139693, #6149, .T. ) ;
#34090 = CARTESIAN_POINT ( 'NONE',  ( -21.53943276465977519, 0.05219959533907696930, 21.24890960531436690 ) ) ;
#34092 = CARTESIAN_POINT ( 'NONE',  ( -14.34966873604972548, 8.224510206698743886, 83.33442372801903275 ) ) ;
#34094 = CARTESIAN_POINT ( 'NONE',  ( -9.564922557960796823, -16.46253265017161027, 57.08224293864769550 ) ) ;
#34093 = CARTESIAN_POINT ( 'NONE',  ( 16.52544592524342804, -4.483927247898539470, 63.54057627198103830 ) ) ;
#34095 = CARTESIAN_POINT ( 'NONE',  ( 15.72974639402176855, 15.80617190586768217, 81.87609039468568994 ) ) ;
#34096 = CARTESIAN_POINT ( 'NONE',  ( -0.05219959533937732626, 21.53943276465977519, 67.50109039468568994 ) ) ;
#34097 = CARTESIAN_POINT ( 'NONE',  ( -19.03943276465977164, -0.05219959533935918106, 98.75109039468567573 ) ) ;
#34098 = CARTESIAN_POINT ( 'NONE',  ( 4.379528057220339221, -16.55341960407611168, 62.70724293864769550 ) ) ;
#34099 = CARTESIAN_POINT ( 'NONE',  ( -18.67979575497178146, -10.72451020669898902, 111.6655762719810525 ) ) ;
#34100 = CARTESIAN_POINT ( 'NONE',  ( -15.80617190586745835, -15.72974639402198527, 66.87390960531436690 ) ) ;
#34102 = CARTESIAN_POINT ( 'NONE',  ( 22.00000000000000000, -1.163414459189985801E-14, 95.00000000000000000 ) ) ;
#34101 = VECTOR ( 'NONE', #166044, 1000.000000000000114 ) ;
#34103 = CARTESIAN_POINT ( 'NONE',  ( -17.81289503416611808, 24.51734667627700404, 141.9500000054623285 ) ) ;
#34104 = CARTESIAN_POINT ( 'NONE',  ( -9.474510206698964154, 16.51473224551069663, 70.41557627198102409 ) ) ;
#34105 = CARTESIAN_POINT ( 'NONE',  ( -16.53943276465976808, 0.05219959533911058130, 36.24890960531435979 ) ) ;
#34106 = CARTESIAN_POINT ( 'NONE',  ( -8.314922557961024197, 14.29746914071037800, 112.9177570613523329 ) ) ;
#34107 = CARTESIAN_POINT ( 'NONE',  ( 4.379528057220092307, 16.55341960407617563, 77.29275706135234714 ) ) ;
#34108 = CARTESIAN_POINT ( 'NONE',  ( -13.97604488694547697, 13.89961937509957934, 33.12609039468566863 ) ) ;
#34109 = DIRECTION ( 'NONE',  ( -1.000000000000000000, -0.000000000000000000, -0.000000000000000000 ) ) ;
#34110 = CARTESIAN_POINT ( 'NONE',  ( 19.02544592524343514, -5.153800228976328945, 93.54057627198102409 ) ) ;
#34111 = CARTESIAN_POINT ( 'NONE',  ( 0.05219959533910956823, 16.53943276465976808, 59.99890960531436690 ) ) ;
#34113 = CARTESIAN_POINT ( 'NONE',  ( 19.02544592524343514, -5.153800228976328945, 113.5405762719810241 ) ) ;
#34112 = CARTESIAN_POINT ( 'NONE',  ( 31.99364916731006048, 4.791014396527177230E-13, 45.00000000000022027 ) ) ;
#34114 = CARTESIAN_POINT ( 'NONE',  ( 15.80617190586746368, 15.72974639402197994, 54.37390960531435979 ) ) ;
#34115 = CARTESIAN_POINT ( 'NONE',  ( 12.06949235617757843, -12.14591786802309237, 103.1239096053143811 ) ) ;
#34116 = CARTESIAN_POINT ( 'NONE',  ( -16.55341960407617563, 4.379528057220093196, 48.54275706135234714 ) ) ;
#34117 = CARTESIAN_POINT ( 'NONE',  ( -14.34966873604960291, -8.224510206698953496, 81.66557627198103830 ) ) ;
#34118 = CARTESIAN_POINT ( 'NONE',  ( -19.53037848336980531, 5.499999999999902300, 64.85532783611449759 ) ) ;
#34119 = CARTESIAN_POINT ( 'NONE',  ( -16.46253265017146816, -9.564922557961047289, 84.16775706135233293 ) ) ;
#34120 = CARTESIAN_POINT ( 'NONE',  ( 21.52544592524344225, -5.823673210054117533, 23.54057627198102765 ) ) ;
#34121 = CARTESIAN_POINT ( 'NONE',  ( -11.40812507854754720, -35.11059874428192273, -6.724999997268813701 ) ) ;
#34122 = CARTESIAN_POINT ( 'NONE',  ( -17.59860650958989936, -7.585241751807033417, 41.57662985737508166 ) ) ;
#34124 = CARTESIAN_POINT ( 'NONE',  ( -14.34966873604960291, -8.224510206698953496, 31.66557627198102054 ) ) ;
#34123 = CARTESIAN_POINT ( 'NONE',  ( 14.34966873604972726, -8.224510206698740333, 30.83442372801902209 ) ) ;
#34125 = CARTESIAN_POINT ( 'NONE',  ( -5.823673210054116645, -21.52544592524344225, 57.29057627198103120 ) ) ;
#34126 = CARTESIAN_POINT ( 'NONE',  ( -16.46253265017146816, -9.564922557961047289, 89.16775706135234714 ) ) ;
#34127 = CARTESIAN_POINT ( 'NONE',  ( -0.05219959533907301413, -21.53943276465977519, 42.49890960531435979 ) ) ;
#34128 = CARTESIAN_POINT ( 'NONE',  ( -5.719274019375665041, -21.55341960407619695, 84.79275706135234714 ) ) ;
#34129 = CARTESIAN_POINT ( 'NONE',  ( 18.83841601638290086, -33.00795687112466936, -25.49111855720866160 ) ) ;
#34130 = CARTESIAN_POINT ( 'NONE',  ( -8.224510206698735004, -14.34966873604973081, 29.58442372801901854 ) ) ;
#34132 = CARTESIAN_POINT ( 'NONE',  ( -13.89961937509977652, 13.97604488694528158, 90.62390960531432427 ) ) ;
#34131 = CARTESIAN_POINT ( 'NONE',  ( -16.51473224551069308, -9.474510206698971260, 36.66557627198102409 ) ) ;
#34133 = CARTESIAN_POINT ( 'NONE',  ( -19.03943276465977164, 0.05219959533909376836, 41.24890960531435269 ) ) ;
#34134 = CARTESIAN_POINT ( 'NONE',  ( 8.224510206698953496, -14.34966873604960469, 102.9155762719810383 ) ) ;
#34135 = ITEM_DEFINED_TRANSFORMATION ( 'NONE', 'NONE', #124223,  #82054 ) ;
#34136 = CARTESIAN_POINT ( 'NONE',  ( -19.02544592524342804, 5.153800228976336051, 101.0405762719810241 ) ) ;
#34137 = ORIENTED_EDGE ( 'NONE', *, *, #16216, .F. ) ;
#34138 = CARTESIAN_POINT ( 'NONE',  ( -16.55341960407617563, 4.379528057220093196, 58.54275706135235424 ) ) ;
#34139 = CARTESIAN_POINT ( 'NONE',  ( 15.80617190586746368, 15.72974639402197994, 94.37390960531436690 ) ) ;
#34140 = CARTESIAN_POINT ( 'NONE',  ( 19.03943276465977164, -0.05219959533909143690, 38.74890960531436690 ) ) ;
#34142 = CARTESIAN_POINT ( 'NONE',  ( -15.80617190586768217, 15.72974639402176855, 33.12609039468569705 ) ) ;
#34141 = CARTESIAN_POINT ( 'NONE',  ( 13.89961937509957401, 13.97604488694547697, 71.87609039468567573 ) ) ;
#34143 = CARTESIAN_POINT ( 'NONE',  ( -16.46253265017160317, 9.564922557960807481, 65.83224293864769550 ) ) ;
#34144 = CARTESIAN_POINT ( 'NONE',  ( -16.51473224551069308, -9.474510206698971260, 101.6655762719810241 ) ) ;
#34145 = EDGE_LOOP ( 'NONE', ( #113933, #104667, #129575, #111356 ) ) ;
#34146 = CARTESIAN_POINT ( 'NONE',  ( 12.14591786802327356, -12.06949235617739191, 35.62609039468568994 ) ) ;
#34147 = CARTESIAN_POINT ( 'NONE',  ( -5.719274019375978568, 21.55341960407610458, 110.2072429386477239 ) ) ;
#34150 = CARTESIAN_POINT ( 'NONE',  ( -5.049401038297874678, -19.05341960407617918, 79.79275706135233293 ) ) ;
#34149 = CARTESIAN_POINT ( 'NONE',  ( -13.89961937509977652, 13.97604488694528158, 90.62390960531432427 ) ) ;
#34148 = CARTESIAN_POINT ( 'NONE',  ( -12.06949235617756955, 12.14591786802309770, 105.6239096053143669 ) ) ;
#34151 = CARTESIAN_POINT ( 'NONE',  ( 10.81492255796078972, 18.62759615963270932, 84.58224293864769550 ) ) ;
#34152 = CARTESIAN_POINT ( 'NONE',  ( -19.02544592524334988, -5.153800228976617603, 23.95942372801900078 ) ) ;
#34153 = CARTESIAN_POINT ( 'NONE',  ( 12.14591786802327356, -12.06949235617739191, 80.62609039468567573 ) ) ;
#34154 = CARTESIAN_POINT ( 'NONE',  ( -19.02544592524342804, 5.153800228976336051, 101.0405762719810241 ) ) ;
#34155 = CARTESIAN_POINT ( 'NONE',  ( -19.05341960407611168, -5.049401038298163336, 51.45724293864770260 ) ) ;
#34156 = CARTESIAN_POINT ( 'NONE',  ( 5.823673210054444382, -21.52544592524334988, 55.20942372801902565 ) ) ;
#34157 = CARTESIAN_POINT ( 'NONE',  ( -21.52544592524334988, -5.823673210054445271, 68.95942372801901854 ) ) ;
#34158 = CARTESIAN_POINT ( 'NONE',  ( 19.03943276465977164, -0.05219959533909143690, 68.74890960531436690 ) ) ;
#34159 = CARTESIAN_POINT ( 'NONE',  ( 5.719274019375673035, 21.55341960407619339, 47.29275706135234003 ) ) ;
#34160 = CARTESIAN_POINT ( 'NONE',  ( 19.05341960407617918, -5.049401038297876454, 91.04275706135234714 ) ) ;
#34161 = CARTESIAN_POINT ( 'NONE',  ( -0.05219959533909027116, -19.03943276465977164, 47.49890960531435979 ) ) ;
#34162 = CARTESIAN_POINT ( 'NONE',  ( -8.314922557961024197, 14.29746914071037800, 92.91775706135236135 ) ) ;
#34163 = CARTESIAN_POINT ( 'NONE',  ( 5.049401038298161559, -19.05341960407611168, 67.70724293864769550 ) ) ;
#34164 = CARTESIAN_POINT ( 'NONE',  ( -30.73962218707678318, 22.33364281372846705, -1.947842220587803874 ) ) ;
#34165 = CARTESIAN_POINT ( 'NONE',  ( -16.51473224551069308, -9.474510206698971260, 46.66557627198102409 ) ) ;
#34166 = CARTESIAN_POINT ( 'NONE',  ( -5.823673210054116645, -21.52544592524344225, 87.29057627198103830 ) ) ;
#34167 = CARTESIAN_POINT ( 'NONE',  ( 16.55341960407618274, -4.379528057220086978, 71.04275706135234714 ) ) ;
#34168 = CARTESIAN_POINT ( 'NONE',  ( -24.72709851008508863, 6.869189314505790733, 167.7661538690215650 ) ) ;
#34169 = CARTESIAN_POINT ( 'NONE',  ( -5.049401038297874678, -19.05341960407617918, 24.79275706135233648 ) ) ;
#34170 = EDGE_CURVE ( 'NONE', #182160, #171657, #149107, .T. ) ;
#34171 = CARTESIAN_POINT ( 'NONE',  ( -16.46253265017160317, 9.564922557960807481, 70.83224293864770971 ) ) ;
#34172 = CARTESIAN_POINT ( 'NONE',  ( 14.29746914071049879, -8.314922557960816363, 63.33224293864770260 ) ) ;
#34173 = CARTESIAN_POINT ( 'NONE',  ( -14.29746914071049879, 8.314922557960819915, 100.8322429386477097 ) ) ;
#34174 = CARTESIAN_POINT ( 'NONE',  ( 5.049401038298161559, -19.05341960407611168, 107.7072429386476955 ) ) ;
#34175 = CARTESIAN_POINT ( 'NONE',  ( -19.02544592524342804, 5.153800228976336051, 96.04057627198103830 ) ) ;
#34176 = CARTESIAN_POINT ( 'NONE',  ( -18.62759615963255300, -10.81492255796106328, 44.16775706135234714 ) ) ;
#34177 = CARTESIAN_POINT ( 'NONE',  ( -19.02544592524342804, 5.153800228976336051, 106.0405762719810241 ) ) ;
#34178 = CARTESIAN_POINT ( 'NONE',  ( -10.81492255796105439, 18.62759615963255655, 112.9177570613523329 ) ) ;
#34179 = CARTESIAN_POINT ( 'NONE',  ( -16.53943276465976808, -0.05219959533934237506, 83.75109039468568994 ) ) ;
#34180 = CARTESIAN_POINT ( 'NONE',  ( -10.81492255796105439, 18.62759615963255655, 42.91775706135235424 ) ) ;
#34181 = CARTESIAN_POINT ( 'NONE',  ( -19.05341960407611168, -5.049401038298163336, 111.4572429386476671 ) ) ;
#34182 = CARTESIAN_POINT ( 'NONE',  ( 18.62759615963271287, -10.81492255796078972, 103.3322429386476955 ) ) ;
#34183 = CARTESIAN_POINT ( 'NONE',  ( 14.29746914071049879, -8.314922557960816363, 58.33224293864768839 ) ) ;
#34184 = CARTESIAN_POINT ( 'NONE',  ( -9.564922557960796823, -16.46253265017161027, 57.08224293864769550 ) ) ;
#34185 = CARTESIAN_POINT ( 'NONE',  ( 4.379528057220339221, -16.55341960407611168, 87.70724293864769550 ) ) ;
#34186 = CARTESIAN_POINT ( 'NONE',  ( -5.823673210054116645, -21.52544592524344225, 37.29057627198102409 ) ) ;
#34187 = CARTESIAN_POINT ( 'NONE',  ( 5.153800228976615827, -19.02544592524334988, 50.20942372801897591 ) ) ;
#34188 = CARTESIAN_POINT ( 'NONE',  ( -16.53943276465976808, 0.05219959533911058130, 111.2489096053143669 ) ) ;
#34189 = ORIENTED_EDGE ( 'NONE', *, *, #90472, .T. ) ;
#34190 = CARTESIAN_POINT ( 'NONE',  ( 12.06949235617739724, 12.14591786802326823, 66.87609039468568994 ) ) ;
#34191 = CARTESIAN_POINT ( 'NONE',  ( 16.51473224551069308, 9.474510206698969483, 69.16557627198102409 ) ) ;
#34192 = CARTESIAN_POINT ( 'NONE',  ( -22.44159573604010305, 16.30477369853692338, 142.6750000027311671 ) ) ;
#34193 = CARTESIAN_POINT ( 'NONE',  ( -16.52544592524342804, 4.483927247898546575, 86.04057627198102409 ) ) ;
#34194 = CARTESIAN_POINT ( 'NONE',  ( -10.81492255796078084, -18.62759615963271287, 42.08224293864769550 ) ) ;
#34195 = CARTESIAN_POINT ( 'NONE',  ( -14.34966873604972548, 8.224510206698743886, 103.3344237280190043 ) ) ;
#34196 = CARTESIAN_POINT ( 'NONE',  ( -9.564922557961040184, 16.46253265017147172, 102.9177570613523329 ) ) ;
#34197 = CARTESIAN_POINT ( 'NONE',  ( 21.55341960407619695, -5.719274019375665929, 81.04275706135236135 ) ) ;
#34198 = CARTESIAN_POINT ( 'NONE',  ( 9.474510206698971260, -16.51473224551069308, 87.91557627198102409 ) ) ;
#34199 = CARTESIAN_POINT ( 'NONE',  ( 21.53943276465977519, -0.05219959533907433946, 103.7489096053143669 ) ) ;
#34200 = CARTESIAN_POINT ( 'NONE',  ( 0.05219959533934541429, -16.53943276465976808, 50.00109039468568994 ) ) ;
#34201 = CARTESIAN_POINT ( 'NONE',  ( -5.153800228976328057, -19.02544592524343514, 27.29057627198103120 ) ) ;
#34202 = CARTESIAN_POINT ( 'NONE',  ( -0.05219959533934338120, 16.53943276465976808, 37.50109039468568284 ) ) ;
#34203 = CARTESIAN_POINT ( 'NONE',  ( 9.564922557961047289, -16.46253265017146816, 100.4177570613523329 ) ) ;
#34204 = CARTESIAN_POINT ( 'NONE',  ( 21.52544592524344225, -5.823673210054117533, 93.54057627198103830 ) ) ;
#34205 = CARTESIAN_POINT ( 'NONE',  ( 19.03943276465977164, 0.05219959533936151252, 51.25109039468567573 ) ) ;
#34206 = CARTESIAN_POINT ( 'NONE',  ( 18.39443945427638738, -5.500000000000021316, 86.01745347608655834 ) ) ;
#34207 = CARTESIAN_POINT ( 'NONE',  ( 15.80617190586746368, 15.72974639402197994, 99.37390960531436690 ) ) ;
#34208 = DIRECTION ( 'NONE',  ( -0.000000000000000000, 0.000000000000000000, 1.000000000000000000 ) ) ;
#34209 = CARTESIAN_POINT ( 'NONE',  ( 16.46253265017160672, -9.564922557960803928, 73.33224293864769550 ) ) ;
#34210 = CARTESIAN_POINT ( 'NONE',  ( 14.34966873604972726, -8.224510206698740333, 35.83442372801901143 ) ) ;
#34211 = DIRECTION ( 'NONE',  ( -1.000000000000000000, -0.000000000000000000, 0.000000000000000000 ) ) ;
#34212 = CARTESIAN_POINT ( 'NONE',  ( 16.51473224551083163, -9.474510206698727899, 65.83442372801900433 ) ) ;
#34214 = CARTESIAN_POINT ( 'NONE',  ( 14.29746914071049879, -8.314922557960816363, 63.33224293864770260 ) ) ;
#34213 = CARTESIAN_POINT ( 'NONE',  ( -10.72451020669898014, 18.67979575497178502, 115.4155762719810241 ) ) ;
#34215 = CARTESIAN_POINT ( 'NONE',  ( -0.05219959533909027116, -19.03943276465977164, 67.49890960531436690 ) ) ;
#34217 = CARTESIAN_POINT ( 'NONE',  ( -9.564922557961040184, 16.46253265017147172, 37.91775706135233293 ) ) ;
#34216 = CARTESIAN_POINT ( 'NONE',  ( -16.52544592524335698, -4.483927247898792601, 33.95942372801901143 ) ) ;
#34218 = CARTESIAN_POINT ( 'NONE',  ( 18.62759615963255655, 10.81492255796105972, 56.66775706135235424 ) ) ;
#34220 = CARTESIAN_POINT ( 'NONE',  ( 5.153800228976615827, -19.02544592524334988, 110.2094237280189901 ) ) ;
#34219 = B_SPLINE_CURVE_WITH_KNOTS ( 'NONE', 3,
 ( #140219, #60398, #124049, #139232, #44255, #106902, #125065 ),
 .UNSPECIFIED., .F., .F.,
 ( 4, 3, 4 ),
 ( -4.508036450095025827E-05, 0.000000000000000000, 0.006877813788783073562 ),
 .UNSPECIFIED. ) ;
#34221 = CARTESIAN_POINT ( 'NONE',  ( 16.51473224551069308, 9.474510206698969483, 49.16557627198102409 ) ) ;
#34222 = CARTESIAN_POINT ( 'NONE',  ( -19.05341960407617563, 5.049401038297882671, 88.54275706135230450 ) ) ;
#34223 = CARTESIAN_POINT ( 'NONE',  ( 10.72451020669871369, 18.67979575497193778, 82.08442372801901854 ) ) ;
#34224 = CARTESIAN_POINT ( 'NONE',  ( -5.153800228976607833, 19.02544592524334988, 62.70942372801899722 ) ) ;
#34225 = CARTESIAN_POINT ( 'NONE',  ( 19.03943276465977164, -0.05219959533909143690, 33.74890960531435979 ) ) ;
#34226 = CARTESIAN_POINT ( 'NONE',  ( 10.72451020669898902, -18.67979575497178502, 57.91557627198103120 ) ) ;
#34228 = CARTESIAN_POINT ( 'NONE',  ( -16.46253265017146816, -9.564922557961047289, 69.16775706135233293 ) ) ;
#34227 = CARTESIAN_POINT ( 'NONE',  ( 14.29746914071049879, -8.314922557960816363, 68.33224293864769550 ) ) ;
#34229 = CARTESIAN_POINT ( 'NONE',  ( -69.65682714487590488, -71.74905178543390605, -10.00000000000000000 ) ) ;
#34230 = CARTESIAN_POINT ( 'NONE',  ( 16.51473224551083163, -9.474510206698727899, 30.83442372801900433 ) ) ;
#34231 = CARTESIAN_POINT ( 'NONE',  ( 12.14591786802327356, -12.06949235617739191, 100.6260903946857184 ) ) ;
#34232 = CARTESIAN_POINT ( 'NONE',  ( 16.55341960407611168, 4.379528057220329451, 48.95724293864770971 ) ) ;
#34234 = CARTESIAN_POINT ( 'NONE',  ( 22.44159573604009594, -16.30477369853687364, 139.6750000027311955 ) ) ;
#34233 = CARTESIAN_POINT ( 'NONE',  ( -15.72974639402176322, -15.80617190586768395, 94.37609039468568994 ) ) ;
#34235 = CARTESIAN_POINT ( 'NONE',  ( 5.719274019375991003, -21.55341960407610458, 92.70724293864770971 ) ) ;
#34236 = CARTESIAN_POINT ( 'NONE',  ( -19.02544592524342804, 5.153800228976336051, 46.04057627198101699 ) ) ;
#34237 = CARTESIAN_POINT ( 'NONE',  ( -15.72974639402176322, -15.80617190586768395, 74.37609039468568994 ) ) ;
#34238 = CARTESIAN_POINT ( 'NONE',  ( -13.89961937509977652, 13.97604488694528158, 55.62390960531434558 ) ) ;
#34239 = ORIENTED_EDGE ( 'NONE', *, *, #197329, .T. ) ;
#34240 = CARTESIAN_POINT ( 'NONE',  ( 5.153800228976335163, 19.02544592524342804, 69.79057627198103830 ) ) ;
#34241 = CARTESIAN_POINT ( 'NONE',  ( -14.29746914071049879, 8.314922557960819915, 105.8322429386476955 ) ) ;
#34242 = CARTESIAN_POINT ( 'NONE',  ( -9.474510206698964154, 16.51473224551069663, 105.4155762719810383 ) ) ;
#34243 = CIRCLE ( 'NONE', #147258, 1.249999999999999778 ) ;
#34244 = CARTESIAN_POINT ( 'NONE',  ( -14.34966873604960291, -8.224510206698953496, 51.66557627198102409 ) ) ;
#34245 = CARTESIAN_POINT ( 'NONE',  ( 9.564922557960805705, 16.46253265017160317, 34.58224293864770260 ) ) ;
#34246 = CARTESIAN_POINT ( 'NONE',  ( 16.52544592524342804, -4.483927247898539470, 83.54057627198102409 ) ) ;
#34247 = CARTESIAN_POINT ( 'NONE',  ( 15.80617190586746368, 15.72974639402197994, 94.37390960531436690 ) ) ;
#34248 = CARTESIAN_POINT ( 'NONE',  ( -10.72451020669870658, -18.67979575497194134, 39.58442372801901143 ) ) ;
#34249 = CARTESIAN_POINT ( 'NONE',  ( -16.51473224551069308, -9.474510206698971260, 21.66557627198102765 ) ) ;
#34250 = CARTESIAN_POINT ( 'NONE',  ( 16.52544592524335698, 4.483927247898782831, 36.45942372801901143 ) ) ;
#34251 = CARTESIAN_POINT ( 'NONE',  ( -5.719274019375978568, 21.55341960407610458, 90.20724293864770971 ) ) ;
#34253 = CARTESIAN_POINT ( 'NONE',  ( -21.55341960407619339, 5.719274019375674811, 108.5427570613523756 ) ) ;
#34252 = UNCERTAINTY_MEASURE_WITH_UNIT (LENGTH_MEASURE( 1.000000000000000082E-05 ), #151525, 'distance_accuracy_value', 'NONE');
#34254 = CARTESIAN_POINT ( 'NONE',  ( 16.46253265017160672, -9.564922557960803928, 88.33224293864769550 ) ) ;
#34255 = CARTESIAN_POINT ( 'NONE',  ( -0.05219959533937732626, 21.53943276465977519, 42.50109039468567573 ) ) ;
#34256 = CARTESIAN_POINT ( 'NONE',  ( 15.72974639402199770, -15.80617190586745480, 33.12390960531435979 ) ) ;
#34257 = CARTESIAN_POINT ( 'NONE',  ( -14.29746914071037622, -8.314922557961029526, 109.1677570613523613 ) ) ;
#34259 = CARTESIAN_POINT ( 'NONE',  ( -10.81492255796105439, 18.62759615963255655, 77.91775706135231871 ) ) ;
#34258 = CARTESIAN_POINT ( 'NONE',  ( -18.62759615963255300, -10.81492255796106328, 54.16775706135235424 ) ) ;
#34260 = CARTESIAN_POINT ( 'NONE',  ( 5.153800228976615827, -19.02544592524334988, 35.20942372801899722 ) ) ;
#34261 = CARTESIAN_POINT ( 'NONE',  ( 16.55341960407618274, -4.379528057220086978, 86.04275706135236135 ) ) ;
#34262 = CARTESIAN_POINT ( 'NONE',  ( 21.53943276465977519, 0.05219959533937863772, 41.25109039468568284 ) ) ;
#34263 = CARTESIAN_POINT ( 'NONE',  ( -13.97604488694527625, -13.89961937509977652, 51.87390960531436690 ) ) ;
#34264 = CARTESIAN_POINT ( 'NONE',  ( -18.62759615963255300, -10.81492255796106328, 99.16775706135234714 ) ) ;
#34265 = CARTESIAN_POINT ( 'NONE',  ( -16.46253265017160317, 9.564922557960807481, 100.8322429386477097 ) ) ;
#34266 = CARTESIAN_POINT ( 'NONE',  ( 5.719274019375991003, -21.55341960407610458, 102.7072429386476955 ) ) ;
#34267 = CARTESIAN_POINT ( 'NONE',  ( -18.67979575497178146, -10.72451020669898902, 76.66557627198103830 ) ) ;
#34269 = CARTESIAN_POINT ( 'NONE',  ( 15.80617190586746368, 15.72974639402197994, 64.37390960531435269 ) ) ;
#34268 = DIRECTION ( 'NONE',  ( 1.000000000000000000, 0.000000000000000000, 0.000000000000000000 ) ) ;
#34271 = CARTESIAN_POINT ( 'NONE',  ( -12.06949235617756955, 12.14591786802309770, 60.62390960531437401 ) ) ;
#34270 = CARTESIAN_POINT ( 'NONE',  ( -14.34966873604972548, 8.224510206698743886, 58.33442372801901143 ) ) ;
#34272 = CYLINDRICAL_SURFACE ( 'NONE', #120879, 5.500000000001017852 ) ;
#34273 = CARTESIAN_POINT ( 'NONE',  ( -5.049401038297874678, -19.05341960407617918, 94.79275706135230450 ) ) ;
#34274 = LINE ( 'NONE', #2933, #150416 ) ;
#34275 = CARTESIAN_POINT ( 'NONE',  ( 16.55341960407618274, -4.379528057220086978, 21.04275706135234714 ) ) ;
#34276 = CARTESIAN_POINT ( 'NONE',  ( 5.823673210054125526, 21.52544592524343514, 104.7905762719810241 ) ) ;
#34277 = CARTESIAN_POINT ( 'NONE',  ( -15.80617190586745835, -15.72974639402198527, 76.87390960531439532 ) ) ;
#34278 = CARTESIAN_POINT ( 'NONE',  ( -15.80617190586745835, -15.72974639402198527, 21.87390960531436690 ) ) ;
#34279 = CARTESIAN_POINT ( 'NONE',  ( 12.06949235617739724, 12.14591786802326823, 56.87609039468568994 ) ) ;
#34280 = CARTESIAN_POINT ( 'NONE',  ( -5.049401038298153566, 19.05341960407611168, 65.20724293864765286 ) ) ;
#34282 = CARTESIAN_POINT ( 'NONE',  ( 16.46253265017146816, 9.564922557961045513, 106.6677570613523471 ) ) ;
#34281 = CARTESIAN_POINT ( 'NONE',  ( -21.52544592524334988, -5.823673210054445271, 48.95942372801902565 ) ) ;
#34283 = CARTESIAN_POINT ( 'NONE',  ( -9.564922557960796823, -16.46253265017161027, 102.0822429386477097 ) ) ;
#34284 = CARTESIAN_POINT ( 'NONE',  ( -0.05219959533909027116, -19.03943276465977164, 97.49890960531436690 ) ) ;
#34285 = CARTESIAN_POINT ( 'NONE',  ( -15.72974639402197994, 15.80617190586746368, 95.62390960531436690 ) ) ;
#34286 = CARTESIAN_POINT ( 'NONE',  ( -9.564922557960796823, -16.46253265017161027, 62.08224293864769550 ) ) ;
#34287 = CARTESIAN_POINT ( 'NONE',  ( -16.81555441253550853, -7.025013491695501600, 59.36314554665745646 ) ) ;
#34288 = CARTESIAN_POINT ( 'NONE',  ( 12.06949235617757843, -12.14591786802309237, 88.12390960531436690 ) ) ;
#34289 = CARTESIAN_POINT ( 'NONE',  ( 9.474510206698971260, -16.51473224551069308, 112.9155762719810383 ) ) ;
#34290 = DIRECTION ( 'NONE',  ( 0.000000000000000000, 0.000000000000000000, 1.000000000000000000 ) ) ;
#34291 = CARTESIAN_POINT ( 'NONE',  ( -10.81492255796078084, -18.62759615963271287, 102.0822429386476955 ) ) ;
#34292 = CARTESIAN_POINT ( 'NONE',  ( -16.46253265017146816, -9.564922557961047289, 69.16775706135233293 ) ) ;
#34293 = CARTESIAN_POINT ( 'NONE',  ( -0.05219959533907301413, -21.53943276465977519, 22.49890960531436335 ) ) ;
#34294 = CARTESIAN_POINT ( 'NONE',  ( 16.46253265017160672, -9.564922557960803928, 28.33224293864769550 ) ) ;
#34295 = CARTESIAN_POINT ( 'NONE',  ( 21.53943276465977519, -0.05219959533907433946, 48.74890960531435979 ) ) ;
#34296 = CARTESIAN_POINT ( 'NONE',  ( 16.46253265017160672, -9.564922557960803928, 98.33224293864769550 ) ) ;
#34297 = CARTESIAN_POINT ( 'NONE',  ( 10.72451020669871369, 18.67979575497193778, 72.08442372801899012 ) ) ;
#34298 = CARTESIAN_POINT ( 'NONE',  ( -5.049401038298153566, 19.05341960407611168, 50.20724293864770260 ) ) ;
#34299 = CARTESIAN_POINT ( 'NONE',  ( -14.34966873604960291, -8.224510206698953496, 91.66557627198103830 ) ) ;
#34300 = CARTESIAN_POINT ( 'NONE',  ( 0.05219959533934541429, -16.53943276465976808, 35.00109039468568284 ) ) ;
#34301 = CARTESIAN_POINT ( 'NONE',  ( 5.823673210054444382, -21.52544592524334988, 60.20942372801902565 ) ) ;
#34302 = ORIENTED_EDGE ( 'NONE', *, *, #62612, .F. ) ;
#34303 = CARTESIAN_POINT ( 'NONE',  ( 16.46253265017146816, 9.564922557961045513, 31.66775706135232937 ) ) ;
#34304 = CARTESIAN_POINT ( 'NONE',  ( -9.564922557961040184, 16.46253265017147172, 77.91775706135234714 ) ) ;
#34305 = CARTESIAN_POINT ( 'NONE',  ( 13.97604488694548053, -13.89961937509957401, 45.62609039468566863 ) ) ;
#34306 = DIRECTION ( 'NONE',  ( 1.000000000000000000, 0.000000000000000000, 0.000000000000000000 ) ) ;
#34307 = CARTESIAN_POINT ( 'NONE',  ( 0.05219959533937995610, -21.53943276465977519, 40.00109039468567573 ) ) ;
#34308 = CARTESIAN_POINT ( 'NONE',  ( 30.74264578624800137, -22.33583958711395212, -2.949999994537626957 ) ) ;
#34309 = CARTESIAN_POINT ( 'NONE',  ( 19.03943276465977164, 0.05219959533936151252, 31.25109039468566863 ) ) ;
#34310 = CARTESIAN_POINT ( 'NONE',  ( -9.564922557960796823, -16.46253265017161027, 62.08224293864769550 ) ) ;
#34311 = CARTESIAN_POINT ( 'NONE',  ( 5.153800228976615827, -19.02544592524334988, 35.20942372801899722 ) ) ;
#34312 = CARTESIAN_POINT ( 'NONE',  ( 16.52544592524335698, 4.483927247898782831, 106.4594237280190328 ) ) ;
#34314 = CARTESIAN_POINT ( 'NONE',  ( 21.55341960407619695, -5.719274019375665929, 91.04275706135236135 ) ) ;
#34313 = CARTESIAN_POINT ( 'NONE',  ( 5.719274019375991003, -21.55341960407610458, 22.70724293864769194 ) ) ;
#34315 = CARTESIAN_POINT ( 'NONE',  ( 3.556970738554033499E-15, -38.81732327939057825, -6.124999997268812280 ) ) ;
#34316 = CARTESIAN_POINT ( 'NONE',  ( -17.50000000000000355, -5.068104630630324792, 34.27181594659972319 ) ) ;
#34317 = CARTESIAN_POINT ( 'NONE',  ( 18.67979575497194134, -10.72451020669871369, 80.83442372801901854 ) ) ;
#34318 = CARTESIAN_POINT ( 'NONE',  ( 21.65131445265850729, -0.9841389949901845347, -58.61993113718296655 ) ) ;
#34319 = CARTESIAN_POINT ( 'NONE',  ( 16.51473224551069308, 9.474510206698969483, 94.16557627198103830 ) ) ;
#34320 = CARTESIAN_POINT ( 'NONE',  ( -1.468823602708420273, -30.74735067906812702, -50.54421433284817056 ) ) ;
#34322 = CARTESIAN_POINT ( 'NONE',  ( -0.05219959533909027116, -19.03943276465977164, 57.49890960531435979 ) ) ;
#34321 = B_SPLINE_CURVE_WITH_KNOTS ( 'NONE', 3,
 ( #54377, #24049, #163560, #86703, #177738, #116049, #69545, #192900, #39207, #147391, #55370, #84691, #118056, #83696, #25060, #6856, #117040, #68535, #133208, #100863 ),
 .UNSPECIFIED., .F., .F.,
 ( 4, 2, 2, 2, 2, 2, 2, 2, 2, 4 ),
 ( 0.004000878361811936561, 0.004499404418915928239, 0.004997930476019919917, 0.005496456533123911595, 0.005994982590227904140, 0.006244245618779899545, 0.006493508647331894951, 0.006992034704435887496, 0.007490560761539879174, 0.007989086818643870852 ),
 .UNSPECIFIED. ) ;
#34324 = EDGE_CURVE ( 'NONE', #22766, #155866, #110733, .T. ) ;
#34323 = CARTESIAN_POINT ( 'NONE',  ( 0.05219959533907565091, 21.53943276465977519, 49.99890960531437401 ) ) ;
#34325 = CARTESIAN_POINT ( 'NONE',  ( 12.06949235617757843, -12.14591786802309237, 28.12390960531435979 ) ) ;
#34327 = CARTESIAN_POINT ( 'NONE',  ( -0.05219959533909027116, -19.03943276465977164, 97.49890960531436690 ) ) ;
#34326 = CARTESIAN_POINT ( 'NONE',  ( 4.483927247898545687, 16.52544592524342804, 94.79057627198105251 ) ) ;
#34328 = CARTESIAN_POINT ( 'NONE',  ( 13.89961937509957401, 13.97604488694547697, 21.87609039468566152 ) ) ;
#34329 = CARTESIAN_POINT ( 'NONE',  ( 12.14591786802309770, 12.06949235617756955, 104.3739096053143669 ) ) ;
#34330 = CARTESIAN_POINT ( 'NONE',  ( -10.81492255796105439, 18.62759615963255655, 52.91775706135235424 ) ) ;
#34331 = CARTESIAN_POINT ( 'NONE',  ( -14.34966873604972548, 8.224510206698743886, 108.3344237280190185 ) ) ;
#34332 = CARTESIAN_POINT ( 'NONE',  ( -16.51473224551082808, 9.474510206698731452, 63.33442372801900433 ) ) ;
#34333 = FACE_OUTER_BOUND ( 'NONE', #131122, .T. ) ;
#34334 = CARTESIAN_POINT ( 'NONE',  ( -19.03943276465977164, 0.05219959533909376836, 111.2489096053143669 ) ) ;
#34335 = CARTESIAN_POINT ( 'NONE',  ( 16.55341960407611168, 4.379528057220329451, 73.95724293864769550 ) ) ;
#34337 = CARTESIAN_POINT ( 'NONE',  ( 13.97604488694548053, -13.89961937509957401, 55.62609039468566863 ) ) ;
#34336 = AXIS2_PLACEMENT_3D ( 'NONE', #9187, #40513, #160858 ) ;
#34338 = CARTESIAN_POINT ( 'NONE',  ( 16.51473224551069308, 9.474510206698969483, 59.16557627198102409 ) ) ;
#34339 = CARTESIAN_POINT ( 'NONE',  ( 4.379528057220339221, -16.55341960407611168, 62.70724293864769550 ) ) ;
#34340 = CARTESIAN_POINT ( 'NONE',  ( -9.474510206698720793, -16.51473224551083518, 89.58442372801900433 ) ) ;
#34341 = CARTESIAN_POINT ( 'NONE',  ( 0.05219959533907565091, 21.53943276465977519, 29.99890960531435979 ) ) ;
#34342 = VERTEX_POINT ( 'NONE', #62029 ) ;
#34343 = CARTESIAN_POINT ( 'NONE',  ( -12.14591786802309592, -12.06949235617757132, 106.8739096053143811 ) ) ;
#34344 = CARTESIAN_POINT ( 'NONE',  ( -17.58332526062525147, -7.635886036038636249, 99.07665040441534643 ) ) ;
#34346 = CARTESIAN_POINT ( 'NONE',  ( -15.80617190586745835, -15.72974639402198527, 61.87390960531436690 ) ) ;
#34345 = CARTESIAN_POINT ( 'NONE',  ( -9.564922557960796823, -16.46253265017161027, 62.08224293864769550 ) ) ;
#34347 = CARTESIAN_POINT ( 'NONE',  ( -13.89961937509977652, 13.97604488694528158, 45.62390960531433848 ) ) ;
#34349 = CARTESIAN_POINT ( 'NONE',  ( 5.153800228976335163, 19.02544592524342804, 79.79057627198102409 ) ) ;
#34348 = CARTESIAN_POINT ( 'NONE',  ( -16.53943276465976808, -0.05219959533934237506, 88.75109039468567573 ) ) ;
#34350 = CARTESIAN_POINT ( 'NONE',  ( -5.153800228976607833, 19.02544592524334988, 47.70942372801900433 ) ) ;
#34351 = CARTESIAN_POINT ( 'NONE',  ( 10.81492255796106328, -18.62759615963255655, 85.41775706135236135 ) ) ;
#34352 = CARTESIAN_POINT ( 'NONE',  ( -5.719274019375978568, 21.55341960407610458, 55.20724293864770260 ) ) ;
#34353 = CARTESIAN_POINT ( 'NONE',  ( 13.97604488694527802, 13.89961937509977652, 104.3739096053143385 ) ) ;
#34354 = CARTESIAN_POINT ( 'NONE',  ( -5.153800228976328057, -19.02544592524343514, 22.29057627198102765 ) ) ;
#34355 = CARTESIAN_POINT ( 'NONE',  ( 12.14591786802327356, -12.06949235617739191, 90.62609039468567573 ) ) ;
#34356 = CARTESIAN_POINT ( 'NONE',  ( 9.564922557961047289, -16.46253265017146816, 105.4177570613523471 ) ) ;
#34357 = CARTESIAN_POINT ( 'NONE',  ( 16.46253265017160672, -9.564922557960803928, 23.33224293864769194 ) ) ;
#34358 = DIRECTION ( 'NONE',  ( -1.000000000000000000, 0.000000000000000000, 0.000000000000000000 ) ) ;
#34359 = CARTESIAN_POINT ( 'NONE',  ( 15.72974639402176855, 15.80617190586768217, 101.8760903946857042 ) ) ;
#34360 = CARTESIAN_POINT ( 'NONE',  ( 4.379528057220339221, -16.55341960407611168, 57.70724293864770260 ) ) ;
#34361 = CARTESIAN_POINT ( 'NONE',  ( 14.29746914071049879, -8.314922557960816363, 68.33224293864769550 ) ) ;
#34362 = CARTESIAN_POINT ( 'NONE',  ( 21.55341960407610458, 5.719274019375980345, 93.95724293864770971 ) ) ;
#34363 = CARTESIAN_POINT ( 'NONE',  ( 5.719274019375991003, -21.55341960407610458, 92.70724293864770971 ) ) ;
#34364 = CARTESIAN_POINT ( 'NONE',  ( 16.88567814943162304, -6.947325034625687401, 96.20998877347413725 ) ) ;
#34365 = CARTESIAN_POINT ( 'NONE',  ( -21.55341960407610458, -5.719274019375992779, 26.45724293864768839 ) ) ;
#34366 = CARTESIAN_POINT ( 'NONE',  ( 8.314922557961029526, -14.29746914071037800, 60.41775706135235424 ) ) ;
#34367 = CARTESIAN_POINT ( 'NONE',  ( -8.224510206698948167, 14.34966873604960824, 85.41557627198102409 ) ) ;
#34368 = CARTESIAN_POINT ( 'NONE',  ( 5.153800228976335163, 19.02544592524342804, 44.79057627198103830 ) ) ;
#34369 =( LENGTH_UNIT ( ) NAMED_UNIT ( * ) SI_UNIT ( .MILLI., .METRE. ) );
#34370 = CARTESIAN_POINT ( 'NONE',  ( 35.02204707441116227, -5.958053119633049732, 40.41886734368968348 ) ) ;
#34371 = CARTESIAN_POINT ( 'NONE',  ( 16.52544592524335698, 4.483927247898782831, 91.45942372801901854 ) ) ;
#34372 = CARTESIAN_POINT ( 'NONE',  ( -15.72974639402176322, -15.80617190586768395, 39.37609039468567573 ) ) ;
#34373 = CARTESIAN_POINT ( 'NONE',  ( 5.049401038298161559, -19.05341960407611168, 82.70724293864770971 ) ) ;
#34374 = CARTESIAN_POINT ( 'NONE',  ( -18.62759615963255300, -10.81492255796106328, 74.16775706135231871 ) ) ;
#34375 = CARTESIAN_POINT ( 'NONE',  ( 19.02544592524343514, -5.153800228976328945, 23.54057627198102054 ) ) ;
#34376 = CARTESIAN_POINT ( 'NONE',  ( -5.153800228976328057, -19.02544592524343514, 27.29057627198103120 ) ) ;
#34377 = VERTEX_POINT ( 'NONE', #46883 ) ;
#34378 = CARTESIAN_POINT ( 'NONE',  ( -18.62759615963255300, -10.81492255796106328, 64.16775706135234714 ) ) ;
#34380 = CARTESIAN_POINT ( 'NONE',  ( -16.46253265017160317, 9.564922557960807481, 110.8322429386476955 ) ) ;
#34379 = CARTESIAN_POINT ( 'NONE',  ( 9.474510206698971260, -16.51473224551069308, 42.91557627198103120 ) ) ;
#34381 = CARTESIAN_POINT ( 'NONE',  ( -19.05341960407611168, -5.049401038298163336, 96.45724293864769550 ) ) ;
#34382 = CARTESIAN_POINT ( 'NONE',  ( 13.89961937509957401, 13.97604488694547697, 66.87609039468567573 ) ) ;
#34383 = CARTESIAN_POINT ( 'NONE',  ( -5.719274019375665041, -21.55341960407619695, 29.79275706135234358 ) ) ;
#34384 = CARTESIAN_POINT ( 'NONE',  ( -9.564922557961040184, 16.46253265017147172, 52.91775706135233293 ) ) ;
#34385 = CARTESIAN_POINT ( 'NONE',  ( 9.474510206698971260, -16.51473224551069308, 42.91557627198103120 ) ) ;
#34386 = CARTESIAN_POINT ( 'NONE',  ( 4.483927247898790824, -16.52544592524335698, 100.2094237280190043 ) ) ;
#34387 = CARTESIAN_POINT ( 'NONE',  ( -19.02544592524334988, -5.153800228976617603, 68.95942372801896170 ) ) ;
#34388 = CARTESIAN_POINT ( 'NONE',  ( -14.29746914071049879, 8.314922557960819915, 30.83224293864770260 ) ) ;
#34390 = ORIENTED_EDGE ( 'NONE', *, *, #125103, .T. ) ;
#34389 = CARTESIAN_POINT ( 'NONE',  ( 9.564922557961047289, -16.46253265017146816, 50.41775706135233293 ) ) ;
#34391 = CARTESIAN_POINT ( 'NONE',  ( -5.049401038298153566, 19.05341960407611168, 95.20724293864770971 ) ) ;
#34392 = CIRCLE ( 'NONE', #50560, 27.29906736325805028 ) ;
#34393 = CARTESIAN_POINT ( 'NONE',  ( -18.67979575497193778, 10.72451020669871902, 93.33442372801901854 ) ) ;
#34394 = CARTESIAN_POINT ( 'NONE',  ( -10.72451020669870658, -18.67979575497194134, 109.5844237280190328 ) ) ;
#34395 = DIRECTION ( 'NONE',  ( 0.000000000000000000, 0.000000000000000000, -1.000000000000000000 ) ) ;
#34396 = CARTESIAN_POINT ( 'NONE',  ( -21.55341960407619339, 5.719274019375674811, 83.54275706135234714 ) ) ;
#34397 = CARTESIAN_POINT ( 'NONE',  ( 16.53943276465976808, 0.05219959533934440121, 26.25109039468567573 ) ) ;
#34398 = CARTESIAN_POINT ( 'NONE',  ( 19.05341960407611168, 5.049401038298154454, 88.95724293864769550 ) ) ;
#34399 = CARTESIAN_POINT ( 'NONE',  ( -26.46959431505283789, -27.26463967846487435, -15.00000000000000178 ) ) ;
#34400 = CARTESIAN_POINT ( 'NONE',  ( 19.02544592524343514, -5.153800228976328945, 83.54057627198100988 ) ) ;
#34401 = DIRECTION ( 'NONE',  ( 1.000000000000000000, 0.000000000000000000, -0.000000000000000000 ) ) ;
#34402 = CARTESIAN_POINT ( 'NONE',  ( 16.46253265017146816, 9.564922557961045513, 76.66775706135234714 ) ) ;
#34403 = CARTESIAN_POINT ( 'NONE',  ( -16.51473224551069308, -9.474510206698971260, 106.6655762719810383 ) ) ;
#34404 = CARTESIAN_POINT ( 'NONE',  ( 21.52544592524334988, 5.823673210054432836, 101.4594237280190185 ) ) ;
#34405 = CARTESIAN_POINT ( 'NONE',  ( 16.53943276465976808, -0.05219959533910856209, 103.7489096053143669 ) ) ;
#34406 = CARTESIAN_POINT ( 'NONE',  ( -10.81492255796078084, -18.62759615963271287, 42.08224293864769550 ) ) ;
#34407 = CARTESIAN_POINT ( 'NONE',  ( 5.823673210054125526, 21.52544592524343514, 39.79057627198103830 ) ) ;
#34408 = CARTESIAN_POINT ( 'NONE',  ( 16.53943276465976808, -0.05219959533910856209, 103.7489096053143669 ) ) ;
#34409 = CARTESIAN_POINT ( 'NONE',  ( -15.29519331188519082, 1.499966876286098927, -61.92990168432675091 ) ) ;
#34410 = CARTESIAN_POINT ( 'NONE',  ( 19.02544592524334988, 5.153800228976608722, 56.45942372801898301 ) ) ;
#34411 = CARTESIAN_POINT ( 'NONE',  ( 16.53943276465976808, -0.05219959533910856209, 28.74890960531435624 ) ) ;
#34412 = CARTESIAN_POINT ( 'NONE',  ( 9.564922557960805705, 16.46253265017160317, 104.5822429386476955 ) ) ;
#34413 = CARTESIAN_POINT ( 'NONE',  ( 15.80617190586769283, -15.72974639402175789, 80.62609039468567573 ) ) ;
#34414 = CARTESIAN_POINT ( 'NONE',  ( 21.55341960407610458, 5.719274019375980345, 73.95724293864769550 ) ) ;
#34415 = CARTESIAN_POINT ( 'NONE',  ( 15.80617190586769283, -15.72974639402175789, 40.62609039468567573 ) ) ;
#34416 = CARTESIAN_POINT ( 'NONE',  ( 15.72974639402199770, -15.80617190586745480, 98.12390960531436690 ) ) ;
#34417 = CARTESIAN_POINT ( 'NONE',  ( 10.81492255796106328, -18.62759615963255655, 55.41775706135234714 ) ) ;
#34418 = CARTESIAN_POINT ( 'NONE',  ( 19.03943276465977164, -0.05219959533909143690, 28.74890960531435624 ) ) ;
#34419 = CARTESIAN_POINT ( 'NONE',  ( -19.05341960407611168, -5.049401038298163336, 86.45724293864769550 ) ) ;
#34420 = CARTESIAN_POINT ( 'NONE',  ( -0.05219959533934338120, 16.53943276465976808, 82.50109039468568994 ) ) ;
#34421 = CARTESIAN_POINT ( 'NONE',  ( -4.379528057220328563, 16.55341960407611168, 110.2072429386477239 ) ) ;
#34422 = CARTESIAN_POINT ( 'NONE',  ( 5.049401038298161559, -19.05341960407611168, 102.7072429386476955 ) ) ;
#34423 = CARTESIAN_POINT ( 'NONE',  ( -12.06949235617756955, 12.14591786802309770, 50.62390960531435979 ) ) ;
#34424 = CARTESIAN_POINT ( 'NONE',  ( 14.29746914071049879, -8.314922557960816363, 23.33224293864769194 ) ) ;
#34425 = CARTESIAN_POINT ( 'NONE',  ( 16.51473224551069308, 9.474510206698969483, 59.16557627198102409 ) ) ;
#34426 = CARTESIAN_POINT ( 'NONE',  ( -5.153800228976328057, -19.02544592524343514, 32.29057627198102409 ) ) ;
#34427 = CARTESIAN_POINT ( 'NONE',  ( 15.80617190586746368, 15.72974639402197994, 39.37390960531436690 ) ) ;
#34428 = CARTESIAN_POINT ( 'NONE',  ( -5.049401038297874678, -19.05341960407617918, 24.79275706135233648 ) ) ;
#34430 = CARTESIAN_POINT ( 'NONE',  ( 8.224510206698953496, -14.34966873604960469, 42.91557627198103120 ) ) ;
#34429 = CARTESIAN_POINT ( 'NONE',  ( 17.50000000000000000, 5.499999999999997335, 120.0000000000000142 ) ) ;
#34431 = CARTESIAN_POINT ( 'NONE',  ( 0.05219959533937995610, -21.53943276465977519, 40.00109039468567573 ) ) ;
#34432 = CARTESIAN_POINT ( 'NONE',  ( -13.89961937509977652, 13.97604488694528158, 115.6239096053143669 ) ) ;
#34433 = CARTESIAN_POINT ( 'NONE',  ( 16.53943276465976808, 0.05219959533934440121, 61.25109039468567573 ) ) ;
#34434 = CARTESIAN_POINT ( 'NONE',  ( 19.05341960407617918, -5.049401038297876454, 61.04275706135232582 ) ) ;
#34435 = CARTESIAN_POINT ( 'NONE',  ( -4.483927247898539470, -16.52544592524342804, 22.29057627198102765 ) ) ;
#34436 = CARTESIAN_POINT ( 'NONE',  ( 17.48853670773245739, -5.747243402303059412, 51.16671299749991420 ) ) ;
#34437 = CARTESIAN_POINT ( 'NONE',  ( 0.05219959533934541429, -16.53943276465976808, 105.0010903946856757 ) ) ;
#34438 = CARTESIAN_POINT ( 'NONE',  ( 13.89961937509977652, -13.97604488694527269, 38.12390960531436690 ) ) ;
#34439 = CARTESIAN_POINT ( 'NONE',  ( -5.049401038298153566, 19.05341960407611168, 60.20724293864768129 ) ) ;
#34440 = CARTESIAN_POINT ( 'NONE',  ( -13.97604488694527625, -13.89961937509977652, 31.87390960531435979 ) ) ;
#34441 = CARTESIAN_POINT ( 'NONE',  ( 0.05219959533937995610, -21.53943276465977519, 30.00109039468568284 ) ) ;
#34442 = CARTESIAN_POINT ( 'NONE',  ( -13.89961937509977652, 13.97604488694528158, 50.62390960531435979 ) ) ;
#34443 = CARTESIAN_POINT ( 'NONE',  ( 4.000000000000000888, -105.0000000000000000, -23.00000000000000000 ) ) ;
#34444 = CARTESIAN_POINT ( 'NONE',  ( 9.564922557960805705, 16.46253265017160317, 49.58224293864770260 ) ) ;
#34445 = CARTESIAN_POINT ( 'NONE',  ( -0.05219959533907301413, -21.53943276465977519, 22.49890960531436335 ) ) ;
#34447 = CARTESIAN_POINT ( 'NONE',  ( -16.52544592524342804, 4.483927247898546575, 111.0405762719810525 ) ) ;
#34446 = CARTESIAN_POINT ( 'NONE',  ( 5.823673210054444382, -21.52544592524334988, 65.20942372801901854 ) ) ;
#34448 = CARTESIAN_POINT ( 'NONE',  ( -19.02544592524342804, 5.153800228976336051, 116.0405762719810383 ) ) ;
#34449 = CARTESIAN_POINT ( 'NONE',  ( -0.05219959533934338120, 16.53943276465976808, 72.50109039468568994 ) ) ;
#34450 = ADVANCED_FACE ( 'NONE', ( #123694, #93363, #198588, #108543 ), #44900, .T. ) ;
#34451 = CARTESIAN_POINT ( 'NONE',  ( 10.72451020669871369, 18.67979575497193778, 92.08442372801901854 ) ) ;
#34452 = CARTESIAN_POINT ( 'NONE',  ( 4.483927247898790824, -16.52544592524335698, 55.20942372801902565 ) ) ;
#34453 = CARTESIAN_POINT ( 'NONE',  ( -16.51473224551069308, -9.474510206698971260, 91.66557627198103830 ) ) ;
#34454 = CARTESIAN_POINT ( 'NONE',  ( 12.14591786802327356, -12.06949235617739191, 35.62609039468568994 ) ) ;
#34455 = CARTESIAN_POINT ( 'NONE',  ( 12.14591786802327356, -12.06949235617739191, 30.62609039468567929 ) ) ;
#34456 = CARTESIAN_POINT ( 'NONE',  ( 8.314922557961029526, -14.29746914071037800, 95.41775706135234714 ) ) ;
#34457 = CARTESIAN_POINT ( 'NONE',  ( 5.049401038297881783, 19.05341960407617563, 107.2927570613523187 ) ) ;
#34458 = CARTESIAN_POINT ( 'NONE',  ( -5.823673210054116645, -21.52544592524344225, 107.2905762719810525 ) ) ;
#34460 = CARTESIAN_POINT ( 'NONE',  ( 0.05219959533936267826, -19.03943276465977164, 105.0010903946856615 ) ) ;
#34459 = CARTESIAN_POINT ( 'NONE',  ( -12.14591786802309592, -12.06949235617757132, 96.87390960531436690 ) ) ;
#34461 = CARTESIAN_POINT ( 'NONE',  ( 0.05219959533934541429, -16.53943276465976808, 75.00109039468568994 ) ) ;
#34462 = LINE ( 'NONE', #66778, #21477 ) ;
#34463 = CARTESIAN_POINT ( 'NONE',  ( 13.89961937509957401, 13.97604488694547697, 66.87609039468567573 ) ) ;
#34464 = CARTESIAN_POINT ( 'NONE',  ( 4.483927247898545687, 16.52544592524342804, 49.79057627198102409 ) ) ;
#34465 = CARTESIAN_POINT ( 'NONE',  ( -8.314922557960811034, -14.29746914071050412, 47.08224293864770260 ) ) ;
#34466 = CARTESIAN_POINT ( 'NONE',  ( 12.14591786802309770, 12.06949235617756955, 94.37390960531436690 ) ) ;
#34468 = CARTESIAN_POINT ( 'NONE',  ( -16.36317988757057407, 7.306389748694917863, 89.09789608363227842 ) ) ;
#34467 = CARTESIAN_POINT ( 'NONE',  ( -19.03943276465977164, -0.05219959533935918106, 28.75109039468566507 ) ) ;
#34469 = CARTESIAN_POINT ( 'NONE',  ( 21.52544592524334988, 5.823673210054432836, 41.45942372801901143 ) ) ;
#34470 = CARTESIAN_POINT ( 'NONE',  ( -5.153800228976607833, 19.02544592524334988, 97.70942372801900433 ) ) ;
#34471 = CARTESIAN_POINT ( 'NONE',  ( -2.802625768539467543, -39.09149893265183806, -33.00000000000000000 ) ) ;
#34472 = CARTESIAN_POINT ( 'NONE',  ( 19.03943276465977164, -0.05219959533909143690, 93.74890960531435269 ) ) ;
#34473 = CARTESIAN_POINT ( 'NONE',  ( -19.05341960407611168, -5.049401038298163336, 91.45724293864766707 ) ) ;
#34474 = CARTESIAN_POINT ( 'NONE',  ( -15.80617190586745835, -15.72974639402198527, 51.87390960531437401 ) ) ;
#34475 = CARTESIAN_POINT ( 'NONE',  ( 4.483927247898545687, 16.52544592524342804, 89.79057627198103830 ) ) ;
#34476 = CARTESIAN_POINT ( 'NONE',  ( 5.049401038298161559, -19.05341960407611168, 72.70724293864768129 ) ) ;
#34477 = CARTESIAN_POINT ( 'NONE',  ( -19.02544592524342804, 5.153800228976336051, 31.04057627198102409 ) ) ;
#34478 = AXIS2_PLACEMENT_3D ( 'NONE', #78214, #89435, #43931 ) ;
#34479 = CARTESIAN_POINT ( 'NONE',  ( -18.62759615963255300, -10.81492255796106328, 44.16775706135234714 ) ) ;
#34480 = CARTESIAN_POINT ( 'NONE',  ( 15.72974639402176855, 15.80617190586768217, 81.87609039468568994 ) ) ;
#34481 = CARTESIAN_POINT ( 'NONE',  ( -19.02544592524342804, 5.153800228976336051, 51.04057627198103120 ) ) ;
#34482 = CARTESIAN_POINT ( 'NONE',  ( 14.34966873604972726, -8.224510206698740333, 90.83442372801901854 ) ) ;
#34483 = CARTESIAN_POINT ( 'NONE',  ( 10.81492255796106328, -18.62759615963255655, 35.41775706135234003 ) ) ;
#34484 = CARTESIAN_POINT ( 'NONE',  ( 18.62759615963255655, 10.81492255796105972, 26.66775706135235424 ) ) ;
#34486 = CARTESIAN_POINT ( 'NONE',  ( -13.89961937509977652, 13.97604488694528158, 80.62390960531436690 ) ) ;
#34485 = CARTESIAN_POINT ( 'NONE',  ( -9.474510206698720793, -16.51473224551083518, 49.58442372801899722 ) ) ;
#34487 = CARTESIAN_POINT ( 'NONE',  ( 19.02544592524334988, 5.153800228976608722, 36.45942372801900433 ) ) ;
#34488 = CARTESIAN_POINT ( 'NONE',  ( 21.55341960407619695, -5.719274019375665929, 86.04275706135236135 ) ) ;
#34489 = CARTESIAN_POINT ( 'NONE',  ( 15.80617190586746368, 15.72974639402197994, 74.37390960531436690 ) ) ;
#34490 = CARTESIAN_POINT ( 'NONE',  ( 0.05219959533910956823, 16.53943276465976808, 44.99890960531435979 ) ) ;
#34492 = CARTESIAN_POINT ( 'NONE',  ( 5.049401038297881783, 19.05341960407617563, 27.29275706135232937 ) ) ;
#34491 = CARTESIAN_POINT ( 'NONE',  ( -15.80617190586768217, 15.72974639402176855, 93.12609039468568994 ) ) ;
#34493 = CARTESIAN_POINT ( 'NONE',  ( 12.14591786802309770, 12.06949235617756955, 69.37390960531436690 ) ) ;
#34494 = CARTESIAN_POINT ( 'NONE',  ( 13.97604488694527802, 13.89961937509977652, 29.37390960531435979 ) ) ;
#34495 = CARTESIAN_POINT ( 'NONE',  ( -0.05219959533936034679, 19.03943276465977164, 67.50109039468566152 ) ) ;
#34496 = CARTESIAN_POINT ( 'NONE',  ( 14.34966873604960469, 8.224510206698951720, 39.16557627198102409 ) ) ;
#34497 = CARTESIAN_POINT ( 'NONE',  ( -21.53943276465977519, -0.05219959533937600094, 83.75109039468568994 ) ) ;
#34498 = CARTESIAN_POINT ( 'NONE',  ( 13.97604488694527802, 13.89961937509977652, 79.37390960531435269 ) ) ;
#34499 = CARTESIAN_POINT ( 'NONE',  ( 5.153800228976615827, -19.02544592524334988, 50.20942372801897591 ) ) ;
#34500 = CARTESIAN_POINT ( 'NONE',  ( -0.05219959533907301413, -21.53943276465977519, 62.49890960531436690 ) ) ;
#34501 = CARTESIAN_POINT ( 'NONE',  ( 18.62759615963271287, -10.81492255796078972, 113.3322429386476955 ) ) ;
#34502 = CARTESIAN_POINT ( 'NONE',  ( 14.29746914071037800, 8.314922557961029526, 21.66775706135235069 ) ) ;
#34503 = CARTESIAN_POINT ( 'NONE',  ( 14.29746914071037800, 8.314922557961029526, 71.66775706135234714 ) ) ;
#34505 = CARTESIAN_POINT ( 'NONE',  ( 21.53943276465977519, -0.05219959533907433946, 103.7489096053143669 ) ) ;
#34504 = CARTESIAN_POINT ( 'NONE',  ( 17.26058549869090442, 6.457015423128627418, 63.87745837476070676 ) ) ;
#34506 = CARTESIAN_POINT ( 'NONE',  ( -12.06949235617756955, 12.14591786802309770, 105.6239096053143669 ) ) ;
#34507 = CARTESIAN_POINT ( 'NONE',  ( 22.81625015709509441, 31.40387420917330275, -9.824999997268811569 ) ) ;
#34508 = CARTESIAN_POINT ( 'NONE',  ( 4.379528057220092307, 16.55341960407617563, 42.29275706135235424 ) ) ;
#34509 = CARTESIAN_POINT ( 'NONE',  ( -21.52544592524343514, 5.823673210054127303, 56.04057627198102409 ) ) ;
#34510 = CARTESIAN_POINT ( 'NONE',  ( -16.52544592524335698, -4.483927247898792601, 108.9594237280190185 ) ) ;
#34511 = CARTESIAN_POINT ( 'NONE',  ( 5.153800228976335163, 19.02544592524342804, 34.79057627198102409 ) ) ;
#34512 = CARTESIAN_POINT ( 'NONE',  ( 16.53943276465976808, 0.05219959533934440121, 66.25109039468567573 ) ) ;
#34513 = CARTESIAN_POINT ( 'NONE',  ( -19.02544592524334988, -5.153800228976617603, 63.95942372801899012 ) ) ;
#34514 = CARTESIAN_POINT ( 'NONE',  ( 5.823673210054444382, -21.52544592524334988, 45.20942372801901854 ) ) ;
#34515 = CARTESIAN_POINT ( 'NONE',  ( 10.81492255796078972, 18.62759615963270932, 54.58224293864769550 ) ) ;
#34516 = CARTESIAN_POINT ( 'NONE',  ( 4.379528057220092307, 16.55341960407617563, 97.29275706135234714 ) ) ;
#34517 = CARTESIAN_POINT ( 'NONE',  ( -18.62759615963255300, -10.81492255796106328, 84.16775706135234714 ) ) ;
#34518 = CARTESIAN_POINT ( 'NONE',  ( -21.52544592524343514, 5.823673210054127303, 51.04057627198103120 ) ) ;
#34519 = CARTESIAN_POINT ( 'NONE',  ( 21.52544592524344225, -5.823673210054117533, 33.54057627198102409 ) ) ;
#34520 = CARTESIAN_POINT ( 'NONE',  ( -12.06949235617739369, -12.14591786802326823, 74.37609039468568994 ) ) ;
#34521 = CARTESIAN_POINT ( 'NONE',  ( -15.80617190586745835, -15.72974639402198527, 51.87390960531437401 ) ) ;
#34522 = ORIENTED_EDGE ( 'NONE', *, *, #30897, .T. ) ;
#34523 = CARTESIAN_POINT ( 'NONE',  ( 19.03943276465977164, -0.05219959533909143690, 103.7489096053143669 ) ) ;
#34524 = CARTESIAN_POINT ( 'NONE',  ( 17.50000000000000000, 4.189786006557876696, 22.00000000000000711 ) ) ;
#34525 = CARTESIAN_POINT ( 'NONE',  ( -19.03943276465977164, 0.05219959533909376836, 31.24890960531435979 ) ) ;
#34526 = CARTESIAN_POINT ( 'NONE',  ( -21.55341960407610458, -5.719274019375992779, 56.45724293864768839 ) ) ;
#34527 = CARTESIAN_POINT ( 'NONE',  ( -0.05219959533934338120, 16.53943276465976808, 87.50109039468568994 ) ) ;
#34528 = CARTESIAN_POINT ( 'NONE',  ( 15.72974639402176855, 15.80617190586768217, 41.87609039468568284 ) ) ;
#34529 = CARTESIAN_POINT ( 'NONE',  ( 5.049401038297881783, 19.05341960407617563, 102.2927570613523045 ) ) ;
#34530 = CARTESIAN_POINT ( 'NONE',  ( 16.55341960407611168, 4.379528057220329451, 108.9572429386476955 ) ) ;
#34531 = CARTESIAN_POINT ( 'NONE',  ( -9.564922557961040184, 16.46253265017147172, 112.9177570613523329 ) ) ;
#34532 = AXIS2_PLACEMENT_3D ( 'NONE', #151543, #29199, #150553 ) ;
#34533 = CARTESIAN_POINT ( 'NONE',  ( -13.89961937509977652, 13.97604488694528158, 45.62390960531433848 ) ) ;
#34534 = CARTESIAN_POINT ( 'NONE',  ( 14.46726734353924648, -1.322814319813029993, -62.26916108939695960 ) ) ;
#34535 = CARTESIAN_POINT ( 'NONE',  ( 16.46253265017160672, -9.564922557960803928, 93.33224293864769550 ) ) ;
#34536 = CARTESIAN_POINT ( 'NONE',  ( -0.05219959533934338120, 16.53943276465976808, 72.50109039468568994 ) ) ;
#34537 = CARTESIAN_POINT ( 'NONE',  ( -21.53943276465977519, -0.05219959533937600094, 103.7510903946857042 ) ) ;
#34538 = CARTESIAN_POINT ( 'NONE',  ( -10.81492255796078084, -18.62759615963271287, 62.08224293864769550 ) ) ;
#34539 = CARTESIAN_POINT ( 'NONE',  ( 4.379528057220092307, 16.55341960407617563, 92.29275706135236135 ) ) ;
#34540 = CARTESIAN_POINT ( 'NONE',  ( -16.51473224551082808, 9.474510206698731452, 83.33442372801899012 ) ) ;
#34541 = CARTESIAN_POINT ( 'NONE',  ( 19.03943276465977164, -0.05219959533909143690, 33.74890960531435979 ) ) ;
#34542 = CARTESIAN_POINT ( 'NONE',  ( 5.049401038298161559, -19.05341960407611168, 82.70724293864770971 ) ) ;
#34543 = CARTESIAN_POINT ( 'NONE',  ( 19.03943276465977164, -0.05219959533909143690, 28.74890960531435624 ) ) ;
#34544 = CARTESIAN_POINT ( 'NONE',  ( 13.97604488694548053, -13.89961937509957401, 70.62609039468567573 ) ) ;
#34545 = CARTESIAN_POINT ( 'NONE',  ( 25.73063820182080264, -8.702599028576591067, 171.6270364942811284 ) ) ;
#34546 = CARTESIAN_POINT ( 'NONE',  ( -19.03943276465977164, 0.05219959533909376836, 106.2489096053143669 ) ) ;
#34547 = CARTESIAN_POINT ( 'NONE',  ( 0.05219959533910956823, 16.53943276465976808, 59.99890960531436690 ) ) ;
#34548 = CARTESIAN_POINT ( 'NONE',  ( 15.72974639402199770, -15.80617190586745480, 58.12390960531435979 ) ) ;
#34549 = CARTESIAN_POINT ( 'NONE',  ( -28.85599147140294463, 2.075228890450760606E-14, 149.6527036446661327 ) ) ;
#34550 = CARTESIAN_POINT ( 'NONE',  ( 0.05219959533936267826, -19.03943276465977164, 30.00109039468566863 ) ) ;
#34551 = PRESENTATION_STYLE_ASSIGNMENT (( #188247 ) ) ;
#34553 = CARTESIAN_POINT ( 'NONE',  ( 13.97604488694527802, 13.89961937509977652, 69.37390960531436690 ) ) ;
#34552 = CARTESIAN_POINT ( 'NONE',  ( -0.05219959533909027116, -19.03943276465977164, 62.49890960531435979 ) ) ;
#34554 = CARTESIAN_POINT ( 'NONE',  ( 4.379528057220092307, 16.55341960407617563, 47.29275706135234003 ) ) ;
#34555 = CARTESIAN_POINT ( 'NONE',  ( -19.25176906914649777, -5.499999999999800160, 100.9992726424227669 ) ) ;
#34556 = CARTESIAN_POINT ( 'NONE',  ( 12.78135187869861511, -34.69226357686214612, -8.000000000000003553 ) ) ;
#34557 = CARTESIAN_POINT ( 'NONE',  ( 16.52544592524335698, 4.483927247898782831, 71.45942372801901854 ) ) ;
#34558 = CARTESIAN_POINT ( 'NONE',  ( 24.81835718235489807, 6.052279806424484931, 168.4265042179603142 ) ) ;
#34560 = EDGE_CURVE ( 'NONE', #86859, #100314, #29730, .T. ) ;
#34559 = CARTESIAN_POINT ( 'NONE',  ( -8.314922557961024197, 14.29746914071037800, 62.91775706135236135 ) ) ;
#34561 =( BOUNDED_CURVE ( )  B_SPLINE_CURVE ( 2, ( #196798, #85593, #58266, #165455, #22936, #84582, #73451, #57279, #40089, #118953, #24952, #70439, #147280 ),
 .UNSPECIFIED., .F., .T. ) 
 B_SPLINE_CURVE_WITH_KNOTS ( ( 3, 2, 2, 2, 2, 2, 3 ),
 ( 0.7656340109859774978, 0.7675438596491228616, 0.7719298245614034659, 0.7763157894736841813, 0.7807017543859648967, 0.7850877192982456121, 0.7870432477834813367 ),
 .UNSPECIFIED. ) 
 CURVE ( )  GEOMETRIC_REPRESENTATION_ITEM ( )  RATIONAL_B_SPLINE_CURVE ( ( 0.9832469066685285419, 0.9851625545550100060, 1.000000000000000000, 0.9659258262890683122, 1.000000000000000000, 0.9659258262890683122, 1.000000000000000000, 0.9659258262890683122, 1.000000000000000000, 0.9659258262890683122, 1.000000000000000000, 0.9848076720550078544, 0.9831626618144001517 ) ) 
 REPRESENTATION_ITEM ( '' )  );
#34562 = CARTESIAN_POINT ( 'NONE',  ( -8.224510206698735004, -14.34966873604973081, 44.58442372801901854 ) ) ;
#34564 = FACE_BOUND ( 'NONE', #47532, .T. ) ;
#34563 = CARTESIAN_POINT ( 'NONE',  ( -9.474510206698964154, 16.51473224551069663, 55.41557627198103120 ) ) ;
#34565 = CARTESIAN_POINT ( 'NONE',  ( 15.72974639402176855, 15.80617190586768217, 56.87609039468568994 ) ) ;
#34566 = CARTESIAN_POINT ( 'NONE',  ( -13.97604488694547697, 13.89961937509957934, 58.12609039468566863 ) ) ;
#34567 = CARTESIAN_POINT ( 'NONE',  ( -18.67979575497193778, 10.72451020669871902, 98.33442372801901854 ) ) ;
#34568 = CARTESIAN_POINT ( 'NONE',  ( -19.03943276465977164, 0.05219959533909376836, 31.24890960531435979 ) ) ;
#34569 = FACE_OUTER_BOUND ( 'NONE', #42514, .T. ) ;
#34570 = CARTESIAN_POINT ( 'NONE',  ( -15.72974639402197994, 15.80617190586746368, 55.62390960531436690 ) ) ;
#34571 = CARTESIAN_POINT ( 'NONE',  ( -13.97604488694527625, -13.89961937509977652, 106.8739096053143669 ) ) ;
#34572 = CARTESIAN_POINT ( 'NONE',  ( 12.06949235617757843, -12.14591786802309237, 108.1239096053143811 ) ) ;
#34573 = CARTESIAN_POINT ( 'NONE',  ( 14.29746914071037800, 8.314922557961029526, 41.66775706135235424 ) ) ;
#34574 = CARTESIAN_POINT ( 'NONE',  ( 12.06949235617757843, -12.14591786802309237, 33.12390960531435979 ) ) ;
#34575 = ORIENTED_EDGE ( 'NONE', *, *, #196054, .T. ) ;
#34576 = CARTESIAN_POINT ( 'NONE',  ( -10.72451020669898014, 18.67979575497178502, 105.4155762719810383 ) ) ;
#34578 = CARTESIAN_POINT ( 'NONE',  ( 5.153800228976335163, 19.02544592524342804, 114.7905762719810241 ) ) ;
#34577 = CARTESIAN_POINT ( 'NONE',  ( 4.483927247898545687, 16.52544592524342804, 39.79057627198103830 ) ) ;
#34579 = CARTESIAN_POINT ( 'NONE',  ( -19.03943276465977164, -0.05219959533935918106, 88.75109039468567573 ) ) ;
#34580 = CARTESIAN_POINT ( 'NONE',  ( 9.474510206698729675, 16.51473224551082808, 32.08442372801900433 ) ) ;
#34581 = CARTESIAN_POINT ( 'NONE',  ( -12.14591786802309592, -12.06949235617757132, 36.87390960531435979 ) ) ;
#34582 = CARTESIAN_POINT ( 'NONE',  ( 5.823673210054125526, 21.52544592524343514, 99.79057627198103830 ) ) ;
#34583 = CARTESIAN_POINT ( 'NONE',  ( -10.81492255796078084, -18.62759615963271287, 57.08224293864769550 ) ) ;
#34584 = CARTESIAN_POINT ( 'NONE',  ( -13.97604488694527625, -13.89961937509977652, 81.87390960531436690 ) ) ;
#34585 = CARTESIAN_POINT ( 'NONE',  ( -4.379528057220328563, 16.55341960407611168, 40.20724293864769550 ) ) ;
#34586 = CARTESIAN_POINT ( 'NONE',  ( 5.049401038298161559, -19.05341960407611168, 87.70724293864769550 ) ) ;
#34587 = CARTESIAN_POINT ( 'NONE',  ( 19.52851543214743302, 5.500000000000026645, 57.89357721762583964 ) ) ;
#34588 = CARTESIAN_POINT ( 'NONE',  ( 0.05219959533936267826, -19.03943276465977164, 40.00109039468566152 ) ) ;
#34589 = CARTESIAN_POINT ( 'NONE',  ( 18.62759615963271287, -10.81492255796078972, 83.33224293864769550 ) ) ;
#34590 = CARTESIAN_POINT ( 'NONE',  ( -16.53943276465976808, 0.05219959533911058130, 106.2489096053143811 ) ) ;
#34591 = CARTESIAN_POINT ( 'NONE',  ( 21.53943276465977519, 0.05219959533937863772, 36.25109039468567573 ) ) ;
#34592 = CARTESIAN_POINT ( 'NONE',  ( -8.571926809382608425, 26.38167802310805854, 142.4750000027312069 ) ) ;
#34593 = CARTESIAN_POINT ( 'NONE',  ( -8.224510206698735004, -14.34966873604973081, 104.5844237280190185 ) ) ;
#34594 = CARTESIAN_POINT ( 'NONE',  ( 5.153800228976335163, 19.02544592524342804, 39.79057627198100988 ) ) ;
#34595 = CARTESIAN_POINT ( 'NONE',  ( -5.049401038298153566, 19.05341960407611168, 90.20724293864766707 ) ) ;
#34596 = CARTESIAN_POINT ( 'NONE',  ( -26.03370437638687918, 6.875205692009823011, 160.5968874236874910 ) ) ;
#34597 = CARTESIAN_POINT ( 'NONE',  ( -19.03943276465977164, 0.05219959533909376836, 26.24890960531435624 ) ) ;
#34598 = CARTESIAN_POINT ( 'NONE',  ( 12.06949235617757843, -12.14591786802309237, 48.12390960531436690 ) ) ;
#34599 = CARTESIAN_POINT ( 'NONE',  ( 18.62759615963255655, 10.81492255796105972, 76.66775706135234714 ) ) ;
#34601 = CARTESIAN_POINT ( 'NONE',  ( -16.52544592524335698, -4.483927247898792601, 73.95942372801901854 ) ) ;
#34600 = CARTESIAN_POINT ( 'NONE',  ( 26.28653040952099218, -27.04268878403684084, -20.33571853020390208 ) ) ;
#34602 = CARTESIAN_POINT ( 'NONE',  ( 5.049401038298161559, -19.05341960407611168, 62.70724293864769550 ) ) ;
#34603 = CARTESIAN_POINT ( 'NONE',  ( -5.049401038298153566, 19.05341960407611168, 70.20724293864769550 ) ) ;
#34604 = VERTEX_POINT ( 'NONE', #124708 ) ;
#34605 = CARTESIAN_POINT ( 'NONE',  ( -21.53943276465977519, -0.05219959533937600094, 108.7510903946857042 ) ) ;
#34606 = CARTESIAN_POINT ( 'NONE',  ( -14.34966873604972548, 8.224510206698743886, 73.33442372801901854 ) ) ;
#34607 = CARTESIAN_POINT ( 'NONE',  ( 10.72451020669871369, 18.67979575497193778, 97.08442372801904696 ) ) ;
#34608 = CARTESIAN_POINT ( 'NONE',  ( 5.049401038298161559, -19.05341960407611168, 67.70724293864769550 ) ) ;
#34609 = CARTESIAN_POINT ( 'NONE',  ( -10.72451020669898014, 18.67979575497178502, 35.41557627198102409 ) ) ;
#34610 = CARTESIAN_POINT ( 'NONE',  ( 19.02544592524334988, 5.153800228976608722, 111.4594237280190043 ) ) ;
#34611 = CARTESIAN_POINT ( 'NONE',  ( -5.719274019375665041, -21.55341960407619695, 74.79275706135234714 ) ) ;
#34612 = CARTESIAN_POINT ( 'NONE',  ( 4.483927247898790824, -16.52544592524335698, 55.20942372801902565 ) ) ;
#34613 = CARTESIAN_POINT ( 'NONE',  ( -5.823673210054116645, -21.52544592524344225, 97.29057627198105251 ) ) ;
#34614 = CARTESIAN_POINT ( 'NONE',  ( -19.05341960407617563, 5.049401038297882671, 93.54275706135234714 ) ) ;
#34615 = CARTESIAN_POINT ( 'NONE',  ( 13.89961937509977652, -13.97604488694527269, 83.12390960531436690 ) ) ;
#34616 = CARTESIAN_POINT ( 'NONE',  ( -16.51473224551082808, 9.474510206698731452, 108.3344237280190043 ) ) ;
#34617 = CARTESIAN_POINT ( 'NONE',  ( -9.564922557961040184, 16.46253265017147172, 112.9177570613523329 ) ) ;
#34618 = CARTESIAN_POINT ( 'NONE',  ( 16.55341960407611168, 4.379528057220329451, 68.95724293864769550 ) ) ;
#34619 = CARTESIAN_POINT ( 'NONE',  ( -14.29746914071037622, -8.314922557961029526, 74.16775706135231871 ) ) ;
#34621 = CARTESIAN_POINT ( 'NONE',  ( -9.474510206698964154, 16.51473224551069663, 50.41557627198102409 ) ) ;
#34620 = CARTESIAN_POINT ( 'NONE',  ( -15.72974639402176322, -15.80617190586768395, 19.37609039468568639 ) ) ;
#34622 = CARTESIAN_POINT ( 'NONE',  ( 5.049401038298161559, -19.05341960407611168, 57.70724293864769550 ) ) ;
#34623 = CARTESIAN_POINT ( 'NONE',  ( -8.224510206698735004, -14.34966873604973081, 74.58442372801901854 ) ) ;
#34624 = CARTESIAN_POINT ( 'NONE',  ( -23.31738231874055245, -16.94106989632524574, 144.4500000054623854 ) ) ;
#34625 = EDGE_LOOP ( 'NONE', ( #118427, #64920, #137199, #118377 ) ) ;
#34626 = CARTESIAN_POINT ( 'NONE',  ( -16.51473224551082808, 9.474510206698731452, 23.33442372801900078 ) ) ;
#34627 = CARTESIAN_POINT ( 'NONE',  ( 16.51473224551069308, 9.474510206698969483, 34.16557627198102409 ) ) ;
#34628 = VERTEX_POINT ( 'NONE', #169215 ) ;
#34629 = CARTESIAN_POINT ( 'NONE',  ( 9.564922557961047289, -16.46253265017146816, 105.4177570613523471 ) ) ;
#34631 = CARTESIAN_POINT ( 'NONE',  ( 4.483927247898790824, -16.52544592524335698, 35.20942372801901854 ) ) ;
#34630 = CARTESIAN_POINT ( 'NONE',  ( -19.03943276465977164, -0.05219959533935918106, 38.75109039468566152 ) ) ;
#34632 = CARTESIAN_POINT ( 'NONE',  ( 9.564922557960805705, 16.46253265017160317, 44.58224293864769550 ) ) ;
#34633 = CARTESIAN_POINT ( 'NONE',  ( 0.05219959533909260263, 19.03943276465977164, 69.99890960531435269 ) ) ;
#34634 = CARTESIAN_POINT ( 'NONE',  ( -5.823673210054116645, -21.52544592524344225, 87.29057627198103830 ) ) ;
#34635 = DIRECTION ( 'NONE',  ( -1.084202172485503448E-15, 1.000000000000000000, 0.000000000000000000 ) ) ;
#34636 = CARTESIAN_POINT ( 'NONE',  ( -13.89961937509977652, 13.97604488694528158, 50.62390960531435979 ) ) ;
#34637 = CARTESIAN_POINT ( 'NONE',  ( -17.49999999999999645, 5.499999999999992895, 93.71769037696437010 ) ) ;
#34638 = CARTESIAN_POINT ( 'NONE',  ( -19.02544592524334988, -5.153800228976617603, 103.9594237280190043 ) ) ;
#34640 = AXIS2_PLACEMENT_3D ( 'NONE', #128532, #21372, #6190 ) ;
#34639 = CARTESIAN_POINT ( 'NONE',  ( 0.05219959533910956823, 16.53943276465976808, 69.99890960531435269 ) ) ;
#34641 = CARTESIAN_POINT ( 'NONE',  ( 13.89961937509957401, 13.97604488694547697, 21.87609039468566152 ) ) ;
#34642 = CARTESIAN_POINT ( 'NONE',  ( 12.06949235617757843, -12.14591786802309237, 58.12390960531435979 ) ) ;
#34643 = CARTESIAN_POINT ( 'NONE',  ( -10.81492255796105439, 18.62759615963255655, 82.91775706135234714 ) ) ;
#34644 = CARTESIAN_POINT ( 'NONE',  ( -19.03943276465977164, 0.05219959533909376836, 26.24890960531435624 ) ) ;
#34645 = CARTESIAN_POINT ( 'NONE',  ( 10.81492255796106328, -18.62759615963255655, 85.41775706135236135 ) ) ;
#34647 = CARTESIAN_POINT ( 'NONE',  ( 21.52544592524334988, 5.823673210054432836, 71.45942372801901854 ) ) ;
#34646 = CARTESIAN_POINT ( 'NONE',  ( 4.379528057220339221, -16.55341960407611168, 32.70724293864770260 ) ) ;
#34648 = CARTESIAN_POINT ( 'NONE',  ( 0.05219959533909260263, 19.03943276465977164, 79.99890960531436690 ) ) ;
#34649 = CARTESIAN_POINT ( 'NONE',  ( -21.52544592524334988, -5.823673210054445271, 38.95942372801901854 ) ) ;
#34650 = CARTESIAN_POINT ( 'NONE',  ( -5.049401038298153566, 19.05341960407611168, 75.20724293864769550 ) ) ;
#34651 = CARTESIAN_POINT ( 'NONE',  ( 16.52544592524342804, -4.483927247898539470, 88.54057627198103830 ) ) ;
#34652 = CARTESIAN_POINT ( 'NONE',  ( -4.483927247898539470, -16.52544592524342804, 57.29057627198103120 ) ) ;
#34653 = CARTESIAN_POINT ( 'NONE',  ( -18.62759615963270932, 10.81492255796079327, 75.83224293864769550 ) ) ;
#34654 = CARTESIAN_POINT ( 'NONE',  ( -16.46253265017160317, 9.564922557960807481, 70.83224293864770971 ) ) ;
#34655 = CARTESIAN_POINT ( 'NONE',  ( 5.719274019375991003, -21.55341960407610458, 82.70724293864770971 ) ) ;
#34656 = CARTESIAN_POINT ( 'NONE',  ( -9.474510206698720793, -16.51473224551083518, 79.58442372801899012 ) ) ;
#34658 = CARTESIAN_POINT ( 'NONE',  ( 16.52544592524342804, -4.483927247898539470, 78.54057627198103830 ) ) ;
#34657 = CARTESIAN_POINT ( 'NONE',  ( -18.22780087662122028, 5.500000000000031086, 38.51540105326107266 ) ) ;
#34659 = AXIS2_PLACEMENT_3D ( 'NONE', #187400, #61040, #153051 ) ;
#34660 = CARTESIAN_POINT ( 'NONE',  ( 5.823673210054125526, 21.52544592524343514, 59.79057627198103120 ) ) ;
#34661 = DIRECTION ( 'NONE',  ( -0.000000000000000000, -0.000000000000000000, 1.000000000000000000 ) ) ;
#34663 = CARTESIAN_POINT ( 'NONE',  ( -17.14385361876520264, -23.59649016807271238, 145.6750000027311671 ) ) ;
#34662 = CARTESIAN_POINT ( 'NONE',  ( -8.224510206698735004, -14.34966873604973081, 104.5844237280190185 ) ) ;
#34664 = CARTESIAN_POINT ( 'NONE',  ( -16.46253265017146816, -9.564922557961047289, 99.16775706135233293 ) ) ;
#34665 = CARTESIAN_POINT ( 'NONE',  ( -16.53943276465976808, 0.05219959533911058130, 66.24890960531436690 ) ) ;
#34666 = CARTESIAN_POINT ( 'NONE',  ( 8.724588103088175117, -0.9974278668897691436, -61.97156292062779670 ) ) ;
#34667 = CARTESIAN_POINT ( 'NONE',  ( 9.564922557960805705, 16.46253265017160317, 64.58224293864769550 ) ) ;
#34668 = CARTESIAN_POINT ( 'NONE',  ( 16.55341960407611168, 4.379528057220329451, 48.95724293864770971 ) ) ;
#34669 = CARTESIAN_POINT ( 'NONE',  ( -5.049401038298153566, 19.05341960407611168, 95.20724293864770971 ) ) ;
#34671 = CARTESIAN_POINT ( 'NONE',  ( -9.564922557960796823, -16.46253265017161027, 72.08224293864770971 ) ) ;
#34670 = CARTESIAN_POINT ( 'NONE',  ( 5.049401038297881783, 19.05341960407617563, 87.29275706135234714 ) ) ;
#34672 = CARTESIAN_POINT ( 'NONE',  ( -9.474510206698964154, 16.51473224551069663, 85.41557627198102409 ) ) ;
#34673 = CARTESIAN_POINT ( 'NONE',  ( 5.153800228976335163, 19.02544592524342804, 84.79057627198099567 ) ) ;
#34674 = CARTESIAN_POINT ( 'NONE',  ( 15.72974639402199770, -15.80617190586745480, 58.12390960531435979 ) ) ;
#34675 = CARTESIAN_POINT ( 'NONE',  ( -8.224510206698735004, -14.34966873604973081, 54.58442372801901143 ) ) ;
#34676 = CARTESIAN_POINT ( 'NONE',  ( 0.000000000000000000, -64.82615989628266107, -23.00000000000000000 ) ) ;
#34677 = CARTESIAN_POINT ( 'NONE',  ( -13.89961937509977652, 13.97604488694528158, 50.62390960531435979 ) ) ;
#34678 = CARTESIAN_POINT ( 'NONE',  ( 10.72451020669898902, -18.67979575497178502, 72.91557627198103830 ) ) ;
#34679 = CARTESIAN_POINT ( 'NONE',  ( 13.89961937509957401, 13.97604488694547697, 96.87609039468566152 ) ) ;
#34681 = CARTESIAN_POINT ( 'NONE',  ( 10.72451020669871369, 18.67979575497193778, 52.08442372801901854 ) ) ;
#34680 = CARTESIAN_POINT ( 'NONE',  ( -16.55341960407611168, -4.379528057220339221, 21.45724293864769550 ) ) ;
#34682 = EDGE_CURVE ( 'NONE', #25217, #173153, #195377, .T. ) ;
#34683 = CARTESIAN_POINT ( 'NONE',  ( -13.89961937509957401, -13.97604488694547875, 39.37609039468566152 ) ) ;
#34685 = CARTESIAN_POINT ( 'NONE',  ( 16.52544592524335698, 4.483927247898782831, 91.45942372801901854 ) ) ;
#34684 = CARTESIAN_POINT ( 'NONE',  ( 12.14591786802327356, -12.06949235617739191, 55.62609039468568284 ) ) ;
#34686 = CARTESIAN_POINT ( 'NONE',  ( 19.26498983726239800, -5.499999999999598543, 43.05319577422001487 ) ) ;
#34687 = CARTESIAN_POINT ( 'NONE',  ( 16.52544592524335698, 4.483927247898782831, 86.45942372801901854 ) ) ;
#34688 = CARTESIAN_POINT ( 'NONE',  ( -8.224510206698735004, -14.34966873604973081, 34.58442372801900433 ) ) ;
#34689 = CARTESIAN_POINT ( 'NONE',  ( -0.05219959533909027116, -19.03943276465977164, 42.49890960531435269 ) ) ;
#34690 = CARTESIAN_POINT ( 'NONE',  ( 19.05341960407611168, 5.049401038298154454, 53.95724293864770260 ) ) ;
#34691 = CARTESIAN_POINT ( 'NONE',  ( 13.97604488694527802, 13.89961937509977652, 64.37390960531436690 ) ) ;
#34692 = CARTESIAN_POINT ( 'NONE',  ( 15.72974639402176855, 15.80617190586768217, 56.87609039468568994 ) ) ;
#34693 = CARTESIAN_POINT ( 'NONE',  ( 8.314922557961029526, -14.29746914071037800, 45.41775706135234003 ) ) ;
#34694 = CARTESIAN_POINT ( 'NONE',  ( -4.483927247898539470, -16.52544592524342804, 22.29057627198102765 ) ) ;
#34695 = CARTESIAN_POINT ( 'NONE',  ( -5.049401038298153566, 19.05341960407611168, 30.20724293864768839 ) ) ;
#34696 = CARTESIAN_POINT ( 'NONE',  ( -19.03943276465977164, -0.05219959533935918106, 18.75109039468567218 ) ) ;
#34697 = CARTESIAN_POINT ( 'NONE',  ( 16.55341960407618274, -4.379528057220086978, 31.04275706135234714 ) ) ;
#34698 = CARTESIAN_POINT ( 'NONE',  ( -16.46253265017146816, -9.564922557961047289, 84.16775706135233293 ) ) ;
#34699 = CARTESIAN_POINT ( 'NONE',  ( 14.34966873604960469, 8.224510206698951720, 84.16557627198103830 ) ) ;
#34700 = CARTESIAN_POINT ( 'NONE',  ( 19.02544592524343514, -5.153800228976328945, 33.54057627198102409 ) ) ;
#34702 = CARTESIAN_POINT ( 'NONE',  ( 16.88567814943163015, -6.947325034625690954, 91.20998877347419409 ) ) ;
#34701 = CARTESIAN_POINT ( 'NONE',  ( -16.46253265017146816, -9.564922557961047289, 74.16775706135234714 ) ) ;
#34703 = CARTESIAN_POINT ( 'NONE',  ( -15.80617190586768217, 15.72974639402176855, 83.12609039468568994 ) ) ;
#34704 = CARTESIAN_POINT ( 'NONE',  ( 16.52544592524335698, 4.483927247898782831, 41.45942372801901143 ) ) ;
#34705 = CARTESIAN_POINT ( 'NONE',  ( 16.31925111598457434, 7.325300261831481308, 37.33575461032752685 ) ) ;
#34706 = CARTESIAN_POINT ( 'NONE',  ( -10.72451020669898014, 18.67979575497178502, 35.41557627198102409 ) ) ;
#34707 = CARTESIAN_POINT ( 'NONE',  ( -8.314922557961024197, 14.29746914071037800, 22.91775706135235069 ) ) ;
#34708 = CARTESIAN_POINT ( 'NONE',  ( -0.05219959533909027116, -19.03943276465977164, 27.49890960531435624 ) ) ;
#34709 = CARTESIAN_POINT ( 'NONE',  ( -19.05341960407617563, 5.049401038297882671, 28.54275706135232937 ) ) ;
#34710 = CARTESIAN_POINT ( 'NONE',  ( -28.98447489709222680, -24.58636592488624117, -17.12158557651119750 ) ) ;
#34711 = CARTESIAN_POINT ( 'NONE',  ( 0.05219959533909260263, 19.03943276465977164, 39.99890960531436690 ) ) ;
#34712 = CARTESIAN_POINT ( 'NONE',  ( -5.000000000000003553, 37.66961640367474473, -15.00000000000000000 ) ) ;
#34713 = CARTESIAN_POINT ( 'NONE',  ( 16.51473224551069308, 9.474510206698969483, 69.16557627198102409 ) ) ;
#34714 = CARTESIAN_POINT ( 'NONE',  ( -19.52217212775660116, 5.499999999999917399, 99.93993709005258097 ) ) ;
#34715 = CARTESIAN_POINT ( 'NONE',  ( 13.97604488694548053, -13.89961937509957401, 25.62609039468566507 ) ) ;
#34716 = CARTESIAN_POINT ( 'NONE',  ( -14.34966873604960291, -8.224510206698953496, 31.66557627198102054 ) ) ;
#34717 = CARTESIAN_POINT ( 'NONE',  ( -16.46253265017160317, 9.564922557960807481, 40.83224293864769550 ) ) ;
#34718 = CARTESIAN_POINT ( 'NONE',  ( -9.564922557960796823, -16.46253265017161027, 87.08224293864769550 ) ) ;
#34719 = CARTESIAN_POINT ( 'NONE',  ( 10.81492255796106328, -18.62759615963255655, 65.41775706135234714 ) ) ;
#34720 = CARTESIAN_POINT ( 'NONE',  ( 5.153800228976335163, 19.02544592524342804, 44.79057627198103830 ) ) ;
#34721 = CARTESIAN_POINT ( 'NONE',  ( 18.67979575497194134, -10.72451020669871369, 60.83442372801901854 ) ) ;
#34722 = CARTESIAN_POINT ( 'NONE',  ( 10.81492255796078972, 18.62759615963270932, 29.58224293864769905 ) ) ;
#34723 = CARTESIAN_POINT ( 'NONE',  ( -13.97604488694527625, -13.89961937509977652, 36.87390960531436690 ) ) ;
#34724 = CARTESIAN_POINT ( 'NONE',  ( 21.52544592524334988, 5.823673210054432836, 21.45942372801901499 ) ) ;
#34725 = CARTESIAN_POINT ( 'NONE',  ( 9.564922557961047289, -16.46253265017146816, 45.41775706135232582 ) ) ;
#34726 = CARTESIAN_POINT ( 'NONE',  ( -4.483927247898539470, -16.52544592524342804, 112.2905762719810241 ) ) ;
#34727 = CARTESIAN_POINT ( 'NONE',  ( -19.02544592524342804, 5.153800228976336051, 61.04057627198103120 ) ) ;
#34728 = CARTESIAN_POINT ( 'NONE',  ( -9.564922557961040184, 16.46253265017147172, 112.9177570613523329 ) ) ;
#34729 = CARTESIAN_POINT ( 'NONE',  ( -8.224510206698948167, 14.34966873604960824, 80.41557627198103830 ) ) ;
#34730 = CARTESIAN_POINT ( 'NONE',  ( 9.564922557960805705, 16.46253265017160317, 114.5822429386476955 ) ) ;
#34731 = CARTESIAN_POINT ( 'NONE',  ( 19.03943276465977164, 0.05219959533936151252, 106.2510903946856615 ) ) ;
#34732 = CARTESIAN_POINT ( 'NONE',  ( -21.53943276465977519, 0.05219959533907696930, 106.2489096053143811 ) ) ;
#34733 = CARTESIAN_POINT ( 'NONE',  ( -5.823673210054431948, 21.52544592524334988, 62.70942372801902565 ) ) ;
#34734 = CARTESIAN_POINT ( 'NONE',  ( -16.55341960407617563, 4.379528057220093196, 58.54275706135235424 ) ) ;
#34735 = CARTESIAN_POINT ( 'NONE',  ( 8.314922557961029526, -14.29746914071037800, 60.41775706135235424 ) ) ;
#34736 = CARTESIAN_POINT ( 'NONE',  ( -10.72451020669898014, 18.67979575497178502, 50.41557627198103120 ) ) ;
#34737 = CARTESIAN_POINT ( 'NONE',  ( 19.02544592524343514, -5.153800228976328945, 48.54057627198103120 ) ) ;
#34738 = CARTESIAN_POINT ( 'NONE',  ( -14.29746914071037622, -8.314922557961029526, 69.16775706135234714 ) ) ;
#34739 = CARTESIAN_POINT ( 'NONE',  ( -10.81492255796078084, -18.62759615963271287, 102.0822429386476955 ) ) ;
#34740 = CARTESIAN_POINT ( 'NONE',  ( -14.34966873604960291, -8.224510206698953496, 56.66557627198103830 ) ) ;
#34741 = CARTESIAN_POINT ( 'NONE',  ( -13.97604488694527625, -13.89961937509977652, 66.87390960531436690 ) ) ;
#34742 = CARTESIAN_POINT ( 'NONE',  ( 16.52544592524335698, 4.483927247898782831, 71.45942372801901854 ) ) ;
#34743 = CARTESIAN_POINT ( 'NONE',  ( 4.379528057220092307, 16.55341960407617563, 22.29275706135235069 ) ) ;
#34744 = CARTESIAN_POINT ( 'NONE',  ( -15.80617190586745835, -15.72974639402198527, 101.8739096053143811 ) ) ;
#34745 = CARTESIAN_POINT ( 'NONE',  ( -4.379528057220328563, 16.55341960407611168, 45.20724293864769550 ) ) ;
#34746 = ORIENTED_EDGE ( 'NONE', *, *, #70721, .T. ) ;
#34747 = CARTESIAN_POINT ( 'NONE',  ( 19.48894818550245844, -5.499999999999908518, 92.60307310435240424 ) ) ;
#34748 = CARTESIAN_POINT ( 'NONE',  ( 15.80617190586746368, 15.72974639402197994, 84.37390960531438111 ) ) ;
#34749 = CARTESIAN_POINT ( 'NONE',  ( 0.05219959533910956823, 16.53943276465976808, 29.99890960531435979 ) ) ;
#34750 = ORIENTED_EDGE ( 'NONE', *, *, #26227, .F. ) ;
#34751 = CARTESIAN_POINT ( 'NONE',  ( 5.000000000000000888, -140.0000000000000000, -15.00000000000000000 ) ) ;
#34752 = CARTESIAN_POINT ( 'NONE',  ( 10.72451020669898902, -18.67979575497178502, 97.91557627198103830 ) ) ;
#34753 = CARTESIAN_POINT ( 'NONE',  ( 19.05341960407611168, 5.049401038298154454, 103.9572429386476671 ) ) ;
#34754 = CARTESIAN_POINT ( 'NONE',  ( -0.05219959533937732626, 21.53943276465977519, 27.50109039468567929 ) ) ;
#34755 = CARTESIAN_POINT ( 'NONE',  ( -8.224510206698948167, 14.34966873604960824, 35.41557627198102409 ) ) ;
#34756 = CARTESIAN_POINT ( 'NONE',  ( 16.55341960407618274, -4.379528057220086978, 46.04275706135234714 ) ) ;
#34757 = AXIS2_PLACEMENT_3D ( 'NONE', #66686, #190046, #97991 ) ;
#34758 = CARTESIAN_POINT ( 'NONE',  ( 5.049401038298161559, -19.05341960407611168, 47.70724293864770260 ) ) ;
#34759 = CARTESIAN_POINT ( 'NONE',  ( -9.564922557961040184, 16.46253265017147172, 52.91775706135233293 ) ) ;
#34760 = CARTESIAN_POINT ( 'NONE',  ( -16.46253265017160317, 9.564922557960807481, 80.83224293864769550 ) ) ;
#34761 = ORIENTED_EDGE ( 'NONE', *, *, #69929, .T. ) ;
#34762 = EDGE_CURVE ( 'NONE', #126376, #111207, #124333, .T. ) ;
#34763 = CARTESIAN_POINT ( 'NONE',  ( 10.81492255796078972, 18.62759615963270932, 29.58224293864769905 ) ) ;
#34764 = CARTESIAN_POINT ( 'NONE',  ( -31.56233167169803622, -22.40491105029811081, -17.28239568967446971 ) ) ;
#34765 = CARTESIAN_POINT ( 'NONE',  ( 8.224510206698742110, 14.34966873604972548, 22.08442372801901143 ) ) ;
#34766 = CARTESIAN_POINT ( 'NONE',  ( 13.97604488694548053, -13.89961937509957401, 55.62609039468566863 ) ) ;
#34767 = CARTESIAN_POINT ( 'NONE',  ( -10.81492255796078084, -18.62759615963271287, 107.0822429386476955 ) ) ;
#34768 = CARTESIAN_POINT ( 'NONE',  ( 0.05219959533910956823, 16.53943276465976808, 29.99890960531435979 ) ) ;
#34769 = CARTESIAN_POINT ( 'NONE',  ( -5.153800228976328057, -19.02544592524343514, 82.29057627198103830 ) ) ;
#34770 = CARTESIAN_POINT ( 'NONE',  ( 5.823673210054125526, 21.52544592524343514, 54.79057627198104541 ) ) ;
#34772 = CARTESIAN_POINT ( 'NONE',  ( -14.34966873604972548, 8.224510206698743886, 28.33442372801902209 ) ) ;
#34771 = CARTESIAN_POINT ( 'NONE',  ( 15.80617190586746368, 15.72974639402197994, 89.37390960531435269 ) ) ;
#34773 = CARTESIAN_POINT ( 'NONE',  ( 21.55341960407610458, 5.719274019375980345, 28.95724293864769905 ) ) ;
#34774 = CARTESIAN_POINT ( 'NONE',  ( -0.05219959533937732626, 21.53943276465977519, 92.50109039468567573 ) ) ;
#34776 = EDGE_CURVE ( 'NONE', #130796, #45831, #1351, .T. ) ;
#34775 = CARTESIAN_POINT ( 'NONE',  ( 19.02544592524343514, -5.153800228976328945, 73.54057627198103830 ) ) ;
#34777 = CARTESIAN_POINT ( 'NONE',  ( 19.05341960407611168, 5.049401038298154454, 28.95724293864769550 ) ) ;
#34778 = CARTESIAN_POINT ( 'NONE',  ( -9.564922557960796823, -16.46253265017161027, 87.08224293864769550 ) ) ;
#34779 = CARTESIAN_POINT ( 'NONE',  ( -12.06949235617756955, 12.14591786802309770, 105.6239096053143669 ) ) ;
#34780 = CARTESIAN_POINT ( 'NONE',  ( 9.474510206698729675, 16.51473224551082808, 107.0844237280190043 ) ) ;
#34781 = DIRECTION ( 'NONE',  ( -1.047444401652940164E-14, -1.000000000000000000, -0.000000000000000000 ) ) ;
#34782 = CARTESIAN_POINT ( 'NONE',  ( 9.564922557960805705, 16.46253265017160317, 69.58224293864770971 ) ) ;
#34783 = AXIS2_PLACEMENT_3D ( 'NONE', #1746, #108929, #154442 ) ;
#34785 = CARTESIAN_POINT ( 'NONE',  ( 19.05341960407611168, 5.049401038298154454, 113.9572429386477097 ) ) ;
#34784 = CARTESIAN_POINT ( 'NONE',  ( -5.823673210054431948, 21.52544592524334988, 97.70942372801904696 ) ) ;
#34786 = CARTESIAN_POINT ( 'NONE',  ( -0.05219959533934338120, 16.53943276465976808, 92.50109039468567573 ) ) ;
#34787 = CARTESIAN_POINT ( 'NONE',  ( -30.59399807301414498, 1.495846735942831351, -47.49088840515941001 ) ) ;
#34788 = CARTESIAN_POINT ( 'NONE',  ( -9.564922557961040184, 16.46253265017147172, 62.91775706135233293 ) ) ;
#34789 = CARTESIAN_POINT ( 'NONE',  ( -13.89961937509957401, -13.97604488694547875, 24.37609039468565442 ) ) ;
#34790 = CARTESIAN_POINT ( 'NONE',  ( -16.88567814943164080, -6.947325034625593254, 46.29001122652586275 ) ) ;
#34791 = CARTESIAN_POINT ( 'NONE',  ( 9.474510206698971260, -16.51473224551069308, 22.91557627198102765 ) ) ;
#34792 = CARTESIAN_POINT ( 'NONE',  ( 14.29746914071037800, 8.314922557961029526, 111.6677570613523613 ) ) ;
#34793 = CARTESIAN_POINT ( 'NONE',  ( -27.73933785331498925, 2.428612866367529932E-14, 148.8750000027311842 ) ) ;
#34794 = CARTESIAN_POINT ( 'NONE',  ( -8.224510206698735004, -14.34966873604973081, 104.5844237280190185 ) ) ;
#34795 = CARTESIAN_POINT ( 'NONE',  ( -15.49999999999999822, -5.500000000000000888, 22.00000000000000711 ) ) ;
#34796 = CARTESIAN_POINT ( 'NONE',  ( 0.05219959533934541429, -16.53943276465976808, 75.00109039468568994 ) ) ;
#34797 = CARTESIAN_POINT ( 'NONE',  ( -13.89961937509977652, 13.97604488694528158, 40.62390960531435979 ) ) ;
#34798 = CARTESIAN_POINT ( 'NONE',  ( -18.62759615963255300, -10.81492255796106328, 99.16775706135234714 ) ) ;
#34799 = CARTESIAN_POINT ( 'NONE',  ( 0.05219959533936267826, -19.03943276465977164, 100.0010903946856757 ) ) ;
#34800 = CARTESIAN_POINT ( 'NONE',  ( -18.62759615963255300, -10.81492255796106328, 69.16775706135234714 ) ) ;
#34801 = CARTESIAN_POINT ( 'NONE',  ( -5.153800228976607833, 19.02544592524334988, 47.70942372801900433 ) ) ;
#34802 = CARTESIAN_POINT ( 'NONE',  ( -0.05219959533909027116, -19.03943276465977164, 82.49890960531436690 ) ) ;
#34803 = CARTESIAN_POINT ( 'NONE',  ( -13.89961937509977652, 13.97604488694528158, 65.62390960531436690 ) ) ;
#34804 = DIRECTION ( 'NONE',  ( -0.000000000000000000, -0.000000000000000000, 1.000000000000000000 ) ) ;
#34805 = CARTESIAN_POINT ( 'NONE',  ( -5.823673210054116645, -21.52544592524344225, 52.29057627198102409 ) ) ;
#34806 = CARTESIAN_POINT ( 'NONE',  ( -19.03943276465977164, 0.05219959533909376836, 41.24890960531435269 ) ) ;
#34808 = CARTESIAN_POINT ( 'NONE',  ( -0.05219959533934338120, 16.53943276465976808, 82.50109039468568994 ) ) ;
#34807 = CARTESIAN_POINT ( 'NONE',  ( -21.52544592524343514, 5.823673210054127303, 81.04057627198102409 ) ) ;
#34809 = EDGE_LOOP ( 'NONE', ( #51909, #180120, #35049, #99705, #63 ) ) ;
#34811 = CARTESIAN_POINT ( 'NONE',  ( 29.86685920354754842, -21.69954338932559068, -3.824999997268813345 ) ) ;
#34810 = CARTESIAN_POINT ( 'NONE',  ( 0.05219959533910956823, 16.53943276465976808, 74.99890960531435269 ) ) ;
#34812 = CARTESIAN_POINT ( 'NONE',  ( 8.224510206698742110, 14.34966873604972548, 37.08442372801901143 ) ) ;
#34813 = CARTESIAN_POINT ( 'NONE',  ( 19.03943276465977164, -0.05219959533909143690, 23.74890960531435269 ) ) ;
#34814 = CARTESIAN_POINT ( 'NONE',  ( -5.153800228976607833, 19.02544592524334988, 67.70942372801900433 ) ) ;
#34815 = CARTESIAN_POINT ( 'NONE',  ( -8.224510206698948167, 14.34966873604960824, 75.41557627198102409 ) ) ;
#34816 = CARTESIAN_POINT ( 'NONE',  ( -0.05219959533937732626, 21.53943276465977519, 47.50109039468568994 ) ) ;
#34818 = CARTESIAN_POINT ( 'NONE',  ( -21.55341960407610458, -5.719274019375992779, 86.45724293864770971 ) ) ;
#34817 = CARTESIAN_POINT ( 'NONE',  ( -9.564922557960796823, -16.46253265017161027, 22.08224293864768839 ) ) ;
#34819 = CARTESIAN_POINT ( 'NONE',  ( -4.500000000000001776, -130.0000000000000000, 15.50000000000000000 ) ) ;
#34820 = CARTESIAN_POINT ( 'NONE',  ( 16.55341960407611168, 4.379528057220329451, 93.95724293864770971 ) ) ;
#34821 = CARTESIAN_POINT ( 'NONE',  ( 15.50653001718876745, -40.92458772717220228, -21.39878705119478042 ) ) ;
#34822 = CARTESIAN_POINT ( 'NONE',  ( -16.51473224551069308, -9.474510206698971260, 41.66557627198103120 ) ) ;
#34823 = CARTESIAN_POINT ( 'NONE',  ( -22.81625015709510507, 31.40387420917330275, -0.9249999972688132122 ) ) ;
#34824 = CARTESIAN_POINT ( 'NONE',  ( -5.153800228976607833, 19.02544592524334988, 77.70942372801900433 ) ) ;
#34825 = CARTESIAN_POINT ( 'NONE',  ( -0.05219959533937732626, 21.53943276465977519, 22.50109039468567573 ) ) ;
#34826 = CARTESIAN_POINT ( 'NONE',  ( -9.474510206698964154, 16.51473224551069663, 75.41557627198103830 ) ) ;
#34827 = CARTESIAN_POINT ( 'NONE',  ( 5.153800228976615827, -19.02544592524334988, 60.20942372801899012 ) ) ;
#34828 = CARTESIAN_POINT ( 'NONE',  ( -19.03943276465977164, 0.05219959533909376836, 41.24890960531435269 ) ) ;
#34829 = CARTESIAN_POINT ( 'NONE',  ( -16.55341960407611168, -4.379528057220339221, 56.45724293864768839 ) ) ;
#34830 = CARTESIAN_POINT ( 'NONE',  ( -12.14591786802309592, -12.06949235617757132, 56.87390960531436690 ) ) ;
#34831 = CARTESIAN_POINT ( 'NONE',  ( -5.049401038298153566, 19.05341960407611168, 80.20724293864769550 ) ) ;
#34832 = CARTESIAN_POINT ( 'NONE',  ( 0.05219959533907565091, 21.53943276465977519, 104.9989096053143669 ) ) ;
#34833 = CARTESIAN_POINT ( 'NONE',  ( 5.049401038298161559, -19.05341960407611168, 72.70724293864768129 ) ) ;
#34834 = CARTESIAN_POINT ( 'NONE',  ( 5.823673210054125526, 21.52544592524343514, 74.79057627198105251 ) ) ;
#34835 = CARTESIAN_POINT ( 'NONE',  ( 16.51473224551083163, -9.474510206698727899, 20.83442372801899722 ) ) ;
#34838 = CARTESIAN_POINT ( 'NONE',  ( -12.06949235617756955, 12.14591786802309770, 95.62390960531436690 ) ) ;
#34837 = CARTESIAN_POINT ( 'NONE',  ( 12.06949235617757843, -12.14591786802309237, 23.12390960531436335 ) ) ;
#34836 = CARTESIAN_POINT ( 'NONE',  ( 9.474510206698971260, -16.51473224551069308, 37.91557627198102409 ) ) ;
#34839 = CARTESIAN_POINT ( 'NONE',  ( 9.474510206698729675, 16.51473224551082808, 107.0844237280190043 ) ) ;
#34840 = VERTEX_POINT ( 'NONE', #184405 ) ;
#34841 = CARTESIAN_POINT ( 'NONE',  ( 15.80617190586769283, -15.72974639402175789, 30.62609039468567929 ) ) ;
#34842 = CARTESIAN_POINT ( 'NONE',  ( 13.89961937509957401, 13.97604488694547697, 46.87609039468565442 ) ) ;
#34843 = CARTESIAN_POINT ( 'NONE',  ( -4.379528057220328563, 16.55341960407611168, 25.20724293864769550 ) ) ;
#34844 = CARTESIAN_POINT ( 'NONE',  ( 18.67979575497178502, 10.72451020669898547, 79.16557627198103830 ) ) ;
#34845 = CARTESIAN_POINT ( 'NONE',  ( 13.97604488694527802, 13.89961937509977652, 104.3739096053143385 ) ) ;
#34846 = CARTESIAN_POINT ( 'NONE',  ( 8.314922557960818139, 14.29746914071049879, 54.58224293864769550 ) ) ;
#34847 = CARTESIAN_POINT ( 'NONE',  ( 16.46253265017160672, -9.564922557960803928, 33.33224293864770260 ) ) ;
#34848 = CARTESIAN_POINT ( 'NONE',  ( 9.474510206698971260, -16.51473224551069308, 27.91557627198103120 ) ) ;
#34849 = CARTESIAN_POINT ( 'NONE',  ( -10.81492255796105439, 18.62759615963255655, 107.9177570613523471 ) ) ;
#34850 = CARTESIAN_POINT ( 'NONE',  ( -12.06949235617739369, -12.14591786802326823, 89.37609039468568994 ) ) ;
#34851 = CARTESIAN_POINT ( 'NONE',  ( 5.823673210054444382, -21.52544592524334988, 45.20942372801901854 ) ) ;
#34852 = CARTESIAN_POINT ( 'NONE',  ( -16.53943276465976808, -0.05219959533934237506, 43.75109039468568284 ) ) ;
#34853 = CARTESIAN_POINT ( 'NONE',  ( 21.53943276465977519, -0.05219959533907433946, 23.74890960531435269 ) ) ;
#34854 = CARTESIAN_POINT ( 'NONE',  ( 13.89961937509977652, -13.97604488694527269, 58.12390960531436690 ) ) ;
#34855 = CARTESIAN_POINT ( 'NONE',  ( -0.05219959533909027116, -19.03943276465977164, 72.49890960531435269 ) ) ;
#34856 = CARTESIAN_POINT ( 'NONE',  ( -16.55341960407617563, 4.379528057220093196, 58.54275706135235424 ) ) ;
#34857 = CARTESIAN_POINT ( 'NONE',  ( -4.379528057220328563, 16.55341960407611168, 100.2072429386476955 ) ) ;
#34858 = CARTESIAN_POINT ( 'NONE',  ( -8.224510206698948167, 14.34966873604960824, 25.41557627198103120 ) ) ;
#34859 = LINE ( 'NONE', #158204, #66850 ) ;
#34862 = CARTESIAN_POINT ( 'NONE',  ( 13.89961937509977652, -13.97604488694527269, 78.12390960531433848 ) ) ;
#34861 = CARTESIAN_POINT ( 'NONE',  ( 5.153800228976335163, 19.02544592524342804, 89.79057627198102409 ) ) ;
#34860 = CARTESIAN_POINT ( 'NONE',  ( 18.67979575497194134, -10.72451020669871369, 50.83442372801901143 ) ) ;
#34863 = CARTESIAN_POINT ( 'NONE',  ( 16.46253265017160672, -9.564922557960803928, 103.3322429386476955 ) ) ;
#34864 = CARTESIAN_POINT ( 'NONE',  ( 4.483927247898545687, 16.52544592524342804, 44.79057627198103120 ) ) ;
#34865 = EDGE_CURVE ( 'NONE', #119129, #29984, #24199, .T. ) ;
#34866 = CARTESIAN_POINT ( 'NONE',  ( -8.314922557961024197, 14.29746914071037800, 107.9177570613523471 ) ) ;
#34867 = CARTESIAN_POINT ( 'NONE',  ( 14.29746914071049879, -8.314922557960816363, 38.33224293864768839 ) ) ;
#34868 = CARTESIAN_POINT ( 'NONE',  ( -15.72645790992315717, -17.57596900401679818, -54.79584306608744271 ) ) ;
#34869 = CARTESIAN_POINT ( 'NONE',  ( -0.05219959533936034679, 19.03943276465977164, 32.50109039468566863 ) ) ;
#34870 = CARTESIAN_POINT ( 'NONE',  ( 0.05219959533909260263, 19.03943276465977164, 74.99890960531435269 ) ) ;
#34871 = CARTESIAN_POINT ( 'NONE',  ( -16.46253265017146816, -9.564922557961047289, 49.16775706135233293 ) ) ;
#34872 = CARTESIAN_POINT ( 'NONE',  ( -5.950531402560715689E-15, 38.81732327939063509, -1.124999997268812946 ) ) ;
#34873 = CARTESIAN_POINT ( 'NONE',  ( -17.49999999999999289, 5.500000000000034639, 55.79690382534172954 ) ) ;
#34875 = CARTESIAN_POINT ( 'NONE',  ( -14.34966873604972548, 8.224510206698743886, 73.33442372801901854 ) ) ;
#34874 = CARTESIAN_POINT ( 'NONE',  ( 19.02544592524334988, 5.153800228976608722, 81.45942372801897591 ) ) ;
#34876 = CARTESIAN_POINT ( 'NONE',  ( 16.21995358207304605, 7.366697692864170754, 92.56448998487842061 ) ) ;
#34877 = CARTESIAN_POINT ( 'NONE',  ( -13.89961937509977652, 13.97604488694528158, 100.6239096053143669 ) ) ;
#34878 = CARTESIAN_POINT ( 'NONE',  ( -21.52544592524334988, -5.823673210054445271, 28.95942372801902209 ) ) ;
#34879 = CARTESIAN_POINT ( 'NONE',  ( 19.02544592524334988, 5.153800228976608722, 96.45942372801897591 ) ) ;
#34881 = CARTESIAN_POINT ( 'NONE',  ( 9.564922557960805705, 16.46253265017160317, 44.58224293864769550 ) ) ;
#34880 = CARTESIAN_POINT ( 'NONE',  ( 19.03943276465977164, -0.05219959533909143690, 113.7489096053143669 ) ) ;
#34882 = CARTESIAN_POINT ( 'NONE',  ( 13.89961937509977652, -13.97604488694527269, 88.12390960531438111 ) ) ;
#34884 = CARTESIAN_POINT ( 'NONE',  ( -16.51473224551069308, -9.474510206698971260, 51.66557627198102409 ) ) ;
#34883 = CARTESIAN_POINT ( 'NONE',  ( -14.34966873604960291, -8.224510206698953496, 66.66557627198102409 ) ) ;
#34885 = CARTESIAN_POINT ( 'NONE',  ( -0.05219959533909027116, -19.03943276465977164, 67.49890960531436690 ) ) ;
#34886 = CARTESIAN_POINT ( 'NONE',  ( 9.564922557961047289, -16.46253265017146816, 70.41775706135233293 ) ) ;
#34887 = CARTESIAN_POINT ( 'NONE',  ( -19.03943276465977164, -0.05219959533935918106, 23.75109039468566152 ) ) ;
#34888 = CARTESIAN_POINT ( 'NONE',  ( 5.153800228976335163, 19.02544592524342804, 64.79057627198100988 ) ) ;
#34889 = CARTESIAN_POINT ( 'NONE',  ( 18.67979575497178502, 10.72451020669898547, 69.16557627198102409 ) ) ;
#34891 = CARTESIAN_POINT ( 'NONE',  ( -16.51473224551082808, 9.474510206698731452, 33.33442372801899722 ) ) ;
#34890 = CARTESIAN_POINT ( 'NONE',  ( 4.379528057220339221, -16.55341960407611168, 72.70724293864769550 ) ) ;
#34892 = CARTESIAN_POINT ( 'NONE',  ( 9.564922557960805705, 16.46253265017160317, 114.5822429386476955 ) ) ;
#34893 = CARTESIAN_POINT ( 'NONE',  ( -18.67979575497178146, -10.72451020669898902, 21.66557627198102409 ) ) ;
#34894 = CARTESIAN_POINT ( 'NONE',  ( 19.03943276465977164, -0.05219959533909143690, 58.74890960531435979 ) ) ;
#34895 = CARTESIAN_POINT ( 'NONE',  ( 19.03943276465977164, -0.05219959533909143690, 33.74890960531435979 ) ) ;
#34896 = CARTESIAN_POINT ( 'NONE',  ( -4.483927247898539470, -16.52544592524342804, 107.2905762719810525 ) ) ;
#34897 = CIRCLE ( 'NONE', #96227, 2.000000000000000000 ) ;
#34898 = CARTESIAN_POINT ( 'NONE',  ( -10.72451020669898014, 18.67979575497178502, 110.4155762719810383 ) ) ;
#34899 = DIRECTION ( 'NONE',  ( -7.855351589328939542E-15, 0.000000000000000000, 1.000000000000000000 ) ) ;
#34900 = CARTESIAN_POINT ( 'NONE',  ( 5.719274019375673035, 21.55341960407619339, 32.29275706135235424 ) ) ;
#34901 = CARTESIAN_POINT ( 'NONE',  ( -16.53943276465976808, 0.05219959533911058130, 111.2489096053143669 ) ) ;
#34902 = CARTESIAN_POINT ( 'NONE',  ( -21.53943276465977519, -0.05219959533937600094, 78.75109039468568994 ) ) ;
#34903 = CARTESIAN_POINT ( 'NONE',  ( -5.823673210054116645, -21.52544592524344225, 87.29057627198103830 ) ) ;
#34904 = CARTESIAN_POINT ( 'NONE',  ( 19.05341960407617918, -5.049401038297876454, 41.04275706135233293 ) ) ;
#34905 = CARTESIAN_POINT ( 'NONE',  ( 18.10062525802553424, -5.500000000000021316, 76.01383468041922242 ) ) ;
#34906 = CARTESIAN_POINT ( 'NONE',  ( -13.97604488694527625, -13.89961937509977830, 51.87390960531437401 ) ) ;
#34907 = CARTESIAN_POINT ( 'NONE',  ( -16.55341960407617563, 4.379528057220093196, 43.54275706135235424 ) ) ;
#34908 = CARTESIAN_POINT ( 'NONE',  ( 14.29746914071049879, -8.314922557960816363, 103.3322429386476955 ) ) ;
#34909 = DIRECTION ( 'NONE',  ( 0.000000000000000000, 0.000000000000000000, -1.000000000000000000 ) ) ;
#34910 = CARTESIAN_POINT ( 'NONE',  ( 19.03943276465977164, -0.05219959533909143690, 73.74890960531435269 ) ) ;
#34911 = CARTESIAN_POINT ( 'NONE',  ( 14.29746914071049879, -8.314922557960816363, 88.33224293864769550 ) ) ;
#34912 = CARTESIAN_POINT ( 'NONE',  ( 10.81492255796078972, 18.62759615963270932, 49.58224293864769550 ) ) ;
#34913 = CARTESIAN_POINT ( 'NONE',  ( -14.29746914071049879, 8.314922557960819915, 60.83224293864769550 ) ) ;
#34914 = CARTESIAN_POINT ( 'NONE',  ( -8.314922557961024197, 14.29746914071037800, 32.91775706135234714 ) ) ;
#34915 = CARTESIAN_POINT ( 'NONE',  ( -10.72451020669870658, -18.67979575497194134, 84.58442372801903275 ) ) ;
#34916 = CARTESIAN_POINT ( 'NONE',  ( -17.59860650958993844, 7.585241751806885979, 63.42337014262494677 ) ) ;
#34917 = CARTESIAN_POINT ( 'NONE',  ( -14.29746914071037622, -8.314922557961029526, 94.16775706135237556 ) ) ;
#34918 = CARTESIAN_POINT ( 'NONE',  ( -12.06949235617756955, 12.14591786802309770, 40.62390960531435269 ) ) ;
#34919 = CARTESIAN_POINT ( 'NONE',  ( 0.05219959533909260263, 19.03943276465977164, 39.99890960531436690 ) ) ;
#34920 = CARTESIAN_POINT ( 'NONE',  ( 18.67979575497194134, -10.72451020669871369, 100.8344237280190185 ) ) ;
#34921 = CARTESIAN_POINT ( 'NONE',  ( -15.72974639402197994, 15.80617190586746368, 105.6239096053143669 ) ) ;
#34922 =( BOUNDED_CURVE ( )  B_SPLINE_CURVE ( 2, ( #103575, #149083, #74233, #10571, #88382, #59040, #57074, #168210, #13541, #48846, #139837 ),
 .UNSPECIFIED., .F., .T. ) 
 B_SPLINE_CURVE_WITH_KNOTS ( ( 3, 2, 2, 2, 2, 3 ),
 ( 0.3000000000000002665, 0.3200000000000002842, 0.3400000000000003020, 0.3600000000000003197, 0.3800000000000003375, 0.4000000000000003553 ),
 .UNSPECIFIED. ) 
 CURVE ( )  GEOMETRIC_REPRESENTATION_ITEM ( )  RATIONAL_B_SPLINE_CURVE ( ( 0.9999999999999993339, 0.9510565162951541973, 1.000000000000000000, 0.9510565162951535312, 1.000000000000000000, 0.9510565162951535312, 1.000000000000000000, 0.9510565162951535312, 1.000000000000000000, 0.9510565162951527540, 1.000000000000000888 ) ) 
 REPRESENTATION_ITEM ( '' )  );
#34923 = CARTESIAN_POINT ( 'NONE',  ( 10.81492255796106328, -18.62759615963255655, 60.41775706135235424 ) ) ;
#34924 = CARTESIAN_POINT ( 'NONE',  ( 4.379528057220092307, 16.55341960407617563, 42.29275706135235424 ) ) ;
#34926 = CARTESIAN_POINT ( 'NONE',  ( -15.80617190586768217, 15.72974639402176855, 83.12609039468568994 ) ) ;
#34925 = CARTESIAN_POINT ( 'NONE',  ( -16.55341960407611168, -4.379528057220339221, 66.45724293864768129 ) ) ;
#34927 = AXIS2_PLACEMENT_3D ( 'NONE', #22358, #98161, #35524 ) ;
#34928 = EDGE_CURVE ( 'NONE', #103031, #128045, #91988, .T. ) ;
#34929 = CARTESIAN_POINT ( 'NONE',  ( 14.29746914071037800, 8.314922557961029526, 106.6677570613523756 ) ) ;
#34930 = CARTESIAN_POINT ( 'NONE',  ( 16.18388926212239909, 7.379444403734401803, 27.93953151366153165 ) ) ;
#34931 = CARTESIAN_POINT ( 'NONE',  ( -19.38985940809734032, -32.68077955211932561, -25.00000000000009592 ) ) ;
#34932 = CARTESIAN_POINT ( 'NONE',  ( 12.14591786802309770, 12.06949235617756955, 29.37390960531435269 ) ) ;
#34933 = CARTESIAN_POINT ( 'NONE',  ( 8.224510206698742110, 14.34966873604972548, 77.08442372801901854 ) ) ;
#34934 = CARTESIAN_POINT ( 'NONE',  ( 19.03943276465977164, -0.05219959533909143690, 88.74890960531436690 ) ) ;
#34935 = CIRCLE ( 'NONE', #112429, 38.00000000000000000 ) ;
#34936 = CARTESIAN_POINT ( 'NONE',  ( 9.474510206698971260, -16.51473224551069308, 102.9155762719810241 ) ) ;
#34937 = CARTESIAN_POINT ( 'NONE',  ( 10.81492255796106328, -18.62759615963255655, 90.41775706135236135 ) ) ;
#34938 = CARTESIAN_POINT ( 'NONE',  ( -16.53943276465976808, -0.05219959533934237506, 93.75109039468567573 ) ) ;
#34939 = CARTESIAN_POINT ( 'NONE',  ( -8.224510206698948167, 14.34966873604960824, 60.41557627198102409 ) ) ;
#34940 = CARTESIAN_POINT ( 'NONE',  ( -5.049401038298153566, 19.05341960407611168, 70.20724293864769550 ) ) ;
#34941 = VERTEX_POINT ( 'NONE', #190364 ) ;
#34942 = CARTESIAN_POINT ( 'NONE',  ( -12.14591786802326823, 12.06949235617739902, 23.12609039468567573 ) ) ;
#34943 = CARTESIAN_POINT ( 'NONE',  ( -5.153800228976328057, -19.02544592524343514, 32.29057627198102409 ) ) ;
#34944 = CARTESIAN_POINT ( 'NONE',  ( -13.97604488694527625, -13.89961937509977652, 91.87390960531432427 ) ) ;
#34946 = CARTESIAN_POINT ( 'NONE',  ( -30.74264578624800492, 22.33583958711400186, -0.1999999999999999001 ) ) ;
#34945 = CARTESIAN_POINT ( 'NONE',  ( -8.314922557961024197, 14.29746914071037800, 22.91775706135235069 ) ) ;
#34947 = CARTESIAN_POINT ( 'NONE',  ( -0.05219959533936034679, 19.03943276465977164, 27.50109039468566507 ) ) ;
#34948 = CARTESIAN_POINT ( 'NONE',  ( 14.29746914071037800, 8.314922557961029526, 96.66775706135234714 ) ) ;
#34949 = CARTESIAN_POINT ( 'NONE',  ( 0.05219959533936267826, -19.03943276465977164, 100.0010903946856757 ) ) ;
#34950 = CARTESIAN_POINT ( 'NONE',  ( -16.46253265017160317, 9.564922557960807481, 25.83224293864769194 ) ) ;
#34951 = CARTESIAN_POINT ( 'NONE',  ( -8.224510206698735004, -14.34966873604973081, 64.58442372801900433 ) ) ;
#34952 = CARTESIAN_POINT ( 'NONE',  ( 12.14591786802327356, -12.06949235617739191, 50.62609039468568994 ) ) ;
#34953 = CARTESIAN_POINT ( 'NONE',  ( 15.58367361853946065, -36.85270801516746531, -13.27795824800661961 ) ) ;
#34954 = CARTESIAN_POINT ( 'NONE',  ( 5.049401038297881783, 19.05341960407617563, 67.29275706135234714 ) ) ;
#34955 = CARTESIAN_POINT ( 'NONE',  ( -0.05219959533937732626, 21.53943276465977519, 112.5010903946857042 ) ) ;
#34956 = CARTESIAN_POINT ( 'NONE',  ( 5.153800228976335163, 19.02544592524342804, 44.79057627198103830 ) ) ;
#34957 = CARTESIAN_POINT ( 'NONE',  ( 13.97604488694527802, 13.89961937509977652, 79.37390960531435269 ) ) ;
#34958 = CARTESIAN_POINT ( 'NONE',  ( -16.55341960407611168, -4.379528057220339221, 66.45724293864768129 ) ) ;
#34959 = EDGE_CURVE ( 'NONE', #47253, #68796, #30535, .T. ) ;
#34960 = CARTESIAN_POINT ( 'NONE',  ( -16.46253265017146816, -9.564922557961047289, 44.16775706135232582 ) ) ;
#34961 = CARTESIAN_POINT ( 'NONE',  ( -21.52544592524343514, 5.823673210054127303, 56.04057627198102409 ) ) ;
#34962 = CARTESIAN_POINT ( 'NONE',  ( 5.823673210054444382, -21.52544592524334988, 110.2094237280190185 ) ) ;
#34963 = CARTESIAN_POINT ( 'NONE',  ( 5.049401038298161559, -19.05341960407611168, 92.70724293864769550 ) ) ;
#34964 = CARTESIAN_POINT ( 'NONE',  ( 15.80617190586769283, -15.72974639402175789, 105.6260903946856899 ) ) ;
#34965 = CARTESIAN_POINT ( 'NONE',  ( -0.05219959533907301413, -21.53943276465977519, 67.49890960531436690 ) ) ;
#34966 = CARTESIAN_POINT ( 'NONE',  ( 19.03943276465977164, -0.05219959533909143690, 93.74890960531435269 ) ) ;
#34967 = CARTESIAN_POINT ( 'NONE',  ( 0.05219959533936267826, -19.03943276465977164, 95.00109039468567573 ) ) ;
#34968 = CARTESIAN_POINT ( 'NONE',  ( -16.51473224551069308, -9.474510206698971260, 106.6655762719810383 ) ) ;
#34969 = CARTESIAN_POINT ( 'NONE',  ( 8.314922557961029526, -14.29746914071037800, 20.41775706135234714 ) ) ;
#34970 = CARTESIAN_POINT ( 'NONE',  ( 9.564922557960805705, 16.46253265017160317, 24.58224293864769194 ) ) ;
#34971 = CARTESIAN_POINT ( 'NONE',  ( 0.05219959533909260263, 19.03943276465977164, 89.99890960531436690 ) ) ;
#34972 = CARTESIAN_POINT ( 'NONE',  ( 10.72451020669898902, -18.67979575497178502, 62.91557627198102409 ) ) ;
#34973 = CARTESIAN_POINT ( 'NONE',  ( -4.379528057220086978, -16.55341960407618274, 44.79275706135234714 ) ) ;
#34974 = CARTESIAN_POINT ( 'NONE',  ( 21.53943276465977519, 0.05219959533937863772, 51.25109039468568994 ) ) ;
#34975 = CARTESIAN_POINT ( 'NONE',  ( 15.80617190586769283, -15.72974639402175789, 95.62609039468568994 ) ) ;
#34976 = CARTESIAN_POINT ( 'NONE',  ( 16.55341960407618274, -4.379528057220086978, 101.0427570613523756 ) ) ;
#34977 = CARTESIAN_POINT ( 'NONE',  ( 19.05341960407611168, 5.049401038298154454, 93.95724293864769550 ) ) ;
#34978 = CARTESIAN_POINT ( 'NONE',  ( 0.05219959533910956823, 16.53943276465976808, 94.99890960531436690 ) ) ;
#34979 = CARTESIAN_POINT ( 'NONE',  ( -0.05219959533934338120, 16.53943276465976808, 112.5010903946857042 ) ) ;
#34980 = CARTESIAN_POINT ( 'NONE',  ( 13.97604488694548053, -13.89961937509957401, 70.62609039468567573 ) ) ;
#34981 = CARTESIAN_POINT ( 'NONE',  ( 10.81492255796106328, -18.62759615963255655, 40.41775706135234714 ) ) ;
#34982 = CARTESIAN_POINT ( 'NONE',  ( -16.52544592524342804, 4.483927247898546575, 86.04057627198102409 ) ) ;
#34983 = CARTESIAN_POINT ( 'NONE',  ( -15.80617190586745835, -15.72974639402198527, 21.87390960531436690 ) ) ;
#34984 = CARTESIAN_POINT ( 'NONE',  ( -16.55341960407611168, -4.379528057220339221, 21.45724293864769550 ) ) ;
#34985 = CARTESIAN_POINT ( 'NONE',  ( 18.67979575497194134, -10.72451020669871369, 90.83442372801901854 ) ) ;
#34986 = CARTESIAN_POINT ( 'NONE',  ( 12.06949235617739724, 12.14591786802326823, 51.87609039468568284 ) ) ;
#34987 = CARTESIAN_POINT ( 'NONE',  ( 18.62759615963255655, 10.81492255796105972, 46.66775706135234714 ) ) ;
#34988 = CARTESIAN_POINT ( 'NONE',  ( -5.823673210054431948, 21.52544592524334988, 32.70942372801900433 ) ) ;
#34989 = CARTESIAN_POINT ( 'NONE',  ( -14.34966873604960291, -8.224510206698953496, 101.6655762719810383 ) ) ;
#34990 = CARTESIAN_POINT ( 'NONE',  ( 16.51473224551069308, 9.474510206698969483, 24.16557627198102765 ) ) ;
#34991 = CARTESIAN_POINT ( 'NONE',  ( -16.55341960407611168, -4.379528057220339221, 71.45724293864769550 ) ) ;
#34992 = CARTESIAN_POINT ( 'NONE',  ( 0.05219959533909260263, 19.03943276465977164, 54.99890960531435979 ) ) ;
#34993 = CARTESIAN_POINT ( 'NONE',  ( 12.14591786802327356, -12.06949235617739191, 110.6260903946857042 ) ) ;
#34994 = CARTESIAN_POINT ( 'NONE',  ( -19.03943276465977164, 0.05219959533909376836, 36.24890960531436690 ) ) ;
#34995 = CARTESIAN_POINT ( 'NONE',  ( 15.72974639402199770, -15.80617190586745480, 38.12390960531436690 ) ) ;
#34996 = CARTESIAN_POINT ( 'NONE',  ( 14.34966873604960469, 8.224510206698951720, 84.16557627198103830 ) ) ;
#34997 = CARTESIAN_POINT ( 'NONE',  ( -10.81492255796078084, -18.62759615963271287, 87.08224293864769550 ) ) ;
#34998 = CARTESIAN_POINT ( 'NONE',  ( 19.03943276465977164, -0.05219959533909143690, 83.74890960531436690 ) ) ;
#35000 = CARTESIAN_POINT ( 'NONE',  ( 5.049401038297881783, 19.05341960407617563, 97.29275706135233293 ) ) ;
#34999 = CARTESIAN_POINT ( 'NONE',  ( -5.049401038298153566, 19.05341960407611168, 55.20724293864769550 ) ) ;
#35001 = CARTESIAN_POINT ( 'NONE',  ( -0.05219959533907301413, -21.53943276465977519, 42.49890960531435979 ) ) ;
#35002 = CARTESIAN_POINT ( 'NONE',  ( 18.67979575497194134, -10.72451020669871369, 70.83442372801901854 ) ) ;
#35003 = CARTESIAN_POINT ( 'NONE',  ( 19.02544592524343514, -5.153800228976328945, 53.54057627198102409 ) ) ;
#35004 = CARTESIAN_POINT ( 'NONE',  ( 13.97604488694527802, 13.89961937509977652, 89.37390960531436690 ) ) ;
#35005 = VERTEX_POINT ( 'NONE', #96343 ) ;
#35006 = CARTESIAN_POINT ( 'NONE',  ( 4.483927247898790824, -16.52544592524335698, 70.20942372801904696 ) ) ;
#35007 = CARTESIAN_POINT ( 'NONE',  ( 18.67979575497194134, -10.72451020669871369, 45.83442372801901854 ) ) ;
#35008 = CARTESIAN_POINT ( 'NONE',  ( 10.72451020669871369, 18.67979575497193778, 77.08442372801901854 ) ) ;
#35009 = CARTESIAN_POINT ( 'NONE',  ( -19.03943276465977164, 0.05219959533909376836, 111.2489096053143669 ) ) ;
#35010 = CARTESIAN_POINT ( 'NONE',  ( 18.67979575497178502, 10.72451020669898547, 104.1655762719810241 ) ) ;
#35012 = CARTESIAN_POINT ( 'NONE',  ( 12.14591786802327356, -12.06949235617739191, 70.62609039468567573 ) ) ;
#35011 = CARTESIAN_POINT ( 'NONE',  ( 18.62759615963255655, 10.81492255796105972, 41.66775706135235424 ) ) ;
#35013 = CARTESIAN_POINT ( 'NONE',  ( 21.52544592524344225, -5.823673210054117533, 68.54057627198103830 ) ) ;
#35014 = CARTESIAN_POINT ( 'NONE',  ( -19.05341960407617563, 5.049401038297882671, 28.54275706135232937 ) ) ;
#35016 = CARTESIAN_POINT ( 'NONE',  ( 16.55341960407618274, -4.379528057220086978, 96.04275706135236135 ) ) ;
#35015 = CARTESIAN_POINT ( 'NONE',  ( -13.97604488694527625, -13.89961937509977652, 66.87390960531436690 ) ) ;
#35017 = CARTESIAN_POINT ( 'NONE',  ( 17.97161686093727795, -5.499999999999969802, 83.49637206859166838 ) ) ;
#35018 = CARTESIAN_POINT ( 'NONE',  ( 9.474510206698971260, -16.51473224551069308, 102.9155762719810241 ) ) ;
#35019 = CARTESIAN_POINT ( 'NONE',  ( -21.46320343559653665, -20.96320343559631638, 5.353553390593267736 ) ) ;
#35020 = CARTESIAN_POINT ( 'NONE',  ( -5.153800228976607833, 19.02544592524334988, 77.70942372801900433 ) ) ;
#35021 = CARTESIAN_POINT ( 'NONE',  ( -10.81492255796078084, -18.62759615963271287, 52.08224293864768839 ) ) ;
#35022 = CARTESIAN_POINT ( 'NONE',  ( 4.483927247898545687, 16.52544592524342804, 34.79057627198103120 ) ) ;
#35023 = CARTESIAN_POINT ( 'NONE',  ( 9.564922557961047289, -16.46253265017146816, 105.4177570613523471 ) ) ;
#35024 = CARTESIAN_POINT ( 'NONE',  ( -19.05341960407611168, -5.049401038298163336, 26.45724293864769550 ) ) ;
#35025 = CARTESIAN_POINT ( 'NONE',  ( 14.34966873604972726, -8.224510206698740333, 20.83442372801901143 ) ) ;
#35027 = CARTESIAN_POINT ( 'NONE',  ( -19.03943276465977164, -0.05219959533935918106, 58.75109039468566863 ) ) ;
#35026 = CARTESIAN_POINT ( 'NONE',  ( 21.52544592524344225, -5.823673210054117533, 83.54057627198102409 ) ) ;
#35028 = CARTESIAN_POINT ( 'NONE',  ( 4.379528057220092307, 16.55341960407617563, 77.29275706135234714 ) ) ;
#35029 = CARTESIAN_POINT ( 'NONE',  ( 9.474510206698971260, -16.51473224551069308, 72.91557627198102409 ) ) ;
#35030 = CARTESIAN_POINT ( 'NONE',  ( -16.52544592524342804, 4.483927247898546575, 81.04057627198102409 ) ) ;
#35031 = CARTESIAN_POINT ( 'NONE',  ( -13.97604488694527625, -13.89961937509977652, 46.87390960531435979 ) ) ;
#35032 = CARTESIAN_POINT ( 'NONE',  ( -12.06949235617756955, 12.14591786802309770, 50.62390960531435979 ) ) ;
#35033 = DIRECTION ( 'NONE',  ( 0.000000000000000000, 0.000000000000000000, -1.000000000000000000 ) ) ;
#35034 = CARTESIAN_POINT ( 'NONE',  ( 31.25074303019345479, -7.456059982492100779, 95.94898436327792979 ) ) ;
#35035 = CARTESIAN_POINT ( 'NONE',  ( 16.52544592524342804, -4.483927247898539470, 28.54057627198103120 ) ) ;
#35036 = CARTESIAN_POINT ( 'NONE',  ( 16.46253265017160672, -9.564922557960803928, 83.33224293864768129 ) ) ;
#35037 = LINE ( 'NONE', #130005, #15336 ) ;
#35038 = CARTESIAN_POINT ( 'NONE',  ( 16.51473224551083163, -9.474510206698727899, 40.83442372801900433 ) ) ;
#35039 = CARTESIAN_POINT ( 'NONE',  ( -16.52544592524335698, -4.483927247898792601, 43.95942372801902565 ) ) ;
#35040 = CARTESIAN_POINT ( 'NONE',  ( 5.719274019375991003, -21.55341960407610458, 47.70724293864770260 ) ) ;
#35041 = CARTESIAN_POINT ( 'NONE',  ( -13.89961937509957401, -13.97604488694547875, 29.37609039468565797 ) ) ;
#35042 = CARTESIAN_POINT ( 'NONE',  ( -19.03943276465977164, 0.05219959533909376836, 81.24890960531436690 ) ) ;
#35043 = CARTESIAN_POINT ( 'NONE',  ( 5.153800228976335163, 19.02544592524342804, 114.7905762719810241 ) ) ;
#35044 = CARTESIAN_POINT ( 'NONE',  ( -13.89961937509977652, 13.97604488694528158, 115.6239096053143669 ) ) ;
#35045 = CARTESIAN_POINT ( 'NONE',  ( -21.53943276465977519, -0.05219959533937600094, 43.75109039468568284 ) ) ;
#35046 = CARTESIAN_POINT ( 'NONE',  ( 8.224510206698953496, -14.34966873604960469, 107.9155762719810241 ) ) ;
#35049 = ORIENTED_EDGE ( 'NONE', *, *, #82833, .F. ) ;
#35048 = CARTESIAN_POINT ( 'NONE',  ( 5.049401038298161559, -19.05341960407611168, 82.70724293864770971 ) ) ;
#35047 = CARTESIAN_POINT ( 'NONE',  ( -15.80617190586745835, -15.72974639402198527, 81.87390960531435269 ) ) ;
#35050 = CARTESIAN_POINT ( 'NONE',  ( 21.52544592524334988, 5.823673210054432836, 31.45942372801901854 ) ) ;
#35051 = ORIENTED_EDGE ( 'NONE', *, *, #181354, .T. ) ;
#35052 = CARTESIAN_POINT ( 'NONE',  ( 9.474510206698971260, -16.51473224551069308, 92.91557627198103830 ) ) ;
#35053 = CARTESIAN_POINT ( 'NONE',  ( 15.06137443927351249, -15.06137443927345210, -64.92279855667830191 ) ) ;
#35055 = CARTESIAN_POINT ( 'NONE',  ( 13.97604488694527802, 13.89961937509977652, 29.37390960531435979 ) ) ;
#35054 = CARTESIAN_POINT ( 'NONE',  ( 13.97604488694527802, 13.89961937509977652, 29.37390960531435979 ) ) ;
#35056 = CARTESIAN_POINT ( 'NONE',  ( 16.46253265017146816, 9.564922557961045513, 101.6677570613523329 ) ) ;
#35057 = CARTESIAN_POINT ( 'NONE',  ( -29.86685920354755552, 21.69954338932564397, -7.324999997268814234 ) ) ;
#35058 = CARTESIAN_POINT ( 'NONE',  ( -16.51473224551069308, -9.474510206698971260, 21.66557627198102765 ) ) ;
#35059 = CARTESIAN_POINT ( 'NONE',  ( -10.72451020669870658, -18.67979575497194134, 79.58442372801903275 ) ) ;
#35061 = CARTESIAN_POINT ( 'NONE',  ( -0.05219959533937732626, 21.53943276465977519, 32.50109039468568284 ) ) ;
#35060 = CARTESIAN_POINT ( 'NONE',  ( 19.03943276465977164, -0.05219959533909143690, 63.74890960531435979 ) ) ;
#35062 = CARTESIAN_POINT ( 'NONE',  ( 0.05219959533937995610, -21.53943276465977519, 20.00109039468568639 ) ) ;
#35063 = CARTESIAN_POINT ( 'NONE',  ( 23.31738231874054890, -16.94106989632523508, 146.7999999999999829 ) ) ;
#35064 = CARTESIAN_POINT ( 'NONE',  ( 5.049401038298161559, -19.05341960407611168, 92.70724293864769550 ) ) ;
#35065 = DIRECTION ( 'NONE',  ( 0.000000000000000000, -1.000000000000000000, 0.000000000000000000 ) ) ;
#35067 = CARTESIAN_POINT ( 'NONE',  ( 5.719274019375991003, -21.55341960407610458, 47.70724293864770260 ) ) ;
#35066 = CARTESIAN_POINT ( 'NONE',  ( 8.224510206698742110, 14.34966873604972548, 22.08442372801901143 ) ) ;
#35068 = CARTESIAN_POINT ( 'NONE',  ( 21.55341960407619695, -5.719274019375665929, 76.04275706135237556 ) ) ;
#35069 = CARTESIAN_POINT ( 'NONE',  ( 9.474510206698971260, -16.51473224551069308, 107.9155762719810383 ) ) ;
#35070 = CARTESIAN_POINT ( 'NONE',  ( -19.03943276465977164, -0.05219959533935918106, 98.75109039468567573 ) ) ;
#35071 = CARTESIAN_POINT ( 'NONE',  ( 13.89961937509977652, -13.97604488694527269, 58.12390960531436690 ) ) ;
#35072 = CARTESIAN_POINT ( 'NONE',  ( -19.03943276465977164, 0.05219959533909376836, 91.24890960531436690 ) ) ;
#35073 = CIRCLE ( 'NONE', #15605, 2.500000000000002220 ) ;
#35074 = CARTESIAN_POINT ( 'NONE',  ( 12.06949235617757843, -12.14591786802309237, 88.12390960531436690 ) ) ;
#35075 = CARTESIAN_POINT ( 'NONE',  ( 14.34966873604960469, 8.224510206698951720, 104.1655762719810241 ) ) ;
#35076 = CARTESIAN_POINT ( 'NONE',  ( 16.51473224551069308, 9.474510206698969483, 114.1655762719810241 ) ) ;
#35077 = CARTESIAN_POINT ( 'NONE',  ( 4.483927247898790824, -16.52544592524335698, 75.20942372801901854 ) ) ;
#35079 = CARTESIAN_POINT ( 'NONE',  ( 0.05219959533909260263, 19.03943276465977164, 39.99890960531436690 ) ) ;
#35078 = CARTESIAN_POINT ( 'NONE',  ( -4.483927247898539470, -16.52544592524342804, 52.29057627198102409 ) ) ;
#35080 = CARTESIAN_POINT ( 'NONE',  ( 15.80617190586769283, -15.72974639402175789, 65.62609039468568994 ) ) ;
#35081 = CARTESIAN_POINT ( 'NONE',  ( -16.46253265017146816, -9.564922557961047289, 89.16775706135234714 ) ) ;
#35082 = CARTESIAN_POINT ( 'NONE',  ( -8.314922557960811034, -14.29746914071050412, 67.08224293864770971 ) ) ;
#35083 = CARTESIAN_POINT ( 'NONE',  ( -21.53943276465977519, 0.05219959533907696930, 106.2489096053143811 ) ) ;
#35084 = CARTESIAN_POINT ( 'NONE',  ( 21.52544592524344225, -5.823673210054117533, 43.54057627198103830 ) ) ;
#35085 = CARTESIAN_POINT ( 'NONE',  ( -0.05219959533909027116, -19.03943276465977164, 112.4989096053143669 ) ) ;
#35086 = CARTESIAN_POINT ( 'NONE',  ( -17.81289503416611808, 24.51734667627700404, 139.9500000054623285 ) ) ;
#35087 = CARTESIAN_POINT ( 'NONE',  ( -9.474510206698964154, 16.51473224551069663, 65.41557627198102409 ) ) ;
#35088 = CARTESIAN_POINT ( 'NONE',  ( 8.314922557960818139, 14.29746914071049879, 39.58224293864769550 ) ) ;
#35089 = CARTESIAN_POINT ( 'NONE',  ( -14.29746914071037622, -8.314922557961029526, 109.1677570613523613 ) ) ;
#35090 = CARTESIAN_POINT ( 'NONE',  ( 0.05219959533934541429, -16.53943276465976808, 85.00109039468568994 ) ) ;
#35091 = CARTESIAN_POINT ( 'NONE',  ( -19.05341960407617563, 5.049401038297882671, 33.54275706135231871 ) ) ;
#35092 = B_SPLINE_CURVE_WITH_KNOTS ( 'NONE', 3,
 ( #84852, #173908, #53530, #35377, #116208, #66703, #68695, #115208, #176900, #70710, #132378, #174891, #193058, #160712, #145534, #194072, #162711, #97029, #24216, #55533, #20199, #147554 ),
 .UNSPECIFIED., .F., .F.,
 ( 4, 2, 2, 2, 2, 2, 2, 2, 2, 2, 4 ),
 ( 2.787258305036405189E-07, 0.0003055402697144840151, 0.0006108018135984643248, 0.001221324901366421800, 0.001831847989134385022, 0.002137109533018368909, 0.002442371076902352580, 0.003052894164670316886, 0.003663417252438281192, 0.004273940340206244630, 0.004884463427974209369 ),
 .UNSPECIFIED. ) ;
#35093 = CARTESIAN_POINT ( 'NONE',  ( 16.88567814943166567, 6.947325034625595030, 48.79001122652586275 ) ) ;
#35094 = CARTESIAN_POINT ( 'NONE',  ( 5.153800228976335163, 19.02544592524342804, 94.79057627198103830 ) ) ;
#35095 = CARTESIAN_POINT ( 'NONE',  ( 9.564922557960805705, 16.46253265017160317, 54.58224293864769550 ) ) ;
#35096 = CARTESIAN_POINT ( 'NONE',  ( 8.314922557960818139, 14.29746914071049879, 59.58224293864770260 ) ) ;
#35098 = CARTESIAN_POINT ( 'NONE',  ( -21.53943276465977519, 0.05219959533907696930, 26.24890960531435624 ) ) ;
#35097 = CARTESIAN_POINT ( 'NONE',  ( 19.05341960407611168, 5.049401038298154454, 23.95724293864769194 ) ) ;
#35099 = CARTESIAN_POINT ( 'NONE',  ( -18.67979575497178146, -10.72451020669898902, 56.66557627198103830 ) ) ;
#35100 = CARTESIAN_POINT ( 'NONE',  ( -14.29746914071049879, 8.314922557960819915, 90.83224293864769550 ) ) ;
#35101 = CARTESIAN_POINT ( 'NONE',  ( -4.379528057220086978, -16.55341960407618274, 44.79275706135234714 ) ) ;
#35102 = EDGE_CURVE ( 'NONE', #6927, #183245, #18360, .T. ) ;
#35103 = CARTESIAN_POINT ( 'NONE',  ( -12.14591786802309592, -12.06949235617757132, 81.87390960531435269 ) ) ;
#35104 = DIRECTION ( 'NONE',  ( -0.000000000000000000, -0.000000000000000000, -1.000000000000000000 ) ) ;
#35105 = CARTESIAN_POINT ( 'NONE',  ( 19.02544592524334988, 5.153800228976608722, 76.45942372801897591 ) ) ;
#35106 = CARTESIAN_POINT ( 'NONE',  ( -13.89961937509977652, 13.97604488694528158, 115.6239096053143669 ) ) ;
#35107 = CARTESIAN_POINT ( 'NONE',  ( 11.40812507854754365, 35.11059874428196537, -1.724999997268813479 ) ) ;
#35108 = LINE ( 'NONE', #65440, #141583 ) ;
#35110 = CARTESIAN_POINT ( 'NONE',  ( -12.14591786802309592, -12.06949235617757132, 21.87390960531436690 ) ) ;
#35109 = CARTESIAN_POINT ( 'NONE',  ( 16.53943276465976808, 0.05219959533934440121, 26.25109039468567573 ) ) ;
#35111 = CARTESIAN_POINT ( 'NONE',  ( 16.46253265017146816, 9.564922557961045513, 76.66775706135234714 ) ) ;
#35112 = CARTESIAN_POINT ( 'NONE',  ( -21.55341960407610458, -5.719274019375992779, 51.45724293864770260 ) ) ;
#35113 = CARTESIAN_POINT ( 'NONE',  ( -21.52544592524334988, -5.823673210054445271, 63.95942372801901854 ) ) ;
#35114 = CYLINDRICAL_SURFACE ( 'NONE', #14428, 1.500000000000001332 ) ;
#35115 = CARTESIAN_POINT ( 'NONE',  ( 4.483927247898790824, -16.52544592524335698, 40.20942372801901854 ) ) ;
#35117 = CARTESIAN_POINT ( 'NONE',  ( -13.97604488694527625, -13.89961937509977652, 91.87390960531432427 ) ) ;
#35116 = CARTESIAN_POINT ( 'NONE',  ( -16.46253265017160317, 9.564922557960807481, 25.83224293864769194 ) ) ;
#35118 = CARTESIAN_POINT ( 'NONE',  ( 9.564922557960805705, 16.46253265017160317, 24.58224293864769194 ) ) ;
#35119 = CARTESIAN_POINT ( 'NONE',  ( 16.52544592524342804, -4.483927247898539470, 98.54057627198105251 ) ) ;
#35120 = APPLICATION_PROTOCOL_DEFINITION ( 'draft international standard', 'automotive_design', 1998, #175865 ) ;
#35121 = CARTESIAN_POINT ( 'NONE',  ( 9.564922557960805705, 16.46253265017160317, 104.5822429386476955 ) ) ;
#35122 = ORIENTED_EDGE ( 'NONE', *, *, #41647, .F. ) ;
#35123 = CARTESIAN_POINT ( 'NONE',  ( 16.55341960407618274, -4.379528057220086978, 61.04275706135234714 ) ) ;
#35124 = CARTESIAN_POINT ( 'NONE',  ( 5.153800228976615827, -19.02544592524334988, 105.2094237280190185 ) ) ;
#35125 = CARTESIAN_POINT ( 'NONE',  ( -15.80617190586745835, -15.72974639402198527, 71.87390960531438111 ) ) ;
#35126 = CARTESIAN_POINT ( 'NONE',  ( -9.564922557960796823, -16.46253265017161027, 37.08224293864768839 ) ) ;
#35128 = CARTESIAN_POINT ( 'NONE',  ( 10.72451020669898902, -18.67979575497178502, 112.9155762719810383 ) ) ;
#35127 = CARTESIAN_POINT ( 'NONE',  ( -16.46253265017146816, -9.564922557961047289, 69.16775706135233293 ) ) ;
#35129 = CARTESIAN_POINT ( 'NONE',  ( -19.03943276465977164, 0.05219959533909376836, 71.24890960531435269 ) ) ;
#35130 = CARTESIAN_POINT ( 'NONE',  ( -13.97604488694527625, -13.89961937509977652, 101.8739096053143811 ) ) ;
#35131 = ORIENTED_EDGE ( 'NONE', *, *, #12432, .F. ) ;
#35132 = CARTESIAN_POINT ( 'NONE',  ( -0.05219959533934338120, 16.53943276465976808, 37.50109039468568284 ) ) ;
#35133 = CARTESIAN_POINT ( 'NONE',  ( -21.55341960407610458, -5.719274019375992779, 106.4572429386477097 ) ) ;
#35136 = CARTESIAN_POINT ( 'NONE',  ( -13.97604488694547697, 13.89961937509957934, 78.12609039468567573 ) ) ;
#35135 = CARTESIAN_POINT ( 'NONE',  ( 5.153800228976335163, 19.02544592524342804, 94.79057627198103830 ) ) ;
#35134 = CARTESIAN_POINT ( 'NONE',  ( -14.29746914071049879, 8.314922557960819915, 110.8322429386476955 ) ) ;
#35137 = CARTESIAN_POINT ( 'NONE',  ( -5.719274019375978568, 21.55341960407610458, 80.20724293864769550 ) ) ;
#35138 = CARTESIAN_POINT ( 'NONE',  ( -8.224510206698948167, 14.34966873604960824, 45.41557627198103830 ) ) ;
#35139 = CARTESIAN_POINT ( 'NONE',  ( 19.05341960407617918, -5.049401038297876454, 26.04275706135233293 ) ) ;
#35140 = CARTESIAN_POINT ( 'NONE',  ( 4.379528057220092307, 16.55341960407617563, 62.29275706135236845 ) ) ;
#35141 = CARTESIAN_POINT ( 'NONE',  ( 16.51473224551069308, 9.474510206698969483, 94.16557627198103830 ) ) ;
#35142 = CARTESIAN_POINT ( 'NONE',  ( 0.05219959533909260263, 19.03943276465977164, 49.99890960531435979 ) ) ;
#35143 = CARTESIAN_POINT ( 'NONE',  ( 10.72451020669871369, 18.67979575497193778, 52.08442372801901854 ) ) ;
#35144 = CARTESIAN_POINT ( 'NONE',  ( -15.72974639402176322, -15.80617190586768395, 64.37609039468568994 ) ) ;
#35145 = CARTESIAN_POINT ( 'NONE',  ( 16.46253265017160672, -9.564922557960803928, 58.33224293864769550 ) ) ;
#35146 = CARTESIAN_POINT ( 'NONE',  ( -21.55341960407619339, 5.719274019375674811, 33.54275706135234714 ) ) ;
#35147 = CARTESIAN_POINT ( 'NONE',  ( 16.51473224551083163, -9.474510206698727899, 80.83442372801899012 ) ) ;
#35148 = CARTESIAN_POINT ( 'NONE',  ( -13.89961937509977652, 13.97604488694528158, 45.62390960531433848 ) ) ;
#35149 = CARTESIAN_POINT ( 'NONE',  ( -4.483927247898782831, 16.52544592524335698, 82.70942372801900433 ) ) ;
#35150 = CARTESIAN_POINT ( 'NONE',  ( -9.474510206698964154, 16.51473224551069663, 70.41557627198102409 ) ) ;
#35151 = CARTESIAN_POINT ( 'NONE',  ( 0.05219959533909260263, 19.03943276465977164, 114.9989096053143669 ) ) ;
#35152 = CARTESIAN_POINT ( 'NONE',  ( -9.474510206698964154, 16.51473224551069663, 35.41557627198102409 ) ) ;
#35153 = CARTESIAN_POINT ( 'NONE',  ( -18.67979575497178146, -10.72451020669898902, 86.66557627198102409 ) ) ;
#35154 = CARTESIAN_POINT ( 'NONE',  ( -8.224510206698735004, -14.34966873604973081, 69.58442372801900433 ) ) ;
#35155 = CARTESIAN_POINT ( 'NONE',  ( -21.93180397000138626, 7.641141194970188621, 169.8616410530809731 ) ) ;
#35156 = CARTESIAN_POINT ( 'NONE',  ( -5.153800228976607833, 19.02544592524334988, 27.70942372801899722 ) ) ;
#35157 = ADVANCED_BREP_SHAPE_REPRESENTATION ( '', ( #142731, #82054 ), #62737 ) ;
#35158 = CARTESIAN_POINT ( 'NONE',  ( -5.049401038298153566, 19.05341960407611168, 60.20724293864768129 ) ) ;
#35159 = CARTESIAN_POINT ( 'NONE',  ( -14.29746914071049879, 8.314922557960819915, 50.83224293864770971 ) ) ;
#35160 = CARTESIAN_POINT ( 'NONE',  ( 4.483927247898545687, 16.52544592524342804, 79.79057627198102409 ) ) ;
#35161 = CIRCLE ( 'NONE', #180547, 25.62086810090349331 ) ;
#35162 = CARTESIAN_POINT ( 'NONE',  ( -9.564922557960796823, -16.46253265017161027, 107.0822429386476955 ) ) ;
#35163 = CARTESIAN_POINT ( 'NONE',  ( -16.46253265017160317, 9.564922557960807481, 90.83224293864769550 ) ) ;
#35164 = CARTESIAN_POINT ( 'NONE',  ( -10.81492255796105439, 18.62759615963255655, 52.91775706135235424 ) ) ;
#35165 = CARTESIAN_POINT ( 'NONE',  ( -5.153800228976328057, -19.02544592524343514, 112.2905762719810099 ) ) ;
#35166 = CARTESIAN_POINT ( 'NONE',  ( -15.72974639402176322, -15.80617190586768395, 99.37609039468568994 ) ) ;
#35167 = CARTESIAN_POINT ( 'NONE',  ( 14.34966873604972726, -8.224510206698740333, 85.83442372801901854 ) ) ;
#35168 = CARTESIAN_POINT ( 'NONE',  ( 21.53943276465977519, 0.05219959533937863772, 31.25109039468568639 ) ) ;
#35169 = CARTESIAN_POINT ( 'NONE',  ( -5.153800228976328057, -19.02544592524343514, 107.2905762719810383 ) ) ;
#35170 = CARTESIAN_POINT ( 'NONE',  ( 21.52544592524344225, -5.823673210054117533, 108.5405762719810241 ) ) ;
#35171 = CARTESIAN_POINT ( 'NONE',  ( 14.29746914071049879, -8.314922557960816363, 63.33224293864770260 ) ) ;
#35172 = CARTESIAN_POINT ( 'NONE',  ( -9.474510206698964154, 16.51473224551069663, 45.41557627198103120 ) ) ;
#35173 = CARTESIAN_POINT ( 'NONE',  ( -16.52544592524342804, 4.483927247898546575, 76.04057627198102409 ) ) ;
#35174 = CARTESIAN_POINT ( 'NONE',  ( -18.67979575497178146, -10.72451020669898902, 26.66557627198103475 ) ) ;
#35175 = CARTESIAN_POINT ( 'NONE',  ( 9.564922557961047289, -16.46253265017146816, 25.41775706135234003 ) ) ;
#35176 = CARTESIAN_POINT ( 'NONE',  ( 16.55341960407611168, 4.379528057220329451, 108.9572429386476955 ) ) ;
#35177 = ORIENTED_EDGE ( 'NONE', *, *, #91919, .F. ) ;
#35178 = CARTESIAN_POINT ( 'NONE',  ( -4.483927247898782831, 16.52544592524335698, 62.70942372801902565 ) ) ;
#35179 = CARTESIAN_POINT ( 'NONE',  ( -13.97604488694527625, -13.89961937509977652, 61.87390960531435979 ) ) ;
#35180 = CARTESIAN_POINT ( 'NONE',  ( 8.571926809382597767, 26.38167802310806209, 140.2750000027311899 ) ) ;
#35181 = CARTESIAN_POINT ( 'NONE',  ( -4.379528057220328563, 16.55341960407611168, 85.20724293864770971 ) ) ;
#35182 = CARTESIAN_POINT ( 'NONE',  ( 0.05219959533907565091, 21.53943276465977519, 34.99890960531435979 ) ) ;
#35183 = ORIENTED_EDGE ( 'NONE', *, *, #161479, .F. ) ;
#35184 = CARTESIAN_POINT ( 'NONE',  ( -12.06949235617739369, -12.14591786802326823, 109.3760903946857042 ) ) ;
#35185 = CARTESIAN_POINT ( 'NONE',  ( -13.97604488694547697, 13.89961937509957934, 108.1260903946856331 ) ) ;
#35186 = CARTESIAN_POINT ( 'NONE',  ( 18.62759615963255655, 10.81492255796105972, 76.66775706135234714 ) ) ;
#35187 = CARTESIAN_POINT ( 'NONE',  ( 9.474510206698971260, -16.51473224551069308, 92.91557627198103830 ) ) ;
#35188 = CARTESIAN_POINT ( 'NONE',  ( -10.72451020669898014, 18.67979575497178502, 105.4155762719810383 ) ) ;
#35189 = CARTESIAN_POINT ( 'NONE',  ( 14.34966873604972726, -8.224510206698740333, 50.83442372801901143 ) ) ;
#35190 = CARTESIAN_POINT ( 'NONE',  ( -13.89961937509977652, 13.97604488694528158, 30.62390960531435269 ) ) ;
#35191 = CARTESIAN_POINT ( 'NONE',  ( 12.14591786802327356, -12.06949235617739191, 25.62609039468567929 ) ) ;
#35192 = EDGE_CURVE ( 'NONE', #35378, #90049, #62896, .T. ) ;
#35193 = CARTESIAN_POINT ( 'NONE',  ( -9.474510206698720793, -16.51473224551083518, 99.58442372801900433 ) ) ;
#35194 = CARTESIAN_POINT ( 'NONE',  ( -10.72451020669898014, 18.67979575497178502, 85.41557627198102409 ) ) ;
#35195 = CARTESIAN_POINT ( 'NONE',  ( 5.049401038297881783, 19.05341960407617563, 52.29275706135234003 ) ) ;
#35196 = DIRECTION ( 'NONE',  ( 0.000000000000000000, -0.3420201433256804813, -0.9396926207859040980 ) ) ;
#35197 = CARTESIAN_POINT ( 'NONE',  ( 5.823673210054125526, 21.52544592524343514, 99.79057627198103830 ) ) ;
#35198 = CARTESIAN_POINT ( 'NONE',  ( 7.500000000000000000, 9.184850993605147944E-16, 4.292893218813446765 ) ) ;
#35199 = CARTESIAN_POINT ( 'NONE',  ( -19.03943276465977164, 0.05219959533909376836, 76.24890960531435269 ) ) ;
#35200 = LINE ( 'NONE', #65531, #85282 ) ;
#35201 = CARTESIAN_POINT ( 'NONE',  ( -8.224510206698735004, -14.34966873604973081, 34.58442372801900433 ) ) ;
#35202 = LINE ( 'NONE', #146352, #171004 ) ;
#35204 = CARTESIAN_POINT ( 'NONE',  ( 16.52544592524342804, -4.483927247898539470, 68.54057627198103830 ) ) ;
#35203 = CARTESIAN_POINT ( 'NONE',  ( -21.55341960407610458, -5.719274019375992779, 111.4572429386476813 ) ) ;
#35205 = CARTESIAN_POINT ( 'NONE',  ( 0.05219959533909260263, 19.03943276465977164, 69.99890960531435269 ) ) ;
#35207 = CARTESIAN_POINT ( 'NONE',  ( 16.51473224551083163, -9.474510206698727899, 45.83442372801900433 ) ) ;
#35206 = CARTESIAN_POINT ( 'NONE',  ( 4.483927247898790824, -16.52544592524335698, 35.20942372801901854 ) ) ;
#35208 = CARTESIAN_POINT ( 'NONE',  ( -18.67979575497193778, 10.72451020669871902, 58.33442372801901143 ) ) ;
#35209 = CARTESIAN_POINT ( 'NONE',  ( 9.474510206698729675, 16.51473224551082808, 107.0844237280190043 ) ) ;
#35210 = CARTESIAN_POINT ( 'NONE',  ( 9.564922557960805705, 16.46253265017160317, 54.58224293864769550 ) ) ;
#35211 = CARTESIAN_POINT ( 'NONE',  ( -5.153800228976607833, 19.02544592524334988, 87.70942372801897591 ) ) ;
#35212 = CARTESIAN_POINT ( 'NONE',  ( -5.719274019375665041, -21.55341960407619695, 89.79275706135236135 ) ) ;
#35213 = CARTESIAN_POINT ( 'NONE',  ( 13.97604488694548053, -13.89961937509957401, 60.62609039468564731 ) ) ;
#35214 = CARTESIAN_POINT ( 'NONE',  ( -19.02544592524342804, 5.153800228976336051, 36.04057627198100988 ) ) ;
#35215 = CARTESIAN_POINT ( 'NONE',  ( -18.62759615963270932, 10.81492255796079327, 55.83224293864770260 ) ) ;
#35216 = CARTESIAN_POINT ( 'NONE',  ( 12.06949235617757843, -12.14591786802309237, 63.12390960531435979 ) ) ;
#35217 = CARTESIAN_POINT ( 'NONE',  ( -17.97214573761833378, -5.499999999999956479, 101.4697004903865718 ) ) ;
#35218 = CARTESIAN_POINT ( 'NONE',  ( 16.46253265017146816, 9.564922557961045513, 36.66775706135233293 ) ) ;
#35219 = CARTESIAN_POINT ( 'NONE',  ( -16.55341960407617563, 4.379528057220093196, 103.5427570613523613 ) ) ;
#35220 = CARTESIAN_POINT ( 'NONE',  ( 14.29746914071049879, -8.314922557960816363, 53.33224293864769550 ) ) ;
#35222 = CARTESIAN_POINT ( 'NONE',  ( 27.73933785331498214, 9.013057229001095294, 139.9750000027311501 ) ) ;
#35221 = CARTESIAN_POINT ( 'NONE',  ( 21.52544592524334988, 5.823673210054432836, 86.45942372801901854 ) ) ;
#35223 = CARTESIAN_POINT ( 'NONE',  ( -21.55341960407619339, 5.719274019375674811, 93.54275706135234714 ) ) ;
#35224 = CARTESIAN_POINT ( 'NONE',  ( 18.67979575497178502, 10.72451020669898547, 89.16557627198102409 ) ) ;
#35225 = CARTESIAN_POINT ( 'NONE',  ( -16.51473224551069308, -9.474510206698971260, 56.66557627198103120 ) ) ;
#35226 = CARTESIAN_POINT ( 'NONE',  ( -5.719274019375665041, -21.55341960407619695, 74.79275706135234714 ) ) ;
#35227 = CARTESIAN_POINT ( 'NONE',  ( -5.153800228976328057, -19.02544592524343514, 52.29057627198100988 ) ) ;
#35228 = CARTESIAN_POINT ( 'NONE',  ( 19.03943276465977164, -0.05219959533909143690, 68.74890960531436690 ) ) ;
#35229 = CARTESIAN_POINT ( 'NONE',  ( 16.55341960407611168, 4.379528057220329451, 108.9572429386476955 ) ) ;
#35230 = CARTESIAN_POINT ( 'NONE',  ( 13.97604488694527802, 13.89961937509977652, 109.3739096053143669 ) ) ;
#35231 = CARTESIAN_POINT ( 'NONE',  ( 16.53943276465976808, -0.05219959533910856209, 48.74890960531435979 ) ) ;
#35232 = CARTESIAN_POINT ( 'NONE',  ( -19.03943276465977164, 0.05219959533909376836, 26.24890960531435624 ) ) ;
#35233 = CARTESIAN_POINT ( 'NONE',  ( -12.06949235617756955, 12.14591786802309770, 75.62390960531439532 ) ) ;
#35234 = CARTESIAN_POINT ( 'NONE',  ( -5.719274019375978568, 21.55341960407610458, 100.2072429386476955 ) ) ;
#35235 = CARTESIAN_POINT ( 'NONE',  ( -10.72451020669870658, -18.67979575497194134, 34.58442372801900433 ) ) ;
#35236 = CARTESIAN_POINT ( 'NONE',  ( 27.96619922901622246, -7.272069078172575196, 160.9422763814157804 ) ) ;
#35237 = CARTESIAN_POINT ( 'NONE',  ( 14.29746914071037800, 8.314922557961029526, 31.66775706135234358 ) ) ;
#35238 = CARTESIAN_POINT ( 'NONE',  ( -15.72974639402197994, 15.80617190586746368, 85.62390960531436690 ) ) ;
#35239 = CARTESIAN_POINT ( 'NONE',  ( 18.67979575497194134, -10.72451020669871369, 105.8344237280190328 ) ) ;
#35240 = CARTESIAN_POINT ( 'NONE',  ( -9.564922557960796823, -16.46253265017161027, 87.08224293864769550 ) ) ;
#35241 = CARTESIAN_POINT ( 'NONE',  ( -18.62759615963255300, -10.81492255796106328, 49.16775706135234003 ) ) ;
#35242 = CARTESIAN_POINT ( 'NONE',  ( 18.67979575497178502, 10.72451020669898547, 24.16557627198103120 ) ) ;
#35243 = CARTESIAN_POINT ( 'NONE',  ( -12.06949235617739369, -12.14591786802326823, 109.3760903946857042 ) ) ;
#35245 = CARTESIAN_POINT ( 'NONE',  ( -21.55341960407619339, 5.719274019375674811, 88.54275706135236135 ) ) ;
#35244 = CARTESIAN_POINT ( 'NONE',  ( 10.72451020669871369, 18.67979575497193778, 52.08442372801901854 ) ) ;
#35246 = B_SPLINE_CURVE_WITH_KNOTS ( 'NONE', 3,
 ( #47320, #34129, #110957, #1793, #93801, #111956, #63471, #125146, #186845, #95788, #157474, #65447, #18967, #143271, #48314, #80613 ),
 .UNSPECIFIED., .F., .F.,
 ( 4, 2, 2, 2, 2, 2, 2, 4 ),
 ( 0.02045126265315338338, 0.02288269579900681361, 0.02531412894486024384, 0.03017699523656709737, 0.03260842838242052066, 0.03382414495534723231, 0.03503986152827393008, 0.03990272781998075585 ),
 .UNSPECIFIED. ) ;
#35247 = CARTESIAN_POINT ( 'NONE',  ( -21.55341960407619339, 5.719274019375674811, 113.5427570613523756 ) ) ;
#35248 = CARTESIAN_POINT ( 'NONE',  ( -16.53943276465976808, -0.05219959533934237506, 83.75109039468568994 ) ) ;
#35249 = CARTESIAN_POINT ( 'NONE',  ( 0.05219959533937995610, -21.53943276465977519, 45.00109039468568284 ) ) ;
#35250 = CARTESIAN_POINT ( 'NONE',  ( -13.89961937509977652, 13.97604488694528158, 35.62390960531435269 ) ) ;
#35251 = CARTESIAN_POINT ( 'NONE',  ( -5.823673210054431948, 21.52544592524334988, 97.70942372801904696 ) ) ;
#35252 = CARTESIAN_POINT ( 'NONE',  ( 19.02544592524343514, -5.153800228976328945, 108.5405762719810383 ) ) ;
#35253 = CARTESIAN_POINT ( 'NONE',  ( 10.72451020669898902, -18.67979575497178502, 97.91557627198103830 ) ) ;
#35255 = CARTESIAN_POINT ( 'NONE',  ( -0.05219959533907301413, -21.53943276465977519, 67.49890960531436690 ) ) ;
#35254 = DIRECTION ( 'NONE',  ( 0.000000000000000000, 0.000000000000000000, -1.000000000000000000 ) ) ;
#35257 = CARTESIAN_POINT ( 'NONE',  ( -8.314922557960811034, -14.29746914071050412, 67.08224293864770971 ) ) ;
#35256 = CARTESIAN_POINT ( 'NONE',  ( 16.52544592524335698, 4.483927247898782831, 56.45942372801902565 ) ) ;
#35258 = FACE_OUTER_BOUND ( 'NONE', #47494, .T. ) ;
#35259 = CARTESIAN_POINT ( 'NONE',  ( 13.89961937509957401, 13.97604488694547697, 86.87609039468567573 ) ) ;
#35260 = FACE_OUTER_BOUND ( 'NONE', #88844, .T. ) ;
#35261 = CARTESIAN_POINT ( 'NONE',  ( 12.06949235617739724, 12.14591786802326823, 26.87609039468567218 ) ) ;
#35262 = CARTESIAN_POINT ( 'NONE',  ( -15.72974639402197994, 15.80617190586746368, 95.62390960531436690 ) ) ;
#35263 = CARTESIAN_POINT ( 'NONE',  ( -10.72451020669898014, 18.67979575497178502, 75.41557627198102409 ) ) ;
#35264 = CARTESIAN_POINT ( 'NONE',  ( 13.97604488694527802, 13.89961937509977652, 114.3739096053143669 ) ) ;
#35265 = CARTESIAN_POINT ( 'NONE',  ( 14.34966873604972726, -8.224510206698740333, 50.83442372801901143 ) ) ;
#35266 = CARTESIAN_POINT ( 'NONE',  ( 9.474510206698971260, -16.51473224551069308, 72.91557627198102409 ) ) ;
#35268 = CARTESIAN_POINT ( 'NONE',  ( -19.05341960407617563, 5.049401038297882671, 98.54275706135233293 ) ) ;
#35267 = CARTESIAN_POINT ( 'NONE',  ( -21.53943276465977519, -0.05219959533937600094, 33.75109039468568284 ) ) ;
#35269 = CARTESIAN_POINT ( 'NONE',  ( 9.474510206698971260, -16.51473224551069308, 107.9155762719810383 ) ) ;
#35270 = CARTESIAN_POINT ( 'NONE',  ( -13.97604488694527625, -13.89961937509977652, 86.87390960531436690 ) ) ;
#35271 = CARTESIAN_POINT ( 'NONE',  ( 21.52544592524344225, -5.823673210054117533, 83.54057627198102409 ) ) ;
#35272 = CARTESIAN_POINT ( 'NONE',  ( 9.564922557960805705, 16.46253265017160317, 64.58224293864769550 ) ) ;
#35273 = CARTESIAN_POINT ( 'NONE',  ( -7.260022482700430047, 2.182060888568184698, 2.110832330245266508 ) ) ;
#35274 = CARTESIAN_POINT ( 'NONE',  ( 16.52544592524342804, -4.483927247898539470, 63.54057627198103830 ) ) ;
#35275 = CARTESIAN_POINT ( 'NONE',  ( 0.05219959533907565091, 21.53943276465977519, 24.99890960531435624 ) ) ;
#35276 = CARTESIAN_POINT ( 'NONE',  ( -17.72517630440429315, 5.500000000000143885, 60.92175719257210886 ) ) ;
#35277 = CARTESIAN_POINT ( 'NONE',  ( -5.823673210054116645, -21.52544592524344225, 107.2905762719810525 ) ) ;
#35278 = CARTESIAN_POINT ( 'NONE',  ( 9.564922557961047289, -16.46253265017146816, 60.41775706135233293 ) ) ;
#35279 = CARTESIAN_POINT ( 'NONE',  ( 16.46253265017160672, -9.564922557960803928, 108.3322429386476955 ) ) ;
#35280 = CARTESIAN_POINT ( 'NONE',  ( 18.56101223717332260, 5.499999999999942268, 68.94978406935678095 ) ) ;
#35281 = CARTESIAN_POINT ( 'NONE',  ( -18.62759615963270932, 10.81492255796079327, 60.83224293864769550 ) ) ;
#35282 = CARTESIAN_POINT ( 'NONE',  ( -13.89961937509977652, 13.97604488694528158, 85.62390960531433848 ) ) ;
#35283 = CARTESIAN_POINT ( 'NONE',  ( -10.72451020669870658, -18.67979575497194134, 84.58442372801903275 ) ) ;
#35284 = CARTESIAN_POINT ( 'NONE',  ( -0.05219959533909027116, -19.03943276465977164, 47.49890960531435979 ) ) ;
#35285 = CARTESIAN_POINT ( 'NONE',  ( -8.224510206698948167, 14.34966873604960824, 85.41557627198102409 ) ) ;
#35286 = CARTESIAN_POINT ( 'NONE',  ( 12.14591786802327356, -12.06949235617739191, 40.62609039468567573 ) ) ;
#35287 = CARTESIAN_POINT ( 'NONE',  ( -21.52544592524334988, -5.823673210054445271, 68.95942372801901854 ) ) ;
#35288 = VERTEX_POINT ( 'NONE', #83166 ) ;
#35289 = CARTESIAN_POINT ( 'NONE',  ( 19.02544592524334988, 5.153800228976608722, 21.45942372801899012 ) ) ;
#35290 = CARTESIAN_POINT ( 'NONE',  ( -16.51473224551082808, 9.474510206698731452, 83.33442372801899012 ) ) ;
#35291 = CARTESIAN_POINT ( 'NONE',  ( 30.12056840655111856, -26.02156742258010880, -20.94459150989510476 ) ) ;
#35292 = CARTESIAN_POINT ( 'NONE',  ( -15.80617190586768217, 15.72974639402176855, 33.12609039468569705 ) ) ;
#35293 = EDGE_CURVE ( 'NONE', #22185, #6817, #160018, .T. ) ;
#35294 = CARTESIAN_POINT ( 'NONE',  ( -19.53091890409952214, -5.500000000000037303, 45.06097431831420153 ) ) ;
#35295 = CARTESIAN_POINT ( 'NONE',  ( 5.049401038297881783, 19.05341960407617563, 37.29275706135232582 ) ) ;
#35296 = CARTESIAN_POINT ( 'NONE',  ( 16.51473224551069308, 9.474510206698969483, 59.16557627198102409 ) ) ;
#35297 = CARTESIAN_POINT ( 'NONE',  ( 9.564922557961047289, -16.46253265017146816, 30.41775706135232937 ) ) ;
#35298 = CARTESIAN_POINT ( 'NONE',  ( -12.14591786802326823, 12.06949235617739902, 98.12609039468570415 ) ) ;
#35300 = CARTESIAN_POINT ( 'NONE',  ( -10.81492255796105439, 18.62759615963255655, 82.91775706135234714 ) ) ;
#35299 = CARTESIAN_POINT ( 'NONE',  ( -13.97604488694527625, -13.89961937509977652, 101.8739096053143811 ) ) ;
#35301 = CIRCLE ( 'NONE', #41821, 2.999999999999999556 ) ;
#35302 = CARTESIAN_POINT ( 'NONE',  ( 36.91746825000000598, -11.99521256947793546, -7.724999997268812812 ) ) ;
#35303 = CARTESIAN_POINT ( 'NONE',  ( -17.50000000000000711, -5.499999999999956479, 36.28230962303565121 ) ) ;
#35304 = CARTESIAN_POINT ( 'NONE',  ( 10.81492255796106328, -18.62759615963255655, 80.41775706135234714 ) ) ;
#35305 = CARTESIAN_POINT ( 'NONE',  ( 17.12812012977025233, -6.668231424566045007, 41.14051240676857191 ) ) ;
#35306 = CARTESIAN_POINT ( 'NONE',  ( 16.51473224551069308, 9.474510206698969483, 99.16557627198102409 ) ) ;
#35307 = EDGE_CURVE ( 'NONE', #119499, #172658, #159009, .T. ) ;
#35308 = LINE ( 'NONE', #190986, #198579 ) ;
#35309 = CARTESIAN_POINT ( 'NONE',  ( 16.46253265017160672, -9.564922557960803928, 58.33224293864769550 ) ) ;
#35310 = CARTESIAN_POINT ( 'NONE',  ( -21.53943276465977519, 0.05219959533907696930, 56.24890960531436690 ) ) ;
#35311 = CARTESIAN_POINT ( 'NONE',  ( 14.29746914071049879, -8.314922557960816363, 28.33224293864769550 ) ) ;
#35313 = CARTESIAN_POINT ( 'NONE',  ( -19.03943276465977164, 0.05219959533909376836, 76.24890960531435269 ) ) ;
#35312 = CARTESIAN_POINT ( 'NONE',  ( 8.224510206698953496, -14.34966873604960469, 92.91557627198103830 ) ) ;
#35314 = CARTESIAN_POINT ( 'NONE',  ( 5.719274019375673035, 21.55341960407619339, 112.2927570613523471 ) ) ;
#35315 = CARTESIAN_POINT ( 'NONE',  ( 13.89961937509977652, -13.97604488694527269, 33.12390960531434558 ) ) ;
#35316 = CARTESIAN_POINT ( 'NONE',  ( -8.314922557960811034, -14.29746914071050412, 97.08224293864770971 ) ) ;
#35317 = CARTESIAN_POINT ( 'NONE',  ( 18.67979575497194134, -10.72451020669871369, 60.83442372801901854 ) ) ;
#35318 = CARTESIAN_POINT ( 'NONE',  ( -15.80617190586745835, -15.72974639402198527, 81.87390960531435269 ) ) ;
#35319 = CARTESIAN_POINT ( 'NONE',  ( 13.97604488694548053, -13.89961937509957401, 60.62609039468564731 ) ) ;
#35320 = CARTESIAN_POINT ( 'NONE',  ( -7.652493125987827050, -39.26116846142902261, -15.00000000000000000 ) ) ;
#35321 = CARTESIAN_POINT ( 'NONE',  ( 16.51473224551069308, 9.474510206698969483, 109.1655762719810383 ) ) ;
#35322 = CARTESIAN_POINT ( 'NONE',  ( 14.29746914071049879, -8.314922557960816363, 83.33224293864769550 ) ) ;
#35323 = CARTESIAN_POINT ( 'NONE',  ( -0.05219959533936034679, 19.03943276465977164, 47.50109039468566863 ) ) ;
#35325 = AXIS2_PLACEMENT_3D ( 'NONE', #185200, #46691, #78005 ) ;
#35324 = CARTESIAN_POINT ( 'NONE',  ( 9.564922557960805705, 16.46253265017160317, 64.58224293864769550 ) ) ;
#35326 = CARTESIAN_POINT ( 'NONE',  ( -14.34966873604960291, -8.224510206698953496, 61.66557627198103120 ) ) ;
#35327 = CARTESIAN_POINT ( 'NONE',  ( 0.05219959533936267826, -19.03943276465977164, 75.00109039468566152 ) ) ;
#35328 = CARTESIAN_POINT ( 'NONE',  ( 17.26058549869090086, 6.457015423128633635, 33.87745837476071387 ) ) ;
#35329 = CARTESIAN_POINT ( 'NONE',  ( -0.05219959533907301413, -21.53943276465977519, 42.49890960531435979 ) ) ;
#35330 = ORIENTED_EDGE ( 'NONE', *, *, #19482, .F. ) ;
#35331 = CARTESIAN_POINT ( 'NONE',  ( -4.379528057220328563, 16.55341960407611168, 100.2072429386476955 ) ) ;
#35332 = DIRECTION ( 'NONE',  ( 0.000000000000000000, 0.000000000000000000, -1.000000000000000000 ) ) ;
#35334 = CARTESIAN_POINT ( 'NONE',  ( 21.53943276465977519, -0.05219959533907433946, 58.74890960531436690 ) ) ;
#35333 = CARTESIAN_POINT ( 'NONE',  ( 5.153800228976335163, 19.02544592524342804, 54.79057627198103120 ) ) ;
#35335 = CARTESIAN_POINT ( 'NONE',  ( 13.89961937509977652, -13.97604488694527269, 38.12390960531436690 ) ) ;
#35337 = CARTESIAN_POINT ( 'NONE',  ( 9.564922557960805705, 16.46253265017160317, 69.58224293864770971 ) ) ;
#35336 = CARTESIAN_POINT ( 'NONE',  ( 8.224510206698742110, 14.34966873604972548, 82.08442372801901854 ) ) ;
#35339 = EDGE_CURVE ( 'NONE', #723, #84463, #144840, .T. ) ;
#35338 = CARTESIAN_POINT ( 'NONE',  ( -13.97604488694547697, 13.89961937509957934, 48.12609039468566863 ) ) ;
#35340 = CARTESIAN_POINT ( 'NONE',  ( -21.52544592524334988, -5.823673210054445271, 63.95942372801901854 ) ) ;
#35341 = ORIENTED_EDGE ( 'NONE', *, *, #3150, .F. ) ;
#35342 = CARTESIAN_POINT ( 'NONE',  ( 5.823673210054125526, 21.52544592524343514, 44.79057627198103120 ) ) ;
#35343 = CARTESIAN_POINT ( 'NONE',  ( -19.05341960407611168, -5.049401038298163336, 21.45724293864768839 ) ) ;
#35344 = CARTESIAN_POINT ( 'NONE',  ( 14.29746914071037800, 8.314922557961029526, 91.66775706135234714 ) ) ;
#35345 = CARTESIAN_POINT ( 'NONE',  ( 19.02544592524334988, 5.153800228976608722, 101.4594237280189759 ) ) ;
#35346 = DIRECTION ( 'NONE',  ( -0.1045284632676537068, 0.000000000000000000, 0.9945218953682734009 ) ) ;
#35347 = CARTESIAN_POINT ( 'NONE',  ( 17.97161686093722466, -5.500000000000139444, 43.49637206859164706 ) ) ;
#35348 = CARTESIAN_POINT ( 'NONE',  ( 18.62759615963255655, 10.81492255796105972, 96.66775706135234714 ) ) ;
#35349 = ORIENTED_EDGE ( 'NONE', *, *, #59756, .F. ) ;
#35350 = CARTESIAN_POINT ( 'NONE',  ( 8.314922557960818139, 14.29746914071049879, 44.58224293864769550 ) ) ;
#35351 = CARTESIAN_POINT ( 'NONE',  ( 16.53943276465976808, -0.05219959533910856209, 73.74890960531433848 ) ) ;
#35352 = CARTESIAN_POINT ( 'NONE',  ( 15.80617190586746368, 15.72974639402197994, 99.37390960531436690 ) ) ;
#35353 = CARTESIAN_POINT ( 'NONE',  ( -5.823673210054116645, -21.52544592524344225, 92.29057627198103830 ) ) ;
#35354 = CARTESIAN_POINT ( 'NONE',  ( -0.2682394567894307302, -31.88110949919181181, -45.67705988491092484 ) ) ;
#35355 = CARTESIAN_POINT ( 'NONE',  ( -21.52544592524343514, 5.823673210054127303, 36.04057627198102409 ) ) ;
#35356 = CARTESIAN_POINT ( 'NONE',  ( 16.52544592524335698, 4.483927247898782831, 71.45942372801901854 ) ) ;
#35357 = CARTESIAN_POINT ( 'NONE',  ( -16.52544592524342804, 4.483927247898546575, 76.04057627198102409 ) ) ;
#35358 = CARTESIAN_POINT ( 'NONE',  ( -5.049401038298153566, 19.05341960407611168, 50.20724293864770260 ) ) ;
#35359 = CARTESIAN_POINT ( 'NONE',  ( 34.40547513665162427, -6.508760260264946140, 48.73452191691476543 ) ) ;
#35360 = CARTESIAN_POINT ( 'NONE',  ( -16.55341960407617563, 4.379528057220093196, 98.54275706135234714 ) ) ;
#35361 = CARTESIAN_POINT ( 'NONE',  ( -5.719274019375665041, -21.55341960407619695, 39.79275706135235424 ) ) ;
#35362 = CARTESIAN_POINT ( 'NONE',  ( 19.03943276465977164, -0.05219959533909143690, 78.74890960531436690 ) ) ;
#35363 = CARTESIAN_POINT ( 'NONE',  ( 21.55341960407619695, -5.719274019375665929, 56.04275706135235424 ) ) ;
#35364 = CARTESIAN_POINT ( 'NONE',  ( -16.51473224551069308, -9.474510206698971260, 106.6655762719810383 ) ) ;
#35365 = CARTESIAN_POINT ( 'NONE',  ( -8.817897698975500020, -38.37206457205380161, -32.07286502659091809 ) ) ;
#35366 = ORIENTED_EDGE ( 'NONE', *, *, #152623, .T. ) ;
#35367 = CARTESIAN_POINT ( 'NONE',  ( 15.80617190586769283, -15.72974639402175789, 55.62609039468568284 ) ) ;
#35369 = CARTESIAN_POINT ( 'NONE',  ( 5.049401038298161559, -19.05341960407611168, 22.70724293864769194 ) ) ;
#35368 = CARTESIAN_POINT ( 'NONE',  ( -19.05341960407611168, -5.049401038298163336, 31.45724293864769550 ) ) ;
#35370 = CARTESIAN_POINT ( 'NONE',  ( 13.97604488694548053, -13.89961937509957401, 70.62609039468567573 ) ) ;
#35371 = CARTESIAN_POINT ( 'NONE',  ( -21.53943276465977519, -0.05219959533937600094, 28.75109039468567929 ) ) ;
#35372 = CARTESIAN_POINT ( 'NONE',  ( 19.02544592524334988, 5.153800228976608722, 61.45942372801900433 ) ) ;
#35373 = CARTESIAN_POINT ( 'NONE',  ( -5.049401038298153566, 19.05341960407611168, 30.20724293864768839 ) ) ;
#35374 = CARTESIAN_POINT ( 'NONE',  ( -12.14591786802326823, 12.06949235617739902, 88.12609039468570415 ) ) ;
#35375 = CARTESIAN_POINT ( 'NONE',  ( -19.03943276465977164, -0.05219959533935918106, 58.75109039468566863 ) ) ;
#35376 = CARTESIAN_POINT ( 'NONE',  ( 4.379528057220092307, 16.55341960407617563, 112.2927570613523471 ) ) ;
#35378 = VERTEX_POINT ( 'NONE', #84159 ) ;
#35377 = CARTESIAN_POINT ( 'NONE',  ( 9.438666190699255054, 10.00917710959072160, -62.55979675456843836 ) ) ;
#35379 = CARTESIAN_POINT ( 'NONE',  ( -19.03943276465977164, 0.05219959533909376836, 81.24890960531436690 ) ) ;
#35380 = CARTESIAN_POINT ( 'NONE',  ( -18.62759615963255300, -10.81492255796106328, 89.16775706135236135 ) ) ;
#35381 = CARTESIAN_POINT ( 'NONE',  ( -15.72974639402176322, -15.80617190586768395, 104.3760903946856899 ) ) ;
#35382 = CARTESIAN_POINT ( 'NONE',  ( -3.573655867282028392E-15, 2.428612866367529932E-14, -25.00000000000000000 ) ) ;
#35383 = CARTESIAN_POINT ( 'NONE',  ( 15.80617190586769283, -15.72974639402175789, 80.62609039468567573 ) ) ;
#35384 = CARTESIAN_POINT ( 'NONE',  ( -12.14591786802326823, 12.06949235617739902, 38.12609039468567573 ) ) ;
#35385 = CARTESIAN_POINT ( 'NONE',  ( -16.46253265017160317, 9.564922557960807481, 80.83224293864769550 ) ) ;
#35386 = CARTESIAN_POINT ( 'NONE',  ( -21.55341960407610458, -5.719274019375992779, 26.45724293864768839 ) ) ;
#35387 = CARTESIAN_POINT ( 'NONE',  ( -27.73933785331498925, 9.013057229001089965, 140.7750000027311899 ) ) ;
#35388 = CARTESIAN_POINT ( 'NONE',  ( 9.474510206698971260, -16.51473224551069308, 82.91557627198103830 ) ) ;
#35389 = CARTESIAN_POINT ( 'NONE',  ( -19.52851543214742591, -5.500000000000036415, 40.39357721762583253 ) ) ;
#35390 = CARTESIAN_POINT ( 'NONE',  ( 5.049401038297881783, 19.05341960407617563, 77.29275706135231871 ) ) ;
#35391 = CARTESIAN_POINT ( 'NONE',  ( -9.474510206698964154, 16.51473224551069663, 105.4155762719810383 ) ) ;
#35392 = CARTESIAN_POINT ( 'NONE',  ( -5.719274019375665041, -21.55341960407619695, 99.79275706135234714 ) ) ;
#35393 = CARTESIAN_POINT ( 'NONE',  ( 8.224510206698953496, -14.34966873604960469, 102.9155762719810383 ) ) ;
#35394 = CARTESIAN_POINT ( 'NONE',  ( 18.67979575497178502, 10.72451020669898547, 49.16557627198102409 ) ) ;
#35395 = CARTESIAN_POINT ( 'NONE',  ( 5.719274019375991003, -21.55341960407610458, 32.70724293864770260 ) ) ;
#35396 = CARTESIAN_POINT ( 'NONE',  ( 12.14591786802309770, 12.06949235617756955, 99.37390960531436690 ) ) ;
#35397 = CARTESIAN_POINT ( 'NONE',  ( -15.01118352434399483, 1.500065973499320027, -62.04667436142315751 ) ) ;
#35398 = CARTESIAN_POINT ( 'NONE',  ( 16.46253265017146816, 9.564922557961045513, 61.66775706135234003 ) ) ;
#35399 = CARTESIAN_POINT ( 'NONE',  ( -16.55341960407611168, -4.379528057220339221, 26.45724293864768839 ) ) ;
#35400 = CARTESIAN_POINT ( 'NONE',  ( 13.97604488694527802, 13.89961937509977652, 99.37390960531436690 ) ) ;
#35401 = CARTESIAN_POINT ( 'NONE',  ( 18.67979575497194134, -10.72451020669871369, 80.83442372801901854 ) ) ;
#35402 = CARTESIAN_POINT ( 'NONE',  ( 5.823673210054125526, 21.52544592524343514, 54.79057627198104541 ) ) ;
#35403 = CARTESIAN_POINT ( 'NONE',  ( -21.52544592524334988, -5.823673210054445271, 43.95942372801902565 ) ) ;
#35404 = CARTESIAN_POINT ( 'NONE',  ( -15.80617190586745835, -15.72974639402198527, 101.8739096053143811 ) ) ;
#35405 = CARTESIAN_POINT ( 'NONE',  ( 5.823673210054444382, -21.52544592524334988, 40.20942372801901854 ) ) ;
#35406 = CARTESIAN_POINT ( 'NONE',  ( -0.05219959533909027116, -19.03943276465977164, 27.49890960531435624 ) ) ;
#35407 = CARTESIAN_POINT ( 'NONE',  ( -13.97604488694527625, -13.89961937509977652, 86.87390960531436690 ) ) ;
#35408 = CARTESIAN_POINT ( 'NONE',  ( -4.379528057220328563, 16.55341960407611168, 100.2072429386476955 ) ) ;
#35409 = CARTESIAN_POINT ( 'NONE',  ( 19.05341960407611168, 5.049401038298154454, 113.9572429386477097 ) ) ;
#35410 = CARTESIAN_POINT ( 'NONE',  ( 12.14591786802309770, 12.06949235617756955, 49.37390960531436690 ) ) ;
#35411 = CARTESIAN_POINT ( 'NONE',  ( -16.53943276465976808, -0.05219959533934237506, 113.7510903946856757 ) ) ;
#35412 = CARTESIAN_POINT ( 'NONE',  ( -9.564922557960796823, -16.46253265017161027, 47.08224293864769550 ) ) ;
#35413 = CARTESIAN_POINT ( 'NONE',  ( 12.14591786802309770, 12.06949235617756955, 114.3739096053143527 ) ) ;
#35414 = CARTESIAN_POINT ( 'NONE',  ( -21.55341960407610458, -5.719274019375992779, 46.45724293864769550 ) ) ;
#35415 = CARTESIAN_POINT ( 'NONE',  ( 16.51473224551083163, -9.474510206698727899, 30.83442372801900433 ) ) ;
#35417 = CARTESIAN_POINT ( 'NONE',  ( -4.483927247898539470, -16.52544592524342804, 42.29057627198103120 ) ) ;
#35416 = CARTESIAN_POINT ( 'NONE',  ( -17.97214573761834799, -5.500000000000018652, 86.46970049038655759 ) ) ;
#35418 = CARTESIAN_POINT ( 'NONE',  ( -5.719274019375665041, -21.55341960407619695, 44.79275706135234714 ) ) ;
#35419 = CARTESIAN_POINT ( 'NONE',  ( 19.03943276465977164, -0.05219959533909143690, 113.7489096053143669 ) ) ;
#35420 = CARTESIAN_POINT ( 'NONE',  ( 8.224510206698742110, 14.34966873604972548, 57.08442372801901854 ) ) ;
#35421 = CARTESIAN_POINT ( 'NONE',  ( -9.474510206698720793, -16.51473224551083518, 64.58442372801900433 ) ) ;
#35422 = CARTESIAN_POINT ( 'NONE',  ( -8.224510206698948167, 14.34966873604960824, 25.41557627198103120 ) ) ;
#35423 = CARTESIAN_POINT ( 'NONE',  ( -14.29746914071037622, -8.314922557961029526, 109.1677570613523613 ) ) ;
#35424 = CARTESIAN_POINT ( 'NONE',  ( 0.05219959533909260263, 19.03943276465977164, 34.99890960531435979 ) ) ;
#35425 = CARTESIAN_POINT ( 'NONE',  ( 5.153800228976335163, 19.02544592524342804, 64.79057627198100988 ) ) ;
#35426 = CARTESIAN_POINT ( 'NONE',  ( -19.03943276465977164, 0.05219959533909376836, 21.24890960531436335 ) ) ;
#35427 = CARTESIAN_POINT ( 'NONE',  ( -15.72974639402176322, -15.80617190586768395, 34.37609039468568284 ) ) ;
#35428 = CARTESIAN_POINT ( 'NONE',  ( 16.46253265017160672, -9.564922557960803928, 43.33224293864769550 ) ) ;
#35429 = CYLINDRICAL_SURFACE ( 'NONE', #109809, 1.499999999999997780 ) ;
#35430 = CARTESIAN_POINT ( 'NONE',  ( -9.564922557960796823, -16.46253265017161027, 37.08224293864768839 ) ) ;
#35431 = CARTESIAN_POINT ( 'NONE',  ( 13.89961937509977652, -13.97604488694527269, 113.1239096053143527 ) ) ;
#35432 = AXIS2_PLACEMENT_3D ( 'NONE', #45867, #43891, #60038 ) ;
#35434 = CARTESIAN_POINT ( 'NONE',  ( -8.224510206698948167, 14.34966873604960824, 100.4155762719810241 ) ) ;
#35433 = CARTESIAN_POINT ( 'NONE',  ( 21.55341960407619695, -5.719274019375665929, 61.04275706135234714 ) ) ;
#35435 = CARTESIAN_POINT ( 'NONE',  ( -19.02544592524342804, 5.153800228976336051, 106.0405762719810241 ) ) ;
#35436 = CARTESIAN_POINT ( 'NONE',  ( -16.55341960407617563, 4.379528057220093196, 78.54275706135236135 ) ) ;
#35437 = CARTESIAN_POINT ( 'NONE',  ( 18.67979575497194134, -10.72451020669871369, 85.83442372801901854 ) ) ;
#35438 = CARTESIAN_POINT ( 'NONE',  ( 12.14591786802327356, -12.06949235617739191, 55.62609039468568284 ) ) ;
#35439 = CARTESIAN_POINT ( 'NONE',  ( -5.153800228976328057, -19.02544592524343514, 97.29057627198099567 ) ) ;
#35440 = CARTESIAN_POINT ( 'NONE',  ( 14.34966873604972726, -8.224510206698740333, 35.83442372801901143 ) ) ;
#35441 = CARTESIAN_POINT ( 'NONE',  ( -16.55341960407617563, 4.379528057220093196, 28.54275706135234358 ) ) ;
#35442 = CARTESIAN_POINT ( 'NONE',  ( 8.224510206698742110, 14.34966873604972548, 87.08442372801901854 ) ) ;
#35443 = CARTESIAN_POINT ( 'NONE',  ( 16.46253265017146816, 9.564922557961045513, 106.6677570613523471 ) ) ;
#35444 = CARTESIAN_POINT ( 'NONE',  ( 18.67979575497178502, 10.72451020669898547, 99.16557627198100988 ) ) ;
#35446 = CARTESIAN_POINT ( 'NONE',  ( 19.03943276465977164, 0.05219959533936151252, 106.2510903946856615 ) ) ;
#35445 = CARTESIAN_POINT ( 'NONE',  ( 14.34966873604960469, 8.224510206698951720, 104.1655762719810241 ) ) ;
#35447 = CARTESIAN_POINT ( 'NONE',  ( 16.52544592524335698, 4.483927247898782831, 71.45942372801901854 ) ) ;
#35448 = CARTESIAN_POINT ( 'NONE',  ( 22.37486833544152631, 13.37560805684319121, 165.5209445320979569 ) ) ;
#35450 = EDGE_CURVE ( 'NONE', #194003, #23884, #22997, .T. ) ;
#35449 = CARTESIAN_POINT ( 'NONE',  ( 19.03943276465977164, 0.05219959533936151252, 71.25109039468566152 ) ) ;
#35451 = CARTESIAN_POINT ( 'NONE',  ( 14.34966873604960469, 8.224510206698951720, 44.16557627198103120 ) ) ;
#35452 = CARTESIAN_POINT ( 'NONE',  ( -12.14591786802309592, -12.06949235617757132, 26.87390960531435979 ) ) ;
#35453 = CARTESIAN_POINT ( 'NONE',  ( 12.06949235617757843, -12.14591786802309237, 88.12390960531436690 ) ) ;
#35455 = CARTESIAN_POINT ( 'NONE',  ( -17.05116617787825106, 6.768360034955818172, 88.65675553259201536 ) ) ;
#35454 = CARTESIAN_POINT ( 'NONE',  ( -0.05219959533936034679, 19.03943276465977164, 27.50109039468566507 ) ) ;
#35456 = CARTESIAN_POINT ( 'NONE',  ( -18.67979575497193778, 10.72451020669871902, 43.33442372801901143 ) ) ;
#35457 = CARTESIAN_POINT ( 'NONE',  ( 19.02544592524334988, 5.153800228976608722, 101.4594237280189759 ) ) ;
#35458 = CARTESIAN_POINT ( 'NONE',  ( -19.03943276465977164, 0.05219959533909376836, 116.2489096053143669 ) ) ;
#35459 = CARTESIAN_POINT ( 'NONE',  ( 9.474510206698971260, -16.51473224551069308, 92.91557627198103830 ) ) ;
#35460 = CARTESIAN_POINT ( 'NONE',  ( -9.564922557960796823, -16.46253265017161027, 92.08224293864769550 ) ) ;
#35461 = CARTESIAN_POINT ( 'NONE',  ( -18.67979575497178146, -10.72451020669898902, 61.66557627198103120 ) ) ;
#35462 = CARTESIAN_POINT ( 'NONE',  ( 12.14591786802309770, 12.06949235617756955, 89.37390960531435269 ) ) ;
#35463 = CARTESIAN_POINT ( 'NONE',  ( 19.02544592524343514, -5.153800228976328945, 73.54057627198103830 ) ) ;
#35464 = CARTESIAN_POINT ( 'NONE',  ( -12.14591786802309592, -12.06949235617757132, 111.8739096053143669 ) ) ;
#35465 = CARTESIAN_POINT ( 'NONE',  ( 5.823673210054444382, -21.52544592524334988, 45.20942372801901854 ) ) ;
#35466 = AXIS2_PLACEMENT_3D ( 'NONE', #125460, #144591, #19281 ) ;
#35467 = B_SPLINE_CURVE_WITH_KNOTS ( 'NONE', 3,
 ( #75598, #32094, #77590, #93751, #34080, #14936, #198959, #155432, #46263, #62409, #186792, #94744, #122100, #124079, #79580, #16922, #78575, #184777, #171600, #2738, #95738, #64415, #187780, #49250, #92749, #183790, #169603, #45277, #31101, #76596, #96720, #146217, #37052, #97702, #5712, #111908, #50252, #83544 ),
 .UNSPECIFIED., .F., .F.,
 ( 4, 2, 2, 2, 2, 2, 2, 2, 2, 2, 2, 2, 2, 2, 2, 2, 2, 2, 4 ),
 ( 0.001405631271041209943, 0.003109748753336292505, 0.004813866235631374633, 0.008222101200221529349, 0.01163033616481168493, 0.01333445364710676533, 0.01503857112940184398, 0.02185504105858216903, 0.02355915854087725289, 0.02526327602317233675, 0.02867151098776249754, 0.03548798091694280871, 0.03719209839923789257, 0.03889621588153296255, 0.04230445084612311640, 0.04571268581071328413, 0.04741680329300836799, 0.04912092077530345186, 0.05593739070448378037 ),
 .UNSPECIFIED. ) ;
#35468 = CARTESIAN_POINT ( 'NONE',  ( 18.67979575497194134, -10.72451020669871369, 80.83442372801901854 ) ) ;
#35469 = CARTESIAN_POINT ( 'NONE',  ( 19.02544592524343514, -5.153800228976328945, 58.54057627198102409 ) ) ;
#35470 = CARTESIAN_POINT ( 'NONE',  ( 4.379528057220092307, 16.55341960407617563, 77.29275706135234714 ) ) ;
#35471 = CARTESIAN_POINT ( 'NONE',  ( 5.719274019375673035, 21.55341960407619339, 32.29275706135235424 ) ) ;
#35472 = CARTESIAN_POINT ( 'NONE',  ( -0.05219959533937732626, 21.53943276465977519, 22.50109039468567573 ) ) ;
#35474 = CARTESIAN_POINT ( 'NONE',  ( -19.05341960407611168, -5.049401038298163336, 76.45724293864769550 ) ) ;
#35473 = CARTESIAN_POINT ( 'NONE',  ( -0.05219959533936034679, 19.03943276465977164, 47.50109039468566863 ) ) ;
#35475 = CARTESIAN_POINT ( 'NONE',  ( -9.564922557961040184, 16.46253265017147172, 27.91775706135232582 ) ) ;
#35476 = CARTESIAN_POINT ( 'NONE',  ( 10.81492255796106328, -18.62759615963255655, 85.41775706135236135 ) ) ;
#35477 = CARTESIAN_POINT ( 'NONE',  ( -21.53943276465977519, 0.05219959533907696930, 66.24890960531436690 ) ) ;
#35478 = CARTESIAN_POINT ( 'NONE',  ( -12.14591786802309592, -12.06949235617757132, 51.87390960531437401 ) ) ;
#35480 = CARTESIAN_POINT ( 'NONE',  ( 5.049401038297881783, 19.05341960407617563, 32.29275706135233293 ) ) ;
#35479 = CARTESIAN_POINT ( 'NONE',  ( 10.81492255796106328, -18.62759615963255655, 90.41775706135236135 ) ) ;
#35481 = CARTESIAN_POINT ( 'NONE',  ( 12.14591786802309770, 12.06949235617756955, 64.37390960531435269 ) ) ;
#35482 = CARTESIAN_POINT ( 'NONE',  ( 9.564922557960805705, 16.46253265017160317, 24.58224293864769194 ) ) ;
#35483 = CARTESIAN_POINT ( 'NONE',  ( 5.049401038297881783, 19.05341960407617563, 72.29275706135234714 ) ) ;
#35484 = CARTESIAN_POINT ( 'NONE',  ( 16.53943276465976808, -0.05219959533910856209, 33.74890960531436690 ) ) ;
#35485 = CARTESIAN_POINT ( 'NONE',  ( -15.72974639402176322, -15.80617190586768395, 84.37609039468570415 ) ) ;
#35486 = CARTESIAN_POINT ( 'NONE',  ( 9.474510206698971260, -16.51473224551069308, 72.91557627198102409 ) ) ;
#35487 = CARTESIAN_POINT ( 'NONE',  ( 5.049401038297881783, 19.05341960407617563, 47.29275706135231161 ) ) ;
#35488 = CARTESIAN_POINT ( 'NONE',  ( 18.67979575497178502, 10.72451020669898547, 54.16557627198103120 ) ) ;
#35489 = CARTESIAN_POINT ( 'NONE',  ( -10.72451020669870658, -18.67979575497194134, 49.58442372801901143 ) ) ;
#35490 = CARTESIAN_POINT ( 'NONE',  ( 21.52544592524344225, -5.823673210054117533, 103.5405762719810383 ) ) ;
#35491 = CARTESIAN_POINT ( 'NONE',  ( -0.05219959533936034679, 19.03943276465977164, 102.5010903946856757 ) ) ;
#35492 = CARTESIAN_POINT ( 'NONE',  ( -8.224510206698735004, -14.34966873604973081, 64.58442372801900433 ) ) ;
#35494 = CARTESIAN_POINT ( 'NONE',  ( -0.05219959533907301413, -21.53943276465977519, 102.4989096053143811 ) ) ;
#35493 = LINE ( 'NONE', #97143, #74187 ) ;
#35495 = CARTESIAN_POINT ( 'NONE',  ( 16.53943276465976808, -0.05219959533910856209, 103.7489096053143669 ) ) ;
#35496 = CYLINDRICAL_SURFACE ( 'NONE', #179082, 28.82186960331498682 ) ;
#35497 = CARTESIAN_POINT ( 'NONE',  ( 12.14591786802327356, -12.06949235617739191, 35.62609039468568994 ) ) ;
#35498 = CARTESIAN_POINT ( 'NONE',  ( 0.05219959533907565091, 21.53943276465977519, 59.99890960531436690 ) ) ;
#35499 = CARTESIAN_POINT ( 'NONE',  ( -0.05219959533934338120, 16.53943276465976808, 102.5010903946856899 ) ) ;
#35500 = CARTESIAN_POINT ( 'NONE',  ( 19.02544592524343514, -5.153800228976328945, 33.54057627198102409 ) ) ;
#35501 = CARTESIAN_POINT ( 'NONE',  ( -12.14591786802326823, 12.06949235617739902, 63.12609039468568994 ) ) ;
#35502 = CARTESIAN_POINT ( 'NONE',  ( 5.153800228976615827, -19.02544592524334988, 60.20942372801899012 ) ) ;
#35503 = CARTESIAN_POINT ( 'NONE',  ( -5.823673210054431948, 21.52544592524334988, 42.70942372801901854 ) ) ;
#35504 = CARTESIAN_POINT ( 'NONE',  ( 21.55341960407610458, 5.719274019375980345, 53.95724293864770260 ) ) ;
#35505 = CARTESIAN_POINT ( 'NONE',  ( -8.314922557961024197, 14.29746914071037800, 92.91775706135236135 ) ) ;
#35506 = CARTESIAN_POINT ( 'NONE',  ( -18.67979575497193778, 10.72451020669871902, 63.33442372801900433 ) ) ;
#35507 = CARTESIAN_POINT ( 'NONE',  ( -15.80617190586745835, -15.72974639402198527, 51.87390960531437401 ) ) ;
#35508 = CARTESIAN_POINT ( 'NONE',  ( 18.62759615963271287, -10.81492255796078972, 28.33224293864769550 ) ) ;
#35509 = ORIENTED_EDGE ( 'NONE', *, *, #47680, .F. ) ;
#35510 = CARTESIAN_POINT ( 'NONE',  ( 4.379528057220092307, 16.55341960407617563, 77.29275706135234714 ) ) ;
#35511 = CARTESIAN_POINT ( 'NONE',  ( -18.67979575497178146, -10.72451020669898902, 26.66557627198103475 ) ) ;
#35512 = ORIENTED_EDGE ( 'NONE', *, *, #178481, .F. ) ;
#35513 = CARTESIAN_POINT ( 'NONE',  ( -13.89961937509977652, 13.97604488694528158, 95.62390960531436690 ) ) ;
#35514 = CARTESIAN_POINT ( 'NONE',  ( -16.53943276465976808, -0.05219959533934237506, 113.7510903946856757 ) ) ;
#35515 = CARTESIAN_POINT ( 'NONE',  ( -26.12113310390730092, 7.698689789033755559, 169.4288210027979460 ) ) ;
#35516 = CARTESIAN_POINT ( 'NONE',  ( 12.14591786802309770, 12.06949235617756955, 104.3739096053143669 ) ) ;
#35517 = CARTESIAN_POINT ( 'NONE',  ( -10.81492255796078084, -18.62759615963271287, 67.08224293864770971 ) ) ;
#35518 = CARTESIAN_POINT ( 'NONE',  ( -12.14591786802326823, 12.06949235617739902, 88.12609039468570415 ) ) ;
#35519 = CARTESIAN_POINT ( 'NONE',  ( -5.823673210054431948, 21.52544592524334988, 52.70942372801902565 ) ) ;
#35520 = CARTESIAN_POINT ( 'NONE',  ( -19.02544592524334988, -5.153800228976617603, 103.9594237280190043 ) ) ;
#35521 = CARTESIAN_POINT ( 'NONE',  ( -4.483927247898539470, -16.52544592524342804, 102.2905762719810383 ) ) ;
#35522 = CARTESIAN_POINT ( 'NONE',  ( 16.51473224551069308, 9.474510206698969483, 49.16557627198102409 ) ) ;
#35523 = CARTESIAN_POINT ( 'NONE',  ( 9.474510206698971260, -16.51473224551069308, 27.91557627198103120 ) ) ;
#35524 = DIRECTION ( 'NONE',  ( 1.000000000000000000, 0.000000000000000000, 0.000000000000000000 ) ) ;
#35525 = CARTESIAN_POINT ( 'NONE',  ( -13.97604488694527625, -13.89961937509977652, 86.87390960531436690 ) ) ;
#35526 = CARTESIAN_POINT ( 'NONE',  ( 8.314922557961029526, -14.29746914071037800, 70.41775706135236135 ) ) ;
#35527 = CARTESIAN_POINT ( 'NONE',  ( -21.55341960407619339, 5.719274019375674811, 108.5427570613523756 ) ) ;
#35528 = CARTESIAN_POINT ( 'NONE',  ( -5.823673210054116645, -21.52544592524344225, 57.29057627198103120 ) ) ;
#35529 = CARTESIAN_POINT ( 'NONE',  ( 16.53943276465976808, 0.05219959533934440121, 91.25109039468568994 ) ) ;
#35530 = CARTESIAN_POINT ( 'NONE',  ( -13.89961937509957401, -13.97604488694547875, 79.37609039468567573 ) ) ;
#35531 = CARTESIAN_POINT ( 'NONE',  ( 0.05219959533909260263, 19.03943276465977164, 29.99890960531435979 ) ) ;
#35532 = CARTESIAN_POINT ( 'NONE',  ( 13.97604488694527802, 13.89961937509977652, 74.37390960531436690 ) ) ;
#35533 = CARTESIAN_POINT ( 'NONE',  ( -13.97604488694527625, -13.89961937509977652, 36.87390960531436690 ) ) ;
#35534 = CARTESIAN_POINT ( 'NONE',  ( 19.03943276465977164, 0.05219959533936151252, 66.25109039468567573 ) ) ;
#35535 = B_SPLINE_CURVE_WITH_KNOTS ( 'NONE', 3,
 ( #96459, #111644, #15669, #2473, #93482, #94477, #47002, #186528, #142963, #170339, #169334, #184522, #65138, #80300, #173329, #156158, #30842, #158146, #19638, #155169, #1471, #109657, #33813, #48002, #110643, #187523, #126795, #92489, #81280, #95473, #16661, #63149 ),
 .UNSPECIFIED., .F., .F.,
 ( 4, 2, 2, 2, 2, 2, 2, 2, 2, 2, 2, 2, 2, 2, 2, 4 ),
 ( 2.625112965618923374E-17, 0.0003712461730036762612, 0.0007424923460073262847, 0.001113738519010976308, 0.001484984692014626332, 0.002227477038021933101, 0.002598723211025603507, 0.002969969384029273914, 0.003341215557032944320, 0.003712461730036614727, 0.004083707903040284699, 0.004454954076043955540, 0.004826200249047625512, 0.005197446422051296352, 0.005568692595054966325, 0.005939938768058637165 ),
 .UNSPECIFIED. ) ;
#35536 = CARTESIAN_POINT ( 'NONE',  ( 26.61723430050320616, -3.645106422947246738, 172.4622069319862590 ) ) ;
#35537 = CARTESIAN_POINT ( 'NONE',  ( -5.049401038298153566, 19.05341960407611168, 95.20724293864770971 ) ) ;
#35538 = CARTESIAN_POINT ( 'NONE',  ( -8.224510206698948167, 14.34966873604960824, 45.41557627198103830 ) ) ;
#35539 = CARTESIAN_POINT ( 'NONE',  ( -18.62759615963270932, 10.81492255796079327, 55.83224293864770260 ) ) ;
#35540 = CARTESIAN_POINT ( 'NONE',  ( 28.96383432292632065, 7.816291847812730786, 151.8521076810907005 ) ) ;
#35541 = CARTESIAN_POINT ( 'NONE',  ( -13.89961937509957401, -13.97604488694547875, 34.37609039468566863 ) ) ;
#35542 = FILL_AREA_STYLE_COLOUR ( '', #147681 ) ;
#35544 = CARTESIAN_POINT ( 'NONE',  ( 19.03943276465977164, -0.05219959533909143690, 73.74890960531435269 ) ) ;
#35543 = CARTESIAN_POINT ( 'NONE',  ( 5.049401038298161559, -19.05341960407611168, 47.70724293864770260 ) ) ;
#35545 = CARTESIAN_POINT ( 'NONE',  ( 8.314922557961029526, -14.29746914071037800, 35.41775706135234003 ) ) ;
#35546 = CARTESIAN_POINT ( 'NONE',  ( -18.56101223717332260, -5.500000000000007994, 101.4497840693567667 ) ) ;
#35547 = FACE_OUTER_BOUND ( 'NONE', #64964, .T. ) ;
#35548 = CARTESIAN_POINT ( 'NONE',  ( -4.379528057220086978, -16.55341960407618274, 69.79275706135234714 ) ) ;
#35549 = CARTESIAN_POINT ( 'NONE',  ( 0.05219959533907565091, 21.53943276465977519, 89.99890960531438111 ) ) ;
#35550 = CARTESIAN_POINT ( 'NONE',  ( -16.52544592524335698, -4.483927247898792601, 43.95942372801902565 ) ) ;
#35552 = FACE_BOUND ( 'NONE', #163398, .T. ) ;
#35551 = CARTESIAN_POINT ( 'NONE',  ( -19.05341960407611168, -5.049401038298163336, 41.45724293864769550 ) ) ;
#35553 = CARTESIAN_POINT ( 'NONE',  ( -21.55341960407619339, 5.719274019375674811, 58.54275706135235424 ) ) ;
#35554 = CARTESIAN_POINT ( 'NONE',  ( -9.564922557961040184, 16.46253265017147172, 57.91775706135233293 ) ) ;
#35555 = CARTESIAN_POINT ( 'NONE',  ( -21.52544592524334988, -5.823673210054445271, 88.95942372801901854 ) ) ;
#35556 = CARTESIAN_POINT ( 'NONE',  ( 16.61371651742602040, 7.165104196376160139, 98.64584930007005426 ) ) ;
#35557 = CARTESIAN_POINT ( 'NONE',  ( -15.92681084339657716, 1.315686079477422554, -59.47631410104521166 ) ) ;
#35558 = CARTESIAN_POINT ( 'NONE',  ( 18.67979575497178502, 10.72451020669898547, 49.16557627198102409 ) ) ;
#35559 = CARTESIAN_POINT ( 'NONE',  ( -27.73933785331498925, 9.013057229001088189, 140.7750000027311899 ) ) ;
#35560 = CARTESIAN_POINT ( 'NONE',  ( -5.153800228976328057, -19.02544592524343514, 97.29057627198099567 ) ) ;
#35561 = CARTESIAN_POINT ( 'NONE',  ( 8.314922557960818139, 14.29746914071049879, 104.5822429386477097 ) ) ;
#35562 = CARTESIAN_POINT ( 'NONE',  ( 8.314922557961029526, -14.29746914071037800, 25.41775706135235779 ) ) ;
#35563 = CARTESIAN_POINT ( 'NONE',  ( 12.06949235617757843, -12.14591786802309237, 23.12390960531436335 ) ) ;
#35564 = ORIENTED_EDGE ( 'NONE', *, *, #133302, .F. ) ;
#35565 = CARTESIAN_POINT ( 'NONE',  ( -21.52544592524343514, 5.823673210054127303, 101.0405762719810383 ) ) ;
#35567 = CARTESIAN_POINT ( 'NONE',  ( 3.766062262543149401E-15, -39.95556452105413570, -9.500000000000001776 ) ) ;
#35566 = CARTESIAN_POINT ( 'NONE',  ( -16.55341960407611168, -4.379528057220339221, 41.45724293864769550 ) ) ;
#35568 = CARTESIAN_POINT ( 'NONE',  ( -5.153800228976607833, 19.02544592524334988, 87.70942372801897591 ) ) ;
#35569 = CARTESIAN_POINT ( 'NONE',  ( -9.474510206698720793, -16.51473224551083518, 19.58442372801899722 ) ) ;
#35570 = CARTESIAN_POINT ( 'NONE',  ( -16.52544592524342804, 4.483927247898546575, 31.04057627198102409 ) ) ;
#35571 = CARTESIAN_POINT ( 'NONE',  ( 5.823673210054125526, 21.52544592524343514, 89.79057627198103830 ) ) ;
#35572 = CARTESIAN_POINT ( 'NONE',  ( -21.52544592524343514, 5.823673210054127303, 46.04057627198103830 ) ) ;
#35573 = CARTESIAN_POINT ( 'NONE',  ( -19.03943276465977164, 0.05219959533909376836, 61.24890960531436690 ) ) ;
#35574 = CARTESIAN_POINT ( 'NONE',  ( -4.483927247898539470, -16.52544592524342804, 32.29057627198102409 ) ) ;
#35575 = CARTESIAN_POINT ( 'NONE',  ( -16.46253265017160317, 9.564922557960807481, 90.83224293864769550 ) ) ;
#35576 = AXIS2_PLACEMENT_3D ( 'NONE', #85517, #100683, #107648 ) ;
#35577 = ORIENTED_EDGE ( 'NONE', *, *, #98904, .F. ) ;
#35578 = CARTESIAN_POINT ( 'NONE',  ( 19.52217212775660471, -5.499999999999922728, 62.43993709005261650 ) ) ;
#35579 = CARTESIAN_POINT ( 'NONE',  ( -9.474510206698720793, -16.51473224551083518, 44.58442372801900433 ) ) ;
#35580 = CARTESIAN_POINT ( 'NONE',  ( -21.53943276465977519, 0.05219959533907696930, 81.24890960531436690 ) ) ;
#35581 = CARTESIAN_POINT ( 'NONE',  ( 12.06949235617757843, -12.14591786802309237, 98.12390960531436690 ) ) ;
#35582 = CARTESIAN_POINT ( 'NONE',  ( 21.52544592524334988, 5.823673210054432836, 41.45942372801901143 ) ) ;
#35583 = CARTESIAN_POINT ( 'NONE',  ( 22.44159573604009594, -16.30477369853687364, 141.6750000027311671 ) ) ;
#35584 = CARTESIAN_POINT ( 'NONE',  ( -4.379528057220086978, -16.55341960407618274, 104.7927570613523898 ) ) ;
#35585 = CARTESIAN_POINT ( 'NONE',  ( 13.89961937509977652, -13.97604488694527269, 33.12390960531434558 ) ) ;
#35586 = CARTESIAN_POINT ( 'NONE',  ( -5.153800228976328057, -19.02544592524343514, 92.29057627198099567 ) ) ;
#35587 = CARTESIAN_POINT ( 'NONE',  ( 17.58332526062525147, 7.635886036038630920, 91.57665040441534643 ) ) ;
#35588 = CARTESIAN_POINT ( 'NONE',  ( -19.02544592524342804, 5.153800228976336051, 31.04057627198102409 ) ) ;
#35589 = CARTESIAN_POINT ( 'NONE',  ( -4.483927247898539470, -16.52544592524342804, 47.29057627198103120 ) ) ;
#35590 = CARTESIAN_POINT ( 'NONE',  ( -10.81492255796105439, 18.62759615963255655, 77.91775706135231871 ) ) ;
#35592 = CARTESIAN_POINT ( 'NONE',  ( 14.29746914071037800, 8.314922557961029526, 66.66775706135234714 ) ) ;
#35591 = FACE_OUTER_BOUND ( 'NONE', #126359, .T. ) ;
#35593 = CARTESIAN_POINT ( 'NONE',  ( -13.97604488694527625, -13.89961937509977652, 41.87390960531435979 ) ) ;
#35594 = CARTESIAN_POINT ( 'NONE',  ( -19.05341960407611168, -5.049401038298163336, 46.45724293864768129 ) ) ;
#35595 = VERTEX_POINT ( 'NONE', #161018 ) ;
#35596 = CARTESIAN_POINT ( 'NONE',  ( -21.52544592524334988, -5.823673210054445271, 103.9594237280190185 ) ) ;
#35597 = CARTESIAN_POINT ( 'NONE',  ( -8.314922557961024197, 14.29746914071037800, 62.91775706135236135 ) ) ;
#35598 = CARTESIAN_POINT ( 'NONE',  ( -18.67979575497193778, 10.72451020669871902, 103.3344237280190043 ) ) ;
#35599 = CARTESIAN_POINT ( 'NONE',  ( -15.80617190586745835, -15.72974639402198527, 36.87390960531435979 ) ) ;
#35600 = CARTESIAN_POINT ( 'NONE',  ( 9.474510206698729675, 16.51473224551082808, 112.0844237280190043 ) ) ;
#35601 = CARTESIAN_POINT ( 'NONE',  ( -10.81492255796105439, 18.62759615963255655, 72.91775706135234714 ) ) ;
#35602 = CARTESIAN_POINT ( 'NONE',  ( 16.53943276465976808, 0.05219959533934440121, 41.25109039468568284 ) ) ;
#35603 = CARTESIAN_POINT ( 'NONE',  ( 21.53943276465977519, -0.05219959533907433946, 98.74890960531438111 ) ) ;
#35604 = CARTESIAN_POINT ( 'NONE',  ( -16.51473224551082808, 9.474510206698731452, 98.33442372801900433 ) ) ;
#35605 = CARTESIAN_POINT ( 'NONE',  ( 5.049401038298161559, -19.05341960407611168, 67.70724293864769550 ) ) ;
#35606 = CARTESIAN_POINT ( 'NONE',  ( -19.03943276465977164, -0.05219959533935918106, 113.7510903946856757 ) ) ;
#35607 = AXIS2_PLACEMENT_3D ( 'NONE', #60057, #182431, #32708 ) ;
#35608 = CARTESIAN_POINT ( 'NONE',  ( 19.03943276465977164, 0.05219959533936151252, 106.2510903946856615 ) ) ;
#35609 = CARTESIAN_POINT ( 'NONE',  ( 12.06949235617757843, -12.14591786802309237, 68.12390960531436690 ) ) ;
#35610 = CARTESIAN_POINT ( 'NONE',  ( -16.52544592524335698, -4.483927247898792601, 73.95942372801901854 ) ) ;
#35612 = CARTESIAN_POINT ( 'NONE',  ( 13.89961937509977652, -13.97604488694527269, 48.12390960531435979 ) ) ;
#35611 = CARTESIAN_POINT ( 'NONE',  ( 21.53943276465977519, 0.05219959533937863772, 21.25109039468567218 ) ) ;
#35613 = CARTESIAN_POINT ( 'NONE',  ( 0.05219959533909260263, 19.03943276465977164, 54.99890960531435979 ) ) ;
#35614 = CARTESIAN_POINT ( 'NONE',  ( -14.29746914071037622, -8.314922557961029526, 69.16775706135234714 ) ) ;
#35615 = CARTESIAN_POINT ( 'NONE',  ( 17.14385361876520264, -23.59649016807271238, 144.0750000027311444 ) ) ;
#35616 = CARTESIAN_POINT ( 'NONE',  ( -8.906447517083060816, 27.41122689804195645, 143.8500000054623911 ) ) ;
#35617 = EDGE_LOOP ( 'NONE', ( #88053, #55741, #147933, #197719 ) ) ;
#35618 = CARTESIAN_POINT ( 'NONE',  ( -13.89961937509957401, -13.97604488694547875, 19.37609039468566507 ) ) ;
#35619 = CARTESIAN_POINT ( 'NONE',  ( -0.05219959533909027116, -19.03943276465977164, 27.49890960531435624 ) ) ;
#35620 = EDGE_LOOP ( 'NONE', ( #175029, #100166 ) ) ;
#35621 = CARTESIAN_POINT ( 'NONE',  ( 4.483927247898790824, -16.52544592524335698, 20.20942372801900788 ) ) ;
#35622 = CARTESIAN_POINT ( 'NONE',  ( -18.67979575497178146, -10.72451020669898902, 56.66557627198103830 ) ) ;
#35624 = CARTESIAN_POINT ( 'NONE',  ( -16.53943276465976808, -0.05219959533934237506, 28.75109039468567929 ) ) ;
#35623 = CARTESIAN_POINT ( 'NONE',  ( -9.474510206698720793, -16.51473224551083518, 44.58442372801900433 ) ) ;
#35625 = CARTESIAN_POINT ( 'NONE',  ( 19.05341960407611168, 5.049401038298154454, 48.95724293864768129 ) ) ;
#35626 = CARTESIAN_POINT ( 'NONE',  ( 5.049401038298161559, -19.05341960407611168, 47.70724293864770260 ) ) ;
#35627 = CARTESIAN_POINT ( 'NONE',  ( -21.53943276465977519, 0.05219959533907696930, 91.24890960531436690 ) ) ;
#35628 = CARTESIAN_POINT ( 'NONE',  ( 13.89961937509977652, -13.97604488694527269, 113.1239096053143527 ) ) ;
#35629 = CARTESIAN_POINT ( 'NONE',  ( 9.564922557960805705, 16.46253265017160317, 44.58224293864769550 ) ) ;
#35630 = CARTESIAN_POINT ( 'NONE',  ( 1.300000000000000044, 0.000000000000000000, 0.000000000000000000 ) ) ;
#35631 = CARTESIAN_POINT ( 'NONE',  ( 5.049401038297881783, 19.05341960407617563, 92.29275706135234714 ) ) ;
#35632 = CARTESIAN_POINT ( 'NONE',  ( 4.379528057220339221, -16.55341960407611168, 62.70724293864769550 ) ) ;
#35633 = CARTESIAN_POINT ( 'NONE',  ( -13.97604488694547697, 13.89961937509957934, 28.12609039468565797 ) ) ;
#35634 = CARTESIAN_POINT ( 'NONE',  ( 21.53943276465977519, -0.05219959533907433946, 103.7489096053143669 ) ) ;
#35635 = CARTESIAN_POINT ( 'NONE',  ( -21.53943276465977519, -0.05219959533937600094, 88.75109039468567573 ) ) ;
#35636 = CARTESIAN_POINT ( 'NONE',  ( -13.97604488694527625, -13.89961937509977652, 31.87390960531435979 ) ) ;
#35637 = CARTESIAN_POINT ( 'NONE',  ( -10.72451020669870658, -18.67979575497194134, 79.58442372801903275 ) ) ;
#35639 = CARTESIAN_POINT ( 'NONE',  ( 5.719274019375673035, 21.55341960407619339, 82.29275706135234714 ) ) ;
#35638 = CARTESIAN_POINT ( 'NONE',  ( 16.55341960407611168, 4.379528057220329451, 28.95724293864769905 ) ) ;
#35640 = CARTESIAN_POINT ( 'NONE',  ( -19.05341960407611168, -5.049401038298163336, 66.45724293864769550 ) ) ;
#35641 = CARTESIAN_POINT ( 'NONE',  ( 18.67979575497194134, -10.72451020669871369, 45.83442372801901854 ) ) ;
#35642 = CARTESIAN_POINT ( 'NONE',  ( -0.05219959533909027116, -19.03943276465977164, 87.49890960531436690 ) ) ;
#35643 = CARTESIAN_POINT ( 'NONE',  ( -12.06949235617756955, 12.14591786802309770, 95.62390960531436690 ) ) ;
#35644 = CARTESIAN_POINT ( 'NONE',  ( -14.29746914071049879, 8.314922557960819915, 55.83224293864770260 ) ) ;
#35645 = CARTESIAN_POINT ( 'NONE',  ( -15.72974639402197994, 15.80617190586746368, 65.62390960531436690 ) ) ;
#35646 = CARTESIAN_POINT ( 'NONE',  ( 19.05341960407611168, 5.049401038298154454, 73.95724293864768129 ) ) ;
#35647 = CARTESIAN_POINT ( 'NONE',  ( 18.62759615963271287, -10.81492255796078972, 88.33224293864769550 ) ) ;
#35648 = CARTESIAN_POINT ( 'NONE',  ( -0.05219959533936034679, 19.03943276465977164, 62.50109039468566863 ) ) ;
#35649 = CARTESIAN_POINT ( 'NONE',  ( 16.53943276465976808, -0.05219959533910856209, 78.74890960531436690 ) ) ;
#35650 = CARTESIAN_POINT ( 'NONE',  ( -0.05219959533907301413, -21.53943276465977519, 47.49890960531435979 ) ) ;
#35651 = EDGE_CURVE ( 'NONE', #84227, #56210, #32664, .T. ) ;
#35653 = CARTESIAN_POINT ( 'NONE',  ( 27.73933785331498569, 2.768321779492822058E-14, 146.3750000027311842 ) ) ;
#35652 = CARTESIAN_POINT ( 'NONE',  ( 16.55341960407618274, -4.379528057220086978, 101.0427570613523756 ) ) ;
#35654 = CARTESIAN_POINT ( 'NONE',  ( -13.97604488694547697, 13.89961937509957934, 108.1260903946856331 ) ) ;
#35655 = CARTESIAN_POINT ( 'NONE',  ( -16.53943276465976808, 0.05219959533911058130, 71.24890960531435269 ) ) ;
#35656 = CARTESIAN_POINT ( 'NONE',  ( -17.50000000000014921, 3.292511757969705855, 35.06520270210535983 ) ) ;
#35657 = CARTESIAN_POINT ( 'NONE',  ( -5.049401038298153566, 19.05341960407611168, 60.20724293864768129 ) ) ;
#35658 = CARTESIAN_POINT ( 'NONE',  ( 0.05219959533910956823, 16.53943276465976808, 59.99890960531436690 ) ) ;
#35659 = CARTESIAN_POINT ( 'NONE',  ( 5.049401038298161559, -19.05341960407611168, 102.7072429386476955 ) ) ;
#35661 = CARTESIAN_POINT ( 'NONE',  ( -13.89961937509977652, 13.97604488694528158, 65.62390960531436690 ) ) ;
#35660 = CARTESIAN_POINT ( 'NONE',  ( 19.02544592524334988, 5.153800228976608722, 76.45942372801897591 ) ) ;
#35662 = CARTESIAN_POINT ( 'NONE',  ( 13.97604488694527802, 13.89961937509977652, 79.37390960531435269 ) ) ;
#35663 = CARTESIAN_POINT ( 'NONE',  ( 0.05219959533909260263, 19.03943276465977164, 79.99890960531436690 ) ) ;
#35664 = CARTESIAN_POINT ( 'NONE',  ( 18.62759615963271287, -10.81492255796078972, 68.33224293864769550 ) ) ;
#35665 = CARTESIAN_POINT ( 'NONE',  ( -8.314922557961024197, 14.29746914071037800, 57.91775706135234714 ) ) ;
#35666 = CARTESIAN_POINT ( 'NONE',  ( 1.784589286804253661, -7.284589286804279418, 1.818019484660534424 ) ) ;
#35667 = CARTESIAN_POINT ( 'NONE',  ( 5.049401038298161559, -19.05341960407611168, 47.70724293864770260 ) ) ;
#35668 = CARTESIAN_POINT ( 'NONE',  ( 15.72974639402199770, -15.80617190586745480, 58.12390960531435979 ) ) ;
#35669 = CARTESIAN_POINT ( 'NONE',  ( 5.049401038297881783, 19.05341960407617563, 92.29275706135234714 ) ) ;
#35671 = CARTESIAN_POINT ( 'NONE',  ( 10.72451020669871369, 18.67979575497193778, 42.08442372801901854 ) ) ;
#35670 = CARTESIAN_POINT ( 'NONE',  ( 14.34966873604960469, 8.224510206698951720, 24.16557627198103120 ) ) ;
#35672 = CARTESIAN_POINT ( 'NONE',  ( -16.46253265017146816, -9.564922557961047289, 34.16775706135233293 ) ) ;
#35674 = CARTESIAN_POINT ( 'NONE',  ( -4.379528057220086978, -16.55341960407618274, 89.79275706135236135 ) ) ;
#35673 = CARTESIAN_POINT ( 'NONE',  ( -4.379528057220086978, -16.55341960407618274, 54.79275706135235424 ) ) ;
#35675 = CARTESIAN_POINT ( 'NONE',  ( 19.49149378614656314, -5.499999999999759304, 41.93757513605356735 ) ) ;
#35676 = CARTESIAN_POINT ( 'NONE',  ( -8.224510206698735004, -14.34966873604973081, 74.58442372801901854 ) ) ;
#35678 = CARTESIAN_POINT ( 'NONE',  ( 14.34966873604972726, -8.224510206698740333, 30.83442372801902209 ) ) ;
#35677 = CARTESIAN_POINT ( 'NONE',  ( 15.72974639402199770, -15.80617190586745480, 23.12390960531436335 ) ) ;
#35679 = CARTESIAN_POINT ( 'NONE',  ( 13.97604488694527802, 13.89961937509977652, 44.37390960531435269 ) ) ;
#35680 = CARTESIAN_POINT ( 'NONE',  ( 19.05341960407611168, 5.049401038298154454, 43.95724293864769550 ) ) ;
#35681 = CARTESIAN_POINT ( 'NONE',  ( 9.474510206698971260, -16.51473224551069308, 57.91557627198103120 ) ) ;
#35682 = CARTESIAN_POINT ( 'NONE',  ( -15.72974639402176322, -15.80617190586768395, 39.37609039468567573 ) ) ;
#35683 = CARTESIAN_POINT ( 'NONE',  ( -8.314922557961024197, 14.29746914071037800, 42.91775706135235424 ) ) ;
#35684 = CARTESIAN_POINT ( 'NONE',  ( 8.224510206698742110, 14.34966873604972548, 107.0844237280190043 ) ) ;
#35685 = CARTESIAN_POINT ( 'NONE',  ( 16.51473224551069308, 9.474510206698969483, 34.16557627198102409 ) ) ;
#35686 = CARTESIAN_POINT ( 'NONE',  ( -10.81492255796105439, 18.62759615963255655, 107.9177570613523471 ) ) ;
#35688 = EDGE_CURVE ( 'NONE', #177515, #172390, #11355, .T. ) ;
#35687 = CARTESIAN_POINT ( 'NONE',  ( 16.55341960407618274, -4.379528057220086978, 21.04275706135234714 ) ) ;
#35689 = CARTESIAN_POINT ( 'NONE',  ( -19.05341960407617563, 5.049401038297882671, 73.54275706135233293 ) ) ;
#35690 = CARTESIAN_POINT ( 'NONE',  ( 8.224510206698953496, -14.34966873604960469, 67.91557627198102409 ) ) ;
#35691 = CARTESIAN_POINT ( 'NONE',  ( 0.05219959533909260263, 19.03943276465977164, 44.99890960531435979 ) ) ;
#35693 = CARTESIAN_POINT ( 'NONE',  ( -22.96528548301343520, -5.795830589372932273, 190.0000000000000000 ) ) ;
#35692 = CARTESIAN_POINT ( 'NONE',  ( 19.03943276465977164, 0.05219959533936151252, 76.25109039468566152 ) ) ;
#35694 = CARTESIAN_POINT ( 'NONE',  ( 15.80617190586769283, -15.72974639402175789, 75.62609039468567573 ) ) ;
#35695 = CARTESIAN_POINT ( 'NONE',  ( 0.05219959533934541429, -16.53943276465976808, 35.00109039468568284 ) ) ;
#35696 = CARTESIAN_POINT ( 'NONE',  ( 16.52216118717208104, 7.221426719304524511, 38.57599021046993926 ) ) ;
#35697 = CARTESIAN_POINT ( 'NONE',  ( -0.05219959533907301413, -21.53943276465977519, 32.49890960531435979 ) ) ;
#35698 = CARTESIAN_POINT ( 'NONE',  ( -8.314922557961024197, 14.29746914071037800, 32.91775706135234714 ) ) ;
#35699 = CARTESIAN_POINT ( 'NONE',  ( 13.89961937509978007, -13.97604488694527269, 28.12390960531435624 ) ) ;
#35700 = CARTESIAN_POINT ( 'NONE',  ( -13.89961937509957401, -13.97604488694547875, 24.37609039468565442 ) ) ;
#35701 = CARTESIAN_POINT ( 'NONE',  ( 18.10062525802554134, -5.500000000000023093, 66.01383468041920821 ) ) ;
#35702 = CARTESIAN_POINT ( 'NONE',  ( 5.049401038298161559, -19.05341960407611168, 32.70724293864768129 ) ) ;
#35703 = CARTESIAN_POINT ( 'NONE',  ( -19.99604614807126524, -21.49604614807087799, -52.16759353428663104 ) ) ;
#35704 = CARTESIAN_POINT ( 'NONE',  ( 9.564922557960805705, 16.46253265017160317, 64.58224293864769550 ) ) ;
#35705 = CARTESIAN_POINT ( 'NONE',  ( -19.26498983726237313, 5.499999999999802824, 100.5531957742200575 ) ) ;
#35706 = CARTESIAN_POINT ( 'NONE',  ( -10.81492255796105439, 18.62759615963255655, 112.9177570613523329 ) ) ;
#35707 = CARTESIAN_POINT ( 'NONE',  ( -14.29746914071049879, 8.314922557960819915, 25.83224293864769194 ) ) ;
#35708 = CARTESIAN_POINT ( 'NONE',  ( -19.03943276465977164, 0.05219959533909376836, 36.24890960531436690 ) ) ;
#35709 = CARTESIAN_POINT ( 'NONE',  ( 13.89961937509977652, -13.97604488694527269, 93.12390960531436690 ) ) ;
#35710 = CARTESIAN_POINT ( 'NONE',  ( -10.81492255796105439, 18.62759615963255655, 67.91775706135234714 ) ) ;
#35711 = CARTESIAN_POINT ( 'NONE',  ( -9.474510206698964154, 16.51473224551069663, 55.41557627198103120 ) ) ;
#35712 = CARTESIAN_POINT ( 'NONE',  ( 10.72451020669871369, 18.67979575497193778, 72.08442372801899012 ) ) ;
#35714 = CARTESIAN_POINT ( 'NONE',  ( -15.80617190586745835, -15.72974639402198527, 21.87390960531436690 ) ) ;
#35713 = CARTESIAN_POINT ( 'NONE',  ( 16.51473224551083163, -9.474510206698727899, 90.83442372801900433 ) ) ;
#35715 = CARTESIAN_POINT ( 'NONE',  ( -16.46253265017160317, 9.564922557960807481, 35.83224293864768839 ) ) ;
#35716 = CARTESIAN_POINT ( 'NONE',  ( 10.72451020669898902, -18.67979575497178502, 107.9155762719810241 ) ) ;
#35717 = CARTESIAN_POINT ( 'NONE',  ( 19.03943276465977164, 0.05219959533936151252, 36.25109039468567573 ) ) ;
#35718 = CARTESIAN_POINT ( 'NONE',  ( -14.29746914071049879, 8.314922557960819915, 110.8322429386476955 ) ) ;
#35719 = CARTESIAN_POINT ( 'NONE',  ( 9.564922557960805705, 16.46253265017160317, 64.58224293864769550 ) ) ;
#35720 = CARTESIAN_POINT ( 'NONE',  ( -13.89961937509957401, -13.97604488694547875, 109.3760903946856331 ) ) ;
#35721 = CARTESIAN_POINT ( 'NONE',  ( -16.55341960407611168, -4.379528057220339221, 76.45724293864769550 ) ) ;
#35722 = CARTESIAN_POINT ( 'NONE',  ( -21.53943276465977519, 0.05219959533907696930, 21.24890960531436690 ) ) ;
#35723 = CARTESIAN_POINT ( 'NONE',  ( -5.049401038297874678, -19.05341960407617918, 84.79275706135233293 ) ) ;
#35724 = CARTESIAN_POINT ( 'NONE',  ( -10.72451020669898014, 18.67979575497178502, 95.41557627198102409 ) ) ;
#35725 = CARTESIAN_POINT ( 'NONE',  ( 18.62759615963255655, 10.81492255796105972, 41.66775706135235424 ) ) ;
#35726 = CARTESIAN_POINT ( 'NONE',  ( 12.06949235617739724, 12.14591786802326823, 56.87609039468568994 ) ) ;
#35728 = CARTESIAN_POINT ( 'NONE',  ( -21.55341960407619339, 5.719274019375674811, 53.54275706135234714 ) ) ;
#35727 = CARTESIAN_POINT ( 'NONE',  ( 0.05219959533934541429, -16.53943276465976808, 55.00109039468568284 ) ) ;
#35729 = CARTESIAN_POINT ( 'NONE',  ( 15.72974639402199770, -15.80617190586745480, 58.12390960531435979 ) ) ;
#35730 = CARTESIAN_POINT ( 'NONE',  ( -19.05341960407611168, -5.049401038298163336, 51.45724293864770260 ) ) ;
#35731 = CARTESIAN_POINT ( 'NONE',  ( 23.48529157249599919, 32.32473071737754111, -2.449999994537626069 ) ) ;
#35732 = CARTESIAN_POINT ( 'NONE',  ( -12.06949235617739369, -12.14591786802326823, 79.37609039468567573 ) ) ;
#35733 = CARTESIAN_POINT ( 'NONE',  ( 15.72974639402199770, -15.80617190586745480, 98.12390960531436690 ) ) ;
#35734 = CARTESIAN_POINT ( 'NONE',  ( 4.483927247898545687, 16.52544592524342804, 49.79057627198102409 ) ) ;
#35735 = CARTESIAN_POINT ( 'NONE',  ( -14.34966873604972548, 8.224510206698743886, 63.33442372801900433 ) ) ;
#35736 = CARTESIAN_POINT ( 'NONE',  ( 13.89961937509957401, 13.97604488694547697, 96.87609039468566152 ) ) ;
#35737 = CARTESIAN_POINT ( 'NONE',  ( -10.81492255796078084, -18.62759615963271287, 97.08224293864770971 ) ) ;
#35738 = CARTESIAN_POINT ( 'NONE',  ( 16.53943276465976808, -0.05219959533910856209, 43.74890960531435979 ) ) ;
#35739 = EDGE_LOOP ( 'NONE', ( #165093, #7576 ) ) ;
#35740 = CARTESIAN_POINT ( 'NONE',  ( 18.39443945427638738, -5.500000000000021316, 91.01745347608654413 ) ) ;
#35741 =( BOUNDED_CURVE ( )  B_SPLINE_CURVE ( 2, ( #76211, #109533, #186403, #137890, #141853, #47880, #30721, #31712, #356, #92368, #95352 ),
 .UNSPECIFIED., .F., .T. ) 
 B_SPLINE_CURVE_WITH_KNOTS ( ( 3, 2, 2, 2, 2, 3 ),
 ( 0.3000000000000002665, 0.3200000000000002842, 0.3400000000000003020, 0.3600000000000003197, 0.3800000000000003375, 0.4000000000000003553 ),
 .UNSPECIFIED. ) 
 CURVE ( )  GEOMETRIC_REPRESENTATION_ITEM ( )  RATIONAL_B_SPLINE_CURVE ( ( 0.9999999999999993339, 0.9510565162951541973, 1.000000000000000000, 0.9510565162951535312, 1.000000000000000000, 0.9510565162951535312, 1.000000000000000000, 0.9510565162951535312, 1.000000000000000000, 0.9510565162951527540, 1.000000000000000888 ) ) 
 REPRESENTATION_ITEM ( '' )  );
#35742 = CARTESIAN_POINT ( 'NONE',  ( -5.823673210054116645, -21.52544592524344225, 72.29057627198102409 ) ) ;
#35743 = CARTESIAN_POINT ( 'NONE',  ( 14.34966873604960469, 8.224510206698951720, 29.16557627198103120 ) ) ;
#35744 = ORIENTED_EDGE ( 'NONE', *, *, #76080, .F. ) ;
#35745 = CARTESIAN_POINT ( 'NONE',  ( -22.49873734152930282, -26.99873734152905058, 8.889087296526001936 ) ) ;
#35746 = CARTESIAN_POINT ( 'NONE',  ( -5.719274019375978568, 21.55341960407610458, 95.20724293864769550 ) ) ;
#35747 = CARTESIAN_POINT ( 'NONE',  ( -21.52544592524334988, -5.823673210054445271, 28.95942372801902209 ) ) ;
#35748 = CARTESIAN_POINT ( 'NONE',  ( 4.379528057220339221, -16.55341960407611168, 32.70724293864770260 ) ) ;
#35749 = CARTESIAN_POINT ( 'NONE',  ( -8.224510206698735004, -14.34966873604973081, 44.58442372801901854 ) ) ;
#35750 = CARTESIAN_POINT ( 'NONE',  ( 0.05219959533909260263, 19.03943276465977164, 49.99890960531435979 ) ) ;
#35751 = CARTESIAN_POINT ( 'NONE',  ( -13.97604488694527625, -13.89961937509977652, 76.87390960531433848 ) ) ;
#35752 = ORIENTED_EDGE ( 'NONE', *, *, #140308, .T. ) ;
#35753 = CARTESIAN_POINT ( 'NONE',  ( 18.67979575497178502, 10.72451020669898547, 39.16557627198102409 ) ) ;
#35754 = CARTESIAN_POINT ( 'NONE',  ( -25.38628342471223576, -27.91043139587360145, -20.44818103819420330 ) ) ;
#35755 = CARTESIAN_POINT ( 'NONE',  ( 12.14591786802327356, -12.06949235617739191, 20.62609039468568639 ) ) ;
#35756 = CARTESIAN_POINT ( 'NONE',  ( 13.89961937509957401, 13.97604488694547697, 51.87609039468566863 ) ) ;
#35757 = CARTESIAN_POINT ( 'NONE',  ( -15.72974639402197994, 15.80617190586746368, 95.62390960531436690 ) ) ;
#35758 = CARTESIAN_POINT ( 'NONE',  ( -4.483927247898539470, -16.52544592524342804, 37.29057627198102409 ) ) ;
#35759 = CARTESIAN_POINT ( 'NONE',  ( 5.153800228976335163, 19.02544592524342804, 79.79057627198102409 ) ) ;
#35760 = CARTESIAN_POINT ( 'NONE',  ( 21.52544592524344225, -5.823673210054117533, 48.54057627198103120 ) ) ;
#35762 = CARTESIAN_POINT ( 'NONE',  ( 8.314922557961029526, -14.29746914071037800, 25.41775706135235779 ) ) ;
#35761 = CARTESIAN_POINT ( 'NONE',  ( -15.72974639402197994, 15.80617190586746368, 85.62390960531436690 ) ) ;
#35763 = CARTESIAN_POINT ( 'NONE',  ( -10.81492255796078084, -18.62759615963271287, 27.08224293864769550 ) ) ;
#35764 = CARTESIAN_POINT ( 'NONE',  ( -10.72451020669870658, -18.67979575497194134, 79.58442372801903275 ) ) ;
#35765 = CARTESIAN_POINT ( 'NONE',  ( -16.46253265017160317, 9.564922557960807481, 70.83224293864770971 ) ) ;
#35766 = CARTESIAN_POINT ( 'NONE',  ( -5.049401038298153566, 19.05341960407611168, 30.20724293864768839 ) ) ;
#35767 = CARTESIAN_POINT ( 'NONE',  ( -13.89961937509977652, 13.97604488694528158, 80.62390960531436690 ) ) ;
#35768 = CARTESIAN_POINT ( 'NONE',  ( -4.483927247898539470, -16.52544592524342804, 87.29057627198103830 ) ) ;
#35769 = VERTEX_POINT ( 'NONE', #89167 ) ;
#35770 = CARTESIAN_POINT ( 'NONE',  ( -16.51473224551082808, 9.474510206698731452, 98.33442372801900433 ) ) ;
#35771 = CARTESIAN_POINT ( 'NONE',  ( 0.000000000000000000, 2.449293598294705428E-16, -1.999999999999999112 ) ) ;
#35772 = CARTESIAN_POINT ( 'NONE',  ( -16.46253265017160317, 9.564922557960807481, 75.83224293864769550 ) ) ;
#35774 = CARTESIAN_POINT ( 'NONE',  ( -0.05219959533909027116, -19.03943276465977164, 112.4989096053143669 ) ) ;
#35773 = CARTESIAN_POINT ( 'NONE',  ( 21.53943276465977519, 0.05219959533937863772, 81.25109039468568994 ) ) ;
#35775 = CARTESIAN_POINT ( 'NONE',  ( 4.483927247898790824, -16.52544592524335698, 80.20942372801901854 ) ) ;
#35776 = CARTESIAN_POINT ( 'NONE',  ( -16.81555441253551919, -7.025013491695478507, 74.36314554665749199 ) ) ;
#35777 = CARTESIAN_POINT ( 'NONE',  ( 13.97604488694548053, -13.89961937509957401, 55.62609039468566863 ) ) ;
#35778 = CARTESIAN_POINT ( 'NONE',  ( 21.52544592524334988, 5.823673210054432836, 111.4594237280190328 ) ) ;
#35779 = CARTESIAN_POINT ( 'NONE',  ( 37.01127658466556625, 5.144934411046667044, 43.04759647146322266 ) ) ;
#35780 = DIRECTION ( 'NONE',  ( 0.000000000000000000, 0.000000000000000000, 1.000000000000000000 ) ) ;
#35781 = CARTESIAN_POINT ( 'NONE',  ( -11.40812507854755609, 35.11059874428196537, -3.524999997268813523 ) ) ;
#35782 = CARTESIAN_POINT ( 'NONE',  ( -4.483927247898539470, -16.52544592524342804, 27.29057627198103120 ) ) ;
#35783 = LINE ( 'NONE', #110632, #8068 ) ;
#35784 = CARTESIAN_POINT ( 'NONE',  ( 0.05219959533934541429, -16.53943276465976808, 100.0010903946857042 ) ) ;
#35785 = CARTESIAN_POINT ( 'NONE',  ( -19.35543954521081389, -5.499999999999486633, 84.58901960356449479 ) ) ;
#35786 = CARTESIAN_POINT ( 'NONE',  ( 16.55341960407618274, -4.379528057220086978, 86.04275706135236135 ) ) ;
#35787 = CARTESIAN_POINT ( 'NONE',  ( -19.05341960407611168, -5.049401038298163336, 21.45724293864768839 ) ) ;
#35788 = CARTESIAN_POINT ( 'NONE',  ( -21.55341960407619339, 5.719274019375674811, 98.54275706135234714 ) ) ;
#35789 = CARTESIAN_POINT ( 'NONE',  ( 16.46253265017146816, 9.564922557961045513, 101.6677570613523329 ) ) ;
#35790 = CARTESIAN_POINT ( 'NONE',  ( -21.55341960407619339, 5.719274019375674811, 68.54275706135234714 ) ) ;
#35791 = CARTESIAN_POINT ( 'NONE',  ( 5.049401038297881783, 19.05341960407617563, 42.29275706135234003 ) ) ;
#35792 = CARTESIAN_POINT ( 'NONE',  ( 5.153800228976335163, 19.02544592524342804, 84.79057627198099567 ) ) ;
#35793 = CARTESIAN_POINT ( 'NONE',  ( -5.049401038298153566, 19.05341960407611168, 70.20724293864769550 ) ) ;
#35794 = DIRECTION ( 'NONE',  ( 1.000000000000000000, 0.000000000000000000, 0.000000000000000000 ) ) ;
#35795 = CARTESIAN_POINT ( 'NONE',  ( 21.52544592524344225, -5.823673210054117533, 53.54057627198103120 ) ) ;
#35796 = CARTESIAN_POINT ( 'NONE',  ( 0.05219959533909260263, 19.03943276465977164, 49.99890960531435979 ) ) ;
#35797 = CARTESIAN_POINT ( 'NONE',  ( -12.06949235617739369, -12.14591786802326823, 79.37609039468567573 ) ) ;
#35798 = UNCERTAINTY_MEASURE_WITH_UNIT (LENGTH_MEASURE( 1.000000000000000082E-05 ), #127353, 'distance_accuracy_value', 'NONE');
#35799 = ORIENTED_EDGE ( 'NONE', *, *, #47298, .T. ) ;
#35801 = CARTESIAN_POINT ( 'NONE',  ( -29.86685920354755552, 21.69954338932564397, -4.824999997268814234 ) ) ;
#35800 = CARTESIAN_POINT ( 'NONE',  ( -4.483927247898539470, -16.52544592524342804, 82.29057627198103830 ) ) ;
#35802 = CARTESIAN_POINT ( 'NONE',  ( -4.483927247898782831, 16.52544592524335698, 37.70942372801900433 ) ) ;
#35803 = CARTESIAN_POINT ( 'NONE',  ( 16.55341960407611168, 4.379528057220329451, 103.9572429386476813 ) ) ;
#35804 = CARTESIAN_POINT ( 'NONE',  ( 19.02544592524334988, 5.153800228976608722, 71.45942372801900433 ) ) ;
#35805 = CARTESIAN_POINT ( 'NONE',  ( 8.224510206698953496, -14.34966873604960469, 72.91557627198103830 ) ) ;
#35806 = CARTESIAN_POINT ( 'NONE',  ( -18.67979575497193778, 10.72451020669871902, 38.33442372801900433 ) ) ;
#35808 = CARTESIAN_POINT ( 'NONE',  ( -21.53943276465977519, 0.05219959533907696930, 91.24890960531436690 ) ) ;
#35807 = CARTESIAN_POINT ( 'NONE',  ( -19.05341960407611168, -5.049401038298163336, 26.45724293864769550 ) ) ;
#35809 = CARTESIAN_POINT ( 'NONE',  ( -19.05341960407611168, -5.049401038298163336, 106.4572429386476955 ) ) ;
#35810 = CARTESIAN_POINT ( 'NONE',  ( -14.34966873604960291, -8.224510206698953496, 71.66557627198100988 ) ) ;
#35811 = CARTESIAN_POINT ( 'NONE',  ( 21.89035704508949465, -33.26311937565159127, -20.38189100991405311 ) ) ;
#35812 = CARTESIAN_POINT ( 'NONE',  ( 19.03943276465977164, -0.05219959533909143690, 48.74890960531435979 ) ) ;
#35813 = CARTESIAN_POINT ( 'NONE',  ( 22.81625015709509441, 31.40387420917330275, -5.324999997268813345 ) ) ;
#35814 = CARTESIAN_POINT ( 'NONE',  ( 19.05341960407617918, -5.049401038297876454, 81.04275706135231871 ) ) ;
#35815 = CARTESIAN_POINT ( 'NONE',  ( -15.80617190586768217, 15.72974639402176855, 23.12609039468567573 ) ) ;
#35816 = CARTESIAN_POINT ( 'NONE',  ( -13.89961937509977652, 13.97604488694528158, 70.62390960531432427 ) ) ;
#35817 = CARTESIAN_POINT ( 'NONE',  ( -13.89961937509957401, -13.97604488694547875, 59.37609039468566863 ) ) ;
#35818 = CARTESIAN_POINT ( 'NONE',  ( -9.564922557960796823, -16.46253265017161027, 47.08224293864769550 ) ) ;
#35819 = ADVANCED_FACE ( 'NONE', ( #181204 ), #53848, .T. ) ;
#35820 = CARTESIAN_POINT ( 'NONE',  ( -0.05219959533910754901, -16.53943276465976808, 62.49890960531436690 ) ) ;
#35821 = CARTESIAN_POINT ( 'NONE',  ( 8.224510206698953496, -14.34966873604960469, 47.91557627198102409 ) ) ;
#35822 = CARTESIAN_POINT ( 'NONE',  ( -13.89961937509977652, 13.97604488694528158, 80.62390960531436690 ) ) ;
#35823 = CARTESIAN_POINT ( 'NONE',  ( -10.81492255796078084, -18.62759615963271287, 87.08224293864769550 ) ) ;
#35824 = CARTESIAN_POINT ( 'NONE',  ( -9.564922557960796823, -16.46253265017161027, 77.08224293864769550 ) ) ;
#35825 = CARTESIAN_POINT ( 'NONE',  ( 15.72974639402199770, -15.80617190586745480, 73.12390960531436690 ) ) ;
#35826 = CARTESIAN_POINT ( 'NONE',  ( 21.53943276465977519, 0.05219959533937863772, 111.2510903946856899 ) ) ;
#35829 = CARTESIAN_POINT ( 'NONE',  ( -14.34966873604960291, -8.224510206698953496, 96.66557627198102409 ) ) ;
#35828 = CARTESIAN_POINT ( 'NONE',  ( -12.14591786802326823, 12.06949235617739902, 113.1260903946856899 ) ) ;
#35827 = CARTESIAN_POINT ( 'NONE',  ( -19.03943276465977164, 0.05219959533909376836, 21.24890960531436335 ) ) ;
#35830 = CARTESIAN_POINT ( 'NONE',  ( 16.51473224551083163, -9.474510206698727899, 100.8344237280190043 ) ) ;
#35831 = VERTEX_POINT ( 'NONE', #115522 ) ;
#35832 = CARTESIAN_POINT ( 'NONE',  ( 10.81492255796078972, 18.62759615963270932, 114.5822429386477097 ) ) ;
#35833 = CARTESIAN_POINT ( 'NONE',  ( -9.564922557961040184, 16.46253265017147172, 47.91775706135233293 ) ) ;
#35834 = CARTESIAN_POINT ( 'NONE',  ( 4.483927247898545687, 16.52544592524342804, 24.79057627198103120 ) ) ;
#35835 = CARTESIAN_POINT ( 'NONE',  ( -5.049401038297874678, -19.05341960407617918, 44.79275706135232582 ) ) ;
#35836 = CARTESIAN_POINT ( 'NONE',  ( 19.05341960407611168, 5.049401038298154454, 108.9572429386477097 ) ) ;
#35837 = CARTESIAN_POINT ( 'NONE',  ( -16.55341960407611168, -4.379528057220339221, 56.45724293864768839 ) ) ;
#35838 = CARTESIAN_POINT ( 'NONE',  ( -28.79475375365586842, 2.428612866367529932E-14, 140.2656553485623760 ) ) ;
#35839 = CARTESIAN_POINT ( 'NONE',  ( 16.51473224551069308, 9.474510206698969483, 34.16557627198102409 ) ) ;
#35840 = CARTESIAN_POINT ( 'NONE',  ( 5.823673210054444382, -21.52544592524334988, 105.2094237280190328 ) ) ;
#35841 = CARTESIAN_POINT ( 'NONE',  ( 8.314922557961029526, -14.29746914071037800, 90.41775706135236135 ) ) ;
#35842 = CARTESIAN_POINT ( 'NONE',  ( 15.72974639402176855, 15.80617190586768217, 46.87609039468568994 ) ) ;
#35843 = CARTESIAN_POINT ( 'NONE',  ( -4.483927247898782831, 16.52544592524335698, 42.70942372801901854 ) ) ;
#35844 = CARTESIAN_POINT ( 'NONE',  ( 21.52544592524344225, -5.823673210054117533, 23.54057627198102765 ) ) ;
#35845 = CARTESIAN_POINT ( 'NONE',  ( -9.564922557960796823, -16.46253265017161027, 57.08224293864769550 ) ) ;
#35846 = CARTESIAN_POINT ( 'NONE',  ( 5.153800228976335163, 19.02544592524342804, 59.79057627198100988 ) ) ;
#35847 = CARTESIAN_POINT ( 'NONE',  ( -4.379528057220086978, -16.55341960407618274, 49.79275706135234714 ) ) ;
#35848 = CARTESIAN_POINT ( 'NONE',  ( 12.14591786802309770, 12.06949235617756955, 99.37390960531436690 ) ) ;
#35849 = CARTESIAN_POINT ( 'NONE',  ( -8.314922557961024197, 14.29746914071037800, 112.9177570613523329 ) ) ;
#35850 = DIRECTION ( 'NONE',  ( 4.336808689942018352E-17, -1.000000000000000000, 0.000000000000000000 ) ) ;
#35853 = CARTESIAN_POINT ( 'NONE',  ( 0.05219959533909260263, 19.03943276465977164, 74.99890960531435269 ) ) ;
#35852 = CARTESIAN_POINT ( 'NONE',  ( 9.564922557960805705, 16.46253265017160317, 89.58224293864769550 ) ) ;
#35851 = CARTESIAN_POINT ( 'NONE',  ( 21.52544592524334988, 5.823673210054432836, 56.45942372801902565 ) ) ;
#35854 = CARTESIAN_POINT ( 'NONE',  ( 16.51473224551069308, 9.474510206698969483, 99.16557627198102409 ) ) ;
#35855 = CARTESIAN_POINT ( 'NONE',  ( -8.224510206698948167, 14.34966873604960824, 40.41557627198103120 ) ) ;
#35856 = CARTESIAN_POINT ( 'NONE',  ( 4.379528057220092307, 16.55341960407617563, 107.2927570613523471 ) ) ;
#35857 = CARTESIAN_POINT ( 'NONE',  ( -4.483927247898539470, -16.52544592524342804, 32.29057627198102409 ) ) ;
#35858 = VERTEX_POINT ( 'NONE', #8341 ) ;
#35859 = FACE_OUTER_BOUND ( 'NONE', #168887, .T. ) ;
#35860 = CARTESIAN_POINT ( 'NONE',  ( -0.05219959533936034679, 19.03943276465977164, 42.50109039468566152 ) ) ;
#35861 = CARTESIAN_POINT ( 'NONE',  ( -19.05341960407611168, -5.049401038298163336, 61.45724293864769550 ) ) ;
#35862 = CARTESIAN_POINT ( 'NONE',  ( 5.153800228976615827, -19.02544592524334988, 55.20942372801899722 ) ) ;
#35863 = CARTESIAN_POINT ( 'NONE',  ( -36.91746825000001309, 11.99521256947798342, -9.224999997268813701 ) ) ;
#35864 = PLANE ( 'NONE',  #76338 ) ;
#35866 = CARTESIAN_POINT ( 'NONE',  ( -12.06949235617739369, -12.14591786802326823, 74.37609039468568994 ) ) ;
#35865 = CARTESIAN_POINT ( 'NONE',  ( 5.153800228976615827, -19.02544592524334988, 90.20942372801900433 ) ) ;
#35867 = CARTESIAN_POINT ( 'NONE',  ( 17.50000000000000711, 5.499999999999976907, 93.78230962303565832 ) ) ;
#35868 = CARTESIAN_POINT ( 'NONE',  ( 0.05219959533909260263, 19.03943276465977164, 99.99890960531436690 ) ) ;
#35869 = CARTESIAN_POINT ( 'NONE',  ( 21.55341960407619695, -5.719274019375665929, 26.04275706135235779 ) ) ;
#35870 = CARTESIAN_POINT ( 'NONE',  ( 9.474510206698729675, 16.51473224551082808, 92.08442372801900433 ) ) ;
#35872 = CARTESIAN_POINT ( 'NONE',  ( 0.05219959533909260263, 19.03943276465977164, 49.99890960531435979 ) ) ;
#35871 = CARTESIAN_POINT ( 'NONE',  ( 17.05116617787825106, 6.768360034955840376, 88.84324446740805570 ) ) ;
#35873 = CARTESIAN_POINT ( 'NONE',  ( 16.46253265017160672, -9.564922557960803928, 88.33224293864769550 ) ) ;
#35875 = CARTESIAN_POINT ( 'NONE',  ( 16.46253265017160672, -9.564922557960803928, 48.33224293864769550 ) ) ;
#35874 = CARTESIAN_POINT ( 'NONE',  ( 16.55341960407611168, 4.379528057220329451, 48.95724293864770971 ) ) ;
#35876 = CARTESIAN_POINT ( 'NONE',  ( 19.05341960407617918, -5.049401038297876454, 71.04275706135234714 ) ) ;
#35877 = CARTESIAN_POINT ( 'NONE',  ( -19.02544592524334988, -5.153800228976617603, 23.95942372801900078 ) ) ;
#35878 = CARTESIAN_POINT ( 'NONE',  ( -13.97604488694527625, -13.89961937509977652, 71.87390960531433848 ) ) ;
#35879 = CARTESIAN_POINT ( 'NONE',  ( 18.62759615963271287, -10.81492255796078972, 58.33224293864768839 ) ) ;
#35881 = CARTESIAN_POINT ( 'NONE',  ( 19.03943276465977164, 0.05219959533936151252, 26.25109039468566507 ) ) ;
#35880 = CARTESIAN_POINT ( 'NONE',  ( 4.483927247898545687, 16.52544592524342804, 69.79057627198102409 ) ) ;
#35882 = CARTESIAN_POINT ( 'NONE',  ( 5.049401038298161559, -19.05341960407611168, 112.7072429386476813 ) ) ;
#35883 = CARTESIAN_POINT ( 'NONE',  ( -18.67979575497178146, -10.72451020669898902, 31.66557627198102054 ) ) ;
#35884 = CARTESIAN_POINT ( 'NONE',  ( 19.03943276465977164, -0.05219959533909143690, 53.74890960531436690 ) ) ;
#35885 = CARTESIAN_POINT ( 'NONE',  ( 16.46253265017160672, -9.564922557960803928, 33.33224293864770260 ) ) ;
#35886 = CARTESIAN_POINT ( 'NONE',  ( 16.52544592524342804, -4.483927247898539470, 98.54057627198105251 ) ) ;
#35887 = CARTESIAN_POINT ( 'NONE',  ( 21.55341960407610458, 5.719274019375980345, 103.9572429386476813 ) ) ;
#35888 = CARTESIAN_POINT ( 'NONE',  ( 25.51209292918185412, -5.276535733812600881, 165.5596888358905687 ) ) ;
#35889 = CARTESIAN_POINT ( 'NONE',  ( -10.81492255796105439, 18.62759615963255655, 27.91775706135234358 ) ) ;
#35890 = CARTESIAN_POINT ( 'NONE',  ( 16.46253265017160672, -9.564922557960803928, 98.33224293864769550 ) ) ;
#35891 = CARTESIAN_POINT ( 'NONE',  ( 8.314922557960818139, 14.29746914071049879, 114.5822429386477097 ) ) ;
#35892 = CARTESIAN_POINT ( 'NONE',  ( 21.52544592524334988, 5.823673210054432836, 76.45942372801901854 ) ) ;
#35893 = CARTESIAN_POINT ( 'NONE',  ( 10.81492255796078972, 18.62759615963270932, 94.58224293864769550 ) ) ;
#35894 = EDGE_CURVE ( 'NONE', #114764, #144280, #118527, .T. ) ;
#35895 = CARTESIAN_POINT ( 'NONE',  ( 17.50000000000000000, -5.500000000000000888, 108.2969038253417153 ) ) ;
#35896 = CARTESIAN_POINT ( 'NONE',  ( 12.24802307403557933, -10.74802307403627921, -61.53034260416801260 ) ) ;
#35897 = DIRECTION ( 'NONE',  ( -0.000000000000000000, -0.000000000000000000, -1.000000000000000000 ) ) ;
#35898 = CARTESIAN_POINT ( 'NONE',  ( -14.34966873604972548, 8.224510206698743886, 53.33442372801901854 ) ) ;
#35899 = CARTESIAN_POINT ( 'NONE',  ( 4.483927247898545687, 16.52544592524342804, 104.7905762719810241 ) ) ;
#35900 = CARTESIAN_POINT ( 'NONE',  ( -25.80209238092669821, -7.370998251473047880, 174.5109820657624766 ) ) ;
#35901 = CARTESIAN_POINT ( 'NONE',  ( 5.153800228976335163, 19.02544592524342804, 54.79057627198103120 ) ) ;
#35902 = CARTESIAN_POINT ( 'NONE',  ( -16.52544592524342804, 4.483927247898546575, 96.04057627198102409 ) ) ;
#35903 = CARTESIAN_POINT ( 'NONE',  ( 10.81492255796078972, 18.62759615963270932, 44.58224293864769550 ) ) ;
#35904 = CARTESIAN_POINT ( 'NONE',  ( -12.06949235617756955, 12.14591786802309770, 70.62390960531436690 ) ) ;
#35905 = CARTESIAN_POINT ( 'NONE',  ( -8.224510206698735004, -14.34966873604973081, 19.58442372801901143 ) ) ;
#35906 = CARTESIAN_POINT ( 'NONE',  ( -18.62759615963255300, -10.81492255796106328, 89.16775706135236135 ) ) ;
#35907 = CARTESIAN_POINT ( 'NONE',  ( 17.12812012977029141, -6.668231424565925991, 76.14051240676856480 ) ) ;
#35908 = CARTESIAN_POINT ( 'NONE',  ( -12.06949235617739369, -12.14591786802326823, 104.3760903946856899 ) ) ;
#35909 = CARTESIAN_POINT ( 'NONE',  ( 16.53943276465976808, -0.05219959533910856209, 38.74890960531435979 ) ) ;
#35910 = CARTESIAN_POINT ( 'NONE',  ( -13.89961937509977652, 13.97604488694528158, 40.62390960531435979 ) ) ;
#35911 = CARTESIAN_POINT ( 'NONE',  ( -16.46253265017160317, 9.564922557960807481, 90.83224293864769550 ) ) ;
#35912 = CARTESIAN_POINT ( 'NONE',  ( -18.62759615963270932, 10.81492255796079327, 90.83224293864769550 ) ) ;
#35913 = CARTESIAN_POINT ( 'NONE',  ( 4.379528057220092307, 16.55341960407617563, 37.29275706135235424 ) ) ;
#35915 = CARTESIAN_POINT ( 'NONE',  ( 10.72451020669871369, 18.67979575497193778, 92.08442372801901854 ) ) ;
#35914 = CARTESIAN_POINT ( 'NONE',  ( 8.224510206698953496, -14.34966873604960469, 67.91557627198102409 ) ) ;
#35916 = CARTESIAN_POINT ( 'NONE',  ( 16.53943276465976808, 0.05219959533934440121, 101.2510903946856757 ) ) ;
#35917 = CARTESIAN_POINT ( 'NONE',  ( 17.31747979337963272, -6.344076630960739926, 46.12055131934818064 ) ) ;
#35918 = CARTESIAN_POINT ( 'NONE',  ( 17.50000000000000000, -7.500000000000000888, 120.0000000000000142 ) ) ;
#35919 = CARTESIAN_POINT ( 'NONE',  ( 0.05219959533910956823, 16.53943276465976808, 29.99890960531435979 ) ) ;
#35920 = CARTESIAN_POINT ( 'NONE',  ( -16.55341960407617563, 4.379528057220093196, 73.54275706135234714 ) ) ;
#35921 = CARTESIAN_POINT ( 'NONE',  ( -13.97604488694527625, -13.89961937509977652, 81.87390960531436690 ) ) ;
#35922 = CARTESIAN_POINT ( 'NONE',  ( -19.05341960407611168, -5.049401038298163336, 101.4572429386476955 ) ) ;
#35923 = CARTESIAN_POINT ( 'NONE',  ( 15.80617190586769283, -15.72974639402175789, 85.62609039468568994 ) ) ;
#35924 = CARTESIAN_POINT ( 'NONE',  ( -12.14591786802326823, 12.06949235617739902, 93.12609039468568994 ) ) ;
#35925 = CARTESIAN_POINT ( 'NONE',  ( 16.55341960407611168, 4.379528057220329451, 58.95724293864770971 ) ) ;
#35926 = CARTESIAN_POINT ( 'NONE',  ( -19.03943276465977164, 0.05219959533909376836, 71.24890960531435269 ) ) ;
#35927 = ORIENTED_EDGE ( 'NONE', *, *, #94206, .T. ) ;
#35928 = CARTESIAN_POINT ( 'NONE',  ( 16.46253265017146816, 9.564922557961045513, 106.6677570613523471 ) ) ;
#35929 = CARTESIAN_POINT ( 'NONE',  ( -0.05219959533909027116, -19.03943276465977164, 32.49890960531435979 ) ) ;
#35930 = CARTESIAN_POINT ( 'NONE',  ( 5.153800228976335163, 19.02544592524342804, 79.79057627198102409 ) ) ;
#35932 = CARTESIAN_POINT ( 'NONE',  ( -29.86685920354755197, -21.69954338932560134, -6.424999997268812990 ) ) ;
#35931 = CARTESIAN_POINT ( 'NONE',  ( -19.03943276465977164, -0.05219959533935918106, 113.7510903946856757 ) ) ;
#35933 = CARTESIAN_POINT ( 'NONE',  ( -16.46253265017146816, -9.564922557961047289, 19.16775706135233293 ) ) ;
#35934 = CARTESIAN_POINT ( 'NONE',  ( 16.55341960407618274, -4.379528057220086978, 76.04275706135237556 ) ) ;
#35935 = CARTESIAN_POINT ( 'NONE',  ( -13.97604488694547697, 13.89961937509957934, 113.1260903946856757 ) ) ;
#35936 = CARTESIAN_POINT ( 'NONE',  ( 5.153800228976335163, 19.02544592524342804, 24.79057627198102765 ) ) ;
#35937 = CARTESIAN_POINT ( 'NONE',  ( 16.55341960407618274, -4.379528057220086978, 61.04275706135234714 ) ) ;
#35938 = CARTESIAN_POINT ( 'NONE',  ( -16.55341960407617563, 4.379528057220093196, 48.54275706135234714 ) ) ;
#35939 = CARTESIAN_POINT ( 'NONE',  ( -9.564922557960796823, -16.46253265017161027, 27.08224293864769550 ) ) ;
#35940 = CARTESIAN_POINT ( 'NONE',  ( 13.97604488694548053, -13.89961937509957401, 70.62609039468567573 ) ) ;
#35941 = CARTESIAN_POINT ( 'NONE',  ( 18.62759615963255655, 10.81492255796105972, 111.6677570613523613 ) ) ;
#35942 = CARTESIAN_POINT ( 'NONE',  ( -5.049401038298153566, 19.05341960407611168, 35.20724293864768839 ) ) ;
#35943 = CARTESIAN_POINT ( 'NONE',  ( 13.97604488694527802, 13.89961937509977652, 74.37390960531436690 ) ) ;
#35944 = CARTESIAN_POINT ( 'NONE',  ( -16.53943276465976808, 0.05219959533911058130, 66.24890960531436690 ) ) ;
#35945 = CARTESIAN_POINT ( 'NONE',  ( 19.05341960407617918, -5.049401038297876454, 36.04275706135234003 ) ) ;
#35946 = CARTESIAN_POINT ( 'NONE',  ( -18.67979575497178146, -10.72451020669898902, 36.66557627198103120 ) ) ;
#35947 = CARTESIAN_POINT ( 'NONE',  ( -21.55341960407619339, 5.719274019375674811, 113.5427570613523756 ) ) ;
#35948 = CARTESIAN_POINT ( 'NONE',  ( 16.46253265017160672, -9.564922557960803928, 93.33224293864769550 ) ) ;
#35949 = CARTESIAN_POINT ( 'NONE',  ( -10.81492255796105439, 18.62759615963255655, 112.9177570613523329 ) ) ;
#35950 = CARTESIAN_POINT ( 'NONE',  ( 15.72974639402199770, -15.80617190586745480, 63.12390960531435979 ) ) ;
#35951 = CARTESIAN_POINT ( 'NONE',  ( -13.89961937509977652, 13.97604488694528158, 100.6239096053143669 ) ) ;
#35952 = CARTESIAN_POINT ( 'NONE',  ( 9.474510206698729675, 16.51473224551082808, 72.08442372801900433 ) ) ;
#35953 = CARTESIAN_POINT ( 'NONE',  ( 13.89961937509977652, -13.97604488694527269, 98.12390960531433848 ) ) ;
#35954 = CARTESIAN_POINT ( 'NONE',  ( 13.97604488694548053, -13.89961937509957401, 95.62609039468563310 ) ) ;
#35955 = CARTESIAN_POINT ( 'NONE',  ( 16.55341960407611168, 4.379528057220329451, 113.9572429386477239 ) ) ;
#35956 = CARTESIAN_POINT ( 'NONE',  ( -19.03943276465977164, 0.05219959533909376836, 81.24890960531436690 ) ) ;
#35957 = CARTESIAN_POINT ( 'NONE',  ( 0.05219959533907565091, 21.53943276465977519, 59.99890960531436690 ) ) ;
#35958 = CARTESIAN_POINT ( 'NONE',  ( -4.379528057220086978, -16.55341960407618274, 29.79275706135234358 ) ) ;
#35959 = CARTESIAN_POINT ( 'NONE',  ( -10.72451020669870658, -18.67979575497194134, 29.58442372801901854 ) ) ;
#35960 = CARTESIAN_POINT ( 'NONE',  ( -21.52544592524334988, -5.823673210054445271, 98.95942372801903275 ) ) ;
#35961 = CARTESIAN_POINT ( 'NONE',  ( 14.29746914071037800, 8.314922557961029526, 101.6677570613523613 ) ) ;
#35962 = CARTESIAN_POINT ( 'NONE',  ( -19.02544592524342804, 5.153800228976336051, 91.04057627198100988 ) ) ;
#35963 = CARTESIAN_POINT ( 'NONE',  ( -12.14591786802309592, -12.06949235617757132, 96.87390960531436690 ) ) ;
#35964 = CARTESIAN_POINT ( 'NONE',  ( -4.483927247898539470, -16.52544592524342804, 27.29057627198103120 ) ) ;
#35965 = CARTESIAN_POINT ( 'NONE',  ( -16.51473224551082808, 9.474510206698731452, 73.33442372801900433 ) ) ;
#35966 = CARTESIAN_POINT ( 'NONE',  ( -21.52544592524334988, -5.823673210054445271, 38.95942372801901854 ) ) ;
#35967 = CARTESIAN_POINT ( 'NONE',  ( 14.29746914071049879, -8.314922557960816363, 88.33224293864769550 ) ) ;
#35968 = CARTESIAN_POINT ( 'NONE',  ( 9.564922557960805705, 16.46253265017160317, 114.5822429386476955 ) ) ;
#35969 = CARTESIAN_POINT ( 'NONE',  ( 8.224510206698742110, 14.34966873604972548, 102.0844237280190185 ) ) ;
#35970 = CARTESIAN_POINT ( 'NONE',  ( 10.72451020669871369, 18.67979575497193778, 82.08442372801901854 ) ) ;
#35971 = CARTESIAN_POINT ( 'NONE',  ( -16.53943276465976808, -0.05219959533934237506, 43.75109039468568284 ) ) ;
#35972 = CARTESIAN_POINT ( 'NONE',  ( 18.67979575497194134, -10.72451020669871369, 35.83442372801901143 ) ) ;
#35973 = EDGE_LOOP ( 'NONE', ( #167141, #159163, #107902, #109361, #191043, #43991 ) ) ;
#35974 = CARTESIAN_POINT ( 'NONE',  ( 5.823673210054125526, 21.52544592524343514, 114.7905762719810383 ) ) ;
#35975 = CARTESIAN_POINT ( 'NONE',  ( 16.53943276465976808, -0.05219959533910856209, 88.74890960531436690 ) ) ;
#35976 = CARTESIAN_POINT ( 'NONE',  ( 17.50000000000002132, -3.850315288878719322, 26.76629130603451046 ) ) ;
#35977 = CARTESIAN_POINT ( 'NONE',  ( 4.379528057220339221, -16.55341960407611168, 72.70724293864769550 ) ) ;
#35978 = CARTESIAN_POINT ( 'NONE',  ( 16.51473224551069308, 9.474510206698969483, 59.16557627198102409 ) ) ;
#35979 = CARTESIAN_POINT ( 'NONE',  ( 0.05219959533934541429, -16.53943276465976808, 100.0010903946857042 ) ) ;
#35980 = CARTESIAN_POINT ( 'NONE',  ( -9.564922557960796823, -16.46253265017161027, 37.08224293864768839 ) ) ;
#35981 = CARTESIAN_POINT ( 'NONE',  ( -5.823673210054116645, -21.52544592524344225, 42.29057627198103120 ) ) ;
#35982 = CARTESIAN_POINT ( 'NONE',  ( 16.53943276465976808, -0.05219959533910856209, 73.74890960531433848 ) ) ;
#35983 = CARTESIAN_POINT ( 'NONE',  ( -10.72451020669898014, 18.67979575497178502, 85.41557627198102409 ) ) ;
#35984 = CARTESIAN_POINT ( 'NONE',  ( 13.89961937509977652, -13.97604488694527269, 88.12390960531438111 ) ) ;
#35986 = CARTESIAN_POINT ( 'NONE',  ( -5.049401038297874678, -19.05341960407617918, 94.79275706135230450 ) ) ;
#35985 = CARTESIAN_POINT ( 'NONE',  ( -5.153800228976328057, -19.02544592524343514, 32.29057627198102409 ) ) ;
#35987 = CARTESIAN_POINT ( 'NONE',  ( 0.05219959533907565091, 21.53943276465977519, 29.99890960531435979 ) ) ;
#35988 = CARTESIAN_POINT ( 'NONE',  ( -15.80617190586768217, 15.72974639402176855, 68.12609039468567573 ) ) ;
#35989 = CARTESIAN_POINT ( 'NONE',  ( -9.474510206698964154, 16.51473224551069663, 50.41557627198102409 ) ) ;
#35990 = CARTESIAN_POINT ( 'NONE',  ( -13.89961937509977652, 13.97604488694528158, 90.62390960531432427 ) ) ;
#35991 = ORIENTED_EDGE ( 'NONE', *, *, #88626, .F. ) ;
#35992 = CARTESIAN_POINT ( 'NONE',  ( -14.34966873604972548, 8.224510206698743886, 58.33442372801901143 ) ) ;
#35993 = CARTESIAN_POINT ( 'NONE',  ( -21.52544592524334988, -5.823673210054445271, 48.95942372801902565 ) ) ;
#35994 = CARTESIAN_POINT ( 'NONE',  ( -18.67979575497193778, 10.72451020669871902, 78.33442372801901854 ) ) ;
#35995 = CARTESIAN_POINT ( 'NONE',  ( 13.97604488694527802, 13.89961937509977652, 114.3739096053143669 ) ) ;
#35996 = CARTESIAN_POINT ( 'NONE',  ( 0.05219959533907565091, 21.53943276465977519, 104.9989096053143669 ) ) ;
#35998 = CARTESIAN_POINT ( 'NONE',  ( 16.55341960407618274, -4.379528057220086978, 71.04275706135234714 ) ) ;
#35997 = CARTESIAN_POINT ( 'NONE',  ( -21.53943276465977519, -0.05219959533937600094, 43.75109039468568284 ) ) ;
#35999 = CARTESIAN_POINT ( 'NONE',  ( 10.81492255796078972, 18.62759615963270932, 64.58224293864769550 ) ) ;
#36000 = CARTESIAN_POINT ( 'NONE',  ( 19.03943276465977164, 0.05219959533936151252, 36.25109039468567573 ) ) ;
#36002 = CARTESIAN_POINT ( 'NONE',  ( -16.52544592524335698, -4.483927247898792601, 108.9594237280190185 ) ) ;
#36001 = CARTESIAN_POINT ( 'NONE',  ( 0.05219959533909260263, 19.03943276465977164, 69.99890960531435269 ) ) ;
#36003 = CARTESIAN_POINT ( 'NONE',  ( -17.49999999999999645, -3.512728167236856436, 104.7719000481888685 ) ) ;
#36004 = CARTESIAN_POINT ( 'NONE',  ( 16.46253265017160672, -9.564922557960803928, 108.3322429386476955 ) ) ;
#36005 = CARTESIAN_POINT ( 'NONE',  ( 21.51934928555110460, 22.99905646750775290, -46.25979504214461713 ) ) ;
#36006 = CARTESIAN_POINT ( 'NONE',  ( 0.05219959533936267826, -19.03943276465977164, 85.00109039468567573 ) ) ;
#36007 = CARTESIAN_POINT ( 'NONE',  ( -21.53943276465977519, 0.05219959533907696930, 61.24890960531435979 ) ) ;
#36008 = CARTESIAN_POINT ( 'NONE',  ( -8.314922557960811034, -14.29746914071050412, 32.08224293864769550 ) ) ;
#36009 = CARTESIAN_POINT ( 'NONE',  ( -16.46253265017146816, -9.564922557961047289, 99.16775706135233293 ) ) ;
#36010 = DIRECTION ( 'NONE',  ( 0.000000000000000000, 0.7071067811865483499, -0.7071067811865466846 ) ) ;
#36011 = CARTESIAN_POINT ( 'NONE',  ( 9.564922557961047289, -16.46253265017146816, 100.4177570613523329 ) ) ;
#36013 = CARTESIAN_POINT ( 'NONE',  ( -5.049401038297874678, -19.05341960407617918, 54.79275706135234003 ) ) ;
#36012 = CARTESIAN_POINT ( 'NONE',  ( -18.67979575497178146, -10.72451020669898902, 91.66557627198103830 ) ) ;
#36014 = CARTESIAN_POINT ( 'NONE',  ( 16.81555441253554406, 7.025013491695466961, 106.8631455466574209 ) ) ;
#36015 = CARTESIAN_POINT ( 'NONE',  ( -5.153800228976328057, -19.02544592524343514, 62.29057627198100988 ) ) ;
#36016 = CARTESIAN_POINT ( 'NONE',  ( 4.483927247898545687, 16.52544592524342804, 59.79057627198103120 ) ) ;
#36017 = CARTESIAN_POINT ( 'NONE',  ( -19.02544592524342804, 5.153800228976336051, 46.04057627198101699 ) ) ;
#36018 = CARTESIAN_POINT ( 'NONE',  ( -4.483927247898539470, -16.52544592524342804, 47.29057627198103120 ) ) ;
#36019 = CARTESIAN_POINT ( 'NONE',  ( -6.180203150055817218, 4.962140900324484960, 6.568406857878972716 ) ) ;
#36020 = CARTESIAN_POINT ( 'NONE',  ( 0.9909172445849734334, 21.65732038466284948, -56.20941306831223727 ) ) ;
#36021 = CARTESIAN_POINT ( 'NONE',  ( -14.29746914071049879, 8.314922557960819915, 30.83224293864770260 ) ) ;
#36022 = CARTESIAN_POINT ( 'NONE',  ( 19.02544592524343514, -5.153800228976328945, 63.54057627198103830 ) ) ;
#36023 = CARTESIAN_POINT ( 'NONE',  ( 0.8613000766925150709, 7.878827036337479939, 3.431593142121015294 ) ) ;
#36024 = CARTESIAN_POINT ( 'NONE',  ( 5.049401038297881783, 19.05341960407617563, 42.29275706135234003 ) ) ;
#36025 = CARTESIAN_POINT ( 'NONE',  ( -12.14591786802326823, 12.06949235617739902, 43.12609039468568284 ) ) ;
#36026 = CARTESIAN_POINT ( 'NONE',  ( -15.72974639402197994, 15.80617190586746368, 55.62390960531436690 ) ) ;
#36027 = CARTESIAN_POINT ( 'NONE',  ( 15.72974639402176855, 15.80617190586768217, 106.8760903946856899 ) ) ;
#36028 = CARTESIAN_POINT ( 'NONE',  ( 0.05219959533909260263, 19.03943276465977164, 74.99890960531435269 ) ) ;
#36029 = CARTESIAN_POINT ( 'NONE',  ( 11.80868324581537543, 11.80868324581533990, -59.13370768023891344 ) ) ;
#36030 = CARTESIAN_POINT ( 'NONE',  ( 5.153800228976335163, 19.02544592524342804, 114.7905762719810241 ) ) ;
#36031 = CARTESIAN_POINT ( 'NONE',  ( -22.81625015709509441, -31.40387420917324590, -4.324999997268813345 ) ) ;
#36032 = CARTESIAN_POINT ( 'NONE',  ( 5.719274019375673035, 21.55341960407619339, 37.29275706135235424 ) ) ;
#36033 = CARTESIAN_POINT ( 'NONE',  ( -16.55341960407611168, -4.379528057220339221, 91.45724293864769550 ) ) ;
#36036 = LINE ( 'NONE', #3706, #107910 ) ;
#36035 = CARTESIAN_POINT ( 'NONE',  ( 5.049401038298161559, -19.05341960407611168, 87.70724293864769550 ) ) ;
#36034 = CARTESIAN_POINT ( 'NONE',  ( -10.72451020669898014, 18.67979575497178502, 90.41557627198103830 ) ) ;
#36037 = CARTESIAN_POINT ( 'NONE',  ( -13.97604488694527625, -13.89961937509977652, 91.87390960531432427 ) ) ;
#36038 = CARTESIAN_POINT ( 'NONE',  ( -5.823673210054431948, 21.52544592524334988, 27.70942372801901854 ) ) ;
#36039 = VERTEX_POINT ( 'NONE', #177210 ) ;
#36040 = CARTESIAN_POINT ( 'NONE',  ( 16.51473224551069308, 9.474510206698969483, 89.16557627198103830 ) ) ;
#36041 = CARTESIAN_POINT ( 'NONE',  ( -18.09918380851993902, -5.499999999999988454, 76.48618307335614475 ) ) ;
#36043 = CARTESIAN_POINT ( 'NONE',  ( -13.97604488694527625, -13.89961937509977652, 31.87390960531435979 ) ) ;
#36042 = CARTESIAN_POINT ( 'NONE',  ( 8.224510206698953496, -14.34966873604960469, 112.9155762719810383 ) ) ;
#36044 = CARTESIAN_POINT ( 'NONE',  ( 16.46253265017146816, 9.564922557961045513, 111.6677570613523329 ) ) ;
#36045 = CARTESIAN_POINT ( 'NONE',  ( 22.81625015709509441, 31.40387420917330275, -7.824999997268813345 ) ) ;
#36046 = CARTESIAN_POINT ( 'NONE',  ( 12.14591786802309770, 12.06949235617756955, 114.3739096053143527 ) ) ;
#36047 = CARTESIAN_POINT ( 'NONE',  ( 21.55341960407619695, -5.719274019375665929, 71.04275706135234714 ) ) ;
#36049 = CARTESIAN_POINT ( 'NONE',  ( -15.72974639402176322, -15.80617190586768395, 39.37609039468567573 ) ) ;
#36048 = CARTESIAN_POINT ( 'NONE',  ( -9.564922557960796823, -16.46253265017161027, 62.08224293864769550 ) ) ;
#36050 = CARTESIAN_POINT ( 'NONE',  ( 21.55341960407610458, 5.719274019375980345, 108.9572429386476955 ) ) ;
#36051 = CARTESIAN_POINT ( 'NONE',  ( -8.906447517083053711, -27.41122689804191026, 146.4000000000000057 ) ) ;
#36052 = CARTESIAN_POINT ( 'NONE',  ( -19.03943276465977164, 0.05219959533909376836, 81.24890960531436690 ) ) ;
#36053 = PLANE ( 'NONE',  #185756 ) ;
#36055 = CARTESIAN_POINT ( 'NONE',  ( -21.52544592524343514, 5.823673210054127303, 46.04057627198103830 ) ) ;
#36054 = CARTESIAN_POINT ( 'NONE',  ( 0.05219959533934541429, -16.53943276465976808, 20.00109039468568639 ) ) ;
#36056 = CARTESIAN_POINT ( 'NONE',  ( -15.80617190586768217, 15.72974639402176855, 68.12609039468567573 ) ) ;
#36057 = CARTESIAN_POINT ( 'NONE',  ( -16.51473224551069308, -9.474510206698971260, 111.6655762719810383 ) ) ;
#36058 = CARTESIAN_POINT ( 'NONE',  ( 19.05341960407617918, -5.049401038297876454, 91.04275706135234714 ) ) ;
#36059 = CARTESIAN_POINT ( 'NONE',  ( -5.153800228976328057, -19.02544592524343514, 62.29057627198100988 ) ) ;
#36060 = CARTESIAN_POINT ( 'NONE',  ( -13.97604488694527625, -13.89961937509977652, 86.87390960531436690 ) ) ;
#36061 = ADVANCED_FACE ( 'NONE', ( #70016 ), #40678, .F. ) ;
#36062 = CARTESIAN_POINT ( 'NONE',  ( 14.34966873604960469, 8.224510206698951720, 89.16557627198102409 ) ) ;
#36063 = CARTESIAN_POINT ( 'NONE',  ( -14.34966873604960291, -8.224510206698953496, 91.66557627198103830 ) ) ;
#36064 = CARTESIAN_POINT ( 'NONE',  ( 16.46253265017160672, -9.564922557960803928, 113.3322429386476955 ) ) ;
#36066 = CARTESIAN_POINT ( 'NONE',  ( 19.02544592524343514, -5.153800228976328945, 43.54057627198103120 ) ) ;
#36065 = CARTESIAN_POINT ( 'NONE',  ( 8.314922557960818139, 14.29746914071049879, 54.58224293864769550 ) ) ;
#36067 = CARTESIAN_POINT ( 'NONE',  ( 21.52544592524334988, 5.823673210054432836, 56.45942372801902565 ) ) ;
#36068 = CARTESIAN_POINT ( 'NONE',  ( 5.049401038297881783, 19.05341960407617563, 97.29275706135233293 ) ) ;
#36069 = CARTESIAN_POINT ( 'NONE',  ( 14.34966873604960469, 8.224510206698951720, 64.16557627198102409 ) ) ;
#36070 = CARTESIAN_POINT ( 'NONE',  ( -5.823673210054116645, -21.52544592524344225, 112.2905762719810241 ) ) ;
#36071 = CARTESIAN_POINT ( 'NONE',  ( -21.52544592524343514, 5.823673210054127303, 46.04057627198103830 ) ) ;
#36072 = CARTESIAN_POINT ( 'NONE',  ( 16.51473224551069308, 9.474510206698969483, 114.1655762719810241 ) ) ;
#36073 = CARTESIAN_POINT ( 'NONE',  ( -23.31738231874055600, 16.94106989632528837, 140.0500000054623513 ) ) ;
#36074 = CARTESIAN_POINT ( 'NONE',  ( -0.05219959533909027116, -19.03943276465977164, 62.49890960531435979 ) ) ;
#36075 = CARTESIAN_POINT ( 'NONE',  ( -14.34966873604960291, -8.224510206698953496, 41.66557627198103120 ) ) ;
#36076 = CARTESIAN_POINT ( 'NONE',  ( 4.483927247898790824, -16.52544592524335698, 100.2094237280190043 ) ) ;
#36077 = CARTESIAN_POINT ( 'NONE',  ( 16.55341960407618274, -4.379528057220086978, 86.04275706135236135 ) ) ;
#36078 = CARTESIAN_POINT ( 'NONE',  ( -19.05341960407617563, 5.049401038297882671, 43.54275706135232582 ) ) ;
#36079 = DIRECTION ( 'NONE',  ( 0.7071067811865512365, 0.7071067811865439090, -0.000000000000000000 ) ) ;
#36080 = CARTESIAN_POINT ( 'NONE',  ( 13.97604488694527802, 13.89961937509977652, 94.37390960531436690 ) ) ;
#36081 = CARTESIAN_POINT ( 'NONE',  ( 13.97604488694527802, 13.89961937509977652, 49.37390960531434558 ) ) ;
#36082 = CARTESIAN_POINT ( 'NONE',  ( 16.55341960407611168, 4.379528057220329451, 58.95724293864770971 ) ) ;
#36084 = CARTESIAN_POINT ( 'NONE',  ( -21.53943276465977519, 0.05219959533907696930, 21.24890960531436690 ) ) ;
#36083 = CARTESIAN_POINT ( 'NONE',  ( 16.18388926212238488, -7.379444403734519042, 102.0604684863385074 ) ) ;
#36085 = CARTESIAN_POINT ( 'NONE',  ( -5.719274019375978568, 21.55341960407610458, 35.20724293864768839 ) ) ;
#36086 = CARTESIAN_POINT ( 'NONE',  ( 8.224510206698953496, -14.34966873604960469, 87.91557627198103830 ) ) ;
#36087 = CARTESIAN_POINT ( 'NONE',  ( 12.14591786802327356, -12.06949235617739191, 40.62609039468567573 ) ) ;
#36088 = CARTESIAN_POINT ( 'NONE',  ( -16.55341960407611168, -4.379528057220339221, 81.45724293864769550 ) ) ;
#36089 = CARTESIAN_POINT ( 'NONE',  ( -19.52217212775657273, 5.500000000000114575, 64.93993709005263781 ) ) ;
#36090 = CARTESIAN_POINT ( 'NONE',  ( 19.03943276465977164, 0.05219959533936151252, 81.25109039468567573 ) ) ;
#36091 = CARTESIAN_POINT ( 'NONE',  ( -0.05219959533909027116, -19.03943276465977164, 112.4989096053143669 ) ) ;
#36092 = CARTESIAN_POINT ( 'NONE',  ( -11.40812507854754720, -35.11059874428192273, -4.724999997268812812 ) ) ;
#36093 = CARTESIAN_POINT ( 'NONE',  ( 13.89961937509978007, -13.97604488694527269, 43.12390960531435269 ) ) ;
#36095 = CARTESIAN_POINT ( 'NONE',  ( -4.379528057220086978, -16.55341960407618274, 104.7927570613523898 ) ) ;
#36094 = CARTESIAN_POINT ( 'NONE',  ( -16.55341960407617563, 4.379528057220093196, 23.54275706135235424 ) ) ;
#36096 = CARTESIAN_POINT ( 'NONE',  ( 5.049401038297881783, 19.05341960407617563, 72.29275706135234714 ) ) ;
#36097 = CARTESIAN_POINT ( 'NONE',  ( 21.52544592524344225, -5.823673210054117533, 48.54057627198103120 ) ) ;
#36098 = CARTESIAN_POINT ( 'NONE',  ( -10.72451020669870658, -18.67979575497194134, 74.58442372801901854 ) ) ;
#36099 = CARTESIAN_POINT ( 'NONE',  ( -21.61802400803983559, -13.75099706318440340, 167.9999999999999432 ) ) ;
#36100 = CARTESIAN_POINT ( 'NONE',  ( -16.55341960407617563, 4.379528057220093196, 28.54275706135234358 ) ) ;
#36102 = CARTESIAN_POINT ( 'NONE',  ( 9.564922557960805705, 16.46253265017160317, 89.58224293864769550 ) ) ;
#36101 = CARTESIAN_POINT ( 'NONE',  ( -0.05219959533909027116, -19.03943276465977164, 22.49890960531436690 ) ) ;
#36103 = CARTESIAN_POINT ( 'NONE',  ( 0.05219959533909260263, 19.03943276465977164, 24.99890960531435269 ) ) ;
#36104 = CARTESIAN_POINT ( 'NONE',  ( 8.224510206698953496, -14.34966873604960469, 92.91557627198103830 ) ) ;
#36105 = ITEM_DEFINED_TRANSFORMATION ( 'NONE', 'NONE', #127393,  #82054 ) ;
#36106 = CARTESIAN_POINT ( 'NONE',  ( -19.02544592524342804, 5.153800228976336051, 96.04057627198103830 ) ) ;
#36107 = VERTEX_POINT ( 'NONE', #56852 ) ;
#36108 = CARTESIAN_POINT ( 'NONE',  ( -0.05219959533936034679, 19.03943276465977164, 102.5010903946856757 ) ) ;
#36109 = CARTESIAN_POINT ( 'NONE',  ( -5.823673210054116645, -21.52544592524344225, 72.29057627198102409 ) ) ;
#36110 = CARTESIAN_POINT ( 'NONE',  ( 16.46253265017160672, -9.564922557960803928, 38.33224293864768839 ) ) ;
#36112 = CARTESIAN_POINT ( 'NONE',  ( -18.67979575497178146, -10.72451020669898902, 111.6655762719810525 ) ) ;
#36111 = CARTESIAN_POINT ( 'NONE',  ( -13.89961937509957401, -13.97604488694547875, 64.37609039468567573 ) ) ;
#36113 = CARTESIAN_POINT ( 'NONE',  ( -9.474510206698964154, 16.51473224551069663, 75.41557627198103830 ) ) ;
#36114 = CARTESIAN_POINT ( 'NONE',  ( 16.51473224551069308, 9.474510206698969483, 104.1655762719810241 ) ) ;
#36115 = ORIENTED_EDGE ( 'NONE', *, *, #176051, .T. ) ;
#36116 = CARTESIAN_POINT ( 'NONE',  ( 12.06949235617739724, 12.14591786802326823, 31.87609039468567929 ) ) ;
#36117 = CARTESIAN_POINT ( 'NONE',  ( -10.81492255796078084, -18.62759615963271287, 97.08224293864770971 ) ) ;
#36120 = CARTESIAN_POINT ( 'NONE',  ( 19.02544592524334988, 5.153800228976608722, 56.45942372801898301 ) ) ;
#36119 = CARTESIAN_POINT ( 'NONE',  ( 16.46253265017160672, -9.564922557960803928, 98.33224293864769550 ) ) ;
#36118 = CARTESIAN_POINT ( 'NONE',  ( -16.52544592524342804, 4.483927247898546575, 106.0405762719810525 ) ) ;
#36121 = CARTESIAN_POINT ( 'NONE',  ( -18.62759615963270932, 10.81492255796079327, 85.83224293864768129 ) ) ;
#36122 = CARTESIAN_POINT ( 'NONE',  ( 8.224510206698953496, -14.34966873604960469, 42.91557627198103120 ) ) ;
#36123 = CARTESIAN_POINT ( 'NONE',  ( 15.72974639402176855, 15.80617190586768217, 111.8760903946856615 ) ) ;
#36124 = CARTESIAN_POINT ( 'NONE',  ( -12.06949235617739369, -12.14591786802326823, 59.37609039468568284 ) ) ;
#36125 = CARTESIAN_POINT ( 'NONE',  ( 9.474510206698971260, -16.51473224551069308, 92.91557627198103830 ) ) ;
#36126 = CARTESIAN_POINT ( 'NONE',  ( -5.049401038298153566, 19.05341960407611168, 50.20724293864770260 ) ) ;
#36127 = CARTESIAN_POINT ( 'NONE',  ( 15.80617190586769283, -15.72974639402175789, 55.62609039468568284 ) ) ;
#36128 = CARTESIAN_POINT ( 'NONE',  ( -10.81492255796105439, 18.62759615963255655, 67.91775706135234714 ) ) ;
#36129 = CARTESIAN_POINT ( 'NONE',  ( -13.97604488694527625, -13.89961937509977652, 66.87390960531436690 ) ) ;
#36130 = CARTESIAN_POINT ( 'NONE',  ( 5.719274019375673035, 21.55341960407619339, 32.29275706135235424 ) ) ;
#36131 = ADVANCED_FACE ( 'NONE', ( #38683 ), #102348, .T. ) ;
#36132 = CARTESIAN_POINT ( 'NONE',  ( -16.46253265017146816, -9.564922557961047289, 69.16775706135233293 ) ) ;
#36133 = CARTESIAN_POINT ( 'NONE',  ( 0.05219959533909260263, 19.03943276465977164, 34.99890960531435979 ) ) ;
#36134 = CARTESIAN_POINT ( 'NONE',  ( 4.379528057220092307, 16.55341960407617563, 82.29275706135234714 ) ) ;
#36135 = CARTESIAN_POINT ( 'NONE',  ( 13.97604488694527802, 13.89961937509977652, 54.37390960531435979 ) ) ;
#36136 = CARTESIAN_POINT ( 'NONE',  ( -16.51473224551069308, -9.474510206698971260, 26.66557627198103120 ) ) ;
#36137 = CARTESIAN_POINT ( 'NONE',  ( -9.564922557960796823, -16.46253265017161027, 112.0822429386476955 ) ) ;
#36138 = CARTESIAN_POINT ( 'NONE',  ( -5.049401038298153566, 19.05341960407611168, 40.20724293864768839 ) ) ;
#36139 = CARTESIAN_POINT ( 'NONE',  ( 21.55341960407610458, 5.719274019375980345, 88.95724293864769550 ) ) ;
#36140 = CARTESIAN_POINT ( 'NONE',  ( 4.483927247898790824, -16.52544592524335698, 75.20942372801901854 ) ) ;
#36141 = CARTESIAN_POINT ( 'NONE',  ( -24.04614410382104595, 5.408324479811685848, 174.2944578187875209 ) ) ;
#36142 = CARTESIAN_POINT ( 'NONE',  ( -19.02544592524334988, -5.153800228976617603, 28.95942372801900433 ) ) ;
#36143 = CARTESIAN_POINT ( 'NONE',  ( 5.153800228976335163, 19.02544592524342804, 54.79057627198103120 ) ) ;
#36144 = CARTESIAN_POINT ( 'NONE',  ( -4.379528057220328563, 16.55341960407611168, 45.20724293864769550 ) ) ;
#36145 = CARTESIAN_POINT ( 'NONE',  ( 8.314922557960818139, 14.29746914071049879, 84.58224293864769550 ) ) ;
#36146 = CARTESIAN_POINT ( 'NONE',  ( 5.049401038298161559, -19.05341960407611168, 97.70724293864766707 ) ) ;
#36147 = CARTESIAN_POINT ( 'NONE',  ( 13.89961937509977652, -13.97604488694527269, 83.12390960531436690 ) ) ;
#36148 = CARTESIAN_POINT ( 'NONE',  ( -18.67979575497193778, 10.72451020669871902, 48.33442372801902565 ) ) ;
#36149 = CARTESIAN_POINT ( 'NONE',  ( -0.05219959533909027116, -19.03943276465977164, 92.49890960531436690 ) ) ;
#36150 = CARTESIAN_POINT ( 'NONE',  ( -21.53943276465977519, -0.05219959533937600094, 93.75109039468567573 ) ) ;
#36151 = CARTESIAN_POINT ( 'NONE',  ( 16.55341960407618274, -4.379528057220086978, 86.04275706135236135 ) ) ;
#36152 = CARTESIAN_POINT ( 'NONE',  ( -10.81492255796105439, 18.62759615963255655, 27.91775706135234358 ) ) ;
#36153 = CARTESIAN_POINT ( 'NONE',  ( 10.81492255796078972, 18.62759615963270932, 109.5822429386476955 ) ) ;
#36154 = CARTESIAN_POINT ( 'NONE',  ( -4.483927247898539470, -16.52544592524342804, 47.29057627198103120 ) ) ;
#36155 = CARTESIAN_POINT ( 'NONE',  ( -16.46253265017160317, 9.564922557960807481, 35.83224293864768839 ) ) ;
#36156 = CARTESIAN_POINT ( 'NONE',  ( 12.14591786802309770, 12.06949235617756955, 64.37390960531435269 ) ) ;
#36157 = CARTESIAN_POINT ( 'NONE',  ( -18.62759615963270932, 10.81492255796079327, 30.83224293864770260 ) ) ;
#36158 = CARTESIAN_POINT ( 'NONE',  ( 19.03943276465977164, 0.05219959533936151252, 36.25109039468567573 ) ) ;
#36159 = CARTESIAN_POINT ( 'NONE',  ( 0.05219959533910956823, 16.53943276465976808, 94.99890960531436690 ) ) ;
#36160 = ORIENTED_EDGE ( 'NONE', *, *, #23790, .T. ) ;
#36161 = CARTESIAN_POINT ( 'NONE',  ( 14.34966873604972726, -8.224510206698740333, 70.83442372801901854 ) ) ;
#36162 = CARTESIAN_POINT ( 'NONE',  ( 16.51473224551069308, 9.474510206698969483, 74.16557627198103830 ) ) ;
#36163 = DIRECTION ( 'NONE',  ( 0.000000000000000000, 0.000000000000000000, -1.000000000000000000 ) ) ;
#36164 = CARTESIAN_POINT ( 'NONE',  ( -18.67979575497178146, -10.72451020669898902, 41.66557627198103120 ) ) ;
#36165 = CARTESIAN_POINT ( 'NONE',  ( 8.224510206698742110, 14.34966873604972548, 97.08442372801904696 ) ) ;
#36166 = CARTESIAN_POINT ( 'NONE',  ( 13.89961937509957401, 13.97604488694547697, 111.8760903946856757 ) ) ;
#36167 = CARTESIAN_POINT ( 'NONE',  ( 15.80617190586769283, -15.72974639402175789, 85.62609039468568994 ) ) ;
#36168 = CARTESIAN_POINT ( 'NONE',  ( -0.05219959533909027116, -19.03943276465977164, 77.49890960531435269 ) ) ;
#36169 = CARTESIAN_POINT ( 'NONE',  ( -10.81492255796078084, -18.62759615963271287, 102.0822429386476955 ) ) ;
#36170 = CARTESIAN_POINT ( 'NONE',  ( 12.14591786802327356, -12.06949235617739191, 55.62609039468568284 ) ) ;
#36171 = CARTESIAN_POINT ( 'NONE',  ( 13.89961937509977652, -13.97604488694527269, 23.12390960531436335 ) ) ;
#36172 = CARTESIAN_POINT ( 'NONE',  ( -8.314922557961024197, 14.29746914071037800, 22.91775706135235069 ) ) ;
#36173 = CARTESIAN_POINT ( 'NONE',  ( -9.564922557961040184, 16.46253265017147172, 82.91775706135233293 ) ) ;
#36174 = CARTESIAN_POINT ( 'NONE',  ( -18.62759615963270932, 10.81492255796079327, 80.83224293864769550 ) ) ;
#36175 = CARTESIAN_POINT ( 'NONE',  ( 19.03943276465977164, 0.05219959533936151252, 56.25109039468566863 ) ) ;
#36176 = DIRECTION ( 'NONE',  ( -0.06104853953485701173, -7.476289853398329258E-18, -0.9981347984218670311 ) ) ;
#36177 = CARTESIAN_POINT ( 'NONE',  ( 15.72974639402199770, -15.80617190586745480, 98.12390960531436690 ) ) ;
#36178 = CARTESIAN_POINT ( 'NONE',  ( 28.82186960331498327, 2.781578969918950771E-14, 149.0000000000000000 ) ) ;
#36179 = CARTESIAN_POINT ( 'NONE',  ( -0.05219959533909027116, -19.03943276465977164, 77.49890960531435269 ) ) ;
#36180 = CARTESIAN_POINT ( 'NONE',  ( -8.314922557961024197, 14.29746914071037800, 27.91775706135234358 ) ) ;
#36181 = CARTESIAN_POINT ( 'NONE',  ( 36.81601778013476434, -3.637449627666672569, 49.14141020753752542 ) ) ;
#36183 = CARTESIAN_POINT ( 'NONE',  ( -16.52544592524342804, 4.483927247898546575, 66.04057627198103830 ) ) ;
#36182 = CARTESIAN_POINT ( 'NONE',  ( 5.719274019375991003, -21.55341960407610458, 97.70724293864772392 ) ) ;
#36184 = CARTESIAN_POINT ( 'NONE',  ( 9.564922557960805705, 16.46253265017160317, 64.58224293864769550 ) ) ;
#36185 = CARTESIAN_POINT ( 'NONE',  ( 10.72451020669871369, 18.67979575497193778, 87.08442372801901854 ) ) ;
#36187 = CARTESIAN_POINT ( 'NONE',  ( -19.03943276465977164, -0.05219959533935918106, 38.75109039468566152 ) ) ;
#36186 = CARTESIAN_POINT ( 'NONE',  ( -12.06949235617739369, -12.14591786802326823, 44.37609039468567573 ) ) ;
#36188 = CARTESIAN_POINT ( 'NONE',  ( -21.53943276465977519, -0.05219959533937600094, 58.75109039468568994 ) ) ;
#36189 = CARTESIAN_POINT ( 'NONE',  ( 21.55341960407610458, 5.719274019375980345, 53.95724293864770260 ) ) ;
#36190 = CARTESIAN_POINT ( 'NONE',  ( 16.46253265017146816, 9.564922557961045513, 111.6677570613523329 ) ) ;
#36191 = CARTESIAN_POINT ( 'NONE',  ( -19.05341960407611168, -5.049401038298163336, 51.45724293864770260 ) ) ;
#36192 = CARTESIAN_POINT ( 'NONE',  ( -19.02544592524334988, -5.153800228976617603, 68.95942372801896170 ) ) ;
#36193 = CARTESIAN_POINT ( 'NONE',  ( -10.81492255796105439, 18.62759615963255655, 87.91775706135234714 ) ) ;
#36194 = CARTESIAN_POINT ( 'NONE',  ( 16.46253265017146816, 9.564922557961045513, 71.66775706135233293 ) ) ;
#36195 = CARTESIAN_POINT ( 'NONE',  ( 9.474510206698971260, -16.51473224551069308, 32.91557627198102409 ) ) ;
#36196 = CARTESIAN_POINT ( 'NONE',  ( 21.52544592524344225, -5.823673210054117533, 63.54057627198103830 ) ) ;
#36197 = CARTESIAN_POINT ( 'NONE',  ( 12.06949235617757843, -12.14591786802309237, 68.12390960531436690 ) ) ;
#36198 = CARTESIAN_POINT ( 'NONE',  ( 21.83923006935332012, 7.858462611068595116, 172.8812894384829519 ) ) ;
#36199 = CARTESIAN_POINT ( 'NONE',  ( -5.049401038297874678, -19.05341960407617918, 34.79275706135233293 ) ) ;
#36200 = CARTESIAN_POINT ( 'NONE',  ( 14.34966873604972726, -8.224510206698740333, 85.83442372801901854 ) ) ;
#36201 = CARTESIAN_POINT ( 'NONE',  ( -16.53943276465976808, 0.05219959533911058130, 56.24890960531436690 ) ) ;
#36202 = CARTESIAN_POINT ( 'NONE',  ( 0.05219959533937995610, -21.53943276465977519, 85.00109039468568994 ) ) ;
#36203 = CARTESIAN_POINT ( 'NONE',  ( -21.55341960407619339, 5.719274019375674811, 78.54275706135236135 ) ) ;
#36204 = CARTESIAN_POINT ( 'NONE',  ( -0.05219959533907301413, -21.53943276465977519, 92.49890960531436690 ) ) ;
#36205 = CARTESIAN_POINT ( 'NONE',  ( 9.474510206698971260, -16.51473224551069308, 47.91557627198102409 ) ) ;
#36206 = CARTESIAN_POINT ( 'NONE',  ( -10.72451020669870658, -18.67979575497194134, 69.58442372801900433 ) ) ;
#36207 = CARTESIAN_POINT ( 'NONE',  ( 19.02544592524343514, -5.153800228976328945, 38.54057627198103120 ) ) ;
#36208 = ORIENTED_EDGE ( 'NONE', *, *, #79274, .F. ) ;
#36209 = CARTESIAN_POINT ( 'NONE',  ( -9.474510206698964154, 16.51473224551069663, 60.41557627198102409 ) ) ;
#36210 = CARTESIAN_POINT ( 'NONE',  ( -12.14591786802309592, -12.06949235617757132, 106.8739096053143811 ) ) ;
#36211 = CARTESIAN_POINT ( 'NONE',  ( -5.049401038298153566, 19.05341960407611168, 95.20724293864770971 ) ) ;
#36212 = CARTESIAN_POINT ( 'NONE',  ( -8.224510206698948167, 14.34966873604960824, 50.41557627198103120 ) ) ;
#36213 = CARTESIAN_POINT ( 'NONE',  ( 12.14591786802309770, 12.06949235617756955, 109.3739096053143811 ) ) ;
#36214 = CARTESIAN_POINT ( 'NONE',  ( 10.81492255796078972, 18.62759615963270932, 84.58224293864769550 ) ) ;
#36215 = CARTESIAN_POINT ( 'NONE',  ( -5.823673210054431948, 21.52544592524334988, 37.70942372801900433 ) ) ;
#36216 = CARTESIAN_POINT ( 'NONE',  ( 7.052343178074640839, -2.552343178074650609, 8.889087296526001936 ) ) ;
#36217 = CARTESIAN_POINT ( 'NONE',  ( -12.06949235617739369, -12.14591786802326823, 39.37609039468567573 ) ) ;
#36218 = CARTESIAN_POINT ( 'NONE',  ( 0.05219959533907565091, 21.53943276465977519, 89.99890960531438111 ) ) ;
#36220 = CARTESIAN_POINT ( 'NONE',  ( 15.72974639402176855, 15.80617190586768217, 101.8760903946857042 ) ) ;
#36219 = PRODUCT_DEFINITION_CONTEXT ( 'detailed design', #66005, 'design' ) ;
#36221 = CARTESIAN_POINT ( 'NONE',  ( -19.05341960407611168, -5.049401038298163336, 96.45724293864769550 ) ) ;
#36222 = CARTESIAN_POINT ( 'NONE',  ( -10.81492255796105439, 18.62759615963255655, 32.91775706135234714 ) ) ;
#36223 = ADVANCED_FACE ( 'NONE', ( #101330 ), #164037, .F. ) ;
#36224 = CARTESIAN_POINT ( 'NONE',  ( 10.72451020669898902, -18.67979575497178502, 32.91557627198102409 ) ) ;
#36225 = CARTESIAN_POINT ( 'NONE',  ( -0.05219959533934338120, 16.53943276465976808, 102.5010903946856899 ) ) ;
#36227 = CARTESIAN_POINT ( 'NONE',  ( -18.67979575497193778, 10.72451020669871902, 88.33442372801901854 ) ) ;
#36226 = CARTESIAN_POINT ( 'NONE',  ( -10.72451020669870658, -18.67979575497194134, 54.58442372801901143 ) ) ;
#36228 = CARTESIAN_POINT ( 'NONE',  ( 16.46253265017146816, 9.564922557961045513, 21.66775706135233648 ) ) ;
#36229 = CARTESIAN_POINT ( 'NONE',  ( 0.05219959533934541429, -16.53943276465976808, 75.00109039468568994 ) ) ;
#36230 = CARTESIAN_POINT ( 'NONE',  ( -18.67979575497193778, 10.72451020669871902, 38.33442372801900433 ) ) ;
#36231 = CARTESIAN_POINT ( 'NONE',  ( -19.03943276465977164, 0.05219959533909376836, 31.24890960531435979 ) ) ;
#36232 = CARTESIAN_POINT ( 'NONE',  ( 18.62759615963255655, 10.81492255796105972, 101.6677570613523613 ) ) ;
#36233 = CARTESIAN_POINT ( 'NONE',  ( 16.51473224551069308, 9.474510206698969483, 104.1655762719810241 ) ) ;
#36234 = CARTESIAN_POINT ( 'NONE',  ( 21.52544592524344225, -5.823673210054117533, 103.5405762719810383 ) ) ;
#36236 = CARTESIAN_POINT ( 'NONE',  ( 18.62759615963271287, -10.81492255796078972, 73.33224293864769550 ) ) ;
#36235 = CARTESIAN_POINT ( 'NONE',  ( -3.503282210674343311, -48.86437366581480291, -22.99999999999999645 ) ) ;
#36238 = CARTESIAN_POINT ( 'NONE',  ( 12.14591786802309770, 12.06949235617756955, 49.37390960531436690 ) ) ;
#36237 = CARTESIAN_POINT ( 'NONE',  ( -12.14591786802326823, 12.06949235617739902, 53.12609039468568284 ) ) ;
#36239 = CARTESIAN_POINT ( 'NONE',  ( 22.03292204642282925, 7.478118144893481478, 173.9941030799743089 ) ) ;
#36240 = CARTESIAN_POINT ( 'NONE',  ( -0.05219959533936034679, 19.03943276465977164, 92.50109039468566152 ) ) ;
#36241 = CARTESIAN_POINT ( 'NONE',  ( -1.491051326732881099, -15.38891197842626468, -61.89130710690760395 ) ) ;
#36242 = CARTESIAN_POINT ( 'NONE',  ( 0.05219959533934541429, -16.53943276465976808, 25.00109039468567218 ) ) ;
#36243 = CARTESIAN_POINT ( 'NONE',  ( 15.72974639402199770, -15.80617190586745480, 98.12390960531436690 ) ) ;
#36244 = CARTESIAN_POINT ( 'NONE',  ( -15.72974639402197994, 15.80617190586746368, 70.62390960531436690 ) ) ;
#36245 = CARTESIAN_POINT ( 'NONE',  ( -0.05219959533909027116, -19.03943276465977164, 107.4989096053143527 ) ) ;
#36246 = CARTESIAN_POINT ( 'NONE',  ( 4.483927247898790824, -16.52544592524335698, 50.20942372801901854 ) ) ;
#36247 = CARTESIAN_POINT ( 'NONE',  ( 5.153800228976335163, 19.02544592524342804, 64.79057627198100988 ) ) ;
#36249 = CARTESIAN_POINT ( 'NONE',  ( 9.564922557961047289, -16.46253265017146816, 100.4177570613523329 ) ) ;
#36248 = CARTESIAN_POINT ( 'NONE',  ( -21.53943276465977519, -0.05219959533937600094, 23.75109039468567929 ) ) ;
#36250 = CARTESIAN_POINT ( 'NONE',  ( 16.46253265017160672, -9.564922557960803928, 113.3322429386476955 ) ) ;
#36251 = CARTESIAN_POINT ( 'NONE',  ( -19.05341960407611168, -5.049401038298163336, 81.45724293864769550 ) ) ;
#36252 = CARTESIAN_POINT ( 'NONE',  ( 10.72451020669898902, -18.67979575497178502, 92.91557627198103830 ) ) ;
#36253 = CARTESIAN_POINT ( 'NONE',  ( -19.03943276465977164, 0.05219959533909376836, 61.24890960531436690 ) ) ;
#36254 = DIRECTION ( 'NONE',  ( 1.000000000000000000, 0.000000000000000000, 0.000000000000000000 ) ) ;
#36255 = CARTESIAN_POINT ( 'NONE',  ( -16.53943276465976808, 0.05219959533911058130, 71.24890960531435269 ) ) ;
#36256 = CARTESIAN_POINT ( 'NONE',  ( 5.049401038298161559, -19.05341960407611168, 112.7072429386476813 ) ) ;
#36257 = CARTESIAN_POINT ( 'NONE',  ( 17.62203461105334767, -16.12203461105336189, -54.55577602037946150 ) ) ;
#36258 = CARTESIAN_POINT ( 'NONE',  ( -21.55341960407610458, -5.719274019375992779, 96.45724293864770971 ) ) ;
#36259 = CARTESIAN_POINT ( 'NONE',  ( 5.049401038297881783, 19.05341960407617563, 47.29275706135231161 ) ) ;
#36260 = CARTESIAN_POINT ( 'NONE',  ( -9.564922557960796823, -16.46253265017161027, 112.0822429386476955 ) ) ;
#36261 = CARTESIAN_POINT ( 'NONE',  ( 10.74802307403555268, -10.74802307403551715, -64.92279855667830191 ) ) ;
#36262 = CARTESIAN_POINT ( 'NONE',  ( -15.80617190586745835, -15.72974639402198527, 51.87390960531437401 ) ) ;
#36263 = CARTESIAN_POINT ( 'NONE',  ( 5.049401038298161559, -19.05341960407611168, 82.70724293864770971 ) ) ;
#36264 = CARTESIAN_POINT ( 'NONE',  ( 5.823673210054444382, -21.52544592524334988, 80.20942372801901854 ) ) ;
#36265 = CARTESIAN_POINT ( 'NONE',  ( -16.51473224551069308, -9.474510206698971260, 36.66557627198102409 ) ) ;
#36266 = CARTESIAN_POINT ( 'NONE',  ( 12.14591786802309770, 12.06949235617756955, 69.37390960531436690 ) ) ;
#36267 = CARTESIAN_POINT ( 'NONE',  ( 8.224510206698742110, 14.34966873604972548, 22.08442372801901143 ) ) ;
#36268 = CARTESIAN_POINT ( 'NONE',  ( 10.72451020669871369, 18.67979575497193778, 62.08442372801901143 ) ) ;
#36269 = ORIENTED_EDGE ( 'NONE', *, *, #24747, .F. ) ;
#36270 = CARTESIAN_POINT ( 'NONE',  ( 16.46253265017146816, 9.564922557961045513, 26.66775706135234003 ) ) ;
#36271 = CARTESIAN_POINT ( 'NONE',  ( 16.46253265017146816, 9.564922557961045513, 76.66775706135234714 ) ) ;
#36272 = CARTESIAN_POINT ( 'NONE',  ( 28.45933917494778953, -27.69424206401129851, -20.18904788101062664 ) ) ;
#36273 = CARTESIAN_POINT ( 'NONE',  ( -21.53943276465977519, -0.05219959533937600094, 18.75109039468568639 ) ) ;
#36274 = CARTESIAN_POINT ( 'NONE',  ( -18.22780087662126647, -5.499999999999827693, 43.98236817873107185 ) ) ;
#36275 = CARTESIAN_POINT ( 'NONE',  ( -21.55341960407619339, 5.719274019375674811, 108.5427570613523756 ) ) ;
#36276 = CARTESIAN_POINT ( 'NONE',  ( 16.51473224551069308, 9.474510206698969483, 54.16557627198103120 ) ) ;
#36277 = CARTESIAN_POINT ( 'NONE',  ( 0.05219959533936267826, -19.03943276465977164, 35.00109039468566863 ) ) ;
#36278 = CARTESIAN_POINT ( 'NONE',  ( -8.224510206698735004, -14.34966873604973081, 109.5844237280190328 ) ) ;
#36280 = CARTESIAN_POINT ( 'NONE',  ( -0.05219959533937732626, 21.53943276465977519, 67.50109039468568994 ) ) ;
#36279 = CARTESIAN_POINT ( 'NONE',  ( -19.05341960407611168, -5.049401038298163336, 101.4572429386476955 ) ) ;
#36281 = CARTESIAN_POINT ( 'NONE',  ( 36.91746825000000598, -11.99521256947793546, -3.724999997268812812 ) ) ;
#36282 = CARTESIAN_POINT ( 'NONE',  ( -33.70615967800006985, 5.466638699193796747, 95.70352821367444562 ) ) ;
#36283 = CARTESIAN_POINT ( 'NONE',  ( 15.72974639402176855, 15.80617190586768217, 81.87609039468568994 ) ) ;
#36284 = CARTESIAN_POINT ( 'NONE',  ( -5.719274019375665041, -21.55341960407619695, 104.7927570613523898 ) ) ;
#36285 = FACE_OUTER_BOUND ( 'NONE', #152991, .T. ) ;
#36286 = CARTESIAN_POINT ( 'NONE',  ( 13.89961937509977652, -13.97604488694527269, 103.1239096053143527 ) ) ;
#36287 = CARTESIAN_POINT ( 'NONE',  ( 5.153800228976615827, -19.02544592524334988, 25.20942372801900433 ) ) ;
#36288 = CARTESIAN_POINT ( 'NONE',  ( 15.50000000000000178, 5.499999999999998224, 118.0000000000000142 ) ) ;
#36289 = CARTESIAN_POINT ( 'NONE',  ( -5.153800228976328057, -19.02544592524343514, 42.29057627198101699 ) ) ;
#36290 = CARTESIAN_POINT ( 'NONE',  ( -21.52544592524343514, 5.823673210054127303, 56.04057627198102409 ) ) ;
#36291 = CARTESIAN_POINT ( 'NONE',  ( 8.314922557960818139, 14.29746914071049879, 24.58224293864768839 ) ) ;
#36293 = CARTESIAN_POINT ( 'NONE',  ( -9.564922557960796823, -16.46253265017161027, 82.08224293864768129 ) ) ;
#36292 = CARTESIAN_POINT ( 'NONE',  ( -12.06949235617756955, 12.14591786802309770, 90.62390960531436690 ) ) ;
#36294 = CARTESIAN_POINT ( 'NONE',  ( -21.52544592524334988, -5.823673210054445271, 108.9594237280190185 ) ) ;
#36295 = EDGE_CURVE ( 'NONE', #129907, #49283, #46983, .T. ) ;
#36296 = CARTESIAN_POINT ( 'NONE',  ( -19.02544592524342804, 5.153800228976336051, 41.04057627198103120 ) ) ;
#36297 = CARTESIAN_POINT ( 'NONE',  ( -12.06949235617756955, 12.14591786802309770, 105.6239096053143669 ) ) ;
#36298 = CARTESIAN_POINT ( 'NONE',  ( -21.55341960407619339, 5.719274019375674811, 58.54275706135235424 ) ) ;
#36299 = CARTESIAN_POINT ( 'NONE',  ( 21.52544592524344225, -5.823673210054117533, 93.54057627198103830 ) ) ;
#36300 = CARTESIAN_POINT ( 'NONE',  ( -13.97604488694547697, 13.89961937509957934, 53.12609039468565442 ) ) ;
#36301 = CARTESIAN_POINT ( 'NONE',  ( -20.27679576775602754, -20.59397618482648440, -49.67367017693150189 ) ) ;
#36302 = CARTESIAN_POINT ( 'NONE',  ( 5.153800228976335163, 19.02544592524342804, 109.7905762719810099 ) ) ;
#36303 = CARTESIAN_POINT ( 'NONE',  ( 4.379528057220339221, -16.55341960407611168, 72.70724293864769550 ) ) ;
#36304 = CARTESIAN_POINT ( 'NONE',  ( -16.51473224551082808, 9.474510206698731452, 43.33442372801900433 ) ) ;
#36305 = CARTESIAN_POINT ( 'NONE',  ( 9.474510206698971260, -16.51473224551069308, 62.91557627198102409 ) ) ;
#36306 = CARTESIAN_POINT ( 'NONE',  ( -14.34966873604960291, -8.224510206698953496, 51.66557627198102409 ) ) ;
#36307 = CARTESIAN_POINT ( 'NONE',  ( 5.049401038297881783, 19.05341960407617563, 77.29275706135231871 ) ) ;
#36308 = CARTESIAN_POINT ( 'NONE',  ( 17.71576930673726835, -5.499999999999973355, 101.0825735056735368 ) ) ;
#36309 = CARTESIAN_POINT ( 'NONE',  ( 15.72974639402199770, -15.80617190586745480, 38.12390960531436690 ) ) ;
#36310 = EDGE_CURVE ( 'NONE', #116832, #52906, #117243, .T. ) ;
#36311 = CARTESIAN_POINT ( 'NONE',  ( 4.483927247898545687, 16.52544592524342804, 94.79057627198105251 ) ) ;
#36312 = DIRECTION ( 'NONE',  ( -1.000000000000000000, 0.000000000000000000, -0.000000000000000000 ) ) ;
#36314 = CARTESIAN_POINT ( 'NONE',  ( 5.719274019375991003, -21.55341960407610458, 62.70724293864769550 ) ) ;
#36313 = CARTESIAN_POINT ( 'NONE',  ( -19.02544592524342804, 5.153800228976336051, 61.04057627198103120 ) ) ;
#36315 = CARTESIAN_POINT ( 'NONE',  ( 16.46253265017160672, -9.564922557960803928, 33.33224293864770260 ) ) ;
#36317 = CARTESIAN_POINT ( 'NONE',  ( 16.46253265017160672, -9.564922557960803928, 58.33224293864769550 ) ) ;
#36316 = CARTESIAN_POINT ( 'NONE',  ( -16.52544592524335698, -4.483927247898792601, 73.95942372801901854 ) ) ;
#36318 = CARTESIAN_POINT ( 'NONE',  ( -19.03943276465977164, -0.05219959533935918106, 48.75109039468566863 ) ) ;
#36319 = CARTESIAN_POINT ( 'NONE',  ( -10.72451020669870658, -18.67979575497194134, 74.58442372801901854 ) ) ;
#36320 = CARTESIAN_POINT ( 'NONE',  ( 21.52544592524344225, -5.823673210054117533, 43.54057627198103830 ) ) ;
#36321 = CARTESIAN_POINT ( 'NONE',  ( 5.049401038298161559, -19.05341960407611168, 27.70724293864769550 ) ) ;
#36322 = CARTESIAN_POINT ( 'NONE',  ( -0.05219959533934338120, 16.53943276465976808, 87.50109039468568994 ) ) ;
#36323 = CARTESIAN_POINT ( 'NONE',  ( 9.564922557961047289, -16.46253265017146816, 100.4177570613523329 ) ) ;
#36324 = DIRECTION ( 'NONE',  ( 0.000000000000000000, 0.000000000000000000, 1.000000000000000000 ) ) ;
#36326 = CARTESIAN_POINT ( 'NONE',  ( -21.53943276465977519, 0.05219959533907696930, 61.24890960531435979 ) ) ;
#36325 = CARTESIAN_POINT ( 'NONE',  ( 19.39720447994795904, 5.499999999999970690, 77.16317477297180005 ) ) ;
#36327 = CARTESIAN_POINT ( 'NONE',  ( 18.67979575497194134, -10.72451020669871369, 95.83442372801903275 ) ) ;
#36328 = ORIENTED_EDGE ( 'NONE', *, *, #72845, .F. ) ;
#36329 = CARTESIAN_POINT ( 'NONE',  ( -12.06949235617756955, 12.14591786802309770, 50.62390960531435979 ) ) ;
#36330 = CARTESIAN_POINT ( 'NONE',  ( -12.06949235617756955, 12.14591786802309770, 60.62390960531437401 ) ) ;
#36331 = CARTESIAN_POINT ( 'NONE',  ( 5.823673210054125526, 21.52544592524343514, 79.79057627198102409 ) ) ;
#36332 = CARTESIAN_POINT ( 'NONE',  ( -5.719274019375978568, 21.55341960407610458, 85.20724293864770971 ) ) ;
#36333 = CARTESIAN_POINT ( 'NONE',  ( 17.50000000000000000, -5.499999999999992895, 76.21769037696435589 ) ) ;
#36334 = CARTESIAN_POINT ( 'NONE',  ( -21.52544592524343514, 5.823673210054127303, 31.04057627198102409 ) ) ;
#36335 = CARTESIAN_POINT ( 'NONE',  ( -12.14591786802326823, 12.06949235617739902, 68.12609039468567573 ) ) ;
#36336 = CARTESIAN_POINT ( 'NONE',  ( 16.55341960407611168, 4.379528057220329451, 73.95724293864769550 ) ) ;
#36337 = CARTESIAN_POINT ( 'NONE',  ( 16.46253265017160672, -9.564922557960803928, 48.33224293864769550 ) ) ;
#36338 = CARTESIAN_POINT ( 'NONE',  ( 34.64437015671236963, -3.766696895669991552, 51.50405731776599083 ) ) ;
#36339 = VERTEX_POINT ( 'NONE', #12353 ) ;
#36340 = CARTESIAN_POINT ( 'NONE',  ( 4.379528057220092307, 16.55341960407617563, 92.29275706135236135 ) ) ;
#36341 = CARTESIAN_POINT ( 'NONE',  ( 18.67979575497194134, -10.72451020669871369, 25.83442372801901499 ) ) ;
#36342 = CARTESIAN_POINT ( 'NONE',  ( 9.474510206698971260, -16.51473224551069308, 77.91557627198103830 ) ) ;
#36343 = CARTESIAN_POINT ( 'NONE',  ( -15.80617190586768217, 15.72974639402176855, 48.12609039468568284 ) ) ;
#36344 = CARTESIAN_POINT ( 'NONE',  ( -0.05219959533909027116, -19.03943276465977164, 107.4989096053143527 ) ) ;
#36345 = CARTESIAN_POINT ( 'NONE',  ( -22.02428569922414781, -33.37003842005439935, -23.53509012974684111 ) ) ;
#36346 = VERTEX_POINT ( 'NONE', #193366 ) ;
#36347 = CARTESIAN_POINT ( 'NONE',  ( 18.62759615963255655, 10.81492255796105972, 51.66775706135234714 ) ) ;
#36349 = CARTESIAN_POINT ( 'NONE',  ( -19.05341960407611168, -5.049401038298163336, 106.4572429386476955 ) ) ;
#36348 = CARTESIAN_POINT ( 'NONE',  ( -5.153800228976328057, -19.02544592524343514, 42.29057627198101699 ) ) ;
#36350 = CARTESIAN_POINT ( 'NONE',  ( 9.564922557961047289, -16.46253265017146816, 55.41775706135234003 ) ) ;
#36351 = CARTESIAN_POINT ( 'NONE',  ( 5.823673210054444382, -21.52544592524334988, 35.20942372801901854 ) ) ;
#36352 = CARTESIAN_POINT ( 'NONE',  ( -19.02544592524334988, -5.153800228976617603, 58.95942372801900433 ) ) ;
#36353 = CARTESIAN_POINT ( 'NONE',  ( -19.03943276465977164, 0.05219959533909376836, 21.24890960531436335 ) ) ;
#36354 = CARTESIAN_POINT ( 'NONE',  ( -16.55341960407617563, 4.379528057220093196, 93.54275706135234714 ) ) ;
#36355 = CARTESIAN_POINT ( 'NONE',  ( 13.89961937509957401, 13.97604488694547697, 66.87609039468567573 ) ) ;
#36356 = CARTESIAN_POINT ( 'NONE',  ( 8.314922557961029526, -14.29746914071037800, 110.4177570613523756 ) ) ;
#36357 = CARTESIAN_POINT ( 'NONE',  ( 18.22780087662122739, 5.500000000000000888, 86.48236817873107896 ) ) ;
#36358 = CARTESIAN_POINT ( 'NONE',  ( 5.049401038298161559, -19.05341960407611168, 87.70724293864769550 ) ) ;
#36359 = CARTESIAN_POINT ( 'NONE',  ( 18.62759615963255655, 10.81492255796105972, 86.66775706135234714 ) ) ;
#36360 = CARTESIAN_POINT ( 'NONE',  ( 5.823673210054444382, -21.52544592524334988, 110.2094237280190185 ) ) ;
#36361 = CARTESIAN_POINT ( 'NONE',  ( -11.74149087413295511, 36.13659316521247433, -4.402157773949823216 ) ) ;
#36362 = CARTESIAN_POINT ( 'NONE',  ( -19.03943276465977164, 0.05219959533909376836, 101.2489096053143669 ) ) ;
#36363 = CARTESIAN_POINT ( 'NONE',  ( 10.81492255796106328, -18.62759615963255655, 70.41775706135236135 ) ) ;
#36364 = CARTESIAN_POINT ( 'NONE',  ( -4.379528057220086978, -16.55341960407618274, 19.79275706135235069 ) ) ;
#36365 = CARTESIAN_POINT ( 'NONE',  ( -19.02544592524342804, 5.153800228976336051, 86.04057627198103830 ) ) ;
#36366 = CARTESIAN_POINT ( 'NONE',  ( -5.823673210054116645, -21.52544592524344225, 32.29057627198102409 ) ) ;
#36367 = CARTESIAN_POINT ( 'NONE',  ( 13.97604488694527802, 13.89961937509977652, 99.37390960531436690 ) ) ;
#36368 = LINE ( 'NONE', #33405, #111259 ) ;
#36369 = CARTESIAN_POINT ( 'NONE',  ( -5.049401038298153566, 19.05341960407611168, 65.20724293864765286 ) ) ;
#36370 = CARTESIAN_POINT ( 'NONE',  ( -16.53943276465976808, -0.05219959533934237506, 113.7510903946856757 ) ) ;
#36371 = CARTESIAN_POINT ( 'NONE',  ( -19.49671883438228903, -5.499999999999981348, 39.89279849105682985 ) ) ;
#36372 = CARTESIAN_POINT ( 'NONE',  ( -19.03943276465977164, -0.05219959533935918106, 73.75109039468566152 ) ) ;
#36373 = CARTESIAN_POINT ( 'NONE',  ( 19.03943276465977164, -0.05219959533909143690, 93.74890960531435269 ) ) ;
#36374 = CARTESIAN_POINT ( 'NONE',  ( -14.29746914071049879, 8.314922557960819915, 85.83224293864768129 ) ) ;
#36375 = CARTESIAN_POINT ( 'NONE',  ( 15.72974639402199770, -15.80617190586745480, 43.12390960531435269 ) ) ;
#36376 = CARTESIAN_POINT ( 'NONE',  ( 15.80617190586746368, 15.72974639402197994, 24.37390960531435979 ) ) ;
#36377 = CARTESIAN_POINT ( 'NONE',  ( -8.314922557960811034, -14.29746914071050412, 107.0822429386476955 ) ) ;
#36378 = CARTESIAN_POINT ( 'NONE',  ( -17.05116617787826883, 6.768360034955680504, 53.65675553259199404 ) ) ;
#36379 = CARTESIAN_POINT ( 'NONE',  ( 5.153800228976615827, -19.02544592524334988, 50.20942372801897591 ) ) ;
#36380 = CARTESIAN_POINT ( 'NONE',  ( -16.55341960407611168, -4.379528057220339221, 31.45724293864769550 ) ) ;
#36381 = CARTESIAN_POINT ( 'NONE',  ( 13.89961937509977652, -13.97604488694527269, 108.1239096053143669 ) ) ;
#36382 = CARTESIAN_POINT ( 'NONE',  ( -10.81492255796105439, 18.62759615963255655, 62.91775706135236135 ) ) ;
#36383 = CARTESIAN_POINT ( 'NONE',  ( 5.823673210054125526, 21.52544592524343514, 59.79057627198103120 ) ) ;
#36384 = CARTESIAN_POINT ( 'NONE',  ( 18.62759615963255655, 10.81492255796105972, 41.66775706135235424 ) ) ;
#36385 = CARTESIAN_POINT ( 'NONE',  ( -5.823673210054116645, -21.52544592524344225, 102.2905762719810383 ) ) ;
#36386 = CARTESIAN_POINT ( 'NONE',  ( 5.719274019375673035, 21.55341960407619339, 37.29275706135235424 ) ) ;
#36387 = CARTESIAN_POINT ( 'NONE',  ( 12.06949235617757843, -12.14591786802309237, 103.1239096053143811 ) ) ;
#36388 = CARTESIAN_POINT ( 'NONE',  ( 19.05341960407617918, -5.049401038297876454, 66.04275706135233293 ) ) ;
#36389 = CARTESIAN_POINT ( 'NONE',  ( -19.05341960407611168, -5.049401038298163336, 41.45724293864769550 ) ) ;
#36390 = CARTESIAN_POINT ( 'NONE',  ( 16.53943276465976808, -0.05219959533910856209, 103.7489096053143669 ) ) ;
#36391 = CARTESIAN_POINT ( 'NONE',  ( -16.46253265017160317, 9.564922557960807481, 105.8322429386476955 ) ) ;
#36392 = CARTESIAN_POINT ( 'NONE',  ( 14.34966873604960469, 8.224510206698951720, 39.16557627198102409 ) ) ;
#36393 = CARTESIAN_POINT ( 'NONE',  ( -12.14591786802326823, 12.06949235617739902, 113.1260903946856899 ) ) ;
#36394 = CARTESIAN_POINT ( 'NONE',  ( -0.05219959533909027116, -19.03943276465977164, 52.49890960531436690 ) ) ;
#36395 = CARTESIAN_POINT ( 'NONE',  ( 19.05341960407611168, 5.049401038298154454, 23.95724293864769194 ) ) ;
#36396 = CARTESIAN_POINT ( 'NONE',  ( -21.53943276465977519, -0.05219959533937600094, 113.7510903946856757 ) ) ;
#36398 = CARTESIAN_POINT ( 'NONE',  ( -16.55341960407611168, -4.379528057220339221, 41.45724293864769550 ) ) ;
#36397 = CARTESIAN_POINT ( 'NONE',  ( 17.72560187377285601, 5.500000000000048850, 51.57814504131321343 ) ) ;
#36399 = CARTESIAN_POINT ( 'NONE',  ( -0.05219959533937732626, 21.53943276465977519, 42.50109039468567573 ) ) ;
#36400 = CARTESIAN_POINT ( 'NONE',  ( -19.38985940809734032, -32.68077955211932561, -25.00000000000009592 ) ) ;
#36401 = CARTESIAN_POINT ( 'NONE',  ( 12.06949235617739724, 12.14591786802326823, 56.87609039468568994 ) ) ;
#36402 = CARTESIAN_POINT ( 'NONE',  ( -14.29746914071049879, 8.314922557960819915, 25.83224293864769194 ) ) ;
#36403 = CARTESIAN_POINT ( 'NONE',  ( 8.224510206698742110, 14.34966873604972548, 102.0844237280190185 ) ) ;
#36404 = CARTESIAN_POINT ( 'NONE',  ( -12.06949235617739369, -12.14591786802326823, 29.37609039468568284 ) ) ;
#36405 = CARTESIAN_POINT ( 'NONE',  ( 9.564922557960805705, 16.46253265017160317, 49.58224293864770260 ) ) ;
#36406 = CARTESIAN_POINT ( 'NONE',  ( -0.05219959533909027116, -19.03943276465977164, 27.49890960531435624 ) ) ;
#36407 = CARTESIAN_POINT ( 'NONE',  ( -5.823673210054431948, 21.52544592524334988, 22.70942372801901499 ) ) ;
#36408 = CARTESIAN_POINT ( 'NONE',  ( -9.564922557960796823, -16.46253265017161027, 42.08224293864769550 ) ) ;
#36409 = CARTESIAN_POINT ( 'NONE',  ( -4.287918369368176386, -6.449379854004495982, -62.20361152659754111 ) ) ;
#36410 = CARTESIAN_POINT ( 'NONE',  ( -19.03943276465977164, 0.05219959533909376836, 36.24890960531436690 ) ) ;
#36411 = ADVANCED_FACE ( 'NONE', ( #163018 ), #88167, .T. ) ;
#36412 = CARTESIAN_POINT ( 'NONE',  ( -15.72974639402197994, 15.80617190586746368, 25.62390960531435624 ) ) ;
#36413 = CARTESIAN_POINT ( 'NONE',  ( 37.99999999999999289, 2.428612866367529932E-14, -25.00000000000000000 ) ) ;
#36415 = CARTESIAN_POINT ( 'NONE',  ( -16.52544592524342804, 4.483927247898546575, 106.0405762719810525 ) ) ;
#36414 = CARTESIAN_POINT ( 'NONE',  ( -5.719274019375665041, -21.55341960407619695, 44.79275706135234714 ) ) ;
#36416 = CARTESIAN_POINT ( 'NONE',  ( -19.05341960407611168, -5.049401038298163336, 106.4572429386476955 ) ) ;
#36417 = CARTESIAN_POINT ( 'NONE',  ( 14.29746914071037800, 8.314922557961029526, 81.66775706135236135 ) ) ;
#36418 = CARTESIAN_POINT ( 'NONE',  ( 5.719274019375673035, 21.55341960407619339, 97.29275706135234714 ) ) ;
#36419 = CARTESIAN_POINT ( 'NONE',  ( -4.379528057220086978, -16.55341960407618274, 59.79275706135234714 ) ) ;
#36420 = CARTESIAN_POINT ( 'NONE',  ( 13.97604488694527802, 13.89961937509977652, 99.37390960531436690 ) ) ;
#36421 = ADVANCED_FACE ( 'NONE', ( #147866 ), #150859, .T. ) ;
#36422 = CARTESIAN_POINT ( 'NONE',  ( 8.314922557961029526, -14.29746914071037800, 45.41775706135234003 ) ) ;
#36423 = CARTESIAN_POINT ( 'NONE',  ( -16.52544592524335698, -4.483927247898792601, 28.95942372801902209 ) ) ;
#36424 = CARTESIAN_POINT ( 'NONE',  ( -4.483927247898782831, 16.52544592524335698, 87.70942372801901854 ) ) ;
#36425 = CARTESIAN_POINT ( 'NONE',  ( -19.03943276465977164, -0.05219959533935918106, 103.7510903946856757 ) ) ;
#36426 = CARTESIAN_POINT ( 'NONE',  ( 13.97604488694527802, 13.89961937509977652, 74.37390960531436690 ) ) ;
#36427 = CARTESIAN_POINT ( 'NONE',  ( 15.72974639402199770, -15.80617190586745480, 93.12390960531436690 ) ) ;
#36429 = CARTESIAN_POINT ( 'NONE',  ( 13.89961937509957401, 13.97604488694547697, 101.8760903946856331 ) ) ;
#36428 = CARTESIAN_POINT ( 'NONE',  ( 8.314922557960818139, 14.29746914071049879, 99.58224293864770971 ) ) ;
#36430 = CARTESIAN_POINT ( 'NONE',  ( 14.29746914071037800, 8.314922557961029526, 76.66775706135234714 ) ) ;
#36431 = CARTESIAN_POINT ( 'NONE',  ( -16.79531203550683216, 7.028104445595353411, 43.74755011779542002 ) ) ;
#36432 = CARTESIAN_POINT ( 'NONE',  ( -0.05219959533936034679, 19.03943276465977164, 72.50109039468566152 ) ) ;
#36433 = CARTESIAN_POINT ( 'NONE',  ( 16.53943276465976808, -0.05219959533910856209, 43.74890960531435979 ) ) ;
#36434 = CARTESIAN_POINT ( 'NONE',  ( -12.14591786802309592, -12.06949235617757132, 96.87390960531436690 ) ) ;
#36436 = CARTESIAN_POINT ( 'NONE',  ( -16.62475595723701005, 7.163666690055240593, 90.52713351810474762 ) ) ;
#36435 = CARTESIAN_POINT ( 'NONE',  ( 13.97604488694548053, -13.89961937509957401, 40.62609039468564731 ) ) ;
#36437 = CARTESIAN_POINT ( 'NONE',  ( -10.81492255796105439, 18.62759615963255655, 42.91775706135235424 ) ) ;
#36438 = CARTESIAN_POINT ( 'NONE',  ( 9.474510206698729675, 16.51473224551082808, 102.0844237280190043 ) ) ;
#36439 = CARTESIAN_POINT ( 'NONE',  ( 19.05341960407611168, 5.049401038298154454, 113.9572429386477097 ) ) ;
#36440 = CARTESIAN_POINT ( 'NONE',  ( 9.564922557960805705, 16.46253265017160317, 89.58224293864769550 ) ) ;
#36441 = CARTESIAN_POINT ( 'NONE',  ( -18.67979575497193778, 10.72451020669871902, 108.3344237280190185 ) ) ;
#36442 = CARTESIAN_POINT ( 'NONE',  ( -19.02544592524342804, 5.153800228976336051, 91.04057627198100988 ) ) ;
#36443 = CARTESIAN_POINT ( 'NONE',  ( 10.81492255796078972, 18.62759615963270932, 39.58224293864769550 ) ) ;
#36444 = CARTESIAN_POINT ( 'NONE',  ( 8.224510206698953496, -14.34966873604960469, 92.91557627198103830 ) ) ;
#36445 = CARTESIAN_POINT ( 'NONE',  ( 13.89961937509977652, -13.97604488694527269, 58.12390960531436690 ) ) ;
#36446 = CARTESIAN_POINT ( 'NONE',  ( 12.14591786802309770, 12.06949235617756955, 109.3739096053143811 ) ) ;
#36447 = CARTESIAN_POINT ( 'NONE',  ( -18.62759615963255300, -10.81492255796106328, 24.16775706135235424 ) ) ;
#36448 = CARTESIAN_POINT ( 'NONE',  ( 0.05219959533937995610, -21.53943276465977519, 75.00109039468568994 ) ) ;
#36449 = CARTESIAN_POINT ( 'NONE',  ( 0.05219959533909260263, 19.03943276465977164, 39.99890960531436690 ) ) ;
#36450 = CARTESIAN_POINT ( 'NONE',  ( -12.14591786802326823, 12.06949235617739902, 73.12609039468567573 ) ) ;
#36451 = CARTESIAN_POINT ( 'NONE',  ( -18.67979575497178146, -10.72451020669898902, 111.6655762719810525 ) ) ;
#36452 = CARTESIAN_POINT ( 'NONE',  ( -21.53943276465977519, -0.05219959533937600094, 23.75109039468567929 ) ) ;
#36454 = CARTESIAN_POINT ( 'NONE',  ( -16.46253265017160317, 9.564922557960807481, 70.83224293864770971 ) ) ;
#36453 = CARTESIAN_POINT ( 'NONE',  ( -13.89961937509957401, -13.97604488694547875, 59.37609039468566863 ) ) ;
#36455 = CARTESIAN_POINT ( 'NONE',  ( -13.97604488694547697, 13.89961937509957934, 33.12609039468566863 ) ) ;
#36456 = CARTESIAN_POINT ( 'NONE',  ( 21.55341960407619695, -5.719274019375665929, 66.04275706135236135 ) ) ;
#36457 = ADVANCED_FACE ( 'NONE', ( #9352 ), #29280, .T. ) ;
#36458 = CARTESIAN_POINT ( 'NONE',  ( -0.05219959533907301413, -21.53943276465977519, 67.49890960531436690 ) ) ;
#36459 = CARTESIAN_POINT ( 'NONE',  ( 16.53943276465976808, -0.05219959533910856209, 48.74890960531435979 ) ) ;
#36461 = CARTESIAN_POINT ( 'NONE',  ( -5.153800228976607833, 19.02544592524334988, 22.70942372801899012 ) ) ;
#36460 = CARTESIAN_POINT ( 'NONE',  ( -18.62759615963255300, -10.81492255796106328, 94.16775706135237556 ) ) ;
#36462 = CARTESIAN_POINT ( 'NONE',  ( -12.06949235617756955, 12.14591786802309770, 70.62390960531436690 ) ) ;
#36463 = CARTESIAN_POINT ( 'NONE',  ( 13.97604488694527802, 13.89961937509977652, 24.37390960531435624 ) ) ;
#36464 = CARTESIAN_POINT ( 'NONE',  ( -19.02544592524334988, -5.153800228976617603, 63.95942372801899012 ) ) ;
#36465 = CARTESIAN_POINT ( 'NONE',  ( 0.05219959533910956823, 16.53943276465976808, 24.99890960531435624 ) ) ;
#36466 = CARTESIAN_POINT ( 'NONE',  ( 21.55341960407619695, -5.719274019375665929, 81.04275706135236135 ) ) ;
#36467 = CARTESIAN_POINT ( 'NONE',  ( -19.05341960407611168, -5.049401038298163336, 76.45724293864769550 ) ) ;
#36468 = CARTESIAN_POINT ( 'NONE',  ( -9.474510206698720793, -16.51473224551083518, 49.58442372801899722 ) ) ;
#36469 = CARTESIAN_POINT ( 'NONE',  ( -10.72451020669898014, 18.67979575497178502, 45.41557627198103830 ) ) ;
#36470 = CARTESIAN_POINT ( 'NONE',  ( -10.81492255796105439, 18.62759615963255655, 42.91775706135235424 ) ) ;
#36471 = CARTESIAN_POINT ( 'NONE',  ( 15.80617190586746368, 15.72974639402197994, 99.37390960531436690 ) ) ;
#36472 = CARTESIAN_POINT ( 'NONE',  ( -9.474510206698720793, -16.51473224551083518, 99.58442372801900433 ) ) ;
#36473 = CARTESIAN_POINT ( 'NONE',  ( 8.314922557961029526, -14.29746914071037800, 70.41775706135236135 ) ) ;
#36475 = CARTESIAN_POINT ( 'NONE',  ( 21.52544592524344225, -5.823673210054117533, 113.5405762719810383 ) ) ;
#36474 = CARTESIAN_POINT ( 'NONE',  ( -17.06285122369598284, -17.30253834197026919, -56.77278709839600879 ) ) ;
#36476 = CARTESIAN_POINT ( 'NONE',  ( 12.14591786802309770, 12.06949235617756955, 84.37390960531438111 ) ) ;
#36477 = CARTESIAN_POINT ( 'NONE',  ( -17.31728774477272736, -6.344390552232389346, 99.18093348310682700 ) ) ;
#36478 = CARTESIAN_POINT ( 'NONE',  ( -8.224510206698735004, -14.34966873604973081, 29.58442372801901854 ) ) ;
#36479 = APPLICATION_CONTEXT ( 'automotive_design' ) ;
#36480 = CARTESIAN_POINT ( 'NONE',  ( 18.62759615963271287, -10.81492255796078972, 58.33224293864768839 ) ) ;
#36481 = CARTESIAN_POINT ( 'NONE',  ( -4.379528057220086978, -16.55341960407618274, 89.79275706135236135 ) ) ;
#36482 = CARTESIAN_POINT ( 'NONE',  ( -16.51473224551069308, -9.474510206698971260, 26.66557627198103120 ) ) ;
#36483 = CARTESIAN_POINT ( 'NONE',  ( 16.52544592524335698, 4.483927247898782831, 71.45942372801901854 ) ) ;
#36484 = CARTESIAN_POINT ( 'NONE',  ( 10.72451020669871369, 18.67979575497193778, 42.08442372801901854 ) ) ;
#36485 = CARTESIAN_POINT ( 'NONE',  ( 10.72451020669898902, -18.67979575497178502, 62.91557627198102409 ) ) ;
#36486 = CARTESIAN_POINT ( 'NONE',  ( 8.314922557961029526, -14.29746914071037800, 90.41775706135236135 ) ) ;
#36487 = CARTESIAN_POINT ( 'NONE',  ( 18.67979575497194134, -10.72451020669871369, 65.83442372801900433 ) ) ;
#36488 = CARTESIAN_POINT ( 'NONE',  ( -5.823673210054116645, -21.52544592524344225, 52.29057627198102409 ) ) ;
#36489 = CARTESIAN_POINT ( 'NONE',  ( 21.52544592524344225, -5.823673210054117533, 38.54057627198103120 ) ) ;
#36490 = EDGE_LOOP ( 'NONE', ( #115957, #52747, #47800, #119586 ) ) ;
#36491 = ORIENTED_EDGE ( 'NONE', *, *, #122650, .F. ) ;
#36492 = CARTESIAN_POINT ( 'NONE',  ( -4.483927247898782831, 16.52544592524335698, 62.70942372801902565 ) ) ;
#36493 = CARTESIAN_POINT ( 'NONE',  ( -21.53943276465977519, 0.05219959533907696930, 26.24890960531435624 ) ) ;
#36494 = ORIENTED_EDGE ( 'NONE', *, *, #163970, .F. ) ;
#36495 = CARTESIAN_POINT ( 'NONE',  ( -5.049401038298153566, 19.05341960407611168, 100.2072429386476955 ) ) ;
#36496 = CARTESIAN_POINT ( 'NONE',  ( -4.379528057220328563, 16.55341960407611168, 25.20724293864769550 ) ) ;
#36497 = CARTESIAN_POINT ( 'NONE',  ( -17.60691670004652210, -5.499999999999993783, 79.13333313366442212 ) ) ;
#36498 = CARTESIAN_POINT ( 'NONE',  ( 16.52544592524342804, -4.483927247898539470, 113.5405762719810383 ) ) ;
#36499 = CARTESIAN_POINT ( 'NONE',  ( 21.52544592524344225, -5.823673210054117533, 58.54057627198103120 ) ) ;
#36500 = CARTESIAN_POINT ( 'NONE',  ( -0.05219959533909027116, -19.03943276465977164, 47.49890960531435979 ) ) ;
#36501 = CARTESIAN_POINT ( 'NONE',  ( 12.06949235617739724, 12.14591786802326823, 91.87609039468568994 ) ) ;
#36502 = CARTESIAN_POINT ( 'NONE',  ( 0.05219959533937995610, -21.53943276465977519, 30.00109039468568284 ) ) ;
#36503 = CARTESIAN_POINT ( 'NONE',  ( 19.02544592524334988, 5.153800228976608722, 106.4594237280190185 ) ) ;
#36504 = CARTESIAN_POINT ( 'NONE',  ( 16.53943276465976808, -0.05219959533910856209, 103.7489096053143669 ) ) ;
#36505 = CARTESIAN_POINT ( 'NONE',  ( -16.46253265017160317, 9.564922557960807481, 50.83224293864770260 ) ) ;
#36506 = CARTESIAN_POINT ( 'NONE',  ( -16.46253265017160317, 9.564922557960807481, 25.83224293864769194 ) ) ;
#36507 = CARTESIAN_POINT ( 'NONE',  ( 17.60728821186571835, -5.499999999999883649, 63.36690927743005375 ) ) ;
#36508 = CARTESIAN_POINT ( 'NONE',  ( 0.05219959533909260263, 19.03943276465977164, 94.99890960531436690 ) ) ;
#36509 = CARTESIAN_POINT ( 'NONE',  ( 14.34966873604972726, -8.224510206698740333, 70.83442372801901854 ) ) ;
#36510 = CARTESIAN_POINT ( 'NONE',  ( -5.823673210054431948, 21.52544592524334988, 112.7094237280190328 ) ) ;
#36511 = CARTESIAN_POINT ( 'NONE',  ( -0.05219959533907301413, -21.53943276465977519, 52.49890960531435979 ) ) ;
#36512 = CARTESIAN_POINT ( 'NONE',  ( -16.55341960407617563, 4.379528057220093196, 78.54275706135236135 ) ) ;
#36513 = CARTESIAN_POINT ( 'NONE',  ( 0.05219959533936267826, -19.03943276465977164, 70.00109039468566152 ) ) ;
#36514 = CARTESIAN_POINT ( 'NONE',  ( 5.049401038298161559, -19.05341960407611168, 32.70724293864768129 ) ) ;
#36515 = CARTESIAN_POINT ( 'NONE',  ( 19.02544592524343514, -5.153800228976328945, 73.54057627198103830 ) ) ;
#36516 = CARTESIAN_POINT ( 'NONE',  ( 19.03943276465977164, -0.05219959533909143690, 38.74890960531436690 ) ) ;
#36517 = CARTESIAN_POINT ( 'NONE',  ( -13.89961937509957401, -13.97604488694547875, 79.37609039468567573 ) ) ;
#36518 = CARTESIAN_POINT ( 'NONE',  ( -19.05341960407611168, -5.049401038298163336, 111.4572429386476671 ) ) ;
#36519 = CARTESIAN_POINT ( 'NONE',  ( -9.564922557960796823, -16.46253265017161027, 92.08224293864769550 ) ) ;
#36520 = CARTESIAN_POINT ( 'NONE',  ( -16.55341960407611168, -4.379528057220339221, 46.45724293864769550 ) ) ;
#36521 = CARTESIAN_POINT ( 'NONE',  ( 15.72974639402199770, -15.80617190586745480, 53.12390960531436690 ) ) ;
#36522 = CARTESIAN_POINT ( 'NONE',  ( -17.49999999999999645, 3.850315288878824571, 104.2662913060345176 ) ) ;
#36523 = AXIS2_PLACEMENT_3D ( 'NONE', #14685, #155180, #78319 ) ;
#36524 = CARTESIAN_POINT ( 'NONE',  ( 5.153800228976615827, -19.02544592524334988, 25.20942372801900433 ) ) ;
#36525 = CARTESIAN_POINT ( 'NONE',  ( -17.31728774477274513, -6.344390552232368030, 79.18093348310681279 ) ) ;
#36526 = CARTESIAN_POINT ( 'NONE',  ( -16.46253265017160317, 9.564922557960807481, 55.83224293864769550 ) ) ;
#36527 = CARTESIAN_POINT ( 'NONE',  ( 12.06949235617739724, 12.14591786802326823, 31.87609039468567929 ) ) ;
#36528 = CARTESIAN_POINT ( 'NONE',  ( -19.53091890409951858, -5.499999999999989342, 100.0609743183141802 ) ) ;
#36529 = CARTESIAN_POINT ( 'NONE',  ( 24.93942350307310107, -7.769968609432603479, 171.2173313942149377 ) ) ;
#36530 = CARTESIAN_POINT ( 'NONE',  ( 16.53943276465976808, 0.05219959533934440121, 76.25109039468568994 ) ) ;
#36531 = CARTESIAN_POINT ( 'NONE',  ( -5.719274019375978568, 21.55341960407610458, 95.20724293864769550 ) ) ;
#36532 = CARTESIAN_POINT ( 'NONE',  ( 9.564922557960805705, 16.46253265017160317, 39.58224293864768839 ) ) ;
#36533 = CARTESIAN_POINT ( 'NONE',  ( 18.67979575497194134, -10.72451020669871369, 45.83442372801901854 ) ) ;
#36534 = CARTESIAN_POINT ( 'NONE',  ( -0.05219959533936034679, 19.03943276465977164, 52.50109039468566863 ) ) ;
#36535 = CARTESIAN_POINT ( 'NONE',  ( -0.05219959533909027116, -19.03943276465977164, 47.49890960531435979 ) ) ;
#36536 = CARTESIAN_POINT ( 'NONE',  ( -5.823673210054431948, 21.52544592524334988, 92.70942372801901854 ) ) ;
#36537 = CARTESIAN_POINT ( 'NONE',  ( 17.13100169013300444, 6.664070546373151771, 96.73210164300149927 ) ) ;
#36538 = CARTESIAN_POINT ( 'NONE',  ( 12.06949235617757843, -12.14591786802309237, 43.12390960531435269 ) ) ;
#36539 = DIRECTION ( 'NONE',  ( 0.000000000000000000, 0.000000000000000000, -1.000000000000000000 ) ) ;
#36540 = CARTESIAN_POINT ( 'NONE',  ( -5.719274019375978568, 21.55341960407610458, 50.20724293864769550 ) ) ;
#36541 = CARTESIAN_POINT ( 'NONE',  ( 8.571926809382603096, -26.38167802310801235, 143.4750000027312069 ) ) ;
#36542 = CARTESIAN_POINT ( 'NONE',  ( -19.05341960407611168, -5.049401038298163336, 101.4572429386476955 ) ) ;
#36543 = CARTESIAN_POINT ( 'NONE',  ( 16.52544592524342804, -4.483927247898539470, 98.54057627198105251 ) ) ;
#36544 = CARTESIAN_POINT ( 'NONE',  ( 16.53943276465976808, 0.05219959533934440121, 26.25109039468567573 ) ) ;
#36545 = CARTESIAN_POINT ( 'NONE',  ( -4.379528057220086978, -16.55341960407618274, 104.7927570613523898 ) ) ;
#36546 = VERTEX_POINT ( 'NONE', #155597 ) ;
#36547 = EDGE_CURVE ( 'NONE', #158282, #75891, #59158, .T. ) ;
#36549 = CARTESIAN_POINT ( 'NONE',  ( 15.80617190586746368, 15.72974639402197994, 104.3739096053143669 ) ) ;
#36548 = CARTESIAN_POINT ( 'NONE',  ( 9.474510206698971260, -16.51473224551069308, 102.9155762719810241 ) ) ;
#36550 = AXIS2_PLACEMENT_3D ( 'NONE', #190587, #37901, #145063 ) ;
#36552 = CARTESIAN_POINT ( 'NONE',  ( -9.564922557960796823, -16.46253265017161027, 102.0822429386477097 ) ) ;
#36551 = CARTESIAN_POINT ( 'NONE',  ( 16.53943276465976808, -0.05219959533910856209, 23.74890960531435269 ) ) ;
#36553 = CARTESIAN_POINT ( 'NONE',  ( -19.02544592524334988, -5.153800228976617603, 98.95942372801900433 ) ) ;
#36554 = CARTESIAN_POINT ( 'NONE',  ( -10.72451020669870658, -18.67979575497194134, 109.5844237280190328 ) ) ;
#36555 = CARTESIAN_POINT ( 'NONE',  ( 10.72451020669898902, -18.67979575497178502, 92.91557627198103830 ) ) ;
#36556 = CARTESIAN_POINT ( 'NONE',  ( 15.72974639402199770, -15.80617190586745480, 53.12390960531436690 ) ) ;
#36557 = CARTESIAN_POINT ( 'NONE',  ( 19.02544592524343514, -5.153800228976328945, 58.54057627198102409 ) ) ;
#36558 = CARTESIAN_POINT ( 'NONE',  ( -4.379528057220328563, 16.55341960407611168, 30.20724293864769550 ) ) ;
#36559 = CARTESIAN_POINT ( 'NONE',  ( -19.05341960407611168, -5.049401038298163336, 81.45724293864769550 ) ) ;
#36560 = VERTEX_POINT ( 'NONE', #154602 ) ;
#36561 = CARTESIAN_POINT ( 'NONE',  ( 19.49149378614661288, -5.499999999999589662, 61.93757513605363130 ) ) ;
#36562 = CARTESIAN_POINT ( 'NONE',  ( 5.153800228976615827, -19.02544592524334988, 40.20942372801898301 ) ) ;
#36563 = CARTESIAN_POINT ( 'NONE',  ( 10.81492255796078972, 18.62759615963270932, 79.58224293864769550 ) ) ;
#36564 = CARTESIAN_POINT ( 'NONE',  ( 14.34966873604960469, 8.224510206698951720, 84.16557627198103830 ) ) ;
#36565 = CARTESIAN_POINT ( 'NONE',  ( -5.719274019375665041, -21.55341960407619695, 34.79275706135235424 ) ) ;
#36566 = CARTESIAN_POINT ( 'NONE',  ( -17.14385361876520264, -23.59649016807271593, 147.6750000027311671 ) ) ;
#36567 = CARTESIAN_POINT ( 'NONE',  ( 16.53943276465976808, 0.05219959533934440121, 106.2510903946856757 ) ) ;
#36568 = CARTESIAN_POINT ( 'NONE',  ( -13.97604488694527625, -13.89961937509977652, 21.87390960531435979 ) ) ;
#36569 = CARTESIAN_POINT ( 'NONE',  ( 5.049401038298161559, -19.05341960407611168, 92.70724293864769550 ) ) ;
#36570 = CARTESIAN_POINT ( 'NONE',  ( 9.474510206698971260, -16.51473224551069308, 22.91557627198102765 ) ) ;
#36571 = CARTESIAN_POINT ( 'NONE',  ( -0.05219959533910754901, -16.53943276465976808, 47.49890960531435979 ) ) ;
#36572 = EDGE_CURVE ( 'NONE', #41844, #115644, #112151, .T. ) ;
#36573 = CARTESIAN_POINT ( 'NONE',  ( 0.05219959533937995610, -21.53943276465977519, 65.00109039468568994 ) ) ;
#36574 = DIRECTION ( 'NONE',  ( 0.000000000000000000, 0.000000000000000000, 1.000000000000000000 ) ) ;
#36575 = CARTESIAN_POINT ( 'NONE',  ( 9.564922557960805705, 16.46253265017160317, 49.58224293864770260 ) ) ;
#36576 = CARTESIAN_POINT ( 'NONE',  ( 16.46253265017160672, -9.564922557960803928, 58.33224293864769550 ) ) ;
#36577 = ORIENTED_EDGE ( 'NONE', *, *, #150310, .T. ) ;
#36578 = CARTESIAN_POINT ( 'NONE',  ( -13.89961937509957401, -13.97604488694547875, 19.37609039468566507 ) ) ;
#36579 = CARTESIAN_POINT ( 'NONE',  ( 16.55341960407618274, -4.379528057220086978, 66.04275706135236135 ) ) ;
#36580 = CARTESIAN_POINT ( 'NONE',  ( -15.72974639402176322, -15.80617190586768395, 89.37609039468568994 ) ) ;
#36581 = CARTESIAN_POINT ( 'NONE',  ( -21.55341960407610458, -5.719274019375992779, 21.45724293864769550 ) ) ;
#36582 = CARTESIAN_POINT ( 'NONE',  ( 5.049401038297881783, 19.05341960407617563, 92.29275706135234714 ) ) ;
#36583 = CARTESIAN_POINT ( 'NONE',  ( 5.823673210054444382, -21.52544592524334988, 75.20942372801901854 ) ) ;
#36584 = CARTESIAN_POINT ( 'NONE',  ( 8.314922557961029526, -14.29746914071037800, 30.41775706135234358 ) ) ;
#36585 = CARTESIAN_POINT ( 'NONE',  ( 18.67979575497178502, 10.72451020669898547, 84.16557627198103830 ) ) ;
#36586 = CARTESIAN_POINT ( 'NONE',  ( 0.05219959533936267826, -19.03943276465977164, 95.00109039468567573 ) ) ;
#36587 = CARTESIAN_POINT ( 'NONE',  ( -19.02544592524342804, 5.153800228976336051, 61.04057627198103120 ) ) ;
#36588 = CARTESIAN_POINT ( 'NONE',  ( -13.97604488694547697, 13.89961937509957934, 113.1260903946856757 ) ) ;
#36589 = CARTESIAN_POINT ( 'NONE',  ( -16.46253265017146816, -9.564922557961047289, 99.16775706135233293 ) ) ;
#36590 = CARTESIAN_POINT ( 'NONE',  ( -4.483927247898539470, -16.52544592524342804, 47.29057627198103120 ) ) ;
#36591 = CARTESIAN_POINT ( 'NONE',  ( 19.05341960407617918, -5.049401038297876454, 81.04275706135231871 ) ) ;
#36592 = CARTESIAN_POINT ( 'NONE',  ( 12.14591786802327356, -12.06949235617739191, 55.62609039468568284 ) ) ;
#36594 = CARTESIAN_POINT ( 'NONE',  ( 5.049401038298161559, -19.05341960407611168, 37.70724293864768839 ) ) ;
#36593 = CARTESIAN_POINT ( 'NONE',  ( -21.53943276465977519, 0.05219959533907696930, 116.2489096053143669 ) ) ;
#36595 = CARTESIAN_POINT ( 'NONE',  ( 9.564922557960805705, 16.46253265017160317, 54.58224293864769550 ) ) ;
#36596 = CARTESIAN_POINT ( 'NONE',  ( 12.14591786802327356, -12.06949235617739191, 60.62609039468567573 ) ) ;
#36597 = CARTESIAN_POINT ( 'NONE',  ( 30.00000000000000355, -0.3535533905932712884, 5.353553390593269512 ) ) ;
#36598 = CARTESIAN_POINT ( 'NONE',  ( 28.82186960331499392, -9.364793116373510529, 143.1500000054623740 ) ) ;
#36599 = CARTESIAN_POINT ( 'NONE',  ( -16.46253265017160317, 9.564922557960807481, 100.8322429386477097 ) ) ;
#36600 = CARTESIAN_POINT ( 'NONE',  ( 0.3535533905931687038, -30.00000000000000355, 4.646446609406718942 ) ) ;
#36601 = ORIENTED_EDGE ( 'NONE', *, *, #48904, .F. ) ;
#36602 = CARTESIAN_POINT ( 'NONE',  ( -16.46253265017146816, -9.564922557961047289, 109.1677570613523471 ) ) ;
#36603 = CARTESIAN_POINT ( 'NONE',  ( 10.81492255796078972, 18.62759615963270932, 44.58224293864769550 ) ) ;
#36605 = CARTESIAN_POINT ( 'NONE',  ( -4.483927247898782831, 16.52544592524335698, 27.70942372801901854 ) ) ;
#36604 = CARTESIAN_POINT ( 'NONE',  ( -19.03943276465977164, -0.05219959533935918106, 43.75109039468566863 ) ) ;
#36606 = CARTESIAN_POINT ( 'NONE',  ( -19.03943276465977164, 0.05219959533909376836, 31.24890960531435979 ) ) ;
#36607 = CARTESIAN_POINT ( 'NONE',  ( 9.474510206698971260, -16.51473224551069308, 52.91557627198102409 ) ) ;
#36608 = CARTESIAN_POINT ( 'NONE',  ( -18.62759615963270932, 10.81492255796079327, 90.83224293864769550 ) ) ;
#36609 = CARTESIAN_POINT ( 'NONE',  ( 9.474510206698971260, -16.51473224551069308, 112.9155762719810383 ) ) ;
#36610 = CIRCLE ( 'NONE', #110819, 0.5000000000000004441 ) ;
#36611 = CARTESIAN_POINT ( 'NONE',  ( 9.564922557960805705, 16.46253265017160317, 54.58224293864769550 ) ) ;
#36612 = CARTESIAN_POINT ( 'NONE',  ( -22.44159573604009950, -16.30477369853688430, 145.5750000027311728 ) ) ;
#36613 = CARTESIAN_POINT ( 'NONE',  ( -16.46253265017146816, -9.564922557961047289, 79.16775706135234714 ) ) ;
#36614 = CARTESIAN_POINT ( 'NONE',  ( -16.53943276465976808, 0.05219959533911058130, 61.24890960531435979 ) ) ;
#36615 = CARTESIAN_POINT ( 'NONE',  ( 18.62759615963255655, 10.81492255796105972, 101.6677570613523613 ) ) ;
#36616 = CARTESIAN_POINT ( 'NONE',  ( -18.67979575497178146, -10.72451020669898902, 91.66557627198103830 ) ) ;
#36617 = CARTESIAN_POINT ( 'NONE',  ( 5.719274019375673035, 21.55341960407619339, 82.29275706135234714 ) ) ;
#36618 = CARTESIAN_POINT ( 'NONE',  ( -16.46253265017160317, 9.564922557960807481, 30.83224293864769550 ) ) ;
#36619 = CARTESIAN_POINT ( 'NONE',  ( 10.72451020669871369, 18.67979575497193778, 72.08442372801899012 ) ) ;
#36620 = CARTESIAN_POINT ( 'NONE',  ( -9.474510206698964154, 16.51473224551069663, 110.4155762719810383 ) ) ;
#36622 = CARTESIAN_POINT ( 'NONE',  ( -10.81492255796105439, 18.62759615963255655, 82.91775706135234714 ) ) ;
#36621 = CARTESIAN_POINT ( 'NONE',  ( -16.55341960407611168, -4.379528057220339221, 26.45724293864768839 ) ) ;
#36623 = CARTESIAN_POINT ( 'NONE',  ( 9.564922557960805705, 16.46253265017160317, 69.58224293864770971 ) ) ;
#36624 = CARTESIAN_POINT ( 'NONE',  ( -15.72974639402176322, -15.80617190586768395, 44.37609039468567573 ) ) ;
#36625 = CARTESIAN_POINT ( 'NONE',  ( -19.02544592524342804, 5.153800228976336051, 76.04057627198102409 ) ) ;
#36626 = CARTESIAN_POINT ( 'NONE',  ( 8.224510206698953496, -14.34966873604960469, 87.91557627198103830 ) ) ;
#36627 = CARTESIAN_POINT ( 'NONE',  ( 0.05219959533910956823, 16.53943276465976808, 59.99890960531436690 ) ) ;
#36628 = CARTESIAN_POINT ( 'NONE',  ( 15.80617190586746368, 15.72974639402197994, 69.37390960531436690 ) ) ;
#36629 = CARTESIAN_POINT ( 'NONE',  ( 0.05219959533909260263, 19.03943276465977164, 59.99890960531436690 ) ) ;
#36630 = CARTESIAN_POINT ( 'NONE',  ( 0.05219959533907565091, 21.53943276465977519, 74.99890960531435269 ) ) ;
#36631 = CARTESIAN_POINT ( 'NONE',  ( 16.46253265017146816, 9.564922557961045513, 66.66775706135233293 ) ) ;
#36633 = CARTESIAN_POINT ( 'NONE',  ( -8.224510206698948167, 14.34966873604960824, 75.41557627198102409 ) ) ;
#36632 = CARTESIAN_POINT ( 'NONE',  ( 9.564922557961047289, -16.46253265017146816, 30.41775706135232937 ) ) ;
#36634 = CARTESIAN_POINT ( 'NONE',  ( 0.05219959533907565091, 21.53943276465977519, 54.99890960531435269 ) ) ;
#36635 = PLANE ( 'NONE',  #178759 ) ;
#36637 = CARTESIAN_POINT ( 'NONE',  ( 27.73933785331498569, 2.768321779492822058E-14, 148.3750000027311842 ) ) ;
#36636 = CARTESIAN_POINT ( 'NONE',  ( -16.52544592524335698, -4.483927247898792601, 93.95942372801903275 ) ) ;
#36638 = CARTESIAN_POINT ( 'NONE',  ( -9.564922557961040184, 16.46253265017147172, 107.9177570613523471 ) ) ;
#36639 = CARTESIAN_POINT ( 'NONE',  ( 14.34966873604960469, 8.224510206698951720, 69.16557627198102409 ) ) ;
#36640 = DIRECTION ( 'NONE',  ( 0.000000000000000000, 0.000000000000000000, -1.000000000000000000 ) ) ;
#36641 = CARTESIAN_POINT ( 'NONE',  ( 9.474510206698971260, -16.51473224551069308, 62.91557627198102409 ) ) ;
#36642 = CARTESIAN_POINT ( 'NONE',  ( 8.224510206698953496, -14.34966873604960469, 57.91557627198103120 ) ) ;
#36643 = CARTESIAN_POINT ( 'NONE',  ( -19.03943276465977164, 0.05219959533909376836, 101.2489096053143669 ) ) ;
#36645 = CARTESIAN_POINT ( 'NONE',  ( 9.474510206698971260, -16.51473224551069308, 62.91557627198102409 ) ) ;
#36644 = CARTESIAN_POINT ( 'NONE',  ( 16.46253265017146816, 9.564922557961045513, 71.66775706135233293 ) ) ;
#36646 = CARTESIAN_POINT ( 'NONE',  ( 13.97604488694527802, 13.89961937509977652, 89.37390960531436690 ) ) ;
#36647 = CARTESIAN_POINT ( 'NONE',  ( 19.05341960407611168, 5.049401038298154454, 68.95724293864769550 ) ) ;
#36648 = EDGE_CURVE ( 'NONE', #130499, #75168, #127503, .T. ) ;
#36649 = CARTESIAN_POINT ( 'NONE',  ( 18.67979575497178502, 10.72451020669898547, 64.16557627198102409 ) ) ;
#36650 = CARTESIAN_POINT ( 'NONE',  ( 16.53943276465976808, 0.05219959533934440121, 61.25109039468567573 ) ) ;
#36651 = CARTESIAN_POINT ( 'NONE',  ( -19.05341960407617918, 5.049401038297883559, 103.5427570613523329 ) ) ;
#36652 = CARTESIAN_POINT ( 'NONE',  ( -5.153800228976328057, -19.02544592524343514, 47.29057627198102409 ) ) ;
#36653 = CARTESIAN_POINT ( 'NONE',  ( -10.72451020669898014, 18.67979575497178502, 55.41557627198102409 ) ) ;
#36654 = CARTESIAN_POINT ( 'NONE',  ( -0.05219959533936034679, 19.03943276465977164, 77.50109039468566152 ) ) ;
#36656 = CARTESIAN_POINT ( 'NONE',  ( 15.72974639402176855, 15.80617190586768217, 31.87609039468567929 ) ) ;
#36655 = CARTESIAN_POINT ( 'NONE',  ( -16.55341960407617563, 4.379528057220093196, 113.5427570613523756 ) ) ;
#36657 = CARTESIAN_POINT ( 'NONE',  ( 19.05341960407617918, -5.049401038297876454, 36.04275706135234003 ) ) ;
#36659 = CARTESIAN_POINT ( 'NONE',  ( 4.379528057220092307, 16.55341960407617563, 87.29275706135236135 ) ) ;
#36658 = CARTESIAN_POINT ( 'NONE',  ( -14.34966873604972548, 8.224510206698743886, 63.33442372801900433 ) ) ;
#36660 = CARTESIAN_POINT ( 'NONE',  ( 4.483927247898790824, -16.52544592524335698, 75.20942372801901854 ) ) ;
#36662 = CARTESIAN_POINT ( 'NONE',  ( -14.29746914071037622, -8.314922557961029526, 39.16775706135235424 ) ) ;
#36661 = CARTESIAN_POINT ( 'NONE',  ( -21.53943276465977519, 0.05219959533907696930, 21.24890960531436690 ) ) ;
#36663 = CARTESIAN_POINT ( 'NONE',  ( 19.05341960407611168, 5.049401038298154454, 48.95724293864768129 ) ) ;
#36664 = CARTESIAN_POINT ( 'NONE',  ( -9.474510206698964154, 16.51473224551069663, 45.41557627198103120 ) ) ;
#36665 = CARTESIAN_POINT ( 'NONE',  ( -19.02544592524342804, 5.153800228976336051, 56.04057627198100988 ) ) ;
#36666 = CARTESIAN_POINT ( 'NONE',  ( 18.67979575497194134, -10.72451020669871369, 45.83442372801901854 ) ) ;
#36667 = CARTESIAN_POINT ( 'NONE',  ( -12.06949235617739369, -12.14591786802326823, 54.37609039468568994 ) ) ;
#36668 = CARTESIAN_POINT ( 'NONE',  ( 12.14591786802327356, -12.06949235617739191, 110.6260903946857042 ) ) ;
#36669 = CARTESIAN_POINT ( 'NONE',  ( -13.89961937509977652, 13.97604488694528158, 25.62390960531434558 ) ) ;
#36670 = CARTESIAN_POINT ( 'NONE',  ( 5.823673210054444382, -21.52544592524334988, 110.2094237280190185 ) ) ;
#36671 = CARTESIAN_POINT ( 'NONE',  ( -19.03943276465977164, -0.05219959533935918106, 103.7510903946856757 ) ) ;
#36672 = CARTESIAN_POINT ( 'NONE',  ( -9.564922557961040184, 16.46253265017147172, 62.91775706135233293 ) ) ;
#36673 = CARTESIAN_POINT ( 'NONE',  ( 16.53943276465976808, -0.05219959533910856209, 68.74890960531435269 ) ) ;
#36674 = CARTESIAN_POINT ( 'NONE',  ( -5.153800228976328057, -19.02544592524343514, 32.29057627198102409 ) ) ;
#36676 = CARTESIAN_POINT ( 'NONE',  ( 17.13100169013299734, -6.664070546373147330, 93.26789835699847231 ) ) ;
#36675 = CARTESIAN_POINT ( 'NONE',  ( 13.89961937509957401, 13.97604488694547697, 76.87609039468566152 ) ) ;
#36677 = CARTESIAN_POINT ( 'NONE',  ( -0.05219959533937732626, 21.53943276465977519, 77.50109039468567573 ) ) ;
#36678 = CARTESIAN_POINT ( 'NONE',  ( 4.483927247898790824, -16.52544592524335698, 40.20942372801901854 ) ) ;
#36679 = CARTESIAN_POINT ( 'NONE',  ( -18.09805431107250229, 5.499999999999981348, 91.01606229291887473 ) ) ;
#36680 = CARTESIAN_POINT ( 'NONE',  ( -18.62759615963270932, 10.81492255796079327, 35.83224293864768839 ) ) ;
#36681 = CARTESIAN_POINT ( 'NONE',  ( -12.14591786802326823, 12.06949235617739902, 33.12609039468569705 ) ) ;
#36682 = CARTESIAN_POINT ( 'NONE',  ( 0.05219959533909260263, 19.03943276465977164, 29.99890960531435979 ) ) ;
#36683 = CARTESIAN_POINT ( 'NONE',  ( 10.81492255796106328, -18.62759615963255655, 110.4177570613523756 ) ) ;
#36684 = CARTESIAN_POINT ( 'NONE',  ( 9.562403590618709259, 11.67169337655810502, -59.87610203618464766 ) ) ;
#36685 = CARTESIAN_POINT ( 'NONE',  ( -5.153800228976328057, -19.02544592524343514, 32.29057627198102409 ) ) ;
#36686 = CARTESIAN_POINT ( 'NONE',  ( 23.29544513554940366, -16.92513159979222337, 143.0656553485623874 ) ) ;
#36687 = CARTESIAN_POINT ( 'NONE',  ( 9.474510206698971260, -16.51473224551069308, 62.91557627198102409 ) ) ;
#36688 = CARTESIAN_POINT ( 'NONE',  ( 10.81492255796106328, -18.62759615963255655, 70.41775706135236135 ) ) ;
#36689 = CARTESIAN_POINT ( 'NONE',  ( -19.02544592524334988, -5.153800228976617603, 18.95942372801899722 ) ) ;
#36690 = CARTESIAN_POINT ( 'NONE',  ( -8.224510206698948167, 14.34966873604960824, 30.41557627198101699 ) ) ;
#36691 = CARTESIAN_POINT ( 'NONE',  ( -19.02544592524342804, 5.153800228976336051, 26.04057627198103120 ) ) ;
#36692 = CARTESIAN_POINT ( 'NONE',  ( 5.049401038298161559, -19.05341960407611168, 92.70724293864769550 ) ) ;
#36693 = CARTESIAN_POINT ( 'NONE',  ( -18.67979575497193778, 10.72451020669871902, 63.33442372801900433 ) ) ;
#36694 = CARTESIAN_POINT ( 'NONE',  ( -19.03943276465977164, 0.05219959533909376836, 31.24890960531435979 ) ) ;
#36695 = CARTESIAN_POINT ( 'NONE',  ( -18.67979575497193778, 10.72451020669871902, 68.33442372801900433 ) ) ;
#36697 = CARTESIAN_POINT ( 'NONE',  ( -16.51473224551069308, -9.474510206698971260, 101.6655762719810241 ) ) ;
#36696 = CARTESIAN_POINT ( 'NONE',  ( -5.153800228976607833, 19.02544592524334988, 92.70942372801901854 ) ) ;
#36698 = CARTESIAN_POINT ( 'NONE',  ( -19.03943276465977164, 0.05219959533909376836, 36.24890960531436690 ) ) ;
#36699 = CARTESIAN_POINT ( 'NONE',  ( 21.55341960407610458, 5.719274019375980345, 113.9572429386477239 ) ) ;
#36700 = CARTESIAN_POINT ( 'NONE',  ( 19.02544592524334988, 5.153800228976608722, 41.45942372801900433 ) ) ;
#36701 = CARTESIAN_POINT ( 'NONE',  ( -16.51473224551069308, -9.474510206698971260, 21.66557627198102765 ) ) ;
#36702 = CARTESIAN_POINT ( 'NONE',  ( -5.049401038298153566, 19.05341960407611168, 60.20724293864768129 ) ) ;
#36703 = CARTESIAN_POINT ( 'NONE',  ( -9.564922557961040184, 16.46253265017147172, 102.9177570613523329 ) ) ;
#36704 = CARTESIAN_POINT ( 'NONE',  ( 4.379528057220339221, -16.55341960407611168, 77.70724293864770971 ) ) ;
#36705 = CARTESIAN_POINT ( 'NONE',  ( -21.52544592524343514, 5.823673210054127303, 26.04057627198103475 ) ) ;
#36706 = CARTESIAN_POINT ( 'NONE',  ( -13.89961937509957401, -13.97604488694547875, 89.37609039468563310 ) ) ;
#36707 = CARTESIAN_POINT ( 'NONE',  ( 18.67979575497178502, 10.72451020669898547, 89.16557627198102409 ) ) ;
#36708 = CARTESIAN_POINT ( 'NONE',  ( 15.72974639402176855, 15.80617190586768217, 46.87609039468568994 ) ) ;
#36709 = CARTESIAN_POINT ( 'NONE',  ( -16.53943276465976808, -0.05219959533934237506, 43.75109039468568284 ) ) ;
#36711 = CARTESIAN_POINT ( 'NONE',  ( 18.67979575497194134, -10.72451020669871369, 50.83442372801901143 ) ) ;
#36710 = CARTESIAN_POINT ( 'NONE',  ( 14.34966873604972726, -8.224510206698740333, 40.83442372801901854 ) ) ;
#36712 = CARTESIAN_POINT ( 'NONE',  ( 18.62759615963271287, -10.81492255796078972, 58.33224293864768839 ) ) ;
#36713 = CARTESIAN_POINT ( 'NONE',  ( 5.049401038298161559, -19.05341960407611168, 47.70724293864770260 ) ) ;
#36714 = CARTESIAN_POINT ( 'NONE',  ( -30.74264578624800492, 22.33583958711400186, -1.949999994537626735 ) ) ;
#36715 = CARTESIAN_POINT ( 'NONE',  ( 16.53943276465976808, 0.05219959533934440121, 71.25109039468568994 ) ) ;
#36716 = B_SPLINE_CURVE_WITH_KNOTS ( 'NONE', 3,
 ( #198930, #48232, #1712, #155403, #105912, #30073, #152415, #185748, #31071, #13903, #17897, #707, #122070, #107887, #14906, #183762, #109887, #167598, #29093, #90732, #169574, #154408, #15902, #16893 ),
 .UNSPECIFIED., .F., .F.,
 ( 4, 2, 2, 2, 2, 2, 2, 2, 2, 2, 2, 4 ),
 ( 1.970462154302192724E-07, 0.0003069708713091119884, 0.0006137446964027936649, 0.001227292346590153549, 0.001534066171683836580, 0.001840839996777519178, 0.002147613821871202210, 0.002454387646964885459, 0.003067935297152254558, 0.003681482947339624525, 0.004295030597526993191, 0.004908578247714363157 ),
 .UNSPECIFIED. ) ;
#36717 = CARTESIAN_POINT ( 'NONE',  ( 10.72451020669898902, -18.67979575497178502, 107.9155762719810241 ) ) ;
#36718 = CARTESIAN_POINT ( 'NONE',  ( -8.224510206698948167, 14.34966873604960824, 45.41557627198103830 ) ) ;
#36719 = CARTESIAN_POINT ( 'NONE',  ( 4.379528057220092307, 16.55341960407617563, 67.29275706135234714 ) ) ;
#36720 = CARTESIAN_POINT ( 'NONE',  ( 5.049401038297881783, 19.05341960407617563, 97.29275706135233293 ) ) ;
#36721 = CARTESIAN_POINT ( 'NONE',  ( -10.72451020669898014, 18.67979575497178502, 95.41557627198102409 ) ) ;
#36722 = CARTESIAN_POINT ( 'NONE',  ( -14.34966873604960291, -8.224510206698953496, 26.66557627198103475 ) ) ;
#36723 = ORIENTED_EDGE ( 'NONE', *, *, #123538, .F. ) ;
#36724 = CARTESIAN_POINT ( 'NONE',  ( -12.14591786802326823, 12.06949235617739902, 73.12609039468567573 ) ) ;
#36725 = CARTESIAN_POINT ( 'NONE',  ( 23.35043118190687750, 14.19381810411953992, 169.8796877288296514 ) ) ;
#36726 = CARTESIAN_POINT ( 'NONE',  ( 0.05219959533907565091, 21.53943276465977519, 79.99890960531435269 ) ) ;
#36727 = CARTESIAN_POINT ( 'NONE',  ( 16.52544592524335698, 4.483927247898782831, 111.4594237280190328 ) ) ;
#36728 = ORIENTED_EDGE ( 'NONE', *, *, #111893, .F. ) ;
#36729 = CARTESIAN_POINT ( 'NONE',  ( -17.49999999999998934, -5.624438216177603422, 54.18329655085358354 ) ) ;
#36730 = CARTESIAN_POINT ( 'NONE',  ( 18.62759615963271287, -10.81492255796078972, 108.3322429386477097 ) ) ;
#36731 = CARTESIAN_POINT ( 'NONE',  ( 21.52544592524344225, -5.823673210054117533, 108.5405762719810241 ) ) ;
#36732 = CARTESIAN_POINT ( 'NONE',  ( -14.34966873604960291, -8.224510206698953496, 31.66557627198102054 ) ) ;
#36733 = CARTESIAN_POINT ( 'NONE',  ( -8.314922557961024197, 14.29746914071037800, 42.91775706135235424 ) ) ;
#36734 = CARTESIAN_POINT ( 'NONE',  ( 13.89961937509977652, -13.97604488694527269, 48.12390960531435979 ) ) ;
#36735 = CARTESIAN_POINT ( 'NONE',  ( -5.049401038298153566, 19.05341960407611168, 65.20724293864765286 ) ) ;
#36736 = ORIENTED_EDGE ( 'NONE', *, *, #81855, .T. ) ;
#36737 = CARTESIAN_POINT ( 'NONE',  ( -19.02544592524342804, 5.153800228976336051, 116.0405762719810383 ) ) ;
#36738 = CARTESIAN_POINT ( 'NONE',  ( -29.42957871419942961, -23.46871120497985785, -19.15262919804619557 ) ) ;
#36739 = CARTESIAN_POINT ( 'NONE',  ( 13.97604488694548053, -13.89961937509957401, 110.6260903946856615 ) ) ;
#36740 = CARTESIAN_POINT ( 'NONE',  ( -9.474510206698720793, -16.51473224551083518, 54.58442372801899722 ) ) ;
#36741 = CARTESIAN_POINT ( 'NONE',  ( 5.823673210054125526, 21.52544592524343514, 84.79057627198102409 ) ) ;
#36742 = CARTESIAN_POINT ( 'NONE',  ( -16.53943276465976808, 0.05219959533911058130, 26.24890960531435624 ) ) ;
#36743 = CARTESIAN_POINT ( 'NONE',  ( 19.05341960407611168, 5.049401038298154454, 73.95724293864768129 ) ) ;
#36744 = CARTESIAN_POINT ( 'NONE',  ( -5.719274019375978568, 21.55341960407610458, 40.20724293864769550 ) ) ;
#36746 = CARTESIAN_POINT ( 'NONE',  ( 16.55341960407618274, -4.379528057220086978, 21.04275706135234714 ) ) ;
#36745 = CARTESIAN_POINT ( 'NONE',  ( -0.05219959533907301413, -21.53943276465977519, 77.49890960531433848 ) ) ;
#36747 = CARTESIAN_POINT ( 'NONE',  ( 15.72974639402199770, -15.80617190586745480, 23.12390960531436335 ) ) ;
#36748 = CARTESIAN_POINT ( 'NONE',  ( 21.52544592524334988, 5.823673210054432836, 71.45942372801901854 ) ) ;
#36749 = CARTESIAN_POINT ( 'NONE',  ( -13.89961937509977652, 13.97604488694528158, 75.62390960531438111 ) ) ;
#36750 = CARTESIAN_POINT ( 'NONE',  ( -9.564922557960796823, -16.46253265017161027, 22.08224293864768839 ) ) ;
#36751 = CARTESIAN_POINT ( 'NONE',  ( 16.51473224551069308, 9.474510206698969483, 64.16557627198102409 ) ) ;
#36752 = CARTESIAN_POINT ( 'NONE',  ( 12.06949235617757843, -12.14591786802309237, 88.12390960531436690 ) ) ;
#36753 = ORIENTED_EDGE ( 'NONE', *, *, #190985, .F. ) ;
#36754 = CARTESIAN_POINT ( 'NONE',  ( -19.05341960407617563, 5.049401038297882671, 98.54275706135233293 ) ) ;
#36755 = AXIS2_PLACEMENT_3D ( 'NONE', #5691, #84520, #24887 ) ;
#36756 = CARTESIAN_POINT ( 'NONE',  ( -11.30153831258470731, -180.0000000000000000, -15.00000000000000000 ) ) ;
#36757 = CARTESIAN_POINT ( 'NONE',  ( -5.153800228976328057, -19.02544592524343514, 67.29057627198102409 ) ) ;
#36759 = CARTESIAN_POINT ( 'NONE',  ( -9.474510206698964154, 16.51473224551069663, 105.4155762719810383 ) ) ;
#36758 = CARTESIAN_POINT ( 'NONE',  ( 0.05219959533937995610, -21.53943276465977519, 80.00109039468568994 ) ) ;
#36760 = CARTESIAN_POINT ( 'NONE',  ( -12.06949235617739369, -12.14591786802326823, 84.37609039468570415 ) ) ;
#36761 = CARTESIAN_POINT ( 'NONE',  ( -16.21995358207302118, -7.366697692864226710, 75.06448998487846325 ) ) ;
#36762 = CARTESIAN_POINT ( 'NONE',  ( -16.51473224551082808, 9.474510206698731452, 63.33442372801900433 ) ) ;
#36763 = CARTESIAN_POINT ( 'NONE',  ( 18.62759615963255655, 10.81492255796105972, 111.6677570613523613 ) ) ;
#36764 = CARTESIAN_POINT ( 'NONE',  ( -8.898068258721467672, -27.38543819252872069, 144.3843446568999980 ) ) ;
#36765 = LINE ( 'NONE', #101437, #153154 ) ;
#36766 = CARTESIAN_POINT ( 'NONE',  ( 22.81625015709510151, -31.40387420917324590, -6.424999997268812102 ) ) ;
#36767 = CARTESIAN_POINT ( 'NONE',  ( -8.314922557960811034, -14.29746914071050412, 22.08224293864769194 ) ) ;
#36768 = CARTESIAN_POINT ( 'NONE',  ( 10.20000000000000107, 0.000000000000000000, 1.610000000000000098 ) ) ;
#36769 = CARTESIAN_POINT ( 'NONE',  ( 12.14591786802327356, -12.06949235617739191, 105.6260903946856899 ) ) ;
#36770 = CARTESIAN_POINT ( 'NONE',  ( 16.79531203550646268, 7.028104445595625194, 68.75244988220443076 ) ) ;
#36771 = CARTESIAN_POINT ( 'NONE',  ( -4.379528057220086978, -16.55341960407618274, 79.79275706135236135 ) ) ;
#36772 = CARTESIAN_POINT ( 'NONE',  ( 15.80617190586769283, -15.72974639402175789, 80.62609039468567573 ) ) ;
#36773 = CARTESIAN_POINT ( 'NONE',  ( -19.02544592524334988, -5.153800228976617603, 98.95942372801900433 ) ) ;
#36774 = CARTESIAN_POINT ( 'NONE',  ( -5.823673210054431948, 21.52544592524334988, 67.70942372801901854 ) ) ;
#36775 = CARTESIAN_POINT ( 'NONE',  ( -13.89961937509957401, -13.97604488694547875, 34.37609039468566863 ) ) ;
#36776 = CARTESIAN_POINT ( 'NONE',  ( -19.02544592524342804, 5.153800228976336051, 76.04057627198102409 ) ) ;
#36777 = CARTESIAN_POINT ( 'NONE',  ( 5.153800228976335163, 19.02544592524342804, 54.79057627198103120 ) ) ;
#36778 = CARTESIAN_POINT ( 'NONE',  ( -5.719274019375978568, 21.55341960407610458, 95.20724293864769550 ) ) ;
#36779 = AXIS2_PLACEMENT_3D ( 'NONE', #50383, #158537, #22024 ) ;
#36780 = EDGE_CURVE ( 'NONE', #75343, #116832, #16098, .T. ) ;
#36781 = CARTESIAN_POINT ( 'NONE',  ( 21.53943276465977519, -0.05219959533907433946, 53.74890960531437401 ) ) ;
#36782 = CARTESIAN_POINT ( 'NONE',  ( -0.05219959533909027116, -19.03943276465977164, 52.49890960531436690 ) ) ;
#36783 = CARTESIAN_POINT ( 'NONE',  ( -14.29746914071037622, -8.314922557961029526, 59.16775706135234714 ) ) ;
#36784 = ORIENTED_EDGE ( 'NONE', *, *, #15442, .T. ) ;
#36785 = CARTESIAN_POINT ( 'NONE',  ( -5.719274019375665041, -21.55341960407619695, 39.79275706135235424 ) ) ;
#36787 = CARTESIAN_POINT ( 'NONE',  ( 3.556970738554033499E-15, -38.81732327939057825, -4.124999997268814056 ) ) ;
#36786 = CARTESIAN_POINT ( 'NONE',  ( 8.314922557960818139, 14.29746914071049879, 64.58224293864769550 ) ) ;
#36788 = CARTESIAN_POINT ( 'NONE',  ( 8.224510206698742110, 14.34966873604972548, 42.08442372801901854 ) ) ;
#36789 = CARTESIAN_POINT ( 'NONE',  ( -12.14591786802309592, -12.06949235617757132, 106.8739096053143811 ) ) ;
#36790 = CARTESIAN_POINT ( 'NONE',  ( -13.89961937509957401, -13.97604488694547875, 59.37609039468566863 ) ) ;
#36791 = CARTESIAN_POINT ( 'NONE',  ( 0.05219959533910956823, 16.53943276465976808, 69.99890960531435269 ) ) ;
#36792 = CARTESIAN_POINT ( 'NONE',  ( 10.72451020669871369, 18.67979575497193778, 37.08442372801901143 ) ) ;
#36793 = EDGE_CURVE ( 'NONE', #180473, #175318, #20372, .T. ) ;
#36795 = CARTESIAN_POINT ( 'NONE',  ( -18.62759615963270932, 10.81492255796079327, 95.83224293864770971 ) ) ;
#36794 = CARTESIAN_POINT ( 'NONE',  ( 16.51473224551069308, 9.474510206698969483, 24.16557627198102765 ) ) ;
#36796 = CARTESIAN_POINT ( 'NONE',  ( 9.564922557960805705, 16.46253265017160317, 109.5822429386476955 ) ) ;
#36797 = CARTESIAN_POINT ( 'NONE',  ( -12.06949235617756955, 12.14591786802309770, 80.62390960531438111 ) ) ;
#36798 = CARTESIAN_POINT ( 'NONE',  ( 30.11221142034223419, -26.30828378221802666, -17.15571736052815410 ) ) ;
#36799 = CARTESIAN_POINT ( 'NONE',  ( -36.91746825000000598, 11.99521256947798520, -4.724999997268811924 ) ) ;
#36800 = CARTESIAN_POINT ( 'NONE',  ( -19.03943276465977164, -0.05219959533935918106, 78.75109039468567573 ) ) ;
#36801 = CARTESIAN_POINT ( 'NONE',  ( -10.81492255796105439, 18.62759615963255655, 27.91775706135234358 ) ) ;
#36802 = CARTESIAN_POINT ( 'NONE',  ( -5.153800228976328057, -19.02544592524343514, 67.29057627198102409 ) ) ;
#36803 = CARTESIAN_POINT ( 'NONE',  ( 9.564922557961047289, -16.46253265017146816, 55.41775706135234003 ) ) ;
#36804 = CARTESIAN_POINT ( 'NONE',  ( -13.97604488694527625, -13.89961937509977652, 31.87390960531435979 ) ) ;
#36805 = CARTESIAN_POINT ( 'NONE',  ( 0.05219959533910956823, 16.53943276465976808, 59.99890960531436690 ) ) ;
#36806 = CARTESIAN_POINT ( 'NONE',  ( -16.55341960407611168, -4.379528057220339221, 56.45724293864768839 ) ) ;
#36807 = CARTESIAN_POINT ( 'NONE',  ( -16.51473224551069308, -9.474510206698971260, 56.66557627198103120 ) ) ;
#36808 = CARTESIAN_POINT ( 'NONE',  ( 10.72451020669898902, -18.67979575497178502, 87.91557627198103830 ) ) ;
#36809 = CARTESIAN_POINT ( 'NONE',  ( 13.89961937509977652, -13.97604488694527269, 63.12390960531435979 ) ) ;
#36810 = CARTESIAN_POINT ( 'NONE',  ( 5.719274019375991003, -21.55341960407610458, 77.70724293864770971 ) ) ;
#36811 = EDGE_CURVE ( 'NONE', #132628, #152161, #72698, .T. ) ;
#36812 = CARTESIAN_POINT ( 'NONE',  ( -10.72451020669870658, -18.67979575497194134, 99.58442372801900433 ) ) ;
#36815 = CARTESIAN_POINT ( 'NONE',  ( 0.05219959533910956823, 16.53943276465976808, 99.99890960531436690 ) ) ;
#36814 = CARTESIAN_POINT ( 'NONE',  ( -16.53943276465976808, -0.05219959533934237506, 113.7510903946856757 ) ) ;
#36813 = CARTESIAN_POINT ( 'NONE',  ( -16.51473224551069308, -9.474510206698971260, 26.66557627198103120 ) ) ;
#36816 = CARTESIAN_POINT ( 'NONE',  ( 19.05341960407617918, -5.049401038297876454, 96.04275706135231871 ) ) ;
#36817 = ORIENTED_EDGE ( 'NONE', *, *, #76459, .T. ) ;
#36818 = CARTESIAN_POINT ( 'NONE',  ( -5.719274019375978568, 21.55341960407610458, 110.2072429386477239 ) ) ;
#36819 = CARTESIAN_POINT ( 'NONE',  ( 5.049401038297881783, 19.05341960407617563, 57.29275706135231871 ) ) ;
#36820 = CARTESIAN_POINT ( 'NONE',  ( 14.29746914071037800, 8.314922557961029526, 101.6677570613523613 ) ) ;
#36821 = CARTESIAN_POINT ( 'NONE',  ( 19.02544592524334988, 5.153800228976608722, 41.45942372801900433 ) ) ;
#36822 = CARTESIAN_POINT ( 'NONE',  ( -0.05219959533909027116, -19.03943276465977164, 107.4989096053143527 ) ) ;
#36823 = CARTESIAN_POINT ( 'NONE',  ( 21.53943276465977519, -0.05219959533907433946, 58.74890960531436690 ) ) ;
#36824 = CARTESIAN_POINT ( 'NONE',  ( -19.48894818550243357, 5.500000000000115463, 50.10307310435241845 ) ) ;
#36825 = CARTESIAN_POINT ( 'NONE',  ( 9.564922557960805705, 16.46253265017160317, 39.58224293864768839 ) ) ;
#36826 = CARTESIAN_POINT ( 'NONE',  ( 5.719274019375673035, 21.55341960407619339, 107.2927570613523471 ) ) ;
#36827 = CARTESIAN_POINT ( 'NONE',  ( -14.34966873604972548, 8.224510206698743886, 78.33442372801901854 ) ) ;
#36828 = CARTESIAN_POINT ( 'NONE',  ( 18.67979575497194134, -10.72451020669871369, 30.83442372801902209 ) ) ;
#36829 = CARTESIAN_POINT ( 'NONE',  ( -12.14591786802326823, 12.06949235617739902, 48.12609039468568284 ) ) ;
#36830 = CARTESIAN_POINT ( 'NONE',  ( 19.05341960407611168, 5.049401038298154454, 103.9572429386476671 ) ) ;
#36831 = CARTESIAN_POINT ( 'NONE',  ( 19.02544592524343514, -5.153800228976328945, 48.54057627198103120 ) ) ;
#36832 = CARTESIAN_POINT ( 'NONE',  ( 16.46253265017160672, -9.564922557960803928, 63.33224293864769550 ) ) ;
#36833 = CARTESIAN_POINT ( 'NONE',  ( -16.52544592524335698, -4.483927247898792601, 48.95942372801902565 ) ) ;
#36834 = CARTESIAN_POINT ( 'NONE',  ( 4.379528057220339221, -16.55341960407611168, 102.7072429386476955 ) ) ;
#36835 = CARTESIAN_POINT ( 'NONE',  ( -12.14591786802326823, 12.06949235617739902, 108.1260903946856757 ) ) ;
#36836 = DIRECTION ( 'NONE',  ( -0.000000000000000000, 0.000000000000000000, 1.000000000000000000 ) ) ;
#36839 = CARTESIAN_POINT ( 'NONE',  ( 16.51473224551069308, 9.474510206698969483, 64.16557627198102409 ) ) ;
#36838 = CARTESIAN_POINT ( 'NONE',  ( -0.05219959533909027116, -19.03943276465977164, 72.49890960531435269 ) ) ;
#36837 = CARTESIAN_POINT ( 'NONE',  ( -5.719274019375665041, -21.55341960407619695, 59.79275706135234714 ) ) ;
#36840 = CARTESIAN_POINT ( 'NONE',  ( -19.05341960407611168, -5.049401038298163336, 91.45724293864766707 ) ) ;
#36841 = CARTESIAN_POINT ( 'NONE',  ( -0.05219959533910754901, -16.53943276465976808, 47.49890960531435979 ) ) ;
#36842 = CARTESIAN_POINT ( 'NONE',  ( -8.314922557961024197, 14.29746914071037800, 112.9177570613523329 ) ) ;
#36843 = AXIS2_PLACEMENT_3D ( 'NONE', #26739, #148076, #41904 ) ;
#36844 = CARTESIAN_POINT ( 'NONE',  ( 12.14591786802309770, 12.06949235617756955, 39.37390960531436690 ) ) ;
#36845 = ORIENTED_EDGE ( 'NONE', *, *, #135302, .T. ) ;
#36846 = DIRECTION ( 'NONE',  ( 0.000000000000000000, 0.000000000000000000, 1.000000000000000000 ) ) ;
#36847 = CARTESIAN_POINT ( 'NONE',  ( -16.51473224551069308, -9.474510206698971260, 61.66557627198103120 ) ) ;
#36848 = CARTESIAN_POINT ( 'NONE',  ( 9.474510206698729675, 16.51473224551082808, 37.08442372801899722 ) ) ;
#36849 = CARTESIAN_POINT ( 'NONE',  ( 36.91746824999999177, 2.880721459617395097E-14, -1.624999997268813390 ) ) ;
#36850 = FACE_OUTER_BOUND ( 'NONE', #163276, .T. ) ;
#36852 = CARTESIAN_POINT ( 'NONE',  ( 12.06949235617739724, 12.14591786802326823, 66.87609039468568994 ) ) ;
#36851 = CARTESIAN_POINT ( 'NONE',  ( 9.564922557961047289, -16.46253265017146816, 80.41775706135234714 ) ) ;
#36853 = CARTESIAN_POINT ( 'NONE',  ( 19.49401214000073779, -12.39993551617566503, 169.9999999999999716 ) ) ;
#36854 = CARTESIAN_POINT ( 'NONE',  ( 19.03943276465977164, -0.05219959533909143690, 93.74890960531435269 ) ) ;
#36855 = CARTESIAN_POINT ( 'NONE',  ( 5.823673210054444382, -21.52544592524334988, 30.20942372801902565 ) ) ;
#36856 = CARTESIAN_POINT ( 'NONE',  ( 16.46253265017146816, 9.564922557961045513, 71.66775706135233293 ) ) ;
#36858 = CARTESIAN_POINT ( 'NONE',  ( -16.51473224551069308, -9.474510206698971260, 46.66557627198102409 ) ) ;
#36857 = CARTESIAN_POINT ( 'NONE',  ( 16.61371651742600619, 7.165104196376166357, 88.64584930007006847 ) ) ;
#36859 = CARTESIAN_POINT ( 'NONE',  ( 13.97604488694527802, 13.89961937509977652, 84.37390960531433848 ) ) ;
#36861 = CARTESIAN_POINT ( 'NONE',  ( 19.05341960407611168, 5.049401038298154454, 48.95724293864768129 ) ) ;
#36860 = CARTESIAN_POINT ( 'NONE',  ( -8.224510206698948167, 14.34966873604960824, 50.41557627198103120 ) ) ;
#36862 = CARTESIAN_POINT ( 'NONE',  ( 5.049401038297881783, 19.05341960407617563, 47.29275706135231161 ) ) ;
#36863 = ORIENTED_EDGE ( 'NONE', *, *, #90031, .F. ) ;
#36864 = CARTESIAN_POINT ( 'NONE',  ( -12.06949235617756955, 12.14591786802309770, 90.62390960531436690 ) ) ;
#36865 = CARTESIAN_POINT ( 'NONE',  ( -13.89961937509957401, -13.97604488694547875, 29.37609039468565797 ) ) ;
#36866 = CARTESIAN_POINT ( 'NONE',  ( -9.564922557960796823, -16.46253265017161027, 67.08224293864769550 ) ) ;
#36867 = AXIS2_PLACEMENT_3D ( 'NONE', #95102, #156791, #30459 ) ;
#36868 = CARTESIAN_POINT ( 'NONE',  ( -10.81492255796078084, -18.62759615963271287, 57.08224293864769550 ) ) ;
#36870 = CARTESIAN_POINT ( 'NONE',  ( 5.049401038297881783, 19.05341960407617563, 27.29275706135232937 ) ) ;
#36869 = CARTESIAN_POINT ( 'NONE',  ( -16.53943276465976808, 0.05219959533911058130, 61.24890960531435979 ) ) ;
#36871 = CARTESIAN_POINT ( 'NONE',  ( 16.46253265017160672, -9.564922557960803928, 108.3322429386476955 ) ) ;
#36872 = CARTESIAN_POINT ( 'NONE',  ( 15.80617190586746368, 15.72974639402197994, 29.37390960531435269 ) ) ;
#36873 = CARTESIAN_POINT ( 'NONE',  ( 13.89961937509977652, -13.97604488694527269, 48.12390960531435979 ) ) ;
#36874 = CARTESIAN_POINT ( 'NONE',  ( 5.049401038298161559, -19.05341960407611168, 42.70724293864767418 ) ) ;
#36875 = CARTESIAN_POINT ( 'NONE',  ( 12.06949235617757843, -12.14591786802309237, 98.12390960531436690 ) ) ;
#36876 = CARTESIAN_POINT ( 'NONE',  ( 21.55341960407610458, 5.719274019375980345, 108.9572429386476955 ) ) ;
#36877 = CARTESIAN_POINT ( 'NONE',  ( -13.97604488694527625, -13.89961937509977652, 106.8739096053143669 ) ) ;
#36878 = CARTESIAN_POINT ( 'NONE',  ( -0.05219959533937732626, 21.53943276465977519, 22.50109039468567573 ) ) ;
#36879 = CARTESIAN_POINT ( 'NONE',  ( 9.474510206698971260, -16.51473224551069308, 107.9155762719810383 ) ) ;
#36880 = CARTESIAN_POINT ( 'NONE',  ( 16.55341960407611168, 4.379528057220329451, 113.9572429386477239 ) ) ;
#36881 = CARTESIAN_POINT ( 'NONE',  ( 5.823673210054444382, -21.52544592524334988, 85.20942372801901854 ) ) ;
#36882 = CARTESIAN_POINT ( 'NONE',  ( -5.823673210054116645, -21.52544592524344225, 92.29057627198103830 ) ) ;
#36883 = LINE ( 'NONE', #15275, #37456 ) ;
#36884 = CARTESIAN_POINT ( 'NONE',  ( -32.00000000000000000, -5.510910596163089556E-15, 39.49999999999996447 ) ) ;
#36885 = CARTESIAN_POINT ( 'NONE',  ( 31.42649584489977244, -1.097581692000379583, -49.72218688481374471 ) ) ;
#36886 = CARTESIAN_POINT ( 'NONE',  ( -12.06949235617739369, -12.14591786802326823, 49.37609039468569705 ) ) ;
#36888 = AXIS2_PLACEMENT_3D ( 'NONE', #52183, #146182, #100678 ) ;
#36887 = CARTESIAN_POINT ( 'NONE',  ( -14.34966873604960291, -8.224510206698953496, 111.6655762719810525 ) ) ;
#36889 = CARTESIAN_POINT ( 'NONE',  ( -17.50000000000002132, -4.049696124445859802, 110.8196032933405775 ) ) ;
#36890 = CARTESIAN_POINT ( 'NONE',  ( 13.89961937509977652, -13.97604488694527269, 58.12390960531436690 ) ) ;
#36891 = CARTESIAN_POINT ( 'NONE',  ( 0.05219959533910956823, 16.53943276465976808, 89.99890960531438111 ) ) ;
#36892 = CARTESIAN_POINT ( 'NONE',  ( 5.719274019375991003, -21.55341960407610458, 47.70724293864770260 ) ) ;
#36893 = CARTESIAN_POINT ( 'NONE',  ( 16.52544592524342804, -4.483927247898539470, 63.54057627198103830 ) ) ;
#36894 = CARTESIAN_POINT ( 'NONE',  ( 12.06949235617739724, 12.14591786802326823, 26.87609039468567218 ) ) ;
#36895 = CARTESIAN_POINT ( 'NONE',  ( 18.62759615963255655, 10.81492255796105972, 71.66775706135234714 ) ) ;
#36896 = AXIS2_PLACEMENT_3D ( 'NONE', #118637, #180329, #17408 ) ;
#36897 = CARTESIAN_POINT ( 'NONE',  ( 17.26172910966779739, -6.454744622555850242, 78.30646908649222837 ) ) ;
#36898 = CARTESIAN_POINT ( 'NONE',  ( 4.379528057220092307, 16.55341960407617563, 92.29275706135236135 ) ) ;
#36899 = CARTESIAN_POINT ( 'NONE',  ( 12.14591786802309770, 12.06949235617756955, 44.37390960531435979 ) ) ;
#36900 = CARTESIAN_POINT ( 'NONE',  ( 9.474510206698971260, -16.51473224551069308, 42.91557627198103120 ) ) ;
#36901 = CARTESIAN_POINT ( 'NONE',  ( 9.474510206698971260, -16.51473224551069308, 92.91557627198103830 ) ) ;
#36902 = CARTESIAN_POINT ( 'NONE',  ( 18.62759615963271287, -10.81492255796078972, 88.33224293864769550 ) ) ;
#36903 = COLOUR_RGB ( '', 0.31764706, 0.68627451, 0.89019608) ;
#36904 = CARTESIAN_POINT ( 'NONE',  ( -12.06949235617739369, -12.14591786802326823, 39.37609039468567573 ) ) ;
#36906 = CARTESIAN_POINT ( 'NONE',  ( -5.719274019375665041, -21.55341960407619695, 69.79275706135234714 ) ) ;
#36905 = CARTESIAN_POINT ( 'NONE',  ( 14.34966873604960469, 8.224510206698951720, 64.16557627198102409 ) ) ;
#36907 = CARTESIAN_POINT ( 'NONE',  ( -14.29746914071037622, -8.314922557961029526, 104.1677570613523471 ) ) ;
#36908 = SPHERICAL_SURFACE ( 'NONE', #172699, 0.5000000000000000000 ) ;
#36909 = DIRECTION ( 'NONE',  ( 1.000000000000000000, 0.000000000000000000, 0.000000000000000000 ) ) ;
#36910 = CARTESIAN_POINT ( 'NONE',  ( 8.314922557960818139, 14.29746914071049879, 24.58224293864768839 ) ) ;
#36911 = CARTESIAN_POINT ( 'NONE',  ( 8.314922557961029526, -14.29746914071037800, 75.41775706135233293 ) ) ;
#36912 = CARTESIAN_POINT ( 'NONE',  ( 9.564922557960805705, 16.46253265017160317, 89.58224293864769550 ) ) ;
#36913 = CARTESIAN_POINT ( 'NONE',  ( -19.02544592524342804, 5.153800228976336051, 101.0405762719810241 ) ) ;
#36914 = CARTESIAN_POINT ( 'NONE',  ( 21.52544592524334988, 5.823673210054432836, 81.45942372801900433 ) ) ;
#36915 = CARTESIAN_POINT ( 'NONE',  ( 8.314922557961029526, -14.29746914071037800, 85.41775706135236135 ) ) ;
#36916 = CARTESIAN_POINT ( 'NONE',  ( -4.379528057220328563, 16.55341960407611168, 55.20724293864770260 ) ) ;
#36917 = CARTESIAN_POINT ( 'NONE',  ( 5.153800228976335163, 19.02544592524342804, 74.79057627198103830 ) ) ;
#36918 = VERTEX_POINT ( 'NONE', #18096 ) ;
#36920 =( BOUNDED_CURVE ( )  B_SPLINE_CURVE ( 2, ( #87042, #133544, #10215, #118390, #88031, #85026, #149719, #196250, #158139, #8203, #19631, #142955, #69878 ),
 .UNSPECIFIED., .F., .T. ) 
 B_SPLINE_CURVE_WITH_KNOTS ( ( 3, 2, 2, 2, 2, 2, 3 ),
 ( 0.3182199101112556661, 0.3201754385964912242, 0.3245614035087719396, 0.3289473684210526550, 0.3333333333333333148, 0.3377192982456140302, 0.3396291469087595050 ),
 .UNSPECIFIED. ) 
 CURVE ( )  GEOMETRIC_REPRESENTATION_ITEM ( )  RATIONAL_B_SPLINE_CURVE ( ( 0.9831626618144004848, 0.9848076720550091867, 1.000000000000000000, 0.9659258262890683122, 1.000000000000000000, 0.9659258262890683122, 1.000000000000000000, 0.9659258262890683122, 1.000000000000000000, 0.9659258262890683122, 1.000000000000000000, 0.9851625545550091179, 0.9832469066685282089 ) ) 
 REPRESENTATION_ITEM ( '' )  );
#36919 = CARTESIAN_POINT ( 'NONE',  ( -5.153800228976607833, 19.02544592524334988, 107.7094237280189759 ) ) ;
#36921 = CARTESIAN_POINT ( 'NONE',  ( -8.314922557960811034, -14.29746914071050412, 112.0822429386477097 ) ) ;
#36922 = CARTESIAN_POINT ( 'NONE',  ( -5.153800228976328057, -19.02544592524343514, 82.29057627198103830 ) ) ;
#36924 = CARTESIAN_POINT ( 'NONE',  ( -22.81625015709509441, -31.40387420917324590, -8.324999997268815122 ) ) ;
#36923 = CARTESIAN_POINT ( 'NONE',  ( -12.06949235617739369, -12.14591786802326823, 24.37609039468567573 ) ) ;
#36925 = CARTESIAN_POINT ( 'NONE',  ( 19.02544592524334988, 5.153800228976608722, 21.45942372801899012 ) ) ;
#36926 = CARTESIAN_POINT ( 'NONE',  ( -16.52544592524335698, -4.483927247898792601, 83.95942372801900433 ) ) ;
#36927 = CARTESIAN_POINT ( 'NONE',  ( -13.89961937509957401, -13.97604488694547875, 94.37609039468566152 ) ) ;
#36928 = CARTESIAN_POINT ( 'NONE',  ( -16.53943276465976808, 0.05219959533911058130, 116.2489096053143669 ) ) ;
#36929 = CARTESIAN_POINT ( 'NONE',  ( 14.29746914071037800, 8.314922557961029526, 66.66775706135234714 ) ) ;
#36930 = CARTESIAN_POINT ( 'NONE',  ( -4.379528057220086978, -16.55341960407618274, 54.79275706135235424 ) ) ;
#36931 = CARTESIAN_POINT ( 'NONE',  ( 27.21324236920355233, -29.31705316289551533, -5.578213269879590541 ) ) ;
#36932 = CARTESIAN_POINT ( 'NONE',  ( -19.03943276465977164, -0.05219959533935918106, 68.75109039468566152 ) ) ;
#36933 = CARTESIAN_POINT ( 'NONE',  ( 18.62759615963255655, 10.81492255796105972, 96.66775706135234714 ) ) ;
#36934 = CARTESIAN_POINT ( 'NONE',  ( -0.05219959533909027116, -19.03943276465977164, 37.49890960531436690 ) ) ;
#36935 = CARTESIAN_POINT ( 'NONE',  ( 16.46253265017160672, -9.564922557960803928, 83.33224293864768129 ) ) ;
#36936 = CARTESIAN_POINT ( 'NONE',  ( 12.06949235617757843, -12.14591786802309237, 78.12390960531436690 ) ) ;
#36937 = AXIS2_PLACEMENT_3D ( 'NONE', #38383, #70723, #132390 ) ;
#36938 = CARTESIAN_POINT ( 'NONE',  ( 10.72451020669871369, 18.67979575497193778, 87.08442372801901854 ) ) ;
#36939 = CARTESIAN_POINT ( 'NONE',  ( -9.564922557961040184, 16.46253265017147172, 37.91775706135233293 ) ) ;
#36940 = CARTESIAN_POINT ( 'NONE',  ( 10.72451020669898902, -18.67979575497178502, 42.91557627198103120 ) ) ;
#36941 = CARTESIAN_POINT ( 'NONE',  ( 15.80617190586769283, -15.72974639402175789, 110.6260903946857042 ) ) ;
#36942 = CARTESIAN_POINT ( 'NONE',  ( 13.89961937509977652, -13.97604488694527269, 78.12390960531433848 ) ) ;
#36943 = CARTESIAN_POINT ( 'NONE',  ( 15.80617190586769283, -15.72974639402175789, 110.6260903946857042 ) ) ;
#36944 = CARTESIAN_POINT ( 'NONE',  ( -18.62759615963270932, 10.81492255796079327, 65.83224293864769550 ) ) ;
#36945 = CARTESIAN_POINT ( 'NONE',  ( 9.564922557960805705, 16.46253265017160317, 99.58224293864770971 ) ) ;
#36946 = CARTESIAN_POINT ( 'NONE',  ( 16.51473224551083163, -9.474510206698727899, 80.83442372801899012 ) ) ;
#36947 = CARTESIAN_POINT ( 'NONE',  ( 5.049401038298161559, -19.05341960407611168, 107.7072429386476955 ) ) ;
#36948 = CARTESIAN_POINT ( 'NONE',  ( -5.049401038297874678, -19.05341960407617918, 89.79275706135230450 ) ) ;
#36949 = CARTESIAN_POINT ( 'NONE',  ( -0.05219959533934338120, 16.53943276465976808, 47.50109039468568994 ) ) ;
#36950 = CARTESIAN_POINT ( 'NONE',  ( -16.52544592524342804, 4.483927247898546575, 116.0405762719810383 ) ) ;
#36951 = CARTESIAN_POINT ( 'NONE',  ( 9.474510206698971260, -16.51473224551069308, 82.91557627198103830 ) ) ;
#36952 = CARTESIAN_POINT ( 'NONE',  ( 5.719274019375991003, -21.55341960407610458, 57.70724293864770260 ) ) ;
#36953 = CARTESIAN_POINT ( 'NONE',  ( -4.483927247898782831, 16.52544592524335698, 27.70942372801901854 ) ) ;
#36954 = CARTESIAN_POINT ( 'NONE',  ( -18.67979575497193778, 10.72451020669871902, 28.33442372801902209 ) ) ;
#36955 = CARTESIAN_POINT ( 'NONE',  ( 15.80617190586769283, -15.72974639402175789, 80.62609039468567573 ) ) ;
#36956 = CARTESIAN_POINT ( 'NONE',  ( -16.52544592524335698, -4.483927247898792601, 88.95942372801901854 ) ) ;
#36957 = CARTESIAN_POINT ( 'NONE',  ( 19.03943276465977164, -0.05219959533909143690, 88.74890960531436690 ) ) ;
#36958 = CARTESIAN_POINT ( 'NONE',  ( 14.29746914071049879, -8.314922557960816363, 73.33224293864769550 ) ) ;
#36959 = CARTESIAN_POINT ( 'NONE',  ( -4.483927247898782831, 16.52544592524335698, 112.7094237280190328 ) ) ;
#36960 = CARTESIAN_POINT ( 'NONE',  ( 5.153800228976615827, -19.02544592524334988, 55.20942372801899722 ) ) ;
#36961 = EDGE_CURVE ( 'NONE', #34941, #114568, #105011, .T. ) ;
#36962 = CARTESIAN_POINT ( 'NONE',  ( 5.823673210054444382, -21.52544592524334988, 45.20942372801901854 ) ) ;
#36963 = CARTESIAN_POINT ( 'NONE',  ( -16.53943276465976808, 0.05219959533911058130, 96.24890960531435269 ) ) ;
#36964 = CARTESIAN_POINT ( 'NONE',  ( -13.89961937509977652, 13.97604488694528158, 110.6239096053143243 ) ) ;
#36965 = CARTESIAN_POINT ( 'NONE',  ( -16.52544592524335698, -4.483927247898792601, 98.95942372801903275 ) ) ;
#36966 = CARTESIAN_POINT ( 'NONE',  ( 0.05219959533937995610, -21.53943276465977519, 90.00109039468567573 ) ) ;
#36967 = CARTESIAN_POINT ( 'NONE',  ( 14.29746914071037800, 8.314922557961029526, 51.66775706135234714 ) ) ;
#36968 = CARTESIAN_POINT ( 'NONE',  ( -0.05219959533937732626, 21.53943276465977519, 42.50109039468567573 ) ) ;
#36969 = ORIENTED_EDGE ( 'NONE', *, *, #58065, .F. ) ;
#36970 = CARTESIAN_POINT ( 'NONE',  ( 5.823673210054444382, -21.52544592524334988, 20.20942372801900788 ) ) ;
#36971 = CARTESIAN_POINT ( 'NONE',  ( 16.55341960407611168, 4.379528057220329451, 93.95724293864770971 ) ) ;
#36972 = CARTESIAN_POINT ( 'NONE',  ( 17.50000000000001421, -3.209263204892543353, 27.26196825606273322 ) ) ;
#36973 = CARTESIAN_POINT ( 'NONE',  ( 8.314922557960818139, 14.29746914071049879, 69.58224293864769550 ) ) ;
#36974 = CARTESIAN_POINT ( 'NONE',  ( -12.06949235617739369, -12.14591786802326823, 99.37609039468568994 ) ) ;
#36975 = CARTESIAN_POINT ( 'NONE',  ( 19.05341960407611168, 5.049401038298154454, 33.95724293864769550 ) ) ;
#36976 = ADVANCED_FACE ( 'NONE', ( #144395 ), #145391, .F. ) ;
#36977 = CARTESIAN_POINT ( 'NONE',  ( -21.55341960407610458, -5.719274019375992779, 46.45724293864769550 ) ) ;
#36978 = CARTESIAN_POINT ( 'NONE',  ( 4.379528057220339221, -16.55341960407611168, 77.70724293864770971 ) ) ;
#36979 = CARTESIAN_POINT ( 'NONE',  ( -5.719274019375978568, 21.55341960407610458, 75.20724293864769550 ) ) ;
#36980 = CARTESIAN_POINT ( 'NONE',  ( -13.89961937509977652, 13.97604488694528158, 90.62390960531432427 ) ) ;
#36982 = CARTESIAN_POINT ( 'NONE',  ( -19.03943276465977164, -0.05219959533935918106, 93.75109039468566152 ) ) ;
#36981 = CARTESIAN_POINT ( 'NONE',  ( 5.049401038298161559, -19.05341960407611168, 32.70724293864768129 ) ) ;
#36983 = CARTESIAN_POINT ( 'NONE',  ( -5.719274019375978568, 21.55341960407610458, 35.20724293864768839 ) ) ;
#36984 = CARTESIAN_POINT ( 'NONE',  ( 10.72451020669871369, 18.67979575497193778, 57.08442372801901854 ) ) ;
#36985 = CARTESIAN_POINT ( 'NONE',  ( 9.564922557960805705, 16.46253265017160317, 59.58224293864769550 ) ) ;
#36986 = CARTESIAN_POINT ( 'NONE',  ( 19.02544592524343514, -5.153800228976328945, 83.54057627198100988 ) ) ;
#36987 = ORIENTED_EDGE ( 'NONE', *, *, #76762, .F. ) ;
#36988 = CARTESIAN_POINT ( 'NONE',  ( -16.52544592524335698, -4.483927247898792601, 48.95942372801902565 ) ) ;
#36989 = CARTESIAN_POINT ( 'NONE',  ( 0.05219959533937995610, -21.53943276465977519, 40.00109039468567573 ) ) ;
#36990 = AXIS2_PLACEMENT_3D ( 'NONE', #84875, #24243, #130374 ) ;
#36991 = CARTESIAN_POINT ( 'NONE',  ( -10.81492255796105439, 18.62759615963255655, 77.91775706135231871 ) ) ;
#36992 = CARTESIAN_POINT ( 'NONE',  ( 19.03943276465977164, -0.05219959533909143690, 113.7489096053143669 ) ) ;
#36993 = CARTESIAN_POINT ( 'NONE',  ( 21.52544592524344225, -5.823673210054117533, 88.54057627198103830 ) ) ;
#36995 = CARTESIAN_POINT ( 'NONE',  ( -14.34966873604972548, 8.224510206698743886, 68.33442372801900433 ) ) ;
#36994 = CARTESIAN_POINT ( 'NONE',  ( 10.81492255796106328, -18.62759615963255655, 30.41775706135234358 ) ) ;
#36996 = CARTESIAN_POINT ( 'NONE',  ( 5.719274019375991003, -21.55341960407610458, 62.70724293864769550 ) ) ;
#36997 = CARTESIAN_POINT ( 'NONE',  ( -0.05219959533937732626, 21.53943276465977519, 112.5010903946857042 ) ) ;
#36999 = CARTESIAN_POINT ( 'NONE',  ( -14.29746914071037622, -8.314922557961029526, 99.16775706135234714 ) ) ;
#36998 = CARTESIAN_POINT ( 'NONE',  ( -9.564922557960796823, -16.46253265017161027, 72.08224293864770971 ) ) ;
#37000 = CARTESIAN_POINT ( 'NONE',  ( -17.49999999999999645, -5.500000000000000888, 104.2030961746582847 ) ) ;
#37001 = CARTESIAN_POINT ( 'NONE',  ( 19.05341960407611168, 5.049401038298154454, 83.95724293864766707 ) ) ;
#37002 = CARTESIAN_POINT ( 'NONE',  ( 17.50000000000005329, 3.734851586428519887, 103.1808203866947480 ) ) ;
#37003 = CARTESIAN_POINT ( 'NONE',  ( -19.05341960407617563, 5.049401038297882671, 78.54275706135233293 ) ) ;
#37004 = CARTESIAN_POINT ( 'NONE',  ( 18.67979575497178502, 10.72451020669898547, 54.16557627198103120 ) ) ;
#37005 = CARTESIAN_POINT ( 'NONE',  ( -16.55341960407611168, -4.379528057220339221, 21.45724293864769550 ) ) ;
#37006 = CARTESIAN_POINT ( 'NONE',  ( 19.03943276465977164, 0.05219959533936151252, 101.2510903946856757 ) ) ;
#37007 = CARTESIAN_POINT ( 'NONE',  ( 0.05219959533909260263, 19.03943276465977164, 39.99890960531436690 ) ) ;
#37008 = CARTESIAN_POINT ( 'NONE',  ( -16.51473224551082808, 9.474510206698731452, 93.33442372801900433 ) ) ;
#37010 = CARTESIAN_POINT ( 'NONE',  ( -19.02544592524334988, -5.153800228976617603, 58.95942372801900433 ) ) ;
#37009 = CARTESIAN_POINT ( 'NONE',  ( 15.80617190586746368, 15.72974639402197994, 89.37390960531435269 ) ) ;
#37011 = CARTESIAN_POINT ( 'NONE',  ( 26.58496454516998142, -7.626754437231455519, 167.9682100371138915 ) ) ;
#37012 = CARTESIAN_POINT ( 'NONE',  ( 0.05219959533909260263, 19.03943276465977164, 49.99890960531435979 ) ) ;
#37013 = CARTESIAN_POINT ( 'NONE',  ( -12.14591786802309592, -12.06949235617757132, 56.87390960531436690 ) ) ;
#37014 = AXIS2_PLACEMENT_3D ( 'NONE', #63551, #45402, #64547 ) ;
#37015 = CARTESIAN_POINT ( 'NONE',  ( -19.05341960407611168, -5.049401038298163336, 46.45724293864768129 ) ) ;
#37016 = CARTESIAN_POINT ( 'NONE',  ( -14.29746914071049879, 8.314922557960819915, 55.83224293864770260 ) ) ;
#37017 = CARTESIAN_POINT ( 'NONE',  ( -30.65641173115115947, -25.45263461537911098, -21.37460845010010146 ) ) ;
#37018 = CARTESIAN_POINT ( 'NONE',  ( 0.4369134036781218144, 21.36090571693007334, -56.42503783362397485 ) ) ;
#37019 = CARTESIAN_POINT ( 'NONE',  ( 16.53943276465976808, -0.05219959533910856209, 28.74890960531435624 ) ) ;
#37020 = CARTESIAN_POINT ( 'NONE',  ( 19.02544592524343514, -5.153800228976328945, 68.54057627198103830 ) ) ;
#37021 = FACE_BOUND ( 'NONE', #112637, .T. ) ;
#37022 = CARTESIAN_POINT ( 'NONE',  ( -19.03943276465977164, -0.05219959533935918106, 38.75109039468566152 ) ) ;
#37023 = CARTESIAN_POINT ( 'NONE',  ( -16.55341960407617563, 4.379528057220093196, 53.54275706135234714 ) ) ;
#37024 = CARTESIAN_POINT ( 'NONE',  ( 15.72974639402199770, -15.80617190586745480, 53.12390960531436690 ) ) ;
#37025 = CARTESIAN_POINT ( 'NONE',  ( 10.81492255796106328, -18.62759615963255655, 105.4177570613523613 ) ) ;
#37026 = CARTESIAN_POINT ( 'NONE',  ( -16.51473224551069308, -9.474510206698971260, 76.66557627198103830 ) ) ;
#37027 = DIRECTION ( 'NONE',  ( -0.000000000000000000, -0.000000000000000000, 1.000000000000000000 ) ) ;
#37028 = CARTESIAN_POINT ( 'NONE',  ( 9.474510206698971260, -16.51473224551069308, 102.9155762719810241 ) ) ;
#37029 = CARTESIAN_POINT ( 'NONE',  ( 11.40812507854754365, 35.11059874428196537, -5.224999997268813701 ) ) ;
#37030 = CARTESIAN_POINT ( 'NONE',  ( 15.72974639402176855, 15.80617190586768217, 26.87609039468567218 ) ) ;
#37031 = CARTESIAN_POINT ( 'NONE',  ( -16.53943276465976808, 0.05219959533911058130, 91.24890960531436690 ) ) ;
#37032 = EDGE_CURVE ( 'NONE', #137833, #66922, #192917, .T. ) ;
#37034 = CARTESIAN_POINT ( 'NONE',  ( 13.97604488694527802, 13.89961937509977652, 84.37390960531433848 ) ) ;
#37033 = CARTESIAN_POINT ( 'NONE',  ( 15.80617190586746368, 15.72974639402197994, 84.37390960531438111 ) ) ;
#37035 = CARTESIAN_POINT ( 'NONE',  ( -19.03943276465977164, 0.05219959533909376836, 91.24890960531436690 ) ) ;
#37036 = CARTESIAN_POINT ( 'NONE',  ( -10.81492255796078084, -18.62759615963271287, 107.0822429386476955 ) ) ;
#37037 = VECTOR ( 'NONE', #118877, 1000.000000000000000 ) ;
#37038 = EDGE_LOOP ( 'NONE', ( #35366, #25455, #100433, #167919, #52391 ) ) ;
#37039 = CARTESIAN_POINT ( 'NONE',  ( 5.153800228976335163, 19.02544592524342804, 79.79057627198102409 ) ) ;
#37040 = DIRECTION ( 'NONE',  ( 0.8660254037844392627, 0.000000000000000000, 0.4999999999999988898 ) ) ;
#37042 = CARTESIAN_POINT ( 'NONE',  ( -16.51473224551069308, -9.474510206698971260, 31.66557627198102054 ) ) ;
#37041 = CARTESIAN_POINT ( 'NONE',  ( 16.53943276465976808, -0.05219959533910856209, 108.7489096053143669 ) ) ;
#37043 = CARTESIAN_POINT ( 'NONE',  ( -16.46253265017146816, -9.564922557961047289, 99.16775706135233293 ) ) ;
#37044 = VECTOR ( 'NONE', #183640, 1000.000000000000000 ) ;
#37045 = CARTESIAN_POINT ( 'NONE',  ( -16.53943276465976808, 0.05219959533911058130, 106.2489096053143811 ) ) ;
#37046 = CARTESIAN_POINT ( 'NONE',  ( -21.53943276465977519, -0.05219959533937600094, 73.75109039468567573 ) ) ;
#37048 = CARTESIAN_POINT ( 'NONE',  ( 15.80617190586769283, -15.72974639402175789, 35.62609039468568994 ) ) ;
#37047 = CARTESIAN_POINT ( 'NONE',  ( -19.02544592524342804, 5.153800228976336051, 66.04057627198103830 ) ) ;
#37049 = CARTESIAN_POINT ( 'NONE',  ( -5.719274019375665041, -21.55341960407619695, 19.79275706135235069 ) ) ;
#37050 = CARTESIAN_POINT ( 'NONE',  ( -5.359611314223446995E-15, 29.16686587814335496, 140.8750000027311842 ) ) ;
#37051 = CARTESIAN_POINT ( 'NONE',  ( 9.564922557960805705, 16.46253265017160317, 84.58224293864769550 ) ) ;
#37052 = CARTESIAN_POINT ( 'NONE',  ( 21.08520368033286729, 18.30394477064738012, 139.9999999999999716 ) ) ;
#37054 = CARTESIAN_POINT ( 'NONE',  ( 15.80617190586746368, 15.72974639402197994, 29.37390960531435269 ) ) ;
#37053 = CARTESIAN_POINT ( 'NONE',  ( 4.483927247898790824, -16.52544592524335698, 25.20942372801901854 ) ) ;
#37055 = CARTESIAN_POINT ( 'NONE',  ( 10.81492255796106328, -18.62759615963255655, 65.41775706135234714 ) ) ;
#37056 = CARTESIAN_POINT ( 'NONE',  ( -19.02544592524342804, 5.153800228976336051, 111.0405762719810099 ) ) ;
#37057 = CARTESIAN_POINT ( 'NONE',  ( 16.46253265017146816, 9.564922557961045513, 101.6677570613523329 ) ) ;
#37058 = CARTESIAN_POINT ( 'NONE',  ( -5.153800228976328057, -19.02544592524343514, 47.29057627198102409 ) ) ;
#37059 = CARTESIAN_POINT ( 'NONE',  ( 0.05219959533909260263, 19.03943276465977164, 79.99890960531436690 ) ) ;
#37060 = CARTESIAN_POINT ( 'NONE',  ( 8.314922557960818139, 14.29746914071049879, 99.58224293864770971 ) ) ;
#37061 = CARTESIAN_POINT ( 'NONE',  ( -16.51473224551069308, -9.474510206698971260, 96.66557627198102409 ) ) ;
#37062 = CARTESIAN_POINT ( 'NONE',  ( -8.224510206698948167, 14.34966873604960824, 90.41557627198103830 ) ) ;
#37063 = CARTESIAN_POINT ( 'NONE',  ( -19.05341960407611168, -5.049401038298163336, 111.4572429386476671 ) ) ;
#37065 = CARTESIAN_POINT ( 'NONE',  ( -19.02544592524342804, 5.153800228976336051, 41.04057627198103120 ) ) ;
#37064 = CARTESIAN_POINT ( 'NONE',  ( -14.34966873604960291, -8.224510206698953496, 56.66557627198103830 ) ) ;
#37066 = CARTESIAN_POINT ( 'NONE',  ( -21.55341960407619339, 5.719274019375674811, 63.54275706135234003 ) ) ;
#37067 = CARTESIAN_POINT ( 'NONE',  ( 9.564922557961047289, -16.46253265017146816, 95.41775706135233293 ) ) ;
#37068 = CARTESIAN_POINT ( 'NONE',  ( 16.52544592524342804, -4.483927247898539470, 48.54057627198103120 ) ) ;
#37069 = CARTESIAN_POINT ( 'NONE',  ( 18.62759615963271287, -10.81492255796078972, 108.3322429386477097 ) ) ;
#37070 = CARTESIAN_POINT ( 'NONE',  ( -15.72974639402197994, 15.80617190586746368, 45.62390960531436690 ) ) ;
#37071 = CARTESIAN_POINT ( 'NONE',  ( 18.22780087662122739, 5.500000000000000888, 71.48236817873106475 ) ) ;
#37072 = CARTESIAN_POINT ( 'NONE',  ( 8.906447517083057264, -27.41122689804191026, 140.8500000054623911 ) ) ;
#37073 = CARTESIAN_POINT ( 'NONE',  ( -19.05341960407611168, -5.049401038298163336, 51.45724293864770260 ) ) ;
#37074 = CARTESIAN_POINT ( 'NONE',  ( -4.483927247898539470, -16.52544592524342804, 22.29057627198102765 ) ) ;
#37075 = AXIS2_PLACEMENT_3D ( 'NONE', #21616, #96448, #143954 ) ;
#37076 = CARTESIAN_POINT ( 'NONE',  ( -14.29746914071037622, -8.314922557961029526, 99.16775706135234714 ) ) ;
#37077 = CARTESIAN_POINT ( 'NONE',  ( -8.224510206698735004, -14.34966873604973081, 84.58442372801903275 ) ) ;
#37078 = CARTESIAN_POINT ( 'NONE',  ( -9.474510206698720793, -16.51473224551083518, 39.58442372801899722 ) ) ;
#37079 = CARTESIAN_POINT ( 'NONE',  ( 35.99626262588764547, 2.869439944428138037E-14, 2.000000000000000000 ) ) ;
#37080 = CARTESIAN_POINT ( 'NONE',  ( -9.564922557960796823, -16.46253265017161027, 97.08224293864769550 ) ) ;
#37081 = CARTESIAN_POINT ( 'NONE',  ( -5.153800228976328057, -19.02544592524343514, 57.29057627198103120 ) ) ;
#37082 = CARTESIAN_POINT ( 'NONE',  ( -14.29746914071049879, 8.314922557960819915, 55.83224293864770260 ) ) ;
#37084 = CARTESIAN_POINT ( 'NONE',  ( 5.153800228976335163, 19.02544592524342804, 109.7905762719810099 ) ) ;
#37083 = CARTESIAN_POINT ( 'NONE',  ( 17.72517630441460312, -5.499999999999972466, 48.42175719257602395 ) ) ;
#37085 = CARTESIAN_POINT ( 'NONE',  ( 5.719274019375991003, -21.55341960407610458, 37.70724293864769550 ) ) ;
#37086 = CARTESIAN_POINT ( 'NONE',  ( -16.52544592524342804, 4.483927247898546575, 86.04057627198102409 ) ) ;
#37087 = CARTESIAN_POINT ( 'NONE',  ( -16.55341960407617563, 4.379528057220093196, 43.54275706135235424 ) ) ;
#37088 = CARTESIAN_POINT ( 'NONE',  ( 8.314922557960818139, 14.29746914071049879, 84.58224293864769550 ) ) ;
#37089 = CARTESIAN_POINT ( 'NONE',  ( 11.30153831258470731, -180.0000000000000000, -15.00000000000000000 ) ) ;
#37090 = CARTESIAN_POINT ( 'NONE',  ( 5.049401038297881783, 19.05341960407617563, 72.29275706135234714 ) ) ;
#37091 = CARTESIAN_POINT ( 'NONE',  ( -0.05219959533909027116, -19.03943276465977164, 97.49890960531436690 ) ) ;
#37092 = CARTESIAN_POINT ( 'NONE',  ( -13.97604488694547697, 13.89961937509957934, 78.12609039468567573 ) ) ;
#37093 = CARTESIAN_POINT ( 'NONE',  ( -20.83652723102587245, 20.12987255291484345, -52.58065409862962269 ) ) ;
#37095 = CARTESIAN_POINT ( 'NONE',  ( 16.53943276465976808, 0.05219959533934440121, 111.2510903946856899 ) ) ;
#37094 = CARTESIAN_POINT ( 'NONE',  ( -16.55341960407617563, 4.379528057220093196, 28.54275706135234358 ) ) ;
#37096 = CARTESIAN_POINT ( 'NONE',  ( -19.02544592524334988, -5.153800228976617603, 73.95942372801900433 ) ) ;
#37097 = CARTESIAN_POINT ( 'NONE',  ( 10.72451020669898902, -18.67979575497178502, 37.91557627198102409 ) ) ;
#37098 = CARTESIAN_POINT ( 'NONE',  ( -15.80617190586768217, 15.72974639402176855, 63.12609039468568994 ) ) ;
#37099 = CARTESIAN_POINT ( 'NONE',  ( -23.34492853952158242, -11.48509598731697068, 165.7658222004386914 ) ) ;
#37100 = CARTESIAN_POINT ( 'NONE',  ( 16.53943276465976808, 0.05219959533934440121, 31.25109039468568639 ) ) ;
#37102 = CARTESIAN_POINT ( 'NONE',  ( -5.049401038298153566, 19.05341960407611168, 90.20724293864766707 ) ) ;
#37101 = CARTESIAN_POINT ( 'NONE',  ( -19.05341960407611168, -5.049401038298163336, 26.45724293864769550 ) ) ;
#37103 = CARTESIAN_POINT ( 'NONE',  ( -9.474510206698964154, 16.51473224551069663, 25.41557627198103120 ) ) ;
#37104 = CARTESIAN_POINT ( 'NONE',  ( 4.379528057220339221, -16.55341960407611168, 82.70724293864770971 ) ) ;
#37105 = CARTESIAN_POINT ( 'NONE',  ( -13.97604488694527625, -13.89961937509977652, 86.87390960531436690 ) ) ;
#37106 = ORIENTED_EDGE ( 'NONE', *, *, #99048, .T. ) ;
#37107 = CARTESIAN_POINT ( 'NONE',  ( -19.02544592524334988, -5.153800228976617603, 98.95942372801900433 ) ) ;
#37108 = CARTESIAN_POINT ( 'NONE',  ( -21.53943276465977519, 0.05219959533907696930, 71.24890960531435269 ) ) ;
#37109 = CARTESIAN_POINT ( 'NONE',  ( -19.05341960407611168, -5.049401038298163336, 41.45724293864769550 ) ) ;
#37111 = CARTESIAN_POINT ( 'NONE',  ( 5.823673210054444382, -21.52544592524334988, 20.20942372801900788 ) ) ;
#37110 = CARTESIAN_POINT ( 'NONE',  ( 13.97604488694548053, -13.89961937509957401, 75.62609039468564731 ) ) ;
#37112 = CARTESIAN_POINT ( 'NONE',  ( -19.02544592524342804, 5.153800228976336051, 66.04057627198103830 ) ) ;
#37113 = CARTESIAN_POINT ( 'NONE',  ( -19.05341960407611168, -5.049401038298163336, 111.4572429386476671 ) ) ;
#37114 = ORIENTED_EDGE ( 'NONE', *, *, #125633, .F. ) ;
#37115 = CARTESIAN_POINT ( 'NONE',  ( 8.314922557961029526, -14.29746914071037800, 40.41775706135234714 ) ) ;
#37116 = CARTESIAN_POINT ( 'NONE',  ( 5.719274019375991003, -21.55341960407610458, 107.7072429386476955 ) ) ;
#37119 = CARTESIAN_POINT ( 'NONE',  ( -19.02544592524334988, -5.153800228976617603, 63.95942372801899012 ) ) ;
#37118 = CARTESIAN_POINT ( 'NONE',  ( -5.153800228976328057, -19.02544592524343514, 97.29057627198099567 ) ) ;
#37117 = CARTESIAN_POINT ( 'NONE',  ( -4.483927247898539470, -16.52544592524342804, 112.2905762719810241 ) ) ;
#37120 = CARTESIAN_POINT ( 'NONE',  ( 0.05219959533907565091, 21.53943276465977519, 84.99890960531436690 ) ) ;
#37121 = CARTESIAN_POINT ( 'NONE',  ( 10.72451020669898902, -18.67979575497178502, 92.91557627198103830 ) ) ;
#37122 = CARTESIAN_POINT ( 'NONE',  ( 16.53943276465976808, -0.05219959533910856209, 48.74890960531435979 ) ) ;
#37123 = CARTESIAN_POINT ( 'NONE',  ( -16.51473224551082808, 9.474510206698731452, 23.33442372801900078 ) ) ;
#37124 = CARTESIAN_POINT ( 'NONE',  ( -0.05219959533934338120, 16.53943276465976808, 62.50109039468568284 ) ) ;
#37125 = CARTESIAN_POINT ( 'NONE',  ( 19.03943276465977164, -0.05219959533909143690, 93.74890960531435269 ) ) ;
#37126 = CARTESIAN_POINT ( 'NONE',  ( -13.89961937509977652, 13.97604488694528158, 40.62390960531435979 ) ) ;
#37127 = CARTESIAN_POINT ( 'NONE',  ( 15.72974639402176855, 15.80617190586768217, 51.87609039468568284 ) ) ;
#37128 = CARTESIAN_POINT ( 'NONE',  ( -0.05219959533937732626, 21.53943276465977519, 72.50109039468568994 ) ) ;
#37129 = CARTESIAN_POINT ( 'NONE',  ( -13.89961937509977652, 13.97604488694528158, 65.62390960531436690 ) ) ;
#37130 = CARTESIAN_POINT ( 'NONE',  ( -5.719274019375665041, -21.55341960407619695, 39.79275706135235424 ) ) ;
#37131 = CARTESIAN_POINT ( 'NONE',  ( -9.474510206698720793, -16.51473224551083518, 74.58442372801900433 ) ) ;
#37132 = CARTESIAN_POINT ( 'NONE',  ( -19.02544592524334988, -5.153800228976617603, 78.95942372801900433 ) ) ;
#37133 = CARTESIAN_POINT ( 'NONE',  ( 9.474510206698971260, -16.51473224551069308, 37.91557627198102409 ) ) ;
#37134 = CARTESIAN_POINT ( 'NONE',  ( -14.34966873604972548, 8.224510206698743886, 88.33442372801901854 ) ) ;
#37135 = CARTESIAN_POINT ( 'NONE',  ( -19.03943276465977164, 0.05219959533909376836, 46.24890960531435979 ) ) ;
#37136 = CARTESIAN_POINT ( 'NONE',  ( 23.19706360625304598, -11.80427776162576592, 165.7059442611692361 ) ) ;
#37137 = CARTESIAN_POINT ( 'NONE',  ( -19.05341960407611168, -5.049401038298163336, 96.45724293864769550 ) ) ;
#37138 = CARTESIAN_POINT ( 'NONE',  ( 16.51473224551069308, 9.474510206698969483, 39.16557627198103120 ) ) ;
#37139 = AXIS2_PLACEMENT_3D ( 'NONE', #40384, #163743, #34899 ) ;
#37140 = CARTESIAN_POINT ( 'NONE',  ( 18.62759615963271287, -10.81492255796078972, 83.33224293864769550 ) ) ;
#37141 = CARTESIAN_POINT ( 'NONE',  ( 12.14591786802327356, -12.06949235617739191, 65.62609039468568994 ) ) ;
#37142 = CARTESIAN_POINT ( 'NONE',  ( 19.02544592524334988, 5.153800228976608722, 31.45942372801900433 ) ) ;
#37143 = CARTESIAN_POINT ( 'NONE',  ( -13.97604488694527625, -13.89961937509977652, 51.87390960531436690 ) ) ;
#37144 = CARTESIAN_POINT ( 'NONE',  ( -0.05219959533910754901, -16.53943276465976808, 47.49890960531435979 ) ) ;
#37145 = CARTESIAN_POINT ( 'NONE',  ( -16.55341960407611168, -4.379528057220339221, 86.45724293864770971 ) ) ;
#37146 = CARTESIAN_POINT ( 'NONE',  ( 9.564922557960805705, 16.46253265017160317, 74.58224293864769550 ) ) ;
#37147 = CARTESIAN_POINT ( 'NONE',  ( 18.67979575497194134, -10.72451020669871369, 30.83442372801902209 ) ) ;
#37148 = CARTESIAN_POINT ( 'NONE',  ( 19.05341960407611168, 5.049401038298154454, 98.95724293864766707 ) ) ;
#37149 = CARTESIAN_POINT ( 'NONE',  ( 5.719274019375673035, 21.55341960407619339, 102.2927570613523613 ) ) ;
#37150 = CARTESIAN_POINT ( 'NONE',  ( -14.34966873604972548, 8.224510206698743886, 83.33442372801903275 ) ) ;
#37151 = CARTESIAN_POINT ( 'NONE',  ( 15.80617190586769283, -15.72974639402175789, 30.62609039468567929 ) ) ;
#37152 = CARTESIAN_POINT ( 'NONE',  ( -5.719274019375978568, 21.55341960407610458, 95.20724293864769550 ) ) ;
#37153 = CARTESIAN_POINT ( 'NONE',  ( 8.224510206698953496, -14.34966873604960469, 42.91557627198103120 ) ) ;
#37155 = CARTESIAN_POINT ( 'NONE',  ( -5.049401038298153566, 19.05341960407611168, 35.20724293864768839 ) ) ;
#37154 = AXIS2_PLACEMENT_3D ( 'NONE', #73026, #86176, #23514 ) ;
#37156 = CARTESIAN_POINT ( 'NONE',  ( 0.05219959533910956823, 16.53943276465976808, 64.99890960531435269 ) ) ;
#37157 = CARTESIAN_POINT ( 'NONE',  ( -15.80617190586745835, -15.72974639402198527, 31.87390960531435979 ) ) ;
#37158 = CARTESIAN_POINT ( 'NONE',  ( 16.46253265017146816, 9.564922557961045513, 31.66775706135232937 ) ) ;
#37159 = CARTESIAN_POINT ( 'NONE',  ( 8.314922557960818139, 14.29746914071049879, 94.58224293864769550 ) ) ;
#37160 = CARTESIAN_POINT ( 'NONE',  ( 19.03943276465977164, -0.05219959533909143690, 113.7489096053143669 ) ) ;
#37161 = ORIENTED_EDGE ( 'NONE', *, *, #99437, .F. ) ;
#37162 = CARTESIAN_POINT ( 'NONE',  ( -16.53943276465976808, -0.05219959533934237506, 48.75109039468568284 ) ) ;
#37163 = CARTESIAN_POINT ( 'NONE',  ( 0.05219959533909260263, 19.03943276465977164, 54.99890960531435979 ) ) ;
#37164 = CARTESIAN_POINT ( 'NONE',  ( -16.66274659544009040, -6.346227724781252633, 20.60845629695331027 ) ) ;
#37165 = CARTESIAN_POINT ( 'NONE',  ( -16.55341960407617563, 4.379528057220093196, 88.54275706135236135 ) ) ;
#37166 = CARTESIAN_POINT ( 'NONE',  ( -13.89961937509957401, -13.97604488694547875, 109.3760903946856331 ) ) ;
#37167 = CARTESIAN_POINT ( 'NONE',  ( 10.81492255796106328, -18.62759615963255655, 85.41775706135236135 ) ) ;
#37168 = CARTESIAN_POINT ( 'NONE',  ( 5.049401038298161559, -19.05341960407611168, 77.70724293864765286 ) ) ;
#37169 = CARTESIAN_POINT ( 'NONE',  ( 18.67979575497178502, 10.72451020669898547, 109.1655762719810383 ) ) ;
#37170 = CARTESIAN_POINT ( 'NONE',  ( -0.05219959533934338120, 16.53943276465976808, 52.50109039468567573 ) ) ;
#37172 = CARTESIAN_POINT ( 'NONE',  ( 16.52544592524342804, -4.483927247898539470, 113.5405762719810383 ) ) ;
#37171 = AXIS2_PLACEMENT_3D ( 'NONE', #50464, #191948, #82760 ) ;
#37173 = CARTESIAN_POINT ( 'NONE',  ( 16.52544592524335698, 4.483927247898782831, 21.45942372801901499 ) ) ;
#37174 = CARTESIAN_POINT ( 'NONE',  ( -16.46253265017146816, -9.564922557961047289, 79.16775706135234714 ) ) ;
#37175 = CARTESIAN_POINT ( 'NONE',  ( -0.05219959533907301413, -21.53943276465977519, 82.49890960531436690 ) ) ;
#37176 = CARTESIAN_POINT ( 'NONE',  ( -16.46253265017146816, -9.564922557961047289, 49.16775706135233293 ) ) ;
#37177 = DIRECTION ( 'NONE',  ( 0.000000000000000000, 0.000000000000000000, -1.000000000000000000 ) ) ;
#37178 = CARTESIAN_POINT ( 'NONE',  ( 15.80617190586746368, 15.72974639402197994, 109.3739096053143811 ) ) ;
#37179 = CARTESIAN_POINT ( 'NONE',  ( 17.49999999999999645, 5.076555817581254182, 28.67951492049776974 ) ) ;
#37180 = CARTESIAN_POINT ( 'NONE',  ( 19.03943276465977164, -0.05219959533909143690, 63.74890960531435979 ) ) ;
#37181 = CIRCLE ( 'NONE', #88878, 0.5000000000000004441 ) ;
#37182 = DIRECTION ( 'NONE',  ( -1.000000000000000000, -0.000000000000000000, -0.000000000000000000 ) ) ;
#37183 = CARTESIAN_POINT ( 'NONE',  ( -8.224510206698735004, -14.34966873604973081, 19.58442372801901143 ) ) ;
#37184 = CARTESIAN_POINT ( 'NONE',  ( 23.71437531004595911, 10.61261859643795091, 165.9743991446059965 ) ) ;
#37185 = CARTESIAN_POINT ( 'NONE',  ( -5.823673210054431948, 21.52544592524334988, 57.70942372801901143 ) ) ;
#37187 = CARTESIAN_POINT ( 'NONE',  ( 0.05219959533910956823, 16.53943276465976808, 69.99890960531435269 ) ) ;
#37186 = CARTESIAN_POINT ( 'NONE',  ( 10.72451020669898902, -18.67979575497178502, 102.9155762719810383 ) ) ;
#37188 = CARTESIAN_POINT ( 'NONE',  ( 13.97604488694527802, 13.89961937509977652, 74.37390960531436690 ) ) ;
#37189 = AXIS2_PLACEMENT_3D ( 'NONE', #162885, #164900, #24394 ) ;
#37190 = CARTESIAN_POINT ( 'NONE',  ( -10.72451020669870658, -18.67979575497194134, 79.58442372801903275 ) ) ;
#37192 = CARTESIAN_POINT ( 'NONE',  ( -16.51473224551082808, 9.474510206698731452, 23.33442372801900078 ) ) ;
#37191 = CARTESIAN_POINT ( 'NONE',  ( -12.14591786802326823, 12.06949235617739902, 28.12609039468568284 ) ) ;
#37193 = CARTESIAN_POINT ( 'NONE',  ( 0.05219959533937995610, -21.53943276465977519, 55.00109039468568284 ) ) ;
#37194 = CARTESIAN_POINT ( 'NONE',  ( 21.53943276465977519, -0.05219959533907433946, 108.7489096053143669 ) ) ;
#37195 = CARTESIAN_POINT ( 'NONE',  ( -15.80617190586745835, -15.72974639402198527, 61.87390960531436690 ) ) ;
#37196 = CARTESIAN_POINT ( 'NONE',  ( -13.97604488694547697, 13.89961937509957934, 108.1260903946856331 ) ) ;
#37197 = EDGE_CURVE ( 'NONE', #147808, #22341, #66563, .T. ) ;
#37198 = CARTESIAN_POINT ( 'NONE',  ( 13.97604488694548053, -13.89961937509957401, 70.62609039468567573 ) ) ;
#37199 = CARTESIAN_POINT ( 'NONE',  ( 18.62759615963255655, 10.81492255796105972, 81.66775706135236135 ) ) ;
#37200 = CARTESIAN_POINT ( 'NONE',  ( 13.97604488694548053, -13.89961937509957401, 55.62609039468566863 ) ) ;
#37201 = CARTESIAN_POINT ( 'NONE',  ( 16.46253265017160672, -9.564922557960803928, 38.33224293864768839 ) ) ;
#37202 = CARTESIAN_POINT ( 'NONE',  ( 18.67979575497178502, 10.72451020669898547, 59.16557627198103120 ) ) ;
#37203 = CARTESIAN_POINT ( 'NONE',  ( -8.224510206698948167, 14.34966873604960824, 55.41557627198102409 ) ) ;
#37204 = CARTESIAN_POINT ( 'NONE',  ( -17.48847506799969054, -5.747544572773709781, 24.17302562156720924 ) ) ;
#37205 = CARTESIAN_POINT ( 'NONE',  ( 16.51473224551083163, -9.474510206698727899, 25.83442372801900078 ) ) ;
#37206 = CARTESIAN_POINT ( 'NONE',  ( 16.52544592524335698, 4.483927247898782831, 81.45942372801900433 ) ) ;
#37207 = CARTESIAN_POINT ( 'NONE',  ( -12.06949235617756955, 12.14591786802309770, 50.62390960531435979 ) ) ;
#37208 = CARTESIAN_POINT ( 'NONE',  ( -10.72451020669870658, -18.67979575497194134, 94.58442372801901854 ) ) ;
#37209 = CARTESIAN_POINT ( 'NONE',  ( 21.52544592524334988, 5.823673210054432836, 81.45942372801900433 ) ) ;
#37210 = CARTESIAN_POINT ( 'NONE',  ( 0.05219959533907565091, 21.53943276465977519, 79.99890960531435269 ) ) ;
#37211 = CARTESIAN_POINT ( 'NONE',  ( -9.474510206698964154, 16.51473224551069663, 45.41557627198103120 ) ) ;
#37212 = CARTESIAN_POINT ( 'NONE',  ( 5.719274019375673035, 21.55341960407619339, 57.29275706135234714 ) ) ;
#37213 = CARTESIAN_POINT ( 'NONE',  ( 9.474510206698971260, -16.51473224551069308, 32.91557627198102409 ) ) ;
#37214 = CARTESIAN_POINT ( 'NONE',  ( 16.51473224551069308, 9.474510206698969483, 54.16557627198103120 ) ) ;
#37215 = CARTESIAN_POINT ( 'NONE',  ( 8.224510206698953496, -14.34966873604960469, 102.9155762719810383 ) ) ;
#37216 = CARTESIAN_POINT ( 'NONE',  ( 16.46253265017160672, -9.564922557960803928, 103.3322429386476955 ) ) ;
#37217 = CARTESIAN_POINT ( 'NONE',  ( 16.52544592524342804, -4.483927247898539470, 48.54057627198103120 ) ) ;
#37218 = CARTESIAN_POINT ( 'NONE',  ( -19.03943276465977164, 0.05219959533909376836, 21.24890960531436335 ) ) ;
#37219 = VECTOR ( 'NONE', #80563, 1000.000000000000000 ) ;
#37220 = CARTESIAN_POINT ( 'NONE',  ( -5.823673210054116645, -21.52544592524344225, 87.29057627198103830 ) ) ;
#37221 = CARTESIAN_POINT ( 'NONE',  ( 15.72974639402176855, 15.80617190586768217, 21.87609039468567573 ) ) ;
#37222 = CARTESIAN_POINT ( 'NONE',  ( -15.70878279763969765, 14.67621740152104870, -56.33456566391307518 ) ) ;
#37223 = CARTESIAN_POINT ( 'NONE',  ( 0.05219959533934541429, -16.53943276465976808, 35.00109039468568284 ) ) ;
#37224 = ORIENTED_EDGE ( 'NONE', *, *, #65894, .T. ) ;
#37225 = CARTESIAN_POINT ( 'NONE',  ( 18.62759615963271287, -10.81492255796078972, 68.33224293864769550 ) ) ;
#37226 = CARTESIAN_POINT ( 'NONE',  ( -5.823673210054431948, 21.52544592524334988, 112.7094237280190328 ) ) ;
#37227 = CARTESIAN_POINT ( 'NONE',  ( 9.474510206698971260, -16.51473224551069308, 92.91557627198103830 ) ) ;
#37228 = CARTESIAN_POINT ( 'NONE',  ( -18.62759615963255300, -10.81492255796106328, 34.16775706135234714 ) ) ;
#37229 = CARTESIAN_POINT ( 'NONE',  ( 10.72451020669898902, -18.67979575497178502, 27.91557627198103830 ) ) ;
#37230 = CARTESIAN_POINT ( 'NONE',  ( 12.14591786802327356, -12.06949235617739191, 105.6260903946856899 ) ) ;
#37232 = CARTESIAN_POINT ( 'NONE',  ( -15.80617190586768217, 15.72974639402176855, 78.12609039468570415 ) ) ;
#37231 = CARTESIAN_POINT ( 'NONE',  ( 10.81492255796106328, -18.62759615963255655, 45.41775706135234003 ) ) ;
#37233 = CARTESIAN_POINT ( 'NONE',  ( -15.80617190586768217, 15.72974639402176855, 113.1260903946856899 ) ) ;
#37234 = CARTESIAN_POINT ( 'NONE',  ( -16.53943276465976808, -0.05219959533934237506, 68.75109039468568994 ) ) ;
#37235 = CARTESIAN_POINT ( 'NONE',  ( -21.52544592524334988, -5.823673210054445271, 33.95942372801901143 ) ) ;
#37236 = CARTESIAN_POINT ( 'NONE',  ( 16.51473224551069308, 9.474510206698969483, 34.16557627198102409 ) ) ;
#37237 = CARTESIAN_POINT ( 'NONE',  ( 5.719274019375673035, 21.55341960407619339, 102.2927570613523613 ) ) ;
#37238 = CARTESIAN_POINT ( 'NONE',  ( 9.564922557960805705, 16.46253265017160317, 104.5822429386476955 ) ) ;
#37239 = CARTESIAN_POINT ( 'NONE',  ( -0.05219959533907301413, -21.53943276465977519, 102.4989096053143811 ) ) ;
#37241 = CARTESIAN_POINT ( 'NONE',  ( 5.719274019375991003, -21.55341960407610458, 62.70724293864769550 ) ) ;
#37240 = CARTESIAN_POINT ( 'NONE',  ( -6.907351198298408157, -38.20768336775255136, -23.99027881317066857 ) ) ;
#37243 = CARTESIAN_POINT ( 'NONE',  ( -12.14591786802309592, -12.06949235617757132, 51.87390960531437401 ) ) ;
#37242 = CARTESIAN_POINT ( 'NONE',  ( -12.06949235617739369, -12.14591786802326823, 54.37609039468568994 ) ) ;
#37244 = CARTESIAN_POINT ( 'NONE',  ( -23.29544513554940721, -16.92513159979223758, 146.4656553485623647 ) ) ;
#37245 = CARTESIAN_POINT ( 'NONE',  ( 16.51473224551083163, -9.474510206698727899, 80.83442372801899012 ) ) ;
#37246 = CARTESIAN_POINT ( 'NONE',  ( -1.464556741314096966, -14.82342540975557021, -62.12362001602810579 ) ) ;
#37247 = CARTESIAN_POINT ( 'NONE',  ( -14.29746914071037622, -8.314922557961029526, 24.16775706135235424 ) ) ;
#37248 = CARTESIAN_POINT ( 'NONE',  ( 0.05219959533907565091, 21.53943276465977519, 94.99890960531436690 ) ) ;
#37249 = CARTESIAN_POINT ( 'NONE',  ( 12.06949235617757843, -12.14591786802309237, 68.12390960531436690 ) ) ;
#37250 = CARTESIAN_POINT ( 'NONE',  ( 18.67979575497178502, 10.72451020669898547, 24.16557627198103120 ) ) ;
#37251 = CARTESIAN_POINT ( 'NONE',  ( 12.14591786802327356, -12.06949235617739191, 45.62609039468567573 ) ) ;
#37252 = CARTESIAN_POINT ( 'NONE',  ( 19.05341960407611168, 5.049401038298154454, 53.95724293864770260 ) ) ;
#37254 = CARTESIAN_POINT ( 'NONE',  ( 16.51473224551083163, -9.474510206698727899, 100.8344237280190043 ) ) ;
#37253 = CARTESIAN_POINT ( 'NONE',  ( 21.53943276465977519, 0.05219959533937863772, 31.25109039468568639 ) ) ;
#37255 = CARTESIAN_POINT ( 'NONE',  ( -13.89961937509977652, 13.97604488694528158, 95.62390960531436690 ) ) ;
#37256 = CARTESIAN_POINT ( 'NONE',  ( -19.03943276465977164, 0.05219959533909376836, 91.24890960531436690 ) ) ;
#37257 = CARTESIAN_POINT ( 'NONE',  ( 21.55341960407610458, 5.719274019375980345, 88.95724293864769550 ) ) ;
#37258 = CARTESIAN_POINT ( 'NONE',  ( 0.05219959533909260263, 19.03943276465977164, 59.99890960531436690 ) ) ;
#37259 = CARTESIAN_POINT ( 'NONE',  ( -17.31728774477270960, -6.344390552232406222, 59.18093348310682700 ) ) ;
#37260 = CARTESIAN_POINT ( 'NONE',  ( 0.05219959533910956823, 16.53943276465976808, 74.99890960531435269 ) ) ;
#37261 = CARTESIAN_POINT ( 'NONE',  ( 0.05219959533909260263, 19.03943276465977164, 104.9989096053143669 ) ) ;
#37262 = CARTESIAN_POINT ( 'NONE',  ( 17.46158047089203791, -15.43343858725516426, -55.01551020149706517 ) ) ;
#37263 = CARTESIAN_POINT ( 'NONE',  ( 9.564922557961047289, -16.46253265017146816, 85.41775706135233293 ) ) ;
#37264 = CARTESIAN_POINT ( 'NONE',  ( -21.52544592524343514, 5.823673210054127303, 91.04057627198103830 ) ) ;
#37265 = CARTESIAN_POINT ( 'NONE',  ( 9.474510206698729675, 16.51473224551082808, 52.08442372801900433 ) ) ;
#37266 = CARTESIAN_POINT ( 'NONE',  ( 21.55341960407610458, 5.719274019375980345, 23.95724293864769550 ) ) ;
#37267 = DIRECTION ( 'NONE',  ( 0.9930308165857338887, -0.1178549842436482226, 0.000000000000000000 ) ) ;
#37268 = CARTESIAN_POINT ( 'NONE',  ( -5.719274019375978568, 21.55341960407610458, 50.20724293864769550 ) ) ;
#37269 = CARTESIAN_POINT ( 'NONE',  ( 19.03943276465977164, -0.05219959533909143690, 88.74890960531436690 ) ) ;
#37270 = CARTESIAN_POINT ( 'NONE',  ( -10.72451020669870658, -18.67979575497194134, 74.58442372801901854 ) ) ;
#37271 = CARTESIAN_POINT ( 'NONE',  ( 9.564922557960805705, 16.46253265017160317, 44.58224293864769550 ) ) ;
#37272 = EDGE_CURVE ( 'NONE', #4246, #95772, #128228, .T. ) ;
#37273 = CARTESIAN_POINT ( 'NONE',  ( -8.224510206698948167, 14.34966873604960824, 70.41557627198102409 ) ) ;
#37274 = CARTESIAN_POINT ( 'NONE',  ( 12.14591786802327356, -12.06949235617739191, 20.62609039468568639 ) ) ;
#37275 = CARTESIAN_POINT ( 'NONE',  ( 10.81492255796106328, -18.62759615963255655, 65.41775706135234714 ) ) ;
#37276 = ORIENTED_EDGE ( 'NONE', *, *, #14918, .F. ) ;
#37277 = CARTESIAN_POINT ( 'NONE',  ( -19.03943276465977164, 0.05219959533909376836, 116.2489096053143669 ) ) ;
#37278 = CARTESIAN_POINT ( 'NONE',  ( 19.05341960407617918, -5.049401038297876454, 86.04275706135233293 ) ) ;
#37279 = DIRECTION ( 'NONE',  ( 1.000000000000000000, 0.000000000000000000, 0.000000000000000000 ) ) ;
#37280 = CARTESIAN_POINT ( 'NONE',  ( 21.55341960407619695, -5.719274019375665929, 21.04275706135234714 ) ) ;
#37281 = CARTESIAN_POINT ( 'NONE',  ( -38.00000000000001421, -12.34694845685042708, -3.649999994537627135 ) ) ;
#37282 = CARTESIAN_POINT ( 'NONE',  ( -0.05219959533936034679, 19.03943276465977164, 22.50109039468566152 ) ) ;
#37283 = CARTESIAN_POINT ( 'NONE',  ( 19.05341960407611168, 5.049401038298154454, 58.95724293864768129 ) ) ;
#37284 = CARTESIAN_POINT ( 'NONE',  ( -19.05341960407617563, 5.049401038297882671, 23.54275706135233648 ) ) ;
#37285 = CARTESIAN_POINT ( 'NONE',  ( 8.314922557961029526, -14.29746914071037800, 105.4177570613523613 ) ) ;
#37287 = CARTESIAN_POINT ( 'NONE',  ( 18.67979575497194134, -10.72451020669871369, 70.83442372801901854 ) ) ;
#37286 = CARTESIAN_POINT ( 'NONE',  ( -0.05219959533909027116, -19.03943276465977164, 97.49890960531436690 ) ) ;
#37288 = CARTESIAN_POINT ( 'NONE',  ( 11.40812507854754365, 35.11059874428196537, -7.224999997268813701 ) ) ;
#37289 = DIRECTION ( 'NONE',  ( 1.000000000000000000, 0.000000000000000000, 0.000000000000000000 ) ) ;
#37290 = CARTESIAN_POINT ( 'NONE',  ( 15.72974639402176855, 15.80617190586768217, 71.87609039468568994 ) ) ;
#37291 = CARTESIAN_POINT ( 'NONE',  ( -10.81492255796105439, 18.62759615963255655, 102.9177570613523756 ) ) ;
#37292 = DIRECTION ( 'NONE',  ( -0.000000000000000000, -0.000000000000000000, 1.000000000000000000 ) ) ;
#37293 = CARTESIAN_POINT ( 'NONE',  ( 13.89961937509977652, -13.97604488694527269, 93.12390960531436690 ) ) ;
#37294 = CARTESIAN_POINT ( 'NONE',  ( -19.03943276465977164, -0.05219959533935918106, 18.75109039468567218 ) ) ;
#37295 = CARTESIAN_POINT ( 'NONE',  ( 26.88621168971713615, -26.45719545518169014, -20.39628335082762334 ) ) ;
#37296 = CARTESIAN_POINT ( 'NONE',  ( -13.89961937509977652, 13.97604488694528158, 40.62390960531435979 ) ) ;
#37297 = CARTESIAN_POINT ( 'NONE',  ( 21.53943276465977519, -0.05219959533907433946, 58.74890960531436690 ) ) ;
#37298 = CARTESIAN_POINT ( 'NONE',  ( 16.52544592524335698, 4.483927247898782831, 101.4594237280190185 ) ) ;
#37300 = CARTESIAN_POINT ( 'NONE',  ( -16.51473224551069308, -9.474510206698971260, 86.66557627198102409 ) ) ;
#37299 = CARTESIAN_POINT ( 'NONE',  ( 16.53943276465976808, -0.05219959533910856209, 93.74890960531436690 ) ) ;
#37301 = CARTESIAN_POINT ( 'NONE',  ( -15.80617190586768217, 15.72974639402176855, 98.12609039468570415 ) ) ;
#37302 = CARTESIAN_POINT ( 'NONE',  ( 19.05341960407611168, 5.049401038298154454, 38.95724293864767418 ) ) ;
#37303 = CARTESIAN_POINT ( 'NONE',  ( -12.14591786802309592, -12.06949235617757132, 106.8739096053143811 ) ) ;
#37304 = CARTESIAN_POINT ( 'NONE',  ( -10.72451020669870658, -18.67979575497194134, 49.58442372801901143 ) ) ;
#37305 = CARTESIAN_POINT ( 'NONE',  ( 10.81492255796078972, 18.62759615963270932, 89.58224293864768129 ) ) ;
#37306 = CARTESIAN_POINT ( 'NONE',  ( 9.474510206698729675, 16.51473224551082808, 47.08442372801900433 ) ) ;
#37307 = CARTESIAN_POINT ( 'NONE',  ( 9.474510206698971260, -16.51473224551069308, 47.91557627198102409 ) ) ;
#37308 = CARTESIAN_POINT ( 'NONE',  ( 13.89961937509977652, -13.97604488694527269, 93.12390960531436690 ) ) ;
#37309 = CARTESIAN_POINT ( 'NONE',  ( -16.53943276465976808, 0.05219959533911058130, 81.24890960531436690 ) ) ;
#37310 = VECTOR ( 'NONE', #105213, 1000.000000000000000 ) ;
#37311 = CARTESIAN_POINT ( 'NONE',  ( 13.97604488694548053, -13.89961937509957401, 45.62609039468566863 ) ) ;
#37312 = CARTESIAN_POINT ( 'NONE',  ( 16.46253265017160672, -9.564922557960803928, 58.33224293864769550 ) ) ;
#37313 = CARTESIAN_POINT ( 'NONE',  ( 12.14591786802309770, 12.06949235617756955, 44.37390960531435979 ) ) ;
#37314 = CARTESIAN_POINT ( 'NONE',  ( -5.153800228976607833, 19.02544592524334988, 72.70942372801900433 ) ) ;
#37315 = CARTESIAN_POINT ( 'NONE',  ( -18.22780087662124160, -5.499999999999927169, 88.98236817873107896 ) ) ;
#37316 = CARTESIAN_POINT ( 'NONE',  ( 21.52544592524344225, -5.823673210054117533, 38.54057627198103120 ) ) ;
#37317 = CARTESIAN_POINT ( 'NONE',  ( -0.05219959533910754901, -16.53943276465976808, 97.49890960531436690 ) ) ;
#37318 = CARTESIAN_POINT ( 'NONE',  ( 22.94331271462294453, 0.000000000000000000, 190.0000000000000000 ) ) ;
#37320 = CARTESIAN_POINT ( 'NONE',  ( -10.81492255796078084, -18.62759615963271287, 62.08224293864769550 ) ) ;
#37319 = CARTESIAN_POINT ( 'NONE',  ( -16.51473224551069308, -9.474510206698971260, 56.66557627198103120 ) ) ;
#37321 = CARTESIAN_POINT ( 'NONE',  ( -9.564922557960796823, -16.46253265017161027, 27.08224293864769550 ) ) ;
#37323 = CARTESIAN_POINT ( 'NONE',  ( -16.46253265017160317, 9.564922557960807481, 60.83224293864769550 ) ) ;
#37322 = CARTESIAN_POINT ( 'NONE',  ( 8.224510206698742110, 14.34966873604972548, 72.08442372801899012 ) ) ;
#37324 = CARTESIAN_POINT ( 'NONE',  ( 9.474510206698729675, 16.51473224551082808, 52.08442372801900433 ) ) ;
#37325 = CARTESIAN_POINT ( 'NONE',  ( 21.53943276465977519, 0.05219959533937863772, 71.25109039468568994 ) ) ;
#37326 = CARTESIAN_POINT ( 'NONE',  ( -18.67979575497178146, -10.72451020669898902, 51.66557627198102409 ) ) ;
#37327 = CARTESIAN_POINT ( 'NONE',  ( 12.06949235617757843, -12.14591786802309237, 113.1239096053143953 ) ) ;
#37328 = CARTESIAN_POINT ( 'NONE',  ( 8.314922557961029526, -14.29746914071037800, 90.41775706135236135 ) ) ;
#37329 = CARTESIAN_POINT ( 'NONE',  ( 19.05341960407617918, -5.049401038297876454, 106.0427570613523471 ) ) ;
#37330 = CARTESIAN_POINT ( 'NONE',  ( -13.97604488694527625, -13.89961937509977652, 21.87390960531435979 ) ) ;
#37332 = CARTESIAN_POINT ( 'NONE',  ( -21.55341960407610458, -5.719274019375992779, 46.45724293864769550 ) ) ;
#37331 = DIRECTION ( 'NONE',  ( 0.000000000000000000, 0.000000000000000000, 1.000000000000000000 ) ) ;
#37333 = CARTESIAN_POINT ( 'NONE',  ( -21.52544592524334988, -5.823673210054445271, 88.95942372801901854 ) ) ;
#37334 = CIRCLE ( 'NONE', #124515, 28.90000000000004476 ) ;
#37335 = CARTESIAN_POINT ( 'NONE',  ( 0.05219959533910956823, 16.53943276465976808, 44.99890960531435979 ) ) ;
#37336 = CARTESIAN_POINT ( 'NONE',  ( 16.52544592524342804, -4.483927247898539470, 58.54057627198103120 ) ) ;
#37337 = CARTESIAN_POINT ( 'NONE',  ( -21.53943276465977519, 0.05219959533907696930, 81.24890960531436690 ) ) ;
#37338 = CARTESIAN_POINT ( 'NONE',  ( -5.719274019375978568, 21.55341960407610458, 90.20724293864770971 ) ) ;
#37339 = CARTESIAN_POINT ( 'NONE',  ( -1.249513161672007433, -29.56482114129871519, -48.84067647644814514 ) ) ;
#37340 = CARTESIAN_POINT ( 'NONE',  ( -18.67979575497178146, -10.72451020669898902, 31.66557627198102054 ) ) ;
#37341 = CARTESIAN_POINT ( 'NONE',  ( -16.53943276465976808, -0.05219959533934237506, 63.75109039468568284 ) ) ;
#37342 = CARTESIAN_POINT ( 'NONE',  ( 12.14591786802309770, 12.06949235617756955, 74.37390960531436690 ) ) ;
#37343 = CARTESIAN_POINT ( 'NONE',  ( 9.564922557960805705, 16.46253265017160317, 29.58224293864769550 ) ) ;
#37344 = CARTESIAN_POINT ( 'NONE',  ( -27.73933785331498925, 2.428612866367529932E-14, 139.3750000027311842 ) ) ;
#37345 = ORIENTED_EDGE ( 'NONE', *, *, #110412, .T. ) ;
#37346 = CARTESIAN_POINT ( 'NONE',  ( 16.55341960407618274, -4.379528057220086978, 81.04275706135236135 ) ) ;
#37347 = CARTESIAN_POINT ( 'NONE',  ( -21.53943276465977519, 0.05219959533907696930, 111.2489096053143669 ) ) ;
#37348 = CARTESIAN_POINT ( 'NONE',  ( -16.51473224551069308, -9.474510206698971260, 76.66557627198103830 ) ) ;
#37349 = CARTESIAN_POINT ( 'NONE',  ( 5.719274019375673035, 21.55341960407619339, 52.29275706135236135 ) ) ;
#37350 = CARTESIAN_POINT ( 'NONE',  ( -9.474510206698964154, 16.51473224551069663, 105.4155762719810383 ) ) ;
#37351 = FACE_OUTER_BOUND ( 'NONE', #13676, .T. ) ;
#37352 = VERTEX_POINT ( 'NONE', #129214 ) ;
#37353 = CARTESIAN_POINT ( 'NONE',  ( 18.67979575497194134, -10.72451020669871369, 40.83442372801901854 ) ) ;
#37355 = CARTESIAN_POINT ( 'NONE',  ( -9.564922557960796823, -16.46253265017161027, 97.08224293864769550 ) ) ;
#37354 = CARTESIAN_POINT ( 'NONE',  ( 19.05341960407611168, 5.049401038298154454, 43.95724293864769550 ) ) ;
#37356 = CARTESIAN_POINT ( 'NONE',  ( -5.153800228976607833, 19.02544592524334988, 52.70942372801900433 ) ) ;
#37357 = CARTESIAN_POINT ( 'NONE',  ( 0.05219959533937995610, -21.53943276465977519, 30.00109039468568284 ) ) ;
#37358 = CARTESIAN_POINT ( 'NONE',  ( -9.564922557961040184, 16.46253265017147172, 47.91775706135233293 ) ) ;
#37359 = CARTESIAN_POINT ( 'NONE',  ( -5.153800228976328057, -19.02544592524343514, 22.29057627198102765 ) ) ;
#37360 = CARTESIAN_POINT ( 'NONE',  ( -8.314922557961024197, 14.29746914071037800, 92.91775706135236135 ) ) ;
#37361 = CARTESIAN_POINT ( 'NONE',  ( 9.474510206698729675, 16.51473224551082808, 62.08442372801899722 ) ) ;
#37362 = CARTESIAN_POINT ( 'NONE',  ( -16.52544592524335698, -4.483927247898792601, 108.9594237280190185 ) ) ;
#37363 = CARTESIAN_POINT ( 'NONE',  ( -10.59477242850411649, -90.60836494048552936, -25.00000000000000000 ) ) ;
#37364 = CARTESIAN_POINT ( 'NONE',  ( 19.05341960407611168, 5.049401038298154454, 83.95724293864766707 ) ) ;
#37365 = AXIS2_PLACEMENT_3D ( 'NONE', #33042, #173550, #125047 ) ;
#37366 = CARTESIAN_POINT ( 'NONE',  ( -21.55341960407619339, 5.719274019375674811, 93.54275706135234714 ) ) ;
#37367 = CARTESIAN_POINT ( 'NONE',  ( 18.62759615963255655, 10.81492255796105972, 111.6677570613523613 ) ) ;
#37368 = CARTESIAN_POINT ( 'NONE',  ( 17.60691670004650433, 5.500000000000063061, 66.63333313366440791 ) ) ;
#37369 = CARTESIAN_POINT ( 'NONE',  ( -16.46253265017160317, 9.564922557960807481, 105.8322429386476955 ) ) ;
#37370 = CARTESIAN_POINT ( 'NONE',  ( -18.62759615963255300, -10.81492255796106328, 69.16775706135234714 ) ) ;
#37371 = CARTESIAN_POINT ( 'NONE',  ( -9.564922557961040184, 16.46253265017147172, 112.9177570613523329 ) ) ;
#37372 = CARTESIAN_POINT ( 'NONE',  ( -16.51473224551069308, -9.474510206698971260, 81.66557627198103830 ) ) ;
#37374 = EDGE_CURVE ( 'NONE', #180340, #196688, #84709, .T. ) ;
#37373 = CARTESIAN_POINT ( 'NONE',  ( -18.62759615963270932, 10.81492255796079327, 25.83224293864769194 ) ) ;
#37375 = CARTESIAN_POINT ( 'NONE',  ( -16.51473224551069308, -9.474510206698971260, 96.66557627198102409 ) ) ;
#37376 = CARTESIAN_POINT ( 'NONE',  ( -16.81555441253553695, -7.025013491695479395, 89.36314554665747778 ) ) ;
#37377 = CARTESIAN_POINT ( 'NONE',  ( -19.03943276465977164, 0.05219959533909376836, 76.24890960531435269 ) ) ;
#37378 = CARTESIAN_POINT ( 'NONE',  ( -19.02544592524342804, 5.153800228976336051, 66.04057627198103830 ) ) ;
#37379 = CARTESIAN_POINT ( 'NONE',  ( 14.29746914071037800, 8.314922557961029526, 106.6677570613523756 ) ) ;
#37380 = CARTESIAN_POINT ( 'NONE',  ( 6.434671708797603529, -6.434671708797564449, -61.89430850415821794 ) ) ;
#37381 = CARTESIAN_POINT ( 'NONE',  ( -13.97604488694547697, 13.89961937509957934, 73.12609039468568994 ) ) ;
#37382 = CARTESIAN_POINT ( 'NONE',  ( 19.05341960407611168, 5.049401038298154454, 93.95724293864769550 ) ) ;
#37383 = CARTESIAN_POINT ( 'NONE',  ( -12.06949235617756955, 12.14591786802309770, 80.62390960531438111 ) ) ;
#37384 = CARTESIAN_POINT ( 'NONE',  ( 5.823673210054125526, 21.52544592524343514, 29.79057627198102409 ) ) ;
#37385 = CARTESIAN_POINT ( 'NONE',  ( -19.03943276465977164, 0.05219959533909376836, 116.2489096053143669 ) ) ;
#37386 = CARTESIAN_POINT ( 'NONE',  ( 16.52544592524342804, -4.483927247898539470, 108.5405762719810241 ) ) ;
#37387 = CARTESIAN_POINT ( 'NONE',  ( -16.38665767535054485, 7.295008042176028162, 55.26400864214549102 ) ) ;
#37388 = CARTESIAN_POINT ( 'NONE',  ( -5.049401038297874678, -19.05341960407617918, 39.79275706135232582 ) ) ;
#37389 = CARTESIAN_POINT ( 'NONE',  ( 4.483927247898545687, 16.52544592524342804, 29.79057627198102409 ) ) ;
#37390 = CARTESIAN_POINT ( 'NONE',  ( 19.02544592524343514, -5.153800228976328945, 98.54057627198100988 ) ) ;
#37391 = CARTESIAN_POINT ( 'NONE',  ( 15.72974639402176855, 15.80617190586768217, 61.87609039468568284 ) ) ;
#37392 = CARTESIAN_POINT ( 'NONE',  ( -21.52544592524343514, 5.823673210054127303, 61.04057627198103120 ) ) ;
#37393 = CARTESIAN_POINT ( 'NONE',  ( -15.80617190586768217, 15.72974639402176855, 38.12609039468567573 ) ) ;
#37394 = CARTESIAN_POINT ( 'NONE',  ( 15.80617190586746368, 15.72974639402197994, 84.37390960531438111 ) ) ;
#37395 = CARTESIAN_POINT ( 'NONE',  ( 18.62759615963255655, 10.81492255796105972, 36.66775706135234714 ) ) ;
#37396 = CARTESIAN_POINT ( 'NONE',  ( -16.53943276465976808, 0.05219959533911058130, 106.2489096053143811 ) ) ;
#37397 = CARTESIAN_POINT ( 'NONE',  ( -16.51473224551082808, 9.474510206698731452, 73.33442372801900433 ) ) ;
#37398 = CARTESIAN_POINT ( 'NONE',  ( 19.05341960407611168, 5.049401038298154454, 48.95724293864768129 ) ) ;
#37400 = CARTESIAN_POINT ( 'NONE',  ( 13.97604488694527802, 13.89961937509977652, 99.37390960531436690 ) ) ;
#37399 = CARTESIAN_POINT ( 'NONE',  ( -4.483927247898539470, -16.52544592524342804, 87.29057627198103830 ) ) ;
#37401 = CARTESIAN_POINT ( 'NONE',  ( 16.51473224551069308, 9.474510206698969483, 109.1655762719810383 ) ) ;
#37402 = CARTESIAN_POINT ( 'NONE',  ( 19.03943276465977164, -0.05219959533909143690, 38.74890960531436690 ) ) ;
#37403 = VECTOR ( 'NONE', #159029, 1000.000000000000000 ) ;
#37404 = CARTESIAN_POINT ( 'NONE',  ( -12.14591786802309592, -12.06949235617757132, 36.87390960531435979 ) ) ;
#37405 = CARTESIAN_POINT ( 'NONE',  ( -8.314922557961024197, 14.29746914071037800, 102.9177570613523756 ) ) ;
#37406 = CARTESIAN_POINT ( 'NONE',  ( 16.46253265017160672, -9.564922557960803928, 58.33224293864769550 ) ) ;
#37407 = CARTESIAN_POINT ( 'NONE',  ( -8.314922557960811034, -14.29746914071050412, 112.0822429386477097 ) ) ;
#37408 = CARTESIAN_POINT ( 'NONE',  ( 9.564922557961047289, -16.46253265017146816, 20.41775706135233293 ) ) ;
#37410 = CARTESIAN_POINT ( 'NONE',  ( 16.55341960407611168, 4.379528057220329451, 28.95724293864769905 ) ) ;
#37409 = CARTESIAN_POINT ( 'NONE',  ( 16.46253265017160672, -9.564922557960803928, 108.3322429386476955 ) ) ;
#37411 = CARTESIAN_POINT ( 'NONE',  ( -21.52544592524334988, -5.823673210054445271, 48.95942372801902565 ) ) ;
#37412 = CARTESIAN_POINT ( 'NONE',  ( -4.483927247898782831, 16.52544592524335698, 52.70942372801902565 ) ) ;
#37413 = CARTESIAN_POINT ( 'NONE',  ( 16.55341960407611168, 4.379528057220329451, 33.95724293864769550 ) ) ;
#37414 = CARTESIAN_POINT ( 'NONE',  ( 8.314922557961029526, -14.29746914071037800, 105.4177570613523613 ) ) ;
#37415 = CARTESIAN_POINT ( 'NONE',  ( 16.52544592524335698, 4.483927247898782831, 21.45942372801901499 ) ) ;
#37416 = CARTESIAN_POINT ( 'NONE',  ( 9.474510206698971260, -16.51473224551069308, 52.91557627198102409 ) ) ;
#37417 = CARTESIAN_POINT ( 'NONE',  ( -14.34966873604960291, -8.224510206698953496, 111.6655762719810525 ) ) ;
#37418 = CARTESIAN_POINT ( 'NONE',  ( 10.72451020669871369, 18.67979575497193778, 22.08442372801901143 ) ) ;
#37419 = CARTESIAN_POINT ( 'NONE',  ( 19.05341960407611168, 5.049401038298154454, 48.95724293864768129 ) ) ;
#37420 = CARTESIAN_POINT ( 'NONE',  ( -5.049401038298153566, 19.05341960407611168, 115.2072429386477097 ) ) ;
#37421 = CARTESIAN_POINT ( 'NONE',  ( -16.51473224551069308, -9.474510206698971260, 26.66557627198103120 ) ) ;
#37422 = CARTESIAN_POINT ( 'NONE',  ( -0.05219959533907301413, -21.53943276465977519, 27.49890960531435269 ) ) ;
#37423 = FACE_OUTER_BOUND ( 'NONE', #483, .T. ) ;
#37424 = CARTESIAN_POINT ( 'NONE',  ( 16.46253265017160672, -9.564922557960803928, 103.3322429386476955 ) ) ;
#37426 = CARTESIAN_POINT ( 'NONE',  ( 12.06949235617757843, -12.14591786802309237, 98.12390960531436690 ) ) ;
#37425 = CARTESIAN_POINT ( 'NONE',  ( 21.55341960407619695, -5.719274019375665929, 41.04275706135236135 ) ) ;
#37427 = CARTESIAN_POINT ( 'NONE',  ( -21.53943276465977519, 0.05219959533907696930, 21.24890960531436690 ) ) ;
#37428 = DIRECTION ( 'NONE',  ( 0.000000000000000000, 0.000000000000000000, -1.000000000000000000 ) ) ;
#37429 = CARTESIAN_POINT ( 'NONE',  ( -8.224510206698735004, -14.34966873604973081, 79.58442372801903275 ) ) ;
#37430 = CARTESIAN_POINT ( 'NONE',  ( -21.52544592524334988, -5.823673210054445271, 88.95942372801901854 ) ) ;
#37431 = CARTESIAN_POINT ( 'NONE',  ( 12.06949235617739724, 12.14591786802326823, 56.87609039468568994 ) ) ;
#37432 = CARTESIAN_POINT ( 'NONE',  ( -13.97604488694527625, -13.89961937509977652, 101.8739096053143811 ) ) ;
#37433 = CARTESIAN_POINT ( 'NONE',  ( 16.55341960407618274, -4.379528057220086978, 46.04275706135234714 ) ) ;
#37434 = CARTESIAN_POINT ( 'NONE',  ( 19.02544592524334988, 5.153800228976608722, 111.4594237280190043 ) ) ;
#37435 = CARTESIAN_POINT ( 'NONE',  ( 4.379528057220092307, 16.55341960407617563, 82.29275706135234714 ) ) ;
#37436 = CARTESIAN_POINT ( 'NONE',  ( -5.049401038297874678, -19.05341960407617918, 99.79275706135234714 ) ) ;
#37437 = CARTESIAN_POINT ( 'NONE',  ( -13.89961937509977652, 13.97604488694528158, 70.62390960531432427 ) ) ;
#37438 = CARTESIAN_POINT ( 'NONE',  ( 10.81492255796078972, 18.62759615963270932, 99.58224293864770971 ) ) ;
#37440 = CARTESIAN_POINT ( 'NONE',  ( 19.02544592524334988, 5.153800228976608722, 106.4594237280190185 ) ) ;
#37439 = CARTESIAN_POINT ( 'NONE',  ( 14.29746914071049879, -8.314922557960816363, 88.33224293864769550 ) ) ;
#37441 = CARTESIAN_POINT ( 'NONE',  ( -4.483927247898782831, 16.52544592524335698, 67.70942372801901854 ) ) ;
#37442 = CARTESIAN_POINT ( 'NONE',  ( 21.61802400803986757, 13.75099706318440340, 167.9999999999999432 ) ) ;
#37443 = CARTESIAN_POINT ( 'NONE',  ( 13.97604488694548053, -13.89961937509957401, 70.62609039468567573 ) ) ;
#37444 = CARTESIAN_POINT ( 'NONE',  ( -14.29746914071049879, 8.314922557960819915, 35.83224293864768839 ) ) ;
#37445 = CARTESIAN_POINT ( 'NONE',  ( -4.379528057220328563, 16.55341960407611168, 95.20724293864769550 ) ) ;
#37446 = CARTESIAN_POINT ( 'NONE',  ( 0.05219959533936267826, -19.03943276465977164, 40.00109039468566152 ) ) ;
#37447 = CARTESIAN_POINT ( 'NONE',  ( 15.72974639402176855, 15.80617190586768217, 26.87609039468567218 ) ) ;
#37448 = CARTESIAN_POINT ( 'NONE',  ( 19.03943276465977164, 0.05219959533936151252, 96.25109039468567573 ) ) ;
#37449 = CARTESIAN_POINT ( 'NONE',  ( 9.474510206698971260, -16.51473224551069308, 112.9155762719810383 ) ) ;
#37450 = CARTESIAN_POINT ( 'NONE',  ( -9.564922557960796823, -16.46253265017161027, 87.08224293864769550 ) ) ;
#37451 = CARTESIAN_POINT ( 'NONE',  ( -5.823673210054431948, 21.52544592524334988, 97.70942372801904696 ) ) ;
#37452 = CARTESIAN_POINT ( 'NONE',  ( 9.474510206698971260, -16.51473224551069308, 72.91557627198102409 ) ) ;
#37453 = CARTESIAN_POINT ( 'NONE',  ( 21.53943276465977519, -0.05219959533907433946, 38.74890960531435979 ) ) ;
#37454 = CARTESIAN_POINT ( 'NONE',  ( -8.314922557960811034, -14.29746914071050412, 97.08224293864770971 ) ) ;
#37455 = CARTESIAN_POINT ( 'NONE',  ( -19.03943276465977164, 0.05219959533909376836, 56.24890960531435979 ) ) ;
#37456 = VECTOR ( 'NONE', #199302, 1000.000000000000114 ) ;
#37457 = CARTESIAN_POINT ( 'NONE',  ( 4.483927247898545687, 16.52544592524342804, 109.7905762719810383 ) ) ;
#37458 = CARTESIAN_POINT ( 'NONE',  ( -15.72974639402176322, -15.80617190586768395, 19.37609039468568639 ) ) ;
#37459 = CARTESIAN_POINT ( 'NONE',  ( -5.823673210054431948, 21.52544592524334988, 67.70942372801901854 ) ) ;
#37460 = CARTESIAN_POINT ( 'NONE',  ( -9.564922557960796823, -16.46253265017161027, 42.08224293864769550 ) ) ;
#37461 = CARTESIAN_POINT ( 'NONE',  ( 12.14591786802327356, -12.06949235617739191, 75.62609039468567573 ) ) ;
#37462 = EDGE_CURVE ( 'NONE', #154699, #126159, #6873, .T. ) ;
#37463 = CARTESIAN_POINT ( 'NONE',  ( 0.05219959533907565091, 21.53943276465977519, 109.9989096053143527 ) ) ;
#37464 = VERTEX_POINT ( 'NONE', #52389 ) ;
#37465 = CARTESIAN_POINT ( 'NONE',  ( -5.719274019375978568, 21.55341960407610458, 105.2072429386477097 ) ) ;
#37467 = CARTESIAN_POINT ( 'NONE',  ( -9.474510206698964154, 16.51473224551069663, 70.41557627198102409 ) ) ;
#37466 = CARTESIAN_POINT ( 'NONE',  ( -9.564922557961040184, 16.46253265017147172, 47.91775706135233293 ) ) ;
#37468 = CARTESIAN_POINT ( 'NONE',  ( 9.474510206698729675, 16.51473224551082808, 37.08442372801899722 ) ) ;
#37469 = CARTESIAN_POINT ( 'NONE',  ( 15.72974639402176855, 15.80617190586768217, 66.87609039468568994 ) ) ;
#37470 = CARTESIAN_POINT ( 'NONE',  ( 21.55341960407610458, 5.719274019375980345, 73.95724293864769550 ) ) ;
#37471 = CARTESIAN_POINT ( 'NONE',  ( -14.34966873604960291, -8.224510206698953496, 46.66557627198102409 ) ) ;
#37473 = CARTESIAN_POINT ( 'NONE',  ( 19.03943276465977164, 0.05219959533936151252, 26.25109039468566507 ) ) ;
#37472 = CARTESIAN_POINT ( 'NONE',  ( 21.53943276465977519, 0.05219959533937863772, 86.25109039468568994 ) ) ;
#37474 = CARTESIAN_POINT ( 'NONE',  ( -16.55341960407611168, -4.379528057220339221, 66.45724293864768129 ) ) ;
#37475 = CARTESIAN_POINT ( 'NONE',  ( 19.02544592524343514, -5.153800228976328945, 28.54057627198102409 ) ) ;
#37476 = CARTESIAN_POINT ( 'NONE',  ( 9.474510206698729675, 16.51473224551082808, 52.08442372801900433 ) ) ;
#37477 = CARTESIAN_POINT ( 'NONE',  ( -14.34966873604972548, 8.224510206698743886, 113.3344237280190328 ) ) ;
#37478 = CARTESIAN_POINT ( 'NONE',  ( 21.55341960407619695, -5.719274019375665929, 86.04275706135236135 ) ) ;
#37479 = CARTESIAN_POINT ( 'NONE',  ( 5.049401038297881783, 19.05341960407617563, 42.29275706135234003 ) ) ;
#37480 = CARTESIAN_POINT ( 'NONE',  ( -10.81492255796078084, -18.62759615963271287, 57.08224293864769550 ) ) ;
#37481 = CARTESIAN_POINT ( 'NONE',  ( -5.719274019375665041, -21.55341960407619695, 44.79275706135234714 ) ) ;
#37482 = CARTESIAN_POINT ( 'NONE',  ( -10.72451020669898014, 18.67979575497178502, 100.4155762719810241 ) ) ;
#37483 = CARTESIAN_POINT ( 'NONE',  ( 16.46253265017146816, 9.564922557961045513, 91.66775706135234714 ) ) ;
#37484 = CARTESIAN_POINT ( 'NONE',  ( 16.52544592524335698, 4.483927247898782831, 61.45942372801901854 ) ) ;
#37486 = CARTESIAN_POINT ( 'NONE',  ( 5.719274019375991003, -21.55341960407610458, 107.7072429386476955 ) ) ;
#37485 = CARTESIAN_POINT ( 'NONE',  ( 5.000000000000000000, -140.0000000000000000, 13.35010376910484275 ) ) ;
#37487 = CARTESIAN_POINT ( 'NONE',  ( 14.34966873604960469, 8.224510206698951720, 94.16557627198103830 ) ) ;
#37488 = CARTESIAN_POINT ( 'NONE',  ( -17.49999999999999645, -5.500000000000000888, 29.20309617465828467 ) ) ;
#37489 = CARTESIAN_POINT ( 'NONE',  ( -14.29746914071037622, -8.314922557961029526, 24.16775706135235424 ) ) ;
#37490 = CARTESIAN_POINT ( 'NONE',  ( 21.53943276465977519, -0.05219959533907433946, 53.74890960531437401 ) ) ;
#37491 = CARTESIAN_POINT ( 'NONE',  ( 16.52544592524335698, 4.483927247898782831, 86.45942372801901854 ) ) ;
#37492 = CARTESIAN_POINT ( 'NONE',  ( 17.50000000000000000, -5.499999999999992895, 36.21769037696435589 ) ) ;
#37493 = CARTESIAN_POINT ( 'NONE',  ( -0.05219959533934338120, 16.53943276465976808, 67.50109039468568994 ) ) ;
#37494 = CARTESIAN_POINT ( 'NONE',  ( -5.823673210054431948, 21.52544592524334988, 37.70942372801900433 ) ) ;
#37495 = CARTESIAN_POINT ( 'NONE',  ( 0.05219959533907565091, 21.53943276465977519, 54.99890960531435269 ) ) ;
#37496 = CARTESIAN_POINT ( 'NONE',  ( -16.55341960407617563, 4.379528057220093196, 88.54275706135236135 ) ) ;
#37497 = CARTESIAN_POINT ( 'NONE',  ( 15.80617190586769283, -15.72974639402175789, 65.62609039468568994 ) ) ;
#37498 = CARTESIAN_POINT ( 'NONE',  ( 18.62759615963271287, -10.81492255796078972, 53.33224293864769550 ) ) ;
#37499 = CARTESIAN_POINT ( 'NONE',  ( 21.53943276465977519, -0.05219959533907433946, 33.74890960531436690 ) ) ;
#37500 = ORIENTED_EDGE ( 'NONE', *, *, #14301, .T. ) ;
#37501 = CARTESIAN_POINT ( 'NONE',  ( -16.53943276465976808, -0.05219959533934237506, 68.75109039468568994 ) ) ;
#37502 = CARTESIAN_POINT ( 'NONE',  ( 18.62759615963271287, -10.81492255796078972, 38.33224293864768839 ) ) ;
#37503 = EDGE_LOOP ( 'NONE', ( #80250, #39779, #2613, #55497 ) ) ;
#37504 = CARTESIAN_POINT ( 'NONE',  ( 19.02544592524343514, -5.153800228976328945, 103.5405762719809957 ) ) ;
#37505 = CARTESIAN_POINT ( 'NONE',  ( 4.379528057220092307, 16.55341960407617563, 112.2927570613523471 ) ) ;
#37506 = CARTESIAN_POINT ( 'NONE',  ( 17.72662750342724536, 5.500000000000079048, 73.90179492283743912 ) ) ;
#37507 = CARTESIAN_POINT ( 'NONE',  ( 0.05219959533910956823, 16.53943276465976808, 109.9989096053143527 ) ) ;
#37508 = CARTESIAN_POINT ( 'NONE',  ( 15.80617190586746368, 15.72974639402197994, 54.37390960531435979 ) ) ;
#37509 = CARTESIAN_POINT ( 'NONE',  ( 16.46253265017160672, -9.564922557960803928, 48.33224293864769550 ) ) ;
#37510 = CARTESIAN_POINT ( 'NONE',  ( 12.14591786802327356, -12.06949235617739191, 90.62609039468567573 ) ) ;
#37511 = CARTESIAN_POINT ( 'NONE',  ( -18.67979575497193778, 10.72451020669871902, 28.33442372801902209 ) ) ;
#37512 = CARTESIAN_POINT ( 'NONE',  ( -13.97604488694547697, 13.89961937509957934, 93.12609039468566152 ) ) ;
#37513 = CARTESIAN_POINT ( 'NONE',  ( -12.14591786802309592, -12.06949235617757132, 96.87390960531436690 ) ) ;
#37514 = CARTESIAN_POINT ( 'NONE',  ( 13.97604488694527802, 13.89961937509977652, 59.37390960531434558 ) ) ;
#37515 = AXIS2_PLACEMENT_3D ( 'NONE', #125327, #2966, #3948 ) ;
#37516 = CARTESIAN_POINT ( 'NONE',  ( -9.474510206698964154, 16.51473224551069663, 25.41557627198103120 ) ) ;
#37517 = CARTESIAN_POINT ( 'NONE',  ( 14.01879992551668863, -0.9453496423219486244, -62.45159313300391091 ) ) ;
#37518 = CARTESIAN_POINT ( 'NONE',  ( 9.474510206698971260, -16.51473224551069308, 77.91557627198103830 ) ) ;
#37519 = CARTESIAN_POINT ( 'NONE',  ( -4.379528057220086978, -16.55341960407618274, 64.79275706135234714 ) ) ;
#37520 = CARTESIAN_POINT ( 'NONE',  ( -21.55341960407619339, 5.719274019375674811, 103.5427570613523613 ) ) ;
#37521 = CARTESIAN_POINT ( 'NONE',  ( -5.719274019375978568, 21.55341960407610458, 50.20724293864769550 ) ) ;
#37522 = CARTESIAN_POINT ( 'NONE',  ( 16.52544592524335698, 4.483927247898782831, 71.45942372801901854 ) ) ;
#37523 = CARTESIAN_POINT ( 'NONE',  ( 9.564922557961047289, -16.46253265017146816, 65.41775706135233293 ) ) ;
#37524 = VERTEX_POINT ( 'NONE', #36216 ) ;
#37525 = CARTESIAN_POINT ( 'NONE',  ( -5.823673210054431948, 21.52544592524334988, 67.70942372801901854 ) ) ;
#37526 = CARTESIAN_POINT ( 'NONE',  ( -0.05219959533909027116, -19.03943276465977164, 62.49890960531435979 ) ) ;
#37527 = CARTESIAN_POINT ( 'NONE',  ( -19.02544592524342804, 5.153800228976336051, 36.04057627198100988 ) ) ;
#37528 = CARTESIAN_POINT ( 'NONE',  ( 16.51473224551083163, -9.474510206698727899, 65.83442372801900433 ) ) ;
#37529 = CARTESIAN_POINT ( 'NONE',  ( 19.02544592524343514, -5.153800228976328945, 108.5405762719810383 ) ) ;
#37530 = CARTESIAN_POINT ( 'NONE',  ( -5.153800228976328057, -19.02544592524343514, 97.29057627198099567 ) ) ;
#37531 = CARTESIAN_POINT ( 'NONE',  ( -8.314922557960811034, -14.29746914071050412, 57.08224293864769550 ) ) ;
#37532 = CARTESIAN_POINT ( 'NONE',  ( 5.719274019375991003, -21.55341960407610458, 42.70724293864770260 ) ) ;
#37533 = DIRECTION ( 'NONE',  ( 0.000000000000000000, 0.000000000000000000, -1.000000000000000000 ) ) ;
#37534 = CARTESIAN_POINT ( 'NONE',  ( -19.02544592524334988, -5.153800228976617603, 23.95942372801900078 ) ) ;
#37535 = CARTESIAN_POINT ( 'NONE',  ( 16.46253265017160672, -9.564922557960803928, 48.33224293864769550 ) ) ;
#37536 = DIRECTION ( 'NONE',  ( -0.000000000000000000, -0.000000000000000000, 1.000000000000000000 ) ) ;
#37537 = CARTESIAN_POINT ( 'NONE',  ( -17.48853670773244318, 5.747243402303103821, 108.6667129974999142 ) ) ;
#37538 = CARTESIAN_POINT ( 'NONE',  ( 16.53943276465976808, 0.05219959533934440121, 81.25109039468568994 ) ) ;
#37539 = CARTESIAN_POINT ( 'NONE',  ( -5.823673210054116645, -21.52544592524344225, 102.2905762719810383 ) ) ;
#37540 = CARTESIAN_POINT ( 'NONE',  ( 14.34966873604960469, 8.224510206698951720, 49.16557627198102409 ) ) ;
#37542 = CARTESIAN_POINT ( 'NONE',  ( -30.74264578624800492, -22.33583958711396278, -5.549999994537627046 ) ) ;
#37541 = CARTESIAN_POINT ( 'NONE',  ( 5.049401038298161559, -19.05341960407611168, 42.70724293864767418 ) ) ;
#37543 = CARTESIAN_POINT ( 'NONE',  ( 10.72451020669871369, 18.67979575497193778, 47.08442372801901854 ) ) ;
#37544 = CARTESIAN_POINT ( 'NONE',  ( -0.05219959533936034679, 19.03943276465977164, 42.50109039468566152 ) ) ;
#37545 = CARTESIAN_POINT ( 'NONE',  ( -19.02544592524342804, 5.153800228976336051, 51.04057627198103120 ) ) ;
#37546 = CARTESIAN_POINT ( 'NONE',  ( -18.62759615963255300, -10.81492255796106328, 94.16775706135237556 ) ) ;
#37547 = VECTOR ( 'NONE', #174337, 1000.000000000000000 ) ;
#37548 = CARTESIAN_POINT ( 'NONE',  ( -21.77012268027506181, -5.483007391792980911, 173.8427694444997371 ) ) ;
#37549 = CARTESIAN_POINT ( 'NONE',  ( -16.53943276465976808, 0.05219959533911058130, 46.24890960531435979 ) ) ;
#37550 = CARTESIAN_POINT ( 'NONE',  ( 19.25918095147781983, 5.499999999999579892, 41.95284276293937609 ) ) ;
#37551 = CARTESIAN_POINT ( 'NONE',  ( -18.67979575497178146, -10.72451020669898902, 36.66557627198103120 ) ) ;
#37552 = CARTESIAN_POINT ( 'NONE',  ( -5.359611314223446995E-15, 29.16686587814335851, 144.3750000027311842 ) ) ;
#37553 = VECTOR ( 'NONE', #181340, 1000.000000000000000 ) ;
#37554 = CARTESIAN_POINT ( 'NONE',  ( 13.97604488694527802, 13.89961937509977652, 104.3739096053143385 ) ) ;
#37555 = CARTESIAN_POINT ( 'NONE',  ( -0.05219959533910754901, -16.53943276465976808, 87.49890960531436690 ) ) ;
#37556 = CARTESIAN_POINT ( 'NONE',  ( -8.314922557961024197, 14.29746914071037800, 22.91775706135235069 ) ) ;
#37557 = CARTESIAN_POINT ( 'NONE',  ( 4.483927247898790824, -16.52544592524335698, 105.2094237280190328 ) ) ;
#37558 = ORIENTED_EDGE ( 'NONE', *, *, #147508, .T. ) ;
#37560 = CARTESIAN_POINT ( 'NONE',  ( -10.81492255796078084, -18.62759615963271287, 102.0822429386476955 ) ) ;
#37559 = CARTESIAN_POINT ( 'NONE',  ( -9.474510206698964154, 16.51473224551069663, 95.41557627198102409 ) ) ;
#37562 = CARTESIAN_POINT ( 'NONE',  ( 5.153800228976335163, 19.02544592524342804, 94.79057627198103830 ) ) ;
#37561 = CARTESIAN_POINT ( 'NONE',  ( -0.05219959533910754901, -16.53943276465976808, 32.49890960531435979 ) ) ;
#37563 = CARTESIAN_POINT ( 'NONE',  ( -9.474510206698720793, -16.51473224551083518, 94.58442372801900433 ) ) ;
#37564 = CARTESIAN_POINT ( 'NONE',  ( 15.80617190586769283, -15.72974639402175789, 110.6260903946857042 ) ) ;
#37565 = CARTESIAN_POINT ( 'NONE',  ( 18.62759615963271287, -10.81492255796078972, 88.33224293864769550 ) ) ;
#37566 = CARTESIAN_POINT ( 'NONE',  ( 0.05219959533907565091, 21.53943276465977519, 44.99890960531435979 ) ) ;
#37567 = CARTESIAN_POINT ( 'NONE',  ( -0.05219959533909027116, -19.03943276465977164, 57.49890960531435979 ) ) ;
#37568 = CARTESIAN_POINT ( 'NONE',  ( 4.483927247898545687, 16.52544592524342804, 34.79057627198103120 ) ) ;
#37569 = CARTESIAN_POINT ( 'NONE',  ( -13.97604488694527625, -13.89961937509977652, 76.87390960531433848 ) ) ;
#37570 = ORIENTED_EDGE ( 'NONE', *, *, #6906, .F. ) ;
#37571 = CARTESIAN_POINT ( 'NONE',  ( 16.51473224551069308, 9.474510206698969483, 79.16557627198103830 ) ) ;
#37572 = CARTESIAN_POINT ( 'NONE',  ( 13.89961937509957401, 13.97604488694547697, 36.87609039468565442 ) ) ;
#37573 = CARTESIAN_POINT ( 'NONE',  ( -14.29746914071049879, 8.314922557960819915, 90.83224293864769550 ) ) ;
#37574 = CARTESIAN_POINT ( 'NONE',  ( 15.80617190586769283, -15.72974639402175789, 25.62609039468567929 ) ) ;
#37575 = CARTESIAN_POINT ( 'NONE',  ( 27.73933785331498214, 9.013057229001095294, 144.4750000027311501 ) ) ;
#37576 = CARTESIAN_POINT ( 'NONE',  ( -16.52544592524335698, -4.483927247898792601, 103.9594237280190185 ) ) ;
#37577 = CARTESIAN_POINT ( 'NONE',  ( -16.53943276465976808, 0.05219959533911058130, 116.2489096053143669 ) ) ;
#37578 = CARTESIAN_POINT ( 'NONE',  ( 13.97604488694527802, 13.89961937509977652, 79.37390960531435269 ) ) ;
#37579 = CARTESIAN_POINT ( 'NONE',  ( -37.99626262588766679, 2.428612866367529932E-14, -0.002157773949821304490 ) ) ;
#37580 = CARTESIAN_POINT ( 'NONE',  ( 13.97604488694527802, 13.89961937509977652, 24.37390960531435624 ) ) ;
#37581 = CARTESIAN_POINT ( 'NONE',  ( 12.14591786802309770, 12.06949235617756955, 44.37390960531435979 ) ) ;
#37582 = EDGE_LOOP ( 'NONE', ( #14136, #9844, #60722, #185549, #37276 ) ) ;
#37583 = CARTESIAN_POINT ( 'NONE',  ( -5.719274019375665041, -21.55341960407619695, 54.79275706135235424 ) ) ;
#37584 = CARTESIAN_POINT ( 'NONE',  ( 30.69486229629358576, -23.16037512311203272, -17.06287707314307411 ) ) ;
#37585 = CARTESIAN_POINT ( 'NONE',  ( -5.823673210054431948, 21.52544592524334988, 97.70942372801904696 ) ) ;
#37586 = CARTESIAN_POINT ( 'NONE',  ( 19.02544592524343514, -5.153800228976328945, 38.54057627198103120 ) ) ;
#37587 = CARTESIAN_POINT ( 'NONE',  ( 9.474510206698971260, -16.51473224551069308, 52.91557627198102409 ) ) ;
#37588 = ORIENTED_EDGE ( 'NONE', *, *, #57273, .T. ) ;
#37589 = CARTESIAN_POINT ( 'NONE',  ( 15.72974639402176855, 15.80617190586768217, 91.87609039468568994 ) ) ;
#37590 = CARTESIAN_POINT ( 'NONE',  ( 8.224510206698742110, 14.34966873604972548, 57.08442372801901854 ) ) ;
#37591 = CARTESIAN_POINT ( 'NONE',  ( 10.81492255796106328, -18.62759615963255655, 90.41775706135236135 ) ) ;
#37592 = CARTESIAN_POINT ( 'NONE',  ( -21.53943276465977519, 0.05219959533907696930, 26.24890960531435624 ) ) ;
#37593 = CARTESIAN_POINT ( 'NONE',  ( 16.46253265017146816, 9.564922557961045513, 91.66775706135234714 ) ) ;
#37594 = CARTESIAN_POINT ( 'NONE',  ( 10.81492255796106328, -18.62759615963255655, 75.41775706135233293 ) ) ;
#37595 = CARTESIAN_POINT ( 'NONE',  ( -14.34966873604972548, 8.224510206698743886, 38.33442372801900433 ) ) ;
#37596 = CARTESIAN_POINT ( 'NONE',  ( 21.53943276465977519, -0.05219959533907433946, 83.74890960531435269 ) ) ;
#37597 = CARTESIAN_POINT ( 'NONE',  ( 16.51473224551083163, -9.474510206698727899, 85.83442372801900433 ) ) ;
#37598 = CARTESIAN_POINT ( 'NONE',  ( -19.05341960407611168, -5.049401038298163336, 61.45724293864769550 ) ) ;
#37599 = CARTESIAN_POINT ( 'NONE',  ( 9.474510206698729675, 16.51473224551082808, 102.0844237280190043 ) ) ;
#37600 = CARTESIAN_POINT ( 'NONE',  ( -16.46253265017146816, -9.564922557961047289, 104.1677570613523329 ) ) ;
#37601 = CARTESIAN_POINT ( 'NONE',  ( 4.379528057220339221, -16.55341960407611168, 52.70724293864769550 ) ) ;
#37602 = CARTESIAN_POINT ( 'NONE',  ( -13.89961937509957401, -13.97604488694547875, 74.37609039468566152 ) ) ;
#37603 = CARTESIAN_POINT ( 'NONE',  ( 12.06949235617739724, 12.14591786802326823, 61.87609039468568284 ) ) ;
#37604 = CARTESIAN_POINT ( 'NONE',  ( -16.51473224551069308, -9.474510206698971260, 41.66557627198103120 ) ) ;
#37605 = CARTESIAN_POINT ( 'NONE',  ( -5.153800228976328057, -19.02544592524343514, 52.29057627198100988 ) ) ;
#37606 = CARTESIAN_POINT ( 'NONE',  ( -8.224510206698735004, -14.34966873604973081, 59.58442372801901854 ) ) ;
#37607 = CARTESIAN_POINT ( 'NONE',  ( 8.571926809382603096, -26.38167802310801235, 139.9750000027311785 ) ) ;
#37608 = ADVANCED_FACE ( 'NONE', ( #175744 ), #146388, .F. ) ;
#37609 = CARTESIAN_POINT ( 'NONE',  ( -28.82186960331499037, 2.428612866367529932E-14, 140.2500000054623683 ) ) ;
#37610 = CARTESIAN_POINT ( 'NONE',  ( 16.51473224551069308, 9.474510206698969483, 99.16557627198102409 ) ) ;
#37611 = DIRECTION ( 'NONE',  ( 0.000000000000000000, 0.000000000000000000, 1.000000000000000000 ) ) ;
#37612 = VERTEX_POINT ( 'NONE', #54394 ) ;
#37613 = CARTESIAN_POINT ( 'NONE',  ( -5.153800228976607833, 19.02544592524334988, 107.7094237280189759 ) ) ;
#37614 = CARTESIAN_POINT ( 'NONE',  ( 18.67979575497178502, 10.72451020669898547, 39.16557627198102409 ) ) ;
#37616 = CARTESIAN_POINT ( 'NONE',  ( -12.06949235617739369, -12.14591786802326823, 29.37609039468568284 ) ) ;
#37615 = CARTESIAN_POINT ( 'NONE',  ( 13.89961937509957401, 13.97604488694547697, 31.87609039468566863 ) ) ;
#37617 = CARTESIAN_POINT ( 'NONE',  ( 16.51473224551069308, 9.474510206698969483, 34.16557627198102409 ) ) ;
#37618 = CARTESIAN_POINT ( 'NONE',  ( -16.46253265017160317, 9.564922557960807481, 45.83224293864769550 ) ) ;
#37619 = CARTESIAN_POINT ( 'NONE',  ( -0.05219959533907301413, -21.53943276465977519, 87.49890960531436690 ) ) ;
#37620 = CARTESIAN_POINT ( 'NONE',  ( 9.564922557960805705, 16.46253265017160317, 104.5822429386476955 ) ) ;
#37621 = CARTESIAN_POINT ( 'NONE',  ( -19.03943276465977164, 0.05219959533909376836, 56.24890960531435979 ) ) ;
#37622 = CARTESIAN_POINT ( 'NONE',  ( -8.571926809382601320, -26.38167802310801591, 145.7750000027311899 ) ) ;
#37623 = CARTESIAN_POINT ( 'NONE',  ( -13.97604488694547697, 13.89961937509957934, 83.12609039468564731 ) ) ;
#37624 = CARTESIAN_POINT ( 'NONE',  ( -16.55341960407611168, -4.379528057220339221, 71.45724293864769550 ) ) ;
#37625 = CARTESIAN_POINT ( 'NONE',  ( 5.719274019375991003, -21.55341960407610458, 47.70724293864770260 ) ) ;
#37626 = CARTESIAN_POINT ( 'NONE',  ( 15.72974639402176855, 15.80617190586768217, 111.8760903946856615 ) ) ;
#37627 = CARTESIAN_POINT ( 'NONE',  ( 21.52544592524344225, -5.823673210054117533, 98.54057627198105251 ) ) ;
#37628 = CARTESIAN_POINT ( 'NONE',  ( -15.80617190586768217, 15.72974639402176855, 68.12609039468567573 ) ) ;
#37629 = CARTESIAN_POINT ( 'NONE',  ( -5.823673210054431948, 21.52544592524334988, 72.70942372801901854 ) ) ;
#37630 = CARTESIAN_POINT ( 'NONE',  ( -5.049401038298153566, 19.05341960407611168, 110.2072429386476671 ) ) ;
#37632 = CARTESIAN_POINT ( 'NONE',  ( -18.67979575497193778, 10.72451020669871902, 73.33442372801901854 ) ) ;
#37631 = CARTESIAN_POINT ( 'NONE',  ( -8.314922557961024197, 14.29746914071037800, 107.9177570613523471 ) ) ;
#37633 = CARTESIAN_POINT ( 'NONE',  ( -9.474510206698964154, 16.51473224551069663, 60.41557627198102409 ) ) ;
#37634 = CARTESIAN_POINT ( 'NONE',  ( 15.72974639402176855, 15.80617190586768217, 26.87609039468567218 ) ) ;
#37635 = CARTESIAN_POINT ( 'NONE',  ( 13.89961937509977652, -13.97604488694527269, 88.12390960531438111 ) ) ;
#37636 = CARTESIAN_POINT ( 'NONE',  ( -8.224510206698948167, 14.34966873604960824, 85.41557627198102409 ) ) ;
#37637 = CARTESIAN_POINT ( 'NONE',  ( -4.483927247898539470, -16.52544592524342804, 52.29057627198102409 ) ) ;
#37638 = CARTESIAN_POINT ( 'NONE',  ( 10.81492255796078972, 18.62759615963270932, 59.58224293864770260 ) ) ;
#37639 = CARTESIAN_POINT ( 'NONE',  ( -9.564922557960796823, -16.46253265017161027, 67.08224293864769550 ) ) ;
#37640 = CARTESIAN_POINT ( 'NONE',  ( -15.80617190586745835, -15.72974639402198527, 76.87390960531439532 ) ) ;
#37641 = CARTESIAN_POINT ( 'NONE',  ( -19.03943276465977164, -0.05219959533935918106, 58.75109039468566863 ) ) ;
#37644 = CARTESIAN_POINT ( 'NONE',  ( -12.14591786802309592, -12.06949235617757132, 76.87390960531439532 ) ) ;
#37643 = CARTESIAN_POINT ( 'NONE',  ( -9.474510206698720793, -16.51473224551083518, 24.58442372801900078 ) ) ;
#37642 = TOROIDAL_SURFACE ( 'NONE', #24698, 1.500000000000001776, 0.5000000000000000000 ) ;
#37645 = CARTESIAN_POINT ( 'NONE',  ( -15.72974639402197994, 15.80617190586746368, 50.62390960531435979 ) ) ;
#37646 = ORIENTED_EDGE ( 'NONE', *, *, #85112, .T. ) ;
#37647 = CARTESIAN_POINT ( 'NONE',  ( -17.49999999999998579, -5.500000000000015099, 41.28230962303565832 ) ) ;
#37649 = CARTESIAN_POINT ( 'NONE',  ( 22.44159573604009239, 16.30477369853692693, 146.5750000027312012 ) ) ;
#37648 = CARTESIAN_POINT ( 'NONE',  ( -16.53943276465976808, -0.05219959533934237506, 93.75109039468567573 ) ) ;
#37650 = CARTESIAN_POINT ( 'NONE',  ( -19.03943276465977164, -0.05219959533935918106, 93.75109039468566152 ) ) ;
#37651 = CARTESIAN_POINT ( 'NONE',  ( 14.29746914071049879, -8.314922557960816363, 63.33224293864770260 ) ) ;
#37652 = CARTESIAN_POINT ( 'NONE',  ( -18.56101223717332260, -5.499999999999947597, 61.44978406935677384 ) ) ;
#37653 = CARTESIAN_POINT ( 'NONE',  ( -9.474510206698964154, 16.51473224551069663, 55.41557627198103120 ) ) ;
#37654 = CARTESIAN_POINT ( 'NONE',  ( 12.06949235617757843, -12.14591786802309237, 53.12390960531436690 ) ) ;
#37655 = CARTESIAN_POINT ( 'NONE',  ( -19.05341960407611168, -5.049401038298163336, 86.45724293864769550 ) ) ;
#37657 = CARTESIAN_POINT ( 'NONE',  ( -5.153800228976328057, -19.02544592524343514, 57.29057627198103120 ) ) ;
#37656 = CARTESIAN_POINT ( 'NONE',  ( -5.049401038297874678, -19.05341960407617918, 79.79275706135233293 ) ) ;
#37658 = CARTESIAN_POINT ( 'NONE',  ( 16.51473224551069308, 9.474510206698969483, 84.16557627198102409 ) ) ;
#37659 = CARTESIAN_POINT ( 'NONE',  ( 13.97604488694527802, 13.89961937509977652, 74.37390960531436690 ) ) ;
#37660 = CARTESIAN_POINT ( 'NONE',  ( 21.55341960407610458, 5.719274019375980345, 63.95724293864770260 ) ) ;
#37661 = CARTESIAN_POINT ( 'NONE',  ( 16.52544592524335698, 4.483927247898782831, 56.45942372801902565 ) ) ;
#37662 = DIRECTION ( 'NONE',  ( 1.000000000000000000, 0.000000000000000000, 0.000000000000000000 ) ) ;
#37663 = CARTESIAN_POINT ( 'NONE',  ( -9.474510206698964154, 16.51473224551069663, 45.41557627198103120 ) ) ;
#37664 = CARTESIAN_POINT ( 'NONE',  ( 18.67979575497178502, 10.72451020669898547, 59.16557627198103120 ) ) ;
#37665 = CARTESIAN_POINT ( 'NONE',  ( -16.51473224551082808, 9.474510206698731452, 83.33442372801899012 ) ) ;
#37666 = CARTESIAN_POINT ( 'NONE',  ( -14.29746914071049879, 8.314922557960819915, 25.83224293864769194 ) ) ;
#37667 = CARTESIAN_POINT ( 'NONE',  ( -9.564922557961040184, 16.46253265017147172, 42.91775706135234003 ) ) ;
#37669 = CARTESIAN_POINT ( 'NONE',  ( -12.06949235617739369, -12.14591786802326823, 89.37609039468568994 ) ) ;
#37668 = CARTESIAN_POINT ( 'NONE',  ( 0.05219959533934541429, -16.53943276465976808, 60.00109039468568284 ) ) ;
#37670 = CARTESIAN_POINT ( 'NONE',  ( -17.60769864724391098, 5.499999999999988454, 73.65024842019163032 ) ) ;
#37671 = CARTESIAN_POINT ( 'NONE',  ( -14.29746914071037622, -8.314922557961029526, 84.16775706135234714 ) ) ;
#37672 = CARTESIAN_POINT ( 'NONE',  ( -18.62759615963270932, 10.81492255796079327, 30.83224293864770260 ) ) ;
#37673 = CARTESIAN_POINT ( 'NONE',  ( 5.153800228976335163, 19.02544592524342804, 39.79057627198100988 ) ) ;
#37674 = CARTESIAN_POINT ( 'NONE',  ( -9.474510206698964154, 16.51473224551069663, 50.41557627198102409 ) ) ;
#37675 = CARTESIAN_POINT ( 'NONE',  ( -19.02544592524342804, 5.153800228976336051, 41.04057627198103120 ) ) ;
#37676 = CARTESIAN_POINT ( 'NONE',  ( -21.53943276465977519, -0.05219959533937600094, 33.75109039468568284 ) ) ;
#37677 = CARTESIAN_POINT ( 'NONE',  ( -14.29746914071037622, -8.314922557961029526, 49.16775706135234003 ) ) ;
#37678 = CARTESIAN_POINT ( 'NONE',  ( -0.05219959533910754901, -16.53943276465976808, 22.49890960531436335 ) ) ;
#37679 = CARTESIAN_POINT ( 'NONE',  ( -16.46253265017160317, 9.564922557960807481, 25.83224293864769194 ) ) ;
#37680 = CARTESIAN_POINT ( 'NONE',  ( 5.153800228976615827, -19.02544592524334988, 20.20942372801899722 ) ) ;
#37681 = CARTESIAN_POINT ( 'NONE',  ( -16.53943276465976808, -0.05219959533934237506, 18.75109039468568639 ) ) ;
#37682 = CARTESIAN_POINT ( 'NONE',  ( -9.474510206698720793, -16.51473224551083518, 69.58442372801901854 ) ) ;
#37683 = CARTESIAN_POINT ( 'NONE',  ( 0.05219959533910956823, 16.53943276465976808, 74.99890960531435269 ) ) ;
#37684 = CARTESIAN_POINT ( 'NONE',  ( -19.02544592524342804, 5.153800228976336051, 36.04057627198100988 ) ) ;
#37686 = CARTESIAN_POINT ( 'NONE',  ( 16.52216118717208815, -7.221426719304493425, 91.42400978953007495 ) ) ;
#37685 = CARTESIAN_POINT ( 'NONE',  ( 0.05219959533936267826, -19.03943276465977164, 75.00109039468566152 ) ) ;
#37687 = CARTESIAN_POINT ( 'NONE',  ( 10.72451020669871369, 18.67979575497193778, 72.08442372801899012 ) ) ;
#37688 = CARTESIAN_POINT ( 'NONE',  ( -16.53943276465976808, -0.05219959533934237506, 43.75109039468568284 ) ) ;
#37689 = DIRECTION ( 'NONE',  ( -0.000000000000000000, -0.000000000000000000, 1.000000000000000000 ) ) ;
#37690 = CARTESIAN_POINT ( 'NONE',  ( -18.67979575497178146, -10.72451020669898902, 41.66557627198103120 ) ) ;
#37691 = CARTESIAN_POINT ( 'NONE',  ( -12.06949235617739369, -12.14591786802326823, 24.37609039468567573 ) ) ;
#37692 = LINE ( 'NONE', #132706, #147502 ) ;
#37693 = CARTESIAN_POINT ( 'NONE',  ( 5.049401038297881783, 19.05341960407617563, 22.29275706135233648 ) ) ;
#37694 = CARTESIAN_POINT ( 'NONE',  ( -25.73063820182138528, 8.702599028576308626, 171.6270364942766946 ) ) ;
#37695 = CARTESIAN_POINT ( 'NONE',  ( -19.02544592524342804, 5.153800228976336051, 41.04057627198103120 ) ) ;
#37696 = CARTESIAN_POINT ( 'NONE',  ( -28.79475375365586842, 2.428612866367529932E-14, 142.2656553485623760 ) ) ;
#37697 = CARTESIAN_POINT ( 'NONE',  ( -0.05219959533909027116, -19.03943276465977164, 52.49890960531436690 ) ) ;
#37699 = CARTESIAN_POINT ( 'NONE',  ( 5.823673210054444382, -21.52544592524334988, 60.20942372801902565 ) ) ;
#37698 = CIRCLE ( 'NONE', #70043, 1.999999999999999112 ) ;
#37700 = CARTESIAN_POINT ( 'NONE',  ( 16.46253265017146816, 9.564922557961045513, 21.66775706135233648 ) ) ;
#37701 = CARTESIAN_POINT ( 'NONE',  ( -4.379528057220328563, 16.55341960407611168, 30.20724293864769550 ) ) ;
#37702 = CARTESIAN_POINT ( 'NONE',  ( 5.153800228976335163, 19.02544592524342804, 29.79057627198102409 ) ) ;
#37703 = EDGE_CURVE ( 'NONE', #54292, #83313, #98474, .T. ) ;
#37704 = CARTESIAN_POINT ( 'NONE',  ( 19.03943276465977164, -0.05219959533909143690, 98.74890960531436690 ) ) ;
#37705 = CARTESIAN_POINT ( 'NONE',  ( 15.72974639402176855, 15.80617190586768217, 51.87609039468568284 ) ) ;
#37706 = CARTESIAN_POINT ( 'NONE',  ( -19.03943276465977164, 0.05219959533909376836, 36.24890960531436690 ) ) ;
#37707 = CARTESIAN_POINT ( 'NONE',  ( 5.719274019375673035, 21.55341960407619339, 72.29275706135236135 ) ) ;
#37709 = CARTESIAN_POINT ( 'NONE',  ( 0.05219959533909260263, 19.03943276465977164, 109.9989096053143669 ) ) ;
#37708 = CARTESIAN_POINT ( 'NONE',  ( -13.89961937509957401, -13.97604488694547875, 94.37609039468566152 ) ) ;
#37710 = CARTESIAN_POINT ( 'NONE',  ( 0.05219959533909260263, 19.03943276465977164, 24.99890960531435269 ) ) ;
#37711 = CARTESIAN_POINT ( 'NONE',  ( 0.05219959533907565091, 21.53943276465977519, 114.9989096053143669 ) ) ;
#37712 = CARTESIAN_POINT ( 'NONE',  ( -19.05341960407617563, 5.049401038297882671, 38.54275706135233293 ) ) ;
#37713 = CARTESIAN_POINT ( 'NONE',  ( 8.314922557960818139, 14.29746914071049879, 114.5822429386477097 ) ) ;
#37714 = CARTESIAN_POINT ( 'NONE',  ( 19.05341960407611168, 5.049401038298154454, 68.95724293864769550 ) ) ;
#37715 = CARTESIAN_POINT ( 'NONE',  ( -16.51473224551082808, 9.474510206698731452, 98.33442372801900433 ) ) ;
#37716 = CARTESIAN_POINT ( 'NONE',  ( -14.34966873604960291, -8.224510206698953496, 66.66557627198102409 ) ) ;
#37717 = CARTESIAN_POINT ( 'NONE',  ( -5.153800228976607833, 19.02544592524334988, 22.70942372801899012 ) ) ;
#37718 = CARTESIAN_POINT ( 'NONE',  ( 0.05219959533909260263, 19.03943276465977164, 114.9989096053143669 ) ) ;
#37719 = CARTESIAN_POINT ( 'NONE',  ( -19.02544592524334988, -5.153800228976617603, 93.95942372801900433 ) ) ;
#37720 = CARTESIAN_POINT ( 'NONE',  ( 21.53943276465977519, -0.05219959533907433946, 88.74890960531436690 ) ) ;
#37721 = CARTESIAN_POINT ( 'NONE',  ( -15.80617190586768217, 15.72974639402176855, 38.12609039468567573 ) ) ;
#37722 = CARTESIAN_POINT ( 'NONE',  ( 4.483927247898790824, -16.52544592524335698, 40.20942372801901854 ) ) ;
#37723 = CARTESIAN_POINT ( 'NONE',  ( 14.29746914071037800, 8.314922557961029526, 106.6677570613523756 ) ) ;
#37725 = CARTESIAN_POINT ( 'NONE',  ( -18.62759615963255300, -10.81492255796106328, 44.16775706135234714 ) ) ;
#37724 = CARTESIAN_POINT ( 'NONE',  ( 16.53943276465976808, 0.05219959533934440121, 36.25109039468567573 ) ) ;
#37726 = CARTESIAN_POINT ( 'NONE',  ( -5.719274019375978568, 21.55341960407610458, 55.20724293864770260 ) ) ;
#37727 = CARTESIAN_POINT ( 'NONE',  ( -0.05219959533909027116, -19.03943276465977164, 37.49890960531436690 ) ) ;
#37728 = CARTESIAN_POINT ( 'NONE',  ( -30.74264578624800492, -22.33583958711396278, -3.549999994537626602 ) ) ;
#37729 = CARTESIAN_POINT ( 'NONE',  ( 16.55341960407618274, -4.379528057220086978, 76.04275706135237556 ) ) ;
#37730 = CARTESIAN_POINT ( 'NONE',  ( 5.823673210054125526, 21.52544592524343514, 84.79057627198102409 ) ) ;
#37731 = CARTESIAN_POINT ( 'NONE',  ( -14.34966873604960291, -8.224510206698953496, 36.66557627198103120 ) ) ;
#37732 = CARTESIAN_POINT ( 'NONE',  ( 16.55341960407618274, -4.379528057220086978, 66.04275706135236135 ) ) ;
#37733 = CARTESIAN_POINT ( 'NONE',  ( -9.474510206698720793, -16.51473224551083518, 94.58442372801900433 ) ) ;
#37734 = CARTESIAN_POINT ( 'NONE',  ( 0.05219959533907565091, 21.53943276465977519, 104.9989096053143669 ) ) ;
#37735 = CARTESIAN_POINT ( 'NONE',  ( -14.29746914071049879, 8.314922557960819915, 30.83224293864770260 ) ) ;
#37736 = ADVANCED_FACE ( 'NONE', ( #39224 ), #100880, .F. ) ;
#37737 = ORIENTED_EDGE ( 'NONE', *, *, #155971, .F. ) ;
#37738 = CARTESIAN_POINT ( 'NONE',  ( 8.224510206698742110, 14.34966873604972548, 82.08442372801901854 ) ) ;
#37739 = CARTESIAN_POINT ( 'NONE',  ( 19.49401214000076976, 12.39993551617566681, 169.9999999999999716 ) ) ;
#37740 = CARTESIAN_POINT ( 'NONE',  ( 15.80617190586746368, 15.72974639402197994, 79.37390960531436690 ) ) ;
#37741 = ORIENTED_EDGE ( 'NONE', *, *, #177539, .F. ) ;
#37742 = CARTESIAN_POINT ( 'NONE',  ( 4.483927247898790824, -16.52544592524335698, 100.2094237280190043 ) ) ;
#37743 = ORIENTED_EDGE ( 'NONE', *, *, #165138, .F. ) ;
#37744 = CARTESIAN_POINT ( 'NONE',  ( 19.39720447994795194, 5.499999999999968914, 87.16317477297175742 ) ) ;
#37745 = CARTESIAN_POINT ( 'NONE',  ( -18.62759615963270932, 10.81492255796079327, 85.83224293864768129 ) ) ;
#37746 = CARTESIAN_POINT ( 'NONE',  ( -10.72451020669898014, 18.67979575497178502, 105.4155762719810383 ) ) ;
#37747 = CARTESIAN_POINT ( 'NONE',  ( 12.06949235617757843, -12.14591786802309237, 43.12390960531435269 ) ) ;
#37748 = CARTESIAN_POINT ( 'NONE',  ( 16.52544592524335698, 4.483927247898782831, 31.45942372801901854 ) ) ;
#37749 = CARTESIAN_POINT ( 'NONE',  ( -9.564922557960796823, -16.46253265017161027, 42.08224293864769550 ) ) ;
#37750 = CARTESIAN_POINT ( 'NONE',  ( -16.46253265017160317, 9.564922557960807481, 60.83224293864769550 ) ) ;
#37751 = ORIENTED_EDGE ( 'NONE', *, *, #111017, .T. ) ;
#37752 = CARTESIAN_POINT ( 'NONE',  ( 0.05219959533909260263, 19.03943276465977164, 114.9989096053143669 ) ) ;
#37753 = CARTESIAN_POINT ( 'NONE',  ( 17.97214573761831247, 5.500000000000080824, 78.96970049038658601 ) ) ;
#37754 = CARTESIAN_POINT ( 'NONE',  ( 9.564922557961047289, -16.46253265017146816, 100.4177570613523329 ) ) ;
#37755 = CARTESIAN_POINT ( 'NONE',  ( -19.05341960407617563, 5.049401038297882671, 53.54275706135231871 ) ) ;
#37756 = CARTESIAN_POINT ( 'NONE',  ( -10.81492255796078084, -18.62759615963271287, 92.08224293864769550 ) ) ;
#37757 = CARTESIAN_POINT ( 'NONE',  ( 12.06949235617739724, 12.14591786802326823, 111.8760903946856615 ) ) ;
#37758 = CARTESIAN_POINT ( 'NONE',  ( 21.53943276465977519, -0.05219959533907433946, 43.74890960531435979 ) ) ;
#37760 = CARTESIAN_POINT ( 'NONE',  ( 0.05219959533936267826, -19.03943276465977164, 105.0010903946856615 ) ) ;
#37759 = CARTESIAN_POINT ( 'NONE',  ( 21.52544592524344225, -5.823673210054117533, 78.54057627198103830 ) ) ;
#37761 = CARTESIAN_POINT ( 'NONE',  ( -16.46253265017160317, 9.564922557960807481, 100.8322429386477097 ) ) ;
#37762 = CARTESIAN_POINT ( 'NONE',  ( -10.72451020669870658, -18.67979575497194134, 74.58442372801901854 ) ) ;
#37763 = CARTESIAN_POINT ( 'NONE',  ( -19.03943276465977164, 0.05219959533909376836, 71.24890960531435269 ) ) ;
#37764 = CARTESIAN_POINT ( 'NONE',  ( 31.37858599332833620, 5.662547894918608549, 99.94225302722350079 ) ) ;
#37765 = CARTESIAN_POINT ( 'NONE',  ( 9.474510206698971260, -16.51473224551069308, 67.91557627198102409 ) ) ;
#37766 = CARTESIAN_POINT ( 'NONE',  ( 8.314922557960818139, 14.29746914071049879, 89.58224293864768129 ) ) ;
#37767 = ORIENTED_EDGE ( 'NONE', *, *, #176141, .T. ) ;
#37768 = CARTESIAN_POINT ( 'NONE',  ( 16.46253265017146816, 9.564922557961045513, 106.6677570613523471 ) ) ;
#37769 = CARTESIAN_POINT ( 'NONE',  ( 17.26172910966779384, -6.454744622555844913, 83.30646908649222837 ) ) ;
#37770 = CARTESIAN_POINT ( 'NONE',  ( 13.97604488694527802, 13.89961937509977652, 74.37390960531436690 ) ) ;
#37772 = CARTESIAN_POINT ( 'NONE',  ( -13.97604488694527625, -13.89961937509977652, 96.87390960531433848 ) ) ;
#37771 = CARTESIAN_POINT ( 'NONE',  ( -10.72451020669870658, -18.67979575497194134, 84.58442372801903275 ) ) ;
#37773 = CARTESIAN_POINT ( 'NONE',  ( 12.14591786802327356, -12.06949235617739191, 75.62609039468567573 ) ) ;
#37774 = CARTESIAN_POINT ( 'NONE',  ( -17.40805194822031154, -6.112264579159315758, 74.16628727489390371 ) ) ;
#37775 = CARTESIAN_POINT ( 'NONE',  ( -0.05219959533936034679, 19.03943276465977164, 57.50109039468566863 ) ) ;
#37776 = CARTESIAN_POINT ( 'NONE',  ( -10.72451020669870658, -18.67979575497194134, 109.5844237280190328 ) ) ;
#37777 = CARTESIAN_POINT ( 'NONE',  ( 4.458020396767582660, 6.565813341170965600, -64.20492216656606388 ) ) ;
#37778 = DIRECTION ( 'NONE',  ( 0.7071067811865466846, -7.406550393246786959E-15, 0.7071067811865484609 ) ) ;
#37779 = CARTESIAN_POINT ( 'NONE',  ( 36.91746824999999887, 11.99521256947799053, -4.024999997268814411 ) ) ;
#37780 = CARTESIAN_POINT ( 'NONE',  ( 4.379528057220339221, -16.55341960407611168, 22.70724293864769194 ) ) ;
#37781 = DIRECTION ( 'NONE',  ( 0.000000000000000000, 0.000000000000000000, -1.000000000000000000 ) ) ;
#37782 = CARTESIAN_POINT ( 'NONE',  ( 14.34966873604972726, -8.224510206698740333, 95.83442372801903275 ) ) ;
#37783 = CARTESIAN_POINT ( 'NONE',  ( -35.00000000000000000, 3.889087296526014814, 1.818019484660534424 ) ) ;
#37784 = CARTESIAN_POINT ( 'NONE',  ( -12.14591786802326823, 12.06949235617739902, 78.12609039468570415 ) ) ;
#37785 = CARTESIAN_POINT ( 'NONE',  ( 10.81492255796106328, -18.62759615963255655, 80.41775706135234714 ) ) ;
#37786 = CARTESIAN_POINT ( 'NONE',  ( 5.049401038297881783, 19.05341960407617563, 87.29275706135234714 ) ) ;
#37787 = CARTESIAN_POINT ( 'NONE',  ( -16.46253265017146816, -9.564922557961047289, 39.16775706135234003 ) ) ;
#37788 = CARTESIAN_POINT ( 'NONE',  ( 19.02544592524343514, -5.153800228976328945, 73.54057627198103830 ) ) ;
#37789 = CARTESIAN_POINT ( 'NONE',  ( -0.05219959533909027116, -19.03943276465977164, 62.49890960531435979 ) ) ;
#37790 = CARTESIAN_POINT ( 'NONE',  ( -19.48894818550241581, 5.500000000000114575, 40.10307310435242556 ) ) ;
#37791 = CARTESIAN_POINT ( 'NONE',  ( 18.62759615963271287, -10.81492255796078972, 98.33224293864769550 ) ) ;
#37792 = VECTOR ( 'NONE', #191542, 1000.000000000000000 ) ;
#37793 = CARTESIAN_POINT ( 'NONE',  ( -10.72451020669898014, 18.67979575497178502, 45.41557627198103830 ) ) ;
#37794 = CARTESIAN_POINT ( 'NONE',  ( -9.564922557960796823, -16.46253265017161027, 27.08224293864769550 ) ) ;
#37795 = CARTESIAN_POINT ( 'NONE',  ( -8.224510206698735004, -14.34966873604973081, 69.58442372801900433 ) ) ;
#37796 = UNCERTAINTY_MEASURE_WITH_UNIT (LENGTH_MEASURE( 1.000000000000000082E-05 ), #190273, 'distance_accuracy_value', 'NONE');
#37797 = EDGE_LOOP ( 'NONE', ( #196772, #74917, #34575, #186341 ) ) ;
#37798 = CARTESIAN_POINT ( 'NONE',  ( 10.81492255796106328, -18.62759615963255655, 50.41775706135235424 ) ) ;
#37800 = CARTESIAN_POINT ( 'NONE',  ( 11.74264578624799427, 36.14014761921585972, -0.5999999999999999778 ) ) ;
#37799 = CARTESIAN_POINT ( 'NONE',  ( 16.52544592524342804, -4.483927247898539470, 68.54057627198103830 ) ) ;
#37801 = CARTESIAN_POINT ( 'NONE',  ( 16.53943276465976808, 0.05219959533934440121, 36.25109039468567573 ) ) ;
#37802 = CARTESIAN_POINT ( 'NONE',  ( -16.52544592524342804, 4.483927247898546575, 106.0405762719810525 ) ) ;
#37803 = CARTESIAN_POINT ( 'NONE',  ( 0.05219959533936267826, -19.03943276465977164, 50.00109039468566863 ) ) ;
#37804 = AXIS2_PLACEMENT_3D ( 'NONE', #119849, #149198, #58182 ) ;
#37805 = CARTESIAN_POINT ( 'NONE',  ( -4.483927247898539470, -16.52544592524342804, 57.29057627198103120 ) ) ;
#37807 = EDGE_CURVE ( 'NONE', #38805, #101645, #68827, .T. ) ;
#37806 = CARTESIAN_POINT ( 'NONE',  ( 18.67979575497194134, -10.72451020669871369, 35.83442372801901143 ) ) ;
#37809 = CARTESIAN_POINT ( 'NONE',  ( -15.80617190586745835, -15.72974639402198527, 96.87390960531436690 ) ) ;
#37808 = CARTESIAN_POINT ( 'NONE',  ( -38.00373040315628970, 1.963201398428686990E-14, -0.1220970790697140096 ) ) ;
#37810 = CARTESIAN_POINT ( 'NONE',  ( -9.474510206698964154, 16.51473224551069663, 100.4155762719810241 ) ) ;
#37811 = CARTESIAN_POINT ( 'NONE',  ( -16.55341960407611168, -4.379528057220339221, 76.45724293864769550 ) ) ;
#37812 = CARTESIAN_POINT ( 'NONE',  ( 9.474510206698971260, -16.51473224551069308, 112.9155762719810383 ) ) ;
#37813 = CARTESIAN_POINT ( 'NONE',  ( 29.86685920354754487, 21.69954338932564752, -3.424999997268813434 ) ) ;
#37814 = CARTESIAN_POINT ( 'NONE',  ( -9.474510206698720793, -16.51473224551083518, 84.58442372801900433 ) ) ;
#37815 = CARTESIAN_POINT ( 'NONE',  ( -21.52544592524334988, -5.823673210054445271, 18.95942372801901143 ) ) ;
#37816 = CARTESIAN_POINT ( 'NONE',  ( 0.05219959533909260263, 19.03943276465977164, 69.99890960531435269 ) ) ;
#37817 = CARTESIAN_POINT ( 'NONE',  ( -0.05219959533936034679, 19.03943276465977164, 62.50109039468566863 ) ) ;
#37818 = CARTESIAN_POINT ( 'NONE',  ( -0.05219959533909027116, -19.03943276465977164, 37.49890960531436690 ) ) ;
#37819 = CARTESIAN_POINT ( 'NONE',  ( 10.81492255796106328, -18.62759615963255655, 65.41775706135234714 ) ) ;
#37820 = CARTESIAN_POINT ( 'NONE',  ( 69.65682714487590488, -71.74905178543389184, -4.999999999999999112 ) ) ;
#37821 = ADVANCED_FACE ( 'NONE', ( #197900 ), #133225, .F. ) ;
#37822 = CARTESIAN_POINT ( 'NONE',  ( -14.29746914071049879, 8.314922557960819915, 60.83224293864769550 ) ) ;
#37823 = CARTESIAN_POINT ( 'NONE',  ( -13.89961937509977652, 13.97604488694528158, 65.62390960531436690 ) ) ;
#37824 = CARTESIAN_POINT ( 'NONE',  ( 21.55341960407610458, 5.719274019375980345, 93.95724293864770971 ) ) ;
#37825 = CARTESIAN_POINT ( 'NONE',  ( -0.05219959533909027116, -19.03943276465977164, 52.49890960531436690 ) ) ;
#37826 = EDGE_LOOP ( 'NONE', ( #149635, #77149 ) ) ;
#37827 = CARTESIAN_POINT ( 'NONE',  ( 15.72974639402199770, -15.80617190586745480, 78.12390960531436690 ) ) ;
#37828 = CARTESIAN_POINT ( 'NONE',  ( 5.719274019375673035, 21.55341960407619339, 97.29275706135234714 ) ) ;
#37831 = CARTESIAN_POINT ( 'NONE',  ( -4.483927247898539470, -16.52544592524342804, 102.2905762719810383 ) ) ;
#37830 = CARTESIAN_POINT ( 'NONE',  ( -16.53943276465976808, -0.05219959533934237506, 93.75109039468567573 ) ) ;
#37829 = LINE ( 'NONE', #181356, #86448 ) ;
#37832 = CARTESIAN_POINT ( 'NONE',  ( 5.153800228976615827, -19.02544592524334988, 90.20942372801900433 ) ) ;
#37833 = ORIENTED_EDGE ( 'NONE', *, *, #143190, .F. ) ;
#37834 = CARTESIAN_POINT ( 'NONE',  ( 15.80617190586769283, -15.72974639402175789, 20.62609039468568639 ) ) ;
#37835 = CARTESIAN_POINT ( 'NONE',  ( -19.03943276465977164, -0.05219959533935918106, 53.75109039468566863 ) ) ;
#37836 = CARTESIAN_POINT ( 'NONE',  ( -4.483927247898782831, 16.52544592524335698, 102.7094237280190185 ) ) ;
#37837 = CARTESIAN_POINT ( 'NONE',  ( 19.02544592524334988, 5.153800228976608722, 36.45942372801900433 ) ) ;
#37838 = CARTESIAN_POINT ( 'NONE',  ( 5.153800228976335163, 19.02544592524342804, 99.79057627198102409 ) ) ;
#37839 = CARTESIAN_POINT ( 'NONE',  ( -21.55341960407610458, -5.719274019375992779, 61.45724293864770260 ) ) ;
#37840 = CARTESIAN_POINT ( 'NONE',  ( -25.41560487745637076, 11.65347601360405605, 166.2639678467665476 ) ) ;
#37841 = CARTESIAN_POINT ( 'NONE',  ( 0.05219959533910956823, 16.53943276465976808, 114.9989096053143669 ) ) ;
#37842 = CARTESIAN_POINT ( 'NONE',  ( -0.05219959533937732626, 21.53943276465977519, 112.5010903946857042 ) ) ;
#37843 = CARTESIAN_POINT ( 'NONE',  ( -12.14591786802326823, 12.06949235617739902, 73.12609039468567573 ) ) ;
#37844 = CARTESIAN_POINT ( 'NONE',  ( -15.80617190586768217, 15.72974639402176855, 33.12609039468569705 ) ) ;
#37845 = CARTESIAN_POINT ( 'NONE',  ( 8.314922557961029526, -14.29746914071037800, 45.41775706135234003 ) ) ;
#37846 = CARTESIAN_POINT ( 'NONE',  ( -9.474510206698964154, 16.51473224551069663, 105.4155762719810383 ) ) ;
#37847 = CARTESIAN_POINT ( 'NONE',  ( 16.51473224551069308, 9.474510206698969483, 44.16557627198103120 ) ) ;
#37848 = CARTESIAN_POINT ( 'NONE',  ( -19.03943276465977164, 0.05219959533909376836, 71.24890960531435269 ) ) ;
#37849 = VECTOR ( 'NONE', #114087, 1000.000000000000000 ) ;
#37850 = CARTESIAN_POINT ( 'NONE',  ( -16.52544592524335698, -4.483927247898792601, 43.95942372801902565 ) ) ;
#37851 = CARTESIAN_POINT ( 'NONE',  ( -0.05219959533910754901, -16.53943276465976808, 92.49890960531436690 ) ) ;
#37852 = CARTESIAN_POINT ( 'NONE',  ( 8.224510206698742110, 14.34966873604972548, 102.0844237280190185 ) ) ;
#37853 = DIRECTION ( 'NONE',  ( 1.000000000000000000, 0.000000000000000000, 0.000000000000000000 ) ) ;
#37856 = CARTESIAN_POINT ( 'NONE',  ( -16.46253265017160317, 9.564922557960807481, 65.83224293864769550 ) ) ;
#37855 = CARTESIAN_POINT ( 'NONE',  ( 5.153800228976335163, 19.02544592524342804, 74.79057627198103830 ) ) ;
#37854 = CARTESIAN_POINT ( 'NONE',  ( 21.55341960407619695, -5.719274019375665929, 61.04275706135234714 ) ) ;
#37857 = CARTESIAN_POINT ( 'NONE',  ( 19.05341960407611168, 5.049401038298154454, 93.95724293864769550 ) ) ;
#37858 = CARTESIAN_POINT ( 'NONE',  ( -14.29746914071049879, 8.314922557960819915, 50.83224293864770971 ) ) ;
#37859 = CARTESIAN_POINT ( 'NONE',  ( -16.53943276465976808, -0.05219959533934237506, 98.75109039468568994 ) ) ;
#37860 = CARTESIAN_POINT ( 'NONE',  ( 4.483927247898545687, 16.52544592524342804, 24.79057627198103120 ) ) ;
#37861 = EDGE_LOOP ( 'NONE', ( #170103, #195316, #173275 ) ) ;
#37862 = CARTESIAN_POINT ( 'NONE',  ( 13.97604488694548053, -13.89961937509957401, 45.62609039468566863 ) ) ;
#37863 = DIRECTION ( 'NONE',  ( 1.000000000000000000, 0.000000000000000000, 0.000000000000000000 ) ) ;
#37864 = CARTESIAN_POINT ( 'NONE',  ( 16.46253265017160672, -9.564922557960803928, 58.33224293864769550 ) ) ;
#37865 = CARTESIAN_POINT ( 'NONE',  ( 16.51473224551083163, -9.474510206698727899, 40.83442372801900433 ) ) ;
#37866 = CARTESIAN_POINT ( 'NONE',  ( -11.40812507854754720, -35.11059874428192273, -2.224999997268813701 ) ) ;
#37867 = DIRECTION ( 'NONE',  ( 0.000000000000000000, 0.000000000000000000, -1.000000000000000000 ) ) ;
#37869 = CARTESIAN_POINT ( 'NONE',  ( -0.05219959533934338120, 16.53943276465976808, 67.50109039468568994 ) ) ;
#37868 = CARTESIAN_POINT ( 'NONE',  ( 16.46253265017146816, 9.564922557961045513, 81.66775706135233293 ) ) ;
#37870 = CARTESIAN_POINT ( 'NONE',  ( 16.20579543436678094, 7.371946100355098785, 93.06520834171877254 ) ) ;
#37871 =( BOUNDED_CURVE ( )  B_SPLINE_CURVE ( 2, ( #101184, #41542, #87032, #69868, #146696, #40534, #162873, #86032, #117368, #165880, #11207, #102205, #103205 ),
 .UNSPECIFIED., .F., .T. ) 
 B_SPLINE_CURVE_WITH_KNOTS ( ( 3, 2, 2, 2, 2, 2, 3 ),
 ( 0.6076935943217820491, 0.6096491228070175517, 0.6140350877192982670, 0.6184210526315789824, 0.6228070175438596978, 0.6271929824561403022, 0.6291028311192857769 ),
 .UNSPECIFIED. ) 
 CURVE ( )  GEOMETRIC_REPRESENTATION_ITEM ( )  RATIONAL_B_SPLINE_CURVE ( ( 0.9831626618144007068, 0.9848076720550096308, 1.000000000000000000, 0.9659258262890683122, 1.000000000000000000, 0.9659258262890683122, 1.000000000000000000, 0.9659258262890683122, 1.000000000000000000, 0.9659258262890683122, 1.000000000000000000, 0.9851625545550091179, 0.9832469066685282089 ) ) 
 REPRESENTATION_ITEM ( '' )  );
#37872 = CARTESIAN_POINT ( 'NONE',  ( 9.474510206698971260, -16.51473224551069308, 92.91557627198103830 ) ) ;
#37873 = CARTESIAN_POINT ( 'NONE',  ( -0.05219959533937732626, 21.53943276465977519, 22.50109039468567573 ) ) ;
#37874 = CARTESIAN_POINT ( 'NONE',  ( 19.05341960407617918, -5.049401038297876454, 76.04275706135230450 ) ) ;
#37876 = CARTESIAN_POINT ( 'NONE',  ( 0.05219959533909260263, 19.03943276465977164, 29.99890960531435979 ) ) ;
#37875 = CARTESIAN_POINT ( 'NONE',  ( 17.49999999999999645, 5.500000000000010658, 88.78230962303567253 ) ) ;
#37877 = CARTESIAN_POINT ( 'NONE',  ( 13.97604488694527802, 13.89961937509977652, 89.37390960531436690 ) ) ;
#37879 = CARTESIAN_POINT ( 'NONE',  ( 9.474510206698971260, -16.51473224551069308, 42.91557627198103120 ) ) ;
#37878 = CARTESIAN_POINT ( 'NONE',  ( 8.224510206698953496, -14.34966873604960469, 52.91557627198103830 ) ) ;
#37880 = CARTESIAN_POINT ( 'NONE',  ( 19.03943276465977164, 0.05219959533936151252, 46.25109039468566863 ) ) ;
#37881 = ORIENTED_EDGE ( 'NONE', *, *, #95942, .F. ) ;
#37882 = CARTESIAN_POINT ( 'NONE',  ( -4.483927247898539470, -16.52544592524342804, 82.29057627198103830 ) ) ;
#37883 = CARTESIAN_POINT ( 'NONE',  ( 9.474510206698729675, 16.51473224551082808, 32.08442372801900433 ) ) ;
#37884 = CARTESIAN_POINT ( 'NONE',  ( -5.153800228976328057, -19.02544592524343514, 72.29057627198102409 ) ) ;
#37885 = CARTESIAN_POINT ( 'NONE',  ( -21.55341960407610458, -5.719274019375992779, 61.45724293864770260 ) ) ;
#37887 = CARTESIAN_POINT ( 'NONE',  ( 13.97604488694548053, -13.89961937509957401, 25.62609039468566507 ) ) ;
#37886 = CARTESIAN_POINT ( 'NONE',  ( 8.224510206698953496, -14.34966873604960469, 52.91557627198103830 ) ) ;
#37888 = CARTESIAN_POINT ( 'NONE',  ( -0.05219959533909027116, -19.03943276465977164, 102.4989096053143669 ) ) ;
#37889 = CARTESIAN_POINT ( 'NONE',  ( 5.719274019375991003, -21.55341960407610458, 22.70724293864769194 ) ) ;
#37890 = CARTESIAN_POINT ( 'NONE',  ( 5.049401038298161559, -19.05341960407611168, 47.70724293864770260 ) ) ;
#37891 = CARTESIAN_POINT ( 'NONE',  ( 16.51473224551069308, 9.474510206698969483, 24.16557627198102765 ) ) ;
#37892 = CARTESIAN_POINT ( 'NONE',  ( -4.379528057220328563, 16.55341960407611168, 95.20724293864769550 ) ) ;
#37893 = CARTESIAN_POINT ( 'NONE',  ( 5.719274019375991003, -21.55341960407610458, 92.70724293864770971 ) ) ;
#37894 = CARTESIAN_POINT ( 'NONE',  ( 9.474510206698971260, -16.51473224551069308, 107.9155762719810383 ) ) ;
#37895 = CARTESIAN_POINT ( 'NONE',  ( -21.52544592524343514, 5.823673210054127303, 106.0405762719810525 ) ) ;
#37896 = CARTESIAN_POINT ( 'NONE',  ( 0.05219959533909260263, 19.03943276465977164, 109.9989096053143669 ) ) ;
#37897 = CARTESIAN_POINT ( 'NONE',  ( -13.89961937509977652, 13.97604488694528158, 25.62390960531434558 ) ) ;
#37898 = CARTESIAN_POINT ( 'NONE',  ( 5.823673210054444382, -21.52544592524334988, 80.20942372801901854 ) ) ;
#37899 = CARTESIAN_POINT ( 'NONE',  ( 21.55341960407610458, 5.719274019375980345, 88.95724293864769550 ) ) ;
#37900 = LINE ( 'NONE', #113719, #124634 ) ;
#37901 = DIRECTION ( 'NONE',  ( 6.391086490440868450E-16, -1.000000000000000000, 0.000000000000000000 ) ) ;
#37902 = CARTESIAN_POINT ( 'NONE',  ( 18.22780087662121673, 5.500000000000056843, 58.98459894673892023 ) ) ;
#37903 = CARTESIAN_POINT ( 'NONE',  ( 12.14591786802327356, -12.06949235617739191, 40.62609039468567573 ) ) ;
#37904 = CARTESIAN_POINT ( 'NONE',  ( -4.483927247898539470, -16.52544592524342804, 112.2905762719810241 ) ) ;
#37905 = CARTESIAN_POINT ( 'NONE',  ( -17.50000000000000355, -3.209263204892571775, 110.2380317439372845 ) ) ;
#37906 = CARTESIAN_POINT ( 'NONE',  ( -5.049401038298153566, 19.05341960407611168, 60.20724293864768129 ) ) ;
#37907 = CARTESIAN_POINT ( 'NONE',  ( 14.29746914071049879, -8.314922557960816363, 93.33224293864769550 ) ) ;
#37908 = CARTESIAN_POINT ( 'NONE',  ( -18.67979575497178146, -10.72451020669898902, 31.66557627198102054 ) ) ;
#37909 = CARTESIAN_POINT ( 'NONE',  ( 8.224510206698953496, -14.34966873604960469, 62.91557627198102409 ) ) ;
#37910 = CARTESIAN_POINT ( 'NONE',  ( 19.02544592524334988, 5.153800228976608722, 111.4594237280190043 ) ) ;
#37911 = CARTESIAN_POINT ( 'NONE',  ( -21.53943276465977519, -0.05219959533937600094, 78.75109039468568994 ) ) ;
#37912 = CARTESIAN_POINT ( 'NONE',  ( 14.34966873604972726, -8.224510206698740333, 100.8344237280190185 ) ) ;
#37913 = CARTESIAN_POINT ( 'NONE',  ( -16.55341960407611168, -4.379528057220339221, 41.45724293864769550 ) ) ;
#37914 = CARTESIAN_POINT ( 'NONE',  ( -19.05341960407611168, -5.049401038298163336, 41.45724293864769550 ) ) ;
#37915 = CARTESIAN_POINT ( 'NONE',  ( 13.97604488694527802, 13.89961937509977652, 89.37390960531436690 ) ) ;
#37916 = CARTESIAN_POINT ( 'NONE',  ( 21.53943276465977519, -0.05219959533907433946, 93.74890960531436690 ) ) ;
#37917 = CARTESIAN_POINT ( 'NONE',  ( -4.379528057220086978, -16.55341960407618274, 29.79275706135234358 ) ) ;
#37919 = CARTESIAN_POINT ( 'NONE',  ( -18.67979575497193778, 10.72451020669871902, 68.33442372801900433 ) ) ;
#37918 = CARTESIAN_POINT ( 'NONE',  ( -12.06949235617756955, 12.14591786802309770, 60.62390960531437401 ) ) ;
#37920 = CARTESIAN_POINT ( 'NONE',  ( -16.55341960407617563, 4.379528057220093196, 98.54275706135234714 ) ) ;
#37921 = CARTESIAN_POINT ( 'NONE',  ( 16.79531203550682505, -7.028104445595340977, 46.24755011779544134 ) ) ;
#37922 = CARTESIAN_POINT ( 'NONE',  ( 28.90000000000004476, -9.625633623500122352E-14, -64.92279855667830191 ) ) ;
#37923 = CARTESIAN_POINT ( 'NONE',  ( 16.52544592524342804, -4.483927247898539470, 28.54057627198103120 ) ) ;
#37924 = CARTESIAN_POINT ( 'NONE',  ( -4.379528057220086978, -16.55341960407618274, 79.79275706135236135 ) ) ;
#37925 = CARTESIAN_POINT ( 'NONE',  ( 13.97604488694527802, 13.89961937509977652, 84.37390960531433848 ) ) ;
#37926 = CARTESIAN_POINT ( 'NONE',  ( -19.05341960407611168, -5.049401038298163336, 81.45724293864769550 ) ) ;
#37927 = CARTESIAN_POINT ( 'NONE',  ( 21.55341960407619695, -5.719274019375665929, 91.04275706135236135 ) ) ;
#37928 = CARTESIAN_POINT ( 'NONE',  ( 12.14591786802327356, -12.06949235617739191, 90.62609039468567573 ) ) ;
#37929 = CARTESIAN_POINT ( 'NONE',  ( 4.379528057220339221, -16.55341960407611168, 57.70724293864770260 ) ) ;
#37930 = CARTESIAN_POINT ( 'NONE',  ( -19.05341960407611168, -5.049401038298163336, 66.45724293864769550 ) ) ;
#37931 = ORIENTED_EDGE ( 'NONE', *, *, #39985, .F. ) ;
#37932 = CARTESIAN_POINT ( 'NONE',  ( -5.049401038297874678, -19.05341960407617918, 109.7927570613523187 ) ) ;
#37933 = CARTESIAN_POINT ( 'NONE',  ( 16.55341960407611168, 4.379528057220329451, 103.9572429386476813 ) ) ;
#37934 = CARTESIAN_POINT ( 'NONE',  ( 16.46253265017160672, -9.564922557960803928, 78.33224293864769550 ) ) ;
#37936 = CARTESIAN_POINT ( 'NONE',  ( -29.86685920354755197, -21.69954338932560134, -10.42499999726881299 ) ) ;
#37935 = CARTESIAN_POINT ( 'NONE',  ( -14.34966873604972548, 8.224510206698743886, 23.33442372801901499 ) ) ;
#37937 = CARTESIAN_POINT ( 'NONE',  ( 9.474510206698729675, 16.51473224551082808, 22.08442372801899722 ) ) ;
#37938 = CARTESIAN_POINT ( 'NONE',  ( 12.06949235617739724, 12.14591786802326823, 81.87609039468568994 ) ) ;
#37939 = CARTESIAN_POINT ( 'NONE',  ( -16.46253265017146816, -9.564922557961047289, 94.16775706135233293 ) ) ;
#37941 = B_SPLINE_CURVE_WITH_KNOTS ( 'NONE', 3,
 ( #112697, #141054, #159191, #83350, #110711, #145026, #52024, #109723, #34868, #4506, #2540, #32893, #144031, #111711, #157227, #172393 ),
 .UNSPECIFIED., .F., .F.,
 ( 4, 2, 2, 2, 2, 2, 2, 4 ),
 ( 0.001225964299381153508, 0.002243048150408413245, 0.002751590075922042029, 0.003260132001435670814, 0.003768673926949299598, 0.004277215852462927514, 0.004785757777976557166, 0.005294299703490185083 ),
 .UNSPECIFIED. ) ;
#37940 = CARTESIAN_POINT ( 'NONE',  ( -9.564922557960796823, -16.46253265017161027, 22.08224293864768839 ) ) ;
#37942 = CARTESIAN_POINT ( 'NONE',  ( 14.34966873604972726, -8.224510206698740333, 60.83442372801901854 ) ) ;
#37943 = CARTESIAN_POINT ( 'NONE',  ( 0.05219959533934541429, -16.53943276465976808, 55.00109039468568284 ) ) ;
#37944 = CARTESIAN_POINT ( 'NONE',  ( -19.03943276465977164, 0.05219959533909376836, 21.24890960531436335 ) ) ;
#37945 = CARTESIAN_POINT ( 'NONE',  ( -5.049401038297874678, -19.05341960407617918, 59.79275706135231871 ) ) ;
#37946 = CARTESIAN_POINT ( 'NONE',  ( 18.62759615963255655, 10.81492255796105972, 91.66775706135234714 ) ) ;
#37947 = CARTESIAN_POINT ( 'NONE',  ( -13.97604488694527625, -13.89961937509977652, 36.87390960531436690 ) ) ;
#37948 = CARTESIAN_POINT ( 'NONE',  ( -9.564922557960796823, -16.46253265017161027, 82.08224293864768129 ) ) ;
#37949 = CARTESIAN_POINT ( 'NONE',  ( -4.483927247898539470, -16.52544592524342804, 77.29057627198102409 ) ) ;
#37950 = AXIS2_PLACEMENT_3D ( 'NONE', #11450, #104437, #137743 ) ;
#37951 = EDGE_CURVE ( 'NONE', #58436, #150593, #179764, .T. ) ;
#37952 = CARTESIAN_POINT ( 'NONE',  ( 18.62759615963255655, 10.81492255796105972, 86.66775706135234714 ) ) ;
#37953 = CARTESIAN_POINT ( 'NONE',  ( -19.03943276465977164, -0.05219959533935918106, 58.75109039468566863 ) ) ;
#37954 = CARTESIAN_POINT ( 'NONE',  ( -16.46253265017146816, -9.564922557961047289, 39.16775706135234003 ) ) ;
#37955 = CARTESIAN_POINT ( 'NONE',  ( 10.72451020669898902, -18.67979575497178502, 32.91557627198102409 ) ) ;
#37956 = CARTESIAN_POINT ( 'NONE',  ( -0.05219959533937732626, 21.53943276465977519, 97.50109039468567573 ) ) ;
#37957 = CARTESIAN_POINT ( 'NONE',  ( 19.05341960407611168, 5.049401038298154454, 83.95724293864766707 ) ) ;
#37958 = CARTESIAN_POINT ( 'NONE',  ( -18.67979575497193778, 10.72451020669871902, 108.3344237280190185 ) ) ;
#37959 = CARTESIAN_POINT ( 'NONE',  ( -21.52544592524343514, 5.823673210054127303, 51.04057627198103120 ) ) ;
#37960 = CARTESIAN_POINT ( 'NONE',  ( -5.153800228976328057, -19.02544592524343514, 97.29057627198099567 ) ) ;
#37961 = CARTESIAN_POINT ( 'NONE',  ( -16.46253265017146816, -9.564922557961047289, 74.16775706135234714 ) ) ;
#37962 = CARTESIAN_POINT ( 'NONE',  ( -9.564922557960796823, -16.46253265017161027, 102.0822429386477097 ) ) ;
#37963 = CARTESIAN_POINT ( 'NONE',  ( 16.51473224551083163, -9.474510206698727899, 100.8344237280190043 ) ) ;
#37964 = CARTESIAN_POINT ( 'NONE',  ( -4.483927247898782831, 16.52544592524335698, 47.70942372801902565 ) ) ;
#37965 = CARTESIAN_POINT ( 'NONE',  ( -4.379528057220328563, 16.55341960407611168, 105.2072429386477097 ) ) ;
#37966 = CARTESIAN_POINT ( 'NONE',  ( 16.46253265017160672, -9.564922557960803928, 88.33224293864769550 ) ) ;
#37967 = CARTESIAN_POINT ( 'NONE',  ( 15.80617190586746368, 15.72974639402197994, 64.37390960531435269 ) ) ;
#37968 = CARTESIAN_POINT ( 'NONE',  ( -14.29746914071037622, -8.314922557961029526, 39.16775706135235424 ) ) ;
#37969 = CARTESIAN_POINT ( 'NONE',  ( -5.719274019375665041, -21.55341960407619695, 39.79275706135235424 ) ) ;
#37970 = CARTESIAN_POINT ( 'NONE',  ( 10.81492255796106328, -18.62759615963255655, 80.41775706135234714 ) ) ;
#37971 = CARTESIAN_POINT ( 'NONE',  ( 4.379528057220092307, 16.55341960407617563, 77.29275706135234714 ) ) ;
#37972 = CARTESIAN_POINT ( 'NONE',  ( -9.474510206698964154, 16.51473224551069663, 70.41557627198102409 ) ) ;
#37973 = CARTESIAN_POINT ( 'NONE',  ( 12.06949235617757843, -12.14591786802309237, 83.12390960531436690 ) ) ;
#37974 = CARTESIAN_POINT ( 'NONE',  ( -8.314922557960811034, -14.29746914071050412, 22.08224293864769194 ) ) ;
#37975 = CARTESIAN_POINT ( 'NONE',  ( -13.89961937509957401, -13.97604488694547875, 54.37609039468565442 ) ) ;
#37976 = VECTOR ( 'NONE', #50487, 1000.000000000000000 ) ;
#37977 = CARTESIAN_POINT ( 'NONE',  ( 10.81492255796106328, -18.62759615963255655, 50.41775706135235424 ) ) ;
#37978 = CARTESIAN_POINT ( 'NONE',  ( 16.52544592524342804, -4.483927247898539470, 83.54057627198102409 ) ) ;
#37979 = CARTESIAN_POINT ( 'NONE',  ( -5.823673210054116645, -21.52544592524344225, 22.29057627198102765 ) ) ;
#37980 = CARTESIAN_POINT ( 'NONE',  ( -16.53943276465976808, -0.05219959533934237506, 108.7510903946857042 ) ) ;
#37981 = CARTESIAN_POINT ( 'NONE',  ( -0.05219959533937732626, 21.53943276465977519, 77.50109039468567573 ) ) ;
#37982 = CARTESIAN_POINT ( 'NONE',  ( 12.14591786802327356, -12.06949235617739191, 40.62609039468567573 ) ) ;
#37983 = CARTESIAN_POINT ( 'NONE',  ( -18.67979575497193778, 10.72451020669871902, 38.33442372801900433 ) ) ;
#37984 = ADVANCED_FACE ( 'NONE', ( #13867 ), #96544, .T. ) ;
#37985 = ORIENTED_EDGE ( 'NONE', *, *, #137680, .T. ) ;
#37986 = CARTESIAN_POINT ( 'NONE',  ( 5.719274019375673035, 21.55341960407619339, 22.29275706135235069 ) ) ;
#37987 = CARTESIAN_POINT ( 'NONE',  ( -0.05219959533910754901, -16.53943276465976808, 97.49890960531436690 ) ) ;
#37988 = CARTESIAN_POINT ( 'NONE',  ( -18.56101223717332260, -5.499999999999950262, 51.44978406935678095 ) ) ;
#37989 = CARTESIAN_POINT ( 'NONE',  ( -16.55341960407611168, -4.379528057220339221, 56.45724293864768839 ) ) ;
#37990 = CARTESIAN_POINT ( 'NONE',  ( 19.05341960407611168, 5.049401038298154454, 28.95724293864769550 ) ) ;
#37991 = CARTESIAN_POINT ( 'NONE',  ( 21.53943276465977519, -0.05219959533907433946, 43.74890960531435979 ) ) ;
#37992 = CARTESIAN_POINT ( 'NONE',  ( -4.483927247898539470, -16.52544592524342804, 77.29057627198102409 ) ) ;
#37993 = AXIS2_PLACEMENT_3D ( 'NONE', #73609, #43256, #9937 ) ;
#37994 = CARTESIAN_POINT ( 'NONE',  ( 10.72451020669898902, -18.67979575497178502, 82.91557627198103830 ) ) ;
#37995 = CARTESIAN_POINT ( 'NONE',  ( -19.05341960407611168, -5.049401038298163336, 81.45724293864769550 ) ) ;
#37997 = CARTESIAN_POINT ( 'NONE',  ( -19.05341960407617563, 5.049401038297882671, 98.54275706135233293 ) ) ;
#37996 = CARTESIAN_POINT ( 'NONE',  ( 0.05219959533909260263, 19.03943276465977164, 39.99890960531436690 ) ) ;
#37998 = CARTESIAN_POINT ( 'NONE',  ( -5.823673210054116645, -21.52544592524344225, 27.29057627198103120 ) ) ;
#38000 = CARTESIAN_POINT ( 'NONE',  ( -21.53943276465977519, 0.05219959533907696930, 61.24890960531435979 ) ) ;
#37999 = CARTESIAN_POINT ( 'NONE',  ( -15.72974639402176322, -15.80617190586768395, 59.37609039468568284 ) ) ;
#38001 = CARTESIAN_POINT ( 'NONE',  ( 5.049401038298161559, -19.05341960407611168, 37.70724293864768839 ) ) ;
#38002 = CARTESIAN_POINT ( 'NONE',  ( -5.153800228976328057, -19.02544592524343514, 77.29057627198099567 ) ) ;
#38003 = VERTEX_POINT ( 'NONE', #186630 ) ;
#38004 = CARTESIAN_POINT ( 'NONE',  ( 8.224510206698742110, 14.34966873604972548, 47.08442372801901854 ) ) ;
#38005 = CARTESIAN_POINT ( 'NONE',  ( -15.72974639402176322, -15.80617190586768395, 29.37609039468568284 ) ) ;
#38006 = CARTESIAN_POINT ( 'NONE',  ( -10.72451020669870658, -18.67979575497194134, 69.58442372801900433 ) ) ;
#38007 = CARTESIAN_POINT ( 'NONE',  ( -21.55341960407610458, -5.719274019375992779, 21.45724293864769550 ) ) ;
#38008 = CARTESIAN_POINT ( 'NONE',  ( 21.53943276465977519, -0.05219959533907433946, 88.74890960531436690 ) ) ;
#38010 = CARTESIAN_POINT ( 'NONE',  ( -4.483927247898782831, 16.52544592524335698, 52.70942372801902565 ) ) ;
#38009 = CARTESIAN_POINT ( 'NONE',  ( -15.72974639402176322, -15.80617190586768395, 29.37609039468568284 ) ) ;
#38011 = CARTESIAN_POINT ( 'NONE',  ( 5.719274019375991003, -21.55341960407610458, 67.70724293864769550 ) ) ;
#38012 = CARTESIAN_POINT ( 'NONE',  ( 13.97604488694548053, -13.89961937509957401, 25.62609039468566507 ) ) ;
#38013 = CARTESIAN_POINT ( 'NONE',  ( -5.049401038298153566, 19.05341960407611168, 50.20724293864770260 ) ) ;
#38014 = CARTESIAN_POINT ( 'NONE',  ( -9.474510206698964154, 16.51473224551069663, 115.4155762719810241 ) ) ;
#38015 = CARTESIAN_POINT ( 'NONE',  ( -19.02544592524342804, 5.153800228976336051, 96.04057627198103830 ) ) ;
#38016 = CARTESIAN_POINT ( 'NONE',  ( 20.99774934350697109, 22.92000981050135877, -46.85949206705566183 ) ) ;
#38017 = CARTESIAN_POINT ( 'NONE',  ( -9.564922557961040184, 16.46253265017147172, 67.91775706135233293 ) ) ;
#38018 = CARTESIAN_POINT ( 'NONE',  ( 18.67979575497178502, 10.72451020669898547, 39.16557627198102409 ) ) ;
#38019 = CARTESIAN_POINT ( 'NONE',  ( 16.52544592524335698, 4.483927247898782831, 111.4594237280190328 ) ) ;
#38020 = CARTESIAN_POINT ( 'NONE',  ( 13.89961937509957401, 13.97604488694547697, 101.8760903946856331 ) ) ;
#38021 = CARTESIAN_POINT ( 'NONE',  ( 16.51473224551069308, 9.474510206698969483, 24.16557627198102765 ) ) ;
#38022 = CARTESIAN_POINT ( 'NONE',  ( 5.153800228976615827, -19.02544592524334988, 25.20942372801900433 ) ) ;
#38023 = CARTESIAN_POINT ( 'NONE',  ( 13.89961937509957401, 13.97604488694547697, 101.8760903946856331 ) ) ;
#38025 = CARTESIAN_POINT ( 'NONE',  ( 5.049401038297881783, 19.05341960407617563, 62.29275706135234003 ) ) ;
#38024 = CARTESIAN_POINT ( 'NONE',  ( 15.72974639402199770, -15.80617190586745480, 88.12390960531436690 ) ) ;
#38026 = LINE ( 'NONE', #97663, #62869 ) ;
#38027 = CARTESIAN_POINT ( 'NONE',  ( -19.05341960407611168, -5.049401038298163336, 56.45724293864768129 ) ) ;
#38028 = CARTESIAN_POINT ( 'NONE',  ( -14.29746914071049879, 8.314922557960819915, 65.83224293864769550 ) ) ;
#38029 = CARTESIAN_POINT ( 'NONE',  ( -16.51473224551069308, -9.474510206698971260, 41.66557627198103120 ) ) ;
#38030 = CARTESIAN_POINT ( 'NONE',  ( 16.55341960407611168, 4.379528057220329451, 58.95724293864770971 ) ) ;
#38031 = DIRECTION ( 'NONE',  ( 0.5000000000000037748, 0.4999999999999950040, 0.7071067811865483499 ) ) ;
#38032 = CARTESIAN_POINT ( 'NONE',  ( -0.05219959533910754901, -16.53943276465976808, 32.49890960531435979 ) ) ;
#38033 = CARTESIAN_POINT ( 'NONE',  ( 0.05219959533909260263, 19.03943276465977164, 59.99890960531436690 ) ) ;
#38034 = CARTESIAN_POINT ( 'NONE',  ( -9.564922557961040184, 16.46253265017147172, 22.91775706135233648 ) ) ;
#38035 = CARTESIAN_POINT ( 'NONE',  ( -16.52544592524335698, -4.483927247898792601, 33.95942372801901143 ) ) ;
#38036 = CARTESIAN_POINT ( 'NONE',  ( -10.81492255796078084, -18.62759615963271287, 47.08224293864770260 ) ) ;
#38038 = VERTEX_POINT ( 'NONE', #172430 ) ;
#38037 = CARTESIAN_POINT ( 'NONE',  ( 15.80617190586769283, -15.72974639402175789, 105.6260903946856899 ) ) ;
#38039 = CARTESIAN_POINT ( 'NONE',  ( -5.049401038298153566, 19.05341960407611168, 65.20724293864765286 ) ) ;
#38040 = DIRECTION ( 'NONE',  ( -0.000000000000000000, -0.000000000000000000, 1.000000000000000000 ) ) ;
#38041 = CARTESIAN_POINT ( 'NONE',  ( 5.153800228976335163, 19.02544592524342804, 99.79057627198102409 ) ) ;
#38042 = CARTESIAN_POINT ( 'NONE',  ( 11.40812507854754365, 35.11059874428196537, -3.224999997268813701 ) ) ;
#38043 = CARTESIAN_POINT ( 'NONE',  ( 5.823673210054444382, -21.52544592524334988, 25.20942372801901854 ) ) ;
#38044 = CARTESIAN_POINT ( 'NONE',  ( 12.14591786802309770, 12.06949235617756955, 99.37390960531436690 ) ) ;
#38046 = CARTESIAN_POINT ( 'NONE',  ( -9.564922557960796823, -16.46253265017161027, 72.08224293864770971 ) ) ;
#38045 = CARTESIAN_POINT ( 'NONE',  ( -10.72451020669898014, 18.67979575497178502, 85.41557627198102409 ) ) ;
#38047 = CARTESIAN_POINT ( 'NONE',  ( -13.89961937509977652, 13.97604488694528158, 90.62390960531432427 ) ) ;
#38048 = CARTESIAN_POINT ( 'NONE',  ( -15.80617190586745835, -15.72974639402198527, 111.8739096053143669 ) ) ;
#38049 = ORIENTED_EDGE ( 'NONE', *, *, #142366, .T. ) ;
#38050 = CARTESIAN_POINT ( 'NONE',  ( -5.153800228976328057, -19.02544592524343514, 67.29057627198102409 ) ) ;
#38051 = CARTESIAN_POINT ( 'NONE',  ( 8.898068258721464119, 27.38543819252877398, 147.3843446568999980 ) ) ;
#38053 = CARTESIAN_POINT ( 'NONE',  ( 5.153800228976335163, 19.02544592524342804, 24.79057627198102765 ) ) ;
#38052 = CARTESIAN_POINT ( 'NONE',  ( 14.29746914071049879, -8.314922557960816363, 108.3322429386477097 ) ) ;
#38054 = CARTESIAN_POINT ( 'NONE',  ( -13.97604488694547697, 13.89961937509957934, 93.12609039468566152 ) ) ;
#38055 = CARTESIAN_POINT ( 'NONE',  ( -9.564922557960796823, -16.46253265017161027, 22.08224293864768839 ) ) ;
#38056 = CARTESIAN_POINT ( 'NONE',  ( 21.52544592524334988, 5.823673210054432836, 71.45942372801901854 ) ) ;
#38058 = CARTESIAN_POINT ( 'NONE',  ( 21.53943276465977519, 0.05219959533937863772, 31.25109039468568639 ) ) ;
#38057 = CARTESIAN_POINT ( 'NONE',  ( 16.51473224551069308, 9.474510206698969483, 64.16557627198102409 ) ) ;
#38059 = CARTESIAN_POINT ( 'NONE',  ( 21.52544592524344225, -5.823673210054117533, 113.5405762719810383 ) ) ;
#38060 = CARTESIAN_POINT ( 'NONE',  ( 17.81289503416611453, -24.51734667627695785, 144.6999999999999886 ) ) ;
#38061 = CARTESIAN_POINT ( 'NONE',  ( 0.05219959533909260263, 19.03943276465977164, 74.99890960531435269 ) ) ;
#38062 = CARTESIAN_POINT ( 'NONE',  ( 27.96784714409925243, 7.240004476324741312, 160.9788157999919918 ) ) ;
#38064 = CARTESIAN_POINT ( 'NONE',  ( -5.719274019375978568, 21.55341960407610458, 35.20724293864768839 ) ) ;
#38063 = CARTESIAN_POINT ( 'NONE',  ( -16.52544592524335698, -4.483927247898792601, 23.95942372801901143 ) ) ;
#38065 = CARTESIAN_POINT ( 'NONE',  ( 21.55341960407619695, -5.719274019375665929, 66.04275706135236135 ) ) ;
#38066 = CARTESIAN_POINT ( 'NONE',  ( 16.46253265017160672, -9.564922557960803928, 113.3322429386476955 ) ) ;
#38067 = CARTESIAN_POINT ( 'NONE',  ( 19.02544592524334988, 5.153800228976608722, 96.45942372801897591 ) ) ;
#38068 = CARTESIAN_POINT ( 'NONE',  ( -16.51473224551069308, -9.474510206698971260, 46.66557627198102409 ) ) ;
#38069 = CARTESIAN_POINT ( 'NONE',  ( -16.46253265017160317, 9.564922557960807481, 70.83224293864770971 ) ) ;
#38070 = CARTESIAN_POINT ( 'NONE',  ( -16.53943276465976808, 0.05219959533911058130, 91.24890960531436690 ) ) ;
#38071 = CARTESIAN_POINT ( 'NONE',  ( 13.89961937509977652, -13.97604488694527269, 108.1239096053143669 ) ) ;
#38072 = CARTESIAN_POINT ( 'NONE',  ( -16.55341960407611168, -4.379528057220339221, 96.45724293864770971 ) ) ;
#38073 = CARTESIAN_POINT ( 'NONE',  ( -19.05341960407611168, -5.049401038298163336, 96.45724293864769550 ) ) ;
#38075 = CARTESIAN_POINT ( 'NONE',  ( 0.05219959533909260263, 19.03943276465977164, 44.99890960531435979 ) ) ;
#38074 = CARTESIAN_POINT ( 'NONE',  ( -16.55341960407611168, -4.379528057220339221, 56.45724293864768839 ) ) ;
#38076 = CARTESIAN_POINT ( 'NONE',  ( 15.72974639402176855, 15.80617190586768217, 51.87609039468568284 ) ) ;
#38077 = CARTESIAN_POINT ( 'NONE',  ( -16.51473224551082808, 9.474510206698731452, 98.33442372801900433 ) ) ;
#38078 = CARTESIAN_POINT ( 'NONE',  ( 14.34966873604960469, 8.224510206698951720, 54.16557627198103120 ) ) ;
#38079 = CARTESIAN_POINT ( 'NONE',  ( 15.72974639402199770, -15.80617190586745480, 93.12390960531436690 ) ) ;
#38080 = CARTESIAN_POINT ( 'NONE',  ( -18.62759615963270932, 10.81492255796079327, 45.83224293864769550 ) ) ;
#38082 = CARTESIAN_POINT ( 'NONE',  ( 16.55341960407611168, 4.379528057220329451, 78.95724293864769550 ) ) ;
#38081 = CARTESIAN_POINT ( 'NONE',  ( 19.35543954521080323, 5.499999999999572786, 72.08901960356452321 ) ) ;
#38083 = CARTESIAN_POINT ( 'NONE',  ( -27.73933785331498925, 2.428612866367529932E-14, 144.8750000027311842 ) ) ;
#38084 = CARTESIAN_POINT ( 'NONE',  ( 0.05219959533909260263, 19.03943276465977164, 49.99890960531435979 ) ) ;
#38085 = CARTESIAN_POINT ( 'NONE',  ( -4.379528057220086978, -16.55341960407618274, 109.7927570613523613 ) ) ;
#38086 = CIRCLE ( 'NONE', #31592, 21.30000000000002913 ) ;
#38087 = CARTESIAN_POINT ( 'NONE',  ( 8.314922557961029526, -14.29746914071037800, 95.41775706135234714 ) ) ;
#38088 = CARTESIAN_POINT ( 'NONE',  ( 4.483927247898790824, -16.52544592524335698, 85.20942372801901854 ) ) ;
#38089 = CARTESIAN_POINT ( 'NONE',  ( 19.03943276465977164, 0.05219959533936151252, 41.25109039468566152 ) ) ;
#38091 = CARTESIAN_POINT ( 'NONE',  ( 5.153800228976335163, 19.02544592524342804, 109.7905762719810099 ) ) ;
#38090 = CARTESIAN_POINT ( 'NONE',  ( -16.62475595723694965, 7.163666690055376485, 70.52713351810469078 ) ) ;
#38092 = CARTESIAN_POINT ( 'NONE',  ( -13.89961937509977652, 13.97604488694528158, 90.62390960531432427 ) ) ;
#38093 = CARTESIAN_POINT ( 'NONE',  ( 5.049401038298161559, -19.05341960407611168, 32.70724293864768129 ) ) ;
#38094 = CARTESIAN_POINT ( 'NONE',  ( 12.06949235617757843, -12.14591786802309237, 43.12390960531435269 ) ) ;
#38096 = CARTESIAN_POINT ( 'NONE',  ( 19.02544592524343514, -5.153800228976328945, 108.5405762719810383 ) ) ;
#38095 = DIRECTION ( 'NONE',  ( 0.000000000000000000, -1.000000000000000000, 0.000000000000000000 ) ) ;
#38097 = CARTESIAN_POINT ( 'NONE',  ( 0.05219959533907565091, 21.53943276465977519, 34.99890960531435979 ) ) ;
#38098 = CARTESIAN_POINT ( 'NONE',  ( -8.314922557960811034, -14.29746914071050412, 87.08224293864769550 ) ) ;
#38099 = CARTESIAN_POINT ( 'NONE',  ( -14.34966873604972548, 8.224510206698743886, 43.33442372801901143 ) ) ;
#38100 = CARTESIAN_POINT ( 'NONE',  ( 4.379528057220339221, -16.55341960407611168, 72.70724293864769550 ) ) ;
#38101 = CARTESIAN_POINT ( 'NONE',  ( 29.79829367730021872, -1.376802789500971347, -48.54110828511540632 ) ) ;
#38102 = CARTESIAN_POINT ( 'NONE',  ( -0.05219959533936034679, 19.03943276465977164, 62.50109039468566863 ) ) ;
#38103 = CARTESIAN_POINT ( 'NONE',  ( -16.51473224551069308, -9.474510206698971260, 96.66557627198102409 ) ) ;
#38104 = CARTESIAN_POINT ( 'NONE',  ( -19.02544592524334988, -5.153800228976617603, 83.95942372801901854 ) ) ;
#38105 = CARTESIAN_POINT ( 'NONE',  ( -22.55670631985092456, 22.55670631985084995, -49.13275782002545355 ) ) ;
#38107 = CARTESIAN_POINT ( 'NONE',  ( -12.06949235617739369, -12.14591786802326823, 109.3760903946857042 ) ) ;
#38106 = CARTESIAN_POINT ( 'NONE',  ( -16.52544592524335698, -4.483927247898792601, 33.95942372801901143 ) ) ;
#38108 = CARTESIAN_POINT ( 'NONE',  ( -13.97604488694547697, 13.89961937509957934, 78.12609039468567573 ) ) ;
#38109 = CARTESIAN_POINT ( 'NONE',  ( -10.81492255796078084, -18.62759615963271287, 32.08224293864769550 ) ) ;
#38110 = CARTESIAN_POINT ( 'NONE',  ( -15.80617190586768217, 15.72974639402176855, 68.12609039468567573 ) ) ;
#38111 = CARTESIAN_POINT ( 'NONE',  ( -19.83802472612924106, -12.02135855756094251, 167.9999999999999716 ) ) ;
#38112 = CARTESIAN_POINT ( 'NONE',  ( 16.46253265017146816, 9.564922557961045513, 111.6677570613523329 ) ) ;
#38114 = CARTESIAN_POINT ( 'NONE',  ( 0.05219959533909260263, 19.03943276465977164, 84.99890960531436690 ) ) ;
#38113 = CARTESIAN_POINT ( 'NONE',  ( 19.03943276465977164, -0.05219959533909143690, 23.74890960531435269 ) ) ;
#38115 = VECTOR ( 'NONE', #153443, 999.9999999999998863 ) ;
#38116 = CARTESIAN_POINT ( 'NONE',  ( -19.02544592524342804, 5.153800228976336051, 26.04057627198103120 ) ) ;
#38118 = CARTESIAN_POINT ( 'NONE',  ( -5.153800228976328057, -19.02544592524343514, 77.29057627198099567 ) ) ;
#38117 = CARTESIAN_POINT ( 'NONE',  ( -12.06949235617756955, 12.14591786802309770, 85.62390960531436690 ) ) ;
#38119 = APPLICATION_PROTOCOL_DEFINITION ( 'draft international standard', 'automotive_design', 1998, #110017 ) ;
#38120 = CARTESIAN_POINT ( 'NONE',  ( -19.03943276465977164, 0.05219959533909376836, 86.24890960531436690 ) ) ;
#38121 = EDGE_LOOP ( 'NONE', ( #191720, #79259, #33762, #109984, #5698, #146204 ) ) ;
#38122 = CARTESIAN_POINT ( 'NONE',  ( 9.564922557961047289, -16.46253265017146816, 90.41775706135234714 ) ) ;
#38123 = CARTESIAN_POINT ( 'NONE',  ( 21.55341960407610458, 5.719274019375980345, 73.95724293864769550 ) ) ;
#38124 = CARTESIAN_POINT ( 'NONE',  ( -9.474510206698964154, 16.51473224551069663, 30.41557627198102054 ) ) ;
#38126 = CARTESIAN_POINT ( 'NONE',  ( -10.72451020669898014, 18.67979575497178502, 115.4155762719810241 ) ) ;
#38125 = CARTESIAN_POINT ( 'NONE',  ( -16.51473224551082808, 9.474510206698731452, 68.33442372801900433 ) ) ;
#38127 = CARTESIAN_POINT ( 'NONE',  ( 9.474510206698971260, -16.51473224551069308, 67.91557627198102409 ) ) ;
#38128 = CARTESIAN_POINT ( 'NONE',  ( -19.02544592524342804, 5.153800228976336051, 106.0405762719810241 ) ) ;
#38129 = ORIENTED_EDGE ( 'NONE', *, *, #35651, .F. ) ;
#38130 =( BOUNDED_CURVE ( )  B_SPLINE_CURVE ( 3, ( #9057, #103057, #42391, #134405 ),
 .UNSPECIFIED., .F., .T. ) 
 B_SPLINE_CURVE_WITH_KNOTS ( ( 4, 4 ),
 ( 1.025647941782810824, 2.008945357379066987 ),
 .UNSPECIFIED. ) 
 CURVE ( )  GEOMETRIC_REPRESENTATION_ITEM ( )  RATIONAL_B_SPLINE_CURVE ( ( 1.000000000000000000, 0.9210371567966664230, 0.9210371567966664230, 1.000000000000000000 ) ) 
 REPRESENTATION_ITEM ( '' )  );
#38131 = CARTESIAN_POINT ( 'NONE',  ( -21.52544592524343514, 5.823673210054127303, 101.0405762719810383 ) ) ;
#38134 = CARTESIAN_POINT ( 'NONE',  ( -5.153800228976607833, 19.02544592524334988, 62.70942372801899722 ) ) ;
#38133 = CARTESIAN_POINT ( 'NONE',  ( 13.97604488694527802, 13.89961937509977652, 84.37390960531433848 ) ) ;
#38132 = CARTESIAN_POINT ( 'NONE',  ( 0.05219959533910956823, 16.53943276465976808, 94.99890960531436690 ) ) ;
#38135 = CARTESIAN_POINT ( 'NONE',  ( -21.53943276465977519, 0.05219959533907696930, 91.24890960531436690 ) ) ;
#38136 = CARTESIAN_POINT ( 'NONE',  ( 18.62759615963271287, -10.81492255796078972, 68.33224293864769550 ) ) ;
#38137 = CARTESIAN_POINT ( 'NONE',  ( -16.55341960407611168, -4.379528057220339221, 41.45724293864769550 ) ) ;
#38138 = CARTESIAN_POINT ( 'NONE',  ( -9.564922557961040184, 16.46253265017147172, 27.91775706135232582 ) ) ;
#38139 = CARTESIAN_POINT ( 'NONE',  ( 12.06949235617739724, 12.14591786802326823, 66.87609039468568994 ) ) ;
#38140 = CARTESIAN_POINT ( 'NONE',  ( 5.153800228976335163, 19.02544592524342804, 94.79057627198103830 ) ) ;
#38141 = CARTESIAN_POINT ( 'NONE',  ( 19.05341960407611168, 5.049401038298154454, 43.95724293864769550 ) ) ;
#38142 = CARTESIAN_POINT ( 'NONE',  ( -0.05219959533937732626, 21.53943276465977519, 47.50109039468568994 ) ) ;
#38143 = CARTESIAN_POINT ( 'NONE',  ( -18.67979575497193778, 10.72451020669871902, 53.33442372801901854 ) ) ;
#38144 = CARTESIAN_POINT ( 'NONE',  ( -13.97604488694527625, -13.89961937509977652, 61.87390960531435979 ) ) ;
#38145 = CARTESIAN_POINT ( 'NONE',  ( -21.53943276465977519, -0.05219959533937600094, 38.75109039468567573 ) ) ;
#38146 = CARTESIAN_POINT ( 'NONE',  ( -19.02544592524334988, -5.153800228976617603, 78.95942372801900433 ) ) ;
#38147 = CARTESIAN_POINT ( 'NONE',  ( 13.97604488694548053, -13.89961937509957401, 70.62609039468567573 ) ) ;
#38148 = CARTESIAN_POINT ( 'NONE',  ( -13.89961937509977652, 13.97604488694528158, 40.62390960531435979 ) ) ;
#38149 = CARTESIAN_POINT ( 'NONE',  ( -12.14591786802326823, 12.06949235617739902, 83.12609039468568994 ) ) ;
#38150 = CARTESIAN_POINT ( 'NONE',  ( -19.03943276465977164, 0.05219959533909376836, 56.24890960531435979 ) ) ;
#38151 = CARTESIAN_POINT ( 'NONE',  ( 24.29042230868020624, -8.936166115090800943, 166.5611006352801553 ) ) ;
#38152 = CARTESIAN_POINT ( 'NONE',  ( 13.89961937509977652, -13.97604488694527269, 103.1239096053143527 ) ) ;
#38153 = CARTESIAN_POINT ( 'NONE',  ( -5.049401038298153566, 19.05341960407611168, 35.20724293864768839 ) ) ;
#38154 = CARTESIAN_POINT ( 'NONE',  ( 5.823673210054125526, 21.52544592524343514, 79.79057627198102409 ) ) ;
#38155 = CARTESIAN_POINT ( 'NONE',  ( 4.483927247898790824, -16.52544592524335698, 55.20942372801902565 ) ) ;
#38156 = CARTESIAN_POINT ( 'NONE',  ( 19.02544592524334988, 5.153800228976608722, 21.45942372801899012 ) ) ;
#38157 = CARTESIAN_POINT ( 'NONE',  ( -9.474510206698964154, 16.51473224551069663, 55.41557627198103120 ) ) ;
#38158 = CARTESIAN_POINT ( 'NONE',  ( 4.379528057220339221, -16.55341960407611168, 47.70724293864770260 ) ) ;
#38159 = CARTESIAN_POINT ( 'NONE',  ( 16.53943276465976808, -0.05219959533910856209, 83.74890960531435269 ) ) ;
#38160 = CARTESIAN_POINT ( 'NONE',  ( 19.03943276465977164, -0.05219959533909143690, 73.74890960531435269 ) ) ;
#38161 = CARTESIAN_POINT ( 'NONE',  ( 5.823673210054444382, -21.52544592524334988, 40.20942372801901854 ) ) ;
#38162 = CARTESIAN_POINT ( 'NONE',  ( 19.02544592524343514, -5.153800228976328945, 98.54057627198100988 ) ) ;
#38163 = CARTESIAN_POINT ( 'NONE',  ( 10.81492255796106328, -18.62759615963255655, 105.4177570613523613 ) ) ;
#38164 = CARTESIAN_POINT ( 'NONE',  ( 4.483927247898790824, -16.52544592524335698, 70.20942372801904696 ) ) ;
#38165 = CARTESIAN_POINT ( 'NONE',  ( -0.05219959533937732626, 21.53943276465977519, 27.50109039468567929 ) ) ;
#38166 = CARTESIAN_POINT ( 'NONE',  ( 5.049401038298161559, -19.05341960407611168, 107.7072429386476955 ) ) ;
#38167 = CARTESIAN_POINT ( 'NONE',  ( -21.55341960407610458, -5.719274019375992779, 91.45724293864769550 ) ) ;
#38168 = CARTESIAN_POINT ( 'NONE',  ( -0.05219959533910754901, -16.53943276465976808, 47.49890960531435979 ) ) ;
#38169 = CARTESIAN_POINT ( 'NONE',  ( 16.51473224551069308, 9.474510206698969483, 39.16557627198103120 ) ) ;
#38170 = CARTESIAN_POINT ( 'NONE',  ( 14.34966873604960469, 8.224510206698951720, 74.16557627198102409 ) ) ;
#38171 = CARTESIAN_POINT ( 'NONE',  ( 5.823673210054125526, 21.52544592524343514, 24.79057627198103120 ) ) ;
#38172 = CARTESIAN_POINT ( 'NONE',  ( 9.474510206698729675, 16.51473224551082808, 32.08442372801900433 ) ) ;
#38173 = CARTESIAN_POINT ( 'NONE',  ( -14.34966873604960291, -8.224510206698953496, 106.6655762719810383 ) ) ;
#38174 = CARTESIAN_POINT ( 'NONE',  ( 13.89961937509977652, -13.97604488694527269, 113.1239096053143527 ) ) ;
#38175 = EDGE_LOOP ( 'NONE', ( #67663, #43732, #128356, #192810 ) ) ;
#38176 = CARTESIAN_POINT ( 'NONE',  ( -14.34966873604972548, 8.224510206698743886, 58.33442372801901143 ) ) ;
#38177 = CARTESIAN_POINT ( 'NONE',  ( -13.89961937509977652, 13.97604488694528158, 50.62390960531435979 ) ) ;
#38178 = CARTESIAN_POINT ( 'NONE',  ( -27.73933785331498925, 2.428612866367529932E-14, 138.8750000027311842 ) ) ;
#38179 = CARTESIAN_POINT ( 'NONE',  ( -12.06949235617739369, -12.14591786802326823, 99.37609039468568994 ) ) ;
#38180 = CARTESIAN_POINT ( 'NONE',  ( -9.474510206698720793, -16.51473224551083518, 94.58442372801900433 ) ) ;
#38181 = CARTESIAN_POINT ( 'NONE',  ( -18.62759615963255300, -10.81492255796106328, 74.16775706135231871 ) ) ;
#38182 = CARTESIAN_POINT ( 'NONE',  ( 13.89961937509977652, -13.97604488694527269, 68.12390960531436690 ) ) ;
#38183 = CARTESIAN_POINT ( 'NONE',  ( -0.05219959533907301413, -21.53943276465977519, 87.49890960531436690 ) ) ;
#38184 = CARTESIAN_POINT ( 'NONE',  ( 16.53943276465976808, 0.05219959533934440121, 46.25109039468567573 ) ) ;
#38185 = CARTESIAN_POINT ( 'NONE',  ( -16.53943276465976808, 0.05219959533911058130, 106.2489096053143811 ) ) ;
#38186 = CARTESIAN_POINT ( 'NONE',  ( 5.049401038297881783, 19.05341960407617563, 77.29275706135231871 ) ) ;
#38187 = CARTESIAN_POINT ( 'NONE',  ( 5.823673210054125526, 21.52544592524343514, 79.79057627198102409 ) ) ;
#38188 = CARTESIAN_POINT ( 'NONE',  ( -16.46253265017146816, -9.564922557961047289, 54.16775706135234003 ) ) ;
#38189 = CARTESIAN_POINT ( 'NONE',  ( 19.03943276465977164, -0.05219959533909143690, 113.7489096053143669 ) ) ;
#38190 = CARTESIAN_POINT ( 'NONE',  ( 18.67979575497178502, 10.72451020669898547, 84.16557627198103830 ) ) ;
#38191 = CARTESIAN_POINT ( 'NONE',  ( 17.49999999999998934, 4.640572885337633124, 26.86211835451159757 ) ) ;
#38192 = CARTESIAN_POINT ( 'NONE',  ( 16.51473224551069308, 9.474510206698969483, 69.16557627198102409 ) ) ;
#38193 = PLANE ( 'NONE',  #69125 ) ;
#38194 = CARTESIAN_POINT ( 'NONE',  ( 4.483927247898790824, -16.52544592524335698, 25.20942372801901854 ) ) ;
#38195 = LINE ( 'NONE', #6838, #141830 ) ;
#38196 = CARTESIAN_POINT ( 'NONE',  ( 5.153800228976335163, 19.02544592524342804, 44.79057627198103830 ) ) ;
#38198 = CARTESIAN_POINT ( 'NONE',  ( -16.52544592524342804, 4.483927247898546575, 56.04057627198102409 ) ) ;
#38197 = CARTESIAN_POINT ( 'NONE',  ( 21.52544592524344225, -5.823673210054117533, 103.5405762719810383 ) ) ;
#38199 = CARTESIAN_POINT ( 'NONE',  ( -16.46253265017160317, 9.564922557960807481, 70.83224293864770971 ) ) ;
#38200 = CARTESIAN_POINT ( 'NONE',  ( 10.81492255796106328, -18.62759615963255655, 80.41775706135234714 ) ) ;
#38202 = CARTESIAN_POINT ( 'NONE',  ( -19.02544592524334988, -5.153800228976617603, 33.95942372801897591 ) ) ;
#38201 = CARTESIAN_POINT ( 'NONE',  ( 12.06949235617739724, 12.14591786802326823, 21.87609039468567573 ) ) ;
#38203 = CARTESIAN_POINT ( 'NONE',  ( -18.62759615963255300, -10.81492255796106328, 39.16775706135235424 ) ) ;
#38204 = CARTESIAN_POINT ( 'NONE',  ( -0.05219959533907301413, -21.53943276465977519, 107.4989096053143669 ) ) ;
#38205 = CARTESIAN_POINT ( 'NONE',  ( -18.62759615963270932, 10.81492255796079327, 55.83224293864770260 ) ) ;
#38206 = CARTESIAN_POINT ( 'NONE',  ( 16.46253265017146816, 9.564922557961045513, 96.66775706135233293 ) ) ;
#38207 = CARTESIAN_POINT ( 'NONE',  ( -16.51473224551082808, 9.474510206698731452, 63.33442372801900433 ) ) ;
#38208 = CARTESIAN_POINT ( 'NONE',  ( -15.80617190586768217, 15.72974639402176855, 83.12609039468568994 ) ) ;
#38209 = CARTESIAN_POINT ( 'NONE',  ( 19.03943276465977164, 0.05219959533936151252, 56.25109039468566863 ) ) ;
#38210 = CARTESIAN_POINT ( 'NONE',  ( 19.05341960407611168, 5.049401038298154454, 28.95724293864769550 ) ) ;
#38211 = CARTESIAN_POINT ( 'NONE',  ( 5.823673210054125526, 21.52544592524343514, 54.79057627198104541 ) ) ;
#38212 = CARTESIAN_POINT ( 'NONE',  ( 12.14591786802309770, 12.06949235617756955, 44.37390960531435979 ) ) ;
#38213 = CARTESIAN_POINT ( 'NONE',  ( -38.00000000000000711, 2.428612866367529932E-14, -1.749999994537626558 ) ) ;
#38214 = CARTESIAN_POINT ( 'NONE',  ( 19.03943276465977164, 0.05219959533936151252, 26.25109039468566507 ) ) ;
#38215 = CARTESIAN_POINT ( 'NONE',  ( -4.379528057220086978, -16.55341960407618274, 89.79275706135236135 ) ) ;
#38216 = CARTESIAN_POINT ( 'NONE',  ( 0.05219959533910956823, 16.53943276465976808, 34.99890960531435979 ) ) ;
#38217 = CARTESIAN_POINT ( 'NONE',  ( 18.62759615963255655, 10.81492255796105972, 81.66775706135236135 ) ) ;
#38218 = CARTESIAN_POINT ( 'NONE',  ( 21.55341960407619695, -5.719274019375665929, 76.04275706135237556 ) ) ;
#38219 = CARTESIAN_POINT ( 'NONE',  ( 10.72451020669898902, -18.67979575497178502, 87.91557627198103830 ) ) ;
#38220 = EDGE_CURVE ( 'NONE', #49306, #101016, #167681, .T. ) ;
#38221 = CARTESIAN_POINT ( 'NONE',  ( -9.564922557960796823, -16.46253265017161027, 42.08224293864769550 ) ) ;
#38222 = CARTESIAN_POINT ( 'NONE',  ( 10.81492255796106328, -18.62759615963255655, 50.41775706135235424 ) ) ;
#38223 = CARTESIAN_POINT ( 'NONE',  ( -19.05341960407611168, -5.049401038298163336, 41.45724293864769550 ) ) ;
#38224 = CARTESIAN_POINT ( 'NONE',  ( -16.46253265017160317, 9.564922557960807481, 45.83224293864769550 ) ) ;
#38225 = CARTESIAN_POINT ( 'NONE',  ( -16.53943276465976808, 0.05219959533911058130, 91.24890960531436690 ) ) ;
#38226 = CARTESIAN_POINT ( 'NONE',  ( -5.049401038298153566, 19.05341960407611168, 105.2072429386476671 ) ) ;
#38227 = CARTESIAN_POINT ( 'NONE',  ( 14.29746914071049879, -8.314922557960816363, 38.33224293864768839 ) ) ;
#38228 = CARTESIAN_POINT ( 'NONE',  ( 14.29746914071049879, -8.314922557960816363, 113.3322429386476955 ) ) ;
#38229 = CARTESIAN_POINT ( 'NONE',  ( -10.81492255796078084, -18.62759615963271287, 87.08224293864769550 ) ) ;
#38230 = CARTESIAN_POINT ( 'NONE',  ( 21.52544592524334988, 5.823673210054432836, 26.45942372801901854 ) ) ;
#38231 = CARTESIAN_POINT ( 'NONE',  ( 27.93385843979449845, -7.419916809875269692, 160.9064084702648643 ) ) ;
#38232 = CARTESIAN_POINT ( 'NONE',  ( 12.06949235617739724, 12.14591786802326823, 31.87609039468567929 ) ) ;
#38233 = CARTESIAN_POINT ( 'NONE',  ( -18.67979575497178146, -10.72451020669898902, 76.66557627198103830 ) ) ;
#38234 = CARTESIAN_POINT ( 'NONE',  ( 18.67979575497194134, -10.72451020669871369, 95.83442372801903275 ) ) ;
#38235 = CARTESIAN_POINT ( 'NONE',  ( 19.05341960407611168, 5.049401038298154454, 93.95724293864769550 ) ) ;
#38236 = CARTESIAN_POINT ( 'NONE',  ( -10.72451020669870658, -18.67979575497194134, 34.58442372801900433 ) ) ;
#38237 = CARTESIAN_POINT ( 'NONE',  ( -21.52544592524343514, 5.823673210054127303, 31.04057627198102409 ) ) ;
#38238 = CARTESIAN_POINT ( 'NONE',  ( -14.34966873604972548, 8.224510206698743886, 93.33442372801901854 ) ) ;
#38239 = CARTESIAN_POINT ( 'NONE',  ( 15.80617190586769283, -15.72974639402175789, 65.62609039468568994 ) ) ;
#38240 = CARTESIAN_POINT ( 'NONE',  ( 21.52544592524334988, 5.823673210054432836, 111.4594237280190328 ) ) ;
#38241 = CARTESIAN_POINT ( 'NONE',  ( 4.379528057220092307, 16.55341960407617563, 72.29275706135236135 ) ) ;
#38242 = CARTESIAN_POINT ( 'NONE',  ( -21.52544592524334988, -5.823673210054445271, 28.95942372801902209 ) ) ;
#38243 = CARTESIAN_POINT ( 'NONE',  ( 13.97604488694527802, 13.89961937509977652, 29.37390960531435979 ) ) ;
#38244 = CARTESIAN_POINT ( 'NONE',  ( -10.72451020669870658, -18.67979575497194134, 109.5844237280190328 ) ) ;
#38245 = CARTESIAN_POINT ( 'NONE',  ( 5.049401038298161559, -19.05341960407611168, 112.7072429386476813 ) ) ;
#38246 = CARTESIAN_POINT ( 'NONE',  ( -21.53943276465977519, 0.05219959533907696930, 106.2489096053143811 ) ) ;
#38248 = CARTESIAN_POINT ( 'NONE',  ( 0.05219959533907565091, 21.53943276465977519, 59.99890960531436690 ) ) ;
#38247 = CARTESIAN_POINT ( 'NONE',  ( -7.282160400437569514, -46.44936954762594183, -22.53643251332787756 ) ) ;
#38250 = CARTESIAN_POINT ( 'NONE',  ( 12.06949235617757843, -12.14591786802309237, 53.12390960531436690 ) ) ;
#38249 = CARTESIAN_POINT ( 'NONE',  ( 12.06949235617739724, 12.14591786802326823, 51.87609039468568284 ) ) ;
#38251 = CARTESIAN_POINT ( 'NONE',  ( 21.58591991293347689, 5.574009794464005019, 173.3850233475172615 ) ) ;
#38252 = CARTESIAN_POINT ( 'NONE',  ( 13.89961937509957401, 13.97604488694547697, 81.87609039468564731 ) ) ;
#38253 = VECTOR ( 'NONE', #194788, 1000.000000000000114 ) ;
#38254 = CARTESIAN_POINT ( 'NONE',  ( -16.31925111598457079, 7.325300261831521276, 105.1642453896725300 ) ) ;
#38255 = CARTESIAN_POINT ( 'NONE',  ( 19.03943276465977164, 0.05219959533936151252, 106.2510903946856615 ) ) ;
#38256 = CARTESIAN_POINT ( 'NONE',  ( 15.72974639402199770, -15.80617190586745480, 88.12390960531436690 ) ) ;
#38257 = CARTESIAN_POINT ( 'NONE',  ( -8.224510206698948167, 14.34966873604960824, 70.41557627198102409 ) ) ;
#38258 = CARTESIAN_POINT ( 'NONE',  ( 13.89961937509977652, -13.97604488694527269, 98.12390960531433848 ) ) ;
#38259 = CARTESIAN_POINT ( 'NONE',  ( 4.379528057220092307, 16.55341960407617563, 47.29275706135234003 ) ) ;
#38260 = CARTESIAN_POINT ( 'NONE',  ( 13.89961937509977652, -13.97604488694527269, 58.12390960531436690 ) ) ;
#38262 = CARTESIAN_POINT ( 'NONE',  ( 9.474510206698729675, 16.51473224551082808, 92.08442372801900433 ) ) ;
#38261 = CARTESIAN_POINT ( 'NONE',  ( 10.72451020669871369, 18.67979575497193778, 32.08442372801901854 ) ) ;
#38263 = CARTESIAN_POINT ( 'NONE',  ( -19.03943276465977164, 0.05219959533909376836, 101.2489096053143669 ) ) ;
#38264 = CARTESIAN_POINT ( 'NONE',  ( 9.564922557960805705, 16.46253265017160317, 84.58224293864769550 ) ) ;
#38265 = CARTESIAN_POINT ( 'NONE',  ( -15.72974639402197994, 15.80617190586746368, 85.62390960531436690 ) ) ;
#38266 = CARTESIAN_POINT ( 'NONE',  ( 5.049401038298161559, -19.05341960407611168, 47.70724293864770260 ) ) ;
#38267 = CARTESIAN_POINT ( 'NONE',  ( -16.52216118717207394, -7.221426719304526287, 61.07599021046993215 ) ) ;
#38268 = CARTESIAN_POINT ( 'NONE',  ( -4.379528057220328563, 16.55341960407611168, 65.20724293864768129 ) ) ;
#38269 = CARTESIAN_POINT ( 'NONE',  ( 16.51473224551069308, 9.474510206698969483, 104.1655762719810241 ) ) ;
#38270 = CARTESIAN_POINT ( 'NONE',  ( -30.74735067906812702, 1.468823602708742238, -50.54421433284819898 ) ) ;
#38271 = CARTESIAN_POINT ( 'NONE',  ( -19.03943276465977164, -0.05219959533935918106, 68.75109039468566152 ) ) ;
#38272 = CARTESIAN_POINT ( 'NONE',  ( -21.53943276465977519, 0.05219959533907696930, 91.24890960531436690 ) ) ;
#38273 = CARTESIAN_POINT ( 'NONE',  ( -13.89961937509957401, -13.97604488694547875, 54.37609039468565442 ) ) ;
#38274 = CARTESIAN_POINT ( 'NONE',  ( 16.51473224551069308, 9.474510206698969483, 99.16557627198102409 ) ) ;
#38275 = CARTESIAN_POINT ( 'NONE',  ( 19.19724070472096145, 5.499999999999974243, 68.56193348274381094 ) ) ;
#38276 = CARTESIAN_POINT ( 'NONE',  ( 21.52544592524344225, -5.823673210054117533, 38.54057627198103120 ) ) ;
#38277 = CARTESIAN_POINT ( 'NONE',  ( -19.02544592524342804, 5.153800228976336051, 91.04057627198100988 ) ) ;
#38278 = CARTESIAN_POINT ( 'NONE',  ( 10.81492255796106328, -18.62759615963255655, 60.41775706135235424 ) ) ;
#38279 = CARTESIAN_POINT ( 'NONE',  ( 16.51473224551069308, 9.474510206698969483, 39.16557627198103120 ) ) ;
#38280 = CARTESIAN_POINT ( 'NONE',  ( 8.314922557960818139, 14.29746914071049879, 79.58224293864769550 ) ) ;
#38281 = CARTESIAN_POINT ( 'NONE',  ( 4.483927247898790824, -16.52544592524335698, 25.20942372801901854 ) ) ;
#38282 = CARTESIAN_POINT ( 'NONE',  ( 21.53943276465977519, 0.05219959533937863772, 56.25109039468568284 ) ) ;
#38283 = VERTEX_POINT ( 'NONE', #154281 ) ;
#38284 = CARTESIAN_POINT ( 'NONE',  ( 13.97604488694527802, 13.89961937509977652, 114.3739096053143669 ) ) ;
#38285 = CARTESIAN_POINT ( 'NONE',  ( 9.474510206698729675, 16.51473224551082808, 67.08442372801900433 ) ) ;
#38286 = DIRECTION ( 'NONE',  ( 0.000000000000000000, 0.000000000000000000, 1.000000000000000000 ) ) ;
#38287 = CARTESIAN_POINT ( 'NONE',  ( -10.72451020669870658, -18.67979575497194134, 24.58442372801901499 ) ) ;
#38288 = CARTESIAN_POINT ( 'NONE',  ( -38.00000000000000711, 2.428612866367529932E-14, -5.749999994537626336 ) ) ;
#38289 = CARTESIAN_POINT ( 'NONE',  ( 5.153800228976615827, -19.02544592524334988, 25.20942372801900433 ) ) ;
#38290 = CARTESIAN_POINT ( 'NONE',  ( -19.02544592524342804, 5.153800228976336051, 61.04057627198103120 ) ) ;
#38291 = CARTESIAN_POINT ( 'NONE',  ( -5.823673210054431948, 21.52544592524334988, 112.7094237280190328 ) ) ;
#38292 = CARTESIAN_POINT ( 'NONE',  ( -4.483927247898782831, 16.52544592524335698, 107.7094237280190328 ) ) ;
#38294 = CARTESIAN_POINT ( 'NONE',  ( -18.62759615963255300, -10.81492255796106328, 79.16775706135234714 ) ) ;
#38293 = CARTESIAN_POINT ( 'NONE',  ( 19.03943276465977164, -0.05219959533909143690, 103.7489096053143669 ) ) ;
#38295 = CARTESIAN_POINT ( 'NONE',  ( 22.81625015709509441, 31.40387420917330275, -9.324999997268813345 ) ) ;
#38296 = LINE ( 'NONE', #39291, #31995 ) ;
#38297 = DIRECTION ( 'NONE',  ( 0.000000000000000000, 0.000000000000000000, 1.000000000000000000 ) ) ;
#38299 = CARTESIAN_POINT ( 'NONE',  ( 21.52544592524334988, 5.823673210054432836, 66.45942372801903275 ) ) ;
#38298 = CARTESIAN_POINT ( 'NONE',  ( -4.483927247898782831, 16.52544592524335698, 72.70942372801901854 ) ) ;
#38300 = CARTESIAN_POINT ( 'NONE',  ( -21.55341960407619339, 5.719274019375674811, 108.5427570613523756 ) ) ;
#38301 = DIRECTION ( 'NONE',  ( 0.000000000000000000, 0.000000000000000000, 1.000000000000000000 ) ) ;
#38302 = CARTESIAN_POINT ( 'NONE',  ( 9.474510206698971260, -16.51473224551069308, 87.91557627198102409 ) ) ;
#38303 = CARTESIAN_POINT ( 'NONE',  ( 19.03943276465977164, -0.05219959533909143690, 113.7489096053143669 ) ) ;
#38304 = ORIENTED_EDGE ( 'NONE', *, *, #77897, .T. ) ;
#38305 = CARTESIAN_POINT ( 'NONE',  ( 25.65937876999948841, -27.64914803190701420, -20.38451907593468349 ) ) ;
#38306 = CARTESIAN_POINT ( 'NONE',  ( -9.474510206698964154, 16.51473224551069663, 40.41557627198103120 ) ) ;
#38307 = CARTESIAN_POINT ( 'NONE',  ( -10.72451020669898014, 18.67979575497178502, 40.41557627198103120 ) ) ;
#38308 = CARTESIAN_POINT ( 'NONE',  ( 12.06949235617739724, 12.14591786802326823, 111.8760903946856615 ) ) ;
#38310 = CARTESIAN_POINT ( 'NONE',  ( 13.97604488694527802, 13.89961937509977652, 84.37390960531433848 ) ) ;
#38309 = CARTESIAN_POINT ( 'NONE',  ( -16.55341960407611168, -4.379528057220339221, 96.45724293864770971 ) ) ;
#38311 = CARTESIAN_POINT ( 'NONE',  ( -0.05219959533937732626, 21.53943276465977519, 102.5010903946856899 ) ) ;
#38312 = CARTESIAN_POINT ( 'NONE',  ( 19.02544592524343514, -5.153800228976328945, 33.54057627198102409 ) ) ;
#38313 = CARTESIAN_POINT ( 'NONE',  ( 12.06949235617757843, -12.14591786802309237, 88.12390960531436690 ) ) ;
#38314 = CARTESIAN_POINT ( 'NONE',  ( -18.62759615963255300, -10.81492255796106328, 54.16775706135235424 ) ) ;
#38315 = CARTESIAN_POINT ( 'NONE',  ( 5.823673210054125526, 21.52544592524343514, 84.79057627198102409 ) ) ;
#38316 = CARTESIAN_POINT ( 'NONE',  ( 9.474510206698729675, 16.51473224551082808, 57.08442372801900433 ) ) ;
#38317 = CARTESIAN_POINT ( 'NONE',  ( -18.22780087662121673, -5.500000000000062172, 46.48459894673893444 ) ) ;
#38318 = CARTESIAN_POINT ( 'NONE',  ( -16.46253265017160317, 9.564922557960807481, 90.83224293864769550 ) ) ;
#38319 = CARTESIAN_POINT ( 'NONE',  ( 4.379528057220339221, -16.55341960407611168, 62.70724293864769550 ) ) ;
#38320 = CARTESIAN_POINT ( 'NONE',  ( 0.05219959533936267826, -19.03943276465977164, 50.00109039468566863 ) ) ;
#38321 = CARTESIAN_POINT ( 'NONE',  ( 0.05219959533910956823, 16.53943276465976808, 44.99890960531435979 ) ) ;
#38322 = CARTESIAN_POINT ( 'NONE',  ( 9.474510206698729675, 16.51473224551082808, 77.08442372801900433 ) ) ;
#38323 = CARTESIAN_POINT ( 'NONE',  ( -18.62759615963270932, 10.81492255796079327, 40.83224293864769550 ) ) ;
#38324 = CARTESIAN_POINT ( 'NONE',  ( 12.06949235617757843, -12.14591786802309237, 103.1239096053143811 ) ) ;
#38325 = CYLINDRICAL_SURFACE ( 'NONE', #70994, 7.000000000000006217 ) ;
#38327 = CARTESIAN_POINT ( 'NONE',  ( 21.55341960407610458, 5.719274019375980345, 43.95724293864769550 ) ) ;
#38326 = CARTESIAN_POINT ( 'NONE',  ( -13.89961937509977652, 13.97604488694528158, 40.62390960531435979 ) ) ;
#38328 = CARTESIAN_POINT ( 'NONE',  ( 13.89961937509977652, -13.97604488694527269, 28.12390960531435624 ) ) ;
#38330 = CARTESIAN_POINT ( 'NONE',  ( -19.05341960407611168, -5.049401038298163336, 61.45724293864769550 ) ) ;
#38329 = CARTESIAN_POINT ( 'NONE',  ( -16.55341960407617563, 4.379528057220093196, 78.54275706135236135 ) ) ;
#38331 = CARTESIAN_POINT ( 'NONE',  ( 19.05341960407617918, -5.049401038297876454, 41.04275706135233293 ) ) ;
#38332 = CARTESIAN_POINT ( 'NONE',  ( -10.81492255796105439, 18.62759615963255655, 72.91775706135234714 ) ) ;
#38333 = CARTESIAN_POINT ( 'NONE',  ( -18.67979575497178146, -10.72451020669898902, 46.66557627198102409 ) ) ;
#38334 = CARTESIAN_POINT ( 'NONE',  ( -19.03943276465977164, 0.05219959533909376836, 26.24890960531435624 ) ) ;
#38335 = CARTESIAN_POINT ( 'NONE',  ( -16.51473224551082808, 9.474510206698731452, 98.33442372801900433 ) ) ;
#38336 = CARTESIAN_POINT ( 'NONE',  ( 27.39399371936739769, 5.109217719438622574, 166.7881433183870001 ) ) ;
#38338 = CARTESIAN_POINT ( 'NONE',  ( -21.55341960407610458, -5.719274019375992779, 41.45724293864769550 ) ) ;
#38337 = CARTESIAN_POINT ( 'NONE',  ( 17.50000000000001421, 3.385507783989948560, 37.35538298664832979 ) ) ;
#38339 = CARTESIAN_POINT ( 'NONE',  ( 9.474510206698971260, -16.51473224551069308, 27.91557627198103120 ) ) ;
#38340 = CARTESIAN_POINT ( 'NONE',  ( 15.80617190586769283, -15.72974639402175789, 80.62609039468567573 ) ) ;
#38341 = CARTESIAN_POINT ( 'NONE',  ( 14.29746914071049879, -8.314922557960816363, 43.33224293864769550 ) ) ;
#38342 = CARTESIAN_POINT ( 'NONE',  ( -14.34966873604960291, -8.224510206698953496, 56.66557627198103830 ) ) ;
#38343 = CARTESIAN_POINT ( 'NONE',  ( -18.67979575497178146, -10.72451020669898902, 81.66557627198103830 ) ) ;
#38344 = CARTESIAN_POINT ( 'NONE',  ( 21.55341960407610458, 5.719274019375980345, 78.95724293864769550 ) ) ;
#38345 = FACE_OUTER_BOUND ( 'NONE', #107153, .T. ) ;
#38347 = EDGE_CURVE ( 'NONE', #158522, #164433, #63253, .T. ) ;
#38346 = CARTESIAN_POINT ( 'NONE',  ( 10.81492255796078972, 18.62759615963270932, 29.58224293864769905 ) ) ;
#38348 = CARTESIAN_POINT ( 'NONE',  ( 16.53943276465976808, 0.05219959533934440121, 51.25109039468568994 ) ) ;
#38349 = CARTESIAN_POINT ( 'NONE',  ( -0.05219959533910754901, -16.53943276465976808, 82.49890960531436690 ) ) ;
#38350 = CARTESIAN_POINT ( 'NONE',  ( -19.05341960407611168, -5.049401038298163336, 66.45724293864769550 ) ) ;
#38351 = CARTESIAN_POINT ( 'NONE',  ( -9.564922557960796823, -16.46253265017161027, 37.08224293864768839 ) ) ;
#38352 = CARTESIAN_POINT ( 'NONE',  ( 18.22780087662121673, 5.500000000000056843, 48.98459894673892734 ) ) ;
#38353 = ORIENTED_EDGE ( 'NONE', *, *, #173030, .T. ) ;
#38354 = CARTESIAN_POINT ( 'NONE',  ( -4.483927247898782831, 16.52544592524335698, 77.70942372801900433 ) ) ;
#38355 = CARTESIAN_POINT ( 'NONE',  ( -5.719274019375665041, -21.55341960407619695, 19.79275706135235069 ) ) ;
#38356 = CARTESIAN_POINT ( 'NONE',  ( -19.05341960407611168, -5.049401038298163336, 86.45724293864769550 ) ) ;
#38357 = CARTESIAN_POINT ( 'NONE',  ( 5.719274019375673035, 21.55341960407619339, 57.29275706135234714 ) ) ;
#38358 = CARTESIAN_POINT ( 'NONE',  ( 19.03943276465977164, -0.05219959533909143690, 108.7489096053143527 ) ) ;
#38359 = CARTESIAN_POINT ( 'NONE',  ( -4.755560754640141496, -48.37114524154433326, -24.99999999999999289 ) ) ;
#38360 = ORIENTED_EDGE ( 'NONE', *, *, #198190, .F. ) ;
#38361 = CARTESIAN_POINT ( 'NONE',  ( -15.72974639402176322, -15.80617190586768395, 39.37609039468567573 ) ) ;
#38363 = CARTESIAN_POINT ( 'NONE',  ( -19.05341960407611168, -5.049401038298163336, 101.4572429386476955 ) ) ;
#38362 = CARTESIAN_POINT ( 'NONE',  ( 0.05219959533909260263, 19.03943276465977164, 24.99890960531435269 ) ) ;
#38364 = CARTESIAN_POINT ( 'NONE',  ( -19.05341960407617563, 5.049401038297882671, 58.54275706135234003 ) ) ;
#38365 = CARTESIAN_POINT ( 'NONE',  ( 21.53943276465977519, -0.05219959533907433946, 108.7489096053143669 ) ) ;
#38366 = CARTESIAN_POINT ( 'NONE',  ( 13.97604488694548053, -13.89961937509957401, 45.62609039468566863 ) ) ;
#38367 = CARTESIAN_POINT ( 'NONE',  ( 5.153800228976335163, 19.02544592524342804, 24.79057627198102765 ) ) ;
#38368 = CARTESIAN_POINT ( 'NONE',  ( -16.53943276465976808, -0.05219959533934237506, 93.75109039468567573 ) ) ;
#38369 = CARTESIAN_POINT ( 'NONE',  ( 13.89961937509957401, 13.97604488694547697, 61.87609039468566863 ) ) ;
#38370 = CARTESIAN_POINT ( 'NONE',  ( -16.52544592524335698, -4.483927247898792601, 98.95942372801903275 ) ) ;
#38372 = ORIENTED_EDGE ( 'NONE', *, *, #155322, .T. ) ;
#38371 = CARTESIAN_POINT ( 'NONE',  ( -5.000000000000000000, -139.5000000000000000, 13.35010376910484631 ) ) ;
#38373 = CARTESIAN_POINT ( 'NONE',  ( -19.02544592524342804, 5.153800228976336051, 91.04057627198100988 ) ) ;
#38374 = CARTESIAN_POINT ( 'NONE',  ( -10.72451020669870658, -18.67979575497194134, 89.58442372801901854 ) ) ;
#38375 = CARTESIAN_POINT ( 'NONE',  ( -18.67979575497193778, 10.72451020669871902, 93.33442372801901854 ) ) ;
#38376 = LINE ( 'NONE', #96053, #21147 ) ;
#38377 = CARTESIAN_POINT ( 'NONE',  ( 13.97604488694527802, 13.89961937509977652, 104.3739096053143385 ) ) ;
#38378 = CARTESIAN_POINT ( 'NONE',  ( 5.823673210054444382, -21.52544592524334988, 80.20942372801901854 ) ) ;
#38379 = CARTESIAN_POINT ( 'NONE',  ( -5.049401038297874678, -19.05341960407617918, 109.7927570613523187 ) ) ;
#38380 = CARTESIAN_POINT ( 'NONE',  ( -5.153800228976328057, -19.02544592524343514, 82.29057627198103830 ) ) ;
#38381 = CARTESIAN_POINT ( 'NONE',  ( -5.719274019375978568, 21.55341960407610458, 35.20724293864768839 ) ) ;
#38382 = CARTESIAN_POINT ( 'NONE',  ( 19.03943276465977164, -0.05219959533909143690, 98.74890960531436690 ) ) ;
#38383 = CARTESIAN_POINT ( 'NONE',  ( 193.3062444957835453, -155.7167183371837496, -4.999999999999999112 ) ) ;
#38384 = CARTESIAN_POINT ( 'NONE',  ( 16.51473224551069308, 9.474510206698969483, 74.16557627198103830 ) ) ;
#38385 = CARTESIAN_POINT ( 'NONE',  ( 13.97604488694527802, 13.89961937509977652, 64.37390960531436690 ) ) ;
#38386 = CARTESIAN_POINT ( 'NONE',  ( -12.06949235617739369, -12.14591786802326823, 94.37609039468568994 ) ) ;
#38387 = DIRECTION ( 'NONE',  ( -1.000000000000000000, 0.000000000000000000, 0.000000000000000000 ) ) ;
#38388 = CARTESIAN_POINT ( 'NONE',  ( -19.02544592524334988, -5.153800228976617603, 58.95942372801900433 ) ) ;
#38389 = CARTESIAN_POINT ( 'NONE',  ( -19.02544592524342804, 5.153800228976336051, 96.04057627198103830 ) ) ;
#38390 = CARTESIAN_POINT ( 'NONE',  ( -16.55341960407611168, -4.379528057220339221, 86.45724293864770971 ) ) ;
#38391 = CARTESIAN_POINT ( 'NONE',  ( -21.52544592524343514, 5.823673210054127303, 36.04057627198102409 ) ) ;
#38392 = CARTESIAN_POINT ( 'NONE',  ( 13.89961937509977652, -13.97604488694527269, 113.1239096053143527 ) ) ;
#38393 = CARTESIAN_POINT ( 'NONE',  ( -12.06949235617756955, 12.14591786802309770, 95.62390960531436690 ) ) ;
#38394 = FACE_BOUND ( 'NONE', #130095, .T. ) ;
#38395 = CARTESIAN_POINT ( 'NONE',  ( 13.89961937509957401, 13.97604488694547697, 46.87609039468565442 ) ) ;
#38396 = CARTESIAN_POINT ( 'NONE',  ( -16.53943276465976808, 0.05219959533911058130, 21.24890960531436690 ) ) ;
#38397 = CARTESIAN_POINT ( 'NONE',  ( 19.02544592524343514, -5.153800228976328945, 108.5405762719810383 ) ) ;
#38398 = CARTESIAN_POINT ( 'NONE',  ( 5.719274019375673035, 21.55341960407619339, 67.29275706135234714 ) ) ;
#38399 = CARTESIAN_POINT ( 'NONE',  ( -10.81492255796078084, -18.62759615963271287, 52.08224293864768839 ) ) ;
#38400 = CARTESIAN_POINT ( 'NONE',  ( 10.72451020669871369, 18.67979575497193778, 37.08442372801901143 ) ) ;
#38401 = CARTESIAN_POINT ( 'NONE',  ( 5.719274019375991003, -21.55341960407610458, 82.70724293864770971 ) ) ;
#38402 = CARTESIAN_POINT ( 'NONE',  ( -5.823673210054431948, 21.52544592524334988, 42.70942372801901854 ) ) ;
#38403 = CARTESIAN_POINT ( 'NONE',  ( 16.53943276465976808, -0.05219959533910856209, 113.7489096053143527 ) ) ;
#38404 = CARTESIAN_POINT ( 'NONE',  ( 19.03943276465977164, 0.05219959533936151252, 71.25109039468566152 ) ) ;
#38405 = CARTESIAN_POINT ( 'NONE',  ( 19.02544592524343514, -5.153800228976328945, 38.54057627198103120 ) ) ;
#38407 = CARTESIAN_POINT ( 'NONE',  ( -9.474510206698964154, 16.51473224551069663, 90.41557627198103830 ) ) ;
#38406 = CARTESIAN_POINT ( 'NONE',  ( 16.52544592524342804, -4.483927247898539470, 88.54057627198103830 ) ) ;
#38408 = CARTESIAN_POINT ( 'NONE',  ( -5.049401038298153566, 19.05341960407611168, 90.20724293864766707 ) ) ;
#38409 = CARTESIAN_POINT ( 'NONE',  ( 8.314922557960818139, 14.29746914071049879, 109.5822429386476955 ) ) ;
#38410 = CARTESIAN_POINT ( 'NONE',  ( -8.224510206698948167, 14.34966873604960824, 35.41557627198102409 ) ) ;
#38411 = CARTESIAN_POINT ( 'NONE',  ( 4.379528057220092307, 16.55341960407617563, 102.2927570613523613 ) ) ;
#38412 = CARTESIAN_POINT ( 'NONE',  ( 19.03943276465977164, -0.05219959533909143690, 53.74890960531436690 ) ) ;
#38413 = CARTESIAN_POINT ( 'NONE',  ( -5.153800228976328057, -19.02544592524343514, 22.29057627198102765 ) ) ;
#38414 = CARTESIAN_POINT ( 'NONE',  ( 13.89961937509957401, 13.97604488694547697, 26.87609039468566507 ) ) ;
#38416 = CARTESIAN_POINT ( 'NONE',  ( -14.29746914071049879, 8.314922557960819915, 25.83224293864769194 ) ) ;
#38415 = CARTESIAN_POINT ( 'NONE',  ( 16.51473224551069308, 9.474510206698969483, 114.1655762719810241 ) ) ;
#38417 = CARTESIAN_POINT ( 'NONE',  ( -18.62759615963255300, -10.81492255796106328, 49.16775706135234003 ) ) ;
#38418 = CARTESIAN_POINT ( 'NONE',  ( 5.153800228976335163, 19.02544592524342804, 99.79057627198102409 ) ) ;
#38419 = CARTESIAN_POINT ( 'NONE',  ( -16.55341960407617563, 4.379528057220093196, 43.54275706135235424 ) ) ;
#38420 = EDGE_CURVE ( 'NONE', #87433, #135144, #27843, .T. ) ;
#38421 = CARTESIAN_POINT ( 'NONE',  ( 12.06949235617739724, 12.14591786802326823, 106.8760903946856899 ) ) ;
#38422 = CARTESIAN_POINT ( 'NONE',  ( -14.29746914071037622, -8.314922557961029526, 94.16775706135237556 ) ) ;
#38423 = CARTESIAN_POINT ( 'NONE',  ( -16.52544592524335698, -4.483927247898792601, 23.95942372801901143 ) ) ;
#38424 = CARTESIAN_POINT ( 'NONE',  ( 16.51473224551069308, 9.474510206698969483, 44.16557627198103120 ) ) ;
#38425 = CARTESIAN_POINT ( 'NONE',  ( -0.05219959533910754901, -16.53943276465976808, 102.4989096053143811 ) ) ;
#38426 = CARTESIAN_POINT ( 'NONE',  ( -5.719274019375665041, -21.55341960407619695, 24.79275706135235779 ) ) ;
#38427 = CARTESIAN_POINT ( 'NONE',  ( -0.05219959533909027116, -19.03943276465977164, 32.49890960531435979 ) ) ;
#38428 = CARTESIAN_POINT ( 'NONE',  ( -5.049401038298153566, 19.05341960407611168, 105.2072429386476671 ) ) ;
#38429 = CARTESIAN_POINT ( 'NONE',  ( -0.05219959533909027116, -19.03943276465977164, 37.49890960531436690 ) ) ;
#38430 = CARTESIAN_POINT ( 'NONE',  ( 9.564922557960805705, 16.46253265017160317, 109.5822429386476955 ) ) ;
#38431 = LINE ( 'NONE', #100087, #97070 ) ;
#38432 = EDGE_CURVE ( 'NONE', #89770, #142110, #98784, .T. ) ;
#38433 = CARTESIAN_POINT ( 'NONE',  ( -13.97604488694527625, -13.89961937509977652, 96.87390960531433848 ) ) ;
#38435 = CARTESIAN_POINT ( 'NONE',  ( -12.06949235617756955, 12.14591786802309770, 110.6239096053143669 ) ) ;
#38434 = CARTESIAN_POINT ( 'NONE',  ( 0.05219959533937995610, -21.53943276465977519, 40.00109039468567573 ) ) ;
#38436 = CARTESIAN_POINT ( 'NONE',  ( 16.51473224551069308, 9.474510206698969483, 114.1655762719810241 ) ) ;
#38437 = CARTESIAN_POINT ( 'NONE',  ( -18.22780087662124160, -5.499999999999927169, 68.98236817873106475 ) ) ;
#38438 = CARTESIAN_POINT ( 'NONE',  ( -12.14591786802326823, 12.06949235617739902, 68.12609039468567573 ) ) ;
#38439 = CARTESIAN_POINT ( 'NONE',  ( -21.53943276465977519, -0.05219959533937600094, 93.75109039468567573 ) ) ;
#38440 = CARTESIAN_POINT ( 'NONE',  ( 0.05219959533934541429, -16.53943276465976808, 35.00109039468568284 ) ) ;
#38441 = CARTESIAN_POINT ( 'NONE',  ( -9.564922557960796823, -16.46253265017161027, 87.08224293864769550 ) ) ;
#38442 = CARTESIAN_POINT ( 'NONE',  ( -9.474510206698720793, -16.51473224551083518, 109.5844237280190043 ) ) ;
#38443 = CARTESIAN_POINT ( 'NONE',  ( -16.53943276465976808, -0.05219959533934237506, 88.75109039468567573 ) ) ;
#38444 = B_SPLINE_CURVE_WITH_KNOTS ( 'NONE', 3,
 ( #91225, #77071, #44761, #78057, #47747, #108408 ),
 .UNSPECIFIED., .F., .F.,
 ( 4, 2, 4 ),
 ( 0.007228050697041513671, 0.007608510107494985755, 0.007988969517948456972 ),
 .UNSPECIFIED. ) ;
#38445 = CARTESIAN_POINT ( 'NONE',  ( -13.89961937509957401, -13.97604488694547875, 99.37609039468567573 ) ) ;
#38446 = CARTESIAN_POINT ( 'NONE',  ( -9.474510206698964154, 16.51473224551069663, 75.41557627198103830 ) ) ;
#38447 = CARTESIAN_POINT ( 'NONE',  ( 15.72974639402199770, -15.80617190586745480, 98.12390960531436690 ) ) ;
#38449 = CARTESIAN_POINT ( 'NONE',  ( 19.03943276465977164, 0.05219959533936151252, 96.25109039468567573 ) ) ;
#38448 = CARTESIAN_POINT ( 'NONE',  ( 16.55341960407611168, 4.379528057220329451, 93.95724293864770971 ) ) ;
#38450 = CARTESIAN_POINT ( 'NONE',  ( -4.483927247898782831, 16.52544592524335698, 57.70942372801901143 ) ) ;
#38451 = CARTESIAN_POINT ( 'NONE',  ( -19.53037848336981241, 5.499999999999899636, 79.85532783611445495 ) ) ;
#38452 = CARTESIAN_POINT ( 'NONE',  ( -5.049401038297874678, -19.05341960407617918, 69.79275706135233293 ) ) ;
#38453 = CARTESIAN_POINT ( 'NONE',  ( -4.379528057220328563, 16.55341960407611168, 30.20724293864769550 ) ) ;
#38454 = CARTESIAN_POINT ( 'NONE',  ( -14.29746914071049879, 8.314922557960819915, 95.83224293864770971 ) ) ;
#38456 = CARTESIAN_POINT ( 'NONE',  ( -17.48847506799948803, 5.747544572775297844, 40.82697437843290800 ) ) ;
#38455 = CARTESIAN_POINT ( 'NONE',  ( -19.05341960407617563, 5.049401038297882671, 23.54275706135233648 ) ) ;
#38457 = CARTESIAN_POINT ( 'NONE',  ( 10.72451020669871369, 18.67979575497193778, 27.08442372801901854 ) ) ;
#38458 = CARTESIAN_POINT ( 'NONE',  ( 4.313351365237961588, -4.313351365237934054, -62.50719930893269805 ) ) ;
#38459 = CARTESIAN_POINT ( 'NONE',  ( -13.97604488694527625, -13.89961937509977652, 71.87390960531433848 ) ) ;
#38460 = CARTESIAN_POINT ( 'NONE',  ( 21.55341960407619695, -5.719274019375665929, 96.04275706135236135 ) ) ;
#38461 = CARTESIAN_POINT ( 'NONE',  ( -9.474510206698964154, 16.51473224551069663, 70.41557627198102409 ) ) ;
#38462 = CARTESIAN_POINT ( 'NONE',  ( 15.80617190586746368, 15.72974639402197994, 44.37390960531435979 ) ) ;
#38463 = CARTESIAN_POINT ( 'NONE',  ( 8.314922557960818139, 14.29746914071049879, 84.58224293864769550 ) ) ;
#38464 = CARTESIAN_POINT ( 'NONE',  ( 0.05219959533909260263, 19.03943276465977164, 59.99890960531436690 ) ) ;
#38465 = CARTESIAN_POINT ( 'NONE',  ( 9.474510206698971260, -16.51473224551069308, 22.91557627198102765 ) ) ;
#38466 = CARTESIAN_POINT ( 'NONE',  ( 21.55341960407619695, -5.719274019375665929, 31.04275706135234714 ) ) ;
#38467 = CARTESIAN_POINT ( 'NONE',  ( -15.72974639402176322, -15.80617190586768395, 64.37609039468568994 ) ) ;
#38468 = CARTESIAN_POINT ( 'NONE',  ( 5.049401038298161559, -19.05341960407611168, 42.70724293864767418 ) ) ;
#38469 = CARTESIAN_POINT ( 'NONE',  ( -16.52544592524335698, -4.483927247898792601, 73.95942372801901854 ) ) ;
#38470 = CARTESIAN_POINT ( 'NONE',  ( 21.53943276465977519, -0.05219959533907433946, 108.7489096053143669 ) ) ;
#38471 = ORIENTED_EDGE ( 'NONE', *, *, #61495, .F. ) ;
#38472 = CARTESIAN_POINT ( 'NONE',  ( 15.80617190586746368, 15.72974639402197994, 109.3739096053143811 ) ) ;
#38474 = CARTESIAN_POINT ( 'NONE',  ( -5.049401038298153566, 19.05341960407611168, 70.20724293864769550 ) ) ;
#38473 = CARTESIAN_POINT ( 'NONE',  ( 5.049401038297881783, 19.05341960407617563, 37.29275706135232582 ) ) ;
#38475 = CARTESIAN_POINT ( 'NONE',  ( -13.89961937509957401, -13.97604488694547875, 29.37609039468565797 ) ) ;
#38476 = CARTESIAN_POINT ( 'NONE',  ( 21.52544592524334988, 5.823673210054432836, 71.45942372801901854 ) ) ;
#38477 = CARTESIAN_POINT ( 'NONE',  ( -15.72974639402197994, 15.80617190586746368, 65.62390960531436690 ) ) ;
#38478 = CARTESIAN_POINT ( 'NONE',  ( 14.34966873604960469, 8.224510206698951720, 34.16557627198102409 ) ) ;
#38480 = CARTESIAN_POINT ( 'NONE',  ( 19.03943276465977164, 0.05219959533936151252, 31.25109039468566863 ) ) ;
#38479 = CARTESIAN_POINT ( 'NONE',  ( 21.55341960407619695, -5.719274019375665929, 96.04275706135236135 ) ) ;
#38481 = CARTESIAN_POINT ( 'NONE',  ( -12.14591786802309592, -12.06949235617757132, 61.87390960531436690 ) ) ;
#38482 = CARTESIAN_POINT ( 'NONE',  ( 12.06949235617757843, -12.14591786802309237, 103.1239096053143811 ) ) ;
#38483 = CARTESIAN_POINT ( 'NONE',  ( -19.05341960407617563, 5.049401038297882671, 63.54275706135234003 ) ) ;
#38484 = CARTESIAN_POINT ( 'NONE',  ( -4.379528057220328563, 16.55341960407611168, 25.20724293864769550 ) ) ;
#38485 = CARTESIAN_POINT ( 'NONE',  ( 18.67979575497194134, -10.72451020669871369, 70.83442372801901854 ) ) ;
#38486 = CARTESIAN_POINT ( 'NONE',  ( -9.564922557960796823, -16.46253265017161027, 77.08224293864769550 ) ) ;
#38487 = CARTESIAN_POINT ( 'NONE',  ( 16.46253265017146816, 9.564922557961045513, 46.66775706135233293 ) ) ;
#38488 = CARTESIAN_POINT ( 'NONE',  ( -21.52544592524343514, 5.823673210054127303, 51.04057627198103120 ) ) ;
#38489 = CARTESIAN_POINT ( 'NONE',  ( -10.81492255796105439, 18.62759615963255655, 47.91775706135234714 ) ) ;
#38490 = CIRCLE ( 'NONE', #80468, 2.000000000000001776 ) ;
#38491 = CARTESIAN_POINT ( 'NONE',  ( -5.719274019375978568, 21.55341960407610458, 100.2072429386476955 ) ) ;
#38492 = CARTESIAN_POINT ( 'NONE',  ( -5.049401038297874678, -19.05341960407617918, 104.7927570613523471 ) ) ;
#38493 = CARTESIAN_POINT ( 'NONE',  ( 14.34966873604972726, -8.224510206698740333, 65.83442372801900433 ) ) ;
#38495 = CARTESIAN_POINT ( 'NONE',  ( -15.72974639402197994, 15.80617190586746368, 100.6239096053143811 ) ) ;
#38494 = CARTESIAN_POINT ( 'NONE',  ( 1.300000000000000044, 0.000000000000000000, 0.000000000000000000 ) ) ;
#38496 = CARTESIAN_POINT ( 'NONE',  ( -12.06949235617756955, 12.14591786802309770, 95.62390960531436690 ) ) ;
#38497 = CARTESIAN_POINT ( 'NONE',  ( -16.19135201231366494, -7.376712067591948419, 100.1868085405203317 ) ) ;
#38498 = CARTESIAN_POINT ( 'NONE',  ( -14.29746914071037622, -8.314922557961029526, 19.16775706135234714 ) ) ;
#38499 = CARTESIAN_POINT ( 'NONE',  ( 5.719274019375991003, -21.55341960407610458, 42.70724293864770260 ) ) ;
#38500 = CARTESIAN_POINT ( 'NONE',  ( 0.05219959533934541429, -16.53943276465976808, 90.00109039468567573 ) ) ;
#38501 = CARTESIAN_POINT ( 'NONE',  ( 35.03251413515944535, -11.89243146578850130, -8.000000000000001776 ) ) ;
#38502 = CARTESIAN_POINT ( 'NONE',  ( -16.55341960407617563, 4.379528057220093196, 63.54275706135234003 ) ) ;
#38503 = CARTESIAN_POINT ( 'NONE',  ( -15.72974639402176322, -15.80617190586768395, 34.37609039468568284 ) ) ;
#38504 = CARTESIAN_POINT ( 'NONE',  ( -5.719274019375978568, 21.55341960407610458, 40.20724293864769550 ) ) ;
#38505 = CARTESIAN_POINT ( 'NONE',  ( -16.53943276465976808, -0.05219959533934237506, 88.75109039468567573 ) ) ;
#38506 = CARTESIAN_POINT ( 'NONE',  ( -13.97604488694527625, -13.89961937509977652, 91.87390960531432427 ) ) ;
#38507 = CARTESIAN_POINT ( 'NONE',  ( 0.05219959533937995610, -21.53943276465977519, 65.00109039468568994 ) ) ;
#38508 = CARTESIAN_POINT ( 'NONE',  ( 15.72974639402199770, -15.80617190586745480, 38.12390960531436690 ) ) ;
#38509 = CARTESIAN_POINT ( 'NONE',  ( -21.52544592524343514, 5.823673210054127303, 36.04057627198102409 ) ) ;
#38510 = ORIENTED_EDGE ( 'NONE', *, *, #48810, .T. ) ;
#38511 = CARTESIAN_POINT ( 'NONE',  ( -19.02544592524334988, -5.153800228976617603, 58.95942372801900433 ) ) ;
#38512 = CARTESIAN_POINT ( 'NONE',  ( -4.483927247898782831, 16.52544592524335698, 67.70942372801901854 ) ) ;
#38513 = CARTESIAN_POINT ( 'NONE',  ( 5.823673210054125526, 21.52544592524343514, 29.79057627198102409 ) ) ;
#38514 = ORIENTED_EDGE ( 'NONE', *, *, #166752, .F. ) ;
#38515 = CARTESIAN_POINT ( 'NONE',  ( 0.05219959533909260263, 19.03943276465977164, 89.99890960531436690 ) ) ;
#38516 = CARTESIAN_POINT ( 'NONE',  ( -16.55341960407611168, -4.379528057220339221, 26.45724293864768839 ) ) ;
#38517 = CARTESIAN_POINT ( 'NONE',  ( -18.09805431107249163, 5.499999999999980460, 86.01606229291887473 ) ) ;
#38518 = CARTESIAN_POINT ( 'NONE',  ( -16.55341960407611168, -4.379528057220339221, 106.4572429386477097 ) ) ;
#38519 = CARTESIAN_POINT ( 'NONE',  ( 10.72451020669898902, -18.67979575497178502, 52.91557627198103830 ) ) ;
#38520 = CARTESIAN_POINT ( 'NONE',  ( -5.049401038298153566, 19.05341960407611168, 50.20724293864770260 ) ) ;
#38521 = CARTESIAN_POINT ( 'NONE',  ( 14.34966873604972726, -8.224510206698740333, 80.83442372801901854 ) ) ;
#38522 = CARTESIAN_POINT ( 'NONE',  ( 10.72451020669871369, 18.67979575497193778, 27.08442372801901854 ) ) ;
#38523 = CARTESIAN_POINT ( 'NONE',  ( -9.474510206698720793, -16.51473224551083518, 84.58442372801900433 ) ) ;
#38524 = CARTESIAN_POINT ( 'NONE',  ( -16.55341960407611168, -4.379528057220339221, 86.45724293864770971 ) ) ;
#38525 = CARTESIAN_POINT ( 'NONE',  ( -0.05219959533909027116, -19.03943276465977164, 57.49890960531435979 ) ) ;
#38526 = CARTESIAN_POINT ( 'NONE',  ( 9.474510206698971260, -16.51473224551069308, 32.91557627198102409 ) ) ;
#38527 = CARTESIAN_POINT ( 'NONE',  ( 15.72974639402176855, 15.80617190586768217, 101.8760903946857042 ) ) ;
#38528 = CARTESIAN_POINT ( 'NONE',  ( 9.474510206698971260, -16.51473224551069308, 82.91557627198103830 ) ) ;
#38529 = CARTESIAN_POINT ( 'NONE',  ( 14.34966873604972726, -8.224510206698740333, 60.83442372801901854 ) ) ;
#38530 = CARTESIAN_POINT ( 'NONE',  ( 15.72974639402176855, 15.80617190586768217, 86.87609039468568994 ) ) ;
#38531 = CARTESIAN_POINT ( 'NONE',  ( -15.72974639402197994, 15.80617190586746368, 50.62390960531435979 ) ) ;
#38532 = CARTESIAN_POINT ( 'NONE',  ( 16.52544592524335698, 4.483927247898782831, 76.45942372801901854 ) ) ;
#38533 = CARTESIAN_POINT ( 'NONE',  ( 9.564922557961047289, -16.46253265017146816, 50.41775706135233293 ) ) ;
#38534 = CARTESIAN_POINT ( 'NONE',  ( -13.89961937509957401, -13.97604488694547875, 64.37609039468567573 ) ) ;
#38535 = ORIENTED_EDGE ( 'NONE', *, *, #142437, .T. ) ;
#38536 = CARTESIAN_POINT ( 'NONE',  ( -15.72974639402176322, -15.80617190586768395, 59.37609039468568284 ) ) ;
#38537 = CARTESIAN_POINT ( 'NONE',  ( -5.153800228976328057, -19.02544592524343514, 62.29057627198100988 ) ) ;
#38538 = CARTESIAN_POINT ( 'NONE',  ( 19.05341960407611168, 5.049401038298154454, 38.95724293864767418 ) ) ;
#38539 = CARTESIAN_POINT ( 'NONE',  ( -5.049401038297874678, -19.05341960407617918, 64.79275706135233293 ) ) ;
#38540 = CARTESIAN_POINT ( 'NONE',  ( 19.03943276465977164, -0.05219959533909143690, 113.7489096053143669 ) ) ;
#38541 = CARTESIAN_POINT ( 'NONE',  ( -19.05341960407611168, -5.049401038298163336, 101.4572429386476955 ) ) ;
#38542 = CARTESIAN_POINT ( 'NONE',  ( 16.52544592524342804, -4.483927247898539470, 48.54057627198103120 ) ) ;
#38543 = CARTESIAN_POINT ( 'NONE',  ( -21.53943276465977519, 0.05219959533907696930, 46.24890960531435979 ) ) ;
#38544 = DIRECTION ( 'NONE',  ( 5.392603844284257652E-33, -1.000000000000000000, 0.000000000000000000 ) ) ;
#38545 = CARTESIAN_POINT ( 'NONE',  ( 18.67979575497194134, -10.72451020669871369, 110.8344237280190043 ) ) ;
#38546 = CARTESIAN_POINT ( 'NONE',  ( -17.12812012977029141, -6.668231424565922438, 81.35948759323146362 ) ) ;
#38547 = CARTESIAN_POINT ( 'NONE',  ( 5.153800228976335163, 19.02544592524342804, 54.79057627198103120 ) ) ;
#38548 = CARTESIAN_POINT ( 'NONE',  ( -33.84943726220063098, -0.7253354391803957801, 100.4638154892406021 ) ) ;
#38549 = FACE_OUTER_BOUND ( 'NONE', #157737, .T. ) ;
#38550 = CARTESIAN_POINT ( 'NONE',  ( -16.55341960407617563, 4.379528057220093196, 78.54275706135236135 ) ) ;
#38551 = CARTESIAN_POINT ( 'NONE',  ( -18.67979575497178146, -10.72451020669898902, 96.66557627198102409 ) ) ;
#38552 = CARTESIAN_POINT ( 'NONE',  ( 4.483927247898545687, 16.52544592524342804, 49.79057627198102409 ) ) ;
#38554 = CARTESIAN_POINT ( 'NONE',  ( 20.96320343559668942, 21.46320343559617427, 4.646446609406719830 ) ) ;
#38553 = CARTESIAN_POINT ( 'NONE',  ( 13.97604488694527802, 13.89961937509977652, 44.37390960531435269 ) ) ;
#38555 = CARTESIAN_POINT ( 'NONE',  ( -15.80617190586768217, 15.72974639402176855, 38.12609039468567573 ) ) ;
#38556 = CARTESIAN_POINT ( 'NONE',  ( 13.89961937509957401, 13.97604488694547697, 51.87609039468566863 ) ) ;
#38557 = CARTESIAN_POINT ( 'NONE',  ( 9.564922557960805705, 16.46253265017160317, 34.58224293864770260 ) ) ;
#38558 = CARTESIAN_POINT ( 'NONE',  ( 0.05219959533937995610, -21.53943276465977519, 90.00109039468567573 ) ) ;
#38559 = CARTESIAN_POINT ( 'NONE',  ( -22.87925077421024156, -5.621762139875928099, 172.5226062014847059 ) ) ;
#38560 = VERTEX_POINT ( 'NONE', #139102 ) ;
#38561 = CARTESIAN_POINT ( 'NONE',  ( 4.379528057220339221, -16.55341960407611168, 37.70724293864769550 ) ) ;
#38562 = CARTESIAN_POINT ( 'NONE',  ( 17.50000000001358913, -5.500000000000039968, 73.29690382535059712 ) ) ;
#38563 = CARTESIAN_POINT ( 'NONE',  ( -10.72451020669898014, 18.67979575497178502, 35.41557627198102409 ) ) ;
#38564 = CARTESIAN_POINT ( 'NONE',  ( 27.73933785331498569, 9.013057229001093518, 141.9750000027311785 ) ) ;
#38565 = CARTESIAN_POINT ( 'NONE',  ( 5.153800228976335163, 19.02544592524342804, 94.79057627198103830 ) ) ;
#38566 = CARTESIAN_POINT ( 'NONE',  ( 4.483927247898545687, 16.52544592524342804, 94.79057627198105251 ) ) ;
#38567 = CARTESIAN_POINT ( 'NONE',  ( 16.55341960407618274, -4.379528057220086978, 26.04275706135235779 ) ) ;
#38568 = CARTESIAN_POINT ( 'NONE',  ( 14.29746914071049879, -8.314922557960816363, 23.33224293864769194 ) ) ;
#38569 = ORIENTED_EDGE ( 'NONE', *, *, #170098, .T. ) ;
#38571 = CARTESIAN_POINT ( 'NONE',  ( -15.72974639402197994, 15.80617190586746368, 85.62390960531436690 ) ) ;
#38570 = CARTESIAN_POINT ( 'NONE',  ( -16.51473224551069308, -9.474510206698971260, 96.66557627198102409 ) ) ;
#38573 = CARTESIAN_POINT ( 'NONE',  ( 16.46253265017160672, -9.564922557960803928, 103.3322429386476955 ) ) ;
#38572 = CARTESIAN_POINT ( 'NONE',  ( -0.05219959533910754901, -16.53943276465976808, 22.49890960531436335 ) ) ;
#38574 = CARTESIAN_POINT ( 'NONE',  ( 19.02544592524334988, 5.153800228976608722, 81.45942372801897591 ) ) ;
#38575 = CARTESIAN_POINT ( 'NONE',  ( -15.80617190586768217, 15.72974639402176855, 108.1260903946856757 ) ) ;
#38576 = CARTESIAN_POINT ( 'NONE',  ( -10.81492255796078084, -18.62759615963271287, 87.08224293864769550 ) ) ;
#38577 = CARTESIAN_POINT ( 'NONE',  ( -21.53943276465977519, 0.05219959533907696930, 41.24890960531435269 ) ) ;
#38578 = CARTESIAN_POINT ( 'NONE',  ( 5.153800228976335163, 19.02544592524342804, 64.79057627198100988 ) ) ;
#38579 = CARTESIAN_POINT ( 'NONE',  ( -16.52544592524342804, 4.483927247898546575, 31.04057627198102409 ) ) ;
#38580 = CARTESIAN_POINT ( 'NONE',  ( -9.474510206698964154, 16.51473224551069663, 75.41557627198103830 ) ) ;
#38581 = ORIENTED_EDGE ( 'NONE', *, *, #76696, .T. ) ;
#38582 = DIRECTION ( 'NONE',  ( 0.000000000000000000, 0.000000000000000000, 1.000000000000000000 ) ) ;
#38583 = CARTESIAN_POINT ( 'NONE',  ( -19.05341960407617563, 5.049401038297882671, 23.54275706135233648 ) ) ;
#38584 = CARTESIAN_POINT ( 'NONE',  ( -8.224510206698948167, 14.34966873604960824, 85.41557627198102409 ) ) ;
#38585 = CARTESIAN_POINT ( 'NONE',  ( 0.05219959533937995610, -21.53943276465977519, 20.00109039468568639 ) ) ;
#38586 = CARTESIAN_POINT ( 'NONE',  ( -27.73933785331498925, 9.013057229001089965, 141.2750000027311614 ) ) ;
#38588 = ADVANCED_FACE ( 'NONE', ( #47105 ), #108765, .T. ) ;
#38587 = CARTESIAN_POINT ( 'NONE',  ( -5.823673210054116645, -21.52544592524344225, 77.29057627198102409 ) ) ;
#38589 = CARTESIAN_POINT ( 'NONE',  ( -14.34966873604972548, 8.224510206698743886, 93.33442372801901854 ) ) ;
#38590 = CARTESIAN_POINT ( 'NONE',  ( 16.46253265017160672, -9.564922557960803928, 28.33224293864769550 ) ) ;
#38591 = CARTESIAN_POINT ( 'NONE',  ( 13.97604488694527802, 13.89961937509977652, 74.37390960531436690 ) ) ;
#38592 = DIRECTION ( 'NONE',  ( 1.000000000000000000, 1.776356839400250465E-15, 0.000000000000000000 ) ) ;
#38593 = CARTESIAN_POINT ( 'NONE',  ( -12.14591786802309592, -12.06949235617757132, 26.87390960531435979 ) ) ;
#38594 = CARTESIAN_POINT ( 'NONE',  ( -0.05219959533937732626, 21.53943276465977519, 62.50109039468568284 ) ) ;
#38595 = CARTESIAN_POINT ( 'NONE',  ( 30.24683373042637768, -22.89668476416391485, -22.64123003231907205 ) ) ;
#38596 = CARTESIAN_POINT ( 'NONE',  ( -21.52544592524334988, -5.823673210054445271, 98.95942372801903275 ) ) ;
#38597 = CARTESIAN_POINT ( 'NONE',  ( -19.03943276465977164, 0.05219959533909376836, 46.24890960531435979 ) ) ;
#38598 = CARTESIAN_POINT ( 'NONE',  ( -9.474510206698964154, 16.51473224551069663, 50.41557627198102409 ) ) ;
#38599 = ORIENTED_EDGE ( 'NONE', *, *, #34776, .F. ) ;
#38600 = CARTESIAN_POINT ( 'NONE',  ( 21.55341960407619695, -5.719274019375665929, 91.04275706135236135 ) ) ;
#38601 = CARTESIAN_POINT ( 'NONE',  ( 8.224510206698742110, 14.34966873604972548, 67.08442372801901854 ) ) ;
#38602 = CARTESIAN_POINT ( 'NONE',  ( -5.719274019375665041, -21.55341960407619695, 89.79275706135236135 ) ) ;
#38603 = CARTESIAN_POINT ( 'NONE',  ( 13.89961937509977652, -13.97604488694527269, 113.1239096053143527 ) ) ;
#38604 = CARTESIAN_POINT ( 'NONE',  ( 5.049401038297881783, 19.05341960407617563, 87.29275706135234714 ) ) ;
#38605 = CARTESIAN_POINT ( 'NONE',  ( -21.52544592524334988, -5.823673210054445271, 68.95942372801901854 ) ) ;
#38606 = CARTESIAN_POINT ( 'NONE',  ( 0.05219959533934541429, -16.53943276465976808, 35.00109039468568284 ) ) ;
#38607 = CARTESIAN_POINT ( 'NONE',  ( -15.80617190586745835, -15.72974639402198527, 86.87390960531438111 ) ) ;
#38608 = CARTESIAN_POINT ( 'NONE',  ( -9.474510206698720793, -16.51473224551083518, 89.58442372801900433 ) ) ;
#38609 = CARTESIAN_POINT ( 'NONE',  ( 19.02544592524343514, -5.153800228976328945, 58.54057627198102409 ) ) ;
#38610 = CARTESIAN_POINT ( 'NONE',  ( -5.049401038297874678, -19.05341960407617918, 99.79275706135234714 ) ) ;
#38611 = CARTESIAN_POINT ( 'NONE',  ( 19.02544592524334988, 5.153800228976608722, 101.4594237280189759 ) ) ;
#38612 = CARTESIAN_POINT ( 'NONE',  ( 12.14591786802309770, 12.06949235617756955, 49.37390960531436690 ) ) ;
#38613 = CARTESIAN_POINT ( 'NONE',  ( 5.153800228976615827, -19.02544592524334988, 80.20942372801901854 ) ) ;
#38614 = CARTESIAN_POINT ( 'NONE',  ( -16.53943276465976808, -0.05219959533934237506, 63.75109039468568284 ) ) ;
#38615 = CARTESIAN_POINT ( 'NONE',  ( 0.05219959533909260263, 19.03943276465977164, 39.99890960531436690 ) ) ;
#38617 = ADVANCED_FACE ( 'NONE', ( #52062, #98549 ), #69229, .F. ) ;
#38616 = CARTESIAN_POINT ( 'NONE',  ( 0.05219959533909260263, 19.03943276465977164, 59.99890960531436690 ) ) ;
#38618 = CARTESIAN_POINT ( 'NONE',  ( -12.06949235617739369, -12.14591786802326823, 64.37609039468568994 ) ) ;
#38619 = CARTESIAN_POINT ( 'NONE',  ( -11.80868324581538253, 11.80868324581533457, -59.13370768023891344 ) ) ;
#38620 = CARTESIAN_POINT ( 'NONE',  ( 17.81289503416611453, -24.51734667627695785, 138.9500000054623570 ) ) ;
#38621 = CARTESIAN_POINT ( 'NONE',  ( -9.564922557960796823, -16.46253265017161027, 107.0822429386476955 ) ) ;
#38622 = CARTESIAN_POINT ( 'NONE',  ( 19.05341960407611168, 5.049401038298154454, 28.95724293864769550 ) ) ;
#38623 = ORIENTED_EDGE ( 'NONE', *, *, #20347, .T. ) ;
#38624 = CARTESIAN_POINT ( 'NONE',  ( 5.049401038297881783, 19.05341960407617563, 112.2927570613523471 ) ) ;
#38626 = CARTESIAN_POINT ( 'NONE',  ( -5.823673210054116645, -21.52544592524344225, 32.29057627198102409 ) ) ;
#38625 = CIRCLE ( 'NONE', #103159, 10.00000000000000000 ) ;
#38628 = CARTESIAN_POINT ( 'NONE',  ( 12.06949235617739724, 12.14591786802326823, 21.87609039468567573 ) ) ;
#38627 = CARTESIAN_POINT ( 'NONE',  ( -9.564922557961040184, 16.46253265017147172, 27.91775706135232582 ) ) ;
#38629 = CARTESIAN_POINT ( 'NONE',  ( 5.049401038298161559, -19.05341960407611168, 32.70724293864768129 ) ) ;
#38630 = CARTESIAN_POINT ( 'NONE',  ( -0.05219959533909027116, -19.03943276465977164, 52.49890960531436690 ) ) ;
#38631 = CARTESIAN_POINT ( 'NONE',  ( 21.52544592524344225, -5.823673210054117533, 78.54057627198103830 ) ) ;
#38632 = CARTESIAN_POINT ( 'NONE',  ( 16.51473224551069308, 9.474510206698969483, 99.16557627198102409 ) ) ;
#38633 = CARTESIAN_POINT ( 'NONE',  ( -16.51473224551069308, -9.474510206698971260, 36.66557627198102409 ) ) ;
#38634 = CARTESIAN_POINT ( 'NONE',  ( 27.73933785331498569, 9.013057229001093518, 146.4750000027311501 ) ) ;
#38635 = CARTESIAN_POINT ( 'NONE',  ( 9.564922557961047289, -16.46253265017146816, 80.41775706135234714 ) ) ;
#38636 = CARTESIAN_POINT ( 'NONE',  ( 14.29746914071049879, -8.314922557960816363, 73.33224293864769550 ) ) ;
#38637 = CARTESIAN_POINT ( 'NONE',  ( 0.05219959533907565091, 21.53943276465977519, 44.99890960531435979 ) ) ;
#38638 = CARTESIAN_POINT ( 'NONE',  ( -18.67979575497193778, 10.72451020669871902, 108.3344237280190185 ) ) ;
#38639 = CARTESIAN_POINT ( 'NONE',  ( -5.719274019375978568, 21.55341960407610458, 95.20724293864769550 ) ) ;
#38640 = CARTESIAN_POINT ( 'NONE',  ( -18.67979575497193778, 10.72451020669871902, 68.33442372801900433 ) ) ;
#38641 = CARTESIAN_POINT ( 'NONE',  ( 10.81492255796106328, -18.62759615963255655, 75.41775706135233293 ) ) ;
#38642 = CARTESIAN_POINT ( 'NONE',  ( 16.51473224551069308, 9.474510206698969483, 109.1655762719810383 ) ) ;
#38644 = CARTESIAN_POINT ( 'NONE',  ( -5.719274019375665041, -21.55341960407619695, 74.79275706135234714 ) ) ;
#38643 = CARTESIAN_POINT ( 'NONE',  ( 14.34966873604972726, -8.224510206698740333, 110.8344237280190043 ) ) ;
#38645 = CARTESIAN_POINT ( 'NONE',  ( 5.153800228976335163, 19.02544592524342804, 69.79057627198103830 ) ) ;
#38646 = CARTESIAN_POINT ( 'NONE',  ( -0.05219959533936034679, 19.03943276465977164, 32.50109039468566863 ) ) ;
#38647 = CARTESIAN_POINT ( 'NONE',  ( 5.823673210054444382, -21.52544592524334988, 25.20942372801901854 ) ) ;
#38648 = CARTESIAN_POINT ( 'NONE',  ( 5.049401038298161559, -19.05341960407611168, 62.70724293864769550 ) ) ;
#38649 = CARTESIAN_POINT ( 'NONE',  ( -8.224510206698948167, 14.34966873604960824, 80.41557627198103830 ) ) ;
#38650 = CARTESIAN_POINT ( 'NONE',  ( -4.483927247898539470, -16.52544592524342804, 42.29057627198103120 ) ) ;
#38651 = CARTESIAN_POINT ( 'NONE',  ( -0.05219959533907301413, -21.53943276465977519, 62.49890960531436690 ) ) ;
#38652 = CARTESIAN_POINT ( 'NONE',  ( -9.564922557960796823, -16.46253265017161027, 62.08224293864769550 ) ) ;
#38653 = CARTESIAN_POINT ( 'NONE',  ( -21.55341960407610458, -5.719274019375992779, 71.45724293864769550 ) ) ;
#38654 = CARTESIAN_POINT ( 'NONE',  ( -13.89961937509957401, -13.97604488694547875, 64.37609039468567573 ) ) ;
#38656 = CARTESIAN_POINT ( 'NONE',  ( 8.314922557960818139, 14.29746914071049879, 69.58224293864769550 ) ) ;
#38655 = CYLINDRICAL_SURFACE ( 'NONE', #81573, 59.99999999999998579 ) ;
#38657 = CARTESIAN_POINT ( 'NONE',  ( -10.72451020669898014, 18.67979575497178502, 45.41557627198103830 ) ) ;
#38658 = ORIENTED_EDGE ( 'NONE', *, *, #8310, .F. ) ;
#38659 = DIRECTION ( 'NONE',  ( -1.000000000000000000, -1.953992523340275511E-14, 0.000000000000000000 ) ) ;
#38661 = CARTESIAN_POINT ( 'NONE',  ( -8.571926809382601320, -26.38167802310801591, 139.7750000027311899 ) ) ;
#38660 = CARTESIAN_POINT ( 'NONE',  ( -4.379528057220086978, -16.55341960407618274, 89.79275706135236135 ) ) ;
#38662 = ADVANCED_FACE ( 'NONE', ( #21732 ), #72997, .T. ) ;
#38663 = CARTESIAN_POINT ( 'NONE',  ( -16.51473224551082808, 9.474510206698731452, 83.33442372801899012 ) ) ;
#38664 = CARTESIAN_POINT ( 'NONE',  ( -12.14591786802309592, -12.06949235617757132, 71.87390960531438111 ) ) ;
#38665 = CARTESIAN_POINT ( 'NONE',  ( -19.25176906914649777, -5.499999999999745093, 60.99927264242280245 ) ) ;
#38666 = CARTESIAN_POINT ( 'NONE',  ( 13.97604488694527802, 13.89961937509977652, 49.37390960531434558 ) ) ;
#38667 = CARTESIAN_POINT ( 'NONE',  ( -14.34966873604960291, -8.224510206698953496, 41.66557627198103120 ) ) ;
#38668 = CARTESIAN_POINT ( 'NONE',  ( 13.97604488694527802, 13.89961937509977652, 89.37390960531436690 ) ) ;
#38670 = CARTESIAN_POINT ( 'NONE',  ( 13.89961937509977652, -13.97604488694527269, 48.12390960531435979 ) ) ;
#38669 = CARTESIAN_POINT ( 'NONE',  ( 0.05219959533936267826, -19.03943276465977164, 80.00109039468567573 ) ) ;
#38671 = CARTESIAN_POINT ( 'NONE',  ( -18.67979575497193778, 10.72451020669871902, 63.33442372801900433 ) ) ;
#38672 = CARTESIAN_POINT ( 'NONE',  ( -9.564922557960796823, -16.46253265017161027, 87.08224293864769550 ) ) ;
#38673 = CARTESIAN_POINT ( 'NONE',  ( -13.97604488694527625, -13.89961937509977652, 21.87390960531435979 ) ) ;
#38674 = CARTESIAN_POINT ( 'NONE',  ( -5.153800228976328057, -19.02544592524343514, 77.29057627198099567 ) ) ;
#38675 = CARTESIAN_POINT ( 'NONE',  ( 10.72451020669898902, -18.67979575497178502, 47.91557627198102409 ) ) ;
#38676 = CARTESIAN_POINT ( 'NONE',  ( 16.46253265017160672, -9.564922557960803928, 53.33224293864768839 ) ) ;
#38677 = CARTESIAN_POINT ( 'NONE',  ( 21.53943276465977519, -0.05219959533907433946, 48.74890960531435979 ) ) ;
#38678 = CARTESIAN_POINT ( 'NONE',  ( 9.564922557961047289, -16.46253265017146816, 85.41775706135233293 ) ) ;
#38679 = CARTESIAN_POINT ( 'NONE',  ( -16.55341960407617563, 4.379528057220093196, 108.5427570613523756 ) ) ;
#38680 = CARTESIAN_POINT ( 'NONE',  ( 16.46253265017146816, 9.564922557961045513, 31.66775706135232937 ) ) ;
#38682 = CARTESIAN_POINT ( 'NONE',  ( -16.53943276465976808, -0.05219959533934237506, 83.75109039468568994 ) ) ;
#38681 = CARTESIAN_POINT ( 'NONE',  ( 14.29746914071037800, 8.314922557961029526, 56.66775706135235424 ) ) ;
#38683 = FACE_OUTER_BOUND ( 'NONE', #2723, .T. ) ;
#38684 = CARTESIAN_POINT ( 'NONE',  ( -14.34966873604972548, 8.224510206698743886, 78.33442372801901854 ) ) ;
#38685 = CARTESIAN_POINT ( 'NONE',  ( -5.719274019375978568, 21.55341960407610458, 25.20724293864769550 ) ) ;
#38686 = CARTESIAN_POINT ( 'NONE',  ( 5.153800228976335163, 19.02544592524342804, 34.79057627198102409 ) ) ;
#38687 = CARTESIAN_POINT ( 'NONE',  ( 12.06949235617739724, 12.14591786802326823, 36.87609039468568994 ) ) ;
#38688 = CARTESIAN_POINT ( 'NONE',  ( -5.153800228976328057, -19.02544592524343514, 52.29057627198100988 ) ) ;
#38689 = CARTESIAN_POINT ( 'NONE',  ( -21.53943276465977519, -0.05219959533937600094, 43.75109039468568284 ) ) ;
#38690 = CARTESIAN_POINT ( 'NONE',  ( 14.34966873604972726, -8.224510206698740333, 30.83442372801902209 ) ) ;
#38691 = CARTESIAN_POINT ( 'NONE',  ( -0.05219959533934338120, 16.53943276465976808, 107.5010903946856899 ) ) ;
#38692 = CARTESIAN_POINT ( 'NONE',  ( 13.97604488694527802, 13.89961937509977652, 34.37390960531436690 ) ) ;
#38693 = CARTESIAN_POINT ( 'NONE',  ( 15.72974639402176855, 15.80617190586768217, 111.8760903946856615 ) ) ;
#38694 = CARTESIAN_POINT ( 'NONE',  ( -16.46253265017146816, -9.564922557961047289, 109.1677570613523471 ) ) ;
#38695 = CARTESIAN_POINT ( 'NONE',  ( 16.51473224551083163, -9.474510206698727899, 70.83442372801900433 ) ) ;
#38696 = CARTESIAN_POINT ( 'NONE',  ( 12.14591786802309770, 12.06949235617756955, 74.37390960531436690 ) ) ;
#38697 = CARTESIAN_POINT ( 'NONE',  ( -13.97604488694527625, -13.89961937509977652, 36.87390960531436690 ) ) ;
#38698 = CARTESIAN_POINT ( 'NONE',  ( -5.049401038297874678, -19.05341960407617918, 79.79275706135233293 ) ) ;
#38699 = CARTESIAN_POINT ( 'NONE',  ( 0.05219959533937995610, -21.53943276465977519, 65.00109039468568994 ) ) ;
#38700 = CARTESIAN_POINT ( 'NONE',  ( -4.483927247898782831, 16.52544592524335698, 37.70942372801900433 ) ) ;
#38701 = CARTESIAN_POINT ( 'NONE',  ( 18.39443945427639449, -5.500000000000022204, 56.01745347608652992 ) ) ;
#38702 = CARTESIAN_POINT ( 'NONE',  ( 5.823673210054125526, 21.52544592524343514, 39.79057627198103830 ) ) ;
#38703 = CARTESIAN_POINT ( 'NONE',  ( 16.53943276465976808, 0.05219959533934440121, 21.25109039468567218 ) ) ;
#38704 = CARTESIAN_POINT ( 'NONE',  ( 16.46253265017160672, -9.564922557960803928, 113.3322429386476955 ) ) ;
#38705 = CARTESIAN_POINT ( 'NONE',  ( -23.03403192006594935, 14.65170476119024201, 169.9999999999999716 ) ) ;
#38706 = CARTESIAN_POINT ( 'NONE',  ( -19.05341960407611168, -5.049401038298163336, 36.45724293864766707 ) ) ;
#38707 = CARTESIAN_POINT ( 'NONE',  ( 15.80617190586769283, -15.72974639402175789, 105.6260903946856899 ) ) ;
#38708 = CARTESIAN_POINT ( 'NONE',  ( 9.564922557960805705, 16.46253265017160317, 59.58224293864769550 ) ) ;
#38709 = CARTESIAN_POINT ( 'NONE',  ( 15.80617190586769283, -15.72974639402175789, 65.62609039468568994 ) ) ;
#38710 = CARTESIAN_POINT ( 'NONE',  ( -18.67979575497193778, 10.72451020669871902, 98.33442372801901854 ) ) ;
#38711 = CARTESIAN_POINT ( 'NONE',  ( 14.29746914071049879, -8.314922557960816363, 28.33224293864769550 ) ) ;
#38712 = CARTESIAN_POINT ( 'NONE',  ( -0.05219959533909027116, -19.03943276465977164, 32.49890960531435979 ) ) ;
#38713 = CARTESIAN_POINT ( 'NONE',  ( -19.02544592524342804, 5.153800228976336051, 86.04057627198103830 ) ) ;
#38714 = CARTESIAN_POINT ( 'NONE',  ( -0.05219959533937732626, 21.53943276465977519, 62.50109039468568284 ) ) ;
#38715 = CARTESIAN_POINT ( 'NONE',  ( -9.564922557960796823, -16.46253265017161027, 42.08224293864769550 ) ) ;
#38716 = CARTESIAN_POINT ( 'NONE',  ( -5.719274019375665041, -21.55341960407619695, 59.79275706135234714 ) ) ;
#38718 = CARTESIAN_POINT ( 'NONE',  ( 5.153800228976335163, 19.02544592524342804, 99.79057627198102409 ) ) ;
#38717 = CARTESIAN_POINT ( 'NONE',  ( -19.05341960407617563, 5.049401038297882671, 88.54275706135230450 ) ) ;
#38719 = CARTESIAN_POINT ( 'NONE',  ( -4.379528057220328563, 16.55341960407611168, 115.2072429386476955 ) ) ;
#38720 = CARTESIAN_POINT ( 'NONE',  ( 21.55341960407610458, 5.719274019375980345, 108.9572429386476955 ) ) ;
#38721 = CARTESIAN_POINT ( 'NONE',  ( 5.049401038297881783, 19.05341960407617563, 32.29275706135233293 ) ) ;
#38722 = CARTESIAN_POINT ( 'NONE',  ( 8.314922557960818139, 14.29746914071049879, 104.5822429386477097 ) ) ;
#38723 = CARTESIAN_POINT ( 'NONE',  ( 19.03943276465977164, -0.05219959533909143690, 53.74890960531436690 ) ) ;
#38724 = CARTESIAN_POINT ( 'NONE',  ( 19.02544592524334988, 5.153800228976608722, 91.45942372801900433 ) ) ;
#38725 = CARTESIAN_POINT ( 'NONE',  ( 0.05219959533910956823, 16.53943276465976808, 59.99890960531436690 ) ) ;
#38726 = CARTESIAN_POINT ( 'NONE',  ( -5.823673210054431948, 21.52544592524334988, 107.7094237280190328 ) ) ;
#38727 = CARTESIAN_POINT ( 'NONE',  ( -15.72974639402197994, 15.80617190586746368, 25.62390960531435624 ) ) ;
#38728 = CARTESIAN_POINT ( 'NONE',  ( 5.153800228976615827, -19.02544592524334988, 85.20942372801900433 ) ) ;
#38729 = CARTESIAN_POINT ( 'NONE',  ( -21.55341960407610458, -5.719274019375992779, 96.45724293864770971 ) ) ;
#38730 = CARTESIAN_POINT ( 'NONE',  ( 5.823673210054444382, -21.52544592524334988, 50.20942372801901854 ) ) ;
#38731 = CARTESIAN_POINT ( 'NONE',  ( -12.14591786802326823, 12.06949235617739902, 48.12609039468568284 ) ) ;
#38732 = CARTESIAN_POINT ( 'NONE',  ( 8.314922557961029526, -14.29746914071037800, 105.4177570613523613 ) ) ;
#38734 = CARTESIAN_POINT ( 'NONE',  ( 15.80617190586769283, -15.72974639402175789, 50.62609039468568994 ) ) ;
#38733 = CARTESIAN_POINT ( 'NONE',  ( 0.05219959533934541429, -16.53943276465976808, 35.00109039468568284 ) ) ;
#38735 = CARTESIAN_POINT ( 'NONE',  ( 5.823673210054125526, 21.52544592524343514, 44.79057627198103120 ) ) ;
#38736 = CARTESIAN_POINT ( 'NONE',  ( -5.049401038298153566, 19.05341960407611168, 30.20724293864768839 ) ) ;
#38737 = CARTESIAN_POINT ( 'NONE',  ( 38.00000000000000711, -12.34694845685040754, -4.849999994537625092 ) ) ;
#38738 = CARTESIAN_POINT ( 'NONE',  ( 16.52544592524335698, 4.483927247898782831, 66.45942372801903275 ) ) ;
#38739 = CARTESIAN_POINT ( 'NONE',  ( -0.05219959533907301413, -21.53943276465977519, 92.49890960531436690 ) ) ;
#38740 = CARTESIAN_POINT ( 'NONE',  ( 12.06949235617757843, -12.14591786802309237, 43.12390960531435269 ) ) ;
#38741 = CARTESIAN_POINT ( 'NONE',  ( 16.53943276465976808, 0.05219959533934440121, 61.25109039468567573 ) ) ;
#38742 = CARTESIAN_POINT ( 'NONE',  ( 19.03943276465977164, 0.05219959533936151252, 96.25109039468567573 ) ) ;
#38743 = CARTESIAN_POINT ( 'NONE',  ( -5.719274019375978568, 21.55341960407610458, 100.2072429386476955 ) ) ;
#38744 = CARTESIAN_POINT ( 'NONE',  ( 4.379528057220339221, -16.55341960407611168, 37.70724293864769550 ) ) ;
#38745 = VERTEX_POINT ( 'NONE', #5549 ) ;
#38746 = CARTESIAN_POINT ( 'NONE',  ( -8.224510206698735004, -14.34966873604973081, 84.58442372801903275 ) ) ;
#38747 = FACE_BOUND ( 'NONE', #124199, .T. ) ;
#38748 = CARTESIAN_POINT ( 'NONE',  ( 5.823673210054125526, 21.52544592524343514, 79.79057627198102409 ) ) ;
#38749 = ORIENTED_EDGE ( 'NONE', *, *, #44126, .T. ) ;
#38750 = CARTESIAN_POINT ( 'NONE',  ( 8.224510206698742110, 14.34966873604972548, 112.0844237280190185 ) ) ;
#38751 = ORIENTED_EDGE ( 'NONE', *, *, #78302, .T. ) ;
#38752 = CARTESIAN_POINT ( 'NONE',  ( 0.000000000000000000, 5.499999999999998224, 120.0000000000000142 ) ) ;
#38753 = CARTESIAN_POINT ( 'NONE',  ( 21.53943276465977519, -0.05219959533907433946, 88.74890960531436690 ) ) ;
#38754 = CARTESIAN_POINT ( 'NONE',  ( 10.72451020669898902, -18.67979575497178502, 112.9155762719810383 ) ) ;
#38755 = CARTESIAN_POINT ( 'NONE',  ( -14.34966873604960291, -8.224510206698953496, 36.66557627198103120 ) ) ;
#38756 = CARTESIAN_POINT ( 'NONE',  ( 16.52544592524335698, 4.483927247898782831, 36.45942372801901143 ) ) ;
#38757 = CARTESIAN_POINT ( 'NONE',  ( -16.51473224551069308, -9.474510206698971260, 36.66557627198102409 ) ) ;
#38758 = CARTESIAN_POINT ( 'NONE',  ( 9.564922557960805705, 16.46253265017160317, 69.58224293864770971 ) ) ;
#38759 = CARTESIAN_POINT ( 'NONE',  ( -10.81492255796078084, -18.62759615963271287, 22.08224293864769194 ) ) ;
#38760 = CARTESIAN_POINT ( 'NONE',  ( 15.50000000000000178, -5.500000000000000888, 118.0000000000000142 ) ) ;
#38761 = CARTESIAN_POINT ( 'NONE',  ( -9.564922557961040184, 16.46253265017147172, 107.9177570613523471 ) ) ;
#38762 = CARTESIAN_POINT ( 'NONE',  ( 5.153800228976615827, -19.02544592524334988, 45.20942372801901143 ) ) ;
#38763 = CARTESIAN_POINT ( 'NONE',  ( 21.52544592524344225, -5.823673210054117533, 93.54057627198103830 ) ) ;
#38764 = EDGE_CURVE ( 'NONE', #179099, #64402, #174823, .T. ) ;
#38765 = CARTESIAN_POINT ( 'NONE',  ( -12.14591786802309592, -12.06949235617757132, 21.87390960531436690 ) ) ;
#38766 = CARTESIAN_POINT ( 'NONE',  ( -15.72974639402197994, 15.80617190586746368, 45.62390960531436690 ) ) ;
#38768 = CARTESIAN_POINT ( 'NONE',  ( 16.51473224551083163, -9.474510206698727899, 105.8344237280190043 ) ) ;
#38767 = CARTESIAN_POINT ( 'NONE',  ( -5.719274019375978568, 21.55341960407610458, 85.20724293864770971 ) ) ;
#38769 = CARTESIAN_POINT ( 'NONE',  ( 16.46253265017160672, -9.564922557960803928, 103.3322429386476955 ) ) ;
#38770 = CARTESIAN_POINT ( 'NONE',  ( -18.62759615963255300, -10.81492255796106328, 79.16775706135234714 ) ) ;
#38771 = CARTESIAN_POINT ( 'NONE',  ( 19.05341960407611168, 5.049401038298154454, 73.95724293864768129 ) ) ;
#38772 = CIRCLE ( 'NONE', #61278, 216.0437394197456342 ) ;
#38773 = CARTESIAN_POINT ( 'NONE',  ( -4.379528057220328563, 16.55341960407611168, 100.2072429386476955 ) ) ;
#38774 = CARTESIAN_POINT ( 'NONE',  ( 31.23840969660177436, 7.314650797970924323, 96.67552899226035379 ) ) ;
#38775 = CARTESIAN_POINT ( 'NONE',  ( 0.05219959533909260263, 19.03943276465977164, 64.99890960531436690 ) ) ;
#38776 = CARTESIAN_POINT ( 'NONE',  ( -12.14591786802309592, -12.06949235617757132, 96.87390960531436690 ) ) ;
#38777 = VERTEX_POINT ( 'NONE', #178423 ) ;
#38778 = CARTESIAN_POINT ( 'NONE',  ( 16.46253265017146816, 9.564922557961045513, 101.6677570613523329 ) ) ;
#38779 = CYLINDRICAL_SURFACE ( 'NONE', #114874, 10.00000000000000000 ) ;
#38780 = CARTESIAN_POINT ( 'NONE',  ( -19.02544592524342804, 5.153800228976336051, 66.04057627198103830 ) ) ;
#38782 = CARTESIAN_POINT ( 'NONE',  ( -13.89961937509977652, 13.97604488694528158, 105.6239096053143527 ) ) ;
#38781 = CARTESIAN_POINT ( 'NONE',  ( -21.53943276465977519, -0.05219959533937600094, 88.75109039468567573 ) ) ;
#38783 = CARTESIAN_POINT ( 'NONE',  ( -16.52544592524335698, -4.483927247898792601, 83.95942372801900433 ) ) ;
#38784 = CARTESIAN_POINT ( 'NONE',  ( -16.88567814943164791, -6.947325034625700724, 76.29001122652587696 ) ) ;
#38785 = CARTESIAN_POINT ( 'NONE',  ( 5.153800228976615827, -19.02544592524334988, 55.20942372801899722 ) ) ;
#38786 = CARTESIAN_POINT ( 'NONE',  ( 21.53943276465977519, 0.05219959533937863772, 106.2510903946856757 ) ) ;
#38787 = CARTESIAN_POINT ( 'NONE',  ( 28.79475375365586132, 2.781246896534039337E-14, 144.9843446568999923 ) ) ;
#38788 = CARTESIAN_POINT ( 'NONE',  ( -11.74264578624799782, -36.14014761921581709, -7.349999994537626868 ) ) ;
#38789 = CARTESIAN_POINT ( 'NONE',  ( -16.55341960407611168, -4.379528057220339221, 21.45724293864769550 ) ) ;
#38790 = CARTESIAN_POINT ( 'NONE',  ( -34.48175918554795771, -5.660046887242175195, 49.94512835368022508 ) ) ;
#38791 = CARTESIAN_POINT ( 'NONE',  ( 16.55341960407618274, -4.379528057220086978, 96.04275706135236135 ) ) ;
#38792 = DIRECTION ( 'NONE',  ( 0.000000000000000000, 0.000000000000000000, 1.000000000000000000 ) ) ;
#38793 = CARTESIAN_POINT ( 'NONE',  ( -0.05219959533934338120, 16.53943276465976808, 72.50109039468568994 ) ) ;
#38794 = CARTESIAN_POINT ( 'NONE',  ( -21.55341960407619339, 5.719274019375674811, 83.54275706135234714 ) ) ;
#38795 = CARTESIAN_POINT ( 'NONE',  ( -19.03943276465977164, -0.05219959533935918106, 88.75109039468567573 ) ) ;
#38796 = CARTESIAN_POINT ( 'NONE',  ( 5.153800228976615827, -19.02544592524334988, 40.20942372801898301 ) ) ;
#38797 = CARTESIAN_POINT ( 'NONE',  ( 16.51473224551069308, 9.474510206698969483, 59.16557627198102409 ) ) ;
#38798 = CARTESIAN_POINT ( 'NONE',  ( -13.89961937509977652, 13.97604488694528158, 60.62390960531436690 ) ) ;
#38799 = FACE_OUTER_BOUND ( 'NONE', #58169, .T. ) ;
#38800 = CARTESIAN_POINT ( 'NONE',  ( -15.80617190586745835, -15.72974639402198527, 81.87390960531435269 ) ) ;
#38801 = AXIS2_PLACEMENT_3D ( 'NONE', #127326, #35332, #36312 ) ;
#38802 = CARTESIAN_POINT ( 'NONE',  ( 5.719274019375991003, -21.55341960407610458, 42.70724293864770260 ) ) ;
#38803 = CARTESIAN_POINT ( 'NONE',  ( 5.153800228976335163, 19.02544592524342804, 34.79057627198102409 ) ) ;
#38804 = CARTESIAN_POINT ( 'NONE',  ( 16.53943276465976808, 0.05219959533934440121, 61.25109039468567573 ) ) ;
#38805 = VERTEX_POINT ( 'NONE', #67228 ) ;
#38806 = CARTESIAN_POINT ( 'NONE',  ( 15.72974639402176855, 15.80617190586768217, 41.87609039468568284 ) ) ;
#38808 = CARTESIAN_POINT ( 'NONE',  ( 22.81625015709510151, -31.40387420917324590, -9.924999997268814766 ) ) ;
#38807 = CARTESIAN_POINT ( 'NONE',  ( -16.55341960407611168, -4.379528057220339221, 61.45724293864770260 ) ) ;
#38809 = CARTESIAN_POINT ( 'NONE',  ( 16.52544592524335698, 4.483927247898782831, 31.45942372801901854 ) ) ;
#38810 = CARTESIAN_POINT ( 'NONE',  ( -13.89961937509957401, -13.97604488694547875, 49.37609039468567573 ) ) ;
#38811 = CARTESIAN_POINT ( 'NONE',  ( 12.06949235617757843, -12.14591786802309237, 63.12390960531435979 ) ) ;
#38812 = CARTESIAN_POINT ( 'NONE',  ( 21.55341960407619695, -5.719274019375665929, 31.04275706135234714 ) ) ;
#38814 = CARTESIAN_POINT ( 'NONE',  ( 21.53943276465977519, -0.05219959533907433946, 88.74890960531436690 ) ) ;
#38813 = FACE_OUTER_BOUND ( 'NONE', #134527, .T. ) ;
#38815 = CARTESIAN_POINT ( 'NONE',  ( -13.97604488694527625, -13.89961937509977652, 106.8739096053143669 ) ) ;
#38816 = CARTESIAN_POINT ( 'NONE',  ( -4.483927247898539470, -16.52544592524342804, 77.29057627198102409 ) ) ;
#38817 = CARTESIAN_POINT ( 'NONE',  ( 28.61471831746382222, -27.54183658529444756, -20.22090314799459776 ) ) ;
#38818 = DIRECTION ( 'NONE',  ( 0.000000000000000000, 0.000000000000000000, -1.000000000000000000 ) ) ;
#38819 = CARTESIAN_POINT ( 'NONE',  ( -19.03943276465977164, -0.05219959533935918106, 63.75109039468566863 ) ) ;
#38820 = CARTESIAN_POINT ( 'NONE',  ( 15.80617190586746368, 15.72974639402197994, 114.3739096053143527 ) ) ;
#38821 = CARTESIAN_POINT ( 'NONE',  ( 5.049401038298161559, -19.05341960407611168, 52.70724293864767418 ) ) ;
#38822 = CARTESIAN_POINT ( 'NONE',  ( 16.46253265017146816, 9.564922557961045513, 41.66775706135234003 ) ) ;
#38823 = CARTESIAN_POINT ( 'NONE',  ( -16.51473224551069308, -9.474510206698971260, 26.66557627198103120 ) ) ;
#38824 = CARTESIAN_POINT ( 'NONE',  ( 5.823673210054444382, -21.52544592524334988, 65.20942372801901854 ) ) ;
#38825 = CARTESIAN_POINT ( 'NONE',  ( -17.26058549869094705, -6.457015423128475540, 71.37745837476069255 ) ) ;
#38826 = CARTESIAN_POINT ( 'NONE',  ( -16.52544592524342804, 4.483927247898546575, 51.04057627198103120 ) ) ;
#38827 = CARTESIAN_POINT ( 'NONE',  ( -13.97604488694527625, -13.89961937509977652, 61.87390960531435979 ) ) ;
#38828 = CARTESIAN_POINT ( 'NONE',  ( 5.719274019375991003, -21.55341960407610458, 92.70724293864770971 ) ) ;
#38829 = CARTESIAN_POINT ( 'NONE',  ( -16.51473224551069308, -9.474510206698971260, 51.66557627198102409 ) ) ;
#38830 = ORIENTED_EDGE ( 'NONE', *, *, #27973, .F. ) ;
#38831 = CARTESIAN_POINT ( 'NONE',  ( -5.719274019375978568, 21.55341960407610458, 70.20724293864769550 ) ) ;
#38832 = CARTESIAN_POINT ( 'NONE',  ( -21.55341960407619339, 5.719274019375674811, 93.54275706135234714 ) ) ;
#38835 = CARTESIAN_POINT ( 'NONE',  ( 14.29746914071049879, -8.314922557960816363, 78.33224293864770971 ) ) ;
#38834 = CARTESIAN_POINT ( 'NONE',  ( 8.224510206698742110, 14.34966873604972548, 92.08442372801901854 ) ) ;
#38833 = CARTESIAN_POINT ( 'NONE',  ( -9.564922557960796823, -16.46253265017161027, 27.08224293864769550 ) ) ;
#38836 = CARTESIAN_POINT ( 'NONE',  ( -0.05219959533936034679, 19.03943276465977164, 92.50109039468566152 ) ) ;
#38837 = ORIENTED_EDGE ( 'NONE', *, *, #52114, .F. ) ;
#38838 = CARTESIAN_POINT ( 'NONE',  ( -0.05219959533907301413, -21.53943276465977519, 112.4989096053143669 ) ) ;
#38839 = CARTESIAN_POINT ( 'NONE',  ( -9.564922557961040184, 16.46253265017147172, 42.91775706135234003 ) ) ;
#38840 = CARTESIAN_POINT ( 'NONE',  ( 8.314922557961029526, -14.29746914071037800, 100.4177570613523471 ) ) ;
#38841 = ADVANCED_FACE ( 'NONE', ( #175415 ), #24748, .F. ) ;
#38842 = CARTESIAN_POINT ( 'NONE',  ( 19.03943276465977164, 0.05219959533936151252, 31.25109039468566863 ) ) ;
#38843 = CARTESIAN_POINT ( 'NONE',  ( -13.97604488694527625, -13.89961937509977652, 86.87390960531436690 ) ) ;
#38844 = CARTESIAN_POINT ( 'NONE',  ( -18.67979575497178146, -10.72451020669898902, 56.66557627198103830 ) ) ;
#38845 = CARTESIAN_POINT ( 'NONE',  ( -18.22780087662114212, 5.499999999999995559, 48.51540105326107266 ) ) ;
#38846 = CARTESIAN_POINT ( 'NONE',  ( -12.06949235617756955, 12.14591786802309770, 115.6239096053143669 ) ) ;
#38847 = CARTESIAN_POINT ( 'NONE',  ( -18.62759615963255300, -10.81492255796106328, 104.1677570613523471 ) ) ;
#38848 = CARTESIAN_POINT ( 'NONE',  ( 12.06949235617739724, 12.14591786802326823, 81.87609039468568994 ) ) ;
#38849 = CARTESIAN_POINT ( 'NONE',  ( 15.72974639402176855, 15.80617190586768217, 26.87609039468567218 ) ) ;
#38850 = CARTESIAN_POINT ( 'NONE',  ( -4.483927247898782831, 16.52544592524335698, 32.70942372801900433 ) ) ;
#38851 = CARTESIAN_POINT ( 'NONE',  ( 9.474510206698971260, -16.51473224551069308, 107.9155762719810383 ) ) ;
#38852 = CARTESIAN_POINT ( 'NONE',  ( 16.46253265017160672, -9.564922557960803928, 38.33224293864768839 ) ) ;
#38853 = CARTESIAN_POINT ( 'NONE',  ( -16.46253265017160317, 9.564922557960807481, 65.83224293864769550 ) ) ;
#38854 = CARTESIAN_POINT ( 'NONE',  ( 4.379528057220092307, 16.55341960407617563, 42.29275706135235424 ) ) ;
#38855 = CARTESIAN_POINT ( 'NONE',  ( -8.314922557960811034, -14.29746914071050412, 97.08224293864770971 ) ) ;
#38856 = CARTESIAN_POINT ( 'NONE',  ( -16.53943276465976808, -0.05219959533934237506, 98.75109039468568994 ) ) ;
#38859 = CARTESIAN_POINT ( 'NONE',  ( 5.049401038298161559, -19.05341960407611168, 62.70724293864769550 ) ) ;
#38858 = CARTESIAN_POINT ( 'NONE',  ( 9.474510206698971260, -16.51473224551069308, 77.91557627198103830 ) ) ;
#38857 = CARTESIAN_POINT ( 'NONE',  ( -10.72451020669870658, -18.67979575497194134, 54.58442372801901143 ) ) ;
#38861 = EDGE_CURVE ( 'NONE', #59419, #106915, #156968, .T. ) ;
#38860 = CARTESIAN_POINT ( 'NONE',  ( 13.89961937509977652, -13.97604488694527269, 98.12390960531433848 ) ) ;
#38862 = CARTESIAN_POINT ( 'NONE',  ( -14.29746914071049879, 8.314922557960819915, 45.83224293864769550 ) ) ;
#38863 = CARTESIAN_POINT ( 'NONE',  ( -12.14591786802326823, 12.06949235617739902, 93.12609039468568994 ) ) ;
#38864 = VERTEX_POINT ( 'NONE', #97541 ) ;
#38865 = CARTESIAN_POINT ( 'NONE',  ( 19.03943276465977164, 0.05219959533936151252, 46.25109039468566863 ) ) ;
#38866 = DIRECTION ( 'NONE',  ( 0.000000000000000000, 0.000000000000000000, 1.000000000000000000 ) ) ;
#38867 = CARTESIAN_POINT ( 'NONE',  ( 5.153800228976335163, 19.02544592524342804, 59.79057627198100988 ) ) ;
#38868 = CARTESIAN_POINT ( 'NONE',  ( 19.02544592524334988, 5.153800228976608722, 36.45942372801900433 ) ) ;
#38869 = CARTESIAN_POINT ( 'NONE',  ( 36.91746825000000598, -11.99521256947793546, -9.724999997268813701 ) ) ;
#38870 = CARTESIAN_POINT ( 'NONE',  ( -16.81555441253549787, -7.025013491695498047, 64.36314554665743515 ) ) ;
#38871 = CARTESIAN_POINT ( 'NONE',  ( 16.53943276465976808, 0.05219959533934440121, 51.25109039468568994 ) ) ;
#38873 = CARTESIAN_POINT ( 'NONE',  ( -8.314922557961024197, 14.29746914071037800, 72.91775706135234714 ) ) ;
#38872 = CARTESIAN_POINT ( 'NONE',  ( 13.89961937509957401, 13.97604488694547697, 76.87609039468566152 ) ) ;
#38874 = CARTESIAN_POINT ( 'NONE',  ( -16.46253265017160317, 9.564922557960807481, 95.83224293864769550 ) ) ;
#38875 = CARTESIAN_POINT ( 'NONE',  ( -0.05219959533907301413, -21.53943276465977519, 107.4989096053143669 ) ) ;
#38876 = CARTESIAN_POINT ( 'NONE',  ( -16.46253265017146816, -9.564922557961047289, 74.16775706135234714 ) ) ;
#38878 = CARTESIAN_POINT ( 'NONE',  ( -13.89961937509977652, 13.97604488694528158, 35.62390960531435269 ) ) ;
#38877 = CARTESIAN_POINT ( 'NONE',  ( 9.564922557960805705, 16.46253265017160317, 99.58224293864770971 ) ) ;
#38879 = CARTESIAN_POINT ( 'NONE',  ( 16.51473224551069308, 9.474510206698969483, 94.16557627198103830 ) ) ;
#38881 = CARTESIAN_POINT ( 'NONE',  ( 19.02544592524343514, -5.153800228976328945, 33.54057627198102409 ) ) ;
#38880 = CARTESIAN_POINT ( 'NONE',  ( 8.314922557960818139, 14.29746914071049879, 49.58224293864769550 ) ) ;
#38882 = CARTESIAN_POINT ( 'NONE',  ( -5.049401038297874678, -19.05341960407617918, 44.79275706135232582 ) ) ;
#38883 = CARTESIAN_POINT ( 'NONE',  ( -16.52544592524342804, 4.483927247898546575, 86.04057627198102409 ) ) ;
#38884 = CARTESIAN_POINT ( 'NONE',  ( 18.62759615963255655, 10.81492255796105972, 111.6677570613523613 ) ) ;
#38885 = CARTESIAN_POINT ( 'NONE',  ( -16.51473224551069308, -9.474510206698971260, 51.66557627198102409 ) ) ;
#38886 = CARTESIAN_POINT ( 'NONE',  ( -15.80617190586745835, -15.72974639402198527, 66.87390960531436690 ) ) ;
#38888 = CARTESIAN_POINT ( 'NONE',  ( 5.049401038297881783, 19.05341960407617563, 22.29275706135233648 ) ) ;
#38887 = CARTESIAN_POINT ( 'NONE',  ( 14.29746914071049879, -8.314922557960816363, 48.33224293864770260 ) ) ;
#38889 = CARTESIAN_POINT ( 'NONE',  ( -19.02544592524342804, 5.153800228976336051, 111.0405762719810099 ) ) ;
#38890 = CARTESIAN_POINT ( 'NONE',  ( -19.05341960407611168, -5.049401038298163336, 106.4572429386476955 ) ) ;
#38891 = CARTESIAN_POINT ( 'NONE',  ( 19.02544592524343514, -5.153800228976328945, 43.54057627198103120 ) ) ;
#38892 = CARTESIAN_POINT ( 'NONE',  ( 19.03943276465977164, -0.05219959533909143690, 23.74890960531435269 ) ) ;
#38893 = CARTESIAN_POINT ( 'NONE',  ( 8.224510206698953496, -14.34966873604960469, 82.91557627198103830 ) ) ;
#38894 = CARTESIAN_POINT ( 'NONE',  ( -10.81492255796078084, -18.62759615963271287, 92.08224293864769550 ) ) ;
#38895 = CARTESIAN_POINT ( 'NONE',  ( -9.564922557960796823, -16.46253265017161027, 107.0822429386476955 ) ) ;
#38896 = CARTESIAN_POINT ( 'NONE',  ( 5.823673210054125526, 21.52544592524343514, 114.7905762719810383 ) ) ;
#38897 = CARTESIAN_POINT ( 'NONE',  ( -13.89961937509977652, 13.97604488694528158, 105.6239096053143527 ) ) ;
#38898 = CARTESIAN_POINT ( 'NONE',  ( -0.05219959533910754901, -16.53943276465976808, 97.49890960531436690 ) ) ;
#38899 = CARTESIAN_POINT ( 'NONE',  ( -21.53943276465977519, -0.05219959533937600094, 73.75109039468567573 ) ) ;
#38900 = CARTESIAN_POINT ( 'NONE',  ( 21.53943276465977519, -0.05219959533907433946, 83.74890960531435269 ) ) ;
#38901 = CARTESIAN_POINT ( 'NONE',  ( 17.48847506799970120, -5.747544572773742644, 108.3269743784328227 ) ) ;
#38902 = PLANE ( 'NONE',  #36550 ) ;
#38903 = FACE_OUTER_BOUND ( 'NONE', #154987, .T. ) ;
#38904 = CARTESIAN_POINT ( 'NONE',  ( -12.14591786802326823, 12.06949235617739902, 28.12609039468568284 ) ) ;
#38905 = CARTESIAN_POINT ( 'NONE',  ( 12.14591786802309770, 12.06949235617756955, 109.3739096053143811 ) ) ;
#38906 = CARTESIAN_POINT ( 'NONE',  ( -17.50000000000146372, -3.254303733634626106, 109.9760410692859267 ) ) ;
#38907 = CARTESIAN_POINT ( 'NONE',  ( -13.89961937509977652, 13.97604488694528158, 65.62390960531436690 ) ) ;
#38908 = CARTESIAN_POINT ( 'NONE',  ( 4.483927247898545687, 16.52544592524342804, 94.79057627198105251 ) ) ;
#38909 = CARTESIAN_POINT ( 'NONE',  ( -10.81492255796078084, -18.62759615963271287, 37.08224293864768129 ) ) ;
#38910 = CARTESIAN_POINT ( 'NONE',  ( 4.483927247898545687, 16.52544592524342804, 69.79057627198102409 ) ) ;
#38911 = CARTESIAN_POINT ( 'NONE',  ( 13.89961937509957401, 13.97604488694547697, 111.8760903946856757 ) ) ;
#38912 = CARTESIAN_POINT ( 'NONE',  ( 21.53943276465977519, 0.05219959533937863772, 76.25109039468568994 ) ) ;
#38913 = CARTESIAN_POINT ( 'NONE',  ( 18.22780087662126647, 5.499999999999818812, 61.48236817873107185 ) ) ;
#38914 = CARTESIAN_POINT ( 'NONE',  ( 19.03943276465977164, -0.05219959533909143690, 113.7489096053143669 ) ) ;
#38915 = CARTESIAN_POINT ( 'NONE',  ( 4.483927247898790824, -16.52544592524335698, 95.20942372801903275 ) ) ;
#38916 = CARTESIAN_POINT ( 'NONE',  ( 13.97604488694527802, 13.89961937509977652, 34.37390960531436690 ) ) ;
#38917 = CARTESIAN_POINT ( 'NONE',  ( 13.89961937509977652, -13.97604488694527269, 83.12390960531436690 ) ) ;
#38918 = CARTESIAN_POINT ( 'NONE',  ( -21.53943276465977519, 0.05219959533907696930, 101.2489096053143669 ) ) ;
#38919 = CARTESIAN_POINT ( 'NONE',  ( -16.53943276465976808, -0.05219959533934237506, 23.75109039468567929 ) ) ;
#38921 = CARTESIAN_POINT ( 'NONE',  ( 21.55341960407619695, -5.719274019375665929, 76.04275706135237556 ) ) ;
#38920 = CARTESIAN_POINT ( 'NONE',  ( -16.52544592524342804, 4.483927247898546575, 46.04057627198103830 ) ) ;
#38922 = CARTESIAN_POINT ( 'NONE',  ( 0.05219959533934541429, -16.53943276465976808, 95.00109039468568994 ) ) ;
#38923 = CARTESIAN_POINT ( 'NONE',  ( 16.61371651742640054, -7.165104196375913226, 46.35415069992970416 ) ) ;
#38924 = CARTESIAN_POINT ( 'NONE',  ( -17.44279575226823198, 5.990770900252464060, 80.83557567514318976 ) ) ;
#38925 = CARTESIAN_POINT ( 'NONE',  ( 12.06949235617757843, -12.14591786802309237, 28.12390960531435979 ) ) ;
#38926 = CARTESIAN_POINT ( 'NONE',  ( 16.55341960407618274, -4.379528057220086978, 56.04275706135235424 ) ) ;
#38927 = CARTESIAN_POINT ( 'NONE',  ( 19.03943276465977164, -0.05219959533909143690, 73.74890960531435269 ) ) ;
#38928 = CARTESIAN_POINT ( 'NONE',  ( 13.89961937509977652, -13.97604488694527269, 88.12390960531438111 ) ) ;
#38929 = CARTESIAN_POINT ( 'NONE',  ( 18.62759615963255655, 10.81492255796105972, 91.66775706135234714 ) ) ;
#38930 = CARTESIAN_POINT ( 'NONE',  ( 0.05219959533934541429, -16.53943276465976808, 95.00109039468568994 ) ) ;
#38931 = CARTESIAN_POINT ( 'NONE',  ( 4.483927247898545687, 16.52544592524342804, 64.79057627198103830 ) ) ;
#38932 = CARTESIAN_POINT ( 'NONE',  ( 19.02544592524343514, -5.153800228976328945, 73.54057627198103830 ) ) ;
#38933 = ORIENTED_EDGE ( 'NONE', *, *, #190368, .T. ) ;
#38934 = CARTESIAN_POINT ( 'NONE',  ( 5.153800228976615827, -19.02544592524334988, 110.2094237280189901 ) ) ;
#38935 = CARTESIAN_POINT ( 'NONE',  ( 12.14591786802309770, 12.06949235617756955, 114.3739096053143527 ) ) ;
#38936 = CARTESIAN_POINT ( 'NONE',  ( 0.05219959533909260263, 19.03943276465977164, 84.99890960531436690 ) ) ;
#38938 = CARTESIAN_POINT ( 'NONE',  ( -36.91746825000000598, 2.428612866367529932E-14, -8.624999997268814056 ) ) ;
#38937 = CARTESIAN_POINT ( 'NONE',  ( -19.02544592524334988, -5.153800228976617603, 108.9594237280189759 ) ) ;
#38939 = CARTESIAN_POINT ( 'NONE',  ( 21.52544592524334988, 5.823673210054432836, 106.4594237280190328 ) ) ;
#38940 = CARTESIAN_POINT ( 'NONE',  ( -16.55341960407617563, 4.379528057220093196, 83.54275706135234714 ) ) ;
#38941 = CARTESIAN_POINT ( 'NONE',  ( -19.03943276465977164, -0.05219959533935918106, 93.75109039468566152 ) ) ;
#38942 = CARTESIAN_POINT ( 'NONE',  ( -12.14591786802309592, -12.06949235617757132, 111.8739096053143669 ) ) ;
#38943 = CARTESIAN_POINT ( 'NONE',  ( 12.14591786802327356, -12.06949235617739191, 70.62609039468567573 ) ) ;
#38944 = CARTESIAN_POINT ( 'NONE',  ( 1.300000000000000044, 0.7216878364870328300, -1.250000000000000000 ) ) ;
#38945 = CARTESIAN_POINT ( 'NONE',  ( 9.564922557961047289, -16.46253265017146816, 55.41775706135234003 ) ) ;
#38946 = CARTESIAN_POINT ( 'NONE',  ( 0.05219959533937995610, -21.53943276465977519, 100.0010903946857042 ) ) ;
#38947 = CARTESIAN_POINT ( 'NONE',  ( 0.05219959533909260263, 19.03943276465977164, 39.99890960531436690 ) ) ;
#38948 = CARTESIAN_POINT ( 'NONE',  ( 0.05219959533909260263, 19.03943276465977164, 74.99890960531435269 ) ) ;
#38949 = CARTESIAN_POINT ( 'NONE',  ( -12.14591786802309592, -12.06949235617757132, 71.87390960531438111 ) ) ;
#38950 = AXIS2_PLACEMENT_3D ( 'NONE', #9598, #11606, #56086 ) ;
#38951 = CARTESIAN_POINT ( 'NONE',  ( 15.80617190586769283, -15.72974639402175789, 85.62609039468568994 ) ) ;
#38952 = CARTESIAN_POINT ( 'NONE',  ( -13.97604488694547697, 13.89961937509957934, 43.12609039468566152 ) ) ;
#38953 = CARTESIAN_POINT ( 'NONE',  ( -16.51473224551082808, 9.474510206698731452, 38.33442372801899722 ) ) ;
#38954 = CARTESIAN_POINT ( 'NONE',  ( -5.719274019375978568, 21.55341960407610458, 40.20724293864769550 ) ) ;
#38955 = CARTESIAN_POINT ( 'NONE',  ( -15.80617190586768217, 15.72974639402176855, 93.12609039468568994 ) ) ;
#38956 = CARTESIAN_POINT ( 'NONE',  ( -5.049401038298153566, 19.05341960407611168, 80.20724293864769550 ) ) ;
#38957 = CARTESIAN_POINT ( 'NONE',  ( 10.81492255796106328, -18.62759615963255655, 95.41775706135234714 ) ) ;
#38958 = CARTESIAN_POINT ( 'NONE',  ( -21.55341960407610458, -5.719274019375992779, 46.45724293864769550 ) ) ;
#38959 = CARTESIAN_POINT ( 'NONE',  ( -5.049401038298153566, 19.05341960407611168, 80.20724293864769550 ) ) ;
#38960 = CARTESIAN_POINT ( 'NONE',  ( 9.474510206698729675, 16.51473224551082808, 77.08442372801900433 ) ) ;
#38961 = CARTESIAN_POINT ( 'NONE',  ( 19.05341960407611168, 5.049401038298154454, 98.95724293864766707 ) ) ;
#38962 = EDGE_CURVE ( 'NONE', #197193, #8593, #20723, .T. ) ;
#38963 = CARTESIAN_POINT ( 'NONE',  ( -0.05219959533936034679, 19.03943276465977164, 92.50109039468566152 ) ) ;
#38964 = CARTESIAN_POINT ( 'NONE',  ( 4.379528057220092307, 16.55341960407617563, 37.29275706135235424 ) ) ;
#38965 = CARTESIAN_POINT ( 'NONE',  ( -14.34966873604960291, -8.224510206698953496, 101.6655762719810383 ) ) ;
#38966 = CARTESIAN_POINT ( 'NONE',  ( -19.05341960407611168, -5.049401038298163336, 71.45724293864766707 ) ) ;
#38967 = CARTESIAN_POINT ( 'NONE',  ( -15.80617190586745835, -15.72974639402198527, 66.87390960531436690 ) ) ;
#38968 = CARTESIAN_POINT ( 'NONE',  ( 14.34966873604972726, -8.224510206698740333, 35.83442372801901143 ) ) ;
#38969 = CARTESIAN_POINT ( 'NONE',  ( 5.719274019375673035, 21.55341960407619339, 37.29275706135235424 ) ) ;
#38970 = CARTESIAN_POINT ( 'NONE',  ( -21.55341960407619339, 5.719274019375674811, 83.54275706135234714 ) ) ;
#38971 = CARTESIAN_POINT ( 'NONE',  ( -8.224510206698735004, -14.34966873604973081, 89.58442372801901854 ) ) ;
#38972 = CARTESIAN_POINT ( 'NONE',  ( 9.564922557960805705, 16.46253265017160317, 69.58224293864770971 ) ) ;
#38973 = CARTESIAN_POINT ( 'NONE',  ( -12.14591786802309592, -12.06949235617757132, 71.87390960531438111 ) ) ;
#38974 = CARTESIAN_POINT ( 'NONE',  ( -14.34966873604972548, 8.224510206698743886, 108.3344237280190185 ) ) ;
#38975 = CARTESIAN_POINT ( 'NONE',  ( 9.564922557961047289, -16.46253265017146816, 50.41775706135233293 ) ) ;
#38976 = CARTESIAN_POINT ( 'NONE',  ( 18.62759615963255655, 10.81492255796105972, 31.66775706135234358 ) ) ;
#38977 = EDGE_CURVE ( 'NONE', #44164, #177566, #37900, .T. ) ;
#38978 = CARTESIAN_POINT ( 'NONE',  ( -16.55341960407611168, -4.379528057220339221, 76.45724293864769550 ) ) ;
#38979 = CARTESIAN_POINT ( 'NONE',  ( -9.564922557960796823, -16.46253265017161027, 97.08224293864769550 ) ) ;
#38980 = CARTESIAN_POINT ( 'NONE',  ( -12.14591786802326823, 12.06949235617739902, 98.12609039468570415 ) ) ;
#38981 = CARTESIAN_POINT ( 'NONE',  ( -10.72451020669870658, -18.67979575497194134, 74.58442372801901854 ) ) ;
#38982 = CARTESIAN_POINT ( 'NONE',  ( -14.29746914071037622, -8.314922557961029526, 44.16775706135234714 ) ) ;
#38983 = CARTESIAN_POINT ( 'NONE',  ( 10.72451020669871369, 18.67979575497193778, 37.08442372801901143 ) ) ;
#38984 = CARTESIAN_POINT ( 'NONE',  ( 4.379528057220339221, -16.55341960407611168, 72.70724293864769550 ) ) ;
#38985 = ORIENTED_EDGE ( 'NONE', *, *, #131013, .F. ) ;
#38986 = CARTESIAN_POINT ( 'NONE',  ( -10.72451020669898014, 18.67979575497178502, 115.4155762719810241 ) ) ;
#38987 = CARTESIAN_POINT ( 'NONE',  ( 17.50000000000001066, -5.076555817581232866, 26.32048507950225869 ) ) ;
#38988 = CARTESIAN_POINT ( 'NONE',  ( -8.224510206698948167, 14.34966873604960824, 55.41557627198102409 ) ) ;
#38989 = CARTESIAN_POINT ( 'NONE',  ( -13.89961937509977652, 13.97604488694528158, 30.62390960531435269 ) ) ;
#38990 = CARTESIAN_POINT ( 'NONE',  ( 18.67979575497178502, 10.72451020669898547, 44.16557627198103120 ) ) ;
#38991 = CARTESIAN_POINT ( 'NONE',  ( 14.29746914071049879, -8.314922557960816363, 78.33224293864770971 ) ) ;
#38992 = CARTESIAN_POINT ( 'NONE',  ( -18.67979575497178146, -10.72451020669898902, 81.66557627198103830 ) ) ;
#38993 = CARTESIAN_POINT ( 'NONE',  ( 9.474510206698971260, -16.51473224551069308, 92.91557627198103830 ) ) ;
#38995 = CARTESIAN_POINT ( 'NONE',  ( -19.02544592524334988, -5.153800228976617603, 78.95942372801900433 ) ) ;
#38994 = CARTESIAN_POINT ( 'NONE',  ( 13.97604488694527802, 13.89961937509977652, 44.37390960531435269 ) ) ;
#38997 = CARTESIAN_POINT ( 'NONE',  ( 21.53943276465977519, -0.05219959533907433946, 63.74890960531435979 ) ) ;
#38996 = CARTESIAN_POINT ( 'NONE',  ( 0.05219959533937995610, -21.53943276465977519, 60.00109039468568284 ) ) ;
#38998 = CARTESIAN_POINT ( 'NONE',  ( 13.97604488694527802, 13.89961937509977652, 34.37390960531436690 ) ) ;
#38999 = CARTESIAN_POINT ( 'NONE',  ( -5.049401038298153566, 19.05341960407611168, 75.20724293864769550 ) ) ;
#39000 = ORIENTED_EDGE ( 'NONE', *, *, #167117, .T. ) ;
#39001 = CARTESIAN_POINT ( 'NONE',  ( 4.379528057220092307, 16.55341960407617563, 52.29275706135236135 ) ) ;
#39002 = CARTESIAN_POINT ( 'NONE',  ( -0.05219959533937732626, 21.53943276465977519, 37.50109039468568284 ) ) ;
#39003 = EDGE_CURVE ( 'NONE', #86859, #41998, #36883, .T. ) ;
#39004 = CARTESIAN_POINT ( 'NONE',  ( -5.823673210054431948, 21.52544592524334988, 72.70942372801901854 ) ) ;
#39005 = CARTESIAN_POINT ( 'NONE',  ( 9.474510206698971260, -16.51473224551069308, 97.91557627198102409 ) ) ;
#39006 = CARTESIAN_POINT ( 'NONE',  ( -18.67979575497178146, -10.72451020669898902, 81.66557627198103830 ) ) ;
#39008 = CARTESIAN_POINT ( 'NONE',  ( 4.483927247898790824, -16.52544592524335698, 50.20942372801901854 ) ) ;
#39007 = CARTESIAN_POINT ( 'NONE',  ( 18.67979575497194134, -10.72451020669871369, 30.83442372801902209 ) ) ;
#39009 = CARTESIAN_POINT ( 'NONE',  ( 10.81492255796078972, 18.62759615963270932, 54.58224293864769550 ) ) ;
#39010 = CARTESIAN_POINT ( 'NONE',  ( -15.72974639402176322, -15.80617190586768395, 109.3760903946857042 ) ) ;
#39011 = CARTESIAN_POINT ( 'NONE',  ( -13.97604488694527625, -13.89961937509977652, 56.87390960531434558 ) ) ;
#39012 = CARTESIAN_POINT ( 'NONE',  ( -16.46253265017160317, 9.564922557960807481, 105.8322429386476955 ) ) ;
#39013 = CARTESIAN_POINT ( 'NONE',  ( 16.51473224551069308, 9.474510206698969483, 94.16557627198103830 ) ) ;
#39014 = DIRECTION ( 'NONE',  ( -0.000000000000000000, -0.000000000000000000, 1.000000000000000000 ) ) ;
#39015 = CARTESIAN_POINT ( 'NONE',  ( 13.89961937509957401, 13.97604488694547697, 61.87609039468566863 ) ) ;
#39016 = CARTESIAN_POINT ( 'NONE',  ( 21.53943276465977519, -0.05219959533907433946, 38.74890960531435979 ) ) ;
#39017 = CARTESIAN_POINT ( 'NONE',  ( 4.379528057220339221, -16.55341960407611168, 27.70724293864769905 ) ) ;
#39018 = CARTESIAN_POINT ( 'NONE',  ( 5.153800228976615827, -19.02544592524334988, 100.2094237280190043 ) ) ;
#39019 = DIRECTION ( 'NONE',  ( -1.000000000000000000, 0.000000000000000000, 0.000000000000000000 ) ) ;
#39020 = CARTESIAN_POINT ( 'NONE',  ( -5.823673210054431948, 21.52544592524334988, 112.7094237280190328 ) ) ;
#39021 = CARTESIAN_POINT ( 'NONE',  ( -9.564922557961040184, 16.46253265017147172, 102.9177570613523329 ) ) ;
#39022 = CARTESIAN_POINT ( 'NONE',  ( 19.05341960407617918, -5.049401038297876454, 61.04275706135232582 ) ) ;
#39023 = CARTESIAN_POINT ( 'NONE',  ( -1.022580077288041090E-15, -16.70000000000002061, -59.13370768023891344 ) ) ;
#39024 = CARTESIAN_POINT ( 'NONE',  ( 13.89961937509977652, -13.97604488694527269, 53.12390960531434558 ) ) ;
#39025 = CARTESIAN_POINT ( 'NONE',  ( -14.34966873604960291, -8.224510206698953496, 61.66557627198103120 ) ) ;
#39026 = CARTESIAN_POINT ( 'NONE',  ( 13.89961937509977652, -13.97604488694527269, 33.12390960531434558 ) ) ;
#39027 = CARTESIAN_POINT ( 'NONE',  ( -4.379528057220328563, 16.55341960407611168, 35.20724293864768839 ) ) ;
#39028 = DIRECTION ( 'NONE',  ( -0.1039620511844979306, -0.1039620511844979306, -0.9891328443778538704 ) ) ;
#39029 = CARTESIAN_POINT ( 'NONE',  ( -12.14591786802326823, 12.06949235617739902, 103.1260903946856757 ) ) ;
#39030 = CARTESIAN_POINT ( 'NONE',  ( -19.05341960407611168, -5.049401038298163336, 66.45724293864769550 ) ) ;
#39031 = CARTESIAN_POINT ( 'NONE',  ( 5.049401038297881783, 19.05341960407617563, 22.29275706135233648 ) ) ;
#39032 = CARTESIAN_POINT ( 'NONE',  ( 14.34966873604972726, -8.224510206698740333, 30.83442372801902209 ) ) ;
#39033 = CARTESIAN_POINT ( 'NONE',  ( -10.81492255796078084, -18.62759615963271287, 52.08224293864768839 ) ) ;
#39034 = CARTESIAN_POINT ( 'NONE',  ( -10.81492255796105439, 18.62759615963255655, 107.9177570613523471 ) ) ;
#39035 = CARTESIAN_POINT ( 'NONE',  ( -9.564922557960796823, -16.46253265017161027, 67.08224293864769550 ) ) ;
#39036 = CARTESIAN_POINT ( 'NONE',  ( -9.564922557960796823, -16.46253265017161027, 102.0822429386477097 ) ) ;
#39037 = CARTESIAN_POINT ( 'NONE',  ( -19.05341960407611168, -5.049401038298163336, 96.45724293864769550 ) ) ;
#39038 = CARTESIAN_POINT ( 'NONE',  ( 18.62759615963255655, 10.81492255796105972, 21.66775706135235069 ) ) ;
#39039 = CARTESIAN_POINT ( 'NONE',  ( -14.34966873604960291, -8.224510206698953496, 91.66557627198103830 ) ) ;
#39041 = CARTESIAN_POINT ( 'NONE',  ( -13.89961937509977652, 13.97604488694528158, 70.62390960531432427 ) ) ;
#39040 = CARTESIAN_POINT ( 'NONE',  ( 10.72451020669898902, -18.67979575497178502, 82.91557627198103830 ) ) ;
#39042 = CARTESIAN_POINT ( 'NONE',  ( -0.05219959533909027116, -19.03943276465977164, 67.49890960531436690 ) ) ;
#39043 = CARTESIAN_POINT ( 'NONE',  ( -10.72451020669898014, 18.67979575497178502, 115.4155762719810241 ) ) ;
#39044 = ORIENTED_EDGE ( 'NONE', *, *, #145326, .T. ) ;
#39045 = CARTESIAN_POINT ( 'NONE',  ( -16.46253265017160317, 9.564922557960807481, 70.83224293864770971 ) ) ;
#39046 = CARTESIAN_POINT ( 'NONE',  ( 19.26498983726236958, -5.499999999999790390, 98.05319577422005750 ) ) ;
#39048 = CARTESIAN_POINT ( 'NONE',  ( -16.51473224551069308, -9.474510206698971260, 21.66557627198102765 ) ) ;
#39047 = CARTESIAN_POINT ( 'NONE',  ( 8.224510206698953496, -14.34966873604960469, 102.9155762719810383 ) ) ;
#39049 = CARTESIAN_POINT ( 'NONE',  ( 9.564922557961047289, -16.46253265017146816, 95.41775706135233293 ) ) ;
#39050 = CARTESIAN_POINT ( 'NONE',  ( -16.53943276465976808, 0.05219959533911058130, 101.2489096053143669 ) ) ;
#39051 = CARTESIAN_POINT ( 'NONE',  ( -21.55341960407619339, 5.719274019375674811, 68.54275706135234714 ) ) ;
#39053 = CARTESIAN_POINT ( 'NONE',  ( -21.52544592524334988, -5.823673210054445271, 28.95942372801902209 ) ) ;
#39052 = CARTESIAN_POINT ( 'NONE',  ( -19.03943276465977164, 0.05219959533909376836, 61.24890960531436690 ) ) ;
#39054 = CARTESIAN_POINT ( 'NONE',  ( 5.823673210054125526, 21.52544592524343514, 109.7905762719810383 ) ) ;
#39055 = DIRECTION ( 'NONE',  ( 0.000000000000000000, 1.000000000000000000, 0.000000000000000000 ) ) ;
#39056 = CARTESIAN_POINT ( 'NONE',  ( -5.153800228976328057, -19.02544592524343514, 67.29057627198102409 ) ) ;
#39057 = CARTESIAN_POINT ( 'NONE',  ( 27.89963664982190750, 6.788868650204036292, 161.9772721943422482 ) ) ;
#39059 = CARTESIAN_POINT ( 'NONE',  ( -21.55341960407610458, -5.719274019375992779, 36.45724293864768839 ) ) ;
#39058 = CARTESIAN_POINT ( 'NONE',  ( 4.379528057220092307, 16.55341960407617563, 22.29275706135235069 ) ) ;
#39060 = CARTESIAN_POINT ( 'NONE',  ( -18.67979575497193778, 10.72451020669871902, 63.33442372801900433 ) ) ;
#39061 = CARTESIAN_POINT ( 'NONE',  ( -19.03943276465977164, 0.05219959533909376836, 116.2489096053143669 ) ) ;
#39062 =( BOUNDED_SURFACE ( )  B_SPLINE_SURFACE ( 3, 2, ( 
 ( #156989, #32658, #2305, #143794, #159968, #96294, #98266, #4279, #157981, #63986, #3299, #142798, #81118, #50807, #128620, #35628, #36609, #94312, #173160, #155990, #65959, #21455, #186356, #189330, #127630, #125656, #6276, #124660, #158961, #188331, #48823, #80136, #18487, #20451, #47836, #79144, #144793, #141806, #17487, #112465, #64971, #187353, #190313, #49810, #110476, #174157, #172158, #95305, #5277, #51789, #113449, #175142, #83116, #179162, #99282, #23463, #37620, #162969, #101279, #161967, #116466, #176150, #8289, #9302, #69967, #70968, #132636, #177159, #117463, #178155, #130619, #131633, #85110, #146796, #191304, #160969, #22463, #194324, #193317, #39620, #52780, #54791, #38632, #100289, #114449, #24475, #86125, #129608, #84111, #145790, #147816, #67954, #55792, #7272, #68956, #192315, #53795, #115470, #39908, #127912, #22750, #84399, #145078, #98565, #114748, #189614, #82396, #85405, #6560, #113735, #174442, #192602, #36901, #146075, #131924, #21749, #129891, #176442, #178440, #68238, #112748, #24766, #35911, #191591, #97557, #23755, #159245, #20740, #144084, #37915, #54085, #147097, #115759, #8582, #193608, #99574, #161256, #101574, #55080, #116750, #53070, #160259, #5565, #7560, #175432, #100574, #67244, #69246, #163264, #51088, #162256, #128903, #130912, #70256, #86413, #83400, #177447, #190603, #52079, #38917, #4560, #66252, #102590, #27763, #151095, #87415, #88401, #57091, #150095, #166264, #9590, #135920, #183409, #71255, #89406, #12586, #11598, #41926, #58083, #132919, #25769, #28750, #73266, #118765, #117759, #196613, #120724, #42914, #44892, #152071, #134935, #105565, #106549, #164274, #136894, #168225, #165267, #149100, #40917, #74251, #119753, #29722, #197591, #10590, #26761, #179451, #43902, #181436, #13556, #72251, #133929, #194606, #195619, #182424, #180454, #104580, #148098, #167251, #90386, #59057, #121716, #103592, #75222, #56078, #198581, #60049, #351, #1342, #170214, #153046, #185384, #110518, #188374, #184397, #171210, #139853, #172199, #173201, #61035, #140856, #199566, #156030, #16537, #78184, #137885, #33684, #48863, #14547, #92363, #107530, #109528, #91354, #79186, #17527, #47875, #95347, #157031, #2345, #18529, #32700, #108535, #63023, #80176, #141848, #3339, #186398, #124701, #111516, #62021, #94351, #31707, #65013, #45877, #30715, #122707, #187395, #64026, #169207, #125696, #126670, #154049, #15544, #77202, #138871, #93356, #49851, #76206, #123685, #46874, #155042, #112505, #192358, #70009, #6317, #8333, #114492, #144833, #174199, #113491, #52823, #191345, #161011, #38676, #145831, #146840, #19513, #21498, #142840, #176194, #131678, #96335, #99328, #83159, #50848, #116509, #34677, #7313, #98310, #159001, #190355, #128660, #68998, #158022, #189371, #54835, #51832, #81158, #22505, #175186, #35667, #177203, #36652, #97315, #84152, #66002, #4319, #20494, #127671, #130664, #23506, #37663, #82142, #143838, #67996, #5317, #53841, #115515, #129649, #100332, #67001, #162010, #85154, #193359, #160010, #105323, #180210, #136649, #150852, #10345, #57844, #26516, #134690, #163012, #132679, #71011, #13321, #196375, #24519, #194367, #59807, #166020, #167011, #119516, #178197, #55834, #149845, #117507, #197352, #74010, #88160, #27520, #179204, #181198, #28512, #42675, #90147, #151831, #41680, #198331, #12346, #72001, #104336, #11349, #89161, #86170, #40672, #102342, #74986, #135680, #58816, #147860, #120484, #103344, #165023, #9346, #182175, #43661, #39662, #164031, #25529, #101323, #87173, #148854, #133675, #195366, #56845, #118521, #73020, #125465, #62779, #138632, #93117, #187162, #140621, #171967, #16300, #169973, #141620, #92119, #154802, #61782, #110285, #14303, #60795, #91121, #17291, #94115, #29488, #155794, #108294, #152810, #75970, #137643, #45640, #123451, #63792, #2111, #122467, #153807, #199330, #184159, #78945, #156802, #77950, #95113, #1103, #31465 ),
 ( #183170, #186157, #139617, #107292, #3109, #121477, #32462, #185143, #168963, #76961, #15301, #48633, #44653, #30469, #106306, #113, #167991, #47636, #46634, #124460, #33454, #109290, #170969, #18295, #79950, #34447, #21264, #38435, #4088, #66763, #173966, #174952, #143597, #126446, #158769, #83916, #161775, #157795, #144597, #113260, #145598, #146593, #96106, #52591, #97086, #82920, #192114, #81904, #190120, #36415, #100091, #128424, #172969, #84914, #19286, #51596, #80933, #7077, #142609, #65766, #127436, #98069, #114251, #68758, #175957, #130415, #53596, #159769, #6083, #23270, #115272, #176965, #5081, #20258, #189142, #67762, #35434, #160777, #50615, #129419, #64785, #188144, #22266, #112274, #191117, #49616, #111279, #37426, #99086, #54593, #24279, #40431, #102102, #72781, #162770, #87921, #11106, #147617, #148614, #117269, #10105, #26279, #69764, #196136, #43425, #131433, #149608, #134451, #71765, #163787, #118280, #193119, #85928, #88925, #133435, #178962, #177957, #56606, #180959, #103104, #105094, #12113, #195124, #165782, #166780, #9104, #197118, #28281, #25288, #70771, #101085, #57607, #179971, #89920, #119276, #132440, #86931, #39425, #104099, #41437, #73776, #194131, #55594, #116267, #164785, #42436, #27277, #150617, #8087, #135449, #58585, #120251, #181942, #124221, #138402, #59567, #182936, #121242, #75732, #153569, #93885, #32227, #152575, #183922, #44419, #29257, #109059, #186929, #123220, #125231, #31233, #61551, #90889, #30235, #169738, #108053, #77723, #155563, #62546, #63557, #136421, #200083, #106072, #92882, #48399, #13093, #16065, #184910, #167759, #33224, #151602, #185918, #15066, #137408, #107060, #45407, #47403, #74759, #14065, #91877, #139389, #168731, #154569, #78712, #76727, #46395, #871, #110056, #170736, #199088, #171736, #60556, #17057, #122231, #140388, #1876, #198101, #64554, #128194, #144361, #175709, #5848, #37187, #83681, #189892, #51367, #191871, #145359, #6841, #35204, #50387, #95877, #113028, #65535, #190879, #126218, #174720, #68520, #18063, #52355, #187914, #36183, #160540, #176725, #173735, #4845, #141387, #111046, #127195, #188907, #159525, #49383, #97837, #21022, #34214, #96857, #3856, #158541, #82677, #156565, #67524, #130174, #79718, #129181, #114011, #20031, #112047, #66531, #2875, #172733, #98845, #81673, #143356, #157560, #22029, #53354, #115032, #94884, #19053, #80700, #142377, #167290, #69528, #23031, #192883, #122746, #28787, #29763, #56359, #38198, #54361, #9868, #116033, #60088, #136933, #148373, #90426, #131193, #118041, #168266, #194885, #91397, #153086, #40183, #199608, #13595, #70531, #179732, #86689, #41202, #84676, #177722, #39190, #76246, #105603, #152112, #146355, #75262, #163546, #25046, #7842, #183449, #198622, #99854, #100848, #162530, #121756, #161538, #44933, #106590, #14590, #137924, #61074, #24034, #85688, #147375, #55356, #71527, #8864, #132200, #193891, #133194, #117026, #178721, #101862, #17568, #124743, #173241, #77241, #123727, #154089, #80215, #157072, #92403, #18568, #171251, #15583, #138909, #389, #108576, #186439, #126708, #65052, #185425, #16576, #62062, #46916, #141886, #19552, #156070, #158061, #64065, #94391, #170253, #63064, #2386, #140900, #110557, #188412, #95386, #96374, #169248, #32739, #31747, #125735, #81196, #45917, #48902, #79229, #93395, #66042, #184437, #3377, #47915, #155082, #139894, #78223, #49889, #4357, #187435, #109569, #172238, #30756, #33723, #1383, #111556, #34716, #142877, #107571, #101359, #67040, #129686, #36690, #37701, #6354, #189410, #21537, #146879, #24556, #20533, #7351, #193395, #38711, #115551, #68034, #177239, #160049, #145868, #54871, #144871, #52859, #99364, #163049, #191383, #35707, #147895, #97354, #114530, #159040, #8371, #82181, #143876, #5357, #161047, #100368, #70046, #162047, #131714, #116545, #22541, #84188, #86205, #178233, #39697, #176231, #83197, #128699 ),
 ( #69035, #130700, #174239, #9381, #85190, #50886, #190396, #51872, #192395, #127709, #23543, #53877, #112544, #113531, #175225, #98350, #75020, #12383, #88195, #42710, #136685, #90183, #121511, #166055, #119551, #91156, #41715, #104371, #11385, #59843, #164066, #10381, #40709, #167045, #43696, #179242, #105358, #57879, #102378, #25565, #87209, #195404, #73055, #13356, #151866, #72038, #103380, #148890, #133711, #28546, #106341, #27556, #44687, #150889, #181234, #56882, #149879, #89196, #74045, #197387, #198367, #182211, #183206, #55869, #135716, #118556, #58852, #120519, #168026, #29522, #134727, #152845, #71046, #165058, #132713, #194401, #117543, #180246, #26551, #196409, #49650, #32498, #63826, #122504, #78981, #139652, #1140, #60829, #156835, #172000, #76005, #15339, #30504, #94150, #14339, #2148, #140656, #171006, #95146, #79985, #125498, #18330, #155829, #31501, #186193, #141653, #33488, #64818, #109325, #62814, #34482, #185180, #47674, #154839, #3144, #107327, #153842, #184194, #110319, #187196, #45676, #48666, #124498, #169000, #92155, #76996, #138668, #16336, #126479, #188178, #148, #46670, #61817, #123487, #111314, #173003, #17326, #96140, #137679, #199365, #108330, #93153, #170010, #77985, #83952, #161808, #68794, #69799, #142643, #144633, #65801, #175992, #54626, #19320, #22301, #6116, #173999, #39457, #157829, #130452, #21299, #81938, #113295, #51631, #192150, #177990, #114290, #82956, #67799, #4121, #145632, #174986, #112309, #100126, #159803, #35470, #7112, #189175, #127469, #97119, #80967, #53631, #146629, #37461, #50648, #158802, #129454, #20291, #177000, #115307, #191153, #38469, #143630, #99123, #84947, #36450, #5114, #23303, #52627, #8121, #66796, #128459, #190155, #98107, #131467, #160813, #193153, #116301, #120286, #135484, #165817, #74792, #70805, #57644, #136454, #40465, #103138, #10140, #11142, #180007, #162804, #195160, #181978, #198135, #194164, #180995, #166815, #12149, #88961, #41474, #150651, #133469, #119310, #28316, #118314, #26315, #72816, #59604, #164820, #9139, #121278, #132475, #87956, #55628, #43461, #117301, #178997, #102137, #134485, #73814, #105129, #197154, #89955, #151635, #196172, #42472, #182971, #13130, #101118, #149644, #56641, #163822, #104134, #71800, #58619, #25323, #27314, #24313, #85962, #147651, #86965, #148651, #110092, #126252, #123254, #154604, #90923, #60591, #76763, #138436, #109094, #199124, #124258, #47437, #183955, #184945, #153606, #46430, #62580, #106108, #32263, #79752, #167793, #185953, #170773, #108089, #200117, #16099, #29293, #122266, #125267, #169773, #15102, #14099, #92918, #17093, #139423, #141422, #48435, #31267, #1913, #2909, #45442, #33259, #64587, #61586, #107095, #137444, #93920, #77757, #44455, #155598, #168765, #78746, #905, #152609, #75767, #30268, #91913, #140423, #186965, #171770, #63592, #94917, #156603, #18097, #145392, #23065, #159560, #161572, #67558, #97870, #65571, #66564, #5881, #144396, #114047, #191904, #98880, #99887, #172770, #174753, #95910, #129215, #84710, #49418, #52390, #36217, #3891, #69563, #187949, #160574, #51401, #112081, #143391, #81707, #22063, #7877, #190913, #113061, #21059, #34250, #175745, #4882, #142413, #130209, #189926, #127230, #37223, #19086, #157594, #188945, #111080, #83714, #176760, #6874, #80734, #50422, #82713, #173771, #68553, #53389, #115068, #38232, #35237, #146389, #96891, #158574, #20063, #128229, #133227, #89722, #103899, #163579, #10899, #179766, #87719, #116068, #85723, #24068, #166582, #149404, #180762, #39225, #195933, #56393, #118075, #177756, #73578, #88724, #192918, #132234, #147410, #72572, #131229, #119080, #57408, #134247, #11915, #196923, #42238, #135251, #165580, #148407, #102896, #58390, #150420, #181744, #26075, #41235, #151407, #101897, #164581, #71562, #120057, #8898, #70566, #100881, #27078, #43226, #162563, #25079, #104893, #28082, #12896, #193926, #55389 ),
 ( #117059, #54396, #178754, #40218, #86722, #9902, #194918, #140182, #139196, #78509, #15866, #91679, #46197, #1675, #93686, #125030, #169535, #123027, #94679, #45214, #107850, #14873, #63353, #167568, #13869, #44223, #170538, #47199, #182739, #108859, #61356, #105881, #29061, #90701, #198898, #76534, #16858, #155369, #75536, #106868, #152384, #137211, #32028, #109851, #31035, #48197, #154372, #184712, #60366, #153371, #92684, #77524, #671, #186726, #185709, #171536, #59371, #62341, #122038, #124011, #33024, #136227, #156358, #74560, #183728, #197902, #121043, #168542, #138210, #30040, #199892, #111841, #52156, #37997, #174519, #143159, #81472, #2675, #144159, #35000, #172530, #160338, #19831, #34016, #5644, #49188, #64352, #95673, #99652, #67321, #6640, #35986, #17860, #157360, #189694, #18854, #36982, #113813, #127991, #128982, #110846, #97633, #145157, #159322, #68318, #129969, #4639, #176521, #190680, #96655, #79516, #173530, #98644, #114827, #80500, #20818, #83479, #175508, #21827, #158342, #191669, #50184, #82474, #53148, #66330, #51166, #112827, #141186, #126021, #187717, #142173, #3657, #65335, #126995, #188702, #192681, #54164, #130989, #194688, #10670, #42007, #72334, #103672, #150180, #56158, #117839, #58166, #11681, #73346, #101655, #116827, #162332, #179532, #132001, #57172, #115837, #41002, #135019, #84474, #118850, #177526, #102669, #26844, #42997, #39984, #71335, #7639, #38995, #193689, #55157, #25850, #100651, #164354, #87493, #23833, #163347, #70334, #24843, #149182, #22828, #134009, #196695, #146152, #195700, #180533, #86492, #178518, #132997, #69323, #85483, #165350, #148177, #9670, #147172, #88485, #119833, #181518, #161336, #8661, #29804, #62106, #139938, #120804, #93438, #1428, #121798, #43984, #197671, #184479, #91440, #186484, #45958, #167334, #183491, #136000, #432, #153128, #108618, #182504, #59136, #166349, #105645, #138953, #75304, #106634, #104664, #123769, #185469, #169291, #78266, #74334, #61116, #63107, #28830, #168307, #13637, #14631, #46959, #90471, #199650, #155125, #27847, #170296, #152154, #137968, #31789, #89488, #44975, #76290, #151178, #136975, #198664, #60130, #30797, #122790, #107613, #92446, #154134, #15626, #77283, #16618, #124785, #12666, #38511, #86004, #171296, #68837, #130496, #188455, #141928, #158103, #32782, #125777, #131507, #49936, #157114, #17613, #96417, #23343, #145672, #147693, #54667, #173285, #8164, #9180, #64111, #39498, #70846, #65095, #187479, #140943, #192192, #34759, #132515, #53673, #110599, #126753, #79272, #146669, #22342, #116341, #48946, #2431, #109612, #172281, #84988, #18611, #111601, #47960, #69840, #193194, #115351, #24353, #33770, #7154, #94434, #95430, #83993, #80258, #177041, #100167, #156115, #3419, #178030, #161849, #101158, #162846, #59643, #105167, #182018, #72858, #43501, #26357, #12188, #121317, #11183, #119353, #104175, #167831, #196215, #102178, #14137, #163866, #57685, #25365, #13168, #87006, #148693, #10181, #27353, #166853, #74831, #28355, #136493, #183009, #88999, #150690, #90960, #44493, #106149, #134528, #149685, #195202, #73853, #164861, #87997, #181037, #58657, #71841, #135523, #197194, #133510, #42511, #103181, #165857, #120323, #55669, #89993, #29332, #117343, #151675, #198173, #152647, #75804, #194204, #179039, #56682, #40507, #118356, #180049, #41518, #77790, #78781, #124292, #156636, #48469, #154640, #63627, #18132, #30307, #171804, #79786, #169809, #153643, #107133, #47472, #16135, #2943, #109129, #76800, #31301, #168803, #140458, #139459, #110126, #91950, #15138, #199162, #138471, #1948, #123290, #92954, #137482, #186999, #125303, #155633, #141458, #200152, #170807, #60629, #61622, #939, #46466, #185989, #62614, #183993, #32300, #33292, #122303, #184982, #17129, #45477, #108126, #93955, #94952, #105805, #150342, #136153, #45137, #135175, #43148, #28004, #91604, #119983, #26004, #138131, #87646 ),
 ( #197828, #106794, #74487, #168468, #29966, #181669, #76454, #90628, #11838, #59294, #166506, #120963, #102825, #72496, #10826, #153293, #182662, #167492, #149332, #44146, #104817, #89644, #164511, #151332, #121960, #134170, #195858, #179690, #57330, #152310, #88646, #12821, #199812, #137135, #13796, #28988, #14794, #119006, #75461, #118001, #180689, #198822, #27001, #60287, #196849, #41162, #73503, #183653, #42165, #103825, #165505, #58315, #172447, #49108, #140103, #110766, #93604, #79435, #188622, #78428, #186646, #171457, #34920, #63269, #169458, #81395, #30959, #124950, #92606, #80420, #154296, #15786, #77446, #94600, #33935, #142093, #95593, #3578, #50103, #156279, #17780, #158265, #111763, #173452, #1594, #16779, #62264, #141106, #31949, #157277, #139117, #2594, #96576, #184638, #18773, #593, #64273, #126916, #143081, #48117, #32945, #107772, #123932, #155289, #109774, #125940, #185630, #187638, #65256, #47122, #19754, #170458, #61280, #122950, #46119, #108780, #173039, #49684, #93188, #111349, #126514, #157865, #2181, #155862, #127506, #78018, #140690, #47708, #96175, #184, #46705, #77031, #3179, #80019, #15375, #141688, #94183, #138703, #61852, #123521, #31535, #109358, #34517, #188212, #108368, #139687, #185214, #170045, #64852, #142678, #79015, #1173, #171040, #189210, #19355, #81004, #172034, #4157, #154873, #63861, #65836, #16370, #32531, #62848, #17360, #186228, #169035, #124532, #107362, #30541, #125532, #187229, #92193, #18366, #95184, #48700, #156870, #110352, #33522, #153877, #67834, #176029, #160849, #24349, #52664, #158839, #70843, #20327, #114326, #81976, #69836, #143670, #5151, #66833, #83989, #100163, #131503, #161845, #193190, #39494, #145668, #7149, #147689, #101154, #162841, #191188, #6154, #51667, #68833, #21335, #146665, #128497, #130492, #86000, #174035, #8160, #190192, #192188, #116337, #132511, #129490, #22338, #97156, #113331, #82993, #144669, #115347, #175024, #53669, #177037, #36487, #37497, #159842, #99159, #38507, #112345, #23339, #84983, #54663, #178026, #9176, #50688, #35506, #98143, #117339, #71836, #74828, #196209, #103176, #163861, #42507, #166849, #88995, #29327, #198169, #119349, #151670, #90956, #10176, #183005, #152643, #11178, #133505, #87001, #73848, #181033, #75800, #135519, #56677, #72853, #25360, #89989, #104171, #59639, #195197, #148688, #55665, #118350, #28351, #180044, #197190, #121313, #105163, #182014, #134523, #43497, #26352, #12184, #44489, #57681, #165853, #27349, #167827, #150686, #102173, #14133, #41513, #58654, #164856, #13164, #87992, #149680, #120320, #136489, #106145, #194200, #179035, #40501, #126282, #32296, #93952, #34281, #187979, #49448, #77786, #92950, #138467, #170804, #108122, #33289, #168799, #155630, #111111, #60625, #94949, #30303, #17126, #2940, #19116, #16131, #47469, #183989, #153639, #169805, #31298, #1944, #91946, #78778, #140454, #76796, #139455, #46462, #936, #63624, #199158, #154636, #125300, #156633, #171801, #186996, #62610, #124289, #109126, #122299, #15134, #18128, #185986, #48466, #107128, #110123, #79783, #141455, #172800, #64620, #95940, #157626, #137478, #200148, #45474, #61618, #123286, #184977, #173801, #160603, #5912, #162594, #22093, #143424, #97901, #112110, #176788, #67589, #84739, #96922, #35267, #142444, #158604, #115096, #51430, #82746, #80766, #99915, #38261, #145422, #54426, #50451, #37253, #116096, #20094, #144426, #189956, #190943, #159592, #3922, #174782, #161600, #177784, #98910, #65602, #68583, #6904, #83743, #23094, #146417, #130239, #127262, #7908, #69592, #66594, #131259, #192947, #39254, #175779, #129247, #100910, #113090, #114078, #21089, #188975, #81738, #4911, #128258, #36248, #53419, #52420, #191935, #10927, #132264, #55418, #193955, #148436, #26103, #166605, #104918, #25109, #56423, #117089, #101926, #181769, #59393, #195961, #197925, #103925, #134274, #163608, #102924, #42265 ),
 ( #40252, #105902, #24099, #135274, #87746, #9931, #179793, #118103, #58414, #44245, #180788, #149431, #72600, #8928, #150443, #41262, #178784, #28105, #57434, #86753, #11939, #71590, #70596, #133256, #85753, #73602, #12917, #165605, #147440, #194947, #119107, #164609, #43250, #120081, #27104, #196946, #88750, #89744, #151430, #74581, #136249, #121067, #182761, #126045, #140207, #199916, #47225, #15891, #124037, #152405, #122060, #60388, #2700, #185736, #16882, #75559, #32053, #92708, #154396, #13892, #109875, #125054, #29083, #168565, #183752, #31060, #91704, #123051, #61380, #1701, #187741, #108884, #77549, #139221, #137235, #93710, #184737, #45238, #171559, #169563, #106892, #155392, #198919, #30063, #153398, #49212, #78533, #156381, #170563, #167588, #14896, #696, #76557, #186751, #63377, #62368, #48221, #138233, #33049, #94704, #17886, #79540, #141210, #64377, #90722, #46222, #107875, #190708, #159350, #67348, #95698, #65360, #3682, #146180, #129008, #160364, #18879, #175535, #36012, #97661, #157386, #53178, #68344, #172555, #111867, #127021, #52181, #110870, #98670, #37009, #113839, #191695, #176548, #21854, #34041, #38024, #114854, #96681, #99680, #129995, #161364, #5672, #20846, #131017, #81498, #144186, #51193, #22855, #188728, #50213, #80525, #6666, #83505, #142199, #145182, #82504, #173557, #35026, #158369, #19858, #112854, #84502, #7665, #143185, #4665, #66357, #128018, #69349, #192707, #189720, #174545, #136751, #167109, #134793, #135782, #75084, #13420, #183271, #60895, #168089, #169068, #41779, #43762, #165124, #198435, #153911, #115863, #121576, #105426, #73124, #138735, #54190, #29586, #180311, #76069, #91217, #44751, #30574, #26616, #59908, #92225, #196474, #58919, #166123, #28610, #197453, #103445, #150956, #137745, #15406, #149946, #106407, #122571, #152908, #14405, #120587, #199429, #89264, #184261, #45743, #74112, #182281, #90248, #77063, #151931, #88259, #11452, #57945, #107395, #119616, #181299, #42777, #104439, #27625, #12450, #49718, #81034, #111383, #142710, #189242, #95217, #156903, #97186, #50720, #112378, #140724, #155896, #1207, #33555, #171073, #96207, #31569, #18399, #174070, #123554, #157896, #93220, #80050, #65868, #82009, #79050, #110386, #46740, #16404, #32563, #94217, #64883, #154905, #141719, #3209, #139719, #2214, #109393, #63895, #126544, #61884, #17394, #188243, #19385, #34548, #173071, #125566, #187263, #172068, #185249, #78050, #4189, #48732, #127540, #170078, #35539, #158872, #20361, #215, #108401, #62884, #124565, #186262, #47740, #132545, #40539, #160883, #83027, #36521, #23375, #68869, #25395, #85020, #6187, #22374, #175057, #39529, #130528, #147724, #159878, #98176, #5185, #21369, #178061, #114360, #145703, #161881, #143703, #131542, #69873, #100199, #24386, #9211, #8198, #66866, #70878, #86037, #129522, #194234, #162878, #55700, #38543, #192225, #163899, #176065, #177072, #84025, #117373, #144701, #67867, #113365, #101189, #116373, #51702, #179070, #53707, #191222, #52696, #37532, #99195, #7185, #102210, #128529, #115384, #146701, #193226, #54700, #190223, #122333, #58685, #60660, #166882, #197223, #164892, #165885, #105195, #43530, #13197, #90990, #198203, #199193, #71870, #73881, #195230, #28383, #184025, #148722, #151704, #135551, #103210, #168833, #87037, #59673, #150719, #11212, #42541, #181066, #121345, #107162, #90021, #12218, #120352, #133538, #74860, #104204, #41547, #29360, #89028, #26386, #136522, #118384, #56711, #88025, #10210, #183038, #75834, #44521, #180078, #149713, #182047, #72887, #106177, #167860, #152677, #14166, #134556, #137512, #45507, #196244, #57713, #119383, #27382, #189007, #2972, #62647, #110155, #78813, #187030, #15170, #185012, #123319, #65634, #48501, #79818, #138500, #94982, #155664, #17160, #76829, #172834, #188011, #91979, #31334, #46497, #34313, #111144, #92985, #124324, #200182, #108158, #49481, #127294 ),
 ( #140492, #61651, #171833, #50482, #153673, #156667, #1980, #169840, #112142, #30338, #141489, #93984, #154670, #186022, #47504, #64652, #16166, #33321, #63660, #125333, #77820, #18162, #109160, #139489, #95976, #32331, #971, #126314, #170839, #157660, #19149, #80799, #142477, #3955, #191967, #55453, #189988, #145455, #128290, #192981, #69626, #83775, #23127, #66626, #53453, #100945, #130272, #162629, #24136, #175813, #132299, #146450, #5944, #115129, #22125, #176821, #158635, #51462, #113124, #8964, #38293, #84772, #81770, #99947, #98943, #160634, #20126, #116129, #131292, #35299, #174814, #36279, #161633, #173834, #7943, #54459, #177818, #39288, #4942, #144459, #85788, #147474, #70633, #193991, #114110, #67620, #6937, #96955, #97934, #143457, #37286, #82778, #159627, #68616, #21122, #129281, #190976, #52453, #42299, #74618, #152441, #133291, #105938, #13927, #134309, #56459, #151465, #137273, #73636, #103960, #180820, #101962, #43283, #195995, #71625, #59430, #119140, #194981, #104952, #148473, #163643, #118138, #198955, #166638, #167623, #135307, #117124, #179827, #88783, #41297, #136284, #12953, #27136, #28140, #9965, #196979, #44280, #58446, #29119, #90758, #165638, #75594, #89780, #149465, #120114, #150476, #181805, #25145, #102958, #164642, #178818, #197960, #121103, #86787, #182797, #11971, #40288, #26138, #87780, #10960, #72634, #57468, #76592, #78570, #60422, #48257, #186787, #154432, #109911, #63414, #126079, #122095, #187775, #2733, #46258, #64410, #79575, #110903, #155427, #108919, #80558, #31096, #93746, #732, #49245, #153434, #199951, #30099, #156419, #33083, #168599, #94739, #47262, #91739, #14932, #138268, #184772, #62404, #172589, #141244, #61415, #92744, #123086, #107913, #17920, #95733, #32089, #34075, #140244, #170599, #169598, #139256, #1736, #16917, #171595, #157419, #18913, #142233, #45272, #125089, #15926, #183786, #106926, #77584, #124074, #185775, #19892, #85546, #3718, #114889, #67384, #128054, #159388, #97697, #7700, #22889, #54224, #98706, #52216, #23893, #174583, #37047, #144223, #192742, #96715, #143220, #173591, #99713, #176583, #111903, #38057, #190742, #35060, #158403, #81533, #189756, #5707, #146212, #84535, #4702, #36048, #66392, #51228, #161397, #39052, #175570, #177585, #83539, #113873, #112889, #82541, #21889, #160400, #130030, #69383, #131052, #115895, #188763, #145218, #20883, #6700, #100710, #65395, #68378, #191729, #129041, #127056, #50247, #162390, #53211, #71393, #102725, #41062, #181573, #167392, #103729, #72393, #10729, #132061, #73405, #164414, #101718, #89546, #149238, #163408, #135076, #178579, #193750, #24904, #28888, #196752, #136052, #165409, #147232, #86551, #118907, #148235, #166408, #43051, #57233, #58219, #40044, #26902, #74387, #88545, #197727, #59193, #134069, #105705, #119888, #179590, #150243, #195759, #11738, #55218, #9729, #133057, #182562, #104717, #27903, #116887, #151232, #180591, #42065, #194747, #12721, #120862, #8724, #56219, #117901, #44045, #70393, #25906, #87551, #184537, #78325, #93500, #156174, #90528, #17673, #32842, #76352, #171354, #91500, #122849, #198721, #168367, #48017, #125835, #62165, #64170, #170356, #492, #29863, #169350, #108678, #47019, #16676, #94492, #1487, #2489, #75361, #77346, #60188, #31848, #187538, #152210, #155186, #139012, #106694, #172339, #13694, #63165, #154195, #14690, #46017, #107673, #124844, #110659, #139998, #15685, #123829, #137031, #186544, #30859, #45036, #79331, #92506, #153187, #109673, #121858, #183550, #138029, #199712, #141001, #49004, #61177, #185527, #49994, #5461, #188517, #52961, #129786, #143980, #83297, #126810, #51973, #161149, #190500, #22646, #84293, #35807, #192496, #6454, #66144, #113632, #82289, #175327, #18668, #111659, #173346, #69138, #36794, #144973, #141987, #98459, #159139, #20636, #80314, #176336, #191483, #95488, #34817, #96472, #160153, #33828, #21644 ) ),
 .UNSPECIFIED., .T., .F., .F. ) 
 B_SPLINE_SURFACE_WITH_KNOTS ( ( 4, 3, 4 ),
 ( 3, 2, 2, 2, 2, 2, 2, 2, 2, 2, 2, 2, 2, 2, 2, 2, 2, 2, 2, 2, 2, 2, 2, 2, 2, 2, 2, 2, 2, 2, 2, 2, 2, 2, 2, 2, 2, 2, 2, 2, 2, 2, 2, 2, 2, 2, 2, 2, 2, 2, 2, 2, 2, 2, 2, 2, 2, 2, 2, 2, 2, 2, 2, 2, 2, 2, 2, 2, 2, 2, 2, 2, 2, 2, 2, 2, 2, 2, 2, 2, 2, 2, 2, 2, 2, 2, 2, 2, 2, 2, 2, 2, 2, 2, 2, 2, 2, 2, 2, 2, 2, 2, 2, 2, 2, 2, 2, 2, 2, 2, 2, 2, 2, 2, 2, 2, 2, 2, 2, 2, 2, 2, 2, 2, 2, 2, 2, 2, 2, 2, 2, 2, 2, 2, 2, 2, 2, 2, 2, 2, 2, 2, 2, 2, 2, 2, 2, 2, 2, 2, 2, 2, 2, 2, 2, 2, 2, 2, 2, 2, 2, 2, 2, 2, 2, 2, 2, 2, 2, 2, 2, 2, 2, 2, 2, 2, 2, 2, 2, 2, 2, 2, 2, 2, 2, 2, 2, 2, 2, 2, 2, 2, 2, 2, 2, 2, 2, 2, 2, 2, 2, 2, 2, 2, 2, 2, 2, 2, 2, 2, 2, 2, 2, 2, 2, 2, 2, 2, 2, 2, 2, 2, 2, 2, 2, 2, 2, 2, 3 ),
 ( 0.000000000000000000, 0.5000000000000000000, 1.000000000000000000 ),
 ( 0.000000000000000000, 0.004385964912280701511, 0.008771929824561403022, 0.01315789473684210453, 0.01754385964912280604, 0.02192982456140350755, 0.02631578947368420907, 0.03070175438596491058, 0.03508771929824561209, 0.03947368421052631360, 0.04385964912280701511, 0.04824561403508771662, 0.05263157894736841813, 0.05701754385964911964, 0.06140350877192982115, 0.06578947368421052266, 0.07017543859649122417, 0.07456140350877192569, 0.07894736842105262720, 0.08333333333333332871, 0.08771929824561403022, 0.09210526315789473173, 0.09649122807017543324, 0.1008771929824561348, 0.1052631578947368363, 0.1096491228070175378, 0.1140350877192982393, 0.1184210526315789408, 0.1228070175438596423, 0.1271929824561403577, 0.1315789473684210453, 0.1359649122807017607, 0.1403508771929824483, 0.1447368421052631637, 0.1491228070175438514, 0.1535087719298245668, 0.1578947368421052544, 0.1622807017543859698, 0.1666666666666666574, 0.1710526315789473728, 0.1754385964912280604, 0.1798245614035087758, 0.1842105263157894635, 0.1885964912280701788, 0.1929824561403508665, 0.1973684210526315819, 0.2017543859649122695, 0.2061403508771929849, 0.2105263157894736725, 0.2149122807017543879, 0.2192982456140350755, 0.2236842105263157909, 0.2280701754385964786, 0.2324561403508771940, 0.2368421052631578816, 0.2412280701754385970, 0.2456140350877192846, 0.2500000000000000000, 0.2543859649122807154, 0.2587719298245614308, 0.2631578947368420907, 0.2675438596491228060, 0.2719298245614035214, 0.2763157894736842368, 0.2807017543859648967, 0.2850877192982456121, 0.2894736842105263275, 0.2938596491228070429, 0.2982456140350877027, 0.3026315789473684181, 0.3070175438596491335, 0.3114035087719298489, 0.3157894736842105088, 0.3201754385964912242, 0.3245614035087719396, 0.3289473684210526550, 0.3333333333333333148, 0.3377192982456140302, 0.3421052631578947456, 0.3464912280701754610, 0.3508771929824561209, 0.3552631578947368363, 0.3596491228070175517, 0.3640350877192982670, 0.3684210526315789269, 0.3728070175438596423, 0.3771929824561403577, 0.3815789473684210731, 0.3859649122807017330, 0.3903508771929824483, 0.3947368421052631637, 0.3991228070175438791, 0.4035087719298245390, 0.4078947368421052544, 0.4122807017543859698, 0.4166666666666666852, 0.4210526315789473450, 0.4254385964912280604, 0.4298245614035087758, 0.4342105263157894912, 0.4385964912280701511, 0.4429824561403508665, 0.4473684210526315819, 0.4517543859649122973, 0.4561403508771929571, 0.4605263157894736725, 0.4649122807017543879, 0.4692982456140351033, 0.4736842105263157632, 0.4780701754385964786, 0.4824561403508771940, 0.4868421052631579093, 0.4912280701754385692, 0.4956140350877192846, 0.5000000000000000000, 0.5043859649122807154, 0.5087719298245614308, 0.5131578947368421462, 0.5175438596491228616, 0.5219298245614034659, 0.5263157894736841813, 0.5307017543859648967, 0.5350877192982456121, 0.5394736842105263275, 0.5438596491228070429, 0.5482456140350877583, 0.5526315789473684736, 0.5570175438596490780, 0.5614035087719297934, 0.5657894736842105088, 0.5701754385964912242, 0.5745614035087719396, 0.5789473684210526550, 0.5833333333333333703, 0.5877192982456140857, 0.5921052631578946901, 0.5964912280701754055, 0.6008771929824561209, 0.6052631578947368363, 0.6096491228070175517, 0.6140350877192982670, 0.6184210526315789824, 0.6228070175438596978, 0.6271929824561403022, 0.6315789473684210176, 0.6359649122807017330, 0.6403508771929824483, 0.6447368421052631637, 0.6491228070175438791, 0.6535087719298245945, 0.6578947368421053099, 0.6622807017543859143, 0.6666666666666666297, 0.6710526315789473450, 0.6754385964912280604, 0.6798245614035087758, 0.6842105263157894912, 0.6885964912280702066, 0.6929824561403509220, 0.6973684210526315264, 0.7017543859649122417, 0.7061403508771929571, 0.7105263157894736725, 0.7149122807017543879, 0.7192982456140351033, 0.7236842105263158187, 0.7280701754385965341, 0.7324561403508771384, 0.7368421052631578538, 0.7412280701754385692, 0.7456140350877192846, 0.7500000000000000000, 0.7543859649122807154, 0.7587719298245614308, 0.7631578947368421462, 0.7675438596491228616, 0.7719298245614034659, 0.7763157894736841813, 0.7807017543859648967, 0.7850877192982456121, 0.7894736842105263275, 0.7938596491228070429, 0.7982456140350877583, 0.8026315789473684736, 0.8070175438596490780, 0.8114035087719297934, 0.8157894736842105088, 0.8201754385964912242, 0.8245614035087719396, 0.8289473684210526550, 0.8333333333333333703, 0.8377192982456140857, 0.8421052631578946901, 0.8464912280701754055, 0.8508771929824561209, 0.8552631578947368363, 0.8596491228070175517, 0.8640350877192982670, 0.8684210526315789824, 0.8728070175438596978, 0.8771929824561403022, 0.8815789473684210176, 0.8859649122807017330, 0.8903508771929824483, 0.8947368421052631637, 0.8991228070175438791, 0.9035087719298245945, 0.9078947368421053099, 0.9122807017543859143, 0.9166666666666666297, 0.9210526315789473450, 0.9254385964912280604, 0.9298245614035087758, 0.9342105263157894912, 0.9385964912280702066, 0.9429824561403509220, 0.9473684210526315264, 0.9517543859649122417, 0.9561403508771929571, 0.9605263157894736725, 0.9649122807017543879, 0.9692982456140351033, 0.9736842105263158187, 0.9780701754385965341, 0.9824561403508771384, 0.9868421052631578538, 0.9912280701754385692, 0.9956140350877192846, 1.000000000000000000 ),
 .UNSPECIFIED. ) 
 GEOMETRIC_REPRESENTATION_ITEM ( )  RATIONAL_B_SPLINE_SURFACE ( (
 ( 1.000000000000000000, 0.9659258262890683122, 1.000000000000000000, 0.9659258262890683122, 1.000000000000000000, 0.9659258262890683122, 1.000000000000000000, 0.9659258262890683122, 1.000000000000000000, 0.9659258262890683122, 1.000000000000000000, 0.9659258262890683122, 1.000000000000000000, 0.9659258262890683122, 1.000000000000000000, 0.9659258262890683122, 1.000000000000000000, 0.9659258262890683122, 1.000000000000000000, 0.9659258262890683122, 1.000000000000000000, 0.9659258262890683122, 1.000000000000000000, 0.9659258262890683122, 1.000000000000000000, 0.9659258262890683122, 1.000000000000000000, 0.9659258262890683122, 1.000000000000000000, 0.9659258262890683122, 1.000000000000000000, 0.9659258262890683122, 1.000000000000000000, 0.9659258262890683122, 1.000000000000000000, 0.9659258262890683122, 1.000000000000000000, 0.9659258262890683122, 1.000000000000000000, 0.9659258262890683122, 1.000000000000000000, 0.9659258262890683122, 1.000000000000000000, 0.9659258262890683122, 1.000000000000000000, 0.9659258262890683122, 1.000000000000000000, 0.9659258262890683122, 1.000000000000000000, 0.9659258262890683122, 1.000000000000000000, 0.9659258262890683122, 1.000000000000000000, 0.9659258262890683122, 1.000000000000000000, 0.9659258262890683122, 1.000000000000000000, 0.9659258262890683122, 1.000000000000000000, 0.9659258262890683122, 1.000000000000000000, 0.9659258262890683122, 1.000000000000000000, 0.9659258262890683122, 1.000000000000000000, 0.9659258262890683122, 1.000000000000000000, 0.9659258262890683122, 1.000000000000000000, 0.9659258262890683122, 1.000000000000000000, 0.9659258262890683122, 1.000000000000000000, 0.9659258262890683122, 1.000000000000000000, 0.9659258262890683122, 1.000000000000000000, 0.9659258262890683122, 1.000000000000000000, 0.9659258262890683122, 1.000000000000000000, 0.9659258262890683122, 1.000000000000000000, 0.9659258262890683122, 1.000000000000000000, 0.9659258262890683122, 1.000000000000000000, 0.9659258262890683122, 1.000000000000000000, 0.9659258262890683122, 1.000000000000000000, 0.9659258262890683122, 1.000000000000000000, 0.9659258262890683122, 1.000000000000000000, 0.9659258262890683122, 1.000000000000000000, 0.9659258262890683122, 1.000000000000000000, 0.9659258262890683122, 1.000000000000000000, 0.9659258262890683122, 1.000000000000000000, 0.9659258262890683122, 1.000000000000000000, 0.9659258262890683122, 1.000000000000000000, 0.9659258262890683122, 1.000000000000000000, 0.9659258262890683122, 1.000000000000000000, 0.9659258262890683122, 1.000000000000000000, 0.9659258262890683122, 1.000000000000000000, 0.9659258262890683122, 1.000000000000000000, 0.9659258262890683122, 1.000000000000000000, 0.9659258262890683122, 1.000000000000000000, 0.9659258262890683122, 1.000000000000000000, 0.9659258262890683122, 1.000000000000000000, 0.9659258262890683122, 1.000000000000000000, 0.9659258262890683122, 1.000000000000000000, 0.9659258262890683122, 1.000000000000000000, 0.9659258262890683122, 1.000000000000000000, 0.9659258262890683122, 1.000000000000000000, 0.9659258262890683122, 1.000000000000000000, 0.9659258262890683122, 1.000000000000000000, 0.9659258262890683122, 1.000000000000000000, 0.9659258262890683122, 1.000000000000000000, 0.9659258262890683122, 1.000000000000000000, 0.9659258262890683122, 1.000000000000000000, 0.9659258262890683122, 1.000000000000000000, 0.9659258262890683122, 1.000000000000000000, 0.9659258262890683122, 1.000000000000000000, 0.9659258262890683122, 1.000000000000000000, 0.9659258262890683122, 1.000000000000000000, 0.9659258262890683122, 1.000000000000000000, 0.9659258262890683122, 1.000000000000000000, 0.9659258262890683122, 1.000000000000000000, 0.9659258262890683122, 1.000000000000000000, 0.9659258262890683122, 1.000000000000000000, 0.9659258262890683122, 1.000000000000000000, 0.9659258262890683122, 1.000000000000000000, 0.9659258262890683122, 1.000000000000000000, 0.9659258262890683122, 1.000000000000000000, 0.9659258262890683122, 1.000000000000000000, 0.9659258262890683122, 1.000000000000000000, 0.9659258262890683122, 1.000000000000000000, 0.9659258262890683122, 1.000000000000000000, 0.9659258262890683122, 1.000000000000000000, 0.9659258262890683122, 1.000000000000000000, 0.9659258262890683122, 1.000000000000000000, 0.9659258262890683122, 1.000000000000000000, 0.9659258262890683122, 1.000000000000000000, 0.9659258262890683122, 1.000000000000000000, 0.9659258262890683122, 1.000000000000000000, 0.9659258262890683122, 1.000000000000000000, 0.9659258262890683122, 1.000000000000000000, 0.9659258262890683122, 1.000000000000000000, 0.9659258262890683122, 1.000000000000000000, 0.9659258262890683122, 1.000000000000000000, 0.9659258262890683122, 1.000000000000000000, 0.9659258262890683122, 1.000000000000000000, 0.9659258262890683122, 1.000000000000000000, 0.9659258262890683122, 1.000000000000000000, 0.9659258262890683122, 1.000000000000000000, 0.9659258262890683122, 1.000000000000000000, 0.9659258262890683122, 1.000000000000000000, 0.9659258262890683122, 1.000000000000000000, 0.9659258262890683122, 1.000000000000000000, 0.9659258262890683122, 1.000000000000000000, 0.9659258262890683122, 1.000000000000000000, 0.9659258262890683122, 1.000000000000000000, 0.9659258262890683122, 1.000000000000000000, 0.9659258262890683122, 1.000000000000000000, 0.9659258262890683122, 1.000000000000000000, 0.9659258262890683122, 1.000000000000000000, 0.9659258262890683122, 1.000000000000000000, 0.9659258262890683122, 1.000000000000000000, 0.9659258262890683122, 1.000000000000000000, 0.9659258262890683122, 1.000000000000000000, 0.9659258262890683122, 1.000000000000000000, 0.9659258262890683122, 1.000000000000000000, 0.9659258262890683122, 1.000000000000000000, 0.9659258262890683122, 1.000000000000000000, 0.9659258262890683122, 1.000000000000000000, 0.9659258262890683122, 1.000000000000000000, 0.9659258262890683122, 1.000000000000000000, 0.9659258262890683122, 1.000000000000000000, 0.9659258262890683122, 1.000000000000000000, 0.9659258262890683122, 1.000000000000000000, 0.9659258262890683122, 1.000000000000000000, 0.9659258262890683122, 1.000000000000000000, 0.9659258262890683122, 1.000000000000000000, 0.9659258262890683122, 1.000000000000000000, 0.9659258262890683122, 1.000000000000000000, 0.9659258262890683122, 1.000000000000000000, 0.9659258262890683122, 1.000000000000000000, 0.9659258262890683122, 1.000000000000000000, 0.9659258262890683122, 1.000000000000000000, 0.9659258262890683122, 1.000000000000000000, 0.9659258262890683122, 1.000000000000000000, 0.9659258262890683122, 1.000000000000000000, 0.9659258262890683122, 1.000000000000000000, 0.9659258262890683122, 1.000000000000000000, 0.9659258262890683122, 1.000000000000000000, 0.9659258262890683122, 1.000000000000000000, 0.9659258262890683122, 1.000000000000000000, 0.9659258262890683122, 1.000000000000000000, 0.9659258262890683122, 1.000000000000000000, 0.9659258262890683122, 1.000000000000000000, 0.9659258262890683122, 1.000000000000000000, 0.9659258262890683122, 1.000000000000000000, 0.9659258262890683122, 1.000000000000000000, 0.9659258262890683122, 1.000000000000000000, 0.9659258262890683122, 1.000000000000000000, 0.9659258262890683122, 1.000000000000000000, 0.9659258262890683122, 1.000000000000000000, 0.9659258262890683122, 1.000000000000000000, 0.9659258262890683122, 1.000000000000000000, 0.9659258262890683122, 1.000000000000000000, 0.9659258262890683122, 1.000000000000000000, 0.9659258262890683122, 1.000000000000000000, 0.9659258262890683122, 1.000000000000000000, 0.9659258262890683122, 1.000000000000000000, 0.9659258262890683122, 1.000000000000000000, 0.9659258262890683122, 1.000000000000000000, 0.9659258262890683122, 1.000000000000000000, 0.9659258262890683122, 1.000000000000000000, 0.9659258262890683122, 1.000000000000000000, 0.9659258262890683122, 1.000000000000000000, 0.9659258262890683122, 1.000000000000000000, 0.9659258262890683122, 1.000000000000000000, 0.9659258262890683122, 1.000000000000000000, 0.9659258262890683122, 1.000000000000000000, 0.9659258262890683122, 1.000000000000000000, 0.9659258262890683122, 1.000000000000000000, 0.9659258262890683122, 1.000000000000000000, 0.9659258262890683122, 1.000000000000000000, 0.9659258262890683122, 1.000000000000000000, 0.9659258262890683122, 1.000000000000000000, 0.9659258262890683122, 1.000000000000000000, 0.9659258262890683122, 1.000000000000000000, 0.9659258262890683122, 1.000000000000000000, 0.9659258262890683122, 1.000000000000000000, 0.9659258262890683122, 1.000000000000000000, 0.9659258262890683122, 1.000000000000000000, 0.9659258262890683122, 1.000000000000000000, 0.9659258262890683122, 1.000000000000000000, 0.9659258262890683122, 1.000000000000000000, 0.9659258262890683122, 1.000000000000000000, 0.9659258262890683122, 1.000000000000000000, 0.9659258262890683122, 1.000000000000000000, 0.9659258262890683122, 1.000000000000000000, 0.9659258262890683122, 1.000000000000000000, 0.9659258262890683122, 1.000000000000000000, 0.9659258262890683122, 1.000000000000000000, 0.9659258262890683122, 1.000000000000000000, 0.9659258262890683122, 1.000000000000000000, 0.9659258262890683122, 1.000000000000000000, 0.9659258262890683122, 1.000000000000000000, 0.9659258262890683122, 1.000000000000000000, 0.9659258262890683122, 1.000000000000000000, 0.9659258262890683122, 1.000000000000000000, 0.9659258262890683122, 1.000000000000000000, 0.9659258262890683122, 1.000000000000000000, 0.9659258262890683122, 1.000000000000000000, 0.9659258262890683122, 1.000000000000000000, 0.9659258262890683122, 1.000000000000000000, 0.9659258262890683122, 1.000000000000000000, 0.9659258262890683122, 1.000000000000000000, 0.9659258262890683122, 1.000000000000000000, 0.9659258262890683122, 1.000000000000000000, 0.9659258262890683122, 1.000000000000000000, 0.9659258262890683122, 1.000000000000000000, 0.9659258262890683122, 1.000000000000000000, 0.9659258262890683122, 1.000000000000000000, 0.9659258262890683122, 1.000000000000000000, 0.9659258262890683122, 1.000000000000000000, 0.9659258262890683122, 1.000000000000000000, 0.9659258262890683122, 1.000000000000000000, 0.9659258262890683122, 1.000000000000000000, 0.9659258262890683122, 1.000000000000000000, 0.9659258262890683122, 1.000000000000000000, 0.9659258262890683122, 1.000000000000000000, 0.9659258262890683122, 1.000000000000000000),
 ( 0.3333333333333333703, 0.3219752754296894559, 0.3333333333333333703, 0.3219752754296894559, 0.3333333333333333703, 0.3219752754296894559, 0.3333333333333333703, 0.3219752754296894559, 0.3333333333333333703, 0.3219752754296894559, 0.3333333333333333703, 0.3219752754296894559, 0.3333333333333333703, 0.3219752754296894559, 0.3333333333333333703, 0.3219752754296894559, 0.3333333333333333703, 0.3219752754296894559, 0.3333333333333333703, 0.3219752754296894559, 0.3333333333333333703, 0.3219752754296894559, 0.3333333333333333703, 0.3219752754296894559, 0.3333333333333333703, 0.3219752754296894559, 0.3333333333333333703, 0.3219752754296894559, 0.3333333333333333703, 0.3219752754296894559, 0.3333333333333333703, 0.3219752754296894559, 0.3333333333333333703, 0.3219752754296894559, 0.3333333333333333703, 0.3219752754296894559, 0.3333333333333333703, 0.3219752754296894559, 0.3333333333333333703, 0.3219752754296894559, 0.3333333333333333703, 0.3219752754296894559, 0.3333333333333333703, 0.3219752754296894559, 0.3333333333333333703, 0.3219752754296894559, 0.3333333333333333703, 0.3219752754296894559, 0.3333333333333333703, 0.3219752754296894559, 0.3333333333333333703, 0.3219752754296894559, 0.3333333333333333703, 0.3219752754296894559, 0.3333333333333333703, 0.3219752754296894559, 0.3333333333333333703, 0.3219752754296894559, 0.3333333333333333703, 0.3219752754296894559, 0.3333333333333333703, 0.3219752754296894559, 0.3333333333333333703, 0.3219752754296894559, 0.3333333333333333703, 0.3219752754296894559, 0.3333333333333333703, 0.3219752754296894559, 0.3333333333333333703, 0.3219752754296894559, 0.3333333333333333703, 0.3219752754296894559, 0.3333333333333333703, 0.3219752754296894559, 0.3333333333333333703, 0.3219752754296894559, 0.3333333333333333703, 0.3219752754296894559, 0.3333333333333333703, 0.3219752754296894559, 0.3333333333333333703, 0.3219752754296894559, 0.3333333333333333703, 0.3219752754296894559, 0.3333333333333333703, 0.3219752754296894559, 0.3333333333333333703, 0.3219752754296894559, 0.3333333333333333703, 0.3219752754296894559, 0.3333333333333333703, 0.3219752754296894559, 0.3333333333333333703, 0.3219752754296894559, 0.3333333333333333703, 0.3219752754296894559, 0.3333333333333333703, 0.3219752754296894559, 0.3333333333333333703, 0.3219752754296894559, 0.3333333333333333703, 0.3219752754296894559, 0.3333333333333333703, 0.3219752754296894559, 0.3333333333333333703, 0.3219752754296894559, 0.3333333333333333703, 0.3219752754296894559, 0.3333333333333333703, 0.3219752754296894559, 0.3333333333333333703, 0.3219752754296894559, 0.3333333333333333703, 0.3219752754296894559, 0.3333333333333333703, 0.3219752754296894559, 0.3333333333333333703, 0.3219752754296894559, 0.3333333333333333703, 0.3219752754296894559, 0.3333333333333333703, 0.3219752754296894559, 0.3333333333333333703, 0.3219752754296894559, 0.3333333333333333703, 0.3219752754296894559, 0.3333333333333333703, 0.3219752754296894559, 0.3333333333333333703, 0.3219752754296894559, 0.3333333333333333703, 0.3219752754296894559, 0.3333333333333333703, 0.3219752754296894559, 0.3333333333333333703, 0.3219752754296894559, 0.3333333333333333703, 0.3219752754296894559, 0.3333333333333333703, 0.3219752754296894559, 0.3333333333333333703, 0.3219752754296894559, 0.3333333333333333703, 0.3219752754296894559, 0.3333333333333333703, 0.3219752754296894559, 0.3333333333333333703, 0.3219752754296894559, 0.3333333333333333703, 0.3219752754296894559, 0.3333333333333333703, 0.3219752754296894559, 0.3333333333333333703, 0.3219752754296894559, 0.3333333333333333703, 0.3219752754296894559, 0.3333333333333333703, 0.3219752754296894559, 0.3333333333333333703, 0.3219752754296894559, 0.3333333333333333703, 0.3219752754296894559, 0.3333333333333333703, 0.3219752754296894559, 0.3333333333333333703, 0.3219752754296894559, 0.3333333333333333703, 0.3219752754296894559, 0.3333333333333333703, 0.3219752754296894559, 0.3333333333333333703, 0.3219752754296894559, 0.3333333333333333703, 0.3219752754296894559, 0.3333333333333333703, 0.3219752754296894559, 0.3333333333333333703, 0.3219752754296894559, 0.3333333333333333703, 0.3219752754296894559, 0.3333333333333333703, 0.3219752754296894559, 0.3333333333333333703, 0.3219752754296894559, 0.3333333333333333703, 0.3219752754296894559, 0.3333333333333333703, 0.3219752754296894559, 0.3333333333333333703, 0.3219752754296894559, 0.3333333333333333703, 0.3219752754296894559, 0.3333333333333333703, 0.3219752754296894559, 0.3333333333333333703, 0.3219752754296894559, 0.3333333333333333703, 0.3219752754296894559, 0.3333333333333333703, 0.3219752754296894559, 0.3333333333333333703, 0.3219752754296894559, 0.3333333333333333703, 0.3219752754296894559, 0.3333333333333333703, 0.3219752754296894559, 0.3333333333333333703, 0.3219752754296894559, 0.3333333333333333703, 0.3219752754296894559, 0.3333333333333333703, 0.3219752754296894559, 0.3333333333333333703, 0.3219752754296894559, 0.3333333333333333703, 0.3219752754296894559, 0.3333333333333333703, 0.3219752754296894559, 0.3333333333333333703, 0.3219752754296894559, 0.3333333333333333703, 0.3219752754296894559, 0.3333333333333333703, 0.3219752754296894559, 0.3333333333333333703, 0.3219752754296894559, 0.3333333333333333703, 0.3219752754296894559, 0.3333333333333333703, 0.3219752754296894559, 0.3333333333333333703, 0.3219752754296894559, 0.3333333333333333703, 0.3219752754296894559, 0.3333333333333333703, 0.3219752754296894559, 0.3333333333333333703, 0.3219752754296894559, 0.3333333333333333703, 0.3219752754296894559, 0.3333333333333333703, 0.3219752754296894559, 0.3333333333333333703, 0.3219752754296894559, 0.3333333333333333703, 0.3219752754296894559, 0.3333333333333333703, 0.3219752754296894559, 0.3333333333333333703, 0.3219752754296894559, 0.3333333333333333703, 0.3219752754296894559, 0.3333333333333333703, 0.3219752754296894559, 0.3333333333333333703, 0.3219752754296894559, 0.3333333333333333703, 0.3219752754296894559, 0.3333333333333333703, 0.3219752754296894559, 0.3333333333333333703, 0.3219752754296894559, 0.3333333333333333703, 0.3219752754296894559, 0.3333333333333333703, 0.3219752754296894559, 0.3333333333333333703, 0.3219752754296894559, 0.3333333333333333703, 0.3219752754296894559, 0.3333333333333333703, 0.3219752754296894559, 0.3333333333333333703, 0.3219752754296894559, 0.3333333333333333703, 0.3219752754296894559, 0.3333333333333333703, 0.3219752754296894559, 0.3333333333333333703, 0.3219752754296894559, 0.3333333333333333703, 0.3219752754296894559, 0.3333333333333333703, 0.3219752754296894559, 0.3333333333333333703, 0.3219752754296894559, 0.3333333333333333703, 0.3219752754296894559, 0.3333333333333333703, 0.3219752754296894559, 0.3333333333333333703, 0.3219752754296894559, 0.3333333333333333703, 0.3219752754296894559, 0.3333333333333333703, 0.3219752754296894559, 0.3333333333333333703, 0.3219752754296894559, 0.3333333333333333703, 0.3219752754296894559, 0.3333333333333333703, 0.3219752754296894559, 0.3333333333333333703, 0.3219752754296894559, 0.3333333333333333703, 0.3219752754296894559, 0.3333333333333333703, 0.3219752754296894559, 0.3333333333333333703, 0.3219752754296894559, 0.3333333333333333703, 0.3219752754296894559, 0.3333333333333333703, 0.3219752754296894559, 0.3333333333333333703, 0.3219752754296894559, 0.3333333333333333703, 0.3219752754296894559, 0.3333333333333333703, 0.3219752754296894559, 0.3333333333333333703, 0.3219752754296894559, 0.3333333333333333703, 0.3219752754296894559, 0.3333333333333333703, 0.3219752754296894559, 0.3333333333333333703, 0.3219752754296894559, 0.3333333333333333703, 0.3219752754296894559, 0.3333333333333333703, 0.3219752754296894559, 0.3333333333333333703, 0.3219752754296894559, 0.3333333333333333703, 0.3219752754296894559, 0.3333333333333333703, 0.3219752754296894559, 0.3333333333333333703, 0.3219752754296894559, 0.3333333333333333703, 0.3219752754296894559, 0.3333333333333333703, 0.3219752754296894559, 0.3333333333333333703, 0.3219752754296894559, 0.3333333333333333703, 0.3219752754296894559, 0.3333333333333333703, 0.3219752754296894559, 0.3333333333333333703, 0.3219752754296894559, 0.3333333333333333703, 0.3219752754296894559, 0.3333333333333333703, 0.3219752754296894559, 0.3333333333333333703, 0.3219752754296894559, 0.3333333333333333703, 0.3219752754296894559, 0.3333333333333333703, 0.3219752754296894559, 0.3333333333333333703, 0.3219752754296894559, 0.3333333333333333703, 0.3219752754296894559, 0.3333333333333333703, 0.3219752754296894559, 0.3333333333333333703, 0.3219752754296894559, 0.3333333333333333703, 0.3219752754296894559, 0.3333333333333333703, 0.3219752754296894559, 0.3333333333333333703, 0.3219752754296894559, 0.3333333333333333703, 0.3219752754296894559, 0.3333333333333333703, 0.3219752754296894559, 0.3333333333333333703, 0.3219752754296894559, 0.3333333333333333703, 0.3219752754296894559, 0.3333333333333333703, 0.3219752754296894559, 0.3333333333333333703, 0.3219752754296894559, 0.3333333333333333703, 0.3219752754296894559, 0.3333333333333333703, 0.3219752754296894559, 0.3333333333333333703, 0.3219752754296894559, 0.3333333333333333703, 0.3219752754296894559, 0.3333333333333333703, 0.3219752754296894559, 0.3333333333333333703, 0.3219752754296894559, 0.3333333333333333703, 0.3219752754296894559, 0.3333333333333333703, 0.3219752754296894559, 0.3333333333333333703, 0.3219752754296894559, 0.3333333333333333703, 0.3219752754296894559, 0.3333333333333333703, 0.3219752754296894559, 0.3333333333333333703, 0.3219752754296894559, 0.3333333333333333703, 0.3219752754296894559, 0.3333333333333333703, 0.3219752754296894559, 0.3333333333333333703, 0.3219752754296894559, 0.3333333333333333703, 0.3219752754296894559, 0.3333333333333333703, 0.3219752754296894559, 0.3333333333333333703, 0.3219752754296894559, 0.3333333333333333703, 0.3219752754296894559, 0.3333333333333333703, 0.3219752754296894559, 0.3333333333333333703, 0.3219752754296894559, 0.3333333333333333703, 0.3219752754296894559, 0.3333333333333333703, 0.3219752754296894559, 0.3333333333333333703, 0.3219752754296894559, 0.3333333333333333703, 0.3219752754296894559, 0.3333333333333333703, 0.3219752754296894559, 0.3333333333333333703, 0.3219752754296894559, 0.3333333333333333703, 0.3219752754296894559, 0.3333333333333333703, 0.3219752754296894559, 0.3333333333333333703, 0.3219752754296894559, 0.3333333333333333703, 0.3219752754296894559, 0.3333333333333333703, 0.3219752754296894559, 0.3333333333333333703, 0.3219752754296894559, 0.3333333333333333703, 0.3219752754296894559, 0.3333333333333333703),
 ( 0.3333333333333333703, 0.3219752754296894559, 0.3333333333333333703, 0.3219752754296894559, 0.3333333333333333703, 0.3219752754296894559, 0.3333333333333333703, 0.3219752754296894559, 0.3333333333333333703, 0.3219752754296894559, 0.3333333333333333703, 0.3219752754296894559, 0.3333333333333333703, 0.3219752754296894559, 0.3333333333333333703, 0.3219752754296894559, 0.3333333333333333703, 0.3219752754296894559, 0.3333333333333333703, 0.3219752754296894559, 0.3333333333333333703, 0.3219752754296894559, 0.3333333333333333703, 0.3219752754296894559, 0.3333333333333333703, 0.3219752754296894559, 0.3333333333333333703, 0.3219752754296894559, 0.3333333333333333703, 0.3219752754296894559, 0.3333333333333333703, 0.3219752754296894559, 0.3333333333333333703, 0.3219752754296894559, 0.3333333333333333703, 0.3219752754296894559, 0.3333333333333333703, 0.3219752754296894559, 0.3333333333333333703, 0.3219752754296894559, 0.3333333333333333703, 0.3219752754296894559, 0.3333333333333333703, 0.3219752754296894559, 0.3333333333333333703, 0.3219752754296894559, 0.3333333333333333703, 0.3219752754296894559, 0.3333333333333333703, 0.3219752754296894559, 0.3333333333333333703, 0.3219752754296894559, 0.3333333333333333703, 0.3219752754296894559, 0.3333333333333333703, 0.3219752754296894559, 0.3333333333333333703, 0.3219752754296894559, 0.3333333333333333703, 0.3219752754296894559, 0.3333333333333333703, 0.3219752754296894559, 0.3333333333333333703, 0.3219752754296894559, 0.3333333333333333703, 0.3219752754296894559, 0.3333333333333333703, 0.3219752754296894559, 0.3333333333333333703, 0.3219752754296894559, 0.3333333333333333703, 0.3219752754296894559, 0.3333333333333333703, 0.3219752754296894559, 0.3333333333333333703, 0.3219752754296894559, 0.3333333333333333703, 0.3219752754296894559, 0.3333333333333333703, 0.3219752754296894559, 0.3333333333333333703, 0.3219752754296894559, 0.3333333333333333703, 0.3219752754296894559, 0.3333333333333333703, 0.3219752754296894559, 0.3333333333333333703, 0.3219752754296894559, 0.3333333333333333703, 0.3219752754296894559, 0.3333333333333333703, 0.3219752754296894559, 0.3333333333333333703, 0.3219752754296894559, 0.3333333333333333703, 0.3219752754296894559, 0.3333333333333333703, 0.3219752754296894559, 0.3333333333333333703, 0.3219752754296894559, 0.3333333333333333703, 0.3219752754296894559, 0.3333333333333333703, 0.3219752754296894559, 0.3333333333333333703, 0.3219752754296894559, 0.3333333333333333703, 0.3219752754296894559, 0.3333333333333333703, 0.3219752754296894559, 0.3333333333333333703, 0.3219752754296894559, 0.3333333333333333703, 0.3219752754296894559, 0.3333333333333333703, 0.3219752754296894559, 0.3333333333333333703, 0.3219752754296894559, 0.3333333333333333703, 0.3219752754296894559, 0.3333333333333333703, 0.3219752754296894559, 0.3333333333333333703, 0.3219752754296894559, 0.3333333333333333703, 0.3219752754296894559, 0.3333333333333333703, 0.3219752754296894559, 0.3333333333333333703, 0.3219752754296894559, 0.3333333333333333703, 0.3219752754296894559, 0.3333333333333333703, 0.3219752754296894559, 0.3333333333333333703, 0.3219752754296894559, 0.3333333333333333703, 0.3219752754296894559, 0.3333333333333333703, 0.3219752754296894559, 0.3333333333333333703, 0.3219752754296894559, 0.3333333333333333703, 0.3219752754296894559, 0.3333333333333333703, 0.3219752754296894559, 0.3333333333333333703, 0.3219752754296894559, 0.3333333333333333703, 0.3219752754296894559, 0.3333333333333333703, 0.3219752754296894559, 0.3333333333333333703, 0.3219752754296894559, 0.3333333333333333703, 0.3219752754296894559, 0.3333333333333333703, 0.3219752754296894559, 0.3333333333333333703, 0.3219752754296894559, 0.3333333333333333703, 0.3219752754296894559, 0.3333333333333333703, 0.3219752754296894559, 0.3333333333333333703, 0.3219752754296894559, 0.3333333333333333703, 0.3219752754296894559, 0.3333333333333333703, 0.3219752754296894559, 0.3333333333333333703, 0.3219752754296894559, 0.3333333333333333703, 0.3219752754296894559, 0.3333333333333333703, 0.3219752754296894559, 0.3333333333333333703, 0.3219752754296894559, 0.3333333333333333703, 0.3219752754296894559, 0.3333333333333333703, 0.3219752754296894559, 0.3333333333333333703, 0.3219752754296894559, 0.3333333333333333703, 0.3219752754296894559, 0.3333333333333333703, 0.3219752754296894559, 0.3333333333333333703, 0.3219752754296894559, 0.3333333333333333703, 0.3219752754296894559, 0.3333333333333333703, 0.3219752754296894559, 0.3333333333333333703, 0.3219752754296894559, 0.3333333333333333703, 0.3219752754296894559, 0.3333333333333333703, 0.3219752754296894559, 0.3333333333333333703, 0.3219752754296894559, 0.3333333333333333703, 0.3219752754296894559, 0.3333333333333333703, 0.3219752754296894559, 0.3333333333333333703, 0.3219752754296894559, 0.3333333333333333703, 0.3219752754296894559, 0.3333333333333333703, 0.3219752754296894559, 0.3333333333333333703, 0.3219752754296894559, 0.3333333333333333703, 0.3219752754296894559, 0.3333333333333333703, 0.3219752754296894559, 0.3333333333333333703, 0.3219752754296894559, 0.3333333333333333703, 0.3219752754296894559, 0.3333333333333333703, 0.3219752754296894559, 0.3333333333333333703, 0.3219752754296894559, 0.3333333333333333703, 0.3219752754296894559, 0.3333333333333333703, 0.3219752754296894559, 0.3333333333333333703, 0.3219752754296894559, 0.3333333333333333703, 0.3219752754296894559, 0.3333333333333333703, 0.3219752754296894559, 0.3333333333333333703, 0.3219752754296894559, 0.3333333333333333703, 0.3219752754296894559, 0.3333333333333333703, 0.3219752754296894559, 0.3333333333333333703, 0.3219752754296894559, 0.3333333333333333703, 0.3219752754296894559, 0.3333333333333333703, 0.3219752754296894559, 0.3333333333333333703, 0.3219752754296894559, 0.3333333333333333703, 0.3219752754296894559, 0.3333333333333333703, 0.3219752754296894559, 0.3333333333333333703, 0.3219752754296894559, 0.3333333333333333703, 0.3219752754296894559, 0.3333333333333333703, 0.3219752754296894559, 0.3333333333333333703, 0.3219752754296894559, 0.3333333333333333703, 0.3219752754296894559, 0.3333333333333333703, 0.3219752754296894559, 0.3333333333333333703, 0.3219752754296894559, 0.3333333333333333703, 0.3219752754296894559, 0.3333333333333333703, 0.3219752754296894559, 0.3333333333333333703, 0.3219752754296894559, 0.3333333333333333703, 0.3219752754296894559, 0.3333333333333333703, 0.3219752754296894559, 0.3333333333333333703, 0.3219752754296894559, 0.3333333333333333703, 0.3219752754296894559, 0.3333333333333333703, 0.3219752754296894559, 0.3333333333333333703, 0.3219752754296894559, 0.3333333333333333703, 0.3219752754296894559, 0.3333333333333333703, 0.3219752754296894559, 0.3333333333333333703, 0.3219752754296894559, 0.3333333333333333703, 0.3219752754296894559, 0.3333333333333333703, 0.3219752754296894559, 0.3333333333333333703, 0.3219752754296894559, 0.3333333333333333703, 0.3219752754296894559, 0.3333333333333333703, 0.3219752754296894559, 0.3333333333333333703, 0.3219752754296894559, 0.3333333333333333703, 0.3219752754296894559, 0.3333333333333333703, 0.3219752754296894559, 0.3333333333333333703, 0.3219752754296894559, 0.3333333333333333703, 0.3219752754296894559, 0.3333333333333333703, 0.3219752754296894559, 0.3333333333333333703, 0.3219752754296894559, 0.3333333333333333703, 0.3219752754296894559, 0.3333333333333333703, 0.3219752754296894559, 0.3333333333333333703, 0.3219752754296894559, 0.3333333333333333703, 0.3219752754296894559, 0.3333333333333333703, 0.3219752754296894559, 0.3333333333333333703, 0.3219752754296894559, 0.3333333333333333703, 0.3219752754296894559, 0.3333333333333333703, 0.3219752754296894559, 0.3333333333333333703, 0.3219752754296894559, 0.3333333333333333703, 0.3219752754296894559, 0.3333333333333333703, 0.3219752754296894559, 0.3333333333333333703, 0.3219752754296894559, 0.3333333333333333703, 0.3219752754296894559, 0.3333333333333333703, 0.3219752754296894559, 0.3333333333333333703, 0.3219752754296894559, 0.3333333333333333703, 0.3219752754296894559, 0.3333333333333333703, 0.3219752754296894559, 0.3333333333333333703, 0.3219752754296894559, 0.3333333333333333703, 0.3219752754296894559, 0.3333333333333333703, 0.3219752754296894559, 0.3333333333333333703, 0.3219752754296894559, 0.3333333333333333703, 0.3219752754296894559, 0.3333333333333333703, 0.3219752754296894559, 0.3333333333333333703, 0.3219752754296894559, 0.3333333333333333703, 0.3219752754296894559, 0.3333333333333333703, 0.3219752754296894559, 0.3333333333333333703, 0.3219752754296894559, 0.3333333333333333703, 0.3219752754296894559, 0.3333333333333333703, 0.3219752754296894559, 0.3333333333333333703, 0.3219752754296894559, 0.3333333333333333703, 0.3219752754296894559, 0.3333333333333333703, 0.3219752754296894559, 0.3333333333333333703, 0.3219752754296894559, 0.3333333333333333703, 0.3219752754296894559, 0.3333333333333333703, 0.3219752754296894559, 0.3333333333333333703, 0.3219752754296894559, 0.3333333333333333703, 0.3219752754296894559, 0.3333333333333333703, 0.3219752754296894559, 0.3333333333333333703, 0.3219752754296894559, 0.3333333333333333703, 0.3219752754296894559, 0.3333333333333333703, 0.3219752754296894559, 0.3333333333333333703, 0.3219752754296894559, 0.3333333333333333703, 0.3219752754296894559, 0.3333333333333333703, 0.3219752754296894559, 0.3333333333333333703, 0.3219752754296894559, 0.3333333333333333703, 0.3219752754296894559, 0.3333333333333333703, 0.3219752754296894559, 0.3333333333333333703, 0.3219752754296894559, 0.3333333333333333703, 0.3219752754296894559, 0.3333333333333333703, 0.3219752754296894559, 0.3333333333333333703, 0.3219752754296894559, 0.3333333333333333703, 0.3219752754296894559, 0.3333333333333333703, 0.3219752754296894559, 0.3333333333333333703, 0.3219752754296894559, 0.3333333333333333703, 0.3219752754296894559, 0.3333333333333333703, 0.3219752754296894559, 0.3333333333333333703, 0.3219752754296894559, 0.3333333333333333703, 0.3219752754296894559, 0.3333333333333333703, 0.3219752754296894559, 0.3333333333333333703, 0.3219752754296894559, 0.3333333333333333703, 0.3219752754296894559, 0.3333333333333333703, 0.3219752754296894559, 0.3333333333333333703, 0.3219752754296894559, 0.3333333333333333703, 0.3219752754296894559, 0.3333333333333333703, 0.3219752754296894559, 0.3333333333333333703, 0.3219752754296894559, 0.3333333333333333703, 0.3219752754296894559, 0.3333333333333333703, 0.3219752754296894559, 0.3333333333333333703, 0.3219752754296894559, 0.3333333333333333703, 0.3219752754296894559, 0.3333333333333333703),
 ( 1.000000000000000000, 0.9659258262890683122, 1.000000000000000000, 0.9659258262890683122, 1.000000000000000000, 0.9659258262890683122, 1.000000000000000000, 0.9659258262890683122, 1.000000000000000000, 0.9659258262890683122, 1.000000000000000000, 0.9659258262890683122, 1.000000000000000000, 0.9659258262890683122, 1.000000000000000000, 0.9659258262890683122, 1.000000000000000000, 0.9659258262890683122, 1.000000000000000000, 0.9659258262890683122, 1.000000000000000000, 0.9659258262890683122, 1.000000000000000000, 0.9659258262890683122, 1.000000000000000000, 0.9659258262890683122, 1.000000000000000000, 0.9659258262890683122, 1.000000000000000000, 0.9659258262890683122, 1.000000000000000000, 0.9659258262890683122, 1.000000000000000000, 0.9659258262890683122, 1.000000000000000000, 0.9659258262890683122, 1.000000000000000000, 0.9659258262890683122, 1.000000000000000000, 0.9659258262890683122, 1.000000000000000000, 0.9659258262890683122, 1.000000000000000000, 0.9659258262890683122, 1.000000000000000000, 0.9659258262890683122, 1.000000000000000000, 0.9659258262890683122, 1.000000000000000000, 0.9659258262890683122, 1.000000000000000000, 0.9659258262890683122, 1.000000000000000000, 0.9659258262890683122, 1.000000000000000000, 0.9659258262890683122, 1.000000000000000000, 0.9659258262890683122, 1.000000000000000000, 0.9659258262890683122, 1.000000000000000000, 0.9659258262890683122, 1.000000000000000000, 0.9659258262890683122, 1.000000000000000000, 0.9659258262890683122, 1.000000000000000000, 0.9659258262890683122, 1.000000000000000000, 0.9659258262890683122, 1.000000000000000000, 0.9659258262890683122, 1.000000000000000000, 0.9659258262890683122, 1.000000000000000000, 0.9659258262890683122, 1.000000000000000000, 0.9659258262890683122, 1.000000000000000000, 0.9659258262890683122, 1.000000000000000000, 0.9659258262890683122, 1.000000000000000000, 0.9659258262890683122, 1.000000000000000000, 0.9659258262890683122, 1.000000000000000000, 0.9659258262890683122, 1.000000000000000000, 0.9659258262890683122, 1.000000000000000000, 0.9659258262890683122, 1.000000000000000000, 0.9659258262890683122, 1.000000000000000000, 0.9659258262890683122, 1.000000000000000000, 0.9659258262890683122, 1.000000000000000000, 0.9659258262890683122, 1.000000000000000000, 0.9659258262890683122, 1.000000000000000000, 0.9659258262890683122, 1.000000000000000000, 0.9659258262890683122, 1.000000000000000000, 0.9659258262890683122, 1.000000000000000000, 0.9659258262890683122, 1.000000000000000000, 0.9659258262890683122, 1.000000000000000000, 0.9659258262890683122, 1.000000000000000000, 0.9659258262890683122, 1.000000000000000000, 0.9659258262890683122, 1.000000000000000000, 0.9659258262890683122, 1.000000000000000000, 0.9659258262890683122, 1.000000000000000000, 0.9659258262890683122, 1.000000000000000000, 0.9659258262890683122, 1.000000000000000000, 0.9659258262890683122, 1.000000000000000000, 0.9659258262890683122, 1.000000000000000000, 0.9659258262890683122, 1.000000000000000000, 0.9659258262890683122, 1.000000000000000000, 0.9659258262890683122, 1.000000000000000000, 0.9659258262890683122, 1.000000000000000000, 0.9659258262890683122, 1.000000000000000000, 0.9659258262890683122, 1.000000000000000000, 0.9659258262890683122, 1.000000000000000000, 0.9659258262890683122, 1.000000000000000000, 0.9659258262890683122, 1.000000000000000000, 0.9659258262890683122, 1.000000000000000000, 0.9659258262890683122, 1.000000000000000000, 0.9659258262890683122, 1.000000000000000000, 0.9659258262890683122, 1.000000000000000000, 0.9659258262890683122, 1.000000000000000000, 0.9659258262890683122, 1.000000000000000000, 0.9659258262890683122, 1.000000000000000000, 0.9659258262890683122, 1.000000000000000000, 0.9659258262890683122, 1.000000000000000000, 0.9659258262890683122, 1.000000000000000000, 0.9659258262890683122, 1.000000000000000000, 0.9659258262890683122, 1.000000000000000000, 0.9659258262890683122, 1.000000000000000000, 0.9659258262890683122, 1.000000000000000000, 0.9659258262890683122, 1.000000000000000000, 0.9659258262890683122, 1.000000000000000000, 0.9659258262890683122, 1.000000000000000000, 0.9659258262890683122, 1.000000000000000000, 0.9659258262890683122, 1.000000000000000000, 0.9659258262890683122, 1.000000000000000000, 0.9659258262890683122, 1.000000000000000000, 0.9659258262890683122, 1.000000000000000000, 0.9659258262890683122, 1.000000000000000000, 0.9659258262890683122, 1.000000000000000000, 0.9659258262890683122, 1.000000000000000000, 0.9659258262890683122, 1.000000000000000000, 0.9659258262890683122, 1.000000000000000000, 0.9659258262890683122, 1.000000000000000000, 0.9659258262890683122, 1.000000000000000000, 0.9659258262890683122, 1.000000000000000000, 0.9659258262890683122, 1.000000000000000000, 0.9659258262890683122, 1.000000000000000000, 0.9659258262890683122, 1.000000000000000000, 0.9659258262890683122, 1.000000000000000000, 0.9659258262890683122, 1.000000000000000000, 0.9659258262890683122, 1.000000000000000000, 0.9659258262890683122, 1.000000000000000000, 0.9659258262890683122, 1.000000000000000000, 0.9659258262890683122, 1.000000000000000000, 0.9659258262890683122, 1.000000000000000000, 0.9659258262890683122, 1.000000000000000000, 0.9659258262890683122, 1.000000000000000000, 0.9659258262890683122, 1.000000000000000000, 0.9659258262890683122, 1.000000000000000000, 0.9659258262890683122, 1.000000000000000000, 0.9659258262890683122, 1.000000000000000000, 0.9659258262890683122, 1.000000000000000000, 0.9659258262890683122, 1.000000000000000000, 0.9659258262890683122, 1.000000000000000000, 0.9659258262890683122, 1.000000000000000000, 0.9659258262890683122, 1.000000000000000000, 0.9659258262890683122, 1.000000000000000000, 0.9659258262890683122, 1.000000000000000000, 0.9659258262890683122, 1.000000000000000000, 0.9659258262890683122, 1.000000000000000000, 0.9659258262890683122, 1.000000000000000000, 0.9659258262890683122, 1.000000000000000000, 0.9659258262890683122, 1.000000000000000000, 0.9659258262890683122, 1.000000000000000000, 0.9659258262890683122, 1.000000000000000000, 0.9659258262890683122, 1.000000000000000000, 0.9659258262890683122, 1.000000000000000000, 0.9659258262890683122, 1.000000000000000000, 0.9659258262890683122, 1.000000000000000000, 0.9659258262890683122, 1.000000000000000000, 0.9659258262890683122, 1.000000000000000000, 0.9659258262890683122, 1.000000000000000000, 0.9659258262890683122, 1.000000000000000000, 0.9659258262890683122, 1.000000000000000000, 0.9659258262890683122, 1.000000000000000000, 0.9659258262890683122, 1.000000000000000000, 0.9659258262890683122, 1.000000000000000000, 0.9659258262890683122, 1.000000000000000000, 0.9659258262890683122, 1.000000000000000000, 0.9659258262890683122, 1.000000000000000000, 0.9659258262890683122, 1.000000000000000000, 0.9659258262890683122, 1.000000000000000000, 0.9659258262890683122, 1.000000000000000000, 0.9659258262890683122, 1.000000000000000000, 0.9659258262890683122, 1.000000000000000000, 0.9659258262890683122, 1.000000000000000000, 0.9659258262890683122, 1.000000000000000000, 0.9659258262890683122, 1.000000000000000000, 0.9659258262890683122, 1.000000000000000000, 0.9659258262890683122, 1.000000000000000000, 0.9659258262890683122, 1.000000000000000000, 0.9659258262890683122, 1.000000000000000000, 0.9659258262890683122, 1.000000000000000000, 0.9659258262890683122, 1.000000000000000000, 0.9659258262890683122, 1.000000000000000000, 0.9659258262890683122, 1.000000000000000000, 0.9659258262890683122, 1.000000000000000000, 0.9659258262890683122, 1.000000000000000000, 0.9659258262890683122, 1.000000000000000000, 0.9659258262890683122, 1.000000000000000000, 0.9659258262890683122, 1.000000000000000000, 0.9659258262890683122, 1.000000000000000000, 0.9659258262890683122, 1.000000000000000000, 0.9659258262890683122, 1.000000000000000000, 0.9659258262890683122, 1.000000000000000000, 0.9659258262890683122, 1.000000000000000000, 0.9659258262890683122, 1.000000000000000000, 0.9659258262890683122, 1.000000000000000000, 0.9659258262890683122, 1.000000000000000000, 0.9659258262890683122, 1.000000000000000000, 0.9659258262890683122, 1.000000000000000000, 0.9659258262890683122, 1.000000000000000000, 0.9659258262890683122, 1.000000000000000000, 0.9659258262890683122, 1.000000000000000000, 0.9659258262890683122, 1.000000000000000000, 0.9659258262890683122, 1.000000000000000000, 0.9659258262890683122, 1.000000000000000000, 0.9659258262890683122, 1.000000000000000000, 0.9659258262890683122, 1.000000000000000000, 0.9659258262890683122, 1.000000000000000000, 0.9659258262890683122, 1.000000000000000000, 0.9659258262890683122, 1.000000000000000000, 0.9659258262890683122, 1.000000000000000000, 0.9659258262890683122, 1.000000000000000000, 0.9659258262890683122, 1.000000000000000000, 0.9659258262890683122, 1.000000000000000000, 0.9659258262890683122, 1.000000000000000000, 0.9659258262890683122, 1.000000000000000000, 0.9659258262890683122, 1.000000000000000000, 0.9659258262890683122, 1.000000000000000000, 0.9659258262890683122, 1.000000000000000000, 0.9659258262890683122, 1.000000000000000000, 0.9659258262890683122, 1.000000000000000000, 0.9659258262890683122, 1.000000000000000000, 0.9659258262890683122, 1.000000000000000000, 0.9659258262890683122, 1.000000000000000000, 0.9659258262890683122, 1.000000000000000000, 0.9659258262890683122, 1.000000000000000000, 0.9659258262890683122, 1.000000000000000000, 0.9659258262890683122, 1.000000000000000000, 0.9659258262890683122, 1.000000000000000000, 0.9659258262890683122, 1.000000000000000000, 0.9659258262890683122, 1.000000000000000000, 0.9659258262890683122, 1.000000000000000000, 0.9659258262890683122, 1.000000000000000000, 0.9659258262890683122, 1.000000000000000000, 0.9659258262890683122, 1.000000000000000000, 0.9659258262890683122, 1.000000000000000000, 0.9659258262890683122, 1.000000000000000000, 0.9659258262890683122, 1.000000000000000000, 0.9659258262890683122, 1.000000000000000000, 0.9659258262890683122, 1.000000000000000000, 0.9659258262890683122, 1.000000000000000000, 0.9659258262890683122, 1.000000000000000000, 0.9659258262890683122, 1.000000000000000000, 0.9659258262890683122, 1.000000000000000000, 0.9659258262890683122, 1.000000000000000000, 0.9659258262890683122, 1.000000000000000000, 0.9659258262890683122, 1.000000000000000000),
 ( 0.3333333333333333703, 0.3219752754296894559, 0.3333333333333333703, 0.3219752754296894559, 0.3333333333333333703, 0.3219752754296894559, 0.3333333333333333703, 0.3219752754296894559, 0.3333333333333333703, 0.3219752754296894559, 0.3333333333333333703, 0.3219752754296894559, 0.3333333333333333703, 0.3219752754296894559, 0.3333333333333333703, 0.3219752754296894559, 0.3333333333333333703, 0.3219752754296894559, 0.3333333333333333703, 0.3219752754296894559, 0.3333333333333333703, 0.3219752754296894559, 0.3333333333333333703, 0.3219752754296894559, 0.3333333333333333703, 0.3219752754296894559, 0.3333333333333333703, 0.3219752754296894559, 0.3333333333333333703, 0.3219752754296894559, 0.3333333333333333703, 0.3219752754296894559, 0.3333333333333333703, 0.3219752754296894559, 0.3333333333333333703, 0.3219752754296894559, 0.3333333333333333703, 0.3219752754296894559, 0.3333333333333333703, 0.3219752754296894559, 0.3333333333333333703, 0.3219752754296894559, 0.3333333333333333703, 0.3219752754296894559, 0.3333333333333333703, 0.3219752754296894559, 0.3333333333333333703, 0.3219752754296894559, 0.3333333333333333703, 0.3219752754296894559, 0.3333333333333333703, 0.3219752754296894559, 0.3333333333333333703, 0.3219752754296894559, 0.3333333333333333703, 0.3219752754296894559, 0.3333333333333333703, 0.3219752754296894559, 0.3333333333333333703, 0.3219752754296894559, 0.3333333333333333703, 0.3219752754296894559, 0.3333333333333333703, 0.3219752754296894559, 0.3333333333333333703, 0.3219752754296894559, 0.3333333333333333703, 0.3219752754296894559, 0.3333333333333333703, 0.3219752754296894559, 0.3333333333333333703, 0.3219752754296894559, 0.3333333333333333703, 0.3219752754296894559, 0.3333333333333333703, 0.3219752754296894559, 0.3333333333333333703, 0.3219752754296894559, 0.3333333333333333703, 0.3219752754296894559, 0.3333333333333333703, 0.3219752754296894559, 0.3333333333333333703, 0.3219752754296894559, 0.3333333333333333703, 0.3219752754296894559, 0.3333333333333333703, 0.3219752754296894559, 0.3333333333333333703, 0.3219752754296894559, 0.3333333333333333703, 0.3219752754296894559, 0.3333333333333333703, 0.3219752754296894559, 0.3333333333333333703, 0.3219752754296894559, 0.3333333333333333703, 0.3219752754296894559, 0.3333333333333333703, 0.3219752754296894559, 0.3333333333333333703, 0.3219752754296894559, 0.3333333333333333703, 0.3219752754296894559, 0.3333333333333333703, 0.3219752754296894559, 0.3333333333333333703, 0.3219752754296894559, 0.3333333333333333703, 0.3219752754296894559, 0.3333333333333333703, 0.3219752754296894559, 0.3333333333333333703, 0.3219752754296894559, 0.3333333333333333703, 0.3219752754296894559, 0.3333333333333333703, 0.3219752754296894559, 0.3333333333333333703, 0.3219752754296894559, 0.3333333333333333703, 0.3219752754296894559, 0.3333333333333333703, 0.3219752754296894559, 0.3333333333333333703, 0.3219752754296894559, 0.3333333333333333703, 0.3219752754296894559, 0.3333333333333333703, 0.3219752754296894559, 0.3333333333333333703, 0.3219752754296894559, 0.3333333333333333703, 0.3219752754296894559, 0.3333333333333333703, 0.3219752754296894559, 0.3333333333333333703, 0.3219752754296894559, 0.3333333333333333703, 0.3219752754296894559, 0.3333333333333333703, 0.3219752754296894559, 0.3333333333333333703, 0.3219752754296894559, 0.3333333333333333703, 0.3219752754296894559, 0.3333333333333333703, 0.3219752754296894559, 0.3333333333333333703, 0.3219752754296894559, 0.3333333333333333703, 0.3219752754296894559, 0.3333333333333333703, 0.3219752754296894559, 0.3333333333333333703, 0.3219752754296894559, 0.3333333333333333703, 0.3219752754296894559, 0.3333333333333333703, 0.3219752754296894559, 0.3333333333333333703, 0.3219752754296894559, 0.3333333333333333703, 0.3219752754296894559, 0.3333333333333333703, 0.3219752754296894559, 0.3333333333333333703, 0.3219752754296894559, 0.3333333333333333703, 0.3219752754296894559, 0.3333333333333333703, 0.3219752754296894559, 0.3333333333333333703, 0.3219752754296894559, 0.3333333333333333703, 0.3219752754296894559, 0.3333333333333333703, 0.3219752754296894559, 0.3333333333333333703, 0.3219752754296894559, 0.3333333333333333703, 0.3219752754296894559, 0.3333333333333333703, 0.3219752754296894559, 0.3333333333333333703, 0.3219752754296894559, 0.3333333333333333703, 0.3219752754296894559, 0.3333333333333333703, 0.3219752754296894559, 0.3333333333333333703, 0.3219752754296894559, 0.3333333333333333703, 0.3219752754296894559, 0.3333333333333333703, 0.3219752754296894559, 0.3333333333333333703, 0.3219752754296894559, 0.3333333333333333703, 0.3219752754296894559, 0.3333333333333333703, 0.3219752754296894559, 0.3333333333333333703, 0.3219752754296894559, 0.3333333333333333703, 0.3219752754296894559, 0.3333333333333333703, 0.3219752754296894559, 0.3333333333333333703, 0.3219752754296894559, 0.3333333333333333703, 0.3219752754296894559, 0.3333333333333333703, 0.3219752754296894559, 0.3333333333333333703, 0.3219752754296894559, 0.3333333333333333703, 0.3219752754296894559, 0.3333333333333333703, 0.3219752754296894559, 0.3333333333333333703, 0.3219752754296894559, 0.3333333333333333703, 0.3219752754296894559, 0.3333333333333333703, 0.3219752754296894559, 0.3333333333333333703, 0.3219752754296894559, 0.3333333333333333703, 0.3219752754296894559, 0.3333333333333333703, 0.3219752754296894559, 0.3333333333333333703, 0.3219752754296894559, 0.3333333333333333703, 0.3219752754296894559, 0.3333333333333333703, 0.3219752754296894559, 0.3333333333333333703, 0.3219752754296894559, 0.3333333333333333703, 0.3219752754296894559, 0.3333333333333333703, 0.3219752754296894559, 0.3333333333333333703, 0.3219752754296894559, 0.3333333333333333703, 0.3219752754296894559, 0.3333333333333333703, 0.3219752754296894559, 0.3333333333333333703, 0.3219752754296894559, 0.3333333333333333703, 0.3219752754296894559, 0.3333333333333333703, 0.3219752754296894559, 0.3333333333333333703, 0.3219752754296894559, 0.3333333333333333703, 0.3219752754296894559, 0.3333333333333333703, 0.3219752754296894559, 0.3333333333333333703, 0.3219752754296894559, 0.3333333333333333703, 0.3219752754296894559, 0.3333333333333333703, 0.3219752754296894559, 0.3333333333333333703, 0.3219752754296894559, 0.3333333333333333703, 0.3219752754296894559, 0.3333333333333333703, 0.3219752754296894559, 0.3333333333333333703, 0.3219752754296894559, 0.3333333333333333703, 0.3219752754296894559, 0.3333333333333333703, 0.3219752754296894559, 0.3333333333333333703, 0.3219752754296894559, 0.3333333333333333703, 0.3219752754296894559, 0.3333333333333333703, 0.3219752754296894559, 0.3333333333333333703, 0.3219752754296894559, 0.3333333333333333703, 0.3219752754296894559, 0.3333333333333333703, 0.3219752754296894559, 0.3333333333333333703, 0.3219752754296894559, 0.3333333333333333703, 0.3219752754296894559, 0.3333333333333333703, 0.3219752754296894559, 0.3333333333333333703, 0.3219752754296894559, 0.3333333333333333703, 0.3219752754296894559, 0.3333333333333333703, 0.3219752754296894559, 0.3333333333333333703, 0.3219752754296894559, 0.3333333333333333703, 0.3219752754296894559, 0.3333333333333333703, 0.3219752754296894559, 0.3333333333333333703, 0.3219752754296894559, 0.3333333333333333703, 0.3219752754296894559, 0.3333333333333333703, 0.3219752754296894559, 0.3333333333333333703, 0.3219752754296894559, 0.3333333333333333703, 0.3219752754296894559, 0.3333333333333333703, 0.3219752754296894559, 0.3333333333333333703, 0.3219752754296894559, 0.3333333333333333703, 0.3219752754296894559, 0.3333333333333333703, 0.3219752754296894559, 0.3333333333333333703, 0.3219752754296894559, 0.3333333333333333703, 0.3219752754296894559, 0.3333333333333333703, 0.3219752754296894559, 0.3333333333333333703, 0.3219752754296894559, 0.3333333333333333703, 0.3219752754296894559, 0.3333333333333333703, 0.3219752754296894559, 0.3333333333333333703, 0.3219752754296894559, 0.3333333333333333703, 0.3219752754296894559, 0.3333333333333333703, 0.3219752754296894559, 0.3333333333333333703, 0.3219752754296894559, 0.3333333333333333703, 0.3219752754296894559, 0.3333333333333333703, 0.3219752754296894559, 0.3333333333333333703, 0.3219752754296894559, 0.3333333333333333703, 0.3219752754296894559, 0.3333333333333333703, 0.3219752754296894559, 0.3333333333333333703, 0.3219752754296894559, 0.3333333333333333703, 0.3219752754296894559, 0.3333333333333333703, 0.3219752754296894559, 0.3333333333333333703, 0.3219752754296894559, 0.3333333333333333703, 0.3219752754296894559, 0.3333333333333333703, 0.3219752754296894559, 0.3333333333333333703, 0.3219752754296894559, 0.3333333333333333703, 0.3219752754296894559, 0.3333333333333333703, 0.3219752754296894559, 0.3333333333333333703, 0.3219752754296894559, 0.3333333333333333703, 0.3219752754296894559, 0.3333333333333333703, 0.3219752754296894559, 0.3333333333333333703, 0.3219752754296894559, 0.3333333333333333703, 0.3219752754296894559, 0.3333333333333333703, 0.3219752754296894559, 0.3333333333333333703, 0.3219752754296894559, 0.3333333333333333703, 0.3219752754296894559, 0.3333333333333333703, 0.3219752754296894559, 0.3333333333333333703, 0.3219752754296894559, 0.3333333333333333703, 0.3219752754296894559, 0.3333333333333333703, 0.3219752754296894559, 0.3333333333333333703, 0.3219752754296894559, 0.3333333333333333703, 0.3219752754296894559, 0.3333333333333333703, 0.3219752754296894559, 0.3333333333333333703, 0.3219752754296894559, 0.3333333333333333703, 0.3219752754296894559, 0.3333333333333333703, 0.3219752754296894559, 0.3333333333333333703, 0.3219752754296894559, 0.3333333333333333703, 0.3219752754296894559, 0.3333333333333333703, 0.3219752754296894559, 0.3333333333333333703, 0.3219752754296894559, 0.3333333333333333703, 0.3219752754296894559, 0.3333333333333333703, 0.3219752754296894559, 0.3333333333333333703, 0.3219752754296894559, 0.3333333333333333703, 0.3219752754296894559, 0.3333333333333333703, 0.3219752754296894559, 0.3333333333333333703, 0.3219752754296894559, 0.3333333333333333703, 0.3219752754296894559, 0.3333333333333333703, 0.3219752754296894559, 0.3333333333333333703, 0.3219752754296894559, 0.3333333333333333703, 0.3219752754296894559, 0.3333333333333333703, 0.3219752754296894559, 0.3333333333333333703, 0.3219752754296894559, 0.3333333333333333703, 0.3219752754296894559, 0.3333333333333333703, 0.3219752754296894559, 0.3333333333333333703, 0.3219752754296894559, 0.3333333333333333703, 0.3219752754296894559, 0.3333333333333333703, 0.3219752754296894559, 0.3333333333333333703, 0.3219752754296894559, 0.3333333333333333703),
 ( 0.3333333333333333703, 0.3219752754296894559, 0.3333333333333333703, 0.3219752754296894559, 0.3333333333333333703, 0.3219752754296894559, 0.3333333333333333703, 0.3219752754296894559, 0.3333333333333333703, 0.3219752754296894559, 0.3333333333333333703, 0.3219752754296894559, 0.3333333333333333703, 0.3219752754296894559, 0.3333333333333333703, 0.3219752754296894559, 0.3333333333333333703, 0.3219752754296894559, 0.3333333333333333703, 0.3219752754296894559, 0.3333333333333333703, 0.3219752754296894559, 0.3333333333333333703, 0.3219752754296894559, 0.3333333333333333703, 0.3219752754296894559, 0.3333333333333333703, 0.3219752754296894559, 0.3333333333333333703, 0.3219752754296894559, 0.3333333333333333703, 0.3219752754296894559, 0.3333333333333333703, 0.3219752754296894559, 0.3333333333333333703, 0.3219752754296894559, 0.3333333333333333703, 0.3219752754296894559, 0.3333333333333333703, 0.3219752754296894559, 0.3333333333333333703, 0.3219752754296894559, 0.3333333333333333703, 0.3219752754296894559, 0.3333333333333333703, 0.3219752754296894559, 0.3333333333333333703, 0.3219752754296894559, 0.3333333333333333703, 0.3219752754296894559, 0.3333333333333333703, 0.3219752754296894559, 0.3333333333333333703, 0.3219752754296894559, 0.3333333333333333703, 0.3219752754296894559, 0.3333333333333333703, 0.3219752754296894559, 0.3333333333333333703, 0.3219752754296894559, 0.3333333333333333703, 0.3219752754296894559, 0.3333333333333333703, 0.3219752754296894559, 0.3333333333333333703, 0.3219752754296894559, 0.3333333333333333703, 0.3219752754296894559, 0.3333333333333333703, 0.3219752754296894559, 0.3333333333333333703, 0.3219752754296894559, 0.3333333333333333703, 0.3219752754296894559, 0.3333333333333333703, 0.3219752754296894559, 0.3333333333333333703, 0.3219752754296894559, 0.3333333333333333703, 0.3219752754296894559, 0.3333333333333333703, 0.3219752754296894559, 0.3333333333333333703, 0.3219752754296894559, 0.3333333333333333703, 0.3219752754296894559, 0.3333333333333333703, 0.3219752754296894559, 0.3333333333333333703, 0.3219752754296894559, 0.3333333333333333703, 0.3219752754296894559, 0.3333333333333333703, 0.3219752754296894559, 0.3333333333333333703, 0.3219752754296894559, 0.3333333333333333703, 0.3219752754296894559, 0.3333333333333333703, 0.3219752754296894559, 0.3333333333333333703, 0.3219752754296894559, 0.3333333333333333703, 0.3219752754296894559, 0.3333333333333333703, 0.3219752754296894559, 0.3333333333333333703, 0.3219752754296894559, 0.3333333333333333703, 0.3219752754296894559, 0.3333333333333333703, 0.3219752754296894559, 0.3333333333333333703, 0.3219752754296894559, 0.3333333333333333703, 0.3219752754296894559, 0.3333333333333333703, 0.3219752754296894559, 0.3333333333333333703, 0.3219752754296894559, 0.3333333333333333703, 0.3219752754296894559, 0.3333333333333333703, 0.3219752754296894559, 0.3333333333333333703, 0.3219752754296894559, 0.3333333333333333703, 0.3219752754296894559, 0.3333333333333333703, 0.3219752754296894559, 0.3333333333333333703, 0.3219752754296894559, 0.3333333333333333703, 0.3219752754296894559, 0.3333333333333333703, 0.3219752754296894559, 0.3333333333333333703, 0.3219752754296894559, 0.3333333333333333703, 0.3219752754296894559, 0.3333333333333333703, 0.3219752754296894559, 0.3333333333333333703, 0.3219752754296894559, 0.3333333333333333703, 0.3219752754296894559, 0.3333333333333333703, 0.3219752754296894559, 0.3333333333333333703, 0.3219752754296894559, 0.3333333333333333703, 0.3219752754296894559, 0.3333333333333333703, 0.3219752754296894559, 0.3333333333333333703, 0.3219752754296894559, 0.3333333333333333703, 0.3219752754296894559, 0.3333333333333333703, 0.3219752754296894559, 0.3333333333333333703, 0.3219752754296894559, 0.3333333333333333703, 0.3219752754296894559, 0.3333333333333333703, 0.3219752754296894559, 0.3333333333333333703, 0.3219752754296894559, 0.3333333333333333703, 0.3219752754296894559, 0.3333333333333333703, 0.3219752754296894559, 0.3333333333333333703, 0.3219752754296894559, 0.3333333333333333703, 0.3219752754296894559, 0.3333333333333333703, 0.3219752754296894559, 0.3333333333333333703, 0.3219752754296894559, 0.3333333333333333703, 0.3219752754296894559, 0.3333333333333333703, 0.3219752754296894559, 0.3333333333333333703, 0.3219752754296894559, 0.3333333333333333703, 0.3219752754296894559, 0.3333333333333333703, 0.3219752754296894559, 0.3333333333333333703, 0.3219752754296894559, 0.3333333333333333703, 0.3219752754296894559, 0.3333333333333333703, 0.3219752754296894559, 0.3333333333333333703, 0.3219752754296894559, 0.3333333333333333703, 0.3219752754296894559, 0.3333333333333333703, 0.3219752754296894559, 0.3333333333333333703, 0.3219752754296894559, 0.3333333333333333703, 0.3219752754296894559, 0.3333333333333333703, 0.3219752754296894559, 0.3333333333333333703, 0.3219752754296894559, 0.3333333333333333703, 0.3219752754296894559, 0.3333333333333333703, 0.3219752754296894559, 0.3333333333333333703, 0.3219752754296894559, 0.3333333333333333703, 0.3219752754296894559, 0.3333333333333333703, 0.3219752754296894559, 0.3333333333333333703, 0.3219752754296894559, 0.3333333333333333703, 0.3219752754296894559, 0.3333333333333333703, 0.3219752754296894559, 0.3333333333333333703, 0.3219752754296894559, 0.3333333333333333703, 0.3219752754296894559, 0.3333333333333333703, 0.3219752754296894559, 0.3333333333333333703, 0.3219752754296894559, 0.3333333333333333703, 0.3219752754296894559, 0.3333333333333333703, 0.3219752754296894559, 0.3333333333333333703, 0.3219752754296894559, 0.3333333333333333703, 0.3219752754296894559, 0.3333333333333333703, 0.3219752754296894559, 0.3333333333333333703, 0.3219752754296894559, 0.3333333333333333703, 0.3219752754296894559, 0.3333333333333333703, 0.3219752754296894559, 0.3333333333333333703, 0.3219752754296894559, 0.3333333333333333703, 0.3219752754296894559, 0.3333333333333333703, 0.3219752754296894559, 0.3333333333333333703, 0.3219752754296894559, 0.3333333333333333703, 0.3219752754296894559, 0.3333333333333333703, 0.3219752754296894559, 0.3333333333333333703, 0.3219752754296894559, 0.3333333333333333703, 0.3219752754296894559, 0.3333333333333333703, 0.3219752754296894559, 0.3333333333333333703, 0.3219752754296894559, 0.3333333333333333703, 0.3219752754296894559, 0.3333333333333333703, 0.3219752754296894559, 0.3333333333333333703, 0.3219752754296894559, 0.3333333333333333703, 0.3219752754296894559, 0.3333333333333333703, 0.3219752754296894559, 0.3333333333333333703, 0.3219752754296894559, 0.3333333333333333703, 0.3219752754296894559, 0.3333333333333333703, 0.3219752754296894559, 0.3333333333333333703, 0.3219752754296894559, 0.3333333333333333703, 0.3219752754296894559, 0.3333333333333333703, 0.3219752754296894559, 0.3333333333333333703, 0.3219752754296894559, 0.3333333333333333703, 0.3219752754296894559, 0.3333333333333333703, 0.3219752754296894559, 0.3333333333333333703, 0.3219752754296894559, 0.3333333333333333703, 0.3219752754296894559, 0.3333333333333333703, 0.3219752754296894559, 0.3333333333333333703, 0.3219752754296894559, 0.3333333333333333703, 0.3219752754296894559, 0.3333333333333333703, 0.3219752754296894559, 0.3333333333333333703, 0.3219752754296894559, 0.3333333333333333703, 0.3219752754296894559, 0.3333333333333333703, 0.3219752754296894559, 0.3333333333333333703, 0.3219752754296894559, 0.3333333333333333703, 0.3219752754296894559, 0.3333333333333333703, 0.3219752754296894559, 0.3333333333333333703, 0.3219752754296894559, 0.3333333333333333703, 0.3219752754296894559, 0.3333333333333333703, 0.3219752754296894559, 0.3333333333333333703, 0.3219752754296894559, 0.3333333333333333703, 0.3219752754296894559, 0.3333333333333333703, 0.3219752754296894559, 0.3333333333333333703, 0.3219752754296894559, 0.3333333333333333703, 0.3219752754296894559, 0.3333333333333333703, 0.3219752754296894559, 0.3333333333333333703, 0.3219752754296894559, 0.3333333333333333703, 0.3219752754296894559, 0.3333333333333333703, 0.3219752754296894559, 0.3333333333333333703, 0.3219752754296894559, 0.3333333333333333703, 0.3219752754296894559, 0.3333333333333333703, 0.3219752754296894559, 0.3333333333333333703, 0.3219752754296894559, 0.3333333333333333703, 0.3219752754296894559, 0.3333333333333333703, 0.3219752754296894559, 0.3333333333333333703, 0.3219752754296894559, 0.3333333333333333703, 0.3219752754296894559, 0.3333333333333333703, 0.3219752754296894559, 0.3333333333333333703, 0.3219752754296894559, 0.3333333333333333703, 0.3219752754296894559, 0.3333333333333333703, 0.3219752754296894559, 0.3333333333333333703, 0.3219752754296894559, 0.3333333333333333703, 0.3219752754296894559, 0.3333333333333333703, 0.3219752754296894559, 0.3333333333333333703, 0.3219752754296894559, 0.3333333333333333703, 0.3219752754296894559, 0.3333333333333333703, 0.3219752754296894559, 0.3333333333333333703, 0.3219752754296894559, 0.3333333333333333703, 0.3219752754296894559, 0.3333333333333333703, 0.3219752754296894559, 0.3333333333333333703, 0.3219752754296894559, 0.3333333333333333703, 0.3219752754296894559, 0.3333333333333333703, 0.3219752754296894559, 0.3333333333333333703, 0.3219752754296894559, 0.3333333333333333703, 0.3219752754296894559, 0.3333333333333333703, 0.3219752754296894559, 0.3333333333333333703, 0.3219752754296894559, 0.3333333333333333703, 0.3219752754296894559, 0.3333333333333333703, 0.3219752754296894559, 0.3333333333333333703, 0.3219752754296894559, 0.3333333333333333703, 0.3219752754296894559, 0.3333333333333333703, 0.3219752754296894559, 0.3333333333333333703, 0.3219752754296894559, 0.3333333333333333703, 0.3219752754296894559, 0.3333333333333333703, 0.3219752754296894559, 0.3333333333333333703, 0.3219752754296894559, 0.3333333333333333703, 0.3219752754296894559, 0.3333333333333333703, 0.3219752754296894559, 0.3333333333333333703, 0.3219752754296894559, 0.3333333333333333703, 0.3219752754296894559, 0.3333333333333333703, 0.3219752754296894559, 0.3333333333333333703, 0.3219752754296894559, 0.3333333333333333703, 0.3219752754296894559, 0.3333333333333333703, 0.3219752754296894559, 0.3333333333333333703, 0.3219752754296894559, 0.3333333333333333703, 0.3219752754296894559, 0.3333333333333333703, 0.3219752754296894559, 0.3333333333333333703, 0.3219752754296894559, 0.3333333333333333703, 0.3219752754296894559, 0.3333333333333333703, 0.3219752754296894559, 0.3333333333333333703, 0.3219752754296894559, 0.3333333333333333703, 0.3219752754296894559, 0.3333333333333333703, 0.3219752754296894559, 0.3333333333333333703, 0.3219752754296894559, 0.3333333333333333703),
 ( 1.000000000000000000, 0.9659258262890683122, 1.000000000000000000, 0.9659258262890683122, 1.000000000000000000, 0.9659258262890683122, 1.000000000000000000, 0.9659258262890683122, 1.000000000000000000, 0.9659258262890683122, 1.000000000000000000, 0.9659258262890683122, 1.000000000000000000, 0.9659258262890683122, 1.000000000000000000, 0.9659258262890683122, 1.000000000000000000, 0.9659258262890683122, 1.000000000000000000, 0.9659258262890683122, 1.000000000000000000, 0.9659258262890683122, 1.000000000000000000, 0.9659258262890683122, 1.000000000000000000, 0.9659258262890683122, 1.000000000000000000, 0.9659258262890683122, 1.000000000000000000, 0.9659258262890683122, 1.000000000000000000, 0.9659258262890683122, 1.000000000000000000, 0.9659258262890683122, 1.000000000000000000, 0.9659258262890683122, 1.000000000000000000, 0.9659258262890683122, 1.000000000000000000, 0.9659258262890683122, 1.000000000000000000, 0.9659258262890683122, 1.000000000000000000, 0.9659258262890683122, 1.000000000000000000, 0.9659258262890683122, 1.000000000000000000, 0.9659258262890683122, 1.000000000000000000, 0.9659258262890683122, 1.000000000000000000, 0.9659258262890683122, 1.000000000000000000, 0.9659258262890683122, 1.000000000000000000, 0.9659258262890683122, 1.000000000000000000, 0.9659258262890683122, 1.000000000000000000, 0.9659258262890683122, 1.000000000000000000, 0.9659258262890683122, 1.000000000000000000, 0.9659258262890683122, 1.000000000000000000, 0.9659258262890683122, 1.000000000000000000, 0.9659258262890683122, 1.000000000000000000, 0.9659258262890683122, 1.000000000000000000, 0.9659258262890683122, 1.000000000000000000, 0.9659258262890683122, 1.000000000000000000, 0.9659258262890683122, 1.000000000000000000, 0.9659258262890683122, 1.000000000000000000, 0.9659258262890683122, 1.000000000000000000, 0.9659258262890683122, 1.000000000000000000, 0.9659258262890683122, 1.000000000000000000, 0.9659258262890683122, 1.000000000000000000, 0.9659258262890683122, 1.000000000000000000, 0.9659258262890683122, 1.000000000000000000, 0.9659258262890683122, 1.000000000000000000, 0.9659258262890683122, 1.000000000000000000, 0.9659258262890683122, 1.000000000000000000, 0.9659258262890683122, 1.000000000000000000, 0.9659258262890683122, 1.000000000000000000, 0.9659258262890683122, 1.000000000000000000, 0.9659258262890683122, 1.000000000000000000, 0.9659258262890683122, 1.000000000000000000, 0.9659258262890683122, 1.000000000000000000, 0.9659258262890683122, 1.000000000000000000, 0.9659258262890683122, 1.000000000000000000, 0.9659258262890683122, 1.000000000000000000, 0.9659258262890683122, 1.000000000000000000, 0.9659258262890683122, 1.000000000000000000, 0.9659258262890683122, 1.000000000000000000, 0.9659258262890683122, 1.000000000000000000, 0.9659258262890683122, 1.000000000000000000, 0.9659258262890683122, 1.000000000000000000, 0.9659258262890683122, 1.000000000000000000, 0.9659258262890683122, 1.000000000000000000, 0.9659258262890683122, 1.000000000000000000, 0.9659258262890683122, 1.000000000000000000, 0.9659258262890683122, 1.000000000000000000, 0.9659258262890683122, 1.000000000000000000, 0.9659258262890683122, 1.000000000000000000, 0.9659258262890683122, 1.000000000000000000, 0.9659258262890683122, 1.000000000000000000, 0.9659258262890683122, 1.000000000000000000, 0.9659258262890683122, 1.000000000000000000, 0.9659258262890683122, 1.000000000000000000, 0.9659258262890683122, 1.000000000000000000, 0.9659258262890683122, 1.000000000000000000, 0.9659258262890683122, 1.000000000000000000, 0.9659258262890683122, 1.000000000000000000, 0.9659258262890683122, 1.000000000000000000, 0.9659258262890683122, 1.000000000000000000, 0.9659258262890683122, 1.000000000000000000, 0.9659258262890683122, 1.000000000000000000, 0.9659258262890683122, 1.000000000000000000, 0.9659258262890683122, 1.000000000000000000, 0.9659258262890683122, 1.000000000000000000, 0.9659258262890683122, 1.000000000000000000, 0.9659258262890683122, 1.000000000000000000, 0.9659258262890683122, 1.000000000000000000, 0.9659258262890683122, 1.000000000000000000, 0.9659258262890683122, 1.000000000000000000, 0.9659258262890683122, 1.000000000000000000, 0.9659258262890683122, 1.000000000000000000, 0.9659258262890683122, 1.000000000000000000, 0.9659258262890683122, 1.000000000000000000, 0.9659258262890683122, 1.000000000000000000, 0.9659258262890683122, 1.000000000000000000, 0.9659258262890683122, 1.000000000000000000, 0.9659258262890683122, 1.000000000000000000, 0.9659258262890683122, 1.000000000000000000, 0.9659258262890683122, 1.000000000000000000, 0.9659258262890683122, 1.000000000000000000, 0.9659258262890683122, 1.000000000000000000, 0.9659258262890683122, 1.000000000000000000, 0.9659258262890683122, 1.000000000000000000, 0.9659258262890683122, 1.000000000000000000, 0.9659258262890683122, 1.000000000000000000, 0.9659258262890683122, 1.000000000000000000, 0.9659258262890683122, 1.000000000000000000, 0.9659258262890683122, 1.000000000000000000, 0.9659258262890683122, 1.000000000000000000, 0.9659258262890683122, 1.000000000000000000, 0.9659258262890683122, 1.000000000000000000, 0.9659258262890683122, 1.000000000000000000, 0.9659258262890683122, 1.000000000000000000, 0.9659258262890683122, 1.000000000000000000, 0.9659258262890683122, 1.000000000000000000, 0.9659258262890683122, 1.000000000000000000, 0.9659258262890683122, 1.000000000000000000, 0.9659258262890683122, 1.000000000000000000, 0.9659258262890683122, 1.000000000000000000, 0.9659258262890683122, 1.000000000000000000, 0.9659258262890683122, 1.000000000000000000, 0.9659258262890683122, 1.000000000000000000, 0.9659258262890683122, 1.000000000000000000, 0.9659258262890683122, 1.000000000000000000, 0.9659258262890683122, 1.000000000000000000, 0.9659258262890683122, 1.000000000000000000, 0.9659258262890683122, 1.000000000000000000, 0.9659258262890683122, 1.000000000000000000, 0.9659258262890683122, 1.000000000000000000, 0.9659258262890683122, 1.000000000000000000, 0.9659258262890683122, 1.000000000000000000, 0.9659258262890683122, 1.000000000000000000, 0.9659258262890683122, 1.000000000000000000, 0.9659258262890683122, 1.000000000000000000, 0.9659258262890683122, 1.000000000000000000, 0.9659258262890683122, 1.000000000000000000, 0.9659258262890683122, 1.000000000000000000, 0.9659258262890683122, 1.000000000000000000, 0.9659258262890683122, 1.000000000000000000, 0.9659258262890683122, 1.000000000000000000, 0.9659258262890683122, 1.000000000000000000, 0.9659258262890683122, 1.000000000000000000, 0.9659258262890683122, 1.000000000000000000, 0.9659258262890683122, 1.000000000000000000, 0.9659258262890683122, 1.000000000000000000, 0.9659258262890683122, 1.000000000000000000, 0.9659258262890683122, 1.000000000000000000, 0.9659258262890683122, 1.000000000000000000, 0.9659258262890683122, 1.000000000000000000, 0.9659258262890683122, 1.000000000000000000, 0.9659258262890683122, 1.000000000000000000, 0.9659258262890683122, 1.000000000000000000, 0.9659258262890683122, 1.000000000000000000, 0.9659258262890683122, 1.000000000000000000, 0.9659258262890683122, 1.000000000000000000, 0.9659258262890683122, 1.000000000000000000, 0.9659258262890683122, 1.000000000000000000, 0.9659258262890683122, 1.000000000000000000, 0.9659258262890683122, 1.000000000000000000, 0.9659258262890683122, 1.000000000000000000, 0.9659258262890683122, 1.000000000000000000, 0.9659258262890683122, 1.000000000000000000, 0.9659258262890683122, 1.000000000000000000, 0.9659258262890683122, 1.000000000000000000, 0.9659258262890683122, 1.000000000000000000, 0.9659258262890683122, 1.000000000000000000, 0.9659258262890683122, 1.000000000000000000, 0.9659258262890683122, 1.000000000000000000, 0.9659258262890683122, 1.000000000000000000, 0.9659258262890683122, 1.000000000000000000, 0.9659258262890683122, 1.000000000000000000, 0.9659258262890683122, 1.000000000000000000, 0.9659258262890683122, 1.000000000000000000, 0.9659258262890683122, 1.000000000000000000, 0.9659258262890683122, 1.000000000000000000, 0.9659258262890683122, 1.000000000000000000, 0.9659258262890683122, 1.000000000000000000, 0.9659258262890683122, 1.000000000000000000, 0.9659258262890683122, 1.000000000000000000, 0.9659258262890683122, 1.000000000000000000, 0.9659258262890683122, 1.000000000000000000, 0.9659258262890683122, 1.000000000000000000, 0.9659258262890683122, 1.000000000000000000, 0.9659258262890683122, 1.000000000000000000, 0.9659258262890683122, 1.000000000000000000, 0.9659258262890683122, 1.000000000000000000, 0.9659258262890683122, 1.000000000000000000, 0.9659258262890683122, 1.000000000000000000, 0.9659258262890683122, 1.000000000000000000, 0.9659258262890683122, 1.000000000000000000, 0.9659258262890683122, 1.000000000000000000, 0.9659258262890683122, 1.000000000000000000, 0.9659258262890683122, 1.000000000000000000, 0.9659258262890683122, 1.000000000000000000, 0.9659258262890683122, 1.000000000000000000, 0.9659258262890683122, 1.000000000000000000, 0.9659258262890683122, 1.000000000000000000, 0.9659258262890683122, 1.000000000000000000, 0.9659258262890683122, 1.000000000000000000, 0.9659258262890683122, 1.000000000000000000, 0.9659258262890683122, 1.000000000000000000, 0.9659258262890683122, 1.000000000000000000, 0.9659258262890683122, 1.000000000000000000, 0.9659258262890683122, 1.000000000000000000, 0.9659258262890683122, 1.000000000000000000, 0.9659258262890683122, 1.000000000000000000, 0.9659258262890683122, 1.000000000000000000, 0.9659258262890683122, 1.000000000000000000, 0.9659258262890683122, 1.000000000000000000, 0.9659258262890683122, 1.000000000000000000, 0.9659258262890683122, 1.000000000000000000, 0.9659258262890683122, 1.000000000000000000, 0.9659258262890683122, 1.000000000000000000, 0.9659258262890683122, 1.000000000000000000, 0.9659258262890683122, 1.000000000000000000, 0.9659258262890683122, 1.000000000000000000, 0.9659258262890683122, 1.000000000000000000, 0.9659258262890683122, 1.000000000000000000, 0.9659258262890683122, 1.000000000000000000, 0.9659258262890683122, 1.000000000000000000, 0.9659258262890683122, 1.000000000000000000, 0.9659258262890683122, 1.000000000000000000, 0.9659258262890683122, 1.000000000000000000, 0.9659258262890683122, 1.000000000000000000, 0.9659258262890683122, 1.000000000000000000, 0.9659258262890683122, 1.000000000000000000) ) ) 
 REPRESENTATION_ITEM ( '' )  SURFACE ( )  );
#39063 = CARTESIAN_POINT ( 'NONE',  ( 16.51473224551083163, -9.474510206698727899, 95.83442372801900433 ) ) ;
#39064 = CARTESIAN_POINT ( 'NONE',  ( 16.51473224551069308, 9.474510206698969483, 44.16557627198103120 ) ) ;
#39065 = CARTESIAN_POINT ( 'NONE',  ( -13.89961937509977652, 13.97604488694528158, 75.62390960531438111 ) ) ;
#39066 = CARTESIAN_POINT ( 'NONE',  ( 16.55341960407611168, 4.379528057220329451, 98.95724293864770971 ) ) ;
#39067 = CARTESIAN_POINT ( 'NONE',  ( 19.02544592524343514, -5.153800228976328945, 98.54057627198100988 ) ) ;
#39068 = CARTESIAN_POINT ( 'NONE',  ( -4.379528057220328563, 16.55341960407611168, 90.20724293864770971 ) ) ;
#39069 = CARTESIAN_POINT ( 'NONE',  ( 13.97604488694527802, 13.89961937509977652, 94.37390960531436690 ) ) ;
#39071 = CARTESIAN_POINT ( 'NONE',  ( -5.049401038298153566, 19.05341960407611168, 40.20724293864768839 ) ) ;
#39070 = CARTESIAN_POINT ( 'NONE',  ( -12.14591786802309592, -12.06949235617757132, 41.87390960531435979 ) ) ;
#39072 = ORIENTED_EDGE ( 'NONE', *, *, #12002, .F. ) ;
#39073 = CARTESIAN_POINT ( 'NONE',  ( 21.53943276465977519, 0.05219959533937863772, 51.25109039468568994 ) ) ;
#39074 = CARTESIAN_POINT ( 'NONE',  ( 9.564922557961047289, -16.46253265017146816, 80.41775706135234714 ) ) ;
#39075 = CARTESIAN_POINT ( 'NONE',  ( 14.29746914071049879, -8.314922557960816363, 48.33224293864770260 ) ) ;
#39076 = CARTESIAN_POINT ( 'NONE',  ( -15.80617190586745835, -15.72974639402198527, 101.8739096053143811 ) ) ;
#39077 = CARTESIAN_POINT ( 'NONE',  ( 15.72974639402199770, -15.80617190586745480, 53.12390960531436690 ) ) ;
#39079 = CARTESIAN_POINT ( 'NONE',  ( -4.483927247898539470, -16.52544592524342804, 82.29057627198103830 ) ) ;
#39078 = CARTESIAN_POINT ( 'NONE',  ( 19.49190055781010500, 5.500000000000047962, 73.06116087098777712 ) ) ;
#39080 = CARTESIAN_POINT ( 'NONE',  ( -5.153800228976328057, -19.02544592524343514, 57.29057627198103120 ) ) ;
#39081 = CARTESIAN_POINT ( 'NONE',  ( -0.05219959533910754901, -16.53943276465976808, 27.49890960531435269 ) ) ;
#39082 = CARTESIAN_POINT ( 'NONE',  ( 4.379528057220092307, 16.55341960407617563, 107.2927570613523471 ) ) ;
#39083 = CARTESIAN_POINT ( 'NONE',  ( -16.53943276465976808, -0.05219959533934237506, 68.75109039468568994 ) ) ;
#39084 = CARTESIAN_POINT ( 'NONE',  ( 9.474510206698729675, 16.51473224551082808, 27.08442372801900433 ) ) ;
#39086 = CARTESIAN_POINT ( 'NONE',  ( 13.97604488694527802, 13.89961937509977652, 109.3739096053143669 ) ) ;
#39085 = DIRECTION ( 'NONE',  ( 1.000000000000000000, 0.000000000000000000, 0.000000000000000000 ) ) ;
#39087 = CARTESIAN_POINT ( 'NONE',  ( -5.153800228976328057, -19.02544592524343514, 82.29057627198103830 ) ) ;
#39088 = CARTESIAN_POINT ( 'NONE',  ( -19.02544592524342804, 5.153800228976336051, 41.04057627198103120 ) ) ;
#39089 = CARTESIAN_POINT ( 'NONE',  ( 4.379528057220339221, -16.55341960407611168, 42.70724293864770260 ) ) ;
#39091 = CARTESIAN_POINT ( 'NONE',  ( -13.89961937509977652, 13.97604488694528158, 100.6239096053143669 ) ) ;
#39090 = CARTESIAN_POINT ( 'NONE',  ( -9.564922557960796823, -16.46253265017161027, 112.0822429386476955 ) ) ;
#39092 = CARTESIAN_POINT ( 'NONE',  ( -21.55341960407610458, -5.719274019375992779, 41.45724293864769550 ) ) ;
#39093 = CARTESIAN_POINT ( 'NONE',  ( -0.05219959533910754901, -16.53943276465976808, 82.49890960531436690 ) ) ;
#39094 = CARTESIAN_POINT ( 'NONE',  ( -4.379528057220086978, -16.55341960407618274, 39.79275706135235424 ) ) ;
#39095 = CARTESIAN_POINT ( 'NONE',  ( 0.05219959533910956823, 16.53943276465976808, 64.99890960531435269 ) ) ;
#39096 = CARTESIAN_POINT ( 'NONE',  ( 35.00000000000000000, -3.889087296526014814, 1.818019484660534424 ) ) ;
#39097 = CARTESIAN_POINT ( 'NONE',  ( 19.02544592524334988, 5.153800228976608722, 66.45942372801899012 ) ) ;
#39098 = CARTESIAN_POINT ( 'NONE',  ( -13.97604488694527625, -13.89961937509977652, 101.8739096053143811 ) ) ;
#39099 = CARTESIAN_POINT ( 'NONE',  ( -19.05341960407617563, 5.049401038297882671, 73.54275706135233293 ) ) ;
#39100 = CARTESIAN_POINT ( 'NONE',  ( -27.73933785331498925, 9.013057229001089965, 147.2750000027311614 ) ) ;
#39102 = CARTESIAN_POINT ( 'NONE',  ( -0.05219959533934338120, 16.53943276465976808, 112.5010903946857042 ) ) ;
#39101 = CARTESIAN_POINT ( 'NONE',  ( -16.46253265017146816, -9.564922557961047289, 109.1677570613523471 ) ) ;
#39103 = CARTESIAN_POINT ( 'NONE',  ( -9.564922557961040184, 16.46253265017147172, 67.91775706135233293 ) ) ;
#39104 = CARTESIAN_POINT ( 'NONE',  ( 5.823673210054125526, 21.52544592524343514, 29.79057627198102409 ) ) ;
#39105 = CARTESIAN_POINT ( 'NONE',  ( 5.823673210054444382, -21.52544592524334988, 70.20942372801904696 ) ) ;
#39106 = CARTESIAN_POINT ( 'NONE',  ( -21.04946095171256104, -10.24435024061084931, 168.3368280404223754 ) ) ;
#39107 = CARTESIAN_POINT ( 'NONE',  ( -0.05219959533934338120, 16.53943276465976808, 27.50109039468567929 ) ) ;
#39109 = CARTESIAN_POINT ( 'NONE',  ( 0.05219959533909260263, 19.03943276465977164, 69.99890960531435269 ) ) ;
#39108 = CARTESIAN_POINT ( 'NONE',  ( 18.22780087662122384, -5.500000000000022204, 56.01540105326107977 ) ) ;
#39110 = CARTESIAN_POINT ( 'NONE',  ( 14.68143632974469881, 16.57870055856060887, -58.31140971112360205 ) ) ;
#39112 = CARTESIAN_POINT ( 'NONE',  ( -16.46253265017160317, 9.564922557960807481, 70.83224293864770971 ) ) ;
#39111 = CARTESIAN_POINT ( 'NONE',  ( 12.14591786802309770, 12.06949235617756955, 89.37390960531435269 ) ) ;
#39113 = CARTESIAN_POINT ( 'NONE',  ( 16.46253265017160672, -9.564922557960803928, 88.33224293864769550 ) ) ;
#39114 = CARTESIAN_POINT ( 'NONE',  ( 0.05219959533936267826, -19.03943276465977164, 95.00109039468567573 ) ) ;
#39115 = CARTESIAN_POINT ( 'NONE',  ( 10.81492255796078972, 18.62759615963270932, 74.58224293864768129 ) ) ;
#39116 = CARTESIAN_POINT ( 'NONE',  ( 0.05219959533909260263, 19.03943276465977164, 24.99890960531435269 ) ) ;
#39117 = CARTESIAN_POINT ( 'NONE',  ( -16.51473224551082808, 9.474510206698731452, 58.33442372801900433 ) ) ;
#39118 = CARTESIAN_POINT ( 'NONE',  ( 16.51473224551069308, 9.474510206698969483, 54.16557627198103120 ) ) ;
#39120 = EDGE_CURVE ( 'NONE', #31542, #82818, #43493, .T. ) ;
#39119 = CARTESIAN_POINT ( 'NONE',  ( 19.02544592524343514, -5.153800228976328945, 88.54057627198102409 ) ) ;
#39121 = ORIENTED_EDGE ( 'NONE', *, *, #68419, .T. ) ;
#39122 = CARTESIAN_POINT ( 'NONE',  ( -5.719274019375978568, 21.55341960407610458, 105.2072429386477097 ) ) ;
#39125 = CARTESIAN_POINT ( 'NONE',  ( -5.049401038297874678, -19.05341960407617918, 59.79275706135231871 ) ) ;
#39124 = CARTESIAN_POINT ( 'NONE',  ( 19.02544592524343514, -5.153800228976328945, 83.54057627198100988 ) ) ;
#39123 = CARTESIAN_POINT ( 'NONE',  ( 4.379528057220339221, -16.55341960407611168, 87.70724293864769550 ) ) ;
#39126 = CARTESIAN_POINT ( 'NONE',  ( -18.67979575497178146, -10.72451020669898902, 86.66557627198102409 ) ) ;
#39127 = CARTESIAN_POINT ( 'NONE',  ( 15.72974639402199770, -15.80617190586745480, 73.12390960531436690 ) ) ;
#39128 = CARTESIAN_POINT ( 'NONE',  ( -0.05219959533910754901, -16.53943276465976808, 32.49890960531435979 ) ) ;
#39129 = CARTESIAN_POINT ( 'NONE',  ( -10.72451020669870658, -18.67979575497194134, 104.5844237280190185 ) ) ;
#39130 = CARTESIAN_POINT ( 'NONE',  ( -8.314922557961024197, 14.29746914071037800, 62.91775706135236135 ) ) ;
#39131 = CARTESIAN_POINT ( 'NONE',  ( -5.049401038298153566, 19.05341960407611168, 95.20724293864770971 ) ) ;
#39132 = CARTESIAN_POINT ( 'NONE',  ( 13.97604488694527802, 13.89961937509977652, 29.37390960531435979 ) ) ;
#39133 = CARTESIAN_POINT ( 'NONE',  ( 15.80617190586769283, -15.72974639402175789, 40.62609039468567573 ) ) ;
#39134 = CARTESIAN_POINT ( 'NONE',  ( -10.72451020669870658, -18.67979575497194134, 49.58442372801901143 ) ) ;
#39135 = CARTESIAN_POINT ( 'NONE',  ( -0.05219959533909027116, -19.03943276465977164, 57.49890960531435979 ) ) ;
#39136 = CARTESIAN_POINT ( 'NONE',  ( 18.67979575497194134, -10.72451020669871369, 35.83442372801901143 ) ) ;
#39137 = CARTESIAN_POINT ( 'NONE',  ( 9.564922557961047289, -16.46253265017146816, 75.41775706135234714 ) ) ;
#39138 = CARTESIAN_POINT ( 'NONE',  ( 13.89961937509957401, 13.97604488694547697, 71.87609039468567573 ) ) ;
#39139 = CARTESIAN_POINT ( 'NONE',  ( 19.03943276465977164, -0.05219959533909143690, 43.74890960531435979 ) ) ;
#39140 = CARTESIAN_POINT ( 'NONE',  ( 16.52544592524335698, 4.483927247898782831, 71.45942372801901854 ) ) ;
#39141 = CARTESIAN_POINT ( 'NONE',  ( 9.474510206698971260, -16.51473224551069308, 52.91557627198102409 ) ) ;
#39142 = CARTESIAN_POINT ( 'NONE',  ( 24.66578506923904968, -3.377805382905422427, 172.1149105766468210 ) ) ;
#39143 = CARTESIAN_POINT ( 'NONE',  ( -16.51473224551069308, -9.474510206698971260, 101.6655762719810241 ) ) ;
#39144 = CARTESIAN_POINT ( 'NONE',  ( -9.474510206698964154, 16.51473224551069663, 40.41557627198103120 ) ) ;
#39145 = CARTESIAN_POINT ( 'NONE',  ( -10.81492255796078084, -18.62759615963271287, 77.08224293864769550 ) ) ;
#39146 = CARTESIAN_POINT ( 'NONE',  ( 8.224510206698742110, 14.34966873604972548, 67.08442372801901854 ) ) ;
#39147 = CARTESIAN_POINT ( 'NONE',  ( -5.823673210054431948, 21.52544592524334988, 112.7094237280190328 ) ) ;
#39148 = CARTESIAN_POINT ( 'NONE',  ( -5.049401038298153566, 19.05341960407611168, 50.20724293864770260 ) ) ;
#39149 = CARTESIAN_POINT ( 'NONE',  ( 0.05219959533910956823, 16.53943276465976808, 39.99890960531436690 ) ) ;
#39150 = CARTESIAN_POINT ( 'NONE',  ( -14.34966873604960291, -8.224510206698953496, 86.66557627198102409 ) ) ;
#39151 = CARTESIAN_POINT ( 'NONE',  ( 19.05341960407611168, 5.049401038298154454, 83.95724293864766707 ) ) ;
#39152 = CARTESIAN_POINT ( 'NONE',  ( 0.05219959533937995610, -21.53943276465977519, 35.00109039468568284 ) ) ;
#39153 = CARTESIAN_POINT ( 'NONE',  ( 13.89961937509977652, -13.97604488694527269, 88.12390960531438111 ) ) ;
#39154 = CARTESIAN_POINT ( 'NONE',  ( 21.55341960407619695, -5.719274019375665929, 101.0427570613523756 ) ) ;
#39155 = CARTESIAN_POINT ( 'NONE',  ( -14.34966873604972548, 8.224510206698743886, 68.33442372801900433 ) ) ;
#39156 = CARTESIAN_POINT ( 'NONE',  ( -16.51473224551069308, -9.474510206698971260, 111.6655762719810383 ) ) ;
#39157 = CARTESIAN_POINT ( 'NONE',  ( 15.72974639402199770, -15.80617190586745480, 88.12390960531436690 ) ) ;
#39158 = CARTESIAN_POINT ( 'NONE',  ( 12.14591786802309770, 12.06949235617756955, 49.37390960531436690 ) ) ;
#39159 = CARTESIAN_POINT ( 'NONE',  ( 16.46253265017160672, -9.564922557960803928, 38.33224293864768839 ) ) ;
#39160 = CARTESIAN_POINT ( 'NONE',  ( 16.53943276465976808, -0.05219959533910856209, 63.74890960531435979 ) ) ;
#39161 = CARTESIAN_POINT ( 'NONE',  ( -5.719274019375978568, 21.55341960407610458, 35.20724293864768839 ) ) ;
#39162 = CARTESIAN_POINT ( 'NONE',  ( -21.52544592524343514, 5.823673210054127303, 26.04057627198103475 ) ) ;
#39163 = CARTESIAN_POINT ( 'NONE',  ( -19.03943276465977164, -0.05219959533935918106, 33.75109039468566863 ) ) ;
#39164 = CARTESIAN_POINT ( 'NONE',  ( 0.05219959533910956823, 16.53943276465976808, 104.9989096053143669 ) ) ;
#39165 = CARTESIAN_POINT ( 'NONE',  ( 16.46253265017160672, -9.564922557960803928, 103.3322429386476955 ) ) ;
#39166 = ORIENTED_EDGE ( 'NONE', *, *, #46412, .T. ) ;
#39167 = CARTESIAN_POINT ( 'NONE',  ( 0.05219959533934541429, -16.53943276465976808, 55.00109039468568284 ) ) ;
#39168 = CARTESIAN_POINT ( 'NONE',  ( -13.89961937509977652, 13.97604488694528158, 60.62390960531436690 ) ) ;
#39169 = CARTESIAN_POINT ( 'NONE',  ( -193.3062444957834884, -155.7167183371838064, -4.999999999999999112 ) ) ;
#39170 = CARTESIAN_POINT ( 'NONE',  ( -9.564922557961040184, 16.46253265017147172, 57.91775706135233293 ) ) ;
#39171 = CARTESIAN_POINT ( 'NONE',  ( -4.379528057220086978, -16.55341960407618274, 94.79275706135234714 ) ) ;
#39172 = CARTESIAN_POINT ( 'NONE',  ( 5.049401038297881783, 19.05341960407617563, 92.29275706135234714 ) ) ;
#39173 = CARTESIAN_POINT ( 'NONE',  ( -15.80617190586768217, 15.72974639402176855, 63.12609039468568994 ) ) ;
#39174 = CARTESIAN_POINT ( 'NONE',  ( -19.05341960407611168, -5.049401038298163336, 71.45724293864766707 ) ) ;
#39175 = CARTESIAN_POINT ( 'NONE',  ( 21.52544592524344225, -5.823673210054117533, 93.54057627198103830 ) ) ;
#39176 = CARTESIAN_POINT ( 'NONE',  ( -12.06949235617756955, 12.14591786802309770, 110.6239096053143669 ) ) ;
#39177 = B_SPLINE_CURVE_WITH_KNOTS ( 'NONE', 3,
 ( #126545, #127542, #96208, #157897, #19386, #81035, #129523, #190224, #191223, #142711, #97187, #5186, #189243, #84026, #82010, #66867, #128530, #36522, #21370, #114361, #68870, #195231 ),
 .UNSPECIFIED., .F., .F.,
 ( 4, 2, 2, 2, 2, 2, 2, 2, 2, 2, 4 ),
 ( 5.204170427930421283E-18, 0.001309639967555401930, 0.001964459951333100401, 0.002291869943221949528, 0.002455574939166360864, 0.002619279935110772201, 0.002782984931055183537, 0.002946689926999595741, 0.003274099918888392392, 0.003928919902666009115, 0.005238559870221241692 ),
 .UNSPECIFIED. ) ;
#39178 = CARTESIAN_POINT ( 'NONE',  ( -19.05341960407617563, 5.049401038297882671, 83.54275706135233293 ) ) ;
#39179 = CARTESIAN_POINT ( 'NONE',  ( -21.53943276465977519, 0.05219959533907696930, 71.24890960531435269 ) ) ;
#39180 = CARTESIAN_POINT ( 'NONE',  ( -0.05219959533936034679, 19.03943276465977164, 47.50109039468566863 ) ) ;
#39181 = CARTESIAN_POINT ( 'NONE',  ( 19.53091890409952569, 5.499999999999982236, 97.56097431831416600 ) ) ;
#39182 = CARTESIAN_POINT ( 'NONE',  ( -5.823673210054116645, -21.52544592524344225, 87.29057627198103830 ) ) ;
#39183 = CARTESIAN_POINT ( 'NONE',  ( 17.49999999999999645, 5.500000000000000888, 28.78230962303566542 ) ) ;
#39184 = CARTESIAN_POINT ( 'NONE',  ( -13.97604488694527625, -13.89961937509977652, 61.87390960531435979 ) ) ;
#39185 = DIRECTION ( 'NONE',  ( 0.000000000000000000, 0.000000000000000000, 1.000000000000000000 ) ) ;
#39186 = CARTESIAN_POINT ( 'NONE',  ( 8.314922557961029526, -14.29746914071037800, 20.41775706135234714 ) ) ;
#39187 = CARTESIAN_POINT ( 'NONE',  ( 36.85371136276476278, -2.758154363750434879, 49.76185830465986015 ) ) ;
#39188 = CARTESIAN_POINT ( 'NONE',  ( -0.05219959533909027116, -19.03943276465977164, 42.49890960531435269 ) ) ;
#39190 = CARTESIAN_POINT ( 'NONE',  ( -16.53943276465976808, 0.05219959533911058130, 51.24890960531436690 ) ) ;
#39189 = CARTESIAN_POINT ( 'NONE',  ( 18.67979575497178502, 10.72451020669898547, 109.1655762719810383 ) ) ;
#39192 = CARTESIAN_POINT ( 'NONE',  ( -5.049401038298153566, 19.05341960407611168, 60.20724293864768129 ) ) ;
#39191 = B_SPLINE_CURVE_WITH_KNOTS ( 'NONE', 3,
 ( #77738, #91893, #46410, #47418, #170753, #93900, #169753, #166795, #153584, #122247, #43440, #107075, #139404, #155578, #58600, #89936, #120266, #183937, #181958, #45422 ),
 .UNSPECIFIED., .F., .F.,
 ( 4, 2, 2, 2, 2, 2, 2, 2, 2, 4 ),
 ( 0.000000000000000000, 0.0004987090165372690164, 0.0009974180330745380327, 0.001246772541343168800, 0.001496127049611799568, 0.001994836066149061320, 0.002493545082686322422, 0.002742899590954955575, 0.002992254099223587861, 0.003989672132298133916 ),
 .UNSPECIFIED. ) ;
#39193 = CARTESIAN_POINT ( 'NONE',  ( 15.80617190586769283, -15.72974639402175789, 80.62609039468567573 ) ) ;
#39195 = CARTESIAN_POINT ( 'NONE',  ( 19.03943276465977164, 0.05219959533936151252, 26.25109039468566507 ) ) ;
#39194 = CARTESIAN_POINT ( 'NONE',  ( -14.34966873604972548, 8.224510206698743886, 23.33442372801901499 ) ) ;
#39196 = CARTESIAN_POINT ( 'NONE',  ( 12.14591786802309770, 12.06949235617756955, 24.37390960531435979 ) ) ;
#39197 = CARTESIAN_POINT ( 'NONE',  ( -21.52544592524334988, -5.823673210054445271, 33.95942372801901143 ) ) ;
#39198 = CARTESIAN_POINT ( 'NONE',  ( -5.719274019375978568, 21.55341960407610458, 115.2072429386476955 ) ) ;
#39199 = CARTESIAN_POINT ( 'NONE',  ( 15.72974639402199770, -15.80617190586745480, 58.12390960531435979 ) ) ;
#39200 = CARTESIAN_POINT ( 'NONE',  ( -9.474510206698720793, -16.51473224551083518, 94.58442372801900433 ) ) ;
#39201 = CARTESIAN_POINT ( 'NONE',  ( -16.46253265017146816, -9.564922557961047289, 69.16775706135233293 ) ) ;
#39202 = CARTESIAN_POINT ( 'NONE',  ( 18.67979575497194134, -10.72451020669871369, 75.83442372801900433 ) ) ;
#39203 = CARTESIAN_POINT ( 'NONE',  ( 9.564922557961047289, -16.46253265017146816, 50.41775706135233293 ) ) ;
#39204 = CARTESIAN_POINT ( 'NONE',  ( -4.379528057220328563, 16.55341960407611168, 115.2072429386476955 ) ) ;
#39205 = CARTESIAN_POINT ( 'NONE',  ( -18.62759615963270932, 10.81492255796079327, 45.83224293864769550 ) ) ;
#39206 = CARTESIAN_POINT ( 'NONE',  ( -4.379528057220328563, 16.55341960407611168, 50.20724293864769550 ) ) ;
#39207 = CARTESIAN_POINT ( 'NONE',  ( -19.52837319214026479, 5.499999999999997335, 94.60471352585537375 ) ) ;
#39208 = CARTESIAN_POINT ( 'NONE',  ( -15.72974639402176322, -15.80617190586768395, 109.3760903946857042 ) ) ;
#39209 = CARTESIAN_POINT ( 'NONE',  ( 4.483927247898790824, -16.52544592524335698, 90.20942372801903275 ) ) ;
#39210 = CARTESIAN_POINT ( 'NONE',  ( 12.06949235617757843, -12.14591786802309237, 43.12390960531435269 ) ) ;
#39211 = CARTESIAN_POINT ( 'NONE',  ( 5.719274019375673035, 21.55341960407619339, 77.29275706135234714 ) ) ;
#39212 = CARTESIAN_POINT ( 'NONE',  ( -15.72974639402176322, -15.80617190586768395, 74.37609039468568994 ) ) ;
#39213 = CARTESIAN_POINT ( 'NONE',  ( -18.67979575497178146, -10.72451020669898902, 86.66557627198102409 ) ) ;
#39214 = CARTESIAN_POINT ( 'NONE',  ( 13.89961937509977652, -13.97604488694527269, 33.12390960531434558 ) ) ;
#39215 = CARTESIAN_POINT ( 'NONE',  ( 15.80617190586769283, -15.72974639402175789, 60.62609039468567573 ) ) ;
#39216 = CARTESIAN_POINT ( 'NONE',  ( -0.05219959533909027116, -19.03943276465977164, 37.49890960531436690 ) ) ;
#39217 = CARTESIAN_POINT ( 'NONE',  ( -19.02544592524342804, 5.153800228976336051, 51.04057627198103120 ) ) ;
#39218 = CARTESIAN_POINT ( 'NONE',  ( -8.314922557960811034, -14.29746914071050412, 87.08224293864769550 ) ) ;
#39219 = CARTESIAN_POINT ( 'NONE',  ( -0.05219959533909027116, -19.03943276465977164, 102.4989096053143669 ) ) ;
#39220 = CARTESIAN_POINT ( 'NONE',  ( 16.53943276465976808, -0.05219959533910856209, 38.74890960531435979 ) ) ;
#39221 = CARTESIAN_POINT ( 'NONE',  ( -16.53943276465976808, 0.05219959533911058130, 116.2489096053143669 ) ) ;
#39222 = CARTESIAN_POINT ( 'NONE',  ( 5.719274019375991003, -21.55341960407610458, 77.70724293864770971 ) ) ;
#39223 = CARTESIAN_POINT ( 'NONE',  ( -21.53943276465977519, -0.05219959533937600094, 18.75109039468568639 ) ) ;
#39224 = FACE_OUTER_BOUND ( 'NONE', #86665, .T. ) ;
#39225 = CARTESIAN_POINT ( 'NONE',  ( -4.483927247898782831, 16.52544592524335698, 27.70942372801901854 ) ) ;
#39226 = CARTESIAN_POINT ( 'NONE',  ( 15.80617190586746368, 15.72974639402197994, 69.37390960531436690 ) ) ;
#39227 = CARTESIAN_POINT ( 'NONE',  ( 21.52544592524334988, 5.823673210054432836, 101.4594237280190185 ) ) ;
#39228 = CARTESIAN_POINT ( 'NONE',  ( 0.05219959533909260263, 19.03943276465977164, 84.99890960531436690 ) ) ;
#39229 = CARTESIAN_POINT ( 'NONE',  ( -21.55341960407619339, 5.719274019375674811, 33.54275706135234714 ) ) ;
#39230 = CARTESIAN_POINT ( 'NONE',  ( 0.05219959533909260263, 19.03943276465977164, 109.9989096053143669 ) ) ;
#39231 = CARTESIAN_POINT ( 'NONE',  ( -16.53943276465976808, -0.05219959533934237506, 93.75109039468567573 ) ) ;
#39232 = CARTESIAN_POINT ( 'NONE',  ( 21.53943276465977519, 0.05219959533937863772, 76.25109039468568994 ) ) ;
#39233 = CARTESIAN_POINT ( 'NONE',  ( 9.564922557961047289, -16.46253265017146816, 20.41775706135233293 ) ) ;
#39234 = CARTESIAN_POINT ( 'NONE',  ( 16.52544592524335698, 4.483927247898782831, 81.45942372801900433 ) ) ;
#39235 = CARTESIAN_POINT ( 'NONE',  ( -10.72451020669870658, -18.67979575497194134, 24.58442372801901499 ) ) ;
#39236 = CARTESIAN_POINT ( 'NONE',  ( 16.46253265017160672, -9.564922557960803928, 38.33224293864768839 ) ) ;
#39237 = CARTESIAN_POINT ( 'NONE',  ( -5.823673210054431948, 21.52544592524334988, 92.70942372801901854 ) ) ;
#39238 = CARTESIAN_POINT ( 'NONE',  ( 19.02544592524343514, -5.153800228976328945, 88.54057627198102409 ) ) ;
#39239 = CARTESIAN_POINT ( 'NONE',  ( -10.72451020669898014, 18.67979575497178502, 90.41557627198103830 ) ) ;
#39240 = CARTESIAN_POINT ( 'NONE',  ( -13.89961937509957401, -13.97604488694547875, 54.37609039468565442 ) ) ;
#39242 = CARTESIAN_POINT ( 'NONE',  ( 15.80617190586746368, 15.72974639402197994, 49.37390960531436690 ) ) ;
#39241 = CARTESIAN_POINT ( 'NONE',  ( 2.973862142520690366, -93.04182470242774627, -15.00000000000000000 ) ) ;
#39244 = CARTESIAN_POINT ( 'NONE',  ( 8.224510206698953496, -14.34966873604960469, 47.91557627198102409 ) ) ;
#39243 = CARTESIAN_POINT ( 'NONE',  ( -9.564922557960796823, -16.46253265017161027, 92.08224293864769550 ) ) ;
#39245 = CARTESIAN_POINT ( 'NONE',  ( 9.797797781461023092, -9.576928023050404803, -62.58071313852363460 ) ) ;
#39246 = CARTESIAN_POINT ( 'NONE',  ( -19.05341960407617563, 5.049401038297882671, 73.54275706135233293 ) ) ;
#39247 = CARTESIAN_POINT ( 'NONE',  ( -17.31728774477273447, 6.344390552232379576, 105.8190665168932014 ) ) ;
#39248 = CARTESIAN_POINT ( 'NONE',  ( -16.46253265017146816, -9.564922557961047289, 104.1677570613523329 ) ) ;
#39249 = CARTESIAN_POINT ( 'NONE',  ( 15.80617190586746368, 15.72974639402197994, 79.37390960531436690 ) ) ;
#39250 = CARTESIAN_POINT ( 'NONE',  ( 0.05219959533910956823, 16.53943276465976808, 69.99890960531435269 ) ) ;
#39251 = CARTESIAN_POINT ( 'NONE',  ( -19.02544592524342804, 5.153800228976336051, 96.04057627198103830 ) ) ;
#39252 = CARTESIAN_POINT ( 'NONE',  ( 14.34966873604972726, -8.224510206698740333, 45.83442372801901854 ) ) ;
#39253 = CARTESIAN_POINT ( 'NONE',  ( -16.46253265017160317, 9.564922557960807481, 60.83224293864769550 ) ) ;
#39255 = CARTESIAN_POINT ( 'NONE',  ( 9.474510206698729675, 16.51473224551082808, 97.08442372801900433 ) ) ;
#39254 = CARTESIAN_POINT ( 'NONE',  ( 21.55341960407619695, -5.719274019375665929, 26.04275706135235779 ) ) ;
#39256 = CARTESIAN_POINT ( 'NONE',  ( -5.153800228976328057, -19.02544592524343514, 92.29057627198099567 ) ) ;
#39257 = CARTESIAN_POINT ( 'NONE',  ( -19.02544592524342804, 5.153800228976336051, 76.04057627198102409 ) ) ;
#39258 = CARTESIAN_POINT ( 'NONE',  ( -15.80617190586745835, -15.72974639402198527, 71.87390960531438111 ) ) ;
#39259 = CARTESIAN_POINT ( 'NONE',  ( 5.153800228976335163, 19.02544592524342804, 44.79057627198103830 ) ) ;
#39260 = CARTESIAN_POINT ( 'NONE',  ( -13.79161361927567597, 35.19715793953689342, -8.000000000000000000 ) ) ;
#39261 = CARTESIAN_POINT ( 'NONE',  ( -16.55341960407611168, -4.379528057220339221, 51.45724293864770260 ) ) ;
#39262 = CARTESIAN_POINT ( 'NONE',  ( 0.05219959533909260263, 19.03943276465977164, 99.99890960531436690 ) ) ;
#39263 = DIRECTION ( 'NONE',  ( -1.000000000000000000, 0.000000000000000000, 0.000000000000000000 ) ) ;
#39264 = CARTESIAN_POINT ( 'NONE',  ( -9.564922557961040184, 16.46253265017147172, 67.91775706135233293 ) ) ;
#39265 = CARTESIAN_POINT ( 'NONE',  ( 0.05219959533907565091, 21.53943276465977519, 94.99890960531436690 ) ) ;
#39266 = CARTESIAN_POINT ( 'NONE',  ( 13.89961937509957401, 13.97604488694547697, 46.87609039468565442 ) ) ;
#39267 = CARTESIAN_POINT ( 'NONE',  ( -19.02544592524342804, 5.153800228976336051, 96.04057627198103830 ) ) ;
#39268 = CARTESIAN_POINT ( 'NONE',  ( 18.89770734986043621, 5.500000000000079936, 66.60214472496636517 ) ) ;
#39269 = CARTESIAN_POINT ( 'NONE',  ( -18.67979575497178146, -10.72451020669898902, 41.66557627198103120 ) ) ;
#39270 = CARTESIAN_POINT ( 'NONE',  ( 9.474510206698971260, -16.51473224551069308, 82.91557627198103830 ) ) ;
#39271 = CARTESIAN_POINT ( 'NONE',  ( -21.52544592524334988, -5.823673210054445271, 68.95942372801901854 ) ) ;
#39272 = CARTESIAN_POINT ( 'NONE',  ( -13.89961937509977652, 13.97604488694528158, 40.62390960531435979 ) ) ;
#39274 = ORIENTED_EDGE ( 'NONE', *, *, #56349, .T. ) ;
#39273 = CARTESIAN_POINT ( 'NONE',  ( 4.483927247898545687, 16.52544592524342804, 79.79057627198102409 ) ) ;
#39275 = CARTESIAN_POINT ( 'NONE',  ( -12.14591786802326823, 12.06949235617739902, 28.12609039468568284 ) ) ;
#39276 = CARTESIAN_POINT ( 'NONE',  ( -0.05219959533937732626, 21.53943276465977519, 47.50109039468568994 ) ) ;
#39277 = VERTEX_POINT ( 'NONE', #184133 ) ;
#39278 = CARTESIAN_POINT ( 'NONE',  ( -25.89282049031357857, -12.30142083841955269, 140.0000000000000000 ) ) ;
#39279 = CARTESIAN_POINT ( 'NONE',  ( 0.05219959533936267826, -19.03943276465977164, 60.00109039468566863 ) ) ;
#39280 = CARTESIAN_POINT ( 'NONE',  ( -20.48541513753863796, 11.15937153969632156, 168.1083253156164119 ) ) ;
#39281 = CARTESIAN_POINT ( 'NONE',  ( 0.05219959533937995610, -21.53943276465977519, 20.00109039468568639 ) ) ;
#39282 = CARTESIAN_POINT ( 'NONE',  ( 9.564922557960805705, 16.46253265017160317, 64.58224293864769550 ) ) ;
#39283 = CARTESIAN_POINT ( 'NONE',  ( 23.48529157249600630, -32.32473071737749137, -9.049999994537627046 ) ) ;
#39284 = CARTESIAN_POINT ( 'NONE',  ( -18.67979575497193778, 10.72451020669871902, 113.3344237280190328 ) ) ;
#39285 = CARTESIAN_POINT ( 'NONE',  ( -16.46253265017160317, 9.564922557960807481, 45.83224293864769550 ) ) ;
#39286 = CARTESIAN_POINT ( 'NONE',  ( -16.51473224551082808, 9.474510206698731452, 23.33442372801900078 ) ) ;
#39287 = CARTESIAN_POINT ( 'NONE',  ( 4.379528057220092307, 16.55341960407617563, 87.29275706135236135 ) ) ;
#39289 = CARTESIAN_POINT ( 'NONE',  ( 21.55341960407619695, -5.719274019375665929, 71.04275706135234714 ) ) ;
#39288 = CARTESIAN_POINT ( 'NONE',  ( -5.049401038298153566, 19.05341960407611168, 100.2072429386476955 ) ) ;
#39290 = CARTESIAN_POINT ( 'NONE',  ( -22.44159573604009950, -16.30477369853688430, 147.5750000027312012 ) ) ;
#39291 = CARTESIAN_POINT ( 'NONE',  ( 24.99873734152946270, 24.49873734152886229, 5.353553390593268624 ) ) ;
#39292 = DIRECTION ( 'NONE',  ( -0.000000000000000000, -0.000000000000000000, 1.000000000000000000 ) ) ;
#39294 = CARTESIAN_POINT ( 'NONE',  ( 5.719274019375673035, 21.55341960407619339, 77.29275706135234714 ) ) ;
#39293 = CARTESIAN_POINT ( 'NONE',  ( 16.52544592524335698, 4.483927247898782831, 71.45942372801901854 ) ) ;
#39295 = CARTESIAN_POINT ( 'NONE',  ( -10.81492255796105439, 18.62759615963255655, 97.91775706135236135 ) ) ;
#39296 = LINE ( 'NONE', #144465, #79954 ) ;
#39297 = CARTESIAN_POINT ( 'NONE',  ( 8.314922557961029526, -14.29746914071037800, 40.41775706135234714 ) ) ;
#39298 = CARTESIAN_POINT ( 'NONE',  ( -0.05219959533909027116, -19.03943276465977164, 82.49890960531436690 ) ) ;
#39299 = CARTESIAN_POINT ( 'NONE',  ( 0.05219959533909260263, 19.03943276465977164, 104.9989096053143669 ) ) ;
#39300 = CARTESIAN_POINT ( 'NONE',  ( 0.000000000000000000, 0.000000000000000000, -52.65483682830183199 ) ) ;
#39301 = CARTESIAN_POINT ( 'NONE',  ( 13.89961937509977652, -13.97604488694527269, 43.12390960531434558 ) ) ;
#39302 = CARTESIAN_POINT ( 'NONE',  ( -10.81492255796078084, -18.62759615963271287, 37.08224293864768129 ) ) ;
#39303 = CARTESIAN_POINT ( 'NONE',  ( 16.52544592524335698, 4.483927247898782831, 111.4594237280190328 ) ) ;
#39305 = CARTESIAN_POINT ( 'NONE',  ( -0.05219959533909027116, -19.03943276465977164, 77.49890960531435269 ) ) ;
#39304 = CARTESIAN_POINT ( 'NONE',  ( 8.224510206698953496, -14.34966873604960469, 77.91557627198102409 ) ) ;
#39306 = CARTESIAN_POINT ( 'NONE',  ( -10.72451020669870658, -18.67979575497194134, 109.5844237280190328 ) ) ;
#39307 = CARTESIAN_POINT ( 'NONE',  ( -16.51473224551069308, -9.474510206698971260, 31.66557627198102054 ) ) ;
#39308 = CARTESIAN_POINT ( 'NONE',  ( 8.314922557960818139, 14.29746914071049879, 84.58224293864769550 ) ) ;
#39309 = CARTESIAN_POINT ( 'NONE',  ( -10.81492255796105439, 18.62759615963255655, 42.91775706135235424 ) ) ;
#39310 = CARTESIAN_POINT ( 'NONE',  ( 21.55341960407610458, 5.719274019375980345, 88.95724293864769550 ) ) ;
#39311 = CARTESIAN_POINT ( 'NONE',  ( -5.049401038297874678, -19.05341960407617918, 54.79275706135234003 ) ) ;
#39312 = LINE ( 'NONE', #120140, #78770 ) ;
#39313 = CARTESIAN_POINT ( 'NONE',  ( -16.46253265017160317, 9.564922557960807481, 100.8322429386477097 ) ) ;
#39314 = CARTESIAN_POINT ( 'NONE',  ( 4.379528057220339221, -16.55341960407611168, 67.70724293864769550 ) ) ;
#39315 = CARTESIAN_POINT ( 'NONE',  ( -0.05219959533910754901, -16.53943276465976808, 52.49890960531435979 ) ) ;
#39316 = CARTESIAN_POINT ( 'NONE',  ( 16.55341960407611168, 4.379528057220329451, 28.95724293864769905 ) ) ;
#39318 = EDGE_CURVE ( 'NONE', #17723, #168659, #164256, .T. ) ;
#39317 = CARTESIAN_POINT ( 'NONE',  ( 19.03943276465977164, 0.05219959533936151252, 76.25109039468566152 ) ) ;
#39319 = CARTESIAN_POINT ( 'NONE',  ( 25.54568634023502582, -20.96320343559646915, 7.533197955354848929 ) ) ;
#39320 = CARTESIAN_POINT ( 'NONE',  ( -0.05219959533907301413, -21.53943276465977519, 27.49890960531435269 ) ) ;
#39321 = CARTESIAN_POINT ( 'NONE',  ( 12.06949235617757843, -12.14591786802309237, 93.12390960531436690 ) ) ;
#39322 = DIRECTION ( 'NONE',  ( -0.1178549842436472511, 0.9930308165857339997, -0.000000000000000000 ) ) ;
#39324 = CARTESIAN_POINT ( 'NONE',  ( 18.62759615963271287, -10.81492255796078972, 43.33224293864769550 ) ) ;
#39323 = CARTESIAN_POINT ( 'NONE',  ( 19.05341960407611168, 5.049401038298154454, 43.95724293864769550 ) ) ;
#39325 = CARTESIAN_POINT ( 'NONE',  ( -13.89961937509977652, 13.97604488694528158, 30.62390960531435269 ) ) ;
#39327 = CARTESIAN_POINT ( 'NONE',  ( 19.02544592524343514, -5.153800228976328945, 58.54057627198102409 ) ) ;
#39326 = CARTESIAN_POINT ( 'NONE',  ( -4.379528057220086978, -16.55341960407618274, 74.79275706135234714 ) ) ;
#39328 = CARTESIAN_POINT ( 'NONE',  ( 0.05219959533936267826, -19.03943276465977164, 45.00109039468566863 ) ) ;
#39329 = CARTESIAN_POINT ( 'NONE',  ( -0.05219959533937732626, 21.53943276465977519, 72.50109039468568994 ) ) ;
#39330 = CARTESIAN_POINT ( 'NONE',  ( -10.72451020669898014, 18.67979575497178502, 40.41557627198103120 ) ) ;
#39331 = CARTESIAN_POINT ( 'NONE',  ( 16.52544592524342804, -4.483927247898539470, 108.5405762719810241 ) ) ;
#39332 = CARTESIAN_POINT ( 'NONE',  ( -19.03943276465977164, -0.05219959533935918106, 88.75109039468567573 ) ) ;
#39333 = CARTESIAN_POINT ( 'NONE',  ( -5.950531402560715689E-15, 38.81732327939063509, -3.624999997268813168 ) ) ;
#39335 = CARTESIAN_POINT ( 'NONE',  ( 10.81492255796078972, 18.62759615963270932, 49.58224293864769550 ) ) ;
#39334 = DIRECTION ( 'NONE',  ( 0.000000000000000000, 0.000000000000000000, -1.000000000000000000 ) ) ;
#39336 = CARTESIAN_POINT ( 'NONE',  ( 9.474510206698971260, -16.51473224551069308, 22.91557627198102765 ) ) ;
#39337 = CARTESIAN_POINT ( 'NONE',  ( -21.52544592524334988, -5.823673210054445271, 83.95942372801900433 ) ) ;
#39338 = CARTESIAN_POINT ( 'NONE',  ( 0.05219959533910956823, 16.53943276465976808, 49.99890960531437401 ) ) ;
#39340 = CARTESIAN_POINT ( 'NONE',  ( -12.06949235617756955, 12.14591786802309770, 50.62390960531435979 ) ) ;
#39339 = CARTESIAN_POINT ( 'NONE',  ( 12.14591786802327356, -12.06949235617739191, 65.62609039468568994 ) ) ;
#39341 = CARTESIAN_POINT ( 'NONE',  ( 5.823673210054125526, 21.52544592524343514, 84.79057627198102409 ) ) ;
#39342 = CARTESIAN_POINT ( 'NONE',  ( 15.80617190586746368, 15.72974639402197994, 79.37390960531436690 ) ) ;
#39343 = CARTESIAN_POINT ( 'NONE',  ( -1.069973119862968947, -29.34370184275725180, -49.12095057784389951 ) ) ;
#39344 = CARTESIAN_POINT ( 'NONE',  ( -18.67979575497178146, -10.72451020669898902, 21.66557627198102409 ) ) ;
#39345 = CARTESIAN_POINT ( 'NONE',  ( 4.379528057220339221, -16.55341960407611168, 82.70724293864770971 ) ) ;
#39346 = CARTESIAN_POINT ( 'NONE',  ( -16.51473224551069308, -9.474510206698971260, 61.66557627198103120 ) ) ;
#39347 = CARTESIAN_POINT ( 'NONE',  ( 0.05219959533909260263, 19.03943276465977164, 34.99890960531435979 ) ) ;
#39348 = SHAPE_REPRESENTATION_RELATIONSHIP ( 'NONE' , 'NONE' ,  #112845, #15828 ) ;
#39349 = CARTESIAN_POINT ( 'NONE',  ( 30.00000000000000355, 3.181980515339470905, 8.889087296526001936 ) ) ;
#39350 = CARTESIAN_POINT ( 'NONE',  ( -4.483927247898782831, 16.52544592524335698, 82.70942372801900433 ) ) ;
#39351 = B_SPLINE_CURVE_WITH_KNOTS ( 'NONE', 3,
 ( #12659, #197664, #105639, #123762, #138945, #170288, #61110, #1420, #13631, #44970, #59130, #60125, #93431, #74326, #120797, #151171, #119826, #181511, #43977, #75298, #42990, #167328, #28824, #78258, #122783, #136969, #104655, #184473, #121792, #198658, #183486, #77276, #27839, #91434, #30791, #106628, #29798, #107607, #168302, #169285, #92439, #154125, #185461, #425, #62099, #46951, #89480, #67078 ),
 .UNSPECIFIED., .F., .F.,
 ( 4, 2, 2, 2, 2, 2, 2, 2, 2, 2, 2, 2, 2, 2, 2, 2, 2, 2, 2, 2, 2, 2, 2, 4 ),
 ( 0.01768515071410577122, 0.01915622216236236713, 0.01989175788649066162, 0.02062729361061895611, 0.02209836505887554162, 0.02283390078300383264, 0.02356943650713212365, 0.02504050795538871610, 0.02651157940364531201, 0.02724711512777359956, 0.02798265085190188711, 0.02945372230015844486, 0.03092479374841500261, 0.03239586519667155690, 0.03313140092079984445, 0.03386693664492812506, 0.03460247236905640567, 0.03533800809318470015, 0.03680907954144128219, 0.03754461526556956974, 0.03828015098969785729, 0.03975122243795443933, 0.04048675816208271994, 0.04122229388621100749 ),
 .UNSPECIFIED. ) ;
#39352 = CARTESIAN_POINT ( 'NONE',  ( 18.62759615963255655, 10.81492255796105972, 26.66775706135235424 ) ) ;
#39353 = CARTESIAN_POINT ( 'NONE',  ( 9.474510206698971260, -16.51473224551069308, 72.91557627198102409 ) ) ;
#39354 = CARTESIAN_POINT ( 'NONE',  ( -15.80617190586768217, 15.72974639402176855, 53.12609039468568284 ) ) ;
#39355 = CARTESIAN_POINT ( 'NONE',  ( 13.97604488694527802, 13.89961937509977652, 109.3739096053143669 ) ) ;
#39357 = EDGE_CURVE ( 'NONE', #64290, #97924, #63303, .T. ) ;
#39356 = CARTESIAN_POINT ( 'NONE',  ( -8.863853373469556374, -46.11448583660600065, -24.15755306339368147 ) ) ;
#39358 = ORIENTED_EDGE ( 'NONE', *, *, #31820, .F. ) ;
#39359 = CARTESIAN_POINT ( 'NONE',  ( 21.52544592524334988, 5.823673210054432836, 46.45942372801901854 ) ) ;
#39361 = CARTESIAN_POINT ( 'NONE',  ( -13.97604488694527625, -13.89961937509977652, 101.8739096053143811 ) ) ;
#39360 = CARTESIAN_POINT ( 'NONE',  ( 13.97604488694527802, 13.89961937509977652, 114.3739096053143669 ) ) ;
#39362 = CARTESIAN_POINT ( 'NONE',  ( -19.02544592524334988, -5.153800228976617603, 48.95942372801900433 ) ) ;
#39363 = CARTESIAN_POINT ( 'NONE',  ( 10.72451020669898902, -18.67979575497178502, 107.9155762719810241 ) ) ;
#39364 = CARTESIAN_POINT ( 'NONE',  ( -19.02544592524334988, -5.153800228976617603, 48.95942372801900433 ) ) ;
#39365 = CARTESIAN_POINT ( 'NONE',  ( -13.97604488694547697, 13.89961937509957934, 48.12609039468566863 ) ) ;
#39366 = CARTESIAN_POINT ( 'NONE',  ( 16.52544592524335698, 4.483927247898782831, 106.4594237280190328 ) ) ;
#39367 = DIRECTION ( 'NONE',  ( 1.000000000000000000, -0.000000000000000000, -0.000000000000000000 ) ) ;
#39368 = CARTESIAN_POINT ( 'NONE',  ( -16.46253265017160317, 9.564922557960807481, 65.83224293864769550 ) ) ;
#39369 = CARTESIAN_POINT ( 'NONE',  ( 10.81492255796106328, -18.62759615963255655, 85.41775706135236135 ) ) ;
#39370 = CARTESIAN_POINT ( 'NONE',  ( 5.823673210054444382, -21.52544592524334988, 100.2094237280190043 ) ) ;
#39371 = CARTESIAN_POINT ( 'NONE',  ( 24.28759355007372989, -0.2213677808126924551, -54.22458008397516949 ) ) ;
#39372 = CARTESIAN_POINT ( 'NONE',  ( -0.05219959533909027116, -19.03943276465977164, 97.49890960531436690 ) ) ;
#39373 = CARTESIAN_POINT ( 'NONE',  ( 18.67979575497194134, -10.72451020669871369, 70.83442372801901854 ) ) ;
#39374 = CARTESIAN_POINT ( 'NONE',  ( -4.379528057220086978, -16.55341960407618274, 24.79275706135235779 ) ) ;
#39375 = CARTESIAN_POINT ( 'NONE',  ( -16.51473224551069308, -9.474510206698971260, 76.66557627198103830 ) ) ;
#39376 = CARTESIAN_POINT ( 'NONE',  ( 10.81492255796078972, 18.62759615963270932, 24.58224293864768839 ) ) ;
#39377 = CARTESIAN_POINT ( 'NONE',  ( 13.89961937509977652, -13.97604488694527269, 98.12390960531433848 ) ) ;
#39378 = CARTESIAN_POINT ( 'NONE',  ( -13.97604488694547520, 13.89961937509957934, 88.12609039468564731 ) ) ;
#39379 = CARTESIAN_POINT ( 'NONE',  ( 16.51473224551069308, 9.474510206698969483, 84.16557627198102409 ) ) ;
#39380 = CARTESIAN_POINT ( 'NONE',  ( 16.51473224551069308, 9.474510206698969483, 64.16557627198102409 ) ) ;
#39381 = CARTESIAN_POINT ( 'NONE',  ( -10.81492255796078084, -18.62759615963271287, 112.0822429386477097 ) ) ;
#39382 = CARTESIAN_POINT ( 'NONE',  ( 8.314922557961029526, -14.29746914071037800, 95.41775706135234714 ) ) ;
#39383 = LINE ( 'NONE', #104054, #69481 ) ;
#39384 = CARTESIAN_POINT ( 'NONE',  ( -0.05219959533936034679, 19.03943276465977164, 62.50109039468566863 ) ) ;
#39385 = CARTESIAN_POINT ( 'NONE',  ( 13.89961937509977652, -13.97604488694527269, 88.12390960531438111 ) ) ;
#39386 = CARTESIAN_POINT ( 'NONE',  ( -12.06949235617756955, 12.14591786802309770, 90.62390960531436690 ) ) ;
#39387 = CARTESIAN_POINT ( 'NONE',  ( -5.719274019375978568, 21.55341960407610458, 30.20724293864769550 ) ) ;
#39388 = CARTESIAN_POINT ( 'NONE',  ( 18.62759615963271287, -10.81492255796078972, 28.33224293864769550 ) ) ;
#39389 = CARTESIAN_POINT ( 'NONE',  ( 16.52544592524342804, -4.483927247898539470, 88.54057627198103830 ) ) ;
#39390 = CARTESIAN_POINT ( 'NONE',  ( -3.573655867282028392E-15, 2.428612866367529932E-14, 167.9999999999999716 ) ) ;
#39391 = CARTESIAN_POINT ( 'NONE',  ( 19.02544592524334988, 5.153800228976608722, 46.45942372801899012 ) ) ;
#39392 = CARTESIAN_POINT ( 'NONE',  ( -12.06949235617739369, -12.14591786802326823, 104.3760903946856899 ) ) ;
#39393 = CARTESIAN_POINT ( 'NONE',  ( -19.02544592524342804, 5.153800228976336051, 86.04057627198103830 ) ) ;
#39394 = CARTESIAN_POINT ( 'NONE',  ( -10.81492255796105439, 18.62759615963255655, 67.91775706135234714 ) ) ;
#39395 = CARTESIAN_POINT ( 'NONE',  ( 15.72974639402199770, -15.80617190586745480, 58.12390960531435979 ) ) ;
#39396 = CARTESIAN_POINT ( 'NONE',  ( -18.67979575497193778, 10.72451020669871902, 28.33442372801902209 ) ) ;
#39397 = CARTESIAN_POINT ( 'NONE',  ( 15.80617190586746368, 15.72974639402197994, 89.37390960531435269 ) ) ;
#39398 = CARTESIAN_POINT ( 'NONE',  ( -16.52544592524342804, 4.483927247898546575, 111.0405762719810525 ) ) ;
#39399 = CARTESIAN_POINT ( 'NONE',  ( 9.474510206698729675, 16.51473224551082808, 72.08442372801900433 ) ) ;
#39400 = CARTESIAN_POINT ( 'NONE',  ( 9.564922557960805705, 16.46253265017160317, 49.58224293864770260 ) ) ;
#39401 = CARTESIAN_POINT ( 'NONE',  ( -13.97604488694527625, -13.89961937509977652, 96.87390960531433848 ) ) ;
#39402 = CARTESIAN_POINT ( 'NONE',  ( -9.564922557960796823, -16.46253265017161027, 92.08224293864769550 ) ) ;
#39403 = CARTESIAN_POINT ( 'NONE',  ( -0.05219959533909027116, -19.03943276465977164, 22.49890960531436690 ) ) ;
#39404 = CARTESIAN_POINT ( 'NONE',  ( -16.52544592524342804, 4.483927247898546575, 46.04057627198103830 ) ) ;
#39405 = CARTESIAN_POINT ( 'NONE',  ( 12.14591786802327356, -12.06949235617739191, 45.62609039468567573 ) ) ;
#39406 = CARTESIAN_POINT ( 'NONE',  ( -15.80617190586768217, 15.72974639402176855, 103.1260903946856757 ) ) ;
#39408 = CARTESIAN_POINT ( 'NONE',  ( -4.483927247898539470, -16.52544592524342804, 27.29057627198103120 ) ) ;
#39407 = CARTESIAN_POINT ( 'NONE',  ( 13.89961937509977652, -13.97604488694527269, 113.1239096053143527 ) ) ;
#39409 = CARTESIAN_POINT ( 'NONE',  ( -21.52544592524334988, -5.823673210054445271, 28.95942372801902209 ) ) ;
#39410 = CARTESIAN_POINT ( 'NONE',  ( 19.02544592524343514, -5.153800228976328945, 98.54057627198100988 ) ) ;
#39411 = CARTESIAN_POINT ( 'NONE',  ( 16.52544592524335698, 4.483927247898782831, 106.4594237280190328 ) ) ;
#39412 = CARTESIAN_POINT ( 'NONE',  ( 14.34966873604972726, -8.224510206698740333, 95.83442372801903275 ) ) ;
#39413 = CARTESIAN_POINT ( 'NONE',  ( 16.55341960407618274, -4.379528057220086978, 26.04275706135235779 ) ) ;
#39415 = B_SPLINE_CURVE_WITH_KNOTS ( 'NONE', 3,
 ( #158021, #128659, #112504, #51831, #19512, #126669 ),
 .UNSPECIFIED., .F., .F.,
 ( 4, 2, 4 ),
 ( 0.007228050697041587397, 0.007608510107495056879, 0.007988969517948526361 ),
 .UNSPECIFIED. ) ;
#39414 = CARTESIAN_POINT ( 'NONE',  ( 13.89961937509977652, -13.97604488694527269, 53.12390960531434558 ) ) ;
#39416 = CARTESIAN_POINT ( 'NONE',  ( 8.314922557960818139, 14.29746914071049879, 104.5822429386477097 ) ) ;
#39417 = CARTESIAN_POINT ( 'NONE',  ( 21.52544592524344225, -5.823673210054117533, 113.5405762719810383 ) ) ;
#39418 = CARTESIAN_POINT ( 'NONE',  ( -5.153800228976328057, -19.02544592524343514, 32.29057627198102409 ) ) ;
#39419 = CARTESIAN_POINT ( 'NONE',  ( 9.474510206698971260, -16.51473224551069308, 107.9155762719810383 ) ) ;
#39420 = CARTESIAN_POINT ( 'NONE',  ( -5.049401038298153566, 19.05341960407611168, 30.20724293864768839 ) ) ;
#39421 = CARTESIAN_POINT ( 'NONE',  ( -19.05341960407611168, -5.049401038298163336, 101.4572429386476955 ) ) ;
#39422 = CARTESIAN_POINT ( 'NONE',  ( -17.40805194822032576, -6.112264579159275790, 34.16628727489390371 ) ) ;
#39423 = CARTESIAN_POINT ( 'NONE',  ( 13.89961937509977652, -13.97604488694527269, 98.12390960531433848 ) ) ;
#39425 = CARTESIAN_POINT ( 'NONE',  ( 4.379528057220339221, -16.55341960407611168, 87.70724293864769550 ) ) ;
#39424 = CARTESIAN_POINT ( 'NONE',  ( -10.81492255796105439, 18.62759615963255655, 47.91775706135234714 ) ) ;
#39426 = CARTESIAN_POINT ( 'NONE',  ( 16.51473224551069308, 9.474510206698969483, 99.16557627198102409 ) ) ;
#39427 = CARTESIAN_POINT ( 'NONE',  ( -27.77709992218201052, -7.633332386735008690, 161.4489275245939268 ) ) ;
#39428 = CARTESIAN_POINT ( 'NONE',  ( -16.53943276465976808, -0.05219959533934237506, 68.75109039468568994 ) ) ;
#39429 = CARTESIAN_POINT ( 'NONE',  ( -10.72451020669870658, -18.67979575497194134, 84.58442372801903275 ) ) ;
#39430 = CARTESIAN_POINT ( 'NONE',  ( 12.06949235617739724, 12.14591786802326823, 41.87609039468568284 ) ) ;
#39431 = CARTESIAN_POINT ( 'NONE',  ( -19.02544592524342804, 5.153800228976336051, 81.04057627198103830 ) ) ;
#39432 = CARTESIAN_POINT ( 'NONE',  ( 5.049401038297881783, 19.05341960407617563, 112.2927570613523471 ) ) ;
#39433 = CARTESIAN_POINT ( 'NONE',  ( -12.06949235617739369, -12.14591786802326823, 79.37609039468567573 ) ) ;
#39434 = CARTESIAN_POINT ( 'NONE',  ( 16.46253265017146816, 9.564922557961045513, 91.66775706135234714 ) ) ;
#39435 = CARTESIAN_POINT ( 'NONE',  ( -5.153800228976328057, -19.02544592524343514, 62.29057627198100988 ) ) ;
#39436 = CARTESIAN_POINT ( 'NONE',  ( -18.67979575497178146, -10.72451020669898902, 101.6655762719810383 ) ) ;
#39438 = CARTESIAN_POINT ( 'NONE',  ( 13.97604488694548053, -13.89961937509957401, 95.62609039468563310 ) ) ;
#39437 = CARTESIAN_POINT ( 'NONE',  ( 16.53943276465976808, -0.05219959533910856209, 88.74890960531436690 ) ) ;
#39439 = CARTESIAN_POINT ( 'NONE',  ( 16.53943276465976808, 0.05219959533934440121, 56.25109039468568284 ) ) ;
#39440 = CARTESIAN_POINT ( 'NONE',  ( 24.30454888808800007, 2.781629622375082267, 174.5654150192188183 ) ) ;
#39441 = CARTESIAN_POINT ( 'NONE',  ( 5.153800228976615827, -19.02544592524334988, 55.20942372801899722 ) ) ;
#39442 = CARTESIAN_POINT ( 'NONE',  ( 16.53943276465976808, -0.05219959533910856209, 38.74890960531435979 ) ) ;
#39443 = CARTESIAN_POINT ( 'NONE',  ( 4.379528057220339221, -16.55341960407611168, 82.70724293864770971 ) ) ;
#39445 = CARTESIAN_POINT ( 'NONE',  ( 4.647474457565486646E-15, -28.90000000000004476, -52.65483682830183199 ) ) ;
#39444 = CARTESIAN_POINT ( 'NONE',  ( 21.55341960407619695, -5.719274019375665929, 111.0427570613523613 ) ) ;
#39446 = CARTESIAN_POINT ( 'NONE',  ( 15.80617190586769283, -15.72974639402175789, 20.62609039468568639 ) ) ;
#39447 = CARTESIAN_POINT ( 'NONE',  ( 19.03943276465977164, -0.05219959533909143690, 73.74890960531435269 ) ) ;
#39448 = CARTESIAN_POINT ( 'NONE',  ( 10.72451020669871369, 18.67979575497193778, 92.08442372801901854 ) ) ;
#39449 = CARTESIAN_POINT ( 'NONE',  ( -19.03943276465977164, 0.05219959533909376836, 76.24890960531435269 ) ) ;
#39450 = CARTESIAN_POINT ( 'NONE',  ( 10.72451020669898902, -18.67979575497178502, 47.91557627198102409 ) ) ;
#39451 = CARTESIAN_POINT ( 'NONE',  ( 8.224510206698953496, -14.34966873604960469, 77.91557627198102409 ) ) ;
#39452 = CARTESIAN_POINT ( 'NONE',  ( 19.05341960407611168, 5.049401038298154454, 58.95724293864768129 ) ) ;
#39453 = CARTESIAN_POINT ( 'NONE',  ( 14.34966873604960469, 8.224510206698951720, 109.1655762719810383 ) ) ;
#39454 = CARTESIAN_POINT ( 'NONE',  ( -5.823673210054431948, 21.52544592524334988, 22.70942372801901499 ) ) ;
#39455 = CARTESIAN_POINT ( 'NONE',  ( -10.81492255796105439, 18.62759615963255655, 67.91775706135234714 ) ) ;
#39456 = CARTESIAN_POINT ( 'NONE',  ( -16.46253265017160317, 9.564922557960807481, 40.83224293864769550 ) ) ;
#39457 = CARTESIAN_POINT ( 'NONE',  ( 16.55341960407618274, -4.379528057220086978, 81.04275706135236135 ) ) ;
#39458 = CARTESIAN_POINT ( 'NONE',  ( -5.719274019375978568, 21.55341960407610458, 115.2072429386476955 ) ) ;
#39459 = CARTESIAN_POINT ( 'NONE',  ( -18.62759615963270932, 10.81492255796079327, 115.8322429386477097 ) ) ;
#39461 = CARTESIAN_POINT ( 'NONE',  ( -16.46253265017160317, 9.564922557960807481, 65.83224293864769550 ) ) ;
#39460 = CARTESIAN_POINT ( 'NONE',  ( -19.03943276465977164, -0.05219959533935918106, 33.75109039468566863 ) ) ;
#39462 = CARTESIAN_POINT ( 'NONE',  ( 10.59477242850415024, -90.60836494048558620, -15.00000000000000000 ) ) ;
#39463 = CARTESIAN_POINT ( 'NONE',  ( 21.55341960407619695, -5.719274019375665929, 71.04275706135234714 ) ) ;
#39464 = CARTESIAN_POINT ( 'NONE',  ( 21.52544592524344225, -5.823673210054117533, 58.54057627198103120 ) ) ;
#39465 = CARTESIAN_POINT ( 'NONE',  ( -8.314922557960811034, -14.29746914071050412, 32.08224293864769550 ) ) ;
#39467 = CARTESIAN_POINT ( 'NONE',  ( 21.55341960407619695, -5.719274019375665929, 106.0427570613523471 ) ) ;
#39466 = CARTESIAN_POINT ( 'NONE',  ( 15.72974639402176855, 15.80617190586768217, 76.87609039468567573 ) ) ;
#39468 = CARTESIAN_POINT ( 'NONE',  ( 12.14591786802309770, 12.06949235617756955, 54.37390960531435979 ) ) ;
#39469 = CARTESIAN_POINT ( 'NONE',  ( 0.05219959533910956823, 16.53943276465976808, 99.99890960531436690 ) ) ;
#39470 = CARTESIAN_POINT ( 'NONE',  ( -5.153800228976607833, 19.02544592524334988, 57.70942372801899012 ) ) ;
#39471 = CARTESIAN_POINT ( 'NONE',  ( 16.53943276465976808, -0.05219959533910856209, 28.74890960531435624 ) ) ;
#39472 = CARTESIAN_POINT ( 'NONE',  ( -0.05219959533937732626, 21.53943276465977519, 67.50109039468568994 ) ) ;
#39473 = CARTESIAN_POINT ( 'NONE',  ( 19.03943276465977164, -0.05219959533909143690, 68.74890960531436690 ) ) ;
#39474 = CARTESIAN_POINT ( 'NONE',  ( 9.564922557961047289, -16.46253265017146816, 30.41775706135232937 ) ) ;
#39475 = CARTESIAN_POINT ( 'NONE',  ( -5.823673210054116645, -21.52544592524344225, 42.29057627198103120 ) ) ;
#39476 = CARTESIAN_POINT ( 'NONE',  ( -0.05219959533937732626, 21.53943276465977519, 42.50109039468567573 ) ) ;
#39477 = CARTESIAN_POINT ( 'NONE',  ( -15.72974639402197994, 15.80617190586746368, 100.6239096053143811 ) ) ;
#39478 = CARTESIAN_POINT ( 'NONE',  ( 19.05341960407617918, -5.049401038297876454, 96.04275706135231871 ) ) ;
#39479 = CARTESIAN_POINT ( 'NONE',  ( 0.05219959533934541429, -16.53943276465976808, 55.00109039468568284 ) ) ;
#39481 = CARTESIAN_POINT ( 'NONE',  ( -15.72974639402197994, 15.80617190586746368, 95.62390960531436690 ) ) ;
#39480 = CARTESIAN_POINT ( 'NONE',  ( -17.18269478283327345, -17.18269478283298568, -56.77278709839600879 ) ) ;
#39482 = CARTESIAN_POINT ( 'NONE',  ( 4.379528057220339221, -16.55341960407611168, 92.70724293864770971 ) ) ;
#39483 = CARTESIAN_POINT ( 'NONE',  ( -16.52216118717206683, -7.221426719304509412, 101.0759902104699108 ) ) ;
#39484 = CARTESIAN_POINT ( 'NONE',  ( -5.153800228976607833, 19.02544592524334988, 112.7094237280190043 ) ) ;
#39485 = EDGE_CURVE ( 'NONE', #178697, #59792, #40899, .T. ) ;
#39486 = CARTESIAN_POINT ( 'NONE',  ( -0.05219959533907301413, -21.53943276465977519, 42.49890960531435979 ) ) ;
#39487 = CARTESIAN_POINT ( 'NONE',  ( -16.55341960407617563, 4.379528057220093196, 88.54275706135236135 ) ) ;
#39488 = DIRECTION ( 'NONE',  ( 0.000000000000000000, 0.000000000000000000, -1.000000000000000000 ) ) ;
#39489 = CARTESIAN_POINT ( 'NONE',  ( -4.379528057220086978, -16.55341960407618274, 49.79275706135234714 ) ) ;
#39490 = CARTESIAN_POINT ( 'NONE',  ( 21.55341960407619695, -5.719274019375665929, 31.04275706135234714 ) ) ;
#39491 = CARTESIAN_POINT ( 'NONE',  ( 21.53943276465977519, -0.05219959533907433946, 38.74890960531435979 ) ) ;
#39492 = CARTESIAN_POINT ( 'NONE',  ( -4.379528057220086978, -16.55341960407618274, 79.79275706135236135 ) ) ;
#39493 = CARTESIAN_POINT ( 'NONE',  ( -5.049401038298153566, 19.05341960407611168, 95.20724293864770971 ) ) ;
#39494 = CARTESIAN_POINT ( 'NONE',  ( 5.719274019375673035, 21.55341960407619339, 72.29275706135236135 ) ) ;
#39495 = CARTESIAN_POINT ( 'NONE',  ( 18.67979575497178502, 10.72451020669898547, 34.16557627198102409 ) ) ;
#39496 = CARTESIAN_POINT ( 'NONE',  ( -18.67979575497178146, -10.72451020669898902, 21.66557627198102409 ) ) ;
#39497 = ORIENTED_EDGE ( 'NONE', *, *, #176927, .T. ) ;
#39498 = CARTESIAN_POINT ( 'NONE',  ( -16.46253265017146816, -9.564922557961047289, 54.16775706135234003 ) ) ;
#39499 = CARTESIAN_POINT ( 'NONE',  ( 12.14591786802327356, -12.06949235617739191, 70.62609039468567573 ) ) ;
#39500 = CARTESIAN_POINT ( 'NONE',  ( 0.05219959533907565091, 21.53943276465977519, 34.99890960531435979 ) ) ;
#39501 = ORIENTED_EDGE ( 'NONE', *, *, #176156, .F. ) ;
#39502 = CARTESIAN_POINT ( 'NONE',  ( 9.474510206698971260, -16.51473224551069308, 87.91557627198102409 ) ) ;
#39503 = CARTESIAN_POINT ( 'NONE',  ( 8.314922557961029526, -14.29746914071037800, 110.4177570613523756 ) ) ;
#39504 = DIRECTION ( 'NONE',  ( -0.000000000000000000, -0.000000000000000000, 1.000000000000000000 ) ) ;
#39505 = CARTESIAN_POINT ( 'NONE',  ( 14.34966873604960469, 8.224510206698951720, 109.1655762719810383 ) ) ;
#39506 = CARTESIAN_POINT ( 'NONE',  ( 5.823673210054125526, 21.52544592524343514, 49.79057627198102409 ) ) ;
#39507 = CARTESIAN_POINT ( 'NONE',  ( 5.153800228976335163, 19.02544592524342804, 44.79057627198103830 ) ) ;
#39508 = CARTESIAN_POINT ( 'NONE',  ( -8.314922557961024197, 14.29746914071037800, 72.91775706135234714 ) ) ;
#39509 = CARTESIAN_POINT ( 'NONE',  ( -0.05219959533937732626, 21.53943276465977519, 32.50109039468568284 ) ) ;
#39510 = CARTESIAN_POINT ( 'NONE',  ( -13.89961937509957401, -13.97604488694547875, 89.37609039468563310 ) ) ;
#39511 = CARTESIAN_POINT ( 'NONE',  ( -14.34966873604960291, -8.224510206698953496, 86.66557627198102409 ) ) ;
#39512 = CARTESIAN_POINT ( 'NONE',  ( -19.05341960407611168, -5.049401038298163336, 51.45724293864770260 ) ) ;
#39513 = CARTESIAN_POINT ( 'NONE',  ( -19.05341960407611168, -5.049401038298163336, 26.45724293864769550 ) ) ;
#39514 = CARTESIAN_POINT ( 'NONE',  ( -10.81492255796105439, 18.62759615963255655, 102.9177570613523756 ) ) ;
#39515 = CARTESIAN_POINT ( 'NONE',  ( 19.05341960407611168, 5.049401038298154454, 83.95724293864766707 ) ) ;
#39516 = CARTESIAN_POINT ( 'NONE',  ( -0.05219959533934338120, 16.53943276465976808, 62.50109039468568284 ) ) ;
#39517 = CARTESIAN_POINT ( 'NONE',  ( 15.80617190586769283, -15.72974639402175789, 90.62609039468567573 ) ) ;
#39518 = CARTESIAN_POINT ( 'NONE',  ( -10.81492255796078084, -18.62759615963271287, 52.08224293864768839 ) ) ;
#39519 = CARTESIAN_POINT ( 'NONE',  ( -16.53943276465976808, -0.05219959533934237506, 73.75109039468567573 ) ) ;
#39520 = CARTESIAN_POINT ( 'NONE',  ( 13.97604488694548053, -13.89961937509957401, 55.62609039468566863 ) ) ;
#39521 = CARTESIAN_POINT ( 'NONE',  ( -19.03943276465977164, -0.05219959533935918106, 68.75109039468566152 ) ) ;
#39522 = CARTESIAN_POINT ( 'NONE',  ( 5.719274019375673035, 21.55341960407619339, 67.29275706135234714 ) ) ;
#39523 = CARTESIAN_POINT ( 'NONE',  ( -19.02544592524342804, 5.153800228976336051, 66.04057627198103830 ) ) ;
#39524 = CARTESIAN_POINT ( 'NONE',  ( -5.153800228976328057, -19.02544592524343514, 22.29057627198102765 ) ) ;
#39525 = CARTESIAN_POINT ( 'NONE',  ( -19.05341960407617563, 5.049401038297882671, 63.54275706135234003 ) ) ;
#39526 = CARTESIAN_POINT ( 'NONE',  ( -3.573655867282028392E-15, 2.428612866367529932E-14, -24.99999999999997868 ) ) ;
#39527 = CARTESIAN_POINT ( 'NONE',  ( 19.05341960407611168, 5.049401038298154454, 98.95724293864766707 ) ) ;
#39528 = CARTESIAN_POINT ( 'NONE',  ( -14.29746914071049879, 8.314922557960819915, 50.83224293864770971 ) ) ;
#39529 = CARTESIAN_POINT ( 'NONE',  ( -21.55341960407610458, -5.719274019375992779, 51.45724293864770260 ) ) ;
#39530 = CARTESIAN_POINT ( 'NONE',  ( 21.44473182883397655, 22.99799039501303355, -49.72310555961296075 ) ) ;
#39531 = CARTESIAN_POINT ( 'NONE',  ( 15.80617190586769283, -15.72974639402175789, 110.6260903946857042 ) ) ;
#39532 = SURFACE_STYLE_FILL_AREA ( #108404 ) ;
#39533 = CARTESIAN_POINT ( 'NONE',  ( -16.51473224551069308, -9.474510206698971260, 46.66557627198102409 ) ) ;
#39534 = CARTESIAN_POINT ( 'NONE',  ( 0.05219959533909260263, 19.03943276465977164, 29.99890960531435979 ) ) ;
#39535 = CARTESIAN_POINT ( 'NONE',  ( -34.42160027699925706, -2.272024392515961555, 89.98798656105711302 ) ) ;
#39536 = CARTESIAN_POINT ( 'NONE',  ( -36.91746825000000598, 2.428612866367529932E-14, -0.8749999972688132788 ) ) ;
#39537 = CARTESIAN_POINT ( 'NONE',  ( -8.314922557961024197, 14.29746914071037800, 67.91775706135234714 ) ) ;
#39538 = CARTESIAN_POINT ( 'NONE',  ( -15.72974639402197994, 15.80617190586746368, 80.62390960531438111 ) ) ;
#39539 = CARTESIAN_POINT ( 'NONE',  ( -12.14591786802309592, -12.06949235617757132, 56.87390960531436690 ) ) ;
#39541 = FACE_OUTER_BOUND ( 'NONE', #150311, .T. ) ;
#39540 = CARTESIAN_POINT ( 'NONE',  ( -9.474510206698964154, 16.51473224551069663, 45.41557627198103120 ) ) ;
#39542 = CARTESIAN_POINT ( 'NONE',  ( -5.823673210054431948, 21.52544592524334988, 42.70942372801901854 ) ) ;
#39543 = CARTESIAN_POINT ( 'NONE',  ( 19.02544592524334988, 5.153800228976608722, 46.45942372801899012 ) ) ;
#39544 = CARTESIAN_POINT ( 'NONE',  ( -9.474510206698964154, 16.51473224551069663, 30.41557627198102054 ) ) ;
#39545 = CARTESIAN_POINT ( 'NONE',  ( 15.72974639402176855, 15.80617190586768217, 76.87609039468567573 ) ) ;
#39546 = CARTESIAN_POINT ( 'NONE',  ( 13.89961937509977652, -13.97604488694527269, 23.12390960531436335 ) ) ;
#39547 = ORIENTED_EDGE ( 'NONE', *, *, #115114, .T. ) ;
#39548 = CARTESIAN_POINT ( 'NONE',  ( -16.52544592524342804, 4.483927247898546575, 41.04057627198103120 ) ) ;
#39549 = CARTESIAN_POINT ( 'NONE',  ( 17.49999999999999645, 3.209263204892637500, 112.7380317439374409 ) ) ;
#39550 = CARTESIAN_POINT ( 'NONE',  ( 18.62759615963271287, -10.81492255796078972, 38.33224293864768839 ) ) ;
#39551 = ORIENTED_EDGE ( 'NONE', *, *, #23933, .T. ) ;
#39552 = DIRECTION ( 'NONE',  ( -1.000000000000000000, -0.000000000000000000, -0.000000000000000000 ) ) ;
#39553 = CARTESIAN_POINT ( 'NONE',  ( -19.02544592524342804, 5.153800228976336051, 96.04057627198103830 ) ) ;
#39554 = CARTESIAN_POINT ( 'NONE',  ( -16.52544592524342804, 4.483927247898546575, 91.04057627198103830 ) ) ;
#39555 = CARTESIAN_POINT ( 'NONE',  ( -16.55341960407617563, 4.379528057220093196, 28.54275706135234358 ) ) ;
#39556 = ADVANCED_FACE ( 'NONE', ( #47609 ), #188116, .T. ) ;
#39557 = CARTESIAN_POINT ( 'NONE',  ( -21.53943276465977519, 0.05219959533907696930, 66.24890960531436690 ) ) ;
#39558 = VERTEX_POINT ( 'NONE', #70121 ) ;
#39559 = CARTESIAN_POINT ( 'NONE',  ( 16.46253265017160672, -9.564922557960803928, 28.33224293864769550 ) ) ;
#39561 = CARTESIAN_POINT ( 'NONE',  ( 5.823673210054125526, 21.52544592524343514, 84.79057627198102409 ) ) ;
#39560 = CARTESIAN_POINT ( 'NONE',  ( 5.153800228976335163, 19.02544592524342804, 84.79057627198099567 ) ) ;
#39563 = CARTESIAN_POINT ( 'NONE',  ( 5.049401038298161559, -19.05341960407611168, 102.7072429386476955 ) ) ;
#39562 = CARTESIAN_POINT ( 'NONE',  ( -4.483927247898539470, -16.52544592524342804, 22.29057627198102765 ) ) ;
#39564 = CARTESIAN_POINT ( 'NONE',  ( -13.89961937509957401, -13.97604488694547875, 79.37609039468567573 ) ) ;
#39565 = CARTESIAN_POINT ( 'NONE',  ( 5.719274019375673035, 21.55341960407619339, 107.2927570613523471 ) ) ;
#39566 = CARTESIAN_POINT ( 'NONE',  ( -5.719274019375978568, 21.55341960407610458, 80.20724293864769550 ) ) ;
#39567 = CARTESIAN_POINT ( 'NONE',  ( -21.55341960407610458, -5.719274019375992779, 31.45724293864769550 ) ) ;
#39568 = CARTESIAN_POINT ( 'NONE',  ( 19.02544592524343514, -5.153800228976328945, 63.54057627198103830 ) ) ;
#39569 = CARTESIAN_POINT ( 'NONE',  ( -12.06949235617739369, -12.14591786802326823, 109.3760903946857042 ) ) ;
#39570 = CARTESIAN_POINT ( 'NONE',  ( -16.46253265017160317, 9.564922557960807481, 80.83224293864769550 ) ) ;
#39571 = CARTESIAN_POINT ( 'NONE',  ( -31.79921067246706201, -6.362367971534558464, 91.02144216243111430 ) ) ;
#39572 = CARTESIAN_POINT ( 'NONE',  ( 13.89961937509957401, 13.97604488694547697, 21.87609039468566152 ) ) ;
#39573 = CARTESIAN_POINT ( 'NONE',  ( 8.224510206698953496, -14.34966873604960469, 87.91557627198103830 ) ) ;
#39574 = CARTESIAN_POINT ( 'NONE',  ( 18.67979575497194134, -10.72451020669871369, 20.83442372801901143 ) ) ;
#39575 = CARTESIAN_POINT ( 'NONE',  ( 8.571926809382597767, 26.38167802310806209, 144.7750000027311899 ) ) ;
#39576 = CARTESIAN_POINT ( 'NONE',  ( 15.80617190586746368, 15.72974639402197994, 74.37390960531436690 ) ) ;
#39577 = CARTESIAN_POINT ( 'NONE',  ( -16.53943276465976808, -0.05219959533934237506, 88.75109039468567573 ) ) ;
#39578 = CARTESIAN_POINT ( 'NONE',  ( 13.97604488694527802, 13.89961937509977652, 24.37390960531435624 ) ) ;
#39579 = CARTESIAN_POINT ( 'NONE',  ( 19.02544592524343514, -5.153800228976328945, 78.54057627198099567 ) ) ;
#39580 = CARTESIAN_POINT ( 'NONE',  ( -17.50000000000000355, -5.499999999999980460, 96.28230962303564411 ) ) ;
#39581 = CARTESIAN_POINT ( 'NONE',  ( 0.000000000000000000, 0.000000000000000000, -56.77278709839600879 ) ) ;
#39582 = CARTESIAN_POINT ( 'NONE',  ( 4.483927247898545687, 16.52544592524342804, 24.79057627198103120 ) ) ;
#39583 = CARTESIAN_POINT ( 'NONE',  ( -5.823673210054431948, 21.52544592524334988, 57.70942372801901143 ) ) ;
#39584 = CARTESIAN_POINT ( 'NONE',  ( -13.97604488694527625, -13.89961937509977652, 111.8739096053143243 ) ) ;
#39585 = CARTESIAN_POINT ( 'NONE',  ( -21.52544592524334988, -5.823673210054445271, 93.95942372801903275 ) ) ;
#39586 = CARTESIAN_POINT ( 'NONE',  ( 19.03943276465977164, -0.05219959533909143690, 48.74890960531435979 ) ) ;
#39587 = CARTESIAN_POINT ( 'NONE',  ( 19.02544592524343514, -5.153800228976328945, 53.54057627198102409 ) ) ;
#39588 = VERTEX_POINT ( 'NONE', #55947 ) ;
#39589 = CARTESIAN_POINT ( 'NONE',  ( 18.62759615963255655, 10.81492255796105972, 91.66775706135234714 ) ) ;
#39590 = CARTESIAN_POINT ( 'NONE',  ( -14.29746914071037622, -8.314922557961029526, 59.16775706135234714 ) ) ;
#39591 = CARTESIAN_POINT ( 'NONE',  ( -21.55341960407619339, 5.719274019375674811, 83.54275706135234714 ) ) ;
#39592 = CARTESIAN_POINT ( 'NONE',  ( 21.53943276465977519, -0.05219959533907433946, 23.74890960531435269 ) ) ;
#39593 = CARTESIAN_POINT ( 'NONE',  ( -16.46253265017146816, -9.564922557961047289, 94.16775706135233293 ) ) ;
#39594 = CARTESIAN_POINT ( 'NONE',  ( 15.80617190586769283, -15.72974639402175789, 60.62609039468567573 ) ) ;
#39595 = CARTESIAN_POINT ( 'NONE',  ( -0.05219959533934338120, 16.53943276465976808, 32.50109039468568284 ) ) ;
#39596 = CARTESIAN_POINT ( 'NONE',  ( -10.81492255796078084, -18.62759615963271287, 87.08224293864769550 ) ) ;
#39597 = CARTESIAN_POINT ( 'NONE',  ( 5.153800228976615827, -19.02544592524334988, 85.20942372801900433 ) ) ;
#39598 = CARTESIAN_POINT ( 'NONE',  ( 9.564922557960805705, 16.46253265017160317, 69.58224293864770971 ) ) ;
#39599 = CARTESIAN_POINT ( 'NONE',  ( 16.51473224551083163, -9.474510206698727899, 95.83442372801900433 ) ) ;
#39600 = CARTESIAN_POINT ( 'NONE',  ( 13.89961937509957401, 13.97604488694547697, 96.87609039468566152 ) ) ;
#39601 = CARTESIAN_POINT ( 'NONE',  ( 16.55341960407611168, 4.379528057220329451, 58.95724293864770971 ) ) ;
#39602 = CARTESIAN_POINT ( 'NONE',  ( -16.51473224551082808, 9.474510206698731452, 83.33442372801899012 ) ) ;
#39603 = CARTESIAN_POINT ( 'NONE',  ( -8.314922557961024197, 14.29746914071037800, 62.91775706135236135 ) ) ;
#39604 = CARTESIAN_POINT ( 'NONE',  ( 5.049401038297881783, 19.05341960407617563, 37.29275706135232582 ) ) ;
#39605 = CARTESIAN_POINT ( 'NONE',  ( -19.02544592524342804, 5.153800228976336051, 36.04057627198100988 ) ) ;
#39606 = CARTESIAN_POINT ( 'NONE',  ( 16.51473224551069308, 9.474510206698969483, 49.16557627198102409 ) ) ;
#39607 = CARTESIAN_POINT ( 'NONE',  ( 4.483927247898790824, -16.52544592524335698, 60.20942372801902565 ) ) ;
#39608 = FACE_OUTER_BOUND ( 'NONE', #92199, .T. ) ;
#39609 = CARTESIAN_POINT ( 'NONE',  ( 28.82186960331498327, 2.781578969918950771E-14, 141.2500000054623683 ) ) ;
#39610 = CARTESIAN_POINT ( 'NONE',  ( 19.03943276465977164, -0.05219959533909143690, 103.7489096053143669 ) ) ;
#39611 = CARTESIAN_POINT ( 'NONE',  ( -5.049401038298153566, 19.05341960407611168, 25.20724293864768484 ) ) ;
#39612 = ORIENTED_EDGE ( 'NONE', *, *, #129926, .T. ) ;
#39613 = CARTESIAN_POINT ( 'NONE',  ( 5.049401038297881783, 19.05341960407617563, 97.29275706135233293 ) ) ;
#39614 = CARTESIAN_POINT ( 'NONE',  ( -15.80617190586745835, -15.72974639402198527, 36.87390960531435979 ) ) ;
#39616 = CARTESIAN_POINT ( 'NONE',  ( -0.05219959533934338120, 16.53943276465976808, 22.50109039468567573 ) ) ;
#39615 = CARTESIAN_POINT ( 'NONE',  ( -13.97604488694547697, 13.89961937509957934, 38.12609039468566152 ) ) ;
#39617 = CARTESIAN_POINT ( 'NONE',  ( 9.564922557960805705, 16.46253265017160317, 34.58224293864770260 ) ) ;
#39618 = CARTESIAN_POINT ( 'NONE',  ( -5.153800228976328057, -19.02544592524343514, 52.29057627198100988 ) ) ;
#39619 = CARTESIAN_POINT ( 'NONE',  ( -10.81492255796078084, -18.62759615963271287, 67.08224293864770971 ) ) ;
#39620 = CARTESIAN_POINT ( 'NONE',  ( 5.153800228976335163, 19.02544592524342804, 99.79057627198102409 ) ) ;
#39621 = CARTESIAN_POINT ( 'NONE',  ( 16.51473224551069308, 9.474510206698969483, 39.16557627198103120 ) ) ;
#39622 = CARTESIAN_POINT ( 'NONE',  ( 22.44159573604009594, -16.30477369853687364, 146.1750000027311671 ) ) ;
#39623 = CARTESIAN_POINT ( 'NONE',  ( 13.97604488694548053, -13.89961937509957401, 90.62609039468567573 ) ) ;
#39624 = CARTESIAN_POINT ( 'NONE',  ( -8.224510206698948167, 14.34966873604960824, 55.41557627198102409 ) ) ;
#39625 = CARTESIAN_POINT ( 'NONE',  ( 10.72451020669898902, -18.67979575497178502, 27.91557627198103830 ) ) ;
#39626 = CARTESIAN_POINT ( 'NONE',  ( 18.62759615963255655, 10.81492255796105972, 106.6677570613523756 ) ) ;
#39627 = CARTESIAN_POINT ( 'NONE',  ( 18.62759615963271287, -10.81492255796078972, 93.33224293864769550 ) ) ;
#39628 = CARTESIAN_POINT ( 'NONE',  ( 15.72974639402176855, 15.80617190586768217, 71.87609039468568994 ) ) ;
#39629 = CARTESIAN_POINT ( 'NONE',  ( -18.67979575497193778, 10.72451020669871902, 78.33442372801901854 ) ) ;
#39630 = CARTESIAN_POINT ( 'NONE',  ( 9.564922557960805705, 16.46253265017160317, 114.5822429386476955 ) ) ;
#39632 = CARTESIAN_POINT ( 'NONE',  ( -21.53943276465977519, -0.05219959533937600094, 63.75109039468568284 ) ) ;
#39631 = CARTESIAN_POINT ( 'NONE',  ( 16.53943276465976808, 0.05219959533934440121, 101.2510903946856757 ) ) ;
#39633 = CARTESIAN_POINT ( 'NONE',  ( -0.05219959533909027116, -19.03943276465977164, 62.49890960531435979 ) ) ;
#39634 = CARTESIAN_POINT ( 'NONE',  ( -13.89961937509957401, -13.97604488694547875, 34.37609039468566863 ) ) ;
#39635 = CARTESIAN_POINT ( 'NONE',  ( 15.80617190586769283, -15.72974639402175789, 25.62609039468567929 ) ) ;
#39636 = CARTESIAN_POINT ( 'NONE',  ( 13.89961937509977652, -13.97604488694527269, 73.12390960531436690 ) ) ;
#39637 = CARTESIAN_POINT ( 'NONE',  ( 8.314922557960818139, 14.29746914071049879, 84.58224293864769550 ) ) ;
#39638 = CARTESIAN_POINT ( 'NONE',  ( 12.06949235617757843, -12.14591786802309237, 53.12390960531436690 ) ) ;
#39639 = CARTESIAN_POINT ( 'NONE',  ( 15.80617190586746368, 15.72974639402197994, 54.37390960531435979 ) ) ;
#39640 = CARTESIAN_POINT ( 'NONE',  ( 19.03943276465977164, -0.05219959533909143690, 63.74890960531435979 ) ) ;
#39641 = CARTESIAN_POINT ( 'NONE',  ( 15.72974639402199770, -15.80617190586745480, 73.12390960531436690 ) ) ;
#39642 = CARTESIAN_POINT ( 'NONE',  ( -13.97604488694547697, 13.89961937509957934, 48.12609039468566863 ) ) ;
#39644 = CARTESIAN_POINT ( 'NONE',  ( -12.06949235617756955, 12.14591786802309770, 60.62390960531437401 ) ) ;
#39643 = CARTESIAN_POINT ( 'NONE',  ( 13.97604488694548053, -13.89961937509957401, 25.62609039468566507 ) ) ;
#39645 = CARTESIAN_POINT ( 'NONE',  ( 21.52544592524344225, -5.823673210054117533, 43.54057627198103830 ) ) ;
#39646 = ORIENTED_EDGE ( 'NONE', *, *, #105416, .F. ) ;
#39647 = DIRECTION ( 'NONE',  ( 0.000000000000000000, -0.8660254037844385966, -0.5000000000000003331 ) ) ;
#39649 = CARTESIAN_POINT ( 'NONE',  ( -8.571926809382601320, -26.38167802310801591, 141.7750000027311899 ) ) ;
#39648 = CARTESIAN_POINT ( 'NONE',  ( -16.52544592524335698, -4.483927247898792601, 78.95942372801901854 ) ) ;
#39650 = CARTESIAN_POINT ( 'NONE',  ( -19.02544592524334988, -5.153800228976617603, 93.95942372801900433 ) ) ;
#39651 = CARTESIAN_POINT ( 'NONE',  ( 8.314922557960818139, 14.29746914071049879, 49.58224293864769550 ) ) ;
#39652 = DIRECTION ( 'NONE',  ( 0.4999999999999967248, -0.5000000000000019984, -0.7071067811865484609 ) ) ;
#39653 = CARTESIAN_POINT ( 'NONE',  ( -13.89961937509977652, 13.97604488694528158, 45.62390960531433848 ) ) ;
#39654 = CARTESIAN_POINT ( 'NONE',  ( -4.483927247898539470, -16.52544592524342804, 37.29057627198102409 ) ) ;
#39655 = CARTESIAN_POINT ( 'NONE',  ( -16.51473224551069308, -9.474510206698971260, 86.66557627198102409 ) ) ;
#39656 = CARTESIAN_POINT ( 'NONE',  ( -0.05219959533909027116, -19.03943276465977164, 52.49890960531436690 ) ) ;
#39657 = CARTESIAN_POINT ( 'NONE',  ( -15.72974639402176322, -15.80617190586768395, 59.37609039468568284 ) ) ;
#39658 = CARTESIAN_POINT ( 'NONE',  ( 13.89961937509977652, -13.97604488694527269, 78.12390960531433848 ) ) ;
#39659 = CARTESIAN_POINT ( 'NONE',  ( -16.51473224551069308, -9.474510206698971260, 31.66557627198102054 ) ) ;
#39660 = CARTESIAN_POINT ( 'NONE',  ( -19.03943276465977164, 0.05219959533909376836, 71.24890960531435269 ) ) ;
#39661 = CARTESIAN_POINT ( 'NONE',  ( -21.53943276465977519, 0.05219959533907696930, 46.24890960531435979 ) ) ;
#39662 = CARTESIAN_POINT ( 'NONE',  ( -19.05341960407611168, -5.049401038298163336, 31.45724293864769550 ) ) ;
#39663 = CARTESIAN_POINT ( 'NONE',  ( 18.62759615963271287, -10.81492255796078972, 58.33224293864768839 ) ) ;
#39664 = CARTESIAN_POINT ( 'NONE',  ( -12.06949235617739369, -12.14591786802326823, 104.3760903946856899 ) ) ;
#39665 = CARTESIAN_POINT ( 'NONE',  ( 9.564922557961047289, -16.46253265017146816, 20.41775706135233293 ) ) ;
#39667 = CARTESIAN_POINT ( 'NONE',  ( 12.14591786802327356, -12.06949235617739191, 80.62609039468567573 ) ) ;
#39666 = CARTESIAN_POINT ( 'NONE',  ( -16.55341960407617563, 4.379528057220093196, 48.54275706135234714 ) ) ;
#39668 = CARTESIAN_POINT ( 'NONE',  ( -17.72696623605159516, 5.500000000000051514, 68.59811031808418136 ) ) ;
#39669 = CARTESIAN_POINT ( 'NONE',  ( -4.483927247898782831, 16.52544592524335698, 67.70942372801901854 ) ) ;
#39670 = CARTESIAN_POINT ( 'NONE',  ( 18.67979575497178502, 10.72451020669898547, 29.16557627198103120 ) ) ;
#39671 = CARTESIAN_POINT ( 'NONE',  ( 9.474510206698971260, -16.51473224551069308, 27.91557627198103120 ) ) ;
#39672 = CARTESIAN_POINT ( 'NONE',  ( -12.14591786802326823, 12.06949235617739902, 38.12609039468567573 ) ) ;
#39673 = CARTESIAN_POINT ( 'NONE',  ( -19.05341960407611168, -5.049401038298163336, 51.45724293864770260 ) ) ;
#39674 = CARTESIAN_POINT ( 'NONE',  ( 21.55341960407619695, -5.719274019375665929, 36.04275706135234714 ) ) ;
#39675 = CARTESIAN_POINT ( 'NONE',  ( 4.379528057220092307, 16.55341960407617563, 42.29275706135235424 ) ) ;
#39676 = CARTESIAN_POINT ( 'NONE',  ( -16.55341960407617563, 4.379528057220093196, 98.54275706135234714 ) ) ;
#39677 = LINE ( 'NONE', #166035, #27890 ) ;
#39678 = CARTESIAN_POINT ( 'NONE',  ( -5.823673210054431948, 21.52544592524334988, 97.70942372801904696 ) ) ;
#39679 = CARTESIAN_POINT ( 'NONE',  ( -19.05341960407617563, 5.049401038297882671, 108.5427570613523187 ) ) ;
#39680 = CARTESIAN_POINT ( 'NONE',  ( 0.05219959533936267826, -19.03943276465977164, 65.00109039468567573 ) ) ;
#39681 = CARTESIAN_POINT ( 'NONE',  ( 4.483927247898545687, 16.52544592524342804, 74.79057627198105251 ) ) ;
#39682 = CARTESIAN_POINT ( 'NONE',  ( -19.05341960407611168, -5.049401038298163336, 26.45724293864769550 ) ) ;
#39684 = PLANE ( 'NONE',  #130858 ) ;
#39683 = CARTESIAN_POINT ( 'NONE',  ( -19.02544592524334988, -5.153800228976617603, 58.95942372801900433 ) ) ;
#39685 = CARTESIAN_POINT ( 'NONE',  ( -18.67979575497193778, 10.72451020669871902, 58.33442372801901143 ) ) ;
#39686 = CARTESIAN_POINT ( 'NONE',  ( 16.52544592524335698, 4.483927247898782831, 26.45942372801901854 ) ) ;
#39687 = FACE_OUTER_BOUND ( 'NONE', #80548, .T. ) ;
#39688 = CARTESIAN_POINT ( 'NONE',  ( -5.823673210054116645, -21.52544592524344225, 22.29057627198102765 ) ) ;
#39689 = CARTESIAN_POINT ( 'NONE',  ( 16.46253265017146816, 9.564922557961045513, 106.6677570613523471 ) ) ;
#39690 = CARTESIAN_POINT ( 'NONE',  ( -5.153800228976328057, -19.02544592524343514, 112.2905762719810099 ) ) ;
#39691 = CARTESIAN_POINT ( 'NONE',  ( -25.93326183087854275, 10.28624940747392991, 166.6531433017870540 ) ) ;
#39692 = CARTESIAN_POINT ( 'NONE',  ( -5.153800228976328057, -19.02544592524343514, 22.29057627198102765 ) ) ;
#39693 = CARTESIAN_POINT ( 'NONE',  ( -18.67979575497193778, 10.72451020669871902, 113.3344237280190328 ) ) ;
#39694 = CARTESIAN_POINT ( 'NONE',  ( 0.05219959533909260263, 19.03943276465977164, 49.99890960531435979 ) ) ;
#39695 = CARTESIAN_POINT ( 'NONE',  ( -18.62759615963255300, -10.81492255796106328, 69.16775706135234714 ) ) ;
#39696 = CARTESIAN_POINT ( 'NONE',  ( 5.719274019375673035, 21.55341960407619339, 102.2927570613523613 ) ) ;
#39697 = CARTESIAN_POINT ( 'NONE',  ( -12.14591786802309592, -12.06949235617757132, 21.87390960531436690 ) ) ;
#39698 = CARTESIAN_POINT ( 'NONE',  ( -9.474510206698964154, 16.51473224551069663, 85.41557627198102409 ) ) ;
#39699 = CARTESIAN_POINT ( 'NONE',  ( -18.67979575497193778, 10.72451020669871902, 58.33442372801901143 ) ) ;
#39700 = CARTESIAN_POINT ( 'NONE',  ( 10.81492255796106328, -18.62759615963255655, 50.41775706135235424 ) ) ;
#39702 = CARTESIAN_POINT ( 'NONE',  ( 19.05341960407611168, 5.049401038298154454, 103.9572429386476671 ) ) ;
#39701 = CARTESIAN_POINT ( 'NONE',  ( -5.153800228976607833, 19.02544592524334988, 77.70942372801900433 ) ) ;
#39703 = CARTESIAN_POINT ( 'NONE',  ( -9.564922557960796823, -16.46253265017161027, 22.08224293864768839 ) ) ;
#39704 = CARTESIAN_POINT ( 'NONE',  ( -15.80617190586745835, -15.72974639402198527, 106.8739096053143811 ) ) ;
#39705 = CARTESIAN_POINT ( 'NONE',  ( -9.474510206698720793, -16.51473224551083518, 39.58442372801899722 ) ) ;
#39706 = CARTESIAN_POINT ( 'NONE',  ( -16.55341960407611168, -4.379528057220339221, 91.45724293864769550 ) ) ;
#39707 = CARTESIAN_POINT ( 'NONE',  ( 19.02544592524343514, -5.153800228976328945, 43.54057627198103120 ) ) ;
#39708 = CARTESIAN_POINT ( 'NONE',  ( -5.153800228976607833, 19.02544592524334988, 102.7094237280189759 ) ) ;
#39709 = CARTESIAN_POINT ( 'NONE',  ( -16.53943276465976808, 0.05219959533911058130, 56.24890960531436690 ) ) ;
#39710 = CARTESIAN_POINT ( 'NONE',  ( -21.53943276465977519, -0.05219959533937600094, 113.7510903946856757 ) ) ;
#39711 = CARTESIAN_POINT ( 'NONE',  ( 0.05219959533909260263, 19.03943276465977164, 99.99890960531436690 ) ) ;
#39712 = CARTESIAN_POINT ( 'NONE',  ( -0.05219959533936034679, 19.03943276465977164, 92.50109039468566152 ) ) ;
#39713 = CARTESIAN_POINT ( 'NONE',  ( -10.81492255796078084, -18.62759615963271287, 92.08224293864769550 ) ) ;
#39714 = CARTESIAN_POINT ( 'NONE',  ( -5.823673210054431948, 21.52544592524334988, 47.70942372801902565 ) ) ;
#39715 = CARTESIAN_POINT ( 'NONE',  ( -14.29746914071037622, -8.314922557961029526, 49.16775706135234003 ) ) ;
#39716 = CARTESIAN_POINT ( 'NONE',  ( 16.55341960407618274, -4.379528057220086978, 106.0427570613523471 ) ) ;
#39718 = CARTESIAN_POINT ( 'NONE',  ( -18.67979575497193778, 10.72451020669871902, 33.33442372801900433 ) ) ;
#39717 = CARTESIAN_POINT ( 'NONE',  ( -14.34966873604972548, 8.224510206698743886, 43.33442372801901143 ) ) ;
#39719 = CARTESIAN_POINT ( 'NONE',  ( 15.72974639402199770, -15.80617190586745480, 48.12390960531436690 ) ) ;
#39720 = CARTESIAN_POINT ( 'NONE',  ( 9.564922557960805705, 16.46253265017160317, 29.58224293864769550 ) ) ;
#39721 = CARTESIAN_POINT ( 'NONE',  ( 11.74264578624800315, -36.14014761921581709, -11.14999999453762669 ) ) ;
#39723 = CIRCLE ( 'NONE', #165742, 2.041999999999999815 ) ;
#39722 = CARTESIAN_POINT ( 'NONE',  ( -4.379528057220086978, -16.55341960407618274, 59.79275706135234714 ) ) ;
#39724 = EDGE_CURVE ( 'NONE', #51296, #74939, #101479, .T. ) ;
#39725 = CARTESIAN_POINT ( 'NONE',  ( 5.823673210054125526, 21.52544592524343514, 94.79057627198105251 ) ) ;
#39726 = CARTESIAN_POINT ( 'NONE',  ( 4.379528057220339221, -16.55341960407611168, 32.70724293864770260 ) ) ;
#39727 = CARTESIAN_POINT ( 'NONE',  ( -16.53943276465976808, -0.05219959533934237506, 68.75109039468568994 ) ) ;
#39728 = CARTESIAN_POINT ( 'NONE',  ( -9.474510206698964154, 16.51473224551069663, 55.41557627198103120 ) ) ;
#39729 = CARTESIAN_POINT ( 'NONE',  ( -16.51473224551082808, 9.474510206698731452, 88.33442372801900433 ) ) ;
#39730 = CARTESIAN_POINT ( 'NONE',  ( 15.72974639402199770, -15.80617190586745480, 88.12390960531436690 ) ) ;
#39731 = CARTESIAN_POINT ( 'NONE',  ( 14.34966873604960469, 8.224510206698951720, 29.16557627198103120 ) ) ;
#39732 = ORIENTED_EDGE ( 'NONE', *, *, #165015, .F. ) ;
#39733 = CARTESIAN_POINT ( 'NONE',  ( 25.93326183087853565, 10.28624940747392991, 166.6531433017870540 ) ) ;
#39734 = CARTESIAN_POINT ( 'NONE',  ( 15.72974639402199770, -15.80617190586745480, 68.12390960531436690 ) ) ;
#39735 = CARTESIAN_POINT ( 'NONE',  ( 14.34966873604972726, -8.224510206698740333, 105.8344237280190328 ) ) ;
#39736 = ORIENTED_EDGE ( 'NONE', *, *, #17849, .F. ) ;
#39737 = CARTESIAN_POINT ( 'NONE',  ( 23.48529157249600630, -32.32473071737748427, -3.299999999999999822 ) ) ;
#39738 = CARTESIAN_POINT ( 'NONE',  ( 5.823673210054125526, 21.52544592524343514, 94.79057627198105251 ) ) ;
#39739 = CARTESIAN_POINT ( 'NONE',  ( 15.72974639402199770, -15.80617190586745480, 113.1239096053143953 ) ) ;
#39740 = CARTESIAN_POINT ( 'NONE',  ( 14.29746914071049879, -8.314922557960816363, 23.33224293864769194 ) ) ;
#39741 = CARTESIAN_POINT ( 'NONE',  ( -8.224510206698735004, -14.34966873604973081, 34.58442372801900433 ) ) ;
#39742 = CARTESIAN_POINT ( 'NONE',  ( -16.51473224551069308, -9.474510206698971260, 31.66557627198102054 ) ) ;
#39743 = CARTESIAN_POINT ( 'NONE',  ( -5.153800228976328057, -19.02544592524343514, 67.29057627198102409 ) ) ;
#39744 = CARTESIAN_POINT ( 'NONE',  ( 28.82186960331499392, -9.364793116373510529, 146.8999999999999773 ) ) ;
#39745 = CARTESIAN_POINT ( 'NONE',  ( 5.153800228976335163, 19.02544592524342804, 114.7905762719810241 ) ) ;
#39746 = FACE_OUTER_BOUND ( 'NONE', #94727, .T. ) ;
#39747 = CARTESIAN_POINT ( 'NONE',  ( 13.89961937509957401, 13.97604488694547697, 111.8760903946856757 ) ) ;
#39748 = CARTESIAN_POINT ( 'NONE',  ( 19.03943276465977164, 0.05219959533936151252, 36.25109039468567573 ) ) ;
#39749 = CARTESIAN_POINT ( 'NONE',  ( 15.80617190586746368, 15.72974639402197994, 89.37390960531435269 ) ) ;
#39750 = CARTESIAN_POINT ( 'NONE',  ( 12.06949235617757843, -12.14591786802309237, 23.12390960531436335 ) ) ;
#39751 = AXIS2_PLACEMENT_3D ( 'NONE', #174676, #128149, #97793 ) ;
#39752 = CARTESIAN_POINT ( 'NONE',  ( 5.719274019375991003, -21.55341960407610458, 52.70724293864769550 ) ) ;
#39754 = CARTESIAN_POINT ( 'NONE',  ( -19.03943276465977164, -0.05219959533935918106, 108.7510903946856615 ) ) ;
#39753 = CARTESIAN_POINT ( 'NONE',  ( -21.52544592524343514, 5.823673210054127303, 86.04057627198102409 ) ) ;
#39755 = CARTESIAN_POINT ( 'NONE',  ( -19.03943276465977164, 0.05219959533909376836, 101.2489096053143669 ) ) ;
#39756 = CARTESIAN_POINT ( 'NONE',  ( 21.53943276465977519, 0.05219959533937863772, 76.25109039468568994 ) ) ;
#39757 = CARTESIAN_POINT ( 'NONE',  ( -13.97604488694527625, -13.89961937509977652, 56.87390960531434558 ) ) ;
#39758 = CARTESIAN_POINT ( 'NONE',  ( -16.55341960407611168, -4.379528057220339221, 106.4572429386477097 ) ) ;
#39759 = CARTESIAN_POINT ( 'NONE',  ( 31.49214409296861206, 4.585214664522583305, 100.9553921309669704 ) ) ;
#39760 = CARTESIAN_POINT ( 'NONE',  ( 5.153800228976335163, 19.02544592524342804, 74.79057627198103830 ) ) ;
#39761 = CARTESIAN_POINT ( 'NONE',  ( -0.05219959533910754901, -16.53943276465976808, 92.49890960531436690 ) ) ;
#39762 = ORIENTED_EDGE ( 'NONE', *, *, #185215, .F. ) ;
#39763 = CARTESIAN_POINT ( 'NONE',  ( -13.97604488694547697, 13.89961937509957934, 93.12609039468566152 ) ) ;
#39764 = CARTESIAN_POINT ( 'NONE',  ( 2.500000000000000000, 2.500728763858895382E-16, -2.041999999999999815 ) ) ;
#39765 = CARTESIAN_POINT ( 'NONE',  ( 19.02544592524343514, -5.153800228976328945, 63.54057627198103830 ) ) ;
#39767 = CARTESIAN_POINT ( 'NONE',  ( 16.51473224551069308, 9.474510206698969483, 99.16557627198102409 ) ) ;
#39766 = CARTESIAN_POINT ( 'NONE',  ( 10.72451020669871369, 18.67979575497193778, 87.08442372801901854 ) ) ;
#39768 = CARTESIAN_POINT ( 'NONE',  ( 16.52544592524335698, 4.483927247898782831, 76.45942372801901854 ) ) ;
#39769 = CARTESIAN_POINT ( 'NONE',  ( -16.36317988757057051, -7.306389748694941844, 50.90210391636774290 ) ) ;
#39770 = CARTESIAN_POINT ( 'NONE',  ( 19.03943276465977164, 0.05219959533936151252, 41.25109039468566152 ) ) ;
#39771 = CARTESIAN_POINT ( 'NONE',  ( -18.67979575497193778, 10.72451020669871902, 93.33442372801901854 ) ) ;
#39772 = CARTESIAN_POINT ( 'NONE',  ( 36.93866063236283281, 5.356020730800094221, 43.73704834337281966 ) ) ;
#39773 = DIRECTION ( 'NONE',  ( -0.000000000000000000, -0.000000000000000000, 1.000000000000000000 ) ) ;
#39774 = CARTESIAN_POINT ( 'NONE',  ( 14.34966873604972726, -8.224510206698740333, 100.8344237280190185 ) ) ;
#39775 = CARTESIAN_POINT ( 'NONE',  ( -34.78522506798721992, -0.4968532545621949237, 52.49999999999998579 ) ) ;
#39776 = CARTESIAN_POINT ( 'NONE',  ( -8.314922557961024197, 14.29746914071037800, 87.91775706135234714 ) ) ;
#39777 = CARTESIAN_POINT ( 'NONE',  ( 17.12812012977028076, 6.668231424565952636, 68.85948759323146362 ) ) ;
#39778 = CARTESIAN_POINT ( 'NONE',  ( -14.34966873604972548, 8.224510206698743886, 73.33442372801901854 ) ) ;
#39779 = ORIENTED_EDGE ( 'NONE', *, *, #124331, .T. ) ;
#39780 = CARTESIAN_POINT ( 'NONE',  ( 10.72451020669871369, 18.67979575497193778, 77.08442372801901854 ) ) ;
#39781 = CARTESIAN_POINT ( 'NONE',  ( -5.153800228976607833, 19.02544592524334988, 92.70942372801901854 ) ) ;
#39782 = CARTESIAN_POINT ( 'NONE',  ( 19.02544592524334988, 5.153800228976608722, 36.45942372801900433 ) ) ;
#39783 = CARTESIAN_POINT ( 'NONE',  ( -13.89961937509977652, 13.97604488694528158, 65.62390960531436690 ) ) ;
#39784 = CARTESIAN_POINT ( 'NONE',  ( -13.89961937509977652, 13.97604488694528158, 55.62390960531434558 ) ) ;
#39785 = LINE ( 'NONE', #159126, #198290 ) ;
#39786 = CARTESIAN_POINT ( 'NONE',  ( -5.719274019375978568, 21.55341960407610458, 75.20724293864769550 ) ) ;
#39787 = CARTESIAN_POINT ( 'NONE',  ( 21.53943276465977519, -0.05219959533907433946, 33.74890960531436690 ) ) ;
#39788 = CARTESIAN_POINT ( 'NONE',  ( -13.89961937509977652, 13.97604488694528158, 30.62390960531435269 ) ) ;
#39789 = CARTESIAN_POINT ( 'NONE',  ( -8.314922557961024197, 14.29746914071037800, 62.91775706135236135 ) ) ;
#39790 = ADVANCED_FACE ( 'NONE', ( #115628 ), #82108, .T. ) ;
#39791 = ORIENTED_EDGE ( 'NONE', *, *, #73698, .F. ) ;
#39792 = CARTESIAN_POINT ( 'NONE',  ( 5.719274019375673035, 21.55341960407619339, 27.29275706135234358 ) ) ;
#39794 = CARTESIAN_POINT ( 'NONE',  ( 3.556970738554033499E-15, -38.81732327939057825, -8.124999997268814056 ) ) ;
#39793 = CARTESIAN_POINT ( 'NONE',  ( -12.06949235617756955, 12.14591786802309770, 70.62390960531436690 ) ) ;
#39795 = CARTESIAN_POINT ( 'NONE',  ( 12.06949235617739724, 12.14591786802326823, 21.87609039468567573 ) ) ;
#39796 = CARTESIAN_POINT ( 'NONE',  ( 13.97604488694548053, -13.89961937509957401, 50.62609039468566152 ) ) ;
#39797 = CARTESIAN_POINT ( 'NONE',  ( -4.483927247898539470, -16.52544592524342804, 62.29057627198102409 ) ) ;
#39798 = CARTESIAN_POINT ( 'NONE',  ( 15.80617190586769283, -15.72974639402175789, 35.62609039468568994 ) ) ;
#39799 = CARTESIAN_POINT ( 'NONE',  ( -10.72451020669898014, 18.67979575497178502, 75.41557627198102409 ) ) ;
#39800 = CARTESIAN_POINT ( 'NONE',  ( -9.474510206698964154, 16.51473224551069663, 105.4155762719810383 ) ) ;
#39801 = CARTESIAN_POINT ( 'NONE',  ( -8.224510206698948167, 14.34966873604960824, 55.41557627198102409 ) ) ;
#39802 = CARTESIAN_POINT ( 'NONE',  ( 16.51473224551069308, 9.474510206698969483, 114.1655762719810241 ) ) ;
#39803 = LINE ( 'NONE', #101469, #166765 ) ;
#39804 = CARTESIAN_POINT ( 'NONE',  ( -5.153800228976607833, 19.02544592524334988, 72.70942372801900433 ) ) ;
#39805 = CARTESIAN_POINT ( 'NONE',  ( -21.55341960407610458, -5.719274019375992779, 106.4572429386477097 ) ) ;
#39806 = CARTESIAN_POINT ( 'NONE',  ( -13.97604488694527625, -13.89961937509977652, 61.87390960531435979 ) ) ;
#39807 = CARTESIAN_POINT ( 'NONE',  ( 13.89961937509957401, 13.97604488694547697, 46.87609039468565442 ) ) ;
#39808 = CARTESIAN_POINT ( 'NONE',  ( -9.564922557960796823, -16.46253265017161027, 27.08224293864769550 ) ) ;
#39809 = AXIS2_PLACEMENT_3D ( 'NONE', #50880, #82175, #112538 ) ;
#39810 = CARTESIAN_POINT ( 'NONE',  ( -0.05219959533937732626, 21.53943276465977519, 57.50109039468568994 ) ) ;
#39811 = CARTESIAN_POINT ( 'NONE',  ( 5.000000000000000000, -116.8122400552013431, 54.87277500418469600 ) ) ;
#39812 = CARTESIAN_POINT ( 'NONE',  ( 12.06949235617757843, -12.14591786802309237, 43.12390960531435269 ) ) ;
#39813 = CARTESIAN_POINT ( 'NONE',  ( -19.05341960407611168, -5.049401038298163336, 61.45724293864769550 ) ) ;
#39814 = CARTESIAN_POINT ( 'NONE',  ( -15.80617190586745835, -15.72974639402198527, 86.87390960531438111 ) ) ;
#39815 = CARTESIAN_POINT ( 'NONE',  ( -5.153800228976328057, -19.02544592524343514, 57.29057627198103120 ) ) ;
#39816 = ORIENTED_EDGE ( 'NONE', *, *, #130059, .F. ) ;
#39817 = CARTESIAN_POINT ( 'NONE',  ( 0.05219959533907565091, 21.53943276465977519, 64.99890960531435269 ) ) ;
#39818 = ORIENTED_EDGE ( 'NONE', *, *, #39120, .F. ) ;
#39819 = CARTESIAN_POINT ( 'NONE',  ( -15.72974639402176322, -15.80617190586768395, 99.37609039468568994 ) ) ;
#39822 = CARTESIAN_POINT ( 'NONE',  ( 8.224510206698953496, -14.34966873604960469, 87.91557627198103830 ) ) ;
#39821 = CARTESIAN_POINT ( 'NONE',  ( -8.224510206698735004, -14.34966873604973081, 99.58442372801900433 ) ) ;
#39820 = CYLINDRICAL_SURFACE ( 'NONE', #25126, 5.500000000001017852 ) ;
#39823 = CARTESIAN_POINT ( 'NONE',  ( -16.51473224551082808, 9.474510206698731452, 93.33442372801900433 ) ) ;
#39824 = EDGE_LOOP ( 'NONE', ( #172271, #61109, #183008, #105635, #98400, #82231 ) ) ;
#39825 = CARTESIAN_POINT ( 'NONE',  ( -16.46253265017146816, -9.564922557961047289, 34.16775706135233293 ) ) ;
#39826 = CARTESIAN_POINT ( 'NONE',  ( 16.55341960407618274, -4.379528057220086978, 96.04275706135236135 ) ) ;
#39827 = CARTESIAN_POINT ( 'NONE',  ( 16.46253265017146816, 9.564922557961045513, 36.66775706135233293 ) ) ;
#39828 = CARTESIAN_POINT ( 'NONE',  ( -9.474510206698964154, 16.51473224551069663, 85.41557627198102409 ) ) ;
#39829 = CARTESIAN_POINT ( 'NONE',  ( -10.72451020669898014, 18.67979575497178502, 60.41557627198102409 ) ) ;
#39830 = CARTESIAN_POINT ( 'NONE',  ( -9.564922557960796823, -16.46253265017161027, 22.08224293864768839 ) ) ;
#39831 = CARTESIAN_POINT ( 'NONE',  ( -19.02544592524342804, 5.153800228976336051, 26.04057627198103120 ) ) ;
#39832 = CARTESIAN_POINT ( 'NONE',  ( 5.823673210054444382, -21.52544592524334988, 95.20942372801903275 ) ) ;
#39833 = CARTESIAN_POINT ( 'NONE',  ( -16.53943276465976808, -0.05219959533934237506, 78.75109039468568994 ) ) ;
#39834 = CARTESIAN_POINT ( 'NONE',  ( 21.53943276465977519, 0.05219959533937863772, 26.25109039468567573 ) ) ;
#39835 = CARTESIAN_POINT ( 'NONE',  ( -14.34966873604972548, 8.224510206698743886, 33.33442372801900433 ) ) ;
#39836 = CARTESIAN_POINT ( 'NONE',  ( 9.564922557960805705, 16.46253265017160317, 104.5822429386476955 ) ) ;
#39837 = CARTESIAN_POINT ( 'NONE',  ( -13.97604488694527625, -13.89961937509977652, 41.87390960531435979 ) ) ;
#39838 = CARTESIAN_POINT ( 'NONE',  ( 16.51473224551069308, 9.474510206698969483, 49.16557627198102409 ) ) ;
#39839 = CARTESIAN_POINT ( 'NONE',  ( 8.224510206698742110, 14.34966873604972548, 42.08442372801901854 ) ) ;
#39840 = CARTESIAN_POINT ( 'NONE',  ( 14.34966873604960469, 8.224510206698951720, 89.16557627198102409 ) ) ;
#39841 = CARTESIAN_POINT ( 'NONE',  ( 12.14591786802327356, -12.06949235617739191, 100.6260903946857184 ) ) ;
#39844 = CARTESIAN_POINT ( 'NONE',  ( 9.474510206698971260, -16.51473224551069308, 62.91557627198102409 ) ) ;
#39843 = CARTESIAN_POINT ( 'NONE',  ( 16.51473224551069308, 9.474510206698969483, 84.16557627198102409 ) ) ;
#39842 = CARTESIAN_POINT ( 'NONE',  ( -0.05219959533937732626, 21.53943276465977519, 42.50109039468567573 ) ) ;
#39845 = CARTESIAN_POINT ( 'NONE',  ( 16.46253265017160672, -9.564922557960803928, 93.33224293864769550 ) ) ;
#39846 = CARTESIAN_POINT ( 'NONE',  ( 4.379528057220339221, -16.55341960407611168, 37.70724293864769550 ) ) ;
#39847 = CARTESIAN_POINT ( 'NONE',  ( -12.14591786802326823, 12.06949235617739902, 98.12609039468570415 ) ) ;
#39848 = ORIENTED_EDGE ( 'NONE', *, *, #194281, .F. ) ;
#39849 = CARTESIAN_POINT ( 'NONE',  ( -5.049401038297874678, -19.05341960407617918, 49.79275706135231871 ) ) ;
#39850 = CARTESIAN_POINT ( 'NONE',  ( -0.05219959533909027116, -19.03943276465977164, 112.4989096053143669 ) ) ;
#39851 = CARTESIAN_POINT ( 'NONE',  ( 19.05341960407611168, 5.049401038298154454, 63.95724293864769550 ) ) ;
#39852 = CARTESIAN_POINT ( 'NONE',  ( 13.97604488694548053, -13.89961937509957401, 35.62609039468567573 ) ) ;
#39853 = CARTESIAN_POINT ( 'NONE',  ( -11.40812507854754720, -35.11059874428192273, -6.224999997268812812 ) ) ;
#39854 = CARTESIAN_POINT ( 'NONE',  ( 19.36337904590692460, -5.499999999999943157, 72.91494137495618588 ) ) ;
#39855 = CARTESIAN_POINT ( 'NONE',  ( 12.14591786802327356, -12.06949235617739191, 45.62609039468567573 ) ) ;
#39857 = CARTESIAN_POINT ( 'NONE',  ( -16.55341960407617563, 4.379528057220093196, 53.54275706135234714 ) ) ;
#39856 = CARTESIAN_POINT ( 'NONE',  ( 19.02544592524334988, 5.153800228976608722, 76.45942372801897591 ) ) ;
#39858 = CARTESIAN_POINT ( 'NONE',  ( 0.05219959533909260263, 19.03943276465977164, 114.9989096053143669 ) ) ;
#39859 = CARTESIAN_POINT ( 'NONE',  ( -13.89961937509977652, 13.97604488694528158, 95.62390960531436690 ) ) ;
#39860 = CARTESIAN_POINT ( 'NONE',  ( 5.719274019375991003, -21.55341960407610458, 112.7072429386476955 ) ) ;
#39861 = CARTESIAN_POINT ( 'NONE',  ( -13.97604488694547697, 13.89961937509957934, 78.12609039468567573 ) ) ;
#39863 = CARTESIAN_POINT ( 'NONE',  ( -13.89961937509977652, 13.97604488694528158, 40.62390960531435979 ) ) ;
#39862 = CARTESIAN_POINT ( 'NONE',  ( 19.05341960407611168, 5.049401038298154454, 98.95724293864766707 ) ) ;
#39864 = CARTESIAN_POINT ( 'NONE',  ( -13.89961937509977652, 13.97604488694528158, 75.62390960531438111 ) ) ;
#39866 = CARTESIAN_POINT ( 'NONE',  ( -9.564922557960796823, -16.46253265017161027, 32.08224293864769550 ) ) ;
#39865 = CARTESIAN_POINT ( 'NONE',  ( 0.05219959533910956823, 16.53943276465976808, 44.99890960531435979 ) ) ;
#39867 = CARTESIAN_POINT ( 'NONE',  ( 16.51473224551083163, -9.474510206698727899, 55.83442372801899722 ) ) ;
#39868 = CARTESIAN_POINT ( 'NONE',  ( -8.224510206698948167, 14.34966873604960824, 85.41557627198102409 ) ) ;
#39869 = CARTESIAN_POINT ( 'NONE',  ( 18.67979575497194134, -10.72451020669871369, 105.8344237280190328 ) ) ;
#39870 = CARTESIAN_POINT ( 'NONE',  ( 13.89961937509977652, -13.97604488694527269, 48.12390960531435979 ) ) ;
#39871 = CARTESIAN_POINT ( 'NONE',  ( -21.55341960407610458, -5.719274019375992779, 51.45724293864770260 ) ) ;
#39873 = CARTESIAN_POINT ( 'NONE',  ( -5.823673210054431948, 21.52544592524334988, 107.7094237280190328 ) ) ;
#39872 = CARTESIAN_POINT ( 'NONE',  ( 12.14591786802309770, 12.06949235617756955, 59.37390960531436690 ) ) ;
#39874 = CARTESIAN_POINT ( 'NONE',  ( -9.564922557960796823, -16.46253265017161027, 112.0822429386476955 ) ) ;
#39875 = CARTESIAN_POINT ( 'NONE',  ( -5.049401038298153566, 19.05341960407611168, 105.2072429386476671 ) ) ;
#39876 = CARTESIAN_POINT ( 'NONE',  ( -19.03943276465977164, 0.05219959533909376836, 41.24890960531435269 ) ) ;
#39877 = CARTESIAN_POINT ( 'NONE',  ( 5.153800228976335163, 19.02544592524342804, 29.79057627198102409 ) ) ;
#39878 = CARTESIAN_POINT ( 'NONE',  ( 14.29746914071049879, -8.314922557960816363, 83.33224293864769550 ) ) ;
#39879 = CARTESIAN_POINT ( 'NONE',  ( -10.81492255796078084, -18.62759615963271287, 97.08224293864770971 ) ) ;
#39880 = CARTESIAN_POINT ( 'NONE',  ( -5.153800228976328057, -19.02544592524343514, 107.2905762719810383 ) ) ;
#39881 = CARTESIAN_POINT ( 'NONE',  ( 10.81492255796106328, -18.62759615963255655, 20.41775706135234714 ) ) ;
#39882 = CARTESIAN_POINT ( 'NONE',  ( -16.51473224551069308, -9.474510206698971260, 101.6655762719810241 ) ) ;
#39884 = CARTESIAN_POINT ( 'NONE',  ( 12.14591786802309770, 12.06949235617756955, 109.3739096053143811 ) ) ;
#39883 = CARTESIAN_POINT ( 'NONE',  ( 18.22780087662122384, -5.500000000000022204, 66.01540105326107266 ) ) ;
#39885 = CARTESIAN_POINT ( 'NONE',  ( -9.564922557960796823, -16.46253265017161027, 72.08224293864770971 ) ) ;
#39886 = CARTESIAN_POINT ( 'NONE',  ( -10.81492255796078084, -18.62759615963271287, 77.08224293864769550 ) ) ;
#39887 = DIRECTION ( 'NONE',  ( -3.709348145883536076E-20, 0.000000000000000000, 1.000000000000000000 ) ) ;
#39888 = CARTESIAN_POINT ( 'NONE',  ( -21.94566984220701755, -7.593969325705130835, 169.8906363267648771 ) ) ;
#39890 = CARTESIAN_POINT ( 'NONE',  ( 19.46398650005389896, -5.499999999999940492, 67.68269651486370719 ) ) ;
#39889 = CARTESIAN_POINT ( 'NONE',  ( 18.67979575497178502, 10.72451020669898547, 24.16557627198103120 ) ) ;
#39891 = CARTESIAN_POINT ( 'NONE',  ( 12.14591786802327356, -12.06949235617739191, 30.62609039468567929 ) ) ;
#39892 = CARTESIAN_POINT ( 'NONE',  ( 4.379528057220339221, -16.55341960407611168, 97.70724293864772392 ) ) ;
#39893 = CARTESIAN_POINT ( 'NONE',  ( 19.35633801406911658, -5.499999999999589662, 51.63373818172766505 ) ) ;
#39894 = CARTESIAN_POINT ( 'NONE',  ( -0.05219959533909027116, -19.03943276465977164, 92.49890960531436690 ) ) ;
#39895 = CARTESIAN_POINT ( 'NONE',  ( 13.97604488694527802, 13.89961937509977652, 64.37390960531436690 ) ) ;
#39897 = ADVANCED_FACE ( 'NONE', ( #177317 ), #192469, .T. ) ;
#39896 = CARTESIAN_POINT ( 'NONE',  ( -4.379528057220328563, 16.55341960407611168, 80.20724293864769550 ) ) ;
#39898 = AXIS2_PLACEMENT_3D ( 'NONE', #85387, #97542, #114733 ) ;
#39900 = B_SPLINE_CURVE_WITH_KNOTS ( 'NONE', 3,
 ( #34558, #17404, #116133, #126554, #115133, #192985, #94227, #79061, #160638, #70637, #130276, #186271 ),
 .UNSPECIFIED., .F., .F.,
 ( 4, 2, 2, 2, 2, 4 ),
 ( -0.003994749848159050501, -0.003130422923337882173, -0.002266095998516713846, -0.0005374421488743771902, 0.001191211700767959465, 0.002919865550410296121 ),
 .UNSPECIFIED. ) ;
#39899 = CARTESIAN_POINT ( 'NONE',  ( -21.55341960407610458, -5.719274019375992779, 36.45724293864768839 ) ) ;
#39901 = CARTESIAN_POINT ( 'NONE',  ( -14.34966873604960291, -8.224510206698953496, 56.66557627198103830 ) ) ;
#39902 = CARTESIAN_POINT ( 'NONE',  ( -14.29746914071037622, -8.314922557961029526, 19.16775706135234714 ) ) ;
#39903 = CARTESIAN_POINT ( 'NONE',  ( 5.719274019375673035, 21.55341960407619339, 77.29275706135234714 ) ) ;
#39904 = CARTESIAN_POINT ( 'NONE',  ( -27.73933785331498925, -9.013057229001049109, 146.9750000027311785 ) ) ;
#39905 = CARTESIAN_POINT ( 'NONE',  ( -10.81492255796078084, -18.62759615963271287, 22.08224293864769194 ) ) ;
#39906 = CARTESIAN_POINT ( 'NONE',  ( -14.34966873604972548, 8.224510206698743886, 78.33442372801901854 ) ) ;
#39907 = CARTESIAN_POINT ( 'NONE',  ( 19.02544592524343514, -5.153800228976328945, 28.54057627198102409 ) ) ;
#39908 = CARTESIAN_POINT ( 'NONE',  ( -16.46253265017160317, 9.564922557960807481, 95.83224293864769550 ) ) ;
#39909 = CARTESIAN_POINT ( 'NONE',  ( 0.05219959533907565091, 21.53943276465977519, 94.99890960531436690 ) ) ;
#39910 = CARTESIAN_POINT ( 'NONE',  ( 12.06949235617739724, 12.14591786802326823, 31.87609039468567929 ) ) ;
#39912 = CARTESIAN_POINT ( 'NONE',  ( -0.05219959533937732626, 21.53943276465977519, 67.50109039468568994 ) ) ;
#39911 = CARTESIAN_POINT ( 'NONE',  ( 16.55341960407611168, 4.379528057220329451, 53.95724293864770260 ) ) ;
#39914 = CARTESIAN_POINT ( 'NONE',  ( -21.55341960407610458, -5.719274019375992779, 21.45724293864769550 ) ) ;
#39913 = CARTESIAN_POINT ( 'NONE',  ( -16.53943276465976808, -0.05219959533934237506, 98.75109039468568994 ) ) ;
#39915 = CARTESIAN_POINT ( 'NONE',  ( -5.049401038298153566, 19.05341960407611168, 110.2072429386476813 ) ) ;
#39916 = CARTESIAN_POINT ( 'NONE',  ( 2.500000000000000000, -2.629050547790028551E-15, -2.041999999999999815 ) ) ;
#39917 = CARTESIAN_POINT ( 'NONE',  ( -16.55341960407617563, 4.379528057220093196, 108.5427570613523756 ) ) ;
#39918 = CARTESIAN_POINT ( 'NONE',  ( -16.52544592524335698, -4.483927247898792601, 53.95942372801900433 ) ) ;
#39919 = CARTESIAN_POINT ( 'NONE',  ( -13.97604488694527625, -13.89961937509977652, 66.87390960531436690 ) ) ;
#39920 = CARTESIAN_POINT ( 'NONE',  ( -19.03943276465977164, 0.05219959533909376836, 81.24890960531436690 ) ) ;
#39921 = CARTESIAN_POINT ( 'NONE',  ( -5.823673210054431948, 21.52544592524334988, 67.70942372801901854 ) ) ;
#39922 = CARTESIAN_POINT ( 'NONE',  ( 8.224510206698742110, 14.34966873604972548, 77.08442372801901854 ) ) ;
#39923 = CARTESIAN_POINT ( 'NONE',  ( 8.224510206698953496, -14.34966873604960469, 47.91557627198102409 ) ) ;
#39924 = CARTESIAN_POINT ( 'NONE',  ( -19.03943276465977164, 0.05219959533909376836, 56.24890960531435979 ) ) ;
#39925 = ORIENTED_EDGE ( 'NONE', *, *, #87651, .F. ) ;
#39926 = CARTESIAN_POINT ( 'NONE',  ( 4.483927247898790824, -16.52544592524335698, 20.20942372801900788 ) ) ;
#39927 = CARTESIAN_POINT ( 'NONE',  ( -8.224510206698948167, 14.34966873604960824, 105.4155762719810383 ) ) ;
#39928 = CARTESIAN_POINT ( 'NONE',  ( 16.51473224551069308, 9.474510206698969483, 74.16557627198103830 ) ) ;
#39930 = CARTESIAN_POINT ( 'NONE',  ( 30.74264578624800137, -22.33583958711395212, -1.200000000000000178 ) ) ;
#39929 = CARTESIAN_POINT ( 'NONE',  ( 16.46253265017146816, 9.564922557961045513, 96.66775706135233293 ) ) ;
#39931 = CARTESIAN_POINT ( 'NONE',  ( -5.823673210054431948, 21.52544592524334988, 97.70942372801904696 ) ) ;
#39932 = CARTESIAN_POINT ( 'NONE',  ( -8.224510206698735004, -14.34966873604973081, 74.58442372801901854 ) ) ;
#39933 = CARTESIAN_POINT ( 'NONE',  ( 16.51473224551083163, -9.474510206698727899, 90.83442372801900433 ) ) ;
#39934 = CARTESIAN_POINT ( 'NONE',  ( -10.81492255796078084, -18.62759615963271287, 57.08224293864769550 ) ) ;
#39935 = CARTESIAN_POINT ( 'NONE',  ( -14.29746914071037622, -8.314922557961029526, 54.16775706135235424 ) ) ;
#39936 = DIRECTION ( 'NONE',  ( -1.000000000000000000, 0.000000000000000000, 0.000000000000000000 ) ) ;
#39937 = CARTESIAN_POINT ( 'NONE',  ( 9.474510206698729675, 16.51473224551082808, 57.08442372801900433 ) ) ;
#39938 = CARTESIAN_POINT ( 'NONE',  ( 10.72451020669871369, 18.67979575497193778, 92.08442372801901854 ) ) ;
#39939 = CARTESIAN_POINT ( 'NONE',  ( -19.05341960407611168, -5.049401038298163336, 31.45724293864769550 ) ) ;
#39940 = CARTESIAN_POINT ( 'NONE',  ( -13.89961937509977652, 13.97604488694528158, 70.62390960531432427 ) ) ;
#39941 = CARTESIAN_POINT ( 'NONE',  ( -8.224510206698948167, 14.34966873604960824, 55.41557627198102409 ) ) ;
#39942 = CARTESIAN_POINT ( 'NONE',  ( 10.72451020669871369, 18.67979575497193778, 92.08442372801901854 ) ) ;
#39943 = CARTESIAN_POINT ( 'NONE',  ( -0.05219959533936034679, 19.03943276465977164, 47.50109039468566863 ) ) ;
#39944 = CARTESIAN_POINT ( 'NONE',  ( -19.03943276465977164, -0.05219959533935918106, 23.75109039468566152 ) ) ;
#39945 = CARTESIAN_POINT ( 'NONE',  ( 0.05219959533909260263, 19.03943276465977164, 114.9989096053143669 ) ) ;
#39946 = CARTESIAN_POINT ( 'NONE',  ( -5.719274019375665041, -21.55341960407619695, 99.79275706135234714 ) ) ;
#39947 = CARTESIAN_POINT ( 'NONE',  ( -16.46253265017160317, 9.564922557960807481, 75.83224293864769550 ) ) ;
#39948 = CARTESIAN_POINT ( 'NONE',  ( 0.05219959533937995610, -21.53943276465977519, 95.00109039468568994 ) ) ;
#39949 = CARTESIAN_POINT ( 'NONE',  ( -21.52544592524343514, 5.823673210054127303, 46.04057627198103830 ) ) ;
#39950 = CARTESIAN_POINT ( 'NONE',  ( 13.97604488694527802, 13.89961937509977652, 79.37390960531435269 ) ) ;
#39951 = CARTESIAN_POINT ( 'NONE',  ( 13.97604488694548053, -13.89961937509957401, 70.62609039468567573 ) ) ;
#39952 = CARTESIAN_POINT ( 'NONE',  ( -5.153800228976328057, -19.02544592524343514, 47.29057627198102409 ) ) ;
#39953 = CARTESIAN_POINT ( 'NONE',  ( 16.46253265017160672, -9.564922557960803928, 88.33224293864769550 ) ) ;
#39954 = CARTESIAN_POINT ( 'NONE',  ( 5.049401038297881783, 19.05341960407617563, 97.29275706135233293 ) ) ;
#39955 = CARTESIAN_POINT ( 'NONE',  ( -12.14591786802326823, 12.06949235617739902, 38.12609039468567573 ) ) ;
#39956 = CARTESIAN_POINT ( 'NONE',  ( -16.53943276465976808, 0.05219959533911058130, 106.2489096053143811 ) ) ;
#39957 = CARTESIAN_POINT ( 'NONE',  ( 19.05341960407611168, 5.049401038298154454, 73.95724293864768129 ) ) ;
#39958 = CARTESIAN_POINT ( 'NONE',  ( 21.55341960407610458, 5.719274019375980345, 48.95724293864770971 ) ) ;
#39959 = CARTESIAN_POINT ( 'NONE',  ( 12.06949235617739724, 12.14591786802326823, 36.87609039468568994 ) ) ;
#39960 = CARTESIAN_POINT ( 'NONE',  ( 18.67979575497194134, -10.72451020669871369, 30.83442372801902209 ) ) ;
#39961 = CARTESIAN_POINT ( 'NONE',  ( -0.05219959533937732626, 21.53943276465977519, 82.50109039468568994 ) ) ;
#39962 = CARTESIAN_POINT ( 'NONE',  ( -14.34966873604972548, 8.224510206698743886, 88.33442372801901854 ) ) ;
#39963 = AXIS2_PLACEMENT_3D ( 'NONE', #83798, #126333, #189027 ) ;
#39964 = CARTESIAN_POINT ( 'NONE',  ( -13.89961937509977652, 13.97604488694528158, 80.62390960531436690 ) ) ;
#39965 = CARTESIAN_POINT ( 'NONE',  ( 14.34966873604972726, -8.224510206698740333, 105.8344237280190328 ) ) ;
#39966 = CARTESIAN_POINT ( 'NONE',  ( 9.474510206698729675, 16.51473224551082808, 57.08442372801900433 ) ) ;
#39967 = CARTESIAN_POINT ( 'NONE',  ( 15.80617190586769283, -15.72974639402175789, 35.62609039468568994 ) ) ;
#39968 = CARTESIAN_POINT ( 'NONE',  ( 16.55341960407611168, 4.379528057220329451, 83.95724293864770971 ) ) ;
#39969 = CARTESIAN_POINT ( 'NONE',  ( -5.153800228976328057, -19.02544592524343514, 102.2905762719810383 ) ) ;
#39970 = CARTESIAN_POINT ( 'NONE',  ( -14.29746914071037622, -8.314922557961029526, 109.1677570613523613 ) ) ;
#39971 = CARTESIAN_POINT ( 'NONE',  ( -21.52544592524334988, -5.823673210054445271, 68.95942372801901854 ) ) ;
#39972 = CARTESIAN_POINT ( 'NONE',  ( -8.224510206698735004, -14.34966873604973081, 39.58442372801901143 ) ) ;
#39973 = CARTESIAN_POINT ( 'NONE',  ( -21.52544592524334988, -5.823673210054445271, 33.95942372801901143 ) ) ;
#39974 = CARTESIAN_POINT ( 'NONE',  ( -16.52544592524342804, 4.483927247898546575, 71.04057627198103830 ) ) ;
#39975 = ORIENTED_EDGE ( 'NONE', *, *, #94686, .T. ) ;
#39976 = CARTESIAN_POINT ( 'NONE',  ( -15.72974639402197994, 15.80617190586746368, 110.6239096053143669 ) ) ;
#39977 = CARTESIAN_POINT ( 'NONE',  ( -12.14591786802309592, -12.06949235617757132, 51.87390960531437401 ) ) ;
#39978 = CARTESIAN_POINT ( 'NONE',  ( -13.89961937509977652, 13.97604488694528158, 25.62390960531434558 ) ) ;
#39979 = CARTESIAN_POINT ( 'NONE',  ( -5.719274019375978568, 21.55341960407610458, 35.20724293864768839 ) ) ;
#39980 = CARTESIAN_POINT ( 'NONE',  ( -12.06949235617756955, 12.14591786802309770, 60.62390960531437401 ) ) ;
#39981 = CARTESIAN_POINT ( 'NONE',  ( -15.80617190586745835, -15.72974639402198527, 81.87390960531435269 ) ) ;
#39982 = CARTESIAN_POINT ( 'NONE',  ( -19.03943276465977164, 0.05219959533909376836, 76.24890960531435269 ) ) ;
#39984 = CARTESIAN_POINT ( 'NONE',  ( -9.474510206698720793, -16.51473224551083518, 79.58442372801899012 ) ) ;
#39983 = CARTESIAN_POINT ( 'NONE',  ( 9.474510206698971260, -16.51473224551069308, 37.91557627198102409 ) ) ;
#39985 = EDGE_CURVE ( 'NONE', #142110, #69099, #82259, .T. ) ;
#39987 = CARTESIAN_POINT ( 'NONE',  ( 21.52544592524344225, -5.823673210054117533, 63.54057627198103830 ) ) ;
#39986 = CARTESIAN_POINT ( 'NONE',  ( 18.67979575497194134, -10.72451020669871369, 60.83442372801901854 ) ) ;
#39988 = CARTESIAN_POINT ( 'NONE',  ( 0.05219959533909260263, 19.03943276465977164, 44.99890960531435979 ) ) ;
#39989 = CARTESIAN_POINT ( 'NONE',  ( -0.05219959533909027116, -19.03943276465977164, 67.49890960531436690 ) ) ;
#39990 = ORIENTED_EDGE ( 'NONE', *, *, #31579, .T. ) ;
#39991 = CARTESIAN_POINT ( 'NONE',  ( -14.34966873604972548, 8.224510206698743886, 48.33442372801902565 ) ) ;
#39992 = CARTESIAN_POINT ( 'NONE',  ( 5.823673210054444382, -21.52544592524334988, 35.20942372801901854 ) ) ;
#39993 = CARTESIAN_POINT ( 'NONE',  ( 15.72974639402176855, 15.80617190586768217, 56.87609039468568994 ) ) ;
#39994 = CARTESIAN_POINT ( 'NONE',  ( 16.51473224551069308, 9.474510206698969483, 104.1655762719810241 ) ) ;
#39995 = CARTESIAN_POINT ( 'NONE',  ( -15.72974639402197994, 15.80617190586746368, 80.62390960531438111 ) ) ;
#39997 = CARTESIAN_POINT ( 'NONE',  ( -4.483927247898782831, 16.52544592524335698, 57.70942372801901143 ) ) ;
#39996 = CARTESIAN_POINT ( 'NONE',  ( 0.05219959533937995610, -21.53943276465977519, 25.00109039468567218 ) ) ;
#39998 = CARTESIAN_POINT ( 'NONE',  ( 15.80617190586746368, 15.72974639402197994, 44.37390960531435979 ) ) ;
#39999 = CARTESIAN_POINT ( 'NONE',  ( 5.719274019375673035, 21.55341960407619339, 112.2927570613523471 ) ) ;
#40000 = CARTESIAN_POINT ( 'NONE',  ( 19.03943276465977164, -0.05219959533909143690, 48.74890960531435979 ) ) ;
#40001 = CARTESIAN_POINT ( 'NONE',  ( -9.564922557960796823, -16.46253265017161027, 107.0822429386476955 ) ) ;
#40002 = CARTESIAN_POINT ( 'NONE',  ( -5.049401038298153566, 19.05341960407611168, 85.20724293864766707 ) ) ;
#40003 = LINE ( 'NONE', #6659, #82972 ) ;
#40004 = CARTESIAN_POINT ( 'NONE',  ( -19.05341960407617563, 5.049401038297882671, 68.54275706135230450 ) ) ;
#40005 = CARTESIAN_POINT ( 'NONE',  ( 0.05219959533907565091, 21.53943276465977519, 49.99890960531437401 ) ) ;
#40006 = CARTESIAN_POINT ( 'NONE',  ( -8.314922557960811034, -14.29746914071050412, 27.08224293864769550 ) ) ;
#40007 = CARTESIAN_POINT ( 'NONE',  ( 19.05341960407617918, -5.049401038297876454, 86.04275706135233293 ) ) ;
#40008 = DIRECTION ( 'NONE',  ( -0.000000000000000000, -0.000000000000000000, 1.000000000000000000 ) ) ;
#40009 = CARTESIAN_POINT ( 'NONE',  ( 15.80617190586769283, -15.72974639402175789, 110.6260903946857042 ) ) ;
#40010 = CARTESIAN_POINT ( 'NONE',  ( 16.46253265017146816, 9.564922557961045513, 101.6677570613523329 ) ) ;
#40011 = CARTESIAN_POINT ( 'NONE',  ( -19.02544592524334988, -5.153800228976617603, 48.95942372801900433 ) ) ;
#40012 = CARTESIAN_POINT ( 'NONE',  ( 16.21995358207305671, 7.366697692864192959, 107.5644899848784206 ) ) ;
#40013 = CARTESIAN_POINT ( 'NONE',  ( 9.564922557960805705, 16.46253265017160317, 49.58224293864770260 ) ) ;
#40014 = CARTESIAN_POINT ( 'NONE',  ( -12.06949235617756955, 12.14591786802309770, 55.62390960531436690 ) ) ;
#40015 = CARTESIAN_POINT ( 'NONE',  ( -16.46253265017160317, 9.564922557960807481, 30.83224293864769550 ) ) ;
#40016 = CARTESIAN_POINT ( 'NONE',  ( 16.55341960407611168, 4.379528057220329451, 33.95724293864769550 ) ) ;
#40017 = CARTESIAN_POINT ( 'NONE',  ( -30.12056840655105461, -26.02156742258015854, -20.94459150989508345 ) ) ;
#40018 = CARTESIAN_POINT ( 'NONE',  ( 16.53943276465976808, 0.05219959533934440121, 111.2510903946856899 ) ) ;
#40019 = CARTESIAN_POINT ( 'NONE',  ( 19.05341960407611168, 5.049401038298154454, 68.95724293864769550 ) ) ;
#40020 = CARTESIAN_POINT ( 'NONE',  ( -19.03943276465977164, -0.05219959533935918106, 28.75109039468566507 ) ) ;
#40021 = CARTESIAN_POINT ( 'NONE',  ( 8.224510206698742110, 14.34966873604972548, 32.08442372801901854 ) ) ;
#40022 = CARTESIAN_POINT ( 'NONE',  ( -5.823673210054116645, -21.52544592524344225, 37.29057627198102409 ) ) ;
#40023 = CARTESIAN_POINT ( 'NONE',  ( 10.72451020669871369, 18.67979575497193778, 102.0844237280190185 ) ) ;
#40024 = CARTESIAN_POINT ( 'NONE',  ( -13.89961937509977652, 13.97604488694528158, 65.62390960531436690 ) ) ;
#40025 = CARTESIAN_POINT ( 'NONE',  ( -13.97604488694527625, -13.89961937509977652, 111.8739096053143243 ) ) ;
#40026 = CARTESIAN_POINT ( 'NONE',  ( 19.02544592524343514, -5.153800228976328945, 103.5405762719809957 ) ) ;
#40027 = CARTESIAN_POINT ( 'NONE',  ( -11.40812507854755609, 35.11059874428196537, -3.024999997268813523 ) ) ;
#40028 = CARTESIAN_POINT ( 'NONE',  ( -5.823673210054431948, 21.52544592524334988, 22.70942372801901499 ) ) ;
#40029 = CARTESIAN_POINT ( 'NONE',  ( 8.314922557960818139, 14.29746914071049879, 89.58224293864768129 ) ) ;
#40031 = CARTESIAN_POINT ( 'NONE',  ( 0.05219959533909260263, 19.03943276465977164, 64.99890960531436690 ) ) ;
#40030 = CARTESIAN_POINT ( 'NONE',  ( -5.719274019375978568, 21.55341960407610458, 80.20724293864769550 ) ) ;
#40032 = CARTESIAN_POINT ( 'NONE',  ( -19.05341960407611168, -5.049401038298163336, 76.45724293864769550 ) ) ;
#40033 = CARTESIAN_POINT ( 'NONE',  ( 5.719274019375991003, -21.55341960407610458, 112.7072429386476955 ) ) ;
#40034 = ORIENTED_EDGE ( 'NONE', *, *, #178675, .F. ) ;
#40035 = CARTESIAN_POINT ( 'NONE',  ( -9.564922557960796823, -16.46253265017161027, 77.08224293864769550 ) ) ;
#40036 = AXIS2_PLACEMENT_3D ( 'NONE', #113385, #86057, #98197 ) ;
#40037 = CARTESIAN_POINT ( 'NONE',  ( 28.79475375365567302, 9.355982642739496313, 147.0843446568999866 ) ) ;
#40039 = CARTESIAN_POINT ( 'NONE',  ( 13.89961937509977652, -13.97604488694527269, 23.12390960531436335 ) ) ;
#40038 = CARTESIAN_POINT ( 'NONE',  ( 16.52544592524342804, -4.483927247898539470, 108.5405762719810241 ) ) ;
#40040 = CARTESIAN_POINT ( 'NONE',  ( 0.05219959533909260263, 19.03943276465977164, 69.99890960531435269 ) ) ;
#40041 = CARTESIAN_POINT ( 'NONE',  ( 9.474510206698729675, 16.51473224551082808, 92.08442372801900433 ) ) ;
#40042 = CARTESIAN_POINT ( 'NONE',  ( 12.14591786802309770, 12.06949235617756955, 104.3739096053143669 ) ) ;
#40043 = CARTESIAN_POINT ( 'NONE',  ( 5.719274019375673035, 21.55341960407619339, 67.29275706135234714 ) ) ;
#40045 = CARTESIAN_POINT ( 'NONE',  ( 10.81492255796106328, -18.62759615963255655, 25.41775706135235779 ) ) ;
#40044 = CARTESIAN_POINT ( 'NONE',  ( 13.97604488694527802, 13.89961937509977652, 49.37390960531434558 ) ) ;
#40046 = CARTESIAN_POINT ( 'NONE',  ( -15.80617190586745835, -15.72974639402198527, 106.8739096053143811 ) ) ;
#40047 = CARTESIAN_POINT ( 'NONE',  ( -28.82186960331499037, 2.428612866367529932E-14, 142.0000000000000000 ) ) ;
#40048 = CARTESIAN_POINT ( 'NONE',  ( 5.049401038298161559, -19.05341960407611168, 77.70724293864765286 ) ) ;
#40050 = CARTESIAN_POINT ( 'NONE',  ( 10.81492255796078972, 18.62759615963270932, 34.58224293864770260 ) ) ;
#40049 = CARTESIAN_POINT ( 'NONE',  ( -0.05219959533936034679, 19.03943276465977164, 102.5010903946856757 ) ) ;
#40051 = CARTESIAN_POINT ( 'NONE',  ( 0.05219959533937995610, -21.53943276465977519, 65.00109039468568994 ) ) ;
#40052 = CARTESIAN_POINT ( 'NONE',  ( -19.03943276465977164, 0.05219959533909376836, 101.2489096053143669 ) ) ;
#40053 = CARTESIAN_POINT ( 'NONE',  ( -5.153800228976607833, 19.02544592524334988, 87.70942372801897591 ) ) ;
#40054 = CARTESIAN_POINT ( 'NONE',  ( -5.049401038298153566, 19.05341960407611168, 45.20724293864769550 ) ) ;
#40055 = CARTESIAN_POINT ( 'NONE',  ( 0.05219959533909260263, 19.03943276465977164, 74.99890960531435269 ) ) ;
#40056 = CARTESIAN_POINT ( 'NONE',  ( 16.52544592524342804, -4.483927247898539470, 78.54057627198103830 ) ) ;
#40057 = CARTESIAN_POINT ( 'NONE',  ( 19.05341960407611168, 5.049401038298154454, 108.9572429386477097 ) ) ;
#40058 = CARTESIAN_POINT ( 'NONE',  ( 8.224510206698953496, -14.34966873604960469, 92.91557627198103830 ) ) ;
#40059 = CARTESIAN_POINT ( 'NONE',  ( -13.89961937509977652, 13.97604488694528158, 95.62390960531436690 ) ) ;
#40061 = CARTESIAN_POINT ( 'NONE',  ( 13.97604488694527802, 13.89961937509977652, 34.37390960531436690 ) ) ;
#40060 = CARTESIAN_POINT ( 'NONE',  ( -14.29746914071049879, 8.314922557960819915, 45.83224293864769550 ) ) ;
#40062 = ORIENTED_EDGE ( 'NONE', *, *, #173531, .T. ) ;
#40063 = CARTESIAN_POINT ( 'NONE',  ( -21.53943276465977519, -0.05219959533937600094, 58.75109039468568994 ) ) ;
#40064 = CARTESIAN_POINT ( 'NONE',  ( -19.02544592524334988, -5.153800228976617603, 73.95942372801900433 ) ) ;
#40065 = CARTESIAN_POINT ( 'NONE',  ( 12.06949235617757843, -12.14591786802309237, 43.12390960531435269 ) ) ;
#40066 = CARTESIAN_POINT ( 'NONE',  ( 21.52544592524344225, -5.823673210054117533, 93.54057627198103830 ) ) ;
#40067 = CARTESIAN_POINT ( 'NONE',  ( 5.823673210054125526, 21.52544592524343514, 34.79057627198103120 ) ) ;
#40068 = CARTESIAN_POINT ( 'NONE',  ( 4.483927247898545687, 16.52544592524342804, 84.79057627198102409 ) ) ;
#40069 = CARTESIAN_POINT ( 'NONE',  ( 16.46253265017160672, -9.564922557960803928, 58.33224293864769550 ) ) ;
#40070 = CARTESIAN_POINT ( 'NONE',  ( 16.53943276465976808, -0.05219959533910856209, 28.74890960531435624 ) ) ;
#40071 = CARTESIAN_POINT ( 'NONE',  ( -12.06949235617739369, -12.14591786802326823, 104.3760903946856899 ) ) ;
#40072 = CARTESIAN_POINT ( 'NONE',  ( -16.55341960407617563, 4.379528057220093196, 68.54275706135234714 ) ) ;
#40073 = CARTESIAN_POINT ( 'NONE',  ( -5.049401038297874678, -19.05341960407617918, 29.79275706135232227 ) ) ;
#40074 = CARTESIAN_POINT ( 'NONE',  ( 19.02544592524343514, -5.153800228976328945, 103.5405762719809957 ) ) ;
#40075 = CARTESIAN_POINT ( 'NONE',  ( -19.05341960407611168, -5.049401038298163336, 76.45724293864769550 ) ) ;
#40076 = CARTESIAN_POINT ( 'NONE',  ( 13.89961937509977652, -13.97604488694527269, 33.12390960531434558 ) ) ;
#40077 = CARTESIAN_POINT ( 'NONE',  ( 8.314922557960818139, 14.29746914071049879, 44.58224293864769550 ) ) ;
#40079 = CARTESIAN_POINT ( 'NONE',  ( 0.05219959533909260263, 19.03943276465977164, 99.99890960531436690 ) ) ;
#40078 = CARTESIAN_POINT ( 'NONE',  ( -13.97604488694527625, -13.89961937509977652, 111.8739096053143243 ) ) ;
#40080 = CARTESIAN_POINT ( 'NONE',  ( -18.67979575497178146, -10.72451020669898902, 36.66557627198103120 ) ) ;
#40081 = CARTESIAN_POINT ( 'NONE',  ( -14.29746914071049879, 8.314922557960819915, 70.83224293864770971 ) ) ;
#40082 = CARTESIAN_POINT ( 'NONE',  ( 14.34966873604972726, -8.224510206698740333, 20.83442372801901143 ) ) ;
#40083 = CARTESIAN_POINT ( 'NONE',  ( -8.224510206698948167, 14.34966873604960824, 65.41557627198102409 ) ) ;
#40085 = AXIS2_PLACEMENT_3D ( 'NONE', #91233, #72124, #195489 ) ;
#40084 = CARTESIAN_POINT ( 'NONE',  ( 30.27664185797779339, -1.503321482105604456, -47.91583118997746027 ) ) ;
#40086 = CARTESIAN_POINT ( 'NONE',  ( -19.03943276465977164, -0.05219959533935918106, 58.75109039468566863 ) ) ;
#40087 = CARTESIAN_POINT ( 'NONE',  ( -16.46253265017160317, 9.564922557960807481, 100.8322429386477097 ) ) ;
#40088 = CARTESIAN_POINT ( 'NONE',  ( 13.97604488694548053, -13.89961937509957401, 80.62609039468567573 ) ) ;
#40089 = CARTESIAN_POINT ( 'NONE',  ( -9.474510206698720793, -16.51473224551083518, 39.58442372801899722 ) ) ;
#40091 = CARTESIAN_POINT ( 'NONE',  ( -16.55341960407617563, 4.379528057220093196, 93.54275706135234714 ) ) ;
#40090 = CARTESIAN_POINT ( 'NONE',  ( 9.474510206698729675, 16.51473224551082808, 107.0844237280190043 ) ) ;
#40092 = CARTESIAN_POINT ( 'NONE',  ( 16.51473224551069308, 9.474510206698969483, 44.16557627198103120 ) ) ;
#40093 = CARTESIAN_POINT ( 'NONE',  ( 15.80617190586746368, 15.72974639402197994, 34.37390960531435979 ) ) ;
#40094 = CARTESIAN_POINT ( 'NONE',  ( -10.72451020669870658, -18.67979575497194134, 49.58442372801901143 ) ) ;
#40095 = CARTESIAN_POINT ( 'NONE',  ( 4.500000000000000888, -126.1226662136678556, 8.481152457036394310 ) ) ;
#40096 = CARTESIAN_POINT ( 'NONE',  ( 16.52544592524335698, 4.483927247898782831, 21.45942372801901499 ) ) ;
#40098 = CARTESIAN_POINT ( 'NONE',  ( 16.51473224551069308, 9.474510206698969483, 79.16557627198103830 ) ) ;
#40097 = CARTESIAN_POINT ( 'NONE',  ( 0.000000000000000000, -64.82615989628266107, -25.00000000000000000 ) ) ;
#40099 = CARTESIAN_POINT ( 'NONE',  ( 17.10449713765564184, 17.26089242801060664, -56.77278709839600879 ) ) ;
#40101 = CARTESIAN_POINT ( 'NONE',  ( -9.564922557960796823, -16.46253265017161027, 72.08224293864770971 ) ) ;
#40100 = CARTESIAN_POINT ( 'NONE',  ( -16.55341960407611168, -4.379528057220339221, 86.45724293864770971 ) ) ;
#40102 = CARTESIAN_POINT ( 'NONE',  ( -19.05341960407611168, -5.049401038298163336, 81.45724293864769550 ) ) ;
#40103 = ORIENTED_EDGE ( 'NONE', *, *, #74517, .F. ) ;
#40104 = CARTESIAN_POINT ( 'NONE',  ( -5.049401038297874678, -19.05341960407617918, 94.79275706135230450 ) ) ;
#40105 = CARTESIAN_POINT ( 'NONE',  ( -18.67979575497178146, -10.72451020669898902, 61.66557627198103120 ) ) ;
#40106 = CARTESIAN_POINT ( 'NONE',  ( 19.02544592524343514, -5.153800228976328945, 23.54057627198102054 ) ) ;
#40107 = CARTESIAN_POINT ( 'NONE',  ( -5.049401038297874678, -19.05341960407617918, 59.79275706135231871 ) ) ;
#40108 = CARTESIAN_POINT ( 'NONE',  ( 19.05341960407611168, 5.049401038298154454, 58.95724293864768129 ) ) ;
#40109 = CARTESIAN_POINT ( 'NONE',  ( -16.51473224551069308, -9.474510206698971260, 91.66557627198103830 ) ) ;
#40110 = ORIENTED_EDGE ( 'NONE', *, *, #19257, .T. ) ;
#40111 = CARTESIAN_POINT ( 'NONE',  ( -5.719274019375978568, 21.55341960407610458, 95.20724293864769550 ) ) ;
#40113 = CARTESIAN_POINT ( 'NONE',  ( 19.05341960407617918, -5.049401038297876454, 61.04275706135232582 ) ) ;
#40112 = CARTESIAN_POINT ( 'NONE',  ( -4.379528057220328563, 16.55341960407611168, 95.20724293864769550 ) ) ;
#40114 = CARTESIAN_POINT ( 'NONE',  ( -21.55341960407610458, -5.719274019375992779, 91.45724293864769550 ) ) ;
#40115 = CARTESIAN_POINT ( 'NONE',  ( -21.52544592524343514, 5.823673210054127303, 71.04057627198103830 ) ) ;
#40116 = CARTESIAN_POINT ( 'NONE',  ( 14.29746914071049879, -8.314922557960816363, 28.33224293864769550 ) ) ;
#40117 = CARTESIAN_POINT ( 'NONE',  ( -10.81492255796105439, 18.62759615963255655, 107.9177570613523471 ) ) ;
#40118 = CARTESIAN_POINT ( 'NONE',  ( 16.53943276465976808, 0.05219959533934440121, 51.25109039468568994 ) ) ;
#40119 = CARTESIAN_POINT ( 'NONE',  ( 9.564922557960805705, 16.46253265017160317, 79.58224293864769550 ) ) ;
#40120 = CARTESIAN_POINT ( 'NONE',  ( -9.564922557960796823, -16.46253265017161027, 37.08224293864768839 ) ) ;
#40121 = VECTOR ( 'NONE', #138782, 1000.000000000000000 ) ;
#40122 = CARTESIAN_POINT ( 'NONE',  ( -15.72974639402176322, -15.80617190586768395, 39.37609039468567573 ) ) ;
#40123 = CARTESIAN_POINT ( 'NONE',  ( -15.72974639402176322, -15.80617190586768395, 54.37609039468568994 ) ) ;
#40124 = CARTESIAN_POINT ( 'NONE',  ( 9.474510206698971260, -16.51473224551069308, 42.91557627198103120 ) ) ;
#40125 = CARTESIAN_POINT ( 'NONE',  ( 15.72974639402176855, 15.80617190586768217, 26.87609039468567218 ) ) ;
#40126 = CARTESIAN_POINT ( 'NONE',  ( -16.46253265017146816, -9.564922557961047289, 64.16775706135233293 ) ) ;
#40127 = CARTESIAN_POINT ( 'NONE',  ( -16.46253265017146816, -9.564922557961047289, 69.16775706135233293 ) ) ;
#40128 = CARTESIAN_POINT ( 'NONE',  ( -0.05219959533934338120, 16.53943276465976808, 32.50109039468568284 ) ) ;
#40129 = CARTESIAN_POINT ( 'NONE',  ( -5.153800228976328057, -19.02544592524343514, 22.29057627198102765 ) ) ;
#40130 = CARTESIAN_POINT ( 'NONE',  ( 16.53943276465976808, 0.05219959533934440121, 71.25109039468568994 ) ) ;
#40131 = CARTESIAN_POINT ( 'NONE',  ( -5.153800228976328057, -19.02544592524343514, 42.29057627198101699 ) ) ;
#40132 = CARTESIAN_POINT ( 'NONE',  ( 21.94905633995417915, -7.481063542984161430, 170.0146117665088923 ) ) ;
#40133 = CARTESIAN_POINT ( 'NONE',  ( -0.05219959533909027116, -19.03943276465977164, 92.49890960531436690 ) ) ;
#40135 = ADVANCED_FACE ( 'NONE', ( #161122 ), #22619, .F. ) ;
#40134 = CARTESIAN_POINT ( 'NONE',  ( 13.89961937509977652, -13.97604488694527269, 28.12390960531435624 ) ) ;
#40136 = CARTESIAN_POINT ( 'NONE',  ( -18.67979575497178146, -10.72451020669898902, 76.66557627198103830 ) ) ;
#40137 = CARTESIAN_POINT ( 'NONE',  ( -4.483927247898782831, 16.52544592524335698, 62.70942372801902565 ) ) ;
#40138 = CARTESIAN_POINT ( 'NONE',  ( -18.67979575497193778, 10.72451020669871902, 113.3344237280190328 ) ) ;
#40139 = CARTESIAN_POINT ( 'NONE',  ( 16.51473224551069308, 9.474510206698969483, 54.16557627198103120 ) ) ;
#40140 = CARTESIAN_POINT ( 'NONE',  ( 14.34966873604960469, 8.224510206698951720, 29.16557627198103120 ) ) ;
#40141 = CARTESIAN_POINT ( 'NONE',  ( -4.379528057220328563, 16.55341960407611168, 65.20724293864768129 ) ) ;
#40142 = CARTESIAN_POINT ( 'NONE',  ( 19.05341960407611168, 5.049401038298154454, 73.95724293864768129 ) ) ;
#40143 = CARTESIAN_POINT ( 'NONE',  ( 21.53943276465977519, 0.05219959533937863772, 41.25109039468568284 ) ) ;
#40144 = CARTESIAN_POINT ( 'NONE',  ( 9.474510206698971260, -16.51473224551069308, 82.91557627198103830 ) ) ;
#40145 = CARTESIAN_POINT ( 'NONE',  ( 15.80617190586769283, -15.72974639402175789, 80.62609039468567573 ) ) ;
#40146 = CARTESIAN_POINT ( 'NONE',  ( 4.483927247898790824, -16.52544592524335698, 60.20942372801902565 ) ) ;
#40147 = CARTESIAN_POINT ( 'NONE',  ( 5.153800228976335163, 19.02544592524342804, 114.7905762719810241 ) ) ;
#40148 = CARTESIAN_POINT ( 'NONE',  ( 5.719274019375991003, -21.55341960407610458, 87.70724293864769550 ) ) ;
#40149 = AXIS2_PLACEMENT_3D ( 'NONE', #159113, #117623, #100445 ) ;
#40150 = CARTESIAN_POINT ( 'NONE',  ( -8.224510206698948167, 14.34966873604960824, 50.41557627198103120 ) ) ;
#40151 = CARTESIAN_POINT ( 'NONE',  ( 16.46253265017160672, -9.564922557960803928, 28.33224293864769550 ) ) ;
#40152 = CARTESIAN_POINT ( 'NONE',  ( 8.314922557961029526, -14.29746914071037800, 55.41775706135234714 ) ) ;
#40153 = CARTESIAN_POINT ( 'NONE',  ( -12.14591786802309592, -12.06949235617757132, 51.87390960531437401 ) ) ;
#40154 = CARTESIAN_POINT ( 'NONE',  ( -15.80617190586745835, -15.72974639402198527, 21.87390960531436690 ) ) ;
#40155 = CARTESIAN_POINT ( 'NONE',  ( -5.719274019375978568, 21.55341960407610458, 35.20724293864768839 ) ) ;
#40156 = CARTESIAN_POINT ( 'NONE',  ( -10.72451020669870658, -18.67979575497194134, 109.5844237280190328 ) ) ;
#40157 = CARTESIAN_POINT ( 'NONE',  ( 12.06949235617757843, -12.14591786802309237, 98.12390960531436690 ) ) ;
#40158 = CARTESIAN_POINT ( 'NONE',  ( 19.05341960407611168, 5.049401038298154454, 93.95724293864769550 ) ) ;
#40159 = ORIENTED_EDGE ( 'NONE', *, *, #55093, .F. ) ;
#40160 = CARTESIAN_POINT ( 'NONE',  ( -8.224510206698735004, -14.34966873604973081, 49.58442372801901143 ) ) ;
#40161 = CARTESIAN_POINT ( 'NONE',  ( 5.153800228976335163, 19.02544592524342804, 54.79057627198103120 ) ) ;
#40162 = CYLINDRICAL_SURFACE ( 'NONE', #143697, 2.500000000000002220 ) ;
#40163 = CARTESIAN_POINT ( 'NONE',  ( -9.474510206698720793, -16.51473224551083518, 44.58442372801900433 ) ) ;
#40164 = CARTESIAN_POINT ( 'NONE',  ( -16.55341960407617563, 4.379528057220093196, 98.54275706135234714 ) ) ;
#40165 = CARTESIAN_POINT ( 'NONE',  ( -5.153800228976607833, 19.02544592524334988, 97.70942372801900433 ) ) ;
#40166 = CARTESIAN_POINT ( 'NONE',  ( 18.67979575497194134, -10.72451020669871369, 60.83442372801901854 ) ) ;
#40167 = CARTESIAN_POINT ( 'NONE',  ( 13.89961937509977652, -13.97604488694527269, 73.12390960531436690 ) ) ;
#40168 = CARTESIAN_POINT ( 'NONE',  ( 21.53943276465977519, -0.05219959533907433946, 88.74890960531436690 ) ) ;
#40169 = CARTESIAN_POINT ( 'NONE',  ( -14.29746914071049879, 8.314922557960819915, 105.8322429386476955 ) ) ;
#40170 = CARTESIAN_POINT ( 'NONE',  ( 13.97604488694548053, -13.89961937509957401, 75.62609039468564731 ) ) ;
#40171 = CARTESIAN_POINT ( 'NONE',  ( -15.72974639402197994, 15.80617190586746368, 80.62390960531438111 ) ) ;
#40172 = CARTESIAN_POINT ( 'NONE',  ( 13.89961937509957401, 13.97604488694547697, 36.87609039468565442 ) ) ;
#40173 = CARTESIAN_POINT ( 'NONE',  ( 19.25176906914649066, 5.499999999999787725, 98.49927264242275271 ) ) ;
#40174 = CARTESIAN_POINT ( 'NONE',  ( -10.81492255796078084, -18.62759615963271287, 87.08224293864769550 ) ) ;
#40175 = CARTESIAN_POINT ( 'NONE',  ( -19.53037848336980886, 5.499999999999903189, 54.85532783611443364 ) ) ;
#40176 = CARTESIAN_POINT ( 'NONE',  ( -9.474510206698964154, 16.51473224551069663, 65.41557627198102409 ) ) ;
#40177 = CARTESIAN_POINT ( 'NONE',  ( -17.60691670004652210, -5.499999999999992006, 89.13333313366439370 ) ) ;
#40178 = CARTESIAN_POINT ( 'NONE',  ( 12.14591786802327356, -12.06949235617739191, 20.62609039468568639 ) ) ;
#40179 = CARTESIAN_POINT ( 'NONE',  ( -18.22780087662119541, 5.500000000000102141, 66.01763182126894947 ) ) ;
#40180 = CARTESIAN_POINT ( 'NONE',  ( 5.049401038298161559, -19.05341960407611168, 42.70724293864767418 ) ) ;
#40181 = CARTESIAN_POINT ( 'NONE',  ( 16.46253265017160672, -9.564922557960803928, 108.3322429386476955 ) ) ;
#40183 = CARTESIAN_POINT ( 'NONE',  ( 12.06949235617757843, -12.14591786802309237, 53.12390960531436690 ) ) ;
#40182 = CARTESIAN_POINT ( 'NONE',  ( 10.81492255796078972, 18.62759615963270932, 104.5822429386477097 ) ) ;
#40184 = CARTESIAN_POINT ( 'NONE',  ( 18.62759615963255655, 10.81492255796105972, 71.66775706135234714 ) ) ;
#40186 = CARTESIAN_POINT ( 'NONE',  ( 0.05219959533936267826, -19.03943276465977164, 35.00109039468566863 ) ) ;
#40185 = CARTESIAN_POINT ( 'NONE',  ( 14.34966873604972726, -8.224510206698740333, 20.83442372801901143 ) ) ;
#40187 = CARTESIAN_POINT ( 'NONE',  ( -14.34966873604960291, -8.224510206698953496, 31.66557627198102054 ) ) ;
#40188 = CARTESIAN_POINT ( 'NONE',  ( -21.55341960407610458, -5.719274019375992779, 111.4572429386476813 ) ) ;
#40189 = CARTESIAN_POINT ( 'NONE',  ( -4.483927247898539470, -16.52544592524342804, 47.29057627198103120 ) ) ;
#40190 = CARTESIAN_POINT ( 'NONE',  ( 9.474510206698729675, 16.51473224551082808, 92.08442372801900433 ) ) ;
#40191 = CARTESIAN_POINT ( 'NONE',  ( 9.474510206698729675, 16.51473224551082808, 67.08442372801900433 ) ) ;
#40193 = B_SPLINE_CURVE_WITH_KNOTS ( 'NONE', 3,
 ( #571, #102058, #92587, #15766, #76434, #61259 ),
 .UNSPECIFIED., .F., .F.,
 ( 4, 2, 4 ),
 ( 0.003989672132298113100, 0.004372778065220548488, 0.004755883998142983876 ),
 .UNSPECIFIED. ) ;
#40192 = CARTESIAN_POINT ( 'NONE',  ( 10.81492255796106328, -18.62759615963255655, 65.41775706135234714 ) ) ;
#40194 = CARTESIAN_POINT ( 'NONE',  ( -16.51473224551082808, 9.474510206698731452, 48.33442372801900433 ) ) ;
#40195 = CARTESIAN_POINT ( 'NONE',  ( 0.05219959533909260263, 19.03943276465977164, 29.99890960531435979 ) ) ;
#40196 = CARTESIAN_POINT ( 'NONE',  ( 10.72451020669898902, -18.67979575497178502, 47.91557627198102409 ) ) ;
#40197 = CARTESIAN_POINT ( 'NONE',  ( 0.05219959533910956823, 16.53943276465976808, 44.99890960531435979 ) ) ;
#40198 = CARTESIAN_POINT ( 'NONE',  ( -17.48853670773243607, -5.747243402303084281, 26.33328700250008936 ) ) ;
#40199 = CARTESIAN_POINT ( 'NONE',  ( -10.81492255796105439, 18.62759615963255655, 112.9177570613523329 ) ) ;
#40200 = CARTESIAN_POINT ( 'NONE',  ( -12.14591786802326823, 12.06949235617739902, 88.12609039468570415 ) ) ;
#40201 = CARTESIAN_POINT ( 'NONE',  ( 16.53943276465976808, -0.05219959533910856209, 33.74890960531436690 ) ) ;
#40202 = CARTESIAN_POINT ( 'NONE',  ( -10.81492255796105439, 18.62759615963255655, 77.91775706135231871 ) ) ;
#40203 = CARTESIAN_POINT ( 'NONE',  ( 18.67979575497194134, -10.72451020669871369, 85.83442372801901854 ) ) ;
#40204 = CARTESIAN_POINT ( 'NONE',  ( -21.55341960407610458, -5.719274019375992779, 86.45724293864770971 ) ) ;
#40205 = AXIS2_PLACEMENT_3D ( 'NONE', #31289, #167818, #168790 ) ;
#40206 = CARTESIAN_POINT ( 'NONE',  ( -0.05219959533909027116, -19.03943276465977164, 42.49890960531435269 ) ) ;
#40207 = CARTESIAN_POINT ( 'NONE',  ( 10.81492255796106328, -18.62759615963255655, 60.41775706135235424 ) ) ;
#40208 = CARTESIAN_POINT ( 'NONE',  ( 16.51473224551069308, 9.474510206698969483, 34.16557627198102409 ) ) ;
#40209 = CARTESIAN_POINT ( 'NONE',  ( 19.03943276465977164, -0.05219959533909143690, 53.74890960531436690 ) ) ;
#40210 = CARTESIAN_POINT ( 'NONE',  ( -8.314922557960811034, -14.29746914071050412, 92.08224293864769550 ) ) ;
#40211 = CARTESIAN_POINT ( 'NONE',  ( -5.153800228976328057, -19.02544592524343514, 102.2905762719810383 ) ) ;
#40212 = CARTESIAN_POINT ( 'NONE',  ( 8.224510206698953496, -14.34966873604960469, 37.91557627198102409 ) ) ;
#40213 = CARTESIAN_POINT ( 'NONE',  ( -19.05341960407611168, -5.049401038298163336, 21.45724293864768839 ) ) ;
#40214 = CARTESIAN_POINT ( 'NONE',  ( 10.72451020669898902, -18.67979575497178502, 67.91557627198102409 ) ) ;
#40215 = CARTESIAN_POINT ( 'NONE',  ( 10.72451020669871369, 18.67979575497193778, 22.08442372801901143 ) ) ;
#40216 = CARTESIAN_POINT ( 'NONE',  ( -15.81114279943209766, 14.65109730209610461, -56.29481432398279139 ) ) ;
#40218 = CARTESIAN_POINT ( 'NONE',  ( -13.97604488694547697, 13.89961937509957934, 113.1260903946856757 ) ) ;
#40217 = CARTESIAN_POINT ( 'NONE',  ( -19.03943276465977164, 0.05219959533909376836, 76.24890960531435269 ) ) ;
#40219 = EDGE_CURVE ( 'NONE', #86241, #26894, #83557, .T. ) ;
#40220 = CARTESIAN_POINT ( 'NONE',  ( -10.81492255796078084, -18.62759615963271287, 67.08224293864770971 ) ) ;
#40221 = CIRCLE ( 'NONE', #62725, 4.500000000000000000 ) ;
#40222 = CARTESIAN_POINT ( 'NONE',  ( 10.72451020669871369, 18.67979575497193778, 97.08442372801904696 ) ) ;
#40223 = CARTESIAN_POINT ( 'NONE',  ( -9.474510206698964154, 16.51473224551069663, 75.41557627198103830 ) ) ;
#40224 = CARTESIAN_POINT ( 'NONE',  ( -18.67979575497193778, 10.72451020669871902, 33.33442372801900433 ) ) ;
#40225 = CARTESIAN_POINT ( 'NONE',  ( -13.89961937509977652, 13.97604488694528158, 110.6239096053143243 ) ) ;
#40226 = CARTESIAN_POINT ( 'NONE',  ( -0.05219959533934338120, 16.53943276465976808, 92.50109039468567573 ) ) ;
#40227 = CARTESIAN_POINT ( 'NONE',  ( -5.719274019375665041, -21.55341960407619695, 64.79275706135234714 ) ) ;
#40228 = CARTESIAN_POINT ( 'NONE',  ( 0.05219959533937995610, -21.53943276465977519, 95.00109039468568994 ) ) ;
#40229 = CARTESIAN_POINT ( 'NONE',  ( -12.06949235617739369, -12.14591786802326823, 79.37609039468567573 ) ) ;
#40230 = CARTESIAN_POINT ( 'NONE',  ( 10.81492255796106328, -18.62759615963255655, 30.41775706135234358 ) ) ;
#40231 = VECTOR ( 'NONE', #78412, 1000.000000000000000 ) ;
#40232 = CARTESIAN_POINT ( 'NONE',  ( 19.02544592524343514, -5.153800228976328945, 23.54057627198102054 ) ) ;
#40233 = CARTESIAN_POINT ( 'NONE',  ( -15.80617190586768217, 15.72974639402176855, 93.12609039468568994 ) ) ;
#40234 = CARTESIAN_POINT ( 'NONE',  ( -9.564922557960796823, -16.46253265017161027, 97.08224293864769550 ) ) ;
#40235 = CARTESIAN_POINT ( 'NONE',  ( 5.823673210054125526, 21.52544592524343514, 84.79057627198102409 ) ) ;
#40236 = CARTESIAN_POINT ( 'NONE',  ( -13.97604488694547697, 13.89961937509957934, 58.12609039468566863 ) ) ;
#40238 = CARTESIAN_POINT ( 'NONE',  ( 10.72451020669898902, -18.67979575497178502, 52.91557627198103830 ) ) ;
#40237 = CARTESIAN_POINT ( 'NONE',  ( -18.37348032455536639, -33.26197007281776052, -21.07589179611765928 ) ) ;
#40240 = CARTESIAN_POINT ( 'NONE',  ( 0.05219959533910956823, 16.53943276465976808, 49.99890960531437401 ) ) ;
#40239 = CARTESIAN_POINT ( 'NONE',  ( 9.564922557960805705, 16.46253265017160317, 94.58224293864769550 ) ) ;
#40241 = CARTESIAN_POINT ( 'NONE',  ( 23.31738231874054534, 16.94106989632529192, 145.1999999999999886 ) ) ;
#40242 = CARTESIAN_POINT ( 'NONE',  ( -16.46253265017146816, -9.564922557961047289, 74.16775706135234714 ) ) ;
#40243 = AXIS2_PLACEMENT_3D ( 'NONE', #141305, #171655, #33144 ) ;
#40244 =( BOUNDED_CURVE ( )  B_SPLINE_CURVE ( 2, ( #105971, #198986, #195014, #60454, #183816, #57501, #168630, #29152, #30130, #166671, #120146, #179859, #180854 ),
 .UNSPECIFIED., .F., .T. ) 
 B_SPLINE_CURVE_WITH_KNOTS ( ( 3, 2, 2, 2, 2, 2, 3 ),
 ( 0.3708971688807142786, 0.3728070175438596423, 0.3771929824561403577, 0.3815789473684210731, 0.3859649122807017330, 0.3903508771929824483, 0.3923064056782181175 ),
 .UNSPECIFIED. ) 
 CURVE ( )  GEOMETRIC_REPRESENTATION_ITEM ( )  RATIONAL_B_SPLINE_CURVE ( ( 0.9832469066685285419, 0.9851625545550100060, 1.000000000000000000, 0.9659258262890683122, 1.000000000000000000, 0.9659258262890683122, 1.000000000000000000, 0.9659258262890683122, 1.000000000000000000, 0.9659258262890683122, 1.000000000000000000, 0.9848076720550082985, 0.9831626618144002627 ) ) 
 REPRESENTATION_ITEM ( '' )  );
#40245 = DIRECTION ( 'NONE',  ( 0.000000000000000000, 0.000000000000000000, 1.000000000000000000 ) ) ;
#40246 = CARTESIAN_POINT ( 'NONE',  ( 19.03943276465977164, 0.05219959533936151252, 111.2510903946856757 ) ) ;
#40247 = CARTESIAN_POINT ( 'NONE',  ( -15.80617190586745835, -15.72974639402198527, 81.87390960531435269 ) ) ;
#40248 = CARTESIAN_POINT ( 'NONE',  ( 4.379528057220339221, -16.55341960407611168, 62.70724293864769550 ) ) ;
#40249 = CARTESIAN_POINT ( 'NONE',  ( 13.97604488694527802, 13.89961937509977652, 99.37390960531436690 ) ) ;
#40250 = CARTESIAN_POINT ( 'NONE',  ( 4.483927247898790824, -16.52544592524335698, 25.20942372801901854 ) ) ;
#40251 = CARTESIAN_POINT ( 'NONE',  ( 5.153800228976335163, 19.02544592524342804, 54.79057627198103120 ) ) ;
#40253 = CARTESIAN_POINT ( 'NONE',  ( -16.46253265017146816, -9.564922557961047289, 84.16775706135233293 ) ) ;
#40252 = CARTESIAN_POINT ( 'NONE',  ( -21.53943276465977519, 0.05219959533907696930, 116.2489096053143669 ) ) ;
#40254 = EDGE_CURVE ( 'NONE', #38777, #89664, #118443, .T. ) ;
#40255 = CARTESIAN_POINT ( 'NONE',  ( -19.03943276465977164, 0.05219959533909376836, 91.24890960531436690 ) ) ;
#40256 = CARTESIAN_POINT ( 'NONE',  ( -19.02544592524342804, 5.153800228976336051, 71.04057627198099567 ) ) ;
#40257 = CARTESIAN_POINT ( 'NONE',  ( -21.53943276465977519, 0.05219959533907696930, 71.24890960531435269 ) ) ;
#40258 = CARTESIAN_POINT ( 'NONE',  ( -5.153800228976328057, -19.02544592524343514, 47.29057627198102409 ) ) ;
#40259 = CARTESIAN_POINT ( 'NONE',  ( 34.12434206616184440, 14.08647367304311260, -8.000000000000001776 ) ) ;
#40260 = CARTESIAN_POINT ( 'NONE',  ( -16.52544592524342804, 4.483927247898546575, 51.04057627198103120 ) ) ;
#40261 = CARTESIAN_POINT ( 'NONE',  ( 9.474510206698971260, -16.51473224551069308, 102.9155762719810241 ) ) ;
#40262 = CARTESIAN_POINT ( 'NONE',  ( 23.31738231874054890, -16.94106989632523508, 141.0500000054623513 ) ) ;
#40263 = CARTESIAN_POINT ( 'NONE',  ( -9.474510206698720793, -16.51473224551083518, 64.58442372801900433 ) ) ;
#40264 = CARTESIAN_POINT ( 'NONE',  ( 21.53943276465977519, -0.05219959533907433946, 88.74890960531436690 ) ) ;
#40265 = CARTESIAN_POINT ( 'NONE',  ( -13.97604488694547697, 13.89961937509957934, 53.12609039468565442 ) ) ;
#40266 = CARTESIAN_POINT ( 'NONE',  ( 19.03943276465977164, -0.05219959533909143690, 98.74890960531436690 ) ) ;
#40267 = CARTESIAN_POINT ( 'NONE',  ( 4.999999999999999112, 11.45643923738960090, -18.00000000000000000 ) ) ;
#40268 = CARTESIAN_POINT ( 'NONE',  ( 0.05219959533907565091, 21.53943276465977519, 44.99890960531435979 ) ) ;
#40269 = AXIS2_PLACEMENT_3D ( 'NONE', #40095, #67436, #129093 ) ;
#40270 = CARTESIAN_POINT ( 'NONE',  ( 19.05341960407611168, 5.049401038298154454, 68.95724293864769550 ) ) ;
#40271 = CARTESIAN_POINT ( 'NONE',  ( -18.67979575497193778, 10.72451020669871902, 68.33442372801900433 ) ) ;
#40272 = CARTESIAN_POINT ( 'NONE',  ( 16.51473224551069308, 9.474510206698969483, 44.16557627198103120 ) ) ;
#40274 = ORIENTED_EDGE ( 'NONE', *, *, #33819, .F. ) ;
#40273 = CARTESIAN_POINT ( 'NONE',  ( 12.14591786802309770, 12.06949235617756955, 79.37390960531436690 ) ) ;
#40275 = CARTESIAN_POINT ( 'NONE',  ( -15.72974639402176322, -15.80617190586768395, 59.37609039468568284 ) ) ;
#40276 = ORIENTED_EDGE ( 'NONE', *, *, #139988, .T. ) ;
#40277 = CARTESIAN_POINT ( 'NONE',  ( 9.564922557960805705, 16.46253265017160317, 109.5822429386476955 ) ) ;
#40278 = CARTESIAN_POINT ( 'NONE',  ( 19.05341960407617918, -5.049401038297876454, 71.04275706135234714 ) ) ;
#40279 = DIRECTION ( 'NONE',  ( -0.000000000000000000, -0.000000000000000000, 1.000000000000000000 ) ) ;
#40280 = CARTESIAN_POINT ( 'NONE',  ( -5.719274019375978568, 21.55341960407610458, 115.2072429386476955 ) ) ;
#40281 = CARTESIAN_POINT ( 'NONE',  ( 16.51473224551069308, 9.474510206698969483, 54.16557627198103120 ) ) ;
#40282 = CARTESIAN_POINT ( 'NONE',  ( 16.52544592524335698, 4.483927247898782831, 36.45942372801901143 ) ) ;
#40283 = CARTESIAN_POINT ( 'NONE',  ( -11.74264578624799782, -36.14014761921581709, -5.349999994537626868 ) ) ;
#40284 = CARTESIAN_POINT ( 'NONE',  ( -19.03943276465977164, -0.05219959533935918106, 23.75109039468566152 ) ) ;
#40285 = CARTESIAN_POINT ( 'NONE',  ( -16.46253265017160317, 9.564922557960807481, 40.83224293864769550 ) ) ;
#40286 = CARTESIAN_POINT ( 'NONE',  ( -13.89961937509957401, -13.97604488694547875, 19.37609039468566507 ) ) ;
#40287 = CARTESIAN_POINT ( 'NONE',  ( -16.52544592524335698, -4.483927247898792601, 88.95942372801901854 ) ) ;
#40289 = CARTESIAN_POINT ( 'NONE',  ( -10.81492255796105439, 18.62759615963255655, 67.91775706135234714 ) ) ;
#40288 = CARTESIAN_POINT ( 'NONE',  ( 19.03943276465977164, -0.05219959533909143690, 83.74890960531436690 ) ) ;
#40290 = CARTESIAN_POINT ( 'NONE',  ( 6.542564195780748548, -4.422302296885995077, -62.17069030305508903 ) ) ;
#40291 = CARTESIAN_POINT ( 'NONE',  ( -13.97604488694527625, -13.89961937509977652, 111.8739096053143243 ) ) ;
#40292 = LINE ( 'NONE', #25149, #179287 ) ;
#40294 = CARTESIAN_POINT ( 'NONE',  ( 18.62759615963255655, 10.81492255796105972, 66.66775706135234714 ) ) ;
#40293 = CARTESIAN_POINT ( 'NONE',  ( 8.314922557961029526, -14.29746914071037800, 55.41775706135234714 ) ) ;
#40295 = CARTESIAN_POINT ( 'NONE',  ( 15.72974639402176855, 15.80617190586768217, 96.87609039468568994 ) ) ;
#40296 = CARTESIAN_POINT ( 'NONE',  ( 26.25049742697153832, -7.664248127782749442, 169.1476266185236454 ) ) ;
#40297 = CARTESIAN_POINT ( 'NONE',  ( -4.483927247898782831, 16.52544592524335698, 32.70942372801900433 ) ) ;
#40298 = CARTESIAN_POINT ( 'NONE',  ( -13.97604488694527625, -13.89961937509977652, 81.87390960531436690 ) ) ;
#40299 = VERTEX_POINT ( 'NONE', #54949 ) ;
#40300 = CARTESIAN_POINT ( 'NONE',  ( -0.8894290736107403061, -29.18776880969891963, -52.33677266386638394 ) ) ;
#40301 = CARTESIAN_POINT ( 'NONE',  ( 19.05341960407611168, 5.049401038298154454, 38.95724293864767418 ) ) ;
#40302 = CARTESIAN_POINT ( 'NONE',  ( 18.67979575497178502, 10.72451020669898547, 49.16557627198102409 ) ) ;
#40303 = CARTESIAN_POINT ( 'NONE',  ( -16.53943276465976808, -0.05219959533934237506, 103.7510903946857042 ) ) ;
#40305 = CARTESIAN_POINT ( 'NONE',  ( -13.89961937509977652, 13.97604488694528158, 70.62390960531432427 ) ) ;
#40304 = CARTESIAN_POINT ( 'NONE',  ( 4.483927247898545687, 16.52544592524342804, 84.79057627198102409 ) ) ;
#40306 = CARTESIAN_POINT ( 'NONE',  ( -15.80617190586768217, 15.72974639402176855, 103.1260903946856757 ) ) ;
#40307 = CARTESIAN_POINT ( 'NONE',  ( 8.314922557961029526, -14.29746914071037800, 25.41775706135235779 ) ) ;
#40308 = CARTESIAN_POINT ( 'NONE',  ( 0.05219959533910956823, 16.53943276465976808, 94.99890960531436690 ) ) ;
#40309 = CARTESIAN_POINT ( 'NONE',  ( 5.719274019375673035, 21.55341960407619339, 47.29275706135234003 ) ) ;
#40310 = CARTESIAN_POINT ( 'NONE',  ( 18.62759615963271287, -10.81492255796078972, 78.33224293864770971 ) ) ;
#40311 = CARTESIAN_POINT ( 'NONE',  ( 0.05219959533936267826, -19.03943276465977164, 55.00109039468566863 ) ) ;
#40312 = CARTESIAN_POINT ( 'NONE',  ( -9.564922557960796823, -16.46253265017161027, 102.0822429386477097 ) ) ;
#40313 = CARTESIAN_POINT ( 'NONE',  ( -16.52544592524342804, 4.483927247898546575, 61.04057627198103120 ) ) ;
#40314 = CARTESIAN_POINT ( 'NONE',  ( -8.224510206698948167, 14.34966873604960824, 50.41557627198103120 ) ) ;
#40315 = CARTESIAN_POINT ( 'NONE',  ( 16.53943276465976808, 0.05219959533934440121, 106.2510903946856757 ) ) ;
#40316 = CARTESIAN_POINT ( 'NONE',  ( 13.97604488694548053, -13.89961937509957401, 70.62609039468567573 ) ) ;
#40317 = CARTESIAN_POINT ( 'NONE',  ( -18.56197773271732032, 5.499999999999903189, 83.55066217314454491 ) ) ;
#40318 = CARTESIAN_POINT ( 'NONE',  ( 10.81492255796078972, 18.62759615963270932, 24.58224293864768839 ) ) ;
#40319 = CARTESIAN_POINT ( 'NONE',  ( 0.05219959533910956823, 16.53943276465976808, 84.99890960531436690 ) ) ;
#40320 = DIRECTION ( 'NONE',  ( 0.000000000000000000, 0.000000000000000000, -1.000000000000000000 ) ) ;
#40322 = CARTESIAN_POINT ( 'NONE',  ( 0.05219959533907565091, 21.53943276465977519, 54.99890960531435269 ) ) ;
#40321 = CARTESIAN_POINT ( 'NONE',  ( -0.05219959533909027116, -19.03943276465977164, 42.49890960531435269 ) ) ;
#40323 = CARTESIAN_POINT ( 'NONE',  ( 21.55341960407610458, 5.719274019375980345, 78.95724293864769550 ) ) ;
#40324 = CARTESIAN_POINT ( 'NONE',  ( 19.05341960407611168, 5.049401038298154454, 23.95724293864769194 ) ) ;
#40326 = CARTESIAN_POINT ( 'NONE',  ( -9.474510206698964154, 16.51473224551069663, 55.41557627198103120 ) ) ;
#40325 = CARTESIAN_POINT ( 'NONE',  ( -8.314922557961024197, 14.29746914071037800, 62.91775706135236135 ) ) ;
#40327 = CARTESIAN_POINT ( 'NONE',  ( 19.03943276465977164, 0.05219959533936151252, 46.25109039468566863 ) ) ;
#40328 = CARTESIAN_POINT ( 'NONE',  ( -15.72974639402176322, -15.80617190586768395, 54.37609039468568994 ) ) ;
#40329 = EDGE_LOOP ( 'NONE', ( #103946, #161702, #108610, #15047 ) ) ;
#40330 = CARTESIAN_POINT ( 'NONE',  ( -14.34966873604960291, -8.224510206698953496, 111.6655762719810525 ) ) ;
#40331 = EDGE_CURVE ( 'NONE', #83841, #177652, #130777, .T. ) ;
#40332 = CARTESIAN_POINT ( 'NONE',  ( 19.03943276465977164, 0.05219959533936151252, 86.25109039468567573 ) ) ;
#40333 = CARTESIAN_POINT ( 'NONE',  ( -11.40812507854755609, 35.11059874428196537, -3.524999997268813523 ) ) ;
#40335 = CARTESIAN_POINT ( 'NONE',  ( 0.05219959533907565091, 21.53943276465977519, 44.99890960531435979 ) ) ;
#40334 = CARTESIAN_POINT ( 'NONE',  ( -30.00000000000000000, 5.499999999999992895, 37.50000000000000000 ) ) ;
#40336 = CARTESIAN_POINT ( 'NONE',  ( 16.62475595723694965, -7.163666690055214836, 68.02713351810464815 ) ) ;
#40337 = CARTESIAN_POINT ( 'NONE',  ( 18.62759615963255655, 10.81492255796105972, 81.66775706135236135 ) ) ;
#40338 = CARTESIAN_POINT ( 'NONE',  ( -4.483927247898539470, -16.52544592524342804, 27.29057627198103120 ) ) ;
#40340 = CARTESIAN_POINT ( 'NONE',  ( 4.379528057220339221, -16.55341960407611168, 62.70724293864769550 ) ) ;
#40339 = CARTESIAN_POINT ( 'NONE',  ( 4.379528057220092307, 16.55341960407617563, 57.29275706135234714 ) ) ;
#40341 = CARTESIAN_POINT ( 'NONE',  ( -10.81492255796078084, -18.62759615963271287, 87.08224293864769550 ) ) ;
#40342 = CARTESIAN_POINT ( 'NONE',  ( 5.823673210054125526, 21.52544592524343514, 69.79057627198102409 ) ) ;
#40343 = DIRECTION ( 'NONE',  ( 1.000000000000000000, 1.776356839400250465E-15, 0.000000000000000000 ) ) ;
#40345 = CARTESIAN_POINT ( 'NONE',  ( 18.62759615963271287, -10.81492255796078972, 23.33224293864769194 ) ) ;
#40344 = CARTESIAN_POINT ( 'NONE',  ( 5.153800228976615827, -19.02544592524334988, 80.20942372801901854 ) ) ;
#40346 = CARTESIAN_POINT ( 'NONE',  ( -9.564922557960796823, -16.46253265017161027, 67.08224293864769550 ) ) ;
#40347 = CARTESIAN_POINT ( 'NONE',  ( -19.02544592524342804, 5.153800228976336051, 31.04057627198102409 ) ) ;
#40348 = CARTESIAN_POINT ( 'NONE',  ( -17.49999999999999645, -7.500000000000000888, 118.0000000000000142 ) ) ;
#40349 = VERTEX_POINT ( 'NONE', #194475 ) ;
#40351 = CARTESIAN_POINT ( 'NONE',  ( 4.379528057220092307, 16.55341960407617563, 82.29275706135234714 ) ) ;
#40350 = AXIS2_PLACEMENT_3D ( 'NONE', #61043, #31715, #155050 ) ;
#40352 = CARTESIAN_POINT ( 'NONE',  ( -5.719274019375978568, 21.55341960407610458, 105.2072429386477097 ) ) ;
#40353 = CARTESIAN_POINT ( 'NONE',  ( -13.97604488694527625, -13.89961937509977652, 71.87390960531433848 ) ) ;
#40354 = CARTESIAN_POINT ( 'NONE',  ( 21.53943276465977519, 0.05219959533937863772, 41.25109039468568284 ) ) ;
#40355 = CARTESIAN_POINT ( 'NONE',  ( -13.97604488694527625, -13.89961937509977652, 96.87390960531433848 ) ) ;
#40356 = CARTESIAN_POINT ( 'NONE',  ( -26.35186391108957338, -29.45501048291157886, -18.59600737860424857 ) ) ;
#40357 = VERTEX_POINT ( 'NONE', #68108 ) ;
#40358 = CARTESIAN_POINT ( 'NONE',  ( -5.823673210054431948, 21.52544592524334988, 47.70942372801902565 ) ) ;
#40360 = CARTESIAN_POINT ( 'NONE',  ( 9.564922557960805705, 16.46253265017160317, 109.5822429386476955 ) ) ;
#40359 = CARTESIAN_POINT ( 'NONE',  ( -19.03943276465977164, 0.05219959533909376836, 21.24890960531436335 ) ) ;
#40361 = CARTESIAN_POINT ( 'NONE',  ( 9.564922557961047289, -16.46253265017146816, 60.41775706135233293 ) ) ;
#40362 = CARTESIAN_POINT ( 'NONE',  ( -5.823673210054116645, -21.52544592524344225, 112.2905762719810241 ) ) ;
#40363 = CARTESIAN_POINT ( 'NONE',  ( 16.51473224551083163, -9.474510206698727899, 50.83442372801899722 ) ) ;
#40364 = CARTESIAN_POINT ( 'NONE',  ( 19.02544592524334988, 5.153800228976608722, 46.45942372801899012 ) ) ;
#40366 = EDGE_LOOP ( 'NONE', ( #109902, #184235, #54907, #2803 ) ) ;
#40365 = CARTESIAN_POINT ( 'NONE',  ( -16.55341960407617563, 4.379528057220093196, 103.5427570613523613 ) ) ;
#40368 = VERTEX_POINT ( 'NONE', #160125 ) ;
#40367 = CARTESIAN_POINT ( 'NONE',  ( 23.84690145917535631, -10.26550538186640082, 166.0764395470883983 ) ) ;
#40369 = CARTESIAN_POINT ( 'NONE',  ( -19.02544592524342804, 5.153800228976336051, 71.04057627198099567 ) ) ;
#40370 = CARTESIAN_POINT ( 'NONE',  ( -5.719274019375665041, -21.55341960407619695, 79.79275706135236135 ) ) ;
#40371 = CARTESIAN_POINT ( 'NONE',  ( 21.52544592524334988, 5.823673210054432836, 91.45942372801901854 ) ) ;
#40372 = CARTESIAN_POINT ( 'NONE',  ( -0.1000365528946621507, -9.100000000000004974, -63.95112321872119310 ) ) ;
#40373 = CARTESIAN_POINT ( 'NONE',  ( 9.564922557960805705, 16.46253265017160317, 84.58224293864769550 ) ) ;
#40374 = CARTESIAN_POINT ( 'NONE',  ( 21.55341960407619695, -5.719274019375665929, 61.04275706135234714 ) ) ;
#40375 = CARTESIAN_POINT ( 'NONE',  ( -19.03943276465977164, -0.05219959533935918106, 113.7510903946856757 ) ) ;
#40376 = CARTESIAN_POINT ( 'NONE',  ( 16.51473224551069308, 9.474510206698969483, 69.16557627198102409 ) ) ;
#40377 = CARTESIAN_POINT ( 'NONE',  ( 5.153800228976335163, 19.02544592524342804, 109.7905762719810099 ) ) ;
#40378 = CARTESIAN_POINT ( 'NONE',  ( -0.05219959533909027116, -19.03943276465977164, 87.49890960531436690 ) ) ;
#40379 = DIRECTION ( 'NONE',  ( 1.000000000000000000, -0.000000000000000000, 0.000000000000000000 ) ) ;
#40380 = CARTESIAN_POINT ( 'NONE',  ( 19.03943276465977164, -0.05219959533909143690, 78.74890960531436690 ) ) ;
#40381 = CARTESIAN_POINT ( 'NONE',  ( 0.05219959533909260263, 19.03943276465977164, 69.99890960531435269 ) ) ;
#40382 = CARTESIAN_POINT ( 'NONE',  ( -18.67979575497178146, -10.72451020669898902, 106.6655762719810383 ) ) ;
#40383 = CARTESIAN_POINT ( 'NONE',  ( 16.53943276465976808, 0.05219959533934440121, 101.2510903946856757 ) ) ;
#40384 = CARTESIAN_POINT ( 'NONE',  ( 31.99364916730971231, 1.011436372600181938E-12, 95.00000000000021316 ) ) ;
#40385 = VECTOR ( 'NONE', #197575, 1000.000000000000000 ) ;
#40386 = CARTESIAN_POINT ( 'NONE',  ( -19.05341960407617563, 5.049401038297882671, 63.54275706135234003 ) ) ;
#40387 = CARTESIAN_POINT ( 'NONE',  ( 13.89961937509977652, -13.97604488694527269, 98.12390960531433848 ) ) ;
#40388 = CARTESIAN_POINT ( 'NONE',  ( 8.314922557960818139, 14.29746914071049879, 69.58224293864769550 ) ) ;
#40389 = CARTESIAN_POINT ( 'NONE',  ( 8.314922557960818139, 14.29746914071049879, 104.5822429386477097 ) ) ;
#40390 = AXIS2_PLACEMENT_3D ( 'NONE', #64891, #137754, #187271 ) ;
#40391 = CARTESIAN_POINT ( 'NONE',  ( -5.823673210054116645, -21.52544592524344225, 37.29057627198102409 ) ) ;
#40392 = CARTESIAN_POINT ( 'NONE',  ( -5.049401038298153566, 19.05341960407611168, 115.2072429386477097 ) ) ;
#40393 = CARTESIAN_POINT ( 'NONE',  ( -21.53943276465977519, 0.05219959533907696930, 21.24890960531436690 ) ) ;
#40394 = CARTESIAN_POINT ( 'NONE',  ( 4.379528057220339221, -16.55341960407611168, 97.70724293864772392 ) ) ;
#40395 = CARTESIAN_POINT ( 'NONE',  ( -16.31925111598457789, 7.325300261831452886, 55.16424538967250157 ) ) ;
#40396 = CARTESIAN_POINT ( 'NONE',  ( -16.51473224551082808, 9.474510206698731452, 38.33442372801899722 ) ) ;
#40397 = CARTESIAN_POINT ( 'NONE',  ( -4.379528057220086978, -16.55341960407618274, 104.7927570613523898 ) ) ;
#40398 = CARTESIAN_POINT ( 'NONE',  ( -16.51473224551069308, -9.474510206698971260, 86.66557627198102409 ) ) ;
#40399 = CARTESIAN_POINT ( 'NONE',  ( 10.72451020669871369, 18.67979575497193778, 57.08442372801901854 ) ) ;
#40400 = CARTESIAN_POINT ( 'NONE',  ( -10.72451020669898014, 18.67979575497178502, 50.41557627198103120 ) ) ;
#40401 = CARTESIAN_POINT ( 'NONE',  ( -5.823673210054431948, 21.52544592524334988, 32.70942372801900433 ) ) ;
#40402 = CARTESIAN_POINT ( 'NONE',  ( 5.823673210054125526, 21.52544592524343514, 79.79057627198102409 ) ) ;
#40403 = CARTESIAN_POINT ( 'NONE',  ( 4.379528057220339221, -16.55341960407611168, 102.7072429386476955 ) ) ;
#40404 = CARTESIAN_POINT ( 'NONE',  ( -19.05341960407617563, 5.049401038297882671, 73.54275706135233293 ) ) ;
#40405 = CARTESIAN_POINT ( 'NONE',  ( 9.564922557960805705, 16.46253265017160317, 39.58224293864768839 ) ) ;
#40406 = CARTESIAN_POINT ( 'NONE',  ( -19.02544592524342804, 5.153800228976336051, 96.04057627198103830 ) ) ;
#40407 = CARTESIAN_POINT ( 'NONE',  ( 16.51473224551069308, 9.474510206698969483, 89.16557627198103830 ) ) ;
#40408 = CARTESIAN_POINT ( 'NONE',  ( -13.89961937509977652, 13.97604488694528158, 25.62390960531434558 ) ) ;
#40409 = CARTESIAN_POINT ( 'NONE',  ( 12.14591786802309770, 12.06949235617756955, 39.37390960531436690 ) ) ;
#40410 = CARTESIAN_POINT ( 'NONE',  ( -14.29746914071037622, -8.314922557961029526, 44.16775706135234714 ) ) ;
#40412 = AXIS2_PLACEMENT_3D ( 'NONE', #179831, #41301, #55457 ) ;
#40411 = CARTESIAN_POINT ( 'NONE',  ( 21.53943276465977519, 0.05219959533937863772, 111.2510903946856899 ) ) ;
#40414 = CARTESIAN_POINT ( 'NONE',  ( 16.55341960407611168, 4.379528057220329451, 23.95724293864769550 ) ) ;
#40413 = DIRECTION ( 'NONE',  ( 1.000000000000000000, 0.000000000000000000, 0.000000000000000000 ) ) ;
#40415 = CARTESIAN_POINT ( 'NONE',  ( -21.55341960407619339, 5.719274019375674811, 28.54275706135234358 ) ) ;
#40416 = CARTESIAN_POINT ( 'NONE',  ( 9.564922557960805705, 16.46253265017160317, 99.58224293864770971 ) ) ;
#40417 = CARTESIAN_POINT ( 'NONE',  ( 16.53943276465976808, 0.05219959533934440121, 101.2510903946856757 ) ) ;
#40418 = CARTESIAN_POINT ( 'NONE',  ( -0.05219959533934338120, 16.53943276465976808, 92.50109039468567573 ) ) ;
#40419 = CARTESIAN_POINT ( 'NONE',  ( -16.55341960407617563, 4.379528057220093196, 23.54275706135235424 ) ) ;
#40420 = CARTESIAN_POINT ( 'NONE',  ( 13.89961937509977652, -13.97604488694527269, 48.12390960531435979 ) ) ;
#40421 = CARTESIAN_POINT ( 'NONE',  ( 16.52544592524342804, -4.483927247898539470, 103.5405762719810383 ) ) ;
#40422 = CARTESIAN_POINT ( 'NONE',  ( 21.55341960407619695, -5.719274019375665929, 26.04275706135235779 ) ) ;
#40423 = CARTESIAN_POINT ( 'NONE',  ( 19.02544592524343514, -5.153800228976328945, 33.54057627198102409 ) ) ;
#40424 = CARTESIAN_POINT ( 'NONE',  ( -0.05219959533909027116, -19.03943276465977164, 107.4989096053143527 ) ) ;
#40425 = CARTESIAN_POINT ( 'NONE',  ( 21.52544592524334988, 5.823673210054432836, 31.45942372801901854 ) ) ;
#40426 = CARTESIAN_POINT ( 'NONE',  ( 23.48298174826589246, 32.32155151706776053, -2.702157773949822595 ) ) ;
#40427 = CARTESIAN_POINT ( 'NONE',  ( 13.89961937509977652, -13.97604488694527269, 103.1239096053143527 ) ) ;
#40428 = SPHERICAL_SURFACE ( 'NONE', #61444, 4.324969328314201888 ) ;
#40429 = CARTESIAN_POINT ( 'NONE',  ( 19.05341960407611168, 5.049401038298154454, 98.95724293864766707 ) ) ;
#40431 = CARTESIAN_POINT ( 'NONE',  ( -4.483927247898539470, -16.52544592524342804, 97.29057627198105251 ) ) ;
#40430 = CARTESIAN_POINT ( 'NONE',  ( -18.67979575497193778, 10.72451020669871902, 43.33442372801901143 ) ) ;
#40432 = CARTESIAN_POINT ( 'NONE',  ( -5.049401038298153566, 19.05341960407611168, 90.20724293864766707 ) ) ;
#40433 = CARTESIAN_POINT ( 'NONE',  ( -8.224510206698735004, -14.34966873604973081, 64.58442372801900433 ) ) ;
#40434 = CARTESIAN_POINT ( 'NONE',  ( 10.72451020669871369, 18.67979575497193778, 77.08442372801901854 ) ) ;
#40435 = CARTESIAN_POINT ( 'NONE',  ( -0.05219959533934338120, 16.53943276465976808, 42.50109039468567573 ) ) ;
#40436 = CARTESIAN_POINT ( 'NONE',  ( 13.97604488694527802, 13.89961937509977652, 79.37390960531435269 ) ) ;
#40437 = CARTESIAN_POINT ( 'NONE',  ( -5.153800228976607833, 19.02544592524334988, 112.7094237280190043 ) ) ;
#40438 = CARTESIAN_POINT ( 'NONE',  ( 4.483927247898790824, -16.52544592524335698, 70.20942372801904696 ) ) ;
#40439 = CARTESIAN_POINT ( 'NONE',  ( 16.51473224551083163, -9.474510206698727899, 90.83442372801900433 ) ) ;
#40440 = CARTESIAN_POINT ( 'NONE',  ( 16.51473224551069308, 9.474510206698969483, 64.16557627198102409 ) ) ;
#40441 = CARTESIAN_POINT ( 'NONE',  ( 21.55341960407610458, 5.719274019375980345, 83.95724293864770971 ) ) ;
#40443 = CARTESIAN_POINT ( 'NONE',  ( -0.05219959533936034679, 19.03943276465977164, 87.50109039468567573 ) ) ;
#40442 = CARTESIAN_POINT ( 'NONE',  ( 16.53943276465976808, -0.05219959533910856209, 93.74890960531436690 ) ) ;
#40444 = CARTESIAN_POINT ( 'NONE',  ( 14.34966873604972726, -8.224510206698740333, 60.83442372801901854 ) ) ;
#40445 = CARTESIAN_POINT ( 'NONE',  ( -18.22780087662123805, 5.499999999999981348, 81.01763182126896368 ) ) ;
#40446 = CARTESIAN_POINT ( 'NONE',  ( -19.02544592524334988, -5.153800228976617603, 53.95942372801898301 ) ) ;
#40447 = CARTESIAN_POINT ( 'NONE',  ( 12.14591786802309770, 12.06949235617756955, 34.37390960531435979 ) ) ;
#40448 = CARTESIAN_POINT ( 'NONE',  ( 12.14591786802309770, 12.06949235617756955, 79.37390960531436690 ) ) ;
#40450 = CARTESIAN_POINT ( 'NONE',  ( -5.000000000000000000, -120.0000000000000142, -13.00000000000000000 ) ) ;
#40449 = CARTESIAN_POINT ( 'NONE',  ( 10.81492255796106328, -18.62759615963255655, 110.4177570613523756 ) ) ;
#40451 = CARTESIAN_POINT ( 'NONE',  ( 5.823673210054444382, -21.52544592524334988, 25.20942372801901854 ) ) ;
#40452 = CARTESIAN_POINT ( 'NONE',  ( -13.89961937509977652, 13.97604488694528158, 95.62390960531436690 ) ) ;
#40453 = CARTESIAN_POINT ( 'NONE',  ( 9.474510206698971260, -16.51473224551069308, 77.91557627198103830 ) ) ;
#40454 = CARTESIAN_POINT ( 'NONE',  ( 18.67979575497194134, -10.72451020669871369, 95.83442372801903275 ) ) ;
#40455 = CARTESIAN_POINT ( 'NONE',  ( 19.02544592524343514, -5.153800228976328945, 78.54057627198099567 ) ) ;
#40456 = CARTESIAN_POINT ( 'NONE',  ( -21.52544592524343514, 5.823673210054127303, 46.04057627198103830 ) ) ;
#40457 = VECTOR ( 'NONE', #87244, 1000.000000000000000 ) ;
#40458 = CARTESIAN_POINT ( 'NONE',  ( -4.379528057220328563, 16.55341960407611168, 75.20724293864769550 ) ) ;
#40459 = CARTESIAN_POINT ( 'NONE',  ( -16.51473224551069308, -9.474510206698971260, 51.66557627198102409 ) ) ;
#40460 = CARTESIAN_POINT ( 'NONE',  ( 12.06949235617757843, -12.14591786802309237, 103.1239096053143811 ) ) ;
#40461 = CARTESIAN_POINT ( 'NONE',  ( -21.53943276465977519, -0.05219959533937600094, 18.75109039468568639 ) ) ;
#40462 = EDGE_CURVE ( 'NONE', #22341, #39558, #127303, .T. ) ;
#40463 = CARTESIAN_POINT ( 'NONE',  ( 15.80617190586769283, -15.72974639402175789, 60.62609039468567573 ) ) ;
#40464 = CARTESIAN_POINT ( 'NONE',  ( -5.153800228976328057, -19.02544592524343514, 47.29057627198102409 ) ) ;
#40465 = CARTESIAN_POINT ( 'NONE',  ( -16.52544592524335698, -4.483927247898792601, 68.95942372801901854 ) ) ;
#40466 = CARTESIAN_POINT ( 'NONE',  ( -15.72974639402197994, 15.80617190586746368, 110.6239096053143669 ) ) ;
#40467 = CARTESIAN_POINT ( 'NONE',  ( -10.72451020669898014, 18.67979575497178502, 115.4155762719810241 ) ) ;
#40469 = CARTESIAN_POINT ( 'NONE',  ( 19.02544592524343514, -5.153800228976328945, 68.54057627198103830 ) ) ;
#40468 = CARTESIAN_POINT ( 'NONE',  ( -19.02544592524334988, -5.153800228976617603, 43.95942372801899012 ) ) ;
#40470 = DIRECTION ( 'NONE',  ( 1.000000000000000000, 1.776356839400250465E-15, 0.000000000000000000 ) ) ;
#40471 = CARTESIAN_POINT ( 'NONE',  ( 5.823673210054444382, -21.52544592524334988, 75.20942372801901854 ) ) ;
#40472 = CARTESIAN_POINT ( 'NONE',  ( 10.72451020669898902, -18.67979575497178502, 57.91557627198103120 ) ) ;
#40473 = CARTESIAN_POINT ( 'NONE',  ( 0.05219959533910956823, 16.53943276465976808, 34.99890960531435979 ) ) ;
#40475 = CARTESIAN_POINT ( 'NONE',  ( 5.823673210054444382, -21.52544592524334988, 110.2094237280190185 ) ) ;
#40474 = CARTESIAN_POINT ( 'NONE',  ( 5.719274019375673035, 21.55341960407619339, 72.29275706135236135 ) ) ;
#40476 = CARTESIAN_POINT ( 'NONE',  ( -16.53943276465976808, 0.05219959533911058130, 56.24890960531436690 ) ) ;
#40477 = CARTESIAN_POINT ( 'NONE',  ( 16.53943276465976808, -0.05219959533910856209, 98.74890960531438111 ) ) ;
#40478 = CARTESIAN_POINT ( 'NONE',  ( -9.474510206698720793, -16.51473224551083518, 49.58442372801899722 ) ) ;
#40479 = CARTESIAN_POINT ( 'NONE',  ( 14.34966873604972726, -8.224510206698740333, 110.8344237280190043 ) ) ;
#40480 = CARTESIAN_POINT ( 'NONE',  ( -0.05219959533937732626, 21.53943276465977519, 72.50109039468568994 ) ) ;
#40481 = CARTESIAN_POINT ( 'NONE',  ( -19.05341960407611168, -5.049401038298163336, 61.45724293864769550 ) ) ;
#40482 = CARTESIAN_POINT ( 'NONE',  ( -13.97604488694547697, 13.89961937509957934, 33.12609039468566863 ) ) ;
#40483 = CARTESIAN_POINT ( 'NONE',  ( -0.05219959533907301413, -21.53943276465977519, 37.49890960531436690 ) ) ;
#40484 = CARTESIAN_POINT ( 'NONE',  ( -0.05219959533937732626, 21.53943276465977519, 37.50109039468568284 ) ) ;
#40485 = CARTESIAN_POINT ( 'NONE',  ( -5.823673210054116645, -21.52544592524344225, 92.29057627198103830 ) ) ;
#40486 = CARTESIAN_POINT ( 'NONE',  ( 19.05341960407617918, -5.049401038297876454, 81.04275706135231871 ) ) ;
#40487 = CARTESIAN_POINT ( 'NONE',  ( 4.379528057220092307, 16.55341960407617563, 47.29275706135234003 ) ) ;
#40489 = CARTESIAN_POINT ( 'NONE',  ( -15.80617190586745835, -15.72974639402198527, 91.87390960531436690 ) ) ;
#40488 = CARTESIAN_POINT ( 'NONE',  ( 11.74264578624799427, 36.14014761921585972, -6.599999999999999645 ) ) ;
#40490 = CARTESIAN_POINT ( 'NONE',  ( 14.29746914071049879, -8.314922557960816363, 83.33224293864769550 ) ) ;
#40491 = CARTESIAN_POINT ( 'NONE',  ( 0.5182397417203463696, 31.81335209757180138, -45.77644358828415250 ) ) ;
#40492 = CARTESIAN_POINT ( 'NONE',  ( -8.314922557961024197, 14.29746914071037800, 22.91775706135235069 ) ) ;
#40493 = CARTESIAN_POINT ( 'NONE',  ( 15.72974639402199770, -15.80617190586745480, 48.12390960531436690 ) ) ;
#40494 = CARTESIAN_POINT ( 'NONE',  ( -12.06949235617739369, -12.14591786802326823, 89.37609039468568994 ) ) ;
#40495 = CARTESIAN_POINT ( 'NONE',  ( -0.05219959533909027116, -19.03943276465977164, 22.49890960531436690 ) ) ;
#40496 = CARTESIAN_POINT ( 'NONE',  ( -4.379528057220086978, -16.55341960407618274, 59.79275706135234714 ) ) ;
#40497 = CARTESIAN_POINT ( 'NONE',  ( 21.53943276465977519, 0.05219959533937863772, 21.25109039468567218 ) ) ;
#40498 = CARTESIAN_POINT ( 'NONE',  ( 21.53943276465977519, -0.05219959533907433946, 48.74890960531435979 ) ) ;
#40499 = CARTESIAN_POINT ( 'NONE',  ( 4.379528057220092307, 16.55341960407617563, 82.29275706135234714 ) ) ;
#40500 = CARTESIAN_POINT ( 'NONE',  ( 9.564922557960805705, 16.46253265017160317, 99.58224293864770971 ) ) ;
#40502 = CARTESIAN_POINT ( 'NONE',  ( 19.02544592524343514, -5.153800228976328945, 23.54057627198102054 ) ) ;
#40501 = CARTESIAN_POINT ( 'NONE',  ( -5.719274019375665041, -21.55341960407619695, 49.79275706135234714 ) ) ;
#40503 = EDGE_CURVE ( 'NONE', #106382, #156928, #36765, .T. ) ;
#40504 = CARTESIAN_POINT ( 'NONE',  ( 21.55341960407610458, 5.719274019375980345, 38.95724293864768839 ) ) ;
#40505 = CARTESIAN_POINT ( 'NONE',  ( -18.67979575497178146, -10.72451020669898902, 26.66557627198103475 ) ) ;
#40506 = VERTEX_POINT ( 'NONE', #86279 ) ;
#40507 = CARTESIAN_POINT ( 'NONE',  ( -13.97604488694547697, 13.89961937509957934, 33.12609039468566863 ) ) ;
#40508 = CARTESIAN_POINT ( 'NONE',  ( -8.224510206698735004, -14.34966873604973081, 64.58442372801900433 ) ) ;
#40509 = CARTESIAN_POINT ( 'NONE',  ( -10.72451020669898014, 18.67979575497178502, 25.41557627198103120 ) ) ;
#40510 = ORIENTED_EDGE ( 'NONE', *, *, #121415, .F. ) ;
#40511 = CARTESIAN_POINT ( 'NONE',  ( 9.564922557960805705, 16.46253265017160317, 79.58224293864769550 ) ) ;
#40512 = CARTESIAN_POINT ( 'NONE',  ( 4.379528057220092307, 16.55341960407617563, 97.29275706135234714 ) ) ;
#40513 = DIRECTION ( 'NONE',  ( -0.000000000000000000, -0.000000000000000000, -1.000000000000000000 ) ) ;
#40514 = CARTESIAN_POINT ( 'NONE',  ( -16.52544592524342804, 4.483927247898546575, 91.04057627198103830 ) ) ;
#40515 = CARTESIAN_POINT ( 'NONE',  ( 0.05219959533907565091, 21.53943276465977519, 44.99890960531435979 ) ) ;
#40516 = CARTESIAN_POINT ( 'NONE',  ( 19.05341960407611168, 5.049401038298154454, 33.95724293864769550 ) ) ;
#40517 = CARTESIAN_POINT ( 'NONE',  ( -16.53943276465976808, -0.05219959533934237506, 83.75109039468568994 ) ) ;
#40518 = CARTESIAN_POINT ( 'NONE',  ( -21.55341960407619339, 5.719274019375674811, 38.54275706135234714 ) ) ;
#40519 = CARTESIAN_POINT ( 'NONE',  ( 0.05219959533936267826, -19.03943276465977164, 85.00109039468567573 ) ) ;
#40520 = CARTESIAN_POINT ( 'NONE',  ( 0.05219959533910956823, 16.53943276465976808, 94.99890960531436690 ) ) ;
#40521 = CARTESIAN_POINT ( 'NONE',  ( -16.51473224551069308, -9.474510206698971260, 36.66557627198102409 ) ) ;
#40522 = CIRCLE ( 'NONE', #153513, 0.5000000000000004441 ) ;
#40523 = CARTESIAN_POINT ( 'NONE',  ( 7.143419655154898962, 2.300691058039359138, 1.353258418600855606 ) ) ;
#40524 = CARTESIAN_POINT ( 'NONE',  ( -21.52544592524334988, -5.823673210054445271, 103.9594237280190185 ) ) ;
#40525 = CARTESIAN_POINT ( 'NONE',  ( -16.51473224551069308, -9.474510206698971260, 76.66557627198103830 ) ) ;
#40526 = CARTESIAN_POINT ( 'NONE',  ( -4.483927247898782831, 16.52544592524335698, 57.70942372801901143 ) ) ;
#40527 = CARTESIAN_POINT ( 'NONE',  ( 21.53943276465977519, 0.05219959533937863772, 91.25109039468568994 ) ) ;
#40528 = CARTESIAN_POINT ( 'NONE',  ( -12.14591786802326823, 12.06949235617739902, 68.12609039468567573 ) ) ;
#40529 = CARTESIAN_POINT ( 'NONE',  ( -13.97604488694547697, 13.89961937509957934, 53.12609039468565442 ) ) ;
#40530 = CARTESIAN_POINT ( 'NONE',  ( 13.89961937509957401, 13.97604488694547697, 71.87609039468567573 ) ) ;
#40531 = ORIENTED_EDGE ( 'NONE', *, *, #93872, .F. ) ;
#40532 = CARTESIAN_POINT ( 'NONE',  ( -18.62759615963255300, -10.81492255796106328, 69.16775706135234714 ) ) ;
#40533 = CARTESIAN_POINT ( 'NONE',  ( -0.05219959533909027116, -19.03943276465977164, 67.49890960531436690 ) ) ;
#40534 = CARTESIAN_POINT ( 'NONE',  ( 5.049401038298163336, -19.05341960407611168, 57.70724293864769550 ) ) ;
#40535 = CARTESIAN_POINT ( 'NONE',  ( -19.05341960407617563, 5.049401038297882671, 58.54275706135234003 ) ) ;
#40536 = CARTESIAN_POINT ( 'NONE',  ( -5.153800228976328057, -19.02544592524343514, 112.2905762719810099 ) ) ;
#40537 = CARTESIAN_POINT ( 'NONE',  ( 0.05219959533909260263, 19.03943276465977164, 84.99890960531436690 ) ) ;
#40538 = CARTESIAN_POINT ( 'NONE',  ( 8.314922557960818139, 14.29746914071049879, 34.58224293864770260 ) ) ;
#40539 = CARTESIAN_POINT ( 'NONE',  ( 21.53943276465977519, -0.05219959533907433946, 53.74890960531437401 ) ) ;
#40540 = AXIS2_PLACEMENT_3D ( 'NONE', #168891, #125392, #188071 ) ;
#40541 = CARTESIAN_POINT ( 'NONE',  ( -17.50000000000000355, -5.499999999999980460, 96.28230962303564411 ) ) ;
#40542 = CARTESIAN_POINT ( 'NONE',  ( 18.67979575497194134, -10.72451020669871369, 105.8344237280190328 ) ) ;
#40543 = LINE ( 'NONE', #10213, #131638 ) ;
#40544 = CARTESIAN_POINT ( 'NONE',  ( -0.05219959533909027116, -19.03943276465977164, 42.49890960531435269 ) ) ;
#40545 = CARTESIAN_POINT ( 'NONE',  ( -22.55670631985092456, 22.55670631985084995, -49.13275782002545355 ) ) ;
#40546 = CLOSED_SHELL ( 'NONE', ( #76335, #33399, #74822, #57481, #190867, #160324, #159714, #69806, #58859, #199293, #143321, #24502, #148472, #56119, #180672, #164208, #196446, #43559, #188878, #71291, #133626, #186837, #127956, #63617, #114807, #31263, #126066, #77190, #174477, #40954, #24020, #42259, #153468, #197319, #46152, #112753, #104846, #27614, #2590, #97525, #95432, #108367, #20485, #1974, #69657, #110248, #164603, #64210, #81082, #153897, #161177, #46895, #25653, #138725, #110024, #54968, #190000, #97654, #153798, #16998, #146823, #171723, #109146, #76948, #146611, #171372, #159534, #160082, #104372, #123909, #170825, #166486, #178238, #112001, #146860, #186014, #722, #21594, #149831, #95180, #103505, #13940, #10682, #85779, #196832, #61320, #185979, #187879, #179456, #99221, #98163, #122343, #24296, #161345, #99828, #166955, #160774, #27944, #42667, #79825, #51155, #188468, #64776, #28572, #75398, #134692, #88676, #184994, #37736, #152432, #104525, #132667, #161301, #159613, #122342, #160562, #144333, #128121, #112277, #74707, #99666, #36131, #91338, #76927, #159804, #191328, #50278, #180767, #74303, #185866, #37821, #54395, #97894, #144962, #137415, #175123, #31555, #22546, #162698, #124120, #158488, #131277, #25829, #65365, #94644, #45288, #113643, #182724, #38841, #185345, #30171, #153602, #189248, #190123, #124477, #190547, #130023, #5079, #86919, #24989, #23022, #193642, #106615, #40874, #6010, #27853, #113957, #130880, #16480, #62499, #128132, #155671, #194812, #157654, #89639, #74609, #170585, #107807, #113512, #173634, #115553, #97465 ) ) ;
#40547 = CARTESIAN_POINT ( 'NONE',  ( -10.70204458709375395, -12.25440978676920700, -59.34122310496267261 ) ) ;
#40548 = CARTESIAN_POINT ( 'NONE',  ( -5.719274019375665041, -21.55341960407619695, 64.79275706135234714 ) ) ;
#40549 = CARTESIAN_POINT ( 'NONE',  ( -37.07204608585244188, -7.847727336691864508, -7.999999999999996447 ) ) ;
#40550 = CARTESIAN_POINT ( 'NONE',  ( 12.06949235617739724, 12.14591786802326823, 66.87609039468568994 ) ) ;
#40551 = CARTESIAN_POINT ( 'NONE',  ( 5.823673210054125526, 21.52544592524343514, 84.79057627198102409 ) ) ;
#40552 = CARTESIAN_POINT ( 'NONE',  ( -8.224510206698948167, 14.34966873604960824, 55.41557627198102409 ) ) ;
#40554 = DIRECTION ( 'NONE',  ( 0.000000000000000000, -0.8164965809277232589, -0.5773502691896295058 ) ) ;
#40553 = CARTESIAN_POINT ( 'NONE',  ( -16.51473224551069308, -9.474510206698971260, 26.66557627198103120 ) ) ;
#40555 = CARTESIAN_POINT ( 'NONE',  ( 21.53943276465977519, 0.05219959533937863772, 46.25109039468567573 ) ) ;
#40556 = CARTESIAN_POINT ( 'NONE',  ( -19.02544592524334988, -5.153800228976617603, 43.95942372801899012 ) ) ;
#40557 = CARTESIAN_POINT ( 'NONE',  ( 16.51473224551069308, 9.474510206698969483, 34.16557627198102409 ) ) ;
#40558 = CARTESIAN_POINT ( 'NONE',  ( 10.81492255796106328, -18.62759615963255655, 80.41775706135234714 ) ) ;
#40559 = LINE ( 'NONE', #195249, #150372 ) ;
#40560 = CARTESIAN_POINT ( 'NONE',  ( 8.224510206698953496, -14.34966873604960469, 32.91557627198102409 ) ) ;
#40561 = CARTESIAN_POINT ( 'NONE',  ( -22.81625015709509441, -31.40387420917324590, -2.824999997268812901 ) ) ;
#40562 = CARTESIAN_POINT ( 'NONE',  ( -21.53943276465977519, 0.05219959533907696930, 41.24890960531435269 ) ) ;
#40563 = CARTESIAN_POINT ( 'NONE',  ( 9.051314012904532191, -0.3916721525565275974, -63.96062167512631191 ) ) ;
#40564 = CARTESIAN_POINT ( 'NONE',  ( -16.51473224551069308, -9.474510206698971260, 91.66557627198103830 ) ) ;
#40565 = CARTESIAN_POINT ( 'NONE',  ( 8.224510206698953496, -14.34966873604960469, 87.91557627198103830 ) ) ;
#40566 = CARTESIAN_POINT ( 'NONE',  ( 13.97604488694548053, -13.89961937509957401, 110.6260903946856615 ) ) ;
#40567 = CARTESIAN_POINT ( 'NONE',  ( 5.823673210054125526, 21.52544592524343514, 69.79057627198102409 ) ) ;
#40568 = ORIENTED_EDGE ( 'NONE', *, *, #118900, .F. ) ;
#40569 = CARTESIAN_POINT ( 'NONE',  ( 5.049401038298161559, -19.05341960407611168, 37.70724293864768839 ) ) ;
#40571 = CARTESIAN_POINT ( 'NONE',  ( -15.72974639402197994, 15.80617190586746368, 95.62390960531436690 ) ) ;
#40570 = CARTESIAN_POINT ( 'NONE',  ( -19.05341960407611168, -5.049401038298163336, 91.45724293864766707 ) ) ;
#40573 = CARTESIAN_POINT ( 'NONE',  ( -9.564922557960796823, -16.46253265017161027, 107.0822429386476955 ) ) ;
#40572 = CARTESIAN_POINT ( 'NONE',  ( 4.483927247898790824, -16.52544592524335698, 110.2094237280190185 ) ) ;
#40574 = CARTESIAN_POINT ( 'NONE',  ( -5.153800228976607833, 19.02544592524334988, 82.70942372801897591 ) ) ;
#40575 = CARTESIAN_POINT ( 'NONE',  ( 21.52544592524334988, 5.823673210054432836, 96.45942372801901854 ) ) ;
#40576 = CARTESIAN_POINT ( 'NONE',  ( -21.52544592524343514, 5.823673210054127303, 76.04057627198102409 ) ) ;
#40577 = CARTESIAN_POINT ( 'NONE',  ( 10.72451020669898902, -18.67979575497178502, 32.91557627198102409 ) ) ;
#40578 = CARTESIAN_POINT ( 'NONE',  ( -9.474510206698964154, 16.51473224551069663, 45.41557627198103120 ) ) ;
#40579 = CARTESIAN_POINT ( 'NONE',  ( 4.379528057220339221, -16.55341960407611168, 27.70724293864769905 ) ) ;
#40580 = CARTESIAN_POINT ( 'NONE',  ( 13.89961937509977652, -13.97604488694527269, 78.12390960531433848 ) ) ;
#40581 = ORIENTED_EDGE ( 'NONE', *, *, #99588, .F. ) ;
#40582 = CARTESIAN_POINT ( 'NONE',  ( -17.49999999999999645, 5.499999999999997335, 110.7969038253417295 ) ) ;
#40583 = CARTESIAN_POINT ( 'NONE',  ( -9.564922557961040184, 16.46253265017147172, 32.91775706135233293 ) ) ;
#40584 = CARTESIAN_POINT ( 'NONE',  ( -12.06949235617756955, 12.14591786802309770, 90.62390960531436690 ) ) ;
#40585 = CARTESIAN_POINT ( 'NONE',  ( 21.53943276465977519, 0.05219959533937863772, 26.25109039468567573 ) ) ;
#40586 = CARTESIAN_POINT ( 'NONE',  ( -27.73933785331498925, 9.013057229001089965, 145.2750000027311899 ) ) ;
#40587 = CARTESIAN_POINT ( 'NONE',  ( 5.823673210054125526, 21.52544592524343514, 59.79057627198103120 ) ) ;
#40588 = CARTESIAN_POINT ( 'NONE',  ( 14.34966873604972726, -8.224510206698740333, 95.83442372801903275 ) ) ;
#40589 = CARTESIAN_POINT ( 'NONE',  ( -14.29746914071049879, 8.314922557960819915, 115.8322429386477097 ) ) ;
#40590 = CARTESIAN_POINT ( 'NONE',  ( -5.153800228976328057, -19.02544592524343514, 77.29057627198099567 ) ) ;
#40591 = CARTESIAN_POINT ( 'NONE',  ( 9.564922557960805705, 16.46253265017160317, 24.58224293864769194 ) ) ;
#40592 = CARTESIAN_POINT ( 'NONE',  ( -16.55341960407611168, -4.379528057220339221, 31.45724293864769550 ) ) ;
#40593 = CARTESIAN_POINT ( 'NONE',  ( 5.719274019375673035, 21.55341960407619339, 62.29275706135236845 ) ) ;
#40594 = CARTESIAN_POINT ( 'NONE',  ( -0.05219959533909027116, -19.03943276465977164, 112.4989096053143669 ) ) ;
#40595 = CARTESIAN_POINT ( 'NONE',  ( -18.62759615963255300, -10.81492255796106328, 99.16775706135234714 ) ) ;
#40596 = CARTESIAN_POINT ( 'NONE',  ( 16.46253265017160672, -9.564922557960803928, 33.33224293864770260 ) ) ;
#40597 = CARTESIAN_POINT ( 'NONE',  ( 19.02544592524343514, -5.153800228976328945, 33.54057627198102409 ) ) ;
#40598 = VERTEX_POINT ( 'NONE', #98428 ) ;
#40599 = CARTESIAN_POINT ( 'NONE',  ( 5.719274019375673035, 21.55341960407619339, 97.29275706135234714 ) ) ;
#40600 = CARTESIAN_POINT ( 'NONE',  ( 12.06949235617739724, 12.14591786802326823, 46.87609039468568994 ) ) ;
#40601 = CARTESIAN_POINT ( 'NONE',  ( 18.67979575497194134, -10.72451020669871369, 85.83442372801901854 ) ) ;
#40602 = CARTESIAN_POINT ( 'NONE',  ( 9.564922557960805705, 16.46253265017160317, 114.5822429386476955 ) ) ;
#40603 = CARTESIAN_POINT ( 'NONE',  ( 5.153800228976615827, -19.02544592524334988, 90.20942372801900433 ) ) ;
#40604 = CARTESIAN_POINT ( 'NONE',  ( 5.719274019375673035, 21.55341960407619339, 57.29275706135234714 ) ) ;
#40605 = CARTESIAN_POINT ( 'NONE',  ( 8.224510206698742110, 14.34966873604972548, 27.08442372801901854 ) ) ;
#40606 = CIRCLE ( 'NONE', #150454, 0.2000000000000057288 ) ;
#40607 = CARTESIAN_POINT ( 'NONE',  ( -5.049401038297874678, -19.05341960407617918, 84.79275706135233293 ) ) ;
#40608 = CARTESIAN_POINT ( 'NONE',  ( 19.05341960407611168, 5.049401038298154454, 48.95724293864768129 ) ) ;
#40609 = CARTESIAN_POINT ( 'NONE',  ( 9.474510206698729675, 16.51473224551082808, 97.08442372801900433 ) ) ;
#40610 = CARTESIAN_POINT ( 'NONE',  ( 16.46253265017146816, 9.564922557961045513, 86.66775706135233293 ) ) ;
#40611 = CARTESIAN_POINT ( 'NONE',  ( -4.483927247898539470, -16.52544592524342804, 57.29057627198103120 ) ) ;
#40612 = CARTESIAN_POINT ( 'NONE',  ( -5.049401038297874678, -19.05341960407617918, 79.79275706135233293 ) ) ;
#40613 = CARTESIAN_POINT ( 'NONE',  ( 8.314922557961029526, -14.29746914071037800, 65.41775706135234714 ) ) ;
#40614 = CARTESIAN_POINT ( 'NONE',  ( -19.03943276465977164, -0.05219959533935918106, 28.75109039468566507 ) ) ;
#40615 = CARTESIAN_POINT ( 'NONE',  ( 19.02544592524343514, -5.153800228976328945, 38.54057627198103120 ) ) ;
#40616 = CARTESIAN_POINT ( 'NONE',  ( -19.03943276465977164, 0.05219959533909376836, 46.24890960531435979 ) ) ;
#40617 = CARTESIAN_POINT ( 'NONE',  ( 0.05219959533934541429, -16.53943276465976808, 65.00109039468568994 ) ) ;
#40618 = CARTESIAN_POINT ( 'NONE',  ( -27.73933785331498925, 9.013057229001089965, 141.2750000027311614 ) ) ;
#40619 = CARTESIAN_POINT ( 'NONE',  ( 8.906447517083057264, -27.41122689804191026, 140.8500000054623911 ) ) ;
#40620 = CARTESIAN_POINT ( 'NONE',  ( 16.51473224551069308, 9.474510206698969483, 109.1655762719810383 ) ) ;
#40621 = CARTESIAN_POINT ( 'NONE',  ( -2.552343178074577779, 7.052343178074668373, 1.110912703473986074 ) ) ;
#40622 = ORIENTED_EDGE ( 'NONE', *, *, #186227, .F. ) ;
#40623 = CARTESIAN_POINT ( 'NONE',  ( -19.05341960407617563, 5.049401038297882671, 93.54275706135234714 ) ) ;
#40624 = CARTESIAN_POINT ( 'NONE',  ( -15.80617190586745835, -15.72974639402198527, 41.87390960531435979 ) ) ;
#40626 = CARTESIAN_POINT ( 'NONE',  ( 5.153800228976615827, -19.02544592524334988, 105.2094237280190185 ) ) ;
#40625 = CARTESIAN_POINT ( 'NONE',  ( -19.02544592524334988, -5.153800228976617603, 28.95942372801900433 ) ) ;
#40627 = CARTESIAN_POINT ( 'NONE',  ( -9.474510206698964154, 16.51473224551069663, 35.41557627198102409 ) ) ;
#40628 = CARTESIAN_POINT ( 'NONE',  ( 16.46253265017160672, -9.564922557960803928, 43.33224293864769550 ) ) ;
#40629 = CARTESIAN_POINT ( 'NONE',  ( -21.55341960407610458, -5.719274019375992779, 76.45724293864769550 ) ) ;
#40630 = EDGE_CURVE ( 'NONE', #135024, #4644, #83271, .T. ) ;
#40631 = CARTESIAN_POINT ( 'NONE',  ( -16.51473224551069308, -9.474510206698971260, 31.66557627198102054 ) ) ;
#40632 = CARTESIAN_POINT ( 'NONE',  ( -8.571926809382601320, -26.38167802310801591, 143.7750000027311899 ) ) ;
#40633 = CARTESIAN_POINT ( 'NONE',  ( -19.02544592524334988, -5.153800228976617603, 83.95942372801901854 ) ) ;
#40634 = CARTESIAN_POINT ( 'NONE',  ( 8.314922557960818139, 14.29746914071049879, 59.58224293864770260 ) ) ;
#40635 = CARTESIAN_POINT ( 'NONE',  ( -5.823673210054116645, -21.52544592524344225, 32.29057627198102409 ) ) ;
#40636 = CARTESIAN_POINT ( 'NONE',  ( 10.72451020669871369, 18.67979575497193778, 107.0844237280190043 ) ) ;
#40637 = CARTESIAN_POINT ( 'NONE',  ( 5.823673210054125526, 21.52544592524343514, 84.79057627198102409 ) ) ;
#40638 = CARTESIAN_POINT ( 'NONE',  ( 15.80617190586769283, -15.72974639402175789, 70.62609039468567573 ) ) ;
#40639 = CARTESIAN_POINT ( 'NONE',  ( 21.52544592524334988, 5.823673210054432836, 61.45942372801901854 ) ) ;
#40640 = CARTESIAN_POINT ( 'NONE',  ( -5.049401038298153566, 19.05341960407611168, 105.2072429386476671 ) ) ;
#40642 = CARTESIAN_POINT ( 'NONE',  ( -5.823673210054431948, 21.52544592524334988, 57.70942372801901143 ) ) ;
#40641 = CARTESIAN_POINT ( 'NONE',  ( 8.224510206698742110, 14.34966873604972548, 107.0844237280190043 ) ) ;
#40643 = CARTESIAN_POINT ( 'NONE',  ( -0.05219959533909027116, -19.03943276465977164, 57.49890960531435979 ) ) ;
#40644 = CARTESIAN_POINT ( 'NONE',  ( -5.153800228976607833, 19.02544592524334988, 32.70942372801899722 ) ) ;
#40645 = CARTESIAN_POINT ( 'NONE',  ( -18.67979575497193778, 10.72451020669871902, 28.33442372801902209 ) ) ;
#40646 = CARTESIAN_POINT ( 'NONE',  ( -19.03943276465977164, 0.05219959533909376836, 66.24890960531436690 ) ) ;
#40647 = CARTESIAN_POINT ( 'NONE',  ( -4.483927247898539470, -16.52544592524342804, 77.29057627198102409 ) ) ;
#40648 = CARTESIAN_POINT ( 'NONE',  ( -0.05219959533910754901, -16.53943276465976808, 47.49890960531435979 ) ) ;
#40649 = CARTESIAN_POINT ( 'NONE',  ( 21.52544592524344225, -5.823673210054117533, 63.54057627198103830 ) ) ;
#40650 = CARTESIAN_POINT ( 'NONE',  ( 16.46253265017160672, -9.564922557960803928, 53.33224293864768839 ) ) ;
#40651 = CARTESIAN_POINT ( 'NONE',  ( -10.81492255796078084, -18.62759615963271287, 72.08224293864769550 ) ) ;
#40652 = CARTESIAN_POINT ( 'NONE',  ( -16.46253265017146816, -9.564922557961047289, 49.16775706135233293 ) ) ;
#40654 = CARTESIAN_POINT ( 'NONE',  ( -16.53943276465976808, 0.05219959533911058130, 61.24890960531435979 ) ) ;
#40653 = DIRECTION ( 'NONE',  ( 0.000000000000000000, 0.000000000000000000, 1.000000000000000000 ) ) ;
#40655 = CARTESIAN_POINT ( 'NONE',  ( 21.53943276465977519, -0.05219959533907433946, 43.74890960531435979 ) ) ;
#40656 = ORIENTED_EDGE ( 'NONE', *, *, #71324, .T. ) ;
#40657 = CARTESIAN_POINT ( 'NONE',  ( 16.29526858892874941, 7.335722546920130149, 103.2967059780020662 ) ) ;
#40659 = CARTESIAN_POINT ( 'NONE',  ( -17.14385361876520264, -23.59649016807271238, 139.6750000027311955 ) ) ;
#40658 = CARTESIAN_POINT ( 'NONE',  ( -8.314922557961024197, 14.29746914071037800, 82.91775706135234714 ) ) ;
#40660 = CARTESIAN_POINT ( 'NONE',  ( 13.89961937509957401, 13.97604488694547697, 91.87609039468567573 ) ) ;
#40661 = CARTESIAN_POINT ( 'NONE',  ( -4.483927247898539470, -16.52544592524342804, 52.29057627198102409 ) ) ;
#40662 = CARTESIAN_POINT ( 'NONE',  ( -18.39639308325436673, -5.500000000000039080, 61.48252246182197212 ) ) ;
#40663 = CARTESIAN_POINT ( 'NONE',  ( 19.05341960407611168, 5.049401038298154454, 43.95724293864769550 ) ) ;
#40664 = CARTESIAN_POINT ( 'NONE',  ( -16.52544592524342804, 4.483927247898546575, 36.04057627198102409 ) ) ;
#40665 = CARTESIAN_POINT ( 'NONE',  ( 13.97604488694527802, 13.89961937509977652, 94.37390960531436690 ) ) ;
#40666 = CARTESIAN_POINT ( 'NONE',  ( -16.51473224551069308, -9.474510206698971260, 56.66557627198103120 ) ) ;
#40667 = CARTESIAN_POINT ( 'NONE',  ( -21.52544592524334988, -5.823673210054445271, 53.95942372801900433 ) ) ;
#40668 = CARTESIAN_POINT ( 'NONE',  ( 19.03943276465977164, -0.05219959533909143690, 68.74890960531436690 ) ) ;
#40669 = CARTESIAN_POINT ( 'NONE',  ( -9.564922557960796823, -16.46253265017161027, 27.08224293864769550 ) ) ;
#40670 = CARTESIAN_POINT ( 'NONE',  ( -0.05219959533909027116, -19.03943276465977164, 72.49890960531435269 ) ) ;
#40671 = CARTESIAN_POINT ( 'NONE',  ( 21.52544592524344225, -5.823673210054117533, 48.54057627198103120 ) ) ;
#40672 = CARTESIAN_POINT ( 'NONE',  ( 19.05341960407611168, 5.049401038298154454, 33.95724293864769550 ) ) ;
#40673 = CARTESIAN_POINT ( 'NONE',  ( 5.823673210054125526, 21.52544592524343514, 34.79057627198103120 ) ) ;
#40674 = CARTESIAN_POINT ( 'NONE',  ( -14.34966873604972548, 8.224510206698743886, 108.3344237280190185 ) ) ;
#40675 = CARTESIAN_POINT ( 'NONE',  ( -16.46253265017146816, -9.564922557961047289, 24.16775706135233648 ) ) ;
#40677 = CARTESIAN_POINT ( 'NONE',  ( 8.224510206698742110, 14.34966873604972548, 87.08442372801901854 ) ) ;
#40676 = CARTESIAN_POINT ( 'NONE',  ( -12.14591786802326823, 12.06949235617739902, 43.12609039468568284 ) ) ;
#40678 = CYLINDRICAL_SURFACE ( 'NONE', #4812, 2.500000000000002220 ) ;
#40679 = CARTESIAN_POINT ( 'NONE',  ( 16.53943276465976808, 0.05219959533934440121, 61.25109039468567573 ) ) ;
#40680 = CARTESIAN_POINT ( 'NONE',  ( -13.97604488694527625, -13.89961937509977652, 106.8739096053143669 ) ) ;
#40681 = CARTESIAN_POINT ( 'NONE',  ( 9.474510206698971260, -16.51473224551069308, 37.91557627198102409 ) ) ;
#40682 = CARTESIAN_POINT ( 'NONE',  ( 14.34966873604972726, -8.224510206698740333, 40.83442372801901854 ) ) ;
#40683 = CARTESIAN_POINT ( 'NONE',  ( -0.05219959533909027116, -19.03943276465977164, 42.49890960531435269 ) ) ;
#40684 = CARTESIAN_POINT ( 'NONE',  ( -10.81492255796105439, 18.62759615963255655, 32.91775706135234714 ) ) ;
#40685 = CARTESIAN_POINT ( 'NONE',  ( -12.06949235617739369, -12.14591786802326823, 29.37609039468568284 ) ) ;
#40686 = CARTESIAN_POINT ( 'NONE',  ( -16.53943276465976808, -0.05219959533934237506, 98.75109039468568994 ) ) ;
#40687 = CARTESIAN_POINT ( 'NONE',  ( 1.348150961071065097E-30, -64.82615989628266107, -15.00000000000000000 ) ) ;
#40688 = CARTESIAN_POINT ( 'NONE',  ( -5.719274019375665041, -21.55341960407619695, 94.79275706135234714 ) ) ;
#40689 = CARTESIAN_POINT ( 'NONE',  ( 19.05341960407617918, -5.049401038297876454, 96.04275706135231871 ) ) ;
#40690 = CARTESIAN_POINT ( 'NONE',  ( -9.564922557961040184, 16.46253265017147172, 57.91775706135233293 ) ) ;
#40691 = CARTESIAN_POINT ( 'NONE',  ( 16.52544592524342804, -4.483927247898539470, 58.54057627198103120 ) ) ;
#40692 = CARTESIAN_POINT ( 'NONE',  ( 16.55341960407611168, 4.379528057220329451, 113.9572429386477239 ) ) ;
#40694 = CARTESIAN_POINT ( 'NONE',  ( 16.31925111598458145, 7.325300261831480420, 77.33575461032749843 ) ) ;
#40693 = CARTESIAN_POINT ( 'NONE',  ( 16.51473224551083163, -9.474510206698727899, 60.83442372801900433 ) ) ;
#40695 = CARTESIAN_POINT ( 'NONE',  ( -21.53943276465977519, -0.05219959533937600094, 63.75109039468568284 ) ) ;
#40696 = CARTESIAN_POINT ( 'NONE',  ( 16.53943276465976808, 0.05219959533934440121, 21.25109039468567218 ) ) ;
#40697 = CARTESIAN_POINT ( 'NONE',  ( -193.3062444957834884, -155.7167183371838064, 0.000000000000000000 ) ) ;
#40698 = CARTESIAN_POINT ( 'NONE',  ( 21.53943276465977519, -0.05219959533907433946, 23.74890960531435269 ) ) ;
#40699 = CARTESIAN_POINT ( 'NONE',  ( 9.474510206698729675, 16.51473224551082808, 107.0844237280190043 ) ) ;
#40700 = CARTESIAN_POINT ( 'NONE',  ( 5.049401038298161559, -19.05341960407611168, 112.7072429386476813 ) ) ;
#40701 = CARTESIAN_POINT ( 'NONE',  ( -25.52568752982265821, 9.519068727184937018, 170.8917780290381927 ) ) ;
#40702 = CARTESIAN_POINT ( 'NONE',  ( 19.03943276465977164, -0.05219959533909143690, 23.74890960531435269 ) ) ;
#40703 = CARTESIAN_POINT ( 'NONE',  ( -0.05219959533937732626, 21.53943276465977519, 102.5010903946856899 ) ) ;
#40704 = CARTESIAN_POINT ( 'NONE',  ( 0.05219959533909260263, 19.03943276465977164, 59.99890960531436690 ) ) ;
#40705 = AXIS2_PLACEMENT_3D ( 'NONE', #120589, #182284, #105428 ) ;
#40706 = CARTESIAN_POINT ( 'NONE',  ( 18.62759615963255655, 10.81492255796105972, 71.66775706135234714 ) ) ;
#40707 = ADVANCED_FACE ( 'NONE', ( #129760 ), #61712, .T. ) ;
#40708 = CARTESIAN_POINT ( 'NONE',  ( -18.62759615963255300, -10.81492255796106328, 104.1677570613523471 ) ) ;
#40709 = CARTESIAN_POINT ( 'NONE',  ( 8.224510206698742110, 14.34966873604972548, 107.0844237280190043 ) ) ;
#40710 = CARTESIAN_POINT ( 'NONE',  ( 9.474510206698971260, -16.51473224551069308, 72.91557627198102409 ) ) ;
#40711 = CARTESIAN_POINT ( 'NONE',  ( 18.62759615963255655, 10.81492255796105972, 51.66775706135234714 ) ) ;
#40712 = CARTESIAN_POINT ( 'NONE',  ( 21.55341960407619695, -5.719274019375665929, 51.04275706135234714 ) ) ;
#40714 = CARTESIAN_POINT ( 'NONE',  ( 9.474510206698971260, -16.51473224551069308, 102.9155762719810241 ) ) ;
#40713 = CARTESIAN_POINT ( 'NONE',  ( -16.46253265017146816, -9.564922557961047289, 84.16775706135233293 ) ) ;
#40715 = CARTESIAN_POINT ( 'NONE',  ( 19.03943276465977164, -0.05219959533909143690, 23.74890960531435269 ) ) ;
#40716 = CARTESIAN_POINT ( 'NONE',  ( 18.62759615963271287, -10.81492255796078972, 103.3322429386476955 ) ) ;
#40717 = CARTESIAN_POINT ( 'NONE',  ( 5.153800228976615827, -19.02544592524334988, 20.20942372801899722 ) ) ;
#40718 = CARTESIAN_POINT ( 'NONE',  ( 16.55341960407611168, 4.379528057220329451, 103.9572429386476813 ) ) ;
#40719 = CARTESIAN_POINT ( 'NONE',  ( -13.89961937509977652, 13.97604488694528158, 50.62390960531435979 ) ) ;
#40720 = CARTESIAN_POINT ( 'NONE',  ( -19.05341960407617563, 5.049401038297882671, 93.54275706135234714 ) ) ;
#40721 = CARTESIAN_POINT ( 'NONE',  ( -4.483927247898539470, -16.52544592524342804, 67.29057627198103830 ) ) ;
#40722 = CARTESIAN_POINT ( 'NONE',  ( 10.81492255796106328, -18.62759615963255655, 105.4177570613523613 ) ) ;
#40723 = CARTESIAN_POINT ( 'NONE',  ( -5.049401038298153566, 19.05341960407611168, 105.2072429386476671 ) ) ;
#40724 = CARTESIAN_POINT ( 'NONE',  ( 19.05341960407617918, -5.049401038297876454, 76.04275706135230450 ) ) ;
#40725 = CARTESIAN_POINT ( 'NONE',  ( -5.823673210054116645, -21.52544592524344225, 82.29057627198103830 ) ) ;
#40726 = CARTESIAN_POINT ( 'NONE',  ( -21.55341960407619339, 5.719274019375674811, 33.54275706135234714 ) ) ;
#40727 = CARTESIAN_POINT ( 'NONE',  ( -4.483927247898782831, 16.52544592524335698, 37.70942372801900433 ) ) ;
#40728 = CARTESIAN_POINT ( 'NONE',  ( 16.55341960407618274, -4.379528057220086978, 96.04275706135236135 ) ) ;
#40730 = CARTESIAN_POINT ( 'NONE',  ( 21.53943276465977519, 0.05219959533937863772, 41.25109039468568284 ) ) ;
#40729 = CARTESIAN_POINT ( 'NONE',  ( -0.05219959533934338120, 16.53943276465976808, 37.50109039468568284 ) ) ;
#40731 = CARTESIAN_POINT ( 'NONE',  ( -21.52544592524343514, 5.823673210054127303, 41.04057627198103120 ) ) ;
#40732 = CARTESIAN_POINT ( 'NONE',  ( -16.46253265017160317, 9.564922557960807481, 35.83224293864768839 ) ) ;
#40733 = CARTESIAN_POINT ( 'NONE',  ( -11.74264578624799782, -36.14014761921581709, -11.34999999453762776 ) ) ;
#40734 = CARTESIAN_POINT ( 'NONE',  ( -0.05219959533934338120, 16.53943276465976808, 62.50109039468568284 ) ) ;
#40735 = CARTESIAN_POINT ( 'NONE',  ( 15.80617190586746368, 15.72974639402197994, 84.37390960531438111 ) ) ;
#40736 = CARTESIAN_POINT ( 'NONE',  ( 8.314922557960818139, 14.29746914071049879, 39.58224293864769550 ) ) ;
#40737 = CARTESIAN_POINT ( 'NONE',  ( -16.53943276465976808, -0.05219959533934237506, 53.75109039468568994 ) ) ;
#40738 = CARTESIAN_POINT ( 'NONE',  ( 5.049401038298161559, -19.05341960407611168, 57.70724293864769550 ) ) ;
#40739 = CARTESIAN_POINT ( 'NONE',  ( 14.34966873604972726, -8.224510206698740333, 90.83442372801901854 ) ) ;
#40740 = CARTESIAN_POINT ( 'NONE',  ( -13.97604488694547697, 13.89961937509957934, 83.12609039468564731 ) ) ;
#40741 = CARTESIAN_POINT ( 'NONE',  ( -5.719274019375978568, 21.55341960407610458, 80.20724293864769550 ) ) ;
#40742 = CARTESIAN_POINT ( 'NONE',  ( 16.55341960407611168, 4.379528057220329451, 28.95724293864769905 ) ) ;
#40743 = ORIENTED_EDGE ( 'NONE', *, *, #8138, .F. ) ;
#40744 = CARTESIAN_POINT ( 'NONE',  ( 19.83801684532418008, 12.12952959760495730, 169.9999999999999716 ) ) ;
#40745 = EDGE_CURVE ( 'NONE', #21338, #141920, #151982, .T. ) ;
#40746 = CARTESIAN_POINT ( 'NONE',  ( 10.72451020669898902, -18.67979575497178502, 57.91557627198103120 ) ) ;
#40747 = CARTESIAN_POINT ( 'NONE',  ( -0.05219959533934338120, 16.53943276465976808, 102.5010903946856899 ) ) ;
#40748 = VERTEX_POINT ( 'NONE', #4663 ) ;
#40749 = CARTESIAN_POINT ( 'NONE',  ( 17.50000000000005684, -3.926509638704657856, 102.9170501086137790 ) ) ;
#40750 = CARTESIAN_POINT ( 'NONE',  ( 18.62759615963271287, -10.81492255796078972, 88.33224293864769550 ) ) ;
#40751 = CIRCLE ( 'NONE', #179615, 2.500000000000002220 ) ;
#40752 = CARTESIAN_POINT ( 'NONE',  ( -16.53943276465976808, 0.05219959533911058130, 21.24890960531436690 ) ) ;
#40753 = CARTESIAN_POINT ( 'NONE',  ( 0.05219959533934541429, -16.53943276465976808, 40.00109039468567573 ) ) ;
#40754 = CARTESIAN_POINT ( 'NONE',  ( -9.474510206698964154, 16.51473224551069663, 30.41557627198102054 ) ) ;
#40755 = CARTESIAN_POINT ( 'NONE',  ( 13.89961937509977652, -13.97604488694527269, 63.12390960531435979 ) ) ;
#40756 = CARTESIAN_POINT ( 'NONE',  ( 23.31738231874054534, 16.94106989632529192, 147.1999999999999886 ) ) ;
#40757 = CARTESIAN_POINT ( 'NONE',  ( -18.62759615963270932, 10.81492255796079327, 25.83224293864769194 ) ) ;
#40758 = CARTESIAN_POINT ( 'NONE',  ( 1.500000000002908562, 30.39999999999990266, -50.95361246531977173 ) ) ;
#40759 = CARTESIAN_POINT ( 'NONE',  ( 14.34966873604972726, -8.224510206698740333, 100.8344237280190185 ) ) ;
#40760 = CARTESIAN_POINT ( 'NONE',  ( 19.05341960407617918, -5.049401038297876454, 101.0427570613523045 ) ) ;
#40761 = CARTESIAN_POINT ( 'NONE',  ( 19.02544592524334988, 5.153800228976608722, 36.45942372801900433 ) ) ;
#40762 = CARTESIAN_POINT ( 'NONE',  ( 15.80617190586746368, 15.72974639402197994, 84.37390960531438111 ) ) ;
#40763 = CARTESIAN_POINT ( 'NONE',  ( 16.55341960407618274, -4.379528057220086978, 111.0427570613523613 ) ) ;
#40764 = CARTESIAN_POINT ( 'NONE',  ( 5.823673210054125526, 21.52544592524343514, 29.79057627198102409 ) ) ;
#40765 = CARTESIAN_POINT ( 'NONE',  ( 13.89961937509957401, 13.97604488694547697, 111.8760903946856757 ) ) ;
#40766 = CARTESIAN_POINT ( 'NONE',  ( 9.564922557960805705, 16.46253265017160317, 109.5822429386476955 ) ) ;
#40767 = CARTESIAN_POINT ( 'NONE',  ( -5.823673210054431948, 21.52544592524334988, 62.70942372801902565 ) ) ;
#40768 = CARTESIAN_POINT ( 'NONE',  ( 16.46253265017160672, -9.564922557960803928, 58.33224293864769550 ) ) ;
#40769 = CARTESIAN_POINT ( 'NONE',  ( -12.06949235617756955, 12.14591786802309770, 95.62390960531436690 ) ) ;
#40770 = CARTESIAN_POINT ( 'NONE',  ( 31.56642711641980625, 3.769985069463992478, 101.5021612967808409 ) ) ;
#40771 = CARTESIAN_POINT ( 'NONE',  ( -16.51473224551069308, -9.474510206698971260, 71.66557627198102409 ) ) ;
#40772 = CARTESIAN_POINT ( 'NONE',  ( 4.379528057220339221, -16.55341960407611168, 72.70724293864769550 ) ) ;
#40773 = ORIENTED_EDGE ( 'NONE', *, *, #96707, .F. ) ;
#40774 = CARTESIAN_POINT ( 'NONE',  ( 16.46253265017146816, 9.564922557961045513, 86.66775706135233293 ) ) ;
#40775 = DIRECTION ( 'NONE',  ( -1.000000000000000000, -0.000000000000000000, -0.000000000000000000 ) ) ;
#40776 = CARTESIAN_POINT ( 'NONE',  ( -19.03943276465977164, 0.05219959533909376836, 66.24890960531436690 ) ) ;
#40777 = CARTESIAN_POINT ( 'NONE',  ( 31.68593437162162019, -6.718755962661552950, 91.65819149638747376 ) ) ;
#40779 = CARTESIAN_POINT ( 'NONE',  ( -19.02544592524342804, 5.153800228976336051, 101.0405762719810241 ) ) ;
#40778 = CARTESIAN_POINT ( 'NONE',  ( -9.564922557960796823, -16.46253265017161027, 72.08224293864770971 ) ) ;
#40780 = CARTESIAN_POINT ( 'NONE',  ( 8.314922557961029526, -14.29746914071037800, 60.41775706135235424 ) ) ;
#40781 = DIRECTION ( 'NONE',  ( 0.000000000000000000, 0.000000000000000000, 1.000000000000000000 ) ) ;
#40782 = CARTESIAN_POINT ( 'NONE',  ( -19.03943276465977164, -0.05219959533935918106, 43.75109039468566863 ) ) ;
#40783 = CARTESIAN_POINT ( 'NONE',  ( 10.72451020669871369, 18.67979575497193778, 97.08442372801904696 ) ) ;
#40784 = CARTESIAN_POINT ( 'NONE',  ( 36.87151287952131185, 2.273789158011782163, 50.01119746921813913 ) ) ;
#40785 = CARTESIAN_POINT ( 'NONE',  ( 5.049401038298161559, -19.05341960407611168, 112.7072429386476813 ) ) ;
#40786 = CARTESIAN_POINT ( 'NONE',  ( -8.224510206698735004, -14.34966873604973081, 99.58442372801900433 ) ) ;
#40787 = CARTESIAN_POINT ( 'NONE',  ( -34.71415419550760362, -2.652640888949080455, 52.01956328305328014 ) ) ;
#40788 = CARTESIAN_POINT ( 'NONE',  ( 16.52544592524335698, 4.483927247898782831, 86.45942372801901854 ) ) ;
#40789 = CARTESIAN_POINT ( 'NONE',  ( 8.898068258721465895, 27.38543819252877398, 145.6656553485624102 ) ) ;
#40790 = CARTESIAN_POINT ( 'NONE',  ( -8.224510206698735004, -14.34966873604973081, 69.58442372801900433 ) ) ;
#40791 = VERTEX_POINT ( 'NONE', #7662 ) ;
#40792 = CARTESIAN_POINT ( 'NONE',  ( -10.72451020669870658, -18.67979575497194134, 79.58442372801903275 ) ) ;
#40793 = CARTESIAN_POINT ( 'NONE',  ( 5.153800228976615827, -19.02544592524334988, 85.20942372801900433 ) ) ;
#40794 = CARTESIAN_POINT ( 'NONE',  ( -0.05219959533936034679, 19.03943276465977164, 32.50109039468566863 ) ) ;
#40795 = CARTESIAN_POINT ( 'NONE',  ( -16.51473224551069308, -9.474510206698971260, 71.66557627198102409 ) ) ;
#40796 = CARTESIAN_POINT ( 'NONE',  ( 5.049401038298161559, -19.05341960407611168, 57.70724293864769550 ) ) ;
#40797 = CARTESIAN_POINT ( 'NONE',  ( 16.45676962205255833, -7.258233047195244758, 22.85181134416914617 ) ) ;
#40798 = CARTESIAN_POINT ( 'NONE',  ( 0.05219959533907565091, 21.53943276465977519, 79.99890960531435269 ) ) ;
#40799 = CARTESIAN_POINT ( 'NONE',  ( 15.72974639402199770, -15.80617190586745480, 38.12390960531436690 ) ) ;
#40800 = CARTESIAN_POINT ( 'NONE',  ( 0.05219959533909260263, 19.03943276465977164, 39.99890960531436690 ) ) ;
#40801 = CARTESIAN_POINT ( 'NONE',  ( 8.314922557961029526, -14.29746914071037800, 65.41775706135234714 ) ) ;
#40802 = EDGE_LOOP ( 'NONE', ( #123635, #84527 ) ) ;
#40803 = CARTESIAN_POINT ( 'NONE',  ( 21.52544592524334988, 5.823673210054432836, 36.45942372801901143 ) ) ;
#40805 = CARTESIAN_POINT ( 'NONE',  ( -36.91746825000001309, 11.99521256947798342, -8.724999997268813701 ) ) ;
#40804 = CARTESIAN_POINT ( 'NONE',  ( -16.53943276465976808, 0.05219959533911058130, 61.24890960531435979 ) ) ;
#40806 = CARTESIAN_POINT ( 'NONE',  ( 0.05219959533934541429, -16.53943276465976808, 20.00109039468568639 ) ) ;
#40807 = CARTESIAN_POINT ( 'NONE',  ( 16.51473224551083163, -9.474510206698727899, 50.83442372801899722 ) ) ;
#40808 = CARTESIAN_POINT ( 'NONE',  ( 16.53943276465976808, -0.05219959533910856209, 53.74890960531437401 ) ) ;
#40809 = CARTESIAN_POINT ( 'NONE',  ( 5.719274019375673035, 21.55341960407619339, 22.29275706135235069 ) ) ;
#40811 = CARTESIAN_POINT ( 'NONE',  ( -5.719274019375978568, 21.55341960407610458, 80.20724293864769550 ) ) ;
#40810 = CARTESIAN_POINT ( 'NONE',  ( 0.05219959533909260263, 19.03943276465977164, 99.99890960531436690 ) ) ;
#40812 = CARTESIAN_POINT ( 'NONE',  ( -19.03943276465977164, 0.05219959533909376836, 86.24890960531436690 ) ) ;
#40813 = CARTESIAN_POINT ( 'NONE',  ( 12.14591786802309770, 12.06949235617756955, 59.37390960531436690 ) ) ;
#40814 = CARTESIAN_POINT ( 'NONE',  ( 32.28837973138387696, -23.54499195901921027, -23.03346093386909743 ) ) ;
#40815 = CARTESIAN_POINT ( 'NONE',  ( 36.91746824999999177, 11.99521256947799230, -7.524999997268813523 ) ) ;
#40816 = CARTESIAN_POINT ( 'NONE',  ( 19.02544592524334988, 5.153800228976608722, 71.45942372801900433 ) ) ;
#40817 = CARTESIAN_POINT ( 'NONE',  ( -15.72974639402197994, 15.80617190586746368, 105.6239096053143669 ) ) ;
#40818 = CARTESIAN_POINT ( 'NONE',  ( -5.153800228976328057, -19.02544592524343514, 62.29057627198100988 ) ) ;
#40819 = CARTESIAN_POINT ( 'NONE',  ( -9.474510206698720793, -16.51473224551083518, 49.58442372801899722 ) ) ;
#40820 = CARTESIAN_POINT ( 'NONE',  ( -16.51473224551069308, -9.474510206698971260, 31.66557627198102054 ) ) ;
#40821 = CARTESIAN_POINT ( 'NONE',  ( 15.72974639402176855, 15.80617190586768217, 61.87609039468568284 ) ) ;
#40822 = PLANE ( 'NONE',  #159466 ) ;
#40823 = CARTESIAN_POINT ( 'NONE',  ( -14.29746914071049879, 8.314922557960819915, 45.83224293864769550 ) ) ;
#40824 = CARTESIAN_POINT ( 'NONE',  ( 19.05341960407611168, 5.049401038298154454, 58.95724293864768129 ) ) ;
#40825 = CARTESIAN_POINT ( 'NONE',  ( -15.72974639402197994, 15.80617190586746368, 70.62390960531436690 ) ) ;
#40826 = CARTESIAN_POINT ( 'NONE',  ( -9.474510206698964154, 16.51473224551069663, 55.41557627198103120 ) ) ;
#40827 = ORIENTED_EDGE ( 'NONE', *, *, #19616, .T. ) ;
#40828 = CARTESIAN_POINT ( 'NONE',  ( -10.72451020669898014, 18.67979575497178502, 65.41557627198102409 ) ) ;
#40829 = CARTESIAN_POINT ( 'NONE',  ( -5.719274019375665041, -21.55341960407619695, 94.79275706135234714 ) ) ;
#40832 = CARTESIAN_POINT ( 'NONE',  ( 0.05219959533910956823, 16.53943276465976808, 84.99890960531436690 ) ) ;
#40831 = CARTESIAN_POINT ( 'NONE',  ( 16.55341960407618274, -4.379528057220086978, 101.0427570613523756 ) ) ;
#40830 = CARTESIAN_POINT ( 'NONE',  ( 18.22780087662121673, 5.500000000000056843, 73.98459894673894155 ) ) ;
#40833 = CARTESIAN_POINT ( 'NONE',  ( -13.97604488694547697, 13.89961937509957934, 88.12609039468563310 ) ) ;
#40834 = VERTEX_POINT ( 'NONE', #19856 ) ;
#40835 = CARTESIAN_POINT ( 'NONE',  ( -13.89961937509957401, -13.97604488694547875, 44.37609039468566863 ) ) ;
#40836 = CARTESIAN_POINT ( 'NONE',  ( 12.06949235617739724, 12.14591786802326823, 106.8760903946856899 ) ) ;
#40837 = CARTESIAN_POINT ( 'NONE',  ( 5.049401038297881783, 19.05341960407617563, 27.29275706135232937 ) ) ;
#40838 = CARTESIAN_POINT ( 'NONE',  ( -19.05341960407611168, -5.049401038298163336, 86.45724293864769550 ) ) ;
#40839 = CARTESIAN_POINT ( 'NONE',  ( -21.53943276465977519, 0.05219959533907696930, 56.24890960531436690 ) ) ;
#40840 = CARTESIAN_POINT ( 'NONE',  ( -18.39635199886965822, 5.500000000000101252, 51.01967076359998998 ) ) ;
#40841 = CARTESIAN_POINT ( 'NONE',  ( 12.06949235617757843, -12.14591786802309237, 113.1239096053143953 ) ) ;
#40842 = CARTESIAN_POINT ( 'NONE',  ( -10.72451020669870658, -18.67979575497194134, 89.58442372801901854 ) ) ;
#40843 = CARTESIAN_POINT ( 'NONE',  ( 16.52544592524335698, 4.483927247898782831, 81.45942372801900433 ) ) ;
#40844 = CARTESIAN_POINT ( 'NONE',  ( -15.72974639402176322, -15.80617190586768395, 24.37609039468567573 ) ) ;
#40845 = CARTESIAN_POINT ( 'NONE',  ( -4.379528057220086978, -16.55341960407618274, 24.79275706135235779 ) ) ;
#40846 = CARTESIAN_POINT ( 'NONE',  ( -19.05341960407611168, -5.049401038298163336, 111.4572429386476671 ) ) ;
#40847 = CARTESIAN_POINT ( 'NONE',  ( 9.564922557960805705, 16.46253265017160317, 44.58224293864769550 ) ) ;
#40848 = CARTESIAN_POINT ( 'NONE',  ( 9.564922557960805705, 16.46253265017160317, 49.58224293864770260 ) ) ;
#40849 = VECTOR ( 'NONE', #101339, 1000.000000000000114 ) ;
#40850 = CARTESIAN_POINT ( 'NONE',  ( -14.34966873604972548, 8.224510206698743886, 33.33442372801900433 ) ) ;
#40851 = CARTESIAN_POINT ( 'NONE',  ( 16.53943276465976808, -0.05219959533910856209, 93.74890960531436690 ) ) ;
#40852 = CARTESIAN_POINT ( 'NONE',  ( -16.55341960407617563, 4.379528057220093196, 98.54275706135234714 ) ) ;
#40855 = CARTESIAN_POINT ( 'NONE',  ( -19.02544592524342804, 5.153800228976336051, 66.04057627198103830 ) ) ;
#40854 = CARTESIAN_POINT ( 'NONE',  ( 5.153800228976335163, 19.02544592524342804, 79.79057627198102409 ) ) ;
#40853 = CARTESIAN_POINT ( 'NONE',  ( 5.719274019375673035, 21.55341960407619339, 37.29275706135235424 ) ) ;
#40856 = CARTESIAN_POINT ( 'NONE',  ( -19.03943276465977164, 0.05219959533909376836, 86.24890960531436690 ) ) ;
#40857 = CARTESIAN_POINT ( 'NONE',  ( -0.05219959533910754901, -16.53943276465976808, 27.49890960531435269 ) ) ;
#40858 = CARTESIAN_POINT ( 'NONE',  ( 14.29746914071037800, 8.314922557961029526, 101.6677570613523613 ) ) ;
#40859 = ORIENTED_EDGE ( 'NONE', *, *, #46300, .T. ) ;
#40860 = CARTESIAN_POINT ( 'NONE',  ( -16.51473224551082808, 9.474510206698731452, 48.33442372801900433 ) ) ;
#40861 = CARTESIAN_POINT ( 'NONE',  ( 19.02544592524343514, -5.153800228976328945, 113.5405762719810241 ) ) ;
#40862 = CARTESIAN_POINT ( 'NONE',  ( 0.05219959533909260263, 19.03943276465977164, 44.99890960531435979 ) ) ;
#40863 = CARTESIAN_POINT ( 'NONE',  ( -13.89961937509957401, -13.97604488694547875, 34.37609039468566863 ) ) ;
#40864 = CARTESIAN_POINT ( 'NONE',  ( 29.86685920354754487, 21.69954338932564752, -5.424999997268813878 ) ) ;
#40865 = CARTESIAN_POINT ( 'NONE',  ( -0.05219959533934338120, 16.53943276465976808, 47.50109039468568994 ) ) ;
#40867 = CARTESIAN_POINT ( 'NONE',  ( 4.379528057220092307, 16.55341960407617563, 52.29275706135236135 ) ) ;
#40866 = CARTESIAN_POINT ( 'NONE',  ( 9.474510206698729675, 16.51473224551082808, 72.08442372801900433 ) ) ;
#40868 = CARTESIAN_POINT ( 'NONE',  ( 6.703913744606314395, -4.665024204860747759, -64.15759393448441017 ) ) ;
#40869 = CARTESIAN_POINT ( 'NONE',  ( -9.564922557960796823, -16.46253265017161027, 92.08224293864769550 ) ) ;
#40870 = CARTESIAN_POINT ( 'NONE',  ( -10.72451020669898014, 18.67979575497178502, 115.4155762719810241 ) ) ;
#40871 = CARTESIAN_POINT ( 'NONE',  ( -13.89961937509957401, -13.97604488694547875, 79.37609039468567573 ) ) ;
#40873 = CARTESIAN_POINT ( 'NONE',  ( 9.474510206698971260, -16.51473224551069308, 32.91557627198102409 ) ) ;
#40872 = CARTESIAN_POINT ( 'NONE',  ( 13.89961937509977652, -13.97604488694527269, 108.1239096053143669 ) ) ;
#40874 = ADVANCED_FACE ( 'NONE', ( #113837 ), #115860, .F. ) ;
#40875 = CARTESIAN_POINT ( 'NONE',  ( -19.03943276465977164, 0.05219959533909376836, 76.24890960531435269 ) ) ;
#40877 = CARTESIAN_POINT ( 'NONE',  ( -19.02544592524342804, 5.153800228976336051, 31.04057627198102409 ) ) ;
#40876 = CARTESIAN_POINT ( 'NONE',  ( 0.05219959533910956823, 16.53943276465976808, 29.99890960531435979 ) ) ;
#40878 = CARTESIAN_POINT ( 'NONE',  ( -0.05219959533936034679, 19.03943276465977164, 52.50109039468566863 ) ) ;
#40879 = CARTESIAN_POINT ( 'NONE',  ( 16.55341960407611168, 4.379528057220329451, 83.95724293864770971 ) ) ;
#40880 = CARTESIAN_POINT ( 'NONE',  ( -15.80617190586768217, 15.72974639402176855, 108.1260903946856757 ) ) ;
#40881 = CARTESIAN_POINT ( 'NONE',  ( 9.564922557960805705, 16.46253265017160317, 49.58224293864770260 ) ) ;
#40882 = CARTESIAN_POINT ( 'NONE',  ( -5.719274019375978568, 21.55341960407610458, 50.20724293864769550 ) ) ;
#40884 = CARTESIAN_POINT ( 'NONE',  ( 10.81492255796106328, -18.62759615963255655, 105.4177570613523613 ) ) ;
#40883 = CARTESIAN_POINT ( 'NONE',  ( -16.55341960407611168, -4.379528057220339221, 56.45724293864768839 ) ) ;
#40885 = CARTESIAN_POINT ( 'NONE',  ( -9.474510206698964154, 16.51473224551069663, 95.41557627198102409 ) ) ;
#40886 = CARTESIAN_POINT ( 'NONE',  ( 9.474510206698971260, -16.51473224551069308, 112.9155762719810383 ) ) ;
#40887 = CARTESIAN_POINT ( 'NONE',  ( 16.51473224551069308, 9.474510206698969483, 44.16557627198103120 ) ) ;
#40888 = CARTESIAN_POINT ( 'NONE',  ( -16.51473224551069308, -9.474510206698971260, 26.66557627198103120 ) ) ;
#40889 = CARTESIAN_POINT ( 'NONE',  ( 4.379528057220339221, -16.55341960407611168, 92.70724293864770971 ) ) ;
#40890 = CARTESIAN_POINT ( 'NONE',  ( -15.72974639402197994, 15.80617190586746368, 90.62390960531436690 ) ) ;
#40891 = CARTESIAN_POINT ( 'NONE',  ( 13.97604488694527802, 13.89961937509977652, 99.37390960531436690 ) ) ;
#40892 = CARTESIAN_POINT ( 'NONE',  ( 15.80617190586769283, -15.72974639402175789, 20.62609039468568639 ) ) ;
#40893 = CARTESIAN_POINT ( 'NONE',  ( -0.05219959533909027116, -19.03943276465977164, 92.49890960531436690 ) ) ;
#40895 = CARTESIAN_POINT ( 'NONE',  ( -14.34966873604960291, -8.224510206698953496, 96.66557627198102409 ) ) ;
#40894 = PLANE ( 'NONE',  #36843 ) ;
#40897 = CARTESIAN_POINT ( 'NONE',  ( -16.51473224551069308, -9.474510206698971260, 76.66557627198103830 ) ) ;
#40896 = VECTOR ( 'NONE', #77106, 1000.000000000000000 ) ;
#40898 = CARTESIAN_POINT ( 'NONE',  ( 21.53943276465977519, -0.05219959533907433946, 78.74890960531436690 ) ) ;
#40899 = LINE ( 'NONE', #124433, #172509 ) ;
#40900 = FACE_OUTER_BOUND ( 'NONE', #52986, .T. ) ;
#40902 = CARTESIAN_POINT ( 'NONE',  ( 18.56197773271731677, -5.499999999999892530, 66.05066217314451649 ) ) ;
#40901 = CARTESIAN_POINT ( 'NONE',  ( -5.823673210054116645, -21.52544592524344225, 32.29057627198102409 ) ) ;
#40903 = CARTESIAN_POINT ( 'NONE',  ( 14.29746914071037800, 8.314922557961029526, 31.66775706135234358 ) ) ;
#40904 = CARTESIAN_POINT ( 'NONE',  ( -12.06949235617756955, 12.14591786802309770, 100.6239096053143811 ) ) ;
#40905 = DIRECTION ( 'NONE',  ( 0.000000000000000000, -0.000000000000000000, -1.000000000000000000 ) ) ;
#40906 = CARTESIAN_POINT ( 'NONE',  ( -9.474510206698964154, 16.51473224551069663, 90.41557627198103830 ) ) ;
#40907 = CARTESIAN_POINT ( 'NONE',  ( -5.049401038298153566, 19.05341960407611168, 50.20724293864770260 ) ) ;
#40908 = CARTESIAN_POINT ( 'NONE',  ( 8.314922557960818139, 14.29746914071049879, 74.58224293864768129 ) ) ;
#40909 = CARTESIAN_POINT ( 'NONE',  ( 18.67979575497178502, 10.72451020669898547, 29.16557627198103120 ) ) ;
#40910 = CARTESIAN_POINT ( 'NONE',  ( 0.05219959533910956823, 16.53943276465976808, 49.99890960531437401 ) ) ;
#40911 = CARTESIAN_POINT ( 'NONE',  ( -19.05341960407617563, 5.049401038297882671, 103.5427570613523329 ) ) ;
#40912 = CARTESIAN_POINT ( 'NONE',  ( -21.55341960407619339, 5.719274019375674811, 68.54275706135234714 ) ) ;
#40913 = CARTESIAN_POINT ( 'NONE',  ( -27.73933785331498925, 9.013057229001088189, 144.7750000027311614 ) ) ;
#40914 = CARTESIAN_POINT ( 'NONE',  ( -5.823673210054116645, -21.52544592524344225, 22.29057627198102765 ) ) ;
#40915 = CARTESIAN_POINT ( 'NONE',  ( -16.53943276465976808, -0.05219959533934237506, 83.75109039468568994 ) ) ;
#40916 = CARTESIAN_POINT ( 'NONE',  ( 9.474510206698971260, -16.51473224551069308, 22.91557627198102765 ) ) ;
#40917 = CARTESIAN_POINT ( 'NONE',  ( 0.05219959533909260263, 19.03943276465977164, 74.99890960531435269 ) ) ;
#40918 = CARTESIAN_POINT ( 'NONE',  ( 15.72974639402199770, -15.80617190586745480, 78.12390960531436690 ) ) ;
#40919 = CARTESIAN_POINT ( 'NONE',  ( 14.29746914071037800, 8.314922557961029526, 31.66775706135234358 ) ) ;
#40921 = CARTESIAN_POINT ( 'NONE',  ( 15.80617190586769283, -15.72974639402175789, 75.62609039468567573 ) ) ;
#40920 = CARTESIAN_POINT ( 'NONE',  ( 4.379528057220339221, -16.55341960407611168, 47.70724293864770260 ) ) ;
#40923 = CARTESIAN_POINT ( 'NONE',  ( -0.05219959533907301413, -21.53943276465977519, 27.49890960531435269 ) ) ;
#40922 = CARTESIAN_POINT ( 'NONE',  ( 16.52544592524335698, 4.483927247898782831, 86.45942372801901854 ) ) ;
#40924 = CARTESIAN_POINT ( 'NONE',  ( 19.03943276465977164, -0.05219959533909143690, 113.7489096053143669 ) ) ;
#40925 = CARTESIAN_POINT ( 'NONE',  ( -16.18388926212238133, 7.379444403734528812, 79.56046848633847901 ) ) ;
#40926 = CARTESIAN_POINT ( 'NONE',  ( 12.06949235617739724, 12.14591786802326823, 106.8760903946856899 ) ) ;
#40927 = CARTESIAN_POINT ( 'NONE',  ( 8.224510206698742110, 14.34966873604972548, 57.08442372801901854 ) ) ;
#40929 = ORIENTED_EDGE ( 'NONE', *, *, #78228, .T. ) ;
#40928 = CARTESIAN_POINT ( 'NONE',  ( -9.564922557960796823, -16.46253265017161027, 72.08224293864770971 ) ) ;
#40930 = CARTESIAN_POINT ( 'NONE',  ( -0.05219959533909027116, -19.03943276465977164, 92.49890960531436690 ) ) ;
#40931 = CARTESIAN_POINT ( 'NONE',  ( -0.05219959533937732626, 21.53943276465977519, 77.50109039468567573 ) ) ;
#40932 = CARTESIAN_POINT ( 'NONE',  ( 8.314922557961029526, -14.29746914071037800, 75.41775706135233293 ) ) ;
#40933 = CARTESIAN_POINT ( 'NONE',  ( 8.224510206698953496, -14.34966873604960469, 52.91557627198103830 ) ) ;
#40934 = CARTESIAN_POINT ( 'NONE',  ( 13.97604488694527802, 13.89961937509977652, 49.37390960531434558 ) ) ;
#40935 = CARTESIAN_POINT ( 'NONE',  ( 13.89961937509977652, -13.97604488694527269, 43.12390960531434558 ) ) ;
#40936 = ORIENTED_EDGE ( 'NONE', *, *, #99054, .F. ) ;
#40937 = CARTESIAN_POINT ( 'NONE',  ( 13.89961937509957401, 13.97604488694547697, 96.87609039468566152 ) ) ;
#40938 = CARTESIAN_POINT ( 'NONE',  ( -16.55341960407611168, -4.379528057220339221, 111.4572429386476813 ) ) ;
#40939 = CARTESIAN_POINT ( 'NONE',  ( -13.97604488694527625, -13.89961937509977652, 61.87390960531435979 ) ) ;
#40941 = CARTESIAN_POINT ( 'NONE',  ( 11.74264578624800315, -36.14014761921581709, -5.400000000000000355 ) ) ;
#40940 = CARTESIAN_POINT ( 'NONE',  ( -16.51473224551082808, 9.474510206698731452, 103.3344237280190043 ) ) ;
#40942 = CARTESIAN_POINT ( 'NONE',  ( -10.81492255796105439, 18.62759615963255655, 107.9177570613523471 ) ) ;
#40943 = CARTESIAN_POINT ( 'NONE',  ( -4.483927247898782831, 16.52544592524335698, 62.70942372801902565 ) ) ;
#40944 = CARTESIAN_POINT ( 'NONE',  ( -19.05341960407617563, 5.049401038297882671, 88.54275706135230450 ) ) ;
#40945 = CARTESIAN_POINT ( 'NONE',  ( -21.55341960407610458, -5.719274019375992779, 56.45724293864768839 ) ) ;
#40946 = CARTESIAN_POINT ( 'NONE',  ( -4.379528057220086978, -16.55341960407618274, 49.79275706135234714 ) ) ;
#40947 = DIRECTION ( 'NONE',  ( 0.000000000000000000, 0.000000000000000000, -1.000000000000000000 ) ) ;
#40948 = CARTESIAN_POINT ( 'NONE',  ( 9.564922557961047289, -16.46253265017146816, 60.41775706135233293 ) ) ;
#40949 = CARTESIAN_POINT ( 'NONE',  ( 18.62759615963255655, 10.81492255796105972, 101.6677570613523613 ) ) ;
#40950 = CARTESIAN_POINT ( 'NONE',  ( -12.14591786802309592, -12.06949235617757132, 111.8739096053143669 ) ) ;
#40951 = CARTESIAN_POINT ( 'NONE',  ( -5.049401038298153566, 19.05341960407611168, 65.20724293864765286 ) ) ;
#40952 = CARTESIAN_POINT ( 'NONE',  ( 4.483927247898545687, 16.52544592524342804, 54.79057627198104541 ) ) ;
#40953 = CARTESIAN_POINT ( 'NONE',  ( 15.72974639402176855, 15.80617190586768217, 86.87609039468568994 ) ) ;
#40954 = ADVANCED_FACE ( 'NONE', ( #66355 ), #101680, .F. ) ;
#40955 = CARTESIAN_POINT ( 'NONE',  ( 0.05219959533936267826, -19.03943276465977164, 45.00109039468566863 ) ) ;
#40956 = CARTESIAN_POINT ( 'NONE',  ( -16.46253265017146816, -9.564922557961047289, 24.16775706135233648 ) ) ;
#40957 = CARTESIAN_POINT ( 'NONE',  ( 21.53943276465977519, -0.05219959533907433946, 23.74890960531435269 ) ) ;
#40958 = CARTESIAN_POINT ( 'NONE',  ( 5.719274019375673035, 21.55341960407619339, 97.29275706135234714 ) ) ;
#40959 = CARTESIAN_POINT ( 'NONE',  ( -0.05219959533909027116, -19.03943276465977164, 72.49890960531435269 ) ) ;
#40960 = CARTESIAN_POINT ( 'NONE',  ( -21.52544592524334988, -5.823673210054445271, 88.95942372801901854 ) ) ;
#40961 = CARTESIAN_POINT ( 'NONE',  ( -10.81492255796078084, -18.62759615963271287, 52.08224293864768839 ) ) ;
#40962 = CARTESIAN_POINT ( 'NONE',  ( -16.46253265017160317, 9.564922557960807481, 85.83224293864769550 ) ) ;
#40963 = CARTESIAN_POINT ( 'NONE',  ( -9.474510206698720793, -16.51473224551083518, 59.58442372801900433 ) ) ;
#40964 = CARTESIAN_POINT ( 'NONE',  ( -13.97604488694527625, -13.89961937509977652, 46.87390960531435979 ) ) ;
#40965 = CARTESIAN_POINT ( 'NONE',  ( -19.02544592524342804, 5.153800228976336051, 96.04057627198103830 ) ) ;
#40966 = CARTESIAN_POINT ( 'NONE',  ( -16.51473224551082808, 9.474510206698731452, 88.33442372801900433 ) ) ;
#40967 = EDGE_CURVE ( 'NONE', #19836, #70507, #117665, .T. ) ;
#40968 = CARTESIAN_POINT ( 'NONE',  ( 12.06949235617739724, 12.14591786802326823, 46.87609039468568994 ) ) ;
#40969 = CARTESIAN_POINT ( 'NONE',  ( -12.14591786802309592, -12.06949235617757132, 101.8739096053143811 ) ) ;
#40970 = CARTESIAN_POINT ( 'NONE',  ( 5.153800228976335163, 19.02544592524342804, 69.79057627198103830 ) ) ;
#40971 = EDGE_CURVE ( 'NONE', #49688, #200018, #175533, .T. ) ;
#40972 = CARTESIAN_POINT ( 'NONE',  ( -15.72974639402197994, 15.80617190586746368, 50.62390960531435979 ) ) ;
#40973 = B_SPLINE_CURVE_WITH_KNOTS ( 'NONE', 3,
 ( #125798, #62128, #107635, #18631, #122810, #48966, #172302, #61138, #169312, #3439, #65115, #126773, #188478, #15647, #46980, #453, #111622, #77306, #138975, #123792, #142939, #81258 ),
 .UNSPECIFIED., .F., .F.,
 ( 4, 2, 2, 2, 2, 2, 2, 2, 2, 2, 4 ),
 ( 2.194270917860438266E-17, 0.001309639967555297629, 0.001964459951332936036, 0.002291869943221755239, 0.002455574939166158335, 0.002619279935110561432, 0.002782984931054964528, 0.002946689926999367624, 0.003274099918888187261, 0.003928919902665813958, 0.005238559870221069087 ),
 .UNSPECIFIED. ) ;
#40974 = CARTESIAN_POINT ( 'NONE',  ( 12.14591786802327356, -12.06949235617739191, 20.62609039468568639 ) ) ;
#40975 = CARTESIAN_POINT ( 'NONE',  ( -15.72974639402176322, -15.80617190586768395, 19.37609039468568639 ) ) ;
#40976 = CARTESIAN_POINT ( 'NONE',  ( -5.823673210054431948, 21.52544592524334988, 82.70942372801900433 ) ) ;
#40977 = CARTESIAN_POINT ( 'NONE',  ( 8.224510206698742110, 14.34966873604972548, 82.08442372801901854 ) ) ;
#40978 = CARTESIAN_POINT ( 'NONE',  ( 5.049401038298161559, -19.05341960407611168, 77.70724293864765286 ) ) ;
#40979 = CARTESIAN_POINT ( 'NONE',  ( 14.34966873604972726, -8.224510206698740333, 95.83442372801903275 ) ) ;
#40980 = CARTESIAN_POINT ( 'NONE',  ( 16.51473224551083163, -9.474510206698727899, 60.83442372801900433 ) ) ;
#40981 = CARTESIAN_POINT ( 'NONE',  ( -21.55341960407619339, 5.719274019375674811, 33.54275706135234714 ) ) ;
#40982 = CARTESIAN_POINT ( 'NONE',  ( -8.224510206698948167, 14.34966873604960824, 75.41557627198102409 ) ) ;
#40983 = CARTESIAN_POINT ( 'NONE',  ( 13.89961937509977652, -13.97604488694527269, 93.12390960531436690 ) ) ;
#40984 = CARTESIAN_POINT ( 'NONE',  ( -16.52544592524335698, -4.483927247898792601, 88.95942372801901854 ) ) ;
#40985 = B_SPLINE_CURVE_WITH_KNOTS ( 'NONE', 3,
 ( #54945, #196483, #11462, #118629, #57953, #150964, #116617, #72113, #74119, #180320, #73133, #178306, #147966, #133787, #101433, #134803, #104448, #165133, #39769, #181307, #166131, #151939, #27633, #102450, #120595, #89274, #148964, #41788, #90256, #163124, #9453, #86275 ),
 .UNSPECIFIED., .F., .F.,
 ( 4, 2, 2, 2, 2, 2, 2, 2, 2, 2, 2, 2, 2, 2, 2, 4 ),
 ( 2.969368287472575283E-17, 0.0003712461730037006557, 0.0007424923460073716043, 0.001113738519011042661, 0.001484984692014713501, 0.002227477038022055399, 0.002598723211025726239, 0.002969969384029397079, 0.003341215557033067919, 0.003712461730036738759, 0.004083707903040409599, 0.004454954076044081307, 0.004826200249047752147, 0.005197446422051422987, 0.005568692595055093827, 0.005939938768058764668 ),
 .UNSPECIFIED. ) ;
#40986 = CARTESIAN_POINT ( 'NONE',  ( -10.81492255796105439, 18.62759615963255655, 67.91775706135234714 ) ) ;
#40987 = CARTESIAN_POINT ( 'NONE',  ( 14.34966873604972726, -8.224510206698740333, 30.83442372801902209 ) ) ;
#40988 = CARTESIAN_POINT ( 'NONE',  ( -18.62759615963255300, -10.81492255796106328, 34.16775706135234714 ) ) ;
#40989 = CARTESIAN_POINT ( 'NONE',  ( -14.34966873604960291, -8.224510206698953496, 66.66557627198102409 ) ) ;
#40990 = VERTEX_POINT ( 'NONE', #162356 ) ;
#40991 = CARTESIAN_POINT ( 'NONE',  ( 21.52544592524344225, -5.823673210054117533, 98.54057627198105251 ) ) ;
#40992 = CARTESIAN_POINT ( 'NONE',  ( -8.224510206698948167, 14.34966873604960824, 50.41557627198103120 ) ) ;
#40993 = VERTEX_POINT ( 'NONE', #23857 ) ;
#40994 = CARTESIAN_POINT ( 'NONE',  ( 9.474510206698971260, -16.51473224551069308, 22.91557627198102765 ) ) ;
#40995 = CARTESIAN_POINT ( 'NONE',  ( 21.55341960407610458, 5.719274019375980345, 23.95724293864769550 ) ) ;
#40996 = CARTESIAN_POINT ( 'NONE',  ( -21.52544592524334988, -5.823673210054445271, 43.95942372801902565 ) ) ;
#40997 = CARTESIAN_POINT ( 'NONE',  ( 4.483927247898545687, 16.52544592524342804, 59.79057627198103120 ) ) ;
#40998 = AXIS2_PLACEMENT_3D ( 'NONE', #133958, #54112, #118796 ) ;
#40999 = CARTESIAN_POINT ( 'NONE',  ( 21.52544592524344225, -5.823673210054117533, 68.54057627198103830 ) ) ;
#41000 = CARTESIAN_POINT ( 'NONE',  ( 13.97604488694527802, 13.89961937509977652, 69.37390960531436690 ) ) ;
#41002 = CARTESIAN_POINT ( 'NONE',  ( 19.03943276465977164, 0.05219959533936151252, 81.25109039468567573 ) ) ;
#41001 = CARTESIAN_POINT ( 'NONE',  ( -19.05341960407611168, -5.049401038298163336, 21.45724293864768839 ) ) ;
#41003 = CARTESIAN_POINT ( 'NONE',  ( -21.52544592524343514, 5.823673210054127303, 61.04057627198103120 ) ) ;
#41004 = CARTESIAN_POINT ( 'NONE',  ( -13.89961937509977652, 13.97604488694528158, 40.62390960531435979 ) ) ;
#41005 = CARTESIAN_POINT ( 'NONE',  ( -16.51473224551069308, -9.474510206698971260, 71.66557627198102409 ) ) ;
#41006 = ORIENTED_EDGE ( 'NONE', *, *, #10071, .F. ) ;
#41007 = CARTESIAN_POINT ( 'NONE',  ( -16.55341960407617563, 4.379528057220093196, 48.54275706135234714 ) ) ;
#41008 = CARTESIAN_POINT ( 'NONE',  ( 15.72974639402176855, 15.80617190586768217, 26.87609039468567218 ) ) ;
#41009 = CARTESIAN_POINT ( 'NONE',  ( 15.80617190586769283, -15.72974639402175789, 55.62609039468568284 ) ) ;
#41010 = CARTESIAN_POINT ( 'NONE',  ( -0.05219959533909027116, -19.03943276465977164, 107.4989096053143527 ) ) ;
#41011 = CARTESIAN_POINT ( 'NONE',  ( -21.52544592524343514, 5.823673210054127303, 86.04057627198102409 ) ) ;
#41013 = CARTESIAN_POINT ( 'NONE',  ( 14.34966873604972726, -8.224510206698740333, 55.83442372801901854 ) ) ;
#41012 = CARTESIAN_POINT ( 'NONE',  ( 21.53943276465977519, 0.05219959533937863772, 21.25109039468567218 ) ) ;
#41014 = AXIS2_PLACEMENT_3D ( 'NONE', #35019, #172548, #64369 ) ;
#41015 = CARTESIAN_POINT ( 'NONE',  ( -18.67979575497178146, -10.72451020669898902, 46.66557627198102409 ) ) ;
#41016 = CARTESIAN_POINT ( 'NONE',  ( -19.02544592524334988, -5.153800228976617603, 23.95942372801900078 ) ) ;
#41017 = CARTESIAN_POINT ( 'NONE',  ( -9.474510206698964154, 16.51473224551069663, 55.41557627198103120 ) ) ;
#41018 = CARTESIAN_POINT ( 'NONE',  ( 19.03943276465977164, -0.05219959533909143690, 113.7489096053143669 ) ) ;
#41019 = CARTESIAN_POINT ( 'NONE',  ( -19.02544592524342804, 5.153800228976336051, 91.04057627198100988 ) ) ;
#41020 = CARTESIAN_POINT ( 'NONE',  ( 17.49999999999999645, -5.624438216177558125, 88.31670344914645909 ) ) ;
#41021 = CARTESIAN_POINT ( 'NONE',  ( 16.51473224551083163, -9.474510206698727899, 65.83442372801900433 ) ) ;
#41022 = CARTESIAN_POINT ( 'NONE',  ( 21.53943276465977519, -0.05219959533907433946, 48.74890960531435979 ) ) ;
#41023 = CARTESIAN_POINT ( 'NONE',  ( 16.52544592524335698, 4.483927247898782831, 101.4594237280190185 ) ) ;
#41024 = CARTESIAN_POINT ( 'NONE',  ( 5.153800228976615827, -19.02544592524334988, 80.20942372801901854 ) ) ;
#41025 = DIRECTION ( 'NONE',  ( 0.000000000000000000, 1.000000000000000000, 0.000000000000000000 ) ) ;
#41026 = CARTESIAN_POINT ( 'NONE',  ( 9.474510206698729675, 16.51473224551082808, 22.08442372801899722 ) ) ;
#41027 = CARTESIAN_POINT ( 'NONE',  ( -13.89961937509957401, -13.97604488694547875, 79.37609039468567573 ) ) ;
#41028 = CARTESIAN_POINT ( 'NONE',  ( -19.02544592524334988, -5.153800228976617603, 43.95942372801899012 ) ) ;
#41029 = CARTESIAN_POINT ( 'NONE',  ( 17.60691670004650788, 5.500000000000063949, 71.63333313366440791 ) ) ;
#41030 = CARTESIAN_POINT ( 'NONE',  ( -16.46253265017160317, 9.564922557960807481, 50.83224293864770260 ) ) ;
#41031 = CARTESIAN_POINT ( 'NONE',  ( -16.52544592524342804, 4.483927247898546575, 51.04057627198103120 ) ) ;
#41032 = CARTESIAN_POINT ( 'NONE',  ( -9.474510206698964154, 16.51473224551069663, 35.41557627198102409 ) ) ;
#41033 = CARTESIAN_POINT ( 'NONE',  ( -16.53943276465976808, 0.05219959533911058130, 41.24890960531435269 ) ) ;
#41034 = DIRECTION ( 'NONE',  ( 0.8164965809277242581, 0.000000000000000000, -0.5773502691896281735 ) ) ;
#41035 = CARTESIAN_POINT ( 'NONE',  ( -16.55341960407617563, 4.379528057220093196, 108.5427570613523756 ) ) ;
#41036 = CARTESIAN_POINT ( 'NONE',  ( 5.049401038298161559, -19.05341960407611168, 52.70724293864767418 ) ) ;
#41037 = CARTESIAN_POINT ( 'NONE',  ( 13.97604488694548053, -13.89961937509957401, 25.62609039468566507 ) ) ;
#41038 = CARTESIAN_POINT ( 'NONE',  ( -16.52544592524335698, -4.483927247898792601, 38.95942372801901854 ) ) ;
#41039 = CARTESIAN_POINT ( 'NONE',  ( 21.53943276465977519, -0.05219959533907433946, 43.74890960531435979 ) ) ;
#41041 = ORIENTED_EDGE ( 'NONE', *, *, #80739, .T. ) ;
#41040 = CARTESIAN_POINT ( 'NONE',  ( -18.62759615963255300, -10.81492255796106328, 89.16775706135236135 ) ) ;
#41042 = CARTESIAN_POINT ( 'NONE',  ( 16.51473224551069308, 9.474510206698969483, 59.16557627198102409 ) ) ;
#41043 = CARTESIAN_POINT ( 'NONE',  ( -5.153800228976328057, -19.02544592524343514, 107.2905762719810383 ) ) ;
#41044 = CARTESIAN_POINT ( 'NONE',  ( -0.05219959533909027116, -19.03943276465977164, 97.49890960531436690 ) ) ;
#41045 = CARTESIAN_POINT ( 'NONE',  ( -33.56243482129945477, -21.76536163099331489, -24.28098042443967586 ) ) ;
#41046 = CARTESIAN_POINT ( 'NONE',  ( -5.719274019375665041, -21.55341960407619695, 24.79275706135235779 ) ) ;
#41047 = AXIS2_PLACEMENT_3D ( 'NONE', #57516, #16715, #119184 ) ;
#41048 = CARTESIAN_POINT ( 'NONE',  ( -8.314922557960811034, -14.29746914071050412, 82.08224293864768129 ) ) ;
#41050 = CARTESIAN_POINT ( 'NONE',  ( 13.89961937509977652, -13.97604488694527269, 68.12390960531436690 ) ) ;
#41049 = CARTESIAN_POINT ( 'NONE',  ( -15.80617190586745835, -15.72974639402198527, 76.87390960531439532 ) ) ;
#41051 = CARTESIAN_POINT ( 'NONE',  ( -0.05219959533909027116, -19.03943276465977164, 77.49890960531435269 ) ) ;
#41052 = CARTESIAN_POINT ( 'NONE',  ( 18.62759615963271287, -10.81492255796078972, 113.3322429386476955 ) ) ;
#41053 = VERTEX_POINT ( 'NONE', #193713 ) ;
#41054 = CARTESIAN_POINT ( 'NONE',  ( -5.049401038298153566, 19.05341960407611168, 80.20724293864769550 ) ) ;
#41055 = ADVANCED_FACE ( 'NONE', ( #85507 ), #147196, .T. ) ;
#41057 = CARTESIAN_POINT ( 'NONE',  ( 27.86273085795036408, -28.69962071417356242, -15.00000000000000178 ) ) ;
#41056 = CARTESIAN_POINT ( 'NONE',  ( 4.379528057220339221, -16.55341960407611168, 107.7072429386476955 ) ) ;
#41058 = CARTESIAN_POINT ( 'NONE',  ( 19.05341960407611168, 5.049401038298154454, 68.95724293864769550 ) ) ;
#41059 = CARTESIAN_POINT ( 'NONE',  ( -0.05219959533936034679, 19.03943276465977164, 87.50109039468567573 ) ) ;
#41060 = CARTESIAN_POINT ( 'NONE',  ( -0.05219959533910754901, -16.53943276465976808, 97.49890960531436690 ) ) ;
#41061 = CARTESIAN_POINT ( 'NONE',  ( -18.62759615963255300, -10.81492255796106328, 54.16775706135235424 ) ) ;
#41063 = CARTESIAN_POINT ( 'NONE',  ( 15.80617190586769283, -15.72974639402175789, 25.62609039468567929 ) ) ;
#41062 = CARTESIAN_POINT ( 'NONE',  ( -9.474510206698964154, 16.51473224551069663, 55.41557627198103120 ) ) ;
#41064 = CARTESIAN_POINT ( 'NONE',  ( 4.483927247898545687, 16.52544592524342804, 99.79057627198103830 ) ) ;
#41065 = CARTESIAN_POINT ( 'NONE',  ( -17.81289503416611808, 24.51734667627700404, 143.7000000000000171 ) ) ;
#41066 = CARTESIAN_POINT ( 'NONE',  ( -9.564922557960796823, -16.46253265017161027, 72.08224293864770971 ) ) ;
#41067 = DIRECTION ( 'NONE',  ( -0.000000000000000000, -0.000000000000000000, 1.000000000000000000 ) ) ;
#41069 = CARTESIAN_POINT ( 'NONE',  ( 10.72451020669898902, -18.67979575497178502, 32.91557627198102409 ) ) ;
#41068 = CARTESIAN_POINT ( 'NONE',  ( -16.53943276465976808, -0.05219959533934237506, 18.75109039468568639 ) ) ;
#41070 = CARTESIAN_POINT ( 'NONE',  ( 21.53943276465977519, 0.05219959533937863772, 51.25109039468568994 ) ) ;
#41071 = CARTESIAN_POINT ( 'NONE',  ( 5.049401038298161559, -19.05341960407611168, 92.70724293864769550 ) ) ;
#41072 = CARTESIAN_POINT ( 'NONE',  ( 9.474510206698729675, 16.51473224551082808, 77.08442372801900433 ) ) ;
#41073 = CARTESIAN_POINT ( 'NONE',  ( -5.153800228976328057, -19.02544592524343514, 77.29057627198099567 ) ) ;
#41074 = CARTESIAN_POINT ( 'NONE',  ( -16.55341960407611168, -4.379528057220339221, 76.45724293864769550 ) ) ;
#41075 = CARTESIAN_POINT ( 'NONE',  ( 16.46253265017160672, -9.564922557960803928, 108.3322429386476955 ) ) ;
#41076 = CARTESIAN_POINT ( 'NONE',  ( -0.05219959533910754901, -16.53943276465976808, 77.49890960531433848 ) ) ;
#41077 = CARTESIAN_POINT ( 'NONE',  ( 19.05341960407611168, 5.049401038298154454, 98.95724293864766707 ) ) ;
#41081 = CARTESIAN_POINT ( 'NONE',  ( 13.89961937509977652, -13.97604488694527269, 33.12390960531434558 ) ) ;
#41080 =( BOUNDED_CURVE ( )  B_SPLINE_CURVE ( 2, ( #41374, #133370, #88860, #163724, #13032, #89860, #86868, #105032, #137349, #120192, #44357 ),
 .UNSPECIFIED., .F., .T. ) 
 B_SPLINE_CURVE_WITH_KNOTS ( ( 3, 2, 2, 2, 2, 3 ),
 ( 0.6000000000000005329, 0.6200000000000005507, 0.6400000000000005684, 0.6600000000000005862, 0.6800000000000006040, 0.7000000000000006217 ),
 .UNSPECIFIED. ) 
 CURVE ( )  GEOMETRIC_REPRESENTATION_ITEM ( )  RATIONAL_B_SPLINE_CURVE ( ( 0.9999999999999986677, 0.9510565162951548634, 1.000000000000000000, 0.9510565162951535312, 1.000000000000000000, 0.9510565162951535312, 1.000000000000000000, 0.9510565162951535312, 1.000000000000000000, 0.9510565162951518658, 1.000000000000001554 ) ) 
 REPRESENTATION_ITEM ( '' )  );
#41079 = CARTESIAN_POINT ( 'NONE',  ( 16.55341960407611168, 4.379528057220329451, 48.95724293864770971 ) ) ;
#41078 = CARTESIAN_POINT ( 'NONE',  ( -5.049401038298153566, 19.05341960407611168, 50.20724293864770260 ) ) ;
#41082 = VERTEX_POINT ( 'NONE', #97659 ) ;
#41083 = CARTESIAN_POINT ( 'NONE',  ( -0.05219959533937732626, 21.53943276465977519, 42.50109039468567573 ) ) ;
#41084 = CARTESIAN_POINT ( 'NONE',  ( 5.049401038297881783, 19.05341960407617563, 82.29275706135229029 ) ) ;
#41085 = CARTESIAN_POINT ( 'NONE',  ( -16.52544592524342804, 4.483927247898546575, 51.04057627198103120 ) ) ;
#41086 = CARTESIAN_POINT ( 'NONE',  ( 10.81492255796078972, 18.62759615963270932, 94.58224293864769550 ) ) ;
#41087 = CARTESIAN_POINT ( 'NONE',  ( -18.62759615963270932, 10.81492255796079327, 35.83224293864768839 ) ) ;
#41088 = CARTESIAN_POINT ( 'NONE',  ( 8.224510206698953496, -14.34966873604960469, 87.91557627198103830 ) ) ;
#41089 = CARTESIAN_POINT ( 'NONE',  ( -19.05341960407611168, -5.049401038298163336, 41.45724293864769550 ) ) ;
#41090 = CARTESIAN_POINT ( 'NONE',  ( 8.314922557960818139, 14.29746914071049879, 29.58224293864769905 ) ) ;
#41091 = CARTESIAN_POINT ( 'NONE',  ( -12.14591786802326823, 12.06949235617739902, 88.12609039468570415 ) ) ;
#41092 = CARTESIAN_POINT ( 'NONE',  ( -8.224510206698735004, -14.34966873604973081, 74.58442372801901854 ) ) ;
#41093 = CARTESIAN_POINT ( 'NONE',  ( 16.51473224551083163, -9.474510206698727899, 20.83442372801899722 ) ) ;
#41094 = CARTESIAN_POINT ( 'NONE',  ( -19.03943276465977164, 0.05219959533909376836, 86.24890960531436690 ) ) ;
#41095 = CARTESIAN_POINT ( 'NONE',  ( -13.97604488694527625, -13.89961937509977652, 81.87390960531436690 ) ) ;
#41096 = CARTESIAN_POINT ( 'NONE',  ( 16.53943276465976808, 0.05219959533934440121, 91.25109039468568994 ) ) ;
#41097 = CARTESIAN_POINT ( 'NONE',  ( 19.02544592524343514, -5.153800228976328945, 43.54057627198103120 ) ) ;
#41098 = CARTESIAN_POINT ( 'NONE',  ( 12.06949235617757843, -12.14591786802309237, 53.12390960531436690 ) ) ;
#41099 = CARTESIAN_POINT ( 'NONE',  ( 13.97604488694527802, 13.89961937509977652, 99.37390960531436690 ) ) ;
#41100 = CARTESIAN_POINT ( 'NONE',  ( -18.62759615963270932, 10.81492255796079327, 30.83224293864770260 ) ) ;
#41101 = CARTESIAN_POINT ( 'NONE',  ( -0.05219959533910754901, -16.53943276465976808, 77.49890960531433848 ) ) ;
#41102 = ORIENTED_EDGE ( 'NONE', *, *, #162015, .F. ) ;
#41103 = CARTESIAN_POINT ( 'NONE',  ( -14.29746914071049879, 8.314922557960819915, 70.83224293864770971 ) ) ;
#41104 = CARTESIAN_POINT ( 'NONE',  ( 31.81624771892550285, -0.5097844185666569050, -45.77220262091589831 ) ) ;
#41105 = CARTESIAN_POINT ( 'NONE',  ( 9.564922557961047289, -16.46253265017146816, 65.41775706135233293 ) ) ;
#41106 = CARTESIAN_POINT ( 'NONE',  ( 16.46253265017160672, -9.564922557960803928, 103.3322429386476955 ) ) ;
#41107 = CARTESIAN_POINT ( 'NONE',  ( -13.97604488694547697, 13.89961937509957934, 83.12609039468564731 ) ) ;
#41108 = CARTESIAN_POINT ( 'NONE',  ( -5.359611314223446995E-15, 29.16686587814335496, 146.8750000027311273 ) ) ;
#41110 = CARTESIAN_POINT ( 'NONE',  ( -8.314922557961024197, 14.29746914071037800, 97.91775706135236135 ) ) ;
#41109 = CARTESIAN_POINT ( 'NONE',  ( 13.97604488694548053, -13.89961937509957401, 105.6260903946856757 ) ) ;
#41111 = CARTESIAN_POINT ( 'NONE',  ( -9.564922557960796823, -16.46253265017161027, 42.08224293864769550 ) ) ;
#41112 = CARTESIAN_POINT ( 'NONE',  ( 21.55341960407610458, 5.719274019375980345, 28.95724293864769905 ) ) ;
#41113 = CARTESIAN_POINT ( 'NONE',  ( -15.72974639402176322, -15.80617190586768395, 54.37609039468568994 ) ) ;
#41114 = CARTESIAN_POINT ( 'NONE',  ( -16.53943276465976808, -0.05219959533934237506, 23.75109039468567929 ) ) ;
#41116 = CARTESIAN_POINT ( 'NONE',  ( 13.89961937509977652, -13.97604488694527269, 73.12390960531436690 ) ) ;
#41115 = PLANE ( 'NONE',  #12145 ) ;
#41117 = EDGE_CURVE ( 'NONE', #142306, #50018, #159348, .T. ) ;
#41118 = CARTESIAN_POINT ( 'NONE',  ( 19.02544592524343514, -5.153800228976328945, 113.5405762719810241 ) ) ;
#41120 = CARTESIAN_POINT ( 'NONE',  ( -16.46253265017160317, 9.564922557960807481, 80.83224293864769550 ) ) ;
#41119 = CARTESIAN_POINT ( 'NONE',  ( -16.53943276465976808, 0.05219959533911058130, 71.24890960531435269 ) ) ;
#41121 = CARTESIAN_POINT ( 'NONE',  ( 9.564922557960805705, 16.46253265017160317, 84.58224293864769550 ) ) ;
#41122 = EDGE_LOOP ( 'NONE', ( #75709, #168171, #165391, #55162 ) ) ;
#41123 = CARTESIAN_POINT ( 'NONE',  ( 16.46253265017146816, 9.564922557961045513, 86.66775706135233293 ) ) ;
#41124 = CARTESIAN_POINT ( 'NONE',  ( 18.67979575497178502, 10.72451020669898547, 59.16557627198103120 ) ) ;
#41125 = CARTESIAN_POINT ( 'NONE',  ( 16.46253265017160672, -9.564922557960803928, 33.33224293864770260 ) ) ;
#41126 = CARTESIAN_POINT ( 'NONE',  ( -13.89961937509957401, -13.97604488694547875, 54.37609039468565442 ) ) ;
#41127 = CARTESIAN_POINT ( 'NONE',  ( -9.564922557960796823, -16.46253265017161027, 62.08224293864769550 ) ) ;
#41128 = CARTESIAN_POINT ( 'NONE',  ( -19.05341960407611168, -5.049401038298163336, 91.45724293864766707 ) ) ;
#41129 = ORIENTED_EDGE ( 'NONE', *, *, #93805, .F. ) ;
#41130 = CARTESIAN_POINT ( 'NONE',  ( -10.72451020669898014, 18.67979575497178502, 90.41557627198103830 ) ) ;
#41132 = CARTESIAN_POINT ( 'NONE',  ( 5.049401038297881783, 19.05341960407617563, 47.29275706135231161 ) ) ;
#41131 = CARTESIAN_POINT ( 'NONE',  ( 16.52544592524342804, -4.483927247898539470, 93.54057627198103830 ) ) ;
#41133 = CARTESIAN_POINT ( 'NONE',  ( -15.72974639402197994, 15.80617190586746368, 90.62390960531436690 ) ) ;
#41134 = CARTESIAN_POINT ( 'NONE',  ( -0.05219959533907301413, -21.53943276465977519, 77.49890960531433848 ) ) ;
#41135 = CARTESIAN_POINT ( 'NONE',  ( 8.224510206698953496, -14.34966873604960469, 32.91557627198102409 ) ) ;
#41136 = CARTESIAN_POINT ( 'NONE',  ( -5.823673210054431948, 21.52544592524334988, 107.7094237280190328 ) ) ;
#41137 = CARTESIAN_POINT ( 'NONE',  ( -0.05219959533934338120, 16.53943276465976808, 47.50109039468568994 ) ) ;
#41138 = CARTESIAN_POINT ( 'NONE',  ( 16.51473224551069308, 9.474510206698969483, 84.16557627198102409 ) ) ;
#41139 = CARTESIAN_POINT ( 'NONE',  ( 9.474510206698971260, -16.51473224551069308, 32.91557627198102409 ) ) ;
#41140 = VECTOR ( 'NONE', #193532, 1000.000000000000000 ) ;
#41141 = CARTESIAN_POINT ( 'NONE',  ( 0.05219959533937995610, -21.53943276465977519, 40.00109039468567573 ) ) ;
#41142 = CARTESIAN_POINT ( 'NONE',  ( -5.823673210054431948, 21.52544592524334988, 52.70942372801902565 ) ) ;
#41143 = CARTESIAN_POINT ( 'NONE',  ( 19.05341960407611168, 5.049401038298154454, 53.95724293864770260 ) ) ;
#41144 = CARTESIAN_POINT ( 'NONE',  ( 10.81492255796078972, 18.62759615963270932, 114.5822429386477097 ) ) ;
#41145 = CARTESIAN_POINT ( 'NONE',  ( -9.564922557961040184, 16.46253265017147172, 62.91775706135233293 ) ) ;
#41146 = EDGE_CURVE ( 'NONE', #68158, #133003, #194626, .T. ) ;
#41147 = CARTESIAN_POINT ( 'NONE',  ( -13.89961937509977652, 13.97604488694528158, 35.62390960531435269 ) ) ;
#41148 = CARTESIAN_POINT ( 'NONE',  ( 12.14591786802327356, -12.06949235617739191, 25.62609039468567929 ) ) ;
#41149 = CARTESIAN_POINT ( 'NONE',  ( -19.03943276465977164, 0.05219959533909376836, 31.24890960531435979 ) ) ;
#41150 = CARTESIAN_POINT ( 'NONE',  ( -0.05219959533934338120, 16.53943276465976808, 72.50109039468568994 ) ) ;
#41151 = CARTESIAN_POINT ( 'NONE',  ( -5.153800228976328057, -19.02544592524343514, 37.29057627198102409 ) ) ;
#41152 = CARTESIAN_POINT ( 'NONE',  ( 24.10884208241212434, -5.471882726980744849, 173.8287385965643352 ) ) ;
#41153 = CARTESIAN_POINT ( 'NONE',  ( 0.05219959533909260263, 19.03943276465977164, 89.99890960531436690 ) ) ;
#41154 = CARTESIAN_POINT ( 'NONE',  ( -16.51473224551069308, -9.474510206698971260, 26.66557627198103120 ) ) ;
#41155 = CARTESIAN_POINT ( 'NONE',  ( -10.81492255796078084, -18.62759615963271287, 72.08224293864769550 ) ) ;
#41156 = CARTESIAN_POINT ( 'NONE',  ( 8.224510206698742110, 14.34966873604972548, 57.08442372801901854 ) ) ;
#41157 = CARTESIAN_POINT ( 'NONE',  ( -0.05219959533937732626, 21.53943276465977519, 107.5010903946856899 ) ) ;
#41158 = CARTESIAN_POINT ( 'NONE',  ( -19.02544592524342804, 5.153800228976336051, 36.04057627198100988 ) ) ;
#41159 = CARTESIAN_POINT ( 'NONE',  ( 16.52544592524342804, -4.483927247898539470, 33.54057627198102409 ) ) ;
#41160 = CARTESIAN_POINT ( 'NONE',  ( -12.14591786802309592, -12.06949235617757132, 61.87390960531436690 ) ) ;
#41161 = CARTESIAN_POINT ( 'NONE',  ( -16.51473224551069308, -9.474510206698971260, 66.66557627198102409 ) ) ;
#41162 = CARTESIAN_POINT ( 'NONE',  ( -15.72974639402176322, -15.80617190586768395, 104.3760903946856899 ) ) ;
#41163 = CARTESIAN_POINT ( 'NONE',  ( 21.55341960407619695, -5.719274019375665929, 36.04275706135234714 ) ) ;
#41164 = CARTESIAN_POINT ( 'NONE',  ( 19.02544592524343514, -5.153800228976328945, 73.54057627198103830 ) ) ;
#41165 = CARTESIAN_POINT ( 'NONE',  ( 15.72974639402176855, 15.80617190586768217, 91.87609039468568994 ) ) ;
#41166 = CARTESIAN_POINT ( 'NONE',  ( 4.379528057220092307, 16.55341960407617563, 62.29275706135236845 ) ) ;
#41167 = CARTESIAN_POINT ( 'NONE',  ( 16.46253265017160672, -9.564922557960803928, 108.3322429386476955 ) ) ;
#41168 = CARTESIAN_POINT ( 'NONE',  ( 16.53943276465976808, -0.05219959533910856209, 38.74890960531435979 ) ) ;
#41169 = CARTESIAN_POINT ( 'NONE',  ( -5.153800228976328057, -19.02544592524343514, 22.29057627198102765 ) ) ;
#41170 = CARTESIAN_POINT ( 'NONE',  ( 0.05219959533934541429, -16.53943276465976808, 55.00109039468568284 ) ) ;
#41171 = CARTESIAN_POINT ( 'NONE',  ( -0.05219959533910754901, -16.53943276465976808, 57.49890960531435979 ) ) ;
#41172 = CARTESIAN_POINT ( 'NONE',  ( 19.05341960407611168, 5.049401038298154454, 108.9572429386477097 ) ) ;
#41173 = CARTESIAN_POINT ( 'NONE',  ( 10.81492255796078972, 18.62759615963270932, 29.58224293864769905 ) ) ;
#41174 = CARTESIAN_POINT ( 'NONE',  ( -5.153800228976607833, 19.02544592524334988, 22.70942372801899012 ) ) ;
#41175 = CARTESIAN_POINT ( 'NONE',  ( 14.29746914071049879, -8.314922557960816363, 88.33224293864769550 ) ) ;
#41176 = CARTESIAN_POINT ( 'NONE',  ( 19.02544592524343514, -5.153800228976328945, 93.54057627198102409 ) ) ;
#41177 = ORIENTED_EDGE ( 'NONE', *, *, #95674, .T. ) ;
#41178 = CARTESIAN_POINT ( 'NONE',  ( -16.53943276465976808, -0.05219959533934237506, 53.75109039468568994 ) ) ;
#41179 = CARTESIAN_POINT ( 'NONE',  ( 0.05219959533909260263, 19.03943276465977164, 49.99890960531435979 ) ) ;
#41180 = CARTESIAN_POINT ( 'NONE',  ( 17.60689202196056158, 5.500000000000022204, 101.6333492360910782 ) ) ;
#41181 = CARTESIAN_POINT ( 'NONE',  ( 9.474510206698729675, 16.51473224551082808, 42.08442372801900433 ) ) ;
#41182 = CARTESIAN_POINT ( 'NONE',  ( -9.474510206698964154, 16.51473224551069663, 45.41557627198103120 ) ) ;
#41183 = CARTESIAN_POINT ( 'NONE',  ( 14.29746914071037800, 8.314922557961029526, 81.66775706135236135 ) ) ;
#41184 = CARTESIAN_POINT ( 'NONE',  ( -13.89961937509957401, -13.97604488694547875, 94.37609039468566152 ) ) ;
#41185 = CARTESIAN_POINT ( 'NONE',  ( -21.55341960407619339, 5.719274019375674811, 68.54275706135234714 ) ) ;
#41186 = CARTESIAN_POINT ( 'NONE',  ( -19.05341960407611168, -5.049401038298163336, 66.45724293864769550 ) ) ;
#41187 = CARTESIAN_POINT ( 'NONE',  ( -0.05219959533907301413, -21.53943276465977519, 97.49890960531436690 ) ) ;
#41188 = CARTESIAN_POINT ( 'NONE',  ( 0.05219959533910956823, 16.53943276465976808, 99.99890960531436690 ) ) ;
#41189 = VECTOR ( 'NONE', #168231, 1000.000000000000000 ) ;
#41190 = CARTESIAN_POINT ( 'NONE',  ( 9.474510206698729675, 16.51473224551082808, 72.08442372801900433 ) ) ;
#41191 = CARTESIAN_POINT ( 'NONE',  ( 0.05219959533907565091, 21.53943276465977519, 69.99890960531435269 ) ) ;
#41192 = CARTESIAN_POINT ( 'NONE',  ( -9.564922557961040184, 16.46253265017147172, 47.91775706135233293 ) ) ;
#41193 = CARTESIAN_POINT ( 'NONE',  ( 13.89961937509977652, -13.97604488694527269, 113.1239096053143527 ) ) ;
#41194 = CARTESIAN_POINT ( 'NONE',  ( -5.719274019375978568, 21.55341960407610458, 95.20724293864769550 ) ) ;
#41195 = CARTESIAN_POINT ( 'NONE',  ( -9.656827144875922642, -71.74905178543390605, -15.00000000000000178 ) ) ;
#41196 = CARTESIAN_POINT ( 'NONE',  ( 14.34966873604972726, -8.224510206698740333, 25.83442372801901499 ) ) ;
#41197 = CARTESIAN_POINT ( 'NONE',  ( 37.19790397533368775, -4.369830079088518282, 41.64077531718624670 ) ) ;
#41198 = CARTESIAN_POINT ( 'NONE',  ( -0.05219959533934338120, 16.53943276465976808, 27.50109039468567929 ) ) ;
#41199 = CARTESIAN_POINT ( 'NONE',  ( 16.51473224551069308, 9.474510206698969483, 49.16557627198102409 ) ) ;
#41200 = CARTESIAN_POINT ( 'NONE',  ( -5.049401038298153566, 19.05341960407611168, 105.2072429386476671 ) ) ;
#41202 = CARTESIAN_POINT ( 'NONE',  ( -12.14591786802309592, -12.06949235617757132, 51.87390960531437401 ) ) ;
#41201 = CARTESIAN_POINT ( 'NONE',  ( 21.53943276465977519, -0.05219959533907433946, 93.74890960531436690 ) ) ;
#41203 = CARTESIAN_POINT ( 'NONE',  ( -5.823673210054431948, 21.52544592524334988, 72.70942372801901854 ) ) ;
#41205 = CARTESIAN_POINT ( 'NONE',  ( -0.05219959533936034679, 19.03943276465977164, 22.50109039468566152 ) ) ;
#41204 = CARTESIAN_POINT ( 'NONE',  ( -8.224510206698735004, -14.34966873604973081, 29.58442372801901854 ) ) ;
#41206 = CARTESIAN_POINT ( 'NONE',  ( 4.379528057220339221, -16.55341960407611168, 32.70724293864770260 ) ) ;
#41207 = CARTESIAN_POINT ( 'NONE',  ( -21.53943276465977519, -0.05219959533937600094, 18.75109039468568639 ) ) ;
#41208 = CARTESIAN_POINT ( 'NONE',  ( -12.06949235617756955, 12.14591786802309770, 45.62390960531436690 ) ) ;
#41209 = CARTESIAN_POINT ( 'NONE',  ( 5.049401038297881783, 19.05341960407617563, 97.29275706135233293 ) ) ;
#41210 = CARTESIAN_POINT ( 'NONE',  ( 16.51473224551083163, -9.474510206698727899, 60.83442372801900433 ) ) ;
#41211 = CARTESIAN_POINT ( 'NONE',  ( 10.81492255796106328, -18.62759615963255655, 70.41775706135236135 ) ) ;
#41212 = CARTESIAN_POINT ( 'NONE',  ( -19.05341960407617563, 5.049401038297882671, 48.54275706135233293 ) ) ;
#41213 = CARTESIAN_POINT ( 'NONE',  ( 9.474510206698971260, -16.51473224551069308, 27.91557627198103120 ) ) ;
#41214 = CARTESIAN_POINT ( 'NONE',  ( 18.62759615963271287, -10.81492255796078972, 38.33224293864768839 ) ) ;
#41215 = CARTESIAN_POINT ( 'NONE',  ( -14.34966873604960291, -8.224510206698953496, 51.66557627198102409 ) ) ;
#41216 = CARTESIAN_POINT ( 'NONE',  ( -16.88567814943161238, -6.947325034625785101, 26.29001122652587696 ) ) ;
#41217 = CARTESIAN_POINT ( 'NONE',  ( 13.89961937509957401, 13.97604488694547697, 21.87609039468566152 ) ) ;
#41218 = CARTESIAN_POINT ( 'NONE',  ( 8.314922557961029526, -14.29746914071037800, 65.41775706135234714 ) ) ;
#41219 = CARTESIAN_POINT ( 'NONE',  ( -4.379528057220328563, 16.55341960407611168, 35.20724293864768839 ) ) ;
#41220 = CARTESIAN_POINT ( 'NONE',  ( -15.72974639402176322, -15.80617190586768395, 74.37609039468568994 ) ) ;
#41221 = CARTESIAN_POINT ( 'NONE',  ( 5.719274019375673035, 21.55341960407619339, 67.29275706135234714 ) ) ;
#41222 = CARTESIAN_POINT ( 'NONE',  ( 5.823673210054125526, 21.52544592524343514, 84.79057627198102409 ) ) ;
#41223 = CARTESIAN_POINT ( 'NONE',  ( -19.05341960407611168, -5.049401038298163336, 41.45724293864769550 ) ) ;
#41224 = CARTESIAN_POINT ( 'NONE',  ( -18.67979575497193778, 10.72451020669871902, 38.33442372801900433 ) ) ;
#41225 = CARTESIAN_POINT ( 'NONE',  ( -4.379528057220328563, 16.55341960407611168, 115.2072429386476955 ) ) ;
#41226 = CARTESIAN_POINT ( 'NONE',  ( -13.89961937509977652, 13.97604488694528158, 55.62390960531434558 ) ) ;
#41227 = CARTESIAN_POINT ( 'NONE',  ( -16.52544592524342804, 4.483927247898546575, 91.04057627198103830 ) ) ;
#41228 = CARTESIAN_POINT ( 'NONE',  ( 13.89961937509977652, -13.97604488694527269, 83.12390960531436690 ) ) ;
#41229 = CARTESIAN_POINT ( 'NONE',  ( 4.379528057220339221, -16.55341960407611168, 42.70724293864770260 ) ) ;
#41230 = CARTESIAN_POINT ( 'NONE',  ( 4.379528057220339221, -16.55341960407611168, 97.70724293864772392 ) ) ;
#41231 = CARTESIAN_POINT ( 'NONE',  ( -18.62759615963270932, 10.81492255796079327, 65.83224293864769550 ) ) ;
#41232 = CARTESIAN_POINT ( 'NONE',  ( 15.80617190586746368, 15.72974639402197994, 114.3739096053143527 ) ) ;
#41233 = CARTESIAN_POINT ( 'NONE',  ( -19.02544592524342804, 5.153800228976336051, 111.0405762719810099 ) ) ;
#41235 = CARTESIAN_POINT ( 'NONE',  ( 4.379528057220092307, 16.55341960407617563, 22.29275706135235069 ) ) ;
#41234 = CARTESIAN_POINT ( 'NONE',  ( -19.02544592524342804, 5.153800228976336051, 61.04057627198103120 ) ) ;
#41236 = CARTESIAN_POINT ( 'NONE',  ( -21.55341960407610458, -5.719274019375992779, 76.45724293864769550 ) ) ;
#41237 = CARTESIAN_POINT ( 'NONE',  ( 0.05219959533937995610, -21.53943276465977519, 90.00109039468567573 ) ) ;
#41238 = CARTESIAN_POINT ( 'NONE',  ( -0.05219959533909027116, -19.03943276465977164, 82.49890960531436690 ) ) ;
#41239 = CARTESIAN_POINT ( 'NONE',  ( -5.823673210054431948, 21.52544592524334988, 22.70942372801901499 ) ) ;
#41240 = CARTESIAN_POINT ( 'NONE',  ( 18.62759615963271287, -10.81492255796078972, 23.33224293864769194 ) ) ;
#41241 = CARTESIAN_POINT ( 'NONE',  ( -4.483927247898782831, 16.52544592524335698, 87.70942372801901854 ) ) ;
#41242 = CARTESIAN_POINT ( 'NONE',  ( 21.53943276465977519, 0.05219959533937863772, 71.25109039468568994 ) ) ;
#41243 = CARTESIAN_POINT ( 'NONE',  ( -18.67979575497193778, 10.72451020669871902, 98.33442372801901854 ) ) ;
#41244 = CARTESIAN_POINT ( 'NONE',  ( -0.05219959533934338120, 16.53943276465976808, 57.50109039468568994 ) ) ;
#41245 = CARTESIAN_POINT ( 'NONE',  ( -18.67979575497193778, 10.72451020669871902, 33.33442372801900433 ) ) ;
#41246 = CARTESIAN_POINT ( 'NONE',  ( 19.05341960407611168, 5.049401038298154454, 23.95724293864769194 ) ) ;
#41247 = CARTESIAN_POINT ( 'NONE',  ( 15.80617190586769283, -15.72974639402175789, 90.62609039468567573 ) ) ;
#41248 = CARTESIAN_POINT ( 'NONE',  ( 13.97604488694527802, 13.89961937509977652, 94.37390960531436690 ) ) ;
#41249 = CARTESIAN_POINT ( 'NONE',  ( -21.55341960407610458, -5.719274019375992779, 96.45724293864770971 ) ) ;
#41250 = CARTESIAN_POINT ( 'NONE',  ( 19.03943276465977164, 0.05219959533936151252, 56.25109039468566863 ) ) ;
#41251 = CARTESIAN_POINT ( 'NONE',  ( -18.67979575497178146, -10.72451020669898902, 51.66557627198102409 ) ) ;
#41253 = CARTESIAN_POINT ( 'NONE',  ( -14.29746914071049879, 8.314922557960819915, 40.83224293864769550 ) ) ;
#41252 = CARTESIAN_POINT ( 'NONE',  ( -19.03943276465977164, 0.05219959533909376836, 101.2489096053143669 ) ) ;
#41254 = LINE ( 'NONE', #178775, #108027 ) ;
#41255 = CARTESIAN_POINT ( 'NONE',  ( 19.03943276465977164, 0.05219959533936151252, 71.25109039468566152 ) ) ;
#41256 = CARTESIAN_POINT ( 'NONE',  ( -18.89770734986048595, -5.500000000000010658, 79.10214472496643623 ) ) ;
#41257 = CARTESIAN_POINT ( 'NONE',  ( -19.05341960407617563, 5.049401038297882671, 108.5427570613523187 ) ) ;
#41258 = CARTESIAN_POINT ( 'NONE',  ( -18.67979575497178146, -10.72451020669898902, 81.66557627198103830 ) ) ;
#41259 = CARTESIAN_POINT ( 'NONE',  ( 4.379528057220339221, -16.55341960407611168, 67.70724293864769550 ) ) ;
#41260 = CARTESIAN_POINT ( 'NONE',  ( 14.34966873604972726, -8.224510206698740333, 30.83442372801902209 ) ) ;
#41261 = CARTESIAN_POINT ( 'NONE',  ( 0.05219959533909260263, 19.03943276465977164, 44.99890960531435979 ) ) ;
#41263 = CARTESIAN_POINT ( 'NONE',  ( -13.97604488694547697, 13.89961937509957934, 78.12609039468567573 ) ) ;
#41262 = CARTESIAN_POINT ( 'NONE',  ( 15.72974639402199770, -15.80617190586745480, 113.1239096053143953 ) ) ;
#41264 = CARTESIAN_POINT ( 'NONE',  ( 0.05219959533909260263, 19.03943276465977164, 89.99890960531436690 ) ) ;
#41265 = CARTESIAN_POINT ( 'NONE',  ( 13.89961937509977652, -13.97604488694527269, 68.12390960531436690 ) ) ;
#41266 = CARTESIAN_POINT ( 'NONE',  ( -10.81492255796078084, -18.62759615963271287, 82.08224293864768129 ) ) ;
#41267 = CARTESIAN_POINT ( 'NONE',  ( -19.03943276465977164, 0.05219959533909376836, 41.24890960531435269 ) ) ;
#41268 = CARTESIAN_POINT ( 'NONE',  ( -18.63871995876255383, 32.95139847355620333, -7.999999999999996447 ) ) ;
#41269 = CARTESIAN_POINT ( 'NONE',  ( 16.53943276465976808, -0.05219959533910856209, 48.74890960531435979 ) ) ;
#41270 = CARTESIAN_POINT ( 'NONE',  ( -5.153800228976328057, -19.02544592524343514, 87.29057627198103830 ) ) ;
#41271 = DIRECTION ( 'NONE',  ( -0.000000000000000000, -0.000000000000000000, -1.000000000000000000 ) ) ;
#41272 = CARTESIAN_POINT ( 'NONE',  ( 13.89961937509957401, 13.97604488694547697, 71.87609039468567573 ) ) ;
#41273 = CARTESIAN_POINT ( 'NONE',  ( 21.53943276465977519, -0.05219959533907433946, 78.74890960531436690 ) ) ;
#41274 = CARTESIAN_POINT ( 'NONE',  ( 13.89961937509957401, 13.97604488694547697, 36.87609039468565442 ) ) ;
#41275 = CARTESIAN_POINT ( 'NONE',  ( -16.46253265017160317, 9.564922557960807481, 105.8322429386476955 ) ) ;
#41276 = CARTESIAN_POINT ( 'NONE',  ( -17.50000000000014211, 3.292511757969745378, 115.0652027021053669 ) ) ;
#41277 = CARTESIAN_POINT ( 'NONE',  ( -0.05219959533907301413, -21.53943276465977519, 37.49890960531436690 ) ) ;
#41278 = AXIS2_PLACEMENT_3D ( 'NONE', #4485, #69170, #66175 ) ;
#41279 = CARTESIAN_POINT ( 'NONE',  ( -16.51473224551069308, -9.474510206698971260, 66.66557627198102409 ) ) ;
#41280 = CARTESIAN_POINT ( 'NONE',  ( 15.80617190586769283, -15.72974639402175789, 70.62609039468567573 ) ) ;
#41281 = CARTESIAN_POINT ( 'NONE',  ( -16.46253265017160317, 9.564922557960807481, 30.83224293864769550 ) ) ;
#41283 = EDGE_LOOP ( 'NONE', ( #53747, #179327, #163086, #55728 ) ) ;
#41282 = CARTESIAN_POINT ( 'NONE',  ( -21.55341960407619339, 5.719274019375674811, 23.54275706135235424 ) ) ;
#41284 = CARTESIAN_POINT ( 'NONE',  ( -21.53943276465977519, -0.05219959533937600094, 48.75109039468568284 ) ) ;
#41285 = ORIENTED_EDGE ( 'NONE', *, *, #8998, .F. ) ;
#41286 = CARTESIAN_POINT ( 'NONE',  ( -28.21656721799290324, -5.378544878440105315, 140.0000000000000568 ) ) ;
#41288 = EDGE_CURVE ( 'NONE', #152161, #28437, #43019, .T. ) ;
#41287 = CARTESIAN_POINT ( 'NONE',  ( -5.153800228976607833, 19.02544592524334988, 72.70942372801900433 ) ) ;
#41289 = DIRECTION ( 'NONE',  ( -0.7071067811865312525, 0.000000000000000000, 0.7071067811865637820 ) ) ;
#41290 = CARTESIAN_POINT ( 'NONE',  ( -18.67979575497178146, -10.72451020669898902, 106.6655762719810383 ) ) ;
#41291 = CARTESIAN_POINT ( 'NONE',  ( -9.474510206698964154, 16.51473224551069663, 65.41557627198102409 ) ) ;
#41292 = CARTESIAN_POINT ( 'NONE',  ( -4.483927247898782831, 16.52544592524335698, 32.70942372801900433 ) ) ;
#41293 = CARTESIAN_POINT ( 'NONE',  ( -30.74264578624800492, -22.33583958711396278, -9.549999994537627046 ) ) ;
#41294 = CARTESIAN_POINT ( 'NONE',  ( -18.62759615963255300, -10.81492255796106328, 104.1677570613523471 ) ) ;
#41295 = CARTESIAN_POINT ( 'NONE',  ( -16.51473224551069308, -9.474510206698971260, 36.66557627198102409 ) ) ;
#41296 = CARTESIAN_POINT ( 'NONE',  ( 18.62759615963255655, 10.81492255796105972, 111.6677570613523613 ) ) ;
#41298 = CARTESIAN_POINT ( 'NONE',  ( 15.80617190586769283, -15.72974639402175789, 65.62609039468568994 ) ) ;
#41297 = CARTESIAN_POINT ( 'NONE',  ( 13.97604488694527802, 13.89961937509977652, 89.37390960531436690 ) ) ;
#41299 = DIRECTION ( 'NONE',  ( -1.000000000000000000, 0.000000000000000000, 0.000000000000000000 ) ) ;
#41300 = CARTESIAN_POINT ( 'NONE',  ( 28.82186960331498327, 2.781578969918950771E-14, 145.2500000054623683 ) ) ;
#41301 = DIRECTION ( 'NONE',  ( -0.7071067811865466846, 7.406550393246786959E-15, -0.7071067811865484609 ) ) ;
#41303 = CARTESIAN_POINT ( 'NONE',  ( 18.67979575497194134, -10.72451020669871369, 75.83442372801900433 ) ) ;
#41302 = CARTESIAN_POINT ( 'NONE',  ( -16.52544592524335698, -4.483927247898792601, 53.95942372801900433 ) ) ;
#41304 = CARTESIAN_POINT ( 'NONE',  ( 0.05219959533937995610, -21.53943276465977519, 90.00109039468567573 ) ) ;
#41305 = CARTESIAN_POINT ( 'NONE',  ( -12.21811429388712966, 11.10918730048719993, -59.22494048452013971 ) ) ;
#41306 = CARTESIAN_POINT ( 'NONE',  ( -16.52544592524335698, -4.483927247898792601, 33.95942372801901143 ) ) ;
#41307 = CARTESIAN_POINT ( 'NONE',  ( -19.02544592524342804, 5.153800228976336051, 86.04057627198103830 ) ) ;
#41308 = CARTESIAN_POINT ( 'NONE',  ( -19.05341960407611168, -5.049401038298163336, 111.4572429386476671 ) ) ;
#41309 = ORIENTED_EDGE ( 'NONE', *, *, #191998, .T. ) ;
#41310 = AXIS2_PLACEMENT_3D ( 'NONE', #158534, #189884, #160531 ) ;
#41311 = CARTESIAN_POINT ( 'NONE',  ( 17.26058549869088665, 6.457015423128626530, 43.87745837476069255 ) ) ;
#41312 = CARTESIAN_POINT ( 'NONE',  ( 16.51473224551069308, 9.474510206698969483, 29.16557627198103475 ) ) ;
#41313 = CARTESIAN_POINT ( 'NONE',  ( -0.05219959533907301413, -21.53943276465977519, 47.49890960531435979 ) ) ;
#41314 = CARTESIAN_POINT ( 'NONE',  ( -12.14591786802326823, 12.06949235617739902, 108.1260903946856757 ) ) ;
#41316 = CARTESIAN_POINT ( 'NONE',  ( 19.05341960407611168, 5.049401038298154454, 63.95724293864769550 ) ) ;
#41315 = CARTESIAN_POINT ( 'NONE',  ( 4.483927247898545687, 16.52544592524342804, 89.79057627198103830 ) ) ;
#41317 = CARTESIAN_POINT ( 'NONE',  ( 21.52544592524334988, 5.823673210054432836, 91.45942372801901854 ) ) ;
#41318 = CARTESIAN_POINT ( 'NONE',  ( -16.55341960407617563, 4.379528057220093196, 23.54275706135235424 ) ) ;
#41319 = CARTESIAN_POINT ( 'NONE',  ( -16.53943276465976808, 0.05219959533911058130, 91.24890960531436690 ) ) ;
#41320 = CARTESIAN_POINT ( 'NONE',  ( -18.67979575497193778, 10.72451020669871902, 48.33442372801902565 ) ) ;
#41321 = CARTESIAN_POINT ( 'NONE',  ( -15.80617190586745835, -15.72974639402198527, 76.87390960531439532 ) ) ;
#41322 = CARTESIAN_POINT ( 'NONE',  ( -19.05341960407617563, 5.049401038297882671, 43.54275706135232582 ) ) ;
#41323 = CARTESIAN_POINT ( 'NONE',  ( -34.48171762721880640, 5.660481407866293502, 49.94458042978408940 ) ) ;
#41324 = CARTESIAN_POINT ( 'NONE',  ( -13.89961937509977652, 13.97604488694528158, 95.62390960531436690 ) ) ;
#41325 = CARTESIAN_POINT ( 'NONE',  ( -4.483927247898539470, -16.52544592524342804, 62.29057627198102409 ) ) ;
#41326 = CARTESIAN_POINT ( 'NONE',  ( -4.483927247898539470, -16.52544592524342804, 37.29057627198102409 ) ) ;
#41327 = CARTESIAN_POINT ( 'NONE',  ( -8.314922557961024197, 14.29746914071037800, 112.9177570613523329 ) ) ;
#41328 = CARTESIAN_POINT ( 'NONE',  ( -5.153800228976607833, 19.02544592524334988, 62.70942372801899722 ) ) ;
#41329 = CARTESIAN_POINT ( 'NONE',  ( -3.573655867282028392E-15, 2.428612866367529932E-14, 1.984260520772446048E-44 ) ) ;
#41330 = CARTESIAN_POINT ( 'NONE',  ( 13.89961937509977652, -13.97604488694527269, 113.1239096053143527 ) ) ;
#41331 = CARTESIAN_POINT ( 'NONE',  ( 16.52544592524342804, -4.483927247898539470, 93.54057627198103830 ) ) ;
#41332 = CARTESIAN_POINT ( 'NONE',  ( -21.38418241377624085, 5.438282248597754887, 174.2683007571264113 ) ) ;
#41334 = CARTESIAN_POINT ( 'NONE',  ( -0.05219959533907301413, -21.53943276465977519, 47.49890960531435979 ) ) ;
#41333 = CARTESIAN_POINT ( 'NONE',  ( -19.05341960407611168, -5.049401038298163336, 51.45724293864770260 ) ) ;
#41335 = CARTESIAN_POINT ( 'NONE',  ( -18.67979575497178146, -10.72451020669898902, 81.66557627198103830 ) ) ;
#41336 = CARTESIAN_POINT ( 'NONE',  ( 9.474510206698971260, -16.51473224551069308, 22.91557627198102765 ) ) ;
#41338 = CARTESIAN_POINT ( 'NONE',  ( -9.564922557960796823, -16.46253265017161027, 42.08224293864769550 ) ) ;
#41337 = CARTESIAN_POINT ( 'NONE',  ( 12.06949235617739724, 12.14591786802326823, 66.87609039468568994 ) ) ;
#41339 = CARTESIAN_POINT ( 'NONE',  ( 10.81492255796106328, -18.62759615963255655, 55.41775706135234714 ) ) ;
#41340 = CARTESIAN_POINT ( 'NONE',  ( -0.05219959533910754901, -16.53943276465976808, 102.4989096053143811 ) ) ;
#41341 = CARTESIAN_POINT ( 'NONE',  ( 0.05219959533936267826, -19.03943276465977164, 85.00109039468567573 ) ) ;
#41342 = CARTESIAN_POINT ( 'NONE',  ( 36.91746824999999177, 11.99521256947799230, -4.024999997268814411 ) ) ;
#41344 = CARTESIAN_POINT ( 'NONE',  ( 21.55341960407610458, 5.719274019375980345, 43.95724293864769550 ) ) ;
#41343 = CARTESIAN_POINT ( 'NONE',  ( 17.49999999999999645, 4.119547552400690371, 37.01912384492517560 ) ) ;
#41345 = CARTESIAN_POINT ( 'NONE',  ( 17.31728774477273447, -6.344390552232384017, 68.31906651689318721 ) ) ;
#41346 = CARTESIAN_POINT ( 'NONE',  ( 10.72451020669871369, 18.67979575497193778, 82.08442372801901854 ) ) ;
#41347 = CARTESIAN_POINT ( 'NONE',  ( -8.314922557960811034, -14.29746914071050412, 32.08224293864769550 ) ) ;
#41349 = CARTESIAN_POINT ( 'NONE',  ( -4.379528057220328563, 16.55341960407611168, 40.20724293864769550 ) ) ;
#41348 = CARTESIAN_POINT ( 'NONE',  ( 16.52544592524335698, 4.483927247898782831, 51.45942372801901854 ) ) ;
#41350 = CARTESIAN_POINT ( 'NONE',  ( 5.823673210054125526, 21.52544592524343514, 64.79057627198103830 ) ) ;
#41351 = CARTESIAN_POINT ( 'NONE',  ( 10.81492255796078972, 18.62759615963270932, 69.58224293864769550 ) ) ;
#41352 = CARTESIAN_POINT ( 'NONE',  ( -21.65274598442066889, 9.891030456500295998, 170.6639841963363438 ) ) ;
#41354 = CARTESIAN_POINT ( 'NONE',  ( 16.46253265017160672, -9.564922557960803928, 108.3322429386476955 ) ) ;
#41353 = CARTESIAN_POINT ( 'NONE',  ( 0.05219959533936267826, -19.03943276465977164, 80.00109039468567573 ) ) ;
#41355 = CARTESIAN_POINT ( 'NONE',  ( -0.05219959533909027116, -19.03943276465977164, 42.49890960531435269 ) ) ;
#41356 = CARTESIAN_POINT ( 'NONE',  ( -4.483927247898539470, -16.52544592524342804, 112.2905762719810241 ) ) ;
#41357 = CARTESIAN_POINT ( 'NONE',  ( -3.573655867282028392E-15, 2.428612866367529932E-14, 155.0000000000000000 ) ) ;
#41358 = ORIENTED_EDGE ( 'NONE', *, *, #102901, .T. ) ;
#41359 = CARTESIAN_POINT ( 'NONE',  ( -0.05219959533934338120, 16.53943276465976808, 87.50109039468568994 ) ) ;
#41360 = CARTESIAN_POINT ( 'NONE',  ( 5.719274019375991003, -21.55341960407610458, 102.7072429386476955 ) ) ;
#41361 = CARTESIAN_POINT ( 'NONE',  ( -13.89961937509977652, 13.97604488694528158, 70.62390960531432427 ) ) ;
#41362 = CARTESIAN_POINT ( 'NONE',  ( 15.80617190586769283, -15.72974639402175789, 35.62609039468568994 ) ) ;
#41363 = CARTESIAN_POINT ( 'NONE',  ( -5.049401038298153566, 19.05341960407611168, 95.20724293864770971 ) ) ;
#41364 = CARTESIAN_POINT ( 'NONE',  ( -22.88436389169415364, -32.73361847831216664, -22.76175135428083962 ) ) ;
#41365 = ORIENTED_EDGE ( 'NONE', *, *, #67877, .F. ) ;
#41366 = CARTESIAN_POINT ( 'NONE',  ( 15.72974639402176855, 15.80617190586768217, 31.87609039468567929 ) ) ;
#41368 = CARTESIAN_POINT ( 'NONE',  ( -19.05341960407617563, 5.049401038297882671, 88.54275706135230450 ) ) ;
#41367 = CARTESIAN_POINT ( 'NONE',  ( -16.46253265017160317, 9.564922557960807481, 30.83224293864769550 ) ) ;
#41369 = CARTESIAN_POINT ( 'NONE',  ( 9.474510206698729675, 16.51473224551082808, 42.08442372801900433 ) ) ;
#41370 = CARTESIAN_POINT ( 'NONE',  ( 10.72451020669898902, -18.67979575497178502, 112.9155762719810383 ) ) ;
#41371 = CARTESIAN_POINT ( 'NONE',  ( 16.51473224551083163, -9.474510206698727899, 45.83442372801900433 ) ) ;
#41372 = CARTESIAN_POINT ( 'NONE',  ( 19.02544592524334988, 5.153800228976608722, 51.45942372801900433 ) ) ;
#41373 = CARTESIAN_POINT ( 'NONE',  ( -4.379528057220086978, -16.55341960407618274, 94.79275706135234714 ) ) ;
#41375 = ORIENTED_EDGE ( 'NONE', *, *, #49532, .F. ) ;
#41374 = CARTESIAN_POINT ( 'NONE',  ( -28.79475375365586842, 2.428612866367530248E-14, 145.9843446568999923 ) ) ;
#41376 = CARTESIAN_POINT ( 'NONE',  ( -16.51473224551069308, -9.474510206698971260, 71.66557627198102409 ) ) ;
#41377 = CARTESIAN_POINT ( 'NONE',  ( -18.62759615963255300, -10.81492255796106328, 84.16775706135234714 ) ) ;
#41378 = CARTESIAN_POINT ( 'NONE',  ( -5.719274019375665041, -21.55341960407619695, 99.79275706135234714 ) ) ;
#41379 = CARTESIAN_POINT ( 'NONE',  ( -1.304723572972834811, -6.853560127763683063, -64.38700459888463001 ) ) ;
#41380 = CARTESIAN_POINT ( 'NONE',  ( 16.51473224551069308, 9.474510206698969483, 89.16557627198103830 ) ) ;
#41381 = CARTESIAN_POINT ( 'NONE',  ( -18.62759615963255300, -10.81492255796106328, 59.16775706135234714 ) ) ;
#41382 = CARTESIAN_POINT ( 'NONE',  ( 9.474510206698729675, 16.51473224551082808, 97.08442372801900433 ) ) ;
#41383 = EDGE_CURVE ( 'NONE', #102181, #34342, #106141, .T. ) ;
#41384 = CARTESIAN_POINT ( 'NONE',  ( -19.03943276465977164, 0.05219959533909376836, 71.24890960531435269 ) ) ;
#41385 = CARTESIAN_POINT ( 'NONE',  ( 9.564922557960805705, 16.46253265017160317, 114.5822429386476955 ) ) ;
#41386 = CARTESIAN_POINT ( 'NONE',  ( -19.03943276465977164, 0.05219959533909376836, 81.24890960531436690 ) ) ;
#41387 = CARTESIAN_POINT ( 'NONE',  ( -17.31728774477274513, -6.344390552232373359, 89.18093348310689805 ) ) ;
#41388 = CARTESIAN_POINT ( 'NONE',  ( 16.51473224551069308, 9.474510206698969483, 69.16557627198102409 ) ) ;
#41389 = CARTESIAN_POINT ( 'NONE',  ( 5.153800228976335163, 19.02544592524342804, 49.79057627198100988 ) ) ;
#41390 = CARTESIAN_POINT ( 'NONE',  ( 5.823673210054444382, -21.52544592524334988, 20.20942372801900788 ) ) ;
#41391 = CARTESIAN_POINT ( 'NONE',  ( 4.379528057220092307, 16.55341960407617563, 97.29275706135234714 ) ) ;
#41392 = CARTESIAN_POINT ( 'NONE',  ( 0.9462312807052283281, 16.38015919949121013, -61.48063308926517578 ) ) ;
#41393 = CARTESIAN_POINT ( 'NONE',  ( -6.856101608890819192E-16, -64.85304063214812231, -12.99999966871702917 ) ) ;
#41394 = CARTESIAN_POINT ( 'NONE',  ( -16.46253265017146816, -9.564922557961047289, 59.16775706135233293 ) ) ;
#41395 = CARTESIAN_POINT ( 'NONE',  ( -16.46253265017160317, 9.564922557960807481, 85.83224293864769550 ) ) ;
#41396 = CARTESIAN_POINT ( 'NONE',  ( -16.55341960407611168, -4.379528057220339221, 76.45724293864769550 ) ) ;
#41397 = CARTESIAN_POINT ( 'NONE',  ( -0.05219959533910754901, -16.53943276465976808, 112.4989096053143669 ) ) ;
#41398 = CARTESIAN_POINT ( 'NONE',  ( -21.53943276465977519, 0.05219959533907696930, 26.24890960531435624 ) ) ;
#41399 = CARTESIAN_POINT ( 'NONE',  ( -19.05341960407611168, -5.049401038298163336, 106.4572429386476955 ) ) ;
#41400 = CARTESIAN_POINT ( 'NONE',  ( 16.53943276465976808, -0.05219959533910856209, 88.74890960531436690 ) ) ;
#41401 = CARTESIAN_POINT ( 'NONE',  ( 9.474510206698971260, -16.51473224551069308, 112.9155762719810383 ) ) ;
#41402 = CARTESIAN_POINT ( 'NONE',  ( -19.05341960407617563, 5.049401038297882671, 33.54275706135231871 ) ) ;
#41403 = CARTESIAN_POINT ( 'NONE',  ( 14.34966873604972726, -8.224510206698740333, 100.8344237280190185 ) ) ;
#41404 = CARTESIAN_POINT ( 'NONE',  ( -0.05219959533909027116, -19.03943276465977164, 82.49890960531436690 ) ) ;
#41405 = CARTESIAN_POINT ( 'NONE',  ( -0.05219959533937732626, 21.53943276465977519, 47.50109039468568994 ) ) ;
#41406 = CARTESIAN_POINT ( 'NONE',  ( -10.72451020669898014, 18.67979575497178502, 40.41557627198103120 ) ) ;
#41407 = CARTESIAN_POINT ( 'NONE',  ( -21.55341960407619339, 5.719274019375674811, 38.54275706135234714 ) ) ;
#41408 = CARTESIAN_POINT ( 'NONE',  ( 21.53943276465977519, -0.05219959533907433946, 83.74890960531435269 ) ) ;
#41409 = CARTESIAN_POINT ( 'NONE',  ( -4.483927247898539470, -16.52544592524342804, 92.29057627198103830 ) ) ;
#41410 = CARTESIAN_POINT ( 'NONE',  ( 19.03943276465977164, 0.05219959533936151252, 56.25109039468566863 ) ) ;
#41411 = CARTESIAN_POINT ( 'NONE',  ( -13.89961937509977652, 13.97604488694528158, 35.62390960531435269 ) ) ;
#41412 = CARTESIAN_POINT ( 'NONE',  ( -19.05341960407611168, -5.049401038298163336, 101.4572429386476955 ) ) ;
#41413 = CARTESIAN_POINT ( 'NONE',  ( -19.02544592524342804, 5.153800228976336051, 101.0405762719810241 ) ) ;
#41414 = CARTESIAN_POINT ( 'NONE',  ( -16.53943276465976808, 0.05219959533911058130, 111.2489096053143669 ) ) ;
#41415 = CARTESIAN_POINT ( 'NONE',  ( -12.14591786802309592, -12.06949235617757132, 26.87390960531435979 ) ) ;
#41416 = CARTESIAN_POINT ( 'NONE',  ( 14.34966873604972726, -8.224510206698740333, 40.83442372801901854 ) ) ;
#41417 = CARTESIAN_POINT ( 'NONE',  ( 18.67979575497194134, -10.72451020669871369, 100.8344237280190185 ) ) ;
#41419 = CARTESIAN_POINT ( 'NONE',  ( 4.483927247898790824, -16.52544592524335698, 110.2094237280190185 ) ) ;
#41418 = CARTESIAN_POINT ( 'NONE',  ( -19.02544592524342804, 5.153800228976336051, 111.0405762719810099 ) ) ;
#41420 = CARTESIAN_POINT ( 'NONE',  ( 5.823673210054444382, -21.52544592524334988, 30.20942372801902565 ) ) ;
#41421 = CARTESIAN_POINT ( 'NONE',  ( 16.51473224551069308, 9.474510206698969483, 49.16557627198102409 ) ) ;
#41422 = CARTESIAN_POINT ( 'NONE',  ( -8.224510206698735004, -14.34966873604973081, 44.58442372801901854 ) ) ;
#41423 = CARTESIAN_POINT ( 'NONE',  ( -16.55341960407617563, 4.379528057220093196, 108.5427570613523756 ) ) ;
#41424 = CARTESIAN_POINT ( 'NONE',  ( -4.483927247898782831, 16.52544592524335698, 97.70942372801904696 ) ) ;
#41425 = CARTESIAN_POINT ( 'NONE',  ( -19.02544592524334988, -5.153800228976617603, 108.9594237280189759 ) ) ;
#41426 = CARTESIAN_POINT ( 'NONE',  ( 9.564922557960805705, 16.46253265017160317, 29.58224293864769550 ) ) ;
#41427 = CARTESIAN_POINT ( 'NONE',  ( 4.483927247898545687, 16.52544592524342804, 109.7905762719810383 ) ) ;
#41428 = CARTESIAN_POINT ( 'NONE',  ( -21.52544592524343514, 5.823673210054127303, 101.0405762719810383 ) ) ;
#41429 = CARTESIAN_POINT ( 'NONE',  ( -13.89961937509977652, 13.97604488694528158, 30.62390960531435269 ) ) ;
#41430 = CARTESIAN_POINT ( 'NONE',  ( -19.05341960407611168, -5.049401038298163336, 106.4572429386476955 ) ) ;
#41431 = CARTESIAN_POINT ( 'NONE',  ( 21.52544592524334988, 5.823673210054432836, 36.45942372801901143 ) ) ;
#41432 = CARTESIAN_POINT ( 'NONE',  ( 0.000000000000000000, 0.000000000000000000, -64.92179855667829713 ) ) ;
#41433 = CARTESIAN_POINT ( 'NONE',  ( -16.46253265017160317, 9.564922557960807481, 110.8322429386476955 ) ) ;
#41434 = CARTESIAN_POINT ( 'NONE',  ( -28.79475375365581158, -9.355982642739276045, 142.0843446569000434 ) ) ;
#41435 = CARTESIAN_POINT ( 'NONE',  ( 5.153800228976335163, 19.02544592524342804, 104.7905762719809957 ) ) ;
#41437 = CARTESIAN_POINT ( 'NONE',  ( -4.483927247898539470, -16.52544592524342804, 87.29057627198103830 ) ) ;
#41436 = CARTESIAN_POINT ( 'NONE',  ( 10.81492255796106328, -18.62759615963255655, 30.41775706135234358 ) ) ;
#41438 = CARTESIAN_POINT ( 'NONE',  ( 16.46253265017160672, -9.564922557960803928, 93.33224293864769550 ) ) ;
#41439 = CARTESIAN_POINT ( 'NONE',  ( 5.153800228976617603, -19.02544592524335343, 70.20942372801900433 ) ) ;
#41441 =( BOUNDED_SURFACE ( )  B_SPLINE_SURFACE ( 3, 2, ( 
 ( #70582, #174769, #36235 ),
 ( #115083, #8914, #159579 ),
 ( #82732, #144413, #193942 ),
 ( #5899, #83730, #190930 ),
 ( #99902, #175764, #38247 ),
 ( #52407, #37240, #98896 ),
 ( #183494, #77286, #138956 ),
 ( #169294, #435, #62110 ),
 ( #167336, #71577, #152156 ),
 ( #30800, #44978, #184483 ),
 ( #163595, #198666, #60133 ),
 ( #136977, #123773, #29807 ),
 ( #199653, #92449, #121801 ),
 ( #45962, #107616, #139942 ),
 ( #1432, #31792, #148423 ),
 ( #154137, #25096, #106638 ),
 ( #63110, #168311, #15629 ),
 ( #124788, #40237, #194935 ),
 ( #9918, #185472, #46962 ),
 ( #133243, #108621, #170299 ),
 ( #93441, #91443, #56411 ),
 ( #122793, #120807, #155128 ),
 ( #16621, #153131, #14634 ),
 ( #78269, #76293, #101913 ),
 ( #137971, #61119, #86738 ),
 ( #75306, #182506, #43986 ),
 ( #105647, #28833, #90474 ),
 ( #13639, #32785, #174284 ),
 ( #35754, #64115, #144919 ),
 ( #3422, #6401, #173290 ),
 ( #94437, #113578, #109615 ),
 ( #68082, #160098, #175272 ),
 ( #126756, #20581, #82233 ),
 ( #112592, #143923, #5404 ),
 ( #110602, #17617, #95434 ),
 ( #97399, #188459, #127755 ),
 ( #171299, #141931, #65098 ),
 ( #140946, #36738, #19599 ),
 ( #67088, #49940, #34764 ),
 ( #128747, #142922, #186487 ),
 ( #96421, #158107, #47963 ),
 ( #33774, #159086, #190444 ),
 ( #156118, #51919, #79276 ),
 ( #111605, #81241, #4404 ) ),
 .UNSPECIFIED., .F., .F., .T. ) 
 B_SPLINE_SURFACE_WITH_KNOTS ( ( 4, 2, 2, 2, 2, 2, 2, 2, 2, 2, 2, 2, 2, 2, 2, 2, 2, 2, 2, 2, 2, 4 ),
 ( 3, 3 ),
 ( 0.1334715276261017047, 0.1400397817209072804, 0.1416818452446086951, 0.1433239087683100821, 0.1466080358157128560, 0.1498921628631156300, 0.1531762899105184039, 0.1564604169579211779, 0.1597445440053239796, 0.1630286710527267813, 0.1646707345764281682, 0.1663127981001295552, 0.1679548616238309422, 0.1695969251475323292, 0.1712389886712337161, 0.1720600204330844096, 0.1728810521949351031, 0.1745231157186364901, 0.1761651792423378771, 0.1794493062897406788, 0.1827334333371434805, 0.1860175603845462544 ),
 ( 0.000000000000000000, 1.000000000000000000 ),
 .UNSPECIFIED. ) 
 GEOMETRIC_REPRESENTATION_ITEM ( )  RATIONAL_B_SPLINE_SURFACE ( (
 ( 1.000000000000000000, 0.7745966692414834043, 1.000000000000000000),
 ( 1.000000000000000000, 0.7873173169476442856, 1.000000000000000000),
 ( 1.000000000000000000, 0.8012080269091595985, 1.000000000000000000),
 ( 1.000000000000000000, 0.8197272276933328383, 1.000000000000000000),
 ( 1.000000000000000000, 0.8234885421913021863, 1.000000000000000000),
 ( 1.000000000000000000, 0.8311157573375610452, 1.000000000000000000),
 ( 1.000000000000000000, 0.8349728938257607869, 1.000000000000000000),
 ( 1.000000000000000000, 0.8465302108189354247, 1.000000000000000000),
 ( 1.000000000000000000, 0.8542644918356914197, 1.000000000000000000),
 ( 1.000000000000000000, 0.8696747091108276706, 1.000000000000000000),
 ( 1.000000000000000000, 0.8773507960691676599, 1.000000000000000000),
 ( 1.000000000000000000, 0.8925002889089016511, 1.000000000000000000),
 ( 1.000000000000000000, 0.8999891582781396338, 1.000000000000000000),
 ( 1.000000000000000000, 0.9145203485641226759, 1.000000000000000000),
 ( 1.000000000000000000, 0.9215166741119587002, 1.000000000000000000),
 ( 1.000000000000000000, 0.9348196634156782370, 1.000000000000000000),
 ( 1.000000000000000000, 0.9411264847296237912, 1.000000000000000000),
 ( 1.000000000000000000, 0.9528821887672441759, 1.000000000000000000),
 ( 1.000000000000000000, 0.9583320463343939499, 1.000000000000000000),
 ( 1.000000000000000000, 0.9657141226242618171, 1.000000000000000000),
 ( 1.000000000000000000, 0.9680424144921330187, 1.000000000000000000),
 ( 1.000000000000000000, 0.9724014971077669101, 1.000000000000000000),
 ( 1.000000000000000000, 0.9744334801158447412, 1.000000000000000000),
 ( 1.000000000000000000, 0.9781204877085358795, 1.000000000000000000),
 ( 1.000000000000000000, 0.9797809101335805959, 1.000000000000000000),
 ( 1.000000000000000000, 0.9826818083352881761, 1.000000000000000000),
 ( 1.000000000000000000, 0.9839230189806127402, 1.000000000000000000),
 ( 1.000000000000000000, 0.9859013487406023124, 1.000000000000000000),
 ( 1.000000000000000000, 0.9866146582094301731, 1.000000000000000000),
 ( 1.000000000000000000, 0.9872250220265939014, 1.000000000000000000),
 ( 1.000000000000000000, 0.9873522598263766437, 1.000000000000000000),
 ( 1.000000000000000000, 0.9874472609175324322, 1.000000000000000000),
 ( 1.000000000000000000, 0.9874138636738953867, 1.000000000000000000),
 ( 1.000000000000000000, 0.9870735186573816877, 1.000000000000000000),
 ( 1.000000000000000000, 0.9865315217161264583, 1.000000000000000000),
 ( 1.000000000000000000, 0.9848873008857174094, 1.000000000000000000),
 ( 1.000000000000000000, 0.9837743821442677117, 1.000000000000000000),
 ( 1.000000000000000000, 0.9797976954002749483, 1.000000000000000000),
 ( 1.000000000000000000, 0.9763000371664851684, 1.000000000000000000),
 ( 1.000000000000000000, 0.9680363503266700143, 1.000000000000000000),
 ( 1.000000000000000000, 0.9632464763793491258, 1.000000000000000000),
 ( 1.000000000000000000, 0.9526889542241591124, 1.000000000000000000),
 ( 1.000000000000000000, 0.9469283804590789000, 1.000000000000000000),
 ( 1.000000000000000000, 0.9407878411039238831, 1.000000000000000000) ) ) 
 REPRESENTATION_ITEM ( '' )  SURFACE ( )  );
#41440 = CARTESIAN_POINT ( 'NONE',  ( 16.55341960407618274, -4.379528057220086978, 61.04275706135234714 ) ) ;
#41442 = CARTESIAN_POINT ( 'NONE',  ( 5.719274019375673035, 21.55341960407619339, 82.29275706135234714 ) ) ;
#41443 = CIRCLE ( 'NONE', #106078, 2.000000000000001776 ) ;
#41444 = CARTESIAN_POINT ( 'NONE',  ( -4.379528057220086978, -16.55341960407618274, 39.79275706135235424 ) ) ;
#41445 = CARTESIAN_POINT ( 'NONE',  ( -19.03943276465977164, 0.05219959533909376836, 76.24890960531435269 ) ) ;
#41446 = CARTESIAN_POINT ( 'NONE',  ( -16.51473224551082808, 9.474510206698731452, 103.3344237280190043 ) ) ;
#41447 = CARTESIAN_POINT ( 'NONE',  ( 0.05219959533934541429, -16.53943276465976808, 75.00109039468568994 ) ) ;
#41448 = CARTESIAN_POINT ( 'NONE',  ( -15.72974639402176322, -15.80617190586768395, 109.3760903946857042 ) ) ;
#41449 = CARTESIAN_POINT ( 'NONE',  ( 19.05341960407617918, -5.049401038297876454, 91.04275706135234714 ) ) ;
#41450 = CARTESIAN_POINT ( 'NONE',  ( 13.89961937509977652, -13.97604488694527269, 68.12390960531436690 ) ) ;
#41451 = CARTESIAN_POINT ( 'NONE',  ( 21.55341960407610458, 5.719274019375980345, 78.95724293864769550 ) ) ;
#41453 = CARTESIAN_POINT ( 'NONE',  ( -13.97604488694547697, 13.89961937509957934, 93.12609039468566152 ) ) ;
#41452 = CARTESIAN_POINT ( 'NONE',  ( 14.29746914071049879, -8.314922557960816363, 93.33224293864769550 ) ) ;
#41454 = CARTESIAN_POINT ( 'NONE',  ( -4.379528057220086978, -16.55341960407618274, 59.79275706135234714 ) ) ;
#41455 = CARTESIAN_POINT ( 'NONE',  ( 21.92083080610932200, 6.374575339256159268, 171.4095429173257514 ) ) ;
#41456 = CARTESIAN_POINT ( 'NONE',  ( -5.049401038297874678, -19.05341960407617918, 54.79275706135234003 ) ) ;
#41457 = CARTESIAN_POINT ( 'NONE',  ( 4.379528057220339221, -16.55341960407611168, 37.70724293864769550 ) ) ;
#41458 = CARTESIAN_POINT ( 'NONE',  ( -4.483927247898539470, -16.52544592524342804, 82.29057627198103830 ) ) ;
#41460 = CARTESIAN_POINT ( 'NONE',  ( -17.58332526062528345, -7.635886036038592728, 44.07665040441535353 ) ) ;
#41459 = CARTESIAN_POINT ( 'NONE',  ( 0.05219959533936267826, -19.03943276465977164, 20.00109039468567218 ) ) ;
#41461 = CARTESIAN_POINT ( 'NONE',  ( -18.62759615963255300, -10.81492255796106328, 19.16775706135234714 ) ) ;
#41462 = CARTESIAN_POINT ( 'NONE',  ( 13.89961937509977652, -13.97604488694527269, 98.12390960531433848 ) ) ;
#41463 = CARTESIAN_POINT ( 'NONE',  ( 16.51473224551069308, 9.474510206698969483, 79.16557627198103830 ) ) ;
#41464 = CARTESIAN_POINT ( 'NONE',  ( 5.719274019375673035, 21.55341960407619339, 92.29275706135236135 ) ) ;
#41465 = CARTESIAN_POINT ( 'NONE',  ( 9.474510206698971260, -16.51473224551069308, 77.91557627198103830 ) ) ;
#41466 = CARTESIAN_POINT ( 'NONE',  ( -0.05219959533907301413, -21.53943276465977519, 32.49890960531435979 ) ) ;
#41467 = CARTESIAN_POINT ( 'NONE',  ( 8.314922557960818139, 14.29746914071049879, 79.58224293864769550 ) ) ;
#41468 = VERTEX_POINT ( 'NONE', #9693 ) ;
#41469 = CARTESIAN_POINT ( 'NONE',  ( 9.564922557960805705, 16.46253265017160317, 44.58224293864769550 ) ) ;
#41470 = CARTESIAN_POINT ( 'NONE',  ( 16.53943276465976808, -0.05219959533910856209, 103.7489096053143669 ) ) ;
#41471 = CARTESIAN_POINT ( 'NONE',  ( -0.05219959533907301413, -21.53943276465977519, 107.4989096053143669 ) ) ;
#41472 = CARTESIAN_POINT ( 'NONE',  ( -18.67979575497193778, 10.72451020669871902, 58.33442372801901143 ) ) ;
#41473 = CARTESIAN_POINT ( 'NONE',  ( 19.02544592524343514, -5.153800228976328945, 28.54057627198102409 ) ) ;
#41474 = CARTESIAN_POINT ( 'NONE',  ( 16.55341960407618274, -4.379528057220086978, 66.04275706135236135 ) ) ;
#41475 = CARTESIAN_POINT ( 'NONE',  ( 15.80617190586746368, 15.72974639402197994, 99.37390960531436690 ) ) ;
#41476 = CARTESIAN_POINT ( 'NONE',  ( 21.55341960407610458, 5.719274019375980345, 113.9572429386477239 ) ) ;
#41478 = CARTESIAN_POINT ( 'NONE',  ( 19.05341960407611168, 5.049401038298154454, 53.95724293864770260 ) ) ;
#41477 = CARTESIAN_POINT ( 'NONE',  ( 5.049401038297881783, 19.05341960407617563, 42.29275706135234003 ) ) ;
#41479 = CARTESIAN_POINT ( 'NONE',  ( 16.51473224551069308, 9.474510206698969483, 114.1655762719810241 ) ) ;
#41480 = CARTESIAN_POINT ( 'NONE',  ( -5.719274019375665041, -21.55341960407619695, 59.79275706135234714 ) ) ;
#41481 = CARTESIAN_POINT ( 'NONE',  ( -10.72451020669898014, 18.67979575497178502, 60.41557627198102409 ) ) ;
#41482 = CARTESIAN_POINT ( 'NONE',  ( -4.483927247898539470, -16.52544592524342804, 42.29057627198103120 ) ) ;
#41484 = CARTESIAN_POINT ( 'NONE',  ( -5.719274019375665041, -21.55341960407619695, 104.7927570613523898 ) ) ;
#41483 = CARTESIAN_POINT ( 'NONE',  ( 18.62759615963255655, 10.81492255796105972, 71.66775706135234714 ) ) ;
#41485 = CARTESIAN_POINT ( 'NONE',  ( 8.224510206698953496, -14.34966873604960469, 52.91557627198103830 ) ) ;
#41486 = CARTESIAN_POINT ( 'NONE',  ( -8.314922557960811034, -14.29746914071050412, 107.0822429386476955 ) ) ;
#41487 = CARTESIAN_POINT ( 'NONE',  ( 13.89961937509957401, 13.97604488694547697, 41.87609039468566152 ) ) ;
#41488 = CARTESIAN_POINT ( 'NONE',  ( 16.55341960407618274, -4.379528057220086978, 101.0427570613523756 ) ) ;
#41490 = ADVANCED_FACE ( 'NONE', ( #148200 ), #89511, .F. ) ;
#41489 = CARTESIAN_POINT ( 'NONE',  ( 21.53943276465977519, 0.05219959533937863772, 71.25109039468568994 ) ) ;
#41491 = CARTESIAN_POINT ( 'NONE',  ( -9.474510206698964154, 16.51473224551069663, 55.41557627198103120 ) ) ;
#41492 = CARTESIAN_POINT ( 'NONE',  ( 16.46253265017146816, 9.564922557961045513, 31.66775706135232937 ) ) ;
#41493 = CARTESIAN_POINT ( 'NONE',  ( -5.719274019375978568, 21.55341960407610458, 40.20724293864769550 ) ) ;
#41494 = B_SPLINE_CURVE_WITH_KNOTS ( 'NONE', 3,
 ( #76982, #107313, #182196, #183191, #92141, #32483, #154823, #155815, #43681, #15323, #167030, #75006, #121497, #28532, #152831, #45662, #168986, #106326, #90168, #123473, #136671, #198353, #168012, #29508, #30490, #153828 ),
 .UNSPECIFIED., .F., .F.,
 ( 4, 2, 2, 2, 2, 2, 2, 2, 2, 2, 2, 2, 4 ),
 ( 1.971416326362521810E-07, 0.0002960211146593206026, 0.0005918450876860049644, 0.0008876690607126895430, 0.001183493033739374230, 0.001775140979792742737, 0.002366788925846110593, 0.002662612898872792570, 0.002958436871899474113, 0.003254260844926156089, 0.003550084817952837632, 0.004141732764006201585, 0.004733380710059564671 ),
 .UNSPECIFIED. ) ;
#41495 = CARTESIAN_POINT ( 'NONE',  ( -18.67979575497193778, 10.72451020669871902, 28.33442372801902209 ) ) ;
#41496 = CARTESIAN_POINT ( 'NONE',  ( -15.72974639402197994, 15.80617190586746368, 85.62390960531436690 ) ) ;
#41497 = CARTESIAN_POINT ( 'NONE',  ( -5.153800228976607833, 19.02544592524334988, 87.70942372801897591 ) ) ;
#41498 = CARTESIAN_POINT ( 'NONE',  ( -12.06949235617739369, -12.14591786802326823, 54.37609039468568994 ) ) ;
#41500 = CARTESIAN_POINT ( 'NONE',  ( -5.823673210054116645, -21.52544592524344225, 92.29057627198103830 ) ) ;
#41499 = CARTESIAN_POINT ( 'NONE',  ( 3.889087296525895354, -35.00000000000001421, 8.181980515339454030 ) ) ;
#41501 = CARTESIAN_POINT ( 'NONE',  ( -12.06949235617756955, 12.14591786802309770, 80.62390960531438111 ) ) ;
#41502 = CARTESIAN_POINT ( 'NONE',  ( -17.50000000000000000, -5.622605283950869115, 101.3120731059611046 ) ) ;
#41503 = CARTESIAN_POINT ( 'NONE',  ( -14.34966873604972548, 8.224510206698743886, 28.33442372801902209 ) ) ;
#41504 = CARTESIAN_POINT ( 'NONE',  ( 5.823673210054125526, 21.52544592524343514, 49.79057627198102409 ) ) ;
#41505 = CARTESIAN_POINT ( 'NONE',  ( -16.52544592524335698, -4.483927247898792601, 73.95942372801901854 ) ) ;
#41506 = CARTESIAN_POINT ( 'NONE',  ( 0.05219959533909260263, 19.03943276465977164, 24.99890960531435269 ) ) ;
#41507 = EDGE_CURVE ( 'NONE', #96464, #7679, #11985, .T. ) ;
#41508 = CARTESIAN_POINT ( 'NONE',  ( -16.55341960407617563, 4.379528057220093196, 58.54275706135235424 ) ) ;
#41509 = CARTESIAN_POINT ( 'NONE',  ( 15.80617190586769283, -15.72974639402175789, 25.62609039468567929 ) ) ;
#41510 = CARTESIAN_POINT ( 'NONE',  ( -18.67979575497178146, -10.72451020669898902, 51.66557627198102409 ) ) ;
#41511 = CARTESIAN_POINT ( 'NONE',  ( 14.34966873604972726, -8.224510206698740333, 70.83442372801901854 ) ) ;
#41512 = CARTESIAN_POINT ( 'NONE',  ( 19.05341960407611168, 5.049401038298154454, 98.95724293864766707 ) ) ;
#41514 = CARTESIAN_POINT ( 'NONE',  ( 5.049401038298161559, -19.05341960407611168, 32.70724293864768129 ) ) ;
#41513 = CARTESIAN_POINT ( 'NONE',  ( 10.72451020669871369, 18.67979575497193778, 52.08442372801901854 ) ) ;
#41515 = CARTESIAN_POINT ( 'NONE',  ( -18.62759615963270932, 10.81492255796079327, 40.83224293864769550 ) ) ;
#41516 = CARTESIAN_POINT ( 'NONE',  ( -10.81492255796078084, -18.62759615963271287, 22.08224293864769194 ) ) ;
#41517 = VERTEX_POINT ( 'NONE', #105672 ) ;
#41518 = CARTESIAN_POINT ( 'NONE',  ( -0.05219959533936034679, 19.03943276465977164, 32.50109039468566863 ) ) ;
#41519 = CARTESIAN_POINT ( 'NONE',  ( -4.483927247898782831, 16.52544592524335698, 52.70942372801902565 ) ) ;
#41520 = CARTESIAN_POINT ( 'NONE',  ( 16.51473224551069308, 9.474510206698969483, 109.1655762719810383 ) ) ;
#41521 = VERTEX_POINT ( 'NONE', #164379 ) ;
#41522 = CARTESIAN_POINT ( 'NONE',  ( 19.02544592524343514, -5.153800228976328945, 83.54057627198100988 ) ) ;
#41523 = CARTESIAN_POINT ( 'NONE',  ( 8.224510206698742110, 14.34966873604972548, 102.0844237280190185 ) ) ;
#41524 = CARTESIAN_POINT ( 'NONE',  ( -28.79475375365490564, 9.355982642740551469, 142.1656553485624102 ) ) ;
#41525 = CARTESIAN_POINT ( 'NONE',  ( 8.314922557960818139, 14.29746914071049879, 89.58224293864768129 ) ) ;
#41526 = CARTESIAN_POINT ( 'NONE',  ( 21.53943276465977519, -0.05219959533907433946, 53.74890960531437401 ) ) ;
#41527 = CARTESIAN_POINT ( 'NONE',  ( 9.474510206698971260, -16.51473224551069308, 37.91557627198102409 ) ) ;
#41528 = CARTESIAN_POINT ( 'NONE',  ( -16.52544592524335698, -4.483927247898792601, 73.95942372801901854 ) ) ;
#41529 = CARTESIAN_POINT ( 'NONE',  ( -5.719274019375665041, -21.55341960407619695, 24.79275706135235779 ) ) ;
#41530 = CARTESIAN_POINT ( 'NONE',  ( -5.049401038297874678, -19.05341960407617918, 89.79275706135230450 ) ) ;
#41531 = CARTESIAN_POINT ( 'NONE',  ( -19.02544592524342804, 5.153800228976336051, 36.04057627198100988 ) ) ;
#41532 = CARTESIAN_POINT ( 'NONE',  ( -28.79475375365586842, 2.428612866367529932E-14, 155.0000000000000000 ) ) ;
#41533 = CARTESIAN_POINT ( 'NONE',  ( -21.53943276465977519, -0.05219959533937600094, 103.7510903946857042 ) ) ;
#41534 = CARTESIAN_POINT ( 'NONE',  ( -9.474510206698964154, 16.51473224551069663, 80.41557627198103830 ) ) ;
#41535 = CARTESIAN_POINT ( 'NONE',  ( 12.06949235617739724, 12.14591786802326823, 61.87609039468568284 ) ) ;
#41536 = CARTESIAN_POINT ( 'NONE',  ( -5.719274019375665041, -21.55341960407619695, 89.79275706135236135 ) ) ;
#41537 = CARTESIAN_POINT ( 'NONE',  ( -19.05341960407617563, 5.049401038297882671, 48.54275706135233293 ) ) ;
#41538 = ADVANCED_FACE ( 'NONE', ( #87516 ), #196719, .T. ) ;
#41539 = CARTESIAN_POINT ( 'NONE',  ( 0.05219959533936267826, -19.03943276465977164, 60.00109039468566863 ) ) ;
#41540 = ORIENTED_EDGE ( 'NONE', *, *, #98398, .F. ) ;
#41541 = CARTESIAN_POINT ( 'NONE',  ( 10.81492255796106328, -18.62759615963255655, 55.41775706135234714 ) ) ;
#41542 = CARTESIAN_POINT ( 'NONE',  ( 17.58332526062526568, -7.635886036038552760, 58.42334959558466778 ) ) ;
#41543 = CARTESIAN_POINT ( 'NONE',  ( 19.02544592524334988, 5.153800228976608722, 51.45942372801900433 ) ) ;
#41544 = CARTESIAN_POINT ( 'NONE',  ( -0.05219959533909027116, -19.03943276465977164, 97.49890960531436690 ) ) ;
#41545 = CARTESIAN_POINT ( 'NONE',  ( 19.05341960407611168, 5.049401038298154454, 78.95724293864769550 ) ) ;
#41546 = CARTESIAN_POINT ( 'NONE',  ( -14.34966873604960291, -8.224510206698953496, 36.66557627198103120 ) ) ;
#41547 = CARTESIAN_POINT ( 'NONE',  ( 10.72451020669898902, -18.67979575497178502, 32.91557627198102409 ) ) ;
#41548 = CARTESIAN_POINT ( 'NONE',  ( -11.40812507854754720, -35.11059874428192273, -2.724999997268813257 ) ) ;
#41549 = CARTESIAN_POINT ( 'NONE',  ( 20.12987255291491095, 20.83652723102580495, -52.58065409862962269 ) ) ;
#41550 = CARTESIAN_POINT ( 'NONE',  ( 21.52544592524334988, 5.823673210054432836, 111.4594237280190328 ) ) ;
#41551 = CARTESIAN_POINT ( 'NONE',  ( -27.46925885783797838, 7.746560145625151605, 162.9586723222901981 ) ) ;
#41552 = CARTESIAN_POINT ( 'NONE',  ( 19.02544592524343514, -5.153800228976328945, 33.54057627198102409 ) ) ;
#41553 = CARTESIAN_POINT ( 'NONE',  ( -13.97604488694527625, -13.89961937509977652, 21.87390960531435979 ) ) ;
#41554 = CARTESIAN_POINT ( 'NONE',  ( 11.74264578624799427, 36.14014761921585972, -4.599999999999999645 ) ) ;
#41555 = CARTESIAN_POINT ( 'NONE',  ( 5.000000000000000000, -140.0000000000000000, 21.32407087589996308 ) ) ;
#41556 = CARTESIAN_POINT ( 'NONE',  ( 16.52544592524335698, 4.483927247898782831, 66.45942372801903275 ) ) ;
#41557 = CARTESIAN_POINT ( 'NONE',  ( -18.62759615963270932, 10.81492255796079327, 80.83224293864769550 ) ) ;
#41558 = CARTESIAN_POINT ( 'NONE',  ( -4.379528057220328563, 16.55341960407611168, 55.20724293864770260 ) ) ;
#41560 = CARTESIAN_POINT ( 'NONE',  ( -19.05341960407611168, -5.049401038298163336, 106.4572429386476955 ) ) ;
#41559 = CARTESIAN_POINT ( 'NONE',  ( 5.049401038298161559, -19.05341960407611168, 22.70724293864769194 ) ) ;
#41561 = CARTESIAN_POINT ( 'NONE',  ( 10.72451020669871369, 18.67979575497193778, 27.08442372801901854 ) ) ;
#41562 = CARTESIAN_POINT ( 'NONE',  ( 16.51473224551083163, -9.474510206698727899, 30.83442372801900433 ) ) ;
#41563 = CARTESIAN_POINT ( 'NONE',  ( 9.474510206698971260, -16.51473224551069308, 32.91557627198102409 ) ) ;
#41564 = CARTESIAN_POINT ( 'NONE',  ( 21.53943276465977519, 0.05219959533937863772, 86.25109039468568994 ) ) ;
#41565 = CARTESIAN_POINT ( 'NONE',  ( 16.79531203550645202, -7.028104445595737992, 31.24755011779557989 ) ) ;
#41566 = CARTESIAN_POINT ( 'NONE',  ( -12.06949235617756955, 12.14591786802309770, 30.62390960531436335 ) ) ;
#41567 = CARTESIAN_POINT ( 'NONE',  ( 36.91746824999999887, -11.99521256947793546, -2.224999997268813701 ) ) ;
#41568 = CARTESIAN_POINT ( 'NONE',  ( -15.80617190586745835, -15.72974639402198527, 36.87390960531435979 ) ) ;
#41569 = CARTESIAN_POINT ( 'NONE',  ( 4.379528057220339221, -16.55341960407611168, 97.70724293864772392 ) ) ;
#41570 = CARTESIAN_POINT ( 'NONE',  ( 25.80819889657193045, -27.69677943096044714, -16.54815200935614428 ) ) ;
#41571 = CARTESIAN_POINT ( 'NONE',  ( -19.03943276465977164, 0.05219959533909376836, 86.24890960531436690 ) ) ;
#41572 = CARTESIAN_POINT ( 'NONE',  ( -16.55341960407611168, -4.379528057220339221, 91.45724293864769550 ) ) ;
#41573 = CARTESIAN_POINT ( 'NONE',  ( -0.05219959533936034679, 19.03943276465977164, 107.5010903946856615 ) ) ;
#41574 = CARTESIAN_POINT ( 'NONE',  ( 18.67979575497178502, 10.72451020669898547, 59.16557627198103120 ) ) ;
#41575 = ORIENTED_EDGE ( 'NONE', *, *, #80930, .F. ) ;
#41576 = CARTESIAN_POINT ( 'NONE',  ( 19.05341960407611168, 5.049401038298154454, 33.95724293864769550 ) ) ;
#41578 = CARTESIAN_POINT ( 'NONE',  ( -18.67979575497178146, -10.72451020669898902, 91.66557627198103830 ) ) ;
#41577 = CARTESIAN_POINT ( 'NONE',  ( 9.564922557960805705, 16.46253265017160317, 89.58224293864769550 ) ) ;
#41580 = CARTESIAN_POINT ( 'NONE',  ( -16.51473224551069308, -9.474510206698971260, 91.66557627198103830 ) ) ;
#41579 = CARTESIAN_POINT ( 'NONE',  ( 16.53943276465976808, 0.05219959533934440121, 106.2510903946856757 ) ) ;
#41581 = CARTESIAN_POINT ( 'NONE',  ( -0.05219959533936034679, 19.03943276465977164, 82.50109039468567573 ) ) ;
#41582 = CARTESIAN_POINT ( 'NONE',  ( 10.81492255796106328, -18.62759615963255655, 90.41775706135236135 ) ) ;
#41583 = CARTESIAN_POINT ( 'NONE',  ( -21.52544592524343514, 5.823673210054127303, 81.04057627198102409 ) ) ;
#41584 = CARTESIAN_POINT ( 'NONE',  ( -18.67979575497178146, -10.72451020669898902, 36.66557627198103120 ) ) ;
#41585 = CARTESIAN_POINT ( 'NONE',  ( -13.97604488694527625, -13.89961937509977652, 56.87390960531434558 ) ) ;
#41586 = CARTESIAN_POINT ( 'NONE',  ( -4.379528057220086978, -16.55341960407618274, 109.7927570613523613 ) ) ;
#41587 = CARTESIAN_POINT ( 'NONE',  ( 13.89961937509977652, -13.97604488694527269, 68.12390960531436690 ) ) ;
#41588 = ORIENTED_EDGE ( 'NONE', *, *, #194310, .T. ) ;
#41589 = CARTESIAN_POINT ( 'NONE',  ( -31.34418352700887311, -5.970234417100033220, 99.56646813413776442 ) ) ;
#41590 = CARTESIAN_POINT ( 'NONE',  ( 9.564922557961047289, -16.46253265017146816, 25.41775706135234003 ) ) ;
#41591 = CARTESIAN_POINT ( 'NONE',  ( 16.55341960407611168, 4.379528057220329451, 73.95724293864769550 ) ) ;
#41592 = CARTESIAN_POINT ( 'NONE',  ( -18.62759615963255300, -10.81492255796106328, 19.16775706135234714 ) ) ;
#41593 = CARTESIAN_POINT ( 'NONE',  ( 27.73933785331498569, 2.768321779492822058E-14, 146.3750000027311842 ) ) ;
#41594 = CARTESIAN_POINT ( 'NONE',  ( -18.62759615963270932, 10.81492255796079327, 65.83224293864769550 ) ) ;
#41595 = CARTESIAN_POINT ( 'NONE',  ( -14.34966873604972548, 8.224510206698743886, 98.33442372801901854 ) ) ;
#41596 = CARTESIAN_POINT ( 'NONE',  ( 4.483927247898545687, 16.52544592524342804, 104.7905762719810241 ) ) ;
#41597 = CARTESIAN_POINT ( 'NONE',  ( 19.02544592524343514, -5.153800228976328945, 68.54057627198103830 ) ) ;
#41598 = FILL_AREA_STYLE_COLOUR ( '', #195127 ) ;
#41599 = CARTESIAN_POINT ( 'NONE',  ( -8.224510206698948167, 14.34966873604960824, 25.41557627198103120 ) ) ;
#41600 = CARTESIAN_POINT ( 'NONE',  ( 21.53943276465977519, 0.05219959533937863772, 46.25109039468567573 ) ) ;
#41601 = CARTESIAN_POINT ( 'NONE',  ( -16.51473224551069308, -9.474510206698971260, 111.6655762719810383 ) ) ;
#41602 = CARTESIAN_POINT ( 'NONE',  ( 21.55341960407619695, -5.719274019375665929, 76.04275706135237556 ) ) ;
#41603 = CARTESIAN_POINT ( 'NONE',  ( 13.97604488694527802, 13.89961937509977652, 34.37390960531436690 ) ) ;
#41604 = CARTESIAN_POINT ( 'NONE',  ( -13.97604488694527625, -13.89961937509977652, 31.87390960531435979 ) ) ;
#41605 = ORIENTED_EDGE ( 'NONE', *, *, #115308, .T. ) ;
#41606 = CARTESIAN_POINT ( 'NONE',  ( -10.81492255796105439, 18.62759615963255655, 92.91775706135236135 ) ) ;
#41607 = CARTESIAN_POINT ( 'NONE',  ( -14.29746914071037622, -8.314922557961029526, 49.16775706135234003 ) ) ;
#41608 = CARTESIAN_POINT ( 'NONE',  ( 21.55341960407619695, -5.719274019375665929, 76.04275706135237556 ) ) ;
#41609 = CARTESIAN_POINT ( 'NONE',  ( 16.46253265017160672, -9.564922557960803928, 98.33224293864769550 ) ) ;
#41610 = CARTESIAN_POINT ( 'NONE',  ( -16.51473224551082808, 9.474510206698731452, 83.33442372801899012 ) ) ;
#41611 = CARTESIAN_POINT ( 'NONE',  ( 21.53943276465977519, 0.05219959533937863772, 61.25109039468567573 ) ) ;
#41612 = CARTESIAN_POINT ( 'NONE',  ( 5.049401038297881783, 19.05341960407617563, 112.2927570613523471 ) ) ;
#41613 = CARTESIAN_POINT ( 'NONE',  ( 16.51473224551083163, -9.474510206698727899, 80.83442372801899012 ) ) ;
#41614 = CARTESIAN_POINT ( 'NONE',  ( 0.05219959533909260263, 19.03943276465977164, 54.99890960531435979 ) ) ;
#41615 = CARTESIAN_POINT ( 'NONE',  ( 19.05341960407617918, -5.049401038297876454, 91.04275706135234714 ) ) ;
#41616 = CARTESIAN_POINT ( 'NONE',  ( -8.314922557960811034, -14.29746914071050412, 27.08224293864769550 ) ) ;
#41617 = CARTESIAN_POINT ( 'NONE',  ( 9.474510206698729675, 16.51473224551082808, 92.08442372801900433 ) ) ;
#41618 = CARTESIAN_POINT ( 'NONE',  ( 16.52544592524342804, -4.483927247898539470, 43.54057627198103830 ) ) ;
#41619 = EDGE_CURVE ( 'NONE', #153939, #132628, #118873, .T. ) ;
#41620 = CARTESIAN_POINT ( 'NONE',  ( -19.03943276465977164, -0.05219959533935918106, 63.75109039468566863 ) ) ;
#41621 = CARTESIAN_POINT ( 'NONE',  ( -4.483927247898782831, 16.52544592524335698, 47.70942372801902565 ) ) ;
#41622 = CARTESIAN_POINT ( 'NONE',  ( 5.153800228976615827, -19.02544592524334988, 30.20942372801900433 ) ) ;
#41623 = CARTESIAN_POINT ( 'NONE',  ( -0.05219959533909027116, -19.03943276465977164, 27.49890960531435624 ) ) ;
#41624 = CARTESIAN_POINT ( 'NONE',  ( -5.153800228976328057, -19.02544592524343514, 47.29057627198102409 ) ) ;
#41625 = CARTESIAN_POINT ( 'NONE',  ( -4.379528057220086978, -16.55341960407618274, 44.79275706135234714 ) ) ;
#41626 = CARTESIAN_POINT ( 'NONE',  ( 8.906447517083050158, 27.41122689804195645, 139.6500000054623740 ) ) ;
#41627 = CARTESIAN_POINT ( 'NONE',  ( 1.784210473542230573E-15, -29.16686587814331588, 147.3750000027311842 ) ) ;
#41628 = CARTESIAN_POINT ( 'NONE',  ( -0.05219959533909027116, -19.03943276465977164, 87.49890960531436690 ) ) ;
#41629 = CARTESIAN_POINT ( 'NONE',  ( 9.564922557961047289, -16.46253265017146816, 85.41775706135233293 ) ) ;
#41630 = VERTEX_POINT ( 'NONE', #122815 ) ;
#41631 = CARTESIAN_POINT ( 'NONE',  ( -9.564922557961040184, 16.46253265017147172, 102.9177570613523329 ) ) ;
#41632 = CARTESIAN_POINT ( 'NONE',  ( -15.80617190586745835, -15.72974639402198527, 31.87390960531435979 ) ) ;
#41634 = CARTESIAN_POINT ( 'NONE',  ( 19.03943276465977164, 0.05219959533936151252, 111.2510903946856757 ) ) ;
#41633 = CARTESIAN_POINT ( 'NONE',  ( 9.474510206698729675, 16.51473224551082808, 27.08442372801900433 ) ) ;
#41635 = CARTESIAN_POINT ( 'NONE',  ( -12.06949235617756955, 12.14591786802309770, 105.6239096053143669 ) ) ;
#41636 = CARTESIAN_POINT ( 'NONE',  ( -9.564922557960796823, -16.46253265017161027, 37.08224293864768839 ) ) ;
#41637 = CARTESIAN_POINT ( 'NONE',  ( 21.53943276465977519, -0.05219959533907433946, 68.74890960531435269 ) ) ;
#41638 = CARTESIAN_POINT ( 'NONE',  ( 5.153800228976335163, 19.02544592524342804, 39.79057627198100988 ) ) ;
#41639 = CARTESIAN_POINT ( 'NONE',  ( 17.81289503416611453, -24.51734667627695785, 142.9500000054624138 ) ) ;
#41640 = CARTESIAN_POINT ( 'NONE',  ( 0.05219959533936267826, -19.03943276465977164, 65.00109039468567573 ) ) ;
#41641 = CARTESIAN_POINT ( 'NONE',  ( 14.34966873604960469, 8.224510206698951720, 59.16557627198103120 ) ) ;
#41642 = CARTESIAN_POINT ( 'NONE',  ( 21.52544592524344225, -5.823673210054117533, 33.54057627198102409 ) ) ;
#41643 = CARTESIAN_POINT ( 'NONE',  ( 21.52544592524334988, 5.823673210054432836, 96.45942372801901854 ) ) ;
#41644 = CARTESIAN_POINT ( 'NONE',  ( 10.72451020669898902, -18.67979575497178502, 77.91557627198102409 ) ) ;
#41645 = CARTESIAN_POINT ( 'NONE',  ( 21.52544592524334988, 5.823673210054432836, 76.45942372801901854 ) ) ;
#41646 = CARTESIAN_POINT ( 'NONE',  ( -21.53943276465977519, -0.05219959533937600094, 58.75109039468568994 ) ) ;
#41647 = EDGE_CURVE ( 'NONE', #99233, #122084, #181060, .T. ) ;
#41648 = CARTESIAN_POINT ( 'NONE',  ( -16.51473224551069308, -9.474510206698971260, 101.6655762719810241 ) ) ;
#41650 = CARTESIAN_POINT ( 'NONE',  ( -15.80617190586768217, 15.72974639402176855, 68.12609039468567573 ) ) ;
#41649 = CARTESIAN_POINT ( 'NONE',  ( -12.14591786802326823, 12.06949235617739902, 93.12609039468568994 ) ) ;
#41651 = CARTESIAN_POINT ( 'NONE',  ( -13.97604488694527625, -13.89961937509977652, 51.87390960531436690 ) ) ;
#41652 = CARTESIAN_POINT ( 'NONE',  ( 18.67979575497194134, -10.72451020669871369, 30.83442372801902209 ) ) ;
#41653 = CARTESIAN_POINT ( 'NONE',  ( 19.03943276465977164, -0.05219959533909143690, 73.74890960531435269 ) ) ;
#41654 = CARTESIAN_POINT ( 'NONE',  ( -16.53943276465976808, 0.05219959533911058130, 76.24890960531435269 ) ) ;
#41655 = CARTESIAN_POINT ( 'NONE',  ( 14.34966873604960469, 8.224510206698951720, 44.16557627198103120 ) ) ;
#41656 = CARTESIAN_POINT ( 'NONE',  ( 21.53943276465977519, -0.05219959533907433946, 63.74890960531435979 ) ) ;
#41657 = ADVANCED_FACE ( 'NONE', ( #64138 ), #47985, .F. ) ;
#41658 = CARTESIAN_POINT ( 'NONE',  ( -0.05219959533909027116, -19.03943276465977164, 42.49890960531435269 ) ) ;
#41659 = CARTESIAN_POINT ( 'NONE',  ( 15.72974639402199770, -15.80617190586745480, 58.12390960531435979 ) ) ;
#41660 = CARTESIAN_POINT ( 'NONE',  ( 0.05219959533936267826, -19.03943276465977164, 50.00109039468566863 ) ) ;
#41662 = CARTESIAN_POINT ( 'NONE',  ( 14.29746914071049879, -8.314922557960816363, 58.33224293864768839 ) ) ;
#41661 = CARTESIAN_POINT ( 'NONE',  ( -5.049401038297874678, -19.05341960407618274, 24.79275706135234358 ) ) ;
#41663 = CARTESIAN_POINT ( 'NONE',  ( 0.05219959533907565091, 21.53943276465977519, 34.99890960531435979 ) ) ;
#41664 = EDGE_LOOP ( 'NONE', ( #143970, #36736, #164631, #100931, #160815 ) ) ;
#41665 = CARTESIAN_POINT ( 'NONE',  ( 17.05116617787824396, 6.768360034955816396, 103.8432444674080273 ) ) ;
#41666 = CARTESIAN_POINT ( 'NONE',  ( -16.55341960407617563, 4.379528057220093196, 83.54275706135234714 ) ) ;
#41667 = CARTESIAN_POINT ( 'NONE',  ( -16.46253265017146816, -9.564922557961047289, 84.16775706135233293 ) ) ;
#41668 = CARTESIAN_POINT ( 'NONE',  ( -16.53943276465976808, 0.05219959533911058130, 56.24890960531436690 ) ) ;
#41669 = DIRECTION ( 'NONE',  ( 0.000000000000000000, 0.000000000000000000, 1.000000000000000000 ) ) ;
#41670 = CARTESIAN_POINT ( 'NONE',  ( 19.02544592524343514, -5.153800228976328945, 53.54057627198102409 ) ) ;
#41671 = CARTESIAN_POINT ( 'NONE',  ( 0.05219959533910956823, 16.53943276465976808, 39.99890960531436690 ) ) ;
#41672 = CARTESIAN_POINT ( 'NONE',  ( 5.153800228976335163, 19.02544592524342804, 94.79057627198103830 ) ) ;
#41673 = CARTESIAN_POINT ( 'NONE',  ( 9.474510206698971260, -16.51473224551069308, 47.91557627198102409 ) ) ;
#41674 = CARTESIAN_POINT ( 'NONE',  ( -21.55341960407619339, 5.719274019375674811, 63.54275706135234003 ) ) ;
#41675 = CARTESIAN_POINT ( 'NONE',  ( -16.46253265017160317, 9.564922557960807481, 75.83224293864769550 ) ) ;
#41676 = CARTESIAN_POINT ( 'NONE',  ( 13.89961937509977652, -13.97604488694527269, 28.12390960531435624 ) ) ;
#41677 = CARTESIAN_POINT ( 'NONE',  ( 19.03943276465977164, -0.05219959533909143690, 63.74890960531435979 ) ) ;
#41678 = CARTESIAN_POINT ( 'NONE',  ( 15.72974639402199770, -15.80617190586745480, 53.12390960531436690 ) ) ;
#41679 = VECTOR ( 'NONE', #181068, 1000.000000000000000 ) ;
#41680 = CARTESIAN_POINT ( 'NONE',  ( -13.89961937509977652, 13.97604488694528158, 35.62390960531435269 ) ) ;
#41681 = CARTESIAN_POINT ( 'NONE',  ( 21.53943276465977519, -0.05219959533907433946, 38.74890960531435979 ) ) ;
#41682 = CARTESIAN_POINT ( 'NONE',  ( -12.14591786802326823, 12.06949235617739902, 108.1260903946856757 ) ) ;
#41683 = CARTESIAN_POINT ( 'NONE',  ( -21.55341960407619339, 5.719274019375674811, 113.5427570613523756 ) ) ;
#41685 = CARTESIAN_POINT ( 'NONE',  ( 4.483927247898790824, -16.52544592524335698, 80.20942372801901854 ) ) ;
#41684 = CARTESIAN_POINT ( 'NONE',  ( -16.53943276465976808, -0.05219959533934237506, 48.75109039468568284 ) ) ;
#41686 = CARTESIAN_POINT ( 'NONE',  ( 20.43538597629128262, -20.43538597629122222, -64.92279855667830191 ) ) ;
#41687 = CARTESIAN_POINT ( 'NONE',  ( -14.34966873604972548, 8.224510206698743886, 68.33442372801900433 ) ) ;
#41688 = CARTESIAN_POINT ( 'NONE',  ( -16.53943276465976808, -0.05219959533934237506, 58.75109039468568994 ) ) ;
#41689 = CARTESIAN_POINT ( 'NONE',  ( -0.05219959533909027116, -19.03943276465977164, 102.4989096053143669 ) ) ;
#41690 = CARTESIAN_POINT ( 'NONE',  ( 9.564922557960805705, 16.46253265017160317, 29.58224293864769550 ) ) ;
#41691 = CARTESIAN_POINT ( 'NONE',  ( 12.06949235617739724, 12.14591786802326823, 41.87609039468568284 ) ) ;
#41692 = CARTESIAN_POINT ( 'NONE',  ( -13.89961937509977652, 13.97604488694528158, 50.62390960531435979 ) ) ;
#41693 = CARTESIAN_POINT ( 'NONE',  ( -21.53943276465977519, -0.05219959533937600094, 28.75109039468567929 ) ) ;
#41694 = CARTESIAN_POINT ( 'NONE',  ( -16.55341960407617563, 4.379528057220093196, 33.54275706135234714 ) ) ;
#41695 = CARTESIAN_POINT ( 'NONE',  ( -14.29746914071037622, -8.314922557961029526, 99.16775706135234714 ) ) ;
#41696 = DIRECTION ( 'NONE',  ( -0.4999999999999966693, 0.5000000000000018874, 0.7071067811865484609 ) ) ;
#41697 = CARTESIAN_POINT ( 'NONE',  ( 21.53943276465977519, 0.05219959533937863772, 101.2510903946856757 ) ) ;
#41698 = CARTESIAN_POINT ( 'NONE',  ( -5.153800228976607833, 19.02544592524334988, 102.7094237280189759 ) ) ;
#41699 = CARTESIAN_POINT ( 'NONE',  ( 14.29746914071049879, -8.314922557960816363, 63.33224293864770260 ) ) ;
#41700 = CARTESIAN_POINT ( 'NONE',  ( 16.51473224551069308, 9.474510206698969483, 29.16557627198103475 ) ) ;
#41702 = CARTESIAN_POINT ( 'NONE',  ( 16.21995358207276894, -7.366697692864364377, 57.43551001512073384 ) ) ;
#41701 = CARTESIAN_POINT ( 'NONE',  ( 19.05341960407617918, -5.049401038297876454, 66.04275706135233293 ) ) ;
#41703 = CARTESIAN_POINT ( 'NONE',  ( 5.719274019375673035, 21.55341960407619339, 67.29275706135234714 ) ) ;
#41704 = CARTESIAN_POINT ( 'NONE',  ( -12.14591786802326823, 12.06949235617739902, 23.12609039468567573 ) ) ;
#41705 = CARTESIAN_POINT ( 'NONE',  ( -17.60769864724391098, 5.499999999999987566, 63.65024842019166584 ) ) ;
#41706 = CARTESIAN_POINT ( 'NONE',  ( 5.153800228976335163, 19.02544592524342804, 114.7905762719810241 ) ) ;
#41707 = CARTESIAN_POINT ( 'NONE',  ( -9.474510206698720793, -16.51473224551083518, 109.5844237280190043 ) ) ;
#41708 = CARTESIAN_POINT ( 'NONE',  ( -9.474510206698964154, 16.51473224551069663, 115.4155762719810241 ) ) ;
#41709 = CARTESIAN_POINT ( 'NONE',  ( -21.35462415990330953, 10.43496131973800090, 170.3924512066482748 ) ) ;
#41710 = CARTESIAN_POINT ( 'NONE',  ( -13.97604488694527625, -13.89961937509977652, 21.87390960531435979 ) ) ;
#41711 = CARTESIAN_POINT ( 'NONE',  ( 18.62759615963255655, 10.81492255796105972, 101.6677570613523613 ) ) ;
#41712 = CARTESIAN_POINT ( 'NONE',  ( -13.97604488694527625, -13.89961937509977652, 36.87390960531436690 ) ) ;
#41713 = CARTESIAN_POINT ( 'NONE',  ( -5.719274019375665041, -21.55341960407619695, 49.79275706135234714 ) ) ;
#41714 = CARTESIAN_POINT ( 'NONE',  ( -15.72974639402176322, -15.80617190586768395, 99.37609039468568994 ) ) ;
#41715 = CARTESIAN_POINT ( 'NONE',  ( -14.34966873604972548, 8.224510206698743886, 108.3344237280190185 ) ) ;
#41717 = B_SPLINE_CURVE_WITH_KNOTS ( 'NONE', 3,
 ( #195606, #13545, #44882, #165255, #121706, #26749, #120711, #57079, #118753, #88388, #183399, #168215, #166250, #41914, #27750, #61025, #89393, #29712, #12572, #74238, #91344, #14535, #90375, #135907, #197578, #59045, #137875, #105554, #136882, #198568, #167240, #156019 ),
 .UNSPECIFIED., .F., .F.,
 ( 4, 2, 2, 2, 2, 2, 2, 2, 2, 2, 2, 2, 2, 2, 2, 4 ),
 ( 1.684111863762029156E-17, 0.0003712461730037040710, 0.0007424923460073912284, 0.001113738519011078657, 0.001484984692014765760, 0.002227477038022137798, 0.002598723211025810373, 0.002969969384029482080, 0.003341215557033154655, 0.003712461730036826363, 0.004083707903040498070, 0.004454954076044169778, 0.004826200249047842353, 0.005197446422051514060, 0.005568692595055185768, 0.005939938768058857475 ),
 .UNSPECIFIED. ) ;
#41716 = CARTESIAN_POINT ( 'NONE',  ( 9.564922557960805705, 16.46253265017160317, 79.58224293864769550 ) ) ;
#41718 = CARTESIAN_POINT ( 'NONE',  ( -10.81492255796105439, 18.62759615963255655, 62.91775706135236135 ) ) ;
#41719 = CARTESIAN_POINT ( 'NONE',  ( -21.55341960407619339, 5.719274019375674811, 48.54275706135234714 ) ) ;
#41721 = CARTESIAN_POINT ( 'NONE',  ( -13.97604488694527625, -13.89961937509977652, 91.87390960531432427 ) ) ;
#41720 = CARTESIAN_POINT ( 'NONE',  ( -13.97604488694547697, 13.89961937509957934, 83.12609039468564731 ) ) ;
#41722 = CARTESIAN_POINT ( 'NONE',  ( 12.14591786802309770, 12.06949235617756955, 114.3739096053143527 ) ) ;
#41723 = CARTESIAN_POINT ( 'NONE',  ( -21.52544592524343514, 5.823673210054127303, 96.04057627198102409 ) ) ;
#41724 = CARTESIAN_POINT ( 'NONE',  ( -9.474510206698720793, -16.51473224551083518, 24.58442372801900078 ) ) ;
#41725 = CARTESIAN_POINT ( 'NONE',  ( -4.483927247898539470, -16.52544592524342804, 92.29057627198103830 ) ) ;
#41726 = CARTESIAN_POINT ( 'NONE',  ( -5.153800228976328057, -19.02544592524343514, 52.29057627198100988 ) ) ;
#41727 = CARTESIAN_POINT ( 'NONE',  ( 19.05341960407617918, -5.049401038297876454, 81.04275706135231871 ) ) ;
#41728 = CARTESIAN_POINT ( 'NONE',  ( -16.53943276465976808, 0.05219959533911058130, 51.24890960531436690 ) ) ;
#41729 = CARTESIAN_POINT ( 'NONE',  ( 10.72451020669871369, 18.67979575497193778, 107.0844237280190043 ) ) ;
#41730 = CARTESIAN_POINT ( 'NONE',  ( -13.97604488694527625, -13.89961937509977652, 106.8739096053143669 ) ) ;
#41731 = CARTESIAN_POINT ( 'NONE',  ( 16.51473224551083163, -9.474510206698727899, 80.83442372801899012 ) ) ;
#41732 = CARTESIAN_POINT ( 'NONE',  ( 10.72451020669898902, -18.67979575497178502, 82.91557627198103830 ) ) ;
#41733 = CARTESIAN_POINT ( 'NONE',  ( -10.72451020669870658, -18.67979575497194134, 34.58442372801900433 ) ) ;
#41734 = CARTESIAN_POINT ( 'NONE',  ( -8.314922557961024197, 14.29746914071037800, 27.91775706135234358 ) ) ;
#41735 = CARTESIAN_POINT ( 'NONE',  ( -8.314922557961024197, 14.29746914071037800, 92.91775706135236135 ) ) ;
#41737 = CARTESIAN_POINT ( 'NONE',  ( 15.72974639402176855, 15.80617190586768217, 36.87609039468568994 ) ) ;
#41736 = CARTESIAN_POINT ( 'NONE',  ( 17.49999999999999289, 5.624438216177601646, 61.68329655085356222 ) ) ;
#41738 = CARTESIAN_POINT ( 'NONE',  ( -5.823673210054116645, -21.52544592524344225, 37.29057627198102409 ) ) ;
#41739 = CARTESIAN_POINT ( 'NONE',  ( -8.224510206698948167, 14.34966873604960824, 110.4155762719810383 ) ) ;
#41740 = CARTESIAN_POINT ( 'NONE',  ( -11.40812507854754720, -35.11059874428192273, -2.724999997268813257 ) ) ;
#41741 = CARTESIAN_POINT ( 'NONE',  ( -14.34966873604972548, 8.224510206698743886, 63.33442372801900433 ) ) ;
#41742 = CARTESIAN_POINT ( 'NONE',  ( -12.06949235617756955, 12.14591786802309770, 90.62390960531436690 ) ) ;
#41743 = CARTESIAN_POINT ( 'NONE',  ( -18.62759615963270932, 10.81492255796079327, 85.83224293864768129 ) ) ;
#41744 = CARTESIAN_POINT ( 'NONE',  ( 12.06949235617757843, -12.14591786802309237, 23.12390960531436335 ) ) ;
#41745 = CARTESIAN_POINT ( 'NONE',  ( -12.14591786802326823, 12.06949235617739902, 48.12609039468568284 ) ) ;
#41746 = CARTESIAN_POINT ( 'NONE',  ( -0.05219959533909027116, -19.03943276465977164, 52.49890960531436690 ) ) ;
#41747 = CARTESIAN_POINT ( 'NONE',  ( -8.314922557961024197, 14.29746914071037800, 87.91775706135234714 ) ) ;
#41748 = CARTESIAN_POINT ( 'NONE',  ( 5.153800228976615827, -19.02544592524334988, 85.20942372801900433 ) ) ;
#41749 = CARTESIAN_POINT ( 'NONE',  ( -18.62759615963270932, 10.81492255796079327, 85.83224293864768129 ) ) ;
#41750 = CARTESIAN_POINT ( 'NONE',  ( 16.52544592524335698, 4.483927247898782831, 106.4594237280190328 ) ) ;
#41751 = ORIENTED_EDGE ( 'NONE', *, *, #94101, .T. ) ;
#41752 = CARTESIAN_POINT ( 'NONE',  ( -21.53943276465977519, 0.05219959533907696930, 66.24890960531436690 ) ) ;
#41753 = CARTESIAN_POINT ( 'NONE',  ( 16.55341960407618274, -4.379528057220086978, 96.04275706135236135 ) ) ;
#41754 = ORIENTED_EDGE ( 'NONE', *, *, #41507, .T. ) ;
#41755 = CARTESIAN_POINT ( 'NONE',  ( 5.823673210054125526, 21.52544592524343514, 24.79057627198103120 ) ) ;
#41756 = CARTESIAN_POINT ( 'NONE',  ( 22.80000000000002913, -8.654466842953076985E-14, -64.92279855667830191 ) ) ;
#41757 = CARTESIAN_POINT ( 'NONE',  ( 10.72451020669898902, -18.67979575497178502, 92.91557627198103830 ) ) ;
#41758 = CARTESIAN_POINT ( 'NONE',  ( -4.483927247898782831, 16.52544592524335698, 112.7094237280190328 ) ) ;
#41759 = CARTESIAN_POINT ( 'NONE',  ( 8.314922557961029526, -14.29746914071037800, 40.41775706135234714 ) ) ;
#41760 = CARTESIAN_POINT ( 'NONE',  ( 19.05341960407611168, 5.049401038298154454, 38.95724293864767418 ) ) ;
#41761 = CARTESIAN_POINT ( 'NONE',  ( 12.14591786802327356, -12.06949235617739191, 35.62609039468568994 ) ) ;
#41762 = CARTESIAN_POINT ( 'NONE',  ( 13.97604488694527802, 13.89961937509977652, 54.37390960531435979 ) ) ;
#41763 = CARTESIAN_POINT ( 'NONE',  ( 17.14385361876520264, -23.59649016807271238, 140.0750000027311728 ) ) ;
#41764 = CARTESIAN_POINT ( 'NONE',  ( 16.51473224551069308, 9.474510206698969483, 109.1655762719810383 ) ) ;
#41765 = CARTESIAN_POINT ( 'NONE',  ( -19.03943276465977164, 0.05219959533909376836, 116.2489096053143669 ) ) ;
#41766 = CARTESIAN_POINT ( 'NONE',  ( 4.483927247898790824, -16.52544592524335698, 105.2094237280190328 ) ) ;
#41767 = CARTESIAN_POINT ( 'NONE',  ( 16.51473224551083163, -9.474510206698727899, 95.83442372801900433 ) ) ;
#41768 = CARTESIAN_POINT ( 'NONE',  ( 5.049401038297881783, 19.05341960407617563, 37.29275706135232582 ) ) ;
#41769 = CARTESIAN_POINT ( 'NONE',  ( 21.55341960407610458, 5.719274019375980345, 73.95724293864769550 ) ) ;
#41770 = CARTESIAN_POINT ( 'NONE',  ( -4.379528057220086978, -16.55341960407618274, 104.7927570613523898 ) ) ;
#41771 = CARTESIAN_POINT ( 'NONE',  ( 10.81492255796078972, 18.62759615963270932, 34.58224293864770260 ) ) ;
#41772 = CARTESIAN_POINT ( 'NONE',  ( 13.89961937509957401, 13.97604488694547697, 101.8760903946856331 ) ) ;
#41773 = CARTESIAN_POINT ( 'NONE',  ( 5.153800228976335163, 19.02544592524342804, 109.7905762719810099 ) ) ;
#41774 = CARTESIAN_POINT ( 'NONE',  ( -18.67979575497193778, 10.72451020669871902, 58.33442372801901143 ) ) ;
#41775 = CARTESIAN_POINT ( 'NONE',  ( 13.89961937509977652, -13.97604488694527269, 58.12390960531436690 ) ) ;
#41776 = CARTESIAN_POINT ( 'NONE',  ( 0.05219959533910956823, 16.53943276465976808, 94.99890960531436690 ) ) ;
#41777 = CARTESIAN_POINT ( 'NONE',  ( 0.000000000000000000, -105.0000000000000000, 12.00000000000000355 ) ) ;
#41778 = CARTESIAN_POINT ( 'NONE',  ( -12.14591786802309592, -12.06949235617757132, 81.87390960531435269 ) ) ;
#41779 = CARTESIAN_POINT ( 'NONE',  ( 21.52544592524344225, -5.823673210054117533, 78.54057627198103830 ) ) ;
#41780 = ORIENTED_EDGE ( 'NONE', *, *, #16626, .T. ) ;
#41781 = CARTESIAN_POINT ( 'NONE',  ( 9.564922557961047289, -16.46253265017146816, 85.41775706135233293 ) ) ;
#41782 = CARTESIAN_POINT ( 'NONE',  ( 18.89770734986048595, 5.499999999999949374, 91.60214472496640781 ) ) ;
#41783 = CARTESIAN_POINT ( 'NONE',  ( -16.51473224551069308, -9.474510206698971260, 66.66557627198102409 ) ) ;
#41784 = CARTESIAN_POINT ( 'NONE',  ( 17.50000000001358913, -5.500000000000039968, 73.29690382535059712 ) ) ;
#41786 = CARTESIAN_POINT ( 'NONE',  ( -5.153800228976328057, -19.02544592524343514, 87.29057627198103830 ) ) ;
#41785 = CARTESIAN_POINT ( 'NONE',  ( -13.89961937509977652, 13.97604488694528158, 80.62390960531436690 ) ) ;
#41787 = CARTESIAN_POINT ( 'NONE',  ( 16.52544592524335698, 4.483927247898782831, 66.45942372801903275 ) ) ;
#41788 = CARTESIAN_POINT ( 'NONE',  ( -17.40861289039001747, -6.110651285853280434, 51.37232470827432707 ) ) ;
#41789 = CARTESIAN_POINT ( 'NONE',  ( -13.89961937509957401, -13.97604488694547875, 49.37609039468567573 ) ) ;
#41790 = DIRECTION ( 'NONE',  ( 1.000000000000000000, 0.000000000000000000, 0.000000000000000000 ) ) ;
#41791 = CARTESIAN_POINT ( 'NONE',  ( -19.02544592524342804, 5.153800228976336051, 106.0405762719810241 ) ) ;
#41792 = CARTESIAN_POINT ( 'NONE',  ( -8.224510206698735004, -14.34966873604973081, 104.5844237280190185 ) ) ;
#41793 = CARTESIAN_POINT ( 'NONE',  ( -35.02204707441116938, -5.958053119633060390, 40.41886734368969059 ) ) ;
#41794 = CARTESIAN_POINT ( 'NONE',  ( 4.483927247898790824, -16.52544592524335698, 95.20942372801903275 ) ) ;
#41795 = CYLINDRICAL_SURFACE ( 'NONE', #77586, 2.000000000000001776 ) ;
#41796 = CARTESIAN_POINT ( 'NONE',  ( -4.379528057220086978, -16.55341960407618274, 69.79275706135234714 ) ) ;
#41797 = CARTESIAN_POINT ( 'NONE',  ( 1.300000000000000044, 0.7216878364870328300, -1.250000000000000000 ) ) ;
#41798 = CARTESIAN_POINT ( 'NONE',  ( -5.823673210054431948, 21.52544592524334988, 67.70942372801901854 ) ) ;
#41799 = CARTESIAN_POINT ( 'NONE',  ( 13.97604488694548053, -13.89961937509957401, 90.62609039468567573 ) ) ;
#41800 = CARTESIAN_POINT ( 'NONE',  ( -9.474510206698720793, -16.51473224551083518, 24.58442372801900078 ) ) ;
#41801 = CARTESIAN_POINT ( 'NONE',  ( -5.049401038298153566, 19.05341960407611168, 60.20724293864768129 ) ) ;
#41802 = CARTESIAN_POINT ( 'NONE',  ( 19.02544592524343514, -5.153800228976328945, 43.54057627198103120 ) ) ;
#41803 = CARTESIAN_POINT ( 'NONE',  ( -14.64368186514533932, -37.22806287882965393, -11.21878843496574518 ) ) ;
#41804 = CARTESIAN_POINT ( 'NONE',  ( 5.719274019375991003, -21.55341960407610458, 82.70724293864770971 ) ) ;
#41805 = CARTESIAN_POINT ( 'NONE',  ( -5.719274019375978568, 21.55341960407610458, 30.20724293864769550 ) ) ;
#41806 = CARTESIAN_POINT ( 'NONE',  ( -9.564922557960796823, -16.46253265017161027, 37.08224293864768839 ) ) ;
#41807 = CARTESIAN_POINT ( 'NONE',  ( -4.483927247898782831, 16.52544592524335698, 52.70942372801902565 ) ) ;
#41808 = ORIENTED_EDGE ( 'NONE', *, *, #145235, .F. ) ;
#41809 = CARTESIAN_POINT ( 'NONE',  ( -15.80617190586768217, 15.72974639402176855, 33.12609039468569705 ) ) ;
#41811 = CARTESIAN_POINT ( 'NONE',  ( -30.74264578624800492, 22.33583958711400186, -0.1999999999999999001 ) ) ;
#41810 = CARTESIAN_POINT ( 'NONE',  ( 14.29746914071049879, -8.314922557960816363, 53.33224293864769550 ) ) ;
#41812 = CARTESIAN_POINT ( 'NONE',  ( 12.14591786802327356, -12.06949235617739191, 25.62609039468567929 ) ) ;
#41813 = CARTESIAN_POINT ( 'NONE',  ( -19.05341960407617563, 5.049401038297882671, 33.54275706135231871 ) ) ;
#41814 = CARTESIAN_POINT ( 'NONE',  ( 0.05219959533910956823, 16.53943276465976808, 54.99890960531435269 ) ) ;
#41815 = CARTESIAN_POINT ( 'NONE',  ( -18.67979575497178146, -10.72451020669898902, 111.6655762719810525 ) ) ;
#41817 = CARTESIAN_POINT ( 'NONE',  ( 21.52544592524344225, -5.823673210054117533, 78.54057627198103830 ) ) ;
#41816 = CARTESIAN_POINT ( 'NONE',  ( 1.300000000000000044, -0.7216878364870318308, 1.249999999999999778 ) ) ;
#41818 = CARTESIAN_POINT ( 'NONE',  ( -16.51473224551069308, -9.474510206698971260, 86.66557627198102409 ) ) ;
#41819 = CARTESIAN_POINT ( 'NONE',  ( -8.314922557960811034, -14.29746914071050412, 57.08224293864769550 ) ) ;
#41820 = CARTESIAN_POINT ( 'NONE',  ( -19.03943276465977164, 0.05219959533909376836, 106.2489096053143669 ) ) ;
#41821 = AXIS2_PLACEMENT_3D ( 'NONE', #91110, #88149, #26506 ) ;
#41822 = CARTESIAN_POINT ( 'NONE',  ( -37.51279278323693234, 1.941191203875217264, 39.85083793614485614 ) ) ;
#41823 = CARTESIAN_POINT ( 'NONE',  ( -9.564922557961040184, 16.46253265017147172, 62.91775706135233293 ) ) ;
#41824 = CARTESIAN_POINT ( 'NONE',  ( 18.62759615963271287, -10.81492255796078972, 108.3322429386477097 ) ) ;
#41825 = CARTESIAN_POINT ( 'NONE',  ( 13.89961937509977652, -13.97604488694527269, 53.12390960531434558 ) ) ;
#41826 = CARTESIAN_POINT ( 'NONE',  ( 5.049401038297881783, 19.05341960407617563, 47.29275706135231161 ) ) ;
#41827 = CARTESIAN_POINT ( 'NONE',  ( -19.05341960407611168, -5.049401038298163336, 21.45724293864768839 ) ) ;
#41828 = CARTESIAN_POINT ( 'NONE',  ( -15.72974639402176322, -15.80617190586768395, 59.37609039468568284 ) ) ;
#41829 = CARTESIAN_POINT ( 'NONE',  ( -17.48853670773247515, -5.747243402303015003, 71.33328700250007159 ) ) ;
#41830 = CARTESIAN_POINT ( 'NONE',  ( -8.314922557960811034, -14.29746914071050412, 37.08224293864768129 ) ) ;
#41831 = CARTESIAN_POINT ( 'NONE',  ( 5.153800228976335163, 19.02544592524342804, 54.79057627198103120 ) ) ;
#41832 = CARTESIAN_POINT ( 'NONE',  ( -18.62759615963270932, 10.81492255796079327, 75.83224293864769550 ) ) ;
#41833 = CARTESIAN_POINT ( 'NONE',  ( -5.359611314223446995E-15, 29.16686587814335496, 144.3750000027311842 ) ) ;
#41834 = CARTESIAN_POINT ( 'NONE',  ( -5.049401038298153566, 19.05341960407611168, 40.20724293864768839 ) ) ;
#41835 = ORIENTED_EDGE ( 'NONE', *, *, #132614, .F. ) ;
#41836 = CARTESIAN_POINT ( 'NONE',  ( -5.823673210054116645, -21.52544592524344225, 72.29057627198102409 ) ) ;
#41837 = ORIENTED_EDGE ( 'NONE', *, *, #61842, .F. ) ;
#41838 = CARTESIAN_POINT ( 'NONE',  ( -10.81492255796105439, 18.62759615963255655, 82.91775706135234714 ) ) ;
#41841 = CARTESIAN_POINT ( 'NONE',  ( 8.224510206698953496, -14.34966873604960469, 82.91557627198103830 ) ) ;
#41840 = CARTESIAN_POINT ( 'NONE',  ( 8.224510206698742110, 14.34966873604972548, 97.08442372801904696 ) ) ;
#41839 = CARTESIAN_POINT ( 'NONE',  ( 6.310639553377889399, -38.36010752038117033, -23.94295717418827252 ) ) ;
#41842 = ORIENTED_EDGE ( 'NONE', *, *, #19937, .F. ) ;
#41843 = CARTESIAN_POINT ( 'NONE',  ( -9.564922557960796823, -16.46253265017161027, 72.08224293864770971 ) ) ;
#41844 = VERTEX_POINT ( 'NONE', #29830 ) ;
#41845 = CARTESIAN_POINT ( 'NONE',  ( 13.97604488694548053, -13.89961937509957401, 45.62609039468566863 ) ) ;
#41846 = CARTESIAN_POINT ( 'NONE',  ( -4.483927247898782831, 16.52544592524335698, 82.70942372801900433 ) ) ;
#41847 = CARTESIAN_POINT ( 'NONE',  ( 5.049401038297881783, 19.05341960407617563, 22.29275706135233648 ) ) ;
#41848 = CARTESIAN_POINT ( 'NONE',  ( 13.89961937509977652, -13.97604488694527269, 88.12390960531438111 ) ) ;
#41849 = CARTESIAN_POINT ( 'NONE',  ( -21.52544592524343514, 5.823673210054127303, 51.04057627198103120 ) ) ;
#41850 = CARTESIAN_POINT ( 'NONE',  ( -10.59477242850411649, -90.60836494048552936, -15.00000000000000000 ) ) ;
#41851 = CARTESIAN_POINT ( 'NONE',  ( -16.46253265017160317, 9.564922557960807481, 25.83224293864769194 ) ) ;
#41852 = CARTESIAN_POINT ( 'NONE',  ( 5.719274019375673035, 21.55341960407619339, 102.2927570613523613 ) ) ;
#41853 = CARTESIAN_POINT ( 'NONE',  ( -4.379528057220086978, -16.55341960407618274, 59.79275706135234714 ) ) ;
#41854 = CARTESIAN_POINT ( 'NONE',  ( 21.53943276465977519, 0.05219959533937863772, 21.25109039468567218 ) ) ;
#41855 = CARTESIAN_POINT ( 'NONE',  ( 4.379528057220092307, 16.55341960407617563, 27.29275706135234358 ) ) ;
#41856 = CARTESIAN_POINT ( 'NONE',  ( 0.05219959533909260263, 19.03943276465977164, 89.99890960531436690 ) ) ;
#41857 = CARTESIAN_POINT ( 'NONE',  ( 13.89961937509977652, -13.97604488694527269, 38.12390960531436690 ) ) ;
#41858 = CARTESIAN_POINT ( 'NONE',  ( 13.97604488694527802, 13.89961937509977652, 54.37390960531435979 ) ) ;
#41859 = VECTOR ( 'NONE', #2927, 1000.000000000000000 ) ;
#41860 = CARTESIAN_POINT ( 'NONE',  ( -12.06949235617739369, -12.14591786802326823, 29.37609039468568284 ) ) ;
#41861 = CARTESIAN_POINT ( 'NONE',  ( 16.55341960407611168, 4.379528057220329451, 88.95724293864769550 ) ) ;
#41862 = CARTESIAN_POINT ( 'NONE',  ( -4.379528057220086978, -16.55341960407618274, 99.79275706135234714 ) ) ;
#41865 = CARTESIAN_POINT ( 'NONE',  ( -16.51473224551069308, -9.474510206698971260, 51.66557627198102409 ) ) ;
#41864 = CARTESIAN_POINT ( 'NONE',  ( -19.03943276465977164, 0.05219959533909376836, 61.24890960531436690 ) ) ;
#41863 = CARTESIAN_POINT ( 'NONE',  ( -21.53943276465977519, -0.05219959533937600094, 48.75109039468568284 ) ) ;
#41866 = CARTESIAN_POINT ( 'NONE',  ( 9.474510206698971260, -16.51473224551069308, 82.91557627198103830 ) ) ;
#41867 = CARTESIAN_POINT ( 'NONE',  ( -8.224510206698948167, 14.34966873604960824, 35.41557627198102409 ) ) ;
#41868 = CARTESIAN_POINT ( 'NONE',  ( 8.314922557961029526, -14.29746914071037800, 105.4177570613523613 ) ) ;
#41869 = EDGE_LOOP ( 'NONE', ( #151698, #146513, #85345, #78076 ) ) ;
#41870 = CARTESIAN_POINT ( 'NONE',  ( -16.51473224551082808, 9.474510206698731452, 28.33442372801900433 ) ) ;
#41871 = CARTESIAN_POINT ( 'NONE',  ( 19.02544592524343514, -5.153800228976328945, 108.5405762719810383 ) ) ;
#41872 = CARTESIAN_POINT ( 'NONE',  ( 9.564922557960805705, 16.46253265017160317, 54.58224293864769550 ) ) ;
#41873 = CARTESIAN_POINT ( 'NONE',  ( -19.05341960407617563, 5.049401038297882671, 28.54275706135232937 ) ) ;
#41874 = CARTESIAN_POINT ( 'NONE',  ( -11.40812507854754720, -35.11059874428192273, -4.224999997268813701 ) ) ;
#41875 = CARTESIAN_POINT ( 'NONE',  ( -16.55341960407617563, 4.379528057220093196, 48.54275706135234714 ) ) ;
#41877 = CARTESIAN_POINT ( 'NONE',  ( 0.05219959533934541429, -16.53943276465976808, 50.00109039468568994 ) ) ;
#41876 = CARTESIAN_POINT ( 'NONE',  ( -19.05341960407617563, 5.049401038297882671, 68.54275706135230450 ) ) ;
#41878 = CARTESIAN_POINT ( 'NONE',  ( 7.500000000000000000, 9.184850993605147944E-16, 4.292893218813446765 ) ) ;
#41879 = CARTESIAN_POINT ( 'NONE',  ( 13.89961937509977652, -13.97604488694527269, 73.12390960531436690 ) ) ;
#41880 = CARTESIAN_POINT ( 'NONE',  ( -18.62759615963270932, 10.81492255796079327, 110.8322429386476955 ) ) ;
#41881 = CARTESIAN_POINT ( 'NONE',  ( 19.05341960407617918, -5.049401038297876454, 66.04275706135233293 ) ) ;
#41883 = CARTESIAN_POINT ( 'NONE',  ( -19.02544592524342804, 5.153800228976336051, 36.04057627198100988 ) ) ;
#41882 = CARTESIAN_POINT ( 'NONE',  ( 19.02544592524343514, -5.153800228976328945, 108.5405762719810383 ) ) ;
#41884 = CARTESIAN_POINT ( 'NONE',  ( 19.03943276465977164, -0.05219959533909143690, 73.74890960531435269 ) ) ;
#41886 = CARTESIAN_POINT ( 'NONE',  ( -13.89961937509977652, 13.97604488694528158, 40.62390960531435979 ) ) ;
#41885 = CARTESIAN_POINT ( 'NONE',  ( -14.34966873604960291, -8.224510206698953496, 36.66557627198103120 ) ) ;
#41887 = CARTESIAN_POINT ( 'NONE',  ( -13.89961937509957401, -13.97604488694547875, 44.37609039468566863 ) ) ;
#41888 = CARTESIAN_POINT ( 'NONE',  ( -8.314922557960811034, -14.29746914071050412, 77.08224293864769550 ) ) ;
#41889 = CARTESIAN_POINT ( 'NONE',  ( 5.719274019375673035, 21.55341960407619339, 112.2927570613523471 ) ) ;
#41890 = CARTESIAN_POINT ( 'NONE',  ( 19.03943276465977164, -0.05219959533909143690, 58.74890960531435979 ) ) ;
#41891 = EDGE_CURVE ( 'NONE', #144280, #57253, #64929, .T. ) ;
#41892 = CARTESIAN_POINT ( 'NONE',  ( 15.72974639402199770, -15.80617190586745480, 48.12390960531436690 ) ) ;
#41894 = CARTESIAN_POINT ( 'NONE',  ( -10.72451020669870658, -18.67979575497194134, 99.58442372801900433 ) ) ;
#41893 = CARTESIAN_POINT ( 'NONE',  ( -8.224510206698948167, 14.34966873604960824, 50.41557627198103120 ) ) ;
#41895 = CARTESIAN_POINT ( 'NONE',  ( -13.89961937509977652, 13.97604488694528158, 95.62390960531436690 ) ) ;
#41896 = CARTESIAN_POINT ( 'NONE',  ( 9.564922557960805705, 16.46253265017160317, 104.5822429386476955 ) ) ;
#41897 = CARTESIAN_POINT ( 'NONE',  ( -9.474510206698964154, 16.51473224551069663, 45.41557627198103120 ) ) ;
#41898 = CARTESIAN_POINT ( 'NONE',  ( 19.02544592524343514, -5.153800228976328945, 28.54057627198102409 ) ) ;
#41899 = CARTESIAN_POINT ( 'NONE',  ( 16.52544592524342804, -4.483927247898539470, 93.54057627198103830 ) ) ;
#41900 = CARTESIAN_POINT ( 'NONE',  ( 18.62759615963271287, -10.81492255796078972, 98.33224293864769550 ) ) ;
#41901 = CARTESIAN_POINT ( 'NONE',  ( -9.564922557960796823, -16.46253265017161027, 82.08224293864768129 ) ) ;
#41902 = CARTESIAN_POINT ( 'NONE',  ( 21.55341960407610458, 5.719274019375980345, 98.95724293864770971 ) ) ;
#41903 = CARTESIAN_POINT ( 'NONE',  ( -16.46253265017160317, 9.564922557960807481, 95.83224293864769550 ) ) ;
#41905 = CARTESIAN_POINT ( 'NONE',  ( -12.06949235617756955, 12.14591786802309770, 105.6239096053143669 ) ) ;
#41904 = DIRECTION ( 'NONE',  ( 1.000000000000000000, 0.000000000000000000, -0.000000000000000000 ) ) ;
#41906 = CARTESIAN_POINT ( 'NONE',  ( 13.89961937509977652, -13.97604488694527269, 68.12390960531436690 ) ) ;
#41907 = CARTESIAN_POINT ( 'NONE',  ( 0.05219959533907565091, 21.53943276465977519, 84.99890960531436690 ) ) ;
#41908 = CARTESIAN_POINT ( 'NONE',  ( -31.28760401664904833, 6.510460035718205418, 98.73157056914054408 ) ) ;
#41909 = LINE ( 'NONE', #102573, #7551 ) ;
#41911 = DIRECTION ( 'NONE',  ( -1.000000000000000000, 0.000000000000000000, 0.000000000000000000 ) ) ;
#41910 = CARTESIAN_POINT ( 'NONE',  ( 21.53943276465977519, -0.05219959533907433946, 28.74890960531435624 ) ) ;
#41912 = CARTESIAN_POINT ( 'NONE',  ( 16.52544592524335698, 4.483927247898782831, 36.45942372801901143 ) ) ;
#41913 = CARTESIAN_POINT ( 'NONE',  ( -4.379528057220328563, 16.55341960407611168, 95.20724293864769550 ) ) ;
#41914 = CARTESIAN_POINT ( 'NONE',  ( -16.21995358207304250, -7.366697692864176084, 95.06448998487844904 ) ) ;
#41915 = CARTESIAN_POINT ( 'NONE',  ( 5.049401038298161559, -19.05341960407611168, 92.70724293864769550 ) ) ;
#41916 = CARTESIAN_POINT ( 'NONE',  ( 19.02544592524343514, -5.153800228976328945, 48.54057627198103120 ) ) ;
#41917 = CARTESIAN_POINT ( 'NONE',  ( -14.29746914071049879, 8.314922557960819915, 80.83224293864769550 ) ) ;
#41918 = CARTESIAN_POINT ( 'NONE',  ( -10.81492255796078084, -18.62759615963271287, 32.08224293864769550 ) ) ;
#41919 = CARTESIAN_POINT ( 'NONE',  ( 16.52544592524342804, -4.483927247898539470, 48.54057627198103120 ) ) ;
#41920 = CARTESIAN_POINT ( 'NONE',  ( -5.153800228976607833, 19.02544592524334988, 102.7094237280189759 ) ) ;
#41921 = CARTESIAN_POINT ( 'NONE',  ( 0.05219959533937995610, -21.53943276465977519, 65.00109039468568994 ) ) ;
#41922 = CARTESIAN_POINT ( 'NONE',  ( -8.571926809382608425, 26.38167802310805854, 146.4750000027311785 ) ) ;
#41923 = CARTESIAN_POINT ( 'NONE',  ( 5.153800228976335163, 19.02544592524342804, 94.79057627198103830 ) ) ;
#41924 = CARTESIAN_POINT ( 'NONE',  ( 8.314922557961029526, -14.29746914071037800, 85.41775706135236135 ) ) ;
#41925 = CARTESIAN_POINT ( 'NONE',  ( -19.03943276465977164, 0.05219959533909376836, 26.24890960531435624 ) ) ;
#41926 = CARTESIAN_POINT ( 'NONE',  ( 13.97604488694527802, 13.89961937509977652, 79.37390960531435269 ) ) ;
#41927 = CARTESIAN_POINT ( 'NONE',  ( -10.72451020669898014, 18.67979575497178502, 75.41557627198102409 ) ) ;
#41928 = CARTESIAN_POINT ( 'NONE',  ( 14.29746914071037800, 8.314922557961029526, 21.66775706135235069 ) ) ;
#41930 = CARTESIAN_POINT ( 'NONE',  ( -5.823673210054431948, 21.52544592524334988, 62.70942372801902565 ) ) ;
#41929 = CARTESIAN_POINT ( 'NONE',  ( -16.52544592524342804, 4.483927247898546575, 51.04057627198103120 ) ) ;
#41932 = CARTESIAN_POINT ( 'NONE',  ( 18.62759615963271287, -10.81492255796078972, 23.33224293864769194 ) ) ;
#41931 = CARTESIAN_POINT ( 'NONE',  ( 4.379528057220092307, 16.55341960407617563, 82.29275706135234714 ) ) ;
#41933 = CARTESIAN_POINT ( 'NONE',  ( 16.88567814943164791, 6.947325034625595030, 28.79001122652586631 ) ) ;
#41934 = CARTESIAN_POINT ( 'NONE',  ( -31.99364916731038022, -1.163414459189985801E-14, 95.00000000000000000 ) ) ;
#41935 = CARTESIAN_POINT ( 'NONE',  ( -12.06949235617739369, -12.14591786802326823, 109.3760903946857042 ) ) ;
#41936 = CARTESIAN_POINT ( 'NONE',  ( 16.55341960407618274, -4.379528057220086978, 66.04275706135236135 ) ) ;
#41937 = CARTESIAN_POINT ( 'NONE',  ( 0.05219959533909260263, 19.03943276465977164, 74.99890960531435269 ) ) ;
#41938 = CARTESIAN_POINT ( 'NONE',  ( 9.474510206698971260, -16.51473224551069308, 92.91557627198103830 ) ) ;
#41939 = CARTESIAN_POINT ( 'NONE',  ( 10.81492255796106328, -18.62759615963255655, 75.41775706135233293 ) ) ;
#41940 = CARTESIAN_POINT ( 'NONE',  ( 14.34966873604972726, -8.224510206698740333, 75.83442372801900433 ) ) ;
#41941 = CARTESIAN_POINT ( 'NONE',  ( -8.224510206698948167, 14.34966873604960824, 45.41557627198103830 ) ) ;
#41942 = CARTESIAN_POINT ( 'NONE',  ( 13.97604488694527802, 13.89961937509977652, 59.37390960531434558 ) ) ;
#41943 = CARTESIAN_POINT ( 'NONE',  ( -5.049401038298153566, 19.05341960407611168, 50.20724293864770260 ) ) ;
#41945 = ORIENTED_EDGE ( 'NONE', *, *, #58944, .T. ) ;
#41944 = CARTESIAN_POINT ( 'NONE',  ( 16.52544592524335698, 4.483927247898782831, 36.45942372801901143 ) ) ;
#41946 = CARTESIAN_POINT ( 'NONE',  ( 19.03943276465977164, 0.05219959533936151252, 96.25109039468567573 ) ) ;
#41947 = CARTESIAN_POINT ( 'NONE',  ( -4.483927247898539470, -16.52544592524342804, 97.29057627198105251 ) ) ;
#41948 = CARTESIAN_POINT ( 'NONE',  ( 16.46253265017160672, -9.564922557960803928, 63.33224293864769550 ) ) ;
#41950 = CARTESIAN_POINT ( 'NONE',  ( -23.48529157249600985, 32.32473071737754111, -4.299999999999999822 ) ) ;
#41949 = CARTESIAN_POINT ( 'NONE',  ( -13.89961937509957401, -13.97604488694547875, 104.3760903946856757 ) ) ;
#41951 = CARTESIAN_POINT ( 'NONE',  ( 0.05219959533937995610, -21.53943276465977519, 110.0010903946856757 ) ) ;
#41952 = CARTESIAN_POINT ( 'NONE',  ( -12.14591786802326823, 12.06949235617739902, 73.12609039468567573 ) ) ;
#41953 = CARTESIAN_POINT ( 'NONE',  ( -30.00000000000000000, -1.163414459189985801E-14, 97.65000000000000568 ) ) ;
#41954 = CARTESIAN_POINT ( 'NONE',  ( 5.719274019375991003, -21.55341960407610458, 62.70724293864769550 ) ) ;
#41955 = CARTESIAN_POINT ( 'NONE',  ( 8.224510206698742110, 14.34966873604972548, 57.08442372801901854 ) ) ;
#41956 = DIRECTION ( 'NONE',  ( 0.000000000000000000, -1.224646799151876092E-16, 1.000000000000000000 ) ) ;
#41957 = CARTESIAN_POINT ( 'NONE',  ( 5.049401038297881783, 19.05341960407617563, 62.29275706135234003 ) ) ;
#41958 = CARTESIAN_POINT ( 'NONE',  ( 16.51473224551069308, 9.474510206698969483, 94.16557627198103830 ) ) ;
#41959 = CARTESIAN_POINT ( 'NONE',  ( 0.05219959533910956823, 16.53943276465976808, 109.9989096053143527 ) ) ;
#41960 = CARTESIAN_POINT ( 'NONE',  ( 16.46253265017160672, -9.564922557960803928, 63.33224293864769550 ) ) ;
#41961 = CARTESIAN_POINT ( 'NONE',  ( 14.29746914071049879, -8.314922557960816363, 53.33224293864769550 ) ) ;
#41962 = CARTESIAN_POINT ( 'NONE',  ( 18.62759615963255655, 10.81492255796105972, 81.66775706135236135 ) ) ;
#41963 = CARTESIAN_POINT ( 'NONE',  ( -13.89961937509957401, -13.97604488694547875, 44.37609039468566863 ) ) ;
#41964 = CARTESIAN_POINT ( 'NONE',  ( -5.049401038297874678, -19.05341960407617918, 34.79275706135233293 ) ) ;
#41965 = CARTESIAN_POINT ( 'NONE',  ( -18.67979575497178146, -10.72451020669898902, 26.66557627198103475 ) ) ;
#41966 = CARTESIAN_POINT ( 'NONE',  ( -5.719274019375665041, -21.55341960407619695, 94.79275706135234714 ) ) ;
#41967 = CARTESIAN_POINT ( 'NONE',  ( -19.05341960407611168, -5.049401038298163336, 66.45724293864769550 ) ) ;
#41968 = CARTESIAN_POINT ( 'NONE',  ( -15.80617190586768217, 15.72974639402176855, 98.12609039468570415 ) ) ;
#41969 = CARTESIAN_POINT ( 'NONE',  ( -18.62759615963270932, 10.81492255796079327, 50.83224293864770971 ) ) ;
#41970 = CARTESIAN_POINT ( 'NONE',  ( -19.03943276465977164, 0.05219959533909376836, 86.24890960531436690 ) ) ;
#41971 = CARTESIAN_POINT ( 'NONE',  ( -9.564922557961040184, 16.46253265017147172, 57.91775706135233293 ) ) ;
#41972 = CARTESIAN_POINT ( 'NONE',  ( 16.51473224551069308, 9.474510206698969483, 39.16557627198103120 ) ) ;
#41973 = CARTESIAN_POINT ( 'NONE',  ( -5.153800228976328057, -19.02544592524343514, 92.29057627198099567 ) ) ;
#41974 = CARTESIAN_POINT ( 'NONE',  ( -13.97604488694547697, 13.89961937509957934, 88.12609039468563310 ) ) ;
#41975 = CARTESIAN_POINT ( 'NONE',  ( -16.52544592524335698, -4.483927247898792601, 33.95942372801901143 ) ) ;
#41976 = CARTESIAN_POINT ( 'NONE',  ( 16.55341960407611168, 4.379528057220329451, 98.95724293864770971 ) ) ;
#41977 = CARTESIAN_POINT ( 'NONE',  ( -19.05341960407611168, -5.049401038298163336, 66.45724293864769550 ) ) ;
#41978 = CARTESIAN_POINT ( 'NONE',  ( 0.05219959533907565091, 21.53943276465977519, 49.99890960531437401 ) ) ;
#41979 = AXIS2_PLACEMENT_3D ( 'NONE', #144582, #21249, #80918 ) ;
#41980 = CARTESIAN_POINT ( 'NONE',  ( -5.049401038297874678, -19.05341960407617918, 109.7927570613523187 ) ) ;
#41981 = CARTESIAN_POINT ( 'NONE',  ( 21.55341960407610458, 5.719274019375980345, 113.9572429386477239 ) ) ;
#41982 = CARTESIAN_POINT ( 'NONE',  ( 21.52544592524334988, 5.823673210054432836, 66.45942372801903275 ) ) ;
#41983 = CARTESIAN_POINT ( 'NONE',  ( 16.53943276465976808, 0.05219959533934440121, 71.25109039468568994 ) ) ;
#41984 = CARTESIAN_POINT ( 'NONE',  ( -19.02544592524342804, 5.153800228976336051, 71.04057627198099567 ) ) ;
#41985 = CARTESIAN_POINT ( 'NONE',  ( -4.379528057220086978, -16.55341960407618274, 99.79275706135234714 ) ) ;
#41986 = CARTESIAN_POINT ( 'NONE',  ( -9.564922557961040184, 16.46253265017147172, 42.91775706135234003 ) ) ;
#41987 = CARTESIAN_POINT ( 'NONE',  ( 5.823673210054444382, -21.52544592524334988, 30.20942372801902565 ) ) ;
#41988 = CARTESIAN_POINT ( 'NONE',  ( 12.06949235617757843, -12.14591786802309237, 73.12390960531436690 ) ) ;
#41989 = CARTESIAN_POINT ( 'NONE',  ( -13.89961937509977652, 13.97604488694528158, 100.6239096053143669 ) ) ;
#41990 = CARTESIAN_POINT ( 'NONE',  ( -0.05219959533934338120, 16.53943276465976808, 87.50109039468568994 ) ) ;
#41991 = CARTESIAN_POINT ( 'NONE',  ( 5.719274019375673035, 21.55341960407619339, 67.29275706135234714 ) ) ;
#41992 = CARTESIAN_POINT ( 'NONE',  ( -12.14591786802326823, 12.06949235617739902, 28.12609039468568284 ) ) ;
#41993 = CARTESIAN_POINT ( 'NONE',  ( 15.80617190586769283, -15.72974639402175789, 25.62609039468567929 ) ) ;
#41994 = CARTESIAN_POINT ( 'NONE',  ( 8.314922557960818139, 14.29746914071049879, 69.58224293864769550 ) ) ;
#41995 = ORIENTED_EDGE ( 'NONE', *, *, #31456, .F. ) ;
#41996 = CARTESIAN_POINT ( 'NONE',  ( 10.81492255796078972, 18.62759615963270932, 94.58224293864769550 ) ) ;
#41997 = CARTESIAN_POINT ( 'NONE',  ( -16.53943276465976808, 0.05219959533911058130, 56.24890960531436690 ) ) ;
#41998 = VERTEX_POINT ( 'NONE', #199678 ) ;
#41999 = CARTESIAN_POINT ( 'NONE',  ( -5.049401038298153566, 19.05341960407611168, 25.20724293864768484 ) ) ;
#42000 = CARTESIAN_POINT ( 'NONE',  ( -10.72451020669898014, 18.67979575497178502, 30.41557627198101699 ) ) ;
#42001 = CARTESIAN_POINT ( 'NONE',  ( -18.62759615963255300, -10.81492255796106328, 39.16775706135235424 ) ) ;
#42002 = CARTESIAN_POINT ( 'NONE',  ( 16.52544592524342804, -4.483927247898539470, 63.54057627198103830 ) ) ;
#42003 = AXIS2_PLACEMENT_3D ( 'NONE', #143837, #37662, #191344 ) ;
#42004 = CARTESIAN_POINT ( 'NONE',  ( -10.72451020669898014, 18.67979575497178502, 70.41557627198102409 ) ) ;
#42005 = CARTESIAN_POINT ( 'NONE',  ( 9.474510206698971260, -16.51473224551069308, 77.91557627198103830 ) ) ;
#42007 = CARTESIAN_POINT ( 'NONE',  ( -9.474510206698720793, -16.51473224551083518, 84.58442372801900433 ) ) ;
#42006 = CARTESIAN_POINT ( 'NONE',  ( -19.02544592524342804, 5.153800228976336051, 31.04057627198102409 ) ) ;
#42008 = CARTESIAN_POINT ( 'NONE',  ( 18.62759615963271287, -10.81492255796078972, 53.33224293864769550 ) ) ;
#42009 = CARTESIAN_POINT ( 'NONE',  ( 5.153800228976335163, 19.02544592524342804, 34.79057627198102409 ) ) ;
#42010 = CARTESIAN_POINT ( 'NONE',  ( 13.89961937509977652, -13.97604488694527269, 73.12390960531436690 ) ) ;
#42011 = ORIENTED_EDGE ( 'NONE', *, *, #151687, .T. ) ;
#42012 = CARTESIAN_POINT ( 'NONE',  ( 8.224510206698742110, 14.34966873604972548, 32.08442372801901854 ) ) ;
#42013 = CARTESIAN_POINT ( 'NONE',  ( -18.62759615963255300, -10.81492255796106328, 29.16775706135234003 ) ) ;
#42014 = CARTESIAN_POINT ( 'NONE',  ( 21.52544592524334988, 5.823673210054432836, 56.45942372801902565 ) ) ;
#42015 = CARTESIAN_POINT ( 'NONE',  ( 9.564922557960805705, 16.46253265017160317, 109.5822429386476955 ) ) ;
#42016 = CARTESIAN_POINT ( 'NONE',  ( -18.67979575497178146, -10.72451020669898902, 66.66557627198102409 ) ) ;
#42018 = CARTESIAN_POINT ( 'NONE',  ( 12.14591786802327356, -12.06949235617739191, 45.62609039468567573 ) ) ;
#42017 = CARTESIAN_POINT ( 'NONE',  ( 5.823673210054125526, 21.52544592524343514, 104.7905762719810241 ) ) ;
#42019 = CARTESIAN_POINT ( 'NONE',  ( -5.719274019375978568, 21.55341960407610458, 55.20724293864770260 ) ) ;
#42020 = CARTESIAN_POINT ( 'NONE',  ( 5.823673210054444382, -21.52544592524334988, 100.2094237280190043 ) ) ;
#42021 = CARTESIAN_POINT ( 'NONE',  ( -13.89961937509977652, 13.97604488694528158, 60.62390960531436690 ) ) ;
#42022 = CARTESIAN_POINT ( 'NONE',  ( 13.97604488694527802, 13.89961937509977652, 104.3739096053143385 ) ) ;
#42023 = CARTESIAN_POINT ( 'NONE',  ( -5.153800228976328057, -19.02544592524343514, 82.29057627198103830 ) ) ;
#42024 = CARTESIAN_POINT ( 'NONE',  ( 16.19135201231354415, -7.376712067591904010, 87.31319145947881566 ) ) ;
#42025 = EDGE_CURVE ( 'NONE', #23117, #188447, #67991, .T. ) ;
#42026 = CARTESIAN_POINT ( 'NONE',  ( 0.05219959533936267826, -19.03943276465977164, 65.00109039468567573 ) ) ;
#42028 = CARTESIAN_POINT ( 'NONE',  ( -18.62759615963270932, 10.81492255796079327, 40.83224293864769550 ) ) ;
#42027 = CARTESIAN_POINT ( 'NONE',  ( 16.46253265017146816, 9.564922557961045513, 21.66775706135233648 ) ) ;
#42029 = CARTESIAN_POINT ( 'NONE',  ( -14.29746914071037622, -8.314922557961029526, 99.16775706135234714 ) ) ;
#42030 = CARTESIAN_POINT ( 'NONE',  ( 0.05219959533936267826, -19.03943276465977164, 85.00109039468567573 ) ) ;
#42031 = DIRECTION ( 'NONE',  ( -0.5000000000000004441, -0.4999999999999986677, 0.7071067811865481278 ) ) ;
#42032 = CARTESIAN_POINT ( 'NONE',  ( -19.05341960407617563, 5.049401038297882671, 23.54275706135233648 ) ) ;
#42033 = CARTESIAN_POINT ( 'NONE',  ( 9.474510206698729675, 16.51473224551082808, 82.08442372801899012 ) ) ;
#42034 = CARTESIAN_POINT ( 'NONE',  ( -9.564922557961040184, 16.46253265017147172, 42.91775706135234003 ) ) ;
#42035 = CARTESIAN_POINT ( 'NONE',  ( 17.44270441346516876, 5.991230190323038940, 108.8633507926423363 ) ) ;
#42036 = CARTESIAN_POINT ( 'NONE',  ( -0.05219959533909027116, -19.03943276465977164, 37.49890960531436690 ) ) ;
#42037 = CARTESIAN_POINT ( 'NONE',  ( -4.483927247898539470, -16.52544592524342804, 47.29057627198103120 ) ) ;
#42038 = CARTESIAN_POINT ( 'NONE',  ( 19.02544592524343514, -5.153800228976328945, 33.54057627198102409 ) ) ;
#42039 = CARTESIAN_POINT ( 'NONE',  ( -16.55341960407611168, -4.379528057220339221, 41.45724293864769550 ) ) ;
#42040 = DIRECTION ( 'NONE',  ( -1.000000000000000000, 0.000000000000000000, 0.000000000000000000 ) ) ;
#42041 = CARTESIAN_POINT ( 'NONE',  ( 14.29746914071037800, 8.314922557961029526, 106.6677570613523756 ) ) ;
#42042 = CARTESIAN_POINT ( 'NONE',  ( -13.89961937509977652, 13.97604488694528158, 55.62390960531434558 ) ) ;
#42043 = CARTESIAN_POINT ( 'NONE',  ( 16.51473224551083163, -9.474510206698727899, 30.83442372801900433 ) ) ;
#42044 = CARTESIAN_POINT ( 'NONE',  ( -16.53943276465976808, -0.05219959533934237506, 38.75109039468567573 ) ) ;
#42045 = CARTESIAN_POINT ( 'NONE',  ( 15.72974639402199770, -15.80617190586745480, 43.12390960531435269 ) ) ;
#42047 = EDGE_LOOP ( 'NONE', ( #13918, #194517, #91810, #48248 ) ) ;
#42046 = CARTESIAN_POINT ( 'NONE',  ( -10.72451020669870658, -18.67979575497194134, 89.58442372801901854 ) ) ;
#42048 = CARTESIAN_POINT ( 'NONE',  ( 19.02544592524343514, -5.153800228976328945, 103.5405762719809957 ) ) ;
#42049 = CARTESIAN_POINT ( 'NONE',  ( 9.474510206698971260, -16.51473224551069308, 87.91557627198102409 ) ) ;
#42050 = CARTESIAN_POINT ( 'NONE',  ( -32.61617023573567309, -23.16041576125357082, -21.42686488341023932 ) ) ;
#42051 = CARTESIAN_POINT ( 'NONE',  ( 21.52544592524344225, -5.823673210054117533, 103.5405762719810383 ) ) ;
#42052 = CARTESIAN_POINT ( 'NONE',  ( -4.379528057220328563, 16.55341960407611168, 80.20724293864769550 ) ) ;
#42054 = CARTESIAN_POINT ( 'NONE',  ( 19.02544592524343514, -5.153800228976328945, 73.54057627198103830 ) ) ;
#42053 = CARTESIAN_POINT ( 'NONE',  ( -21.52544592524343514, 5.823673210054127303, 81.04057627198102409 ) ) ;
#42055 = CARTESIAN_POINT ( 'NONE',  ( 5.049401038298161559, -19.05341960407611168, 72.70724293864768129 ) ) ;
#42056 = CARTESIAN_POINT ( 'NONE',  ( 15.80617190586746368, 15.72974639402197994, 94.37390960531436690 ) ) ;
#42057 = VERTEX_POINT ( 'NONE', #172307 ) ;
#42058 = CARTESIAN_POINT ( 'NONE',  ( 0.05219959533909260263, 19.03943276465977164, 54.99890960531435979 ) ) ;
#42060 = DIRECTION ( 'NONE',  ( -0.9526137857479314297, -0.3041824702427711746, 0.000000000000000000 ) ) ;
#42059 = CARTESIAN_POINT ( 'NONE',  ( -16.55341960407611168, -4.379528057220339221, 96.45724293864770971 ) ) ;
#42061 = CARTESIAN_POINT ( 'NONE',  ( -5.049401038298153566, 19.05341960407611168, 65.20724293864765286 ) ) ;
#42062 = CARTESIAN_POINT ( 'NONE',  ( -16.51473224551082808, 9.474510206698731452, 78.33442372801900433 ) ) ;
#42063 = CARTESIAN_POINT ( 'NONE',  ( -0.05219959533910754901, -16.53943276465976808, 92.49890960531436690 ) ) ;
#42064 = CARTESIAN_POINT ( 'NONE',  ( 10.72451020669871369, 18.67979575497193778, 57.08442372801901854 ) ) ;
#42066 = CARTESIAN_POINT ( 'NONE',  ( 10.72451020669871369, 18.67979575497193778, 22.08442372801901143 ) ) ;
#42065 = CARTESIAN_POINT ( 'NONE',  ( 5.153800228976335163, 19.02544592524342804, 44.79057627198103830 ) ) ;
#42067 = CARTESIAN_POINT ( 'NONE',  ( 12.06949235617757843, -12.14591786802309237, 103.1239096053143811 ) ) ;
#42068 = CARTESIAN_POINT ( 'NONE',  ( 11.26676076908655766, -37.89014424912599566, -31.17854569212329707 ) ) ;
#42069 = CARTESIAN_POINT ( 'NONE',  ( 19.05341960407611168, 5.049401038298154454, 68.95724293864769550 ) ) ;
#42070 = CARTESIAN_POINT ( 'NONE',  ( 17.31728774477275579, 6.344390552232371583, 111.6809334831068270 ) ) ;
#42072 = CARTESIAN_POINT ( 'NONE',  ( -0.05219959533909027116, -19.03943276465977164, 107.4989096053143527 ) ) ;
#42071 = CARTESIAN_POINT ( 'NONE',  ( 16.46253265017146816, 9.564922557961045513, 111.6677570613523329 ) ) ;
#42073 = CARTESIAN_POINT ( 'NONE',  ( 21.52544592524334988, 5.823673210054432836, 46.45942372801901854 ) ) ;
#42074 = CARTESIAN_POINT ( 'NONE',  ( -0.05219959533909027116, -19.03943276465977164, 92.49890960531436690 ) ) ;
#42075 = CARTESIAN_POINT ( 'NONE',  ( -13.97604488694547697, 13.89961937509957934, 83.12609039468564731 ) ) ;
#42076 = CARTESIAN_POINT ( 'NONE',  ( -5.049401038298153566, 19.05341960407611168, 65.20724293864765286 ) ) ;
#42077 = CARTESIAN_POINT ( 'NONE',  ( -14.34966873604960291, -8.224510206698953496, 81.66557627198103830 ) ) ;
#42078 = CARTESIAN_POINT ( 'NONE',  ( -19.03943276465977164, 0.05219959533909376836, 101.2489096053143669 ) ) ;
#42079 = CARTESIAN_POINT ( 'NONE',  ( -12.14591786802309592, -12.06949235617757132, 76.87390960531439532 ) ) ;
#42080 = CARTESIAN_POINT ( 'NONE',  ( 5.153800228976335163, 19.02544592524342804, 104.7905762719809957 ) ) ;
#42081 = CARTESIAN_POINT ( 'NONE',  ( -19.05341960407617563, 5.049401038297882671, 48.54275706135233293 ) ) ;
#42084 = CARTESIAN_POINT ( 'NONE',  ( 9.564922557960805705, 16.46253265017160317, 24.58224293864769194 ) ) ;
#42083 = CARTESIAN_POINT ( 'NONE',  ( -0.05219959533910754901, -16.53943276465976808, 42.49890960531435979 ) ) ;
#42082 = CARTESIAN_POINT ( 'NONE',  ( 9.564922557960805705, 16.46253265017160317, 44.58224293864769550 ) ) ;
#42085 = ORIENTED_EDGE ( 'NONE', *, *, #164773, .F. ) ;
#42086 = CARTESIAN_POINT ( 'NONE',  ( 18.62759615963255655, 10.81492255796105972, 46.66775706135234714 ) ) ;
#42087 = CARTESIAN_POINT ( 'NONE',  ( -0.05219959533936034679, 19.03943276465977164, 82.50109039468567573 ) ) ;
#42088 = CARTESIAN_POINT ( 'NONE',  ( 14.34966873604960469, 8.224510206698951720, 34.16557627198102409 ) ) ;
#42089 = CARTESIAN_POINT ( 'NONE',  ( 18.67979575497178502, 10.72451020669898547, 94.16557627198103830 ) ) ;
#42090 = CARTESIAN_POINT ( 'NONE',  ( -5.719274019375978568, 21.55341960407610458, 40.20724293864769550 ) ) ;
#42091 = CARTESIAN_POINT ( 'NONE',  ( 14.34966873604960469, 8.224510206698951720, 79.16557627198103830 ) ) ;
#42092 = CARTESIAN_POINT ( 'NONE',  ( -13.97604488694527625, -13.89961937509977652, 36.87390960531436690 ) ) ;
#42093 = CARTESIAN_POINT ( 'NONE',  ( -16.53943276465976808, -0.05219959533934237506, 108.7510903946857042 ) ) ;
#42094 = CARTESIAN_POINT ( 'NONE',  ( -12.06949235617739369, -12.14591786802326823, 69.37609039468567573 ) ) ;
#42095 = CARTESIAN_POINT ( 'NONE',  ( -13.89961937509957401, -13.97604488694547875, 24.37609039468565442 ) ) ;
#42096 = CARTESIAN_POINT ( 'NONE',  ( 9.474510206698971260, -16.51473224551069308, 92.91557627198103830 ) ) ;
#42097 = CARTESIAN_POINT ( 'NONE',  ( 13.89961937509977652, -13.97604488694527269, 73.12390960531436690 ) ) ;
#42098 = CARTESIAN_POINT ( 'NONE',  ( -16.53943276465976808, -0.05219959533934237506, 78.75109039468568994 ) ) ;
#42099 = CARTESIAN_POINT ( 'NONE',  ( -0.05219959533909027116, -19.03943276465977164, 32.49890960531435979 ) ) ;
#42100 = EDGE_CURVE ( 'NONE', #70273, #130796, #105442, .T. ) ;
#42101 = CARTESIAN_POINT ( 'NONE',  ( 8.224510206698953496, -14.34966873604960469, 52.91557627198103830 ) ) ;
#42103 = CARTESIAN_POINT ( 'NONE',  ( -19.02544592524342804, 5.153800228976336051, 86.04057627198103830 ) ) ;
#42102 = CARTESIAN_POINT ( 'NONE',  ( -16.46253265017160317, 9.564922557960807481, 115.8322429386477097 ) ) ;
#42104 = CARTESIAN_POINT ( 'NONE',  ( 5.719274019375991003, -21.55341960407610458, 27.70724293864769905 ) ) ;
#42105 = CARTESIAN_POINT ( 'NONE',  ( 16.52544592524342804, -4.483927247898539470, 78.54057627198103830 ) ) ;
#42106 = B_SPLINE_CURVE_WITH_KNOTS ( 'NONE', 3,
 ( #138987, #123804, #185502, #156149, #46993, #108652, #170330, #32817, #17647, #140976, #2464, #64146, #125810, #191461, #68113, #21618, #129765, #117627, #145951, #178314, #9463, #36770, #194479, #52939, #39777, #98434, #160130, #163132, #24635, #114613, #176312, #55951 ),
 .UNSPECIFIED., .F., .F.,
 ( 4, 2, 2, 2, 2, 2, 2, 2, 2, 2, 2, 2, 2, 2, 2, 4 ),
 ( 2.625112965618923374E-17, 0.0003712461730037037999, 0.0007424923460073813621, 0.001113738519011058924, 0.001484984692014736487, 0.002227477038022089659, 0.002598723211025752260, 0.002969969384029414426, 0.003341215557033077026, 0.003712461730036739193, 0.004083707903040401793, 0.004454954076044063092, 0.004826200249047726126, 0.005197446422051388293, 0.005568692595055050459, 0.005939938768058712626 ),
 .UNSPECIFIED. ) ;
#42107 = ORIENTED_EDGE ( 'NONE', *, *, #116672, .T. ) ;
#42108 = CARTESIAN_POINT ( 'NONE',  ( -8.224510206698948167, 14.34966873604960824, 60.41557627198102409 ) ) ;
#42110 = CARTESIAN_POINT ( 'NONE',  ( 17.97182807773871360, -5.500000000000039080, 86.03038844047287625 ) ) ;
#42109 = CARTESIAN_POINT ( 'NONE',  ( -8.224510206698735004, -14.34966873604973081, 49.58442372801901143 ) ) ;
#42111 = CARTESIAN_POINT ( 'NONE',  ( -9.474510206698720793, -16.51473224551083518, 69.58442372801901854 ) ) ;
#42112 = CARTESIAN_POINT ( 'NONE',  ( -16.51473224551069308, -9.474510206698971260, 86.66557627198102409 ) ) ;
#42113 = CARTESIAN_POINT ( 'NONE',  ( -13.89961937509957401, -13.97604488694547875, 64.37609039468567573 ) ) ;
#42114 = CARTESIAN_POINT ( 'NONE',  ( -17.14385361876520619, 23.59649016807275856, 149.0750000027311728 ) ) ;
#42116 = CARTESIAN_POINT ( 'NONE',  ( -12.06949235617739369, -12.14591786802326823, 99.37609039468568994 ) ) ;
#42115 = CARTESIAN_POINT ( 'NONE',  ( -4.483927247898782831, 16.52544592524335698, 22.70942372801901499 ) ) ;
#42117 = CARTESIAN_POINT ( 'NONE',  ( -0.05219959533909027116, -19.03943276465977164, 42.49890960531435269 ) ) ;
#42118 = CARTESIAN_POINT ( 'NONE',  ( -15.72974639402197994, 15.80617190586746368, 25.62390960531435624 ) ) ;
#42119 = CARTESIAN_POINT ( 'NONE',  ( -21.55341960407619339, 5.719274019375674811, 48.54275706135234714 ) ) ;
#42120 = CARTESIAN_POINT ( 'NONE',  ( -14.29746914071037622, -8.314922557961029526, 24.16775706135235424 ) ) ;
#42122 = CARTESIAN_POINT ( 'NONE',  ( 13.97604488694527802, 13.89961937509977652, 74.37390960531436690 ) ) ;
#42121 = DIRECTION ( 'NONE',  ( -0.000000000000000000, -0.000000000000000000, 1.000000000000000000 ) ) ;
#42123 = CARTESIAN_POINT ( 'NONE',  ( -9.474510206698964154, 16.51473224551069663, 115.4155762719810241 ) ) ;
#42125 = CARTESIAN_POINT ( 'NONE',  ( 13.89961937509977652, -13.97604488694527269, 83.12390960531436690 ) ) ;
#42124 = CARTESIAN_POINT ( 'NONE',  ( 12.06949235617757843, -12.14591786802309237, 68.12390960531436690 ) ) ;
#42127 = EDGE_CURVE ( 'NONE', #199942, #99274, #157141, .T. ) ;
#42126 = CARTESIAN_POINT ( 'NONE',  ( -19.02544592524342804, 5.153800228976336051, 71.04057627198099567 ) ) ;
#42128 = CARTESIAN_POINT ( 'NONE',  ( 16.51473224551083163, -9.474510206698727899, 95.83442372801900433 ) ) ;
#42129 = CARTESIAN_POINT ( 'NONE',  ( 15.72974639402199770, -15.80617190586745480, 68.12390960531436690 ) ) ;
#42130 = CARTESIAN_POINT ( 'NONE',  ( 19.05341960407611168, 5.049401038298154454, 28.95724293864769550 ) ) ;
#42131 = CARTESIAN_POINT ( 'NONE',  ( -9.474510206698720793, -16.51473224551083518, 59.58442372801900433 ) ) ;
#42132 = CARTESIAN_POINT ( 'NONE',  ( 5.049401038298161559, -19.05341960407611168, 57.70724293864769550 ) ) ;
#42133 = CARTESIAN_POINT ( 'NONE',  ( 16.51473224551069308, 9.474510206698969483, 89.16557627198103830 ) ) ;
#42134 = ORIENTED_EDGE ( 'NONE', *, *, #152270, .F. ) ;
#42135 = CARTESIAN_POINT ( 'NONE',  ( 18.67979575497178502, 10.72451020669898547, 84.16557627198103830 ) ) ;
#42137 = CARTESIAN_POINT ( 'NONE',  ( -9.474510206698720793, -16.51473224551083518, 44.58442372801900433 ) ) ;
#42136 = CARTESIAN_POINT ( 'NONE',  ( -8.314922557960811034, -14.29746914071050412, 92.08224293864769550 ) ) ;
#42138 = CARTESIAN_POINT ( 'NONE',  ( 0.05219959533907565091, 21.53943276465977519, 69.99890960531435269 ) ) ;
#42139 = CARTESIAN_POINT ( 'NONE',  ( 15.80617190586746368, 15.72974639402197994, 74.37390960531436690 ) ) ;
#42140 = CARTESIAN_POINT ( 'NONE',  ( -14.34966873604960291, -8.224510206698953496, 31.66557627198102054 ) ) ;
#42141 = CARTESIAN_POINT ( 'NONE',  ( -5.719274019375665041, -21.55341960407619695, 109.7927570613523613 ) ) ;
#42142 = CARTESIAN_POINT ( 'NONE',  ( 16.46253265017160672, -9.564922557960803928, 73.33224293864769550 ) ) ;
#42143 = CARTESIAN_POINT ( 'NONE',  ( 13.89961937509977652, -13.97604488694527269, 38.12390960531436690 ) ) ;
#42144 = AXIS2_PLACEMENT_3D ( 'NONE', #98572, #187646, #49117 ) ;
#42145 = CARTESIAN_POINT ( 'NONE',  ( 0.05219959533937995610, -21.53943276465977519, 35.00109039468568284 ) ) ;
#42146 = CARTESIAN_POINT ( 'NONE',  ( 10.81492255796106328, -18.62759615963255655, 50.41775706135235424 ) ) ;
#42147 = CARTESIAN_POINT ( 'NONE',  ( -9.474510206698964154, 16.51473224551069663, 50.41557627198102409 ) ) ;
#42148 = CARTESIAN_POINT ( 'NONE',  ( 18.67979575497178502, 10.72451020669898547, 114.1655762719810383 ) ) ;
#42149 = CARTESIAN_POINT ( 'NONE',  ( -16.46253265017146816, -9.564922557961047289, 59.16775706135233293 ) ) ;
#42150 = CARTESIAN_POINT ( 'NONE',  ( 19.02544592524343514, -5.153800228976328945, 33.54057627198102409 ) ) ;
#42151 = CARTESIAN_POINT ( 'NONE',  ( -8.314922557961024197, 14.29746914071037800, 32.91775706135234714 ) ) ;
#42152 = CARTESIAN_POINT ( 'NONE',  ( -16.51473224551069308, -9.474510206698971260, 21.66557627198102765 ) ) ;
#42153 = CARTESIAN_POINT ( 'NONE',  ( 8.314922557961029526, -14.29746914071037800, 75.41775706135233293 ) ) ;
#42154 = CARTESIAN_POINT ( 'NONE',  ( -16.51473224551069308, -9.474510206698971260, 41.66557627198103120 ) ) ;
#42155 = CARTESIAN_POINT ( 'NONE',  ( 21.88033147701266046, -7.974798826776969385, 169.5716465351769955 ) ) ;
#42156 = CARTESIAN_POINT ( 'NONE',  ( -5.153800228976328057, -19.02544592524343514, 87.29057627198103830 ) ) ;
#42157 = CARTESIAN_POINT ( 'NONE',  ( -13.97604488694527625, -13.89961937509977652, 26.87390960531434558 ) ) ;
#42158 = CARTESIAN_POINT ( 'NONE',  ( 18.62759615963271287, -10.81492255796078972, 73.33224293864769550 ) ) ;
#42159 = CARTESIAN_POINT ( 'NONE',  ( 16.55341960407618274, -4.379528057220086978, 51.04275706135234714 ) ) ;
#42160 = CARTESIAN_POINT ( 'NONE',  ( -5.153800228976607833, 19.02544592524334988, 22.70942372801899012 ) ) ;
#42161 = CARTESIAN_POINT ( 'NONE',  ( 5.153800228976335163, 19.02544592524342804, 39.79057627198100988 ) ) ;
#42162 = CARTESIAN_POINT ( 'NONE',  ( -16.55341960407611168, -4.379528057220339221, 36.45724293864768839 ) ) ;
#42163 = CARTESIAN_POINT ( 'NONE',  ( -16.52544592524342804, 4.483927247898546575, 66.04057627198103830 ) ) ;
#42164 = CARTESIAN_POINT ( 'NONE',  ( -19.05341960407611168, -5.049401038298163336, 61.45724293864769550 ) ) ;
#42165 = CARTESIAN_POINT ( 'NONE',  ( -21.53943276465977519, -0.05219959533937600094, 103.7510903946857042 ) ) ;
#42166 = CARTESIAN_POINT ( 'NONE',  ( 5.823673210054444382, -21.52544592524334988, 30.20942372801902565 ) ) ;
#42167 = CARTESIAN_POINT ( 'NONE',  ( -16.46253265017160317, 9.564922557960807481, 75.83224293864769550 ) ) ;
#42168 = CARTESIAN_POINT ( 'NONE',  ( -5.719274019375665041, -21.55341960407619695, 84.79275706135234714 ) ) ;
#42169 = CARTESIAN_POINT ( 'NONE',  ( 16.53943276465976808, 0.05219959533934440121, 71.25109039468568994 ) ) ;
#42170 = CARTESIAN_POINT ( 'NONE',  ( -12.06949235617739369, -12.14591786802326823, 34.37609039468568284 ) ) ;
#42172 = CARTESIAN_POINT ( 'NONE',  ( -13.97604488694527625, -13.89961937509977652, 111.8739096053143243 ) ) ;
#42171 = CARTESIAN_POINT ( 'NONE',  ( 14.34966873604960469, 8.224510206698951720, 94.16557627198103830 ) ) ;
#42173 = CARTESIAN_POINT ( 'NONE',  ( -4.483927247898539470, -16.52544592524342804, 27.29057627198103120 ) ) ;
#42174 = CARTESIAN_POINT ( 'NONE',  ( 16.46253265017160672, -9.564922557960803928, 23.33224293864769194 ) ) ;
#42175 = CARTESIAN_POINT ( 'NONE',  ( -14.34966873604972548, 8.224510206698743886, 48.33442372801902565 ) ) ;
#42176 = CARTESIAN_POINT ( 'NONE',  ( -16.52544592524342804, 4.483927247898546575, 61.04057627198103120 ) ) ;
#42177 = CARTESIAN_POINT ( 'NONE',  ( 4.483927247898790824, -16.52544592524335698, 105.2094237280190328 ) ) ;
#42178 = CARTESIAN_POINT ( 'NONE',  ( 13.97604488694527802, 13.89961937509977652, 114.3739096053143669 ) ) ;
#42179 = CARTESIAN_POINT ( 'NONE',  ( -0.05219959533907301413, -21.53943276465977519, 27.49890960531435269 ) ) ;
#42180 = CARTESIAN_POINT ( 'NONE',  ( 15.80617190586769283, -15.72974639402175789, 110.6260903946857042 ) ) ;
#42181 = CARTESIAN_POINT ( 'NONE',  ( -16.55341960407611168, -4.379528057220339221, 86.45724293864770971 ) ) ;
#42182 = CARTESIAN_POINT ( 'NONE',  ( 19.05341960407611168, 5.049401038298154454, 88.95724293864769550 ) ) ;
#42183 = ORIENTED_EDGE ( 'NONE', *, *, #157696, .T. ) ;
#42184 = CARTESIAN_POINT ( 'NONE',  ( -0.05219959533934338120, 16.53943276465976808, 37.50109039468568284 ) ) ;
#42185 = CARTESIAN_POINT ( 'NONE',  ( -16.46253265017160317, 9.564922557960807481, 40.83224293864769550 ) ) ;
#42187 = DIRECTION ( 'NONE',  ( -0.4999999999999933942, 0.5000000000000055511, -0.7071067811865484609 ) ) ;
#42186 = CARTESIAN_POINT ( 'NONE',  ( -8.224510206698735004, -14.34966873604973081, 39.58442372801901143 ) ) ;
#42188 = CARTESIAN_POINT ( 'NONE',  ( 5.153800228976615827, -19.02544592524334988, 45.20942372801901143 ) ) ;
#42189 = CARTESIAN_POINT ( 'NONE',  ( 16.51473224551069308, 9.474510206698969483, 49.16557627198102409 ) ) ;
#42190 = CARTESIAN_POINT ( 'NONE',  ( -16.52544592524335698, -4.483927247898792601, 73.95942372801901854 ) ) ;
#42191 = CARTESIAN_POINT ( 'NONE',  ( 0.05219959533936267826, -19.03943276465977164, 100.0010903946856757 ) ) ;
#42192 = CARTESIAN_POINT ( 'NONE',  ( -19.03943276465977164, 0.05219959533909376836, 61.24890960531436690 ) ) ;
#42193 = CARTESIAN_POINT ( 'NONE',  ( 0.05219959533910956823, 16.53943276465976808, 104.9989096053143669 ) ) ;
#42194 = CARTESIAN_POINT ( 'NONE',  ( -5.049401038297874678, -19.05341960407617918, 69.79275706135233293 ) ) ;
#42195 = CARTESIAN_POINT ( 'NONE',  ( -5.823673210054116645, -21.52544592524344225, 57.29057627198103120 ) ) ;
#42196 = CARTESIAN_POINT ( 'NONE',  ( 13.89961937509957401, 13.97604488694547697, 46.87609039468565442 ) ) ;
#42197 = CARTESIAN_POINT ( 'NONE',  ( 19.20446147854524810, 5.499999999999942268, 96.88999695167673565 ) ) ;
#42198 = CARTESIAN_POINT ( 'NONE',  ( -18.62759615963270932, 10.81492255796079327, 95.83224293864770971 ) ) ;
#42199 = CARTESIAN_POINT ( 'NONE',  ( -17.12812012977029497, 6.668231424565929544, 83.64051240676855059 ) ) ;
#42200 = AXIS2_PLACEMENT_3D ( 'NONE', #80283, #141955, #62132 ) ;
#42201 = CARTESIAN_POINT ( 'NONE',  ( 16.51473224551083163, -9.474510206698727899, 105.8344237280190043 ) ) ;
#42202 = CARTESIAN_POINT ( 'NONE',  ( -18.39635199886966177, 5.500000000000101252, 61.01967076359998998 ) ) ;
#42203 = CARTESIAN_POINT ( 'NONE',  ( 16.55341960407618274, -4.379528057220086978, 31.04275706135234714 ) ) ;
#42204 = CARTESIAN_POINT ( 'NONE',  ( -9.564922557960796823, -16.46253265017161027, 47.08224293864769550 ) ) ;
#42205 = CARTESIAN_POINT ( 'NONE',  ( -13.89961937509977652, 13.97604488694528158, 110.6239096053143243 ) ) ;
#42206 = CARTESIAN_POINT ( 'NONE',  ( 21.55341960407610458, 5.719274019375980345, 88.95724293864769550 ) ) ;
#42207 = CARTESIAN_POINT ( 'NONE',  ( 10.72451020669871369, 18.67979575497193778, 67.08442372801901854 ) ) ;
#42209 = CARTESIAN_POINT ( 'NONE',  ( 13.97604488694548053, -13.89961937509957401, 20.62609039468567573 ) ) ;
#42208 = CARTESIAN_POINT ( 'NONE',  ( -9.564922557961040184, 16.46253265017147172, 112.9177570613523329 ) ) ;
#42210 = CARTESIAN_POINT ( 'NONE',  ( -8.224510206698948167, 14.34966873604960824, 35.41557627198102409 ) ) ;
#42211 = CARTESIAN_POINT ( 'NONE',  ( -0.05219959533907301413, -21.53943276465977519, 102.4989096053143811 ) ) ;
#42212 = CARTESIAN_POINT ( 'NONE',  ( -8.314922557960811034, -14.29746914071050412, 47.08224293864770260 ) ) ;
#42213 = CARTESIAN_POINT ( 'NONE',  ( -19.05341960407617563, 5.049401038297882671, 88.54275706135230450 ) ) ;
#42214 = CARTESIAN_POINT ( 'NONE',  ( -0.05219959533936034679, 19.03943276465977164, 52.50109039468566863 ) ) ;
#42215 = CARTESIAN_POINT ( 'NONE',  ( -21.55341960407619339, 5.719274019375674811, 68.54275706135234714 ) ) ;
#42216 = CARTESIAN_POINT ( 'NONE',  ( 19.03943276465977164, 0.05219959533936151252, 41.25109039468566152 ) ) ;
#42217 = CARTESIAN_POINT ( 'NONE',  ( -9.564922557960796823, -16.46253265017161027, 27.08224293864769550 ) ) ;
#42218 = CARTESIAN_POINT ( 'NONE',  ( -10.81492255796078084, -18.62759615963271287, 42.08224293864769550 ) ) ;
#42219 = CARTESIAN_POINT ( 'NONE',  ( -4.379528057220328563, 16.55341960407611168, 40.20724293864769550 ) ) ;
#42220 = CARTESIAN_POINT ( 'NONE',  ( -0.05219959533937732626, 21.53943276465977519, 107.5010903946856899 ) ) ;
#42221 = CARTESIAN_POINT ( 'NONE',  ( -14.34966873604972548, 8.224510206698743886, 73.33442372801901854 ) ) ;
#42222 = CARTESIAN_POINT ( 'NONE',  ( -8.224510206698948167, 14.34966873604960824, 35.41557627198102409 ) ) ;
#42223 = CARTESIAN_POINT ( 'NONE',  ( 5.823673210054444382, -21.52544592524334988, 70.20942372801904696 ) ) ;
#42224 = CARTESIAN_POINT ( 'NONE',  ( -10.81492255796105439, 18.62759615963255655, 72.91775706135234714 ) ) ;
#42225 = CARTESIAN_POINT ( 'NONE',  ( -18.67979575497178146, -10.72451020669898902, 71.66557627198100988 ) ) ;
#42226 = CARTESIAN_POINT ( 'NONE',  ( 9.564922557960805705, 16.46253265017160317, 44.58224293864769550 ) ) ;
#42227 = CARTESIAN_POINT ( 'NONE',  ( -5.823673210054431948, 21.52544592524334988, 37.70942372801900433 ) ) ;
#42228 = CARTESIAN_POINT ( 'NONE',  ( 14.29746914071049879, -8.314922557960816363, 113.3322429386476955 ) ) ;
#42229 = CARTESIAN_POINT ( 'NONE',  ( 19.05341960407611168, 5.049401038298154454, 33.95724293864769550 ) ) ;
#42230 = CARTESIAN_POINT ( 'NONE',  ( 4.379528057220339221, -16.55341960407611168, 97.70724293864772392 ) ) ;
#42231 = CARTESIAN_POINT ( 'NONE',  ( 16.46253265017160672, -9.564922557960803928, 88.33224293864769550 ) ) ;
#42232 = CARTESIAN_POINT ( 'NONE',  ( 12.06949235617757843, -12.14591786802309237, 43.12390960531435269 ) ) ;
#42233 = CARTESIAN_POINT ( 'NONE',  ( 12.06949235617757843, -12.14591786802309237, 98.12390960531436690 ) ) ;
#42234 = CARTESIAN_POINT ( 'NONE',  ( 5.823673210054125526, 21.52544592524343514, 64.79057627198103830 ) ) ;
#42235 = CARTESIAN_POINT ( 'NONE',  ( -21.53943276465977519, 0.05219959533907696930, 101.2489096053143669 ) ) ;
#42236 = CARTESIAN_POINT ( 'NONE',  ( -40.00000000000002842, 1.938754146708588393E-14, 0.000000000000000000 ) ) ;
#42238 = CARTESIAN_POINT ( 'NONE',  ( -14.29746914071037622, -8.314922557961029526, 24.16775706135235424 ) ) ;
#42237 = CARTESIAN_POINT ( 'NONE',  ( -13.97604488694527625, -13.89961937509977652, 61.87390960531435979 ) ) ;
#42239 = CARTESIAN_POINT ( 'NONE',  ( 5.719274019375991003, -21.55341960407610458, 57.70724293864770260 ) ) ;
#42240 = CARTESIAN_POINT ( 'NONE',  ( 15.80617190586769283, -15.72974639402175789, 95.62609039468568994 ) ) ;
#42241 = CARTESIAN_POINT ( 'NONE',  ( 19.03943276465977164, -0.05219959533909143690, 73.74890960531435269 ) ) ;
#42242 = CARTESIAN_POINT ( 'NONE',  ( 18.67979575497178502, 10.72451020669898547, 114.1655762719810383 ) ) ;
#42243 = CARTESIAN_POINT ( 'NONE',  ( 9.474510206698971260, -16.51473224551069308, 107.9155762719810383 ) ) ;
#42244 = CARTESIAN_POINT ( 'NONE',  ( -12.14591786802326823, 12.06949235617739902, 93.12609039468568994 ) ) ;
#42245 = CARTESIAN_POINT ( 'NONE',  ( 18.62759615963255655, 10.81492255796105972, 71.66775706135234714 ) ) ;
#42246 = CARTESIAN_POINT ( 'NONE',  ( 15.80617190586769283, -15.72974639402175789, 95.62609039468568994 ) ) ;
#42247 = CARTESIAN_POINT ( 'NONE',  ( 8.314922557961029526, -14.29746914071037800, 55.41775706135234714 ) ) ;
#42248 = CARTESIAN_POINT ( 'NONE',  ( 18.67979575497194134, -10.72451020669871369, 20.83442372801901143 ) ) ;
#42249 = CARTESIAN_POINT ( 'NONE',  ( -19.03943276465977164, 0.05219959533909376836, 21.24890960531436335 ) ) ;
#42250 = CARTESIAN_POINT ( 'NONE',  ( 10.81492255796106328, -18.62759615963255655, 85.41775706135236135 ) ) ;
#42251 = CARTESIAN_POINT ( 'NONE',  ( 15.80617190586746368, 15.72974639402197994, 89.37390960531435269 ) ) ;
#42252 = CARTESIAN_POINT ( 'NONE',  ( -16.46253265017146816, -9.564922557961047289, 49.16775706135233293 ) ) ;
#42253 = CARTESIAN_POINT ( 'NONE',  ( 5.719274019375991003, -21.55341960407610458, 57.70724293864770260 ) ) ;
#42256 = B_SPLINE_CURVE_WITH_KNOTS ( 'NONE', 3,
 ( #28405, #91014, #14189, #150741, #57736, #90044, #102232, #103233, #164915, #137535, #13219, #42564, #181089, #199216, #119406, #58706 ),
 .UNSPECIFIED., .F., .F.,
 ( 4, 2, 2, 2, 2, 2, 2, 4 ),
 ( 0.001176332860010937233, 0.001620974858810565918, 0.002065616857610193952, 0.002954900855209450887, 0.003399542854009075452, 0.003844184852808700016, 0.004288826851608324581, 0.004733468850407949145 ),
 .UNSPECIFIED. ) ;
#42255 = CARTESIAN_POINT ( 'NONE',  ( -12.06949235617756955, 12.14591786802309770, 40.62390960531435269 ) ) ;
#42254 = CARTESIAN_POINT ( 'NONE',  ( -5.049401038298153566, 19.05341960407611168, 100.2072429386476955 ) ) ;
#42257 = DIRECTION ( 'NONE',  ( -0.000000000000000000, -0.6427876096865403621, -0.7660444431189770143 ) ) ;
#42258 = CARTESIAN_POINT ( 'NONE',  ( -19.53091890409952924, -5.499999999999945821, 80.06097431831415179 ) ) ;
#42259 = ADVANCED_FACE ( 'NONE', ( #92472 ), #15652, .F. ) ;
#42260 = CARTESIAN_POINT ( 'NONE',  ( 5.049401038297881783, 19.05341960407617563, 102.2927570613523045 ) ) ;
#42261 = CARTESIAN_POINT ( 'NONE',  ( -21.53943276465977519, 0.05219959533907696930, 91.24890960531436690 ) ) ;
#42262 = CARTESIAN_POINT ( 'NONE',  ( -0.05219959533910754901, -16.53943276465976808, 52.49890960531435979 ) ) ;
#42263 = CARTESIAN_POINT ( 'NONE',  ( -16.55341960407617563, 4.379528057220093196, 28.54275706135234358 ) ) ;
#42264 = CARTESIAN_POINT ( 'NONE',  ( -19.05341960407611168, -5.049401038298163336, 46.45724293864768129 ) ) ;
#42266 = CARTESIAN_POINT ( 'NONE',  ( -19.05341960407617563, 5.049401038297882671, 83.54275706135233293 ) ) ;
#42265 = CARTESIAN_POINT ( 'NONE',  ( -21.53943276465977519, -0.05219959533937600094, 18.75109039468568639 ) ) ;
#42267 = CARTESIAN_POINT ( 'NONE',  ( 9.564922557960805705, 16.46253265017160317, 84.58224293864769550 ) ) ;
#42268 = CARTESIAN_POINT ( 'NONE',  ( -12.14591786802326823, 12.06949235617739902, 28.12609039468568284 ) ) ;
#42269 =( BOUNDED_CURVE ( )  B_SPLINE_CURVE ( 2, ( #121208, #182899, #44383, #106038, #11066, #87882, #29222, #90855, #196101, #72744, #71727, #119241, #14028 ),
 .UNSPECIFIED., .F., .F. ) 
 B_SPLINE_CURVE_WITH_KNOTS ( ( 3, 2, 2, 2, 2, 2, 3 ),
 ( 0.3445356995849399029, 0.3464912280701754610, 0.3508771929824561209, 0.3552631578947368363, 0.3596491228070175517, 0.3640350877192982670, 0.3659449363824437418 ),
 .UNSPECIFIED. ) 
 CURVE ( )  GEOMETRIC_REPRESENTATION_ITEM ( )  RATIONAL_B_SPLINE_CURVE ( ( 0.9831626618144004848, 0.9848076720550091867, 1.000000000000000000, 0.9659258262890683122, 1.000000000000000000, 0.9659258262890683122, 1.000000000000000000, 0.9659258262890683122, 1.000000000000000000, 0.9659258262890683122, 1.000000000000000000, 0.9851625545550088958, 0.9832469066685279868 ) ) 
 REPRESENTATION_ITEM ( '' )  );
#42270 = CARTESIAN_POINT ( 'NONE',  ( 5.153800228976335163, 19.02544592524342804, 74.79057627198103830 ) ) ;
#42271 = CARTESIAN_POINT ( 'NONE',  ( 15.72974639402199770, -15.80617190586745480, 78.12390960531436690 ) ) ;
#42272 = CARTESIAN_POINT ( 'NONE',  ( -16.46253265017160317, 9.564922557960807481, 30.83224293864769550 ) ) ;
#42273 = CARTESIAN_POINT ( 'NONE',  ( 27.87032660475913204, 24.53198321425060158, -8.000000000000003553 ) ) ;
#42274 = CARTESIAN_POINT ( 'NONE',  ( -16.55341960407611168, -4.379528057220339221, 56.45724293864768839 ) ) ;
#42275 = CARTESIAN_POINT ( 'NONE',  ( -19.05341960407611168, -5.049401038298163336, 96.45724293864769550 ) ) ;
#42276 = CARTESIAN_POINT ( 'NONE',  ( 28.82186960331498327, 2.781578969918950771E-14, 141.2500000054623683 ) ) ;
#42277 = CARTESIAN_POINT ( 'NONE',  ( -5.049401038297874678, -19.05341960407617918, 64.79275706135233293 ) ) ;
#42278 = CARTESIAN_POINT ( 'NONE',  ( -21.52544592524343514, 5.823673210054127303, 71.04057627198103830 ) ) ;
#42279 = CARTESIAN_POINT ( 'NONE',  ( 9.474510206698729675, 16.51473224551082808, 42.08442372801900433 ) ) ;
#42280 = CARTESIAN_POINT ( 'NONE',  ( -16.51473224551069308, -9.474510206698971260, 101.6655762719810241 ) ) ;
#42281 = DIRECTION ( 'NONE',  ( 0.000000000000000000, 0.04175967627138096189, 0.9991276842514722478 ) ) ;
#42282 = CARTESIAN_POINT ( 'NONE',  ( -21.53943276465977519, 0.05219959533907696930, 46.24890960531435979 ) ) ;
#42283 = CARTESIAN_POINT ( 'NONE',  ( -19.03943276465977164, 0.05219959533909376836, 76.24890960531435269 ) ) ;
#42284 = CARTESIAN_POINT ( 'NONE',  ( 21.55341960407619695, -5.719274019375665929, 61.04275706135234714 ) ) ;
#42285 = CARTESIAN_POINT ( 'NONE',  ( 9.474510206698971260, -16.51473224551069308, 27.91557627198103120 ) ) ;
#42287 = ORIENTED_EDGE ( 'NONE', *, *, #160293, .T. ) ;
#42286 = CARTESIAN_POINT ( 'NONE',  ( -15.80617190586768217, 15.72974639402176855, 23.12609039468567573 ) ) ;
#42288 = CARTESIAN_POINT ( 'NONE',  ( -21.52544592524334988, -5.823673210054445271, 48.95942372801902565 ) ) ;
#42289 = ORIENTED_EDGE ( 'NONE', *, *, #143629, .T. ) ;
#42290 = CARTESIAN_POINT ( 'NONE',  ( 19.02544592524343514, -5.153800228976328945, 98.54057627198100988 ) ) ;
#42291 = CARTESIAN_POINT ( 'NONE',  ( -20.96320343559624177, 21.46320343559660770, 5.353553390593268624 ) ) ;
#42292 = CARTESIAN_POINT ( 'NONE',  ( -5.823673210054116645, -21.52544592524344225, 102.2905762719810383 ) ) ;
#42293 = CARTESIAN_POINT ( 'NONE',  ( -16.46253265017160317, 9.564922557960807481, 55.83224293864769550 ) ) ;
#42294 = CARTESIAN_POINT ( 'NONE',  ( 12.06949235617739724, 12.14591786802326823, 36.87609039468568994 ) ) ;
#42295 = CARTESIAN_POINT ( 'NONE',  ( 23.48529157249599919, 32.32473071737754111, -10.44999999453762385 ) ) ;
#42296 = CARTESIAN_POINT ( 'NONE',  ( -5.719274019375665041, -21.55341960407619695, 104.7927570613523898 ) ) ;
#42297 = CARTESIAN_POINT ( 'NONE',  ( 16.46253265017160672, -9.564922557960803928, 43.33224293864769550 ) ) ;
#42298 = CARTESIAN_POINT ( 'NONE',  ( -10.81492255796105439, 18.62759615963255655, 102.9177570613523756 ) ) ;
#42300 = CARTESIAN_POINT ( 'NONE',  ( -10.72451020669870658, -18.67979575497194134, 59.58442372801901854 ) ) ;
#42299 = CARTESIAN_POINT ( 'NONE',  ( -16.46253265017160317, 9.564922557960807481, 95.83224293864769550 ) ) ;
#42301 = CARTESIAN_POINT ( 'NONE',  ( 4.803421339707764304, -3.978740937077453577, -62.48491958522772904 ) ) ;
#42302 = CARTESIAN_POINT ( 'NONE',  ( -19.05341960407611168, -5.049401038298163336, 111.4572429386476671 ) ) ;
#42303 = CARTESIAN_POINT ( 'NONE',  ( -17.50000000000000711, 4.640572885337600262, 30.63788164548843085 ) ) ;
#42305 = CARTESIAN_POINT ( 'NONE',  ( 10.72451020669871369, 18.67979575497193778, 62.08442372801901143 ) ) ;
#42304 = CARTESIAN_POINT ( 'NONE',  ( 16.52544592524335698, 4.483927247898782831, 46.45942372801901854 ) ) ;
#42306 = CARTESIAN_POINT ( 'NONE',  ( 18.62759615963255655, 10.81492255796105972, 86.66775706135234714 ) ) ;
#42307 = CARTESIAN_POINT ( 'NONE',  ( -40.00200000000003087, -1.163414459189985801E-14, 95.00000000000000000 ) ) ;
#42308 = CARTESIAN_POINT ( 'NONE',  ( -16.52544592524335698, -4.483927247898792601, 23.95942372801901143 ) ) ;
#42309 = CARTESIAN_POINT ( 'NONE',  ( -5.153800228976328057, -19.02544592524343514, 67.29057627198102409 ) ) ;
#42310 = CARTESIAN_POINT ( 'NONE',  ( 9.564922557960805705, 16.46253265017160317, 114.5822429386476955 ) ) ;
#42311 = DIRECTION ( 'NONE',  ( -1.000000000000000000, -0.000000000000000000, -0.000000000000000000 ) ) ;
#42312 = CARTESIAN_POINT ( 'NONE',  ( -13.97604488694527625, -13.89961937509977652, 26.87390960531434558 ) ) ;
#42313 = CARTESIAN_POINT ( 'NONE',  ( -21.52544592524343514, 5.823673210054127303, 41.04057627198103120 ) ) ;
#42314 = CARTESIAN_POINT ( 'NONE',  ( -14.34966873604972548, 8.224510206698743886, 93.33442372801901854 ) ) ;
#42316 = CARTESIAN_POINT ( 'NONE',  ( 16.46253265017160672, -9.564922557960803928, 63.33224293864769550 ) ) ;
#42315 = CARTESIAN_POINT ( 'NONE',  ( -14.29746914071049879, 8.314922557960819915, 80.83224293864769550 ) ) ;
#42317 = CARTESIAN_POINT ( 'NONE',  ( -21.55341960407619339, 5.719274019375674811, 88.54275706135236135 ) ) ;
#42318 = CARTESIAN_POINT ( 'NONE',  ( -69.65682714487590488, -71.74905178543390605, -15.00000000000000000 ) ) ;
#42319 = CARTESIAN_POINT ( 'NONE',  ( 16.55341960407618274, -4.379528057220086978, 26.04275706135235779 ) ) ;
#42320 = CARTESIAN_POINT ( 'NONE',  ( -16.52544592524342804, 4.483927247898546575, 91.04057627198103830 ) ) ;
#42321 = CARTESIAN_POINT ( 'NONE',  ( 10.81492255796106328, -18.62759615963255655, 45.41775706135234003 ) ) ;
#42322 = CARTESIAN_POINT ( 'NONE',  ( -10.72451020669898014, 18.67979575497178502, 75.41557627198102409 ) ) ;
#42323 = CARTESIAN_POINT ( 'NONE',  ( -5.049401038297874678, -19.05341960407617918, 34.79275706135233293 ) ) ;
#42324 = LINE ( 'NONE', #58473, #165976 ) ;
#42325 = CARTESIAN_POINT ( 'NONE',  ( 19.05341960407611168, 5.049401038298154454, 88.95724293864769550 ) ) ;
#42326 = CARTESIAN_POINT ( 'NONE',  ( 16.55341960407611168, 4.379528057220329451, 58.95724293864770971 ) ) ;
#42327 = CARTESIAN_POINT ( 'NONE',  ( -12.06949235617756955, 12.14591786802309770, 30.62390960531436335 ) ) ;
#42328 = CARTESIAN_POINT ( 'NONE',  ( 16.55341960407618274, -4.379528057220086978, 111.0427570613523613 ) ) ;
#42329 = CARTESIAN_POINT ( 'NONE',  ( -0.05219959533936034679, 19.03943276465977164, 67.50109039468566152 ) ) ;
#42330 = CARTESIAN_POINT ( 'NONE',  ( 17.13100169013298668, 6.664070546373165982, 46.73210164300152059 ) ) ;
#42331 = CARTESIAN_POINT ( 'NONE',  ( 13.97604488694527802, 13.89961937509977652, 114.3739096053143669 ) ) ;
#42332 = ADVANCED_FACE ( 'NONE', ( #123796 ), #46985, .F. ) ;
#42333 = CARTESIAN_POINT ( 'NONE',  ( 8.314922557960818139, 14.29746914071049879, 94.58224293864769550 ) ) ;
#42334 = CARTESIAN_POINT ( 'NONE',  ( -17.60769864724390388, 5.499999999999984013, 58.65024842019164453 ) ) ;
#42336 = CARTESIAN_POINT ( 'NONE',  ( 0.05219959533907565091, 21.53943276465977519, 49.99890960531437401 ) ) ;
#42335 = CARTESIAN_POINT ( 'NONE',  ( -16.46253265017160317, 9.564922557960807481, 45.83224293864769550 ) ) ;
#42337 = CARTESIAN_POINT ( 'NONE',  ( -15.72974639402197994, 15.80617190586746368, 65.62390960531436690 ) ) ;
#42338 = CARTESIAN_POINT ( 'NONE',  ( -12.06949235617756955, 12.14591786802309770, 115.6239096053143669 ) ) ;
#42340 = CARTESIAN_POINT ( 'NONE',  ( -19.02544592524342804, 5.153800228976336051, 46.04057627198101699 ) ) ;
#42339 = CARTESIAN_POINT ( 'NONE',  ( -16.53943276465976808, -0.05219959533934237506, 58.75109039468568994 ) ) ;
#42341 = CARTESIAN_POINT ( 'NONE',  ( -18.67979575497193778, 10.72451020669871902, 58.33442372801901143 ) ) ;
#42342 = CARTESIAN_POINT ( 'NONE',  ( 16.55341960407611168, 4.379528057220329451, 108.9572429386476955 ) ) ;
#42343 = CARTESIAN_POINT ( 'NONE',  ( -5.049401038297874678, -19.05341960407617918, 94.79275706135230450 ) ) ;
#42344 = CARTESIAN_POINT ( 'NONE',  ( -36.91746825000000598, 11.99521256947798520, -7.224999997268813701 ) ) ;
#42346 = CARTESIAN_POINT ( 'NONE',  ( 10.72451020669898902, -18.67979575497178502, 27.91557627198103830 ) ) ;
#42345 = CYLINDRICAL_SURFACE ( 'NONE', #157214, 12.50000000000000000 ) ;
#42347 = CARTESIAN_POINT ( 'NONE',  ( 19.03943276465977164, -0.05219959533909143690, 23.74890960531435269 ) ) ;
#42348 = CARTESIAN_POINT ( 'NONE',  ( -15.80617190586768217, 15.72974639402176855, 68.12609039468567573 ) ) ;
#42350 = CARTESIAN_POINT ( 'NONE',  ( 16.53943276465976808, -0.05219959533910856209, 48.74890960531435979 ) ) ;
#42349 = CARTESIAN_POINT ( 'NONE',  ( -8.314922557961024197, 14.29746914071037800, 62.91775706135236135 ) ) ;
#42351 = CARTESIAN_POINT ( 'NONE',  ( 18.62759615963271287, -10.81492255796078972, 63.33224293864770260 ) ) ;
#42352 = CARTESIAN_POINT ( 'NONE',  ( -18.67979575497178146, -10.72451020669898902, 61.66557627198103120 ) ) ;
#42353 = CARTESIAN_POINT ( 'NONE',  ( 28.98398574327581301, -24.58691951735649894, -17.12116358423670448 ) ) ;
#42355 = CARTESIAN_POINT ( 'NONE',  ( -13.89961937509977652, 13.97604488694528158, 110.6239096053143243 ) ) ;
#42354 = CARTESIAN_POINT ( 'NONE',  ( -16.51473224551082808, 9.474510206698731452, 88.33442372801900433 ) ) ;
#42356 = CARTESIAN_POINT ( 'NONE',  ( 5.153800228976335163, 19.02544592524342804, 54.79057627198103120 ) ) ;
#42357 = CARTESIAN_POINT ( 'NONE',  ( -16.52544592524342804, 4.483927247898546575, 111.0405762719810525 ) ) ;
#42358 = CARTESIAN_POINT ( 'NONE',  ( -13.89961937509977652, 13.97604488694528158, 110.6239096053143243 ) ) ;
#42359 = VERTEX_POINT ( 'NONE', #156141 ) ;
#42360 = CARTESIAN_POINT ( 'NONE',  ( -8.314922557961024197, 14.29746914071037800, 67.91775706135234714 ) ) ;
#42361 = CARTESIAN_POINT ( 'NONE',  ( 10.81492255796078972, 18.62759615963270932, 104.5822429386477097 ) ) ;
#42362 = CARTESIAN_POINT ( 'NONE',  ( 16.51473224551069308, 9.474510206698969483, 64.16557627198102409 ) ) ;
#42363 = CARTESIAN_POINT ( 'NONE',  ( -10.72451020669870658, -18.67979575497194134, 34.58442372801900433 ) ) ;
#42364 = CARTESIAN_POINT ( 'NONE',  ( -19.05341960407611168, -5.049401038298163336, 101.4572429386476955 ) ) ;
#42365 = CARTESIAN_POINT ( 'NONE',  ( -22.23580286100235526, -34.17069428431420874, -18.13567467416600820 ) ) ;
#42366 = VERTEX_POINT ( 'NONE', #3444 ) ;
#42367 = CARTESIAN_POINT ( 'NONE',  ( 18.62759615963255655, 10.81492255796105972, 36.66775706135234714 ) ) ;
#42369 = CARTESIAN_POINT ( 'NONE',  ( -9.564922557961040184, 16.46253265017147172, 87.91775706135233293 ) ) ;
#42368 = CARTESIAN_POINT ( 'NONE',  ( 19.03943276465977164, -0.05219959533909143690, 28.74890960531435624 ) ) ;
#42370 = CARTESIAN_POINT ( 'NONE',  ( 19.05341960407617918, -5.049401038297876454, 46.04275706135233293 ) ) ;
#42371 = CARTESIAN_POINT ( 'NONE',  ( -0.05219959533907301413, -21.53943276465977519, 112.4989096053143669 ) ) ;
#42372 = CARTESIAN_POINT ( 'NONE',  ( 13.97604488694548053, -13.89961937509957401, 35.62609039468567573 ) ) ;
#42373 = CARTESIAN_POINT ( 'NONE',  ( -13.97604488694547697, 13.89961937509957934, 53.12609039468565442 ) ) ;
#42374 = CARTESIAN_POINT ( 'NONE',  ( -4.483927247898782831, 16.52544592524335698, 87.70942372801901854 ) ) ;
#42375 = CARTESIAN_POINT ( 'NONE',  ( 24.81835880841864039, -6.052260367207979996, 168.4265213779230521 ) ) ;
#42376 = CARTESIAN_POINT ( 'NONE',  ( 13.97604488694527802, 13.89961937509977652, 69.37390960531436690 ) ) ;
#42377 = CARTESIAN_POINT ( 'NONE',  ( 18.62759615963255655, 10.81492255796105972, 81.66775706135236135 ) ) ;
#42378 = CARTESIAN_POINT ( 'NONE',  ( 15.80617190586769283, -15.72974639402175789, 95.62609039468568994 ) ) ;
#42379 = DIRECTION ( 'NONE',  ( 0.000000000000000000, -3.469446951953611428E-15, -1.000000000000000000 ) ) ;
#42380 = CARTESIAN_POINT ( 'NONE',  ( -5.153800228976328057, -19.02544592524343514, 92.29057627198099567 ) ) ;
#42381 = CARTESIAN_POINT ( 'NONE',  ( 5.719274019375673035, 21.55341960407619339, 67.29275706135234714 ) ) ;
#42382 = CARTESIAN_POINT ( 'NONE',  ( 19.05341960407617918, -5.049401038297876454, 96.04275706135231871 ) ) ;
#42383 = CARTESIAN_POINT ( 'NONE',  ( -5.049401038298153566, 19.05341960407611168, 60.20724293864768129 ) ) ;
#42384 = CARTESIAN_POINT ( 'NONE',  ( -0.05219959533909027116, -19.03943276465977164, 112.4989096053143669 ) ) ;
#42385 = CARTESIAN_POINT ( 'NONE',  ( -19.03943276465977164, 0.05219959533909376836, 76.24890960531435269 ) ) ;
#42386 = CARTESIAN_POINT ( 'NONE',  ( 17.50000000000003553, -5.001413817666677808, 23.20927153282391942 ) ) ;
#42387 = CARTESIAN_POINT ( 'NONE',  ( -16.46253265017160317, 9.564922557960807481, 65.83224293864769550 ) ) ;
#42388 = CARTESIAN_POINT ( 'NONE',  ( -16.51473224551069308, -9.474510206698971260, 46.66557627198102409 ) ) ;
#42389 = CARTESIAN_POINT ( 'NONE',  ( 21.52544592524334988, 5.823673210054432836, 21.45942372801901499 ) ) ;
#42390 = CARTESIAN_POINT ( 'NONE',  ( -4.483927247898782831, 16.52544592524335698, 87.70942372801901854 ) ) ;
#42391 = CARTESIAN_POINT ( 'NONE',  ( 6.180203150055848305, -4.962140900324442327, 6.568406857878970939 ) ) ;
#42392 = CARTESIAN_POINT ( 'NONE',  ( 6.292920404648722155, -0.7621229312825326119, -64.49503546857651770 ) ) ;
#42393 = CARTESIAN_POINT ( 'NONE',  ( -9.564922557961040184, 16.46253265017147172, 57.91775706135233293 ) ) ;
#42394 = CARTESIAN_POINT ( 'NONE',  ( -9.474510206698964154, 16.51473224551069663, 85.41557627198102409 ) ) ;
#42395 = CARTESIAN_POINT ( 'NONE',  ( 4.379528057220339221, -16.55341960407611168, 67.70724293864769550 ) ) ;
#42396 = CARTESIAN_POINT ( 'NONE',  ( 12.06949235617757843, -12.14591786802309237, 103.1239096053143811 ) ) ;
#42397 = CARTESIAN_POINT ( 'NONE',  ( 16.51473224551069308, 9.474510206698969483, 109.1655762719810383 ) ) ;
#42398 = CARTESIAN_POINT ( 'NONE',  ( 16.51473224551069308, 9.474510206698969483, 99.16557627198102409 ) ) ;
#42399 = CARTESIAN_POINT ( 'NONE',  ( -4.483927247898539470, -16.52544592524342804, 87.29057627198103830 ) ) ;
#42400 = CARTESIAN_POINT ( 'NONE',  ( -19.03943276465977164, 0.05219959533909376836, 116.2489096053143669 ) ) ;
#42401 = CARTESIAN_POINT ( 'NONE',  ( -19.03943276465977164, -0.05219959533935918106, 28.75109039468566507 ) ) ;
#42402 = CARTESIAN_POINT ( 'NONE',  ( -16.55341960407617563, 4.379528057220093196, 108.5427570613523756 ) ) ;
#42403 = CARTESIAN_POINT ( 'NONE',  ( -5.049401038298153566, 19.05341960407611168, 95.20724293864770971 ) ) ;
#42404 = CARTESIAN_POINT ( 'NONE',  ( 0.05219959533937995610, -21.53943276465977519, 55.00109039468568284 ) ) ;
#42405 = CARTESIAN_POINT ( 'NONE',  ( 21.53943276465977519, -0.05219959533907433946, 43.74890960531435979 ) ) ;
#42406 = CARTESIAN_POINT ( 'NONE',  ( 21.52544592524334988, 5.823673210054432836, 21.45942372801901499 ) ) ;
#42407 = CARTESIAN_POINT ( 'NONE',  ( -5.719274019375978568, 21.55341960407610458, 70.20724293864769550 ) ) ;
#42408 = CARTESIAN_POINT ( 'NONE',  ( 14.34966873604960469, 8.224510206698951720, 89.16557627198102409 ) ) ;
#42409 = CARTESIAN_POINT ( 'NONE',  ( -9.564922557961040184, 16.46253265017147172, 62.91775706135233293 ) ) ;
#42410 = CARTESIAN_POINT ( 'NONE',  ( -13.97604488694527625, -13.89961937509977652, 26.87390960531434558 ) ) ;
#42411 = CARTESIAN_POINT ( 'NONE',  ( 5.049401038298161559, -19.05341960407611168, 87.70724293864769550 ) ) ;
#42412 = CARTESIAN_POINT ( 'NONE',  ( -5.049401038298153566, 19.05341960407611168, 95.20724293864770971 ) ) ;
#42413 = CARTESIAN_POINT ( 'NONE',  ( 14.29746914071049879, -8.314922557960816363, 113.3322429386476955 ) ) ;
#42414 = ORIENTED_EDGE ( 'NONE', *, *, #156518, .T. ) ;
#42415 = CARTESIAN_POINT ( 'NONE',  ( -16.53943276465976808, -0.05219959533934237506, 113.7510903946856757 ) ) ;
#42416 = CARTESIAN_POINT ( 'NONE',  ( 12.06949235617739724, 12.14591786802326823, 41.87609039468568284 ) ) ;
#42417 = CARTESIAN_POINT ( 'NONE',  ( -21.55341960407619339, 5.719274019375674811, 103.5427570613523613 ) ) ;
#42418 = CARTESIAN_POINT ( 'NONE',  ( -5.153800228976328057, -19.02544592524343514, 102.2905762719810383 ) ) ;
#42419 = CARTESIAN_POINT ( 'NONE',  ( -5.823673210054431948, 21.52544592524334988, 27.70942372801901854 ) ) ;
#42420 = CARTESIAN_POINT ( 'NONE',  ( 0.05219959533909260263, 19.03943276465977164, 49.99890960531435979 ) ) ;
#42421 = CARTESIAN_POINT ( 'NONE',  ( -12.06949235617739369, -12.14591786802326823, 49.37609039468569705 ) ) ;
#42422 = CARTESIAN_POINT ( 'NONE',  ( 8.314922557961029526, -14.29746914071037800, 95.41775706135234714 ) ) ;
#42423 = CARTESIAN_POINT ( 'NONE',  ( -5.049401038297874678, -19.05341960407617918, 109.7927570613523187 ) ) ;
#42424 = ADVANCED_FACE ( 'NONE', ( #177313 ), #8444, .T. ) ;
#42425 = CARTESIAN_POINT ( 'NONE',  ( 16.46253265017160672, -9.564922557960803928, 28.33224293864769550 ) ) ;
#42426 = CARTESIAN_POINT ( 'NONE',  ( 8.224510206698953496, -14.34966873604960469, 92.91557627198103830 ) ) ;
#42427 = CARTESIAN_POINT ( 'NONE',  ( 15.72974639402199770, -15.80617190586745480, 98.12390960531436690 ) ) ;
#42428 = CARTESIAN_POINT ( 'NONE',  ( 16.46253265017146816, 9.564922557961045513, 86.66775706135233293 ) ) ;
#42429 = CARTESIAN_POINT ( 'NONE',  ( 13.97604488694527802, 13.89961937509977652, 34.37390960531436690 ) ) ;
#42430 = CARTESIAN_POINT ( 'NONE',  ( -16.46253265017160317, 9.564922557960807481, 100.8322429386477097 ) ) ;
#42431 = CARTESIAN_POINT ( 'NONE',  ( -21.53943276465977519, -0.05219959533937600094, 38.75109039468567573 ) ) ;
#42432 = CARTESIAN_POINT ( 'NONE',  ( -5.049401038298153566, 19.05341960407611168, 100.2072429386476955 ) ) ;
#42433 = CARTESIAN_POINT ( 'NONE',  ( 0.000000000000000000, 1.178949249685212974, -2.042000000000001148 ) ) ;
#42434 = CARTESIAN_POINT ( 'NONE',  ( -9.474510206698964154, 16.51473224551069663, 85.41557627198102409 ) ) ;
#42436 = CARTESIAN_POINT ( 'NONE',  ( -16.52544592524342804, 4.483927247898546575, 86.04057627198102409 ) ) ;
#42435 = CARTESIAN_POINT ( 'NONE',  ( 21.53943276465977519, 0.05219959533937863772, 26.25109039468567573 ) ) ;
#42437 = CARTESIAN_POINT ( 'NONE',  ( -16.51473224551069308, -9.474510206698971260, 91.66557627198103830 ) ) ;
#42438 = CARTESIAN_POINT ( 'NONE',  ( -5.049401038297874678, -19.05341960407617918, 19.79275706135233293 ) ) ;
#42439 = CARTESIAN_POINT ( 'NONE',  ( -0.05219959533934338120, 16.53943276465976808, 57.50109039468568994 ) ) ;
#42440 = CARTESIAN_POINT ( 'NONE',  ( -18.62759615963255300, -10.81492255796106328, 84.16775706135234714 ) ) ;
#42441 = CARTESIAN_POINT ( 'NONE',  ( 4.379528057220092307, 16.55341960407617563, 42.29275706135235424 ) ) ;
#42442 = CARTESIAN_POINT ( 'NONE',  ( -19.05341960407611168, -5.049401038298163336, 86.45724293864769550 ) ) ;
#42443 = CARTESIAN_POINT ( 'NONE',  ( -9.474510206698720793, -16.51473224551083518, 99.58442372801900433 ) ) ;
#42444 = CARTESIAN_POINT ( 'NONE',  ( -16.55341960407617563, 4.379528057220093196, 68.54275706135234714 ) ) ;
#42445 = CARTESIAN_POINT ( 'NONE',  ( -15.80617190586768217, 15.72974639402176855, 113.1260903946856899 ) ) ;
#42446 = CARTESIAN_POINT ( 'NONE',  ( -9.474510206698720793, -16.51473224551083518, 79.58442372801899012 ) ) ;
#42447 = CARTESIAN_POINT ( 'NONE',  ( 5.153800228976335163, 19.02544592524342804, 59.79057627198100988 ) ) ;
#42448 = CARTESIAN_POINT ( 'NONE',  ( 15.80617190586746368, 15.72974639402197994, 79.37390960531436690 ) ) ;
#42450 = CARTESIAN_POINT ( 'NONE',  ( -0.05219959533936034679, 19.03943276465977164, 97.50109039468567573 ) ) ;
#42449 = CARTESIAN_POINT ( 'NONE',  ( 12.14591786802309770, 12.06949235617756955, 74.37390960531436690 ) ) ;
#42451 = CARTESIAN_POINT ( 'NONE',  ( 24.83221077041948988, 4.296110748034003279, 170.3917201292229322 ) ) ;
#42452 = CARTESIAN_POINT ( 'NONE',  ( -5.153800228976607833, 19.02544592524334988, 52.70942372801900433 ) ) ;
#42453 = CARTESIAN_POINT ( 'NONE',  ( -0.05219959533934338120, 16.53943276465976808, 107.5010903946856899 ) ) ;
#42454 = CARTESIAN_POINT ( 'NONE',  ( -8.314922557960811034, -14.29746914071050412, 82.08224293864768129 ) ) ;
#42456 = CARTESIAN_POINT ( 'NONE',  ( 0.05219959533936267826, -19.03943276465977164, 45.00109039468566863 ) ) ;
#42455 = CARTESIAN_POINT ( 'NONE',  ( 5.823673210054444382, -21.52544592524334988, 110.2094237280190185 ) ) ;
#42457 = CARTESIAN_POINT ( 'NONE',  ( 18.62759615963271287, -10.81492255796078972, 108.3322429386477097 ) ) ;
#42458 = CARTESIAN_POINT ( 'NONE',  ( -9.474510206698964154, 16.51473224551069663, 105.4155762719810383 ) ) ;
#42459 = CARTESIAN_POINT ( 'NONE',  ( -5.153800228976328057, -19.02544592524343514, 82.29057627198103830 ) ) ;
#42460 = CARTESIAN_POINT ( 'NONE',  ( -10.72451020669870658, -18.67979575497194134, 84.58442372801903275 ) ) ;
#42461 = CARTESIAN_POINT ( 'NONE',  ( -9.474510206698964154, 16.51473224551069663, 60.41557627198102409 ) ) ;
#42462 = VERTEX_POINT ( 'NONE', #111627 ) ;
#42463 = CARTESIAN_POINT ( 'NONE',  ( 19.03943276465977164, -0.05219959533909143690, 43.74890960531435979 ) ) ;
#42464 = CARTESIAN_POINT ( 'NONE',  ( -15.80617190586745835, -15.72974639402198527, 26.87390960531435979 ) ) ;
#42465 = CARTESIAN_POINT ( 'NONE',  ( -16.52544592524342804, 4.483927247898546575, 81.04057627198102409 ) ) ;
#42466 = CARTESIAN_POINT ( 'NONE',  ( -13.89961937509977652, 13.97604488694528158, 45.62390960531433848 ) ) ;
#42467 = CARTESIAN_POINT ( 'NONE',  ( 14.29746914071049879, -8.314922557960816363, 93.33224293864769550 ) ) ;
#42468 = EDGE_CURVE ( 'NONE', #163715, #60746, #86801, .T. ) ;
#42469 = CARTESIAN_POINT ( 'NONE',  ( -18.62759615963270932, 10.81492255796079327, 105.8322429386476955 ) ) ;
#42470 = CARTESIAN_POINT ( 'NONE',  ( -10.72451020669870658, -18.67979575497194134, 54.58442372801901143 ) ) ;
#42471 = CARTESIAN_POINT ( 'NONE',  ( 16.51473224551069308, 9.474510206698969483, 29.16557627198103475 ) ) ;
#42472 = CARTESIAN_POINT ( 'NONE',  ( 12.14591786802327356, -12.06949235617739191, 60.62609039468567573 ) ) ;
#42473 = CARTESIAN_POINT ( 'NONE',  ( -18.62759615963270932, 10.81492255796079327, 105.8322429386476955 ) ) ;
#42474 = CARTESIAN_POINT ( 'NONE',  ( 5.823673210054125526, 21.52544592524343514, 94.79057627198105251 ) ) ;
#42476 = CARTESIAN_POINT ( 'NONE',  ( 9.564922557960805705, 16.46253265017160317, 49.58224293864770260 ) ) ;
#42475 = CARTESIAN_POINT ( 'NONE',  ( 19.03943276465977164, 0.05219959533936151252, 41.25109039468566152 ) ) ;
#42477 = CARTESIAN_POINT ( 'NONE',  ( 0.000000000000000000, 0.000000000000000000, -54.21489346206828230 ) ) ;
#42478 = CARTESIAN_POINT ( 'NONE',  ( 21.53943276465977519, 0.05219959533937863772, 51.25109039468568994 ) ) ;
#42479 = CARTESIAN_POINT ( 'NONE',  ( 15.72974639402199770, -15.80617190586745480, 58.12390960531435979 ) ) ;
#42480 = CARTESIAN_POINT ( 'NONE',  ( 16.55341960407611168, 4.379528057220329451, 43.95724293864769550 ) ) ;
#42482 = CARTESIAN_POINT ( 'NONE',  ( -5.823673210054431948, 21.52544592524334988, 107.7094237280190328 ) ) ;
#42481 = CARTESIAN_POINT ( 'NONE',  ( 15.72974639402176855, 15.80617190586768217, 81.87609039468568994 ) ) ;
#42483 = CARTESIAN_POINT ( 'NONE',  ( 8.224510206698953496, -14.34966873604960469, 102.9155762719810383 ) ) ;
#42484 = CARTESIAN_POINT ( 'NONE',  ( -0.05219959533936034679, 19.03943276465977164, 42.50109039468566152 ) ) ;
#42485 = CARTESIAN_POINT ( 'NONE',  ( -8.314922557961024197, 14.29746914071037800, 107.9177570613523471 ) ) ;
#42486 = CARTESIAN_POINT ( 'NONE',  ( 21.55341960407619695, -5.719274019375665929, 71.04275706135234714 ) ) ;
#42487 = CARTESIAN_POINT ( 'NONE',  ( 5.153800228976335163, 19.02544592524342804, 54.79057627198103120 ) ) ;
#42488 = CARTESIAN_POINT ( 'NONE',  ( -5.049401038297874678, -19.05341960407617918, 29.79275706135232227 ) ) ;
#42489 = CARTESIAN_POINT ( 'NONE',  ( -21.52544592524343514, 5.823673210054127303, 36.04057627198102409 ) ) ;
#42490 = CARTESIAN_POINT ( 'NONE',  ( -18.67979575497193778, 10.72451020669871902, 33.33442372801900433 ) ) ;
#42491 = CARTESIAN_POINT ( 'NONE',  ( -10.81492255796078084, -18.62759615963271287, 92.08224293864769550 ) ) ;
#42492 = CARTESIAN_POINT ( 'NONE',  ( -13.97604488694547697, 13.89961937509957934, 83.12609039468564731 ) ) ;
#42493 = CARTESIAN_POINT ( 'NONE',  ( 4.379528057220092307, 16.55341960407617563, 57.29275706135234714 ) ) ;
#42495 = CARTESIAN_POINT ( 'NONE',  ( -21.55341960407610458, -5.719274019375992779, 91.45724293864769550 ) ) ;
#42494 = CARTESIAN_POINT ( 'NONE',  ( 17.72662750342724891, 5.500000000000081712, 63.90179492283743201 ) ) ;
#42497 = CARTESIAN_POINT ( 'NONE',  ( 12.06949235617757843, -12.14591786802309237, 83.12390960531436690 ) ) ;
#42496 = CARTESIAN_POINT ( 'NONE',  ( 4.483927247898790824, -16.52544592524335698, 75.20942372801901854 ) ) ;
#42498 = CARTESIAN_POINT ( 'NONE',  ( -19.38985940809734032, -32.68077955211932561, -25.00000000000009592 ) ) ;
#42499 = CARTESIAN_POINT ( 'NONE',  ( 16.51473224551083163, -9.474510206698727899, 110.8344237280190043 ) ) ;
#42500 = CARTESIAN_POINT ( 'NONE',  ( -0.05219959533907301413, -21.53943276465977519, 32.49890960531435979 ) ) ;
#42501 = DIRECTION ( 'NONE',  ( -0.4999999999999967248, 0.5000000000000019984, 0.7071067811865485719 ) ) ;
#42502 = CARTESIAN_POINT ( 'NONE',  ( -0.05219959533934338120, 16.53943276465976808, 57.50109039468568994 ) ) ;
#42503 = CARTESIAN_POINT ( 'NONE',  ( -21.52544592524334988, -5.823673210054445271, 23.95942372801901143 ) ) ;
#42504 = CARTESIAN_POINT ( 'NONE',  ( -18.67979575497178146, -10.72451020669898902, 41.66557627198103120 ) ) ;
#42505 = CARTESIAN_POINT ( 'NONE',  ( 4.379528057220092307, 16.55341960407617563, 77.29275706135234714 ) ) ;
#42506 = CARTESIAN_POINT ( 'NONE',  ( -19.03943276465977164, 0.05219959533909376836, 81.24890960531436690 ) ) ;
#42508 = CARTESIAN_POINT ( 'NONE',  ( 5.049401038298161559, -19.05341960407611168, 22.70724293864769194 ) ) ;
#42507 = CARTESIAN_POINT ( 'NONE',  ( 18.62759615963255655, 10.81492255796105972, 61.66775706135235424 ) ) ;
#42509 = CARTESIAN_POINT ( 'NONE',  ( 18.62759615963271287, -10.81492255796078972, 38.33224293864768839 ) ) ;
#42510 = VERTEX_POINT ( 'NONE', #70117 ) ;
#42511 = CARTESIAN_POINT ( 'NONE',  ( 19.03943276465977164, 0.05219959533936151252, 36.25109039468567573 ) ) ;
#42512 = CARTESIAN_POINT ( 'NONE',  ( -0.05219959533934338120, 16.53943276465976808, 57.50109039468568994 ) ) ;
#42513 = CARTESIAN_POINT ( 'NONE',  ( 16.51473224551069308, 9.474510206698969483, 114.1655762719810241 ) ) ;
#42514 = EDGE_LOOP ( 'NONE', ( #152231, #142466 ) ) ;
#42515 = EDGE_CURVE ( 'NONE', #21583, #125361, #9454, .T. ) ;
#42516 = CARTESIAN_POINT ( 'NONE',  ( -5.153800228976328057, -19.02544592524343514, 87.29057627198103830 ) ) ;
#42517 = CARTESIAN_POINT ( 'NONE',  ( -12.06949235617739369, -12.14591786802326823, 99.37609039468568994 ) ) ;
#42518 = CARTESIAN_POINT ( 'NONE',  ( -19.03943276465977164, 0.05219959533909376836, 116.2489096053143669 ) ) ;
#42519 = CARTESIAN_POINT ( 'NONE',  ( 12.06949235617757843, -12.14591786802309237, 98.12390960531436690 ) ) ;
#42520 = CARTESIAN_POINT ( 'NONE',  ( 0.05219959533907565091, 21.53943276465977519, 39.99890960531436690 ) ) ;
#42521 = CARTESIAN_POINT ( 'NONE',  ( -13.89961937509977652, 13.97604488694528158, 25.62390960531434558 ) ) ;
#42522 = CARTESIAN_POINT ( 'NONE',  ( 14.34966873604972726, -8.224510206698740333, 75.83442372801900433 ) ) ;
#42523 = CARTESIAN_POINT ( 'NONE',  ( 5.719274019375991003, -21.55341960407610458, 112.7072429386476955 ) ) ;
#42524 = CARTESIAN_POINT ( 'NONE',  ( 19.02544592524334988, 5.153800228976608722, 71.45942372801900433 ) ) ;
#42525 = CARTESIAN_POINT ( 'NONE',  ( 5.153800228976335163, 19.02544592524342804, 34.79057627198102409 ) ) ;
#42526 = DIRECTION ( 'NONE',  ( 0.4999999999999967248, -0.5000000000000019984, -0.7071067811865485719 ) ) ;
#42527 = CARTESIAN_POINT ( 'NONE',  ( 5.823673210054444382, -21.52544592524334988, 100.2094237280190043 ) ) ;
#42528 = CARTESIAN_POINT ( 'NONE',  ( -19.03943276465977164, 0.05219959533909376836, 61.24890960531436690 ) ) ;
#42529 = EDGE_CURVE ( 'NONE', #15380, #38864, #93839, .T. ) ;
#42530 = CARTESIAN_POINT ( 'NONE',  ( -16.55341960407617563, 4.379528057220093196, 53.54275706135234714 ) ) ;
#42531 = CARTESIAN_POINT ( 'NONE',  ( 5.719274019375673035, 21.55341960407619339, 87.29275706135236135 ) ) ;
#42532 = CARTESIAN_POINT ( 'NONE',  ( 13.97604488694548053, -13.89961937509957401, 40.62609039468564731 ) ) ;
#42533 = CARTESIAN_POINT ( 'NONE',  ( -13.97604488694547697, 13.89961937509957934, 53.12609039468565442 ) ) ;
#42534 = VERTEX_POINT ( 'NONE', #55943 ) ;
#42535 = CARTESIAN_POINT ( 'NONE',  ( -5.823673210054431948, 21.52544592524334988, 47.70942372801902565 ) ) ;
#42536 = CARTESIAN_POINT ( 'NONE',  ( 193.3062444957835453, -155.7167183371837496, -15.00000000000000178 ) ) ;
#42537 = CARTESIAN_POINT ( 'NONE',  ( -19.03943276465977164, -0.05219959533935918106, 48.75109039468566863 ) ) ;
#42538 = CARTESIAN_POINT ( 'NONE',  ( 16.51473224551069308, 9.474510206698969483, 94.16557627198103830 ) ) ;
#42539 = CARTESIAN_POINT ( 'NONE',  ( -16.51473224551069308, -9.474510206698971260, 86.66557627198102409 ) ) ;
#42540 = CARTESIAN_POINT ( 'NONE',  ( -14.34966873604960291, -8.224510206698953496, 41.66557627198103120 ) ) ;
#42541 = CARTESIAN_POINT ( 'NONE',  ( 0.05219959533907565091, 21.53943276465977519, 34.99890960531435979 ) ) ;
#42542 = CARTESIAN_POINT ( 'NONE',  ( 3.556970738554033499E-15, -38.81732327939057825, -4.624999997268814056 ) ) ;
#42543 = CARTESIAN_POINT ( 'NONE',  ( 21.84063423829474715, 22.96000461283902894, -49.40985016368630767 ) ) ;
#42544 = CARTESIAN_POINT ( 'NONE',  ( 10.72451020669871369, 18.67979575497193778, 107.0844237280190043 ) ) ;
#42545 = CARTESIAN_POINT ( 'NONE',  ( -36.91746825000000598, 2.428612866367529932E-14, -11.12499999726881228 ) ) ;
#42546 = CARTESIAN_POINT ( 'NONE',  ( -9.474510206698964154, 16.51473224551069663, 35.41557627198102409 ) ) ;
#42547 = CARTESIAN_POINT ( 'NONE',  ( 19.05341960407611168, 5.049401038298154454, 23.95724293864769194 ) ) ;
#42548 = CARTESIAN_POINT ( 'NONE',  ( -5.000000000000000000, 6.123233995736766282E-16, -15.00000000000000000 ) ) ;
#42549 = CARTESIAN_POINT ( 'NONE',  ( -15.54838543842805443, -33.98976552189215283, -7.999999999999996447 ) ) ;
#42550 = CARTESIAN_POINT ( 'NONE',  ( -16.55341960407617563, 4.379528057220093196, 58.54275706135235424 ) ) ;
#42551 = CARTESIAN_POINT ( 'NONE',  ( -10.72451020669898014, 18.67979575497178502, 80.41557627198103830 ) ) ;
#42552 = CARTESIAN_POINT ( 'NONE',  ( 14.34966873604960469, 8.224510206698951720, 39.16557627198102409 ) ) ;
#42554 = CARTESIAN_POINT ( 'NONE',  ( -9.474510206698964154, 16.51473224551069663, 110.4155762719810383 ) ) ;
#42553 = CARTESIAN_POINT ( 'NONE',  ( 13.97604488694527802, 13.89961937509977652, 34.37390960531436690 ) ) ;
#42555 = CARTESIAN_POINT ( 'NONE',  ( 18.62759615963255655, 10.81492255796105972, 26.66775706135235424 ) ) ;
#42556 = CARTESIAN_POINT ( 'NONE',  ( 13.89961937509957401, 13.97604488694547697, 31.87609039468566863 ) ) ;
#42557 = CARTESIAN_POINT ( 'NONE',  ( 5.049401038298161559, -19.05341960407611168, 32.70724293864768129 ) ) ;
#42558 = CARTESIAN_POINT ( 'NONE',  ( -10.72451020669870658, -18.67979575497194134, 79.58442372801903275 ) ) ;
#42559 = LINE ( 'NONE', #104222, #169681 ) ;
#42560 = CARTESIAN_POINT ( 'NONE',  ( 8.314922557960818139, 14.29746914071049879, 24.58224293864768839 ) ) ;
#42561 = CARTESIAN_POINT ( 'NONE',  ( 17.50000000000000000, 3.305555262949673612, 112.8748284784341251 ) ) ;
#42562 = CARTESIAN_POINT ( 'NONE',  ( 10.72451020669898902, -18.67979575497178502, 32.91557627198102409 ) ) ;
#42563 = CARTESIAN_POINT ( 'NONE',  ( 14.34966873604960469, 8.224510206698951720, 109.1655762719810383 ) ) ;
#42564 = CARTESIAN_POINT ( 'NONE',  ( -5.802100494052803370, -6.819150417750785564, -63.98534035886881099 ) ) ;
#42565 = CARTESIAN_POINT ( 'NONE',  ( 19.05341960407611168, 5.049401038298154454, 83.95724293864766707 ) ) ;
#42566 = CARTESIAN_POINT ( 'NONE',  ( -16.52544592524342804, 4.483927247898546575, 76.04057627198102409 ) ) ;
#42567 = CARTESIAN_POINT ( 'NONE',  ( -19.02544592524334988, -5.153800228976617603, 108.9594237280189759 ) ) ;
#42568 = CARTESIAN_POINT ( 'NONE',  ( -10.81492255796078084, -18.62759615963271287, 57.08224293864769550 ) ) ;
#42569 = ORIENTED_EDGE ( 'NONE', *, *, #179632, .T. ) ;
#42570 = CARTESIAN_POINT ( 'NONE',  ( 9.564922557960805705, 16.46253265017160317, 34.58224293864770260 ) ) ;
#42572 = CARTESIAN_POINT ( 'NONE',  ( 0.05219959533907565091, 21.53943276465977519, 94.99890960531436690 ) ) ;
#42571 = CARTESIAN_POINT ( 'NONE',  ( 0.05219959533909260263, 19.03943276465977164, 84.99890960531436690 ) ) ;
#42574 = CARTESIAN_POINT ( 'NONE',  ( -19.03943276465977164, 0.05219959533909376836, 86.24890960531436690 ) ) ;
#42573 = CARTESIAN_POINT ( 'NONE',  ( 16.55341960407618274, -4.379528057220086978, 111.0427570613523613 ) ) ;
#42575 = CARTESIAN_POINT ( 'NONE',  ( -13.97604488694547697, 13.89961937509957934, 78.12609039468567573 ) ) ;
#42576 = CARTESIAN_POINT ( 'NONE',  ( -5.823673210054431948, 21.52544592524334988, 92.70942372801901854 ) ) ;
#42577 = CARTESIAN_POINT ( 'NONE',  ( 5.719274019375991003, -21.55341960407610458, 77.70724293864770971 ) ) ;
#42578 = CARTESIAN_POINT ( 'NONE',  ( -5.719274019375978568, 21.55341960407610458, 35.20724293864768839 ) ) ;
#42579 = CARTESIAN_POINT ( 'NONE',  ( -9.474510206698964154, 16.51473224551069663, 50.41557627198102409 ) ) ;
#42580 = CARTESIAN_POINT ( 'NONE',  ( -12.14591786802309592, -12.06949235617757132, 21.87390960531436690 ) ) ;
#42581 = CARTESIAN_POINT ( 'NONE',  ( 19.03943276465977164, -0.05219959533909143690, 58.74890960531435979 ) ) ;
#42582 = CARTESIAN_POINT ( 'NONE',  ( -31.76083434626056956, -6.487688756757402864, 91.22915654580295097 ) ) ;
#42583 = CARTESIAN_POINT ( 'NONE',  ( -5.049401038297874678, -19.05341960407617918, 24.79275706135233648 ) ) ;
#42584 = CARTESIAN_POINT ( 'NONE',  ( 12.06949235617757843, -12.14591786802309237, 73.12390960531436690 ) ) ;
#42585 = CARTESIAN_POINT ( 'NONE',  ( -0.05219959533907301413, -21.53943276465977519, 107.4989096053143669 ) ) ;
#42586 = CARTESIAN_POINT ( 'NONE',  ( -5.823673210054116645, -21.52544592524344225, 112.2905762719810241 ) ) ;
#42587 = CARTESIAN_POINT ( 'NONE',  ( -6.434671708797603529, 6.434671708797564449, -63.95112321872120731 ) ) ;
#42588 = CARTESIAN_POINT ( 'NONE',  ( 10.72451020669898902, -18.67979575497178502, 52.91557627198103830 ) ) ;
#42589 = CARTESIAN_POINT ( 'NONE',  ( 14.34966873604972726, -8.224510206698740333, 90.83442372801901854 ) ) ;
#42590 = CARTESIAN_POINT ( 'NONE',  ( -12.06949235617756955, 12.14591786802309770, 100.6239096053143811 ) ) ;
#42591 = CARTESIAN_POINT ( 'NONE',  ( -5.153800228976328057, -19.02544592524343514, 57.29057627198103120 ) ) ;
#42592 = CARTESIAN_POINT ( 'NONE',  ( -14.29746914071049879, 8.314922557960819915, 25.83224293864769194 ) ) ;
#42593 = ORIENTED_EDGE ( 'NONE', *, *, #47203, .T. ) ;
#42594 = CARTESIAN_POINT ( 'NONE',  ( -15.80617190586768217, 15.72974639402176855, 48.12609039468568284 ) ) ;
#42595 = CARTESIAN_POINT ( 'NONE',  ( 19.05341960407611168, 5.049401038298154454, 108.9572429386477097 ) ) ;
#42596 = CARTESIAN_POINT ( 'NONE',  ( 18.62759615963255655, 10.81492255796105972, 76.66775706135234714 ) ) ;
#42597 = CARTESIAN_POINT ( 'NONE',  ( -19.05341960407611168, -5.049401038298163336, 36.45724293864766707 ) ) ;
#42598 = CARTESIAN_POINT ( 'NONE',  ( 13.97604488694527802, 13.89961937509977652, 44.37390960531435269 ) ) ;
#42599 = ORIENTED_EDGE ( 'NONE', *, *, #7273, .T. ) ;
#42600 = CARTESIAN_POINT ( 'NONE',  ( 18.62759615963255655, 10.81492255796105972, 86.66775706135234714 ) ) ;
#42601 = CARTESIAN_POINT ( 'NONE',  ( -16.52544592524335698, -4.483927247898792601, 48.95942372801902565 ) ) ;
#42602 = CARTESIAN_POINT ( 'NONE',  ( -18.67979575497193778, 10.72451020669871902, 73.33442372801901854 ) ) ;
#42603 = CARTESIAN_POINT ( 'NONE',  ( 9.474510206698971260, -16.51473224551069308, 102.9155762719810241 ) ) ;
#42604 = CARTESIAN_POINT ( 'NONE',  ( 0.05219959533936267826, -19.03943276465977164, 80.00109039468567573 ) ) ;
#42605 = CARTESIAN_POINT ( 'NONE',  ( -21.55341960407619339, 5.719274019375674811, 58.54275706135235424 ) ) ;
#42606 = CARTESIAN_POINT ( 'NONE',  ( 14.34966873604972726, -8.224510206698740333, 20.83442372801901143 ) ) ;
#42607 = CARTESIAN_POINT ( 'NONE',  ( -13.97604488694547697, 13.89961937509957934, 78.12609039468567573 ) ) ;
#42608 = CARTESIAN_POINT ( 'NONE',  ( -5.153800228976328057, -19.02544592524343514, 52.29057627198100988 ) ) ;
#42609 = CARTESIAN_POINT ( 'NONE',  ( 19.03943276465977164, 0.05219959533936151252, 86.25109039468567573 ) ) ;
#42610 = CARTESIAN_POINT ( 'NONE',  ( -12.14591786802309592, -12.06949235617757132, 21.87390960531436690 ) ) ;
#42611 = CARTESIAN_POINT ( 'NONE',  ( -13.89961937509957401, -13.97604488694547875, 84.37609039468567573 ) ) ;
#42612 = CARTESIAN_POINT ( 'NONE',  ( 12.14591786802309770, 12.06949235617756955, 34.37390960531435979 ) ) ;
#42613 = CARTESIAN_POINT ( 'NONE',  ( -19.05341960407617563, 5.049401038297882671, 68.54275706135230450 ) ) ;
#42614 = CARTESIAN_POINT ( 'NONE',  ( 14.29746914071037800, 8.314922557961029526, 46.66775706135234714 ) ) ;
#42615 = CARTESIAN_POINT ( 'NONE',  ( 5.153800228976615827, -19.02544592524334988, 20.20942372801899722 ) ) ;
#42616 = CARTESIAN_POINT ( 'NONE',  ( 13.97604488694527802, 13.89961937509977652, 39.37390960531435269 ) ) ;
#42617 = CARTESIAN_POINT ( 'NONE',  ( 8.314922557961029526, -14.29746914071037800, 40.41775706135234714 ) ) ;
#42618 = FACE_OUTER_BOUND ( 'NONE', #125018, .T. ) ;
#42620 = CIRCLE ( 'NONE', #181481, 2.000000000000001776 ) ;
#42619 = CARTESIAN_POINT ( 'NONE',  ( -17.14385361876520264, -23.59649016807271593, 145.1750000027311387 ) ) ;
#42621 = CARTESIAN_POINT ( 'NONE',  ( -19.03943276465977164, 0.05219959533909376836, 96.24890960531436690 ) ) ;
#42622 = EDGE_CURVE ( 'NONE', #165429, #58517, #195479, .T. ) ;
#42623 = LINE ( 'NONE', #198281, #197634 ) ;
#42624 = CARTESIAN_POINT ( 'NONE',  ( 16.46253265017146816, 9.564922557961045513, 101.6677570613523329 ) ) ;
#42625 = CARTESIAN_POINT ( 'NONE',  ( 19.05341960407611168, 5.049401038298154454, 113.9572429386477097 ) ) ;
#42627 = CARTESIAN_POINT ( 'NONE',  ( 16.53943276465976808, 0.05219959533934440121, 21.25109039468567218 ) ) ;
#42626 = CARTESIAN_POINT ( 'NONE',  ( -19.05341960407617563, 5.049401038297882671, 23.54275706135233648 ) ) ;
#42628 = CARTESIAN_POINT ( 'NONE',  ( 13.89961937509977652, -13.97604488694527269, 23.12390960531436335 ) ) ;
#42629 = CARTESIAN_POINT ( 'NONE',  ( 9.474510206698971260, -16.51473224551069308, 37.91557627198102409 ) ) ;
#42630 = CARTESIAN_POINT ( 'NONE',  ( 21.55341960407610458, 5.719274019375980345, 68.95724293864769550 ) ) ;
#42631 =( BOUNDED_CURVE ( )  B_SPLINE_CURVE ( 2, ( #114314, #99147, #9163, #194187, #70830, #179020, #40488, #102160, #27336, #134509, #90943 ),
 .UNSPECIFIED., .F., .F. ) 
 B_SPLINE_CURVE_WITH_KNOTS ( ( 3, 2, 2, 2, 2, 3 ),
 ( 0.6000000000000000888, 0.6200000000000001066, 0.6400000000000001243, 0.6600000000000001421, 0.6800000000000001599, 0.7000000000000000666 ),
 .UNSPECIFIED. ) 
 CURVE ( )  GEOMETRIC_REPRESENTATION_ITEM ( )  RATIONAL_B_SPLINE_CURVE ( ( 0.9999999999999997780, 0.9510565162951537532, 1.000000000000000000, 0.9510565162951535312, 1.000000000000000000, 0.9510565162951535312, 1.000000000000000000, 0.9510565162951535312, 1.000000000000000000, 0.9510565162951533091, 1.000000000000000222 ) ) 
 REPRESENTATION_ITEM ( '' )  );
#42632 = CARTESIAN_POINT ( 'NONE',  ( -19.03943276465977164, 0.05219959533909376836, 41.24890960531435269 ) ) ;
#42633 = CARTESIAN_POINT ( 'NONE',  ( -5.153800228976607833, 19.02544592524335343, 47.70942372801900433 ) ) ;
#42634 = CARTESIAN_POINT ( 'NONE',  ( -5.049401038297874678, -19.05341960407617918, 64.79275706135233293 ) ) ;
#42635 = CARTESIAN_POINT ( 'NONE',  ( 12.14591786802309770, 12.06949235617756955, 49.37390960531436690 ) ) ;
#42636 = CARTESIAN_POINT ( 'NONE',  ( -21.55341960407610458, -5.719274019375992779, 31.45724293864769550 ) ) ;
#42637 = CARTESIAN_POINT ( 'NONE',  ( -10.72451020669870658, -18.67979575497194134, 94.58442372801901854 ) ) ;
#42638 = EDGE_CURVE ( 'NONE', #111352, #198671, #40985, .T. ) ;
#42639 = CARTESIAN_POINT ( 'NONE',  ( -18.62759615963270932, 10.81492255796079327, 80.83224293864769550 ) ) ;
#42640 = CARTESIAN_POINT ( 'NONE',  ( -18.67979575497193778, 10.72451020669871902, 53.33442372801901854 ) ) ;
#42641 = CARTESIAN_POINT ( 'NONE',  ( -15.72974639402176322, -15.80617190586768395, 64.37609039468568994 ) ) ;
#42642 = CARTESIAN_POINT ( 'NONE',  ( -13.97604488694527625, -13.89961937509977652, 101.8739096053143811 ) ) ;
#42644 = CARTESIAN_POINT ( 'NONE',  ( 21.52544592524334988, 5.823673210054432836, 61.45942372801901854 ) ) ;
#42643 = CARTESIAN_POINT ( 'NONE',  ( -8.314922557961024197, 14.29746914071037800, 87.91775706135234714 ) ) ;
#42645 = CARTESIAN_POINT ( 'NONE',  ( 9.474510206698971260, -16.51473224551069308, 57.91557627198103120 ) ) ;
#42646 = CARTESIAN_POINT ( 'NONE',  ( 19.05341960407611168, 5.049401038298154454, 23.95724293864769194 ) ) ;
#42647 = CARTESIAN_POINT ( 'NONE',  ( 9.564922557960805705, 16.46253265017160317, 54.58224293864769550 ) ) ;
#42648 = CARTESIAN_POINT ( 'NONE',  ( 16.55341960407611168, 4.379528057220329451, 68.95724293864769550 ) ) ;
#42649 = CARTESIAN_POINT ( 'NONE',  ( -16.53943276465976808, 0.05219959533911058130, 36.24890960531435979 ) ) ;
#42650 = CARTESIAN_POINT ( 'NONE',  ( -10.81492255796078084, -18.62759615963271287, 47.08224293864770260 ) ) ;
#42651 = CARTESIAN_POINT ( 'NONE',  ( -19.02544592524342804, 5.153800228976336051, 51.04057627198103120 ) ) ;
#42652 = CARTESIAN_POINT ( 'NONE',  ( 15.80617190586746368, 15.72974639402197994, 59.37390960531436690 ) ) ;
#42653 = CARTESIAN_POINT ( 'NONE',  ( 9.564922557961047289, -16.46253265017146816, 50.41775706135233293 ) ) ;
#42655 = CARTESIAN_POINT ( 'NONE',  ( -14.34966873604960291, -8.224510206698953496, 61.66557627198103120 ) ) ;
#42654 = DIRECTION ( 'NONE',  ( -0.000000000000000000, -0.000000000000000000, 1.000000000000000000 ) ) ;
#42656 = CARTESIAN_POINT ( 'NONE',  ( 18.67979575497178502, 10.72451020669898547, 39.16557627198102409 ) ) ;
#42657 = VERTEX_POINT ( 'NONE', #13428 ) ;
#42658 = ORIENTED_EDGE ( 'NONE', *, *, #190013, .F. ) ;
#42659 = CARTESIAN_POINT ( 'NONE',  ( 16.18388926212237422, 7.379444403734533253, 102.9395315136615210 ) ) ;
#42660 = CARTESIAN_POINT ( 'NONE',  ( 4.379528057220092307, 16.55341960407617563, 82.29275706135234714 ) ) ;
#42661 = CARTESIAN_POINT ( 'NONE',  ( -5.049401038297874678, -19.05341960407617918, 69.79275706135233293 ) ) ;
#42662 = CARTESIAN_POINT ( 'NONE',  ( 4.483927247898545687, 16.52544592524342804, 49.79057627198102409 ) ) ;
#42663 = DIRECTION ( 'NONE',  ( 0.000000000000000000, -1.224646799146988112E-16, 1.000000000000000000 ) ) ;
#42664 = CARTESIAN_POINT ( 'NONE',  ( -9.564922557960796823, -16.46253265017161027, 52.08224293864768839 ) ) ;
#42665 = CARTESIAN_POINT ( 'NONE',  ( -16.55341960407611168, -4.379528057220339221, 41.45724293864769550 ) ) ;
#42666 = CARTESIAN_POINT ( 'NONE',  ( -9.474510206698964154, 16.51473224551069663, 50.41557627198102409 ) ) ;
#42667 = ADVANCED_FACE ( 'NONE', ( #12459 ), #25635, .F. ) ;
#42668 = CARTESIAN_POINT ( 'NONE',  ( 5.153800228976335163, 19.02544592524342804, 69.79057627198103830 ) ) ;
#42669 = CARTESIAN_POINT ( 'NONE',  ( -16.51473224551069308, -9.474510206698971260, 36.66557627198102409 ) ) ;
#42670 = CARTESIAN_POINT ( 'NONE',  ( 0.05219959533937995610, -21.53943276465977519, 45.00109039468568284 ) ) ;
#42671 = CARTESIAN_POINT ( 'NONE',  ( 5.049401038298161559, -19.05341960407611168, 77.70724293864765286 ) ) ;
#42672 = CARTESIAN_POINT ( 'NONE',  ( 13.97604488694527802, 13.89961937509977652, 29.37390960531435979 ) ) ;
#42673 = CARTESIAN_POINT ( 'NONE',  ( 16.46253265017160672, -9.564922557960803928, 58.33224293864769550 ) ) ;
#42674 = CARTESIAN_POINT ( 'NONE',  ( 10.81492255796078972, 18.62759615963270932, 44.58224293864769550 ) ) ;
#42675 = CARTESIAN_POINT ( 'NONE',  ( -19.03943276465977164, 0.05219959533909376836, 36.24890960531436690 ) ) ;
#42676 = CARTESIAN_POINT ( 'NONE',  ( -10.72451020669898014, 18.67979575497178502, 40.41557627198103120 ) ) ;
#42677 = CARTESIAN_POINT ( 'NONE',  ( -14.34966873604972548, 8.224510206698743886, 98.33442372801901854 ) ) ;
#42678 = CARTESIAN_POINT ( 'NONE',  ( -16.46253265017146816, -9.564922557961047289, 29.16775706135232937 ) ) ;
#42680 = CARTESIAN_POINT ( 'NONE',  ( 16.52544592524335698, 4.483927247898782831, 81.45942372801900433 ) ) ;
#42679 = CARTESIAN_POINT ( 'NONE',  ( 12.14591786802327356, -12.06949235617739191, 50.62609039468568994 ) ) ;
#42681 = CARTESIAN_POINT ( 'NONE',  ( -18.22780087662122028, 5.500000000000031086, 68.51540105326107266 ) ) ;
#42682 = CARTESIAN_POINT ( 'NONE',  ( -14.29746914071037622, -8.314922557961029526, 69.16775706135234714 ) ) ;
#42683 = CARTESIAN_POINT ( 'NONE',  ( 12.06949235617739724, 12.14591786802326823, 46.87609039468568994 ) ) ;
#42684 = CARTESIAN_POINT ( 'NONE',  ( -19.05341960407611168, -5.049401038298163336, 111.4572429386476671 ) ) ;
#42685 = CARTESIAN_POINT ( 'NONE',  ( 16.52544592524335698, 4.483927247898782831, 36.45942372801901143 ) ) ;
#42686 = CARTESIAN_POINT ( 'NONE',  ( -5.049401038298153566, 19.05341960407611168, 30.20724293864768839 ) ) ;
#42687 = CARTESIAN_POINT ( 'NONE',  ( -10.81492255796105439, 18.62759615963255655, 22.91775706135235069 ) ) ;
#42688 = CARTESIAN_POINT ( 'NONE',  ( 8.314922557961029526, -14.29746914071037800, 30.41775706135234358 ) ) ;
#42689 = CARTESIAN_POINT ( 'NONE',  ( -14.34966873604972548, 8.224510206698743886, 98.33442372801901854 ) ) ;
#42690 = CARTESIAN_POINT ( 'NONE',  ( -18.09918380851993902, -5.499999999999988454, 71.48618307335610211 ) ) ;
#42691 = CARTESIAN_POINT ( 'NONE',  ( 21.55341960407619695, -5.719274019375665929, 106.0427570613523471 ) ) ;
#42692 = CARTESIAN_POINT ( 'NONE',  ( -19.03943276465977164, -0.05219959533935918106, 98.75109039468567573 ) ) ;
#42693 = CARTESIAN_POINT ( 'NONE',  ( -16.55341960407611168, -4.379528057220339221, 61.45724293864770260 ) ) ;
#42694 = CARTESIAN_POINT ( 'NONE',  ( -19.03943276465977164, 0.05219959533909376836, 26.24890960531435624 ) ) ;
#42696 = CARTESIAN_POINT ( 'NONE',  ( 16.29526858892876007, 7.335722546920145248, 78.29670597800209464 ) ) ;
#42695 = CARTESIAN_POINT ( 'NONE',  ( -19.05341960407617563, 5.049401038297882671, 58.54275706135234003 ) ) ;
#42697 = CARTESIAN_POINT ( 'NONE',  ( -15.72974639402176322, -15.80617190586768395, 59.37609039468568284 ) ) ;
#42698 = CARTESIAN_POINT ( 'NONE',  ( -16.53943276465976808, -0.05219959533934237506, 28.75109039468567929 ) ) ;
#42699 = CARTESIAN_POINT ( 'NONE',  ( 30.00000000000000000, -5.510910596163089556E-15, 45.00000000000000000 ) ) ;
#42700 = CARTESIAN_POINT ( 'NONE',  ( 19.02544592524343514, -5.153800228976328945, 113.5405762719810241 ) ) ;
#42701 = CARTESIAN_POINT ( 'NONE',  ( 15.72974639402199770, -15.80617190586745480, 78.12390960531436690 ) ) ;
#42702 = CARTESIAN_POINT ( 'NONE',  ( -16.51473224551082808, 9.474510206698731452, 113.3344237280190043 ) ) ;
#42703 = CARTESIAN_POINT ( 'NONE',  ( 16.46253265017160672, -9.564922557960803928, 108.3322429386476955 ) ) ;
#42704 = CARTESIAN_POINT ( 'NONE',  ( 3.071040654511329571, -27.74725471568222801, 139.9999999999999716 ) ) ;
#42705 = CARTESIAN_POINT ( 'NONE',  ( 0.05219959533910956823, 16.53943276465976808, 114.9989096053143669 ) ) ;
#42706 = CARTESIAN_POINT ( 'NONE',  ( -10.72451020669870658, -18.67979575497194134, 109.5844237280190328 ) ) ;
#42707 = CARTESIAN_POINT ( 'NONE',  ( 19.02544592524343514, -5.153800228976328945, 48.54057627198103120 ) ) ;
#42708 = CARTESIAN_POINT ( 'NONE',  ( 10.81492255796106328, -18.62759615963255655, 55.41775706135234714 ) ) ;
#42709 = CARTESIAN_POINT ( 'NONE',  ( -18.62759615963255300, -10.81492255796106328, 99.16775706135234714 ) ) ;
#42710 = CARTESIAN_POINT ( 'NONE',  ( -4.379528057220086978, -16.55341960407618274, 109.7927570613523613 ) ) ;
#42711 = CARTESIAN_POINT ( 'NONE',  ( -0.05219959533909027116, -19.03943276465977164, 77.49890960531435269 ) ) ;
#42712 = CARTESIAN_POINT ( 'NONE',  ( -10.81492255796105439, 18.62759615963255655, 42.91775706135235424 ) ) ;
#42713 = CARTESIAN_POINT ( 'NONE',  ( 5.823673210054444382, -21.52544592524334988, 55.20942372801902565 ) ) ;
#42715 = CARTESIAN_POINT ( 'NONE',  ( -9.564922557960796823, -16.46253265017161027, 87.08224293864769550 ) ) ;
#42714 = CARTESIAN_POINT ( 'NONE',  ( 9.474510206698729675, 16.51473224551082808, 82.08442372801899012 ) ) ;
#42716 = CARTESIAN_POINT ( 'NONE',  ( 8.314922557960818139, 14.29746914071049879, 109.5822429386476955 ) ) ;
#42717 = CARTESIAN_POINT ( 'NONE',  ( 15.72974639402199770, -15.80617190586745480, 93.12390960531436690 ) ) ;
#42718 = CARTESIAN_POINT ( 'NONE',  ( -8.314922557960811034, -14.29746914071050412, 72.08224293864769550 ) ) ;
#42719 = CARTESIAN_POINT ( 'NONE',  ( 18.62759615963255655, 10.81492255796105972, 111.6677570613523613 ) ) ;
#42720 = CARTESIAN_POINT ( 'NONE',  ( 16.52544592524342804, -4.483927247898539470, 98.54057627198105251 ) ) ;
#42721 = CARTESIAN_POINT ( 'NONE',  ( 0.05219959533909260263, 19.03943276465977164, 44.99890960531435979 ) ) ;
#42722 = CARTESIAN_POINT ( 'NONE',  ( -5.049401038297874678, -19.05341960407617918, 79.79275706135233293 ) ) ;
#42723 = CARTESIAN_POINT ( 'NONE',  ( 4.379528057220339221, -16.55341960407611168, 47.70724293864770260 ) ) ;
#42724 = CARTESIAN_POINT ( 'NONE',  ( -0.05219959533937732626, 21.53943276465977519, 112.5010903946857042 ) ) ;
#42725 = CARTESIAN_POINT ( 'NONE',  ( 13.97604488694527802, 13.89961937509977652, 104.3739096053143385 ) ) ;
#42726 = CARTESIAN_POINT ( 'NONE',  ( 9.564922557961047289, -16.46253265017146816, 80.41775706135234714 ) ) ;
#42727 = CARTESIAN_POINT ( 'NONE',  ( -10.72451020669898014, 18.67979575497178502, 75.41557627198102409 ) ) ;
#42728 = CARTESIAN_POINT ( 'NONE',  ( 10.72451020669871369, 18.67979575497193778, 27.08442372801901854 ) ) ;
#42729 = CARTESIAN_POINT ( 'NONE',  ( -16.53943276465976808, -0.05219959533934237506, 33.75109039468568284 ) ) ;
#42730 = CARTESIAN_POINT ( 'NONE',  ( 14.29746914071037800, 8.314922557961029526, 96.66775706135234714 ) ) ;
#42732 = CARTESIAN_POINT ( 'NONE',  ( -21.52544592524334988, -5.823673210054445271, 33.95942372801901143 ) ) ;
#42731 = CARTESIAN_POINT ( 'NONE',  ( 17.40805194822031154, 6.112264579159360167, 61.66628727489387529 ) ) ;
#42733 = CARTESIAN_POINT ( 'NONE',  ( -10.81492255796078084, -18.62759615963271287, 47.08224293864770260 ) ) ;
#42734 = CARTESIAN_POINT ( 'NONE',  ( -8.224510206698948167, 14.34966873604960824, 115.4155762719810241 ) ) ;
#42735 = CARTESIAN_POINT ( 'NONE',  ( 37.99999999999999289, 2.893978650043524126E-14, -8.749999994537628112 ) ) ;
#42736 = CARTESIAN_POINT ( 'NONE',  ( -4.483927247898782831, 16.52544592524335698, 67.70942372801901854 ) ) ;
#42737 = CARTESIAN_POINT ( 'NONE',  ( 4.379528057220339221, -16.55341960407611168, 97.70724293864772392 ) ) ;
#42738 = CARTESIAN_POINT ( 'NONE',  ( -18.67979575497178146, -10.72451020669898902, 76.66557627198103830 ) ) ;
#42739 = CARTESIAN_POINT ( 'NONE',  ( 8.314922557960818139, 14.29746914071049879, 29.58224293864769905 ) ) ;
#42740 = CARTESIAN_POINT ( 'NONE',  ( 8.224510206698742110, 14.34966873604972548, 52.08442372801901854 ) ) ;
#42741 = CARTESIAN_POINT ( 'NONE',  ( 9.564922557960805705, 16.46253265017160317, 44.58224293864769550 ) ) ;
#42742 = CARTESIAN_POINT ( 'NONE',  ( 16.53943276465976808, 0.05219959533934440121, 96.25109039468568994 ) ) ;
#42743 = CARTESIAN_POINT ( 'NONE',  ( 13.89961937509957401, 13.97604488694547697, 91.87609039468567573 ) ) ;
#42744 = CARTESIAN_POINT ( 'NONE',  ( -0.05219959533907301413, -21.53943276465977519, 87.49890960531436690 ) ) ;
#42745 = CARTESIAN_POINT ( 'NONE',  ( 0.05219959533934541429, -16.53943276465976808, 105.0010903946856757 ) ) ;
#42746 = ORIENTED_EDGE ( 'NONE', *, *, #48034, .T. ) ;
#42747 = CARTESIAN_POINT ( 'NONE',  ( 19.03943276465977164, -0.05219959533909143690, 113.7489096053143669 ) ) ;
#42748 = CARTESIAN_POINT ( 'NONE',  ( -18.62759615963270932, 10.81492255796079327, 55.83224293864770260 ) ) ;
#42749 = CARTESIAN_POINT ( 'NONE',  ( -8.314922557961024197, 14.29746914071037800, 97.91775706135236135 ) ) ;
#42750 = ORIENTED_EDGE ( 'NONE', *, *, #106636, .T. ) ;
#42751 = CARTESIAN_POINT ( 'NONE',  ( 10.81492255796078972, 18.62759615963270932, 24.58224293864768839 ) ) ;
#42752 = CARTESIAN_POINT ( 'NONE',  ( -18.87075004821565472, 5.500000000000079048, 73.67408112101047379 ) ) ;
#42753 = CARTESIAN_POINT ( 'NONE',  ( -18.62759615963270932, 10.81492255796079327, 80.83224293864769550 ) ) ;
#42754 = CARTESIAN_POINT ( 'NONE',  ( -4.379528057220328563, 16.55341960407611168, 30.20724293864769550 ) ) ;
#42755 = CARTESIAN_POINT ( 'NONE',  ( -4.379528057220086978, -16.55341960407618274, 19.79275706135235069 ) ) ;
#42756 = CARTESIAN_POINT ( 'NONE',  ( 13.89961937509977652, -13.97604488694527269, 38.12390960531436690 ) ) ;
#42757 = CARTESIAN_POINT ( 'NONE',  ( 14.34966873604972726, -8.224510206698740333, 30.83442372801902209 ) ) ;
#42758 = CARTESIAN_POINT ( 'NONE',  ( 0.05219959533909260263, 19.03943276465977164, 54.99890960531435979 ) ) ;
#42759 = CARTESIAN_POINT ( 'NONE',  ( 27.73933785331498214, 9.013057229001095294, 140.4750000027311785 ) ) ;
#42760 = CARTESIAN_POINT ( 'NONE',  ( -16.51473224551069308, -9.474510206698971260, 106.6655762719810383 ) ) ;
#42761 = CARTESIAN_POINT ( 'NONE',  ( -19.05341960407611168, -5.049401038298163336, 106.4572429386476955 ) ) ;
#42762 = EDGE_CURVE ( 'NONE', #176889, #197513, #34935, .T. ) ;
#42763 = CARTESIAN_POINT ( 'NONE',  ( -14.34966873604972548, 8.224510206698743886, 83.33442372801903275 ) ) ;
#42764 = CARTESIAN_POINT ( 'NONE',  ( 19.03943276465977164, 0.05219959533936151252, 96.25109039468567573 ) ) ;
#42765 = CARTESIAN_POINT ( 'NONE',  ( -5.153800228976607833, 19.02544592524334988, 42.70942372801901143 ) ) ;
#42766 = CARTESIAN_POINT ( 'NONE',  ( -21.52544592524343514, 5.823673210054127303, 71.04057627198103830 ) ) ;
#42767 = CARTESIAN_POINT ( 'NONE',  ( -4.483927247898782831, 16.52544592524335698, 97.70942372801904696 ) ) ;
#42768 = CARTESIAN_POINT ( 'NONE',  ( -0.05219959533907301413, -21.53943276465977519, 27.49890960531435269 ) ) ;
#42769 = CARTESIAN_POINT ( 'NONE',  ( 9.474510206698729675, 16.51473224551082808, 87.08442372801900433 ) ) ;
#42770 = CARTESIAN_POINT ( 'NONE',  ( -5.049401038298153566, 19.05341960407611168, 50.20724293864770260 ) ) ;
#42771 = CARTESIAN_POINT ( 'NONE',  ( 0.05219959533909260263, 19.03943276465977164, 94.99890960531436690 ) ) ;
#42772 = CARTESIAN_POINT ( 'NONE',  ( -0.05219959533937732626, 21.53943276465977519, 57.50109039468568994 ) ) ;
#42773 = CARTESIAN_POINT ( 'NONE',  ( 19.02544592524343514, -5.153800228976328945, 58.54057627198102409 ) ) ;
#42774 = CARTESIAN_POINT ( 'NONE',  ( 14.29746914071049879, -8.314922557960816363, 103.3322429386476955 ) ) ;
#42775 = CARTESIAN_POINT ( 'NONE',  ( -17.40805194822031865, -6.112264579159316646, 84.16628727489391792 ) ) ;
#42776 = CARTESIAN_POINT ( 'NONE',  ( 8.224510206698953496, -14.34966873604960469, 82.91557627198103830 ) ) ;
#42777 = CARTESIAN_POINT ( 'NONE',  ( 15.72974639402199770, -15.80617190586745480, 68.12390960531436690 ) ) ;
#42778 = CARTESIAN_POINT ( 'NONE',  ( -16.51473224551082808, 9.474510206698731452, 88.33442372801900433 ) ) ;
#42779 = LINE ( 'NONE', #39764, #124679 ) ;
#42780 = CARTESIAN_POINT ( 'NONE',  ( 19.05341960407611168, 5.049401038298154454, 58.95724293864768129 ) ) ;
#42781 = CARTESIAN_POINT ( 'NONE',  ( -3.889087296526120507, -29.99999999999998579, 1.818019484660534868 ) ) ;
#42783 = CARTESIAN_POINT ( 'NONE',  ( -13.97604488694527625, -13.89961937509977652, 81.87390960531436690 ) ) ;
#42782 = CARTESIAN_POINT ( 'NONE',  ( -19.03943276465977164, 0.05219959533909376836, 81.24890960531436690 ) ) ;
#42784 = CARTESIAN_POINT ( 'NONE',  ( -16.52544592524335698, -4.483927247898792601, 63.95942372801901854 ) ) ;
#42785 = CARTESIAN_POINT ( 'NONE',  ( -28.90000000000004476, 2.980639576201346218E-13, -49.67367017693150189 ) ) ;
#42786 = CARTESIAN_POINT ( 'NONE',  ( 0.05219959533936267826, -19.03943276465977164, 45.00109039468566863 ) ) ;
#42787 = CARTESIAN_POINT ( 'NONE',  ( 36.79349492566039714, 4.147684444183153296, 48.62988885745598111 ) ) ;
#42788 = CARTESIAN_POINT ( 'NONE',  ( 19.03943276465977164, -0.05219959533909143690, 113.7489096053143669 ) ) ;
#42789 = CARTESIAN_POINT ( 'NONE',  ( -4.379528057220086978, -16.55341960407618274, 104.7927570613523898 ) ) ;
#42790 = EDGE_CURVE ( 'NONE', #84237, #42534, #2607, .T. ) ;
#42791 = CARTESIAN_POINT ( 'NONE',  ( -1.250870343808723417, -21.94965239947791247, -55.99511580764671237 ) ) ;
#42792 = CARTESIAN_POINT ( 'NONE',  ( -12.14591786802326823, 12.06949235617739902, 78.12609039468570415 ) ) ;
#42793 = CARTESIAN_POINT ( 'NONE',  ( -16.88567814943165857, 6.947325034625572826, 28.70998877347415501 ) ) ;
#42794 = CARTESIAN_POINT ( 'NONE',  ( 16.55341960407618274, -4.379528057220086978, 56.04275706135235424 ) ) ;
#42795 = CARTESIAN_POINT ( 'NONE',  ( -5.049401038298153566, 19.05341960407611168, 75.20724293864769550 ) ) ;
#42796 = CARTESIAN_POINT ( 'NONE',  ( -18.67979575497193778, 10.72451020669871902, 63.33442372801900433 ) ) ;
#42797 = CARTESIAN_POINT ( 'NONE',  ( -5.049401038297874678, -19.05341960407617918, 74.79275706135231871 ) ) ;
#42798 = CARTESIAN_POINT ( 'NONE',  ( 5.153800228976615827, -19.02544592524334988, 30.20942372801900433 ) ) ;
#42799 = CARTESIAN_POINT ( 'NONE',  ( -13.89961937509977652, 13.97604488694528158, 70.62390960531432427 ) ) ;
#42800 = CARTESIAN_POINT ( 'NONE',  ( 19.03943276465977164, -0.05219959533909143690, 38.74890960531436690 ) ) ;
#42801 = CARTESIAN_POINT ( 'NONE',  ( 17.29445255458983510, -6.392944142058904156, 23.31418393918777454 ) ) ;
#42802 = CARTESIAN_POINT ( 'NONE',  ( 21.53943276465977519, -0.05219959533907433946, 83.74890960531435269 ) ) ;
#42803 = CARTESIAN_POINT ( 'NONE',  ( -10.72451020669898014, 18.67979575497178502, 30.41557627198101699 ) ) ;
#42804 = CARTESIAN_POINT ( 'NONE',  ( -19.02544592524342804, 5.153800228976336051, 26.04057627198103120 ) ) ;
#42805 = CARTESIAN_POINT ( 'NONE',  ( 0.05219959533934541429, -16.53943276465976808, 55.00109039468568284 ) ) ;
#42806 = ORIENTED_EDGE ( 'NONE', *, *, #178304, .T. ) ;
#42807 = CARTESIAN_POINT ( 'NONE',  ( -5.719274019375665041, -21.55341960407619695, 34.79275706135235424 ) ) ;
#42809 = CARTESIAN_POINT ( 'NONE',  ( 11.74264578624799427, 36.14014761921585972, -8.599999999999999645 ) ) ;
#42808 = CARTESIAN_POINT ( 'NONE',  ( 12.14591786802309770, 12.06949235617756955, 49.37390960531436690 ) ) ;
#42810 = CARTESIAN_POINT ( 'NONE',  ( -16.53943276465976808, -0.05219959533934237506, 23.75109039468567929 ) ) ;
#42811 = CARTESIAN_POINT ( 'NONE',  ( -9.474510206698720793, -16.51473224551083518, 34.58442372801899722 ) ) ;
#42812 = CARTESIAN_POINT ( 'NONE',  ( 8.224510206698953496, -14.34966873604960469, 47.91557627198102409 ) ) ;
#42813 = CARTESIAN_POINT ( 'NONE',  ( 10.72451020669898902, -18.67979575497178502, 112.9155762719810383 ) ) ;
#42815 = CARTESIAN_POINT ( 'NONE',  ( -21.55341960407610458, -5.719274019375992779, 81.45724293864769550 ) ) ;
#42814 = DIRECTION ( 'NONE',  ( 0.000000000000000000, 0.000000000000000000, 1.000000000000000000 ) ) ;
#42816 = CARTESIAN_POINT ( 'NONE',  ( 5.153800228976335163, 19.02544592524342804, 94.79057627198103830 ) ) ;
#42817 = CARTESIAN_POINT ( 'NONE',  ( -12.14591786802309592, -12.06949235617757132, 66.87390960531436690 ) ) ;
#42818 = CARTESIAN_POINT ( 'NONE',  ( 5.049401038298161559, -19.05341960407611168, 97.70724293864766707 ) ) ;
#42819 = CARTESIAN_POINT ( 'NONE',  ( -36.81781682666242972, 5.501098665926424935, 45.34601664933740039 ) ) ;
#42820 = CARTESIAN_POINT ( 'NONE',  ( -5.153800228976607833, 19.02544592524334988, 67.70942372801900433 ) ) ;
#42821 = CARTESIAN_POINT ( 'NONE',  ( 5.719274019375991003, -21.55341960407610458, 107.7072429386476955 ) ) ;
#42822 = CARTESIAN_POINT ( 'NONE',  ( 19.02544592524343514, -5.153800228976328945, 58.54057627198102409 ) ) ;
#42823 = CARTESIAN_POINT ( 'NONE',  ( -5.153800228976328057, -19.02544592524343514, 22.29057627198102765 ) ) ;
#42824 = CARTESIAN_POINT ( 'NONE',  ( 21.52544592524334988, 5.823673210054432836, 46.45942372801901854 ) ) ;
#42825 = CARTESIAN_POINT ( 'NONE',  ( 17.14385361876520264, 23.59649016807275856, 148.1750000027311955 ) ) ;
#42826 = CARTESIAN_POINT ( 'NONE',  ( -14.29746914071049879, 8.314922557960819915, 35.83224293864768839 ) ) ;
#42827 = CARTESIAN_POINT ( 'NONE',  ( 5.049401038298161559, -19.05341960407611168, 47.70724293864770260 ) ) ;
#42828 = CARTESIAN_POINT ( 'NONE',  ( -9.564922557960796823, -16.46253265017161027, 102.0822429386477097 ) ) ;
#42829 = CARTESIAN_POINT ( 'NONE',  ( 18.62759615963271287, -10.81492255796078972, 78.33224293864770971 ) ) ;
#42830 = CARTESIAN_POINT ( 'NONE',  ( 8.571926809382603096, -26.38167802310801235, 143.4750000027312069 ) ) ;
#42831 = CARTESIAN_POINT ( 'NONE',  ( -0.05219959533909027116, -19.03943276465977164, 42.49890960531435269 ) ) ;
#42832 = VERTEX_POINT ( 'NONE', #87279 ) ;
#42833 = CARTESIAN_POINT ( 'NONE',  ( 5.823673210054125526, 21.52544592524343514, 64.79057627198103830 ) ) ;
#42834 = CARTESIAN_POINT ( 'NONE',  ( -21.53943276465977519, -0.05219959533937600094, 88.75109039468567573 ) ) ;
#42837 = CARTESIAN_POINT ( 'NONE',  ( 14.29746914071049879, -8.314922557960816363, 83.33224293864769550 ) ) ;
#42836 = CARTESIAN_POINT ( 'NONE',  ( 16.55341960407618274, -4.379528057220086978, 86.04275706135236135 ) ) ;
#42835 = CARTESIAN_POINT ( 'NONE',  ( -28.82186960331499037, 2.428612866367529932E-14, 139.1250000027311842 ) ) ;
#42838 = CARTESIAN_POINT ( 'NONE',  ( -9.474510206698964154, 16.51473224551069663, 70.41557627198102409 ) ) ;
#42839 = EDGE_LOOP ( 'NONE', ( #192307, #164191 ) ) ;
#42840 = CARTESIAN_POINT ( 'NONE',  ( 16.46253265017146816, 9.564922557961045513, 36.66775706135233293 ) ) ;
#42841 = CARTESIAN_POINT ( 'NONE',  ( 8.314922557961029526, -14.29746914071037800, 90.41775706135236135 ) ) ;
#42842 = CARTESIAN_POINT ( 'NONE',  ( -15.72974639402176322, -15.80617190586768395, 109.3760903946857042 ) ) ;
#42843 = CARTESIAN_POINT ( 'NONE',  ( -13.97604488694527625, -13.89961937509977652, 91.87390960531432427 ) ) ;
#42844 = CARTESIAN_POINT ( 'NONE',  ( -15.72974639402197994, 15.80617190586746368, 50.62390960531435979 ) ) ;
#42845 = CARTESIAN_POINT ( 'NONE',  ( -5.823673210054431948, 21.52544592524334988, 92.70942372801901854 ) ) ;
#42846 = CARTESIAN_POINT ( 'NONE',  ( -8.314922557961024197, 14.29746914071037800, 57.91775706135234714 ) ) ;
#42847 = CARTESIAN_POINT ( 'NONE',  ( 18.67979575497194134, -10.72451020669871369, 20.83442372801901143 ) ) ;
#42848 = CARTESIAN_POINT ( 'NONE',  ( 8.314922557961029526, -14.29746914071037800, 25.41775706135235779 ) ) ;
#42849 = CARTESIAN_POINT ( 'NONE',  ( -13.97604488694527625, -13.89961937509977652, 86.87390960531436690 ) ) ;
#42850 = CARTESIAN_POINT ( 'NONE',  ( -8.314922557961024197, 14.29746914071037800, 27.91775706135234358 ) ) ;
#42851 = CARTESIAN_POINT ( 'NONE',  ( -9.474510206698964154, 16.51473224551069663, 50.41557627198102409 ) ) ;
#42852 = CARTESIAN_POINT ( 'NONE',  ( -8.224510206698735004, -14.34966873604973081, 34.58442372801900433 ) ) ;
#42853 = CARTESIAN_POINT ( 'NONE',  ( -8.224510206698948167, 14.34966873604960824, 80.41557627198103830 ) ) ;
#42854 = CARTESIAN_POINT ( 'NONE',  ( -12.14591786802326823, 12.06949235617739902, 88.12609039468570415 ) ) ;
#42856 = CARTESIAN_POINT ( 'NONE',  ( 9.564922557960805705, 16.46253265017160317, 64.58224293864769550 ) ) ;
#42855 = CARTESIAN_POINT ( 'NONE',  ( -18.67979575497193778, 10.72451020669871902, 43.33442372801901143 ) ) ;
#42857 = CARTESIAN_POINT ( 'NONE',  ( 19.02544592524343514, -5.153800228976328945, 83.54057627198100988 ) ) ;
#42858 = CARTESIAN_POINT ( 'NONE',  ( 0.05219959533910956823, 16.53943276465976808, 29.99890960531435979 ) ) ;
#42859 = CARTESIAN_POINT ( 'NONE',  ( 8.314922557961029526, -14.29746914071037800, 85.41775706135236135 ) ) ;
#42860 = VERTEX_POINT ( 'NONE', #75092 ) ;
#42861 = CARTESIAN_POINT ( 'NONE',  ( 0.05219959533936267826, -19.03943276465977164, 25.00109039468566152 ) ) ;
#42862 = CARTESIAN_POINT ( 'NONE',  ( 9.564922557960805705, 16.46253265017160317, 94.58224293864769550 ) ) ;
#42863 = EDGE_CURVE ( 'NONE', #103252, #144934, #84261, .T. ) ;
#42864 = CARTESIAN_POINT ( 'NONE',  ( 9.474510206698971260, -16.51473224551069308, 42.91557627198103120 ) ) ;
#42865 = CARTESIAN_POINT ( 'NONE',  ( 0.05219959533909260263, 19.03943276465977164, 114.9989096053143669 ) ) ;
#42866 = CARTESIAN_POINT ( 'NONE',  ( 8.224510206698742110, 14.34966873604972548, 42.08442372801901854 ) ) ;
#42868 = CARTESIAN_POINT ( 'NONE',  ( 14.29746914071037800, 8.314922557961029526, 56.66775706135235424 ) ) ;
#42867 = CARTESIAN_POINT ( 'NONE',  ( 19.05341960407617918, -5.049401038297876454, 71.04275706135234714 ) ) ;
#42869 = CARTESIAN_POINT ( 'NONE',  ( 7.128481858827108830, 2.709097808555399833, 7.001991027368838161 ) ) ;
#42870 = CARTESIAN_POINT ( 'NONE',  ( 19.05341960407611168, 5.049401038298154454, 83.95724293864766707 ) ) ;
#42871 = CARTESIAN_POINT ( 'NONE',  ( 5.823673210054125526, 21.52544592524343514, 109.7905762719810383 ) ) ;
#42872 = CARTESIAN_POINT ( 'NONE',  ( 16.46253265017146816, 9.564922557961045513, 66.66775706135233293 ) ) ;
#42874 = DIRECTION ( 'NONE',  ( 1.000000000000000000, 0.000000000000000000, 0.000000000000000000 ) ) ;
#42873 = CARTESIAN_POINT ( 'NONE',  ( -16.46253265017160317, 9.564922557960807481, 110.8322429386476955 ) ) ;
#42875 = CARTESIAN_POINT ( 'NONE',  ( -5.153800228976328057, -19.02544592524343514, 72.29057627198102409 ) ) ;
#42877 = FACE_OUTER_BOUND ( 'NONE', #77092, .T. ) ;
#42876 = CARTESIAN_POINT ( 'NONE',  ( -12.06949235617756955, 12.14591786802309770, 35.62390960531437401 ) ) ;
#42878 = CARTESIAN_POINT ( 'NONE',  ( 9.474510206698729675, 16.51473224551082808, 32.08442372801900433 ) ) ;
#42879 = CARTESIAN_POINT ( 'NONE',  ( -4.379528057220328563, 16.55341960407611168, 80.20724293864769550 ) ) ;
#42880 = CARTESIAN_POINT ( 'NONE',  ( 15.80617190586769283, -15.72974639402175789, 110.6260903946857042 ) ) ;
#42881 = CARTESIAN_POINT ( 'NONE',  ( -19.02544592524342804, 5.153800228976336051, 51.04057627198103120 ) ) ;
#42883 = CARTESIAN_POINT ( 'NONE',  ( 21.53943276465977519, 0.05219959533937863772, 101.2510903946856757 ) ) ;
#42882 = CARTESIAN_POINT ( 'NONE',  ( 4.483927247898545687, 16.52544592524342804, 39.79057627198103830 ) ) ;
#42884 = CARTESIAN_POINT ( 'NONE',  ( 16.51473224551069308, 9.474510206698969483, 94.16557627198103830 ) ) ;
#42885 = CARTESIAN_POINT ( 'NONE',  ( -9.564922557960796823, -16.46253265017161027, 107.0822429386476955 ) ) ;
#42886 = CARTESIAN_POINT ( 'NONE',  ( -5.153800228976328057, -19.02544592524343514, 37.29057627198102409 ) ) ;
#42887 = CARTESIAN_POINT ( 'NONE',  ( -8.314922557960811034, -14.29746914071050412, 102.0822429386476955 ) ) ;
#42888 = CARTESIAN_POINT ( 'NONE',  ( -12.06949235617756955, 12.14591786802309770, 70.62390960531436690 ) ) ;
#42889 = CARTESIAN_POINT ( 'NONE',  ( -10.81492255796078084, -18.62759615963271287, 87.08224293864769550 ) ) ;
#42890 = CARTESIAN_POINT ( 'NONE',  ( -19.02544592524342804, 5.153800228976336051, 86.04057627198103830 ) ) ;
#42891 = CARTESIAN_POINT ( 'NONE',  ( -21.52544592524343514, 5.823673210054127303, 101.0405762719810383 ) ) ;
#42892 = CARTESIAN_POINT ( 'NONE',  ( -9.564922557960796823, -16.46253265017161027, 87.08224293864769550 ) ) ;
#42894 = CARTESIAN_POINT ( 'NONE',  ( -16.52544592524342804, 4.483927247898546575, 106.0405762719810525 ) ) ;
#42893 = CYLINDRICAL_SURFACE ( 'NONE', #29958, 2.649999999999999911 ) ;
#42895 = CARTESIAN_POINT ( 'NONE',  ( -5.153800228976328057, -19.02544592524343514, 72.29057627198102409 ) ) ;
#42896 = CARTESIAN_POINT ( 'NONE',  ( -15.72974639402197994, 15.80617190586746368, 80.62390960531438111 ) ) ;
#42897 = CARTESIAN_POINT ( 'NONE',  ( -21.82220748998223669, -8.288476145941629625, 169.3167957967150983 ) ) ;
#42899 = FILL_AREA_STYLE_COLOUR ( '', #143549 ) ;
#42898 = CARTESIAN_POINT ( 'NONE',  ( -0.05219959533907301413, -21.53943276465977519, 32.49890960531435979 ) ) ;
#42900 = CARTESIAN_POINT ( 'NONE',  ( 4.379528057220092307, 16.55341960407617563, 27.29275706135234358 ) ) ;
#42901 = CARTESIAN_POINT ( 'NONE',  ( -8.224510206698948167, 14.34966873604960824, 90.41557627198103830 ) ) ;
#42902 = CARTESIAN_POINT ( 'NONE',  ( -17.72662750342724891, -5.500000000000086153, 46.40179492283740359 ) ) ;
#42903 = CARTESIAN_POINT ( 'NONE',  ( 0.05219959533909260263, 19.03943276465977164, 89.99890960531436690 ) ) ;
#42904 = CARTESIAN_POINT ( 'NONE',  ( 19.03943276465977164, -0.05219959533909143690, 48.74890960531435979 ) ) ;
#42905 = CARTESIAN_POINT ( 'NONE',  ( -16.52544592524342804, 4.483927247898546575, 86.04057627198102409 ) ) ;
#42906 = CARTESIAN_POINT ( 'NONE',  ( 0.05219959533907565091, 21.53943276465977519, 24.99890960531435624 ) ) ;
#42907 = CARTESIAN_POINT ( 'NONE',  ( -16.53943276465976808, 0.05219959533911058130, 51.24890960531436690 ) ) ;
#42908 = CARTESIAN_POINT ( 'NONE',  ( -5.049401038297874678, -19.05341960407617918, 104.7927570613523471 ) ) ;
#42909 = CARTESIAN_POINT ( 'NONE',  ( 21.53943276465977519, 0.05219959533937863772, 66.25109039468567573 ) ) ;
#42910 = DIRECTION ( 'NONE',  ( 0.000000000000000000, 0.000000000000000000, 1.000000000000000000 ) ) ;
#42911 = CARTESIAN_POINT ( 'NONE',  ( 19.02544592524343514, -5.153800228976328945, 98.54057627198100988 ) ) ;
#42912 = CARTESIAN_POINT ( 'NONE',  ( -8.314922557961024197, 14.29746914071037800, 87.91775706135234714 ) ) ;
#42913 = CARTESIAN_POINT ( 'NONE',  ( -19.03943276465977164, 0.05219959533909376836, 31.24890960531435979 ) ) ;
#42914 = CARTESIAN_POINT ( 'NONE',  ( -5.153800228976328057, -19.02544592524343514, 77.29057627198099567 ) ) ;
#42915 = CARTESIAN_POINT ( 'NONE',  ( -21.53943276465977519, 0.05219959533907696930, 81.24890960531436690 ) ) ;
#42916 = CARTESIAN_POINT ( 'NONE',  ( -12.06949235617739369, -12.14591786802326823, 19.37609039468568639 ) ) ;
#42917 = VECTOR ( 'NONE', #780, 1000.000000000000000 ) ;
#42919 = CARTESIAN_POINT ( 'NONE',  ( 10.81492255796106328, -18.62759615963255655, 55.41775706135234714 ) ) ;
#42918 = CARTESIAN_POINT ( 'NONE',  ( 4.483927247898545687, 16.52544592524342804, 49.79057627198102409 ) ) ;
#42921 = CARTESIAN_POINT ( 'NONE',  ( -5.823673210054116645, -21.52544592524344225, 22.29057627198102765 ) ) ;
#42920 = CARTESIAN_POINT ( 'NONE',  ( 8.314922557961029526, -14.29746914071037800, 80.41775706135234714 ) ) ;
#42922 = CARTESIAN_POINT ( 'NONE',  ( -9.474510206698964154, 16.51473224551069663, 115.4155762719810241 ) ) ;
#42923 = DIRECTION ( 'NONE',  ( 0.000000000000000000, 0.9396926207859095381, -0.3420201433256656043 ) ) ;
#42924 = CARTESIAN_POINT ( 'NONE',  ( -4.483927247898782831, 16.52544592524335698, 112.7094237280190328 ) ) ;
#42925 = CARTESIAN_POINT ( 'NONE',  ( -12.14591786802326823, 12.06949235617739902, 58.12609039468568994 ) ) ;
#42926 = CARTESIAN_POINT ( 'NONE',  ( -13.97604488694527625, -13.89961937509977652, 71.87390960531433848 ) ) ;
#42927 = CARTESIAN_POINT ( 'NONE',  ( -5.049401038298153566, 19.05341960407611168, 75.20724293864769550 ) ) ;
#42928 = CARTESIAN_POINT ( 'NONE',  ( 21.53943276465977519, 0.05219959533937863772, 76.25109039468568994 ) ) ;
#42929 = CARTESIAN_POINT ( 'NONE',  ( -12.14591786802326823, 12.06949235617739902, 78.12609039468570415 ) ) ;
#42930 = CARTESIAN_POINT ( 'NONE',  ( 14.29746914071049879, -8.314922557960816363, 53.33224293864769550 ) ) ;
#42931 = CARTESIAN_POINT ( 'NONE',  ( -5.049401038298153566, 19.05341960407611168, 55.20724293864769550 ) ) ;
#42932 = CARTESIAN_POINT ( 'NONE',  ( -5.153800228976328057, -19.02544592524343514, 47.29057627198102409 ) ) ;
#42934 = ORIENTED_EDGE ( 'NONE', *, *, #70410, .F. ) ;
#42933 = CARTESIAN_POINT ( 'NONE',  ( 12.06949235617739724, 12.14591786802326823, 36.87609039468568994 ) ) ;
#42935 = CARTESIAN_POINT ( 'NONE',  ( 0.05219959533936267826, -19.03943276465977164, 100.0010903946856757 ) ) ;
#42936 = CARTESIAN_POINT ( 'NONE',  ( -8.314922557960811034, -14.29746914071050412, 92.08224293864769550 ) ) ;
#42937 = CARTESIAN_POINT ( 'NONE',  ( -19.03943276465977164, 0.05219959533909376836, 66.24890960531436690 ) ) ;
#42939 = CARTESIAN_POINT ( 'NONE',  ( -30.74264578624800492, -22.33583958711396278, -1.800000000000000044 ) ) ;
#42938 = CARTESIAN_POINT ( 'NONE',  ( -5.049401038297874678, -19.05341960407617918, 99.79275706135234714 ) ) ;
#42940 = CARTESIAN_POINT ( 'NONE',  ( 15.80617190586769283, -15.72974639402175789, 100.6260903946857184 ) ) ;
#42941 = CARTESIAN_POINT ( 'NONE',  ( -12.06949235617739369, -12.14591786802326823, 64.37609039468568994 ) ) ;
#42942 = DIRECTION ( 'NONE',  ( -0.000000000000000000, 1.000000000000000000, 0.000000000000000000 ) ) ;
#42943 = CARTESIAN_POINT ( 'NONE',  ( 0.05219959533907565091, 21.53943276465977519, 64.99890960531435269 ) ) ;
#42944 = CARTESIAN_POINT ( 'NONE',  ( -8.314922557961024197, 14.29746914071037800, 52.91775706135235424 ) ) ;
#42945 = CARTESIAN_POINT ( 'NONE',  ( 1.784589286804354247, 7.284589286804251884, 8.181980515339454030 ) ) ;
#42946 = CARTESIAN_POINT ( 'NONE',  ( -9.474510206698720793, -16.51473224551083518, 44.58442372801900433 ) ) ;
#42947 = CARTESIAN_POINT ( 'NONE',  ( 19.03943276465977164, -0.05219959533909143690, 83.74890960531436690 ) ) ;
#42948 = CARTESIAN_POINT ( 'NONE',  ( -16.51473224551069308, -9.474510206698971260, 21.66557627198102765 ) ) ;
#42949 = CARTESIAN_POINT ( 'NONE',  ( -16.46253265017160317, 9.564922557960807481, 70.83224293864770971 ) ) ;
#42950 = CARTESIAN_POINT ( 'NONE',  ( 15.80617190586769283, -15.72974639402175789, 70.62609039468567573 ) ) ;
#42951 = CARTESIAN_POINT ( 'NONE',  ( 13.97604488694548053, -13.89961937509957401, 40.62609039468564731 ) ) ;
#42952 = CARTESIAN_POINT ( 'NONE',  ( 9.474510206698729675, 16.51473224551082808, 27.08442372801900433 ) ) ;
#42953 = CARTESIAN_POINT ( 'NONE',  ( -0.05219959533909027116, -19.03943276465977164, 57.49890960531435979 ) ) ;
#42954 = CARTESIAN_POINT ( 'NONE',  ( 9.564922557960805705, 16.46253265017160317, 114.5822429386476955 ) ) ;
#42955 = CARTESIAN_POINT ( 'NONE',  ( 5.823673210054444382, -21.52544592524334988, 80.20942372801901854 ) ) ;
#42956 = CARTESIAN_POINT ( 'NONE',  ( 5.153800228976335163, 19.02544592524342804, 64.79057627198100988 ) ) ;
#42957 = VECTOR ( 'NONE', #136873, 1000.000000000000000 ) ;
#42958 = CARTESIAN_POINT ( 'NONE',  ( -10.72451020669870658, -18.67979575497194134, 99.58442372801900433 ) ) ;
#42959 = CARTESIAN_POINT ( 'NONE',  ( 15.72974639402199770, -15.80617190586745480, 38.12390960531436690 ) ) ;
#42960 = CARTESIAN_POINT ( 'NONE',  ( 13.97604488694527802, 13.89961937509977652, 84.37390960531433848 ) ) ;
#42961 = CARTESIAN_POINT ( 'NONE',  ( 5.719274019375673035, 21.55341960407619339, 42.29275706135235424 ) ) ;
#42962 = CARTESIAN_POINT ( 'NONE',  ( 19.05341960407617918, -5.049401038297876454, 61.04275706135232582 ) ) ;
#42963 = CARTESIAN_POINT ( 'NONE',  ( 0.05219959533909260263, 19.03943276465977164, 39.99890960531436690 ) ) ;
#42964 = CARTESIAN_POINT ( 'NONE',  ( 5.049401038298161559, -19.05341960407611168, 92.70724293864769550 ) ) ;
#42965 = CARTESIAN_POINT ( 'NONE',  ( 16.53943276465976808, 0.05219959533934440121, 26.25109039468567573 ) ) ;
#42966 = CARTESIAN_POINT ( 'NONE',  ( -4.379528057220328563, 16.55341960407611168, 85.20724293864770971 ) ) ;
#42967 = CARTESIAN_POINT ( 'NONE',  ( -5.049401038298153566, 19.05341960407611168, 65.20724293864765286 ) ) ;
#42968 = CARTESIAN_POINT ( 'NONE',  ( 15.80617190586746368, 15.72974639402197994, 54.37390960531435979 ) ) ;
#42969 = CARTESIAN_POINT ( 'NONE',  ( 16.55341960407618274, -4.379528057220086978, 21.04275706135234714 ) ) ;
#42970 = CARTESIAN_POINT ( 'NONE',  ( 21.53943276465977519, -0.05219959533907433946, 113.7489096053143527 ) ) ;
#42971 = CARTESIAN_POINT ( 'NONE',  ( 18.62759615963255655, 10.81492255796105972, 66.66775706135234714 ) ) ;
#42972 = CARTESIAN_POINT ( 'NONE',  ( 0.05219959533934541429, -16.53943276465976808, 75.00109039468568994 ) ) ;
#42973 = CARTESIAN_POINT ( 'NONE',  ( -14.29746914071037622, -8.314922557961029526, 64.16775706135234714 ) ) ;
#42974 = CARTESIAN_POINT ( 'NONE',  ( -5.049401038298153566, 19.05341960407611168, 65.20724293864765286 ) ) ;
#42975 = CARTESIAN_POINT ( 'NONE',  ( 12.06949235617739724, 12.14591786802326823, 96.87609039468568994 ) ) ;
#42976 = CARTESIAN_POINT ( 'NONE',  ( -19.03943276465977164, -0.05219959533935918106, 48.75109039468566863 ) ) ;
#42977 = CARTESIAN_POINT ( 'NONE',  ( -0.05219959533907301413, -21.53943276465977519, 112.4989096053143669 ) ) ;
#42978 = CARTESIAN_POINT ( 'NONE',  ( -12.14591786802309592, -12.06949235617757132, 71.87390960531438111 ) ) ;
#42979 = CARTESIAN_POINT ( 'NONE',  ( 5.153800228976335163, 19.02544592524342804, 94.79057627198103830 ) ) ;
#42980 = CARTESIAN_POINT ( 'NONE',  ( 0.05219959533934541429, -16.53943276465976808, 95.00109039468568994 ) ) ;
#42981 = CARTESIAN_POINT ( 'NONE',  ( -15.80617190586768217, 15.72974639402176855, 58.12609039468568994 ) ) ;
#42982 = CARTESIAN_POINT ( 'NONE',  ( -8.314922557961024197, 14.29746914071037800, 32.91775706135234714 ) ) ;
#42983 = CARTESIAN_POINT ( 'NONE',  ( 10.72451020669871369, 18.67979575497193778, 22.08442372801901143 ) ) ;
#42984 = CARTESIAN_POINT ( 'NONE',  ( -8.314922557960811034, -14.29746914071050412, 52.08224293864768839 ) ) ;
#42985 = ORIENTED_EDGE ( 'NONE', *, *, #34928, .T. ) ;
#42986 = CARTESIAN_POINT ( 'NONE',  ( 15.80617190586746368, 15.72974639402197994, 99.37390960531436690 ) ) ;
#42987 = B_SPLINE_CURVE_WITH_KNOTS ( 'NONE', 3,
 ( #97740, #18956, #143260, #157463, #113915, #156464, #112930, #175613, #67426, #17964 ),
 .UNSPECIFIED., .F., .F.,
 ( 4, 2, 2, 2, 4 ),
 ( 3.469446951953614189E-18, 0.0009160790699533124387, 0.001832158139906621408, 0.002748237209859930377, 0.003664316279813239347 ),
 .UNSPECIFIED. ) ;
#42988 = CARTESIAN_POINT ( 'NONE',  ( 16.55341960407611168, 4.379528057220329451, 33.95724293864769550 ) ) ;
#42989 = EDGE_LOOP ( 'NONE', ( #109000, #132938, #121788, #48322, #24378 ) ) ;
#42990 = CARTESIAN_POINT ( 'NONE',  ( 34.37178856895486234, 7.314363934749350094, 46.67665261413966959 ) ) ;
#42991 = CARTESIAN_POINT ( 'NONE',  ( -10.72451020669898014, 18.67979575497178502, 35.41557627198102409 ) ) ;
#42992 = CARTESIAN_POINT ( 'NONE',  ( 18.67979575497194134, -10.72451020669871369, 30.83442372801902209 ) ) ;
#42993 = CARTESIAN_POINT ( 'NONE',  ( -16.52544592524342804, 4.483927247898546575, 71.04057627198103830 ) ) ;
#42994 = CARTESIAN_POINT ( 'NONE',  ( 15.72974639402199770, -15.80617190586745480, 73.12390960531436690 ) ) ;
#42995 = CARTESIAN_POINT ( 'NONE',  ( -16.51473224551069308, -9.474510206698971260, 76.66557627198103830 ) ) ;
#42997 = CARTESIAN_POINT ( 'NONE',  ( -5.049401038297874678, -19.05341960407617918, 79.79275706135233293 ) ) ;
#42996 = CARTESIAN_POINT ( 'NONE',  ( -13.89961937509977652, 13.97604488694528158, 25.62390960531434558 ) ) ;
#42998 = CARTESIAN_POINT ( 'NONE',  ( -15.80617190586745835, -15.72974639402198527, 51.87390960531437401 ) ) ;
#42999 = CARTESIAN_POINT ( 'NONE',  ( -19.03943276465977164, 0.05219959533909376836, 61.24890960531436690 ) ) ;
#43000 = ORIENTED_EDGE ( 'NONE', *, *, #85306, .F. ) ;
#43001 = CARTESIAN_POINT ( 'NONE',  ( 8.314922557961029526, -14.29746914071037800, 40.41775706135234714 ) ) ;
#43002 = CARTESIAN_POINT ( 'NONE',  ( -10.72451020669898014, 18.67979575497178502, 110.4155762719810383 ) ) ;
#43003 = CARTESIAN_POINT ( 'NONE',  ( 14.29746914071049879, -8.314922557960816363, 43.33224293864769550 ) ) ;
#43004 = CARTESIAN_POINT ( 'NONE',  ( -19.02544592524342804, 5.153800228976336051, 101.0405762719810241 ) ) ;
#43005 = CARTESIAN_POINT ( 'NONE',  ( 21.52544592524344225, -5.823673210054117533, 78.54057627198103830 ) ) ;
#43007 = CARTESIAN_POINT ( 'NONE',  ( -16.55341960407617563, 4.379528057220093196, 38.54275706135234714 ) ) ;
#43006 = CARTESIAN_POINT ( 'NONE',  ( 0.05219959533907565091, 21.53943276465977519, 104.9989096053143669 ) ) ;
#43008 = CARTESIAN_POINT ( 'NONE',  ( -21.53943276465977519, 0.05219959533907696930, 46.24890960531435979 ) ) ;
#43009 = CARTESIAN_POINT ( 'NONE',  ( 10.72451020669871369, 18.67979575497193778, 97.08442372801904696 ) ) ;
#43010 = CARTESIAN_POINT ( 'NONE',  ( -9.564922557960796823, -16.46253265017161027, 42.08224293864769550 ) ) ;
#43011 = CARTESIAN_POINT ( 'NONE',  ( 16.46253265017160672, -9.564922557960803928, 103.3322429386476955 ) ) ;
#43012 = CARTESIAN_POINT ( 'NONE',  ( 5.049401038298161559, -19.05341960407611168, 82.70724293864770971 ) ) ;
#43013 = CARTESIAN_POINT ( 'NONE',  ( 17.40805194821984259, -6.112264579160781253, 88.33371272510609629 ) ) ;
#43014 = CARTESIAN_POINT ( 'NONE',  ( -5.049401038297874678, -19.05341960407617918, 54.79275706135234003 ) ) ;
#43016 = CARTESIAN_POINT ( 'NONE',  ( 21.52544592524344225, -5.823673210054117533, 28.54057627198103120 ) ) ;
#43015 = CARTESIAN_POINT ( 'NONE',  ( 10.72451020669871369, 18.67979575497193778, 112.0844237280190185 ) ) ;
#43017 = CARTESIAN_POINT ( 'NONE',  ( -14.34966873604972548, 8.224510206698743886, 98.33442372801901854 ) ) ;
#43018 = CARTESIAN_POINT ( 'NONE',  ( 9.564922557961047289, -16.46253265017146816, 80.41775706135234714 ) ) ;
#43019 = LINE ( 'NONE', #104686, #14313 ) ;
#43020 = CARTESIAN_POINT ( 'NONE',  ( -19.02544592524334988, -5.153800228976617603, 88.95942372801897591 ) ) ;
#43021 = CARTESIAN_POINT ( 'NONE',  ( -9.474510206698720793, -16.51473224551083518, 44.58442372801900433 ) ) ;
#43022 = CARTESIAN_POINT ( 'NONE',  ( -16.31925111598457079, -7.325300261831483084, 44.83575461032751264 ) ) ;
#43023 = CARTESIAN_POINT ( 'NONE',  ( 19.03943276465977164, -0.05219959533909143690, 43.74890960531435979 ) ) ;
#43024 = CARTESIAN_POINT ( 'NONE',  ( -8.224510206698948167, 14.34966873604960824, 55.41557627198102409 ) ) ;
#43025 = EDGE_CURVE ( 'NONE', #43345, #156405, #9121, .T. ) ;
#43026 = CARTESIAN_POINT ( 'NONE',  ( 16.51473224551069308, 9.474510206698969483, 29.16557627198103475 ) ) ;
#43027 = CARTESIAN_POINT ( 'NONE',  ( -16.52544592524342804, 4.483927247898546575, 36.04057627198102409 ) ) ;
#43028 = DIRECTION ( 'NONE',  ( 0.000000000000000000, 0.7071067811865466846, 0.7071067811865484609 ) ) ;
#43029 = CARTESIAN_POINT ( 'NONE',  ( -12.06949235617739369, -12.14591786802326823, 109.3760903946857042 ) ) ;
#43030 = CARTESIAN_POINT ( 'NONE',  ( 16.51473224551069308, 9.474510206698969483, 54.16557627198103120 ) ) ;
#43031 = CARTESIAN_POINT ( 'NONE',  ( 0.05219959533937995610, -21.53943276465977519, 105.0010903946856757 ) ) ;
#43032 = CARTESIAN_POINT ( 'NONE',  ( 4.379528057220092307, 16.55341960407617563, 22.29275706135235069 ) ) ;
#43033 = CARTESIAN_POINT ( 'NONE',  ( 10.81492255796078972, 18.62759615963270932, 39.58224293864769550 ) ) ;
#43034 = CARTESIAN_POINT ( 'NONE',  ( 21.55341960407619695, -5.719274019375665929, 86.04275706135236135 ) ) ;
#43035 = CARTESIAN_POINT ( 'NONE',  ( -13.89961937509977652, 13.97604488694528158, 100.6239096053143669 ) ) ;
#43036 = CARTESIAN_POINT ( 'NONE',  ( 5.153800228976335163, 19.02544592524342804, 79.79057627198102409 ) ) ;
#43037 = CARTESIAN_POINT ( 'NONE',  ( -29.86685920354755197, -21.69954338932560134, -8.424999997268812990 ) ) ;
#43038 = CARTESIAN_POINT ( 'NONE',  ( -21.53943276465977519, 0.05219959533907696930, 106.2489096053143811 ) ) ;
#43039 = CARTESIAN_POINT ( 'NONE',  ( 12.14591786802309770, 12.06949235617756955, 84.37390960531438111 ) ) ;
#43040 = CARTESIAN_POINT ( 'NONE',  ( -5.823673210054116645, -21.52544592524344225, 72.29057627198102409 ) ) ;
#43041 = CARTESIAN_POINT ( 'NONE',  ( 19.05341960407611168, 5.049401038298154454, 78.95724293864769550 ) ) ;
#43042 = CARTESIAN_POINT ( 'NONE',  ( 10.72451020669898902, -18.67979575497178502, 97.91557627198103830 ) ) ;
#43043 = ORIENTED_EDGE ( 'NONE', *, *, #74692, .T. ) ;
#43044 = CARTESIAN_POINT ( 'NONE',  ( -19.05341960407611168, -5.049401038298163336, 66.45724293864769550 ) ) ;
#43046 = CARTESIAN_POINT ( 'NONE',  ( 21.48948823426665911, -5.485118590273156514, 173.8226827327241608 ) ) ;
#43045 = CARTESIAN_POINT ( 'NONE',  ( -14.34966873604960291, -8.224510206698953496, 91.66557627198103830 ) ) ;
#43047 = CARTESIAN_POINT ( 'NONE',  ( 19.02544592524343514, -5.153800228976328945, 63.54057627198103830 ) ) ;
#43048 = CARTESIAN_POINT ( 'NONE',  ( -16.46253265017146816, -9.564922557961047289, 74.16775706135234714 ) ) ;
#43049 = CARTESIAN_POINT ( 'NONE',  ( -16.55341960407611168, -4.379528057220339221, 96.45724293864770971 ) ) ;
#43050 = CARTESIAN_POINT ( 'NONE',  ( 21.53943276465977519, 0.05219959533937863772, 56.25109039468568284 ) ) ;
#43052 = CARTESIAN_POINT ( 'NONE',  ( 5.719274019375673035, 21.55341960407619339, 22.29275706135235069 ) ) ;
#43051 = CARTESIAN_POINT ( 'NONE',  ( 0.05219959533909260263, 19.03943276465977164, 49.99890960531435979 ) ) ;
#43053 = CARTESIAN_POINT ( 'NONE',  ( -14.34966873604960291, -8.224510206698953496, 106.6655762719810383 ) ) ;
#43054 = CARTESIAN_POINT ( 'NONE',  ( 12.04662589228224689, -37.70593178236023846, -30.82293284779730769 ) ) ;
#43055 = CARTESIAN_POINT ( 'NONE',  ( -16.46253265017160317, 9.564922557960807481, 60.83224293864769550 ) ) ;
#43056 = CARTESIAN_POINT ( 'NONE',  ( 17.50000000000000355, 5.624438216177583882, 111.6832965508535551 ) ) ;
#43058 = CARTESIAN_POINT ( 'NONE',  ( -16.46253265017160317, 9.564922557960807481, 115.8322429386477097 ) ) ;
#43057 = CARTESIAN_POINT ( 'NONE',  ( -19.03943276465977164, -0.05219959533935918106, 103.7510903946856757 ) ) ;
#43059 = CARTESIAN_POINT ( 'NONE',  ( 21.55341960407619695, -5.719274019375665929, 56.04275706135235424 ) ) ;
#43060 = CARTESIAN_POINT ( 'NONE',  ( 0.05219959533909260263, 19.03943276465977164, 94.99890960531436690 ) ) ;
#43061 = CARTESIAN_POINT ( 'NONE',  ( -16.51473224551082808, 9.474510206698731452, 83.33442372801899012 ) ) ;
#43062 = CARTESIAN_POINT ( 'NONE',  ( 13.89961937509977652, -13.97604488694527269, 58.12390960531436690 ) ) ;
#43063 = CARTESIAN_POINT ( 'NONE',  ( -16.55341960407611168, -4.379528057220339221, 81.45724293864769550 ) ) ;
#43064 = CARTESIAN_POINT ( 'NONE',  ( -13.89961937509977652, 13.97604488694528158, 85.62390960531433848 ) ) ;
#43065 = CARTESIAN_POINT ( 'NONE',  ( 12.06949235617757843, -12.14591786802309237, 83.12390960531436690 ) ) ;
#43066 = CARTESIAN_POINT ( 'NONE',  ( 9.564922557960805705, 16.46253265017160317, 84.58224293864769550 ) ) ;
#43067 = CARTESIAN_POINT ( 'NONE',  ( -0.05219959533936034679, 19.03943276465977164, 37.50109039468567573 ) ) ;
#43070 = CARTESIAN_POINT ( 'NONE',  ( -0.05219959533909027116, -19.03943276465977164, 22.49890960531436690 ) ) ;
#43069 = CARTESIAN_POINT ( 'NONE',  ( -16.52544592524342804, 4.483927247898546575, 46.04057627198103830 ) ) ;
#43068 = CARTESIAN_POINT ( 'NONE',  ( -9.474510206698964154, 16.51473224551069663, 45.41557627198103120 ) ) ;
#43071 = ORIENTED_EDGE ( 'NONE', *, *, #155738, .T. ) ;
#43072 = CARTESIAN_POINT ( 'NONE',  ( 5.823673210054444382, -21.52544592524334988, 40.20942372801901854 ) ) ;
#43073 = CARTESIAN_POINT ( 'NONE',  ( 0.05219959533936267826, -19.03943276465977164, 80.00109039468567573 ) ) ;
#43074 = CARTESIAN_POINT ( 'NONE',  ( 14.34966873604960469, 8.224510206698951720, 29.16557627198103120 ) ) ;
#43075 = CARTESIAN_POINT ( 'NONE',  ( -10.81492255796078084, -18.62759615963271287, 92.08224293864769550 ) ) ;
#43076 = CARTESIAN_POINT ( 'NONE',  ( -10.81492255796078084, -18.62759615963271287, 37.08224293864768129 ) ) ;
#43077 = CARTESIAN_POINT ( 'NONE',  ( -16.52544592524342804, 4.483927247898546575, 66.04057627198103830 ) ) ;
#43078 = CARTESIAN_POINT ( 'NONE',  ( 13.89961937509977652, -13.97604488694527269, 43.12390960531434558 ) ) ;
#43079 = CARTESIAN_POINT ( 'NONE',  ( -14.29746914071037622, -8.314922557961029526, 104.1677570613523471 ) ) ;
#43080 = CARTESIAN_POINT ( 'NONE',  ( 8.224510206698742110, 14.34966873604972548, 77.08442372801901854 ) ) ;
#43081 = CARTESIAN_POINT ( 'NONE',  ( -5.719274019375978568, 21.55341960407610458, 35.20724293864768839 ) ) ;
#43082 = CARTESIAN_POINT ( 'NONE',  ( 16.46253265017146816, 9.564922557961045513, 21.66775706135233648 ) ) ;
#43083 = CARTESIAN_POINT ( 'NONE',  ( 16.51473224551069308, 9.474510206698969483, 94.16557627198103830 ) ) ;
#43084 = CARTESIAN_POINT ( 'NONE',  ( -19.03943276465977164, 0.05219959533909376836, 71.24890960531435269 ) ) ;
#43085 = CARTESIAN_POINT ( 'NONE',  ( -16.55341960407617563, 4.379528057220093196, 78.54275706135236135 ) ) ;
#43086 = CARTESIAN_POINT ( 'NONE',  ( 9.474510206698971260, -16.51473224551069308, 22.91557627198102765 ) ) ;
#43087 = CARTESIAN_POINT ( 'NONE',  ( -8.224510206698948167, 14.34966873604960824, 30.41557627198101699 ) ) ;
#43089 = CARTESIAN_POINT ( 'NONE',  ( 16.51473224551069308, 9.474510206698969483, 89.16557627198103830 ) ) ;
#43088 = CARTESIAN_POINT ( 'NONE',  ( -5.153800228976328057, -19.02544592524343514, 107.2905762719810383 ) ) ;
#43090 = CARTESIAN_POINT ( 'NONE',  ( 15.80617190586746368, 15.72974639402197994, 24.37390960531435979 ) ) ;
#43091 = CARTESIAN_POINT ( 'NONE',  ( -14.34966873604960291, -8.224510206698953496, 76.66557627198103830 ) ) ;
#43092 = AXIS2_PLACEMENT_3D ( 'NONE', #165008, #88144, #38659 ) ;
#43093 = CARTESIAN_POINT ( 'NONE',  ( 4.483927247898545687, 16.52544592524342804, 64.79057627198103830 ) ) ;
#43095 = CARTESIAN_POINT ( 'NONE',  ( -18.22780087662121673, -5.500000000000063061, 56.48459894673892734 ) ) ;
#43094 = CARTESIAN_POINT ( 'NONE',  ( -12.06949235617739369, -12.14591786802326823, 59.37609039468568284 ) ) ;
#43096 = CARTESIAN_POINT ( 'NONE',  ( -19.02544592524334988, -5.153800228976617603, 53.95942372801898301 ) ) ;
#43097 = CARTESIAN_POINT ( 'NONE',  ( -19.05341960407611168, -5.049401038298163336, 91.45724293864766707 ) ) ;
#43098 = CARTESIAN_POINT ( 'NONE',  ( -5.049401038297874678, -19.05341960407617918, 59.79275706135231871 ) ) ;
#43100 = CARTESIAN_POINT ( 'NONE',  ( -27.73933785331498925, -9.013057229001049109, 143.4750000027311785 ) ) ;
#43099 = B_SPLINE_CURVE_WITH_KNOTS ( 'NONE', 3,
 ( #63653, #5937, #158628, #141483, #49474, #50475 ),
 .UNSPECIFIED., .F., .F.,
 ( 4, 2, 4 ),
 ( 0.007228050697041690613, 0.007608510107495180044, 0.007988969517948670343 ),
 .UNSPECIFIED. ) ;
#43102 = CARTESIAN_POINT ( 'NONE',  ( -4.483927247898782831, 16.52544592524335698, 92.70942372801901854 ) ) ;
#43101 = CARTESIAN_POINT ( 'NONE',  ( 16.51473224551083163, -9.474510206698727899, 110.8344237280190043 ) ) ;
#43103 = CARTESIAN_POINT ( 'NONE',  ( -16.46253265017160317, 9.564922557960807481, 35.83224293864768839 ) ) ;
#43104 = CARTESIAN_POINT ( 'NONE',  ( 10.72451020669898902, -18.67979575497178502, 27.91557627198103830 ) ) ;
#43105 = CARTESIAN_POINT ( 'NONE',  ( 10.72451020669871369, 18.67979575497193778, 57.08442372801901854 ) ) ;
#43106 = CARTESIAN_POINT ( 'NONE',  ( -5.049401038297874678, -19.05341960407617918, 99.79275706135234714 ) ) ;
#43108 = CARTESIAN_POINT ( 'NONE',  ( 5.049401038298161559, -19.05341960407611168, 77.70724293864765286 ) ) ;
#43107 = CARTESIAN_POINT ( 'NONE',  ( -9.474510206698720793, -16.51473224551083518, 54.58442372801899722 ) ) ;
#43109 = CARTESIAN_POINT ( 'NONE',  ( 37.99626262588764547, 12.34573411038917357, -0.9021577739498228832 ) ) ;
#43111 = CARTESIAN_POINT ( 'NONE',  ( 5.049401038298161559, -19.05341960407611168, 67.70724293864769550 ) ) ;
#43110 = CARTESIAN_POINT ( 'NONE',  ( -12.14591786802309592, -12.06949235617757132, 71.87390960531438111 ) ) ;
#43112 = CARTESIAN_POINT ( 'NONE',  ( 9.474510206698971260, -16.51473224551069308, 72.91557627198102409 ) ) ;
#43113 = CARTESIAN_POINT ( 'NONE',  ( -13.89961937509957401, -13.97604488694547875, 84.37609039468567573 ) ) ;
#43114 = CARTESIAN_POINT ( 'NONE',  ( -15.80617190586745835, -15.72974639402198527, 66.87390960531436690 ) ) ;
#43115 = CARTESIAN_POINT ( 'NONE',  ( -13.97604488694527625, -13.89961937509977652, 21.87390960531435979 ) ) ;
#43116 = CARTESIAN_POINT ( 'NONE',  ( -16.46253265017146816, -9.564922557961047289, 59.16775706135233293 ) ) ;
#43117 = CARTESIAN_POINT ( 'NONE',  ( 13.89961937509977652, -13.97604488694527269, 58.12390960531436690 ) ) ;
#43118 = CARTESIAN_POINT ( 'NONE',  ( 5.049401038298161559, -19.05341960407611168, 92.70724293864769550 ) ) ;
#43119 = CARTESIAN_POINT ( 'NONE',  ( -15.80617190586745835, -15.72974639402198527, 86.87390960531438111 ) ) ;
#43121 = CARTESIAN_POINT ( 'NONE',  ( -13.97604488694547697, 13.89961937509957934, 48.12609039468566863 ) ) ;
#43120 = CARTESIAN_POINT ( 'NONE',  ( 12.14591786802309770, 12.06949235617756955, 74.37390960531436690 ) ) ;
#43122 = CARTESIAN_POINT ( 'NONE',  ( 10.72451020669898902, -18.67979575497178502, 82.91557627198103830 ) ) ;
#43123 = CARTESIAN_POINT ( 'NONE',  ( -21.52544592524343514, 5.823673210054127303, 66.04057627198103830 ) ) ;
#43124 = CARTESIAN_POINT ( 'NONE',  ( 4.379528057220339221, -16.55341960407611168, 37.70724293864769550 ) ) ;
#43125 = CARTESIAN_POINT ( 'NONE',  ( -15.72974639402176322, -15.80617190586768395, 99.37609039468568994 ) ) ;
#43126 = CARTESIAN_POINT ( 'NONE',  ( -13.97604488694527625, -13.89961937509977652, 76.87390960531433848 ) ) ;
#43127 = CARTESIAN_POINT ( 'NONE',  ( 16.46253265017160672, -9.564922557960803928, 38.33224293864768839 ) ) ;
#43128 = CARTESIAN_POINT ( 'NONE',  ( -5.823673210054431948, 21.52544592524334988, 37.70942372801900433 ) ) ;
#43129 = CARTESIAN_POINT ( 'NONE',  ( 18.67979575497194134, -10.72451020669871369, 40.83442372801901854 ) ) ;
#43130 = CARTESIAN_POINT ( 'NONE',  ( -19.05341960407611168, -5.049401038298163336, 46.45724293864768129 ) ) ;
#43131 = CARTESIAN_POINT ( 'NONE',  ( -0.05219959533937732626, 21.53943276465977519, 27.50109039468567929 ) ) ;
#43132 = CARTESIAN_POINT ( 'NONE',  ( -19.03943276465977164, -0.05219959533935918106, 63.75109039468566863 ) ) ;
#43133 = CARTESIAN_POINT ( 'NONE',  ( -19.02544592524342804, 5.153800228976336051, 36.04057627198100988 ) ) ;
#43134 = CARTESIAN_POINT ( 'NONE',  ( 8.224510206698742110, 14.34966873604972548, 27.08442372801901854 ) ) ;
#43135 = CARTESIAN_POINT ( 'NONE',  ( -19.05341960407611168, -5.049401038298163336, 21.45724293864768839 ) ) ;
#43136 = CARTESIAN_POINT ( 'NONE',  ( -14.34966873604972548, 8.224510206698743886, 73.33442372801901854 ) ) ;
#43137 = CARTESIAN_POINT ( 'NONE',  ( 16.46253265017160672, -9.564922557960803928, 38.33224293864768839 ) ) ;
#43138 = CARTESIAN_POINT ( 'NONE',  ( -24.44405923433090067, -13.71792739260092731, 165.9118100595187286 ) ) ;
#43139 = CARTESIAN_POINT ( 'NONE',  ( -9.564922557960796823, -16.46253265017161027, 92.08224293864769550 ) ) ;
#43140 = CARTESIAN_POINT ( 'NONE',  ( -16.51473224551069308, -9.474510206698971260, 21.66557627198102765 ) ) ;
#43141 = CARTESIAN_POINT ( 'NONE',  ( -10.72451020669898014, 18.67979575497178502, 65.41557627198102409 ) ) ;
#43142 = CARTESIAN_POINT ( 'NONE',  ( -16.55341960407617563, 4.379528057220093196, 48.54275706135234714 ) ) ;
#43143 = CARTESIAN_POINT ( 'NONE',  ( -21.53943276465977519, -0.05219959533937600094, 103.7510903946857042 ) ) ;
#43144 = CARTESIAN_POINT ( 'NONE',  ( 9.564922557960805705, 16.46253265017160317, 34.58224293864770260 ) ) ;
#43145 = CARTESIAN_POINT ( 'NONE',  ( 16.55341960407611168, 4.379528057220329451, 33.95724293864769550 ) ) ;
#43146 = CARTESIAN_POINT ( 'NONE',  ( -4.483927247898539470, -16.52544592524342804, 67.29057627198103830 ) ) ;
#43147 = CARTESIAN_POINT ( 'NONE',  ( 19.05341960407611168, 5.049401038298154454, 58.95724293864768129 ) ) ;
#43148 = CARTESIAN_POINT ( 'NONE',  ( 0.05219959533936267826, -19.03943276465977164, 20.00109039468567218 ) ) ;
#43149 = CARTESIAN_POINT ( 'NONE',  ( -10.72451020669870658, -18.67979575497194134, 24.58442372801901499 ) ) ;
#43150 = CARTESIAN_POINT ( 'NONE',  ( -19.03943276465977164, 0.05219959533909376836, 81.24890960531436690 ) ) ;
#43151 = VECTOR ( 'NONE', #82773, 1000.000000000000000 ) ;
#43152 = CARTESIAN_POINT ( 'NONE',  ( -15.80617190586768217, 15.72974639402176855, 88.12609039468570415 ) ) ;
#43153 = CARTESIAN_POINT ( 'NONE',  ( 4.379528057220092307, 16.55341960407617563, 57.29275706135234714 ) ) ;
#43154 = CARTESIAN_POINT ( 'NONE',  ( 4.379528057220092307, 16.55341960407617563, 32.29275706135235424 ) ) ;
#43155 = EDGE_CURVE ( 'NONE', #131752, #56947, #14412, .T. ) ;
#43157 = CARTESIAN_POINT ( 'NONE',  ( -15.80617190586768217, 15.72974639402176855, 98.12609039468570415 ) ) ;
#43156 = CARTESIAN_POINT ( 'NONE',  ( 14.29746914071049879, -8.314922557960816363, 88.33224293864769550 ) ) ;
#43158 = CARTESIAN_POINT ( 'NONE',  ( -4.379528057220328563, 16.55341960407611168, 35.20724293864768839 ) ) ;
#43159 = CARTESIAN_POINT ( 'NONE',  ( -9.474510206698964154, 16.51473224551069663, 25.41557627198103120 ) ) ;
#43160 = CARTESIAN_POINT ( 'NONE',  ( -12.14591786802326823, 12.06949235617739902, 58.12609039468568994 ) ) ;
#43161 = CARTESIAN_POINT ( 'NONE',  ( 4.483927247898545687, 16.52544592524342804, 59.79057627198103120 ) ) ;
#43162 = CARTESIAN_POINT ( 'NONE',  ( -16.55341960407617563, 4.379528057220093196, 103.5427570613523613 ) ) ;
#43163 = CARTESIAN_POINT ( 'NONE',  ( 13.97604488694527802, 13.89961937509977652, 109.3739096053143669 ) ) ;
#43164 = CARTESIAN_POINT ( 'NONE',  ( 5.823673210054125526, 21.52544592524343514, 34.79057627198103120 ) ) ;
#43165 = CARTESIAN_POINT ( 'NONE',  ( 10.72451020669871369, 18.67979575497193778, 112.0844237280190185 ) ) ;
#43166 = CARTESIAN_POINT ( 'NONE',  ( -4.379528057220328563, 16.55341960407611168, 80.20724293864769550 ) ) ;
#43167 = CARTESIAN_POINT ( 'NONE',  ( -5.049401038298153566, 19.05341960407611168, 95.20724293864770971 ) ) ;
#43168 = ORIENTED_EDGE ( 'NONE', *, *, #157696, .F. ) ;
#43169 = CARTESIAN_POINT ( 'NONE',  ( 16.52544592524335698, 4.483927247898782831, 46.45942372801901854 ) ) ;
#43170 = CARTESIAN_POINT ( 'NONE',  ( -13.89961937509977652, 13.97604488694528158, 35.62390960531435269 ) ) ;
#43171 = CARTESIAN_POINT ( 'NONE',  ( -4.483927247898782831, 16.52544592524335698, 47.70942372801902565 ) ) ;
#43172 = CARTESIAN_POINT ( 'NONE',  ( -13.89961937509957401, -13.97604488694547875, 49.37609039468567573 ) ) ;
#43173 = CARTESIAN_POINT ( 'NONE',  ( 0.05219959533909260263, 19.03943276465977164, 44.99890960531435979 ) ) ;
#43174 = CARTESIAN_POINT ( 'NONE',  ( -8.224510206698735004, -14.34966873604973081, 84.58442372801903275 ) ) ;
#43175 = CARTESIAN_POINT ( 'NONE',  ( 9.474510206698729675, 16.51473224551082808, 77.08442372801900433 ) ) ;
#43176 = CARTESIAN_POINT ( 'NONE',  ( 9.564922557961047289, -16.46253265017146816, 35.41775706135233293 ) ) ;
#43177 = CARTESIAN_POINT ( 'NONE',  ( -16.46253265017160317, 9.564922557960807481, 60.83224293864769550 ) ) ;
#43178 = CARTESIAN_POINT ( 'NONE',  ( -0.05219959533910754901, -16.53943276465976808, 92.49890960531436690 ) ) ;
#43179 = CARTESIAN_POINT ( 'NONE',  ( 16.51473224551083163, -9.474510206698727899, 65.83442372801900433 ) ) ;
#43180 = CARTESIAN_POINT ( 'NONE',  ( 21.53943276465977519, -0.05219959533907433946, 68.74890960531435269 ) ) ;
#43181 = CARTESIAN_POINT ( 'NONE',  ( -13.89961937509957401, -13.97604488694547875, 44.37609039468566863 ) ) ;
#43182 = CARTESIAN_POINT ( 'NONE',  ( 16.51473224551069308, 9.474510206698969483, 99.16557627198102409 ) ) ;
#43183 = CARTESIAN_POINT ( 'NONE',  ( 18.62759615963271287, -10.81492255796078972, 73.33224293864769550 ) ) ;
#43184 = CARTESIAN_POINT ( 'NONE',  ( -16.38665767535055195, 7.295008042176048590, 85.26400864214548392 ) ) ;
#43185 = CARTESIAN_POINT ( 'NONE',  ( 9.564922557961047289, -16.46253265017146816, 105.4177570613523471 ) ) ;
#43186 = CARTESIAN_POINT ( 'NONE',  ( 18.22780087662123805, 5.499999999999960032, 96.48236817873105053 ) ) ;
#43187 = CARTESIAN_POINT ( 'NONE',  ( 16.52544592524335698, 4.483927247898782831, 31.45942372801901854 ) ) ;
#43188 = CARTESIAN_POINT ( 'NONE',  ( 5.049401038298161559, -19.05341960407611168, 37.70724293864768839 ) ) ;
#43189 = CARTESIAN_POINT ( 'NONE',  ( 19.05341960407611168, 5.049401038298154454, 113.9572429386477097 ) ) ;
#43190 = CARTESIAN_POINT ( 'NONE',  ( -10.72451020669898014, 18.67979575497178502, 85.41557627198102409 ) ) ;
#43191 = CARTESIAN_POINT ( 'NONE',  ( 10.81492255796106328, -18.62759615963255655, 55.41775706135234714 ) ) ;
#43194 = CARTESIAN_POINT ( 'NONE',  ( 19.03943276465977164, 0.05219959533936151252, 21.25109039468565797 ) ) ;
#43193 = CARTESIAN_POINT ( 'NONE',  ( 5.049401038297881783, 19.05341960407617563, 102.2927570613523045 ) ) ;
#43192 =( BOUNDED_CURVE ( )  B_SPLINE_CURVE ( 2, ( #68363, #192725, #130014, #54209, #7683, #100694, #193734, #159369, #191713, #86536, #53197, #101700, #67367, #8707, #131036, #20866, #56202, #113858, #69367, #177570, #9714, #82523, #162375, #133042, #40027, #97680, #38042, #23877, #71378, #178562, #70377, #144205, #174564, #85528, #132045, #148220, #147216, #36031, #114872, #55202, #52200, #116871, #160384, #99698, #175554, #83524, #37029, #98690, #21874, #137015, #168352, #12707, #25891, #153172, #76336, #11722, #58205, #106679, #10714, #57217, #182546, #44028, #121841, #87536, #138012, #90513, #150226, #119874, #167376, #28872, #60172, #135062, #149223, #164399, #120847, #183535, #197713, #196738, #43037, #73390, #105689, #59178, #181559, #104703, #29848, #91485, #72377, #199696, #74373, #75346, #166392, #152195, #118891, #180576, #13679, #198705, #134051, #136038, #14674, #45019, #117884 ),
 .UNSPECIFIED., .F., .T. ) 
 B_SPLINE_CURVE_WITH_KNOTS ( ( 3, 2, 2, 2, 2, 2, 2, 2, 2, 2, 2, 2, 2, 2, 2, 2, 2, 2, 2, 2, 2, 2, 2, 2, 2, 2, 2, 2, 2, 2, 2, 2, 2, 2, 2, 2, 2, 2, 2, 2, 2, 2, 2, 2, 2, 2, 2, 2, 2, 2, 3 ),
 ( 0.000000000000000000, 0.02000000000000000042, 0.04000000000000000083, 0.05999999999999999778, 0.08000000000000000167, 0.1000000000000000056, 0.1199999999999999956, 0.1400000000000000133, 0.1600000000000000033, 0.1799999999999999933, 0.2000000000000000111, 0.2200000000000000011, 0.2399999999999999911, 0.2600000000000000089, 0.2800000000000000266, 0.2999999999999999889, 0.3200000000000000067, 0.3400000000000000244, 0.3599999999999999867, 0.3800000000000000044, 0.4000000000000000222, 0.4199999999999999845, 0.4400000000000000022, 0.4600000000000000200, 0.4799999999999999822, 0.5000000000000000000, 0.5200000000000000178, 0.5400000000000000355, 0.5600000000000000533, 0.5799999999999999600, 0.5999999999999999778, 0.6199999999999999956, 0.6400000000000000133, 0.6600000000000000311, 0.6800000000000000488, 0.6999999999999999556, 0.7199999999999999734, 0.7399999999999999911, 0.7600000000000000089, 0.7800000000000000266, 0.8000000000000000444, 0.8199999999999999512, 0.8399999999999999689, 0.8599999999999999867, 0.8800000000000000044, 0.9000000000000000222, 0.9200000000000000400, 0.9399999999999999467, 0.9599999999999999645, 0.9799999999999999822, 1.000000000000000000 ),
 .UNSPECIFIED. ) 
 CURVE ( )  GEOMETRIC_REPRESENTATION_ITEM ( )  RATIONAL_B_SPLINE_CURVE ( ( 1.000000000000000000, 0.9510565162951535312, 1.000000000000000000, 0.9510565162951535312, 1.000000000000000000, 0.9510565162951535312, 1.000000000000000000, 0.9510565162951535312, 1.000000000000000000, 0.9510565162951535312, 1.000000000000000000, 0.9510565162951535312, 1.000000000000000000, 0.9510565162951535312, 1.000000000000000000, 0.9510565162951535312, 1.000000000000000000, 0.9510565162951535312, 1.000000000000000000, 0.9510565162951535312, 1.000000000000000000, 0.9510565162951535312, 1.000000000000000000, 0.9510565162951535312, 1.000000000000000000, 0.9510565162951535312, 1.000000000000000000, 0.9510565162951535312, 1.000000000000000000, 0.9510565162951535312, 1.000000000000000000, 0.9510565162951535312, 1.000000000000000000, 0.9510565162951535312, 1.000000000000000000, 0.9510565162951535312, 1.000000000000000000, 0.9510565162951535312, 1.000000000000000000, 0.9510565162951535312, 1.000000000000000000, 0.9510565162951535312, 1.000000000000000000, 0.9510565162951535312, 1.000000000000000000, 0.9510565162951535312, 1.000000000000000000, 0.9510565162951535312, 1.000000000000000000, 0.9510565162951535312, 1.000000000000000000, 0.9510565162951535312, 1.000000000000000000, 0.9510565162951535312, 1.000000000000000000, 0.9510565162951535312, 1.000000000000000000, 0.9510565162951535312, 1.000000000000000000, 0.9510565162951535312, 1.000000000000000000, 0.9510565162951535312, 1.000000000000000000, 0.9510565162951535312, 1.000000000000000000, 0.9510565162951535312, 1.000000000000000000, 0.9510565162951535312, 1.000000000000000000, 0.9510565162951535312, 1.000000000000000000, 0.9510565162951535312, 1.000000000000000000, 0.9510565162951535312, 1.000000000000000000, 0.9510565162951535312, 1.000000000000000000, 0.9510565162951535312, 1.000000000000000000, 0.9510565162951535312, 1.000000000000000000, 0.9510565162951535312, 1.000000000000000000, 0.9510565162951535312, 1.000000000000000000, 0.9510565162951535312, 1.000000000000000000, 0.9510565162951535312, 1.000000000000000000, 0.9510565162951535312, 1.000000000000000000, 0.9510565162951535312, 1.000000000000000000, 0.9510565162951535312, 1.000000000000000000, 0.9510565162951535312, 1.000000000000000000, 0.9510565162951535312, 1.000000000000000000, 0.9510565162951535312, 1.000000000000000000 ) ) 
 REPRESENTATION_ITEM ( '' )  );
#43195 = CARTESIAN_POINT ( 'NONE',  ( 8.224510206698742110, 14.34966873604972548, 107.0844237280190043 ) ) ;
#43196 = EDGE_CURVE ( 'NONE', #85848, #1176, #104262, .T. ) ;
#43197 = CARTESIAN_POINT ( 'NONE',  ( -21.52544592524343514, 5.823673210054127303, 101.0405762719810383 ) ) ;
#43198 = CARTESIAN_POINT ( 'NONE',  ( -8.224510206698948167, 14.34966873604960824, 45.41557627198103830 ) ) ;
#43199 = CARTESIAN_POINT ( 'NONE',  ( 5.049401038297881783, 19.05341960407617563, 77.29275706135231871 ) ) ;
#43200 = CARTESIAN_POINT ( 'NONE',  ( -9.564922557961040184, 16.46253265017147172, 52.91775706135233293 ) ) ;
#43201 = CARTESIAN_POINT ( 'NONE',  ( 18.62759615963255655, 10.81492255796105972, 71.66775706135234714 ) ) ;
#43202 = CARTESIAN_POINT ( 'NONE',  ( 16.46253265017146816, 9.564922557961045513, 36.66775706135233293 ) ) ;
#43203 = CARTESIAN_POINT ( 'NONE',  ( 4.483927247898545687, 16.52544592524342804, 104.7905762719810241 ) ) ;
#43204 = CARTESIAN_POINT ( 'NONE',  ( -15.72974639402197994, 15.80617190586746368, 50.62390960531435979 ) ) ;
#43205 = CARTESIAN_POINT ( 'NONE',  ( -4.379528057220328563, 16.55341960407611168, 30.20724293864769550 ) ) ;
#43206 = CARTESIAN_POINT ( 'NONE',  ( 19.03943276465977164, 0.05219959533936151252, 21.25109039468565797 ) ) ;
#43207 = CARTESIAN_POINT ( 'NONE',  ( -12.06949235617739369, -12.14591786802326823, 74.37609039468568994 ) ) ;
#43208 = CARTESIAN_POINT ( 'NONE',  ( 4.483927247898545687, 16.52544592524342804, 24.79057627198103120 ) ) ;
#43209 = CARTESIAN_POINT ( 'NONE',  ( -18.67979575497193778, 10.72451020669871902, 63.33442372801900433 ) ) ;
#43210 = CARTESIAN_POINT ( 'NONE',  ( 15.80617190586769283, -15.72974639402175789, 65.62609039468568994 ) ) ;
#43211 = CARTESIAN_POINT ( 'NONE',  ( -15.72974639402197994, 15.80617190586746368, 70.62390960531436690 ) ) ;
#43212 = VERTEX_POINT ( 'NONE', #110393 ) ;
#43213 = CARTESIAN_POINT ( 'NONE',  ( -16.51473224551069308, -9.474510206698971260, 26.66557627198103120 ) ) ;
#43214 = CARTESIAN_POINT ( 'NONE',  ( 10.72451020669871369, 18.67979575497193778, 47.08442372801901854 ) ) ;
#43215 = CARTESIAN_POINT ( 'NONE',  ( -16.46253265017160317, 9.564922557960807481, 25.83224293864769194 ) ) ;
#43216 = CARTESIAN_POINT ( 'NONE',  ( -0.05219959533909027116, -19.03943276465977164, 42.49890960531435269 ) ) ;
#43217 = CARTESIAN_POINT ( 'NONE',  ( -12.14591786802309592, -12.06949235617757132, 76.87390960531439532 ) ) ;
#43218 = CARTESIAN_POINT ( 'NONE',  ( 9.564922557960805705, 16.46253265017160317, 84.58224293864769550 ) ) ;
#43219 = CARTESIAN_POINT ( 'NONE',  ( 0.05219959533910956823, 16.53943276465976808, 24.99890960531435624 ) ) ;
#43220 = CARTESIAN_POINT ( 'NONE',  ( -8.314922557960811034, -14.29746914071050412, 102.0822429386476955 ) ) ;
#43221 = CARTESIAN_POINT ( 'NONE',  ( 21.55341960407610458, 5.719274019375980345, 68.95724293864769550 ) ) ;
#43222 = CARTESIAN_POINT ( 'NONE',  ( 10.72451020669898902, -18.67979575497178502, 102.9155762719810383 ) ) ;
#43223 = CARTESIAN_POINT ( 'NONE',  ( -0.05219959533909027116, -19.03943276465977164, 112.4989096053143669 ) ) ;
#43224 = EDGE_CURVE ( 'NONE', #104654, #86900, #38444, .T. ) ;
#43226 = CARTESIAN_POINT ( 'NONE',  ( 4.483927247898790824, -16.52544592524335698, 20.20942372801900788 ) ) ;
#43225 = CARTESIAN_POINT ( 'NONE',  ( 13.97604488694527802, 13.89961937509977652, 69.37390960531436690 ) ) ;
#43227 = CARTESIAN_POINT ( 'NONE',  ( 18.62759615963271287, -10.81492255796078972, 53.33224293864769550 ) ) ;
#43228 = CARTESIAN_POINT ( 'NONE',  ( -10.72451020669870658, -18.67979575497194134, 79.58442372801903275 ) ) ;
#43229 = CARTESIAN_POINT ( 'NONE',  ( 5.153800228976335163, 19.02544592524342804, 84.79057627198099567 ) ) ;
#43230 = AXIS2_PLACEMENT_3D ( 'NONE', #99950, #102960, #41299 ) ;
#43231 = CARTESIAN_POINT ( 'NONE',  ( -18.67979575497178146, -10.72451020669898902, 21.66557627198102409 ) ) ;
#43232 = CARTESIAN_POINT ( 'NONE',  ( -14.34966873604972548, 8.224510206698743886, 78.33442372801901854 ) ) ;
#43233 = CARTESIAN_POINT ( 'NONE',  ( 5.719274019375673035, 21.55341960407619339, 52.29275706135236135 ) ) ;
#43234 = CARTESIAN_POINT ( 'NONE',  ( -18.62759615963255300, -10.81492255796106328, 99.16775706135234714 ) ) ;
#43235 = CARTESIAN_POINT ( 'NONE',  ( 16.55341960407618274, -4.379528057220086978, 66.04275706135236135 ) ) ;
#43236 = CARTESIAN_POINT ( 'NONE',  ( 21.53943276465977519, -0.05219959533907433946, 108.7489096053143669 ) ) ;
#43237 = CARTESIAN_POINT ( 'NONE',  ( -19.03943276465977164, 0.05219959533909376836, 116.2489096053143669 ) ) ;
#43238 = CARTESIAN_POINT ( 'NONE',  ( 5.719274019375991003, -21.55341960407610458, 87.70724293864769550 ) ) ;
#43239 = CARTESIAN_POINT ( 'NONE',  ( -5.153800228976607833, 19.02544592524334988, 52.70942372801900433 ) ) ;
#43240 = CARTESIAN_POINT ( 'NONE',  ( 10.72451020669898902, -18.67979575497178502, 42.91557627198103120 ) ) ;
#43242 = CARTESIAN_POINT ( 'NONE',  ( 16.53943276465976808, -0.05219959533910856209, 38.74890960531435979 ) ) ;
#43241 = CARTESIAN_POINT ( 'NONE',  ( 0.05219959533909260263, 19.03943276465977164, 94.99890960531436690 ) ) ;
#43243 = CARTESIAN_POINT ( 'NONE',  ( -16.62475595723697452, 7.163666690055237041, 65.52713351810467657 ) ) ;
#43244 = DIRECTION ( 'NONE',  ( -0.000000000000000000, 0.000000000000000000, 1.000000000000000000 ) ) ;
#43245 = CARTESIAN_POINT ( 'NONE',  ( -13.89961937509957401, -13.97604488694547875, 99.37609039468567573 ) ) ;
#43246 = CARTESIAN_POINT ( 'NONE',  ( -5.823673210054116645, -21.52544592524344225, 77.29057627198102409 ) ) ;
#43247 = CARTESIAN_POINT ( 'NONE',  ( -14.34966873604960291, -8.224510206698953496, 51.66557627198102409 ) ) ;
#43248 = CARTESIAN_POINT ( 'NONE',  ( 16.53943276465976808, 0.05219959533934440121, 36.25109039468567573 ) ) ;
#43249 = CARTESIAN_POINT ( 'NONE',  ( 5.049401038298161559, -19.05341960407611168, 42.70724293864767418 ) ) ;
#43251 = CARTESIAN_POINT ( 'NONE',  ( -5.049401038297874678, -19.05341960407617918, 79.79275706135233293 ) ) ;
#43250 = CARTESIAN_POINT ( 'NONE',  ( 10.81492255796078972, 18.62759615963270932, 109.5822429386476955 ) ) ;
#43252 = CARTESIAN_POINT ( 'NONE',  ( 5.049401038298161559, -19.05341960407611168, 77.70724293864765286 ) ) ;
#43253 = CARTESIAN_POINT ( 'NONE',  ( -5.153800228976328057, -19.02544592524343514, 77.29057627198099567 ) ) ;
#43254 = CARTESIAN_POINT ( 'NONE',  ( -15.72974639402197994, 15.80617190586746368, 75.62390960531439532 ) ) ;
#43255 = CARTESIAN_POINT ( 'NONE',  ( 5.049401038298161559, -19.05341960407611168, 37.70724293864768839 ) ) ;
#43256 = DIRECTION ( 'NONE',  ( 0.000000000000000000, 0.000000000000000000, 1.000000000000000000 ) ) ;
#43257 = CARTESIAN_POINT ( 'NONE',  ( 0.05219959533910956823, 16.53943276465976808, 59.99890960531436690 ) ) ;
#43258 = CARTESIAN_POINT ( 'NONE',  ( 0.05219959533909260263, 19.03943276465977164, 94.99890960531436690 ) ) ;
#43259 = CARTESIAN_POINT ( 'NONE',  ( -3.573655867282028392E-15, 2.428612866367529932E-14, -8.000000000000000000 ) ) ;
#43260 = CARTESIAN_POINT ( 'NONE',  ( -19.03943276465977164, -0.05219959533935918106, 58.75109039468566863 ) ) ;
#43261 = CARTESIAN_POINT ( 'NONE',  ( -15.72974639402197994, 15.80617190586746368, 80.62390960531438111 ) ) ;
#43262 = CARTESIAN_POINT ( 'NONE',  ( -9.564922557961040184, 16.46253265017147172, 32.91775706135233293 ) ) ;
#43263 = CARTESIAN_POINT ( 'NONE',  ( -9.564922557960796823, -16.46253265017161027, 87.08224293864769550 ) ) ;
#43264 = CARTESIAN_POINT ( 'NONE',  ( 10.19492084563873391, -9.320932348315787763, -60.40172357148235704 ) ) ;
#43265 = CARTESIAN_POINT ( 'NONE',  ( 5.823673210054125526, 21.52544592524343514, 24.79057627198103120 ) ) ;
#43266 = CARTESIAN_POINT ( 'NONE',  ( -19.05341960407611168, -5.049401038298163336, 76.45724293864769550 ) ) ;
#43267 = CARTESIAN_POINT ( 'NONE',  ( 15.72974639402176855, 15.80617190586768217, 46.87609039468568994 ) ) ;
#43268 = CARTESIAN_POINT ( 'NONE',  ( -19.05341960407611168, -5.049401038298163336, 31.45724293864769550 ) ) ;
#43271 = ORIENTED_EDGE ( 'NONE', *, *, #170016, .F. ) ;
#43270 = CARTESIAN_POINT ( 'NONE',  ( -16.51473224551069308, -9.474510206698971260, 96.66557627198102409 ) ) ;
#43269 = CARTESIAN_POINT ( 'NONE',  ( 21.55341960407610458, 5.719274019375980345, 108.9572429386476955 ) ) ;
#43272 = CARTESIAN_POINT ( 'NONE',  ( 0.05219959533937995610, -21.53943276465977519, 35.00109039468568284 ) ) ;
#43273 = ORIENTED_EDGE ( 'NONE', *, *, #128725, .T. ) ;
#43274 = CARTESIAN_POINT ( 'NONE',  ( -19.05341960407611168, -5.049401038298163336, 106.4572429386476955 ) ) ;
#43275 = CARTESIAN_POINT ( 'NONE',  ( 0.05219959533909260263, 19.03943276465977164, 89.99890960531436690 ) ) ;
#43276 = CARTESIAN_POINT ( 'NONE',  ( -10.81492255796078084, -18.62759615963271287, 107.0822429386476955 ) ) ;
#43277 = CARTESIAN_POINT ( 'NONE',  ( -19.03943276465977164, 0.05219959533909376836, 61.24890960531436690 ) ) ;
#43278 = CARTESIAN_POINT ( 'NONE',  ( 16.55341960407618274, -4.379528057220086978, 26.04275706135235779 ) ) ;
#43279 = CARTESIAN_POINT ( 'NONE',  ( 38.00000000000000000, 12.34694845685046616, -10.64999999453762491 ) ) ;
#43280 = CARTESIAN_POINT ( 'NONE',  ( 18.67979575497194134, -10.72451020669871369, 100.8344237280190185 ) ) ;
#43281 = CARTESIAN_POINT ( 'NONE',  ( 19.03943276465977164, -0.05219959533909143690, 38.74890960531436690 ) ) ;
#43282 = CARTESIAN_POINT ( 'NONE',  ( 10.81492255796106328, -18.62759615963255655, 95.41775706135234714 ) ) ;
#43284 = CARTESIAN_POINT ( 'NONE',  ( 18.67979575497194134, -10.72451020669871369, 60.83442372801901854 ) ) ;
#43283 = CARTESIAN_POINT ( 'NONE',  ( 9.474510206698971260, -16.51473224551069308, 92.91557627198103830 ) ) ;
#43285 = CARTESIAN_POINT ( 'NONE',  ( -5.359611314223446995E-15, 29.16686587814335496, 142.8750000027311842 ) ) ;
#43286 = CARTESIAN_POINT ( 'NONE',  ( -16.51473224551069308, -9.474510206698971260, 101.6655762719810241 ) ) ;
#43287 = DIRECTION ( 'NONE',  ( -1.000000000000000000, -0.000000000000000000, -0.000000000000000000 ) ) ;
#43290 = CARTESIAN_POINT ( 'NONE',  ( -10.81492255796105439, 18.62759615963255655, 52.91775706135235424 ) ) ;
#43289 = CARTESIAN_POINT ( 'NONE',  ( 4.379528057220092307, 16.55341960407617563, 67.29275706135234714 ) ) ;
#43288 = CARTESIAN_POINT ( 'NONE',  ( -4.379528057220086978, -16.55341960407618274, 49.79275706135234714 ) ) ;
#43291 = CARTESIAN_POINT ( 'NONE',  ( 10.72451020669871369, 18.67979575497193778, 87.08442372801901854 ) ) ;
#43292 = VECTOR ( 'NONE', #23423, 1000.000000000000000 ) ;
#43293 = DIRECTION ( 'NONE',  ( 1.000000000000000000, 0.000000000000000000, 0.000000000000000000 ) ) ;
#43294 = CARTESIAN_POINT ( 'NONE',  ( -16.53943276465976808, -0.05219959533934237506, 33.75109039468568284 ) ) ;
#43295 = CARTESIAN_POINT ( 'NONE',  ( -16.51473224551069308, -9.474510206698971260, 76.66557627198103830 ) ) ;
#43296 = CARTESIAN_POINT ( 'NONE',  ( -19.05341960407611168, -5.049401038298163336, 91.45724293864766707 ) ) ;
#43297 = DIRECTION ( 'NONE',  ( 0.000000000000000000, 0.000000000000000000, -1.000000000000000000 ) ) ;
#43298 = CARTESIAN_POINT ( 'NONE',  ( -9.564922557960796823, -16.46253265017161027, 27.08224293864769550 ) ) ;
#43299 = CARTESIAN_POINT ( 'NONE',  ( 18.67979575497178502, 10.72451020669898547, 34.16557627198102409 ) ) ;
#43300 = CARTESIAN_POINT ( 'NONE',  ( -12.14591786802326823, 12.06949235617739902, 88.12609039468570415 ) ) ;
#43302 = CARTESIAN_POINT ( 'NONE',  ( 13.89961937509977652, -13.97604488694527269, 68.12390960531436690 ) ) ;
#43301 = CARTESIAN_POINT ( 'NONE',  ( 16.52544592524342804, -4.483927247898539470, 88.54057627198103830 ) ) ;
#43303 = CARTESIAN_POINT ( 'NONE',  ( 21.55341960407619695, -5.719274019375665929, 96.04275706135236135 ) ) ;
#43304 = CARTESIAN_POINT ( 'NONE',  ( -21.65131445265848598, 0.9841389949903269763, -58.61993113718295945 ) ) ;
#43305 = CARTESIAN_POINT ( 'NONE',  ( -8.224510206698735004, -14.34966873604973081, 29.58442372801901854 ) ) ;
#43306 = CARTESIAN_POINT ( 'NONE',  ( -8.224510206698948167, 14.34966873604960824, 80.41557627198103830 ) ) ;
#43307 = CARTESIAN_POINT ( 'NONE',  ( 18.62759615963255655, 10.81492255796105972, 36.66775706135234714 ) ) ;
#43308 = CARTESIAN_POINT ( 'NONE',  ( 10.72451020669898902, -18.67979575497178502, 67.91557627198102409 ) ) ;
#43309 = CARTESIAN_POINT ( 'NONE',  ( 9.474510206698729675, 16.51473224551082808, 42.08442372801900433 ) ) ;
#43310 = CARTESIAN_POINT ( 'NONE',  ( -34.77165353390495284, 6.824181688848569571, 41.87898302971510844 ) ) ;
#43311 = CARTESIAN_POINT ( 'NONE',  ( -19.05341960407611168, -5.049401038298163336, 76.45724293864769550 ) ) ;
#43312 = CARTESIAN_POINT ( 'NONE',  ( -8.314922557960811034, -14.29746914071050412, 47.08224293864770260 ) ) ;
#43313 = CIRCLE ( 'NONE', #175652, 40.00000000000000711 ) ;
#43314 = CARTESIAN_POINT ( 'NONE',  ( 12.14591786802309770, 12.06949235617756955, 29.37390960531435269 ) ) ;
#43315 = CARTESIAN_POINT ( 'NONE',  ( 12.06949235617739724, 12.14591786802326823, 106.8760903946856899 ) ) ;
#43316 = CARTESIAN_POINT ( 'NONE',  ( -16.51473224551082808, 9.474510206698731452, 68.33442372801900433 ) ) ;
#43317 = CARTESIAN_POINT ( 'NONE',  ( 17.49999999999999645, 5.624438216177601646, 46.68329655085357643 ) ) ;
#43318 = CARTESIAN_POINT ( 'NONE',  ( 10.72451020669898902, -18.67979575497178502, 22.91557627198102765 ) ) ;
#43319 = CARTESIAN_POINT ( 'NONE',  ( 4.483927247898545687, 16.52544592524342804, 84.79057627198102409 ) ) ;
#43320 = CARTESIAN_POINT ( 'NONE',  ( 18.22780087662122384, 5.500000000000018652, 93.98459894673892734 ) ) ;
#43322 = CARTESIAN_POINT ( 'NONE',  ( 18.62759615963271287, -10.81492255796078972, 38.33224293864768839 ) ) ;
#43321 = CARTESIAN_POINT ( 'NONE',  ( 5.049401038298161559, -19.05341960407611168, 27.70724293864769550 ) ) ;
#43323 = CARTESIAN_POINT ( 'NONE',  ( -10.81492255796078084, -18.62759615963271287, 72.08224293864769550 ) ) ;
#43324 = CARTESIAN_POINT ( 'NONE',  ( -8.224510206698948167, 14.34966873604960824, 115.4155762719810241 ) ) ;
#43326 = CARTESIAN_POINT ( 'NONE',  ( -9.564922557960796823, -16.46253265017161027, 52.08224293864768839 ) ) ;
#43325 = CARTESIAN_POINT ( 'NONE',  ( -16.52544592524335698, -4.483927247898792601, 68.95942372801901854 ) ) ;
#43327 = CARTESIAN_POINT ( 'NONE',  ( 18.67979575497194134, -10.72451020669871369, 50.83442372801901143 ) ) ;
#43328 = CARTESIAN_POINT ( 'NONE',  ( -0.05219959533910754901, -16.53943276465976808, 107.4989096053143669 ) ) ;
#43329 = CARTESIAN_POINT ( 'NONE',  ( -16.46253265017146816, -9.564922557961047289, 89.16775706135234714 ) ) ;
#43330 = CARTESIAN_POINT ( 'NONE',  ( 29.86685920354754487, 21.69954338932564752, -5.924999997268813878 ) ) ;
#43332 = CARTESIAN_POINT ( 'NONE',  ( -18.62759615963270932, 10.81492255796079327, 35.83224293864768839 ) ) ;
#43331 = CARTESIAN_POINT ( 'NONE',  ( -38.00000000000000711, 2.428612866367529932E-14, -8.000000000000000000 ) ) ;
#43333 = LINE ( 'NONE', #90805, #162401 ) ;
#43334 = CARTESIAN_POINT ( 'NONE',  ( -15.72974639402176322, -15.80617190586768395, 64.37609039468568994 ) ) ;
#43336 = CARTESIAN_POINT ( 'NONE',  ( -16.53943276465976808, 0.05219959533911058130, 41.24890960531435269 ) ) ;
#43335 = CARTESIAN_POINT ( 'NONE',  ( -12.06949235617739369, -12.14591786802326823, 54.37609039468568994 ) ) ;
#43337 = CARTESIAN_POINT ( 'NONE',  ( 15.80617190586746368, 15.72974639402197994, 64.37390960531435269 ) ) ;
#43338 = CARTESIAN_POINT ( 'NONE',  ( -21.53943276465977519, 0.05219959533907696930, 66.24890960531436690 ) ) ;
#43339 = CARTESIAN_POINT ( 'NONE',  ( -21.93653645885848746, -8.192071713419743162, 172.2938920027118002 ) ) ;
#43341 = CARTESIAN_POINT ( 'NONE',  ( -19.05341960407611168, -5.049401038298163336, 111.4572429386476671 ) ) ;
#43340 = CARTESIAN_POINT ( 'NONE',  ( 16.51473224551083163, -9.474510206698727899, 80.83442372801899012 ) ) ;
#43342 = CARTESIAN_POINT ( 'NONE',  ( 16.46253265017160672, -9.564922557960803928, 48.33224293864769550 ) ) ;
#43343 = CARTESIAN_POINT ( 'NONE',  ( 12.14591786802309770, 12.06949235617756955, 109.3739096053143811 ) ) ;
#43344 = CARTESIAN_POINT ( 'NONE',  ( -3.573655867282028392E-15, 2.428612866367529932E-14, 139.9999999999999716 ) ) ;
#43345 = VERTEX_POINT ( 'NONE', #92233 ) ;
#43346 = CARTESIAN_POINT ( 'NONE',  ( 12.14591786802327356, -12.06949235617739191, 65.62609039468568994 ) ) ;
#43347 = CARTESIAN_POINT ( 'NONE',  ( -21.53943276465977519, 0.05219959533907696930, 101.2489096053143669 ) ) ;
#43348 = CARTESIAN_POINT ( 'NONE',  ( -19.03943276465977164, 0.05219959533909376836, 56.24890960531435979 ) ) ;
#43349 = CARTESIAN_POINT ( 'NONE',  ( 5.719274019375673035, 21.55341960407619339, 47.29275706135234003 ) ) ;
#43350 = CARTESIAN_POINT ( 'NONE',  ( 9.564922557960805705, 16.46253265017160317, 94.58224293864769550 ) ) ;
#43351 = CARTESIAN_POINT ( 'NONE',  ( -27.83073679762865638, -28.30972371523964881, -20.09501658340063557 ) ) ;
#43352 = ORIENTED_EDGE ( 'NONE', *, *, #109475, .F. ) ;
#43353 = CARTESIAN_POINT ( 'NONE',  ( -10.72451020669870658, -18.67979575497194134, 34.58442372801900433 ) ) ;
#43355 = CARTESIAN_POINT ( 'NONE',  ( 9.474510206698729675, 16.51473224551082808, 92.08442372801900433 ) ) ;
#43354 = CARTESIAN_POINT ( 'NONE',  ( -13.97604488694527625, -13.89961937509977652, 101.8739096053143811 ) ) ;
#43356 = CARTESIAN_POINT ( 'NONE',  ( -9.564922557961040184, 16.46253265017147172, 42.91775706135234003 ) ) ;
#43357 = CARTESIAN_POINT ( 'NONE',  ( 10.81492255796078972, 18.62759615963270932, 104.5822429386477097 ) ) ;
#43358 = CARTESIAN_POINT ( 'NONE',  ( -13.89961937509957401, -13.97604488694547875, 34.37609039468566863 ) ) ;
#43359 = CARTESIAN_POINT ( 'NONE',  ( 19.05341960407617918, -5.049401038297876454, 51.04275706135231871 ) ) ;
#43360 = CARTESIAN_POINT ( 'NONE',  ( -4.483927247898782831, 16.52544592524335698, 97.70942372801904696 ) ) ;
#43361 = CARTESIAN_POINT ( 'NONE',  ( 24.39441179196515463, -8.562450407400064023, 166.7298547261019053 ) ) ;
#43362 = CARTESIAN_POINT ( 'NONE',  ( 13.97604488694527802, 13.89961937509977652, 74.37390960531436690 ) ) ;
#43363 = CARTESIAN_POINT ( 'NONE',  ( -15.72974639402176322, -15.80617190586768395, 79.37609039468567573 ) ) ;
#43364 = CARTESIAN_POINT ( 'NONE',  ( -10.72451020669870658, -18.67979575497194134, 79.58442372801903275 ) ) ;
#43365 = CARTESIAN_POINT ( 'NONE',  ( -0.6701480022146820703, -8.945614359730862830, -63.98123544873404711 ) ) ;
#43366 = CARTESIAN_POINT ( 'NONE',  ( -16.51473224551069308, -9.474510206698971260, 86.66557627198102409 ) ) ;
#43367 = CARTESIAN_POINT ( 'NONE',  ( 18.62759615963255655, 10.81492255796105972, 56.66775706135235424 ) ) ;
#43368 = CARTESIAN_POINT ( 'NONE',  ( 16.51473224551083163, -9.474510206698727899, 100.8344237280190043 ) ) ;
#43369 = CARTESIAN_POINT ( 'NONE',  ( -0.05219959533909027116, -19.03943276465977164, 72.49890960531435269 ) ) ;
#43370 = CARTESIAN_POINT ( 'NONE',  ( 19.05341960407611168, 5.049401038298154454, 108.9572429386477097 ) ) ;
#43371 = CARTESIAN_POINT ( 'NONE',  ( 9.564922557960805705, 16.46253265017160317, 79.58224293864769550 ) ) ;
#43372 = CARTESIAN_POINT ( 'NONE',  ( 17.49999999999997158, -3.354790192122885539, 22.07749092806899682 ) ) ;
#43373 = CARTESIAN_POINT ( 'NONE',  ( 5.153800228976335163, 19.02544592524342804, 69.79057627198103830 ) ) ;
#43374 = CARTESIAN_POINT ( 'NONE',  ( -0.05219959533909027116, -19.03943276465977164, 52.49890960531436690 ) ) ;
#43375 = CARTESIAN_POINT ( 'NONE',  ( -21.55341960407610458, -5.719274019375992779, 111.4572429386476813 ) ) ;
#43376 = CARTESIAN_POINT ( 'NONE',  ( 14.29746914071037800, 8.314922557961029526, 81.66775706135236135 ) ) ;
#43377 = FACE_OUTER_BOUND ( 'NONE', #65455, .T. ) ;
#43378 = CARTESIAN_POINT ( 'NONE',  ( 19.03943276465977164, 0.05219959533936151252, 46.25109039468566863 ) ) ;
#43379 = CARTESIAN_POINT ( 'NONE',  ( 19.03943276465977164, -0.05219959533909143690, 78.74890960531436690 ) ) ;
#43380 = CARTESIAN_POINT ( 'NONE',  ( 12.06949235617757843, -12.14591786802309237, 78.12390960531436690 ) ) ;
#43381 = CARTESIAN_POINT ( 'NONE',  ( -16.53943276465976808, 0.05219959533911058130, 106.2489096053143811 ) ) ;
#43382 = CARTESIAN_POINT ( 'NONE',  ( -10.81492255796078084, -18.62759615963271287, 22.08224293864769194 ) ) ;
#43383 = ORIENTED_EDGE ( 'NONE', *, *, #190970, .T. ) ;
#43384 = CARTESIAN_POINT ( 'NONE',  ( 19.02544592524343514, -5.153800228976328945, 103.5405762719809957 ) ) ;
#43385 = CARTESIAN_POINT ( 'NONE',  ( 16.55341960407611168, 4.379528057220329451, 83.95724293864770971 ) ) ;
#43386 = DIRECTION ( 'NONE',  ( -1.000000000000000000, 0.000000000000000000, 0.000000000000000000 ) ) ;
#43387 = CARTESIAN_POINT ( 'NONE',  ( -5.153800228976607833, 19.02544592524334988, 27.70942372801899722 ) ) ;
#43388 = CARTESIAN_POINT ( 'NONE',  ( -4.483927247898782831, 16.52544592524335698, 87.70942372801901854 ) ) ;
#43390 = EDGE_CURVE ( 'NONE', #57160, #166090, #145569, .T. ) ;
#43389 = CARTESIAN_POINT ( 'NONE',  ( 16.51473224551069308, 9.474510206698969483, 89.16557627198103830 ) ) ;
#43391 = CARTESIAN_POINT ( 'NONE',  ( -5.823673210054431948, 21.52544592524334988, 52.70942372801902565 ) ) ;
#43392 = CARTESIAN_POINT ( 'NONE',  ( -18.62759615963270932, 10.81492255796079327, 40.83224293864769550 ) ) ;
#43393 = CARTESIAN_POINT ( 'NONE',  ( 5.823673210054125526, 21.52544592524343514, 114.7905762719810383 ) ) ;
#43394 = CARTESIAN_POINT ( 'NONE',  ( 21.52544592524344225, -5.823673210054117533, 68.54057627198103830 ) ) ;
#43395 = CARTESIAN_POINT ( 'NONE',  ( 4.379528057220339221, -16.55341960407611168, 97.70724293864772392 ) ) ;
#43396 = CARTESIAN_POINT ( 'NONE',  ( -19.02544592524334988, -5.153800228976617603, 53.95942372801898301 ) ) ;
#43397 = AXIS2_PLACEMENT_3D ( 'NONE', #176257, #175249, #146908 ) ;
#43398 = CARTESIAN_POINT ( 'NONE',  ( -9.564922557960796823, -16.46253265017161027, 37.08224293864768839 ) ) ;
#43399 = CARTESIAN_POINT ( 'NONE',  ( -5.153800228976328057, -19.02544592524343514, 82.29057627198103830 ) ) ;
#43400 = CARTESIAN_POINT ( 'NONE',  ( 5.153800228976335163, 19.02544592524342804, 84.79057627198099567 ) ) ;
#43401 = CARTESIAN_POINT ( 'NONE',  ( 12.06949235617757843, -12.14591786802309237, 103.1239096053143811 ) ) ;
#43402 = ORIENTED_EDGE ( 'NONE', *, *, #6742, .F. ) ;
#43403 = CARTESIAN_POINT ( 'NONE',  ( 8.224510206698953496, -14.34966873604960469, 22.91557627198102765 ) ) ;
#43404 = CARTESIAN_POINT ( 'NONE',  ( 16.55341960407618274, -4.379528057220086978, 36.04275706135234714 ) ) ;
#43405 = CARTESIAN_POINT ( 'NONE',  ( 15.80617190586769283, -15.72974639402175789, 100.6260903946857184 ) ) ;
#43406 = CARTESIAN_POINT ( 'NONE',  ( 0.05219959533909260263, 19.03943276465977164, 94.99890960531436690 ) ) ;
#43407 = CARTESIAN_POINT ( 'NONE',  ( 18.67979575497194134, -10.72451020669871369, 35.83442372801901143 ) ) ;
#43408 = CARTESIAN_POINT ( 'NONE',  ( 19.02544592524343514, -5.153800228976328945, 48.54057627198103120 ) ) ;
#43409 = CARTESIAN_POINT ( 'NONE',  ( 14.29746914071037800, 8.314922557961029526, 41.66775706135235424 ) ) ;
#43410 = AXIS2_PLACEMENT_3D ( 'NONE', #67943, #161955, #177147 ) ;
#43411 = CARTESIAN_POINT ( 'NONE',  ( 16.51473224551083163, -9.474510206698727899, 110.8344237280190043 ) ) ;
#43412 = CARTESIAN_POINT ( 'NONE',  ( 19.03943276465977164, -0.05219959533909143690, 38.74890960531436690 ) ) ;
#43413 = CARTESIAN_POINT ( 'NONE',  ( 4.483927247898545687, 16.52544592524342804, 99.79057627198103830 ) ) ;
#43414 = CARTESIAN_POINT ( 'NONE',  ( -21.55341960407610458, -5.719274019375992779, 106.4572429386477097 ) ) ;
#43415 = CARTESIAN_POINT ( 'NONE',  ( -19.02544592524334988, -5.153800228976617603, 83.95942372801901854 ) ) ;
#43416 = SURFACE_STYLE_FILL_AREA ( #135441 ) ;
#43417 = CARTESIAN_POINT ( 'NONE',  ( 13.89961937509977652, -13.97604488694527269, 88.12390960531438111 ) ) ;
#43418 = CARTESIAN_POINT ( 'NONE',  ( 15.80617190586769283, -15.72974639402175789, 30.62609039468567929 ) ) ;
#43419 = CARTESIAN_POINT ( 'NONE',  ( -5.049401038298153566, 19.05341960407611168, 25.20724293864768484 ) ) ;
#43420 = CARTESIAN_POINT ( 'NONE',  ( 5.153800228976335163, 19.02544592524342804, 89.79057627198102409 ) ) ;
#43421 = CIRCLE ( 'NONE', #75728, 21.30000000000002913 ) ;
#43422 = CARTESIAN_POINT ( 'NONE',  ( 16.79531203550644847, -7.028104445595642957, 111.2475501177955977 ) ) ;
#43423 = CARTESIAN_POINT ( 'NONE',  ( 9.474510206698971260, -16.51473224551069308, 82.91557627198103830 ) ) ;
#43425 = CARTESIAN_POINT ( 'NONE',  ( 8.314922557960818139, 14.29746914071049879, 94.58224293864769550 ) ) ;
#43424 = CARTESIAN_POINT ( 'NONE',  ( 18.62759615963255655, 10.81492255796105972, 36.66775706135234714 ) ) ;
#43426 = CARTESIAN_POINT ( 'NONE',  ( -9.474510206698964154, 16.51473224551069663, 100.4155762719810241 ) ) ;
#43427 = CARTESIAN_POINT ( 'NONE',  ( 13.89961937509957401, 13.97604488694547697, 21.87609039468566152 ) ) ;
#43428 = CARTESIAN_POINT ( 'NONE',  ( -12.14591786802326823, 12.06949235617739902, 53.12609039468568284 ) ) ;
#43429 = CARTESIAN_POINT ( 'NONE',  ( 21.53943276465977519, 0.05219959533937863772, 76.25109039468568994 ) ) ;
#43430 = CARTESIAN_POINT ( 'NONE',  ( 4.483927247898790824, -16.52544592524335698, 30.20942372801902565 ) ) ;
#43431 = CARTESIAN_POINT ( 'NONE',  ( -5.153800228976328057, -19.02544592524343514, 67.29057627198102409 ) ) ;
#43432 = CARTESIAN_POINT ( 'NONE',  ( 19.02544592524334988, 5.153800228976608722, 96.45942372801897591 ) ) ;
#43433 = CARTESIAN_POINT ( 'NONE',  ( -14.29746914071037622, -8.314922557961029526, 74.16775706135231871 ) ) ;
#43434 = CARTESIAN_POINT ( 'NONE',  ( 15.80617190586769283, -15.72974639402175789, 110.6260903946857042 ) ) ;
#43435 = CARTESIAN_POINT ( 'NONE',  ( 13.97604488694548053, -13.89961937509957401, 80.62609039468567573 ) ) ;
#43436 = CARTESIAN_POINT ( 'NONE',  ( -9.564922557960796823, -16.46253265017161027, 62.08224293864769550 ) ) ;
#43437 = CARTESIAN_POINT ( 'NONE',  ( -15.80617190586745835, -15.72974639402198527, 81.87390960531435269 ) ) ;
#43439 = CARTESIAN_POINT ( 'NONE',  ( 13.97604488694548053, -13.89961937509957401, 75.62609039468564731 ) ) ;
#43438 = CARTESIAN_POINT ( 'NONE',  ( 8.224510206698953496, -14.34966873604960469, 77.91557627198102409 ) ) ;
#43440 = CARTESIAN_POINT ( 'NONE',  ( -19.52851543214745078, -5.499999999999944045, 70.39357721762578990 ) ) ;
#43441 = CARTESIAN_POINT ( 'NONE',  ( 16.51473224551083163, -9.474510206698727899, 50.83442372801899722 ) ) ;
#43442 = CARTESIAN_POINT ( 'NONE',  ( 16.55341960407618274, -4.379528057220086978, 106.0427570613523471 ) ) ;
#43443 = CARTESIAN_POINT ( 'NONE',  ( -14.29746914071049879, 8.314922557960819915, 80.83224293864769550 ) ) ;
#43445 = CARTESIAN_POINT ( 'NONE',  ( 22.44159573604009594, -16.30477369853687364, 145.6750000027311671 ) ) ;
#43444 = CARTESIAN_POINT ( 'NONE',  ( -0.05219959533937732626, 21.53943276465977519, 102.5010903946856899 ) ) ;
#43446 = CARTESIAN_POINT ( 'NONE',  ( 21.53943276465977519, -0.05219959533907433946, 113.7489096053143527 ) ) ;
#43447 =( BOUNDED_SURFACE ( )  B_SPLINE_SURFACE ( 3, 2, ( 
 ( #145350, #194875, #23021, #55346, #56348, #146346, #10859, #68511, #72528, #131184, #26033, #118031, #38189, #179722, #161529, #41193, #87678, #134204, #195892, #57367, #7833, #6832, #130165, #191862, #53344, #176716, #12856, #153328, #122986, #88681, #168504, #30002, #13829, #75495, #104850, #181701, #152344, #150377, #44181, #137168, #138169, #92642, #15822, #45174, #77483, #14830, #76492, #27036, #30993, #199850, #136186, #151365, #167526, #74521, #198857, #60323, #61316, #73537, #197861, #105839, #58348, #121998, #183688, #106829, #629, #123970, #166540, #184673, #90662, #91640, #62300, #46156, #11873, #107811, #185667, #135210, #169493, #154332, #47158, #196882, #29022, #28038, #43182, #139152, #120016, #165539, #89679, #59328, #120997, #182696, #173490, #158304, #189653, #94638, #141145, #66291, #78466, #79477, #128941, #51127, #187677, #112787, #33974, #188663, #2635, #49147, #95631, #65295, #156318, #16816, #35948, #31986, #125979, #34963, #17819, #18814, #174481, #126954, #19792, #97594, #159282, #143119, #93643, #64311, #140141, #96615, #80458, #4599, #110805, #50142, #172487, #81433, #127950, #155328, #111801, #20779, #157318, #142132, #48155, #124989, #3616, #1633, #82434, #144122, #5603, #67282, #190642, #108817, #170496, #63310, #186685, #109813, #171496, #32985, #22790, #37957, #54124, #161295, #162295, #85445, #86454, #160298, #84437, #130951, #145116, #147135, #8623, #70295, #87455, #10631, #191630, #24805, #177487, #38956, #149141, #193648, #113774, #178480, #72292, #175470, #131963, #116789, #133970, #36942, #115797, #53110, #68280, #23795, #98604, #148139, #9630, #21788, #71297, #55120, #39947, #101618, #132960, #99615, #146115, #194648, #83439, #7599, #52118, #56118, #192641, #117801, #100612, #163307, #69285, #179494, #40959, #102631, #164316, #6601, #25809, #129931, #114788, #176481, #181478, #105607, #61078, #152116, #106594, #137928, #76250, #29767, #180495, #104620, #26804, #60092, #167294, #88445, #92407, #75266, #196656, #182464, #89446, #58125, #184441, #41967, #122750, #166309, #199612, #120763, #11641, #198626, #134979, #42956, #45921, #107575, #169253, #28791, #73308, #119794, #57133, #27806, #150140, #168270, #151136, #136937, #12627, #90430, #13599, #121760, #91401, #74292, #183453, #135961, #44937, #30760, #154093, #103634, #153090, #43945, #118809, #197631, #14594, #15587, #165311, #59097, #77245, #195662, #20537, #80219, #138913, #393, #95390, #65056, #32743, #16580, #141890, #3381, #35711, #126713, #48907, #62066, #47919, #2390, #186443, #159044, #127713, #185430, #108580, #19556, #155086, #123731, #81200, #187439, #94395, #109573, #142881, #125739, #50890, #46920, #156074, #63068, #17572, #170257, #1387, #124747, #97358, #96378, #4362, #18572, #78227, #66046, #31751, #189414, #157076, #140904, #171256, #93400, #188416, #112548, #139898, #79233, #110561, #49894, #111560, #64069, #172242, #173245, #33728, #34720, #158065, #174243, #5361, #114535, #42463, #165808, #73804, #131718, #160054, #43452, #84192, #104126, #38715, #175229, #27305, #105120, #85194, #99368, #88952, #58611, #21541, #70050, #120278, #176235, #83201, #100372, #116549, #144875, #8375, #178237, #150643, #145872, #6358, #113535, #143880, #115556, #192399, #54875, #12140, #69039, #37706, #68038, #135476, #128703, #197145, #191387, #181970, #7355, #98355, #146883, #129690, #52863, #166807, #82187, #67044, #53881, #161051, #22545, #190400, #51876, #130704, #162051, #177243, #193400, #36694, #23547, #31258, #92909, #76753, #138428, #167785, #44446, #15094, #13121, #107086, #200109, #897, #155590, #78738, #108080, #140414, #77749, #16091, #89947, #93912, #62571, #199115, #14091, #30260, #137435, #61577, #123246, #124249, #136446, #60582, #168757, #121269, #184937, #46422, #169764, #63584, #186956, #29284, #185944, #153596, #154595, #125258, #139415, #151627, #47429, #48427, #74784, #109085 ),
 ( #110083, #170765, #182963, #122258, #91904, #32254, #198127, #183947, #17085, #1904, #28307, #59595, #106100, #90915, #152601, #75758, #45433, #64579, #52383, #191897, #174746, #188936, #175738, #145385, #49409, #159553, #6867, #3883, #172761, #189919, #5874, #111072, #97863, #67551, #129208, #35229, #95902, #2901, #33251, #4874, #81699, #144389, #156594, #80726, #126244, #36210, #143382, #187940, #68546, #51394, #34241, #158566, #65562, #157586, #160567, #18088, #98871, #142405, #114040, #96883, #19078, #21050, #127222, #50413, #37215, #22056, #83707, #66557, #112073, #173762, #94909, #190906, #20055, #113054, #128222, #82705, #130202, #79744, #53382, #171762, #141413, #25071, #54388, #131220, #101889, #99880, #193918, #86714, #87710, #42230, #165571, #194910, #27070, #164573, #102888, #176752, #180754, #149396, #85716, #100874, #117051, #24061, #148399, #9893, #10891, #23058, #147402, #55381, #7870, #71554, #133219, #56385, #150411, #73570, #116061, #72564, #40210, #163571, #11906, #118067, #38225, #41227, #135243, #161565, #179757, #26067, #196915, #84703, #178746, #177749, #192911, #134239, #146382, #195924, #57400, #69556, #119072, #103891, #88716, #115059, #39218, #162556, #8890, #70558, #132225, #29054, #78501, #139188, #137204, #663, #183721, #138202, #152377, #198890, #45207, #14864, #105873, #166573, #185701, #181736, #75529, #123019, #44214, #168535, #124003, #76525, #169526, #62333, #47190, #92676, #108850, #106861, #74552, #61348, #197894, #167560, #170530, #32020, #93678, #30033, #136219, #59363, #120049, #154364, #60358, #199884, #90694, #46189, #15858, #43217, #184704, #107842, #91671, #153362, #121032, #182730, #31026, #104885, #122031, #77516, #155361, #16850, #140174, #58382, #28073, #89714, #151399, #12889, #13862, #35977, #172521, #187707, #3648, #110837, #111831, #34991, #97624, #109843, #34006, #80490, #94671, #96645, #158333, #19822, #36973, #160329, #141176, #174510, #126986, #188693, #98634, #143149, #63345, #127981, #21819, #125022, #81463, #66320, #83471, #186718, #65326, #2666, #17851, #173520, #48188, #159314, #20809, #171528, #82465, #4630, #189684, #51157, #144151, #49179, #95663, #5636, #33016, #157350, #1667, #67313, #142164, #128973, #50174, #112817, #18845, #190672, #52148, #113805, #175500, #156350, #79507, #64343, #126012, #9660, #130982, #55150, #10661, #101647, #56149, #87484, #25840, #179523, #129961, #54156, #176511, #71327, #116820, #37989, #41997, #24834, #146145, #131994, #38988, #7632, #134000, #191661, #72324, #115829, #163339, #192673, #132989, #102660, #68310, #148169, #194680, #193680, #178511, #84467, #161328, #39977, #53140, #23826, #86484, #117830, #195691, #57162, #40992, #118841, #164345, #149172, #6632, #180524, #103663, #177518, #100644, #147165, #162325, #165341, #26834, #145148, #114819, #85476, #8653, #99645, #22821, #69316, #70327, #123760, #46949, #27837, #61108, #13629, #75296, #185459, #29796, #150171, #14623, #108609, #11671, #44968, #153119, #170286, #73337, #90462, #89478, #104653, #60123, #135010, #184471, #122781, #58156, #45950, #121790, #76280, #137959, #169283, #74324, #120795, #107605, #119824, #59128, #88474, #30789, #167326, #92437, #136967, #168300, #182495, #28822, #198656, #106626, #135991, #196687, #15617, #181509, #105637, #199642, #197662, #183484, #154123, #91432, #77274, #138943, #423, #62097, #42988, #43975, #166339, #151169, #12657, #152146, #128736, #111590, #32773, #18601, #125768, #94425, #20569, #78256, #159075, #140934, #112580, #157105, #47951, #34749, #171286, #79262, #174274, #35743, #82221, #141919, #109602, #156106, #93429, #66077, #33761, #173276, #17603, #97389, #1418, #143911, #188446, #95421, #2421, #155115, #158095, #5393, #190432, #187468, #80249, #49926, #96408, #64101, #113567, #19587, #124776, #48937, #3410, #65085, #16609, #110590, #189445, #67076, #51908, #81230, #172272, #31780 ),
 ( #126744, #142911, #4393, #127743, #50922, #139929, #63097, #186474, #38750, #99402, #6391, #36727, #8411, #85231, #147932, #55908, #7391, #68070, #9418, #145906, #54911, #129724, #146921, #70084, #131753, #71083, #53916, #116583, #115590, #178272, #25602, #133751, #160087, #193435, #23583, #98389, #191421, #132750, #39735, #21574, #22580, #194437, #117582, #56920, #101397, #175261, #83233, #163090, #24594, #69075, #52897, #86242, #179282, #72077, #40747, #102416, #144908, #84228, #100407, #130741, #195445, #164103, #114572, #176270, #87246, #37742, #161085, #148929, #10419, #192433, #177279, #162088, #105398, #30545, #187, #12422, #42749, #74085, #118595, #181272, #104412, #77035, #76044, #184233, #134765, #41753, #199404, #167084, #135755, #166095, #60867, #28586, #92197, #180285, #88233, #152883, #183246, #122543, #43737, #90222, #153881, #59884, #103418, #44727, #15378, #165097, #75059, #106383, #26590, #149918, #120558, #57918, #196448, #151906, #11424, #14378, #91193, #73094, #137720, #13395, #168064, #29562, #45714, #27597, #150929, #107367, #119589, #89235, #138706, #169039, #197426, #58892, #136725, #198407, #182252, #121550, #187233, #18370, #109362, #170049, #189213, #185219, #79019, #126517, #47712, #172038, #127509, #80022, #173043, #4161, #142682, #96180, #46710, #171044, #93192, #188216, #33525, #154877, #158843, #141691, #62854, #48703, #155867, #124536, #50692, #108373, #112350, #32534, #65839, #110356, #78022, #64855, #1177, #94187, #174041, #35510, #97159, #95187, #139691, #186233, #123525, #157869, #63866, #3182, #17364, #49689, #19358, #31540, #111354, #34520, #156873, #81007, #140694, #2184, #20331, #16375, #125537, #81980, #143673, #61856, #55670, #84989, #117344, #54668, #193195, #66837, #70847, #39499, #176033, #191192, #7155, #116342, #178031, #128500, #132516, #101159, #37501, #52668, #68838, #114330, #115352, #38512, #162847, #113335, #99163, #83994, #98146, #100168, #161850, #23344, #175027, #24354, #69841, #147694, #130497, #192193, #40508, #146670, #190195, #131508, #102179, #51673, #8165, #86005, #87007, #36492, #53674, #144672, #21339, #177042, #159846, #9181, #194205, #82997, #179040, #163867, #25366, #5154, #6157, #160853, #22343, #67837, #129494, #145673, #168804, #29333, #27354, #90961, #73854, #28356, #42512, #89000, #135524, #105168, #196216, #56683, #75805, #71842, #165858, #13169, #134529, #58658, #14138, #166854, #59644, #152648, #137483, #183010, #133511, #57686, #180050, #74832, #120324, #41519, #45478, #89994, #149686, #197195, #104176, #11184, #199163, #195203, #60630, #119354, #122304, #182019, #164862, #151676, #87998, #181038, #183995, #107134, #30308, #43502, #26358, #72859, #10182, #44494, #150691, #136494, #12189, #198174, #106150, #118357, #121318, #167832, #148694, #103182, #184983, #123291, #124293, #15139, #139460, #47473, #63628, #33293, #97652, #93956, #159342, #140459, #78782, #91951, #20838, #125304, #154641, #31302, #62615, #92955, #109130, #170808, #187000, #138472, #16136, #940, #61623, #32301, #155635, #17130, #200153, #48470, #1949, #171805, #185990, #110127, #82495, #144178, #76801, #5664, #153644, #46467, #108127, #169811, #77791, #57335, #74492, #11843, #88651, #44150, #134175, #168472, #45141, #42170, #106798, #105809, #137139, #121964, #153297, #58320, #104822, #29970, #103830, #43154, #95341, #14798, #151337, #76458, #197833, #152314, #166511, #12826, #59299, #28992, #119988, #180694, #199816, #195863, #89649, #198826, #181674, #182666, #138135, #90632, #183657, #61284, #125691, #91609, #119011, #28009, #165510, #60291, #167496, #27007, #172194, #13800, #73508, #120967, #136158, #135180, #187390, #150347, #48858, #75466, #110513, #33679, #196854, #157026, #72501, #94950, #62611, #108123, #139456, #142445, #168800, #93953, #32297, #45475, #138468, #156634, #155631, #107129, #31299, #2941, #141456, #65603, #125301, #183990, #30304 ),
 ( #186997, #937, #187980, #157627, #61619, #171802, #19117, #16132, #184978, #1945, #18129, #123287, #110124, #79784, #64621, #47470, #169806, #15135, #91947, #17127, #78779, #126283, #49449, #77787, #76797, #111112, #154637, #63625, #200149, #140455, #48467, #33290, #172801, #124290, #34282, #185987, #92951, #109127, #3923, #153640, #95941, #80767, #46463, #170805, #99916, #175780, #188976, #174783, #146418, #84740, #8929, #68584, #127263, #50452, #83744, #53420, #21090, #4912, #130240, #191936, #24100, #115097, #37254, #112111, #36249, #190944, #97902, #147441, #116097, #173802, #96923, #7909, #143425, #35268, #69593, #98911, #82747, #159593, #131260, #114079, #39255, #158605, #160604, #22094, #20095, #144427, #189957, #51431, #85754, #192948, #54427, #6905, #66595, #177785, #81739, #100911, #145423, #129248, #113091, #128259, #176789, #162595, #5913, #67590, #38262, #161601, #23095, #52421, #152406, #88751, #163609, #102925, #72601, #134275, #193956, #164610, #28106, #151431, #59394, #120082, #148437, #29084, #195962, #89745, #27105, #118104, #12918, #57435, #182762, #70597, #119108, #180789, #178785, #87747, #133257, #194948, #90723, #74582, #136250, #150444, #86754, #197926, #40253, #121068, #11940, #42266, #56424, #132265, #196947, #44246, #167589, #26104, #103926, #73603, #135275, #149432, #55419, #58415, #25110, #10928, #165606, #181770, #117090, #43251, #105903, #101927, #9932, #104919, #71591, #179794, #166606, #41263, #170564, #106893, #94705, #34042, #16883, #31061, #17887, #187742, #91705, #1702, #49213, #46223, #14897, #32054, #48222, #153399, #140208, #109876, #171560, #77550, #138234, #45239, #75560, #47226, #124038, #186752, #156382, #107876, #168566, #33050, #184738, #93711, #30064, #185737, #108885, #155393, #79541, #92709, #125055, #154397, #199917, #169564, #172556, #198920, #78534, #62369, #137236, #76558, #141211, #63378, #60389, #61381, #2701, #64378, #95699, #126046, #13893, #122061, #110871, #183753, #15892, #123052, #139222, #697, #54191, #145183, #67349, #80526, #66358, #20847, #4666, #177553, #146181, #3683, #127022, #38025, #173558, #142200, #99681, #5673, #51194, #39022, #144187, #129009, #65361, #174546, #19859, #81499, #115864, #114855, #22856, #37010, #35027, #84503, #188729, #7666, #113840, #159351, #143186, #18880, #83506, #69350, #157387, #112855, #190709, #175536, #98671, #189721, #50214, #160365, #111868, #36013, #82505, #52182, #96682, #97662, #176549, #161365, #131018, #6667, #158370, #128019, #21855, #192708, #68345, #129996, #191696, #53179, #103698, #117868, #104688, #74357, #178545, #88514, #136023, #133025, #101684, #118876, #135046, #40011, #26871, #196722, #58190, #164382, #24870, #132027, #162359, #134035, #10698, #73374, #181542, #194715, #193716, #119858, #71361, #180560, #55185, #72361, #195728, #57201, #43021, #179558, #11707, #41028, #86519, #56184, #59163, #85511, #42034, #149207, #23860, #116854, #166376, #165377, #147199, #148203, #27872, #89513, #182531, #150210, #100677, #8690, #151203, #12691, #102694, #163373, #197697, #120831, #70360, #9696, #25875, #87519, #153157, #107642, #91469, #64140, #32811, #90498, #13664, #124813, #60157, #167360, #186513, #92474, #137996, #14658, #47987, #30826, #156143, #137002, #138981, #459, #62134, #75331, #78293, #108646, #109640, #169319, #154162, #79301, #185496, #105674, #170324, #140970, #28858, #123798, #31816, #125804, #152180, #45987, #183520, #121826, #15654, #198690, #139967, #16646, #45003, #1456, #77313, #93467, #155154, #171323, #29832, #76318, #63134, #106663, #199680, #44013, #94462, #122817, #17641, #46987, #2458, #61145, #184507, #168336, #143949, #34789, #95458, #114607, #110628, #4428, #51943, #173314, #97425, #52932, #5429, #98426, #129758, #68106, #21611, #172309, #96444, #18639, #113603, #159111, #80285, #84263, #67113, #188486, #174309, #81265, #49965, #176304, #33798 ),
 ( #65122, #48973, #83269, #189480, #128771, #158131, #175297, #144943, #157143, #190470, #36763, #35778, #20605, #126780, #3446, #82257, #141957, #66115, #160123, #6425, #37776, #99440, #191455, #161120, #22617, #145944, #111629, #7425, #69109, #19623, #142946, #50958, #127780, #187506, #112617, #167861, #38786, #163126, #9456, #24629, #15171, #148966, #23620, #86277, #132786, #194473, #53950, #147968, #90991, #14167, #122334, #183039, #8446, #91980, #55945, #152678, #87281, #85267, #75835, #153674, #133789, #71120, #137513, #107163, #70119, #121346, #168834, #117621, #131790, #10455, #29361, #193470, #59674, #199194, #60661, #179319, #54947, #162123, #192467, #164140, #40783, #106178, #184026, #102452, #146958, #45508, #101435, #72116, #116619, #25637, #195481, #44522, #30339, #130775, #115626, #177315, #178308, #100443, #39771, #61652, #187031, #125334, #138501, #31335, #49482, #48502, #200183, #124325, #95977, #34314, #158636, #18163, #76830, #123320, #33322, #2973, #170840, #154671, #79819, #141490, #173835, #64653, #110156, #185013, #186023, #140493, #47505, #96956, #65635, #46498, #108159, #157661, #92986, #169841, #19150, #171834, #32332, #109161, #80800, #63661, #189008, #16167, #94983, #156668, #77821, #93985, #139490, #972, #35300, #142478, #3956, #126315, #62648, #127295, #155665, #50483, #188012, #78814, #17161, #1981, #111145, #112143, #172835, #114111, #68617, #176822, #38294, #54460, #190977, #5945, #22126, #129282, #130273, #53454, #116130, #128291, #52454, #98944, #113125, #115130, #99948, #161634, #189989, #177819, #84773, #162630, #145456, #6938, #55454, #23128, #81771, #146451, #117125, #143458, #7944, #69627, #101963, #82779, #4943, #131293, #147475, #178819, #175814, #191968, #192982, #39289, #37287, #20127, #100946, #174815, #160635, #83776, #24137, #66627, #85789, #8965, #70634, #132300, #193992, #97935, #40289, #51463, #36280, #159628, #21123, #144460, #67621, #166639, #180821, #167624, #137274, #41298, #151466, #198956, #195996, #164643, #181806, #197961, #102959, #89781, #59431, #121104, #27137, #87781, #194982, #25146, #196980, #73637, #136285, #44281, #57469, #56460, #182798, #134310, #43284, #118139, #135308, #58447, #120115, #105939, #42300, #74619, #103961, #149466, #119141, #122096, #148474, #104953, #11972, #86788, #179828, #29120, #28141, #9966, #10961, #90759, #152442, #45273, #12954, #163644, #71626, #13928, #75595, #165639, #26139, #60423, #183787, #133292, #72635, #88784, #150477, #15927, #170600, #154433, #127057, #63415, #17921, #49246, #187776, #141245, #91740, #77585, #138269, #171596, #16918, #199952, #3719, #186788, #107914, #93747, #733, #169599, #95734, #153435, #34076, #139257, #110904, #32090, #123087, #109912, #46259, #62405, #14933, #172590, #33084, #106927, #184773, #31097, #168600, #2734, #108920, #125090, #124075, #94740, #64411, #30100, #156420, #79576, #155428, #78571, #92745, #185776, #140245, #76593, #47263, #1737, #126080, #157420, #18914, #48258, #80559, #142234, #65396, #61416, #188764, #84536, #20884, #36049, #52217, #159389, #160401, #83540, #146213, #158404, #82542, #129042, #143221, #145219, #6701, #68379, #19893, #7701, #114890, #192743, #175571, #37048, #85547, #191730, #111904, #176584, #147233, #173592, #81534, #144224, #113874, #70394, #98707, #189757, #66393, #21890, #35061, #69384, #22890, #4703, #131053, #130031, #38058, #99714, #54225, #97698, #5708, #115896, #128055, #67385, #132062, #177586, #190743, #39053, #53212, #161398, #100711, #162391, #23894, #8725, #50248, #51229, #96716, #112890, #174584, #58220, #179591, #103730, #59194, #41063, #40045, #136053, #119889, #193751, #71394, #133058, #55219, #27904, #195760, #11739, #102726, #181574, #151233, #116888, #196753, #43052, #42066, #165410, #194748, #9730, #180592, #178580, #72394, #26903, #166409, #120863, #44046, #73406, #105706, #104718, #89547, #101719, #182563 ),
 ( #167393, #75362, #88546, #150244, #163409, #10730, #56220, #117902, #152211, #12722, #28889, #135077, #164415, #90529, #74388, #197728, #134070, #57234, #25907, #24905, #13695, #86552, #148236, #87552, #149239, #118908, #155187, #169351, #18669, #16677, #29864, #30860, #139013, #493, #60189, #92507, #94493, #17674, #125836, #186545, #14691, #95489, #62166, #156175, #93501, #91501, #79332, #157175, #139999, #154196, #141002, #110660, #76353, #124845, #172340, #15686, #138030, #78326, #171355, #199713, #63166, #32843, #2490, #123830, #61178, #168368, #198722, #170357, #47020, #109674, #64171, #77347, #153188, #187539, #107674, #1488, #122850, #108679, #31849, #48018, #49005, #185528, #137032, #121859, #33829, #183551, #45037, #184538, #106695, #46018, #141988, #127808, #99470, #37809, #162151, #21645, #80315, #3476, #36795, #6455, #174338, #158161, #83298, #144974, #177343, #68136, #190501, #65153, #189512, #143981, #50986, #100472, #69139, #126811, #49995, #161150, #96473, #188518, #22647, #128802, #35808, #112646, #84294, #67144, #192497, #111660, #51974, #113633, #173347, #97454, #142978, #4456, #38814, #145973, #7455, #160154, #19653, #130806, #175328, #191484, #159140, #20637, #66145, #34818, #129787, #53981, #81294, #82290, #98460, #52962, #114639, #5462, #176337, #115654, #116647, #55974, #25666, #87311, #146987, #117651, #181336, #104478, #12487, #73163, #101464, #182322, #148995, #42815, #180349, #178337, #166162, #43801, #26656, #40811, #27663, #197490, #163155, #11492, #58957, #179348, #24658, #41817, #57982, #86307, #149986, #119654, #89303, #10484, #147996, #54977, #85295, #56984, #133820, #196512, #150995, #102481, #39799, #74148, #194501, #103485, #9485, #195511, #118658, #165163, #135820, #164168, #134833, #72144, #71149, #120625, #105464, #88298, #132815, #23647, #8474, #70149, #131819, #193499, #29621, #28649, #93256, #94253, #63929, #60934, #15444, #123591, #185285, #199467, #48767, #46777, #59947, #122608, #169104, #30611, #90285, #184298, #124601, #47776, #155933, #16438, #44791, #125598, #92264, #186296, #108436, #121614, #109429, #187295, #170112, #45780, #171109, #140758, #106444, #154941, #2246, #107432, #168125, #31606, #1242, #91253, #78087, #62921, #32600, #153948, #152944, #198475, #151969, #252, #77102, #139755, #17428, #138771, #183309, #79085, #137782, #167150, #14443, #61921, #13457, #75121, #136789, #76106, #21403, #189277, #34583, #65902, #68904, #95251, #20397, #158906, #172102, #64916, #83061, #82045, #33588, #157928, #129554, #67901, #192261, #51736, #110421, #156936, #66901, #36556, #4224, #188278, #113398, #175088, #7219, #98210, #143741, #18433, #19418, #174103, #81066, #130563, #99229, #80083, #141752, #191254, #126577, #3242, #52729, #5220, #127576, #142744, #114394, #97220, #22409, #49751, #128564, #190259, #111420, #50753, #173106, #96240, #112411, #35572, #159914, #144735, #6222, #176096, #37566, #160916, #84060, #145738, #26423, #24422, #133578, #85057, #163935, #87073, #148758, #88063, #132582, #164930, #194270, #178097, #9247, #12255, #38577, #25432, #102247, #115417, #8234, #149750, #10247, #177106, #101225, #72926, #11252, #135587, #195268, #53743, #100233, #71906, #180116, #147761, #131578, #56752, #118423, #150757, #41584, #103248, #161915, #162914, #117411, #86071, #73917, #42578, #23409, #146738, #134595, #69912, #193262, #196281, #57750, #70914, #55737, #119420, #40577, #165924, #54736, #181104, #104241, #116408, #179108, #39567, #27420, #89066, #154711, #62683, #76867, #13233, #124364, #168870, #108198, #75873, #14205, #59711, #58721, #123358, #186060, #94020, #91028, #45545, #153712, #15208, #29398, #78850, #138537, #90058, #152714, #199232, #60697, #120390, #137549, #16204, #77859, #47543, #46539, #74896, #155701, #122373, #139526, #15, #151740, #1009, #17196, #61689, #184062, #109197, #170876, #136559, #185051, #32367, #107200 ),
 ( #197259, #169880, #30375, #182084, #43567, #198240, #31373, #105232, #92019, #121384, #93023, #166920, #183076, #28421, #44559, #106214, #167898, #64691, #171870, #2018, #176616, #50522, #115928, #23924, #172872, #33359, #177618, #111182, #22922, #95018, #114923, #38091, #99746, #39086, #19189, #54257, #80838, #126352, #96014, #101752, #125372, #161430, #189047, #63697, #156706, #100742, #84568, #187068, #188049, #162423, #85579, #24937, #146246, #140528, #48538, #7732, #69418, #34353, #18200, #131084, #192773, #40074, #147265, #8755, #110192, #49519, #3993, #157699, #163440, #132092, #79858, #141526, #70426, #3014, #142515, #193781, #55250, #65673, #127335, #116918, #178611, #198757, #168402, #73436, #135107, #194777, #103761, #149269, #10761, #45070, #44080, #152244, #166441, #102758, #13729, #58251, #197760, #165440, #26935, #72425, #148267, #12755, #75395, #183585, #180624, #196783, #43083, #104750, #118939, #86583, #27936, #179622, #42096, #88577, #150275, #9759, #11771, #105739, #167426, #137067, #136086, #164445, #106728, #151265, #119919, #117933, #71423, #89579, #87582, #181605, #74420, #134103, #60222, #133087, #121892, #195793, #28922, #59227, #25939, #120896, #57265, #182596, #56251, #90562, #41094, #29897, #107707, #169386, #91535, #64207, #31883, #48054, #77380, #17712, #187574, #153222, #32880, #94530, #78361, #140035, #30894, #46052, #16711, #14727, #108713, #1524, #2527, #157213, #80354, #109710, #142026, #79369, #141040, #76387, #95527, #125874, #528, #15720, #93537, #139048, #63202, #124882, #49042, #138064, #62200, #170392, #122883, #186581, #171393, #156212, #199745, #110697, #172377, #33867, #155222, #18707, #65191, #3515, #61211, #126850, #188556, #184571, #92541, #123864, #50034, #111698, #154230, #185562, #47056, #145012, #34855, #69179, #146011, #143015, #7494, #6493, #37848, #22685, #54019, #159178, #5498, #130845, #4493, #144017, #193540, #115693, #52011, #177381, #98498, #53001, #67181, #113670, #160191, #129825, #20673, #81332, #100510, #96510, #190537, #99508, #82327, #83335, #38853, #191524, #84332, #162189, #23687, #192536, #158200, #128838, #66183, #85335, #127845, #175364, #36832, #189551, #68173, #114679, #176375, #51023, #147027, #161189, #8511, #21681, #70189, #131857, #55014, #19690, #173385, #112684, #174376, #35846, #97492, #180388, #136830, #118696, #56011, #132852, #88335, #178374, #12522, #89339, #86346, #151031, #150026, #181373, #166197, #197526, #102522, #149034, #74186, #148033, #87348, #198513, #58995, #195549, #120661, #41858, #196549, #10522, #75158, #103525, #182359, #116684, #119689, #133859, #43837, #90321, #194540, #104516, #152007, #72185, #117689, #134871, #135856, #179386, #42851, #105501, #167187, #165200, #40848, #9522, #39838, #11531, #26695, #28686, #13493, #57023, #71188, #101504, #73201, #58019, #164205, #27698, #163193, #24697, #25703, #92303, #139791, #153986, #199505, #169144, #63965, #183346, #61959, #290, #121651, #91291, #1279, #123626, #44828, #122645, #186331, #124637, #125635, #31643, #59984, #106483, #154977, #62956, #77140, #184335, #47814, #109463, #168162, #171146, #93292, #152982, #15483, #46812, #138809, #29659, #14481, #60971, #45817, #76143, #30649, #107468, #137821, #108471, #32635, #185321, #170149, #16473, #78122, #94289, #155967, #17464, #79121, #140794, #2282, #121314, #60626, #43498, #57682, #44490, #14134, #118351, #28352, #75801, #72854, #41514, #58655, #74829, #180045, #166850, #136490, #198170, #104172, #164857, #71837, #102174, #73849, #150687, #13165, #183006, #134524, #133506, #59640, #11179, #120321, #195198, #12185, #135520, #197191, #106146, #119350, #151671, #181034, #26353, #196210, #199159, #25361, #182015, #88996, #163862, #56678, #167828, #105164, #87002, #87993, #29328, #90957, #122300, #89990, #40502, #148689, #152644, #137479, #42508, #103177, #10177, #149681, #165854, #27350, #103971, #102969 ) ),
 .UNSPECIFIED., .T., .F., .F. ) 
 B_SPLINE_SURFACE_WITH_KNOTS ( ( 4, 3, 4 ),
 ( 3, 2, 2, 2, 2, 2, 2, 2, 2, 2, 2, 2, 2, 2, 2, 2, 2, 2, 2, 2, 2, 2, 2, 2, 2, 2, 2, 2, 2, 2, 2, 2, 2, 2, 2, 2, 2, 2, 2, 2, 2, 2, 2, 2, 2, 2, 2, 2, 2, 2, 2, 2, 2, 2, 2, 2, 2, 2, 2, 2, 2, 2, 2, 2, 2, 2, 2, 2, 2, 2, 2, 2, 2, 2, 2, 2, 2, 2, 2, 2, 2, 2, 2, 2, 2, 2, 2, 2, 2, 2, 2, 2, 2, 2, 2, 2, 2, 2, 2, 2, 2, 2, 2, 2, 2, 2, 2, 2, 2, 2, 2, 2, 2, 2, 2, 2, 2, 2, 2, 2, 2, 2, 2, 2, 2, 2, 2, 2, 2, 2, 2, 2, 2, 2, 2, 2, 2, 2, 2, 2, 2, 2, 2, 2, 2, 2, 2, 2, 2, 2, 2, 2, 2, 2, 2, 2, 2, 2, 2, 2, 2, 2, 2, 2, 2, 2, 2, 2, 2, 2, 2, 2, 2, 2, 2, 2, 2, 2, 2, 2, 2, 2, 2, 2, 2, 2, 2, 2, 2, 2, 2, 2, 2, 2, 2, 2, 2, 2, 2, 2, 2, 2, 2, 2, 2, 2, 2, 2, 2, 2, 2, 2, 2, 2, 2, 2, 2, 2, 2, 2, 2, 2, 2, 2, 2, 2, 2, 2, 3 ),
 ( 0.000000000000000000, 0.5000000000000000000, 1.000000000000000000 ),
 ( 0.000000000000000000, 0.004385964912280701511, 0.008771929824561403022, 0.01315789473684210453, 0.01754385964912280604, 0.02192982456140350755, 0.02631578947368420907, 0.03070175438596491058, 0.03508771929824561209, 0.03947368421052631360, 0.04385964912280701511, 0.04824561403508771662, 0.05263157894736841813, 0.05701754385964911964, 0.06140350877192982115, 0.06578947368421052266, 0.07017543859649122417, 0.07456140350877192569, 0.07894736842105262720, 0.08333333333333332871, 0.08771929824561403022, 0.09210526315789473173, 0.09649122807017543324, 0.1008771929824561348, 0.1052631578947368363, 0.1096491228070175378, 0.1140350877192982393, 0.1184210526315789408, 0.1228070175438596423, 0.1271929824561403577, 0.1315789473684210453, 0.1359649122807017607, 0.1403508771929824483, 0.1447368421052631637, 0.1491228070175438514, 0.1535087719298245668, 0.1578947368421052544, 0.1622807017543859698, 0.1666666666666666574, 0.1710526315789473728, 0.1754385964912280604, 0.1798245614035087758, 0.1842105263157894635, 0.1885964912280701788, 0.1929824561403508665, 0.1973684210526315819, 0.2017543859649122695, 0.2061403508771929849, 0.2105263157894736725, 0.2149122807017543879, 0.2192982456140350755, 0.2236842105263157909, 0.2280701754385964786, 0.2324561403508771940, 0.2368421052631578816, 0.2412280701754385970, 0.2456140350877192846, 0.2500000000000000000, 0.2543859649122807154, 0.2587719298245614308, 0.2631578947368420907, 0.2675438596491228060, 0.2719298245614035214, 0.2763157894736842368, 0.2807017543859648967, 0.2850877192982456121, 0.2894736842105263275, 0.2938596491228070429, 0.2982456140350877027, 0.3026315789473684181, 0.3070175438596491335, 0.3114035087719298489, 0.3157894736842105088, 0.3201754385964912242, 0.3245614035087719396, 0.3289473684210526550, 0.3333333333333333148, 0.3377192982456140302, 0.3421052631578947456, 0.3464912280701754610, 0.3508771929824561209, 0.3552631578947368363, 0.3596491228070175517, 0.3640350877192982670, 0.3684210526315789269, 0.3728070175438596423, 0.3771929824561403577, 0.3815789473684210731, 0.3859649122807017330, 0.3903508771929824483, 0.3947368421052631637, 0.3991228070175438791, 0.4035087719298245390, 0.4078947368421052544, 0.4122807017543859698, 0.4166666666666666852, 0.4210526315789473450, 0.4254385964912280604, 0.4298245614035087758, 0.4342105263157894912, 0.4385964912280701511, 0.4429824561403508665, 0.4473684210526315819, 0.4517543859649122973, 0.4561403508771929571, 0.4605263157894736725, 0.4649122807017543879, 0.4692982456140351033, 0.4736842105263157632, 0.4780701754385964786, 0.4824561403508771940, 0.4868421052631579093, 0.4912280701754385692, 0.4956140350877192846, 0.5000000000000000000, 0.5043859649122807154, 0.5087719298245614308, 0.5131578947368421462, 0.5175438596491228616, 0.5219298245614034659, 0.5263157894736841813, 0.5307017543859648967, 0.5350877192982456121, 0.5394736842105263275, 0.5438596491228070429, 0.5482456140350877583, 0.5526315789473684736, 0.5570175438596490780, 0.5614035087719297934, 0.5657894736842105088, 0.5701754385964912242, 0.5745614035087719396, 0.5789473684210526550, 0.5833333333333333703, 0.5877192982456140857, 0.5921052631578946901, 0.5964912280701754055, 0.6008771929824561209, 0.6052631578947368363, 0.6096491228070175517, 0.6140350877192982670, 0.6184210526315789824, 0.6228070175438596978, 0.6271929824561403022, 0.6315789473684210176, 0.6359649122807017330, 0.6403508771929824483, 0.6447368421052631637, 0.6491228070175438791, 0.6535087719298245945, 0.6578947368421053099, 0.6622807017543859143, 0.6666666666666666297, 0.6710526315789473450, 0.6754385964912280604, 0.6798245614035087758, 0.6842105263157894912, 0.6885964912280702066, 0.6929824561403509220, 0.6973684210526315264, 0.7017543859649122417, 0.7061403508771929571, 0.7105263157894736725, 0.7149122807017543879, 0.7192982456140351033, 0.7236842105263158187, 0.7280701754385965341, 0.7324561403508771384, 0.7368421052631578538, 0.7412280701754385692, 0.7456140350877192846, 0.7500000000000000000, 0.7543859649122807154, 0.7587719298245614308, 0.7631578947368421462, 0.7675438596491228616, 0.7719298245614034659, 0.7763157894736841813, 0.7807017543859648967, 0.7850877192982456121, 0.7894736842105263275, 0.7938596491228070429, 0.7982456140350877583, 0.8026315789473684736, 0.8070175438596490780, 0.8114035087719297934, 0.8157894736842105088, 0.8201754385964912242, 0.8245614035087719396, 0.8289473684210526550, 0.8333333333333333703, 0.8377192982456140857, 0.8421052631578946901, 0.8464912280701754055, 0.8508771929824561209, 0.8552631578947368363, 0.8596491228070175517, 0.8640350877192982670, 0.8684210526315789824, 0.8728070175438596978, 0.8771929824561403022, 0.8815789473684210176, 0.8859649122807017330, 0.8903508771929824483, 0.8947368421052631637, 0.8991228070175438791, 0.9035087719298245945, 0.9078947368421053099, 0.9122807017543859143, 0.9166666666666666297, 0.9210526315789473450, 0.9254385964912280604, 0.9298245614035087758, 0.9342105263157894912, 0.9385964912280702066, 0.9429824561403509220, 0.9473684210526315264, 0.9517543859649122417, 0.9561403508771929571, 0.9605263157894736725, 0.9649122807017543879, 0.9692982456140351033, 0.9736842105263158187, 0.9780701754385965341, 0.9824561403508771384, 0.9868421052631578538, 0.9912280701754385692, 0.9956140350877192846, 1.000000000000000000 ),
 .UNSPECIFIED. ) 
 GEOMETRIC_REPRESENTATION_ITEM ( )  RATIONAL_B_SPLINE_SURFACE ( (
 ( 1.000000000000000000, 0.9659258262890683122, 1.000000000000000000, 0.9659258262890683122, 1.000000000000000000, 0.9659258262890683122, 1.000000000000000000, 0.9659258262890683122, 1.000000000000000000, 0.9659258262890683122, 1.000000000000000000, 0.9659258262890683122, 1.000000000000000000, 0.9659258262890683122, 1.000000000000000000, 0.9659258262890683122, 1.000000000000000000, 0.9659258262890683122, 1.000000000000000000, 0.9659258262890683122, 1.000000000000000000, 0.9659258262890683122, 1.000000000000000000, 0.9659258262890683122, 1.000000000000000000, 0.9659258262890683122, 1.000000000000000000, 0.9659258262890683122, 1.000000000000000000, 0.9659258262890683122, 1.000000000000000000, 0.9659258262890683122, 1.000000000000000000, 0.9659258262890683122, 1.000000000000000000, 0.9659258262890683122, 1.000000000000000000, 0.9659258262890683122, 1.000000000000000000, 0.9659258262890683122, 1.000000000000000000, 0.9659258262890683122, 1.000000000000000000, 0.9659258262890683122, 1.000000000000000000, 0.9659258262890683122, 1.000000000000000000, 0.9659258262890683122, 1.000000000000000000, 0.9659258262890683122, 1.000000000000000000, 0.9659258262890683122, 1.000000000000000000, 0.9659258262890683122, 1.000000000000000000, 0.9659258262890683122, 1.000000000000000000, 0.9659258262890683122, 1.000000000000000000, 0.9659258262890683122, 1.000000000000000000, 0.9659258262890683122, 1.000000000000000000, 0.9659258262890683122, 1.000000000000000000, 0.9659258262890683122, 1.000000000000000000, 0.9659258262890683122, 1.000000000000000000, 0.9659258262890683122, 1.000000000000000000, 0.9659258262890683122, 1.000000000000000000, 0.9659258262890683122, 1.000000000000000000, 0.9659258262890683122, 1.000000000000000000, 0.9659258262890683122, 1.000000000000000000, 0.9659258262890683122, 1.000000000000000000, 0.9659258262890683122, 1.000000000000000000, 0.9659258262890683122, 1.000000000000000000, 0.9659258262890683122, 1.000000000000000000, 0.9659258262890683122, 1.000000000000000000, 0.9659258262890683122, 1.000000000000000000, 0.9659258262890683122, 1.000000000000000000, 0.9659258262890683122, 1.000000000000000000, 0.9659258262890683122, 1.000000000000000000, 0.9659258262890683122, 1.000000000000000000, 0.9659258262890683122, 1.000000000000000000, 0.9659258262890683122, 1.000000000000000000, 0.9659258262890683122, 1.000000000000000000, 0.9659258262890683122, 1.000000000000000000, 0.9659258262890683122, 1.000000000000000000, 0.9659258262890683122, 1.000000000000000000, 0.9659258262890683122, 1.000000000000000000, 0.9659258262890683122, 1.000000000000000000, 0.9659258262890683122, 1.000000000000000000, 0.9659258262890683122, 1.000000000000000000, 0.9659258262890683122, 1.000000000000000000, 0.9659258262890683122, 1.000000000000000000, 0.9659258262890683122, 1.000000000000000000, 0.9659258262890683122, 1.000000000000000000, 0.9659258262890683122, 1.000000000000000000, 0.9659258262890683122, 1.000000000000000000, 0.9659258262890683122, 1.000000000000000000, 0.9659258262890683122, 1.000000000000000000, 0.9659258262890683122, 1.000000000000000000, 0.9659258262890683122, 1.000000000000000000, 0.9659258262890683122, 1.000000000000000000, 0.9659258262890683122, 1.000000000000000000, 0.9659258262890683122, 1.000000000000000000, 0.9659258262890683122, 1.000000000000000000, 0.9659258262890683122, 1.000000000000000000, 0.9659258262890683122, 1.000000000000000000, 0.9659258262890683122, 1.000000000000000000, 0.9659258262890683122, 1.000000000000000000, 0.9659258262890683122, 1.000000000000000000, 0.9659258262890683122, 1.000000000000000000, 0.9659258262890683122, 1.000000000000000000, 0.9659258262890683122, 1.000000000000000000, 0.9659258262890683122, 1.000000000000000000, 0.9659258262890683122, 1.000000000000000000, 0.9659258262890683122, 1.000000000000000000, 0.9659258262890683122, 1.000000000000000000, 0.9659258262890683122, 1.000000000000000000, 0.9659258262890683122, 1.000000000000000000, 0.9659258262890683122, 1.000000000000000000, 0.9659258262890683122, 1.000000000000000000, 0.9659258262890683122, 1.000000000000000000, 0.9659258262890683122, 1.000000000000000000, 0.9659258262890683122, 1.000000000000000000, 0.9659258262890683122, 1.000000000000000000, 0.9659258262890683122, 1.000000000000000000, 0.9659258262890683122, 1.000000000000000000, 0.9659258262890683122, 1.000000000000000000, 0.9659258262890683122, 1.000000000000000000, 0.9659258262890683122, 1.000000000000000000, 0.9659258262890683122, 1.000000000000000000, 0.9659258262890683122, 1.000000000000000000, 0.9659258262890683122, 1.000000000000000000, 0.9659258262890683122, 1.000000000000000000, 0.9659258262890683122, 1.000000000000000000, 0.9659258262890683122, 1.000000000000000000, 0.9659258262890683122, 1.000000000000000000, 0.9659258262890683122, 1.000000000000000000, 0.9659258262890683122, 1.000000000000000000, 0.9659258262890683122, 1.000000000000000000, 0.9659258262890683122, 1.000000000000000000, 0.9659258262890683122, 1.000000000000000000, 0.9659258262890683122, 1.000000000000000000, 0.9659258262890683122, 1.000000000000000000, 0.9659258262890683122, 1.000000000000000000, 0.9659258262890683122, 1.000000000000000000, 0.9659258262890683122, 1.000000000000000000, 0.9659258262890683122, 1.000000000000000000, 0.9659258262890683122, 1.000000000000000000, 0.9659258262890683122, 1.000000000000000000, 0.9659258262890683122, 1.000000000000000000, 0.9659258262890683122, 1.000000000000000000, 0.9659258262890683122, 1.000000000000000000, 0.9659258262890683122, 1.000000000000000000, 0.9659258262890683122, 1.000000000000000000, 0.9659258262890683122, 1.000000000000000000, 0.9659258262890683122, 1.000000000000000000, 0.9659258262890683122, 1.000000000000000000, 0.9659258262890683122, 1.000000000000000000, 0.9659258262890683122, 1.000000000000000000, 0.9659258262890683122, 1.000000000000000000, 0.9659258262890683122, 1.000000000000000000, 0.9659258262890683122, 1.000000000000000000, 0.9659258262890683122, 1.000000000000000000, 0.9659258262890683122, 1.000000000000000000, 0.9659258262890683122, 1.000000000000000000, 0.9659258262890683122, 1.000000000000000000, 0.9659258262890683122, 1.000000000000000000, 0.9659258262890683122, 1.000000000000000000, 0.9659258262890683122, 1.000000000000000000, 0.9659258262890683122, 1.000000000000000000, 0.9659258262890683122, 1.000000000000000000, 0.9659258262890683122, 1.000000000000000000, 0.9659258262890683122, 1.000000000000000000, 0.9659258262890683122, 1.000000000000000000, 0.9659258262890683122, 1.000000000000000000, 0.9659258262890683122, 1.000000000000000000, 0.9659258262890683122, 1.000000000000000000, 0.9659258262890683122, 1.000000000000000000, 0.9659258262890683122, 1.000000000000000000, 0.9659258262890683122, 1.000000000000000000, 0.9659258262890683122, 1.000000000000000000, 0.9659258262890683122, 1.000000000000000000, 0.9659258262890683122, 1.000000000000000000, 0.9659258262890683122, 1.000000000000000000, 0.9659258262890683122, 1.000000000000000000, 0.9659258262890683122, 1.000000000000000000, 0.9659258262890683122, 1.000000000000000000, 0.9659258262890683122, 1.000000000000000000, 0.9659258262890683122, 1.000000000000000000, 0.9659258262890683122, 1.000000000000000000, 0.9659258262890683122, 1.000000000000000000, 0.9659258262890683122, 1.000000000000000000, 0.9659258262890683122, 1.000000000000000000, 0.9659258262890683122, 1.000000000000000000, 0.9659258262890683122, 1.000000000000000000, 0.9659258262890683122, 1.000000000000000000, 0.9659258262890683122, 1.000000000000000000, 0.9659258262890683122, 1.000000000000000000, 0.9659258262890683122, 1.000000000000000000, 0.9659258262890683122, 1.000000000000000000, 0.9659258262890683122, 1.000000000000000000, 0.9659258262890683122, 1.000000000000000000, 0.9659258262890683122, 1.000000000000000000, 0.9659258262890683122, 1.000000000000000000, 0.9659258262890683122, 1.000000000000000000, 0.9659258262890683122, 1.000000000000000000, 0.9659258262890683122, 1.000000000000000000, 0.9659258262890683122, 1.000000000000000000, 0.9659258262890683122, 1.000000000000000000, 0.9659258262890683122, 1.000000000000000000, 0.9659258262890683122, 1.000000000000000000, 0.9659258262890683122, 1.000000000000000000, 0.9659258262890683122, 1.000000000000000000, 0.9659258262890683122, 1.000000000000000000, 0.9659258262890683122, 1.000000000000000000, 0.9659258262890683122, 1.000000000000000000, 0.9659258262890683122, 1.000000000000000000, 0.9659258262890683122, 1.000000000000000000, 0.9659258262890683122, 1.000000000000000000, 0.9659258262890683122, 1.000000000000000000, 0.9659258262890683122, 1.000000000000000000, 0.9659258262890683122, 1.000000000000000000, 0.9659258262890683122, 1.000000000000000000, 0.9659258262890683122, 1.000000000000000000, 0.9659258262890683122, 1.000000000000000000, 0.9659258262890683122, 1.000000000000000000, 0.9659258262890683122, 1.000000000000000000, 0.9659258262890683122, 1.000000000000000000, 0.9659258262890683122, 1.000000000000000000, 0.9659258262890683122, 1.000000000000000000, 0.9659258262890683122, 1.000000000000000000, 0.9659258262890683122, 1.000000000000000000, 0.9659258262890683122, 1.000000000000000000, 0.9659258262890683122, 1.000000000000000000, 0.9659258262890683122, 1.000000000000000000, 0.9659258262890683122, 1.000000000000000000, 0.9659258262890683122, 1.000000000000000000, 0.9659258262890683122, 1.000000000000000000, 0.9659258262890683122, 1.000000000000000000, 0.9659258262890683122, 1.000000000000000000, 0.9659258262890683122, 1.000000000000000000, 0.9659258262890683122, 1.000000000000000000, 0.9659258262890683122, 1.000000000000000000, 0.9659258262890683122, 1.000000000000000000, 0.9659258262890683122, 1.000000000000000000, 0.9659258262890683122, 1.000000000000000000, 0.9659258262890683122, 1.000000000000000000, 0.9659258262890683122, 1.000000000000000000, 0.9659258262890683122, 1.000000000000000000, 0.9659258262890683122, 1.000000000000000000, 0.9659258262890683122, 1.000000000000000000, 0.9659258262890683122, 1.000000000000000000, 0.9659258262890683122, 1.000000000000000000, 0.9659258262890683122, 1.000000000000000000, 0.9659258262890683122, 1.000000000000000000, 0.9659258262890683122, 1.000000000000000000, 0.9659258262890683122, 1.000000000000000000, 0.9659258262890683122, 1.000000000000000000, 0.9659258262890683122, 1.000000000000000000),
 ( 0.3333333333333333703, 0.3219752754296894559, 0.3333333333333333703, 0.3219752754296894559, 0.3333333333333333703, 0.3219752754296894559, 0.3333333333333333703, 0.3219752754296894559, 0.3333333333333333703, 0.3219752754296894559, 0.3333333333333333703, 0.3219752754296894559, 0.3333333333333333703, 0.3219752754296894559, 0.3333333333333333703, 0.3219752754296894559, 0.3333333333333333703, 0.3219752754296894559, 0.3333333333333333703, 0.3219752754296894559, 0.3333333333333333703, 0.3219752754296894559, 0.3333333333333333703, 0.3219752754296894559, 0.3333333333333333703, 0.3219752754296894559, 0.3333333333333333703, 0.3219752754296894559, 0.3333333333333333703, 0.3219752754296894559, 0.3333333333333333703, 0.3219752754296894559, 0.3333333333333333703, 0.3219752754296894559, 0.3333333333333333703, 0.3219752754296894559, 0.3333333333333333703, 0.3219752754296894559, 0.3333333333333333703, 0.3219752754296894559, 0.3333333333333333703, 0.3219752754296894559, 0.3333333333333333703, 0.3219752754296894559, 0.3333333333333333703, 0.3219752754296894559, 0.3333333333333333703, 0.3219752754296894559, 0.3333333333333333703, 0.3219752754296894559, 0.3333333333333333703, 0.3219752754296894559, 0.3333333333333333703, 0.3219752754296894559, 0.3333333333333333703, 0.3219752754296894559, 0.3333333333333333703, 0.3219752754296894559, 0.3333333333333333703, 0.3219752754296894559, 0.3333333333333333703, 0.3219752754296894559, 0.3333333333333333703, 0.3219752754296894559, 0.3333333333333333703, 0.3219752754296894559, 0.3333333333333333703, 0.3219752754296894559, 0.3333333333333333703, 0.3219752754296894559, 0.3333333333333333703, 0.3219752754296894559, 0.3333333333333333703, 0.3219752754296894559, 0.3333333333333333703, 0.3219752754296894559, 0.3333333333333333703, 0.3219752754296894559, 0.3333333333333333703, 0.3219752754296894559, 0.3333333333333333703, 0.3219752754296894559, 0.3333333333333333703, 0.3219752754296894559, 0.3333333333333333703, 0.3219752754296894559, 0.3333333333333333703, 0.3219752754296894559, 0.3333333333333333703, 0.3219752754296894559, 0.3333333333333333703, 0.3219752754296894559, 0.3333333333333333703, 0.3219752754296894559, 0.3333333333333333703, 0.3219752754296894559, 0.3333333333333333703, 0.3219752754296894559, 0.3333333333333333703, 0.3219752754296894559, 0.3333333333333333703, 0.3219752754296894559, 0.3333333333333333703, 0.3219752754296894559, 0.3333333333333333703, 0.3219752754296894559, 0.3333333333333333703, 0.3219752754296894559, 0.3333333333333333703, 0.3219752754296894559, 0.3333333333333333703, 0.3219752754296894559, 0.3333333333333333703, 0.3219752754296894559, 0.3333333333333333703, 0.3219752754296894559, 0.3333333333333333703, 0.3219752754296894559, 0.3333333333333333703, 0.3219752754296894559, 0.3333333333333333703, 0.3219752754296894559, 0.3333333333333333703, 0.3219752754296894559, 0.3333333333333333703, 0.3219752754296894559, 0.3333333333333333703, 0.3219752754296894559, 0.3333333333333333703, 0.3219752754296894559, 0.3333333333333333703, 0.3219752754296894559, 0.3333333333333333703, 0.3219752754296894559, 0.3333333333333333703, 0.3219752754296894559, 0.3333333333333333703, 0.3219752754296894559, 0.3333333333333333703, 0.3219752754296894559, 0.3333333333333333703, 0.3219752754296894559, 0.3333333333333333703, 0.3219752754296894559, 0.3333333333333333703, 0.3219752754296894559, 0.3333333333333333703, 0.3219752754296894559, 0.3333333333333333703, 0.3219752754296894559, 0.3333333333333333703, 0.3219752754296894559, 0.3333333333333333703, 0.3219752754296894559, 0.3333333333333333703, 0.3219752754296894559, 0.3333333333333333703, 0.3219752754296894559, 0.3333333333333333703, 0.3219752754296894559, 0.3333333333333333703, 0.3219752754296894559, 0.3333333333333333703, 0.3219752754296894559, 0.3333333333333333703, 0.3219752754296894559, 0.3333333333333333703, 0.3219752754296894559, 0.3333333333333333703, 0.3219752754296894559, 0.3333333333333333703, 0.3219752754296894559, 0.3333333333333333703, 0.3219752754296894559, 0.3333333333333333703, 0.3219752754296894559, 0.3333333333333333703, 0.3219752754296894559, 0.3333333333333333703, 0.3219752754296894559, 0.3333333333333333703, 0.3219752754296894559, 0.3333333333333333703, 0.3219752754296894559, 0.3333333333333333703, 0.3219752754296894559, 0.3333333333333333703, 0.3219752754296894559, 0.3333333333333333703, 0.3219752754296894559, 0.3333333333333333703, 0.3219752754296894559, 0.3333333333333333703, 0.3219752754296894559, 0.3333333333333333703, 0.3219752754296894559, 0.3333333333333333703, 0.3219752754296894559, 0.3333333333333333703, 0.3219752754296894559, 0.3333333333333333703, 0.3219752754296894559, 0.3333333333333333703, 0.3219752754296894559, 0.3333333333333333703, 0.3219752754296894559, 0.3333333333333333703, 0.3219752754296894559, 0.3333333333333333703, 0.3219752754296894559, 0.3333333333333333703, 0.3219752754296894559, 0.3333333333333333703, 0.3219752754296894559, 0.3333333333333333703, 0.3219752754296894559, 0.3333333333333333703, 0.3219752754296894559, 0.3333333333333333703, 0.3219752754296894559, 0.3333333333333333703, 0.3219752754296894559, 0.3333333333333333703, 0.3219752754296894559, 0.3333333333333333703, 0.3219752754296894559, 0.3333333333333333703, 0.3219752754296894559, 0.3333333333333333703, 0.3219752754296894559, 0.3333333333333333703, 0.3219752754296894559, 0.3333333333333333703, 0.3219752754296894559, 0.3333333333333333703, 0.3219752754296894559, 0.3333333333333333703, 0.3219752754296894559, 0.3333333333333333703, 0.3219752754296894559, 0.3333333333333333703, 0.3219752754296894559, 0.3333333333333333703, 0.3219752754296894559, 0.3333333333333333703, 0.3219752754296894559, 0.3333333333333333703, 0.3219752754296894559, 0.3333333333333333703, 0.3219752754296894559, 0.3333333333333333703, 0.3219752754296894559, 0.3333333333333333703, 0.3219752754296894559, 0.3333333333333333703, 0.3219752754296894559, 0.3333333333333333703, 0.3219752754296894559, 0.3333333333333333703, 0.3219752754296894559, 0.3333333333333333703, 0.3219752754296894559, 0.3333333333333333703, 0.3219752754296894559, 0.3333333333333333703, 0.3219752754296894559, 0.3333333333333333703, 0.3219752754296894559, 0.3333333333333333703, 0.3219752754296894559, 0.3333333333333333703, 0.3219752754296894559, 0.3333333333333333703, 0.3219752754296894559, 0.3333333333333333703, 0.3219752754296894559, 0.3333333333333333703, 0.3219752754296894559, 0.3333333333333333703, 0.3219752754296894559, 0.3333333333333333703, 0.3219752754296894559, 0.3333333333333333703, 0.3219752754296894559, 0.3333333333333333703, 0.3219752754296894559, 0.3333333333333333703, 0.3219752754296894559, 0.3333333333333333703, 0.3219752754296894559, 0.3333333333333333703, 0.3219752754296894559, 0.3333333333333333703, 0.3219752754296894559, 0.3333333333333333703, 0.3219752754296894559, 0.3333333333333333703, 0.3219752754296894559, 0.3333333333333333703, 0.3219752754296894559, 0.3333333333333333703, 0.3219752754296894559, 0.3333333333333333703, 0.3219752754296894559, 0.3333333333333333703, 0.3219752754296894559, 0.3333333333333333703, 0.3219752754296894559, 0.3333333333333333703, 0.3219752754296894559, 0.3333333333333333703, 0.3219752754296894559, 0.3333333333333333703, 0.3219752754296894559, 0.3333333333333333703, 0.3219752754296894559, 0.3333333333333333703, 0.3219752754296894559, 0.3333333333333333703, 0.3219752754296894559, 0.3333333333333333703, 0.3219752754296894559, 0.3333333333333333703, 0.3219752754296894559, 0.3333333333333333703, 0.3219752754296894559, 0.3333333333333333703, 0.3219752754296894559, 0.3333333333333333703, 0.3219752754296894559, 0.3333333333333333703, 0.3219752754296894559, 0.3333333333333333703, 0.3219752754296894559, 0.3333333333333333703, 0.3219752754296894559, 0.3333333333333333703, 0.3219752754296894559, 0.3333333333333333703, 0.3219752754296894559, 0.3333333333333333703, 0.3219752754296894559, 0.3333333333333333703, 0.3219752754296894559, 0.3333333333333333703, 0.3219752754296894559, 0.3333333333333333703, 0.3219752754296894559, 0.3333333333333333703, 0.3219752754296894559, 0.3333333333333333703, 0.3219752754296894559, 0.3333333333333333703, 0.3219752754296894559, 0.3333333333333333703, 0.3219752754296894559, 0.3333333333333333703, 0.3219752754296894559, 0.3333333333333333703, 0.3219752754296894559, 0.3333333333333333703, 0.3219752754296894559, 0.3333333333333333703, 0.3219752754296894559, 0.3333333333333333703, 0.3219752754296894559, 0.3333333333333333703, 0.3219752754296894559, 0.3333333333333333703, 0.3219752754296894559, 0.3333333333333333703, 0.3219752754296894559, 0.3333333333333333703, 0.3219752754296894559, 0.3333333333333333703, 0.3219752754296894559, 0.3333333333333333703, 0.3219752754296894559, 0.3333333333333333703, 0.3219752754296894559, 0.3333333333333333703, 0.3219752754296894559, 0.3333333333333333703, 0.3219752754296894559, 0.3333333333333333703, 0.3219752754296894559, 0.3333333333333333703, 0.3219752754296894559, 0.3333333333333333703, 0.3219752754296894559, 0.3333333333333333703, 0.3219752754296894559, 0.3333333333333333703, 0.3219752754296894559, 0.3333333333333333703, 0.3219752754296894559, 0.3333333333333333703, 0.3219752754296894559, 0.3333333333333333703, 0.3219752754296894559, 0.3333333333333333703, 0.3219752754296894559, 0.3333333333333333703, 0.3219752754296894559, 0.3333333333333333703, 0.3219752754296894559, 0.3333333333333333703, 0.3219752754296894559, 0.3333333333333333703, 0.3219752754296894559, 0.3333333333333333703, 0.3219752754296894559, 0.3333333333333333703, 0.3219752754296894559, 0.3333333333333333703, 0.3219752754296894559, 0.3333333333333333703, 0.3219752754296894559, 0.3333333333333333703, 0.3219752754296894559, 0.3333333333333333703, 0.3219752754296894559, 0.3333333333333333703, 0.3219752754296894559, 0.3333333333333333703, 0.3219752754296894559, 0.3333333333333333703, 0.3219752754296894559, 0.3333333333333333703, 0.3219752754296894559, 0.3333333333333333703, 0.3219752754296894559, 0.3333333333333333703, 0.3219752754296894559, 0.3333333333333333703, 0.3219752754296894559, 0.3333333333333333703, 0.3219752754296894559, 0.3333333333333333703, 0.3219752754296894559, 0.3333333333333333703, 0.3219752754296894559, 0.3333333333333333703, 0.3219752754296894559, 0.3333333333333333703, 0.3219752754296894559, 0.3333333333333333703, 0.3219752754296894559, 0.3333333333333333703, 0.3219752754296894559, 0.3333333333333333703, 0.3219752754296894559, 0.3333333333333333703, 0.3219752754296894559, 0.3333333333333333703, 0.3219752754296894559, 0.3333333333333333703),
 ( 0.3333333333333333703, 0.3219752754296894559, 0.3333333333333333703, 0.3219752754296894559, 0.3333333333333333703, 0.3219752754296894559, 0.3333333333333333703, 0.3219752754296894559, 0.3333333333333333703, 0.3219752754296894559, 0.3333333333333333703, 0.3219752754296894559, 0.3333333333333333703, 0.3219752754296894559, 0.3333333333333333703, 0.3219752754296894559, 0.3333333333333333703, 0.3219752754296894559, 0.3333333333333333703, 0.3219752754296894559, 0.3333333333333333703, 0.3219752754296894559, 0.3333333333333333703, 0.3219752754296894559, 0.3333333333333333703, 0.3219752754296894559, 0.3333333333333333703, 0.3219752754296894559, 0.3333333333333333703, 0.3219752754296894559, 0.3333333333333333703, 0.3219752754296894559, 0.3333333333333333703, 0.3219752754296894559, 0.3333333333333333703, 0.3219752754296894559, 0.3333333333333333703, 0.3219752754296894559, 0.3333333333333333703, 0.3219752754296894559, 0.3333333333333333703, 0.3219752754296894559, 0.3333333333333333703, 0.3219752754296894559, 0.3333333333333333703, 0.3219752754296894559, 0.3333333333333333703, 0.3219752754296894559, 0.3333333333333333703, 0.3219752754296894559, 0.3333333333333333703, 0.3219752754296894559, 0.3333333333333333703, 0.3219752754296894559, 0.3333333333333333703, 0.3219752754296894559, 0.3333333333333333703, 0.3219752754296894559, 0.3333333333333333703, 0.3219752754296894559, 0.3333333333333333703, 0.3219752754296894559, 0.3333333333333333703, 0.3219752754296894559, 0.3333333333333333703, 0.3219752754296894559, 0.3333333333333333703, 0.3219752754296894559, 0.3333333333333333703, 0.3219752754296894559, 0.3333333333333333703, 0.3219752754296894559, 0.3333333333333333703, 0.3219752754296894559, 0.3333333333333333703, 0.3219752754296894559, 0.3333333333333333703, 0.3219752754296894559, 0.3333333333333333703, 0.3219752754296894559, 0.3333333333333333703, 0.3219752754296894559, 0.3333333333333333703, 0.3219752754296894559, 0.3333333333333333703, 0.3219752754296894559, 0.3333333333333333703, 0.3219752754296894559, 0.3333333333333333703, 0.3219752754296894559, 0.3333333333333333703, 0.3219752754296894559, 0.3333333333333333703, 0.3219752754296894559, 0.3333333333333333703, 0.3219752754296894559, 0.3333333333333333703, 0.3219752754296894559, 0.3333333333333333703, 0.3219752754296894559, 0.3333333333333333703, 0.3219752754296894559, 0.3333333333333333703, 0.3219752754296894559, 0.3333333333333333703, 0.3219752754296894559, 0.3333333333333333703, 0.3219752754296894559, 0.3333333333333333703, 0.3219752754296894559, 0.3333333333333333703, 0.3219752754296894559, 0.3333333333333333703, 0.3219752754296894559, 0.3333333333333333703, 0.3219752754296894559, 0.3333333333333333703, 0.3219752754296894559, 0.3333333333333333703, 0.3219752754296894559, 0.3333333333333333703, 0.3219752754296894559, 0.3333333333333333703, 0.3219752754296894559, 0.3333333333333333703, 0.3219752754296894559, 0.3333333333333333703, 0.3219752754296894559, 0.3333333333333333703, 0.3219752754296894559, 0.3333333333333333703, 0.3219752754296894559, 0.3333333333333333703, 0.3219752754296894559, 0.3333333333333333703, 0.3219752754296894559, 0.3333333333333333703, 0.3219752754296894559, 0.3333333333333333703, 0.3219752754296894559, 0.3333333333333333703, 0.3219752754296894559, 0.3333333333333333703, 0.3219752754296894559, 0.3333333333333333703, 0.3219752754296894559, 0.3333333333333333703, 0.3219752754296894559, 0.3333333333333333703, 0.3219752754296894559, 0.3333333333333333703, 0.3219752754296894559, 0.3333333333333333703, 0.3219752754296894559, 0.3333333333333333703, 0.3219752754296894559, 0.3333333333333333703, 0.3219752754296894559, 0.3333333333333333703, 0.3219752754296894559, 0.3333333333333333703, 0.3219752754296894559, 0.3333333333333333703, 0.3219752754296894559, 0.3333333333333333703, 0.3219752754296894559, 0.3333333333333333703, 0.3219752754296894559, 0.3333333333333333703, 0.3219752754296894559, 0.3333333333333333703, 0.3219752754296894559, 0.3333333333333333703, 0.3219752754296894559, 0.3333333333333333703, 0.3219752754296894559, 0.3333333333333333703, 0.3219752754296894559, 0.3333333333333333703, 0.3219752754296894559, 0.3333333333333333703, 0.3219752754296894559, 0.3333333333333333703, 0.3219752754296894559, 0.3333333333333333703, 0.3219752754296894559, 0.3333333333333333703, 0.3219752754296894559, 0.3333333333333333703, 0.3219752754296894559, 0.3333333333333333703, 0.3219752754296894559, 0.3333333333333333703, 0.3219752754296894559, 0.3333333333333333703, 0.3219752754296894559, 0.3333333333333333703, 0.3219752754296894559, 0.3333333333333333703, 0.3219752754296894559, 0.3333333333333333703, 0.3219752754296894559, 0.3333333333333333703, 0.3219752754296894559, 0.3333333333333333703, 0.3219752754296894559, 0.3333333333333333703, 0.3219752754296894559, 0.3333333333333333703, 0.3219752754296894559, 0.3333333333333333703, 0.3219752754296894559, 0.3333333333333333703, 0.3219752754296894559, 0.3333333333333333703, 0.3219752754296894559, 0.3333333333333333703, 0.3219752754296894559, 0.3333333333333333703, 0.3219752754296894559, 0.3333333333333333703, 0.3219752754296894559, 0.3333333333333333703, 0.3219752754296894559, 0.3333333333333333703, 0.3219752754296894559, 0.3333333333333333703, 0.3219752754296894559, 0.3333333333333333703, 0.3219752754296894559, 0.3333333333333333703, 0.3219752754296894559, 0.3333333333333333703, 0.3219752754296894559, 0.3333333333333333703, 0.3219752754296894559, 0.3333333333333333703, 0.3219752754296894559, 0.3333333333333333703, 0.3219752754296894559, 0.3333333333333333703, 0.3219752754296894559, 0.3333333333333333703, 0.3219752754296894559, 0.3333333333333333703, 0.3219752754296894559, 0.3333333333333333703, 0.3219752754296894559, 0.3333333333333333703, 0.3219752754296894559, 0.3333333333333333703, 0.3219752754296894559, 0.3333333333333333703, 0.3219752754296894559, 0.3333333333333333703, 0.3219752754296894559, 0.3333333333333333703, 0.3219752754296894559, 0.3333333333333333703, 0.3219752754296894559, 0.3333333333333333703, 0.3219752754296894559, 0.3333333333333333703, 0.3219752754296894559, 0.3333333333333333703, 0.3219752754296894559, 0.3333333333333333703, 0.3219752754296894559, 0.3333333333333333703, 0.3219752754296894559, 0.3333333333333333703, 0.3219752754296894559, 0.3333333333333333703, 0.3219752754296894559, 0.3333333333333333703, 0.3219752754296894559, 0.3333333333333333703, 0.3219752754296894559, 0.3333333333333333703, 0.3219752754296894559, 0.3333333333333333703, 0.3219752754296894559, 0.3333333333333333703, 0.3219752754296894559, 0.3333333333333333703, 0.3219752754296894559, 0.3333333333333333703, 0.3219752754296894559, 0.3333333333333333703, 0.3219752754296894559, 0.3333333333333333703, 0.3219752754296894559, 0.3333333333333333703, 0.3219752754296894559, 0.3333333333333333703, 0.3219752754296894559, 0.3333333333333333703, 0.3219752754296894559, 0.3333333333333333703, 0.3219752754296894559, 0.3333333333333333703, 0.3219752754296894559, 0.3333333333333333703, 0.3219752754296894559, 0.3333333333333333703, 0.3219752754296894559, 0.3333333333333333703, 0.3219752754296894559, 0.3333333333333333703, 0.3219752754296894559, 0.3333333333333333703, 0.3219752754296894559, 0.3333333333333333703, 0.3219752754296894559, 0.3333333333333333703, 0.3219752754296894559, 0.3333333333333333703, 0.3219752754296894559, 0.3333333333333333703, 0.3219752754296894559, 0.3333333333333333703, 0.3219752754296894559, 0.3333333333333333703, 0.3219752754296894559, 0.3333333333333333703, 0.3219752754296894559, 0.3333333333333333703, 0.3219752754296894559, 0.3333333333333333703, 0.3219752754296894559, 0.3333333333333333703, 0.3219752754296894559, 0.3333333333333333703, 0.3219752754296894559, 0.3333333333333333703, 0.3219752754296894559, 0.3333333333333333703, 0.3219752754296894559, 0.3333333333333333703, 0.3219752754296894559, 0.3333333333333333703, 0.3219752754296894559, 0.3333333333333333703, 0.3219752754296894559, 0.3333333333333333703, 0.3219752754296894559, 0.3333333333333333703, 0.3219752754296894559, 0.3333333333333333703, 0.3219752754296894559, 0.3333333333333333703, 0.3219752754296894559, 0.3333333333333333703, 0.3219752754296894559, 0.3333333333333333703, 0.3219752754296894559, 0.3333333333333333703, 0.3219752754296894559, 0.3333333333333333703, 0.3219752754296894559, 0.3333333333333333703, 0.3219752754296894559, 0.3333333333333333703, 0.3219752754296894559, 0.3333333333333333703, 0.3219752754296894559, 0.3333333333333333703, 0.3219752754296894559, 0.3333333333333333703, 0.3219752754296894559, 0.3333333333333333703, 0.3219752754296894559, 0.3333333333333333703, 0.3219752754296894559, 0.3333333333333333703, 0.3219752754296894559, 0.3333333333333333703, 0.3219752754296894559, 0.3333333333333333703, 0.3219752754296894559, 0.3333333333333333703, 0.3219752754296894559, 0.3333333333333333703, 0.3219752754296894559, 0.3333333333333333703, 0.3219752754296894559, 0.3333333333333333703, 0.3219752754296894559, 0.3333333333333333703, 0.3219752754296894559, 0.3333333333333333703, 0.3219752754296894559, 0.3333333333333333703, 0.3219752754296894559, 0.3333333333333333703, 0.3219752754296894559, 0.3333333333333333703, 0.3219752754296894559, 0.3333333333333333703, 0.3219752754296894559, 0.3333333333333333703, 0.3219752754296894559, 0.3333333333333333703, 0.3219752754296894559, 0.3333333333333333703, 0.3219752754296894559, 0.3333333333333333703, 0.3219752754296894559, 0.3333333333333333703, 0.3219752754296894559, 0.3333333333333333703, 0.3219752754296894559, 0.3333333333333333703, 0.3219752754296894559, 0.3333333333333333703, 0.3219752754296894559, 0.3333333333333333703, 0.3219752754296894559, 0.3333333333333333703, 0.3219752754296894559, 0.3333333333333333703, 0.3219752754296894559, 0.3333333333333333703, 0.3219752754296894559, 0.3333333333333333703, 0.3219752754296894559, 0.3333333333333333703, 0.3219752754296894559, 0.3333333333333333703, 0.3219752754296894559, 0.3333333333333333703, 0.3219752754296894559, 0.3333333333333333703, 0.3219752754296894559, 0.3333333333333333703, 0.3219752754296894559, 0.3333333333333333703, 0.3219752754296894559, 0.3333333333333333703, 0.3219752754296894559, 0.3333333333333333703, 0.3219752754296894559, 0.3333333333333333703, 0.3219752754296894559, 0.3333333333333333703, 0.3219752754296894559, 0.3333333333333333703, 0.3219752754296894559, 0.3333333333333333703, 0.3219752754296894559, 0.3333333333333333703, 0.3219752754296894559, 0.3333333333333333703, 0.3219752754296894559, 0.3333333333333333703, 0.3219752754296894559, 0.3333333333333333703),
 ( 1.000000000000000000, 0.9659258262890683122, 1.000000000000000000, 0.9659258262890683122, 1.000000000000000000, 0.9659258262890683122, 1.000000000000000000, 0.9659258262890683122, 1.000000000000000000, 0.9659258262890683122, 1.000000000000000000, 0.9659258262890683122, 1.000000000000000000, 0.9659258262890683122, 1.000000000000000000, 0.9659258262890683122, 1.000000000000000000, 0.9659258262890683122, 1.000000000000000000, 0.9659258262890683122, 1.000000000000000000, 0.9659258262890683122, 1.000000000000000000, 0.9659258262890683122, 1.000000000000000000, 0.9659258262890683122, 1.000000000000000000, 0.9659258262890683122, 1.000000000000000000, 0.9659258262890683122, 1.000000000000000000, 0.9659258262890683122, 1.000000000000000000, 0.9659258262890683122, 1.000000000000000000, 0.9659258262890683122, 1.000000000000000000, 0.9659258262890683122, 1.000000000000000000, 0.9659258262890683122, 1.000000000000000000, 0.9659258262890683122, 1.000000000000000000, 0.9659258262890683122, 1.000000000000000000, 0.9659258262890683122, 1.000000000000000000, 0.9659258262890683122, 1.000000000000000000, 0.9659258262890683122, 1.000000000000000000, 0.9659258262890683122, 1.000000000000000000, 0.9659258262890683122, 1.000000000000000000, 0.9659258262890683122, 1.000000000000000000, 0.9659258262890683122, 1.000000000000000000, 0.9659258262890683122, 1.000000000000000000, 0.9659258262890683122, 1.000000000000000000, 0.9659258262890683122, 1.000000000000000000, 0.9659258262890683122, 1.000000000000000000, 0.9659258262890683122, 1.000000000000000000, 0.9659258262890683122, 1.000000000000000000, 0.9659258262890683122, 1.000000000000000000, 0.9659258262890683122, 1.000000000000000000, 0.9659258262890683122, 1.000000000000000000, 0.9659258262890683122, 1.000000000000000000, 0.9659258262890683122, 1.000000000000000000, 0.9659258262890683122, 1.000000000000000000, 0.9659258262890683122, 1.000000000000000000, 0.9659258262890683122, 1.000000000000000000, 0.9659258262890683122, 1.000000000000000000, 0.9659258262890683122, 1.000000000000000000, 0.9659258262890683122, 1.000000000000000000, 0.9659258262890683122, 1.000000000000000000, 0.9659258262890683122, 1.000000000000000000, 0.9659258262890683122, 1.000000000000000000, 0.9659258262890683122, 1.000000000000000000, 0.9659258262890683122, 1.000000000000000000, 0.9659258262890683122, 1.000000000000000000, 0.9659258262890683122, 1.000000000000000000, 0.9659258262890683122, 1.000000000000000000, 0.9659258262890683122, 1.000000000000000000, 0.9659258262890683122, 1.000000000000000000, 0.9659258262890683122, 1.000000000000000000, 0.9659258262890683122, 1.000000000000000000, 0.9659258262890683122, 1.000000000000000000, 0.9659258262890683122, 1.000000000000000000, 0.9659258262890683122, 1.000000000000000000, 0.9659258262890683122, 1.000000000000000000, 0.9659258262890683122, 1.000000000000000000, 0.9659258262890683122, 1.000000000000000000, 0.9659258262890683122, 1.000000000000000000, 0.9659258262890683122, 1.000000000000000000, 0.9659258262890683122, 1.000000000000000000, 0.9659258262890683122, 1.000000000000000000, 0.9659258262890683122, 1.000000000000000000, 0.9659258262890683122, 1.000000000000000000, 0.9659258262890683122, 1.000000000000000000, 0.9659258262890683122, 1.000000000000000000, 0.9659258262890683122, 1.000000000000000000, 0.9659258262890683122, 1.000000000000000000, 0.9659258262890683122, 1.000000000000000000, 0.9659258262890683122, 1.000000000000000000, 0.9659258262890683122, 1.000000000000000000, 0.9659258262890683122, 1.000000000000000000, 0.9659258262890683122, 1.000000000000000000, 0.9659258262890683122, 1.000000000000000000, 0.9659258262890683122, 1.000000000000000000, 0.9659258262890683122, 1.000000000000000000, 0.9659258262890683122, 1.000000000000000000, 0.9659258262890683122, 1.000000000000000000, 0.9659258262890683122, 1.000000000000000000, 0.9659258262890683122, 1.000000000000000000, 0.9659258262890683122, 1.000000000000000000, 0.9659258262890683122, 1.000000000000000000, 0.9659258262890683122, 1.000000000000000000, 0.9659258262890683122, 1.000000000000000000, 0.9659258262890683122, 1.000000000000000000, 0.9659258262890683122, 1.000000000000000000, 0.9659258262890683122, 1.000000000000000000, 0.9659258262890683122, 1.000000000000000000, 0.9659258262890683122, 1.000000000000000000, 0.9659258262890683122, 1.000000000000000000, 0.9659258262890683122, 1.000000000000000000, 0.9659258262890683122, 1.000000000000000000, 0.9659258262890683122, 1.000000000000000000, 0.9659258262890683122, 1.000000000000000000, 0.9659258262890683122, 1.000000000000000000, 0.9659258262890683122, 1.000000000000000000, 0.9659258262890683122, 1.000000000000000000, 0.9659258262890683122, 1.000000000000000000, 0.9659258262890683122, 1.000000000000000000, 0.9659258262890683122, 1.000000000000000000, 0.9659258262890683122, 1.000000000000000000, 0.9659258262890683122, 1.000000000000000000, 0.9659258262890683122, 1.000000000000000000, 0.9659258262890683122, 1.000000000000000000, 0.9659258262890683122, 1.000000000000000000, 0.9659258262890683122, 1.000000000000000000, 0.9659258262890683122, 1.000000000000000000, 0.9659258262890683122, 1.000000000000000000, 0.9659258262890683122, 1.000000000000000000, 0.9659258262890683122, 1.000000000000000000, 0.9659258262890683122, 1.000000000000000000, 0.9659258262890683122, 1.000000000000000000, 0.9659258262890683122, 1.000000000000000000, 0.9659258262890683122, 1.000000000000000000, 0.9659258262890683122, 1.000000000000000000, 0.9659258262890683122, 1.000000000000000000, 0.9659258262890683122, 1.000000000000000000, 0.9659258262890683122, 1.000000000000000000, 0.9659258262890683122, 1.000000000000000000, 0.9659258262890683122, 1.000000000000000000, 0.9659258262890683122, 1.000000000000000000, 0.9659258262890683122, 1.000000000000000000, 0.9659258262890683122, 1.000000000000000000, 0.9659258262890683122, 1.000000000000000000, 0.9659258262890683122, 1.000000000000000000, 0.9659258262890683122, 1.000000000000000000, 0.9659258262890683122, 1.000000000000000000, 0.9659258262890683122, 1.000000000000000000, 0.9659258262890683122, 1.000000000000000000, 0.9659258262890683122, 1.000000000000000000, 0.9659258262890683122, 1.000000000000000000, 0.9659258262890683122, 1.000000000000000000, 0.9659258262890683122, 1.000000000000000000, 0.9659258262890683122, 1.000000000000000000, 0.9659258262890683122, 1.000000000000000000, 0.9659258262890683122, 1.000000000000000000, 0.9659258262890683122, 1.000000000000000000, 0.9659258262890683122, 1.000000000000000000, 0.9659258262890683122, 1.000000000000000000, 0.9659258262890683122, 1.000000000000000000, 0.9659258262890683122, 1.000000000000000000, 0.9659258262890683122, 1.000000000000000000, 0.9659258262890683122, 1.000000000000000000, 0.9659258262890683122, 1.000000000000000000, 0.9659258262890683122, 1.000000000000000000, 0.9659258262890683122, 1.000000000000000000, 0.9659258262890683122, 1.000000000000000000, 0.9659258262890683122, 1.000000000000000000, 0.9659258262890683122, 1.000000000000000000, 0.9659258262890683122, 1.000000000000000000, 0.9659258262890683122, 1.000000000000000000, 0.9659258262890683122, 1.000000000000000000, 0.9659258262890683122, 1.000000000000000000, 0.9659258262890683122, 1.000000000000000000, 0.9659258262890683122, 1.000000000000000000, 0.9659258262890683122, 1.000000000000000000, 0.9659258262890683122, 1.000000000000000000, 0.9659258262890683122, 1.000000000000000000, 0.9659258262890683122, 1.000000000000000000, 0.9659258262890683122, 1.000000000000000000, 0.9659258262890683122, 1.000000000000000000, 0.9659258262890683122, 1.000000000000000000, 0.9659258262890683122, 1.000000000000000000, 0.9659258262890683122, 1.000000000000000000, 0.9659258262890683122, 1.000000000000000000, 0.9659258262890683122, 1.000000000000000000, 0.9659258262890683122, 1.000000000000000000, 0.9659258262890683122, 1.000000000000000000, 0.9659258262890683122, 1.000000000000000000, 0.9659258262890683122, 1.000000000000000000, 0.9659258262890683122, 1.000000000000000000, 0.9659258262890683122, 1.000000000000000000, 0.9659258262890683122, 1.000000000000000000, 0.9659258262890683122, 1.000000000000000000, 0.9659258262890683122, 1.000000000000000000, 0.9659258262890683122, 1.000000000000000000, 0.9659258262890683122, 1.000000000000000000, 0.9659258262890683122, 1.000000000000000000, 0.9659258262890683122, 1.000000000000000000, 0.9659258262890683122, 1.000000000000000000, 0.9659258262890683122, 1.000000000000000000, 0.9659258262890683122, 1.000000000000000000, 0.9659258262890683122, 1.000000000000000000, 0.9659258262890683122, 1.000000000000000000, 0.9659258262890683122, 1.000000000000000000, 0.9659258262890683122, 1.000000000000000000, 0.9659258262890683122, 1.000000000000000000, 0.9659258262890683122, 1.000000000000000000, 0.9659258262890683122, 1.000000000000000000, 0.9659258262890683122, 1.000000000000000000, 0.9659258262890683122, 1.000000000000000000, 0.9659258262890683122, 1.000000000000000000, 0.9659258262890683122, 1.000000000000000000, 0.9659258262890683122, 1.000000000000000000, 0.9659258262890683122, 1.000000000000000000, 0.9659258262890683122, 1.000000000000000000, 0.9659258262890683122, 1.000000000000000000, 0.9659258262890683122, 1.000000000000000000, 0.9659258262890683122, 1.000000000000000000, 0.9659258262890683122, 1.000000000000000000, 0.9659258262890683122, 1.000000000000000000, 0.9659258262890683122, 1.000000000000000000, 0.9659258262890683122, 1.000000000000000000, 0.9659258262890683122, 1.000000000000000000, 0.9659258262890683122, 1.000000000000000000, 0.9659258262890683122, 1.000000000000000000, 0.9659258262890683122, 1.000000000000000000, 0.9659258262890683122, 1.000000000000000000, 0.9659258262890683122, 1.000000000000000000, 0.9659258262890683122, 1.000000000000000000, 0.9659258262890683122, 1.000000000000000000, 0.9659258262890683122, 1.000000000000000000, 0.9659258262890683122, 1.000000000000000000, 0.9659258262890683122, 1.000000000000000000, 0.9659258262890683122, 1.000000000000000000, 0.9659258262890683122, 1.000000000000000000, 0.9659258262890683122, 1.000000000000000000, 0.9659258262890683122, 1.000000000000000000, 0.9659258262890683122, 1.000000000000000000, 0.9659258262890683122, 1.000000000000000000, 0.9659258262890683122, 1.000000000000000000, 0.9659258262890683122, 1.000000000000000000),
 ( 0.3333333333333333703, 0.3219752754296894559, 0.3333333333333333703, 0.3219752754296894559, 0.3333333333333333703, 0.3219752754296894559, 0.3333333333333333703, 0.3219752754296894559, 0.3333333333333333703, 0.3219752754296894559, 0.3333333333333333703, 0.3219752754296894559, 0.3333333333333333703, 0.3219752754296894559, 0.3333333333333333703, 0.3219752754296894559, 0.3333333333333333703, 0.3219752754296894559, 0.3333333333333333703, 0.3219752754296894559, 0.3333333333333333703, 0.3219752754296894559, 0.3333333333333333703, 0.3219752754296894559, 0.3333333333333333703, 0.3219752754296894559, 0.3333333333333333703, 0.3219752754296894559, 0.3333333333333333703, 0.3219752754296894559, 0.3333333333333333703, 0.3219752754296894559, 0.3333333333333333703, 0.3219752754296894559, 0.3333333333333333703, 0.3219752754296894559, 0.3333333333333333703, 0.3219752754296894559, 0.3333333333333333703, 0.3219752754296894559, 0.3333333333333333703, 0.3219752754296894559, 0.3333333333333333703, 0.3219752754296894559, 0.3333333333333333703, 0.3219752754296894559, 0.3333333333333333703, 0.3219752754296894559, 0.3333333333333333703, 0.3219752754296894559, 0.3333333333333333703, 0.3219752754296894559, 0.3333333333333333703, 0.3219752754296894559, 0.3333333333333333703, 0.3219752754296894559, 0.3333333333333333703, 0.3219752754296894559, 0.3333333333333333703, 0.3219752754296894559, 0.3333333333333333703, 0.3219752754296894559, 0.3333333333333333703, 0.3219752754296894559, 0.3333333333333333703, 0.3219752754296894559, 0.3333333333333333703, 0.3219752754296894559, 0.3333333333333333703, 0.3219752754296894559, 0.3333333333333333703, 0.3219752754296894559, 0.3333333333333333703, 0.3219752754296894559, 0.3333333333333333703, 0.3219752754296894559, 0.3333333333333333703, 0.3219752754296894559, 0.3333333333333333703, 0.3219752754296894559, 0.3333333333333333703, 0.3219752754296894559, 0.3333333333333333703, 0.3219752754296894559, 0.3333333333333333703, 0.3219752754296894559, 0.3333333333333333703, 0.3219752754296894559, 0.3333333333333333703, 0.3219752754296894559, 0.3333333333333333703, 0.3219752754296894559, 0.3333333333333333703, 0.3219752754296894559, 0.3333333333333333703, 0.3219752754296894559, 0.3333333333333333703, 0.3219752754296894559, 0.3333333333333333703, 0.3219752754296894559, 0.3333333333333333703, 0.3219752754296894559, 0.3333333333333333703, 0.3219752754296894559, 0.3333333333333333703, 0.3219752754296894559, 0.3333333333333333703, 0.3219752754296894559, 0.3333333333333333703, 0.3219752754296894559, 0.3333333333333333703, 0.3219752754296894559, 0.3333333333333333703, 0.3219752754296894559, 0.3333333333333333703, 0.3219752754296894559, 0.3333333333333333703, 0.3219752754296894559, 0.3333333333333333703, 0.3219752754296894559, 0.3333333333333333703, 0.3219752754296894559, 0.3333333333333333703, 0.3219752754296894559, 0.3333333333333333703, 0.3219752754296894559, 0.3333333333333333703, 0.3219752754296894559, 0.3333333333333333703, 0.3219752754296894559, 0.3333333333333333703, 0.3219752754296894559, 0.3333333333333333703, 0.3219752754296894559, 0.3333333333333333703, 0.3219752754296894559, 0.3333333333333333703, 0.3219752754296894559, 0.3333333333333333703, 0.3219752754296894559, 0.3333333333333333703, 0.3219752754296894559, 0.3333333333333333703, 0.3219752754296894559, 0.3333333333333333703, 0.3219752754296894559, 0.3333333333333333703, 0.3219752754296894559, 0.3333333333333333703, 0.3219752754296894559, 0.3333333333333333703, 0.3219752754296894559, 0.3333333333333333703, 0.3219752754296894559, 0.3333333333333333703, 0.3219752754296894559, 0.3333333333333333703, 0.3219752754296894559, 0.3333333333333333703, 0.3219752754296894559, 0.3333333333333333703, 0.3219752754296894559, 0.3333333333333333703, 0.3219752754296894559, 0.3333333333333333703, 0.3219752754296894559, 0.3333333333333333703, 0.3219752754296894559, 0.3333333333333333703, 0.3219752754296894559, 0.3333333333333333703, 0.3219752754296894559, 0.3333333333333333703, 0.3219752754296894559, 0.3333333333333333703, 0.3219752754296894559, 0.3333333333333333703, 0.3219752754296894559, 0.3333333333333333703, 0.3219752754296894559, 0.3333333333333333703, 0.3219752754296894559, 0.3333333333333333703, 0.3219752754296894559, 0.3333333333333333703, 0.3219752754296894559, 0.3333333333333333703, 0.3219752754296894559, 0.3333333333333333703, 0.3219752754296894559, 0.3333333333333333703, 0.3219752754296894559, 0.3333333333333333703, 0.3219752754296894559, 0.3333333333333333703, 0.3219752754296894559, 0.3333333333333333703, 0.3219752754296894559, 0.3333333333333333703, 0.3219752754296894559, 0.3333333333333333703, 0.3219752754296894559, 0.3333333333333333703, 0.3219752754296894559, 0.3333333333333333703, 0.3219752754296894559, 0.3333333333333333703, 0.3219752754296894559, 0.3333333333333333703, 0.3219752754296894559, 0.3333333333333333703, 0.3219752754296894559, 0.3333333333333333703, 0.3219752754296894559, 0.3333333333333333703, 0.3219752754296894559, 0.3333333333333333703, 0.3219752754296894559, 0.3333333333333333703, 0.3219752754296894559, 0.3333333333333333703, 0.3219752754296894559, 0.3333333333333333703, 0.3219752754296894559, 0.3333333333333333703, 0.3219752754296894559, 0.3333333333333333703, 0.3219752754296894559, 0.3333333333333333703, 0.3219752754296894559, 0.3333333333333333703, 0.3219752754296894559, 0.3333333333333333703, 0.3219752754296894559, 0.3333333333333333703, 0.3219752754296894559, 0.3333333333333333703, 0.3219752754296894559, 0.3333333333333333703, 0.3219752754296894559, 0.3333333333333333703, 0.3219752754296894559, 0.3333333333333333703, 0.3219752754296894559, 0.3333333333333333703, 0.3219752754296894559, 0.3333333333333333703, 0.3219752754296894559, 0.3333333333333333703, 0.3219752754296894559, 0.3333333333333333703, 0.3219752754296894559, 0.3333333333333333703, 0.3219752754296894559, 0.3333333333333333703, 0.3219752754296894559, 0.3333333333333333703, 0.3219752754296894559, 0.3333333333333333703, 0.3219752754296894559, 0.3333333333333333703, 0.3219752754296894559, 0.3333333333333333703, 0.3219752754296894559, 0.3333333333333333703, 0.3219752754296894559, 0.3333333333333333703, 0.3219752754296894559, 0.3333333333333333703, 0.3219752754296894559, 0.3333333333333333703, 0.3219752754296894559, 0.3333333333333333703, 0.3219752754296894559, 0.3333333333333333703, 0.3219752754296894559, 0.3333333333333333703, 0.3219752754296894559, 0.3333333333333333703, 0.3219752754296894559, 0.3333333333333333703, 0.3219752754296894559, 0.3333333333333333703, 0.3219752754296894559, 0.3333333333333333703, 0.3219752754296894559, 0.3333333333333333703, 0.3219752754296894559, 0.3333333333333333703, 0.3219752754296894559, 0.3333333333333333703, 0.3219752754296894559, 0.3333333333333333703, 0.3219752754296894559, 0.3333333333333333703, 0.3219752754296894559, 0.3333333333333333703, 0.3219752754296894559, 0.3333333333333333703, 0.3219752754296894559, 0.3333333333333333703, 0.3219752754296894559, 0.3333333333333333703, 0.3219752754296894559, 0.3333333333333333703, 0.3219752754296894559, 0.3333333333333333703, 0.3219752754296894559, 0.3333333333333333703, 0.3219752754296894559, 0.3333333333333333703, 0.3219752754296894559, 0.3333333333333333703, 0.3219752754296894559, 0.3333333333333333703, 0.3219752754296894559, 0.3333333333333333703, 0.3219752754296894559, 0.3333333333333333703, 0.3219752754296894559, 0.3333333333333333703, 0.3219752754296894559, 0.3333333333333333703, 0.3219752754296894559, 0.3333333333333333703, 0.3219752754296894559, 0.3333333333333333703, 0.3219752754296894559, 0.3333333333333333703, 0.3219752754296894559, 0.3333333333333333703, 0.3219752754296894559, 0.3333333333333333703, 0.3219752754296894559, 0.3333333333333333703, 0.3219752754296894559, 0.3333333333333333703, 0.3219752754296894559, 0.3333333333333333703, 0.3219752754296894559, 0.3333333333333333703, 0.3219752754296894559, 0.3333333333333333703, 0.3219752754296894559, 0.3333333333333333703, 0.3219752754296894559, 0.3333333333333333703, 0.3219752754296894559, 0.3333333333333333703, 0.3219752754296894559, 0.3333333333333333703, 0.3219752754296894559, 0.3333333333333333703, 0.3219752754296894559, 0.3333333333333333703, 0.3219752754296894559, 0.3333333333333333703, 0.3219752754296894559, 0.3333333333333333703, 0.3219752754296894559, 0.3333333333333333703, 0.3219752754296894559, 0.3333333333333333703, 0.3219752754296894559, 0.3333333333333333703, 0.3219752754296894559, 0.3333333333333333703, 0.3219752754296894559, 0.3333333333333333703, 0.3219752754296894559, 0.3333333333333333703, 0.3219752754296894559, 0.3333333333333333703, 0.3219752754296894559, 0.3333333333333333703, 0.3219752754296894559, 0.3333333333333333703, 0.3219752754296894559, 0.3333333333333333703, 0.3219752754296894559, 0.3333333333333333703, 0.3219752754296894559, 0.3333333333333333703, 0.3219752754296894559, 0.3333333333333333703, 0.3219752754296894559, 0.3333333333333333703, 0.3219752754296894559, 0.3333333333333333703, 0.3219752754296894559, 0.3333333333333333703, 0.3219752754296894559, 0.3333333333333333703, 0.3219752754296894559, 0.3333333333333333703, 0.3219752754296894559, 0.3333333333333333703, 0.3219752754296894559, 0.3333333333333333703, 0.3219752754296894559, 0.3333333333333333703, 0.3219752754296894559, 0.3333333333333333703, 0.3219752754296894559, 0.3333333333333333703, 0.3219752754296894559, 0.3333333333333333703, 0.3219752754296894559, 0.3333333333333333703, 0.3219752754296894559, 0.3333333333333333703, 0.3219752754296894559, 0.3333333333333333703, 0.3219752754296894559, 0.3333333333333333703, 0.3219752754296894559, 0.3333333333333333703, 0.3219752754296894559, 0.3333333333333333703, 0.3219752754296894559, 0.3333333333333333703, 0.3219752754296894559, 0.3333333333333333703, 0.3219752754296894559, 0.3333333333333333703, 0.3219752754296894559, 0.3333333333333333703, 0.3219752754296894559, 0.3333333333333333703, 0.3219752754296894559, 0.3333333333333333703, 0.3219752754296894559, 0.3333333333333333703, 0.3219752754296894559, 0.3333333333333333703, 0.3219752754296894559, 0.3333333333333333703, 0.3219752754296894559, 0.3333333333333333703, 0.3219752754296894559, 0.3333333333333333703, 0.3219752754296894559, 0.3333333333333333703, 0.3219752754296894559, 0.3333333333333333703, 0.3219752754296894559, 0.3333333333333333703, 0.3219752754296894559, 0.3333333333333333703, 0.3219752754296894559, 0.3333333333333333703, 0.3219752754296894559, 0.3333333333333333703, 0.3219752754296894559, 0.3333333333333333703, 0.3219752754296894559, 0.3333333333333333703),
 ( 0.3333333333333333703, 0.3219752754296894559, 0.3333333333333333703, 0.3219752754296894559, 0.3333333333333333703, 0.3219752754296894559, 0.3333333333333333703, 0.3219752754296894559, 0.3333333333333333703, 0.3219752754296894559, 0.3333333333333333703, 0.3219752754296894559, 0.3333333333333333703, 0.3219752754296894559, 0.3333333333333333703, 0.3219752754296894559, 0.3333333333333333703, 0.3219752754296894559, 0.3333333333333333703, 0.3219752754296894559, 0.3333333333333333703, 0.3219752754296894559, 0.3333333333333333703, 0.3219752754296894559, 0.3333333333333333703, 0.3219752754296894559, 0.3333333333333333703, 0.3219752754296894559, 0.3333333333333333703, 0.3219752754296894559, 0.3333333333333333703, 0.3219752754296894559, 0.3333333333333333703, 0.3219752754296894559, 0.3333333333333333703, 0.3219752754296894559, 0.3333333333333333703, 0.3219752754296894559, 0.3333333333333333703, 0.3219752754296894559, 0.3333333333333333703, 0.3219752754296894559, 0.3333333333333333703, 0.3219752754296894559, 0.3333333333333333703, 0.3219752754296894559, 0.3333333333333333703, 0.3219752754296894559, 0.3333333333333333703, 0.3219752754296894559, 0.3333333333333333703, 0.3219752754296894559, 0.3333333333333333703, 0.3219752754296894559, 0.3333333333333333703, 0.3219752754296894559, 0.3333333333333333703, 0.3219752754296894559, 0.3333333333333333703, 0.3219752754296894559, 0.3333333333333333703, 0.3219752754296894559, 0.3333333333333333703, 0.3219752754296894559, 0.3333333333333333703, 0.3219752754296894559, 0.3333333333333333703, 0.3219752754296894559, 0.3333333333333333703, 0.3219752754296894559, 0.3333333333333333703, 0.3219752754296894559, 0.3333333333333333703, 0.3219752754296894559, 0.3333333333333333703, 0.3219752754296894559, 0.3333333333333333703, 0.3219752754296894559, 0.3333333333333333703, 0.3219752754296894559, 0.3333333333333333703, 0.3219752754296894559, 0.3333333333333333703, 0.3219752754296894559, 0.3333333333333333703, 0.3219752754296894559, 0.3333333333333333703, 0.3219752754296894559, 0.3333333333333333703, 0.3219752754296894559, 0.3333333333333333703, 0.3219752754296894559, 0.3333333333333333703, 0.3219752754296894559, 0.3333333333333333703, 0.3219752754296894559, 0.3333333333333333703, 0.3219752754296894559, 0.3333333333333333703, 0.3219752754296894559, 0.3333333333333333703, 0.3219752754296894559, 0.3333333333333333703, 0.3219752754296894559, 0.3333333333333333703, 0.3219752754296894559, 0.3333333333333333703, 0.3219752754296894559, 0.3333333333333333703, 0.3219752754296894559, 0.3333333333333333703, 0.3219752754296894559, 0.3333333333333333703, 0.3219752754296894559, 0.3333333333333333703, 0.3219752754296894559, 0.3333333333333333703, 0.3219752754296894559, 0.3333333333333333703, 0.3219752754296894559, 0.3333333333333333703, 0.3219752754296894559, 0.3333333333333333703, 0.3219752754296894559, 0.3333333333333333703, 0.3219752754296894559, 0.3333333333333333703, 0.3219752754296894559, 0.3333333333333333703, 0.3219752754296894559, 0.3333333333333333703, 0.3219752754296894559, 0.3333333333333333703, 0.3219752754296894559, 0.3333333333333333703, 0.3219752754296894559, 0.3333333333333333703, 0.3219752754296894559, 0.3333333333333333703, 0.3219752754296894559, 0.3333333333333333703, 0.3219752754296894559, 0.3333333333333333703, 0.3219752754296894559, 0.3333333333333333703, 0.3219752754296894559, 0.3333333333333333703, 0.3219752754296894559, 0.3333333333333333703, 0.3219752754296894559, 0.3333333333333333703, 0.3219752754296894559, 0.3333333333333333703, 0.3219752754296894559, 0.3333333333333333703, 0.3219752754296894559, 0.3333333333333333703, 0.3219752754296894559, 0.3333333333333333703, 0.3219752754296894559, 0.3333333333333333703, 0.3219752754296894559, 0.3333333333333333703, 0.3219752754296894559, 0.3333333333333333703, 0.3219752754296894559, 0.3333333333333333703, 0.3219752754296894559, 0.3333333333333333703, 0.3219752754296894559, 0.3333333333333333703, 0.3219752754296894559, 0.3333333333333333703, 0.3219752754296894559, 0.3333333333333333703, 0.3219752754296894559, 0.3333333333333333703, 0.3219752754296894559, 0.3333333333333333703, 0.3219752754296894559, 0.3333333333333333703, 0.3219752754296894559, 0.3333333333333333703, 0.3219752754296894559, 0.3333333333333333703, 0.3219752754296894559, 0.3333333333333333703, 0.3219752754296894559, 0.3333333333333333703, 0.3219752754296894559, 0.3333333333333333703, 0.3219752754296894559, 0.3333333333333333703, 0.3219752754296894559, 0.3333333333333333703, 0.3219752754296894559, 0.3333333333333333703, 0.3219752754296894559, 0.3333333333333333703, 0.3219752754296894559, 0.3333333333333333703, 0.3219752754296894559, 0.3333333333333333703, 0.3219752754296894559, 0.3333333333333333703, 0.3219752754296894559, 0.3333333333333333703, 0.3219752754296894559, 0.3333333333333333703, 0.3219752754296894559, 0.3333333333333333703, 0.3219752754296894559, 0.3333333333333333703, 0.3219752754296894559, 0.3333333333333333703, 0.3219752754296894559, 0.3333333333333333703, 0.3219752754296894559, 0.3333333333333333703, 0.3219752754296894559, 0.3333333333333333703, 0.3219752754296894559, 0.3333333333333333703, 0.3219752754296894559, 0.3333333333333333703, 0.3219752754296894559, 0.3333333333333333703, 0.3219752754296894559, 0.3333333333333333703, 0.3219752754296894559, 0.3333333333333333703, 0.3219752754296894559, 0.3333333333333333703, 0.3219752754296894559, 0.3333333333333333703, 0.3219752754296894559, 0.3333333333333333703, 0.3219752754296894559, 0.3333333333333333703, 0.3219752754296894559, 0.3333333333333333703, 0.3219752754296894559, 0.3333333333333333703, 0.3219752754296894559, 0.3333333333333333703, 0.3219752754296894559, 0.3333333333333333703, 0.3219752754296894559, 0.3333333333333333703, 0.3219752754296894559, 0.3333333333333333703, 0.3219752754296894559, 0.3333333333333333703, 0.3219752754296894559, 0.3333333333333333703, 0.3219752754296894559, 0.3333333333333333703, 0.3219752754296894559, 0.3333333333333333703, 0.3219752754296894559, 0.3333333333333333703, 0.3219752754296894559, 0.3333333333333333703, 0.3219752754296894559, 0.3333333333333333703, 0.3219752754296894559, 0.3333333333333333703, 0.3219752754296894559, 0.3333333333333333703, 0.3219752754296894559, 0.3333333333333333703, 0.3219752754296894559, 0.3333333333333333703, 0.3219752754296894559, 0.3333333333333333703, 0.3219752754296894559, 0.3333333333333333703, 0.3219752754296894559, 0.3333333333333333703, 0.3219752754296894559, 0.3333333333333333703, 0.3219752754296894559, 0.3333333333333333703, 0.3219752754296894559, 0.3333333333333333703, 0.3219752754296894559, 0.3333333333333333703, 0.3219752754296894559, 0.3333333333333333703, 0.3219752754296894559, 0.3333333333333333703, 0.3219752754296894559, 0.3333333333333333703, 0.3219752754296894559, 0.3333333333333333703, 0.3219752754296894559, 0.3333333333333333703, 0.3219752754296894559, 0.3333333333333333703, 0.3219752754296894559, 0.3333333333333333703, 0.3219752754296894559, 0.3333333333333333703, 0.3219752754296894559, 0.3333333333333333703, 0.3219752754296894559, 0.3333333333333333703, 0.3219752754296894559, 0.3333333333333333703, 0.3219752754296894559, 0.3333333333333333703, 0.3219752754296894559, 0.3333333333333333703, 0.3219752754296894559, 0.3333333333333333703, 0.3219752754296894559, 0.3333333333333333703, 0.3219752754296894559, 0.3333333333333333703, 0.3219752754296894559, 0.3333333333333333703, 0.3219752754296894559, 0.3333333333333333703, 0.3219752754296894559, 0.3333333333333333703, 0.3219752754296894559, 0.3333333333333333703, 0.3219752754296894559, 0.3333333333333333703, 0.3219752754296894559, 0.3333333333333333703, 0.3219752754296894559, 0.3333333333333333703, 0.3219752754296894559, 0.3333333333333333703, 0.3219752754296894559, 0.3333333333333333703, 0.3219752754296894559, 0.3333333333333333703, 0.3219752754296894559, 0.3333333333333333703, 0.3219752754296894559, 0.3333333333333333703, 0.3219752754296894559, 0.3333333333333333703, 0.3219752754296894559, 0.3333333333333333703, 0.3219752754296894559, 0.3333333333333333703, 0.3219752754296894559, 0.3333333333333333703, 0.3219752754296894559, 0.3333333333333333703, 0.3219752754296894559, 0.3333333333333333703, 0.3219752754296894559, 0.3333333333333333703, 0.3219752754296894559, 0.3333333333333333703, 0.3219752754296894559, 0.3333333333333333703, 0.3219752754296894559, 0.3333333333333333703, 0.3219752754296894559, 0.3333333333333333703, 0.3219752754296894559, 0.3333333333333333703, 0.3219752754296894559, 0.3333333333333333703, 0.3219752754296894559, 0.3333333333333333703, 0.3219752754296894559, 0.3333333333333333703, 0.3219752754296894559, 0.3333333333333333703, 0.3219752754296894559, 0.3333333333333333703, 0.3219752754296894559, 0.3333333333333333703, 0.3219752754296894559, 0.3333333333333333703, 0.3219752754296894559, 0.3333333333333333703, 0.3219752754296894559, 0.3333333333333333703, 0.3219752754296894559, 0.3333333333333333703, 0.3219752754296894559, 0.3333333333333333703, 0.3219752754296894559, 0.3333333333333333703, 0.3219752754296894559, 0.3333333333333333703, 0.3219752754296894559, 0.3333333333333333703, 0.3219752754296894559, 0.3333333333333333703, 0.3219752754296894559, 0.3333333333333333703, 0.3219752754296894559, 0.3333333333333333703, 0.3219752754296894559, 0.3333333333333333703, 0.3219752754296894559, 0.3333333333333333703, 0.3219752754296894559, 0.3333333333333333703, 0.3219752754296894559, 0.3333333333333333703, 0.3219752754296894559, 0.3333333333333333703, 0.3219752754296894559, 0.3333333333333333703, 0.3219752754296894559, 0.3333333333333333703, 0.3219752754296894559, 0.3333333333333333703, 0.3219752754296894559, 0.3333333333333333703, 0.3219752754296894559, 0.3333333333333333703, 0.3219752754296894559, 0.3333333333333333703, 0.3219752754296894559, 0.3333333333333333703, 0.3219752754296894559, 0.3333333333333333703, 0.3219752754296894559, 0.3333333333333333703, 0.3219752754296894559, 0.3333333333333333703, 0.3219752754296894559, 0.3333333333333333703, 0.3219752754296894559, 0.3333333333333333703, 0.3219752754296894559, 0.3333333333333333703, 0.3219752754296894559, 0.3333333333333333703, 0.3219752754296894559, 0.3333333333333333703, 0.3219752754296894559, 0.3333333333333333703, 0.3219752754296894559, 0.3333333333333333703, 0.3219752754296894559, 0.3333333333333333703, 0.3219752754296894559, 0.3333333333333333703, 0.3219752754296894559, 0.3333333333333333703, 0.3219752754296894559, 0.3333333333333333703, 0.3219752754296894559, 0.3333333333333333703, 0.3219752754296894559, 0.3333333333333333703),
 ( 1.000000000000000000, 0.9659258262890683122, 1.000000000000000000, 0.9659258262890683122, 1.000000000000000000, 0.9659258262890683122, 1.000000000000000000, 0.9659258262890683122, 1.000000000000000000, 0.9659258262890683122, 1.000000000000000000, 0.9659258262890683122, 1.000000000000000000, 0.9659258262890683122, 1.000000000000000000, 0.9659258262890683122, 1.000000000000000000, 0.9659258262890683122, 1.000000000000000000, 0.9659258262890683122, 1.000000000000000000, 0.9659258262890683122, 1.000000000000000000, 0.9659258262890683122, 1.000000000000000000, 0.9659258262890683122, 1.000000000000000000, 0.9659258262890683122, 1.000000000000000000, 0.9659258262890683122, 1.000000000000000000, 0.9659258262890683122, 1.000000000000000000, 0.9659258262890683122, 1.000000000000000000, 0.9659258262890683122, 1.000000000000000000, 0.9659258262890683122, 1.000000000000000000, 0.9659258262890683122, 1.000000000000000000, 0.9659258262890683122, 1.000000000000000000, 0.9659258262890683122, 1.000000000000000000, 0.9659258262890683122, 1.000000000000000000, 0.9659258262890683122, 1.000000000000000000, 0.9659258262890683122, 1.000000000000000000, 0.9659258262890683122, 1.000000000000000000, 0.9659258262890683122, 1.000000000000000000, 0.9659258262890683122, 1.000000000000000000, 0.9659258262890683122, 1.000000000000000000, 0.9659258262890683122, 1.000000000000000000, 0.9659258262890683122, 1.000000000000000000, 0.9659258262890683122, 1.000000000000000000, 0.9659258262890683122, 1.000000000000000000, 0.9659258262890683122, 1.000000000000000000, 0.9659258262890683122, 1.000000000000000000, 0.9659258262890683122, 1.000000000000000000, 0.9659258262890683122, 1.000000000000000000, 0.9659258262890683122, 1.000000000000000000, 0.9659258262890683122, 1.000000000000000000, 0.9659258262890683122, 1.000000000000000000, 0.9659258262890683122, 1.000000000000000000, 0.9659258262890683122, 1.000000000000000000, 0.9659258262890683122, 1.000000000000000000, 0.9659258262890683122, 1.000000000000000000, 0.9659258262890683122, 1.000000000000000000, 0.9659258262890683122, 1.000000000000000000, 0.9659258262890683122, 1.000000000000000000, 0.9659258262890683122, 1.000000000000000000, 0.9659258262890683122, 1.000000000000000000, 0.9659258262890683122, 1.000000000000000000, 0.9659258262890683122, 1.000000000000000000, 0.9659258262890683122, 1.000000000000000000, 0.9659258262890683122, 1.000000000000000000, 0.9659258262890683122, 1.000000000000000000, 0.9659258262890683122, 1.000000000000000000, 0.9659258262890683122, 1.000000000000000000, 0.9659258262890683122, 1.000000000000000000, 0.9659258262890683122, 1.000000000000000000, 0.9659258262890683122, 1.000000000000000000, 0.9659258262890683122, 1.000000000000000000, 0.9659258262890683122, 1.000000000000000000, 0.9659258262890683122, 1.000000000000000000, 0.9659258262890683122, 1.000000000000000000, 0.9659258262890683122, 1.000000000000000000, 0.9659258262890683122, 1.000000000000000000, 0.9659258262890683122, 1.000000000000000000, 0.9659258262890683122, 1.000000000000000000, 0.9659258262890683122, 1.000000000000000000, 0.9659258262890683122, 1.000000000000000000, 0.9659258262890683122, 1.000000000000000000, 0.9659258262890683122, 1.000000000000000000, 0.9659258262890683122, 1.000000000000000000, 0.9659258262890683122, 1.000000000000000000, 0.9659258262890683122, 1.000000000000000000, 0.9659258262890683122, 1.000000000000000000, 0.9659258262890683122, 1.000000000000000000, 0.9659258262890683122, 1.000000000000000000, 0.9659258262890683122, 1.000000000000000000, 0.9659258262890683122, 1.000000000000000000, 0.9659258262890683122, 1.000000000000000000, 0.9659258262890683122, 1.000000000000000000, 0.9659258262890683122, 1.000000000000000000, 0.9659258262890683122, 1.000000000000000000, 0.9659258262890683122, 1.000000000000000000, 0.9659258262890683122, 1.000000000000000000, 0.9659258262890683122, 1.000000000000000000, 0.9659258262890683122, 1.000000000000000000, 0.9659258262890683122, 1.000000000000000000, 0.9659258262890683122, 1.000000000000000000, 0.9659258262890683122, 1.000000000000000000, 0.9659258262890683122, 1.000000000000000000, 0.9659258262890683122, 1.000000000000000000, 0.9659258262890683122, 1.000000000000000000, 0.9659258262890683122, 1.000000000000000000, 0.9659258262890683122, 1.000000000000000000, 0.9659258262890683122, 1.000000000000000000, 0.9659258262890683122, 1.000000000000000000, 0.9659258262890683122, 1.000000000000000000, 0.9659258262890683122, 1.000000000000000000, 0.9659258262890683122, 1.000000000000000000, 0.9659258262890683122, 1.000000000000000000, 0.9659258262890683122, 1.000000000000000000, 0.9659258262890683122, 1.000000000000000000, 0.9659258262890683122, 1.000000000000000000, 0.9659258262890683122, 1.000000000000000000, 0.9659258262890683122, 1.000000000000000000, 0.9659258262890683122, 1.000000000000000000, 0.9659258262890683122, 1.000000000000000000, 0.9659258262890683122, 1.000000000000000000, 0.9659258262890683122, 1.000000000000000000, 0.9659258262890683122, 1.000000000000000000, 0.9659258262890683122, 1.000000000000000000, 0.9659258262890683122, 1.000000000000000000, 0.9659258262890683122, 1.000000000000000000, 0.9659258262890683122, 1.000000000000000000, 0.9659258262890683122, 1.000000000000000000, 0.9659258262890683122, 1.000000000000000000, 0.9659258262890683122, 1.000000000000000000, 0.9659258262890683122, 1.000000000000000000, 0.9659258262890683122, 1.000000000000000000, 0.9659258262890683122, 1.000000000000000000, 0.9659258262890683122, 1.000000000000000000, 0.9659258262890683122, 1.000000000000000000, 0.9659258262890683122, 1.000000000000000000, 0.9659258262890683122, 1.000000000000000000, 0.9659258262890683122, 1.000000000000000000, 0.9659258262890683122, 1.000000000000000000, 0.9659258262890683122, 1.000000000000000000, 0.9659258262890683122, 1.000000000000000000, 0.9659258262890683122, 1.000000000000000000, 0.9659258262890683122, 1.000000000000000000, 0.9659258262890683122, 1.000000000000000000, 0.9659258262890683122, 1.000000000000000000, 0.9659258262890683122, 1.000000000000000000, 0.9659258262890683122, 1.000000000000000000, 0.9659258262890683122, 1.000000000000000000, 0.9659258262890683122, 1.000000000000000000, 0.9659258262890683122, 1.000000000000000000, 0.9659258262890683122, 1.000000000000000000, 0.9659258262890683122, 1.000000000000000000, 0.9659258262890683122, 1.000000000000000000, 0.9659258262890683122, 1.000000000000000000, 0.9659258262890683122, 1.000000000000000000, 0.9659258262890683122, 1.000000000000000000, 0.9659258262890683122, 1.000000000000000000, 0.9659258262890683122, 1.000000000000000000, 0.9659258262890683122, 1.000000000000000000, 0.9659258262890683122, 1.000000000000000000, 0.9659258262890683122, 1.000000000000000000, 0.9659258262890683122, 1.000000000000000000, 0.9659258262890683122, 1.000000000000000000, 0.9659258262890683122, 1.000000000000000000, 0.9659258262890683122, 1.000000000000000000, 0.9659258262890683122, 1.000000000000000000, 0.9659258262890683122, 1.000000000000000000, 0.9659258262890683122, 1.000000000000000000, 0.9659258262890683122, 1.000000000000000000, 0.9659258262890683122, 1.000000000000000000, 0.9659258262890683122, 1.000000000000000000, 0.9659258262890683122, 1.000000000000000000, 0.9659258262890683122, 1.000000000000000000, 0.9659258262890683122, 1.000000000000000000, 0.9659258262890683122, 1.000000000000000000, 0.9659258262890683122, 1.000000000000000000, 0.9659258262890683122, 1.000000000000000000, 0.9659258262890683122, 1.000000000000000000, 0.9659258262890683122, 1.000000000000000000, 0.9659258262890683122, 1.000000000000000000, 0.9659258262890683122, 1.000000000000000000, 0.9659258262890683122, 1.000000000000000000, 0.9659258262890683122, 1.000000000000000000, 0.9659258262890683122, 1.000000000000000000, 0.9659258262890683122, 1.000000000000000000, 0.9659258262890683122, 1.000000000000000000, 0.9659258262890683122, 1.000000000000000000, 0.9659258262890683122, 1.000000000000000000, 0.9659258262890683122, 1.000000000000000000, 0.9659258262890683122, 1.000000000000000000, 0.9659258262890683122, 1.000000000000000000, 0.9659258262890683122, 1.000000000000000000, 0.9659258262890683122, 1.000000000000000000, 0.9659258262890683122, 1.000000000000000000, 0.9659258262890683122, 1.000000000000000000, 0.9659258262890683122, 1.000000000000000000, 0.9659258262890683122, 1.000000000000000000, 0.9659258262890683122, 1.000000000000000000, 0.9659258262890683122, 1.000000000000000000, 0.9659258262890683122, 1.000000000000000000, 0.9659258262890683122, 1.000000000000000000, 0.9659258262890683122, 1.000000000000000000, 0.9659258262890683122, 1.000000000000000000, 0.9659258262890683122, 1.000000000000000000, 0.9659258262890683122, 1.000000000000000000, 0.9659258262890683122, 1.000000000000000000, 0.9659258262890683122, 1.000000000000000000, 0.9659258262890683122, 1.000000000000000000, 0.9659258262890683122, 1.000000000000000000, 0.9659258262890683122, 1.000000000000000000, 0.9659258262890683122, 1.000000000000000000, 0.9659258262890683122, 1.000000000000000000, 0.9659258262890683122, 1.000000000000000000, 0.9659258262890683122, 1.000000000000000000, 0.9659258262890683122, 1.000000000000000000, 0.9659258262890683122, 1.000000000000000000, 0.9659258262890683122, 1.000000000000000000, 0.9659258262890683122, 1.000000000000000000, 0.9659258262890683122, 1.000000000000000000, 0.9659258262890683122, 1.000000000000000000, 0.9659258262890683122, 1.000000000000000000, 0.9659258262890683122, 1.000000000000000000, 0.9659258262890683122, 1.000000000000000000, 0.9659258262890683122, 1.000000000000000000, 0.9659258262890683122, 1.000000000000000000, 0.9659258262890683122, 1.000000000000000000, 0.9659258262890683122, 1.000000000000000000, 0.9659258262890683122, 1.000000000000000000, 0.9659258262890683122, 1.000000000000000000, 0.9659258262890683122, 1.000000000000000000, 0.9659258262890683122, 1.000000000000000000, 0.9659258262890683122, 1.000000000000000000, 0.9659258262890683122, 1.000000000000000000, 0.9659258262890683122, 1.000000000000000000, 0.9659258262890683122, 1.000000000000000000, 0.9659258262890683122, 1.000000000000000000, 0.9659258262890683122, 1.000000000000000000, 0.9659258262890683122, 1.000000000000000000, 0.9659258262890683122, 1.000000000000000000, 0.9659258262890683122, 1.000000000000000000) ) ) 
 REPRESENTATION_ITEM ( '' )  SURFACE ( )  );
#43448 = CARTESIAN_POINT ( 'NONE',  ( 9.474510206698971260, -16.51473224551069308, 102.9155762719810241 ) ) ;
#43449 = CARTESIAN_POINT ( 'NONE',  ( 5.049401038298161559, -19.05341960407611168, 67.70724293864769550 ) ) ;
#43450 = CARTESIAN_POINT ( 'NONE',  ( 15.72974639402176855, 15.80617190586768217, 81.87609039468568994 ) ) ;
#43451 = CARTESIAN_POINT ( 'NONE',  ( -13.97604488694527625, -13.89961937509977652, 56.87390960531434558 ) ) ;
#43452 = CARTESIAN_POINT ( 'NONE',  ( 5.049401038298161559, -19.05341960407611168, 42.70724293864767418 ) ) ;
#43453 = CARTESIAN_POINT ( 'NONE',  ( 10.81492255796078972, 18.62759615963270932, 24.58224293864768839 ) ) ;
#43454 = CARTESIAN_POINT ( 'NONE',  ( -8.224510206698948167, 14.34966873604960824, 65.41557627198102409 ) ) ;
#43455 = CARTESIAN_POINT ( 'NONE',  ( -9.474510206698964154, 16.51473224551069663, 40.41557627198103120 ) ) ;
#43456 = CARTESIAN_POINT ( 'NONE',  ( 4.379528057220339221, -16.55341960407611168, 97.70724293864772392 ) ) ;
#43457 = CARTESIAN_POINT ( 'NONE',  ( 0.05219959533907565091, 21.53943276465977519, 109.9989096053143527 ) ) ;
#43458 = CARTESIAN_POINT ( 'NONE',  ( -21.53943276465977519, -0.05219959533937600094, 43.75109039468568284 ) ) ;
#43459 = CARTESIAN_POINT ( 'NONE',  ( 5.153800228976335163, 19.02544592524342804, 34.79057627198102409 ) ) ;
#43460 = EDGE_CURVE ( 'NONE', #85102, #116714, #74632, .T. ) ;
#43461 = CARTESIAN_POINT ( 'NONE',  ( -8.314922557961024197, 14.29746914071037800, 62.91775706135236135 ) ) ;
#43462 = CARTESIAN_POINT ( 'NONE',  ( -10.72451020669898014, 18.67979575497178502, 100.4155762719810241 ) ) ;
#43463 = CARTESIAN_POINT ( 'NONE',  ( -18.67979575497178146, -10.72451020669898902, 96.66557627198102409 ) ) ;
#43465 = CARTESIAN_POINT ( 'NONE',  ( 19.02544592524343514, -5.153800228976328945, 48.54057627198103120 ) ) ;
#43464 = CARTESIAN_POINT ( 'NONE',  ( 9.474510206698729675, 16.51473224551082808, 32.08442372801900433 ) ) ;
#43466 = CARTESIAN_POINT ( 'NONE',  ( 9.809999999999998721, 0.000000000000000000, 0.000000000000000000 ) ) ;
#43467 = CARTESIAN_POINT ( 'NONE',  ( -10.72451020669870658, -18.67979575497194134, 54.58442372801901143 ) ) ;
#43468 = CARTESIAN_POINT ( 'NONE',  ( -5.823673210054116645, -21.52544592524344225, 62.29057627198102409 ) ) ;
#43469 = CARTESIAN_POINT ( 'NONE',  ( 12.14591786802309770, 12.06949235617756955, 29.37390960531435269 ) ) ;
#43471 = CARTESIAN_POINT ( 'NONE',  ( 18.62759615963255655, 10.81492255796105972, 106.6677570613523756 ) ) ;
#43470 = CARTESIAN_POINT ( 'NONE',  ( 15.80617190586769283, -15.72974639402175789, 75.62609039468567573 ) ) ;
#43472 = CARTESIAN_POINT ( 'NONE',  ( -9.474510206698720793, -16.51473224551083518, 44.58442372801900433 ) ) ;
#43473 = CARTESIAN_POINT ( 'NONE',  ( 8.224510206698742110, 14.34966873604972548, 97.08442372801904696 ) ) ;
#43474 = CARTESIAN_POINT ( 'NONE',  ( 18.67979575497194134, -10.72451020669871369, 55.83442372801901854 ) ) ;
#43475 = CARTESIAN_POINT ( 'NONE',  ( 5.049401038298161559, -19.05341960407611168, 62.70724293864769550 ) ) ;
#43476 = CARTESIAN_POINT ( 'NONE',  ( -13.89961937509957401, -13.97604488694547875, 39.37609039468566152 ) ) ;
#43477 = CARTESIAN_POINT ( 'NONE',  ( 15.80617190586746368, 15.72974639402197994, 44.37390960531435979 ) ) ;
#43478 = EDGE_CURVE ( 'NONE', #164159, #132746, #23972, .T. ) ;
#43479 = CARTESIAN_POINT ( 'NONE',  ( -15.80617190586768217, 15.72974639402176855, 33.12609039468569705 ) ) ;
#43480 = CARTESIAN_POINT ( 'NONE',  ( 0.05219959533907565091, 21.53943276465977519, 89.99890960531438111 ) ) ;
#43481 = CARTESIAN_POINT ( 'NONE',  ( 19.02544592524334988, 5.153800228976608722, 91.45942372801900433 ) ) ;
#43482 = CARTESIAN_POINT ( 'NONE',  ( 14.29746914071037800, 8.314922557961029526, 51.66775706135234714 ) ) ;
#43484 = CARTESIAN_POINT ( 'NONE',  ( 18.67979575497178502, 10.72451020669898547, 89.16557627198102409 ) ) ;
#43483 = CARTESIAN_POINT ( 'NONE',  ( -6.837351365824967608, 5.758699013978442416, -61.93409818843132797 ) ) ;
#43486 = CARTESIAN_POINT ( 'NONE',  ( 14.29746914071049879, -8.314922557960816363, 73.33224293864769550 ) ) ;
#43485 = CARTESIAN_POINT ( 'NONE',  ( 14.34966873604972726, -8.224510206698740333, 80.83442372801901854 ) ) ;
#43487 = CARTESIAN_POINT ( 'NONE',  ( -25.96435248595175693, -27.35529834266888116, -20.33897993952049887 ) ) ;
#43488 = CARTESIAN_POINT ( 'NONE',  ( -5.153800228976607833, 19.02544592524334988, 102.7094237280189759 ) ) ;
#43489 = CARTESIAN_POINT ( 'NONE',  ( -21.55341960407610458, -5.719274019375992779, 36.45724293864768839 ) ) ;
#43490 = CARTESIAN_POINT ( 'NONE',  ( -3.573655867282028392E-15, 2.428612866367529932E-14, 164.9999999999999716 ) ) ;
#43491 = CARTESIAN_POINT ( 'NONE',  ( -0.05219959533934338120, 16.53943276465976808, 52.50109039468567573 ) ) ;
#43492 = CARTESIAN_POINT ( 'NONE',  ( -18.62759615963270932, 10.81492255796079327, 110.8322429386476955 ) ) ;
#43493 = B_SPLINE_CURVE_WITH_KNOTS ( 'NONE', 3,
 ( #152783, #71237, #45615, #26743, #118747, #107267, #14274, #76935, #149082, #32434, #194589, #75943, #25751, #153780, #41908, #180436, #132900, #155767, #138604, #10570, #86, #185117, #168938, #56059, #61756, #123424, #169947, #109263, #60769, #139592, #92091, #62753, #46607, #117738, #1078, #30445, #91095, #103574, #165249, #137618, #122441, #108268, #31438, #154776 ),
 .UNSPECIFIED., .F., .F.,
 ( 4, 2, 2, 2, 2, 2, 2, 2, 2, 2, 2, 2, 2, 2, 2, 2, 2, 2, 2, 2, 2, 4 ),
 ( 0.01750047681075390590, 0.01897230708297386464, 0.01970822221908384228, 0.02044413735519382339, 0.02191596762741378213, 0.02338779789963374087, 0.02485962817185370308, 0.02559554330796365990, 0.02633145844407362365, 0.02706737358018358394, 0.02780328871629354423, 0.02927511898851346828, 0.03074694926073338885, 0.03221877953295330943, 0.03295469466906329054, 0.03369060980517327164, 0.03516244007739323385, 0.03663427034961320300, 0.03737018548572319798, 0.03810610062183318603, 0.03957793089405317599, 0.04104976116627316596 ),
 .UNSPECIFIED. ) ;
#43494 = CARTESIAN_POINT ( 'NONE',  ( 5.719274019375991003, -21.55341960407610458, 37.70724293864769550 ) ) ;
#43495 = CARTESIAN_POINT ( 'NONE',  ( -8.314922557961024197, 14.29746914071037800, 67.91775706135234714 ) ) ;
#43496 = CARTESIAN_POINT ( 'NONE',  ( 19.02544592524343514, -5.153800228976328945, 88.54057627198102409 ) ) ;
#43498 = CARTESIAN_POINT ( 'NONE',  ( 13.97604488694527802, 13.89961937509977652, 34.37390960531436690 ) ) ;
#43497 = CARTESIAN_POINT ( 'NONE',  ( -15.72974639402176322, -15.80617190586768395, 54.37609039468568994 ) ) ;
#43499 = CARTESIAN_POINT ( 'NONE',  ( -15.72974639402197994, 15.80617190586746368, 25.62390960531435624 ) ) ;
#43500 = ORIENTED_EDGE ( 'NONE', *, *, #128552, .T. ) ;
#43501 = CARTESIAN_POINT ( 'NONE',  ( -5.049401038297874678, -19.05341960407617918, 44.79275706135232582 ) ) ;
#43502 = CARTESIAN_POINT ( 'NONE',  ( -16.55341960407617563, 4.379528057220093196, 48.54275706135234714 ) ) ;
#43503 = CARTESIAN_POINT ( 'NONE',  ( 19.02544592524343514, -5.153800228976328945, 113.5405762719810241 ) ) ;
#43504 = CARTESIAN_POINT ( 'NONE',  ( 16.46253265017160672, -9.564922557960803928, 73.33224293864769550 ) ) ;
#43505 = CARTESIAN_POINT ( 'NONE',  ( 16.55341960407618274, -4.379528057220086978, 106.0427570613523471 ) ) ;
#43506 = CYLINDRICAL_SURFACE ( 'NONE', #18184, 1.500000000000001332 ) ;
#43507 = CARTESIAN_POINT ( 'NONE',  ( 0.05219959533910956823, 16.53943276465976808, 94.99890960531436690 ) ) ;
#43508 = CARTESIAN_POINT ( 'NONE',  ( 15.80617190586746368, 15.72974639402197994, 34.37390960531435979 ) ) ;
#43509 = CARTESIAN_POINT ( 'NONE',  ( -19.03943276465977164, 0.05219959533909376836, 26.24890960531435624 ) ) ;
#43510 = CARTESIAN_POINT ( 'NONE',  ( -4.379528057220086978, -16.55341960407618274, 69.79275706135234714 ) ) ;
#43511 = CARTESIAN_POINT ( 'NONE',  ( -21.52544592524343514, 5.823673210054127303, 116.0405762719810383 ) ) ;
#43512 = CARTESIAN_POINT ( 'NONE',  ( -13.89961937509957401, -13.97604488694547875, 74.37609039468566152 ) ) ;
#43513 = CARTESIAN_POINT ( 'NONE',  ( -19.05341960407611168, -5.049401038298163336, 41.45724293864769550 ) ) ;
#43514 = CARTESIAN_POINT ( 'NONE',  ( -21.55341960407610458, -5.719274019375992779, 71.45724293864769550 ) ) ;
#43515 = CYLINDRICAL_SURFACE ( 'NONE', #179855, 4.999999999999999112 ) ;
#43516 = CARTESIAN_POINT ( 'NONE',  ( 15.80617190586769283, -15.72974639402175789, 85.62609039468568994 ) ) ;
#43517 = CARTESIAN_POINT ( 'NONE',  ( 5.049401038298161559, -19.05341960407611168, 67.70724293864769550 ) ) ;
#43518 = CARTESIAN_POINT ( 'NONE',  ( 4.483927247898790824, -16.52544592524335698, 50.20942372801901854 ) ) ;
#43519 = CARTESIAN_POINT ( 'NONE',  ( 21.53943276465977519, 0.05219959533937863772, 76.25109039468568994 ) ) ;
#43520 = CARTESIAN_POINT ( 'NONE',  ( -13.97604488694547697, 13.89961937509957934, 43.12609039468566152 ) ) ;
#43521 = CIRCLE ( 'NONE', #11203, 25.62086810090349331 ) ;
#43522 = CARTESIAN_POINT ( 'NONE',  ( 19.03943276465977164, 0.05219959533936151252, 56.25109039468566863 ) ) ;
#43523 = VERTEX_POINT ( 'NONE', #6193 ) ;
#43524 = CARTESIAN_POINT ( 'NONE',  ( 18.67979575497194134, -10.72451020669871369, 55.83442372801901854 ) ) ;
#43525 = CARTESIAN_POINT ( 'NONE',  ( 13.97604488694527802, 13.89961937509977652, 24.37390960531435624 ) ) ;
#43526 = CARTESIAN_POINT ( 'NONE',  ( -0.05219959533936034679, 19.03943276465977164, 52.50109039468566863 ) ) ;
#43527 = CARTESIAN_POINT ( 'NONE',  ( -16.51473224551069308, -9.474510206698971260, 96.66557627198102409 ) ) ;
#43528 = CARTESIAN_POINT ( 'NONE',  ( 13.89961937509977652, -13.97604488694527269, 78.12390960531433848 ) ) ;
#43529 = CARTESIAN_POINT ( 'NONE',  ( 16.52544592524342804, -4.483927247898539470, 43.54057627198103830 ) ) ;
#43530 = CARTESIAN_POINT ( 'NONE',  ( 21.55341960407610458, 5.719274019375980345, 38.95724293864768839 ) ) ;
#43531 = CARTESIAN_POINT ( 'NONE',  ( -36.91746825000001309, -11.99521256947794789, -11.02499999726881263 ) ) ;
#43532 = CARTESIAN_POINT ( 'NONE',  ( 19.98428748653497422, 21.47640361312187096, -52.19293734151717956 ) ) ;
#43533 = CARTESIAN_POINT ( 'NONE',  ( -21.55341960407619339, 5.719274019375674811, 98.54275706135234714 ) ) ;
#43534 = CARTESIAN_POINT ( 'NONE',  ( 4.999999999999999112, 11.45643923738960090, -15.00000000000000000 ) ) ;
#43535 = CARTESIAN_POINT ( 'NONE',  ( 16.46253265017160672, -9.564922557960803928, 38.33224293864768839 ) ) ;
#43536 = CARTESIAN_POINT ( 'NONE',  ( -0.05219959533909027116, -19.03943276465977164, 107.4989096053143527 ) ) ;
#43537 = CARTESIAN_POINT ( 'NONE',  ( -37.38060010999600280, -6.349431928853577212, -7.999999999999996447 ) ) ;
#43538 = CARTESIAN_POINT ( 'NONE',  ( 12.14591786802327356, -12.06949235617739191, 55.62609039468568284 ) ) ;
#43539 = CARTESIAN_POINT ( 'NONE',  ( 5.719274019375991003, -21.55341960407610458, 87.70724293864769550 ) ) ;
#43540 = CARTESIAN_POINT ( 'NONE',  ( 8.314922557960818139, 14.29746914071049879, 34.58224293864770260 ) ) ;
#43542 = CARTESIAN_POINT ( 'NONE',  ( 9.564922557960805705, 16.46253265017160317, 104.5822429386476955 ) ) ;
#43541 = CARTESIAN_POINT ( 'NONE',  ( -0.05219959533909027116, -19.03943276465977164, 27.49890960531435624 ) ) ;
#43543 = CARTESIAN_POINT ( 'NONE',  ( 21.55341960407619695, -5.719274019375665929, 31.04275706135234714 ) ) ;
#43544 = CARTESIAN_POINT ( 'NONE',  ( -19.02544592524334988, -5.153800228976617603, 28.95942372801900433 ) ) ;
#43545 = CARTESIAN_POINT ( 'NONE',  ( -19.03943276465977164, 0.05219959533909376836, 26.24890960531435624 ) ) ;
#43546 = CARTESIAN_POINT ( 'NONE',  ( 21.52544592524334988, 5.823673210054432836, 76.45942372801901854 ) ) ;
#43547 = CARTESIAN_POINT ( 'NONE',  ( 17.50000000000002132, 5.499999999999984013, 98.78230962303568674 ) ) ;
#43548 = CARTESIAN_POINT ( 'NONE',  ( 16.55341960407611168, 4.379528057220329451, 33.95724293864769550 ) ) ;
#43549 = CARTESIAN_POINT ( 'NONE',  ( 22.81625015709509441, 31.40387420917330275, -3.824999997268813345 ) ) ;
#43550 = CARTESIAN_POINT ( 'NONE',  ( -18.67979575497178146, -10.72451020669898902, 21.66557627198102409 ) ) ;
#43551 = CARTESIAN_POINT ( 'NONE',  ( 14.29746914071049879, -8.314922557960816363, 88.33224293864769550 ) ) ;
#43552 = CARTESIAN_POINT ( 'NONE',  ( 23.23284429171615884, -30.31406682163549959, -16.83429831496583873 ) ) ;
#43553 = CARTESIAN_POINT ( 'NONE',  ( 16.51473224551069308, 9.474510206698969483, 79.16557627198103830 ) ) ;
#43554 = CARTESIAN_POINT ( 'NONE',  ( -8.224510206698948167, 14.34966873604960824, 70.41557627198102409 ) ) ;
#43555 = CARTESIAN_POINT ( 'NONE',  ( 13.97604488694548053, -13.89961937509957401, 105.6260903946856757 ) ) ;
#43556 = CARTESIAN_POINT ( 'NONE',  ( -15.72974639402197994, 15.80617190586746368, 65.62390960531436690 ) ) ;
#43557 = ORIENTED_EDGE ( 'NONE', *, *, #142600, .F. ) ;
#43558 = CARTESIAN_POINT ( 'NONE',  ( -16.46253265017160317, 9.564922557960807481, 30.83224293864769550 ) ) ;
#43559 = ADVANCED_FACE ( 'NONE', ( #188251 ), #145708, .F. ) ;
#43561 = CARTESIAN_POINT ( 'NONE',  ( 10.72451020669898902, -18.67979575497178502, 72.91557627198103830 ) ) ;
#43560 = CARTESIAN_POINT ( 'NONE',  ( 13.89961937509977652, -13.97604488694527269, 83.12390960531436690 ) ) ;
#43563 = CARTESIAN_POINT ( 'NONE',  ( 5.049401038298161559, -19.05341960407611168, 87.70724293864769550 ) ) ;
#43562 = CARTESIAN_POINT ( 'NONE',  ( -8.314922557961024197, 14.29746914071037800, 107.9177570613523471 ) ) ;
#43564 = CARTESIAN_POINT ( 'NONE',  ( 19.02544592524334988, 5.153800228976608722, 61.45942372801900433 ) ) ;
#43565 = CARTESIAN_POINT ( 'NONE',  ( -18.67979575497193778, 10.72451020669871902, 98.33442372801901854 ) ) ;
#43566 = CARTESIAN_POINT ( 'NONE',  ( -10.81492255796078084, -18.62759615963271287, 82.08224293864768129 ) ) ;
#43567 = CARTESIAN_POINT ( 'NONE',  ( -9.474510206698964154, 16.51473224551069663, 115.4155762719810241 ) ) ;
#43568 = CARTESIAN_POINT ( 'NONE',  ( -19.02544592524342804, 5.153800228976336051, 46.04057627198101699 ) ) ;
#43569 = CARTESIAN_POINT ( 'NONE',  ( 16.52544592524335698, 4.483927247898782831, 111.4594237280190328 ) ) ;
#43570 = CARTESIAN_POINT ( 'NONE',  ( 9.474510206698971260, -16.51473224551069308, 57.91557627198103120 ) ) ;
#43571 = CARTESIAN_POINT ( 'NONE',  ( -31.45337032948814482, -4.959272002022346193, 100.6317495573355245 ) ) ;
#43572 = CARTESIAN_POINT ( 'NONE',  ( -10.72451020669870658, -18.67979575497194134, 104.5844237280190185 ) ) ;
#43573 = CIRCLE ( 'NONE', #140535, 21.30000000000002913 ) ;
#43574 = CARTESIAN_POINT ( 'NONE',  ( 14.34966873604960469, 8.224510206698951720, 74.16557627198102409 ) ) ;
#43575 = CARTESIAN_POINT ( 'NONE',  ( -10.72451020669898014, 18.67979575497178502, 110.4155762719810383 ) ) ;
#43576 = CARTESIAN_POINT ( 'NONE',  ( -21.52544592524343514, 5.823673210054127303, 101.0405762719810383 ) ) ;
#43577 = CARTESIAN_POINT ( 'NONE',  ( -4.713425861958496554, 4.023676584314499038, -64.51712888360829368 ) ) ;
#43578 = CARTESIAN_POINT ( 'NONE',  ( -10.72451020669898014, 18.67979575497178502, 60.41557627198102409 ) ) ;
#43579 = CARTESIAN_POINT ( 'NONE',  ( 12.06949235617739724, 12.14591786802326823, 86.87609039468568994 ) ) ;
#43580 = CARTESIAN_POINT ( 'NONE',  ( -8.224510206698948167, 14.34966873604960824, 110.4155762719810383 ) ) ;
#43581 = CARTESIAN_POINT ( 'NONE',  ( 16.46253265017160672, -9.564922557960803928, 53.33224293864768839 ) ) ;
#43582 = CARTESIAN_POINT ( 'NONE',  ( -8.314922557961024197, 14.29746914071037800, 102.9177570613523756 ) ) ;
#43583 = CARTESIAN_POINT ( 'NONE',  ( 10.81492255796106328, -18.62759615963255655, 50.41775706135235424 ) ) ;
#43584 = CARTESIAN_POINT ( 'NONE',  ( -9.474510206698964154, 16.51473224551069663, 115.4155762719810241 ) ) ;
#43585 = CARTESIAN_POINT ( 'NONE',  ( 10.81492255796106328, -18.62759615963255655, 85.41775706135236135 ) ) ;
#43586 = CARTESIAN_POINT ( 'NONE',  ( -19.03943276465977164, 0.05219959533909376836, 36.24890960531436690 ) ) ;
#43587 = CARTESIAN_POINT ( 'NONE',  ( 5.153800228976335163, 19.02544592524342804, 44.79057627198103830 ) ) ;
#43588 = ORIENTED_EDGE ( 'NONE', *, *, #51079, .T. ) ;
#43589 = CARTESIAN_POINT ( 'NONE',  ( 21.53943276465977519, 0.05219959533937863772, 71.25109039468568994 ) ) ;
#43590 = CARTESIAN_POINT ( 'NONE',  ( 19.02544592524343514, -5.153800228976328945, 103.5405762719809957 ) ) ;
#43591 = CARTESIAN_POINT ( 'NONE',  ( 9.564922557961047289, -16.46253265017146816, 75.41775706135234714 ) ) ;
#43592 = CARTESIAN_POINT ( 'NONE',  ( 21.52544592524334988, 5.823673210054432836, 51.45942372801901854 ) ) ;
#43593 = CARTESIAN_POINT ( 'NONE',  ( -16.52544592524335698, -4.483927247898792601, 23.95942372801901143 ) ) ;
#43594 = CARTESIAN_POINT ( 'NONE',  ( 19.03943276465977164, 0.05219959533936151252, 71.25109039468566152 ) ) ;
#43595 = CARTESIAN_POINT ( 'NONE',  ( 5.049401038298161559, -19.05341960407611168, 47.70724293864770260 ) ) ;
#43596 = CARTESIAN_POINT ( 'NONE',  ( 16.46253265017146816, 9.564922557961045513, 86.66775706135233293 ) ) ;
#43597 = EDGE_CURVE ( 'NONE', #155866, #52144, #192804, .T. ) ;
#43598 = CARTESIAN_POINT ( 'NONE',  ( -8.224510206698948167, 14.34966873604960824, 30.41557627198101699 ) ) ;
#43599 = CARTESIAN_POINT ( 'NONE',  ( -19.05341960407617563, 5.049401038297882671, 93.54275706135234714 ) ) ;
#43600 = CARTESIAN_POINT ( 'NONE',  ( -4.483927247898539470, -16.52544592524342804, 37.29057627198102409 ) ) ;
#43601 = CARTESIAN_POINT ( 'NONE',  ( 19.05341960407617918, -5.049401038297876454, 66.04275706135233293 ) ) ;
#43602 = CARTESIAN_POINT ( 'NONE',  ( 0.05219959533934541429, -16.53943276465976808, 45.00109039468568284 ) ) ;
#43603 = CARTESIAN_POINT ( 'NONE',  ( 5.049401038297881783, 19.05341960407617563, 22.29275706135233648 ) ) ;
#43604 = CARTESIAN_POINT ( 'NONE',  ( -16.46253265017160317, 9.564922557960807481, 40.83224293864769550 ) ) ;
#43605 = CARTESIAN_POINT ( 'NONE',  ( -3.573655867282028392E-15, 2.428612866367529932E-14, 2.000000000000000000 ) ) ;
#43606 = CARTESIAN_POINT ( 'NONE',  ( 14.34966873604972726, -8.224510206698740333, 45.83442372801901854 ) ) ;
#43607 = CARTESIAN_POINT ( 'NONE',  ( 0.000000000000000000, 0.000000000000000000, -25.00000000000000000 ) ) ;
#43608 = CARTESIAN_POINT ( 'NONE',  ( -8.571926809382601320, -26.38167802310801591, 145.2750000027311899 ) ) ;
#43609 = CARTESIAN_POINT ( 'NONE',  ( 5.049401038298161559, -19.05341960407611168, 92.70724293864769550 ) ) ;
#43610 = CARTESIAN_POINT ( 'NONE',  ( 18.22780087662122384, -5.500000000000022204, 86.01540105326108687 ) ) ;
#43611 = ORIENTED_EDGE ( 'NONE', *, *, #162842, .F. ) ;
#43612 = CARTESIAN_POINT ( 'NONE',  ( 9.474510206698729675, 16.51473224551082808, 87.08442372801900433 ) ) ;
#43613 = CARTESIAN_POINT ( 'NONE',  ( 9.564922557960805705, 16.46253265017160317, 114.5822429386476955 ) ) ;
#43615 = CARTESIAN_POINT ( 'NONE',  ( -19.05341960407617563, 5.049401038297882671, 98.54275706135233293 ) ) ;
#43614 = CARTESIAN_POINT ( 'NONE',  ( 16.46253265017146816, 9.564922557961045513, 21.66775706135233648 ) ) ;
#43616 = CARTESIAN_POINT ( 'NONE',  ( 12.06949235617757843, -12.14591786802309237, 113.1239096053143953 ) ) ;
#43617 = CARTESIAN_POINT ( 'NONE',  ( -19.05341960407611168, -5.049401038298163336, 41.45724293864769550 ) ) ;
#43618 = CARTESIAN_POINT ( 'NONE',  ( 21.55341960407610458, 5.719274019375980345, 53.95724293864770260 ) ) ;
#43619 = CARTESIAN_POINT ( 'NONE',  ( -0.05219959533909027116, -19.03943276465977164, 22.49890960531436690 ) ) ;
#43620 = DIRECTION ( 'NONE',  ( -1.000000000000000000, 0.000000000000000000, 0.000000000000000000 ) ) ;
#43621 = CARTESIAN_POINT ( 'NONE',  ( -0.05219959533936034679, 19.03943276465977164, 67.50109039468566152 ) ) ;
#43622 = CARTESIAN_POINT ( 'NONE',  ( -16.55341960407611168, -4.379528057220339221, 51.45724293864770260 ) ) ;
#43624 = EDGE_CURVE ( 'NONE', #164433, #133568, #59459, .T. ) ;
#43623 = CARTESIAN_POINT ( 'NONE',  ( -15.72974639402197994, 15.80617190586746368, 35.62390960531437401 ) ) ;
#43625 = CARTESIAN_POINT ( 'NONE',  ( -5.719274019375665041, -21.55341960407619695, 94.79275706135234714 ) ) ;
#43626 = CARTESIAN_POINT ( 'NONE',  ( 0.05219959533907565091, 21.53943276465977519, 79.99890960531435269 ) ) ;
#43627 = CARTESIAN_POINT ( 'NONE',  ( 5.719274019375673035, 21.55341960407619339, 62.29275706135236845 ) ) ;
#43628 = CARTESIAN_POINT ( 'NONE',  ( -21.52544592524334988, -5.823673210054445271, 63.95942372801901854 ) ) ;
#43629 = CARTESIAN_POINT ( 'NONE',  ( 16.51473224551069308, 9.474510206698969483, 94.16557627198103830 ) ) ;
#43631 = CARTESIAN_POINT ( 'NONE',  ( -15.72974639402176322, -15.80617190586768395, 69.37609039468567573 ) ) ;
#43630 = CARTESIAN_POINT ( 'NONE',  ( -12.14591786802326823, 12.06949235617739902, 98.12609039468570415 ) ) ;
#43632 = CARTESIAN_POINT ( 'NONE',  ( -14.29746914071049879, 8.314922557960819915, 115.8322429386477097 ) ) ;
#43633 = AXIS2_PLACEMENT_3D ( 'NONE', #136722, #134763, #103416 ) ;
#43634 = CARTESIAN_POINT ( 'NONE',  ( -4.483927247898539470, -16.52544592524342804, 62.29057627198102409 ) ) ;
#43635 = CARTESIAN_POINT ( 'NONE',  ( 4.379528057220339221, -16.55341960407611168, 32.70724293864770260 ) ) ;
#43636 = CARTESIAN_POINT ( 'NONE',  ( 21.55341960407610458, 5.719274019375980345, 38.95724293864768839 ) ) ;
#43637 = CARTESIAN_POINT ( 'NONE',  ( 0.05219959533909260263, 19.03943276465977164, 44.99890960531435979 ) ) ;
#43638 = CARTESIAN_POINT ( 'NONE',  ( -21.53943276465977519, 0.05219959533907696930, 61.24890960531435979 ) ) ;
#43639 = CARTESIAN_POINT ( 'NONE',  ( -5.049401038297874678, -19.05341960407617918, 54.79275706135234003 ) ) ;
#43641 = CARTESIAN_POINT ( 'NONE',  ( 12.14591786802309770, 12.06949235617756955, 44.37390960531435979 ) ) ;
#43640 = CARTESIAN_POINT ( 'NONE',  ( -16.21995358207306026, -7.366697692864122793, 40.06448998487842772 ) ) ;
#43642 = CARTESIAN_POINT ( 'NONE',  ( -5.719274019375978568, 21.55341960407610458, 30.20724293864769550 ) ) ;
#43643 = ORIENTED_EDGE ( 'NONE', *, *, #60477, .F. ) ;
#43644 = ORIENTED_EDGE ( 'NONE', *, *, #31456, .T. ) ;
#43645 = CARTESIAN_POINT ( 'NONE',  ( 30.20036327792367814, -26.22857331006468584, -17.18026671435356434 ) ) ;
#43646 = CARTESIAN_POINT ( 'NONE',  ( -12.06949235617739369, -12.14591786802326823, 74.37609039468568994 ) ) ;
#43647 = CARTESIAN_POINT ( 'NONE',  ( -19.02544592524334988, -5.153800228976617603, 78.95942372801900433 ) ) ;
#43648 = EDGE_CURVE ( 'NONE', #130010, #116580, #190230, .T. ) ;
#43649 = CARTESIAN_POINT ( 'NONE',  ( 8.314922557960818139, 14.29746914071049879, 44.58224293864769550 ) ) ;
#43650 = CARTESIAN_POINT ( 'NONE',  ( 17.05587630539789146, -6.762274262135623992, 53.24180309037312497 ) ) ;
#43651 = CARTESIAN_POINT ( 'NONE',  ( 16.53943276465976808, -0.05219959533910856209, 23.74890960531435269 ) ) ;
#43652 = CARTESIAN_POINT ( 'NONE',  ( -13.97604488694527625, -13.89961937509977652, 46.87390960531435979 ) ) ;
#43653 = CARTESIAN_POINT ( 'NONE',  ( -0.05219959533909027116, -19.03943276465977164, 72.49890960531435269 ) ) ;
#43654 = AXIS2_PLACEMENT_3D ( 'NONE', #27724, #151056, #174160 ) ;
#43655 = CARTESIAN_POINT ( 'NONE',  ( 19.02544592524343514, -5.153800228976328945, 43.54057627198103120 ) ) ;
#43656 = CARTESIAN_POINT ( 'NONE',  ( -15.72974639402176322, -15.80617190586768395, 49.37609039468569705 ) ) ;
#43657 = CARTESIAN_POINT ( 'NONE',  ( -19.05341960407611168, -5.049401038298163336, 66.45724293864769550 ) ) ;
#43658 = CARTESIAN_POINT ( 'NONE',  ( 5.000000000000000000, -126.2936762853306902, 8.011306146643438097 ) ) ;
#43659 = CARTESIAN_POINT ( 'NONE',  ( 9.564922557960805705, 16.46253265017160317, 64.58224293864769550 ) ) ;
#43660 = CARTESIAN_POINT ( 'NONE',  ( 10.72451020669898902, -18.67979575497178502, 42.91557627198103120 ) ) ;
#43661 = CARTESIAN_POINT ( 'NONE',  ( -16.51473224551069308, -9.474510206698971260, 31.66557627198102054 ) ) ;
#43662 = CARTESIAN_POINT ( 'NONE',  ( -18.67979575497178146, -10.72451020669898902, 41.66557627198103120 ) ) ;
#43663 = CARTESIAN_POINT ( 'NONE',  ( -4.483927247898782831, 16.52544592524335698, 92.70942372801901854 ) ) ;
#43664 = CARTESIAN_POINT ( 'NONE',  ( -9.564922557961040184, 16.46253265017147172, 27.91775706135232582 ) ) ;
#43665 = CARTESIAN_POINT ( 'NONE',  ( -14.34966873604972548, 8.224510206698743886, 73.33442372801901854 ) ) ;
#43666 = CARTESIAN_POINT ( 'NONE',  ( 0.05219959533909260263, 19.03943276465977164, 114.9989096053143669 ) ) ;
#43667 = CARTESIAN_POINT ( 'NONE',  ( -4.483927247898782831, 16.52544592524335698, 47.70942372801902565 ) ) ;
#43668 = CARTESIAN_POINT ( 'NONE',  ( 4.483927247898790824, -16.52544592524335698, 35.20942372801901854 ) ) ;
#43669 = CARTESIAN_POINT ( 'NONE',  ( 13.97604488694527802, 13.89961937509977652, 109.3739096053143669 ) ) ;
#43670 = CARTESIAN_POINT ( 'NONE',  ( 8.314922557961029526, -14.29746914071037800, 30.41775706135234358 ) ) ;
#43671 = CARTESIAN_POINT ( 'NONE',  ( 9.564922557960805705, 16.46253265017160317, 39.58224293864768839 ) ) ;
#43672 = CARTESIAN_POINT ( 'NONE',  ( -10.72451020669870658, -18.67979575497194134, 29.58442372801901854 ) ) ;
#43673 = CARTESIAN_POINT ( 'NONE',  ( 9.474510206698729675, 16.51473224551082808, 112.0844237280190043 ) ) ;
#43674 = CARTESIAN_POINT ( 'NONE',  ( 8.314922557961029526, -14.29746914071037800, 105.4177570613523613 ) ) ;
#43675 = DIRECTION ( 'NONE',  ( 0.000000000000000000, 0.000000000000000000, 1.000000000000000000 ) ) ;
#43676 = CARTESIAN_POINT ( 'NONE',  ( 0.05219959533937995610, -21.53943276465977519, 105.0010903946856757 ) ) ;
#43677 = CARTESIAN_POINT ( 'NONE',  ( -0.05219959533936034679, 19.03943276465977164, 92.50109039468566152 ) ) ;
#43678 = CARTESIAN_POINT ( 'NONE',  ( 16.55341960407611168, 4.379528057220329451, 53.95724293864770260 ) ) ;
#43679 = CARTESIAN_POINT ( 'NONE',  ( -14.29746914071049879, 8.314922557960819915, 115.8322429386477097 ) ) ;
#43681 = CARTESIAN_POINT ( 'NONE',  ( -8.725106586199771641, 0.9968436689773673143, -64.02420483255114902 ) ) ;
#43680 = CARTESIAN_POINT ( 'NONE',  ( -19.05341960407617563, 5.049401038297882671, 63.54275706135234003 ) ) ;
#43682 = CARTESIAN_POINT ( 'NONE',  ( 10.72451020669871369, 18.67979575497193778, 47.08442372801901854 ) ) ;
#43683 = CARTESIAN_POINT ( 'NONE',  ( -16.55341960407617563, 4.379528057220093196, 23.54275706135235424 ) ) ;
#43684 = CARTESIAN_POINT ( 'NONE',  ( 3.889087296526329229, 29.99999999999996092, 1.818019484660534868 ) ) ;
#43685 = CARTESIAN_POINT ( 'NONE',  ( -9.564922557960796823, -16.46253265017161027, 112.0822429386476955 ) ) ;
#43686 = CARTESIAN_POINT ( 'NONE',  ( 21.55341960407610458, 5.719274019375980345, 73.95724293864769550 ) ) ;
#43687 = CARTESIAN_POINT ( 'NONE',  ( -19.03943276465977164, -0.05219959533935918106, 108.7510903946856615 ) ) ;
#43688 = CARTESIAN_POINT ( 'NONE',  ( -16.51473224551069308, -9.474510206698971260, 96.66557627198102409 ) ) ;
#43689 = CARTESIAN_POINT ( 'NONE',  ( -17.17579732620334454, -22.53935769174907122, 140.0000000000000000 ) ) ;
#43690 = CARTESIAN_POINT ( 'NONE',  ( -16.46253265017160317, 9.564922557960807481, 30.83224293864769550 ) ) ;
#43691 = CARTESIAN_POINT ( 'NONE',  ( -0.05219959533937732626, 21.53943276465977519, 97.50109039468567573 ) ) ;
#43692 = CARTESIAN_POINT ( 'NONE',  ( 16.51473224551069308, 9.474510206698969483, 44.16557627198103120 ) ) ;
#43693 = AXIS2_PLACEMENT_3D ( 'NONE', #156399, #17903, #34058 ) ;
#43694 = CARTESIAN_POINT ( 'NONE',  ( 15.80617190586769283, -15.72974639402175789, 45.62609039468567573 ) ) ;
#43695 = CARTESIAN_POINT ( 'NONE',  ( 15.72974639402176855, 15.80617190586768217, 91.87609039468568994 ) ) ;
#43696 = CARTESIAN_POINT ( 'NONE',  ( 14.29746914071037800, 8.314922557961029526, 106.6677570613523756 ) ) ;
#43697 = CARTESIAN_POINT ( 'NONE',  ( -5.153800228976328057, -19.02544592524343514, 77.29057627198099567 ) ) ;
#43698 = CARTESIAN_POINT ( 'NONE',  ( -15.72974639402176322, -15.80617190586768395, 49.37609039468569705 ) ) ;
#43699 = CARTESIAN_POINT ( 'NONE',  ( 15.80617190586769283, -15.72974639402175789, 35.62609039468568994 ) ) ;
#43701 = CARTESIAN_POINT ( 'NONE',  ( -19.05341960407611168, -5.049401038298163336, 86.45724293864769550 ) ) ;
#43700 = CARTESIAN_POINT ( 'NONE',  ( 13.89961937509957401, 13.97604488694547697, 76.87609039468566152 ) ) ;
#43702 = CARTESIAN_POINT ( 'NONE',  ( -0.05219959533910754901, -16.53943276465976808, 102.4989096053143811 ) ) ;
#43703 = CARTESIAN_POINT ( 'NONE',  ( 18.67979575497178502, 10.72451020669898547, 94.16557627198103830 ) ) ;
#43704 = CARTESIAN_POINT ( 'NONE',  ( -8.314922557960811034, -14.29746914071050412, 77.08224293864769550 ) ) ;
#43705 = CARTESIAN_POINT ( 'NONE',  ( 21.55341960407619695, -5.719274019375665929, 111.0427570613523613 ) ) ;
#43706 = CARTESIAN_POINT ( 'NONE',  ( 16.53943276465976808, -0.05219959533910856209, 98.74890960531438111 ) ) ;
#43707 = CARTESIAN_POINT ( 'NONE',  ( 13.89961937509977652, -13.97604488694527269, 33.12390960531434558 ) ) ;
#43709 = CIRCLE ( 'NONE', #156707, 2.000000000000001776 ) ;
#43708 = CARTESIAN_POINT ( 'NONE',  ( 5.049401038297881783, 19.05341960407617563, 82.29275706135229029 ) ) ;
#43710 = CARTESIAN_POINT ( 'NONE',  ( 4.379528057220339221, -16.55341960407611168, 42.70724293864770260 ) ) ;
#43711 = CARTESIAN_POINT ( 'NONE',  ( -21.52544592524334988, -5.823673210054445271, 93.95942372801903275 ) ) ;
#43712 = CARTESIAN_POINT ( 'NONE',  ( 9.474510206698971260, -16.51473224551069308, 107.9155762719810383 ) ) ;
#43713 = CARTESIAN_POINT ( 'NONE',  ( 0.05219959533936267826, -19.03943276465977164, 70.00109039468566152 ) ) ;
#43714 = CARTESIAN_POINT ( 'NONE',  ( 21.55341960407610458, 5.719274019375980345, 83.95724293864770971 ) ) ;
#43715 = CARTESIAN_POINT ( 'NONE',  ( 0.05219959533937995610, -21.53943276465977519, 30.00109039468568284 ) ) ;
#43716 = CARTESIAN_POINT ( 'NONE',  ( -16.52544592524335698, -4.483927247898792601, 23.95942372801901143 ) ) ;
#43717 = CARTESIAN_POINT ( 'NONE',  ( -8.224510206698735004, -14.34966873604973081, 89.58442372801901854 ) ) ;
#43719 = CARTESIAN_POINT ( 'NONE',  ( -21.55341960407619339, 5.719274019375674811, 38.54275706135234714 ) ) ;
#43718 = CARTESIAN_POINT ( 'NONE',  ( -13.89961937509977652, 13.97604488694528158, 30.62390960531435269 ) ) ;
#43720 = CARTESIAN_POINT ( 'NONE',  ( 13.97604488694527802, 13.89961937509977652, 24.37390960531435624 ) ) ;
#43721 = CARTESIAN_POINT ( 'NONE',  ( 38.00000000000000711, -12.34694845685040754, -8.849999994537625980 ) ) ;
#43722 = CARTESIAN_POINT ( 'NONE',  ( -12.14591786802326823, 12.06949235617739902, 53.12609039468568284 ) ) ;
#43723 = CARTESIAN_POINT ( 'NONE',  ( -14.29746914071049879, 8.314922557960819915, 80.83224293864769550 ) ) ;
#43724 = CARTESIAN_POINT ( 'NONE',  ( 18.67979575497178502, 10.72451020669898547, 74.16557627198102409 ) ) ;
#43725 = CARTESIAN_POINT ( 'NONE',  ( -14.34966873604960291, -8.224510206698953496, 31.66557627198102054 ) ) ;
#43726 = CARTESIAN_POINT ( 'NONE',  ( -8.314922557961024197, 14.29746914071037800, 52.91775706135235424 ) ) ;
#43727 = CARTESIAN_POINT ( 'NONE',  ( 9.474510206698971260, -16.51473224551069308, 42.91557627198103120 ) ) ;
#43728 = CARTESIAN_POINT ( 'NONE',  ( 14.29746914071037800, 8.314922557961029526, 91.66775706135234714 ) ) ;
#43729 = CARTESIAN_POINT ( 'NONE',  ( -13.89961937509957401, -13.97604488694547875, 89.37609039468563310 ) ) ;
#43730 = CARTESIAN_POINT ( 'NONE',  ( 21.52544592524344225, -5.823673210054117533, 88.54057627198103830 ) ) ;
#43731 = CARTESIAN_POINT ( 'NONE',  ( 16.53943276465976808, 0.05219959533934440121, 111.2510903946856899 ) ) ;
#43732 = ORIENTED_EDGE ( 'NONE', *, *, #155029, .T. ) ;
#43733 = CARTESIAN_POINT ( 'NONE',  ( 26.36463166569312477, 3.076743934663749069, 174.2851114983683942 ) ) ;
#43734 = CARTESIAN_POINT ( 'NONE',  ( -0.05219959533907301413, -21.53943276465977519, 57.49890960531435979 ) ) ;
#43735 = ORIENTED_EDGE ( 'NONE', *, *, #44529, .F. ) ;
#43736 = ORIENTED_EDGE ( 'NONE', *, *, #53248, .F. ) ;
#43737 = CARTESIAN_POINT ( 'NONE',  ( -14.34966873604972548, 8.224510206698743886, 93.33442372801901854 ) ) ;
#43738 = ORIENTED_EDGE ( 'NONE', *, *, #124684, .F. ) ;
#43739 = CARTESIAN_POINT ( 'NONE',  ( -5.823673210054116645, -21.52544592524344225, 22.29057627198102765 ) ) ;
#43740 = CARTESIAN_POINT ( 'NONE',  ( -38.00000000000000711, 2.428612866367529932E-14, -7.749999994537626336 ) ) ;
#43741 = CARTESIAN_POINT ( 'NONE',  ( -0.05219959533907301413, -21.53943276465977519, 72.49890960531435269 ) ) ;
#43742 = CARTESIAN_POINT ( 'NONE',  ( -8.314922557961024197, 14.29746914071037800, 112.9177570613523329 ) ) ;
#43743 = CARTESIAN_POINT ( 'NONE',  ( -12.06949235617739369, -12.14591786802326823, 24.37609039468567573 ) ) ;
#43744 = CARTESIAN_POINT ( 'NONE',  ( -12.06949235617756955, 12.14591786802309770, 115.6239096053143669 ) ) ;
#43745 = CARTESIAN_POINT ( 'NONE',  ( 8.224510206698742110, 14.34966873604972548, 32.08442372801901854 ) ) ;
#43746 = CARTESIAN_POINT ( 'NONE',  ( 19.02544592524343514, -5.153800228976328945, 58.54057627198102409 ) ) ;
#43747 = CARTESIAN_POINT ( 'NONE',  ( -28.82186960331499392, -9.364793116373526516, 142.0999999999999659 ) ) ;
#43748 = CARTESIAN_POINT ( 'NONE',  ( 19.03943276465977164, -0.05219959533909143690, 103.7489096053143669 ) ) ;
#43749 = CARTESIAN_POINT ( 'NONE',  ( -16.55341960407617563, 4.379528057220093196, 93.54275706135234714 ) ) ;
#43750 = CARTESIAN_POINT ( 'NONE',  ( 0.05219959533936267826, -19.03943276465977164, 95.00109039468567573 ) ) ;
#43751 = CARTESIAN_POINT ( 'NONE',  ( -16.46253265017146816, -9.564922557961047289, 24.16775706135233648 ) ) ;
#43752 = CARTESIAN_POINT ( 'NONE',  ( 21.53943276465977519, -0.05219959533907433946, 73.74890960531433848 ) ) ;
#43753 = CARTESIAN_POINT ( 'NONE',  ( 0.05219959533934541429, -16.53943276465976808, 95.00109039468568994 ) ) ;
#43754 = CARTESIAN_POINT ( 'NONE',  ( -9.564922557961040184, 16.46253265017147172, 92.91775706135233293 ) ) ;
#43755 = CARTESIAN_POINT ( 'NONE',  ( 16.51473224551069308, 9.474510206698969483, 44.16557627198103120 ) ) ;
#43756 = CARTESIAN_POINT ( 'NONE',  ( -5.049401038298153566, 19.05341960407611168, 85.20724293864766707 ) ) ;
#43757 = CARTESIAN_POINT ( 'NONE',  ( 10.72451020669871369, 18.67979575497193778, 62.08442372801901143 ) ) ;
#43758 = CARTESIAN_POINT ( 'NONE',  ( -9.474510206698964154, 16.51473224551069663, 65.41557627198102409 ) ) ;
#43759 = CARTESIAN_POINT ( 'NONE',  ( -14.29746914071049879, 8.314922557960819915, 80.83224293864769550 ) ) ;
#43760 = CARTESIAN_POINT ( 'NONE',  ( -16.20579543436679160, -7.371946100355097897, 85.56520834171882939 ) ) ;
#43761 = CARTESIAN_POINT ( 'NONE',  ( 8.314922557960818139, 14.29746914071049879, 79.58224293864769550 ) ) ;
#43762 = CARTESIAN_POINT ( 'NONE',  ( 18.62759615963271287, -10.81492255796078972, 78.33224293864770971 ) ) ;
#43763 = CARTESIAN_POINT ( 'NONE',  ( -5.049401038297874678, -19.05341960407617918, 89.79275706135230450 ) ) ;
#43764 = FACE_OUTER_BOUND ( 'NONE', #83531, .T. ) ;
#43765 = CARTESIAN_POINT ( 'NONE',  ( -16.51473224551082808, 9.474510206698731452, 43.33442372801900433 ) ) ;
#43766 = CARTESIAN_POINT ( 'NONE',  ( 31.68374724557848765, -1.945525369148856987, 102.2474955886453643 ) ) ;
#43768 = CARTESIAN_POINT ( 'NONE',  ( -9.474510206698964154, 16.51473224551069663, 80.41557627198103830 ) ) ;
#43767 = CARTESIAN_POINT ( 'NONE',  ( 13.97604488694527802, 13.89961937509977652, 79.37390960531435269 ) ) ;
#43769 = CARTESIAN_POINT ( 'NONE',  ( -12.14591786802326823, 12.06949235617739902, 63.12609039468568994 ) ) ;
#43770 = CARTESIAN_POINT ( 'NONE',  ( -22.32889156691206622, 5.550768075871975071, 173.1969276168243823 ) ) ;
#43771 = CARTESIAN_POINT ( 'NONE',  ( -19.02544592524334988, -5.153800228976617603, 48.95942372801900433 ) ) ;
#43772 = CARTESIAN_POINT ( 'NONE',  ( -17.49999999999999645, 5.499999999999992895, 98.71769037696435589 ) ) ;
#43773 = CARTESIAN_POINT ( 'NONE',  ( -16.51473224551069308, -9.474510206698971260, 106.6655762719810383 ) ) ;
#43774 = CARTESIAN_POINT ( 'NONE',  ( 12.06949235617739724, 12.14591786802326823, 96.87609039468568994 ) ) ;
#43775 = CARTESIAN_POINT ( 'NONE',  ( -19.99999999999998224, -188.0000000000000000, -15.00000000000000000 ) ) ;
#43776 = CARTESIAN_POINT ( 'NONE',  ( 4.483927247898790824, -16.52544592524335698, 75.20942372801901854 ) ) ;
#43777 = CARTESIAN_POINT ( 'NONE',  ( -16.81555441253551564, 7.025013491695477619, 30.63685445334257551 ) ) ;
#43778 = CARTESIAN_POINT ( 'NONE',  ( -16.52544592524335698, -4.483927247898792601, 48.95942372801902565 ) ) ;
#43779 = CARTESIAN_POINT ( 'NONE',  ( 16.51473224551069308, 9.474510206698969483, 74.16557627198103830 ) ) ;
#43780 = CARTESIAN_POINT ( 'NONE',  ( 21.53943276465977519, 0.05219959533937863772, 71.25109039468568994 ) ) ;
#43781 = CARTESIAN_POINT ( 'NONE',  ( -9.474510206698720793, -16.51473224551083518, 69.58442372801901854 ) ) ;
#43782 = CARTESIAN_POINT ( 'NONE',  ( 19.05341960407617918, -5.049401038297876454, 21.04275706135232582 ) ) ;
#43783 = AXIS2_PLACEMENT_3D ( 'NONE', #17316, #139641, #3134 ) ;
#43784 = CARTESIAN_POINT ( 'NONE',  ( 5.049401038298161559, -19.05341960407611168, 57.70724293864769550 ) ) ;
#43785 = CARTESIAN_POINT ( 'NONE',  ( 0.05219959533909260263, 19.03943276465977164, 49.99890960531435979 ) ) ;
#43786 = DIRECTION ( 'NONE',  ( 0.000000000000000000, 0.000000000000000000, -1.000000000000000000 ) ) ;
#43787 = CARTESIAN_POINT ( 'NONE',  ( -5.823673210054116645, -21.52544592524344225, 67.29057627198103830 ) ) ;
#43788 = CARTESIAN_POINT ( 'NONE',  ( -15.72974639402197994, 15.80617190586746368, 35.62390960531437401 ) ) ;
#43789 = CARTESIAN_POINT ( 'NONE',  ( 19.03943276465977164, -0.05219959533909143690, 23.74890960531435269 ) ) ;
#43790 = CARTESIAN_POINT ( 'NONE',  ( -12.06949235617739369, -12.14591786802326823, 49.37609039468569705 ) ) ;
#43791 = EDGE_LOOP ( 'NONE', ( #62971, #160380, #75656, #168823 ) ) ;
#43792 = EDGE_CURVE ( 'NONE', #60746, #8743, #141726, .T. ) ;
#43793 = CARTESIAN_POINT ( 'NONE',  ( -15.72974639402176322, -15.80617190586768395, 34.37609039468568284 ) ) ;
#43795 = CARTESIAN_POINT ( 'NONE',  ( 11.74264578624799427, 36.14014761921585972, -6.599999999999999645 ) ) ;
#43794 = CARTESIAN_POINT ( 'NONE',  ( -0.05219959533910754901, -16.53943276465976808, 47.49890960531435979 ) ) ;
#43796 = CARTESIAN_POINT ( 'NONE',  ( -0.05219959533936034679, 19.03943276465977164, 102.5010903946856757 ) ) ;
#43797 = CARTESIAN_POINT ( 'NONE',  ( 16.46253265017146816, 9.564922557961045513, 36.66775706135233293 ) ) ;
#43798 = CARTESIAN_POINT ( 'NONE',  ( 8.224510206698953496, -14.34966873604960469, 42.91557627198103120 ) ) ;
#43799 = CARTESIAN_POINT ( 'NONE',  ( -21.52544592524343514, 5.823673210054127303, 116.0405762719810383 ) ) ;
#43801 = CARTESIAN_POINT ( 'NONE',  ( -15.72974639402197994, 15.80617190586746368, 80.62390960531438111 ) ) ;
#43800 = DIRECTION ( 'NONE',  ( 0.000000000000000000, 0.000000000000000000, 1.000000000000000000 ) ) ;
#43802 = CARTESIAN_POINT ( 'NONE',  ( 13.97604488694527802, 13.89961937509977652, 89.37390960531436690 ) ) ;
#43803 = CARTESIAN_POINT ( 'NONE',  ( 16.52544592524342804, -4.483927247898539470, 58.54057627198103120 ) ) ;
#43804 = CARTESIAN_POINT ( 'NONE',  ( -9.564922557960796823, -16.46253265017161027, 102.0822429386477097 ) ) ;
#43805 = CARTESIAN_POINT ( 'NONE',  ( -193.3062444957834884, -155.7167183371838064, -23.00000000000000000 ) ) ;
#43806 = CARTESIAN_POINT ( 'NONE',  ( 0.05219959533936267826, -19.03943276465977164, 50.00109039468566863 ) ) ;
#43807 = CARTESIAN_POINT ( 'NONE',  ( -10.81492255796078084, -18.62759615963271287, 112.0822429386477097 ) ) ;
#43808 = CARTESIAN_POINT ( 'NONE',  ( 5.049401038298161559, -19.05341960407611168, 42.70724293864767418 ) ) ;
#43809 = CARTESIAN_POINT ( 'NONE',  ( -9.564922557960796823, -16.46253265017161027, 22.08224293864768839 ) ) ;
#43810 = CARTESIAN_POINT ( 'NONE',  ( -5.823673210054431948, 21.52544592524334988, 52.70942372801902565 ) ) ;
#43811 = CARTESIAN_POINT ( 'NONE',  ( -8.571926809382608425, 26.38167802310805854, 146.4750000027311785 ) ) ;
#43812 = CARTESIAN_POINT ( 'NONE',  ( 14.34966873604960469, 8.224510206698951720, 44.16557627198103120 ) ) ;
#43813 = CARTESIAN_POINT ( 'NONE',  ( 13.97604488694527802, 13.89961937509977652, 49.37390960531434558 ) ) ;
#43814 = CARTESIAN_POINT ( 'NONE',  ( -13.89961937509977652, 13.97604488694528158, 95.62390960531436690 ) ) ;
#43815 = CARTESIAN_POINT ( 'NONE',  ( -5.719274019375978568, 21.55341960407610458, 75.20724293864769550 ) ) ;
#43816 = CARTESIAN_POINT ( 'NONE',  ( -27.73933785331498925, 9.013057229001089965, 144.7750000027311614 ) ) ;
#43817 = CARTESIAN_POINT ( 'NONE',  ( -19.05341960407611168, -5.049401038298163336, 51.45724293864770260 ) ) ;
#43818 = CARTESIAN_POINT ( 'NONE',  ( -18.67979575497178146, -10.72451020669898902, 56.66557627198103830 ) ) ;
#43819 = CARTESIAN_POINT ( 'NONE',  ( -15.72974639402176322, -15.80617190586768395, 84.37609039468570415 ) ) ;
#43822 = CARTESIAN_POINT ( 'NONE',  ( -0.05219959533910754901, -16.53943276465976808, 72.49890960531435269 ) ) ;
#43821 = CARTESIAN_POINT ( 'NONE',  ( -4.483927247898782831, 16.52544592524335698, 77.70942372801900433 ) ) ;
#43820 = DIRECTION ( 'NONE',  ( 1.000000000000000000, 0.000000000000000000, 0.000000000000000000 ) ) ;
#43823 = CARTESIAN_POINT ( 'NONE',  ( -16.46253265017160317, 9.564922557960807481, 70.83224293864770971 ) ) ;
#43824 = VERTEX_POINT ( 'NONE', #80056 ) ;
#43825 = CARTESIAN_POINT ( 'NONE',  ( -5.153800228976607833, 19.02544592524334988, 22.70942372801899012 ) ) ;
#43826 = CARTESIAN_POINT ( 'NONE',  ( 16.52544592524335698, 4.483927247898782831, 91.45942372801901854 ) ) ;
#43827 = CARTESIAN_POINT ( 'NONE',  ( -16.46253265017146816, -9.564922557961047289, 19.16775706135233293 ) ) ;
#43828 = CARTESIAN_POINT ( 'NONE',  ( 19.05341960407611168, 5.049401038298154454, 73.95724293864768129 ) ) ;
#43829 = CARTESIAN_POINT ( 'NONE',  ( 5.719274019375991003, -21.55341960407610458, 52.70724293864769550 ) ) ;
#43830 = CARTESIAN_POINT ( 'NONE',  ( 14.29746914071037800, 8.314922557961029526, 31.66775706135234358 ) ) ;
#43831 = CARTESIAN_POINT ( 'NONE',  ( -10.81492255796105439, 18.62759615963255655, 97.91775706135236135 ) ) ;
#43832 = CARTESIAN_POINT ( 'NONE',  ( -16.52544592524335698, -4.483927247898792601, 58.95942372801902565 ) ) ;
#43833 = CARTESIAN_POINT ( 'NONE',  ( 0.05219959533907565091, 21.53943276465977519, 109.9989096053143527 ) ) ;
#43834 = CARTESIAN_POINT ( 'NONE',  ( 5.153800228976615827, -19.02544592524334988, 110.2094237280189901 ) ) ;
#43835 = CARTESIAN_POINT ( 'NONE',  ( 19.05341960407611168, 5.049401038298154454, 93.95724293864769550 ) ) ;
#43836 = CARTESIAN_POINT ( 'NONE',  ( 14.29746914071037800, 8.314922557961029526, 31.66775706135234358 ) ) ;
#43837 = CARTESIAN_POINT ( 'NONE',  ( -0.05219959533909027116, -19.03943276465977164, 52.49890960531436690 ) ) ;
#43838 = CARTESIAN_POINT ( 'NONE',  ( -12.06949235617739369, -12.14591786802326823, 34.37609039468568284 ) ) ;
#43839 = CARTESIAN_POINT ( 'NONE',  ( 12.06949235617757843, -12.14591786802309237, 73.12390960531436690 ) ) ;
#43840 = CARTESIAN_POINT ( 'NONE',  ( 16.55341960407618274, -4.379528057220086978, 86.04275706135236135 ) ) ;
#43842 = CARTESIAN_POINT ( 'NONE',  ( 13.89961937509977652, -13.97604488694527269, 63.12390960531435979 ) ) ;
#43841 = CARTESIAN_POINT ( 'NONE',  ( -10.81492255796105439, 18.62759615963255655, 42.91775706135235424 ) ) ;
#43843 = CARTESIAN_POINT ( 'NONE',  ( -19.03943276465977164, 0.05219959533909376836, 81.24890960531436690 ) ) ;
#43844 = CARTESIAN_POINT ( 'NONE',  ( 12.06949235617739724, 12.14591786802326823, 86.87609039468568994 ) ) ;
#43846 = ORIENTED_EDGE ( 'NONE', *, *, #88147, .F. ) ;
#43845 = CARTESIAN_POINT ( 'NONE',  ( -21.75836449082842705, -8.509082329565398339, 169.1767350484829251 ) ) ;
#43847 = ORIENTED_EDGE ( 'NONE', *, *, #191998, .F. ) ;
#43848 = CARTESIAN_POINT ( 'NONE',  ( 0.05219959533936267826, -19.03943276465977164, 35.00109039468566863 ) ) ;
#43849 = CARTESIAN_POINT ( 'NONE',  ( 16.46253265017160672, -9.564922557960803928, 93.33224293864769550 ) ) ;
#43850 = CARTESIAN_POINT ( 'NONE',  ( 5.049401038298161559, -19.05341960407611168, 47.70724293864770260 ) ) ;
#43851 = CARTESIAN_POINT ( 'NONE',  ( 16.46253265017160672, -9.564922557960803928, 108.3322429386476955 ) ) ;
#43852 = CARTESIAN_POINT ( 'NONE',  ( -0.05219959533934338120, 16.53943276465976808, 37.50109039468568284 ) ) ;
#43853 = B_SPLINE_CURVE_WITH_KNOTS ( 'NONE', 3,
 ( #29922, #108741, #153250, #75421, #186606, #15746, #198781, #109734, #137095, #91562, #141066, #77405, #76413, #140062, #60247, #199770, #121918, #14752, #47080, #184597, #46078, #185590 ),
 .UNSPECIFIED., .F., .F.,
 ( 4, 2, 2, 2, 2, 2, 2, 2, 2, 2, 4 ),
 ( 2.602085213965211027E-18, 0.001309639967555396075, 0.001964459951333086523, 0.002291869943221923507, 0.002455574939166342216, 0.002619279935110760058, 0.002782984931055178333, 0.002946689926999596608, 0.003274099918888406270, 0.003928919902666004778, 0.005238559870221203528 ),
 .UNSPECIFIED. ) ;
#43855 = CARTESIAN_POINT ( 'NONE',  ( -4.379528057220086978, -16.55341960407618274, 59.79275706135234714 ) ) ;
#43854 = CARTESIAN_POINT ( 'NONE',  ( -19.02544592524334988, -5.153800228976617603, 58.95942372801900433 ) ) ;
#43856 = CARTESIAN_POINT ( 'NONE',  ( 16.46253265017160672, -9.564922557960803928, 108.3322429386476955 ) ) ;
#43857 = CARTESIAN_POINT ( 'NONE',  ( -19.05341960407611168, -5.049401038298163336, 76.45724293864769550 ) ) ;
#43858 = CARTESIAN_POINT ( 'NONE',  ( -15.72974639402197994, 15.80617190586746368, 100.6239096053143811 ) ) ;
#43859 = CARTESIAN_POINT ( 'NONE',  ( -16.51473224551082808, 9.474510206698731452, 63.33442372801900433 ) ) ;
#43861 = DIRECTION ( 'NONE',  ( 1.000000000000000000, -0.000000000000000000, -0.000000000000000000 ) ) ;
#43860 = CARTESIAN_POINT ( 'NONE',  ( -19.02544592524342804, 5.153800228976336051, 96.04057627198103830 ) ) ;
#43862 = CARTESIAN_POINT ( 'NONE',  ( 13.89961937509977652, -13.97604488694527269, 78.12390960531433848 ) ) ;
#43864 = CARTESIAN_POINT ( 'NONE',  ( -19.05341960407611168, -5.049401038298163336, 26.45724293864769550 ) ) ;
#43863 = CARTESIAN_POINT ( 'NONE',  ( -12.06949235617756955, 12.14591786802309770, 30.62390960531436335 ) ) ;
#43865 = CARTESIAN_POINT ( 'NONE',  ( 19.02544592524334988, 5.153800228976608722, 41.45942372801900433 ) ) ;
#43866 = CARTESIAN_POINT ( 'NONE',  ( 0.05219959533910956823, 16.53943276465976808, 74.99890960531435269 ) ) ;
#43867 = CARTESIAN_POINT ( 'NONE',  ( 10.81492255796106328, -18.62759615963255655, 100.4177570613523471 ) ) ;
#43868 = CARTESIAN_POINT ( 'NONE',  ( -0.05219959533909027116, -19.03943276465977164, 42.49890960531435269 ) ) ;
#43870 = CARTESIAN_POINT ( 'NONE',  ( 0.05219959533937995610, -21.53943276465977519, 110.0010903946856757 ) ) ;
#43869 = CARTESIAN_POINT ( 'NONE',  ( 8.314922557960818139, 14.29746914071049879, 34.58224293864770260 ) ) ;
#43871 = CARTESIAN_POINT ( 'NONE',  ( 13.97604488694527802, 13.89961937509977652, 94.37390960531436690 ) ) ;
#43872 = CARTESIAN_POINT ( 'NONE',  ( -5.153800228976328057, -19.02544592524343514, 92.29057627198099567 ) ) ;
#43873 = CARTESIAN_POINT ( 'NONE',  ( -19.02544592524342804, 5.153800228976336051, 31.04057627198102409 ) ) ;
#43874 = CARTESIAN_POINT ( 'NONE',  ( 12.06949235617757843, -12.14591786802309237, 113.1239096053143953 ) ) ;
#43875 = CARTESIAN_POINT ( 'NONE',  ( 4.483927247898545687, 16.52544592524342804, 79.79057627198102409 ) ) ;
#43876 = CARTESIAN_POINT ( 'NONE',  ( -21.55341960407610458, -5.719274019375992779, 81.45724293864769550 ) ) ;
#43877 = CARTESIAN_POINT ( 'NONE',  ( 19.05341960407611168, 5.049401038298154454, 88.95724293864769550 ) ) ;
#43878 = CARTESIAN_POINT ( 'NONE',  ( -5.823673210054116645, -21.52544592524344225, 92.29057627198103830 ) ) ;
#43879 = CARTESIAN_POINT ( 'NONE',  ( 5.153800228976335163, 19.02544592524342804, 84.79057627198099567 ) ) ;
#43882 = CARTESIAN_POINT ( 'NONE',  ( 14.34966873604960469, 8.224510206698951720, 89.16557627198102409 ) ) ;
#43881 = CARTESIAN_POINT ( 'NONE',  ( -18.22780087662126647, -5.499999999999827693, 63.98236817873107185 ) ) ;
#43880 = VECTOR ( 'NONE', #159620, 1000.000000000000000 ) ;
#43883 = CARTESIAN_POINT ( 'NONE',  ( 16.51473224551069308, 9.474510206698969483, 69.16557627198102409 ) ) ;
#43884 = CARTESIAN_POINT ( 'NONE',  ( 18.62759615963271287, -10.81492255796078972, 68.33224293864769550 ) ) ;
#43885 = CARTESIAN_POINT ( 'NONE',  ( -21.75500197730213259, -5.836128546636254910, 172.5265712840238734 ) ) ;
#43887 = FACE_OUTER_BOUND ( 'NONE', #24683, .T. ) ;
#43886 = CARTESIAN_POINT ( 'NONE',  ( -10.72451020669898014, 18.67979575497178502, 35.41557627198102409 ) ) ;
#43888 = CARTESIAN_POINT ( 'NONE',  ( -12.14591786802326823, 12.06949235617739902, 23.12609039468567573 ) ) ;
#43889 = EDGE_CURVE ( 'NONE', #9032, #58436, #93947, .T. ) ;
#43890 = CARTESIAN_POINT ( 'NONE',  ( 0.05219959533910956823, 16.53943276465976808, 94.99890960531436690 ) ) ;
#43891 = DIRECTION ( 'NONE',  ( -1.000000000000000000, -0.000000000000000000, -3.709348145883536076E-20 ) ) ;
#43892 = CARTESIAN_POINT ( 'NONE',  ( 5.153800228976335163, 19.02544592524342804, 84.79057627198099567 ) ) ;
#43893 = CARTESIAN_POINT ( 'NONE',  ( -9.474510206698964154, 16.51473224551069663, 50.41557627198102409 ) ) ;
#43894 = CARTESIAN_POINT ( 'NONE',  ( -14.34966873604960291, -8.224510206698953496, 81.66557627198103830 ) ) ;
#43895 = CARTESIAN_POINT ( 'NONE',  ( 5.153800228976335163, 19.02544592524342804, 109.7905762719810099 ) ) ;
#43896 = CARTESIAN_POINT ( 'NONE',  ( 0.05219959533936267826, -19.03943276465977164, 105.0010903946856615 ) ) ;
#43897 = CARTESIAN_POINT ( 'NONE',  ( -21.52544592524334988, -5.823673210054445271, 58.95942372801902565 ) ) ;
#43898 = CARTESIAN_POINT ( 'NONE',  ( 19.02544592524343514, -5.153800228976328945, 93.54057627198102409 ) ) ;
#43899 = CARTESIAN_POINT ( 'NONE',  ( -21.53943276465977519, 0.05219959533907696930, 81.24890960531436690 ) ) ;
#43900 = CARTESIAN_POINT ( 'NONE',  ( 16.55341960407618274, -4.379528057220086978, 66.04275706135236135 ) ) ;
#43901 = CARTESIAN_POINT ( 'NONE',  ( 0.05219959533909260263, 19.03943276465977164, 24.99890960531435269 ) ) ;
#43902 = CARTESIAN_POINT ( 'NONE',  ( 16.46253265017160672, -9.564922557960803928, 73.33224293864769550 ) ) ;
#43903 = CARTESIAN_POINT ( 'NONE',  ( -21.52544592524343514, 5.823673210054127303, 81.04057627198102409 ) ) ;
#43904 = CARTESIAN_POINT ( 'NONE',  ( 19.02544592524334988, 5.153800228976608722, 111.4594237280190043 ) ) ;
#43906 = CARTESIAN_POINT ( 'NONE',  ( -18.62759615963255300, -10.81492255796106328, 54.16775706135235424 ) ) ;
#43905 = CARTESIAN_POINT ( 'NONE',  ( -14.29746914071049879, 8.314922557960819915, 40.83224293864769550 ) ) ;
#43907 = B_SPLINE_CURVE_WITH_KNOTS ( 'NONE', 3,
 ( #185389, #157037, #18534, #3344, #65019, #139464, #94956, #122308, #2947, #137487 ),
 .UNSPECIFIED., .F., .F.,
 ( 4, 2, 2, 2, 4 ),
 ( 2.788259402197439630E-07, 0.0002944003759562778284, 0.0005885219259723359700, 0.0008826434759883940032, 0.001176765026004452036 ),
 .UNSPECIFIED. ) ;
#43909 = CARTESIAN_POINT ( 'NONE',  ( -19.03943276465977164, 0.05219959533909376836, 116.2489096053143669 ) ) ;
#43908 = CARTESIAN_POINT ( 'NONE',  ( 4.483927247898790824, -16.52544592524335698, 90.20942372801903275 ) ) ;
#43910 = DIRECTION ( 'NONE',  ( 0.000000000000000000, 0.000000000000000000, -1.000000000000000000 ) ) ;
#43911 = CARTESIAN_POINT ( 'NONE',  ( -16.36317988757059183, 7.306389748694926745, 79.09789608363225000 ) ) ;
#43912 = CARTESIAN_POINT ( 'NONE',  ( 14.29746914071037800, 8.314922557961029526, 101.6677570613523613 ) ) ;
#43913 = CARTESIAN_POINT ( 'NONE',  ( -0.05219959533934338120, 16.53943276465976808, 47.50109039468568994 ) ) ;
#43914 = CARTESIAN_POINT ( 'NONE',  ( 19.05341960407611168, 5.049401038298154454, 63.95724293864769550 ) ) ;
#43915 = CARTESIAN_POINT ( 'NONE',  ( 16.51473224551069308, 9.474510206698969483, 69.16557627198102409 ) ) ;
#43916 = CARTESIAN_POINT ( 'NONE',  ( 12.06949235617739724, 12.14591786802326823, 71.87609039468568994 ) ) ;
#43917 = CARTESIAN_POINT ( 'NONE',  ( 0.05219959533910956823, 16.53943276465976808, 49.99890960531437401 ) ) ;
#43918 = CARTESIAN_POINT ( 'NONE',  ( -5.153800228976328057, -19.02544592524343514, 52.29057627198100988 ) ) ;
#43919 = CARTESIAN_POINT ( 'NONE',  ( -0.05219959533909027116, -19.03943276465977164, 52.49890960531436690 ) ) ;
#43920 = CARTESIAN_POINT ( 'NONE',  ( 16.55341960407618274, -4.379528057220086978, 46.04275706135234714 ) ) ;
#43921 = CARTESIAN_POINT ( 'NONE',  ( -5.049401038297874678, -19.05341960407617918, 99.79275706135234714 ) ) ;
#43922 = CARTESIAN_POINT ( 'NONE',  ( -16.53943276465976808, 0.05219959533911058130, 101.2489096053143669 ) ) ;
#43923 = CARTESIAN_POINT ( 'NONE',  ( 5.153800228976335163, 19.02544592524342804, 59.79057627198100988 ) ) ;
#43925 = CARTESIAN_POINT ( 'NONE',  ( 23.48529157249600630, -32.32473071737749137, -5.300000000000000711 ) ) ;
#43924 = CARTESIAN_POINT ( 'NONE',  ( 19.05341960407617918, -5.049401038297876454, 101.0427570613523045 ) ) ;
#43926 = CARTESIAN_POINT ( 'NONE',  ( 18.62759615963255655, 10.81492255796105972, 96.66775706135234714 ) ) ;
#43927 = CARTESIAN_POINT ( 'NONE',  ( 0.05219959533934541429, -16.53943276465976808, 65.00109039468568994 ) ) ;
#43928 = CARTESIAN_POINT ( 'NONE',  ( -193.3062444957834884, -155.7167183371838064, 0.000000000000000000 ) ) ;
#43929 = CARTESIAN_POINT ( 'NONE',  ( 18.67979575497178502, 10.72451020669898547, 64.16557627198102409 ) ) ;
#43930 = CARTESIAN_POINT ( 'NONE',  ( -16.52544592524335698, -4.483927247898792601, 48.95942372801902565 ) ) ;
#43931 = DIRECTION ( 'NONE',  ( 0.000000000000000000, 0.000000000000000000, 1.000000000000000000 ) ) ;
#43932 = CARTESIAN_POINT ( 'NONE',  ( -0.05219959533936034679, 19.03943276465977164, 42.50109039468566152 ) ) ;
#43933 = AXIS2_PLACEMENT_3D ( 'NONE', #72143, #165162, #74147 ) ;
#43934 = CARTESIAN_POINT ( 'NONE',  ( 13.97604488694527802, 13.89961937509977652, 89.37390960531436690 ) ) ;
#43935 = CARTESIAN_POINT ( 'NONE',  ( -19.03943276465977164, 0.05219959533909376836, 26.24890960531435624 ) ) ;
#43936 = CARTESIAN_POINT ( 'NONE',  ( -19.05341960407611168, -5.049401038298163336, 71.45724293864766707 ) ) ;
#43937 = DIRECTION ( 'NONE',  ( 0.000000000000000000, 0.000000000000000000, -1.000000000000000000 ) ) ;
#43938 = CARTESIAN_POINT ( 'NONE',  ( -10.72451020669870658, -18.67979575497194134, 74.58442372801901854 ) ) ;
#43939 = CARTESIAN_POINT ( 'NONE',  ( 9.474510206698971260, -16.51473224551069308, 92.91557627198103830 ) ) ;
#43940 = CARTESIAN_POINT ( 'NONE',  ( 13.89961937509957401, 13.97604488694547697, 31.87609039468566863 ) ) ;
#43941 = CARTESIAN_POINT ( 'NONE',  ( 5.153800228976615827, -19.02544592524334988, 30.20942372801900433 ) ) ;
#43942 = CARTESIAN_POINT ( 'NONE',  ( -19.03943276465977164, 0.05219959533909376836, 61.24890960531436690 ) ) ;
#43943 = CARTESIAN_POINT ( 'NONE',  ( 21.55341960407610458, 5.719274019375980345, 28.95724293864769905 ) ) ;
#43944 = CARTESIAN_POINT ( 'NONE',  ( 21.53943276465977519, 0.05219959533937863772, 81.25109039468568994 ) ) ;
#43945 = CARTESIAN_POINT ( 'NONE',  ( 13.97604488694527802, 13.89961937509977652, 59.37390960531434558 ) ) ;
#43946 = CARTESIAN_POINT ( 'NONE',  ( -18.62759615963255300, -10.81492255796106328, 84.16775706135234714 ) ) ;
#43947 = CARTESIAN_POINT ( 'NONE',  ( 21.55341960407610458, 5.719274019375980345, 33.95724293864769550 ) ) ;
#43948 = CARTESIAN_POINT ( 'NONE',  ( -19.05341960407611168, -5.049401038298163336, 76.45724293864769550 ) ) ;
#43949 = CARTESIAN_POINT ( 'NONE',  ( -10.72451020669870658, -18.67979575497194134, 39.58442372801901143 ) ) ;
#43950 = CARTESIAN_POINT ( 'NONE',  ( 16.51473224551083163, -9.474510206698727899, 65.83442372801900433 ) ) ;
#43951 = CARTESIAN_POINT ( 'NONE',  ( -0.05219959533909027116, -19.03943276465977164, 42.49890960531435269 ) ) ;
#43952 = CARTESIAN_POINT ( 'NONE',  ( 13.97604488694527802, 13.89961937509977652, 89.37390960531436690 ) ) ;
#43953 = CARTESIAN_POINT ( 'NONE',  ( 14.34966873604972726, -8.224510206698740333, 25.83442372801901499 ) ) ;
#43954 = CARTESIAN_POINT ( 'NONE',  ( 12.06949235617757843, -12.14591786802309237, 83.12390960531436690 ) ) ;
#43955 = CARTESIAN_POINT ( 'NONE',  ( 0.05219959533909260263, 19.03943276465977164, 54.99890960531435979 ) ) ;
#43956 = CARTESIAN_POINT ( 'NONE',  ( -10.72451020669898014, 18.67979575497178502, 55.41557627198102409 ) ) ;
#43957 = CARTESIAN_POINT ( 'NONE',  ( 0.05219959533934541429, -16.53943276465976808, 20.00109039468568639 ) ) ;
#43958 = CARTESIAN_POINT ( 'NONE',  ( 18.67979575497194134, -10.72451020669871369, 20.83442372801901143 ) ) ;
#43959 = CARTESIAN_POINT ( 'NONE',  ( -0.05219959533937732626, 21.53943276465977519, 67.50109039468568994 ) ) ;
#43960 = CARTESIAN_POINT ( 'NONE',  ( -12.06949235617739369, -12.14591786802326823, 69.37609039468567573 ) ) ;
#43961 = CARTESIAN_POINT ( 'NONE',  ( 14.34966873604972726, -8.224510206698740333, 70.83442372801901854 ) ) ;
#43962 = CARTESIAN_POINT ( 'NONE',  ( -9.474510206698964154, 16.51473224551069663, 65.41557627198102409 ) ) ;
#43963 = CARTESIAN_POINT ( 'NONE',  ( 8.314922557961029526, -14.29746914071037800, 95.41775706135234714 ) ) ;
#43964 = CARTESIAN_POINT ( 'NONE',  ( -19.05341960407617563, 5.049401038297882671, 48.54275706135233293 ) ) ;
#43965 = CARTESIAN_POINT ( 'NONE',  ( 10.81492255796078972, 18.62759615963270932, 109.5822429386476955 ) ) ;
#43966 = CARTESIAN_POINT ( 'NONE',  ( 4.483927247898545687, 16.52544592524342804, 59.79057627198103120 ) ) ;
#43967 = CARTESIAN_POINT ( 'NONE',  ( -16.46253265017160317, 9.564922557960807481, 85.83224293864769550 ) ) ;
#43968 = CARTESIAN_POINT ( 'NONE',  ( -16.55341960407617563, 4.379528057220093196, 88.54275706135236135 ) ) ;
#43969 = CARTESIAN_POINT ( 'NONE',  ( 5.719274019375673035, 21.55341960407619339, 52.29275706135236135 ) ) ;
#43970 = CARTESIAN_POINT ( 'NONE',  ( 4.483927247898790824, -16.52544592524335698, 35.20942372801901854 ) ) ;
#43971 = CARTESIAN_POINT ( 'NONE',  ( 21.53943276465977519, 0.05219959533937863772, 26.25109039468567573 ) ) ;
#43972 = CARTESIAN_POINT ( 'NONE',  ( 14.34966873604960469, 8.224510206698951720, 64.16557627198102409 ) ) ;
#43973 = ORIENTED_EDGE ( 'NONE', *, *, #133150, .T. ) ;
#43974 = CARTESIAN_POINT ( 'NONE',  ( -21.53943276465977519, 0.05219959533907696930, 96.24890960531435269 ) ) ;
#43975 = CARTESIAN_POINT ( 'NONE',  ( 16.53943276465976808, -0.05219959533910856209, 33.74890960531436690 ) ) ;
#43976 = ORIENTED_EDGE ( 'NONE', *, *, #7317, .F. ) ;
#43977 = CARTESIAN_POINT ( 'NONE',  ( 34.36946425582527098, 7.112708652184213776, 47.39170078794326457 ) ) ;
#43978 = CARTESIAN_POINT ( 'NONE',  ( -15.80617190586745835, -15.72974639402198527, 26.87390960531435979 ) ) ;
#43979 = CARTESIAN_POINT ( 'NONE',  ( 18.67979575497194134, -10.72451020669871369, 40.83442372801901854 ) ) ;
#43980 = CARTESIAN_POINT ( 'NONE',  ( 4.379528057220339221, -16.55341960407611168, 67.70724293864769550 ) ) ;
#43981 = AXIS2_PLACEMENT_3D ( 'NONE', #51071, #101554, #86396 ) ;
#43982 = CARTESIAN_POINT ( 'NONE',  ( -16.46253265017160317, 9.564922557960807481, 80.83224293864769550 ) ) ;
#43984 = CARTESIAN_POINT ( 'NONE',  ( 16.51473224551083163, -9.474510206698727899, 70.83442372801900433 ) ) ;
#43983 = CARTESIAN_POINT ( 'NONE',  ( -13.97604488694527625, -13.89961937509977652, 26.87390960531434558 ) ) ;
#43985 = CARTESIAN_POINT ( 'NONE',  ( 5.823673210054125526, 21.52544592524343514, 44.79057627198103120 ) ) ;
#43986 = CARTESIAN_POINT ( 'NONE',  ( -23.14280555631616210, -30.41650385747668750, -16.87365452859015136 ) ) ;
#43987 = CARTESIAN_POINT ( 'NONE',  ( -16.46253265017160317, 9.564922557960807481, 60.83224293864769550 ) ) ;
#43988 = CARTESIAN_POINT ( 'NONE',  ( 16.55341960407618274, -4.379528057220086978, 31.04275706135234714 ) ) ;
#43989 = CARTESIAN_POINT ( 'NONE',  ( -5.719274019375978568, 21.55341960407610458, 115.2072429386476955 ) ) ;
#43990 = CARTESIAN_POINT ( 'NONE',  ( 8.314922557960818139, 14.29746914071049879, 49.58224293864769550 ) ) ;
#43991 = ORIENTED_EDGE ( 'NONE', *, *, #194548, .F. ) ;
#43992 = CARTESIAN_POINT ( 'NONE',  ( -19.02544592524342804, 5.153800228976336051, 86.04057627198103830 ) ) ;
#43993 = CARTESIAN_POINT ( 'NONE',  ( 21.52544592524344225, -5.823673210054117533, 68.54057627198103830 ) ) ;
#43995 = CARTESIAN_POINT ( 'NONE',  ( 8.224510206698742110, 14.34966873604972548, 32.08442372801901854 ) ) ;
#43994 = CARTESIAN_POINT ( 'NONE',  ( -21.55341960407610458, -5.719274019375992779, 106.4572429386477097 ) ) ;
#43996 = EDGE_CURVE ( 'NONE', #65708, #70507, #27389, .T. ) ;
#43997 = CARTESIAN_POINT ( 'NONE',  ( 5.719274019375991003, -21.55341960407610458, 42.70724293864770260 ) ) ;
#43998 = CARTESIAN_POINT ( 'NONE',  ( -0.05219959533937732626, 21.53943276465977519, 102.5010903946856899 ) ) ;
#43999 = CARTESIAN_POINT ( 'NONE',  ( 5.153800228976335163, 19.02544592524342804, 99.79057627198102409 ) ) ;
#44000 = B_SPLINE_CURVE_WITH_KNOTS ( 'NONE', 3,
 ( #94585, #106780, #4544, #172432, #114734, #7545 ),
 .UNSPECIFIED., .F., .F.,
 ( 4, 2, 4 ),
 ( 0.003693721832073882522, 0.004289092630022420076, 0.004884463427970957630 ),
 .UNSPECIFIED. ) ;
#44001 = CARTESIAN_POINT ( 'NONE',  ( 19.05341960407611168, 5.049401038298154454, 38.95724293864767418 ) ) ;
#44002 = CARTESIAN_POINT ( 'NONE',  ( 19.02544592524343514, -5.153800228976328945, 93.54057627198102409 ) ) ;
#44003 = CARTESIAN_POINT ( 'NONE',  ( 0.05219959533909260263, 19.03943276465977164, 74.99890960531435269 ) ) ;
#44004 = CARTESIAN_POINT ( 'NONE',  ( -18.36170132746697803, -35.61590944478785303, -18.35554273634631528 ) ) ;
#44005 = CARTESIAN_POINT ( 'NONE',  ( 13.89961937509957401, 13.97604488694547697, 56.87609039468564731 ) ) ;
#44007 = CARTESIAN_POINT ( 'NONE',  ( -5.719274019375978568, 21.55341960407610458, 35.20724293864768839 ) ) ;
#44006 = CARTESIAN_POINT ( 'NONE',  ( -10.72451020669870658, -18.67979575497194134, 109.5844237280190328 ) ) ;
#44009 = EDGE_CURVE ( 'NONE', #194071, #21815, #45609, .T. ) ;
#44008 = CARTESIAN_POINT ( 'NONE',  ( -14.34966873604972548, 8.224510206698743886, 108.3344237280190185 ) ) ;
#44010 = CARTESIAN_POINT ( 'NONE',  ( -9.474510206698720793, -16.51473224551083518, 84.58442372801900433 ) ) ;
#44011 = CARTESIAN_POINT ( 'NONE',  ( -16.18388926212240975, 7.379444403734375157, 59.56046848633847191 ) ) ;
#44012 = CARTESIAN_POINT ( 'NONE',  ( 13.89961937509957401, 13.97604488694547697, 81.87609039468564731 ) ) ;
#44013 = CARTESIAN_POINT ( 'NONE',  ( 19.02544592524334988, 5.153800228976608722, 26.45942372801899722 ) ) ;
#44014 = CARTESIAN_POINT ( 'NONE',  ( -14.76558643118678305, -15.47416251488300887, -56.40920624782621928 ) ) ;
#44015 = CARTESIAN_POINT ( 'NONE',  ( -9.564922557960796823, -16.46253265017161027, 37.08224293864768839 ) ) ;
#44016 = CARTESIAN_POINT ( 'NONE',  ( 8.314922557960818139, 14.29746914071049879, 49.58224293864769550 ) ) ;
#44017 = CARTESIAN_POINT ( 'NONE',  ( -17.48853670773245028, -5.747243402303093163, 111.3332870025001000 ) ) ;
#44018 = CARTESIAN_POINT ( 'NONE',  ( -16.53943276465976808, 0.05219959533911058130, 26.24890960531435624 ) ) ;
#44019 = DIRECTION ( 'NONE',  ( 0.000000000000000000, 0.000000000000000000, 1.000000000000000000 ) ) ;
#44020 = CARTESIAN_POINT ( 'NONE',  ( -12.06949235617739369, -12.14591786802326823, 89.37609039468568994 ) ) ;
#44021 = CARTESIAN_POINT ( 'NONE',  ( -19.02544592524342804, 5.153800228976336051, 46.04057627198101699 ) ) ;
#44022 = CARTESIAN_POINT ( 'NONE',  ( -21.55341960407619339, 5.719274019375674811, 113.5427570613523756 ) ) ;
#44023 = CARTESIAN_POINT ( 'NONE',  ( 9.474510206698729675, 16.51473224551082808, 112.0844237280190043 ) ) ;
#44025 = VERTEX_POINT ( 'NONE', #42548 ) ;
#44024 = CARTESIAN_POINT ( 'NONE',  ( -21.55341960407619339, 5.719274019375674811, 93.54275706135234714 ) ) ;
#44026 = CARTESIAN_POINT ( 'NONE',  ( -19.03943276465977164, 0.05219959533909376836, 96.24890960531436690 ) ) ;
#44027 = CARTESIAN_POINT ( 'NONE',  ( -16.46253265017160317, 9.564922557960807481, 80.83224293864769550 ) ) ;
#44028 = CARTESIAN_POINT ( 'NONE',  ( -36.91746825000000598, 11.99521256947798520, -6.724999997268813701 ) ) ;
#44029 = CARTESIAN_POINT ( 'NONE',  ( 21.52544592524344225, -5.823673210054117533, 108.5405762719810241 ) ) ;
#44030 = AXIS2_PLACEMENT_3D ( 'NONE', #121322, #90966, #29337 ) ;
#44031 = CARTESIAN_POINT ( 'NONE',  ( -14.29746914071049879, 8.314922557960819915, 80.83224293864769550 ) ) ;
#44032 = CARTESIAN_POINT ( 'NONE',  ( 15.72974639402199770, -15.80617190586745480, 73.12390960531436690 ) ) ;
#44033 = CARTESIAN_POINT ( 'NONE',  ( -5.049401038298153566, 19.05341960407611168, 60.20724293864768129 ) ) ;
#44035 = CARTESIAN_POINT ( 'NONE',  ( 8.314922557961029526, -14.29746914071037800, 90.41775706135236135 ) ) ;
#44034 = CARTESIAN_POINT ( 'NONE',  ( -0.05219959533907301413, -21.53943276465977519, 102.4989096053143811 ) ) ;
#44036 = ORIENTED_EDGE ( 'NONE', *, *, #12998, .F. ) ;
#44037 = CARTESIAN_POINT ( 'NONE',  ( -19.02544592524342804, 5.153800228976336051, 66.04057627198103830 ) ) ;
#44038 = EDGE_CURVE ( 'NONE', #117777, #172040, #166286, .T. ) ;
#44040 = CARTESIAN_POINT ( 'NONE',  ( 21.58577566615618082, -5.573877917343201815, 173.3856758005497056 ) ) ;
#44039 = CARTESIAN_POINT ( 'NONE',  ( -16.53943276465976808, 0.05219959533911058130, 91.24890960531436690 ) ) ;
#44041 = CARTESIAN_POINT ( 'NONE',  ( -5.153800228976328057, -19.02544592524343514, 62.29057627198100988 ) ) ;
#44042 = CARTESIAN_POINT ( 'NONE',  ( -16.51473224551082808, 9.474510206698731452, 73.33442372801900433 ) ) ;
#44043 = CARTESIAN_POINT ( 'NONE',  ( -14.34966873604960291, -8.224510206698953496, 81.66557627198103830 ) ) ;
#44044 = CARTESIAN_POINT ( 'NONE',  ( 18.67979575497194134, -10.72451020669871369, 55.83442372801901854 ) ) ;
#44046 = CARTESIAN_POINT ( 'NONE',  ( 0.05219959533937995610, -21.53943276465977519, 20.00109039468568639 ) ) ;
#44045 = CARTESIAN_POINT ( 'NONE',  ( 16.46253265017160672, -9.564922557960803928, 43.33224293864769550 ) ) ;
#44047 = CARTESIAN_POINT ( 'NONE',  ( -4.483927247898539470, -16.52544592524342804, 107.2905762719810525 ) ) ;
#44048 = CARTESIAN_POINT ( 'NONE',  ( 8.817897698974592302, -38.37206457205375187, -32.07286502659245286 ) ) ;
#44049 = CARTESIAN_POINT ( 'NONE',  ( -19.05341960407611168, -5.049401038298163336, 56.45724293864768129 ) ) ;
#44050 = CARTESIAN_POINT ( 'NONE',  ( 28.82186960331498327, 2.781578969918950771E-14, 143.2500000054623683 ) ) ;
#44052 = CARTESIAN_POINT ( 'NONE',  ( 5.153800228976335163, 19.02544592524342804, 109.7905762719810099 ) ) ;
#44051 = CARTESIAN_POINT ( 'NONE',  ( 0.05219959533936267826, -19.03943276465977164, 95.00109039468567573 ) ) ;
#44053 = CARTESIAN_POINT ( 'NONE',  ( -15.80617190586768217, 15.72974639402176855, 53.12609039468568284 ) ) ;
#44054 = CARTESIAN_POINT ( 'NONE',  ( 19.03943276465977164, -0.05219959533909143690, 88.74890960531436690 ) ) ;
#44055 = CARTESIAN_POINT ( 'NONE',  ( -9.474510206698720793, -16.51473224551083518, 79.58442372801899012 ) ) ;
#44056 = CARTESIAN_POINT ( 'NONE',  ( 16.51473224551069308, 9.474510206698969483, 54.16557627198103120 ) ) ;
#44057 = CARTESIAN_POINT ( 'NONE',  ( -16.52544592524342804, 4.483927247898546575, 71.04057627198103830 ) ) ;
#44058 = CARTESIAN_POINT ( 'NONE',  ( -12.06949235617756955, 12.14591786802309770, 75.62390960531439532 ) ) ;
#44059 = CARTESIAN_POINT ( 'NONE',  ( -16.51473224551069308, -9.474510206698971260, 86.66557627198102409 ) ) ;
#44060 = CARTESIAN_POINT ( 'NONE',  ( 12.14591786802309770, 12.06949235617756955, 79.37390960531436690 ) ) ;
#44061 = CARTESIAN_POINT ( 'NONE',  ( -13.89961937509977652, 13.97604488694528158, 90.62390960531432427 ) ) ;
#44062 = CARTESIAN_POINT ( 'NONE',  ( -9.564922557961040184, 16.46253265017147172, 37.91775706135233293 ) ) ;
#44065 = CARTESIAN_POINT ( 'NONE',  ( -9.564922557960796823, -16.46253265017161027, 27.08224293864769550 ) ) ;
#44064 = CARTESIAN_POINT ( 'NONE',  ( -14.29746914071049879, 8.314922557960819915, 25.83224293864769194 ) ) ;
#44063 = CARTESIAN_POINT ( 'NONE',  ( -13.97604488694527625, -13.89961937509977652, 51.87390960531436690 ) ) ;
#44066 = ORIENTED_EDGE ( 'NONE', *, *, #143733, .T. ) ;
#44067 = CARTESIAN_POINT ( 'NONE',  ( -5.823673210054431948, 21.52544592524334988, 47.70942372801902565 ) ) ;
#44068 = CARTESIAN_POINT ( 'NONE',  ( 13.97604488694548053, -13.89961937509957401, 70.62609039468567573 ) ) ;
#44069 = CARTESIAN_POINT ( 'NONE',  ( -12.14591786802309592, -12.06949235617757132, 41.87390960531435979 ) ) ;
#44070 = CARTESIAN_POINT ( 'NONE',  ( 18.62759615963271287, -10.81492255796078972, 83.33224293864769550 ) ) ;
#44071 = CARTESIAN_POINT ( 'NONE',  ( 0.05219959533909260263, 19.03943276465977164, 114.9989096053143669 ) ) ;
#44073 = CARTESIAN_POINT ( 'NONE',  ( -4.379528057220328563, 16.55341960407611168, 70.20724293864769550 ) ) ;
#44072 = TOROIDAL_SURFACE ( 'NONE', #79554, 206.0437394197456911, 8.000000000000000000 ) ;
#44074 = CARTESIAN_POINT ( 'NONE',  ( -19.02544592524342804, 5.153800228976336051, 46.04057627198101699 ) ) ;
#44075 = CARTESIAN_POINT ( 'NONE',  ( 16.46253265017146816, 9.564922557961045513, 36.66775706135233293 ) ) ;
#44076 = CARTESIAN_POINT ( 'NONE',  ( 8.224510206698742110, 14.34966873604972548, 107.0844237280190043 ) ) ;
#44077 = CARTESIAN_POINT ( 'NONE',  ( -12.14591786802326823, 12.06949235617739902, 63.12609039468568994 ) ) ;
#44078 = CARTESIAN_POINT ( 'NONE',  ( 15.72974639402199770, -15.80617190586745480, 43.12390960531435269 ) ) ;
#44079 = CARTESIAN_POINT ( 'NONE',  ( -19.02544592524334988, -5.153800228976617603, 18.95942372801899722 ) ) ;
#44080 = CARTESIAN_POINT ( 'NONE',  ( -0.05219959533909027116, -19.03943276465977164, 97.49890960531436690 ) ) ;
#44081 = AXIS2_PLACEMENT_3D ( 'NONE', #161920, #9252, #68909 ) ;
#44082 = CARTESIAN_POINT ( 'NONE',  ( -0.05219959533934338120, 16.53943276465976808, 72.50109039468568994 ) ) ;
#44083 = CARTESIAN_POINT ( 'NONE',  ( 8.314922557960818139, 14.29746914071049879, 114.5822429386477097 ) ) ;
#44084 = CARTESIAN_POINT ( 'NONE',  ( -12.06949235617756955, 12.14591786802309770, 30.62390960531436335 ) ) ;
#44086 = CARTESIAN_POINT ( 'NONE',  ( -13.97604488694527625, -13.89961937509977652, 86.87390960531436690 ) ) ;
#44085 = CARTESIAN_POINT ( 'NONE',  ( 19.05341960407611168, 5.049401038298154454, 98.95724293864766707 ) ) ;
#44087 = CARTESIAN_POINT ( 'NONE',  ( -21.55341960407610458, -5.719274019375992779, 31.45724293864769550 ) ) ;
#44088 = CARTESIAN_POINT ( 'NONE',  ( -12.14591786802309592, -12.06949235617757132, 71.87390960531438111 ) ) ;
#44089 = B_SPLINE_CURVE_WITH_KNOTS ( 'NONE', 3,
 ( #64606, #187966, #110110, #112097, #138454, #63610 ),
 .UNSPECIFIED., .F., .F.,
 ( 4, 2, 4 ),
 ( 0.007228050697041590866, 0.007608510107495068155, 0.007988969517948545443 ),
 .UNSPECIFIED. ) ;
#44090 = CARTESIAN_POINT ( 'NONE',  ( -8.224510206698948167, 14.34966873604960824, 50.41557627198103120 ) ) ;
#44092 = CARTESIAN_POINT ( 'NONE',  ( -17.60779699588839264, -5.500000000000014211, 56.34981316670103979 ) ) ;
#44091 = CARTESIAN_POINT ( 'NONE',  ( 14.29746914071037800, 8.314922557961029526, 56.66775706135235424 ) ) ;
#44093 = CARTESIAN_POINT ( 'NONE',  ( 13.97604488694548053, -13.89961937509957401, 55.62609039468566863 ) ) ;
#44094 = CARTESIAN_POINT ( 'NONE',  ( -5.153800228976328057, -19.02544592524343514, 92.29057627198099567 ) ) ;
#44095 = CARTESIAN_POINT ( 'NONE',  ( -9.564922557961040184, 16.46253265017147172, 67.91775706135233293 ) ) ;
#44096 = CARTESIAN_POINT ( 'NONE',  ( -22.44159573604009950, -16.30477369853688430, 141.5750000027311728 ) ) ;
#44097 = CARTESIAN_POINT ( 'NONE',  ( -19.05341960407617563, 5.049401038297882671, 53.54275706135231871 ) ) ;
#44099 = CARTESIAN_POINT ( 'NONE',  ( -8.224510206698735004, -14.34966873604973081, 94.58442372801901854 ) ) ;
#44098 = CARTESIAN_POINT ( 'NONE',  ( -16.46253265017146816, -9.564922557961047289, 99.16775706135233293 ) ) ;
#44100 = CARTESIAN_POINT ( 'NONE',  ( 17.14385361876520264, 23.59649016807275856, 144.6750000027311671 ) ) ;
#44101 = CARTESIAN_POINT ( 'NONE',  ( -16.51473224551069308, -9.474510206698971260, 41.66557627198103120 ) ) ;
#44102 = CARTESIAN_POINT ( 'NONE',  ( -19.02544592524342804, 5.153800228976336051, 111.0405762719810099 ) ) ;
#44103 = CARTESIAN_POINT ( 'NONE',  ( -21.52544592524334988, -5.823673210054445271, 53.95942372801900433 ) ) ;
#44104 = CARTESIAN_POINT ( 'NONE',  ( 9.474510206698729675, 16.51473224551082808, 97.08442372801900433 ) ) ;
#44106 = CARTESIAN_POINT ( 'NONE',  ( -13.89961937509977652, 13.97604488694528158, 60.62390960531436690 ) ) ;
#44105 = CARTESIAN_POINT ( 'NONE',  ( 4.999999999999996447, 5.000000000000003553, -18.00000000000000000 ) ) ;
#44107 = CARTESIAN_POINT ( 'NONE',  ( -4.500000000000001776, -140.0000000000000000, 13.35010376910484275 ) ) ;
#44109 = CARTESIAN_POINT ( 'NONE',  ( 19.03943276465977164, -0.05219959533909143690, 68.74890960531436690 ) ) ;
#44108 = CARTESIAN_POINT ( 'NONE',  ( 12.14591786802309770, 12.06949235617756955, 74.37390960531436690 ) ) ;
#44110 = CARTESIAN_POINT ( 'NONE',  ( -19.02544592524342804, 5.153800228976336051, 81.04057627198103830 ) ) ;
#44111 = CARTESIAN_POINT ( 'NONE',  ( -5.153800228976607833, 19.02544592524334988, 82.70942372801897591 ) ) ;
#44112 = CARTESIAN_POINT ( 'NONE',  ( -21.52544592524343514, 5.823673210054127303, 66.04057627198103830 ) ) ;
#44113 = CARTESIAN_POINT ( 'NONE',  ( 16.55341960407611168, 4.379528057220329451, 113.9572429386477239 ) ) ;
#44114 = CARTESIAN_POINT ( 'NONE',  ( 19.05341960407617918, -5.049401038297876454, 41.04275706135233293 ) ) ;
#44115 = CARTESIAN_POINT ( 'NONE',  ( -16.46253265017160317, 9.564922557960807481, 80.83224293864769550 ) ) ;
#44116 = CARTESIAN_POINT ( 'NONE',  ( 15.72974639402199770, -15.80617190586745480, 88.12390960531436690 ) ) ;
#44118 = CARTESIAN_POINT ( 'NONE',  ( -5.049401038297874678, -19.05341960407617918, 44.79275706135232582 ) ) ;
#44117 = CARTESIAN_POINT ( 'NONE',  ( -12.14591786802309592, -12.06949235617757132, 76.87390960531439532 ) ) ;
#44119 = CARTESIAN_POINT ( 'NONE',  ( -5.823673210054116645, -21.52544592524344225, 77.29057627198102409 ) ) ;
#44120 = CARTESIAN_POINT ( 'NONE',  ( 18.67979575497178502, 10.72451020669898547, 64.16557627198102409 ) ) ;
#44121 = CARTESIAN_POINT ( 'NONE',  ( -18.62759615963270932, 10.81492255796079327, 40.83224293864769550 ) ) ;
#44122 = CARTESIAN_POINT ( 'NONE',  ( -21.53943276465977519, -0.05219959533937600094, 93.75109039468567573 ) ) ;
#44123 = CARTESIAN_POINT ( 'NONE',  ( 13.97604488694527802, 13.89961937509977652, 84.37390960531433848 ) ) ;
#44124 = CARTESIAN_POINT ( 'NONE',  ( -19.03943276465977164, 0.05219959533909376836, 21.24890960531436335 ) ) ;
#44125 = CARTESIAN_POINT ( 'NONE',  ( 0.05219959533937995610, -21.53943276465977519, 30.00109039468568284 ) ) ;
#44126 = EDGE_CURVE ( 'NONE', #179372, #105638, #9152, .T. ) ;
#44127 = CARTESIAN_POINT ( 'NONE',  ( 10.72451020669871369, 18.67979575497193778, 42.08442372801901854 ) ) ;
#44128 = CARTESIAN_POINT ( 'NONE',  ( 16.46253265017160672, -9.564922557960803928, 53.33224293864768839 ) ) ;
#44129 = CARTESIAN_POINT ( 'NONE',  ( -15.72974639402176322, -15.80617190586768395, 24.37609039468567573 ) ) ;
#44130 = CARTESIAN_POINT ( 'NONE',  ( 16.46253265017146816, 9.564922557961045513, 61.66775706135234003 ) ) ;
#44131 = CARTESIAN_POINT ( 'NONE',  ( -16.46253265017160317, 9.564922557960807481, 35.83224293864768839 ) ) ;
#44132 = CARTESIAN_POINT ( 'NONE',  ( -4.379528057220086978, -16.55341960407618274, 24.79275706135235779 ) ) ;
#44133 = CARTESIAN_POINT ( 'NONE',  ( 0.05219959533909260263, 19.03943276465977164, 29.99890960531435979 ) ) ;
#44134 = CARTESIAN_POINT ( 'NONE',  ( 4.379528057220092307, 16.55341960407617563, 57.29275706135234714 ) ) ;
#44135 = CARTESIAN_POINT ( 'NONE',  ( 9.474510206698971260, -16.51473224551069308, 37.91557627198102409 ) ) ;
#44136 = CARTESIAN_POINT ( 'NONE',  ( -20.93662873023658122, -11.00447265502299210, 170.1964094900432372 ) ) ;
#44137 = CARTESIAN_POINT ( 'NONE',  ( -19.03943276465977164, 0.05219959533909376836, 91.24890960531436690 ) ) ;
#44138 = CARTESIAN_POINT ( 'NONE',  ( -9.564922557960796823, -16.46253265017161027, 22.08224293864768839 ) ) ;
#44139 = CARTESIAN_POINT ( 'NONE',  ( -15.80617190586745835, -15.72974639402198527, 56.87390960531436690 ) ) ;
#44140 = CARTESIAN_POINT ( 'NONE',  ( -8.224510206698735004, -14.34966873604973081, 49.58442372801901143 ) ) ;
#44141 = CARTESIAN_POINT ( 'NONE',  ( 0.05219959533937995610, -21.53943276465977519, 100.0010903946857042 ) ) ;
#44142 = CARTESIAN_POINT ( 'NONE',  ( -0.05219959533909027116, -19.03943276465977164, 37.49890960531436690 ) ) ;
#44143 = CARTESIAN_POINT ( 'NONE',  ( 8.314922557960818139, 14.29746914071049879, 29.58224293864769905 ) ) ;
#44144 = CARTESIAN_POINT ( 'NONE',  ( -4.483927247898539470, -16.52544592524342804, 62.29057627198102409 ) ) ;
#44145 = CARTESIAN_POINT ( 'NONE',  ( 9.474510206698971260, -16.51473224551069308, 67.91557627198102409 ) ) ;
#44146 = CARTESIAN_POINT ( 'NONE',  ( -5.719274019375665041, -21.55341960407619695, 109.7927570613523613 ) ) ;
#44147 = CARTESIAN_POINT ( 'NONE',  ( -10.72451020669870658, -18.67979575497194134, 29.58442372801901854 ) ) ;
#44148 = CARTESIAN_POINT ( 'NONE',  ( -15.80617190586768217, 15.72974639402176855, 83.12609039468568994 ) ) ;
#44149 = CARTESIAN_POINT ( 'NONE',  ( 14.34966873604972726, -8.224510206698740333, 50.83442372801901143 ) ) ;
#44150 = CARTESIAN_POINT ( 'NONE',  ( 4.483927247898790824, -16.52544592524335698, 35.20942372801901854 ) ) ;
#44152 = CARTESIAN_POINT ( 'NONE',  ( -10.81492255796105439, 18.62759615963255655, 97.91775706135236135 ) ) ;
#44151 = CARTESIAN_POINT ( 'NONE',  ( 8.224510206698953496, -14.34966873604960469, 92.91557627198103830 ) ) ;
#44153 = CARTESIAN_POINT ( 'NONE',  ( 12.06949235617757843, -12.14591786802309237, 38.12390960531436690 ) ) ;
#44154 = CARTESIAN_POINT ( 'NONE',  ( 13.89961937509977652, -13.97604488694527269, 23.12390960531436335 ) ) ;
#44155 = CARTESIAN_POINT ( 'NONE',  ( -8.224510206698735004, -14.34966873604973081, 39.58442372801901143 ) ) ;
#44156 = CARTESIAN_POINT ( 'NONE',  ( 12.14591786802309770, 12.06949235617756955, 59.37390960531436690 ) ) ;
#44157 = CARTESIAN_POINT ( 'NONE',  ( 8.314922557961029526, -14.29746914071037800, 105.4177570613523613 ) ) ;
#44158 = CARTESIAN_POINT ( 'NONE',  ( -19.03943276465977164, 0.05219959533909376836, 101.2489096053143669 ) ) ;
#44159 = CARTESIAN_POINT ( 'NONE',  ( -5.153800228976328057, -19.02544592524343514, 107.2905762719810383 ) ) ;
#44160 = CARTESIAN_POINT ( 'NONE',  ( -21.55341960407619339, 5.719274019375674811, 108.5427570613523756 ) ) ;
#44161 = ADVANCED_FACE ( 'NONE', ( #7837 ), #38193, .F. ) ;
#44162 = CARTESIAN_POINT ( 'NONE',  ( 8.314922557960818139, 14.29746914071049879, 89.58224293864768129 ) ) ;
#44163 = CARTESIAN_POINT ( 'NONE',  ( -19.05341960407611168, -5.049401038298163336, 96.45724293864769550 ) ) ;
#44164 = VERTEX_POINT ( 'NONE', #192878 ) ;
#44165 = CARTESIAN_POINT ( 'NONE',  ( -12.14591786802326823, 12.06949235617739902, 38.12609039468567573 ) ) ;
#44166 = CARTESIAN_POINT ( 'NONE',  ( -0.05219959533909027116, -19.03943276465977164, 42.49890960531435269 ) ) ;
#44167 = CARTESIAN_POINT ( 'NONE',  ( 19.03943276465977164, -0.05219959533909143690, 103.7489096053143669 ) ) ;
#44169 = CARTESIAN_POINT ( 'NONE',  ( 20.96320343559668942, 21.46320343559617427, 4.646446609406719830 ) ) ;
#44168 = CARTESIAN_POINT ( 'NONE',  ( -0.05219959533934338120, 16.53943276465976808, 42.50109039468567573 ) ) ;
#44170 = CARTESIAN_POINT ( 'NONE',  ( 19.05341960407617918, -5.049401038297876454, 46.04275706135233293 ) ) ;
#44171 = CARTESIAN_POINT ( 'NONE',  ( -16.51473224551069308, -9.474510206698971260, 41.66557627198103120 ) ) ;
#44172 = CARTESIAN_POINT ( 'NONE',  ( -4.483927247898782831, 16.52544592524335698, 77.70942372801900433 ) ) ;
#44173 = CARTESIAN_POINT ( 'NONE',  ( -16.46253265017146816, -9.564922557961047289, 89.16775706135234714 ) ) ;
#44174 = CARTESIAN_POINT ( 'NONE',  ( 5.049401038297881783, 19.05341960407617563, 27.29275706135232937 ) ) ;
#44175 = CARTESIAN_POINT ( 'NONE',  ( 0.05219959533909260263, 19.03943276465977164, 64.99890960531436690 ) ) ;
#44176 = CARTESIAN_POINT ( 'NONE',  ( -12.06949235617756955, 12.14591786802309770, 100.6239096053143811 ) ) ;
#44177 = AXIS2_PLACEMENT_3D ( 'NONE', #125969, #175460, #141135 ) ;
#44178 = CARTESIAN_POINT ( 'NONE',  ( 9.474510206698729675, 16.51473224551082808, 67.08442372801900433 ) ) ;
#44179 = CARTESIAN_POINT ( 'NONE',  ( 5.823673210054125526, 21.52544592524343514, 59.79057627198103120 ) ) ;
#44180 = CARTESIAN_POINT ( 'NONE',  ( 16.46253265017146816, 9.564922557961045513, 31.66775706135232937 ) ) ;
#44181 = CARTESIAN_POINT ( 'NONE',  ( 16.46253265017160672, -9.564922557960803928, 108.3322429386476955 ) ) ;
#44182 = CARTESIAN_POINT ( 'NONE',  ( 5.719274019375991003, -21.55341960407610458, 72.70724293864769550 ) ) ;
#44183 = CARTESIAN_POINT ( 'NONE',  ( -17.48853670773246805, 5.747243402303039872, 83.66671299749991420 ) ) ;
#44184 = CARTESIAN_POINT ( 'NONE',  ( -9.564922557961040184, 16.46253265017147172, 107.9177570613523471 ) ) ;
#44185 = CARTESIAN_POINT ( 'NONE',  ( 37.32596994906252519, -3.631267627803086206, 40.85341334860915907 ) ) ;
#44186 = CARTESIAN_POINT ( 'NONE',  ( -16.52544592524335698, -4.483927247898792601, 28.95942372801902209 ) ) ;
#44187 = CARTESIAN_POINT ( 'NONE',  ( 13.89961937509977652, -13.97604488694527269, 33.12390960531434558 ) ) ;
#44188 = CARTESIAN_POINT ( 'NONE',  ( 19.02544592524343514, -5.153800228976328945, 113.5405762719810241 ) ) ;
#44189 = CARTESIAN_POINT ( 'NONE',  ( 15.80617190586746368, 15.72974639402197994, 94.37390960531436690 ) ) ;
#44190 = CARTESIAN_POINT ( 'NONE',  ( 21.52544592524334988, 5.823673210054432836, 61.45942372801901854 ) ) ;
#44192 = CARTESIAN_POINT ( 'NONE',  ( 15.80617190586769283, -15.72974639402175789, 105.6260903946856899 ) ) ;
#44191 = CARTESIAN_POINT ( 'NONE',  ( -19.02544592524334988, -5.153800228976617603, 103.9594237280190043 ) ) ;
#44193 = CARTESIAN_POINT ( 'NONE',  ( -16.55341960407617563, 4.379528057220093196, 113.5427570613523756 ) ) ;
#44194 = CARTESIAN_POINT ( 'NONE',  ( 21.52544592524344225, -5.823673210054117533, 103.5405762719810383 ) ) ;
#44195 = CARTESIAN_POINT ( 'NONE',  ( 4.483927247898545687, 16.52544592524342804, 54.79057627198104541 ) ) ;
#44196 = CARTESIAN_POINT ( 'NONE',  ( -19.03943276465977164, -0.05219959533935918106, 83.75109039468567573 ) ) ;
#44197 = CARTESIAN_POINT ( 'NONE',  ( -19.03943276465977164, -0.05219959533935918106, 58.75109039468566863 ) ) ;
#44198 = CARTESIAN_POINT ( 'NONE',  ( 5.719274019375673035, 21.55341960407619339, 62.29275706135236845 ) ) ;
#44199 = CARTESIAN_POINT ( 'NONE',  ( -19.05341960407617563, 5.049401038297882671, 38.54275706135233293 ) ) ;
#44200 = CARTESIAN_POINT ( 'NONE',  ( 4.483927247898545687, 16.52544592524342804, 99.79057627198103830 ) ) ;
#44201 = CARTESIAN_POINT ( 'NONE',  ( -15.72974639402197994, 15.80617190586746368, 35.62390960531437401 ) ) ;
#44202 = CARTESIAN_POINT ( 'NONE',  ( 16.55341960407611168, 4.379528057220329451, 33.95724293864769550 ) ) ;
#44203 = CARTESIAN_POINT ( 'NONE',  ( -21.52544592524334988, -5.823673210054445271, 93.95942372801903275 ) ) ;
#44204 = CARTESIAN_POINT ( 'NONE',  ( -8.314922557961024197, 14.29746914071037800, 72.91775706135234714 ) ) ;
#44205 = CARTESIAN_POINT ( 'NONE',  ( -12.06949235617756955, 12.14591786802309770, 30.62390960531436335 ) ) ;
#44206 = CARTESIAN_POINT ( 'NONE',  ( 0.05219959533937995610, -21.53943276465977519, 60.00109039468568284 ) ) ;
#44207 = CARTESIAN_POINT ( 'NONE',  ( -15.80617190586768217, 15.72974639402176855, 73.12609039468567573 ) ) ;
#44208 = CARTESIAN_POINT ( 'NONE',  ( -0.05219959533907301413, -21.53943276465977519, 67.49890960531436690 ) ) ;
#44209 = ORIENTED_EDGE ( 'NONE', *, *, #36793, .T. ) ;
#44210 = CARTESIAN_POINT ( 'NONE',  ( 9.564922557960805705, 16.46253265017160317, 24.58224293864769194 ) ) ;
#44211 = CARTESIAN_POINT ( 'NONE',  ( 5.823673210054444382, -21.52544592524334988, 45.20942372801901854 ) ) ;
#44212 = CARTESIAN_POINT ( 'NONE',  ( -13.97604488694527625, -13.89961937509977652, 21.87390960531435979 ) ) ;
#44213 = CARTESIAN_POINT ( 'NONE',  ( -16.51473224551069308, -9.474510206698971260, 36.66557627198102409 ) ) ;
#44214 = CARTESIAN_POINT ( 'NONE',  ( -0.05219959533910754901, -16.53943276465976808, 82.49890960531436690 ) ) ;
#44215 = CARTESIAN_POINT ( 'NONE',  ( -13.97604488694527625, -13.89961937509977652, 91.87390960531432427 ) ) ;
#44216 = CARTESIAN_POINT ( 'NONE',  ( -16.55341960407611168, -4.379528057220339221, 26.45724293864768839 ) ) ;
#44217 = CARTESIAN_POINT ( 'NONE',  ( -16.52544592524342804, 4.483927247898546575, 96.04057627198102409 ) ) ;
#44218 = CARTESIAN_POINT ( 'NONE',  ( -21.53943276465977519, 0.05219959533907696930, 66.24890960531436690 ) ) ;
#44219 = AXIS2_PLACEMENT_3D ( 'NONE', #103040, #27214, #56539 ) ;
#44220 = CARTESIAN_POINT ( 'NONE',  ( -10.72451020669898014, 18.67979575497178502, 105.4155762719810383 ) ) ;
#44221 = CARTESIAN_POINT ( 'NONE',  ( -19.03943276465977164, 0.05219959533909376836, 111.2489096053143669 ) ) ;
#44223 = CARTESIAN_POINT ( 'NONE',  ( -19.05341960407617563, 5.049401038297882671, 108.5427570613523187 ) ) ;
#44222 = CARTESIAN_POINT ( 'NONE',  ( -5.153800228976328057, -19.02544592524343514, 62.29057627198100988 ) ) ;
#44224 = CARTESIAN_POINT ( 'NONE',  ( -5.823673210054116645, -21.52544592524344225, 62.29057627198102409 ) ) ;
#44225 = CARTESIAN_POINT ( 'NONE',  ( -0.05219959533937732626, 21.53943276465977519, 82.50109039468568994 ) ) ;
#44226 = B_SPLINE_CURVE_WITH_KNOTS ( 'NONE', 3,
 ( #192591, #131913, #146064, #194594, #7548, #193597, #39893, #101561, #52067, #24754, #148086, #179439, #164262, #175420, #28738, #11586, #184386, #103580, #106538, #119741 ),
 .UNSPECIFIED., .F., .F.,
 ( 4, 2, 2, 2, 2, 2, 2, 2, 2, 4 ),
 ( 0.004000878361811995541, 0.004499404418916006301, 0.004997930476020017061, 0.005496456533124027821, 0.005994982590228037714, 0.006244245618780033119, 0.006493508647332028524, 0.006992034704436018468, 0.007490560761540008411, 0.007989086818643999222 ),
 .UNSPECIFIED. ) ;
#44227 = CARTESIAN_POINT ( 'NONE',  ( -13.89961937509977652, 13.97604488694528158, 70.62390960531432427 ) ) ;
#44228 = CARTESIAN_POINT ( 'NONE',  ( 16.51473224551069308, 9.474510206698969483, 104.1655762719810241 ) ) ;
#44229 = CARTESIAN_POINT ( 'NONE',  ( -8.224510206698735004, -14.34966873604973081, 79.58442372801903275 ) ) ;
#44230 = CARTESIAN_POINT ( 'NONE',  ( 21.52544592524334988, 5.823673210054432836, 61.45942372801901854 ) ) ;
#44231 = CARTESIAN_POINT ( 'NONE',  ( -18.67979575497193778, 10.72451020669871902, 103.3344237280190043 ) ) ;
#44232 = CARTESIAN_POINT ( 'NONE',  ( -15.72974639402197994, 15.80617190586746368, 115.6239096053143669 ) ) ;
#44233 = CARTESIAN_POINT ( 'NONE',  ( 5.823673210054125526, 21.52544592524343514, 79.79057627198102409 ) ) ;
#44234 = CARTESIAN_POINT ( 'NONE',  ( -9.564922557961040184, 16.46253265017147172, 42.91775706135234003 ) ) ;
#44235 = CARTESIAN_POINT ( 'NONE',  ( 5.823673210054125526, 21.52544592524343514, 39.79057627198103830 ) ) ;
#44237 = CARTESIAN_POINT ( 'NONE',  ( 14.34966873604960469, 8.224510206698951720, 39.16557627198102409 ) ) ;
#44236 = CARTESIAN_POINT ( 'NONE',  ( -16.46253265017160317, 9.564922557960807481, 80.83224293864769550 ) ) ;
#44238 = CARTESIAN_POINT ( 'NONE',  ( -16.36317988757060249, 7.306389748694932962, 64.09789608363229263 ) ) ;
#44239 = DIRECTION ( 'NONE',  ( 0.7071067811865512365, 0.7071067811865439090, -0.000000000000000000 ) ) ;
#44240 = CARTESIAN_POINT ( 'NONE',  ( -16.51473224551082808, 9.474510206698731452, 93.33442372801900433 ) ) ;
#44241 = CARTESIAN_POINT ( 'NONE',  ( -21.52544592524343514, 5.823673210054127303, 71.04057627198103830 ) ) ;
#44242 = CARTESIAN_POINT ( 'NONE',  ( 4.483927247898545687, 16.52544592524342804, 54.79057627198104541 ) ) ;
#44243 = CARTESIAN_POINT ( 'NONE',  ( 16.55341960407618274, -4.379528057220086978, 26.04275706135235779 ) ) ;
#44244 = CARTESIAN_POINT ( 'NONE',  ( -9.564922557960796823, -16.46253265017161027, 47.08224293864769550 ) ) ;
#44246 = CARTESIAN_POINT ( 'NONE',  ( -5.153800228976607833, 19.02544592524334988, 82.70942372801897591 ) ) ;
#44245 = CARTESIAN_POINT ( 'NONE',  ( 15.80617190586746368, 15.72974639402197994, 114.3739096053143527 ) ) ;
#44247 = CARTESIAN_POINT ( 'NONE',  ( -19.02544592524342804, 5.153800228976336051, 86.04057627198103830 ) ) ;
#44248 = CARTESIAN_POINT ( 'NONE',  ( -16.53943276465976808, 0.05219959533911058130, 86.24890960531436690 ) ) ;
#44249 = CARTESIAN_POINT ( 'NONE',  ( -0.05219959533909027116, -19.03943276465977164, 67.49890960531436690 ) ) ;
#44250 = CARTESIAN_POINT ( 'NONE',  ( -4.483927247898539470, -16.52544592524342804, 72.29057627198102409 ) ) ;
#44251 = CARTESIAN_POINT ( 'NONE',  ( -19.03943276465977164, 0.05219959533909376836, 26.24890960531435624 ) ) ;
#44252 = CARTESIAN_POINT ( 'NONE',  ( -37.57652299961961262, -0.7251171387572962201, 39.53617709569547856 ) ) ;
#44253 = CARTESIAN_POINT ( 'NONE',  ( -4.483927247898539470, -16.52544592524342804, 37.29057627198102409 ) ) ;
#44254 = CARTESIAN_POINT ( 'NONE',  ( -19.02544592524342804, 5.153800228976336051, 96.04057627198103830 ) ) ;
#44255 = CARTESIAN_POINT ( 'NONE',  ( -1.114781414664558017E-12, -67.16384485484803690, -14.99989890117360503 ) ) ;
#44256 = CARTESIAN_POINT ( 'NONE',  ( 19.03943276465977164, 0.05219959533936151252, 51.25109039468567573 ) ) ;
#44257 = CARTESIAN_POINT ( 'NONE',  ( 16.52544592524335698, 4.483927247898782831, 66.45942372801903275 ) ) ;
#44258 = CARTESIAN_POINT ( 'NONE',  ( 18.62759615963271287, -10.81492255796078972, 78.33224293864770971 ) ) ;
#44259 = CARTESIAN_POINT ( 'NONE',  ( 9.474510206698729675, 16.51473224551082808, 37.08442372801899722 ) ) ;
#44260 = CARTESIAN_POINT ( 'NONE',  ( 13.97604488694527802, 13.89961937509977652, 89.37390960531436690 ) ) ;
#44261 = CARTESIAN_POINT ( 'NONE',  ( -17.50000000000014566, 3.417042746626947736, 115.1738039623247403 ) ) ;
#44262 = CARTESIAN_POINT ( 'NONE',  ( 0.05219959533907565091, 21.53943276465977519, 34.99890960531435979 ) ) ;
#44263 = CARTESIAN_POINT ( 'NONE',  ( 5.153800228976335163, 19.02544592524342804, 74.79057627198103830 ) ) ;
#44264 = CARTESIAN_POINT ( 'NONE',  ( 21.53943276465977519, 0.05219959533937863772, 51.25109039468568994 ) ) ;
#44265 = CARTESIAN_POINT ( 'NONE',  ( 0.05219959533910956823, 16.53943276465976808, 114.9989096053143669 ) ) ;
#44268 = EDGE_LOOP ( 'NONE', ( #199754, #69163, #135578, #66704 ) ) ;
#44267 = CARTESIAN_POINT ( 'NONE',  ( 16.51473224551069308, 9.474510206698969483, 99.16557627198102409 ) ) ;
#44266 = CARTESIAN_POINT ( 'NONE',  ( -18.67979575497193778, 10.72451020669871902, 23.33442372801901499 ) ) ;
#44269 = CARTESIAN_POINT ( 'NONE',  ( -18.67979575497193778, 10.72451020669871902, 38.33442372801900433 ) ) ;
#44270 = ORIENTED_EDGE ( 'NONE', *, *, #81855, .F. ) ;
#44271 = CARTESIAN_POINT ( 'NONE',  ( 19.05341960407611168, 5.049401038298154454, 93.95724293864769550 ) ) ;
#44272 = LINE ( 'NONE', #57459, #27004 ) ;
#44273 = CARTESIAN_POINT ( 'NONE',  ( 18.62759615963271287, -10.81492255796078972, 108.3322429386477097 ) ) ;
#44274 = CARTESIAN_POINT ( 'NONE',  ( 5.049401038298161559, -19.05341960407611168, 47.70724293864770260 ) ) ;
#44275 = CARTESIAN_POINT ( 'NONE',  ( -4.379528057220086978, -16.55341960407618274, 24.79275706135235779 ) ) ;
#44276 = CARTESIAN_POINT ( 'NONE',  ( 22.81625015709509441, 31.40387420917330275, -5.824999997268813345 ) ) ;
#44277 = CARTESIAN_POINT ( 'NONE',  ( -15.72974639402176322, -15.80617190586768395, 99.37609039468568994 ) ) ;
#44278 = CARTESIAN_POINT ( 'NONE',  ( 19.02544592524343514, -5.153800228976328945, 28.54057627198102409 ) ) ;
#44279 = CARTESIAN_POINT ( 'NONE',  ( -21.53943276465977519, -0.05219959533937600094, 103.7510903946857042 ) ) ;
#44281 = CARTESIAN_POINT ( 'NONE',  ( 15.72974639402176855, 15.80617190586768217, 61.87609039468568284 ) ) ;
#44280 = CARTESIAN_POINT ( 'NONE',  ( 9.474510206698971260, -16.51473224551069308, 87.91557627198102409 ) ) ;
#44282 = CARTESIAN_POINT ( 'NONE',  ( 27.73933785331498569, 2.768321779492822058E-14, 146.3750000027311842 ) ) ;
#44283 = CARTESIAN_POINT ( 'NONE',  ( 13.89961937509977652, -13.97604488694527269, 98.12390960531433848 ) ) ;
#44284 = CARTESIAN_POINT ( 'NONE',  ( 22.94331271462294097, -3.784814030245898575, 190.0000000000000000 ) ) ;
#44287 = CARTESIAN_POINT ( 'NONE',  ( 5.823673210054444382, -21.52544592524334988, 55.20942372801902565 ) ) ;
#44286 = CARTESIAN_POINT ( 'NONE',  ( 4.483927247898790824, -16.52544592524335698, 65.20942372801901854 ) ) ;
#44285 = CARTESIAN_POINT ( 'NONE',  ( 12.06949235617739724, 12.14591786802326823, 56.87609039468568994 ) ) ;
#44288 = CARTESIAN_POINT ( 'NONE',  ( 18.62759615963255655, 10.81492255796105972, 91.66775706135234714 ) ) ;
#44289 = DIRECTION ( 'NONE',  ( 1.075492293517917348E-15, -0.9946471445771457587, 0.1033298494363120851 ) ) ;
#44290 = CARTESIAN_POINT ( 'NONE',  ( -0.05219959533934338120, 16.53943276465976808, 32.50109039468568284 ) ) ;
#44291 = CARTESIAN_POINT ( 'NONE',  ( 19.02544592524343514, -5.153800228976328945, 68.54057627198103830 ) ) ;
#44292 = CARTESIAN_POINT ( 'NONE',  ( 9.564922557960805705, 16.46253265017160317, 94.58224293864769550 ) ) ;
#44293 = CARTESIAN_POINT ( 'NONE',  ( -16.46253265017160317, 9.564922557960807481, 110.8322429386476955 ) ) ;
#44294 = CARTESIAN_POINT ( 'NONE',  ( -0.05219959533909027116, -19.03943276465977164, 27.49890960531435624 ) ) ;
#44295 = CARTESIAN_POINT ( 'NONE',  ( 5.823673210054125526, 21.52544592524343514, 34.79057627198103120 ) ) ;
#44296 = CARTESIAN_POINT ( 'NONE',  ( 16.53943276465976808, 0.05219959533934440121, 86.25109039468568994 ) ) ;
#44298 = CARTESIAN_POINT ( 'NONE',  ( 5.153800228976335163, 19.02544592524342804, 69.79057627198103830 ) ) ;
#44297 = CARTESIAN_POINT ( 'NONE',  ( -16.52544592524342804, 4.483927247898546575, 66.04057627198103830 ) ) ;
#44299 = CARTESIAN_POINT ( 'NONE',  ( -5.823673210054431948, 21.52544592524334988, 92.70942372801901854 ) ) ;
#44300 = CARTESIAN_POINT ( 'NONE',  ( -24.06642195515787108, 0.8101246706336291403, -56.93999021579660536 ) ) ;
#44301 = CARTESIAN_POINT ( 'NONE',  ( 16.55341960407618274, -4.379528057220086978, 21.04275706135234714 ) ) ;
#44302 = CARTESIAN_POINT ( 'NONE',  ( 14.34966873604960469, 8.224510206698951720, 69.16557627198102409 ) ) ;
#44303 = CARTESIAN_POINT ( 'NONE',  ( -15.80617190586768217, 15.72974639402176855, 33.12609039468569705 ) ) ;
#44304 = CARTESIAN_POINT ( 'NONE',  ( -18.67979575497178146, -10.72451020669898902, 71.66557627198100988 ) ) ;
#44305 = CARTESIAN_POINT ( 'NONE',  ( -0.05219959533936034679, 19.03943276465977164, 32.50109039468566863 ) ) ;
#44306 = CARTESIAN_POINT ( 'NONE',  ( -35.70266437024451989, 0.2453497911276154020, 37.50000000000000711 ) ) ;
#44307 = CARTESIAN_POINT ( 'NONE',  ( 19.02544592524343514, -5.153800228976328945, 88.54057627198102409 ) ) ;
#44308 = CARTESIAN_POINT ( 'NONE',  ( -16.52544592524342804, 4.483927247898546575, 56.04057627198102409 ) ) ;
#44309 = CARTESIAN_POINT ( 'NONE',  ( -12.14591786802309592, -12.06949235617757132, 31.87390960531435979 ) ) ;
#44310 = CARTESIAN_POINT ( 'NONE',  ( 12.06949235617739724, 12.14591786802326823, 111.8760903946856615 ) ) ;
#44311 = CARTESIAN_POINT ( 'NONE',  ( 0.05219959533936267826, -19.03943276465977164, 60.00109039468566863 ) ) ;
#44312 = CARTESIAN_POINT ( 'NONE',  ( -11.80868324581538253, 11.80868324581533457, -65.00100000000003320 ) ) ;
#44313 = CARTESIAN_POINT ( 'NONE',  ( 5.153800228976335163, 19.02544592524342804, 99.79057627198102409 ) ) ;
#44314 = CARTESIAN_POINT ( 'NONE',  ( -16.55341960407611168, -4.379528057220339221, 76.45724293864769550 ) ) ;
#44315 = DIRECTION ( 'NONE',  ( 0.000000000000000000, 0.000000000000000000, -1.000000000000000000 ) ) ;
#44317 = CARTESIAN_POINT ( 'NONE',  ( 21.52544592524344225, -5.823673210054117533, 38.54057627198103120 ) ) ;
#44316 = CARTESIAN_POINT ( 'NONE',  ( -19.03943276465977164, 0.05219959533909376836, 26.24890960531435624 ) ) ;
#44318 = CARTESIAN_POINT ( 'NONE',  ( -10.72451020669898014, 18.67979575497178502, 65.41557627198102409 ) ) ;
#44319 = CARTESIAN_POINT ( 'NONE',  ( -0.05219959533909027116, -19.03943276465977164, 22.49890960531436690 ) ) ;
#44321 = CARTESIAN_POINT ( 'NONE',  ( 16.46253265017160672, -9.564922557960803928, 48.33224293864769550 ) ) ;
#44320 = CARTESIAN_POINT ( 'NONE',  ( 12.06949235617739724, 12.14591786802326823, 71.87609039468568994 ) ) ;
#44322 = CARTESIAN_POINT ( 'NONE',  ( 5.823673210054444382, -21.52544592524334988, 55.20942372801902565 ) ) ;
#44323 = VECTOR ( 'NONE', #104912, 1000.000000000000114 ) ;
#44324 = CARTESIAN_POINT ( 'NONE',  ( -16.52544592524342804, 4.483927247898546575, 91.04057627198103830 ) ) ;
#44325 = DIRECTION ( 'NONE',  ( -0.000000000000000000, -0.000000000000000000, 1.000000000000000000 ) ) ;
#44326 = CARTESIAN_POINT ( 'NONE',  ( -36.91746825000000598, 11.99521256947798520, -9.224999997268813701 ) ) ;
#44327 = CARTESIAN_POINT ( 'NONE',  ( -18.62759615963270932, 10.81492255796079327, 40.83224293864769550 ) ) ;
#44328 = CARTESIAN_POINT ( 'NONE',  ( -11.80868324581538253, 11.80868324581533457, -61.34707691135562868 ) ) ;
#44330 = CARTESIAN_POINT ( 'NONE',  ( 0.6703450422171775003, 8.945518415904238907, -63.98125415533367999 ) ) ;
#44329 = CARTESIAN_POINT ( 'NONE',  ( -5.823673210054431948, 21.52544592524334988, 72.70942372801901854 ) ) ;
#44332 = CARTESIAN_POINT ( 'NONE',  ( -4.379528057220328563, 16.55341960407611168, 45.20724293864769550 ) ) ;
#44331 = CARTESIAN_POINT ( 'NONE',  ( 8.224510206698742110, 14.34966873604972548, 57.08442372801901854 ) ) ;
#44333 = CARTESIAN_POINT ( 'NONE',  ( 15.72974639402199770, -15.80617190586745480, 73.12390960531436690 ) ) ;
#44334 = CARTESIAN_POINT ( 'NONE',  ( -21.55341960407610458, -5.719274019375992779, 56.45724293864768839 ) ) ;
#44335 = CARTESIAN_POINT ( 'NONE',  ( -21.64434376887846767, -9.890319055725230513, 170.6724019390509568 ) ) ;
#44337 = CARTESIAN_POINT ( 'NONE',  ( -13.89961937509977652, 13.97604488694528158, 95.62390960531436690 ) ) ;
#44336 = CARTESIAN_POINT ( 'NONE',  ( -16.51473224551082808, 9.474510206698731452, 78.33442372801900433 ) ) ;
#44338 = CARTESIAN_POINT ( 'NONE',  ( 5.153800228976335163, 19.02544592524342804, 44.79057627198103830 ) ) ;
#44339 = CARTESIAN_POINT ( 'NONE',  ( 16.46253265017160672, -9.564922557960803928, 23.33224293864769194 ) ) ;
#44340 = CARTESIAN_POINT ( 'NONE',  ( 13.97604488694527802, 13.89961937509977652, 109.3739096053143669 ) ) ;
#44341 = ORIENTED_EDGE ( 'NONE', *, *, #136647, .F. ) ;
#44342 = CARTESIAN_POINT ( 'NONE',  ( -8.314922557961024197, 14.29746914071037800, 62.91775706135236135 ) ) ;
#44343 = CARTESIAN_POINT ( 'NONE',  ( -5.719274019375978568, 21.55341960407610458, 100.2072429386476955 ) ) ;
#44344 = CARTESIAN_POINT ( 'NONE',  ( -13.89961937509977652, 13.97604488694528158, 50.62390960531435979 ) ) ;
#44345 = CARTESIAN_POINT ( 'NONE',  ( -18.62759615963255300, -10.81492255796106328, 44.16775706135234714 ) ) ;
#44346 = CARTESIAN_POINT ( 'NONE',  ( -13.97604488694527625, -13.89961937509977652, 91.87390960531432427 ) ) ;
#44347 = CARTESIAN_POINT ( 'NONE',  ( -21.89035704509619862, -33.26311937564968702, -20.38189100991792557 ) ) ;
#44348 = VERTEX_POINT ( 'NONE', #144357 ) ;
#44349 = CARTESIAN_POINT ( 'NONE',  ( 10.72451020669871369, 18.67979575497193778, 37.08442372801901143 ) ) ;
#44351 = CARTESIAN_POINT ( 'NONE',  ( -19.02544592524334988, -5.153800228976617603, 93.95942372801900433 ) ) ;
#44350 = CARTESIAN_POINT ( 'NONE',  ( -16.46253265017160317, 9.564922557960807481, 100.8322429386477097 ) ) ;
#44352 = CARTESIAN_POINT ( 'NONE',  ( -19.03943276465977164, -0.05219959533935918106, 38.75109039468566152 ) ) ;
#44353 = CARTESIAN_POINT ( 'NONE',  ( 21.52544592524344225, -5.823673210054117533, 93.54057627198103830 ) ) ;
#44354 = CARTESIAN_POINT ( 'NONE',  ( -9.474510206698720793, -16.51473224551083518, 34.58442372801899722 ) ) ;
#44355 = CARTESIAN_POINT ( 'NONE',  ( -0.05219959533936034679, 19.03943276465977164, 42.50109039468566152 ) ) ;
#44356 = CARTESIAN_POINT ( 'NONE',  ( -14.29746914071037622, -8.314922557961029526, 94.16775706135237556 ) ) ;
#44357 = CARTESIAN_POINT ( 'NONE',  ( 28.79475375365586132, 2.781246896534039337E-14, 146.9843446568999923 ) ) ;
#44358 = CARTESIAN_POINT ( 'NONE',  ( 16.51473224551069308, 9.474510206698969483, 59.16557627198102409 ) ) ;
#44359 = CIRCLE ( 'NONE', #109002, 69.99999999999998579 ) ;
#44360 = CARTESIAN_POINT ( 'NONE',  ( 0.05219959533937995610, -21.53943276465977519, 70.00109039468568994 ) ) ;
#44361 = EDGE_CURVE ( 'NONE', #144525, #30159, #35200, .T. ) ;
#44362 = CARTESIAN_POINT ( 'NONE',  ( 10.81492255796106328, -18.62759615963255655, 85.41775706135236135 ) ) ;
#44363 = CARTESIAN_POINT ( 'NONE',  ( 37.99999999999999289, 2.893978650043524126E-14, -10.74999999453762811 ) ) ;
#44364 = CARTESIAN_POINT ( 'NONE',  ( 16.46253265017160672, -9.564922557960803928, 88.33224293864769550 ) ) ;
#44365 = CARTESIAN_POINT ( 'NONE',  ( 10.72451020669871369, 18.67979575497193778, 57.08442372801901854 ) ) ;
#44366 = CARTESIAN_POINT ( 'NONE',  ( -16.46253265017146816, -9.564922557961047289, 104.1677570613523329 ) ) ;
#44367 = CARTESIAN_POINT ( 'NONE',  ( -19.05341960407611168, -5.049401038298163336, 61.45724293864769550 ) ) ;
#44368 = CARTESIAN_POINT ( 'NONE',  ( -13.89961937509977652, 13.97604488694528158, 110.6239096053143243 ) ) ;
#44369 = CARTESIAN_POINT ( 'NONE',  ( 19.03943276465977164, -0.05219959533909143690, 78.74890960531436690 ) ) ;
#44370 = DIRECTION ( 'NONE',  ( 0.000000000000000000, 0.000000000000000000, -1.000000000000000000 ) ) ;
#44371 = CARTESIAN_POINT ( 'NONE',  ( -9.564922557960796823, -16.46253265017161027, 67.08224293864769550 ) ) ;
#44372 = CARTESIAN_POINT ( 'NONE',  ( 19.05341960407611168, 5.049401038298154454, 48.95724293864768129 ) ) ;
#44373 = CARTESIAN_POINT ( 'NONE',  ( 15.80617190586746368, 15.72974639402197994, 94.37390960531436690 ) ) ;
#44374 = CARTESIAN_POINT ( 'NONE',  ( 4.379528057220092307, 16.55341960407617563, 92.29275706135236135 ) ) ;
#44375 = CARTESIAN_POINT ( 'NONE',  ( 6.139823915386828368, -0.3964520562363907374, -64.52448473163055098 ) ) ;
#44376 = CARTESIAN_POINT ( 'NONE',  ( 13.97604488694548053, -13.89961937509957401, 50.62609039468566152 ) ) ;
#44377 = CARTESIAN_POINT ( 'NONE',  ( -9.474510206698964154, 16.51473224551069663, 80.41557627198103830 ) ) ;
#44378 = CARTESIAN_POINT ( 'NONE',  ( -12.14591786802309592, -12.06949235617757132, 71.87390960531438111 ) ) ;
#44379 = CARTESIAN_POINT ( 'NONE',  ( 12.14591786802309770, 12.06949235617756955, 109.3739096053143811 ) ) ;
#44380 = CARTESIAN_POINT ( 'NONE',  ( -16.51473224551069308, -9.474510206698971260, 111.6655762719810383 ) ) ;
#44381 =( BOUNDED_CURVE ( )  B_SPLINE_CURVE ( 2, ( #156949, #31621, #32614, #169121, #80097, #15461, #138787, #46791, #108450, #178112, #22422, #35587, #162928 ),
 .UNSPECIFIED., .F., .T. ) 
 B_SPLINE_CURVE_WITH_KNOTS ( ( 3, 2, 2, 2, 2, 2, 3 ),
 ( 0.2130024320386090242, 0.2149122807017543879, 0.2192982456140350755, 0.2236842105263157909, 0.2280701754385964786, 0.2324561403508771940, 0.2344116688361128631 ),
 .UNSPECIFIED. ) 
 CURVE ( )  GEOMETRIC_REPRESENTATION_ITEM ( )  RATIONAL_B_SPLINE_CURVE ( ( 0.9832469066685285419, 0.9851625545550100060, 1.000000000000000000, 0.9659258262890683122, 1.000000000000000000, 0.9659258262890683122, 1.000000000000000000, 0.9659258262890683122, 1.000000000000000000, 0.9659258262890683122, 1.000000000000000000, 0.9848076720550082985, 0.9831626618144004848 ) ) 
 REPRESENTATION_ITEM ( '' )  );
#44382 = CARTESIAN_POINT ( 'NONE',  ( -13.89961937509977652, 13.97604488694528158, 100.6239096053143669 ) ) ;
#44383 = CARTESIAN_POINT ( 'NONE',  ( 16.46253265017160672, -9.564922557960803928, 83.33224293864768129 ) ) ;
#44384 = CARTESIAN_POINT ( 'NONE',  ( -16.51473224551082808, 9.474510206698731452, 33.33442372801899722 ) ) ;
#44385 = CARTESIAN_POINT ( 'NONE',  ( 0.05219959533934541429, -16.53943276465976808, 90.00109039468567573 ) ) ;
#44386 = CARTESIAN_POINT ( 'NONE',  ( -9.564922557960796823, -16.46253265017161027, 72.08224293864770971 ) ) ;
#44387 = CARTESIAN_POINT ( 'NONE',  ( -5.719274019375665041, -21.55341960407619695, 49.79275706135234714 ) ) ;
#44388 = CARTESIAN_POINT ( 'NONE',  ( 21.53943276465977519, -0.05219959533907433946, 38.74890960531435979 ) ) ;
#44389 = CARTESIAN_POINT ( 'NONE',  ( -15.72974639402176322, -15.80617190586768395, 19.37609039468568639 ) ) ;
#44390 = CARTESIAN_POINT ( 'NONE',  ( 21.55341960407610458, 5.719274019375980345, 68.95724293864769550 ) ) ;
#44391 = CARTESIAN_POINT ( 'NONE',  ( 4.483927247898545687, 16.52544592524342804, 94.79057627198105251 ) ) ;
#44392 = CARTESIAN_POINT ( 'NONE',  ( 19.03943276465977164, 0.05219959533936151252, 51.25109039468567573 ) ) ;
#44393 = EDGE_CURVE ( 'NONE', #3755, #42366, #188903, .T. ) ;
#44394 = CARTESIAN_POINT ( 'NONE',  ( -19.02544592524342804, 5.153800228976336051, 36.04057627198100988 ) ) ;
#44395 = CARTESIAN_POINT ( 'NONE',  ( 5.153800228976335163, 19.02544592524342804, 79.79057627198102409 ) ) ;
#44396 = CARTESIAN_POINT ( 'NONE',  ( -5.153800228976328057, -19.02544592524343514, 82.29057627198103830 ) ) ;
#44397 = CARTESIAN_POINT ( 'NONE',  ( -22.44159573604010305, 16.30477369853692338, 141.1750000027311671 ) ) ;
#44398 = CARTESIAN_POINT ( 'NONE',  ( -14.34966873604960291, -8.224510206698953496, 106.6655762719810383 ) ) ;
#44399 = ORIENTED_EDGE ( 'NONE', *, *, #15491, .F. ) ;
#44400 = CARTESIAN_POINT ( 'NONE',  ( 4.379528057220339221, -16.55341960407611168, 22.70724293864769194 ) ) ;
#44401 = CARTESIAN_POINT ( 'NONE',  ( -12.14591786802326823, 12.06949235617739902, 33.12609039468569705 ) ) ;
#44402 = CARTESIAN_POINT ( 'NONE',  ( -18.67979575497193778, 10.72451020669871902, 93.33442372801901854 ) ) ;
#44403 = CARTESIAN_POINT ( 'NONE',  ( 19.02544592524343514, -5.153800228976328945, 103.5405762719809957 ) ) ;
#44404 = CARTESIAN_POINT ( 'NONE',  ( 10.72451020669898902, -18.67979575497178502, 112.9155762719810383 ) ) ;
#44405 = CARTESIAN_POINT ( 'NONE',  ( 16.46253265017160672, -9.564922557960803928, 43.33224293864769550 ) ) ;
#44406 = CARTESIAN_POINT ( 'NONE',  ( -14.29746914071037622, -8.314922557961029526, 49.16775706135234003 ) ) ;
#44407 = CARTESIAN_POINT ( 'NONE',  ( 16.46253265017146816, 9.564922557961045513, 111.6677570613523329 ) ) ;
#44408 = CARTESIAN_POINT ( 'NONE',  ( 16.51473224551069308, 9.474510206698969483, 39.16557627198103120 ) ) ;
#44409 = CARTESIAN_POINT ( 'NONE',  ( -0.05219959533910754901, -16.53943276465976808, 92.49890960531436690 ) ) ;
#44410 = CARTESIAN_POINT ( 'NONE',  ( -10.81492255796078084, -18.62759615963271287, 107.0822429386476955 ) ) ;
#44411 = CARTESIAN_POINT ( 'NONE',  ( -19.03943276465977164, -0.05219959533935918106, 68.75109039468566152 ) ) ;
#44412 = CARTESIAN_POINT ( 'NONE',  ( -0.05219959533909027116, -19.03943276465977164, 22.49890960531436690 ) ) ;
#44413 = CARTESIAN_POINT ( 'NONE',  ( -10.72451020669870658, -18.67979575497194134, 19.58442372801901143 ) ) ;
#44414 = DIRECTION ( 'NONE',  ( 1.000000000000000000, 0.000000000000000000, 0.000000000000000000 ) ) ;
#44415 = CARTESIAN_POINT ( 'NONE',  ( 13.97604488694527802, 13.89961937509977652, 94.37390960531436690 ) ) ;
#44416 = LINE ( 'NONE', #14061, #55114 ) ;
#44417 = CARTESIAN_POINT ( 'NONE',  ( -5.153800228976328057, -19.02544592524343514, 87.29057627198103830 ) ) ;
#44419 = CARTESIAN_POINT ( 'NONE',  ( -8.314922557960811034, -14.29746914071050412, 82.08224293864768129 ) ) ;
#44418 = CARTESIAN_POINT ( 'NONE',  ( 5.823673210054444382, -21.52544592524334988, 30.20942372801902565 ) ) ;
#44420 = CARTESIAN_POINT ( 'NONE',  ( -0.05219959533909027116, -19.03943276465977164, 77.49890960531435269 ) ) ;
#44421 = CARTESIAN_POINT ( 'NONE',  ( 13.89961937509957401, 13.97604488694547697, 26.87609039468566507 ) ) ;
#44423 = CARTESIAN_POINT ( 'NONE',  ( 19.03943276465977164, 0.05219959533936151252, 56.25109039468566863 ) ) ;
#44422 = CARTESIAN_POINT ( 'NONE',  ( -14.29746914071037622, -8.314922557961029526, 49.16775706135234003 ) ) ;
#44424 = CARTESIAN_POINT ( 'NONE',  ( 18.67979575497194134, -10.72451020669871369, 60.83442372801901854 ) ) ;
#44425 = CARTESIAN_POINT ( 'NONE',  ( -12.06949235617739369, -12.14591786802326823, 29.37609039468568284 ) ) ;
#44426 = CARTESIAN_POINT ( 'NONE',  ( -19.03943276465977164, 0.05219959533909376836, 71.24890960531435269 ) ) ;
#44427 = CARTESIAN_POINT ( 'NONE',  ( 19.03943276465977164, 0.05219959533936151252, 96.25109039468567573 ) ) ;
#44428 = CARTESIAN_POINT ( 'NONE',  ( 4.483927247898790824, -16.52544592524335698, 65.20942372801901854 ) ) ;
#44429 = CARTESIAN_POINT ( 'NONE',  ( -21.52544592524334988, -5.823673210054445271, 103.9594237280190185 ) ) ;
#44430 = CARTESIAN_POINT ( 'NONE',  ( -0.05219959533936034679, 19.03943276465977164, 82.50109039468567573 ) ) ;
#44431 = CARTESIAN_POINT ( 'NONE',  ( -9.474510206698964154, 16.51473224551069663, 50.41557627198102409 ) ) ;
#44432 = CARTESIAN_POINT ( 'NONE',  ( 10.81492255796078972, 18.62759615963270932, 84.58224293864769550 ) ) ;
#44434 = CARTESIAN_POINT ( 'NONE',  ( 9.474510206698729675, 16.51473224551082808, 82.08442372801899012 ) ) ;
#44433 = CARTESIAN_POINT ( 'NONE',  ( -12.06949235617756955, 12.14591786802309770, 80.62390960531438111 ) ) ;
#44435 = CARTESIAN_POINT ( 'NONE',  ( 17.50000000000004263, -5.622605283950769639, 61.18792689403890961 ) ) ;
#44436 = CARTESIAN_POINT ( 'NONE',  ( 19.02544592524334988, 5.153800228976608722, 46.45942372801899012 ) ) ;
#44437 = CARTESIAN_POINT ( 'NONE',  ( -0.05219959533910754901, -16.53943276465976808, 22.49890960531436335 ) ) ;
#44438 = CARTESIAN_POINT ( 'NONE',  ( 0.05219959533910956823, 16.53943276465976808, 69.99890960531435269 ) ) ;
#44440 = CARTESIAN_POINT ( 'NONE',  ( 27.73933785331498214, 9.013057229001095294, 145.9750000027311785 ) ) ;
#44439 = CARTESIAN_POINT ( 'NONE',  ( 5.719274019375673035, 21.55341960407619339, 97.29275706135234714 ) ) ;
#44441 = CARTESIAN_POINT ( 'NONE',  ( 21.52544592524344225, -5.823673210054117533, 103.5405762719810383 ) ) ;
#44442 = CARTESIAN_POINT ( 'NONE',  ( -19.05341960407611168, -5.049401038298163336, 71.45724293864766707 ) ) ;
#44443 = CARTESIAN_POINT ( 'NONE',  ( -21.52544592524334988, -5.823673210054445271, 78.95942372801901854 ) ) ;
#44444 = CARTESIAN_POINT ( 'NONE',  ( 13.89961937509977652, -13.97604488694527269, 68.12390960531436690 ) ) ;
#44445 = EDGE_LOOP ( 'NONE', ( #108669, #151253, #116948, #54910 ) ) ;
#44446 = CARTESIAN_POINT ( 'NONE',  ( 5.153800228976335163, 19.02544592524342804, 29.79057627198102409 ) ) ;
#44447 = CARTESIAN_POINT ( 'NONE',  ( 10.81492255796078972, 18.62759615963270932, 34.58224293864770260 ) ) ;
#44448 = CARTESIAN_POINT ( 'NONE',  ( -4.483927247898539470, -16.52544592524342804, 62.29057627198102409 ) ) ;
#44449 = CARTESIAN_POINT ( 'NONE',  ( -19.05341960407611168, -5.049401038298163336, 46.45724293864768129 ) ) ;
#44450 = CARTESIAN_POINT ( 'NONE',  ( 14.34966873604960469, 8.224510206698951720, 99.16557627198100988 ) ) ;
#44451 = VECTOR ( 'NONE', #74680, 1000.000000000000000 ) ;
#44452 = CARTESIAN_POINT ( 'NONE',  ( -21.55341960407610458, -5.719274019375992779, 111.4572429386476813 ) ) ;
#44453 = CARTESIAN_POINT ( 'NONE',  ( -21.52544592524334988, -5.823673210054445271, 53.95942372801900433 ) ) ;
#44454 = CARTESIAN_POINT ( 'NONE',  ( -13.97604488694527625, -13.89961937509977652, 36.87390960531436690 ) ) ;
#44455 = CARTESIAN_POINT ( 'NONE',  ( 8.224510206698742110, 14.34966873604972548, 47.08442372801901854 ) ) ;
#44456 = CARTESIAN_POINT ( 'NONE',  ( 5.719274019375991003, -21.55341960407610458, 102.7072429386476955 ) ) ;
#44457 = CARTESIAN_POINT ( 'NONE',  ( -18.67979575497178146, -10.72451020669898902, 91.66557627198103830 ) ) ;
#44459 = CARTESIAN_POINT ( 'NONE',  ( -19.02544592524342804, 5.153800228976336051, 56.04057627198100988 ) ) ;
#44458 = CARTESIAN_POINT ( 'NONE',  ( -19.03943276465977164, -0.05219959533935918106, 23.75109039468566152 ) ) ;
#44460 = CARTESIAN_POINT ( 'NONE',  ( -5.153800228976328057, -19.02544592524343514, 112.2905762719810099 ) ) ;
#44461 = CARTESIAN_POINT ( 'NONE',  ( -21.55341960407619339, 5.719274019375674811, 58.54275706135235424 ) ) ;
#44462 = CARTESIAN_POINT ( 'NONE',  ( 18.67979575497178502, 10.72451020669898547, 44.16557627198103120 ) ) ;
#44463 = CARTESIAN_POINT ( 'NONE',  ( -4.483927247898782831, 16.52544592524335698, 112.7094237280190328 ) ) ;
#44465 = CARTESIAN_POINT ( 'NONE',  ( 21.53943276465977519, 0.05219959533937863772, 101.2510903946856757 ) ) ;
#44464 = CARTESIAN_POINT ( 'NONE',  ( -18.67979575497193778, 10.72451020669871902, 63.33442372801900433 ) ) ;
#44466 = CARTESIAN_POINT ( 'NONE',  ( -19.03943276465977164, -0.05219959533935918106, 38.75109039468566152 ) ) ;
#44467 = CARTESIAN_POINT ( 'NONE',  ( -16.52544592524335698, -4.483927247898792601, 103.9594237280190185 ) ) ;
#44468 = CARTESIAN_POINT ( 'NONE',  ( -18.62759615963255300, -10.81492255796106328, 49.16775706135234003 ) ) ;
#44469 = CARTESIAN_POINT ( 'NONE',  ( 16.46253265017160672, -9.564922557960803928, 58.33224293864769550 ) ) ;
#44470 = CARTESIAN_POINT ( 'NONE',  ( -13.89961937509957401, -13.97604488694547875, 19.37609039468566507 ) ) ;
#44471 = CARTESIAN_POINT ( 'NONE',  ( -19.02544592524342804, 5.153800228976336051, 116.0405762719810383 ) ) ;
#44472 = CARTESIAN_POINT ( 'NONE',  ( 10.72451020669871369, 18.67979575497193778, 32.08442372801901854 ) ) ;
#44473 = CARTESIAN_POINT ( 'NONE',  ( -21.53943276465977519, 0.05219959533907696930, 86.24890960531436690 ) ) ;
#44474 = CARTESIAN_POINT ( 'NONE',  ( 12.14591786802327356, -12.06949235617739191, 40.62609039468567573 ) ) ;
#44476 = CARTESIAN_POINT ( 'NONE',  ( -10.72451020669898014, 18.67979575497178502, 75.41557627198102409 ) ) ;
#44475 = CARTESIAN_POINT ( 'NONE',  ( 17.50000000000000000, 5.499999999999997335, 31.70309617465830243 ) ) ;
#44478 = CARTESIAN_POINT ( 'NONE',  ( -12.14591786802309592, -12.06949235617757132, 71.87390960531438111 ) ) ;
#44477 = CARTESIAN_POINT ( 'NONE',  ( 8.224510206698742110, 14.34966873604972548, 62.08442372801901143 ) ) ;
#44479 = DIRECTION ( 'NONE',  ( -0.8437662581494470571, 0.5367108174878540972, 0.000000000000000000 ) ) ;
#44480 = CARTESIAN_POINT ( 'NONE',  ( -5.153800228976607833, 19.02544592524334988, 97.70942372801900433 ) ) ;
#44481 = CARTESIAN_POINT ( 'NONE',  ( -21.52544592524343514, 5.823673210054127303, 36.04057627198102409 ) ) ;
#44482 = VECTOR ( 'NONE', #14171, 1000.000000000000000 ) ;
#44483 = FACE_OUTER_BOUND ( 'NONE', #166911, .T. ) ;
#44484 = CARTESIAN_POINT ( 'NONE',  ( 16.52544592524335698, 4.483927247898782831, 36.45942372801901143 ) ) ;
#44485 = CARTESIAN_POINT ( 'NONE',  ( -18.67979575497178146, -10.72451020669898902, 106.6655762719810383 ) ) ;
#44486 = CARTESIAN_POINT ( 'NONE',  ( 18.62759615963271287, -10.81492255796078972, 33.33224293864769550 ) ) ;
#44487 = CARTESIAN_POINT ( 'NONE',  ( -16.53943276465976808, -0.05219959533934237506, 73.75109039468567573 ) ) ;
#44488 = CARTESIAN_POINT ( 'NONE',  ( -16.51473224551069308, -9.474510206698971260, 81.66557627198103830 ) ) ;
#44490 = CARTESIAN_POINT ( 'NONE',  ( 19.05341960407611168, 5.049401038298154454, 33.95724293864769550 ) ) ;
#44489 = CARTESIAN_POINT ( 'NONE',  ( -21.53943276465977519, -0.05219959533937600094, 53.75109039468568994 ) ) ;
#44491 = CARTESIAN_POINT ( 'NONE',  ( -13.89961937509977652, 13.97604488694528158, 115.6239096053143669 ) ) ;
#44492 = ORIENTED_EDGE ( 'NONE', *, *, #103099, .T. ) ;
#44493 = CARTESIAN_POINT ( 'NONE',  ( -16.46253265017146816, -9.564922557961047289, 39.16775706135234003 ) ) ;
#44494 = CARTESIAN_POINT ( 'NONE',  ( -4.483927247898782831, 16.52544592524335698, 47.70942372801902565 ) ) ;
#44495 = CARTESIAN_POINT ( 'NONE',  ( 5.153800228976335163, 19.02544592524342804, 114.7905762719810241 ) ) ;
#44496 = CARTESIAN_POINT ( 'NONE',  ( -13.89961937509977652, 13.97604488694528158, 70.62390960531432427 ) ) ;
#44497 = CARTESIAN_POINT ( 'NONE',  ( 8.224510206698742110, 14.34966873604972548, 97.08442372801904696 ) ) ;
#44498 = PLANE ( 'NONE',  #127987 ) ;
#44499 = CARTESIAN_POINT ( 'NONE',  ( 4.379528057220339221, -16.55341960407611168, 97.70724293864772392 ) ) ;
#44500 = CARTESIAN_POINT ( 'NONE',  ( 5.823673210054125526, 21.52544592524343514, 34.79057627198103120 ) ) ;
#44501 = CARTESIAN_POINT ( 'NONE',  ( -9.564922557960796823, -16.46253265017161027, 37.08224293864768839 ) ) ;
#44502 = CARTESIAN_POINT ( 'NONE',  ( 16.55341960407618274, -4.379528057220086978, 61.04275706135234714 ) ) ;
#44503 = CARTESIAN_POINT ( 'NONE',  ( -21.53943276465977519, 0.05219959533907696930, 116.2489096053143669 ) ) ;
#44504 = CARTESIAN_POINT ( 'NONE',  ( 5.049401038297881783, 19.05341960407617563, 72.29275706135234714 ) ) ;
#44505 = CARTESIAN_POINT ( 'NONE',  ( 16.46253265017160672, -9.564922557960803928, 38.33224293864768839 ) ) ;
#44506 = CARTESIAN_POINT ( 'NONE',  ( 0.05219959533907565091, 21.53943276465977519, 64.99890960531435269 ) ) ;
#44507 = CARTESIAN_POINT ( 'NONE',  ( -9.474510206698964154, 16.51473224551069663, 115.4155762719810241 ) ) ;
#44508 = CARTESIAN_POINT ( 'NONE',  ( 21.52544592524334988, 5.823673210054432836, 91.45942372801901854 ) ) ;
#44509 = CARTESIAN_POINT ( 'NONE',  ( 13.97604488694527802, 13.89961937509977652, 64.37390960531436690 ) ) ;
#44510 = CARTESIAN_POINT ( 'NONE',  ( 12.14591786802327356, -12.06949235617739191, 55.62609039468568284 ) ) ;
#44511 = CARTESIAN_POINT ( 'NONE',  ( 13.89961937509977652, -13.97604488694527269, 63.12390960531435979 ) ) ;
#44512 = CARTESIAN_POINT ( 'NONE',  ( -10.72451020669870658, -18.67979575497194134, 84.58442372801903275 ) ) ;
#44513 = CARTESIAN_POINT ( 'NONE',  ( 16.46253265017146816, 9.564922557961045513, 41.66775706135234003 ) ) ;
#44514 = CARTESIAN_POINT ( 'NONE',  ( -9.474510206698720793, -16.51473224551083518, 54.58442372801899722 ) ) ;
#44515 = CARTESIAN_POINT ( 'NONE',  ( 0.05219959533937995610, -21.53943276465977519, 55.00109039468568284 ) ) ;
#44516 = CARTESIAN_POINT ( 'NONE',  ( -5.427562675786936573E-15, 30.27659582821221207, 143.4843446568999639 ) ) ;
#44517 = CARTESIAN_POINT ( 'NONE',  ( -9.474510206698720793, -16.51473224551083518, 44.58442372801900433 ) ) ;
#44518 = CARTESIAN_POINT ( 'NONE',  ( -9.474510206698964154, 16.51473224551069663, 95.41557627198102409 ) ) ;
#44519 = CARTESIAN_POINT ( 'NONE',  ( 13.89961937509977652, -13.97604488694527269, 83.12390960531436690 ) ) ;
#44520 = CARTESIAN_POINT ( 'NONE',  ( -0.05219959533910754901, -16.53943276465976808, 32.49890960531435979 ) ) ;
#44522 = CARTESIAN_POINT ( 'NONE',  ( -5.719274019375665041, -21.55341960407619695, 94.79275706135234714 ) ) ;
#44521 = CARTESIAN_POINT ( 'NONE',  ( -15.72974639402197994, 15.80617190586746368, 30.62390960531436335 ) ) ;
#44523 = CARTESIAN_POINT ( 'NONE',  ( 36.91746824999999887, 11.99521256947799053, -1.524999997268813745 ) ) ;
#44524 = CARTESIAN_POINT ( 'NONE',  ( -34.52594549653172606, 0.3596637467104419339, 89.49999999999899103 ) ) ;
#44525 = CARTESIAN_POINT ( 'NONE',  ( 10.72451020669871369, 18.67979575497193778, 92.08442372801901854 ) ) ;
#44526 = CARTESIAN_POINT ( 'NONE',  ( -26.70613957415103101, 7.662257527287501979, 167.2521143936661474 ) ) ;
#44527 = CARTESIAN_POINT ( 'NONE',  ( 9.564922557960805705, 16.46253265017160317, 34.58224293864770260 ) ) ;
#44528 = DIRECTION ( 'NONE',  ( 0.000000000000000000, 0.000000000000000000, 1.000000000000000000 ) ) ;
#44529 = EDGE_CURVE ( 'NONE', #142736, #3830, #81669, .T. ) ;
#44530 = CARTESIAN_POINT ( 'NONE',  ( 33.72265478998905053, 5.501106843017430137, 95.34580731367215378 ) ) ;
#44531 = CARTESIAN_POINT ( 'NONE',  ( 0.05219959533934541429, -16.53943276465976808, 45.00109039468568284 ) ) ;
#44532 = CARTESIAN_POINT ( 'NONE',  ( -18.62759615963270932, 10.81492255796079327, 65.83224293864769550 ) ) ;
#44533 = CARTESIAN_POINT ( 'NONE',  ( 8.314922557960818139, 14.29746914071049879, 44.58224293864769550 ) ) ;
#44535 = CARTESIAN_POINT ( 'NONE',  ( 16.46253265017160672, -9.564922557960803928, 113.3322429386476955 ) ) ;
#44534 = CARTESIAN_POINT ( 'NONE',  ( 16.55341960407611168, 4.379528057220329451, 108.9572429386476955 ) ) ;
#44536 = CARTESIAN_POINT ( 'NONE',  ( 0.05219959533937995610, -21.53943276465977519, 25.00109039468567218 ) ) ;
#44537 = CARTESIAN_POINT ( 'NONE',  ( 13.89961937509957401, 13.97604488694547697, 41.87609039468566152 ) ) ;
#44538 = CARTESIAN_POINT ( 'NONE',  ( -14.29746914071049879, 8.314922557960819915, 115.8322429386477097 ) ) ;
#44539 = CARTESIAN_POINT ( 'NONE',  ( 15.72974639402176855, 15.80617190586768217, 61.87609039468568284 ) ) ;
#44540 = CARTESIAN_POINT ( 'NONE',  ( 17.40861289039004944, -6.110651285853252901, 31.12767529172569780 ) ) ;
#44541 = CARTESIAN_POINT ( 'NONE',  ( -8.314922557960811034, -14.29746914071050412, 27.08224293864769550 ) ) ;
#44542 = CARTESIAN_POINT ( 'NONE',  ( -0.05219959533936034679, 19.03943276465977164, 67.50109039468566152 ) ) ;
#44543 = CARTESIAN_POINT ( 'NONE',  ( 21.52544592524344225, -5.823673210054117533, 23.54057627198102765 ) ) ;
#44544 = CARTESIAN_POINT ( 'NONE',  ( -8.224510206698948167, 14.34966873604960824, 85.41557627198102409 ) ) ;
#44545 = CARTESIAN_POINT ( 'NONE',  ( 27.39934578958845179, -26.16170490841984630, -16.57183124570353172 ) ) ;
#44546 = CARTESIAN_POINT ( 'NONE',  ( -5.153800228976328057, -19.02544592524343514, 72.29057627198102409 ) ) ;
#44547 = CARTESIAN_POINT ( 'NONE',  ( 0.05219959533910956823, 16.53943276465976808, 69.99890960531435269 ) ) ;
#44548 = CARTESIAN_POINT ( 'NONE',  ( -0.05219959533936034679, 19.03943276465977164, 102.5010903946856757 ) ) ;
#44549 = CARTESIAN_POINT ( 'NONE',  ( -5.719274019375978568, 21.55341960407610458, 45.20724293864769550 ) ) ;
#44550 = ORIENTED_EDGE ( 'NONE', *, *, #192276, .T. ) ;
#44551 = CARTESIAN_POINT ( 'NONE',  ( 12.06949235617757843, -12.14591786802309237, 113.1239096053143953 ) ) ;
#44553 = CARTESIAN_POINT ( 'NONE',  ( 10.81492255796078972, 18.62759615963270932, 79.58224293864769550 ) ) ;
#44552 = CARTESIAN_POINT ( 'NONE',  ( -13.97604488694527625, -13.89961937509977652, 66.87390960531436690 ) ) ;
#44555 = CARTESIAN_POINT ( 'NONE',  ( -19.03943276465977164, 0.05219959533909376836, 91.24890960531436690 ) ) ;
#44554 = CARTESIAN_POINT ( 'NONE',  ( 16.52544592524335698, 4.483927247898782831, 111.4594237280190328 ) ) ;
#44556 = CARTESIAN_POINT ( 'NONE',  ( -19.03943276465977164, -0.05219959533935918106, 73.75109039468566152 ) ) ;
#44557 = CARTESIAN_POINT ( 'NONE',  ( -21.52544592524334988, -5.823673210054445271, 93.95942372801903275 ) ) ;
#44558 = CARTESIAN_POINT ( 'NONE',  ( 21.53943276465977519, -0.05219959533907433946, 68.74890960531435269 ) ) ;
#44559 = CARTESIAN_POINT ( 'NONE',  ( 16.46253265017160672, -9.564922557960803928, 113.3322429386476955 ) ) ;
#44560 = CARTESIAN_POINT ( 'NONE',  ( 13.89961937509977652, -13.97604488694527269, 53.12390960531434558 ) ) ;
#44561 = CARTESIAN_POINT ( 'NONE',  ( 12.06949235617739724, 12.14591786802326823, 101.8760903946857042 ) ) ;
#44562 = CARTESIAN_POINT ( 'NONE',  ( -16.51473224551069308, -9.474510206698971260, 66.66557627198102409 ) ) ;
#44563 = CARTESIAN_POINT ( 'NONE',  ( -8.314922557961024197, 14.29746914071037800, 22.91775706135235069 ) ) ;
#44564 = CARTESIAN_POINT ( 'NONE',  ( -31.68374724557850541, -1.945525369148830563, 102.2474955886453785 ) ) ;
#44565 = CARTESIAN_POINT ( 'NONE',  ( 18.62759615963255655, 10.81492255796105972, 111.6677570613523613 ) ) ;
#44566 = CARTESIAN_POINT ( 'NONE',  ( 14.29746914071049879, -8.314922557960816363, 78.33224293864770971 ) ) ;
#44567 = CARTESIAN_POINT ( 'NONE',  ( -15.72974639402197994, 15.80617190586746368, 105.6239096053143669 ) ) ;
#44568 = CARTESIAN_POINT ( 'NONE',  ( 21.55341960407610458, 5.719274019375980345, 98.95724293864770971 ) ) ;
#44569 = DIRECTION ( 'NONE',  ( 0.000000000000000000, 0.000000000000000000, -1.000000000000000000 ) ) ;
#44570 = CARTESIAN_POINT ( 'NONE',  ( 0.05219959533907565091, 21.53943276465977519, 64.99890960531435269 ) ) ;
#44571 = CARTESIAN_POINT ( 'NONE',  ( -0.05219959533934338120, 16.53943276465976808, 77.50109039468567573 ) ) ;
#44572 = CARTESIAN_POINT ( 'NONE',  ( 12.06949235617757843, -12.14591786802309237, 103.1239096053143811 ) ) ;
#44573 = CARTESIAN_POINT ( 'NONE',  ( -13.97604488694527625, -13.89961937509977652, 61.87390960531435979 ) ) ;
#44574 = CARTESIAN_POINT ( 'NONE',  ( -16.55341960407611168, -4.379528057220339221, 21.45724293864769550 ) ) ;
#44575 = CARTESIAN_POINT ( 'NONE',  ( -5.823673210054431948, 21.52544592524334988, 47.70942372801902565 ) ) ;
#44576 = CARTESIAN_POINT ( 'NONE',  ( -19.05341960407611168, -5.049401038298163336, 101.4572429386476955 ) ) ;
#44577 = CARTESIAN_POINT ( 'NONE',  ( 10.81492255796106328, -18.62759615963255655, 80.41775706135234714 ) ) ;
#44578 = CARTESIAN_POINT ( 'NONE',  ( 19.02544592524343514, -5.153800228976328945, 33.54057627198102409 ) ) ;
#44579 = CARTESIAN_POINT ( 'NONE',  ( -16.51473224551069308, -9.474510206698971260, 41.66557627198103120 ) ) ;
#44580 = VERTEX_POINT ( 'NONE', #145354 ) ;
#44581 = CARTESIAN_POINT ( 'NONE',  ( -15.80617190586768217, 15.72974639402176855, 78.12609039468570415 ) ) ;
#44582 = CARTESIAN_POINT ( 'NONE',  ( -5.153800228976328057, -19.02544592524343514, 102.2905762719810383 ) ) ;
#44583 = CARTESIAN_POINT ( 'NONE',  ( 5.153800228976615827, -19.02544592524334988, 80.20942372801901854 ) ) ;
#44584 = CARTESIAN_POINT ( 'NONE',  ( -15.80617190586768217, 15.72974639402176855, 38.12609039468567573 ) ) ;
#44585 = CARTESIAN_POINT ( 'NONE',  ( -8.314922557961024197, 14.29746914071037800, 22.91775706135235069 ) ) ;
#44586 = CARTESIAN_POINT ( 'NONE',  ( -5.153800228976607833, 19.02544592524334988, 72.70942372801900433 ) ) ;
#44587 = CARTESIAN_POINT ( 'NONE',  ( -19.02544592524342804, 5.153800228976336051, 51.04057627198103120 ) ) ;
#44588 = CARTESIAN_POINT ( 'NONE',  ( -13.89961937509957401, -13.97604488694547875, 84.37609039468567573 ) ) ;
#44589 = CIRCLE ( 'NONE', #105920, 0.5000000000000004441 ) ;
#44590 = CARTESIAN_POINT ( 'NONE',  ( 12.14591786802309770, 12.06949235617756955, 24.37390960531435979 ) ) ;
#44591 = CARTESIAN_POINT ( 'NONE',  ( 19.05341960407617918, -5.049401038297876454, 91.04275706135234714 ) ) ;
#44592 = CARTESIAN_POINT ( 'NONE',  ( 0.05219959533910956823, 16.53943276465976808, 34.99890960531435979 ) ) ;
#44593 = CARTESIAN_POINT ( 'NONE',  ( -0.05219959533936034679, 19.03943276465977164, 67.50109039468566152 ) ) ;
#44594 = CARTESIAN_POINT ( 'NONE',  ( -4.483927247898782831, 16.52544592524335698, 42.70942372801901854 ) ) ;
#44595 = CARTESIAN_POINT ( 'NONE',  ( 9.564922557961047289, -16.46253265017146816, 30.41775706135232937 ) ) ;
#44596 = EDGE_CURVE ( 'NONE', #151167, #36346, #51363, .T. ) ;
#44597 = CARTESIAN_POINT ( 'NONE',  ( 16.46253265017160672, -9.564922557960803928, 28.33224293864769550 ) ) ;
#44598 = CARTESIAN_POINT ( 'NONE',  ( 18.56197773271727769, -5.500000000000078160, 71.05066217314453070 ) ) ;
#44599 = CARTESIAN_POINT ( 'NONE',  ( 12.06949235617739724, 12.14591786802326823, 51.87609039468568284 ) ) ;
#44600 = DIRECTION ( 'NONE',  ( 0.000000000000000000, 1.000000000000000000, 0.000000000000000000 ) ) ;
#44601 = CARTESIAN_POINT ( 'NONE',  ( 1.784210473542230573E-15, -29.16686587814331588, 141.3750000027311557 ) ) ;
#44602 = CARTESIAN_POINT ( 'NONE',  ( -13.89961937509977652, 13.97604488694528158, 90.62390960531432427 ) ) ;
#44603 = DIRECTION ( 'NONE',  ( -1.000000000000000000, 0.000000000000000000, 0.000000000000000000 ) ) ;
#44604 = ORIENTED_EDGE ( 'NONE', *, *, #130089, .F. ) ;
#44605 = CARTESIAN_POINT ( 'NONE',  ( -19.02544592524334988, -5.153800228976617603, 78.95942372801900433 ) ) ;
#44606 = CARTESIAN_POINT ( 'NONE',  ( -5.719274019375978568, 21.55341960407610458, 30.20724293864769550 ) ) ;
#44608 = CARTESIAN_POINT ( 'NONE',  ( 19.03943276465977164, 0.05219959533936151252, 96.25109039468567573 ) ) ;
#44607 = CARTESIAN_POINT ( 'NONE',  ( -19.03943276465977164, -0.05219959533935918106, 23.75109039468566152 ) ) ;
#44609 = CARTESIAN_POINT ( 'NONE',  ( 14.34966873604960469, 8.224510206698951720, 109.1655762719810383 ) ) ;
#44610 = CARTESIAN_POINT ( 'NONE',  ( -13.89961937509977652, 13.97604488694528158, 40.62390960531435979 ) ) ;
#44611 = CARTESIAN_POINT ( 'NONE',  ( 18.67979575497178502, 10.72451020669898547, 59.16557627198103120 ) ) ;
#44612 = CARTESIAN_POINT ( 'NONE',  ( -0.05219959533910754901, -16.53943276465976808, 112.4989096053143669 ) ) ;
#44613 = CARTESIAN_POINT ( 'NONE',  ( 23.46320343559666100, 18.96320343559613875, 1.110912703473986074 ) ) ;
#44614 = CARTESIAN_POINT ( 'NONE',  ( 16.46253265017146816, 9.564922557961045513, 66.66775706135233293 ) ) ;
#44616 = VECTOR ( 'NONE', #52347, 1000.000000000000000 ) ;
#44615 = CARTESIAN_POINT ( 'NONE',  ( -4.379528057220328563, 16.55341960407611168, 35.20724293864768839 ) ) ;
#44617 = CARTESIAN_POINT ( 'NONE',  ( 13.97604488694527802, 13.89961937509977652, 109.3739096053143669 ) ) ;
#44618 = CARTESIAN_POINT ( 'NONE',  ( 10.81492255796106328, -18.62759615963255655, 90.41775706135236135 ) ) ;
#44619 = CARTESIAN_POINT ( 'NONE',  ( -21.55341960407610458, -5.719274019375992779, 86.45724293864770971 ) ) ;
#44620 = CARTESIAN_POINT ( 'NONE',  ( -5.719274019375665041, -21.55341960407619695, 54.79275706135235424 ) ) ;
#44621 = CARTESIAN_POINT ( 'NONE',  ( 18.62759615963255655, 10.81492255796105972, 61.66775706135235424 ) ) ;
#44622 = CARTESIAN_POINT ( 'NONE',  ( 9.564922557960805705, 16.46253265017160317, 94.58224293864769550 ) ) ;
#44624 = CARTESIAN_POINT ( 'NONE',  ( -5.823673210054431948, 21.52544592524334988, 47.70942372801902565 ) ) ;
#44623 = CARTESIAN_POINT ( 'NONE',  ( -0.05219959533934338120, 16.53943276465976808, 92.50109039468567573 ) ) ;
#44625 =( BOUNDED_CURVE ( )  B_SPLINE_CURVE ( 2, ( #11310, #196335, #57803, #119474, #181157, #42633, #104296, #27479, #12306, #58775, #120443, #50578, #126407 ),
 .UNSPECIFIED., .F., .T. ) 
 B_SPLINE_CURVE_WITH_KNOTS ( ( 3, 2, 2, 2, 2, 2, 3 ),
 ( 0.6866866425649248429, 0.6885964912280702066, 0.6929824561403509220, 0.6973684210526315264, 0.7017543859649122417, 0.7061403508771929571, 0.7080958793624286818 ),
 .UNSPECIFIED. ) 
 CURVE ( )  GEOMETRIC_REPRESENTATION_ITEM ( )  RATIONAL_B_SPLINE_CURVE ( ( 0.9832469066685285419, 0.9851625545550100060, 1.000000000000000000, 0.9659258262890683122, 1.000000000000000000, 0.9659258262890683122, 1.000000000000000000, 0.9659258262890683122, 1.000000000000000000, 0.9659258262890683122, 1.000000000000000000, 0.9848076720550078544, 0.9831626618144001517 ) ) 
 REPRESENTATION_ITEM ( '' )  );
#44626 = CARTESIAN_POINT ( 'NONE',  ( 12.06949235617757843, -12.14591786802309237, 113.1239096053143953 ) ) ;
#44627 = CARTESIAN_POINT ( 'NONE',  ( -8.314922557960811034, -14.29746914071050412, 72.08224293864769550 ) ) ;
#44628 = CARTESIAN_POINT ( 'NONE',  ( 16.52544592524342804, -4.483927247898539470, 38.54057627198103120 ) ) ;
#44629 = CARTESIAN_POINT ( 'NONE',  ( -0.05219959533907301413, -21.53943276465977519, 42.49890960531435979 ) ) ;
#44630 = CARTESIAN_POINT ( 'NONE',  ( -19.05341960407611168, -5.049401038298163336, 66.45724293864769550 ) ) ;
#44631 = CARTESIAN_POINT ( 'NONE',  ( -16.51473224551069308, -9.474510206698971260, 46.66557627198102409 ) ) ;
#44632 = CARTESIAN_POINT ( 'NONE',  ( -5.719274019375978568, 21.55341960407610458, 60.20724293864768839 ) ) ;
#44633 = CARTESIAN_POINT ( 'NONE',  ( -19.05341960407617563, 5.049401038297882671, 43.54275706135232582 ) ) ;
#44635 = CARTESIAN_POINT ( 'NONE',  ( 14.34966873604960469, 8.224510206698951720, 49.16557627198102409 ) ) ;
#44634 = FACE_OUTER_BOUND ( 'NONE', #54338, .T. ) ;
#44636 = CARTESIAN_POINT ( 'NONE',  ( 5.823673210054125526, 21.52544592524343514, 24.79057627198103120 ) ) ;
#44637 = ORIENTED_EDGE ( 'NONE', *, *, #188177, .F. ) ;
#44638 = VERTEX_POINT ( 'NONE', #99849 ) ;
#44639 = CARTESIAN_POINT ( 'NONE',  ( -32.00000000000000711, -5.510910596163089556E-15, 45.00000000000000000 ) ) ;
#44640 = CARTESIAN_POINT ( 'NONE',  ( -14.29746914071037622, -8.314922557961029526, 69.16775706135234714 ) ) ;
#44641 = CARTESIAN_POINT ( 'NONE',  ( -13.89961937509957401, -13.97604488694547875, 79.37609039468567573 ) ) ;
#44642 = CARTESIAN_POINT ( 'NONE',  ( -16.52544592524342804, 4.483927247898546575, 41.04057627198103120 ) ) ;
#44643 = CARTESIAN_POINT ( 'NONE',  ( -19.53091890409952214, -5.500000000000036415, 60.06097431831418731 ) ) ;
#44644 = CARTESIAN_POINT ( 'NONE',  ( 16.52544592524342804, -4.483927247898539470, 33.54057627198102409 ) ) ;
#44645 = CARTESIAN_POINT ( 'NONE',  ( -5.049401038298153566, 19.05341960407611168, 55.20724293864769550 ) ) ;
#44646 = CARTESIAN_POINT ( 'NONE',  ( 9.474510206698971260, -16.51473224551069308, 77.91557627198103830 ) ) ;
#44647 = CARTESIAN_POINT ( 'NONE',  ( 5.049401038298161559, -19.05341960407611168, 42.70724293864767418 ) ) ;
#44648 = CARTESIAN_POINT ( 'NONE',  ( 15.80617190586769283, -15.72974639402175789, 50.62609039468568994 ) ) ;
#44649 = CARTESIAN_POINT ( 'NONE',  ( -5.153800228976328057, -19.02544592524343514, 62.29057627198100988 ) ) ;
#44650 = FACE_BOUND ( 'NONE', #107983, .T. ) ;
#44651 = CARTESIAN_POINT ( 'NONE',  ( 0.05219959533909260263, 19.03943276465977164, 64.99890960531436690 ) ) ;
#44652 = CARTESIAN_POINT ( 'NONE',  ( -21.55341960407610458, -5.719274019375992779, 31.45724293864769550 ) ) ;
#44653 = CARTESIAN_POINT ( 'NONE',  ( 16.53943276465976808, -0.05219959533910856209, 113.7489096053143527 ) ) ;
#44654 = CARTESIAN_POINT ( 'NONE',  ( 18.62759615963271287, -10.81492255796078972, 43.33224293864769550 ) ) ;
#44655 = CARTESIAN_POINT ( 'NONE',  ( 16.55341960407618274, -4.379528057220086978, 86.04275706135236135 ) ) ;
#44656 = CARTESIAN_POINT ( 'NONE',  ( -21.55341960407619339, 5.719274019375674811, 103.5427570613523613 ) ) ;
#44657 = CARTESIAN_POINT ( 'NONE',  ( -16.53943276465976808, -0.05219959533934237506, 68.75109039468568994 ) ) ;
#44658 = CARTESIAN_POINT ( 'NONE',  ( 19.03943276465977164, -0.05219959533909143690, 108.7489096053143527 ) ) ;
#44659 = CARTESIAN_POINT ( 'NONE',  ( -12.06949235617739369, -12.14591786802326823, 54.37609039468568994 ) ) ;
#44660 = CARTESIAN_POINT ( 'NONE',  ( -14.29746914071037622, -8.314922557961029526, 34.16775706135234714 ) ) ;
#44661 = CARTESIAN_POINT ( 'NONE',  ( -19.02544592524342804, 5.153800228976336051, 111.0405762719810099 ) ) ;
#44662 = CARTESIAN_POINT ( 'NONE',  ( -4.379528057220086978, -16.55341960407618274, 29.79275706135234358 ) ) ;
#44663 = CARTESIAN_POINT ( 'NONE',  ( -13.89961937509977652, 13.97604488694528158, 35.62390960531435269 ) ) ;
#44664 = CARTESIAN_POINT ( 'NONE',  ( -21.55341960407619339, 5.719274019375674811, 28.54275706135234358 ) ) ;
#44665 = CARTESIAN_POINT ( 'NONE',  ( -8.224510206698735004, -14.34966873604973081, 24.58442372801901499 ) ) ;
#44666 = CARTESIAN_POINT ( 'NONE',  ( 0.05219959533934541429, -16.53943276465976808, 80.00109039468568994 ) ) ;
#44667 = DIRECTION ( 'NONE',  ( -9.445700745138859830E-17, 1.000000000000000000, 0.000000000000000000 ) ) ;
#44668 = CARTESIAN_POINT ( 'NONE',  ( -18.67979575497193778, 10.72451020669871902, 93.33442372801901854 ) ) ;
#44669 = CARTESIAN_POINT ( 'NONE',  ( -9.474510206698720793, -16.51473224551083518, 99.58442372801900433 ) ) ;
#44670 = CARTESIAN_POINT ( 'NONE',  ( -4.483927247898539470, -16.52544592524342804, 57.29057627198103120 ) ) ;
#44671 = CARTESIAN_POINT ( 'NONE',  ( 0.05219959533910956823, 16.53943276465976808, 109.9989096053143527 ) ) ;
#44673 = CARTESIAN_POINT ( 'NONE',  ( 17.40861289039009918, -6.110651285853051284, 56.12767529172571557 ) ) ;
#44672 = CARTESIAN_POINT ( 'NONE',  ( -19.05341960407617563, 5.049401038297882671, 53.54275706135231871 ) ) ;
#44674 = CARTESIAN_POINT ( 'NONE',  ( -0.05219959533937732626, 21.53943276465977519, 52.50109039468567573 ) ) ;
#44675 = CARTESIAN_POINT ( 'NONE',  ( -19.03943276465977164, -0.05219959533935918106, 103.7510903946856757 ) ) ;
#44676 = DIRECTION ( 'NONE',  ( 1.000000000000000000, 0.000000000000000000, 3.709348145883536076E-20 ) ) ;
#44677 = CARTESIAN_POINT ( 'NONE',  ( 9.564922557960805705, 16.46253265017160317, 109.5822429386476955 ) ) ;
#44678 = CARTESIAN_POINT ( 'NONE',  ( 18.67979575497178502, 10.72451020669898547, 79.16557627198103830 ) ) ;
#44679 = CARTESIAN_POINT ( 'NONE',  ( -13.89961937509957401, -13.97604488694547875, 99.37609039468567573 ) ) ;
#44680 = CARTESIAN_POINT ( 'NONE',  ( 5.049401038298161559, -19.05341960407611168, 107.7072429386476955 ) ) ;
#44681 = CARTESIAN_POINT ( 'NONE',  ( 6.377275439838900439, -27.11046330701184459, 140.0000000000000000 ) ) ;
#44682 = CARTESIAN_POINT ( 'NONE',  ( -8.224510206698948167, 14.34966873604960824, 110.4155762719810383 ) ) ;
#44683 = CARTESIAN_POINT ( 'NONE',  ( 18.67979575497194134, -10.72451020669871369, 95.83442372801903275 ) ) ;
#44684 = CARTESIAN_POINT ( 'NONE',  ( -19.03943276465977164, 0.05219959533909376836, 41.24890960531435269 ) ) ;
#44685 = CARTESIAN_POINT ( 'NONE',  ( 21.55341960407619695, -5.719274019375665929, 56.04275706135235424 ) ) ;
#44686 = CARTESIAN_POINT ( 'NONE',  ( -15.80617190586768217, 15.72974639402176855, 88.12609039468570415 ) ) ;
#44687 = CARTESIAN_POINT ( 'NONE',  ( -8.314922557961024197, 14.29746914071037800, 102.9177570613523756 ) ) ;
#44688 = CARTESIAN_POINT ( 'NONE',  ( -19.02544592524342804, 5.153800228976336051, 71.04057627198099567 ) ) ;
#44689 = CARTESIAN_POINT ( 'NONE',  ( 21.52544592524334988, 5.823673210054432836, 41.45942372801901143 ) ) ;
#44690 = CARTESIAN_POINT ( 'NONE',  ( -5.823673210054431948, 21.52544592524334988, 37.70942372801900433 ) ) ;
#44692 = CARTESIAN_POINT ( 'NONE',  ( 19.03943276465977164, -0.05219959533909143690, 93.74890960531435269 ) ) ;
#44691 = CARTESIAN_POINT ( 'NONE',  ( 19.02544592524334988, 5.153800228976608722, 66.45942372801899012 ) ) ;
#44693 = CARTESIAN_POINT ( 'NONE',  ( 0.05219959533910956823, 16.53943276465976808, 109.9989096053143527 ) ) ;
#44694 = CARTESIAN_POINT ( 'NONE',  ( -18.62759615963270932, 10.81492255796079327, 100.8322429386477097 ) ) ;
#44695 = CARTESIAN_POINT ( 'NONE',  ( 16.53943276465976808, -0.05219959533910856209, 68.74890960531435269 ) ) ;
#44696 = CARTESIAN_POINT ( 'NONE',  ( 9.474510206698729675, 16.51473224551082808, 22.08442372801899722 ) ) ;
#44697 = CARTESIAN_POINT ( 'NONE',  ( 8.224510206698953496, -14.34966873604960469, 82.91557627198103830 ) ) ;
#44698 = CARTESIAN_POINT ( 'NONE',  ( -5.049401038298153566, 19.05341960407611168, 30.20724293864768839 ) ) ;
#44699 = CARTESIAN_POINT ( 'NONE',  ( -19.02544592524334988, -5.153800228976617603, 88.95942372801897591 ) ) ;
#44700 = CARTESIAN_POINT ( 'NONE',  ( -8.314922557960811034, -14.29746914071050412, 52.08224293864768839 ) ) ;
#44701 = CARTESIAN_POINT ( 'NONE',  ( -15.80617190586768217, 15.72974639402176855, 98.12609039468570415 ) ) ;
#44702 = CARTESIAN_POINT ( 'NONE',  ( -13.97604488694527625, -13.89961937509977652, 91.87390960531432427 ) ) ;
#44703 = CARTESIAN_POINT ( 'NONE',  ( 9.474510206698729675, 16.51473224551082808, 62.08442372801899722 ) ) ;
#44704 = CARTESIAN_POINT ( 'NONE',  ( -21.53943276465977519, 0.05219959533907696930, 76.24890960531435269 ) ) ;
#44705 = CARTESIAN_POINT ( 'NONE',  ( -21.53943276465977519, -0.05219959533937600094, 33.75109039468568284 ) ) ;
#44706 = CARTESIAN_POINT ( 'NONE',  ( 12.06949235617739724, 12.14591786802326823, 31.87609039468567929 ) ) ;
#44707 = CARTESIAN_POINT ( 'NONE',  ( -8.224510206698735004, -14.34966873604973081, 99.58442372801900433 ) ) ;
#44709 = CARTESIAN_POINT ( 'NONE',  ( -21.53943276465977519, -0.05219959533937600094, 18.75109039468568639 ) ) ;
#44708 = CARTESIAN_POINT ( 'NONE',  ( -19.02544592524342804, 5.153800228976336051, 31.04057627198102409 ) ) ;
#44710 = CARTESIAN_POINT ( 'NONE',  ( -5.049401038298153566, 19.05341960407611168, 25.20724293864768484 ) ) ;
#44711 = CARTESIAN_POINT ( 'NONE',  ( 36.91746824999999887, 11.99521256947799053, -4.024999997268814411 ) ) ;
#44712 = CARTESIAN_POINT ( 'NONE',  ( -16.52544592524335698, -4.483927247898792601, 43.95942372801902565 ) ) ;
#44713 = CARTESIAN_POINT ( 'NONE',  ( -0.05219959533910754901, -16.53943276465976808, 77.49890960531433848 ) ) ;
#44714 = CARTESIAN_POINT ( 'NONE',  ( -18.62759615963270932, 10.81492255796079327, 75.83224293864769550 ) ) ;
#44715 = CARTESIAN_POINT ( 'NONE',  ( -12.14591786802309592, -12.06949235617757132, 26.87390960531435979 ) ) ;
#44716 = CARTESIAN_POINT ( 'NONE',  ( -14.34966873604972548, 8.224510206698743886, 48.33442372801902565 ) ) ;
#44717 = CARTESIAN_POINT ( 'NONE',  ( 16.46253265017160672, -9.564922557960803928, 43.33224293864769550 ) ) ;
#44718 = CARTESIAN_POINT ( 'NONE',  ( -16.52544592524335698, -4.483927247898792601, 83.95942372801900433 ) ) ;
#44719 = CARTESIAN_POINT ( 'NONE',  ( -16.46253265017146816, -9.564922557961047289, 69.16775706135233293 ) ) ;
#44720 = CARTESIAN_POINT ( 'NONE',  ( 10.72451020669898902, -18.67979575497178502, 67.91557627198102409 ) ) ;
#44721 = CARTESIAN_POINT ( 'NONE',  ( -16.53943276465976808, -0.05219959533934237506, 108.7510903946857042 ) ) ;
#44722 = ORIENTED_EDGE ( 'NONE', *, *, #62577, .T. ) ;
#44723 = CARTESIAN_POINT ( 'NONE',  ( 26.79623349963134871, 5.044589688426436069, 170.2051123914324080 ) ) ;
#44724 = CARTESIAN_POINT ( 'NONE',  ( 18.62759615963271287, -10.81492255796078972, 43.33224293864769550 ) ) ;
#44725 = VERTEX_POINT ( 'NONE', #98840 ) ;
#44726 = ORIENTED_EDGE ( 'NONE', *, *, #45727, .F. ) ;
#44727 = CARTESIAN_POINT ( 'NONE',  ( 4.379528057220092307, 16.55341960407617563, 92.29275706135236135 ) ) ;
#44728 = ORIENTED_EDGE ( 'NONE', *, *, #17351, .T. ) ;
#44729 = CARTESIAN_POINT ( 'NONE',  ( 19.05341960407611168, 5.049401038298154454, 113.9572429386477097 ) ) ;
#44730 = CARTESIAN_POINT ( 'NONE',  ( 17.50000000000001066, -3.242565516153302241, 102.5000000000090807 ) ) ;
#44731 = CARTESIAN_POINT ( 'NONE',  ( 21.53943276465977519, -0.05219959533907433946, 68.74890960531435269 ) ) ;
#44732 = CARTESIAN_POINT ( 'NONE',  ( -8.224510206698735004, -14.34966873604973081, 104.5844237280190185 ) ) ;
#44733 = CARTESIAN_POINT ( 'NONE',  ( -0.05219959533934338120, 16.53943276465976808, 27.50109039468567929 ) ) ;
#44734 = CARTESIAN_POINT ( 'NONE',  ( 16.51473224551069308, 9.474510206698969483, 24.16557627198102765 ) ) ;
#44735 = CARTESIAN_POINT ( 'NONE',  ( -4.379528057220086978, -16.55341960407618274, 24.79275706135235779 ) ) ;
#44736 = CARTESIAN_POINT ( 'NONE',  ( -5.049401038298153566, 19.05341960407611168, 60.20724293864768129 ) ) ;
#44737 = CARTESIAN_POINT ( 'NONE',  ( -8.906447517083053711, -27.41122689804191026, 140.4000000000000057 ) ) ;
#44738 = CARTESIAN_POINT ( 'NONE',  ( -19.03943276465977164, 0.05219959533909376836, 101.2489096053143669 ) ) ;
#44739 = CARTESIAN_POINT ( 'NONE',  ( 16.53943276465976808, 0.05219959533934440121, 91.25109039468568994 ) ) ;
#44740 = CARTESIAN_POINT ( 'NONE',  ( 19.05341960407617918, -5.049401038297876454, 86.04275706135233293 ) ) ;
#44741 = CARTESIAN_POINT ( 'NONE',  ( -19.03943276465977164, -0.05219959533935918106, 28.75109039468566507 ) ) ;
#44742 = CARTESIAN_POINT ( 'NONE',  ( 18.62759615963271287, -10.81492255796078972, 78.33224293864770971 ) ) ;
#44743 = CARTESIAN_POINT ( 'NONE',  ( -8.224510206698735004, -14.34966873604973081, 104.5844237280190185 ) ) ;
#44744 = CARTESIAN_POINT ( 'NONE',  ( -5.049401038297874678, -19.05341960407617918, 94.79275706135230450 ) ) ;
#44745 = CARTESIAN_POINT ( 'NONE',  ( -9.474510206698964154, 16.51473224551069663, 45.41557627198103120 ) ) ;
#44746 = CARTESIAN_POINT ( 'NONE',  ( -19.02544592524342804, 5.153800228976336051, 91.04057627198100988 ) ) ;
#44747 = CARTESIAN_POINT ( 'NONE',  ( 15.80617190586769283, -15.72974639402175789, 55.62609039468568284 ) ) ;
#44748 = CARTESIAN_POINT ( 'NONE',  ( -16.46253265017160317, 9.564922557960807481, 45.83224293864769550 ) ) ;
#44749 = CARTESIAN_POINT ( 'NONE',  ( -16.31925111598453881, -7.325300261831592330, 84.83575461032749843 ) ) ;
#44750 = CARTESIAN_POINT ( 'NONE',  ( 4.483927247898545687, 16.52544592524342804, 79.79057627198102409 ) ) ;
#44751 = CARTESIAN_POINT ( 'NONE',  ( -10.72451020669898014, 18.67979575497178502, 75.41557627198102409 ) ) ;
#44752 = CARTESIAN_POINT ( 'NONE',  ( -27.73933785331498925, 2.428612866367529932E-14, 149.1250000027311842 ) ) ;
#44753 = CARTESIAN_POINT ( 'NONE',  ( -38.00000000000000711, 12.34694845685046438, -5.849999994537627757 ) ) ;
#44754 = CARTESIAN_POINT ( 'NONE',  ( -5.153800228976607833, 19.02544592524334988, 37.70942372801899722 ) ) ;
#44755 = CARTESIAN_POINT ( 'NONE',  ( 31.71843943275782962, -0.9850135343614644379, 102.4512077271823642 ) ) ;
#44756 = AXIS2_PLACEMENT_3D ( 'NONE', #129087, #112934, #191777 ) ;
#44758 = CARTESIAN_POINT ( 'NONE',  ( 5.153800228976335163, 19.02544592524342804, 89.79057627198102409 ) ) ;
#44757 = CARTESIAN_POINT ( 'NONE',  ( -13.89961937509977652, 13.97604488694528158, 75.62390960531438111 ) ) ;
#44759 = ADVANCED_FACE ( 'NONE', ( #190875, #83676 ), #67520, .F. ) ;
#44760 = CARTESIAN_POINT ( 'NONE',  ( -12.14591786802326823, 12.06949235617739902, 68.12609039468567573 ) ) ;
#44761 = CARTESIAN_POINT ( 'NONE',  ( -17.72662750342725957, -5.500000000000095923, 66.40179492283743912 ) ) ;
#44762 = CARTESIAN_POINT ( 'NONE',  ( 19.05341960407617918, -5.049401038297876454, 31.04275706135232227 ) ) ;
#44763 = CARTESIAN_POINT ( 'NONE',  ( -16.31925111598457079, 7.325300261831543480, 110.1642453896725442 ) ) ;
#44764 = CARTESIAN_POINT ( 'NONE',  ( 19.05341960407611168, 5.049401038298154454, 113.9572429386477097 ) ) ;
#44765 = CARTESIAN_POINT ( 'NONE',  ( -0.05219959533934338120, 16.53943276465976808, 87.50109039468568994 ) ) ;
#44766 = CARTESIAN_POINT ( 'NONE',  ( 14.46985881644522465, -1.324169127979137883, -60.11284999819414310 ) ) ;
#44767 = CARTESIAN_POINT ( 'NONE',  ( -14.34966873604972548, 8.224510206698743886, 73.33442372801901854 ) ) ;
#44768 = CARTESIAN_POINT ( 'NONE',  ( -16.29526858892872809, 7.335722546920264264, 29.20329402199793378 ) ) ;
#44769 = CARTESIAN_POINT ( 'NONE',  ( 8.314922557961029526, -14.29746914071037800, 60.41775706135235424 ) ) ;
#44770 = CARTESIAN_POINT ( 'NONE',  ( -20.41037832431298682, -34.40082058117823749, -25.00000000000009592 ) ) ;
#44771 = CARTESIAN_POINT ( 'NONE',  ( -18.62759615963255300, -10.81492255796106328, 69.16775706135234714 ) ) ;
#44772 = CARTESIAN_POINT ( 'NONE',  ( -19.02544592524334988, -5.153800228976617603, 78.95942372801900433 ) ) ;
#44773 = CARTESIAN_POINT ( 'NONE',  ( -9.474510206698720793, -16.51473224551083518, 29.58442372801900433 ) ) ;
#44774 = CARTESIAN_POINT ( 'NONE',  ( -16.46253265017160317, 9.564922557960807481, 45.83224293864769550 ) ) ;
#44775 = CARTESIAN_POINT ( 'NONE',  ( 0.05219959533909260263, 19.03943276465977164, 44.99890960531435979 ) ) ;
#44776 = CARTESIAN_POINT ( 'NONE',  ( 16.54732454198001790, -7.207534646770589859, 22.94022044411182293 ) ) ;
#44777 = CARTESIAN_POINT ( 'NONE',  ( 21.52544592524344225, -5.823673210054117533, 73.54057627198102409 ) ) ;
#44778 = CARTESIAN_POINT ( 'NONE',  ( -18.62759615963270932, 10.81492255796079327, 25.83224293864769194 ) ) ;
#44779 = CARTESIAN_POINT ( 'NONE',  ( -19.03943276465977164, 0.05219959533909376836, 21.24890960531436335 ) ) ;
#44780 = CARTESIAN_POINT ( 'NONE',  ( 8.314922557961029526, -14.29746914071037800, 45.41775706135234003 ) ) ;
#44781 = ADVANCED_FACE ( 'NONE', ( #175705 ), #112043, .F. ) ;
#44782 = ORIENTED_EDGE ( 'NONE', *, *, #193684, .F. ) ;
#44783 = CARTESIAN_POINT ( 'NONE',  ( -15.72974639402197994, 15.80617190586746368, 115.6239096053143669 ) ) ;
#44785 = CARTESIAN_POINT ( 'NONE',  ( -6.020228577223754586E-15, 39.95556452105416412, -2.500000000000000444 ) ) ;
#44784 = CARTESIAN_POINT ( 'NONE',  ( -8.224510206698948167, 14.34966873604960824, 50.41557627198103120 ) ) ;
#44786 = CARTESIAN_POINT ( 'NONE',  ( -5.153800228976607833, 19.02544592524334988, 107.7094237280189759 ) ) ;
#44787 = CARTESIAN_POINT ( 'NONE',  ( -16.46253265017146816, -9.564922557961047289, 34.16775706135233293 ) ) ;
#44788 = CARTESIAN_POINT ( 'NONE',  ( 8.314922557960818139, 14.29746914071049879, 39.58224293864769550 ) ) ;
#44789 = CARTESIAN_POINT ( 'NONE',  ( -10.72451020669870658, -18.67979575497194134, 24.58442372801901499 ) ) ;
#44791 = CARTESIAN_POINT ( 'NONE',  ( -21.53943276465977519, 0.05219959533907696930, 66.24890960531436690 ) ) ;
#44790 = CARTESIAN_POINT ( 'NONE',  ( 17.50000000000000000, 5.499999999999997335, 120.0000000000000142 ) ) ;
#44792 = CARTESIAN_POINT ( 'NONE',  ( 13.89961937509977652, -13.97604488694527269, 93.12390960531436690 ) ) ;
#44793 = CARTESIAN_POINT ( 'NONE',  ( 16.52544592524342804, -4.483927247898539470, 43.54057627198103830 ) ) ;
#44794 = CARTESIAN_POINT ( 'NONE',  ( -13.97604488694527625, -13.89961937509977652, 101.8739096053143811 ) ) ;
#44795 = CARTESIAN_POINT ( 'NONE',  ( -28.82186960331499037, 2.428612866367529932E-14, 146.2500000054623683 ) ) ;
#44796 = CARTESIAN_POINT ( 'NONE',  ( -19.02544592524334988, -5.153800228976617603, 53.95942372801898301 ) ) ;
#44797 = CARTESIAN_POINT ( 'NONE',  ( -21.55341960407610458, -5.719274019375992779, 96.45724293864770971 ) ) ;
#44798 = CARTESIAN_POINT ( 'NONE',  ( 13.89961937509977652, -13.97604488694527269, 43.12390960531434558 ) ) ;
#44799 = CARTESIAN_POINT ( 'NONE',  ( 14.34966873604960469, 8.224510206698951720, 109.1655762719810383 ) ) ;
#44800 = CARTESIAN_POINT ( 'NONE',  ( -15.72974639402176322, -15.80617190586768395, 44.37609039468567573 ) ) ;
#44801 = CARTESIAN_POINT ( 'NONE',  ( 8.571926809382603096, -26.38167802310801235, 147.4750000027311785 ) ) ;
#44802 = CARTESIAN_POINT ( 'NONE',  ( 4.379528057220339221, -16.55341960407611168, 22.70724293864769194 ) ) ;
#44803 = CARTESIAN_POINT ( 'NONE',  ( 19.02544592524343514, -5.153800228976328945, 48.54057627198103120 ) ) ;
#44804 = CARTESIAN_POINT ( 'NONE',  ( -0.05219959533909027116, -19.03943276465977164, 102.4989096053143669 ) ) ;
#44805 = CARTESIAN_POINT ( 'NONE',  ( 15.80617190586746368, 15.72974639402197994, 69.37390960531436690 ) ) ;
#44806 = CARTESIAN_POINT ( 'NONE',  ( -27.73933785331498925, 2.428612866367529932E-14, 146.8750000027311842 ) ) ;
#44807 = CARTESIAN_POINT ( 'NONE',  ( 5.153800228976335163, 19.02544592524342804, 44.79057627198103830 ) ) ;
#44808 = CARTESIAN_POINT ( 'NONE',  ( 0.05219959533907565091, 21.53943276465977519, 49.99890960531437401 ) ) ;
#44809 = CARTESIAN_POINT ( 'NONE',  ( -21.55341960407619339, 5.719274019375674811, 88.54275706135236135 ) ) ;
#44812 = CARTESIAN_POINT ( 'NONE',  ( 14.29746914071049879, -8.314922557960816363, 63.33224293864770260 ) ) ;
#44811 = CARTESIAN_POINT ( 'NONE',  ( -14.34966873604972548, 8.224510206698743886, 83.33442372801903275 ) ) ;
#44810 = CARTESIAN_POINT ( 'NONE',  ( 11.22590306719470377, -43.10241010958339558, -21.31070173013108260 ) ) ;
#44813 = CARTESIAN_POINT ( 'NONE',  ( -8.224510206698735004, -14.34966873604973081, 89.58442372801901854 ) ) ;
#44814 = CARTESIAN_POINT ( 'NONE',  ( 13.89961937509977652, -13.97604488694527269, 73.12390960531436690 ) ) ;
#44815 = VERTEX_POINT ( 'NONE', #161533 ) ;
#44816 = CARTESIAN_POINT ( 'NONE',  ( 13.97604488694548053, -13.89961937509957401, 20.62609039468567573 ) ) ;
#44817 = CARTESIAN_POINT ( 'NONE',  ( -4.379528057220086978, -16.55341960407618274, 84.79275706135234714 ) ) ;
#44818 = CARTESIAN_POINT ( 'NONE',  ( -18.62759615963255300, -10.81492255796106328, 109.1677570613523613 ) ) ;
#44819 = CARTESIAN_POINT ( 'NONE',  ( 5.153800228976335163, 19.02544592524342804, 79.79057627198102409 ) ) ;
#44820 = CARTESIAN_POINT ( 'NONE',  ( -0.05219959533907301413, -21.53943276465977519, 42.49890960531435979 ) ) ;
#44821 = CARTESIAN_POINT ( 'NONE',  ( -0.05219959533934338120, 16.53943276465976808, 22.50109039468567573 ) ) ;
#44822 = CARTESIAN_POINT ( 'NONE',  ( -21.55341960407619339, 5.719274019375674811, 88.54275706135236135 ) ) ;
#44823 = CARTESIAN_POINT ( 'NONE',  ( -16.52544592524335698, -4.483927247898792601, 68.95942372801901854 ) ) ;
#44824 = CARTESIAN_POINT ( 'NONE',  ( 18.67979575497178502, 10.72451020669898547, 109.1655762719810383 ) ) ;
#44825 = CARTESIAN_POINT ( 'NONE',  ( -13.97604488694547697, 13.89961937509957934, 108.1260903946856331 ) ) ;
#44826 = CARTESIAN_POINT ( 'NONE',  ( 9.474510206698971260, -16.51473224551069308, 97.91557627198102409 ) ) ;
#44827 = CARTESIAN_POINT ( 'NONE',  ( -12.14591786802326823, 12.06949235617739902, 28.12609039468568284 ) ) ;
#44828 = CARTESIAN_POINT ( 'NONE',  ( 16.46253265017160672, -9.564922557960803928, 43.33224293864769550 ) ) ;
#44829 = CARTESIAN_POINT ( 'NONE',  ( 14.29746914071037800, 8.314922557961029526, 36.66775706135234714 ) ) ;
#44830 = CARTESIAN_POINT ( 'NONE',  ( -16.55341960407611168, -4.379528057220339221, 76.45724293864769550 ) ) ;
#44831 = CARTESIAN_POINT ( 'NONE',  ( -16.55341960407617563, 4.379528057220093196, 83.54275706135234714 ) ) ;
#44832 = EDGE_CURVE ( 'NONE', #71451, #99831, #188659, .T. ) ;
#44834 = CARTESIAN_POINT ( 'NONE',  ( -9.564922557960796823, -16.46253265017161027, 62.08224293864769550 ) ) ;
#44833 = CARTESIAN_POINT ( 'NONE',  ( -5.823673210054431948, 21.52544592524334988, 32.70942372801900433 ) ) ;
#44835 = CARTESIAN_POINT ( 'NONE',  ( -19.02544592524342804, 5.153800228976336051, 86.04057627198103830 ) ) ;
#44836 = CARTESIAN_POINT ( 'NONE',  ( -0.05219959533934338120, 16.53943276465976808, 82.50109039468568994 ) ) ;
#44838 = VERTEX_POINT ( 'NONE', #162525 ) ;
#44837 = LINE ( 'NONE', #168170, #143440 ) ;
#44839 = ORIENTED_EDGE ( 'NONE', *, *, #91376, .F. ) ;
#44840 = CARTESIAN_POINT ( 'NONE',  ( -9.474510206698720793, -16.51473224551083518, 29.58442372801900433 ) ) ;
#44841 = CARTESIAN_POINT ( 'NONE',  ( 19.02544592524343514, -5.153800228976328945, 93.54057627198102409 ) ) ;
#44842 = CARTESIAN_POINT ( 'NONE',  ( -19.02544592524342804, 5.153800228976336051, 51.04057627198103120 ) ) ;
#44844 = ORIENTED_EDGE ( 'NONE', *, *, #20020, .F. ) ;
#44843 = CARTESIAN_POINT ( 'NONE',  ( 5.153800228976335163, 19.02544592524342804, 114.7905762719810241 ) ) ;
#44845 = CARTESIAN_POINT ( 'NONE',  ( 14.34966873604972726, -8.224510206698740333, 30.83442372801902209 ) ) ;
#44847 = CARTESIAN_POINT ( 'NONE',  ( 4.483927247898790824, -16.52544592524335698, 40.20942372801901854 ) ) ;
#44846 = CARTESIAN_POINT ( 'NONE',  ( 0.05219959533936267826, -19.03943276465977164, 55.00109039468566863 ) ) ;
#44848 = CARTESIAN_POINT ( 'NONE',  ( -0.05219959533909027116, -19.03943276465977164, 107.4989096053143527 ) ) ;
#44849 = CARTESIAN_POINT ( 'NONE',  ( -19.02544592524342804, 5.153800228976336051, 71.04057627198099567 ) ) ;
#44850 = CARTESIAN_POINT ( 'NONE',  ( 10.81492255796078972, 18.62759615963270932, 94.58224293864769550 ) ) ;
#44851 = CARTESIAN_POINT ( 'NONE',  ( -5.049401038297874678, -19.05341960407617918, 59.79275706135231871 ) ) ;
#44853 = CARTESIAN_POINT ( 'NONE',  ( -19.05341960407611168, -5.049401038298163336, 21.45724293864768839 ) ) ;
#44852 = CARTESIAN_POINT ( 'NONE',  ( -19.02544592524342804, 5.153800228976336051, 86.04057627198103830 ) ) ;
#44854 = CARTESIAN_POINT ( 'NONE',  ( -13.97604488694527625, -13.89961937509977652, 61.87390960531435979 ) ) ;
#44856 = CARTESIAN_POINT ( 'NONE',  ( 9.564922557960805705, 16.46253265017160317, 69.58224293864770971 ) ) ;
#44855 = CARTESIAN_POINT ( 'NONE',  ( -16.55341960407617563, 4.379528057220093196, 108.5427570613523756 ) ) ;
#44857 = CARTESIAN_POINT ( 'NONE',  ( 13.89961937509957401, 13.97604488694547697, 36.87609039468565442 ) ) ;
#44858 = B_SPLINE_CURVE_WITH_KNOTS ( 'NONE', 3,
 ( #76463, #64280, #121969, #60295, #183661, #123939, #109781, #79443, #16786, #95600, #62271, #108787, #94607, #168476, #46126, #137143, #45146, #93611, #107780, #198831, #78436, #169465, #106802, #47129, #157285, #75470, #29974, #1601, #91613, #14802, #185637, #138140 ),
 .UNSPECIFIED., .F., .F.,
 ( 4, 2, 2, 2, 2, 2, 2, 2, 2, 2, 2, 2, 2, 2, 2, 4 ),
 ( 8.673617379884034509E-19, 0.0003712461730036735507, 0.0007424923460073462340, 0.001113738519011018809, 0.001484984692014691601, 0.002227477038022048893, 0.002598723211025715830, 0.002969969384029382767, 0.003341215557033050138, 0.003712461730036717509, 0.004083707903040385313, 0.004454954076044052684, 0.004826200249047720055, 0.005197446422051387425, 0.005568692595055054796, 0.005939938768058721300 ),
 .UNSPECIFIED. ) ;
#44859 = CARTESIAN_POINT ( 'NONE',  ( -4.483927247898539470, -16.52544592524342804, 72.29057627198102409 ) ) ;
#44860 = CARTESIAN_POINT ( 'NONE',  ( -21.52544592524334988, -5.823673210054445271, 93.95942372801903275 ) ) ;
#44861 = CARTESIAN_POINT ( 'NONE',  ( 9.474510206698971260, -16.51473224551069308, 32.91557627198102409 ) ) ;
#44862 = CARTESIAN_POINT ( 'NONE',  ( 8.314922557961029526, -14.29746914071037800, 55.41775706135234714 ) ) ;
#44864 = CARTESIAN_POINT ( 'NONE',  ( 21.55341960407619695, -5.719274019375665929, 91.04275706135236135 ) ) ;
#44863 = CARTESIAN_POINT ( 'NONE',  ( -4.379528057220328563, 16.55341960407611168, 40.20724293864769550 ) ) ;
#44865 = CARTESIAN_POINT ( 'NONE',  ( 16.46253265017160672, -9.564922557960803928, 88.33224293864769550 ) ) ;
#44866 = CARTESIAN_POINT ( 'NONE',  ( -19.05341960407611168, -5.049401038298163336, 96.45724293864769550 ) ) ;
#44867 = CARTESIAN_POINT ( 'NONE',  ( 12.06949235617757843, -12.14591786802309237, 103.1239096053143811 ) ) ;
#44868 = CARTESIAN_POINT ( 'NONE',  ( -8.224510206698948167, 14.34966873604960824, 80.41557627198103830 ) ) ;
#44869 = CARTESIAN_POINT ( 'NONE',  ( -18.62759615963270932, 10.81492255796079327, 85.83224293864768129 ) ) ;
#44870 = CARTESIAN_POINT ( 'NONE',  ( 19.05341960407611168, 5.049401038298154454, 93.95724293864769550 ) ) ;
#44871 = CARTESIAN_POINT ( 'NONE',  ( 15.80617190586746368, 15.72974639402197994, 104.3739096053143669 ) ) ;
#44872 = CARTESIAN_POINT ( 'NONE',  ( -19.02544592524342804, 5.153800228976336051, 96.04057627198103830 ) ) ;
#44874 = CARTESIAN_POINT ( 'NONE',  ( 16.53943276465976808, -0.05219959533910856209, 93.74890960531436690 ) ) ;
#44873 = CARTESIAN_POINT ( 'NONE',  ( -18.22780087662123094, -5.499999999999984901, 91.48459894673894155 ) ) ;
#44875 = CARTESIAN_POINT ( 'NONE',  ( 16.46253265017160672, -9.564922557960803928, 63.33224293864769550 ) ) ;
#44876 = CARTESIAN_POINT ( 'NONE',  ( 10.81492255796078972, 18.62759615963270932, 64.58224293864769550 ) ) ;
#44877 = CARTESIAN_POINT ( 'NONE',  ( 17.12812012977024878, -6.668231424566041454, 26.14051240676857191 ) ) ;
#44879 = CARTESIAN_POINT ( 'NONE',  ( 17.50000000000000000, -5.500000000000000888, 120.0000000000000142 ) ) ;
#44878 = CARTESIAN_POINT ( 'NONE',  ( -8.314922557961024197, 14.29746914071037800, 112.9177570613523329 ) ) ;
#44880 = CARTESIAN_POINT ( 'NONE',  ( -12.06949235617739369, -12.14591786802326823, 19.37609039468568639 ) ) ;
#44881 = CARTESIAN_POINT ( 'NONE',  ( 14.34966873604960469, 8.224510206698951720, 84.16557627198103830 ) ) ;
#44882 = CARTESIAN_POINT ( 'NONE',  ( -17.48847506799967633, -5.747544572773783500, 94.17302562156720569 ) ) ;
#44883 = CARTESIAN_POINT ( 'NONE',  ( 19.05341960407611168, 5.049401038298154454, 78.95724293864769550 ) ) ;
#44884 = CARTESIAN_POINT ( 'NONE',  ( -9.474510206698964154, 16.51473224551069663, 40.41557627198103120 ) ) ;
#44885 = CARTESIAN_POINT ( 'NONE',  ( -12.06949235617756955, 12.14591786802309770, 60.62390960531437401 ) ) ;
#44886 = CARTESIAN_POINT ( 'NONE',  ( 9.564922557960805705, 16.46253265017160317, 109.5822429386476955 ) ) ;
#44887 = CARTESIAN_POINT ( 'NONE',  ( 5.049401038297881783, 19.05341960407617563, 102.2927570613523045 ) ) ;
#44888 = CARTESIAN_POINT ( 'NONE',  ( -5.049401038298153566, 19.05341960407611168, 95.20724293864770971 ) ) ;
#44889 = CARTESIAN_POINT ( 'NONE',  ( 10.72451020669898902, -18.67979575497178502, 72.91557627198103830 ) ) ;
#44890 = CARTESIAN_POINT ( 'NONE',  ( 0.05219959533934541429, -16.53943276465976808, 70.00109039468568994 ) ) ;
#44891 = CARTESIAN_POINT ( 'NONE',  ( -5.153800228976607833, 19.02544592524335343, 107.7094237280189901 ) ) ;
#44892 = CARTESIAN_POINT ( 'NONE',  ( -9.564922557960796823, -16.46253265017161027, 77.08224293864769550 ) ) ;
#44893 = CARTESIAN_POINT ( 'NONE',  ( -21.55341960407610458, -5.719274019375992779, 86.45724293864770971 ) ) ;
#44894 = CARTESIAN_POINT ( 'NONE',  ( -9.474510206698720793, -16.51473224551083518, 109.5844237280190043 ) ) ;
#44896 = CARTESIAN_POINT ( 'NONE',  ( -21.55341960407619339, 5.719274019375674811, 53.54275706135234714 ) ) ;
#44895 = CARTESIAN_POINT ( 'NONE',  ( -14.29746914071049879, 8.314922557960819915, 35.83224293864768839 ) ) ;
#44897 = FACE_OUTER_BOUND ( 'NONE', #175080, .T. ) ;
#44899 = CARTESIAN_POINT ( 'NONE',  ( -5.153800228976328057, -19.02544592524343514, 107.2905762719810383 ) ) ;
#44898 = CARTESIAN_POINT ( 'NONE',  ( -16.55341960407617563, 4.379528057220093196, 83.54275706135234714 ) ) ;
#44900 = CYLINDRICAL_SURFACE ( 'NONE', #111346, 7.500000000000000000 ) ;
#44901 = CARTESIAN_POINT ( 'NONE',  ( -16.52216118717209170, 7.221426719304500530, 78.92400978953006074 ) ) ;
#44902 = CARTESIAN_POINT ( 'NONE',  ( 14.34966873604972726, -8.224510206698740333, 100.8344237280190185 ) ) ;
#44903 = CARTESIAN_POINT ( 'NONE',  ( 16.55341960407618274, -4.379528057220086978, 41.04275706135236135 ) ) ;
#44904 = CARTESIAN_POINT ( 'NONE',  ( -5.049401038298153566, 19.05341960407611168, 60.20724293864768129 ) ) ;
#44905 = CARTESIAN_POINT ( 'NONE',  ( -9.474510206698964154, 16.51473224551069663, 75.41557627198103830 ) ) ;
#44906 = CARTESIAN_POINT ( 'NONE',  ( -21.55341960407619339, 5.719274019375674811, 63.54275706135234003 ) ) ;
#44907 = CARTESIAN_POINT ( 'NONE',  ( -8.314922557961024197, 14.29746914071037800, 57.91775706135234714 ) ) ;
#44908 = CARTESIAN_POINT ( 'NONE',  ( 8.224510206698953496, -14.34966873604960469, 37.91557627198102409 ) ) ;
#44909 = CARTESIAN_POINT ( 'NONE',  ( 19.02544592524343514, -5.153800228976328945, 43.54057627198103120 ) ) ;
#44910 = CARTESIAN_POINT ( 'NONE',  ( 13.97604488694527802, 13.89961937509977652, 44.37390960531435269 ) ) ;
#44912 = ORIENTED_EDGE ( 'NONE', *, *, #13873, .T. ) ;
#44911 = CARTESIAN_POINT ( 'NONE',  ( 12.06949235617739724, 12.14591786802326823, 41.87609039468568284 ) ) ;
#44913 = CARTESIAN_POINT ( 'NONE',  ( 16.51473224551083163, -9.474510206698727899, 90.83442372801900433 ) ) ;
#44914 = CARTESIAN_POINT ( 'NONE',  ( -8.314922557960811034, -14.29746914071050412, 102.0822429386476955 ) ) ;
#44915 = CARTESIAN_POINT ( 'NONE',  ( -13.89961937509977652, 13.97604488694528158, 55.62390960531434558 ) ) ;
#44917 = CARTESIAN_POINT ( 'NONE',  ( 11.74264578624799427, 36.14014761921585972, -8.599999999999999645 ) ) ;
#44916 = CARTESIAN_POINT ( 'NONE',  ( 9.564922557961047289, -16.46253265017146816, 85.41775706135233293 ) ) ;
#44918 = CARTESIAN_POINT ( 'NONE',  ( -15.80617190586768217, 15.72974639402176855, 88.12609039468570415 ) ) ;
#44919 = CARTESIAN_POINT ( 'NONE',  ( -16.53943276465976808, -0.05219959533934237506, 73.75109039468567573 ) ) ;
#44920 = CARTESIAN_POINT ( 'NONE',  ( -28.79475375365586842, 2.428612866367529932E-14, 150.0000000000000000 ) ) ;
#44921 = CARTESIAN_POINT ( 'NONE',  ( -10.72451020669898014, 18.67979575497178502, 55.41557627198102409 ) ) ;
#44922 = CARTESIAN_POINT ( 'NONE',  ( 4.483927247898790824, -16.52544592524335698, 35.20942372801901854 ) ) ;
#44923 = CARTESIAN_POINT ( 'NONE',  ( -19.52837319214027545, 5.499999999999899636, 69.60471352585538796 ) ) ;
#44924 = CARTESIAN_POINT ( 'NONE',  ( -9.564922557961040184, 16.46253265017147172, 42.91775706135234003 ) ) ;
#44925 = CARTESIAN_POINT ( 'NONE',  ( 5.153800228976335163, 19.02544592524342804, 94.79057627198103830 ) ) ;
#44926 = CARTESIAN_POINT ( 'NONE',  ( -13.97604488694527625, -13.89961937509977652, 21.87390960531435979 ) ) ;
#44927 = CARTESIAN_POINT ( 'NONE',  ( 9.474510206698971260, -16.51473224551069308, 57.91557627198103120 ) ) ;
#44928 = CARTESIAN_POINT ( 'NONE',  ( 16.23105266556536463, 17.63037570847457047, -54.49189616393496749 ) ) ;
#44929 = CARTESIAN_POINT ( 'NONE',  ( 18.62759615963255655, 10.81492255796105972, 71.66775706135234714 ) ) ;
#44930 = DIRECTION ( 'NONE',  ( 0.000000000000000000, 0.000000000000000000, -1.000000000000000000 ) ) ;
#44931 = CARTESIAN_POINT ( 'NONE',  ( -16.51473224551082808, 9.474510206698731452, 28.33442372801900433 ) ) ;
#44932 = CARTESIAN_POINT ( 'NONE',  ( 15.80617190586769283, -15.72974639402175789, 110.6260903946857042 ) ) ;
#44933 = CARTESIAN_POINT ( 'NONE',  ( 8.224510206698953496, -14.34966873604960469, 47.91557627198102409 ) ) ;
#44934 = CARTESIAN_POINT ( 'NONE',  ( -16.46253265017160317, 9.564922557960807481, 50.83224293864770260 ) ) ;
#44935 = CARTESIAN_POINT ( 'NONE',  ( 16.46253265017160672, -9.564922557960803928, 103.3322429386476955 ) ) ;
#44936 = CARTESIAN_POINT ( 'NONE',  ( 15.72974639402176855, 15.80617190586768217, 76.87609039468567573 ) ) ;
#44937 = CARTESIAN_POINT ( 'NONE',  ( -9.474510206698964154, 16.51473224551069663, 60.41557627198102409 ) ) ;
#44938 = EDGE_CURVE ( 'NONE', #10027, #114473, #130169, .T. ) ;
#44939 = CARTESIAN_POINT ( 'NONE',  ( -21.52544592524334988, -5.823673210054445271, 73.95942372801901854 ) ) ;
#44940 = CARTESIAN_POINT ( 'NONE',  ( -18.62759615963270932, 10.81492255796079327, 40.83224293864769550 ) ) ;
#44941 = B_SPLINE_CURVE_WITH_KNOTS ( 'NONE', 3,
 ( #168687, #30188, #42386, #91830, #104049, #165729, #153523, #15020, #76681, #184864, #88873, #28232, #58538, #89872, #12065, #43372, #13044, #74711 ),
 .UNSPECIFIED., .F., .F.,
 ( 4, 2, 2, 2, 2, 2, 2, 2, 4 ),
 ( 8.542522420166516410E-18, 0.0007580895335617857762, 0.001516179067123562879, 0.001895223833904452785, 0.002274268600685342909, 0.002463790984075790898, 0.002653313367466239320, 0.002842835750856687743, 0.003032358134247136166 ),
 .UNSPECIFIED. ) ;
#44942 = CARTESIAN_POINT ( 'NONE',  ( 5.823673210054444382, -21.52544592524334988, 40.20942372801901854 ) ) ;
#44943 = CARTESIAN_POINT ( 'NONE',  ( -16.51473224551082808, 9.474510206698731452, 63.33442372801900433 ) ) ;
#44944 = CARTESIAN_POINT ( 'NONE',  ( 13.97604488694527802, 13.89961937509977652, 34.37390960531436690 ) ) ;
#44945 = CARTESIAN_POINT ( 'NONE',  ( -19.05341960407611168, -5.049401038298163336, 76.45724293864769550 ) ) ;
#44946 = CARTESIAN_POINT ( 'NONE',  ( -12.14591786802326823, 12.06949235617739902, 33.12609039468569705 ) ) ;
#44947 = CARTESIAN_POINT ( 'NONE',  ( -16.55341960407611168, -4.379528057220339221, 91.45724293864769550 ) ) ;
#44948 = CARTESIAN_POINT ( 'NONE',  ( 5.049401038298161559, -19.05341960407611168, 57.70724293864769550 ) ) ;
#44949 = CARTESIAN_POINT ( 'NONE',  ( -21.52544592524343514, 5.823673210054127303, 36.04057627198102409 ) ) ;
#44950 = CARTESIAN_POINT ( 'NONE',  ( 16.51473224551083163, -9.474510206698727899, 110.8344237280190043 ) ) ;
#44951 = CARTESIAN_POINT ( 'NONE',  ( -21.52544592524334988, -5.823673210054445271, 18.95942372801901143 ) ) ;
#44952 = CARTESIAN_POINT ( 'NONE',  ( -18.67979575497193778, 10.72451020669871902, 68.33442372801900433 ) ) ;
#44953 = CARTESIAN_POINT ( 'NONE',  ( 16.55341960407618274, -4.379528057220086978, 66.04275706135236135 ) ) ;
#44954 = CARTESIAN_POINT ( 'NONE',  ( 0.05219959533934541429, -16.53943276465976808, 70.00109039468568994 ) ) ;
#44955 = CARTESIAN_POINT ( 'NONE',  ( 5.153800228976335163, 19.02544592524342804, 59.79057627198100988 ) ) ;
#44956 = CARTESIAN_POINT ( 'NONE',  ( 0.05219959533934541429, -16.53943276465976808, 85.00109039468568994 ) ) ;
#44957 = CARTESIAN_POINT ( 'NONE',  ( 19.02544592524334988, 5.153800228976608722, 36.45942372801900433 ) ) ;
#44958 = CARTESIAN_POINT ( 'NONE',  ( -18.62759615963255300, -10.81492255796106328, 24.16775706135235424 ) ) ;
#44959 = CARTESIAN_POINT ( 'NONE',  ( 16.55341960407611168, 4.379528057220329451, 58.95724293864770971 ) ) ;
#44960 = CARTESIAN_POINT ( 'NONE',  ( -16.46253265017160317, 9.564922557960807481, 80.83224293864769550 ) ) ;
#44961 = CARTESIAN_POINT ( 'NONE',  ( 12.06949235617739724, 12.14591786802326823, 86.87609039468568994 ) ) ;
#44962 = CARTESIAN_POINT ( 'NONE',  ( 10.72451020669871369, 18.67979575497193778, 62.08442372801901143 ) ) ;
#44963 = CARTESIAN_POINT ( 'NONE',  ( 12.06949235617739724, 12.14591786802326823, 31.87609039468567929 ) ) ;
#44964 = CARTESIAN_POINT ( 'NONE',  ( -15.72974639402176322, -15.80617190586768395, 19.37609039468568639 ) ) ;
#44965 = CARTESIAN_POINT ( 'NONE',  ( 12.06949235617757843, -12.14591786802309237, 58.12390960531435979 ) ) ;
#44966 = ORIENTED_EDGE ( 'NONE', *, *, #136135, .T. ) ;
#44967 = CARTESIAN_POINT ( 'NONE',  ( -21.55341960407610458, -5.719274019375992779, 101.4572429386476955 ) ) ;
#44968 = CARTESIAN_POINT ( 'NONE',  ( 16.52544592524342804, -4.483927247898539470, 43.54057627198103830 ) ) ;
#44969 = ORIENTED_EDGE ( 'NONE', *, *, #148455, .F. ) ;
#44970 = CARTESIAN_POINT ( 'NONE',  ( 34.59574315510280940, 4.379613810579301436, 51.09339236891210589 ) ) ;
#44971 = CARTESIAN_POINT ( 'NONE',  ( 5.049401038298161559, -19.05341960407611168, 112.7072429386476813 ) ) ;
#44972 = CARTESIAN_POINT ( 'NONE',  ( -15.72974639402176322, -15.80617190586768395, 34.37609039468568284 ) ) ;
#44973 = CARTESIAN_POINT ( 'NONE',  ( -4.483927247898539470, -16.52544592524342804, 52.29057627198102409 ) ) ;
#44974 = CARTESIAN_POINT ( 'NONE',  ( -13.97604488694527625, -13.89961937509977652, 66.87390960531436690 ) ) ;
#44975 = CARTESIAN_POINT ( 'NONE',  ( 5.049401038297881783, 19.05341960407617563, 62.29275706135234003 ) ) ;
#44976 = CARTESIAN_POINT ( 'NONE',  ( -13.97604488694527625, -13.89961937509977652, 91.87390960531432427 ) ) ;
#44977 = CARTESIAN_POINT ( 'NONE',  ( -21.55341960407610458, -5.719274019375992779, 51.45724293864770260 ) ) ;
#44978 = CARTESIAN_POINT ( 'NONE',  ( -10.08838716500075883, -37.25234734385823998, -23.84483522324640958 ) ) ;
#44979 = CARTESIAN_POINT ( 'NONE',  ( -0.05219959533909027116, -19.03943276465977164, 62.49890960531435979 ) ) ;
#44980 = CARTESIAN_POINT ( 'NONE',  ( -16.55341960407617563, 4.379528057220093196, 43.54275706135235424 ) ) ;
#44981 = CARTESIAN_POINT ( 'NONE',  ( 16.51473224551083163, -9.474510206698727899, 65.83442372801900433 ) ) ;
#44982 = CARTESIAN_POINT ( 'NONE',  ( 21.53943276465977519, -0.05219959533907433946, 108.7489096053143669 ) ) ;
#44983 = CARTESIAN_POINT ( 'NONE',  ( 16.52544592524342804, -4.483927247898539470, 48.54057627198103120 ) ) ;
#44984 = ORIENTED_EDGE ( 'NONE', *, *, #18810, .F. ) ;
#44985 = CARTESIAN_POINT ( 'NONE',  ( -9.564922557960796823, -16.46253265017161027, 97.08224293864769550 ) ) ;
#44986 = CARTESIAN_POINT ( 'NONE',  ( 15.72974639402199770, -15.80617190586745480, 78.12390960531436690 ) ) ;
#44988 = CARTESIAN_POINT ( 'NONE',  ( -4.483927247898782831, 16.52544592524335698, 37.70942372801900433 ) ) ;
#44987 = CARTESIAN_POINT ( 'NONE',  ( 21.53943276465977519, -0.05219959533907433946, 108.7489096053143669 ) ) ;
#44989 = CARTESIAN_POINT ( 'NONE',  ( 18.67979575497178502, 10.72451020669898547, 34.16557627198102409 ) ) ;
#44990 = CARTESIAN_POINT ( 'NONE',  ( 0.05219959533937995610, -21.53943276465977519, 105.0010903946856757 ) ) ;
#44991 = CARTESIAN_POINT ( 'NONE',  ( 9.564922557960805705, 16.46253265017160317, 99.58224293864770971 ) ) ;
#44992 = VECTOR ( 'NONE', #175058, 1000.000000000000000 ) ;
#44993 = CARTESIAN_POINT ( 'NONE',  ( 19.03943276465977164, -0.05219959533909143690, 43.74890960531435979 ) ) ;
#44994 = CARTESIAN_POINT ( 'NONE',  ( -0.05219959533909027116, -19.03943276465977164, 97.49890960531436690 ) ) ;
#44995 = CARTESIAN_POINT ( 'NONE',  ( -9.564922557960796823, -16.46253265017161027, 77.08224293864769550 ) ) ;
#44996 = CARTESIAN_POINT ( 'NONE',  ( 17.26172910966714369, -6.454744622557084810, 88.30646908649210047 ) ) ;
#44997 = CARTESIAN_POINT ( 'NONE',  ( -9.564922557961040184, 16.46253265017147172, 57.91775706135233293 ) ) ;
#44999 = CARTESIAN_POINT ( 'NONE',  ( 5.719274019375991003, -21.55341960407610458, 32.70724293864770260 ) ) ;
#44998 = CARTESIAN_POINT ( 'NONE',  ( -5.719274019375665041, -21.55341960407619695, 109.7927570613523613 ) ) ;
#45000 = CARTESIAN_POINT ( 'NONE',  ( 8.314922557961029526, -14.29746914071037800, 110.4177570613523756 ) ) ;
#45001 = CARTESIAN_POINT ( 'NONE',  ( 16.51473224551069308, 9.474510206698969483, 39.16557627198103120 ) ) ;
#45002 = CARTESIAN_POINT ( 'NONE',  ( 16.51473224551083163, -9.474510206698727899, 80.83442372801899012 ) ) ;
#45003 = CARTESIAN_POINT ( 'NONE',  ( -19.03943276465977164, -0.05219959533935918106, 28.75109039468566507 ) ) ;
#45004 = CARTESIAN_POINT ( 'NONE',  ( -17.31728774477270250, -6.344390552232404445, 44.18093348310681989 ) ) ;
#45005 = CARTESIAN_POINT ( 'NONE',  ( -19.03943276465977164, 0.05219959533909376836, 36.24890960531436690 ) ) ;
#45006 = CARTESIAN_POINT ( 'NONE',  ( 14.34966873604960469, 8.224510206698951720, 39.16557627198102409 ) ) ;
#45007 = CARTESIAN_POINT ( 'NONE',  ( -16.29526858892874586, -7.335722546920139031, 110.7967059780020662 ) ) ;
#45008 = CARTESIAN_POINT ( 'NONE',  ( 14.34966873604960469, 8.224510206698951720, 24.16557627198103120 ) ) ;
#45009 = CARTESIAN_POINT ( 'NONE',  ( 20.50626127892844863, -20.36451067365405976, -52.65483682830183909 ) ) ;
#45010 = CARTESIAN_POINT ( 'NONE',  ( -12.14591786802326823, 12.06949235617739902, 88.12609039468570415 ) ) ;
#45011 = CARTESIAN_POINT ( 'NONE',  ( -9.474510206698964154, 16.51473224551069663, 50.41557627198102409 ) ) ;
#45012 = EDGE_CURVE ( 'NONE', #82818, #44725, #3852, .T. ) ;
#45013 = CARTESIAN_POINT ( 'NONE',  ( -5.823673210054431948, 21.52544592524334988, 102.7094237280190185 ) ) ;
#45014 = CARTESIAN_POINT ( 'NONE',  ( -19.02544592524334988, -5.153800228976617603, 108.9594237280189759 ) ) ;
#45015 = CARTESIAN_POINT ( 'NONE',  ( -5.823673210054431948, 21.52544592524334988, 87.70942372801901854 ) ) ;
#45016 = CARTESIAN_POINT ( 'NONE',  ( 16.51473224551083163, -9.474510206698727899, 70.83442372801900433 ) ) ;
#45017 = CARTESIAN_POINT ( 'NONE',  ( -13.97604488694527625, -13.89961937509977652, 86.87390960531436690 ) ) ;
#45018 = CARTESIAN_POINT ( 'NONE',  ( -0.05219959533909027116, -19.03943276465977164, 87.49890960531436690 ) ) ;
#45019 = CARTESIAN_POINT ( 'NONE',  ( -36.91746825000000598, -11.99521256947794789, -10.52499999726881441 ) ) ;
#45020 = CARTESIAN_POINT ( 'NONE',  ( -21.55341960407610458, -5.719274019375992779, 111.4572429386476813 ) ) ;
#45021 = AXIS2_PLACEMENT_3D ( 'NONE', #173787, #140441, #34268 ) ;
#45022 = CARTESIAN_POINT ( 'NONE',  ( 8.314922557960818139, 14.29746914071049879, 84.58224293864769550 ) ) ;
#45023 = CARTESIAN_POINT ( 'NONE',  ( -5.823673210054116645, -21.52544592524344225, 57.29057627198103120 ) ) ;
#45024 = CARTESIAN_POINT ( 'NONE',  ( -9.474510206698964154, 16.51473224551069663, 55.41557627198103120 ) ) ;
#45026 = CARTESIAN_POINT ( 'NONE',  ( -8.224510206698735004, -14.34966873604973081, 84.58442372801903275 ) ) ;
#45025 = CARTESIAN_POINT ( 'NONE',  ( 15.80617190586746368, 15.72974639402197994, 99.37390960531436690 ) ) ;
#45027 = EDGE_CURVE ( 'NONE', #199255, #15707, #117637, .T. ) ;
#45028 = ORIENTED_EDGE ( 'NONE', *, *, #197329, .F. ) ;
#45029 = CARTESIAN_POINT ( 'NONE',  ( -0.05219959533909027116, -19.03943276465977164, 62.49890960531435979 ) ) ;
#45031 = DIRECTION ( 'NONE',  ( -0.000000000000000000, -0.000000000000000000, 1.000000000000000000 ) ) ;
#45030 = CARTESIAN_POINT ( 'NONE',  ( 8.314922557960818139, 14.29746914071049879, 94.58224293864769550 ) ) ;
#45032 = CARTESIAN_POINT ( 'NONE',  ( -9.564922557960796823, -16.46253265017161027, 52.08224293864768839 ) ) ;
#45033 = CARTESIAN_POINT ( 'NONE',  ( 9.564922557961047289, -16.46253265017146816, 85.41775706135233293 ) ) ;
#45034 = CARTESIAN_POINT ( 'NONE',  ( 4.483927247898545687, 16.52544592524342804, 84.79057627198102409 ) ) ;
#45035 = CARTESIAN_POINT ( 'NONE',  ( 15.80617190586769283, -15.72974639402175789, 55.62609039468568284 ) ) ;
#45037 = CARTESIAN_POINT ( 'NONE',  ( 18.62759615963271287, -10.81492255796078972, 98.33224293864769550 ) ) ;
#45036 = CARTESIAN_POINT ( 'NONE',  ( -13.97604488694527625, -13.89961937509977652, 31.87390960531435979 ) ) ;
#45038 = CARTESIAN_POINT ( 'NONE',  ( 14.29746914071049879, -8.314922557960816363, 103.3322429386476955 ) ) ;
#45039 = CARTESIAN_POINT ( 'NONE',  ( 28.82186960331500813, 9.364793116373537174, 147.3500000054623627 ) ) ;
#45040 = CARTESIAN_POINT ( 'NONE',  ( -19.03943276465977164, 0.05219959533909376836, 56.24890960531435979 ) ) ;
#45041 = CARTESIAN_POINT ( 'NONE',  ( -9.248023074035630842, -11.04433579861080084, -62.31744588651325500 ) ) ;
#45043 = CARTESIAN_POINT ( 'NONE',  ( -19.05341960407611168, -5.049401038298163336, 111.4572429386476671 ) ) ;
#45042 = CARTESIAN_POINT ( 'NONE',  ( -9.474510206698720793, -16.51473224551083518, 99.58442372801900433 ) ) ;
#45044 = CARTESIAN_POINT ( 'NONE',  ( 15.80617190586769283, -15.72974639402175789, 55.62609039468568284 ) ) ;
#45045 = CARTESIAN_POINT ( 'NONE',  ( -9.474510206698964154, 16.51473224551069663, 80.41557627198103830 ) ) ;
#45046 = CARTESIAN_POINT ( 'NONE',  ( 9.474510206698729675, 16.51473224551082808, 67.08442372801900433 ) ) ;
#45047 = CARTESIAN_POINT ( 'NONE',  ( -5.049401038298153566, 19.05341960407611168, 60.20724293864768129 ) ) ;
#45048 = CARTESIAN_POINT ( 'NONE',  ( -4.379528057220328563, 16.55341960407611168, 80.20724293864769550 ) ) ;
#45049 = CARTESIAN_POINT ( 'NONE',  ( 16.52544592524342804, -4.483927247898539470, 68.54057627198103830 ) ) ;
#45050 = CARTESIAN_POINT ( 'NONE',  ( -13.89961937509977652, 13.97604488694528158, 90.62390960531432427 ) ) ;
#45051 = CARTESIAN_POINT ( 'NONE',  ( 16.55341960407611168, 4.379528057220329451, 83.95724293864770971 ) ) ;
#45052 = CARTESIAN_POINT ( 'NONE',  ( -13.97604488694527625, -13.89961937509977652, 81.87390960531436690 ) ) ;
#45053 = CARTESIAN_POINT ( 'NONE',  ( 19.05341960407617918, -5.049401038297876454, 26.04275706135233293 ) ) ;
#45056 = CARTESIAN_POINT ( 'NONE',  ( -0.05219959533910754901, -16.53943276465976808, 112.4989096053143669 ) ) ;
#45055 = CARTESIAN_POINT ( 'NONE',  ( 12.06949235617757843, -12.14591786802309237, 33.12390960531435979 ) ) ;
#45054 = CARTESIAN_POINT ( 'NONE',  ( 13.97604488694527802, 13.89961937509977652, 54.37390960531435979 ) ) ;
#45057 = ORIENTED_EDGE ( 'NONE', *, *, #10333, .F. ) ;
#45058 = CARTESIAN_POINT ( 'NONE',  ( -10.72451020669870658, -18.67979575497194134, 39.58442372801901143 ) ) ;
#45059 = CARTESIAN_POINT ( 'NONE',  ( 9.474510206698729675, 16.51473224551082808, 67.08442372801900433 ) ) ;
#45060 = CARTESIAN_POINT ( 'NONE',  ( -4.379528057220328563, 16.55341960407611168, 40.20724293864769550 ) ) ;
#45061 = CARTESIAN_POINT ( 'NONE',  ( 10.81492255796078972, 18.62759615963270932, 84.58224293864769550 ) ) ;
#45062 = CARTESIAN_POINT ( 'NONE',  ( 5.049401038298161559, -19.05341960407611168, 112.7072429386476813 ) ) ;
#45063 = CARTESIAN_POINT ( 'NONE',  ( -8.224510206698948167, 14.34966873604960824, 65.41557627198102409 ) ) ;
#45064 = CARTESIAN_POINT ( 'NONE',  ( 19.05341960407611168, 5.049401038298154454, 38.95724293864767418 ) ) ;
#45065 = CARTESIAN_POINT ( 'NONE',  ( 13.89961937509957401, 13.97604488694547697, 31.87609039468566863 ) ) ;
#45066 = CARTESIAN_POINT ( 'NONE',  ( -14.34966873604972548, 8.224510206698743886, 98.33442372801901854 ) ) ;
#45067 = CARTESIAN_POINT ( 'NONE',  ( 4.483927247898790824, -16.52544592524335698, 60.20942372801902565 ) ) ;
#45068 = CARTESIAN_POINT ( 'NONE',  ( -21.52544592524343514, 5.823673210054127303, 31.04057627198102409 ) ) ;
#45069 = CARTESIAN_POINT ( 'NONE',  ( 18.62759615963255655, 10.81492255796105972, 101.6677570613523613 ) ) ;
#45070 = CARTESIAN_POINT ( 'NONE',  ( 5.049401038298161559, -19.05341960407611168, 97.70724293864766707 ) ) ;
#45071 = CARTESIAN_POINT ( 'NONE',  ( 8.224510206698742110, 14.34966873604972548, 77.08442372801901854 ) ) ;
#45072 = CARTESIAN_POINT ( 'NONE',  ( 16.55341960407611168, 4.379528057220329451, 113.9572429386477239 ) ) ;
#45073 = CARTESIAN_POINT ( 'NONE',  ( 16.55341960407611168, 4.379528057220329451, 28.95724293864769905 ) ) ;
#45075 = CARTESIAN_POINT ( 'NONE',  ( -19.05341960407611168, -5.049401038298163336, 86.45724293864769550 ) ) ;
#45074 = CARTESIAN_POINT ( 'NONE',  ( 16.51473224551069308, 9.474510206698969483, 109.1655762719810383 ) ) ;
#45076 = CARTESIAN_POINT ( 'NONE',  ( -0.05219959533907301413, -21.53943276465977519, 27.49890960531435269 ) ) ;
#45077 = CARTESIAN_POINT ( 'NONE',  ( -4.379528057220328563, 16.55341960407611168, 55.20724293864770260 ) ) ;
#45078 = CARTESIAN_POINT ( 'NONE',  ( -14.34966873604960291, -8.224510206698953496, 36.66557627198103120 ) ) ;
#45079 = VERTEX_POINT ( 'NONE', #174716 ) ;
#45080 = CARTESIAN_POINT ( 'NONE',  ( -8.224510206698948167, 14.34966873604960824, 55.41557627198102409 ) ) ;
#45082 = CARTESIAN_POINT ( 'NONE',  ( -7.052343178074647945, -2.552343178074588437, 1.110912703473986074 ) ) ;
#45081 = CARTESIAN_POINT ( 'NONE',  ( 14.34966873604972726, -8.224510206698740333, 55.83442372801901854 ) ) ;
#45083 = CARTESIAN_POINT ( 'NONE',  ( -16.51473224551082808, 9.474510206698731452, 48.33442372801900433 ) ) ;
#45084 = CARTESIAN_POINT ( 'NONE',  ( -19.02544592524342804, 5.153800228976336051, 91.04057627198100988 ) ) ;
#45085 = CARTESIAN_POINT ( 'NONE',  ( 16.51473224551083163, -9.474510206698727899, 65.83442372801900433 ) ) ;
#45086 = CARTESIAN_POINT ( 'NONE',  ( -27.73933785331498925, 9.013057229001089965, 143.2750000027311899 ) ) ;
#45087 = CARTESIAN_POINT ( 'NONE',  ( 0.05219959533936267826, -19.03943276465977164, 55.00109039468566863 ) ) ;
#45089 = CARTESIAN_POINT ( 'NONE',  ( -0.05219959533934338120, 16.53943276465976808, 77.50109039468567573 ) ) ;
#45088 = CARTESIAN_POINT ( 'NONE',  ( -13.97604488694547697, 13.89961937509957934, 93.12609039468566152 ) ) ;
#45090 = CARTESIAN_POINT ( 'NONE',  ( -5.359611314223446995E-15, 29.16686587814335496, 148.8750000027311842 ) ) ;
#45091 = CARTESIAN_POINT ( 'NONE',  ( -19.05341960407611168, -5.049401038298163336, 26.45724293864769550 ) ) ;
#45092 = CARTESIAN_POINT ( 'NONE',  ( -5.049401038298153566, 19.05341960407611168, 115.2072429386477097 ) ) ;
#45093 = CARTESIAN_POINT ( 'NONE',  ( 21.55341960407619695, -5.719274019375665929, 46.04275706135234714 ) ) ;
#45094 = CARTESIAN_POINT ( 'NONE',  ( 16.46253265017146816, 9.564922557961045513, 101.6677570613523329 ) ) ;
#45096 = CARTESIAN_POINT ( 'NONE',  ( 19.05341960407611168, 5.049401038298154454, 58.95724293864768129 ) ) ;
#45095 = CARTESIAN_POINT ( 'NONE',  ( 11.74264578624799427, 36.14014761921585972, -2.600000000000000533 ) ) ;
#45097 = CARTESIAN_POINT ( 'NONE',  ( 19.05341960407611168, 5.049401038298154454, 98.95724293864766707 ) ) ;
#45099 = CARTESIAN_POINT ( 'NONE',  ( 16.51473224551069308, 9.474510206698969483, 59.16557627198102409 ) ) ;
#45098 = CARTESIAN_POINT ( 'NONE',  ( 0.05219959533910956823, 16.53943276465976808, 69.99890960531435269 ) ) ;
#45100 = CARTESIAN_POINT ( 'NONE',  ( -13.97604488694527625, -13.89961937509977652, 76.87390960531433848 ) ) ;
#45101 = CARTESIAN_POINT ( 'NONE',  ( 19.02544592524334988, 5.153800228976608722, 81.45942372801897591 ) ) ;
#45102 = CARTESIAN_POINT ( 'NONE',  ( -0.05219959533907301413, -21.53943276465977519, 52.49890960531435979 ) ) ;
#45103 = CARTESIAN_POINT ( 'NONE',  ( -4.379528057220328563, 16.55341960407611168, 110.2072429386477239 ) ) ;
#45104 = CARTESIAN_POINT ( 'NONE',  ( 19.03943276465977164, 0.05219959533936151252, 41.25109039468566152 ) ) ;
#45105 = CARTESIAN_POINT ( 'NONE',  ( 5.049401038298161559, -19.05341960407611168, 77.70724293864765286 ) ) ;
#45106 = CARTESIAN_POINT ( 'NONE',  ( 21.55341960407610458, 5.719274019375980345, 78.95724293864769550 ) ) ;
#45108 = CARTESIAN_POINT ( 'NONE',  ( -19.03943276465977164, -0.05219959533935918106, 53.75109039468566863 ) ) ;
#45107 = CARTESIAN_POINT ( 'NONE',  ( 14.34966873604960469, 8.224510206698951720, 84.16557627198103830 ) ) ;
#45109 = CARTESIAN_POINT ( 'NONE',  ( 15.72974639402199770, -15.80617190586745480, 73.12390960531436690 ) ) ;
#45110 = CARTESIAN_POINT ( 'NONE',  ( -18.67979575497178146, -10.72451020669898902, 66.66557627198102409 ) ) ;
#45111 = CARTESIAN_POINT ( 'NONE',  ( -10.72451020669898014, 18.67979575497178502, 35.41557627198102409 ) ) ;
#45112 = CARTESIAN_POINT ( 'NONE',  ( -5.719274019375665041, -21.55341960407619695, 94.79275706135234714 ) ) ;
#45113 = CARTESIAN_POINT ( 'NONE',  ( 19.05341960407611168, 5.049401038298154454, 63.95724293864769550 ) ) ;
#45114 = CARTESIAN_POINT ( 'NONE',  ( -8.314922557960811034, -14.29746914071050412, 112.0822429386477097 ) ) ;
#45115 = CARTESIAN_POINT ( 'NONE',  ( 0.05219959533937995610, -21.53943276465977519, 20.00109039468568639 ) ) ;
#45116 = CARTESIAN_POINT ( 'NONE',  ( -10.72451020669870658, -18.67979575497194134, 39.58442372801901143 ) ) ;
#45117 = CARTESIAN_POINT ( 'NONE',  ( 13.89961937509977652, -13.97604488694527269, 28.12390960531435624 ) ) ;
#45118 = CARTESIAN_POINT ( 'NONE',  ( -5.719274019375978568, 21.55341960407610458, 105.2072429386477097 ) ) ;
#45119 = CARTESIAN_POINT ( 'NONE',  ( -5.049401038297874678, -19.05341960407617918, 44.79275706135232582 ) ) ;
#45120 = CARTESIAN_POINT ( 'NONE',  ( -16.46253265017160317, 9.564922557960807481, 40.83224293864769550 ) ) ;
#45121 = CARTESIAN_POINT ( 'NONE',  ( -5.153800228976328057, -19.02544592524343514, 22.29057627198102765 ) ) ;
#45122 = DIRECTION ( 'NONE',  ( 0.000000000000000000, -0.000000000000000000, -1.000000000000000000 ) ) ;
#45123 = CARTESIAN_POINT ( 'NONE',  ( -12.14591786802326823, 12.06949235617739902, 58.12609039468568994 ) ) ;
#45124 = CARTESIAN_POINT ( 'NONE',  ( -9.564922557960796823, -16.46253265017161027, 27.08224293864769550 ) ) ;
#45125 = CARTESIAN_POINT ( 'NONE',  ( -24.06609220500524415, -14.38661408136937148, 165.8682408874374232 ) ) ;
#45126 = CARTESIAN_POINT ( 'NONE',  ( -19.05341960407611168, -5.049401038298163336, 81.45724293864769550 ) ) ;
#45127 = CARTESIAN_POINT ( 'NONE',  ( -0.05219959533910754901, -16.53943276465976808, 102.4989096053143811 ) ) ;
#45128 = CARTESIAN_POINT ( 'NONE',  ( -15.72974639402197994, 15.80617190586746368, 55.62390960531436690 ) ) ;
#45129 = CARTESIAN_POINT ( 'NONE',  ( -16.52544592524335698, -4.483927247898792601, 43.95942372801902565 ) ) ;
#45130 = CARTESIAN_POINT ( 'NONE',  ( -10.81492255796105439, 18.62759615963255655, 97.91775706135236135 ) ) ;
#45131 = EDGE_CURVE ( 'NONE', #166995, #86859, #100843, .T. ) ;
#45132 = CARTESIAN_POINT ( 'NONE',  ( -9.474510206698964154, 16.51473224551069663, 40.41557627198103120 ) ) ;
#45133 = CARTESIAN_POINT ( 'NONE',  ( -14.29746914071037622, -8.314922557961029526, 109.1677570613523613 ) ) ;
#45134 = CARTESIAN_POINT ( 'NONE',  ( -12.06949235617756955, 12.14591786802309770, 55.62390960531436690 ) ) ;
#45135 = CIRCLE ( 'NONE', #138630, 2.500000000000002220 ) ;
#45136 = CARTESIAN_POINT ( 'NONE',  ( -9.474510206698964154, 16.51473224551069663, 70.41557627198102409 ) ) ;
#45137 = CARTESIAN_POINT ( 'NONE',  ( 9.564922557961047289, -16.46253265017146816, 20.41775706135233293 ) ) ;
#45138 = CARTESIAN_POINT ( 'NONE',  ( 21.53943276465977519, 0.05219959533937863772, 26.25109039468567573 ) ) ;
#45139 = CARTESIAN_POINT ( 'NONE',  ( 10.81492255796106328, -18.62759615963255655, 75.41775706135233293 ) ) ;
#45140 = CARTESIAN_POINT ( 'NONE',  ( 16.55341960407618274, -4.379528057220086978, 51.04275706135234714 ) ) ;
#45141 = CARTESIAN_POINT ( 'NONE',  ( -8.224510206698735004, -14.34966873604973081, 34.58442372801900433 ) ) ;
#45143 = CARTESIAN_POINT ( 'NONE',  ( 18.67979575497194134, -10.72451020669871369, 105.8344237280190328 ) ) ;
#45142 = CARTESIAN_POINT ( 'NONE',  ( -8.314922557960811034, -14.29746914071050412, 77.08224293864769550 ) ) ;
#45144 = EDGE_CURVE ( 'NONE', #115376, #99310, #4595, .T. ) ;
#45145 = CARTESIAN_POINT ( 'NONE',  ( -4.379528057220328563, 16.55341960407611168, 30.20724293864769550 ) ) ;
#45146 = CARTESIAN_POINT ( 'NONE',  ( -16.20579543436677383, 7.371946100355101450, 114.4347916582812985 ) ) ;
#45147 = CARTESIAN_POINT ( 'NONE',  ( 16.55341960407618274, -4.379528057220086978, 36.04275706135234714 ) ) ;
#45148 = CARTESIAN_POINT ( 'NONE',  ( -8.314922557960811034, -14.29746914071050412, 47.08224293864770260 ) ) ;
#45149 = CARTESIAN_POINT ( 'NONE',  ( -12.14591786802326823, 12.06949235617739902, 83.12609039468568994 ) ) ;
#45150 = CARTESIAN_POINT ( 'NONE',  ( -5.049401038298153566, 19.05341960407611168, 100.2072429386476955 ) ) ;
#45151 = CARTESIAN_POINT ( 'NONE',  ( -19.03943276465977164, 0.05219959533909376836, 111.2489096053143669 ) ) ;
#45152 = CARTESIAN_POINT ( 'NONE',  ( 5.719274019375673035, 21.55341960407619339, 102.2927570613523613 ) ) ;
#45153 = CARTESIAN_POINT ( 'NONE',  ( -8.314922557961024197, 14.29746914071037800, 102.9177570613523756 ) ) ;
#45154 = CARTESIAN_POINT ( 'NONE',  ( -12.14591786802309592, -12.06949235617757132, 91.87390960531436690 ) ) ;
#45155 = CARTESIAN_POINT ( 'NONE',  ( -0.05219959533909027116, -19.03943276465977164, 87.49890960531436690 ) ) ;
#45156 = ORIENTED_EDGE ( 'NONE', *, *, #6979, .F. ) ;
#45157 = CARTESIAN_POINT ( 'NONE',  ( 14.29746914071037800, 8.314922557961029526, 36.66775706135234714 ) ) ;
#45158 = CARTESIAN_POINT ( 'NONE',  ( 19.02544592524343514, -5.153800228976328945, 38.54057627198103120 ) ) ;
#45159 = CARTESIAN_POINT ( 'NONE',  ( -19.03943276465977164, 0.05219959533909376836, 111.2489096053143669 ) ) ;
#45161 = CARTESIAN_POINT ( 'NONE',  ( 29.86685920354754842, -21.69954338932559068, -1.824999997268813345 ) ) ;
#45160 = CARTESIAN_POINT ( 'NONE',  ( 14.34966873604972726, -8.224510206698740333, 45.83442372801901854 ) ) ;
#45162 = CARTESIAN_POINT ( 'NONE',  ( -13.97604488694547697, 13.89961937509957934, 38.12609039468566152 ) ) ;
#45163 = CARTESIAN_POINT ( 'NONE',  ( -14.34966873604972548, 8.224510206698743886, 103.3344237280190043 ) ) ;
#45164 = CARTESIAN_POINT ( 'NONE',  ( -19.03943276465977164, 0.05219959533909376836, 31.24890960531435979 ) ) ;
#45165 = CARTESIAN_POINT ( 'NONE',  ( 16.53943276465976808, 0.05219959533934440121, 76.25109039468568994 ) ) ;
#45166 = CARTESIAN_POINT ( 'NONE',  ( 16.51473224551083163, -9.474510206698727899, 85.83442372801900433 ) ) ;
#45167 = CARTESIAN_POINT ( 'NONE',  ( -5.153800228976607833, 19.02544592524334988, 22.70942372801899012 ) ) ;
#45168 = CARTESIAN_POINT ( 'NONE',  ( -5.049401038298153566, 19.05341960407611168, 65.20724293864765286 ) ) ;
#45169 = CARTESIAN_POINT ( 'NONE',  ( 8.314922557960818139, 14.29746914071049879, 94.58224293864769550 ) ) ;
#45170 = VECTOR ( 'NONE', #175951, 1000.000000000000000 ) ;
#45171 = CARTESIAN_POINT ( 'NONE',  ( -5.153800228976607833, 19.02544592524334988, 62.70942372801899722 ) ) ;
#45172 = CARTESIAN_POINT ( 'NONE',  ( -18.67979575497178146, -10.72451020669898902, 66.66557627198102409 ) ) ;
#45173 = CARTESIAN_POINT ( 'NONE',  ( 13.97604488694548053, -13.89961937509957401, 25.62609039468566507 ) ) ;
#45174 = CARTESIAN_POINT ( 'NONE',  ( -5.153800228976328057, -19.02544592524343514, 107.2905762719810383 ) ) ;
#45175 = EDGE_CURVE ( 'NONE', #120193, #182074, #126097, .T. ) ;
#45176 = CARTESIAN_POINT ( 'NONE',  ( -0.05219959533907301413, -21.53943276465977519, 82.49890960531436690 ) ) ;
#45177 = CARTESIAN_POINT ( 'NONE',  ( -19.02544592524342804, 5.153800228976336051, 116.0405762719810383 ) ) ;
#45178 = CARTESIAN_POINT ( 'NONE',  ( 13.97604488694548053, -13.89961937509957401, 105.6260903946856757 ) ) ;
#45179 = CARTESIAN_POINT ( 'NONE',  ( -2.552343178074661267, -7.052343178074616858, 8.889087296526001936 ) ) ;
#45180 = CARTESIAN_POINT ( 'NONE',  ( -4.483927247898782831, 16.52544592524335698, 27.70942372801901854 ) ) ;
#45181 = CARTESIAN_POINT ( 'NONE',  ( -0.05219959533909027116, -19.03943276465977164, 27.49890960531435624 ) ) ;
#45182 = CARTESIAN_POINT ( 'NONE',  ( 5.049401038298161559, -19.05341960407611168, 92.70724293864769550 ) ) ;
#45183 = CARTESIAN_POINT ( 'NONE',  ( 0.05219959533907565091, 21.53943276465977519, 94.99890960531436690 ) ) ;
#45184 = CARTESIAN_POINT ( 'NONE',  ( 4.483927247898790824, -16.52544592524335698, 60.20942372801902565 ) ) ;
#45185 = CARTESIAN_POINT ( 'NONE',  ( -21.53943276465977519, -0.05219959533937600094, 58.75109039468568994 ) ) ;
#45187 = CARTESIAN_POINT ( 'NONE',  ( 21.52544592524334988, 5.823673210054432836, 111.4594237280190328 ) ) ;
#45186 = CARTESIAN_POINT ( 'NONE',  ( 19.05341960407617918, -5.049401038297876454, 101.0427570613523045 ) ) ;
#45188 = CARTESIAN_POINT ( 'NONE',  ( -12.06949235617739369, -12.14591786802326823, 109.3760903946857042 ) ) ;
#45189 = CARTESIAN_POINT ( 'NONE',  ( 0.05219959533907565091, 21.53943276465977519, 94.99890960531436690 ) ) ;
#45190 = CARTESIAN_POINT ( 'NONE',  ( 14.29746914071049879, -8.314922557960816363, 33.33224293864769550 ) ) ;
#45191 = CARTESIAN_POINT ( 'NONE',  ( -0.05219959533936034679, 19.03943276465977164, 87.50109039468567573 ) ) ;
#45192 = CARTESIAN_POINT ( 'NONE',  ( -10.72451020669870658, -18.67979575497194134, 59.58442372801901854 ) ) ;
#45193 = CARTESIAN_POINT ( 'NONE',  ( 19.05341960407617918, -5.049401038297876454, 36.04275706135234003 ) ) ;
#45194 = CARTESIAN_POINT ( 'NONE',  ( 12.06949235617757843, -12.14591786802309237, 108.1239096053143811 ) ) ;
#45195 = CARTESIAN_POINT ( 'NONE',  ( -10.81492255796078084, -18.62759615963271287, 32.08224293864769550 ) ) ;
#45196 = CARTESIAN_POINT ( 'NONE',  ( -16.53943276465976808, 0.05219959533911058130, 36.24890960531435979 ) ) ;
#45197 = CARTESIAN_POINT ( 'NONE',  ( 5.719274019375673035, 21.55341960407619339, 92.29275706135236135 ) ) ;
#45198 = CARTESIAN_POINT ( 'NONE',  ( -16.55341960407617563, 4.379528057220093196, 73.54275706135234714 ) ) ;
#45199 = CARTESIAN_POINT ( 'NONE',  ( 8.224510206698953496, -14.34966873604960469, 27.91557627198103830 ) ) ;
#45200 = CARTESIAN_POINT ( 'NONE',  ( -18.67979575497193778, 10.72451020669871902, 68.33442372801900433 ) ) ;
#45201 = CARTESIAN_POINT ( 'NONE',  ( -0.05219959533937732626, 21.53943276465977519, 57.50109039468568994 ) ) ;
#45202 = VERTEX_POINT ( 'NONE', #137921 ) ;
#45203 = CARTESIAN_POINT ( 'NONE',  ( 13.89961937509978007, -13.97604488694527269, 63.12390960531435979 ) ) ;
#45204 = CARTESIAN_POINT ( 'NONE',  ( 15.80617190586769283, -15.72974639402175789, 40.62609039468567573 ) ) ;
#45205 = CARTESIAN_POINT ( 'NONE',  ( 19.05341960407611168, 5.049401038298154454, 28.95724293864769550 ) ) ;
#45206 = CARTESIAN_POINT ( 'NONE',  ( -19.02544592524342804, 5.153800228976336051, 41.04057627198103120 ) ) ;
#45207 = CARTESIAN_POINT ( 'NONE',  ( 14.34966873604960469, 8.224510206698951720, 84.16557627198103830 ) ) ;
#45208 = CARTESIAN_POINT ( 'NONE',  ( -9.474510206698964154, 16.51473224551069663, 90.41557627198103830 ) ) ;
#45209 = CARTESIAN_POINT ( 'NONE',  ( -4.483927247898539470, -16.52544592524342804, 27.29057627198103120 ) ) ;
#45210 = CARTESIAN_POINT ( 'NONE',  ( -5.719274019375978568, 21.55341960407610458, 60.20724293864768839 ) ) ;
#45211 = CARTESIAN_POINT ( 'NONE',  ( -21.52544592524343514, 5.823673210054127303, 106.0405762719810525 ) ) ;
#45212 = CARTESIAN_POINT ( 'NONE',  ( 0.05219959533909260263, 19.03943276465977164, 99.99890960531436690 ) ) ;
#45214 = CARTESIAN_POINT ( 'NONE',  ( -5.049401038297874678, -19.05341960407617918, 109.7927570613523187 ) ) ;
#45213 = CARTESIAN_POINT ( 'NONE',  ( -9.474510206698964154, 16.51473224551069663, 65.41557627198102409 ) ) ;
#45215 = CARTESIAN_POINT ( 'NONE',  ( 21.53943276465977519, -0.05219959533907433946, 53.74890960531437401 ) ) ;
#45216 = CARTESIAN_POINT ( 'NONE',  ( -5.823673210054431948, 21.52544592524334988, 82.70942372801900433 ) ) ;
#45217 = CARTESIAN_POINT ( 'NONE',  ( -5.049401038298153566, 19.05341960407611168, 65.20724293864765286 ) ) ;
#45218 = CARTESIAN_POINT ( 'NONE',  ( -5.153800228976328057, -19.02544592524343514, 92.29057627198099567 ) ) ;
#45219 = CARTESIAN_POINT ( 'NONE',  ( 12.14591786802327356, -12.06949235617739191, 70.62609039468567573 ) ) ;
#45220 = CARTESIAN_POINT ( 'NONE',  ( -18.62759615963255300, -10.81492255796106328, 64.16775706135234714 ) ) ;
#45221 = CARTESIAN_POINT ( 'NONE',  ( -10.81492255796105439, 18.62759615963255655, 82.91775706135234714 ) ) ;
#45222 = CARTESIAN_POINT ( 'NONE',  ( 5.823673210054125526, 21.52544592524343514, 114.7905762719810383 ) ) ;
#45223 = CARTESIAN_POINT ( 'NONE',  ( -14.29746914071037622, -8.314922557961029526, 84.16775706135234714 ) ) ;
#45225 = CARTESIAN_POINT ( 'NONE',  ( -18.67979575497178146, -10.72451020669898902, 76.66557627198103830 ) ) ;
#45224 = B_SPLINE_CURVE_WITH_KNOTS ( 'NONE', 3,
 ( #146197, #163390, #129026, #22873, #6685, #176567 ),
 .UNSPECIFIED., .F., .F.,
 ( 4, 2, 4 ),
 ( 0.003989672132298099222, 0.004372778065220536345, 0.004755883998142972600 ),
 .UNSPECIFIED. ) ;
#45226 = CARTESIAN_POINT ( 'NONE',  ( -9.564922557961040184, 16.46253265017147172, 52.91775706135233293 ) ) ;
#45227 = CARTESIAN_POINT ( 'NONE',  ( 15.80617190586746368, 15.72974639402197994, 44.37390960531435979 ) ) ;
#45229 = CARTESIAN_POINT ( 'NONE',  ( 4.379528057220339221, -16.55341960407611168, 27.70724293864769905 ) ) ;
#45228 = CARTESIAN_POINT ( 'NONE',  ( 13.89961937509977652, -13.97604488694527269, 88.12390960531438111 ) ) ;
#45230 = CARTESIAN_POINT ( 'NONE',  ( 4.999999999999997335, 3.306546357697854226E-16, 2.700000000000000622 ) ) ;
#45231 = CARTESIAN_POINT ( 'NONE',  ( 15.72974639402199770, -15.80617190586745480, 23.12390960531436335 ) ) ;
#45232 = CARTESIAN_POINT ( 'NONE',  ( 1.500000000000000888, 15.20000000000002061, -59.79525829764741474 ) ) ;
#45233 = CARTESIAN_POINT ( 'NONE',  ( -9.474510206698720793, -16.51473224551083518, 89.58442372801900433 ) ) ;
#45234 = CARTESIAN_POINT ( 'NONE',  ( 5.823673210054125526, 21.52544592524343514, 74.79057627198105251 ) ) ;
#45235 = CARTESIAN_POINT ( 'NONE',  ( 14.29746914071049879, -8.314922557960816363, 53.33224293864769550 ) ) ;
#45236 = CARTESIAN_POINT ( 'NONE',  ( -19.03943276465977164, -0.05219959533935918106, 113.7510903946856757 ) ) ;
#45237 = CARTESIAN_POINT ( 'NONE',  ( -5.049401038298153566, 19.05341960407611168, 40.20724293864768839 ) ) ;
#45239 = CARTESIAN_POINT ( 'NONE',  ( -19.05341960407617563, 5.049401038297882671, 73.54275706135233293 ) ) ;
#45238 = CARTESIAN_POINT ( 'NONE',  ( -5.719274019375978568, 21.55341960407610458, 100.2072429386476955 ) ) ;
#45240 = CARTESIAN_POINT ( 'NONE',  ( 0.05219959533909260263, 19.03943276465977164, 84.99890960531436690 ) ) ;
#45241 = CARTESIAN_POINT ( 'NONE',  ( 16.55341960407611168, 4.379528057220329451, 83.95724293864770971 ) ) ;
#45242 = CARTESIAN_POINT ( 'NONE',  ( -5.153800228976328057, -19.02544592524343514, 57.29057627198103120 ) ) ;
#45243 = CARTESIAN_POINT ( 'NONE',  ( -8.314922557960811034, -14.29746914071050412, 62.08224293864769550 ) ) ;
#45244 = CARTESIAN_POINT ( 'NONE',  ( 13.89961937509977652, -13.97604488694527269, 28.12390960531435624 ) ) ;
#45245 = CARTESIAN_POINT ( 'NONE',  ( -17.01956338556749415, -5.458179474447081070, 20.69910624262117338 ) ) ;
#45246 = CARTESIAN_POINT ( 'NONE',  ( -14.34966873604960291, -8.224510206698953496, 41.66557627198103120 ) ) ;
#45247 = CARTESIAN_POINT ( 'NONE',  ( 13.97604488694527802, 13.89961937509977652, 89.37390960531436690 ) ) ;
#45248 = FACE_BOUND ( 'NONE', #109084, .T. ) ;
#45249 = CARTESIAN_POINT ( 'NONE',  ( -5.153800228976607833, 19.02544592524334988, 52.70942372801900433 ) ) ;
#45250 = CARTESIAN_POINT ( 'NONE',  ( -16.52544592524335698, -4.483927247898792601, 53.95942372801900433 ) ) ;
#45251 = CARTESIAN_POINT ( 'NONE',  ( -21.55341960407610458, -5.719274019375992779, 76.45724293864769550 ) ) ;
#45252 = CARTESIAN_POINT ( 'NONE',  ( 5.049401038297881783, 19.05341960407617563, 32.29275706135233293 ) ) ;
#45253 = CARTESIAN_POINT ( 'NONE',  ( 0.05219959533909260263, 19.03943276465977164, 89.99890960531436690 ) ) ;
#45254 = CARTESIAN_POINT ( 'NONE',  ( 0.2208081763724077662, 21.31244378140432971, -58.84882290019458395 ) ) ;
#45255 = CARTESIAN_POINT ( 'NONE',  ( -15.80617190586745835, -15.72974639402198527, 26.87390960531435979 ) ) ;
#45256 = CARTESIAN_POINT ( 'NONE',  ( 16.46253265017160672, -9.564922557960803928, 58.33224293864769550 ) ) ;
#45257 = CARTESIAN_POINT ( 'NONE',  ( -21.53943276465977519, -0.05219959533937600094, 48.75109039468568284 ) ) ;
#45258 = CARTESIAN_POINT ( 'NONE',  ( 16.46253265017160672, -9.564922557960803928, 23.33224293864769194 ) ) ;
#45261 = VERTEX_POINT ( 'NONE', #56353 ) ;
#45260 = CARTESIAN_POINT ( 'NONE',  ( 9.564922557960805705, 16.46253265017160317, 89.58224293864769550 ) ) ;
#45259 = CARTESIAN_POINT ( 'NONE',  ( 10.81492255796106328, -18.62759615963255655, 20.41775706135234714 ) ) ;
#45262 = CARTESIAN_POINT ( 'NONE',  ( 15.72974639402176855, 15.80617190586768217, 36.87609039468568994 ) ) ;
#45263 = ORIENTED_EDGE ( 'NONE', *, *, #151687, .F. ) ;
#45264 = CARTESIAN_POINT ( 'NONE',  ( -19.05341960407611168, -5.049401038298163336, 96.45724293864769550 ) ) ;
#45265 = CARTESIAN_POINT ( 'NONE',  ( -5.049401038298153566, 19.05341960407611168, 90.20724293864768129 ) ) ;
#45266 = CARTESIAN_POINT ( 'NONE',  ( 10.81492255796078972, 18.62759615963270932, 104.5822429386477097 ) ) ;
#45267 = CARTESIAN_POINT ( 'NONE',  ( 5.153800228976335163, 19.02544592524342804, 49.79057627198100988 ) ) ;
#45268 = CARTESIAN_POINT ( 'NONE',  ( 8.314922557961029526, -14.29746914071037800, 25.41775706135235779 ) ) ;
#45269 = CARTESIAN_POINT ( 'NONE',  ( 3.556970738554033499E-15, -38.81732327939057825, -2.624999997268812724 ) ) ;
#45270 = CARTESIAN_POINT ( 'NONE',  ( -13.89961937509977652, 13.97604488694528158, 25.62390960531434558 ) ) ;
#45271 = CARTESIAN_POINT ( 'NONE',  ( -15.80617190586768217, 15.72974639402176855, 103.1260903946856757 ) ) ;
#45273 = CARTESIAN_POINT ( 'NONE',  ( 21.55341960407619695, -5.719274019375665929, 56.04275706135235424 ) ) ;
#45272 = CARTESIAN_POINT ( 'NONE',  ( -16.46253265017160317, 9.564922557960807481, 70.83224293864770971 ) ) ;
#45274 = AXIS2_PLACEMENT_3D ( 'NONE', #53186, #101690, #129015 ) ;
#45275 = CARTESIAN_POINT ( 'NONE',  ( -22.44159573604010305, 16.30477369853692338, 147.1750000027311671 ) ) ;
#45276 = CARTESIAN_POINT ( 'NONE',  ( 0.05219959533909260263, 19.03943276465977164, 94.99890960531436690 ) ) ;
#45277 = CARTESIAN_POINT ( 'NONE',  ( 16.18341559714236055, 22.93862090151660382, 139.9999999999999716 ) ) ;
#45280 = CARTESIAN_POINT ( 'NONE',  ( -0.05219959533937732626, 21.53943276465977519, 62.50109039468568284 ) ) ;
#45279 = CARTESIAN_POINT ( 'NONE',  ( 14.34966873604972726, -8.224510206698740333, 65.83442372801900433 ) ) ;
#45278 = CARTESIAN_POINT ( 'NONE',  ( -14.29746914071037622, -8.314922557961029526, 39.16775706135235424 ) ) ;
#45281 = CARTESIAN_POINT ( 'NONE',  ( 5.719274019375673035, 21.55341960407619339, 87.29275706135236135 ) ) ;
#45282 = CARTESIAN_POINT ( 'NONE',  ( 4.070616889113809478, 4.625078002628068674, -62.49731305256334224 ) ) ;
#45283 = CARTESIAN_POINT ( 'NONE',  ( -16.53943276465976808, -0.05219959533934237506, 18.75109039468568639 ) ) ;
#45284 = CARTESIAN_POINT ( 'NONE',  ( -19.05341960407611168, -5.049401038298163336, 76.45724293864769550 ) ) ;
#45285 = CARTESIAN_POINT ( 'NONE',  ( 16.51473224551069308, 9.474510206698969483, 99.16557627198102409 ) ) ;
#45286 = CARTESIAN_POINT ( 'NONE',  ( 16.53943276465976808, -0.05219959533910856209, 113.7489096053143527 ) ) ;
#45288 = ADVANCED_FACE ( 'NONE', ( #153083 ), #198618, .T. ) ;
#45287 = CARTESIAN_POINT ( 'NONE',  ( 10.72451020669898902, -18.67979575497178502, 32.91557627198102409 ) ) ;
#45289 = CARTESIAN_POINT ( 'NONE',  ( -16.55341960407617563, 4.379528057220093196, 93.54275706135234714 ) ) ;
#45291 = CARTESIAN_POINT ( 'NONE',  ( 16.46253265017160672, -9.564922557960803928, 58.33224293864769550 ) ) ;
#45290 = CARTESIAN_POINT ( 'NONE',  ( 14.29746914071049879, -8.314922557960816363, 73.33224293864769550 ) ) ;
#45292 = CARTESIAN_POINT ( 'NONE',  ( -21.52544592524334988, -5.823673210054445271, 88.95942372801901854 ) ) ;
#45293 = CARTESIAN_POINT ( 'NONE',  ( -28.79475375365586842, 2.428612866367529932E-14, 144.2656553485623760 ) ) ;
#45294 = CARTESIAN_POINT ( 'NONE',  ( -16.51473224551082808, 9.474510206698731452, 103.3344237280190043 ) ) ;
#45295 = CARTESIAN_POINT ( 'NONE',  ( -8.224510206698948167, 14.34966873604960824, 75.41557627198102409 ) ) ;
#45296 = CARTESIAN_POINT ( 'NONE',  ( -18.62759615963255300, -10.81492255796106328, 34.16775706135234714 ) ) ;
#45297 = CARTESIAN_POINT ( 'NONE',  ( 18.62759615963271287, -10.81492255796078972, 63.33224293864770260 ) ) ;
#45298 = CARTESIAN_POINT ( 'NONE',  ( 13.89961937509957401, 13.97604488694547697, 36.87609039468565442 ) ) ;
#45299 = CARTESIAN_POINT ( 'NONE',  ( -35.63758492646881137, 1.954004632199960012, 37.74231687961064807 ) ) ;
#45300 = CARTESIAN_POINT ( 'NONE',  ( 19.03943276465977164, -0.05219959533909143690, 83.74890960531436690 ) ) ;
#45301 = CARTESIAN_POINT ( 'NONE',  ( -8.314922557960811034, -14.29746914071050412, 52.08224293864768839 ) ) ;
#45302 = CIRCLE ( 'NONE', #96, 1.999999999999999112 ) ;
#45303 = CARTESIAN_POINT ( 'NONE',  ( 8.314922557960818139, 14.29746914071049879, 34.58224293864770260 ) ) ;
#45304 = CARTESIAN_POINT ( 'NONE',  ( 14.29746914071037800, 8.314922557961029526, 96.66775706135234714 ) ) ;
#45305 = CARTESIAN_POINT ( 'NONE',  ( -13.97604488694547697, 13.89961937509957934, 48.12609039468566863 ) ) ;
#45306 = DIRECTION ( 'NONE',  ( 0.1039620511844979445, 0.1039620511844979445, -0.9891328443778539814 ) ) ;
#45307 = CARTESIAN_POINT ( 'NONE',  ( 19.05341960407611168, 5.049401038298154454, 103.9572429386476671 ) ) ;
#45308 = CARTESIAN_POINT ( 'NONE',  ( 16.53943276465976808, -0.05219959533910856209, 78.74890960531436690 ) ) ;
#45309 = CARTESIAN_POINT ( 'NONE',  ( -16.51473224551082808, 9.474510206698731452, 38.33442372801899722 ) ) ;
#45311 = CARTESIAN_POINT ( 'NONE',  ( 21.55341960407610458, 5.719274019375980345, 38.95724293864768839 ) ) ;
#45310 = CARTESIAN_POINT ( 'NONE',  ( 16.51473224551069308, 9.474510206698969483, 29.16557627198103475 ) ) ;
#45312 = CARTESIAN_POINT ( 'NONE',  ( 10.81492255796078972, 18.62759615963270932, 69.58224293864769550 ) ) ;
#45313 = CARTESIAN_POINT ( 'NONE',  ( -8.314922557960811034, -14.29746914071050412, 112.0822429386477097 ) ) ;
#45314 = CARTESIAN_POINT ( 'NONE',  ( -16.55341960407617563, 4.379528057220093196, 58.54275706135235424 ) ) ;
#45315 = CARTESIAN_POINT ( 'NONE',  ( 18.67979575497194134, -10.72451020669871369, 40.83442372801901854 ) ) ;
#45316 = B_SPLINE_CURVE_WITH_KNOTS ( 'NONE', 3,
 ( #13592, #75259, #65050, #93392, #33721, #171247, #5355, #143874, #79226, #3375, #32736, #20531, #96371, #186436, #126706, #156067, #112542, #63059, #47912, #109566 ),
 .UNSPECIFIED., .F., .F.,
 ( 4, 2, 2, 2, 2, 2, 2, 2, 2, 4 ),
 ( 0.000000000000000000, 0.0004987090165372804005, 0.0009974180330745608010, 0.001246772541343200893, 0.001496127049611841201, 0.001994836066149102520, 0.002493545082686363622, 0.002742899590954984632, 0.002992254099223606075, 0.003989672132298083609 ),
 .UNSPECIFIED. ) ;
#45317 = CARTESIAN_POINT ( 'NONE',  ( -14.29746914071049879, 8.314922557960819915, 85.83224293864768129 ) ) ;
#45318 = CYLINDRICAL_SURFACE ( 'NONE', #112421, 0.4999999999999995559 ) ;
#45319 = CARTESIAN_POINT ( 'NONE',  ( -17.49999999999999645, 5.499999999999997335, 25.79690382534172244 ) ) ;
#45320 = CARTESIAN_POINT ( 'NONE',  ( 21.55341960407610458, 5.719274019375980345, 33.95724293864769550 ) ) ;
#45321 = FACE_OUTER_BOUND ( 'NONE', #92008, .T. ) ;
#45322 = CARTESIAN_POINT ( 'NONE',  ( -37.99626262588766679, 2.428612866367529932E-14, -7.747842220587803475 ) ) ;
#45324 = CARTESIAN_POINT ( 'NONE',  ( -8.224510206698948167, 14.34966873604960824, 40.41557627198103120 ) ) ;
#45323 = CARTESIAN_POINT ( 'NONE',  ( -12.14591786802326823, 12.06949235617739902, 48.12609039468568284 ) ) ;
#45325 = CARTESIAN_POINT ( 'NONE',  ( -15.80617190586745835, -15.72974639402198527, 66.87390960531436690 ) ) ;
#45326 = CARTESIAN_POINT ( 'NONE',  ( 19.03943276465977164, 0.05219959533936151252, 81.25109039468567573 ) ) ;
#45327 = CARTESIAN_POINT ( 'NONE',  ( -15.72974639402197994, 15.80617190586746368, 55.62390960531436690 ) ) ;
#45328 = CARTESIAN_POINT ( 'NONE',  ( 30.98370104197785224, -22.00508125442255647, -21.15278651796061382 ) ) ;
#45330 = CARTESIAN_POINT ( 'NONE',  ( 19.03943276465977164, -0.05219959533909143690, 98.74890960531436690 ) ) ;
#45329 = CARTESIAN_POINT ( 'NONE',  ( 19.03943276465977164, -0.05219959533909143690, 43.74890960531435979 ) ) ;
#45331 = CARTESIAN_POINT ( 'NONE',  ( 13.97604488694527802, 13.89961937509977652, 49.37390960531434558 ) ) ;
#45332 = CARTESIAN_POINT ( 'NONE',  ( 16.52544592524342804, -4.483927247898539470, 108.5405762719810241 ) ) ;
#45333 = CARTESIAN_POINT ( 'NONE',  ( 19.03943276465977164, -0.05219959533909143690, 113.7489096053143669 ) ) ;
#45334 = ORIENTED_EDGE ( 'NONE', *, *, #142600, .T. ) ;
#45335 = CARTESIAN_POINT ( 'NONE',  ( 14.29746914071037800, 8.314922557961029526, 66.66775706135234714 ) ) ;
#45336 = CARTESIAN_POINT ( 'NONE',  ( 18.67979575497178502, 10.72451020669898547, 89.16557627198102409 ) ) ;
#45337 = CARTESIAN_POINT ( 'NONE',  ( 19.03943276465977164, -0.05219959533909143690, 58.74890960531435979 ) ) ;
#45338 = CARTESIAN_POINT ( 'NONE',  ( 0.05219959533937995610, -21.53943276465977519, 25.00109039468567218 ) ) ;
#45339 = CARTESIAN_POINT ( 'NONE',  ( 5.153800228976335163, 19.02544592524342804, 89.79057627198102409 ) ) ;
#45340 = CARTESIAN_POINT ( 'NONE',  ( -37.91032098691104579, -19.19859865632797025, -20.09511994390769729 ) ) ;
#45341 = EDGE_LOOP ( 'NONE', ( #152192, #180986, #168348, #117968, #16483 ) ) ;
#45342 = CARTESIAN_POINT ( 'NONE',  ( -10.72451020669870658, -18.67979575497194134, 19.58442372801901143 ) ) ;
#45345 = CARTESIAN_POINT ( 'NONE',  ( -9.564922557961040184, 16.46253265017147172, 82.91775706135233293 ) ) ;
#45344 = CARTESIAN_POINT ( 'NONE',  ( -19.03943276465977164, 0.05219959533909376836, 101.2489096053143669 ) ) ;
#45343 = CARTESIAN_POINT ( 'NONE',  ( -9.474510206698964154, 16.51473224551069663, 30.41557627198102054 ) ) ;
#45346 = CARTESIAN_POINT ( 'NONE',  ( -19.05341960407617563, 5.049401038297882671, 43.54275706135232582 ) ) ;
#45347 = CARTESIAN_POINT ( 'NONE',  ( 18.67979575497178502, 10.72451020669898547, 104.1655762719810241 ) ) ;
#45348 = CARTESIAN_POINT ( 'NONE',  ( 9.564922557961047289, -16.46253265017146816, 35.41775706135233293 ) ) ;
#45349 = CARTESIAN_POINT ( 'NONE',  ( 16.46253265017146816, 9.564922557961045513, 31.66775706135232937 ) ) ;
#45350 = CARTESIAN_POINT ( 'NONE',  ( 16.53943276465976808, 0.05219959533934440121, 96.25109039468568994 ) ) ;
#45351 = CARTESIAN_POINT ( 'NONE',  ( -13.89961937509977652, 13.97604488694528158, 110.6239096053143243 ) ) ;
#45352 = CARTESIAN_POINT ( 'NONE',  ( 16.51473224551069308, 9.474510206698969483, 54.16557627198103120 ) ) ;
#45353 = CARTESIAN_POINT ( 'NONE',  ( 15.72974639402176855, 15.80617190586768217, 61.87609039468568284 ) ) ;
#45354 = CARTESIAN_POINT ( 'NONE',  ( 0.05219959533937995610, -21.53943276465977519, 75.00109039468568994 ) ) ;
#45355 = CARTESIAN_POINT ( 'NONE',  ( -9.474510206698964154, 16.51473224551069663, 115.4155762719810241 ) ) ;
#45356 = CARTESIAN_POINT ( 'NONE',  ( 19.05341960407611168, 5.049401038298154454, 78.95724293864769550 ) ) ;
#45357 = CARTESIAN_POINT ( 'NONE',  ( 10.72451020669871369, 18.67979575497193778, 47.08442372801901854 ) ) ;
#45358 = CARTESIAN_POINT ( 'NONE',  ( 5.049401038297881783, 19.05341960407617563, 102.2927570613523045 ) ) ;
#45359 = CARTESIAN_POINT ( 'NONE',  ( -19.05341960407611168, -5.049401038298163336, 51.45724293864770260 ) ) ;
#45360 = CARTESIAN_POINT ( 'NONE',  ( 19.05341960407611168, 5.049401038298154454, 103.9572429386476671 ) ) ;
#45361 = CARTESIAN_POINT ( 'NONE',  ( -16.46253265017160317, 9.564922557960807481, 80.83224293864769550 ) ) ;
#45362 = LINE ( 'NONE', #27225, #140419 ) ;
#45363 = CARTESIAN_POINT ( 'NONE',  ( 5.153800228976335163, 19.02544592524342804, 59.79057627198100988 ) ) ;
#45364 = CARTESIAN_POINT ( 'NONE',  ( -18.62759615963270932, 10.81492255796079327, 95.83224293864770971 ) ) ;
#45365 = CARTESIAN_POINT ( 'NONE',  ( -14.29746914071037622, -8.314922557961029526, 84.16775706135234714 ) ) ;
#45366 = CARTESIAN_POINT ( 'NONE',  ( 27.88129983271499768, 6.733757357597986548, 162.1517353552272880 ) ) ;
#45367 = CARTESIAN_POINT ( 'NONE',  ( 5.153800228976615827, -19.02544592524334988, 50.20942372801897591 ) ) ;
#45368 = CARTESIAN_POINT ( 'NONE',  ( -16.51473224551069308, -9.474510206698971260, 81.66557627198103830 ) ) ;
#45369 = CARTESIAN_POINT ( 'NONE',  ( -12.14591786802309592, -12.06949235617757132, 51.87390960531437401 ) ) ;
#45370 = CARTESIAN_POINT ( 'NONE',  ( 8.314922557960818139, 14.29746914071049879, 94.58224293864769550 ) ) ;
#45371 = CARTESIAN_POINT ( 'NONE',  ( -0.05219959533907301413, -21.53943276465977519, 22.49890960531436335 ) ) ;
#45372 = CARTESIAN_POINT ( 'NONE',  ( -19.05341960407611168, -5.049401038298163336, 111.4572429386476671 ) ) ;
#45373 = CARTESIAN_POINT ( 'NONE',  ( 5.153800228976335163, 19.02544592524342804, 114.7905762719810241 ) ) ;
#45374 = CARTESIAN_POINT ( 'NONE',  ( 19.02544592524334988, 5.153800228976608722, 36.45942372801900433 ) ) ;
#45375 = CARTESIAN_POINT ( 'NONE',  ( 14.29746914071037800, 8.314922557961029526, 91.66775706135234714 ) ) ;
#45376 = CARTESIAN_POINT ( 'NONE',  ( -9.474510206698964154, 16.51473224551069663, 75.41557627198103830 ) ) ;
#45377 = CARTESIAN_POINT ( 'NONE',  ( -5.719274019375665041, -21.55341960407619695, 34.79275706135235424 ) ) ;
#45378 = CARTESIAN_POINT ( 'NONE',  ( -10.81492255796078084, -18.62759615963271287, 32.08224293864769550 ) ) ;
#45379 = CARTESIAN_POINT ( 'NONE',  ( 18.67979575497178502, 10.72451020669898547, 114.1655762719810383 ) ) ;
#45380 = CARTESIAN_POINT ( 'NONE',  ( 10.81492255796078972, 18.62759615963270932, 69.58224293864769550 ) ) ;
#45381 = CARTESIAN_POINT ( 'NONE',  ( -8.224510206698948167, 14.34966873604960824, 95.41557627198102409 ) ) ;
#45382 = CARTESIAN_POINT ( 'NONE',  ( 13.97604488694548053, -13.89961937509957401, 50.62609039468566152 ) ) ;
#45383 = CARTESIAN_POINT ( 'NONE',  ( -9.564922557960796823, -16.46253265017161027, 32.08224293864769550 ) ) ;
#45384 = CARTESIAN_POINT ( 'NONE',  ( -5.049401038298153566, 19.05341960407611168, 90.20724293864766707 ) ) ;
#45385 = CARTESIAN_POINT ( 'NONE',  ( -9.564922557960796823, -16.46253265017161027, 82.08224293864768129 ) ) ;
#45386 = CARTESIAN_POINT ( 'NONE',  ( -27.73933785331498925, 2.428612866367529932E-14, 148.8750000027311842 ) ) ;
#45387 = CARTESIAN_POINT ( 'NONE',  ( -4.379528057220328563, 16.55341960407611168, 105.2072429386477097 ) ) ;
#45388 = VERTEX_POINT ( 'NONE', #60085 ) ;
#45389 = CARTESIAN_POINT ( 'NONE',  ( -14.29746914071049879, 8.314922557960819915, 30.83224293864770260 ) ) ;
#45390 = CARTESIAN_POINT ( 'NONE',  ( 16.55341960407618274, -4.379528057220086978, 21.04275706135234714 ) ) ;
#45391 = CARTESIAN_POINT ( 'NONE',  ( -5.719274019375665041, -21.55341960407619695, 99.79275706135234714 ) ) ;
#45392 = CARTESIAN_POINT ( 'NONE',  ( 16.46253265017160672, -9.564922557960803928, 98.33224293864769550 ) ) ;
#45393 = CARTESIAN_POINT ( 'NONE',  ( -18.67979575497178146, -10.72451020669898902, 111.6655762719810525 ) ) ;
#45394 = CARTESIAN_POINT ( 'NONE',  ( -9.474510206698964154, 16.51473224551069663, 45.41557627198103120 ) ) ;
#45395 = CARTESIAN_POINT ( 'NONE',  ( -8.314922557961024197, 14.29746914071037800, 42.91775706135235424 ) ) ;
#45396 = CARTESIAN_POINT ( 'NONE',  ( -16.53943276465976808, -0.05219959533934237506, 18.75109039468568639 ) ) ;
#45397 = CARTESIAN_POINT ( 'NONE',  ( -4.379528057220328563, 16.55341960407611168, 100.2072429386476955 ) ) ;
#45398 = CARTESIAN_POINT ( 'NONE',  ( 0.05219959533907565091, 21.53943276465977519, 104.9989096053143669 ) ) ;
#45399 = CARTESIAN_POINT ( 'NONE',  ( 13.89961937509957401, 13.97604488694547697, 66.87609039468567573 ) ) ;
#45400 = LINE ( 'NONE', #17049, #147821 ) ;
#45401 = CARTESIAN_POINT ( 'NONE',  ( -15.72974639402197994, 15.80617190586746368, 115.6239096053143669 ) ) ;
#45402 = DIRECTION ( 'NONE',  ( 0.000000000000000000, 0.000000000000000000, -1.000000000000000000 ) ) ;
#45403 = CARTESIAN_POINT ( 'NONE',  ( -5.153800228976328057, -19.02544592524343514, 92.29057627198099567 ) ) ;
#45404 = CARTESIAN_POINT ( 'NONE',  ( 17.48847506799970120, -5.747544572773743532, 113.3269743784328227 ) ) ;
#45405 = CARTESIAN_POINT ( 'NONE',  ( 19.05341960407611168, 5.049401038298154454, 78.95724293864769550 ) ) ;
#45407 = CARTESIAN_POINT ( 'NONE',  ( -12.06949235617756955, 12.14591786802309770, 75.62390960531439532 ) ) ;
#45406 = CARTESIAN_POINT ( 'NONE',  ( 21.53943276465977519, 0.05219959533937863772, 31.25109039468568639 ) ) ;
#45408 = CARTESIAN_POINT ( 'NONE',  ( 19.05341960407611168, 5.049401038298154454, 88.95724293864769550 ) ) ;
#45410 = CARTESIAN_POINT ( 'NONE',  ( 16.46253265017146816, 9.564922557961045513, 56.66775706135233293 ) ) ;
#45409 = CARTESIAN_POINT ( 'NONE',  ( 4.483927247898790824, -16.52544592524335698, 50.20942372801901854 ) ) ;
#45411 = CARTESIAN_POINT ( 'NONE',  ( 15.80617190586769283, -15.72974639402175789, 65.62609039468568994 ) ) ;
#45412 = CARTESIAN_POINT ( 'NONE',  ( -0.05219959533934338120, 16.53943276465976808, 27.50109039468567929 ) ) ;
#45413 = CARTESIAN_POINT ( 'NONE',  ( 13.97604488694527802, 13.89961937509977652, 74.37390960531436690 ) ) ;
#45414 = CARTESIAN_POINT ( 'NONE',  ( 5.049401038297881783, 19.05341960407617563, 97.29275706135233293 ) ) ;
#45415 = CARTESIAN_POINT ( 'NONE',  ( 14.34966873604972726, -8.224510206698740333, 60.83442372801901854 ) ) ;
#45416 = CARTESIAN_POINT ( 'NONE',  ( -10.81492255796105439, 18.62759615963255655, 102.9177570613523756 ) ) ;
#45417 = CARTESIAN_POINT ( 'NONE',  ( -19.03943276465977164, -0.05219959533935918106, 83.75109039468567573 ) ) ;
#45418 = CARTESIAN_POINT ( 'NONE',  ( 19.02544592524343514, -5.153800228976328945, 48.54057627198103120 ) ) ;
#45419 = CARTESIAN_POINT ( 'NONE',  ( -15.72974639402197994, 15.80617190586746368, 70.62390960531436690 ) ) ;
#45421 = CARTESIAN_POINT ( 'NONE',  ( 16.46253265017146816, 9.564922557961045513, 81.66775706135233293 ) ) ;
#45420 = CARTESIAN_POINT ( 'NONE',  ( 12.06949235617757843, -12.14591786802309237, 78.12390960531436690 ) ) ;
#45422 = CARTESIAN_POINT ( 'NONE',  ( -18.22780087662124160, -5.499999999999927169, 68.98236817873106475 ) ) ;
#45423 = CARTESIAN_POINT ( 'NONE',  ( 5.049401038297881783, 19.05341960407617563, 37.29275706135232582 ) ) ;
#45424 = CARTESIAN_POINT ( 'NONE',  ( -4.483927247898782831, 16.52544592524335698, 112.7094237280190328 ) ) ;
#45425 = CARTESIAN_POINT ( 'NONE',  ( -12.06949235617756955, 12.14591786802309770, 65.62390960531436690 ) ) ;
#45427 = CARTESIAN_POINT ( 'NONE',  ( -27.73933785331498925, 9.013057229001089965, 144.7750000027311614 ) ) ;
#45426 = CARTESIAN_POINT ( 'NONE',  ( -21.55341960407619339, 5.719274019375674811, 108.5427570613523756 ) ) ;
#45428 = CARTESIAN_POINT ( 'NONE',  ( 10.81492255796078972, 18.62759615963270932, 114.5822429386477097 ) ) ;
#45429 = CARTESIAN_POINT ( 'NONE',  ( 19.02544592524343514, -5.153800228976328945, 63.54057627198103830 ) ) ;
#45430 = CARTESIAN_POINT ( 'NONE',  ( -10.81492255796105439, 18.62759615963255655, 87.91775706135234714 ) ) ;
#45431 = CARTESIAN_POINT ( 'NONE',  ( 19.05341960407611168, 5.049401038298154454, 68.95724293864769550 ) ) ;
#45432 = ORIENTED_EDGE ( 'NONE', *, *, #125504, .T. ) ;
#45433 = CARTESIAN_POINT ( 'NONE',  ( 8.224510206698953496, -14.34966873604960469, 112.9155762719810383 ) ) ;
#45434 = CARTESIAN_POINT ( 'NONE',  ( -15.72974639402197994, 15.80617190586746368, 35.62390960531437401 ) ) ;
#45435 = CARTESIAN_POINT ( 'NONE',  ( -16.52544592524342804, 4.483927247898546575, 66.04057627198103830 ) ) ;
#45436 = CARTESIAN_POINT ( 'NONE',  ( -19.03943276465977164, 0.05219959533909376836, 46.24890960531435979 ) ) ;
#45437 = CARTESIAN_POINT ( 'NONE',  ( -12.06949235617756955, 12.14591786802309770, 85.62390960531436690 ) ) ;
#45438 = CARTESIAN_POINT ( 'NONE',  ( 18.62759615963271287, -10.81492255796078972, 113.3322429386476955 ) ) ;
#45439 = AXIS2_PLACEMENT_3D ( 'NONE', #160773, #22263, #83912 ) ;
#45440 = CARTESIAN_POINT ( 'NONE',  ( 15.72974639402176855, 15.80617190586768217, 51.87609039468568284 ) ) ;
#45441 = CARTESIAN_POINT ( 'NONE',  ( -5.153800228976328057, -19.02544592524343514, 37.29057627198102409 ) ) ;
#45442 = CARTESIAN_POINT ( 'NONE',  ( -16.53943276465976808, -0.05219959533934237506, 48.75109039468568284 ) ) ;
#45443 = CARTESIAN_POINT ( 'NONE',  ( -5.823673210054116645, -21.52544592524344225, 92.29057627198103830 ) ) ;
#45445 = CARTESIAN_POINT ( 'NONE',  ( -13.97604488694527625, -13.89961937509977652, 56.87390960531434558 ) ) ;
#45444 = CARTESIAN_POINT ( 'NONE',  ( 5.049401038297881783, 19.05341960407617563, 27.29275706135232937 ) ) ;
#45446 = CARTESIAN_POINT ( 'NONE',  ( -5.153800228976328057, -19.02544592524343514, 107.2905762719810383 ) ) ;
#45447 = CARTESIAN_POINT ( 'NONE',  ( 0.05219959533937995610, -21.53943276465977519, 55.00109039468568284 ) ) ;
#45448 = CARTESIAN_POINT ( 'NONE',  ( 15.72974639402199770, -15.80617190586745480, 48.12390960531436690 ) ) ;
#45449 = CARTESIAN_POINT ( 'NONE',  ( 16.55341960407611168, 4.379528057220329451, 28.95724293864769905 ) ) ;
#45451 = CARTESIAN_POINT ( 'NONE',  ( -15.72974639402176322, -15.80617190586768395, 99.37609039468568994 ) ) ;
#45450 = CARTESIAN_POINT ( 'NONE',  ( -0.05219959533937732626, 21.53943276465977519, 62.50109039468568284 ) ) ;
#45452 = CARTESIAN_POINT ( 'NONE',  ( -19.02544592524334988, -5.153800228976617603, 33.95942372801897591 ) ) ;
#45453 = CARTESIAN_POINT ( 'NONE',  ( -16.55341960407617563, 4.379528057220093196, 98.54275706135234714 ) ) ;
#45454 = CARTESIAN_POINT ( 'NONE',  ( -15.72974639402176322, -15.80617190586768395, 59.37609039468568284 ) ) ;
#45455 = CARTESIAN_POINT ( 'NONE',  ( 5.049401038298161559, -19.05341960407611168, 52.70724293864767418 ) ) ;
#45456 = CARTESIAN_POINT ( 'NONE',  ( -15.80617190586768217, 15.72974639402176855, 113.1260903946856899 ) ) ;
#45457 = CARTESIAN_POINT ( 'NONE',  ( 5.153800228976335163, 19.02544592524342804, 114.7905762719810241 ) ) ;
#45458 = CARTESIAN_POINT ( 'NONE',  ( -15.72974639402197994, 15.80617190586746368, 110.6239096053143669 ) ) ;
#45459 = CARTESIAN_POINT ( 'NONE',  ( -21.53943276465977519, 0.05219959533907696930, 71.24890960531435269 ) ) ;
#45460 = CARTESIAN_POINT ( 'NONE',  ( -4.379528057220086978, -16.55341960407618274, 44.79275706135234714 ) ) ;
#45462 = CARTESIAN_POINT ( 'NONE',  ( -18.67979575497178146, -10.72451020669898902, 81.66557627198103830 ) ) ;
#45461 = CARTESIAN_POINT ( 'NONE',  ( -6.576301504920873953, 6.293041912674299354, -61.89430850415822505 ) ) ;
#45464 = CARTESIAN_POINT ( 'NONE',  ( -16.55341960407611168, -4.379528057220339221, 81.45724293864769550 ) ) ;
#45463 = CARTESIAN_POINT ( 'NONE',  ( 12.14591786802327356, -12.06949235617739191, 60.62609039468567573 ) ) ;
#45465 = CARTESIAN_POINT ( 'NONE',  ( -20.53125566280828806, 20.33951628977422743, -49.67367017693150189 ) ) ;
#45466 = CARTESIAN_POINT ( 'NONE',  ( -13.97604488694547697, 13.89961937509957934, 108.1260903946856331 ) ) ;
#45467 = CARTESIAN_POINT ( 'NONE',  ( -5.719274019375978568, 21.55341960407610458, 30.20724293864769550 ) ) ;
#45468 = CARTESIAN_POINT ( 'NONE',  ( 14.18669005401828187, -34.08280046153741694, -8.000000000000001776 ) ) ;
#45469 = CARTESIAN_POINT ( 'NONE',  ( -16.55341960407617563, 4.379528057220093196, 43.54275706135235424 ) ) ;
#45470 = CARTESIAN_POINT ( 'NONE',  ( 15.80617190586746368, 15.72974639402197994, 114.3739096053143527 ) ) ;
#45471 = CARTESIAN_POINT ( 'NONE',  ( -21.52544592524343514, 5.823673210054127303, 36.04057627198102409 ) ) ;
#45472 = CARTESIAN_POINT ( 'NONE',  ( 14.29746914071037800, 8.314922557961029526, 71.66775706135234714 ) ) ;
#45473 = CARTESIAN_POINT ( 'NONE',  ( 9.564922557960805705, 16.46253265017160317, 79.58224293864769550 ) ) ;
#45475 = CARTESIAN_POINT ( 'NONE',  ( 16.55341960407618274, -4.379528057220086978, 21.04275706135234714 ) ) ;
#45474 = CARTESIAN_POINT ( 'NONE',  ( 10.72451020669871369, 18.67979575497193778, 37.08442372801901143 ) ) ;
#45476 = CARTESIAN_POINT ( 'NONE',  ( -10.81492255796078084, -18.62759615963271287, 32.08224293864769550 ) ) ;
#45477 = CARTESIAN_POINT ( 'NONE',  ( 13.89961937509957401, 13.97604488694547697, 21.87609039468566152 ) ) ;
#45478 = CARTESIAN_POINT ( 'NONE',  ( -0.05219959533934338120, 16.53943276465976808, 52.50109039468567573 ) ) ;
#45479 = CARTESIAN_POINT ( 'NONE',  ( -19.03943276465977164, 0.05219959533909376836, 101.2489096053143669 ) ) ;
#45480 = CARTESIAN_POINT ( 'NONE',  ( 10.72451020669898902, -18.67979575497178502, 107.9155762719810241 ) ) ;
#45481 = CARTESIAN_POINT ( 'NONE',  ( -9.564922557960796823, -16.46253265017161027, 72.08224293864770971 ) ) ;
#45482 = DIRECTION ( 'NONE',  ( -0.000000000000000000, -0.000000000000000000, 1.000000000000000000 ) ) ;
#45483 = FACE_BOUND ( 'NONE', #200173, .T. ) ;
#45484 = CARTESIAN_POINT ( 'NONE',  ( -16.52544592524342804, 4.483927247898546575, 86.04057627198102409 ) ) ;
#45485 = CARTESIAN_POINT ( 'NONE',  ( -21.52544592524343514, 5.823673210054127303, 36.04057627198102409 ) ) ;
#45486 = CARTESIAN_POINT ( 'NONE',  ( -17.44279575226823908, 5.990770900252464948, 35.83557567514318976 ) ) ;
#45487 = CARTESIAN_POINT ( 'NONE',  ( 4.483927247898790824, -16.52544592524335698, 60.20942372801902565 ) ) ;
#45488 = CARTESIAN_POINT ( 'NONE',  ( -21.53943276465977519, -0.05219959533937600094, 18.75109039468568639 ) ) ;
#45489 = CARTESIAN_POINT ( 'NONE',  ( 19.05341960407617918, -5.049401038297876454, 81.04275706135231871 ) ) ;
#45490 = FACE_OUTER_BOUND ( 'NONE', #86062, .T. ) ;
#45491 = CARTESIAN_POINT ( 'NONE',  ( 5.719274019375991003, -21.55341960407610458, 62.70724293864769550 ) ) ;
#45492 = CARTESIAN_POINT ( 'NONE',  ( -13.89961937509977652, 13.97604488694528158, 100.6239096053143669 ) ) ;
#45493 = CARTESIAN_POINT ( 'NONE',  ( -21.53943276465977519, -0.05219959533937600094, 93.75109039468567573 ) ) ;
#45494 = CARTESIAN_POINT ( 'NONE',  ( 9.564922557960805705, 16.46253265017160317, 64.58224293864769550 ) ) ;
#45495 = CARTESIAN_POINT ( 'NONE',  ( -8.224510206698735004, -14.34966873604973081, 49.58442372801901143 ) ) ;
#45496 = CARTESIAN_POINT ( 'NONE',  ( 0.05219959533909260263, 19.03943276465977164, 59.99890960531436690 ) ) ;
#45497 = CARTESIAN_POINT ( 'NONE',  ( 21.55341960407619695, -5.719274019375665929, 81.04275706135236135 ) ) ;
#45498 = ORIENTED_EDGE ( 'NONE', *, *, #174403, .T. ) ;
#45499 = CARTESIAN_POINT ( 'NONE',  ( -16.46253265017146816, -9.564922557961047289, 39.16775706135234003 ) ) ;
#45500 = CARTESIAN_POINT ( 'NONE',  ( -13.89961937509957401, -13.97604488694547875, 54.37609039468565442 ) ) ;
#45501 = CARTESIAN_POINT ( 'NONE',  ( 15.72974639402176855, 15.80617190586768217, 46.87609039468568994 ) ) ;
#45502 = CARTESIAN_POINT ( 'NONE',  ( 18.22780087662121673, 5.500000000000056843, 53.98459894673893444 ) ) ;
#45503 = CARTESIAN_POINT ( 'NONE',  ( 13.89961937509957401, 13.97604488694547697, 51.87609039468566863 ) ) ;
#45504 = CARTESIAN_POINT ( 'NONE',  ( 16.46253265017160672, -9.564922557960803928, 98.33224293864769550 ) ) ;
#45505 = CARTESIAN_POINT ( 'NONE',  ( -0.05219959533909027116, -19.03943276465977164, 72.49890960531435269 ) ) ;
#45506 = CARTESIAN_POINT ( 'NONE',  ( -14.34966873604960291, -8.224510206698953496, 26.66557627198103475 ) ) ;
#45508 = CARTESIAN_POINT ( 'NONE',  ( 21.55341960407619695, -5.719274019375665929, 96.04275706135236135 ) ) ;
#45507 = CARTESIAN_POINT ( 'NONE',  ( 18.62759615963271287, -10.81492255796078972, 28.33224293864769550 ) ) ;
#45509 = CARTESIAN_POINT ( 'NONE',  ( -36.91746825000001309, -11.99521256947794789, -9.024999997268812635 ) ) ;
#45510 = CARTESIAN_POINT ( 'NONE',  ( -34.25194412823100976, 3.632597792548372340, 90.85486465461549699 ) ) ;
#45511 = CARTESIAN_POINT ( 'NONE',  ( -18.67979575497193778, 10.72451020669871902, 103.3344237280190043 ) ) ;
#45512 = CARTESIAN_POINT ( 'NONE',  ( 22.10131684062755042, -1.340157125434722429, -58.31342218742626216 ) ) ;
#45513 = CARTESIAN_POINT ( 'NONE',  ( 9.474510206698971260, -16.51473224551069308, 22.91557627198102765 ) ) ;
#45514 = CARTESIAN_POINT ( 'NONE',  ( 9.474510206698971260, -16.51473224551069308, 112.9155762719810383 ) ) ;
#45515 = CARTESIAN_POINT ( 'NONE',  ( 33.80093248007431583, 2.440252113607736195, 99.94207534358628209 ) ) ;
#45516 = CARTESIAN_POINT ( 'NONE',  ( 0.05219959533934541429, -16.53943276465976808, 50.00109039468568994 ) ) ;
#45518 = EDGE_CURVE ( 'NONE', #68306, #155416, #61071, .T. ) ;
#45517 = CARTESIAN_POINT ( 'NONE',  ( 15.72974639402199770, -15.80617190586745480, 73.12390960531436690 ) ) ;
#45519 = CARTESIAN_POINT ( 'NONE',  ( 8.314922557960818139, 14.29746914071049879, 39.58224293864769550 ) ) ;
#45521 = CARTESIAN_POINT ( 'NONE',  ( -19.03943276465977164, 0.05219959533909376836, 96.24890960531436690 ) ) ;
#45520 = CARTESIAN_POINT ( 'NONE',  ( -16.52544592524342804, 4.483927247898546575, 106.0405762719810525 ) ) ;
#45522 = CARTESIAN_POINT ( 'NONE',  ( 5.153800228976615827, -19.02544592524334988, 35.20942372801899722 ) ) ;
#45523 = CARTESIAN_POINT ( 'NONE',  ( -9.564922557960796823, -16.46253265017161027, 22.08224293864768839 ) ) ;
#45524 = CARTESIAN_POINT ( 'NONE',  ( -5.823673210054431948, 21.52544592524334988, 62.70942372801902565 ) ) ;
#45525 = CARTESIAN_POINT ( 'NONE',  ( 18.22780087662123805, -5.499999999999976019, 98.51763182126896368 ) ) ;
#45526 = CARTESIAN_POINT ( 'NONE',  ( 12.06949235617739724, 12.14591786802326823, 111.8760903946856615 ) ) ;
#45527 = CYLINDRICAL_SURFACE ( 'NONE', #46454, 40.00000000000002132 ) ;
#45528 = CARTESIAN_POINT ( 'NONE',  ( -10.81492255796078084, -18.62759615963271287, 27.08224293864769550 ) ) ;
#45529 = CARTESIAN_POINT ( 'NONE',  ( 0.05219959533910956823, 16.53943276465976808, 94.99890960531436690 ) ) ;
#45530 = CARTESIAN_POINT ( 'NONE',  ( -5.153800228976607833, 19.02544592524334988, 57.70942372801899012 ) ) ;
#45531 = CARTESIAN_POINT ( 'NONE',  ( 0.05219959533909260263, 19.03943276465977164, 79.99890960531436690 ) ) ;
#45532 = CARTESIAN_POINT ( 'NONE',  ( 12.06949235617757843, -12.14591786802309237, 78.12390960531436690 ) ) ;
#45533 = CARTESIAN_POINT ( 'NONE',  ( 5.153800228976615827, -19.02544592524334988, 90.20942372801900433 ) ) ;
#45534 = CARTESIAN_POINT ( 'NONE',  ( 18.67979575497178502, 10.72451020669898547, 44.16557627198103120 ) ) ;
#45535 = ORIENTED_EDGE ( 'NONE', *, *, #73081, .T. ) ;
#45536 = CARTESIAN_POINT ( 'NONE',  ( -5.049401038298153566, 19.05341960407611168, 25.20724293864768484 ) ) ;
#45537 = CARTESIAN_POINT ( 'NONE',  ( -16.46253265017146816, -9.564922557961047289, 99.16775706135233293 ) ) ;
#45539 = CARTESIAN_POINT ( 'NONE',  ( -21.52544592524343514, 5.823673210054127303, 81.04057627198102409 ) ) ;
#45538 = CARTESIAN_POINT ( 'NONE',  ( -9.564922557960796823, -16.46253265017161027, 67.08224293864769550 ) ) ;
#45541 = CARTESIAN_POINT ( 'NONE',  ( 13.89961937509977652, -13.97604488694527269, 83.12390960531436690 ) ) ;
#45540 = CARTESIAN_POINT ( 'NONE',  ( 8.314922557961029526, -14.29746914071037800, 85.41775706135236135 ) ) ;
#45542 = CARTESIAN_POINT ( 'NONE',  ( -19.05341960407617563, 5.049401038297882671, 68.54275706135230450 ) ) ;
#45543 = CARTESIAN_POINT ( 'NONE',  ( -15.72974639402176322, -15.80617190586768395, 84.37609039468570415 ) ) ;
#45544 = CARTESIAN_POINT ( 'NONE',  ( 5.823673210054125526, 21.52544592524343514, 59.79057627198103120 ) ) ;
#45545 = CARTESIAN_POINT ( 'NONE',  ( 5.719274019375991003, -21.55341960407610458, 27.70724293864769905 ) ) ;
#45546 = CARTESIAN_POINT ( 'NONE',  ( 5.153800228976335163, 19.02544592524342804, 39.79057627198100988 ) ) ;
#45547 = CARTESIAN_POINT ( 'NONE',  ( 16.52544592524335698, 4.483927247898782831, 106.4594237280190328 ) ) ;
#45548 = CARTESIAN_POINT ( 'NONE',  ( 5.153800228976335163, 19.02544592524342804, 44.79057627198103830 ) ) ;
#45549 = CARTESIAN_POINT ( 'NONE',  ( -16.51473224551082808, 9.474510206698731452, 113.3344237280190043 ) ) ;
#45550 = LINE ( 'NONE', #89070, #173238 ) ;
#45551 = CARTESIAN_POINT ( 'NONE',  ( -15.72974639402176322, -15.80617190586768395, 109.3760903946857042 ) ) ;
#45552 = CARTESIAN_POINT ( 'NONE',  ( 14.34966873604960469, 8.224510206698951720, 79.16557627198103830 ) ) ;
#45553 =( BOUNDED_CURVE ( )  B_SPLINE_CURVE ( 3, ( #192198, #101164, #69846, #132521 ),
 .UNSPECIFIED., .F., .T. ) 
 B_SPLINE_CURVE_WITH_KNOTS ( ( 4, 4 ),
 ( 1.132647296210725241, 2.115944711806982959 ),
 .UNSPECIFIED. ) 
 CURVE ( )  GEOMETRIC_REPRESENTATION_ITEM ( )  RATIONAL_B_SPLINE_CURVE ( ( 1.000000000000000000, 0.9210371567966660900, 0.9210371567966660900, 1.000000000000000000 ) ) 
 REPRESENTATION_ITEM ( '' )  );
#45554 = CARTESIAN_POINT ( 'NONE',  ( 0.05219959533907565091, 21.53943276465977519, 104.9989096053143669 ) ) ;
#45555 = CARTESIAN_POINT ( 'NONE',  ( 0.05219959533907565091, 21.53943276465977519, 104.9989096053143669 ) ) ;
#45556 = CARTESIAN_POINT ( 'NONE',  ( -27.73933785331498925, -9.013057229001049109, 139.4750000027311785 ) ) ;
#45557 = CARTESIAN_POINT ( 'NONE',  ( -5.823673210054116645, -21.52544592524344225, 47.29057627198103120 ) ) ;
#45558 = CARTESIAN_POINT ( 'NONE',  ( -16.53943276465976808, -0.05219959533934237506, 78.75109039468568994 ) ) ;
#45559 = CARTESIAN_POINT ( 'NONE',  ( -0.05219959533910754901, -16.53943276465976808, 107.4989096053143669 ) ) ;
#45560 = CARTESIAN_POINT ( 'NONE',  ( 5.153800228976335163, 19.02544592524342804, 54.79057627198103120 ) ) ;
#45561 = CARTESIAN_POINT ( 'NONE',  ( -18.56453257813361191, 5.500000000000043521, 50.99000423690686290 ) ) ;
#45562 = CARTESIAN_POINT ( 'NONE',  ( -8.314922557960811034, -14.29746914071050412, 22.08224293864769194 ) ) ;
#45563 = VERTEX_POINT ( 'NONE', #193885 ) ;
#45564 = CARTESIAN_POINT ( 'NONE',  ( -18.67979575497193778, 10.72451020669871902, 53.33442372801901854 ) ) ;
#45565 = CARTESIAN_POINT ( 'NONE',  ( -16.51473224551069308, -9.474510206698971260, 91.66557627198103830 ) ) ;
#45566 = CARTESIAN_POINT ( 'NONE',  ( 15.72974639402176855, 15.80617190586768217, 86.87609039468568994 ) ) ;
#45567 = CARTESIAN_POINT ( 'NONE',  ( -13.97604488694527625, -13.89961937509977652, 21.87390960531435979 ) ) ;
#45568 = CARTESIAN_POINT ( 'NONE',  ( 9.474510206698971260, -16.51473224551069308, 22.91557627198102765 ) ) ;
#45569 = VERTEX_POINT ( 'NONE', #14586 ) ;
#45570 = CARTESIAN_POINT ( 'NONE',  ( 10.72451020669871369, 18.67979575497193778, 72.08442372801899012 ) ) ;
#45571 = CARTESIAN_POINT ( 'NONE',  ( -19.02544592524342804, 5.153800228976336051, 51.04057627198103120 ) ) ;
#45572 = CARTESIAN_POINT ( 'NONE',  ( 0.05219959533909260263, 19.03943276465977164, 99.99890960531436690 ) ) ;
#45573 = CARTESIAN_POINT ( 'NONE',  ( 13.97604488694548053, -13.89961937509957401, 80.62609039468567573 ) ) ;
#45574 = CARTESIAN_POINT ( 'NONE',  ( -18.67979575497193778, 10.72451020669871902, 38.33442372801900433 ) ) ;
#45575 = CARTESIAN_POINT ( 'NONE',  ( -19.03943276465977164, -0.05219959533935918106, 103.7510903946856757 ) ) ;
#45576 = CARTESIAN_POINT ( 'NONE',  ( 13.89961937509957401, 13.97604488694547697, 71.87609039468567573 ) ) ;
#45577 = CARTESIAN_POINT ( 'NONE',  ( 19.05341960407611168, 5.049401038298154454, 43.95724293864769550 ) ) ;
#45578 = CARTESIAN_POINT ( 'NONE',  ( -16.46253265017146816, -9.564922557961047289, 89.16775706135234714 ) ) ;
#45579 = CARTESIAN_POINT ( 'NONE',  ( 4.379528057220092307, 16.55341960407617563, 107.2927570613523471 ) ) ;
#45580 = CARTESIAN_POINT ( 'NONE',  ( 0.05219959533936267826, -19.03943276465977164, 75.00109039468566152 ) ) ;
#45581 = CARTESIAN_POINT ( 'NONE',  ( -4.483927247898539470, -16.52544592524342804, 42.29057627198103120 ) ) ;
#45582 = CARTESIAN_POINT ( 'NONE',  ( -5.153800228976607833, 19.02544592524334988, 67.70942372801900433 ) ) ;
#45583 = CARTESIAN_POINT ( 'NONE',  ( 21.53943276465977519, 0.05219959533937863772, 101.2510903946856757 ) ) ;
#45584 = CARTESIAN_POINT ( 'NONE',  ( -16.46253265017146816, -9.564922557961047289, 24.16775706135233648 ) ) ;
#45585 = CARTESIAN_POINT ( 'NONE',  ( 19.02544592524343514, -5.153800228976328945, 33.54057627198102409 ) ) ;
#45586 = CARTESIAN_POINT ( 'NONE',  ( 15.06137443927351072, -15.06137443927345210, -56.46919128290398504 ) ) ;
#45587 = CARTESIAN_POINT ( 'NONE',  ( -8.314922557961024197, 14.29746914071037800, 42.91775706135235424 ) ) ;
#45588 = DIRECTION ( 'NONE',  ( 1.000000000000000000, 0.000000000000000000, 0.000000000000000000 ) ) ;
#45589 = CARTESIAN_POINT ( 'NONE',  ( -22.44159573604009950, -16.30477369853688430, 143.0750000027311728 ) ) ;
#45590 = CARTESIAN_POINT ( 'NONE',  ( 13.97604488694527802, 13.89961937509977652, 94.37390960531436690 ) ) ;
#45591 = CARTESIAN_POINT ( 'NONE',  ( 11.30153831258470731, -190.0000000000000000, -15.00000000000000000 ) ) ;
#45592 = ORIENTED_EDGE ( 'NONE', *, *, #186506, .T. ) ;
#45593 = CARTESIAN_POINT ( 'NONE',  ( -19.02544592524334988, -5.153800228976617603, 83.95942372801901854 ) ) ;
#45594 = B_SPLINE_CURVE_WITH_KNOTS ( 'NONE', 3,
 ( #122054, #61373, #136243, #28099, #151424, #10921, #199909, #195955, #26097, #181763, #197918, #42258, #183746, #59387, #179787, #121061, #73596, #41256, #168559, #58408 ),
 .UNSPECIFIED., .F., .F.,
 ( 4, 2, 2, 2, 2, 2, 2, 2, 2, 4 ),
 ( 3.469446951953614189E-18, 0.0004987090165372655469, 0.0009974180330745276244, 0.001246772541343162512, 0.001496127049611797183, 0.001994836066149062188, 0.002493545082686327626, 0.002742899590954957743, 0.002992254099223588728, 0.003989672132298103559 ),
 .UNSPECIFIED. ) ;
#45595 = CARTESIAN_POINT ( 'NONE',  ( -15.80617190586745835, -15.72974639402198527, 26.87390960531435979 ) ) ;
#45597 = CARTESIAN_POINT ( 'NONE',  ( 16.46253265017146816, 9.564922557961045513, 101.6677570613523329 ) ) ;
#45596 = CARTESIAN_POINT ( 'NONE',  ( 19.05341960407617918, -5.049401038297876454, 21.04275706135232582 ) ) ;
#45598 = CARTESIAN_POINT ( 'NONE',  ( 4.483927247898545687, 16.52544592524342804, 114.7905762719810383 ) ) ;
#45599 = CARTESIAN_POINT ( 'NONE',  ( -9.564922557960796823, -16.46253265017161027, 27.08224293864769550 ) ) ;
#45600 = CARTESIAN_POINT ( 'NONE',  ( 15.80617190586746368, 15.72974639402197994, 64.37390960531435269 ) ) ;
#45601 = CARTESIAN_POINT ( 'NONE',  ( 18.67979575497178502, 10.72451020669898547, 54.16557627198103120 ) ) ;
#45602 = CARTESIAN_POINT ( 'NONE',  ( -16.46253265017160317, 9.564922557960807481, 25.83224293864769194 ) ) ;
#45603 = CYLINDRICAL_SURFACE ( 'NONE', #195359, 1.000000000000000888 ) ;
#45604 = CARTESIAN_POINT ( 'NONE',  ( -9.564922557961040184, 16.46253265017147172, 72.91775706135233293 ) ) ;
#45605 = CARTESIAN_POINT ( 'NONE',  ( 16.52544592524342804, -4.483927247898539470, 38.54057627198103120 ) ) ;
#45606 = CARTESIAN_POINT ( 'NONE',  ( 10.81492255796078972, 18.62759615963270932, 24.58224293864768839 ) ) ;
#45607 = CARTESIAN_POINT ( 'NONE',  ( -0.05219959533937732626, 21.53943276465977519, 87.50109039468568994 ) ) ;
#45608 = CARTESIAN_POINT ( 'NONE',  ( -21.52544592524343514, 5.823673210054127303, 76.04057627198102409 ) ) ;
#45609 = B_SPLINE_CURVE_WITH_KNOTS ( 'NONE', 3,
 ( #133546, #132552, #102216, #118391, #88032, #85027 ),
 .UNSPECIFIED., .F., .F.,
 ( 4, 2, 4 ),
 ( 3.469446951953613804E-18, 0.0003837532665635201958, 0.0007675065331270369221 ),
 .UNSPECIFIED. ) ;
#45610 = CARTESIAN_POINT ( 'NONE',  ( -18.62759615963255300, -10.81492255796106328, 64.16775706135234714 ) ) ;
#45611 = CARTESIAN_POINT ( 'NONE',  ( 0.05219959533937995610, -21.53943276465977519, 50.00109039468568994 ) ) ;
#45612 = CARTESIAN_POINT ( 'NONE',  ( -13.97604488694527625, -13.89961937509977652, 96.87390960531433848 ) ) ;
#45613 = CARTESIAN_POINT ( 'NONE',  ( 14.29746914071037800, 8.314922557961029526, 91.66775706135234714 ) ) ;
#45614 = CARTESIAN_POINT ( 'NONE',  ( 13.89961937509977652, -13.97604488694527269, 23.12390960531436335 ) ) ;
#45615 = CARTESIAN_POINT ( 'NONE',  ( -31.71835025711374101, 0.9887710624358323486, 102.4506977131440237 ) ) ;
#45616 = CARTESIAN_POINT ( 'NONE',  ( 8.224510206698953496, -14.34966873604960469, 67.91557627198102409 ) ) ;
#45617 = CARTESIAN_POINT ( 'NONE',  ( 4.483927247898545687, 16.52544592524342804, 34.79057627198103120 ) ) ;
#45618 = CARTESIAN_POINT ( 'NONE',  ( 9.474510206698971260, -16.51473224551069308, 62.91557627198102409 ) ) ;
#45619 = CARTESIAN_POINT ( 'NONE',  ( 0.05219959533909260263, 19.03943276465977164, 29.99890960531435979 ) ) ;
#45620 = CARTESIAN_POINT ( 'NONE',  ( -21.55341960407610458, -5.719274019375992779, 61.45724293864770260 ) ) ;
#45621 = CARTESIAN_POINT ( 'NONE',  ( 19.03943276465977164, 0.05219959533936151252, 36.25109039468567573 ) ) ;
#45623 = CARTESIAN_POINT ( 'NONE',  ( -14.29746914071049879, 8.314922557960819915, 45.83224293864769550 ) ) ;
#45622 = CYLINDRICAL_SURFACE ( 'NONE', #133281, 28.82186960331498682 ) ;
#45624 = CARTESIAN_POINT ( 'NONE',  ( -10.72451020669898014, 18.67979575497178502, 25.41557627198103120 ) ) ;
#45625 = ORIENTED_EDGE ( 'NONE', *, *, #156075, .F. ) ;
#45626 = DIRECTION ( 'NONE',  ( -0.000000000000000000, 0.000000000000000000, 1.000000000000000000 ) ) ;
#45627 = CARTESIAN_POINT ( 'NONE',  ( -8.224510206698735004, -14.34966873604973081, 74.58442372801901854 ) ) ;
#45628 = CARTESIAN_POINT ( 'NONE',  ( 9.474510206698729675, 16.51473224551082808, 72.08442372801900433 ) ) ;
#45629 = CARTESIAN_POINT ( 'NONE',  ( -4.379528057220328563, 16.55341960407611168, 40.20724293864769550 ) ) ;
#45630 = CARTESIAN_POINT ( 'NONE',  ( 16.38665767535058038, -7.295008042175997076, 52.76400864214550523 ) ) ;
#45631 = CARTESIAN_POINT ( 'NONE',  ( 16.53943276465976808, -0.05219959533910856209, 33.74890960531436690 ) ) ;
#45632 = CARTESIAN_POINT ( 'NONE',  ( -16.46253265017160317, 9.564922557960807481, 50.83224293864770260 ) ) ;
#45633 = CARTESIAN_POINT ( 'NONE',  ( 13.89961937509977652, -13.97604488694527269, 78.12390960531433848 ) ) ;
#45634 = CARTESIAN_POINT ( 'NONE',  ( 9.474510206698971260, -16.51473224551069308, 42.91557627198103120 ) ) ;
#45635 = CARTESIAN_POINT ( 'NONE',  ( -15.80617190586768217, 15.72974639402176855, 43.12609039468568284 ) ) ;
#45636 = CARTESIAN_POINT ( 'NONE',  ( -5.049401038298153566, 19.05341960407611168, 55.20724293864769550 ) ) ;
#45637 = CARTESIAN_POINT ( 'NONE',  ( -3.889087296525651105, 35.00000000000004263, 8.181980515339454030 ) ) ;
#45638 = CARTESIAN_POINT ( 'NONE',  ( -16.51473224551069308, -9.474510206698971260, 56.66557627198103120 ) ) ;
#45639 = CARTESIAN_POINT ( 'NONE',  ( 10.72451020669898902, -18.67979575497178502, 32.91557627198102409 ) ) ;
#45640 = CARTESIAN_POINT ( 'NONE',  ( 19.05341960407611168, 5.049401038298154454, 23.95724293864769194 ) ) ;
#45641 = CARTESIAN_POINT ( 'NONE',  ( -18.62759615963270932, 10.81492255796079327, 25.83224293864769194 ) ) ;
#45642 = CARTESIAN_POINT ( 'NONE',  ( -8.314922557961024197, 14.29746914071037800, 87.91775706135234714 ) ) ;
#45643 = ADVANCED_FACE ( 'NONE', ( #121753 ), #55350, .T. ) ;
#45644 = CARTESIAN_POINT ( 'NONE',  ( 5.823673210054444382, -21.52544592524334988, 105.2094237280190328 ) ) ;
#45645 = CARTESIAN_POINT ( 'NONE',  ( 8.314922557961029526, -14.29746914071037800, 70.41775706135236135 ) ) ;
#45646 = CARTESIAN_POINT ( 'NONE',  ( -16.51473224551069308, -9.474510206698971260, 106.6655762719810383 ) ) ;
#45647 = CARTESIAN_POINT ( 'NONE',  ( 14.34966873604972726, -8.224510206698740333, 50.83442372801901143 ) ) ;
#45648 = CARTESIAN_POINT ( 'NONE',  ( -14.34966873604972548, 8.224510206698743886, 38.33442372801900433 ) ) ;
#45649 = CARTESIAN_POINT ( 'NONE',  ( 14.29746914071037800, 8.314922557961029526, 101.6677570613523613 ) ) ;
#45650 = CARTESIAN_POINT ( 'NONE',  ( -12.06949235617739369, -12.14591786802326823, 29.37609039468568284 ) ) ;
#45651 = CARTESIAN_POINT ( 'NONE',  ( -16.51473224551069308, -9.474510206698971260, 36.66557627198102409 ) ) ;
#45652 = CARTESIAN_POINT ( 'NONE',  ( 15.80617190586746368, 15.72974639402197994, 104.3739096053143669 ) ) ;
#45653 = CARTESIAN_POINT ( 'NONE',  ( -12.06949235617739369, -12.14591786802326823, 19.37609039468568639 ) ) ;
#45654 = CARTESIAN_POINT ( 'NONE',  ( 12.06949235617739724, 12.14591786802326823, 91.87609039468568994 ) ) ;
#45655 = CARTESIAN_POINT ( 'NONE',  ( -17.13100169013226193, 6.664070546374124326, 45.76789835699824494 ) ) ;
#45656 = CARTESIAN_POINT ( 'NONE',  ( -18.67979575497193778, 10.72451020669871902, 88.33442372801901854 ) ) ;
#45657 = CARTESIAN_POINT ( 'NONE',  ( -16.46253265017146816, -9.564922557961047289, 84.16775706135233293 ) ) ;
#45658 = CARTESIAN_POINT ( 'NONE',  ( 8.224510206698953496, -14.34966873604960469, 57.91557627198103120 ) ) ;
#45659 = CARTESIAN_POINT ( 'NONE',  ( 12.06949235617757843, -12.14591786802309237, 43.12390960531435269 ) ) ;
#45660 = CARTESIAN_POINT ( 'NONE',  ( -16.55341960407611168, -4.379528057220339221, 101.4572429386476955 ) ) ;
#45662 = CARTESIAN_POINT ( 'NONE',  ( -7.214655873249279594, 1.452908486251215381, -64.31726809345073548 ) ) ;
#45661 = CARTESIAN_POINT ( 'NONE',  ( 16.46253265017146816, 9.564922557961045513, 41.66775706135234003 ) ) ;
#45663 = CARTESIAN_POINT ( 'NONE',  ( 0.05219959533937995610, -21.53943276465977519, 50.00109039468568994 ) ) ;
#45664 = CARTESIAN_POINT ( 'NONE',  ( -9.564922557961040184, 16.46253265017147172, 102.9177570613523329 ) ) ;
#45665 = CARTESIAN_POINT ( 'NONE',  ( 17.48847506799968343, 5.747544572773809257, 81.67302562156720569 ) ) ;
#45666 = CARTESIAN_POINT ( 'NONE',  ( -13.89961937509977652, 13.97604488694528158, 110.6239096053143243 ) ) ;
#45667 = CARTESIAN_POINT ( 'NONE',  ( -5.719274019375978568, 21.55341960407610458, 70.20724293864769550 ) ) ;
#45668 = CARTESIAN_POINT ( 'NONE',  ( -19.03943276465977164, -0.05219959533935918106, 98.75109039468567573 ) ) ;
#45669 = CARTESIAN_POINT ( 'NONE',  ( -9.564922557960796823, -16.46253265017161027, 107.0822429386476955 ) ) ;
#45670 = CARTESIAN_POINT ( 'NONE',  ( -5.049401038297874678, -19.05341960407618274, 49.79275706135232582 ) ) ;
#45671 = CARTESIAN_POINT ( 'NONE',  ( -14.29746914071049879, 8.314922557960819915, 105.8322429386476955 ) ) ;
#45672 = CARTESIAN_POINT ( 'NONE',  ( 15.80617190586769283, -15.72974639402175789, 100.6260903946857184 ) ) ;
#45673 = CARTESIAN_POINT ( 'NONE',  ( 9.474510206698971260, -16.51473224551069308, 37.91557627198102409 ) ) ;
#45674 = CARTESIAN_POINT ( 'NONE',  ( -15.80617190586768217, 15.72974639402176855, 48.12609039468568284 ) ) ;
#45675 = CARTESIAN_POINT ( 'NONE',  ( -10.81492255796105439, 18.62759615963255655, 87.91775706135234714 ) ) ;
#45676 = CARTESIAN_POINT ( 'NONE',  ( -16.53943276465976808, -0.05219959533934237506, 88.75109039468567573 ) ) ;
#45677 = CARTESIAN_POINT ( 'NONE',  ( 5.719274019375673035, 21.55341960407619339, 47.29275706135234003 ) ) ;
#45678 = CARTESIAN_POINT ( 'NONE',  ( 21.52544592524334988, 5.823673210054432836, 46.45942372801901854 ) ) ;
#45680 = CARTESIAN_POINT ( 'NONE',  ( -16.46253265017160317, 9.564922557960807481, 95.83224293864769550 ) ) ;
#45679 = CARTESIAN_POINT ( 'NONE',  ( -16.51473224551082808, 9.474510206698731452, 63.33442372801900433 ) ) ;
#45681 = CARTESIAN_POINT ( 'NONE',  ( -16.55341960407611168, -4.379528057220339221, 101.4572429386476955 ) ) ;
#45682 = CARTESIAN_POINT ( 'NONE',  ( 21.52544592524344225, -5.823673210054117533, 88.54057627198103830 ) ) ;
#45683 = CARTESIAN_POINT ( 'NONE',  ( 16.52544592524342804, -4.483927247898539470, 63.54057627198103830 ) ) ;
#45684 = CARTESIAN_POINT ( 'NONE',  ( 10.81492255796106328, -18.62759615963255655, 105.4177570613523613 ) ) ;
#45685 = CARTESIAN_POINT ( 'NONE',  ( -8.314922557960811034, -14.29746914071050412, 87.08224293864769550 ) ) ;
#45686 = CARTESIAN_POINT ( 'NONE',  ( 16.51473224551069308, 9.474510206698969483, 34.16557627198102409 ) ) ;
#45687 = CARTESIAN_POINT ( 'NONE',  ( 5.153800228976615827, -19.02544592524334988, 80.20942372801901854 ) ) ;
#45688 = CARTESIAN_POINT ( 'NONE',  ( 12.06949235617757843, -12.14591786802309237, 48.12390960531436690 ) ) ;
#45689 = CARTESIAN_POINT ( 'NONE',  ( 0.05219959533937995610, -21.53943276465977519, 90.00109039468567573 ) ) ;
#45690 = CARTESIAN_POINT ( 'NONE',  ( -0.05219959533909027116, -19.03943276465977164, 92.49890960531436690 ) ) ;
#45691 = CARTESIAN_POINT ( 'NONE',  ( 9.474510206698729675, 16.51473224551082808, 57.08442372801900433 ) ) ;
#45692 = CARTESIAN_POINT ( 'NONE',  ( -15.72974639402197994, 15.80617190586746368, 70.62390960531436690 ) ) ;
#45693 = CARTESIAN_POINT ( 'NONE',  ( 18.67979575497194134, -10.72451020669871369, 20.83442372801901143 ) ) ;
#45694 = CARTESIAN_POINT ( 'NONE',  ( 16.53943276465976808, 0.05219959533934440121, 26.25109039468567573 ) ) ;
#45695 = CARTESIAN_POINT ( 'NONE',  ( -16.52544592524335698, -4.483927247898792601, 83.95942372801900433 ) ) ;
#45697 = CARTESIAN_POINT ( 'NONE',  ( 10.72451020669871369, 18.67979575497193778, 27.08442372801901854 ) ) ;
#45696 = CARTESIAN_POINT ( 'NONE',  ( 5.153800228976335163, 19.02544592524342804, 24.79057627198102765 ) ) ;
#45698 = CARTESIAN_POINT ( 'NONE',  ( -14.29746914071049879, 8.314922557960819915, 115.8322429386477097 ) ) ;
#45699 = CARTESIAN_POINT ( 'NONE',  ( 22.81625015709510151, -31.40387420917324590, -4.424999997268812990 ) ) ;
#45700 = CARTESIAN_POINT ( 'NONE',  ( -8.314922557961024197, 14.29746914071037800, 52.91775706135235424 ) ) ;
#45701 = CARTESIAN_POINT ( 'NONE',  ( 14.29746914071049879, -8.314922557960816363, 78.33224293864770971 ) ) ;
#45702 = CARTESIAN_POINT ( 'NONE',  ( -15.80617190586745835, -15.72974639402198527, 81.87390960531435269 ) ) ;
#45703 = CARTESIAN_POINT ( 'NONE',  ( -16.52544592524342804, 4.483927247898546575, 31.04057627198102409 ) ) ;
#45704 = CARTESIAN_POINT ( 'NONE',  ( -16.52544592524335698, -4.483927247898792601, 33.95942372801901143 ) ) ;
#45705 = CARTESIAN_POINT ( 'NONE',  ( -19.05341960407611168, -5.049401038298163336, 46.45724293864768129 ) ) ;
#45706 = CARTESIAN_POINT ( 'NONE',  ( 4.483927247898790824, -16.52544592524335698, 75.20942372801901854 ) ) ;
#45707 = CARTESIAN_POINT ( 'NONE',  ( 5.153800228976615827, -19.02544592524334988, 80.20942372801901854 ) ) ;
#45708 = CARTESIAN_POINT ( 'NONE',  ( -18.67979575497178146, -10.72451020669898902, 71.66557627198100988 ) ) ;
#45709 = CARTESIAN_POINT ( 'NONE',  ( -8.314922557961024197, 14.29746914071037800, 107.9177570613523471 ) ) ;
#45710 = ORIENTED_EDGE ( 'NONE', *, *, #74806, .T. ) ;
#45711 = CARTESIAN_POINT ( 'NONE',  ( 20.43538597629129328, 20.43538597629121156, -52.65483682830182488 ) ) ;
#45712 = CARTESIAN_POINT ( 'NONE',  ( -5.719274019375978568, 21.55341960407610458, 45.20724293864769550 ) ) ;
#45713 = VERTEX_POINT ( 'NONE', #184434 ) ;
#45714 = CARTESIAN_POINT ( 'NONE',  ( -14.34966873604972548, 8.224510206698743886, 88.33442372801901854 ) ) ;
#45715 = CARTESIAN_POINT ( 'NONE',  ( 15.80617190586746368, 15.72974639402197994, 49.37390960531436690 ) ) ;
#45716 = VERTEX_POINT ( 'NONE', #170250 ) ;
#45717 = CARTESIAN_POINT ( 'NONE',  ( -19.05341960407611168, -5.049401038298163336, 111.4572429386476671 ) ) ;
#45718 = CARTESIAN_POINT ( 'NONE',  ( -6.020228577223754586E-15, 39.95556452105416412, -8.249999994537626336 ) ) ;
#45719 = CARTESIAN_POINT ( 'NONE',  ( 5.153800228976335163, 19.02544592524342804, 24.79057627198102765 ) ) ;
#45720 = CARTESIAN_POINT ( 'NONE',  ( 21.53943276465977519, -0.05219959533907433946, 73.74890960531433848 ) ) ;
#45721 = CARTESIAN_POINT ( 'NONE',  ( -16.53943276465976808, -0.05219959533934237506, 103.7510903946857042 ) ) ;
#45722 = CARTESIAN_POINT ( 'NONE',  ( 10.72451020669871369, 18.67979575497193778, 62.08442372801901143 ) ) ;
#45723 = CARTESIAN_POINT ( 'NONE',  ( -16.55341960407617563, 4.379528057220093196, 23.54275706135235424 ) ) ;
#45724 = CARTESIAN_POINT ( 'NONE',  ( -16.46253265017160317, 9.564922557960807481, 25.83224293864769194 ) ) ;
#45725 = CARTESIAN_POINT ( 'NONE',  ( -16.52544592524335698, -4.483927247898792601, 33.95942372801901143 ) ) ;
#45726 = CARTESIAN_POINT ( 'NONE',  ( -19.05341960407611168, -5.049401038298163336, 46.45724293864768129 ) ) ;
#45727 = EDGE_CURVE ( 'NONE', #15160, #151905, #133188, .T. ) ;
#45728 = CARTESIAN_POINT ( 'NONE',  ( 16.38029848613153661, -0.9460486868805465521, -61.48057501744755626 ) ) ;
#45729 = CARTESIAN_POINT ( 'NONE',  ( -19.05341960407611168, -5.049401038298163336, 111.4572429386476671 ) ) ;
#45730 = CARTESIAN_POINT ( 'NONE',  ( -14.34966873604972548, 8.224510206698743886, 88.33442372801901854 ) ) ;
#45731 = CARTESIAN_POINT ( 'NONE',  ( 13.97604488694548053, -13.89961937509957401, 95.62609039468563310 ) ) ;
#45732 = CARTESIAN_POINT ( 'NONE',  ( -15.80617190586768217, 15.72974639402176855, 113.1260903946856899 ) ) ;
#45733 = CARTESIAN_POINT ( 'NONE',  ( -21.52544592524343514, 5.823673210054127303, 81.04057627198102409 ) ) ;
#45734 = CARTESIAN_POINT ( 'NONE',  ( 8.314922557961029526, -14.29746914071037800, 100.4177570613523471 ) ) ;
#45735 = CARTESIAN_POINT ( 'NONE',  ( -9.474510206698720793, -16.51473224551083518, 99.58442372801900433 ) ) ;
#45736 = CARTESIAN_POINT ( 'NONE',  ( -13.97604488694527625, -13.89961937509977652, 51.87390960531436690 ) ) ;
#45737 = CARTESIAN_POINT ( 'NONE',  ( -9.474510206698964154, 16.51473224551069663, 90.41557627198103830 ) ) ;
#45738 = CARTESIAN_POINT ( 'NONE',  ( 5.823673210054444382, -21.52544592524334988, 50.20942372801901854 ) ) ;
#45739 = CARTESIAN_POINT ( 'NONE',  ( 9.564922557960805705, 16.46253265017160317, 49.58224293864770260 ) ) ;
#45740 = DIRECTION ( 'NONE',  ( -0.5000000000000002220, -0.4999999999999985012, 0.7071067811865483499 ) ) ;
#45741 = CARTESIAN_POINT ( 'NONE',  ( 19.02544592524343514, -5.153800228976328945, 113.5405762719810241 ) ) ;
#45742 = CARTESIAN_POINT ( 'NONE',  ( -16.52544592524342804, 4.483927247898546575, 71.04057627198103830 ) ) ;
#45743 = CARTESIAN_POINT ( 'NONE',  ( -15.72974639402197994, 15.80617190586746368, 70.62390960531436690 ) ) ;
#45744 = DIRECTION ( 'NONE',  ( 1.000000000000000000, 0.000000000000000000, 0.000000000000000000 ) ) ;
#45745 = CARTESIAN_POINT ( 'NONE',  ( 19.02544592524334988, 5.153800228976608722, 36.45942372801900433 ) ) ;
#45746 = CARTESIAN_POINT ( 'NONE',  ( -4.500000000000001776, -139.5000000000000000, 21.32407087589996664 ) ) ;
#45748 = CARTESIAN_POINT ( 'NONE',  ( -9.474510206698964154, 16.51473224551069663, 90.41557627198103830 ) ) ;
#45747 = CARTESIAN_POINT ( 'NONE',  ( 9.474510206698971260, -16.51473224551069308, 67.91557627198102409 ) ) ;
#45749 = CARTESIAN_POINT ( 'NONE',  ( -14.29746914071037622, -8.314922557961029526, 49.16775706135234003 ) ) ;
#45750 = CARTESIAN_POINT ( 'NONE',  ( 3.503282210674363295, -48.86437366581479580, -25.00000000000000000 ) ) ;
#45751 = CARTESIAN_POINT ( 'NONE',  ( 19.05341960407617918, -5.049401038297876454, 26.04275706135233293 ) ) ;
#45752 = LINE ( 'NONE', #78058, #4847 ) ;
#45753 = CARTESIAN_POINT ( 'NONE',  ( -14.34966873604972548, 8.224510206698743886, 88.33442372801901854 ) ) ;
#45754 = CARTESIAN_POINT ( 'NONE',  ( -0.1123844339349781840, -21.30000000000003268, -56.46919128290401346 ) ) ;
#45755 = CARTESIAN_POINT ( 'NONE',  ( 0.05219959533934541429, -16.53943276465976808, 85.00109039468568994 ) ) ;
#45756 = CARTESIAN_POINT ( 'NONE',  ( -4.483927247898782831, 16.52544592524335698, 57.70942372801901143 ) ) ;
#45757 = CARTESIAN_POINT ( 'NONE',  ( -13.89961937509957401, -13.97604488694547875, 29.37609039468565797 ) ) ;
#45759 = DIRECTION ( 'NONE',  ( -0.000000000000000000, -0.000000000000000000, 1.000000000000000000 ) ) ;
#45758 = CARTESIAN_POINT ( 'NONE',  ( 16.51473224551069308, 9.474510206698969483, 59.16557627198102409 ) ) ;
#45760 = CARTESIAN_POINT ( 'NONE',  ( 21.52544592524334988, 5.823673210054432836, 71.45942372801901854 ) ) ;
#45761 = CARTESIAN_POINT ( 'NONE',  ( 5.153800228976615827, -19.02544592524334988, 80.20942372801901854 ) ) ;
#45762 = CARTESIAN_POINT ( 'NONE',  ( 0.05219959533937995610, -21.53943276465977519, 110.0010903946856757 ) ) ;
#45763 = CARTESIAN_POINT ( 'NONE',  ( -9.564922557960796823, -16.46253265017161027, 47.08224293864769550 ) ) ;
#45764 = CARTESIAN_POINT ( 'NONE',  ( -15.69994562750274447, 14.67883866103742463, -58.73507448357034377 ) ) ;
#45765 = CARTESIAN_POINT ( 'NONE',  ( -18.62759615963270932, 10.81492255796079327, 70.83224293864770971 ) ) ;
#45766 = CARTESIAN_POINT ( 'NONE',  ( -21.53943276465977519, 0.05219959533907696930, 21.24890960531436690 ) ) ;
#45767 = CARTESIAN_POINT ( 'NONE',  ( 12.06949235617757843, -12.14591786802309237, 113.1239096053143953 ) ) ;
#45768 = CARTESIAN_POINT ( 'NONE',  ( 14.29746914071037800, 8.314922557961029526, 51.66775706135234714 ) ) ;
#45769 = CARTESIAN_POINT ( 'NONE',  ( 16.55341960407611168, 4.379528057220329451, 28.95724293864769905 ) ) ;
#45770 = VERTEX_POINT ( 'NONE', #199605 ) ;
#45771 = CARTESIAN_POINT ( 'NONE',  ( -10.72451020669870658, -18.67979575497194134, 19.58442372801901143 ) ) ;
#45773 = CARTESIAN_POINT ( 'NONE',  ( 23.48529157249599919, 32.32473071737754111, -6.700000000000001066 ) ) ;
#45772 = CARTESIAN_POINT ( 'NONE',  ( -16.55341960407611168, -4.379528057220339221, 46.45724293864769550 ) ) ;
#45774 = CIRCLE ( 'NONE', #68420, 59.99999999999998579 ) ;
#45775 = CARTESIAN_POINT ( 'NONE',  ( -19.03943276465977164, -0.05219959533935918106, 103.7510903946856757 ) ) ;
#45776 = CARTESIAN_POINT ( 'NONE',  ( 13.89961937509957401, 13.97604488694547697, 41.87609039468566152 ) ) ;
#45777 = CARTESIAN_POINT ( 'NONE',  ( -8.224510206698948167, 14.34966873604960824, 45.41557627198103830 ) ) ;
#45778 = CARTESIAN_POINT ( 'NONE',  ( -18.62759615963270932, 10.81492255796079327, 100.8322429386477097 ) ) ;
#45780 = CARTESIAN_POINT ( 'NONE',  ( 15.80617190586746368, 15.72974639402197994, 64.37390960531435269 ) ) ;
#45779 = CARTESIAN_POINT ( 'NONE',  ( 16.79531203550651242, 7.028104445595491079, 33.75244988220442366 ) ) ;
#45781 = CARTESIAN_POINT ( 'NONE',  ( 16.51473224551069308, 9.474510206698969483, 79.16557627198103830 ) ) ;
#45782 = CARTESIAN_POINT ( 'NONE',  ( -16.52544592524342804, 4.483927247898546575, 51.04057627198103120 ) ) ;
#45783 = CARTESIAN_POINT ( 'NONE',  ( 5.153800228976335163, 19.02544592524342804, 99.79057627198102409 ) ) ;
#45784 = CARTESIAN_POINT ( 'NONE',  ( -17.49999999999999645, 5.499999999999997335, 120.0000000000000142 ) ) ;
#45785 = CARTESIAN_POINT ( 'NONE',  ( -16.46253265017146816, -9.564922557961047289, 54.16775706135234003 ) ) ;
#45786 = CARTESIAN_POINT ( 'NONE',  ( 10.72451020669898902, -18.67979575497178502, 92.91557627198103830 ) ) ;
#45787 = CARTESIAN_POINT ( 'NONE',  ( 19.02544592524343514, -5.153800228976328945, 43.54057627198103120 ) ) ;
#45788 = CARTESIAN_POINT ( 'NONE',  ( -12.14591786802309592, -12.06949235617757132, 111.8739096053143669 ) ) ;
#45789 = CARTESIAN_POINT ( 'NONE',  ( -0.05219959533937732626, 21.53943276465977519, 52.50109039468567573 ) ) ;
#45790 = CARTESIAN_POINT ( 'NONE',  ( 8.571926809382597767, 26.38167802310806209, 146.2750000027311899 ) ) ;
#45791 = CARTESIAN_POINT ( 'NONE',  ( 8.314922557960818139, 14.29746914071049879, 24.58224293864768839 ) ) ;
#45792 = CARTESIAN_POINT ( 'NONE',  ( 19.05341960407611168, 5.049401038298154454, 48.95724293864768129 ) ) ;
#45793 = CARTESIAN_POINT ( 'NONE',  ( -5.153800228976328057, -19.02544592524343514, 97.29057627198099567 ) ) ;
#45794 = CARTESIAN_POINT ( 'NONE',  ( 10.81492255796078972, 18.62759615963270932, 59.58224293864770260 ) ) ;
#45795 = CARTESIAN_POINT ( 'NONE',  ( -19.02130022317637525, 5.499999999999598543, 45.78188669246576836 ) ) ;
#45796 = CARTESIAN_POINT ( 'NONE',  ( -19.05341960407611168, -5.049401038298163336, 41.45724293864769550 ) ) ;
#45797 = CARTESIAN_POINT ( 'NONE',  ( 10.81492255796078972, 18.62759615963270932, 49.58224293864769550 ) ) ;
#45798 = CARTESIAN_POINT ( 'NONE',  ( -15.80617190586768217, 15.72974639402176855, 88.12609039468570415 ) ) ;
#45800 = CARTESIAN_POINT ( 'NONE',  ( -14.34966873604972548, 8.224510206698743886, 88.33442372801901854 ) ) ;
#45799 = CARTESIAN_POINT ( 'NONE',  ( 19.25015247713429289, -32.77362114220795064, -25.12817986193741859 ) ) ;
#45801 = CARTESIAN_POINT ( 'NONE',  ( 16.52544592524335698, 4.483927247898782831, 91.45942372801901854 ) ) ;
#45802 = CARTESIAN_POINT ( 'NONE',  ( -13.97604488694527625, -13.89961937509977652, 66.87390960531436690 ) ) ;
#45803 =( BOUNDED_CURVE ( )  B_SPLINE_CURVE ( 2, ( #63742, #75920, #46584, #61735, #170919, #125416, #111230, #172922, #33407, #48584, #123403 ),
 .UNSPECIFIED., .F., .T. ) 
 B_SPLINE_CURVE_WITH_KNOTS ( ( 3, 2, 2, 2, 2, 3 ),
 ( 0.8000000000000007105, 0.8200000000000006173, 0.8400000000000006350, 0.8600000000000007638, 0.8800000000000007816, 0.9000000000000007994 ),
 .UNSPECIFIED. ) 
 CURVE ( )  GEOMETRIC_REPRESENTATION_ITEM ( )  RATIONAL_B_SPLINE_CURVE ( ( 0.9999999999999983347, 0.9510565162951551965, 1.000000000000000000, 0.9510565162951535312, 1.000000000000000000, 0.9510565162951535312, 1.000000000000000000, 0.9510565162951535312, 1.000000000000000000, 0.9510565162951516438, 1.000000000000001998 ) ) 
 REPRESENTATION_ITEM ( '' )  );
#45804 = ORIENTED_EDGE ( 'NONE', *, *, #35688, .T. ) ;
#45805 = CARTESIAN_POINT ( 'NONE',  ( -9.564922557961040184, 16.46253265017147172, 22.91775706135233648 ) ) ;
#45806 = CARTESIAN_POINT ( 'NONE',  ( -12.14591786802326823, 12.06949235617739902, 88.12609039468570415 ) ) ;
#45807 = CARTESIAN_POINT ( 'NONE',  ( 21.52544592524334988, 5.823673210054432836, 111.4594237280190328 ) ) ;
#45808 = CARTESIAN_POINT ( 'NONE',  ( 9.564922557960805705, 16.46253265017160317, 79.58224293864769550 ) ) ;
#45809 = CARTESIAN_POINT ( 'NONE',  ( 10.81492255796078972, 18.62759615963270932, 54.58224293864769550 ) ) ;
#45810 = CARTESIAN_POINT ( 'NONE',  ( 4.379528057220092307, 16.55341960407617563, 22.29275706135235069 ) ) ;
#45811 = CARTESIAN_POINT ( 'NONE',  ( 21.52544592524334988, 5.823673210054432836, 76.45942372801901854 ) ) ;
#45812 = CARTESIAN_POINT ( 'NONE',  ( -8.314922557961024197, 14.29746914071037800, 62.91775706135236135 ) ) ;
#45813 = CARTESIAN_POINT ( 'NONE',  ( -5.719274019375978568, 21.55341960407610458, 115.2072429386476955 ) ) ;
#45814 = CARTESIAN_POINT ( 'NONE',  ( 19.02544592524334988, 5.153800228976608722, 106.4594237280190185 ) ) ;
#45815 = CARTESIAN_POINT ( 'NONE',  ( 13.97604488694527802, 13.89961937509977652, 74.37390960531436690 ) ) ;
#45816 = CARTESIAN_POINT ( 'NONE',  ( 0.05219959533934541429, -16.53943276465976808, 30.00109039468568284 ) ) ;
#45817 = CARTESIAN_POINT ( 'NONE',  ( 16.46253265017160672, -9.564922557960803928, 38.33224293864768839 ) ) ;
#45818 = CARTESIAN_POINT ( 'NONE',  ( -5.153800228976607833, 19.02544592524334988, 112.7094237280190043 ) ) ;
#45819 = CARTESIAN_POINT ( 'NONE',  ( 14.29746914071049879, -8.314922557960816363, 78.33224293864770971 ) ) ;
#45820 = CARTESIAN_POINT ( 'NONE',  ( -8.224510206698735004, -14.34966873604973081, 84.58442372801903275 ) ) ;
#45822 = CARTESIAN_POINT ( 'NONE',  ( -19.05341960407611168, -5.049401038298163336, 66.45724293864769550 ) ) ;
#45821 = CARTESIAN_POINT ( 'NONE',  ( -21.52544592524334988, -5.823673210054445271, 33.95942372801901143 ) ) ;
#45823 = CARTESIAN_POINT ( 'NONE',  ( 19.02544592524343514, -5.153800228976328945, 63.54057627198103830 ) ) ;
#45824 = CARTESIAN_POINT ( 'NONE',  ( 8.314922557961029526, -14.29746914071037800, 80.41775706135234714 ) ) ;
#45826 = ORIENTED_EDGE ( 'NONE', *, *, #34324, .T. ) ;
#45825 = CARTESIAN_POINT ( 'NONE',  ( -21.95653654802831412, -6.613221094984323756, 171.0358100525039902 ) ) ;
#45827 = VERTEX_POINT ( 'NONE', #122743 ) ;
#45828 = CARTESIAN_POINT ( 'NONE',  ( 19.03943276465977164, 0.05219959533936151252, 26.25109039468566507 ) ) ;
#45829 = CARTESIAN_POINT ( 'NONE',  ( -13.97604488694527625, -13.89961937509977652, 41.87390960531435979 ) ) ;
#45831 = VERTEX_POINT ( 'NONE', #107567 ) ;
#45830 = CARTESIAN_POINT ( 'NONE',  ( 1.464443979261886630, 14.82300492994660068, -62.12379213640164721 ) ) ;
#45832 = CARTESIAN_POINT ( 'NONE',  ( 0.05219959533934541429, -16.53943276465976808, 30.00109039468568284 ) ) ;
#45834 = CARTESIAN_POINT ( 'NONE',  ( -8.314922557961024197, 14.29746914071037800, 42.91775706135235424 ) ) ;
#45833 = CARTESIAN_POINT ( 'NONE',  ( -19.03943276465977164, -0.05219959533935918106, 58.75109039468566863 ) ) ;
#45835 = CARTESIAN_POINT ( 'NONE',  ( 5.049401038298161559, -19.05341960407611168, 102.7072429386476955 ) ) ;
#45836 = CARTESIAN_POINT ( 'NONE',  ( 13.89961937509977652, -13.97604488694527269, 63.12390960531435979 ) ) ;
#45837 = CARTESIAN_POINT ( 'NONE',  ( -18.62759615963270932, 10.81492255796079327, 105.8322429386476955 ) ) ;
#45839 = CARTESIAN_POINT ( 'NONE',  ( -2.649999999999999911, -105.0000000000000000, -15.00000000000000000 ) ) ;
#45838 = CARTESIAN_POINT ( 'NONE',  ( -16.46253265017160317, 9.564922557960807481, 95.83224293864769550 ) ) ;
#45840 = CARTESIAN_POINT ( 'NONE',  ( -9.564922557960796823, -16.46253265017161027, 62.08224293864769550 ) ) ;
#45842 = CARTESIAN_POINT ( 'NONE',  ( -19.02544592524342804, 5.153800228976336051, 26.04057627198103120 ) ) ;
#45841 = CARTESIAN_POINT ( 'NONE',  ( -12.14591786802309592, -12.06949235617757132, 26.87390960531435979 ) ) ;
#45843 = CARTESIAN_POINT ( 'NONE',  ( -19.05341960407617563, 5.049401038297882671, 33.54275706135231871 ) ) ;
#45844 = CARTESIAN_POINT ( 'NONE',  ( 12.06949235617757843, -12.14591786802309237, 68.12390960531436690 ) ) ;
#45845 = CARTESIAN_POINT ( 'NONE',  ( -0.05219959533937732626, 21.53943276465977519, 92.50109039468567573 ) ) ;
#45846 = CARTESIAN_POINT ( 'NONE',  ( 13.97604488694527802, 13.89961937509977652, 44.37390960531435269 ) ) ;
#45847 = CARTESIAN_POINT ( 'NONE',  ( 12.14591786802327356, -12.06949235617739191, 50.62609039468568994 ) ) ;
#45849 = CARTESIAN_POINT ( 'NONE',  ( -18.62759615963255300, -10.81492255796106328, 89.16775706135236135 ) ) ;
#45848 = CARTESIAN_POINT ( 'NONE',  ( 14.34966873604960469, 8.224510206698951720, 39.16557627198102409 ) ) ;
#45850 = CARTESIAN_POINT ( 'NONE',  ( 5.049401038298161559, -19.05341960407611168, 77.70724293864765286 ) ) ;
#45851 = CARTESIAN_POINT ( 'NONE',  ( 5.153800228976335163, 19.02544592524342804, 99.79057627198102409 ) ) ;
#45852 = CARTESIAN_POINT ( 'NONE',  ( 8.224510206698953496, -14.34966873604960469, 112.9155762719810383 ) ) ;
#45853 = CARTESIAN_POINT ( 'NONE',  ( -14.29746914071049879, 8.314922557960819915, 75.83224293864769550 ) ) ;
#45854 = CARTESIAN_POINT ( 'NONE',  ( 18.62759615963271287, -10.81492255796078972, 88.33224293864769550 ) ) ;
#45855 = CARTESIAN_POINT ( 'NONE',  ( 9.474510206698971260, -16.51473224551069308, 82.91557627198103830 ) ) ;
#45856 = CARTESIAN_POINT ( 'NONE',  ( -15.80617190586745835, -15.72974639402198527, 101.8739096053143811 ) ) ;
#45857 = CARTESIAN_POINT ( 'NONE',  ( -9.564922557961040184, 16.46253265017147172, 72.91775706135233293 ) ) ;
#45859 = CARTESIAN_POINT ( 'NONE',  ( -12.06949235617756955, 12.14591786802309770, 85.62390960531436690 ) ) ;
#45858 = CARTESIAN_POINT ( 'NONE',  ( 18.39635199886966532, -5.500000000000095035, 48.51967076359998288 ) ) ;
#45860 = CARTESIAN_POINT ( 'NONE',  ( -9.564922557960796823, -16.46253265017161027, 52.08224293864768839 ) ) ;
#45861 = CARTESIAN_POINT ( 'NONE',  ( -10.72451020669898014, 18.67979575497178502, 65.41557627198102409 ) ) ;
#45862 = CARTESIAN_POINT ( 'NONE',  ( -25.31005825231498818, -7.802036135343648482, 170.7258689498729325 ) ) ;
#45864 = CARTESIAN_POINT ( 'NONE',  ( 17.14385361876520264, 23.59649016807275856, 148.6750000027311387 ) ) ;
#45863 = CARTESIAN_POINT ( 'NONE',  ( -14.29746914071049879, 8.314922557960819915, 25.83224293864769194 ) ) ;
#45865 = CARTESIAN_POINT ( 'NONE',  ( -16.51473224551082808, 9.474510206698731452, 113.3344237280190043 ) ) ;
#45866 = CARTESIAN_POINT ( 'NONE',  ( -16.53943276465976808, 0.05219959533911058130, 76.24890960531435269 ) ) ;
#45867 = CARTESIAN_POINT ( 'NONE',  ( -30.00000000000000000, -1.163414459189985801E-14, 95.00000000000000000 ) ) ;
#45868 = CARTESIAN_POINT ( 'NONE',  ( 0.05219959533909260263, 19.03943276465977164, 69.99890960531435269 ) ) ;
#45869 = CARTESIAN_POINT ( 'NONE',  ( 5.049401038298161559, -19.05341960407611168, 27.70724293864769550 ) ) ;
#45870 = CARTESIAN_POINT ( 'NONE',  ( -14.34966873604960291, -8.224510206698953496, 71.66557627198100988 ) ) ;
#45871 = CARTESIAN_POINT ( 'NONE',  ( 5.049401038298161559, -19.05341960407611168, 112.7072429386476813 ) ) ;
#45872 = CARTESIAN_POINT ( 'NONE',  ( -5.153800228976607833, 19.02544592524334988, 82.70942372801897591 ) ) ;
#45873 = CARTESIAN_POINT ( 'NONE',  ( 0.05219959533909260263, 19.03943276465977164, 104.9989096053143669 ) ) ;
#45874 = CARTESIAN_POINT ( 'NONE',  ( -21.53943276465977519, 0.05219959533907696930, 71.24890960531435269 ) ) ;
#45875 = CARTESIAN_POINT ( 'NONE',  ( 12.14591786802327356, -12.06949235617739191, 70.62609039468567573 ) ) ;
#45876 = CARTESIAN_POINT ( 'NONE',  ( 19.05341960407618274, -5.049401038297876454, 106.0427570613523471 ) ) ;
#45877 = CARTESIAN_POINT ( 'NONE',  ( 9.564922557960805705, 16.46253265017160317, 59.58224293864769550 ) ) ;
#45878 = CARTESIAN_POINT ( 'NONE',  ( 10.72451020669898902, -18.67979575497178502, 62.91557627198102409 ) ) ;
#45879 = CARTESIAN_POINT ( 'NONE',  ( -19.03943276465977164, -0.05219959533935918106, 108.7510903946856615 ) ) ;
#45881 = CARTESIAN_POINT ( 'NONE',  ( -21.53943276465977519, -0.05219959533937600094, 58.75109039468568994 ) ) ;
#45880 = CARTESIAN_POINT ( 'NONE',  ( -12.06949235617756955, 12.14591786802309770, 35.62390960531437401 ) ) ;
#45882 = EDGE_CURVE ( 'NONE', #15494, #63455, #152090, .T. ) ;
#45883 = DIRECTION ( 'NONE',  ( 1.000000000000000000, 0.000000000000000000, 0.000000000000000000 ) ) ;
#45885 = CARTESIAN_POINT ( 'NONE',  ( 9.564922557960805705, 16.46253265017160317, 104.5822429386476955 ) ) ;
#45884 = CARTESIAN_POINT ( 'NONE',  ( -12.06949235617739369, -12.14591786802326823, 79.37609039468567573 ) ) ;
#45886 = CARTESIAN_POINT ( 'NONE',  ( -15.49999999999999822, -5.500000000000000888, 118.0000000000000142 ) ) ;
#45887 = DIRECTION ( 'NONE',  ( 1.000000000000000000, 0.000000000000000000, -0.000000000000000000 ) ) ;
#45888 = CARTESIAN_POINT ( 'NONE',  ( 4.379528057220092307, 16.55341960407617563, 92.29275706135236135 ) ) ;
#45889 = CARTESIAN_POINT ( 'NONE',  ( 12.06949235617739724, 12.14591786802326823, 46.87609039468568994 ) ) ;
#45890 = CARTESIAN_POINT ( 'NONE',  ( 5.049401038298161559, -19.05341960407611168, 57.70724293864769550 ) ) ;
#45891 = CARTESIAN_POINT ( 'NONE',  ( 19.05341960407611168, 5.049401038298154454, 73.95724293864768129 ) ) ;
#45892 = CARTESIAN_POINT ( 'NONE',  ( -10.72451020669870658, -18.67979575497194134, 54.58442372801901143 ) ) ;
#45893 = CARTESIAN_POINT ( 'NONE',  ( 12.06949235617739724, 12.14591786802326823, 66.87609039468568994 ) ) ;
#45894 = CARTESIAN_POINT ( 'NONE',  ( 16.52544592524342804, -4.483927247898539470, 28.54057627198103120 ) ) ;
#45895 = CARTESIAN_POINT ( 'NONE',  ( -5.153800228976328057, -19.02544592524343514, 42.29057627198101699 ) ) ;
#45896 = CARTESIAN_POINT ( 'NONE',  ( -19.02544592524342804, 5.153800228976336051, 41.04057627198103120 ) ) ;
#45897 = CARTESIAN_POINT ( 'NONE',  ( 4.379528057220092307, 16.55341960407617563, 27.29275706135234358 ) ) ;
#45898 = CARTESIAN_POINT ( 'NONE',  ( 5.049401038297881783, 19.05341960407617563, 77.29275706135231871 ) ) ;
#45899 = CARTESIAN_POINT ( 'NONE',  ( -16.55341960407611168, -4.379528057220339221, 101.4572429386476955 ) ) ;
#45900 = CARTESIAN_POINT ( 'NONE',  ( -19.02544592524342804, 5.153800228976336051, 51.04057627198103120 ) ) ;
#45902 = CARTESIAN_POINT ( 'NONE',  ( -11.74264578624799782, -36.14014761921581709, -9.600000000000001421 ) ) ;
#45901 = CARTESIAN_POINT ( 'NONE',  ( 5.049401038297881783, 19.05341960407617563, 82.29275706135229029 ) ) ;
#45903 = CARTESIAN_POINT ( 'NONE',  ( -5.719274019375665041, -21.55341960407619695, 89.79275706135236135 ) ) ;
#45904 = CARTESIAN_POINT ( 'NONE',  ( 16.53943276465976808, 0.05219959533934440121, 56.25109039468568284 ) ) ;
#45905 = DIRECTION ( 'NONE',  ( 1.000000000000000000, 0.000000000000000000, 0.000000000000000000 ) ) ;
#45906 = CARTESIAN_POINT ( 'NONE',  ( -21.52544592524343514, 5.823673210054127303, 51.04057627198103120 ) ) ;
#45907 = CARTESIAN_POINT ( 'NONE',  ( 16.53943276465976808, 0.05219959533934440121, 41.25109039468568284 ) ) ;
#45908 = CARTESIAN_POINT ( 'NONE',  ( -19.02544592524342804, 5.153800228976336939, 36.04057627198101699 ) ) ;
#45909 = CARTESIAN_POINT ( 'NONE',  ( 16.46253265017146816, 9.564922557961045513, 41.66775706135234003 ) ) ;
#45910 = CARTESIAN_POINT ( 'NONE',  ( 19.02544592524343514, -5.153800228976328945, 88.54057627198102409 ) ) ;
#45911 = CARTESIAN_POINT ( 'NONE',  ( 19.02544592524343514, -5.153800228976328945, 48.54057627198103120 ) ) ;
#45912 = CARTESIAN_POINT ( 'NONE',  ( 14.61887724323083937, 16.11132338694242350, -56.15647863711520671 ) ) ;
#45913 = CARTESIAN_POINT ( 'NONE',  ( 21.52544592524334988, 5.823673210054432836, 71.45942372801901854 ) ) ;
#45914 = CARTESIAN_POINT ( 'NONE',  ( -11.74264578624799782, -36.14014761921581709, -11.34999999453762776 ) ) ;
#45915 = CARTESIAN_POINT ( 'NONE',  ( 5.049401038297881783, 19.05341960407617563, 37.29275706135232582 ) ) ;
#45916 = CARTESIAN_POINT ( 'NONE',  ( 15.80617190586769283, -15.72974639402175789, 105.6260903946856899 ) ) ;
#45917 = CARTESIAN_POINT ( 'NONE',  ( -14.29746914071049879, 8.314922557960819915, 35.83224293864768839 ) ) ;
#45918 = CARTESIAN_POINT ( 'NONE',  ( -9.474510206698964154, 16.51473224551069663, 60.41557627198102409 ) ) ;
#45919 = CARTESIAN_POINT ( 'NONE',  ( -16.46253265017160317, 9.564922557960807481, 105.8322429386476955 ) ) ;
#45920 = CARTESIAN_POINT ( 'NONE',  ( -21.52544592524334988, -5.823673210054445271, 88.95942372801901854 ) ) ;
#45921 = CARTESIAN_POINT ( 'NONE',  ( 9.564922557960805705, 16.46253265017160317, 64.58224293864769550 ) ) ;
#45922 = CARTESIAN_POINT ( 'NONE',  ( -0.05219959533937732626, 21.53943276465977519, 77.50109039468567573 ) ) ;
#45923 = CARTESIAN_POINT ( 'NONE',  ( 10.72451020669898902, -18.67979575497178502, 42.91557627198103120 ) ) ;
#45924 = CARTESIAN_POINT ( 'NONE',  ( -18.62759615963255300, -10.81492255796106328, 29.16775706135234003 ) ) ;
#45925 = CARTESIAN_POINT ( 'NONE',  ( -9.564922557961040184, 16.46253265017147172, 47.91775706135233293 ) ) ;
#45926 = CARTESIAN_POINT ( 'NONE',  ( -13.97604488694527625, -13.89961937509977652, 31.87390960531435979 ) ) ;
#45927 = CARTESIAN_POINT ( 'NONE',  ( -19.05341960407611168, -5.049401038298163336, 81.45724293864769550 ) ) ;
#45928 = CARTESIAN_POINT ( 'NONE',  ( 16.55341960407618274, -4.379528057220086978, 31.04275706135234714 ) ) ;
#45929 = CARTESIAN_POINT ( 'NONE',  ( 16.52544592524342804, -4.483927247898539470, 93.54057627198103830 ) ) ;
#45930 = CARTESIAN_POINT ( 'NONE',  ( 19.03943276465977164, -0.05219959533909143690, 58.74890960531435979 ) ) ;
#45931 = CARTESIAN_POINT ( 'NONE',  ( -10.81492255796078084, -18.62759615963271287, 32.08224293864769550 ) ) ;
#45932 = CARTESIAN_POINT ( 'NONE',  ( 13.89961937509957401, 13.97604488694547697, 96.87609039468566152 ) ) ;
#45933 = CARTESIAN_POINT ( 'NONE',  ( -21.52544592524343514, 5.823673210054127303, 106.0405762719810525 ) ) ;
#45934 = CARTESIAN_POINT ( 'NONE',  ( 5.823673210054444382, -21.52544592524334988, 70.20942372801904696 ) ) ;
#45935 = CARTESIAN_POINT ( 'NONE',  ( 8.224510206698742110, 14.34966873604972548, 67.08442372801901854 ) ) ;
#45936 = CARTESIAN_POINT ( 'NONE',  ( 0.05219959533934541429, -16.53943276465976808, 65.00109039468568994 ) ) ;
#45937 = CARTESIAN_POINT ( 'NONE',  ( 19.03943276465977164, -0.05219959533909143690, 58.74890960531435979 ) ) ;
#45938 = CARTESIAN_POINT ( 'NONE',  ( -16.52544592524335698, -4.483927247898792601, 83.95942372801900433 ) ) ;
#45939 = CARTESIAN_POINT ( 'NONE',  ( -19.02544592524334988, -5.153800228976617603, 48.95942372801900433 ) ) ;
#45940 = CARTESIAN_POINT ( 'NONE',  ( -21.53943276465977519, -0.05219959533937600094, 23.75109039468567929 ) ) ;
#45941 = CARTESIAN_POINT ( 'NONE',  ( 8.314922557960818139, 14.29746914071049879, 64.58224293864769550 ) ) ;
#45942 = CARTESIAN_POINT ( 'NONE',  ( -19.03943276465977164, 0.05219959533909376836, 81.24890960531436690 ) ) ;
#45943 = CARTESIAN_POINT ( 'NONE',  ( 16.53943276465976808, 0.05219959533934440121, 71.25109039468568994 ) ) ;
#45944 = CARTESIAN_POINT ( 'NONE',  ( -21.53943276465977519, -0.05219959533937600094, 63.75109039468568284 ) ) ;
#45945 = CARTESIAN_POINT ( 'NONE',  ( 8.224510206698742110, 14.34966873604972548, 22.08442372801901143 ) ) ;
#45946 = CARTESIAN_POINT ( 'NONE',  ( -15.72974639402197994, 15.80617190586746368, 115.6239096053143669 ) ) ;
#45947 = CARTESIAN_POINT ( 'NONE',  ( 16.52544592524342804, -4.483927247898539470, 58.54057627198103120 ) ) ;
#45948 = VERTEX_POINT ( 'NONE', #30752 ) ;
#45949 = CARTESIAN_POINT ( 'NONE',  ( 21.55341960407610458, 5.719274019375980345, 88.95724293864769550 ) ) ;
#45950 = CARTESIAN_POINT ( 'NONE',  ( -16.52544592524342804, 4.483927247898546575, 41.04057627198103120 ) ) ;
#45951 = VERTEX_POINT ( 'NONE', #92400 ) ;
#45952 = DIRECTION ( 'NONE',  ( 0.000000000000000000, 0.000000000000000000, -1.000000000000000000 ) ) ;
#45953 = CARTESIAN_POINT ( 'NONE',  ( -0.05219959533907301413, -21.53943276465977519, 112.4989096053143669 ) ) ;
#45954 = CARTESIAN_POINT ( 'NONE',  ( -19.02544592524342804, 5.153800228976336051, 111.0405762719810099 ) ) ;
#45955 = CARTESIAN_POINT ( 'NONE',  ( 15.72974639402176855, 15.80617190586768217, 36.87609039468568994 ) ) ;
#45956 = CARTESIAN_POINT ( 'NONE',  ( -12.06949235617756955, 12.14591786802309770, 45.62390960531436690 ) ) ;
#45957 = CARTESIAN_POINT ( 'NONE',  ( 9.474510206698971260, -16.51473224551069308, 62.91557627198102409 ) ) ;
#45958 = CARTESIAN_POINT ( 'NONE',  ( -5.049401038297874678, -19.05341960407617918, 69.79275706135233293 ) ) ;
#45959 = CARTESIAN_POINT ( 'NONE',  ( -13.89961937509977652, 13.97604488694528158, 95.62390960531436690 ) ) ;
#45960 = EDGE_CURVE ( 'NONE', #132514, #55277, #124794, .T. ) ;
#45961 = CARTESIAN_POINT ( 'NONE',  ( 21.55341960407610458, 5.719274019375980345, 48.95724293864770971 ) ) ;
#45962 = CARTESIAN_POINT ( 'NONE',  ( -16.87022414723119113, -33.99382086345450915, -27.12615631800879967 ) ) ;
#45963 = CARTESIAN_POINT ( 'NONE',  ( 9.474510206698971260, -16.51473224551069308, 62.91557627198102409 ) ) ;
#45964 = CARTESIAN_POINT ( 'NONE',  ( 14.34966873604972726, -8.224510206698740333, 35.83442372801901143 ) ) ;
#45965 = CARTESIAN_POINT ( 'NONE',  ( -9.474510206698720793, -16.51473224551083518, 64.58442372801900433 ) ) ;
#45966 = CARTESIAN_POINT ( 'NONE',  ( 15.80617190586746368, 15.72974639402197994, 109.3739096053143811 ) ) ;
#45967 = CARTESIAN_POINT ( 'NONE',  ( -16.55341960407611168, -4.379528057220339221, 46.45724293864769550 ) ) ;
#45968 = CARTESIAN_POINT ( 'NONE',  ( -13.89961937509977652, 13.97604488694528158, 95.62390960531436690 ) ) ;
#45969 = CARTESIAN_POINT ( 'NONE',  ( 21.53943276465977519, -0.05219959533907433946, 78.74890960531436690 ) ) ;
#45971 = CARTESIAN_POINT ( 'NONE',  ( -4.379528057220086978, -16.55341960407618274, 39.79275706135235424 ) ) ;
#45970 = CARTESIAN_POINT ( 'NONE',  ( 15.80617190586746368, 15.72974639402197994, 94.37390960531436690 ) ) ;
#45972 = CARTESIAN_POINT ( 'NONE',  ( 15.72974639402199770, -15.80617190586745480, 38.12390960531436690 ) ) ;
#45973 = CARTESIAN_POINT ( 'NONE',  ( -15.72974639402176322, -15.80617190586768395, 94.37609039468568994 ) ) ;
#45974 = CARTESIAN_POINT ( 'NONE',  ( -19.05341960407611168, -5.049401038298163336, 86.45724293864769550 ) ) ;
#45975 = CARTESIAN_POINT ( 'NONE',  ( 0.05219959533909260263, 19.03943276465977164, 44.99890960531435979 ) ) ;
#45976 = CARTESIAN_POINT ( 'NONE',  ( 13.89961937509977652, -13.97604488694527269, 93.12390960531436690 ) ) ;
#45977 = CARTESIAN_POINT ( 'NONE',  ( -8.224510206698948167, 14.34966873604960824, 105.4155762719810383 ) ) ;
#45978 = CARTESIAN_POINT ( 'NONE',  ( -16.46253265017160317, 9.564922557960807481, 70.83224293864770971 ) ) ;
#45979 = CARTESIAN_POINT ( 'NONE',  ( -16.51473224551082808, 9.474510206698731452, 113.3344237280190043 ) ) ;
#45980 = CARTESIAN_POINT ( 'NONE',  ( 18.22780087662126647, 5.499999999999818812, 41.48236817873107185 ) ) ;
#45981 = CARTESIAN_POINT ( 'NONE',  ( -16.46253265017146816, -9.564922557961047289, 59.16775706135233293 ) ) ;
#45983 = CARTESIAN_POINT ( 'NONE',  ( -18.62759615963270932, 10.81492255796079327, 35.83224293864768839 ) ) ;
#45982 = CARTESIAN_POINT ( 'NONE',  ( -0.05219959533937732626, 21.53943276465977519, 112.5010903946857042 ) ) ;
#45984 = CARTESIAN_POINT ( 'NONE',  ( 8.314922557961029526, -14.29746914071037800, 90.41775706135236135 ) ) ;
#45985 = CARTESIAN_POINT ( 'NONE',  ( 23.48529157249600630, -32.32473071737748427, -9.300000000000000711 ) ) ;
#45986 = CARTESIAN_POINT ( 'NONE',  ( 13.89961937509957401, 13.97604488694547697, 71.87609039468567573 ) ) ;
#45987 = CARTESIAN_POINT ( 'NONE',  ( 5.153800228976615827, -19.02544592524334988, 30.20942372801900433 ) ) ;
#45988 = CARTESIAN_POINT ( 'NONE',  ( -17.26058549869089376, -6.457015423128631859, 46.37745837476068544 ) ) ;
#45989 = CARTESIAN_POINT ( 'NONE',  ( 19.05341960407611168, 5.049401038298154454, 43.95724293864769550 ) ) ;
#45990 = CARTESIAN_POINT ( 'NONE',  ( 14.34966873604960469, 8.224510206698951720, 34.16557627198102409 ) ) ;
#45991 = CARTESIAN_POINT ( 'NONE',  ( -9.474510206698964154, 16.51473224551069663, 25.41557627198103120 ) ) ;
#45992 = CARTESIAN_POINT ( 'NONE',  ( 4.379528057220339221, -16.55341960407611168, 27.70724293864769905 ) ) ;
#45993 = LINE ( 'NONE', #118882, #119466 ) ;
#45994 = CARTESIAN_POINT ( 'NONE',  ( 8.314922557961029526, -14.29746914071037800, 95.41775706135234714 ) ) ;
#45995 = CARTESIAN_POINT ( 'NONE',  ( 19.02544592524343514, -5.153800228976328945, 38.54057627198103120 ) ) ;
#45996 = CARTESIAN_POINT ( 'NONE',  ( -21.53943276465977519, -0.05219959533937600094, 103.7510903946857042 ) ) ;
#45997 = CARTESIAN_POINT ( 'NONE',  ( 8.224510206698742110, 14.34966873604972548, 22.08442372801901143 ) ) ;
#45998 = CARTESIAN_POINT ( 'NONE',  ( -10.81492255796105439, 18.62759615963255655, 72.91775706135234714 ) ) ;
#45999 = CARTESIAN_POINT ( 'NONE',  ( 9.474510206698729675, 16.51473224551082808, 52.08442372801900433 ) ) ;
#46000 = CARTESIAN_POINT ( 'NONE',  ( -0.05219959533909027116, -19.03943276465977164, 92.49890960531436690 ) ) ;
#46001 = CARTESIAN_POINT ( 'NONE',  ( 16.46253265017160672, -9.564922557960803928, 88.33224293864769550 ) ) ;
#46002 = CARTESIAN_POINT ( 'NONE',  ( -18.39443945427638738, 5.500000000000030198, 38.51745347608652281 ) ) ;
#46003 = CARTESIAN_POINT ( 'NONE',  ( 10.81492255796078972, 18.62759615963270932, 104.5822429386477097 ) ) ;
#46004 = CARTESIAN_POINT ( 'NONE',  ( -8.224510206698948167, 14.34966873604960824, 65.41557627198102409 ) ) ;
#46005 = CARTESIAN_POINT ( 'NONE',  ( 10.81492255796078972, 18.62759615963270932, 59.58224293864770260 ) ) ;
#46006 = CARTESIAN_POINT ( 'NONE',  ( -0.05219959533909027116, -19.03943276465977164, 57.49890960531435979 ) ) ;
#46008 = CARTESIAN_POINT ( 'NONE',  ( -14.34966873604972548, 8.224510206698743886, 93.33442372801901854 ) ) ;
#46007 = CARTESIAN_POINT ( 'NONE',  ( -15.72974639402197994, 15.80617190586746368, 95.62390960531436690 ) ) ;
#46009 = ORIENTED_EDGE ( 'NONE', *, *, #31131, .T. ) ;
#46010 = CARTESIAN_POINT ( 'NONE',  ( -5.153800228976328057, -19.02544592524343514, 42.29057627198101699 ) ) ;
#46012 = DIRECTION ( 'NONE',  ( -0.000000000000000000, -0.000000000000000000, 1.000000000000000000 ) ) ;
#46011 = CARTESIAN_POINT ( 'NONE',  ( 14.29746914071049879, -8.314922557960816363, 93.33224293864769550 ) ) ;
#46013 = CARTESIAN_POINT ( 'NONE',  ( 13.89961937509977652, -13.97604488694527269, 53.12390960531434558 ) ) ;
#46014 = CARTESIAN_POINT ( 'NONE',  ( 19.05341960407617918, -5.049401038297876454, 86.04275706135233293 ) ) ;
#46015 = CARTESIAN_POINT ( 'NONE',  ( 8.314922557960818139, 14.29746914071049879, 89.58224293864768129 ) ) ;
#46016 = CARTESIAN_POINT ( 'NONE',  ( -10.72451020669870658, -18.67979575497194134, 49.58442372801901143 ) ) ;
#46018 = CARTESIAN_POINT ( 'NONE',  ( 5.719274019375991003, -21.55341960407610458, 97.70724293864772392 ) ) ;
#46017 = CARTESIAN_POINT ( 'NONE',  ( 19.05341960407611168, 5.049401038298154454, 33.95724293864769550 ) ) ;
#46019 = CARTESIAN_POINT ( 'NONE',  ( 8.314922557960818139, 14.29746914071049879, 94.58224293864769550 ) ) ;
#46020 = CARTESIAN_POINT ( 'NONE',  ( 8.543935154430876366, -46.31530851241901559, -24.25021605108609535 ) ) ;
#46021 = CARTESIAN_POINT ( 'NONE',  ( -0.05219959533909027116, -19.03943276465977164, 62.49890960531435979 ) ) ;
#46022 = CARTESIAN_POINT ( 'NONE',  ( 17.48853670773245028, 5.747243402303095827, 113.8332870025000716 ) ) ;
#46024 = CARTESIAN_POINT ( 'NONE',  ( 9.564922557960805705, 16.46253265017160317, 109.5822429386476955 ) ) ;
#46023 = CARTESIAN_POINT ( 'NONE',  ( -5.153800228976607833, 19.02544592524334988, 97.70942372801900433 ) ) ;
#46025 = CARTESIAN_POINT ( 'NONE',  ( -0.05219959533937732626, 21.53943276465977519, 42.50109039468567573 ) ) ;
#46026 = CARTESIAN_POINT ( 'NONE',  ( 13.97604488694527802, 13.89961937509977652, 79.37390960531435269 ) ) ;
#46027 = CARTESIAN_POINT ( 'NONE',  ( -16.46253265017146816, -9.564922557961047289, 64.16775706135233293 ) ) ;
#46028 = CARTESIAN_POINT ( 'NONE',  ( -19.02544592524342804, 5.153800228976336051, 61.04057627198103120 ) ) ;
#46029 = B_SPLINE_CURVE_WITH_KNOTS ( 'NONE', 3,
 ( #92990, #154676, #16171, #126319, #976, #184030, #171839, #2978, #124329, #33326, #64657, #188016, #109165, #170845, #155669, #107167, #17165, #78818, #156672, #91984, #1985, #94987, #173839, #112147, #35305, #175819, #161641, #143462, #130280, #66631, #174820, #23135 ),
 .UNSPECIFIED., .F., .F.,
 ( 4, 2, 2, 2, 2, 2, 2, 2, 2, 2, 2, 2, 2, 2, 2, 4 ),
 ( 7.806255641895631925E-18, 0.0003712461730036880790, 0.0007424923460073683517, 0.001113738519011048516, 0.001484984692014728897, 0.002227477038022087057, 0.002598723211025766571, 0.002969969384029446085, 0.003341215557033124731, 0.003712461730036803811, 0.004083707903040482458, 0.004454954076044161104, 0.004826200249047840618, 0.005197446422051519264, 0.005568692595055198778, 0.005939938768058877425 ),
 .UNSPECIFIED. ) ;
#46030 = CARTESIAN_POINT ( 'NONE',  ( 0.05219959533910956823, 16.53943276465976808, 74.99890960531435269 ) ) ;
#46031 = CARTESIAN_POINT ( 'NONE',  ( -14.34966873604960291, -8.224510206698953496, 61.66557627198103120 ) ) ;
#46032 = CARTESIAN_POINT ( 'NONE',  ( 0.05219959533909260263, 19.03943276465977164, 84.99890960531436690 ) ) ;
#46033 = CARTESIAN_POINT ( 'NONE',  ( -10.81492255796078084, -18.62759615963271287, 97.08224293864770971 ) ) ;
#46034 = CARTESIAN_POINT ( 'NONE',  ( -13.89961937509977652, 13.97604488694528158, 85.62390960531433848 ) ) ;
#46035 = CARTESIAN_POINT ( 'NONE',  ( -19.02544592524334988, -5.153800228976617603, 28.95942372801900433 ) ) ;
#46038 = CARTESIAN_POINT ( 'NONE',  ( -12.06949235617756955, 12.14591786802309770, 110.6239096053143669 ) ) ;
#46037 = CARTESIAN_POINT ( 'NONE',  ( 12.14591786802309770, 12.06949235617756955, 34.37390960531435979 ) ) ;
#46036 = CARTESIAN_POINT ( 'NONE',  ( -19.02544592524342804, 5.153800228976336051, 41.04057627198103120 ) ) ;
#46039 = VERTEX_POINT ( 'NONE', #86683 ) ;
#46040 = CARTESIAN_POINT ( 'NONE',  ( 10.81492255796106328, -18.62759615963255655, 35.41775706135234003 ) ) ;
#46041 = CARTESIAN_POINT ( 'NONE',  ( -19.02544592524334988, -5.153800228976617603, 63.95942372801899012 ) ) ;
#46042 = CARTESIAN_POINT ( 'NONE',  ( -12.14591786802309592, -12.06949235617757132, 31.87390960531435979 ) ) ;
#46043 = CARTESIAN_POINT ( 'NONE',  ( -21.55341960407610458, -5.719274019375992779, 91.45724293864769550 ) ) ;
#46044 = CARTESIAN_POINT ( 'NONE',  ( 15.80617190586746368, 15.72974639402197994, 24.37390960531435979 ) ) ;
#46045 = CARTESIAN_POINT ( 'NONE',  ( 4.379528057220339221, -16.55341960407611168, 67.70724293864769550 ) ) ;
#46046 = CARTESIAN_POINT ( 'NONE',  ( 19.03943276465977164, -0.05219959533909143690, 33.74890960531435979 ) ) ;
#46047 = CARTESIAN_POINT ( 'NONE',  ( 9.474510206698729675, 16.51473224551082808, 32.08442372801900433 ) ) ;
#46048 = CARTESIAN_POINT ( 'NONE',  ( -16.52544592524335698, -4.483927247898792601, 108.9594237280190185 ) ) ;
#46049 = CARTESIAN_POINT ( 'NONE',  ( 4.483927247898790824, -16.52544592524335698, 55.20942372801902565 ) ) ;
#46050 = CARTESIAN_POINT ( 'NONE',  ( 10.72451020669898902, -18.67979575497178502, 42.91557627198103120 ) ) ;
#46051 = CARTESIAN_POINT ( 'NONE',  ( -5.823673210054431948, 21.52544592524334988, 112.7094237280190328 ) ) ;
#46052 = CARTESIAN_POINT ( 'NONE',  ( 5.049401038298161559, -19.05341960407611168, 82.70724293864770971 ) ) ;
#46053 = CARTESIAN_POINT ( 'NONE',  ( 12.14591786802327356, -12.06949235617739191, 55.62609039468568284 ) ) ;
#46054 = CARTESIAN_POINT ( 'NONE',  ( 0.05219959533909260263, 19.03943276465977164, 29.99890960531435979 ) ) ;
#46055 = CARTESIAN_POINT ( 'NONE',  ( 12.14591786802309770, 12.06949235617756955, 34.37390960531435979 ) ) ;
#46057 = CARTESIAN_POINT ( 'NONE',  ( 9.474510206698971260, -16.51473224551069308, 87.91557627198102409 ) ) ;
#46056 = CARTESIAN_POINT ( 'NONE',  ( 19.05341960407611168, 5.049401038298154454, 108.9572429386477097 ) ) ;
#46058 = CARTESIAN_POINT ( 'NONE',  ( 5.049401038298161559, -19.05341960407611168, 102.7072429386476955 ) ) ;
#46059 = CARTESIAN_POINT ( 'NONE',  ( 12.06949235617757843, -12.14591786802309237, 53.12390960531436690 ) ) ;
#46060 = EDGE_CURVE ( 'NONE', #145210, #138331, #77238, .T. ) ;
#46061 = CARTESIAN_POINT ( 'NONE',  ( 8.224510206698953496, -14.34966873604960469, 27.91557627198103830 ) ) ;
#46062 = VERTEX_POINT ( 'NONE', #123724 ) ;
#46063 = CARTESIAN_POINT ( 'NONE',  ( 16.55341960407611168, 4.379528057220329451, 48.95724293864770971 ) ) ;
#46065 = PLANE ( 'NONE',  #70588 ) ;
#46064 = CARTESIAN_POINT ( 'NONE',  ( 16.52544592524335698, 4.483927247898782831, 41.45942372801901143 ) ) ;
#46066 = CARTESIAN_POINT ( 'NONE',  ( 9.474510206698729675, 16.51473224551082808, 47.08442372801900433 ) ) ;
#46067 = CARTESIAN_POINT ( 'NONE',  ( -5.049401038298153566, 19.05341960407611168, 85.20724293864766707 ) ) ;
#46068 = CARTESIAN_POINT ( 'NONE',  ( 19.02544592524334988, 5.153800228976608722, 71.45942372801900433 ) ) ;
#46069 = CARTESIAN_POINT ( 'NONE',  ( 8.571926809382603096, -26.38167802310801235, 143.9750000027312069 ) ) ;
#46070 = CARTESIAN_POINT ( 'NONE',  ( -5.153800228976607833, 19.02544592524334988, 52.70942372801900433 ) ) ;
#46072 = CARTESIAN_POINT ( 'NONE',  ( -16.53943276465976808, -0.05219959533934237506, 83.75109039468568994 ) ) ;
#46071 = CARTESIAN_POINT ( 'NONE',  ( 19.02544592524334988, 5.153800228976608722, 96.45942372801897591 ) ) ;
#46073 = CARTESIAN_POINT ( 'NONE',  ( -27.73933785331498925, 9.013057229001089965, 147.2750000027311614 ) ) ;
#46074 = CARTESIAN_POINT ( 'NONE',  ( -19.05341960407611168, -5.049401038298163336, 21.45724293864768839 ) ) ;
#46075 = CARTESIAN_POINT ( 'NONE',  ( -16.46253265017160317, 9.564922557960807481, 110.8322429386476955 ) ) ;
#46076 = CARTESIAN_POINT ( 'NONE',  ( -10.81492255796105439, 18.62759615963255655, 42.91775706135235424 ) ) ;
#46077 = CARTESIAN_POINT ( 'NONE',  ( -16.46253265017146816, -9.564922557961047289, 104.1677570613523329 ) ) ;
#46079 = CARTESIAN_POINT ( 'NONE',  ( -19.05341960407611168, -5.049401038298163336, 61.45724293864769550 ) ) ;
#46078 = CARTESIAN_POINT ( 'NONE',  ( 17.49999999999999645, -5.076555817581239083, 106.3204850795022764 ) ) ;
#46080 = CARTESIAN_POINT ( 'NONE',  ( -0.05219959533909027116, -19.03943276465977164, 97.49890960531436690 ) ) ;
#46082 = CARTESIAN_POINT ( 'NONE',  ( -19.02544592524342804, 5.153800228976336051, 61.04057627198103120 ) ) ;
#46081 = CARTESIAN_POINT ( 'NONE',  ( -16.53943276465976808, 0.05219959533911058130, 66.24890960531436690 ) ) ;
#46083 = CARTESIAN_POINT ( 'NONE',  ( -9.474510206698964154, 16.51473224551069663, 80.41557627198103830 ) ) ;
#46084 = CARTESIAN_POINT ( 'NONE',  ( 16.51473224551083163, -9.474510206698727899, 75.83442372801900433 ) ) ;
#46085 = CARTESIAN_POINT ( 'NONE',  ( 10.72451020669898902, -18.67979575497178502, 52.91557627198103830 ) ) ;
#46086 = CARTESIAN_POINT ( 'NONE',  ( -8.224510206698948167, 14.34966873604960824, 115.4155762719810241 ) ) ;
#46087 = CARTESIAN_POINT ( 'NONE',  ( 19.02544592524334988, 5.153800228976608722, 41.45942372801900433 ) ) ;
#46088 = CARTESIAN_POINT ( 'NONE',  ( -0.05219959533909027116, -19.03943276465977164, 82.49890960531436690 ) ) ;
#46089 = CARTESIAN_POINT ( 'NONE',  ( 21.52544592524344225, -5.823673210054117533, 78.54057627198103830 ) ) ;
#46091 = CARTESIAN_POINT ( 'NONE',  ( -16.46253265017146816, -9.564922557961047289, 29.16775706135232937 ) ) ;
#46090 = CARTESIAN_POINT ( 'NONE',  ( -14.34966873604960291, -8.224510206698953496, 81.66557627198103830 ) ) ;
#46092 = CARTESIAN_POINT ( 'NONE',  ( 18.62759615963271287, -10.81492255796078972, 58.33224293864768839 ) ) ;
#46093 = CARTESIAN_POINT ( 'NONE',  ( -21.55341960407610458, -5.719274019375992779, 36.45724293864768839 ) ) ;
#46094 = CARTESIAN_POINT ( 'NONE',  ( 5.719274019375673035, 21.55341960407619339, 97.29275706135234714 ) ) ;
#46095 = CARTESIAN_POINT ( 'NONE',  ( -5.153800228976328057, -19.02544592524343514, 62.29057627198100988 ) ) ;
#46096 = CARTESIAN_POINT ( 'NONE',  ( 0.05219959533910956823, 16.53943276465976808, 109.9989096053143527 ) ) ;
#46097 = CARTESIAN_POINT ( 'NONE',  ( -21.55341960407619339, 5.719274019375674811, 28.54275706135234358 ) ) ;
#46098 = CARTESIAN_POINT ( 'NONE',  ( -19.20446147854528718, -5.499999999999909406, 39.38999695167677118 ) ) ;
#46099 = CARTESIAN_POINT ( 'NONE',  ( -15.72974639402176322, -15.80617190586768395, 39.37609039468567573 ) ) ;
#46100 = CARTESIAN_POINT ( 'NONE',  ( 19.03943276465977164, -0.05219959533909143690, 38.74890960531436690 ) ) ;
#46101 = CARTESIAN_POINT ( 'NONE',  ( 15.72974639402199770, -15.80617190586745480, 108.1239096053143811 ) ) ;
#46102 = CARTESIAN_POINT ( 'NONE',  ( 16.51473224551083163, -9.474510206698727899, 50.83442372801899722 ) ) ;
#46103 = CARTESIAN_POINT ( 'NONE',  ( -19.03943276465977164, 0.05219959533909376836, 21.24890960531436335 ) ) ;
#46104 = CARTESIAN_POINT ( 'NONE',  ( 9.474510206698971260, -16.51473224551069308, 22.91557627198102765 ) ) ;
#46105 = CYLINDRICAL_SURFACE ( 'NONE', #62730, 2.500000000000002220 ) ;
#46106 = CARTESIAN_POINT ( 'NONE',  ( -8.314922557961024197, 14.29746914071037800, 57.91775706135234714 ) ) ;
#46107 = CARTESIAN_POINT ( 'NONE',  ( 19.03943276465977164, -0.05219959533909143690, 28.74890960531435624 ) ) ;
#46108 = CARTESIAN_POINT ( 'NONE',  ( -25.27727188472087505, -10.29814791481089387, 170.4127952078933106 ) ) ;
#46109 = CARTESIAN_POINT ( 'NONE',  ( 0.05219959533909260263, 19.03943276465977164, 69.99890960531435269 ) ) ;
#46110 = CARTESIAN_POINT ( 'NONE',  ( -16.52544592524342804, 4.483927247898546575, 101.0405762719810383 ) ) ;
#46111 = CIRCLE ( 'NONE', #159091, 1.999999999999999556 ) ;
#46112 = CARTESIAN_POINT ( 'NONE',  ( -10.72451020669898014, 18.67979575497178502, 55.41557627198102409 ) ) ;
#46113 = CARTESIAN_POINT ( 'NONE',  ( 12.06949235617739724, 12.14591786802326823, 41.87609039468568284 ) ) ;
#46114 = CARTESIAN_POINT ( 'NONE',  ( 21.55341960407619695, -5.719274019375665929, 106.0427570613523471 ) ) ;
#46115 = CARTESIAN_POINT ( 'NONE',  ( 19.03943276465977164, -0.05219959533909143690, 23.74890960531435269 ) ) ;
#46116 = CARTESIAN_POINT ( 'NONE',  ( 12.14591786802309770, 12.06949235617756955, 24.37390960531435979 ) ) ;
#46117 = CARTESIAN_POINT ( 'NONE',  ( -4.379528057220328563, 16.55341960407611168, 50.20724293864769550 ) ) ;
#46118 = CARTESIAN_POINT ( 'NONE',  ( -9.564922557960796823, -16.46253265017161027, 47.08224293864769550 ) ) ;
#46119 = CARTESIAN_POINT ( 'NONE',  ( 0.05219959533937995610, -21.53943276465977519, 90.00109039468567573 ) ) ;
#46120 = CARTESIAN_POINT ( 'NONE',  ( 18.67979575497178502, 10.72451020669898547, 109.1655762719810383 ) ) ;
#46121 = CARTESIAN_POINT ( 'NONE',  ( 5.719274019375673035, 21.55341960407619339, 72.29275706135236135 ) ) ;
#46122 = CARTESIAN_POINT ( 'NONE',  ( 16.55341960407618274, -4.379528057220086978, 56.04275706135235424 ) ) ;
#46124 = CARTESIAN_POINT ( 'NONE',  ( -15.80617190586768217, 15.72974639402176855, 103.1260903946856757 ) ) ;
#46123 = CARTESIAN_POINT ( 'NONE',  ( 4.379528057220339221, -16.55341960407611168, 77.70724293864770971 ) ) ;
#46125 = CARTESIAN_POINT ( 'NONE',  ( -16.55341960407611168, -4.379528057220339221, 21.45724293864769550 ) ) ;
#46126 = CARTESIAN_POINT ( 'NONE',  ( -16.19135201231366850, 7.376712067591915556, 114.8131914594797394 ) ) ;
#46127 = CARTESIAN_POINT ( 'NONE',  ( -16.52544592524335698, -4.483927247898792601, 33.95942372801901143 ) ) ;
#46128 = CARTESIAN_POINT ( 'NONE',  ( -4.379528057220328563, 16.55341960407611168, 40.20724293864769550 ) ) ;
#46130 = CARTESIAN_POINT ( 'NONE',  ( -16.55341960407617563, 4.379528057220093196, 83.54275706135234714 ) ) ;
#46129 = B_SPLINE_CURVE_WITH_KNOTS ( 'NONE', 3,
 ( #20044, #175725, #37204, #98860, #156582, #143369, #63572, #157574, #18077, #79732, #141401, #187928, #111060, #19067, #142392, #3871, #65550, #23046, #176740, #85705, #160555, #164562, #41216, #101878, #56373, #22045, #9882, #148388, #145374, #40198, #178735, #7858 ),
 .UNSPECIFIED., .F., .F.,
 ( 4, 2, 2, 2, 2, 2, 2, 2, 2, 2, 2, 2, 2, 2, 2, 4 ),
 ( 2.883244014823444873E-17, 0.0003712461730037120398, 0.0007424923460073952399, 0.001113738519011078440, 0.001484984692014761640, 0.002227477038022125221, 0.002598723211025809939, 0.002969969384029495525, 0.003341215557033180676, 0.003712461730036866261, 0.004083707903040550979, 0.004454954076044235697, 0.004826200249047921283, 0.005197446422051606868, 0.005568692595055292453, 0.005939938768058977171 ),
 .UNSPECIFIED. ) ;
#46131 = CARTESIAN_POINT ( 'NONE',  ( -13.89961937509977652, 13.97604488694528158, 105.6239096053143527 ) ) ;
#46132 = CARTESIAN_POINT ( 'NONE',  ( -9.474510206698964154, 16.51473224551069663, 110.4155762719810383 ) ) ;
#46133 = CARTESIAN_POINT ( 'NONE',  ( -21.52544592524334988, -5.823673210054445271, 93.95942372801903275 ) ) ;
#46134 = CARTESIAN_POINT ( 'NONE',  ( 16.55341960407618274, -4.379528057220086978, 106.0427570613523471 ) ) ;
#46135 = CARTESIAN_POINT ( 'NONE',  ( 16.53943276465976808, -0.05219959533910856209, 68.74890960531435269 ) ) ;
#46136 = CARTESIAN_POINT ( 'NONE',  ( 9.564922557960805705, 16.46253265017160317, 79.58224293864769550 ) ) ;
#46137 = ORIENTED_EDGE ( 'NONE', *, *, #21608, .T. ) ;
#46138 = CARTESIAN_POINT ( 'NONE',  ( 16.53943276465976808, 0.05219959533934440121, 46.25109039468567573 ) ) ;
#46139 = CARTESIAN_POINT ( 'NONE',  ( -9.564922557960796823, -16.46253265017161027, 37.08224293864768839 ) ) ;
#46140 = CARTESIAN_POINT ( 'NONE',  ( 9.474510206698971260, -16.51473224551069308, 92.91557627198103830 ) ) ;
#46142 = DIRECTION ( 'NONE',  ( -0.000000000000000000, -0.000000000000000000, 1.000000000000000000 ) ) ;
#46141 = CARTESIAN_POINT ( 'NONE',  ( -14.34966873604972548, 8.224510206698743886, 38.33442372801900433 ) ) ;
#46143 = CARTESIAN_POINT ( 'NONE',  ( 13.89961937509957401, 13.97604488694547697, 31.87609039468566863 ) ) ;
#46144 = CARTESIAN_POINT ( 'NONE',  ( 16.52544592524335698, 4.483927247898782831, 96.45942372801901854 ) ) ;
#46145 = CARTESIAN_POINT ( 'NONE',  ( -9.564922557960796823, -16.46253265017161027, 37.08224293864768839 ) ) ;
#46146 = CARTESIAN_POINT ( 'NONE',  ( -16.53943276465976808, -0.05219959533934237506, 78.75109039468568994 ) ) ;
#46147 = CARTESIAN_POINT ( 'NONE',  ( 8.314922557961029526, -14.29746914071037800, 70.41775706135236135 ) ) ;
#46148 = CARTESIAN_POINT ( 'NONE',  ( -13.89961937509957401, -13.97604488694547875, 84.37609039468567573 ) ) ;
#46149 = CARTESIAN_POINT ( 'NONE',  ( 19.05341960407617918, -5.049401038297876454, 26.04275706135233293 ) ) ;
#46150 = CARTESIAN_POINT ( 'NONE',  ( -9.564922557960796823, -16.46253265017161027, 52.08224293864768839 ) ) ;
#46151 = CARTESIAN_POINT ( 'NONE',  ( -8.314922557960811034, -14.29746914071050412, 87.08224293864769550 ) ) ;
#46152 = ADVANCED_FACE ( 'NONE', ( #118034 ), #70525, .F. ) ;
#46153 = CARTESIAN_POINT ( 'NONE',  ( -13.89961937509957401, -13.97604488694547875, 54.37609039468565442 ) ) ;
#46154 = CARTESIAN_POINT ( 'NONE',  ( 21.52544592524344225, -5.823673210054117533, 53.54057627198103120 ) ) ;
#46155 = CARTESIAN_POINT ( 'NONE',  ( -19.03943276465977164, -0.05219959533935918106, 33.75109039468566863 ) ) ;
#46156 = CARTESIAN_POINT ( 'NONE',  ( -19.05341960407611168, -5.049401038298163336, 101.4572429386476955 ) ) ;
#46157 = CARTESIAN_POINT ( 'NONE',  ( -15.72974639402197994, 15.80617190586746368, 80.62390960531438111 ) ) ;
#46158 = CARTESIAN_POINT ( 'NONE',  ( 9.474510206698971260, -16.51473224551069308, 112.9155762719810383 ) ) ;
#46159 = CARTESIAN_POINT ( 'NONE',  ( -5.153800228976607833, 19.02544592524334988, 102.7094237280189759 ) ) ;
#46160 = CARTESIAN_POINT ( 'NONE',  ( 9.474510206698971260, -16.51473224551069308, 112.9155762719810383 ) ) ;
#46161 = CARTESIAN_POINT ( 'NONE',  ( 9.474510206698729675, 16.51473224551082808, 107.0844237280190043 ) ) ;
#46162 = CARTESIAN_POINT ( 'NONE',  ( -16.46253265017160317, 9.564922557960807481, 35.83224293864768839 ) ) ;
#46163 = CARTESIAN_POINT ( 'NONE',  ( -19.02544592524342804, 5.153800228976336051, 101.0405762719810241 ) ) ;
#46164 = CARTESIAN_POINT ( 'NONE',  ( 21.55341960407610458, 5.719274019375980345, 73.95724293864769550 ) ) ;
#46165 = CARTESIAN_POINT ( 'NONE',  ( -8.224510206698735004, -14.34966873604973081, 49.58442372801901143 ) ) ;
#46166 = CARTESIAN_POINT ( 'NONE',  ( -21.53943276465977519, -0.05219959533937600094, 63.75109039468568284 ) ) ;
#46168 = CARTESIAN_POINT ( 'NONE',  ( 18.62759615963255655, 10.81492255796105972, 111.6677570613523613 ) ) ;
#46167 = CARTESIAN_POINT ( 'NONE',  ( 19.02544592524334988, 5.153800228976608722, 101.4594237280189759 ) ) ;
#46169 = CARTESIAN_POINT ( 'NONE',  ( 12.14591786802327356, -12.06949235617739191, 105.6260903946856899 ) ) ;
#46170 = PRODUCT_RELATED_PRODUCT_CATEGORY ( 'part', '', ( #184101 ) ) ;
#46171 = CARTESIAN_POINT ( 'NONE',  ( 21.52544592524344225, -5.823673210054117533, 98.54057627198105251 ) ) ;
#46172 = CARTESIAN_POINT ( 'NONE',  ( 12.14591786802309770, 12.06949235617756955, 39.37390960531436690 ) ) ;
#46173 = CARTESIAN_POINT ( 'NONE',  ( 13.89961937509957401, 13.97604488694547697, 86.87609039468567573 ) ) ;
#46174 = CARTESIAN_POINT ( 'NONE',  ( 18.62759615963255655, 10.81492255796105972, 56.66775706135235424 ) ) ;
#46175 = CARTESIAN_POINT ( 'NONE',  ( -16.46253265017146816, -9.564922557961047289, 44.16775706135232582 ) ) ;
#46176 = CARTESIAN_POINT ( 'NONE',  ( -4.379528057220328563, 16.55341960407611168, 100.2072429386476955 ) ) ;
#46177 = CARTESIAN_POINT ( 'NONE',  ( 21.55341960407610458, 5.719274019375980345, 28.95724293864769905 ) ) ;
#46178 = CARTESIAN_POINT ( 'NONE',  ( 4.379528057220339221, -16.55341960407611168, 32.70724293864770260 ) ) ;
#46179 = CARTESIAN_POINT ( 'NONE',  ( -10.72451020669870658, -18.67979575497194134, 104.5844237280190185 ) ) ;
#46180 = CARTESIAN_POINT ( 'NONE',  ( 14.29746914071037800, 8.314922557961029526, 56.66775706135235424 ) ) ;
#46181 = CARTESIAN_POINT ( 'NONE',  ( -16.55341960407617563, 4.379528057220093196, 113.5427570613523756 ) ) ;
#46182 = CARTESIAN_POINT ( 'NONE',  ( 18.67979575497194134, -10.72451020669871369, 60.83442372801901854 ) ) ;
#46183 = CARTESIAN_POINT ( 'NONE',  ( -18.62759615963255300, -10.81492255796106328, 59.16775706135234714 ) ) ;
#46184 = ORIENTED_EDGE ( 'NONE', *, *, #97135, .F. ) ;
#46185 = CARTESIAN_POINT ( 'NONE',  ( -13.89961937509977652, 13.97604488694528158, 30.62390960531435269 ) ) ;
#46186 = CARTESIAN_POINT ( 'NONE',  ( 10.81492255796106328, -18.62759615963255655, 25.41775706135235779 ) ) ;
#46187 = CARTESIAN_POINT ( 'NONE',  ( -12.06949235617756955, 12.14591786802309770, 105.6239096053143669 ) ) ;
#46188 = CARTESIAN_POINT ( 'NONE',  ( 20.02699684519809509, -3.713461942911806979, 37.50000000000000000 ) ) ;
#46189 = CARTESIAN_POINT ( 'NONE',  ( -4.483927247898539470, -16.52544592524342804, 77.29057627198102409 ) ) ;
#46190 = CARTESIAN_POINT ( 'NONE',  ( -13.89961937509977652, 13.97604488694528158, 70.62390960531432427 ) ) ;
#46191 = CARTESIAN_POINT ( 'NONE',  ( 12.14591786802309770, 12.06949235617756955, 24.37390960531435979 ) ) ;
#46192 = CARTESIAN_POINT ( 'NONE',  ( 5.719274019375991003, -21.55341960407610458, 57.70724293864770260 ) ) ;
#46193 = CARTESIAN_POINT ( 'NONE',  ( 16.55341960407611168, 4.379528057220329451, 88.95724293864769550 ) ) ;
#46194 = CARTESIAN_POINT ( 'NONE',  ( -15.80617190586745835, -15.72974639402198527, 101.8739096053143811 ) ) ;
#46195 = CARTESIAN_POINT ( 'NONE',  ( -13.97604488694527625, -13.89961937509977652, 96.87390960531433848 ) ) ;
#46197 = CARTESIAN_POINT ( 'NONE',  ( 19.03943276465977164, 0.05219959533936151252, 111.2510903946856757 ) ) ;
#46196 = CARTESIAN_POINT ( 'NONE',  ( 9.564922557960805705, 16.46253265017160317, 49.58224293864770260 ) ) ;
#46198 = CARTESIAN_POINT ( 'NONE',  ( -21.53943276465977519, 0.05219959533907696930, 61.24890960531435979 ) ) ;
#46199 = CARTESIAN_POINT ( 'NONE',  ( 18.62759615963255655, 10.81492255796105972, 81.66775706135236135 ) ) ;
#46200 = CARTESIAN_POINT ( 'NONE',  ( -5.153800228976328057, -19.02544592524343514, 72.29057627198102409 ) ) ;
#46201 = CARTESIAN_POINT ( 'NONE',  ( 9.564922557960805705, 16.46253265017160317, 99.58224293864770971 ) ) ;
#46202 = CARTESIAN_POINT ( 'NONE',  ( 12.14591786802327356, -12.06949235617739191, 80.62609039468567573 ) ) ;
#46203 = CARTESIAN_POINT ( 'NONE',  ( -18.62759615963255300, -10.81492255796106328, 54.16775706135235424 ) ) ;
#46204 = CARTESIAN_POINT ( 'NONE',  ( -0.05219959533937732626, 21.53943276465977519, 87.50109039468568994 ) ) ;
#46205 = CARTESIAN_POINT ( 'NONE',  ( -10.72451020669898014, 18.67979575497178502, 115.4155762719810241 ) ) ;
#46206 = CARTESIAN_POINT ( 'NONE',  ( 14.29746914071037800, 8.314922557961029526, 81.66775706135236135 ) ) ;
#46207 = CARTESIAN_POINT ( 'NONE',  ( 10.72451020669898902, -18.67979575497178502, 77.91557627198102409 ) ) ;
#46208 = CARTESIAN_POINT ( 'NONE',  ( 16.51473224551083163, -9.474510206698727899, 40.83442372801900433 ) ) ;
#46209 = CARTESIAN_POINT ( 'NONE',  ( -21.55341960407610458, -5.719274019375992779, 36.45724293864768839 ) ) ;
#46211 = CARTESIAN_POINT ( 'NONE',  ( -14.34966873604960291, -8.224510206698953496, 21.66557627198102409 ) ) ;
#46210 = CARTESIAN_POINT ( 'NONE',  ( 0.05219959533909260263, 19.03943276465977164, 84.99890960531436690 ) ) ;
#46212 = DIRECTION ( 'NONE',  ( 0.000000000000000000, 0.000000000000000000, -1.000000000000000000 ) ) ;
#46214 = VECTOR ( 'NONE', #61172, 1000.000000000000114 ) ;
#46213 = CARTESIAN_POINT ( 'NONE',  ( -13.97604488694527625, -13.89961937509977652, 111.8739096053143243 ) ) ;
#46215 = CARTESIAN_POINT ( 'NONE',  ( 37.58407650405589351, 2.428612866815129610E-14, 39.49999999999996447 ) ) ;
#46216 = CARTESIAN_POINT ( 'NONE',  ( -5.049401038297874678, -19.05341960407617918, 99.79275706135234714 ) ) ;
#46217 = CARTESIAN_POINT ( 'NONE',  ( 5.823673210054125526, 21.52544592524343514, 69.79057627198102409 ) ) ;
#46218 = CARTESIAN_POINT ( 'NONE',  ( -0.05219959533910754901, -16.53943276465976808, 47.49890960531435979 ) ) ;
#46219 = CARTESIAN_POINT ( 'NONE',  ( 9.564922557961047289, -16.46253265017146816, 110.4177570613523471 ) ) ;
#46220 = CARTESIAN_POINT ( 'NONE',  ( 9.564922557960805705, 16.46253265017160317, 29.58224293864769550 ) ) ;
#46221 = CARTESIAN_POINT ( 'NONE',  ( 0.05219959533936267826, -19.03943276465977164, 110.0010903946856757 ) ) ;
#46223 = CARTESIAN_POINT ( 'NONE',  ( 13.97604488694548053, -13.89961937509957401, 75.62609039468564731 ) ) ;
#46222 = CARTESIAN_POINT ( 'NONE',  ( 15.80617190586746368, 15.72974639402197994, 94.37390960531436690 ) ) ;
#46224 = CARTESIAN_POINT ( 'NONE',  ( 4.379528057220092307, 16.55341960407617563, 82.29275706135234714 ) ) ;
#46225 = CARTESIAN_POINT ( 'NONE',  ( -19.02544592524342804, 5.153800228976336051, 81.04057627198103830 ) ) ;
#46226 = CARTESIAN_POINT ( 'NONE',  ( 8.224510206698953496, -14.34966873604960469, 82.91557627198103830 ) ) ;
#46227 = CARTESIAN_POINT ( 'NONE',  ( -16.51473224551069308, -9.474510206698971260, 56.66557627198103120 ) ) ;
#46228 = CARTESIAN_POINT ( 'NONE',  ( -16.53943276465976808, 0.05219959533911058130, 66.24890960531436690 ) ) ;
#46229 = CARTESIAN_POINT ( 'NONE',  ( -9.564922557960796823, -16.46253265017161027, 27.08224293864769550 ) ) ;
#46230 = CARTESIAN_POINT ( 'NONE',  ( -36.87149605698876087, -2.274342727564272693, 50.01098105774816105 ) ) ;
#46231 = CARTESIAN_POINT ( 'NONE',  ( -4.483927247898539470, -16.52544592524342804, 42.29057627198103120 ) ) ;
#46232 = CARTESIAN_POINT ( 'NONE',  ( 9.564922557960805705, 16.46253265017160317, 79.58224293864769550 ) ) ;
#46233 = FACE_BOUND ( 'NONE', #23007, .T. ) ;
#46234 = CARTESIAN_POINT ( 'NONE',  ( 19.03943276465977164, 0.05219959533936151252, 56.25109039468566863 ) ) ;
#46235 = CARTESIAN_POINT ( 'NONE',  ( -14.34966873604972548, 8.224510206698743886, 63.33442372801900433 ) ) ;
#46236 = CARTESIAN_POINT ( 'NONE',  ( -21.52544592524343514, 5.823673210054127303, 66.04057627198103830 ) ) ;
#46237 = CARTESIAN_POINT ( 'NONE',  ( 19.03943276465977164, 0.05219959533936151252, 26.25109039468566507 ) ) ;
#46238 = CARTESIAN_POINT ( 'NONE',  ( 19.02544592524343514, -5.153800228976328945, 88.54057627198102409 ) ) ;
#46239 = CARTESIAN_POINT ( 'NONE',  ( -20.10180177043494254, -22.06666061677796975, -48.51647576933254413 ) ) ;
#46240 = CARTESIAN_POINT ( 'NONE',  ( 15.80617190586746368, 15.72974639402197994, 24.37390960531435979 ) ) ;
#46241 = CARTESIAN_POINT ( 'NONE',  ( 16.51473224551069308, 9.474510206698969483, 59.16557627198102409 ) ) ;
#46242 = CARTESIAN_POINT ( 'NONE',  ( 21.55341960407619695, -5.719274019375665929, 56.04275706135235424 ) ) ;
#46243 = CARTESIAN_POINT ( 'NONE',  ( -8.314922557960811034, -14.29746914071050412, 112.0822429386477097 ) ) ;
#46246 = ORIENTED_EDGE ( 'NONE', *, *, #26316, .F. ) ;
#46245 = CARTESIAN_POINT ( 'NONE',  ( 19.05341960407611168, 5.049401038298154454, 98.95724293864766707 ) ) ;
#46244 = CARTESIAN_POINT ( 'NONE',  ( 15.72974639402199770, -15.80617190586745480, 103.1239096053143811 ) ) ;
#46247 = CARTESIAN_POINT ( 'NONE',  ( -21.52544592524334988, -5.823673210054445271, 33.95942372801901143 ) ) ;
#46248 = VERTEX_POINT ( 'NONE', #152108 ) ;
#46249 = CARTESIAN_POINT ( 'NONE',  ( 9.474510206698971260, -16.51473224551069308, 97.91557627198102409 ) ) ;
#46250 = AXIS2_PLACEMENT_3D ( 'NONE', #173436, #53053, #96561 ) ;
#46251 = CYLINDRICAL_SURFACE ( 'NONE', #81775, 1.999999999999999112 ) ;
#46252 = CARTESIAN_POINT ( 'NONE',  ( -18.62759615963270932, 10.81492255796079327, 90.83224293864769550 ) ) ;
#46253 = CARTESIAN_POINT ( 'NONE',  ( 9.564922557960805705, 16.46253265017160317, 44.58224293864769550 ) ) ;
#46254 = CARTESIAN_POINT ( 'NONE',  ( -0.05219959533934338120, 16.53943276465976808, 27.50109039468567929 ) ) ;
#46255 = CARTESIAN_POINT ( 'NONE',  ( -36.91746825000000598, 2.428612866367529932E-14, -5.124999997268813168 ) ) ;
#46256 = CARTESIAN_POINT ( 'NONE',  ( -5.049401038298153566, 19.05341960407611168, 25.20724293864768484 ) ) ;
#46257 = CARTESIAN_POINT ( 'NONE',  ( 0.05219959533937995610, -21.53943276465977519, 100.0010903946857042 ) ) ;
#46259 = CARTESIAN_POINT ( 'NONE',  ( 10.72451020669871369, 18.67979575497193778, 47.08442372801901854 ) ) ;
#46258 = CARTESIAN_POINT ( 'NONE',  ( 0.05219959533909260263, 19.03943276465977164, 79.99890960531436690 ) ) ;
#46260 = CARTESIAN_POINT ( 'NONE',  ( 10.72451020669871369, 18.67979575497193778, 27.08442372801901854 ) ) ;
#46261 = CARTESIAN_POINT ( 'NONE',  ( -8.571926809382608425, 26.38167802310805854, 146.9750000027311785 ) ) ;
#46262 = CARTESIAN_POINT ( 'NONE',  ( -9.564922557960796823, -16.46253265017161027, 97.08224293864769550 ) ) ;
#46263 = CARTESIAN_POINT ( 'NONE',  ( -11.70006521384596709, 26.14342653898853541, 139.9999999999999716 ) ) ;
#46266 = CARTESIAN_POINT ( 'NONE',  ( -15.80617190586768217, 15.72974639402176855, 58.12609039468568994 ) ) ;
#46265 = CARTESIAN_POINT ( 'NONE',  ( -14.29746914071037622, -8.314922557961029526, 74.16775706135231871 ) ) ;
#46264 = CARTESIAN_POINT ( 'NONE',  ( 16.55341960407618274, -4.379528057220086978, 46.04275706135234714 ) ) ;
#46267 = CARTESIAN_POINT ( 'NONE',  ( -10.81492255796105439, 18.62759615963255655, 77.91775706135231871 ) ) ;
#46268 = DIRECTION ( 'NONE',  ( -0.000000000000000000, -0.000000000000000000, 1.000000000000000000 ) ) ;
#46269 = CARTESIAN_POINT ( 'NONE',  ( -16.46253265017146816, -9.564922557961047289, 109.1677570613523471 ) ) ;
#46270 = CARTESIAN_POINT ( 'NONE',  ( -16.51473224551069308, -9.474510206698971260, 71.66557627198102409 ) ) ;
#46271 = CARTESIAN_POINT ( 'NONE',  ( -5.049401038298153566, 19.05341960407611168, 100.2072429386476955 ) ) ;
#46272 = CARTESIAN_POINT ( 'NONE',  ( 4.379528057220339221, -16.55341960407611168, 107.7072429386476955 ) ) ;
#46273 = CARTESIAN_POINT ( 'NONE',  ( -15.72974639402197994, 15.80617190586746368, 35.62390960531437401 ) ) ;
#46274 = CARTESIAN_POINT ( 'NONE',  ( 0.05219959533934541429, -16.53943276465976808, 95.00109039468568994 ) ) ;
#46276 = CARTESIAN_POINT ( 'NONE',  ( -13.89961937509977652, 13.97604488694528158, 50.62390960531435979 ) ) ;
#46275 = CARTESIAN_POINT ( 'NONE',  ( -12.06949235617756955, 12.14591786802309770, 70.62390960531436690 ) ) ;
#46277 = CARTESIAN_POINT ( 'NONE',  ( -21.53943276465977519, -0.05219959533937600094, 73.75109039468567573 ) ) ;
#46278 = LINE ( 'NONE', #199970, #98639 ) ;
#46279 = CARTESIAN_POINT ( 'NONE',  ( 9.474510206698729675, 16.51473224551082808, 102.0844237280190043 ) ) ;
#46280 = CARTESIAN_POINT ( 'NONE',  ( -12.14591786802309592, -12.06949235617757132, 81.87390960531435269 ) ) ;
#46281 = CARTESIAN_POINT ( 'NONE',  ( 21.52544592524334988, 5.823673210054432836, 26.45942372801901854 ) ) ;
#46282 = CARTESIAN_POINT ( 'NONE',  ( -21.55341960407610458, -5.719274019375992779, 61.45724293864770260 ) ) ;
#46283 = CARTESIAN_POINT ( 'NONE',  ( -16.31925111598456724, -7.325300261831553250, 104.8357546103274842 ) ) ;
#46284 = CARTESIAN_POINT ( 'NONE',  ( -35.41256452865198412, 3.967314244253445032, 38.63057146076392456 ) ) ;
#46285 = CARTESIAN_POINT ( 'NONE',  ( 5.153800228976335163, 19.02544592524342804, 84.79057627198099567 ) ) ;
#46286 = CARTESIAN_POINT ( 'NONE',  ( 16.53943276465976808, -0.05219959533910856209, 48.74890960531435979 ) ) ;
#46287 = CARTESIAN_POINT ( 'NONE',  ( 14.29746914071049879, -8.314922557960816363, 28.33224293864769550 ) ) ;
#46288 = CARTESIAN_POINT ( 'NONE',  ( -12.14591786802326823, 12.06949235617739902, 93.12609039468568994 ) ) ;
#46289 = CARTESIAN_POINT ( 'NONE',  ( 19.02544592524334988, 5.153800228976608722, 46.45942372801899012 ) ) ;
#46290 = CARTESIAN_POINT ( 'NONE',  ( 16.36317988757058117, 7.306389748694953390, 48.40210391636776421 ) ) ;
#46291 = CARTESIAN_POINT ( 'NONE',  ( -5.049401038298153566, 19.05341960407611168, 110.2072429386476671 ) ) ;
#46292 = CARTESIAN_POINT ( 'NONE',  ( 16.53943276465976808, -0.05219959533910856209, 73.74890960531433848 ) ) ;
#46293 = CARTESIAN_POINT ( 'NONE',  ( 19.03943276465977164, 0.05219959533936151252, 46.25109039468566863 ) ) ;
#46295 = CARTESIAN_POINT ( 'NONE',  ( -21.53943276465977519, 0.05219959533907696930, 41.24890960531435269 ) ) ;
#46294 = CARTESIAN_POINT ( 'NONE',  ( -0.05219959533909027116, -19.03943276465977164, 32.49890960531435979 ) ) ;
#46297 = ORIENTED_EDGE ( 'NONE', *, *, #73681, .F. ) ;
#46296 = CARTESIAN_POINT ( 'NONE',  ( 21.55341960407610458, 5.719274019375980345, 68.95724293864769550 ) ) ;
#46298 = CARTESIAN_POINT ( 'NONE',  ( -0.05219959533910754901, -16.53943276465976808, 97.49890960531436690 ) ) ;
#46299 = CARTESIAN_POINT ( 'NONE',  ( 12.14591786802327356, -12.06949235617739191, 55.62609039468568284 ) ) ;
#46300 = EDGE_CURVE ( 'NONE', #160624, #46248, #45316, .T. ) ;
#46301 = CARTESIAN_POINT ( 'NONE',  ( -12.06949235617756955, 12.14591786802309770, 90.62390960531436690 ) ) ;
#46302 = CARTESIAN_POINT ( 'NONE',  ( 17.44270441346514389, -5.991230190323080684, 36.13664920735772768 ) ) ;
#46303 = CARTESIAN_POINT ( 'NONE',  ( 11.40812507854755253, -35.11059874428192273, -10.52499999726881263 ) ) ;
#46304 = CARTESIAN_POINT ( 'NONE',  ( 15.80617190586746368, 15.72974639402197994, 39.37390960531436690 ) ) ;
#46305 = DIRECTION ( 'NONE',  ( 1.000000000000000000, 0.000000000000000000, 0.000000000000000000 ) ) ;
#46306 = CARTESIAN_POINT ( 'NONE',  ( 0.9201939147134639008, 8.788676749360311291, -64.01182165210214237 ) ) ;
#46308 = CARTESIAN_POINT ( 'NONE',  ( -8.314922557960811034, -14.29746914071050412, 27.08224293864769550 ) ) ;
#46307 = CARTESIAN_POINT ( 'NONE',  ( 8.224510206698742110, 14.34966873604972548, 37.08442372801901143 ) ) ;
#46309 = CARTESIAN_POINT ( 'NONE',  ( -21.52544592524343514, 5.823673210054127303, 56.04057627198102409 ) ) ;
#46311 = CARTESIAN_POINT ( 'NONE',  ( 0.05219959533936267826, -19.03943276465977164, 80.00109039468567573 ) ) ;
#46310 = AXIS2_PLACEMENT_3D ( 'NONE', #71865, #133533, #72882 ) ;
#46312 = CARTESIAN_POINT ( 'NONE',  ( -18.67979575497178146, -10.72451020669898902, 66.66557627198102409 ) ) ;
#46313 = CARTESIAN_POINT ( 'NONE',  ( 15.72974639402176855, 15.80617190586768217, 76.87609039468567573 ) ) ;
#46314 = CARTESIAN_POINT ( 'NONE',  ( -12.06727048284065340, 11.49022483853021903, -61.36479237366228290 ) ) ;
#46315 = CARTESIAN_POINT ( 'NONE',  ( -16.55341960407617563, 4.379528057220093196, 43.54275706135235424 ) ) ;
#46317 = CARTESIAN_POINT ( 'NONE',  ( -5.153800228976328057, -19.02544592524343514, 97.29057627198099567 ) ) ;
#46316 = CARTESIAN_POINT ( 'NONE',  ( 5.049401038298161559, -19.05341960407611168, 42.70724293864767418 ) ) ;
#46318 = CARTESIAN_POINT ( 'NONE',  ( -13.97604488694527625, -13.89961937509977652, 36.87390960531436690 ) ) ;
#46319 = CARTESIAN_POINT ( 'NONE',  ( -14.34966873604960291, -8.224510206698953496, 106.6655762719810383 ) ) ;
#46320 = APPLICATION_PROTOCOL_DEFINITION ( 'draft international standard', 'automotive_design', 1998, #138369 ) ;
#46321 = FACE_BOUND ( 'NONE', #104468, .T. ) ;
#46322 = EDGE_LOOP ( 'NONE', ( #178316, #191055, #25603, #56540 ) ) ;
#46323 = CARTESIAN_POINT ( 'NONE',  ( 4.483927247898790824, -16.52544592524335698, 75.20942372801901854 ) ) ;
#46324 = CARTESIAN_POINT ( 'NONE',  ( -5.823673210054116645, -21.52544592524344225, 87.29057627198103830 ) ) ;
#46325 = CARTESIAN_POINT ( 'NONE',  ( 19.02544592524343514, -5.153800228976328945, 53.54057627198102409 ) ) ;
#46326 = CARTESIAN_POINT ( 'NONE',  ( -5.719274019375665041, -21.55341960407619695, 24.79275706135235779 ) ) ;
#46327 = CARTESIAN_POINT ( 'NONE',  ( 0.05219959533909260263, 19.03943276465977164, 79.99890960531436690 ) ) ;
#46328 = ORIENTED_EDGE ( 'NONE', *, *, #195370, .T. ) ;
#46329 = CARTESIAN_POINT ( 'NONE',  ( 0.05219959533937995610, -21.53943276465977519, 20.00109039468568639 ) ) ;
#46332 = CARTESIAN_POINT ( 'NONE',  ( 9.564922557961047289, -16.46253265017146816, 75.41775706135234714 ) ) ;
#46331 = CARTESIAN_POINT ( 'NONE',  ( -13.89961937509977652, 13.97604488694528158, 105.6239096053143527 ) ) ;
#46330 = CARTESIAN_POINT ( 'NONE',  ( 19.05341960407611168, 5.049401038298154454, 23.95724293864769194 ) ) ;
#46333 = CARTESIAN_POINT ( 'NONE',  ( -19.02544592524334988, -5.153800228976617603, 28.95942372801900433 ) ) ;
#46334 = CARTESIAN_POINT ( 'NONE',  ( 21.53943276465977519, -0.05219959533907433946, 98.74890960531438111 ) ) ;
#46335 = CARTESIAN_POINT ( 'NONE',  ( 9.474510206698729675, 16.51473224551082808, 37.08442372801899722 ) ) ;
#46336 = CARTESIAN_POINT ( 'NONE',  ( 14.29746914071037800, 8.314922557961029526, 81.66775706135236135 ) ) ;
#46337 = CARTESIAN_POINT ( 'NONE',  ( 13.97604488694527802, 13.89961937509977652, 109.3739096053143669 ) ) ;
#46338 = CARTESIAN_POINT ( 'NONE',  ( 9.474510206698971260, -16.51473224551069308, 57.91557627198103120 ) ) ;
#46339 = CARTESIAN_POINT ( 'NONE',  ( 18.67979575497194134, -10.72451020669871369, 60.83442372801901854 ) ) ;
#46340 = CARTESIAN_POINT ( 'NONE',  ( 10.72451020669871369, 18.67979575497193778, 82.08442372801901854 ) ) ;
#46341 = CARTESIAN_POINT ( 'NONE',  ( 0.05219959533909260263, 19.03943276465977164, 79.99890960531436690 ) ) ;
#46342 = CARTESIAN_POINT ( 'NONE',  ( -15.80617190586768217, 15.72974639402176855, 43.12609039468568284 ) ) ;
#46343 = CARTESIAN_POINT ( 'NONE',  ( 13.97604488694548053, -13.89961937509957401, 85.62609039468568994 ) ) ;
#46344 = CARTESIAN_POINT ( 'NONE',  ( 19.05341960407611168, 5.049401038298154454, 53.95724293864770260 ) ) ;
#46345 = CARTESIAN_POINT ( 'NONE',  ( 19.05341960407611168, 5.049401038298154454, 98.95724293864766707 ) ) ;
#46346 = CARTESIAN_POINT ( 'NONE',  ( 5.153800228976335163, 19.02544592524342804, 59.79057627198100988 ) ) ;
#46347 = CARTESIAN_POINT ( 'NONE',  ( 17.58332526062529411, -7.635886036038496805, 78.42334959558466778 ) ) ;
#46348 = CARTESIAN_POINT ( 'NONE',  ( -13.97604488694527625, -13.89961937509977652, 46.87390960531435979 ) ) ;
#46349 = CARTESIAN_POINT ( 'NONE',  ( -15.72974639402197994, 15.80617190586746368, 100.6239096053143811 ) ) ;
#46350 = CARTESIAN_POINT ( 'NONE',  ( 12.14591786802327356, -12.06949235617739191, 85.62609039468568994 ) ) ;
#46351 = CARTESIAN_POINT ( 'NONE',  ( -24.79447686064998635, 6.332871904607505265, 168.1804317516294134 ) ) ;
#46352 = CARTESIAN_POINT ( 'NONE',  ( 9.474510206698729675, 16.51473224551082808, 42.08442372801900433 ) ) ;
#46353 = CARTESIAN_POINT ( 'NONE',  ( 9.474510206698971260, -16.51473224551069308, 62.91557627198102409 ) ) ;
#46354 = CARTESIAN_POINT ( 'NONE',  ( 16.52544592524342804, -4.483927247898539470, 63.54057627198103830 ) ) ;
#46355 = CARTESIAN_POINT ( 'NONE',  ( -8.224510206698948167, 14.34966873604960824, 90.41557627198103830 ) ) ;
#46356 = CARTESIAN_POINT ( 'NONE',  ( 19.03943276465977164, -0.05219959533909143690, 113.7489096053143669 ) ) ;
#46357 = CARTESIAN_POINT ( 'NONE',  ( 5.049401038298161559, -19.05341960407611168, 97.70724293864766707 ) ) ;
#46358 = CARTESIAN_POINT ( 'NONE',  ( -19.03943276465977164, 0.05219959533909376836, 101.2489096053143669 ) ) ;
#46359 = CARTESIAN_POINT ( 'NONE',  ( -19.05341960407617563, 5.049401038297882671, 23.54275706135233648 ) ) ;
#46360 = CARTESIAN_POINT ( 'NONE',  ( -14.29746914071037622, -8.314922557961029526, 99.16775706135234714 ) ) ;
#46361 = CARTESIAN_POINT ( 'NONE',  ( 5.153800228976335163, 19.02544592524342804, 74.79057627198103830 ) ) ;
#46362 = CARTESIAN_POINT ( 'NONE',  ( -18.62759615963255300, -10.81492255796106328, 34.16775706135234714 ) ) ;
#46363 = CARTESIAN_POINT ( 'NONE',  ( -21.55341960407610458, -5.719274019375992779, 26.45724293864768839 ) ) ;
#46364 = CARTESIAN_POINT ( 'NONE',  ( 21.55341960407610458, 5.719274019375980345, 113.9572429386477239 ) ) ;
#46365 = CARTESIAN_POINT ( 'NONE',  ( 21.53943276465977519, -0.05219959533907433946, 73.74890960531433848 ) ) ;
#46366 = CARTESIAN_POINT ( 'NONE',  ( -5.049401038298153566, 19.05341960407611168, 50.20724293864770260 ) ) ;
#46367 = CARTESIAN_POINT ( 'NONE',  ( -16.55341960407611168, -4.379528057220339221, 81.45724293864769550 ) ) ;
#46368 = CARTESIAN_POINT ( 'NONE',  ( -19.02544592524334988, -5.153800228976617603, 48.95942372801900433 ) ) ;
#46369 = CARTESIAN_POINT ( 'NONE',  ( 9.474510206698971260, -16.51473224551069308, 22.91557627198102765 ) ) ;
#46370 = CARTESIAN_POINT ( 'NONE',  ( 19.03943276465977164, -0.05219959533909143690, 88.74890960531436690 ) ) ;
#46371 = CARTESIAN_POINT ( 'NONE',  ( 9.474510206698971260, -16.51473224551069308, 77.91557627198103830 ) ) ;
#46372 = CARTESIAN_POINT ( 'NONE',  ( -17.14385361876520975, 23.59649016807275856, 146.5750000027311728 ) ) ;
#46373 = CARTESIAN_POINT ( 'NONE',  ( 4.483927247898545687, 16.52544592524342804, 94.79057627198105251 ) ) ;
#46374 = VERTEX_POINT ( 'NONE', #155078 ) ;
#46375 = CARTESIAN_POINT ( 'NONE',  ( -4.379528057220086978, -16.55341960407618274, 104.7927570613523898 ) ) ;
#46376 = CARTESIAN_POINT ( 'NONE',  ( 12.06949235617739724, 12.14591786802326823, 21.87609039468567573 ) ) ;
#46377 = CARTESIAN_POINT ( 'NONE',  ( 5.719274019375673035, 21.55341960407619339, 97.29275706135234714 ) ) ;
#46378 = CARTESIAN_POINT ( 'NONE',  ( -9.564922557960796823, -16.46253265017161027, 97.08224293864769550 ) ) ;
#46379 = CARTESIAN_POINT ( 'NONE',  ( 18.62759615963255655, 10.81492255796105972, 21.66775706135235069 ) ) ;
#46380 = CARTESIAN_POINT ( 'NONE',  ( -9.474510206698964154, 16.51473224551069663, 25.41557627198103120 ) ) ;
#46381 = CARTESIAN_POINT ( 'NONE',  ( 12.14591786802327356, -12.06949235617739191, 30.62609039468567929 ) ) ;
#46382 = EDGE_CURVE ( 'NONE', #93673, #115190, #134498, .T. ) ;
#46383 = CARTESIAN_POINT ( 'NONE',  ( 19.05341960407617918, -5.049401038297876454, 101.0427570613523045 ) ) ;
#46384 = VECTOR ( 'NONE', #120353, 1000.000000000000000 ) ;
#46385 = CARTESIAN_POINT ( 'NONE',  ( 5.823673210054125526, 21.52544592524343514, 89.79057627198103830 ) ) ;
#46386 = CARTESIAN_POINT ( 'NONE',  ( -19.05341960407617563, 5.049401038297882671, 63.54275706135234003 ) ) ;
#46387 = CARTESIAN_POINT ( 'NONE',  ( -18.22780087662126647, -5.499999999999827693, 63.98236817873107185 ) ) ;
#46388 = CARTESIAN_POINT ( 'NONE',  ( -21.52544592524334988, -5.823673210054445271, 23.95942372801901143 ) ) ;
#46389 = CARTESIAN_POINT ( 'NONE',  ( 6.791538853603070081, -3.181980515339468241, 1.110912703473986074 ) ) ;
#46390 = CARTESIAN_POINT ( 'NONE',  ( 19.02544592524343514, -5.153800228976328945, 88.54057627198102409 ) ) ;
#46391 = CARTESIAN_POINT ( 'NONE',  ( 14.29746914071037800, 8.314922557961029526, 51.66775706135234714 ) ) ;
#46392 = DIRECTION ( 'NONE',  ( 0.06104853953485701173, 0.000000000000000000, -0.9981347984218670311 ) ) ;
#46393 = CARTESIAN_POINT ( 'NONE',  ( -9.474510206698720793, -16.51473224551083518, 64.58442372801900433 ) ) ;
#46395 = CARTESIAN_POINT ( 'NONE',  ( 16.52544592524342804, -4.483927247898539470, 73.54057627198102409 ) ) ;
#46394 = CARTESIAN_POINT ( 'NONE',  ( -21.53943276465977519, 0.05219959533907696930, 111.2489096053143669 ) ) ;
#46396 = CARTESIAN_POINT ( 'NONE',  ( 9.564922557960805705, 16.46253265017160317, 89.58224293864769550 ) ) ;
#46398 = CARTESIAN_POINT ( 'NONE',  ( -19.02544592524334988, -5.153800228976617603, 58.95942372801900433 ) ) ;
#46397 = CARTESIAN_POINT ( 'NONE',  ( -4.379528057220086978, -16.55341960407618274, 49.79275706135234714 ) ) ;
#46399 = CARTESIAN_POINT ( 'NONE',  ( -18.62759615963255300, -10.81492255796106328, 64.16775706135234714 ) ) ;
#46400 = CARTESIAN_POINT ( 'NONE',  ( 16.55341960407618274, -4.379528057220086978, 31.04275706135234714 ) ) ;
#46401 = CARTESIAN_POINT ( 'NONE',  ( -19.02544592524342804, 5.153800228976336051, 66.04057627198103830 ) ) ;
#46402 = CARTESIAN_POINT ( 'NONE',  ( -13.97604488694547697, 13.89961937509957934, 93.12609039468566152 ) ) ;
#46403 = CARTESIAN_POINT ( 'NONE',  ( -4.379528057220086978, -16.55341960407618274, 49.79275706135234714 ) ) ;
#46404 = CARTESIAN_POINT ( 'NONE',  ( -15.72974639402176322, -15.80617190586768395, 104.3760903946856899 ) ) ;
#46405 = CARTESIAN_POINT ( 'NONE',  ( 0.05219959533936267826, -19.03943276465977164, 75.00109039468566152 ) ) ;
#46406 = CARTESIAN_POINT ( 'NONE',  ( 19.03943276465977164, -0.05219959533909143690, 43.74890960531435979 ) ) ;
#46407 = CARTESIAN_POINT ( 'NONE',  ( 21.55341960407610458, 5.719274019375980345, 68.95724293864769550 ) ) ;
#46409 = CARTESIAN_POINT ( 'NONE',  ( 16.46253265017146816, 9.564922557961045513, 76.66775706135234714 ) ) ;
#46408 = CARTESIAN_POINT ( 'NONE',  ( -0.05219959533910754901, -16.53943276465976808, 72.49890960531435269 ) ) ;
#46410 = CARTESIAN_POINT ( 'NONE',  ( -18.56101223717332260, -5.500000000000061284, 71.44978406935676674 ) ) ;
#46412 = EDGE_CURVE ( 'NONE', #53443, #176653, #91117, .T. ) ;
#46411 = CARTESIAN_POINT ( 'NONE',  ( -19.02544592524334988, -5.153800228976617603, 38.95942372801900433 ) ) ;
#46413 = CARTESIAN_POINT ( 'NONE',  ( -14.34966873604972548, 8.224510206698743886, 108.3344237280190185 ) ) ;
#46414 = CARTESIAN_POINT ( 'NONE',  ( 14.29746914071049879, -8.314922557960816363, 68.33224293864769550 ) ) ;
#46416 = CARTESIAN_POINT ( 'NONE',  ( 17.14385361876520264, -23.59649016807271238, 145.5750000027312012 ) ) ;
#46415 = CARTESIAN_POINT ( 'NONE',  ( 10.81492255796106328, -18.62759615963255655, 100.4177570613523471 ) ) ;
#46417 = CARTESIAN_POINT ( 'NONE',  ( 0.05219959533907565091, 21.53943276465977519, 104.9989096053143669 ) ) ;
#46418 = CARTESIAN_POINT ( 'NONE',  ( 5.153800228976335163, 19.02544592524342804, 59.79057627198100988 ) ) ;
#46419 = CARTESIAN_POINT ( 'NONE',  ( -21.53943276465977519, -0.05219959533937600094, 83.75109039468568994 ) ) ;
#46420 = CARTESIAN_POINT ( 'NONE',  ( -9.564922557960796823, -16.46253265017161027, 67.08224293864769550 ) ) ;
#46421 = ORIENTED_EDGE ( 'NONE', *, *, #43648, .F. ) ;
#46422 = CARTESIAN_POINT ( 'NONE',  ( 16.51473224551069308, 9.474510206698969483, 24.16557627198102765 ) ) ;
#46423 = CARTESIAN_POINT ( 'NONE',  ( -13.89961937509977652, 13.97604488694528158, 115.6239096053143669 ) ) ;
#46424 = CARTESIAN_POINT ( 'NONE',  ( -0.05219959533910754901, -16.53943276465976808, 67.49890960531436690 ) ) ;
#46425 = CARTESIAN_POINT ( 'NONE',  ( -5.153800228976328057, -19.02544592524343514, 27.29057627198103120 ) ) ;
#46426 = CARTESIAN_POINT ( 'NONE',  ( 12.06949235617757843, -12.14591786802309237, 88.12390960531436690 ) ) ;
#46427 = CARTESIAN_POINT ( 'NONE',  ( 21.53943276465977519, -0.05219959533907433946, 93.74890960531436690 ) ) ;
#46428 = CARTESIAN_POINT ( 'NONE',  ( -0.05219959533937732626, 21.53943276465977519, 47.50109039468568994 ) ) ;
#46429 = CARTESIAN_POINT ( 'NONE',  ( 27.94727395831375460, -6.976223361892288644, 161.4607800657734344 ) ) ;
#46430 = CARTESIAN_POINT ( 'NONE',  ( -16.52544592524335698, -4.483927247898792601, 53.95942372801900433 ) ) ;
#46431 = CARTESIAN_POINT ( 'NONE',  ( 15.80617190586746368, 15.72974639402197994, 94.37390960531436690 ) ) ;
#46432 = CARTESIAN_POINT ( 'NONE',  ( -5.153800228976607833, 19.02544592524334988, 22.70942372801899012 ) ) ;
#46433 = CARTESIAN_POINT ( 'NONE',  ( -9.474510206698964154, 16.51473224551069663, 110.4155762719810383 ) ) ;
#46434 = CARTESIAN_POINT ( 'NONE',  ( 15.80617190586769283, -15.72974639402175789, 45.62609039468567573 ) ) ;
#46435 = CARTESIAN_POINT ( 'NONE',  ( 21.52544592524344225, -5.823673210054117533, 43.54057627198103830 ) ) ;
#46436 = CARTESIAN_POINT ( 'NONE',  ( -8.314922557960811034, -14.29746914071050412, 27.08224293864769550 ) ) ;
#46438 = CARTESIAN_POINT ( 'NONE',  ( 21.55341960407619695, -5.719274019375665929, 91.04275706135236135 ) ) ;
#46437 = CARTESIAN_POINT ( 'NONE',  ( -15.80617190586768217, 15.72974639402176855, 68.12609039468567573 ) ) ;
#46439 = CARTESIAN_POINT ( 'NONE',  ( -5.153800228976607833, 19.02544592524334988, 32.70942372801899722 ) ) ;
#46440 = CARTESIAN_POINT ( 'NONE',  ( -14.29746914071037622, -8.314922557961029526, 84.16775706135234714 ) ) ;
#46441 = CARTESIAN_POINT ( 'NONE',  ( 10.72451020669871369, 18.67979575497193778, 57.08442372801901854 ) ) ;
#46442 = CARTESIAN_POINT ( 'NONE',  ( -5.153800228976328057, -19.02544592524343514, 47.29057627198102409 ) ) ;
#46443 = CARTESIAN_POINT ( 'NONE',  ( 0.05219959533936267826, -19.03943276465977164, 25.00109039468566152 ) ) ;
#46444 = CARTESIAN_POINT ( 'NONE',  ( 5.823673210054125526, 21.52544592524343514, 29.79057627198102409 ) ) ;
#46445 = CARTESIAN_POINT ( 'NONE',  ( 21.55341960407610458, 5.719274019375980345, 113.9572429386477239 ) ) ;
#46446 = CARTESIAN_POINT ( 'NONE',  ( 21.52544592524344225, -5.823673210054117533, 68.54057627198103830 ) ) ;
#46447 = CARTESIAN_POINT ( 'NONE',  ( -16.53943276465976808, -0.05219959533934237506, 43.75109039468568284 ) ) ;
#46449 = CARTESIAN_POINT ( 'NONE',  ( 10.81492255796078972, 18.62759615963270932, 74.58224293864768129 ) ) ;
#46448 = DIRECTION ( 'NONE',  ( -1.000000000000000000, -0.000000000000000000, 0.000000000000000000 ) ) ;
#46451 = CARTESIAN_POINT ( 'NONE',  ( 12.06949235617757843, -12.14591786802309237, 63.12390960531435979 ) ) ;
#46450 = CARTESIAN_POINT ( 'NONE',  ( -16.52544592524335698, -4.483927247898792601, 63.95942372801901854 ) ) ;
#46452 = CARTESIAN_POINT ( 'NONE',  ( -22.92000981050143338, 20.99774934350689648, -46.85949206705567605 ) ) ;
#46453 = CARTESIAN_POINT ( 'NONE',  ( 0.05219959533936267826, -19.03943276465977164, 110.0010903946856757 ) ) ;
#46454 = AXIS2_PLACEMENT_3D ( 'NONE', #107181, #168852, #21026 ) ;
#46455 = CARTESIAN_POINT ( 'NONE',  ( 5.719274019375991003, -21.55341960407610458, 22.70724293864769194 ) ) ;
#46456 = DIRECTION ( 'NONE',  ( 1.000000000000000000, 1.776356839400250465E-15, 0.000000000000000000 ) ) ;
#46457 = CARTESIAN_POINT ( 'NONE',  ( -12.14591786802326823, 12.06949235617739902, 43.12609039468568284 ) ) ;
#46458 = CARTESIAN_POINT ( 'NONE',  ( -10.72451020669898014, 18.67979575497178502, 115.4155762719810241 ) ) ;
#46459 = CARTESIAN_POINT ( 'NONE',  ( -18.67979575497178146, -10.72451020669898902, 26.66557627198103475 ) ) ;
#46460 = CARTESIAN_POINT ( 'NONE',  ( 14.34966873604972726, -8.224510206698740333, 60.83442372801901854 ) ) ;
#46461 = CARTESIAN_POINT ( 'NONE',  ( -19.03943276465977164, 0.05219959533909376836, 71.24890960531435269 ) ) ;
#46463 = CARTESIAN_POINT ( 'NONE',  ( 0.05219959533936267826, -19.03943276465977164, 105.0010903946856615 ) ) ;
#46462 = CARTESIAN_POINT ( 'NONE',  ( -5.823673210054431948, 21.52544592524334988, 42.70942372801901854 ) ) ;
#46464 = CARTESIAN_POINT ( 'NONE',  ( 5.823673210054125526, 21.52544592524343514, 24.79057627198103120 ) ) ;
#46465 = VERTEX_POINT ( 'NONE', #110555 ) ;
#46466 = CARTESIAN_POINT ( 'NONE',  ( -19.03943276465977164, -0.05219959533935918106, 23.75109039468566152 ) ) ;
#46467 = CARTESIAN_POINT ( 'NONE',  ( 12.06949235617739724, 12.14591786802326823, 36.87609039468568994 ) ) ;
#46468 = CARTESIAN_POINT ( 'NONE',  ( 0.05219959533909260263, 19.03943276465977164, 94.99890960531436690 ) ) ;
#46469 = CARTESIAN_POINT ( 'NONE',  ( -21.52544592524343514, 5.823673210054127303, 101.0405762719810383 ) ) ;
#46470 = CARTESIAN_POINT ( 'NONE',  ( 0.05219959533909260263, 19.03943276465977164, 69.99890960531435269 ) ) ;
#46471 = DIRECTION ( 'NONE',  ( 1.000000000000000000, 0.000000000000000000, 0.000000000000000000 ) ) ;
#46472 = CARTESIAN_POINT ( 'NONE',  ( 8.314922557960818139, 14.29746914071049879, 79.58224293864769550 ) ) ;
#46473 = CARTESIAN_POINT ( 'NONE',  ( 18.67979575497178502, 10.72451020669898547, 34.16557627198102409 ) ) ;
#46474 = DIRECTION ( 'NONE',  ( -1.000000000000000000, -0.000000000000000000, -0.000000000000000000 ) ) ;
#46475 = CARTESIAN_POINT ( 'NONE',  ( 8.314922557961029526, -14.29746914071037800, 60.41775706135235424 ) ) ;
#46476 = CARTESIAN_POINT ( 'NONE',  ( 21.52544592524344225, -5.823673210054117533, 108.5405762719810241 ) ) ;
#46477 = CARTESIAN_POINT ( 'NONE',  ( 5.153800228976615827, -19.02544592524334988, 80.20942372801901854 ) ) ;
#46478 = CARTESIAN_POINT ( 'NONE',  ( 0.05219959533907565091, 21.53943276465977519, 34.99890960531435979 ) ) ;
#46479 = CARTESIAN_POINT ( 'NONE',  ( -5.153800228976328057, -19.02544592524343514, 32.29057627198102409 ) ) ;
#46480 = CARTESIAN_POINT ( 'NONE',  ( 18.62759615963271287, -10.81492255796078972, 68.33224293864769550 ) ) ;
#46481 = CARTESIAN_POINT ( 'NONE',  ( 16.51473224551069308, 9.474510206698969483, 99.16557627198102409 ) ) ;
#46482 = CARTESIAN_POINT ( 'NONE',  ( -21.55341960407619339, 5.719274019375674811, 98.54275706135234714 ) ) ;
#46483 = CARTESIAN_POINT ( 'NONE',  ( -0.05219959533909027116, -19.03943276465977164, 57.49890960531435979 ) ) ;
#46484 = CARTESIAN_POINT ( 'NONE',  ( 14.34966873604972726, -8.224510206698740333, 55.83442372801901854 ) ) ;
#46485 = CARTESIAN_POINT ( 'NONE',  ( 19.03943276465977164, -0.05219959533909143690, 63.74890960531435979 ) ) ;
#46486 = CARTESIAN_POINT ( 'NONE',  ( 5.823673210054444382, -21.52544592524334988, 80.20942372801901854 ) ) ;
#46487 = ORIENTED_EDGE ( 'NONE', *, *, #37462, .F. ) ;
#46488 = CARTESIAN_POINT ( 'NONE',  ( 19.02544592524334988, 5.153800228976608722, 36.45942372801900433 ) ) ;
#46489 = CARTESIAN_POINT ( 'NONE',  ( -9.564922557961040184, 16.46253265017147172, 37.91775706135233293 ) ) ;
#46490 = CARTESIAN_POINT ( 'NONE',  ( -15.80617190586768217, 15.72974639402176855, 43.12609039468568284 ) ) ;
#46491 = EDGE_CURVE ( 'NONE', #4215, #36339, #131967, .T. ) ;
#46492 = CARTESIAN_POINT ( 'NONE',  ( -7.122238460089373113, 1.425225664899916866, -62.29949481927938137 ) ) ;
#46493 = CARTESIAN_POINT ( 'NONE',  ( -19.03943276465977164, -0.05219959533935918106, 33.75109039468566863 ) ) ;
#46494 = CARTESIAN_POINT ( 'NONE',  ( 5.049401038298161559, -19.05341960407611168, 92.70724293864769550 ) ) ;
#46495 = CARTESIAN_POINT ( 'NONE',  ( 19.05341960407611168, 5.049401038298154454, 63.95724293864769550 ) ) ;
#46496 = CARTESIAN_POINT ( 'NONE',  ( -4.379528057220328563, 16.55341960407611168, 30.20724293864769550 ) ) ;
#46499 = B_SPLINE_CURVE_WITH_KNOTS ( 'NONE', 3,
 ( #70242, #118750, #40902, #85389, #149085, #165252, #135904, #131910, #119738, #104564, #166246, #180439, #39890, #150078, #54071, #101557, #195603, #71240, #163249, #133912 ),
 .UNSPECIFIED., .F., .F.,
 ( 4, 2, 2, 2, 2, 2, 2, 2, 2, 4 ),
 ( 0.004000878361811928755, 0.004499404418915960331, 0.004997930476019991908, 0.005496456533124022617, 0.005994982590228054194, 0.006244245618780048732, 0.006493508647332044137, 0.006992034704436029743, 0.007490560761540015350, 0.007989086818644000956 ),
 .UNSPECIFIED. ) ;
#46498 = CARTESIAN_POINT ( 'NONE',  ( 15.72974639402176855, 15.80617190586768217, 86.87609039468568994 ) ) ;
#46497 = CARTESIAN_POINT ( 'NONE',  ( 10.72451020669898902, -18.67979575497178502, 22.91557627198102765 ) ) ;
#46500 = CARTESIAN_POINT ( 'NONE',  ( -22.81625015709509441, -31.40387420917324590, -10.82499999726881157 ) ) ;
#46501 = CARTESIAN_POINT ( 'NONE',  ( 17.49999999999999645, 5.500000000000009770, 58.78230962303567253 ) ) ;
#46502 = CARTESIAN_POINT ( 'NONE',  ( -0.05219959533937732626, 21.53943276465977519, 102.5010903946856899 ) ) ;
#46503 = CARTESIAN_POINT ( 'NONE',  ( 24.28797299941339816, -0.2180554607492743435, -56.78142080721293894 ) ) ;
#46504 = CARTESIAN_POINT ( 'NONE',  ( -5.049401038298153566, 19.05341960407611168, 30.20724293864768839 ) ) ;
#46505 = CARTESIAN_POINT ( 'NONE',  ( 5.153800228976335163, 19.02544592524342804, 109.7905762719810099 ) ) ;
#46506 = EDGE_CURVE ( 'NONE', #74166, #101229, #117487, .T. ) ;
#46507 = CARTESIAN_POINT ( 'NONE',  ( 30.00000000000000000, -1.163414459189985801E-14, 95.00000000000000000 ) ) ;
#46508 = CARTESIAN_POINT ( 'NONE',  ( 12.06949235617739724, 12.14591786802326823, 46.87609039468568994 ) ) ;
#46509 = B_SPLINE_CURVE_WITH_KNOTS ( 'NONE', 3,
 ( #25371, #176038, #37506, #55675, #145678, #99168 ),
 .UNSPECIFIED., .F., .F.,
 ( 4, 2, 4 ),
 ( 0.007228050697041520610, 0.007608510107494992694, 0.007988969517948463911 ),
 .UNSPECIFIED. ) ;
#46510 = CARTESIAN_POINT ( 'NONE',  ( -0.05219959533907301413, -21.53943276465977519, 72.49890960531435269 ) ) ;
#46511 = CARTESIAN_POINT ( 'NONE',  ( -12.14591786802309592, -12.06949235617757132, 36.87390960531435979 ) ) ;
#46513 = CARTESIAN_POINT ( 'NONE',  ( -19.03943276465977164, 0.05219959533909376836, 91.24890960531436690 ) ) ;
#46512 = CARTESIAN_POINT ( 'NONE',  ( 14.34966873604960469, 8.224510206698951720, 104.1655762719810241 ) ) ;
#46514 = CARTESIAN_POINT ( 'NONE',  ( -16.51473224551082808, 9.474510206698731452, 23.33442372801900078 ) ) ;
#46515 = CARTESIAN_POINT ( 'NONE',  ( 4.483927247898545687, 16.52544592524342804, 114.7905762719810383 ) ) ;
#46516 = CARTESIAN_POINT ( 'NONE',  ( 0.05219959533937995610, -21.53943276465977519, 65.00109039468568994 ) ) ;
#46517 = CARTESIAN_POINT ( 'NONE',  ( -13.97604488694527625, -13.89961937509977652, 111.8739096053143243 ) ) ;
#46518 = CARTESIAN_POINT ( 'NONE',  ( 0.05219959533934541429, -16.53943276465976808, 105.0010903946856757 ) ) ;
#46519 = CARTESIAN_POINT ( 'NONE',  ( 9.474510206698729675, 16.51473224551082808, 62.08442372801899722 ) ) ;
#46520 = CARTESIAN_POINT ( 'NONE',  ( -22.81625015709509441, -31.40387420917324590, -6.824999997268814234 ) ) ;
#46521 = CARTESIAN_POINT ( 'NONE',  ( 5.719274019375991003, -21.55341960407610458, 22.70724293864769194 ) ) ;
#46522 = CARTESIAN_POINT ( 'NONE',  ( 14.29746914071049879, -8.314922557960816363, 93.33224293864769550 ) ) ;
#46523 = CARTESIAN_POINT ( 'NONE',  ( -9.564922557961040184, 16.46253265017147172, 52.91775706135233293 ) ) ;
#46524 = CARTESIAN_POINT ( 'NONE',  ( 9.474510206698971260, -16.51473224551069308, 72.91557627198102409 ) ) ;
#46525 = CARTESIAN_POINT ( 'NONE',  ( 16.53943276465976808, -0.05219959533910856209, 68.74890960531435269 ) ) ;
#46526 = CARTESIAN_POINT ( 'NONE',  ( -0.05219959533936034679, 19.03943276465977164, 92.50109039468566152 ) ) ;
#46527 = CARTESIAN_POINT ( 'NONE',  ( -5.823673210054116645, -21.52544592524344225, 52.29057627198102409 ) ) ;
#46528 = EDGE_LOOP ( 'NONE', ( #19196, #118842, #67309, #158152 ) ) ;
#46529 = CARTESIAN_POINT ( 'NONE',  ( 13.89961937509977652, -13.97604488694527269, 23.12390960531436335 ) ) ;
#46530 = CARTESIAN_POINT ( 'NONE',  ( -16.61371651742602396, -7.165104196376045564, 31.14584930007003294 ) ) ;
#46532 = CARTESIAN_POINT ( 'NONE',  ( -15.80617190586745835, -15.72974639402198527, 76.87390960531439532 ) ) ;
#46531 = CARTESIAN_POINT ( 'NONE',  ( -9.564922557960796823, -16.46253265017161027, 72.08224293864770971 ) ) ;
#46533 = VECTOR ( 'NONE', #87393, 1000.000000000000000 ) ;
#46535 = CARTESIAN_POINT ( 'NONE',  ( 19.03943276465977164, -0.05219959533909143690, 73.74890960531435269 ) ) ;
#46534 = CARTESIAN_POINT ( 'NONE',  ( -12.14591786802326823, 12.06949235617739902, 93.12609039468568994 ) ) ;
#46536 = CARTESIAN_POINT ( 'NONE',  ( 5.153800228976615827, -19.02544592524334988, 65.20942372801900433 ) ) ;
#46537 = CARTESIAN_POINT ( 'NONE',  ( 0.05219959533937995610, -21.53943276465977519, 85.00109039468568994 ) ) ;
#46538 = CARTESIAN_POINT ( 'NONE',  ( 18.67979575497178502, 10.72451020669898547, 69.16557627198102409 ) ) ;
#46539 = CARTESIAN_POINT ( 'NONE',  ( 10.81492255796078972, 18.62759615963270932, 24.58224293864768839 ) ) ;
#46540 = CARTESIAN_POINT ( 'NONE',  ( 5.049401038298161559, -19.05341960407611168, 32.70724293864768129 ) ) ;
#46541 = CARTESIAN_POINT ( 'NONE',  ( 16.53943276465976808, 0.05219959533934440121, 101.2510903946856757 ) ) ;
#46542 = CARTESIAN_POINT ( 'NONE',  ( -9.564922557960796823, -16.46253265017161027, 47.08224293864769550 ) ) ;
#46543 = CARTESIAN_POINT ( 'NONE',  ( -16.52544592524335698, -4.483927247898792601, 23.95942372801901143 ) ) ;
#46544 = CARTESIAN_POINT ( 'NONE',  ( -9.564922557961040184, 16.46253265017147172, 82.91775706135233293 ) ) ;
#46545 = CARTESIAN_POINT ( 'NONE',  ( 21.55341960407619695, -5.719274019375665929, 106.0427570613523471 ) ) ;
#46546 = CARTESIAN_POINT ( 'NONE',  ( 14.34966873604960469, 8.224510206698951720, 64.16557627198102409 ) ) ;
#46547 = CARTESIAN_POINT ( 'NONE',  ( -15.80617190586745835, -15.72974639402198527, 101.8739096053143811 ) ) ;
#46548 = CARTESIAN_POINT ( 'NONE',  ( 5.719274019375991003, -21.55341960407610458, 102.7072429386476955 ) ) ;
#46549 = CARTESIAN_POINT ( 'NONE',  ( 22.44159573604009594, -16.30477369853687364, 140.1750000027311955 ) ) ;
#46550 = CARTESIAN_POINT ( 'NONE',  ( 15.72974639402199770, -15.80617190586745480, 43.12390960531435269 ) ) ;
#46551 = CARTESIAN_POINT ( 'NONE',  ( 4.483927247898790824, -16.52544592524335698, 85.20942372801901854 ) ) ;
#46552 = CARTESIAN_POINT ( 'NONE',  ( 8.224510206698953496, -14.34966873604960469, 87.91557627198103830 ) ) ;
#46553 = CARTESIAN_POINT ( 'NONE',  ( 19.05341960407611168, 5.049401038298154454, 58.95724293864768129 ) ) ;
#46554 = CARTESIAN_POINT ( 'NONE',  ( -19.26498983726239089, 5.499999999999603872, 50.55319577422003618 ) ) ;
#46555 = CARTESIAN_POINT ( 'NONE',  ( 0.05219959533934541429, -16.53943276465976808, 105.0010903946856757 ) ) ;
#46556 = CARTESIAN_POINT ( 'NONE',  ( 21.55341960407619695, -5.719274019375665929, 31.04275706135234714 ) ) ;
#46557 = CARTESIAN_POINT ( 'NONE',  ( 5.153800228976335163, 19.02544592524342804, 99.79057627198102409 ) ) ;
#46558 = CARTESIAN_POINT ( 'NONE',  ( -21.53943276465977519, -0.05219959533937600094, 68.75109039468568994 ) ) ;
#46559 = CARTESIAN_POINT ( 'NONE',  ( 9.474510206698971260, -16.51473224551069308, 22.91557627198102765 ) ) ;
#46560 = CARTESIAN_POINT ( 'NONE',  ( -9.474510206698964154, 16.51473224551069663, 25.41557627198103120 ) ) ;
#46561 = CIRCLE ( 'NONE', #137351, 7.999999999999998224 ) ;
#46562 = EDGE_LOOP ( 'NONE', ( #140120, #80075, #117583, #109420 ) ) ;
#46563 = CARTESIAN_POINT ( 'NONE',  ( 15.80617190586769283, -15.72974639402175789, 65.62609039468568994 ) ) ;
#46564 = CARTESIAN_POINT ( 'NONE',  ( -9.564922557960796823, -16.46253265017161027, 47.08224293864769550 ) ) ;
#46565 = CARTESIAN_POINT ( 'NONE',  ( 16.51473224551069308, 9.474510206698969483, 84.16557627198102409 ) ) ;
#46566 = CARTESIAN_POINT ( 'NONE',  ( 19.02544592524334988, 5.153800228976608722, 71.45942372801900433 ) ) ;
#46567 = CARTESIAN_POINT ( 'NONE',  ( -18.67979575497193778, 10.72451020669871902, 48.33442372801902565 ) ) ;
#46568 = CARTESIAN_POINT ( 'NONE',  ( 16.46253265017146816, 9.564922557961045513, 106.6677570613523471 ) ) ;
#46569 = CARTESIAN_POINT ( 'NONE',  ( 5.049401038297881783, 19.05341960407617563, 72.29275706135234714 ) ) ;
#46570 = CARTESIAN_POINT ( 'NONE',  ( -0.05219959533909027116, -19.03943276465977164, 37.49890960531436690 ) ) ;
#46571 = CARTESIAN_POINT ( 'NONE',  ( -16.46253265017146816, -9.564922557961047289, 84.16775706135233293 ) ) ;
#46572 = CARTESIAN_POINT ( 'NONE',  ( 16.53943276465976808, 0.05219959533934440121, 106.2510903946856757 ) ) ;
#46573 = CARTESIAN_POINT ( 'NONE',  ( -16.51473224551082808, 9.474510206698731452, 78.33442372801900433 ) ) ;
#46574 = CARTESIAN_POINT ( 'NONE',  ( -4.483927247898539470, -16.52544592524342804, 32.29057627198102409 ) ) ;
#46575 = CARTESIAN_POINT ( 'NONE',  ( 16.46253265017146816, 9.564922557961045513, 51.66775706135233293 ) ) ;
#46576 = CARTESIAN_POINT ( 'NONE',  ( 5.823673210054444382, -21.52544592524334988, 100.2094237280190043 ) ) ;
#46577 = CARTESIAN_POINT ( 'NONE',  ( -16.46253265017146816, -9.564922557961047289, 19.16775706135233293 ) ) ;
#46578 = CARTESIAN_POINT ( 'NONE',  ( 19.03943276465977164, -0.05219959533909143690, 23.74890960531435269 ) ) ;
#46579 = CARTESIAN_POINT ( 'NONE',  ( 18.62759615963255655, 10.81492255796105972, 86.66775706135234714 ) ) ;
#46580 = CARTESIAN_POINT ( 'NONE',  ( -16.55341960407617563, 4.379528057220093196, 38.54275706135234714 ) ) ;
#46581 = CARTESIAN_POINT ( 'NONE',  ( -19.03943276465977164, 0.05219959533909376836, 91.24890960531436690 ) ) ;
#46582 = CARTESIAN_POINT ( 'NONE',  ( 17.14385361876520264, -23.59649016807271238, 141.5750000027312012 ) ) ;
#46583 = CARTESIAN_POINT ( 'NONE',  ( -19.03943276465977164, 0.05219959533909376836, 81.24890960531436690 ) ) ;
#46584 = CARTESIAN_POINT ( 'NONE',  ( -23.31738231874055600, 16.94106989632528837, 141.7999999999999829 ) ) ;
#46585 = CIRCLE ( 'NONE', #40085, 5.000000000000000000 ) ;
#46586 = CARTESIAN_POINT ( 'NONE',  ( -13.89961937509957401, -13.97604488694547875, 84.37609039468567573 ) ) ;
#46587 = CARTESIAN_POINT ( 'NONE',  ( 9.564922557960805705, 16.46253265017160317, 109.5822429386476955 ) ) ;
#46589 = CARTESIAN_POINT ( 'NONE',  ( -19.02544592524334988, -5.153800228976617603, 103.9594237280190043 ) ) ;
#46588 = CARTESIAN_POINT ( 'NONE',  ( 19.02544592524334988, 5.153800228976608722, 21.45942372801899012 ) ) ;
#46590 = CARTESIAN_POINT ( 'NONE',  ( 16.53943276465976808, -0.05219959533910856209, 93.74890960531436690 ) ) ;
#46591 = CARTESIAN_POINT ( 'NONE',  ( -19.05341960407611168, -5.049401038298163336, 21.45724293864768839 ) ) ;
#46592 = CARTESIAN_POINT ( 'NONE',  ( 15.80617190586746368, 15.72974639402197994, 59.37390960531436690 ) ) ;
#46593 =( GEOMETRIC_REPRESENTATION_CONTEXT ( 3 ) GLOBAL_UNCERTAINTY_ASSIGNED_CONTEXT ( ( #175317 ) ) GLOBAL_UNIT_ASSIGNED_CONTEXT ( ( #66915, #189290, #128579 ) ) REPRESENTATION_CONTEXT ( 'NONE', 'WORKASPACE' ) );
#46594 = CARTESIAN_POINT ( 'NONE',  ( -21.55341960407610458, -5.719274019375992779, 46.45724293864769550 ) ) ;
#46595 = CARTESIAN_POINT ( 'NONE',  ( 12.14591786802309770, 12.06949235617756955, 114.3739096053143527 ) ) ;
#46596 = CARTESIAN_POINT ( 'NONE',  ( -16.70000000000002061, 1.759457951533292443E-13, -61.34707691135562868 ) ) ;
#46597 = CARTESIAN_POINT ( 'NONE',  ( 19.02544592524334988, 5.153800228976608722, 51.45942372801900433 ) ) ;
#46598 = CARTESIAN_POINT ( 'NONE',  ( -8.314922557960811034, -14.29746914071050412, 42.08224293864769550 ) ) ;
#46599 = CARTESIAN_POINT ( 'NONE',  ( -9.474510206698964154, 16.51473224551069663, 110.4155762719810383 ) ) ;
#46600 = CARTESIAN_POINT ( 'NONE',  ( 10.81492255796106328, -18.62759615963255655, 75.41775706135233293 ) ) ;
#46601 = CARTESIAN_POINT ( 'NONE',  ( 10.81492255796078972, 18.62759615963270932, 64.58224293864769550 ) ) ;
#46602 = CARTESIAN_POINT ( 'NONE',  ( -15.72974639402176322, -15.80617190586768395, 54.37609039468568994 ) ) ;
#46603 = CARTESIAN_POINT ( 'NONE',  ( -0.05219959533937732626, 21.53943276465977519, 57.50109039468568994 ) ) ;
#46604 = CARTESIAN_POINT ( 'NONE',  ( 9.564922557960805705, 16.46253265017160317, 89.58224293864769550 ) ) ;
#46605 = CARTESIAN_POINT ( 'NONE',  ( -4.379528057220086978, -16.55341960407618274, 79.79275706135236135 ) ) ;
#46606 = CARTESIAN_POINT ( 'NONE',  ( -8.224510206698948167, 14.34966873604960824, 115.4155762719810241 ) ) ;
#46607 = CARTESIAN_POINT ( 'NONE',  ( -31.99745974829804140, 5.643669518723349654, 90.03617080843918075 ) ) ;
#46608 = CARTESIAN_POINT ( 'NONE',  ( 12.06949235617757843, -12.14591786802309237, 68.12390960531436690 ) ) ;
#46609 = CARTESIAN_POINT ( 'NONE',  ( 12.14591786802309770, 12.06949235617756955, 29.37390960531435269 ) ) ;
#46610 = CARTESIAN_POINT ( 'NONE',  ( 5.049401038298161559, -19.05341960407611168, 67.70724293864769550 ) ) ;
#46611 = CARTESIAN_POINT ( 'NONE',  ( 19.02544592524343514, -5.153800228976328945, 33.54057627198102409 ) ) ;
#46612 = CARTESIAN_POINT ( 'NONE',  ( 0.05219959533907565091, 21.53943276465977519, 39.99890960531436690 ) ) ;
#46614 = CIRCLE ( 'NONE', #120942, 59.99999999999998579 ) ;
#46613 = CARTESIAN_POINT ( 'NONE',  ( 9.474510206698729675, 16.51473224551082808, 32.08442372801900433 ) ) ;
#46616 = CARTESIAN_POINT ( 'NONE',  ( 8.314922557960818139, 14.29746914071049879, 54.58224293864769550 ) ) ;
#46615 = DIRECTION ( 'NONE',  ( -0.000000000000000000, -0.000000000000000000, 1.000000000000000000 ) ) ;
#46617 = CARTESIAN_POINT ( 'NONE',  ( -18.62759615963270932, 10.81492255796079327, 30.83224293864770260 ) ) ;
#46618 = CARTESIAN_POINT ( 'NONE',  ( 17.66907692000827979, 2.165031582823986778, 37.50000000000000000 ) ) ;
#46619 = CARTESIAN_POINT ( 'NONE',  ( 8.314922557961029526, -14.29746914071037800, 70.41775706135236135 ) ) ;
#46620 = CARTESIAN_POINT ( 'NONE',  ( -16.46253265017146816, -9.564922557961047289, 74.16775706135234714 ) ) ;
#46621 = CARTESIAN_POINT ( 'NONE',  ( 14.34966873604960469, 8.224510206698951720, 44.16557627198103120 ) ) ;
#46622 = ORIENTED_EDGE ( 'NONE', *, *, #19336, .F. ) ;
#46623 = CARTESIAN_POINT ( 'NONE',  ( -19.49190055781011921, -5.499999999999968026, 75.56116087098783396 ) ) ;
#46624 = CARTESIAN_POINT ( 'NONE',  ( 16.55341960407611168, 4.379528057220329451, 23.95724293864769550 ) ) ;
#46625 = CARTESIAN_POINT ( 'NONE',  ( -16.51473224551069308, -9.474510206698971260, 56.66557627198103120 ) ) ;
#46626 = CARTESIAN_POINT ( 'NONE',  ( -5.153800228976328057, -19.02544592524343514, 57.29057627198103120 ) ) ;
#46627 = CARTESIAN_POINT ( 'NONE',  ( 5.153800228976335163, 19.02544592524342804, 39.79057627198100988 ) ) ;
#46628 = CARTESIAN_POINT ( 'NONE',  ( 10.72451020669871369, 18.67979575497193778, 47.08442372801901854 ) ) ;
#46629 = CARTESIAN_POINT ( 'NONE',  ( -19.03943276465977164, 0.05219959533909376836, 61.24890960531436690 ) ) ;
#46630 = CARTESIAN_POINT ( 'NONE',  ( 17.60769864724391098, -5.499999999999979572, 81.15024842019167295 ) ) ;
#46631 = CARTESIAN_POINT ( 'NONE',  ( -13.97604488694527625, -13.89961937509977652, 41.87390960531435979 ) ) ;
#46632 = CARTESIAN_POINT ( 'NONE',  ( -15.72974639402197994, 15.80617190586746368, 40.62390960531435269 ) ) ;
#46634 = CARTESIAN_POINT ( 'NONE',  ( -0.05219959533910754901, -16.53943276465976808, 112.4989096053143669 ) ) ;
#46633 = CARTESIAN_POINT ( 'NONE',  ( -5.823673210054431948, 21.52544592524334988, 77.70942372801900433 ) ) ;
#46635 = CARTESIAN_POINT ( 'NONE',  ( 18.67979575497178502, 10.72451020669898547, 34.16557627198102409 ) ) ;
#46636 = CARTESIAN_POINT ( 'NONE',  ( -12.06949235617739369, -12.14591786802326823, 94.37609039468568994 ) ) ;
#46637 = CARTESIAN_POINT ( 'NONE',  ( -0.05219959533937732626, 21.53943276465977519, 102.5010903946856899 ) ) ;
#46638 = CARTESIAN_POINT ( 'NONE',  ( 4.379528057220092307, 16.55341960407617563, 72.29275706135236135 ) ) ;
#46639 = CARTESIAN_POINT ( 'NONE',  ( 19.03943276465977164, -0.05219959533909143690, 103.7489096053143669 ) ) ;
#46640 = CARTESIAN_POINT ( 'NONE',  ( -4.379528057220086978, -16.55341960407618274, 49.79275706135234714 ) ) ;
#46641 = CARTESIAN_POINT ( 'NONE',  ( -8.224510206698735004, -14.34966873604973081, 39.58442372801901143 ) ) ;
#46642 = CARTESIAN_POINT ( 'NONE',  ( -12.06949235617739369, -12.14591786802326823, 99.37609039468568994 ) ) ;
#46643 = CARTESIAN_POINT ( 'NONE',  ( -10.81492255796105439, 18.62759615963255655, 57.91775706135234714 ) ) ;
#46644 = CARTESIAN_POINT ( 'NONE',  ( -8.314922557961024197, 14.29746914071037800, 22.91775706135235069 ) ) ;
#46645 = CARTESIAN_POINT ( 'NONE',  ( -10.81492255796078084, -18.62759615963271287, 112.0822429386477097 ) ) ;
#46646 = CARTESIAN_POINT ( 'NONE',  ( 14.34966873604972726, -8.224510206698740333, 25.83442372801901499 ) ) ;
#46647 = CARTESIAN_POINT ( 'NONE',  ( 8.314922557961029526, -14.29746914071037800, 80.41775706135234714 ) ) ;
#46648 = CARTESIAN_POINT ( 'NONE',  ( -17.48847506799950224, 5.747544572775299621, 45.82697437843291510 ) ) ;
#46649 = CARTESIAN_POINT ( 'NONE',  ( 21.52544592524334988, 5.823673210054432836, 91.45942372801901854 ) ) ;
#46651 = EDGE_CURVE ( 'NONE', #157648, #82035, #81934, .T. ) ;
#46650 = CARTESIAN_POINT ( 'NONE',  ( -13.89961937509957401, -13.97604488694547875, 89.37609039468563310 ) ) ;
#46652 = CARTESIAN_POINT ( 'NONE',  ( 14.34966873604960469, 8.224510206698951720, 54.16557627198103120 ) ) ;
#46653 = CARTESIAN_POINT ( 'NONE',  ( 4.379528057220339221, -16.55341960407611168, 37.70724293864769550 ) ) ;
#46654 = CARTESIAN_POINT ( 'NONE',  ( -16.52544592524342804, 4.483927247898546575, 111.0405762719810525 ) ) ;
#46656 = FILL_AREA_STYLE_COLOUR ( '', #79181 ) ;
#46655 = CARTESIAN_POINT ( 'NONE',  ( 5.153800228976615827, -19.02544592524334988, 50.20942372801897591 ) ) ;
#46657 = CARTESIAN_POINT ( 'NONE',  ( 21.52544592524334988, 5.823673210054432836, 51.45942372801901854 ) ) ;
#46658 = CARTESIAN_POINT ( 'NONE',  ( 13.97604488694548053, -13.89961937509957401, 105.6260903946856757 ) ) ;
#46659 = LINE ( 'NONE', #141644, #156776 ) ;
#46660 = CARTESIAN_POINT ( 'NONE',  ( 19.03943276465977164, -0.05219959533909143690, 108.7489096053143527 ) ) ;
#46661 = CARTESIAN_POINT ( 'NONE',  ( 21.52544592524344225, -5.823673210054117533, 78.54057627198103830 ) ) ;
#46662 = CARTESIAN_POINT ( 'NONE',  ( -13.97604488694547697, 13.89961937509957934, 98.12609039468566152 ) ) ;
#46663 = CARTESIAN_POINT ( 'NONE',  ( -13.89961937509977652, 13.97604488694528158, 100.6239096053143669 ) ) ;
#46664 = CARTESIAN_POINT ( 'NONE',  ( -26.77313074627685907, 4.631999166354653141, 170.7390164845645870 ) ) ;
#46665 = CARTESIAN_POINT ( 'NONE',  ( 0.05219959533910956823, 16.53943276465976808, 104.9989096053143669 ) ) ;
#46666 = CARTESIAN_POINT ( 'NONE',  ( -0.05219959533937732626, 21.53943276465977519, 92.50109039468567573 ) ) ;
#46667 = CARTESIAN_POINT ( 'NONE',  ( -13.89961937509977652, 13.97604488694528158, 25.62390960531434558 ) ) ;
#46668 = CARTESIAN_POINT ( 'NONE',  ( -15.72974639402176322, -15.80617190586768395, 39.37609039468567573 ) ) ;
#46669 = CARTESIAN_POINT ( 'NONE',  ( -5.719274019375665041, -21.55341960407619695, 89.79275706135236135 ) ) ;
#46670 = CARTESIAN_POINT ( 'NONE',  ( 16.52544592524335698, 4.483927247898782831, 86.45942372801901854 ) ) ;
#46671 = CARTESIAN_POINT ( 'NONE',  ( -21.52544592524334988, -5.823673210054445271, 48.95942372801902565 ) ) ;
#46672 = CARTESIAN_POINT ( 'NONE',  ( 15.80617190586769283, -15.72974639402175789, 45.62609039468567573 ) ) ;
#46674 = CARTESIAN_POINT ( 'NONE',  ( 16.51473224551069308, 9.474510206698969483, 84.16557627198102409 ) ) ;
#46673 = CARTESIAN_POINT ( 'NONE',  ( -5.049401038297874678, -19.05341960407617918, 64.79275706135233293 ) ) ;
#46675 = CARTESIAN_POINT ( 'NONE',  ( 16.53943276465976808, -0.05219959533910856209, 98.74890960531438111 ) ) ;
#46676 = AXIS2_PLACEMENT_3D ( 'NONE', #62740, #185106, #170929 ) ;
#46677 = CARTESIAN_POINT ( 'NONE',  ( 5.823673210054125526, 21.52544592524343514, 84.79057627198102409 ) ) ;
#46678 = CARTESIAN_POINT ( 'NONE',  ( -8.314922557960811034, -14.29746914071050412, 62.08224293864769550 ) ) ;
#46679 = CARTESIAN_POINT ( 'NONE',  ( -15.72974639402176322, -15.80617190586768395, 109.3760903946857042 ) ) ;
#46680 = CARTESIAN_POINT ( 'NONE',  ( 16.53943276465976808, -0.05219959533910856209, 88.74890960531436690 ) ) ;
#46681 = CARTESIAN_POINT ( 'NONE',  ( 9.474510206698971260, -16.51473224551069308, 42.91557627198103120 ) ) ;
#46682 = CARTESIAN_POINT ( 'NONE',  ( -0.05219959533936034679, 19.03943276465977164, 77.50109039468566152 ) ) ;
#46683 = CARTESIAN_POINT ( 'NONE',  ( -8.224510206698948167, 14.34966873604960824, 30.41557627198101699 ) ) ;
#46684 = CARTESIAN_POINT ( 'NONE',  ( -5.719274019375665041, -21.55341960407619695, 94.79275706135234714 ) ) ;
#46685 = CARTESIAN_POINT ( 'NONE',  ( -16.51473224551069308, -9.474510206698971260, 86.66557627198102409 ) ) ;
#46686 = CARTESIAN_POINT ( 'NONE',  ( -5.049401038297874678, -19.05341960407617918, 59.79275706135231871 ) ) ;
#46687 = CARTESIAN_POINT ( 'NONE',  ( 21.52544592524344225, -5.823673210054117533, 63.54057627198103830 ) ) ;
#46688 = CARTESIAN_POINT ( 'NONE',  ( 21.52544592524344225, -5.823673210054117533, 108.5405762719810241 ) ) ;
#46689 = CARTESIAN_POINT ( 'NONE',  ( -13.89961937509957401, -13.97604488694547875, 109.3760903946856331 ) ) ;
#46690 = CARTESIAN_POINT ( 'NONE',  ( 16.52544592524335698, 4.483927247898782831, 76.45942372801901854 ) ) ;
#46692 = CARTESIAN_POINT ( 'NONE',  ( -18.62759615963270932, 10.81492255796079327, 115.8322429386477097 ) ) ;
#46691 = DIRECTION ( 'NONE',  ( -0.7071067811865466846, 2.468850131082262977E-15, 0.7071067811865484609 ) ) ;
#46693 = CARTESIAN_POINT ( 'NONE',  ( 12.14591786802309770, 12.06949235617756955, 104.3739096053143669 ) ) ;
#46694 = CARTESIAN_POINT ( 'NONE',  ( -22.81625015709510507, 31.40387420917330275, -9.424999997268812990 ) ) ;
#46695 = CARTESIAN_POINT ( 'NONE',  ( -8.314922557961024197, 14.29746914071037800, 47.91775706135234714 ) ) ;
#46696 = CARTESIAN_POINT ( 'NONE',  ( -12.06949235617756955, 12.14591786802309770, 75.62390960531439532 ) ) ;
#46697 = CARTESIAN_POINT ( 'NONE',  ( 5.719274019375991003, -21.55341960407610458, 72.70724293864769550 ) ) ;
#46698 = CARTESIAN_POINT ( 'NONE',  ( 8.314922557961029526, -14.29746914071037800, 100.4177570613523471 ) ) ;
#46699 = CARTESIAN_POINT ( 'NONE',  ( 14.34966873604972726, -8.224510206698740333, 35.83442372801901143 ) ) ;
#46700 = CARTESIAN_POINT ( 'NONE',  ( -5.049401038298153566, 19.05341960407611168, 45.20724293864769550 ) ) ;
#46701 = CARTESIAN_POINT ( 'NONE',  ( -14.29746914071037622, -8.314922557961029526, 84.16775706135234714 ) ) ;
#46702 = CARTESIAN_POINT ( 'NONE',  ( 16.51473224551083163, -9.474510206698727899, 75.83442372801900433 ) ) ;
#46703 = CARTESIAN_POINT ( 'NONE',  ( -10.81492255796078084, -18.62759615963271287, 72.08224293864769550 ) ) ;
#46704 = CARTESIAN_POINT ( 'NONE',  ( -16.53943276465976808, -0.05219959533934237506, 103.7510903946857042 ) ) ;
#46705 = CARTESIAN_POINT ( 'NONE',  ( 18.62759615963255655, 10.81492255796105972, 86.66775706135234714 ) ) ;
#46706 = AXIS2_PLACEMENT_3D ( 'NONE', #134024, #193705, #23850 ) ;
#46707 = CARTESIAN_POINT ( 'NONE',  ( 15.72974639402199770, -15.80617190586745480, 63.12390960531435979 ) ) ;
#46708 = CARTESIAN_POINT ( 'NONE',  ( 18.67979575497178502, 10.72451020669898547, 49.16557627198102409 ) ) ;
#46709 = ORIENTED_EDGE ( 'NONE', *, *, #152294, .F. ) ;
#46710 = CARTESIAN_POINT ( 'NONE',  ( 8.224510206698742110, 14.34966873604972548, 82.08442372801901854 ) ) ;
#46711 = CARTESIAN_POINT ( 'NONE',  ( 21.53943276465977519, -0.05219959533907433946, 43.74890960531435979 ) ) ;
#46712 = VERTEX_POINT ( 'NONE', #70161 ) ;
#46713 = CARTESIAN_POINT ( 'NONE',  ( -19.02544592524342804, 5.153800228976336051, 111.0405762719810099 ) ) ;
#46714 = CARTESIAN_POINT ( 'NONE',  ( 37.99999999999999289, 2.893978650043524126E-14, -8.749999994537628112 ) ) ;
#46715 = CARTESIAN_POINT ( 'NONE',  ( 16.46253265017160672, -9.564922557960803928, 23.33224293864769194 ) ) ;
#46716 = CARTESIAN_POINT ( 'NONE',  ( -5.823673210054116645, -21.52544592524344225, 72.29057627198102409 ) ) ;
#46717 = CARTESIAN_POINT ( 'NONE',  ( 0.05219959533934541429, -16.53943276465976808, 100.0010903946857042 ) ) ;
#46718 = CARTESIAN_POINT ( 'NONE',  ( 10.72451020669871369, 18.67979575497193778, 47.08442372801901854 ) ) ;
#46719 = CARTESIAN_POINT ( 'NONE',  ( -8.224510206698735004, -14.34966873604973081, 19.58442372801901143 ) ) ;
#46720 = CARTESIAN_POINT ( 'NONE',  ( -0.05219959533909027116, -19.03943276465977164, 22.49890960531436690 ) ) ;
#46721 = CARTESIAN_POINT ( 'NONE',  ( 5.049401038297881783, 19.05341960407617563, 112.2927570613523471 ) ) ;
#46722 = CARTESIAN_POINT ( 'NONE',  ( 13.97604488694527802, 13.89961937509977652, 34.37390960531436690 ) ) ;
#46723 = CARTESIAN_POINT ( 'NONE',  ( -28.82186960331499392, 9.364793116373565596, 141.9000000000000057 ) ) ;
#46724 = CARTESIAN_POINT ( 'NONE',  ( -13.97604488694527625, -13.89961937509977652, 101.8739096053143811 ) ) ;
#46725 = VECTOR ( 'NONE', #178142, 1000.000000000000000 ) ;
#46726 = CARTESIAN_POINT ( 'NONE',  ( -8.314922557961024197, 14.29746914071037800, 82.91775706135234714 ) ) ;
#46727 = CARTESIAN_POINT ( 'NONE',  ( -0.05219959533936034679, 19.03943276465977164, 77.50109039468566152 ) ) ;
#46728 = CARTESIAN_POINT ( 'NONE',  ( -9.564922557961040184, 16.46253265017147172, 22.91775706135233648 ) ) ;
#46729 = CARTESIAN_POINT ( 'NONE',  ( -18.67979575497178146, -10.72451020669898902, 56.66557627198103830 ) ) ;
#46730 = CARTESIAN_POINT ( 'NONE',  ( -0.05219959533934338120, 16.53943276465976808, 87.50109039468568994 ) ) ;
#46731 = CARTESIAN_POINT ( 'NONE',  ( 9.474510206698729675, 16.51473224551082808, 92.08442372801900433 ) ) ;
#46732 = CARTESIAN_POINT ( 'NONE',  ( 13.97604488694527802, 13.89961937509977652, 54.37390960531435979 ) ) ;
#46734 = CIRCLE ( 'NONE', #17581, 23.10356920737165254 ) ;
#46733 = CARTESIAN_POINT ( 'NONE',  ( -13.89961937509977652, 13.97604488694528158, 85.62390960531433848 ) ) ;
#46735 = CARTESIAN_POINT ( 'NONE',  ( 21.52544592524334988, 5.823673210054432836, 46.45942372801901854 ) ) ;
#46736 = CARTESIAN_POINT ( 'NONE',  ( -13.97604488694527625, -13.89961937509977652, 41.87390960531435979 ) ) ;
#46737 = CARTESIAN_POINT ( 'NONE',  ( -16.36317988757060249, -7.306389748694939179, 85.90210391636776421 ) ) ;
#46738 = CARTESIAN_POINT ( 'NONE',  ( 19.03943276465977164, -0.05219959533909143690, 103.7489096053143669 ) ) ;
#46739 = CARTESIAN_POINT ( 'NONE',  ( -12.06949235617756955, 12.14591786802309770, 70.62390960531436690 ) ) ;
#46740 = CARTESIAN_POINT ( 'NONE',  ( -18.67979575497178146, -10.72451020669898902, 61.66557627198103120 ) ) ;
#46741 = CARTESIAN_POINT ( 'NONE',  ( -12.49999999999997691, -89.99999999999997158, -15.00000000000000178 ) ) ;
#46742 = MECHANICAL_DESIGN_GEOMETRIC_PRESENTATION_REPRESENTATION (  '', ( #91879 ), #53220 ) ;
#46743 =( BOUNDED_SURFACE ( )  B_SPLINE_SURFACE ( 3, 2, ( 
 ( #147779, #11269, #55754, #197275, #43584, #54754, #163953, #9265, #87091, #88081, #25451, #149767, #180132, #70931, #118439, #24439, #90074, #58738, #40594, #120407, #101243, #39584, #41601, #165941, #105250, #132598, #103266, #72942, #166936, #28439, #196296, #134612, #57766, #148776, #10265, #42595, #102265, #150775, #164946, #151757, #162932, #26439, #69931, #71924, #119436, #131595, #193280, #86088, #181121, #133594, #104258, #117428, #195286, #116428, #179126, #178116, #194288, #73935, #89083, #56767, #27441, #12270, #135604, #171891, #107218, #153730, #2035, #106232, #152733, #77877, #122392, #44576, #155718, #185069, #167915, #17215, #74913, #95036, #16225, #46557, #61707, #13250, #168889, #124384, #14223, #33378, #139544, #78867, #29415, #59732, #140547, #15226, #63715, #125390, #48557, #136576, #62701, #183095, #198256, #91046, #121401, #76885, #123377, #75893, #187087, #108219, #137568, #93042, #30394, #199251, #110210, #92041, #60718, #184081, #169899, #170893, #138556, #1029, #45565, #34, #186079, #47561, #109214, #31392, #154729, #32385, #94040, #49540, #128351, #83836, #126372, #66689, #145518, #112203, #97995, #192033, #6998, #111202, #159688, #189070, #190049, #142535, #81830, #38356, #65692, #64710, #79876, #160697, #175876, #68680, #51524, #188069, #53515, #115193, #50542, #97014, #130335, #172894, #96033, #21186, #127357, #34373, #99006, #113187, #157720, #22188, #18220, #156727, #82842, #174876, #5006, #141545, #173893, #67686, #19209, #176885, #144521, #3034, #80859, #4014, #35362, #158695, #20184, #143517, #36342, #6006, #129344, #191039, #52512, #114173, #37348, #102028, #10030, #162696, #104025, #133357, #100011, #179895, #194058, #161697, #88847, #178885, #27201, #181869, #195047, #57533, #117192, #26204, #39353, #101012, #87843, #149531, #134374, #40353, #163710, #86855, #193045, #54522, #177884, #41361, #85851, #150539, #12039, #84837, #55519, #24202, #25213, #118204, #148539, #103027, #71690, #147540, #56526, #116195, #120179, #73703, #70697, #135375, #131356, #69689, #164709, #196060, #197045, #9028, #11026, #72701, #58513, #23194, #119202, #180887, #42362, #165704, #146516, #8006, #132365, #124145, #169667, #108986, #125157, #107979, #13992, #74684, #47331, #89847, #199016, #1803, #92812, #800, #170667, #30162, #63481, #60485, #153498, #140313, #138334, #121169, #45337, #106989, #185844, #168662, #91806, #61481, #183849, #137336, #14995, #182863, #76655, #139320, #43348, #152503, #13019, #200014, #15994, #123152, #154499, #31162, #32155, #184840, #122160, #93812, #105019, #46325, #77652, #62473, #155492, #59494, #151530, #16984, #166703, #78638, #75659, #28206, #106002, #136350, #198026, #44344, #167689, #29186, #90820, #142301, #110968, #3781, #17988, #33149, #189819, #129105, #66454, #65458, #111967, #80624, #51291, #67447, #145282, #21953, #97762, #175635, #186856, #5772, #144283, #109980, #174645, #83603, #112952, #4767, #127121, #20945, #50311, #141310, #94807, #173659, #171660, #159449, #156486, #79641, #48325, #98768, #68444, #187840, #158467, #37109, #2799, #190804, #6765, #64477, #128116, #126144, #82602, #81597, #49309, #52278, #113936, #172652, #34140, #160462, #36110, #95799, #19955, #157485, #18978, #188827, #35126, #96778, #143281, #9792, #54288, #147298, #161463, #176648, #133119, #72460, #71454, #8787, #55280, #23956, #194808, #10792, #88610, #165471, #41125, #118971, #130098, #149298, #87612, #53276, #117964, #26967, #56282, #148298, #85611, #164475, #193815, #84601, #38124, #116951, #114955, #102789, #99778, #22953, #191795, #42130, #11803, #131117, #101784, #180654, #146280, #134134, #150306, #7767, #179655, #69450, #25969, #24969, #192806, #195823, #57294, #115960, #177648, #103791, #39116, #100772, #163472, #162455, #70457, #132122, #178643, #40106, #86615, #183620, #168435, #184605, #139083, #29931, #59260, #43115, #122917, #58281, #182628 ),
 ( #73467, #120929, #181635, #196814, #46086, #61245, #30927, #60255, #104783, #15754, #77413, #44113, #28954, #92575, #166471, #151298, #91570, #105771, #27969, #107741, #198789, #89609, #169422, #135140, #119950, #154263, #138097, #153258, #12787, #45103, #74452, #152277, #136118, #197794, #167458, #121926, #75429, #90595, #13761, #137103, #106760, #14760, #76421, #199778, #195469, #86264, #87268, #39758, #179305, #135779, #163113, #162110, #177301, #57942, #73121, #104436, #148952, #23607, #89261, #12447, #147954, #194459, #42774, #146945, #193457, #118618, #24616, #85253, #196472, #25623, #8434, #119613, #115612, #53937, #56944, #10442, #102438, #38773, #9441, #165121, #54934, #74109, #180308, #181296, #70106, #100429, #166120, #55930, #27622, #150953, #131775, #116606, #103442, #178294, #101421, #71106, #132772, #117605, #164125, #40769, #72102, #133775, #41776, #26613, #88256, #149943, #11449, #134790, #127280, #81757, #94969, #157645, #17146, #126301, #136748, #958, #187997, #49467, #34299, #140477, #78799, #187017, #90245, #151928, #75081, #141475, #186008, #188993, #112129, #182278, #93971, #62634, #1965, #18149, #155651, #79803, #110142, #124310, #48488, #13417, #20113, #50469, #170826, #173820, #28607, #167106, #171821, #95961, #35285, #47490, #33309, #2959, #96941, #158622, #111130, #64639, #172819, #63645, #125320, #19134, #32318, #80785, #156653, #197450, #109147, #142463, #58916, #3941, #65620, #120584, #43759, #105423, #25130, #84759, #21110, #39273, #38280, #40273, #147459, #85772, #143444, #82765, #24119, #23114, #7928, #176808, #51449, #162614, #4930, #113110, #144446, #178803, #146437, #69612, #8949, #66613, #131278, #114097, #174800, #70617, #189974, #98930, #101946, #192966, #100930, #132283, #130258, #163627, #160621, #53440, #128277, #99934, #5931, #145442, #6924, #193975, #68602, #191954, #161620, #83762, #37273, #115115, #67607, #54445, #55437, #36266, #52439, #97921, #116115, #177804, #117108, #159614, #129268, #190962, #175800, #22112, #171703, #128162, #189862, #111012, #141355, #156532, #108023, #1844, #19022, #109029, #66499, #172698, #50355, #843, #154541, #112014, #48368, #173703, #35171, #143325, #31203, #157528, #77694, #169710, #124188, #16036, #110025, #18031, #170708, #96826, #2842, #92854, #187883, #63526, #139362, #158510, #186897, #19997, #62516, #64520, #65503, #125201, #34183, #47374, #32198, #95844, #80668, #142344, #33192, #94851, #79685, #185889, #93855, #155532, #49350, #17027, #81641, #4811, #78680, #126187, #140356, #3824, #127164, #188872, #6810, #175679, #68488, #82645, #97806, #54330, #193857, #131161, #130143, #176694, #145328, #116001, #132166, #9835, #86655, #162498, #40150, #51336, #70498, #8830, #174690, #39158, #148339, #177690, #69496, #191840, #85655, #115000, #5817, #159495, #38168, #36154, #23999, #20990, #144328, #112996, #163513, #133160, #52324, #23000, #101826, #67493, #55322, #71494, #129150, #192851, #190847, #147342, #146323, #113981, #116993, #178688, #37153, #98813, #25012, #100815, #160507, #84646, #21997, #83650, #53321, #99823, #161508, #7812, #74495, #120971, #60294, #76462, #59302, #165514, #26010, #198830, #41168, #150350, #153300, #44153, #152317, #121968, #181677, #14801, #11847, #104825, #91612, #89654, #72504, #196857, #58323, #75469, #119991, #43158, #12829, #135183, #88654, #166514, #134179, #28012, #90635, #194852, #103833, #164517, #151340, #167500, #136161, #105813, #182669, #183660, #87653, #56325, #28995, #27010, #197836, #13803, #137142, #45145, #10834, #102831, #106801, #118007, #168475, #73512, #29973, #57339, #179696, #149338, #195866, #119014, #180697, #42173, #107779, #16785, #1600, #158271, #19760, #141112, #171463, #186653, #138139, #31955, #49115, #139123, #96582, #2601, #80426, #30965, #184644, #142099, #78435, #3584, #65262, #173458, #61287, #187644, #169464, #199819, #154303, #46125, #140109 ),
 ( #95599, #155295, #64279, #77452, #600, #125946, #110772, #172454, #63276, #124956, #48123, #92612, #15792, #62270, #79442, #123938, #126922, #50109, #122957, #93610, #185636, #109780, #156286, #32951, #17786, #94606, #47128, #33941, #108786, #170465, #188629, #157284, #111769, #18780, #34929, #129896, #177452, #70261, #20746, #114753, #22755, #116755, #193613, #7565, #84404, #146081, #36907, #21754, #54090, #113741, #162261, #53075, #8587, #51094, #191596, #131930, #98570, #69251, #178446, #55085, #35916, #130917, #175437, #176447, #67250, #6566, #163269, #190609, #189620, #4566, #85410, #100579, #39913, #37920, #112754, #101581, #81401, #160264, #83406, #143087, #174447, #82401, #192608, #52084, #66258, #127918, #115765, #97562, #159250, #23761, #38922, #144089, #147102, #5570, #128908, #99580, #145083, #68245, #161261, #179457, #132924, #88406, #9595, #135926, #71260, #56083, #24771, #136899, #106555, #25774, #196618, #75228, #194611, #43908, #183414, #86418, #166270, #102595, #120729, #119758, #121722, #28755, #167256, #148104, #164281, #105570, #104585, #89411, #58088, #117764, #90392, #40922, #87420, #149105, #60054, #27768, #151100, #152076, #10595, #12592, #195624, #72256, #13561, #133934, #180459, #44898, #74256, #182429, #198586, #11603, #57097, #41931, #134941, #118771, #181442, #103597, #26766, #150102, #165272, #73271, #42920, #197596, #59062, #62027, #78190, #45884, #16543, #64032, #65020, #77208, #137891, #139860, #140862, #93361, #17533, #94357, #172205, #199572, #126676, #2351, #357, #108541, #32705, #109534, #171216, #184403, #76212, #124706, #188380, #155048, #138877, #170220, #30722, #185390, #1349, #153052, #91361, #122713, #125702, #123692, #92369, #46881, #61041, #14554, #156036, #110524, #47881, #31713, #63029, #186404, #79193, #48869, #107537, #187401, #29728, #169213, #154055, #3345, #33690, #95353, #157038, #49857, #18535, #80182, #15550, #141854, #168232, #67007, #70014, #161016, #69003, #115520, #98316, #131683, #128666, #21503, #8339, #6322, #189377, #113497, #175192, #192363, #36658, #160016, #129654, #51838, #5323, #83164, #50854, #144838, #7319, #193364, #20500, #81164, #68002, #84157, #191350, #22510, #37668, #177208, #142846, #111523, #145837, #143844, #52828, #176199, #114497, #99333, #127677, #19519, #130669, #173208, #53846, #82148, #38681, #174205, #190362, #100337, #96341, #34684, #66009, #162016, #23512, #35673, #85159, #4325, #158028, #146845, #112512, #97321, #159007, #180214, #148858, #119520, #135684, #16061, #92878, #166024, #46391, #54840, #74014, #12351, #178202, #42679, #154565, #181202, #73024, #10349, #89165, #118525, #9350, #163016, #41684, #39666, #27524, #101328, #86174, #116515, #169734, #139385, #55838, #26520, #108049, #24523, #197356, #77719, #147864, #196379, #132683, #150857, #149849, #71015, #58820, #120488, #194371, #117512, #182179, #134696, #179209, #40676, #104340, #25533, #102346, #31229, #164035, #72006, #87177, #133679, #195371, #56850, #103348, #165027, #88165, #11353, #57848, #95873, #78708, #2871, #64549, #81670, #126214, #187910, #19049, #141383, #94880, #111042, #140385, #49379, #96854, #97834, #110052, #170732, #172729, #173732, #34210, #50384, #127192, #4842, #32223, #159522, #35201, #33220, #157556, #65532, #142373, #3853, #17053, #109055, #80696, #21019, #188904, #171732, #112044, #63553, #18059, #158538, #185914, #124217, #155559, #20028, #156561, #125227, #79714, #93881, #47399, #143353, #66528, #128191, #189889, #51364, #113025, #174717, #36180, #82674, #867, #62542, #1872, #186925, #48395, #101857, #67521, #132195, #41196, #70526, #162526, #38194, #178716, #7838, #98841, #52352, #69524, #129178, #55351, #190876, #175706, #144358, #56354, #26036, #145355, #116029, #194880, #114008, #163541, #102858, #5845, #85683, #22025, #40178, #39186, #164544, #148368, #86684, #37183, #83677, #99850, #8859, #25041 ),
 ( #146351, #131189, #24029, #84672, #161534, #54357, #6837, #192879, #9863, #160536, #53350, #68516, #177718, #117021, #100844, #193886, #71522, #133189, #130170, #191867, #118035, #176721, #147370, #179726, #115028, #23027, #103861, #195895, #44184, #184676, #74524, #58352, #89683, #150380, #104854, #121001, #72531, #10862, #42201, #45178, #43185, #11877, #166543, #119043, #134208, #90665, #30005, #167530, #28041, #12859, #181704, #152347, #168507, #46159, #122990, #198860, #76496, #87681, #106832, #91643, #57370, #75498, #107814, #13832, #105842, #151368, #122001, #136189, #165542, #180725, #197864, #27039, #60327, #88685, #73540, #149366, #199853, #169497, #135213, #59331, #138172, #196885, #153332, #120019, #182699, #29025, #137172, #183691, #14833, #61319, #34967, #173494, #112791, #170499, #124994, #95635, #50146, #47161, #139155, #111806, #92645, #633, #108820, #66295, #110809, #157323, #96619, #30996, #18818, #1637, #62303, #158308, #77486, #186689, #189658, #80462, #188667, #19796, #17823, #51131, #48159, #141150, #127954, #125983, #31989, #32989, #156323, #49151, #171500, #109817, #2639, #93647, #79481, #126958, #154334, #140145, #123973, #64315, #3620, #187681, #142136, #65299, #81437, #185670, #15825, #143123, #63314, #94642, #4603, #172491, #33979, #155332, #16820, #78471, #71301, #161299, #145121, #176485, #36946, #191634, #7603, #159286, #97598, #128945, #131968, #129935, #98608, #53114, #5607, #20783, #177491, #116793, #54128, #114792, #99619, #68284, #38960, #55124, #132964, #9634, #85449, #163311, #174485, #193652, #178485, #82438, #162299, #194653, #100617, #192645, #37961, #8627, #22795, #190646, #144126, #84441, #67287, #147139, #52122, #113778, #35952, #86458, #56123, #175474, #146119, #24809, #160302, #39951, #21792, #83443, #115801, #6605, #70299, #69289, #130955, #101622, #148143, #23799, #57137, #11646, #182469, #136941, #133975, #25813, #198630, #179498, #87459, #195666, #153094, #197637, #43950, #183457, #199616, #105612, #88449, #149146, #121764, #164320, #73312, #76254, #167300, #75271, #44943, #104625, #137932, #134983, #27811, #14598, #12632, #118813, #119799, #181484, #60096, #42962, #10636, #106598, #72296, #196661, #166314, #117805, #40963, #120768, #151141, #89452, #102635, #58130, #28796, #180499, #41971, #90435, #168274, #103638, #165316, #29771, #74297, #91406, #26809, #150144, #135966, #152121, #59103, #13603, #77249, #107580, #63073, #171261, #123735, #65061, #94400, #61082, #140909, #155090, #122755, #49899, #139903, #188422, #142886, #156081, #18577, #78232, #187444, #398, #62070, #48912, #110566, #95395, #1392, #124752, #47924, #154097, #15591, #138917, #2395, #46924, #111566, #173250, #45925, #16584, #185434, #186448, #79238, #109578, #64074, #32749, #108584, #17577, #170261, #81205, #34725, #31755, #96383, #92411, #157081, #125744, #169257, #184445, #93404, #172247, #33734, #158070, #19561, #80224, #141895, #3386, #126718, #30764, #177249, #36700, #85201, #176241, #131724, #174249, #114541, #193406, #160060, #145878, #39705, #54881, #159050, #7361, #98361, #37712, #190406, #129696, #86213, #113541, #112554, #127719, #8381, #23553, #116555, #99374, #35717, #101368, #163057, #21547, #144882, #178244, #97364, #143886, #69046, #175235, #83207, #161057, #82193, #52870, #100379, #24564, #6364, #20544, #22552, #38721, #191393, #53887, #130711, #70056, #5367, #4368, #162057, #68044, #84198, #192405, #115562, #146889, #67051, #128709, #66051, #189421, #50896, #51882, #149887, #10389, #165066, #181242, #132721, #71055, #102386, #105367, #103388, #72046, #26560, #179251, #194409, #150898, #90192, #27565, #88203, #73063, #41724, #12392, #28555, #106350, #183215, #58862, #136695, #147903, #167054, #151875, #55879, #135725, #44696, #74054, #166064, #11393, #182221, #134735, #164074, #117552, #196417, #40717, #120528, #25573, #87217, #9389, #59853, #29531, #148899 ),
 ( #133720, #195412, #57887, #197396, #13365, #56890, #118564, #75029, #180254, #119559, #42719, #168034, #89205, #43705, #198376, #104381, #121520, #61825, #122512, #95155, #137688, #46679, #49658, #140664, #48675, #156843, #77993, #111322, #108338, #1148, #188186, #186201, #169008, #93162, #154847, #172008, #16344, #139660, #109333, #31509, #45684, #32506, #123495, #124506, #77004, #62823, #173012, #156, #199373, #14348, #18338, #110327, #141661, #47683, #60837, #126488, #91164, #185188, #171015, #79993, #184202, #30512, #155837, #170019, #107335, #33496, #92164, #94158, #17334, #152853, #76013, #78990, #2156, #63834, #153850, #125507, #187204, #15348, #138676, #3153, #64826, #127479, #80977, #177010, #174995, #38479, #100136, #69809, #157838, #83962, #4131, #193163, #50657, #142652, #36460, #144643, #97128, #161817, #67809, #34491, #114301, #128468, #96149, #23312, #113304, #84956, #116310, #129464, #192161, #51640, #160823, #174008, #35479, #22311, #145642, #68804, #98117, #159814, #21309, #189184, #112318, #158812, #176003, #20300, #146638, #8131, #19329, #190164, #81948, #82966, #52636, #6126, #37472, #191163, #143640, #99133, #5123, #54635, #131476, #66805, #65810, #7122, #130463, #53641, #115318, #59614, #117310, #11151, #119319, #13139, #89964, #104144, #181006, #42481, #133477, #118323, #150660, #10149, #58629, #149653, #105138, #147661, #87965, #166824, #195169, #165826, #74801, #28325, #120295, #177999, #179006, #71809, #27323, #197163, #194173, #85971, #181988, #39466, #9148, #55637, #136464, #57653, #88970, #43470, #101127, #12158, #148661, #70815, #151644, #24322, #56650, #198144, #73823, #135493, #162813, #164829, #132484, #180016, #72825, #40474, #134494, #102146, #41483, #103148, #163831, #26325, #196181, #25333, #86974, #15110, #31274, #199133, #169781, #17101, #18105, #30276, #90932, #92925, #93927, #46437, #170780, #47445, #125275, #152618, #79759, #155606, #153614, #61593, #185960, #62587, #124265, #137454, #29302, #77764, #141430, #108096, #91922, #123262, #183963, #138443, #154611, #106118, #44464, #75776, #78753, #76771, #45450, #200124, #14109, #167802, #109101, #63599, #913, #184953, #16106, #139431, #32270, #1920, #2917, #156610, #140430, #110099, #121287, #186972, #48442, #60600, #171778, #182980, #33266, #94925, #122275, #107104, #168774, #19093, #172777, #128236, #49426, #175754, #111087, #95917, #64595, #179527, #149176, #65579, #36226, #117834, #34258, #86487, #25844, #126259, #5890, #142420, #163342, #159569, #164349, #71330, #35244, #157602, #132992, #80742, #20071, #87488, #114057, #24837, #194683, #51408, #187956, #81715, #174760, #3899, #21067, #127238, #66571, #189933, #148172, #113068, #97878, #82723, #4889, #158582, #144404, #188952, #67566, #9663, #50429, #173778, #112088, #129224, #37231, #190921, #101650, #52398, #56152, #96898, #143400, #40996, #102664, #151173, #75300, #152150, #13633, #26838, #118845, #167330, #107610, #197666, #181513, #12661, #73341, #27841, #43979, #195695, #134004, #165345, #168304, #166344, #135014, #89482, #42001, #57166, #136971, #153124, #90466, #74328, #135995, #104657, #198661, #91437, #169288, #45955, #121794, #199647, #10665, #29801, #14628, #180528, #60127, #30794, #183488, #28826, #59132, #44972, #120799, #88478, #103667, #182500, #150175, #106630, #11675, #196691, #72328, #122786, #92442, #58160, #105641, #61113, #119828, #76285, #42992, #137964, #184476, #31785, #49931, #48942, #50926, #158099, #96413, #35747, #93434, #47956, #18606, #173281, #170291, #62102, #34754, #15622, #123765, #155120, #189449, #33766, #80254, #19591, #154128, #141924, #77279, #81234, #142915, #4397, #110595, #185464, #112584, #174278, #109607, #94430, #66081, #46955, #16614, #3415, #63103, #108614, #127748, #78261, #32778, #17608, #138948, #428, #157110, #187473, #2426, #139934, #171291, #65090, #1423, #124781, #126749, #186479, #156111 ),
 ( #95426, #79268, #140939, #64106, #188451, #125773, #172277, #111596, #177283, #131757, #97393, #85235, #23587, #20573, #115594, #39739, #38754, #7395, #6395, #162092, #114576, #190436, #5397, #176275, #82225, #100411, #143916, #128740, #159079, #67080, #51912, #191425, #146925, #113571, #21578, #101401, #175265, #36731, #70088, #52901, #163094, #8416, #98393, #160092, #83236, #144912, #84232, #193439, #68074, #129728, #130745, #145910, #37746, #161089, #69079, #53920, #99406, #22584, #192438, #54915, #116587, #178276, #48600, #109257, #81875, #124427, #33422, #36385, #127403, #35404, #143567, #64752, #98039, #95081, #188111, #174921, #172937, #155761, #79916, #141588, #158738, #3076, #159736, #77920, #19254, #17259, #173936, #34416, #139587, #5049, #20227, #1072, #78912, #171933, #142578, #97055, #94082, #186123, #66735, #62747, #47603, #140589, #113231, #157764, #4057, #128395, #170936, #65735, #110252, #32428, #190092, #2079, #156769, #63758, #189112, #51567, #125432, #126414, #187128, #18263, #49583, #111246, #96075, #80901, #50585, #112245, #102073, #23238, #146561, #39397, #161743, #115239, #131402, #99052, #69734, #117239, #118250, #130381, #191084, #193090, #194103, #8056, #70743, #147588, #25258, #52557, #179941, #55565, #53561, #84882, #85900, #162742, #24250, #37394, #129388, #177930, #41408, #54566, #192079, #116238, #83882, #38401, #101057, #6052, #144566, #175923, #178932, #176931, #145564, #100058, #114218, #67730, #9073, #163758, #132411, #40402, #86901, #148584, #10076, #71734, #103073, #56576, #133404, #195093, #21233, #82888, #160741, #22233, #7042, #68724, #90862, #182906, #58558, #199059, #28253, #119248, #72751, #89892, #149577, #75700, #11073, #196108, #164755, #76700, #46365, #165752, #136394, #15039, #134422, #183895, #120224, #123194, #14035, #122203, #168705, #151575, #184883, #181914, #74730, #61525, #59537, #42407, #166749, #13064, #45380, #198071, #121216, #44390, #105065, #43394, #106045, #104070, #167731, #60528, #26250, #73748, #57578, #29229, #137380, #152547, #107033, #30207, #91849, #180932, #87891, #153542, #197091, #138376, #200056, #27245, #88894, #150586, #12085, #135420, #17320, #128452, #172996, #112302, #62808, #16329, #173992, #110312, #35461, #97112, #5107, #93147, #19312, #139646, #190148, #186186, #77979, #171994, #79979, #32491, #158795, #3137, #170003, #49644, #63819, #31494, #20284, #48660, #81930, #51623, #64812, #127462, #187189, #96133, #109319, #170999, #157822, #80960, #4114, #33482, #95140, #156829, #124490, #47667, #94144, #111307, #155823, #143622, #66788, #154831, #125492, #78975, #18322, #188171, #141647, #34474, #126473, #140650, #142636, #2140, #1134, #65793, #189168, #50640, #144626, #147643, #69791, #159796, #195152, #52620, #146621, #54618, #148643, #25316, #39450, #116293, #177983, #68786, #53623, #85955, #145625, #194157, #84940, #40456, #161801, #9132, #10132, #22294, #82948, #23296, #70798, #38462, #162797, #101111, #117294, #6109, #71793, #132466, #7105, #115299, #24306, #55621, #178989, #130444, #8113, #102130, #67791, #100118, #83945, #176992, #175985, #192142, #131459, #98098, #36443, #129447, #163814, #193146, #37453, #86958, #191146, #21291, #133462, #113288, #174979, #114282, #99114, #160806, #121270, #137436, #15095, #91905, #167786, #45434, #56633, #75759, #14092, #179999, #44447, #153597, #182964, #74785, #150644, #90916, #120279, #11134, #164812, #181971, #41466, #29285, #103131, #87948, #118307, #168758, #138429, #57637, #28308, #107087, #26308, #199116, #76754, #149636, #198128, #134478, #152602, #151628, #72808, #60583, #122259, #196163, #119303, #12141, #106101, #183948, #180987, #42464, #30261, #104127, #165809, #27306, #88953, #136447, #73805, #135477, #197146, #58612, #43453, #105121, #166808, #89948, #13122, #59596, #49410, #157587, #3884, #186957, #20056, #17086, #110084, #96884, #94910, #77750, #1905 ),
 ( #63585, #184938, #111073, #46423, #31259, #200110, #112074, #81700, #898, #171763, #50414, #108081, #19079, #158567, #61578, #141414, #139416, #95903, #156595, #123247, #65563, #142406, #169765, #62572, #93913, #64580, #80727, #16092, #92910, #127223, #154596, #124250, #185945, #35230, #79745, #126245, #188937, #47430, #187941, #170766, #109086, #173763, #32255, #155591, #78739, #172762, #140415, #125259, #48428, #33252, #18089, #2902, #34242, #38226, #21051, #145386, #6868, #24062, #68547, #130203, #161566, #83708, #37216, #53383, #82706, #191898, #39219, #40211, #52384, #113055, #115060, #116062, #176753, #192912, #69557, #147403, #174747, #101890, #177750, #175739, #99881, #7871, #84704, #146383, #98872, #23059, #132226, #97864, #131221, #114041, #54389, #5875, #160568, #100875, #128223, #66558, #159554, #162557, #22057, #67552, #85717, #36211, #189920, #8891, #70559, #193919, #55382, #117052, #178747, #163572, #25072, #143383, #4875, #51395, #144390, #129209, #190907, #44215, #9894, #74553, #183722, #12890, #104886, #180755, #45208, #181737, #164574, #88717, #150412, #167561, #11907, #73571, #166574, #27071, #42231, #196916, #26068, #135244, #182731, #106862, #195925, #56386, #58383, #59364, #120050, #136220, #197895, #90695, #118068, #168536, #121033, #119073, #43218, #151400, #28074, #89715, #103892, #105874, #75530, #41228, #29055, #57401, #152378, #149397, #165572, #13863, #71555, #133220, #102889, #137205, #198891, #10892, #60359, #179758, #194911, #122032, #86715, #148400, #87711, #72565, #134240, #94672, #110838, #188694, #65327, #141177, #18846, #30034, #49180, #187708, #153363, #17852, #126987, #156351, #48189, #124004, #64344, #93679, #184705, #138203, #155362, #14865, #2667, #76526, #61349, #91672, #142165, #111832, #31027, #1668, #80491, #199885, #172522, #50175, #123020, #171529, #107843, #126013, #125023, #46190, #34007, #95664, #169527, #92677, #185702, #79508, #157351, #154365, #15859, #3649, #77517, #139189, #664, #62334, #109844, #47191, #108851, #170531, #32021, #16851, #78502, #140175, #63346, #186719, #33017, #25594, #133741, #180276, #163082, #196439, #193427, #86234, #103410, #88225, #158334, #70077, #112818, #54902, #194430, #131745, #55901, #147924, #174511, #24586, #127982, #57909, #165088, #146913, #26582, #4631, #10410, #132742, #19823, #173521, #35978, #9410, #117574, #11416, #149909, #102408, #179274, #40738, #116576, #178265, #148921, #8402, #56911, #71076, #73086, #143150, #164095, #134757, #39728, #87238, #34992, #96646, #189685, #72068, #101389, #195436, #162080, #118586, #81464, #85222, #66321, #51158, #41746, #97625, #23574, #14369, #27588, #154868, #78013, #13386, #59875, #108362, #12413, #58883, #184224, #28577, #150920, #61847, #89226, #198397, #183236, #139681, #1168, #122533, #152874, #168055, #106373, #120549, #75050, #167075, #119581, #45705, #123516, #74075, #166085, #185209, #121541, #46700, #170040, #16365, #42741, #169029, #135746, #181264, #197417, #182242, #44717, #29552, #43727, #31530, #76035, #104403, #199394, #136716, #105388, #93183, #91185, #90213, #151896, #137710, #77025, #60858, #107356, #30534, #92187, #153871, #15369, #138697, #179, #141682, #49678, #155857, #17355, #140684, #4151, #48695, #2176, #64846, #126508, #143662, #188206, #111342, #80997, #3173, #156864, #173033, #63856, #34511, #158833, #159836, #172029, #32526, #96169, #35500, #157859, #112339, #189204, #66827, #94178, #21330, #97150, #95177, #19349, #127499, #65830, #50681, #18359, #142672, #51661, #79010, #174029, #33517, #20321, #125527, #80013, #81970, #47703, #186222, #187224, #5145, #128491, #110347, #190186, #113325, #109353, #175017, #36482, #98138, #82988, #144664, #62843, #124527, #171035, #164850, #41506, #117333, #195191, #6148, #25354, #163854, #129485, #194194, #103170, #132505, #24343, #100157, #40495, #69830, #160843, #114321, #131497, #191183, #179027 ) ),
 .UNSPECIFIED., .T., .F., .F. ) 
 B_SPLINE_SURFACE_WITH_KNOTS ( ( 4, 3, 4 ),
 ( 3, 2, 2, 2, 2, 2, 2, 2, 2, 2, 2, 2, 2, 2, 2, 2, 2, 2, 2, 2, 2, 2, 2, 2, 2, 2, 2, 2, 2, 2, 2, 2, 2, 2, 2, 2, 2, 2, 2, 2, 2, 2, 2, 2, 2, 2, 2, 2, 2, 2, 2, 2, 2, 2, 2, 2, 2, 2, 2, 2, 2, 2, 2, 2, 2, 2, 2, 2, 2, 2, 2, 2, 2, 2, 2, 2, 2, 2, 2, 2, 2, 2, 2, 2, 2, 2, 2, 2, 2, 2, 2, 2, 2, 2, 2, 2, 2, 2, 2, 2, 2, 2, 2, 2, 2, 2, 2, 2, 2, 2, 2, 2, 2, 2, 2, 2, 2, 2, 2, 2, 2, 2, 2, 2, 2, 2, 2, 2, 2, 2, 2, 2, 2, 2, 2, 2, 2, 2, 2, 2, 2, 2, 2, 2, 2, 2, 2, 2, 2, 2, 2, 2, 2, 2, 2, 2, 2, 2, 2, 2, 2, 2, 2, 2, 2, 2, 2, 2, 2, 2, 2, 2, 2, 2, 2, 2, 2, 2, 2, 2, 2, 2, 2, 2, 2, 2, 2, 2, 2, 2, 2, 2, 2, 2, 2, 2, 2, 2, 2, 2, 2, 2, 2, 2, 2, 2, 2, 2, 2, 2, 2, 2, 2, 2, 2, 2, 2, 2, 2, 2, 2, 2, 2, 2, 2, 2, 2, 2, 3 ),
 ( 0.000000000000000000, 0.5000000000000000000, 1.000000000000000000 ),
 ( 0.000000000000000000, 0.004385964912280701511, 0.008771929824561403022, 0.01315789473684210453, 0.01754385964912280604, 0.02192982456140350755, 0.02631578947368420907, 0.03070175438596491058, 0.03508771929824561209, 0.03947368421052631360, 0.04385964912280701511, 0.04824561403508771662, 0.05263157894736841813, 0.05701754385964911964, 0.06140350877192982115, 0.06578947368421052266, 0.07017543859649122417, 0.07456140350877192569, 0.07894736842105262720, 0.08333333333333332871, 0.08771929824561403022, 0.09210526315789473173, 0.09649122807017543324, 0.1008771929824561348, 0.1052631578947368363, 0.1096491228070175378, 0.1140350877192982393, 0.1184210526315789408, 0.1228070175438596423, 0.1271929824561403577, 0.1315789473684210453, 0.1359649122807017607, 0.1403508771929824483, 0.1447368421052631637, 0.1491228070175438514, 0.1535087719298245668, 0.1578947368421052544, 0.1622807017543859698, 0.1666666666666666574, 0.1710526315789473728, 0.1754385964912280604, 0.1798245614035087758, 0.1842105263157894635, 0.1885964912280701788, 0.1929824561403508665, 0.1973684210526315819, 0.2017543859649122695, 0.2061403508771929849, 0.2105263157894736725, 0.2149122807017543879, 0.2192982456140350755, 0.2236842105263157909, 0.2280701754385964786, 0.2324561403508771940, 0.2368421052631578816, 0.2412280701754385970, 0.2456140350877192846, 0.2500000000000000000, 0.2543859649122807154, 0.2587719298245614308, 0.2631578947368420907, 0.2675438596491228060, 0.2719298245614035214, 0.2763157894736842368, 0.2807017543859648967, 0.2850877192982456121, 0.2894736842105263275, 0.2938596491228070429, 0.2982456140350877027, 0.3026315789473684181, 0.3070175438596491335, 0.3114035087719298489, 0.3157894736842105088, 0.3201754385964912242, 0.3245614035087719396, 0.3289473684210526550, 0.3333333333333333148, 0.3377192982456140302, 0.3421052631578947456, 0.3464912280701754610, 0.3508771929824561209, 0.3552631578947368363, 0.3596491228070175517, 0.3640350877192982670, 0.3684210526315789269, 0.3728070175438596423, 0.3771929824561403577, 0.3815789473684210731, 0.3859649122807017330, 0.3903508771929824483, 0.3947368421052631637, 0.3991228070175438791, 0.4035087719298245390, 0.4078947368421052544, 0.4122807017543859698, 0.4166666666666666852, 0.4210526315789473450, 0.4254385964912280604, 0.4298245614035087758, 0.4342105263157894912, 0.4385964912280701511, 0.4429824561403508665, 0.4473684210526315819, 0.4517543859649122973, 0.4561403508771929571, 0.4605263157894736725, 0.4649122807017543879, 0.4692982456140351033, 0.4736842105263157632, 0.4780701754385964786, 0.4824561403508771940, 0.4868421052631579093, 0.4912280701754385692, 0.4956140350877192846, 0.5000000000000000000, 0.5043859649122807154, 0.5087719298245614308, 0.5131578947368421462, 0.5175438596491228616, 0.5219298245614034659, 0.5263157894736841813, 0.5307017543859648967, 0.5350877192982456121, 0.5394736842105263275, 0.5438596491228070429, 0.5482456140350877583, 0.5526315789473684736, 0.5570175438596490780, 0.5614035087719297934, 0.5657894736842105088, 0.5701754385964912242, 0.5745614035087719396, 0.5789473684210526550, 0.5833333333333333703, 0.5877192982456140857, 0.5921052631578946901, 0.5964912280701754055, 0.6008771929824561209, 0.6052631578947368363, 0.6096491228070175517, 0.6140350877192982670, 0.6184210526315789824, 0.6228070175438596978, 0.6271929824561403022, 0.6315789473684210176, 0.6359649122807017330, 0.6403508771929824483, 0.6447368421052631637, 0.6491228070175438791, 0.6535087719298245945, 0.6578947368421053099, 0.6622807017543859143, 0.6666666666666666297, 0.6710526315789473450, 0.6754385964912280604, 0.6798245614035087758, 0.6842105263157894912, 0.6885964912280702066, 0.6929824561403509220, 0.6973684210526315264, 0.7017543859649122417, 0.7061403508771929571, 0.7105263157894736725, 0.7149122807017543879, 0.7192982456140351033, 0.7236842105263158187, 0.7280701754385965341, 0.7324561403508771384, 0.7368421052631578538, 0.7412280701754385692, 0.7456140350877192846, 0.7500000000000000000, 0.7543859649122807154, 0.7587719298245614308, 0.7631578947368421462, 0.7675438596491228616, 0.7719298245614034659, 0.7763157894736841813, 0.7807017543859648967, 0.7850877192982456121, 0.7894736842105263275, 0.7938596491228070429, 0.7982456140350877583, 0.8026315789473684736, 0.8070175438596490780, 0.8114035087719297934, 0.8157894736842105088, 0.8201754385964912242, 0.8245614035087719396, 0.8289473684210526550, 0.8333333333333333703, 0.8377192982456140857, 0.8421052631578946901, 0.8464912280701754055, 0.8508771929824561209, 0.8552631578947368363, 0.8596491228070175517, 0.8640350877192982670, 0.8684210526315789824, 0.8728070175438596978, 0.8771929824561403022, 0.8815789473684210176, 0.8859649122807017330, 0.8903508771929824483, 0.8947368421052631637, 0.8991228070175438791, 0.9035087719298245945, 0.9078947368421053099, 0.9122807017543859143, 0.9166666666666666297, 0.9210526315789473450, 0.9254385964912280604, 0.9298245614035087758, 0.9342105263157894912, 0.9385964912280702066, 0.9429824561403509220, 0.9473684210526315264, 0.9517543859649122417, 0.9561403508771929571, 0.9605263157894736725, 0.9649122807017543879, 0.9692982456140351033, 0.9736842105263158187, 0.9780701754385965341, 0.9824561403508771384, 0.9868421052631578538, 0.9912280701754385692, 0.9956140350877192846, 1.000000000000000000 ),
 .UNSPECIFIED. ) 
 GEOMETRIC_REPRESENTATION_ITEM ( )  RATIONAL_B_SPLINE_SURFACE ( (
 ( 1.000000000000000000, 0.9659258262890683122, 1.000000000000000000, 0.9659258262890683122, 1.000000000000000000, 0.9659258262890683122, 1.000000000000000000, 0.9659258262890683122, 1.000000000000000000, 0.9659258262890683122, 1.000000000000000000, 0.9659258262890683122, 1.000000000000000000, 0.9659258262890683122, 1.000000000000000000, 0.9659258262890683122, 1.000000000000000000, 0.9659258262890683122, 1.000000000000000000, 0.9659258262890683122, 1.000000000000000000, 0.9659258262890683122, 1.000000000000000000, 0.9659258262890683122, 1.000000000000000000, 0.9659258262890683122, 1.000000000000000000, 0.9659258262890683122, 1.000000000000000000, 0.9659258262890683122, 1.000000000000000000, 0.9659258262890683122, 1.000000000000000000, 0.9659258262890683122, 1.000000000000000000, 0.9659258262890683122, 1.000000000000000000, 0.9659258262890683122, 1.000000000000000000, 0.9659258262890683122, 1.000000000000000000, 0.9659258262890683122, 1.000000000000000000, 0.9659258262890683122, 1.000000000000000000, 0.9659258262890683122, 1.000000000000000000, 0.9659258262890683122, 1.000000000000000000, 0.9659258262890683122, 1.000000000000000000, 0.9659258262890683122, 1.000000000000000000, 0.9659258262890683122, 1.000000000000000000, 0.9659258262890683122, 1.000000000000000000, 0.9659258262890683122, 1.000000000000000000, 0.9659258262890683122, 1.000000000000000000, 0.9659258262890683122, 1.000000000000000000, 0.9659258262890683122, 1.000000000000000000, 0.9659258262890683122, 1.000000000000000000, 0.9659258262890683122, 1.000000000000000000, 0.9659258262890683122, 1.000000000000000000, 0.9659258262890683122, 1.000000000000000000, 0.9659258262890683122, 1.000000000000000000, 0.9659258262890683122, 1.000000000000000000, 0.9659258262890683122, 1.000000000000000000, 0.9659258262890683122, 1.000000000000000000, 0.9659258262890683122, 1.000000000000000000, 0.9659258262890683122, 1.000000000000000000, 0.9659258262890683122, 1.000000000000000000, 0.9659258262890683122, 1.000000000000000000, 0.9659258262890683122, 1.000000000000000000, 0.9659258262890683122, 1.000000000000000000, 0.9659258262890683122, 1.000000000000000000, 0.9659258262890683122, 1.000000000000000000, 0.9659258262890683122, 1.000000000000000000, 0.9659258262890683122, 1.000000000000000000, 0.9659258262890683122, 1.000000000000000000, 0.9659258262890683122, 1.000000000000000000, 0.9659258262890683122, 1.000000000000000000, 0.9659258262890683122, 1.000000000000000000, 0.9659258262890683122, 1.000000000000000000, 0.9659258262890683122, 1.000000000000000000, 0.9659258262890683122, 1.000000000000000000, 0.9659258262890683122, 1.000000000000000000, 0.9659258262890683122, 1.000000000000000000, 0.9659258262890683122, 1.000000000000000000, 0.9659258262890683122, 1.000000000000000000, 0.9659258262890683122, 1.000000000000000000, 0.9659258262890683122, 1.000000000000000000, 0.9659258262890683122, 1.000000000000000000, 0.9659258262890683122, 1.000000000000000000, 0.9659258262890683122, 1.000000000000000000, 0.9659258262890683122, 1.000000000000000000, 0.9659258262890683122, 1.000000000000000000, 0.9659258262890683122, 1.000000000000000000, 0.9659258262890683122, 1.000000000000000000, 0.9659258262890683122, 1.000000000000000000, 0.9659258262890683122, 1.000000000000000000, 0.9659258262890683122, 1.000000000000000000, 0.9659258262890683122, 1.000000000000000000, 0.9659258262890683122, 1.000000000000000000, 0.9659258262890683122, 1.000000000000000000, 0.9659258262890683122, 1.000000000000000000, 0.9659258262890683122, 1.000000000000000000, 0.9659258262890683122, 1.000000000000000000, 0.9659258262890683122, 1.000000000000000000, 0.9659258262890683122, 1.000000000000000000, 0.9659258262890683122, 1.000000000000000000, 0.9659258262890683122, 1.000000000000000000, 0.9659258262890683122, 1.000000000000000000, 0.9659258262890683122, 1.000000000000000000, 0.9659258262890683122, 1.000000000000000000, 0.9659258262890683122, 1.000000000000000000, 0.9659258262890683122, 1.000000000000000000, 0.9659258262890683122, 1.000000000000000000, 0.9659258262890683122, 1.000000000000000000, 0.9659258262890683122, 1.000000000000000000, 0.9659258262890683122, 1.000000000000000000, 0.9659258262890683122, 1.000000000000000000, 0.9659258262890683122, 1.000000000000000000, 0.9659258262890683122, 1.000000000000000000, 0.9659258262890683122, 1.000000000000000000, 0.9659258262890683122, 1.000000000000000000, 0.9659258262890683122, 1.000000000000000000, 0.9659258262890683122, 1.000000000000000000, 0.9659258262890683122, 1.000000000000000000, 0.9659258262890683122, 1.000000000000000000, 0.9659258262890683122, 1.000000000000000000, 0.9659258262890683122, 1.000000000000000000, 0.9659258262890683122, 1.000000000000000000, 0.9659258262890683122, 1.000000000000000000, 0.9659258262890683122, 1.000000000000000000, 0.9659258262890683122, 1.000000000000000000, 0.9659258262890683122, 1.000000000000000000, 0.9659258262890683122, 1.000000000000000000, 0.9659258262890683122, 1.000000000000000000, 0.9659258262890683122, 1.000000000000000000, 0.9659258262890683122, 1.000000000000000000, 0.9659258262890683122, 1.000000000000000000, 0.9659258262890683122, 1.000000000000000000, 0.9659258262890683122, 1.000000000000000000, 0.9659258262890683122, 1.000000000000000000, 0.9659258262890683122, 1.000000000000000000, 0.9659258262890683122, 1.000000000000000000, 0.9659258262890683122, 1.000000000000000000, 0.9659258262890683122, 1.000000000000000000, 0.9659258262890683122, 1.000000000000000000, 0.9659258262890683122, 1.000000000000000000, 0.9659258262890683122, 1.000000000000000000, 0.9659258262890683122, 1.000000000000000000, 0.9659258262890683122, 1.000000000000000000, 0.9659258262890683122, 1.000000000000000000, 0.9659258262890683122, 1.000000000000000000, 0.9659258262890683122, 1.000000000000000000, 0.9659258262890683122, 1.000000000000000000, 0.9659258262890683122, 1.000000000000000000, 0.9659258262890683122, 1.000000000000000000, 0.9659258262890683122, 1.000000000000000000, 0.9659258262890683122, 1.000000000000000000, 0.9659258262890683122, 1.000000000000000000, 0.9659258262890683122, 1.000000000000000000, 0.9659258262890683122, 1.000000000000000000, 0.9659258262890683122, 1.000000000000000000, 0.9659258262890683122, 1.000000000000000000, 0.9659258262890683122, 1.000000000000000000, 0.9659258262890683122, 1.000000000000000000, 0.9659258262890683122, 1.000000000000000000, 0.9659258262890683122, 1.000000000000000000, 0.9659258262890683122, 1.000000000000000000, 0.9659258262890683122, 1.000000000000000000, 0.9659258262890683122, 1.000000000000000000, 0.9659258262890683122, 1.000000000000000000, 0.9659258262890683122, 1.000000000000000000, 0.9659258262890683122, 1.000000000000000000, 0.9659258262890683122, 1.000000000000000000, 0.9659258262890683122, 1.000000000000000000, 0.9659258262890683122, 1.000000000000000000, 0.9659258262890683122, 1.000000000000000000, 0.9659258262890683122, 1.000000000000000000, 0.9659258262890683122, 1.000000000000000000, 0.9659258262890683122, 1.000000000000000000, 0.9659258262890683122, 1.000000000000000000, 0.9659258262890683122, 1.000000000000000000, 0.9659258262890683122, 1.000000000000000000, 0.9659258262890683122, 1.000000000000000000, 0.9659258262890683122, 1.000000000000000000, 0.9659258262890683122, 1.000000000000000000, 0.9659258262890683122, 1.000000000000000000, 0.9659258262890683122, 1.000000000000000000, 0.9659258262890683122, 1.000000000000000000, 0.9659258262890683122, 1.000000000000000000, 0.9659258262890683122, 1.000000000000000000, 0.9659258262890683122, 1.000000000000000000, 0.9659258262890683122, 1.000000000000000000, 0.9659258262890683122, 1.000000000000000000, 0.9659258262890683122, 1.000000000000000000, 0.9659258262890683122, 1.000000000000000000, 0.9659258262890683122, 1.000000000000000000, 0.9659258262890683122, 1.000000000000000000, 0.9659258262890683122, 1.000000000000000000, 0.9659258262890683122, 1.000000000000000000, 0.9659258262890683122, 1.000000000000000000, 0.9659258262890683122, 1.000000000000000000, 0.9659258262890683122, 1.000000000000000000, 0.9659258262890683122, 1.000000000000000000, 0.9659258262890683122, 1.000000000000000000, 0.9659258262890683122, 1.000000000000000000, 0.9659258262890683122, 1.000000000000000000, 0.9659258262890683122, 1.000000000000000000, 0.9659258262890683122, 1.000000000000000000, 0.9659258262890683122, 1.000000000000000000, 0.9659258262890683122, 1.000000000000000000, 0.9659258262890683122, 1.000000000000000000, 0.9659258262890683122, 1.000000000000000000, 0.9659258262890683122, 1.000000000000000000, 0.9659258262890683122, 1.000000000000000000, 0.9659258262890683122, 1.000000000000000000, 0.9659258262890683122, 1.000000000000000000, 0.9659258262890683122, 1.000000000000000000, 0.9659258262890683122, 1.000000000000000000, 0.9659258262890683122, 1.000000000000000000, 0.9659258262890683122, 1.000000000000000000, 0.9659258262890683122, 1.000000000000000000, 0.9659258262890683122, 1.000000000000000000, 0.9659258262890683122, 1.000000000000000000, 0.9659258262890683122, 1.000000000000000000, 0.9659258262890683122, 1.000000000000000000, 0.9659258262890683122, 1.000000000000000000, 0.9659258262890683122, 1.000000000000000000, 0.9659258262890683122, 1.000000000000000000, 0.9659258262890683122, 1.000000000000000000, 0.9659258262890683122, 1.000000000000000000, 0.9659258262890683122, 1.000000000000000000, 0.9659258262890683122, 1.000000000000000000, 0.9659258262890683122, 1.000000000000000000, 0.9659258262890683122, 1.000000000000000000, 0.9659258262890683122, 1.000000000000000000, 0.9659258262890683122, 1.000000000000000000, 0.9659258262890683122, 1.000000000000000000, 0.9659258262890683122, 1.000000000000000000, 0.9659258262890683122, 1.000000000000000000, 0.9659258262890683122, 1.000000000000000000, 0.9659258262890683122, 1.000000000000000000, 0.9659258262890683122, 1.000000000000000000, 0.9659258262890683122, 1.000000000000000000, 0.9659258262890683122, 1.000000000000000000, 0.9659258262890683122, 1.000000000000000000, 0.9659258262890683122, 1.000000000000000000, 0.9659258262890683122, 1.000000000000000000, 0.9659258262890683122, 1.000000000000000000, 0.9659258262890683122, 1.000000000000000000, 0.9659258262890683122, 1.000000000000000000, 0.9659258262890683122, 1.000000000000000000, 0.9659258262890683122, 1.000000000000000000),
 ( 0.3333333333333333703, 0.3219752754296894559, 0.3333333333333333703, 0.3219752754296894559, 0.3333333333333333703, 0.3219752754296894559, 0.3333333333333333703, 0.3219752754296894559, 0.3333333333333333703, 0.3219752754296894559, 0.3333333333333333703, 0.3219752754296894559, 0.3333333333333333703, 0.3219752754296894559, 0.3333333333333333703, 0.3219752754296894559, 0.3333333333333333703, 0.3219752754296894559, 0.3333333333333333703, 0.3219752754296894559, 0.3333333333333333703, 0.3219752754296894559, 0.3333333333333333703, 0.3219752754296894559, 0.3333333333333333703, 0.3219752754296894559, 0.3333333333333333703, 0.3219752754296894559, 0.3333333333333333703, 0.3219752754296894559, 0.3333333333333333703, 0.3219752754296894559, 0.3333333333333333703, 0.3219752754296894559, 0.3333333333333333703, 0.3219752754296894559, 0.3333333333333333703, 0.3219752754296894559, 0.3333333333333333703, 0.3219752754296894559, 0.3333333333333333703, 0.3219752754296894559, 0.3333333333333333703, 0.3219752754296894559, 0.3333333333333333703, 0.3219752754296894559, 0.3333333333333333703, 0.3219752754296894559, 0.3333333333333333703, 0.3219752754296894559, 0.3333333333333333703, 0.3219752754296894559, 0.3333333333333333703, 0.3219752754296894559, 0.3333333333333333703, 0.3219752754296894559, 0.3333333333333333703, 0.3219752754296894559, 0.3333333333333333703, 0.3219752754296894559, 0.3333333333333333703, 0.3219752754296894559, 0.3333333333333333703, 0.3219752754296894559, 0.3333333333333333703, 0.3219752754296894559, 0.3333333333333333703, 0.3219752754296894559, 0.3333333333333333703, 0.3219752754296894559, 0.3333333333333333703, 0.3219752754296894559, 0.3333333333333333703, 0.3219752754296894559, 0.3333333333333333703, 0.3219752754296894559, 0.3333333333333333703, 0.3219752754296894559, 0.3333333333333333703, 0.3219752754296894559, 0.3333333333333333703, 0.3219752754296894559, 0.3333333333333333703, 0.3219752754296894559, 0.3333333333333333703, 0.3219752754296894559, 0.3333333333333333703, 0.3219752754296894559, 0.3333333333333333703, 0.3219752754296894559, 0.3333333333333333703, 0.3219752754296894559, 0.3333333333333333703, 0.3219752754296894559, 0.3333333333333333703, 0.3219752754296894559, 0.3333333333333333703, 0.3219752754296894559, 0.3333333333333333703, 0.3219752754296894559, 0.3333333333333333703, 0.3219752754296894559, 0.3333333333333333703, 0.3219752754296894559, 0.3333333333333333703, 0.3219752754296894559, 0.3333333333333333703, 0.3219752754296894559, 0.3333333333333333703, 0.3219752754296894559, 0.3333333333333333703, 0.3219752754296894559, 0.3333333333333333703, 0.3219752754296894559, 0.3333333333333333703, 0.3219752754296894559, 0.3333333333333333703, 0.3219752754296894559, 0.3333333333333333703, 0.3219752754296894559, 0.3333333333333333703, 0.3219752754296894559, 0.3333333333333333703, 0.3219752754296894559, 0.3333333333333333703, 0.3219752754296894559, 0.3333333333333333703, 0.3219752754296894559, 0.3333333333333333703, 0.3219752754296894559, 0.3333333333333333703, 0.3219752754296894559, 0.3333333333333333703, 0.3219752754296894559, 0.3333333333333333703, 0.3219752754296894559, 0.3333333333333333703, 0.3219752754296894559, 0.3333333333333333703, 0.3219752754296894559, 0.3333333333333333703, 0.3219752754296894559, 0.3333333333333333703, 0.3219752754296894559, 0.3333333333333333703, 0.3219752754296894559, 0.3333333333333333703, 0.3219752754296894559, 0.3333333333333333703, 0.3219752754296894559, 0.3333333333333333703, 0.3219752754296894559, 0.3333333333333333703, 0.3219752754296894559, 0.3333333333333333703, 0.3219752754296894559, 0.3333333333333333703, 0.3219752754296894559, 0.3333333333333333703, 0.3219752754296894559, 0.3333333333333333703, 0.3219752754296894559, 0.3333333333333333703, 0.3219752754296894559, 0.3333333333333333703, 0.3219752754296894559, 0.3333333333333333703, 0.3219752754296894559, 0.3333333333333333703, 0.3219752754296894559, 0.3333333333333333703, 0.3219752754296894559, 0.3333333333333333703, 0.3219752754296894559, 0.3333333333333333703, 0.3219752754296894559, 0.3333333333333333703, 0.3219752754296894559, 0.3333333333333333703, 0.3219752754296894559, 0.3333333333333333703, 0.3219752754296894559, 0.3333333333333333703, 0.3219752754296894559, 0.3333333333333333703, 0.3219752754296894559, 0.3333333333333333703, 0.3219752754296894559, 0.3333333333333333703, 0.3219752754296894559, 0.3333333333333333703, 0.3219752754296894559, 0.3333333333333333703, 0.3219752754296894559, 0.3333333333333333703, 0.3219752754296894559, 0.3333333333333333703, 0.3219752754296894559, 0.3333333333333333703, 0.3219752754296894559, 0.3333333333333333703, 0.3219752754296894559, 0.3333333333333333703, 0.3219752754296894559, 0.3333333333333333703, 0.3219752754296894559, 0.3333333333333333703, 0.3219752754296894559, 0.3333333333333333703, 0.3219752754296894559, 0.3333333333333333703, 0.3219752754296894559, 0.3333333333333333703, 0.3219752754296894559, 0.3333333333333333703, 0.3219752754296894559, 0.3333333333333333703, 0.3219752754296894559, 0.3333333333333333703, 0.3219752754296894559, 0.3333333333333333703, 0.3219752754296894559, 0.3333333333333333703, 0.3219752754296894559, 0.3333333333333333703, 0.3219752754296894559, 0.3333333333333333703, 0.3219752754296894559, 0.3333333333333333703, 0.3219752754296894559, 0.3333333333333333703, 0.3219752754296894559, 0.3333333333333333703, 0.3219752754296894559, 0.3333333333333333703, 0.3219752754296894559, 0.3333333333333333703, 0.3219752754296894559, 0.3333333333333333703, 0.3219752754296894559, 0.3333333333333333703, 0.3219752754296894559, 0.3333333333333333703, 0.3219752754296894559, 0.3333333333333333703, 0.3219752754296894559, 0.3333333333333333703, 0.3219752754296894559, 0.3333333333333333703, 0.3219752754296894559, 0.3333333333333333703, 0.3219752754296894559, 0.3333333333333333703, 0.3219752754296894559, 0.3333333333333333703, 0.3219752754296894559, 0.3333333333333333703, 0.3219752754296894559, 0.3333333333333333703, 0.3219752754296894559, 0.3333333333333333703, 0.3219752754296894559, 0.3333333333333333703, 0.3219752754296894559, 0.3333333333333333703, 0.3219752754296894559, 0.3333333333333333703, 0.3219752754296894559, 0.3333333333333333703, 0.3219752754296894559, 0.3333333333333333703, 0.3219752754296894559, 0.3333333333333333703, 0.3219752754296894559, 0.3333333333333333703, 0.3219752754296894559, 0.3333333333333333703, 0.3219752754296894559, 0.3333333333333333703, 0.3219752754296894559, 0.3333333333333333703, 0.3219752754296894559, 0.3333333333333333703, 0.3219752754296894559, 0.3333333333333333703, 0.3219752754296894559, 0.3333333333333333703, 0.3219752754296894559, 0.3333333333333333703, 0.3219752754296894559, 0.3333333333333333703, 0.3219752754296894559, 0.3333333333333333703, 0.3219752754296894559, 0.3333333333333333703, 0.3219752754296894559, 0.3333333333333333703, 0.3219752754296894559, 0.3333333333333333703, 0.3219752754296894559, 0.3333333333333333703, 0.3219752754296894559, 0.3333333333333333703, 0.3219752754296894559, 0.3333333333333333703, 0.3219752754296894559, 0.3333333333333333703, 0.3219752754296894559, 0.3333333333333333703, 0.3219752754296894559, 0.3333333333333333703, 0.3219752754296894559, 0.3333333333333333703, 0.3219752754296894559, 0.3333333333333333703, 0.3219752754296894559, 0.3333333333333333703, 0.3219752754296894559, 0.3333333333333333703, 0.3219752754296894559, 0.3333333333333333703, 0.3219752754296894559, 0.3333333333333333703, 0.3219752754296894559, 0.3333333333333333703, 0.3219752754296894559, 0.3333333333333333703, 0.3219752754296894559, 0.3333333333333333703, 0.3219752754296894559, 0.3333333333333333703, 0.3219752754296894559, 0.3333333333333333703, 0.3219752754296894559, 0.3333333333333333703, 0.3219752754296894559, 0.3333333333333333703, 0.3219752754296894559, 0.3333333333333333703, 0.3219752754296894559, 0.3333333333333333703, 0.3219752754296894559, 0.3333333333333333703, 0.3219752754296894559, 0.3333333333333333703, 0.3219752754296894559, 0.3333333333333333703, 0.3219752754296894559, 0.3333333333333333703, 0.3219752754296894559, 0.3333333333333333703, 0.3219752754296894559, 0.3333333333333333703, 0.3219752754296894559, 0.3333333333333333703, 0.3219752754296894559, 0.3333333333333333703, 0.3219752754296894559, 0.3333333333333333703, 0.3219752754296894559, 0.3333333333333333703, 0.3219752754296894559, 0.3333333333333333703, 0.3219752754296894559, 0.3333333333333333703, 0.3219752754296894559, 0.3333333333333333703, 0.3219752754296894559, 0.3333333333333333703, 0.3219752754296894559, 0.3333333333333333703, 0.3219752754296894559, 0.3333333333333333703, 0.3219752754296894559, 0.3333333333333333703, 0.3219752754296894559, 0.3333333333333333703, 0.3219752754296894559, 0.3333333333333333703, 0.3219752754296894559, 0.3333333333333333703, 0.3219752754296894559, 0.3333333333333333703, 0.3219752754296894559, 0.3333333333333333703, 0.3219752754296894559, 0.3333333333333333703, 0.3219752754296894559, 0.3333333333333333703, 0.3219752754296894559, 0.3333333333333333703, 0.3219752754296894559, 0.3333333333333333703, 0.3219752754296894559, 0.3333333333333333703, 0.3219752754296894559, 0.3333333333333333703, 0.3219752754296894559, 0.3333333333333333703, 0.3219752754296894559, 0.3333333333333333703, 0.3219752754296894559, 0.3333333333333333703, 0.3219752754296894559, 0.3333333333333333703, 0.3219752754296894559, 0.3333333333333333703, 0.3219752754296894559, 0.3333333333333333703, 0.3219752754296894559, 0.3333333333333333703, 0.3219752754296894559, 0.3333333333333333703, 0.3219752754296894559, 0.3333333333333333703, 0.3219752754296894559, 0.3333333333333333703, 0.3219752754296894559, 0.3333333333333333703, 0.3219752754296894559, 0.3333333333333333703, 0.3219752754296894559, 0.3333333333333333703, 0.3219752754296894559, 0.3333333333333333703, 0.3219752754296894559, 0.3333333333333333703, 0.3219752754296894559, 0.3333333333333333703, 0.3219752754296894559, 0.3333333333333333703, 0.3219752754296894559, 0.3333333333333333703, 0.3219752754296894559, 0.3333333333333333703, 0.3219752754296894559, 0.3333333333333333703, 0.3219752754296894559, 0.3333333333333333703, 0.3219752754296894559, 0.3333333333333333703, 0.3219752754296894559, 0.3333333333333333703, 0.3219752754296894559, 0.3333333333333333703, 0.3219752754296894559, 0.3333333333333333703, 0.3219752754296894559, 0.3333333333333333703, 0.3219752754296894559, 0.3333333333333333703, 0.3219752754296894559, 0.3333333333333333703, 0.3219752754296894559, 0.3333333333333333703, 0.3219752754296894559, 0.3333333333333333703),
 ( 0.3333333333333333703, 0.3219752754296894559, 0.3333333333333333703, 0.3219752754296894559, 0.3333333333333333703, 0.3219752754296894559, 0.3333333333333333703, 0.3219752754296894559, 0.3333333333333333703, 0.3219752754296894559, 0.3333333333333333703, 0.3219752754296894559, 0.3333333333333333703, 0.3219752754296894559, 0.3333333333333333703, 0.3219752754296894559, 0.3333333333333333703, 0.3219752754296894559, 0.3333333333333333703, 0.3219752754296894559, 0.3333333333333333703, 0.3219752754296894559, 0.3333333333333333703, 0.3219752754296894559, 0.3333333333333333703, 0.3219752754296894559, 0.3333333333333333703, 0.3219752754296894559, 0.3333333333333333703, 0.3219752754296894559, 0.3333333333333333703, 0.3219752754296894559, 0.3333333333333333703, 0.3219752754296894559, 0.3333333333333333703, 0.3219752754296894559, 0.3333333333333333703, 0.3219752754296894559, 0.3333333333333333703, 0.3219752754296894559, 0.3333333333333333703, 0.3219752754296894559, 0.3333333333333333703, 0.3219752754296894559, 0.3333333333333333703, 0.3219752754296894559, 0.3333333333333333703, 0.3219752754296894559, 0.3333333333333333703, 0.3219752754296894559, 0.3333333333333333703, 0.3219752754296894559, 0.3333333333333333703, 0.3219752754296894559, 0.3333333333333333703, 0.3219752754296894559, 0.3333333333333333703, 0.3219752754296894559, 0.3333333333333333703, 0.3219752754296894559, 0.3333333333333333703, 0.3219752754296894559, 0.3333333333333333703, 0.3219752754296894559, 0.3333333333333333703, 0.3219752754296894559, 0.3333333333333333703, 0.3219752754296894559, 0.3333333333333333703, 0.3219752754296894559, 0.3333333333333333703, 0.3219752754296894559, 0.3333333333333333703, 0.3219752754296894559, 0.3333333333333333703, 0.3219752754296894559, 0.3333333333333333703, 0.3219752754296894559, 0.3333333333333333703, 0.3219752754296894559, 0.3333333333333333703, 0.3219752754296894559, 0.3333333333333333703, 0.3219752754296894559, 0.3333333333333333703, 0.3219752754296894559, 0.3333333333333333703, 0.3219752754296894559, 0.3333333333333333703, 0.3219752754296894559, 0.3333333333333333703, 0.3219752754296894559, 0.3333333333333333703, 0.3219752754296894559, 0.3333333333333333703, 0.3219752754296894559, 0.3333333333333333703, 0.3219752754296894559, 0.3333333333333333703, 0.3219752754296894559, 0.3333333333333333703, 0.3219752754296894559, 0.3333333333333333703, 0.3219752754296894559, 0.3333333333333333703, 0.3219752754296894559, 0.3333333333333333703, 0.3219752754296894559, 0.3333333333333333703, 0.3219752754296894559, 0.3333333333333333703, 0.3219752754296894559, 0.3333333333333333703, 0.3219752754296894559, 0.3333333333333333703, 0.3219752754296894559, 0.3333333333333333703, 0.3219752754296894559, 0.3333333333333333703, 0.3219752754296894559, 0.3333333333333333703, 0.3219752754296894559, 0.3333333333333333703, 0.3219752754296894559, 0.3333333333333333703, 0.3219752754296894559, 0.3333333333333333703, 0.3219752754296894559, 0.3333333333333333703, 0.3219752754296894559, 0.3333333333333333703, 0.3219752754296894559, 0.3333333333333333703, 0.3219752754296894559, 0.3333333333333333703, 0.3219752754296894559, 0.3333333333333333703, 0.3219752754296894559, 0.3333333333333333703, 0.3219752754296894559, 0.3333333333333333703, 0.3219752754296894559, 0.3333333333333333703, 0.3219752754296894559, 0.3333333333333333703, 0.3219752754296894559, 0.3333333333333333703, 0.3219752754296894559, 0.3333333333333333703, 0.3219752754296894559, 0.3333333333333333703, 0.3219752754296894559, 0.3333333333333333703, 0.3219752754296894559, 0.3333333333333333703, 0.3219752754296894559, 0.3333333333333333703, 0.3219752754296894559, 0.3333333333333333703, 0.3219752754296894559, 0.3333333333333333703, 0.3219752754296894559, 0.3333333333333333703, 0.3219752754296894559, 0.3333333333333333703, 0.3219752754296894559, 0.3333333333333333703, 0.3219752754296894559, 0.3333333333333333703, 0.3219752754296894559, 0.3333333333333333703, 0.3219752754296894559, 0.3333333333333333703, 0.3219752754296894559, 0.3333333333333333703, 0.3219752754296894559, 0.3333333333333333703, 0.3219752754296894559, 0.3333333333333333703, 0.3219752754296894559, 0.3333333333333333703, 0.3219752754296894559, 0.3333333333333333703, 0.3219752754296894559, 0.3333333333333333703, 0.3219752754296894559, 0.3333333333333333703, 0.3219752754296894559, 0.3333333333333333703, 0.3219752754296894559, 0.3333333333333333703, 0.3219752754296894559, 0.3333333333333333703, 0.3219752754296894559, 0.3333333333333333703, 0.3219752754296894559, 0.3333333333333333703, 0.3219752754296894559, 0.3333333333333333703, 0.3219752754296894559, 0.3333333333333333703, 0.3219752754296894559, 0.3333333333333333703, 0.3219752754296894559, 0.3333333333333333703, 0.3219752754296894559, 0.3333333333333333703, 0.3219752754296894559, 0.3333333333333333703, 0.3219752754296894559, 0.3333333333333333703, 0.3219752754296894559, 0.3333333333333333703, 0.3219752754296894559, 0.3333333333333333703, 0.3219752754296894559, 0.3333333333333333703, 0.3219752754296894559, 0.3333333333333333703, 0.3219752754296894559, 0.3333333333333333703, 0.3219752754296894559, 0.3333333333333333703, 0.3219752754296894559, 0.3333333333333333703, 0.3219752754296894559, 0.3333333333333333703, 0.3219752754296894559, 0.3333333333333333703, 0.3219752754296894559, 0.3333333333333333703, 0.3219752754296894559, 0.3333333333333333703, 0.3219752754296894559, 0.3333333333333333703, 0.3219752754296894559, 0.3333333333333333703, 0.3219752754296894559, 0.3333333333333333703, 0.3219752754296894559, 0.3333333333333333703, 0.3219752754296894559, 0.3333333333333333703, 0.3219752754296894559, 0.3333333333333333703, 0.3219752754296894559, 0.3333333333333333703, 0.3219752754296894559, 0.3333333333333333703, 0.3219752754296894559, 0.3333333333333333703, 0.3219752754296894559, 0.3333333333333333703, 0.3219752754296894559, 0.3333333333333333703, 0.3219752754296894559, 0.3333333333333333703, 0.3219752754296894559, 0.3333333333333333703, 0.3219752754296894559, 0.3333333333333333703, 0.3219752754296894559, 0.3333333333333333703, 0.3219752754296894559, 0.3333333333333333703, 0.3219752754296894559, 0.3333333333333333703, 0.3219752754296894559, 0.3333333333333333703, 0.3219752754296894559, 0.3333333333333333703, 0.3219752754296894559, 0.3333333333333333703, 0.3219752754296894559, 0.3333333333333333703, 0.3219752754296894559, 0.3333333333333333703, 0.3219752754296894559, 0.3333333333333333703, 0.3219752754296894559, 0.3333333333333333703, 0.3219752754296894559, 0.3333333333333333703, 0.3219752754296894559, 0.3333333333333333703, 0.3219752754296894559, 0.3333333333333333703, 0.3219752754296894559, 0.3333333333333333703, 0.3219752754296894559, 0.3333333333333333703, 0.3219752754296894559, 0.3333333333333333703, 0.3219752754296894559, 0.3333333333333333703, 0.3219752754296894559, 0.3333333333333333703, 0.3219752754296894559, 0.3333333333333333703, 0.3219752754296894559, 0.3333333333333333703, 0.3219752754296894559, 0.3333333333333333703, 0.3219752754296894559, 0.3333333333333333703, 0.3219752754296894559, 0.3333333333333333703, 0.3219752754296894559, 0.3333333333333333703, 0.3219752754296894559, 0.3333333333333333703, 0.3219752754296894559, 0.3333333333333333703, 0.3219752754296894559, 0.3333333333333333703, 0.3219752754296894559, 0.3333333333333333703, 0.3219752754296894559, 0.3333333333333333703, 0.3219752754296894559, 0.3333333333333333703, 0.3219752754296894559, 0.3333333333333333703, 0.3219752754296894559, 0.3333333333333333703, 0.3219752754296894559, 0.3333333333333333703, 0.3219752754296894559, 0.3333333333333333703, 0.3219752754296894559, 0.3333333333333333703, 0.3219752754296894559, 0.3333333333333333703, 0.3219752754296894559, 0.3333333333333333703, 0.3219752754296894559, 0.3333333333333333703, 0.3219752754296894559, 0.3333333333333333703, 0.3219752754296894559, 0.3333333333333333703, 0.3219752754296894559, 0.3333333333333333703, 0.3219752754296894559, 0.3333333333333333703, 0.3219752754296894559, 0.3333333333333333703, 0.3219752754296894559, 0.3333333333333333703, 0.3219752754296894559, 0.3333333333333333703, 0.3219752754296894559, 0.3333333333333333703, 0.3219752754296894559, 0.3333333333333333703, 0.3219752754296894559, 0.3333333333333333703, 0.3219752754296894559, 0.3333333333333333703, 0.3219752754296894559, 0.3333333333333333703, 0.3219752754296894559, 0.3333333333333333703, 0.3219752754296894559, 0.3333333333333333703, 0.3219752754296894559, 0.3333333333333333703, 0.3219752754296894559, 0.3333333333333333703, 0.3219752754296894559, 0.3333333333333333703, 0.3219752754296894559, 0.3333333333333333703, 0.3219752754296894559, 0.3333333333333333703, 0.3219752754296894559, 0.3333333333333333703, 0.3219752754296894559, 0.3333333333333333703, 0.3219752754296894559, 0.3333333333333333703, 0.3219752754296894559, 0.3333333333333333703, 0.3219752754296894559, 0.3333333333333333703, 0.3219752754296894559, 0.3333333333333333703, 0.3219752754296894559, 0.3333333333333333703, 0.3219752754296894559, 0.3333333333333333703, 0.3219752754296894559, 0.3333333333333333703, 0.3219752754296894559, 0.3333333333333333703, 0.3219752754296894559, 0.3333333333333333703, 0.3219752754296894559, 0.3333333333333333703, 0.3219752754296894559, 0.3333333333333333703, 0.3219752754296894559, 0.3333333333333333703, 0.3219752754296894559, 0.3333333333333333703, 0.3219752754296894559, 0.3333333333333333703, 0.3219752754296894559, 0.3333333333333333703, 0.3219752754296894559, 0.3333333333333333703, 0.3219752754296894559, 0.3333333333333333703, 0.3219752754296894559, 0.3333333333333333703, 0.3219752754296894559, 0.3333333333333333703, 0.3219752754296894559, 0.3333333333333333703, 0.3219752754296894559, 0.3333333333333333703, 0.3219752754296894559, 0.3333333333333333703, 0.3219752754296894559, 0.3333333333333333703, 0.3219752754296894559, 0.3333333333333333703, 0.3219752754296894559, 0.3333333333333333703, 0.3219752754296894559, 0.3333333333333333703, 0.3219752754296894559, 0.3333333333333333703, 0.3219752754296894559, 0.3333333333333333703, 0.3219752754296894559, 0.3333333333333333703, 0.3219752754296894559, 0.3333333333333333703, 0.3219752754296894559, 0.3333333333333333703, 0.3219752754296894559, 0.3333333333333333703, 0.3219752754296894559, 0.3333333333333333703, 0.3219752754296894559, 0.3333333333333333703, 0.3219752754296894559, 0.3333333333333333703, 0.3219752754296894559, 0.3333333333333333703, 0.3219752754296894559, 0.3333333333333333703, 0.3219752754296894559, 0.3333333333333333703, 0.3219752754296894559, 0.3333333333333333703),
 ( 1.000000000000000000, 0.9659258262890683122, 1.000000000000000000, 0.9659258262890683122, 1.000000000000000000, 0.9659258262890683122, 1.000000000000000000, 0.9659258262890683122, 1.000000000000000000, 0.9659258262890683122, 1.000000000000000000, 0.9659258262890683122, 1.000000000000000000, 0.9659258262890683122, 1.000000000000000000, 0.9659258262890683122, 1.000000000000000000, 0.9659258262890683122, 1.000000000000000000, 0.9659258262890683122, 1.000000000000000000, 0.9659258262890683122, 1.000000000000000000, 0.9659258262890683122, 1.000000000000000000, 0.9659258262890683122, 1.000000000000000000, 0.9659258262890683122, 1.000000000000000000, 0.9659258262890683122, 1.000000000000000000, 0.9659258262890683122, 1.000000000000000000, 0.9659258262890683122, 1.000000000000000000, 0.9659258262890683122, 1.000000000000000000, 0.9659258262890683122, 1.000000000000000000, 0.9659258262890683122, 1.000000000000000000, 0.9659258262890683122, 1.000000000000000000, 0.9659258262890683122, 1.000000000000000000, 0.9659258262890683122, 1.000000000000000000, 0.9659258262890683122, 1.000000000000000000, 0.9659258262890683122, 1.000000000000000000, 0.9659258262890683122, 1.000000000000000000, 0.9659258262890683122, 1.000000000000000000, 0.9659258262890683122, 1.000000000000000000, 0.9659258262890683122, 1.000000000000000000, 0.9659258262890683122, 1.000000000000000000, 0.9659258262890683122, 1.000000000000000000, 0.9659258262890683122, 1.000000000000000000, 0.9659258262890683122, 1.000000000000000000, 0.9659258262890683122, 1.000000000000000000, 0.9659258262890683122, 1.000000000000000000, 0.9659258262890683122, 1.000000000000000000, 0.9659258262890683122, 1.000000000000000000, 0.9659258262890683122, 1.000000000000000000, 0.9659258262890683122, 1.000000000000000000, 0.9659258262890683122, 1.000000000000000000, 0.9659258262890683122, 1.000000000000000000, 0.9659258262890683122, 1.000000000000000000, 0.9659258262890683122, 1.000000000000000000, 0.9659258262890683122, 1.000000000000000000, 0.9659258262890683122, 1.000000000000000000, 0.9659258262890683122, 1.000000000000000000, 0.9659258262890683122, 1.000000000000000000, 0.9659258262890683122, 1.000000000000000000, 0.9659258262890683122, 1.000000000000000000, 0.9659258262890683122, 1.000000000000000000, 0.9659258262890683122, 1.000000000000000000, 0.9659258262890683122, 1.000000000000000000, 0.9659258262890683122, 1.000000000000000000, 0.9659258262890683122, 1.000000000000000000, 0.9659258262890683122, 1.000000000000000000, 0.9659258262890683122, 1.000000000000000000, 0.9659258262890683122, 1.000000000000000000, 0.9659258262890683122, 1.000000000000000000, 0.9659258262890683122, 1.000000000000000000, 0.9659258262890683122, 1.000000000000000000, 0.9659258262890683122, 1.000000000000000000, 0.9659258262890683122, 1.000000000000000000, 0.9659258262890683122, 1.000000000000000000, 0.9659258262890683122, 1.000000000000000000, 0.9659258262890683122, 1.000000000000000000, 0.9659258262890683122, 1.000000000000000000, 0.9659258262890683122, 1.000000000000000000, 0.9659258262890683122, 1.000000000000000000, 0.9659258262890683122, 1.000000000000000000, 0.9659258262890683122, 1.000000000000000000, 0.9659258262890683122, 1.000000000000000000, 0.9659258262890683122, 1.000000000000000000, 0.9659258262890683122, 1.000000000000000000, 0.9659258262890683122, 1.000000000000000000, 0.9659258262890683122, 1.000000000000000000, 0.9659258262890683122, 1.000000000000000000, 0.9659258262890683122, 1.000000000000000000, 0.9659258262890683122, 1.000000000000000000, 0.9659258262890683122, 1.000000000000000000, 0.9659258262890683122, 1.000000000000000000, 0.9659258262890683122, 1.000000000000000000, 0.9659258262890683122, 1.000000000000000000, 0.9659258262890683122, 1.000000000000000000, 0.9659258262890683122, 1.000000000000000000, 0.9659258262890683122, 1.000000000000000000, 0.9659258262890683122, 1.000000000000000000, 0.9659258262890683122, 1.000000000000000000, 0.9659258262890683122, 1.000000000000000000, 0.9659258262890683122, 1.000000000000000000, 0.9659258262890683122, 1.000000000000000000, 0.9659258262890683122, 1.000000000000000000, 0.9659258262890683122, 1.000000000000000000, 0.9659258262890683122, 1.000000000000000000, 0.9659258262890683122, 1.000000000000000000, 0.9659258262890683122, 1.000000000000000000, 0.9659258262890683122, 1.000000000000000000, 0.9659258262890683122, 1.000000000000000000, 0.9659258262890683122, 1.000000000000000000, 0.9659258262890683122, 1.000000000000000000, 0.9659258262890683122, 1.000000000000000000, 0.9659258262890683122, 1.000000000000000000, 0.9659258262890683122, 1.000000000000000000, 0.9659258262890683122, 1.000000000000000000, 0.9659258262890683122, 1.000000000000000000, 0.9659258262890683122, 1.000000000000000000, 0.9659258262890683122, 1.000000000000000000, 0.9659258262890683122, 1.000000000000000000, 0.9659258262890683122, 1.000000000000000000, 0.9659258262890683122, 1.000000000000000000, 0.9659258262890683122, 1.000000000000000000, 0.9659258262890683122, 1.000000000000000000, 0.9659258262890683122, 1.000000000000000000, 0.9659258262890683122, 1.000000000000000000, 0.9659258262890683122, 1.000000000000000000, 0.9659258262890683122, 1.000000000000000000, 0.9659258262890683122, 1.000000000000000000, 0.9659258262890683122, 1.000000000000000000, 0.9659258262890683122, 1.000000000000000000, 0.9659258262890683122, 1.000000000000000000, 0.9659258262890683122, 1.000000000000000000, 0.9659258262890683122, 1.000000000000000000, 0.9659258262890683122, 1.000000000000000000, 0.9659258262890683122, 1.000000000000000000, 0.9659258262890683122, 1.000000000000000000, 0.9659258262890683122, 1.000000000000000000, 0.9659258262890683122, 1.000000000000000000, 0.9659258262890683122, 1.000000000000000000, 0.9659258262890683122, 1.000000000000000000, 0.9659258262890683122, 1.000000000000000000, 0.9659258262890683122, 1.000000000000000000, 0.9659258262890683122, 1.000000000000000000, 0.9659258262890683122, 1.000000000000000000, 0.9659258262890683122, 1.000000000000000000, 0.9659258262890683122, 1.000000000000000000, 0.9659258262890683122, 1.000000000000000000, 0.9659258262890683122, 1.000000000000000000, 0.9659258262890683122, 1.000000000000000000, 0.9659258262890683122, 1.000000000000000000, 0.9659258262890683122, 1.000000000000000000, 0.9659258262890683122, 1.000000000000000000, 0.9659258262890683122, 1.000000000000000000, 0.9659258262890683122, 1.000000000000000000, 0.9659258262890683122, 1.000000000000000000, 0.9659258262890683122, 1.000000000000000000, 0.9659258262890683122, 1.000000000000000000, 0.9659258262890683122, 1.000000000000000000, 0.9659258262890683122, 1.000000000000000000, 0.9659258262890683122, 1.000000000000000000, 0.9659258262890683122, 1.000000000000000000, 0.9659258262890683122, 1.000000000000000000, 0.9659258262890683122, 1.000000000000000000, 0.9659258262890683122, 1.000000000000000000, 0.9659258262890683122, 1.000000000000000000, 0.9659258262890683122, 1.000000000000000000, 0.9659258262890683122, 1.000000000000000000, 0.9659258262890683122, 1.000000000000000000, 0.9659258262890683122, 1.000000000000000000, 0.9659258262890683122, 1.000000000000000000, 0.9659258262890683122, 1.000000000000000000, 0.9659258262890683122, 1.000000000000000000, 0.9659258262890683122, 1.000000000000000000, 0.9659258262890683122, 1.000000000000000000, 0.9659258262890683122, 1.000000000000000000, 0.9659258262890683122, 1.000000000000000000, 0.9659258262890683122, 1.000000000000000000, 0.9659258262890683122, 1.000000000000000000, 0.9659258262890683122, 1.000000000000000000, 0.9659258262890683122, 1.000000000000000000, 0.9659258262890683122, 1.000000000000000000, 0.9659258262890683122, 1.000000000000000000, 0.9659258262890683122, 1.000000000000000000, 0.9659258262890683122, 1.000000000000000000, 0.9659258262890683122, 1.000000000000000000, 0.9659258262890683122, 1.000000000000000000, 0.9659258262890683122, 1.000000000000000000, 0.9659258262890683122, 1.000000000000000000, 0.9659258262890683122, 1.000000000000000000, 0.9659258262890683122, 1.000000000000000000, 0.9659258262890683122, 1.000000000000000000, 0.9659258262890683122, 1.000000000000000000, 0.9659258262890683122, 1.000000000000000000, 0.9659258262890683122, 1.000000000000000000, 0.9659258262890683122, 1.000000000000000000, 0.9659258262890683122, 1.000000000000000000, 0.9659258262890683122, 1.000000000000000000, 0.9659258262890683122, 1.000000000000000000, 0.9659258262890683122, 1.000000000000000000, 0.9659258262890683122, 1.000000000000000000, 0.9659258262890683122, 1.000000000000000000, 0.9659258262890683122, 1.000000000000000000, 0.9659258262890683122, 1.000000000000000000, 0.9659258262890683122, 1.000000000000000000, 0.9659258262890683122, 1.000000000000000000, 0.9659258262890683122, 1.000000000000000000, 0.9659258262890683122, 1.000000000000000000, 0.9659258262890683122, 1.000000000000000000, 0.9659258262890683122, 1.000000000000000000, 0.9659258262890683122, 1.000000000000000000, 0.9659258262890683122, 1.000000000000000000, 0.9659258262890683122, 1.000000000000000000, 0.9659258262890683122, 1.000000000000000000, 0.9659258262890683122, 1.000000000000000000, 0.9659258262890683122, 1.000000000000000000, 0.9659258262890683122, 1.000000000000000000, 0.9659258262890683122, 1.000000000000000000, 0.9659258262890683122, 1.000000000000000000, 0.9659258262890683122, 1.000000000000000000, 0.9659258262890683122, 1.000000000000000000, 0.9659258262890683122, 1.000000000000000000, 0.9659258262890683122, 1.000000000000000000, 0.9659258262890683122, 1.000000000000000000, 0.9659258262890683122, 1.000000000000000000, 0.9659258262890683122, 1.000000000000000000, 0.9659258262890683122, 1.000000000000000000, 0.9659258262890683122, 1.000000000000000000, 0.9659258262890683122, 1.000000000000000000, 0.9659258262890683122, 1.000000000000000000, 0.9659258262890683122, 1.000000000000000000, 0.9659258262890683122, 1.000000000000000000, 0.9659258262890683122, 1.000000000000000000, 0.9659258262890683122, 1.000000000000000000, 0.9659258262890683122, 1.000000000000000000, 0.9659258262890683122, 1.000000000000000000, 0.9659258262890683122, 1.000000000000000000, 0.9659258262890683122, 1.000000000000000000, 0.9659258262890683122, 1.000000000000000000, 0.9659258262890683122, 1.000000000000000000, 0.9659258262890683122, 1.000000000000000000),
 ( 0.3333333333333333703, 0.3219752754296894559, 0.3333333333333333703, 0.3219752754296894559, 0.3333333333333333703, 0.3219752754296894559, 0.3333333333333333703, 0.3219752754296894559, 0.3333333333333333703, 0.3219752754296894559, 0.3333333333333333703, 0.3219752754296894559, 0.3333333333333333703, 0.3219752754296894559, 0.3333333333333333703, 0.3219752754296894559, 0.3333333333333333703, 0.3219752754296894559, 0.3333333333333333703, 0.3219752754296894559, 0.3333333333333333703, 0.3219752754296894559, 0.3333333333333333703, 0.3219752754296894559, 0.3333333333333333703, 0.3219752754296894559, 0.3333333333333333703, 0.3219752754296894559, 0.3333333333333333703, 0.3219752754296894559, 0.3333333333333333703, 0.3219752754296894559, 0.3333333333333333703, 0.3219752754296894559, 0.3333333333333333703, 0.3219752754296894559, 0.3333333333333333703, 0.3219752754296894559, 0.3333333333333333703, 0.3219752754296894559, 0.3333333333333333703, 0.3219752754296894559, 0.3333333333333333703, 0.3219752754296894559, 0.3333333333333333703, 0.3219752754296894559, 0.3333333333333333703, 0.3219752754296894559, 0.3333333333333333703, 0.3219752754296894559, 0.3333333333333333703, 0.3219752754296894559, 0.3333333333333333703, 0.3219752754296894559, 0.3333333333333333703, 0.3219752754296894559, 0.3333333333333333703, 0.3219752754296894559, 0.3333333333333333703, 0.3219752754296894559, 0.3333333333333333703, 0.3219752754296894559, 0.3333333333333333703, 0.3219752754296894559, 0.3333333333333333703, 0.3219752754296894559, 0.3333333333333333703, 0.3219752754296894559, 0.3333333333333333703, 0.3219752754296894559, 0.3333333333333333703, 0.3219752754296894559, 0.3333333333333333703, 0.3219752754296894559, 0.3333333333333333703, 0.3219752754296894559, 0.3333333333333333703, 0.3219752754296894559, 0.3333333333333333703, 0.3219752754296894559, 0.3333333333333333703, 0.3219752754296894559, 0.3333333333333333703, 0.3219752754296894559, 0.3333333333333333703, 0.3219752754296894559, 0.3333333333333333703, 0.3219752754296894559, 0.3333333333333333703, 0.3219752754296894559, 0.3333333333333333703, 0.3219752754296894559, 0.3333333333333333703, 0.3219752754296894559, 0.3333333333333333703, 0.3219752754296894559, 0.3333333333333333703, 0.3219752754296894559, 0.3333333333333333703, 0.3219752754296894559, 0.3333333333333333703, 0.3219752754296894559, 0.3333333333333333703, 0.3219752754296894559, 0.3333333333333333703, 0.3219752754296894559, 0.3333333333333333703, 0.3219752754296894559, 0.3333333333333333703, 0.3219752754296894559, 0.3333333333333333703, 0.3219752754296894559, 0.3333333333333333703, 0.3219752754296894559, 0.3333333333333333703, 0.3219752754296894559, 0.3333333333333333703, 0.3219752754296894559, 0.3333333333333333703, 0.3219752754296894559, 0.3333333333333333703, 0.3219752754296894559, 0.3333333333333333703, 0.3219752754296894559, 0.3333333333333333703, 0.3219752754296894559, 0.3333333333333333703, 0.3219752754296894559, 0.3333333333333333703, 0.3219752754296894559, 0.3333333333333333703, 0.3219752754296894559, 0.3333333333333333703, 0.3219752754296894559, 0.3333333333333333703, 0.3219752754296894559, 0.3333333333333333703, 0.3219752754296894559, 0.3333333333333333703, 0.3219752754296894559, 0.3333333333333333703, 0.3219752754296894559, 0.3333333333333333703, 0.3219752754296894559, 0.3333333333333333703, 0.3219752754296894559, 0.3333333333333333703, 0.3219752754296894559, 0.3333333333333333703, 0.3219752754296894559, 0.3333333333333333703, 0.3219752754296894559, 0.3333333333333333703, 0.3219752754296894559, 0.3333333333333333703, 0.3219752754296894559, 0.3333333333333333703, 0.3219752754296894559, 0.3333333333333333703, 0.3219752754296894559, 0.3333333333333333703, 0.3219752754296894559, 0.3333333333333333703, 0.3219752754296894559, 0.3333333333333333703, 0.3219752754296894559, 0.3333333333333333703, 0.3219752754296894559, 0.3333333333333333703, 0.3219752754296894559, 0.3333333333333333703, 0.3219752754296894559, 0.3333333333333333703, 0.3219752754296894559, 0.3333333333333333703, 0.3219752754296894559, 0.3333333333333333703, 0.3219752754296894559, 0.3333333333333333703, 0.3219752754296894559, 0.3333333333333333703, 0.3219752754296894559, 0.3333333333333333703, 0.3219752754296894559, 0.3333333333333333703, 0.3219752754296894559, 0.3333333333333333703, 0.3219752754296894559, 0.3333333333333333703, 0.3219752754296894559, 0.3333333333333333703, 0.3219752754296894559, 0.3333333333333333703, 0.3219752754296894559, 0.3333333333333333703, 0.3219752754296894559, 0.3333333333333333703, 0.3219752754296894559, 0.3333333333333333703, 0.3219752754296894559, 0.3333333333333333703, 0.3219752754296894559, 0.3333333333333333703, 0.3219752754296894559, 0.3333333333333333703, 0.3219752754296894559, 0.3333333333333333703, 0.3219752754296894559, 0.3333333333333333703, 0.3219752754296894559, 0.3333333333333333703, 0.3219752754296894559, 0.3333333333333333703, 0.3219752754296894559, 0.3333333333333333703, 0.3219752754296894559, 0.3333333333333333703, 0.3219752754296894559, 0.3333333333333333703, 0.3219752754296894559, 0.3333333333333333703, 0.3219752754296894559, 0.3333333333333333703, 0.3219752754296894559, 0.3333333333333333703, 0.3219752754296894559, 0.3333333333333333703, 0.3219752754296894559, 0.3333333333333333703, 0.3219752754296894559, 0.3333333333333333703, 0.3219752754296894559, 0.3333333333333333703, 0.3219752754296894559, 0.3333333333333333703, 0.3219752754296894559, 0.3333333333333333703, 0.3219752754296894559, 0.3333333333333333703, 0.3219752754296894559, 0.3333333333333333703, 0.3219752754296894559, 0.3333333333333333703, 0.3219752754296894559, 0.3333333333333333703, 0.3219752754296894559, 0.3333333333333333703, 0.3219752754296894559, 0.3333333333333333703, 0.3219752754296894559, 0.3333333333333333703, 0.3219752754296894559, 0.3333333333333333703, 0.3219752754296894559, 0.3333333333333333703, 0.3219752754296894559, 0.3333333333333333703, 0.3219752754296894559, 0.3333333333333333703, 0.3219752754296894559, 0.3333333333333333703, 0.3219752754296894559, 0.3333333333333333703, 0.3219752754296894559, 0.3333333333333333703, 0.3219752754296894559, 0.3333333333333333703, 0.3219752754296894559, 0.3333333333333333703, 0.3219752754296894559, 0.3333333333333333703, 0.3219752754296894559, 0.3333333333333333703, 0.3219752754296894559, 0.3333333333333333703, 0.3219752754296894559, 0.3333333333333333703, 0.3219752754296894559, 0.3333333333333333703, 0.3219752754296894559, 0.3333333333333333703, 0.3219752754296894559, 0.3333333333333333703, 0.3219752754296894559, 0.3333333333333333703, 0.3219752754296894559, 0.3333333333333333703, 0.3219752754296894559, 0.3333333333333333703, 0.3219752754296894559, 0.3333333333333333703, 0.3219752754296894559, 0.3333333333333333703, 0.3219752754296894559, 0.3333333333333333703, 0.3219752754296894559, 0.3333333333333333703, 0.3219752754296894559, 0.3333333333333333703, 0.3219752754296894559, 0.3333333333333333703, 0.3219752754296894559, 0.3333333333333333703, 0.3219752754296894559, 0.3333333333333333703, 0.3219752754296894559, 0.3333333333333333703, 0.3219752754296894559, 0.3333333333333333703, 0.3219752754296894559, 0.3333333333333333703, 0.3219752754296894559, 0.3333333333333333703, 0.3219752754296894559, 0.3333333333333333703, 0.3219752754296894559, 0.3333333333333333703, 0.3219752754296894559, 0.3333333333333333703, 0.3219752754296894559, 0.3333333333333333703, 0.3219752754296894559, 0.3333333333333333703, 0.3219752754296894559, 0.3333333333333333703, 0.3219752754296894559, 0.3333333333333333703, 0.3219752754296894559, 0.3333333333333333703, 0.3219752754296894559, 0.3333333333333333703, 0.3219752754296894559, 0.3333333333333333703, 0.3219752754296894559, 0.3333333333333333703, 0.3219752754296894559, 0.3333333333333333703, 0.3219752754296894559, 0.3333333333333333703, 0.3219752754296894559, 0.3333333333333333703, 0.3219752754296894559, 0.3333333333333333703, 0.3219752754296894559, 0.3333333333333333703, 0.3219752754296894559, 0.3333333333333333703, 0.3219752754296894559, 0.3333333333333333703, 0.3219752754296894559, 0.3333333333333333703, 0.3219752754296894559, 0.3333333333333333703, 0.3219752754296894559, 0.3333333333333333703, 0.3219752754296894559, 0.3333333333333333703, 0.3219752754296894559, 0.3333333333333333703, 0.3219752754296894559, 0.3333333333333333703, 0.3219752754296894559, 0.3333333333333333703, 0.3219752754296894559, 0.3333333333333333703, 0.3219752754296894559, 0.3333333333333333703, 0.3219752754296894559, 0.3333333333333333703, 0.3219752754296894559, 0.3333333333333333703, 0.3219752754296894559, 0.3333333333333333703, 0.3219752754296894559, 0.3333333333333333703, 0.3219752754296894559, 0.3333333333333333703, 0.3219752754296894559, 0.3333333333333333703, 0.3219752754296894559, 0.3333333333333333703, 0.3219752754296894559, 0.3333333333333333703, 0.3219752754296894559, 0.3333333333333333703, 0.3219752754296894559, 0.3333333333333333703, 0.3219752754296894559, 0.3333333333333333703, 0.3219752754296894559, 0.3333333333333333703, 0.3219752754296894559, 0.3333333333333333703, 0.3219752754296894559, 0.3333333333333333703, 0.3219752754296894559, 0.3333333333333333703, 0.3219752754296894559, 0.3333333333333333703, 0.3219752754296894559, 0.3333333333333333703, 0.3219752754296894559, 0.3333333333333333703, 0.3219752754296894559, 0.3333333333333333703, 0.3219752754296894559, 0.3333333333333333703, 0.3219752754296894559, 0.3333333333333333703, 0.3219752754296894559, 0.3333333333333333703, 0.3219752754296894559, 0.3333333333333333703, 0.3219752754296894559, 0.3333333333333333703, 0.3219752754296894559, 0.3333333333333333703, 0.3219752754296894559, 0.3333333333333333703, 0.3219752754296894559, 0.3333333333333333703, 0.3219752754296894559, 0.3333333333333333703, 0.3219752754296894559, 0.3333333333333333703, 0.3219752754296894559, 0.3333333333333333703, 0.3219752754296894559, 0.3333333333333333703, 0.3219752754296894559, 0.3333333333333333703, 0.3219752754296894559, 0.3333333333333333703, 0.3219752754296894559, 0.3333333333333333703, 0.3219752754296894559, 0.3333333333333333703, 0.3219752754296894559, 0.3333333333333333703, 0.3219752754296894559, 0.3333333333333333703, 0.3219752754296894559, 0.3333333333333333703, 0.3219752754296894559, 0.3333333333333333703, 0.3219752754296894559, 0.3333333333333333703, 0.3219752754296894559, 0.3333333333333333703, 0.3219752754296894559, 0.3333333333333333703, 0.3219752754296894559, 0.3333333333333333703, 0.3219752754296894559, 0.3333333333333333703, 0.3219752754296894559, 0.3333333333333333703),
 ( 0.3333333333333333703, 0.3219752754296894559, 0.3333333333333333703, 0.3219752754296894559, 0.3333333333333333703, 0.3219752754296894559, 0.3333333333333333703, 0.3219752754296894559, 0.3333333333333333703, 0.3219752754296894559, 0.3333333333333333703, 0.3219752754296894559, 0.3333333333333333703, 0.3219752754296894559, 0.3333333333333333703, 0.3219752754296894559, 0.3333333333333333703, 0.3219752754296894559, 0.3333333333333333703, 0.3219752754296894559, 0.3333333333333333703, 0.3219752754296894559, 0.3333333333333333703, 0.3219752754296894559, 0.3333333333333333703, 0.3219752754296894559, 0.3333333333333333703, 0.3219752754296894559, 0.3333333333333333703, 0.3219752754296894559, 0.3333333333333333703, 0.3219752754296894559, 0.3333333333333333703, 0.3219752754296894559, 0.3333333333333333703, 0.3219752754296894559, 0.3333333333333333703, 0.3219752754296894559, 0.3333333333333333703, 0.3219752754296894559, 0.3333333333333333703, 0.3219752754296894559, 0.3333333333333333703, 0.3219752754296894559, 0.3333333333333333703, 0.3219752754296894559, 0.3333333333333333703, 0.3219752754296894559, 0.3333333333333333703, 0.3219752754296894559, 0.3333333333333333703, 0.3219752754296894559, 0.3333333333333333703, 0.3219752754296894559, 0.3333333333333333703, 0.3219752754296894559, 0.3333333333333333703, 0.3219752754296894559, 0.3333333333333333703, 0.3219752754296894559, 0.3333333333333333703, 0.3219752754296894559, 0.3333333333333333703, 0.3219752754296894559, 0.3333333333333333703, 0.3219752754296894559, 0.3333333333333333703, 0.3219752754296894559, 0.3333333333333333703, 0.3219752754296894559, 0.3333333333333333703, 0.3219752754296894559, 0.3333333333333333703, 0.3219752754296894559, 0.3333333333333333703, 0.3219752754296894559, 0.3333333333333333703, 0.3219752754296894559, 0.3333333333333333703, 0.3219752754296894559, 0.3333333333333333703, 0.3219752754296894559, 0.3333333333333333703, 0.3219752754296894559, 0.3333333333333333703, 0.3219752754296894559, 0.3333333333333333703, 0.3219752754296894559, 0.3333333333333333703, 0.3219752754296894559, 0.3333333333333333703, 0.3219752754296894559, 0.3333333333333333703, 0.3219752754296894559, 0.3333333333333333703, 0.3219752754296894559, 0.3333333333333333703, 0.3219752754296894559, 0.3333333333333333703, 0.3219752754296894559, 0.3333333333333333703, 0.3219752754296894559, 0.3333333333333333703, 0.3219752754296894559, 0.3333333333333333703, 0.3219752754296894559, 0.3333333333333333703, 0.3219752754296894559, 0.3333333333333333703, 0.3219752754296894559, 0.3333333333333333703, 0.3219752754296894559, 0.3333333333333333703, 0.3219752754296894559, 0.3333333333333333703, 0.3219752754296894559, 0.3333333333333333703, 0.3219752754296894559, 0.3333333333333333703, 0.3219752754296894559, 0.3333333333333333703, 0.3219752754296894559, 0.3333333333333333703, 0.3219752754296894559, 0.3333333333333333703, 0.3219752754296894559, 0.3333333333333333703, 0.3219752754296894559, 0.3333333333333333703, 0.3219752754296894559, 0.3333333333333333703, 0.3219752754296894559, 0.3333333333333333703, 0.3219752754296894559, 0.3333333333333333703, 0.3219752754296894559, 0.3333333333333333703, 0.3219752754296894559, 0.3333333333333333703, 0.3219752754296894559, 0.3333333333333333703, 0.3219752754296894559, 0.3333333333333333703, 0.3219752754296894559, 0.3333333333333333703, 0.3219752754296894559, 0.3333333333333333703, 0.3219752754296894559, 0.3333333333333333703, 0.3219752754296894559, 0.3333333333333333703, 0.3219752754296894559, 0.3333333333333333703, 0.3219752754296894559, 0.3333333333333333703, 0.3219752754296894559, 0.3333333333333333703, 0.3219752754296894559, 0.3333333333333333703, 0.3219752754296894559, 0.3333333333333333703, 0.3219752754296894559, 0.3333333333333333703, 0.3219752754296894559, 0.3333333333333333703, 0.3219752754296894559, 0.3333333333333333703, 0.3219752754296894559, 0.3333333333333333703, 0.3219752754296894559, 0.3333333333333333703, 0.3219752754296894559, 0.3333333333333333703, 0.3219752754296894559, 0.3333333333333333703, 0.3219752754296894559, 0.3333333333333333703, 0.3219752754296894559, 0.3333333333333333703, 0.3219752754296894559, 0.3333333333333333703, 0.3219752754296894559, 0.3333333333333333703, 0.3219752754296894559, 0.3333333333333333703, 0.3219752754296894559, 0.3333333333333333703, 0.3219752754296894559, 0.3333333333333333703, 0.3219752754296894559, 0.3333333333333333703, 0.3219752754296894559, 0.3333333333333333703, 0.3219752754296894559, 0.3333333333333333703, 0.3219752754296894559, 0.3333333333333333703, 0.3219752754296894559, 0.3333333333333333703, 0.3219752754296894559, 0.3333333333333333703, 0.3219752754296894559, 0.3333333333333333703, 0.3219752754296894559, 0.3333333333333333703, 0.3219752754296894559, 0.3333333333333333703, 0.3219752754296894559, 0.3333333333333333703, 0.3219752754296894559, 0.3333333333333333703, 0.3219752754296894559, 0.3333333333333333703, 0.3219752754296894559, 0.3333333333333333703, 0.3219752754296894559, 0.3333333333333333703, 0.3219752754296894559, 0.3333333333333333703, 0.3219752754296894559, 0.3333333333333333703, 0.3219752754296894559, 0.3333333333333333703, 0.3219752754296894559, 0.3333333333333333703, 0.3219752754296894559, 0.3333333333333333703, 0.3219752754296894559, 0.3333333333333333703, 0.3219752754296894559, 0.3333333333333333703, 0.3219752754296894559, 0.3333333333333333703, 0.3219752754296894559, 0.3333333333333333703, 0.3219752754296894559, 0.3333333333333333703, 0.3219752754296894559, 0.3333333333333333703, 0.3219752754296894559, 0.3333333333333333703, 0.3219752754296894559, 0.3333333333333333703, 0.3219752754296894559, 0.3333333333333333703, 0.3219752754296894559, 0.3333333333333333703, 0.3219752754296894559, 0.3333333333333333703, 0.3219752754296894559, 0.3333333333333333703, 0.3219752754296894559, 0.3333333333333333703, 0.3219752754296894559, 0.3333333333333333703, 0.3219752754296894559, 0.3333333333333333703, 0.3219752754296894559, 0.3333333333333333703, 0.3219752754296894559, 0.3333333333333333703, 0.3219752754296894559, 0.3333333333333333703, 0.3219752754296894559, 0.3333333333333333703, 0.3219752754296894559, 0.3333333333333333703, 0.3219752754296894559, 0.3333333333333333703, 0.3219752754296894559, 0.3333333333333333703, 0.3219752754296894559, 0.3333333333333333703, 0.3219752754296894559, 0.3333333333333333703, 0.3219752754296894559, 0.3333333333333333703, 0.3219752754296894559, 0.3333333333333333703, 0.3219752754296894559, 0.3333333333333333703, 0.3219752754296894559, 0.3333333333333333703, 0.3219752754296894559, 0.3333333333333333703, 0.3219752754296894559, 0.3333333333333333703, 0.3219752754296894559, 0.3333333333333333703, 0.3219752754296894559, 0.3333333333333333703, 0.3219752754296894559, 0.3333333333333333703, 0.3219752754296894559, 0.3333333333333333703, 0.3219752754296894559, 0.3333333333333333703, 0.3219752754296894559, 0.3333333333333333703, 0.3219752754296894559, 0.3333333333333333703, 0.3219752754296894559, 0.3333333333333333703, 0.3219752754296894559, 0.3333333333333333703, 0.3219752754296894559, 0.3333333333333333703, 0.3219752754296894559, 0.3333333333333333703, 0.3219752754296894559, 0.3333333333333333703, 0.3219752754296894559, 0.3333333333333333703, 0.3219752754296894559, 0.3333333333333333703, 0.3219752754296894559, 0.3333333333333333703, 0.3219752754296894559, 0.3333333333333333703, 0.3219752754296894559, 0.3333333333333333703, 0.3219752754296894559, 0.3333333333333333703, 0.3219752754296894559, 0.3333333333333333703, 0.3219752754296894559, 0.3333333333333333703, 0.3219752754296894559, 0.3333333333333333703, 0.3219752754296894559, 0.3333333333333333703, 0.3219752754296894559, 0.3333333333333333703, 0.3219752754296894559, 0.3333333333333333703, 0.3219752754296894559, 0.3333333333333333703, 0.3219752754296894559, 0.3333333333333333703, 0.3219752754296894559, 0.3333333333333333703, 0.3219752754296894559, 0.3333333333333333703, 0.3219752754296894559, 0.3333333333333333703, 0.3219752754296894559, 0.3333333333333333703, 0.3219752754296894559, 0.3333333333333333703, 0.3219752754296894559, 0.3333333333333333703, 0.3219752754296894559, 0.3333333333333333703, 0.3219752754296894559, 0.3333333333333333703, 0.3219752754296894559, 0.3333333333333333703, 0.3219752754296894559, 0.3333333333333333703, 0.3219752754296894559, 0.3333333333333333703, 0.3219752754296894559, 0.3333333333333333703, 0.3219752754296894559, 0.3333333333333333703, 0.3219752754296894559, 0.3333333333333333703, 0.3219752754296894559, 0.3333333333333333703, 0.3219752754296894559, 0.3333333333333333703, 0.3219752754296894559, 0.3333333333333333703, 0.3219752754296894559, 0.3333333333333333703, 0.3219752754296894559, 0.3333333333333333703, 0.3219752754296894559, 0.3333333333333333703, 0.3219752754296894559, 0.3333333333333333703, 0.3219752754296894559, 0.3333333333333333703, 0.3219752754296894559, 0.3333333333333333703, 0.3219752754296894559, 0.3333333333333333703, 0.3219752754296894559, 0.3333333333333333703, 0.3219752754296894559, 0.3333333333333333703, 0.3219752754296894559, 0.3333333333333333703, 0.3219752754296894559, 0.3333333333333333703, 0.3219752754296894559, 0.3333333333333333703, 0.3219752754296894559, 0.3333333333333333703, 0.3219752754296894559, 0.3333333333333333703, 0.3219752754296894559, 0.3333333333333333703, 0.3219752754296894559, 0.3333333333333333703, 0.3219752754296894559, 0.3333333333333333703, 0.3219752754296894559, 0.3333333333333333703, 0.3219752754296894559, 0.3333333333333333703, 0.3219752754296894559, 0.3333333333333333703, 0.3219752754296894559, 0.3333333333333333703, 0.3219752754296894559, 0.3333333333333333703, 0.3219752754296894559, 0.3333333333333333703, 0.3219752754296894559, 0.3333333333333333703, 0.3219752754296894559, 0.3333333333333333703, 0.3219752754296894559, 0.3333333333333333703, 0.3219752754296894559, 0.3333333333333333703, 0.3219752754296894559, 0.3333333333333333703, 0.3219752754296894559, 0.3333333333333333703, 0.3219752754296894559, 0.3333333333333333703, 0.3219752754296894559, 0.3333333333333333703, 0.3219752754296894559, 0.3333333333333333703, 0.3219752754296894559, 0.3333333333333333703, 0.3219752754296894559, 0.3333333333333333703, 0.3219752754296894559, 0.3333333333333333703, 0.3219752754296894559, 0.3333333333333333703, 0.3219752754296894559, 0.3333333333333333703, 0.3219752754296894559, 0.3333333333333333703, 0.3219752754296894559, 0.3333333333333333703, 0.3219752754296894559, 0.3333333333333333703, 0.3219752754296894559, 0.3333333333333333703, 0.3219752754296894559, 0.3333333333333333703),
 ( 1.000000000000000000, 0.9659258262890683122, 1.000000000000000000, 0.9659258262890683122, 1.000000000000000000, 0.9659258262890683122, 1.000000000000000000, 0.9659258262890683122, 1.000000000000000000, 0.9659258262890683122, 1.000000000000000000, 0.9659258262890683122, 1.000000000000000000, 0.9659258262890683122, 1.000000000000000000, 0.9659258262890683122, 1.000000000000000000, 0.9659258262890683122, 1.000000000000000000, 0.9659258262890683122, 1.000000000000000000, 0.9659258262890683122, 1.000000000000000000, 0.9659258262890683122, 1.000000000000000000, 0.9659258262890683122, 1.000000000000000000, 0.9659258262890683122, 1.000000000000000000, 0.9659258262890683122, 1.000000000000000000, 0.9659258262890683122, 1.000000000000000000, 0.9659258262890683122, 1.000000000000000000, 0.9659258262890683122, 1.000000000000000000, 0.9659258262890683122, 1.000000000000000000, 0.9659258262890683122, 1.000000000000000000, 0.9659258262890683122, 1.000000000000000000, 0.9659258262890683122, 1.000000000000000000, 0.9659258262890683122, 1.000000000000000000, 0.9659258262890683122, 1.000000000000000000, 0.9659258262890683122, 1.000000000000000000, 0.9659258262890683122, 1.000000000000000000, 0.9659258262890683122, 1.000000000000000000, 0.9659258262890683122, 1.000000000000000000, 0.9659258262890683122, 1.000000000000000000, 0.9659258262890683122, 1.000000000000000000, 0.9659258262890683122, 1.000000000000000000, 0.9659258262890683122, 1.000000000000000000, 0.9659258262890683122, 1.000000000000000000, 0.9659258262890683122, 1.000000000000000000, 0.9659258262890683122, 1.000000000000000000, 0.9659258262890683122, 1.000000000000000000, 0.9659258262890683122, 1.000000000000000000, 0.9659258262890683122, 1.000000000000000000, 0.9659258262890683122, 1.000000000000000000, 0.9659258262890683122, 1.000000000000000000, 0.9659258262890683122, 1.000000000000000000, 0.9659258262890683122, 1.000000000000000000, 0.9659258262890683122, 1.000000000000000000, 0.9659258262890683122, 1.000000000000000000, 0.9659258262890683122, 1.000000000000000000, 0.9659258262890683122, 1.000000000000000000, 0.9659258262890683122, 1.000000000000000000, 0.9659258262890683122, 1.000000000000000000, 0.9659258262890683122, 1.000000000000000000, 0.9659258262890683122, 1.000000000000000000, 0.9659258262890683122, 1.000000000000000000, 0.9659258262890683122, 1.000000000000000000, 0.9659258262890683122, 1.000000000000000000, 0.9659258262890683122, 1.000000000000000000, 0.9659258262890683122, 1.000000000000000000, 0.9659258262890683122, 1.000000000000000000, 0.9659258262890683122, 1.000000000000000000, 0.9659258262890683122, 1.000000000000000000, 0.9659258262890683122, 1.000000000000000000, 0.9659258262890683122, 1.000000000000000000, 0.9659258262890683122, 1.000000000000000000, 0.9659258262890683122, 1.000000000000000000, 0.9659258262890683122, 1.000000000000000000, 0.9659258262890683122, 1.000000000000000000, 0.9659258262890683122, 1.000000000000000000, 0.9659258262890683122, 1.000000000000000000, 0.9659258262890683122, 1.000000000000000000, 0.9659258262890683122, 1.000000000000000000, 0.9659258262890683122, 1.000000000000000000, 0.9659258262890683122, 1.000000000000000000, 0.9659258262890683122, 1.000000000000000000, 0.9659258262890683122, 1.000000000000000000, 0.9659258262890683122, 1.000000000000000000, 0.9659258262890683122, 1.000000000000000000, 0.9659258262890683122, 1.000000000000000000, 0.9659258262890683122, 1.000000000000000000, 0.9659258262890683122, 1.000000000000000000, 0.9659258262890683122, 1.000000000000000000, 0.9659258262890683122, 1.000000000000000000, 0.9659258262890683122, 1.000000000000000000, 0.9659258262890683122, 1.000000000000000000, 0.9659258262890683122, 1.000000000000000000, 0.9659258262890683122, 1.000000000000000000, 0.9659258262890683122, 1.000000000000000000, 0.9659258262890683122, 1.000000000000000000, 0.9659258262890683122, 1.000000000000000000, 0.9659258262890683122, 1.000000000000000000, 0.9659258262890683122, 1.000000000000000000, 0.9659258262890683122, 1.000000000000000000, 0.9659258262890683122, 1.000000000000000000, 0.9659258262890683122, 1.000000000000000000, 0.9659258262890683122, 1.000000000000000000, 0.9659258262890683122, 1.000000000000000000, 0.9659258262890683122, 1.000000000000000000, 0.9659258262890683122, 1.000000000000000000, 0.9659258262890683122, 1.000000000000000000, 0.9659258262890683122, 1.000000000000000000, 0.9659258262890683122, 1.000000000000000000, 0.9659258262890683122, 1.000000000000000000, 0.9659258262890683122, 1.000000000000000000, 0.9659258262890683122, 1.000000000000000000, 0.9659258262890683122, 1.000000000000000000, 0.9659258262890683122, 1.000000000000000000, 0.9659258262890683122, 1.000000000000000000, 0.9659258262890683122, 1.000000000000000000, 0.9659258262890683122, 1.000000000000000000, 0.9659258262890683122, 1.000000000000000000, 0.9659258262890683122, 1.000000000000000000, 0.9659258262890683122, 1.000000000000000000, 0.9659258262890683122, 1.000000000000000000, 0.9659258262890683122, 1.000000000000000000, 0.9659258262890683122, 1.000000000000000000, 0.9659258262890683122, 1.000000000000000000, 0.9659258262890683122, 1.000000000000000000, 0.9659258262890683122, 1.000000000000000000, 0.9659258262890683122, 1.000000000000000000, 0.9659258262890683122, 1.000000000000000000, 0.9659258262890683122, 1.000000000000000000, 0.9659258262890683122, 1.000000000000000000, 0.9659258262890683122, 1.000000000000000000, 0.9659258262890683122, 1.000000000000000000, 0.9659258262890683122, 1.000000000000000000, 0.9659258262890683122, 1.000000000000000000, 0.9659258262890683122, 1.000000000000000000, 0.9659258262890683122, 1.000000000000000000, 0.9659258262890683122, 1.000000000000000000, 0.9659258262890683122, 1.000000000000000000, 0.9659258262890683122, 1.000000000000000000, 0.9659258262890683122, 1.000000000000000000, 0.9659258262890683122, 1.000000000000000000, 0.9659258262890683122, 1.000000000000000000, 0.9659258262890683122, 1.000000000000000000, 0.9659258262890683122, 1.000000000000000000, 0.9659258262890683122, 1.000000000000000000, 0.9659258262890683122, 1.000000000000000000, 0.9659258262890683122, 1.000000000000000000, 0.9659258262890683122, 1.000000000000000000, 0.9659258262890683122, 1.000000000000000000, 0.9659258262890683122, 1.000000000000000000, 0.9659258262890683122, 1.000000000000000000, 0.9659258262890683122, 1.000000000000000000, 0.9659258262890683122, 1.000000000000000000, 0.9659258262890683122, 1.000000000000000000, 0.9659258262890683122, 1.000000000000000000, 0.9659258262890683122, 1.000000000000000000, 0.9659258262890683122, 1.000000000000000000, 0.9659258262890683122, 1.000000000000000000, 0.9659258262890683122, 1.000000000000000000, 0.9659258262890683122, 1.000000000000000000, 0.9659258262890683122, 1.000000000000000000, 0.9659258262890683122, 1.000000000000000000, 0.9659258262890683122, 1.000000000000000000, 0.9659258262890683122, 1.000000000000000000, 0.9659258262890683122, 1.000000000000000000, 0.9659258262890683122, 1.000000000000000000, 0.9659258262890683122, 1.000000000000000000, 0.9659258262890683122, 1.000000000000000000, 0.9659258262890683122, 1.000000000000000000, 0.9659258262890683122, 1.000000000000000000, 0.9659258262890683122, 1.000000000000000000, 0.9659258262890683122, 1.000000000000000000, 0.9659258262890683122, 1.000000000000000000, 0.9659258262890683122, 1.000000000000000000, 0.9659258262890683122, 1.000000000000000000, 0.9659258262890683122, 1.000000000000000000, 0.9659258262890683122, 1.000000000000000000, 0.9659258262890683122, 1.000000000000000000, 0.9659258262890683122, 1.000000000000000000, 0.9659258262890683122, 1.000000000000000000, 0.9659258262890683122, 1.000000000000000000, 0.9659258262890683122, 1.000000000000000000, 0.9659258262890683122, 1.000000000000000000, 0.9659258262890683122, 1.000000000000000000, 0.9659258262890683122, 1.000000000000000000, 0.9659258262890683122, 1.000000000000000000, 0.9659258262890683122, 1.000000000000000000, 0.9659258262890683122, 1.000000000000000000, 0.9659258262890683122, 1.000000000000000000, 0.9659258262890683122, 1.000000000000000000, 0.9659258262890683122, 1.000000000000000000, 0.9659258262890683122, 1.000000000000000000, 0.9659258262890683122, 1.000000000000000000, 0.9659258262890683122, 1.000000000000000000, 0.9659258262890683122, 1.000000000000000000, 0.9659258262890683122, 1.000000000000000000, 0.9659258262890683122, 1.000000000000000000, 0.9659258262890683122, 1.000000000000000000, 0.9659258262890683122, 1.000000000000000000, 0.9659258262890683122, 1.000000000000000000, 0.9659258262890683122, 1.000000000000000000, 0.9659258262890683122, 1.000000000000000000, 0.9659258262890683122, 1.000000000000000000, 0.9659258262890683122, 1.000000000000000000, 0.9659258262890683122, 1.000000000000000000, 0.9659258262890683122, 1.000000000000000000, 0.9659258262890683122, 1.000000000000000000, 0.9659258262890683122, 1.000000000000000000, 0.9659258262890683122, 1.000000000000000000, 0.9659258262890683122, 1.000000000000000000, 0.9659258262890683122, 1.000000000000000000, 0.9659258262890683122, 1.000000000000000000, 0.9659258262890683122, 1.000000000000000000, 0.9659258262890683122, 1.000000000000000000, 0.9659258262890683122, 1.000000000000000000, 0.9659258262890683122, 1.000000000000000000, 0.9659258262890683122, 1.000000000000000000, 0.9659258262890683122, 1.000000000000000000, 0.9659258262890683122, 1.000000000000000000, 0.9659258262890683122, 1.000000000000000000, 0.9659258262890683122, 1.000000000000000000, 0.9659258262890683122, 1.000000000000000000, 0.9659258262890683122, 1.000000000000000000, 0.9659258262890683122, 1.000000000000000000, 0.9659258262890683122, 1.000000000000000000, 0.9659258262890683122, 1.000000000000000000, 0.9659258262890683122, 1.000000000000000000, 0.9659258262890683122, 1.000000000000000000, 0.9659258262890683122, 1.000000000000000000, 0.9659258262890683122, 1.000000000000000000, 0.9659258262890683122, 1.000000000000000000, 0.9659258262890683122, 1.000000000000000000, 0.9659258262890683122, 1.000000000000000000, 0.9659258262890683122, 1.000000000000000000, 0.9659258262890683122, 1.000000000000000000, 0.9659258262890683122, 1.000000000000000000, 0.9659258262890683122, 1.000000000000000000, 0.9659258262890683122, 1.000000000000000000, 0.9659258262890683122, 1.000000000000000000) ) ) 
 REPRESENTATION_ITEM ( '' )  SURFACE ( )  );
#46744 = CARTESIAN_POINT ( 'NONE',  ( 0.05219959533936267826, -19.03943276465977164, 45.00109039468566863 ) ) ;
#46745 = CARTESIAN_POINT ( 'NONE',  ( 21.92644707618960709, -9.078916001213698905, 171.2473621415418847 ) ) ;
#46747 = CARTESIAN_POINT ( 'NONE',  ( 13.97604488694527802, 13.89961937509977652, 79.37390960531435269 ) ) ;
#46746 = CARTESIAN_POINT ( 'NONE',  ( 5.153800228976335163, 19.02544592524342804, 64.79057627198100988 ) ) ;
#46748 = CARTESIAN_POINT ( 'NONE',  ( 8.314922557961029526, -14.29746914071037800, 55.41775706135234714 ) ) ;
#46749 = CARTESIAN_POINT ( 'NONE',  ( 18.22780087662122384, -5.500000000000022204, 81.01540105326105845 ) ) ;
#46750 = CARTESIAN_POINT ( 'NONE',  ( -17.48847506799969409, 5.747544572773746197, 110.8269743784328512 ) ) ;
#46751 = CARTESIAN_POINT ( 'NONE',  ( 12.14591786802327356, -12.06949235617739191, 85.62609039468568994 ) ) ;
#46752 = CARTESIAN_POINT ( 'NONE',  ( -1.051486528467078463, -23.87412888849584647, -54.54543624665773649 ) ) ;
#46753 = CARTESIAN_POINT ( 'NONE',  ( 4.379528057220092307, 16.55341960407617563, 82.29275706135234714 ) ) ;
#46754 = CARTESIAN_POINT ( 'NONE',  ( 16.53943276465976808, 0.05219959533934440121, 51.25109039468568994 ) ) ;
#46755 = CARTESIAN_POINT ( 'NONE',  ( -9.474510206698720793, -16.51473224551083518, 29.58442372801900433 ) ) ;
#46757 = CARTESIAN_POINT ( 'NONE',  ( 17.55127066232087429, -16.58784780708363371, -56.88740615283250435 ) ) ;
#46756 = CARTESIAN_POINT ( 'NONE',  ( 5.153800228976335163, 19.02544592524342804, 49.79057627198100988 ) ) ;
#46758 = CARTESIAN_POINT ( 'NONE',  ( -21.52544592524334988, -5.823673210054445271, 48.95942372801902565 ) ) ;
#46759 = CARTESIAN_POINT ( 'NONE',  ( -13.89961937509957401, -13.97604488694547875, 79.37609039468567573 ) ) ;
#46760 = CARTESIAN_POINT ( 'NONE',  ( -10.81492255796105439, 18.62759615963255655, 102.9177570613523756 ) ) ;
#46761 = CARTESIAN_POINT ( 'NONE',  ( 9.474510206698971260, -16.51473224551069308, 32.91557627198102409 ) ) ;
#46762 = CARTESIAN_POINT ( 'NONE',  ( -15.22409499613346640, 14.91565869316874959, -58.84910547483664800 ) ) ;
#46763 = CARTESIAN_POINT ( 'NONE',  ( 18.67979575497178502, 10.72451020669898547, 69.16557627198102409 ) ) ;
#46764 = CARTESIAN_POINT ( 'NONE',  ( 13.97604488694527802, 13.89961937509977652, 114.3739096053143669 ) ) ;
#46765 = CARTESIAN_POINT ( 'NONE',  ( 16.46253265017160672, -9.564922557960803928, 23.33224293864769194 ) ) ;
#46766 = CARTESIAN_POINT ( 'NONE',  ( 4.379528057220092307, 16.55341960407617563, 32.29275706135235424 ) ) ;
#46767 = CARTESIAN_POINT ( 'NONE',  ( 16.53943276465976808, -0.05219959533910856209, 33.74890960531436690 ) ) ;
#46768 = ORIENTED_EDGE ( 'NONE', *, *, #154789, .F. ) ;
#46769 = CARTESIAN_POINT ( 'NONE',  ( 5.823673210054444382, -21.52544592524334988, 20.20942372801900788 ) ) ;
#46771 = CARTESIAN_POINT ( 'NONE',  ( 38.00000000000000711, -12.34694845685040754, -7.100000000000000533 ) ) ;
#46770 = CARTESIAN_POINT ( 'NONE',  ( 0.05219959533910956823, 16.53943276465976808, 39.99890960531436690 ) ) ;
#46772 = CARTESIAN_POINT ( 'NONE',  ( 5.153800228976615827, -19.02544592524334988, 105.2094237280190185 ) ) ;
#46773 = CARTESIAN_POINT ( 'NONE',  ( 16.51473224551083163, -9.474510206698727899, 20.83442372801899722 ) ) ;
#46774 = CARTESIAN_POINT ( 'NONE',  ( 8.224510206698953496, -14.34966873604960469, 37.91557627198102409 ) ) ;
#46775 = CARTESIAN_POINT ( 'NONE',  ( -0.05219959533907301413, -21.53943276465977519, 107.4989096053143669 ) ) ;
#46777 = CARTESIAN_POINT ( 'NONE',  ( 21.52544592524344225, -5.823673210054117533, 68.54057627198103830 ) ) ;
#46776 = FACE_OUTER_BOUND ( 'NONE', #71687, .T. ) ;
#46778 = CARTESIAN_POINT ( 'NONE',  ( 0.05219959533909260263, 19.03943276465977164, 74.99890960531435269 ) ) ;
#46779 = CARTESIAN_POINT ( 'NONE',  ( -8.314922557960811034, -14.29746914071050412, 52.08224293864768839 ) ) ;
#46780 = CARTESIAN_POINT ( 'NONE',  ( -5.153800228976328057, -19.02544592524343514, 87.29057627198103830 ) ) ;
#46781 = DIRECTION ( 'NONE',  ( 0.000000000000000000, 0.000000000000000000, -1.000000000000000000 ) ) ;
#46782 = CARTESIAN_POINT ( 'NONE',  ( 9.474510206698729675, 16.51473224551082808, 52.08442372801900433 ) ) ;
#46783 = CARTESIAN_POINT ( 'NONE',  ( -18.62759615963270932, 10.81492255796079327, 95.83224293864770971 ) ) ;
#46784 = CARTESIAN_POINT ( 'NONE',  ( -12.14591786802309592, -12.06949235617757132, 101.8739096053143811 ) ) ;
#46785 = CARTESIAN_POINT ( 'NONE',  ( 18.67979575497194134, -10.72451020669871369, 50.83442372801901143 ) ) ;
#46786 = CARTESIAN_POINT ( 'NONE',  ( -5.359611314223446995E-15, 29.16686587814335496, 148.3750000027311842 ) ) ;
#46787 = CARTESIAN_POINT ( 'NONE',  ( 14.34966873604960469, 8.224510206698951720, 29.16557627198103120 ) ) ;
#46788 = CARTESIAN_POINT ( 'NONE',  ( 16.51473224551069308, 9.474510206698969483, 39.16557627198103120 ) ) ;
#46789 = CARTESIAN_POINT ( 'NONE',  ( 13.97604488694527802, 13.89961937509977652, 94.37390960531436690 ) ) ;
#46790 = CARTESIAN_POINT ( 'NONE',  ( 10.81492255796078972, 18.62759615963270932, 54.58224293864769550 ) ) ;
#46791 = CARTESIAN_POINT ( 'NONE',  ( 5.049401038297881783, 19.05341960407617918, 92.29275706135234714 ) ) ;
#46792 = CARTESIAN_POINT ( 'NONE',  ( 5.153800228976335163, 19.02544592524342804, 34.79057627198102409 ) ) ;
#46793 = CARTESIAN_POINT ( 'NONE',  ( 21.55341960407610458, 5.719274019375980345, 53.95724293864770260 ) ) ;
#46794 = CARTESIAN_POINT ( 'NONE',  ( -21.53943276465977519, -0.05219959533937600094, 68.75109039468568994 ) ) ;
#46796 = CARTESIAN_POINT ( 'NONE',  ( 0.05219959533934541429, -16.53943276465976808, 85.00109039468568994 ) ) ;
#46795 = CARTESIAN_POINT ( 'NONE',  ( 16.63682861930254120, -37.51503513662888878, -19.06746308534681233 ) ) ;
#46797 = CARTESIAN_POINT ( 'NONE',  ( -5.153800228976328057, -19.02544592524343514, 52.29057627198100988 ) ) ;
#46798 = CARTESIAN_POINT ( 'NONE',  ( -5.049401038298153566, 19.05341960407611168, 60.20724293864768129 ) ) ;
#46799 = ORIENTED_EDGE ( 'NONE', *, *, #148993, .F. ) ;
#46800 = CARTESIAN_POINT ( 'NONE',  ( -5.153800228976607833, 19.02544592524334988, 32.70942372801899722 ) ) ;
#46801 = CARTESIAN_POINT ( 'NONE',  ( -12.14591786802326823, 12.06949235617739902, 73.12609039468567573 ) ) ;
#46802 = CARTESIAN_POINT ( 'NONE',  ( -21.55341960407619339, 5.719274019375674811, 98.54275706135234714 ) ) ;
#46803 = CARTESIAN_POINT ( 'NONE',  ( -16.46253265017160317, 9.564922557960807481, 70.83224293864770971 ) ) ;
#46804 = CARTESIAN_POINT ( 'NONE',  ( 10.72451020669898902, -18.67979575497178502, 32.91557627198102409 ) ) ;
#46805 = CARTESIAN_POINT ( 'NONE',  ( -13.89961937509957401, -13.97604488694547875, 104.3760903946856757 ) ) ;
#46806 = CARTESIAN_POINT ( 'NONE',  ( 15.72974639402176855, 15.80617190586768217, 81.87609039468568994 ) ) ;
#46807 = CARTESIAN_POINT ( 'NONE',  ( 16.52544592524335698, 4.483927247898782831, 46.45942372801901854 ) ) ;
#46808 = CARTESIAN_POINT ( 'NONE',  ( -15.72974639402197994, 15.80617190586746368, 95.62390960531436690 ) ) ;
#46809 = CARTESIAN_POINT ( 'NONE',  ( -5.153800228976607833, 19.02544592524334988, 107.7094237280189759 ) ) ;
#46810 = CARTESIAN_POINT ( 'NONE',  ( 9.564922557960805705, 16.46253265017160317, 79.58224293864769550 ) ) ;
#46811 = CARTESIAN_POINT ( 'NONE',  ( -14.29746914071037622, -8.314922557961029526, 34.16775706135234714 ) ) ;
#46812 = CARTESIAN_POINT ( 'NONE',  ( 13.97604488694527802, 13.89961937509977652, 39.37390960531435269 ) ) ;
#46813 = CARTESIAN_POINT ( 'NONE',  ( 16.51473224551083163, -9.474510206698727899, 110.8344237280190043 ) ) ;
#46814 = CARTESIAN_POINT ( 'NONE',  ( 12.14591786802309770, 12.06949235617756955, 84.37390960531438111 ) ) ;
#46815 = CARTESIAN_POINT ( 'NONE',  ( 16.52544592524335698, 4.483927247898782831, 86.45942372801901854 ) ) ;
#46817 = CARTESIAN_POINT ( 'NONE',  ( -16.46253265017160317, 9.564922557960807481, 55.83224293864769550 ) ) ;
#46816 = CARTESIAN_POINT ( 'NONE',  ( 21.53943276465977519, 0.05219959533937863772, 36.25109039468567573 ) ) ;
#46818 = CARTESIAN_POINT ( 'NONE',  ( -19.03943276465977164, 0.05219959533909376836, 66.24890960531436690 ) ) ;
#46819 = CARTESIAN_POINT ( 'NONE',  ( 16.55341960407618274, -4.379528057220086978, 91.04275706135236135 ) ) ;
#46820 = CIRCLE ( 'NONE', #37139, 2.649999999999999467 ) ;
#46821 = CARTESIAN_POINT ( 'NONE',  ( -24.24393946302878078, -5.863316274098051117, 172.4343578713344982 ) ) ;
#46822 = VERTEX_POINT ( 'NONE', #55986 ) ;
#46823 = CARTESIAN_POINT ( 'NONE',  ( 16.51473224551083163, -9.474510206698727899, 20.83442372801899722 ) ) ;
#46824 = CARTESIAN_POINT ( 'NONE',  ( -19.05341960407611168, -5.049401038298163336, 41.45724293864769550 ) ) ;
#46826 = ORIENTED_EDGE ( 'NONE', *, *, #149391, .F. ) ;
#46825 = CARTESIAN_POINT ( 'NONE',  ( 16.51473224551069308, 9.474510206698969483, 109.1655762719810383 ) ) ;
#46827 = CARTESIAN_POINT ( 'NONE',  ( -14.29746914071037622, -8.314922557961029526, 34.16775706135234714 ) ) ;
#46829 = CARTESIAN_POINT ( 'NONE',  ( 12.14591786802327356, -12.06949235617739191, 40.62609039468567573 ) ) ;
#46828 = CARTESIAN_POINT ( 'NONE',  ( -16.51473224551082808, 9.474510206698731452, 63.33442372801900433 ) ) ;
#46830 = CARTESIAN_POINT ( 'NONE',  ( 19.03943276465977164, -0.05219959533909143690, 43.74890960531435979 ) ) ;
#46831 = CARTESIAN_POINT ( 'NONE',  ( 16.46253265017160672, -9.564922557960803928, 103.3322429386476955 ) ) ;
#46832 = CARTESIAN_POINT ( 'NONE',  ( 5.049401038298161559, -19.05341960407611168, 67.70724293864769550 ) ) ;
#46833 = CARTESIAN_POINT ( 'NONE',  ( 5.823673210054125526, 21.52544592524343514, 99.79057627198103830 ) ) ;
#46835 = PLANE ( 'NONE',  #153741 ) ;
#46834 = CARTESIAN_POINT ( 'NONE',  ( -0.05219959533909027116, -19.03943276465977164, 92.49890960531436690 ) ) ;
#46836 = CARTESIAN_POINT ( 'NONE',  ( 0.05219959533909260263, 19.03943276465977164, 59.99890960531436690 ) ) ;
#46838 = CARTESIAN_POINT ( 'NONE',  ( 16.46253265017160672, -9.564922557960803928, 28.33224293864769550 ) ) ;
#46837 = CARTESIAN_POINT ( 'NONE',  ( -12.14591786802326823, 12.06949235617739902, 108.1260903946856757 ) ) ;
#46839 = CARTESIAN_POINT ( 'NONE',  ( -19.05341960407617563, 5.049401038297882671, 23.54275706135233648 ) ) ;
#46840 = VECTOR ( 'NONE', #189925, 1000.000000000000000 ) ;
#46841 = CARTESIAN_POINT ( 'NONE',  ( -14.34966873604960291, -8.224510206698953496, 61.66557627198103120 ) ) ;
#46842 = CARTESIAN_POINT ( 'NONE',  ( 21.52544592524334988, 5.823673210054432836, 101.4594237280190185 ) ) ;
#46843 = CARTESIAN_POINT ( 'NONE',  ( -9.564922557960796823, -16.46253265017161027, 37.08224293864768839 ) ) ;
#46845 = CARTESIAN_POINT ( 'NONE',  ( 21.53943276465977519, 0.05219959533937863772, 96.25109039468568994 ) ) ;
#46844 = CARTESIAN_POINT ( 'NONE',  ( 14.29746914071049879, -8.314922557960816363, 43.33224293864769550 ) ) ;
#46846 = CARTESIAN_POINT ( 'NONE',  ( 19.03943276465977164, -0.05219959533909143690, 83.74890960531436690 ) ) ;
#46847 = CARTESIAN_POINT ( 'NONE',  ( -9.474510206698964154, 16.51473224551069663, 90.41557627198103830 ) ) ;
#46848 = CARTESIAN_POINT ( 'NONE',  ( -14.34966873604960291, -8.224510206698953496, 111.6655762719810525 ) ) ;
#46849 = CARTESIAN_POINT ( 'NONE',  ( 16.55341960407611168, 4.379528057220329451, 73.95724293864769550 ) ) ;
#46850 = CARTESIAN_POINT ( 'NONE',  ( 10.72451020669898902, -18.67979575497178502, 87.91557627198103830 ) ) ;
#46851 = CARTESIAN_POINT ( 'NONE',  ( 13.97604488694527802, 13.89961937509977652, 69.37390960531436690 ) ) ;
#46852 = CARTESIAN_POINT ( 'NONE',  ( 10.72451020669898902, -18.67979575497178502, 82.91557627198103830 ) ) ;
#46853 = PRESENTATION_LAYER_ASSIGNMENT (  '', '', ( #88862 ) ) ;
#46854 = CARTESIAN_POINT ( 'NONE',  ( -16.46253265017146816, -9.564922557961047289, 79.16775706135234714 ) ) ;
#46856 = CARTESIAN_POINT ( 'NONE',  ( -4.483927247898539470, -16.52544592524342804, 87.29057627198103830 ) ) ;
#46855 = CARTESIAN_POINT ( 'NONE',  ( 5.153800228976617603, -19.02544592524335343, 65.20942372801899012 ) ) ;
#46857 = CARTESIAN_POINT ( 'NONE',  ( 19.05341960407611168, 5.049401038298154454, 63.95724293864769550 ) ) ;
#46858 = CARTESIAN_POINT ( 'NONE',  ( 0.05219959533907565091, 21.53943276465977519, 64.99890960531435269 ) ) ;
#46859 = CARTESIAN_POINT ( 'NONE',  ( -17.60691670004652565, -5.499999999999996447, 84.13333313366439370 ) ) ;
#46860 = CARTESIAN_POINT ( 'NONE',  ( 4.379528057220092307, 16.55341960407617563, 112.2927570613523471 ) ) ;
#46861 = CARTESIAN_POINT ( 'NONE',  ( 4.483927247898790824, -16.52544592524335698, 25.20942372801901854 ) ) ;
#46862 = CARTESIAN_POINT ( 'NONE',  ( 0.05219959533910956823, 16.53943276465976808, 74.99890960531435269 ) ) ;
#46863 = CARTESIAN_POINT ( 'NONE',  ( -18.89770734986048950, -5.499999999999954703, 94.10214472496637939 ) ) ;
#46864 = CARTESIAN_POINT ( 'NONE',  ( -13.97604488694527625, -13.89961937509977652, 76.87390960531433848 ) ) ;
#46865 = CARTESIAN_POINT ( 'NONE',  ( -9.474510206698964154, 16.51473224551069663, 30.41557627198102054 ) ) ;
#46866 = CARTESIAN_POINT ( 'NONE',  ( 16.52544592524342804, -4.483927247898539470, 68.54057627198103830 ) ) ;
#46867 = CARTESIAN_POINT ( 'NONE',  ( -5.153800228976328057, -19.02544592524343514, 112.2905762719810099 ) ) ;
#46869 = CARTESIAN_POINT ( 'NONE',  ( -13.89961937509977652, 13.97604488694528158, 80.62390960531436690 ) ) ;
#46868 = CARTESIAN_POINT ( 'NONE',  ( 19.03943276465977164, 0.05219959533936151252, 86.25109039468567573 ) ) ;
#46870 = TOROIDAL_SURFACE ( 'NONE', #156560, 2.700000000000000622, 0.2000000000000000111 ) ;
#46871 = CARTESIAN_POINT ( 'NONE',  ( 0.05219959533909260263, 19.03943276465977164, 89.99890960531436690 ) ) ;
#46872 = CARTESIAN_POINT ( 'NONE',  ( -15.80617190586745835, -15.72974639402198527, 76.87390960531439532 ) ) ;
#46873 = CARTESIAN_POINT ( 'NONE',  ( -8.224510206698735004, -14.34966873604973081, 69.58442372801900433 ) ) ;
#46874 = CARTESIAN_POINT ( 'NONE',  ( -19.03943276465977164, 0.05219959533909376836, 56.24890960531435979 ) ) ;
#46875 = CARTESIAN_POINT ( 'NONE',  ( 21.53943276465977519, -0.05219959533907433946, 68.74890960531435269 ) ) ;
#46876 = CARTESIAN_POINT ( 'NONE',  ( -21.52544592524334988, -5.823673210054445271, 73.95942372801901854 ) ) ;
#46877 = CARTESIAN_POINT ( 'NONE',  ( 19.05341960407617918, -5.049401038297876454, 91.04275706135234714 ) ) ;
#46879 = CARTESIAN_POINT ( 'NONE',  ( 10.81492255796106328, -18.62759615963255655, 40.41775706135234714 ) ) ;
#46878 = CARTESIAN_POINT ( 'NONE',  ( -4.483927247898539470, -16.52544592524342804, 42.29057627198103120 ) ) ;
#46880 = DIRECTION ( 'NONE',  ( 0.000000000000000000, -0.1045284632676537068, 0.9945218953682734009 ) ) ;
#46882 = CARTESIAN_POINT ( 'NONE',  ( -16.51473224551069308, -9.474510206698971260, 106.6655762719810383 ) ) ;
#46881 = CARTESIAN_POINT ( 'NONE',  ( 12.06949235617739724, 12.14591786802326823, 71.87609039468568994 ) ) ;
#46883 = CARTESIAN_POINT ( 'NONE',  ( 5.000000000000000000, -139.5000000000000000, 13.35010376910484098 ) ) ;
#46884 = DIRECTION ( 'NONE',  ( -1.000000000000000000, -0.000000000000000000, -0.000000000000000000 ) ) ;
#46885 = CARTESIAN_POINT ( 'NONE',  ( 0.05219959533934541429, -16.53943276465976808, 90.00109039468567573 ) ) ;
#46886 = CARTESIAN_POINT ( 'NONE',  ( -12.06949235617739369, -12.14591786802326823, 49.37609039468569705 ) ) ;
#46887 = CARTESIAN_POINT ( 'NONE',  ( -19.05341960407611168, -5.049401038298163336, 61.45724293864769550 ) ) ;
#46888 = CARTESIAN_POINT ( 'NONE',  ( 9.474510206698971260, -16.51473224551069308, 77.91557627198103830 ) ) ;
#46889 = CARTESIAN_POINT ( 'NONE',  ( -5.719274019375665041, -21.55341960407619695, 59.79275706135234714 ) ) ;
#46890 = CARTESIAN_POINT ( 'NONE',  ( -12.06949235617739369, -12.14591786802326823, 64.37609039468568994 ) ) ;
#46891 = CARTESIAN_POINT ( 'NONE',  ( -12.14591786802309592, -12.06949235617757132, 26.87390960531435979 ) ) ;
#46892 = CARTESIAN_POINT ( 'NONE',  ( -9.564922557960796823, -16.46253265017161027, 37.08224293864768839 ) ) ;
#46893 = CARTESIAN_POINT ( 'NONE',  ( 5.153800228976335163, 19.02544592524342804, 29.79057627198102409 ) ) ;
#46895 = ADVANCED_FACE ( 'NONE', ( #22658 ), #40822, .T. ) ;
#46894 = CARTESIAN_POINT ( 'NONE',  ( -16.52544592524335698, -4.483927247898792601, 23.95942372801901143 ) ) ;
#46896 = CARTESIAN_POINT ( 'NONE',  ( -13.97604488694547697, 13.89961937509957934, 83.12609039468564731 ) ) ;
#46897 = CARTESIAN_POINT ( 'NONE',  ( 4.379528057220339221, -16.55341960407611168, 82.70724293864770971 ) ) ;
#46898 = CARTESIAN_POINT ( 'NONE',  ( -9.474510206698964154, 16.51473224551069663, 45.41557627198103120 ) ) ;
#46900 = CARTESIAN_POINT ( 'NONE',  ( 1.988064558232696151E-15, -30.27659582821216588, 148.4843446568999923 ) ) ;
#46899 = CARTESIAN_POINT ( 'NONE',  ( 16.51473224551083163, -9.474510206698727899, 90.83442372801900433 ) ) ;
#46901 = CARTESIAN_POINT ( 'NONE',  ( -21.55341960407619339, 5.719274019375674811, 93.54275706135234714 ) ) ;
#46902 = CARTESIAN_POINT ( 'NONE',  ( -4.483927247898782831, 16.52544592524335698, 47.70942372801902565 ) ) ;
#46903 = CARTESIAN_POINT ( 'NONE',  ( 16.62475595723696387, 7.163666690055258357, 36.97286648189536606 ) ) ;
#46904 = CARTESIAN_POINT ( 'NONE',  ( -15.72974639402197994, 15.80617190586746368, 50.62390960531435979 ) ) ;
#46905 = CARTESIAN_POINT ( 'NONE',  ( -0.05219959533934338120, 16.53943276465976808, 42.50109039468567573 ) ) ;
#46906 = CARTESIAN_POINT ( 'NONE',  ( 13.97604488694527802, 13.89961937509977830, 34.37390960531435979 ) ) ;
#46907 = CARTESIAN_POINT ( 'NONE',  ( -13.97604488694547697, 13.89961937509957934, 48.12609039468566863 ) ) ;
#46908 = CARTESIAN_POINT ( 'NONE',  ( 16.46253265017160672, -9.564922557960803928, 83.33224293864768129 ) ) ;
#46909 = CARTESIAN_POINT ( 'NONE',  ( -13.97604488694527625, -13.89961937509977652, 51.87390960531436690 ) ) ;
#46910 = VECTOR ( 'NONE', #84540, 1000.000000000000000 ) ;
#46911 = CARTESIAN_POINT ( 'NONE',  ( 17.18269478283314911, 17.18269478283310647, -54.21489346206828230 ) ) ;
#46912 = CARTESIAN_POINT ( 'NONE',  ( 19.05341960407611168, 5.049401038298154454, 63.95724293864769550 ) ) ;
#46913 = DIRECTION ( 'NONE',  ( -0.000000000000000000, -0.000000000000000000, 1.000000000000000000 ) ) ;
#46914 = CARTESIAN_POINT ( 'NONE',  ( -9.564922557961040184, 16.46253265017147172, 37.91775706135233293 ) ) ;
#46915 = CARTESIAN_POINT ( 'NONE',  ( 0.05219959533937995610, -21.53943276465977519, 105.0010903946856757 ) ) ;
#46916 = CARTESIAN_POINT ( 'NONE',  ( 0.05219959533910956823, 16.53943276465976808, 39.99890960531436690 ) ) ;
#46917 = CARTESIAN_POINT ( 'NONE',  ( -9.564922557960796823, -16.46253265017161027, 47.08224293864769550 ) ) ;
#46918 = CARTESIAN_POINT ( 'NONE',  ( -19.02544592524342804, 5.153800228976336051, 111.0405762719810099 ) ) ;
#46919 = CARTESIAN_POINT ( 'NONE',  ( -15.72974639402176322, -15.80617190586768395, 79.37609039468567573 ) ) ;
#46920 = CARTESIAN_POINT ( 'NONE',  ( -19.02544592524342804, 5.153800228976336051, 51.04057627198103120 ) ) ;
#46921 = CARTESIAN_POINT ( 'NONE',  ( 10.81492255796106328, -18.62759615963255655, 85.41775706135236135 ) ) ;
#46922 = CARTESIAN_POINT ( 'NONE',  ( -15.72974639402197994, 15.80617190586746368, 35.62390960531437401 ) ) ;
#46923 = CARTESIAN_POINT ( 'NONE',  ( -0.05219959533937732626, 21.53943276465977519, 22.50109039468567573 ) ) ;
#46924 = CARTESIAN_POINT ( 'NONE',  ( -19.05341960407617563, 5.049401038297882671, 48.54275706135233293 ) ) ;
#46925 = CARTESIAN_POINT ( 'NONE',  ( 9.564922557960805705, 16.46253265017160317, 34.58224293864770260 ) ) ;
#46926 = CARTESIAN_POINT ( 'NONE',  ( -9.564922557960796823, -16.46253265017161027, 77.08224293864769550 ) ) ;
#46927 = CARTESIAN_POINT ( 'NONE',  ( 13.89961937509957401, 13.97604488694547697, 111.8760903946856757 ) ) ;
#46928 = CARTESIAN_POINT ( 'NONE',  ( -4.483927247898539470, -16.52544592524342804, 87.29057627198103830 ) ) ;
#46929 = CARTESIAN_POINT ( 'NONE',  ( -13.97604488694527625, -13.89961937509977652, 51.87390960531436690 ) ) ;
#46930 = CARTESIAN_POINT ( 'NONE',  ( -5.823673210054116645, -21.52544592524344225, 32.29057627198102409 ) ) ;
#46931 = CARTESIAN_POINT ( 'NONE',  ( 19.05341960407617918, -5.049401038297876454, 96.04275706135231871 ) ) ;
#46932 = CARTESIAN_POINT ( 'NONE',  ( 5.823673210054125526, 21.52544592524343514, 99.79057627198103830 ) ) ;
#46933 = CARTESIAN_POINT ( 'NONE',  ( 15.72974639402176855, 15.80617190586768217, 61.87609039468568284 ) ) ;
#46934 = CARTESIAN_POINT ( 'NONE',  ( 0.05219959533934541429, -16.53943276465976808, 60.00109039468568284 ) ) ;
#46935 = CARTESIAN_POINT ( 'NONE',  ( 8.314922557961029526, -14.29746914071037800, 70.41775706135236135 ) ) ;
#46936 = CARTESIAN_POINT ( 'NONE',  ( 9.564922557960805705, 16.46253265017160317, 64.58224293864769550 ) ) ;
#46937 = CARTESIAN_POINT ( 'NONE',  ( -0.05219959533934338120, 16.53943276465976808, 92.50109039468567573 ) ) ;
#46938 = CARTESIAN_POINT ( 'NONE',  ( -21.53943276465977519, 0.05219959533907696930, 111.2489096053143669 ) ) ;
#46939 = CARTESIAN_POINT ( 'NONE',  ( -14.34966873604960291, -8.224510206698953496, 71.66557627198100988 ) ) ;
#46940 = CARTESIAN_POINT ( 'NONE',  ( 19.03943276465977164, -0.05219959533909143690, 83.74890960531436690 ) ) ;
#46941 = CARTESIAN_POINT ( 'NONE',  ( 12.14591786802327356, -12.06949235617739191, 70.62609039468567573 ) ) ;
#46942 = CARTESIAN_POINT ( 'NONE',  ( 15.72974639402176855, 15.80617190586768217, 61.87609039468568284 ) ) ;
#46943 = CARTESIAN_POINT ( 'NONE',  ( -9.474510206698720793, -16.51473224551083518, 109.5844237280190043 ) ) ;
#46944 = CARTESIAN_POINT ( 'NONE',  ( -15.72974639402197994, 15.80617190586746368, 110.6239096053143669 ) ) ;
#46945 = CARTESIAN_POINT ( 'NONE',  ( 8.224510206698953496, -14.34966873604960469, 62.91557627198102409 ) ) ;
#46946 = ORIENTED_EDGE ( 'NONE', *, *, #137445, .F. ) ;
#46947 = CARTESIAN_POINT ( 'NONE',  ( -17.49999999999999645, 5.499999999999992895, 68.71769037696435589 ) ) ;
#46948 = CARTESIAN_POINT ( 'NONE',  ( 21.52544592524344225, -5.823673210054117533, 83.54057627198102409 ) ) ;
#46949 = CARTESIAN_POINT ( 'NONE',  ( -14.29746914071049879, 8.314922557960819915, 45.83224293864769550 ) ) ;
#46950 = ORIENTED_EDGE ( 'NONE', *, *, #6641, .T. ) ;
#46951 = CARTESIAN_POINT ( 'NONE',  ( 35.69940131823276630, 0.4911691522782191677, 37.51200899188186355 ) ) ;
#46952 = CARTESIAN_POINT ( 'NONE',  ( 21.52544592524334988, 5.823673210054432836, 21.45942372801901499 ) ) ;
#46953 = VECTOR ( 'NONE', #7393, 1000.000000000000000 ) ;
#46954 = CARTESIAN_POINT ( 'NONE',  ( -21.55341960407610458, -5.719274019375992779, 21.45724293864769550 ) ) ;
#46955 = CARTESIAN_POINT ( 'NONE',  ( -15.80617190586768217, 15.72974639402176855, 23.12609039468567573 ) ) ;
#46956 = CARTESIAN_POINT ( 'NONE',  ( 14.29746914071049879, -8.314922557960816363, 53.33224293864769550 ) ) ;
#46957 = CARTESIAN_POINT ( 'NONE',  ( 0.05219959533934541429, -16.53943276465976808, 65.00109039468568994 ) ) ;
#46958 = CARTESIAN_POINT ( 'NONE',  ( 19.03943276465977164, -0.05219959533909143690, 58.74890960531435979 ) ) ;
#46959 = CARTESIAN_POINT ( 'NONE',  ( -13.89961937509957401, -13.97604488694547875, 64.37609039468567573 ) ) ;
#46960 = CARTESIAN_POINT ( 'NONE',  ( 0.05219959533909260263, 19.03943276465977164, 74.99890960531435269 ) ) ;
#46961 = CARTESIAN_POINT ( 'NONE',  ( 5.823673210054125526, 21.52544592524343514, 34.79057627198103120 ) ) ;
#46962 = CARTESIAN_POINT ( 'NONE',  ( -18.60204571914025706, -35.35091242066509665, -18.26754506500681430 ) ) ;
#46963 = CARTESIAN_POINT ( 'NONE',  ( 16.51473224551069308, 9.474510206698969483, 59.16557627198102409 ) ) ;
#46964 = CARTESIAN_POINT ( 'NONE',  ( -16.53943276465976808, -0.05219959533934237506, 28.75109039468567929 ) ) ;
#46965 = CARTESIAN_POINT ( 'NONE',  ( 9.564922557961047289, -16.46253265017146816, 65.41775706135233293 ) ) ;
#46966 = CARTESIAN_POINT ( 'NONE',  ( -21.53943276465977519, -0.05219959533937600094, 23.75109039468567929 ) ) ;
#46967 = CARTESIAN_POINT ( 'NONE',  ( 16.52544592524342804, -4.483927247898539470, 28.54057627198103120 ) ) ;
#46968 = CARTESIAN_POINT ( 'NONE',  ( 16.51473224551069308, 9.474510206698969483, 89.16557627198103830 ) ) ;
#46969 = CARTESIAN_POINT ( 'NONE',  ( -21.55341960407610458, -5.719274019375992779, 61.45724293864770260 ) ) ;
#46971 = CARTESIAN_POINT ( 'NONE',  ( 0.05219959533934541429, -16.53943276465976808, 35.00109039468568284 ) ) ;
#46970 = CARTESIAN_POINT ( 'NONE',  ( -15.80617190586745835, -15.72974639402198527, 91.87390960531436690 ) ) ;
#46972 = CARTESIAN_POINT ( 'NONE',  ( 0.05219959533907565091, 21.53943276465977519, 39.99890960531436690 ) ) ;
#46973 = CARTESIAN_POINT ( 'NONE',  ( -18.62759615963255300, -10.81492255796106328, 89.16775706135236135 ) ) ;
#46974 = CARTESIAN_POINT ( 'NONE',  ( -5.153800228976328057, -19.02544592524343514, 82.29057627198103830 ) ) ;
#46975 = CARTESIAN_POINT ( 'NONE',  ( -9.474510206698964154, 16.51473224551069663, 45.41557627198103120 ) ) ;
#46976 = CARTESIAN_POINT ( 'NONE',  ( -9.474510206698964154, 16.51473224551069663, 95.41557627198102409 ) ) ;
#46977 = CARTESIAN_POINT ( 'NONE',  ( -16.55341960407611168, -4.379528057220339221, 101.4572429386476955 ) ) ;
#46978 = CARTESIAN_POINT ( 'NONE',  ( 19.05341960407611168, 5.049401038298154454, 58.95724293864768129 ) ) ;
#46979 = CARTESIAN_POINT ( 'NONE',  ( -4.379528057220086978, -16.55341960407618274, 24.79275706135235779 ) ) ;
#46980 = CARTESIAN_POINT ( 'NONE',  ( 17.50000000000001066, 3.345213924137313555, 32.91231376905654571 ) ) ;
#46982 = CARTESIAN_POINT ( 'NONE',  ( 5.153800228976335163, 19.02544592524342804, 109.7905762719810099 ) ) ;
#46981 = CARTESIAN_POINT ( 'NONE',  ( 21.52544592524334988, 5.823673210054432836, 101.4594237280190185 ) ) ;
#46983 = B_SPLINE_CURVE_WITH_KNOTS ( 'NONE', 3,
 ( #100339, #194373, #39668, #131685, #180216, #42681 ),
 .UNSPECIFIED., .F., .F.,
 ( 4, 2, 4 ),
 ( 0.003239945802372296794, 0.003620412082092151589, 0.004000878361812006817 ),
 .UNSPECIFIED. ) ;
#46984 = CARTESIAN_POINT ( 'NONE',  ( 14.34966873604972726, -8.224510206698740333, 95.83442372801903275 ) ) ;
#46985 = PLANE ( 'NONE',  #129321 ) ;
#46986 = CARTESIAN_POINT ( 'NONE',  ( -19.03943276465977164, -0.05219959533935918106, 68.75109039468566152 ) ) ;
#46987 = CARTESIAN_POINT ( 'NONE',  ( 13.97604488694548053, -13.89961937509957401, 25.62609039468566507 ) ) ;
#46988 = CARTESIAN_POINT ( 'NONE',  ( 3.915140329348349990, 5.773271879485236013, -64.38756054665736883 ) ) ;
#46989 = CARTESIAN_POINT ( 'NONE',  ( -13.89961937509977652, 13.97604488694528158, 25.62390960531434558 ) ) ;
#46990 = CARTESIAN_POINT ( 'NONE',  ( -4.483927247898539470, -16.52544592524342804, 32.29057627198102409 ) ) ;
#46991 = CARTESIAN_POINT ( 'NONE',  ( -17.26172910966780094, -6.454744622555835143, 109.1935309135077716 ) ) ;
#46992 = CARTESIAN_POINT ( 'NONE',  ( -16.55341960407617563, 4.379528057220093196, 113.5427570613523756 ) ) ;
#46993 = CARTESIAN_POINT ( 'NONE',  ( 17.40805194822030444, 6.112264579159358391, 66.66628727489390371 ) ) ;
#46994 = CARTESIAN_POINT ( 'NONE',  ( 12.06949235617739724, 12.14591786802326823, 91.87609039468568994 ) ) ;
#46995 = CARTESIAN_POINT ( 'NONE',  ( -5.153800228976328057, -19.02544592524343514, 32.29057627198102409 ) ) ;
#46996 = CARTESIAN_POINT ( 'NONE',  ( 15.80617190586769283, -15.72974639402175789, 105.6260903946856899 ) ) ;
#46997 = CARTESIAN_POINT ( 'NONE',  ( 16.55341960407618274, -4.379528057220086978, 21.04275706135234714 ) ) ;
#46998 = CARTESIAN_POINT ( 'NONE',  ( 5.719274019375673035, 21.55341960407619339, 72.29275706135236135 ) ) ;
#46999 = CARTESIAN_POINT ( 'NONE',  ( -16.46253265017146816, -9.564922557961047289, 49.16775706135233293 ) ) ;
#47000 = CARTESIAN_POINT ( 'NONE',  ( 13.89961937509977652, -13.97604488694527269, 98.12390960531433848 ) ) ;
#47001 = CARTESIAN_POINT ( 'NONE',  ( -19.02544592524342804, 5.153800228976336051, 71.04057627198099567 ) ) ;
#47002 = CARTESIAN_POINT ( 'NONE',  ( 17.26172910966777962, 6.454744622555869782, 71.69353091350775742 ) ) ;
#47003 = CARTESIAN_POINT ( 'NONE',  ( 5.823673210054125526, 21.52544592524343514, 94.79057627198105251 ) ) ;
#47004 = AXIS2_PLACEMENT_3D ( 'NONE', #175896, #34395, #67705 ) ;
#47005 = CARTESIAN_POINT ( 'NONE',  ( -8.224510206698948167, 14.34966873604960824, 60.41557627198102409 ) ) ;
#47006 = CARTESIAN_POINT ( 'NONE',  ( 15.80617190586746368, 15.72974639402197994, 59.37390960531436690 ) ) ;
#47007 = CARTESIAN_POINT ( 'NONE',  ( 9.474510206698971260, -16.51473224551069308, 57.91557627198103120 ) ) ;
#47009 = CARTESIAN_POINT ( 'NONE',  ( -16.55341960407617563, 4.379528057220093196, 78.54275706135236135 ) ) ;
#47008 = CARTESIAN_POINT ( 'NONE',  ( 18.62759615963271287, -10.81492255796078972, 88.33224293864769550 ) ) ;
#47010 = ORIENTED_EDGE ( 'NONE', *, *, #56442, .T. ) ;
#47011 = CARTESIAN_POINT ( 'NONE',  ( -19.03943276465977164, 0.05219959533909376836, 41.24890960531435269 ) ) ;
#47013 = CARTESIAN_POINT ( 'NONE',  ( 21.96434091948367850, -6.687777057363585520, 170.9277123045938822 ) ) ;
#47012 = CARTESIAN_POINT ( 'NONE',  ( -8.314922557960811034, -14.29746914071050412, 82.08224293864768129 ) ) ;
#47014 = CARTESIAN_POINT ( 'NONE',  ( 16.51473224551069308, 9.474510206698969483, 49.16557627198102409 ) ) ;
#47015 = CARTESIAN_POINT ( 'NONE',  ( 14.29746914071049879, -8.314922557960816363, 113.3322429386476955 ) ) ;
#47016 = CARTESIAN_POINT ( 'NONE',  ( 19.05341960407617918, -5.049401038297876454, 61.04275706135232582 ) ) ;
#47017 = CARTESIAN_POINT ( 'NONE',  ( -16.52544592524342804, 4.483927247898546575, 81.04057627198102409 ) ) ;
#47018 = CARTESIAN_POINT ( 'NONE',  ( -15.72974639402176322, -15.80617190586768395, 44.37609039468567573 ) ) ;
#47020 = CARTESIAN_POINT ( 'NONE',  ( -10.81492255796078084, -18.62759615963271287, 102.0822429386476955 ) ) ;
#47019 = CARTESIAN_POINT ( 'NONE',  ( 9.474510206698971260, -16.51473224551069308, 37.91557627198102409 ) ) ;
#47021 = CARTESIAN_POINT ( 'NONE',  ( 14.29746914071049879, -8.314922557960816363, 83.33224293864769550 ) ) ;
#47022 = CARTESIAN_POINT ( 'NONE',  ( 22.02428569922084023, -33.37003842005633203, -23.53509012974128112 ) ) ;
#47023 = CARTESIAN_POINT ( 'NONE',  ( 16.51473224551069308, 9.474510206698969483, 64.16557627198102409 ) ) ;
#47024 = AXIS2_PLACEMENT_3D ( 'NONE', #59478, #89832, #73686 ) ;
#47025 = FACE_OUTER_BOUND ( 'NONE', #152969, .T. ) ;
#47027 = CARTESIAN_POINT ( 'NONE',  ( -16.46253265017160317, 9.564922557960807481, 95.83224293864769550 ) ) ;
#47026 = CARTESIAN_POINT ( 'NONE',  ( -13.97604488694547697, 13.89961937509957934, 93.12609039468566152 ) ) ;
#47028 = CARTESIAN_POINT ( 'NONE',  ( 21.52544592524334988, 5.823673210054432836, 41.45942372801901143 ) ) ;
#47029 = CARTESIAN_POINT ( 'NONE',  ( 9.564922557960805705, 16.46253265017160317, 89.58224293864769550 ) ) ;
#47030 = CARTESIAN_POINT ( 'NONE',  ( 5.153800228976615827, -19.02544592524334988, 70.20942372801899012 ) ) ;
#47031 = CARTESIAN_POINT ( 'NONE',  ( 19.02544592524343514, -5.153800228976328945, 38.54057627198103120 ) ) ;
#47032 = ADVANCED_FACE ( 'NONE', ( #84305 ), #8485, .T. ) ;
#47033 = CARTESIAN_POINT ( 'NONE',  ( 16.52544592524342804, -4.483927247898539470, 73.54057627198102409 ) ) ;
#47034 = CARTESIAN_POINT ( 'NONE',  ( -14.34966873604960291, -8.224510206698953496, 71.66557627198100988 ) ) ;
#47035 = CARTESIAN_POINT ( 'NONE',  ( 19.02544592524343514, -5.153800228976328945, 88.54057627198102409 ) ) ;
#47036 = CARTESIAN_POINT ( 'NONE',  ( 10.81492255796078972, 18.62759615963270932, 104.5822429386477097 ) ) ;
#47037 = CARTESIAN_POINT ( 'NONE',  ( -19.02544592524342804, 5.153800228976336051, 91.04057627198100988 ) ) ;
#47038 = CARTESIAN_POINT ( 'NONE',  ( -13.97604488694547697, 13.89961937509957934, 33.12609039468566863 ) ) ;
#47041 = CARTESIAN_POINT ( 'NONE',  ( -16.53943276465976808, 0.05219959533911058130, 116.2489096053143669 ) ) ;
#47040 = CARTESIAN_POINT ( 'NONE',  ( -0.05219959533910754901, -16.53943276465976808, 27.49890960531435269 ) ) ;
#47039 = CARTESIAN_POINT ( 'NONE',  ( -16.46253265017160317, 9.564922557960807481, 35.83224293864768839 ) ) ;
#47042 = CARTESIAN_POINT ( 'NONE',  ( 16.51473224551083163, -9.474510206698727899, 105.8344237280190043 ) ) ;
#47043 = ORIENTED_EDGE ( 'NONE', *, *, #8188, .T. ) ;
#47044 = CARTESIAN_POINT ( 'NONE',  ( -0.05219959533937732626, 21.53943276465977519, 27.50109039468567929 ) ) ;
#47045 = CARTESIAN_POINT ( 'NONE',  ( -0.05219959533936034679, 19.03943276465977164, 72.50109039468566152 ) ) ;
#47046 = CARTESIAN_POINT ( 'NONE',  ( 16.55341960407611168, 4.379528057220329451, 28.95724293864769905 ) ) ;
#47047 = CARTESIAN_POINT ( 'NONE',  ( -21.53943276465977519, 0.05219959533907696930, 91.24890960531436690 ) ) ;
#47048 = CARTESIAN_POINT ( 'NONE',  ( -5.049401038298153566, 19.05341960407611168, 110.2072429386476671 ) ) ;
#47049 = CARTESIAN_POINT ( 'NONE',  ( 0.05219959533910956823, 16.53943276465976808, 64.99890960531435269 ) ) ;
#47050 = CARTESIAN_POINT ( 'NONE',  ( 13.89961937509977652, -13.97604488694527269, 23.12390960531436335 ) ) ;
#47051 = CARTESIAN_POINT ( 'NONE',  ( -19.05341960407617563, 5.049401038297882671, 23.54275706135233648 ) ) ;
#47052 = CARTESIAN_POINT ( 'NONE',  ( 4.483927247898790824, -16.52544592524335698, 85.20942372801901854 ) ) ;
#47053 = CARTESIAN_POINT ( 'NONE',  ( 0.05219959533934541429, -16.53943276465976808, 60.00109039468568284 ) ) ;
#47054 = CARTESIAN_POINT ( 'NONE',  ( 10.72451020669898902, -18.67979575497178502, 22.91557627198102765 ) ) ;
#47055 = CARTESIAN_POINT ( 'NONE',  ( -21.55341960407619339, 5.719274019375674811, 108.5427570613523756 ) ) ;
#47056 = CARTESIAN_POINT ( 'NONE',  ( 9.474510206698971260, -16.51473224551069308, 72.91557627198102409 ) ) ;
#47057 = CARTESIAN_POINT ( 'NONE',  ( 16.55341960407618274, -4.379528057220086978, 56.04275706135235424 ) ) ;
#47058 = CARTESIAN_POINT ( 'NONE',  ( 5.049401038298161559, -19.05341960407611168, 27.70724293864769550 ) ) ;
#47059 = CARTESIAN_POINT ( 'NONE',  ( -12.06949235617756955, 12.14591786802309770, 40.62390960531435269 ) ) ;
#47060 = CARTESIAN_POINT ( 'NONE',  ( -17.49999999999999289, 5.500000000000032863, 70.79690382534172954 ) ) ;
#47062 = CARTESIAN_POINT ( 'NONE',  ( 16.51473224551069308, 9.474510206698969483, 74.16557627198103830 ) ) ;
#47061 = CARTESIAN_POINT ( 'NONE',  ( -9.564922557960796823, -16.46253265017161027, 102.0822429386477097 ) ) ;
#47063 = CARTESIAN_POINT ( 'NONE',  ( -16.46253265017160317, 9.564922557960807481, 110.8322429386476955 ) ) ;
#47064 = CARTESIAN_POINT ( 'NONE',  ( -16.52544592524342804, 4.483927247898546575, 56.04057627198102409 ) ) ;
#47065 = CARTESIAN_POINT ( 'NONE',  ( -8.224510206698948167, 14.34966873604960824, 35.41557627198102409 ) ) ;
#47066 = CARTESIAN_POINT ( 'NONE',  ( 0.05219959533910956823, 16.53943276465976808, 49.99890960531437401 ) ) ;
#47068 = CARTESIAN_POINT ( 'NONE',  ( -18.09918380851992481, -5.500000000000040856, 56.48618307335612343 ) ) ;
#47067 = CARTESIAN_POINT ( 'NONE',  ( 8.314922557961029526, -14.29746914071037800, 45.41775706135234003 ) ) ;
#47069 = CARTESIAN_POINT ( 'NONE',  ( -0.05219959533936034679, 19.03943276465977164, 52.50109039468566863 ) ) ;
#47070 = CARTESIAN_POINT ( 'NONE',  ( -16.46253265017160317, 9.564922557960807481, 70.83224293864770971 ) ) ;
#47071 = CARTESIAN_POINT ( 'NONE',  ( -19.02544592524334988, -5.153800228976617603, 48.95942372801900433 ) ) ;
#47072 = CARTESIAN_POINT ( 'NONE',  ( 19.03943276465977164, 0.05219959533936151252, 56.25109039468566863 ) ) ;
#47074 = CARTESIAN_POINT ( 'NONE',  ( -14.34966873604972548, 8.224510206698743886, 88.33442372801901854 ) ) ;
#47073 = CARTESIAN_POINT ( 'NONE',  ( -13.89961937509957401, -13.97604488694547875, 94.37609039468566152 ) ) ;
#47075 = CARTESIAN_POINT ( 'NONE',  ( -27.73933785331498925, 9.013057229001089965, 143.2750000027311899 ) ) ;
#47076 = CARTESIAN_POINT ( 'NONE',  ( 16.51473224551069308, 9.474510206698969483, 24.16557627198102765 ) ) ;
#47077 = CARTESIAN_POINT ( 'NONE',  ( -0.05219959533909027116, -19.03943276465977164, 107.4989096053143527 ) ) ;
#47078 = CARTESIAN_POINT ( 'NONE',  ( 10.72451020669871369, 18.67979575497193778, 47.08442372801901854 ) ) ;
#47079 = CARTESIAN_POINT ( 'NONE',  ( 19.02544592524334988, 5.153800228976608722, 106.4594237280190185 ) ) ;
#47081 = CARTESIAN_POINT ( 'NONE',  ( -13.97604488694527625, -13.89961937509977652, 61.87390960531435979 ) ) ;
#47080 = CARTESIAN_POINT ( 'NONE',  ( 17.50000000000002132, -4.049696124445863354, 106.6803967066595078 ) ) ;
#47082 = CARTESIAN_POINT ( 'NONE',  ( -13.89961937509977652, 13.97604488694528158, 100.6239096053143669 ) ) ;
#47084 = CARTESIAN_POINT ( 'NONE',  ( 9.474510206698971260, -16.51473224551069308, 62.91557627198102409 ) ) ;
#47083 = CARTESIAN_POINT ( 'NONE',  ( 16.55341960407611168, 4.379528057220329451, 58.95724293864770971 ) ) ;
#47085 = CARTESIAN_POINT ( 'NONE',  ( 5.049401038298161559, -19.05341960407611168, 57.70724293864769550 ) ) ;
#47086 = CARTESIAN_POINT ( 'NONE',  ( -9.564922557961040184, 16.46253265017147172, 77.91775706135234714 ) ) ;
#47087 = CARTESIAN_POINT ( 'NONE',  ( 5.719274019375991003, -21.55341960407610458, 52.70724293864769550 ) ) ;
#47088 = CARTESIAN_POINT ( 'NONE',  ( -19.03943276465977164, -0.05219959533935918106, 38.75109039468566152 ) ) ;
#47089 = CARTESIAN_POINT ( 'NONE',  ( 19.03943276465977164, -0.05219959533909143690, 83.74890960531436690 ) ) ;
#47090 = CARTESIAN_POINT ( 'NONE',  ( 10.81492255796078972, 18.62759615963270932, 79.58224293864769550 ) ) ;
#47092 = CARTESIAN_POINT ( 'NONE',  ( 19.03943276465977164, 0.05219959533936151252, 31.25109039468566863 ) ) ;
#47091 = CARTESIAN_POINT ( 'NONE',  ( 8.224510206698953496, -14.34966873604960469, 77.91557627198102409 ) ) ;
#47093 = CARTESIAN_POINT ( 'NONE',  ( 21.53943276465977519, -0.05219959533907433946, 63.74890960531435979 ) ) ;
#47094 = VECTOR ( 'NONE', #183435, 1000.000000000000000 ) ;
#47095 = CARTESIAN_POINT ( 'NONE',  ( -15.72974639402197994, 15.80617190586746368, 40.62390960531435269 ) ) ;
#47096 = CARTESIAN_POINT ( 'NONE',  ( 5.049401038298161559, -19.05341960407611168, 67.70724293864769550 ) ) ;
#47097 = CARTESIAN_POINT ( 'NONE',  ( -16.52544592524342804, 4.483927247898546575, 111.0405762719810525 ) ) ;
#47098 = CARTESIAN_POINT ( 'NONE',  ( 5.719274019375673035, 21.55341960407619339, 32.29275706135235424 ) ) ;
#47099 = CARTESIAN_POINT ( 'NONE',  ( 9.564922557960805705, 16.46253265017160317, 114.5822429386476955 ) ) ;
#47100 = CARTESIAN_POINT ( 'NONE',  ( 21.53943276465977519, 0.05219959533937863772, 41.25109039468568284 ) ) ;
#47101 = CARTESIAN_POINT ( 'NONE',  ( -19.02544592524342804, 5.153800228976336051, 31.04057627198102409 ) ) ;
#47102 = CARTESIAN_POINT ( 'NONE',  ( -21.55341960407610458, -5.719274019375992779, 111.4572429386476813 ) ) ;
#47103 = EDGE_CURVE ( 'NONE', #100170, #16229, #26667, .T. ) ;
#47104 = CARTESIAN_POINT ( 'NONE',  ( -9.564922557961040184, 16.46253265017147172, 42.91775706135234003 ) ) ;
#47105 = FACE_OUTER_BOUND ( 'NONE', #22670, .T. ) ;
#47106 = CARTESIAN_POINT ( 'NONE',  ( -16.51473224551069308, -9.474510206698971260, 26.66557627198103120 ) ) ;
#47107 =( NAMED_UNIT ( * ) SI_UNIT ( $, .STERADIAN. ) SOLID_ANGLE_UNIT ( ) );
#47108 = CARTESIAN_POINT ( 'NONE',  ( 16.55341960407618274, -4.379528057220086978, 56.04275706135235424 ) ) ;
#47109 = CARTESIAN_POINT ( 'NONE',  ( -13.89961937509977652, 13.97604488694528158, 30.62390960531435269 ) ) ;
#47110 = CARTESIAN_POINT ( 'NONE',  ( -21.04946095171256104, -10.86023174791543866, 170.2405914574444239 ) ) ;
#47111 = CARTESIAN_POINT ( 'NONE',  ( 0.05219959533909260263, 19.03943276465977164, 74.99890960531435269 ) ) ;
#47112 = CARTESIAN_POINT ( 'NONE',  ( 4.483927247898545687, 16.52544592524342804, 109.7905762719810383 ) ) ;
#47113 = CARTESIAN_POINT ( 'NONE',  ( 18.67979575497178502, 10.72451020669898547, 59.16557627198103120 ) ) ;
#47114 = CARTESIAN_POINT ( 'NONE',  ( 12.14591786802309770, 12.06949235617756955, 84.37390960531438111 ) ) ;
#47115 = CARTESIAN_POINT ( 'NONE',  ( 12.06949235617739724, 12.14591786802326823, 31.87609039468567929 ) ) ;
#47116 = CARTESIAN_POINT ( 'NONE',  ( -10.81492255796105439, 18.62759615963255655, 92.91775706135236135 ) ) ;
#47117 = CARTESIAN_POINT ( 'NONE',  ( -16.51473224551069308, -9.474510206698971260, 21.66557627198102765 ) ) ;
#47118 = EDGE_CURVE ( 'NONE', #49927, #87243, #127276, .T. ) ;
#47119 = CARTESIAN_POINT ( 'NONE',  ( 14.34966873604972726, -8.224510206698740333, 105.8344237280190328 ) ) ;
#47120 = CARTESIAN_POINT ( 'NONE',  ( 16.52544592524342804, -4.483927247898539470, 53.54057627198103120 ) ) ;
#47121 = CARTESIAN_POINT ( 'NONE',  ( 9.474510206698971260, -16.51473224551069308, 52.91557627198102409 ) ) ;
#47122 = CARTESIAN_POINT ( 'NONE',  ( 21.55341960407619695, -5.719274019375665929, 91.04275706135236135 ) ) ;
#47123 = CARTESIAN_POINT ( 'NONE',  ( 0.05219959533907565091, 21.53943276465977519, 104.9989096053143669 ) ) ;
#47124 = CARTESIAN_POINT ( 'NONE',  ( -21.55341960407619339, 5.719274019375674811, 73.54275706135234714 ) ) ;
#47125 = CARTESIAN_POINT ( 'NONE',  ( -12.14591786802326823, 12.06949235617739902, 48.12609039468568284 ) ) ;
#47127 = CARTESIAN_POINT ( 'NONE',  ( 18.67979575497194134, -10.72451020669871369, 85.83442372801901854 ) ) ;
#47126 = CARTESIAN_POINT ( 'NONE',  ( 16.52544592524342804, -4.483927247898539470, 78.54057627198103830 ) ) ;
#47128 = CARTESIAN_POINT ( 'NONE',  ( -14.34966873604972548, 8.224510206698743886, 108.3344237280190185 ) ) ;
#47129 = CARTESIAN_POINT ( 'NONE',  ( -17.05116617787822975, 6.768360034955819948, 113.6567555325920296 ) ) ;
#47130 = CARTESIAN_POINT ( 'NONE',  ( -16.53943276465976808, -0.05219959533934237506, 43.75109039468568284 ) ) ;
#47131 = CARTESIAN_POINT ( 'NONE',  ( 8.314922557960818139, 14.29746914071049879, 44.58224293864769550 ) ) ;
#47132 = CARTESIAN_POINT ( 'NONE',  ( -8.314922557961024197, 14.29746914071037800, 82.91775706135234714 ) ) ;
#47133 = CARTESIAN_POINT ( 'NONE',  ( -0.05219959533909027116, -19.03943276465977164, 102.4989096053143669 ) ) ;
#47134 = CARTESIAN_POINT ( 'NONE',  ( -19.03943276465977164, 0.05219959533909376836, 116.2489096053143669 ) ) ;
#47135 = CARTESIAN_POINT ( 'NONE',  ( -0.05219959533937732626, 21.53943276465977519, 97.50109039468567573 ) ) ;
#47136 = CARTESIAN_POINT ( 'NONE',  ( 12.06949235617739724, 12.14591786802326823, 96.87609039468568994 ) ) ;
#47137 = CARTESIAN_POINT ( 'NONE',  ( -8.224510206698948167, 14.34966873604960824, 75.41557627198102409 ) ) ;
#47138 = CARTESIAN_POINT ( 'NONE',  ( -19.02544592524342804, 5.153800228976336051, 86.04057627198103830 ) ) ;
#47139 = VERTEX_POINT ( 'NONE', #145984 ) ;
#47140 = CARTESIAN_POINT ( 'NONE',  ( 16.52544592524335698, 4.483927247898782831, 21.45942372801901499 ) ) ;
#47141 = CARTESIAN_POINT ( 'NONE',  ( -19.03943276465977164, 0.05219959533909376836, 31.24890960531435979 ) ) ;
#47142 = CARTESIAN_POINT ( 'NONE',  ( -0.05219959533909027116, -19.03943276465977164, 87.49890960531436690 ) ) ;
#47144 = CARTESIAN_POINT ( 'NONE',  ( 29.86685920354754487, 21.69954338932564752, -3.424999997268813434 ) ) ;
#47143 = CARTESIAN_POINT ( 'NONE',  ( -16.52544592524335698, -4.483927247898792601, 28.95942372801902209 ) ) ;
#47145 = CARTESIAN_POINT ( 'NONE',  ( -9.564922557961040184, 16.46253265017147172, 32.91775706135233293 ) ) ;
#47146 = CARTESIAN_POINT ( 'NONE',  ( -12.14591786802326823, 12.06949235617739902, 88.12609039468570415 ) ) ;
#47147 = CARTESIAN_POINT ( 'NONE',  ( -16.51473224551069308, -9.474510206698971260, 31.66557627198102054 ) ) ;
#47148 = CARTESIAN_POINT ( 'NONE',  ( -4.379528057220086978, -16.55341960407618274, 74.79275706135234714 ) ) ;
#47149 = CARTESIAN_POINT ( 'NONE',  ( -16.53943276465976808, -0.05219959533934237506, 68.75109039468568994 ) ) ;
#47150 = CARTESIAN_POINT ( 'NONE',  ( -19.05341960407617563, 5.049401038297882671, 78.54275706135233293 ) ) ;
#47151 = CARTESIAN_POINT ( 'NONE',  ( -10.81492255796105439, 18.62759615963255655, 112.9177570613523329 ) ) ;
#47152 = CARTESIAN_POINT ( 'NONE',  ( -5.153800228976328057, -19.02544592524343514, 52.29057627198100988 ) ) ;
#47153 = CARTESIAN_POINT ( 'NONE',  ( -5.049401038298153566, 19.05341960407611168, 90.20724293864766707 ) ) ;
#47154 = CARTESIAN_POINT ( 'NONE',  ( -4.379528057220328563, 16.55341960407611168, 90.20724293864770971 ) ) ;
#47155 = CARTESIAN_POINT ( 'NONE',  ( -5.049401038297874678, -19.05341960407617918, 49.79275706135231871 ) ) ;
#47156 = CARTESIAN_POINT ( 'NONE',  ( 0.05219959533907565091, 21.53943276465977519, 44.99890960531435979 ) ) ;
#47157 = CARTESIAN_POINT ( 'NONE',  ( -19.05341960407617563, 5.049401038297882671, 33.54275706135231871 ) ) ;
#47158 = CARTESIAN_POINT ( 'NONE',  ( 0.05219959533909260263, 19.03943276465977164, 99.99890960531436690 ) ) ;
#47159 = CARTESIAN_POINT ( 'NONE',  ( -15.72974639402197994, 15.80617190586746368, 75.62390960531439532 ) ) ;
#47160 = CARTESIAN_POINT ( 'NONE',  ( -5.153800228976328057, -19.02544592524343514, 112.2905762719810099 ) ) ;
#47161 = CARTESIAN_POINT ( 'NONE',  ( -19.05341960407617563, 5.049401038297882671, 93.54275706135234714 ) ) ;
#47162 = CARTESIAN_POINT ( 'NONE',  ( -17.50000000000014566, 3.292511757969728947, 110.0652027021053243 ) ) ;
#47163 = CARTESIAN_POINT ( 'NONE',  ( -19.03943276465977164, -0.05219959533935918106, 108.7510903946856615 ) ) ;
#47164 = CARTESIAN_POINT ( 'NONE',  ( 0.05219959533909260263, 19.03943276465977164, 29.99890960531435979 ) ) ;
#47165 = CARTESIAN_POINT ( 'NONE',  ( -0.05219959533909027116, -19.03943276465977164, 97.49890960531436690 ) ) ;
#47166 = CARTESIAN_POINT ( 'NONE',  ( 15.80617190586746368, 15.72974639402197994, 74.37390960531436690 ) ) ;
#47167 = CARTESIAN_POINT ( 'NONE',  ( 8.224510206698742110, 14.34966873604972548, 47.08442372801901854 ) ) ;
#47168 = CARTESIAN_POINT ( 'NONE',  ( 10.81492255796106328, -18.62759615963255655, 50.41775706135235424 ) ) ;
#47170 = CARTESIAN_POINT ( 'NONE',  ( -21.53943276465977519, -0.05219959533937600094, 103.7510903946857042 ) ) ;
#47169 = CARTESIAN_POINT ( 'NONE',  ( 13.97604488694548053, -13.89961937509957401, 90.62609039468567573 ) ) ;
#47171 = CARTESIAN_POINT ( 'NONE',  ( 4.379528057220092307, 16.55341960407617563, 112.2927570613523471 ) ) ;
#47172 = CARTESIAN_POINT ( 'NONE',  ( 16.51473224551069308, 9.474510206698969483, 99.16557627198102409 ) ) ;
#47173 = CARTESIAN_POINT ( 'NONE',  ( 8.314922557960818139, 14.29746914071049879, 94.58224293864769550 ) ) ;
#47174 = CARTESIAN_POINT ( 'NONE',  ( -8.224510206698948167, 14.34966873604960824, 40.41557627198103120 ) ) ;
#47175 = CARTESIAN_POINT ( 'NONE',  ( 0.05219959533936267826, -19.03943276465977164, 70.00109039468566152 ) ) ;
#47176 = CARTESIAN_POINT ( 'NONE',  ( 5.823673210054444382, -21.52544592524334988, 60.20942372801902565 ) ) ;
#47177 = CARTESIAN_POINT ( 'NONE',  ( -13.97604488694547697, 13.89961937509957934, 23.12609039468565442 ) ) ;
#47178 = CARTESIAN_POINT ( 'NONE',  ( 4.483927247898545687, 16.52544592524342804, 109.7905762719810383 ) ) ;
#47179 = CARTESIAN_POINT ( 'NONE',  ( -21.52544592524343514, 5.823673210054127303, 31.04057627198102409 ) ) ;
#47180 = CARTESIAN_POINT ( 'NONE',  ( 12.06949235617739724, 12.14591786802326823, 111.8760903946856615 ) ) ;
#47181 = CARTESIAN_POINT ( 'NONE',  ( -10.72451020669870658, -18.67979575497194134, 99.58442372801900433 ) ) ;
#47182 = CARTESIAN_POINT ( 'NONE',  ( -12.06949235617739369, -12.14591786802326823, 54.37609039468568994 ) ) ;
#47183 = CARTESIAN_POINT ( 'NONE',  ( -16.53943276465976808, 0.05219959533911058130, 26.24890960531435624 ) ) ;
#47184 = CARTESIAN_POINT ( 'NONE',  ( 18.67979575497194134, -10.72451020669871369, 65.83442372801900433 ) ) ;
#47185 = CARTESIAN_POINT ( 'NONE',  ( -21.55341960407619339, 5.719274019375674811, 58.54275706135235424 ) ) ;
#47186 = CARTESIAN_POINT ( 'NONE',  ( 9.564922557960805705, 16.46253265017160317, 29.58224293864769550 ) ) ;
#47187 = CARTESIAN_POINT ( 'NONE',  ( -18.62759615963255300, -10.81492255796106328, 24.16775706135235424 ) ) ;
#47188 = CARTESIAN_POINT ( 'NONE',  ( -8.224510206698948167, 14.34966873604960824, 100.4155762719810241 ) ) ;
#47189 = CARTESIAN_POINT ( 'NONE',  ( 13.89961937509977652, -13.97604488694527269, 28.12390960531435624 ) ) ;
#47190 = CARTESIAN_POINT ( 'NONE',  ( -16.53943276465976808, 0.05219959533911058130, 81.24890960531436690 ) ) ;
#47191 = CARTESIAN_POINT ( 'NONE',  ( -5.153800228976328057, -19.02544592524343514, 67.29057627198102409 ) ) ;
#47192 = CARTESIAN_POINT ( 'NONE',  ( 8.224510206698953496, -14.34966873604960469, 22.91557627198102765 ) ) ;
#47193 = CARTESIAN_POINT ( 'NONE',  ( 18.67979575497178502, 10.72451020669898547, 54.16557627198103120 ) ) ;
#47194 = CARTESIAN_POINT ( 'NONE',  ( -16.55341960407611168, -4.379528057220339221, 91.45724293864769550 ) ) ;
#47195 = CIRCLE ( 'NONE', #98831, 2.649999999999999467 ) ;
#47196 = CARTESIAN_POINT ( 'NONE',  ( -21.55341960407610458, -5.719274019375992779, 96.45724293864770971 ) ) ;
#47197 = CARTESIAN_POINT ( 'NONE',  ( 19.02544592524343514, -5.153800228976328945, 98.54057627198100988 ) ) ;
#47199 = CARTESIAN_POINT ( 'NONE',  ( -13.97604488694547697, 13.89961937509957934, 108.1260903946856331 ) ) ;
#47198 = CARTESIAN_POINT ( 'NONE',  ( 16.46253265017160672, -9.564922557960803928, 58.33224293864769550 ) ) ;
#47200 = CARTESIAN_POINT ( 'NONE',  ( -5.719274019375978568, 21.55341960407610458, 40.20724293864769550 ) ) ;
#47201 = CARTESIAN_POINT ( 'NONE',  ( -10.81492255796105439, 18.62759615963255655, 87.91775706135234714 ) ) ;
#47202 = CARTESIAN_POINT ( 'NONE',  ( -0.05219959533909027116, -19.03943276465977164, 67.49890960531436690 ) ) ;
#47203 = EDGE_CURVE ( 'NONE', #111651, #194969, #33125, .T. ) ;
#47204 = CARTESIAN_POINT ( 'NONE',  ( -5.049401038298153566, 19.05341960407611168, 105.2072429386476671 ) ) ;
#47205 = CARTESIAN_POINT ( 'NONE',  ( -12.06949235617739369, -12.14591786802326823, 74.37609039468568994 ) ) ;
#47206 = CARTESIAN_POINT ( 'NONE',  ( -18.67979575497193778, 10.72451020669871902, 63.33442372801900433 ) ) ;
#47207 = CARTESIAN_POINT ( 'NONE',  ( 5.719274019375673035, 21.55341960407619339, 92.29275706135236135 ) ) ;
#47208 = CARTESIAN_POINT ( 'NONE',  ( -15.72974639402197994, 15.80617190586746368, 95.62390960531436690 ) ) ;
#47210 = CARTESIAN_POINT ( 'NONE',  ( -4.379528057220086978, -16.55341960407618274, 74.79275706135234714 ) ) ;
#47209 = CARTESIAN_POINT ( 'NONE',  ( -5.823673210054431948, 21.52544592524334988, 37.70942372801900433 ) ) ;
#47211 = CARTESIAN_POINT ( 'NONE',  ( -21.52544592524343514, 5.823673210054127303, 76.04057627198102409 ) ) ;
#47212 = CARTESIAN_POINT ( 'NONE',  ( 13.89961937509957401, 13.97604488694547697, 31.87609039468566863 ) ) ;
#47213 = CARTESIAN_POINT ( 'NONE',  ( 10.81492255796078972, 18.62759615963270932, 44.58224293864769550 ) ) ;
#47215 = CARTESIAN_POINT ( 'NONE',  ( 14.34966873604960469, 8.224510206698951720, 24.16557627198103120 ) ) ;
#47214 = CARTESIAN_POINT ( 'NONE',  ( 9.474510206698971260, -16.51473224551069308, 82.91557627198103830 ) ) ;
#47216 = CARTESIAN_POINT ( 'NONE',  ( -16.18388926212242396, 7.379444403734377822, 64.56046848633850743 ) ) ;
#47217 = CARTESIAN_POINT ( 'NONE',  ( -16.46253265017160317, 9.564922557960807481, 105.8322429386476955 ) ) ;
#47218 = DIRECTION ( 'NONE',  ( 0.000000000000000000, 0.000000000000000000, -1.000000000000000000 ) ) ;
#47219 = CARTESIAN_POINT ( 'NONE',  ( -16.46253265017146816, -9.564922557961047289, 94.16775706135233293 ) ) ;
#47220 = CARTESIAN_POINT ( 'NONE',  ( 21.52544592524344225, -5.823673210054117533, 73.54057627198102409 ) ) ;
#47221 = CARTESIAN_POINT ( 'NONE',  ( 12.06949235617757843, -12.14591786802309237, 43.12390960531435269 ) ) ;
#47222 = CARTESIAN_POINT ( 'NONE',  ( -13.97604488694547697, 13.89961937509957934, 108.1260903946856331 ) ) ;
#47223 = CARTESIAN_POINT ( 'NONE',  ( -5.153800228976328057, -19.02544592524343514, 37.29057627198102409 ) ) ;
#47224 = CARTESIAN_POINT ( 'NONE',  ( 9.564922557961047289, -16.46253265017146816, 105.4177570613523471 ) ) ;
#47226 = CARTESIAN_POINT ( 'NONE',  ( -13.97604488694547697, 13.89961937509957934, 73.12609039468568994 ) ) ;
#47225 = CARTESIAN_POINT ( 'NONE',  ( -18.67979575497178146, -10.72451020669898902, 106.6655762719810383 ) ) ;
#47227 = CARTESIAN_POINT ( 'NONE',  ( -14.34966873604972548, 8.224510206698743886, 83.33442372801903275 ) ) ;
#47228 = CARTESIAN_POINT ( 'NONE',  ( 19.05341960407611168, 5.049401038298154454, 68.95724293864769550 ) ) ;
#47229 = CARTESIAN_POINT ( 'NONE',  ( -16.55341960407611168, -4.379528057220339221, 76.45724293864769550 ) ) ;
#47230 = CARTESIAN_POINT ( 'NONE',  ( -9.564922557960796823, -16.46253265017161027, 67.08224293864769550 ) ) ;
#47231 = CARTESIAN_POINT ( 'NONE',  ( -14.29746914071049879, 8.314922557960819915, 65.83224293864769550 ) ) ;
#47232 = CARTESIAN_POINT ( 'NONE',  ( 19.02544592524343514, -5.153800228976328945, 23.54057627198102054 ) ) ;
#47233 = DIRECTION ( 'NONE',  ( -0.8660254037844410391, -0.000000000000000000, -0.4999999999999958367 ) ) ;
#47234 = CARTESIAN_POINT ( 'NONE',  ( -12.06949235617756955, 12.14591786802309770, 45.62390960531436690 ) ) ;
#47235 = CARTESIAN_POINT ( 'NONE',  ( -9.564922557960796823, -16.46253265017161027, 82.08224293864768129 ) ) ;
#47236 = FACE_BOUND ( 'NONE', #72263, .T. ) ;
#47237 = CARTESIAN_POINT ( 'NONE',  ( 13.97604488694548053, -13.89961937509957401, 45.62609039468566863 ) ) ;
#47238 = CARTESIAN_POINT ( 'NONE',  ( 16.53943276465976808, 0.05219959533934440121, 66.25109039468567573 ) ) ;
#47239 = AXIS2_PLACEMENT_3D ( 'NONE', #101463, #9484, #10483 ) ;
#47240 = CARTESIAN_POINT ( 'NONE',  ( 0.05219959533907565091, 21.53943276465977519, 64.99890960531435269 ) ) ;
#47241 = CARTESIAN_POINT ( 'NONE',  ( 0.05219959533936267826, -19.03943276465977164, 20.00109039468567218 ) ) ;
#47242 = CARTESIAN_POINT ( 'NONE',  ( -16.51473224551069308, -9.474510206698971260, 91.66557627198103830 ) ) ;
#47243 = CARTESIAN_POINT ( 'NONE',  ( -3.573655867282028392E-15, 2.428612866367529932E-14, 139.9999999999999716 ) ) ;
#47244 = CARTESIAN_POINT ( 'NONE',  ( 18.62759615963271287, -10.81492255796078972, 33.33224293864769550 ) ) ;
#47245 = CARTESIAN_POINT ( 'NONE',  ( 5.153800228976335163, 19.02544592524342804, 64.79057627198100988 ) ) ;
#47246 = CARTESIAN_POINT ( 'NONE',  ( -21.55341960407619339, 5.719274019375674811, 33.54275706135234714 ) ) ;
#47247 = AXIS2_PLACEMENT_3D ( 'NONE', #26660, #9490, #118662 ) ;
#47248 = CARTESIAN_POINT ( 'NONE',  ( 12.14591786802309770, 12.06949235617756955, 109.3739096053143811 ) ) ;
#47251 = ORIENTED_EDGE ( 'NONE', *, *, #115833, .T. ) ;
#47250 = CARTESIAN_POINT ( 'NONE',  ( 5.049401038298161559, -19.05341960407611168, 97.70724293864766707 ) ) ;
#47249 = CARTESIAN_POINT ( 'NONE',  ( -15.80617190586745835, -15.72974639402198527, 101.8739096053143811 ) ) ;
#47252 = CARTESIAN_POINT ( 'NONE',  ( 15.80617190586769283, -15.72974639402175789, 30.62609039468567929 ) ) ;
#47253 = VERTEX_POINT ( 'NONE', #23659 ) ;
#47254 = CARTESIAN_POINT ( 'NONE',  ( 13.97604488694527802, 13.89961937509977652, 89.37390960531436690 ) ) ;
#47255 = CARTESIAN_POINT ( 'NONE',  ( 18.87580814761074777, -5.500000000000045297, 83.37172394265758157 ) ) ;
#47256 = CARTESIAN_POINT ( 'NONE',  ( -21.53943276465977519, 0.05219959533907696930, 91.24890960531436690 ) ) ;
#47257 = CARTESIAN_POINT ( 'NONE',  ( -0.05219959533909027116, -19.03943276465977164, 47.49890960531435979 ) ) ;
#47258 = CARTESIAN_POINT ( 'NONE',  ( -5.153800228976607833, 19.02544592524334988, 112.7094237280190043 ) ) ;
#47259 = CARTESIAN_POINT ( 'NONE',  ( -22.81625015709509441, -31.40387420917324590, -2.824999997268812901 ) ) ;
#47260 = CARTESIAN_POINT ( 'NONE',  ( 19.05341960407611168, 5.049401038298154454, 33.95724293864769550 ) ) ;
#47261 = CARTESIAN_POINT ( 'NONE',  ( 15.72974639402176855, 15.80617190586768217, 81.87609039468568994 ) ) ;
#47263 = CARTESIAN_POINT ( 'NONE',  ( 10.72451020669871369, 18.67979575497193778, 42.08442372801901854 ) ) ;
#47262 = CARTESIAN_POINT ( 'NONE',  ( -19.03943276465977164, 0.05219959533909376836, 76.24890960531435269 ) ) ;
#47264 = CARTESIAN_POINT ( 'NONE',  ( -15.80617190586768217, 15.72974639402176855, 23.12609039468567573 ) ) ;
#47265 = CARTESIAN_POINT ( 'NONE',  ( 27.73933785331498569, 2.768321779492822058E-14, 142.3750000027311842 ) ) ;
#47266 = CARTESIAN_POINT ( 'NONE',  ( 5.049401038298161559, -19.05341960407611168, 97.70724293864766707 ) ) ;
#47267 = CARTESIAN_POINT ( 'NONE',  ( 19.19724070472091526, 5.500000000000158096, 63.56193348274384647 ) ) ;
#47270 = CARTESIAN_POINT ( 'NONE',  ( 10.72451020669871369, 18.67979575497193778, 42.08442372801901854 ) ) ;
#47269 = CARTESIAN_POINT ( 'NONE',  ( 4.483927247898790824, -16.52544592524335698, 70.20942372801904696 ) ) ;
#47268 = CARTESIAN_POINT ( 'NONE',  ( -4.379528057220086978, -16.55341960407618274, 34.79275706135235424 ) ) ;
#47271 = CARTESIAN_POINT ( 'NONE',  ( 21.52544592524334988, 5.823673210054432836, 81.45942372801900433 ) ) ;
#47272 = DIRECTION ( 'NONE',  ( 0.000000000000000000, 0.5000000000000011102, 0.8660254037844379305 ) ) ;
#47273 = CARTESIAN_POINT ( 'NONE',  ( 5.153800228976615827, -19.02544592524334988, 110.2094237280189901 ) ) ;
#47274 = CARTESIAN_POINT ( 'NONE',  ( 19.03943276465977164, -0.05219959533909143690, 58.74890960531435979 ) ) ;
#47275 = CARTESIAN_POINT ( 'NONE',  ( 19.05341960407611168, 5.049401038298154454, 103.9572429386476671 ) ) ;
#47276 = EDGE_CURVE ( 'NONE', #197536, #150928, #146999, .T. ) ;
#47277 = CARTESIAN_POINT ( 'NONE',  ( -8.224510206698948167, 14.34966873604960824, 110.4155762719810383 ) ) ;
#47278 = CARTESIAN_POINT ( 'NONE',  ( 16.53943276465976808, -0.05219959533910856209, 108.7489096053143669 ) ) ;
#47279 = CARTESIAN_POINT ( 'NONE',  ( 18.62759615963271287, -10.81492255796078972, 28.33224293864769550 ) ) ;
#47280 = CARTESIAN_POINT ( 'NONE',  ( 12.14591786802327356, -12.06949235617739191, 80.62609039468567573 ) ) ;
#47282 = CARTESIAN_POINT ( 'NONE',  ( -13.97604488694527625, -13.89961937509977652, 56.87390960531434558 ) ) ;
#47281 = CARTESIAN_POINT ( 'NONE',  ( -8.314922557960811034, -14.29746914071050412, 67.08224293864770971 ) ) ;
#47283 = CARTESIAN_POINT ( 'NONE',  ( 10.72451020669871369, 18.67979575497193778, 72.08442372801899012 ) ) ;
#47284 = CARTESIAN_POINT ( 'NONE',  ( 18.62759615963255655, 10.81492255796105972, 66.66775706135234714 ) ) ;
#47285 = CARTESIAN_POINT ( 'NONE',  ( -19.05341960407617563, 5.049401038297882671, 103.5427570613523329 ) ) ;
#47286 = CARTESIAN_POINT ( 'NONE',  ( -8.314922557960811034, -14.29746914071050412, 72.08224293864769550 ) ) ;
#47287 = CARTESIAN_POINT ( 'NONE',  ( 21.52544592524334988, 5.823673210054432836, 31.45942372801901854 ) ) ;
#47288 = CARTESIAN_POINT ( 'NONE',  ( -5.823673210054116645, -21.52544592524344225, 57.29057627198103120 ) ) ;
#47289 = CARTESIAN_POINT ( 'NONE',  ( 8.906447517083057264, -27.41122689804191026, 140.5999999999999943 ) ) ;
#47290 = CARTESIAN_POINT ( 'NONE',  ( 8.906447517083050158, 27.41122689804195645, 143.6500000054623740 ) ) ;
#47291 = CARTESIAN_POINT ( 'NONE',  ( -16.51473224551069308, -9.474510206698971260, 66.66557627198102409 ) ) ;
#47292 = CARTESIAN_POINT ( 'NONE',  ( -16.52544592524342804, 4.483927247898546575, 46.04057627198103830 ) ) ;
#47293 = CARTESIAN_POINT ( 'NONE',  ( 16.52544592524335698, 4.483927247898782831, 111.4594237280190328 ) ) ;
#47294 = CARTESIAN_POINT ( 'NONE',  ( -16.52544592524335698, -4.483927247898792601, 98.95942372801903275 ) ) ;
#47295 = CARTESIAN_POINT ( 'NONE',  ( -13.97604488694547697, 13.89961937509957934, 53.12609039468565442 ) ) ;
#47296 = CARTESIAN_POINT ( 'NONE',  ( 17.40861289039005300, 6.110651285853281323, 48.87232470827434128 ) ) ;
#47297 = CARTESIAN_POINT ( 'NONE',  ( -0.05219959533909027116, -19.03943276465977164, 102.4989096053143669 ) ) ;
#47298 = EDGE_CURVE ( 'NONE', #104408, #140931, #185322, .T. ) ;
#47299 = CARTESIAN_POINT ( 'NONE',  ( -16.52544592524342804, 4.483927247898546575, 81.04057627198102409 ) ) ;
#47300 = CARTESIAN_POINT ( 'NONE',  ( -9.474510206698720793, -16.51473224551083518, 49.58442372801899722 ) ) ;
#47302 = CARTESIAN_POINT ( 'NONE',  ( 15.72974639402199770, -15.80617190586745480, 33.12390960531435979 ) ) ;
#47301 = CARTESIAN_POINT ( 'NONE',  ( 19.03943276465977164, -0.05219959533909143690, 38.74890960531436690 ) ) ;
#47304 = ORIENTED_EDGE ( 'NONE', *, *, #5230, .F. ) ;
#47303 = CARTESIAN_POINT ( 'NONE',  ( 21.53943276465977519, -0.05219959533907433946, 58.74890960531436690 ) ) ;
#47305 = CARTESIAN_POINT ( 'NONE',  ( 4.379528057220339221, -16.55341960407611168, 92.70724293864770971 ) ) ;
#47306 = CARTESIAN_POINT ( 'NONE',  ( -12.14591786802326823, 12.06949235617739902, 53.12609039468568284 ) ) ;
#47307 = CARTESIAN_POINT ( 'NONE',  ( 12.06949235617757843, -12.14591786802309237, 88.12390960531436690 ) ) ;
#47308 = CARTESIAN_POINT ( 'NONE',  ( -28.81842663310010266, -24.98430004053108178, -11.52348593588107484 ) ) ;
#47309 = CARTESIAN_POINT ( 'NONE',  ( -17.48847506799968698, 5.747544572773789717, 50.82697437843282273 ) ) ;
#47310 = CARTESIAN_POINT ( 'NONE',  ( -19.02544592524342804, 5.153800228976336051, 111.0405762719810099 ) ) ;
#47311 = CARTESIAN_POINT ( 'NONE',  ( 17.60728821186566151, -5.500000000000016875, 78.36690927743003954 ) ) ;
#47312 = CARTESIAN_POINT ( 'NONE',  ( 18.22780087662122739, 5.500000000000000888, 86.48236817873107896 ) ) ;
#47313 = ORIENTED_EDGE ( 'NONE', *, *, #85455, .T. ) ;
#47315 = CARTESIAN_POINT ( 'NONE',  ( -8.314922557960811034, -14.29746914071050412, 32.08224293864769550 ) ) ;
#47314 = CARTESIAN_POINT ( 'NONE',  ( -16.55341960407617563, 4.379528057220093196, 43.54275706135235424 ) ) ;
#47316 = CARTESIAN_POINT ( 'NONE',  ( -15.72974639402197994, 15.80617190586746368, 50.62390960531435979 ) ) ;
#47317 = CARTESIAN_POINT ( 'NONE',  ( -19.05341960407617563, 5.049401038297882671, 88.54275706135230450 ) ) ;
#47318 = CARTESIAN_POINT ( 'NONE',  ( 15.72974639402199770, -15.80617190586745480, 43.12390960531435269 ) ) ;
#47319 = CARTESIAN_POINT ( 'NONE',  ( 21.52544592524334988, 5.823673210054432836, 81.45942372801900433 ) ) ;
#47320 = CARTESIAN_POINT ( 'NONE',  ( 19.38985940809749309, -32.68077955211924035, -24.99999999999992895 ) ) ;
#47321 = CARTESIAN_POINT ( 'NONE',  ( 16.55341960407618274, -4.379528057220086978, 51.04275706135234714 ) ) ;
#47323 = CARTESIAN_POINT ( 'NONE',  ( -9.564922557960796823, -16.46253265017161027, 107.0822429386476955 ) ) ;
#47322 = CARTESIAN_POINT ( 'NONE',  ( 19.05341960407611168, 5.049401038298154454, 38.95724293864767418 ) ) ;
#47324 = CARTESIAN_POINT ( 'NONE',  ( 5.153800228976335163, 19.02544592524342804, 34.79057627198102409 ) ) ;
#47325 = CARTESIAN_POINT ( 'NONE',  ( -8.224510206698948167, 14.34966873604960824, 100.4155762719810241 ) ) ;
#47326 = DIRECTION ( 'NONE',  ( 1.000000000000000000, 9.714451465470120961E-17, 5.551115123125775923E-17 ) ) ;
#47327 = CARTESIAN_POINT ( 'NONE',  ( -9.474510206698964154, 16.51473224551069663, 105.4155762719810383 ) ) ;
#47328 = ORIENTED_EDGE ( 'NONE', *, *, #168827, .F. ) ;
#47329 = CARTESIAN_POINT ( 'NONE',  ( -4.483927247898782831, 16.52544592524335698, 62.70942372801902565 ) ) ;
#47330 = CARTESIAN_POINT ( 'NONE',  ( -18.62759615963270932, 10.81492255796079327, 90.83224293864769550 ) ) ;
#47331 = CARTESIAN_POINT ( 'NONE',  ( -16.51473224551069308, -9.474510206698971260, 61.66557627198103120 ) ) ;
#47332 = CARTESIAN_POINT ( 'NONE',  ( -0.05219959533937732626, 21.53943276465977519, 22.50109039468567573 ) ) ;
#47333 = CARTESIAN_POINT ( 'NONE',  ( 9.474510206698971260, -16.51473224551069308, 82.91557627198103830 ) ) ;
#47334 = CARTESIAN_POINT ( 'NONE',  ( 17.79613651744293534, 24.49428055684532524, 145.2843446568999752 ) ) ;
#47335 = ORIENTED_EDGE ( 'NONE', *, *, #26374, .T. ) ;
#47336 = CARTESIAN_POINT ( 'NONE',  ( 10.81492255796078972, 18.62759615963270932, 114.5822429386477097 ) ) ;
#47339 = CARTESIAN_POINT ( 'NONE',  ( -5.153800228976607833, 19.02544592524334988, 77.70942372801900433 ) ) ;
#47338 = CARTESIAN_POINT ( 'NONE',  ( -16.51473224551069308, -9.474510206698971260, 111.6655762719810383 ) ) ;
#47337 = CARTESIAN_POINT ( 'NONE',  ( 19.02544592524343514, -5.153800228976328945, 23.54057627198102054 ) ) ;
#47340 = CARTESIAN_POINT ( 'NONE',  ( -16.46253265017146816, -9.564922557961047289, 29.16775706135232937 ) ) ;
#47341 = CARTESIAN_POINT ( 'NONE',  ( 10.72451020669898902, -18.67979575497178502, 97.91557627198103830 ) ) ;
#47342 = CARTESIAN_POINT ( 'NONE',  ( -19.02544592524334988, -5.153800228976617603, 38.95942372801900433 ) ) ;
#47343 = CARTESIAN_POINT ( 'NONE',  ( -8.314922557961024197, 14.29746914071037800, 72.91775706135234714 ) ) ;
#47344 = CARTESIAN_POINT ( 'NONE',  ( 9.474510206698971260, -16.51473224551069308, 107.9155762719810383 ) ) ;
#47345 = CARTESIAN_POINT ( 'NONE',  ( -9.474510206698964154, 16.51473224551069663, 60.41557627198102409 ) ) ;
#47346 = AXIS2_PLACEMENT_3D ( 'NONE', #29502, #47653, #13335 ) ;
#47347 = CARTESIAN_POINT ( 'NONE',  ( -15.80617190586768217, 15.72974639402176855, 68.12609039468567573 ) ) ;
#47348 = CARTESIAN_POINT ( 'NONE',  ( -10.72451020669870658, -18.67979575497194134, 84.58442372801903275 ) ) ;
#47349 = CARTESIAN_POINT ( 'NONE',  ( 19.03943276465977164, -0.05219959533909143690, 73.74890960531435269 ) ) ;
#47350 = CARTESIAN_POINT ( 'NONE',  ( -18.62759615963255300, -10.81492255796106328, 49.16775706135234003 ) ) ;
#47351 = ADVANCED_FACE ( 'NONE', ( #57994 ), #15089, .F. ) ;
#47352 = CARTESIAN_POINT ( 'NONE',  ( -19.03943276465977164, -0.05219959533935918106, 88.75109039468567573 ) ) ;
#47353 = CARTESIAN_POINT ( 'NONE',  ( 19.05341960407611168, 5.049401038298154454, 48.95724293864768129 ) ) ;
#47354 = CARTESIAN_POINT ( 'NONE',  ( 16.51473224551069308, 9.474510206698969483, 99.16557627198102409 ) ) ;
#47355 = CARTESIAN_POINT ( 'NONE',  ( -16.51473224551069308, -9.474510206698971260, 66.66557627198102409 ) ) ;
#47356 = CARTESIAN_POINT ( 'NONE',  ( -5.153800228976328057, -19.02544592524343514, 107.2905762719810383 ) ) ;
#47357 = CARTESIAN_POINT ( 'NONE',  ( 19.03943276465977164, -0.05219959533909143690, 48.74890960531435979 ) ) ;
#47358 = CARTESIAN_POINT ( 'NONE',  ( -18.67979575497178146, -10.72451020669898902, 101.6655762719810383 ) ) ;
#47359 = CARTESIAN_POINT ( 'NONE',  ( -16.52544592524335698, -4.483927247898792601, 78.95942372801901854 ) ) ;
#47360 = CARTESIAN_POINT ( 'NONE',  ( -24.24385185424182154, 7.025880200331685366, 170.5073520790474504 ) ) ;
#47361 = CARTESIAN_POINT ( 'NONE',  ( -9.564922557961040184, 16.46253265017147172, 47.91775706135233293 ) ) ;
#47362 = CARTESIAN_POINT ( 'NONE',  ( 19.02544592524343514, -5.153800228976328945, 63.54057627198103830 ) ) ;
#47363 = CARTESIAN_POINT ( 'NONE',  ( -8.314922557960811034, -14.29746914071050412, 52.08224293864768839 ) ) ;
#47364 = CARTESIAN_POINT ( 'NONE',  ( 16.55341960407611168, 4.379528057220329451, 88.95724293864769550 ) ) ;
#47365 = CARTESIAN_POINT ( 'NONE',  ( -13.97604488694527625, -13.89961937509977652, 106.8739096053143669 ) ) ;
#47366 = CARTESIAN_POINT ( 'NONE',  ( -9.474510206698964154, 16.51473224551069663, 85.41557627198102409 ) ) ;
#47367 = CARTESIAN_POINT ( 'NONE',  ( -5.153800228976328057, -19.02544592524343514, 107.2905762719810383 ) ) ;
#47368 = CARTESIAN_POINT ( 'NONE',  ( 21.52544592524334988, 5.823673210054432836, 106.4594237280190328 ) ) ;
#47369 = CARTESIAN_POINT ( 'NONE',  ( 16.55341960407618274, -4.379528057220086978, 91.04275706135236135 ) ) ;
#47370 = CARTESIAN_POINT ( 'NONE',  ( 16.46253265017160672, -9.564922557960803928, 73.33224293864769550 ) ) ;
#47371 = CARTESIAN_POINT ( 'NONE',  ( 0.05219959533937995610, -21.53943276465977519, 45.00109039468568284 ) ) ;
#47372 = CARTESIAN_POINT ( 'NONE',  ( 0.05219959533907565091, 21.53943276465977519, 29.99890960531435979 ) ) ;
#47373 = CARTESIAN_POINT ( 'NONE',  ( 10.72451020669898902, -18.67979575497178502, 102.9155762719810383 ) ) ;
#47374 = CARTESIAN_POINT ( 'NONE',  ( 12.06949235617757843, -12.14591786802309237, 58.12390960531435979 ) ) ;
#47375 = CARTESIAN_POINT ( 'NONE',  ( -19.03943276465977164, 0.05219959533909376836, 61.24890960531436690 ) ) ;
#47376 = CARTESIAN_POINT ( 'NONE',  ( -8.314922557960811034, -14.29746914071050412, 87.08224293864769550 ) ) ;
#47377 = CARTESIAN_POINT ( 'NONE',  ( -9.564922557961040184, 16.46253265017147172, 47.91775706135233293 ) ) ;
#47378 = CARTESIAN_POINT ( 'NONE',  ( 4.483927247898545687, 16.52544592524342804, 109.7905762719810383 ) ) ;
#47379 = CARTESIAN_POINT ( 'NONE',  ( 4.379528057220092307, 16.55341960407617563, 72.29275706135236135 ) ) ;
#47380 = CARTESIAN_POINT ( 'NONE',  ( -9.564922557960796823, -16.46253265017161027, 62.08224293864769550 ) ) ;
#47381 = CARTESIAN_POINT ( 'NONE',  ( 27.73933785331498925, -9.013057229001034898, 141.7750000027311899 ) ) ;
#47382 = CARTESIAN_POINT ( 'NONE',  ( -4.483927247898539470, -16.52544592524342804, 92.29057627198103830 ) ) ;
#47383 = CARTESIAN_POINT ( 'NONE',  ( 15.72974639402199770, -15.80617190586745480, 38.12390960531436690 ) ) ;
#47384 = EDGE_LOOP ( 'NONE', ( #170476, #79382, #115140, #179154, #163179 ) ) ;
#47385 = CARTESIAN_POINT ( 'NONE',  ( 12.14591786802327356, -12.06949235617739191, 100.6260903946857184 ) ) ;
#47386 = CARTESIAN_POINT ( 'NONE',  ( 0.05219959533934541429, -16.53943276465976808, 30.00109039468568284 ) ) ;
#47387 = CARTESIAN_POINT ( 'NONE',  ( 0.05219959533937995610, -21.53943276465977519, 95.00109039468568994 ) ) ;
#47388 = CARTESIAN_POINT ( 'NONE',  ( 9.474510206698971260, -16.51473224551069308, 82.91557627198103830 ) ) ;
#47389 = CARTESIAN_POINT ( 'NONE',  ( 10.81492255796106328, -18.62759615963255655, 20.41775706135234714 ) ) ;
#47390 = CARTESIAN_POINT ( 'NONE',  ( 19.05341960407611168, 5.049401038298154454, 33.95724293864769550 ) ) ;
#47391 = VECTOR ( 'NONE', #132819, 1000.000000000000114 ) ;
#47392 = CARTESIAN_POINT ( 'NONE',  ( 0.05219959533934541429, -16.53943276465976808, 35.00109039468568284 ) ) ;
#47393 = CARTESIAN_POINT ( 'NONE',  ( 16.46253265017146816, 9.564922557961045513, 96.66775706135233293 ) ) ;
#47394 = CARTESIAN_POINT ( 'NONE',  ( 5.823673210054125526, 21.52544592524343514, 84.79057627198102409 ) ) ;
#47395 = CARTESIAN_POINT ( 'NONE',  ( 19.05341960407617918, -5.049401038297876454, 66.04275706135233293 ) ) ;
#47396 = CARTESIAN_POINT ( 'NONE',  ( 21.53943276465977519, 0.05219959533937863772, 21.25109039468567218 ) ) ;
#47397 = CARTESIAN_POINT ( 'NONE',  ( -13.97604488694527625, -13.89961937509977830, 71.87390960531435269 ) ) ;
#47398 = CARTESIAN_POINT ( 'NONE',  ( -13.97604488694527625, -13.89961937509977652, 71.87390960531433848 ) ) ;
#47399 = CARTESIAN_POINT ( 'NONE',  ( -8.224510206698735004, -14.34966873604973081, 29.58442372801901854 ) ) ;
#47400 = CARTESIAN_POINT ( 'NONE',  ( 30.73962218707677607, 22.33364281372847060, -6.802157773949823572 ) ) ;
#47401 = CARTESIAN_POINT ( 'NONE',  ( -5.049401038297874678, -19.05341960407617918, 54.79275706135234003 ) ) ;
#47403 = CARTESIAN_POINT ( 'NONE',  ( -8.224510206698948167, 14.34966873604960824, 75.41557627198102409 ) ) ;
#47402 = CARTESIAN_POINT ( 'NONE',  ( -18.62759615963255300, -10.81492255796106328, 24.16775706135235424 ) ) ;
#47404 = CARTESIAN_POINT ( 'NONE',  ( 19.05341960407611168, 5.049401038298154454, 83.95724293864766707 ) ) ;
#47406 = CARTESIAN_POINT ( 'NONE',  ( 16.46253265017146816, 9.564922557961045513, 51.66775706135233293 ) ) ;
#47405 = CARTESIAN_POINT ( 'NONE',  ( 12.14591786802327356, -12.06949235617739191, 40.62609039468567573 ) ) ;
#47407 = CARTESIAN_POINT ( 'NONE',  ( -15.80617190586768217, 15.72974639402176855, 68.12609039468567573 ) ) ;
#47408 = CARTESIAN_POINT ( 'NONE',  ( -16.53943276465976808, -0.05219959533934237506, 23.75109039468567929 ) ) ;
#47409 = CARTESIAN_POINT ( 'NONE',  ( 5.049401038298161559, -19.05341960407611168, 67.70724293864769550 ) ) ;
#47410 = CARTESIAN_POINT ( 'NONE',  ( -13.97604488694547697, 13.89961937509957934, 88.12609039468563310 ) ) ;
#47411 = CARTESIAN_POINT ( 'NONE',  ( -8.314922557961024197, 14.29746914071037800, 57.91775706135234714 ) ) ;
#47412 = CARTESIAN_POINT ( 'NONE',  ( 10.72451020669871369, 18.67979575497193778, 102.0844237280190185 ) ) ;
#47413 = CARTESIAN_POINT ( 'NONE',  ( -13.89961937509957401, -13.97604488694547875, 64.37609039468567573 ) ) ;
#47414 = CARTESIAN_POINT ( 'NONE',  ( 9.564922557960805705, 16.46253265017160317, 49.58224293864770260 ) ) ;
#47415 = CARTESIAN_POINT ( 'NONE',  ( 15.72974639402199770, -15.80617190586745480, 68.12390960531436690 ) ) ;
#47417 = CARTESIAN_POINT ( 'NONE',  ( -19.05341960407617563, 5.049401038297882671, 73.54275706135233293 ) ) ;
#47416 = CARTESIAN_POINT ( 'NONE',  ( -16.55341960407611168, -4.379528057220339221, 66.45724293864768129 ) ) ;
#47418 = CARTESIAN_POINT ( 'NONE',  ( -18.87255363501903105, -5.500000000000063061, 71.32513748171827217 ) ) ;
#47419 = CARTESIAN_POINT ( 'NONE',  ( -0.05219959533936034679, 19.03943276465977164, 42.50109039468566152 ) ) ;
#47420 = CARTESIAN_POINT ( 'NONE',  ( -8.224510206698735004, -14.34966873604973081, 99.58442372801900433 ) ) ;
#47421 = CARTESIAN_POINT ( 'NONE',  ( 16.55341960407611168, 4.379528057220329451, 63.95724293864770260 ) ) ;
#47423 = CARTESIAN_POINT ( 'NONE',  ( 27.73933785331498569, 2.768321779492822058E-14, 145.8750000027311842 ) ) ;
#47422 = CARTESIAN_POINT ( 'NONE',  ( -21.53943276465977519, -0.05219959533937600094, 98.75109039468568994 ) ) ;
#47424 = CARTESIAN_POINT ( 'NONE',  ( 10.72451020669898902, -18.67979575497178502, 92.91557627198103830 ) ) ;
#47425 = CARTESIAN_POINT ( 'NONE',  ( -16.51473224551069308, -9.474510206698971260, 61.66557627198103120 ) ) ;
#47426 = CARTESIAN_POINT ( 'NONE',  ( -5.823673210054431948, 21.52544592524334988, 72.70942372801901854 ) ) ;
#47427 = CARTESIAN_POINT ( 'NONE',  ( -19.03943276465977164, 0.05219959533909376836, 51.24890960531436690 ) ) ;
#47428 = ORIENTED_EDGE ( 'NONE', *, *, #196038, .F. ) ;
#47429 = CARTESIAN_POINT ( 'NONE',  ( -13.97604488694527625, -13.89961937509977652, 21.87390960531435979 ) ) ;
#47430 = CARTESIAN_POINT ( 'NONE',  ( 19.02544592524343514, -5.153800228976328945, 108.5405762719810383 ) ) ;
#47431 = CARTESIAN_POINT ( 'NONE',  ( -14.34966873604960291, -8.224510206698953496, 71.66557627198100988 ) ) ;
#47432 = CARTESIAN_POINT ( 'NONE',  ( -13.89961937509977652, 13.97604488694528158, 30.62390960531435269 ) ) ;
#47433 = CARTESIAN_POINT ( 'NONE',  ( 14.34966873604960469, 8.224510206698951720, 79.16557627198103830 ) ) ;
#47434 = CARTESIAN_POINT ( 'NONE',  ( 21.55341960407610458, 5.719274019375980345, 98.95724293864770971 ) ) ;
#47435 = CARTESIAN_POINT ( 'NONE',  ( -5.719274019375665041, -21.55341960407619695, 34.79275706135235424 ) ) ;
#47436 = DIRECTION ( 'NONE',  ( -0.7071067811865561215, -0.7071067811865389130, -0.000000000000000000 ) ) ;
#47437 = CARTESIAN_POINT ( 'NONE',  ( -4.379528057220086978, -16.55341960407618274, 54.79275706135235424 ) ) ;
#47438 = CARTESIAN_POINT ( 'NONE',  ( -10.72451020669898014, 18.67979575497178502, 85.41557627198102409 ) ) ;
#47439 = CARTESIAN_POINT ( 'NONE',  ( 16.46253265017146816, 9.564922557961045513, 21.66775706135233648 ) ) ;
#47440 = CARTESIAN_POINT ( 'NONE',  ( -13.97604488694527625, -13.89961937509977652, 101.8739096053143811 ) ) ;
#47441 = CARTESIAN_POINT ( 'NONE',  ( -18.62759615963255300, -10.81492255796106328, 39.16775706135235424 ) ) ;
#47442 = EDGE_CURVE ( 'NONE', #7679, #165187, #136569, .T. ) ;
#47443 = CARTESIAN_POINT ( 'NONE',  ( 21.53943276465977519, -0.05219959533907433946, 38.74890960531435979 ) ) ;
#47444 = CARTESIAN_POINT ( 'NONE',  ( 12.06949235617757843, -12.14591786802309237, 28.12390960531435979 ) ) ;
#47446 = CARTESIAN_POINT ( 'NONE',  ( -10.72451020669870658, -18.67979575497194134, 94.58442372801901854 ) ) ;
#47445 = CARTESIAN_POINT ( 'NONE',  ( -5.823673210054431948, 21.52544592524334988, 67.70942372801901854 ) ) ;
#47447 = CARTESIAN_POINT ( 'NONE',  ( 5.153800228976615827, -19.02544592524334988, 25.20942372801900433 ) ) ;
#47448 = CARTESIAN_POINT ( 'NONE',  ( -14.29746914071037622, -8.314922557961029526, 94.16775706135237556 ) ) ;
#47449 = CARTESIAN_POINT ( 'NONE',  ( -18.62759615963255300, -10.81492255796106328, 59.16775706135234714 ) ) ;
#47450 = CARTESIAN_POINT ( 'NONE',  ( 0.05219959533909260263, 19.03943276465977164, 39.99890960531436690 ) ) ;
#47451 = CARTESIAN_POINT ( 'NONE',  ( 5.153800228976615827, -19.02544592524334988, 25.20942372801900433 ) ) ;
#47452 = CARTESIAN_POINT ( 'NONE',  ( -10.72451020669898014, 18.67979575497178502, 25.41557627198103120 ) ) ;
#47453 = CARTESIAN_POINT ( 'NONE',  ( 10.72451020669898902, -18.67979575497178502, 112.9155762719810383 ) ) ;
#47454 = CARTESIAN_POINT ( 'NONE',  ( -18.62759615963270932, 10.81492255796079327, 80.83224293864769550 ) ) ;
#47455 = CARTESIAN_POINT ( 'NONE',  ( 16.55341960407618274, -4.379528057220086978, 36.04275706135234714 ) ) ;
#47457 = CARTESIAN_POINT ( 'NONE',  ( -21.53943276465977519, 0.05219959533907696930, 81.24890960531436690 ) ) ;
#47456 = FACE_OUTER_BOUND ( 'NONE', #157868, .T. ) ;
#47459 = CARTESIAN_POINT ( 'NONE',  ( -4.379528057220328563, 16.55341960407611168, 60.20724293864768839 ) ) ;
#47458 = CARTESIAN_POINT ( 'NONE',  ( -4.379528057220086978, -16.55341960407618274, 64.79275706135234714 ) ) ;
#47460 = CARTESIAN_POINT ( 'NONE',  ( -19.49401214000077331, 12.39993551617566858, 164.9999999999999716 ) ) ;
#47461 = CARTESIAN_POINT ( 'NONE',  ( 19.05341960407617918, -5.049401038297876454, 96.04275706135231871 ) ) ;
#47462 = CARTESIAN_POINT ( 'NONE',  ( -24.06132300323553252, 0.8180345313833771170, -54.40060964255544462 ) ) ;
#47463 = CARTESIAN_POINT ( 'NONE',  ( 12.14591786802327356, -12.06949235617739191, 35.62609039468568994 ) ) ;
#47464 = CARTESIAN_POINT ( 'NONE',  ( 18.67979575497178502, 10.72451020669898547, 109.1655762719810383 ) ) ;
#47465 = CARTESIAN_POINT ( 'NONE',  ( 15.80617190586746368, 15.72974639402197994, 74.37390960531436690 ) ) ;
#47466 = CARTESIAN_POINT ( 'NONE',  ( 0.05219959533907565091, 21.53943276465977519, 34.99890960531435979 ) ) ;
#47467 = CARTESIAN_POINT ( 'NONE',  ( 16.55341960407618274, -4.379528057220086978, 56.04275706135235424 ) ) ;
#47468 = CARTESIAN_POINT ( 'NONE',  ( -13.97604488694527625, -13.89961937509977652, 66.87390960531436690 ) ) ;
#47470 = CARTESIAN_POINT ( 'NONE',  ( 13.97604488694548053, -13.89961937509957401, 110.6260903946856615 ) ) ;
#47469 = CARTESIAN_POINT ( 'NONE',  ( 0.05219959533937995610, -21.53943276465977519, 45.00109039468568284 ) ) ;
#47471 = CARTESIAN_POINT ( 'NONE',  ( 10.81492255796078972, 18.62759615963270932, 29.58224293864769905 ) ) ;
#47472 = CARTESIAN_POINT ( 'NONE',  ( -13.89961937509957401, -13.97604488694547875, 29.37609039468565797 ) ) ;
#47473 = CARTESIAN_POINT ( 'NONE',  ( -12.06949235617739369, -12.14591786802326823, 44.37609039468567573 ) ) ;
#47474 = CARTESIAN_POINT ( 'NONE',  ( -19.02544592524342804, 5.153800228976336051, 101.0405762719810241 ) ) ;
#47475 = CARTESIAN_POINT ( 'NONE',  ( 10.81492255796078972, 18.62759615963270932, 109.5822429386476955 ) ) ;
#47476 = CARTESIAN_POINT ( 'NONE',  ( 0.05219959533909260263, 19.03943276465977164, 74.99890960531435269 ) ) ;
#47477 = CARTESIAN_POINT ( 'NONE',  ( -17.50000000000000355, 5.622605283950871780, 23.68792689403890606 ) ) ;
#47478 = CARTESIAN_POINT ( 'NONE',  ( 8.224510206698953496, -14.34966873604960469, 82.91557627198103830 ) ) ;
#47479 = CARTESIAN_POINT ( 'NONE',  ( -21.53943276465977519, 0.05219959533907696930, 21.24890960531436690 ) ) ;
#47480 = CARTESIAN_POINT ( 'NONE',  ( 19.03943276465977164, -0.05219959533909143690, 23.74890960531435269 ) ) ;
#47481 = CARTESIAN_POINT ( 'NONE',  ( 21.55341960407610458, 5.719274019375980345, 103.9572429386476813 ) ) ;
#47482 = CARTESIAN_POINT ( 'NONE',  ( 16.51473224551083163, -9.474510206698727899, 65.83442372801900433 ) ) ;
#47483 = CARTESIAN_POINT ( 'NONE',  ( -21.52544592524343514, 5.823673210054127303, 31.04057627198102409 ) ) ;
#47484 = CARTESIAN_POINT ( 'NONE',  ( -13.89961937509977652, 13.97604488694528158, 25.62390960531434558 ) ) ;
#47485 = CARTESIAN_POINT ( 'NONE',  ( -10.72451020669898014, 18.67979575497178502, 70.41557627198102409 ) ) ;
#47486 = AXIS2_PLACEMENT_3D ( 'NONE', #174394, #96527, #64227 ) ;
#47487 = CARTESIAN_POINT ( 'NONE',  ( 9.474510206698971260, -16.51473224551069308, 92.91557627198103830 ) ) ;
#47488 = CARTESIAN_POINT ( 'NONE',  ( -5.823673210054431948, 21.52544592524334988, 92.70942372801901854 ) ) ;
#47489 = CARTESIAN_POINT ( 'NONE',  ( -19.02544592524342804, 5.153800228976336051, 51.04057627198103120 ) ) ;
#47490 = CARTESIAN_POINT ( 'NONE',  ( -4.379528057220328563, 16.55341960407611168, 85.20724293864770971 ) ) ;
#47491 = CARTESIAN_POINT ( 'NONE',  ( 14.34966873604972726, -8.224510206698740333, 40.83442372801901854 ) ) ;
#47492 = CARTESIAN_POINT ( 'NONE',  ( 16.46253265017160672, -9.564922557960803928, 58.33224293864769550 ) ) ;
#47493 = CARTESIAN_POINT ( 'NONE',  ( -5.823673210054431948, 21.52544592524334988, 77.70942372801900433 ) ) ;
#47494 = EDGE_LOOP ( 'NONE', ( #149638, #5003, #60952, #27895 ) ) ;
#47495 = CARTESIAN_POINT ( 'NONE',  ( 19.02544592524334988, 5.153800228976608722, 26.45942372801899722 ) ) ;
#47496 = CARTESIAN_POINT ( 'NONE',  ( 16.51473224551083163, -9.474510206698727899, 35.83442372801899722 ) ) ;
#47497 = CARTESIAN_POINT ( 'NONE',  ( 21.55341960407619695, -5.719274019375665929, 31.04275706135234714 ) ) ;
#47498 = AXIS2_PLACEMENT_3D ( 'NONE', #165368, #168329, #59154 ) ;
#47499 = CARTESIAN_POINT ( 'NONE',  ( 20.43538597629129328, 20.43538597629121156, -64.92279855667830191 ) ) ;
#47500 = CARTESIAN_POINT ( 'NONE',  ( 0.05219959533936267826, -19.03943276465977164, 35.00109039468566863 ) ) ;
#47501 = CARTESIAN_POINT ( 'NONE',  ( 13.97604488694527802, 13.89961937509977652, 84.37390960531433848 ) ) ;
#47502 = CARTESIAN_POINT ( 'NONE',  ( 0.05219959533909260263, 19.03943276465977164, 69.99890960531435269 ) ) ;
#47503 = CARTESIAN_POINT ( 'NONE',  ( 8.224510206698953496, -14.34966873604960469, 27.91557627198103830 ) ) ;
#47505 = CARTESIAN_POINT ( 'NONE',  ( -0.05219959533937732626, 21.53943276465977519, 87.50109039468568994 ) ) ;
#47504 = CARTESIAN_POINT ( 'NONE',  ( 16.46253265017160672, -9.564922557960803928, 113.3322429386476955 ) ) ;
#47506 = CARTESIAN_POINT ( 'NONE',  ( 29.86685920354754487, 21.69954338932564752, -7.924999997268814766 ) ) ;
#47507 = CARTESIAN_POINT ( 'NONE',  ( 17.49999999999999645, 5.500000000000000888, 28.78230962303566542 ) ) ;
#47508 = CARTESIAN_POINT ( 'NONE',  ( -18.67979575497193778, 10.72451020669871902, 93.33442372801901854 ) ) ;
#47509 = CARTESIAN_POINT ( 'NONE',  ( 17.50000000000000000, 5.499999999999992895, 61.70309617465829177 ) ) ;
#47510 = CARTESIAN_POINT ( 'NONE',  ( 19.03943276465977164, -0.05219959533909143690, 98.74890960531436690 ) ) ;
#47511 = CARTESIAN_POINT ( 'NONE',  ( 34.46456012332993879, 1.775814316247266156, 89.78225565739066383 ) ) ;
#47512 = CARTESIAN_POINT ( 'NONE',  ( 12.14591786802327356, -12.06949235617739191, 45.62609039468567573 ) ) ;
#47513 = CARTESIAN_POINT ( 'NONE',  ( 5.823673210054125526, 21.52544592524343514, 74.79057627198105251 ) ) ;
#47514 = CARTESIAN_POINT ( 'NONE',  ( 16.52544592524342804, -4.483927247898539470, 23.54057627198102765 ) ) ;
#47516 = CARTESIAN_POINT ( 'NONE',  ( 16.51473224551069308, 9.474510206698969483, 94.16557627198103830 ) ) ;
#47515 = CARTESIAN_POINT ( 'NONE',  ( 16.52544592524342804, -4.483927247898539470, 113.5405762719810383 ) ) ;
#47517 = CARTESIAN_POINT ( 'NONE',  ( -15.80617190586768217, 15.72974639402176855, 113.1260903946856899 ) ) ;
#47518 = CARTESIAN_POINT ( 'NONE',  ( 0.05219959533910956823, 16.53943276465976808, 109.9989096053143527 ) ) ;
#47519 = CARTESIAN_POINT ( 'NONE',  ( 10.72451020669871369, 18.67979575497193778, 67.08442372801901854 ) ) ;
#47520 = CARTESIAN_POINT ( 'NONE',  ( -9.474510206698964154, 16.51473224551069663, 110.4155762719810383 ) ) ;
#47521 = CARTESIAN_POINT ( 'NONE',  ( -12.14591786802326823, 12.06949235617739902, 108.1260903946856757 ) ) ;
#47522 = CARTESIAN_POINT ( 'NONE',  ( -13.97604488694547697, 13.89961937509957934, 58.12609039468566863 ) ) ;
#47523 = CARTESIAN_POINT ( 'NONE',  ( -9.564922557961040184, 16.46253265017147172, 67.91775706135233293 ) ) ;
#47524 = CARTESIAN_POINT ( 'NONE',  ( -13.97604488694527625, -13.89961937509977652, 111.8739096053143243 ) ) ;
#47525 = CARTESIAN_POINT ( 'NONE',  ( 8.314922557960818139, 14.29746914071049879, 94.58224293864769550 ) ) ;
#47526 = CARTESIAN_POINT ( 'NONE',  ( -0.05219959533936034679, 19.03943276465977164, 57.50109039468566863 ) ) ;
#47527 = AXIS2_PLACEMENT_3D ( 'NONE', #68177, #53005, #113674 ) ;
#47528 = CARTESIAN_POINT ( 'NONE',  ( 5.049401038298161559, -19.05341960407611168, 82.70724293864770971 ) ) ;
#47529 = CARTESIAN_POINT ( 'NONE',  ( 12.14591786802309770, 12.06949235617756955, 64.37390960531435269 ) ) ;
#47530 = CARTESIAN_POINT ( 'NONE',  ( -19.02544592524334988, -5.153800228976617603, 93.95942372801900433 ) ) ;
#47531 = CARTESIAN_POINT ( 'NONE',  ( -21.55341960407610458, -5.719274019375992779, 51.45724293864770260 ) ) ;
#47532 = EDGE_LOOP ( 'NONE', ( #56147, #187469, #49026, #38749, #75582 ) ) ;
#47533 = EDGE_CURVE ( 'NONE', #56239, #183247, #7784, .T. ) ;
#47534 = CARTESIAN_POINT ( 'NONE',  ( 12.14591786802309770, 12.06949235617756955, 114.3739096053143527 ) ) ;
#47535 = CARTESIAN_POINT ( 'NONE',  ( -16.81555441253549432, -7.025013491695499823, 29.36314554665745646 ) ) ;
#47537 = CARTESIAN_POINT ( 'NONE',  ( -21.55341960407610458, -5.719274019375992779, 71.45724293864769550 ) ) ;
#47536 = CARTESIAN_POINT ( 'NONE',  ( 13.97604488694527802, 13.89961937509977652, 69.37390960531436690 ) ) ;
#47539 = CARTESIAN_POINT ( 'NONE',  ( -16.46253265017160317, 9.564922557960807481, 75.83224293864769550 ) ) ;
#47538 = CARTESIAN_POINT ( 'NONE',  ( 16.55341960407618274, -4.379528057220086978, 91.04275706135236135 ) ) ;
#47540 = CARTESIAN_POINT ( 'NONE',  ( -9.564922557961040184, 16.46253265017147172, 62.91775706135233293 ) ) ;
#47541 = CARTESIAN_POINT ( 'NONE',  ( -15.80617190586768217, 15.72974639402176855, 83.12609039468568994 ) ) ;
#47542 = CARTESIAN_POINT ( 'NONE',  ( 5.823673210054125526, 21.52544592524343514, 64.79057627198103830 ) ) ;
#47543 = CARTESIAN_POINT ( 'NONE',  ( 5.823673210054125526, 21.52544592524343514, 24.79057627198103120 ) ) ;
#47544 = CARTESIAN_POINT ( 'NONE',  ( 19.03943276465977164, -0.05219959533909143690, 38.74890960531436690 ) ) ;
#47545 = CARTESIAN_POINT ( 'NONE',  ( 12.14591786802327356, -12.06949235617739191, 100.6260903946857184 ) ) ;
#47546 = CARTESIAN_POINT ( 'NONE',  ( -9.474510206698964154, 16.51473224551069663, 55.41557627198103120 ) ) ;
#47547 = CARTESIAN_POINT ( 'NONE',  ( 12.06949235617739724, 12.14591786802326823, 26.87609039468567218 ) ) ;
#47548 = CARTESIAN_POINT ( 'NONE',  ( 16.46253265017146816, 9.564922557961045513, 81.66775706135233293 ) ) ;
#47549 = CARTESIAN_POINT ( 'NONE',  ( 21.53943276465977519, 0.05219959533937863772, 96.25109039468568994 ) ) ;
#47550 = CARTESIAN_POINT ( 'NONE',  ( 14.34966873604960469, 8.224510206698951720, 54.16557627198103120 ) ) ;
#47551 = CARTESIAN_POINT ( 'NONE',  ( -21.55341960407610458, -5.719274019375992779, 101.4572429386476955 ) ) ;
#47552 = CARTESIAN_POINT ( 'NONE',  ( 10.72451020669898902, -18.67979575497178502, 102.9155762719810383 ) ) ;
#47553 = CARTESIAN_POINT ( 'NONE',  ( 28.79475375365563750, 9.355982642739540722, 149.0843446568999866 ) ) ;
#47554 = CARTESIAN_POINT ( 'NONE',  ( 5.823673210054125526, 21.52544592524343514, 49.79057627198102409 ) ) ;
#47555 = CARTESIAN_POINT ( 'NONE',  ( -8.224510206698735004, -14.34966873604973081, 74.58442372801901854 ) ) ;
#47556 = CARTESIAN_POINT ( 'NONE',  ( -12.06949235617756955, 12.14591786802309770, 90.62390960531436690 ) ) ;
#47557 = CARTESIAN_POINT ( 'NONE',  ( 13.89961937509977652, -13.97604488694527269, 43.12390960531434558 ) ) ;
#47558 = CARTESIAN_POINT ( 'NONE',  ( -22.72061570927963459, -33.65877872499205381, -17.91763856381928477 ) ) ;
#47559 = CARTESIAN_POINT ( 'NONE',  ( 0.05219959533934541429, -16.53943276465976808, 110.0010903946856757 ) ) ;
#47560 = CARTESIAN_POINT ( 'NONE',  ( -15.80617190586768217, 15.72974639402176855, 38.12609039468567573 ) ) ;
#47561 = CARTESIAN_POINT ( 'NONE',  ( -19.02544592524342804, 5.153800228976336051, 91.04057627198100988 ) ) ;
#47562 = CARTESIAN_POINT ( 'NONE',  ( 15.72974639402176855, 15.80617190586768217, 61.87609039468568284 ) ) ;
#47563 = CARTESIAN_POINT ( 'NONE',  ( 17.50000000000000000, -5.499999999999992895, 51.21769037696435589 ) ) ;
#47564 = CARTESIAN_POINT ( 'NONE',  ( -11.45643923738960446, -4.999999999999992895, -15.00000000000000000 ) ) ;
#47565 =( BOUNDED_CURVE ( )  B_SPLINE_CURVE ( 2, ( #88803, #150496, #153453, #123107, #14951, #11993, #73656, #152461, #90777, #107934, #45293 ),
 .UNSPECIFIED., .F., .T. ) 
 B_SPLINE_CURVE_WITH_KNOTS ( ( 3, 2, 2, 2, 2, 3 ),
 ( 0.3000000000000030420, 0.3200000000000030598, 0.3400000000000030775, 0.3600000000000030953, 0.3800000000000031131, 0.4000000000000031308 ),
 .UNSPECIFIED. ) 
 CURVE ( )  GEOMETRIC_REPRESENTATION_ITEM ( )  RATIONAL_B_SPLINE_CURVE ( ( 0.9999999999999925615, 0.9510565162951609697, 1.000000000000000000, 0.9510565162951535312, 1.000000000000000000, 0.9510565162951535312, 1.000000000000000000, 0.9510565162951535312, 1.000000000000000000, 0.9510565162951458706, 1.000000000000007550 ) ) 
 REPRESENTATION_ITEM ( '' )  );
#47566 = ORIENTED_EDGE ( 'NONE', *, *, #19851, .T. ) ;
#47567 = CARTESIAN_POINT ( 'NONE',  ( -10.81492255796105439, 18.62759615963255655, 52.91775706135235424 ) ) ;
#47569 = LINE ( 'NONE', #173900, #156416 ) ;
#47568 = CARTESIAN_POINT ( 'NONE',  ( 19.05341960407611168, 5.049401038298154454, 53.95724293864770260 ) ) ;
#47570 = CARTESIAN_POINT ( 'NONE',  ( -13.89961937509977652, 13.97604488694528158, 85.62390960531433848 ) ) ;
#47571 = CARTESIAN_POINT ( 'NONE',  ( -5.153800228976607833, 19.02544592524334988, 72.70942372801900433 ) ) ;
#47572 = CARTESIAN_POINT ( 'NONE',  ( 18.62759615963255655, 10.81492255796105972, 46.66775706135234714 ) ) ;
#47573 = CARTESIAN_POINT ( 'NONE',  ( 13.97604488694548053, -13.89961937509957401, 65.62609039468567573 ) ) ;
#47574 = CARTESIAN_POINT ( 'NONE',  ( 9.564922557960805705, 16.46253265017160317, 39.58224293864768839 ) ) ;
#47575 = CARTESIAN_POINT ( 'NONE',  ( 8.224510206698742110, 14.34966873604972548, 102.0844237280190185 ) ) ;
#47576 = CARTESIAN_POINT ( 'NONE',  ( 13.89961937509957401, 13.97604488694547697, 71.87609039468567573 ) ) ;
#47577 = CARTESIAN_POINT ( 'NONE',  ( 4.483927247898545687, 16.52544592524342804, 29.79057627198102409 ) ) ;
#47578 = CARTESIAN_POINT ( 'NONE',  ( -13.89961937509957401, -13.97604488694547875, 44.37609039468566863 ) ) ;
#47579 = CARTESIAN_POINT ( 'NONE',  ( 18.62759615963255655, 10.81492255796105972, 111.6677570613523613 ) ) ;
#47580 = CARTESIAN_POINT ( 'NONE',  ( 16.46253265017146816, 9.564922557961045513, 31.66775706135232937 ) ) ;
#47581 = CARTESIAN_POINT ( 'NONE',  ( 19.05341960407611168, 5.049401038298154454, 33.95724293864769550 ) ) ;
#47582 = CARTESIAN_POINT ( 'NONE',  ( -5.719274019375665041, -21.55341960407619695, 94.79275706135234714 ) ) ;
#47583 = CARTESIAN_POINT ( 'NONE',  ( -14.29746914071037622, -8.314922557961029526, 39.16775706135235424 ) ) ;
#47584 = CARTESIAN_POINT ( 'NONE',  ( -5.153800228976328057, -19.02544592524343514, 92.29057627198099567 ) ) ;
#47585 = CARTESIAN_POINT ( 'NONE',  ( -27.74069374691375955, 6.311165852667651066, 163.4895129000220209 ) ) ;
#47586 = CARTESIAN_POINT ( 'NONE',  ( -5.049401038298153566, 19.05341960407611168, 75.20724293864769550 ) ) ;
#47587 = CARTESIAN_POINT ( 'NONE',  ( 69.65682714487590488, -71.74905178543389184, -4.999999999999999112 ) ) ;
#47588 = CARTESIAN_POINT ( 'NONE',  ( 13.97604488694548053, -13.89961937509957401, 90.62609039468567573 ) ) ;
#47589 = CARTESIAN_POINT ( 'NONE',  ( 9.564922557960805705, 16.46253265017160317, 104.5822429386476955 ) ) ;
#47590 = CARTESIAN_POINT ( 'NONE',  ( -0.05219959533937732626, 21.53943276465977519, 97.50109039468567573 ) ) ;
#47591 = CARTESIAN_POINT ( 'NONE',  ( 0.05219959533910956823, 16.53943276465976808, 94.99890960531436690 ) ) ;
#47592 = CARTESIAN_POINT ( 'NONE',  ( -19.03943276465977164, 0.05219959533909376836, 26.24890960531435624 ) ) ;
#47593 = CARTESIAN_POINT ( 'NONE',  ( -21.53943276465977519, 0.05219959533907696930, 56.24890960531436690 ) ) ;
#47594 = CARTESIAN_POINT ( 'NONE',  ( 18.62759615963271287, -10.81492255796078972, 38.33224293864768839 ) ) ;
#47595 = CARTESIAN_POINT ( 'NONE',  ( -0.05219959533909027116, -19.03943276465977164, 27.49890960531435624 ) ) ;
#47596 = CARTESIAN_POINT ( 'NONE',  ( 17.50000000000000000, -5.500000000000000888, 120.0000000000000142 ) ) ;
#47597 = CARTESIAN_POINT ( 'NONE',  ( 19.05341960407617918, -5.049401038297876454, 61.04275706135232582 ) ) ;
#47598 = CARTESIAN_POINT ( 'NONE',  ( -4.379528057220328563, 16.55341960407611168, 45.20724293864769550 ) ) ;
#47599 = CARTESIAN_POINT ( 'NONE',  ( 16.51473224551069308, 9.474510206698969483, 114.1655762719810241 ) ) ;
#47600 = CARTESIAN_POINT ( 'NONE',  ( -18.62759615963255300, -10.81492255796106328, 84.16775706135234714 ) ) ;
#47601 = CARTESIAN_POINT ( 'NONE',  ( 18.62759615963271287, -10.81492255796078972, 68.33224293864769550 ) ) ;
#47602 = CARTESIAN_POINT ( 'NONE',  ( 10.72451020669871369, 18.67979575497193778, 47.08442372801901854 ) ) ;
#47603 = CARTESIAN_POINT ( 'NONE',  ( -10.72451020669898014, 18.67979575497178502, 95.41557627198102409 ) ) ;
#47604 = CARTESIAN_POINT ( 'NONE',  ( 18.67979575497194134, -10.72451020669871369, 45.83442372801901854 ) ) ;
#47605 = CARTESIAN_POINT ( 'NONE',  ( -13.97604488694527625, -13.89961937509977652, 26.87390960531434558 ) ) ;
#47606 = CARTESIAN_POINT ( 'NONE',  ( -0.05219959533909027116, -19.03943276465977164, 77.49890960531435269 ) ) ;
#47607 = CARTESIAN_POINT ( 'NONE',  ( -12.14591786802326823, 12.06949235617739902, 78.12609039468570415 ) ) ;
#47608 = CARTESIAN_POINT ( 'NONE',  ( 4.379528057220339221, -16.55341960407611168, 102.7072429386476955 ) ) ;
#47609 = FACE_OUTER_BOUND ( 'NONE', #188300, .T. ) ;
#47610 = CARTESIAN_POINT ( 'NONE',  ( -16.52544592524342804, 4.483927247898546575, 51.04057627198103120 ) ) ;
#47611 = CARTESIAN_POINT ( 'NONE',  ( 4.379528057220092307, 16.55341960407617563, 107.2927570613523471 ) ) ;
#47612 = CARTESIAN_POINT ( 'NONE',  ( -16.51473224551069308, -9.474510206698971260, 71.66557627198102409 ) ) ;
#47613 = CARTESIAN_POINT ( 'NONE',  ( 19.05341960407611168, 5.049401038298154454, 33.95724293864769550 ) ) ;
#47614 = CARTESIAN_POINT ( 'NONE',  ( 21.52544592524344225, -5.823673210054117533, 48.54057627198103120 ) ) ;
#47615 = CARTESIAN_POINT ( 'NONE',  ( 13.89961937509957401, 13.97604488694547697, 36.87609039468565442 ) ) ;
#47617 = CARTESIAN_POINT ( 'NONE',  ( 16.53943276465976808, -0.05219959533910856209, 53.74890960531437401 ) ) ;
#47616 = FACE_OUTER_BOUND ( 'NONE', #98820, .T. ) ;
#47618 = CARTESIAN_POINT ( 'NONE',  ( 21.53943276465977519, -0.05219959533907433946, 28.74890960531435624 ) ) ;
#47619 = CARTESIAN_POINT ( 'NONE',  ( 18.67979575497194134, -10.72451020669871369, 65.83442372801900433 ) ) ;
#47620 = DIRECTION ( 'NONE',  ( 0.7071067811865414665, -0.7071067811865536790, -0.000000000000000000 ) ) ;
#47621 = CARTESIAN_POINT ( 'NONE',  ( 14.29746914071037800, 8.314922557961029526, 66.66775706135234714 ) ) ;
#47622 = CARTESIAN_POINT ( 'NONE',  ( 13.89961937509957401, 13.97604488694547697, 56.87609039468564731 ) ) ;
#47623 = CARTESIAN_POINT ( 'NONE',  ( -16.55341960407611168, -4.379528057220339221, 41.45724293864769550 ) ) ;
#47624 = DIRECTION ( 'NONE',  ( 0.000000000000000000, -1.000000000000000000, -0.000000000000000000 ) ) ;
#47625 = CARTESIAN_POINT ( 'NONE',  ( 16.55341960407611168, 4.379528057220329451, 28.95724293864769905 ) ) ;
#47626 = CARTESIAN_POINT ( 'NONE',  ( 16.46253265017160672, -9.564922557960803928, 38.33224293864768839 ) ) ;
#47627 = CARTESIAN_POINT ( 'NONE',  ( -19.05341960407611168, -5.049401038298163336, 56.45724293864768129 ) ) ;
#47628 = CARTESIAN_POINT ( 'NONE',  ( -8.224510206698948167, 14.34966873604960824, 115.4155762719810241 ) ) ;
#47629 = CARTESIAN_POINT ( 'NONE',  ( 18.67979575497194134, -10.72451020669871369, 35.83442372801901143 ) ) ;
#47630 = CARTESIAN_POINT ( 'NONE',  ( -19.03943276465977164, 0.05219959533909376836, 56.24890960531435979 ) ) ;
#47631 = DIRECTION ( 'NONE',  ( 0.000000000000000000, 0.000000000000000000, -1.000000000000000000 ) ) ;
#47632 = CARTESIAN_POINT ( 'NONE',  ( 13.89961937509977652, -13.97604488694527269, 48.12390960531435979 ) ) ;
#47633 = EDGE_CURVE ( 'NONE', #177280, #143210, #13788, .T. ) ;
#47634 = CARTESIAN_POINT ( 'NONE',  ( -5.719274019375978568, 21.55341960407610458, 35.20724293864768839 ) ) ;
#47636 = CARTESIAN_POINT ( 'NONE',  ( 4.379528057220339221, -16.55341960407611168, 112.7072429386476955 ) ) ;
#47635 = CARTESIAN_POINT ( 'NONE',  ( 5.823673210054444382, -21.52544592524334988, 55.20942372801902565 ) ) ;
#47637 = CARTESIAN_POINT ( 'NONE',  ( -21.53943276465977519, 0.05219959533907696930, 31.24890960531435979 ) ) ;
#47638 = B_SPLINE_CURVE_WITH_KNOTS ( 'NONE', 3,
 ( #34471, #65790, #48657, #64809, #185168, #33479, #127459, #173989, #31489, #189165, #94139, #50637, #112299, #124485, #95137, #156826 ),
 .UNSPECIFIED., .F., .F.,
 ( 4, 2, 2, 2, 2, 2, 2, 4 ),
 ( 4.336808689942017736E-19, 0.005088736175617444152, 0.006360920219521812996, 0.007633104263426180106, 0.01017747235123490218, 0.01526620852685233766, 0.01781057661466104933, 0.02035494470246975926 ),
 .UNSPECIFIED. ) ;
#47639 = CARTESIAN_POINT ( 'NONE',  ( 12.06949235617739724, 12.14591786802326823, 96.87609039468568994 ) ) ;
#47640 = CARTESIAN_POINT ( 'NONE',  ( 21.52544592524334988, 5.823673210054432836, 111.4594237280190328 ) ) ;
#47641 = VECTOR ( 'NONE', #21129, 1000.000000000000000 ) ;
#47642 = CARTESIAN_POINT ( 'NONE',  ( -8.314922557961024197, 14.29746914071037800, 62.91775706135236135 ) ) ;
#47643 = CARTESIAN_POINT ( 'NONE',  ( 0.05219959533909260263, 19.03943276465977164, 109.9989096053143669 ) ) ;
#47644 = EDGE_CURVE ( 'NONE', #22185, #126159, #43313, .T. ) ;
#47645 = CARTESIAN_POINT ( 'NONE',  ( -14.29746914071037622, -8.314922557961029526, 49.16775706135234003 ) ) ;
#47646 = CARTESIAN_POINT ( 'NONE',  ( 12.14591786802327356, -12.06949235617739191, 25.62609039468567929 ) ) ;
#47647 = CARTESIAN_POINT ( 'NONE',  ( 12.06949235617739724, 12.14591786802326823, 96.87609039468568994 ) ) ;
#47648 = CARTESIAN_POINT ( 'NONE',  ( 5.719274019375673035, 21.55341960407619339, 52.29275706135236135 ) ) ;
#47649 = CARTESIAN_POINT ( 'NONE',  ( -16.55341960407617563, 4.379528057220093196, 28.54275706135234358 ) ) ;
#47650 = CARTESIAN_POINT ( 'NONE',  ( 18.67979575497178502, 10.72451020669898547, 114.1655762719810383 ) ) ;
#47651 = CARTESIAN_POINT ( 'NONE',  ( 4.379528057220092307, 16.55341960407617563, 22.29275706135235069 ) ) ;
#47652 = CARTESIAN_POINT ( 'NONE',  ( -12.14591786802326823, 12.06949235617739902, 88.12609039468570415 ) ) ;
#47653 = DIRECTION ( 'NONE',  ( -0.000000000000000000, 0.000000000000000000, 1.000000000000000000 ) ) ;
#47654 = CARTESIAN_POINT ( 'NONE',  ( 21.53943276465977519, 0.05219959533937863772, 86.25109039468568994 ) ) ;
#47655 = CARTESIAN_POINT ( 'NONE',  ( -16.51473224551082808, 9.474510206698731452, 83.33442372801899012 ) ) ;
#47656 = CARTESIAN_POINT ( 'NONE',  ( -12.14591786802309592, -12.06949235617757132, 41.87390960531435979 ) ) ;
#47657 = CARTESIAN_POINT ( 'NONE',  ( -0.05219959533910754901, -16.53943276465976808, 42.49890960531435979 ) ) ;
#47658 = CARTESIAN_POINT ( 'NONE',  ( 4.379528057220339221, -16.55341960407611168, 112.7072429386476955 ) ) ;
#47660 = CARTESIAN_POINT ( 'NONE',  ( 2.500000000000000000, 0.000000000000000000, 0.000000000000000000 ) ) ;
#47659 = CARTESIAN_POINT ( 'NONE',  ( 0.05219959533936267826, -19.03943276465977164, 45.00109039468566863 ) ) ;
#47661 = CARTESIAN_POINT ( 'NONE',  ( 18.62759615963255655, 10.81492255796105972, 51.66775706135234714 ) ) ;
#47662 = CARTESIAN_POINT ( 'NONE',  ( -9.474510206698720793, -16.51473224551083518, 104.5844237280190043 ) ) ;
#47663 = CARTESIAN_POINT ( 'NONE',  ( 9.474510206698971260, -16.51473224551069308, 107.9155762719810383 ) ) ;
#47664 = CARTESIAN_POINT ( 'NONE',  ( 18.62759615963271287, -10.81492255796078972, 53.33224293864769550 ) ) ;
#47665 = CARTESIAN_POINT ( 'NONE',  ( -5.049401038297874678, -19.05341960407617918, 94.79275706135230450 ) ) ;
#47666 = CARTESIAN_POINT ( 'NONE',  ( 5.153800228976335163, 19.02544592524342804, 89.79057627198102409 ) ) ;
#47667 = CARTESIAN_POINT ( 'NONE',  ( 15.80617190586746368, 15.72974639402197994, 54.37390960531435979 ) ) ;
#47668 = CARTESIAN_POINT ( 'NONE',  ( 12.06949235617757843, -12.14591786802309237, 113.1239096053143953 ) ) ;
#47669 = CARTESIAN_POINT ( 'NONE',  ( 9.564922557960805705, 16.46253265017160317, 64.58224293864769550 ) ) ;
#47670 = CARTESIAN_POINT ( 'NONE',  ( -19.03943276465977164, 0.05219959533909376836, 26.24890960531435624 ) ) ;
#47672 = CARTESIAN_POINT ( 'NONE',  ( -21.52544592524334988, -5.823673210054445271, 33.95942372801901143 ) ) ;
#47671 = AXIS2_PLACEMENT_3D ( 'NONE', #33297, #45482, #14142 ) ;
#47673 = CARTESIAN_POINT ( 'NONE',  ( 15.80617190586769283, -15.72974639402175789, 85.62609039468568994 ) ) ;
#47674 = CARTESIAN_POINT ( 'NONE',  ( 8.314922557961029526, -14.29746914071037800, 90.41775706135236135 ) ) ;
#47675 = CARTESIAN_POINT ( 'NONE',  ( -15.80617190586768217, 15.72974639402176855, 28.12609039468568284 ) ) ;
#47676 = CARTESIAN_POINT ( 'NONE',  ( -5.823673210054431948, 21.52544592524334988, 42.70942372801901854 ) ) ;
#47678 = CARTESIAN_POINT ( 'NONE',  ( -0.05219959533909027116, -19.03943276465977164, 72.49890960531435269 ) ) ;
#47677 = CARTESIAN_POINT ( 'NONE',  ( -0.05219959533936034679, 19.03943276465977164, 62.50109039468566863 ) ) ;
#47679 = CARTESIAN_POINT ( 'NONE',  ( -18.62759615963255300, -10.81492255796106328, 84.16775706135234714 ) ) ;
#47680 = EDGE_CURVE ( 'NONE', #35288, #198944, #153126, .T. ) ;
#47681 = CARTESIAN_POINT ( 'NONE',  ( -0.05219959533907301413, -21.53943276465977519, 87.49890960531436690 ) ) ;
#47682 = CARTESIAN_POINT ( 'NONE',  ( -14.34966873604960291, -8.224510206698953496, 66.66557627198102409 ) ) ;
#47683 = CARTESIAN_POINT ( 'NONE',  ( -5.823673210054431948, 21.52544592524334988, 102.7094237280190185 ) ) ;
#47684 = CARTESIAN_POINT ( 'NONE',  ( -16.55341960407611168, -4.379528057220339221, 81.45724293864769550 ) ) ;
#47685 = CARTESIAN_POINT ( 'NONE',  ( 0.05219959533909260263, 19.03943276465977164, 34.99890960531435979 ) ) ;
#47686 = CARTESIAN_POINT ( 'NONE',  ( -16.51473224551082808, 9.474510206698731452, 73.33442372801900433 ) ) ;
#47687 = CARTESIAN_POINT ( 'NONE',  ( 4.483927247898545687, 16.52544592524342804, 29.79057627198102409 ) ) ;
#47688 = CARTESIAN_POINT ( 'NONE',  ( 18.67979575497194134, -10.72451020669871369, 90.83442372801901854 ) ) ;
#47689 = CARTESIAN_POINT ( 'NONE',  ( 19.03943276465977164, -0.05219959533909143690, 93.74890960531435269 ) ) ;
#47690 = CARTESIAN_POINT ( 'NONE',  ( -0.05219959533936034679, 19.03943276465977164, 62.50109039468566863 ) ) ;
#47691 = CARTESIAN_POINT ( 'NONE',  ( 18.67979575497178502, 10.72451020669898547, 64.16557627198102409 ) ) ;
#47692 = CARTESIAN_POINT ( 'NONE',  ( 5.823673210054125526, 21.52544592524343514, 114.7905762719810383 ) ) ;
#47693 = CARTESIAN_POINT ( 'NONE',  ( 5.153800228976615827, -19.02544592524334988, 105.2094237280190185 ) ) ;
#47694 = CARTESIAN_POINT ( 'NONE',  ( -16.52544592524335698, -4.483927247898792601, 78.95942372801901854 ) ) ;
#47696 = CARTESIAN_POINT ( 'NONE',  ( -18.62759615963255300, -10.81492255796106328, 19.16775706135234714 ) ) ;
#47695 = FACE_OUTER_BOUND ( 'NONE', #145024, .T. ) ;
#47697 = CARTESIAN_POINT ( 'NONE',  ( 16.55341960407611168, 4.379528057220329451, 98.95724293864770971 ) ) ;
#47698 = CARTESIAN_POINT ( 'NONE',  ( -5.950531402560715689E-15, 38.81732327939063509, -7.624999997268814056 ) ) ;
#47699 = CARTESIAN_POINT ( 'NONE',  ( 16.55341960407618274, -4.379528057220086978, 51.04275706135234714 ) ) ;
#47700 = CARTESIAN_POINT ( 'NONE',  ( 5.719274019375991003, -21.55341960407610458, 67.70724293864769550 ) ) ;
#47701 = CARTESIAN_POINT ( 'NONE',  ( -0.05219959533934338120, 16.53943276465976808, 107.5010903946856899 ) ) ;
#47702 = CARTESIAN_POINT ( 'NONE',  ( -14.34966873604972548, 8.224510206698743886, 33.33442372801900433 ) ) ;
#47703 = CARTESIAN_POINT ( 'NONE',  ( 19.03943276465977164, -0.05219959533909143690, 28.74890960531435624 ) ) ;
#47704 = CARTESIAN_POINT ( 'NONE',  ( 4.379528057220092307, 16.55341960407617563, 82.29275706135234714 ) ) ;
#47705 = CARTESIAN_POINT ( 'NONE',  ( -13.89961937509957401, -13.97604488694547875, 69.37609039468564731 ) ) ;
#47706 = CARTESIAN_POINT ( 'NONE',  ( 5.719274019375991003, -21.55341960407610458, 77.70724293864770971 ) ) ;
#47707 = CARTESIAN_POINT ( 'NONE',  ( 12.06949235617739724, 12.14591786802326823, 96.87609039468568994 ) ) ;
#47708 = CARTESIAN_POINT ( 'NONE',  ( 5.719274019375673035, 21.55341960407619339, 87.29275706135236135 ) ) ;
#47709 = CARTESIAN_POINT ( 'NONE',  ( -0.05219959533907301413, -21.53943276465977519, 62.49890960531436690 ) ) ;
#47710 = CARTESIAN_POINT ( 'NONE',  ( 21.55341960407610458, 5.719274019375980345, 48.95724293864770971 ) ) ;
#47711 = ORIENTED_EDGE ( 'NONE', *, *, #82905, .T. ) ;
#47712 = CARTESIAN_POINT ( 'NONE',  ( -16.53943276465976808, -0.05219959533934237506, 83.75109039468568994 ) ) ;
#47713 = CARTESIAN_POINT ( 'NONE',  ( 5.719274019375991003, -21.55341960407610458, 42.70724293864770260 ) ) ;
#47714 = ORIENTED_EDGE ( 'NONE', *, *, #168500, .F. ) ;
#47715 = CARTESIAN_POINT ( 'NONE',  ( 19.02544592524343514, -5.153800228976328945, 113.5405762719810241 ) ) ;
#47716 = CARTESIAN_POINT ( 'NONE',  ( -19.02544592524342804, 5.153800228976336051, 31.04057627198102409 ) ) ;
#47717 = CARTESIAN_POINT ( 'NONE',  ( 0.05219959533907565091, 21.53943276465977519, 64.99890960531435269 ) ) ;
#47718 = CARTESIAN_POINT ( 'NONE',  ( -4.379528057220086978, -16.55341960407618274, 99.79275706135234714 ) ) ;
#47719 = CARTESIAN_POINT ( 'NONE',  ( -10.81492255796105439, 18.62759615963255655, 42.91775706135235424 ) ) ;
#47720 = CARTESIAN_POINT ( 'NONE',  ( -19.03943276465977164, -0.05219959533935918106, 108.7510903946856615 ) ) ;
#47721 = CARTESIAN_POINT ( 'NONE',  ( -16.51473224551069308, -9.474510206698971260, 21.66557627198102765 ) ) ;
#47722 = CARTESIAN_POINT ( 'NONE',  ( -12.06949235617739369, -12.14591786802326823, 19.37609039468568639 ) ) ;
#47723 = CARTESIAN_POINT ( 'NONE',  ( 19.03943276465977164, -0.05219959533909143690, 43.74890960531435979 ) ) ;
#47724 = CARTESIAN_POINT ( 'NONE',  ( -8.906447517083053711, -27.41122689804191026, 142.4000000000000057 ) ) ;
#47725 = CARTESIAN_POINT ( 'NONE',  ( 9.564922557960805705, 16.46253265017160317, 89.58224293864769550 ) ) ;
#47726 = CARTESIAN_POINT ( 'NONE',  ( 8.224510206698742110, 14.34966873604972548, 82.08442372801901854 ) ) ;
#47727 = CARTESIAN_POINT ( 'NONE',  ( 9.564922557961047289, -16.46253265017146816, 75.41775706135234714 ) ) ;
#47728 = CARTESIAN_POINT ( 'NONE',  ( -5.049401038297874678, -19.05341960407617918, 19.79275706135233293 ) ) ;
#47729 = CARTESIAN_POINT ( 'NONE',  ( -0.05219959533907301413, -21.53943276465977519, 67.49890960531436690 ) ) ;
#47730 = CARTESIAN_POINT ( 'NONE',  ( -8.314922557961024197, 14.29746914071037800, 82.91775706135234714 ) ) ;
#47731 = CARTESIAN_POINT ( 'NONE',  ( -19.03943276465977164, -0.05219959533935918106, 78.75109039468567573 ) ) ;
#47732 = CARTESIAN_POINT ( 'NONE',  ( 9.474510206698971260, -16.51473224551069308, 42.91557627198103120 ) ) ;
#47733 = CARTESIAN_POINT ( 'NONE',  ( 16.46253265017160672, -9.564922557960803928, 78.33224293864769550 ) ) ;
#47734 = CARTESIAN_POINT ( 'NONE',  ( -21.55341960407619339, 5.719274019375674811, 53.54275706135234714 ) ) ;
#47735 = CARTESIAN_POINT ( 'NONE',  ( 9.474510206698971260, -16.51473224551069308, 47.91557627198102409 ) ) ;
#47736 = CARTESIAN_POINT ( 'NONE',  ( 19.02544592524334988, 5.153800228976608722, 76.45942372801897591 ) ) ;
#47737 = CARTESIAN_POINT ( 'NONE',  ( 26.62494319856317304, -7.396441074661128212, 168.1134502243652094 ) ) ;
#47738 = CARTESIAN_POINT ( 'NONE',  ( -9.474510206698964154, 16.51473224551069663, 110.4155762719810383 ) ) ;
#47739 = CARTESIAN_POINT ( 'NONE',  ( 4.483927247898545687, 16.52544592524342804, 59.79057627198103120 ) ) ;
#47740 = CARTESIAN_POINT ( 'NONE',  ( 18.67979575497178502, 10.72451020669898547, 54.16557627198103120 ) ) ;
#47741 = CARTESIAN_POINT ( 'NONE',  ( -3.660253528765646358, -6.551653823223124284, 1.589185716900144207 ) ) ;
#47742 = CARTESIAN_POINT ( 'NONE',  ( 9.474510206698729675, 16.51473224551082808, 42.08442372801900433 ) ) ;
#47743 = CARTESIAN_POINT ( 'NONE',  ( 21.83922654085338877, -7.858455564366274793, 172.8813051029758299 ) ) ;
#47745 = CARTESIAN_POINT ( 'NONE',  ( 9.564922557960805705, 16.46253265017160317, 74.58224293864769550 ) ) ;
#47744 = CARTESIAN_POINT ( 'NONE',  ( 19.03943276465977164, -0.05219959533909143690, 63.74890960531435979 ) ) ;
#47746 = CARTESIAN_POINT ( 'NONE',  ( -4.483927247898782831, 16.52544592524335698, 47.70942372801902565 ) ) ;
#47747 = CARTESIAN_POINT ( 'NONE',  ( -18.09918380851993192, -5.500000000000040856, 66.48618307335613054 ) ) ;
#47748 = CARTESIAN_POINT ( 'NONE',  ( 21.46320343559668231, 20.96320343559617072, 5.353553390593268624 ) ) ;
#47749 = CARTESIAN_POINT ( 'NONE',  ( -4.483927247898782831, 16.52544592524335698, 82.70942372801900433 ) ) ;
#47750 = FACE_OUTER_BOUND ( 'NONE', #144784, .T. ) ;
#47751 = CARTESIAN_POINT ( 'NONE',  ( -16.55341960407617563, 4.379528057220093196, 68.54275706135234714 ) ) ;
#47752 = CARTESIAN_POINT ( 'NONE',  ( -14.29746914071037622, -8.314922557961029526, 39.16775706135235424 ) ) ;
#47753 = CARTESIAN_POINT ( 'NONE',  ( 19.02544592524334988, 5.153800228976608722, 26.45942372801899722 ) ) ;
#47755 = FACE_BOUND ( 'NONE', #143164, .T. ) ;
#47754 = CARTESIAN_POINT ( 'NONE',  ( 16.51473224551069308, 9.474510206698969483, 54.16557627198103120 ) ) ;
#47756 = CARTESIAN_POINT ( 'NONE',  ( 5.823673210054444382, -21.52544592524334988, 55.20942372801902565 ) ) ;
#47757 = CARTESIAN_POINT ( 'NONE',  ( 9.564922557961047289, -16.46253265017146816, 65.41775706135233293 ) ) ;
#47758 = CARTESIAN_POINT ( 'NONE',  ( 18.62759615963255655, 10.81492255796105972, 106.6677570613523756 ) ) ;
#47759 = CARTESIAN_POINT ( 'NONE',  ( -13.97604488694527625, -13.89961937509977652, 31.87390960531435979 ) ) ;
#47760 = CARTESIAN_POINT ( 'NONE',  ( -11.74149087413294623, -36.13659316521243881, -7.602157773949822506 ) ) ;
#47761 = CARTESIAN_POINT ( 'NONE',  ( 0.05219959533907565091, 21.53943276465977519, 49.99890960531437401 ) ) ;
#47762 = CIRCLE ( 'NONE', #80070, 2.000000000000000000 ) ;
#47763 = CARTESIAN_POINT ( 'NONE',  ( 0.05219959533909260263, 19.03943276465977164, 114.9989096053143669 ) ) ;
#47764 = CARTESIAN_POINT ( 'NONE',  ( -12.06949235617756955, 12.14591786802309770, 100.6239096053143811 ) ) ;
#47765 = CARTESIAN_POINT ( 'NONE',  ( 16.55341960407618274, -4.379528057220086978, 31.04275706135234714 ) ) ;
#47766 = CARTESIAN_POINT ( 'NONE',  ( -12.06949235617756955, 12.14591786802309770, 35.62390960531437401 ) ) ;
#47767 = ORIENTED_EDGE ( 'NONE', *, *, #133168, .T. ) ;
#47768 = CARTESIAN_POINT ( 'NONE',  ( -21.55341960407610458, -5.719274019375992779, 111.4572429386476813 ) ) ;
#47770 = CARTESIAN_POINT ( 'NONE',  ( 9.564922557960805705, 16.46253265017160317, 109.5822429386476955 ) ) ;
#47769 = CARTESIAN_POINT ( 'NONE',  ( -16.53943276465976808, 0.05219959533911058130, 36.24890960531435979 ) ) ;
#47771 = CARTESIAN_POINT ( 'NONE',  ( 16.51473224551083163, -9.474510206698727899, 110.8344237280190043 ) ) ;
#47772 = CARTESIAN_POINT ( 'NONE',  ( 9.564922557961047289, -16.46253265017146816, 25.41775706135234003 ) ) ;
#47773 = CARTESIAN_POINT ( 'NONE',  ( -16.53943276465976808, 0.05219959533911058130, 36.24890960531435979 ) ) ;
#47774 = CARTESIAN_POINT ( 'NONE',  ( -21.53943276465977519, 0.05219959533907696930, 101.2489096053143669 ) ) ;
#47776 = CARTESIAN_POINT ( 'NONE',  ( -15.80617190586745835, -15.72974639402198527, 66.87390960531436690 ) ) ;
#47775 = CARTESIAN_POINT ( 'NONE',  ( 17.40805194822031865, 6.112264579159358391, 31.66628727489388595 ) ) ;
#47777 = CARTESIAN_POINT ( 'NONE',  ( -5.153800228976328057, -19.02544592524343514, 82.29057627198103830 ) ) ;
#47778 = CARTESIAN_POINT ( 'NONE',  ( 16.55341960407611168, 4.379528057220329451, 43.95724293864769550 ) ) ;
#47779 = CARTESIAN_POINT ( 'NONE',  ( 13.97604488694527802, 13.89961937509977652, 94.37390960531436690 ) ) ;
#47780 = CARTESIAN_POINT ( 'NONE',  ( 32.00000000000000000, -5.510910596163089556E-15, 45.00000000000000000 ) ) ;
#47781 = CARTESIAN_POINT ( 'NONE',  ( -19.03943276465977164, -0.05219959533935918106, 58.75109039468566863 ) ) ;
#47782 = CARTESIAN_POINT ( 'NONE',  ( 21.55341960407610458, 5.719274019375980345, 98.95724293864770971 ) ) ;
#47783 = CARTESIAN_POINT ( 'NONE',  ( 16.55341960407611168, 4.379528057220329451, 93.95724293864770971 ) ) ;
#47784 = CARTESIAN_POINT ( 'NONE',  ( 10.81492255796106328, -18.62759615963255655, 35.41775706135234003 ) ) ;
#47785 = CIRCLE ( 'NONE', #83263, 26.05799246640827960 ) ;
#47786 = CARTESIAN_POINT ( 'NONE',  ( 22.44159573604009239, 16.30477369853692693, 142.0750000027311728 ) ) ;
#47787 = CARTESIAN_POINT ( 'NONE',  ( -4.379528057220328563, 16.55341960407611168, 30.20724293864769550 ) ) ;
#47788 = CARTESIAN_POINT ( 'NONE',  ( 13.97604488694527802, 13.89961937509977652, 34.37390960531436690 ) ) ;
#47789 = CARTESIAN_POINT ( 'NONE',  ( -19.05341960407611168, -5.049401038298163336, 81.45724293864769550 ) ) ;
#47790 = CARTESIAN_POINT ( 'NONE',  ( 21.55341960407610458, 5.719274019375980345, 63.95724293864770260 ) ) ;
#47791 = DIRECTION ( 'NONE',  ( 0.9526137857479322069, -0.3041824702427683991, 0.000000000000000000 ) ) ;
#47792 = CARTESIAN_POINT ( 'NONE',  ( -19.02544592524342804, 5.153800228976336051, 36.04057627198100988 ) ) ;
#47793 = CARTESIAN_POINT ( 'NONE',  ( 21.55341960407610458, 5.719274019375980345, 48.95724293864770971 ) ) ;
#47794 = EDGE_CURVE ( 'NONE', #170159, #53763, #151749, .T. ) ;
#47795 = CARTESIAN_POINT ( 'NONE',  ( 10.72451020669871369, 18.67979575497193778, 72.08442372801899012 ) ) ;
#47797 = CARTESIAN_POINT ( 'NONE',  ( -12.06949235617739369, -12.14591786802326823, 64.37609039468568994 ) ) ;
#47796 = CARTESIAN_POINT ( 'NONE',  ( 8.779096689230840411, -37.67883572780987578, -23.98624440746760911 ) ) ;
#47798 = CARTESIAN_POINT ( 'NONE',  ( -9.564922557960796823, -16.46253265017161027, 52.08224293864768839 ) ) ;
#47799 = CARTESIAN_POINT ( 'NONE',  ( 19.03943276465977164, -0.05219959533909143690, 58.74890960531435979 ) ) ;
#47800 = ORIENTED_EDGE ( 'NONE', *, *, #71198, .F. ) ;
#47801 = CARTESIAN_POINT ( 'NONE',  ( 9.564922557961047289, -16.46253265017146816, 20.41775706135233293 ) ) ;
#47802 = CARTESIAN_POINT ( 'NONE',  ( 16.55341960407618274, -4.379528057220086978, 76.04275706135237556 ) ) ;
#47803 = CARTESIAN_POINT ( 'NONE',  ( 10.81492255796106328, -18.62759615963255655, 95.41775706135234714 ) ) ;
#47804 = CARTESIAN_POINT ( 'NONE',  ( 0.05219959533909260263, 19.03943276465977164, 79.99890960531436690 ) ) ;
#47805 = CARTESIAN_POINT ( 'NONE',  ( 21.55341960407610458, 5.719274019375980345, 38.95724293864768839 ) ) ;
#47806 = CARTESIAN_POINT ( 'NONE',  ( -19.05341960407617563, 5.049401038297882671, 113.5427570613523471 ) ) ;
#47807 = CARTESIAN_POINT ( 'NONE',  ( 18.62759615963255655, 10.81492255796105972, 81.66775706135236135 ) ) ;
#47808 = CARTESIAN_POINT ( 'NONE',  ( -14.34966873604972548, 8.224510206698743886, 43.33442372801901143 ) ) ;
#47809 = CARTESIAN_POINT ( 'NONE',  ( 21.55341960407610458, 5.719274019375980345, 93.95724293864770971 ) ) ;
#47810 = CARTESIAN_POINT ( 'NONE',  ( -13.89961937509957401, -13.97604488694547875, 109.3760903946856331 ) ) ;
#47812 = EDGE_CURVE ( 'NONE', #41630, #40834, #165999, .T. ) ;
#47811 = CARTESIAN_POINT ( 'NONE',  ( -5.153800228976328057, -19.02544592524343514, 77.29057627198099567 ) ) ;
#47813 = CARTESIAN_POINT ( 'NONE',  ( -9.564922557961040184, 16.46253265017147172, 112.9177570613523329 ) ) ;
#47814 = CARTESIAN_POINT ( 'NONE',  ( -16.46253265017160317, 9.564922557960807481, 40.83224293864769550 ) ) ;
#47815 = CARTESIAN_POINT ( 'NONE',  ( -16.53943276465976808, -0.05219959533934237506, 23.75109039468567929 ) ) ;
#47816 = CARTESIAN_POINT ( 'NONE',  ( -16.52544592524342804, 4.483927247898546575, 66.04057627198103830 ) ) ;
#47817 = CARTESIAN_POINT ( 'NONE',  ( 8.314922557961029526, -14.29746914071037800, 75.41775706135233293 ) ) ;
#47819 = CARTESIAN_POINT ( 'NONE',  ( -19.02544592524342804, 5.153800228976336051, 46.04057627198101699 ) ) ;
#47818 = CARTESIAN_POINT ( 'NONE',  ( 18.62759615963255655, 10.81492255796105972, 26.66775706135235424 ) ) ;
#47820 = CARTESIAN_POINT ( 'NONE',  ( -13.97604488694527625, -13.89961937509977652, 66.87390960531436690 ) ) ;
#47821 = CARTESIAN_POINT ( 'NONE',  ( 4.483927247898790824, -16.52544592524335698, 70.20942372801904696 ) ) ;
#47822 = CYLINDRICAL_SURFACE ( 'NONE', #20775, 1.500000000000001332 ) ;
#47823 = ORIENTED_EDGE ( 'NONE', *, *, #186744, .T. ) ;
#47824 = CARTESIAN_POINT ( 'NONE',  ( -0.05219959533936034679, 19.03943276465977164, 22.50109039468566152 ) ) ;
#47825 = CARTESIAN_POINT ( 'NONE',  ( 0.05219959533909260263, 19.03943276465977164, 34.99890960531435979 ) ) ;
#47827 = ORIENTED_EDGE ( 'NONE', *, *, #116452, .F. ) ;
#47826 = CARTESIAN_POINT ( 'NONE',  ( 5.153800228976335163, 19.02544592524342804, 104.7905762719809957 ) ) ;
#47828 = CARTESIAN_POINT ( 'NONE',  ( 8.314922557961029526, -14.29746914071037800, 35.41775706135234003 ) ) ;
#47830 = CARTESIAN_POINT ( 'NONE',  ( -0.05219959533934338120, 16.53943276465976808, 37.50109039468568284 ) ) ;
#47829 = CARTESIAN_POINT ( 'NONE',  ( 5.153800228976615827, -19.02544592524334988, 55.20942372801899722 ) ) ;
#47831 = CARTESIAN_POINT ( 'NONE',  ( -13.97604488694527625, -13.89961937509977652, 36.87390960531436690 ) ) ;
#47832 = CARTESIAN_POINT ( 'NONE',  ( -9.474510206698964154, 16.51473224551069663, 110.4155762719810383 ) ) ;
#47833 = CARTESIAN_POINT ( 'NONE',  ( 13.89961937509977652, -13.97604488694527269, 58.12390960531436690 ) ) ;
#47834 = CARTESIAN_POINT ( 'NONE',  ( 18.62759615963271287, -10.81492255796078972, 103.3322429386476955 ) ) ;
#47836 = CARTESIAN_POINT ( 'NONE',  ( 16.51473224551069308, 9.474510206698969483, 109.1655762719810383 ) ) ;
#47835 = CARTESIAN_POINT ( 'NONE',  ( 9.564922557960805705, 16.46253265017160317, 89.58224293864769550 ) ) ;
#47837 = CARTESIAN_POINT ( 'NONE',  ( 19.05341960407611168, 5.049401038298154454, 58.95724293864768129 ) ) ;
#47839 = CARTESIAN_POINT ( 'NONE',  ( -18.22780087662122028, 5.500000000000031086, 93.51540105326107266 ) ) ;
#47838 = CARTESIAN_POINT ( 'NONE',  ( 4.483927247898790824, -16.52544592524335698, 110.2094237280190185 ) ) ;
#47840 = CARTESIAN_POINT ( 'NONE',  ( -9.474510206698720793, -16.51473224551083518, 99.58442372801900433 ) ) ;
#47841 = CARTESIAN_POINT ( 'NONE',  ( 5.153800228976615827, -19.02544592524334988, 20.20942372801899722 ) ) ;
#47842 = CARTESIAN_POINT ( 'NONE',  ( 4.483927247898545687, 16.52544592524342804, 54.79057627198104541 ) ) ;
#47843 = CARTESIAN_POINT ( 'NONE',  ( -18.67979575497193778, 10.72451020669871902, 93.33442372801901854 ) ) ;
#47844 = CARTESIAN_POINT ( 'NONE',  ( -5.049401038298153566, 19.05341960407611168, 40.20724293864768839 ) ) ;
#47846 = CARTESIAN_POINT ( 'NONE',  ( -21.52544592524334988, -5.823673210054445271, 88.95942372801901854 ) ) ;
#47845 = CARTESIAN_POINT ( 'NONE',  ( -8.224510206698948167, 14.34966873604960824, 25.41557627198103120 ) ) ;
#47847 = CARTESIAN_POINT ( 'NONE',  ( -19.02544592524342804, 5.153800228976336051, 76.04057627198102409 ) ) ;
#47848 = CARTESIAN_POINT ( 'NONE',  ( 0.05219959533909260263, 19.03943276465977164, 89.99890960531436690 ) ) ;
#47849 = CARTESIAN_POINT ( 'NONE',  ( 8.224510206698953496, -14.34966873604960469, 97.91557627198103830 ) ) ;
#47850 = CARTESIAN_POINT ( 'NONE',  ( 14.29746914071049879, -8.314922557960816363, 63.33224293864770260 ) ) ;
#47851 = CARTESIAN_POINT ( 'NONE',  ( 18.62759615963271287, -10.81492255796078972, 68.33224293864769550 ) ) ;
#47852 = CARTESIAN_POINT ( 'NONE',  ( 0.05219959533909260263, 19.03943276465977164, 79.99890960531436690 ) ) ;
#47853 = CARTESIAN_POINT ( 'NONE',  ( 21.53943276465977519, -0.05219959533907433946, 88.74890960531436690 ) ) ;
#47854 = CARTESIAN_POINT ( 'NONE',  ( 16.51473224551083163, -9.474510206698727899, 80.83442372801899012 ) ) ;
#47856 = CARTESIAN_POINT ( 'NONE',  ( 8.224510206698953496, -14.34966873604960469, 92.91557627198103830 ) ) ;
#47855 = PLANE ( 'NONE',  #191436 ) ;
#47857 = CARTESIAN_POINT ( 'NONE',  ( 5.153800228976335163, 19.02544592524342804, 54.79057627198103120 ) ) ;
#47858 = CARTESIAN_POINT ( 'NONE',  ( 5.823673210054125526, 21.52544592524343514, 64.79057627198103830 ) ) ;
#47859 = CARTESIAN_POINT ( 'NONE',  ( 16.19135201231362586, -7.376712067592066546, 27.31319145947968607 ) ) ;
#47861 = DIRECTION ( 'NONE',  ( 1.000000000000000000, 0.000000000000000000, 0.000000000000000000 ) ) ;
#47860 = CARTESIAN_POINT ( 'NONE',  ( -14.34966873604972548, 8.224510206698743886, 113.3344237280190328 ) ) ;
#47862 = CARTESIAN_POINT ( 'NONE',  ( 9.474510206698729675, 16.51473224551082808, 112.0844237280190043 ) ) ;
#47863 = CARTESIAN_POINT ( 'NONE',  ( 4.483927247898545687, 16.52544592524342804, 79.79057627198102409 ) ) ;
#47864 = CARTESIAN_POINT ( 'NONE',  ( -19.25918095147779852, -5.499999999999533706, 94.45284276293934056 ) ) ;
#47865 = CARTESIAN_POINT ( 'NONE',  ( 13.89961937509977652, -13.97604488694527269, 73.12390960531436690 ) ) ;
#47866 = CARTESIAN_POINT ( 'NONE',  ( 16.46253265017160672, -9.564922557960803928, 38.33224293864768839 ) ) ;
#47867 = CARTESIAN_POINT ( 'NONE',  ( 12.06949235617757843, -12.14591786802309237, 63.12390960531435979 ) ) ;
#47868 = CARTESIAN_POINT ( 'NONE',  ( 19.03943276465977164, -0.05219959533909143690, 98.74890960531436690 ) ) ;
#47870 = CARTESIAN_POINT ( 'NONE',  ( 19.03943276465977164, -0.05219959533909143690, 68.74890960531436690 ) ) ;
#47869 = CARTESIAN_POINT ( 'NONE',  ( -19.03943276465977164, -0.05219959533935918106, 93.75109039468566152 ) ) ;
#47871 = CARTESIAN_POINT ( 'NONE',  ( 19.05341960407611168, 5.049401038298154454, 88.95724293864769550 ) ) ;
#47872 = CARTESIAN_POINT ( 'NONE',  ( 0.05219959533907565091, 21.53943276465977519, 74.99890960531435269 ) ) ;
#47873 = CARTESIAN_POINT ( 'NONE',  ( -12.06949235617739369, -12.14591786802326823, 69.37609039468567573 ) ) ;
#47874 = CARTESIAN_POINT ( 'NONE',  ( -5.049401038297874678, -19.05341960407618274, 109.7927570613523329 ) ) ;
#47875 = CARTESIAN_POINT ( 'NONE',  ( 16.46253265017160672, -9.564922557960803928, 63.33224293864769550 ) ) ;
#47876 = CARTESIAN_POINT ( 'NONE',  ( 15.72974639402199770, -15.80617190586745480, 73.12390960531436690 ) ) ;
#47877 = CARTESIAN_POINT ( 'NONE',  ( 19.03943276465977164, 0.05219959533936151252, 91.25109039468566152 ) ) ;
#47879 = CARTESIAN_POINT ( 'NONE',  ( -21.52544592524334988, -5.823673210054445271, 43.95942372801902565 ) ) ;
#47878 = CARTESIAN_POINT ( 'NONE',  ( -16.52544592524342804, 4.483927247898546575, 41.04057627198103120 ) ) ;
#47880 = CARTESIAN_POINT ( 'NONE',  ( 1.993301997531345686E-15, -30.30510711980685556, 144.7500000054623399 ) ) ;
#47882 = CARTESIAN_POINT ( 'NONE',  ( 19.02544592524343514, -5.153800228976328945, 108.5405762719810383 ) ) ;
#47881 = CARTESIAN_POINT ( 'NONE',  ( 14.34966873604972726, -8.224510206698740333, 70.83442372801901854 ) ) ;
#47883 = CARTESIAN_POINT ( 'NONE',  ( -19.03943276465977164, 0.05219959533909376836, 106.2489096053143669 ) ) ;
#47884 = CARTESIAN_POINT ( 'NONE',  ( -3.573655867282028392E-15, -12.39993551617566503, 175.0000000000000000 ) ) ;
#47885 = CARTESIAN_POINT ( 'NONE',  ( -8.314922557961024197, 14.29746914071037800, 87.91775706135234714 ) ) ;
#47886 = CARTESIAN_POINT ( 'NONE',  ( 12.14591786802327356, -12.06949235617739191, 45.62609039468567573 ) ) ;
#47887 = CARTESIAN_POINT ( 'NONE',  ( -5.049401038298153566, 19.05341960407611168, 55.20724293864769550 ) ) ;
#47888 = CARTESIAN_POINT ( 'NONE',  ( -16.51473224551069308, -9.474510206698971260, 56.66557627198103120 ) ) ;
#47889 = CARTESIAN_POINT ( 'NONE',  ( -15.80617190586768217, 15.72974639402176855, 48.12609039468568284 ) ) ;
#47890 = CARTESIAN_POINT ( 'NONE',  ( 8.314922557961029526, -14.29746914071037800, 60.41775706135235424 ) ) ;
#47891 = CARTESIAN_POINT ( 'NONE',  ( 0.05219959533910956823, 16.53943276465976808, 39.99890960531436690 ) ) ;
#47892 = CARTESIAN_POINT ( 'NONE',  ( -5.049401038298153566, 19.05341960407611168, 45.20724293864769550 ) ) ;
#47893 = CARTESIAN_POINT ( 'NONE',  ( -19.03943276465977164, 0.05219959533909376836, 31.24890960531435979 ) ) ;
#47894 = CARTESIAN_POINT ( 'NONE',  ( -16.53943276465976808, -0.05219959533934237506, 33.75109039468568284 ) ) ;
#47895 = CARTESIAN_POINT ( 'NONE',  ( 19.03943276465977164, 0.05219959533936151252, 76.25109039468566152 ) ) ;
#47896 = CARTESIAN_POINT ( 'NONE',  ( -16.55341960407611168, -4.379528057220339221, 81.45724293864769550 ) ) ;
#47897 = CARTESIAN_POINT ( 'NONE',  ( -13.97604488694527625, -13.89961937509977652, 51.87390960531436690 ) ) ;
#47899 = DIRECTION ( 'NONE',  ( -1.000000000000000000, 0.000000000000000000, 0.000000000000000000 ) ) ;
#47898 = CARTESIAN_POINT ( 'NONE',  ( -19.05341960407617563, 5.049401038297882671, 83.54275706135233293 ) ) ;
#47900 = CARTESIAN_POINT ( 'NONE',  ( 21.52544592524334988, 5.823673210054432836, 86.45942372801901854 ) ) ;
#47901 = CARTESIAN_POINT ( 'NONE',  ( -14.34966873604972548, 8.224510206698743886, 58.33442372801901143 ) ) ;
#47902 = CARTESIAN_POINT ( 'NONE',  ( 16.79531203550649820, 7.028104445595489302, 38.75244988220443787 ) ) ;
#47903 = CARTESIAN_POINT ( 'NONE',  ( -10.72451020669898014, 18.67979575497178502, 45.41557627198103830 ) ) ;
#47904 = CARTESIAN_POINT ( 'NONE',  ( -14.34966873604972548, 8.224510206698743886, 43.33442372801901143 ) ) ;
#47905 = CARTESIAN_POINT ( 'NONE',  ( -31.74999999999995737, 5.204748896376250699E-16, -4.250000000000000000 ) ) ;
#47906 = CARTESIAN_POINT ( 'NONE',  ( 13.97604488694548053, -13.89961937509957401, 25.62609039468566507 ) ) ;
#47907 = CARTESIAN_POINT ( 'NONE',  ( -19.05341960407611168, -5.049401038298163336, 71.45724293864766707 ) ) ;
#47908 = CARTESIAN_POINT ( 'NONE',  ( -28.47622644277399928, -25.16156846422451920, -16.68312038616162951 ) ) ;
#47909 = CARTESIAN_POINT ( 'NONE',  ( 19.05341960407611168, 5.049401038298154454, 53.95724293864770260 ) ) ;
#47910 = CARTESIAN_POINT ( 'NONE',  ( 14.74842737557653116, 15.51017872335176762, -56.39952970130667609 ) ) ;
#47911 = CARTESIAN_POINT ( 'NONE',  ( -16.46253265017160317, 9.564922557960807481, 65.83224293864769550 ) ) ;
#47912 = CARTESIAN_POINT ( 'NONE',  ( -18.56399227203345603, -5.499999999999828582, 53.97830131249904184 ) ) ;
#47913 = CARTESIAN_POINT ( 'NONE',  ( 19.02544592524334988, 5.153800228976608722, 31.45942372801900433 ) ) ;
#47914 = CARTESIAN_POINT ( 'NONE',  ( 21.55341960407619695, -5.719274019375665929, 111.0427570613523613 ) ) ;
#47915 = CARTESIAN_POINT ( 'NONE',  ( 12.14591786802309770, 12.06949235617756955, 34.37390960531435979 ) ) ;
#47916 = CARTESIAN_POINT ( 'NONE',  ( -16.46253265017160317, 9.564922557960807481, 45.83224293864769550 ) ) ;
#47917 = CARTESIAN_POINT ( 'NONE',  ( 13.89961937509977652, -13.97604488694527269, 103.1239096053143527 ) ) ;
#47918 = CARTESIAN_POINT ( 'NONE',  ( 21.52544592524334988, 5.823673210054432836, 76.45942372801901854 ) ) ;
#47919 = CARTESIAN_POINT ( 'NONE',  ( 9.564922557960805705, 16.46253265017160317, 54.58224293864769550 ) ) ;
#47920 = CARTESIAN_POINT ( 'NONE',  ( 21.55341960407619695, -5.719274019375665929, 81.04275706135236135 ) ) ;
#47921 = CARTESIAN_POINT ( 'NONE',  ( -21.55341960407610458, -5.719274019375992779, 21.45724293864769550 ) ) ;
#47922 = CARTESIAN_POINT ( 'NONE',  ( 9.474510206698971260, -16.51473224551069308, 32.91557627198102409 ) ) ;
#47923 = CARTESIAN_POINT ( 'NONE',  ( -5.719274019375665041, -21.55341960407619695, 29.79275706135234358 ) ) ;
#47924 = CARTESIAN_POINT ( 'NONE',  ( -9.474510206698720793, -16.51473224551083518, 49.58442372801899722 ) ) ;
#47925 = CARTESIAN_POINT ( 'NONE',  ( 0.05219959533909260263, 19.03943276465977164, 34.99890960531435979 ) ) ;
#47926 = CARTESIAN_POINT ( 'NONE',  ( 5.049401038298161559, -19.05341960407611168, 77.70724293864765286 ) ) ;
#47927 = CARTESIAN_POINT ( 'NONE',  ( 19.02544592524334988, 5.153800228976608722, 111.4594237280190043 ) ) ;
#47928 = CARTESIAN_POINT ( 'NONE',  ( 16.55341960407611168, 4.379528057220329451, 73.95724293864769550 ) ) ;
#47929 = CARTESIAN_POINT ( 'NONE',  ( 15.80617190586746368, 15.72974639402197994, 34.37390960531435979 ) ) ;
#47930 = CARTESIAN_POINT ( 'NONE',  ( 16.51473224551083163, -9.474510206698727899, 105.8344237280190043 ) ) ;
#47931 = CARTESIAN_POINT ( 'NONE',  ( 21.52544592524344225, -5.823673210054117533, 98.54057627198105251 ) ) ;
#47932 = CARTESIAN_POINT ( 'NONE',  ( -18.67979575497193778, 10.72451020669871902, 58.33442372801901143 ) ) ;
#47933 = CARTESIAN_POINT ( 'NONE',  ( 16.52544592524335698, 4.483927247898782831, 51.45942372801901854 ) ) ;
#47934 = CARTESIAN_POINT ( 'NONE',  ( -14.29746914071037622, -8.314922557961029526, 59.16775706135234714 ) ) ;
#47935 = CARTESIAN_POINT ( 'NONE',  ( -18.67979575497178146, -10.72451020669898902, 66.66557627198102409 ) ) ;
#47936 = EDGE_LOOP ( 'NONE', ( #45535, #23772 ) ) ;
#47937 =( BOUNDED_SURFACE ( )  B_SPLINE_SURFACE ( 3, 2, ( 
 ( #91823, #157250, #18744, #60503, #45355, #122178, #183870, #173422, #34892, #107007, #153516, #15013, #200032, #49080, #61500, #71224, #68211, #35882, #99546, #114720, #39874, #86383, #101541, #98536, #175403, #38889, #177418, #132887, #23724, #161228, #5537, #55050, #67216, #100546, #20711, #22722, #144055, #193578, #36871, #84370, #24733, #128874, #85373, #176412, #160229, #7531, #129863, #162225, #82367, #148067, #146047, #147066, #83373, #130884, #9558, #159216, #131894, #190574, #69216, #163233, #117725, #194576, #52050, #113706, #54057, #56046, #37888, #191561, #97529, #8549, #21720, #192573, #70226, #115731, #116721, #178410, #53040, #145050, #6531, #74220, #14517, #58052, #153018, #61008, #13527, #12554, #87384, #150063, #198550, #90357, #76178, #137858, #135888, #25738, #165236, #133896, #199538, #179420, #166231, #41895, #40885, #59027, #26730, #102558, #72221, #43871, #42884, #164243, #197560, #10557, #152042, #134905, #149069, #75193, #120694, #60020, #182393, #195587, #57059, #136864, #11568, #118734, #180422, #121687, #105536, #28720, #73234, #103561, #183383, #88369, #91326, #196582, #119723, #181406, #44865, #104549, #27731, #89374, #151063, #167222, #106520, #168198, #29695, #32670, #93328, #4291, #125667, #123658, #107503, #156001, #126642, #17498, #138844, #111487, #30685, #33655, #46846, #187365, #62993, #324, #61992, #185355, #108506, #110487, #170185, #49823, #172170, #173172, #157001, #1314, #140826, #79155, #48834, #139825, #34648, #142811, #96307, #122680, #94323, #92336, #154022, #81130, #186368, #141818, #95316, #45850, #109500, #31679, #155013, #16509, #78157, #124671, #18499, #47847, #171182, #15517, #188344, #77174, #80147, #64984, #2315, #169179, #63997, #157993, #3311, #19485, #184369, #116479, #145803, #53809, #54804, #84124, #147830, #7286, #127642, #23476, #189342, #177172, #158973, #69980, #100302, #66972, #20465, #38645, #36623, #50820, #112477, #128632, #86139, #129621, #115484, #99296, #8303, #174170, #82115, #143806, #101293, #68970, #161980, #35640, #130634, #97286, #191316, #65972, #193330, #5289, #192328, #85125, #51803, #178168, #24488, #190326, #146809, #144805, #159981, #113462, #131648, #175156, #39633, #162983, #98280, #21467, #83129, #6288, #67967, #52793, #114461, #176163, #37633, #160982, #22476, #149815, #120455, #72991, #9316, #165990, #132649, #181168, #179175, #89133, #42645, #25498, #40643, #104307, #71972, #70981, #117477, #148825, #194337, #26489, #27490, #134660, #12318, #102312, #87141, #10315, #55805, #150821, #73983, #133646, #135652, #195337, #196346, #164002, #56817, #103315, #118491, #180182, #119486, #41651, #164995, #197323, #58786, #88131, #11321, #57814, #119260, #151587, #42420, #30221, #135433, #122218, #41421, #181927, #73761, #43408, #87904, #137393, #180944, #149590, #166764, #27259, #138389, #59551, #57590, #103087, #89904, #60542, #13076, #72765, #45394, #164768, #167745, #104083, #121229, #197104, #134435, #196120, #165765, #88909, #44405, #150600, #183909, #106059, #107047, #90876, #58571, #74743, #136406, #182920, #120236, #168719, #76714, #91863, #56590, #28266, #26263, #11088, #15053, #105078, #75715, #29243, #179954, #198084, #12098, #152560, #14049, #199073, #153556, #118264, #157546, #139376, #125218, #188893, #92869, #49368, #140375, #124205, #171722, #32215, #2861, #184898, #50373, #48386, #64539, #47390, #94870, #112033, #123208, #95863, #154556, #33211, #65522, #81660, #127182, #16051, #169725, #18050, #158529, #1862, #155550, #35190, #79703, #126205, #858, #63544, #186915, #141374, #110043, #17044, #93871, #20017, #170723, #3843, #78698, #173722, #200071, #34201, #156551, #108039, #187901, #19040, #111032, #96844, #61539, #172719, #46380, #185905, #77710, #31218, #62532, #80687, #109045, #142363, #23017, #190865, #25031, #36171, #7829, #6827, #178707, #99841, #174707, #54348, #98830, #189879, #116019 ),
 ( #115017, #51354, #113014, #101845, #68505, #162517, #146341, #66518, #130160, #5835, #52342, #67511, #160524, #37172, #177709, #22015, #83667, #97823, #147361, #159512, #131180, #85674, #129168, #21008, #82663, #8849, #144347, #39176, #70517, #193876, #84663, #192869, #132185, #161525, #143343, #69515, #4831, #100834, #176711, #113998, #175696, #163531, #191857, #24019, #55342, #128180, #53339, #145345, #38185, #117012, #40169, #180717, #120993, #165535, #42193, #56344, #90657, #179716, #74516, #29017, #10855, #133181, #194871, #152339, #118026, #59324, #13825, #137164, #166536, #136182, #75491, #104845, #168499, #28033, #148358, #44176, #9854, #197857, #41188, #198853, #182691, #87674, #102851, #105835, #57361, #71513, #164536, #149358, #106825, #150373, #167522, #120012, #60317, #26029, #72524, #134199, #121994, #89674, #183684, #195887, #151361, #119035, #11868, #86675, #45169, #103854, #12850, #27031, #88677, #73533, #135205, #196877, #58344, #181697, #43178, #153324, #79472, #92637, #124984, #15817, #3612, #108812, #95627, #14826, #155324, #47154, #16812, #61312, #110801, #154328, #122982, #140136, #625, #111797, #32980, #30989, #76487, #63305, #33970, #186681, #46151, #18809, #138164, #141140, #77478, #94634, #170491, #107805, #169489, #139148, #62296, #17815, #123964, #157312, #2630, #80454, #64307, #31982, #48151, #109808, #156313, #93638, #142127, #50138, #65291, #29997, #171491, #125974, #185662, #126950, #78462, #91636, #1628, #187673, #188658, #199846, #184669, #49143, #172482, #176475, #114782, #70289, #161289, #36936, #143115, #192635, #4594, #37949, #158299, #98599, #81429, #130945, #112782, #160292, #162288, #66287, #22783, #113769, #97590, #145111, #5598, #99609, #19788, #23788, #21783, #84431, #20774, #68273, #85438, #96610, #69278, #127946, #6594, #38949, #55113, #100606, #189648, #51123, #191624, #131957, #175465, #128936, #8616, #53103, #146108, #174475, #83434, #129924, #7592, #54117, #190637, #67278, #193641, #144118, #177480, #52112, #147129, #173485, #115791, #34958, #35944, #159278, #82430, #30486, #93134, #154819, #150132, #163300, #102624, #71289, #16317, #77967, #103627, #179488, #139634, #196648, #164310, #1122, #9624, #184176, #180489, #116783, #73301, #148133, #92137, #72286, #24799, #153824, #58118, #130, #134971, #178474, #132954, #15319, #87449, #101610, #86447, #76978, #194642, #138649, #45658, #11634, #57127, #122485, #107309, #169991, #133963, #56112, #10625, #168982, #61799, #123469, #39941, #117793, #108311, #40952, #185161, #25803, #46652, #118801, #149134, #195655, #41961, #165303, #31482, #26796, #88438, #50631, #113278, #97102, #141637, #80950, #19302, #189158, #79969, #174969, #82938, #190138, #144616, #34464, #170986, #32479, #21281, #126463, #81920, #65783, #186174, #49634, #125483, #171984, #187179, #18312, #156820, #158786, #3127, #64802, #94132, #66780, #155811, #112292, #5097, #48650, #109307, #17309, #128441, #78964, #35451, #51613, #36433, #142625, #173982, #98088, #4104, #62796, #127452, #124478, #20274, #47656, #143613, #140639, #159786, #2129, #63810, #110302, #33472, #95130, #188161, #111297, #172986, #96123, #157812, #194148, #39442, #148633, #191136, #160796, #99104, #41457, #24297, #55612, #114271, #70789, #175975, #131450, #26298, #133453, #37444, #132457, #178980, #192133, #85945, #6100, #117286, #40447, #102121, #176983, #129437, #163805, #68777, #101102, #53614, #179990, #84931, #71783, #52609, #193137, #23287, #54610, #22284, #86949, #130434, #83935, #116284, #38453, #87939, #9123, #7095, #145616, #162788, #10123, #147634, #115290, #25307, #195143, #56624, #100108, #161792, #146612, #103122, #118298, #164803, #8104, #67780, #69782, #177974, #169755, #76745, #57627, #75749, #122249, #135467, #167777, #149626, #137426, #199106, #60573, #120268, #72799, #183939, #12130, #44437, #197135, #123237, #28298, #15084, #134469, #74776 ),
 ( #153586, #182954, #165799, #138420, #119294, #45424, #73794, #152592, #89938, #27296, #88943, #58602, #150634, #107077, #181960, #200100, #168749, #61568, #30252, #151619, #29275, #106091, #91895, #166797, #184928, #31250, #46413, #11124, #121260, #180977, #42453, #108071, #13112, #196154, #14083, #104117, #136438, #43442, #105111, #198119, #59586, #90907, #127211, #171753, #186946, #62563, #96872, #185935, #80716, #35219, #17075, #139406, #888, #158556, #124240, #65552, #20046, #143371, #172750, #142394, #81689, #111062, #174737, #34231, #154586, #50403, #16082, #3873, #47420, #4863, #188925, #93902, #109076, #112063, #63574, #77740, #170755, #155580, #113045, #156584, #173751, #32244, #18079, #66548, #78729, #128212, #33242, #140405, #64570, #125248, #95893, #1894, #189909, #141403, #157576, #48417, #187930, #51384, #110073, #92900, #94900, #126235, #79734, #2891, #49399, #19069, #5865, #54379, #194901, #176742, #191888, #71544, #116051, #39209, #175727, #38215, #161555, #177740, #23048, #53372, #130192, #56375, #6858, #40200, #115050, #9884, #118058, #70549, #69547, #144378, #68537, #55372, #147393, #133210, #36200, #131211, #82694, #22047, #190897, #97854, #159543, #84693, #98862, #21041, #100865, #83698, #67541, #129199, #162547, #99871, #52373, #192902, #114030, #8881, #146373, #37206, #132216, #24051, #117042, #85707, #160557, #145376, #193908, #7860, #178737, #101880, #163562, #25062, #86705, #148390, #12879, #120039, #59353, #182719, #30025, #135233, #26058, #73560, #29045, #167550, #198880, #76516, #72552, #121022, #136209, #57390, #14855, #11897, #179748, #43207, #58372, #183712, #91663, #45198, #42221, #119063, #44204, #105863, #138192, #90685, #104874, #149386, #60347, #10882, #152367, #164564, #166563, #87701, #134230, #122021, #195915, #13852, #180745, #28062, #103882, #137194, #165562, #89703, #168527, #27059, #75519, #181726, #88705, #151389, #196905, #106852, #150401, #153353, #74544, #199875, #197884, #61339, #41218, #102879, #18838, #15848, #156343, #188687, #4623, #50167, #77507, #92667, #141170, #81457, #63337, #78493, #158327, #2659, #126005, #62324, #125014, #48181, #64336, #109837, #140166, #16843, #143143, #93668, #126978, #1659, #96639, #123010, #157343, #17843, #31017, #155353, #142157, #33999, #19816, #184696, #79501, #169517, #108841, #139178, #46180, #107833, #171520, #185692, #154355, #187701, #170522, #654, #123994, #49171, #186710, #47182, #110830, #32011, #95655, #33009, #94664, #80483, #172514, #3641, #65319, #111825, #173513, #34986, #36967, #51150, #174504, #23820, #82458, #85470, #130975, #99639, #6625, #146139, #69309, #116815, #21813, #112811, #160322, #115822, #54149, #147159, #163333, #159308, #7625, #22815, #144146, #101642, #98628, #66314, #129955, #145142, #70321, #178506, #131988, #128966, #5630, #192666, #177512, #24829, #38982, #191655, #35971, #97618, #86479, #53134, #8647, #100638, #189678, #114813, #190666, #175494, #52142, #83465, #68304, #162319, #176505, #37982, #20803, #193673, #67307, #55144, #39972, #113799, #161322, #84461, #148164, #127975, #182489, #136962, #60117, #89473, #197657, #198651, #27832, #91427, #151164, #71321, #167321, #132984, #120789, #102655, #13624, #43970, #10656, #164340, #105632, #180519, #194675, #56144, #72319, #29791, #73332, #59123, #42982, #152141, #117825, #25835, #87479, #44963, #12652, #28817, #179518, #74319, #40987, #135004, #9655, #121785, #149166, #135986, #90457, #195686, #75291, #133995, #183479, #106621, #168295, #41992, #57157, #118836, #103658, #165336, #26828, #88469, #150166, #11666, #196682, #104647, #58151, #119819, #181504, #166334, #126737, #188440, #186468, #199636, #138937, #107600, #49919, #111584, #139923, #15611, #173269, #32767, #417, #34743, #45945, #17597, #16603, #153114, #109596, #184466, #64094, #108603, #61103, #125762, #94419, #33755, #171279, #14618, #169278, #187462, #123754 ),
 ( #3404, #156099, #140928, #141913, #79256, #76275, #2414, #137953, #110584, #122776, #48930, #30784, #157099, #172265, #154118, #92431, #95414, #185453, #77268, #62091, #46943, #170280, #78250, #18595, #47945, #80243, #31774, #93422, #155109, #1412, #65079, #63091, #124770, #161078, #66071, #21566, #116577, #23575, #4386, #22573, #69067, #82214, #114565, #96402, #84220, #145899, #7383, #67070, #19581, #130734, #192426, #129717, #85223, #144901, #175254, #162081, #81224, #83226, #113560, #6384, #127737, #177271, #20563, #189439, #68063, #128729, #178266, #99395, #97383, #142905, #191414, #100400, #52890, #112574, #146914, #50916, #53908, #143905, #115583, #36720, #174268, #35736, #159069, #5387, #38742, #190425, #8403, #70078, #131746, #193428, #98382, #176262, #37733, #54904, #160079, #158089, #51901, #167077, #121543, #11418, #147925, #9411, #198399, #103412, #58885, #42743, #163083, #26584, #102410, #148923, #164097, #195438, #133743, #74077, #118588, #56913, #71077, #43729, #132743, #27590, #182244, #25596, #39729, #89228, #166087, #150922, #10412, #24587, #12415, #135748, #73088, #28579, #88227, #180278, #105391, #86235, #165090, #41748, #149911, #194431, #120551, #87240, #55902, #134759, #72070, #101390, #104405, #40740, #117575, #196441, #90215, #57911, #179275, #151898, #119583, #197419, #181266, #13388, #75052, #136718, #59877, #45707, #122535, #171037, #169031, #110349, #32528, #33519, #17357, #61849, #1170, #139683, #109355, #181, #95179, #3175, #172031, #64848, #154870, #91187, #152876, #141684, #46702, #2178, #186224, #106375, #170042, #107358, #92189, #30537, #138699, #77027, #79012, #123518, #185211, #14371, #187226, #76037, #94180, #125529, #153873, #29554, #137712, #48697, #199396, #155859, #156866, #18362, #62845, #140686, #80015, #124529, #183238, #47705, #44719, #63858, #168057, #60860, #184226, #15371, #108364, #31532, #93185, #16367, #78015, #188208, #173035, #127501, #149419, #190188, #117074, #162580, #71576, #111344, #81000, #19351, #164596, #147426, #178770, #34513, #193941, #96171, #51663, #10915, #56410, #157861, #55404, #101912, #112341, #8913, #87734, #113327, #148422, #132250, #49680, #175020, #189206, #35502, #50683, #81972, #20323, #163594, #5147, #143665, #142674, #133242, #4153, #40236, #194934, #174031, #65832, #97152, #118091, #158835, #25095, #179781, #41250, #70581, #86737, #102912, #9917, #126510, #26090, #66829, #128493, #39240, #100896, #24084, #85739, #106880, #73591, #27092, #45226, #43239, #134262, #119095, #135264, #92695, #136238, #60376, #105891, #14884, #57422, #88738, #165594, #107862, #90711, #122048, #180777, #137222, #42252, #197912, #154383, #199903, #103914, #198908, #168553, #58403, #152394, #72588, #183739, #30051, #91692, #104906, #195949, #153383, #76545, #167578, #61367, #121055, #151419, #138221, #150432, #59382, #89733, #182750, #11927, #123038, #196935, #120069, #44234, #166594, #181757, #75547, #28094, #12906, #29072, #184724, #13880, #74570, #46208, #169547, #31046, #140195, #18867, #156370, #93698, #32041, #78521, #155381, #3670, #1688, #143173, #65348, #66344, #50199, #94692, #34028, #172543, #142186, #33037, #128006, #36000, #4653, #97647, #187729, #124024, #185722, #127008, #188716, #186738, #139208, #111855, #173545, #49200, #189708, #64364, #17874, #81486, #683, #141198, #79528, #2687, #47212, #96669, #63365, #108871, #126033, #48209, #15878, #80513, #16870, #62354, #110858, #19845, #95686, #125042, #51181, #170551, #35014, #109863, #158357, #157373, #171548, #112841, #174533, #77536, #147186, #145171, #86506, #8676, #9684, #193702, #38012, #177541, #115851, #85498, #176536, #71349, #179546, #148190, #41016, #131003, #67335, #128997, #117853, #22843, #178532, #162347, #82489, #146168, #21842, #68333, #83494, #114842, #53164, #55172, #99668, #161352, #190695, #163361, #52170, #70348, #101671, #6655, #5659, #113827 ),
 ( #144173, #132015, #175522, #24857, #116842, #160352, #36997, #39999, #129983, #20833, #98658, #191683, #159336, #84490, #133013, #192695, #194703, #7653, #69337, #54178, #56172, #39010, #100665, #23848, #167347, #72348, #27860, #122804, #29819, #10684, #28844, #75317, #88500, #120818, #102682, #90485, #181530, #196708, #134022, #106650, #195714, #152167, #44990, #26858, #149194, #57187, #168322, #118863, #136988, #91455, #153143, #182518, #13650, #14645, #43998, #184494, #105660, #164367, #60144, #25862, #198677, #180546, #76305, #121812, #103685, #42020, #183507, #73361, #87506, #165364, #150196, #11694, #166363, #137983, #136011, #199666, #135033, #58178, #119845, #61131, #43009, #104676, #89501, #151190, #12678, #74345, #197683, #59148, #154148, #172295, #18624, #31803, #64126, #45973, #33784, #95444, #157128, #16633, #169305, #80271, #141941, #79287, #34774, #94449, #124800, #111615, #30811, #171310, #63121, #32797, #77298, #126766, #170310, #138968, #156129, #78280, #127766, #48959, #46973, #92460, #140957, #49951, #2444, #62121, #96431, #15640, #3432, #93452, #110613, #186498, #123784, #185483, #108632, #155140, #65108, #139953, #173300, #188470, #158117, #19609, #47974, #125791, #187493, #81251, #109626, #142933, #66100, #4414, #107627, #17628, #446, #1443, #147952, #52917, #8432, #192453, #112602, #176290, #51929, #98412, #113589, #144929, #83254, #23605, #35764, #6410, #38770, #177299, #70104, #86262, #82243, #69094, #145928, #67098, #24614, #21596, #189466, #114593, #68091, #193455, #39756, #54931, #175283, #128757, #53935, #130761, #9438, #100427, #37762, #159097, #131773, #20591, #115610, #174294, #99424, #97410, #146942, #190454, #161106, #178292, #143934, #162108, #129744, #36748, #22601, #191441, #85251, #5415, #101419, #84248, #116604, #160108, #7411, #163111, #71103, #50944, #25621, #166118, #198431, #14401, #59904, #87265, #102436, #150951, #91213, #73119, #88254, #168085, #12445, #135777, #72100, #134788, #57940, #74107, #119611, #149941, #27620, #152904, #75079, #117603, #11447, #106403, #132770, #167104, #89259, #40767, #103439, #151926, #43757, #29582, #194457, #197448, #179303, #118616, #148950, #55928, #164123, #181294, #195467, #10440, #58914, #180306, #133773, #56942, #120582, #196470, #41774, #182276, #165119, #105421, #42772, #26611, #28605, #90243, #13415, #136746, #104434, #121572, #183267, #44747, #199425, #122566, #140718, #169063, #2208, #171067, #1202, #170073, #186256, #47734, #172062, #185243, #109387, #76066, #63889, #60890, #17388, #107390, #48726, #125560, #15401, #30569, #79044, #123549, #184256, #45738, #153906, #141713, #154900, #94211, #62879, #187257, #92220, #77058, #138730, #18393, #32557, #155890, #210, #110379, #61879, #16399, #137741, #46735, #78045, #108396, #31564, #33549, #93215, #139714, #124559, #95211, #156897, #80044, #77533, #110855, #35997, #158353, #680, #94689, #189705, #97644, #50196, #49197, #124021, #186735, #35011, #127005, #51178, #112838, #172540, #62351, #1685, #170547, #174530, #15875, #2684, #78518, #139205, #95683, #63362, #185719, #108868, #80510, #79525, #47209, #34025, #32038, #188713, #171545, #93695, #111852, #157370, #96666, #18864, #155378, #16867, #173542, #48206, #140192, #125039, #19842, #109860, #81483, #142183, #3667, #156367, #65345, #143170, #66341, #33033, #17871, #141195, #4650, #128003, #64361, #126030, #187726, #39007, #115848, #36994, #194700, #191680, #159333, #22840, #38009, #163358, #9681, #24854, #21838, #98655, #162344, #100662, #56169, #147183, #84487, #128994, #178529, #190692, #23845, #71346, #114839, #5656, #53161, #8672, #70345, #39996, #117850, #52167, #85495, #177537, #160349, #179543, #176533, #20830, #146164, #99664, #86503, #133009, #148187, #83491, #145168, #132012, #193699, #41012, #55168, #7650, #113824, #101668, #175519, #116839, #144170, #69334, #67332, #82486, #6652, #131000 ),
 ( #68330, #129980, #161349, #192692, #54175, #120815, #152164, #10680, #167344, #72345, #27857, #122801, #29816, #134019, #28841, #75314, #88496, #182515, #102679, #90482, #13647, #59145, #183504, #168319, #136985, #198674, #136008, #91452, #151187, #181527, #153140, #87503, #89497, #119842, #12675, #195711, #44987, #26855, #57183, #74342, #73357, #184491, #105656, #103682, #149191, #197680, #106647, #43994, #118860, #14642, #180543, #60141, #150193, #121808, #43006, #42017, #165361, #11691, #135030, #76302, #137980, #199662, #61128, #164364, #25859, #196705, #58175, #104673, #166359, #154145, #3429, #62118, #65105, #110609, #79284, #186495, #125788, #15637, #64123, #4411, #47971, #1440, #81248, #187490, #48956, #185480, #109623, #155136, #171307, #172292, #107624, #140954, #66096, #188466, #30808, #124797, #19606, #127763, #80268, #2441, #77294, #16630, #126763, #157125, #142930, #45970, #33781, #92457, #31800, #443, #169302, #138965, #32793, #108629, #123781, #95441, #93449, #46970, #170307, #18621, #94446, #78277, #141938, #156126, #17625, #139950, #49948, #111612, #173297, #34771, #96428, #63118, #158114, #23602, #160105, #174291, #97407, #146939, #5412, #8429, #53932, #22598, #129741, #69091, #192450, #39753, #144926, #35761, #83251, #38767, #177296, #70101, #86259, #82240, #130758, #145925, #67095, #24611, #21592, #189463, #52914, #68088, #193452, #101415, #54928, #51926, #128754, #115607, #100424, #147949, #162105, #114590, #159094, #131770, #20588, #85248, #143930, #176287, #190451, #116601, #113586, #37759, #178289, #175280, #163108, #191438, #36745, #161103, #6407, #9435, #98409, #71100, #99420, #50941, #84245, #7408, #112599, #58670, #31315, #28368, #168816, #953, #17142, #62629, #90006, #169824, #14151, #29345, #105180, #139473, #151689, #123303, #77804, #59656, #182031, #43514, #124306, #166866, #108140, #186004, #47485, #15151, #184996, #109142, #153656, #132767, #76813, #197207, #92968, #120336, #46480, #13180, #170821, #154654, #136506, #74843, #16149, #106162, #198186, #121330, #183022, #155647, #199176, #32313, #30320, #93967, #44506, #167844, #90974, #152661, #138484, #75818, #137496, #200165, #60643, #122317, #184008, #45491, #107146, #61635, #91963, #64634, #96936, #78794, #66608, #4926, #35281, #159607, #144441, #143439, #174796, #112124, #67603, #127275, #157641, #5927, #63640, #3936, #95956, #65616, #110138, #21106, #2955, #171817, #188989, #49463, #160617, #81752, #79798, #125316, #173816, #82761, #158618, #94964, #129263, #187012, #189970, #126296, #128272, #19130, #156649, #18145, #48482, #51445, #33305, #141471, #190958, #113105, #52435, #36262, #80780, #20108, #97916, #114093, #142458, #175794, #98926, #37268, #140473, #50465, #187993, #111125, #1961, #172815, #34295, #25124, #145437, #8943, #84755, #131273, #146433, #177799, #116111, #86768, #191949, #147455, #42282, #149446, #130254, #148451, #194962, #7923, #40268, #22108, #9946, #71605, #178799, #102939, #87761, #133271, #118120, #55433, #10942, #70612, #100925, #72615, #6920, #132279, #39269, #193970, #53435, #164624, #69608, #115110, #117104, #192961, #103940, #56439, #23109, #68598, #101942, #26118, #163623, #38276, #134290, #176803, #179808, #54440, #41277, #162610, #99930, #161615, #24114, #195977, #85768, #57449, #119122, #180803, #83758, #199934, #44262, #183769, #122077, #91721, #182779, #15909, #185755, #92726, #47244, #137252, #73618, #135289, #124056, #29100, #184755, #168582, #88766, #152422, #28122, #74598, #89761, #121084, #59410, #61397, #105919, #167605, #196961, #169581, #58429, #153415, #107894, #151447, #11954, #120096, #31079, #181784, #138250, #154415, #77567, #45255, #14914, #139239, #106909, #165620, #30080, #27119, #123069, #150459, #76575, #43265, #714, #46240, #166620, #104933, #62386, #136266, #12934, #197941, #90739, #13910, #75576, #198938, #60405, #51211, #93728, #63395, #1719 ),
 ( #187760, #127039, #65379, #35044, #126063, #159368, #129025, #36030, #190726, #80543, #16900, #78551, #67366, #172573, #128036, #111885, #32072, #95717, #171578, #17904, #33067, #64395, #2718, #143203, #49230, #110888, #140226, #112872, #125072, #96698, #174563, #94722, #155410, #186769, #97679, #48239, #81516, #20865, #82522, #188746, #158387, #144204, #50231, #108902, #173575, #170581, #66376, #109894, #19876, #156400, #5690, #4684, #79559, #141227, #189738, #34059, #157404, #18897, #142217, #3700, #115879, #40026, #85527, #194731, #37028, #6684, #145201, #87535, #70376, #101699, #160383, #116870, #21873, #177569, #72376, #179574, #83523, #178561, #24886, #38041, #132044, #52199, #163389, #86535, #8706, #133041, #117883, #148219, #9713, #147215, #41044, #100693, #131035, #102709, #98689, #39037, #69366, #162374, #68362, #56201, #176566, #130013, #23876, #22872, #134050, #55201, #53196, #191712, #193733, #164398, #71377, #114871, #25890, #99697, #149222, #161381, #10713, #192724, #84519, #113857, #175553, #146196, #7682, #54208, #180575, #103713, #153171, #11721, #14673, #60171, #28871, #136037, #75345, #198704, #46001, #151217, #42049, #89529, #45018, #183534, #76334, #92488, #88529, #137014, #152194, #73389, #30841, #27887, #195742, #59177, #74372, #199695, #107656, #61160, #58204, #135061, #121840, #106678, #154177, #168351, #120846, #165393, #138011, #26886, #29847, #150225, #182545, #196737, #122832, #119873, #44027, #184521, #181558, #91484, #197712, #43036, #167375, #12706, #169333, #104702, #15668, #105688, #77327, #166391, #90512, #57216, #118890, #13678, #31831, #172323, #4441, #20621, #66129, #93481, #108660, #157158, #97440, #79315, #94476, #174323, #18653, #141971, #78308, #140984, #48001, #2472, #80299, #474, #33812, #159125, #81279, #123812, #17655, #112631, #138995, #173328, #95472, #47001, #109655, #158145, #49979, #35793, #62148, #3460, #185510, #124827, #155168, #170338, #16660, #125818, #1470, #139981, #65137, #186527, #63148, #171337, #126794, #64154, #32825, #188500, #187521, #48987, #156157, #34803, #111643, #96458, #19637, #110642, #142961, #127794, #189494, #50972, #146971, #115638, #22629, #162135, #85279, #132799, #37789, #128785, #176319, #131804, #70132, #101448, #179333, #175311, #23631, #38798, #160137, #117634, #114620, #82271, #145957, #161133, #86291, #194486, #147981, #144956, #21625, #8459, #193483, #40796, #54960, #7438, #51957, #163140, #113617, #116632, #67127, #69122, #190485, #39784, #83282, #130789, #71133, #36777, #178321, #84276, #6437, #53963, #99453, #24643, #98442, #55958, #192480, #9470, #129771, #177327, #102465, #5443, #164153, #68119, #100455, #143963, #191467, #52945, #180334, #195495, #43785, #184280, #166145, #181321, #60917, #105449, #28633, #165148, #27648, #134817, #89287, #167133, #87295, #120610, #45763, #168109, #10468, #104462, #199449, #107415, #59931, #58941, #133803, #196497, #44775, #136773, #122592, #25650, #182304, #72129, #11476, #41802, #148979, #56969, #12472, #88282, #118642, #90270, #73147, #103469, #26639, #151953, #150978, #149970, #13442, #74133, #135804, #57967, #121598, #198459, #75106, #106428, #183293, #119638, #42800, #29606, #197475, #91238, #152928, #14425, #76090, #137765, #77085, #126562, #185269, #188262, #33573, #2231, #109413, #48751, #172086, #19403, #124585, #15426, #62904, #18418, #156921, #49736, #65886, #61903, #110404, #125583, #46761, #4208, #1226, #169088, #32583, #47759, #173090, #81052, #34568, #31589, #108420, #95235, #80067, #127560, #141737, #94236, #138754, #111404, #236, #3227, #153932, #155917, #123574, #96224, #170095, #17412, #157913, #93239, #64901, #171092, #154924, #140743, #186280, #142728, #16422, #189262, #79069, #50737, #78069, #63913, #30594, #92247, #139737, #187281, #145720, #178079, #194252, #39546, #66883, #82026, #130545, #70896, #52711, #67884, #147742, #192243, #115400 ) ),
 .UNSPECIFIED., .T., .F., .T. ) 
 B_SPLINE_SURFACE_WITH_KNOTS ( ( 4, 3, 4 ),
 ( 3, 2, 2, 2, 2, 2, 2, 2, 2, 2, 2, 2, 2, 2, 2, 2, 2, 2, 2, 2, 2, 2, 2, 2, 2, 2, 2, 2, 2, 2, 2, 2, 2, 2, 2, 2, 2, 2, 2, 2, 2, 2, 2, 2, 2, 2, 2, 2, 2, 2, 2, 2, 2, 2, 2, 2, 2, 2, 2, 2, 2, 2, 2, 2, 2, 2, 2, 2, 2, 2, 2, 2, 2, 2, 2, 2, 2, 2, 2, 2, 2, 2, 2, 2, 2, 2, 2, 2, 2, 2, 2, 2, 2, 2, 2, 2, 2, 2, 2, 2, 2, 2, 2, 2, 2, 2, 2, 2, 2, 2, 2, 2, 2, 2, 2, 2, 2, 2, 2, 2, 2, 2, 2, 2, 2, 2, 2, 2, 2, 2, 2, 2, 2, 2, 2, 2, 2, 2, 2, 2, 2, 2, 2, 2, 2, 2, 2, 2, 2, 2, 2, 2, 2, 2, 2, 2, 2, 2, 2, 2, 2, 2, 2, 2, 2, 2, 2, 2, 2, 2, 2, 2, 2, 2, 2, 2, 2, 2, 2, 2, 2, 2, 2, 2, 2, 2, 2, 2, 2, 2, 2, 2, 2, 2, 2, 2, 2, 2, 2, 2, 2, 2, 2, 2, 2, 2, 2, 2, 2, 2, 2, 2, 2, 2, 2, 2, 2, 2, 2, 2, 2, 2, 2, 2, 2, 2, 2, 2, 3 ),
 ( 0.000000000000000000, 0.5000000000000000000, 1.000000000000000000 ),
 ( 0.000000000000000000, 0.004385964912280701511, 0.008771929824561403022, 0.01315789473684210453, 0.01754385964912280604, 0.02192982456140350755, 0.02631578947368420907, 0.03070175438596491058, 0.03508771929824561209, 0.03947368421052631360, 0.04385964912280701511, 0.04824561403508771662, 0.05263157894736841813, 0.05701754385964911964, 0.06140350877192982115, 0.06578947368421052266, 0.07017543859649122417, 0.07456140350877192569, 0.07894736842105262720, 0.08333333333333332871, 0.08771929824561403022, 0.09210526315789473173, 0.09649122807017543324, 0.1008771929824561348, 0.1052631578947368363, 0.1096491228070175378, 0.1140350877192982393, 0.1184210526315789408, 0.1228070175438596423, 0.1271929824561403577, 0.1315789473684210453, 0.1359649122807017607, 0.1403508771929824483, 0.1447368421052631637, 0.1491228070175438514, 0.1535087719298245668, 0.1578947368421052544, 0.1622807017543859698, 0.1666666666666666574, 0.1710526315789473728, 0.1754385964912280604, 0.1798245614035087758, 0.1842105263157894635, 0.1885964912280701788, 0.1929824561403508665, 0.1973684210526315819, 0.2017543859649122695, 0.2061403508771929849, 0.2105263157894736725, 0.2149122807017543879, 0.2192982456140350755, 0.2236842105263157909, 0.2280701754385964786, 0.2324561403508771940, 0.2368421052631578816, 0.2412280701754385970, 0.2456140350877192846, 0.2500000000000000000, 0.2543859649122807154, 0.2587719298245614308, 0.2631578947368420907, 0.2675438596491228060, 0.2719298245614035214, 0.2763157894736842368, 0.2807017543859648967, 0.2850877192982456121, 0.2894736842105263275, 0.2938596491228070429, 0.2982456140350877027, 0.3026315789473684181, 0.3070175438596491335, 0.3114035087719298489, 0.3157894736842105088, 0.3201754385964912242, 0.3245614035087719396, 0.3289473684210526550, 0.3333333333333333148, 0.3377192982456140302, 0.3421052631578947456, 0.3464912280701754610, 0.3508771929824561209, 0.3552631578947368363, 0.3596491228070175517, 0.3640350877192982670, 0.3684210526315789269, 0.3728070175438596423, 0.3771929824561403577, 0.3815789473684210731, 0.3859649122807017330, 0.3903508771929824483, 0.3947368421052631637, 0.3991228070175438791, 0.4035087719298245390, 0.4078947368421052544, 0.4122807017543859698, 0.4166666666666666852, 0.4210526315789473450, 0.4254385964912280604, 0.4298245614035087758, 0.4342105263157894912, 0.4385964912280701511, 0.4429824561403508665, 0.4473684210526315819, 0.4517543859649122973, 0.4561403508771929571, 0.4605263157894736725, 0.4649122807017543879, 0.4692982456140351033, 0.4736842105263157632, 0.4780701754385964786, 0.4824561403508771940, 0.4868421052631579093, 0.4912280701754385692, 0.4956140350877192846, 0.5000000000000000000, 0.5043859649122807154, 0.5087719298245614308, 0.5131578947368421462, 0.5175438596491228616, 0.5219298245614034659, 0.5263157894736841813, 0.5307017543859648967, 0.5350877192982456121, 0.5394736842105263275, 0.5438596491228070429, 0.5482456140350877583, 0.5526315789473684736, 0.5570175438596490780, 0.5614035087719297934, 0.5657894736842105088, 0.5701754385964912242, 0.5745614035087719396, 0.5789473684210526550, 0.5833333333333333703, 0.5877192982456140857, 0.5921052631578946901, 0.5964912280701754055, 0.6008771929824561209, 0.6052631578947368363, 0.6096491228070175517, 0.6140350877192982670, 0.6184210526315789824, 0.6228070175438596978, 0.6271929824561403022, 0.6315789473684210176, 0.6359649122807017330, 0.6403508771929824483, 0.6447368421052631637, 0.6491228070175438791, 0.6535087719298245945, 0.6578947368421053099, 0.6622807017543859143, 0.6666666666666666297, 0.6710526315789473450, 0.6754385964912280604, 0.6798245614035087758, 0.6842105263157894912, 0.6885964912280702066, 0.6929824561403509220, 0.6973684210526315264, 0.7017543859649122417, 0.7061403508771929571, 0.7105263157894736725, 0.7149122807017543879, 0.7192982456140351033, 0.7236842105263158187, 0.7280701754385965341, 0.7324561403508771384, 0.7368421052631578538, 0.7412280701754385692, 0.7456140350877192846, 0.7500000000000000000, 0.7543859649122807154, 0.7587719298245614308, 0.7631578947368421462, 0.7675438596491228616, 0.7719298245614034659, 0.7763157894736841813, 0.7807017543859648967, 0.7850877192982456121, 0.7894736842105263275, 0.7938596491228070429, 0.7982456140350877583, 0.8026315789473684736, 0.8070175438596490780, 0.8114035087719297934, 0.8157894736842105088, 0.8201754385964912242, 0.8245614035087719396, 0.8289473684210526550, 0.8333333333333333703, 0.8377192982456140857, 0.8421052631578946901, 0.8464912280701754055, 0.8508771929824561209, 0.8552631578947368363, 0.8596491228070175517, 0.8640350877192982670, 0.8684210526315789824, 0.8728070175438596978, 0.8771929824561403022, 0.8815789473684210176, 0.8859649122807017330, 0.8903508771929824483, 0.8947368421052631637, 0.8991228070175438791, 0.9035087719298245945, 0.9078947368421053099, 0.9122807017543859143, 0.9166666666666666297, 0.9210526315789473450, 0.9254385964912280604, 0.9298245614035087758, 0.9342105263157894912, 0.9385964912280702066, 0.9429824561403509220, 0.9473684210526315264, 0.9517543859649122417, 0.9561403508771929571, 0.9605263157894736725, 0.9649122807017543879, 0.9692982456140351033, 0.9736842105263158187, 0.9780701754385965341, 0.9824561403508771384, 0.9868421052631578538, 0.9912280701754385692, 0.9956140350877192846, 1.000000000000000000 ),
 .UNSPECIFIED. ) 
 GEOMETRIC_REPRESENTATION_ITEM ( )  RATIONAL_B_SPLINE_SURFACE ( (
 ( 1.000000000000000000, 0.9659258262890683122, 1.000000000000000000, 0.9659258262890683122, 1.000000000000000000, 0.9659258262890683122, 1.000000000000000000, 0.9659258262890683122, 1.000000000000000000, 0.9659258262890683122, 1.000000000000000000, 0.9659258262890683122, 1.000000000000000000, 0.9659258262890683122, 1.000000000000000000, 0.9659258262890683122, 1.000000000000000000, 0.9659258262890683122, 1.000000000000000000, 0.9659258262890683122, 1.000000000000000000, 0.9659258262890683122, 1.000000000000000000, 0.9659258262890683122, 1.000000000000000000, 0.9659258262890683122, 1.000000000000000000, 0.9659258262890683122, 1.000000000000000000, 0.9659258262890683122, 1.000000000000000000, 0.9659258262890683122, 1.000000000000000000, 0.9659258262890683122, 1.000000000000000000, 0.9659258262890683122, 1.000000000000000000, 0.9659258262890683122, 1.000000000000000000, 0.9659258262890683122, 1.000000000000000000, 0.9659258262890683122, 1.000000000000000000, 0.9659258262890683122, 1.000000000000000000, 0.9659258262890683122, 1.000000000000000000, 0.9659258262890683122, 1.000000000000000000, 0.9659258262890683122, 1.000000000000000000, 0.9659258262890683122, 1.000000000000000000, 0.9659258262890683122, 1.000000000000000000, 0.9659258262890683122, 1.000000000000000000, 0.9659258262890683122, 1.000000000000000000, 0.9659258262890683122, 1.000000000000000000, 0.9659258262890683122, 1.000000000000000000, 0.9659258262890683122, 1.000000000000000000, 0.9659258262890683122, 1.000000000000000000, 0.9659258262890683122, 1.000000000000000000, 0.9659258262890683122, 1.000000000000000000, 0.9659258262890683122, 1.000000000000000000, 0.9659258262890683122, 1.000000000000000000, 0.9659258262890683122, 1.000000000000000000, 0.9659258262890683122, 1.000000000000000000, 0.9659258262890683122, 1.000000000000000000, 0.9659258262890683122, 1.000000000000000000, 0.9659258262890683122, 1.000000000000000000, 0.9659258262890683122, 1.000000000000000000, 0.9659258262890683122, 1.000000000000000000, 0.9659258262890683122, 1.000000000000000000, 0.9659258262890683122, 1.000000000000000000, 0.9659258262890683122, 1.000000000000000000, 0.9659258262890683122, 1.000000000000000000, 0.9659258262890683122, 1.000000000000000000, 0.9659258262890683122, 1.000000000000000000, 0.9659258262890683122, 1.000000000000000000, 0.9659258262890683122, 1.000000000000000000, 0.9659258262890683122, 1.000000000000000000, 0.9659258262890683122, 1.000000000000000000, 0.9659258262890683122, 1.000000000000000000, 0.9659258262890683122, 1.000000000000000000, 0.9659258262890683122, 1.000000000000000000, 0.9659258262890683122, 1.000000000000000000, 0.9659258262890683122, 1.000000000000000000, 0.9659258262890683122, 1.000000000000000000, 0.9659258262890683122, 1.000000000000000000, 0.9659258262890683122, 1.000000000000000000, 0.9659258262890683122, 1.000000000000000000, 0.9659258262890683122, 1.000000000000000000, 0.9659258262890683122, 1.000000000000000000, 0.9659258262890683122, 1.000000000000000000, 0.9659258262890683122, 1.000000000000000000, 0.9659258262890683122, 1.000000000000000000, 0.9659258262890683122, 1.000000000000000000, 0.9659258262890683122, 1.000000000000000000, 0.9659258262890683122, 1.000000000000000000, 0.9659258262890683122, 1.000000000000000000, 0.9659258262890683122, 1.000000000000000000, 0.9659258262890683122, 1.000000000000000000, 0.9659258262890683122, 1.000000000000000000, 0.9659258262890683122, 1.000000000000000000, 0.9659258262890683122, 1.000000000000000000, 0.9659258262890683122, 1.000000000000000000, 0.9659258262890683122, 1.000000000000000000, 0.9659258262890683122, 1.000000000000000000, 0.9659258262890683122, 1.000000000000000000, 0.9659258262890683122, 1.000000000000000000, 0.9659258262890683122, 1.000000000000000000, 0.9659258262890683122, 1.000000000000000000, 0.9659258262890683122, 1.000000000000000000, 0.9659258262890683122, 1.000000000000000000, 0.9659258262890683122, 1.000000000000000000, 0.9659258262890683122, 1.000000000000000000, 0.9659258262890683122, 1.000000000000000000, 0.9659258262890683122, 1.000000000000000000, 0.9659258262890683122, 1.000000000000000000, 0.9659258262890683122, 1.000000000000000000, 0.9659258262890683122, 1.000000000000000000, 0.9659258262890683122, 1.000000000000000000, 0.9659258262890683122, 1.000000000000000000, 0.9659258262890683122, 1.000000000000000000, 0.9659258262890683122, 1.000000000000000000, 0.9659258262890683122, 1.000000000000000000, 0.9659258262890683122, 1.000000000000000000, 0.9659258262890683122, 1.000000000000000000, 0.9659258262890683122, 1.000000000000000000, 0.9659258262890683122, 1.000000000000000000, 0.9659258262890683122, 1.000000000000000000, 0.9659258262890683122, 1.000000000000000000, 0.9659258262890683122, 1.000000000000000000, 0.9659258262890683122, 1.000000000000000000, 0.9659258262890683122, 1.000000000000000000, 0.9659258262890683122, 1.000000000000000000, 0.9659258262890683122, 1.000000000000000000, 0.9659258262890683122, 1.000000000000000000, 0.9659258262890683122, 1.000000000000000000, 0.9659258262890683122, 1.000000000000000000, 0.9659258262890683122, 1.000000000000000000, 0.9659258262890683122, 1.000000000000000000, 0.9659258262890683122, 1.000000000000000000, 0.9659258262890683122, 1.000000000000000000, 0.9659258262890683122, 1.000000000000000000, 0.9659258262890683122, 1.000000000000000000, 0.9659258262890683122, 1.000000000000000000, 0.9659258262890683122, 1.000000000000000000, 0.9659258262890683122, 1.000000000000000000, 0.9659258262890683122, 1.000000000000000000, 0.9659258262890683122, 1.000000000000000000, 0.9659258262890683122, 1.000000000000000000, 0.9659258262890683122, 1.000000000000000000, 0.9659258262890683122, 1.000000000000000000, 0.9659258262890683122, 1.000000000000000000, 0.9659258262890683122, 1.000000000000000000, 0.9659258262890683122, 1.000000000000000000, 0.9659258262890683122, 1.000000000000000000, 0.9659258262890683122, 1.000000000000000000, 0.9659258262890683122, 1.000000000000000000, 0.9659258262890683122, 1.000000000000000000, 0.9659258262890683122, 1.000000000000000000, 0.9659258262890683122, 1.000000000000000000, 0.9659258262890683122, 1.000000000000000000, 0.9659258262890683122, 1.000000000000000000, 0.9659258262890683122, 1.000000000000000000, 0.9659258262890683122, 1.000000000000000000, 0.9659258262890683122, 1.000000000000000000, 0.9659258262890683122, 1.000000000000000000, 0.9659258262890683122, 1.000000000000000000, 0.9659258262890683122, 1.000000000000000000, 0.9659258262890683122, 1.000000000000000000, 0.9659258262890683122, 1.000000000000000000, 0.9659258262890683122, 1.000000000000000000, 0.9659258262890683122, 1.000000000000000000, 0.9659258262890683122, 1.000000000000000000, 0.9659258262890683122, 1.000000000000000000, 0.9659258262890683122, 1.000000000000000000, 0.9659258262890683122, 1.000000000000000000, 0.9659258262890683122, 1.000000000000000000, 0.9659258262890683122, 1.000000000000000000, 0.9659258262890683122, 1.000000000000000000, 0.9659258262890683122, 1.000000000000000000, 0.9659258262890683122, 1.000000000000000000, 0.9659258262890683122, 1.000000000000000000, 0.9659258262890683122, 1.000000000000000000, 0.9659258262890683122, 1.000000000000000000, 0.9659258262890683122, 1.000000000000000000, 0.9659258262890683122, 1.000000000000000000, 0.9659258262890683122, 1.000000000000000000, 0.9659258262890683122, 1.000000000000000000, 0.9659258262890683122, 1.000000000000000000, 0.9659258262890683122, 1.000000000000000000, 0.9659258262890683122, 1.000000000000000000, 0.9659258262890683122, 1.000000000000000000, 0.9659258262890683122, 1.000000000000000000, 0.9659258262890683122, 1.000000000000000000, 0.9659258262890683122, 1.000000000000000000, 0.9659258262890683122, 1.000000000000000000, 0.9659258262890683122, 1.000000000000000000, 0.9659258262890683122, 1.000000000000000000, 0.9659258262890683122, 1.000000000000000000, 0.9659258262890683122, 1.000000000000000000, 0.9659258262890683122, 1.000000000000000000, 0.9659258262890683122, 1.000000000000000000, 0.9659258262890683122, 1.000000000000000000, 0.9659258262890683122, 1.000000000000000000, 0.9659258262890683122, 1.000000000000000000, 0.9659258262890683122, 1.000000000000000000, 0.9659258262890683122, 1.000000000000000000, 0.9659258262890683122, 1.000000000000000000, 0.9659258262890683122, 1.000000000000000000, 0.9659258262890683122, 1.000000000000000000, 0.9659258262890683122, 1.000000000000000000, 0.9659258262890683122, 1.000000000000000000, 0.9659258262890683122, 1.000000000000000000, 0.9659258262890683122, 1.000000000000000000, 0.9659258262890683122, 1.000000000000000000, 0.9659258262890683122, 1.000000000000000000, 0.9659258262890683122, 1.000000000000000000, 0.9659258262890683122, 1.000000000000000000, 0.9659258262890683122, 1.000000000000000000, 0.9659258262890683122, 1.000000000000000000, 0.9659258262890683122, 1.000000000000000000, 0.9659258262890683122, 1.000000000000000000, 0.9659258262890683122, 1.000000000000000000, 0.9659258262890683122, 1.000000000000000000, 0.9659258262890683122, 1.000000000000000000, 0.9659258262890683122, 1.000000000000000000, 0.9659258262890683122, 1.000000000000000000, 0.9659258262890683122, 1.000000000000000000, 0.9659258262890683122, 1.000000000000000000, 0.9659258262890683122, 1.000000000000000000, 0.9659258262890683122, 1.000000000000000000, 0.9659258262890683122, 1.000000000000000000, 0.9659258262890683122, 1.000000000000000000, 0.9659258262890683122, 1.000000000000000000, 0.9659258262890683122, 1.000000000000000000, 0.9659258262890683122, 1.000000000000000000, 0.9659258262890683122, 1.000000000000000000, 0.9659258262890683122, 1.000000000000000000, 0.9659258262890683122, 1.000000000000000000, 0.9659258262890683122, 1.000000000000000000, 0.9659258262890683122, 1.000000000000000000, 0.9659258262890683122, 1.000000000000000000, 0.9659258262890683122, 1.000000000000000000, 0.9659258262890683122, 1.000000000000000000, 0.9659258262890683122, 1.000000000000000000, 0.9659258262890683122, 1.000000000000000000, 0.9659258262890683122, 1.000000000000000000, 0.9659258262890683122, 1.000000000000000000, 0.9659258262890683122, 1.000000000000000000, 0.9659258262890683122, 1.000000000000000000, 0.9659258262890683122, 1.000000000000000000, 0.9659258262890683122, 1.000000000000000000, 0.9659258262890683122, 1.000000000000000000),
 ( 0.3333333333333333703, 0.3219752754296894559, 0.3333333333333333703, 0.3219752754296894559, 0.3333333333333333703, 0.3219752754296894559, 0.3333333333333333703, 0.3219752754296894559, 0.3333333333333333703, 0.3219752754296894559, 0.3333333333333333703, 0.3219752754296894559, 0.3333333333333333703, 0.3219752754296894559, 0.3333333333333333703, 0.3219752754296894559, 0.3333333333333333703, 0.3219752754296894559, 0.3333333333333333703, 0.3219752754296894559, 0.3333333333333333703, 0.3219752754296894559, 0.3333333333333333703, 0.3219752754296894559, 0.3333333333333333703, 0.3219752754296894559, 0.3333333333333333703, 0.3219752754296894559, 0.3333333333333333703, 0.3219752754296894559, 0.3333333333333333703, 0.3219752754296894559, 0.3333333333333333703, 0.3219752754296894559, 0.3333333333333333703, 0.3219752754296894559, 0.3333333333333333703, 0.3219752754296894559, 0.3333333333333333703, 0.3219752754296894559, 0.3333333333333333703, 0.3219752754296894559, 0.3333333333333333703, 0.3219752754296894559, 0.3333333333333333703, 0.3219752754296894559, 0.3333333333333333703, 0.3219752754296894559, 0.3333333333333333703, 0.3219752754296894559, 0.3333333333333333703, 0.3219752754296894559, 0.3333333333333333703, 0.3219752754296894559, 0.3333333333333333703, 0.3219752754296894559, 0.3333333333333333703, 0.3219752754296894559, 0.3333333333333333703, 0.3219752754296894559, 0.3333333333333333703, 0.3219752754296894559, 0.3333333333333333703, 0.3219752754296894559, 0.3333333333333333703, 0.3219752754296894559, 0.3333333333333333703, 0.3219752754296894559, 0.3333333333333333703, 0.3219752754296894559, 0.3333333333333333703, 0.3219752754296894559, 0.3333333333333333703, 0.3219752754296894559, 0.3333333333333333703, 0.3219752754296894559, 0.3333333333333333703, 0.3219752754296894559, 0.3333333333333333703, 0.3219752754296894559, 0.3333333333333333703, 0.3219752754296894559, 0.3333333333333333703, 0.3219752754296894559, 0.3333333333333333703, 0.3219752754296894559, 0.3333333333333333703, 0.3219752754296894559, 0.3333333333333333703, 0.3219752754296894559, 0.3333333333333333703, 0.3219752754296894559, 0.3333333333333333703, 0.3219752754296894559, 0.3333333333333333703, 0.3219752754296894559, 0.3333333333333333703, 0.3219752754296894559, 0.3333333333333333703, 0.3219752754296894559, 0.3333333333333333703, 0.3219752754296894559, 0.3333333333333333703, 0.3219752754296894559, 0.3333333333333333703, 0.3219752754296894559, 0.3333333333333333703, 0.3219752754296894559, 0.3333333333333333703, 0.3219752754296894559, 0.3333333333333333703, 0.3219752754296894559, 0.3333333333333333703, 0.3219752754296894559, 0.3333333333333333703, 0.3219752754296894559, 0.3333333333333333703, 0.3219752754296894559, 0.3333333333333333703, 0.3219752754296894559, 0.3333333333333333703, 0.3219752754296894559, 0.3333333333333333703, 0.3219752754296894559, 0.3333333333333333703, 0.3219752754296894559, 0.3333333333333333703, 0.3219752754296894559, 0.3333333333333333703, 0.3219752754296894559, 0.3333333333333333703, 0.3219752754296894559, 0.3333333333333333703, 0.3219752754296894559, 0.3333333333333333703, 0.3219752754296894559, 0.3333333333333333703, 0.3219752754296894559, 0.3333333333333333703, 0.3219752754296894559, 0.3333333333333333703, 0.3219752754296894559, 0.3333333333333333703, 0.3219752754296894559, 0.3333333333333333703, 0.3219752754296894559, 0.3333333333333333703, 0.3219752754296894559, 0.3333333333333333703, 0.3219752754296894559, 0.3333333333333333703, 0.3219752754296894559, 0.3333333333333333703, 0.3219752754296894559, 0.3333333333333333703, 0.3219752754296894559, 0.3333333333333333703, 0.3219752754296894559, 0.3333333333333333703, 0.3219752754296894559, 0.3333333333333333703, 0.3219752754296894559, 0.3333333333333333703, 0.3219752754296894559, 0.3333333333333333703, 0.3219752754296894559, 0.3333333333333333703, 0.3219752754296894559, 0.3333333333333333703, 0.3219752754296894559, 0.3333333333333333703, 0.3219752754296894559, 0.3333333333333333703, 0.3219752754296894559, 0.3333333333333333703, 0.3219752754296894559, 0.3333333333333333703, 0.3219752754296894559, 0.3333333333333333703, 0.3219752754296894559, 0.3333333333333333703, 0.3219752754296894559, 0.3333333333333333703, 0.3219752754296894559, 0.3333333333333333703, 0.3219752754296894559, 0.3333333333333333703, 0.3219752754296894559, 0.3333333333333333703, 0.3219752754296894559, 0.3333333333333333703, 0.3219752754296894559, 0.3333333333333333703, 0.3219752754296894559, 0.3333333333333333703, 0.3219752754296894559, 0.3333333333333333703, 0.3219752754296894559, 0.3333333333333333703, 0.3219752754296894559, 0.3333333333333333703, 0.3219752754296894559, 0.3333333333333333703, 0.3219752754296894559, 0.3333333333333333703, 0.3219752754296894559, 0.3333333333333333703, 0.3219752754296894559, 0.3333333333333333703, 0.3219752754296894559, 0.3333333333333333703, 0.3219752754296894559, 0.3333333333333333703, 0.3219752754296894559, 0.3333333333333333703, 0.3219752754296894559, 0.3333333333333333703, 0.3219752754296894559, 0.3333333333333333703, 0.3219752754296894559, 0.3333333333333333703, 0.3219752754296894559, 0.3333333333333333703, 0.3219752754296894559, 0.3333333333333333703, 0.3219752754296894559, 0.3333333333333333703, 0.3219752754296894559, 0.3333333333333333703, 0.3219752754296894559, 0.3333333333333333703, 0.3219752754296894559, 0.3333333333333333703, 0.3219752754296894559, 0.3333333333333333703, 0.3219752754296894559, 0.3333333333333333703, 0.3219752754296894559, 0.3333333333333333703, 0.3219752754296894559, 0.3333333333333333703, 0.3219752754296894559, 0.3333333333333333703, 0.3219752754296894559, 0.3333333333333333703, 0.3219752754296894559, 0.3333333333333333703, 0.3219752754296894559, 0.3333333333333333703, 0.3219752754296894559, 0.3333333333333333703, 0.3219752754296894559, 0.3333333333333333703, 0.3219752754296894559, 0.3333333333333333703, 0.3219752754296894559, 0.3333333333333333703, 0.3219752754296894559, 0.3333333333333333703, 0.3219752754296894559, 0.3333333333333333703, 0.3219752754296894559, 0.3333333333333333703, 0.3219752754296894559, 0.3333333333333333703, 0.3219752754296894559, 0.3333333333333333703, 0.3219752754296894559, 0.3333333333333333703, 0.3219752754296894559, 0.3333333333333333703, 0.3219752754296894559, 0.3333333333333333703, 0.3219752754296894559, 0.3333333333333333703, 0.3219752754296894559, 0.3333333333333333703, 0.3219752754296894559, 0.3333333333333333703, 0.3219752754296894559, 0.3333333333333333703, 0.3219752754296894559, 0.3333333333333333703, 0.3219752754296894559, 0.3333333333333333703, 0.3219752754296894559, 0.3333333333333333703, 0.3219752754296894559, 0.3333333333333333703, 0.3219752754296894559, 0.3333333333333333703, 0.3219752754296894559, 0.3333333333333333703, 0.3219752754296894559, 0.3333333333333333703, 0.3219752754296894559, 0.3333333333333333703, 0.3219752754296894559, 0.3333333333333333703, 0.3219752754296894559, 0.3333333333333333703, 0.3219752754296894559, 0.3333333333333333703, 0.3219752754296894559, 0.3333333333333333703, 0.3219752754296894559, 0.3333333333333333703, 0.3219752754296894559, 0.3333333333333333703, 0.3219752754296894559, 0.3333333333333333703, 0.3219752754296894559, 0.3333333333333333703, 0.3219752754296894559, 0.3333333333333333703, 0.3219752754296894559, 0.3333333333333333703, 0.3219752754296894559, 0.3333333333333333703, 0.3219752754296894559, 0.3333333333333333703, 0.3219752754296894559, 0.3333333333333333703, 0.3219752754296894559, 0.3333333333333333703, 0.3219752754296894559, 0.3333333333333333703, 0.3219752754296894559, 0.3333333333333333703, 0.3219752754296894559, 0.3333333333333333703, 0.3219752754296894559, 0.3333333333333333703, 0.3219752754296894559, 0.3333333333333333703, 0.3219752754296894559, 0.3333333333333333703, 0.3219752754296894559, 0.3333333333333333703, 0.3219752754296894559, 0.3333333333333333703, 0.3219752754296894559, 0.3333333333333333703, 0.3219752754296894559, 0.3333333333333333703, 0.3219752754296894559, 0.3333333333333333703, 0.3219752754296894559, 0.3333333333333333703, 0.3219752754296894559, 0.3333333333333333703, 0.3219752754296894559, 0.3333333333333333703, 0.3219752754296894559, 0.3333333333333333703, 0.3219752754296894559, 0.3333333333333333703, 0.3219752754296894559, 0.3333333333333333703, 0.3219752754296894559, 0.3333333333333333703, 0.3219752754296894559, 0.3333333333333333703, 0.3219752754296894559, 0.3333333333333333703, 0.3219752754296894559, 0.3333333333333333703, 0.3219752754296894559, 0.3333333333333333703, 0.3219752754296894559, 0.3333333333333333703, 0.3219752754296894559, 0.3333333333333333703, 0.3219752754296894559, 0.3333333333333333703, 0.3219752754296894559, 0.3333333333333333703, 0.3219752754296894559, 0.3333333333333333703, 0.3219752754296894559, 0.3333333333333333703, 0.3219752754296894559, 0.3333333333333333703, 0.3219752754296894559, 0.3333333333333333703, 0.3219752754296894559, 0.3333333333333333703, 0.3219752754296894559, 0.3333333333333333703, 0.3219752754296894559, 0.3333333333333333703, 0.3219752754296894559, 0.3333333333333333703, 0.3219752754296894559, 0.3333333333333333703, 0.3219752754296894559, 0.3333333333333333703, 0.3219752754296894559, 0.3333333333333333703, 0.3219752754296894559, 0.3333333333333333703, 0.3219752754296894559, 0.3333333333333333703, 0.3219752754296894559, 0.3333333333333333703, 0.3219752754296894559, 0.3333333333333333703, 0.3219752754296894559, 0.3333333333333333703, 0.3219752754296894559, 0.3333333333333333703, 0.3219752754296894559, 0.3333333333333333703, 0.3219752754296894559, 0.3333333333333333703, 0.3219752754296894559, 0.3333333333333333703, 0.3219752754296894559, 0.3333333333333333703, 0.3219752754296894559, 0.3333333333333333703, 0.3219752754296894559, 0.3333333333333333703, 0.3219752754296894559, 0.3333333333333333703, 0.3219752754296894559, 0.3333333333333333703, 0.3219752754296894559, 0.3333333333333333703, 0.3219752754296894559, 0.3333333333333333703, 0.3219752754296894559, 0.3333333333333333703, 0.3219752754296894559, 0.3333333333333333703, 0.3219752754296894559, 0.3333333333333333703, 0.3219752754296894559, 0.3333333333333333703, 0.3219752754296894559, 0.3333333333333333703, 0.3219752754296894559, 0.3333333333333333703, 0.3219752754296894559, 0.3333333333333333703, 0.3219752754296894559, 0.3333333333333333703, 0.3219752754296894559, 0.3333333333333333703, 0.3219752754296894559, 0.3333333333333333703, 0.3219752754296894559, 0.3333333333333333703, 0.3219752754296894559, 0.3333333333333333703, 0.3219752754296894559, 0.3333333333333333703),
 ( 0.3333333333333333703, 0.3219752754296894559, 0.3333333333333333703, 0.3219752754296894559, 0.3333333333333333703, 0.3219752754296894559, 0.3333333333333333703, 0.3219752754296894559, 0.3333333333333333703, 0.3219752754296894559, 0.3333333333333333703, 0.3219752754296894559, 0.3333333333333333703, 0.3219752754296894559, 0.3333333333333333703, 0.3219752754296894559, 0.3333333333333333703, 0.3219752754296894559, 0.3333333333333333703, 0.3219752754296894559, 0.3333333333333333703, 0.3219752754296894559, 0.3333333333333333703, 0.3219752754296894559, 0.3333333333333333703, 0.3219752754296894559, 0.3333333333333333703, 0.3219752754296894559, 0.3333333333333333703, 0.3219752754296894559, 0.3333333333333333703, 0.3219752754296894559, 0.3333333333333333703, 0.3219752754296894559, 0.3333333333333333703, 0.3219752754296894559, 0.3333333333333333703, 0.3219752754296894559, 0.3333333333333333703, 0.3219752754296894559, 0.3333333333333333703, 0.3219752754296894559, 0.3333333333333333703, 0.3219752754296894559, 0.3333333333333333703, 0.3219752754296894559, 0.3333333333333333703, 0.3219752754296894559, 0.3333333333333333703, 0.3219752754296894559, 0.3333333333333333703, 0.3219752754296894559, 0.3333333333333333703, 0.3219752754296894559, 0.3333333333333333703, 0.3219752754296894559, 0.3333333333333333703, 0.3219752754296894559, 0.3333333333333333703, 0.3219752754296894559, 0.3333333333333333703, 0.3219752754296894559, 0.3333333333333333703, 0.3219752754296894559, 0.3333333333333333703, 0.3219752754296894559, 0.3333333333333333703, 0.3219752754296894559, 0.3333333333333333703, 0.3219752754296894559, 0.3333333333333333703, 0.3219752754296894559, 0.3333333333333333703, 0.3219752754296894559, 0.3333333333333333703, 0.3219752754296894559, 0.3333333333333333703, 0.3219752754296894559, 0.3333333333333333703, 0.3219752754296894559, 0.3333333333333333703, 0.3219752754296894559, 0.3333333333333333703, 0.3219752754296894559, 0.3333333333333333703, 0.3219752754296894559, 0.3333333333333333703, 0.3219752754296894559, 0.3333333333333333703, 0.3219752754296894559, 0.3333333333333333703, 0.3219752754296894559, 0.3333333333333333703, 0.3219752754296894559, 0.3333333333333333703, 0.3219752754296894559, 0.3333333333333333703, 0.3219752754296894559, 0.3333333333333333703, 0.3219752754296894559, 0.3333333333333333703, 0.3219752754296894559, 0.3333333333333333703, 0.3219752754296894559, 0.3333333333333333703, 0.3219752754296894559, 0.3333333333333333703, 0.3219752754296894559, 0.3333333333333333703, 0.3219752754296894559, 0.3333333333333333703, 0.3219752754296894559, 0.3333333333333333703, 0.3219752754296894559, 0.3333333333333333703, 0.3219752754296894559, 0.3333333333333333703, 0.3219752754296894559, 0.3333333333333333703, 0.3219752754296894559, 0.3333333333333333703, 0.3219752754296894559, 0.3333333333333333703, 0.3219752754296894559, 0.3333333333333333703, 0.3219752754296894559, 0.3333333333333333703, 0.3219752754296894559, 0.3333333333333333703, 0.3219752754296894559, 0.3333333333333333703, 0.3219752754296894559, 0.3333333333333333703, 0.3219752754296894559, 0.3333333333333333703, 0.3219752754296894559, 0.3333333333333333703, 0.3219752754296894559, 0.3333333333333333703, 0.3219752754296894559, 0.3333333333333333703, 0.3219752754296894559, 0.3333333333333333703, 0.3219752754296894559, 0.3333333333333333703, 0.3219752754296894559, 0.3333333333333333703, 0.3219752754296894559, 0.3333333333333333703, 0.3219752754296894559, 0.3333333333333333703, 0.3219752754296894559, 0.3333333333333333703, 0.3219752754296894559, 0.3333333333333333703, 0.3219752754296894559, 0.3333333333333333703, 0.3219752754296894559, 0.3333333333333333703, 0.3219752754296894559, 0.3333333333333333703, 0.3219752754296894559, 0.3333333333333333703, 0.3219752754296894559, 0.3333333333333333703, 0.3219752754296894559, 0.3333333333333333703, 0.3219752754296894559, 0.3333333333333333703, 0.3219752754296894559, 0.3333333333333333703, 0.3219752754296894559, 0.3333333333333333703, 0.3219752754296894559, 0.3333333333333333703, 0.3219752754296894559, 0.3333333333333333703, 0.3219752754296894559, 0.3333333333333333703, 0.3219752754296894559, 0.3333333333333333703, 0.3219752754296894559, 0.3333333333333333703, 0.3219752754296894559, 0.3333333333333333703, 0.3219752754296894559, 0.3333333333333333703, 0.3219752754296894559, 0.3333333333333333703, 0.3219752754296894559, 0.3333333333333333703, 0.3219752754296894559, 0.3333333333333333703, 0.3219752754296894559, 0.3333333333333333703, 0.3219752754296894559, 0.3333333333333333703, 0.3219752754296894559, 0.3333333333333333703, 0.3219752754296894559, 0.3333333333333333703, 0.3219752754296894559, 0.3333333333333333703, 0.3219752754296894559, 0.3333333333333333703, 0.3219752754296894559, 0.3333333333333333703, 0.3219752754296894559, 0.3333333333333333703, 0.3219752754296894559, 0.3333333333333333703, 0.3219752754296894559, 0.3333333333333333703, 0.3219752754296894559, 0.3333333333333333703, 0.3219752754296894559, 0.3333333333333333703, 0.3219752754296894559, 0.3333333333333333703, 0.3219752754296894559, 0.3333333333333333703, 0.3219752754296894559, 0.3333333333333333703, 0.3219752754296894559, 0.3333333333333333703, 0.3219752754296894559, 0.3333333333333333703, 0.3219752754296894559, 0.3333333333333333703, 0.3219752754296894559, 0.3333333333333333703, 0.3219752754296894559, 0.3333333333333333703, 0.3219752754296894559, 0.3333333333333333703, 0.3219752754296894559, 0.3333333333333333703, 0.3219752754296894559, 0.3333333333333333703, 0.3219752754296894559, 0.3333333333333333703, 0.3219752754296894559, 0.3333333333333333703, 0.3219752754296894559, 0.3333333333333333703, 0.3219752754296894559, 0.3333333333333333703, 0.3219752754296894559, 0.3333333333333333703, 0.3219752754296894559, 0.3333333333333333703, 0.3219752754296894559, 0.3333333333333333703, 0.3219752754296894559, 0.3333333333333333703, 0.3219752754296894559, 0.3333333333333333703, 0.3219752754296894559, 0.3333333333333333703, 0.3219752754296894559, 0.3333333333333333703, 0.3219752754296894559, 0.3333333333333333703, 0.3219752754296894559, 0.3333333333333333703, 0.3219752754296894559, 0.3333333333333333703, 0.3219752754296894559, 0.3333333333333333703, 0.3219752754296894559, 0.3333333333333333703, 0.3219752754296894559, 0.3333333333333333703, 0.3219752754296894559, 0.3333333333333333703, 0.3219752754296894559, 0.3333333333333333703, 0.3219752754296894559, 0.3333333333333333703, 0.3219752754296894559, 0.3333333333333333703, 0.3219752754296894559, 0.3333333333333333703, 0.3219752754296894559, 0.3333333333333333703, 0.3219752754296894559, 0.3333333333333333703, 0.3219752754296894559, 0.3333333333333333703, 0.3219752754296894559, 0.3333333333333333703, 0.3219752754296894559, 0.3333333333333333703, 0.3219752754296894559, 0.3333333333333333703, 0.3219752754296894559, 0.3333333333333333703, 0.3219752754296894559, 0.3333333333333333703, 0.3219752754296894559, 0.3333333333333333703, 0.3219752754296894559, 0.3333333333333333703, 0.3219752754296894559, 0.3333333333333333703, 0.3219752754296894559, 0.3333333333333333703, 0.3219752754296894559, 0.3333333333333333703, 0.3219752754296894559, 0.3333333333333333703, 0.3219752754296894559, 0.3333333333333333703, 0.3219752754296894559, 0.3333333333333333703, 0.3219752754296894559, 0.3333333333333333703, 0.3219752754296894559, 0.3333333333333333703, 0.3219752754296894559, 0.3333333333333333703, 0.3219752754296894559, 0.3333333333333333703, 0.3219752754296894559, 0.3333333333333333703, 0.3219752754296894559, 0.3333333333333333703, 0.3219752754296894559, 0.3333333333333333703, 0.3219752754296894559, 0.3333333333333333703, 0.3219752754296894559, 0.3333333333333333703, 0.3219752754296894559, 0.3333333333333333703, 0.3219752754296894559, 0.3333333333333333703, 0.3219752754296894559, 0.3333333333333333703, 0.3219752754296894559, 0.3333333333333333703, 0.3219752754296894559, 0.3333333333333333703, 0.3219752754296894559, 0.3333333333333333703, 0.3219752754296894559, 0.3333333333333333703, 0.3219752754296894559, 0.3333333333333333703, 0.3219752754296894559, 0.3333333333333333703, 0.3219752754296894559, 0.3333333333333333703, 0.3219752754296894559, 0.3333333333333333703, 0.3219752754296894559, 0.3333333333333333703, 0.3219752754296894559, 0.3333333333333333703, 0.3219752754296894559, 0.3333333333333333703, 0.3219752754296894559, 0.3333333333333333703, 0.3219752754296894559, 0.3333333333333333703, 0.3219752754296894559, 0.3333333333333333703, 0.3219752754296894559, 0.3333333333333333703, 0.3219752754296894559, 0.3333333333333333703, 0.3219752754296894559, 0.3333333333333333703, 0.3219752754296894559, 0.3333333333333333703, 0.3219752754296894559, 0.3333333333333333703, 0.3219752754296894559, 0.3333333333333333703, 0.3219752754296894559, 0.3333333333333333703, 0.3219752754296894559, 0.3333333333333333703, 0.3219752754296894559, 0.3333333333333333703, 0.3219752754296894559, 0.3333333333333333703, 0.3219752754296894559, 0.3333333333333333703, 0.3219752754296894559, 0.3333333333333333703, 0.3219752754296894559, 0.3333333333333333703, 0.3219752754296894559, 0.3333333333333333703, 0.3219752754296894559, 0.3333333333333333703, 0.3219752754296894559, 0.3333333333333333703, 0.3219752754296894559, 0.3333333333333333703, 0.3219752754296894559, 0.3333333333333333703, 0.3219752754296894559, 0.3333333333333333703, 0.3219752754296894559, 0.3333333333333333703, 0.3219752754296894559, 0.3333333333333333703, 0.3219752754296894559, 0.3333333333333333703, 0.3219752754296894559, 0.3333333333333333703, 0.3219752754296894559, 0.3333333333333333703, 0.3219752754296894559, 0.3333333333333333703, 0.3219752754296894559, 0.3333333333333333703, 0.3219752754296894559, 0.3333333333333333703, 0.3219752754296894559, 0.3333333333333333703, 0.3219752754296894559, 0.3333333333333333703, 0.3219752754296894559, 0.3333333333333333703, 0.3219752754296894559, 0.3333333333333333703, 0.3219752754296894559, 0.3333333333333333703, 0.3219752754296894559, 0.3333333333333333703, 0.3219752754296894559, 0.3333333333333333703, 0.3219752754296894559, 0.3333333333333333703, 0.3219752754296894559, 0.3333333333333333703, 0.3219752754296894559, 0.3333333333333333703, 0.3219752754296894559, 0.3333333333333333703, 0.3219752754296894559, 0.3333333333333333703, 0.3219752754296894559, 0.3333333333333333703, 0.3219752754296894559, 0.3333333333333333703, 0.3219752754296894559, 0.3333333333333333703, 0.3219752754296894559, 0.3333333333333333703, 0.3219752754296894559, 0.3333333333333333703, 0.3219752754296894559, 0.3333333333333333703),
 ( 1.000000000000000000, 0.9659258262890683122, 1.000000000000000000, 0.9659258262890683122, 1.000000000000000000, 0.9659258262890683122, 1.000000000000000000, 0.9659258262890683122, 1.000000000000000000, 0.9659258262890683122, 1.000000000000000000, 0.9659258262890683122, 1.000000000000000000, 0.9659258262890683122, 1.000000000000000000, 0.9659258262890683122, 1.000000000000000000, 0.9659258262890683122, 1.000000000000000000, 0.9659258262890683122, 1.000000000000000000, 0.9659258262890683122, 1.000000000000000000, 0.9659258262890683122, 1.000000000000000000, 0.9659258262890683122, 1.000000000000000000, 0.9659258262890683122, 1.000000000000000000, 0.9659258262890683122, 1.000000000000000000, 0.9659258262890683122, 1.000000000000000000, 0.9659258262890683122, 1.000000000000000000, 0.9659258262890683122, 1.000000000000000000, 0.9659258262890683122, 1.000000000000000000, 0.9659258262890683122, 1.000000000000000000, 0.9659258262890683122, 1.000000000000000000, 0.9659258262890683122, 1.000000000000000000, 0.9659258262890683122, 1.000000000000000000, 0.9659258262890683122, 1.000000000000000000, 0.9659258262890683122, 1.000000000000000000, 0.9659258262890683122, 1.000000000000000000, 0.9659258262890683122, 1.000000000000000000, 0.9659258262890683122, 1.000000000000000000, 0.9659258262890683122, 1.000000000000000000, 0.9659258262890683122, 1.000000000000000000, 0.9659258262890683122, 1.000000000000000000, 0.9659258262890683122, 1.000000000000000000, 0.9659258262890683122, 1.000000000000000000, 0.9659258262890683122, 1.000000000000000000, 0.9659258262890683122, 1.000000000000000000, 0.9659258262890683122, 1.000000000000000000, 0.9659258262890683122, 1.000000000000000000, 0.9659258262890683122, 1.000000000000000000, 0.9659258262890683122, 1.000000000000000000, 0.9659258262890683122, 1.000000000000000000, 0.9659258262890683122, 1.000000000000000000, 0.9659258262890683122, 1.000000000000000000, 0.9659258262890683122, 1.000000000000000000, 0.9659258262890683122, 1.000000000000000000, 0.9659258262890683122, 1.000000000000000000, 0.9659258262890683122, 1.000000000000000000, 0.9659258262890683122, 1.000000000000000000, 0.9659258262890683122, 1.000000000000000000, 0.9659258262890683122, 1.000000000000000000, 0.9659258262890683122, 1.000000000000000000, 0.9659258262890683122, 1.000000000000000000, 0.9659258262890683122, 1.000000000000000000, 0.9659258262890683122, 1.000000000000000000, 0.9659258262890683122, 1.000000000000000000, 0.9659258262890683122, 1.000000000000000000, 0.9659258262890683122, 1.000000000000000000, 0.9659258262890683122, 1.000000000000000000, 0.9659258262890683122, 1.000000000000000000, 0.9659258262890683122, 1.000000000000000000, 0.9659258262890683122, 1.000000000000000000, 0.9659258262890683122, 1.000000000000000000, 0.9659258262890683122, 1.000000000000000000, 0.9659258262890683122, 1.000000000000000000, 0.9659258262890683122, 1.000000000000000000, 0.9659258262890683122, 1.000000000000000000, 0.9659258262890683122, 1.000000000000000000, 0.9659258262890683122, 1.000000000000000000, 0.9659258262890683122, 1.000000000000000000, 0.9659258262890683122, 1.000000000000000000, 0.9659258262890683122, 1.000000000000000000, 0.9659258262890683122, 1.000000000000000000, 0.9659258262890683122, 1.000000000000000000, 0.9659258262890683122, 1.000000000000000000, 0.9659258262890683122, 1.000000000000000000, 0.9659258262890683122, 1.000000000000000000, 0.9659258262890683122, 1.000000000000000000, 0.9659258262890683122, 1.000000000000000000, 0.9659258262890683122, 1.000000000000000000, 0.9659258262890683122, 1.000000000000000000, 0.9659258262890683122, 1.000000000000000000, 0.9659258262890683122, 1.000000000000000000, 0.9659258262890683122, 1.000000000000000000, 0.9659258262890683122, 1.000000000000000000, 0.9659258262890683122, 1.000000000000000000, 0.9659258262890683122, 1.000000000000000000, 0.9659258262890683122, 1.000000000000000000, 0.9659258262890683122, 1.000000000000000000, 0.9659258262890683122, 1.000000000000000000, 0.9659258262890683122, 1.000000000000000000, 0.9659258262890683122, 1.000000000000000000, 0.9659258262890683122, 1.000000000000000000, 0.9659258262890683122, 1.000000000000000000, 0.9659258262890683122, 1.000000000000000000, 0.9659258262890683122, 1.000000000000000000, 0.9659258262890683122, 1.000000000000000000, 0.9659258262890683122, 1.000000000000000000, 0.9659258262890683122, 1.000000000000000000, 0.9659258262890683122, 1.000000000000000000, 0.9659258262890683122, 1.000000000000000000, 0.9659258262890683122, 1.000000000000000000, 0.9659258262890683122, 1.000000000000000000, 0.9659258262890683122, 1.000000000000000000, 0.9659258262890683122, 1.000000000000000000, 0.9659258262890683122, 1.000000000000000000, 0.9659258262890683122, 1.000000000000000000, 0.9659258262890683122, 1.000000000000000000, 0.9659258262890683122, 1.000000000000000000, 0.9659258262890683122, 1.000000000000000000, 0.9659258262890683122, 1.000000000000000000, 0.9659258262890683122, 1.000000000000000000, 0.9659258262890683122, 1.000000000000000000, 0.9659258262890683122, 1.000000000000000000, 0.9659258262890683122, 1.000000000000000000, 0.9659258262890683122, 1.000000000000000000, 0.9659258262890683122, 1.000000000000000000, 0.9659258262890683122, 1.000000000000000000, 0.9659258262890683122, 1.000000000000000000, 0.9659258262890683122, 1.000000000000000000, 0.9659258262890683122, 1.000000000000000000, 0.9659258262890683122, 1.000000000000000000, 0.9659258262890683122, 1.000000000000000000, 0.9659258262890683122, 1.000000000000000000, 0.9659258262890683122, 1.000000000000000000, 0.9659258262890683122, 1.000000000000000000, 0.9659258262890683122, 1.000000000000000000, 0.9659258262890683122, 1.000000000000000000, 0.9659258262890683122, 1.000000000000000000, 0.9659258262890683122, 1.000000000000000000, 0.9659258262890683122, 1.000000000000000000, 0.9659258262890683122, 1.000000000000000000, 0.9659258262890683122, 1.000000000000000000, 0.9659258262890683122, 1.000000000000000000, 0.9659258262890683122, 1.000000000000000000, 0.9659258262890683122, 1.000000000000000000, 0.9659258262890683122, 1.000000000000000000, 0.9659258262890683122, 1.000000000000000000, 0.9659258262890683122, 1.000000000000000000, 0.9659258262890683122, 1.000000000000000000, 0.9659258262890683122, 1.000000000000000000, 0.9659258262890683122, 1.000000000000000000, 0.9659258262890683122, 1.000000000000000000, 0.9659258262890683122, 1.000000000000000000, 0.9659258262890683122, 1.000000000000000000, 0.9659258262890683122, 1.000000000000000000, 0.9659258262890683122, 1.000000000000000000, 0.9659258262890683122, 1.000000000000000000, 0.9659258262890683122, 1.000000000000000000, 0.9659258262890683122, 1.000000000000000000, 0.9659258262890683122, 1.000000000000000000, 0.9659258262890683122, 1.000000000000000000, 0.9659258262890683122, 1.000000000000000000, 0.9659258262890683122, 1.000000000000000000, 0.9659258262890683122, 1.000000000000000000, 0.9659258262890683122, 1.000000000000000000, 0.9659258262890683122, 1.000000000000000000, 0.9659258262890683122, 1.000000000000000000, 0.9659258262890683122, 1.000000000000000000, 0.9659258262890683122, 1.000000000000000000, 0.9659258262890683122, 1.000000000000000000, 0.9659258262890683122, 1.000000000000000000, 0.9659258262890683122, 1.000000000000000000, 0.9659258262890683122, 1.000000000000000000, 0.9659258262890683122, 1.000000000000000000, 0.9659258262890683122, 1.000000000000000000, 0.9659258262890683122, 1.000000000000000000, 0.9659258262890683122, 1.000000000000000000, 0.9659258262890683122, 1.000000000000000000, 0.9659258262890683122, 1.000000000000000000, 0.9659258262890683122, 1.000000000000000000, 0.9659258262890683122, 1.000000000000000000, 0.9659258262890683122, 1.000000000000000000, 0.9659258262890683122, 1.000000000000000000, 0.9659258262890683122, 1.000000000000000000, 0.9659258262890683122, 1.000000000000000000, 0.9659258262890683122, 1.000000000000000000, 0.9659258262890683122, 1.000000000000000000, 0.9659258262890683122, 1.000000000000000000, 0.9659258262890683122, 1.000000000000000000, 0.9659258262890683122, 1.000000000000000000, 0.9659258262890683122, 1.000000000000000000, 0.9659258262890683122, 1.000000000000000000, 0.9659258262890683122, 1.000000000000000000, 0.9659258262890683122, 1.000000000000000000, 0.9659258262890683122, 1.000000000000000000, 0.9659258262890683122, 1.000000000000000000, 0.9659258262890683122, 1.000000000000000000, 0.9659258262890683122, 1.000000000000000000, 0.9659258262890683122, 1.000000000000000000, 0.9659258262890683122, 1.000000000000000000, 0.9659258262890683122, 1.000000000000000000, 0.9659258262890683122, 1.000000000000000000, 0.9659258262890683122, 1.000000000000000000, 0.9659258262890683122, 1.000000000000000000, 0.9659258262890683122, 1.000000000000000000, 0.9659258262890683122, 1.000000000000000000, 0.9659258262890683122, 1.000000000000000000, 0.9659258262890683122, 1.000000000000000000, 0.9659258262890683122, 1.000000000000000000, 0.9659258262890683122, 1.000000000000000000, 0.9659258262890683122, 1.000000000000000000, 0.9659258262890683122, 1.000000000000000000, 0.9659258262890683122, 1.000000000000000000, 0.9659258262890683122, 1.000000000000000000, 0.9659258262890683122, 1.000000000000000000, 0.9659258262890683122, 1.000000000000000000, 0.9659258262890683122, 1.000000000000000000, 0.9659258262890683122, 1.000000000000000000, 0.9659258262890683122, 1.000000000000000000, 0.9659258262890683122, 1.000000000000000000, 0.9659258262890683122, 1.000000000000000000, 0.9659258262890683122, 1.000000000000000000, 0.9659258262890683122, 1.000000000000000000, 0.9659258262890683122, 1.000000000000000000, 0.9659258262890683122, 1.000000000000000000, 0.9659258262890683122, 1.000000000000000000, 0.9659258262890683122, 1.000000000000000000, 0.9659258262890683122, 1.000000000000000000, 0.9659258262890683122, 1.000000000000000000, 0.9659258262890683122, 1.000000000000000000, 0.9659258262890683122, 1.000000000000000000, 0.9659258262890683122, 1.000000000000000000, 0.9659258262890683122, 1.000000000000000000, 0.9659258262890683122, 1.000000000000000000, 0.9659258262890683122, 1.000000000000000000, 0.9659258262890683122, 1.000000000000000000, 0.9659258262890683122, 1.000000000000000000, 0.9659258262890683122, 1.000000000000000000, 0.9659258262890683122, 1.000000000000000000),
 ( 0.3333333333333333703, 0.3219752754296894559, 0.3333333333333333703, 0.3219752754296894559, 0.3333333333333333703, 0.3219752754296894559, 0.3333333333333333703, 0.3219752754296894559, 0.3333333333333333703, 0.3219752754296894559, 0.3333333333333333703, 0.3219752754296894559, 0.3333333333333333703, 0.3219752754296894559, 0.3333333333333333703, 0.3219752754296894559, 0.3333333333333333703, 0.3219752754296894559, 0.3333333333333333703, 0.3219752754296894559, 0.3333333333333333703, 0.3219752754296894559, 0.3333333333333333703, 0.3219752754296894559, 0.3333333333333333703, 0.3219752754296894559, 0.3333333333333333703, 0.3219752754296894559, 0.3333333333333333703, 0.3219752754296894559, 0.3333333333333333703, 0.3219752754296894559, 0.3333333333333333703, 0.3219752754296894559, 0.3333333333333333703, 0.3219752754296894559, 0.3333333333333333703, 0.3219752754296894559, 0.3333333333333333703, 0.3219752754296894559, 0.3333333333333333703, 0.3219752754296894559, 0.3333333333333333703, 0.3219752754296894559, 0.3333333333333333703, 0.3219752754296894559, 0.3333333333333333703, 0.3219752754296894559, 0.3333333333333333703, 0.3219752754296894559, 0.3333333333333333703, 0.3219752754296894559, 0.3333333333333333703, 0.3219752754296894559, 0.3333333333333333703, 0.3219752754296894559, 0.3333333333333333703, 0.3219752754296894559, 0.3333333333333333703, 0.3219752754296894559, 0.3333333333333333703, 0.3219752754296894559, 0.3333333333333333703, 0.3219752754296894559, 0.3333333333333333703, 0.3219752754296894559, 0.3333333333333333703, 0.3219752754296894559, 0.3333333333333333703, 0.3219752754296894559, 0.3333333333333333703, 0.3219752754296894559, 0.3333333333333333703, 0.3219752754296894559, 0.3333333333333333703, 0.3219752754296894559, 0.3333333333333333703, 0.3219752754296894559, 0.3333333333333333703, 0.3219752754296894559, 0.3333333333333333703, 0.3219752754296894559, 0.3333333333333333703, 0.3219752754296894559, 0.3333333333333333703, 0.3219752754296894559, 0.3333333333333333703, 0.3219752754296894559, 0.3333333333333333703, 0.3219752754296894559, 0.3333333333333333703, 0.3219752754296894559, 0.3333333333333333703, 0.3219752754296894559, 0.3333333333333333703, 0.3219752754296894559, 0.3333333333333333703, 0.3219752754296894559, 0.3333333333333333703, 0.3219752754296894559, 0.3333333333333333703, 0.3219752754296894559, 0.3333333333333333703, 0.3219752754296894559, 0.3333333333333333703, 0.3219752754296894559, 0.3333333333333333703, 0.3219752754296894559, 0.3333333333333333703, 0.3219752754296894559, 0.3333333333333333703, 0.3219752754296894559, 0.3333333333333333703, 0.3219752754296894559, 0.3333333333333333703, 0.3219752754296894559, 0.3333333333333333703, 0.3219752754296894559, 0.3333333333333333703, 0.3219752754296894559, 0.3333333333333333703, 0.3219752754296894559, 0.3333333333333333703, 0.3219752754296894559, 0.3333333333333333703, 0.3219752754296894559, 0.3333333333333333703, 0.3219752754296894559, 0.3333333333333333703, 0.3219752754296894559, 0.3333333333333333703, 0.3219752754296894559, 0.3333333333333333703, 0.3219752754296894559, 0.3333333333333333703, 0.3219752754296894559, 0.3333333333333333703, 0.3219752754296894559, 0.3333333333333333703, 0.3219752754296894559, 0.3333333333333333703, 0.3219752754296894559, 0.3333333333333333703, 0.3219752754296894559, 0.3333333333333333703, 0.3219752754296894559, 0.3333333333333333703, 0.3219752754296894559, 0.3333333333333333703, 0.3219752754296894559, 0.3333333333333333703, 0.3219752754296894559, 0.3333333333333333703, 0.3219752754296894559, 0.3333333333333333703, 0.3219752754296894559, 0.3333333333333333703, 0.3219752754296894559, 0.3333333333333333703, 0.3219752754296894559, 0.3333333333333333703, 0.3219752754296894559, 0.3333333333333333703, 0.3219752754296894559, 0.3333333333333333703, 0.3219752754296894559, 0.3333333333333333703, 0.3219752754296894559, 0.3333333333333333703, 0.3219752754296894559, 0.3333333333333333703, 0.3219752754296894559, 0.3333333333333333703, 0.3219752754296894559, 0.3333333333333333703, 0.3219752754296894559, 0.3333333333333333703, 0.3219752754296894559, 0.3333333333333333703, 0.3219752754296894559, 0.3333333333333333703, 0.3219752754296894559, 0.3333333333333333703, 0.3219752754296894559, 0.3333333333333333703, 0.3219752754296894559, 0.3333333333333333703, 0.3219752754296894559, 0.3333333333333333703, 0.3219752754296894559, 0.3333333333333333703, 0.3219752754296894559, 0.3333333333333333703, 0.3219752754296894559, 0.3333333333333333703, 0.3219752754296894559, 0.3333333333333333703, 0.3219752754296894559, 0.3333333333333333703, 0.3219752754296894559, 0.3333333333333333703, 0.3219752754296894559, 0.3333333333333333703, 0.3219752754296894559, 0.3333333333333333703, 0.3219752754296894559, 0.3333333333333333703, 0.3219752754296894559, 0.3333333333333333703, 0.3219752754296894559, 0.3333333333333333703, 0.3219752754296894559, 0.3333333333333333703, 0.3219752754296894559, 0.3333333333333333703, 0.3219752754296894559, 0.3333333333333333703, 0.3219752754296894559, 0.3333333333333333703, 0.3219752754296894559, 0.3333333333333333703, 0.3219752754296894559, 0.3333333333333333703, 0.3219752754296894559, 0.3333333333333333703, 0.3219752754296894559, 0.3333333333333333703, 0.3219752754296894559, 0.3333333333333333703, 0.3219752754296894559, 0.3333333333333333703, 0.3219752754296894559, 0.3333333333333333703, 0.3219752754296894559, 0.3333333333333333703, 0.3219752754296894559, 0.3333333333333333703, 0.3219752754296894559, 0.3333333333333333703, 0.3219752754296894559, 0.3333333333333333703, 0.3219752754296894559, 0.3333333333333333703, 0.3219752754296894559, 0.3333333333333333703, 0.3219752754296894559, 0.3333333333333333703, 0.3219752754296894559, 0.3333333333333333703, 0.3219752754296894559, 0.3333333333333333703, 0.3219752754296894559, 0.3333333333333333703, 0.3219752754296894559, 0.3333333333333333703, 0.3219752754296894559, 0.3333333333333333703, 0.3219752754296894559, 0.3333333333333333703, 0.3219752754296894559, 0.3333333333333333703, 0.3219752754296894559, 0.3333333333333333703, 0.3219752754296894559, 0.3333333333333333703, 0.3219752754296894559, 0.3333333333333333703, 0.3219752754296894559, 0.3333333333333333703, 0.3219752754296894559, 0.3333333333333333703, 0.3219752754296894559, 0.3333333333333333703, 0.3219752754296894559, 0.3333333333333333703, 0.3219752754296894559, 0.3333333333333333703, 0.3219752754296894559, 0.3333333333333333703, 0.3219752754296894559, 0.3333333333333333703, 0.3219752754296894559, 0.3333333333333333703, 0.3219752754296894559, 0.3333333333333333703, 0.3219752754296894559, 0.3333333333333333703, 0.3219752754296894559, 0.3333333333333333703, 0.3219752754296894559, 0.3333333333333333703, 0.3219752754296894559, 0.3333333333333333703, 0.3219752754296894559, 0.3333333333333333703, 0.3219752754296894559, 0.3333333333333333703, 0.3219752754296894559, 0.3333333333333333703, 0.3219752754296894559, 0.3333333333333333703, 0.3219752754296894559, 0.3333333333333333703, 0.3219752754296894559, 0.3333333333333333703, 0.3219752754296894559, 0.3333333333333333703, 0.3219752754296894559, 0.3333333333333333703, 0.3219752754296894559, 0.3333333333333333703, 0.3219752754296894559, 0.3333333333333333703, 0.3219752754296894559, 0.3333333333333333703, 0.3219752754296894559, 0.3333333333333333703, 0.3219752754296894559, 0.3333333333333333703, 0.3219752754296894559, 0.3333333333333333703, 0.3219752754296894559, 0.3333333333333333703, 0.3219752754296894559, 0.3333333333333333703, 0.3219752754296894559, 0.3333333333333333703, 0.3219752754296894559, 0.3333333333333333703, 0.3219752754296894559, 0.3333333333333333703, 0.3219752754296894559, 0.3333333333333333703, 0.3219752754296894559, 0.3333333333333333703, 0.3219752754296894559, 0.3333333333333333703, 0.3219752754296894559, 0.3333333333333333703, 0.3219752754296894559, 0.3333333333333333703, 0.3219752754296894559, 0.3333333333333333703, 0.3219752754296894559, 0.3333333333333333703, 0.3219752754296894559, 0.3333333333333333703, 0.3219752754296894559, 0.3333333333333333703, 0.3219752754296894559, 0.3333333333333333703, 0.3219752754296894559, 0.3333333333333333703, 0.3219752754296894559, 0.3333333333333333703, 0.3219752754296894559, 0.3333333333333333703, 0.3219752754296894559, 0.3333333333333333703, 0.3219752754296894559, 0.3333333333333333703, 0.3219752754296894559, 0.3333333333333333703, 0.3219752754296894559, 0.3333333333333333703, 0.3219752754296894559, 0.3333333333333333703, 0.3219752754296894559, 0.3333333333333333703, 0.3219752754296894559, 0.3333333333333333703, 0.3219752754296894559, 0.3333333333333333703, 0.3219752754296894559, 0.3333333333333333703, 0.3219752754296894559, 0.3333333333333333703, 0.3219752754296894559, 0.3333333333333333703, 0.3219752754296894559, 0.3333333333333333703, 0.3219752754296894559, 0.3333333333333333703, 0.3219752754296894559, 0.3333333333333333703, 0.3219752754296894559, 0.3333333333333333703, 0.3219752754296894559, 0.3333333333333333703, 0.3219752754296894559, 0.3333333333333333703, 0.3219752754296894559, 0.3333333333333333703, 0.3219752754296894559, 0.3333333333333333703, 0.3219752754296894559, 0.3333333333333333703, 0.3219752754296894559, 0.3333333333333333703, 0.3219752754296894559, 0.3333333333333333703, 0.3219752754296894559, 0.3333333333333333703, 0.3219752754296894559, 0.3333333333333333703, 0.3219752754296894559, 0.3333333333333333703, 0.3219752754296894559, 0.3333333333333333703, 0.3219752754296894559, 0.3333333333333333703, 0.3219752754296894559, 0.3333333333333333703, 0.3219752754296894559, 0.3333333333333333703, 0.3219752754296894559, 0.3333333333333333703, 0.3219752754296894559, 0.3333333333333333703, 0.3219752754296894559, 0.3333333333333333703, 0.3219752754296894559, 0.3333333333333333703, 0.3219752754296894559, 0.3333333333333333703, 0.3219752754296894559, 0.3333333333333333703, 0.3219752754296894559, 0.3333333333333333703, 0.3219752754296894559, 0.3333333333333333703, 0.3219752754296894559, 0.3333333333333333703, 0.3219752754296894559, 0.3333333333333333703, 0.3219752754296894559, 0.3333333333333333703, 0.3219752754296894559, 0.3333333333333333703, 0.3219752754296894559, 0.3333333333333333703, 0.3219752754296894559, 0.3333333333333333703, 0.3219752754296894559, 0.3333333333333333703, 0.3219752754296894559, 0.3333333333333333703, 0.3219752754296894559, 0.3333333333333333703, 0.3219752754296894559, 0.3333333333333333703, 0.3219752754296894559, 0.3333333333333333703, 0.3219752754296894559, 0.3333333333333333703, 0.3219752754296894559, 0.3333333333333333703),
 ( 0.3333333333333333703, 0.3219752754296894559, 0.3333333333333333703, 0.3219752754296894559, 0.3333333333333333703, 0.3219752754296894559, 0.3333333333333333703, 0.3219752754296894559, 0.3333333333333333703, 0.3219752754296894559, 0.3333333333333333703, 0.3219752754296894559, 0.3333333333333333703, 0.3219752754296894559, 0.3333333333333333703, 0.3219752754296894559, 0.3333333333333333703, 0.3219752754296894559, 0.3333333333333333703, 0.3219752754296894559, 0.3333333333333333703, 0.3219752754296894559, 0.3333333333333333703, 0.3219752754296894559, 0.3333333333333333703, 0.3219752754296894559, 0.3333333333333333703, 0.3219752754296894559, 0.3333333333333333703, 0.3219752754296894559, 0.3333333333333333703, 0.3219752754296894559, 0.3333333333333333703, 0.3219752754296894559, 0.3333333333333333703, 0.3219752754296894559, 0.3333333333333333703, 0.3219752754296894559, 0.3333333333333333703, 0.3219752754296894559, 0.3333333333333333703, 0.3219752754296894559, 0.3333333333333333703, 0.3219752754296894559, 0.3333333333333333703, 0.3219752754296894559, 0.3333333333333333703, 0.3219752754296894559, 0.3333333333333333703, 0.3219752754296894559, 0.3333333333333333703, 0.3219752754296894559, 0.3333333333333333703, 0.3219752754296894559, 0.3333333333333333703, 0.3219752754296894559, 0.3333333333333333703, 0.3219752754296894559, 0.3333333333333333703, 0.3219752754296894559, 0.3333333333333333703, 0.3219752754296894559, 0.3333333333333333703, 0.3219752754296894559, 0.3333333333333333703, 0.3219752754296894559, 0.3333333333333333703, 0.3219752754296894559, 0.3333333333333333703, 0.3219752754296894559, 0.3333333333333333703, 0.3219752754296894559, 0.3333333333333333703, 0.3219752754296894559, 0.3333333333333333703, 0.3219752754296894559, 0.3333333333333333703, 0.3219752754296894559, 0.3333333333333333703, 0.3219752754296894559, 0.3333333333333333703, 0.3219752754296894559, 0.3333333333333333703, 0.3219752754296894559, 0.3333333333333333703, 0.3219752754296894559, 0.3333333333333333703, 0.3219752754296894559, 0.3333333333333333703, 0.3219752754296894559, 0.3333333333333333703, 0.3219752754296894559, 0.3333333333333333703, 0.3219752754296894559, 0.3333333333333333703, 0.3219752754296894559, 0.3333333333333333703, 0.3219752754296894559, 0.3333333333333333703, 0.3219752754296894559, 0.3333333333333333703, 0.3219752754296894559, 0.3333333333333333703, 0.3219752754296894559, 0.3333333333333333703, 0.3219752754296894559, 0.3333333333333333703, 0.3219752754296894559, 0.3333333333333333703, 0.3219752754296894559, 0.3333333333333333703, 0.3219752754296894559, 0.3333333333333333703, 0.3219752754296894559, 0.3333333333333333703, 0.3219752754296894559, 0.3333333333333333703, 0.3219752754296894559, 0.3333333333333333703, 0.3219752754296894559, 0.3333333333333333703, 0.3219752754296894559, 0.3333333333333333703, 0.3219752754296894559, 0.3333333333333333703, 0.3219752754296894559, 0.3333333333333333703, 0.3219752754296894559, 0.3333333333333333703, 0.3219752754296894559, 0.3333333333333333703, 0.3219752754296894559, 0.3333333333333333703, 0.3219752754296894559, 0.3333333333333333703, 0.3219752754296894559, 0.3333333333333333703, 0.3219752754296894559, 0.3333333333333333703, 0.3219752754296894559, 0.3333333333333333703, 0.3219752754296894559, 0.3333333333333333703, 0.3219752754296894559, 0.3333333333333333703, 0.3219752754296894559, 0.3333333333333333703, 0.3219752754296894559, 0.3333333333333333703, 0.3219752754296894559, 0.3333333333333333703, 0.3219752754296894559, 0.3333333333333333703, 0.3219752754296894559, 0.3333333333333333703, 0.3219752754296894559, 0.3333333333333333703, 0.3219752754296894559, 0.3333333333333333703, 0.3219752754296894559, 0.3333333333333333703, 0.3219752754296894559, 0.3333333333333333703, 0.3219752754296894559, 0.3333333333333333703, 0.3219752754296894559, 0.3333333333333333703, 0.3219752754296894559, 0.3333333333333333703, 0.3219752754296894559, 0.3333333333333333703, 0.3219752754296894559, 0.3333333333333333703, 0.3219752754296894559, 0.3333333333333333703, 0.3219752754296894559, 0.3333333333333333703, 0.3219752754296894559, 0.3333333333333333703, 0.3219752754296894559, 0.3333333333333333703, 0.3219752754296894559, 0.3333333333333333703, 0.3219752754296894559, 0.3333333333333333703, 0.3219752754296894559, 0.3333333333333333703, 0.3219752754296894559, 0.3333333333333333703, 0.3219752754296894559, 0.3333333333333333703, 0.3219752754296894559, 0.3333333333333333703, 0.3219752754296894559, 0.3333333333333333703, 0.3219752754296894559, 0.3333333333333333703, 0.3219752754296894559, 0.3333333333333333703, 0.3219752754296894559, 0.3333333333333333703, 0.3219752754296894559, 0.3333333333333333703, 0.3219752754296894559, 0.3333333333333333703, 0.3219752754296894559, 0.3333333333333333703, 0.3219752754296894559, 0.3333333333333333703, 0.3219752754296894559, 0.3333333333333333703, 0.3219752754296894559, 0.3333333333333333703, 0.3219752754296894559, 0.3333333333333333703, 0.3219752754296894559, 0.3333333333333333703, 0.3219752754296894559, 0.3333333333333333703, 0.3219752754296894559, 0.3333333333333333703, 0.3219752754296894559, 0.3333333333333333703, 0.3219752754296894559, 0.3333333333333333703, 0.3219752754296894559, 0.3333333333333333703, 0.3219752754296894559, 0.3333333333333333703, 0.3219752754296894559, 0.3333333333333333703, 0.3219752754296894559, 0.3333333333333333703, 0.3219752754296894559, 0.3333333333333333703, 0.3219752754296894559, 0.3333333333333333703, 0.3219752754296894559, 0.3333333333333333703, 0.3219752754296894559, 0.3333333333333333703, 0.3219752754296894559, 0.3333333333333333703, 0.3219752754296894559, 0.3333333333333333703, 0.3219752754296894559, 0.3333333333333333703, 0.3219752754296894559, 0.3333333333333333703, 0.3219752754296894559, 0.3333333333333333703, 0.3219752754296894559, 0.3333333333333333703, 0.3219752754296894559, 0.3333333333333333703, 0.3219752754296894559, 0.3333333333333333703, 0.3219752754296894559, 0.3333333333333333703, 0.3219752754296894559, 0.3333333333333333703, 0.3219752754296894559, 0.3333333333333333703, 0.3219752754296894559, 0.3333333333333333703, 0.3219752754296894559, 0.3333333333333333703, 0.3219752754296894559, 0.3333333333333333703, 0.3219752754296894559, 0.3333333333333333703, 0.3219752754296894559, 0.3333333333333333703, 0.3219752754296894559, 0.3333333333333333703, 0.3219752754296894559, 0.3333333333333333703, 0.3219752754296894559, 0.3333333333333333703, 0.3219752754296894559, 0.3333333333333333703, 0.3219752754296894559, 0.3333333333333333703, 0.3219752754296894559, 0.3333333333333333703, 0.3219752754296894559, 0.3333333333333333703, 0.3219752754296894559, 0.3333333333333333703, 0.3219752754296894559, 0.3333333333333333703, 0.3219752754296894559, 0.3333333333333333703, 0.3219752754296894559, 0.3333333333333333703, 0.3219752754296894559, 0.3333333333333333703, 0.3219752754296894559, 0.3333333333333333703, 0.3219752754296894559, 0.3333333333333333703, 0.3219752754296894559, 0.3333333333333333703, 0.3219752754296894559, 0.3333333333333333703, 0.3219752754296894559, 0.3333333333333333703, 0.3219752754296894559, 0.3333333333333333703, 0.3219752754296894559, 0.3333333333333333703, 0.3219752754296894559, 0.3333333333333333703, 0.3219752754296894559, 0.3333333333333333703, 0.3219752754296894559, 0.3333333333333333703, 0.3219752754296894559, 0.3333333333333333703, 0.3219752754296894559, 0.3333333333333333703, 0.3219752754296894559, 0.3333333333333333703, 0.3219752754296894559, 0.3333333333333333703, 0.3219752754296894559, 0.3333333333333333703, 0.3219752754296894559, 0.3333333333333333703, 0.3219752754296894559, 0.3333333333333333703, 0.3219752754296894559, 0.3333333333333333703, 0.3219752754296894559, 0.3333333333333333703, 0.3219752754296894559, 0.3333333333333333703, 0.3219752754296894559, 0.3333333333333333703, 0.3219752754296894559, 0.3333333333333333703, 0.3219752754296894559, 0.3333333333333333703, 0.3219752754296894559, 0.3333333333333333703, 0.3219752754296894559, 0.3333333333333333703, 0.3219752754296894559, 0.3333333333333333703, 0.3219752754296894559, 0.3333333333333333703, 0.3219752754296894559, 0.3333333333333333703, 0.3219752754296894559, 0.3333333333333333703, 0.3219752754296894559, 0.3333333333333333703, 0.3219752754296894559, 0.3333333333333333703, 0.3219752754296894559, 0.3333333333333333703, 0.3219752754296894559, 0.3333333333333333703, 0.3219752754296894559, 0.3333333333333333703, 0.3219752754296894559, 0.3333333333333333703, 0.3219752754296894559, 0.3333333333333333703, 0.3219752754296894559, 0.3333333333333333703, 0.3219752754296894559, 0.3333333333333333703, 0.3219752754296894559, 0.3333333333333333703, 0.3219752754296894559, 0.3333333333333333703, 0.3219752754296894559, 0.3333333333333333703, 0.3219752754296894559, 0.3333333333333333703, 0.3219752754296894559, 0.3333333333333333703, 0.3219752754296894559, 0.3333333333333333703, 0.3219752754296894559, 0.3333333333333333703, 0.3219752754296894559, 0.3333333333333333703, 0.3219752754296894559, 0.3333333333333333703, 0.3219752754296894559, 0.3333333333333333703, 0.3219752754296894559, 0.3333333333333333703, 0.3219752754296894559, 0.3333333333333333703, 0.3219752754296894559, 0.3333333333333333703, 0.3219752754296894559, 0.3333333333333333703, 0.3219752754296894559, 0.3333333333333333703, 0.3219752754296894559, 0.3333333333333333703, 0.3219752754296894559, 0.3333333333333333703, 0.3219752754296894559, 0.3333333333333333703, 0.3219752754296894559, 0.3333333333333333703, 0.3219752754296894559, 0.3333333333333333703, 0.3219752754296894559, 0.3333333333333333703, 0.3219752754296894559, 0.3333333333333333703, 0.3219752754296894559, 0.3333333333333333703, 0.3219752754296894559, 0.3333333333333333703, 0.3219752754296894559, 0.3333333333333333703, 0.3219752754296894559, 0.3333333333333333703, 0.3219752754296894559, 0.3333333333333333703, 0.3219752754296894559, 0.3333333333333333703, 0.3219752754296894559, 0.3333333333333333703, 0.3219752754296894559, 0.3333333333333333703, 0.3219752754296894559, 0.3333333333333333703, 0.3219752754296894559, 0.3333333333333333703, 0.3219752754296894559, 0.3333333333333333703, 0.3219752754296894559, 0.3333333333333333703, 0.3219752754296894559, 0.3333333333333333703, 0.3219752754296894559, 0.3333333333333333703, 0.3219752754296894559, 0.3333333333333333703, 0.3219752754296894559, 0.3333333333333333703, 0.3219752754296894559, 0.3333333333333333703, 0.3219752754296894559, 0.3333333333333333703, 0.3219752754296894559, 0.3333333333333333703, 0.3219752754296894559, 0.3333333333333333703),
 ( 1.000000000000000000, 0.9659258262890683122, 1.000000000000000000, 0.9659258262890683122, 1.000000000000000000, 0.9659258262890683122, 1.000000000000000000, 0.9659258262890683122, 1.000000000000000000, 0.9659258262890683122, 1.000000000000000000, 0.9659258262890683122, 1.000000000000000000, 0.9659258262890683122, 1.000000000000000000, 0.9659258262890683122, 1.000000000000000000, 0.9659258262890683122, 1.000000000000000000, 0.9659258262890683122, 1.000000000000000000, 0.9659258262890683122, 1.000000000000000000, 0.9659258262890683122, 1.000000000000000000, 0.9659258262890683122, 1.000000000000000000, 0.9659258262890683122, 1.000000000000000000, 0.9659258262890683122, 1.000000000000000000, 0.9659258262890683122, 1.000000000000000000, 0.9659258262890683122, 1.000000000000000000, 0.9659258262890683122, 1.000000000000000000, 0.9659258262890683122, 1.000000000000000000, 0.9659258262890683122, 1.000000000000000000, 0.9659258262890683122, 1.000000000000000000, 0.9659258262890683122, 1.000000000000000000, 0.9659258262890683122, 1.000000000000000000, 0.9659258262890683122, 1.000000000000000000, 0.9659258262890683122, 1.000000000000000000, 0.9659258262890683122, 1.000000000000000000, 0.9659258262890683122, 1.000000000000000000, 0.9659258262890683122, 1.000000000000000000, 0.9659258262890683122, 1.000000000000000000, 0.9659258262890683122, 1.000000000000000000, 0.9659258262890683122, 1.000000000000000000, 0.9659258262890683122, 1.000000000000000000, 0.9659258262890683122, 1.000000000000000000, 0.9659258262890683122, 1.000000000000000000, 0.9659258262890683122, 1.000000000000000000, 0.9659258262890683122, 1.000000000000000000, 0.9659258262890683122, 1.000000000000000000, 0.9659258262890683122, 1.000000000000000000, 0.9659258262890683122, 1.000000000000000000, 0.9659258262890683122, 1.000000000000000000, 0.9659258262890683122, 1.000000000000000000, 0.9659258262890683122, 1.000000000000000000, 0.9659258262890683122, 1.000000000000000000, 0.9659258262890683122, 1.000000000000000000, 0.9659258262890683122, 1.000000000000000000, 0.9659258262890683122, 1.000000000000000000, 0.9659258262890683122, 1.000000000000000000, 0.9659258262890683122, 1.000000000000000000, 0.9659258262890683122, 1.000000000000000000, 0.9659258262890683122, 1.000000000000000000, 0.9659258262890683122, 1.000000000000000000, 0.9659258262890683122, 1.000000000000000000, 0.9659258262890683122, 1.000000000000000000, 0.9659258262890683122, 1.000000000000000000, 0.9659258262890683122, 1.000000000000000000, 0.9659258262890683122, 1.000000000000000000, 0.9659258262890683122, 1.000000000000000000, 0.9659258262890683122, 1.000000000000000000, 0.9659258262890683122, 1.000000000000000000, 0.9659258262890683122, 1.000000000000000000, 0.9659258262890683122, 1.000000000000000000, 0.9659258262890683122, 1.000000000000000000, 0.9659258262890683122, 1.000000000000000000, 0.9659258262890683122, 1.000000000000000000, 0.9659258262890683122, 1.000000000000000000, 0.9659258262890683122, 1.000000000000000000, 0.9659258262890683122, 1.000000000000000000, 0.9659258262890683122, 1.000000000000000000, 0.9659258262890683122, 1.000000000000000000, 0.9659258262890683122, 1.000000000000000000, 0.9659258262890683122, 1.000000000000000000, 0.9659258262890683122, 1.000000000000000000, 0.9659258262890683122, 1.000000000000000000, 0.9659258262890683122, 1.000000000000000000, 0.9659258262890683122, 1.000000000000000000, 0.9659258262890683122, 1.000000000000000000, 0.9659258262890683122, 1.000000000000000000, 0.9659258262890683122, 1.000000000000000000, 0.9659258262890683122, 1.000000000000000000, 0.9659258262890683122, 1.000000000000000000, 0.9659258262890683122, 1.000000000000000000, 0.9659258262890683122, 1.000000000000000000, 0.9659258262890683122, 1.000000000000000000, 0.9659258262890683122, 1.000000000000000000, 0.9659258262890683122, 1.000000000000000000, 0.9659258262890683122, 1.000000000000000000, 0.9659258262890683122, 1.000000000000000000, 0.9659258262890683122, 1.000000000000000000, 0.9659258262890683122, 1.000000000000000000, 0.9659258262890683122, 1.000000000000000000, 0.9659258262890683122, 1.000000000000000000, 0.9659258262890683122, 1.000000000000000000, 0.9659258262890683122, 1.000000000000000000, 0.9659258262890683122, 1.000000000000000000, 0.9659258262890683122, 1.000000000000000000, 0.9659258262890683122, 1.000000000000000000, 0.9659258262890683122, 1.000000000000000000, 0.9659258262890683122, 1.000000000000000000, 0.9659258262890683122, 1.000000000000000000, 0.9659258262890683122, 1.000000000000000000, 0.9659258262890683122, 1.000000000000000000, 0.9659258262890683122, 1.000000000000000000, 0.9659258262890683122, 1.000000000000000000, 0.9659258262890683122, 1.000000000000000000, 0.9659258262890683122, 1.000000000000000000, 0.9659258262890683122, 1.000000000000000000, 0.9659258262890683122, 1.000000000000000000, 0.9659258262890683122, 1.000000000000000000, 0.9659258262890683122, 1.000000000000000000, 0.9659258262890683122, 1.000000000000000000, 0.9659258262890683122, 1.000000000000000000, 0.9659258262890683122, 1.000000000000000000, 0.9659258262890683122, 1.000000000000000000, 0.9659258262890683122, 1.000000000000000000, 0.9659258262890683122, 1.000000000000000000, 0.9659258262890683122, 1.000000000000000000, 0.9659258262890683122, 1.000000000000000000, 0.9659258262890683122, 1.000000000000000000, 0.9659258262890683122, 1.000000000000000000, 0.9659258262890683122, 1.000000000000000000, 0.9659258262890683122, 1.000000000000000000, 0.9659258262890683122, 1.000000000000000000, 0.9659258262890683122, 1.000000000000000000, 0.9659258262890683122, 1.000000000000000000, 0.9659258262890683122, 1.000000000000000000, 0.9659258262890683122, 1.000000000000000000, 0.9659258262890683122, 1.000000000000000000, 0.9659258262890683122, 1.000000000000000000, 0.9659258262890683122, 1.000000000000000000, 0.9659258262890683122, 1.000000000000000000, 0.9659258262890683122, 1.000000000000000000, 0.9659258262890683122, 1.000000000000000000, 0.9659258262890683122, 1.000000000000000000, 0.9659258262890683122, 1.000000000000000000, 0.9659258262890683122, 1.000000000000000000, 0.9659258262890683122, 1.000000000000000000, 0.9659258262890683122, 1.000000000000000000, 0.9659258262890683122, 1.000000000000000000, 0.9659258262890683122, 1.000000000000000000, 0.9659258262890683122, 1.000000000000000000, 0.9659258262890683122, 1.000000000000000000, 0.9659258262890683122, 1.000000000000000000, 0.9659258262890683122, 1.000000000000000000, 0.9659258262890683122, 1.000000000000000000, 0.9659258262890683122, 1.000000000000000000, 0.9659258262890683122, 1.000000000000000000, 0.9659258262890683122, 1.000000000000000000, 0.9659258262890683122, 1.000000000000000000, 0.9659258262890683122, 1.000000000000000000, 0.9659258262890683122, 1.000000000000000000, 0.9659258262890683122, 1.000000000000000000, 0.9659258262890683122, 1.000000000000000000, 0.9659258262890683122, 1.000000000000000000, 0.9659258262890683122, 1.000000000000000000, 0.9659258262890683122, 1.000000000000000000, 0.9659258262890683122, 1.000000000000000000, 0.9659258262890683122, 1.000000000000000000, 0.9659258262890683122, 1.000000000000000000, 0.9659258262890683122, 1.000000000000000000, 0.9659258262890683122, 1.000000000000000000, 0.9659258262890683122, 1.000000000000000000, 0.9659258262890683122, 1.000000000000000000, 0.9659258262890683122, 1.000000000000000000, 0.9659258262890683122, 1.000000000000000000, 0.9659258262890683122, 1.000000000000000000, 0.9659258262890683122, 1.000000000000000000, 0.9659258262890683122, 1.000000000000000000, 0.9659258262890683122, 1.000000000000000000, 0.9659258262890683122, 1.000000000000000000, 0.9659258262890683122, 1.000000000000000000, 0.9659258262890683122, 1.000000000000000000, 0.9659258262890683122, 1.000000000000000000, 0.9659258262890683122, 1.000000000000000000, 0.9659258262890683122, 1.000000000000000000, 0.9659258262890683122, 1.000000000000000000, 0.9659258262890683122, 1.000000000000000000, 0.9659258262890683122, 1.000000000000000000, 0.9659258262890683122, 1.000000000000000000, 0.9659258262890683122, 1.000000000000000000, 0.9659258262890683122, 1.000000000000000000, 0.9659258262890683122, 1.000000000000000000, 0.9659258262890683122, 1.000000000000000000, 0.9659258262890683122, 1.000000000000000000, 0.9659258262890683122, 1.000000000000000000, 0.9659258262890683122, 1.000000000000000000, 0.9659258262890683122, 1.000000000000000000, 0.9659258262890683122, 1.000000000000000000, 0.9659258262890683122, 1.000000000000000000, 0.9659258262890683122, 1.000000000000000000, 0.9659258262890683122, 1.000000000000000000, 0.9659258262890683122, 1.000000000000000000, 0.9659258262890683122, 1.000000000000000000, 0.9659258262890683122, 1.000000000000000000, 0.9659258262890683122, 1.000000000000000000, 0.9659258262890683122, 1.000000000000000000, 0.9659258262890683122, 1.000000000000000000, 0.9659258262890683122, 1.000000000000000000, 0.9659258262890683122, 1.000000000000000000, 0.9659258262890683122, 1.000000000000000000, 0.9659258262890683122, 1.000000000000000000, 0.9659258262890683122, 1.000000000000000000, 0.9659258262890683122, 1.000000000000000000, 0.9659258262890683122, 1.000000000000000000, 0.9659258262890683122, 1.000000000000000000, 0.9659258262890683122, 1.000000000000000000, 0.9659258262890683122, 1.000000000000000000, 0.9659258262890683122, 1.000000000000000000, 0.9659258262890683122, 1.000000000000000000, 0.9659258262890683122, 1.000000000000000000, 0.9659258262890683122, 1.000000000000000000, 0.9659258262890683122, 1.000000000000000000, 0.9659258262890683122, 1.000000000000000000, 0.9659258262890683122, 1.000000000000000000, 0.9659258262890683122, 1.000000000000000000, 0.9659258262890683122, 1.000000000000000000, 0.9659258262890683122, 1.000000000000000000, 0.9659258262890683122, 1.000000000000000000, 0.9659258262890683122, 1.000000000000000000, 0.9659258262890683122, 1.000000000000000000, 0.9659258262890683122, 1.000000000000000000, 0.9659258262890683122, 1.000000000000000000, 0.9659258262890683122, 1.000000000000000000, 0.9659258262890683122, 1.000000000000000000, 0.9659258262890683122, 1.000000000000000000, 0.9659258262890683122, 1.000000000000000000, 0.9659258262890683122, 1.000000000000000000, 0.9659258262890683122, 1.000000000000000000, 0.9659258262890683122, 1.000000000000000000) ) ) 
 REPRESENTATION_ITEM ( '' )  SURFACE ( )  );
#47938 = CARTESIAN_POINT ( 'NONE',  ( -16.46253265017160317, 9.564922557960807481, 45.83224293864769550 ) ) ;
#47939 = CARTESIAN_POINT ( 'NONE',  ( -8.314922557961024197, 14.29746914071037800, 92.91775706135236135 ) ) ;
#47940 = CIRCLE ( 'NONE', #131929, 216.0437394197456342 ) ;
#47941 = CARTESIAN_POINT ( 'NONE',  ( 10.81492255796078972, 18.62759615963270932, 99.58224293864770971 ) ) ;
#47942 = CARTESIAN_POINT ( 'NONE',  ( -12.14591786802309592, -12.06949235617757132, 46.87390960531435979 ) ) ;
#47943 = CARTESIAN_POINT ( 'NONE',  ( -19.05341960407611168, -5.049401038298163336, 86.45724293864769550 ) ) ;
#47944 = CARTESIAN_POINT ( 'NONE',  ( 0.05219959533934541429, -16.53943276465976808, 80.00109039468568994 ) ) ;
#47945 = CARTESIAN_POINT ( 'NONE',  ( -19.03943276465977164, -0.05219959533935918106, 108.7510903946856615 ) ) ;
#47946 = CARTESIAN_POINT ( 'NONE',  ( -21.52544592524334988, -5.823673210054445271, 18.95942372801901143 ) ) ;
#47947 = CARTESIAN_POINT ( 'NONE',  ( 14.29746914071049879, -8.314922557960816363, 43.33224293864769550 ) ) ;
#47948 = ORIENTED_EDGE ( 'NONE', *, *, #58065, .T. ) ;
#47949 = CARTESIAN_POINT ( 'NONE',  ( -17.12812012977029141, 6.668231424565931320, 68.64051240676857901 ) ) ;
#47950 = CARTESIAN_POINT ( 'NONE',  ( -21.55341960407610458, -5.719274019375992779, 86.45724293864770971 ) ) ;
#47951 = CARTESIAN_POINT ( 'NONE',  ( -4.379528057220328563, 16.55341960407611168, 30.20724293864769550 ) ) ;
#47952 = VERTEX_POINT ( 'NONE', #14215 ) ;
#47953 = CARTESIAN_POINT ( 'NONE',  ( -17.13100169013299379, -6.664070546373171311, 54.23210164300153480 ) ) ;
#47954 = CARTESIAN_POINT ( 'NONE',  ( 10.81492255796078972, 18.62759615963270932, 114.5822429386477097 ) ) ;
#47955 = CARTESIAN_POINT ( 'NONE',  ( -13.89961937509977652, 13.97604488694528158, 110.6239096053143243 ) ) ;
#47956 = CARTESIAN_POINT ( 'NONE',  ( -21.55341960407619339, 5.719274019375674811, 28.54275706135234358 ) ) ;
#47957 = CARTESIAN_POINT ( 'NONE',  ( -16.53943276465976808, 0.05219959533911058130, 56.24890960531436690 ) ) ;
#47958 = CARTESIAN_POINT ( 'NONE',  ( 8.224510206698742110, 14.34966873604972548, 42.08442372801901854 ) ) ;
#47959 = CARTESIAN_POINT ( 'NONE',  ( 5.153800228976335163, 19.02544592524342804, 59.79057627198100988 ) ) ;
#47960 = CARTESIAN_POINT ( 'NONE',  ( -9.474510206698720793, -16.51473224551083518, 49.58442372801899722 ) ) ;
#47961 = CARTESIAN_POINT ( 'NONE',  ( 19.03943276465977164, -0.05219959533909143690, 73.74890960531435269 ) ) ;
#47962 = CARTESIAN_POINT ( 'NONE',  ( -18.62759615963270932, 10.81492255796079327, 35.83224293864768839 ) ) ;
#47963 = CARTESIAN_POINT ( 'NONE',  ( -34.03190083852857128, -20.28298779506915750, -18.01673046680507184 ) ) ;
#47964 = CARTESIAN_POINT ( 'NONE',  ( -0.05219959533909027116, -19.03943276465977164, 42.49890960531435269 ) ) ;
#47965 = CARTESIAN_POINT ( 'NONE',  ( -4.379528057220086978, -16.55341960407618274, 19.79275706135235069 ) ) ;
#47966 = CARTESIAN_POINT ( 'NONE',  ( 19.02544592524334988, 5.153800228976608722, 66.45942372801899012 ) ) ;
#47967 = CARTESIAN_POINT ( 'NONE',  ( 18.62759615963271287, -10.81492255796078972, 98.33224293864769550 ) ) ;
#47968 = CARTESIAN_POINT ( 'NONE',  ( -12.06949235617756955, 12.14591786802309770, 35.62390960531437401 ) ) ;
#47969 = CARTESIAN_POINT ( 'NONE',  ( -16.46253265017160317, 9.564922557960807481, 90.83224293864769550 ) ) ;
#47970 = CARTESIAN_POINT ( 'NONE',  ( 18.62759615963271287, -10.81492255796078972, 53.33224293864769550 ) ) ;
#47972 = CARTESIAN_POINT ( 'NONE',  ( -8.224510206698735004, -14.34966873604973081, 24.58442372801901499 ) ) ;
#47971 = CARTESIAN_POINT ( 'NONE',  ( 10.81492255796078972, 18.62759615963270932, 99.58224293864770971 ) ) ;
#47973 = CARTESIAN_POINT ( 'NONE',  ( -21.52544592524343514, 5.823673210054127303, 36.04057627198102409 ) ) ;
#47974 = CARTESIAN_POINT ( 'NONE',  ( -10.72451020669870658, -18.67979575497194134, 84.58442372801903275 ) ) ;
#47975 = CARTESIAN_POINT ( 'NONE',  ( 9.564922557960805705, 16.46253265017160317, 89.58224293864769550 ) ) ;
#47976 = CARTESIAN_POINT ( 'NONE',  ( 5.153800228976335163, 19.02544592524342804, 34.79057627198102409 ) ) ;
#47977 = CARTESIAN_POINT ( 'NONE',  ( 19.03943276465977164, -0.05219959533909143690, 88.74890960531436690 ) ) ;
#47978 = CARTESIAN_POINT ( 'NONE',  ( 16.53943276465976808, -0.05219959533910856209, 98.74890960531438111 ) ) ;
#47979 = CARTESIAN_POINT ( 'NONE',  ( -5.153800228976328057, -19.02544592524343514, 67.29057627198102409 ) ) ;
#47980 = CARTESIAN_POINT ( 'NONE',  ( -16.52544592524335698, -4.483927247898792601, 28.95942372801902209 ) ) ;
#47981 = CARTESIAN_POINT ( 'NONE',  ( 17.40861289039007431, -6.110651285853167636, 86.12767529172568004 ) ) ;
#47983 = CARTESIAN_POINT ( 'NONE',  ( 5.049401038298161559, -19.05341960407611168, 107.7072429386476955 ) ) ;
#47982 = CARTESIAN_POINT ( 'NONE',  ( -0.05219959533937732626, 21.53943276465977519, 92.50109039468567573 ) ) ;
#47984 = CARTESIAN_POINT ( 'NONE',  ( 12.06949235617739724, 12.14591786802326823, 86.87609039468568994 ) ) ;
#47985 = PLANE ( 'NONE',  #113166 ) ;
#47986 = CARTESIAN_POINT ( 'NONE',  ( -0.05219959533936034679, 19.03943276465977164, 72.50109039468566152 ) ) ;
#47987 = CARTESIAN_POINT ( 'NONE',  ( 0.05219959533936267826, -19.03943276465977164, 35.00109039468566863 ) ) ;
#47988 = CARTESIAN_POINT ( 'NONE',  ( 18.22780087662123805, -5.499999999999976019, 93.51763182126896368 ) ) ;
#47989 = CARTESIAN_POINT ( 'NONE',  ( 19.05341960407611168, 5.049401038298154454, 23.95724293864769194 ) ) ;
#47990 = CARTESIAN_POINT ( 'NONE',  ( -16.55341960407611168, -4.379528057220339221, 41.45724293864769550 ) ) ;
#47991 = CARTESIAN_POINT ( 'NONE',  ( -16.51473224551069308, -9.474510206698971260, 21.66557627198102765 ) ) ;
#47992 = CARTESIAN_POINT ( 'NONE',  ( -14.29746914071049879, 8.314922557960819915, 30.83224293864770260 ) ) ;
#47993 = CARTESIAN_POINT ( 'NONE',  ( -19.49190055781010855, -5.499999999999973355, 85.56116087098779133 ) ) ;
#47994 = CARTESIAN_POINT ( 'NONE',  ( 16.53943276465976808, 0.05219959533934440121, 101.2510903946856757 ) ) ;
#47995 = CARTESIAN_POINT ( 'NONE',  ( 0.05219959533909260263, 19.03943276465977164, 34.99890960531435979 ) ) ;
#47996 = CARTESIAN_POINT ( 'NONE',  ( -18.62759615963255300, -10.81492255796106328, 94.16775706135237556 ) ) ;
#47997 = CARTESIAN_POINT ( 'NONE',  ( 5.153800228976615827, -19.02544592524334988, 105.2094237280190185 ) ) ;
#47998 = CARTESIAN_POINT ( 'NONE',  ( 5.823673210054444382, -21.52544592524334988, 85.20942372801901854 ) ) ;
#47999 = CARTESIAN_POINT ( 'NONE',  ( 5.153800228976615827, -19.02544592524334988, 55.20942372801899722 ) ) ;
#48000 = CARTESIAN_POINT ( 'NONE',  ( -19.03943276465977164, 0.05219959533909376836, 91.24890960531436690 ) ) ;
#48001 = CARTESIAN_POINT ( 'NONE',  ( 19.03943276465977164, -0.05219959533909143690, 73.74890960531435269 ) ) ;
#48002 = CARTESIAN_POINT ( 'NONE',  ( 17.05116617787822975, 6.768360034955830606, 73.84324446740798464 ) ) ;
#48003 = CARTESIAN_POINT ( 'NONE',  ( -12.06949235617756955, 12.14591786802309770, 70.62390960531436690 ) ) ;
#48004 = CARTESIAN_POINT ( 'NONE',  ( 21.52544592524344225, -5.823673210054117533, 63.54057627198103830 ) ) ;
#48005 = CARTESIAN_POINT ( 'NONE',  ( -13.89961937509977652, 13.97604488694528158, 60.62390960531436690 ) ) ;
#48007 = CARTESIAN_POINT ( 'NONE',  ( 8.224510206698742110, 14.34966873604972548, 72.08442372801899012 ) ) ;
#48006 = CARTESIAN_POINT ( 'NONE',  ( 0.05219959533907565091, 21.53943276465977519, 79.99890960531435269 ) ) ;
#48008 = ORIENTED_EDGE ( 'NONE', *, *, #165748, .F. ) ;
#48009 = CARTESIAN_POINT ( 'NONE',  ( -5.049401038298153566, 19.05341960407611168, 50.20724293864770260 ) ) ;
#48011 = CARTESIAN_POINT ( 'NONE',  ( 22.81625015709509441, 31.40387420917330275, -5.324999997268812457 ) ) ;
#48010 = CARTESIAN_POINT ( 'NONE',  ( 12.14591786802309770, 12.06949235617756955, 84.37390960531438111 ) ) ;
#48012 = CARTESIAN_POINT ( 'NONE',  ( -9.564922557960796823, -16.46253265017161027, 57.08224293864769550 ) ) ;
#48013 = CARTESIAN_POINT ( 'NONE',  ( -8.224510206698948167, 14.34966873604960824, 110.4155762719810383 ) ) ;
#48014 = CARTESIAN_POINT ( 'NONE',  ( -19.02544592524334988, -5.153800228976617603, 68.95942372801896170 ) ) ;
#48015 = CARTESIAN_POINT ( 'NONE',  ( 16.53943276465976808, -0.05219959533910856209, 88.74890960531436690 ) ) ;
#48016 = CARTESIAN_POINT ( 'NONE',  ( -15.72974639402176322, -15.80617190586768395, 39.37609039468567573 ) ) ;
#48018 = CARTESIAN_POINT ( 'NONE',  ( 5.823673210054125526, 21.52544592524343514, 99.79057627198103830 ) ) ;
#48017 = CARTESIAN_POINT ( 'NONE',  ( 5.153800228976335163, 19.02544592524342804, 39.79057627198100988 ) ) ;
#48019 = CARTESIAN_POINT ( 'NONE',  ( -4.483927247898539470, -16.52544592524342804, 87.29057627198103830 ) ) ;
#48020 = CARTESIAN_POINT ( 'NONE',  ( 20.26331839697992265, -34.49854857074736714, -25.13492617046049560 ) ) ;
#48021 = CARTESIAN_POINT ( 'NONE',  ( 9.474510206698971260, -16.51473224551069308, 42.91557627198103120 ) ) ;
#48022 = CARTESIAN_POINT ( 'NONE',  ( 19.49190055781009079, 5.500000000000041744, 48.06116087098784817 ) ) ;
#48024 = CARTESIAN_POINT ( 'NONE',  ( 19.03943276465977164, -0.05219959533909143690, 103.7489096053143669 ) ) ;
#48023 = CARTESIAN_POINT ( 'NONE',  ( -5.049401038297874678, -19.05341960407617918, 99.79275706135234714 ) ) ;
#48025 = CARTESIAN_POINT ( 'NONE',  ( -21.52544592524334988, -5.823673210054445271, 33.95942372801901143 ) ) ;
#48026 = CARTESIAN_POINT ( 'NONE',  ( 19.03943276465977164, -0.05219959533909143690, 78.74890960531436690 ) ) ;
#48027 = CARTESIAN_POINT ( 'NONE',  ( 16.51473224551083163, -9.474510206698727899, 70.83442372801900433 ) ) ;
#48028 = CARTESIAN_POINT ( 'NONE',  ( 9.474510206698971260, -16.51473224551069308, 47.91557627198102409 ) ) ;
#48029 = CARTESIAN_POINT ( 'NONE',  ( -8.224510206698948167, 14.34966873604960824, 75.41557627198102409 ) ) ;
#48030 = CARTESIAN_POINT ( 'NONE',  ( -12.14591786802309592, -12.06949235617757132, 66.87390960531436690 ) ) ;
#48031 = CARTESIAN_POINT ( 'NONE',  ( -5.153800228976328057, -19.02544592524343514, 77.29057627198099567 ) ) ;
#48032 = CARTESIAN_POINT ( 'NONE',  ( 18.62759615963271287, -10.81492255796078972, 103.3322429386476955 ) ) ;
#48033 = CARTESIAN_POINT ( 'NONE',  ( -9.474510206698964154, 16.51473224551069663, 70.41557627198102409 ) ) ;
#48034 = EDGE_CURVE ( 'NONE', #95422, #115310, #189981, .T. ) ;
#48035 = CARTESIAN_POINT ( 'NONE',  ( -15.80617190586768217, 15.72974639402176855, 113.1260903946856899 ) ) ;
#48038 = CARTESIAN_POINT ( 'NONE',  ( 4.483927247898545687, 16.52544592524342804, 114.7905762719810383 ) ) ;
#48037 = CARTESIAN_POINT ( 'NONE',  ( 12.14591786802327356, -12.06949235617739191, 105.6260903946856899 ) ) ;
#48036 = CARTESIAN_POINT ( 'NONE',  ( 5.049401038298161559, -19.05341960407611168, 37.70724293864768839 ) ) ;
#48039 = CARTESIAN_POINT ( 'NONE',  ( 19.05341960407617918, -5.049401038297876454, 101.0427570613523045 ) ) ;
#48040 = VERTEX_POINT ( 'NONE', #188060 ) ;
#48041 = CARTESIAN_POINT ( 'NONE',  ( 21.55341960407619695, -5.719274019375665929, 31.04275706135234714 ) ) ;
#48042 = CARTESIAN_POINT ( 'NONE',  ( 16.51473224551083163, -9.474510206698727899, 60.83442372801900433 ) ) ;
#48043 = CARTESIAN_POINT ( 'NONE',  ( 16.53943276465976808, 0.05219959533934440121, 111.2510903946856899 ) ) ;
#48044 = CARTESIAN_POINT ( 'NONE',  ( -10.81492255796078084, -18.62759615963271287, 67.08224293864770971 ) ) ;
#48045 = CARTESIAN_POINT ( 'NONE',  ( -13.97604488694527625, -13.89961937509977652, 111.8739096053143243 ) ) ;
#48046 = CARTESIAN_POINT ( 'NONE',  ( -14.34966873604960291, -8.224510206698953496, 51.66557627198102409 ) ) ;
#48047 = CARTESIAN_POINT ( 'NONE',  ( -9.474510206698964154, 16.51473224551069663, 25.41557627198103120 ) ) ;
#48048 = CARTESIAN_POINT ( 'NONE',  ( 19.05341960407611168, 5.049401038298154454, 43.95724293864769550 ) ) ;
#48049 = CARTESIAN_POINT ( 'NONE',  ( 5.153800228976615827, -19.02544592524334988, 25.20942372801900433 ) ) ;
#48050 = CARTESIAN_POINT ( 'NONE',  ( -14.34966873604972548, 8.224510206698743886, 83.33442372801903275 ) ) ;
#48051 = CARTESIAN_POINT ( 'NONE',  ( 8.224510206698742110, 14.34966873604972548, 62.08442372801901143 ) ) ;
#48052 = CARTESIAN_POINT ( 'NONE',  ( 13.97604488694527802, 13.89961937509977652, 114.3739096053143669 ) ) ;
#48053 = CARTESIAN_POINT ( 'NONE',  ( 18.67979575497194134, -10.72451020669871369, 110.8344237280190043 ) ) ;
#48054 = CARTESIAN_POINT ( 'NONE',  ( 5.153800228976335163, 19.02544592524342804, 84.79057627198099567 ) ) ;
#48055 = CARTESIAN_POINT ( 'NONE',  ( -4.483927247898782831, 16.52544592524335698, 57.70942372801901143 ) ) ;
#48056 = CARTESIAN_POINT ( 'NONE',  ( -0.05219959533910754901, -16.53943276465976808, 112.4989096053143669 ) ) ;
#48057 = CARTESIAN_POINT ( 'NONE',  ( -16.53943276465976808, -0.05219959533934237506, 108.7510903946857042 ) ) ;
#48058 = PLANE ( 'NONE',  #41047 ) ;
#48061 = CARTESIAN_POINT ( 'NONE',  ( -5.153800228976328057, -19.02544592524343514, 72.29057627198102409 ) ) ;
#48060 = CARTESIAN_POINT ( 'NONE',  ( 13.89961937509977652, -13.97604488694527269, 98.12390960531433848 ) ) ;
#48059 = CARTESIAN_POINT ( 'NONE',  ( -15.80617190586768217, 15.72974639402176855, 73.12609039468567573 ) ) ;
#48062 = CARTESIAN_POINT ( 'NONE',  ( -9.564922557960796823, -16.46253265017161027, 107.0822429386476955 ) ) ;
#48063 = CARTESIAN_POINT ( 'NONE',  ( 16.53943276465976808, -0.05219959533910856209, 53.74890960531437401 ) ) ;
#48064 = CARTESIAN_POINT ( 'NONE',  ( 16.53943276465976808, 0.05219959533934440121, 106.2510903946856757 ) ) ;
#48065 = CARTESIAN_POINT ( 'NONE',  ( -14.34966873604960291, -8.224510206698953496, 51.66557627198102409 ) ) ;
#48067 = DIRECTION ( 'NONE',  ( 0.000000000000000000, 1.000000000000000000, 0.000000000000000000 ) ) ;
#48066 = CARTESIAN_POINT ( 'NONE',  ( -14.34966873604972548, 8.224510206698743886, 43.33442372801901143 ) ) ;
#48068 = CARTESIAN_POINT ( 'NONE',  ( 0.05219959533936267826, -19.03943276465977164, 35.00109039468566863 ) ) ;
#48069 = CARTESIAN_POINT ( 'NONE',  ( -9.564922557960796823, -16.46253265017161027, 72.08224293864770971 ) ) ;
#48070 = CARTESIAN_POINT ( 'NONE',  ( -9.474510206698720793, -16.51473224551083518, 54.58442372801899722 ) ) ;
#48071 = CARTESIAN_POINT ( 'NONE',  ( 13.89961937509957401, 13.97604488694547697, 56.87609039468564731 ) ) ;
#48073 = CARTESIAN_POINT ( 'NONE',  ( 16.55341960407618274, -4.379528057220086978, 86.04275706135236135 ) ) ;
#48072 = CARTESIAN_POINT ( 'NONE',  ( -13.97604488694547697, 13.89961937509957934, 103.1260903946856473 ) ) ;
#48074 = CARTESIAN_POINT ( 'NONE',  ( -16.51473224551069308, -9.474510206698971260, 31.66557627198102054 ) ) ;
#48075 = CARTESIAN_POINT ( 'NONE',  ( 9.474510206698971260, -16.51473224551069308, 102.9155762719810241 ) ) ;
#48076 = CARTESIAN_POINT ( 'NONE',  ( 21.55341960407619695, -5.719274019375665929, 41.04275706135236135 ) ) ;
#48077 = CARTESIAN_POINT ( 'NONE',  ( 5.049401038297881783, 19.05341960407617563, 87.29275706135234714 ) ) ;
#48079 = CARTESIAN_POINT ( 'NONE',  ( -13.89961937509977652, 13.97604488694528158, 55.62390960531434558 ) ) ;
#48078 = CARTESIAN_POINT ( 'NONE',  ( 2.500000000000000000, -105.0000000000000000, 7.000000000000003553 ) ) ;
#48080 = CARTESIAN_POINT ( 'NONE',  ( 13.89961937509977652, -13.97604488694527269, 98.12390960531433848 ) ) ;
#48082 = CARTESIAN_POINT ( 'NONE',  ( 5.049401038298161559, -19.05341960407611168, 47.70724293864770260 ) ) ;
#48081 = CARTESIAN_POINT ( 'NONE',  ( -8.224510206698948167, 14.34966873604960824, 60.41557627198102409 ) ) ;
#48083 = CARTESIAN_POINT ( 'NONE',  ( -13.89961937509977652, 13.97604488694528158, 65.62390960531436690 ) ) ;
#48084 = CARTESIAN_POINT ( 'NONE',  ( -5.153800228976607833, 19.02544592524334988, 67.70942372801900433 ) ) ;
#48085 = CARTESIAN_POINT ( 'NONE',  ( -16.46253265017146816, -9.564922557961047289, 49.16775706135233293 ) ) ;
#48086 = CARTESIAN_POINT ( 'NONE',  ( 16.51473224551069308, 9.474510206698969483, 84.16557627198102409 ) ) ;
#48087 = CARTESIAN_POINT ( 'NONE',  ( -5.719274019375978568, 21.55341960407610458, 75.20724293864769550 ) ) ;
#48089 = CARTESIAN_POINT ( 'NONE',  ( -16.46253265017146816, -9.564922557961047289, 39.16775706135234003 ) ) ;
#48088 = CARTESIAN_POINT ( 'NONE',  ( -0.05219959533910754901, -16.53943276465976808, 72.49890960531435269 ) ) ;
#48090 = CARTESIAN_POINT ( 'NONE',  ( -21.55341960407610458, -5.719274019375992779, 46.45724293864769550 ) ) ;
#48091 = CARTESIAN_POINT ( 'NONE',  ( -15.72974639402197994, 15.80617190586746368, 45.62390960531436690 ) ) ;
#48092 = CARTESIAN_POINT ( 'NONE',  ( -0.05219959533909027116, -19.03943276465977164, 62.49890960531435979 ) ) ;
#48093 = CARTESIAN_POINT ( 'NONE',  ( -9.474510206698964154, 16.51473224551069663, 45.41557627198103120 ) ) ;
#48094 = CARTESIAN_POINT ( 'NONE',  ( 8.224510206698953496, -14.34966873604960469, 107.9155762719810241 ) ) ;
#48095 = CARTESIAN_POINT ( 'NONE',  ( 5.823673210054444382, -21.52544592524334988, 20.20942372801900788 ) ) ;
#48096 = CARTESIAN_POINT ( 'NONE',  ( -9.474510206698964154, 16.51473224551069663, 115.4155762719810241 ) ) ;
#48097 = CARTESIAN_POINT ( 'NONE',  ( 5.719274019375673035, 21.55341960407619339, 22.29275706135235069 ) ) ;
#48098 = CARTESIAN_POINT ( 'NONE',  ( 19.02544592524343514, -5.153800228976328945, 33.54057627198102409 ) ) ;
#48099 = CARTESIAN_POINT ( 'NONE',  ( -15.72974639402197994, 15.80617190586746368, 100.6239096053143811 ) ) ;
#48100 = CARTESIAN_POINT ( 'NONE',  ( -16.46253265017146816, -9.564922557961047289, 44.16775706135232582 ) ) ;
#48101 = DIRECTION ( 'NONE',  ( 1.000000000000000000, 0.000000000000000000, 0.000000000000000000 ) ) ;
#48102 = CARTESIAN_POINT ( 'NONE',  ( -5.049401038298153566, 19.05341960407611168, 25.20724293864768484 ) ) ;
#48103 = DIRECTION ( 'NONE',  ( -1.000000000000000000, -4.336808689942018352E-17, 3.574525976782710619E-31 ) ) ;
#48104 = CARTESIAN_POINT ( 'NONE',  ( -12.06949235617739369, -12.14591786802326823, 64.37609039468568994 ) ) ;
#48105 = CARTESIAN_POINT ( 'NONE',  ( -19.03943276465977164, 0.05219959533909376836, 31.24890960531435979 ) ) ;
#48106 = CARTESIAN_POINT ( 'NONE',  ( -21.47376810973161199, -7.452933495370250405, 174.2084625793504244 ) ) ;
#48107 = CARTESIAN_POINT ( 'NONE',  ( 9.474510206698971260, -16.51473224551069308, 77.91557627198103830 ) ) ;
#48108 = CARTESIAN_POINT ( 'NONE',  ( -4.379528057220328563, 16.55341960407611168, 110.2072429386477239 ) ) ;
#48109 = CARTESIAN_POINT ( 'NONE',  ( 18.62759615963271287, -10.81492255796078972, 48.33224293864770260 ) ) ;
#48110 = CARTESIAN_POINT ( 'NONE',  ( 12.06949235617757843, -12.14591786802309237, 83.12390960531436690 ) ) ;
#48111 = CARTESIAN_POINT ( 'NONE',  ( -4.483927247898782831, 16.52544592524335698, 27.70942372801901854 ) ) ;
#48112 = CARTESIAN_POINT ( 'NONE',  ( -21.55341960407619339, 5.719274019375674811, 83.54275706135234714 ) ) ;
#48113 = CARTESIAN_POINT ( 'NONE',  ( 13.89961937509977652, -13.97604488694527269, 23.12390960531436335 ) ) ;
#48114 = CARTESIAN_POINT ( 'NONE',  ( -4.379528057220086978, -16.55341960407618274, 109.7927570613523613 ) ) ;
#48115 = CARTESIAN_POINT ( 'NONE',  ( -4.379528057220328563, 16.55341960407611168, 60.20724293864768839 ) ) ;
#48116 = CARTESIAN_POINT ( 'NONE',  ( -16.51473224551069308, -9.474510206698971260, 51.66557627198102409 ) ) ;
#48117 = CARTESIAN_POINT ( 'NONE',  ( -15.80617190586768217, 15.72974639402176855, 93.12609039468568994 ) ) ;
#48118 = CARTESIAN_POINT ( 'NONE',  ( 10.81492255796078972, 18.62759615963270932, 114.5822429386477097 ) ) ;
#48119 = CARTESIAN_POINT ( 'NONE',  ( 18.62759615963255655, 10.81492255796105972, 71.66775706135234714 ) ) ;
#48120 = CARTESIAN_POINT ( 'NONE',  ( 14.29746914071037800, 8.314922557961029526, 36.66775706135234714 ) ) ;
#48122 = CARTESIAN_POINT ( 'NONE',  ( 21.52544592524334988, 5.823673210054432836, 91.45942372801901854 ) ) ;
#48121 = CARTESIAN_POINT ( 'NONE',  ( -8.314922557960811034, -14.29746914071050412, 72.08224293864769550 ) ) ;
#48123 = CARTESIAN_POINT ( 'NONE',  ( 14.29746914071037800, 8.314922557961029526, 111.6677570613523613 ) ) ;
#48124 = CARTESIAN_POINT ( 'NONE',  ( 17.72696623605160227, -5.500000000000079048, 61.09811031808416004 ) ) ;
#48125 = CARTESIAN_POINT ( 'NONE',  ( -16.55341960407617563, 4.379528057220093196, 38.54275706135234714 ) ) ;
#48126 = CARTESIAN_POINT ( 'NONE',  ( -14.29746914071049879, 8.314922557960819915, 45.83224293864769550 ) ) ;
#48127 = CARTESIAN_POINT ( 'NONE',  ( -8.314922557961024197, 14.29746914071037800, 87.91775706135234714 ) ) ;
#48128 = CARTESIAN_POINT ( 'NONE',  ( -9.564922557960796823, -16.46253265017161027, 102.0822429386477097 ) ) ;
#48129 = CARTESIAN_POINT ( 'NONE',  ( -5.049401038298153566, 19.05341960407611168, 100.2072429386476955 ) ) ;
#48130 = CARTESIAN_POINT ( 'NONE',  ( -21.53943276465977519, -0.05219959533937600094, 98.75109039468568994 ) ) ;
#48131 = CARTESIAN_POINT ( 'NONE',  ( -14.34966873604972548, 8.224510206698743886, 108.3344237280190185 ) ) ;
#48132 = CARTESIAN_POINT ( 'NONE',  ( 12.06949235617757843, -12.14591786802309237, 78.12390960531436690 ) ) ;
#48133 = CARTESIAN_POINT ( 'NONE',  ( -9.564922557960796823, -16.46253265017161027, 87.08224293864769550 ) ) ;
#48134 = VERTEX_POINT ( 'NONE', #141537 ) ;
#48135 = CARTESIAN_POINT ( 'NONE',  ( 8.224510206698742110, 14.34966873604972548, 22.08442372801901143 ) ) ;
#48136 = CARTESIAN_POINT ( 'NONE',  ( 19.02544592524343514, -5.153800228976328945, 33.54057627198102409 ) ) ;
#48137 = CARTESIAN_POINT ( 'NONE',  ( -13.97604488694527625, -13.89961937509977652, 96.87390960531433848 ) ) ;
#48139 = CARTESIAN_POINT ( 'NONE',  ( -11.40812507854755609, 35.11059874428196537, -5.024999997268813523 ) ) ;
#48138 = CARTESIAN_POINT ( 'NONE',  ( 8.224510206698742110, 14.34966873604972548, 32.08442372801901854 ) ) ;
#48140 = CARTESIAN_POINT ( 'NONE',  ( 9.564922557961047289, -16.46253265017146816, 35.41775706135233293 ) ) ;
#48141 = CARTESIAN_POINT ( 'NONE',  ( 4.379528057220092307, 16.55341960407617563, 97.29275706135234714 ) ) ;
#48142 = CARTESIAN_POINT ( 'NONE',  ( -0.05219959533936034679, 19.03943276465977164, 107.5010903946856615 ) ) ;
#48143 = CARTESIAN_POINT ( 'NONE',  ( -5.153800228976328057, -19.02544592524343514, 37.29057627198102409 ) ) ;
#48144 = CARTESIAN_POINT ( 'NONE',  ( 16.52544592524335698, 4.483927247898782831, 86.45942372801901854 ) ) ;
#48145 = CARTESIAN_POINT ( 'NONE',  ( 16.55341960407618274, -4.379528057220086978, 71.04275706135234714 ) ) ;
#48146 = CARTESIAN_POINT ( 'NONE',  ( -19.05341960407611168, -5.049401038298163336, 41.45724293864769550 ) ) ;
#48147 = CARTESIAN_POINT ( 'NONE',  ( -9.564922557961040184, 16.46253265017147172, 72.91775706135233293 ) ) ;
#48148 = CARTESIAN_POINT ( 'NONE',  ( -5.823673210054431948, 21.52544592524334988, 112.7094237280190328 ) ) ;
#48149 = CARTESIAN_POINT ( 'NONE',  ( 9.474510206698971260, -16.51473224551069308, 52.91557627198102409 ) ) ;
#48150 = CARTESIAN_POINT ( 'NONE',  ( -19.05341960407611168, -5.049401038298163336, 96.45724293864769550 ) ) ;
#48151 = CARTESIAN_POINT ( 'NONE',  ( 14.29746914071049879, -8.314922557960816363, 83.33224293864769550 ) ) ;
#48152 = CARTESIAN_POINT ( 'NONE',  ( -9.474510206698720793, -16.51473224551083518, 59.58442372801900433 ) ) ;
#48153 = CARTESIAN_POINT ( 'NONE',  ( -15.72974639402197994, 15.80617190586746368, 45.62390960531436690 ) ) ;
#48154 = CARTESIAN_POINT ( 'NONE',  ( -16.51473224551082808, 9.474510206698731452, 23.33442372801900078 ) ) ;
#48155 = CARTESIAN_POINT ( 'NONE',  ( -0.05219959533909027116, -19.03943276465977164, 87.49890960531436690 ) ) ;
#48156 = CARTESIAN_POINT ( 'NONE',  ( -9.474510206698720793, -16.51473224551083518, 19.58442372801899722 ) ) ;
#48157 = CARTESIAN_POINT ( 'NONE',  ( 10.81492255796078972, 18.62759615963270932, 64.58224293864769550 ) ) ;
#48158 = CARTESIAN_POINT ( 'NONE',  ( 5.049401038298161559, -19.05341960407611168, 112.7072429386476813 ) ) ;
#48159 = CARTESIAN_POINT ( 'NONE',  ( -19.03943276465977164, -0.05219959533935918106, 88.75109039468567573 ) ) ;
#48160 = CARTESIAN_POINT ( 'NONE',  ( -17.50000000000000000, 3.345213924137382389, 109.5876862309435040 ) ) ;
#48161 = CARTESIAN_POINT ( 'NONE',  ( 19.05341960407617918, -5.049401038297876454, 106.0427570613523471 ) ) ;
#48162 = CARTESIAN_POINT ( 'NONE',  ( 13.89961937509977652, -13.97604488694527269, 23.12390960531436335 ) ) ;
#48163 = CARTESIAN_POINT ( 'NONE',  ( -19.03943276465977164, 0.05219959533909376836, 101.2489096053143669 ) ) ;
#48164 = CARTESIAN_POINT ( 'NONE',  ( 18.62759615963271287, -10.81492255796078972, 73.33224293864769550 ) ) ;
#48165 = AXIS2_PLACEMENT_3D ( 'NONE', #67764, #37428, #175959 ) ;
#48166 = CARTESIAN_POINT ( 'NONE',  ( 4.483927247898790824, -16.52544592524335698, 45.20942372801901854 ) ) ;
#48167 = CARTESIAN_POINT ( 'NONE',  ( 21.55341960407619695, -5.719274019375665929, 51.04275706135234714 ) ) ;
#48168 = CARTESIAN_POINT ( 'NONE',  ( 21.52544592524334988, 5.823673210054432836, 101.4594237280190185 ) ) ;
#48169 = CARTESIAN_POINT ( 'NONE',  ( 12.14591786802327356, -12.06949235617739191, 90.62609039468567573 ) ) ;
#48170 = CARTESIAN_POINT ( 'NONE',  ( 19.03943276465977164, -0.05219959533909143690, 93.74890960531435269 ) ) ;
#48171 = CARTESIAN_POINT ( 'NONE',  ( 16.53943276465976808, -0.05219959533910856209, 93.74890960531436690 ) ) ;
#48172 = CARTESIAN_POINT ( 'NONE',  ( -4.483927247898539470, -16.52544592524342804, 42.29057627198103120 ) ) ;
#48173 = CARTESIAN_POINT ( 'NONE',  ( 16.51473224551083163, -9.474510206698727899, 65.83442372801900433 ) ) ;
#48174 = EDGE_CURVE ( 'NONE', #51216, #51307, #48744, .T. ) ;
#48175 = CARTESIAN_POINT ( 'NONE',  ( 18.62759615963255655, 10.81492255796105972, 51.66775706135234714 ) ) ;
#48176 = CARTESIAN_POINT ( 'NONE',  ( -19.05341960407617563, 5.049401038297882671, 28.54275706135232937 ) ) ;
#48177 = CARTESIAN_POINT ( 'NONE',  ( 0.05219959533910956823, 16.53943276465976808, 89.99890960531438111 ) ) ;
#48178 = CARTESIAN_POINT ( 'NONE',  ( -18.67979575497178146, -10.72451020669898902, 31.66557627198102054 ) ) ;
#48179 = CARTESIAN_POINT ( 'NONE',  ( 14.29746914071049879, -8.314922557960816363, 28.33224293864769550 ) ) ;
#48180 = CARTESIAN_POINT ( 'NONE',  ( 15.80617190586769283, -15.72974639402175789, 95.62609039468568994 ) ) ;
#48181 = CARTESIAN_POINT ( 'NONE',  ( 16.52544592524335698, 4.483927247898782831, 61.45942372801901854 ) ) ;
#48182 = CARTESIAN_POINT ( 'NONE',  ( 8.314922557961029526, -14.29746914071037800, 110.4177570613523756 ) ) ;
#48183 = CARTESIAN_POINT ( 'NONE',  ( 21.55341960407619695, -5.719274019375665929, 56.04275706135235424 ) ) ;
#48184 = ORIENTED_EDGE ( 'NONE', *, *, #146255, .T. ) ;
#48185 = CARTESIAN_POINT ( 'NONE',  ( 21.52544592524334988, 5.823673210054432836, 36.45942372801901143 ) ) ;
#48186 = CARTESIAN_POINT ( 'NONE',  ( 16.53943276465976808, -0.05219959533910856209, 98.74890960531438111 ) ) ;
#48187 = CARTESIAN_POINT ( 'NONE',  ( -5.049401038298153566, 19.05341960407611168, 30.20724293864768839 ) ) ;
#48188 = CARTESIAN_POINT ( 'NONE',  ( -8.224510206698948167, 14.34966873604960824, 65.41557627198102409 ) ) ;
#48189 = CARTESIAN_POINT ( 'NONE',  ( -16.46253265017160317, 9.564922557960807481, 75.83224293864769550 ) ) ;
#48190 = CARTESIAN_POINT ( 'NONE',  ( 16.53943276465976808, 0.05219959533934440121, 106.2510903946856757 ) ) ;
#48191 = EDGE_CURVE ( 'NONE', #23117, #171657, #120801, .T. ) ;
#48192 = CARTESIAN_POINT ( 'NONE',  ( 18.62759615963271287, -10.81492255796078972, 58.33224293864768839 ) ) ;
#48193 = CARTESIAN_POINT ( 'NONE',  ( -12.06949235617756955, 12.14591786802309770, 85.62390960531436690 ) ) ;
#48194 = CARTESIAN_POINT ( 'NONE',  ( 15.72974639402199770, -15.80617190586745480, 98.12390960531436690 ) ) ;
#48195 = CARTESIAN_POINT ( 'NONE',  ( 9.474510206698971260, -16.51473224551069308, 97.91557627198102409 ) ) ;
#48197 = CARTESIAN_POINT ( 'NONE',  ( -13.89961937509957401, -13.97604488694547875, 104.3760903946856757 ) ) ;
#48196 = CARTESIAN_POINT ( 'NONE',  ( 16.51473224551069308, 9.474510206698969483, 54.16557627198103120 ) ) ;
#48198 = CARTESIAN_POINT ( 'NONE',  ( 18.62759615963271287, -10.81492255796078972, 38.33224293864768839 ) ) ;
#48199 = CARTESIAN_POINT ( 'NONE',  ( 21.53943276465977519, 0.05219959533937863772, 71.25109039468568994 ) ) ;
#48200 = CARTESIAN_POINT ( 'NONE',  ( 16.51473224551069308, 9.474510206698969483, 64.16557627198102409 ) ) ;
#48201 = CARTESIAN_POINT ( 'NONE',  ( -19.02544592524342804, 5.153800228976336051, 96.04057627198103830 ) ) ;
#48202 = CARTESIAN_POINT ( 'NONE',  ( -16.55341960407617563, 4.379528057220093196, 58.54275706135235424 ) ) ;
#48203 = CARTESIAN_POINT ( 'NONE',  ( 21.53943276465977519, 0.05219959533937863772, 41.25109039468568284 ) ) ;
#48204 = CARTESIAN_POINT ( 'NONE',  ( 21.55341960407619695, -5.719274019375665929, 86.04275706135236135 ) ) ;
#48205 = CARTESIAN_POINT ( 'NONE',  ( 15.80617190586746368, 15.72974639402197994, 104.3739096053143669 ) ) ;
#48207 = CARTESIAN_POINT ( 'NONE',  ( 4.483927247898790824, -16.52544592524335698, 80.20942372801901854 ) ) ;
#48206 = CARTESIAN_POINT ( 'NONE',  ( 0.05219959533937995610, -21.53943276465977519, 35.00109039468568284 ) ) ;
#48208 = CARTESIAN_POINT ( 'NONE',  ( 5.823673210054125526, 21.52544592524343514, 74.79057627198105251 ) ) ;
#48209 = CARTESIAN_POINT ( 'NONE',  ( 16.51473224551083163, -9.474510206698727899, 30.83442372801900433 ) ) ;
#48211 = CARTESIAN_POINT ( 'NONE',  ( 0.05219959533910956823, 16.53943276465976808, 24.99890960531435624 ) ) ;
#48210 = CARTESIAN_POINT ( 'NONE',  ( 9.564922557960805705, 16.46253265017160317, 74.58224293864769550 ) ) ;
#48212 = FACE_OUTER_BOUND ( 'NONE', #773, .T. ) ;
#48213 = CARTESIAN_POINT ( 'NONE',  ( -9.474510206698964154, 16.51473224551069663, 100.4155762719810241 ) ) ;
#48214 = CYLINDRICAL_SURFACE ( 'NONE', #124993, 1.000000000000000888 ) ;
#48215 = CARTESIAN_POINT ( 'NONE',  ( -16.46253265017146816, -9.564922557961047289, 79.16775706135234714 ) ) ;
#48216 = CARTESIAN_POINT ( 'NONE',  ( -5.823673210054116645, -21.52544592524344225, 57.29057627198103120 ) ) ;
#48217 = CARTESIAN_POINT ( 'NONE',  ( 16.52544592524342804, -4.483927247898539470, 38.54057627198103120 ) ) ;
#48218 = CARTESIAN_POINT ( 'NONE',  ( -12.14591786802326823, 12.06949235617739902, 23.12609039468567573 ) ) ;
#48219 = CARTESIAN_POINT ( 'NONE',  ( -9.474510206698964154, 16.51473224551069663, 30.41557627198102054 ) ) ;
#48220 = CARTESIAN_POINT ( 'NONE',  ( -16.46253265017146816, -9.564922557961047289, 104.1677570613523329 ) ) ;
#48222 = CARTESIAN_POINT ( 'NONE',  ( 0.05219959533936267826, -19.03943276465977164, 75.00109039468566152 ) ) ;
#48221 = CARTESIAN_POINT ( 'NONE',  ( -21.53943276465977519, 0.05219959533907696930, 96.24890960531435269 ) ) ;
#48223 = CARTESIAN_POINT ( 'NONE',  ( 8.314922557961029526, -14.29746914071037800, 85.41775706135236135 ) ) ;
#48224 = CARTESIAN_POINT ( 'NONE',  ( 0.05219959533909260263, 19.03943276465977164, 69.99890960531435269 ) ) ;
#48225 = CARTESIAN_POINT ( 'NONE',  ( -14.29746914071049879, 8.314922557960819915, 70.83224293864770971 ) ) ;
#48226 = CARTESIAN_POINT ( 'NONE',  ( 5.153800228976335163, 19.02544592524342804, 64.79057627198100988 ) ) ;
#48227 = CARTESIAN_POINT ( 'NONE',  ( 16.53943276465976808, -0.05219959533910856209, 63.74890960531435979 ) ) ;
#48228 = DIRECTION ( 'NONE',  ( -1.000000000000000000, 0.000000000000000000, 0.000000000000000000 ) ) ;
#48229 = CARTESIAN_POINT ( 'NONE',  ( 17.55241889863238569, -16.58432793727737575, -54.34081276845726904 ) ) ;
#48230 = CARTESIAN_POINT ( 'NONE',  ( -8.224510206698948167, 14.34966873604960824, 35.41557627198102409 ) ) ;
#48231 = CARTESIAN_POINT ( 'NONE',  ( -16.46253265017160317, 9.564922557960807481, 75.83224293864769550 ) ) ;
#48232 = CARTESIAN_POINT ( 'NONE',  ( -0.1037895044722853544, -16.70000000000002061, -59.13370768023892055 ) ) ;
#48233 = CARTESIAN_POINT ( 'NONE',  ( 9.564922557961047289, -16.46253265017146816, 45.41775706135232582 ) ) ;
#48234 = CARTESIAN_POINT ( 'NONE',  ( -8.314922557961024197, 14.29746914071037800, 62.91775706135236135 ) ) ;
#48235 = CARTESIAN_POINT ( 'NONE',  ( 21.53943276465977519, -0.05219959533907433946, 63.74890960531435979 ) ) ;
#48236 = CARTESIAN_POINT ( 'NONE',  ( -16.46253265017146816, -9.564922557961047289, 24.16775706135233648 ) ) ;
#48237 = CARTESIAN_POINT ( 'NONE',  ( 9.564922557960805705, 16.46253265017160317, 79.58224293864769550 ) ) ;
#48238 = CARTESIAN_POINT ( 'NONE',  ( 20.43538597629128262, -20.43538597629122222, -49.67367017693150189 ) ) ;
#48239 = CARTESIAN_POINT ( 'NONE',  ( 19.05341960407611168, 5.049401038298154454, 108.9572429386477097 ) ) ;
#48240 = CARTESIAN_POINT ( 'NONE',  ( 19.03943276465977164, -0.05219959533909143690, 63.74890960531435979 ) ) ;
#48241 = CARTESIAN_POINT ( 'NONE',  ( -10.81492255796105439, 18.62759615963255655, 32.91775706135234714 ) ) ;
#48242 = CARTESIAN_POINT ( 'NONE',  ( 12.06949235617757843, -12.14591786802309237, 113.1239096053143953 ) ) ;
#48243 = EDGE_CURVE ( 'NONE', #165210, #188443, #20624, .T. ) ;
#48246 = ORIENTED_EDGE ( 'NONE', *, *, #69903, .T. ) ;
#48245 = CARTESIAN_POINT ( 'NONE',  ( 16.51473224551069308, 9.474510206698969483, 84.16557627198102409 ) ) ;
#48244 = CARTESIAN_POINT ( 'NONE',  ( -18.67979575497178146, -10.72451020669898902, 96.66557627198102409 ) ) ;
#48247 = CARTESIAN_POINT ( 'NONE',  ( 15.72974639402176855, 15.80617190586768217, 21.87609039468567573 ) ) ;
#48248 = ORIENTED_EDGE ( 'NONE', *, *, #74471, .F. ) ;
#48249 = CARTESIAN_POINT ( 'NONE',  ( -16.51473224551069308, -9.474510206698971260, 81.66557627198103830 ) ) ;
#48250 = LINE ( 'NONE', #17913, #68957 ) ;
#48251 = CARTESIAN_POINT ( 'NONE',  ( -21.52544592524343514, 5.823673210054127303, 96.04057627198102409 ) ) ;
#48252 = CARTESIAN_POINT ( 'NONE',  ( -13.89961937509977652, 13.97604488694528158, 40.62390960531435979 ) ) ;
#48253 = CARTESIAN_POINT ( 'NONE',  ( 19.05341960407617918, -5.049401038297876454, 101.0427570613523045 ) ) ;
#48254 = CARTESIAN_POINT ( 'NONE',  ( -29.86685920354755197, -21.69954338932560134, -10.92499999726881299 ) ) ;
#48255 = CARTESIAN_POINT ( 'NONE',  ( -9.474510206698964154, 16.51473224551069663, 25.41557627198103120 ) ) ;
#48256 = CARTESIAN_POINT ( 'NONE',  ( -21.52544592524334988, -5.823673210054445271, 88.95942372801901854 ) ) ;
#48259 = B_SPLINE_CURVE_WITH_KNOTS ( 'NONE', 3,
 ( #37011, #86520, #22857, #189722, #20848, #131020, #53180, #159352, #99682, #115865, #148204, #82506, #70361, #116855 ),
 .UNSPECIFIED., .F., .F.,
 ( 4, 2, 2, 2, 2, 2, 4 ),
 ( -0.0006136969902427243540, 0.0004464899733162487790, 0.001506676936875221912, 0.003627050863993200487, 0.004687237827552194654, 0.005747424791111188820, 0.007867798718229178020 ),
 .UNSPECIFIED. ) ;
#48258 = CARTESIAN_POINT ( 'NONE',  ( 21.55341960407619695, -5.719274019375665929, 41.04275706135236135 ) ) ;
#48257 = CARTESIAN_POINT ( 'NONE',  ( -13.97604488694527625, -13.89961937509977652, 81.87390960531436690 ) ) ;
#48260 = CARTESIAN_POINT ( 'NONE',  ( 21.52544592524334988, 5.823673210054432836, 26.45942372801901854 ) ) ;
#48261 = CARTESIAN_POINT ( 'NONE',  ( 8.906447517083057264, -27.41122689804191026, 148.5999999999999943 ) ) ;
#48262 = CARTESIAN_POINT ( 'NONE',  ( 16.46253265017160672, -9.564922557960803928, 88.33224293864769550 ) ) ;
#48263 = CARTESIAN_POINT ( 'NONE',  ( 19.25176906914649422, 5.499999999999733546, 63.49927264242280245 ) ) ;
#48266 = CARTESIAN_POINT ( 'NONE',  ( -0.05219959533937732626, 21.53943276465977519, 47.50109039468568994 ) ) ;
#48265 = CARTESIAN_POINT ( 'NONE',  ( -21.53943276465977519, 0.05219959533907696930, 46.24890960531435979 ) ) ;
#48264 = CARTESIAN_POINT ( 'NONE',  ( -4.483927247898782831, 16.52544592524335698, 42.70942372801901854 ) ) ;
#48267 = CARTESIAN_POINT ( 'NONE',  ( 15.80617190586769283, -15.72974639402175789, 70.62609039468567573 ) ) ;
#48268 = CARTESIAN_POINT ( 'NONE',  ( 4.313351365237948265, 4.313351365237946489, -62.50719930893269805 ) ) ;
#48269 = CARTESIAN_POINT ( 'NONE',  ( 9.474510206698729675, 16.51473224551082808, 107.0844237280190043 ) ) ;
#48270 = CARTESIAN_POINT ( 'NONE',  ( -16.51473224551069308, -9.474510206698971260, 56.66557627198103120 ) ) ;
#48271 = CARTESIAN_POINT ( 'NONE',  ( -13.89961937509977652, 13.97604488694528158, 80.62390960531436690 ) ) ;
#48272 = CARTESIAN_POINT ( 'NONE',  ( -8.314922557960811034, -14.29746914071050412, 102.0822429386476955 ) ) ;
#48273 = CARTESIAN_POINT ( 'NONE',  ( 4.483927247898545687, 16.52544592524342804, 109.7905762719810383 ) ) ;
#48274 = CARTESIAN_POINT ( 'NONE',  ( 0.05219959533909260263, 19.03943276465977164, 114.9989096053143669 ) ) ;
#48275 = CARTESIAN_POINT ( 'NONE',  ( -12.14591786802326823, 12.06949235617739902, 78.12609039468570415 ) ) ;
#48277 = CARTESIAN_POINT ( 'NONE',  ( 16.46253265017160672, -9.564922557960803928, 53.33224293864768839 ) ) ;
#48276 = CARTESIAN_POINT ( 'NONE',  ( -12.14591786802309592, -12.06949235617757132, 71.87390960531438111 ) ) ;
#48278 = CARTESIAN_POINT ( 'NONE',  ( 10.81492255796106328, -18.62759615963255655, 80.41775706135234714 ) ) ;
#48279 = CARTESIAN_POINT ( 'NONE',  ( 18.67979575497194134, -10.72451020669871369, 65.83442372801900433 ) ) ;
#48280 = CARTESIAN_POINT ( 'NONE',  ( 19.05341960407617918, -5.049401038297876454, 101.0427570613523045 ) ) ;
#48281 = CARTESIAN_POINT ( 'NONE',  ( -12.14591786802309592, -12.06949235617757132, 66.87390960531436690 ) ) ;
#48282 = CARTESIAN_POINT ( 'NONE',  ( 10.72451020669871369, 18.67979575497193778, 22.08442372801901143 ) ) ;
#48283 = CARTESIAN_POINT ( 'NONE',  ( -21.52544592524343514, 5.823673210054127303, 61.04057627198103120 ) ) ;
#48284 = DIRECTION ( 'NONE',  ( 0.000000000000000000, 0.000000000000000000, -1.000000000000000000 ) ) ;
#48285 = CARTESIAN_POINT ( 'NONE',  ( 28.82186960331498327, 9.364793116373570925, 143.3500000054623342 ) ) ;
#48286 = CARTESIAN_POINT ( 'NONE',  ( 19.02544592524343514, -5.153800228976328945, 68.54057627198103830 ) ) ;
#48287 = CARTESIAN_POINT ( 'NONE',  ( -4.379528057220328563, 16.55341960407611168, 35.20724293864768839 ) ) ;
#48288 = CARTESIAN_POINT ( 'NONE',  ( -16.52544592524342804, 4.483927247898546575, 26.04057627198103475 ) ) ;
#48289 = CARTESIAN_POINT ( 'NONE',  ( -12.14591786802326823, 12.06949235617739902, 98.12609039468570415 ) ) ;
#48290 = CARTESIAN_POINT ( 'NONE',  ( 16.51473224551083163, -9.474510206698727899, 50.83442372801899722 ) ) ;
#48291 = CARTESIAN_POINT ( 'NONE',  ( -4.313351365237961588, 4.313351365237934942, -65.00100000000003320 ) ) ;
#48292 = CARTESIAN_POINT ( 'NONE',  ( 5.153800228976335163, 19.02544592524342804, 109.7905762719810099 ) ) ;
#48293 = CARTESIAN_POINT ( 'NONE',  ( -16.53943276465976808, 0.05219959533911058130, 71.24890960531435269 ) ) ;
#48294 = CARTESIAN_POINT ( 'NONE',  ( -19.03943276465977164, -0.05219959533935918106, 48.75109039468566863 ) ) ;
#48296 = CARTESIAN_POINT ( 'NONE',  ( 9.474510206698971260, -16.51473224551069308, 112.9155762719810383 ) ) ;
#48295 = CARTESIAN_POINT ( 'NONE',  ( 16.61371651742600264, -7.165104196376133494, 101.3541506999299884 ) ) ;
#48297 = CARTESIAN_POINT ( 'NONE',  ( -5.823673210054116645, -21.52544592524344225, 57.29057627198103120 ) ) ;
#48298 = CARTESIAN_POINT ( 'NONE',  ( -8.224510206698948167, 14.34966873604960824, 100.4155762719810241 ) ) ;
#48299 = CARTESIAN_POINT ( 'NONE',  ( 16.55341960407618274, -4.379528057220086978, 46.04275706135234714 ) ) ;
#48300 = CARTESIAN_POINT ( 'NONE',  ( -14.34966873604960291, -8.224510206698953496, 91.66557627198103830 ) ) ;
#48301 = CARTESIAN_POINT ( 'NONE',  ( 17.26058549869089731, -6.457015423128600773, 36.12254162523932877 ) ) ;
#48302 = CARTESIAN_POINT ( 'NONE',  ( -17.12812012977025589, 6.668231424566045007, 48.64051240676857901 ) ) ;
#48303 = CARTESIAN_POINT ( 'NONE',  ( -21.53943276465977519, 0.05219959533907696930, 26.24890960531435624 ) ) ;
#48304 = CARTESIAN_POINT ( 'NONE',  ( -36.91746825000001309, 11.99521256947798342, -7.224999997268814589 ) ) ;
#48305 = CARTESIAN_POINT ( 'NONE',  ( 2.577820198429831642E-15, 9.100000000000001421, -63.95112321872120731 ) ) ;
#48307 = VERTEX_POINT ( 'NONE', #127347 ) ;
#48306 = CIRCLE ( 'NONE', #193659, 0.1999999999999987899 ) ;
#48309 = CARTESIAN_POINT ( 'NONE',  ( 4.483927247898545687, 16.52544592524342804, 24.79057627198103120 ) ) ;
#48308 = CARTESIAN_POINT ( 'NONE',  ( -16.53943276465976808, -0.05219959533934237506, 43.75109039468568284 ) ) ;
#48310 = CARTESIAN_POINT ( 'NONE',  ( 15.80617190586746368, 15.72974639402197994, 59.37390960531436690 ) ) ;
#48311 = CARTESIAN_POINT ( 'NONE',  ( 9.564922557961047289, -16.46253265017146816, 90.41775706135234714 ) ) ;
#48312 = CARTESIAN_POINT ( 'NONE',  ( 18.67979575497178502, 10.72451020669898547, 49.16557627198102409 ) ) ;
#48313 = CARTESIAN_POINT ( 'NONE',  ( -21.53943276465977519, -0.05219959533937600094, 78.75109039468568994 ) ) ;
#48314 = CARTESIAN_POINT ( 'NONE',  ( 4.295634330582102756, -37.01983766409436072, -32.59999999999998721 ) ) ;
#48315 = CARTESIAN_POINT ( 'NONE',  ( 16.53943276465976808, 0.05219959533934440121, 41.25109039468568284 ) ) ;
#48317 = CARTESIAN_POINT ( 'NONE',  ( -16.51473224551069308, -9.474510206698971260, 106.6655762719810383 ) ) ;
#48316 = CARTESIAN_POINT ( 'NONE',  ( -5.153800228976328057, -19.02544592524343514, 37.29057627198102409 ) ) ;
#48318 = CARTESIAN_POINT ( 'NONE',  ( -19.05341960407611168, -5.049401038298163336, 41.45724293864769550 ) ) ;
#48319 = CARTESIAN_POINT ( 'NONE',  ( 8.224510206698953496, -14.34966873604960469, 97.91557627198103830 ) ) ;
#48320 = CARTESIAN_POINT ( 'NONE',  ( 0.000000000000000000, 0.000000000000000000, 0.000000000000000000 ) ) ;
#48321 = CARTESIAN_POINT ( 'NONE',  ( 9.564922557960805705, 16.46253265017160317, 94.58224293864769550 ) ) ;
#48322 = ORIENTED_EDGE ( 'NONE', *, *, #28066, .T. ) ;
#48323 = CARTESIAN_POINT ( 'NONE',  ( 8.314922557961029526, -14.29746914071037800, 50.41775706135235424 ) ) ;
#48324 = CARTESIAN_POINT ( 'NONE',  ( -15.80617190586745835, -15.72974639402198527, 96.87390960531436690 ) ) ;
#48325 = CARTESIAN_POINT ( 'NONE',  ( -0.05219959533909027116, -19.03943276465977164, 42.49890960531435269 ) ) ;
#48326 = CARTESIAN_POINT ( 'NONE',  ( -5.823673210054431948, 21.52544592524334988, 27.70942372801901854 ) ) ;
#48327 = CARTESIAN_POINT ( 'NONE',  ( -16.51473224551069308, -9.474510206698971260, 81.66557627198103830 ) ) ;
#48328 = CARTESIAN_POINT ( 'NONE',  ( -9.474510206698964154, 16.51473224551069663, 115.4155762719810241 ) ) ;
#48329 = ORIENTED_EDGE ( 'NONE', *, *, #181003, .F. ) ;
#48330 = CARTESIAN_POINT ( 'NONE',  ( 12.06949235617739724, 12.14591786802326823, 41.87609039468568284 ) ) ;
#48331 = CARTESIAN_POINT ( 'NONE',  ( 18.62759615963255655, 10.81492255796105972, 21.66775706135235069 ) ) ;
#48334 = CARTESIAN_POINT ( 'NONE',  ( -5.049401038297874678, -19.05341960407617918, 69.79275706135233293 ) ) ;
#48333 = CARTESIAN_POINT ( 'NONE',  ( -9.474510206698964154, 16.51473224551069663, 90.41557627198103830 ) ) ;
#48332 = CARTESIAN_POINT ( 'NONE',  ( -16.53943276465976808, 0.05219959533911058130, 116.2489096053143669 ) ) ;
#48335 = CARTESIAN_POINT ( 'NONE',  ( -5.049401038297874678, -19.05341960407617918, 29.79275706135232227 ) ) ;
#48336 = CARTESIAN_POINT ( 'NONE',  ( -21.52544592524343514, 5.823673210054127303, 91.04057627198103830 ) ) ;
#48337 = CARTESIAN_POINT ( 'NONE',  ( -19.03943276465977164, -0.05219959533935918106, 33.75109039468566863 ) ) ;
#48338 = CARTESIAN_POINT ( 'NONE',  ( 4.379528057220092307, 16.55341960407617563, 72.29275706135236135 ) ) ;
#48339 = CARTESIAN_POINT ( 'NONE',  ( -16.51473224551069308, -9.474510206698971260, 111.6655762719810383 ) ) ;
#48340 = CARTESIAN_POINT ( 'NONE',  ( -9.564922557960796823, -16.46253265017161027, 62.08224293864769550 ) ) ;
#48341 = AXIS2_PLACEMENT_3D ( 'NONE', #79770, #46448, #141440 ) ;
#48342 = CARTESIAN_POINT ( 'NONE',  ( -5.823673210054431948, 21.52544592524334988, 67.70942372801901854 ) ) ;
#48343 = CARTESIAN_POINT ( 'NONE',  ( 10.72451020669871369, 18.67979575497193778, 62.08442372801901143 ) ) ;
#48344 = CARTESIAN_POINT ( 'NONE',  ( -9.474510206698964154, 16.51473224551069663, 80.41557627198103830 ) ) ;
#48345 = CARTESIAN_POINT ( 'NONE',  ( 15.80617190586769283, -15.72974639402175789, 45.62609039468567573 ) ) ;
#48346 = CARTESIAN_POINT ( 'NONE',  ( 19.02544592524334988, 5.153800228976608722, 81.45942372801897591 ) ) ;
#48347 = CARTESIAN_POINT ( 'NONE',  ( -19.02544592524342804, 5.153800228976336051, 51.04057627198103120 ) ) ;
#48348 = CARTESIAN_POINT ( 'NONE',  ( 9.564922557960805705, 16.46253265017160317, 99.58224293864770971 ) ) ;
#48349 = CARTESIAN_POINT ( 'NONE',  ( -13.89961937509977652, 13.97604488694528158, 65.62390960531436690 ) ) ;
#48350 = CARTESIAN_POINT ( 'NONE',  ( 19.05341960407611168, 5.049401038298154454, 108.9572429386477097 ) ) ;
#48351 = CARTESIAN_POINT ( 'NONE',  ( 19.05341960407611168, 5.049401038298154454, 53.95724293864770260 ) ) ;
#48352 = CARTESIAN_POINT ( 'NONE',  ( -5.719274019375978568, 21.55341960407610458, 100.2072429386476955 ) ) ;
#48353 = CARTESIAN_POINT ( 'NONE',  ( -0.05219959533934338120, 16.53943276465976808, 72.50109039468568994 ) ) ;
#48354 = CARTESIAN_POINT ( 'NONE',  ( -21.88033147701267822, 7.974798826780869376, 169.5716465351736133 ) ) ;
#48355 = CARTESIAN_POINT ( 'NONE',  ( -19.05341960407617563, 5.049401038297882671, 28.54275706135232937 ) ) ;
#48356 = CARTESIAN_POINT ( 'NONE',  ( 13.89961937509977652, -13.97604488694527269, 68.12390960531436690 ) ) ;
#48357 = CARTESIAN_POINT ( 'NONE',  ( 8.314922557960818139, 14.29746914071049879, 64.58224293864769550 ) ) ;
#48358 = CARTESIAN_POINT ( 'NONE',  ( 16.55341960407611168, 4.379528057220329451, 93.95724293864770971 ) ) ;
#48359 = CARTESIAN_POINT ( 'NONE',  ( -16.51473224551069308, -9.474510206698971260, 101.6655762719810241 ) ) ;
#48360 = CARTESIAN_POINT ( 'NONE',  ( 5.153800228976335163, 19.02544592524342804, 94.79057627198103830 ) ) ;
#48361 = CARTESIAN_POINT ( 'NONE',  ( -21.52544592524334988, -5.823673210054445271, 48.95942372801902565 ) ) ;
#48362 = CARTESIAN_POINT ( 'NONE',  ( 16.46253265017160672, -9.564922557960803928, 108.3322429386476955 ) ) ;
#48363 = CARTESIAN_POINT ( 'NONE',  ( 13.89961937509957401, 13.97604488694547697, 21.87609039468566152 ) ) ;
#48364 = CARTESIAN_POINT ( 'NONE',  ( -16.53943276465976808, -0.05219959533934237506, 78.75109039468568994 ) ) ;
#48365 = CARTESIAN_POINT ( 'NONE',  ( -21.53943276465977519, -0.05219959533937600094, 43.75109039468568284 ) ) ;
#48366 = CARTESIAN_POINT ( 'NONE',  ( -0.05219959533907301413, -21.53943276465977519, 37.49890960531436690 ) ) ;
#48367 = CARTESIAN_POINT ( 'NONE',  ( -5.719274019375978568, 21.55341960407610458, 105.2072429386477097 ) ) ;
#48368 = CARTESIAN_POINT ( 'NONE',  ( 16.53943276465976808, -0.05219959533910856209, 63.74890960531435979 ) ) ;
#48369 = CARTESIAN_POINT ( 'NONE',  ( -16.46253265017160317, 9.564922557960807481, 55.83224293864769550 ) ) ;
#48370 = CARTESIAN_POINT ( 'NONE',  ( -4.483927247898539470, -16.52544592524342804, 82.29057627198103830 ) ) ;
#48371 = CARTESIAN_POINT ( 'NONE',  ( 5.719274019375991003, -21.55341960407610458, 47.70724293864770260 ) ) ;
#48372 = CARTESIAN_POINT ( 'NONE',  ( 16.46253265017146816, 9.564922557961045513, 46.66775706135233293 ) ) ;
#48373 = CARTESIAN_POINT ( 'NONE',  ( -19.05341960407611168, -5.049401038298163336, 21.45724293864768839 ) ) ;
#48374 = ORIENTED_EDGE ( 'NONE', *, *, #186584, .F. ) ;
#48375 = CARTESIAN_POINT ( 'NONE',  ( -0.05219959533934338120, 16.53943276465976808, 62.50109039468568284 ) ) ;
#48376 = CARTESIAN_POINT ( 'NONE',  ( -19.03943276465977164, 0.05219959533909376836, 71.24890960531435269 ) ) ;
#48377 = CARTESIAN_POINT ( 'NONE',  ( 8.571926809382603096, -26.38167802310801235, 143.4750000027312069 ) ) ;
#48378 = CARTESIAN_POINT ( 'NONE',  ( 8.224510206698953496, -14.34966873604960469, 87.91557627198103830 ) ) ;
#48379 = CARTESIAN_POINT ( 'NONE',  ( 21.52544592524344225, -5.823673210054117533, 33.54057627198102409 ) ) ;
#48380 = CARTESIAN_POINT ( 'NONE',  ( 16.55341960407618274, -4.379528057220086978, 111.0427570613523613 ) ) ;
#48381 = CARTESIAN_POINT ( 'NONE',  ( 14.29746914071037800, 8.314922557961029526, 21.66775706135235069 ) ) ;
#48382 = CARTESIAN_POINT ( 'NONE',  ( 5.823673210054444382, -21.52544592524334988, 95.20942372801903275 ) ) ;
#48383 = CARTESIAN_POINT ( 'NONE',  ( -9.564922557960796823, -16.46253265017161027, 92.08224293864769550 ) ) ;
#48384 = CARTESIAN_POINT ( 'NONE',  ( 21.53943276465977519, -0.05219959533907433946, 113.7489096053143527 ) ) ;
#48385 = CARTESIAN_POINT ( 'NONE',  ( 14.29746914071037800, 8.314922557961029526, 61.66775706135235424 ) ) ;
#48386 = CARTESIAN_POINT ( 'NONE',  ( 13.97604488694527802, 13.89961937509977652, 34.37390960531436690 ) ) ;
#48387 = CARTESIAN_POINT ( 'NONE',  ( -16.53943276465976808, -0.05219959533934237506, 28.75109039468567929 ) ) ;
#48388 = CARTESIAN_POINT ( 'NONE',  ( 19.03943276465977164, 0.05219959533936151252, 101.2510903946856757 ) ) ;
#48389 = CARTESIAN_POINT ( 'NONE',  ( -15.80617190586745835, -15.72974639402198527, 96.87390960531436690 ) ) ;
#48390 = CARTESIAN_POINT ( 'NONE',  ( -9.474510206698720793, -16.51473224551083518, 64.58442372801900433 ) ) ;
#48391 = CARTESIAN_POINT ( 'NONE',  ( 18.22780087662122384, -5.500000000000022204, 86.01540105326108687 ) ) ;
#48392 = CARTESIAN_POINT ( 'NONE',  ( 21.55341960407610458, 5.719274019375980345, 113.9572429386477239 ) ) ;
#48393 = CARTESIAN_POINT ( 'NONE',  ( -23.31738231874055600, 16.94106989632528837, 142.0500000054623513 ) ) ;
#48394 = CARTESIAN_POINT ( 'NONE',  ( 19.05341960407611168, 5.049401038298154454, 78.95724293864769550 ) ) ;
#48395 = CARTESIAN_POINT ( 'NONE',  ( 14.29746914071037800, 8.314922557961029526, 26.66775706135235424 ) ) ;
#48396 = CARTESIAN_POINT ( 'NONE',  ( 16.30563709075146761, -36.53016886171239719, -10.22897874253568773 ) ) ;
#48397 = CARTESIAN_POINT ( 'NONE',  ( -9.564922557961040184, 16.46253265017147172, 62.91775706135233293 ) ) ;
#48399 = CARTESIAN_POINT ( 'NONE',  ( 8.224510206698953496, -14.34966873604960469, 77.91557627198102409 ) ) ;
#48398 = CARTESIAN_POINT ( 'NONE',  ( -5.823673210054116645, -21.52544592524344225, 112.2905762719810241 ) ) ;
#48400 = CARTESIAN_POINT ( 'NONE',  ( 13.89961937509977652, -13.97604488694527269, 78.12390960531433848 ) ) ;
#48402 = CARTESIAN_POINT ( 'NONE',  ( 19.03943276465977164, 0.05219959533936151252, 36.25109039468567573 ) ) ;
#48401 = CARTESIAN_POINT ( 'NONE',  ( 14.29746914071037800, 8.314922557961029526, 41.66775706135235424 ) ) ;
#48403 = CARTESIAN_POINT ( 'NONE',  ( -10.81492255796105439, 18.62759615963255655, 57.91775706135234714 ) ) ;
#48404 = CARTESIAN_POINT ( 'NONE',  ( -19.02544592524334988, -5.153800228976617603, 108.9594237280189759 ) ) ;
#48406 = EDGE_CURVE ( 'NONE', #1611, #197947, #11297, .T. ) ;
#48405 = CARTESIAN_POINT ( 'NONE',  ( -19.03943276465977164, 0.05219959533909376836, 56.24890960531435979 ) ) ;
#48407 = CARTESIAN_POINT ( 'NONE',  ( 5.153800228976615827, -19.02544592524334988, 80.20942372801901854 ) ) ;
#48408 = CARTESIAN_POINT ( 'NONE',  ( 4.483927247898790824, -16.52544592524335698, 55.20942372801902565 ) ) ;
#48409 = CARTESIAN_POINT ( 'NONE',  ( 0.05219959533937995610, -21.53943276465977519, 100.0010903946857042 ) ) ;
#48410 = CARTESIAN_POINT ( 'NONE',  ( -16.51473224551082808, 9.474510206698731452, 68.33442372801900433 ) ) ;
#48411 = CARTESIAN_POINT ( 'NONE',  ( -5.049401038298153566, 19.05341960407611168, 45.20724293864769550 ) ) ;
#48412 = CARTESIAN_POINT ( 'NONE',  ( -5.719274019375978568, 21.55341960407610458, 65.20724293864768129 ) ) ;
#48414 = CARTESIAN_POINT ( 'NONE',  ( 19.05341960407617918, -5.049401038297876454, 71.04275706135234714 ) ) ;
#48413 = CARTESIAN_POINT ( 'NONE',  ( 14.29746914071049879, -8.314922557960816363, 63.33224293864770260 ) ) ;
#48415 = CARTESIAN_POINT ( 'NONE',  ( 21.81018892176227908, 9.477090470496801089, 170.9397748289983099 ) ) ;
#48416 = CARTESIAN_POINT ( 'NONE',  ( -19.05341960407617563, 5.049401038297882671, 38.54275706135233293 ) ) ;
#48417 = CARTESIAN_POINT ( 'NONE',  ( -16.52544592524335698, -4.483927247898792601, 93.95942372801903275 ) ) ;
#48418 = CARTESIAN_POINT ( 'NONE',  ( 8.224510206698953496, -14.34966873604960469, 52.91557627198103830 ) ) ;
#48420 = CARTESIAN_POINT ( 'NONE',  ( 27.73933785331498569, 2.768321779492822058E-14, 141.8750000027311842 ) ) ;
#48419 = CARTESIAN_POINT ( 'NONE',  ( 15.72974639402176855, 15.80617190586768217, 86.87609039468568994 ) ) ;
#48421 = CARTESIAN_POINT ( 'NONE',  ( 21.55341960407610458, 5.719274019375980345, 98.95724293864770971 ) ) ;
#48422 = CARTESIAN_POINT ( 'NONE',  ( 5.153800228976335163, 19.02544592524342804, 54.79057627198103120 ) ) ;
#48423 = CARTESIAN_POINT ( 'NONE',  ( 10.72451020669871369, 18.67979575497193778, 67.08442372801901854 ) ) ;
#48424 = CARTESIAN_POINT ( 'NONE',  ( 19.03943276465977164, -0.05219959533909143690, 43.74890960531435979 ) ) ;
#48425 = ORIENTED_EDGE ( 'NONE', *, *, #140289, .T. ) ;
#48426 = CARTESIAN_POINT ( 'NONE',  ( -19.02544592524342804, 5.153800228976336051, 66.04057627198103830 ) ) ;
#48427 = CARTESIAN_POINT ( 'NONE',  ( -16.51473224551069308, -9.474510206698971260, 21.66557627198102765 ) ) ;
#48428 = CARTESIAN_POINT ( 'NONE',  ( -19.03943276465977164, 0.05219959533909376836, 106.2489096053143669 ) ) ;
#48429 = CARTESIAN_POINT ( 'NONE',  ( 4.379528057220339221, -16.55341960407611168, 57.70724293864770260 ) ) ;
#48430 = CARTESIAN_POINT ( 'NONE',  ( 16.51473224551069308, 9.474510206698969483, 34.16557627198102409 ) ) ;
#48431 = CARTESIAN_POINT ( 'NONE',  ( -8.224510206698948167, 14.34966873604960824, 80.41557627198103830 ) ) ;
#48432 = CARTESIAN_POINT ( 'NONE',  ( 18.67979575497178502, 10.72451020669898547, 94.16557627198103830 ) ) ;
#48433 = CARTESIAN_POINT ( 'NONE',  ( 15.80617190586769283, -15.72974639402175789, 30.62609039468567929 ) ) ;
#48434 = CARTESIAN_POINT ( 'NONE',  ( -5.153800228976328057, -19.02544592524343514, 22.29057627198102765 ) ) ;
#48435 = CARTESIAN_POINT ( 'NONE',  ( -8.224510206698735004, -14.34966873604973081, 49.58442372801901143 ) ) ;
#48436 = CARTESIAN_POINT ( 'NONE',  ( 5.719274019375991003, -21.55341960407610458, 77.70724293864770971 ) ) ;
#48437 = CARTESIAN_POINT ( 'NONE',  ( 10.81492255796106328, -18.62759615963255655, 105.4177570613523613 ) ) ;
#48438 = CARTESIAN_POINT ( 'NONE',  ( 9.564922557960805705, 16.46253265017160317, 104.5822429386476955 ) ) ;
#48439 = CARTESIAN_POINT ( 'NONE',  ( -5.823673210054431948, 21.52544592524334988, 47.70942372801902565 ) ) ;
#48440 = CARTESIAN_POINT ( 'NONE',  ( 15.80617190586746368, 15.72974639402197994, 39.37390960531436690 ) ) ;
#48441 = CARTESIAN_POINT ( 'NONE',  ( -4.483927247898782831, 16.52544592524335698, 97.70942372801904696 ) ) ;
#48443 = CARTESIAN_POINT ( 'NONE',  ( 10.72451020669871369, 18.67979575497193778, 87.08442372801901854 ) ) ;
#48442 = CARTESIAN_POINT ( 'NONE',  ( -21.53943276465977519, -0.05219959533937600094, 58.75109039468568994 ) ) ;
#48444 = CARTESIAN_POINT ( 'NONE',  ( 9.564922557961047289, -16.46253265017146816, 35.41775706135233293 ) ) ;
#48445 = CARTESIAN_POINT ( 'NONE',  ( 0.05219959533934541429, -16.53943276465976808, 85.00109039468568994 ) ) ;
#48446 = CARTESIAN_POINT ( 'NONE',  ( -21.53943276465977519, -0.05219959533937600094, 38.75109039468567573 ) ) ;
#48447 = CARTESIAN_POINT ( 'NONE',  ( -16.46253265017160317, 9.564922557960807481, 45.83224293864769550 ) ) ;
#48448 = CARTESIAN_POINT ( 'NONE',  ( 21.55341960407619695, -5.719274019375665929, 111.0427570613523613 ) ) ;
#48449 = CARTESIAN_POINT ( 'NONE',  ( -19.03943276465977164, 0.05219959533909376836, 116.2489096053143669 ) ) ;
#48450 = CARTESIAN_POINT ( 'NONE',  ( -5.719274019375665041, -21.55341960407619695, 24.79275706135235779 ) ) ;
#48451 = CIRCLE ( 'NONE', #138775, 2.500000000000002220 ) ;
#48452 = CARTESIAN_POINT ( 'NONE',  ( -10.81492255796078084, -18.62759615963271287, 77.08224293864769550 ) ) ;
#48454 = CARTESIAN_POINT ( 'NONE',  ( -15.80617190586745835, -15.72974639402198527, 81.87390960531435269 ) ) ;
#48453 = CARTESIAN_POINT ( 'NONE',  ( 69.65682714487590488, -71.74905178543389184, -15.00000000000000178 ) ) ;
#48456 = CARTESIAN_POINT ( 'NONE',  ( -8.224510206698948167, 14.34966873604960824, 65.41557627198102409 ) ) ;
#48455 = CARTESIAN_POINT ( 'NONE',  ( 4.483927247898790824, -16.52544592524335698, 60.20942372801902565 ) ) ;
#48457 = CARTESIAN_POINT ( 'NONE',  ( 24.43795752428853518, 7.704305290315001997, 171.8420761435737631 ) ) ;
#48458 = CARTESIAN_POINT ( 'NONE',  ( 9.564922557961047289, -16.46253265017146816, 90.41775706135234714 ) ) ;
#48459 = CARTESIAN_POINT ( 'NONE',  ( -21.36119649488922079, 0.4379334789938477690, -56.42482690868972384 ) ) ;
#48460 = CARTESIAN_POINT ( 'NONE',  ( 8.314922557961029526, -14.29746914071037800, 40.41775706135234714 ) ) ;
#48461 = CARTESIAN_POINT ( 'NONE',  ( 15.72974639402199770, -15.80617190586745480, 93.12390960531436690 ) ) ;
#48462 = CARTESIAN_POINT ( 'NONE',  ( -10.81492255796078084, -18.62759615963271287, 77.08224293864769550 ) ) ;
#48463 = CARTESIAN_POINT ( 'NONE',  ( 15.80617190586746368, 15.72974639402197994, 24.37390960531435979 ) ) ;
#48464 = CARTESIAN_POINT ( 'NONE',  ( 16.53943276465976808, 0.05219959533934440121, 56.25109039468568284 ) ) ;
#48465 = CARTESIAN_POINT ( 'NONE',  ( -16.51473224551069308, -9.474510206698971260, 76.66557627198103830 ) ) ;
#48467 = CARTESIAN_POINT ( 'NONE',  ( -0.05219959533936034679, 19.03943276465977164, 107.5010903946856615 ) ) ;
#48466 = CARTESIAN_POINT ( 'NONE',  ( -15.72974639402176322, -15.80617190586768395, 39.37609039468567573 ) ) ;
#48468 = CARTESIAN_POINT ( 'NONE',  ( 19.03943276465977164, -0.05219959533909143690, 113.7489096053143669 ) ) ;
#48469 = CARTESIAN_POINT ( 'NONE',  ( 19.02544592524334988, 5.153800228976608722, 31.45942372801900433 ) ) ;
#48470 = CARTESIAN_POINT ( 'NONE',  ( -16.52544592524335698, -4.483927247898792601, 38.95942372801901854 ) ) ;
#48471 = CARTESIAN_POINT ( 'NONE',  ( 5.049401038298161559, -19.05341960407611168, 97.70724293864766707 ) ) ;
#48472 = CARTESIAN_POINT ( 'NONE',  ( 5.823673210054125526, 21.52544592524343514, 99.79057627198103830 ) ) ;
#48473 = CARTESIAN_POINT ( 'NONE',  ( 16.46253265017160672, -9.564922557960803928, 58.33224293864769550 ) ) ;
#48474 = LINE ( 'NONE', #108131, #99308 ) ;
#48475 = CARTESIAN_POINT ( 'NONE',  ( -8.314922557960811034, -14.29746914071050412, 77.08224293864769550 ) ) ;
#48476 = CARTESIAN_POINT ( 'NONE',  ( 13.97604488694527802, 13.89961937509977652, 114.3739096053143669 ) ) ;
#48477 = CARTESIAN_POINT ( 'NONE',  ( 19.05341960407611168, 5.049401038298154454, 23.95724293864769194 ) ) ;
#48478 = CARTESIAN_POINT ( 'NONE',  ( 5.719274019375991003, -21.55341960407610458, 97.70724293864772392 ) ) ;
#48479 = CARTESIAN_POINT ( 'NONE',  ( 9.474510206698729675, 16.51473224551082808, 57.08442372801900433 ) ) ;
#48480 = CARTESIAN_POINT ( 'NONE',  ( 16.51473224551069308, 9.474510206698969483, 114.1655762719810241 ) ) ;
#48481 = CARTESIAN_POINT ( 'NONE',  ( 19.05341960407611168, 5.049401038298154454, 28.95724293864769550 ) ) ;
#48482 = CARTESIAN_POINT ( 'NONE',  ( 18.62759615963271287, -10.81492255796078972, 53.33224293864769550 ) ) ;
#48483 = AXIS2_PLACEMENT_3D ( 'NONE', #81802, #7975, #69659 ) ;
#48484 = CARTESIAN_POINT ( 'NONE',  ( 19.05341960407611168, 5.049401038298154454, 98.95724293864766707 ) ) ;
#48485 = CARTESIAN_POINT ( 'NONE',  ( -18.62759615963255300, -10.81492255796106328, 74.16775706135231871 ) ) ;
#48486 = CARTESIAN_POINT ( 'NONE',  ( -5.153800228976328057, -19.02544592524343514, 47.29057627198102409 ) ) ;
#48487 = EDGE_CURVE ( 'NONE', #122541, #169284, #174867, .T. ) ;
#48488 = CARTESIAN_POINT ( 'NONE',  ( -0.05219959533910754901, -16.53943276465976808, 87.49890960531436690 ) ) ;
#48489 = CARTESIAN_POINT ( 'NONE',  ( 16.52544592524335698, 4.483927247898782831, 31.45942372801901854 ) ) ;
#48490 = CARTESIAN_POINT ( 'NONE',  ( -18.62759615963255300, -10.81492255796106328, 64.16775706135234714 ) ) ;
#48491 = ORIENTED_EDGE ( 'NONE', *, *, #10333, .T. ) ;
#48492 = CARTESIAN_POINT ( 'NONE',  ( -13.89961937509957401, -13.97604488694547875, 24.37609039468565442 ) ) ;
#48493 = CARTESIAN_POINT ( 'NONE',  ( 19.02544592524334988, 5.153800228976608722, 81.45942372801897591 ) ) ;
#48494 = CARTESIAN_POINT ( 'NONE',  ( 19.02544592524334988, 5.153800228976608722, 41.45942372801900433 ) ) ;
#48495 = CARTESIAN_POINT ( 'NONE',  ( -30.74264578624800492, 22.33583958711400186, -5.949999994537626513 ) ) ;
#48496 = CARTESIAN_POINT ( 'NONE',  ( -5.823673210054431948, 21.52544592524334988, 37.70942372801900433 ) ) ;
#48497 = CARTESIAN_POINT ( 'NONE',  ( 17.59860650958989936, 7.585241751807028088, 54.07662985737508876 ) ) ;
#48498 = CARTESIAN_POINT ( 'NONE',  ( -13.89961937509957401, -13.97604488694547875, 39.37609039468566152 ) ) ;
#48499 = CARTESIAN_POINT ( 'NONE',  ( 13.89961937509977652, -13.97604488694527269, 63.12390960531435979 ) ) ;
#48500 = CARTESIAN_POINT ( 'NONE',  ( 4.379528057220339221, -16.55341960407611168, 27.70724293864769905 ) ) ;
#48502 = CARTESIAN_POINT ( 'NONE',  ( 15.72974639402176855, 15.80617190586768217, 91.87609039468568994 ) ) ;
#48501 = CARTESIAN_POINT ( 'NONE',  ( -5.719274019375978568, 21.55341960407610458, 25.20724293864769550 ) ) ;
#48503 = CARTESIAN_POINT ( 'NONE',  ( -11.40812507854754720, -35.11059874428192273, -6.224999997268812812 ) ) ;
#48504 = CARTESIAN_POINT ( 'NONE',  ( -27.73933785331498925, 2.428612866367529932E-14, 149.1250000027311842 ) ) ;
#48505 = CARTESIAN_POINT ( 'NONE',  ( 18.67979575497194134, -10.72451020669871369, 85.83442372801901854 ) ) ;
#48506 = CARTESIAN_POINT ( 'NONE',  ( 21.30000000000002203, -0.1105695005019232124, -58.85720012050612127 ) ) ;
#48507 = CARTESIAN_POINT ( 'NONE',  ( 16.46253265017160672, -9.564922557960803928, 103.3322429386476955 ) ) ;
#48508 = CARTESIAN_POINT ( 'NONE',  ( -24.02723517065431125, -14.44770145514793036, 165.8682408883346397 ) ) ;
#48509 = CARTESIAN_POINT ( 'NONE',  ( -16.51473224551069308, -9.474510206698971260, 56.66557627198103120 ) ) ;
#48510 = CARTESIAN_POINT ( 'NONE',  ( 21.53943276465977519, -0.05219959533907433946, 63.74890960531435979 ) ) ;
#48511 = CARTESIAN_POINT ( 'NONE',  ( -16.52544592524342804, 4.483927247898546575, 31.04057627198102409 ) ) ;
#48513 = CARTESIAN_POINT ( 'NONE',  ( -5.153800228976328057, -19.02544592524343514, 97.29057627198099567 ) ) ;
#48512 = CARTESIAN_POINT ( 'NONE',  ( -16.55341960407611168, -4.379528057220339221, 111.4572429386476813 ) ) ;
#48514 = CARTESIAN_POINT ( 'NONE',  ( -16.51473224551082808, 9.474510206698731452, 28.33442372801900433 ) ) ;
#48515 = CARTESIAN_POINT ( 'NONE',  ( -12.06949235617756955, 12.14591786802309770, 100.6239096053143811 ) ) ;
#48516 = CARTESIAN_POINT ( 'NONE',  ( 21.52544592524334988, 5.823673210054432836, 71.45942372801901854 ) ) ;
#48517 = CARTESIAN_POINT ( 'NONE',  ( 16.46253265017160672, -9.564922557960803928, 98.33224293864769550 ) ) ;
#48518 = CARTESIAN_POINT ( 'NONE',  ( -12.14591786802326823, 12.06949235617739902, 113.1260903946856899 ) ) ;
#48519 = CARTESIAN_POINT ( 'NONE',  ( 19.05341960407617918, -5.049401038297876454, 61.04275706135232582 ) ) ;
#48520 = CARTESIAN_POINT ( 'NONE',  ( -11.40812507854754720, -35.11059874428192273, -4.724999997268812812 ) ) ;
#48521 = CARTESIAN_POINT ( 'NONE',  ( 5.049401038298161559, -19.05341960407611168, 107.7072429386476955 ) ) ;
#48522 = CARTESIAN_POINT ( 'NONE',  ( -16.52544592524342804, 4.483927247898546575, 71.04057627198103830 ) ) ;
#48523 = CARTESIAN_POINT ( 'NONE',  ( -19.02544592524334988, -5.153800228976617603, 58.95942372801900433 ) ) ;
#48524 = CARTESIAN_POINT ( 'NONE',  ( 13.89961937509977652, -13.97604488694527269, 58.12390960531436690 ) ) ;
#48525 = CARTESIAN_POINT ( 'NONE',  ( -0.05219959533910754901, -16.53943276465976808, 62.49890960531436690 ) ) ;
#48526 = CARTESIAN_POINT ( 'NONE',  ( -9.564922557961040184, 16.46253265017147172, 87.91775706135233293 ) ) ;
#48527 = CARTESIAN_POINT ( 'NONE',  ( -18.62759615963270932, 10.81492255796079327, 45.83224293864769550 ) ) ;
#48528 = ORIENTED_EDGE ( 'NONE', *, *, #30819, .T. ) ;
#48529 = CARTESIAN_POINT ( 'NONE',  ( 5.049401038298161559, -19.05341960407611168, 22.70724293864769194 ) ) ;
#48530 = CARTESIAN_POINT ( 'NONE',  ( -16.20579543436681647, -7.371946100354982434, 30.56520834171878320 ) ) ;
#48532 = CARTESIAN_POINT ( 'NONE',  ( -21.55341960407610458, -5.719274019375992779, 61.45724293864770260 ) ) ;
#48531 = CARTESIAN_POINT ( 'NONE',  ( 5.153800228976335163, 19.02544592524342804, 69.79057627198103830 ) ) ;
#48534 = CARTESIAN_POINT ( 'NONE',  ( 19.05341960407611168, 5.049401038298154454, 73.95724293864768129 ) ) ;
#48533 = CARTESIAN_POINT ( 'NONE',  ( 4.483927247898790824, -16.52544592524335698, 90.20942372801903275 ) ) ;
#48535 = CARTESIAN_POINT ( 'NONE',  ( -0.05219959533936034679, 19.03943276465977164, 52.50109039468566863 ) ) ;
#48536 = CARTESIAN_POINT ( 'NONE',  ( -5.719274019375665041, -21.55341960407619695, 84.79275706135234714 ) ) ;
#48537 = CARTESIAN_POINT ( 'NONE',  ( -15.80617190586745835, -15.72974639402198527, 61.87390960531436690 ) ) ;
#48538 = CARTESIAN_POINT ( 'NONE',  ( 0.05219959533909260263, 19.03943276465977164, 104.9989096053143669 ) ) ;
#48539 = CARTESIAN_POINT ( 'NONE',  ( -13.89961937509977652, 13.97604488694528158, 35.62390960531435269 ) ) ;
#48540 = CARTESIAN_POINT ( 'NONE',  ( 8.314922557961029526, -14.29746914071037800, 105.4177570613523613 ) ) ;
#48541 = CARTESIAN_POINT ( 'NONE',  ( -19.03943276465977164, -0.05219959533935918106, 113.7510903946856757 ) ) ;
#48542 = CARTESIAN_POINT ( 'NONE',  ( 19.25176906914651553, 5.499999999999744205, 78.49927264242278113 ) ) ;
#48543 = CARTESIAN_POINT ( 'NONE',  ( 15.80617190586769283, -15.72974639402175789, 90.62609039468567573 ) ) ;
#48544 = CARTESIAN_POINT ( 'NONE',  ( -8.224510206698948167, 14.34966873604960824, 60.41557627198102409 ) ) ;
#48545 = CARTESIAN_POINT ( 'NONE',  ( 12.06949235617757843, -12.14591786802309237, 68.12390960531436690 ) ) ;
#48546 = CARTESIAN_POINT ( 'NONE',  ( 15.80617190586746368, 15.72974639402197994, 89.37390960531435269 ) ) ;
#48547 = CARTESIAN_POINT ( 'NONE',  ( -10.72451020669898014, 18.67979575497178502, 95.41557627198102409 ) ) ;
#48548 = CARTESIAN_POINT ( 'NONE',  ( -1.467638476639070655, -30.74964850363294033, -47.27948696604328660 ) ) ;
#48549 = CARTESIAN_POINT ( 'NONE',  ( 21.52544592524344225, -5.823673210054117533, 48.54057627198103120 ) ) ;
#48550 = CARTESIAN_POINT ( 'NONE',  ( 4.379528057220092307, 16.55341960407617563, 67.29275706135234714 ) ) ;
#48551 = CARTESIAN_POINT ( 'NONE',  ( -8.314922557960811034, -14.29746914071050412, 97.08224293864770971 ) ) ;
#48552 = CARTESIAN_POINT ( 'NONE',  ( -13.97604488694527625, -13.89961937509977652, 41.87390960531435979 ) ) ;
#48553 =( NAMED_UNIT ( * ) SI_UNIT ( $, .STERADIAN. ) SOLID_ANGLE_UNIT ( ) );
#48554 = CARTESIAN_POINT ( 'NONE',  ( 35.24470855014509141, -4.955302550156627461, 39.34877664276073261 ) ) ;
#48555 = CARTESIAN_POINT ( 'NONE',  ( 4.483927247898790824, -16.52544592524335698, 100.2094237280190043 ) ) ;
#48556 = CARTESIAN_POINT ( 'NONE',  ( 5.823673210054444382, -21.52544592524334988, 30.20942372801902565 ) ) ;
#48557 = CARTESIAN_POINT ( 'NONE',  ( -16.51473224551069308, -9.474510206698971260, 96.66557627198102409 ) ) ;
#48558 = CARTESIAN_POINT ( 'NONE',  ( -21.53943276465977519, -0.05219959533937600094, 63.75109039468568284 ) ) ;
#48559 = CYLINDRICAL_SURFACE ( 'NONE', #198726, 28.82186960331498682 ) ;
#48560 = CARTESIAN_POINT ( 'NONE',  ( 19.03943276465977164, -0.05219959533909143690, 28.74890960531435624 ) ) ;
#48561 = VERTEX_POINT ( 'NONE', #178876 ) ;
#48562 = CARTESIAN_POINT ( 'NONE',  ( 18.62759615963255655, 10.81492255796105972, 56.66775706135235424 ) ) ;
#48564 = CARTESIAN_POINT ( 'NONE',  ( 9.474510206698971260, -16.51473224551069308, 22.91557627198102765 ) ) ;
#48563 = CARTESIAN_POINT ( 'NONE',  ( 9.474510206698971260, -16.51473224551069308, 47.91557627198102409 ) ) ;
#48565 = CARTESIAN_POINT ( 'NONE',  ( -9.564922557960796823, -16.46253265017161027, 92.08224293864769550 ) ) ;
#48566 = CARTESIAN_POINT ( 'NONE',  ( 19.02544592524334988, 5.153800228976608722, 66.45942372801899012 ) ) ;
#48567 = CARTESIAN_POINT ( 'NONE',  ( -10.81492255796105439, 18.62759615963255655, 27.91775706135234358 ) ) ;
#48568 = CARTESIAN_POINT ( 'NONE',  ( 19.03943276465977164, 0.05219959533936151252, 61.25109039468566863 ) ) ;
#48569 = CARTESIAN_POINT ( 'NONE',  ( 13.89961937509977652, -13.97604488694527269, 43.12390960531434558 ) ) ;
#48570 = CARTESIAN_POINT ( 'NONE',  ( -12.14591786802326823, 12.06949235617739902, 108.1260903946856757 ) ) ;
#48571 = CARTESIAN_POINT ( 'NONE',  ( -5.049401038297874678, -19.05341960407617918, 74.79275706135231871 ) ) ;
#48572 = CARTESIAN_POINT ( 'NONE',  ( -12.14591786802309592, -12.06949235617757132, 21.87390960531436690 ) ) ;
#48573 = CARTESIAN_POINT ( 'NONE',  ( 5.153800228976615827, -19.02544592524334988, 45.20942372801901143 ) ) ;
#48574 = CARTESIAN_POINT ( 'NONE',  ( -5.153800228976328057, -19.02544592524343514, 102.2905762719810383 ) ) ;
#48575 = CARTESIAN_POINT ( 'NONE',  ( 21.52544592524334988, 5.823673210054432836, 106.4594237280190328 ) ) ;
#48576 = CARTESIAN_POINT ( 'NONE',  ( 9.474510206698729675, 16.51473224551082808, 22.08442372801899722 ) ) ;
#48577 = CARTESIAN_POINT ( 'NONE',  ( -19.05341960407611168, -5.049401038298163336, 31.45724293864769550 ) ) ;
#48578 = CARTESIAN_POINT ( 'NONE',  ( 21.52544592524334988, 5.823673210054432836, 91.45942372801901854 ) ) ;
#48579 = CARTESIAN_POINT ( 'NONE',  ( 4.379528057220092307, 16.55341960407617563, 37.29275706135235424 ) ) ;
#48580 = CARTESIAN_POINT ( 'NONE',  ( -16.51473224551069308, -9.474510206698971260, 96.66557627198102409 ) ) ;
#48581 = EDGE_CURVE ( 'NONE', #74939, #166806, #88480, .T. ) ;
#48582 = CARTESIAN_POINT ( 'NONE',  ( 32.00000000000000000, -5.510910596163089556E-15, 45.00000000000000000 ) ) ;
#48583 = CARTESIAN_POINT ( 'NONE',  ( -9.474510206698964154, 16.51473224551069663, 75.41557627198103830 ) ) ;
#48584 = CARTESIAN_POINT ( 'NONE',  ( 28.82186960331521419, 9.364793116373263615, 141.0999999999999943 ) ) ;
#48585 = CARTESIAN_POINT ( 'NONE',  ( -16.51473224551082808, 9.474510206698731452, 68.33442372801900433 ) ) ;
#48586 = CARTESIAN_POINT ( 'NONE',  ( 19.05341960407611168, 5.049401038298154454, 108.9572429386477097 ) ) ;
#48587 = CARTESIAN_POINT ( 'NONE',  ( 15.72974639402176855, 15.80617190586768217, 96.87609039468568994 ) ) ;
#48588 = CARTESIAN_POINT ( 'NONE',  ( 8.314922557960818139, 14.29746914071049879, 94.58224293864769550 ) ) ;
#48589 = CARTESIAN_POINT ( 'NONE',  ( 0.05219959533909260263, 19.03943276465977164, 24.99890960531435269 ) ) ;
#48590 = CARTESIAN_POINT ( 'NONE',  ( 21.55341960407610458, 5.719274019375980345, 43.95724293864769550 ) ) ;
#48591 = CARTESIAN_POINT ( 'NONE',  ( 10.81492255796078972, 18.62759615963270932, 34.58224293864770260 ) ) ;
#48592 = CARTESIAN_POINT ( 'NONE',  ( 14.29746914071049879, -8.314922557960816363, 103.3322429386476955 ) ) ;
#48593 = CARTESIAN_POINT ( 'NONE',  ( -13.90353822939980688, 0.7813480796680551954, -62.49831333862086780 ) ) ;
#48594 = CARTESIAN_POINT ( 'NONE',  ( 19.05341960407617918, -5.049401038297876454, 56.04275706135234714 ) ) ;
#48595 = CARTESIAN_POINT ( 'NONE',  ( -16.53943276465976808, 0.05219959533911058130, 46.24890960531435979 ) ) ;
#48596 = CARTESIAN_POINT ( 'NONE',  ( -19.03943276465977164, 0.05219959533909376836, 111.2489096053143669 ) ) ;
#48597 = CARTESIAN_POINT ( 'NONE',  ( 21.55341960407619695, -5.719274019375665929, 86.04275706135236135 ) ) ;
#48598 = CARTESIAN_POINT ( 'NONE',  ( -15.72974639402197994, 15.80617190586746368, 75.62390960531439532 ) ) ;
#48599 = CARTESIAN_POINT ( 'NONE',  ( -10.81492255796105439, 18.62759615963255655, 42.91775706135235424 ) ) ;
#48600 = CARTESIAN_POINT ( 'NONE',  ( 18.62759615963271287, -10.81492255796078972, 103.3322429386476955 ) ) ;
#48601 = CARTESIAN_POINT ( 'NONE',  ( -10.72451020669870658, -18.67979575497194134, 49.58442372801901143 ) ) ;
#48602 = CARTESIAN_POINT ( 'NONE',  ( -16.51473224551069308, -9.474510206698971260, 21.66557627198102765 ) ) ;
#48603 = CARTESIAN_POINT ( 'NONE',  ( 16.46253265017160672, -9.564922557960803928, 83.33224293864768129 ) ) ;
#48604 = CARTESIAN_POINT ( 'NONE',  ( -12.06949235617739369, -12.14591786802326823, 84.37609039468570415 ) ) ;
#48605 = CARTESIAN_POINT ( 'NONE',  ( -12.06949235617756955, 12.14591786802309770, 100.6239096053143811 ) ) ;
#48606 = CARTESIAN_POINT ( 'NONE',  ( 9.474510206698971260, -16.51473224551069308, 107.9155762719810383 ) ) ;
#48607 = CARTESIAN_POINT ( 'NONE',  ( -4.483927247898539470, -16.52544592524342804, 57.29057627198103120 ) ) ;
#48608 = CARTESIAN_POINT ( 'NONE',  ( -16.55341960407617563, 4.379528057220093196, 113.5427570613523756 ) ) ;
#48609 = CARTESIAN_POINT ( 'NONE',  ( -9.474510206698964154, 16.51473224551069663, 70.41557627198102409 ) ) ;
#48610 = CARTESIAN_POINT ( 'NONE',  ( 0.05219959533909260263, 19.03943276465977164, 34.99890960531435979 ) ) ;
#48611 = CARTESIAN_POINT ( 'NONE',  ( 0.05219959533907565091, 21.53943276465977519, 49.99890960531437401 ) ) ;
#48612 = CARTESIAN_POINT ( 'NONE',  ( -9.564922557961040184, 16.46253265017147172, 32.91775706135233293 ) ) ;
#48614 = CARTESIAN_POINT ( 'NONE',  ( -12.06949235617756955, 12.14591786802309770, 30.62390960531436335 ) ) ;
#48613 = CARTESIAN_POINT ( 'NONE',  ( -17.49999999999999645, -5.499999999999992895, 49.20309617465830598 ) ) ;
#48616 = CIRCLE ( 'NONE', #77615, 2.649999999999999467 ) ;
#48615 = CARTESIAN_POINT ( 'NONE',  ( -0.05219959533909027116, -19.03943276465977164, 102.4989096053143669 ) ) ;
#48617 = CARTESIAN_POINT ( 'NONE',  ( -10.72451020669870658, -18.67979575497194134, 54.58442372801901143 ) ) ;
#48618 = CARTESIAN_POINT ( 'NONE',  ( -0.05219959533909027116, -19.03943276465977164, 112.4989096053143669 ) ) ;
#48619 = CARTESIAN_POINT ( 'NONE',  ( -16.52544592524335698, -4.483927247898792601, 58.95942372801902565 ) ) ;
#48620 = CARTESIAN_POINT ( 'NONE',  ( 16.51473224551083163, -9.474510206698727899, 65.83442372801900433 ) ) ;
#48621 = CARTESIAN_POINT ( 'NONE',  ( 16.55341960407611168, 4.379528057220329451, 28.95724293864769905 ) ) ;
#48622 = CARTESIAN_POINT ( 'NONE',  ( -19.39720447994793773, -5.500000000000083489, 74.66317477297180005 ) ) ;
#48623 = CARTESIAN_POINT ( 'NONE',  ( 8.314922557961029526, -14.29746914071037800, 100.4177570613523471 ) ) ;
#48624 = CARTESIAN_POINT ( 'NONE',  ( 19.02544592524343514, -5.153800228976328945, 43.54057627198103120 ) ) ;
#48625 = CARTESIAN_POINT ( 'NONE',  ( 0.05219959533909260263, 19.03943276465977164, 54.99890960531435979 ) ) ;
#48626 = CARTESIAN_POINT ( 'NONE',  ( -19.05341960407611168, -5.049401038298163336, 26.45724293864769550 ) ) ;
#48627 = CARTESIAN_POINT ( 'NONE',  ( 5.719274019375673035, 21.55341960407619339, 27.29275706135234358 ) ) ;
#48628 = CARTESIAN_POINT ( 'NONE',  ( -19.02544592524342804, 5.153800228976336051, 51.04057627198103120 ) ) ;
#48629 = CARTESIAN_POINT ( 'NONE',  ( -3.874011537017815421, -5.374011537017722162, -62.41807096325323556 ) ) ;
#48630 = CARTESIAN_POINT ( 'NONE',  ( -19.02544592524342804, 5.153800228976336051, 41.04057627198103120 ) ) ;
#48631 = CARTESIAN_POINT ( 'NONE',  ( 15.72974639402199770, -15.80617190586745480, 28.12390960531435979 ) ) ;
#48633 = CARTESIAN_POINT ( 'NONE',  ( 16.55341960407611168, 4.379528057220329451, 113.9572429386477239 ) ) ;
#48632 = CARTESIAN_POINT ( 'NONE',  ( -18.67979575497193778, 10.72451020669871902, 53.33442372801901854 ) ) ;
#48634 = CARTESIAN_POINT ( 'NONE',  ( -5.823673210054116645, -21.52544592524344225, 27.29057627198103120 ) ) ;
#48635 = CARTESIAN_POINT ( 'NONE',  ( -16.53943276465976808, -0.05219959533934237506, 73.75109039468567573 ) ) ;
#48636 = CARTESIAN_POINT ( 'NONE',  ( -10.81492255796105439, 18.62759615963255655, 102.9177570613523756 ) ) ;
#48637 = CARTESIAN_POINT ( 'NONE',  ( -16.55341960407617563, 4.379528057220093196, 53.54275706135234714 ) ) ;
#48638 = CARTESIAN_POINT ( 'NONE',  ( -13.97604488694527625, -13.89961937509977652, 91.87390960531432427 ) ) ;
#48639 = CARTESIAN_POINT ( 'NONE',  ( 12.14591786802327356, -12.06949235617739191, 40.62609039468567573 ) ) ;
#48640 = CARTESIAN_POINT ( 'NONE',  ( 16.55341960407618274, -4.379528057220086978, 31.04275706135234714 ) ) ;
#48641 = CARTESIAN_POINT ( 'NONE',  ( 12.06949235617739724, 12.14591786802326823, 91.87609039468568994 ) ) ;
#48642 = CARTESIAN_POINT ( 'NONE',  ( -21.55341960407619339, 5.719274019375674811, 53.54275706135234714 ) ) ;
#48643 = CARTESIAN_POINT ( 'NONE',  ( 5.049401038297881783, 19.05341960407617563, 102.2927570613523045 ) ) ;
#48644 = CARTESIAN_POINT ( 'NONE',  ( 5.823673210054125526, 21.52544592524343514, 109.7905762719810383 ) ) ;
#48646 = CARTESIAN_POINT ( 'NONE',  ( -5.153800228976607833, 19.02544592524334988, 107.7094237280189759 ) ) ;
#48645 = CARTESIAN_POINT ( 'NONE',  ( -16.55341960407611168, -4.379528057220339221, 106.4572429386477097 ) ) ;
#48647 = CARTESIAN_POINT ( 'NONE',  ( 16.55341960407618274, -4.379528057220086978, 91.04275706135236135 ) ) ;
#48648 = CARTESIAN_POINT ( 'NONE',  ( -17.48853670773247870, 5.747243402302952830, 43.66671299749993551 ) ) ;
#48649 = CARTESIAN_POINT ( 'NONE',  ( -0.05219959533936034679, 19.03943276465977164, 82.50109039468567573 ) ) ;
#48650 = CARTESIAN_POINT ( 'NONE',  ( -4.379528057220328563, 16.55341960407611168, 45.20724293864769550 ) ) ;
#48651 = CARTESIAN_POINT ( 'NONE',  ( 14.34966873604960469, 8.224510206698951720, 44.16557627198103120 ) ) ;
#48652 = CARTESIAN_POINT ( 'NONE',  ( -14.34966873604960291, -8.224510206698953496, 106.6655762719810383 ) ) ;
#48654 = CARTESIAN_POINT ( 'NONE',  ( -17.44279575226822843, 5.990770900252461395, 90.83557567514318976 ) ) ;
#48653 = CARTESIAN_POINT ( 'NONE',  ( 19.03943276465977164, 0.05219959533936151252, 46.25109039468566863 ) ) ;
#48655 = CARTESIAN_POINT ( 'NONE',  ( 21.55341960407619695, -5.719274019375665929, 41.04275706135236135 ) ) ;
#48656 = CARTESIAN_POINT ( 'NONE',  ( 9.564922557961047289, -16.46253265017146816, 105.4177570613523471 ) ) ;
#48657 = CARTESIAN_POINT ( 'NONE',  ( -6.193113236902241248, -38.78391156914231175, -32.76858701579858035 ) ) ;
#48658 = CARTESIAN_POINT ( 'NONE',  ( -0.05219959533909027116, -19.03943276465977164, 92.49890960531436690 ) ) ;
#48659 = CARTESIAN_POINT ( 'NONE',  ( 19.02544592524343514, -5.153800228976328945, 83.54057627198100988 ) ) ;
#48660 = CARTESIAN_POINT ( 'NONE',  ( 5.719274019375991003, -21.55341960407610458, 57.70724293864770260 ) ) ;
#48661 = CARTESIAN_POINT ( 'NONE',  ( -12.14591786802309592, -12.06949235617757132, 111.8739096053143669 ) ) ;
#48662 = CARTESIAN_POINT ( 'NONE',  ( 16.51473224551069308, 9.474510206698969483, 69.16557627198102409 ) ) ;
#48663 = CARTESIAN_POINT ( 'NONE',  ( -19.05341960407611168, -5.049401038298163336, 26.45724293864769550 ) ) ;
#48664 = CARTESIAN_POINT ( 'NONE',  ( 5.823673210054444382, -21.52544592524334988, 40.20942372801901854 ) ) ;
#48665 = CARTESIAN_POINT ( 'NONE',  ( -21.53943276465977519, -0.05219959533937600094, 73.75109039468567573 ) ) ;
#48666 = CARTESIAN_POINT ( 'NONE',  ( -16.55341960407617563, 4.379528057220093196, 88.54275706135236135 ) ) ;
#48667 = EDGE_CURVE ( 'NONE', #128792, #30636, #137115, .T. ) ;
#48668 = CARTESIAN_POINT ( 'NONE',  ( -18.62759615963255300, -10.81492255796106328, 24.16775706135235424 ) ) ;
#48669 = CARTESIAN_POINT ( 'NONE',  ( -21.52544592524334988, -5.823673210054445271, 23.95942372801901143 ) ) ;
#48671 = CARTESIAN_POINT ( 'NONE',  ( 19.03943276465977164, -0.05219959533909143690, 78.74890960531436690 ) ) ;
#48670 = CARTESIAN_POINT ( 'NONE',  ( 19.02544592524334988, 5.153800228976608722, 56.45942372801898301 ) ) ;
#48672 = CARTESIAN_POINT ( 'NONE',  ( 0.05219959533937995610, -21.53943276465977519, 90.00109039468567573 ) ) ;
#48673 = CARTESIAN_POINT ( 'NONE',  ( -21.55341960407610458, -5.719274019375992779, 86.45724293864770971 ) ) ;
#48674 = CARTESIAN_POINT ( 'NONE',  ( 8.224510206698953496, -14.34966873604960469, 47.91557627198102409 ) ) ;
#48675 = CARTESIAN_POINT ( 'NONE',  ( -21.53943276465977519, -0.05219959533937600094, 108.7510903946857042 ) ) ;
#48676 = CARTESIAN_POINT ( 'NONE',  ( 16.53943276465976808, -0.05219959533910856209, 83.74890960531435269 ) ) ;
#48677 = CARTESIAN_POINT ( 'NONE',  ( 4.483927247898545687, 16.52544592524342804, 114.7905762719810383 ) ) ;
#48678 = CARTESIAN_POINT ( 'NONE',  ( 9.474510206698729675, 16.51473224551082808, 72.08442372801900433 ) ) ;
#48679 = CARTESIAN_POINT ( 'NONE',  ( -12.14591786802309592, -12.06949235617757132, 41.87390960531435979 ) ) ;
#48680 = CARTESIAN_POINT ( 'NONE',  ( -5.719274019375665041, -21.55341960407619695, 84.79275706135234714 ) ) ;
#48681 = CARTESIAN_POINT ( 'NONE',  ( 0.05219959533909260263, 19.03943276465977164, 94.99890960531436690 ) ) ;
#48682 = CARTESIAN_POINT ( 'NONE',  ( -16.46253265017146816, -9.564922557961047289, 59.16775706135233293 ) ) ;
#48683 = CARTESIAN_POINT ( 'NONE',  ( -21.53943276465977519, 0.05219959533907696930, 61.24890960531435979 ) ) ;
#48684 = CARTESIAN_POINT ( 'NONE',  ( -0.05219959533907301413, -21.53943276465977519, 112.4989096053143669 ) ) ;
#48685 = CARTESIAN_POINT ( 'NONE',  ( 4.379528057220092307, 16.55341960407617563, 22.29275706135235069 ) ) ;
#48686 = CARTESIAN_POINT ( 'NONE',  ( 12.14591786802327356, -12.06949235617739191, 75.62609039468567573 ) ) ;
#48687 = CARTESIAN_POINT ( 'NONE',  ( -21.52544592524334988, -5.823673210054445271, 28.95942372801902209 ) ) ;
#48688 = CARTESIAN_POINT ( 'NONE',  ( 14.34966873604960469, 8.224510206698951720, 109.1655762719810383 ) ) ;
#48689 = CARTESIAN_POINT ( 'NONE',  ( 22.81625015709509441, 31.40387420917330275, -7.824999997268813345 ) ) ;
#48690 = CARTESIAN_POINT ( 'NONE',  ( 0.05219959533934541429, -16.53943276465976808, 30.00109039468568284 ) ) ;
#48691 = PRODUCT_DEFINITION ( 'UNKNOWN', '', #82349, #3893 ) ;
#48692 = CARTESIAN_POINT ( 'NONE',  ( -18.67979575497178146, -10.72451020669898902, 56.66557627198103830 ) ) ;
#48693 = CARTESIAN_POINT ( 'NONE',  ( -12.06949235617739369, -12.14591786802326823, 99.37609039468568994 ) ) ;
#48694 = CARTESIAN_POINT ( 'NONE',  ( 8.314922557961029526, -14.29746914071037800, 40.41775706135234714 ) ) ;
#48695 = CARTESIAN_POINT ( 'NONE',  ( -5.153800228976328057, -19.02544592524343514, 37.29057627198102409 ) ) ;
#48696 = CARTESIAN_POINT ( 'NONE',  ( 16.52544592524335698, 4.483927247898782831, 86.45942372801901854 ) ) ;
#48697 = CARTESIAN_POINT ( 'NONE',  ( 19.02544592524334988, 5.153800228976608722, 71.45942372801900433 ) ) ;
#48698 = CARTESIAN_POINT ( 'NONE',  ( 21.53943276465977519, -0.05219959533907433946, 58.74890960531436690 ) ) ;
#48699 = CARTESIAN_POINT ( 'NONE',  ( 16.55341960407618274, -4.379528057220086978, 101.0427570613523756 ) ) ;
#48700 = CARTESIAN_POINT ( 'NONE',  ( 5.719274019375673035, 21.55341960407619339, 77.29275706135234714 ) ) ;
#48701 = CARTESIAN_POINT ( 'NONE',  ( -21.55341960407610458, -5.719274019375992779, 56.45724293864768839 ) ) ;
#48702 = CARTESIAN_POINT ( 'NONE',  ( -21.55341960407610458, -5.719274019375992779, 46.45724293864769550 ) ) ;
#48703 = CARTESIAN_POINT ( 'NONE',  ( 4.483927247898790824, -16.52544592524335698, 80.20942372801901854 ) ) ;
#48704 = CARTESIAN_POINT ( 'NONE',  ( -15.72974639402197994, 15.80617190586746368, 40.62390960531435269 ) ) ;
#48705 = ORIENTED_EDGE ( 'NONE', *, *, #2143, .F. ) ;
#48706 = CARTESIAN_POINT ( 'NONE',  ( 13.97604488694527802, 13.89961937509977652, 99.37390960531436690 ) ) ;
#48707 = CARTESIAN_POINT ( 'NONE',  ( -21.70980307670620846, -7.452553642297963243, 174.2373330747589932 ) ) ;
#48708 = CARTESIAN_POINT ( 'NONE',  ( -9.564922557960796823, -16.46253265017161027, 22.08224293864768839 ) ) ;
#48709 = CARTESIAN_POINT ( 'NONE',  ( 5.719274019375991003, -21.55341960407610458, 67.70724293864769550 ) ) ;
#48710 = CARTESIAN_POINT ( 'NONE',  ( -14.29746914071037622, -8.314922557961029526, 109.1677570613523613 ) ) ;
#48711 = CARTESIAN_POINT ( 'NONE',  ( -21.52544592524334988, -5.823673210054445271, 48.95942372801902565 ) ) ;
#48712 = CARTESIAN_POINT ( 'NONE',  ( 19.05341960407617918, -5.049401038297876454, 101.0427570613523045 ) ) ;
#48713 = CARTESIAN_POINT ( 'NONE',  ( 14.34966873604960469, 8.224510206698951720, 109.1655762719810383 ) ) ;
#48714 = CARTESIAN_POINT ( 'NONE',  ( -16.51473224551082808, 9.474510206698731452, 108.3344237280190043 ) ) ;
#48715 = CARTESIAN_POINT ( 'NONE',  ( 0.05219959533909260263, 19.03943276465977164, 39.99890960531436690 ) ) ;
#48716 = CARTESIAN_POINT ( 'NONE',  ( 10.20000000000000107, 2.210487472460972205E-16, -1.610000000000000098 ) ) ;
#48717 = CARTESIAN_POINT ( 'NONE',  ( -5.153800228976328057, -19.02544592524343514, 87.29057627198103830 ) ) ;
#48718 = CARTESIAN_POINT ( 'NONE',  ( -16.53943276465976808, -0.05219959533934237506, 78.75109039468568994 ) ) ;
#48719 = CARTESIAN_POINT ( 'NONE',  ( -9.474510206698720793, -16.51473224551083518, 74.58442372801900433 ) ) ;
#48720 = CARTESIAN_POINT ( 'NONE',  ( 10.72451020669871369, 18.67979575497193778, 107.0844237280190043 ) ) ;
#48721 = CARTESIAN_POINT ( 'NONE',  ( 21.52544592524344225, -5.823673210054117533, 63.54057627198103830 ) ) ;
#48722 = CARTESIAN_POINT ( 'NONE',  ( -12.06949235617739369, -12.14591786802326823, 84.37609039468570415 ) ) ;
#48723 = CARTESIAN_POINT ( 'NONE',  ( 9.564922557961047289, -16.46253265017146816, 75.41775706135234714 ) ) ;
#48724 = CARTESIAN_POINT ( 'NONE',  ( 19.05341960407611168, 5.049401038298154454, 38.95724293864767418 ) ) ;
#48725 = CARTESIAN_POINT ( 'NONE',  ( -5.153800228976328057, -19.02544592524343514, 72.29057627198102409 ) ) ;
#48726 = CARTESIAN_POINT ( 'NONE',  ( 18.62759615963255655, 10.81492255796105972, 51.66775706135234714 ) ) ;
#48727 = CARTESIAN_POINT ( 'NONE',  ( 5.049401038298161559, -19.05341960407611168, 52.70724293864767418 ) ) ;
#48728 = CARTESIAN_POINT ( 'NONE',  ( 5.153800228976615827, -19.02544592524334988, 70.20942372801899012 ) ) ;
#48729 = CARTESIAN_POINT ( 'NONE',  ( 20.69372460268611746, -11.29034304323151794, 170.1224388339879567 ) ) ;
#48730 = CARTESIAN_POINT ( 'NONE',  ( 16.46253265017160672, -9.564922557960803928, 103.3322429386476955 ) ) ;
#48731 = CARTESIAN_POINT ( 'NONE',  ( -14.34966873604960291, -8.224510206698953496, 66.66557627198102409 ) ) ;
#48732 = CARTESIAN_POINT ( 'NONE',  ( -21.55341960407610458, -5.719274019375992779, 56.45724293864768839 ) ) ;
#48733 = CARTESIAN_POINT ( 'NONE',  ( -5.427562675786936573E-15, 30.27659582821221207, 143.7656553485623476 ) ) ;
#48734 = CARTESIAN_POINT ( 'NONE',  ( -13.97604488694547697, 13.89961937509957934, 28.12609039468565797 ) ) ;
#48735 = CARTESIAN_POINT ( 'NONE',  ( 10.59477242850415024, -90.60836494048558620, -4.999999999999999112 ) ) ;
#48737 = CARTESIAN_POINT ( 'NONE',  ( 9.564922557960805705, 16.46253265017160317, 79.58224293864769550 ) ) ;
#48736 = CARTESIAN_POINT ( 'NONE',  ( 19.02544592524343514, -5.153800228976328945, 68.54057627198103830 ) ) ;
#48738 = CARTESIAN_POINT ( 'NONE',  ( 4.379528057220092307, 16.55341960407617563, 57.29275706135234714 ) ) ;
#48739 = CARTESIAN_POINT ( 'NONE',  ( 5.153800228976617603, -19.02544592524335343, 80.20942372801900433 ) ) ;
#48740 = CARTESIAN_POINT ( 'NONE',  ( -17.13100169013301510, 6.664070546373130455, 110.7678983569984723 ) ) ;
#48741 = CARTESIAN_POINT ( 'NONE',  ( 4.379528057220092307, 16.55341960407617563, 87.29275706135236135 ) ) ;
#48742 = CYLINDRICAL_SURFACE ( 'NONE', #17757, 1.500000000000001332 ) ;
#48743 = CARTESIAN_POINT ( 'NONE',  ( -14.34966873604972548, 8.224510206698743886, 63.33442372801900433 ) ) ;
#48744 =( BOUNDED_CURVE ( )  B_SPLINE_CURVE ( 2, ( #16214, #47553, #64702, #62693, #19201, #4005, #126364, #124375, #49530, #32377, #143509 ),
 .UNSPECIFIED., .F., .F. ) 
 B_SPLINE_CURVE_WITH_KNOTS ( ( 3, 2, 2, 2, 2, 3 ),
 ( 0.9000000000000007994, 0.9200000000000007061, 0.9400000000000003908, 0.9600000000000002975, 0.9800000000000002043, 1.000000000000000000 ),
 .UNSPECIFIED. ) 
 CURVE ( )  GEOMETRIC_REPRESENTATION_ITEM ( )  RATIONAL_B_SPLINE_CURVE ( ( 0.9999999999999981126, 0.9510565162951554186, 1.000000000000000000, 0.9510565162951535312, 1.000000000000000000, 0.9510565162951535312, 1.000000000000000000, 0.9510565162951535312, 1.000000000000000000, 0.9510565162951535312, 1.000000000000000000 ) ) 
 REPRESENTATION_ITEM ( '' )  );
#48745 = CARTESIAN_POINT ( 'NONE',  ( 8.224510206698742110, 14.34966873604972548, 37.08442372801901143 ) ) ;
#48747 = DIRECTION ( 'NONE',  ( -1.000000000000000000, 0.000000000000000000, 0.000000000000000000 ) ) ;
#48746 = CARTESIAN_POINT ( 'NONE',  ( -19.02544592524342804, 5.153800228976336051, 56.04057627198100988 ) ) ;
#48748 = CARTESIAN_POINT ( 'NONE',  ( -15.72974639402176322, -15.80617190586768395, 59.37609039468568284 ) ) ;
#48749 = CARTESIAN_POINT ( 'NONE',  ( -9.564922557961040184, 16.46253265017147172, 67.91775706135233293 ) ) ;
#48750 = CARTESIAN_POINT ( 'NONE',  ( -15.72974639402176322, -15.80617190586768395, 109.3760903946857042 ) ) ;
#48751 = CARTESIAN_POINT ( 'NONE',  ( -13.89961937509977652, 13.97604488694528158, 35.62390960531435269 ) ) ;
#48752 = CARTESIAN_POINT ( 'NONE',  ( -17.49999999999999645, -5.500000000000005329, 31.28230962303567253 ) ) ;
#48753 = CARTESIAN_POINT ( 'NONE',  ( 21.52544592524344225, -5.823673210054117533, 48.54057627198103120 ) ) ;
#48754 = CARTESIAN_POINT ( 'NONE',  ( 18.62759615963271287, -10.81492255796078972, 23.33224293864769194 ) ) ;
#48755 = CARTESIAN_POINT ( 'NONE',  ( -8.224510206698948167, 14.34966873604960824, 100.4155762719810241 ) ) ;
#48756 = CARTESIAN_POINT ( 'NONE',  ( 14.34966873604972726, -8.224510206698740333, 35.83442372801901143 ) ) ;
#48757 = CARTESIAN_POINT ( 'NONE',  ( 8.224510206698953496, -14.34966873604960469, 32.91557627198102409 ) ) ;
#48758 = ORIENTED_EDGE ( 'NONE', *, *, #32194, .F. ) ;
#48759 = CARTESIAN_POINT ( 'NONE',  ( -15.72974639402176322, -15.80617190586768395, 19.37609039468568639 ) ) ;
#48761 = CARTESIAN_POINT ( 'NONE',  ( 38.00000000000000711, -12.34694845685040754, -9.100000000000001421 ) ) ;
#48760 = CARTESIAN_POINT ( 'NONE',  ( -0.05219959533910754901, -16.53943276465976808, 37.49890960531436690 ) ) ;
#48762 = CARTESIAN_POINT ( 'NONE',  ( -9.564922557961040184, 16.46253265017147172, 97.91775706135233293 ) ) ;
#48763 = CARTESIAN_POINT ( 'NONE',  ( -0.05219959533936034679, 19.03943276465977164, 32.50109039468566863 ) ) ;
#48764 = CARTESIAN_POINT ( 'NONE',  ( -14.29746914071049879, 8.314922557960819915, 30.83224293864770260 ) ) ;
#48766 = EDGE_CURVE ( 'NONE', #29006, #51296, #25997, .T. ) ;
#48765 = CARTESIAN_POINT ( 'NONE',  ( -15.72974639402197994, 15.80617190586746368, 100.6239096053143811 ) ) ;
#48767 = CARTESIAN_POINT ( 'NONE',  ( 21.53943276465977519, -0.05219959533907433946, 68.74890960531435269 ) ) ;
#48768 = CARTESIAN_POINT ( 'NONE',  ( 13.89961937509977652, -13.97604488694527269, 78.12390960531433848 ) ) ;
#48769 = CARTESIAN_POINT ( 'NONE',  ( 14.34966873604960469, 8.224510206698951720, 49.16557627198102409 ) ) ;
#48770 = CARTESIAN_POINT ( 'NONE',  ( -19.03943276465977164, 0.05219959533909376836, 96.24890960531436690 ) ) ;
#48771 = DIRECTION ( 'NONE',  ( 0.06104853953485701173, 0.000000000000000000, -0.9981347984218670311 ) ) ;
#48772 = CARTESIAN_POINT ( 'NONE',  ( 16.46253265017146816, 9.564922557961045513, 46.66775706135233293 ) ) ;
#48773 = CARTESIAN_POINT ( 'NONE',  ( -18.62759615963270932, 10.81492255796079327, 90.83224293864769550 ) ) ;
#48774 = CARTESIAN_POINT ( 'NONE',  ( 14.34966873604960469, 8.224510206698951720, 99.16557627198100988 ) ) ;
#48775 = CARTESIAN_POINT ( 'NONE',  ( 21.53943276465977519, 0.05219959533937863772, 41.25109039468568284 ) ) ;
#48776 = CARTESIAN_POINT ( 'NONE',  ( 27.73933785331498214, 9.013057229001095294, 139.9750000027311501 ) ) ;
#48777 = EDGE_CURVE ( 'NONE', #76374, #111025, #193035, .T. ) ;
#48778 = CARTESIAN_POINT ( 'NONE',  ( 8.314922557961029526, -14.29746914071037800, 105.4177570613523613 ) ) ;
#48779 = CARTESIAN_POINT ( 'NONE',  ( -19.02544592524342804, 5.153800228976336051, 31.04057627198102409 ) ) ;
#48780 = CARTESIAN_POINT ( 'NONE',  ( -13.89961937509977652, 13.97604488694528158, 90.62390960531432427 ) ) ;
#48781 = CARTESIAN_POINT ( 'NONE',  ( 10.72451020669898902, -18.67979575497178502, 57.91557627198103120 ) ) ;
#48782 = CARTESIAN_POINT ( 'NONE',  ( 17.14385361876520264, -23.59649016807271238, 139.5750000027311444 ) ) ;
#48783 = CARTESIAN_POINT ( 'NONE',  ( -5.153800228976328057, -19.02544592524343514, 37.29057627198102409 ) ) ;
#48784 = CARTESIAN_POINT ( 'NONE',  ( -8.314922557960811034, -14.29746914071050412, 42.08224293864769550 ) ) ;
#48785 = CARTESIAN_POINT ( 'NONE',  ( 5.719274019375673035, 21.55341960407619339, 67.29275706135234714 ) ) ;
#48787 = CARTESIAN_POINT ( 'NONE',  ( 8.224510206698742110, 14.34966873604972548, 67.08442372801901854 ) ) ;
#48786 = CARTESIAN_POINT ( 'NONE',  ( 23.57492084471138583, -29.96337447970307721, -16.79025860370820666 ) ) ;
#48788 = CARTESIAN_POINT ( 'NONE',  ( -19.03943276465977164, 0.05219959533909376836, 51.24890960531436690 ) ) ;
#48789 = CARTESIAN_POINT ( 'NONE',  ( -19.03943276465977164, 0.05219959533909376836, 66.24890960531436690 ) ) ;
#48790 = ORIENTED_EDGE ( 'NONE', *, *, #62255, .T. ) ;
#48791 = CARTESIAN_POINT ( 'NONE',  ( -15.72974639402176322, -15.80617190586768395, 104.3760903946856899 ) ) ;
#48792 = CARTESIAN_POINT ( 'NONE',  ( 12.14591786802327356, -12.06949235617739191, 70.62609039468567573 ) ) ;
#48793 = CARTESIAN_POINT ( 'NONE',  ( -21.53943276465977519, -0.05219959533937600094, 93.75109039468567573 ) ) ;
#48794 = CARTESIAN_POINT ( 'NONE',  ( 9.474510206698971260, -16.51473224551069308, 67.91557627198102409 ) ) ;
#48795 = CARTESIAN_POINT ( 'NONE',  ( -21.55341960407610458, -5.719274019375992779, 36.45724293864768839 ) ) ;
#48796 = CARTESIAN_POINT ( 'NONE',  ( 16.46253265017146816, 9.564922557961045513, 101.6677570613523329 ) ) ;
#48797 = CARTESIAN_POINT ( 'NONE',  ( 21.52544592524334988, 5.823673210054432836, 86.45942372801901854 ) ) ;
#48798 = CARTESIAN_POINT ( 'NONE',  ( 8.314922557961029526, -14.29746914071037800, 55.41775706135234714 ) ) ;
#48799 = CARTESIAN_POINT ( 'NONE',  ( 18.62759615963271287, -10.81492255796078972, 98.33224293864769550 ) ) ;
#48800 = CARTESIAN_POINT ( 'NONE',  ( -0.05219959533936034679, 19.03943276465977164, 97.50109039468567573 ) ) ;
#48801 = CARTESIAN_POINT ( 'NONE',  ( 16.46253265017160672, -9.564922557960803928, 83.33224293864768129 ) ) ;
#48802 = CARTESIAN_POINT ( 'NONE',  ( 19.05341960407617918, -5.049401038297876454, 106.0427570613523471 ) ) ;
#48803 = CARTESIAN_POINT ( 'NONE',  ( 8.224510206698742110, 14.34966873604972548, 22.08442372801901143 ) ) ;
#48804 = CARTESIAN_POINT ( 'NONE',  ( -12.06949235617756955, 12.14591786802309770, 60.62390960531437401 ) ) ;
#48805 = CARTESIAN_POINT ( 'NONE',  ( -16.55341960407617563, 4.379528057220093196, 68.54275706135234714 ) ) ;
#48807 = CARTESIAN_POINT ( 'NONE',  ( -9.564922557960796823, -16.46253265017161027, 47.08224293864769550 ) ) ;
#48806 = CARTESIAN_POINT ( 'NONE',  ( -5.719274019375665041, -21.55341960407619695, 29.79275706135234358 ) ) ;
#48808 = CARTESIAN_POINT ( 'NONE',  ( 9.474510206698971260, -16.51473224551069308, 72.91557627198102409 ) ) ;
#48809 = CARTESIAN_POINT ( 'NONE',  ( -0.05219959533934338120, 16.53943276465976808, 72.50109039468568994 ) ) ;
#48810 = EDGE_CURVE ( 'NONE', #170287, #64113, #162687, .T. ) ;
#48811 = CARTESIAN_POINT ( 'NONE',  ( 17.81289503416611453, -24.51734667627695785, 144.9500000054623854 ) ) ;
#48812 = VERTEX_POINT ( 'NONE', #176876 ) ;
#48813 = CARTESIAN_POINT ( 'NONE',  ( 10.81492255796106328, -18.62759615963255655, 110.4177570613523756 ) ) ;
#48814 = CARTESIAN_POINT ( 'NONE',  ( 9.564922557960805705, 16.46253265017160317, 34.58224293864770260 ) ) ;
#48815 = ORIENTED_EDGE ( 'NONE', *, *, #173030, .F. ) ;
#48816 = CARTESIAN_POINT ( 'NONE',  ( 4.483927247898790824, -16.52544592524335698, 35.20942372801901854 ) ) ;
#48818 = CARTESIAN_POINT ( 'NONE',  ( 8.224510206698742110, 14.34966873604972548, 47.08442372801901854 ) ) ;
#48817 = CARTESIAN_POINT ( 'NONE',  ( -16.46253265017146816, -9.564922557961047289, 44.16775706135232582 ) ) ;
#48819 = CARTESIAN_POINT ( 'NONE',  ( 5.153800228976335163, 19.02544592524342804, 49.79057627198100988 ) ) ;
#48820 = CARTESIAN_POINT ( 'NONE',  ( 13.97604488694527802, 13.89961937509977652, 64.37390960531436690 ) ) ;
#48821 = CARTESIAN_POINT ( 'NONE',  ( 10.81492255796078972, 18.62759615963270932, 89.58224293864768129 ) ) ;
#48823 = CARTESIAN_POINT ( 'NONE',  ( 0.05219959533909260263, 19.03943276465977164, 109.9989096053143669 ) ) ;
#48822 = CARTESIAN_POINT ( 'NONE',  ( -5.049401038298153566, 19.05341960407611168, 80.20724293864769550 ) ) ;
#48824 = CARTESIAN_POINT ( 'NONE',  ( -13.89961937509977652, 13.97604488694528158, 60.62390960531436690 ) ) ;
#48825 = CARTESIAN_POINT ( 'NONE',  ( 12.50000000000001066, -90.00000000000005684, 0.000000000000000000 ) ) ;
#48826 = CARTESIAN_POINT ( 'NONE',  ( 16.46253265017146816, 9.564922557961045513, 101.6677570613523329 ) ) ;
#48827 = CARTESIAN_POINT ( 'NONE',  ( 10.81492255796078972, 18.62759615963270932, 79.58224293864769550 ) ) ;
#48828 = CARTESIAN_POINT ( 'NONE',  ( -9.474510206698720793, -16.51473224551083518, 29.58442372801900433 ) ) ;
#48829 = CARTESIAN_POINT ( 'NONE',  ( -4.483927247898539470, -16.52544592524342804, 67.29057627198103830 ) ) ;
#48830 = CARTESIAN_POINT ( 'NONE',  ( -21.55341960407619339, 5.719274019375674811, 88.54275706135236135 ) ) ;
#48831 = CARTESIAN_POINT ( 'NONE',  ( -8.224510206698948167, 14.34966873604960824, 115.4155762719810241 ) ) ;
#48833 = CARTESIAN_POINT ( 'NONE',  ( 10.81492255796106328, -18.62759615963255655, 95.41775706135234714 ) ) ;
#48832 = CARTESIAN_POINT ( 'NONE',  ( 4.483927247898545687, 16.52544592524342804, 29.79057627198102409 ) ) ;
#48834 = CARTESIAN_POINT ( 'NONE',  ( -9.474510206698964154, 16.51473224551069663, 80.41557627198103830 ) ) ;
#48835 = CARTESIAN_POINT ( 'NONE',  ( 5.719274019375673035, 21.55341960407619339, 42.29275706135235424 ) ) ;
#48836 = CARTESIAN_POINT ( 'NONE',  ( 13.89961937509977652, -13.97604488694527269, 78.12390960531433848 ) ) ;
#48837 = CARTESIAN_POINT ( 'NONE',  ( 0.05219959533910956823, 16.53943276465976808, 99.99890960531436690 ) ) ;
#48838 = CARTESIAN_POINT ( 'NONE',  ( 14.29746914071049879, -8.314922557960816363, 58.33224293864768839 ) ) ;
#48839 = CARTESIAN_POINT ( 'NONE',  ( -10.72451020669898014, 18.67979575497178502, 70.41557627198102409 ) ) ;
#48840 = CARTESIAN_POINT ( 'NONE',  ( 16.46253265017160672, -9.564922557960803928, 68.33224293864770971 ) ) ;
#48841 = CARTESIAN_POINT ( 'NONE',  ( -15.72974639402197994, 15.80617190586746368, 80.62390960531438111 ) ) ;
#48842 = CARTESIAN_POINT ( 'NONE',  ( 13.97604488694548053, -13.89961937509957401, 80.62609039468567573 ) ) ;
#48844 = CARTESIAN_POINT ( 'NONE',  ( -16.53943276465976808, 0.05219959533911058130, 71.24890960531435269 ) ) ;
#48843 = CARTESIAN_POINT ( 'NONE',  ( -19.03943276465977164, -0.05219959533935918106, 33.75109039468566863 ) ) ;
#48845 = CARTESIAN_POINT ( 'NONE',  ( 15.72974639402199770, -15.80617190586745480, 53.12390960531436690 ) ) ;
#48846 = CARTESIAN_POINT ( 'NONE',  ( -28.82186960331508985, -9.364793116373393289, 146.0999999999999659 ) ) ;
#48848 = CARTESIAN_POINT ( 'NONE',  ( 8.571926809382603096, -26.38167802310801235, 145.9750000027311785 ) ) ;
#48847 = CARTESIAN_POINT ( 'NONE',  ( -12.06949235617739369, -12.14591786802326823, 99.37609039468568994 ) ) ;
#48849 = CARTESIAN_POINT ( 'NONE',  ( -19.02544592524334988, -5.153800228976617603, 103.9594237280190043 ) ) ;
#48850 = CARTESIAN_POINT ( 'NONE',  ( 14.29746914071049879, -8.314922557960816363, 78.33224293864770971 ) ) ;
#48851 = CARTESIAN_POINT ( 'NONE',  ( -17.50000000000147793, 3.254303733634561269, 35.02395893071405197 ) ) ;
#48852 = CARTESIAN_POINT ( 'NONE',  ( -19.05341960407611168, -5.049401038298163336, 71.45724293864766707 ) ) ;
#48853 = CARTESIAN_POINT ( 'NONE',  ( -13.97604488694527625, -13.89961937509977652, 36.87390960531436690 ) ) ;
#48854 = CARTESIAN_POINT ( 'NONE',  ( -14.34966873604960291, -8.224510206698953496, 61.66557627198103120 ) ) ;
#48855 = CARTESIAN_POINT ( 'NONE',  ( -0.05219959533909027116, -19.03943276465977164, 97.49890960531436690 ) ) ;
#48857 = CARTESIAN_POINT ( 'NONE',  ( -9.474510206698964154, 16.51473224551069663, 60.41557627198102409 ) ) ;
#48856 = CARTESIAN_POINT ( 'NONE',  ( 16.51473224551083163, -9.474510206698727899, 95.83442372801900433 ) ) ;
#48858 = CARTESIAN_POINT ( 'NONE',  ( -14.29746914071037622, -8.314922557961029526, 24.16775706135235424 ) ) ;
#48859 = CARTESIAN_POINT ( 'NONE',  ( -5.153800228976328057, -19.02544592524343514, 92.29057627198099567 ) ) ;
#48860 = CARTESIAN_POINT ( 'NONE',  ( -18.67979575497178146, -10.72451020669898902, 66.66557627198102409 ) ) ;
#48861 = CARTESIAN_POINT ( 'NONE',  ( -4.483927247898782831, 16.52544592524335698, 52.70942372801902565 ) ) ;
#48862 = CARTESIAN_POINT ( 'NONE',  ( -17.26058549869103942, 6.457015423128297016, 93.62254162523932166 ) ) ;
#48863 = CARTESIAN_POINT ( 'NONE',  ( 0.05219959533909260263, 19.03943276465977164, 64.99890960531436690 ) ) ;
#48864 = CARTESIAN_POINT ( 'NONE',  ( -15.72974639402197994, 15.80617190586746368, 65.62390960531436690 ) ) ;
#48865 = CARTESIAN_POINT ( 'NONE',  ( -9.564922557961040184, 16.46253265017147172, 92.91775706135233293 ) ) ;
#48867 = CARTESIAN_POINT ( 'NONE',  ( 18.62759615963255655, 10.81492255796105972, 51.66775706135234714 ) ) ;
#48866 = CARTESIAN_POINT ( 'NONE',  ( -4.483927247898782831, 16.52544592524335698, 112.7094237280190328 ) ) ;
#48868 = CARTESIAN_POINT ( 'NONE',  ( -4.500000000000000888, -139.5000000000000000, 21.32407087589996308 ) ) ;
#48870 = CARTESIAN_POINT ( 'NONE',  ( 19.02544592524343514, -5.153800228976328945, 103.5405762719809957 ) ) ;
#48869 = CARTESIAN_POINT ( 'NONE',  ( -4.379528057220086978, -16.55341960407618274, 69.79275706135234714 ) ) ;
#48871 = CARTESIAN_POINT ( 'NONE',  ( 18.87075004821566537, -5.499999999999866773, 41.17408112101043116 ) ) ;
#48872 = CARTESIAN_POINT ( 'NONE',  ( -16.21995358207307092, -7.366697692864072167, 35.06448998487840640 ) ) ;
#48873 = CARTESIAN_POINT ( 'NONE',  ( 14.34966873604972726, -8.224510206698740333, 90.83442372801901854 ) ) ;
#48874 = CARTESIAN_POINT ( 'NONE',  ( 14.29746914071037800, 8.314922557961029526, 36.66775706135234714 ) ) ;
#48875 = CARTESIAN_POINT ( 'NONE',  ( -9.474510206698964154, 16.51473224551069663, 50.41557627198102409 ) ) ;
#48876 = CARTESIAN_POINT ( 'NONE',  ( -5.153800228976328057, -19.02544592524343514, 47.29057627198102409 ) ) ;
#48877 = CARTESIAN_POINT ( 'NONE',  ( -5.153800228976328057, -19.02544592524343514, 57.29057627198103120 ) ) ;
#48878 = CARTESIAN_POINT ( 'NONE',  ( 15.72974639402176855, 15.80617190586768217, 46.87609039468568994 ) ) ;
#48879 = CARTESIAN_POINT ( 'NONE',  ( -12.14591786802326823, 12.06949235617739902, 58.12609039468568994 ) ) ;
#48880 = CARTESIAN_POINT ( 'NONE',  ( -12.14591786802309592, -12.06949235617757132, 31.87390960531435979 ) ) ;
#48881 = CARTESIAN_POINT ( 'NONE',  ( -16.51473224551069308, -9.474510206698971260, 46.66557627198102409 ) ) ;
#48882 = CARTESIAN_POINT ( 'NONE',  ( -13.89961937509977652, 13.97604488694528158, 40.62390960531435979 ) ) ;
#48883 = CARTESIAN_POINT ( 'NONE',  ( 14.34966873604972726, -8.224510206698740333, 30.83442372801902209 ) ) ;
#48884 = CARTESIAN_POINT ( 'NONE',  ( -0.05219959533936034679, 19.03943276465977164, 87.50109039468567573 ) ) ;
#48885 = CARTESIAN_POINT ( 'NONE',  ( 4.483927247898545687, 16.52544592524342804, 89.79057627198103830 ) ) ;
#48886 = CARTESIAN_POINT ( 'NONE',  ( 0.05219959533909260263, 19.03943276465977164, 49.99890960531435979 ) ) ;
#48888 = DIRECTION ( 'NONE',  ( 1.000000000000000000, 0.000000000000000000, 0.000000000000000000 ) ) ;
#48887 = CARTESIAN_POINT ( 'NONE',  ( 13.89961937509957401, 13.97604488694547697, 91.87609039468567573 ) ) ;
#48889 = CARTESIAN_POINT ( 'NONE',  ( 21.52544592524334988, 5.823673210054432836, 71.45942372801901854 ) ) ;
#48890 = CARTESIAN_POINT ( 'NONE',  ( -0.05219959533934338120, 16.53943276465976808, 57.50109039468568994 ) ) ;
#48891 = DIRECTION ( 'NONE',  ( 0.000000000000000000, 1.000000000000000000, -1.287488025362403787E-15 ) ) ;
#48892 = CARTESIAN_POINT ( 'NONE',  ( -5.823673210054116645, -21.52544592524344225, 47.29057627198103120 ) ) ;
#48893 = CARTESIAN_POINT ( 'NONE',  ( 14.34966873604972726, -8.224510206698740333, 40.83442372801901854 ) ) ;
#48894 = CARTESIAN_POINT ( 'NONE',  ( 16.51473224551069308, 9.474510206698969483, 24.16557627198102765 ) ) ;
#48895 = CARTESIAN_POINT ( 'NONE',  ( 13.89961937509957401, 13.97604488694547697, 26.87609039468566507 ) ) ;
#48896 = CARTESIAN_POINT ( 'NONE',  ( 9.613975513199033429, 9.760750291312396243, -60.44446360152739572 ) ) ;
#48897 = CARTESIAN_POINT ( 'NONE',  ( -9.564922557960796823, -16.46253265017161027, 47.08224293864769550 ) ) ;
#48898 = DIRECTION ( 'NONE',  ( 0.000000000000000000, 0.000000000000000000, -1.000000000000000000 ) ) ;
#48899 = CARTESIAN_POINT ( 'NONE',  ( 16.51473224551069308, 9.474510206698969483, 74.16557627198103830 ) ) ;
#48900 = CARTESIAN_POINT ( 'NONE',  ( 17.50000000000000000, -3.805241302050221819, 112.8735247278258953 ) ) ;
#48901 = CARTESIAN_POINT ( 'NONE',  ( 5.719274019375673035, 21.55341960407619339, 112.2927570613523471 ) ) ;
#48902 = CARTESIAN_POINT ( 'NONE',  ( -12.06949235617756955, 12.14591786802309770, 35.62390960531437401 ) ) ;
#48903 = CARTESIAN_POINT ( 'NONE',  ( 0.05219959533909260263, 19.03943276465977164, 39.99890960531436690 ) ) ;
#48904 = EDGE_CURVE ( 'NONE', #145335, #55466, #127416, .T. ) ;
#48905 = CARTESIAN_POINT ( 'NONE',  ( -13.97604488694527625, -13.89961937509977652, 106.8739096053143669 ) ) ;
#48906 = CARTESIAN_POINT ( 'NONE',  ( -10.72451020669870658, -18.67979575497194134, 74.58442372801901854 ) ) ;
#48907 = CARTESIAN_POINT ( 'NONE',  ( 0.05219959533909260263, 19.03943276465977164, 54.99890960531435979 ) ) ;
#48908 = CARTESIAN_POINT ( 'NONE',  ( -21.55341960407619339, 5.719274019375674811, 68.54275706135234714 ) ) ;
#48909 = CARTESIAN_POINT ( 'NONE',  ( -9.474510206698964154, 16.51473224551069663, 115.4155762719810241 ) ) ;
#48910 = CARTESIAN_POINT ( 'NONE',  ( -19.05341960407611168, -5.049401038298163336, 31.45724293864769550 ) ) ;
#48911 = CARTESIAN_POINT ( 'NONE',  ( -5.823673210054431948, 21.52544592524334988, 22.70942372801901499 ) ) ;
#48912 = CARTESIAN_POINT ( 'NONE',  ( 13.97604488694548053, -13.89961937509957401, 50.62609039468566152 ) ) ;
#48913 = CARTESIAN_POINT ( 'NONE',  ( -5.049401038298153566, 19.05341960407611168, 25.20724293864768484 ) ) ;
#48914 = CARTESIAN_POINT ( 'NONE',  ( 5.153800228976335163, 19.02544592524342804, 74.79057627198103830 ) ) ;
#48915 = CARTESIAN_POINT ( 'NONE',  ( 5.049401038297881783, 19.05341960407617563, 107.2927570613523187 ) ) ;
#48916 = CARTESIAN_POINT ( 'NONE',  ( -4.379528057220328563, 16.55341960407611168, 70.20724293864769550 ) ) ;
#48917 = CARTESIAN_POINT ( 'NONE',  ( -5.719274019375978568, 21.55341960407610458, 35.20724293864768839 ) ) ;
#48918 = CARTESIAN_POINT ( 'NONE',  ( 13.89961937509957401, 13.97604488694547697, 106.8760903946856757 ) ) ;
#48919 = CARTESIAN_POINT ( 'NONE',  ( 18.62759615963271287, -10.81492255796078972, 103.3322429386476955 ) ) ;
#48920 = CARTESIAN_POINT ( 'NONE',  ( -18.62759615963255300, -10.81492255796106328, 54.16775706135235424 ) ) ;
#48921 = CARTESIAN_POINT ( 'NONE',  ( 4.483927247898790824, -16.52544592524335698, 55.20942372801902565 ) ) ;
#48922 = CARTESIAN_POINT ( 'NONE',  ( -4.379528057220086978, -16.55341960407618274, 59.79275706135234714 ) ) ;
#48923 = CARTESIAN_POINT ( 'NONE',  ( -21.55341960407610458, -5.719274019375992779, 71.45724293864769550 ) ) ;
#48924 = CARTESIAN_POINT ( 'NONE',  ( 9.564922557960805705, 16.46253265017160317, 44.58224293864769550 ) ) ;
#48925 = CARTESIAN_POINT ( 'NONE',  ( -4.483927247898782831, 16.52544592524335698, 72.70942372801901854 ) ) ;
#48926 = CARTESIAN_POINT ( 'NONE',  ( 21.53943276465977519, -0.05219959533907433946, 98.74890960531438111 ) ) ;
#48927 = CARTESIAN_POINT ( 'NONE',  ( 4.483927247898545687, 16.52544592524342804, 54.79057627198104541 ) ) ;
#48928 = CARTESIAN_POINT ( 'NONE',  ( 13.89961937509977652, -13.97604488694527269, 73.12390960531436690 ) ) ;
#48929 = CARTESIAN_POINT ( 'NONE',  ( 14.34966873604972726, -8.224510206698740333, 80.83442372801901854 ) ) ;
#48930 = CARTESIAN_POINT ( 'NONE',  ( 16.46253265017146816, 9.564922557961045513, 111.6677570613523329 ) ) ;
#48931 = CARTESIAN_POINT ( 'NONE',  ( -10.81492255796078084, -18.62759615963271287, 107.0822429386476955 ) ) ;
#48932 = CARTESIAN_POINT ( 'NONE',  ( 12.14591786802309770, 12.06949235617756955, 39.37390960531436690 ) ) ;
#48933 = EDGE_CURVE ( 'NONE', #2480, #102413, #98244, .T. ) ;
#48934 = ORIENTED_EDGE ( 'NONE', *, *, #136064, .T. ) ;
#48935 = CARTESIAN_POINT ( 'NONE',  ( -16.19135201231366139, 7.376712067591930655, 74.81319145947973936 ) ) ;
#48936 = CARTESIAN_POINT ( 'NONE',  ( 10.81492255796078972, 18.62759615963270932, 89.58224293864768129 ) ) ;
#48937 = CARTESIAN_POINT ( 'NONE',  ( 14.29746914071049879, -8.314922557960816363, 23.33224293864769194 ) ) ;
#48938 = ORIENTED_EDGE ( 'NONE', *, *, #18014, .F. ) ;
#48939 = DIRECTION ( 'NONE',  ( -1.000000000000000000, -0.000000000000000000, -0.000000000000000000 ) ) ;
#48940 = CARTESIAN_POINT ( 'NONE',  ( 10.81492255796078972, 18.62759615963270932, 99.58224293864770971 ) ) ;
#48941 = CARTESIAN_POINT ( 'NONE',  ( -0.05219959533909027116, -19.03943276465977164, 112.4989096053143669 ) ) ;
#48942 = CARTESIAN_POINT ( 'NONE',  ( -5.719274019375665041, -21.55341960407619695, 29.79275706135234358 ) ) ;
#48943 = CARTESIAN_POINT ( 'NONE',  ( 12.06949235617757843, -12.14591786802309237, 48.12390960531436690 ) ) ;
#48944 = CARTESIAN_POINT ( 'NONE',  ( -0.05219959533934338120, 16.53943276465976808, 47.50109039468568994 ) ) ;
#48945 = CARTESIAN_POINT ( 'NONE',  ( 5.153800228976335163, 19.02544592524342804, 54.79057627198103120 ) ) ;
#48946 = CARTESIAN_POINT ( 'NONE',  ( 19.05341960407617918, -5.049401038297876454, 51.04275706135231871 ) ) ;
#48947 = CARTESIAN_POINT ( 'NONE',  ( 9.474510206698971260, -16.51473224551069308, 82.91557627198103830 ) ) ;
#48948 = CARTESIAN_POINT ( 'NONE',  ( 21.55341960407610458, 5.719274019375980345, 38.95724293864768839 ) ) ;
#48949 = CARTESIAN_POINT ( 'NONE',  ( 5.153800228976335163, 19.02544592524342804, 64.79057627198102409 ) ) ;
#48950 = CARTESIAN_POINT ( 'NONE',  ( -14.34966873604972548, 8.224510206698743886, 28.33442372801902209 ) ) ;
#48951 = CARTESIAN_POINT ( 'NONE',  ( -19.02544592524334988, -5.153800228976617603, 68.95942372801896170 ) ) ;
#48952 = CARTESIAN_POINT ( 'NONE',  ( -5.719274019375978568, 21.55341960407610458, 100.2072429386476955 ) ) ;
#48953 = CARTESIAN_POINT ( 'NONE',  ( -16.52544592524342804, 4.483927247898546575, 36.04057627198102409 ) ) ;
#48954 = CARTESIAN_POINT ( 'NONE',  ( 5.049401038298161559, -19.05341960407611168, 82.70724293864770971 ) ) ;
#48955 = CARTESIAN_POINT ( 'NONE',  ( 18.67979575497178502, 10.72451020669898547, 64.16557627198102409 ) ) ;
#48957 = CARTESIAN_POINT ( 'NONE',  ( -4.483927247898782831, 16.52544592524335698, 22.70942372801901499 ) ) ;
#48956 = CARTESIAN_POINT ( 'NONE',  ( 21.53943276465977519, -0.05219959533907433946, 98.74890960531438111 ) ) ;
#48958 = CARTESIAN_POINT ( 'NONE',  ( 10.81492255796078972, 18.62759615963270932, 29.58224293864769905 ) ) ;
#48959 = CARTESIAN_POINT ( 'NONE',  ( -15.72974639402176322, -15.80617190586768395, 89.37609039468568994 ) ) ;
#48960 = CARTESIAN_POINT ( 'NONE',  ( -13.89961937509977652, 13.97604488694528158, 80.62390960531436690 ) ) ;
#48961 = CARTESIAN_POINT ( 'NONE',  ( 16.46253265017160672, -9.564922557960803928, 23.33224293864769194 ) ) ;
#48962 = CARTESIAN_POINT ( 'NONE',  ( 16.46253265017160672, -9.564922557960803928, 78.33224293864769550 ) ) ;
#48963 = CARTESIAN_POINT ( 'NONE',  ( 4.483927247898545687, 16.52544592524342804, 109.7905762719810383 ) ) ;
#48964 = CARTESIAN_POINT ( 'NONE',  ( 5.153800228976335163, 19.02544592524342804, 64.79057627198100988 ) ) ;
#48965 = CARTESIAN_POINT ( 'NONE',  ( 4.483927247898790824, -16.52544592524335698, 25.20942372801901854 ) ) ;
#48966 = CARTESIAN_POINT ( 'NONE',  ( 17.49999999999998224, 3.512728167237055388, 32.27190004818874769 ) ) ;
#48967 = CARTESIAN_POINT ( 'NONE',  ( 16.51473224551069308, 9.474510206698969483, 74.16557627198103830 ) ) ;
#48969 = CARTESIAN_POINT ( 'NONE',  ( 18.62759615963271287, -10.81492255796078972, 23.33224293864769194 ) ) ;
#48968 = CARTESIAN_POINT ( 'NONE',  ( 15.72974639402176855, 15.80617190586768217, 101.8760903946857042 ) ) ;
#48970 = CARTESIAN_POINT ( 'NONE',  ( 4.379528057220092307, 16.55341960407617563, 97.29275706135234714 ) ) ;
#48971 = CARTESIAN_POINT ( 'NONE',  ( 21.11545612445405240, -20.04257545866360957, -49.42219586766479722 ) ) ;
#48972 = CARTESIAN_POINT ( 'NONE',  ( 19.02544592524334988, 5.153800228976608722, 66.45942372801899012 ) ) ;
#48973 = CARTESIAN_POINT ( 'NONE',  ( -21.55341960407619339, 5.719274019375674811, 113.5427570613523756 ) ) ;
#48974 = CARTESIAN_POINT ( 'NONE',  ( 4.070821633784378335, 4.624734593510421377, -64.52277792523199196 ) ) ;
#48975 = CARTESIAN_POINT ( 'NONE',  ( 9.564922557960805705, 16.46253265017160317, 34.58224293864770260 ) ) ;
#48976 = CARTESIAN_POINT ( 'NONE',  ( 12.14591786802309770, 12.06949235617756955, 34.37390960531435979 ) ) ;
#48977 = DIRECTION ( 'NONE',  ( -0.000000000000000000, -0.000000000000000000, 1.000000000000000000 ) ) ;
#48978 = CARTESIAN_POINT ( 'NONE',  ( -14.29746914071037622, -8.314922557961029526, 109.1677570613523613 ) ) ;
#48979 = CARTESIAN_POINT ( 'NONE',  ( 22.89887992856522558, -20.94821244432957386, -50.23592918571483068 ) ) ;
#48980 = CARTESIAN_POINT ( 'NONE',  ( 4.379528057220092307, 16.55341960407617563, 87.29275706135236135 ) ) ;
#48981 = CARTESIAN_POINT ( 'NONE',  ( -13.89961937509977652, 13.97604488694528158, 35.62390960531435269 ) ) ;
#48982 = CARTESIAN_POINT ( 'NONE',  ( -5.719274019375665041, -21.55341960407619695, 94.79275706135234714 ) ) ;
#48983 = CARTESIAN_POINT ( 'NONE',  ( 16.46253265017146816, 9.564922557961045513, 96.66775706135233293 ) ) ;
#48984 = CARTESIAN_POINT ( 'NONE',  ( 18.67979575497194134, -10.72451020669871369, 80.83442372801901854 ) ) ;
#48985 = CARTESIAN_POINT ( 'NONE',  ( 0.05219959533936267826, -19.03943276465977164, 55.00109039468566863 ) ) ;
#48986 = CARTESIAN_POINT ( 'NONE',  ( 16.51473224551069308, 9.474510206698969483, 79.16557627198103830 ) ) ;
#48987 = CARTESIAN_POINT ( 'NONE',  ( -19.02544592524342804, 5.153800228976336051, 66.04057627198103830 ) ) ;
#48988 = DIRECTION ( 'NONE',  ( 1.000000000000000000, 0.000000000000000000, 0.000000000000000000 ) ) ;
#48989 = CARTESIAN_POINT ( 'NONE',  ( -8.224510206698948167, 14.34966873604960824, 70.41557627198102409 ) ) ;
#48990 = CARTESIAN_POINT ( 'NONE',  ( -5.719274019375978568, 21.55341960407610458, 65.20724293864768129 ) ) ;
#48991 = CARTESIAN_POINT ( 'NONE',  ( 19.03943276465977164, -0.05219959533909143690, 43.74890960531435979 ) ) ;
#48993 = CARTESIAN_POINT ( 'NONE',  ( -16.53943276465976808, -0.05219959533934237506, 73.75109039468567573 ) ) ;
#48992 = CARTESIAN_POINT ( 'NONE',  ( 21.55341960407610458, 5.719274019375980345, 83.95724293864770971 ) ) ;
#48994 = VERTEX_POINT ( 'NONE', #130325 ) ;
#48995 = CARTESIAN_POINT ( 'NONE',  ( -16.51473224551069308, -9.474510206698971260, 51.66557627198102409 ) ) ;
#48997 = CARTESIAN_POINT ( 'NONE',  ( -5.950531402560715689E-15, 38.81732327939063509, -5.124999997268813168 ) ) ;
#48996 = CARTESIAN_POINT ( 'NONE',  ( -8.224510206698948167, 14.34966873604960824, 85.41557627198102409 ) ) ;
#48998 = CARTESIAN_POINT ( 'NONE',  ( -5.049401038298153566, 19.05341960407611168, 45.20724293864769550 ) ) ;
#48999 = CARTESIAN_POINT ( 'NONE',  ( 0.05219959533909260263, 19.03943276465977164, 24.99890960531435269 ) ) ;
#49000 = CARTESIAN_POINT ( 'NONE',  ( 0.05219959533936267826, -19.03943276465977164, 65.00109039468567573 ) ) ;
#49001 = CARTESIAN_POINT ( 'NONE',  ( 4.379528057220339221, -16.55341960407611168, 77.70724293864770971 ) ) ;
#49003 = EDGE_CURVE ( 'NONE', #110784, #143487, #75763, .T. ) ;
#49002 = CARTESIAN_POINT ( 'NONE',  ( -5.823673210054431948, 21.52544592524334988, 42.70942372801901854 ) ) ;
#49005 = CARTESIAN_POINT ( 'NONE',  ( 10.81492255796078972, 18.62759615963270932, 99.58224293864770971 ) ) ;
#49004 = CARTESIAN_POINT ( 'NONE',  ( 5.153800228976335163, 19.02544592524342804, 29.79057627198102409 ) ) ;
#49006 = DIRECTION ( 'NONE',  ( 1.000000000000000000, 0.000000000000000000, 0.000000000000000000 ) ) ;
#49007 = CARTESIAN_POINT ( 'NONE',  ( -0.05219959533910754901, -16.53943276465976808, 82.49890960531436690 ) ) ;
#49008 = CARTESIAN_POINT ( 'NONE',  ( 16.25089620724480000, -36.76456463896338533, -23.32760966624454468 ) ) ;
#49009 = CARTESIAN_POINT ( 'NONE',  ( -9.474510206698964154, 16.51473224551069663, 40.41557627198103120 ) ) ;
#49010 = CARTESIAN_POINT ( 'NONE',  ( 29.86685920354754487, 21.69954338932564752, -1.424999997268813212 ) ) ;
#49011 = CARTESIAN_POINT ( 'NONE',  ( 13.89961937509957401, 13.97604488694547697, 76.87609039468566152 ) ) ;
#49012 = CARTESIAN_POINT ( 'NONE',  ( 21.53943276465977519, 0.05219959533937863772, 31.25109039468568639 ) ) ;
#49013 = CARTESIAN_POINT ( 'NONE',  ( -16.51473224551069308, -9.474510206698971260, 66.66557627198102409 ) ) ;
#49014 = CARTESIAN_POINT ( 'NONE',  ( -16.46253265017146816, -9.564922557961047289, 59.16775706135233293 ) ) ;
#49015 = CARTESIAN_POINT ( 'NONE',  ( 16.46253265017160672, -9.564922557960803928, 43.33224293864769550 ) ) ;
#49016 = CARTESIAN_POINT ( 'NONE',  ( -4.379528057220328563, 16.55341960407611168, 60.20724293864768839 ) ) ;
#49017 = CARTESIAN_POINT ( 'NONE',  ( -4.483927247898539470, -16.52544592524342804, 62.29057627198102409 ) ) ;
#49018 = CARTESIAN_POINT ( 'NONE',  ( -19.02544592524342804, 5.153800228976336051, 71.04057627198099567 ) ) ;
#49019 = CARTESIAN_POINT ( 'NONE',  ( -0.05219959533907301413, -21.53943276465977519, 102.4989096053143811 ) ) ;
#49020 = CARTESIAN_POINT ( 'NONE',  ( 5.153800228976335163, 19.02544592524342804, 74.79057627198103830 ) ) ;
#49021 = CARTESIAN_POINT ( 'NONE',  ( -13.97604488694547697, 13.89961937509957934, 23.12609039468565442 ) ) ;
#49024 = CARTESIAN_POINT ( 'NONE',  ( 16.52544592524342804, -4.483927247898539470, 98.54057627198105251 ) ) ;
#49023 = CARTESIAN_POINT ( 'NONE',  ( -8.314922557960811034, -14.29746914071050412, 22.08224293864769194 ) ) ;
#49022 = CARTESIAN_POINT ( 'NONE',  ( 0.05219959533909260263, 19.03943276465977164, 34.99890960531435979 ) ) ;
#49025 = CARTESIAN_POINT ( 'NONE',  ( -13.89961937509957401, -13.97604488694547875, 104.3760903946856757 ) ) ;
#49026 = ORIENTED_EDGE ( 'NONE', *, *, #181589, .T. ) ;
#49027 = CARTESIAN_POINT ( 'NONE',  ( 5.823673210054444382, -21.52544592524334988, 30.20942372801902565 ) ) ;
#49028 = CARTESIAN_POINT ( 'NONE',  ( -16.51473224551082808, 9.474510206698731452, 58.33442372801900433 ) ) ;
#49029 = CARTESIAN_POINT ( 'NONE',  ( 16.52544592524335698, 4.483927247898782831, 111.4594237280190328 ) ) ;
#49030 = CARTESIAN_POINT ( 'NONE',  ( -15.72974639402197994, 15.80617190586746368, 70.62390960531436690 ) ) ;
#49031 = CARTESIAN_POINT ( 'NONE',  ( 9.474510206698971260, -16.51473224551069308, 107.9155762719810383 ) ) ;
#49032 = CARTESIAN_POINT ( 'NONE',  ( -8.224510206698948167, 14.34966873604960824, 50.41557627198103120 ) ) ;
#49033 = CARTESIAN_POINT ( 'NONE',  ( 9.474510206698971260, -16.51473224551069308, 27.91557627198103120 ) ) ;
#49034 = CARTESIAN_POINT ( 'NONE',  ( -9.474510206698964154, 16.51473224551069663, 30.41557627198102054 ) ) ;
#49035 = CARTESIAN_POINT ( 'NONE',  ( -16.46253265017146816, -9.564922557961047289, 29.16775706135232937 ) ) ;
#49036 = CARTESIAN_POINT ( 'NONE',  ( -14.34966873604972548, 8.224510206698743886, 93.33442372801901854 ) ) ;
#49037 = CARTESIAN_POINT ( 'NONE',  ( -10.81492255796105439, 18.62759615963255655, 42.91775706135235424 ) ) ;
#49038 = CARTESIAN_POINT ( 'NONE',  ( -8.314922557961024197, 14.29746914071037800, 42.91775706135235424 ) ) ;
#49039 = CARTESIAN_POINT ( 'NONE',  ( -10.81492255796078084, -18.62759615963271287, 22.08224293864769194 ) ) ;
#49041 = CARTESIAN_POINT ( 'NONE',  ( -10.72451020669870658, -18.67979575497194134, 94.58442372801901854 ) ) ;
#49040 = CARTESIAN_POINT ( 'NONE',  ( -13.89961937509977652, 13.97604488694528158, 55.62390960531434558 ) ) ;
#49042 = CARTESIAN_POINT ( 'NONE',  ( 16.46253265017160672, -9.564922557960803928, 78.33224293864769550 ) ) ;
#49043 = CARTESIAN_POINT ( 'NONE',  ( 16.52544592524335698, 4.483927247898782831, 66.45942372801903275 ) ) ;
#49044 = CARTESIAN_POINT ( 'NONE',  ( 12.06949235617757843, -12.14591786802309237, 103.1239096053143811 ) ) ;
#49045 = CARTESIAN_POINT ( 'NONE',  ( -12.14591786802309592, -12.06949235617757132, 21.87390960531436690 ) ) ;
#49046 = CARTESIAN_POINT ( 'NONE',  ( 17.50000000000000000, -5.500000000000001776, 106.2176903769643417 ) ) ;
#49049 = CARTESIAN_POINT ( 'NONE',  ( 16.46253265017160672, -9.564922557960803928, 83.33224293864768129 ) ) ;
#49048 = CARTESIAN_POINT ( 'NONE',  ( -9.474510206698964154, 16.51473224551069663, 85.41557627198102409 ) ) ;
#49047 = CARTESIAN_POINT ( 'NONE',  ( 10.81492255796106328, -18.62759615963255655, 75.41775706135233293 ) ) ;
#49050 = CARTESIAN_POINT ( 'NONE',  ( 0.05219959533909260263, 19.03943276465977164, 109.9989096053143669 ) ) ;
#49051 = CARTESIAN_POINT ( 'NONE',  ( 16.53943276465976808, -0.05219959533910856209, 63.74890960531435979 ) ) ;
#49052 = CARTESIAN_POINT ( 'NONE',  ( 16.55341960407618274, -4.379528057220086978, 111.0427570613523613 ) ) ;
#49053 = ORIENTED_EDGE ( 'NONE', *, *, #163318, .T. ) ;
#49054 = CARTESIAN_POINT ( 'NONE',  ( 14.34966873604960469, 8.224510206698951720, 44.16557627198103120 ) ) ;
#49056 = CARTESIAN_POINT ( 'NONE',  ( 17.50000000000000000, 5.499999999999992895, 56.70309617465829888 ) ) ;
#49055 = CARTESIAN_POINT ( 'NONE',  ( -14.34966873604972548, 8.224510206698743886, 38.33442372801900433 ) ) ;
#49057 = CARTESIAN_POINT ( 'NONE',  ( 19.05341960407617918, -5.049401038297876454, 36.04275706135234003 ) ) ;
#49058 = CARTESIAN_POINT ( 'NONE',  ( 9.564922557960805705, 16.46253265017160317, 74.58224293864769550 ) ) ;
#49059 = CARTESIAN_POINT ( 'NONE',  ( 19.05341960407617918, -5.049401038297876454, 56.04275706135234714 ) ) ;
#49060 = CARTESIAN_POINT ( 'NONE',  ( 36.91746824999999887, 11.99521256947799053, -8.024999997268814411 ) ) ;
#49061 = CARTESIAN_POINT ( 'NONE',  ( -30.00000000000000000, -5.204748896376250896E-15, 42.49999999999999289 ) ) ;
#49063 = CARTESIAN_POINT ( 'NONE',  ( -14.29746914071037622, -8.314922557961029526, 79.16775706135234714 ) ) ;
#49062 = CARTESIAN_POINT ( 'NONE',  ( -13.89961937509957401, -13.97604488694547875, 79.37609039468567573 ) ) ;
#49064 = DIRECTION ( 'NONE',  ( 1.000000000000000000, 0.000000000000000000, 0.000000000000000000 ) ) ;
#49065 = CARTESIAN_POINT ( 'NONE',  ( -9.474510206698964154, 16.51473224551069663, 105.4155762719810383 ) ) ;
#49066 = CARTESIAN_POINT ( 'NONE',  ( 5.719274019375673035, 21.55341960407619339, 42.29275706135235424 ) ) ;
#49067 = CARTESIAN_POINT ( 'NONE',  ( -9.474510206698720793, -16.51473224551083518, 94.58442372801900433 ) ) ;
#49069 = CARTESIAN_POINT ( 'NONE',  ( 16.46253265017160672, -9.564922557960803928, 48.33224293864769550 ) ) ;
#49068 = CARTESIAN_POINT ( 'NONE',  ( 17.05587630539785238, 6.762274262135713698, 86.75819690962691766 ) ) ;
#49070 = CARTESIAN_POINT ( 'NONE',  ( 9.564922557960805705, 16.46253265017160317, 104.5822429386476955 ) ) ;
#49072 = CARTESIAN_POINT ( 'NONE',  ( -9.564922557960796823, -16.46253265017161027, 52.08224293864768839 ) ) ;
#49071 = CARTESIAN_POINT ( 'NONE',  ( 0.05219959533910956823, 16.53943276465976808, 59.99890960531436690 ) ) ;
#49073 = CARTESIAN_POINT ( 'NONE',  ( -0.05219959533909027116, -19.03943276465977164, 62.49890960531435979 ) ) ;
#49074 = CARTESIAN_POINT ( 'NONE',  ( -5.049401038297874678, -19.05341960407617918, 59.79275706135231871 ) ) ;
#49075 = CARTESIAN_POINT ( 'NONE',  ( 9.474510206698729675, 16.51473224551082808, 27.08442372801900433 ) ) ;
#49076 = CARTESIAN_POINT ( 'NONE',  ( -19.05341960407611168, -5.049401038298163336, 61.45724293864769550 ) ) ;
#49077 = CARTESIAN_POINT ( 'NONE',  ( 18.62759615963271287, -10.81492255796078972, 78.33224293864770971 ) ) ;
#49079 = CARTESIAN_POINT ( 'NONE',  ( 19.02544592524334988, 5.153800228976608722, 41.45942372801900433 ) ) ;
#49078 = CARTESIAN_POINT ( 'NONE',  ( 8.314922557960818139, 14.29746914071049879, 64.58224293864769550 ) ) ;
#49080 = CARTESIAN_POINT ( 'NONE',  ( 19.02544592524343514, -5.153800228976328945, 113.5405762719810241 ) ) ;
#49081 = CARTESIAN_POINT ( 'NONE',  ( -10.81492255796078084, -18.62759615963271287, 47.08224293864770260 ) ) ;
#49082 = CARTESIAN_POINT ( 'NONE',  ( 21.53943276465977519, -0.05219959533907433946, 28.74890960531435624 ) ) ;
#49083 = CARTESIAN_POINT ( 'NONE',  ( -19.02544592524342804, 5.153800228976336051, 71.04057627198099567 ) ) ;
#49084 = CARTESIAN_POINT ( 'NONE',  ( -19.05341960407611168, -5.049401038298163336, 41.45724293864769550 ) ) ;
#49085 = CARTESIAN_POINT ( 'NONE',  ( -14.29746914071049879, 8.314922557960819915, 105.8322429386476955 ) ) ;
#49086 = CARTESIAN_POINT ( 'NONE',  ( 15.80617190586746368, 15.72974639402197994, 104.3739096053143669 ) ) ;
#49087 = CARTESIAN_POINT ( 'NONE',  ( 0.000000000000000000, -105.0000000000000000, 7.000000000000003553 ) ) ;
#49088 = CARTESIAN_POINT ( 'NONE',  ( 21.52544592524334988, 5.823673210054432836, 21.45942372801901499 ) ) ;
#49089 = CARTESIAN_POINT ( 'NONE',  ( 5.049401038298161559, -19.05341960407611168, 27.70724293864769550 ) ) ;
#49090 = CARTESIAN_POINT ( 'NONE',  ( 10.72451020669898902, -18.67979575497178502, 102.9155762719810383 ) ) ;
#49091 = CARTESIAN_POINT ( 'NONE',  ( 9.564922557961047289, -16.46253265017146816, 45.41775706135232582 ) ) ;
#49092 = CARTESIAN_POINT ( 'NONE',  ( -19.05341960407611168, -5.049401038298163336, 21.45724293864768839 ) ) ;
#49093 = CARTESIAN_POINT ( 'NONE',  ( 0.05219959533909260263, 19.03943276465977164, 29.99890960531435979 ) ) ;
#49094 = DIRECTION ( 'NONE',  ( 0.000000000000000000, 0.000000000000000000, 1.000000000000000000 ) ) ;
#49095 = CARTESIAN_POINT ( 'NONE',  ( 16.55341960407618274, -4.379528057220086978, 51.04275706135234714 ) ) ;
#49096 = CARTESIAN_POINT ( 'NONE',  ( 5.049401038298161559, -19.05341960407611168, 32.70724293864768129 ) ) ;
#49097 = CARTESIAN_POINT ( 'NONE',  ( 34.29482437030766562, -3.353353130260861459, 90.62592007927790405 ) ) ;
#49098 = CARTESIAN_POINT ( 'NONE',  ( -9.474510206698964154, 16.51473224551069663, 75.41557627198103830 ) ) ;
#49099 = CARTESIAN_POINT ( 'NONE',  ( -0.05219959533910754901, -16.53943276465976808, 112.4989096053143669 ) ) ;
#49100 = CARTESIAN_POINT ( 'NONE',  ( -18.62759615963270932, 10.81492255796079327, 50.83224293864770971 ) ) ;
#49101 = CARTESIAN_POINT ( 'NONE',  ( 8.314922557960818139, 14.29746914071049879, 74.58224293864768129 ) ) ;
#49102 = CARTESIAN_POINT ( 'NONE',  ( -12.06949235617739369, -12.14591786802326823, 39.37609039468567573 ) ) ;
#49103 = CARTESIAN_POINT ( 'NONE',  ( 5.823673210054444382, -21.52544592524334988, 80.20942372801901854 ) ) ;
#49104 = CARTESIAN_POINT ( 'NONE',  ( -0.05219959533909027116, -19.03943276465977164, 22.49890960531436690 ) ) ;
#49105 = CARTESIAN_POINT ( 'NONE',  ( -8.224510206698735004, -14.34966873604973081, 109.5844237280190328 ) ) ;
#49106 = CARTESIAN_POINT ( 'NONE',  ( 0.05219959533910956823, 16.53943276465976808, 54.99890960531435269 ) ) ;
#49107 = CARTESIAN_POINT ( 'NONE',  ( 19.02544592524343514, -5.153800228976328945, 48.54057627198103120 ) ) ;
#49108 = CARTESIAN_POINT ( 'NONE',  ( -5.823673210054431948, 21.52544592524334988, 102.7094237280190185 ) ) ;
#49109 = CARTESIAN_POINT ( 'NONE',  ( -10.81492255796078084, -18.62759615963271287, 112.0822429386477097 ) ) ;
#49110 =( BOUNDED_CURVE ( )  B_SPLINE_CURVE ( 2, ( #59359, #121028, #659, #45203, #107838, #198886, #31022, #60354, #106857, #27066, #77512, #139184, #62329 ),
 .UNSPECIFIED., .F., .F. ) 
 B_SPLINE_CURVE_WITH_KNOTS ( ( 3, 2, 2, 2, 2, 2, 3 ),
 ( 0.5550620153744135754, 0.5570175438596490780, 0.5614035087719297934, 0.5657894736842105088, 0.5701754385964912242, 0.5745614035087719396, 0.5764712521719174143 ),
 .UNSPECIFIED. ) 
 CURVE ( )  GEOMETRIC_REPRESENTATION_ITEM ( )  RATIONAL_B_SPLINE_CURVE ( ( 0.9831626618144004848, 0.9848076720550091867, 1.000000000000000000, 0.9659258262890683122, 1.000000000000000000, 0.9659258262890683122, 1.000000000000000000, 0.9659258262890683122, 1.000000000000000000, 0.9659258262890683122, 1.000000000000000000, 0.9851625545550091179, 0.9832469066685282089 ) ) 
 REPRESENTATION_ITEM ( '' )  );
#49111 = CARTESIAN_POINT ( 'NONE',  ( -10.72451020669870658, -18.67979575497194134, 69.58442372801900433 ) ) ;
#49112 = CARTESIAN_POINT ( 'NONE',  ( 16.55341960407618274, -4.379528057220086978, 46.04275706135234714 ) ) ;
#49114 = CARTESIAN_POINT ( 'NONE',  ( -15.72974639402176322, -15.80617190586768395, 84.37609039468570415 ) ) ;
#49113 = CARTESIAN_POINT ( 'NONE',  ( 12.06949235617757843, -12.14591786802309237, 78.12390960531436690 ) ) ;
#49115 = CARTESIAN_POINT ( 'NONE',  ( 0.05219959533910956823, 16.53943276465976808, 24.99890960531435624 ) ) ;
#49116 = CARTESIAN_POINT ( 'NONE',  ( 1.988064558232696151E-15, -30.27659582821216588, 140.7656553485623760 ) ) ;
#49117 = DIRECTION ( 'NONE',  ( 0.000000000000000000, -0.8164965809277251463, 0.5773502691896268413 ) ) ;
#49118 = CARTESIAN_POINT ( 'NONE',  ( 12.14591786802309770, 12.06949235617756955, 39.37390960531436690 ) ) ;
#49119 = CARTESIAN_POINT ( 'NONE',  ( -0.05219959533934338120, 16.53943276465976808, 67.50109039468568994 ) ) ;
#49120 = CARTESIAN_POINT ( 'NONE',  ( -5.153800228976328057, -19.02544592524343514, 92.29057627198099567 ) ) ;
#49121 = CARTESIAN_POINT ( 'NONE',  ( -9.564922557960796823, -16.46253265017161027, 107.0822429386476955 ) ) ;
#49122 = CARTESIAN_POINT ( 'NONE',  ( -21.53943276465977519, -0.05219959533937600094, 103.7510903946857042 ) ) ;
#49123 = CARTESIAN_POINT ( 'NONE',  ( 8.314922557961029526, -14.29746914071037800, 105.4177570613523613 ) ) ;
#49124 = CARTESIAN_POINT ( 'NONE',  ( 8.314922557960818139, 14.29746914071049879, 79.58224293864769550 ) ) ;
#49125 = CARTESIAN_POINT ( 'NONE',  ( 13.97604488694527802, 13.89961937509977652, 79.37390960531435269 ) ) ;
#49126 = ORIENTED_EDGE ( 'NONE', *, *, #121041, .F. ) ;
#49127 = CARTESIAN_POINT ( 'NONE',  ( -16.55341960407617563, 4.379528057220093196, 28.54275706135234358 ) ) ;
#49128 = CARTESIAN_POINT ( 'NONE',  ( 16.46253265017160672, -9.564922557960803928, 28.33224293864769550 ) ) ;
#49129 = CARTESIAN_POINT ( 'NONE',  ( 16.51473224551069308, 9.474510206698969483, 94.16557627198103830 ) ) ;
#49131 = CARTESIAN_POINT ( 'NONE',  ( 29.86685920354754842, -21.69954338932559068, -3.824999997268813345 ) ) ;
#49130 = CARTESIAN_POINT ( 'NONE',  ( 14.34966873604972726, -8.224510206698740333, 30.83442372801902209 ) ) ;
#49132 = CARTESIAN_POINT ( 'NONE',  ( -5.049401038297874678, -19.05341960407617918, 39.79275706135232582 ) ) ;
#49133 = CARTESIAN_POINT ( 'NONE',  ( -0.05219959533934338120, 16.53943276465976808, 97.50109039468567573 ) ) ;
#49134 = CARTESIAN_POINT ( 'NONE',  ( 13.97604488694548053, -13.89961937509957401, 100.6260903946856615 ) ) ;
#49135 = CARTESIAN_POINT ( 'NONE',  ( -19.03943276465977164, 0.05219959533909376836, 36.24890960531436690 ) ) ;
#49136 = CARTESIAN_POINT ( 'NONE',  ( -4.483927247898782831, 16.52544592524335698, 82.70942372801900433 ) ) ;
#49137 = CARTESIAN_POINT ( 'NONE',  ( 16.52544592524335698, 4.483927247898782831, 61.45942372801901854 ) ) ;
#49138 = CARTESIAN_POINT ( 'NONE',  ( 27.86273085795036408, -28.69962071417356242, -4.999999999999999112 ) ) ;
#49139 = CARTESIAN_POINT ( 'NONE',  ( -13.97604488694547697, 13.89961937509957934, 63.12609039468566152 ) ) ;
#49140 = CARTESIAN_POINT ( 'NONE',  ( 18.67979575497194134, -10.72451020669871369, 105.8344237280190328 ) ) ;
#49141 = CARTESIAN_POINT ( 'NONE',  ( 0.05219959533909260263, 19.03943276465977164, 49.99890960531435979 ) ) ;
#49142 = CARTESIAN_POINT ( 'NONE',  ( 5.049401038298161559, -19.05341960407611168, 87.70724293864769550 ) ) ;
#49143 = CARTESIAN_POINT ( 'NONE',  ( 12.14591786802309770, 12.06949235617756955, 79.37390960531436690 ) ) ;
#49144 = CARTESIAN_POINT ( 'NONE',  ( 19.02544592524334988, 5.153800228976608722, 61.45942372801900433 ) ) ;
#49145 = CARTESIAN_POINT ( 'NONE',  ( 18.67979575497178502, 10.72451020669898547, 54.16557627198103120 ) ) ;
#49146 = CARTESIAN_POINT ( 'NONE',  ( 5.823673210054444382, -21.52544592524334988, 105.2094237280190328 ) ) ;
#49147 = CARTESIAN_POINT ( 'NONE',  ( 13.97604488694527802, 13.89961937509977652, 94.37390960531436690 ) ) ;
#49148 = CARTESIAN_POINT ( 'NONE',  ( 19.03943276465977164, 0.05219959533936151252, 21.25109039468565797 ) ) ;
#49149 = CARTESIAN_POINT ( 'NONE',  ( 10.72451020669898902, -18.67979575497178502, 67.91557627198102409 ) ) ;
#49150 = CARTESIAN_POINT ( 'NONE',  ( 16.51473224551069308, 9.474510206698969483, 109.1655762719810383 ) ) ;
#49151 = CARTESIAN_POINT ( 'NONE',  ( 5.049401038297881783, 19.05341960407617563, 87.29275706135234714 ) ) ;
#49152 = CARTESIAN_POINT ( 'NONE',  ( -17.50000000000147438, 3.254303733634575924, 110.0239589307140307 ) ) ;
#49153 = CARTESIAN_POINT ( 'NONE',  ( -5.049401038297874678, -19.05341960407617918, 109.7927570613523187 ) ) ;
#49154 = CARTESIAN_POINT ( 'NONE',  ( -13.89961937509977652, 13.97604488694528158, 25.62390960531434558 ) ) ;
#49155 = CARTESIAN_POINT ( 'NONE',  ( 16.51473224551069308, 9.474510206698969483, 104.1655762719810241 ) ) ;
#49156 = CARTESIAN_POINT ( 'NONE',  ( -5.823673210054116645, -21.52544592524344225, 82.29057627198103830 ) ) ;
#49157 = CARTESIAN_POINT ( 'NONE',  ( -4.483927247898782831, 16.52544592524335698, 47.70942372801902565 ) ) ;
#49158 = CARTESIAN_POINT ( 'NONE',  ( -15.80617190586768217, 15.72974639402176855, 53.12609039468568284 ) ) ;
#49159 = CARTESIAN_POINT ( 'NONE',  ( -5.719274019375665041, -21.55341960407619695, 99.79275706135234714 ) ) ;
#49160 = CARTESIAN_POINT ( 'NONE',  ( -4.379528057220086978, -16.55341960407618274, 99.79275706135234714 ) ) ;
#49161 = CARTESIAN_POINT ( 'NONE',  ( -16.46253265017160317, 9.564922557960807481, 85.83224293864769550 ) ) ;
#49162 = CARTESIAN_POINT ( 'NONE',  ( -12.14591786802309592, -12.06949235617757132, 91.87390960531436690 ) ) ;
#49163 = CARTESIAN_POINT ( 'NONE',  ( -4.483927247898539470, -16.52544592524342804, 32.29057627198102409 ) ) ;
#49164 = CARTESIAN_POINT ( 'NONE',  ( 9.474510206698729675, 16.51473224551082808, 72.08442372801900433 ) ) ;
#49165 = CARTESIAN_POINT ( 'NONE',  ( 21.55341960407619695, -5.719274019375665929, 51.04275706135234714 ) ) ;
#49166 = CARTESIAN_POINT ( 'NONE',  ( -19.03943276465977164, -0.05219959533935918106, 28.75109039468566507 ) ) ;
#49167 = CARTESIAN_POINT ( 'NONE',  ( -4.483927247898539470, -16.52544592524342804, 87.29057627198103830 ) ) ;
#49168 = CARTESIAN_POINT ( 'NONE',  ( 5.719274019375991003, -21.55341960407610458, 22.70724293864769194 ) ) ;
#49169 = CARTESIAN_POINT ( 'NONE',  ( 4.483927247898545687, 16.52544592524342804, 29.79057627198102409 ) ) ;
#49170 = CARTESIAN_POINT ( 'NONE',  ( 5.719274019375673035, 21.55341960407619339, 82.29275706135234714 ) ) ;
#49171 = CARTESIAN_POINT ( 'NONE',  ( -4.379528057220086978, -16.55341960407618274, 54.79275706135235424 ) ) ;
#49172 = CARTESIAN_POINT ( 'NONE',  ( 16.55341960407618274, -4.379528057220086978, 101.0427570613523756 ) ) ;
#49173 = CARTESIAN_POINT ( 'NONE',  ( -18.67979575497193778, 10.72451020669871902, 53.33442372801901854 ) ) ;
#49174 = EDGE_CURVE ( 'NONE', #120001, #149477, #117795, .T. ) ;
#49175 = ORIENTED_EDGE ( 'NONE', *, *, #193069, .T. ) ;
#49176 = CARTESIAN_POINT ( 'NONE',  ( -21.53943276465977519, -0.05219959533937600094, 28.75109039468567929 ) ) ;
#49177 = CARTESIAN_POINT ( 'NONE',  ( 0.05219959533910956823, 16.53943276465976808, 104.9989096053143669 ) ) ;
#49178 = CARTESIAN_POINT ( 'NONE',  ( 20.28951144177218424, -1.856485852971755390, 37.50000000000002842 ) ) ;
#49179 = CARTESIAN_POINT ( 'NONE',  ( 16.52544592524342804, -4.483927247898539470, 63.54057627198103830 ) ) ;
#49180 = CARTESIAN_POINT ( 'NONE',  ( -9.564922557960796823, -16.46253265017161027, 77.08224293864769550 ) ) ;
#49181 = CARTESIAN_POINT ( 'NONE',  ( -4.483927247898782831, 16.52544592524335698, 107.7094237280190328 ) ) ;
#49182 = CARTESIAN_POINT ( 'NONE',  ( 0.05219959533909260263, 19.03943276465977164, 39.99890960531436690 ) ) ;
#49183 = CARTESIAN_POINT ( 'NONE',  ( -18.62759615963270932, 10.81492255796079327, 50.83224293864770971 ) ) ;
#49184 = CARTESIAN_POINT ( 'NONE',  ( -4.379528057220328563, 16.55341960407611168, 90.20724293864770971 ) ) ;
#49185 = CARTESIAN_POINT ( 'NONE',  ( 21.55341960407610458, 5.719274019375980345, 93.95724293864770971 ) ) ;
#49186 = CARTESIAN_POINT ( 'NONE',  ( -16.46253265017160317, 9.564922557960807481, 105.8322429386476955 ) ) ;
#49188 = CARTESIAN_POINT ( 'NONE',  ( 19.05341960407617918, -5.049401038297876454, 96.04275706135231871 ) ) ;
#49187 = CARTESIAN_POINT ( 'NONE',  ( 0.05219959533909260263, 19.03943276465977164, 54.99890960531435979 ) ) ;
#49189 = CARTESIAN_POINT ( 'NONE',  ( -21.55341960407610458, -5.719274019375992779, 41.45724293864769550 ) ) ;
#49190 = CARTESIAN_POINT ( 'NONE',  ( 5.823673210054444382, -21.52544592524334988, 65.20942372801901854 ) ) ;
#49191 = CARTESIAN_POINT ( 'NONE',  ( -0.05219959533909027116, -19.03943276465977164, 57.49890960531435979 ) ) ;
#49192 = CARTESIAN_POINT ( 'NONE',  ( -16.51473224551069308, -9.474510206698971260, 91.66557627198103830 ) ) ;
#49193 = CARTESIAN_POINT ( 'NONE',  ( -8.314922557961024197, 14.29746914071037800, 62.91775706135236135 ) ) ;
#49194 = CARTESIAN_POINT ( 'NONE',  ( -10.81492255796105439, 18.62759615963255655, 42.91775706135235424 ) ) ;
#49195 = CARTESIAN_POINT ( 'NONE',  ( 15.72974639402176855, 15.80617190586768217, 91.87609039468568994 ) ) ;
#49196 = CARTESIAN_POINT ( 'NONE',  ( -15.72974639402197994, 15.80617190586746368, 100.6239096053143811 ) ) ;
#49198 = CARTESIAN_POINT ( 'NONE',  ( 16.55341960407618274, -4.379528057220086978, 61.04275706135234714 ) ) ;
#49197 = CARTESIAN_POINT ( 'NONE',  ( 5.719274019375673035, 21.55341960407619339, 42.29275706135235424 ) ) ;
#49199 = CARTESIAN_POINT ( 'NONE',  ( -15.72974639402197994, 15.80617190586746368, 60.62390960531437401 ) ) ;
#49200 = CARTESIAN_POINT ( 'NONE',  ( -19.03943276465977164, -0.05219959533935918106, 33.75109039468566863 ) ) ;
#49202 = CARTESIAN_POINT ( 'NONE',  ( 16.53943276465976808, 0.05219959533934440121, 111.2510903946856899 ) ) ;
#49201 = CARTESIAN_POINT ( 'NONE',  ( -5.049401038298153566, 19.05341960407611168, 70.20724293864769550 ) ) ;
#49203 = CYLINDRICAL_SURFACE ( 'NONE', #198404, 2.649999999999999467 ) ;
#49204 = CARTESIAN_POINT ( 'NONE',  ( -13.97604488694527625, -13.89961937509977652, 106.8739096053143669 ) ) ;
#49205 = CARTESIAN_POINT ( 'NONE',  ( -3.573655867282028392E-15, 2.428612866367529932E-14, 139.9999999999999716 ) ) ;
#49206 = CARTESIAN_POINT ( 'NONE',  ( -13.89961937509957401, -13.97604488694547875, 84.37609039468567573 ) ) ;
#49207 = CARTESIAN_POINT ( 'NONE',  ( -10.81492255796078084, -18.62759615963271287, 62.08224293864769550 ) ) ;
#49208 = CARTESIAN_POINT ( 'NONE',  ( 14.34966873604960469, 8.224510206698951720, 39.16557627198102409 ) ) ;
#49209 = CARTESIAN_POINT ( 'NONE',  ( -13.97604488694547697, 13.89961937509957934, 113.1260903946856757 ) ) ;
#49210 = CARTESIAN_POINT ( 'NONE',  ( 19.05341960407611168, 5.049401038298154454, 28.95724293864769550 ) ) ;
#49211 = CARTESIAN_POINT ( 'NONE',  ( -9.474510206698720793, -16.51473224551083518, 109.5844237280190043 ) ) ;
#49213 = CARTESIAN_POINT ( 'NONE',  ( 16.51473224551083163, -9.474510206698727899, 75.83442372801900433 ) ) ;
#49212 = CARTESIAN_POINT ( 'NONE',  ( 21.52544592524344225, -5.823673210054117533, 98.54057627198105251 ) ) ;
#49214 = CARTESIAN_POINT ( 'NONE',  ( 4.483927247898790824, -16.52544592524335698, 85.20942372801901854 ) ) ;
#49215 = CARTESIAN_POINT ( 'NONE',  ( -13.97604488694527625, -13.89961937509977652, 66.87390960531436690 ) ) ;
#49216 = CARTESIAN_POINT ( 'NONE',  ( -16.52544592524342804, 4.483927247898546575, 76.04057627198102409 ) ) ;
#49217 = CARTESIAN_POINT ( 'NONE',  ( -16.46253265017160317, 9.564922557960807481, 50.83224293864770260 ) ) ;
#49218 = CARTESIAN_POINT ( 'NONE',  ( 16.55341960407611168, 4.379528057220329451, 53.95724293864770260 ) ) ;
#49219 = CARTESIAN_POINT ( 'NONE',  ( -30.73962218707678318, 22.33364281372846705, -5.947842220587803652 ) ) ;
#49220 = CARTESIAN_POINT ( 'NONE',  ( 1.500000000001822542, 22.62338797783493760, -55.49559142602143424 ) ) ;
#49221 = CARTESIAN_POINT ( 'NONE',  ( 14.34966873604960469, 8.224510206698951720, 24.16557627198103120 ) ) ;
#49222 = CARTESIAN_POINT ( 'NONE',  ( -16.46253265017160317, 9.564922557960807481, 80.83224293864769550 ) ) ;
#49223 = CARTESIAN_POINT ( 'NONE',  ( 21.49604614807110536, -21.49604614807103786, -64.92279855667830191 ) ) ;
#49224 = CARTESIAN_POINT ( 'NONE',  ( -5.153800228976607833, 19.02544592524334988, 37.70942372801899722 ) ) ;
#49225 = CARTESIAN_POINT ( 'NONE',  ( -12.06949235617739369, -12.14591786802326823, 44.37609039468567573 ) ) ;
#49226 = CARTESIAN_POINT ( 'NONE',  ( 15.80617190586746368, 15.72974639402197994, 59.37390960531436690 ) ) ;
#49227 = CARTESIAN_POINT ( 'NONE',  ( -5.153800228976607833, 19.02544592524334988, 27.70942372801899722 ) ) ;
#49228 = CARTESIAN_POINT ( 'NONE',  ( 19.05341960407611168, 5.049401038298154454, 68.95724293864769550 ) ) ;
#49229 = DIRECTION ( 'NONE',  ( -0.000000000000000000, 0.000000000000000000, 1.000000000000000000 ) ) ;
#49230 = CARTESIAN_POINT ( 'NONE',  ( -19.03943276465977164, 0.05219959533909376836, 111.2489096053143669 ) ) ;
#49231 = CARTESIAN_POINT ( 'NONE',  ( -18.62759615963255300, -10.81492255796106328, 34.16775706135234714 ) ) ;
#49232 = CARTESIAN_POINT ( 'NONE',  ( -0.05219959533910754901, -16.53943276465976808, 107.4989096053143669 ) ) ;
#49235 = VERTEX_POINT ( 'NONE', #56515 ) ;
#49234 = CARTESIAN_POINT ( 'NONE',  ( -13.97604488694527625, -13.89961937509977652, 76.87390960531433848 ) ) ;
#49233 = CARTESIAN_POINT ( 'NONE',  ( 0.05219959533907565091, 21.53943276465977519, 94.99890960531436690 ) ) ;
#49236 = CARTESIAN_POINT ( 'NONE',  ( 5.719274019375673035, 21.55341960407619339, 27.29275706135234358 ) ) ;
#49237 = ORIENTED_EDGE ( 'NONE', *, *, #107092, .F. ) ;
#49238 = CARTESIAN_POINT ( 'NONE',  ( -16.51473224551069308, -9.474510206698971260, 86.66557627198102409 ) ) ;
#49239 = CARTESIAN_POINT ( 'NONE',  ( 19.46398650005391318, -5.499999999999942268, 82.68269651486370719 ) ) ;
#49240 = CARTESIAN_POINT ( 'NONE',  ( 5.153800228976335163, 19.02544592524342804, 39.79057627198100988 ) ) ;
#49241 = CARTESIAN_POINT ( 'NONE',  ( 16.51473224551083163, -9.474510206698727899, 105.8344237280190043 ) ) ;
#49242 = CARTESIAN_POINT ( 'NONE',  ( -5.950531402560715689E-15, 38.81732327939063509, -7.624999997268814056 ) ) ;
#49243 = CARTESIAN_POINT ( 'NONE',  ( -0.05219959533909027116, -19.03943276465977164, 22.49890960531436690 ) ) ;
#49244 = CARTESIAN_POINT ( 'NONE',  ( 21.55341960407619695, -5.719274019375665929, 91.04275706135236135 ) ) ;
#49246 = CARTESIAN_POINT ( 'NONE',  ( 15.72974639402176855, 15.80617190586768217, 51.87609039468568284 ) ) ;
#49245 = CARTESIAN_POINT ( 'NONE',  ( 9.474510206698971260, -16.51473224551069308, 77.91557627198103830 ) ) ;
#49247 = CARTESIAN_POINT ( 'NONE',  ( -21.53943276465977519, -0.05219959533937600094, 23.75109039468567929 ) ) ;
#49248 = CARTESIAN_POINT ( 'NONE',  ( 22.44159573604009594, -16.30477369853687364, 140.1750000027311955 ) ) ;
#49249 = CARTESIAN_POINT ( 'NONE',  ( -13.97604488694527625, -13.89961937509977652, 91.87390960531432427 ) ) ;
#49250 = CARTESIAN_POINT ( 'NONE',  ( 12.83293741674485133, 25.03729200590208848, 139.9999999999999716 ) ) ;
#49252 = CARTESIAN_POINT ( 'NONE',  ( -0.05219959533907301413, -21.53943276465977519, 47.49890960531435979 ) ) ;
#49251 = CARTESIAN_POINT ( 'NONE',  ( -14.34966873604972548, 8.224510206698743886, 33.33442372801900433 ) ) ;
#49253 = CARTESIAN_POINT ( 'NONE',  ( 18.62759615963255655, 10.81492255796105972, 81.66775706135236135 ) ) ;
#49254 = CARTESIAN_POINT ( 'NONE',  ( -17.49999999999999645, -5.500000000000000888, 24.20309617465829533 ) ) ;
#49255 = CARTESIAN_POINT ( 'NONE',  ( -19.05341960407617563, 5.049401038297882671, 113.5427570613523471 ) ) ;
#49256 = CARTESIAN_POINT ( 'NONE',  ( 0.05219959533909260263, 19.03943276465977164, 59.99890960531436690 ) ) ;
#49257 = CARTESIAN_POINT ( 'NONE',  ( 13.97604488694527802, 13.89961937509977652, 84.37390960531433848 ) ) ;
#49258 = CARTESIAN_POINT ( 'NONE',  ( -14.34966873604960291, -8.224510206698953496, 111.6655762719810525 ) ) ;
#49259 = CARTESIAN_POINT ( 'NONE',  ( -4.379528057220328563, 16.55341960407611168, 110.2072429386477239 ) ) ;
#49260 = CARTESIAN_POINT ( 'NONE',  ( -0.05219959533909027116, -19.03943276465977164, 107.4989096053143527 ) ) ;
#49261 = CARTESIAN_POINT ( 'NONE',  ( 14.29746914071037800, 8.314922557961029526, 76.66775706135234714 ) ) ;
#49263 = CARTESIAN_POINT ( 'NONE',  ( -16.51473224551069308, -9.474510206698971260, 56.66557627198103120 ) ) ;
#49262 = CARTESIAN_POINT ( 'NONE',  ( -4.379528057220328563, 16.55341960407611168, 55.20724293864770260 ) ) ;
#49264 = CARTESIAN_POINT ( 'NONE',  ( 18.62759615963255655, 10.81492255796105972, 81.66775706135236135 ) ) ;
#49265 = CARTESIAN_POINT ( 'NONE',  ( 5.823673210054444382, -21.52544592524334988, 75.20942372801901854 ) ) ;
#49266 = CARTESIAN_POINT ( 'NONE',  ( 13.97604488694548053, -13.89961937509957401, 90.62609039468567573 ) ) ;
#49267 = CARTESIAN_POINT ( 'NONE',  ( -14.29746914071049879, 8.314922557960819915, 65.83224293864769550 ) ) ;
#49268 = CARTESIAN_POINT ( 'NONE',  ( -21.53943276465977519, 0.05219959533907696930, 116.2489096053143669 ) ) ;
#49269 = CARTESIAN_POINT ( 'NONE',  ( -18.67979575497178146, -10.72451020669898902, 61.66557627198103120 ) ) ;
#49270 = CARTESIAN_POINT ( 'NONE',  ( -5.000000000000000000, -126.3477085785529823, 8.212957410198603370 ) ) ;
#49271 = CARTESIAN_POINT ( 'NONE',  ( -5.359611314223446995E-15, 29.16686587814335496, 148.3750000027311842 ) ) ;
#49272 = CARTESIAN_POINT ( 'NONE',  ( -5.049401038298153566, 19.05341960407611168, 65.20724293864765286 ) ) ;
#49273 = CARTESIAN_POINT ( 'NONE',  ( 8.314922557960818139, 14.29746914071049879, 34.58224293864770260 ) ) ;
#49274 = CARTESIAN_POINT ( 'NONE',  ( 14.34966873604972726, -8.224510206698740333, 110.8344237280190043 ) ) ;
#49275 = CARTESIAN_POINT ( 'NONE',  ( 16.53943276465976808, 0.05219959533934440121, 96.25109039468568994 ) ) ;
#49276 = CARTESIAN_POINT ( 'NONE',  ( -5.049401038297874678, -19.05341960407617918, 49.79275706135231871 ) ) ;
#49277 = DIRECTION ( 'NONE',  ( 0.9930308165857338887, 0.1178549842436489581, 0.000000000000000000 ) ) ;
#49278 = CARTESIAN_POINT ( 'NONE',  ( -16.46253265017160317, 9.564922557960807481, 95.83224293864769550 ) ) ;
#49279 = CARTESIAN_POINT ( 'NONE',  ( 16.53943276465976808, -0.05219959533910856209, 58.74890960531436690 ) ) ;
#49281 = CARTESIAN_POINT ( 'NONE',  ( -5.823673210054116645, -21.52544592524344225, 22.29057627198102765 ) ) ;
#49280 = CARTESIAN_POINT ( 'NONE',  ( 20.73749492396215288, -155.7167183371838064, -4.999999999999999112 ) ) ;
#49283 = VERTEX_POINT ( 'NONE', #71680 ) ;
#49282 = CARTESIAN_POINT ( 'NONE',  ( 10.72451020669898902, -18.67979575497178502, 47.91557627198102409 ) ) ;
#49284 = CARTESIAN_POINT ( 'NONE',  ( -0.05219959533910754901, -16.53943276465976808, 92.49890960531436690 ) ) ;
#49285 = CARTESIAN_POINT ( 'NONE',  ( 16.55341960407618274, -4.379528057220086978, 51.04275706135234714 ) ) ;
#49286 = CARTESIAN_POINT ( 'NONE',  ( 16.52544592524342804, -4.483927247898539470, 83.54057627198102409 ) ) ;
#49287 = CARTESIAN_POINT ( 'NONE',  ( -19.52837319214027900, 5.499999999999901412, 64.60471352585541638 ) ) ;
#49288 = CARTESIAN_POINT ( 'NONE',  ( 19.03943276465977164, 0.05219959533936151252, 76.25109039468566152 ) ) ;
#49289 = CARTESIAN_POINT ( 'NONE',  ( 0.05219959533909260263, 19.03943276465977164, 114.9989096053143669 ) ) ;
#49290 = CARTESIAN_POINT ( 'NONE',  ( -29.86685920354755552, 21.69954338932564397, -5.324999997268814234 ) ) ;
#49291 = CARTESIAN_POINT ( 'NONE',  ( 16.46253265017160672, -9.564922557960803928, 43.33224293864769550 ) ) ;
#49293 = CARTESIAN_POINT ( 'NONE',  ( -16.52544592524342804, 4.483927247898546575, 36.04057627198102409 ) ) ;
#49292 = CARTESIAN_POINT ( 'NONE',  ( -8.224510206698735004, -14.34966873604973081, 39.58442372801901143 ) ) ;
#49294 = CARTESIAN_POINT ( 'NONE',  ( 5.719274019375991003, -21.55341960407610458, 52.70724293864769550 ) ) ;
#49295 = CARTESIAN_POINT ( 'NONE',  ( -19.02544592524334988, -5.153800228976617603, 78.95942372801900433 ) ) ;
#49296 = CARTESIAN_POINT ( 'NONE',  ( -15.80617190586745835, -15.72974639402198527, 46.87390960531435979 ) ) ;
#49297 = CARTESIAN_POINT ( 'NONE',  ( 10.81492255796106328, -18.62759615963255655, 85.41775706135236135 ) ) ;
#49298 = LINE ( 'NONE', #31152, #101611 ) ;
#49299 = CARTESIAN_POINT ( 'NONE',  ( 4.379528057220092307, 16.55341960407617563, 32.29275706135235424 ) ) ;
#49302 = EDGE_CURVE ( 'NONE', #77271, #97477, #27310, .T. ) ;
#49301 = CARTESIAN_POINT ( 'NONE',  ( -16.46253265017160317, 9.564922557960807481, 85.83224293864769550 ) ) ;
#49300 = CARTESIAN_POINT ( 'NONE',  ( -19.02544592524342804, 5.153800228976336051, 36.04057627198100988 ) ) ;
#49303 = CARTESIAN_POINT ( 'NONE',  ( -0.05219959533909027116, -19.03943276465977164, 37.49890960531436690 ) ) ;
#49304 = CARTESIAN_POINT ( 'NONE',  ( 14.34966873604960469, 8.224510206698951720, 99.16557627198100988 ) ) ;
#49305 = CARTESIAN_POINT ( 'NONE',  ( 5.153800228976335163, 19.02544592524342804, 104.7905762719809957 ) ) ;
#49306 = VERTEX_POINT ( 'NONE', #36333 ) ;
#49307 = CARTESIAN_POINT ( 'NONE',  ( -16.53943276465976808, -0.05219959533934237506, 58.75109039468568994 ) ) ;
#49308 = CARTESIAN_POINT ( 'NONE',  ( 15.72974639402199770, -15.80617190586745480, 93.12390960531436690 ) ) ;
#49309 = CARTESIAN_POINT ( 'NONE',  ( 9.564922557960805705, 16.46253265017160317, 39.58224293864768839 ) ) ;
#49310 = CARTESIAN_POINT ( 'NONE',  ( 18.67979575497194134, -10.72451020669871369, 25.83442372801901499 ) ) ;
#49311 = CARTESIAN_POINT ( 'NONE',  ( -9.564922557960796823, -16.46253265017161027, 77.08224293864769550 ) ) ;
#49312 = CARTESIAN_POINT ( 'NONE',  ( 19.02544592524343514, -5.153800228976328945, 108.5405762719810383 ) ) ;
#49313 = VERTEX_POINT ( 'NONE', #117181 ) ;
#49314 = CARTESIAN_POINT ( 'NONE',  ( 0.05219959533934541429, -16.53943276465976808, 30.00109039468568284 ) ) ;
#49315 = CARTESIAN_POINT ( 'NONE',  ( -18.62759615963270932, 10.81492255796079327, 110.8322429386476955 ) ) ;
#49318 = CARTESIAN_POINT ( 'NONE',  ( -19.05341960407617563, 5.049401038297882671, 68.54275706135230450 ) ) ;
#49317 = CARTESIAN_POINT ( 'NONE',  ( 5.153800228976335163, 19.02544592524342804, 99.79057627198102409 ) ) ;
#49316 = CARTESIAN_POINT ( 'NONE',  ( 16.52544592524342804, -4.483927247898539470, 108.5405762719810241 ) ) ;
#49319 = CARTESIAN_POINT ( 'NONE',  ( 0.05219959533936267826, -19.03943276465977164, 25.00109039468566152 ) ) ;
#49320 = CARTESIAN_POINT ( 'NONE',  ( -18.67979575497178146, -10.72451020669898902, 91.66557627198103830 ) ) ;
#49321 = CARTESIAN_POINT ( 'NONE',  ( -13.97604488694547697, 13.89961937509957934, 28.12609039468565797 ) ) ;
#49322 = CARTESIAN_POINT ( 'NONE',  ( 14.34966873604972726, -8.224510206698740333, 80.83442372801901854 ) ) ;
#49323 = CARTESIAN_POINT ( 'NONE',  ( 9.564922557960805705, 16.46253265017160317, 104.5822429386476955 ) ) ;
#49324 = CARTESIAN_POINT ( 'NONE',  ( -19.02544592524342804, 5.153800228976336051, 51.04057627198103120 ) ) ;
#49325 = CARTESIAN_POINT ( 'NONE',  ( 21.52544592524334988, 5.823673210054432836, 56.45942372801902565 ) ) ;
#49326 = CARTESIAN_POINT ( 'NONE',  ( -15.80617190586768217, 15.72974639402176855, 68.12609039468567573 ) ) ;
#49327 = CARTESIAN_POINT ( 'NONE',  ( 0.05219959533909260263, 19.03943276465977164, 69.99890960531435269 ) ) ;
#49328 = CARTESIAN_POINT ( 'NONE',  ( 5.823673210054444382, -21.52544592524334988, 55.20942372801902565 ) ) ;
#49329 = CARTESIAN_POINT ( 'NONE',  ( 13.89961937509957401, 13.97604488694547697, 86.87609039468567573 ) ) ;
#49330 = CARTESIAN_POINT ( 'NONE',  ( 0.05219959533909260263, 19.03943276465977164, 54.99890960531435979 ) ) ;
#49331 = CARTESIAN_POINT ( 'NONE',  ( 4.483927247898790824, -16.52544592524335698, 90.20942372801903275 ) ) ;
#49332 = CARTESIAN_POINT ( 'NONE',  ( -19.02544592524342804, 5.153800228976336051, 71.04057627198099567 ) ) ;
#49333 = CARTESIAN_POINT ( 'NONE',  ( 16.51473224551069308, 9.474510206698969483, 54.16557627198103120 ) ) ;
#49334 = CARTESIAN_POINT ( 'NONE',  ( -10.81492255796078084, -18.62759615963271287, 92.08224293864769550 ) ) ;
#49335 = CARTESIAN_POINT ( 'NONE',  ( -8.224510206698735004, -14.34966873604973081, 74.58442372801901854 ) ) ;
#49336 = CARTESIAN_POINT ( 'NONE',  ( -24.57691432906752382, 7.727872488968269948, 167.2019946024466890 ) ) ;
#49337 = CARTESIAN_POINT ( 'NONE',  ( 9.564922557961047289, -16.46253265017146816, 25.41775706135234003 ) ) ;
#49338 = CARTESIAN_POINT ( 'NONE',  ( 5.153800228976335163, 19.02544592524342804, 69.79057627198103830 ) ) ;
#49339 = CARTESIAN_POINT ( 'NONE',  ( 8.314922557960818139, 14.29746914071049879, 54.58224293864769550 ) ) ;
#49340 = CARTESIAN_POINT ( 'NONE',  ( -12.06949235617756955, 12.14591786802309770, 90.62390960531436690 ) ) ;
#49341 = CARTESIAN_POINT ( 'NONE',  ( -13.89961937509977652, 13.97604488694528158, 95.62390960531436690 ) ) ;
#49342 = CARTESIAN_POINT ( 'NONE',  ( -16.46253265017160317, 9.564922557960807481, 95.83224293864769550 ) ) ;
#49343 = CARTESIAN_POINT ( 'NONE',  ( -15.72974639402176322, -15.80617190586768395, 49.37609039468569705 ) ) ;
#49344 = CARTESIAN_POINT ( 'NONE',  ( -13.97604488694527625, -13.89961937509977652, 106.8739096053143669 ) ) ;
#49345 = CARTESIAN_POINT ( 'NONE',  ( 16.51473224551083163, -9.474510206698727899, 20.83442372801899722 ) ) ;
#49346 = CARTESIAN_POINT ( 'NONE',  ( -16.52544592524335698, -4.483927247898792601, 73.95942372801901854 ) ) ;
#49347 = CARTESIAN_POINT ( 'NONE',  ( 21.53943276465977519, 0.05219959533937863772, 41.25109039468568284 ) ) ;
#49348 = CARTESIAN_POINT ( 'NONE',  ( -18.67979575497178146, -10.72451020669898902, 36.66557627198103120 ) ) ;
#49349 = CARTESIAN_POINT ( 'NONE',  ( -10.81492255796078084, -18.62759615963271287, 97.08224293864770971 ) ) ;
#49350 = CARTESIAN_POINT ( 'NONE',  ( -14.29746914071049879, 8.314922557960819915, 55.83224293864770260 ) ) ;
#49351 = CARTESIAN_POINT ( 'NONE',  ( -19.02544592524342804, 5.153800228976336051, 61.04057627198103120 ) ) ;
#49352 = CARTESIAN_POINT ( 'NONE',  ( -16.53943276465976808, 0.05219959533911058130, 81.24890960531436690 ) ) ;
#49353 = CARTESIAN_POINT ( 'NONE',  ( -0.05219959533907301413, -21.53943276465977519, 37.49890960531436690 ) ) ;
#49354 = CARTESIAN_POINT ( 'NONE',  ( -13.97604488694547697, 13.89961937509957934, 43.12609039468566152 ) ) ;
#49355 = CARTESIAN_POINT ( 'NONE',  ( -16.55341960407611168, -4.379528057220339221, 111.4572429386476813 ) ) ;
#49356 = ORIENTED_EDGE ( 'NONE', *, *, #25125, .F. ) ;
#49357 = CARTESIAN_POINT ( 'NONE',  ( -0.05219959533934338120, 16.53943276465976808, 67.50109039468568994 ) ) ;
#49358 = CARTESIAN_POINT ( 'NONE',  ( -16.46253265017160317, 9.564922557960807481, 65.83224293864769550 ) ) ;
#49359 = CARTESIAN_POINT ( 'NONE',  ( 17.14385361876520264, -23.59649016807270883, 141.5750000027311728 ) ) ;
#49360 = CARTESIAN_POINT ( 'NONE',  ( 16.52544592524342804, -4.483927247898539470, 88.54057627198103830 ) ) ;
#49361 = CARTESIAN_POINT ( 'NONE',  ( -10.72451020669898014, 18.67979575497178502, 40.41557627198103120 ) ) ;
#49362 = CARTESIAN_POINT ( 'NONE',  ( 16.52544592524335698, 4.483927247898782831, 111.4594237280190328 ) ) ;
#49363 = CARTESIAN_POINT ( 'NONE',  ( -19.05341960407617563, 5.049401038297882671, 103.5427570613523329 ) ) ;
#49364 = CARTESIAN_POINT ( 'NONE',  ( 5.719274019375673035, 21.55341960407619339, 82.29275706135234714 ) ) ;
#49365 = CARTESIAN_POINT ( 'NONE',  ( 0.05219959533909260263, 19.03943276465977164, 84.99890960531436690 ) ) ;
#49366 = CARTESIAN_POINT ( 'NONE',  ( -18.62759615963270932, 10.81492255796079327, 110.8322429386476955 ) ) ;
#49367 = CARTESIAN_POINT ( 'NONE',  ( 8.314922557961029526, -14.29746914071037800, 50.41775706135235424 ) ) ;
#49368 = CARTESIAN_POINT ( 'NONE',  ( -19.02544592524342804, 5.153800228976336051, 36.04057627198100988 ) ) ;
#49369 = ADVANCED_FACE ( 'NONE', ( #22178 ), #163701, .F. ) ;
#49370 = EDGE_CURVE ( 'NONE', #50285, #14250, #21176, .T. ) ;
#49371 = CARTESIAN_POINT ( 'NONE',  ( 8.314922557961029526, -14.29746914071037800, 35.41775706135234003 ) ) ;
#49372 = CARTESIAN_POINT ( 'NONE',  ( 16.51473224551083163, -9.474510206698727899, 95.83442372801900433 ) ) ;
#49373 = CARTESIAN_POINT ( 'NONE',  ( 21.53943276465977519, -0.05219959533907433946, 88.74890960531436690 ) ) ;
#49374 = CARTESIAN_POINT ( 'NONE',  ( -9.474510206698720793, -16.51473224551083518, 54.58442372801899722 ) ) ;
#49375 = LINE ( 'NONE', #110048, #63938 ) ;
#49376 = CARTESIAN_POINT ( 'NONE',  ( -10.72451020669898014, 18.67979575497178502, 100.4155762719810241 ) ) ;
#49377 = CARTESIAN_POINT ( 'NONE',  ( 8.906447517083050158, 27.41122689804195645, 141.6500000054623740 ) ) ;
#49378 = CARTESIAN_POINT ( 'NONE',  ( -5.049401038298153566, 19.05341960407611168, 75.20724293864769550 ) ) ;
#49379 = CARTESIAN_POINT ( 'NONE',  ( 4.379528057220092307, 16.55341960407617563, 37.29275706135235424 ) ) ;
#49380 = CARTESIAN_POINT ( 'NONE',  ( -18.22780087662123805, 5.499999999999981348, 96.01763182126897789 ) ) ;
#49381 = CARTESIAN_POINT ( 'NONE',  ( 19.02544592524334988, 5.153800228976608722, 66.45942372801899012 ) ) ;
#49383 = CARTESIAN_POINT ( 'NONE',  ( 16.55341960407611168, 4.379528057220329451, 63.95724293864770260 ) ) ;
#49382 = CARTESIAN_POINT ( 'NONE',  ( -15.72974639402197994, 15.80617190586746368, 115.6239096053143669 ) ) ;
#49384 = CARTESIAN_POINT ( 'NONE',  ( 9.564922557960805705, 16.46253265017160317, 69.58224293864770971 ) ) ;
#49386 = CARTESIAN_POINT ( 'NONE',  ( -0.05219959533936034679, 19.03943276465977164, 47.50109039468566863 ) ) ;
#49385 = CARTESIAN_POINT ( 'NONE',  ( -8.224510206698735004, -14.34966873604973081, 34.58442372801900433 ) ) ;
#49387 = CARTESIAN_POINT ( 'NONE',  ( -21.55341960407619339, 5.719274019375674811, 48.54275706135234714 ) ) ;
#49388 = CARTESIAN_POINT ( 'NONE',  ( -5.153800228976607833, 19.02544592524334988, 102.7094237280189759 ) ) ;
#49389 = CARTESIAN_POINT ( 'NONE',  ( 9.564922557960805705, 16.46253265017160317, 49.58224293864770260 ) ) ;
#49390 = CARTESIAN_POINT ( 'NONE',  ( -13.97604488694547697, 13.89961937509957934, 83.12609039468564731 ) ) ;
#49391 = CARTESIAN_POINT ( 'NONE',  ( 0.05219959533937995610, -21.53943276465977519, 90.00109039468567573 ) ) ;
#49392 = CARTESIAN_POINT ( 'NONE',  ( -13.97604488694547697, 13.89961937509957934, 63.12609039468566152 ) ) ;
#49393 = CARTESIAN_POINT ( 'NONE',  ( 19.02544592524343514, -5.153800228976328945, 38.54057627198103120 ) ) ;
#49394 = CARTESIAN_POINT ( 'NONE',  ( -5.823673210054116645, -21.52544592524344225, 52.29057627198102409 ) ) ;
#49396 = CARTESIAN_POINT ( 'NONE',  ( 16.51473224551083163, -9.474510206698727899, 65.83442372801900433 ) ) ;
#49395 = CARTESIAN_POINT ( 'NONE',  ( -0.05219959533910754901, -16.53943276465976808, 67.49890960531436690 ) ) ;
#49397 = CARTESIAN_POINT ( 'NONE',  ( 20.74379371951214424, 11.24248911466463774, 170.1280252572803420 ) ) ;
#49398 = CARTESIAN_POINT ( 'NONE',  ( 16.46253265017146816, 9.564922557961045513, 31.66775706135232937 ) ) ;
#49399 = CARTESIAN_POINT ( 'NONE',  ( 8.224510206698742110, 14.34966873604972548, 92.08442372801901854 ) ) ;
#49400 = CARTESIAN_POINT ( 'NONE',  ( 14.34966873604960469, 8.224510206698951720, 59.16557627198103120 ) ) ;
#49402 = CARTESIAN_POINT ( 'NONE',  ( 17.14385361876520264, 23.59649016807275856, 142.1750000027311671 ) ) ;
#49401 = CARTESIAN_POINT ( 'NONE',  ( -5.823673210054431948, 21.52544592524334988, 82.70942372801900433 ) ) ;
#49403 = CARTESIAN_POINT ( 'NONE',  ( -15.72974639402197994, 15.80617190586746368, 100.6239096053143811 ) ) ;
#49404 = CARTESIAN_POINT ( 'NONE',  ( 16.46253265017160672, -9.564922557960803928, 48.33224293864769550 ) ) ;
#49405 = CARTESIAN_POINT ( 'NONE',  ( -10.72451020669870658, -18.67979575497194134, 64.58442372801900433 ) ) ;
#49406 = CARTESIAN_POINT ( 'NONE',  ( -13.89961937509977652, 13.97604488694528158, 45.62390960531433848 ) ) ;
#49407 = EDGE_LOOP ( 'NONE', ( #187767, #6471, #4772, #33611 ) ) ;
#49408 = CARTESIAN_POINT ( 'NONE',  ( 5.049401038298161559, -19.05341960407611168, 67.70724293864769550 ) ) ;
#49409 = CARTESIAN_POINT ( 'NONE',  ( -16.53943276465976808, 0.05219959533911058130, 111.2489096053143669 ) ) ;
#49410 = CARTESIAN_POINT ( 'NONE',  ( 18.62759615963271287, -10.81492255796078972, 23.33224293864769194 ) ) ;
#49411 = CARTESIAN_POINT ( 'NONE',  ( 4.483927247898545687, 16.52544592524342804, 54.79057627198104541 ) ) ;
#49412 = CARTESIAN_POINT ( 'NONE',  ( 0.05219959533909260263, 19.03943276465977164, 29.99890960531435979 ) ) ;
#49413 = CARTESIAN_POINT ( 'NONE',  ( 0.05219959533910956823, 16.53943276465976808, 84.99890960531436690 ) ) ;
#49414 = CARTESIAN_POINT ( 'NONE',  ( 10.72451020669898902, -18.67979575497178502, 102.9155762719810383 ) ) ;
#49415 = B_SPLINE_CURVE_WITH_KNOTS ( 'NONE', 3,
 ( #4229, #65908, #98216, #99234, #80088, #52733, #174108, #36561, #127581, #5224, #35578, #82050, #159919, #21408, #156940, #114400, #144740, #176101, #160921, #95257 ),
 .UNSPECIFIED., .F., .F.,
 ( 4, 2, 2, 2, 2, 2, 2, 2, 2, 4 ),
 ( 0.004000878361812020695, 0.004499404418916028853, 0.004997930476020036143, 0.005496456533124044301, 0.005994982590228051592, 0.006244245618780055671, 0.006493508647332038933, 0.006992034704436043621, 0.007490560761540048310, 0.007989086818644052998 ),
 .UNSPECIFIED. ) ;
#49416 = CARTESIAN_POINT ( 'NONE',  ( -10.81492255796105439, 18.62759615963255655, 37.91775706135235424 ) ) ;
#49417 = CARTESIAN_POINT ( 'NONE',  ( 16.46253265017160672, -9.564922557960803928, 23.33224293864769194 ) ) ;
#49418 = CARTESIAN_POINT ( 'NONE',  ( -4.379528057220086978, -16.55341960407618274, 39.79275706135235424 ) ) ;
#49419 = CARTESIAN_POINT ( 'NONE',  ( 15.80617190586746368, 15.72974639402197994, 89.37390960531435269 ) ) ;
#49420 = CARTESIAN_POINT ( 'NONE',  ( -13.89961937509957401, -13.97604488694547875, 19.37609039468566507 ) ) ;
#49421 = CARTESIAN_POINT ( 'NONE',  ( 19.05341960407611168, 5.049401038298154454, 88.95724293864769550 ) ) ;
#49422 = CARTESIAN_POINT ( 'NONE',  ( -10.72451020669870658, -18.67979575497194134, 44.58442372801901854 ) ) ;
#49423 = AXIS2_PLACEMENT_3D ( 'NONE', #110265, #186137, #66747 ) ;
#49424 = CARTESIAN_POINT ( 'NONE',  ( 0.05219959533907565091, 21.53943276465977519, 29.99890960531435979 ) ) ;
#49425 = CARTESIAN_POINT ( 'NONE',  ( 16.53943276465976808, 0.05219959533934440121, 101.2510903946856757 ) ) ;
#49427 = CARTESIAN_POINT ( 'NONE',  ( -21.52544592524334988, -5.823673210054445271, 83.95942372801900433 ) ) ;
#49426 = CARTESIAN_POINT ( 'NONE',  ( 21.53943276465977519, 0.05219959533937863772, 56.25109039468568284 ) ) ;
#49428 = CARTESIAN_POINT ( 'NONE',  ( 5.049401038297881783, 19.05341960407617563, 27.29275706135232937 ) ) ;
#49429 = CARTESIAN_POINT ( 'NONE',  ( 8.224510206698742110, 14.34966873604972548, 87.08442372801901854 ) ) ;
#49430 = CARTESIAN_POINT ( 'NONE',  ( 5.823673210054444382, -21.52544592524334988, 40.20942372801901854 ) ) ;
#49431 = CARTESIAN_POINT ( 'NONE',  ( -19.05341960407611168, -5.049401038298163336, 51.45724293864770260 ) ) ;
#49432 = CARTESIAN_POINT ( 'NONE',  ( 21.53943276465977519, 0.05219959533937863772, 101.2510903946856757 ) ) ;
#49433 = CARTESIAN_POINT ( 'NONE',  ( -19.03943276465977164, 0.05219959533909376836, 106.2489096053143669 ) ) ;
#49434 = CARTESIAN_POINT ( 'NONE',  ( -21.52544592524334988, -5.823673210054445271, 23.95942372801901143 ) ) ;
#49435 = CARTESIAN_POINT ( 'NONE',  ( 15.72974639402199770, -15.80617190586745480, 78.12390960531436690 ) ) ;
#49437 = CARTESIAN_POINT ( 'NONE',  ( -10.72451020669898014, 18.67979575497178502, 65.41557627198102409 ) ) ;
#49436 = PLANE ( 'NONE',  #51489 ) ;
#49439 = CARTESIAN_POINT ( 'NONE',  ( -16.55341960407611168, -4.379528057220339221, 61.45724293864770260 ) ) ;
#49438 = CARTESIAN_POINT ( 'NONE',  ( 16.55341960407618274, -4.379528057220086978, 51.04275706135234714 ) ) ;
#49440 = CARTESIAN_POINT ( 'NONE',  ( -0.05219959533936034679, 19.03943276465977164, 87.50109039468567573 ) ) ;
#49441 = CARTESIAN_POINT ( 'NONE',  ( 6.874011537017776341, -5.374011537017756801, -61.98469907122333922 ) ) ;
#49442 = CARTESIAN_POINT ( 'NONE',  ( 8.224510206698742110, 14.34966873604972548, 32.08442372801901854 ) ) ;
#49443 = CARTESIAN_POINT ( 'NONE',  ( -18.62759615963270932, 10.81492255796079327, 100.8322429386477097 ) ) ;
#49444 = CARTESIAN_POINT ( 'NONE',  ( -21.55341960407610458, -5.719274019375992779, 71.45724293864769550 ) ) ;
#49445 = CARTESIAN_POINT ( 'NONE',  ( 19.02544592524343514, -5.153800228976328945, 108.5405762719810383 ) ) ;
#49446 = CARTESIAN_POINT ( 'NONE',  ( 16.52544592524335698, 4.483927247898782831, 61.45942372801901854 ) ) ;
#49447 = CARTESIAN_POINT ( 'NONE',  ( -5.153800228976328057, -19.02544592524343514, 77.29057627198099567 ) ) ;
#49449 = CARTESIAN_POINT ( 'NONE',  ( -16.46253265017146816, -9.564922557961047289, 109.1677570613523471 ) ) ;
#49448 = CARTESIAN_POINT ( 'NONE',  ( -21.55341960407619339, 5.719274019375674811, 48.54275706135234714 ) ) ;
#49450 = CARTESIAN_POINT ( 'NONE',  ( -0.05219959533909027116, -19.03943276465977164, 102.4989096053143669 ) ) ;
#49451 = ORIENTED_EDGE ( 'NONE', *, *, #171492, .T. ) ;
#49452 = CARTESIAN_POINT ( 'NONE',  ( 16.51473224551069308, 9.474510206698969483, 99.16557627198102409 ) ) ;
#49453 = CARTESIAN_POINT ( 'NONE',  ( 0.05219959533907565091, 21.53943276465977519, 104.9989096053143669 ) ) ;
#49454 = CARTESIAN_POINT ( 'NONE',  ( -13.97604488694527625, -13.89961937509977652, 61.87390960531435979 ) ) ;
#49455 = FACE_OUTER_BOUND ( 'NONE', #173897, .T. ) ;
#49456 = CARTESIAN_POINT ( 'NONE',  ( -16.52544592524342804, 4.483927247898546575, 76.04057627198102409 ) ) ;
#49457 = CARTESIAN_POINT ( 'NONE',  ( -21.55341960407610458, -5.719274019375992779, 21.45724293864769550 ) ) ;
#49458 = CARTESIAN_POINT ( 'NONE',  ( 13.97604488694527802, 13.89961937509977652, 24.37390960531435624 ) ) ;
#49459 = CARTESIAN_POINT ( 'NONE',  ( 18.62759615963271287, -10.81492255796078972, 108.3322429386477097 ) ) ;
#49460 = CARTESIAN_POINT ( 'NONE',  ( -16.46253265017146816, -9.564922557961047289, 59.16775706135233293 ) ) ;
#49461 = CARTESIAN_POINT ( 'NONE',  ( 10.72451020669898902, -18.67979575497178502, 22.91557627198102765 ) ) ;
#49462 = CARTESIAN_POINT ( 'NONE',  ( 19.05341960407611168, 5.049401038298154454, 23.95724293864769194 ) ) ;
#49463 = CARTESIAN_POINT ( 'NONE',  ( -15.80617190586745835, -15.72974639402198527, 56.87390960531436690 ) ) ;
#49464 = CARTESIAN_POINT ( 'NONE',  ( -9.564922557960796823, -16.46253265017161027, 102.0822429386477097 ) ) ;
#49465 = CARTESIAN_POINT ( 'NONE',  ( -5.823673210054431948, 21.52544592524334988, 77.70942372801900433 ) ) ;
#49466 = CARTESIAN_POINT ( 'NONE',  ( -5.049401038298153566, 19.05341960407611168, 45.20724293864769550 ) ) ;
#49467 = CARTESIAN_POINT ( 'NONE',  ( -12.14591786802309592, -12.06949235617757132, 91.87390960531436690 ) ) ;
#49468 = CARTESIAN_POINT ( 'NONE',  ( -12.14591786802326823, 12.06949235617739902, 38.12609039468567573 ) ) ;
#49469 = CARTESIAN_POINT ( 'NONE',  ( 21.55341960407619695, -5.719274019375665929, 61.04275706135234714 ) ) ;
#49470 = ORIENTED_EDGE ( 'NONE', *, *, #193512, .T. ) ;
#49471 = CARTESIAN_POINT ( 'NONE',  ( 16.51473224551083163, -9.474510206698727899, 25.83442372801900078 ) ) ;
#49472 = CARTESIAN_POINT ( 'NONE',  ( 5.049401038297881783, 19.05341960407617563, 82.29275706135229029 ) ) ;
#49473 = CARTESIAN_POINT ( 'NONE',  ( 9.474510206698729675, 16.51473224551082808, 37.08442372801899722 ) ) ;
#49474 = CARTESIAN_POINT ( 'NONE',  ( -18.09918380851993547, -5.499999999999988454, 91.48618307335611632 ) ) ;
#49475 = CARTESIAN_POINT ( 'NONE',  ( -0.05219959533937732626, 21.53943276465977519, 32.50109039468568284 ) ) ;
#49476 = CARTESIAN_POINT ( 'NONE',  ( 30.74264578624799782, 22.33583958711400541, -2.549999994537626602 ) ) ;
#49477 = CARTESIAN_POINT ( 'NONE',  ( 0.05219959533936267826, -19.03943276465977164, 30.00109039468566863 ) ) ;
#49478 = CARTESIAN_POINT ( 'NONE',  ( 0.05219959533909260263, 19.03943276465977164, 54.99890960531435979 ) ) ;
#49479 = CARTESIAN_POINT ( 'NONE',  ( -13.89961937509957401, -13.97604488694547875, 34.37609039468566863 ) ) ;
#49480 = CARTESIAN_POINT ( 'NONE',  ( 12.06949235617739724, 12.14591786802326823, 106.8760903946856899 ) ) ;
#49482 = CARTESIAN_POINT ( 'NONE',  ( 10.72451020669871369, 18.67979575497193778, 92.08442372801901854 ) ) ;
#49481 = CARTESIAN_POINT ( 'NONE',  ( -21.55341960407610458, -5.719274019375992779, 21.45724293864769550 ) ) ;
#49483 = CARTESIAN_POINT ( 'NONE',  ( 22.81625015709510151, -31.40387420917324590, -5.924999997268812990 ) ) ;
#49484 = CARTESIAN_POINT ( 'NONE',  ( -33.85315667487628133, 0.3602237081833374321, 100.5000000000010516 ) ) ;
#49485 = CARTESIAN_POINT ( 'NONE',  ( -18.67979575497193778, 10.72451020669871902, 78.33442372801901854 ) ) ;
#49486 = VECTOR ( 'NONE', #123722, 1000.000000000000114 ) ;
#49487 = CARTESIAN_POINT ( 'NONE',  ( 24.06642195515791371, -0.8101246706333994352, -56.93999021579657693 ) ) ;
#49488 = CARTESIAN_POINT ( 'NONE',  ( -13.97604488694527625, -13.89961937509977652, 101.8739096053143811 ) ) ;
#49489 = ADVANCED_FACE ( 'NONE', ( #38345 ), #6990, .F. ) ;
#49490 = CARTESIAN_POINT ( 'NONE',  ( -1.272595016298593507, -31.21487366219225734, -49.98150452412668443 ) ) ;
#49491 = CARTESIAN_POINT ( 'NONE',  ( -19.05341960407611168, -5.049401038298163336, 46.45724293864768129 ) ) ;
#49492 = CARTESIAN_POINT ( 'NONE',  ( -5.719274019375978568, 21.55341960407610458, 60.20724293864768839 ) ) ;
#49493 = CARTESIAN_POINT ( 'NONE',  ( -16.52544592524342804, 4.483927247898546575, 26.04057627198103475 ) ) ;
#49495 = CARTESIAN_POINT ( 'NONE',  ( -9.474510206698964154, 16.51473224551069663, 100.4155762719810241 ) ) ;
#49494 = CARTESIAN_POINT ( 'NONE',  ( 4.483927247898545687, 16.52544592524342804, 99.79057627198103830 ) ) ;
#49496 = CARTESIAN_POINT ( 'NONE',  ( -13.97604488694547697, 13.89961937509957934, 23.12609039468565442 ) ) ;
#49497 = CARTESIAN_POINT ( 'NONE',  ( -14.34966873604960291, -8.224510206698953496, 106.6655762719810383 ) ) ;
#49498 = CARTESIAN_POINT ( 'NONE',  ( 21.53943276465977519, 0.05219959533937863772, 51.25109039468568994 ) ) ;
#49499 = CARTESIAN_POINT ( 'NONE',  ( -14.29746914071037622, -8.314922557961029526, 104.1677570613523471 ) ) ;
#49500 = CARTESIAN_POINT ( 'NONE',  ( -0.05219959533936034679, 19.03943276465977164, 67.50109039468566152 ) ) ;
#49501 = CARTESIAN_POINT ( 'NONE',  ( 13.89961937509977652, -13.97604488694527269, 113.1239096053143527 ) ) ;
#49502 = CARTESIAN_POINT ( 'NONE',  ( -12.14591786802309592, -12.06949235617757132, 81.87390960531435269 ) ) ;
#49503 = CARTESIAN_POINT ( 'NONE',  ( 19.03943276465977164, 0.05219959533936151252, 61.25109039468566863 ) ) ;
#49504 = CARTESIAN_POINT ( 'NONE',  ( -9.564922557960796823, -16.46253265017161027, 57.08224293864769550 ) ) ;
#49505 = CARTESIAN_POINT ( 'NONE',  ( -4.483927247898539470, -16.52544592524342804, 67.29057627198103830 ) ) ;
#49506 = CARTESIAN_POINT ( 'NONE',  ( 13.89961937509957401, 13.97604488694547697, 96.87609039468566152 ) ) ;
#49507 = CARTESIAN_POINT ( 'NONE',  ( -18.67979575497178146, -10.72451020669898902, 41.66557627198103120 ) ) ;
#49508 = ORIENTED_EDGE ( 'NONE', *, *, #14461, .T. ) ;
#49509 = CARTESIAN_POINT ( 'NONE',  ( -8.314922557960811034, -14.29746914071050412, 97.08224293864770971 ) ) ;
#49510 = CARTESIAN_POINT ( 'NONE',  ( -17.05116617787826172, -6.768360034955703597, 31.34324446740801307 ) ) ;
#49512 = CARTESIAN_POINT ( 'NONE',  ( 21.52544592524344225, -5.823673210054117533, 63.54057627198103830 ) ) ;
#49511 = CARTESIAN_POINT ( 'NONE',  ( 5.049401038298161559, -19.05341960407611168, 62.70724293864769550 ) ) ;
#49513 = CARTESIAN_POINT ( 'NONE',  ( -9.564922557960796823, -16.46253265017161027, 42.08224293864769550 ) ) ;
#49515 = CARTESIAN_POINT ( 'NONE',  ( -13.89961937509977652, 13.97604488694528158, 70.62390960531432427 ) ) ;
#49514 = CARTESIAN_POINT ( 'NONE',  ( -4.483927247898782831, 16.52544592524335698, 92.70942372801901854 ) ) ;
#49516 = CARTESIAN_POINT ( 'NONE',  ( -9.564922557961040184, 16.46253265017147172, 52.91775706135233293 ) ) ;
#49517 = CARTESIAN_POINT ( 'NONE',  ( 15.72974639402176855, 15.80617190586768217, 76.87609039468567573 ) ) ;
#49518 = CARTESIAN_POINT ( 'NONE',  ( -21.53943276465977519, 0.05219959533907696930, 46.24890960531435979 ) ) ;
#49519 = CARTESIAN_POINT ( 'NONE',  ( 5.049401038298161559, -19.05341960407611168, 102.7072429386476955 ) ) ;
#49520 = CARTESIAN_POINT ( 'NONE',  ( -19.02544592524342804, 5.153800228976336051, 26.04057627198103120 ) ) ;
#49521 = CARTESIAN_POINT ( 'NONE',  ( 12.06949235617739724, 12.14591786802326823, 86.87609039468568994 ) ) ;
#49522 = CARTESIAN_POINT ( 'NONE',  ( -9.474510206698720793, -16.51473224551083518, 109.5844237280190043 ) ) ;
#49523 = CARTESIAN_POINT ( 'NONE',  ( -16.51473224551069308, -9.474510206698971260, 26.66557627198103120 ) ) ;
#49524 = FACE_OUTER_BOUND ( 'NONE', #130766, .T. ) ;
#49525 = CARTESIAN_POINT ( 'NONE',  ( -21.53943276465977519, -0.05219959533937600094, 93.75109039468567573 ) ) ;
#49526 = CARTESIAN_POINT ( 'NONE',  ( 14.29746914071049879, -8.314922557960816363, 58.33224293864768839 ) ) ;
#49527 = CARTESIAN_POINT ( 'NONE',  ( 12.06949235617757843, -12.14591786802309237, 73.12390960531436690 ) ) ;
#49528 = CARTESIAN_POINT ( 'NONE',  ( -10.81492255796078084, -18.62759615963271287, 97.08224293864770971 ) ) ;
#49529 = CARTESIAN_POINT ( 'NONE',  ( -0.05219959533907301413, -21.53943276465977519, 87.49890960531436690 ) ) ;
#49530 = CARTESIAN_POINT ( 'NONE',  ( -23.29544513554941076, 16.92513159979227666, 149.7843446568999752 ) ) ;
#49532 = EDGE_CURVE ( 'NONE', #40299, #56239, #179963, .T. ) ;
#49531 = CARTESIAN_POINT ( 'NONE',  ( 10.72451020669898902, -18.67979575497178502, 42.91557627198103120 ) ) ;
#49533 = CARTESIAN_POINT ( 'NONE',  ( -16.55341960407617563, 4.379528057220093196, 68.54275706135234714 ) ) ;
#49534 = CARTESIAN_POINT ( 'NONE',  ( -8.314922557960811034, -14.29746914071050412, 92.08224293864769550 ) ) ;
#49535 = CARTESIAN_POINT ( 'NONE',  ( -5.049401038298153566, 19.05341960407611168, 40.20724293864768839 ) ) ;
#49536 =( NAMED_UNIT ( * ) SI_UNIT ( $, .STERADIAN. ) SOLID_ANGLE_UNIT ( ) );
#49537 = DIRECTION ( 'NONE',  ( 0.000000000000000000, -0.5000000000000013323, -0.8660254037844380415 ) ) ;
#49538 = CARTESIAN_POINT ( 'NONE',  ( 8.224510206698742110, 14.34966873604972548, 92.08442372801901854 ) ) ;
#49539 = CARTESIAN_POINT ( 'NONE',  ( -21.53943276465977519, -0.05219959533937600094, 28.75109039468567929 ) ) ;
#49540 = CARTESIAN_POINT ( 'NONE',  ( 5.153800228976335163, 19.02544592524342804, 89.79057627198102409 ) ) ;
#49541 = CARTESIAN_POINT ( 'NONE',  ( -15.72974639402176322, -15.80617190586768395, 74.37609039468568994 ) ) ;
#49542 = CARTESIAN_POINT ( 'NONE',  ( -3.573655867282028392E-15, 2.428612866367529932E-14, 2.000000000000000000 ) ) ;
#49543 = DIRECTION ( 'NONE',  ( 0.000000000000000000, 0.000000000000000000, 1.000000000000000000 ) ) ;
#49544 = ORIENTED_EDGE ( 'NONE', *, *, #166153, .T. ) ;
#49545 = CARTESIAN_POINT ( 'NONE',  ( 0.05219959533937995610, -21.53943276465977519, 60.00109039468568284 ) ) ;
#49547 = CARTESIAN_POINT ( 'NONE',  ( -9.564922557960796823, -16.46253265017161027, 112.0822429386476955 ) ) ;
#49546 = CARTESIAN_POINT ( 'NONE',  ( -19.02544592524342804, 5.153800228976336051, 41.04057627198103120 ) ) ;
#49548 = CARTESIAN_POINT ( 'NONE',  ( -0.05219959533909027116, -19.03943276465977164, 92.49890960531436690 ) ) ;
#49549 = CARTESIAN_POINT ( 'NONE',  ( 5.153800228976615827, -19.02544592524334988, 65.20942372801900433 ) ) ;
#49550 = CARTESIAN_POINT ( 'NONE',  ( -21.52544592524334988, -5.823673210054445271, 23.95942372801901143 ) ) ;
#49551 = CARTESIAN_POINT ( 'NONE',  ( -19.05341960407617563, 5.049401038297882671, 58.54275706135234003 ) ) ;
#49552 = CARTESIAN_POINT ( 'NONE',  ( -19.02544592524342804, 5.153800228976336051, 41.04057627198103120 ) ) ;
#49553 = CARTESIAN_POINT ( 'NONE',  ( 16.55341960407618274, -4.379528057220086978, 111.0427570613523613 ) ) ;
#49554 = CARTESIAN_POINT ( 'NONE',  ( 19.02544592524334988, 5.153800228976608722, 61.45942372801900433 ) ) ;
#49555 = CARTESIAN_POINT ( 'NONE',  ( 16.55341960407611168, 4.379528057220329451, 23.95724293864769550 ) ) ;
#49556 = CARTESIAN_POINT ( 'NONE',  ( -9.564922557961040184, 16.46253265017147172, 52.91775706135233293 ) ) ;
#49557 = CARTESIAN_POINT ( 'NONE',  ( -16.51473224551069308, -9.474510206698971260, 96.66557627198102409 ) ) ;
#49558 = CARTESIAN_POINT ( 'NONE',  ( -0.05219959533937732626, 21.53943276465977519, 107.5010903946856899 ) ) ;
#49559 = CARTESIAN_POINT ( 'NONE',  ( 15.72974639402176855, 15.80617190586768217, 111.8760903946856615 ) ) ;
#49560 = DIRECTION ( 'NONE',  ( -1.000000000000000000, 0.000000000000000000, 0.000000000000000000 ) ) ;
#49561 = CARTESIAN_POINT ( 'NONE',  ( -5.719274019375665041, -21.55341960407619695, 84.79275706135234714 ) ) ;
#49562 = CARTESIAN_POINT ( 'NONE',  ( -12.14591786802326823, 12.06949235617739902, 28.12609039468568284 ) ) ;
#49563 = CARTESIAN_POINT ( 'NONE',  ( 19.02544592524343514, -5.153800228976328945, 93.54057627198102409 ) ) ;
#49564 = AXIS2_PLACEMENT_3D ( 'NONE', #176177, #129633, #80159 ) ;
#49565 = CARTESIAN_POINT ( 'NONE',  ( -27.32543223595603266, 4.845308524273425732, 167.4404622590849385 ) ) ;
#49566 = B_SPLINE_CURVE_WITH_KNOTS ( 'NONE', 3,
 ( #1288, #14490, #61967, #108480, #139799, #62965 ),
 .UNSPECIFIED., .F., .F.,
 ( 4, 2, 4 ),
 ( 0.007228050697041494589, 0.007608510107494984021, 0.007988969517948474319 ),
 .UNSPECIFIED. ) ;
#49567 = CARTESIAN_POINT ( 'NONE',  ( -0.05219959533909027116, -19.03943276465977164, 72.49890960531435269 ) ) ;
#49568 = CARTESIAN_POINT ( 'NONE',  ( 6.412877669190332419, 3.889087296526017479, 8.181980515339454030 ) ) ;
#49569 = CARTESIAN_POINT ( 'NONE',  ( 13.97604488694548053, -13.89961937509957401, 70.62609039468567573 ) ) ;
#49570 = CARTESIAN_POINT ( 'NONE',  ( -13.89961937509977652, 13.97604488694528158, 105.6239096053143527 ) ) ;
#49571 = CARTESIAN_POINT ( 'NONE',  ( -10.81492255796105439, 18.62759615963255655, 102.9177570613523756 ) ) ;
#49572 = CARTESIAN_POINT ( 'NONE',  ( 12.14591786802309770, 12.06949235617756955, 104.3739096053143669 ) ) ;
#49573 = CARTESIAN_POINT ( 'NONE',  ( -15.80617190586745835, -15.72974639402198527, 41.87390960531435979 ) ) ;
#49574 = CARTESIAN_POINT ( 'NONE',  ( -0.05219959533907301413, -21.53943276465977519, 42.49890960531435979 ) ) ;
#49575 = CARTESIAN_POINT ( 'NONE',  ( -14.34966873604960291, -8.224510206698953496, 101.6655762719810383 ) ) ;
#49576 = CARTESIAN_POINT ( 'NONE',  ( 15.20000000000001883, -5.133579287443888301E-14, -64.92279855667830191 ) ) ;
#49577 = CARTESIAN_POINT ( 'NONE',  ( -16.51473224551082808, 9.474510206698731452, 53.33442372801900433 ) ) ;
#49578 = CARTESIAN_POINT ( 'NONE',  ( 12.14591786802309770, 12.06949235617756955, 29.37390960531435269 ) ) ;
#49579 = CARTESIAN_POINT ( 'NONE',  ( -19.05341960407611168, -5.049401038298163336, 106.4572429386476955 ) ) ;
#49580 = CARTESIAN_POINT ( 'NONE',  ( -18.67979575497193778, 10.72451020669871902, 83.33442372801903275 ) ) ;
#49581 = CARTESIAN_POINT ( 'NONE',  ( -21.55341960407610458, -5.719274019375992779, 76.45724293864769550 ) ) ;
#49582 = CARTESIAN_POINT ( 'NONE',  ( 21.52544592524334988, 5.823673210054432836, 41.45942372801901143 ) ) ;
#49583 = CARTESIAN_POINT ( 'NONE',  ( -21.53943276465977519, 0.05219959533907696930, 91.24890960531436690 ) ) ;
#49584 = CARTESIAN_POINT ( 'NONE',  ( 10.81492255796106328, -18.62759615963255655, 50.41775706135235424 ) ) ;
#49585 = CARTESIAN_POINT ( 'NONE',  ( 5.049401038298161559, -19.05341960407611168, 32.70724293864768129 ) ) ;
#49586 = CARTESIAN_POINT ( 'NONE',  ( 5.049401038298161559, -19.05341960407611168, 82.70724293864770971 ) ) ;
#49587 = CARTESIAN_POINT ( 'NONE',  ( -4.379528057220086978, -16.55341960407618274, 84.79275706135234714 ) ) ;
#49588 = CARTESIAN_POINT ( 'NONE',  ( 8.314922557960818139, 14.29746914071049879, 99.58224293864770971 ) ) ;
#49589 = CARTESIAN_POINT ( 'NONE',  ( 16.46253265017160672, -9.564922557960803928, 103.3322429386476955 ) ) ;
#49590 = CARTESIAN_POINT ( 'NONE',  ( 4.483927247898545687, 16.52544592524342804, 54.79057627198104541 ) ) ;
#49591 = CARTESIAN_POINT ( 'NONE',  ( -14.34966873604972548, 8.224510206698743886, 108.3344237280190185 ) ) ;
#49592 = CARTESIAN_POINT ( 'NONE',  ( -19.03943276465977164, 0.05219959533909376836, 51.24890960531436690 ) ) ;
#49593 = CARTESIAN_POINT ( 'NONE',  ( 19.03943276465977164, -0.05219959533909143690, 33.74890960531435979 ) ) ;
#49594 = CARTESIAN_POINT ( 'NONE',  ( 0.05219959533907565091, 21.53943276465977519, 44.99890960531435979 ) ) ;
#49595 = CARTESIAN_POINT ( 'NONE',  ( 16.51473224551083163, -9.474510206698727899, 25.83442372801900078 ) ) ;
#49597 = CARTESIAN_POINT ( 'NONE',  ( -4.379528057220328563, 16.55341960407611168, 40.20724293864769550 ) ) ;
#49596 = CARTESIAN_POINT ( 'NONE',  ( -3.573655867282028392E-15, 2.428612866367529932E-14, -25.00000000000000000 ) ) ;
#49598 = CARTESIAN_POINT ( 'NONE',  ( 15.72974639402176855, 15.80617190586768217, 41.87609039468568284 ) ) ;
#49599 = CARTESIAN_POINT ( 'NONE',  ( -5.883457575057126299, -36.84471599068518799, -32.38015766500866732 ) ) ;
#49600 = CARTESIAN_POINT ( 'NONE',  ( 16.55341960407618274, -4.379528057220086978, 61.04275706135234714 ) ) ;
#49601 = ADVANCED_FACE ( 'NONE', ( #182852 ), #29175, .T. ) ;
#49602 = CARTESIAN_POINT ( 'NONE',  ( -13.97604488694547697, 13.89961937509957934, 63.12609039468566152 ) ) ;
#49603 = CARTESIAN_POINT ( 'NONE',  ( 12.06949235617757843, -12.14591786802309237, 28.12390960531435979 ) ) ;
#49604 = CARTESIAN_POINT ( 'NONE',  ( -19.52851543214745789, -5.499999999999945821, 75.39357721762580411 ) ) ;
#49605 = CARTESIAN_POINT ( 'NONE',  ( 8.224510206698742110, 14.34966873604972548, 107.0844237280190043 ) ) ;
#49606 = CARTESIAN_POINT ( 'NONE',  ( 9.564922557960805705, 16.46253265017160317, 39.58224293864768839 ) ) ;
#49607 = CARTESIAN_POINT ( 'NONE',  ( 13.97604488694527802, 13.89961937509977652, 64.37390960531436690 ) ) ;
#49608 = CARTESIAN_POINT ( 'NONE',  ( 19.05341960407611168, 5.049401038298154454, 23.95724293864769194 ) ) ;
#49609 = CARTESIAN_POINT ( 'NONE',  ( 21.53943276465977519, 0.05219959533937863772, 31.25109039468568639 ) ) ;
#49610 = CARTESIAN_POINT ( 'NONE',  ( -19.03943276465977164, 0.05219959533909376836, 41.24890960531435269 ) ) ;
#49611 = CARTESIAN_POINT ( 'NONE',  ( 8.673617379884035472E-16, -7.600000000000007638, -64.92279855667830191 ) ) ;
#49612 = CARTESIAN_POINT ( 'NONE',  ( 5.153800228976335163, 19.02544592524342804, 49.79057627198100988 ) ) ;
#49613 = CARTESIAN_POINT ( 'NONE',  ( -18.67979575497178146, -10.72451020669898902, 26.66557627198103475 ) ) ;
#49614 = ADVANCED_FACE ( 'NONE', ( #59485 ), #90811, .F. ) ;
#49616 = CARTESIAN_POINT ( 'NONE',  ( 16.52544592524342804, -4.483927247898539470, 98.54057627198105251 ) ) ;
#49615 = CARTESIAN_POINT ( 'NONE',  ( 21.55341960407619695, -5.719274019375665929, 56.04275706135235424 ) ) ;
#49617 = CARTESIAN_POINT ( 'NONE',  ( -9.474510206698964154, 16.51473224551069663, 115.4155762719810241 ) ) ;
#49618 = VECTOR ( 'NONE', #43786, 1000.000000000000000 ) ;
#49619 = CARTESIAN_POINT ( 'NONE',  ( 12.14591786802327356, -12.06949235617739191, 80.62609039468567573 ) ) ;
#49620 = CARTESIAN_POINT ( 'NONE',  ( 18.62759615963255655, 10.81492255796105972, 91.66775706135234714 ) ) ;
#49621 = CARTESIAN_POINT ( 'NONE',  ( -4.483927247898782831, 16.52544592524335698, 57.70942372801901143 ) ) ;
#49622 = CARTESIAN_POINT ( 'NONE',  ( -19.05341960407611168, -5.049401038298163336, 96.45724293864769550 ) ) ;
#49623 = CARTESIAN_POINT ( 'NONE',  ( -14.34966873604972548, 8.224510206698743886, 38.33442372801900433 ) ) ;
#49624 = CARTESIAN_POINT ( 'NONE',  ( -0.05219959533934338120, 16.53943276465976808, 22.50109039468567573 ) ) ;
#49625 = CARTESIAN_POINT ( 'NONE',  ( -4.483927247898782831, 16.52544592524335698, 102.7094237280190185 ) ) ;
#49626 = CARTESIAN_POINT ( 'NONE',  ( 15.80617190586769283, -15.72974639402175789, 50.62609039468568994 ) ) ;
#49627 = CARTESIAN_POINT ( 'NONE',  ( 9.564922557961047289, -16.46253265017146816, 100.4177570613523329 ) ) ;
#49628 = CARTESIAN_POINT ( 'NONE',  ( -15.72974639402197994, 15.80617190586746368, 115.6239096053143669 ) ) ;
#49630 = CARTESIAN_POINT ( 'NONE',  ( -0.05219959533936034679, 19.03943276465977164, 102.5010903946856757 ) ) ;
#49629 = CARTESIAN_POINT ( 'NONE',  ( 14.34966873604960469, 8.224510206698951720, 109.1655762719810383 ) ) ;
#49631 = CARTESIAN_POINT ( 'NONE',  ( -16.52544592524335698, -4.483927247898792601, 68.95942372801901854 ) ) ;
#49632 = CARTESIAN_POINT ( 'NONE',  ( 21.94381615377240280, 13.26253372808201902, 167.9278110240112767 ) ) ;
#49633 = CARTESIAN_POINT ( 'NONE',  ( 16.51473224551083163, -9.474510206698727899, 70.83442372801900433 ) ) ;
#49634 = CARTESIAN_POINT ( 'NONE',  ( 12.06949235617757843, -12.14591786802309237, 48.12390960531436690 ) ) ;
#49635 = CARTESIAN_POINT ( 'NONE',  ( -4.379528057220328563, 16.55341960407611168, 45.20724293864769550 ) ) ;
#49636 = CARTESIAN_POINT ( 'NONE',  ( 16.52544592524342804, -4.483927247898539470, 93.54057627198103830 ) ) ;
#49638 = PRESENTATION_STYLE_ASSIGNMENT (( #139638 ) ) ;
#49637 = CARTESIAN_POINT ( 'NONE',  ( -16.46253265017146816, -9.564922557961047289, 29.16775706135232937 ) ) ;
#49639 = CARTESIAN_POINT ( 'NONE',  ( -15.80617190586768217, 15.72974639402176855, 43.12609039468568284 ) ) ;
#49640 = CARTESIAN_POINT ( 'NONE',  ( -16.46253265017146816, -9.564922557961047289, 99.16775706135233293 ) ) ;
#49641 = DIRECTION ( 'NONE',  ( 0.000000000000000000, 0.000000000000000000, 1.000000000000000000 ) ) ;
#49642 = CARTESIAN_POINT ( 'NONE',  ( -19.03943276465977164, 0.05219959533909376836, 86.24890960531436690 ) ) ;
#49643 = CARTESIAN_POINT ( 'NONE',  ( -5.153800228976328057, -19.02544592524343514, 92.29057627198099567 ) ) ;
#49644 = CARTESIAN_POINT ( 'NONE',  ( 21.52544592524344225, -5.823673210054117533, 58.54057627198103120 ) ) ;
#49645 = CARTESIAN_POINT ( 'NONE',  ( -12.06949235617756955, 12.14591786802309770, 90.62390960531436690 ) ) ;
#49646 = CARTESIAN_POINT ( 'NONE',  ( 9.564922557960805705, 16.46253265017160317, 74.58224293864769550 ) ) ;
#49647 = CARTESIAN_POINT ( 'NONE',  ( 13.89961937509977652, -13.97604488694527269, 23.12390960531436335 ) ) ;
#49648 = CARTESIAN_POINT ( 'NONE',  ( -18.62759615963255300, -10.81492255796106328, 39.16775706135235424 ) ) ;
#49649 = CARTESIAN_POINT ( 'NONE',  ( -21.52544592524334988, -5.823673210054445271, 73.95942372801901854 ) ) ;
#49650 = CARTESIAN_POINT ( 'NONE',  ( 8.224510206698742110, 14.34966873604972548, 97.08442372801904696 ) ) ;
#49651 = CARTESIAN_POINT ( 'NONE',  ( -21.55341960407619339, 5.719274019375674811, 33.54275706135234714 ) ) ;
#49652 = CARTESIAN_POINT ( 'NONE',  ( 5.719274019375673035, 21.55341960407619339, 27.29275706135234358 ) ) ;
#49654 = CARTESIAN_POINT ( 'NONE',  ( 5.153800228976335163, 19.02544592524342804, 74.79057627198103830 ) ) ;
#49653 = CARTESIAN_POINT ( 'NONE',  ( 16.51473224551083163, -9.474510206698727899, 55.83442372801899722 ) ) ;
#49655 = CARTESIAN_POINT ( 'NONE',  ( -10.72451020669870658, -18.67979575497194134, 79.58442372801903275 ) ) ;
#49656 = CARTESIAN_POINT ( 'NONE',  ( 18.62759615963271287, -10.81492255796078972, 78.33224293864770971 ) ) ;
#49657 = CARTESIAN_POINT ( 'NONE',  ( -8.314922557960811034, -14.29746914071050412, 57.08224293864769550 ) ) ;
#49659 = CARTESIAN_POINT ( 'NONE',  ( 9.474510206698729675, 16.51473224551082808, 32.08442372801900433 ) ) ;
#49658 = CARTESIAN_POINT ( 'NONE',  ( -18.62759615963255300, -10.81492255796106328, 109.1677570613523613 ) ) ;
#49660 = CARTESIAN_POINT ( 'NONE',  ( -4.483927247898539470, -16.52544592524342804, 77.29057627198102409 ) ) ;
#49661 = CARTESIAN_POINT ( 'NONE',  ( -5.153800228976328057, -19.02544592524343514, 27.29057627198103120 ) ) ;
#49662 = CARTESIAN_POINT ( 'NONE',  ( -9.564922557961040184, 16.46253265017147172, 67.91775706135233293 ) ) ;
#49663 = CARTESIAN_POINT ( 'NONE',  ( -12.06949235617756955, 12.14591786802309770, 35.62390960531437401 ) ) ;
#49664 = CARTESIAN_POINT ( 'NONE',  ( 21.55341960407619695, -5.719274019375665929, 76.04275706135237556 ) ) ;
#49665 = CARTESIAN_POINT ( 'NONE',  ( -5.049401038298153566, 19.05341960407611168, 75.20724293864769550 ) ) ;
#49666 = CARTESIAN_POINT ( 'NONE',  ( 9.474510206698729675, 16.51473224551082808, 47.08442372801900433 ) ) ;
#49667 = CARTESIAN_POINT ( 'NONE',  ( -18.67979575497178146, -10.72451020669898902, 61.66557627198103120 ) ) ;
#49668 = CARTESIAN_POINT ( 'NONE',  ( -18.67979575497178146, -10.72451020669898902, 111.6655762719810525 ) ) ;
#49669 = CARTESIAN_POINT ( 'NONE',  ( -5.153800228976607833, 19.02544592524334988, 107.7094237280189759 ) ) ;
#49670 = CARTESIAN_POINT ( 'NONE',  ( -16.53943276465976808, -0.05219959533934237506, 73.75109039468567573 ) ) ;
#49672 = CARTESIAN_POINT ( 'NONE',  ( 21.55341960407610458, 5.719274019375980345, 108.9572429386476955 ) ) ;
#49671 = DIRECTION ( 'NONE',  ( -1.000000000000000000, 0.000000000000000000, 0.000000000000000000 ) ) ;
#49673 = CARTESIAN_POINT ( 'NONE',  ( 8.314922557960818139, 14.29746914071049879, 104.5822429386477097 ) ) ;
#49674 = CARTESIAN_POINT ( 'NONE',  ( 22.81625015709510151, -31.40387420917324590, -10.42499999726881477 ) ) ;
#49675 = CARTESIAN_POINT ( 'NONE',  ( -16.52544592524335698, -4.483927247898792601, 38.95942372801901854 ) ) ;
#49676 = CARTESIAN_POINT ( 'NONE',  ( -10.72451020669898014, 18.67979575497178502, 60.41557627198102409 ) ) ;
#49677 = CARTESIAN_POINT ( 'NONE',  ( -16.53943276465976808, -0.05219959533934237506, 103.7510903946857042 ) ) ;
#49678 = CARTESIAN_POINT ( 'NONE',  ( 16.46253265017160672, -9.564922557960803928, 38.33224293864768839 ) ) ;
#49679 = CARTESIAN_POINT ( 'NONE',  ( 4.379528057220092307, 16.55341960407617563, 67.29275706135234714 ) ) ;
#49680 = CARTESIAN_POINT ( 'NONE',  ( 16.51473224551083163, -9.474510206698727899, 60.83442372801900433 ) ) ;
#49681 = CARTESIAN_POINT ( 'NONE',  ( 21.55341960407619695, -5.719274019375665929, 46.04275706135234714 ) ) ;
#49682 = CARTESIAN_POINT ( 'NONE',  ( 15.80617190586746368, 15.72974639402197994, 59.37390960531436690 ) ) ;
#49683 = CARTESIAN_POINT ( 'NONE',  ( 16.55341960407618274, -4.379528057220086978, 96.04275706135236135 ) ) ;
#49684 = CARTESIAN_POINT ( 'NONE',  ( -15.72974639402176322, -15.80617190586768395, 89.37609039468568994 ) ) ;
#49685 = CARTESIAN_POINT ( 'NONE',  ( -10.81492255796078084, -18.62759615963271287, 47.08224293864770260 ) ) ;
#49686 = CARTESIAN_POINT ( 'NONE',  ( -21.53943276465977519, 0.05219959533907696930, 31.24890960531435979 ) ) ;
#49687 = ORIENTED_EDGE ( 'NONE', *, *, #78467, .T. ) ;
#49688 = VERTEX_POINT ( 'NONE', #13982 ) ;
#49689 = CARTESIAN_POINT ( 'NONE',  ( 4.483927247898790824, -16.52544592524335698, 75.20942372801901854 ) ) ;
#49690 = CARTESIAN_POINT ( 'NONE',  ( -21.55341960407610458, -5.719274019375992779, 46.45724293864769550 ) ) ;
#49691 = EDGE_LOOP ( 'NONE', ( #104651, #47711, #14714, #37751, #160204, #100824, #32649, #121405 ) ) ;
#49692 = CARTESIAN_POINT ( 'NONE',  ( 19.03943276465977164, -0.05219959533909143690, 93.74890960531435269 ) ) ;
#49693 = CARTESIAN_POINT ( 'NONE',  ( 0.000000000000000000, 0.000000000000000000, -64.92279855667830191 ) ) ;
#49694 = CARTESIAN_POINT ( 'NONE',  ( 5.153800228976335163, 19.02544592524342804, 29.79057627198102409 ) ) ;
#49695 = CARTESIAN_POINT ( 'NONE',  ( 15.72974639402199770, -15.80617190586745480, 58.12390960531435979 ) ) ;
#49696 = CARTESIAN_POINT ( 'NONE',  ( -16.52544592524335698, -4.483927247898792601, 88.95942372801901854 ) ) ;
#49697 = CARTESIAN_POINT ( 'NONE',  ( -18.62759615963255300, -10.81492255796106328, 44.16775706135234714 ) ) ;
#49698 = CARTESIAN_POINT ( 'NONE',  ( 19.03943276465977164, 0.05219959533936151252, 106.2510903946856615 ) ) ;
#49699 = CARTESIAN_POINT ( 'NONE',  ( 16.53943276465976808, -0.05219959533910856209, 108.7489096053143669 ) ) ;
#49700 = CARTESIAN_POINT ( 'NONE',  ( -19.03943276465977164, -0.05219959533935918106, 108.7510903946856615 ) ) ;
#49701 = CARTESIAN_POINT ( 'NONE',  ( -5.153800228976328057, -19.02544592524343514, 37.29057627198102409 ) ) ;
#49702 = CARTESIAN_POINT ( 'NONE',  ( 17.50000000000002132, -5.499999999999878320, 63.29690382534172954 ) ) ;
#49703 = CARTESIAN_POINT ( 'NONE',  ( 19.02544592524343514, -5.153800228976328945, 93.54057627198102409 ) ) ;
#49704 = CARTESIAN_POINT ( 'NONE',  ( 16.55341960407618274, -4.379528057220086978, 81.04275706135236135 ) ) ;
#49705 = CARTESIAN_POINT ( 'NONE',  ( 5.823673210054444382, -21.52544592524334988, 110.2094237280190185 ) ) ;
#49706 = CARTESIAN_POINT ( 'NONE',  ( 10.81492255796078972, 18.62759615963270932, 59.58224293864770260 ) ) ;
#49707 = EDGE_CURVE ( 'NONE', #146141, #66087, #71433, .T. ) ;
#49708 = CARTESIAN_POINT ( 'NONE',  ( 16.55341960407618274, -4.379528057220086978, 91.04275706135236135 ) ) ;
#49709 = AXIS2_PLACEMENT_3D ( 'NONE', #158220, #126870, #144038 ) ;
#49710 = CARTESIAN_POINT ( 'NONE',  ( 19.02544592524334988, 5.153800228976608722, 76.45942372801897591 ) ) ;
#49711 = CARTESIAN_POINT ( 'NONE',  ( 16.51473224551069308, 9.474510206698969483, 34.16557627198102409 ) ) ;
#49712 = CARTESIAN_POINT ( 'NONE',  ( 5.153800228976335163, 19.02544592524342804, 74.79057627198103830 ) ) ;
#49713 = CARTESIAN_POINT ( 'NONE',  ( -13.89961937509977652, 13.97604488694528158, 30.62390960531435269 ) ) ;
#49714 = CARTESIAN_POINT ( 'NONE',  ( -9.564922557961040184, 16.46253265017147172, 77.91775706135234714 ) ) ;
#49715 = CARTESIAN_POINT ( 'NONE',  ( 25.85392304583073297, -7.514126903509208866, 173.7688241862487644 ) ) ;
#49716 = CARTESIAN_POINT ( 'NONE',  ( 19.02544592524343514, -5.153800228976328945, 108.5405762719810383 ) ) ;
#49717 = CARTESIAN_POINT ( 'NONE',  ( -16.53943276465976808, 0.05219959533911058130, 61.24890960531435979 ) ) ;
#49718 = CARTESIAN_POINT ( 'NONE',  ( -5.823673210054116645, -21.52544592524344225, 67.29057627198103830 ) ) ;
#49719 = DIRECTION ( 'NONE',  ( -1.000000000000000000, -0.000000000000000000, -0.000000000000000000 ) ) ;
#49720 = CARTESIAN_POINT ( 'NONE',  ( 19.05341960407617918, -5.049401038297876454, 31.04275706135232227 ) ) ;
#49721 = CARTESIAN_POINT ( 'NONE',  ( 20.51334883519569985, -11.49142661404781229, 170.0774692710818101 ) ) ;
#49723 = CARTESIAN_POINT ( 'NONE',  ( 5.153800228976335163, 19.02544592524342804, 79.79057627198102409 ) ) ;
#49722 = CARTESIAN_POINT ( 'NONE',  ( 16.51473224551069308, 9.474510206698969483, 59.16557627198102409 ) ) ;
#49724 = CARTESIAN_POINT ( 'NONE',  ( 16.55341960407618274, -4.379528057220086978, 51.04275706135234714 ) ) ;
#49725 = CARTESIAN_POINT ( 'NONE',  ( -19.19724070472095079, -5.500000000000031086, 101.0619334827438109 ) ) ;
#49726 = CARTESIAN_POINT ( 'NONE',  ( -16.18388926212237422, 7.379444403734519931, 109.5604684863385074 ) ) ;
#49727 = CARTESIAN_POINT ( 'NONE',  ( 16.52544592524335698, 4.483927247898782831, 76.45942372801901854 ) ) ;
#49728 = CARTESIAN_POINT ( 'NONE',  ( 22.82566123211450915, -22.19887561992280567, -45.74155842934298022 ) ) ;
#49729 = CARTESIAN_POINT ( 'NONE',  ( 4.483927247898790824, -16.52544592524335698, 60.20942372801902565 ) ) ;
#49730 = CARTESIAN_POINT ( 'NONE',  ( 14.29746914071037800, 8.314922557961029526, 46.66775706135234714 ) ) ;
#49732 = FACE_BOUND ( 'NONE', #136721, .T. ) ;
#49731 = CARTESIAN_POINT ( 'NONE',  ( -13.89961937509977652, 13.97604488694528158, 55.62390960531434558 ) ) ;
#49733 = CARTESIAN_POINT ( 'NONE',  ( 18.67979575497194134, -10.72451020669871369, 50.83442372801901143 ) ) ;
#49734 = CARTESIAN_POINT ( 'NONE',  ( 0.05219959533936267826, -19.03943276465977164, 65.00109039468567573 ) ) ;
#49735 = CARTESIAN_POINT ( 'NONE',  ( 10.81492255796106328, -18.62759615963255655, 105.4177570613523613 ) ) ;
#49736 = CARTESIAN_POINT ( 'NONE',  ( 19.05341960407611168, 5.049401038298154454, 33.95724293864769550 ) ) ;
#49737 = CARTESIAN_POINT ( 'NONE',  ( 16.73912658984721702, 7.076536648759412351, 23.72892465253222127 ) ) ;
#49738 = CARTESIAN_POINT ( 'NONE',  ( -5.719274019375978568, 21.55341960407610458, 55.20724293864770260 ) ) ;
#49739 = CARTESIAN_POINT ( 'NONE',  ( -5.153800228976328057, -19.02544592524343514, 102.2905762719810383 ) ) ;
#49740 = CARTESIAN_POINT ( 'NONE',  ( 4.483927247898545687, 16.52544592524342804, 99.79057627198103830 ) ) ;
#49741 = CARTESIAN_POINT ( 'NONE',  ( 12.06949235617739724, 12.14591786802326823, 36.87609039468568994 ) ) ;
#49742 = CARTESIAN_POINT ( 'NONE',  ( -14.29746914071049879, 8.314922557960819915, 35.83224293864768839 ) ) ;
#49743 = ORIENTED_EDGE ( 'NONE', *, *, #148158, .T. ) ;
#49744 = CARTESIAN_POINT ( 'NONE',  ( 18.62759615963271287, -10.81492255796078972, 103.3322429386476955 ) ) ;
#49746 = CARTESIAN_POINT ( 'NONE',  ( 5.000000000000000888, -140.0000000000000000, -13.00000000000000000 ) ) ;
#49745 = CARTESIAN_POINT ( 'NONE',  ( -14.34966873604960291, -8.224510206698953496, 36.66557627198103120 ) ) ;
#49747 = CARTESIAN_POINT ( 'NONE',  ( -13.89961937509957401, -13.97604488694547875, 89.37609039468563310 ) ) ;
#49748 = CARTESIAN_POINT ( 'NONE',  ( 19.02544592524334988, 5.153800228976608722, 31.45942372801900433 ) ) ;
#49749 = CARTESIAN_POINT ( 'NONE',  ( -16.52544592524342804, 4.483927247898546575, 26.04057627198103475 ) ) ;
#49750 = CARTESIAN_POINT ( 'NONE',  ( -18.67979575497178146, -10.72451020669898902, 106.6655762719810383 ) ) ;
#49751 = CARTESIAN_POINT ( 'NONE',  ( 5.719274019375991003, -21.55341960407610458, 47.70724293864770260 ) ) ;
#49752 = AXIS2_PLACEMENT_3D ( 'NONE', #117386, #7196, #130540 ) ;
#49753 = CARTESIAN_POINT ( 'NONE',  ( -0.05219959533909027116, -19.03943276465977164, 82.49890960531436690 ) ) ;
#49754 = CARTESIAN_POINT ( 'NONE',  ( 16.53943276465976808, -0.05219959533910856209, 33.74890960531436690 ) ) ;
#49755 = CARTESIAN_POINT ( 'NONE',  ( 0.05219959533909260263, 19.03943276465977164, 94.99890960531436690 ) ) ;
#49756 = VERTEX_POINT ( 'NONE', #167678 ) ;
#49757 = CARTESIAN_POINT ( 'NONE',  ( 17.59860650958989936, 7.585241751807028088, 79.07662985737508166 ) ) ;
#49758 = CARTESIAN_POINT ( 'NONE',  ( -0.05219959533936034679, 19.03943276465977164, 47.50109039468566863 ) ) ;
#49759 = CARTESIAN_POINT ( 'NONE',  ( -10.81492255796078084, -18.62759615963271287, 82.08224293864768129 ) ) ;
#49760 = B_SPLINE_CURVE_WITH_KNOTS ( 'NONE', 3,
 ( #108435, #123590, #186295, #120624, #47775, #62920, #106443, #124600, #139754, #171108, #15443, #169103, #143485, #91252, #153947, #60933, #109428, #13456, #59946, #90284, #16437, #45779, #78086, #158662, #136788, #35328, #20153, #137781, #121613, #75120, #251, #107431 ),
 .UNSPECIFIED., .F., .F.,
 ( 4, 2, 2, 2, 2, 2, 2, 2, 2, 2, 2, 2, 2, 2, 2, 4 ),
 ( 2.281672496420497557E-17, 0.0003712461730037045046, 0.0007424923460073861326, 0.001113738519011067598, 0.001484984692014749497, 0.002227477038022112645, 0.002598723211025787388, 0.002969969384029461697, 0.003341215557033136441, 0.003712461730036810750, 0.004083707903040485060, 0.004454954076044158502, 0.004826200249047832812, 0.005197446422051507989, 0.005568692595055182298, 0.005939938768058856608 ),
 .UNSPECIFIED. ) ;
#49761 = CARTESIAN_POINT ( 'NONE',  ( -12.06949235617756955, 12.14591786802309770, 95.62390960531436690 ) ) ;
#49762 =( GEOMETRIC_REPRESENTATION_CONTEXT ( 3 ) GLOBAL_UNCERTAINTY_ASSIGNED_CONTEXT ( ( #146977 ) ) GLOBAL_UNIT_ASSIGNED_CONTEXT ( ( #89080, #10261, #149764 ) ) REPRESENTATION_CONTEXT ( 'NONE', 'WORKASPACE' ) );
#49763 = CARTESIAN_POINT ( 'NONE',  ( -0.05219959533937732626, 21.53943276465977519, 42.50109039468567573 ) ) ;
#49764 = CARTESIAN_POINT ( 'NONE',  ( 27.73933785331498925, -9.013057229001033122, 141.7750000027311899 ) ) ;
#49765 = ADVANCED_FACE ( 'NONE', ( #11017 ), #49933, .T. ) ;
#49766 = CARTESIAN_POINT ( 'NONE',  ( 16.55341960407618274, -4.379528057220086978, 111.0427570613523613 ) ) ;
#49767 = CARTESIAN_POINT ( 'NONE',  ( -0.05219959533909027116, -19.03943276465977164, 42.49890960531435269 ) ) ;
#49768 = CARTESIAN_POINT ( 'NONE',  ( -19.03943276465977164, 0.05219959533909376836, 91.24890960531436690 ) ) ;
#49769 = CARTESIAN_POINT ( 'NONE',  ( -19.53037848336980886, 5.499999999999904077, 44.85532783611448338 ) ) ;
#49770 = CARTESIAN_POINT ( 'NONE',  ( 9.474510206698971260, -16.51473224551069308, 32.91557627198102409 ) ) ;
#49771 = CARTESIAN_POINT ( 'NONE',  ( 8.314922557960818139, 14.29746914071049879, 44.58224293864769550 ) ) ;
#49772 = CARTESIAN_POINT ( 'NONE',  ( 21.53943276465977519, 0.05219959533937863772, 71.25109039468568994 ) ) ;
#49774 = CARTESIAN_POINT ( 'NONE',  ( -12.14591786802326823, 12.06949235617739902, 68.12609039468567573 ) ) ;
#49773 = CARTESIAN_POINT ( 'NONE',  ( 34.03190083852023662, -20.28298779507398208, -18.01673046680643253 ) ) ;
#49775 = CARTESIAN_POINT ( 'NONE',  ( -13.89961937509977652, 13.97604488694528158, 50.62390960531435979 ) ) ;
#49776 = CARTESIAN_POINT ( 'NONE',  ( -0.05219959533909027116, -19.03943276465977164, 67.49890960531436690 ) ) ;
#49777 = ORIENTED_EDGE ( 'NONE', *, *, #28831, .F. ) ;
#49778 = CARTESIAN_POINT ( 'NONE',  ( 21.53943276465977519, 0.05219959533937863772, 106.2510903946856757 ) ) ;
#49779 = CARTESIAN_POINT ( 'NONE',  ( -16.53943276465976808, -0.05219959533934237506, 68.75109039468568994 ) ) ;
#49780 = CARTESIAN_POINT ( 'NONE',  ( -0.05219959533937732626, 21.53943276465977519, 97.50109039468567573 ) ) ;
#49781 = CARTESIAN_POINT ( 'NONE',  ( -5.153800228976328057, -19.02544592524343514, 62.29057627198100988 ) ) ;
#49782 = CARTESIAN_POINT ( 'NONE',  ( -0.05219959533907301413, -21.53943276465977519, 37.49890960531436690 ) ) ;
#49783 = CARTESIAN_POINT ( 'NONE',  ( 13.97604488694548053, -13.89961937509957401, 105.6260903946856757 ) ) ;
#49784 = CARTESIAN_POINT ( 'NONE',  ( -18.67979575497193778, 10.72451020669871902, 63.33442372801900433 ) ) ;
#49785 = CARTESIAN_POINT ( 'NONE',  ( 12.06949235617739724, 12.14591786802326823, 51.87609039468568284 ) ) ;
#49786 = CARTESIAN_POINT ( 'NONE',  ( -15.72974639402197994, 15.80617190586746368, 105.6239096053143669 ) ) ;
#49787 = CARTESIAN_POINT ( 'NONE',  ( -9.474510206698720793, -16.51473224551083518, 94.58442372801900433 ) ) ;
#49788 = CARTESIAN_POINT ( 'NONE',  ( 13.97604488694527802, 13.89961937509977652, 79.37390960531435269 ) ) ;
#49789 = CARTESIAN_POINT ( 'NONE',  ( -16.46253265017146816, -9.564922557961047289, 104.1677570613523329 ) ) ;
#49790 = CARTESIAN_POINT ( 'NONE',  ( -16.51473224551082808, 9.474510206698731452, 113.3344237280190043 ) ) ;
#49791 = CARTESIAN_POINT ( 'NONE',  ( -0.05219959533910754901, -16.53943276465976808, 67.49890960531436690 ) ) ;
#49792 = B_SPLINE_CURVE_WITH_KNOTS ( 'NONE', 3,
 ( #139261, #199955, #168603, #137277, #108924, #47267, #48263, #156424, #107918, #30103, #109917, #737, #1741, #170604, #138272, #172594, #91743, #17925, #63419, #61420 ),
 .UNSPECIFIED., .F., .F.,
 ( 4, 2, 2, 2, 2, 2, 2, 2, 2, 4 ),
 ( 0.000000000000000000, 0.0004987090165372609933, 0.0009974180330745219866, 0.001246772541343152537, 0.001496127049611783088, 0.001994836066149048310, 0.002493545082686314182, 0.002742899590954939095, 0.002992254099223564442, 0.003989672132298079273 ),
 .UNSPECIFIED. ) ;
#49793 = CARTESIAN_POINT ( 'NONE',  ( 14.34966873604972726, -8.224510206698740333, 75.83442372801900433 ) ) ;
#49795 = CARTESIAN_POINT ( 'NONE',  ( -9.564922557960796823, -16.46253265017161027, 52.08224293864768839 ) ) ;
#49794 = CARTESIAN_POINT ( 'NONE',  ( -18.67979575497178146, -10.72451020669898902, 111.6655762719810525 ) ) ;
#49797 = EDGE_CURVE ( 'NONE', #33758, #95658, #107578, .T. ) ;
#49796 = CARTESIAN_POINT ( 'NONE',  ( -16.46253265017160317, 9.564922557960807481, 65.83224293864769550 ) ) ;
#49798 = CARTESIAN_POINT ( 'NONE',  ( 12.06949235617739724, 12.14591786802326823, 71.87609039468568994 ) ) ;
#49799 = CYLINDRICAL_SURFACE ( 'NONE', #133806, 2.000000000000000000 ) ;
#49800 = ORIENTED_EDGE ( 'NONE', *, *, #69228, .F. ) ;
#49801 = CARTESIAN_POINT ( 'NONE',  ( -21.53943276465977519, -0.05219959533937600094, 113.7510903946856757 ) ) ;
#49802 = CARTESIAN_POINT ( 'NONE',  ( -9.564922557960796823, -16.46253265017161027, 37.08224293864768839 ) ) ;
#49803 = ORIENTED_EDGE ( 'NONE', *, *, #15852, .T. ) ;
#49804 = CARTESIAN_POINT ( 'NONE',  ( 16.51473224551083163, -9.474510206698727899, 105.8344237280190043 ) ) ;
#49806 = CARTESIAN_POINT ( 'NONE',  ( -8.314922557961024197, 14.29746914071037800, 22.91775706135235069 ) ) ;
#49805 = CARTESIAN_POINT ( 'NONE',  ( -13.89961937509957401, -13.97604488694547875, 39.37609039468566152 ) ) ;
#49807 = CARTESIAN_POINT ( 'NONE',  ( 0.05219959533909260263, 19.03943276465977164, 44.99890960531435979 ) ) ;
#49808 = CARTESIAN_POINT ( 'NONE',  ( 13.89961937509977652, -13.97604488694527269, 68.12390960531436690 ) ) ;
#49809 = CARTESIAN_POINT ( 'NONE',  ( -18.62759615963270932, 10.81492255796079327, 80.83224293864769550 ) ) ;
#49810 = CARTESIAN_POINT ( 'NONE',  ( -5.153800228976328057, -19.02544592524343514, 107.2905762719810383 ) ) ;
#49811 = CARTESIAN_POINT ( 'NONE',  ( 13.89961937509977652, -13.97604488694527269, 48.12390960531435979 ) ) ;
#49812 = CARTESIAN_POINT ( 'NONE',  ( -27.73933785331498925, 9.013057229001088189, 149.2750000027311614 ) ) ;
#49813 = CARTESIAN_POINT ( 'NONE',  ( -19.02544592524334988, -5.153800228976617603, 93.95942372801900433 ) ) ;
#49814 = CARTESIAN_POINT ( 'NONE',  ( -14.34966873604960291, -8.224510206698953496, 71.66557627198100988 ) ) ;
#49815 = CARTESIAN_POINT ( 'NONE',  ( 19.03943276465977164, 0.05219959533936151252, 31.25109039468566863 ) ) ;
#49816 = AXIS2_PLACEMENT_3D ( 'NONE', #178310, #39773, #175299 ) ;
#49817 = CARTESIAN_POINT ( 'NONE',  ( 16.55341960407611168, 4.379528057220329451, 58.95724293864770971 ) ) ;
#49818 = CARTESIAN_POINT ( 'NONE',  ( -21.53943276465977519, -0.05219959533937600094, 83.75109039468568994 ) ) ;
#49819 = CARTESIAN_POINT ( 'NONE',  ( 19.03943276465977164, -0.05219959533909143690, 28.74890960531435624 ) ) ;
#49820 = CARTESIAN_POINT ( 'NONE',  ( -21.55341960407619339, 5.719274019375674811, 93.54275706135234714 ) ) ;
#49822 = CARTESIAN_POINT ( 'NONE',  ( -21.53943276465977519, -0.05219959533937600094, 78.75109039468568994 ) ) ;
#49821 = CARTESIAN_POINT ( 'NONE',  ( -16.52544592524342804, 4.483927247898546575, 31.04057627198102409 ) ) ;
#49823 = CARTESIAN_POINT ( 'NONE',  ( -13.97604488694527625, -13.89961937509977652, 81.87390960531436690 ) ) ;
#49824 = CARTESIAN_POINT ( 'NONE',  ( 0.05219959533937995610, -21.53943276465977519, 40.00109039468567573 ) ) ;
#49825 = CARTESIAN_POINT ( 'NONE',  ( -13.89961937509977652, 13.97604488694528158, 80.62390960531436690 ) ) ;
#49826 = CARTESIAN_POINT ( 'NONE',  ( 16.52544592524342804, -4.483927247898539470, 98.54057627198105251 ) ) ;
#49827 = CARTESIAN_POINT ( 'NONE',  ( 8.314922557960818139, 14.29746914071049879, 59.58224293864770260 ) ) ;
#49828 = CARTESIAN_POINT ( 'NONE',  ( 21.55341960407610458, 5.719274019375980345, 68.95724293864769550 ) ) ;
#49829 = CARTESIAN_POINT ( 'NONE',  ( -19.03943276465977164, 0.05219959533909376836, 71.24890960531435269 ) ) ;
#49830 = CARTESIAN_POINT ( 'NONE',  ( -21.52544592524343514, 5.823673210054127303, 91.04057627198103830 ) ) ;
#49831 = CARTESIAN_POINT ( 'NONE',  ( 5.049401038297881783, 19.05341960407617563, 77.29275706135231871 ) ) ;
#49833 = CARTESIAN_POINT ( 'NONE',  ( 4.483927247898545687, 16.52544592524342804, 74.79057627198105251 ) ) ;
#49832 = CARTESIAN_POINT ( 'NONE',  ( 5.049401038297881783, 19.05341960407617918, 27.29275706135232582 ) ) ;
#49834 = CARTESIAN_POINT ( 'NONE',  ( 18.67979575497178502, 10.72451020669898547, 49.16557627198102409 ) ) ;
#49835 = FACE_OUTER_BOUND ( 'NONE', #3595, .T. ) ;
#49837 = CARTESIAN_POINT ( 'NONE',  ( 1.784210473542230573E-15, -29.16686587814331588, 147.8750000027311273 ) ) ;
#49836 = CARTESIAN_POINT ( 'NONE',  ( 12.14591786802327356, -12.06949235617739191, 95.62609039468568994 ) ) ;
#49838 = CARTESIAN_POINT ( 'NONE',  ( -16.51473224551082808, 9.474510206698731452, 98.33442372801900433 ) ) ;
#49839 = CARTESIAN_POINT ( 'NONE',  ( -0.05219959533910754901, -16.53943276465976808, 72.49890960531435269 ) ) ;
#49840 = CARTESIAN_POINT ( 'NONE',  ( -18.39639308325438449, -5.500000000000017764, 96.48252246182198633 ) ) ;
#49841 = CARTESIAN_POINT ( 'NONE',  ( 5.049401038298161559, -19.05341960407611168, 57.70724293864769550 ) ) ;
#49842 = CARTESIAN_POINT ( 'NONE',  ( -14.34966873604960291, -8.224510206698953496, 56.66557627198103830 ) ) ;
#49843 = CARTESIAN_POINT ( 'NONE',  ( -16.51473224551069308, -9.474510206698971260, 106.6655762719810383 ) ) ;
#49845 = CARTESIAN_POINT ( 'NONE',  ( 9.564922557960805705, 16.46253265017160317, 59.58224293864769550 ) ) ;
#49844 = CARTESIAN_POINT ( 'NONE',  ( -19.03943276465977164, -0.05219959533935918106, 88.75109039468567573 ) ) ;
#49846 = CARTESIAN_POINT ( 'NONE',  ( -13.97604488694527625, -13.89961937509977652, 81.87390960531436690 ) ) ;
#49847 = CARTESIAN_POINT ( 'NONE',  ( -0.05219959533909027116, -19.03943276465977164, 87.49890960531436690 ) ) ;
#49848 = CARTESIAN_POINT ( 'NONE',  ( 15.72974639402199770, -15.80617190586745480, 68.12390960531436690 ) ) ;
#49849 = CARTESIAN_POINT ( 'NONE',  ( 12.06949235617739724, 12.14591786802326823, 51.87609039468568284 ) ) ;
#49850 = LINE ( 'NONE', #52822, #54817 ) ;
#49851 = CARTESIAN_POINT ( 'NONE',  ( -13.97604488694527625, -13.89961937509977652, 56.87390960531434558 ) ) ;
#49852 = CARTESIAN_POINT ( 'NONE',  ( 21.53943276465977519, -0.05219959533907433946, 73.74890960531433848 ) ) ;
#49853 = CARTESIAN_POINT ( 'NONE',  ( -13.97604488694547697, 13.89961937509957934, 98.12609039468566152 ) ) ;
#49855 = CARTESIAN_POINT ( 'NONE',  ( -21.55341960407619339, 5.719274019375674811, 43.54275706135235424 ) ) ;
#49854 = CARTESIAN_POINT ( 'NONE',  ( 16.55341960407611168, 4.379528057220329451, 23.95724293864769550 ) ) ;
#49856 = CARTESIAN_POINT ( 'NONE',  ( -19.03943276465977164, -0.05219959533935918106, 43.75109039468566863 ) ) ;
#49858 = CARTESIAN_POINT ( 'NONE',  ( 8.224510206698742110, 14.34966873604972548, 97.08442372801904696 ) ) ;
#49857 = CARTESIAN_POINT ( 'NONE',  ( -4.483927247898782831, 16.52544592524335698, 67.70942372801901854 ) ) ;
#49859 = CARTESIAN_POINT ( 'NONE',  ( -17.49999999999999645, 5.499999999999992895, 73.71769037696435589 ) ) ;
#49860 = CARTESIAN_POINT ( 'NONE',  ( -16.53943276465976808, -0.05219959533934237506, 83.75109039468568994 ) ) ;
#49861 = CARTESIAN_POINT ( 'NONE',  ( 0.05219959533934541429, -16.53943276465976808, 40.00109039468567573 ) ) ;
#49862 = CARTESIAN_POINT ( 'NONE',  ( 16.46253265017160672, -9.564922557960803928, 43.33224293864769550 ) ) ;
#49863 = CARTESIAN_POINT ( 'NONE',  ( -19.05341960407611168, -5.049401038298163336, 56.45724293864768129 ) ) ;
#49864 = CARTESIAN_POINT ( 'NONE',  ( -13.89961937509977652, 13.97604488694528158, 55.62390960531434558 ) ) ;
#49865 = CARTESIAN_POINT ( 'NONE',  ( -21.53943276465977519, -0.05219959533937600094, 48.75109039468568284 ) ) ;
#49866 = CARTESIAN_POINT ( 'NONE',  ( 0.05219959533934541429, -16.53943276465976808, 50.00109039468568994 ) ) ;
#49867 = CARTESIAN_POINT ( 'NONE',  ( 16.55341960407611168, 4.379528057220329451, 23.95724293864769550 ) ) ;
#49868 = CARTESIAN_POINT ( 'NONE',  ( 0.05219959533909260263, 19.03943276465977164, 34.99890960531435979 ) ) ;
#49869 = CARTESIAN_POINT ( 'NONE',  ( 9.474510206698971260, -16.51473224551069308, 32.91557627198102409 ) ) ;
#49870 = CARTESIAN_POINT ( 'NONE',  ( 0.05219959533934541429, -16.53943276465976808, 25.00109039468567218 ) ) ;
#49871 = VECTOR ( 'NONE', #19047, 1000.000000000000000 ) ;
#49872 = CARTESIAN_POINT ( 'NONE',  ( -9.564922557961040184, 16.46253265017147172, 87.91775706135233293 ) ) ;
#49873 = CARTESIAN_POINT ( 'NONE',  ( -4.483927247898539470, -16.52544592524342804, 87.29057627198103830 ) ) ;
#49874 = CARTESIAN_POINT ( 'NONE',  ( 5.153800228976335163, 19.02544592524342804, 39.79057627198100988 ) ) ;
#49876 = CARTESIAN_POINT ( 'NONE',  ( 17.31728774477272736, 6.344390552232407998, 76.68093348310681279 ) ) ;
#49875 = CARTESIAN_POINT ( 'NONE',  ( 19.05341960407617918, -5.049401038297876454, 71.04275706135234714 ) ) ;
#49877 = CARTESIAN_POINT ( 'NONE',  ( 18.67979575497194134, -10.72451020669871369, 70.83442372801901854 ) ) ;
#49878 = CARTESIAN_POINT ( 'NONE',  ( 14.29746914071037800, 8.314922557961029526, 46.66775706135234714 ) ) ;
#49879 = CARTESIAN_POINT ( 'NONE',  ( 16.38665767535053774, 7.295008042176047702, 37.23599135785455871 ) ) ;
#49880 = CARTESIAN_POINT ( 'NONE',  ( -5.823673210054116645, -21.52544592524344225, 32.29057627198102409 ) ) ;
#49881 = CARTESIAN_POINT ( 'NONE',  ( 12.06949235617739724, 12.14591786802326823, 21.87609039468567573 ) ) ;
#49882 = CARTESIAN_POINT ( 'NONE',  ( 19.03943276465977164, -0.05219959533909143690, 28.74890960531435624 ) ) ;
#49883 = CARTESIAN_POINT ( 'NONE',  ( -5.049401038297874678, -19.05341960407617918, 34.79275706135233293 ) ) ;
#49884 = CARTESIAN_POINT ( 'NONE',  ( 11.48863819084122184, 12.06828707866188921, -59.15275318406540350 ) ) ;
#49885 = CARTESIAN_POINT ( 'NONE',  ( 5.153800228976335163, 19.02544592524342804, 34.79057627198102409 ) ) ;
#49886 = CARTESIAN_POINT ( 'NONE',  ( -5.049401038298153566, 19.05341960407611168, 70.20724293864769550 ) ) ;
#49887 = CARTESIAN_POINT ( 'NONE',  ( 17.50000000000000000, -3.471454075611709822, 111.9833258114436063 ) ) ;
#49888 = CARTESIAN_POINT ( 'NONE',  ( -5.719274019375665041, -21.55341960407619695, 109.7927570613523613 ) ) ;
#49889 = CARTESIAN_POINT ( 'NONE',  ( 16.52544592524342804, -4.483927247898539470, 33.54057627198102409 ) ) ;
#49890 = CARTESIAN_POINT ( 'NONE',  ( -9.564922557960796823, -16.46253265017161027, 37.08224293864768839 ) ) ;
#49891 = PRESENTATION_LAYER_ASSIGNMENT (  '', '', ( #101560 ) ) ;
#49892 = CARTESIAN_POINT ( 'NONE',  ( -19.02544592524342804, 5.153800228976336051, 91.04057627198100988 ) ) ;
#49893 = CARTESIAN_POINT ( 'NONE',  ( 0.05219959533937995610, -21.53943276465977519, 65.00109039468568994 ) ) ;
#49894 = CARTESIAN_POINT ( 'NONE',  ( -19.02544592524342804, 5.153800228976336051, 46.04057627198101699 ) ) ;
#49895 = CARTESIAN_POINT ( 'NONE',  ( 21.52544592524334988, 5.823673210054432836, 61.45942372801901854 ) ) ;
#49896 = CARTESIAN_POINT ( 'NONE',  ( 5.823673210054125526, 21.52544592524343514, 29.79057627198102409 ) ) ;
#49897 = CARTESIAN_POINT ( 'NONE',  ( 5.153800228976335163, 19.02544592524342804, 29.79057627198102409 ) ) ;
#49898 = CARTESIAN_POINT ( 'NONE',  ( 5.719274019375673035, 21.55341960407619339, 22.29275706135235069 ) ) ;
#49899 = CARTESIAN_POINT ( 'NONE',  ( -5.153800228976607833, 19.02544592524334988, 52.70942372801900433 ) ) ;
#49900 = CARTESIAN_POINT ( 'NONE',  ( -16.52544592524342804, 4.483927247898546575, 116.0405762719810383 ) ) ;
#49901 = CARTESIAN_POINT ( 'NONE',  ( 13.97604488694527802, 13.89961937509977652, 59.37390960531434558 ) ) ;
#49903 = AXIS2_PLACEMENT_3D ( 'NONE', #154283, #48103, #109759 ) ;
#49902 = CARTESIAN_POINT ( 'NONE',  ( -8.224510206698735004, -14.34966873604973081, 19.58442372801901143 ) ) ;
#49904 = CARTESIAN_POINT ( 'NONE',  ( 16.52544592524342804, -4.483927247898539470, 78.54057627198103830 ) ) ;
#49905 = CARTESIAN_POINT ( 'NONE',  ( 21.53943276465977519, -0.05219959533907433946, 28.74890960531435624 ) ) ;
#49906 = CARTESIAN_POINT ( 'NONE',  ( 0.05219959533936267826, -19.03943276465977164, 100.0010903946856757 ) ) ;
#49907 = CARTESIAN_POINT ( 'NONE',  ( -5.719274019375978568, 21.55341960407610458, 105.2072429386477097 ) ) ;
#49908 = CARTESIAN_POINT ( 'NONE',  ( 10.72451020669871369, 18.67979575497193778, 52.08442372801901854 ) ) ;
#49909 = CARTESIAN_POINT ( 'NONE',  ( -16.53943276465976808, -0.05219959533934237506, 53.75109039468568994 ) ) ;
#49910 = CARTESIAN_POINT ( 'NONE',  ( 4.379528057220092307, 16.55341960407617563, 57.29275706135234714 ) ) ;
#49911 = CARTESIAN_POINT ( 'NONE',  ( -21.55341960407610458, -5.719274019375992779, 56.45724293864768839 ) ) ;
#49912 = AXIS2_PLACEMENT_3D ( 'NONE', #75653, #107975, #168657 ) ;
#49913 = CARTESIAN_POINT ( 'NONE',  ( 13.97604488694527802, 13.89961937509977652, 49.37390960531434558 ) ) ;
#49914 = CARTESIAN_POINT ( 'NONE',  ( 12.06949235617739724, 12.14591786802326823, 71.87609039468568994 ) ) ;
#49915 = CARTESIAN_POINT ( 'NONE',  ( 15.72974639402199770, -15.80617190586745480, 108.1239096053143811 ) ) ;
#49916 = CARTESIAN_POINT ( 'NONE',  ( -16.53943276465976808, 0.05219959533911058130, 46.24890960531435979 ) ) ;
#49917 = CARTESIAN_POINT ( 'NONE',  ( -16.51473224551069308, -9.474510206698971260, 76.66557627198103830 ) ) ;
#49918 = CARTESIAN_POINT ( 'NONE',  ( -12.06949235617739369, -12.14591786802326823, 79.37609039468567573 ) ) ;
#49919 = CARTESIAN_POINT ( 'NONE',  ( -16.53943276465976808, -0.05219959533934237506, 23.75109039468567929 ) ) ;
#49920 = CARTESIAN_POINT ( 'NONE',  ( 18.67979575497178502, 10.72451020669898547, 99.16557627198100988 ) ) ;
#49921 = CARTESIAN_POINT ( 'NONE',  ( -16.52544592524342804, 4.483927247898546575, 51.04057627198103120 ) ) ;
#49922 = VERTEX_POINT ( 'NONE', #126134 ) ;
#49923 = CARTESIAN_POINT ( 'NONE',  ( 19.52217212775660116, -5.499999999999906741, 92.43993709005263781 ) ) ;
#49924 =( BOUNDED_SURFACE ( )  B_SPLINE_SURFACE ( 3, 2, ( 
 ( #6753, #36099, #146268 ),
 ( #38111, #97751, #68432 ),
 ( #101773, #159439, #190793 ),
 ( #52267, #113925, #7754 ),
 ( #99766, #175625, #37099 ),
 ( #161451, #98758, #160451 ),
 ( #39106, #22942, #21942 ),
 ( #69438, #131106, #100762 ),
 ( #162444, #23945, #8776 ),
 ( #85599, #147286, #70445 ),
 ( #43845, #121660, #28694 ),
 ( #199513, #182369, #16482 ),
 ( #77148, #154986, #197535 ),
 ( #137831, #32643, #92311 ),
 ( #167197, #105511, #91299 ),
 ( #123634, #122655, #31651 ),
 ( #90330, #185330, #76151 ),
 ( #45825, #13501, #152015 ),
 ( #78131, #171156, #75166 ),
 ( #186340, #46821, #109471 ),
 ( #60980, #184343, #136838 ),
 ( #107476, #12530, #198522 ),
 ( #170158, #106493, #169154 ),
 ( #59993, #183355, #30658 ) ),
 .UNSPECIFIED., .F., .F., .T. ) 
 B_SPLINE_SURFACE_WITH_KNOTS ( ( 4, 2, 2, 2, 2, 2, 2, 2, 2, 2, 2, 4 ),
 ( 3, 3 ),
 ( 0.000000000000000000, 0.001899702839891690993, 0.002849554259837536706, 0.003799405679783381985, 0.005699108519675073412, 0.006648959939620918691, 0.007598811359566763970, 0.008548662779512609250, 0.009498514199458456264, 0.01139821703935014682, 0.01329791987924183738, 0.01519762271913352794 ),
 ( 0.000000000000000000, 1.000000000000000000 ),
 .UNSPECIFIED. ) 
 GEOMETRIC_REPRESENTATION_ITEM ( )  RATIONAL_B_SPLINE_SURFACE ( (
 ( 1.000000000000000000, 0.7660444431189795678, 1.000000000000000000),
 ( 1.000000000000000000, 0.7753720600382140171, 1.000000000000000000),
 ( 1.000000000000000000, 0.7832595754286290068, 1.000000000000000000),
 ( 1.000000000000000000, 0.7928595458705313126, 1.000000000000000000),
 ( 1.000000000000000000, 0.7956872332516286006, 1.000000000000000000),
 ( 1.000000000000000000, 0.8005750596157429344, 1.000000000000000000),
 ( 1.000000000000000000, 0.8026302056541707586, 1.000000000000000000),
 ( 1.000000000000000000, 0.8075080643848452366, 1.000000000000000000),
 ( 1.000000000000000000, 0.8091143015810108308, 1.000000000000000000),
 ( 1.000000000000000000, 0.8093067629632920701, 1.000000000000000000),
 ( 1.000000000000000000, 0.8089952915731790650, 1.000000000000000000),
 ( 1.000000000000000000, 0.8076919994862170604, 1.000000000000000000),
 ( 1.000000000000000000, 0.8067078407649250771, 1.000000000000000000),
 ( 1.000000000000000000, 0.8041786842467109064, 1.000000000000000000),
 ( 1.000000000000000000, 0.8026334674877432240, 1.000000000000000000),
 ( 1.000000000000000000, 0.7990747329468971261, 1.000000000000000000),
 ( 1.000000000000000000, 0.7970509760942148247, 1.000000000000000000),
 ( 1.000000000000000000, 0.7904793850862690263, 1.000000000000000000),
 ( 1.000000000000000000, 0.7855040224313801778, 1.000000000000000000),
 ( 1.000000000000000000, 0.7751942650507522847, 1.000000000000000000),
 ( 1.000000000000000000, 0.7698260778212435707, 1.000000000000000000),
 ( 1.000000000000000000, 0.7598259884960076871, 1.000000000000000000),
 ( 1.000000000000000000, 0.7551428682220966415, 1.000000000000000000),
 ( 1.000000000000000000, 0.7510191126010865581, 1.000000000000000000) ) ) 
 REPRESENTATION_ITEM ( '' )  SURFACE ( )  );
#49925 = CARTESIAN_POINT ( 'NONE',  ( -10.72451020669898014, 18.67979575497178502, 85.41557627198102409 ) ) ;
#49926 = CARTESIAN_POINT ( 'NONE',  ( 8.314922557960818139, 14.29746914071049879, 24.58224293864768839 ) ) ;
#49927 = VERTEX_POINT ( 'NONE', #94796 ) ;
#49928 = CARTESIAN_POINT ( 'NONE',  ( -16.20579543436680936, -7.371946100354977105, 55.56520834171877254 ) ) ;
#49929 = CARTESIAN_POINT ( 'NONE',  ( -18.67979575497178146, -10.72451020669898902, 106.6655762719810383 ) ) ;
#49930 = CARTESIAN_POINT ( 'NONE',  ( -0.05219959533909027116, -19.03943276465977164, 97.49890960531436690 ) ) ;
#49931 = CARTESIAN_POINT ( 'NONE',  ( 0.05219959533937995610, -21.53943276465977519, 30.00109039468568284 ) ) ;
#49932 = CARTESIAN_POINT ( 'NONE',  ( 4.379528057220339221, -16.55341960407611168, 37.70724293864769550 ) ) ;
#49934 = CARTESIAN_POINT ( 'NONE',  ( -16.52544592524335698, -4.483927247898792601, 43.95942372801902565 ) ) ;
#49933 = TOROIDAL_SURFACE ( 'NONE', #72475, 2.700000000000000622, 0.2000000000000000111 ) ;
#49935 = CARTESIAN_POINT ( 'NONE',  ( 5.153800228976335163, 19.02544592524342804, 49.79057627198100988 ) ) ;
#49936 = CARTESIAN_POINT ( 'NONE',  ( 16.46253265017146816, 9.564922557961045513, 56.66775706135233293 ) ) ;
#49937 = CARTESIAN_POINT ( 'NONE',  ( 13.97604488694527802, 13.89961937509977652, 79.37390960531435269 ) ) ;
#49938 = ORIENTED_EDGE ( 'NONE', *, *, #112694, .F. ) ;
#49939 = CARTESIAN_POINT ( 'NONE',  ( -0.05219959533907301413, -21.53943276465977519, 32.49890960531435979 ) ) ;
#49940 = CARTESIAN_POINT ( 'NONE',  ( -30.04893132686769519, -22.76590847478283663, -19.45433810172459488 ) ) ;
#49941 = CARTESIAN_POINT ( 'NONE',  ( 16.52544592524335698, 4.483927247898782831, 26.45942372801901854 ) ) ;
#49942 = CARTESIAN_POINT ( 'NONE',  ( 19.05341960407617918, -5.049401038297876454, 56.04275706135234714 ) ) ;
#49943 = CARTESIAN_POINT ( 'NONE',  ( -21.53943276465977519, 0.05219959533907696930, 96.24890960531435269 ) ) ;
#49944 = EDGE_CURVE ( 'NONE', #76374, #22413, #199276, .T. ) ;
#49945 = CARTESIAN_POINT ( 'NONE',  ( -16.52544592524342804, 4.483927247898546575, 31.04057627198102409 ) ) ;
#49946 = CARTESIAN_POINT ( 'NONE',  ( -19.03943276465977164, 0.05219959533909376836, 76.24890960531435269 ) ) ;
#49947 = CARTESIAN_POINT ( 'NONE',  ( 21.53943276465977519, -0.05219959533907433946, 58.74890960531436690 ) ) ;
#49949 = CARTESIAN_POINT ( 'NONE',  ( -16.52544592524335698, -4.483927247898792601, 18.95942372801901143 ) ) ;
#49948 = CARTESIAN_POINT ( 'NONE',  ( 0.05219959533907565091, 21.53943276465977519, 89.99890960531438111 ) ) ;
#49950 = CARTESIAN_POINT ( 'NONE',  ( 21.53943276465977519, -0.05219959533907433946, 23.74890960531435269 ) ) ;
#49951 = CARTESIAN_POINT ( 'NONE',  ( -21.55341960407619339, 5.719274019375674811, 88.54275706135236135 ) ) ;
#49952 = CARTESIAN_POINT ( 'NONE',  ( -0.05219959533909027116, -19.03943276465977164, 92.49890960531436690 ) ) ;
#49953 = CARTESIAN_POINT ( 'NONE',  ( -13.97604488694527625, -13.89961937509977652, 26.87390960531434558 ) ) ;
#49954 = CARTESIAN_POINT ( 'NONE',  ( 16.51473224551069308, 9.474510206698969483, 89.16557627198103830 ) ) ;
#49955 = CARTESIAN_POINT ( 'NONE',  ( 4.379528057220339221, -16.55341960407611168, 107.7072429386476955 ) ) ;
#49956 = CARTESIAN_POINT ( 'NONE',  ( 16.46253265017160672, -9.564922557960803928, 63.33224293864769550 ) ) ;
#49957 = CARTESIAN_POINT ( 'NONE',  ( 9.564922557961047289, -16.46253265017146816, 110.4177570613523471 ) ) ;
#49958 = CARTESIAN_POINT ( 'NONE',  ( 17.31747979337957233, -6.344076630960846508, 86.12055131934816643 ) ) ;
#49959 = CARTESIAN_POINT ( 'NONE',  ( -19.03943276465977164, 0.05219959533909376836, 71.24890960531435269 ) ) ;
#49961 = CARTESIAN_POINT ( 'NONE',  ( 0.05219959533907565091, 21.53943276465977519, 24.99890960531435624 ) ) ;
#49960 = CARTESIAN_POINT ( 'NONE',  ( 10.81492255796106328, -18.62759615963255655, 100.4177570613523471 ) ) ;
#49962 = CARTESIAN_POINT ( 'NONE',  ( -8.314922557961024197, 14.29746914071037800, 97.91775706135236135 ) ) ;
#49963 = CARTESIAN_POINT ( 'NONE',  ( -31.81624771892549575, 0.5097844185668732875, -45.77220262091587699 ) ) ;
#49964 = CARTESIAN_POINT ( 'NONE',  ( 9.564922557961047289, -16.46253265017146816, 75.41775706135234714 ) ) ;
#49965 = CARTESIAN_POINT ( 'NONE',  ( -16.46253265017146816, -9.564922557961047289, 19.16775706135233293 ) ) ;
#49966 = CARTESIAN_POINT ( 'NONE',  ( 4.242615737635166973, 4.384086992840732222, -64.53213882399994361 ) ) ;
#49967 = CARTESIAN_POINT ( 'NONE',  ( 19.03943276465977164, -0.05219959533909143690, 23.74890960531435269 ) ) ;
#49968 = CARTESIAN_POINT ( 'NONE',  ( -16.52544592524342804, 4.483927247898546575, 26.04057627198103475 ) ) ;
#49969 = FACE_OUTER_BOUND ( 'NONE', #79263, .T. ) ;
#49970 = CARTESIAN_POINT ( 'NONE',  ( 12.14591786802327356, -12.06949235617739191, 100.6260903946857184 ) ) ;
#49971 = CARTESIAN_POINT ( 'NONE',  ( 22.11731296686191328, -20.12440949879982455, -51.56823826216871254 ) ) ;
#49972 = CARTESIAN_POINT ( 'NONE',  ( 12.14591786802327356, -12.06949235617739191, 75.62609039468567573 ) ) ;
#49973 = CARTESIAN_POINT ( 'NONE',  ( -5.049401038298153566, 19.05341960407611168, 35.20724293864768839 ) ) ;
#49974 = CARTESIAN_POINT ( 'NONE',  ( 5.719274019375673035, 21.55341960407619339, 92.29275706135236135 ) ) ;
#49975 = CARTESIAN_POINT ( 'NONE',  ( 16.51473224551083163, -9.474510206698727899, 100.8344237280190043 ) ) ;
#49976 = CARTESIAN_POINT ( 'NONE',  ( -21.53943276465977519, -0.05219959533937600094, 73.75109039468567573 ) ) ;
#49977 = CARTESIAN_POINT ( 'NONE',  ( -13.97604488694547697, 13.89961937509957934, 48.12609039468566863 ) ) ;
#49978 = CARTESIAN_POINT ( 'NONE',  ( 9.474510206698971260, -16.51473224551069308, 72.91557627198102409 ) ) ;
#49979 = CARTESIAN_POINT ( 'NONE',  ( -9.474510206698964154, 16.51473224551069663, 70.41557627198102409 ) ) ;
#49980 = CARTESIAN_POINT ( 'NONE',  ( 24.49873734152912519, -24.99873734152920690, 5.353553390593271288 ) ) ;
#49981 = CARTESIAN_POINT ( 'NONE',  ( 14.29746914071049879, -8.314922557960816363, 53.33224293864769550 ) ) ;
#49982 = CARTESIAN_POINT ( 'NONE',  ( -15.80617190586745835, -15.72974639402198527, 51.87390960531437401 ) ) ;
#49983 = CARTESIAN_POINT ( 'NONE',  ( 0.05219959533909260263, 19.03943276465977164, 44.99890960531435979 ) ) ;
#49985 = CARTESIAN_POINT ( 'NONE',  ( 16.55341960407618274, -4.379528057220086978, 71.04275706135234714 ) ) ;
#49984 = CARTESIAN_POINT ( 'NONE',  ( 10.72451020669898902, -18.67979575497178502, 82.91557627198103830 ) ) ;
#49986 = ORIENTED_EDGE ( 'NONE', *, *, #3940, .T. ) ;
#49988 = CARTESIAN_POINT ( 'NONE',  ( -11.40812507854755609, 35.11059874428196537, -5.024999997268813523 ) ) ;
#49987 = CARTESIAN_POINT ( 'NONE',  ( -14.29746914071049879, 8.314922557960819915, 75.83224293864769550 ) ) ;
#49989 = CARTESIAN_POINT ( 'NONE',  ( 16.52544592524335698, 4.483927247898782831, 41.45942372801901143 ) ) ;
#49990 = CARTESIAN_POINT ( 'NONE',  ( -16.51473224551069308, -9.474510206698971260, 26.66557627198103120 ) ) ;
#49991 = CARTESIAN_POINT ( 'NONE',  ( -19.05341960407617563, 5.049401038297882671, 63.54275706135234003 ) ) ;
#49992 = CARTESIAN_POINT ( 'NONE',  ( 16.53943276465976808, -0.05219959533910856209, 73.74890960531433848 ) ) ;
#49993 = CARTESIAN_POINT ( 'NONE',  ( -18.67979575497193778, 10.72451020669871902, 48.33442372801902565 ) ) ;
#49995 = CARTESIAN_POINT ( 'NONE',  ( -0.05219959533907301413, -21.53943276465977519, 92.49890960531436690 ) ) ;
#49994 = CARTESIAN_POINT ( 'NONE',  ( 16.51473224551069308, 9.474510206698969483, 29.16557627198103475 ) ) ;
#49996 = CARTESIAN_POINT ( 'NONE',  ( -13.97604488694527625, -13.89961937509977652, 111.8739096053143243 ) ) ;
#49997 = CARTESIAN_POINT ( 'NONE',  ( 14.34966873604960469, 8.224510206698951720, 89.16557627198102409 ) ) ;
#49998 = CARTESIAN_POINT ( 'NONE',  ( 17.75813068129455274, -35.78296932995310442, -27.23805928211041660 ) ) ;
#49999 = CARTESIAN_POINT ( 'NONE',  ( 16.46253265017160672, -9.564922557960803928, 48.33224293864769550 ) ) ;
#50000 = CARTESIAN_POINT ( 'NONE',  ( 22.81625015709510151, -31.40387420917324590, -3.924999997268812102 ) ) ;
#50001 = CARTESIAN_POINT ( 'NONE',  ( 19.05341960407617918, -5.049401038297876454, 76.04275706135230450 ) ) ;
#50002 = CARTESIAN_POINT ( 'NONE',  ( -15.80617190586768217, 15.72974639402176855, 28.12609039468568284 ) ) ;
#50003 = CARTESIAN_POINT ( 'NONE',  ( -5.049401038298153566, 19.05341960407611168, 70.20724293864769550 ) ) ;
#50004 = CARTESIAN_POINT ( 'NONE',  ( -13.97604488694547697, 13.89961937509957934, 58.12609039468566863 ) ) ;
#50005 = CARTESIAN_POINT ( 'NONE',  ( 19.03943276465977164, -0.05219959533909143690, 38.74890960531436690 ) ) ;
#50006 = CARTESIAN_POINT ( 'NONE',  ( -0.05219959533910754901, -16.53943276465976808, 57.49890960531435979 ) ) ;
#50007 = CARTESIAN_POINT ( 'NONE',  ( -8.224510206698948167, 14.34966873604960824, 50.41557627198103120 ) ) ;
#50008 = CARTESIAN_POINT ( 'NONE',  ( -5.153800228976328057, -19.02544592524343514, 82.29057627198103830 ) ) ;
#50009 = AXIS2_PLACEMENT_3D ( 'NONE', #61288, #170466, #122958 ) ;
#50010 = CARTESIAN_POINT ( 'NONE',  ( -21.53943276465977519, 0.05219959533907696930, 96.24890960531435269 ) ) ;
#50011 = CARTESIAN_POINT ( 'NONE',  ( 13.89961937509977652, -13.97604488694527269, 78.12390960531433848 ) ) ;
#50012 = CARTESIAN_POINT ( 'NONE',  ( -18.62759615963270932, 10.81492255796079327, 75.83224293864769550 ) ) ;
#50013 = CARTESIAN_POINT ( 'NONE',  ( -19.03943276465977164, -0.05219959533935918106, 23.75109039468566152 ) ) ;
#50016 = CARTESIAN_POINT ( 'NONE',  ( -16.53943276465976808, 0.05219959533911058130, 96.24890960531435269 ) ) ;
#50015 = CARTESIAN_POINT ( 'NONE',  ( -16.55341960407617563, 4.379528057220093196, 103.5427570613523613 ) ) ;
#50014 = CARTESIAN_POINT ( 'NONE',  ( -16.46253265017160317, 9.564922557960807481, 40.83224293864769550 ) ) ;
#50017 = CARTESIAN_POINT ( 'NONE',  ( -5.153800228976607833, 19.02544592524334988, 107.7094237280189759 ) ) ;
#50018 = VERTEX_POINT ( 'NONE', #2788 ) ;
#50019 = CARTESIAN_POINT ( 'NONE',  ( -0.05219959533937732626, 21.53943276465977519, 37.50109039468568284 ) ) ;
#50020 = CARTESIAN_POINT ( 'NONE',  ( 9.474510206698729675, 16.51473224551082808, 57.08442372801900433 ) ) ;
#50021 = CARTESIAN_POINT ( 'NONE',  ( -8.224510206698735004, -14.34966873604973081, 109.5844237280190328 ) ) ;
#50022 = CARTESIAN_POINT ( 'NONE',  ( -0.05219959533907301413, -21.53943276465977519, 67.49890960531436690 ) ) ;
#50023 = CARTESIAN_POINT ( 'NONE',  ( 19.02544592524343514, -5.153800228976328945, 108.5405762719810383 ) ) ;
#50024 = CARTESIAN_POINT ( 'NONE',  ( -12.06949235617756955, 12.14591786802309770, 55.62390960531436690 ) ) ;
#50025 = CARTESIAN_POINT ( 'NONE',  ( -13.89961937509977652, 13.97604488694528158, 25.62390960531434558 ) ) ;
#50026 = CARTESIAN_POINT ( 'NONE',  ( 16.46253265017160672, -9.564922557960803928, 28.33224293864769550 ) ) ;
#50027 = CARTESIAN_POINT ( 'NONE',  ( 10.81492255796106328, -18.62759615963255655, 105.4177570613523613 ) ) ;
#50028 = CARTESIAN_POINT ( 'NONE',  ( -14.34966873604972548, 8.224510206698743886, 88.33442372801901854 ) ) ;
#50029 = CARTESIAN_POINT ( 'NONE',  ( -10.81492255796105439, 18.62759615963255655, 47.91775706135234714 ) ) ;
#50030 = CARTESIAN_POINT ( 'NONE',  ( 12.14591786802327356, -12.06949235617739191, 40.62609039468567573 ) ) ;
#50031 = CARTESIAN_POINT ( 'NONE',  ( 21.52544592524344225, -5.823673210054117533, 28.54057627198103120 ) ) ;
#50033 = CARTESIAN_POINT ( 'NONE',  ( -5.719274019375665041, -21.55341960407619695, 94.79275706135234714 ) ) ;
#50032 = CARTESIAN_POINT ( 'NONE',  ( -0.05219959533909027116, -19.03943276465977164, 57.49890960531435979 ) ) ;
#50034 = CARTESIAN_POINT ( 'NONE',  ( 19.03943276465977164, -0.05219959533909143690, 73.74890960531435269 ) ) ;
#50035 = VECTOR ( 'NONE', #65378, 1000.000000000000000 ) ;
#50036 = CARTESIAN_POINT ( 'NONE',  ( -16.53943276465976808, -0.05219959533934237506, 58.75109039468568994 ) ) ;
#50037 = CARTESIAN_POINT ( 'NONE',  ( -14.29746914071049879, 8.314922557960819915, 100.8322429386477097 ) ) ;
#50038 = CARTESIAN_POINT ( 'NONE',  ( 16.52544592524335698, 4.483927247898782831, 111.4594237280190328 ) ) ;
#50039 = CARTESIAN_POINT ( 'NONE',  ( 16.51473224551069308, 9.474510206698969483, 49.16557627198102409 ) ) ;
#50042 = CARTESIAN_POINT ( 'NONE',  ( 5.153800228976335163, 19.02544592524342804, 74.79057627198103830 ) ) ;
#50041 = CARTESIAN_POINT ( 'NONE',  ( 13.89961937509977652, -13.97604488694527269, 93.12390960531436690 ) ) ;
#50040 = CARTESIAN_POINT ( 'NONE',  ( 21.55341960407619695, -5.719274019375665929, 51.04275706135234714 ) ) ;
#50044 = EDGE_CURVE ( 'NONE', #100590, #137833, #49298, .T. ) ;
#50043 = CARTESIAN_POINT ( 'NONE',  ( 5.153800228976335163, 19.02544592524342804, 109.7905762719810099 ) ) ;
#50045 = CARTESIAN_POINT ( 'NONE',  ( 14.29746914071049879, -8.314922557960816363, 43.33224293864769550 ) ) ;
#50046 = CARTESIAN_POINT ( 'NONE',  ( -14.34966873604972548, 8.224510206698743886, 113.3344237280190328 ) ) ;
#50047 = CARTESIAN_POINT ( 'NONE',  ( 12.14591786802309770, 12.06949235617756955, 34.37390960531435979 ) ) ;
#50049 = AXIS2_PLACEMENT_3D ( 'NONE', #30700, #16523, #152057 ) ;
#50048 = CARTESIAN_POINT ( 'NONE',  ( -4.962140900324383708, 6.180203150055898931, 3.431593142121020623 ) ) ;
#50050 = CARTESIAN_POINT ( 'NONE',  ( -16.51473224551082808, 9.474510206698731452, 38.33442372801899722 ) ) ;
#50051 = CARTESIAN_POINT ( 'NONE',  ( -9.474510206698964154, 16.51473224551069663, 75.41557627198103830 ) ) ;
#50052 = CARTESIAN_POINT ( 'NONE',  ( -5.153800228976607833, 19.02544592524334988, 52.70942372801900433 ) ) ;
#50053 = CARTESIAN_POINT ( 'NONE',  ( 29.86685920354754487, 21.69954338932564752, -1.424999997268813212 ) ) ;
#50054 = CARTESIAN_POINT ( 'NONE',  ( -16.51473224551069308, -9.474510206698971260, 66.66557627198102409 ) ) ;
#50056 = CARTESIAN_POINT ( 'NONE',  ( 4.379528057220092307, 16.55341960407617563, 72.29275706135236135 ) ) ;
#50055 = CARTESIAN_POINT ( 'NONE',  ( -13.97604488694547697, 13.89961937509957934, 88.12609039468563310 ) ) ;
#50058 = CARTESIAN_POINT ( 'NONE',  ( -22.03588254365376997, 7.477584490969214848, 173.9991804579021277 ) ) ;
#50057 =( GEOMETRIC_REPRESENTATION_CONTEXT ( 3 ) GLOBAL_UNCERTAINTY_ASSIGNED_CONTEXT ( ( #159130 ) ) GLOBAL_UNIT_ASSIGNED_CONTEXT ( ( #82837, #6002, #23189 ) ) REPRESENTATION_CONTEXT ( 'NONE', 'WORKASPACE' ) );
#50059 = CARTESIAN_POINT ( 'NONE',  ( 16.51473224551069308, 9.474510206698969483, 104.1655762719810241 ) ) ;
#50060 = CARTESIAN_POINT ( 'NONE',  ( 15.80617190586769283, -15.72974639402175789, 25.62609039468567929 ) ) ;
#50061 = CARTESIAN_POINT ( 'NONE',  ( -16.51473224551082808, 9.474510206698731452, 88.33442372801900433 ) ) ;
#50063 = CARTESIAN_POINT ( 'NONE',  ( 19.02544592524343514, -5.153800228976328945, 43.54057627198103120 ) ) ;
#50062 = CARTESIAN_POINT ( 'NONE',  ( 17.48847506799967633, 5.747544572773806593, 86.67302562156719148 ) ) ;
#50064 = CARTESIAN_POINT ( 'NONE',  ( 9.474510206698971260, -16.51473224551069308, 87.91557627198102409 ) ) ;
#50066 = CARTESIAN_POINT ( 'NONE',  ( -16.46253265017160317, 9.564922557960807481, 50.83224293864770260 ) ) ;
#50065 = CARTESIAN_POINT ( 'NONE',  ( 14.29746914071049879, -8.314922557960816363, 63.33224293864770260 ) ) ;
#50067 = CARTESIAN_POINT ( 'NONE',  ( 19.02544592524343514, -5.153800228976328945, 58.54057627198102409 ) ) ;
#50068 = CARTESIAN_POINT ( 'NONE',  ( 13.89961937509957401, 13.97604488694547697, 66.87609039468567573 ) ) ;
#50069 = CARTESIAN_POINT ( 'NONE',  ( -5.153800228976607833, 19.02544592524334988, 27.70942372801899722 ) ) ;
#50070 = CARTESIAN_POINT ( 'NONE',  ( 5.153800228976335163, 19.02544592524342804, 59.79057627198100988 ) ) ;
#50071 = CARTESIAN_POINT ( 'NONE',  ( 10.81492255796078972, 18.62759615963270932, 64.58224293864769550 ) ) ;
#50073 = CARTESIAN_POINT ( 'NONE',  ( 9.474510206698729675, 16.51473224551082808, 37.08442372801899722 ) ) ;
#50072 = CARTESIAN_POINT ( 'NONE',  ( -16.52544592524342804, 4.483927247898546575, 66.04057627198103830 ) ) ;
#50074 = CARTESIAN_POINT ( 'NONE',  ( 18.22780087662122384, -5.500000000000022204, 86.01540105326108687 ) ) ;
#50075 = CARTESIAN_POINT ( 'NONE',  ( -21.55341960407610458, -5.719274019375992779, 51.45724293864770260 ) ) ;
#50076 = CARTESIAN_POINT ( 'NONE',  ( 15.72974639402199770, -15.80617190586745480, 28.12390960531435979 ) ) ;
#50077 = CARTESIAN_POINT ( 'NONE',  ( 5.153800228976335163, 19.02544592524342804, 54.79057627198103120 ) ) ;
#50078 = CARTESIAN_POINT ( 'NONE',  ( 16.51473224551069308, 9.474510206698969483, 39.16557627198103120 ) ) ;
#50079 = CARTESIAN_POINT ( 'NONE',  ( -0.05219959533910754901, -16.53943276465976808, 107.4989096053143669 ) ) ;
#50080 = CARTESIAN_POINT ( 'NONE',  ( -21.53943276465977519, 0.05219959533907696930, 106.2489096053143811 ) ) ;
#50081 = CARTESIAN_POINT ( 'NONE',  ( -40.00200000000003087, -5.510910596163089556E-15, 45.00000000000000000 ) ) ;
#50082 = CARTESIAN_POINT ( 'NONE',  ( 21.53943276465977519, 0.05219959533937863772, 31.25109039468568639 ) ) ;
#50083 = CARTESIAN_POINT ( 'NONE',  ( -8.224510206698948167, 14.34966873604960824, 110.4155762719810383 ) ) ;
#50084 = CARTESIAN_POINT ( 'NONE',  ( 18.62759615963255655, 10.81492255796105972, 81.66775706135236135 ) ) ;
#50085 = CARTESIAN_POINT ( 'NONE',  ( -0.05219959533907301413, -21.53943276465977519, 87.49890960531436690 ) ) ;
#50086 = CARTESIAN_POINT ( 'NONE',  ( 19.02544592524334988, 5.153800228976608722, 36.45942372801900433 ) ) ;
#50087 = CARTESIAN_POINT ( 'NONE',  ( 16.51473224551069308, 9.474510206698969483, 29.16557627198103475 ) ) ;
#50088 = DIRECTION ( 'NONE',  ( 0.7071067811865467956, -2.468850131082262977E-15, -0.7071067811865483499 ) ) ;
#50089 = CARTESIAN_POINT ( 'NONE',  ( -38.00000000000000711, -12.34694845685042708, -1.899999999999999689 ) ) ;
#50090 = CARTESIAN_POINT ( 'NONE',  ( 0.05219959533934541429, -16.53943276465976808, 45.00109039468568284 ) ) ;
#50091 = CARTESIAN_POINT ( 'NONE',  ( 4.379528057220339221, -16.55341960407611168, 112.7072429386476955 ) ) ;
#50092 = CYLINDRICAL_SURFACE ( 'NONE', #19284, 26.79475375365586487 ) ;
#50093 = CARTESIAN_POINT ( 'NONE',  ( -9.564922557960796823, -16.46253265017161027, 72.08224293864770971 ) ) ;
#50094 = CARTESIAN_POINT ( 'NONE',  ( 16.53943276465976808, -0.05219959533910856209, 93.74890960531436690 ) ) ;
#50095 = CARTESIAN_POINT ( 'NONE',  ( -21.55341960407610458, -5.719274019375992779, 46.45724293864769550 ) ) ;
#50096 = CARTESIAN_POINT ( 'NONE',  ( 16.53943276465976808, -0.05219959533910856209, 83.74890960531435269 ) ) ;
#50097 = CARTESIAN_POINT ( 'NONE',  ( 8.314922557961029526, -14.29746914071037800, 35.41775706135234003 ) ) ;
#50098 = CARTESIAN_POINT ( 'NONE',  ( 21.52544592524334988, 5.823673210054432836, 91.45942372801901854 ) ) ;
#50099 = CARTESIAN_POINT ( 'NONE',  ( -9.564922557961040184, 16.46253265017147172, 62.91775706135233293 ) ) ;
#50100 = CARTESIAN_POINT ( 'NONE',  ( -4.379528057220086978, -16.55341960407618274, 99.79275706135234714 ) ) ;
#50101 = CARTESIAN_POINT ( 'NONE',  ( -8.314922557960811034, -14.29746914071050412, 42.08224293864769550 ) ) ;
#50102 = CARTESIAN_POINT ( 'NONE',  ( 13.89961937509977652, -13.97604488694527269, 48.12390960531435979 ) ) ;
#50103 = CARTESIAN_POINT ( 'NONE',  ( -0.05219959533937732626, 21.53943276465977519, 97.50109039468567573 ) ) ;
#50104 = CARTESIAN_POINT ( 'NONE',  ( -21.52544592524343514, 5.823673210054127303, 111.0405762719810525 ) ) ;
#50105 = CARTESIAN_POINT ( 'NONE',  ( -21.55341960407619339, 5.719274019375674811, 53.54275706135234714 ) ) ;
#50106 = CARTESIAN_POINT ( 'NONE',  ( -16.55341960407617563, 4.379528057220093196, 43.54275706135235424 ) ) ;
#50108 = CARTESIAN_POINT ( 'NONE',  ( 5.823673210054444382, -21.52544592524334988, 85.20942372801901854 ) ) ;
#50107 = CARTESIAN_POINT ( 'NONE',  ( 8.314922557960818139, 14.29746914071049879, 64.58224293864769550 ) ) ;
#50109 = CARTESIAN_POINT ( 'NONE',  ( 4.483927247898790824, -16.52544592524335698, 110.2094237280190185 ) ) ;
#50110 = CARTESIAN_POINT ( 'NONE',  ( 16.20579543436696213, -7.371946100355080134, 46.93479165828048849 ) ) ;
#50111 = DIRECTION ( 'NONE',  ( -0.000000000000000000, 0.000000000000000000, -1.000000000000000000 ) ) ;
#50112 = CARTESIAN_POINT ( 'NONE',  ( 16.55341960407611168, 4.379528057220329451, 33.95724293864769550 ) ) ;
#50113 = CARTESIAN_POINT ( 'NONE',  ( 0.05219959533934541429, -16.53943276465976808, 80.00109039468568994 ) ) ;
#50114 = CARTESIAN_POINT ( 'NONE',  ( -5.049401038298153566, 19.05341960407611168, 80.20724293864769550 ) ) ;
#50115 = CARTESIAN_POINT ( 'NONE',  ( -13.97604488694527625, -13.89961937509977652, 96.87390960531433848 ) ) ;
#50116 = CARTESIAN_POINT ( 'NONE',  ( -21.52544592524334988, -5.823673210054445271, 88.95942372801901854 ) ) ;
#50117 = CARTESIAN_POINT ( 'NONE',  ( -16.55341960407617563, 4.379528057220093196, 83.54275706135234714 ) ) ;
#50118 = CARTESIAN_POINT ( 'NONE',  ( 4.483927247898545687, 16.52544592524342804, 79.79057627198102409 ) ) ;
#50119 = CARTESIAN_POINT ( 'NONE',  ( 16.46253265017160672, -9.564922557960803928, 73.33224293864769550 ) ) ;
#50120 = ORIENTED_EDGE ( 'NONE', *, *, #168447, .T. ) ;
#50121 = CARTESIAN_POINT ( 'NONE',  ( -14.29746914071037622, -8.314922557961029526, 24.16775706135235424 ) ) ;
#50122 = CARTESIAN_POINT ( 'NONE',  ( -5.153800228976328057, -19.02544592524343514, 22.29057627198102765 ) ) ;
#50123 = CARTESIAN_POINT ( 'NONE',  ( 13.89961937509977652, -13.97604488694527269, 98.12390960531433848 ) ) ;
#50125 = CARTESIAN_POINT ( 'NONE',  ( -11.40812507854754720, -35.11059874428192273, -10.22499999726881548 ) ) ;
#50124 = CARTESIAN_POINT ( 'NONE',  ( 14.34966873604972726, -8.224510206698740333, 25.83442372801901499 ) ) ;
#50126 = CARTESIAN_POINT ( 'NONE',  ( -13.89961937509957401, -13.97604488694547875, 24.37609039468565442 ) ) ;
#50127 = CARTESIAN_POINT ( 'NONE',  ( -14.29746914071037622, -8.314922557961029526, 94.16775706135237556 ) ) ;
#50128 = CARTESIAN_POINT ( 'NONE',  ( 9.564922557961047289, -16.46253265017146816, 105.4177570613523471 ) ) ;
#50129 = CARTESIAN_POINT ( 'NONE',  ( 16.52544592524342804, -4.483927247898539470, 113.5405762719810383 ) ) ;
#50130 = CARTESIAN_POINT ( 'NONE',  ( 4.379528057220092307, 16.55341960407617563, 77.29275706135234714 ) ) ;
#50131 = CARTESIAN_POINT ( 'NONE',  ( -16.55341960407617563, 4.379528057220093196, 73.54275706135234714 ) ) ;
#50132 = CARTESIAN_POINT ( 'NONE',  ( 0.000000000000000000, -105.0000000000000000, -23.00000000000000000 ) ) ;
#50133 = CARTESIAN_POINT ( 'NONE',  ( -5.153800228976607833, 19.02544592524334988, 72.70942372801900433 ) ) ;
#50134 = AXIS2_PLACEMENT_3D ( 'NONE', #148170, #166341, #135993 ) ;
#50135 = CARTESIAN_POINT ( 'NONE',  ( -21.53943276465977519, -0.05219959533937600094, 113.7510903946856757 ) ) ;
#50136 = CARTESIAN_POINT ( 'NONE',  ( 16.51473224551069308, 9.474510206698969483, 54.16557627198103120 ) ) ;
#50137 = CARTESIAN_POINT ( 'NONE',  ( 13.89961937509977652, -13.97604488694527269, 78.12390960531433848 ) ) ;
#50138 = CARTESIAN_POINT ( 'NONE',  ( -4.483927247898539470, -16.52544592524342804, 82.29057627198103830 ) ) ;
#50139 = CARTESIAN_POINT ( 'NONE',  ( 19.05341960407617918, -5.049401038297876454, 61.04275706135232582 ) ) ;
#50140 = CARTESIAN_POINT ( 'NONE',  ( -21.52544592524343514, 5.823673210054127303, 46.04057627198103830 ) ) ;
#50141 = CARTESIAN_POINT ( 'NONE',  ( 15.80617190586769283, -15.72974639402175789, 105.6260903946856899 ) ) ;
#50142 = CARTESIAN_POINT ( 'NONE',  ( 13.97604488694527802, 13.89961937509977652, 89.37390960531436690 ) ) ;
#50143 = CARTESIAN_POINT ( 'NONE',  ( 0.05219959533937995610, -21.53943276465977519, 105.0010903946856757 ) ) ;
#50144 = CARTESIAN_POINT ( 'NONE',  ( 21.52544592524344225, -5.823673210054117533, 58.54057627198103120 ) ) ;
#50145 = CARTESIAN_POINT ( 'NONE',  ( 19.02544592524343514, -5.153800228976328945, 103.5405762719809957 ) ) ;
#50146 = CARTESIAN_POINT ( 'NONE',  ( -19.03943276465977164, -0.05219959533935918106, 93.75109039468566152 ) ) ;
#50147 = CARTESIAN_POINT ( 'NONE',  ( -0.05219959533909027116, -19.03943276465977164, 107.4989096053143527 ) ) ;
#50148 = ADVANCED_FACE ( 'NONE', ( #81585 ), #184828, .T. ) ;
#50149 = CARTESIAN_POINT ( 'NONE',  ( -19.02544592524334988, -5.153800228976617603, 103.9594237280190043 ) ) ;
#50150 = CARTESIAN_POINT ( 'NONE',  ( 12.14591786802309770, 12.06949235617756955, 114.3739096053143527 ) ) ;
#50151 = CARTESIAN_POINT ( 'NONE',  ( -13.97604488694527625, -13.89961937509977652, 86.87390960531436690 ) ) ;
#50152 = CARTESIAN_POINT ( 'NONE',  ( -15.80617190586745835, -15.72974639402198527, 76.87390960531439532 ) ) ;
#50153 = CARTESIAN_POINT ( 'NONE',  ( 0.05219959533934541429, -16.53943276465976808, 40.00109039468567573 ) ) ;
#50154 = CARTESIAN_POINT ( 'NONE',  ( -18.67979575497193778, 10.72451020669871902, 48.33442372801902565 ) ) ;
#50155 = CARTESIAN_POINT ( 'NONE',  ( -18.67979575497193778, 10.72451020669871902, 103.3344237280190043 ) ) ;
#50156 = CARTESIAN_POINT ( 'NONE',  ( 16.53943276465976808, 0.05219959533934440121, 96.25109039468568994 ) ) ;
#50157 = CARTESIAN_POINT ( 'NONE',  ( -19.05341960407611168, -5.049401038298163336, 91.45724293864766707 ) ) ;
#50158 = CARTESIAN_POINT ( 'NONE',  ( -8.224510206698948167, 14.34966873604960824, 95.41557627198102409 ) ) ;
#50159 = CARTESIAN_POINT ( 'NONE',  ( -12.14591786802326823, 12.06949235617739902, 113.1260903946856899 ) ) ;
#50160 = CARTESIAN_POINT ( 'NONE',  ( -16.46253265017146816, -9.564922557961047289, 69.16775706135233293 ) ) ;
#50161 = CARTESIAN_POINT ( 'NONE',  ( -10.72451020669870658, -18.67979575497194134, 44.58442372801901854 ) ) ;
#50162 = EDGE_CURVE ( 'NONE', #23346, #48561, #35246, .T. ) ;
#50163 = CARTESIAN_POINT ( 'NONE',  ( 16.55341960407611168, 4.379528057220329451, 88.95724293864769550 ) ) ;
#50164 = CARTESIAN_POINT ( 'NONE',  ( -13.89961937509977652, 13.97604488694528158, 115.6239096053143669 ) ) ;
#50165 = CARTESIAN_POINT ( 'NONE',  ( 14.29746914071049879, -8.314922557960816363, 23.33224293864769194 ) ) ;
#50166 = CARTESIAN_POINT ( 'NONE',  ( -18.62759615963255300, -10.81492255796106328, 89.16775706135236135 ) ) ;
#50167 = CARTESIAN_POINT ( 'NONE',  ( -16.52544592524335698, -4.483927247898792601, 63.95942372801901854 ) ) ;
#50168 = CARTESIAN_POINT ( 'NONE',  ( 16.52544592524335698, 4.483927247898782831, 111.4594237280190328 ) ) ;
#50169 = CARTESIAN_POINT ( 'NONE',  ( -5.823673210054431948, 21.52544592524334988, 37.70942372801900433 ) ) ;
#50170 = ORIENTED_EDGE ( 'NONE', *, *, #5739, .T. ) ;
#50171 = CARTESIAN_POINT ( 'NONE',  ( 15.72974639402176855, 15.80617190586768217, 31.87609039468567929 ) ) ;
#50172 = CARTESIAN_POINT ( 'NONE',  ( 16.53943276465976808, -0.05219959533910856209, 103.7489096053143669 ) ) ;
#50173 = CARTESIAN_POINT ( 'NONE',  ( -13.97604488694527625, -13.89961937509977652, 26.87390960531434558 ) ) ;
#50174 = CARTESIAN_POINT ( 'NONE',  ( -14.34966873604960291, -8.224510206698953496, 61.66557627198103120 ) ) ;
#50175 = CARTESIAN_POINT ( 'NONE',  ( -13.97604488694527625, -13.89961937509977652, 71.87390960531433848 ) ) ;
#50176 = CARTESIAN_POINT ( 'NONE',  ( 16.55341960407618274, -4.379528057220086978, 101.0427570613523756 ) ) ;
#50177 = CARTESIAN_POINT ( 'NONE',  ( 19.02544592524343514, -5.153800228976328945, 38.54057627198103120 ) ) ;
#50178 = CARTESIAN_POINT ( 'NONE',  ( 21.52544592524344225, -5.823673210054117533, 43.54057627198103830 ) ) ;
#50179 = CARTESIAN_POINT ( 'NONE',  ( -14.34966873604960291, -8.224510206698953496, 91.66557627198103830 ) ) ;
#50180 = AXIS2_PLACEMENT_3D ( 'NONE', #69708, #42379, #101030 ) ;
#50181 = CARTESIAN_POINT ( 'NONE',  ( 15.80617190586746368, 15.72974639402197994, 89.37390960531435269 ) ) ;
#50182 = CARTESIAN_POINT ( 'NONE',  ( -19.05341960407611168, -5.049401038298163336, 86.45724293864769550 ) ) ;
#50184 = CARTESIAN_POINT ( 'NONE',  ( -19.05341960407617563, 5.049401038297882671, 88.54275706135230450 ) ) ;
#50183 = CARTESIAN_POINT ( 'NONE',  ( -19.03943276465977164, 0.05219959533909376836, 46.24890960531435979 ) ) ;
#50185 = CARTESIAN_POINT ( 'NONE',  ( -18.62759615963270932, 10.81492255796079327, 50.83224293864770971 ) ) ;
#50186 = CARTESIAN_POINT ( 'NONE',  ( -5.719274019375665041, -21.55341960407619695, 74.79275706135234714 ) ) ;
#50187 = CARTESIAN_POINT ( 'NONE',  ( -5.049401038298153566, 19.05341960407611168, 50.20724293864770260 ) ) ;
#50188 = CARTESIAN_POINT ( 'NONE',  ( 16.51473224551069308, 9.474510206698969483, 79.16557627198103830 ) ) ;
#50189 = ORIENTED_EDGE ( 'NONE', *, *, #92009, .F. ) ;
#50190 = CARTESIAN_POINT ( 'NONE',  ( -12.14591786802326823, 12.06949235617739902, 58.12609039468568994 ) ) ;
#50191 = CARTESIAN_POINT ( 'NONE',  ( -21.55341960407619339, 5.719274019375674811, 48.54275706135234714 ) ) ;
#50192 = EDGE_CURVE ( 'NONE', #57973, #60209, #149973, .T. ) ;
#50193 = CARTESIAN_POINT ( 'NONE',  ( -15.72974639402176322, -15.80617190586768395, 79.37609039468567573 ) ) ;
#50194 = CARTESIAN_POINT ( 'NONE',  ( -19.05341960407611168, -5.049401038298163336, 111.4572429386476671 ) ) ;
#50195 = CARTESIAN_POINT ( 'NONE',  ( 15.80617190586746368, 15.72974639402197994, 94.37390960531436690 ) ) ;
#50197 = CARTESIAN_POINT ( 'NONE',  ( -8.224510206698735004, -14.34966873604973081, 69.58442372801900433 ) ) ;
#50196 = CARTESIAN_POINT ( 'NONE',  ( -0.05219959533937732626, 21.53943276465977519, 42.50109039468567573 ) ) ;
#50198 = CARTESIAN_POINT ( 'NONE',  ( 10.81492255796078972, 18.62759615963270932, 59.58224293864770260 ) ) ;
#50199 = CARTESIAN_POINT ( 'NONE',  ( -5.153800228976607833, 19.02544592524334988, 37.70942372801899722 ) ) ;
#50200 = AXIS2_PLACEMENT_3D ( 'NONE', #36288, #112152, #53464 ) ;
#50202 = CARTESIAN_POINT ( 'NONE',  ( 12.06949235617739724, 12.14591786802326823, 106.8760903946856899 ) ) ;
#50201 = CARTESIAN_POINT ( 'NONE',  ( 19.05341960407611168, 5.049401038298154454, 73.95724293864768129 ) ) ;
#50203 = DIRECTION ( 'NONE',  ( 0.000000000000000000, 0.000000000000000000, -1.000000000000000000 ) ) ;
#50204 = CARTESIAN_POINT ( 'NONE',  ( -9.564922557960796823, -16.46253265017161027, 107.0822429386476955 ) ) ;
#50205 = DIRECTION ( 'NONE',  ( 0.000000000000000000, 0.000000000000000000, 1.000000000000000000 ) ) ;
#50206 = CARTESIAN_POINT ( 'NONE',  ( -19.03943276465977164, -0.05219959533935918106, 78.75109039468567573 ) ) ;
#50207 = CIRCLE ( 'NONE', #143405, 2.041999999999999815 ) ;
#50208 = CARTESIAN_POINT ( 'NONE',  ( -18.62759615963270932, 10.81492255796079327, 55.83224293864770260 ) ) ;
#50209 = CARTESIAN_POINT ( 'NONE',  ( -4.379528057220328563, 16.55341960407611168, 35.20724293864768839 ) ) ;
#50210 = CARTESIAN_POINT ( 'NONE',  ( -16.46253265017146816, -9.564922557961047289, 94.16775706135233293 ) ) ;
#50211 = CARTESIAN_POINT ( 'NONE',  ( 13.89961937509977652, -13.97604488694527269, 28.12390960531435624 ) ) ;
#50212 = CARTESIAN_POINT ( 'NONE',  ( -13.97604488694547697, 13.89961937509957934, 113.1260903946856757 ) ) ;
#50214 = CARTESIAN_POINT ( 'NONE',  ( 9.564922557961047289, -16.46253265017146816, 55.41775706135234003 ) ) ;
#50213 = CARTESIAN_POINT ( 'NONE',  ( -5.719274019375978568, 21.55341960407610458, 85.20724293864770971 ) ) ;
#50215 = CARTESIAN_POINT ( 'NONE',  ( -0.05219959533934338120, 16.53943276465976808, 82.50109039468568994 ) ) ;
#50216 = CARTESIAN_POINT ( 'NONE',  ( -13.89961937509977652, 13.97604488694528158, 65.62390960531436690 ) ) ;
#50217 = CARTESIAN_POINT ( 'NONE',  ( -14.34966873604960291, -8.224510206698953496, 76.66557627198103830 ) ) ;
#50218 = CARTESIAN_POINT ( 'NONE',  ( -0.05219959533909027116, -19.03943276465977164, 47.49890960531435979 ) ) ;
#50219 = CARTESIAN_POINT ( 'NONE',  ( 12.14591786802309770, 12.06949235617756955, 49.37390960531436690 ) ) ;
#50220 = CARTESIAN_POINT ( 'NONE',  ( -6.019987952026119621E-15, 39.95163481335720235, -6.247842220587802586 ) ) ;
#50221 = CARTESIAN_POINT ( 'NONE',  ( 32.50820986112747590, -2.649538386493603515, 87.97934651352352375 ) ) ;
#50222 = CARTESIAN_POINT ( 'NONE',  ( -12.14591786802309592, -12.06949235617757132, 26.87390960531435979 ) ) ;
#50223 = CARTESIAN_POINT ( 'NONE',  ( 0.05219959533909260263, 19.03943276465977164, 74.99890960531435269 ) ) ;
#50224 = DIRECTION ( 'NONE',  ( 0.8164965809277242581, 0.000000000000000000, -0.5773502691896281735 ) ) ;
#50225 = CARTESIAN_POINT ( 'NONE',  ( 19.03943276465977164, 0.05219959533936151252, 36.25109039468567573 ) ) ;
#50226 = CARTESIAN_POINT ( 'NONE',  ( -4.483927247898782831, 16.52544592524335698, 52.70942372801902565 ) ) ;
#50227 = CARTESIAN_POINT ( 'NONE',  ( -15.72974639402197994, 15.80617190586746368, 50.62390960531435979 ) ) ;
#50228 = CARTESIAN_POINT ( 'NONE',  ( -10.81492255796105439, 18.62759615963255655, 112.9177570613523329 ) ) ;
#50229 = CARTESIAN_POINT ( 'NONE',  ( -19.03943276465977164, 0.05219959533909376836, 76.24890960531435269 ) ) ;
#50230 = CARTESIAN_POINT ( 'NONE',  ( -5.049401038298153566, 19.05341960407611168, 115.2072429386477097 ) ) ;
#50231 = CARTESIAN_POINT ( 'NONE',  ( -0.05219959533909027116, -19.03943276465977164, 107.4989096053143527 ) ) ;
#50232 = CARTESIAN_POINT ( 'NONE',  ( -5.719274019375665041, -21.55341960407619695, 44.79275706135234714 ) ) ;
#50233 = CARTESIAN_POINT ( 'NONE',  ( -4.483927247898539470, -16.52544592524342804, 112.2905762719810241 ) ) ;
#50236 = EDGE_LOOP ( 'NONE', ( #27782, #81088 ) ) ;
#50235 = CARTESIAN_POINT ( 'NONE',  ( -19.03943276465977164, 0.05219959533909376836, 76.24890960531435269 ) ) ;
#50234 = CARTESIAN_POINT ( 'NONE',  ( -18.62759615963270932, 10.81492255796079327, 100.8322429386477097 ) ) ;
#50237 = CARTESIAN_POINT ( 'NONE',  ( -0.05219959533937732626, 21.53943276465977519, 32.50109039468568284 ) ) ;
#50238 = VERTEX_POINT ( 'NONE', #127109 ) ;
#50239 = CARTESIAN_POINT ( 'NONE',  ( 19.05341960407611168, 5.049401038298154454, 83.95724293864766707 ) ) ;
#50240 = CARTESIAN_POINT ( 'NONE',  ( 19.52837319214028611, -5.499999999999892530, 82.10471352585541638 ) ) ;
#50242 = CARTESIAN_POINT ( 'NONE',  ( -13.89961937509977652, 13.97604488694528158, 30.62390960531435269 ) ) ;
#50241 = CARTESIAN_POINT ( 'NONE',  ( -16.53943276465976808, 0.05219959533911058130, 116.2489096053143669 ) ) ;
#50243 = CARTESIAN_POINT ( 'NONE',  ( -19.02544592524334988, -5.153800228976617603, 103.9594237280190043 ) ) ;
#50244 = CARTESIAN_POINT ( 'NONE',  ( -11.40812507854755609, 35.11059874428196537, -9.524999997268816188 ) ) ;
#50245 = CARTESIAN_POINT ( 'NONE',  ( -8.224510206698948167, 14.34966873604960824, 115.4155762719810241 ) ) ;
#50246 = CARTESIAN_POINT ( 'NONE',  ( 10.81492255796106328, -18.62759615963255655, 80.41775706135234714 ) ) ;
#50248 = CARTESIAN_POINT ( 'NONE',  ( -0.05219959533937732626, 21.53943276465977519, 27.50109039468567929 ) ) ;
#50247 = CARTESIAN_POINT ( 'NONE',  ( -19.05341960407611168, -5.049401038298163336, 56.45724293864768129 ) ) ;
#50249 = CARTESIAN_POINT ( 'NONE',  ( 10.72451020669871369, 18.67979575497193778, 32.08442372801901854 ) ) ;
#50250 = CARTESIAN_POINT ( 'NONE',  ( 28.82186960331498327, 2.781578969918950771E-14, 147.0000000000000000 ) ) ;
#50251 = CARTESIAN_POINT ( 'NONE',  ( 19.05341960407611168, 5.049401038298154454, 83.95724293864766707 ) ) ;
#50252 = CARTESIAN_POINT ( 'NONE',  ( 24.81492239413702805, 12.70475479534830043, 139.9999999999999716 ) ) ;
#50254 = CARTESIAN_POINT ( 'NONE',  ( 21.55341960407610458, 5.719274019375980345, 38.95724293864768839 ) ) ;
#50253 = CARTESIAN_POINT ( 'NONE',  ( -8.224510206698735004, -14.34966873604973081, 29.58442372801901854 ) ) ;
#50255 = CARTESIAN_POINT ( 'NONE',  ( -18.62759615963255300, -10.81492255796106328, 74.16775706135231871 ) ) ;
#50256 = CARTESIAN_POINT ( 'NONE',  ( -16.51473224551069308, -9.474510206698971260, 106.6655762719810383 ) ) ;
#50257 = CARTESIAN_POINT ( 'NONE',  ( -19.03943276465977164, -0.05219959533935918106, 93.75109039468566152 ) ) ;
#50258 = CARTESIAN_POINT ( 'NONE',  ( -19.02544592524342804, 5.153800228976336051, 61.04057627198103120 ) ) ;
#50259 = CARTESIAN_POINT ( 'NONE',  ( -5.049401038298153566, 19.05341960407611168, 85.20724293864766707 ) ) ;
#50260 = CARTESIAN_POINT ( 'NONE',  ( 16.52544592524342804, -4.483927247898539470, 88.54057627198103830 ) ) ;
#50261 = CARTESIAN_POINT ( 'NONE',  ( 16.52544592524342804, -4.483927247898539470, 103.5405762719810383 ) ) ;
#50262 = CARTESIAN_POINT ( 'NONE',  ( -13.89961937509977652, 13.97604488694528158, 105.6239096053143527 ) ) ;
#50263 = CARTESIAN_POINT ( 'NONE',  ( 14.34966873604972726, -8.224510206698740333, 75.83442372801900433 ) ) ;
#50265 = CARTESIAN_POINT ( 'NONE',  ( 9.564922557960805705, 16.46253265017160317, 44.58224293864769550 ) ) ;
#50264 = CARTESIAN_POINT ( 'NONE',  ( 4.483927247898545687, 16.52544592524342804, 54.79057627198104541 ) ) ;
#50266 = CARTESIAN_POINT ( 'NONE',  ( -5.719274019375665041, -21.55341960407619695, 69.79275706135234714 ) ) ;
#50267 = CARTESIAN_POINT ( 'NONE',  ( 13.97604488694548053, -13.89961937509957401, 95.62609039468563310 ) ) ;
#50268 = CARTESIAN_POINT ( 'NONE',  ( 8.314922557960818139, 14.29746914071049879, 64.58224293864769550 ) ) ;
#50269 = CARTESIAN_POINT ( 'NONE',  ( 18.62759615963255655, 10.81492255796105972, 21.66775706135235069 ) ) ;
#50270 = CARTESIAN_POINT ( 'NONE',  ( -15.72974639402197994, 15.80617190586746368, 50.62390960531435979 ) ) ;
#50271 = CARTESIAN_POINT ( 'NONE',  ( 23.31738231874054890, -16.94106989632523508, 140.7999999999999829 ) ) ;
#50272 = CARTESIAN_POINT ( 'NONE',  ( 8.906447517083057264, -27.41122689804191026, 142.8500000054623911 ) ) ;
#50273 = CARTESIAN_POINT ( 'NONE',  ( 19.05341960407611168, 5.049401038298154454, 73.95724293864768129 ) ) ;
#50274 = CARTESIAN_POINT ( 'NONE',  ( -12.14591786802309592, -12.06949235617757132, 36.87390960531435979 ) ) ;
#50275 = CARTESIAN_POINT ( 'NONE',  ( 12.06949235617739724, 12.14591786802326823, 111.8760903946856615 ) ) ;
#50276 = CARTESIAN_POINT ( 'NONE',  ( 4.379528057220092307, 16.55341960407617563, 87.29275706135236135 ) ) ;
#50278 = ADVANCED_FACE ( 'NONE', ( #173645 ), #35114, .F. ) ;
#50277 = CARTESIAN_POINT ( 'NONE',  ( 5.153800228976615827, -19.02544592524334988, 35.20942372801899722 ) ) ;
#50279 = CARTESIAN_POINT ( 'NONE',  ( 193.3062444957835453, -155.7167183371837496, -4.999999999999999112 ) ) ;
#50280 = CARTESIAN_POINT ( 'NONE',  ( -13.97604488694527625, -13.89961937509977652, 96.87390960531433848 ) ) ;
#50281 = CARTESIAN_POINT ( 'NONE',  ( -8.314922557960811034, -14.29746914071050412, 67.08224293864770971 ) ) ;
#50283 = CARTESIAN_POINT ( 'NONE',  ( -18.67979575497178146, -10.72451020669898902, 21.66557627198102409 ) ) ;
#50282 = CARTESIAN_POINT ( 'NONE',  ( 0.05219959533909260263, 19.03943276465977164, 24.99890960531435269 ) ) ;
#50285 = VERTEX_POINT ( 'NONE', #55270 ) ;
#50284 = CARTESIAN_POINT ( 'NONE',  ( -5.719274019375978568, 21.55341960407610458, 50.20724293864769550 ) ) ;
#50286 = CARTESIAN_POINT ( 'NONE',  ( 16.53943276465976808, -0.05219959533910856209, 78.74890960531436690 ) ) ;
#50287 = CARTESIAN_POINT ( 'NONE',  ( -16.52544592524335698, -4.483927247898792601, 33.95942372801901143 ) ) ;
#50288 = CARTESIAN_POINT ( 'NONE',  ( 12.06949235617757843, -12.14591786802309237, 83.12390960531436690 ) ) ;
#50289 = CARTESIAN_POINT ( 'NONE',  ( -17.49999999999999645, -5.500000000000000888, 120.0000000000000142 ) ) ;
#50290 = CARTESIAN_POINT ( 'NONE',  ( -19.02544592524334988, -5.153800228976617603, 83.95942372801901854 ) ) ;
#50291 = CARTESIAN_POINT ( 'NONE',  ( -5.719274019375978568, 21.55341960407610458, 25.20724293864769550 ) ) ;
#50292 = CARTESIAN_POINT ( 'NONE',  ( 29.86685920354754487, 21.69954338932564752, -1.924999997268813212 ) ) ;
#50293 = CARTESIAN_POINT ( 'NONE',  ( -28.82186960331518932, -9.364793116373263615, 142.0999999999999943 ) ) ;
#50295 = CARTESIAN_POINT ( 'NONE',  ( 16.52544592524342804, -4.483927247898539470, 33.54057627198102409 ) ) ;
#50294 = CARTESIAN_POINT ( 'NONE',  ( 4.379528057220092307, 16.55341960407617563, 27.29275706135234358 ) ) ;
#50296 = CARTESIAN_POINT ( 'NONE',  ( 19.02544592524334988, 5.153800228976608722, 66.45942372801899012 ) ) ;
#50297 = CARTESIAN_POINT ( 'NONE',  ( 5.719274019375991003, -21.55341960407610458, 47.70724293864770260 ) ) ;
#50298 = CARTESIAN_POINT ( 'NONE',  ( -18.67979575497193778, 10.72451020669871902, 68.33442372801900433 ) ) ;
#50299 = CARTESIAN_POINT ( 'NONE',  ( -12.25159394783734434, 10.91551912637959276, -61.48002405683646288 ) ) ;
#50300 = CARTESIAN_POINT ( 'NONE',  ( -12.14591786802326823, 12.06949235617739902, 33.12609039468569705 ) ) ;
#50302 = CARTESIAN_POINT ( 'NONE',  ( 16.46253265017160672, -9.564922557960803928, 83.33224293864768129 ) ) ;
#50301 = CARTESIAN_POINT ( 'NONE',  ( -13.89961937509977652, 13.97604488694528158, 25.62390960531434558 ) ) ;
#50303 = CARTESIAN_POINT ( 'NONE',  ( 19.03943276465977164, -0.05219959533909143690, 28.74890960531435624 ) ) ;
#50304 = CARTESIAN_POINT ( 'NONE',  ( 16.55341960407611168, 4.379528057220329451, 98.95724293864770971 ) ) ;
#50305 = APPLICATION_PROTOCOL_DEFINITION ( 'draft international standard', 'automotive_design', 1998, #50677 ) ;
#50306 = CARTESIAN_POINT ( 'NONE',  ( 16.51473224551069308, 9.474510206698969483, 104.1655762719810241 ) ) ;
#50307 = ORIENTED_EDGE ( 'NONE', *, *, #199845, .T. ) ;
#50308 = CARTESIAN_POINT ( 'NONE',  ( -4.483927247898782831, 16.52544592524335698, 57.70942372801901143 ) ) ;
#50309 = CARTESIAN_POINT ( 'NONE',  ( 16.51473224551083163, -9.474510206698727899, 110.8344237280190043 ) ) ;
#50310 = CARTESIAN_POINT ( 'NONE',  ( 18.62759615963271287, -10.81492255796078972, 73.33224293864769550 ) ) ;
#50311 = CARTESIAN_POINT ( 'NONE',  ( 16.51473224551069308, 9.474510206698969483, 44.16557627198103120 ) ) ;
#50313 = CARTESIAN_POINT ( 'NONE',  ( 10.72451020669898902, -18.67979575497178502, 107.9155762719810241 ) ) ;
#50312 = CARTESIAN_POINT ( 'NONE',  ( 16.51473224551083163, -9.474510206698727899, 70.83442372801900433 ) ) ;
#50314 = CARTESIAN_POINT ( 'NONE',  ( -13.97604488694527625, -13.89961937509977652, 66.87390960531436690 ) ) ;
#50316 = EDGE_CURVE ( 'NONE', #133003, #43212, #23073, .T. ) ;
#50315 = CARTESIAN_POINT ( 'NONE',  ( -9.474510206698964154, 16.51473224551069663, 100.4155762719810241 ) ) ;
#50317 = ORIENTED_EDGE ( 'NONE', *, *, #157780, .F. ) ;
#50318 = CARTESIAN_POINT ( 'NONE',  ( 16.55341960407618274, -4.379528057220086978, 36.04275706135234714 ) ) ;
#50319 = CARTESIAN_POINT ( 'NONE',  ( 10.72451020669898902, -18.67979575497178502, 97.91557627198103830 ) ) ;
#50322 = CARTESIAN_POINT ( 'NONE',  ( -16.51473224551082808, 9.474510206698731452, 78.33442372801900433 ) ) ;
#50321 = CARTESIAN_POINT ( 'NONE',  ( 19.03943276465977164, -0.05219959533909143690, 88.74890960531436690 ) ) ;
#50320 = CARTESIAN_POINT ( 'NONE',  ( -12.06949235617756955, 12.14591786802309770, 110.6239096053143669 ) ) ;
#50323 = CARTESIAN_POINT ( 'NONE',  ( -15.72974639402197994, 15.80617190586746368, 80.62390960531438111 ) ) ;
#50324 = CARTESIAN_POINT ( 'NONE',  ( 4.379528057220339221, -16.55341960407611168, 47.70724293864770260 ) ) ;
#50325 = CARTESIAN_POINT ( 'NONE',  ( -21.53943276465977519, -0.05219959533937600094, 113.7510903946856757 ) ) ;
#50326 = CARTESIAN_POINT ( 'NONE',  ( -4.483927247898782831, 16.52544592524335698, 77.70942372801900433 ) ) ;
#50327 = CARTESIAN_POINT ( 'NONE',  ( 19.05341960407611168, 5.049401038298154454, 88.95724293864769550 ) ) ;
#50328 = CARTESIAN_POINT ( 'NONE',  ( -13.97604488694527625, -13.89961937509977652, 51.87390960531436690 ) ) ;
#50329 = CARTESIAN_POINT ( 'NONE',  ( -15.80617190586768217, 15.72974639402176855, 58.12609039468568994 ) ) ;
#50330 = CARTESIAN_POINT ( 'NONE',  ( 5.823673210054444382, -21.52544592524334988, 70.20942372801904696 ) ) ;
#50331 = CARTESIAN_POINT ( 'NONE',  ( -9.564922557960796823, -16.46253265017161027, 67.08224293864769550 ) ) ;
#50332 = CARTESIAN_POINT ( 'NONE',  ( -5.719274019375665041, -21.55341960407619695, 34.79275706135235424 ) ) ;
#50333 = CARTESIAN_POINT ( 'NONE',  ( 16.46253265017146816, 9.564922557961045513, 91.66775706135234714 ) ) ;
#50334 = CARTESIAN_POINT ( 'NONE',  ( -16.46253265017160317, 9.564922557960807481, 35.83224293864768839 ) ) ;
#50335 = CARTESIAN_POINT ( 'NONE',  ( -4.379528057220086978, -16.55341960407618274, 84.79275706135234714 ) ) ;
#50336 = CARTESIAN_POINT ( 'NONE',  ( -0.05219959533909027116, -19.03943276465977164, 62.49890960531435979 ) ) ;
#50337 = CARTESIAN_POINT ( 'NONE',  ( 9.474510206698971260, -16.51473224551069308, 107.9155762719810383 ) ) ;
#50338 = CARTESIAN_POINT ( 'NONE',  ( -9.564922557960796823, -16.46253265017161027, 37.08224293864768839 ) ) ;
#50339 = CARTESIAN_POINT ( 'NONE',  ( -10.72451020669898014, 18.67979575497178502, 80.41557627198103830 ) ) ;
#50340 = CARTESIAN_POINT ( 'NONE',  ( -4.483927247898782831, 16.52544592524335698, 77.70942372801900433 ) ) ;
#50341 = CARTESIAN_POINT ( 'NONE',  ( -24.81886791266634873, 6.075537473402705224, 168.3989613422507432 ) ) ;
#50342 = CARTESIAN_POINT ( 'NONE',  ( -13.97604488694547697, 13.89961937509957934, 33.12609039468566863 ) ) ;
#50343 = CARTESIAN_POINT ( 'NONE',  ( 19.05341960407611168, 5.049401038298154454, 68.95724293864769550 ) ) ;
#50344 = CARTESIAN_POINT ( 'NONE',  ( -14.34966873604960291, -8.224510206698953496, 46.66557627198102409 ) ) ;
#50345 = CARTESIAN_POINT ( 'NONE',  ( -16.53943276465976808, 0.05219959533911058130, 81.24890960531436690 ) ) ;
#50346 = CARTESIAN_POINT ( 'NONE',  ( -19.02544592524342804, 5.153800228976336051, 101.0405762719810241 ) ) ;
#50347 = CARTESIAN_POINT ( 'NONE',  ( 19.02544592524343514, -5.153800228976328945, 93.54057627198102409 ) ) ;
#50348 = CARTESIAN_POINT ( 'NONE',  ( -21.55341960407619339, 5.719274019375674811, 48.54275706135234714 ) ) ;
#50349 = CARTESIAN_POINT ( 'NONE',  ( 16.51473224551069308, 9.474510206698969483, 109.1655762719810383 ) ) ;
#50350 = CARTESIAN_POINT ( 'NONE',  ( -21.52544592524334988, -5.823673210054445271, 108.9594237280190185 ) ) ;
#50351 = CARTESIAN_POINT ( 'NONE',  ( -14.29746914071037622, -8.314922557961029526, 79.16775706135234714 ) ) ;
#50352 = CARTESIAN_POINT ( 'NONE',  ( 10.72451020669871369, 18.67979575497193778, 27.08442372801901854 ) ) ;
#50353 = CARTESIAN_POINT ( 'NONE',  ( 13.89961937509977652, -13.97604488694527269, 108.1239096053143669 ) ) ;
#50354 = CARTESIAN_POINT ( 'NONE',  ( 5.719274019375991003, -21.55341960407610458, 107.7072429386476955 ) ) ;
#50355 = CARTESIAN_POINT ( 'NONE',  ( 8.314922557960818139, 14.29746914071049879, 64.58224293864769550 ) ) ;
#50356 = CARTESIAN_POINT ( 'NONE',  ( 5.049401038298161559, -19.05341960407611168, 47.70724293864770260 ) ) ;
#50357 = CARTESIAN_POINT ( 'NONE',  ( -4.379528057220328563, 16.55341960407611168, 80.20724293864769550 ) ) ;
#50358 = CARTESIAN_POINT ( 'NONE',  ( 5.823673210054125526, 21.52544592524343514, 29.79057627198102409 ) ) ;
#50359 = CARTESIAN_POINT ( 'NONE',  ( 19.05341960407617918, -5.049401038297876454, 26.04275706135233293 ) ) ;
#50360 = CARTESIAN_POINT ( 'NONE',  ( 16.46253265017160672, -9.564922557960803928, 23.33224293864769194 ) ) ;
#50361 = ORIENTED_EDGE ( 'NONE', *, *, #133623, .T. ) ;
#50362 = CARTESIAN_POINT ( 'NONE',  ( 14.34966873604972726, -8.224510206698740333, 60.83442372801901854 ) ) ;
#50363 = CARTESIAN_POINT ( 'NONE',  ( 9.564922557960805705, 16.46253265017160317, 64.58224293864769550 ) ) ;
#50364 = CARTESIAN_POINT ( 'NONE',  ( -22.44159573604010305, 16.30477369853692338, 146.6750000027311671 ) ) ;
#50365 = CARTESIAN_POINT ( 'NONE',  ( 14.29746914071049879, -8.314922557960816363, 88.33224293864769550 ) ) ;
#50366 = CARTESIAN_POINT ( 'NONE',  ( -10.81492255796078084, -18.62759615963271287, 37.08224293864768129 ) ) ;
#50367 = CARTESIAN_POINT ( 'NONE',  ( -12.14591786802326823, 12.06949235617739902, 113.1260903946856899 ) ) ;
#50368 = CARTESIAN_POINT ( 'NONE',  ( 0.05219959533936267826, -19.03943276465977164, 110.0010903946856757 ) ) ;
#50369 = CARTESIAN_POINT ( 'NONE',  ( -10.81492255796105439, 18.62759615963255655, 77.91775706135231871 ) ) ;
#50370 = CARTESIAN_POINT ( 'NONE',  ( 16.46253265017160672, -9.564922557960803928, 83.33224293864768129 ) ) ;
#50371 = CARTESIAN_POINT ( 'NONE',  ( -10.81492255796078084, -18.62759615963271287, 107.0822429386476955 ) ) ;
#50372 = CARTESIAN_POINT ( 'NONE',  ( 8.224510206698742110, 14.34966873604972548, 57.08442372801901854 ) ) ;
#50373 = CARTESIAN_POINT ( 'NONE',  ( 9.564922557960805705, 16.46253265017160317, 34.58224293864770260 ) ) ;
#50374 = CIRCLE ( 'NONE', #150556, 6.100000000000006750 ) ;
#50375 = CARTESIAN_POINT ( 'NONE',  ( 16.55341960407618274, -4.379528057220086978, 31.04275706135234714 ) ) ;
#50376 = CARTESIAN_POINT ( 'NONE',  ( -19.02544592524334988, -5.153800228976617603, 93.95942372801900433 ) ) ;
#50377 = CARTESIAN_POINT ( 'NONE',  ( 5.719274019375991003, -21.55341960407610458, 87.70724293864769550 ) ) ;
#50378 = CARTESIAN_POINT ( 'NONE',  ( 16.51473224551083163, -9.474510206698727899, 50.83442372801899722 ) ) ;
#50379 = CARTESIAN_POINT ( 'NONE',  ( 19.01533133064925352, -5.499999999999441336, 86.26586590595742621 ) ) ;
#50380 = CARTESIAN_POINT ( 'NONE',  ( 21.55341960407610458, 5.719274019375980345, 103.9572429386476813 ) ) ;
#50381 = CARTESIAN_POINT ( 'NONE',  ( 8.906447517083057264, -27.41122689804191026, 148.5999999999999943 ) ) ;
#50382 = CARTESIAN_POINT ( 'NONE',  ( 13.97604488694527802, 13.89961937509977652, 74.37390960531436690 ) ) ;
#50383 = CARTESIAN_POINT ( 'NONE',  ( 0.000000000000000000, 0.000000000000000000, -15.00000000000000000 ) ) ;
#50384 = CARTESIAN_POINT ( 'NONE',  ( 12.14591786802327356, -12.06949235617739191, 35.62609039468568994 ) ) ;
#50385 = CARTESIAN_POINT ( 'NONE',  ( 36.80065496640121836, -5.465942522010069027, 45.70922642070194541 ) ) ;
#50387 = CARTESIAN_POINT ( 'NONE',  ( 14.29746914071049879, -8.314922557960816363, 68.33224293864769550 ) ) ;
#50386 = CARTESIAN_POINT ( 'NONE',  ( -15.72974639402176322, -15.80617190586768395, 19.37609039468568639 ) ) ;
#50388 = CARTESIAN_POINT ( 'NONE',  ( -19.02544592524342804, 5.153800228976336051, 66.04057627198103830 ) ) ;
#50390 = CARTESIAN_POINT ( 'NONE',  ( 5.153800228976615827, -19.02544592524334988, 45.20942372801901143 ) ) ;
#50389 = CARTESIAN_POINT ( 'NONE',  ( -8.314922557961024197, 14.29746914071037800, 37.91775706135235424 ) ) ;
#50391 = CARTESIAN_POINT ( 'NONE',  ( -15.80617190586768217, 15.72974639402176855, 48.12609039468568284 ) ) ;
#50392 = CARTESIAN_POINT ( 'NONE',  ( -9.564922557961040184, 16.46253265017147172, 107.9177570613523471 ) ) ;
#50393 = CARTESIAN_POINT ( 'NONE',  ( -13.89961937509977652, 13.97604488694528158, 60.62390960531436690 ) ) ;
#50394 = CARTESIAN_POINT ( 'NONE',  ( 5.153800228976615827, -19.02544592524334988, 85.20942372801900433 ) ) ;
#50395 = CARTESIAN_POINT ( 'NONE',  ( -21.55341960407619339, 5.719274019375674811, 83.54275706135234714 ) ) ;
#50396 = CARTESIAN_POINT ( 'NONE',  ( -19.03943276465977164, -0.05219959533935918106, 63.75109039468566863 ) ) ;
#50397 = CARTESIAN_POINT ( 'NONE',  ( 5.049401038298161559, -19.05341960407611168, 37.70724293864768839 ) ) ;
#50398 = CARTESIAN_POINT ( 'NONE',  ( -21.52544592524343514, 5.823673210054127303, 61.04057627198103120 ) ) ;
#50400 = CARTESIAN_POINT ( 'NONE',  ( 13.97604488694548053, -13.89961937509957401, 70.62609039468567573 ) ) ;
#50399 = CARTESIAN_POINT ( 'NONE',  ( -12.06949235617756955, 12.14591786802309770, 60.62390960531437401 ) ) ;
#50401 = CARTESIAN_POINT ( 'NONE',  ( 4.000000000000000888, -165.0000000000000000, 12.00000000000000355 ) ) ;
#50402 = CARTESIAN_POINT ( 'NONE',  ( 9.474510206698729675, 16.51473224551082808, 27.08442372801900433 ) ) ;
#50403 = CARTESIAN_POINT ( 'NONE',  ( 4.483927247898790824, -16.52544592524335698, 100.2094237280190043 ) ) ;
#50404 = CARTESIAN_POINT ( 'NONE',  ( -16.55341960407611168, -4.379528057220339221, 51.45724293864770260 ) ) ;
#50406 = CARTESIAN_POINT ( 'NONE',  ( -27.73933785331498925, 2.428612866367529932E-14, 140.8750000027311842 ) ) ;
#50405 = CARTESIAN_POINT ( 'NONE',  ( -10.81492255796105439, 18.62759615963255655, 87.91775706135234714 ) ) ;
#50407 = CARTESIAN_POINT ( 'NONE',  ( 21.55341960407619695, -5.719274019375665929, 91.04275706135236135 ) ) ;
#50408 = CARTESIAN_POINT ( 'NONE',  ( -10.72451020669898014, 18.67979575497178502, 90.41557627198103830 ) ) ;
#50409 = CARTESIAN_POINT ( 'NONE',  ( 9.564922557960805705, 16.46253265017160317, 49.58224293864770260 ) ) ;
#50410 = CARTESIAN_POINT ( 'NONE',  ( -18.67979575497193778, 10.72451020669871902, 68.33442372801900433 ) ) ;
#50411 = CARTESIAN_POINT ( 'NONE',  ( 19.03943276465977164, -0.05219959533909143690, 48.74890960531435979 ) ) ;
#50412 = CARTESIAN_POINT ( 'NONE',  ( -0.05219959533909027116, -19.03943276465977164, 62.49890960531435979 ) ) ;
#50413 = CARTESIAN_POINT ( 'NONE',  ( 12.06949235617757843, -12.14591786802309237, 103.1239096053143811 ) ) ;
#50414 = CARTESIAN_POINT ( 'NONE',  ( 16.51473224551069308, 9.474510206698969483, 114.1655762719810241 ) ) ;
#50415 = AXIS2_PLACEMENT_3D ( 'NONE', #184297, #105463, #154940 ) ;
#50416 = CARTESIAN_POINT ( 'NONE',  ( 14.29746914071049879, -8.314922557960816363, 58.33224293864768839 ) ) ;
#50417 = CARTESIAN_POINT ( 'NONE',  ( -16.51473224551069308, -9.474510206698971260, 36.66557627198102409 ) ) ;
#50418 = CARTESIAN_POINT ( 'NONE',  ( -4.379528057220328563, 16.55341960407611168, 70.20724293864769550 ) ) ;
#50419 = CARTESIAN_POINT ( 'NONE',  ( 15.72974639402199770, -15.80617190586745480, 98.12390960531436690 ) ) ;
#50420 = CARTESIAN_POINT ( 'NONE',  ( 10.72451020669871369, 18.67979575497193778, 42.08442372801901854 ) ) ;
#50421 = CARTESIAN_POINT ( 'NONE',  ( 28.82186960331498327, 2.781578969918950771E-14, 149.0000000000000000 ) ) ;
#50422 = CARTESIAN_POINT ( 'NONE',  ( -12.14591786802326823, 12.06949235617739902, 33.12609039468569705 ) ) ;
#50423 = CARTESIAN_POINT ( 'NONE',  ( 5.823673210054125526, 21.52544592524343514, 79.79057627198102409 ) ) ;
#50424 = CARTESIAN_POINT ( 'NONE',  ( 10.81492255796106328, -18.62759615963255655, 110.4177570613523756 ) ) ;
#50425 = CARTESIAN_POINT ( 'NONE',  ( -5.153800228976328057, -19.02544592524343514, 87.29057627198103830 ) ) ;
#50426 = CARTESIAN_POINT ( 'NONE',  ( -21.53943276465977519, -0.05219959533937600094, 43.75109039468568284 ) ) ;
#50427 = CARTESIAN_POINT ( 'NONE',  ( 10.81492255796078972, 18.62759615963270932, 34.58224293864770260 ) ) ;
#50428 = CARTESIAN_POINT ( 'NONE',  ( 16.55341960407618274, -4.379528057220086978, 106.0427570613523471 ) ) ;
#50430 = CARTESIAN_POINT ( 'NONE',  ( 10.81492255796106328, -18.62759615963255655, 90.41775706135236135 ) ) ;
#50429 = CARTESIAN_POINT ( 'NONE',  ( 21.53943276465977519, 0.05219959533937863772, 46.25109039468567573 ) ) ;
#50431 = CARTESIAN_POINT ( 'NONE',  ( -5.719274019375665041, -21.55341960407619695, 109.7927570613523613 ) ) ;
#50432 = CARTESIAN_POINT ( 'NONE',  ( 4.483927247898790824, -16.52544592524335698, 85.20942372801901854 ) ) ;
#50433 = CARTESIAN_POINT ( 'NONE',  ( -21.53943276465977519, -0.05219959533937600094, 43.75109039468568284 ) ) ;
#50434 = CARTESIAN_POINT ( 'NONE',  ( 13.89961937509977652, -13.97604488694527269, 33.12390960531434558 ) ) ;
#50435 = CARTESIAN_POINT ( 'NONE',  ( 15.72974639402176855, 15.80617190586768217, 101.8760903946857042 ) ) ;
#50436 = CARTESIAN_POINT ( 'NONE',  ( 9.474510206698971260, -16.51473224551069308, 102.9155762719810241 ) ) ;
#50437 = CARTESIAN_POINT ( 'NONE',  ( -15.72974639402197994, 15.80617190586746368, 100.6239096053143811 ) ) ;
#50439 = CARTESIAN_POINT ( 'NONE',  ( -5.823673210054116645, -21.52544592524344225, 72.29057627198102409 ) ) ;
#50438 = DIRECTION ( 'NONE',  ( 6.391086490440865492E-16, 1.000000000000000000, -0.000000000000000000 ) ) ;
#50441 = CARTESIAN_POINT ( 'NONE',  ( -14.34966873604960291, -8.224510206698953496, 66.66557627198102409 ) ) ;
#50440 = CARTESIAN_POINT ( 'NONE',  ( 0.05219959533934541429, -16.53943276465976808, 50.00109039468568994 ) ) ;
#50442 = CARTESIAN_POINT ( 'NONE',  ( 18.93472913878447983, -5.500000000000005329, 101.2198988386846423 ) ) ;
#50443 = CARTESIAN_POINT ( 'NONE',  ( 5.049401038297881783, 19.05341960407617563, 87.29275706135234714 ) ) ;
#50444 = CARTESIAN_POINT ( 'NONE',  ( 24.49873734152912874, -24.99873734152920690, 5.353553390593267736 ) ) ;
#50445 = CARTESIAN_POINT ( 'NONE',  ( -8.314922557961024197, 14.29746914071037800, 27.91775706135234358 ) ) ;
#50446 = CARTESIAN_POINT ( 'NONE',  ( -10.81492255796078084, -18.62759615963271287, 92.08224293864769550 ) ) ;
#50447 = CARTESIAN_POINT ( 'NONE',  ( -21.52544592524343514, 5.823673210054127303, 76.04057627198102409 ) ) ;
#50448 = CARTESIAN_POINT ( 'NONE',  ( 13.97604488694527802, 13.89961937509977652, 109.3739096053143669 ) ) ;
#50449 = CARTESIAN_POINT ( 'NONE',  ( 8.224510206698742110, 14.34966873604972548, 62.08442372801901143 ) ) ;
#50450 = CARTESIAN_POINT ( 'NONE',  ( -19.05341960407611168, -5.049401038298163336, 76.45724293864769550 ) ) ;
#50452 = CARTESIAN_POINT ( 'NONE',  ( -5.153800228976607833, 19.02544592524334988, 102.7094237280189759 ) ) ;
#50451 = CARTESIAN_POINT ( 'NONE',  ( 21.52544592524334988, 5.823673210054432836, 31.45942372801901854 ) ) ;
#50453 = CARTESIAN_POINT ( 'NONE',  ( -9.564922557960796823, -16.46253265017161027, 107.0822429386476955 ) ) ;
#50454 = CARTESIAN_POINT ( 'NONE',  ( -13.97604488694527625, -13.89961937509977652, 81.87390960531436690 ) ) ;
#50455 = CARTESIAN_POINT ( 'NONE',  ( 15.80617190586746368, 15.72974639402197994, 84.37390960531438111 ) ) ;
#50456 = CARTESIAN_POINT ( 'NONE',  ( -19.03943276465977164, 0.05219959533909376836, 56.24890960531435979 ) ) ;
#50457 = CARTESIAN_POINT ( 'NONE',  ( -7.500000000000001776, 1.104226503365435264, 3.188666715448012834 ) ) ;
#50458 = CARTESIAN_POINT ( 'NONE',  ( -8.224510206698948167, 14.34966873604960824, 65.41557627198102409 ) ) ;
#50459 = CARTESIAN_POINT ( 'NONE',  ( 9.564922557960805705, 16.46253265017160317, 114.5822429386476955 ) ) ;
#50460 = CARTESIAN_POINT ( 'NONE',  ( 15.18304462349147599, -14.93970425505549038, -56.46919128290398504 ) ) ;
#50461 = CARTESIAN_POINT ( 'NONE',  ( 15.80617190586746368, 15.72974639402197994, 104.3739096053143669 ) ) ;
#50462 = CARTESIAN_POINT ( 'NONE',  ( -9.564922557961040184, 16.46253265017147172, 67.91775706135233293 ) ) ;
#50463 = CARTESIAN_POINT ( 'NONE',  ( 5.153800228976335163, 19.02544592524342804, 114.7905762719810241 ) ) ;
#50464 = CARTESIAN_POINT ( 'NONE',  ( -3.573655867282028392E-15, 2.428612866367529932E-14, 2.000000000000000000 ) ) ;
#50465 = CARTESIAN_POINT ( 'NONE',  ( 5.823673210054125526, 21.52544592524343514, 49.79057627198102409 ) ) ;
#50466 = CARTESIAN_POINT ( 'NONE',  ( -5.153800228976328057, -19.02544592524343514, 92.29057627198099567 ) ) ;
#50467 = CARTESIAN_POINT ( 'NONE',  ( 15.80617190586769283, -15.72974639402175789, 75.62609039468567573 ) ) ;
#50468 = CARTESIAN_POINT ( 'NONE',  ( 16.46253265017160672, -9.564922557960803928, 48.33224293864769550 ) ) ;
#50469 = CARTESIAN_POINT ( 'NONE',  ( -12.14591786802309592, -12.06949235617757132, 86.87390960531438111 ) ) ;
#50470 = CARTESIAN_POINT ( 'NONE',  ( 14.29746914071037800, 8.314922557961029526, 36.66775706135234714 ) ) ;
#50471 = CARTESIAN_POINT ( 'NONE',  ( 21.53943276465977519, 0.05219959533937863772, 61.25109039468567573 ) ) ;
#50472 = ORIENTED_EDGE ( 'NONE', *, *, #174667, .F. ) ;
#50473 = CARTESIAN_POINT ( 'NONE',  ( 9.564922557961047289, -16.46253265017146816, 30.41775706135232937 ) ) ;
#50474 = CARTESIAN_POINT ( 'NONE',  ( 16.46253265017146816, 9.564922557961045513, 81.66775706135233293 ) ) ;
#50475 = CARTESIAN_POINT ( 'NONE',  ( -18.22780087662123094, -5.499999999999984901, 91.48459894673894155 ) ) ;
#50476 = CARTESIAN_POINT ( 'NONE',  ( 15.72974639402176855, 15.80617190586768217, 41.87609039468568284 ) ) ;
#50477 = CARTESIAN_POINT ( 'NONE',  ( -30.74264578624800492, 22.33583958711400186, -3.949999994537626957 ) ) ;
#50478 = CARTESIAN_POINT ( 'NONE',  ( -0.05219959533936034679, 19.03943276465977164, 27.50109039468566507 ) ) ;
#50479 = CARTESIAN_POINT ( 'NONE',  ( -5.153800228976328057, -19.02544592524343514, 62.29057627198100988 ) ) ;
#50480 = CARTESIAN_POINT ( 'NONE',  ( -13.89961937509957401, -13.97604488694547875, 29.37609039468565797 ) ) ;
#50481 = CARTESIAN_POINT ( 'NONE',  ( -14.34966873604972548, 8.224510206698743886, 98.33442372801901854 ) ) ;
#50483 = CARTESIAN_POINT ( 'NONE',  ( 21.52544592524334988, 5.823673210054432836, 81.45942372801900433 ) ) ;
#50482 = CARTESIAN_POINT ( 'NONE',  ( -13.89961937509977652, 13.97604488694528158, 115.6239096053143669 ) ) ;
#50484 = CARTESIAN_POINT ( 'NONE',  ( -29.86685920354755552, 21.69954338932564397, -4.824999997268814234 ) ) ;
#50485 = CARTESIAN_POINT ( 'NONE',  ( -17.50000000000003197, -3.305555262949710915, 35.37482847843423883 ) ) ;
#50486 = CARTESIAN_POINT ( 'NONE',  ( 21.52544592524334988, 5.823673210054432836, 91.45942372801901854 ) ) ;
#50487 = DIRECTION ( 'NONE',  ( -0.000000000000000000, -0.000000000000000000, -1.000000000000000000 ) ) ;
#50488 = CARTESIAN_POINT ( 'NONE',  ( 19.03943276465977164, -0.05219959533909143690, 103.7489096053143669 ) ) ;
#50489 = CARTESIAN_POINT ( 'NONE',  ( -1.478515647795532795, -30.09553654342102291, -51.30846887466859840 ) ) ;
#50490 = CARTESIAN_POINT ( 'NONE',  ( -16.46253265017160317, 9.564922557960807481, 50.83224293864770260 ) ) ;
#50491 = CARTESIAN_POINT ( 'NONE',  ( -5.719274019375978568, 21.55341960407610458, 55.20724293864770260 ) ) ;
#50492 = CARTESIAN_POINT ( 'NONE',  ( 14.29746914071049879, -8.314922557960816363, 33.33224293864769550 ) ) ;
#50494 = CARTESIAN_POINT ( 'NONE',  ( -5.153800228976328057, -19.02544592524343514, 82.29057627198103830 ) ) ;
#50493 = CARTESIAN_POINT ( 'NONE',  ( 16.55341960407611168, 4.379528057220329451, 93.95724293864770971 ) ) ;
#50495 = CARTESIAN_POINT ( 'NONE',  ( -19.03943276465977164, -0.05219959533935918106, 28.75109039468566507 ) ) ;
#50496 = CARTESIAN_POINT ( 'NONE',  ( 9.474510206698971260, -16.51473224551069308, 32.91557627198102409 ) ) ;
#50497 = CARTESIAN_POINT ( 'NONE',  ( 12.06949235617757843, -12.14591786802309237, 98.12390960531436690 ) ) ;
#50498 = CARTESIAN_POINT ( 'NONE',  ( -15.72974639402176322, -15.80617190586768395, 59.37609039468568284 ) ) ;
#50499 = CARTESIAN_POINT ( 'NONE',  ( -21.52544592524343514, 5.823673210054127303, 91.04057627198103830 ) ) ;
#50500 = CARTESIAN_POINT ( 'NONE',  ( 19.02544592524334988, 5.153800228976608722, 61.45942372801900433 ) ) ;
#50501 = CARTESIAN_POINT ( 'NONE',  ( -20.03347751555784839, -21.15125157081075002, -49.39869787917044874 ) ) ;
#50502 = CARTESIAN_POINT ( 'NONE',  ( 9.474510206698971260, -16.51473224551069308, 112.9155762719810383 ) ) ;
#50503 = CARTESIAN_POINT ( 'NONE',  ( -0.05219959533910754901, -16.53943276465976808, 77.49890960531433848 ) ) ;
#50505 = CARTESIAN_POINT ( 'NONE',  ( -19.02544592524334988, -5.153800228976617603, 48.95942372801900433 ) ) ;
#50504 = AXIS2_PLACEMENT_3D ( 'NONE', #179746, #130190, #191886 ) ;
#50506 = CARTESIAN_POINT ( 'NONE',  ( 5.049401038298161559, -19.05341960407611168, 67.70724293864769550 ) ) ;
#50507 = CARTESIAN_POINT ( 'NONE',  ( 8.224510206698953496, -14.34966873604960469, 67.91557627198102409 ) ) ;
#50509 = EDGE_CURVE ( 'NONE', #187938, #60305, #139087, .T. ) ;
#50508 = CARTESIAN_POINT ( 'NONE',  ( 5.153800228976615827, -19.02544592524334988, 75.20942372801896170 ) ) ;
#50510 = CARTESIAN_POINT ( 'NONE',  ( 21.55341960407610458, 5.719274019375980345, 33.95724293864769550 ) ) ;
#50511 = ORIENTED_EDGE ( 'NONE', *, *, #182922, .T. ) ;
#50512 = CARTESIAN_POINT ( 'NONE',  ( -12.14591786802309592, -12.06949235617757132, 101.8739096053143811 ) ) ;
#50513 = CARTESIAN_POINT ( 'NONE',  ( -20.96320343559654020, -21.46320343559631638, 4.646446609406719830 ) ) ;
#50515 = CARTESIAN_POINT ( 'NONE',  ( 15.72974639402199770, -15.80617190586745480, 63.12390960531435979 ) ) ;
#50514 = CARTESIAN_POINT ( 'NONE',  ( -0.05219959533909027116, -19.03943276465977164, 57.49890960531435979 ) ) ;
#50516 = CARTESIAN_POINT ( 'NONE',  ( -19.03943276465977164, 0.05219959533909376836, 41.24890960531435269 ) ) ;
#50518 = CARTESIAN_POINT ( 'NONE',  ( -16.51473224551069308, -9.474510206698971260, 76.66557627198103830 ) ) ;
#50517 = CARTESIAN_POINT ( 'NONE',  ( 8.224510206698742110, 14.34966873604972548, 77.08442372801901854 ) ) ;
#50519 = CARTESIAN_POINT ( 'NONE',  ( 5.153800228976615827, -19.02544592524334988, 55.20942372801899722 ) ) ;
#50520 = CARTESIAN_POINT ( 'NONE',  ( -21.52544592524334988, -5.823673210054445271, 68.95942372801901854 ) ) ;
#50521 = CARTESIAN_POINT ( 'NONE',  ( 10.81492255796078972, 18.62759615963270932, 49.58224293864769550 ) ) ;
#50522 = CARTESIAN_POINT ( 'NONE',  ( -13.97604488694527625, -13.89961937509977652, 111.8739096053143243 ) ) ;
#50523 = CARTESIAN_POINT ( 'NONE',  ( 16.53943276465976808, -0.05219959533910856209, 113.7489096053143527 ) ) ;
#50524 = CARTESIAN_POINT ( 'NONE',  ( 16.53943276465976808, 0.05219959533934440121, 81.25109039468568994 ) ) ;
#50525 = CARTESIAN_POINT ( 'NONE',  ( -19.03943276465977164, -0.05219959533935918106, 108.7510903946856615 ) ) ;
#50526 = CARTESIAN_POINT ( 'NONE',  ( 27.16945489364049848, -10.00000000000000000, 149.7909430734646890 ) ) ;
#50527 = DIRECTION ( 'NONE',  ( 2.126200446592120372E-14, -0.6427876096865389188, -0.7660444431189784575 ) ) ;
#50528 = CARTESIAN_POINT ( 'NONE',  ( 15.72974639402176855, 15.80617190586768217, 91.87609039468568994 ) ) ;
#50529 = CARTESIAN_POINT ( 'NONE',  ( -4.379528057220328563, 16.55341960407611168, 45.20724293864769550 ) ) ;
#50530 = CARTESIAN_POINT ( 'NONE',  ( -12.14591786802309592, -12.06949235617757132, 66.87390960531436690 ) ) ;
#50531 = CARTESIAN_POINT ( 'NONE',  ( -21.55341960407610458, -5.719274019375992779, 96.45724293864770971 ) ) ;
#50532 = CARTESIAN_POINT ( 'NONE',  ( -5.823673210054116645, -21.52544592524344225, 82.29057627198103830 ) ) ;
#50533 = CARTESIAN_POINT ( 'NONE',  ( -0.1356448107282722249, -31.90000000000003411, -45.64921306006599622 ) ) ;
#50534 = CARTESIAN_POINT ( 'NONE',  ( 18.67979575497178502, 10.72451020669898547, 34.16557627198102409 ) ) ;
#50535 = CARTESIAN_POINT ( 'NONE',  ( -14.34966873604972548, 8.224510206698743886, 63.33442372801900433 ) ) ;
#50536 = CARTESIAN_POINT ( 'NONE',  ( 14.34966873604960469, 8.224510206698951720, 94.16557627198103830 ) ) ;
#50537 = CARTESIAN_POINT ( 'NONE',  ( 5.153800228976335163, 19.02544592524342804, 39.79057627198100988 ) ) ;
#50538 = SURFACE_STYLE_FILL_AREA ( #97010 ) ;
#50539 = CARTESIAN_POINT ( 'NONE',  ( 34.54531151325587501, -4.968019249220454903, 50.63996542006481860 ) ) ;
#50540 = CARTESIAN_POINT ( 'NONE',  ( 16.52544592524335698, 4.483927247898782831, 96.45942372801901854 ) ) ;
#50541 = CARTESIAN_POINT ( 'NONE',  ( 5.719274019375673035, 21.55341960407619339, 37.29275706135235424 ) ) ;
#50542 = CARTESIAN_POINT ( 'NONE',  ( 16.51473224551069308, 9.474510206698969483, 84.16557627198102409 ) ) ;
#50543 = CARTESIAN_POINT ( 'NONE',  ( -21.55341960407619339, 5.719274019375674811, 68.54275706135234714 ) ) ;
#50544 = CARTESIAN_POINT ( 'NONE',  ( 19.02544592524343514, -5.153800228976328945, 108.5405762719810383 ) ) ;
#50546 = EDGE_CURVE ( 'NONE', #72196, #146762, #166148, .T. ) ;
#50545 = CARTESIAN_POINT ( 'NONE',  ( -13.37225149056313356, -38.04021455642293859, -24.47500528307575962 ) ) ;
#50547 = ORIENTED_EDGE ( 'NONE', *, *, #33328, .F. ) ;
#50548 = CARTESIAN_POINT ( 'NONE',  ( -18.62759615963255300, -10.81492255796106328, 59.16775706135234714 ) ) ;
#50550 = CARTESIAN_POINT ( 'NONE',  ( -13.89961937509977652, 13.97604488694528158, 115.6239096053143669 ) ) ;
#50549 = CARTESIAN_POINT ( 'NONE',  ( -13.97604488694527625, -13.89961937509977652, 41.87390960531435979 ) ) ;
#50551 = CARTESIAN_POINT ( 'NONE',  ( 9.474510206698729675, 16.51473224551082808, 72.08442372801900433 ) ) ;
#50552 = CARTESIAN_POINT ( 'NONE',  ( 5.719274019375673035, 21.55341960407619339, 27.29275706135234358 ) ) ;
#50553 = CARTESIAN_POINT ( 'NONE',  ( 0.05219959533936267826, -19.03943276465977164, 65.00109039468567573 ) ) ;
#50554 = CARTESIAN_POINT ( 'NONE',  ( -13.89961937509977652, 13.97604488694528158, 25.62390960531434558 ) ) ;
#50555 = CARTESIAN_POINT ( 'NONE',  ( 0.05219959533934541429, -16.53943276465976808, 95.00109039468568994 ) ) ;
#50556 = CARTESIAN_POINT ( 'NONE',  ( -19.02544592524334988, -5.153800228976617603, 58.95942372801900433 ) ) ;
#50557 = CARTESIAN_POINT ( 'NONE',  ( -0.05219959533934338120, 16.53943276465976808, 112.5010903946857042 ) ) ;
#50558 = CARTESIAN_POINT ( 'NONE',  ( 19.05341960407617918, -5.049401038297876454, 46.04275706135233293 ) ) ;
#50559 = CARTESIAN_POINT ( 'NONE',  ( -9.474510206698964154, 16.51473224551069663, 85.41557627198102409 ) ) ;
#50560 = AXIS2_PLACEMENT_3D ( 'NONE', #75878, #105236, #182088 ) ;
#50561 = CARTESIAN_POINT ( 'NONE',  ( 5.823673210054444382, -21.52544592524334988, 95.20942372801903275 ) ) ;
#50562 = CARTESIAN_POINT ( 'NONE',  ( 0.05219959533937995610, -21.53943276465977519, 105.0010903946856757 ) ) ;
#50563 = DIRECTION ( 'NONE',  ( 0.000000000000000000, 0.000000000000000000, 1.000000000000000000 ) ) ;
#50564 = CARTESIAN_POINT ( 'NONE',  ( -10.81492255796105439, 18.62759615963255655, 87.91775706135234714 ) ) ;
#50565 = CARTESIAN_POINT ( 'NONE',  ( 12.06949235617739724, 12.14591786802326823, 31.87609039468567929 ) ) ;
#50566 = CARTESIAN_POINT ( 'NONE',  ( 0.05219959533909260263, 19.03943276465977164, 84.99890960531436690 ) ) ;
#50567 = CARTESIAN_POINT ( 'NONE',  ( 5.823673210054125526, 21.52544592524343514, 29.79057627198102409 ) ) ;
#50568 = DIRECTION ( 'NONE',  ( 1.000000000000000000, 0.000000000000000000, 0.000000000000000000 ) ) ;
#50569 = CARTESIAN_POINT ( 'NONE',  ( -0.05219959533909027116, -19.03943276465977164, 77.49890960531435269 ) ) ;
#50570 = CARTESIAN_POINT ( 'NONE',  ( -19.39056639909673407, -5.500000000000056843, 40.78948781074345931 ) ) ;
#50571 = CARTESIAN_POINT ( 'NONE',  ( -16.51473224551082808, 9.474510206698731452, 73.33442372801900433 ) ) ;
#50572 = CARTESIAN_POINT ( 'NONE',  ( -5.049401038298153566, 19.05341960407611168, 105.2072429386476671 ) ) ;
#50573 = CARTESIAN_POINT ( 'NONE',  ( 15.72974639402176855, 15.80617190586768217, 101.8760903946857042 ) ) ;
#50574 = CARTESIAN_POINT ( 'NONE',  ( -16.53943276465976808, 0.05219959533911058130, 96.24890960531435269 ) ) ;
#50575 = CARTESIAN_POINT ( 'NONE',  ( -18.67979575497178146, -10.72451020669898902, 51.66557627198102409 ) ) ;
#50576 = CARTESIAN_POINT ( 'NONE',  ( 10.72451020669898902, -18.67979575497178502, 32.91557627198102409 ) ) ;
#50577 = CARTESIAN_POINT ( 'NONE',  ( -16.52544592524342804, 4.483927247898546575, 101.0405762719810383 ) ) ;
#50578 = CARTESIAN_POINT ( 'NONE',  ( 17.58332526062528345, 7.635886036038587399, 46.57665040441534643 ) ) ;
#50579 = CARTESIAN_POINT ( 'NONE',  ( -0.05219959533936034679, 19.03943276465977164, 52.50109039468566863 ) ) ;
#50580 = CARTESIAN_POINT ( 'NONE',  ( -8.224510206698948167, 14.34966873604960824, 30.41557627198101699 ) ) ;
#50581 = CARTESIAN_POINT ( 'NONE',  ( 13.89961937509977652, -13.97604488694527269, 98.12390960531433848 ) ) ;
#50582 = CARTESIAN_POINT ( 'NONE',  ( 21.53943276465977519, 0.05219959533937863772, 86.25109039468568994 ) ) ;
#50583 = CARTESIAN_POINT ( 'NONE',  ( -10.72451020669898014, 18.67979575497178502, 55.41557627198102409 ) ) ;
#50584 = CARTESIAN_POINT ( 'NONE',  ( -21.52544592524334988, -5.823673210054445271, 48.95942372801902565 ) ) ;
#50585 = CARTESIAN_POINT ( 'NONE',  ( -10.72451020669898014, 18.67979575497178502, 90.41557627198103830 ) ) ;
#50586 = CARTESIAN_POINT ( 'NONE',  ( -21.52544592524334988, -5.823673210054445271, 43.95942372801902565 ) ) ;
#50587 = CARTESIAN_POINT ( 'NONE',  ( 5.153800228976335163, 19.02544592524342804, 24.79057627198102765 ) ) ;
#50588 = CARTESIAN_POINT ( 'NONE',  ( -0.05219959533909027116, -19.03943276465977164, 87.49890960531436690 ) ) ;
#50589 = CARTESIAN_POINT ( 'NONE',  ( 14.29746914071037800, 8.314922557961029526, 81.66775706135236135 ) ) ;
#50590 = CARTESIAN_POINT ( 'NONE',  ( -16.52544592524342804, 4.483927247898546575, 101.0405762719810383 ) ) ;
#50591 = CARTESIAN_POINT ( 'NONE',  ( -19.03943276465977164, 0.05219959533909376836, 111.2489096053143669 ) ) ;
#50592 = CARTESIAN_POINT ( 'NONE',  ( 16.53943276465976808, -0.05219959533910856209, 58.74890960531436690 ) ) ;
#50593 = CARTESIAN_POINT ( 'NONE',  ( -4.379528057220328563, 16.55341960407611168, 25.20724293864769550 ) ) ;
#50594 = CARTESIAN_POINT ( 'NONE',  ( -16.46253265017160317, 9.564922557960807481, 55.83224293864769550 ) ) ;
#50595 = CARTESIAN_POINT ( 'NONE',  ( -19.02544592524342804, 5.153800228976336051, 26.04057627198103120 ) ) ;
#50596 = CARTESIAN_POINT ( 'NONE',  ( -18.67979575497178146, -10.72451020669898902, 51.66557627198102409 ) ) ;
#50597 = CARTESIAN_POINT ( 'NONE',  ( -5.153800228976607833, 19.02544592524334988, 22.70942372801899012 ) ) ;
#50599 = CARTESIAN_POINT ( 'NONE',  ( -12.14591786802309592, -12.06949235617757132, 41.87390960531435979 ) ) ;
#50598 = CARTESIAN_POINT ( 'NONE',  ( -17.44270441346512968, -5.991230190323103777, 41.36335079264229364 ) ) ;
#50600 = CARTESIAN_POINT ( 'NONE',  ( 5.823673210054444382, -21.52544592524334988, 50.20942372801901854 ) ) ;
#50601 = CARTESIAN_POINT ( 'NONE',  ( 21.62954880396029367, -5.465688001471229462, 174.0035134771793253 ) ) ;
#50602 = CARTESIAN_POINT ( 'NONE',  ( -14.29746914071037622, -8.314922557961029526, 64.16775706135234714 ) ) ;
#50603 = CARTESIAN_POINT ( 'NONE',  ( -5.049401038297874678, -19.05341960407617918, 59.79275706135231871 ) ) ;
#50604 = CARTESIAN_POINT ( 'NONE',  ( -8.224510206698948167, 14.34966873604960824, 30.41557627198101699 ) ) ;
#50605 = CARTESIAN_POINT ( 'NONE',  ( -12.14591786802326823, 12.06949235617739902, 113.1260903946856899 ) ) ;
#50606 = CARTESIAN_POINT ( 'NONE',  ( -5.049401038298153566, 19.05341960407611168, 40.20724293864768839 ) ) ;
#50607 = CARTESIAN_POINT ( 'NONE',  ( -9.564922557960796823, -16.46253265017161027, 62.08224293864769550 ) ) ;
#50608 = CARTESIAN_POINT ( 'NONE',  ( -16.53943276465976808, 0.05219959533911058130, 116.2489096053143669 ) ) ;
#50609 = CARTESIAN_POINT ( 'NONE',  ( 21.52544592524334988, 5.823673210054432836, 36.45942372801901143 ) ) ;
#50610 = CARTESIAN_POINT ( 'NONE',  ( 19.02544592524343514, -5.153800228976328945, 48.54057627198103120 ) ) ;
#50611 = CARTESIAN_POINT ( 'NONE',  ( -9.474510206698964154, 16.51473224551069663, 115.4155762719810241 ) ) ;
#50612 = CARTESIAN_POINT ( 'NONE',  ( -16.46253265017160317, 9.564922557960807481, 45.83224293864769550 ) ) ;
#50613 = CARTESIAN_POINT ( 'NONE',  ( -5.049401038298153566, 19.05341960407611168, 115.2072429386477097 ) ) ;
#50615 = CARTESIAN_POINT ( 'NONE',  ( 0.05219959533910956823, 16.53943276465976808, 99.99890960531436690 ) ) ;
#50614 = CARTESIAN_POINT ( 'NONE',  ( 0.05219959533937995610, -21.53943276465977519, 65.00109039468568994 ) ) ;
#50616 = CARTESIAN_POINT ( 'NONE',  ( -5.153800228976328057, -19.02544592524343514, 107.2905762719810383 ) ) ;
#50617 = CARTESIAN_POINT ( 'NONE',  ( -0.05219959533934338120, 16.53943276465976808, 82.50109039468568994 ) ) ;
#50618 = CARTESIAN_POINT ( 'NONE',  ( -21.52544592524334988, -5.823673210054445271, 98.95942372801903275 ) ) ;
#50619 = CARTESIAN_POINT ( 'NONE',  ( -14.34966873604972548, 8.224510206698743886, 48.33442372801902565 ) ) ;
#50620 = CARTESIAN_POINT ( 'NONE',  ( -16.51473224551069308, -9.474510206698971260, 101.6655762719810241 ) ) ;
#50621 = CARTESIAN_POINT ( 'NONE',  ( 16.53943276465976808, 0.05219959533934440121, 41.25109039468568284 ) ) ;
#50622 = CARTESIAN_POINT ( 'NONE',  ( 8.224510206698742110, 14.34966873604972548, 22.08442372801901143 ) ) ;
#50623 = CARTESIAN_POINT ( 'NONE',  ( -8.224510206698735004, -14.34966873604973081, 84.58442372801903275 ) ) ;
#50624 = CARTESIAN_POINT ( 'NONE',  ( -5.153800228976607833, 19.02544592524334988, 112.7094237280190043 ) ) ;
#50625 = CARTESIAN_POINT ( 'NONE',  ( 21.55341960407610458, 5.719274019375980345, 93.95724293864770971 ) ) ;
#50627 = CARTESIAN_POINT ( 'NONE',  ( -13.89961937509957401, -13.97604488694547875, 99.37609039468567573 ) ) ;
#50626 = CARTESIAN_POINT ( 'NONE',  ( -0.05219959533910754901, -16.53943276465976808, 107.4989096053143669 ) ) ;
#50628 = CARTESIAN_POINT ( 'NONE',  ( -8.314922557961024197, 14.29746914071037800, 72.91775706135234714 ) ) ;
#50629 = CARTESIAN_POINT ( 'NONE',  ( 21.93180397000027781, 7.641141194973617878, 169.8616410530779604 ) ) ;
#50630 = CARTESIAN_POINT ( 'NONE',  ( 13.97604488694548053, -13.89961937509957401, 65.62609039468567573 ) ) ;
#50631 = CARTESIAN_POINT ( 'NONE',  ( -4.483927247898539470, -16.52544592524342804, 52.29057627198102409 ) ) ;
#50632 = CARTESIAN_POINT ( 'NONE',  ( -4.483927247898539470, -16.52544592524342804, 27.29057627198103120 ) ) ;
#50633 = CARTESIAN_POINT ( 'NONE',  ( 16.53943276465976808, -0.05219959533910856209, 88.74890960531436690 ) ) ;
#50634 = CARTESIAN_POINT ( 'NONE',  ( -5.153800228976607833, 19.02544592524334988, 27.70942372801899722 ) ) ;
#50635 = CARTESIAN_POINT ( 'NONE',  ( -0.05219959533937732626, 21.53943276465977519, 32.50109039468568284 ) ) ;
#50636 = CARTESIAN_POINT ( 'NONE',  ( 16.46253265017146816, 9.564922557961045513, 91.66775706135234714 ) ) ;
#50637 = CARTESIAN_POINT ( 'NONE',  ( -17.36633513277073249, -35.95409897417807343, -27.53902325179330646 ) ) ;
#50638 = CARTESIAN_POINT ( 'NONE',  ( -13.89961937509977652, 13.97604488694528158, 90.62390960531432427 ) ) ;
#50639 = CARTESIAN_POINT ( 'NONE',  ( 19.02544592524343514, -5.153800228976328945, 93.54057627198102409 ) ) ;
#50640 = CARTESIAN_POINT ( 'NONE',  ( -5.719274019375978568, 21.55341960407610458, 50.20724293864769550 ) ) ;
#50641 = CARTESIAN_POINT ( 'NONE',  ( 4.379528057220339221, -16.55341960407611168, 97.70724293864772392 ) ) ;
#50642 = CARTESIAN_POINT ( 'NONE',  ( 19.02544592524343514, -5.153800228976328945, 68.54057627198103830 ) ) ;
#50643 = CARTESIAN_POINT ( 'NONE',  ( -13.97604488694527625, -13.89961937509977652, 31.87390960531435979 ) ) ;
#50644 = AXIS2_PLACEMENT_3D ( 'NONE', #147656, #104140, #9144 ) ;
#50645 = CARTESIAN_POINT ( 'NONE',  ( -5.719274019375665041, -21.55341960407619695, 34.79275706135235424 ) ) ;
#50646 = CARTESIAN_POINT ( 'NONE',  ( 21.53943276465977519, 0.05219959533937863772, 81.25109039468568994 ) ) ;
#50647 = CARTESIAN_POINT ( 'NONE',  ( -9.474510206698964154, 16.51473224551069663, 55.41557627198103120 ) ) ;
#50648 = CARTESIAN_POINT ( 'NONE',  ( 8.314922557961029526, -14.29746914071037800, 75.41775706135233293 ) ) ;
#50649 = CARTESIAN_POINT ( 'NONE',  ( -0.05219959533937732626, 21.53943276465977519, 32.50109039468568284 ) ) ;
#50650 = CARTESIAN_POINT ( 'NONE',  ( 21.53943276465977519, 0.05219959533937863772, 26.25109039468567573 ) ) ;
#50652 = CARTESIAN_POINT ( 'NONE',  ( 16.46253265017160672, -9.564922557960803928, 78.33224293864769550 ) ) ;
#50651 = CARTESIAN_POINT ( 'NONE',  ( 16.46253265017146816, 9.564922557961045513, 46.66775706135233293 ) ) ;
#50653 = CARTESIAN_POINT ( 'NONE',  ( -16.51473224551082808, 9.474510206698731452, 28.33442372801900433 ) ) ;
#50654 = CARTESIAN_POINT ( 'NONE',  ( -21.55341960407619339, 5.719274019375674811, 78.54275706135236135 ) ) ;
#50655 = CARTESIAN_POINT ( 'NONE',  ( -18.62759615963270932, 10.81492255796079327, 75.83224293864769550 ) ) ;
#50656 = CARTESIAN_POINT ( 'NONE',  ( -12.06949235617756955, 12.14591786802309770, 55.62390960531436690 ) ) ;
#50658 = CARTESIAN_POINT ( 'NONE',  ( 16.51473224551083163, -9.474510206698727899, 25.83442372801900078 ) ) ;
#50657 = CARTESIAN_POINT ( 'NONE',  ( -10.72451020669870658, -18.67979575497194134, 94.58442372801901854 ) ) ;
#50659 = CARTESIAN_POINT ( 'NONE',  ( -8.314922557960811034, -14.29746914071050412, 67.08224293864770971 ) ) ;
#50660 = CARTESIAN_POINT ( 'NONE',  ( 5.049401038298161559, -19.05341960407611168, 22.70724293864769194 ) ) ;
#50661 = CARTESIAN_POINT ( 'NONE',  ( -19.05341960407617563, 5.049401038297882671, 68.54275706135230450 ) ) ;
#50662 = CARTESIAN_POINT ( 'NONE',  ( 0.05219959533910956823, 16.53943276465976808, 34.99890960531435979 ) ) ;
#50663 = AXIS2_PLACEMENT_3D ( 'NONE', #154389, #169556, #187734 ) ;
#50664 = CARTESIAN_POINT ( 'NONE',  ( 21.53943276465977519, 0.05219959533937863772, 81.25109039468568994 ) ) ;
#50665 = CARTESIAN_POINT ( 'NONE',  ( 16.46253265017160672, -9.564922557960803928, 73.33224293864769550 ) ) ;
#50666 = CARTESIAN_POINT ( 'NONE',  ( -5.153800228976607833, 19.02544592524334988, 52.70942372801900433 ) ) ;
#50667 = CARTESIAN_POINT ( 'NONE',  ( 15.72974639402199770, -15.80617190586745480, 53.12390960531436690 ) ) ;
#50668 = CARTESIAN_POINT ( 'NONE',  ( -5.719274019375665041, -21.55341960407619695, 39.79275706135235424 ) ) ;
#50669 = CARTESIAN_POINT ( 'NONE',  ( -10.81492255796078084, -18.62759615963271287, 107.0822429386476955 ) ) ;
#50670 = CARTESIAN_POINT ( 'NONE',  ( 13.89961937509957401, 13.97604488694547697, 111.8760903946856757 ) ) ;
#50671 = CARTESIAN_POINT ( 'NONE',  ( 4.483927247898790824, -16.52544592524335698, 65.20942372801901854 ) ) ;
#50673 = CARTESIAN_POINT ( 'NONE',  ( 5.823673210054125526, 21.52544592524343514, 104.7905762719810241 ) ) ;
#50672 = CARTESIAN_POINT ( 'NONE',  ( 17.05116617787826527, 6.768360034955703597, 63.84324446740807701 ) ) ;
#50674 = CARTESIAN_POINT ( 'NONE',  ( -14.29746914071049879, 8.314922557960819915, 100.8322429386477097 ) ) ;
#50675 = CARTESIAN_POINT ( 'NONE',  ( 20.49784845243110709, -1.163414459189985801E-14, 95.00000000000000000 ) ) ;
#50676 = CARTESIAN_POINT ( 'NONE',  ( -4.379528057220086978, -16.55341960407618274, 39.79275706135235424 ) ) ;
#50677 = APPLICATION_CONTEXT ( 'automotive_design' ) ;
#50678 = EDGE_CURVE ( 'NONE', #41630, #151273, #130085, .T. ) ;
#50679 = CARTESIAN_POINT ( 'NONE',  ( 18.62759615963271287, -10.81492255796078972, 68.33224293864769550 ) ) ;
#50680 = CARTESIAN_POINT ( 'NONE',  ( -12.06949235617739369, -12.14591786802326823, 104.3760903946856899 ) ) ;
#50681 = CARTESIAN_POINT ( 'NONE',  ( -19.02544592524342804, 5.153800228976336051, 31.04057627198102409 ) ) ;
#50682 = CARTESIAN_POINT ( 'NONE',  ( -14.29746914071037622, -8.314922557961029526, 69.16775706135234714 ) ) ;
#50683 = CARTESIAN_POINT ( 'NONE',  ( 0.05219959533936267826, -19.03943276465977164, 60.00109039468566863 ) ) ;
#50684 = CARTESIAN_POINT ( 'NONE',  ( -0.05219959533937732626, 21.53943276465977519, 37.50109039468568284 ) ) ;
#50685 = ADVANCED_FACE ( 'NONE', ( #174634 ), #49924, .F. ) ;
#50686 = CARTESIAN_POINT ( 'NONE',  ( 18.62759615963271287, -10.81492255796078972, 53.33224293864769550 ) ) ;
#50687 = CARTESIAN_POINT ( 'NONE',  ( -8.224510206698735004, -14.34966873604973081, 99.58442372801900433 ) ) ;
#50688 = CARTESIAN_POINT ( 'NONE',  ( -21.55341960407619339, 5.719274019375674811, 63.54275706135234003 ) ) ;
#50689 = CARTESIAN_POINT ( 'NONE',  ( -18.62759615963270932, 10.81492255796079327, 55.83224293864770260 ) ) ;
#50690 = CARTESIAN_POINT ( 'NONE',  ( 21.52544592524344225, -5.823673210054117533, 28.54057627198103120 ) ) ;
#50691 = ORIENTED_EDGE ( 'NONE', *, *, #33197, .F. ) ;
#50692 = CARTESIAN_POINT ( 'NONE',  ( -8.224510206698735004, -14.34966873604973081, 79.58442372801903275 ) ) ;
#50693 = CARTESIAN_POINT ( 'NONE',  ( 10.72451020669898902, -18.67979575497178502, 27.91557627198103830 ) ) ;
#50694 = VERTEX_POINT ( 'NONE', #74195 ) ;
#50695 = CARTESIAN_POINT ( 'NONE',  ( 19.03943276465977164, -0.05219959533909143690, 98.74890960531436690 ) ) ;
#50696 = CARTESIAN_POINT ( 'NONE',  ( -16.53943276465976808, -0.05219959533934237506, 108.7510903946857042 ) ) ;
#50697 = CARTESIAN_POINT ( 'NONE',  ( -14.29746914071049879, 8.314922557960819915, 105.8322429386476955 ) ) ;
#50698 = CARTESIAN_POINT ( 'NONE',  ( -21.55341960407610458, -5.719274019375992779, 66.45724293864768129 ) ) ;
#50699 = CARTESIAN_POINT ( 'NONE',  ( -0.05219959533934338120, 16.53943276465976808, 97.50109039468567573 ) ) ;
#50700 = CARTESIAN_POINT ( 'NONE',  ( 18.62759615963255655, 10.81492255796105972, 41.66775706135235424 ) ) ;
#50701 = CARTESIAN_POINT ( 'NONE',  ( -13.97604488694547697, 13.89961937509957934, 103.1260903946856473 ) ) ;
#50702 = CARTESIAN_POINT ( 'NONE',  ( -16.52544592524342804, 4.483927247898546575, 101.0405762719810383 ) ) ;
#50703 = CARTESIAN_POINT ( 'NONE',  ( 19.03943276465977164, 0.05219959533936151252, 106.2510903946856615 ) ) ;
#50704 = AXIS2_PLACEMENT_3D ( 'NONE', #193026, #178867, #56506 ) ;
#50705 = CARTESIAN_POINT ( 'NONE',  ( 13.89961937509977652, -13.97604488694527269, 23.12390960531436335 ) ) ;
#50706 = CARTESIAN_POINT ( 'NONE',  ( 15.93273212980866482, -1.322671946311529290, -61.66661032175887414 ) ) ;
#50707 = CARTESIAN_POINT ( 'NONE',  ( 16.46253265017160672, -9.564922557960803928, 88.33224293864769550 ) ) ;
#50708 = CARTESIAN_POINT ( 'NONE',  ( 14.29746914071037800, 8.314922557961029526, 71.66775706135234714 ) ) ;
#50709 = CARTESIAN_POINT ( 'NONE',  ( -5.823673210054431948, 21.52544592524334988, 107.7094237280190328 ) ) ;
#50710 = CARTESIAN_POINT ( 'NONE',  ( 10.72451020669898902, -18.67979575497178502, 62.91557627198102409 ) ) ;
#50711 = CARTESIAN_POINT ( 'NONE',  ( -14.29746914071037622, -8.314922557961029526, 84.16775706135234714 ) ) ;
#50712 = CARTESIAN_POINT ( 'NONE',  ( -5.049401038297874678, -19.05341960407617918, 79.79275706135233293 ) ) ;
#50713 = CARTESIAN_POINT ( 'NONE',  ( -9.474510206698964154, 16.51473224551069663, 30.41557627198102054 ) ) ;
#50714 = CARTESIAN_POINT ( 'NONE',  ( -5.153800228976328057, -19.02544592524343514, 77.29057627198099567 ) ) ;
#50715 = CARTESIAN_POINT ( 'NONE',  ( -13.89961937509977652, 13.97604488694528158, 35.62390960531435269 ) ) ;
#50716 = CARTESIAN_POINT ( 'NONE',  ( 16.46253265017146816, 9.564922557961045513, 66.66775706135233293 ) ) ;
#50717 = CARTESIAN_POINT ( 'NONE',  ( 26.70292545465252942, -6.820347898103277018, 168.5277281069534752 ) ) ;
#50718 = CARTESIAN_POINT ( 'NONE',  ( -9.564922557960796823, -16.46253265017161027, 97.08224293864769550 ) ) ;
#50719 = CARTESIAN_POINT ( 'NONE',  ( -16.53943276465976808, 0.05219959533911058130, 46.24890960531435979 ) ) ;
#50720 = CARTESIAN_POINT ( 'NONE',  ( -15.72974639402197994, 15.80617190586746368, 65.62390960531436690 ) ) ;
#50721 = CARTESIAN_POINT ( 'NONE',  ( 17.50000000000000355, -7.500000000000000888, 22.00000000000000711 ) ) ;
#50722 = CARTESIAN_POINT ( 'NONE',  ( -19.05341960407617563, 5.049401038297882671, 33.54275706135231871 ) ) ;
#50723 = DIRECTION ( 'NONE',  ( -0.000000000000000000, -0.000000000000000000, 1.000000000000000000 ) ) ;
#50725 = CARTESIAN_POINT ( 'NONE',  ( -13.97604488694527625, -13.89961937509977652, 71.87390960531433848 ) ) ;
#50724 = CARTESIAN_POINT ( 'NONE',  ( -5.049401038298153566, 19.05341960407611168, 50.20724293864770260 ) ) ;
#50726 = CARTESIAN_POINT ( 'NONE',  ( -8.224510206698735004, -14.34966873604973081, 44.58442372801901854 ) ) ;
#50727 = CARTESIAN_POINT ( 'NONE',  ( -33.70211957050084095, -4.378872343537607570, 98.34732289368837144 ) ) ;
#50728 = CARTESIAN_POINT ( 'NONE',  ( 1.601920565550454256, -37.08308084913829816, -8.000000000000000000 ) ) ;
#50729 = CARTESIAN_POINT ( 'NONE',  ( 14.34966873604972726, -8.224510206698740333, 70.83442372801901854 ) ) ;
#50730 = CARTESIAN_POINT ( 'NONE',  ( 5.719274019375991003, -21.55341960407610458, 97.70724293864772392 ) ) ;
#50731 = CARTESIAN_POINT ( 'NONE',  ( 12.06949235617739724, 12.14591786802326823, 41.87609039468568284 ) ) ;
#50733 = DIRECTION ( 'NONE',  ( 0.000000000000000000, 0.000000000000000000, -1.000000000000000000 ) ) ;
#50732 = CARTESIAN_POINT ( 'NONE',  ( 0.05219959533909260263, 19.03943276465977164, 44.99890960531435979 ) ) ;
#50734 = CARTESIAN_POINT ( 'NONE',  ( 15.80617190586769283, -15.72974639402175789, 50.62609039468568994 ) ) ;
#50735 = CARTESIAN_POINT ( 'NONE',  ( -19.05341960407617563, 5.049401038297882671, 58.54275706135234003 ) ) ;
#50736 = CARTESIAN_POINT ( 'NONE',  ( 0.05219959533937995610, -21.53943276465977519, 95.00109039468568994 ) ) ;
#50737 = CARTESIAN_POINT ( 'NONE',  ( -5.049401038298153566, 19.05341960407611168, 25.20724293864768484 ) ) ;
#50738 = CARTESIAN_POINT ( 'NONE',  ( -13.70000000000001528, 1.443387660838688656E-13, -60.44446360152740283 ) ) ;
#50739 = CARTESIAN_POINT ( 'NONE',  ( -0.05219959533907301413, -21.53943276465977519, 52.49890960531435979 ) ) ;
#50740 = CARTESIAN_POINT ( 'NONE',  ( 16.46253265017160672, -9.564922557960803928, 98.33224293864769550 ) ) ;
#50741 = CARTESIAN_POINT ( 'NONE',  ( 4.483927247898545687, 16.52544592524342804, 104.7905762719810241 ) ) ;
#50742 = CARTESIAN_POINT ( 'NONE',  ( -16.55341960407617563, 4.379528057220093196, 33.54275706135234714 ) ) ;
#50743 = EDGE_CURVE ( 'NONE', #37464, #49927, #44837, .T. ) ;
#50744 = CARTESIAN_POINT ( 'NONE',  ( -16.53943276465976808, -0.05219959533934237506, 108.7510903946857042 ) ) ;
#50745 = ORIENTED_EDGE ( 'NONE', *, *, #107988, .T. ) ;
#50746 = CARTESIAN_POINT ( 'NONE',  ( -10.81492255796078084, -18.62759615963271287, 97.08224293864770971 ) ) ;
#50748 = CARTESIAN_POINT ( 'NONE',  ( 19.05341960407611168, 5.049401038298154454, 108.9572429386477097 ) ) ;
#50747 = CARTESIAN_POINT ( 'NONE',  ( -8.314922557960811034, -14.29746914071050412, 42.08224293864769550 ) ) ;
#50749 = CARTESIAN_POINT ( 'NONE',  ( 5.153800228976615827, -19.02544592524334988, 100.2094237280190043 ) ) ;
#50750 = CARTESIAN_POINT ( 'NONE',  ( 10.81492255796106328, -18.62759615963255655, 110.4177570613523756 ) ) ;
#50751 = CARTESIAN_POINT ( 'NONE',  ( -16.52544592524342804, 4.483927247898546575, 36.04057627198102409 ) ) ;
#50752 = CARTESIAN_POINT ( 'NONE',  ( -21.53943276465977519, 0.05219959533907696930, 91.24890960531436690 ) ) ;
#50753 = CARTESIAN_POINT ( 'NONE',  ( -15.80617190586745835, -15.72974639402198527, 46.87390960531435979 ) ) ;
#50754 = CARTESIAN_POINT ( 'NONE',  ( 13.89961937509977652, -13.97604488694527269, 63.12390960531435979 ) ) ;
#50755 = CARTESIAN_POINT ( 'NONE',  ( 14.29746914071049879, -8.314922557960816363, 33.33224293864769550 ) ) ;
#50756 = CARTESIAN_POINT ( 'NONE',  ( 19.02544592524343514, -5.153800228976328945, 93.54057627198102409 ) ) ;
#50757 = B_SPLINE_CURVE_WITH_KNOTS ( 'NONE', 3,
 ( #174547, #129010, #98672, #162360, #55186, #67350, #6668, #160366, #68346, #36014, #84504, #114856, #192709, #40012, #23861, #178546, #176550, #85512, #147200, #120832, #59164, #75332, #71362, #104689, #91470, #164383, #149208, #13665, #42035, #26872, #180561, #10699 ),
 .UNSPECIFIED., .F., .F.,
 ( 4, 2, 2, 2, 2, 2, 2, 2, 2, 2, 2, 2, 2, 2, 2, 4 ),
 ( 0.000000000000000000, 0.0003712461730036594018, 0.0007424923460073188037, 0.001113738519010978260, 0.001484984692014637607, 0.002227477038021972566, 0.002598723211025655115, 0.002969969384029337665, 0.003341215557033020214, 0.003712461730036702330, 0.004083707903040385313, 0.004454954076044067429, 0.004826200249047749545, 0.005197446422051432528, 0.005568692595055114644, 0.005939938768058796760 ),
 .UNSPECIFIED. ) ;
#50758 = ORIENTED_EDGE ( 'NONE', *, *, #70314, .T. ) ;
#50759 = CARTESIAN_POINT ( 'NONE',  ( 18.39639308325435252, 5.500000000000036415, 58.98252246182193659 ) ) ;
#50760 = CARTESIAN_POINT ( 'NONE',  ( -5.153800228976607833, 19.02544592524334988, 47.70942372801900433 ) ) ;
#50761 = CARTESIAN_POINT ( 'NONE',  ( -10.81492255796078084, -18.62759615963271287, 77.08224293864769550 ) ) ;
#50762 = CARTESIAN_POINT ( 'NONE',  ( -8.224510206698948167, 14.34966873604960824, 95.41557627198102409 ) ) ;
#50763 = CARTESIAN_POINT ( 'NONE',  ( 15.80617190586769283, -15.72974639402175789, 40.62609039468567573 ) ) ;
#50764 = CARTESIAN_POINT ( 'NONE',  ( -27.73933785331498925, 9.013057229001089965, 149.2750000027311330 ) ) ;
#50765 = CARTESIAN_POINT ( 'NONE',  ( 14.29746914071037800, 8.314922557961029526, 111.6677570613523613 ) ) ;
#50766 = CARTESIAN_POINT ( 'NONE',  ( -5.153800228976328057, -19.02544592524343514, 42.29057627198101699 ) ) ;
#50767 = CARTESIAN_POINT ( 'NONE',  ( 13.97604488694527802, 13.89961937509977652, 89.37390960531436690 ) ) ;
#50768 = CARTESIAN_POINT ( 'NONE',  ( -19.05341960407611168, -5.049401038298163336, 26.45724293864769550 ) ) ;
#50769 = CARTESIAN_POINT ( 'NONE',  ( 16.55341960407611168, 4.379528057220329451, 38.95724293864768839 ) ) ;
#50770 = CARTESIAN_POINT ( 'NONE',  ( -0.05219959533937732626, 21.53943276465977519, 67.50109039468568994 ) ) ;
#50772 = CARTESIAN_POINT ( 'NONE',  ( -4.483927247898782831, 16.52544592524335698, 67.70942372801901854 ) ) ;
#50771 = DIRECTION ( 'NONE',  ( 1.000000000000000000, -0.000000000000000000, -0.000000000000000000 ) ) ;
#50773 = CARTESIAN_POINT ( 'NONE',  ( 19.02544592524343514, -5.153800228976328945, 63.54057627198103830 ) ) ;
#50774 = CARTESIAN_POINT ( 'NONE',  ( 0.05219959533909260263, 19.03943276465977164, 49.99890960531435979 ) ) ;
#50775 = VERTEX_POINT ( 'NONE', #29667 ) ;
#50776 = CARTESIAN_POINT ( 'NONE',  ( -5.823673210054431948, 21.52544592524334988, 107.7094237280190328 ) ) ;
#50777 = CARTESIAN_POINT ( 'NONE',  ( 8.314922557961029526, -14.29746914071037800, 80.41775706135234714 ) ) ;
#50778 = CARTESIAN_POINT ( 'NONE',  ( -0.05219959533937732626, 21.53943276465977519, 102.5010903946856899 ) ) ;
#50779 = CARTESIAN_POINT ( 'NONE',  ( 15.80617190586746368, 15.72974639402197994, 34.37390960531435979 ) ) ;
#50780 = CARTESIAN_POINT ( 'NONE',  ( -16.51473224551082808, 9.474510206698731452, 113.3344237280190043 ) ) ;
#50781 = CARTESIAN_POINT ( 'NONE',  ( -0.05219959533937732626, 21.53943276465977519, 62.50109039468568284 ) ) ;
#50782 = CARTESIAN_POINT ( 'NONE',  ( -4.483927247898782831, 16.52544592524335698, 47.70942372801902565 ) ) ;
#50783 = CARTESIAN_POINT ( 'NONE',  ( -21.53943276465977519, 0.05219959533907696930, 101.2489096053143669 ) ) ;
#50784 = CARTESIAN_POINT ( 'NONE',  ( -9.564922557961040184, 16.46253265017147172, 102.9177570613523329 ) ) ;
#50785 = CARTESIAN_POINT ( 'NONE',  ( 5.049401038298161559, -19.05341960407611168, 62.70724293864769550 ) ) ;
#50786 = CARTESIAN_POINT ( 'NONE',  ( -9.474510206698720793, -16.51473224551083518, 109.5844237280190043 ) ) ;
#50787 = TOROIDAL_SURFACE ( 'NONE', #70135, 69.99999999999998579, 10.00000000000000000 ) ;
#50788 = CARTESIAN_POINT ( 'NONE',  ( 5.049401038297881783, 19.05341960407617563, 102.2927570613523045 ) ) ;
#50789 = CARTESIAN_POINT ( 'NONE',  ( -14.34966873604960291, -8.224510206698953496, 66.66557627198102409 ) ) ;
#50790 = CARTESIAN_POINT ( 'NONE',  ( 4.483927247898790824, -16.52544592524335698, 75.20942372801901854 ) ) ;
#50792 = CARTESIAN_POINT ( 'NONE',  ( 5.153800228976335163, 19.02544592524342804, 54.79057627198103120 ) ) ;
#50791 = CARTESIAN_POINT ( 'NONE',  ( 0.05219959533907565091, 21.53943276465977519, 109.9989096053143527 ) ) ;
#50793 = CARTESIAN_POINT ( 'NONE',  ( -5.049401038298153566, 19.05341960407611168, 55.20724293864769550 ) ) ;
#50794 = CARTESIAN_POINT ( 'NONE',  ( -14.29746914071037622, -8.314922557961029526, 74.16775706135231871 ) ) ;
#50795 = CARTESIAN_POINT ( 'NONE',  ( -17.14385361876520619, 23.59649016807275856, 149.0750000027311728 ) ) ;
#50796 = CARTESIAN_POINT ( 'NONE',  ( 1.993301997531345292E-15, -30.30510711980685912, 144.7500000054623399 ) ) ;
#50797 = CARTESIAN_POINT ( 'NONE',  ( -21.55341960407619339, 5.719274019375674811, 108.5427570613523756 ) ) ;
#50798 = CARTESIAN_POINT ( 'NONE',  ( 13.97604488694527802, 13.89961937509977652, 29.37390960531435979 ) ) ;
#50799 = ORIENTED_EDGE ( 'NONE', *, *, #121415, .T. ) ;
#50800 = CARTESIAN_POINT ( 'NONE',  ( 9.474510206698729675, 16.51473224551082808, 107.0844237280190043 ) ) ;
#50801 = CARTESIAN_POINT ( 'NONE',  ( 0.05219959533907565091, 21.53943276465977519, 49.99890960531437401 ) ) ;
#50803 = CARTESIAN_POINT ( 'NONE',  ( -16.52544592524335698, -4.483927247898792601, 28.95942372801902209 ) ) ;
#50802 = CARTESIAN_POINT ( 'NONE',  ( -19.05341960407617563, 5.049401038297882671, 48.54275706135233293 ) ) ;
#50804 = CARTESIAN_POINT ( 'NONE',  ( -19.05341960407611168, -5.049401038298163336, 46.45724293864768129 ) ) ;
#50805 = CARTESIAN_POINT ( 'NONE',  ( 16.51473224551069308, 9.474510206698969483, 49.16557627198102409 ) ) ;
#50806 = CARTESIAN_POINT ( 'NONE',  ( -5.823673210054116645, -21.52544592524344225, 82.29057627198103830 ) ) ;
#50807 = CARTESIAN_POINT ( 'NONE',  ( 19.02544592524343514, -5.153800228976328945, 113.5405762719810241 ) ) ;
#50808 = CARTESIAN_POINT ( 'NONE',  ( 16.51473224551069308, 9.474510206698969483, 49.16557627198102409 ) ) ;
#50809 = CARTESIAN_POINT ( 'NONE',  ( -18.10062525802553779, 5.500000000000031086, 93.51383468041922242 ) ) ;
#50810 = CARTESIAN_POINT ( 'NONE',  ( -13.89961937509957401, -13.97604488694547875, 94.37609039468566152 ) ) ;
#50812 = AXIS2_PLACEMENT_3D ( 'NONE', #13201, #103214, #122339 ) ;
#50811 = CARTESIAN_POINT ( 'NONE',  ( 8.314922557960818139, 14.29746914071049879, 64.58224293864769550 ) ) ;
#50813 = CARTESIAN_POINT ( 'NONE',  ( 9.564922557961047289, -16.46253265017146816, 20.41775706135233293 ) ) ;
#50814 = CARTESIAN_POINT ( 'NONE',  ( -16.53943276465976808, 0.05219959533911058130, 66.24890960531436690 ) ) ;
#50815 = CARTESIAN_POINT ( 'NONE',  ( 18.67979575497194134, -10.72451020669871369, 80.83442372801901854 ) ) ;
#50816 = CARTESIAN_POINT ( 'NONE',  ( 9.564922557960805705, 16.46253265017160317, 29.58224293864769550 ) ) ;
#50817 = CARTESIAN_POINT ( 'NONE',  ( -15.72974639402176322, -15.80617190586768395, 94.37609039468568994 ) ) ;
#50819 = CARTESIAN_POINT ( 'NONE',  ( -18.62759615963255300, -10.81492255796106328, 79.16775706135234714 ) ) ;
#50818 = CARTESIAN_POINT ( 'NONE',  ( 16.53943276465976808, -0.05219959533910856209, 23.74890960531435269 ) ) ;
#50820 = CARTESIAN_POINT ( 'NONE',  ( 13.97604488694527802, 13.89961937509977652, 69.37390960531436690 ) ) ;
#50821 = CARTESIAN_POINT ( 'NONE',  ( -15.72974639402176322, -15.80617190586768395, 39.37609039468567573 ) ) ;
#50822 = CARTESIAN_POINT ( 'NONE',  ( -19.03943276465977164, 0.05219959533909376836, 81.24890960531436690 ) ) ;
#50823 = CARTESIAN_POINT ( 'NONE',  ( 12.06949235617757843, -12.14591786802309237, 88.12390960531436690 ) ) ;
#50824 = CARTESIAN_POINT ( 'NONE',  ( 12.14591786802309770, 12.06949235617756955, 64.37390960531435269 ) ) ;
#50825 = CARTESIAN_POINT ( 'NONE',  ( -5.719274019375978568, 21.55341960407610458, 70.20724293864769550 ) ) ;
#50826 = CARTESIAN_POINT ( 'NONE',  ( 16.51473224551069308, 9.474510206698969483, 79.16557627198103830 ) ) ;
#50827 = CARTESIAN_POINT ( 'NONE',  ( 10.72451020669898902, -18.67979575497178502, 87.91557627198103830 ) ) ;
#50828 = CARTESIAN_POINT ( 'NONE',  ( -0.05219959533936034679, 19.03943276465977164, 67.50109039468566152 ) ) ;
#50830 = CARTESIAN_POINT ( 'NONE',  ( 8.314922557960818139, 14.29746914071049879, 74.58224293864768129 ) ) ;
#50829 = CARTESIAN_POINT ( 'NONE',  ( 9.564922557961047289, -16.46253265017146816, 35.41775706135233293 ) ) ;
#50831 = CARTESIAN_POINT ( 'NONE',  ( -5.823673210054116645, -21.52544592524344225, 52.29057627198102409 ) ) ;
#50832 = CARTESIAN_POINT ( 'NONE',  ( -18.22780087662121673, -5.500000000000063061, 41.48459894673893444 ) ) ;
#50834 = CARTESIAN_POINT ( 'NONE',  ( 27.73933785331498925, -9.013057229001034898, 142.2750000027311899 ) ) ;
#50833 = CARTESIAN_POINT ( 'NONE',  ( -0.05219959533934338120, 16.53943276465976808, 102.5010903946856899 ) ) ;
#50835 = CARTESIAN_POINT ( 'NONE',  ( 19.03943276465977164, 0.05219959533936151252, 101.2510903946856757 ) ) ;
#50836 = CARTESIAN_POINT ( 'NONE',  ( -8.224510206698948167, 14.34966873604960824, 70.41557627198102409 ) ) ;
#50837 = CARTESIAN_POINT ( 'NONE',  ( -17.50000000000002132, 3.345213924137298012, 34.58768623094346140 ) ) ;
#50838 = CARTESIAN_POINT ( 'NONE',  ( 19.02544592524343514, -5.153800228976328945, 63.54057627198103830 ) ) ;
#50839 = CARTESIAN_POINT ( 'NONE',  ( -4.483927247898539470, -16.52544592524342804, 57.29057627198103120 ) ) ;
#50840 = CARTESIAN_POINT ( 'NONE',  ( 13.89961937509977652, -13.97604488694527269, 103.1239096053143527 ) ) ;
#50842 = CARTESIAN_POINT ( 'NONE',  ( 19.05341960407611168, 5.049401038298154454, 63.95724293864769550 ) ) ;
#50841 = CARTESIAN_POINT ( 'NONE',  ( 0.05219959533936267826, -19.03943276465977164, 75.00109039468566152 ) ) ;
#50843 = CARTESIAN_POINT ( 'NONE',  ( -9.474510206698964154, 16.51473224551069663, 90.41557627198103830 ) ) ;
#50844 = CARTESIAN_POINT ( 'NONE',  ( -5.153800228976328057, -19.02544592524343514, 87.29057627198103830 ) ) ;
#50845 = CARTESIAN_POINT ( 'NONE',  ( 18.62759615963271287, -10.81492255796078972, 63.33224293864770260 ) ) ;
#50846 = CARTESIAN_POINT ( 'NONE',  ( 16.52544592524335698, 4.483927247898782831, 51.45942372801901854 ) ) ;
#50847 = CARTESIAN_POINT ( 'NONE',  ( 2.552343178074615970, -7.052343178074640839, 1.110912703473986074 ) ) ;
#50848 = CARTESIAN_POINT ( 'NONE',  ( -19.02544592524342804, 5.153800228976336051, 51.04057627198103120 ) ) ;
#50849 = CARTESIAN_POINT ( 'NONE',  ( -5.823673210054116645, -21.52544592524344225, 52.29057627198102409 ) ) ;
#50850 = CARTESIAN_POINT ( 'NONE',  ( -5.153800228976607833, 19.02544592524334988, 92.70942372801901854 ) ) ;
#50852 = CARTESIAN_POINT ( 'NONE',  ( -5.823673210054431948, 21.52544592524334988, 42.70942372801901854 ) ) ;
#50851 = CARTESIAN_POINT ( 'NONE',  ( 8.314922557960818139, 14.29746914071049879, 24.58224293864768839 ) ) ;
#50853 = CARTESIAN_POINT ( 'NONE',  ( 16.51473224551083163, -9.474510206698727899, 35.83442372801899722 ) ) ;
#50855 = CARTESIAN_POINT ( 'NONE',  ( 4.379528057220092307, 16.55341960407617563, 97.29275706135234714 ) ) ;
#50854 = CARTESIAN_POINT ( 'NONE',  ( 8.224510206698742110, 14.34966873604972548, 62.08442372801901143 ) ) ;
#50856 = CARTESIAN_POINT ( 'NONE',  ( -17.72696623605163424, 5.499999999999871214, 53.59811031808416715 ) ) ;
#50857 = CARTESIAN_POINT ( 'NONE',  ( 8.224510206698742110, 14.34966873604972548, 77.08442372801901854 ) ) ;
#50858 = CARTESIAN_POINT ( 'NONE',  ( 12.14591786802327356, -12.06949235617739191, 35.62609039468568994 ) ) ;
#50859 = CARTESIAN_POINT ( 'NONE',  ( 5.049401038298161559, -19.05341960407611168, 42.70724293864767418 ) ) ;
#50860 = CARTESIAN_POINT ( 'NONE',  ( -19.05341960407611168, -5.049401038298163336, 46.45724293864768129 ) ) ;
#50861 = CARTESIAN_POINT ( 'NONE',  ( 9.564922557960805705, 16.46253265017160317, 59.58224293864769550 ) ) ;
#50862 = CARTESIAN_POINT ( 'NONE',  ( -5.823673210054431948, 21.52544592524334988, 42.70942372801901854 ) ) ;
#50863 = CARTESIAN_POINT ( 'NONE',  ( -14.34966873604972548, 8.224510206698743886, 53.33442372801901854 ) ) ;
#50864 = CARTESIAN_POINT ( 'NONE',  ( -8.314922557961024197, 14.29746914071037800, 107.9177570613523471 ) ) ;
#50865 = CARTESIAN_POINT ( 'NONE',  ( 13.89961937509977652, -13.97604488694527269, 33.12390960531434558 ) ) ;
#50866 = CARTESIAN_POINT ( 'NONE',  ( -21.55341960407619339, 5.719274019375674811, 108.5427570613523756 ) ) ;
#50867 = CARTESIAN_POINT ( 'NONE',  ( 13.97604488694548053, -13.89961937509957401, 105.6260903946856757 ) ) ;
#50868 = CARTESIAN_POINT ( 'NONE',  ( -16.46253265017146816, -9.564922557961047289, 64.16775706135233293 ) ) ;
#50869 = CARTESIAN_POINT ( 'NONE',  ( -16.55341960407611168, -4.379528057220339221, 76.45724293864769550 ) ) ;
#50870 = CARTESIAN_POINT ( 'NONE',  ( 16.46253265017160672, -9.564922557960803928, 43.33224293864769550 ) ) ;
#50872 = CARTESIAN_POINT ( 'NONE',  ( 17.40861289039003168, -6.110651285853313297, 91.12767529172569425 ) ) ;
#50871 = CARTESIAN_POINT ( 'NONE',  ( -5.153800228976607833, 19.02544592524334988, 67.70942372801900433 ) ) ;
#50873 = CARTESIAN_POINT ( 'NONE',  ( 5.719274019375673035, 21.55341960407619339, 72.29275706135236135 ) ) ;
#50874 = CARTESIAN_POINT ( 'NONE',  ( 16.53943276465976808, 0.05219959533934440121, 41.25109039468568284 ) ) ;
#50875 = CARTESIAN_POINT ( 'NONE',  ( -17.50000000000001066, 4.658240926743144605, 23.94470417816805963 ) ) ;
#50876 = CARTESIAN_POINT ( 'NONE',  ( 0.05219959533907565091, 21.53943276465977519, 34.99890960531435979 ) ) ;
#50877 = CARTESIAN_POINT ( 'NONE',  ( 16.52544592524335698, 4.483927247898782831, 21.45942372801901499 ) ) ;
#50878 = CARTESIAN_POINT ( 'NONE',  ( -19.05341960407611168, -5.049401038298164224, 26.45724293864769550 ) ) ;
#50879 = CARTESIAN_POINT ( 'NONE',  ( -5.153800228976607833, 19.02544592524334988, 32.70942372801899722 ) ) ;
#50880 = CARTESIAN_POINT ( 'NONE',  ( -3.573655867282028392E-15, 2.428612866367529932E-14, 155.0000000000000000 ) ) ;
#50881 = CARTESIAN_POINT ( 'NONE',  ( 16.46253265017160672, -9.564922557960803928, 33.33224293864770260 ) ) ;
#50882 = CARTESIAN_POINT ( 'NONE',  ( -20.17688442456149644, -20.77425831086903329, -52.59230516607028250 ) ) ;
#50883 = CARTESIAN_POINT ( 'NONE',  ( 13.89961937509977652, -13.97604488694527269, 68.12390960531436690 ) ) ;
#50884 = CARTESIAN_POINT ( 'NONE',  ( -19.46398650005391318, 5.499999999999953815, 100.1826965148636646 ) ) ;
#50885 = CARTESIAN_POINT ( 'NONE',  ( -5.153800228976607833, 19.02544592524334988, 22.70942372801899012 ) ) ;
#50886 = CARTESIAN_POINT ( 'NONE',  ( -4.483927247898782831, 16.52544592524335698, 112.7094237280190328 ) ) ;
#50887 = CARTESIAN_POINT ( 'NONE',  ( 13.97604488694527802, 13.89961937509977652, 44.37390960531435269 ) ) ;
#50888 = CARTESIAN_POINT ( 'NONE',  ( 5.153800228976335163, 19.02544592524342804, 89.79057627198102409 ) ) ;
#50889 = CARTESIAN_POINT ( 'NONE',  ( -21.55341960407619339, 5.719274019375674811, 68.54275706135234714 ) ) ;
#50890 = CARTESIAN_POINT ( 'NONE',  ( -19.03943276465977164, 0.05219959533909376836, 51.24890960531436690 ) ) ;
#50891 = CARTESIAN_POINT ( 'NONE',  ( 10.72451020669871369, 18.67979575497193778, 62.08442372801901143 ) ) ;
#50893 = CARTESIAN_POINT ( 'NONE',  ( -18.62759615963270932, 10.81492255796079327, 25.83224293864769194 ) ) ;
#50892 = CARTESIAN_POINT ( 'NONE',  ( 19.03943276465977164, 0.05219959533936151252, 96.25109039468567573 ) ) ;
#50894 = CARTESIAN_POINT ( 'NONE',  ( 19.05341960407611168, 5.049401038298154454, 38.95724293864767418 ) ) ;
#50895 = CARTESIAN_POINT ( 'NONE',  ( 10.81492255796078972, 18.62759615963270932, 109.5822429386476955 ) ) ;
#50896 = CARTESIAN_POINT ( 'NONE',  ( -19.03943276465977164, -0.05219959533935918106, 28.75109039468566507 ) ) ;
#50897 = CARTESIAN_POINT ( 'NONE',  ( -8.224510206698948167, 14.34966873604960824, 105.4155762719810383 ) ) ;
#50898 = CARTESIAN_POINT ( 'NONE',  ( -5.049401038298153566, 19.05341960407611168, 65.20724293864765286 ) ) ;
#50899 = CARTESIAN_POINT ( 'NONE',  ( 9.474510206698729675, 16.51473224551082808, 112.0844237280190043 ) ) ;
#50900 = CARTESIAN_POINT ( 'NONE',  ( 14.29746914071049879, -8.314922557960816363, 73.33224293864769550 ) ) ;
#50901 = CARTESIAN_POINT ( 'NONE',  ( -5.823673210054116645, -21.52544592524344225, 27.29057627198103120 ) ) ;
#50902 = CARTESIAN_POINT ( 'NONE',  ( 9.564922557961047289, -16.46253265017146816, 90.41775706135234714 ) ) ;
#50903 = CARTESIAN_POINT ( 'NONE',  ( 10.72451020669898902, -18.67979575497178502, 87.91557627198103830 ) ) ;
#50904 = CARTESIAN_POINT ( 'NONE',  ( -18.67979575497193778, 10.72451020669871902, 53.33442372801901854 ) ) ;
#50905 = CARTESIAN_POINT ( 'NONE',  ( -12.14591786802326823, 12.06949235617739902, 58.12609039468568994 ) ) ;
#50907 = CARTESIAN_POINT ( 'NONE',  ( 21.55341960407619695, -5.719274019375665929, 51.04275706135234714 ) ) ;
#50906 = CARTESIAN_POINT ( 'NONE',  ( -4.483927247898782831, 16.52544592524335698, 52.70942372801902565 ) ) ;
#50908 = CARTESIAN_POINT ( 'NONE',  ( 10.81492255796078972, 18.62759615963270932, 49.58224293864769550 ) ) ;
#50909 = CARTESIAN_POINT ( 'NONE',  ( -16.46253265017160317, 9.564922557960807481, 50.83224293864770260 ) ) ;
#50910 = CARTESIAN_POINT ( 'NONE',  ( 38.00000000000000000, 12.34694845685046616, -4.649999994537627579 ) ) ;
#50911 = CARTESIAN_POINT ( 'NONE',  ( -12.14591786802326823, 12.06949235617739902, 73.12609039468567573 ) ) ;
#50912 = EDGE_CURVE ( 'NONE', #39277, #90572, #153271, .T. ) ;
#50913 = CARTESIAN_POINT ( 'NONE',  ( -10.72451020669898014, 18.67979575497178502, 105.4155762719810383 ) ) ;
#50914 = CARTESIAN_POINT ( 'NONE',  ( -0.05219959533910754901, -16.53943276465976808, 47.49890960531435979 ) ) ;
#50915 = CARTESIAN_POINT ( 'NONE',  ( -14.29746914071037622, -8.314922557961029526, 64.16775706135234714 ) ) ;
#50916 = CARTESIAN_POINT ( 'NONE',  ( -13.97604488694547697, 13.89961937509957934, 98.12609039468566152 ) ) ;
#50917 = CARTESIAN_POINT ( 'NONE',  ( 10.72451020669898902, -18.67979575497178502, 92.91557627198103830 ) ) ;
#50918 = CARTESIAN_POINT ( 'NONE',  ( -4.483927247898539470, -16.52544592524342804, 47.29057627198103120 ) ) ;
#50919 = ORIENTED_EDGE ( 'NONE', *, *, #55537, .T. ) ;
#50920 = CARTESIAN_POINT ( 'NONE',  ( -17.05116617787824751, 6.768360034955817284, 73.65675553259202957 ) ) ;
#50921 = CARTESIAN_POINT ( 'NONE',  ( 0.05219959533907565091, 21.53943276465977519, 74.99890960531435269 ) ) ;
#50922 = CARTESIAN_POINT ( 'NONE',  ( -8.314922557961024197, 14.29746914071037800, 112.9177570613523329 ) ) ;
#50923 = VERTEX_POINT ( 'NONE', #152990 ) ;
#50924 = LINE ( 'NONE', #35745, #85622 ) ;
#50925 = CARTESIAN_POINT ( 'NONE',  ( -15.72974639402197994, 15.80617190586746368, 95.62390960531436690 ) ) ;
#50926 = CARTESIAN_POINT ( 'NONE',  ( -10.72451020669870658, -18.67979575497194134, 29.58442372801901854 ) ) ;
#50927 = CARTESIAN_POINT ( 'NONE',  ( 4.483927247898545687, 16.52544592524342804, 44.79057627198103120 ) ) ;
#50928 = CARTESIAN_POINT ( 'NONE',  ( 4.379528057220092307, 16.55341960407617563, 47.29275706135234003 ) ) ;
#50929 = CIRCLE ( 'NONE', #118802, 10.00000000000000000 ) ;
#50930 = CARTESIAN_POINT ( 'NONE',  ( -16.51473224551069308, -9.474510206698971260, 51.66557627198102409 ) ) ;
#50931 = CARTESIAN_POINT ( 'NONE',  ( -9.474510206698964154, 16.51473224551069663, 80.41557627198103830 ) ) ;
#50932 = ORIENTED_EDGE ( 'NONE', *, *, #150147, .F. ) ;
#50933 = CARTESIAN_POINT ( 'NONE',  ( 0.05219959533907565091, 21.53943276465977519, 34.99890960531435979 ) ) ;
#50934 = CARTESIAN_POINT ( 'NONE',  ( 9.564922557960805705, 16.46253265017160317, 64.58224293864769550 ) ) ;
#50935 = CARTESIAN_POINT ( 'NONE',  ( -0.05219959533934338120, 16.53943276465976808, 27.50109039468567929 ) ) ;
#50936 = CARTESIAN_POINT ( 'NONE',  ( -19.03943276465977164, -0.05219959533935918106, 48.75109039468566863 ) ) ;
#50937 = CARTESIAN_POINT ( 'NONE',  ( -5.823673210054116645, -21.52544592524344225, 102.2905762719810383 ) ) ;
#50938 = CARTESIAN_POINT ( 'NONE',  ( 16.55341960407611168, 4.379528057220329451, 33.95724293864769550 ) ) ;
#50939 = CARTESIAN_POINT ( 'NONE',  ( -19.05341960407611168, -5.049401038298163336, 76.45724293864769550 ) ) ;
#50940 = CARTESIAN_POINT ( 'NONE',  ( -18.62759615963270932, 10.81492255796079327, 65.83224293864769550 ) ) ;
#50942 = CARTESIAN_POINT ( 'NONE',  ( -4.483927247898782831, 16.52544592524335698, 27.70942372801901854 ) ) ;
#50941 = CARTESIAN_POINT ( 'NONE',  ( -21.52544592524343514, 5.823673210054127303, 76.04057627198102409 ) ) ;
#50943 = CARTESIAN_POINT ( 'NONE',  ( 21.52544592524344225, -5.823673210054117533, 23.54057627198102765 ) ) ;
#50944 = CARTESIAN_POINT ( 'NONE',  ( -21.52544592524334988, -5.823673210054445271, 68.95942372801901854 ) ) ;
#50945 = CARTESIAN_POINT ( 'NONE',  ( 19.02544592524343514, -5.153800228976328945, 78.54057627198099567 ) ) ;
#50946 = CARTESIAN_POINT ( 'NONE',  ( 9.564922557960805705, 16.46253265017160317, 34.58224293864770260 ) ) ;
#50947 = CARTESIAN_POINT ( 'NONE',  ( 13.89961937509977652, -13.97604488694527269, 88.12390960531438111 ) ) ;
#50948 = CARTESIAN_POINT ( 'NONE',  ( 16.53943276465976808, -0.05219959533910856209, 88.74890960531436690 ) ) ;
#50949 = ORIENTED_EDGE ( 'NONE', *, *, #85306, .T. ) ;
#50950 = CARTESIAN_POINT ( 'NONE',  ( 5.153800228976615827, -19.02544592524334988, 100.2094237280190043 ) ) ;
#50951 = CARTESIAN_POINT ( 'NONE',  ( -3.573655867282028392E-15, 2.428612866367529932E-14, -18.00000000000000000 ) ) ;
#50952 = CARTESIAN_POINT ( 'NONE',  ( 13.97604488694527802, 13.89961937509977652, 69.37390960531436690 ) ) ;
#50954 = CARTESIAN_POINT ( 'NONE',  ( 15.72974639402199770, -15.80617190586745480, 23.12390960531436335 ) ) ;
#50953 = CARTESIAN_POINT ( 'NONE',  ( -21.52544592524334988, -5.823673210054445271, 93.95942372801903275 ) ) ;
#50955 = CARTESIAN_POINT ( 'NONE',  ( 8.224510206698742110, 14.34966873604972548, 72.08442372801899012 ) ) ;
#50956 = CARTESIAN_POINT ( 'NONE',  ( -29.14368513529649007, 0.8274645171316362680, -49.37167794572891211 ) ) ;
#50957 = CARTESIAN_POINT ( 'NONE',  ( 5.049401038297881783, 19.05341960407617563, 57.29275706135231871 ) ) ;
#50958 = CARTESIAN_POINT ( 'NONE',  ( 5.719274019375673035, 21.55341960407619339, 107.2927570613523471 ) ) ;
#50959 = CARTESIAN_POINT ( 'NONE',  ( 1.988064558232696151E-15, -30.27659582821216588, 144.4843446568999639 ) ) ;
#50960 = CARTESIAN_POINT ( 'NONE',  ( -13.89961937509977652, 13.97604488694528158, 30.62390960531435269 ) ) ;
#50961 = CARTESIAN_POINT ( 'NONE',  ( -8.314922557961024197, 14.29746914071037800, 112.9177570613523329 ) ) ;
#50962 = DIRECTION ( 'NONE',  ( 0.000000000000000000, 0.000000000000000000, 1.000000000000000000 ) ) ;
#50963 = CARTESIAN_POINT ( 'NONE',  ( 16.53943276465976808, 0.05219959533934440121, 106.2510903946856757 ) ) ;
#50964 = CARTESIAN_POINT ( 'NONE',  ( -19.39056639909675894, -5.499999999999976019, 85.78948781074340957 ) ) ;
#50965 = CARTESIAN_POINT ( 'NONE',  ( 14.29746914071037800, 8.314922557961029526, 81.66775706135236135 ) ) ;
#50966 = CARTESIAN_POINT ( 'NONE',  ( -19.02544592524342804, 5.153800228976336051, 26.04057627198103120 ) ) ;
#50967 = CARTESIAN_POINT ( 'NONE',  ( 18.67979575497194134, -10.72451020669871369, 90.83442372801901854 ) ) ;
#50968 = CARTESIAN_POINT ( 'NONE',  ( -0.05219959533936034679, 19.03943276465977164, 102.5010903946856757 ) ) ;
#50969 = CARTESIAN_POINT ( 'NONE',  ( -10.81492255796105439, 18.62759615963255655, 62.91775706135236135 ) ) ;
#50970 = CARTESIAN_POINT ( 'NONE',  ( -19.03943276465977164, -0.05219959533935918106, 43.75109039468566863 ) ) ;
#50971 = CARTESIAN_POINT ( 'NONE',  ( -19.02544592524342804, 5.153800228976336051, 81.04057627198103830 ) ) ;
#50972 = CARTESIAN_POINT ( 'NONE',  ( 19.05341960407611168, 5.049401038298154454, 63.95724293864769550 ) ) ;
#50973 = CARTESIAN_POINT ( 'NONE',  ( 18.67979575497178502, 10.72451020669898547, 54.16557627198103120 ) ) ;
#50974 = CARTESIAN_POINT ( 'NONE',  ( 5.153800228976335163, 19.02544592524342804, 44.79057627198103830 ) ) ;
#50975 = CARTESIAN_POINT ( 'NONE',  ( 14.29746914071037800, 8.314922557961029526, 81.66775706135236135 ) ) ;
#50976 = EDGE_CURVE ( 'NONE', #30088, #36346, #46614, .T. ) ;
#50977 = VERTEX_POINT ( 'NONE', #153994 ) ;
#50979 = CARTESIAN_POINT ( 'NONE',  ( 29.86685920354754487, 21.69954338932564752, -1.424999997268813212 ) ) ;
#50978 = CARTESIAN_POINT ( 'NONE',  ( -14.29746914071049879, 8.314922557960819915, 80.83224293864769550 ) ) ;
#50980 = CARTESIAN_POINT ( 'NONE',  ( 4.379528057220092307, 16.55341960407617563, 42.29275706135235424 ) ) ;
#50981 = CARTESIAN_POINT ( 'NONE',  ( 4.483927247898545687, 16.52544592524342804, 99.79057627198103830 ) ) ;
#50982 = CARTESIAN_POINT ( 'NONE',  ( 13.89961937509957401, 13.97604488694547697, 61.87609039468566863 ) ) ;
#50983 = CARTESIAN_POINT ( 'NONE',  ( -4.483927247898539470, -16.52544592524342804, 77.29057627198102409 ) ) ;
#50984 = CARTESIAN_POINT ( 'NONE',  ( 18.62759615963255655, 10.81492255796105972, 31.66775706135234358 ) ) ;
#50986 = CARTESIAN_POINT ( 'NONE',  ( 18.62759615963271287, -10.81492255796078972, 93.33224293864769550 ) ) ;
#50985 = CARTESIAN_POINT ( 'NONE',  ( 69.65682714487590488, -71.74905178543389184, -4.999999999999999112 ) ) ;
#50987 = CARTESIAN_POINT ( 'NONE',  ( -5.153800228976328057, -19.02544592524343514, 97.29057627198099567 ) ) ;
#50988 = CARTESIAN_POINT ( 'NONE',  ( 4.483927247898545687, 16.52544592524342804, 69.79057627198102409 ) ) ;
#50989 = CARTESIAN_POINT ( 'NONE',  ( 27.75718128995143630, -28.53842127824106356, -16.93139376985908129 ) ) ;
#50990 = CARTESIAN_POINT ( 'NONE',  ( 16.46253265017160672, -9.564922557960803928, 43.33224293864769550 ) ) ;
#50991 = CARTESIAN_POINT ( 'NONE',  ( 36.91746824999999177, 2.880721459617395097E-14, -3.624999997268813168 ) ) ;
#50992 = CARTESIAN_POINT ( 'NONE',  ( -19.02544592524334988, -5.153800228976617603, 83.95942372801901854 ) ) ;
#50993 = CARTESIAN_POINT ( 'NONE',  ( 0.05219959533937995610, -21.53943276465977519, 20.00109039468568639 ) ) ;
#50994 = CARTESIAN_POINT ( 'NONE',  ( -19.03943276465977164, 0.05219959533909376836, 66.24890960531436690 ) ) ;
#50995 = CARTESIAN_POINT ( 'NONE',  ( 5.153800228976615827, -19.02544592524334988, 50.20942372801897591 ) ) ;
#50996 = CARTESIAN_POINT ( 'NONE',  ( -19.03943276465977164, 0.05219959533909376836, 46.24890960531435979 ) ) ;
#50997 = CARTESIAN_POINT ( 'NONE',  ( 12.14591786802309770, 12.06949235617756955, 69.37390960531436690 ) ) ;
#50998 = CARTESIAN_POINT ( 'NONE',  ( 12.06949235617757843, -12.14591786802309237, 58.12390960531435979 ) ) ;
#50999 = CARTESIAN_POINT ( 'NONE',  ( 5.153800228976335163, 19.02544592524342804, 74.79057627198103830 ) ) ;
#51000 = CARTESIAN_POINT ( 'NONE',  ( -5.823673210054116645, -21.52544592524344225, 82.29057627198103830 ) ) ;
#51001 = CARTESIAN_POINT ( 'NONE',  ( -19.03943276465977164, 0.05219959533909376836, 71.24890960531435269 ) ) ;
#51002 = CARTESIAN_POINT ( 'NONE',  ( 21.52544592524344225, -5.823673210054117533, 73.54057627198102409 ) ) ;
#51003 = CARTESIAN_POINT ( 'NONE',  ( 5.719274019375673035, 21.55341960407619339, 112.2927570613523471 ) ) ;
#51006 = CARTESIAN_POINT ( 'NONE',  ( 14.29746914071049879, -8.314922557960816363, 93.33224293864769550 ) ) ;
#51005 = CARTESIAN_POINT ( 'NONE',  ( -14.34966873604972548, 8.224510206698743886, 108.3344237280190185 ) ) ;
#51004 = CARTESIAN_POINT ( 'NONE',  ( 19.03943276465977164, -0.05219959533909143690, 28.74890960531435624 ) ) ;
#51007 = CARTESIAN_POINT ( 'NONE',  ( -9.564922557961040184, 16.46253265017147172, 102.9177570613523329 ) ) ;
#51008 = VERTEX_POINT ( 'NONE', #299 ) ;
#51009 = CARTESIAN_POINT ( 'NONE',  ( -21.52544592524334988, -5.823673210054445271, 23.95942372801901143 ) ) ;
#51010 = CARTESIAN_POINT ( 'NONE',  ( 16.51473224551083163, -9.474510206698727899, 55.83442372801899722 ) ) ;
#51011 = CARTESIAN_POINT ( 'NONE',  ( 14.29746914071049879, -8.314922557960816363, 28.33224293864769550 ) ) ;
#51012 = CARTESIAN_POINT ( 'NONE',  ( 5.823673210054125526, 21.52544592524343514, 69.79057627198102409 ) ) ;
#51013 = CARTESIAN_POINT ( 'NONE',  ( 19.05341960407611168, 5.049401038298154454, 98.95724293864766707 ) ) ;
#51014 = CARTESIAN_POINT ( 'NONE',  ( -14.29746914071049879, 8.314922557960819915, 60.83224293864769550 ) ) ;
#51015 = CARTESIAN_POINT ( 'NONE',  ( -18.87075004821565472, 5.499999999999873879, 48.67408112101043827 ) ) ;
#51016 = CARTESIAN_POINT ( 'NONE',  ( -5.049401038298153566, 19.05341960407611168, 35.20724293864768839 ) ) ;
#51017 = CARTESIAN_POINT ( 'NONE',  ( -15.80617190586768217, 15.72974639402176855, 103.1260903946856757 ) ) ;
#51018 = CARTESIAN_POINT ( 'NONE',  ( 16.52544592524335698, 4.483927247898782831, 91.45942372801901854 ) ) ;
#51019 = CARTESIAN_POINT ( 'NONE',  ( 15.80617190586769283, -15.72974639402175789, 40.62609039468567573 ) ) ;
#51020 = CARTESIAN_POINT ( 'NONE',  ( -4.483927247898782831, 16.52544592524335698, 37.70942372801900433 ) ) ;
#51021 = CARTESIAN_POINT ( 'NONE',  ( -10.72451020669898014, 18.67979575497178502, 25.41557627198103120 ) ) ;
#51022 = CARTESIAN_POINT ( 'NONE',  ( -16.46253265017160317, 9.564922557960807481, 50.83224293864770260 ) ) ;
#51023 = CARTESIAN_POINT ( 'NONE',  ( -5.153800228976328057, -19.02544592524343514, 62.29057627198100988 ) ) ;
#51024 = CARTESIAN_POINT ( 'NONE',  ( -16.55341960407617563, 4.379528057220093196, 48.54275706135234714 ) ) ;
#51025 = CARTESIAN_POINT ( 'NONE',  ( -16.55341960407611168, -4.379528057220339221, 101.4572429386476955 ) ) ;
#51026 = CARTESIAN_POINT ( 'NONE',  ( -16.55341960407617563, 4.379528057220093196, 108.5427570613523756 ) ) ;
#51027 = CARTESIAN_POINT ( 'NONE',  ( -5.049401038298153566, 19.05341960407611168, 50.20724293864770260 ) ) ;
#51030 = CARTESIAN_POINT ( 'NONE',  ( -13.97604488694527625, -13.89961937509977652, 81.87390960531436690 ) ) ;
#51029 = CARTESIAN_POINT ( 'NONE',  ( -0.05219959533909027116, -19.03943276465977164, 97.49890960531436690 ) ) ;
#51028 = CARTESIAN_POINT ( 'NONE',  ( -10.81492255796105439, 18.62759615963255655, 52.91775706135235424 ) ) ;
#51031 = CARTESIAN_POINT ( 'NONE',  ( -0.05219959533909027116, -19.03943276465977164, 102.4989096053143669 ) ) ;
#51032 = CARTESIAN_POINT ( 'NONE',  ( -16.53943276465976808, 0.05219959533911058130, 41.24890960531435269 ) ) ;
#51033 = CARTESIAN_POINT ( 'NONE',  ( -0.05219959533934338120, 16.53943276465976808, 107.5010903946856899 ) ) ;
#51034 = CARTESIAN_POINT ( 'NONE',  ( 16.52544592524342804, -4.483927247898539470, 43.54057627198103830 ) ) ;
#51035 = CARTESIAN_POINT ( 'NONE',  ( 5.000000000000000000, -139.5000000000000000, 21.32407087589995953 ) ) ;
#51036 = CARTESIAN_POINT ( 'NONE',  ( -19.02544592524334988, -5.153800228976617603, 38.95942372801900433 ) ) ;
#51037 = CARTESIAN_POINT ( 'NONE',  ( -19.05341960407611168, -5.049401038298163336, 71.45724293864766707 ) ) ;
#51038 = CARTESIAN_POINT ( 'NONE',  ( 13.89961937509957401, 13.97604488694547697, 46.87609039468565442 ) ) ;
#51039 = CARTESIAN_POINT ( 'NONE',  ( 11.40812507854754365, 35.11059874428196537, -9.724999997268813701 ) ) ;
#51040 = CARTESIAN_POINT ( 'NONE',  ( 2.500000000000000000, -1.178949249685218970, -2.041999999999998039 ) ) ;
#51042 = CARTESIAN_POINT ( 'NONE',  ( -8.224510206698735004, -14.34966873604973081, 64.58442372801900433 ) ) ;
#51041 = CARTESIAN_POINT ( 'NONE',  ( -19.03943276465977164, -0.05219959533935918106, 83.75109039468567573 ) ) ;
#51043 = CARTESIAN_POINT ( 'NONE',  ( 16.61371651742600619, 7.165104196376149481, 93.64584930007004004 ) ) ;
#51044 = CARTESIAN_POINT ( 'NONE',  ( -5.049401038298153566, 19.05341960407611168, 100.2072429386476955 ) ) ;
#51045 = CARTESIAN_POINT ( 'NONE',  ( 10.72451020669871369, 18.67979575497193778, 27.08442372801901854 ) ) ;
#51046 = CARTESIAN_POINT ( 'NONE',  ( -9.474510206698720793, -16.51473224551083518, 89.58442372801900433 ) ) ;
#51048 = CARTESIAN_POINT ( 'NONE',  ( -16.46253265017160317, 9.564922557960807481, 45.83224293864769550 ) ) ;
#51047 = FACE_OUTER_BOUND ( 'NONE', #128586, .T. ) ;
#51049 = CARTESIAN_POINT ( 'NONE',  ( -13.89961937509977652, 13.97604488694528158, 90.62390960531432427 ) ) ;
#51051 = CARTESIAN_POINT ( 'NONE',  ( -5.153800228976328057, -19.02544592524343514, 52.29057627198100988 ) ) ;
#51050 = CARTESIAN_POINT ( 'NONE',  ( -14.34966873604960291, -8.224510206698953496, 46.66557627198102409 ) ) ;
#51052 = CARTESIAN_POINT ( 'NONE',  ( -13.97604488694547697, 13.89961937509957934, 68.12609039468563310 ) ) ;
#51053 = CARTESIAN_POINT ( 'NONE',  ( -5.049401038297874678, -19.05341960407617918, 34.79275706135233293 ) ) ;
#51054 = CARTESIAN_POINT ( 'NONE',  ( 9.564922557960805705, 16.46253265017160317, 59.58224293864769550 ) ) ;
#51055 = CARTESIAN_POINT ( 'NONE',  ( -15.80617190586745835, -15.72974639402198527, 61.87390960531436690 ) ) ;
#51057 = CARTESIAN_POINT ( 'NONE',  ( 15.72974639402176855, 15.80617190586768217, 111.8760903946856615 ) ) ;
#51056 = CARTESIAN_POINT ( 'NONE',  ( -16.55341960407611168, -4.379528057220339221, 71.45724293864769550 ) ) ;
#51058 = DIRECTION ( 'NONE',  ( 1.000000000000000000, 0.000000000000000000, 0.000000000000000000 ) ) ;
#51059 = CARTESIAN_POINT ( 'NONE',  ( 0.05219959533909260263, 19.03943276465977164, 114.9989096053143669 ) ) ;
#51060 = CARTESIAN_POINT ( 'NONE',  ( -0.05219959533909027116, -19.03943276465977164, 52.49890960531436690 ) ) ;
#51061 = CARTESIAN_POINT ( 'NONE',  ( 9.564922557960805705, 16.46253265017160317, 34.58224293864770260 ) ) ;
#51062 = CARTESIAN_POINT ( 'NONE',  ( -16.55341960407611168, -4.379528057220339221, 101.4572429386476955 ) ) ;
#51063 = VECTOR ( 'NONE', #9170, 1000.000000000000000 ) ;
#51064 = CARTESIAN_POINT ( 'NONE',  ( -21.52544592524343514, 5.823673210054127303, 106.0405762719810525 ) ) ;
#51065 = CARTESIAN_POINT ( 'NONE',  ( 13.97604488694527802, 13.89961937509977652, 114.3739096053143669 ) ) ;
#51066 = CARTESIAN_POINT ( 'NONE',  ( 10.72451020669871369, 18.67979575497193778, 32.08442372801901854 ) ) ;
#51067 = CARTESIAN_POINT ( 'NONE',  ( 13.97604488694527802, 13.89961937509977652, 99.37390960531436690 ) ) ;
#51068 = CARTESIAN_POINT ( 'NONE',  ( -19.05341960407611168, -5.049401038298163336, 21.45724293864768839 ) ) ;
#51069 = CARTESIAN_POINT ( 'NONE',  ( -10.81492255796105439, 18.62759615963255655, 72.91775706135234714 ) ) ;
#51070 = CARTESIAN_POINT ( 'NONE',  ( 21.52544592524344225, -5.823673210054117533, 98.54057627198105251 ) ) ;
#51071 = CARTESIAN_POINT ( 'NONE',  ( -30.40000000000003766, 3.080147572466333233E-13, -64.92279855667830191 ) ) ;
#51072 = PLANE ( 'NONE',  #194786 ) ;
#51073 = CARTESIAN_POINT ( 'NONE',  ( 28.90000000000004476, 0.000000000000000000, -52.65483682830183199 ) ) ;
#51074 = CARTESIAN_POINT ( 'NONE',  ( 12.06949235617739724, 12.14591786802326823, 51.87609039468568284 ) ) ;
#51075 = CARTESIAN_POINT ( 'NONE',  ( 16.52544592524342804, -4.483927247898539470, 113.5405762719810383 ) ) ;
#51076 = DIRECTION ( 'NONE',  ( -1.000000000000000000, 0.000000000000000000, 0.000000000000000000 ) ) ;
#51077 = CARTESIAN_POINT ( 'NONE',  ( 19.02544592524343514, -5.153800228976328945, 58.54057627198102409 ) ) ;
#51079 = EDGE_CURVE ( 'NONE', #92102, #72646, #49566, .T. ) ;
#51078 = CARTESIAN_POINT ( 'NONE',  ( 8.224510206698953496, -14.34966873604960469, 92.91557627198103830 ) ) ;
#51080 = CARTESIAN_POINT ( 'NONE',  ( -5.719274019375978568, 21.55341960407610458, 45.20724293864769550 ) ) ;
#51081 = CARTESIAN_POINT ( 'NONE',  ( 16.55341960407611168, 4.379528057220329451, 63.95724293864770260 ) ) ;
#51082 = CARTESIAN_POINT ( 'NONE',  ( -13.97604488694547697, 13.89961937509957934, 113.1260903946856757 ) ) ;
#51083 = CARTESIAN_POINT ( 'NONE',  ( -5.719274019375665041, -21.55341960407619695, 84.79275706135234714 ) ) ;
#51084 = CARTESIAN_POINT ( 'NONE',  ( 16.21995358207303539, -7.366697692864228486, 77.43551001512156517 ) ) ;
#51085 = CARTESIAN_POINT ( 'NONE',  ( -4.379528057220086978, -16.55341960407618274, 94.79275706135234714 ) ) ;
#51086 = CARTESIAN_POINT ( 'NONE',  ( 8.314922557960818139, 14.29746914071049879, 39.58224293864769550 ) ) ;
#51087 = CARTESIAN_POINT ( 'NONE',  ( 19.02544592524343514, -5.153800228976328945, 33.54057627198102409 ) ) ;
#51088 = CARTESIAN_POINT ( 'NONE',  ( -5.049401038298153566, 19.05341960407611168, 85.20724293864766707 ) ) ;
#51089 = CARTESIAN_POINT ( 'NONE',  ( 18.67979575497178502, 10.72451020669898547, 99.16557627198100988 ) ) ;
#51090 = CARTESIAN_POINT ( 'NONE',  ( -12.14591786802326823, 12.06949235617739902, 38.12609039468567573 ) ) ;
#51092 = CARTESIAN_POINT ( 'NONE',  ( 5.823673210054444382, -21.52544592524334988, 80.20942372801901854 ) ) ;
#51091 = CARTESIAN_POINT ( 'NONE',  ( 12.06949235617757843, -12.14591786802309237, 63.12390960531435979 ) ) ;
#51093 = VECTOR ( 'NONE', #21931, 1000.000000000000000 ) ;
#51094 = CARTESIAN_POINT ( 'NONE',  ( -4.483927247898782831, 16.52544592524335698, 102.7094237280190185 ) ) ;
#51095 = CARTESIAN_POINT ( 'NONE',  ( 4.500000000000000888, -139.5000000000000000, 21.32407087589996308 ) ) ;
#51096 = DIRECTION ( 'NONE',  ( -0.7071067811865467956, 0.000000000000000000, -0.7071067811865483499 ) ) ;
#51097 = CARTESIAN_POINT ( 'NONE',  ( -12.14591786802309592, -12.06949235617757132, 26.87390960531435979 ) ) ;
#51098 = CARTESIAN_POINT ( 'NONE',  ( 16.55341960407618274, -4.379528057220086978, 76.04275706135237556 ) ) ;
#51099 = CARTESIAN_POINT ( 'NONE',  ( -5.153800228976328057, -19.02544592524343514, 87.29057627198103830 ) ) ;
#51100 = CARTESIAN_POINT ( 'NONE',  ( -16.51473224551069308, -9.474510206698971260, 106.6655762719810383 ) ) ;
#51101 = CARTESIAN_POINT ( 'NONE',  ( -10.72451020669870658, -18.67979575497194134, 89.58442372801901854 ) ) ;
#51102 = CARTESIAN_POINT ( 'NONE',  ( 14.29746914071037800, 8.314922557961029526, 86.66775706135234714 ) ) ;
#51103 = CARTESIAN_POINT ( 'NONE',  ( -4.379528057220328563, 16.55341960407611168, 65.20724293864768129 ) ) ;
#51104 = CARTESIAN_POINT ( 'NONE',  ( 13.97604488694527802, 13.89961937509977652, 64.37390960531436690 ) ) ;
#51105 = ORIENTED_EDGE ( 'NONE', *, *, #115652, .F. ) ;
#51107 =( BOUNDED_SURFACE ( )  B_SPLINE_SURFACE ( 3, 2, ( 
 ( #78875, #142542, #140554, #50550, #112210, #143525, #66695, #4021, #62709, #109221, #65699, #128359, #2042, #190055, #3041, #141552, #113194, #93049, #126379, #188076, #49547, #174883, #172902, #1036, #170900, #189077, #34380, #154736, #186086, #25220, #146522, #129351, #40360, #86862, #148546, #162704, #22195, #132372, #56533, #83844, #177891, #53522, #145526, #116202, #70704, #8013, #84844, #36349, #99013, #24209, #159696, #10037, #160704, #7005, #68687, #178892, #71697, #85858, #192041, #69696, #147547, #176892, #131363, #23201, #117200, #130342, #175884, #98002, #115200, #39361, #193052, #38363, #133364, #191046, #102035, #195055, #118211, #9035, #100018, #194065, #21193, #161705, #101019, #54529, #55526, #163718, #82849, #144528, #6014, #67693, #52519, #114180, #37355, #26793, #183440, #104611, #136925, #27796, #195652, #137917, #30747, #12618, #28779, #44925, #120754, #88435, #41958, #76239, #107563, #166299, #105595, #119785, #198612, #92396, #135952, #184430, #197622, #89437, #57124, #151125, #150129, #154082, #74282, #182453, #60080, #199600, #29754, #59087, #90418, #43934, #15576, #196645, #167281, #45910, #168258, #61067, #153078, #103624, #165300, #180486, #73298, #122739, #152103, #13587, #75254, #134968, #118798, #121748, #169241, #106581, #133960, #91389, #14580, #11631, #58115, #181469, #42947, #2379, #46908, #100101, #93388, #113270, #170246, #31740, #130427, #17560, #79220, #51606, #160789, #83928, #161785, #140890, #21274, #32731, #7088, #66773, #128434, #155074, #77234, #22277, #176976, #190131, #191128, #159779, #82931, #144609, #62055, #94383, #108569, #138903, #16569, #67773, #383, #192126, #174962, #68769, #38446, #6094, #123720, #156062, #185417, #36426, #78216, #139886, #129430, #98081, #53607, #1375, #115283, #52602, #63054, #145609, #124734, #186431, #114264, #47907, #175968, #109561, #171242, #37437, #99097, #9115, #103115, #57619, #195136, #71776, #23280, #85938, #149619, #146604, #84924, #41450, #72792, #147627, #165793, #197129, #134462, #178973, #56617, #11117, #163798, #118291, #10116, #104111, #70782, #162781, #8097, #132450, #164796, #179982, #40440, #120262, #194141, #55605, #196147, #88937, #54603, #102113, #177967, #39435, #43436, #26291, #87932, #119287, #27290, #24289, #12124, #181954, #150628, #73788, #180970, #42447, #25300, #86942, #105105, #135460, #58596, #69775, #131443, #148626, #117279, #193130, #116277, #133446, #101095, #154580, #16076, #1887, #90900, #198113, #182948, #89932, #60567, #108065, #93896, #138414, #139400, #59580, #28292, #63568, #151613, #13105, #74770, #136432, #882, #76739, #155574, #29269, #31244, #152586, #124233, #185929, #109070, #170749, #77734, #121254, #44431, #62557, #140399, #106085, #47414, #200094, #137420, #17069, #166791, #45418, #61562, #14077, #199100, #169749, #122243, #167771, #32238, #125242, #107071, #123231, #78723, #153580, #75743, #183933, #186940, #48411, #168742, #184922, #30246, #92894, #91889, #15078, #46406, #112057, #80710, #33236, #127205, #2885, #130187, #65546, #96867, #174732, #114025, #5860, #142388, #66543, #158551, #191883, #172744, #81684, #160552, #144373, #175722, #129194, #79728, #141397, #156578, #49393, #37201, #3867, #188919, #50397, #111056, #94894, #113040, #98857, #173745, #52368, #143366, #35214, #68532, #67536, #128207, #22042, #20041, #64564, #110067, #126229, #4858, #187924, #34225, #83693, #189904, #51379, #36195, #190892, #145371, #171747, #97849, #159538, #21036, #6853, #82689, #18073, #95887, #157570, #19063, #150397, #40195, #164559, #133205, #56370, #118053, #38210, #8876, #84688, #53367, #192897, #41213, #73556, #165558, #117037, #42217, #11893, #179743, #176737, #132212, #54374, #102874, #26053, #99866, #103878, #70544, #135229, #25057, #27055, #146368, #162542, #115045, #87697, #161550, #116046, #149382, #10878, #88701, #85702, #23043, #72548, #7855, #134226, #69542 ),
 ( #195911, #131206, #177735, #57386, #119059, #39204, #147388, #100860, #180741, #24046, #193903, #55367, #178732, #101875, #163557, #86700, #148385, #9879, #71539, #194896, #183708, #151385, #104870, #139174, #170518, #167546, #168523, #182715, #199871, #93664, #198876, #47178, #60343, #29041, #120035, #13848, #89699, #16839, #152363, #45194, #61335, #650, #92663, #90681, #153348, #106848, #78489, #59349, #30021, #108837, #31013, #62320, #15844, #166559, #28058, #43203, #136205, #123990, #75515, #137189, #122017, #197880, #181721, #123006, #185688, #91659, #32007, #14850, #76512, #155349, #154351, #138188, #196901, #184692, #12875, #58368, #74540, #46176, #121017, #44200, #105859, #107829, #169513, #77503, #20799, #144142, #21809, #80479, #81453, #95651, #67303, #65315, #3637, #17839, #160318, #82454, #36963, #126974, #51146, #19812, #143139, #4619, #125010, #157339, #171516, #140162, #79497, #127971, #1654, #52138, #188683, #128962, #98624, #66310, #64332, #33005, #156339, #63332, #33995, #189674, #190662, #111821, #112807, #94660, #186706, #175490, #48177, #109833, #141166, #2655, #174500, #50163, #113795, #126000, #35967, #187697, #97614, #159304, #5626, #49167, #110826, #172510, #18834, #142153, #173509, #34982, #96635, #158323, #54145, #72315, #83461, #162315, #116811, #130971, #103654, #39968, #6621, #37978, #148160, #70317, #10652, #84457, #133991, #193669, #176501, #87475, #195682, #57153, #9651, #69305, #179514, #165332, #192662, #24825, #100634, #115818, #163329, #117821, #55140, #131984, #145138, #146135, #71317, #68300, #129951, #101638, #132980, #7621, #25831, #118832, #194671, #38978, #178502, #56140, #23816, #86475, #40982, #164336, #177508, #22811, #191651, #85466, #102651, #149162, #147155, #180515, #8643, #41988, #53130, #114809, #99635, #161318, #181500, #42978, #46939, #121781, #198647, #168291, #169274, #27828, #15607, #185449, #92427, #77264, #137949, #76271, #28813, #90453, #123750, #199632, #122772, #154113, #138933, #167317, #151160, #60113, #184462, #59119, #413, #14614, #61099, #62087, #152137, #104643, #108599, #30780, #26824, #13620, #45941, #106617, #29787, #91423, #11662, #182485, #58147, #88465, #166330, #107596, #150162, #73328, #75287, #135000, #196678, #153110, #119815, #105628, #89469, #12648, #74315, #135982, #197653, #43966, #120785, #183475, #136958, #44959, #79253, #128727, #96399, #155105, #32764, #158086, #19578, #143903, #2411, #5385, #34740, #63087, #81221, #140925, #173266, #64091, #31770, #174266, #67068, #48927, #65076, #142902, #157096, #124766, #78246, #112572, #190423, #125759, #141910, #156096, #4384, #51899, #172262, #20561, #33752, #187459, #93418, #110581, #186464, #170276, #95411, #18592, #66069, #35734, #127735, #80240, #126734, #3401, #16598, #94416, #188437, #82212, #189437, #97381, #50914, #139919, #1408, #47942, #109593, #159067, #49916, #111581, #171276, #17594, #36718, #116574, #179272, #69065, #55899, #85220, #115581, #72066, #147922, #131743, #25592, #38740, #83224, #133739, #129715, #146911, #6382, #68061, #164093, #53906, #177269, #8400, #194428, #117572, #195434, #100398, #54900, #130732, #40736, #162078, #191412, #175252, #148919, #98380, #160077, #21564, #144899, #9408, #23572, #102406, #176260, #178263, #37731, #71074, #132740, #87236, #10408, #24584, #52888, #114563, #101387, #113558, #99393, #161076, #70075, #84218, #22571, #145897, #192424, #193425, #7381, #39726, #163080, #86232, #11414, #121539, #43725, #184222, #57907, #45703, #167073, #149907, #60856, #107354, #169027, #183234, #42739, #152872, #77023, #104401, #198395, #74073, #166083, #136714, #91183, #28575, #105386, #56909, #119579, #44715, #180274, #118584, #75048, #106371, #181262, #199392, #30532, #168053, #12411, #90211, #29550, #197415, #151894, #13384, #137708, #27586, #196437, #41744, #89224, #59873, #14367, #135744, #153869, #150918, #58881, #76033, #122531 ),
 ( #120547, #92185, #15367, #138695, #103408, #165086, #26580, #88223, #73084, #182240, #134755, #32524, #17353, #171033, #1166, #123514, #3172, #65829, #155855, #142671, #172027, #2174, #158832, #34510, #18357, #112338, #125525, #170038, #20320, #62841, #47701, #111341, #127498, #31528, #79008, #154866, #16363, #81969, #95175, #33515, #141681, #4150, #124525, #189203, #177, #50680, #174028, #173032, #49677, #63854, #187222, #97149, #96168, #157858, #35499, #61845, #140682, #186220, #156862, #19348, #94176, #185207, #188205, #80996, #46698, #109351, #93181, #78011, #108360, #48693, #64845, #139679, #80012, #110345, #126507, #5144, #179026, #66826, #128490, #190185, #51660, #178019, #53662, #132504, #6147, #8152, #67828, #101147, #162833, #85992, #147682, #54656, #113324, #98137, #131496, #117332, #82987, #24342, #115340, #114320, #194193, #143661, #22331, #177030, #191182, #163853, #100156, #175016, #159835, #69829, #130484, #70836, #144663, #55658, #38500, #36481, #9169, #40494, #102166, #193183, #129484, #39487, #25353, #52657, #84976, #160842, #176022, #23332, #21329, #161838, #192181, #37491, #99153, #116330, #83982, #145661, #146658, #7142, #68825, #32039, #63363, #139206, #45223, #61365, #15876, #30049, #123036, #76543, #170548, #11171, #26345, #148681, #134516, #31044, #46206, #106878, #186736, #109861, #1686, #153381, #78519, #48207, #92693, #10169, #168551, #87985, #681, #154381, #71829, #140193, #91690, #171546, #184722, #125040, #118343, #196202, #86994, #77534, #133498, #149673, #62352, #124022, #195190, #119341, #56670, #185720, #180037, #47210, #57674, #108869, #183737, #41505, #93696, #103169, #14882, #107860, #155379, #138219, #164849, #72847, #16868, #199901, #169545, #4651, #18865, #35998, #129981, #35012, #83492, #96667, #3668, #156368, #50197, #126031, #53162, #188714, #19843, #97645, #36995, #128995, #65346, #189706, #81484, #114840, #95684, #66342, #145169, #67333, #98656, #52168, #2685, #64362, #79526, #172541, #160350, #127006, #111853, #173543, #34026, #17872, #159334, #21839, #158354, #175520, #128004, #143171, #191681, #190693, #51179, #6653, #112839, #187727, #33034, #49198, #174531, #110856, #157371, #68331, #20831, #82487, #144171, #113825, #94690, #141196, #5657, #80511, #142184, #103683, #101669, #39997, #54176, #196706, #118861, #73358, #163359, #87504, #56170, #179544, #41013, #161350, #132013, #7651, #176534, #115849, #164365, #58176, #116840, #117851, #193700, #165362, #24855, #86504, #177538, #38010, #180544, #135031, #148188, #149192, #102680, #25860, #10681, #22841, #55169, #69335, #99665, #39008, #72346, #84488, #88497, #9682, #26856, #146165, #134020, #131001, #178530, #100663, #195712, #57184, #192693, #150194, #71347, #162345, #133010, #11692, #23846, #85496, #147184, #42018, #8673, #70346, #194701, #169303, #93450, #152165, #155137, #184492, #12676, #30809, #90483, #122802, #13648, #181528, #123782, #16631, #198675, #14643, #92458, #106648, #74343, #27858, #62119, #78278, #75315, #91453, #105657, #45971, #139951, #121809, #170308, #183505, #136986, #43007, #60142, #136009, #1441, #44988, #168320, #107625, #185481, #15638, #29817, #76303, #153141, #119843, #182516, #137981, #31801, #154146, #46971, #138966, #89498, #151188, #166360, #59146, #108630, #199663, #61129, #77295, #120816, #104674, #444, #197681, #43995, #167345, #28842, #65106, #21593, #97408, #81249, #175281, #188467, #32794, #83252, #79285, #96429, #156127, #17626, #113587, #3430, #126764, #34772, #143931, #67096, #50942, #112600, #98410, #187491, #94447, #140955, #186496, #157126, #4412, #190452, #158115, #35762, #2442, #124798, #160106, #47972, #109624, #171308, #64124, #159095, #173298, #51927, #125789, #127764, #48957, #20589, #82241, #5413, #128755, #174292, #110610, #172293, #36746, #144927, #33782, #63119, #19607, #95442, #18622, #80269, #141939, #142931, #49949, #111613 ),
 ( #189464, #66097, #102434, #26609, #192451, #147950, #23603, #53933, #86260, #40765, #178290, #54929, #6408, #69092, #132768, #129742, #68089, #24612, #55926, #130759, #148948, #180304, #117600, #162106, #39754, #194455, #146940, #101416, #193453, #87263, #115608, #145926, #191439, #177297, #9436, #163109, #85249, #103437, #38768, #100425, #179301, #72098, #37760, #8430, #161104, #22599, #88252, #71101, #164121, #25619, #10438, #7409, #195465, #165117, #133770, #56940, #118614, #41772, #70102, #131771, #52915, #114591, #176288, #99421, #84246, #116602, #74104, #183264, #45735, #182272, #207, #135774, #91210, #167101, #197445, #29579, #184253, #121569, #198427, #149938, #12442, #76063, #73116, #11444, #168082, #199422, #58911, #92217, #123546, #60887, #105418, #44744, #137738, #90240, #106400, #136743, #30566, #120579, #89256, #134785, #43754, #152901, #14397, #28602, #46731, #151923, #13412, #122563, #15398, #181291, #75076, #104431, #166114, #170070, #107387, #169060, #153903, #77055, #150948, #138727, #108393, #61876, #185240, #31561, #196467, #59901, #57937, #119608, #42769, #27617, #158863, #20352, #33546, #17385, #126536, #189234, #125557, #143693, #81026, #142702, #128520, #79040, #124556, #109384, #16396, #187254, #34540, #82000, #64875, #65860, #186253, #154897, #190215, #78042, #139711, #1199, #62875, #127531, #3201, #5176, #155887, #157888, #140715, #50712, #112370, #35530, #97178, #4181, #47731, #171064, #174062, #66858, #32554, #51694, #188235, #63886, #113356, #93212, #172059, #49710, #2205, #175048, #111374, #94208, #48723, #19377, #80041, #110376, #95207, #156894, #173063, #18390, #141710, #96199, #148713, #162869, #22365, #132537, #56703, #8189, #117365, #40530, #118376, #177064, #178053, #192215, #163890, #161872, #100190, #114351, #36513, #179061, #133530, #23366, #147716, #116364, #39521, #101181, #21361, #53698, #67858, #98168, #176056, #24377, #159868, #10201, #85012, #25386, #195222, #86028, #83019, #115375, #37523, #9204, #70869, #144693, #87028, #38534, #6178, #69864, #71861, #129513, #145695, #191213, #194226, #52688, #99186, #55691, #102201, #160875, #68860, #84017, #7177, #130519, #146692, #131533, #193217, #54691, #41539, #184018, #76822, #58677, #74852, #90982, #166874, #134547, #88017, #122326, #153666, #150711, #151697, #165877, #183031, #138493, #182039, #30331, #43522, #12210, #103202, #197215, #72879, #200175, #135543, #28375, #44514, #45500, #75827, #73873, #136514, #90013, #61644, #42533, #13188, #91972, #14159, #107155, #199185, #149705, #11204, #26378, #119375, #168825, #120344, #105187, #198195, #181057, #164883, #106170, #15162, #59665, #180070, #121338, #167853, #196236, #137505, #29353, #57705, #152670, #104196, #27374, #89020, #60653, #154663, #16159, #19141, #17152, #78805, #34305, #170832, #155657, #109153, #139482, #185005, #156660, #95967, #32324, #172826, #187023, #140484, #127286, #126307, #171827, #80791, #1971, #31326, #188999, #77813, #48494, #964, #62640, #142469, #63652, #125326, #110148, #111136, #157651, #123312, #33315, #18155, #94975, #3947, #79809, #141482, #124316, #46489, #65626, #108151, #2965, #49473, #64645, #188003, #169833, #186015, #92978, #47496, #93977, #43176, #91634, #123961, #15815, #167520, #92635, #623, #106823, #27029, #182689, #104843, #153322, #168497, #88674, #154326, #120991, #62294, #75489, #77476, #135203, #12848, #185659, #29995, #150370, #166534, #14824, #76485, #139146, #136180, #103852, #138162, #196875, #199843, #74514, #61310, #197855, #165533, #107803, #11866, #44174, #198851, #122980, #90655, #58342, #73531, #46149, #120010, #59322, #137162, #89672, #184667, #181695, #105833, #28031, #29015, #152337, #151359, #13823, #60315, #121991, #183682, #45167, #169487, #30987, #143112, #17812, #3609, #33967, #128933, #109805, #18806, #97587, #81426, #112779, #66284, #16809, #78459, #93635, #186678, #111794, #171488 ),
 ( #50135, #31979, #2627, #140133, #47151, #48148, #34955, #67275, #159275, #110798, #35941, #144115, #173482, #170488, #125971, #32977, #96607, #158296, #155320, #20771, #64304, #5595, #80451, #82427, #1625, #156310, #108809, #19785, #63301, #94631, #4591, #127943, #124981, #79468, #141137, #189645, #187670, #51120, #49140, #174472, #172479, #95624, #157309, #142124, #65288, #126947, #188655, #177477, #145108, #98596, #132951, #164307, #161286, #162285, #176472, #193638, #87446, #192632, #40949, #54114, #22780, #113766, #7589, #83431, #10622, #146105, #38946, #55110, #194639, #86444, #84428, #147126, #100603, #72283, #53100, #23785, #102621, #24796, #56109, #9621, #160289, #21780, #36933, #129921, #117790, #69275, #130942, #115788, #191621, #175462, #116780, #179485, #85435, #25800, #8613, #70286, #149131, #148130, #131954, #190634, #178471, #6591, #52109, #68270, #39938, #114779, #37946, #99606, #101607, #163297, #71286, #187201, #186198, #81945, #48672, #190161, #3149, #143636, #62819, #140661, #51637, #157835, #16341, #94155, #19326, #80973, #5120, #63831, #66802, #96146, #124503, #142649, #2153, #34488, #125503, #93159, #35476, #128465, #110324, #126485, #4128, #18335, #47679, #139657, #174005, #113301, #172005, #64823, #17331, #65807, #31506, #33493, #154844, #95151, #156840, #77990, #79990, #109330, #1145, #141658, #188183, #127475, #97125, #189181, #49655, #111319, #173009, #171012, #155834, #50654, #32503, #112315, #158808, #20297, #78986, #6123, #21306, #114297, #179003, #7119, #192157, #145639, #175999, #98114, #177996, #40471, #130460, #117307, #146635, #177007, #133474, #9145, #193160, #86971, #100133, #144640, #195166, #191160, #8127, #67806, #129461, #25329, #115315, #38476, #69805, #39463, #148658, #161814, #68801, #116307, #53638, #102143, #23309, #84953, #52633, #56647, #163828, #71806, #131473, #85968, #54632, #101124, #162810, #159811, #24319, #37469, #174992, #99130, #147657, #36456, #10146, #70812, #82963, #160820, #132481, #22308, #194170, #83959, #55634, #182977, #103144, #15107, #197160, #13136, #29299, #105135, #72822, #26322, #60597, #91918, #88967, #89961, #104141, #121284, #76768, #120292, #168770, #181985, #150657, #41480, #135490, #11148, #138440, #73820, #166821, #44461, #122272, #14105, #12155, #74798, #28322, #200121, #181002, #151641, #30273, #152615, #183960, #137451, #87962, #149650, #164826, #57650, #45447, #58625, #43467, #136460, #119316, #134491, #106115, #107100, #198141, #153611, #59611, #167799, #118320, #75773, #90929, #180013, #199130, #196178, #42478, #165823, #27320, #154608, #16103, #112085, #1917, #63596, #33263, #64592, #35241, #125271, #32267, #2913, #17097, #188949, #186969, #48439, #139427, #81711, #3896, #158578, #110096, #172774, #141427, #126256, #187953, #46434, #78750, #92922, #61590, #909, #49422, #143397, #173775, #171774, #50426, #20068, #111084, #184949, #140427, #62584, #34255, #95914, #108093, #96895, #94922, #123258, #156607, #169777, #77761, #170777, #31271, #157598, #124262, #185957, #19090, #80738, #47441, #93924, #109098, #142417, #155602, #65575, #18102, #127235, #79756, #66568, #8902, #116072, #54400, #6880, #68558, #101901, #177760, #100885, #70570, #132238, #145397, #129221, #38236, #162568, #37228, #55393, #192922, #39229, #40224, #190918, #36222, #21064, #128233, #98885, #146393, #193930, #176764, #24072, #97874, #189930, #163583, #51405, #113065, #174757, #159566, #85727, #115072, #160579, #82719, #161576, #117063, #147414, #178758, #25083, #86726, #4886, #144401, #5887, #67563, #52395, #114052, #175751, #99891, #22068, #83719, #130214, #191909, #23069, #53394, #84715, #7882, #69567, #131234, #15620, #137962, #78259, #149408, #139932, #61111, #41239, #155118, #1421, #63100, #77277, #134251, #46952, #171289, #195938, #92440, #165584, #57412, #30792, #185462, #122784, #199645, #148411, #10903, #138946, #71566 ),
 ( #31783, #72577, #87723, #9906, #119085, #154126, #107608, #103903, #47954, #180766, #42242, #62100, #16612, #179770, #29799, #102900, #164585, #32776, #45953, #184474, #426, #93432, #91435, #124779, #109605, #186477, #133231, #123763, #194922, #153122, #14626, #108612, #76283, #56398, #169286, #170289, #26079, #118080, #36730, #191424, #81233, #5396, #174277, #97392, #159078, #79265, #49929, #125771, #94428, #33764, #82224, #114575, #6394, #158098, #83235, #52900, #20572, #17606, #173279, #95424, #143914, #67079, #140937, #144911, #111593, #176273, #66080, #68073, #187471, #3413, #156109, #128739, #2424, #157108, #190435, #51911, #129727, #126747, #64104, #113570, #48940, #175264, #65088, #98392, #188449, #110593, #160090, #172275, #34752, #189448, #21577, #142914, #18604, #80252, #141922, #96411, #19590, #127746, #4396, #50925, #112583, #35746, #88237, #39738, #8414, #161088, #54914, #130744, #57922, #193438, #24597, #102419, #41757, #133755, #70087, #194440, #86245, #119593, #100410, #9421, #149922, #72081, #103422, #56923, #7394, #69078, #84231, #177282, #165101, #131756, #116586, #178275, #38753, #22583, #40750, #26594, #101400, #180289, #71086, #163093, #196452, #195449, #55911, #11428, #147935, #192436, #37745, #53919, #132753, #115593, #162091, #73098, #117585, #179285, #164106, #25605, #134769, #87249, #148933, #99405, #23586, #85234, #146924, #145909, #10423, #118599, #108379, #152887, #153887, #74089, #42753, #16381, #104416, #166099, #27601, #89239, #15384, #91197, #136729, #135759, #137724, #93198, #138712, #193, #123531, #185225, #92203, #150933, #197430, #169045, #154883, #120562, #61862, #14382, #151910, #170055, #181276, #59888, #76048, #28589, #1183, #199408, #12426, #58896, #45720, #168068, #31546, #182256, #78028, #60872, #43741, #46716, #139697, #62860, #107373, #167088, #77041, #105402, #90226, #122549, #198411, #13399, #184239, #75063, #30551, #29566, #121554, #183250, #44731, #106387, #186239, #142688, #174048, #48709, #66844, #98153, #35517, #80028, #96186, #50698, #64861, #157875, #111360, #5161, #110362, #63872, #47717, #172044, #65846, #81013, #141697, #21346, #187239, #33531, #97165, #190202, #155873, #3188, #79025, #140700, #144679, #19364, #4168, #127516, #128507, #125543, #113342, #83004, #51680, #175034, #158850, #20338, #126523, #188222, #6164, #81987, #143680, #36499, #159853, #49695, #95193, #189220, #124542, #109368, #171050, #32540, #94193, #34526, #173049, #2190, #112357, #17370, #156879, #18376, #10189, #71849, #179047, #37508, #22350, #55677, #41526, #7162, #25373, #178038, #38519, #56690, #67844, #146677, #101166, #115359, #88005, #24361, #191199, #84001, #132523, #54675, #195210, #68845, #118364, #39506, #160860, #133518, #180057, #103189, #194212, #53682, #163874, #149693, #177049, #9189, #84996, #100175, #147701, #102186, #162854, #116349, #129499, #130504, #117351, #52674, #114337, #86012, #40515, #192200, #164870, #26365, #87015, #23351, #70854, #148701, #8172, #176040, #99170, #145680, #161857, #69848, #131516, #193202, #152655, #167838, #166860, #108133, #73861, #58664, #122311, #76807, #42520, #28362, #165865, #27361, #31308, #106156, #183016, #14145, #153650, #12196, #200159, #169817, #138478, #61629, #184002, #60637, #13174, #74837, #92961, #45485, #107140, #123297, #184989, #151682, #135530, #44500, #168810, #43508, #46473, #199170, #30314, #11191, #197201, #104183, #89007, #134535, #105174, #75812, #72866, #29339, #91957, #150698, #196223, #57693, #119361, #137490, #181045, #90968, #15145, #120330, #182025, #90000, #136500, #198180, #59650, #121324, #188983, #64628, #110132, #109136, #111119, #66602, #112118, #173810, #96930, #158612, #65610, #124299, #170815, #142452, #128266, #93961, #35275, #126290, #125310, #143433, #154647, #33299, #187987, #1955, #174790, #172808, #77797, #32307, #19124, #141465, #81746, #155641, #4919, #49457, #47479 ),
 ( #17136, #80774, #3930, #189964, #187006, #51439, #127270, #78788, #50459, #48476, #157635, #171811, #16142, #20102, #113099, #94958, #34289, #36256, #2949, #140465, #62621, #139466, #946, #156642, #95950, #63634, #185996, #18138, #79792, #148444, #99923, #68591, #21098, #115104, #190951, #118112, #53427, #84748, #162603, #101934, #193963, #130247, #54434, #146426, #179801, #160611, #69600, #9939, #132272, #163616, #117097, #67597, #129256, #144434, #37261, #25117, #191942, #176796, #38269, #98919, #82754, #100918, #86761, #161608, #40261, #131267, #23102, #56432, #55426, #7916, #52428, #97909, #192955, #116104, #24107, #71598, #178792, #177792, #39262, #85761, #159600, #22101, #147448, #133264, #194955, #5920, #114086, #175787, #83751, #145430, #6913, #8936, #70605, #58422, #11947, #42275, #164617, #44254, #106901, #196954, #183761, #12926, #43258, #199926, #75568, #59402, #153407, #166613, #10935, #61389, #57442, #74590, #134282, #195970, #91713, #181777, #104926, #136258, #105911, #14905, #28115, #73611, #182770, #120089, #168574, #89753, #151439, #119115, #123061, #45247, #138242, #197934, #152414, #121076, #167597, #29092, #26111, #90731, #72608, #41270, #180796, #13902, #102932, #76567, #137244, #30072, #87754, #198929, #149439, #60397, #103933, #122069, #165613, #27112, #88758, #150451, #135282, #156392, #35036, #15901, #93720, #143196, #110880, #169573, #47235, #172565, #34051, #158379, #16892, #19868, #49222, #77559, #95708, #155402, #187752, #78543, #46232, #188738, #81508, #63387, #79550, #157396, #171570, #139231, #92718, #127031, #4676, #140218, #17896, #170573, #18889, #66368, #186761, #96691, #48231, #1711, #107886, #184747, #50223, #31070, #33059, #80535, #64387, #142209, #3692, #154407, #125064, #706, #62378, #124048, #65371, #185747, #108894, #109886, #173567, #32064, #111877, #94714, #141219, #2710, #126055, #192716, #112864, #178553, #145192, #86527, #99689, #40019, #159360, #37020, #148211, #54200, #174555, #190718, #115872, #177561, #101692, #160374, #163381, #39030, #20857, #100685, #98681, #131027, #21865, #189730, #132036, #24878, #6675, #22864, #162367, #114863, #82514, #36022, #70368, #9705, #83515, #161373, #113849, #23868, #128028, #130004, #51203, #191704, #68353, #97671, #53188, #144196, #5682, #176558, #38033, #85519, #193725, #147207, #84511, #146189, #7674, #67358, #52191, #69358, #129018, #8698, #55193, #116862, #175545, #102702, #117876, #10706, #75339, #103706, #88522, #42042, #72369, #194723, #74365, #137009, #26879, #13672, #43030, #73382, #29840, #105682, #89521, #183528, #196730, #41036, #91477, #87528, #104696, #164390, #25883, #121834, #11715, #135054, #166384, #136031, #45011, #58198, #165386, #12699, #150218, #198699, #119866, #181551, #149215, #134043, #60165, #27880, #151211, #197705, #195736, #56193, #59171, #106671, #120840, #168344, #182539, #44021, #153165, #167368, #28866, #71369, #90506, #57209, #133033, #118884, #152188, #180568, #179566, #65131, #155162, #16654, #186521, #17649, #188494, #78301, #185504, #156151, #170332, #141965, #139975, #1464, #92482, #34797, #157152, #111637, #63142, #125812, #94470, #79309, #140978, #199688, #31825, #45995, #14666, #154171, #2466, #96452, #126788, #124821, #3454, #173322, #64148, #138004, #93475, #15662, #187515, #48981, #61153, #49973, #47995, #76327, #109649, #122825, #107650, #123806, #184515, #110636, #169327, #77321, #172317, #33806, #30834, #46995, #138989, #95466, #467, #18647, #108654, #80293, #171331, #62142, #32819, #57719, #39534, #55705, #71875, #147729, #112625, #66123, #103216, #134562, #131547, #132551, #146706, #163904, #119389, #162883, #11218, #24392, #193232, #81273, #178066, #50966, #181072, #116377, #9216, #25400, #164898, #56718, #54705, #117378, #70883, #42547, #20615, #194239, #72894, #195235, #26392, #180084, #127788, #189488, #4435, #41553, #174317, #35787, #97434 ) ),
 .UNSPECIFIED., .T., .F., .T. ) 
 B_SPLINE_SURFACE_WITH_KNOTS ( ( 4, 3, 4 ),
 ( 3, 2, 2, 2, 2, 2, 2, 2, 2, 2, 2, 2, 2, 2, 2, 2, 2, 2, 2, 2, 2, 2, 2, 2, 2, 2, 2, 2, 2, 2, 2, 2, 2, 2, 2, 2, 2, 2, 2, 2, 2, 2, 2, 2, 2, 2, 2, 2, 2, 2, 2, 2, 2, 2, 2, 2, 2, 2, 2, 2, 2, 2, 2, 2, 2, 2, 2, 2, 2, 2, 2, 2, 2, 2, 2, 2, 2, 2, 2, 2, 2, 2, 2, 2, 2, 2, 2, 2, 2, 2, 2, 2, 2, 2, 2, 2, 2, 2, 2, 2, 2, 2, 2, 2, 2, 2, 2, 2, 2, 2, 2, 2, 2, 2, 2, 2, 2, 2, 2, 2, 2, 2, 2, 2, 2, 2, 2, 2, 2, 2, 2, 2, 2, 2, 2, 2, 2, 2, 2, 2, 2, 2, 2, 2, 2, 2, 2, 2, 2, 2, 2, 2, 2, 2, 2, 2, 2, 2, 2, 2, 2, 2, 2, 2, 2, 2, 2, 2, 2, 2, 2, 2, 2, 2, 2, 2, 2, 2, 2, 2, 2, 2, 2, 2, 2, 2, 2, 2, 2, 2, 2, 2, 2, 2, 2, 2, 2, 2, 2, 2, 2, 2, 2, 2, 2, 2, 2, 2, 2, 2, 2, 2, 2, 2, 2, 2, 2, 2, 2, 2, 2, 2, 2, 2, 2, 2, 2, 2, 3 ),
 ( 0.000000000000000000, 0.5000000000000000000, 1.000000000000000000 ),
 ( 0.000000000000000000, 0.004385964912280701511, 0.008771929824561403022, 0.01315789473684210453, 0.01754385964912280604, 0.02192982456140350755, 0.02631578947368420907, 0.03070175438596491058, 0.03508771929824561209, 0.03947368421052631360, 0.04385964912280701511, 0.04824561403508771662, 0.05263157894736841813, 0.05701754385964911964, 0.06140350877192982115, 0.06578947368421052266, 0.07017543859649122417, 0.07456140350877192569, 0.07894736842105262720, 0.08333333333333332871, 0.08771929824561403022, 0.09210526315789473173, 0.09649122807017543324, 0.1008771929824561348, 0.1052631578947368363, 0.1096491228070175378, 0.1140350877192982393, 0.1184210526315789408, 0.1228070175438596423, 0.1271929824561403577, 0.1315789473684210453, 0.1359649122807017607, 0.1403508771929824483, 0.1447368421052631637, 0.1491228070175438514, 0.1535087719298245668, 0.1578947368421052544, 0.1622807017543859698, 0.1666666666666666574, 0.1710526315789473728, 0.1754385964912280604, 0.1798245614035087758, 0.1842105263157894635, 0.1885964912280701788, 0.1929824561403508665, 0.1973684210526315819, 0.2017543859649122695, 0.2061403508771929849, 0.2105263157894736725, 0.2149122807017543879, 0.2192982456140350755, 0.2236842105263157909, 0.2280701754385964786, 0.2324561403508771940, 0.2368421052631578816, 0.2412280701754385970, 0.2456140350877192846, 0.2500000000000000000, 0.2543859649122807154, 0.2587719298245614308, 0.2631578947368420907, 0.2675438596491228060, 0.2719298245614035214, 0.2763157894736842368, 0.2807017543859648967, 0.2850877192982456121, 0.2894736842105263275, 0.2938596491228070429, 0.2982456140350877027, 0.3026315789473684181, 0.3070175438596491335, 0.3114035087719298489, 0.3157894736842105088, 0.3201754385964912242, 0.3245614035087719396, 0.3289473684210526550, 0.3333333333333333148, 0.3377192982456140302, 0.3421052631578947456, 0.3464912280701754610, 0.3508771929824561209, 0.3552631578947368363, 0.3596491228070175517, 0.3640350877192982670, 0.3684210526315789269, 0.3728070175438596423, 0.3771929824561403577, 0.3815789473684210731, 0.3859649122807017330, 0.3903508771929824483, 0.3947368421052631637, 0.3991228070175438791, 0.4035087719298245390, 0.4078947368421052544, 0.4122807017543859698, 0.4166666666666666852, 0.4210526315789473450, 0.4254385964912280604, 0.4298245614035087758, 0.4342105263157894912, 0.4385964912280701511, 0.4429824561403508665, 0.4473684210526315819, 0.4517543859649122973, 0.4561403508771929571, 0.4605263157894736725, 0.4649122807017543879, 0.4692982456140351033, 0.4736842105263157632, 0.4780701754385964786, 0.4824561403508771940, 0.4868421052631579093, 0.4912280701754385692, 0.4956140350877192846, 0.5000000000000000000, 0.5043859649122807154, 0.5087719298245614308, 0.5131578947368421462, 0.5175438596491228616, 0.5219298245614034659, 0.5263157894736841813, 0.5307017543859648967, 0.5350877192982456121, 0.5394736842105263275, 0.5438596491228070429, 0.5482456140350877583, 0.5526315789473684736, 0.5570175438596490780, 0.5614035087719297934, 0.5657894736842105088, 0.5701754385964912242, 0.5745614035087719396, 0.5789473684210526550, 0.5833333333333333703, 0.5877192982456140857, 0.5921052631578946901, 0.5964912280701754055, 0.6008771929824561209, 0.6052631578947368363, 0.6096491228070175517, 0.6140350877192982670, 0.6184210526315789824, 0.6228070175438596978, 0.6271929824561403022, 0.6315789473684210176, 0.6359649122807017330, 0.6403508771929824483, 0.6447368421052631637, 0.6491228070175438791, 0.6535087719298245945, 0.6578947368421053099, 0.6622807017543859143, 0.6666666666666666297, 0.6710526315789473450, 0.6754385964912280604, 0.6798245614035087758, 0.6842105263157894912, 0.6885964912280702066, 0.6929824561403509220, 0.6973684210526315264, 0.7017543859649122417, 0.7061403508771929571, 0.7105263157894736725, 0.7149122807017543879, 0.7192982456140351033, 0.7236842105263158187, 0.7280701754385965341, 0.7324561403508771384, 0.7368421052631578538, 0.7412280701754385692, 0.7456140350877192846, 0.7500000000000000000, 0.7543859649122807154, 0.7587719298245614308, 0.7631578947368421462, 0.7675438596491228616, 0.7719298245614034659, 0.7763157894736841813, 0.7807017543859648967, 0.7850877192982456121, 0.7894736842105263275, 0.7938596491228070429, 0.7982456140350877583, 0.8026315789473684736, 0.8070175438596490780, 0.8114035087719297934, 0.8157894736842105088, 0.8201754385964912242, 0.8245614035087719396, 0.8289473684210526550, 0.8333333333333333703, 0.8377192982456140857, 0.8421052631578946901, 0.8464912280701754055, 0.8508771929824561209, 0.8552631578947368363, 0.8596491228070175517, 0.8640350877192982670, 0.8684210526315789824, 0.8728070175438596978, 0.8771929824561403022, 0.8815789473684210176, 0.8859649122807017330, 0.8903508771929824483, 0.8947368421052631637, 0.8991228070175438791, 0.9035087719298245945, 0.9078947368421053099, 0.9122807017543859143, 0.9166666666666666297, 0.9210526315789473450, 0.9254385964912280604, 0.9298245614035087758, 0.9342105263157894912, 0.9385964912280702066, 0.9429824561403509220, 0.9473684210526315264, 0.9517543859649122417, 0.9561403508771929571, 0.9605263157894736725, 0.9649122807017543879, 0.9692982456140351033, 0.9736842105263158187, 0.9780701754385965341, 0.9824561403508771384, 0.9868421052631578538, 0.9912280701754385692, 0.9956140350877192846, 1.000000000000000000 ),
 .UNSPECIFIED. ) 
 GEOMETRIC_REPRESENTATION_ITEM ( )  RATIONAL_B_SPLINE_SURFACE ( (
 ( 1.000000000000000000, 0.9659258262890683122, 1.000000000000000000, 0.9659258262890683122, 1.000000000000000000, 0.9659258262890683122, 1.000000000000000000, 0.9659258262890683122, 1.000000000000000000, 0.9659258262890683122, 1.000000000000000000, 0.9659258262890683122, 1.000000000000000000, 0.9659258262890683122, 1.000000000000000000, 0.9659258262890683122, 1.000000000000000000, 0.9659258262890683122, 1.000000000000000000, 0.9659258262890683122, 1.000000000000000000, 0.9659258262890683122, 1.000000000000000000, 0.9659258262890683122, 1.000000000000000000, 0.9659258262890683122, 1.000000000000000000, 0.9659258262890683122, 1.000000000000000000, 0.9659258262890683122, 1.000000000000000000, 0.9659258262890683122, 1.000000000000000000, 0.9659258262890683122, 1.000000000000000000, 0.9659258262890683122, 1.000000000000000000, 0.9659258262890683122, 1.000000000000000000, 0.9659258262890683122, 1.000000000000000000, 0.9659258262890683122, 1.000000000000000000, 0.9659258262890683122, 1.000000000000000000, 0.9659258262890683122, 1.000000000000000000, 0.9659258262890683122, 1.000000000000000000, 0.9659258262890683122, 1.000000000000000000, 0.9659258262890683122, 1.000000000000000000, 0.9659258262890683122, 1.000000000000000000, 0.9659258262890683122, 1.000000000000000000, 0.9659258262890683122, 1.000000000000000000, 0.9659258262890683122, 1.000000000000000000, 0.9659258262890683122, 1.000000000000000000, 0.9659258262890683122, 1.000000000000000000, 0.9659258262890683122, 1.000000000000000000, 0.9659258262890683122, 1.000000000000000000, 0.9659258262890683122, 1.000000000000000000, 0.9659258262890683122, 1.000000000000000000, 0.9659258262890683122, 1.000000000000000000, 0.9659258262890683122, 1.000000000000000000, 0.9659258262890683122, 1.000000000000000000, 0.9659258262890683122, 1.000000000000000000, 0.9659258262890683122, 1.000000000000000000, 0.9659258262890683122, 1.000000000000000000, 0.9659258262890683122, 1.000000000000000000, 0.9659258262890683122, 1.000000000000000000, 0.9659258262890683122, 1.000000000000000000, 0.9659258262890683122, 1.000000000000000000, 0.9659258262890683122, 1.000000000000000000, 0.9659258262890683122, 1.000000000000000000, 0.9659258262890683122, 1.000000000000000000, 0.9659258262890683122, 1.000000000000000000, 0.9659258262890683122, 1.000000000000000000, 0.9659258262890683122, 1.000000000000000000, 0.9659258262890683122, 1.000000000000000000, 0.9659258262890683122, 1.000000000000000000, 0.9659258262890683122, 1.000000000000000000, 0.9659258262890683122, 1.000000000000000000, 0.9659258262890683122, 1.000000000000000000, 0.9659258262890683122, 1.000000000000000000, 0.9659258262890683122, 1.000000000000000000, 0.9659258262890683122, 1.000000000000000000, 0.9659258262890683122, 1.000000000000000000, 0.9659258262890683122, 1.000000000000000000, 0.9659258262890683122, 1.000000000000000000, 0.9659258262890683122, 1.000000000000000000, 0.9659258262890683122, 1.000000000000000000, 0.9659258262890683122, 1.000000000000000000, 0.9659258262890683122, 1.000000000000000000, 0.9659258262890683122, 1.000000000000000000, 0.9659258262890683122, 1.000000000000000000, 0.9659258262890683122, 1.000000000000000000, 0.9659258262890683122, 1.000000000000000000, 0.9659258262890683122, 1.000000000000000000, 0.9659258262890683122, 1.000000000000000000, 0.9659258262890683122, 1.000000000000000000, 0.9659258262890683122, 1.000000000000000000, 0.9659258262890683122, 1.000000000000000000, 0.9659258262890683122, 1.000000000000000000, 0.9659258262890683122, 1.000000000000000000, 0.9659258262890683122, 1.000000000000000000, 0.9659258262890683122, 1.000000000000000000, 0.9659258262890683122, 1.000000000000000000, 0.9659258262890683122, 1.000000000000000000, 0.9659258262890683122, 1.000000000000000000, 0.9659258262890683122, 1.000000000000000000, 0.9659258262890683122, 1.000000000000000000, 0.9659258262890683122, 1.000000000000000000, 0.9659258262890683122, 1.000000000000000000, 0.9659258262890683122, 1.000000000000000000, 0.9659258262890683122, 1.000000000000000000, 0.9659258262890683122, 1.000000000000000000, 0.9659258262890683122, 1.000000000000000000, 0.9659258262890683122, 1.000000000000000000, 0.9659258262890683122, 1.000000000000000000, 0.9659258262890683122, 1.000000000000000000, 0.9659258262890683122, 1.000000000000000000, 0.9659258262890683122, 1.000000000000000000, 0.9659258262890683122, 1.000000000000000000, 0.9659258262890683122, 1.000000000000000000, 0.9659258262890683122, 1.000000000000000000, 0.9659258262890683122, 1.000000000000000000, 0.9659258262890683122, 1.000000000000000000, 0.9659258262890683122, 1.000000000000000000, 0.9659258262890683122, 1.000000000000000000, 0.9659258262890683122, 1.000000000000000000, 0.9659258262890683122, 1.000000000000000000, 0.9659258262890683122, 1.000000000000000000, 0.9659258262890683122, 1.000000000000000000, 0.9659258262890683122, 1.000000000000000000, 0.9659258262890683122, 1.000000000000000000, 0.9659258262890683122, 1.000000000000000000, 0.9659258262890683122, 1.000000000000000000, 0.9659258262890683122, 1.000000000000000000, 0.9659258262890683122, 1.000000000000000000, 0.9659258262890683122, 1.000000000000000000, 0.9659258262890683122, 1.000000000000000000, 0.9659258262890683122, 1.000000000000000000, 0.9659258262890683122, 1.000000000000000000, 0.9659258262890683122, 1.000000000000000000, 0.9659258262890683122, 1.000000000000000000, 0.9659258262890683122, 1.000000000000000000, 0.9659258262890683122, 1.000000000000000000, 0.9659258262890683122, 1.000000000000000000, 0.9659258262890683122, 1.000000000000000000, 0.9659258262890683122, 1.000000000000000000, 0.9659258262890683122, 1.000000000000000000, 0.9659258262890683122, 1.000000000000000000, 0.9659258262890683122, 1.000000000000000000, 0.9659258262890683122, 1.000000000000000000, 0.9659258262890683122, 1.000000000000000000, 0.9659258262890683122, 1.000000000000000000, 0.9659258262890683122, 1.000000000000000000, 0.9659258262890683122, 1.000000000000000000, 0.9659258262890683122, 1.000000000000000000, 0.9659258262890683122, 1.000000000000000000, 0.9659258262890683122, 1.000000000000000000, 0.9659258262890683122, 1.000000000000000000, 0.9659258262890683122, 1.000000000000000000, 0.9659258262890683122, 1.000000000000000000, 0.9659258262890683122, 1.000000000000000000, 0.9659258262890683122, 1.000000000000000000, 0.9659258262890683122, 1.000000000000000000, 0.9659258262890683122, 1.000000000000000000, 0.9659258262890683122, 1.000000000000000000, 0.9659258262890683122, 1.000000000000000000, 0.9659258262890683122, 1.000000000000000000, 0.9659258262890683122, 1.000000000000000000, 0.9659258262890683122, 1.000000000000000000, 0.9659258262890683122, 1.000000000000000000, 0.9659258262890683122, 1.000000000000000000, 0.9659258262890683122, 1.000000000000000000, 0.9659258262890683122, 1.000000000000000000, 0.9659258262890683122, 1.000000000000000000, 0.9659258262890683122, 1.000000000000000000, 0.9659258262890683122, 1.000000000000000000, 0.9659258262890683122, 1.000000000000000000, 0.9659258262890683122, 1.000000000000000000, 0.9659258262890683122, 1.000000000000000000, 0.9659258262890683122, 1.000000000000000000, 0.9659258262890683122, 1.000000000000000000, 0.9659258262890683122, 1.000000000000000000, 0.9659258262890683122, 1.000000000000000000, 0.9659258262890683122, 1.000000000000000000, 0.9659258262890683122, 1.000000000000000000, 0.9659258262890683122, 1.000000000000000000, 0.9659258262890683122, 1.000000000000000000, 0.9659258262890683122, 1.000000000000000000, 0.9659258262890683122, 1.000000000000000000, 0.9659258262890683122, 1.000000000000000000, 0.9659258262890683122, 1.000000000000000000, 0.9659258262890683122, 1.000000000000000000, 0.9659258262890683122, 1.000000000000000000, 0.9659258262890683122, 1.000000000000000000, 0.9659258262890683122, 1.000000000000000000, 0.9659258262890683122, 1.000000000000000000, 0.9659258262890683122, 1.000000000000000000, 0.9659258262890683122, 1.000000000000000000, 0.9659258262890683122, 1.000000000000000000, 0.9659258262890683122, 1.000000000000000000, 0.9659258262890683122, 1.000000000000000000, 0.9659258262890683122, 1.000000000000000000, 0.9659258262890683122, 1.000000000000000000, 0.9659258262890683122, 1.000000000000000000, 0.9659258262890683122, 1.000000000000000000, 0.9659258262890683122, 1.000000000000000000, 0.9659258262890683122, 1.000000000000000000, 0.9659258262890683122, 1.000000000000000000, 0.9659258262890683122, 1.000000000000000000, 0.9659258262890683122, 1.000000000000000000, 0.9659258262890683122, 1.000000000000000000, 0.9659258262890683122, 1.000000000000000000, 0.9659258262890683122, 1.000000000000000000, 0.9659258262890683122, 1.000000000000000000, 0.9659258262890683122, 1.000000000000000000, 0.9659258262890683122, 1.000000000000000000, 0.9659258262890683122, 1.000000000000000000, 0.9659258262890683122, 1.000000000000000000, 0.9659258262890683122, 1.000000000000000000, 0.9659258262890683122, 1.000000000000000000, 0.9659258262890683122, 1.000000000000000000, 0.9659258262890683122, 1.000000000000000000, 0.9659258262890683122, 1.000000000000000000, 0.9659258262890683122, 1.000000000000000000, 0.9659258262890683122, 1.000000000000000000, 0.9659258262890683122, 1.000000000000000000, 0.9659258262890683122, 1.000000000000000000, 0.9659258262890683122, 1.000000000000000000, 0.9659258262890683122, 1.000000000000000000, 0.9659258262890683122, 1.000000000000000000, 0.9659258262890683122, 1.000000000000000000, 0.9659258262890683122, 1.000000000000000000, 0.9659258262890683122, 1.000000000000000000, 0.9659258262890683122, 1.000000000000000000, 0.9659258262890683122, 1.000000000000000000, 0.9659258262890683122, 1.000000000000000000, 0.9659258262890683122, 1.000000000000000000, 0.9659258262890683122, 1.000000000000000000, 0.9659258262890683122, 1.000000000000000000, 0.9659258262890683122, 1.000000000000000000, 0.9659258262890683122, 1.000000000000000000, 0.9659258262890683122, 1.000000000000000000, 0.9659258262890683122, 1.000000000000000000, 0.9659258262890683122, 1.000000000000000000, 0.9659258262890683122, 1.000000000000000000, 0.9659258262890683122, 1.000000000000000000, 0.9659258262890683122, 1.000000000000000000, 0.9659258262890683122, 1.000000000000000000, 0.9659258262890683122, 1.000000000000000000, 0.9659258262890683122, 1.000000000000000000),
 ( 0.3333333333333333703, 0.3219752754296894559, 0.3333333333333333703, 0.3219752754296894559, 0.3333333333333333703, 0.3219752754296894559, 0.3333333333333333703, 0.3219752754296894559, 0.3333333333333333703, 0.3219752754296894559, 0.3333333333333333703, 0.3219752754296894559, 0.3333333333333333703, 0.3219752754296894559, 0.3333333333333333703, 0.3219752754296894559, 0.3333333333333333703, 0.3219752754296894559, 0.3333333333333333703, 0.3219752754296894559, 0.3333333333333333703, 0.3219752754296894559, 0.3333333333333333703, 0.3219752754296894559, 0.3333333333333333703, 0.3219752754296894559, 0.3333333333333333703, 0.3219752754296894559, 0.3333333333333333703, 0.3219752754296894559, 0.3333333333333333703, 0.3219752754296894559, 0.3333333333333333703, 0.3219752754296894559, 0.3333333333333333703, 0.3219752754296894559, 0.3333333333333333703, 0.3219752754296894559, 0.3333333333333333703, 0.3219752754296894559, 0.3333333333333333703, 0.3219752754296894559, 0.3333333333333333703, 0.3219752754296894559, 0.3333333333333333703, 0.3219752754296894559, 0.3333333333333333703, 0.3219752754296894559, 0.3333333333333333703, 0.3219752754296894559, 0.3333333333333333703, 0.3219752754296894559, 0.3333333333333333703, 0.3219752754296894559, 0.3333333333333333703, 0.3219752754296894559, 0.3333333333333333703, 0.3219752754296894559, 0.3333333333333333703, 0.3219752754296894559, 0.3333333333333333703, 0.3219752754296894559, 0.3333333333333333703, 0.3219752754296894559, 0.3333333333333333703, 0.3219752754296894559, 0.3333333333333333703, 0.3219752754296894559, 0.3333333333333333703, 0.3219752754296894559, 0.3333333333333333703, 0.3219752754296894559, 0.3333333333333333703, 0.3219752754296894559, 0.3333333333333333703, 0.3219752754296894559, 0.3333333333333333703, 0.3219752754296894559, 0.3333333333333333703, 0.3219752754296894559, 0.3333333333333333703, 0.3219752754296894559, 0.3333333333333333703, 0.3219752754296894559, 0.3333333333333333703, 0.3219752754296894559, 0.3333333333333333703, 0.3219752754296894559, 0.3333333333333333703, 0.3219752754296894559, 0.3333333333333333703, 0.3219752754296894559, 0.3333333333333333703, 0.3219752754296894559, 0.3333333333333333703, 0.3219752754296894559, 0.3333333333333333703, 0.3219752754296894559, 0.3333333333333333703, 0.3219752754296894559, 0.3333333333333333703, 0.3219752754296894559, 0.3333333333333333703, 0.3219752754296894559, 0.3333333333333333703, 0.3219752754296894559, 0.3333333333333333703, 0.3219752754296894559, 0.3333333333333333703, 0.3219752754296894559, 0.3333333333333333703, 0.3219752754296894559, 0.3333333333333333703, 0.3219752754296894559, 0.3333333333333333703, 0.3219752754296894559, 0.3333333333333333703, 0.3219752754296894559, 0.3333333333333333703, 0.3219752754296894559, 0.3333333333333333703, 0.3219752754296894559, 0.3333333333333333703, 0.3219752754296894559, 0.3333333333333333703, 0.3219752754296894559, 0.3333333333333333703, 0.3219752754296894559, 0.3333333333333333703, 0.3219752754296894559, 0.3333333333333333703, 0.3219752754296894559, 0.3333333333333333703, 0.3219752754296894559, 0.3333333333333333703, 0.3219752754296894559, 0.3333333333333333703, 0.3219752754296894559, 0.3333333333333333703, 0.3219752754296894559, 0.3333333333333333703, 0.3219752754296894559, 0.3333333333333333703, 0.3219752754296894559, 0.3333333333333333703, 0.3219752754296894559, 0.3333333333333333703, 0.3219752754296894559, 0.3333333333333333703, 0.3219752754296894559, 0.3333333333333333703, 0.3219752754296894559, 0.3333333333333333703, 0.3219752754296894559, 0.3333333333333333703, 0.3219752754296894559, 0.3333333333333333703, 0.3219752754296894559, 0.3333333333333333703, 0.3219752754296894559, 0.3333333333333333703, 0.3219752754296894559, 0.3333333333333333703, 0.3219752754296894559, 0.3333333333333333703, 0.3219752754296894559, 0.3333333333333333703, 0.3219752754296894559, 0.3333333333333333703, 0.3219752754296894559, 0.3333333333333333703, 0.3219752754296894559, 0.3333333333333333703, 0.3219752754296894559, 0.3333333333333333703, 0.3219752754296894559, 0.3333333333333333703, 0.3219752754296894559, 0.3333333333333333703, 0.3219752754296894559, 0.3333333333333333703, 0.3219752754296894559, 0.3333333333333333703, 0.3219752754296894559, 0.3333333333333333703, 0.3219752754296894559, 0.3333333333333333703, 0.3219752754296894559, 0.3333333333333333703, 0.3219752754296894559, 0.3333333333333333703, 0.3219752754296894559, 0.3333333333333333703, 0.3219752754296894559, 0.3333333333333333703, 0.3219752754296894559, 0.3333333333333333703, 0.3219752754296894559, 0.3333333333333333703, 0.3219752754296894559, 0.3333333333333333703, 0.3219752754296894559, 0.3333333333333333703, 0.3219752754296894559, 0.3333333333333333703, 0.3219752754296894559, 0.3333333333333333703, 0.3219752754296894559, 0.3333333333333333703, 0.3219752754296894559, 0.3333333333333333703, 0.3219752754296894559, 0.3333333333333333703, 0.3219752754296894559, 0.3333333333333333703, 0.3219752754296894559, 0.3333333333333333703, 0.3219752754296894559, 0.3333333333333333703, 0.3219752754296894559, 0.3333333333333333703, 0.3219752754296894559, 0.3333333333333333703, 0.3219752754296894559, 0.3333333333333333703, 0.3219752754296894559, 0.3333333333333333703, 0.3219752754296894559, 0.3333333333333333703, 0.3219752754296894559, 0.3333333333333333703, 0.3219752754296894559, 0.3333333333333333703, 0.3219752754296894559, 0.3333333333333333703, 0.3219752754296894559, 0.3333333333333333703, 0.3219752754296894559, 0.3333333333333333703, 0.3219752754296894559, 0.3333333333333333703, 0.3219752754296894559, 0.3333333333333333703, 0.3219752754296894559, 0.3333333333333333703, 0.3219752754296894559, 0.3333333333333333703, 0.3219752754296894559, 0.3333333333333333703, 0.3219752754296894559, 0.3333333333333333703, 0.3219752754296894559, 0.3333333333333333703, 0.3219752754296894559, 0.3333333333333333703, 0.3219752754296894559, 0.3333333333333333703, 0.3219752754296894559, 0.3333333333333333703, 0.3219752754296894559, 0.3333333333333333703, 0.3219752754296894559, 0.3333333333333333703, 0.3219752754296894559, 0.3333333333333333703, 0.3219752754296894559, 0.3333333333333333703, 0.3219752754296894559, 0.3333333333333333703, 0.3219752754296894559, 0.3333333333333333703, 0.3219752754296894559, 0.3333333333333333703, 0.3219752754296894559, 0.3333333333333333703, 0.3219752754296894559, 0.3333333333333333703, 0.3219752754296894559, 0.3333333333333333703, 0.3219752754296894559, 0.3333333333333333703, 0.3219752754296894559, 0.3333333333333333703, 0.3219752754296894559, 0.3333333333333333703, 0.3219752754296894559, 0.3333333333333333703, 0.3219752754296894559, 0.3333333333333333703, 0.3219752754296894559, 0.3333333333333333703, 0.3219752754296894559, 0.3333333333333333703, 0.3219752754296894559, 0.3333333333333333703, 0.3219752754296894559, 0.3333333333333333703, 0.3219752754296894559, 0.3333333333333333703, 0.3219752754296894559, 0.3333333333333333703, 0.3219752754296894559, 0.3333333333333333703, 0.3219752754296894559, 0.3333333333333333703, 0.3219752754296894559, 0.3333333333333333703, 0.3219752754296894559, 0.3333333333333333703, 0.3219752754296894559, 0.3333333333333333703, 0.3219752754296894559, 0.3333333333333333703, 0.3219752754296894559, 0.3333333333333333703, 0.3219752754296894559, 0.3333333333333333703, 0.3219752754296894559, 0.3333333333333333703, 0.3219752754296894559, 0.3333333333333333703, 0.3219752754296894559, 0.3333333333333333703, 0.3219752754296894559, 0.3333333333333333703, 0.3219752754296894559, 0.3333333333333333703, 0.3219752754296894559, 0.3333333333333333703, 0.3219752754296894559, 0.3333333333333333703, 0.3219752754296894559, 0.3333333333333333703, 0.3219752754296894559, 0.3333333333333333703, 0.3219752754296894559, 0.3333333333333333703, 0.3219752754296894559, 0.3333333333333333703, 0.3219752754296894559, 0.3333333333333333703, 0.3219752754296894559, 0.3333333333333333703, 0.3219752754296894559, 0.3333333333333333703, 0.3219752754296894559, 0.3333333333333333703, 0.3219752754296894559, 0.3333333333333333703, 0.3219752754296894559, 0.3333333333333333703, 0.3219752754296894559, 0.3333333333333333703, 0.3219752754296894559, 0.3333333333333333703, 0.3219752754296894559, 0.3333333333333333703, 0.3219752754296894559, 0.3333333333333333703, 0.3219752754296894559, 0.3333333333333333703, 0.3219752754296894559, 0.3333333333333333703, 0.3219752754296894559, 0.3333333333333333703, 0.3219752754296894559, 0.3333333333333333703, 0.3219752754296894559, 0.3333333333333333703, 0.3219752754296894559, 0.3333333333333333703, 0.3219752754296894559, 0.3333333333333333703, 0.3219752754296894559, 0.3333333333333333703, 0.3219752754296894559, 0.3333333333333333703, 0.3219752754296894559, 0.3333333333333333703, 0.3219752754296894559, 0.3333333333333333703, 0.3219752754296894559, 0.3333333333333333703, 0.3219752754296894559, 0.3333333333333333703, 0.3219752754296894559, 0.3333333333333333703, 0.3219752754296894559, 0.3333333333333333703, 0.3219752754296894559, 0.3333333333333333703, 0.3219752754296894559, 0.3333333333333333703, 0.3219752754296894559, 0.3333333333333333703, 0.3219752754296894559, 0.3333333333333333703, 0.3219752754296894559, 0.3333333333333333703, 0.3219752754296894559, 0.3333333333333333703, 0.3219752754296894559, 0.3333333333333333703, 0.3219752754296894559, 0.3333333333333333703, 0.3219752754296894559, 0.3333333333333333703, 0.3219752754296894559, 0.3333333333333333703, 0.3219752754296894559, 0.3333333333333333703, 0.3219752754296894559, 0.3333333333333333703, 0.3219752754296894559, 0.3333333333333333703, 0.3219752754296894559, 0.3333333333333333703, 0.3219752754296894559, 0.3333333333333333703, 0.3219752754296894559, 0.3333333333333333703, 0.3219752754296894559, 0.3333333333333333703, 0.3219752754296894559, 0.3333333333333333703, 0.3219752754296894559, 0.3333333333333333703, 0.3219752754296894559, 0.3333333333333333703, 0.3219752754296894559, 0.3333333333333333703, 0.3219752754296894559, 0.3333333333333333703, 0.3219752754296894559, 0.3333333333333333703, 0.3219752754296894559, 0.3333333333333333703, 0.3219752754296894559, 0.3333333333333333703, 0.3219752754296894559, 0.3333333333333333703, 0.3219752754296894559, 0.3333333333333333703, 0.3219752754296894559, 0.3333333333333333703, 0.3219752754296894559, 0.3333333333333333703, 0.3219752754296894559, 0.3333333333333333703, 0.3219752754296894559, 0.3333333333333333703, 0.3219752754296894559, 0.3333333333333333703, 0.3219752754296894559, 0.3333333333333333703, 0.3219752754296894559, 0.3333333333333333703),
 ( 0.3333333333333333703, 0.3219752754296894559, 0.3333333333333333703, 0.3219752754296894559, 0.3333333333333333703, 0.3219752754296894559, 0.3333333333333333703, 0.3219752754296894559, 0.3333333333333333703, 0.3219752754296894559, 0.3333333333333333703, 0.3219752754296894559, 0.3333333333333333703, 0.3219752754296894559, 0.3333333333333333703, 0.3219752754296894559, 0.3333333333333333703, 0.3219752754296894559, 0.3333333333333333703, 0.3219752754296894559, 0.3333333333333333703, 0.3219752754296894559, 0.3333333333333333703, 0.3219752754296894559, 0.3333333333333333703, 0.3219752754296894559, 0.3333333333333333703, 0.3219752754296894559, 0.3333333333333333703, 0.3219752754296894559, 0.3333333333333333703, 0.3219752754296894559, 0.3333333333333333703, 0.3219752754296894559, 0.3333333333333333703, 0.3219752754296894559, 0.3333333333333333703, 0.3219752754296894559, 0.3333333333333333703, 0.3219752754296894559, 0.3333333333333333703, 0.3219752754296894559, 0.3333333333333333703, 0.3219752754296894559, 0.3333333333333333703, 0.3219752754296894559, 0.3333333333333333703, 0.3219752754296894559, 0.3333333333333333703, 0.3219752754296894559, 0.3333333333333333703, 0.3219752754296894559, 0.3333333333333333703, 0.3219752754296894559, 0.3333333333333333703, 0.3219752754296894559, 0.3333333333333333703, 0.3219752754296894559, 0.3333333333333333703, 0.3219752754296894559, 0.3333333333333333703, 0.3219752754296894559, 0.3333333333333333703, 0.3219752754296894559, 0.3333333333333333703, 0.3219752754296894559, 0.3333333333333333703, 0.3219752754296894559, 0.3333333333333333703, 0.3219752754296894559, 0.3333333333333333703, 0.3219752754296894559, 0.3333333333333333703, 0.3219752754296894559, 0.3333333333333333703, 0.3219752754296894559, 0.3333333333333333703, 0.3219752754296894559, 0.3333333333333333703, 0.3219752754296894559, 0.3333333333333333703, 0.3219752754296894559, 0.3333333333333333703, 0.3219752754296894559, 0.3333333333333333703, 0.3219752754296894559, 0.3333333333333333703, 0.3219752754296894559, 0.3333333333333333703, 0.3219752754296894559, 0.3333333333333333703, 0.3219752754296894559, 0.3333333333333333703, 0.3219752754296894559, 0.3333333333333333703, 0.3219752754296894559, 0.3333333333333333703, 0.3219752754296894559, 0.3333333333333333703, 0.3219752754296894559, 0.3333333333333333703, 0.3219752754296894559, 0.3333333333333333703, 0.3219752754296894559, 0.3333333333333333703, 0.3219752754296894559, 0.3333333333333333703, 0.3219752754296894559, 0.3333333333333333703, 0.3219752754296894559, 0.3333333333333333703, 0.3219752754296894559, 0.3333333333333333703, 0.3219752754296894559, 0.3333333333333333703, 0.3219752754296894559, 0.3333333333333333703, 0.3219752754296894559, 0.3333333333333333703, 0.3219752754296894559, 0.3333333333333333703, 0.3219752754296894559, 0.3333333333333333703, 0.3219752754296894559, 0.3333333333333333703, 0.3219752754296894559, 0.3333333333333333703, 0.3219752754296894559, 0.3333333333333333703, 0.3219752754296894559, 0.3333333333333333703, 0.3219752754296894559, 0.3333333333333333703, 0.3219752754296894559, 0.3333333333333333703, 0.3219752754296894559, 0.3333333333333333703, 0.3219752754296894559, 0.3333333333333333703, 0.3219752754296894559, 0.3333333333333333703, 0.3219752754296894559, 0.3333333333333333703, 0.3219752754296894559, 0.3333333333333333703, 0.3219752754296894559, 0.3333333333333333703, 0.3219752754296894559, 0.3333333333333333703, 0.3219752754296894559, 0.3333333333333333703, 0.3219752754296894559, 0.3333333333333333703, 0.3219752754296894559, 0.3333333333333333703, 0.3219752754296894559, 0.3333333333333333703, 0.3219752754296894559, 0.3333333333333333703, 0.3219752754296894559, 0.3333333333333333703, 0.3219752754296894559, 0.3333333333333333703, 0.3219752754296894559, 0.3333333333333333703, 0.3219752754296894559, 0.3333333333333333703, 0.3219752754296894559, 0.3333333333333333703, 0.3219752754296894559, 0.3333333333333333703, 0.3219752754296894559, 0.3333333333333333703, 0.3219752754296894559, 0.3333333333333333703, 0.3219752754296894559, 0.3333333333333333703, 0.3219752754296894559, 0.3333333333333333703, 0.3219752754296894559, 0.3333333333333333703, 0.3219752754296894559, 0.3333333333333333703, 0.3219752754296894559, 0.3333333333333333703, 0.3219752754296894559, 0.3333333333333333703, 0.3219752754296894559, 0.3333333333333333703, 0.3219752754296894559, 0.3333333333333333703, 0.3219752754296894559, 0.3333333333333333703, 0.3219752754296894559, 0.3333333333333333703, 0.3219752754296894559, 0.3333333333333333703, 0.3219752754296894559, 0.3333333333333333703, 0.3219752754296894559, 0.3333333333333333703, 0.3219752754296894559, 0.3333333333333333703, 0.3219752754296894559, 0.3333333333333333703, 0.3219752754296894559, 0.3333333333333333703, 0.3219752754296894559, 0.3333333333333333703, 0.3219752754296894559, 0.3333333333333333703, 0.3219752754296894559, 0.3333333333333333703, 0.3219752754296894559, 0.3333333333333333703, 0.3219752754296894559, 0.3333333333333333703, 0.3219752754296894559, 0.3333333333333333703, 0.3219752754296894559, 0.3333333333333333703, 0.3219752754296894559, 0.3333333333333333703, 0.3219752754296894559, 0.3333333333333333703, 0.3219752754296894559, 0.3333333333333333703, 0.3219752754296894559, 0.3333333333333333703, 0.3219752754296894559, 0.3333333333333333703, 0.3219752754296894559, 0.3333333333333333703, 0.3219752754296894559, 0.3333333333333333703, 0.3219752754296894559, 0.3333333333333333703, 0.3219752754296894559, 0.3333333333333333703, 0.3219752754296894559, 0.3333333333333333703, 0.3219752754296894559, 0.3333333333333333703, 0.3219752754296894559, 0.3333333333333333703, 0.3219752754296894559, 0.3333333333333333703, 0.3219752754296894559, 0.3333333333333333703, 0.3219752754296894559, 0.3333333333333333703, 0.3219752754296894559, 0.3333333333333333703, 0.3219752754296894559, 0.3333333333333333703, 0.3219752754296894559, 0.3333333333333333703, 0.3219752754296894559, 0.3333333333333333703, 0.3219752754296894559, 0.3333333333333333703, 0.3219752754296894559, 0.3333333333333333703, 0.3219752754296894559, 0.3333333333333333703, 0.3219752754296894559, 0.3333333333333333703, 0.3219752754296894559, 0.3333333333333333703, 0.3219752754296894559, 0.3333333333333333703, 0.3219752754296894559, 0.3333333333333333703, 0.3219752754296894559, 0.3333333333333333703, 0.3219752754296894559, 0.3333333333333333703, 0.3219752754296894559, 0.3333333333333333703, 0.3219752754296894559, 0.3333333333333333703, 0.3219752754296894559, 0.3333333333333333703, 0.3219752754296894559, 0.3333333333333333703, 0.3219752754296894559, 0.3333333333333333703, 0.3219752754296894559, 0.3333333333333333703, 0.3219752754296894559, 0.3333333333333333703, 0.3219752754296894559, 0.3333333333333333703, 0.3219752754296894559, 0.3333333333333333703, 0.3219752754296894559, 0.3333333333333333703, 0.3219752754296894559, 0.3333333333333333703, 0.3219752754296894559, 0.3333333333333333703, 0.3219752754296894559, 0.3333333333333333703, 0.3219752754296894559, 0.3333333333333333703, 0.3219752754296894559, 0.3333333333333333703, 0.3219752754296894559, 0.3333333333333333703, 0.3219752754296894559, 0.3333333333333333703, 0.3219752754296894559, 0.3333333333333333703, 0.3219752754296894559, 0.3333333333333333703, 0.3219752754296894559, 0.3333333333333333703, 0.3219752754296894559, 0.3333333333333333703, 0.3219752754296894559, 0.3333333333333333703, 0.3219752754296894559, 0.3333333333333333703, 0.3219752754296894559, 0.3333333333333333703, 0.3219752754296894559, 0.3333333333333333703, 0.3219752754296894559, 0.3333333333333333703, 0.3219752754296894559, 0.3333333333333333703, 0.3219752754296894559, 0.3333333333333333703, 0.3219752754296894559, 0.3333333333333333703, 0.3219752754296894559, 0.3333333333333333703, 0.3219752754296894559, 0.3333333333333333703, 0.3219752754296894559, 0.3333333333333333703, 0.3219752754296894559, 0.3333333333333333703, 0.3219752754296894559, 0.3333333333333333703, 0.3219752754296894559, 0.3333333333333333703, 0.3219752754296894559, 0.3333333333333333703, 0.3219752754296894559, 0.3333333333333333703, 0.3219752754296894559, 0.3333333333333333703, 0.3219752754296894559, 0.3333333333333333703, 0.3219752754296894559, 0.3333333333333333703, 0.3219752754296894559, 0.3333333333333333703, 0.3219752754296894559, 0.3333333333333333703, 0.3219752754296894559, 0.3333333333333333703, 0.3219752754296894559, 0.3333333333333333703, 0.3219752754296894559, 0.3333333333333333703, 0.3219752754296894559, 0.3333333333333333703, 0.3219752754296894559, 0.3333333333333333703, 0.3219752754296894559, 0.3333333333333333703, 0.3219752754296894559, 0.3333333333333333703, 0.3219752754296894559, 0.3333333333333333703, 0.3219752754296894559, 0.3333333333333333703, 0.3219752754296894559, 0.3333333333333333703, 0.3219752754296894559, 0.3333333333333333703, 0.3219752754296894559, 0.3333333333333333703, 0.3219752754296894559, 0.3333333333333333703, 0.3219752754296894559, 0.3333333333333333703, 0.3219752754296894559, 0.3333333333333333703, 0.3219752754296894559, 0.3333333333333333703, 0.3219752754296894559, 0.3333333333333333703, 0.3219752754296894559, 0.3333333333333333703, 0.3219752754296894559, 0.3333333333333333703, 0.3219752754296894559, 0.3333333333333333703, 0.3219752754296894559, 0.3333333333333333703, 0.3219752754296894559, 0.3333333333333333703, 0.3219752754296894559, 0.3333333333333333703, 0.3219752754296894559, 0.3333333333333333703, 0.3219752754296894559, 0.3333333333333333703, 0.3219752754296894559, 0.3333333333333333703, 0.3219752754296894559, 0.3333333333333333703, 0.3219752754296894559, 0.3333333333333333703, 0.3219752754296894559, 0.3333333333333333703, 0.3219752754296894559, 0.3333333333333333703, 0.3219752754296894559, 0.3333333333333333703, 0.3219752754296894559, 0.3333333333333333703, 0.3219752754296894559, 0.3333333333333333703, 0.3219752754296894559, 0.3333333333333333703, 0.3219752754296894559, 0.3333333333333333703, 0.3219752754296894559, 0.3333333333333333703, 0.3219752754296894559, 0.3333333333333333703, 0.3219752754296894559, 0.3333333333333333703, 0.3219752754296894559, 0.3333333333333333703, 0.3219752754296894559, 0.3333333333333333703, 0.3219752754296894559, 0.3333333333333333703, 0.3219752754296894559, 0.3333333333333333703, 0.3219752754296894559, 0.3333333333333333703, 0.3219752754296894559, 0.3333333333333333703, 0.3219752754296894559, 0.3333333333333333703, 0.3219752754296894559, 0.3333333333333333703, 0.3219752754296894559, 0.3333333333333333703, 0.3219752754296894559, 0.3333333333333333703),
 ( 1.000000000000000000, 0.9659258262890683122, 1.000000000000000000, 0.9659258262890683122, 1.000000000000000000, 0.9659258262890683122, 1.000000000000000000, 0.9659258262890683122, 1.000000000000000000, 0.9659258262890683122, 1.000000000000000000, 0.9659258262890683122, 1.000000000000000000, 0.9659258262890683122, 1.000000000000000000, 0.9659258262890683122, 1.000000000000000000, 0.9659258262890683122, 1.000000000000000000, 0.9659258262890683122, 1.000000000000000000, 0.9659258262890683122, 1.000000000000000000, 0.9659258262890683122, 1.000000000000000000, 0.9659258262890683122, 1.000000000000000000, 0.9659258262890683122, 1.000000000000000000, 0.9659258262890683122, 1.000000000000000000, 0.9659258262890683122, 1.000000000000000000, 0.9659258262890683122, 1.000000000000000000, 0.9659258262890683122, 1.000000000000000000, 0.9659258262890683122, 1.000000000000000000, 0.9659258262890683122, 1.000000000000000000, 0.9659258262890683122, 1.000000000000000000, 0.9659258262890683122, 1.000000000000000000, 0.9659258262890683122, 1.000000000000000000, 0.9659258262890683122, 1.000000000000000000, 0.9659258262890683122, 1.000000000000000000, 0.9659258262890683122, 1.000000000000000000, 0.9659258262890683122, 1.000000000000000000, 0.9659258262890683122, 1.000000000000000000, 0.9659258262890683122, 1.000000000000000000, 0.9659258262890683122, 1.000000000000000000, 0.9659258262890683122, 1.000000000000000000, 0.9659258262890683122, 1.000000000000000000, 0.9659258262890683122, 1.000000000000000000, 0.9659258262890683122, 1.000000000000000000, 0.9659258262890683122, 1.000000000000000000, 0.9659258262890683122, 1.000000000000000000, 0.9659258262890683122, 1.000000000000000000, 0.9659258262890683122, 1.000000000000000000, 0.9659258262890683122, 1.000000000000000000, 0.9659258262890683122, 1.000000000000000000, 0.9659258262890683122, 1.000000000000000000, 0.9659258262890683122, 1.000000000000000000, 0.9659258262890683122, 1.000000000000000000, 0.9659258262890683122, 1.000000000000000000, 0.9659258262890683122, 1.000000000000000000, 0.9659258262890683122, 1.000000000000000000, 0.9659258262890683122, 1.000000000000000000, 0.9659258262890683122, 1.000000000000000000, 0.9659258262890683122, 1.000000000000000000, 0.9659258262890683122, 1.000000000000000000, 0.9659258262890683122, 1.000000000000000000, 0.9659258262890683122, 1.000000000000000000, 0.9659258262890683122, 1.000000000000000000, 0.9659258262890683122, 1.000000000000000000, 0.9659258262890683122, 1.000000000000000000, 0.9659258262890683122, 1.000000000000000000, 0.9659258262890683122, 1.000000000000000000, 0.9659258262890683122, 1.000000000000000000, 0.9659258262890683122, 1.000000000000000000, 0.9659258262890683122, 1.000000000000000000, 0.9659258262890683122, 1.000000000000000000, 0.9659258262890683122, 1.000000000000000000, 0.9659258262890683122, 1.000000000000000000, 0.9659258262890683122, 1.000000000000000000, 0.9659258262890683122, 1.000000000000000000, 0.9659258262890683122, 1.000000000000000000, 0.9659258262890683122, 1.000000000000000000, 0.9659258262890683122, 1.000000000000000000, 0.9659258262890683122, 1.000000000000000000, 0.9659258262890683122, 1.000000000000000000, 0.9659258262890683122, 1.000000000000000000, 0.9659258262890683122, 1.000000000000000000, 0.9659258262890683122, 1.000000000000000000, 0.9659258262890683122, 1.000000000000000000, 0.9659258262890683122, 1.000000000000000000, 0.9659258262890683122, 1.000000000000000000, 0.9659258262890683122, 1.000000000000000000, 0.9659258262890683122, 1.000000000000000000, 0.9659258262890683122, 1.000000000000000000, 0.9659258262890683122, 1.000000000000000000, 0.9659258262890683122, 1.000000000000000000, 0.9659258262890683122, 1.000000000000000000, 0.9659258262890683122, 1.000000000000000000, 0.9659258262890683122, 1.000000000000000000, 0.9659258262890683122, 1.000000000000000000, 0.9659258262890683122, 1.000000000000000000, 0.9659258262890683122, 1.000000000000000000, 0.9659258262890683122, 1.000000000000000000, 0.9659258262890683122, 1.000000000000000000, 0.9659258262890683122, 1.000000000000000000, 0.9659258262890683122, 1.000000000000000000, 0.9659258262890683122, 1.000000000000000000, 0.9659258262890683122, 1.000000000000000000, 0.9659258262890683122, 1.000000000000000000, 0.9659258262890683122, 1.000000000000000000, 0.9659258262890683122, 1.000000000000000000, 0.9659258262890683122, 1.000000000000000000, 0.9659258262890683122, 1.000000000000000000, 0.9659258262890683122, 1.000000000000000000, 0.9659258262890683122, 1.000000000000000000, 0.9659258262890683122, 1.000000000000000000, 0.9659258262890683122, 1.000000000000000000, 0.9659258262890683122, 1.000000000000000000, 0.9659258262890683122, 1.000000000000000000, 0.9659258262890683122, 1.000000000000000000, 0.9659258262890683122, 1.000000000000000000, 0.9659258262890683122, 1.000000000000000000, 0.9659258262890683122, 1.000000000000000000, 0.9659258262890683122, 1.000000000000000000, 0.9659258262890683122, 1.000000000000000000, 0.9659258262890683122, 1.000000000000000000, 0.9659258262890683122, 1.000000000000000000, 0.9659258262890683122, 1.000000000000000000, 0.9659258262890683122, 1.000000000000000000, 0.9659258262890683122, 1.000000000000000000, 0.9659258262890683122, 1.000000000000000000, 0.9659258262890683122, 1.000000000000000000, 0.9659258262890683122, 1.000000000000000000, 0.9659258262890683122, 1.000000000000000000, 0.9659258262890683122, 1.000000000000000000, 0.9659258262890683122, 1.000000000000000000, 0.9659258262890683122, 1.000000000000000000, 0.9659258262890683122, 1.000000000000000000, 0.9659258262890683122, 1.000000000000000000, 0.9659258262890683122, 1.000000000000000000, 0.9659258262890683122, 1.000000000000000000, 0.9659258262890683122, 1.000000000000000000, 0.9659258262890683122, 1.000000000000000000, 0.9659258262890683122, 1.000000000000000000, 0.9659258262890683122, 1.000000000000000000, 0.9659258262890683122, 1.000000000000000000, 0.9659258262890683122, 1.000000000000000000, 0.9659258262890683122, 1.000000000000000000, 0.9659258262890683122, 1.000000000000000000, 0.9659258262890683122, 1.000000000000000000, 0.9659258262890683122, 1.000000000000000000, 0.9659258262890683122, 1.000000000000000000, 0.9659258262890683122, 1.000000000000000000, 0.9659258262890683122, 1.000000000000000000, 0.9659258262890683122, 1.000000000000000000, 0.9659258262890683122, 1.000000000000000000, 0.9659258262890683122, 1.000000000000000000, 0.9659258262890683122, 1.000000000000000000, 0.9659258262890683122, 1.000000000000000000, 0.9659258262890683122, 1.000000000000000000, 0.9659258262890683122, 1.000000000000000000, 0.9659258262890683122, 1.000000000000000000, 0.9659258262890683122, 1.000000000000000000, 0.9659258262890683122, 1.000000000000000000, 0.9659258262890683122, 1.000000000000000000, 0.9659258262890683122, 1.000000000000000000, 0.9659258262890683122, 1.000000000000000000, 0.9659258262890683122, 1.000000000000000000, 0.9659258262890683122, 1.000000000000000000, 0.9659258262890683122, 1.000000000000000000, 0.9659258262890683122, 1.000000000000000000, 0.9659258262890683122, 1.000000000000000000, 0.9659258262890683122, 1.000000000000000000, 0.9659258262890683122, 1.000000000000000000, 0.9659258262890683122, 1.000000000000000000, 0.9659258262890683122, 1.000000000000000000, 0.9659258262890683122, 1.000000000000000000, 0.9659258262890683122, 1.000000000000000000, 0.9659258262890683122, 1.000000000000000000, 0.9659258262890683122, 1.000000000000000000, 0.9659258262890683122, 1.000000000000000000, 0.9659258262890683122, 1.000000000000000000, 0.9659258262890683122, 1.000000000000000000, 0.9659258262890683122, 1.000000000000000000, 0.9659258262890683122, 1.000000000000000000, 0.9659258262890683122, 1.000000000000000000, 0.9659258262890683122, 1.000000000000000000, 0.9659258262890683122, 1.000000000000000000, 0.9659258262890683122, 1.000000000000000000, 0.9659258262890683122, 1.000000000000000000, 0.9659258262890683122, 1.000000000000000000, 0.9659258262890683122, 1.000000000000000000, 0.9659258262890683122, 1.000000000000000000, 0.9659258262890683122, 1.000000000000000000, 0.9659258262890683122, 1.000000000000000000, 0.9659258262890683122, 1.000000000000000000, 0.9659258262890683122, 1.000000000000000000, 0.9659258262890683122, 1.000000000000000000, 0.9659258262890683122, 1.000000000000000000, 0.9659258262890683122, 1.000000000000000000, 0.9659258262890683122, 1.000000000000000000, 0.9659258262890683122, 1.000000000000000000, 0.9659258262890683122, 1.000000000000000000, 0.9659258262890683122, 1.000000000000000000, 0.9659258262890683122, 1.000000000000000000, 0.9659258262890683122, 1.000000000000000000, 0.9659258262890683122, 1.000000000000000000, 0.9659258262890683122, 1.000000000000000000, 0.9659258262890683122, 1.000000000000000000, 0.9659258262890683122, 1.000000000000000000, 0.9659258262890683122, 1.000000000000000000, 0.9659258262890683122, 1.000000000000000000, 0.9659258262890683122, 1.000000000000000000, 0.9659258262890683122, 1.000000000000000000, 0.9659258262890683122, 1.000000000000000000, 0.9659258262890683122, 1.000000000000000000, 0.9659258262890683122, 1.000000000000000000, 0.9659258262890683122, 1.000000000000000000, 0.9659258262890683122, 1.000000000000000000, 0.9659258262890683122, 1.000000000000000000, 0.9659258262890683122, 1.000000000000000000, 0.9659258262890683122, 1.000000000000000000, 0.9659258262890683122, 1.000000000000000000, 0.9659258262890683122, 1.000000000000000000, 0.9659258262890683122, 1.000000000000000000, 0.9659258262890683122, 1.000000000000000000, 0.9659258262890683122, 1.000000000000000000, 0.9659258262890683122, 1.000000000000000000, 0.9659258262890683122, 1.000000000000000000, 0.9659258262890683122, 1.000000000000000000, 0.9659258262890683122, 1.000000000000000000, 0.9659258262890683122, 1.000000000000000000, 0.9659258262890683122, 1.000000000000000000, 0.9659258262890683122, 1.000000000000000000, 0.9659258262890683122, 1.000000000000000000, 0.9659258262890683122, 1.000000000000000000, 0.9659258262890683122, 1.000000000000000000, 0.9659258262890683122, 1.000000000000000000, 0.9659258262890683122, 1.000000000000000000, 0.9659258262890683122, 1.000000000000000000, 0.9659258262890683122, 1.000000000000000000, 0.9659258262890683122, 1.000000000000000000, 0.9659258262890683122, 1.000000000000000000),
 ( 0.3333333333333333703, 0.3219752754296894559, 0.3333333333333333703, 0.3219752754296894559, 0.3333333333333333703, 0.3219752754296894559, 0.3333333333333333703, 0.3219752754296894559, 0.3333333333333333703, 0.3219752754296894559, 0.3333333333333333703, 0.3219752754296894559, 0.3333333333333333703, 0.3219752754296894559, 0.3333333333333333703, 0.3219752754296894559, 0.3333333333333333703, 0.3219752754296894559, 0.3333333333333333703, 0.3219752754296894559, 0.3333333333333333703, 0.3219752754296894559, 0.3333333333333333703, 0.3219752754296894559, 0.3333333333333333703, 0.3219752754296894559, 0.3333333333333333703, 0.3219752754296894559, 0.3333333333333333703, 0.3219752754296894559, 0.3333333333333333703, 0.3219752754296894559, 0.3333333333333333703, 0.3219752754296894559, 0.3333333333333333703, 0.3219752754296894559, 0.3333333333333333703, 0.3219752754296894559, 0.3333333333333333703, 0.3219752754296894559, 0.3333333333333333703, 0.3219752754296894559, 0.3333333333333333703, 0.3219752754296894559, 0.3333333333333333703, 0.3219752754296894559, 0.3333333333333333703, 0.3219752754296894559, 0.3333333333333333703, 0.3219752754296894559, 0.3333333333333333703, 0.3219752754296894559, 0.3333333333333333703, 0.3219752754296894559, 0.3333333333333333703, 0.3219752754296894559, 0.3333333333333333703, 0.3219752754296894559, 0.3333333333333333703, 0.3219752754296894559, 0.3333333333333333703, 0.3219752754296894559, 0.3333333333333333703, 0.3219752754296894559, 0.3333333333333333703, 0.3219752754296894559, 0.3333333333333333703, 0.3219752754296894559, 0.3333333333333333703, 0.3219752754296894559, 0.3333333333333333703, 0.3219752754296894559, 0.3333333333333333703, 0.3219752754296894559, 0.3333333333333333703, 0.3219752754296894559, 0.3333333333333333703, 0.3219752754296894559, 0.3333333333333333703, 0.3219752754296894559, 0.3333333333333333703, 0.3219752754296894559, 0.3333333333333333703, 0.3219752754296894559, 0.3333333333333333703, 0.3219752754296894559, 0.3333333333333333703, 0.3219752754296894559, 0.3333333333333333703, 0.3219752754296894559, 0.3333333333333333703, 0.3219752754296894559, 0.3333333333333333703, 0.3219752754296894559, 0.3333333333333333703, 0.3219752754296894559, 0.3333333333333333703, 0.3219752754296894559, 0.3333333333333333703, 0.3219752754296894559, 0.3333333333333333703, 0.3219752754296894559, 0.3333333333333333703, 0.3219752754296894559, 0.3333333333333333703, 0.3219752754296894559, 0.3333333333333333703, 0.3219752754296894559, 0.3333333333333333703, 0.3219752754296894559, 0.3333333333333333703, 0.3219752754296894559, 0.3333333333333333703, 0.3219752754296894559, 0.3333333333333333703, 0.3219752754296894559, 0.3333333333333333703, 0.3219752754296894559, 0.3333333333333333703, 0.3219752754296894559, 0.3333333333333333703, 0.3219752754296894559, 0.3333333333333333703, 0.3219752754296894559, 0.3333333333333333703, 0.3219752754296894559, 0.3333333333333333703, 0.3219752754296894559, 0.3333333333333333703, 0.3219752754296894559, 0.3333333333333333703, 0.3219752754296894559, 0.3333333333333333703, 0.3219752754296894559, 0.3333333333333333703, 0.3219752754296894559, 0.3333333333333333703, 0.3219752754296894559, 0.3333333333333333703, 0.3219752754296894559, 0.3333333333333333703, 0.3219752754296894559, 0.3333333333333333703, 0.3219752754296894559, 0.3333333333333333703, 0.3219752754296894559, 0.3333333333333333703, 0.3219752754296894559, 0.3333333333333333703, 0.3219752754296894559, 0.3333333333333333703, 0.3219752754296894559, 0.3333333333333333703, 0.3219752754296894559, 0.3333333333333333703, 0.3219752754296894559, 0.3333333333333333703, 0.3219752754296894559, 0.3333333333333333703, 0.3219752754296894559, 0.3333333333333333703, 0.3219752754296894559, 0.3333333333333333703, 0.3219752754296894559, 0.3333333333333333703, 0.3219752754296894559, 0.3333333333333333703, 0.3219752754296894559, 0.3333333333333333703, 0.3219752754296894559, 0.3333333333333333703, 0.3219752754296894559, 0.3333333333333333703, 0.3219752754296894559, 0.3333333333333333703, 0.3219752754296894559, 0.3333333333333333703, 0.3219752754296894559, 0.3333333333333333703, 0.3219752754296894559, 0.3333333333333333703, 0.3219752754296894559, 0.3333333333333333703, 0.3219752754296894559, 0.3333333333333333703, 0.3219752754296894559, 0.3333333333333333703, 0.3219752754296894559, 0.3333333333333333703, 0.3219752754296894559, 0.3333333333333333703, 0.3219752754296894559, 0.3333333333333333703, 0.3219752754296894559, 0.3333333333333333703, 0.3219752754296894559, 0.3333333333333333703, 0.3219752754296894559, 0.3333333333333333703, 0.3219752754296894559, 0.3333333333333333703, 0.3219752754296894559, 0.3333333333333333703, 0.3219752754296894559, 0.3333333333333333703, 0.3219752754296894559, 0.3333333333333333703, 0.3219752754296894559, 0.3333333333333333703, 0.3219752754296894559, 0.3333333333333333703, 0.3219752754296894559, 0.3333333333333333703, 0.3219752754296894559, 0.3333333333333333703, 0.3219752754296894559, 0.3333333333333333703, 0.3219752754296894559, 0.3333333333333333703, 0.3219752754296894559, 0.3333333333333333703, 0.3219752754296894559, 0.3333333333333333703, 0.3219752754296894559, 0.3333333333333333703, 0.3219752754296894559, 0.3333333333333333703, 0.3219752754296894559, 0.3333333333333333703, 0.3219752754296894559, 0.3333333333333333703, 0.3219752754296894559, 0.3333333333333333703, 0.3219752754296894559, 0.3333333333333333703, 0.3219752754296894559, 0.3333333333333333703, 0.3219752754296894559, 0.3333333333333333703, 0.3219752754296894559, 0.3333333333333333703, 0.3219752754296894559, 0.3333333333333333703, 0.3219752754296894559, 0.3333333333333333703, 0.3219752754296894559, 0.3333333333333333703, 0.3219752754296894559, 0.3333333333333333703, 0.3219752754296894559, 0.3333333333333333703, 0.3219752754296894559, 0.3333333333333333703, 0.3219752754296894559, 0.3333333333333333703, 0.3219752754296894559, 0.3333333333333333703, 0.3219752754296894559, 0.3333333333333333703, 0.3219752754296894559, 0.3333333333333333703, 0.3219752754296894559, 0.3333333333333333703, 0.3219752754296894559, 0.3333333333333333703, 0.3219752754296894559, 0.3333333333333333703, 0.3219752754296894559, 0.3333333333333333703, 0.3219752754296894559, 0.3333333333333333703, 0.3219752754296894559, 0.3333333333333333703, 0.3219752754296894559, 0.3333333333333333703, 0.3219752754296894559, 0.3333333333333333703, 0.3219752754296894559, 0.3333333333333333703, 0.3219752754296894559, 0.3333333333333333703, 0.3219752754296894559, 0.3333333333333333703, 0.3219752754296894559, 0.3333333333333333703, 0.3219752754296894559, 0.3333333333333333703, 0.3219752754296894559, 0.3333333333333333703, 0.3219752754296894559, 0.3333333333333333703, 0.3219752754296894559, 0.3333333333333333703, 0.3219752754296894559, 0.3333333333333333703, 0.3219752754296894559, 0.3333333333333333703, 0.3219752754296894559, 0.3333333333333333703, 0.3219752754296894559, 0.3333333333333333703, 0.3219752754296894559, 0.3333333333333333703, 0.3219752754296894559, 0.3333333333333333703, 0.3219752754296894559, 0.3333333333333333703, 0.3219752754296894559, 0.3333333333333333703, 0.3219752754296894559, 0.3333333333333333703, 0.3219752754296894559, 0.3333333333333333703, 0.3219752754296894559, 0.3333333333333333703, 0.3219752754296894559, 0.3333333333333333703, 0.3219752754296894559, 0.3333333333333333703, 0.3219752754296894559, 0.3333333333333333703, 0.3219752754296894559, 0.3333333333333333703, 0.3219752754296894559, 0.3333333333333333703, 0.3219752754296894559, 0.3333333333333333703, 0.3219752754296894559, 0.3333333333333333703, 0.3219752754296894559, 0.3333333333333333703, 0.3219752754296894559, 0.3333333333333333703, 0.3219752754296894559, 0.3333333333333333703, 0.3219752754296894559, 0.3333333333333333703, 0.3219752754296894559, 0.3333333333333333703, 0.3219752754296894559, 0.3333333333333333703, 0.3219752754296894559, 0.3333333333333333703, 0.3219752754296894559, 0.3333333333333333703, 0.3219752754296894559, 0.3333333333333333703, 0.3219752754296894559, 0.3333333333333333703, 0.3219752754296894559, 0.3333333333333333703, 0.3219752754296894559, 0.3333333333333333703, 0.3219752754296894559, 0.3333333333333333703, 0.3219752754296894559, 0.3333333333333333703, 0.3219752754296894559, 0.3333333333333333703, 0.3219752754296894559, 0.3333333333333333703, 0.3219752754296894559, 0.3333333333333333703, 0.3219752754296894559, 0.3333333333333333703, 0.3219752754296894559, 0.3333333333333333703, 0.3219752754296894559, 0.3333333333333333703, 0.3219752754296894559, 0.3333333333333333703, 0.3219752754296894559, 0.3333333333333333703, 0.3219752754296894559, 0.3333333333333333703, 0.3219752754296894559, 0.3333333333333333703, 0.3219752754296894559, 0.3333333333333333703, 0.3219752754296894559, 0.3333333333333333703, 0.3219752754296894559, 0.3333333333333333703, 0.3219752754296894559, 0.3333333333333333703, 0.3219752754296894559, 0.3333333333333333703, 0.3219752754296894559, 0.3333333333333333703, 0.3219752754296894559, 0.3333333333333333703, 0.3219752754296894559, 0.3333333333333333703, 0.3219752754296894559, 0.3333333333333333703, 0.3219752754296894559, 0.3333333333333333703, 0.3219752754296894559, 0.3333333333333333703, 0.3219752754296894559, 0.3333333333333333703, 0.3219752754296894559, 0.3333333333333333703, 0.3219752754296894559, 0.3333333333333333703, 0.3219752754296894559, 0.3333333333333333703, 0.3219752754296894559, 0.3333333333333333703, 0.3219752754296894559, 0.3333333333333333703, 0.3219752754296894559, 0.3333333333333333703, 0.3219752754296894559, 0.3333333333333333703, 0.3219752754296894559, 0.3333333333333333703, 0.3219752754296894559, 0.3333333333333333703, 0.3219752754296894559, 0.3333333333333333703, 0.3219752754296894559, 0.3333333333333333703, 0.3219752754296894559, 0.3333333333333333703, 0.3219752754296894559, 0.3333333333333333703, 0.3219752754296894559, 0.3333333333333333703, 0.3219752754296894559, 0.3333333333333333703, 0.3219752754296894559, 0.3333333333333333703, 0.3219752754296894559, 0.3333333333333333703, 0.3219752754296894559, 0.3333333333333333703, 0.3219752754296894559, 0.3333333333333333703, 0.3219752754296894559, 0.3333333333333333703, 0.3219752754296894559, 0.3333333333333333703, 0.3219752754296894559, 0.3333333333333333703, 0.3219752754296894559, 0.3333333333333333703, 0.3219752754296894559, 0.3333333333333333703, 0.3219752754296894559, 0.3333333333333333703, 0.3219752754296894559, 0.3333333333333333703, 0.3219752754296894559, 0.3333333333333333703, 0.3219752754296894559, 0.3333333333333333703),
 ( 0.3333333333333333703, 0.3219752754296894559, 0.3333333333333333703, 0.3219752754296894559, 0.3333333333333333703, 0.3219752754296894559, 0.3333333333333333703, 0.3219752754296894559, 0.3333333333333333703, 0.3219752754296894559, 0.3333333333333333703, 0.3219752754296894559, 0.3333333333333333703, 0.3219752754296894559, 0.3333333333333333703, 0.3219752754296894559, 0.3333333333333333703, 0.3219752754296894559, 0.3333333333333333703, 0.3219752754296894559, 0.3333333333333333703, 0.3219752754296894559, 0.3333333333333333703, 0.3219752754296894559, 0.3333333333333333703, 0.3219752754296894559, 0.3333333333333333703, 0.3219752754296894559, 0.3333333333333333703, 0.3219752754296894559, 0.3333333333333333703, 0.3219752754296894559, 0.3333333333333333703, 0.3219752754296894559, 0.3333333333333333703, 0.3219752754296894559, 0.3333333333333333703, 0.3219752754296894559, 0.3333333333333333703, 0.3219752754296894559, 0.3333333333333333703, 0.3219752754296894559, 0.3333333333333333703, 0.3219752754296894559, 0.3333333333333333703, 0.3219752754296894559, 0.3333333333333333703, 0.3219752754296894559, 0.3333333333333333703, 0.3219752754296894559, 0.3333333333333333703, 0.3219752754296894559, 0.3333333333333333703, 0.3219752754296894559, 0.3333333333333333703, 0.3219752754296894559, 0.3333333333333333703, 0.3219752754296894559, 0.3333333333333333703, 0.3219752754296894559, 0.3333333333333333703, 0.3219752754296894559, 0.3333333333333333703, 0.3219752754296894559, 0.3333333333333333703, 0.3219752754296894559, 0.3333333333333333703, 0.3219752754296894559, 0.3333333333333333703, 0.3219752754296894559, 0.3333333333333333703, 0.3219752754296894559, 0.3333333333333333703, 0.3219752754296894559, 0.3333333333333333703, 0.3219752754296894559, 0.3333333333333333703, 0.3219752754296894559, 0.3333333333333333703, 0.3219752754296894559, 0.3333333333333333703, 0.3219752754296894559, 0.3333333333333333703, 0.3219752754296894559, 0.3333333333333333703, 0.3219752754296894559, 0.3333333333333333703, 0.3219752754296894559, 0.3333333333333333703, 0.3219752754296894559, 0.3333333333333333703, 0.3219752754296894559, 0.3333333333333333703, 0.3219752754296894559, 0.3333333333333333703, 0.3219752754296894559, 0.3333333333333333703, 0.3219752754296894559, 0.3333333333333333703, 0.3219752754296894559, 0.3333333333333333703, 0.3219752754296894559, 0.3333333333333333703, 0.3219752754296894559, 0.3333333333333333703, 0.3219752754296894559, 0.3333333333333333703, 0.3219752754296894559, 0.3333333333333333703, 0.3219752754296894559, 0.3333333333333333703, 0.3219752754296894559, 0.3333333333333333703, 0.3219752754296894559, 0.3333333333333333703, 0.3219752754296894559, 0.3333333333333333703, 0.3219752754296894559, 0.3333333333333333703, 0.3219752754296894559, 0.3333333333333333703, 0.3219752754296894559, 0.3333333333333333703, 0.3219752754296894559, 0.3333333333333333703, 0.3219752754296894559, 0.3333333333333333703, 0.3219752754296894559, 0.3333333333333333703, 0.3219752754296894559, 0.3333333333333333703, 0.3219752754296894559, 0.3333333333333333703, 0.3219752754296894559, 0.3333333333333333703, 0.3219752754296894559, 0.3333333333333333703, 0.3219752754296894559, 0.3333333333333333703, 0.3219752754296894559, 0.3333333333333333703, 0.3219752754296894559, 0.3333333333333333703, 0.3219752754296894559, 0.3333333333333333703, 0.3219752754296894559, 0.3333333333333333703, 0.3219752754296894559, 0.3333333333333333703, 0.3219752754296894559, 0.3333333333333333703, 0.3219752754296894559, 0.3333333333333333703, 0.3219752754296894559, 0.3333333333333333703, 0.3219752754296894559, 0.3333333333333333703, 0.3219752754296894559, 0.3333333333333333703, 0.3219752754296894559, 0.3333333333333333703, 0.3219752754296894559, 0.3333333333333333703, 0.3219752754296894559, 0.3333333333333333703, 0.3219752754296894559, 0.3333333333333333703, 0.3219752754296894559, 0.3333333333333333703, 0.3219752754296894559, 0.3333333333333333703, 0.3219752754296894559, 0.3333333333333333703, 0.3219752754296894559, 0.3333333333333333703, 0.3219752754296894559, 0.3333333333333333703, 0.3219752754296894559, 0.3333333333333333703, 0.3219752754296894559, 0.3333333333333333703, 0.3219752754296894559, 0.3333333333333333703, 0.3219752754296894559, 0.3333333333333333703, 0.3219752754296894559, 0.3333333333333333703, 0.3219752754296894559, 0.3333333333333333703, 0.3219752754296894559, 0.3333333333333333703, 0.3219752754296894559, 0.3333333333333333703, 0.3219752754296894559, 0.3333333333333333703, 0.3219752754296894559, 0.3333333333333333703, 0.3219752754296894559, 0.3333333333333333703, 0.3219752754296894559, 0.3333333333333333703, 0.3219752754296894559, 0.3333333333333333703, 0.3219752754296894559, 0.3333333333333333703, 0.3219752754296894559, 0.3333333333333333703, 0.3219752754296894559, 0.3333333333333333703, 0.3219752754296894559, 0.3333333333333333703, 0.3219752754296894559, 0.3333333333333333703, 0.3219752754296894559, 0.3333333333333333703, 0.3219752754296894559, 0.3333333333333333703, 0.3219752754296894559, 0.3333333333333333703, 0.3219752754296894559, 0.3333333333333333703, 0.3219752754296894559, 0.3333333333333333703, 0.3219752754296894559, 0.3333333333333333703, 0.3219752754296894559, 0.3333333333333333703, 0.3219752754296894559, 0.3333333333333333703, 0.3219752754296894559, 0.3333333333333333703, 0.3219752754296894559, 0.3333333333333333703, 0.3219752754296894559, 0.3333333333333333703, 0.3219752754296894559, 0.3333333333333333703, 0.3219752754296894559, 0.3333333333333333703, 0.3219752754296894559, 0.3333333333333333703, 0.3219752754296894559, 0.3333333333333333703, 0.3219752754296894559, 0.3333333333333333703, 0.3219752754296894559, 0.3333333333333333703, 0.3219752754296894559, 0.3333333333333333703, 0.3219752754296894559, 0.3333333333333333703, 0.3219752754296894559, 0.3333333333333333703, 0.3219752754296894559, 0.3333333333333333703, 0.3219752754296894559, 0.3333333333333333703, 0.3219752754296894559, 0.3333333333333333703, 0.3219752754296894559, 0.3333333333333333703, 0.3219752754296894559, 0.3333333333333333703, 0.3219752754296894559, 0.3333333333333333703, 0.3219752754296894559, 0.3333333333333333703, 0.3219752754296894559, 0.3333333333333333703, 0.3219752754296894559, 0.3333333333333333703, 0.3219752754296894559, 0.3333333333333333703, 0.3219752754296894559, 0.3333333333333333703, 0.3219752754296894559, 0.3333333333333333703, 0.3219752754296894559, 0.3333333333333333703, 0.3219752754296894559, 0.3333333333333333703, 0.3219752754296894559, 0.3333333333333333703, 0.3219752754296894559, 0.3333333333333333703, 0.3219752754296894559, 0.3333333333333333703, 0.3219752754296894559, 0.3333333333333333703, 0.3219752754296894559, 0.3333333333333333703, 0.3219752754296894559, 0.3333333333333333703, 0.3219752754296894559, 0.3333333333333333703, 0.3219752754296894559, 0.3333333333333333703, 0.3219752754296894559, 0.3333333333333333703, 0.3219752754296894559, 0.3333333333333333703, 0.3219752754296894559, 0.3333333333333333703, 0.3219752754296894559, 0.3333333333333333703, 0.3219752754296894559, 0.3333333333333333703, 0.3219752754296894559, 0.3333333333333333703, 0.3219752754296894559, 0.3333333333333333703, 0.3219752754296894559, 0.3333333333333333703, 0.3219752754296894559, 0.3333333333333333703, 0.3219752754296894559, 0.3333333333333333703, 0.3219752754296894559, 0.3333333333333333703, 0.3219752754296894559, 0.3333333333333333703, 0.3219752754296894559, 0.3333333333333333703, 0.3219752754296894559, 0.3333333333333333703, 0.3219752754296894559, 0.3333333333333333703, 0.3219752754296894559, 0.3333333333333333703, 0.3219752754296894559, 0.3333333333333333703, 0.3219752754296894559, 0.3333333333333333703, 0.3219752754296894559, 0.3333333333333333703, 0.3219752754296894559, 0.3333333333333333703, 0.3219752754296894559, 0.3333333333333333703, 0.3219752754296894559, 0.3333333333333333703, 0.3219752754296894559, 0.3333333333333333703, 0.3219752754296894559, 0.3333333333333333703, 0.3219752754296894559, 0.3333333333333333703, 0.3219752754296894559, 0.3333333333333333703, 0.3219752754296894559, 0.3333333333333333703, 0.3219752754296894559, 0.3333333333333333703, 0.3219752754296894559, 0.3333333333333333703, 0.3219752754296894559, 0.3333333333333333703, 0.3219752754296894559, 0.3333333333333333703, 0.3219752754296894559, 0.3333333333333333703, 0.3219752754296894559, 0.3333333333333333703, 0.3219752754296894559, 0.3333333333333333703, 0.3219752754296894559, 0.3333333333333333703, 0.3219752754296894559, 0.3333333333333333703, 0.3219752754296894559, 0.3333333333333333703, 0.3219752754296894559, 0.3333333333333333703, 0.3219752754296894559, 0.3333333333333333703, 0.3219752754296894559, 0.3333333333333333703, 0.3219752754296894559, 0.3333333333333333703, 0.3219752754296894559, 0.3333333333333333703, 0.3219752754296894559, 0.3333333333333333703, 0.3219752754296894559, 0.3333333333333333703, 0.3219752754296894559, 0.3333333333333333703, 0.3219752754296894559, 0.3333333333333333703, 0.3219752754296894559, 0.3333333333333333703, 0.3219752754296894559, 0.3333333333333333703, 0.3219752754296894559, 0.3333333333333333703, 0.3219752754296894559, 0.3333333333333333703, 0.3219752754296894559, 0.3333333333333333703, 0.3219752754296894559, 0.3333333333333333703, 0.3219752754296894559, 0.3333333333333333703, 0.3219752754296894559, 0.3333333333333333703, 0.3219752754296894559, 0.3333333333333333703, 0.3219752754296894559, 0.3333333333333333703, 0.3219752754296894559, 0.3333333333333333703, 0.3219752754296894559, 0.3333333333333333703, 0.3219752754296894559, 0.3333333333333333703, 0.3219752754296894559, 0.3333333333333333703, 0.3219752754296894559, 0.3333333333333333703, 0.3219752754296894559, 0.3333333333333333703, 0.3219752754296894559, 0.3333333333333333703, 0.3219752754296894559, 0.3333333333333333703, 0.3219752754296894559, 0.3333333333333333703, 0.3219752754296894559, 0.3333333333333333703, 0.3219752754296894559, 0.3333333333333333703, 0.3219752754296894559, 0.3333333333333333703, 0.3219752754296894559, 0.3333333333333333703, 0.3219752754296894559, 0.3333333333333333703, 0.3219752754296894559, 0.3333333333333333703, 0.3219752754296894559, 0.3333333333333333703, 0.3219752754296894559, 0.3333333333333333703, 0.3219752754296894559, 0.3333333333333333703, 0.3219752754296894559, 0.3333333333333333703, 0.3219752754296894559, 0.3333333333333333703, 0.3219752754296894559, 0.3333333333333333703, 0.3219752754296894559, 0.3333333333333333703, 0.3219752754296894559, 0.3333333333333333703, 0.3219752754296894559, 0.3333333333333333703),
 ( 1.000000000000000000, 0.9659258262890683122, 1.000000000000000000, 0.9659258262890683122, 1.000000000000000000, 0.9659258262890683122, 1.000000000000000000, 0.9659258262890683122, 1.000000000000000000, 0.9659258262890683122, 1.000000000000000000, 0.9659258262890683122, 1.000000000000000000, 0.9659258262890683122, 1.000000000000000000, 0.9659258262890683122, 1.000000000000000000, 0.9659258262890683122, 1.000000000000000000, 0.9659258262890683122, 1.000000000000000000, 0.9659258262890683122, 1.000000000000000000, 0.9659258262890683122, 1.000000000000000000, 0.9659258262890683122, 1.000000000000000000, 0.9659258262890683122, 1.000000000000000000, 0.9659258262890683122, 1.000000000000000000, 0.9659258262890683122, 1.000000000000000000, 0.9659258262890683122, 1.000000000000000000, 0.9659258262890683122, 1.000000000000000000, 0.9659258262890683122, 1.000000000000000000, 0.9659258262890683122, 1.000000000000000000, 0.9659258262890683122, 1.000000000000000000, 0.9659258262890683122, 1.000000000000000000, 0.9659258262890683122, 1.000000000000000000, 0.9659258262890683122, 1.000000000000000000, 0.9659258262890683122, 1.000000000000000000, 0.9659258262890683122, 1.000000000000000000, 0.9659258262890683122, 1.000000000000000000, 0.9659258262890683122, 1.000000000000000000, 0.9659258262890683122, 1.000000000000000000, 0.9659258262890683122, 1.000000000000000000, 0.9659258262890683122, 1.000000000000000000, 0.9659258262890683122, 1.000000000000000000, 0.9659258262890683122, 1.000000000000000000, 0.9659258262890683122, 1.000000000000000000, 0.9659258262890683122, 1.000000000000000000, 0.9659258262890683122, 1.000000000000000000, 0.9659258262890683122, 1.000000000000000000, 0.9659258262890683122, 1.000000000000000000, 0.9659258262890683122, 1.000000000000000000, 0.9659258262890683122, 1.000000000000000000, 0.9659258262890683122, 1.000000000000000000, 0.9659258262890683122, 1.000000000000000000, 0.9659258262890683122, 1.000000000000000000, 0.9659258262890683122, 1.000000000000000000, 0.9659258262890683122, 1.000000000000000000, 0.9659258262890683122, 1.000000000000000000, 0.9659258262890683122, 1.000000000000000000, 0.9659258262890683122, 1.000000000000000000, 0.9659258262890683122, 1.000000000000000000, 0.9659258262890683122, 1.000000000000000000, 0.9659258262890683122, 1.000000000000000000, 0.9659258262890683122, 1.000000000000000000, 0.9659258262890683122, 1.000000000000000000, 0.9659258262890683122, 1.000000000000000000, 0.9659258262890683122, 1.000000000000000000, 0.9659258262890683122, 1.000000000000000000, 0.9659258262890683122, 1.000000000000000000, 0.9659258262890683122, 1.000000000000000000, 0.9659258262890683122, 1.000000000000000000, 0.9659258262890683122, 1.000000000000000000, 0.9659258262890683122, 1.000000000000000000, 0.9659258262890683122, 1.000000000000000000, 0.9659258262890683122, 1.000000000000000000, 0.9659258262890683122, 1.000000000000000000, 0.9659258262890683122, 1.000000000000000000, 0.9659258262890683122, 1.000000000000000000, 0.9659258262890683122, 1.000000000000000000, 0.9659258262890683122, 1.000000000000000000, 0.9659258262890683122, 1.000000000000000000, 0.9659258262890683122, 1.000000000000000000, 0.9659258262890683122, 1.000000000000000000, 0.9659258262890683122, 1.000000000000000000, 0.9659258262890683122, 1.000000000000000000, 0.9659258262890683122, 1.000000000000000000, 0.9659258262890683122, 1.000000000000000000, 0.9659258262890683122, 1.000000000000000000, 0.9659258262890683122, 1.000000000000000000, 0.9659258262890683122, 1.000000000000000000, 0.9659258262890683122, 1.000000000000000000, 0.9659258262890683122, 1.000000000000000000, 0.9659258262890683122, 1.000000000000000000, 0.9659258262890683122, 1.000000000000000000, 0.9659258262890683122, 1.000000000000000000, 0.9659258262890683122, 1.000000000000000000, 0.9659258262890683122, 1.000000000000000000, 0.9659258262890683122, 1.000000000000000000, 0.9659258262890683122, 1.000000000000000000, 0.9659258262890683122, 1.000000000000000000, 0.9659258262890683122, 1.000000000000000000, 0.9659258262890683122, 1.000000000000000000, 0.9659258262890683122, 1.000000000000000000, 0.9659258262890683122, 1.000000000000000000, 0.9659258262890683122, 1.000000000000000000, 0.9659258262890683122, 1.000000000000000000, 0.9659258262890683122, 1.000000000000000000, 0.9659258262890683122, 1.000000000000000000, 0.9659258262890683122, 1.000000000000000000, 0.9659258262890683122, 1.000000000000000000, 0.9659258262890683122, 1.000000000000000000, 0.9659258262890683122, 1.000000000000000000, 0.9659258262890683122, 1.000000000000000000, 0.9659258262890683122, 1.000000000000000000, 0.9659258262890683122, 1.000000000000000000, 0.9659258262890683122, 1.000000000000000000, 0.9659258262890683122, 1.000000000000000000, 0.9659258262890683122, 1.000000000000000000, 0.9659258262890683122, 1.000000000000000000, 0.9659258262890683122, 1.000000000000000000, 0.9659258262890683122, 1.000000000000000000, 0.9659258262890683122, 1.000000000000000000, 0.9659258262890683122, 1.000000000000000000, 0.9659258262890683122, 1.000000000000000000, 0.9659258262890683122, 1.000000000000000000, 0.9659258262890683122, 1.000000000000000000, 0.9659258262890683122, 1.000000000000000000, 0.9659258262890683122, 1.000000000000000000, 0.9659258262890683122, 1.000000000000000000, 0.9659258262890683122, 1.000000000000000000, 0.9659258262890683122, 1.000000000000000000, 0.9659258262890683122, 1.000000000000000000, 0.9659258262890683122, 1.000000000000000000, 0.9659258262890683122, 1.000000000000000000, 0.9659258262890683122, 1.000000000000000000, 0.9659258262890683122, 1.000000000000000000, 0.9659258262890683122, 1.000000000000000000, 0.9659258262890683122, 1.000000000000000000, 0.9659258262890683122, 1.000000000000000000, 0.9659258262890683122, 1.000000000000000000, 0.9659258262890683122, 1.000000000000000000, 0.9659258262890683122, 1.000000000000000000, 0.9659258262890683122, 1.000000000000000000, 0.9659258262890683122, 1.000000000000000000, 0.9659258262890683122, 1.000000000000000000, 0.9659258262890683122, 1.000000000000000000, 0.9659258262890683122, 1.000000000000000000, 0.9659258262890683122, 1.000000000000000000, 0.9659258262890683122, 1.000000000000000000, 0.9659258262890683122, 1.000000000000000000, 0.9659258262890683122, 1.000000000000000000, 0.9659258262890683122, 1.000000000000000000, 0.9659258262890683122, 1.000000000000000000, 0.9659258262890683122, 1.000000000000000000, 0.9659258262890683122, 1.000000000000000000, 0.9659258262890683122, 1.000000000000000000, 0.9659258262890683122, 1.000000000000000000, 0.9659258262890683122, 1.000000000000000000, 0.9659258262890683122, 1.000000000000000000, 0.9659258262890683122, 1.000000000000000000, 0.9659258262890683122, 1.000000000000000000, 0.9659258262890683122, 1.000000000000000000, 0.9659258262890683122, 1.000000000000000000, 0.9659258262890683122, 1.000000000000000000, 0.9659258262890683122, 1.000000000000000000, 0.9659258262890683122, 1.000000000000000000, 0.9659258262890683122, 1.000000000000000000, 0.9659258262890683122, 1.000000000000000000, 0.9659258262890683122, 1.000000000000000000, 0.9659258262890683122, 1.000000000000000000, 0.9659258262890683122, 1.000000000000000000, 0.9659258262890683122, 1.000000000000000000, 0.9659258262890683122, 1.000000000000000000, 0.9659258262890683122, 1.000000000000000000, 0.9659258262890683122, 1.000000000000000000, 0.9659258262890683122, 1.000000000000000000, 0.9659258262890683122, 1.000000000000000000, 0.9659258262890683122, 1.000000000000000000, 0.9659258262890683122, 1.000000000000000000, 0.9659258262890683122, 1.000000000000000000, 0.9659258262890683122, 1.000000000000000000, 0.9659258262890683122, 1.000000000000000000, 0.9659258262890683122, 1.000000000000000000, 0.9659258262890683122, 1.000000000000000000, 0.9659258262890683122, 1.000000000000000000, 0.9659258262890683122, 1.000000000000000000, 0.9659258262890683122, 1.000000000000000000, 0.9659258262890683122, 1.000000000000000000, 0.9659258262890683122, 1.000000000000000000, 0.9659258262890683122, 1.000000000000000000, 0.9659258262890683122, 1.000000000000000000, 0.9659258262890683122, 1.000000000000000000, 0.9659258262890683122, 1.000000000000000000, 0.9659258262890683122, 1.000000000000000000, 0.9659258262890683122, 1.000000000000000000, 0.9659258262890683122, 1.000000000000000000, 0.9659258262890683122, 1.000000000000000000, 0.9659258262890683122, 1.000000000000000000, 0.9659258262890683122, 1.000000000000000000, 0.9659258262890683122, 1.000000000000000000, 0.9659258262890683122, 1.000000000000000000, 0.9659258262890683122, 1.000000000000000000, 0.9659258262890683122, 1.000000000000000000, 0.9659258262890683122, 1.000000000000000000, 0.9659258262890683122, 1.000000000000000000, 0.9659258262890683122, 1.000000000000000000, 0.9659258262890683122, 1.000000000000000000, 0.9659258262890683122, 1.000000000000000000, 0.9659258262890683122, 1.000000000000000000, 0.9659258262890683122, 1.000000000000000000, 0.9659258262890683122, 1.000000000000000000, 0.9659258262890683122, 1.000000000000000000, 0.9659258262890683122, 1.000000000000000000, 0.9659258262890683122, 1.000000000000000000, 0.9659258262890683122, 1.000000000000000000, 0.9659258262890683122, 1.000000000000000000, 0.9659258262890683122, 1.000000000000000000, 0.9659258262890683122, 1.000000000000000000, 0.9659258262890683122, 1.000000000000000000, 0.9659258262890683122, 1.000000000000000000, 0.9659258262890683122, 1.000000000000000000, 0.9659258262890683122, 1.000000000000000000, 0.9659258262890683122, 1.000000000000000000, 0.9659258262890683122, 1.000000000000000000, 0.9659258262890683122, 1.000000000000000000, 0.9659258262890683122, 1.000000000000000000, 0.9659258262890683122, 1.000000000000000000, 0.9659258262890683122, 1.000000000000000000, 0.9659258262890683122, 1.000000000000000000, 0.9659258262890683122, 1.000000000000000000, 0.9659258262890683122, 1.000000000000000000, 0.9659258262890683122, 1.000000000000000000, 0.9659258262890683122, 1.000000000000000000, 0.9659258262890683122, 1.000000000000000000, 0.9659258262890683122, 1.000000000000000000, 0.9659258262890683122, 1.000000000000000000, 0.9659258262890683122, 1.000000000000000000, 0.9659258262890683122, 1.000000000000000000, 0.9659258262890683122, 1.000000000000000000, 0.9659258262890683122, 1.000000000000000000) ) ) 
 REPRESENTATION_ITEM ( '' )  SURFACE ( )  );
#51106 = CARTESIAN_POINT ( 'NONE',  ( 16.53943276465976808, 0.05219959533934440121, 31.25109039468568639 ) ) ;
#51108 = CARTESIAN_POINT ( 'NONE',  ( 0.05219959533909260263, 19.03943276465977164, 24.99890960531435269 ) ) ;
#51109 = CARTESIAN_POINT ( 'NONE',  ( -9.564922557960796823, -16.46253265017161027, 82.08224293864768129 ) ) ;
#51111 = CARTESIAN_POINT ( 'NONE',  ( 36.91746824999999887, 11.99521256947799053, -7.524999997268814411 ) ) ;
#51110 = CARTESIAN_POINT ( 'NONE',  ( 16.51473224551083163, -9.474510206698727899, 110.8344237280190043 ) ) ;
#51112 = CARTESIAN_POINT ( 'NONE',  ( 19.05341960407617918, -5.049401038297876454, 21.04275706135232582 ) ) ;
#51113 = CARTESIAN_POINT ( 'NONE',  ( -0.05219959533934338120, 16.53943276465976808, 77.50109039468567573 ) ) ;
#51114 = CARTESIAN_POINT ( 'NONE',  ( -9.564922557961040184, 16.46253265017147172, 112.9177570613523329 ) ) ;
#51115 = CARTESIAN_POINT ( 'NONE',  ( 12.06949235617757843, -12.14591786802309237, 113.1239096053143953 ) ) ;
#51116 = CARTESIAN_POINT ( 'NONE',  ( -8.314922557961024197, 14.29746914071037800, 72.91775706135234714 ) ) ;
#51117 = CARTESIAN_POINT ( 'NONE',  ( -14.29746914071037622, -8.314922557961029526, 49.16775706135234003 ) ) ;
#51118 = CARTESIAN_POINT ( 'NONE',  ( 13.89961937509977652, -13.97604488694527269, 23.12390960531436335 ) ) ;
#51119 = CARTESIAN_POINT ( 'NONE',  ( -16.46253265017146816, -9.564922557961047289, 74.16775706135234714 ) ) ;
#51120 = CARTESIAN_POINT ( 'NONE',  ( 21.55341960407619695, -5.719274019375665929, 106.0427570613523471 ) ) ;
#51121 = CARTESIAN_POINT ( 'NONE',  ( -5.049401038298153566, 19.05341960407611168, 30.20724293864768839 ) ) ;
#51122 = CARTESIAN_POINT ( 'NONE',  ( -16.46253265017160317, 9.564922557960807481, 75.83224293864769550 ) ) ;
#51123 = CARTESIAN_POINT ( 'NONE',  ( -16.52544592524342804, 4.483927247898546575, 71.04057627198103830 ) ) ;
#51124 = CARTESIAN_POINT ( 'NONE',  ( 0.05219959533936267826, -19.03943276465977164, 40.00109039468566152 ) ) ;
#51125 = CARTESIAN_POINT ( 'NONE',  ( -18.67979575497178146, -10.72451020669898902, 41.66557627198103120 ) ) ;
#51126 = CARTESIAN_POINT ( 'NONE',  ( -21.53943276465977519, -0.05219959533937600094, 108.7510903946857042 ) ) ;
#51127 = CARTESIAN_POINT ( 'NONE',  ( -13.89961937509977652, 13.97604488694528158, 95.62390960531436690 ) ) ;
#51128 = CARTESIAN_POINT ( 'NONE',  ( 15.72974639402176855, 15.80617190586768217, 101.8760903946857042 ) ) ;
#51129 = CARTESIAN_POINT ( 'NONE',  ( -5.823673210054116645, -21.52544592524344225, 67.29057627198103830 ) ) ;
#51130 = CARTESIAN_POINT ( 'NONE',  ( -16.46253265017160317, 9.564922557960807481, 95.83224293864769550 ) ) ;
#51131 = CARTESIAN_POINT ( 'NONE',  ( -19.02544592524334988, -5.153800228976617603, 88.95942372801897591 ) ) ;
#51132 = CARTESIAN_POINT ( 'NONE',  ( 19.05341960407611168, 5.049401038298154454, 103.9572429386476671 ) ) ;
#51133 = CARTESIAN_POINT ( 'NONE',  ( -9.474510206698720793, -16.51473224551083518, 94.58442372801900433 ) ) ;
#51134 = CARTESIAN_POINT ( 'NONE',  ( -4.483927247898539470, -16.52544592524342804, 112.2905762719810241 ) ) ;
#51135 = CARTESIAN_POINT ( 'NONE',  ( 13.97604488694527802, 13.89961937509977652, 84.37390960531433848 ) ) ;
#51136 = CARTESIAN_POINT ( 'NONE',  ( -21.55341960407610458, -5.719274019375992779, 61.45724293864770260 ) ) ;
#51137 = CARTESIAN_POINT ( 'NONE',  ( 16.55341960407618274, -4.379528057220086978, 31.04275706135234714 ) ) ;
#51138 = CARTESIAN_POINT ( 'NONE',  ( -21.55341960407619339, 5.719274019375674811, 53.54275706135234714 ) ) ;
#51139 = CARTESIAN_POINT ( 'NONE',  ( 21.55341960407619695, -5.719274019375665929, 91.04275706135236135 ) ) ;
#51140 = CARTESIAN_POINT ( 'NONE',  ( 0.05219959533934541429, -16.53943276465976808, 100.0010903946857042 ) ) ;
#51141 = CARTESIAN_POINT ( 'NONE',  ( 5.153800228976335163, 19.02544592524342804, 84.79057627198099567 ) ) ;
#51142 = CARTESIAN_POINT ( 'NONE',  ( 12.06949235617757843, -12.14591786802309237, 88.12390960531436690 ) ) ;
#51143 = CARTESIAN_POINT ( 'NONE',  ( -14.29746914071037622, -8.314922557961029526, 109.1677570613523613 ) ) ;
#51144 = CARTESIAN_POINT ( 'NONE',  ( -0.05219959533936034679, 19.03943276465977164, 62.50109039468566863 ) ) ;
#51145 = CARTESIAN_POINT ( 'NONE',  ( -21.52544592524334988, -5.823673210054445271, 43.95942372801902565 ) ) ;
#51146 = CARTESIAN_POINT ( 'NONE',  ( -14.29746914071049879, 8.314922557960819915, 95.83224293864770971 ) ) ;
#51147 = CARTESIAN_POINT ( 'NONE',  ( -19.03943276465977164, 0.05219959533909376836, 106.2489096053143669 ) ) ;
#51148 = CARTESIAN_POINT ( 'NONE',  ( 4.379528057220339221, -16.55341960407611168, 27.70724293864769905 ) ) ;
#51149 = CARTESIAN_POINT ( 'NONE',  ( 5.823673210054444382, -21.52544592524334988, 85.20942372801901854 ) ) ;
#51150 = CARTESIAN_POINT ( 'NONE',  ( 16.52544592524335698, 4.483927247898782831, 51.45942372801901854 ) ) ;
#51151 = CARTESIAN_POINT ( 'NONE',  ( -15.72974639402176322, -15.80617190586768395, 39.37609039468567573 ) ) ;
#51152 = ORIENTED_EDGE ( 'NONE', *, *, #143946, .F. ) ;
#51153 = CARTESIAN_POINT ( 'NONE',  ( -21.52544592524334988, -5.823673210054445271, 18.95942372801901143 ) ) ;
#51154 = CARTESIAN_POINT ( 'NONE',  ( 0.05219959533910956823, 16.53943276465976808, 89.99890960531438111 ) ) ;
#51155 = ADVANCED_FACE ( 'NONE', ( #124645 ), #47822, .F. ) ;
#51156 = CARTESIAN_POINT ( 'NONE',  ( -19.01529144963331674, -5.500000000000165201, 51.23431955728442233 ) ) ;
#51157 = CARTESIAN_POINT ( 'NONE',  ( 16.55341960407611168, 4.379528057220329451, 63.95724293864770260 ) ) ;
#51158 = CARTESIAN_POINT ( 'NONE',  ( 5.049401038298161559, -19.05341960407611168, 52.70724293864767418 ) ) ;
#51159 = CARTESIAN_POINT ( 'NONE',  ( 14.29746914071037800, 8.314922557961029526, 111.6677570613523613 ) ) ;
#51160 = CARTESIAN_POINT ( 'NONE',  ( -5.153800228976328057, -19.02544592524343514, 42.29057627198101699 ) ) ;
#51161 = CARTESIAN_POINT ( 'NONE',  ( -0.05219959533907301413, -21.53943276465977519, 37.49890960531436690 ) ) ;
#51162 = CARTESIAN_POINT ( 'NONE',  ( 8.314922557960818139, 14.29746914071049879, 84.58224293864769550 ) ) ;
#51163 = CARTESIAN_POINT ( 'NONE',  ( 10.81492255796078972, 18.62759615963270932, 94.58224293864769550 ) ) ;
#51164 = CARTESIAN_POINT ( 'NONE',  ( 13.97604488694527802, 13.89961937509977652, 84.37390960531433848 ) ) ;
#51166 = CARTESIAN_POINT ( 'NONE',  ( -5.153800228976607833, 19.02544592524334988, 87.70942372801897591 ) ) ;
#51165 = CARTESIAN_POINT ( 'NONE',  ( 19.02544592524343514, -5.153800228976328945, 38.54057627198103120 ) ) ;
#51167 = ADVANCED_FACE ( 'NONE', ( #176139 ), #49799, .T. ) ;
#51168 = CARTESIAN_POINT ( 'NONE',  ( 10.72451020669898902, -18.67979575497178502, 47.91557627198102409 ) ) ;
#51169 = CARTESIAN_POINT ( 'NONE',  ( -15.80617190586768217, 15.72974639402176855, 73.12609039468567573 ) ) ;
#51170 = CARTESIAN_POINT ( 'NONE',  ( -19.03943276465977164, 0.05219959533909376836, 51.24890960531436690 ) ) ;
#51171 = CARTESIAN_POINT ( 'NONE',  ( 19.05341960407611168, 5.049401038298154454, 78.95724293864769550 ) ) ;
#51172 = ORIENTED_EDGE ( 'NONE', *, *, #45882, .F. ) ;
#51173 = CARTESIAN_POINT ( 'NONE',  ( 8.314922557961029526, -14.29746914071037800, 65.41775706135234714 ) ) ;
#51174 = CARTESIAN_POINT ( 'NONE',  ( -18.67979575497193778, 10.72451020669871902, 48.33442372801902565 ) ) ;
#51175 = CARTESIAN_POINT ( 'NONE',  ( -18.67979575497193778, 10.72451020669871902, 73.33442372801901854 ) ) ;
#51176 = CARTESIAN_POINT ( 'NONE',  ( 5.153800228976335163, 19.02544592524342804, 114.7905762719810241 ) ) ;
#51177 = CARTESIAN_POINT ( 'NONE',  ( 18.62759615963271287, -10.81492255796078972, 98.33224293864769550 ) ) ;
#51179 = CARTESIAN_POINT ( 'NONE',  ( 8.224510206698742110, 14.34966873604972548, 62.08442372801901143 ) ) ;
#51178 = CARTESIAN_POINT ( 'NONE',  ( 21.53943276465977519, 0.05219959533937863772, 41.25109039468568284 ) ) ;
#51180 = CARTESIAN_POINT ( 'NONE',  ( 21.52544592524344225, -5.823673210054117533, 58.54057627198103120 ) ) ;
#51181 = CARTESIAN_POINT ( 'NONE',  ( -19.02544592524334988, -5.153800228976617603, 28.95942372801900433 ) ) ;
#51183 = CARTESIAN_POINT ( 'NONE',  ( 16.53943276465976808, 0.05219959533934440121, 101.2510903946856757 ) ) ;
#51182 = CARTESIAN_POINT ( 'NONE',  ( -19.02544592524342804, 5.153800228976336051, 66.04057627198103830 ) ) ;
#51184 = DIRECTION ( 'NONE',  ( 1.000000000000000000, 0.000000000000000000, 0.000000000000000000 ) ) ;
#51185 = CARTESIAN_POINT ( 'NONE',  ( 13.97604488694527802, 13.89961937509977652, 99.37390960531436690 ) ) ;
#51186 = CARTESIAN_POINT ( 'NONE',  ( 19.99074948409479902, 21.30378117525434334, -49.30207733784023105 ) ) ;
#51187 = CARTESIAN_POINT ( 'NONE',  ( -19.02544592524334988, -5.153800228976617603, 78.95942372801900433 ) ) ;
#51188 = CARTESIAN_POINT ( 'NONE',  ( 0.05219959533907565091, 21.53943276465977519, 59.99890960531436690 ) ) ;
#51189 = CARTESIAN_POINT ( 'NONE',  ( 12.06949235617757843, -12.14591786802309237, 33.12390960531435979 ) ) ;
#51190 = CARTESIAN_POINT ( 'NONE',  ( 19.02544592524334988, 5.153800228976608722, 101.4594237280189759 ) ) ;
#51191 = DIRECTION ( 'NONE',  ( 0.000000000000000000, 0.000000000000000000, 1.000000000000000000 ) ) ;
#51192 = CARTESIAN_POINT ( 'NONE',  ( -16.51473224551082808, 9.474510206698731452, 103.3344237280190043 ) ) ;
#51194 = CARTESIAN_POINT ( 'NONE',  ( 19.03943276465977164, 0.05219959533936151252, 61.25109039468566863 ) ) ;
#51193 = CARTESIAN_POINT ( 'NONE',  ( -18.62759615963270932, 10.81492255796079327, 85.83224293864768129 ) ) ;
#51195 = DIRECTION ( 'NONE',  ( -1.000000000000000000, 0.000000000000000000, 0.000000000000000000 ) ) ;
#51196 = CARTESIAN_POINT ( 'NONE',  ( 9.474510206698971260, -16.51473224551069308, 62.91557627198102409 ) ) ;
#51197 = CARTESIAN_POINT ( 'NONE',  ( -16.53943276465976808, 0.05219959533911058130, 61.24890960531435979 ) ) ;
#51198 = CARTESIAN_POINT ( 'NONE',  ( 19.02544592524343514, -5.153800228976328945, 48.54057627198103120 ) ) ;
#51199 = CARTESIAN_POINT ( 'NONE',  ( 8.314922557960818139, 14.29746914071049879, 49.58224293864769550 ) ) ;
#51200 = DIRECTION ( 'NONE',  ( 0.000000000000000000, 0.000000000000000000, -1.000000000000000000 ) ) ;
#51201 = CARTESIAN_POINT ( 'NONE',  ( 31.43434485161623826, -5.140865793513109239, 100.4663950908259125 ) ) ;
#51202 = CARTESIAN_POINT ( 'NONE',  ( 4.379528057220339221, -16.55341960407611168, 27.70724293864769905 ) ) ;
#51203 = CARTESIAN_POINT ( 'NONE',  ( -16.51473224551069308, -9.474510206698971260, 61.66557627198103120 ) ) ;
#51204 = DIRECTION ( 'NONE',  ( 1.000000000000000000, 0.000000000000000000, 3.469446951953612217E-15 ) ) ;
#51205 = CARTESIAN_POINT ( 'NONE',  ( -5.049401038297874678, -19.05341960407617918, 34.79275706135233293 ) ) ;
#51206 = CARTESIAN_POINT ( 'NONE',  ( 12.14591786802327356, -12.06949235617739191, 45.62609039468567573 ) ) ;
#51207 = CARTESIAN_POINT ( 'NONE',  ( 15.72974639402199770, -15.80617190586745480, 48.12390960531436690 ) ) ;
#51208 = CARTESIAN_POINT ( 'NONE',  ( 15.80617190586769283, -15.72974639402175789, 110.6260903946857042 ) ) ;
#51209 = CARTESIAN_POINT ( 'NONE',  ( -16.46253265017160317, 9.564922557960807481, 80.83224293864769550 ) ) ;
#51210 = CARTESIAN_POINT ( 'NONE',  ( 22.99604614807110181, -21.49604614807103786, -64.92279855667830191 ) ) ;
#51211 = CARTESIAN_POINT ( 'NONE',  ( -15.80617190586745835, -15.72974639402198527, 21.87390960531436690 ) ) ;
#51212 = CARTESIAN_POINT ( 'NONE',  ( -15.72974639402176322, -15.80617190586768395, 44.37609039468567573 ) ) ;
#51213 = CARTESIAN_POINT ( 'NONE',  ( 8.314922557960818139, 14.29746914071049879, 94.58224293864769550 ) ) ;
#51216 = VERTEX_POINT ( 'NONE', #64959 ) ;
#51215 = CARTESIAN_POINT ( 'NONE',  ( 19.03943276465977164, -0.05219959533909143690, 78.74890960531436690 ) ) ;
#51214 = CARTESIAN_POINT ( 'NONE',  ( -15.80617190586745835, -15.72974639402198527, 91.87390960531436690 ) ) ;
#51217 = CARTESIAN_POINT ( 'NONE',  ( 9.474510206698971260, -16.51473224551069308, 87.91557627198102409 ) ) ;
#51218 = CARTESIAN_POINT ( 'NONE',  ( 0.05219959533937995610, -21.53943276465977519, 20.00109039468568639 ) ) ;
#51219 = ORIENTED_EDGE ( 'NONE', *, *, #14429, .F. ) ;
#51220 = CARTESIAN_POINT ( 'NONE',  ( -13.89961937509977652, 13.97604488694528158, 80.62390960531436690 ) ) ;
#51221 = DIRECTION ( 'NONE',  ( -1.000000000000000000, -0.000000000000000000, -0.000000000000000000 ) ) ;
#51223 = CARTESIAN_POINT ( 'NONE',  ( 16.51473224551069308, 9.474510206698969483, 39.16557627198103120 ) ) ;
#51222 = CARTESIAN_POINT ( 'NONE',  ( -9.564922557960796823, -16.46253265017161027, 27.08224293864769550 ) ) ;
#51224 = CARTESIAN_POINT ( 'NONE',  ( 9.564922557961047289, -16.46253265017146816, 110.4177570613523471 ) ) ;
#51225 = CARTESIAN_POINT ( 'NONE',  ( 36.91746824999999177, 2.880721459617395097E-14, -10.12499999726881583 ) ) ;
#51226 = CARTESIAN_POINT ( 'NONE',  ( -8.224510206698948167, 14.34966873604960824, 105.4155762719810383 ) ) ;
#51227 = CARTESIAN_POINT ( 'NONE',  ( -10.81492255796105439, 18.62759615963255655, 82.91775706135234714 ) ) ;
#51229 = CARTESIAN_POINT ( 'NONE',  ( 5.719274019375673035, 21.55341960407619339, 27.29275706135234358 ) ) ;
#51228 = CARTESIAN_POINT ( 'NONE',  ( -16.51473224551069308, -9.474510206698971260, 61.66557627198103120 ) ) ;
#51230 = CARTESIAN_POINT ( 'NONE',  ( -21.52544592524343514, 5.823673210054127303, 106.0405762719810525 ) ) ;
#51231 = CARTESIAN_POINT ( 'NONE',  ( -8.906447517083060816, 27.41122689804195645, 147.5999999999999943 ) ) ;
#51232 = CARTESIAN_POINT ( 'NONE',  ( -9.564922557960796823, -16.46253265017161027, 92.08224293864769550 ) ) ;
#51233 = LINE ( 'NONE', #100715, #21054 ) ;
#51235 = CARTESIAN_POINT ( 'NONE',  ( -21.53943276465977519, 0.05219959533907696930, 41.24890960531435269 ) ) ;
#51234 = CARTESIAN_POINT ( 'NONE',  ( 12.14591786802327356, -12.06949235617739191, 20.62609039468568639 ) ) ;
#51236 = CARTESIAN_POINT ( 'NONE',  ( -15.72974639402176322, -15.80617190586768395, 59.37609039468568284 ) ) ;
#51237 = CARTESIAN_POINT ( 'NONE',  ( -16.46253265017160317, 9.564922557960807481, 110.8322429386476955 ) ) ;
#51238 = CARTESIAN_POINT ( 'NONE',  ( -0.05219959533936034679, 19.03943276465977164, 92.50109039468566152 ) ) ;
#51239 = CARTESIAN_POINT ( 'NONE',  ( 5.153800228976335163, 19.02544592524342804, 59.79057627198100988 ) ) ;
#51240 = CARTESIAN_POINT ( 'NONE',  ( -9.564922557960796823, -16.46253265017161027, 87.08224293864769550 ) ) ;
#51241 = AXIS2_PLACEMENT_3D ( 'NONE', #190551, #48067, #80366 ) ;
#51242 = CARTESIAN_POINT ( 'NONE',  ( 8.314922557960818139, 14.29746914071049879, 89.58224293864768129 ) ) ;
#51243 = CARTESIAN_POINT ( 'NONE',  ( 14.34966873604960469, 8.224510206698951720, 89.16557627198102409 ) ) ;
#51244 = CARTESIAN_POINT ( 'NONE',  ( 9.564922557960805705, 16.46253265017160317, 109.5822429386476955 ) ) ;
#51246 = CARTESIAN_POINT ( 'NONE',  ( 19.03943276465977164, -0.05219959533909143690, 43.74890960531435979 ) ) ;
#51245 = CARTESIAN_POINT ( 'NONE',  ( -12.06949235617756955, 12.14591786802309770, 50.62390960531435979 ) ) ;
#51247 = CARTESIAN_POINT ( 'NONE',  ( 5.823673210054444382, -21.52544592524334988, 65.20942372801901854 ) ) ;
#51248 = CARTESIAN_POINT ( 'NONE',  ( -5.153800228976607833, 19.02544592524334988, 87.70942372801897591 ) ) ;
#51249 = CARTESIAN_POINT ( 'NONE',  ( -0.05219959533910754901, -16.53943276465976808, 57.49890960531435979 ) ) ;
#51250 = CARTESIAN_POINT ( 'NONE',  ( 10.81492255796106328, -18.62759615963255655, 20.41775706135234714 ) ) ;
#51251 = CARTESIAN_POINT ( 'NONE',  ( -18.67979575497178146, -10.72451020669898902, 51.66557627198102409 ) ) ;
#51252 = FACE_OUTER_BOUND ( 'NONE', #88537, .T. ) ;
#51253 = CARTESIAN_POINT ( 'NONE',  ( 23.31738231874054534, 16.94106989632529192, 141.4500000054623854 ) ) ;
#51254 = CARTESIAN_POINT ( 'NONE',  ( 13.89961937509977652, -13.97604488694527269, 58.12390960531436690 ) ) ;
#51255 = CARTESIAN_POINT ( 'NONE',  ( 16.52544592524342804, -4.483927247898539470, 33.54057627198102409 ) ) ;
#51256 = CARTESIAN_POINT ( 'NONE',  ( 0.05219959533934541429, -16.53943276465976808, 100.0010903946857042 ) ) ;
#51257 = CARTESIAN_POINT ( 'NONE',  ( 14.34966873604972726, -8.224510206698740333, 85.83442372801901854 ) ) ;
#51258 = CARTESIAN_POINT ( 'NONE',  ( -9.564922557961040184, 16.46253265017147172, 37.91775706135233293 ) ) ;
#51259 = CARTESIAN_POINT ( 'NONE',  ( -17.49999999999999289, 5.500000000000032863, 70.79690382534172954 ) ) ;
#51260 = CARTESIAN_POINT ( 'NONE',  ( -5.153800228976328057, -19.02544592524343514, 92.29057627198099567 ) ) ;
#51261 = CARTESIAN_POINT ( 'NONE',  ( -19.02544592524342804, 5.153800228976336051, 56.04057627198100988 ) ) ;
#51262 = CARTESIAN_POINT ( 'NONE',  ( -8.224510206698948167, 14.34966873604960824, 65.41557627198102409 ) ) ;
#51264 = CARTESIAN_POINT ( 'NONE',  ( -5.049401038298153566, 19.05341960407611168, 115.2072429386477097 ) ) ;
#51263 = CARTESIAN_POINT ( 'NONE',  ( 17.40861289039002813, -6.110651285853312409, 101.1276752917256658 ) ) ;
#51265 = CARTESIAN_POINT ( 'NONE',  ( 10.81492255796078972, 18.62759615963270932, 49.58224293864769550 ) ) ;
#51266 = CARTESIAN_POINT ( 'NONE',  ( -14.29746914071049879, 8.314922557960819915, 80.83224293864769550 ) ) ;
#51267 = CARTESIAN_POINT ( 'NONE',  ( -12.06949235617739369, -12.14591786802326823, 39.37609039468567573 ) ) ;
#51268 = CARTESIAN_POINT ( 'NONE',  ( 14.34966873604960469, 8.224510206698951720, 84.16557627198103830 ) ) ;
#51269 = ADVANCED_FACE ( 'NONE', ( #79130 ), #84743, .T. ) ;
#51270 = CARTESIAN_POINT ( 'NONE',  ( -18.39635199886966177, 5.500000000000102141, 66.01967076359997577 ) ) ;
#51271 = CARTESIAN_POINT ( 'NONE',  ( -16.51473224551082808, 9.474510206698731452, 83.33442372801899012 ) ) ;
#51272 = CARTESIAN_POINT ( 'NONE',  ( 21.55341960407610458, 5.719274019375980345, 23.95724293864769550 ) ) ;
#51273 = CARTESIAN_POINT ( 'NONE',  ( 22.81625015709510151, -31.40387420917324590, -6.424999997268812102 ) ) ;
#51274 = CARTESIAN_POINT ( 'NONE',  ( 19.27311148717737055, 5.499999999999991118, 101.9602859708923575 ) ) ;
#51276 = CARTESIAN_POINT ( 'NONE',  ( 12.06949235617757843, -12.14591786802309237, 23.12390960531436335 ) ) ;
#51275 = CARTESIAN_POINT ( 'NONE',  ( -12.06949235617739369, -12.14591786802326823, 24.37609039468567573 ) ) ;
#51277 = CARTESIAN_POINT ( 'NONE',  ( -13.89961937509957401, -13.97604488694547875, 74.37609039468566152 ) ) ;
#51278 = CARTESIAN_POINT ( 'NONE',  ( 21.53943276465977519, -0.05219959533907433946, 48.74890960531435979 ) ) ;
#51279 = CARTESIAN_POINT ( 'NONE',  ( 10.72451020669871369, 18.67979575497193778, 62.08442372801901143 ) ) ;
#51280 = CARTESIAN_POINT ( 'NONE',  ( -2.649999999999999911, -105.0000000000000000, -15.00000000000000000 ) ) ;
#51281 = CARTESIAN_POINT ( 'NONE',  ( 12.14591786802327356, -12.06949235617739191, 30.62609039468567929 ) ) ;
#51283 = CARTESIAN_POINT ( 'NONE',  ( 19.03943276465977164, -0.05219959533909143690, 88.74890960531436690 ) ) ;
#51282 = CARTESIAN_POINT ( 'NONE',  ( -5.153800228976328057, -19.02544592524343514, 27.29057627198103120 ) ) ;
#51284 = CARTESIAN_POINT ( 'NONE',  ( 14.75151636811257916, 15.50344475828853064, -58.79419791951498553 ) ) ;
#51286 = EDGE_CURVE ( 'NONE', #31542, #44815, #142561, .T. ) ;
#51285 = CARTESIAN_POINT ( 'NONE',  ( -16.53943276465976808, 0.05219959533911058130, 86.24890960531436690 ) ) ;
#51287 = CARTESIAN_POINT ( 'NONE',  ( 13.89961937509977652, -13.97604488694527269, 103.1239096053143527 ) ) ;
#51288 = ORIENTED_EDGE ( 'NONE', *, *, #16052, .T. ) ;
#51289 = CARTESIAN_POINT ( 'NONE',  ( 9.564922557961047289, -16.46253265017146816, 100.4177570613523329 ) ) ;
#51290 = CARTESIAN_POINT ( 'NONE',  ( -5.823673210054116645, -21.52544592524344225, 82.29057627198103830 ) ) ;
#51291 = CARTESIAN_POINT ( 'NONE',  ( -0.05219959533909027116, -19.03943276465977164, 47.49890960531435979 ) ) ;
#51293 = CARTESIAN_POINT ( 'NONE',  ( -21.52544592524343514, 5.823673210054127303, 116.0405762719810383 ) ) ;
#51292 = CARTESIAN_POINT ( 'NONE',  ( -5.049401038297874678, -19.05341960407617918, 64.79275706135233293 ) ) ;
#51294 = CARTESIAN_POINT ( 'NONE',  ( 16.51473224551069308, 9.474510206698969483, 64.16557627198102409 ) ) ;
#51295 = CARTESIAN_POINT ( 'NONE',  ( -19.03943276465977164, 0.05219959533909376836, 111.2489096053143669 ) ) ;
#51296 = VERTEX_POINT ( 'NONE', #34399 ) ;
#51297 = CARTESIAN_POINT ( 'NONE',  ( 0.05219959533934541429, -16.53943276465976808, 35.00109039468568284 ) ) ;
#51298 = CARTESIAN_POINT ( 'NONE',  ( 5.719274019375991003, -21.55341960407610458, 97.70724293864772392 ) ) ;
#51301 = CARTESIAN_POINT ( 'NONE',  ( 16.46253265017146816, 9.564922557961045513, 61.66775706135234003 ) ) ;
#51300 = CARTESIAN_POINT ( 'NONE',  ( 0.05219959533909260263, 19.03943276465977164, 89.99890960531436690 ) ) ;
#51299 = CARTESIAN_POINT ( 'NONE',  ( 12.14591786802309770, 12.06949235617756955, 109.3739096053143811 ) ) ;
#51302 = CARTESIAN_POINT ( 'NONE',  ( -18.67979575497178146, -10.72451020669898902, 86.66557627198102409 ) ) ;
#51303 = CARTESIAN_POINT ( 'NONE',  ( -14.34966873604960291, -8.224510206698953496, 46.66557627198102409 ) ) ;
#51304 = CARTESIAN_POINT ( 'NONE',  ( -19.05341960407617563, 5.049401038297882671, 28.54275706135232937 ) ) ;
#51305 = CARTESIAN_POINT ( 'NONE',  ( 14.34966873604972726, -8.224510206698740333, 60.83442372801901854 ) ) ;
#51307 = VERTEX_POINT ( 'NONE', #127384 ) ;
#51306 = CARTESIAN_POINT ( 'NONE',  ( -19.03943276465977164, 0.05219959533909376836, 91.24890960531436690 ) ) ;
#51308 = CARTESIAN_POINT ( 'NONE',  ( 16.46253265017160672, -9.564922557960803928, 43.33224293864769550 ) ) ;
#51309 = CARTESIAN_POINT ( 'NONE',  ( 0.05219959533937995610, -21.53943276465977519, 50.00109039468568994 ) ) ;
#51310 = CARTESIAN_POINT ( 'NONE',  ( 0.05219959533937995610, -21.53943276465977519, 70.00109039468568994 ) ) ;
#51311 = CARTESIAN_POINT ( 'NONE',  ( -19.05341960407611168, -5.049401038298163336, 61.45724293864769550 ) ) ;
#51312 = CARTESIAN_POINT ( 'NONE',  ( -15.72974639402176322, -15.80617190586768395, 29.37609039468568284 ) ) ;
#51313 = CARTESIAN_POINT ( 'NONE',  ( 19.05341960407617918, -5.049401038297876454, 81.04275706135231871 ) ) ;
#51314 = CARTESIAN_POINT ( 'NONE',  ( 9.564922557960805705, 16.46253265017160317, 34.58224293864770260 ) ) ;
#51315 = CARTESIAN_POINT ( 'NONE',  ( -12.06949235617739369, -12.14591786802326823, 84.37609039468570415 ) ) ;
#51316 = CARTESIAN_POINT ( 'NONE',  ( 9.564922557960805705, 16.46253265017160317, 54.58224293864769550 ) ) ;
#51317 = CARTESIAN_POINT ( 'NONE',  ( 30.73962218707677252, 22.33364281372847060, -2.547842220587803297 ) ) ;
#51319 = EDGE_CURVE ( 'NONE', #16229, #25364, #52071, .T. ) ;
#51318 = CARTESIAN_POINT ( 'NONE',  ( 19.05341960407611168, 5.049401038298154454, 33.95724293864769550 ) ) ;
#51320 = CARTESIAN_POINT ( 'NONE',  ( 10.72451020669898902, -18.67979575497178502, 92.91557627198103830 ) ) ;
#51321 = CARTESIAN_POINT ( 'NONE',  ( 16.55341960407618274, -4.379528057220086978, 76.04275706135237556 ) ) ;
#51322 = DIRECTION ( 'NONE',  ( 1.908195823574487804E-15, 0.000000000000000000, -1.000000000000000000 ) ) ;
#51323 = CARTESIAN_POINT ( 'NONE',  ( 9.474510206698729675, 16.51473224551082808, 27.08442372801900433 ) ) ;
#51324 = CARTESIAN_POINT ( 'NONE',  ( 13.97604488694527802, 13.89961937509977652, 59.37390960531434558 ) ) ;
#51325 = CARTESIAN_POINT ( 'NONE',  ( 12.14591786802309770, 12.06949235617756955, 49.37390960531436690 ) ) ;
#51326 = CARTESIAN_POINT ( 'NONE',  ( 14.29746914071049879, -8.314922557960816363, 83.33224293864769550 ) ) ;
#51327 = AXIS2_PLACEMENT_3D ( 'NONE', #1208, #184262, #45744 ) ;
#51328 = CARTESIAN_POINT ( 'NONE',  ( -19.03943276465977164, 0.05219959533909376836, 101.2489096053143669 ) ) ;
#51329 = CARTESIAN_POINT ( 'NONE',  ( 5.049401038298161559, -19.05341960407611168, 82.70724293864770971 ) ) ;
#51330 = CARTESIAN_POINT ( 'NONE',  ( 10.81492255796106328, -18.62759615963255655, 55.41775706135234714 ) ) ;
#51331 = CARTESIAN_POINT ( 'NONE',  ( 16.51473224551069308, 9.474510206698969483, 99.16557627198102409 ) ) ;
#51332 = CARTESIAN_POINT ( 'NONE',  ( -21.55341960407619339, 5.719274019375674811, 103.5427570613523613 ) ) ;
#51333 = CARTESIAN_POINT ( 'NONE',  ( -16.52544592524335698, -4.483927247898792601, 83.95942372801900433 ) ) ;
#51334 = CARTESIAN_POINT ( 'NONE',  ( -5.823673210054431948, 21.52544592524334988, 22.70942372801901499 ) ) ;
#51335 = CARTESIAN_POINT ( 'NONE',  ( -21.53943276465977519, 0.05219959533907696930, 101.2489096053143669 ) ) ;
#51336 = CARTESIAN_POINT ( 'NONE',  ( -4.379528057220328563, 16.55341960407611168, 50.20724293864769550 ) ) ;
#51337 = CARTESIAN_POINT ( 'NONE',  ( -16.51473224551069308, -9.474510206698971260, 36.66557627198102409 ) ) ;
#51338 = CARTESIAN_POINT ( 'NONE',  ( 14.34966873604960469, 8.224510206698951720, 64.16557627198102409 ) ) ;
#51339 = CARTESIAN_POINT ( 'NONE',  ( 15.80617190586746368, 15.72974639402197994, 29.37390960531435269 ) ) ;
#51340 = CARTESIAN_POINT ( 'NONE',  ( -9.474510206698720793, -16.51473224551083518, 24.58442372801900078 ) ) ;
#51341 = CARTESIAN_POINT ( 'NONE',  ( -14.29746914071049879, 8.314922557960819915, 105.8322429386476955 ) ) ;
#51342 = ORIENTED_EDGE ( 'NONE', *, *, #113885, .T. ) ;
#51343 = CARTESIAN_POINT ( 'NONE',  ( 14.29746914071037800, 8.314922557961029526, 66.66775706135234714 ) ) ;
#51344 = CARTESIAN_POINT ( 'NONE',  ( 5.153800228976335163, 19.02544592524342804, 69.79057627198103830 ) ) ;
#51345 = CARTESIAN_POINT ( 'NONE',  ( -16.90269667309137347, -6.687378500144563809, 21.20804624429822383 ) ) ;
#51346 = CARTESIAN_POINT ( 'NONE',  ( 12.06949235617757843, -12.14591786802309237, 83.12390960531436690 ) ) ;
#51347 = CARTESIAN_POINT ( 'NONE',  ( -5.719274019375978568, 21.55341960407610458, 40.20724293864769550 ) ) ;
#51348 = CARTESIAN_POINT ( 'NONE',  ( -8.224510206698735004, -14.34966873604973081, 89.58442372801901854 ) ) ;
#51349 = CARTESIAN_POINT ( 'NONE',  ( -5.153800228976607833, 19.02544592524334988, 112.7094237280190043 ) ) ;
#51350 = CARTESIAN_POINT ( 'NONE',  ( 18.67979575497194134, -10.72451020669871369, 80.83442372801901854 ) ) ;
#51351 = CARTESIAN_POINT ( 'NONE',  ( 5.049401038298161559, -19.05341960407611168, 92.70724293864769550 ) ) ;
#51352 = CARTESIAN_POINT ( 'NONE',  ( -5.719274019375978568, 21.55341960407610458, 100.2072429386476955 ) ) ;
#51353 = CARTESIAN_POINT ( 'NONE',  ( 14.29746914071037800, 8.314922557961029526, 51.66775706135234714 ) ) ;
#51354 = CARTESIAN_POINT ( 'NONE',  ( -16.52544592524342804, 4.483927247898546575, 116.0405762719810383 ) ) ;
#51355 = CARTESIAN_POINT ( 'NONE',  ( -0.05219959533936034679, 19.03943276465977164, 112.5010903946856757 ) ) ;
#51356 = CARTESIAN_POINT ( 'NONE',  ( 9.474510206698729675, 16.51473224551082808, 87.08442372801900433 ) ) ;
#51357 = CARTESIAN_POINT ( 'NONE',  ( -21.52544592524343514, 5.823673210054127303, 71.04057627198103830 ) ) ;
#51358 = CARTESIAN_POINT ( 'NONE',  ( -5.049401038297874678, -19.05341960407617918, 54.79275706135234003 ) ) ;
#51359 = LINE ( 'NONE', #174712, #180173 ) ;
#51360 = CARTESIAN_POINT ( 'NONE',  ( 5.823673210054125526, 21.52544592524343514, 104.7905762719810241 ) ) ;
#51361 = CARTESIAN_POINT ( 'NONE',  ( 17.49999999999998934, 4.013004640162652237, 27.05394279005593461 ) ) ;
#51362 = CARTESIAN_POINT ( 'NONE',  ( 9.474510206698971260, -16.51473224551069308, 72.91557627198102409 ) ) ;
#51363 = LINE ( 'NONE', #160535, #198310 ) ;
#51364 = CARTESIAN_POINT ( 'NONE',  ( -16.55341960407617563, 4.379528057220093196, 28.54275706135234358 ) ) ;
#51365 = CARTESIAN_POINT ( 'NONE',  ( 36.86261346499075131, -5.499032313789902204, 44.62661474502113634 ) ) ;
#51367 = CARTESIAN_POINT ( 'NONE',  ( 12.14591786802309770, 12.06949235617756955, 69.37390960531436690 ) ) ;
#51366 = CARTESIAN_POINT ( 'NONE',  ( 10.72451020669898902, -18.67979575497178502, 97.91557627198103830 ) ) ;
#51368 = CARTESIAN_POINT ( 'NONE',  ( -16.51473224551069308, -9.474510206698971260, 71.66557627198102409 ) ) ;
#51369 = CARTESIAN_POINT ( 'NONE',  ( 15.80617190586769283, -15.72974639402175789, 85.62609039468568994 ) ) ;
#51371 = CARTESIAN_POINT ( 'NONE',  ( -16.46253265017146816, -9.564922557961047289, 39.16775706135234003 ) ) ;
#51370 = CARTESIAN_POINT ( 'NONE',  ( 16.53943276465976808, 0.05219959533934440121, 36.25109039468567573 ) ) ;
#51372 = CARTESIAN_POINT ( 'NONE',  ( -21.53943276465977519, -0.05219959533937600094, 48.75109039468568284 ) ) ;
#51373 = CARTESIAN_POINT ( 'NONE',  ( 5.823673210054125526, 21.52544592524343514, 64.79057627198103830 ) ) ;
#51374 = CARTESIAN_POINT ( 'NONE',  ( 0.05219959533936267826, -19.03943276465977164, 105.0010903946856615 ) ) ;
#51375 = CARTESIAN_POINT ( 'NONE',  ( -9.564922557960796823, -16.46253265017161027, 52.08224293864768839 ) ) ;
#51376 = CARTESIAN_POINT ( 'NONE',  ( -19.02544592524334988, -5.153800228976617603, 78.95942372801900433 ) ) ;
#51377 = CARTESIAN_POINT ( 'NONE',  ( -10.72451020669870658, -18.67979575497194134, 79.58442372801903275 ) ) ;
#51378 = CARTESIAN_POINT ( 'NONE',  ( -9.564922557961040184, 16.46253265017147172, 62.91775706135233293 ) ) ;
#51379 = CARTESIAN_POINT ( 'NONE',  ( 13.89961937509977652, -13.97604488694527269, 33.12390960531434558 ) ) ;
#51380 = CARTESIAN_POINT ( 'NONE',  ( -21.52544592524343514, 5.823673210054127303, 56.04057627198102409 ) ) ;
#51381 = CARTESIAN_POINT ( 'NONE',  ( 8.314922557960818139, 14.29746914071049879, 69.58224293864769550 ) ) ;
#51382 = CARTESIAN_POINT ( 'NONE',  ( 21.76075944043963872, 9.615265036675765487, 170.8440536485302346 ) ) ;
#51383 = CARTESIAN_POINT ( 'NONE',  ( -5.049401038297874678, -19.05341960407617918, 24.79275706135233648 ) ) ;
#51384 = CARTESIAN_POINT ( 'NONE',  ( -16.55341960407617563, 4.379528057220093196, 93.54275706135234714 ) ) ;
#51385 = CARTESIAN_POINT ( 'NONE',  ( -8.224510206698948167, 14.34966873604960824, 55.41557627198102409 ) ) ;
#51386 = CARTESIAN_POINT ( 'NONE',  ( -21.55341960407619339, 5.719274019375674811, 88.54275706135236135 ) ) ;
#51387 = CARTESIAN_POINT ( 'NONE',  ( -10.81492255796105439, 18.62759615963255655, 82.91775706135234714 ) ) ;
#51388 = CARTESIAN_POINT ( 'NONE',  ( -5.823673210054116645, -21.52544592524344225, 97.29057627198105251 ) ) ;
#51389 = CARTESIAN_POINT ( 'NONE',  ( 19.02544592524343514, -5.153800228976328945, 53.54057627198102409 ) ) ;
#51390 = CARTESIAN_POINT ( 'NONE',  ( -21.55341960407619339, 5.719274019375674811, 63.54275706135234003 ) ) ;
#51391 = CARTESIAN_POINT ( 'NONE',  ( -0.05219959533909027116, -19.03943276465977164, 52.49890960531436690 ) ) ;
#51392 = ORIENTED_EDGE ( 'NONE', *, *, #159956, .F. ) ;
#51393 = CARTESIAN_POINT ( 'NONE',  ( 9.564922557960805705, 16.46253265017160317, 64.58224293864769550 ) ) ;
#51394 = CARTESIAN_POINT ( 'NONE',  ( -16.52544592524342804, 4.483927247898546575, 106.0405762719810525 ) ) ;
#51395 = CARTESIAN_POINT ( 'NONE',  ( 5.049401038298161559, -19.05341960407611168, 92.70724293864769550 ) ) ;
#51396 = CARTESIAN_POINT ( 'NONE',  ( -8.224510206698948167, 14.34966873604960824, 60.41557627198102409 ) ) ;
#51397 = CARTESIAN_POINT ( 'NONE',  ( -9.564922557960796823, -16.46253265017161027, 22.08224293864768839 ) ) ;
#51398 = CARTESIAN_POINT ( 'NONE',  ( -21.52544592524343514, 5.823673210054127303, 81.04057627198102409 ) ) ;
#51399 = CARTESIAN_POINT ( 'NONE',  ( 21.52544592524334988, 5.823673210054432836, 41.45942372801901143 ) ) ;
#51400 = CARTESIAN_POINT ( 'NONE',  ( 27.07812102864233239, -7.738729533396120353, 165.1046384229466355 ) ) ;
#51401 = CARTESIAN_POINT ( 'NONE',  ( -14.34966873604972548, 8.224510206698743886, 38.33442372801900433 ) ) ;
#51402 = CARTESIAN_POINT ( 'NONE',  ( 0.05219959533907565091, 21.53943276465977519, 84.99890960531436690 ) ) ;
#51403 = CARTESIAN_POINT ( 'NONE',  ( -18.67979575497193778, 10.72451020669871902, 108.3344237280190185 ) ) ;
#51404 = CARTESIAN_POINT ( 'NONE',  ( -13.97604488694527625, -13.89961937509977652, 96.87390960531433848 ) ) ;
#51405 = CARTESIAN_POINT ( 'NONE',  ( 15.80617190586769283, -15.72974639402175789, 30.62609039468567929 ) ) ;
#51406 = CARTESIAN_POINT ( 'NONE',  ( 15.80617190586746368, 15.72974639402197994, 34.37390960531435979 ) ) ;
#51407 = CARTESIAN_POINT ( 'NONE',  ( 0.05219959533934541429, -16.53943276465976808, 105.0010903946856757 ) ) ;
#51409 = CARTESIAN_POINT ( 'NONE',  ( 18.67979575497194134, -10.72451020669871369, 90.83442372801901854 ) ) ;
#51408 = CARTESIAN_POINT ( 'NONE',  ( 5.823673210054444382, -21.52544592524334988, 50.20942372801901854 ) ) ;
#51410 = CARTESIAN_POINT ( 'NONE',  ( -15.80617190586768217, 15.72974639402176855, 108.1260903946856757 ) ) ;
#51411 = CARTESIAN_POINT ( 'NONE',  ( 8.314922557961029526, -14.29746914071037800, 80.41775706135234714 ) ) ;
#51412 = CARTESIAN_POINT ( 'NONE',  ( -5.719274019375665041, -21.55341960407619695, 39.79275706135235424 ) ) ;
#51413 = CARTESIAN_POINT ( 'NONE',  ( 5.049401038298161559, -19.05341960407611168, 32.70724293864768129 ) ) ;
#51414 = CARTESIAN_POINT ( 'NONE',  ( 0.05219959533937995610, -21.53943276465977519, 100.0010903946857042 ) ) ;
#51415 = CARTESIAN_POINT ( 'NONE',  ( -0.05219959533909027116, -19.03943276465977164, 112.4989096053143669 ) ) ;
#51416 = CARTESIAN_POINT ( 'NONE',  ( -18.62759615963270932, 10.81492255796079327, 105.8322429386476955 ) ) ;
#51418 = CARTESIAN_POINT ( 'NONE',  ( -15.80617190586745835, -15.72974639402198527, 66.87390960531436690 ) ) ;
#51417 = DIRECTION ( 'NONE',  ( -0.5150380737757255245, 0.000000000000000000, 0.8571673013836856869 ) ) ;
#51420 = CARTESIAN_POINT ( 'NONE',  ( 14.29746914071049879, -8.314922557960816363, 53.33224293864769550 ) ) ;
#51419 = CARTESIAN_POINT ( 'NONE',  ( 16.53943276465976808, 0.05219959533934440121, 46.25109039468567573 ) ) ;
#51421 = CARTESIAN_POINT ( 'NONE',  ( -27.73933785331498925, 2.428612866367529932E-14, 139.1250000027311842 ) ) ;
#51422 = CARTESIAN_POINT ( 'NONE',  ( -13.97604488694547697, 13.89961937509957934, 93.12609039468566152 ) ) ;
#51423 = CARTESIAN_POINT ( 'NONE',  ( -9.248023074035629065, -10.74802307403544077, -60.25555373585994090 ) ) ;
#51424 = CARTESIAN_POINT ( 'NONE',  ( 14.34966873604972726, -8.224510206698740333, 25.83442372801901499 ) ) ;
#51425 = CARTESIAN_POINT ( 'NONE',  ( -21.53943276465977519, 0.05219959533907696930, 101.2489096053143669 ) ) ;
#51426 = CARTESIAN_POINT ( 'NONE',  ( -18.67979575497178146, -10.72451020669898902, 71.66557627198100988 ) ) ;
#51427 = CARTESIAN_POINT ( 'NONE',  ( 13.89961937509977652, -13.97604488694527269, 108.1239096053143669 ) ) ;
#51428 = CARTESIAN_POINT ( 'NONE',  ( 16.55341960407618274, -4.379528057220086978, 41.04275706135236135 ) ) ;
#51429 = CARTESIAN_POINT ( 'NONE',  ( 19.02544592524343514, -5.153800228976328945, 63.54057627198103830 ) ) ;
#51431 = CARTESIAN_POINT ( 'NONE',  ( 13.97604488694548053, -13.89961937509957401, 95.62609039468563310 ) ) ;
#51430 = CARTESIAN_POINT ( 'NONE',  ( -10.81492255796105439, 18.62759615963255655, 32.91775706135234714 ) ) ;
#51432 = EDGE_CURVE ( 'NONE', #133752, #6681, #159608, .T. ) ;
#51433 = CARTESIAN_POINT ( 'NONE',  ( -19.05341960407611168, -5.049401038298163336, 106.4572429386476955 ) ) ;
#51434 = CARTESIAN_POINT ( 'NONE',  ( 5.153800228976335163, 19.02544592524342804, 84.79057627198099567 ) ) ;
#51435 = CARTESIAN_POINT ( 'NONE',  ( 21.52544592524344225, -5.823673210054117533, 93.54057627198103830 ) ) ;
#51436 = CARTESIAN_POINT ( 'NONE',  ( 9.474510206698971260, -16.51473224551069308, 52.91557627198102409 ) ) ;
#51437 = CARTESIAN_POINT ( 'NONE',  ( -17.12812012977024523, -6.668231424566068988, 61.35948759323143520 ) ) ;
#51438 = CARTESIAN_POINT ( 'NONE',  ( 14.34966873604960469, 8.224510206698951720, 69.16557627198102409 ) ) ;
#51439 = CARTESIAN_POINT ( 'NONE',  ( -5.049401038298153566, 19.05341960407611168, 115.2072429386477097 ) ) ;
#51440 = CARTESIAN_POINT ( 'NONE',  ( -29.02171288343480526, 0.6023940538451412197, -52.52077797743537246 ) ) ;
#51441 = CARTESIAN_POINT ( 'NONE',  ( 18.67979575497178502, 10.72451020669898547, 89.16557627198102409 ) ) ;
#51442 = CARTESIAN_POINT ( 'NONE',  ( -19.03943276465977164, -0.05219959533935918106, 48.75109039468566863 ) ) ;
#51443 = CARTESIAN_POINT ( 'NONE',  ( 9.564922557960805705, 16.46253265017160317, 114.5822429386476955 ) ) ;
#51444 = DIRECTION ( 'NONE',  ( -1.000000000000000000, -0.000000000000000000, -0.000000000000000000 ) ) ;
#51445 = CARTESIAN_POINT ( 'NONE',  ( 15.72974639402199770, -15.80617190586745480, 53.12390960531436690 ) ) ;
#51446 = CARTESIAN_POINT ( 'NONE',  ( -16.46253265017160317, 9.564922557960807481, 80.83224293864769550 ) ) ;
#51447 = CARTESIAN_POINT ( 'NONE',  ( 0.05219959533937995610, -21.53943276465977519, 85.00109039468568994 ) ) ;
#51448 = CARTESIAN_POINT ( 'NONE',  ( 13.89961937509977652, -13.97604488694527269, 43.12390960531434558 ) ) ;
#51449 = CARTESIAN_POINT ( 'NONE',  ( -0.05219959533910754901, -16.53943276465976808, 77.49890960531433848 ) ) ;
#51450 = CARTESIAN_POINT ( 'NONE',  ( -12.14591786802326823, 12.06949235617739902, 23.12609039468567573 ) ) ;
#51451 = CARTESIAN_POINT ( 'NONE',  ( 15.72974639402176855, 15.80617190586768217, 66.87609039468568994 ) ) ;
#51452 = ORIENTED_EDGE ( 'NONE', *, *, #145235, .T. ) ;
#51453 = CARTESIAN_POINT ( 'NONE',  ( -16.46253265017146816, -9.564922557961047289, 29.16775706135232937 ) ) ;
#51454 = CARTESIAN_POINT ( 'NONE',  ( -5.153800228976607833, 19.02544592524334988, 77.70942372801900433 ) ) ;
#51455 = FACE_OUTER_BOUND ( 'NONE', #171861, .T. ) ;
#51456 = CARTESIAN_POINT ( 'NONE',  ( -10.72451020669870658, -18.67979575497194134, 29.58442372801901854 ) ) ;
#51457 = LINE ( 'NONE', #191962, #117329 ) ;
#51458 = CARTESIAN_POINT ( 'NONE',  ( -10.72451020669870658, -18.67979575497194134, 109.5844237280190328 ) ) ;
#51459 = CARTESIAN_POINT ( 'NONE',  ( 5.049401038298161559, -19.05341960407611168, 52.70724293864767418 ) ) ;
#51460 = CARTESIAN_POINT ( 'NONE',  ( -0.05219959533936034679, 19.03943276465977164, 27.50109039468566507 ) ) ;
#51461 = CARTESIAN_POINT ( 'NONE',  ( 12.06949235617739724, 12.14591786802326823, 101.8760903946857042 ) ) ;
#51463 = CARTESIAN_POINT ( 'NONE',  ( -5.823673210054431948, 21.52544592524334988, 67.70942372801901854 ) ) ;
#51462 = CARTESIAN_POINT ( 'NONE',  ( 13.97604488694527802, 13.89961937509977652, 104.3739096053143385 ) ) ;
#51464 = CIRCLE ( 'NONE', #148475, 38.00000000000000000 ) ;
#51465 = CARTESIAN_POINT ( 'NONE',  ( 36.91746824999999887, 11.99521256947799053, -5.524999997268812635 ) ) ;
#51466 = CARTESIAN_POINT ( 'NONE',  ( -33.79632059884287543, 5.461862605997785280, 94.26112944759005075 ) ) ;
#51467 = CARTESIAN_POINT ( 'NONE',  ( 5.823673210054444382, -21.52544592524334988, 85.20942372801901854 ) ) ;
#51468 = CARTESIAN_POINT ( 'NONE',  ( -21.52544592524334988, -5.823673210054445271, 103.9594237280190185 ) ) ;
#51469 = CARTESIAN_POINT ( 'NONE',  ( 2.500000000000000000, 1.178949249685212974, -2.042000000000001148 ) ) ;
#51470 = CARTESIAN_POINT ( 'NONE',  ( 13.97604488694527802, 13.89961937509977652, 94.37390960531436690 ) ) ;
#51471 = CARTESIAN_POINT ( 'NONE',  ( -16.46253265017146816, -9.564922557961047289, 19.16775706135233293 ) ) ;
#51472 = CARTESIAN_POINT ( 'NONE',  ( 19.96964676835936459, -32.33678545050543107, -24.48363814647527548 ) ) ;
#51473 = CARTESIAN_POINT ( 'NONE',  ( -0.05219959533909027116, -19.03943276465977164, 42.49890960531435269 ) ) ;
#51474 = CARTESIAN_POINT ( 'NONE',  ( 15.72974639402199770, -15.80617190586745480, 53.12390960531436690 ) ) ;
#51475 = CARTESIAN_POINT ( 'NONE',  ( -8.224510206698948167, 14.34966873604960824, 25.41557627198103120 ) ) ;
#51477 = CARTESIAN_POINT ( 'NONE',  ( -19.03943276465977164, 0.05219959533909376836, 86.24890960531436690 ) ) ;
#51476 = CARTESIAN_POINT ( 'NONE',  ( 16.53943276465976808, -0.05219959533910856209, 98.74890960531438111 ) ) ;
#51478 = CARTESIAN_POINT ( 'NONE',  ( 0.05219959533937995610, -21.53943276465977519, 105.0010903946856757 ) ) ;
#51479 = CARTESIAN_POINT ( 'NONE',  ( 0.05219959533909260263, 19.03943276465977164, 39.99890960531436690 ) ) ;
#51480 = CARTESIAN_POINT ( 'NONE',  ( 16.55341960407611168, 4.379528057220329451, 98.95724293864770971 ) ) ;
#51481 = CARTESIAN_POINT ( 'NONE',  ( 18.62759615963255655, 10.81492255796105972, 61.66775706135235424 ) ) ;
#51482 = CARTESIAN_POINT ( 'NONE',  ( 10.81492255796078972, 18.62759615963270932, 84.58224293864769550 ) ) ;
#51483 = CARTESIAN_POINT ( 'NONE',  ( -16.51473224551082808, 9.474510206698731452, 53.33442372801900433 ) ) ;
#51484 = CARTESIAN_POINT ( 'NONE',  ( -20.76432162245589907, -34.24133103601445072, -10.56798276756222599 ) ) ;
#51485 = CARTESIAN_POINT ( 'NONE',  ( 13.97604488694527802, 13.89961937509977652, 104.3739096053143385 ) ) ;
#51486 = CARTESIAN_POINT ( 'NONE',  ( 8.224510206698953496, -14.34966873604960469, 77.91557627198102409 ) ) ;
#51487 = CARTESIAN_POINT ( 'NONE',  ( -9.474510206698720793, -16.51473224551083518, 44.58442372801900433 ) ) ;
#51489 = AXIS2_PLACEMENT_3D ( 'NONE', #32283, #108108, #186982 ) ;
#51488 = CARTESIAN_POINT ( 'NONE',  ( 5.153800228976335163, 19.02544592524342804, 59.79057627198100988 ) ) ;
#51490 = CARTESIAN_POINT ( 'NONE',  ( 8.224510206698953496, -14.34966873604960469, 57.91557627198103120 ) ) ;
#51491 = CARTESIAN_POINT ( 'NONE',  ( -9.564922557961040184, 16.46253265017147172, 77.91775706135234714 ) ) ;
#51492 = CARTESIAN_POINT ( 'NONE',  ( 18.22780087662122384, -5.500000000000022204, 91.01540105326107266 ) ) ;
#51493 = CARTESIAN_POINT ( 'NONE',  ( -5.823673210054116645, -21.52544592524344225, 32.29057627198102409 ) ) ;
#51494 = ORIENTED_EDGE ( 'NONE', *, *, #171107, .F. ) ;
#51495 = CARTESIAN_POINT ( 'NONE',  ( 0.05219959533910956823, 16.53943276465976808, 94.99890960531436690 ) ) ;
#51496 = FACE_OUTER_BOUND ( 'NONE', #76820, .T. ) ;
#51498 = CARTESIAN_POINT ( 'NONE',  ( -18.62759615963270932, 10.81492255796079327, 65.83224293864769550 ) ) ;
#51497 = CARTESIAN_POINT ( 'NONE',  ( -5.153800228976328057, -19.02544592524343514, 57.29057627198103120 ) ) ;
#51499 = CARTESIAN_POINT ( 'NONE',  ( 5.049401038298161559, -19.05341960407611168, 27.70724293864769550 ) ) ;
#51501 = CARTESIAN_POINT ( 'NONE',  ( 5.049401038298161559, -19.05341960407611168, 57.70724293864769550 ) ) ;
#51500 = CARTESIAN_POINT ( 'NONE',  ( 14.34966873604972726, -8.224510206698740333, 75.83442372801900433 ) ) ;
#51502 = CARTESIAN_POINT ( 'NONE',  ( -19.02544592524334988, -5.153800228976617603, 58.95942372801900433 ) ) ;
#51503 = CARTESIAN_POINT ( 'NONE',  ( 0.05219959533937995610, -21.53943276465977519, 70.00109039468568994 ) ) ;
#51504 = CARTESIAN_POINT ( 'NONE',  ( 18.67979575497178502, 10.72451020669898547, 49.16557627198102409 ) ) ;
#51505 = CARTESIAN_POINT ( 'NONE',  ( 4.483927247898545687, 16.52544592524342804, 114.7905762719810383 ) ) ;
#51506 = CARTESIAN_POINT ( 'NONE',  ( -0.05219959533934338120, 16.53943276465976808, 92.50109039468567573 ) ) ;
#51507 = CARTESIAN_POINT ( 'NONE',  ( 13.97604488694548053, -13.89961937509957401, 100.6260903946856615 ) ) ;
#51508 = CARTESIAN_POINT ( 'NONE',  ( -15.49999999999999822, -5.500000000000000888, 22.00000000000000711 ) ) ;
#51509 = CARTESIAN_POINT ( 'NONE',  ( 16.52216118717208104, 7.221426719304520958, 53.57599021046992505 ) ) ;
#51510 = CARTESIAN_POINT ( 'NONE',  ( -5.823673210054431948, 21.52544592524334988, 102.7094237280190185 ) ) ;
#51511 = CARTESIAN_POINT ( 'NONE',  ( 4.379528057220339221, -16.55341960407611168, 42.70724293864770260 ) ) ;
#51512 = CARTESIAN_POINT ( 'NONE',  ( -14.34966873604960291, -8.224510206698953496, 61.66557627198103120 ) ) ;
#51513 = CARTESIAN_POINT ( 'NONE',  ( -18.67979575497178146, -10.72451020669898902, 91.66557627198103830 ) ) ;
#51514 = CARTESIAN_POINT ( 'NONE',  ( 5.823673210054125526, 21.52544592524343514, 89.79057627198103830 ) ) ;
#51515 = CARTESIAN_POINT ( 'NONE',  ( -1.481880339025519300, -30.11448378070094734, -48.12989299794422493 ) ) ;
#51516 = CARTESIAN_POINT ( 'NONE',  ( 21.53943276465977519, -0.05219959533907433946, 28.74890960531435624 ) ) ;
#51517 = CARTESIAN_POINT ( 'NONE',  ( -4.483927247898782831, 16.52544592524335698, 72.70942372801901854 ) ) ;
#51518 = CARTESIAN_POINT ( 'NONE',  ( -16.53943276465976808, 0.05219959533911058130, 76.24890960531435269 ) ) ;
#51519 = CARTESIAN_POINT ( 'NONE',  ( -16.46253265017160317, 9.564922557960807481, 50.83224293864770260 ) ) ;
#51520 = SURFACE_SIDE_STYLE ('',( #50538 ) ) ;
#51521 = CARTESIAN_POINT ( 'NONE',  ( 34.91229673954796908, -6.363315211036958630, 41.02293916657587403 ) ) ;
#51522 = CARTESIAN_POINT ( 'NONE',  ( -4.483927247898782831, 16.52544592524335698, 97.70942372801904696 ) ) ;
#51523 = CARTESIAN_POINT ( 'NONE',  ( 21.52544592524334988, 5.823673210054432836, 26.45942372801901854 ) ) ;
#51524 = CARTESIAN_POINT ( 'NONE',  ( 0.05219959533909260263, 19.03943276465977164, 84.99890960531436690 ) ) ;
#51525 = CARTESIAN_POINT ( 'NONE',  ( -5.719274019375665041, -21.55341960407619695, 49.79275706135234714 ) ) ;
#51526 = CARTESIAN_POINT ( 'NONE',  ( 5.153800228976335163, 19.02544592524342804, 114.7905762719810241 ) ) ;
#51527 = CARTESIAN_POINT ( 'NONE',  ( -21.44681783660697860, -33.76292609719497761, -24.06782133911154631 ) ) ;
#51528 = EDGE_LOOP ( 'NONE', ( #52381, #44726, #70373, #76520 ) ) ;
#51529 = CARTESIAN_POINT ( 'NONE',  ( -21.52544592524334988, -5.823673210054445271, 48.95942372801902565 ) ) ;
#51531 = CARTESIAN_POINT ( 'NONE',  ( -9.564922557960796823, -16.46253265017161027, 22.08224293864768839 ) ) ;
#51530 = CARTESIAN_POINT ( 'NONE',  ( -9.564922557960796823, -16.46253265017161027, 42.08224293864769550 ) ) ;
#51532 = CARTESIAN_POINT ( 'NONE',  ( 13.89961937509957401, 13.97604488694547697, 56.87609039468564731 ) ) ;
#51533 = CARTESIAN_POINT ( 'NONE',  ( -18.62759615963255300, -10.81492255796106328, 34.16775706135234714 ) ) ;
#51534 = CARTESIAN_POINT ( 'NONE',  ( -5.153800228976607833, 19.02544592524334988, 52.70942372801900433 ) ) ;
#51535 = CARTESIAN_POINT ( 'NONE',  ( -19.05341960407611168, -5.049401038298163336, 21.45724293864768839 ) ) ;
#51536 = CARTESIAN_POINT ( 'NONE',  ( 12.06949235617739724, 12.14591786802326823, 96.87609039468568994 ) ) ;
#51537 = CARTESIAN_POINT ( 'NONE',  ( -13.97604488694547697, 13.89961937509957934, 58.12609039468566863 ) ) ;
#51538 = CARTESIAN_POINT ( 'NONE',  ( 14.29746914071037800, 8.314922557961029526, 111.6677570613523613 ) ) ;
#51539 = CARTESIAN_POINT ( 'NONE',  ( 6.434671708797603529, -6.434671708797564449, -63.95112321872120731 ) ) ;
#51540 = CARTESIAN_POINT ( 'NONE',  ( -13.97604488694527625, -13.89961937509977652, 86.87390960531436690 ) ) ;
#51541 = CARTESIAN_POINT ( 'NONE',  ( 10.72451020669871369, 18.67979575497193778, 87.08442372801901854 ) ) ;
#51542 = CARTESIAN_POINT ( 'NONE',  ( -21.53943276465977519, -0.05219959533937600094, 103.7510903946857042 ) ) ;
#51543 = DIRECTION ( 'NONE',  ( 0.000000000000000000, 0.000000000000000000, 1.000000000000000000 ) ) ;
#51544 = CARTESIAN_POINT ( 'NONE',  ( -5.049401038298153566, 19.05341960407611168, 100.2072429386476955 ) ) ;
#51545 = CARTESIAN_POINT ( 'NONE',  ( 21.53943276465977519, 0.05219959533937863772, 71.25109039468568994 ) ) ;
#51546 = CARTESIAN_POINT ( 'NONE',  ( 12.14591786802327356, -12.06949235617739191, 20.62609039468568639 ) ) ;
#51547 = CARTESIAN_POINT ( 'NONE',  ( 9.474510206698971260, -16.51473224551069308, 72.91557627198102409 ) ) ;
#51548 = CARTESIAN_POINT ( 'NONE',  ( -10.81492255796078084, -18.62759615963271287, 27.08224293864769550 ) ) ;
#51549 = CARTESIAN_POINT ( 'NONE',  ( 9.474510206698971260, -16.51473224551069308, 97.91557627198102409 ) ) ;
#51550 = CARTESIAN_POINT ( 'NONE',  ( 37.99999999999991473, -12.34694845685052833, -8.849999994537625980 ) ) ;
#51551 = CARTESIAN_POINT ( 'NONE',  ( -13.97604488694527625, -13.89961937509977652, 66.87390960531436690 ) ) ;
#51552 = CARTESIAN_POINT ( 'NONE',  ( 8.314922557961029526, -14.29746914071037800, 110.4177570613523756 ) ) ;
#51553 = CARTESIAN_POINT ( 'NONE',  ( -3.573655867282028392E-15, 2.428612866367529932E-14, 169.9999999999999716 ) ) ;
#51554 = CARTESIAN_POINT ( 'NONE',  ( 13.97604488694548053, -13.89961937509957401, 75.62609039468564731 ) ) ;
#51555 = CARTESIAN_POINT ( 'NONE',  ( -16.51473224551069308, -9.474510206698971260, 96.66557627198102409 ) ) ;
#51556 = CARTESIAN_POINT ( 'NONE',  ( -14.29746914071049879, 8.314922557960819915, 90.83224293864769550 ) ) ;
#51557 = CARTESIAN_POINT ( 'NONE',  ( 15.72974639402199770, -15.80617190586745480, 48.12390960531436690 ) ) ;
#51558 = CARTESIAN_POINT ( 'NONE',  ( 5.823673210054125526, 21.52544592524343514, 24.79057627198103120 ) ) ;
#51559 = CARTESIAN_POINT ( 'NONE',  ( -4.379528057220328563, 16.55341960407611168, 105.2072429386477097 ) ) ;
#51560 = CARTESIAN_POINT ( 'NONE',  ( 28.79475375365586132, 2.781246896534039337E-14, 141.2656553485623760 ) ) ;
#51561 = CARTESIAN_POINT ( 'NONE',  ( -13.89961937509957401, -13.97604488694547875, 39.37609039468566152 ) ) ;
#51562 = CARTESIAN_POINT ( 'NONE',  ( -16.53943276465976808, 0.05219959533911058130, 26.24890960531435624 ) ) ;
#51563 = CARTESIAN_POINT ( 'NONE',  ( -16.51473224551069308, -9.474510206698971260, 101.6655762719810241 ) ) ;
#51564 = CARTESIAN_POINT ( 'NONE',  ( 18.67979575497194134, -10.72451020669871369, 70.83442372801901854 ) ) ;
#51565 = CARTESIAN_POINT ( 'NONE',  ( -15.80617190586745835, -15.72974639402198527, 61.87390960531436690 ) ) ;
#51566 = CARTESIAN_POINT ( 'NONE',  ( -21.53943276465977519, -0.05219959533937600094, 43.75109039468568284 ) ) ;
#51567 = CARTESIAN_POINT ( 'NONE',  ( -5.823673210054116645, -21.52544592524344225, 92.29057627198103830 ) ) ;
#51568 = CARTESIAN_POINT ( 'NONE',  ( 21.52544592524334988, 5.823673210054432836, 41.45942372801901143 ) ) ;
#51569 = CARTESIAN_POINT ( 'NONE',  ( -8.314922557960811034, -14.29746914071050412, 107.0822429386476955 ) ) ;
#51570 = CARTESIAN_POINT ( 'NONE',  ( 13.97604488694548053, -13.89961937509957401, 65.62609039468567573 ) ) ;
#51571 = CARTESIAN_POINT ( 'NONE',  ( 16.51473224551069308, 9.474510206698969483, 59.16557627198102409 ) ) ;
#51572 = CARTESIAN_POINT ( 'NONE',  ( -14.34966873604960291, -8.224510206698953496, 111.6655762719810525 ) ) ;
#51573 = CARTESIAN_POINT ( 'NONE',  ( 5.049401038298161559, -19.05341960407611168, 112.7072429386476813 ) ) ;
#51574 = CARTESIAN_POINT ( 'NONE',  ( -4.379528057220328563, 16.55341960407611168, 40.20724293864769550 ) ) ;
#51575 = CARTESIAN_POINT ( 'NONE',  ( -4.379528057220086978, -16.55341960407618274, 109.7927570613523613 ) ) ;
#51576 = CARTESIAN_POINT ( 'NONE',  ( 19.05341960407611168, 5.049401038298154454, 53.95724293864770260 ) ) ;
#51577 = CARTESIAN_POINT ( 'NONE',  ( -9.474510206698964154, 16.51473224551069663, 25.41557627198103120 ) ) ;
#51578 = CARTESIAN_POINT ( 'NONE',  ( -9.474510206698720793, -16.51473224551083518, 19.58442372801899722 ) ) ;
#51580 = CARTESIAN_POINT ( 'NONE',  ( -14.29746914071049879, 8.314922557960819915, 40.83224293864769550 ) ) ;
#51579 = CARTESIAN_POINT ( 'NONE',  ( 0.000000000000000000, 0.000000000000000000, -49.67367017693150189 ) ) ;
#51581 = CARTESIAN_POINT ( 'NONE',  ( 0.05219959533937995610, -21.53943276465977519, 45.00109039468568284 ) ) ;
#51582 = CARTESIAN_POINT ( 'NONE',  ( -7.819668024151573249, -36.54656901728082374, -31.88218832179850182 ) ) ;
#51583 = CARTESIAN_POINT ( 'NONE',  ( 0.05219959533934541429, -16.53943276465976808, 60.00109039468568284 ) ) ;
#51584 = CARTESIAN_POINT ( 'NONE',  ( 14.29746914071049879, -8.314922557960816363, 28.33224293864769550 ) ) ;
#51585 = CARTESIAN_POINT ( 'NONE',  ( -12.14591786802326823, 12.06949235617739902, 103.1260903946856757 ) ) ;
#51586 = CARTESIAN_POINT ( 'NONE',  ( -5.153800228976328057, -19.02544592524343514, 32.29057627198102409 ) ) ;
#51587 = CARTESIAN_POINT ( 'NONE',  ( -0.05219959533909027116, -19.03943276465977164, 42.49890960531435269 ) ) ;
#51588 = CARTESIAN_POINT ( 'NONE',  ( -16.52544592524342804, 4.483927247898546575, 116.0405762719810383 ) ) ;
#51589 = CARTESIAN_POINT ( 'NONE',  ( -10.72451020669870658, -18.67979575497194134, 29.58442372801901854 ) ) ;
#51590 = CARTESIAN_POINT ( 'NONE',  ( -19.02544592524342804, 5.153800228976336051, 46.04057627198101699 ) ) ;
#51591 = CARTESIAN_POINT ( 'NONE',  ( 18.22780087662122384, -5.500000000000022204, 81.01540105326105845 ) ) ;
#51592 = CARTESIAN_POINT ( 'NONE',  ( 16.51473224551069308, 9.474510206698969483, 39.16557627198103120 ) ) ;
#51593 = CARTESIAN_POINT ( 'NONE',  ( -5.823673210054116645, -21.52544592524344225, 27.29057627198103120 ) ) ;
#51594 = VECTOR ( 'NONE', #82511, 1000.000000000000000 ) ;
#51596 = CARTESIAN_POINT ( 'NONE',  ( 4.483927247898545687, 16.52544592524342804, 104.7905762719810241 ) ) ;
#51595 = CARTESIAN_POINT ( 'NONE',  ( -5.719274019375665041, -21.55341960407619695, 59.79275706135234714 ) ) ;
#51597 = CARTESIAN_POINT ( 'NONE',  ( 0.05219959533909260263, 19.03943276465977164, 104.9989096053143669 ) ) ;
#51598 = CARTESIAN_POINT ( 'NONE',  ( -4.379528057220086978, -16.55341960407618274, 79.79275706135236135 ) ) ;
#51599 = CARTESIAN_POINT ( 'NONE',  ( -15.80617190586768217, 15.72974639402176855, 98.12609039468570415 ) ) ;
#51600 = CARTESIAN_POINT ( 'NONE',  ( 4.379528057220092307, 16.55341960407617563, 47.29275706135234003 ) ) ;
#51601 = CARTESIAN_POINT ( 'NONE',  ( -16.46253265017160317, 9.564922557960807481, 95.83224293864769550 ) ) ;
#51602 = CARTESIAN_POINT ( 'NONE',  ( -12.14591786802326823, 12.06949235617739902, 43.12609039468568284 ) ) ;
#51603 = CARTESIAN_POINT ( 'NONE',  ( -14.29746914071037622, -8.314922557961029526, 24.16775706135235424 ) ) ;
#51604 = CARTESIAN_POINT ( 'NONE',  ( -14.29746914071037622, -8.314922557961029526, 79.16775706135234714 ) ) ;
#51605 = CARTESIAN_POINT ( 'NONE',  ( -13.89961937509957401, -13.97604488694547875, 104.3760903946856757 ) ) ;
#51606 = CARTESIAN_POINT ( 'NONE',  ( -19.05341960407611168, -5.049401038298163336, 81.45724293864769550 ) ) ;
#51607 = CARTESIAN_POINT ( 'NONE',  ( 0.05219959533907565091, 21.53943276465977519, 94.99890960531436690 ) ) ;
#51609 = CARTESIAN_POINT ( 'NONE',  ( -13.97604488694547697, 13.89961937509957934, 108.1260903946856331 ) ) ;
#51608 = CARTESIAN_POINT ( 'NONE',  ( -4.483927247898539470, -16.52544592524342804, 107.2905762719810525 ) ) ;
#51610 = CARTESIAN_POINT ( 'NONE',  ( 12.06949235617739724, 12.14591786802326823, 71.87609039468568994 ) ) ;
#51611 = CARTESIAN_POINT ( 'NONE',  ( -17.05116617787848554, 6.768360034955530402, 43.65675553259193720 ) ) ;
#51612 = CARTESIAN_POINT ( 'NONE',  ( -19.03943276465977164, -0.05219959533935918106, 73.75109039468566152 ) ) ;
#51613 = CARTESIAN_POINT ( 'NONE',  ( 16.55341960407611168, 4.379528057220329451, 43.95724293864769550 ) ) ;
#51614 = CARTESIAN_POINT ( 'NONE',  ( -8.314922557960811034, -14.29746914071050412, 87.08224293864769550 ) ) ;
#51616 = CARTESIAN_POINT ( 'NONE',  ( -17.13100169013301155, 6.664070546373155324, 90.76789835699851494 ) ) ;
#51615 = CARTESIAN_POINT ( 'NONE',  ( 13.97604488694548053, -13.89961937509957401, 30.62609039468566863 ) ) ;
#51617 = CARTESIAN_POINT ( 'NONE',  ( -5.823673210054431948, 21.52544592524334988, 37.70942372801900433 ) ) ;
#51618 = CARTESIAN_POINT ( 'NONE',  ( -0.05219959533936034679, 19.03943276465977164, 102.5010903946856757 ) ) ;
#51619 = CARTESIAN_POINT ( 'NONE',  ( -3.889087296526037463, -6.412877669190318208, 1.818019484660534424 ) ) ;
#51620 = CARTESIAN_POINT ( 'NONE',  ( -5.153800228976328057, -19.02544592524343514, 97.29057627198099567 ) ) ;
#51621 = CARTESIAN_POINT ( 'NONE',  ( -5.049401038297874678, -19.05341960407617918, 19.79275706135233293 ) ) ;
#51622 = CARTESIAN_POINT ( 'NONE',  ( 19.05341960407611168, 5.049401038298154454, 93.95724293864769550 ) ) ;
#51623 = CARTESIAN_POINT ( 'NONE',  ( -5.823673210054116645, -21.52544592524344225, 57.29057627198103120 ) ) ;
#51624 = CARTESIAN_POINT ( 'NONE',  ( -12.06949235617756955, 12.14591786802309770, 95.62390960531436690 ) ) ;
#51625 = CARTESIAN_POINT ( 'NONE',  ( 5.049401038298161559, -19.05341960407611168, 62.70724293864769550 ) ) ;
#51626 = CARTESIAN_POINT ( 'NONE',  ( -4.379528057220328563, 16.55341960407611168, 110.2072429386477239 ) ) ;
#51627 = CARTESIAN_POINT ( 'NONE',  ( 18.62759615963255655, 10.81492255796105972, 26.66775706135235424 ) ) ;
#51628 = VECTOR ( 'NONE', #110184, 1000.000000000000000 ) ;
#51629 = CARTESIAN_POINT ( 'NONE',  ( -21.52544592524334988, -5.823673210054445271, 78.95942372801901854 ) ) ;
#51630 = CARTESIAN_POINT ( 'NONE',  ( 19.05341960407611168, 5.049401038298154454, 38.95724293864767418 ) ) ;
#51631 = CARTESIAN_POINT ( 'NONE',  ( -4.379528057220086978, -16.55341960407618274, 79.79275706135236135 ) ) ;
#51632 = CARTESIAN_POINT ( 'NONE',  ( -21.55341960407619339, 5.719274019375674811, 28.54275706135234358 ) ) ;
#51633 = CARTESIAN_POINT ( 'NONE',  ( 5.823673210054444382, -21.52544592524334988, 30.20942372801902565 ) ) ;
#51635 = CARTESIAN_POINT ( 'NONE',  ( -5.153800228976328057, -19.02544592524343514, 67.29057627198102409 ) ) ;
#51634 = CARTESIAN_POINT ( 'NONE',  ( -9.564922557961040184, 16.46253265017147172, 52.91775706135233293 ) ) ;
#51636 = CARTESIAN_POINT ( 'NONE',  ( 19.05341960407617918, -5.049401038297876454, 26.04275706135233293 ) ) ;
#51637 = CARTESIAN_POINT ( 'NONE',  ( -21.53943276465977519, -0.05219959533937600094, 88.75109039468567573 ) ) ;
#51638 = CARTESIAN_POINT ( 'NONE',  ( 18.67979575497178502, 10.72451020669898547, 64.16557627198102409 ) ) ;
#51639 = CARTESIAN_POINT ( 'NONE',  ( -14.34966873604960291, -8.224510206698953496, 56.66557627198103830 ) ) ;
#51641 = CARTESIAN_POINT ( 'NONE',  ( -13.97604488694547697, 13.89961937509957934, 23.12609039468565442 ) ) ;
#51640 = CARTESIAN_POINT ( 'NONE',  ( 21.55341960407619695, -5.719274019375665929, 91.04275706135236135 ) ) ;
#51642 = CARTESIAN_POINT ( 'NONE',  ( -16.52544592524342804, 4.483927247898546575, 71.04057627198103830 ) ) ;
#51643 = CARTESIAN_POINT ( 'NONE',  ( 19.03943276465977164, -0.05219959533909143690, 23.74890960531435269 ) ) ;
#51644 = CARTESIAN_POINT ( 'NONE',  ( -9.564922557961040184, 16.46253265017147172, 62.91775706135233293 ) ) ;
#51645 = CARTESIAN_POINT ( 'NONE',  ( -16.52544592524335698, -4.483927247898792601, 108.9594237280190185 ) ) ;
#51646 = CARTESIAN_POINT ( 'NONE',  ( 21.52544592524334988, 5.823673210054432836, 86.45942372801901854 ) ) ;
#51647 = CARTESIAN_POINT ( 'NONE',  ( -5.153800228976328057, -19.02544592524343514, 82.29057627198103830 ) ) ;
#51648 = CARTESIAN_POINT ( 'NONE',  ( 5.153800228976615827, -19.02544592524334988, 45.20942372801901143 ) ) ;
#51649 = CARTESIAN_POINT ( 'NONE',  ( -5.823673210054116645, -21.52544592524344225, 57.29057627198103120 ) ) ;
#51650 = CARTESIAN_POINT ( 'NONE',  ( 0.05219959533937995610, -21.53943276465977519, 50.00109039468568994 ) ) ;
#51651 = CARTESIAN_POINT ( 'NONE',  ( -21.53943276465977519, 0.05219959533907696930, 101.2489096053143669 ) ) ;
#51652 = CARTESIAN_POINT ( 'NONE',  ( -16.51473224551082808, 9.474510206698731452, 93.33442372801900433 ) ) ;
#51653 = CARTESIAN_POINT ( 'NONE',  ( 16.55341960407618274, -4.379528057220086978, 61.04275706135234714 ) ) ;
#51655 = CARTESIAN_POINT ( 'NONE',  ( 0.05219959533907565091, 21.53943276465977519, 109.9989096053143527 ) ) ;
#51654 = CARTESIAN_POINT ( 'NONE',  ( -17.97161686093721400, 5.500000000000146549, 55.99637206859166128 ) ) ;
#51656 = CARTESIAN_POINT ( 'NONE',  ( -8.224510206698948167, 14.34966873604960824, 95.41557627198102409 ) ) ;
#51657 = CARTESIAN_POINT ( 'NONE',  ( -17.44279575226822132, -5.990770900252460507, 99.16442432485683867 ) ) ;
#51658 = CARTESIAN_POINT ( 'NONE',  ( 12.14591786802327356, -12.06949235617739191, 30.62609039468567929 ) ) ;
#51659 = CARTESIAN_POINT ( 'NONE',  ( -18.67979575497178146, -10.72451020669898902, 61.66557627198103120 ) ) ;
#51660 = CARTESIAN_POINT ( 'NONE',  ( 8.224510206698742110, 14.34966873604972548, 97.08442372801904696 ) ) ;
#51661 = CARTESIAN_POINT ( 'NONE',  ( -9.474510206698964154, 16.51473224551069663, 30.41557627198102054 ) ) ;
#51662 = CARTESIAN_POINT ( 'NONE',  ( 8.314922557961029526, -14.29746914071037800, 60.41775706135235424 ) ) ;
#51663 = CARTESIAN_POINT ( 'NONE',  ( -16.51473224551082808, 9.474510206698731452, 63.33442372801900433 ) ) ;
#51664 = CARTESIAN_POINT ( 'NONE',  ( 21.55341960407619695, -5.719274019375665929, 41.04275706135236135 ) ) ;
#51665 = CARTESIAN_POINT ( 'NONE',  ( 10.72451020669898902, -18.67979575497178502, 57.91557627198103120 ) ) ;
#51666 = CARTESIAN_POINT ( 'NONE',  ( 14.29746914071037800, 8.314922557961029526, 86.66775706135234714 ) ) ;
#51667 = CARTESIAN_POINT ( 'NONE',  ( 15.80617190586769283, -15.72974639402175789, 70.62609039468567573 ) ) ;
#51668 = EDGE_CURVE ( 'NONE', #44025, #243, #11138, .T. ) ;
#51669 = CARTESIAN_POINT ( 'NONE',  ( 21.53943276465977519, -0.05219959533907433946, 53.74890960531437401 ) ) ;
#51670 = CARTESIAN_POINT ( 'NONE',  ( -21.53943276465977519, 0.05219959533907696930, 36.24890960531435979 ) ) ;
#51671 = ORIENTED_EDGE ( 'NONE', *, *, #74956, .F. ) ;
#51672 = ORIENTED_EDGE ( 'NONE', *, *, #194116, .T. ) ;
#51673 = CARTESIAN_POINT ( 'NONE',  ( -16.55341960407617563, 4.379528057220093196, 63.54275706135234003 ) ) ;
#51674 = CARTESIAN_POINT ( 'NONE',  ( 15.72974639402199770, -15.80617190586745480, 28.12390960531435979 ) ) ;
#51675 = ORIENTED_EDGE ( 'NONE', *, *, #79934, .T. ) ;
#51676 = CARTESIAN_POINT ( 'NONE',  ( -0.05219959533909027116, -19.03943276465977164, 97.49890960531436690 ) ) ;
#51677 = CARTESIAN_POINT ( 'NONE',  ( -4.483927247898539470, -16.52544592524342804, 22.29057627198102765 ) ) ;
#51678 = CARTESIAN_POINT ( 'NONE',  ( -25.31021317688466254, 7.802057701675677137, 170.7256852586636171 ) ) ;
#51679 = CARTESIAN_POINT ( 'NONE',  ( -0.05219959533910754901, -16.53943276465976808, 112.4989096053143669 ) ) ;
#51680 = CARTESIAN_POINT ( 'NONE',  ( -10.72451020669898014, 18.67979575497178502, 60.41557627198102409 ) ) ;
#51681 = CARTESIAN_POINT ( 'NONE',  ( -5.049401038298153566, 19.05341960407611168, 40.20724293864768839 ) ) ;
#51682 = CARTESIAN_POINT ( 'NONE',  ( -12.06949235617739369, -12.14591786802326823, 84.37609039468570415 ) ) ;
#51683 = CARTESIAN_POINT ( 'NONE',  ( 5.719274019375673035, 21.55341960407619339, 37.29275706135235424 ) ) ;
#51684 = CARTESIAN_POINT ( 'NONE',  ( -13.89961937509957401, -13.97604488694547875, 104.3760903946856757 ) ) ;
#51685 = CARTESIAN_POINT ( 'NONE',  ( -4.379528057220328563, 16.55341960407611168, 100.2072429386476955 ) ) ;
#51686 = CARTESIAN_POINT ( 'NONE',  ( 0.05219959533909260263, 19.03943276465977164, 59.99890960531436690 ) ) ;
#51687 = CARTESIAN_POINT ( 'NONE',  ( -5.153800228976328057, -19.02544592524343514, 22.29057627198102765 ) ) ;
#51688 = CARTESIAN_POINT ( 'NONE',  ( 0.4356378768753526032, 24.23951953793845249, -54.26206177644314010 ) ) ;
#51689 = CARTESIAN_POINT ( 'NONE',  ( -16.46253265017160317, 9.564922557960807481, 85.83224293864769550 ) ) ;
#51690 = CARTESIAN_POINT ( 'NONE',  ( 12.06949235617739724, 12.14591786802326823, 81.87609039468568994 ) ) ;
#51691 = CARTESIAN_POINT ( 'NONE',  ( -21.52544592524334988, -5.823673210054445271, 108.9594237280190185 ) ) ;
#51692 = CARTESIAN_POINT ( 'NONE',  ( 21.53943276465977519, -0.05219959533907433946, 53.74890960531437401 ) ) ;
#51693 = CARTESIAN_POINT ( 'NONE',  ( -12.06949235617739369, -12.14591786802326823, 74.37609039468568994 ) ) ;
#51694 = CARTESIAN_POINT ( 'NONE',  ( -5.153800228976607833, 19.02544592524334988, 77.70942372801900433 ) ) ;
#51695 = CARTESIAN_POINT ( 'NONE',  ( 13.89961937509977652, -13.97604488694527269, 43.12390960531434558 ) ) ;
#51696 = CARTESIAN_POINT ( 'NONE',  ( 0.05219959533909260263, 19.03943276465977164, 74.99890960531435269 ) ) ;
#51697 = CARTESIAN_POINT ( 'NONE',  ( 16.51473224551069308, 9.474510206698969483, 39.16557627198103120 ) ) ;
#51698 = CARTESIAN_POINT ( 'NONE',  ( -9.474510206698720793, -16.51473224551083518, 69.58442372801901854 ) ) ;
#51699 = CARTESIAN_POINT ( 'NONE',  ( 9.564922557960805705, 16.46253265017160317, 114.5822429386476955 ) ) ;
#51700 = CARTESIAN_POINT ( 'NONE',  ( 5.153800228976335163, 19.02544592524342804, 94.79057627198103830 ) ) ;
#51701 = CARTESIAN_POINT ( 'NONE',  ( -12.14591786802309592, -12.06949235617757132, 56.87390960531436690 ) ) ;
#51702 = CARTESIAN_POINT ( 'NONE',  ( 21.53943276465977519, -0.05219959533907433946, 43.74890960531435979 ) ) ;
#51703 = DIRECTION ( 'NONE',  ( 0.000000000000000000, 0.000000000000000000, 1.000000000000000000 ) ) ;
#51704 = CARTESIAN_POINT ( 'NONE',  ( 19.02544592524334988, 5.153800228976608722, 31.45942372801900433 ) ) ;
#51705 = CARTESIAN_POINT ( 'NONE',  ( -17.49999999999999645, -5.624438216177581218, 79.18329655085355512 ) ) ;
#51706 = CARTESIAN_POINT ( 'NONE',  ( -5.153800228976328057, -19.02544592524343514, 52.29057627198100988 ) ) ;
#51707 = CARTESIAN_POINT ( 'NONE',  ( 8.314922557961029526, -14.29746914071037800, 40.41775706135234714 ) ) ;
#51708 = DIRECTION ( 'NONE',  ( 0.000000000000000000, 0.000000000000000000, -1.000000000000000000 ) ) ;
#51709 = CARTESIAN_POINT ( 'NONE',  ( 21.38418241377623019, -7.427326039334300134, 174.4773576836617224 ) ) ;
#51710 = CARTESIAN_POINT ( 'NONE',  ( -12.14591786802326823, 12.06949235617739902, 78.12609039468570415 ) ) ;
#51711 = CARTESIAN_POINT ( 'NONE',  ( 0.05219959533907565091, 21.53943276465977519, 99.99890960531436690 ) ) ;
#51712 = CARTESIAN_POINT ( 'NONE',  ( -8.224510206698735004, -14.34966873604973081, 39.58442372801901143 ) ) ;
#51714 = DIRECTION ( 'NONE',  ( -0.4999999999999978906, 0.5000000000000033307, -0.7071067811865466846 ) ) ;
#51713 = CARTESIAN_POINT ( 'NONE',  ( -16.51473224551069308, -9.474510206698971260, 46.66557627198102409 ) ) ;
#51715 = CARTESIAN_POINT ( 'NONE',  ( -18.67979575497193778, 10.72451020669871902, 43.33442372801901143 ) ) ;
#51716 = CARTESIAN_POINT ( 'NONE',  ( -19.02544592524334988, -5.153800228976617603, 63.95942372801899012 ) ) ;
#51717 = CARTESIAN_POINT ( 'NONE',  ( 5.823673210054444382, -21.52544592524334988, 100.2094237280190043 ) ) ;
#51718 = DIRECTION ( 'NONE',  ( 1.000000000000000000, 0.000000000000000000, -6.938893903907222067E-15 ) ) ;
#51719 = CARTESIAN_POINT ( 'NONE',  ( 12.14591786802309770, 12.06949235617756955, 39.37390960531436690 ) ) ;
#51720 = CARTESIAN_POINT ( 'NONE',  ( 18.89770734986050726, 5.499999999999904077, 41.60214472496639360 ) ) ;
#51721 = CARTESIAN_POINT ( 'NONE',  ( 18.62759615963271287, -10.81492255796078972, 58.33224293864768839 ) ) ;
#51722 = CARTESIAN_POINT ( 'NONE',  ( 22.44159573604009239, 16.30477369853692693, 142.0750000027311728 ) ) ;
#51723 = CARTESIAN_POINT ( 'NONE',  ( 5.153800228976335163, 19.02544592524342804, 109.7905762719810099 ) ) ;
#51724 = CARTESIAN_POINT ( 'NONE',  ( 4.379528057220339221, -16.55341960407611168, 102.7072429386476955 ) ) ;
#51725 = CARTESIAN_POINT ( 'NONE',  ( 8.224510206698742110, 14.34966873604972548, 27.08442372801901854 ) ) ;
#51726 = CARTESIAN_POINT ( 'NONE',  ( -0.05219959533934338120, 16.53943276465976808, 112.5010903946857042 ) ) ;
#51727 = ORIENTED_EDGE ( 'NONE', *, *, #26464, .F. ) ;
#51729 = CARTESIAN_POINT ( 'NONE',  ( 15.72974639402199770, -15.80617190586745480, 108.1239096053143811 ) ) ;
#51728 = CARTESIAN_POINT ( 'NONE',  ( -19.05341960407611168, -5.049401038298163336, 101.4572429386476955 ) ) ;
#51731 = CARTESIAN_POINT ( 'NONE',  ( -16.51473224551069308, -9.474510206698971260, 111.6655762719810383 ) ) ;
#51730 = CARTESIAN_POINT ( 'NONE',  ( -16.55341960407611168, -4.379528057220339221, 26.45724293864768839 ) ) ;
#51732 = CARTESIAN_POINT ( 'NONE',  ( 5.049401038297881783, 19.05341960407617563, 97.29275706135233293 ) ) ;
#51733 = CARTESIAN_POINT ( 'NONE',  ( 15.72974639402176855, 15.80617190586768217, 101.8760903946857042 ) ) ;
#51734 = CARTESIAN_POINT ( 'NONE',  ( -8.314922557960811034, -14.29746914071050412, 32.08224293864769550 ) ) ;
#51735 = CARTESIAN_POINT ( 'NONE',  ( -18.62759615963270932, 10.81492255796079327, 85.83224293864768129 ) ) ;
#51736 = CARTESIAN_POINT ( 'NONE',  ( 21.55341960407610458, 5.719274019375980345, 53.95724293864770260 ) ) ;
#51737 = CARTESIAN_POINT ( 'NONE',  ( 13.97604488694527802, 13.89961937509977652, 64.37390960531436690 ) ) ;
#51738 = CARTESIAN_POINT ( 'NONE',  ( 8.314922557960818139, 14.29746914071049879, 39.58224293864769550 ) ) ;
#51739 = CARTESIAN_POINT ( 'NONE',  ( -19.02544592524342804, 5.153800228976336051, 76.04057627198102409 ) ) ;
#51740 = AXIS2_PLACEMENT_3D ( 'NONE', #54953, #99447, #5436 ) ;
#51741 = CARTESIAN_POINT ( 'NONE',  ( 18.56101223717331905, 5.499999999999942268, 58.94978406935675252 ) ) ;
#51742 = CARTESIAN_POINT ( 'NONE',  ( -19.03943276465977164, -0.05219959533935918106, 38.75109039468566152 ) ) ;
#51743 = CARTESIAN_POINT ( 'NONE',  ( -18.62759615963270932, 10.81492255796079327, 85.83224293864768129 ) ) ;
#51744 = CARTESIAN_POINT ( 'NONE',  ( 8.314922557960818139, 14.29746914071049879, 89.58224293864768129 ) ) ;
#51745 = CARTESIAN_POINT ( 'NONE',  ( -21.52544592524334988, -5.823673210054445271, 38.95942372801901854 ) ) ;
#51746 = CARTESIAN_POINT ( 'NONE',  ( -8.571926809382601320, -26.38167802310801591, 147.7750000027311899 ) ) ;
#51747 = CARTESIAN_POINT ( 'NONE',  ( 16.55341960407618274, -4.379528057220086978, 101.0427570613523756 ) ) ;
#51748 = CARTESIAN_POINT ( 'NONE',  ( -16.46253265017160317, 9.564922557960807481, 25.83224293864769194 ) ) ;
#51749 = CARTESIAN_POINT ( 'NONE',  ( -19.03943276465977164, 0.05219959533909376836, 86.24890960531436690 ) ) ;
#51750 = CARTESIAN_POINT ( 'NONE',  ( -30.74264578624800492, 22.33583958711400186, -9.949999994537627401 ) ) ;
#51751 = CARTESIAN_POINT ( 'NONE',  ( 14.34966873604960469, 8.224510206698951720, 49.16557627198102409 ) ) ;
#51752 = CARTESIAN_POINT ( 'NONE',  ( 15.80617190586769283, -15.72974639402175789, 60.62609039468567573 ) ) ;
#51753 = CARTESIAN_POINT ( 'NONE',  ( 25.83444802367794679, -27.47999234037484939, -20.36589038153131881 ) ) ;
#51754 = CARTESIAN_POINT ( 'NONE',  ( 16.46253265017160672, -9.564922557960803928, 38.33224293864768839 ) ) ;
#51755 = CARTESIAN_POINT ( 'NONE',  ( -0.05219959533909027116, -19.03943276465977164, 47.49890960531435979 ) ) ;
#51756 = ORIENTED_EDGE ( 'NONE', *, *, #42529, .F. ) ;
#51757 = CARTESIAN_POINT ( 'NONE',  ( -15.80617190586768217, 15.72974639402176855, 103.1260903946856757 ) ) ;
#51758 = CARTESIAN_POINT ( 'NONE',  ( 12.06949235617739724, 12.14591786802326823, 66.87609039468568994 ) ) ;
#51759 = CARTESIAN_POINT ( 'NONE',  ( -21.52544592524334988, -5.823673210054445271, 83.95942372801900433 ) ) ;
#51760 = CARTESIAN_POINT ( 'NONE',  ( -15.80617190586745835, -15.72974639402198527, 21.87390960531436690 ) ) ;
#51761 = CARTESIAN_POINT ( 'NONE',  ( -13.97604488694547697, 13.89961937509957934, 93.12609039468566152 ) ) ;
#51762 = CARTESIAN_POINT ( 'NONE',  ( 15.80617190586769283, -15.72974639402175789, 75.62609039468567573 ) ) ;
#51763 = CARTESIAN_POINT ( 'NONE',  ( 14.34966873604972726, -8.224510206698740333, 30.83442372801902209 ) ) ;
#51764 = CARTESIAN_POINT ( 'NONE',  ( 5.719274019375991003, -21.55341960407610458, 92.70724293864770971 ) ) ;
#51765 = CARTESIAN_POINT ( 'NONE',  ( -19.03943276465977164, -0.05219959533935918106, 103.7510903946856757 ) ) ;
#51766 = CARTESIAN_POINT ( 'NONE',  ( 19.02544592524343514, -5.153800228976328945, 63.54057627198103830 ) ) ;
#51767 = CARTESIAN_POINT ( 'NONE',  ( 13.97604488694548053, -13.89961937509957401, 105.6260903946856757 ) ) ;
#51768 = AXIS2_PLACEMENT_3D ( 'NONE', #50526, #173876, #35346 ) ;
#51769 = CARTESIAN_POINT ( 'NONE',  ( -19.05341960407617563, 5.049401038297882671, 98.54275706135233293 ) ) ;
#51770 = CARTESIAN_POINT ( 'NONE',  ( -0.05219959533910754901, -16.53943276465976808, 47.49890960531435979 ) ) ;
#51771 = CARTESIAN_POINT ( 'NONE',  ( 19.05341960407617918, -5.049401038297876454, 76.04275706135230450 ) ) ;
#51772 = CARTESIAN_POINT ( 'NONE',  ( -4.379528057220086978, -16.55341960407618274, 74.79275706135234714 ) ) ;
#51774 = CARTESIAN_POINT ( 'NONE',  ( -19.05341960407611168, -5.049401038298163336, 41.45724293864769550 ) ) ;
#51773 = CARTESIAN_POINT ( 'NONE',  ( 10.81492255796078972, 18.62759615963270932, 114.5822429386477097 ) ) ;
#51775 = CARTESIAN_POINT ( 'NONE',  ( -9.564922557960796823, -16.46253265017161027, 62.08224293864769550 ) ) ;
#51776 = CARTESIAN_POINT ( 'NONE',  ( -8.314922557961024197, 14.29746914071037800, 72.91775706135234714 ) ) ;
#51777 = CARTESIAN_POINT ( 'NONE',  ( -17.14385361876520264, -23.59649016807271593, 141.6750000027311103 ) ) ;
#51778 = CARTESIAN_POINT ( 'NONE',  ( 23.31738231874054534, 16.94106989632529192, 145.4500000054623854 ) ) ;
#51779 = CARTESIAN_POINT ( 'NONE',  ( -9.474510206698964154, 16.51473224551069663, 105.4155762719810383 ) ) ;
#51780 = DIRECTION ( 'NONE',  ( 0.7071067811865466846, -2.468850131082262977E-15, -0.7071067811865484609 ) ) ;
#51781 = ORIENTED_EDGE ( 'NONE', *, *, #112155, .F. ) ;
#51782 = CARTESIAN_POINT ( 'NONE',  ( 9.474510206698729675, 16.51473224551082808, 112.0844237280190043 ) ) ;
#51783 = CARTESIAN_POINT ( 'NONE',  ( -18.62759615963270932, 10.81492255796079327, 55.83224293864770260 ) ) ;
#51785 = CARTESIAN_POINT ( 'NONE',  ( -12.14591786802326823, 12.06949235617739902, 28.12609039468568284 ) ) ;
#51784 = CARTESIAN_POINT ( 'NONE',  ( 16.51473224551083163, -9.474510206698727899, 45.83442372801900433 ) ) ;
#51786 = CARTESIAN_POINT ( 'NONE',  ( 19.03943276465977164, -0.05219959533909143690, 33.74890960531435979 ) ) ;
#51787 = CARTESIAN_POINT ( 'NONE',  ( 19.02544592524343514, -5.153800228976328945, 53.54057627198102409 ) ) ;
#51788 = CARTESIAN_POINT ( 'NONE',  ( 18.67979575497178502, 10.72451020669898547, 89.16557627198102409 ) ) ;
#51789 = CARTESIAN_POINT ( 'NONE',  ( -19.02544592524342804, 5.153800228976336051, 106.0405762719810241 ) ) ;
#51790 = EDGE_CURVE ( 'NONE', #171099, #33122, #59600, .T. ) ;
#51791 = CARTESIAN_POINT ( 'NONE',  ( 19.02544592524343514, -5.153800228976328945, 53.54057627198102409 ) ) ;
#51792 = LINE ( 'NONE', #111477, #188855 ) ;
#51793 = CARTESIAN_POINT ( 'NONE',  ( -16.51473224551082808, 9.474510206698731452, 103.3344237280190043 ) ) ;
#51794 = CARTESIAN_POINT ( 'NONE',  ( -16.53943276465976808, 0.05219959533911058130, 66.24890960531436690 ) ) ;
#51795 = CARTESIAN_POINT ( 'NONE',  ( 5.823673210054444382, -21.52544592524334988, 105.2094237280190328 ) ) ;
#51796 = CARTESIAN_POINT ( 'NONE',  ( -0.05219959533907301413, -21.53943276465977519, 92.49890960531436690 ) ) ;
#51797 = CARTESIAN_POINT ( 'NONE',  ( -15.72974639402176322, -15.80617190586768395, 84.37609039468570415 ) ) ;
#51798 = CARTESIAN_POINT ( 'NONE',  ( 5.049401038298161559, -19.05341960407611168, 22.70724293864769194 ) ) ;
#51799 = CARTESIAN_POINT ( 'NONE',  ( -10.81492255796105439, 18.62759615963255655, 77.91775706135231871 ) ) ;
#51800 = CARTESIAN_POINT ( 'NONE',  ( 16.51473224551069308, 9.474510206698969483, 104.1655762719810241 ) ) ;
#51802 = CARTESIAN_POINT ( 'NONE',  ( 5.719274019375673035, 21.55341960407619339, 72.29275706135236135 ) ) ;
#51801 = CARTESIAN_POINT ( 'NONE',  ( 4.483927247898545687, 16.52544592524342804, 24.79057627198103120 ) ) ;
#51803 = CARTESIAN_POINT ( 'NONE',  ( 9.564922557960805705, 16.46253265017160317, 64.58224293864769550 ) ) ;
#51804 = CARTESIAN_POINT ( 'NONE',  ( -10.81492255796105439, 18.62759615963255655, 47.91775706135234714 ) ) ;
#51805 = CARTESIAN_POINT ( 'NONE',  ( 13.97604488694527802, 13.89961937509977652, 79.37390960531435269 ) ) ;
#51806 = CARTESIAN_POINT ( 'NONE',  ( -12.14591786802309592, -12.06949235617757132, 91.87390960531436690 ) ) ;
#51807 = CARTESIAN_POINT ( 'NONE',  ( 8.224510206698953496, -14.34966873604960469, 62.91557627198102409 ) ) ;
#51808 = CARTESIAN_POINT ( 'NONE',  ( -5.719274019375978568, 21.55341960407610458, 75.20724293864769550 ) ) ;
#51809 = CARTESIAN_POINT ( 'NONE',  ( 19.05341960407611168, 5.049401038298154454, 63.95724293864769550 ) ) ;
#51810 = CARTESIAN_POINT ( 'NONE',  ( 15.80617190586746368, 15.72974639402197994, 74.37390960531436690 ) ) ;
#51811 = CARTESIAN_POINT ( 'NONE',  ( 19.02544592524334988, 5.153800228976608722, 66.45942372801899012 ) ) ;
#51813 = CARTESIAN_POINT ( 'NONE',  ( 4.379528057220339221, -16.55341960407611168, 77.70724293864770971 ) ) ;
#51812 = CARTESIAN_POINT ( 'NONE',  ( 19.03943276465977164, 0.05219959533936151252, 31.25109039468566863 ) ) ;
#51814 = CARTESIAN_POINT ( 'NONE',  ( -15.80617190586745835, -15.72974639402198527, 46.87390960531435979 ) ) ;
#51815 = CARTESIAN_POINT ( 'NONE',  ( 17.26172910966779384, 6.454744622555852906, 101.6935309135077716 ) ) ;
#51817 = CARTESIAN_POINT ( 'NONE',  ( 27.73933785331498925, -9.013057229001034898, 146.2750000027311899 ) ) ;
#51816 = CARTESIAN_POINT ( 'NONE',  ( -4.483927247898782831, 16.52544592524335698, 97.70942372801904696 ) ) ;
#51818 = CARTESIAN_POINT ( 'NONE',  ( -13.89961937509957401, -13.97604488694547875, 99.37609039468567573 ) ) ;
#51819 = CARTESIAN_POINT ( 'NONE',  ( -14.34966873604960291, -8.224510206698953496, 71.66557627198100988 ) ) ;
#51820 = DIRECTION ( 'NONE',  ( -0.000000000000000000, -0.000000000000000000, 1.000000000000000000 ) ) ;
#51821 = CARTESIAN_POINT ( 'NONE',  ( -13.89961937509977652, 13.97604488694528158, 65.62390960531436690 ) ) ;
#51822 = CARTESIAN_POINT ( 'NONE',  ( -4.379528057220328563, 16.55341960407611168, 55.20724293864770260 ) ) ;
#51823 = CARTESIAN_POINT ( 'NONE',  ( 16.51473224551069308, 9.474510206698969483, 104.1655762719810241 ) ) ;
#51825 = CARTESIAN_POINT ( 'NONE',  ( -16.46253265017160317, 9.564922557960807481, 65.83224293864769550 ) ) ;
#51824 = CARTESIAN_POINT ( 'NONE',  ( 13.89961937509957401, 13.97604488694547697, 71.87609039468567573 ) ) ;
#51826 = CARTESIAN_POINT ( 'NONE',  ( -19.02544592524342804, 5.153800228976336051, 91.04057627198100988 ) ) ;
#51827 = AXIS2_PLACEMENT_3D ( 'NONE', #28856, #58188, #149204 ) ;
#51828 = CARTESIAN_POINT ( 'NONE',  ( 13.89961937509977652, -13.97604488694527269, 68.12390960531436690 ) ) ;
#51829 = CARTESIAN_POINT ( 'NONE',  ( 10.72451020669898902, -18.67979575497178502, 67.91557627198102409 ) ) ;
#51830 = CARTESIAN_POINT ( 'NONE',  ( 12.06949235617739724, 12.14591786802326823, 61.87609039468568284 ) ) ;
#51831 = CARTESIAN_POINT ( 'NONE',  ( 17.97214573761834089, 5.499999999999959144, 98.96970049038660022 ) ) ;
#51832 = CARTESIAN_POINT ( 'NONE',  ( 19.02544592524343514, -5.153800228976328945, 48.54057627198103120 ) ) ;
#51833 = CARTESIAN_POINT ( 'NONE',  ( 18.62759615963271287, -10.81492255796078972, 48.33224293864770260 ) ) ;
#51834 = CARTESIAN_POINT ( 'NONE',  ( -16.51473224551082808, 9.474510206698731452, 78.33442372801900433 ) ) ;
#51836 = CARTESIAN_POINT ( 'NONE',  ( -21.55341960407619339, 5.719274019375674811, 38.54275706135234714 ) ) ;
#51835 = CARTESIAN_POINT ( 'NONE',  ( 16.55341960407611168, 4.379528057220329451, 28.95724293864769905 ) ) ;
#51837 = CARTESIAN_POINT ( 'NONE',  ( 19.05341960407617918, -5.049401038297876454, 31.04275706135232227 ) ) ;
#51839 = CARTESIAN_POINT ( 'NONE',  ( 12.06949235617739724, 12.14591786802326823, 96.87609039468568994 ) ) ;
#51838 = CARTESIAN_POINT ( 'NONE',  ( -4.483927247898782831, 16.52544592524335698, 62.70942372801902565 ) ) ;
#51840 = CARTESIAN_POINT ( 'NONE',  ( 19.01533133064921088, -5.499999999999425349, 41.26586590595739068 ) ) ;
#51841 = CARTESIAN_POINT ( 'NONE',  ( -8.314922557961024197, 14.29746914071037800, 82.91775706135234714 ) ) ;
#51843 = CARTESIAN_POINT ( 'NONE',  ( -14.34966873604972548, 8.224510206698743886, 38.33442372801900433 ) ) ;
#51842 = CARTESIAN_POINT ( 'NONE',  ( 15.80617190586746368, 15.72974639402197994, 24.37390960531435979 ) ) ;
#51844 = CARTESIAN_POINT ( 'NONE',  ( -19.02544592524342804, 5.153800228976336051, 51.04057627198103120 ) ) ;
#51845 = CARTESIAN_POINT ( 'NONE',  ( 13.89961937509977652, -13.97604488694527269, 53.12390960531434558 ) ) ;
#51846 = CARTESIAN_POINT ( 'NONE',  ( 19.02544592524343514, -5.153800228976328945, 63.54057627198103830 ) ) ;
#51847 = CARTESIAN_POINT ( 'NONE',  ( 21.52544592524334988, 5.823673210054432836, 46.45942372801901854 ) ) ;
#51848 = CARTESIAN_POINT ( 'NONE',  ( 12.06949235617739724, 12.14591786802326823, 46.87609039468568994 ) ) ;
#51849 = CARTESIAN_POINT ( 'NONE',  ( -16.52544592524342804, 4.483927247898546575, 26.04057627198103475 ) ) ;
#51850 = CARTESIAN_POINT ( 'NONE',  ( 13.97604488694527802, 13.89961937509977652, 29.37390960531435979 ) ) ;
#51851 = CARTESIAN_POINT ( 'NONE',  ( -5.823673210054431948, 21.52544592524334988, 112.7094237280190328 ) ) ;
#51852 = CARTESIAN_POINT ( 'NONE',  ( -16.46253265017146816, -9.564922557961047289, 104.1677570613523329 ) ) ;
#51853 = CARTESIAN_POINT ( 'NONE',  ( -19.03943276465977164, -0.05219959533935918106, 68.75109039468566152 ) ) ;
#51854 = CARTESIAN_POINT ( 'NONE',  ( -8.224510206698948167, 14.34966873604960824, 65.41557627198102409 ) ) ;
#51855 = CARTESIAN_POINT ( 'NONE',  ( -9.564922557960796823, -16.46253265017161027, 32.08224293864769550 ) ) ;
#51857 = CARTESIAN_POINT ( 'NONE',  ( 0.000000000000000000, 2.357898499370431722, -2.818925648462311528E-15 ) ) ;
#51856 = CARTESIAN_POINT ( 'NONE',  ( -9.564922557961040184, 16.46253265017147172, 67.91775706135233293 ) ) ;
#51858 = CARTESIAN_POINT ( 'NONE',  ( 21.52544592524334988, 5.823673210054432836, 81.45942372801900433 ) ) ;
#51859 = CARTESIAN_POINT ( 'NONE',  ( -14.29746914071037622, -8.314922557961029526, 34.16775706135234714 ) ) ;
#51860 = DIRECTION ( 'NONE',  ( 0.000000000000000000, 0.000000000000000000, 1.000000000000000000 ) ) ;
#51861 = CARTESIAN_POINT ( 'NONE',  ( -5.823673210054116645, -21.52544592524344225, 42.29057627198103120 ) ) ;
#51862 = CARTESIAN_POINT ( 'NONE',  ( 14.29746914071037800, 8.314922557961029526, 21.66775706135235069 ) ) ;
#51863 = CARTESIAN_POINT ( 'NONE',  ( 13.97604488694527802, 13.89961937509977830, 24.37390960531435269 ) ) ;
#51864 = CARTESIAN_POINT ( 'NONE',  ( -9.564922557961040184, 16.46253265017147172, 27.91775706135232582 ) ) ;
#51865 = CARTESIAN_POINT ( 'NONE',  ( 9.278585747845305320, 10.38518860439147495, -60.35672204601533508 ) ) ;
#51866 = CARTESIAN_POINT ( 'NONE',  ( 16.51473224551069308, 9.474510206698969483, 39.16557627198103120 ) ) ;
#51867 = DIRECTION ( 'NONE',  ( -0.000000000000000000, -0.000000000000000000, 1.000000000000000000 ) ) ;
#51868 = CARTESIAN_POINT ( 'NONE',  ( -5.153800228976328057, -19.02544592524343514, 52.29057627198100988 ) ) ;
#51869 = CARTESIAN_POINT ( 'NONE',  ( -18.39443945427638738, 5.500000000000031974, 98.51745347608651571 ) ) ;
#51870 = ADVANCED_FACE ( 'NONE', ( #112228, #173918 ), #110234, .F. ) ;
#51871 = CARTESIAN_POINT ( 'NONE',  ( 16.51473224551083163, -9.474510206698727899, 25.83442372801900078 ) ) ;
#51872 = CARTESIAN_POINT ( 'NONE',  ( 4.379528057220092307, 16.55341960407617563, 112.2927570613523471 ) ) ;
#51873 = CARTESIAN_POINT ( 'NONE',  ( -19.02544592524342804, 5.153800228976336051, 36.04057627198100988 ) ) ;
#51874 = CARTESIAN_POINT ( 'NONE',  ( -9.564922557960796823, -16.46253265017161027, 97.08224293864769550 ) ) ;
#51875 = CARTESIAN_POINT ( 'NONE',  ( 10.81492255796106328, -18.62759615963255655, 70.41775706135236135 ) ) ;
#51876 = CARTESIAN_POINT ( 'NONE',  ( -5.153800228976328057, -19.02544592524343514, 32.29057627198102409 ) ) ;
#51877 = CARTESIAN_POINT ( 'NONE',  ( -18.62759615963255300, -10.81492255796106328, 69.16775706135234714 ) ) ;
#51879 = CARTESIAN_POINT ( 'NONE',  ( -21.55341960407610458, -5.719274019375992779, 26.45724293864768839 ) ) ;
#51878 = CARTESIAN_POINT ( 'NONE',  ( 19.05341960407617918, -5.049401038297876454, 96.04275706135231871 ) ) ;
#51880 = CARTESIAN_POINT ( 'NONE',  ( -5.153800228976328057, -19.02544592524343514, 42.29057627198101699 ) ) ;
#51881 = CARTESIAN_POINT ( 'NONE',  ( 10.81492255796078972, 18.62759615963270932, 104.5822429386477097 ) ) ;
#51882 = CARTESIAN_POINT ( 'NONE',  ( -19.05341960407617563, 5.049401038297882671, 28.54275706135232937 ) ) ;
#51883 = CARTESIAN_POINT ( 'NONE',  ( -14.29746914071049879, 8.314922557960819915, 105.8322429386476955 ) ) ;
#51884 = CARTESIAN_POINT ( 'NONE',  ( -13.89961937509977652, 13.97604488694528158, 65.62390960531436690 ) ) ;
#51885 = CARTESIAN_POINT ( 'NONE',  ( -0.05219959533936034679, 19.03943276465977164, 92.50109039468566152 ) ) ;
#51886 = CARTESIAN_POINT ( 'NONE',  ( 8.224510206698953496, -14.34966873604960469, 77.91557627198102409 ) ) ;
#51887 = CARTESIAN_POINT ( 'NONE',  ( -0.05219959533907301413, -21.53943276465977519, 27.49890960531435269 ) ) ;
#51888 = CARTESIAN_POINT ( 'NONE',  ( 5.049401038297881783, 19.05341960407617563, 82.29275706135229029 ) ) ;
#51889 = CARTESIAN_POINT ( 'NONE',  ( -18.67979575497178146, -10.72451020669898902, 86.66557627198102409 ) ) ;
#51890 = CARTESIAN_POINT ( 'NONE',  ( -5.719274019375665041, -21.55341960407619695, 39.79275706135235424 ) ) ;
#51891 = CARTESIAN_POINT ( 'NONE',  ( 16.55341960407618274, -4.379528057220086978, 46.04275706135234714 ) ) ;
#51893 = CARTESIAN_POINT ( 'NONE',  ( -5.719274019375665041, -21.55341960407619695, 54.79275706135235424 ) ) ;
#51892 = CARTESIAN_POINT ( 'NONE',  ( 8.224510206698742110, 14.34966873604972548, 57.08442372801901854 ) ) ;
#51894 = CARTESIAN_POINT ( 'NONE',  ( 21.55341960407610458, 5.719274019375980345, 58.95724293864770971 ) ) ;
#51895 = CARTESIAN_POINT ( 'NONE',  ( -5.049401038298153566, 19.05341960407611168, 45.20724293864769550 ) ) ;
#51896 = CARTESIAN_POINT ( 'NONE',  ( -11.74264578624800670, 36.14014761921585972, -4.149999994537627579 ) ) ;
#51897 = CARTESIAN_POINT ( 'NONE',  ( -14.34966873604972548, 8.224510206698743886, 73.33442372801901854 ) ) ;
#51898 = CARTESIAN_POINT ( 'NONE',  ( -15.80617190586745835, -15.72974639402198527, 96.87390960531436690 ) ) ;
#51899 = CARTESIAN_POINT ( 'NONE',  ( -4.483927247898539470, -16.52544592524342804, 52.29057627198102409 ) ) ;
#51900 = CARTESIAN_POINT ( 'NONE',  ( 8.224510206698742110, 14.34966873604972548, 57.08442372801901854 ) ) ;
#51901 = CARTESIAN_POINT ( 'NONE',  ( -19.03943276465977164, -0.05219959533935918106, 93.75109039468566152 ) ) ;
#51902 = CARTESIAN_POINT ( 'NONE',  ( -18.62759615963270932, 10.81492255796079327, 95.83224293864770971 ) ) ;
#51903 = CARTESIAN_POINT ( 'NONE',  ( -16.52544592524342804, 4.483927247898546575, 46.04057627198103830 ) ) ;
#51904 = VERTEX_POINT ( 'NONE', #140571 ) ;
#51905 = CARTESIAN_POINT ( 'NONE',  ( -4.483927247898782831, 16.52544592524335698, 77.70942372801900433 ) ) ;
#51906 = CARTESIAN_POINT ( 'NONE',  ( 19.02130022317636815, -5.499999999999793943, 93.28188669246577547 ) ) ;
#51907 = CARTESIAN_POINT ( 'NONE',  ( -10.81492255796078084, -18.62759615963271287, 72.08224293864769550 ) ) ;
#51908 = CARTESIAN_POINT ( 'NONE',  ( -12.14591786802309592, -12.06949235617757132, 21.87390960531436690 ) ) ;
#51909 = ORIENTED_EDGE ( 'NONE', *, *, #90658, .F. ) ;
#51910 = CARTESIAN_POINT ( 'NONE',  ( -5.000000000000000888, 4.999999999999999112, -18.00000000000000000 ) ) ;
#51911 = CARTESIAN_POINT ( 'NONE',  ( -15.72974639402197994, 15.80617190586746368, 100.6239096053143811 ) ) ;
#51912 = CARTESIAN_POINT ( 'NONE',  ( 0.05219959533907565091, 21.53943276465977519, 109.9989096053143527 ) ) ;
#51913 = CARTESIAN_POINT ( 'NONE',  ( 16.52544592524342804, -4.483927247898539470, 33.54057627198102409 ) ) ;
#51914 = CARTESIAN_POINT ( 'NONE',  ( -4.483927247898782831, 16.52544592524335698, 52.70942372801902565 ) ) ;
#51915 = CARTESIAN_POINT ( 'NONE',  ( 19.03943276465977164, -0.05219959533909143690, 43.74890960531435979 ) ) ;
#51916 = CARTESIAN_POINT ( 'NONE',  ( -16.51473224551069308, -9.474510206698971260, 71.66557627198102409 ) ) ;
#51917 = ORIENTED_EDGE ( 'NONE', *, *, #42762, .F. ) ;
#51918 = CARTESIAN_POINT ( 'NONE',  ( 19.02544592524343514, -5.153800228976328945, 113.5405762719810241 ) ) ;
#51919 = CARTESIAN_POINT ( 'NONE',  ( -33.17841651221153398, -18.64421535752885362, -21.40882326906567812 ) ) ;
#51920 = CARTESIAN_POINT ( 'NONE',  ( 16.51473224551083163, -9.474510206698727899, 110.8344237280190043 ) ) ;
#51921 = CARTESIAN_POINT ( 'NONE',  ( 16.46253265017146816, 9.564922557961045513, 51.66775706135233293 ) ) ;
#51922 = CARTESIAN_POINT ( 'NONE',  ( 15.72974639402199770, -15.80617190586745480, 88.12390960531436690 ) ) ;
#51923 = CARTESIAN_POINT ( 'NONE',  ( -14.29746914071037622, -8.314922557961029526, 109.1677570613523613 ) ) ;
#51924 = CARTESIAN_POINT ( 'NONE',  ( -5.153800228976328057, -19.02544592524343514, 77.29057627198099567 ) ) ;
#51925 = CARTESIAN_POINT ( 'NONE',  ( -21.52544592524343514, 5.823673210054127303, 41.04057627198103120 ) ) ;
#51927 = CARTESIAN_POINT ( 'NONE',  ( -14.34966873604972548, 8.224510206698743886, 23.33442372801901499 ) ) ;
#51926 = CARTESIAN_POINT ( 'NONE',  ( -15.80617190586745835, -15.72974639402198527, 81.87390960531435269 ) ) ;
#51928 = CARTESIAN_POINT ( 'NONE',  ( 21.52544592524344225, -5.823673210054117533, 28.54057627198103120 ) ) ;
#51929 = CARTESIAN_POINT ( 'NONE',  ( 18.67979575497194134, -10.72451020669871369, 80.83442372801901854 ) ) ;
#51930 = CARTESIAN_POINT ( 'NONE',  ( -16.51473224551069308, -9.474510206698971260, 76.66557627198103830 ) ) ;
#51931 = CARTESIAN_POINT ( 'NONE',  ( -5.049401038298153566, 19.05341960407611168, 25.20724293864768484 ) ) ;
#51932 = CARTESIAN_POINT ( 'NONE',  ( -13.89961937509977652, 13.97604488694528158, 85.62390960531433848 ) ) ;
#51933 = CARTESIAN_POINT ( 'NONE',  ( 0.05219959533910956823, 16.53943276465976808, 89.99890960531438111 ) ) ;
#51934 = EDGE_LOOP ( 'NONE', ( #94812, #15197 ) ) ;
#51935 = CARTESIAN_POINT ( 'NONE',  ( 9.474510206698729675, 16.51473224551082808, 102.0844237280190043 ) ) ;
#51936 = DIRECTION ( 'NONE',  ( 0.000000000000000000, 1.000000000000000000, 0.000000000000000000 ) ) ;
#51937 = CARTESIAN_POINT ( 'NONE',  ( 19.02544592524343514, -5.153800228976328945, 78.54057627198099567 ) ) ;
#51939 = CARTESIAN_POINT ( 'NONE',  ( -9.474510206698964154, 16.51473224551069663, 100.4155762719810241 ) ) ;
#51938 = CARTESIAN_POINT ( 'NONE',  ( 15.80617190586769283, -15.72974639402175789, 80.62609039468567573 ) ) ;
#51940 = CARTESIAN_POINT ( 'NONE',  ( -4.379528057220086978, -16.55341960407618274, 79.79275706135236135 ) ) ;
#51941 = CARTESIAN_POINT ( 'NONE',  ( -17.48853670773247160, -5.747243402303015891, 76.33328700250010002 ) ) ;
#51942 = CARTESIAN_POINT ( 'NONE',  ( 13.89961937509957401, 13.97604488694547697, 51.87609039468566863 ) ) ;
#51943 = CARTESIAN_POINT ( 'NONE',  ( -16.51473224551082808, 9.474510206698731452, 23.33442372801900078 ) ) ;
#51944 = CARTESIAN_POINT ( 'NONE',  ( 4.704672000039139768, 6.719938155502468646, -64.14994679864911120 ) ) ;
#51945 = CARTESIAN_POINT ( 'NONE',  ( -38.00000000000004263, -12.34694845685037023, -7.649999994537626691 ) ) ;
#51946 = CARTESIAN_POINT ( 'NONE',  ( 29.86685920354754842, -21.69954338932559068, -6.324999997268814234 ) ) ;
#51947 = CARTESIAN_POINT ( 'NONE',  ( 16.53943276465976808, -0.05219959533910856209, 23.74890960531435269 ) ) ;
#51948 = DIRECTION ( 'NONE',  ( 1.000000000000000000, 0.000000000000000000, 0.000000000000000000 ) ) ;
#51949 = CARTESIAN_POINT ( 'NONE',  ( 12.06949235617739724, 12.14591786802326823, 111.8760903946856615 ) ) ;
#51950 = CARTESIAN_POINT ( 'NONE',  ( 23.29544513554940011, 16.92513159979228021, 145.4656553485623647 ) ) ;
#51951 = CARTESIAN_POINT ( 'NONE',  ( -8.314922557961024197, 14.29746914071037800, 87.91775706135234714 ) ) ;
#51952 = CARTESIAN_POINT ( 'NONE',  ( 15.80617190586769283, -15.72974639402175789, 95.62609039468568994 ) ) ;
#51953 = CARTESIAN_POINT ( 'NONE',  ( 5.153800228976615827, -19.02544592524334988, 100.2094237280190043 ) ) ;
#51954 = CARTESIAN_POINT ( 'NONE',  ( 18.62759615963255655, 10.81492255796105972, 66.66775706135234714 ) ) ;
#51955 = CARTESIAN_POINT ( 'NONE',  ( 0.05219959533936267826, -19.03943276465977164, 45.00109039468566863 ) ) ;
#51956 = CARTESIAN_POINT ( 'NONE',  ( -13.97604488694527625, -13.89961937509977652, 76.87390960531433848 ) ) ;
#51957 = CARTESIAN_POINT ( 'NONE',  ( -9.564922557960796823, -16.46253265017161027, 57.08224293864769550 ) ) ;
#51958 = CARTESIAN_POINT ( 'NONE',  ( -18.87580814761071935, 5.500000000000042633, 40.87172394265763842 ) ) ;
#51959 = CARTESIAN_POINT ( 'NONE',  ( -10.81492255796078084, -18.62759615963271287, 97.08224293864770971 ) ) ;
#51960 = CARTESIAN_POINT ( 'NONE',  ( 18.62759615963271287, -10.81492255796078972, 48.33224293864770260 ) ) ;
#51961 = CARTESIAN_POINT ( 'NONE',  ( -5.153800228976328057, -19.02544592524343514, 47.29057627198102409 ) ) ;
#51962 = CARTESIAN_POINT ( 'NONE',  ( 12.14591786802327356, -12.06949235617739191, 60.62609039468567573 ) ) ;
#51963 = UNCERTAINTY_MEASURE_WITH_UNIT (LENGTH_MEASURE( 1.000000000000000082E-05 ), #93038, 'distance_accuracy_value', 'NONE');
#51964 = ORIENTED_EDGE ( 'NONE', *, *, #154401, .T. ) ;
#51965 = CARTESIAN_POINT ( 'NONE',  ( -21.55341960407619339, 5.719274019375674811, 48.54275706135234714 ) ) ;
#51967 = CARTESIAN_POINT ( 'NONE',  ( -5.950531402560715689E-15, 38.81732327939063509, -1.124999997268812946 ) ) ;
#51966 = CARTESIAN_POINT ( 'NONE',  ( 14.29746914071049879, -8.314922557960816363, 68.33224293864769550 ) ) ;
#51968 = CARTESIAN_POINT ( 'NONE',  ( -12.14591786802326823, 12.06949235617739902, 43.12609039468568284 ) ) ;
#51969 = CARTESIAN_POINT ( 'NONE',  ( -4.379528057220328563, 16.55341960407611168, 100.2072429386476955 ) ) ;
#51970 = CARTESIAN_POINT ( 'NONE',  ( -19.05341960407617563, 5.049401038297882671, 48.54275706135233293 ) ) ;
#51971 = CARTESIAN_POINT ( 'NONE',  ( -4.379528057220328563, 16.55341960407611168, 65.20724293864768129 ) ) ;
#51972 = CARTESIAN_POINT ( 'NONE',  ( 21.52544592524334988, 5.823673210054432836, 26.45942372801901854 ) ) ;
#51974 = CARTESIAN_POINT ( 'NONE',  ( 0.05219959533907565091, 21.53943276465977519, 89.99890960531438111 ) ) ;
#51973 = CARTESIAN_POINT ( 'NONE',  ( -0.05219959533909027116, -19.03943276465977164, 27.49890960531435624 ) ) ;
#51975 = ADVANCED_BREP_SHAPE_REPRESENTATION ( '', ( #74599, #82054 ), #17734 ) ;
#51976 = CARTESIAN_POINT ( 'NONE',  ( -13.89961937509977652, 13.97604488694528158, 105.6239096053143527 ) ) ;
#51977 = CARTESIAN_POINT ( 'NONE',  ( -14.29746914071049879, 8.314922557960819915, 75.83224293864769550 ) ) ;
#51978 = CARTESIAN_POINT ( 'NONE',  ( 31.90410663231038768, -24.66877891592865879, -17.57859634139417082 ) ) ;
#51979 = CARTESIAN_POINT ( 'NONE',  ( 36.91746824999999177, 11.99521256947799230, -3.524999997268813079 ) ) ;
#51980 = CARTESIAN_POINT ( 'NONE',  ( -13.97604488694547697, 13.89961937509957934, 83.12609039468564731 ) ) ;
#51981 = CARTESIAN_POINT ( 'NONE',  ( -10.72451020669870658, -18.67979575497194134, 19.58442372801901143 ) ) ;
#51982 = CARTESIAN_POINT ( 'NONE',  ( 13.97604488694527802, 13.89961937509977652, 74.37390960531436690 ) ) ;
#51983 = CARTESIAN_POINT ( 'NONE',  ( 16.51473224551083163, -9.474510206698727899, 55.83442372801899722 ) ) ;
#51984 = CARTESIAN_POINT ( 'NONE',  ( 19.03943276465977164, -0.05219959533909143690, 28.74890960531435624 ) ) ;
#51985 = CARTESIAN_POINT ( 'NONE',  ( 8.224510206698953496, -14.34966873604960469, 57.91557627198103120 ) ) ;
#51986 = CARTESIAN_POINT ( 'NONE',  ( 4.483927247898545687, 16.52544592524342804, 59.79057627198103120 ) ) ;
#51987 = CARTESIAN_POINT ( 'NONE',  ( 19.03943276465977164, -0.05219959533909143690, 78.74890960531436690 ) ) ;
#51988 = CARTESIAN_POINT ( 'NONE',  ( 18.62759615963271287, -10.81492255796078972, 93.33224293864769550 ) ) ;
#51989 = CARTESIAN_POINT ( 'NONE',  ( 9.474510206698971260, -16.51473224551069308, 72.91557627198102409 ) ) ;
#51990 = CARTESIAN_POINT ( 'NONE',  ( 18.62759615963271287, -10.81492255796078972, 78.33224293864770971 ) ) ;
#51991 = CARTESIAN_POINT ( 'NONE',  ( 19.05341960407617918, -5.049401038297876454, 21.04275706135232582 ) ) ;
#51994 = CARTESIAN_POINT ( 'NONE',  ( 0.05219959533910956823, 16.53943276465976808, 89.99890960531438111 ) ) ;
#51993 = CARTESIAN_POINT ( 'NONE',  ( 16.52544592524335698, 4.483927247898782831, 111.4594237280190328 ) ) ;
#51992 = CARTESIAN_POINT ( 'NONE',  ( 16.46253265017160672, -9.564922557960803928, 28.33224293864769550 ) ) ;
#51995 = CARTESIAN_POINT ( 'NONE',  ( -5.153800228976607833, 19.02544592524334988, 92.70942372801901854 ) ) ;
#51996 = ORIENTED_EDGE ( 'NONE', *, *, #69172, .T. ) ;
#51997 = CARTESIAN_POINT ( 'NONE',  ( -21.53943276465977519, 0.05219959533907696930, 116.2489096053143669 ) ) ;
#51998 = CARTESIAN_POINT ( 'NONE',  ( 19.05341960407617918, -5.049401038297876454, 51.04275706135231871 ) ) ;
#51999 = CARTESIAN_POINT ( 'NONE',  ( -4.379528057220086978, -16.55341960407618274, 104.7927570613523898 ) ) ;
#52000 = CARTESIAN_POINT ( 'NONE',  ( -19.02544592524334988, -5.153800228976617603, 38.95942372801900433 ) ) ;
#52001 = CARTESIAN_POINT ( 'NONE',  ( -5.153800228976328057, -19.02544592524343514, 97.29057627198099567 ) ) ;
#52002 = CARTESIAN_POINT ( 'NONE',  ( -12.14591786802309592, -12.06949235617757132, 51.87390960531437401 ) ) ;
#52003 = CARTESIAN_POINT ( 'NONE',  ( -19.52217212775657984, 5.500000000000114575, 49.93993709005260939 ) ) ;
#52004 = CARTESIAN_POINT ( 'NONE',  ( -19.05341960407611168, -5.049401038298163336, 31.45724293864769550 ) ) ;
#52005 = CARTESIAN_POINT ( 'NONE',  ( -18.62759615963255300, -10.81492255796106328, 109.1677570613523613 ) ) ;
#52006 = CARTESIAN_POINT ( 'NONE',  ( 4.483927247898790824, -16.52544592524335698, 80.20942372801901854 ) ) ;
#52007 = CARTESIAN_POINT ( 'NONE',  ( 21.53943276465977519, 0.05219959533937863772, 36.25109039468567573 ) ) ;
#52008 = CARTESIAN_POINT ( 'NONE',  ( 8.224510206698742110, 14.34966873604972548, 47.08442372801901854 ) ) ;
#52009 = CARTESIAN_POINT ( 'NONE',  ( -16.51473224551069308, -9.474510206698971260, 101.6655762719810241 ) ) ;
#52010 = CARTESIAN_POINT ( 'NONE',  ( -19.05341960407611168, -5.049401038298163336, 51.45724293864770260 ) ) ;
#52011 = CARTESIAN_POINT ( 'NONE',  ( 16.51473224551069308, 9.474510206698969483, 69.16557627198102409 ) ) ;
#52012 = CARTESIAN_POINT ( 'NONE',  ( -8.224510206698735004, -14.34966873604973081, 44.58442372801901854 ) ) ;
#52013 = CARTESIAN_POINT ( 'NONE',  ( -16.53943276465976808, 0.05219959533911058130, 106.2489096053143811 ) ) ;
#52014 = CARTESIAN_POINT ( 'NONE',  ( 4.379528057220339221, -16.55341960407611168, 22.70724293864769194 ) ) ;
#52015 = FACE_OUTER_BOUND ( 'NONE', #24120, .T. ) ;
#52018 = CARTESIAN_POINT ( 'NONE',  ( 0.05219959533909260263, 19.03943276465977164, 64.99890960531436690 ) ) ;
#52017 = CARTESIAN_POINT ( 'NONE',  ( 9.474510206698971260, -16.51473224551069308, 87.91557627198102409 ) ) ;
#52016 = CARTESIAN_POINT ( 'NONE',  ( -21.52544592524334988, -5.823673210054445271, 53.95942372801900433 ) ) ;
#52019 = CARTESIAN_POINT ( 'NONE',  ( -13.97604488694527625, -13.89961937509977652, 91.87390960531432427 ) ) ;
#52020 = CARTESIAN_POINT ( 'NONE',  ( -8.224510206698948167, 14.34966873604960824, 45.41557627198103830 ) ) ;
#52021 = CARTESIAN_POINT ( 'NONE',  ( -12.06949235617739369, -12.14591786802326823, 109.3760903946857042 ) ) ;
#52022 = CARTESIAN_POINT ( 'NONE',  ( -0.05219959533910754901, -16.53943276465976808, 37.49890960531436690 ) ) ;
#52023 = ORIENTED_EDGE ( 'NONE', *, *, #102359, .T. ) ;
#52024 = CARTESIAN_POINT ( 'NONE',  ( -15.34294242576431522, -17.41135957075415774, -55.09099524710079976 ) ) ;
#52025 = CARTESIAN_POINT ( 'NONE',  ( -19.03943276465977164, 0.05219959533909376836, 66.24890960531436690 ) ) ;
#52026 = CARTESIAN_POINT ( 'NONE',  ( -19.02544592524334988, -5.153800228976617603, 33.95942372801897591 ) ) ;
#52027 = CARTESIAN_POINT ( 'NONE',  ( -29.86685920354755552, 21.69954338932564397, -9.324999997268813345 ) ) ;
#52028 = LINE ( 'NONE', #51040, #82952 ) ;
#52030 = CARTESIAN_POINT ( 'NONE',  ( 4.379528057220092307, 16.55341960407617563, 67.29275706135234714 ) ) ;
#52029 = CARTESIAN_POINT ( 'NONE',  ( -16.46253265017146816, -9.564922557961047289, 84.16775706135233293 ) ) ;
#52031 = FACE_OUTER_BOUND ( 'NONE', #19960, .T. ) ;
#52032 =( BOUNDED_CURVE ( )  B_SPLINE_CURVE ( 3, ( #191239, #81053, #116391, #174088 ),
 .UNSPECIFIED., .F., .T. ) 
 B_SPLINE_CURVE_WITH_KNOTS ( ( 4, 4 ),
 ( 1.132647296210725907, 2.115944711806982959 ),
 .UNSPECIFIED. ) 
 CURVE ( )  GEOMETRIC_REPRESENTATION_ITEM ( )  RATIONAL_B_SPLINE_CURVE ( ( 1.000000000000000000, 0.9210371567966660900, 0.9210371567966660900, 1.000000000000000000 ) ) 
 REPRESENTATION_ITEM ( '' )  );
#52033 = CARTESIAN_POINT ( 'NONE',  ( -13.89961937509977652, 13.97604488694528158, 90.62390960531432427 ) ) ;
#52034 = CARTESIAN_POINT ( 'NONE',  ( -10.72451020669870658, -18.67979575497194134, 29.58442372801901854 ) ) ;
#52035 = CARTESIAN_POINT ( 'NONE',  ( 9.474510206698729675, 16.51473224551082808, 87.08442372801900433 ) ) ;
#52037 = CARTESIAN_POINT ( 'NONE',  ( -5.153800228976328057, -19.02544592524343514, 52.29057627198100988 ) ) ;
#52036 = CARTESIAN_POINT ( 'NONE',  ( 5.049401038298161559, -19.05341960407611168, 112.7072429386476813 ) ) ;
#52038 = EDGE_CURVE ( 'NONE', #65463, #45569, #36368, .T. ) ;
#52039 = CARTESIAN_POINT ( 'NONE',  ( 19.05341960407611168, 5.049401038298154454, 93.95724293864769550 ) ) ;
#52041 = CARTESIAN_POINT ( 'NONE',  ( 0.05219959533909260263, 19.03943276465977164, 54.99890960531435979 ) ) ;
#52040 = CARTESIAN_POINT ( 'NONE',  ( -4.379528057220328563, 16.55341960407611168, 50.20724293864769550 ) ) ;
#52042 = CARTESIAN_POINT ( 'NONE',  ( 16.46253265017146816, 9.564922557961045513, 61.66775706135234003 ) ) ;
#52043 = ORIENTED_EDGE ( 'NONE', *, *, #83840, .T. ) ;
#52044 = CARTESIAN_POINT ( 'NONE',  ( 0.05219959533910956823, 16.53943276465976808, 84.99890960531436690 ) ) ;
#52045 = CARTESIAN_POINT ( 'NONE',  ( -16.51473224551082808, 9.474510206698731452, 33.33442372801899722 ) ) ;
#52046 = CARTESIAN_POINT ( 'NONE',  ( 0.05219959533909260263, 19.03943276465977164, 64.99890960531436690 ) ) ;
#52047 = CARTESIAN_POINT ( 'NONE',  ( 15.72974639402199770, -15.80617190586745480, 68.12390960531436690 ) ) ;
#52049 = CARTESIAN_POINT ( 'NONE',  ( -9.564922557961040184, 16.46253265017147172, 27.91775706135232582 ) ) ;
#52048 = CARTESIAN_POINT ( 'NONE',  ( -12.14591786802309592, -12.06949235617757132, 61.87390960531436690 ) ) ;
#52050 = CARTESIAN_POINT ( 'NONE',  ( 16.46253265017160672, -9.564922557960803928, 103.3322429386476955 ) ) ;
#52051 = CARTESIAN_POINT ( 'NONE',  ( -10.81492255796078084, -18.62759615963271287, 27.08224293864769550 ) ) ;
#52052 = CARTESIAN_POINT ( 'NONE',  ( -9.564922557960796823, -16.46253265017161027, 52.08224293864768839 ) ) ;
#52053 = CARTESIAN_POINT ( 'NONE',  ( 9.564922557960805705, 16.46253265017160317, 44.58224293864769550 ) ) ;
#52054 = CARTESIAN_POINT ( 'NONE',  ( 4.379528057220339221, -16.55341960407611168, 102.7072429386476955 ) ) ;
#52055 = CARTESIAN_POINT ( 'NONE',  ( 21.52544592524344225, -5.823673210054117533, 113.5405762719810383 ) ) ;
#52056 = CARTESIAN_POINT ( 'NONE',  ( -13.97604488694527625, -13.89961937509977652, 101.8739096053143811 ) ) ;
#52057 = CARTESIAN_POINT ( 'NONE',  ( 21.53943276465977519, 0.05219959533937863772, 26.25109039468567573 ) ) ;
#52058 = CARTESIAN_POINT ( 'NONE',  ( -9.474510206698964154, 16.51473224551069663, 105.4155762719810383 ) ) ;
#52059 = CARTESIAN_POINT ( 'NONE',  ( 19.05341960407611168, 5.049401038298154454, 23.95724293864769194 ) ) ;
#52060 = CARTESIAN_POINT ( 'NONE',  ( -10.72451020669870658, -18.67979575497194134, 79.58442372801903275 ) ) ;
#52061 = CARTESIAN_POINT ( 'NONE',  ( 10.81492255796078972, 18.62759615963270932, 99.58224293864770971 ) ) ;
#52062 = FACE_BOUND ( 'NONE', #14682, .T. ) ;
#52063 = CARTESIAN_POINT ( 'NONE',  ( 18.22780087662123805, -5.499999999999989342, 53.51763182126895657 ) ) ;
#52064 = CARTESIAN_POINT ( 'NONE',  ( 0.05219959533909260263, 19.03943276465977164, 59.99890960531436690 ) ) ;
#52065 = CARTESIAN_POINT ( 'NONE',  ( 16.53943276465976808, 0.05219959533934440121, 51.25109039468568994 ) ) ;
#52066 = CARTESIAN_POINT ( 'NONE',  ( -16.55341960407611168, -4.379528057220339221, 101.4572429386476955 ) ) ;
#52067 = CARTESIAN_POINT ( 'NONE',  ( 19.52837319214024703, -5.500000000000095923, 52.10471352585538796 ) ) ;
#52068 = CARTESIAN_POINT ( 'NONE',  ( 19.03943276465977164, -0.05219959533909143690, 63.74890960531435979 ) ) ;
#52069 = CARTESIAN_POINT ( 'NONE',  ( 16.52544592524342804, -4.483927247898539470, 93.54057627198103830 ) ) ;
#52071 = B_SPLINE_CURVE_WITH_KNOTS ( 'NONE', 3,
 ( #143545, #47585, #3058, #5031, #49565, #4040, #124410, #78892 ),
 .UNSPECIFIED., .F., .F.,
 ( 4, 2, 2, 4 ),
 ( 0.01263483034531157588, 0.01686471550494908489, 0.01897965808476779689, 0.02109460066458651237 ),
 .UNSPECIFIED. ) ;
#52070 = CARTESIAN_POINT ( 'NONE',  ( -5.823673210054116645, -21.52544592524344225, 42.29057627198103120 ) ) ;
#52072 = CARTESIAN_POINT ( 'NONE',  ( 12.06949235617757843, -12.14591786802309237, 68.12390960531436690 ) ) ;
#52073 = CARTESIAN_POINT ( 'NONE',  ( 14.34966873604972726, -8.224510206698740333, 20.83442372801901143 ) ) ;
#52074 = CARTESIAN_POINT ( 'NONE',  ( -21.52544592524334988, -5.823673210054445271, 78.95942372801901854 ) ) ;
#52075 = DIRECTION ( 'NONE',  ( 1.000000000000000000, -0.000000000000000000, -0.000000000000000000 ) ) ;
#52076 = CARTESIAN_POINT ( 'NONE',  ( -8.314922557961024197, 14.29746914071037800, 102.9177570613523756 ) ) ;
#52077 = CARTESIAN_POINT ( 'NONE',  ( 8.224510206698953496, -14.34966873604960469, 47.91557627198102409 ) ) ;
#52078 = CARTESIAN_POINT ( 'NONE',  ( 13.97604488694527802, 13.89961937509977652, 44.37390960531435269 ) ) ;
#52079 = CARTESIAN_POINT ( 'NONE',  ( 16.46253265017160672, -9.564922557960803928, 83.33224293864768129 ) ) ;
#52080 = CARTESIAN_POINT ( 'NONE',  ( -18.67979575497178146, -10.72451020669898902, 91.66557627198103830 ) ) ;
#52081 = CARTESIAN_POINT ( 'NONE',  ( 16.52544592524335698, 4.483927247898782831, 41.45942372801901143 ) ) ;
#52083 = CARTESIAN_POINT ( 'NONE',  ( 10.72451020669871369, 18.67979575497193778, 77.08442372801901854 ) ) ;
#52082 = CARTESIAN_POINT ( 'NONE',  ( -16.53943276465976808, 0.05219959533911058130, 71.24890960531435269 ) ) ;
#52084 = CARTESIAN_POINT ( 'NONE',  ( 16.52544592524335698, 4.483927247898782831, 96.45942372801901854 ) ) ;
#52085 = CARTESIAN_POINT ( 'NONE',  ( 17.50000000001358558, -5.500000000000039968, 48.29690382535059001 ) ) ;
#52086 = CARTESIAN_POINT ( 'NONE',  ( 0.000000000000000000, -2.357898499370432610, 3.252606517456513302E-15 ) ) ;
#52087 = CARTESIAN_POINT ( 'NONE',  ( -12.14591786802309592, -12.06949235617757132, 21.87390960531436690 ) ) ;
#52088 = CARTESIAN_POINT ( 'NONE',  ( -14.34966873604972548, 8.224510206698743886, 78.33442372801901854 ) ) ;
#52089 = CARTESIAN_POINT ( 'NONE',  ( -5.049401038298153566, 19.05341960407611168, 90.20724293864766707 ) ) ;
#52090 = CARTESIAN_POINT ( 'NONE',  ( -0.05219959533909027116, -19.03943276465977164, 102.4989096053143669 ) ) ;
#52091 = CARTESIAN_POINT ( 'NONE',  ( -0.05219959533937732626, 21.53943276465977519, 82.50109039468568994 ) ) ;
#52092 = CARTESIAN_POINT ( 'NONE',  ( 4.483927247898790824, -16.52544592524335698, 90.20942372801903275 ) ) ;
#52093 = CARTESIAN_POINT ( 'NONE',  ( 14.34966873604960469, 8.224510206698951720, 54.16557627198103120 ) ) ;
#52094 = CARTESIAN_POINT ( 'NONE',  ( -0.05219959533909027116, -19.03943276465977164, 62.49890960531435979 ) ) ;
#52095 = ORIENTED_EDGE ( 'NONE', *, *, #109475, .T. ) ;
#52096 = CARTESIAN_POINT ( 'NONE',  ( -5.049401038297874678, -19.05341960407617918, 104.7927570613523471 ) ) ;
#52097 = CARTESIAN_POINT ( 'NONE',  ( 14.29746914071049879, -8.314922557960816363, 113.3322429386476955 ) ) ;
#52098 = CARTESIAN_POINT ( 'NONE',  ( 19.05341960407611168, 5.049401038298154454, 83.95724293864766707 ) ) ;
#52100 = CARTESIAN_POINT ( 'NONE',  ( -22.81625015709509441, -31.40387420917324590, -10.32499999726881157 ) ) ;
#52099 = CARTESIAN_POINT ( 'NONE',  ( -16.46253265017146816, -9.564922557961047289, 109.1677570613523471 ) ) ;
#52101 = CARTESIAN_POINT ( 'NONE',  ( -16.51473224551082808, 9.474510206698731452, 28.33442372801900433 ) ) ;
#52102 = CARTESIAN_POINT ( 'NONE',  ( 4.483927247898790824, -16.52544592524335698, 85.20942372801901854 ) ) ;
#52103 = CARTESIAN_POINT ( 'NONE',  ( 9.474510206698729675, 16.51473224551082808, 112.0844237280190043 ) ) ;
#52104 = CARTESIAN_POINT ( 'NONE',  ( 4.483927247898545687, 16.52544592524342804, 109.7905762719810383 ) ) ;
#52105 = CARTESIAN_POINT ( 'NONE',  ( 8.224510206698742110, 14.34966873604972548, 62.08442372801901143 ) ) ;
#52106 = CARTESIAN_POINT ( 'NONE',  ( -16.52544592524335698, -4.483927247898792601, 48.95942372801902565 ) ) ;
#52107 = CARTESIAN_POINT ( 'NONE',  ( 37.99999999999999289, 2.893978650043524126E-14, -3.000000000000000000 ) ) ;
#52108 = CARTESIAN_POINT ( 'NONE',  ( -19.02544592524334988, -5.153800228976617603, 63.95942372801899012 ) ) ;
#52109 = CARTESIAN_POINT ( 'NONE',  ( -0.05219959533937732626, 21.53943276465977519, 92.50109039468567573 ) ) ;
#52110 = CARTESIAN_POINT ( 'NONE',  ( 19.05341960407611168, 5.049401038298154454, 28.95724293864769550 ) ) ;
#52111 = CARTESIAN_POINT ( 'NONE',  ( -0.05219959533909027116, -19.03943276465977164, 72.49890960531435269 ) ) ;
#52112 = CARTESIAN_POINT ( 'NONE',  ( -4.483927247898539470, -16.52544592524342804, 67.29057627198103830 ) ) ;
#52113 = CARTESIAN_POINT ( 'NONE',  ( -10.72451020669870658, -18.67979575497194134, 94.58442372801901854 ) ) ;
#52114 = EDGE_CURVE ( 'NONE', #106917, #45831, #137905, .T. ) ;
#52115 = CARTESIAN_POINT ( 'NONE',  ( -19.05341960407617563, 5.049401038297882671, 43.54275706135232582 ) ) ;
#52116 = CARTESIAN_POINT ( 'NONE',  ( -15.72974639402197994, 15.80617190586746368, 35.62390960531437401 ) ) ;
#52117 = CARTESIAN_POINT ( 'NONE',  ( -15.72974639402176322, -15.80617190586768395, 109.3760903946857042 ) ) ;
#52118 = CARTESIAN_POINT ( 'NONE',  ( 16.51473224551069308, 9.474510206698969483, 74.16557627198103830 ) ) ;
#52119 = CARTESIAN_POINT ( 'NONE',  ( -0.05219959533937732626, 21.53943276465977519, 102.5010903946856899 ) ) ;
#52120 = CARTESIAN_POINT ( 'NONE',  ( -10.72451020669898014, 18.67979575497178502, 70.41557627198102409 ) ) ;
#52121 = CARTESIAN_POINT ( 'NONE',  ( -16.46253265017160317, 9.564922557960807481, 100.8322429386477097 ) ) ;
#52122 = CARTESIAN_POINT ( 'NONE',  ( -0.05219959533936034679, 19.03943276465977164, 72.50109039468566152 ) ) ;
#52123 = CARTESIAN_POINT ( 'NONE',  ( -19.05341960407611168, -5.049401038298163336, 101.4572429386476955 ) ) ;
#52124 = CARTESIAN_POINT ( 'NONE',  ( 5.153800228976615827, -19.02544592524334988, 90.20942372801900433 ) ) ;
#52125 = CARTESIAN_POINT ( 'NONE',  ( -12.14591786802326823, 12.06949235617739902, 58.12609039468568994 ) ) ;
#52126 = CARTESIAN_POINT ( 'NONE',  ( -0.05219959533909027116, -19.03943276465977164, 22.49890960531436690 ) ) ;
#52127 = CARTESIAN_POINT ( 'NONE',  ( 19.03943276465977164, -0.05219959533909143690, 88.74890960531436690 ) ) ;
#52128 = CARTESIAN_POINT ( 'NONE',  ( 15.80617190586746368, 15.72974639402197994, 59.37390960531436690 ) ) ;
#52129 = CARTESIAN_POINT ( 'NONE',  ( -12.14591786802326823, 12.06949235617739902, 28.12609039468568284 ) ) ;
#52130 = CARTESIAN_POINT ( 'NONE',  ( -15.80617190586768217, 15.72974639402176855, 33.12609039468569705 ) ) ;
#52131 = CARTESIAN_POINT ( 'NONE',  ( 10.72451020669871369, 18.67979575497193778, 82.08442372801901854 ) ) ;
#52132 = CARTESIAN_POINT ( 'NONE',  ( -8.314922557961024197, 14.29746914071037800, 102.9177570613523756 ) ) ;
#52133 = CARTESIAN_POINT ( 'NONE',  ( 13.97604488694527802, 13.89961937509977652, 84.37390960531433848 ) ) ;
#52134 = CARTESIAN_POINT ( 'NONE',  ( 16.52544592524342804, -4.483927247898539470, 78.54057627198103830 ) ) ;
#52135 = CARTESIAN_POINT ( 'NONE',  ( -16.53943276465976808, 0.05219959533911058130, 21.24890960531436690 ) ) ;
#52136 = CARTESIAN_POINT ( 'NONE',  ( 13.89961937509957401, 13.97604488694547697, 56.87609039468564731 ) ) ;
#52137 = CARTESIAN_POINT ( 'NONE',  ( -10.81492255796105439, 18.62759615963255655, 42.91775706135235424 ) ) ;
#52138 = CARTESIAN_POINT ( 'NONE',  ( 16.52544592524342804, -4.483927247898539470, 93.54057627198103830 ) ) ;
#52139 = CARTESIAN_POINT ( 'NONE',  ( -16.46253265017160317, 9.564922557960807481, 110.8322429386476955 ) ) ;
#52140 = CARTESIAN_POINT ( 'NONE',  ( -14.34966873604972548, 8.224510206698743886, 108.3344237280190185 ) ) ;
#52141 = CARTESIAN_POINT ( 'NONE',  ( 21.55341960407619695, -5.719274019375665929, 86.04275706135236135 ) ) ;
#52142 = CARTESIAN_POINT ( 'NONE',  ( 14.29746914071037800, 8.314922557961029526, 41.66775706135235424 ) ) ;
#52143 = CARTESIAN_POINT ( 'NONE',  ( -18.62759615963255300, -10.81492255796106328, 39.16775706135235424 ) ) ;
#52144 = VERTEX_POINT ( 'NONE', #193071 ) ;
#52145 = CARTESIAN_POINT ( 'NONE',  ( -18.67979575497193778, 10.72451020669871902, 23.33442372801901499 ) ) ;
#52146 = CARTESIAN_POINT ( 'NONE',  ( -16.53943276465976808, 0.05219959533911058130, 91.24890960531436690 ) ) ;
#52147 = CARTESIAN_POINT ( 'NONE',  ( -19.35543954521081034, -5.499999999999584332, 49.58901960356452321 ) ) ;
#52148 = CARTESIAN_POINT ( 'NONE',  ( -14.29746914071049879, 8.314922557960819915, 60.83224293864769550 ) ) ;
#52149 = CARTESIAN_POINT ( 'NONE',  ( -16.52544592524335698, -4.483927247898792601, 103.9594237280190185 ) ) ;
#52150 = CARTESIAN_POINT ( 'NONE',  ( 9.474510206698971260, -16.51473224551069308, 42.91557627198103120 ) ) ;
#52151 = CARTESIAN_POINT ( 'NONE',  ( 18.67979575497178502, 10.72451020669898547, 39.16557627198102409 ) ) ;
#52152 = CARTESIAN_POINT ( 'NONE',  ( -8.314922557960811034, -14.29746914071050412, 82.08224293864768129 ) ) ;
#52153 = CARTESIAN_POINT ( 'NONE',  ( 5.719274019375991003, -21.55341960407610458, 77.70724293864770971 ) ) ;
#52154 = CARTESIAN_POINT ( 'NONE',  ( 19.05341960407611168, 5.049401038298154454, 83.95724293864766707 ) ) ;
#52156 = CARTESIAN_POINT ( 'NONE',  ( -19.03943276465977164, -0.05219959533935918106, 98.75109039468567573 ) ) ;
#52155 = CARTESIAN_POINT ( 'NONE',  ( 19.02544592524343514, -5.153800228976328945, 33.54057627198102409 ) ) ;
#52157 = CARTESIAN_POINT ( 'NONE',  ( 5.823673210054125526, 21.52544592524343514, 34.79057627198103120 ) ) ;
#52158 = CARTESIAN_POINT ( 'NONE',  ( -15.80617190586768217, 15.72974639402176855, 53.12609039468568284 ) ) ;
#52159 = CARTESIAN_POINT ( 'NONE',  ( 19.03943276465977164, -0.05219959533909143690, 58.74890960531435979 ) ) ;
#52160 = CARTESIAN_POINT ( 'NONE',  ( 9.474510206698971260, -16.51473224551069308, 87.91557627198102409 ) ) ;
#52161 = EDGE_LOOP ( 'NONE', ( #134378, #82222, #75294, #67690 ) ) ;
#52162 = CARTESIAN_POINT ( 'NONE',  ( -4.483927247898782831, 16.52544592524335698, 47.70942372801902565 ) ) ;
#52163 = CARTESIAN_POINT ( 'NONE',  ( 10.81492255796106328, -18.62759615963255655, 40.41775706135234714 ) ) ;
#52164 = CARTESIAN_POINT ( 'NONE',  ( 5.823673210054444382, -21.52544592524334988, 75.20942372801901854 ) ) ;
#52165 = CARTESIAN_POINT ( 'NONE',  ( -5.823673210054116645, -21.52544592524344225, 22.29057627198102765 ) ) ;
#52166 = CARTESIAN_POINT ( 'NONE',  ( -10.72451020669898014, 18.67979575497178502, 85.41557627198102409 ) ) ;
#52168 = CARTESIAN_POINT ( 'NONE',  ( 16.55341960407618274, -4.379528057220086978, 66.04275706135236135 ) ) ;
#52167 = CARTESIAN_POINT ( 'NONE',  ( -10.72451020669870658, -18.67979575497194134, 24.58442372801901499 ) ) ;
#52169 = CARTESIAN_POINT ( 'NONE',  ( 15.72974639402199770, -15.80617190586745480, 58.12390960531435979 ) ) ;
#52170 = CARTESIAN_POINT ( 'NONE',  ( -5.049401038297874678, -19.05341960407617918, 19.79275706135233293 ) ) ;
#52172 = CARTESIAN_POINT ( 'NONE',  ( -12.14591786802326823, 12.06949235617739902, 103.1260903946856757 ) ) ;
#52171 = CARTESIAN_POINT ( 'NONE',  ( 16.46253265017160672, -9.564922557960803928, 73.33224293864769550 ) ) ;
#52173 = CARTESIAN_POINT ( 'NONE',  ( -17.49999999999999645, -5.076555817581251517, 106.1795149204977378 ) ) ;
#52174 = CARTESIAN_POINT ( 'NONE',  ( -19.02544592524342804, 5.153800228976336051, 86.04057627198103830 ) ) ;
#52175 = CARTESIAN_POINT ( 'NONE',  ( 13.89961937509957401, 13.97604488694547697, 86.87609039468567573 ) ) ;
#52176 = CARTESIAN_POINT ( 'NONE',  ( 18.67979575497178502, 10.72451020669898547, 59.16557627198103120 ) ) ;
#52177 = CARTESIAN_POINT ( 'NONE',  ( -16.55341960407617563, 4.379528057220093196, 113.5427570613523756 ) ) ;
#52178 = CARTESIAN_POINT ( 'NONE',  ( -19.02544592524334988, -5.153800228976617603, 98.95942372801900433 ) ) ;
#52179 = CARTESIAN_POINT ( 'NONE',  ( -5.049401038298153566, 19.05341960407611168, 40.20724293864768839 ) ) ;
#52180 = CARTESIAN_POINT ( 'NONE',  ( 13.97604488694548053, -13.89961937509957401, 90.62609039468567573 ) ) ;
#52182 = CARTESIAN_POINT ( 'NONE',  ( -13.89961937509957401, -13.97604488694547875, 54.37609039468565442 ) ) ;
#52181 = CARTESIAN_POINT ( 'NONE',  ( 0.05219959533907565091, 21.53943276465977519, 89.99890960531438111 ) ) ;
#52183 = CARTESIAN_POINT ( 'NONE',  ( 13.00000000000000000, 2.055000000000000160, 0.000000000000000000 ) ) ;
#52184 = CARTESIAN_POINT ( 'NONE',  ( 16.51473224551069308, 9.474510206698969483, 49.16557627198102409 ) ) ;
#52185 = CARTESIAN_POINT ( 'NONE',  ( -0.05219959533910754901, -16.53943276465976808, 57.49890960531435979 ) ) ;
#52186 = CARTESIAN_POINT ( 'NONE',  ( -9.564922557960796823, -16.46253265017161027, 47.08224293864769550 ) ) ;
#52187 = CARTESIAN_POINT ( 'NONE',  ( -16.55341960407611168, -4.379528057220339221, 56.45724293864768839 ) ) ;
#52188 = CARTESIAN_POINT ( 'NONE',  ( -15.49999999999999822, -7.500000000000000888, 22.00000000000000711 ) ) ;
#52189 = CARTESIAN_POINT ( 'NONE',  ( 31.54463713289763049, -7.108708273820915302, 92.55936662351712130 ) ) ;
#52190 = CARTESIAN_POINT ( 'NONE',  ( 4.483927247898545687, 16.52544592524342804, 34.79057627198103120 ) ) ;
#52191 = CARTESIAN_POINT ( 'NONE',  ( 16.46253265017160672, -9.564922557960803928, 58.33224293864769550 ) ) ;
#52192 = CARTESIAN_POINT ( 'NONE',  ( -0.05219959533936034679, 19.03943276465977164, 72.50109039468566152 ) ) ;
#52193 = CARTESIAN_POINT ( 'NONE',  ( 5.153800228976615827, -19.02544592524334988, 40.20942372801898301 ) ) ;
#52194 = CARTESIAN_POINT ( 'NONE',  ( -8.224510206698735004, -14.34966873604973081, 49.58442372801901143 ) ) ;
#52195 = CARTESIAN_POINT ( 'NONE',  ( -21.53943276465977519, 0.05219959533907696930, 46.24890960531435979 ) ) ;
#52196 = CARTESIAN_POINT ( 'NONE',  ( -5.719274019375665041, -21.55341960407619695, 109.7927570613523613 ) ) ;
#52197 = CARTESIAN_POINT ( 'NONE',  ( 5.153800228976335163, 19.02544592524342804, 74.79057627198103830 ) ) ;
#52198 = CARTESIAN_POINT ( 'NONE',  ( -17.49999999999999645, -5.500000000000000888, 120.0000000000000142 ) ) ;
#52199 = CARTESIAN_POINT ( 'NONE',  ( 13.97604488694527802, 13.89961937509977652, 99.37390960531436690 ) ) ;
#52200 = CARTESIAN_POINT ( 'NONE',  ( -36.91746825000000598, 2.428612866367529932E-14, -4.624999997268814056 ) ) ;
#52201 = CARTESIAN_POINT ( 'NONE',  ( -21.53943276465977519, -0.05219959533937600094, 23.75109039468567929 ) ) ;
#52202 = CARTESIAN_POINT ( 'NONE',  ( -12.14591786802309592, -12.06949235617757132, 86.87390960531438111 ) ) ;
#52204 = CARTESIAN_POINT ( 'NONE',  ( 9.564922557960805705, 16.46253265017160317, 79.58224293864769550 ) ) ;
#52203 = CARTESIAN_POINT ( 'NONE',  ( 5.719274019375991003, -21.55341960407610458, 92.70724293864770971 ) ) ;
#52205 = CARTESIAN_POINT ( 'NONE',  ( 16.46253265017160672, -9.564922557960803928, 83.33224293864768129 ) ) ;
#52206 = CARTESIAN_POINT ( 'NONE',  ( -5.823673210054116645, -21.52544592524344225, 112.2905762719810241 ) ) ;
#52207 = EDGE_LOOP ( 'NONE', ( #12421, #148348, #17220, #34239, #195689 ) ) ;
#52208 = CARTESIAN_POINT ( 'NONE',  ( 19.05341960407611168, 5.049401038298154454, 73.95724293864768129 ) ) ;
#52209 = EDGE_CURVE ( 'NONE', #188443, #27470, #164734, .T. ) ;
#52210 = CARTESIAN_POINT ( 'NONE',  ( -8.898068258721474777, 27.38543819252877043, 147.5843446568999866 ) ) ;
#52212 = CARTESIAN_POINT ( 'NONE',  ( -19.03943276465977164, 0.05219959533909376836, 31.24890960531435979 ) ) ;
#52211 = CARTESIAN_POINT ( 'NONE',  ( -19.03943276465977164, 0.05219959533909376836, 21.24890960531436335 ) ) ;
#52213 = CARTESIAN_POINT ( 'NONE',  ( -0.05219959533936034679, 19.03943276465977164, 92.50109039468566152 ) ) ;
#52214 = CARTESIAN_POINT ( 'NONE',  ( 12.06949235617757843, -12.14591786802309237, 108.1239096053143811 ) ) ;
#52215 = CARTESIAN_POINT ( 'NONE',  ( -5.719274019375665041, -21.55341960407619695, 69.79275706135234714 ) ) ;
#52217 = CARTESIAN_POINT ( 'NONE',  ( -18.62759615963255300, -10.81492255796106328, 39.16775706135235424 ) ) ;
#52216 = CARTESIAN_POINT ( 'NONE',  ( -16.51473224551069308, -9.474510206698971260, 66.66557627198102409 ) ) ;
#52218 = CARTESIAN_POINT ( 'NONE',  ( 21.55341960407610458, 5.719274019375980345, 113.9572429386477239 ) ) ;
#52219 = CARTESIAN_POINT ( 'NONE',  ( 8.571926809382603096, -26.38167802310801235, 139.9750000027311785 ) ) ;
#52220 = CARTESIAN_POINT ( 'NONE',  ( -9.474510206698964154, 16.51473224551069663, 85.41557627198102409 ) ) ;
#52221 = CARTESIAN_POINT ( 'NONE',  ( 27.94130797166919322, 7.397772140654549133, 160.8977822374800155 ) ) ;
#52223 = CARTESIAN_POINT ( 'NONE',  ( 5.823673210054125526, 21.52544592524343514, 34.79057627198103120 ) ) ;
#52222 = CARTESIAN_POINT ( 'NONE',  ( -0.05219959533934338120, 16.53943276465976808, 27.50109039468567929 ) ) ;
#52224 = CARTESIAN_POINT ( 'NONE',  ( 15.72974639402176855, 15.80617190586768217, 61.87609039468568284 ) ) ;
#52225 = CARTESIAN_POINT ( 'NONE',  ( 13.89961937509977652, -13.97604488694527269, 108.1239096053143669 ) ) ;
#52226 = CARTESIAN_POINT ( 'NONE',  ( -13.97604488694547697, 13.89961937509957934, 103.1260903946856473 ) ) ;
#52227 = CARTESIAN_POINT ( 'NONE',  ( -19.05341960407611168, -5.049401038298163336, 51.45724293864770260 ) ) ;
#52228 = CARTESIAN_POINT ( 'NONE',  ( -13.97604488694527625, -13.89961937509977652, 81.87390960531436690 ) ) ;
#52229 = CARTESIAN_POINT ( 'NONE',  ( 4.483927247898545687, 16.52544592524342804, 94.79057627198105251 ) ) ;
#52230 = DIRECTION ( 'NONE',  ( -0.000000000000000000, -0.000000000000000000, 1.000000000000000000 ) ) ;
#52231 = CARTESIAN_POINT ( 'NONE',  ( -14.29746914071049879, 8.314922557960819915, 85.83224293864768129 ) ) ;
#52232 = CARTESIAN_POINT ( 'NONE',  ( -9.564922557960796823, -16.46253265017161027, 107.0822429386476955 ) ) ;
#52234 = CARTESIAN_POINT ( 'NONE',  ( -13.97604488694527625, -13.89961937509977652, 41.87390960531435979 ) ) ;
#52233 = CARTESIAN_POINT ( 'NONE',  ( -8.224510206698948167, 14.34966873604960824, 60.41557627198102409 ) ) ;
#52235 = CARTESIAN_POINT ( 'NONE',  ( -21.55341960407619339, 5.719274019375674811, 58.54275706135235424 ) ) ;
#52236 = CARTESIAN_POINT ( 'NONE',  ( -19.05341960407617563, 5.049401038297882671, 93.54275706135234714 ) ) ;
#52237 = CARTESIAN_POINT ( 'NONE',  ( 16.53943276465976808, -0.05219959533910856209, 48.74890960531435979 ) ) ;
#52238 = CARTESIAN_POINT ( 'NONE',  ( -15.72974639402197994, 15.80617190586746368, 115.6239096053143669 ) ) ;
#52239 = CARTESIAN_POINT ( 'NONE',  ( 10.81492255796078972, 18.62759615963270932, 44.58224293864769550 ) ) ;
#52240 = CARTESIAN_POINT ( 'NONE',  ( 9.474510206698971260, -16.51473224551069308, 112.9155762719810383 ) ) ;
#52241 = CARTESIAN_POINT ( 'NONE',  ( -28.82186960331499037, 2.428612866367529932E-14, 142.2500000054623683 ) ) ;
#52242 = CARTESIAN_POINT ( 'NONE',  ( 19.03943276465977164, -0.05219959533909143690, 53.74890960531436690 ) ) ;
#52243 = CARTESIAN_POINT ( 'NONE',  ( -16.52544592524342804, 4.483927247898546575, 31.04057627198102409 ) ) ;
#52244 = CARTESIAN_POINT ( 'NONE',  ( 16.55341960407618274, -4.379528057220086978, 96.04275706135236135 ) ) ;
#52245 = CARTESIAN_POINT ( 'NONE',  ( 4.483927247898790824, -16.52544592524335698, 90.20942372801903275 ) ) ;
#52246 = CARTESIAN_POINT ( 'NONE',  ( 5.049401038297881783, 19.05341960407617563, 42.29275706135234003 ) ) ;
#52247 = CARTESIAN_POINT ( 'NONE',  ( -17.40805194822030799, 6.112264579159339739, 70.83371272510613892 ) ) ;
#52248 = CARTESIAN_POINT ( 'NONE',  ( 16.46253265017160672, -9.564922557960803928, 88.33224293864769550 ) ) ;
#52249 = CARTESIAN_POINT ( 'NONE',  ( -16.51473224551069308, -9.474510206698971260, 56.66557627198103120 ) ) ;
#52250 = CARTESIAN_POINT ( 'NONE',  ( -0.05219959533910754901, -16.53943276465976808, 62.49890960531436690 ) ) ;
#52252 = CARTESIAN_POINT ( 'NONE',  ( 18.67979575497178502, 10.72451020669898547, 29.16557627198103120 ) ) ;
#52251 = CARTESIAN_POINT ( 'NONE',  ( 9.474510206698971260, -16.51473224551069308, 22.91557627198102765 ) ) ;
#52253 = CARTESIAN_POINT ( 'NONE',  ( 5.823673210054125526, 21.52544592524343514, 39.79057627198103830 ) ) ;
#52254 = CARTESIAN_POINT ( 'NONE',  ( -12.06949235617756955, 12.14591786802309770, 90.62390960531436690 ) ) ;
#52255 = CARTESIAN_POINT ( 'NONE',  ( 16.55341960407618274, -4.379528057220086978, 41.04275706135236135 ) ) ;
#52256 = CARTESIAN_POINT ( 'NONE',  ( 16.55341960407611168, 4.379528057220329451, 83.95724293864770971 ) ) ;
#52257 = CARTESIAN_POINT ( 'NONE',  ( 31.90000000000003411, -0.1356448107283860505, -45.64921306006599622 ) ) ;
#52258 = CARTESIAN_POINT ( 'NONE',  ( -19.03943276465977164, -0.05219959533935918106, 83.75109039468567573 ) ) ;
#52259 = CARTESIAN_POINT ( 'NONE',  ( 13.89961937509977652, -13.97604488694527269, 108.1239096053143669 ) ) ;
#52260 = CARTESIAN_POINT ( 'NONE',  ( -22.81625015709510507, 31.40387420917330275, -3.424999997268813434 ) ) ;
#52261 = CARTESIAN_POINT ( 'NONE',  ( -22.97983228106267362, 21.73741105231462711, -49.48322453030140622 ) ) ;
#52263 = CARTESIAN_POINT ( 'NONE',  ( 8.224510206698742110, 14.34966873604972548, 112.0844237280190185 ) ) ;
#52262 = CARTESIAN_POINT ( 'NONE',  ( 12.14591786802327356, -12.06949235617739191, 30.62609039468567929 ) ) ;
#52264 = CARTESIAN_POINT ( 'NONE',  ( 19.05341960407617918, -5.049401038297876454, 66.04275706135233293 ) ) ;
#52265 = CARTESIAN_POINT ( 'NONE',  ( -21.55341960407610458, -5.719274019375992779, 41.45724293864769550 ) ) ;
#52266 = CARTESIAN_POINT ( 'NONE',  ( -15.72974639402176322, -15.80617190586768395, 64.37609039468568994 ) ) ;
#52267 = CARTESIAN_POINT ( 'NONE',  ( -20.56371838171433097, -11.04494471775294961, 168.1294998094270454 ) ) ;
#52268 = CARTESIAN_POINT ( 'NONE',  ( 8.314922557961029526, -14.29746914071037800, 35.41775706135234003 ) ) ;
#52270 = CARTESIAN_POINT ( 'NONE',  ( -19.05341960407611168, -5.049401038298163336, 86.45724293864769550 ) ) ;
#52269 = CARTESIAN_POINT ( 'NONE',  ( -5.153800228976328057, -19.02544592524343514, 22.29057627198102765 ) ) ;
#52271 = CARTESIAN_POINT ( 'NONE',  ( 14.79957802611874662, 15.40597107458649973, -58.81775317265829273 ) ) ;
#52272 = CARTESIAN_POINT ( 'NONE',  ( -4.483927247898539470, -16.52544592524342804, 87.29057627198103830 ) ) ;
#52273 = SHAPE_DEFINITION_REPRESENTATION ( #19550, #125845 ) ;
#52274 = CARTESIAN_POINT ( 'NONE',  ( 13.97604488694527802, 13.89961937509977652, 89.37390960531436690 ) ) ;
#52275 = ORIENTED_EDGE ( 'NONE', *, *, #143324, .F. ) ;
#52276 = CARTESIAN_POINT ( 'NONE',  ( -19.02544592524334988, -5.153800228976617603, 108.9594237280189759 ) ) ;
#52277 = CARTESIAN_POINT ( 'NONE',  ( -0.05219959533907301413, -21.53943276465977519, 82.49890960531436690 ) ) ;
#52278 = CARTESIAN_POINT ( 'NONE',  ( 13.97604488694527802, 13.89961937509977652, 39.37390960531435269 ) ) ;
#52280 = CARTESIAN_POINT ( 'NONE',  ( -18.62759615963270932, 10.81492255796079327, 115.8322429386477097 ) ) ;
#52279 = CARTESIAN_POINT ( 'NONE',  ( -19.05341960407617563, 5.049401038297882671, 63.54275706135234003 ) ) ;
#52281 = CARTESIAN_POINT ( 'NONE',  ( 16.46253265017160672, -9.564922557960803928, 63.33224293864769550 ) ) ;
#52282 = CARTESIAN_POINT ( 'NONE',  ( -5.049401038298153566, 19.05341960407611168, 105.2072429386476671 ) ) ;
#52283 = EDGE_LOOP ( 'NONE', ( #192030, #90332, #25436, #165878, #150554, #6692 ) ) ;
#52284 = CARTESIAN_POINT ( 'NONE',  ( 12.06949235617739724, 12.14591786802326823, 36.87609039468568994 ) ) ;
#52285 =( BOUNDED_CURVE ( )  B_SPLINE_CURVE ( 2, ( #171081, #32572, #18408, #107404, #122582, #93228, #92235, #15415, #140732, #110394, #139726 ),
 .UNSPECIFIED., .F., .F. ) 
 B_SPLINE_CURVE_WITH_KNOTS ( ( 3, 2, 2, 2, 2, 3 ),
 ( 0.2000000000000001776, 0.2200000000000001954, 0.2400000000000002132, 0.2600000000000002309, 0.2800000000000003042, 0.3000000000000002665 ),
 .UNSPECIFIED. ) 
 CURVE ( )  GEOMETRIC_REPRESENTATION_ITEM ( )  RATIONAL_B_SPLINE_CURVE ( ( 0.9999999999999995559, 0.9510565162951539753, 1.000000000000000000, 0.9510565162951535312, 1.000000000000000000, 0.9510565162951535312, 1.000000000000000000, 0.9510565162951535312, 1.000000000000000000, 0.9510565162951528650, 1.000000000000000666 ) ) 
 REPRESENTATION_ITEM ( '' )  );
#52286 = CARTESIAN_POINT ( 'NONE',  ( 5.823673210054125526, 21.52544592524343514, 109.7905762719810383 ) ) ;
#52289 = CARTESIAN_POINT ( 'NONE',  ( -9.474510206698720793, -16.51473224551083518, 64.58442372801900433 ) ) ;
#52288 = CARTESIAN_POINT ( 'NONE',  ( 13.89961937509977652, -13.97604488694527269, 88.12390960531438111 ) ) ;
#52287 = CARTESIAN_POINT ( 'NONE',  ( 16.53943276465976808, -0.05219959533910856209, 108.7489096053143669 ) ) ;
#52290 = CARTESIAN_POINT ( 'NONE',  ( -15.80617190586745835, -15.72974639402198527, 81.87390960531435269 ) ) ;
#52291 = CARTESIAN_POINT ( 'NONE',  ( -12.14591786802309592, -12.06949235617757132, 46.87390960531435979 ) ) ;
#52292 = CARTESIAN_POINT ( 'NONE',  ( -13.89961937509957401, -13.97604488694547875, 19.37609039468566507 ) ) ;
#52293 = CARTESIAN_POINT ( 'NONE',  ( 12.14591786802327356, -12.06949235617739191, 65.62609039468568994 ) ) ;
#52294 = CARTESIAN_POINT ( 'NONE',  ( -5.153800228976328057, -19.02544592524343514, 87.29057627198103830 ) ) ;
#52295 = CARTESIAN_POINT ( 'NONE',  ( 13.89961937509977652, -13.97604488694527269, 48.12390960531435979 ) ) ;
#52296 = CARTESIAN_POINT ( 'NONE',  ( 5.823673210054444382, -21.52544592524334988, 50.20942372801901854 ) ) ;
#52297 = CARTESIAN_POINT ( 'NONE',  ( -10.81492255796105439, 18.62759615963255655, 72.91775706135234714 ) ) ;
#52298 = CARTESIAN_POINT ( 'NONE',  ( 19.05341960407611168, 5.049401038298154454, 58.95724293864768129 ) ) ;
#52299 = CARTESIAN_POINT ( 'NONE',  ( 5.823673210054444382, -21.52544592524334988, 40.20942372801901854 ) ) ;
#52300 = CARTESIAN_POINT ( 'NONE',  ( -0.05219959533936034679, 19.03943276465977164, 77.50109039468566152 ) ) ;
#52301 = EDGE_CURVE ( 'NONE', #189322, #81647, #70599, .T. ) ;
#52302 = CARTESIAN_POINT ( 'NONE',  ( -9.474510206698720793, -16.51473224551083518, 69.58442372801901854 ) ) ;
#52303 = CARTESIAN_POINT ( 'NONE',  ( 16.51473224551069308, 9.474510206698969483, 44.16557627198103120 ) ) ;
#52304 = CARTESIAN_POINT ( 'NONE',  ( -16.52544592524335698, -4.483927247898792601, 88.95942372801901854 ) ) ;
#52305 = CARTESIAN_POINT ( 'NONE',  ( -16.51473224551069308, -9.474510206698971260, 46.66557627198102409 ) ) ;
#52306 = CARTESIAN_POINT ( 'NONE',  ( 22.37486833544087617, -13.37560805684410070, 165.5209445320981558 ) ) ;
#52307 = CARTESIAN_POINT ( 'NONE',  ( -9.564922557960796823, -16.46253265017161027, 97.08224293864769550 ) ) ;
#52308 = CARTESIAN_POINT ( 'NONE',  ( 5.049401038298161559, -19.05341960407611168, 37.70724293864768839 ) ) ;
#52309 = CARTESIAN_POINT ( 'NONE',  ( 21.55341960407610458, 5.719274019375980345, 83.95724293864770971 ) ) ;
#52310 = CARTESIAN_POINT ( 'NONE',  ( 16.52544592524335698, 4.483927247898782831, 56.45942372801902565 ) ) ;
#52311 = CARTESIAN_POINT ( 'NONE',  ( -0.05219959533936034679, 19.03943276465977164, 27.50109039468566507 ) ) ;
#52312 = CARTESIAN_POINT ( 'NONE',  ( -13.97604488694527625, -13.89961937509977652, 56.87390960531434558 ) ) ;
#52313 = CARTESIAN_POINT ( 'NONE',  ( 16.55341960407611168, 4.379528057220329451, 38.95724293864768839 ) ) ;
#52314 = CARTESIAN_POINT ( 'NONE',  ( -12.14591786802309592, -12.06949235617757132, 86.87390960531438111 ) ) ;
#52315 = CARTESIAN_POINT ( 'NONE',  ( 5.153800228976335163, 19.02544592524342804, 89.79057627198102409 ) ) ;
#52316 = CARTESIAN_POINT ( 'NONE',  ( 16.51473224551069308, 9.474510206698969483, 79.16557627198103830 ) ) ;
#52317 = CARTESIAN_POINT ( 'NONE',  ( 21.55341960407619695, -5.719274019375665929, 31.04275706135234714 ) ) ;
#52318 = CARTESIAN_POINT ( 'NONE',  ( -9.474510206698964154, 16.51473224551069663, 90.41557627198103830 ) ) ;
#52319 = CARTESIAN_POINT ( 'NONE',  ( 15.72974639402176855, 15.80617190586768217, 101.8760903946857042 ) ) ;
#52320 = CARTESIAN_POINT ( 'NONE',  ( 4.379528057220092307, 16.55341960407617563, 82.29275706135234714 ) ) ;
#52321 = PRODUCT_DEFINITION ( 'UNKNOWN', '', #134078, #159563 ) ;
#52322 = CARTESIAN_POINT ( 'NONE',  ( 10.72451020669871369, 18.67979575497193778, 32.08442372801901854 ) ) ;
#52323 = CARTESIAN_POINT ( 'NONE',  ( -18.62759615963270932, 10.81492255796079327, 90.83224293864769550 ) ) ;
#52324 = CARTESIAN_POINT ( 'NONE',  ( -14.29746914071049879, 8.314922557960819915, 45.83224293864769550 ) ) ;
#52325 = CARTESIAN_POINT ( 'NONE',  ( -19.02544592524342804, 5.153800228976336051, 36.04057627198100988 ) ) ;
#52326 = CARTESIAN_POINT ( 'NONE',  ( 12.14591786802309770, 12.06949235617756955, 69.37390960531436690 ) ) ;
#52327 = CARTESIAN_POINT ( 'NONE',  ( 18.67979575497178502, 10.72451020669898547, 29.16557627198103120 ) ) ;
#52328 = CARTESIAN_POINT ( 'NONE',  ( 5.153800228976615827, -19.02544592524334988, 25.20942372801900433 ) ) ;
#52329 = CARTESIAN_POINT ( 'NONE',  ( -16.53943276465976808, 0.05219959533911058130, 96.24890960531435269 ) ) ;
#52330 = CARTESIAN_POINT ( 'NONE',  ( 19.02544592524343514, -5.153800228976328945, 108.5405762719810383 ) ) ;
#52331 = ORIENTED_EDGE ( 'NONE', *, *, #54728, .T. ) ;
#52332 = CARTESIAN_POINT ( 'NONE',  ( 0.05219959533934541429, -16.53943276465976808, 50.00109039468568994 ) ) ;
#52333 = CARTESIAN_POINT ( 'NONE',  ( -5.153800228976328057, -19.02544592524343514, 57.29057627198103120 ) ) ;
#52334 = CARTESIAN_POINT ( 'NONE',  ( 27.73933785331498569, 9.013057229001093518, 139.9750000027311785 ) ) ;
#52335 = CARTESIAN_POINT ( 'NONE',  ( -21.53943276465977519, 0.05219959533907696930, 21.24890960531436690 ) ) ;
#52336 = CARTESIAN_POINT ( 'NONE',  ( 8.314922557961029526, -14.29746914071037800, 90.41775706135236135 ) ) ;
#52337 = CARTESIAN_POINT ( 'NONE',  ( -9.474510206698720793, -16.51473224551083518, 109.5844237280190043 ) ) ;
#52338 = CARTESIAN_POINT ( 'NONE',  ( 21.53943276465977519, 0.05219959533937863772, 86.25109039468568994 ) ) ;
#52339 = CARTESIAN_POINT ( 'NONE',  ( 19.03943276465977164, -0.05219959533909143690, 78.74890960531436690 ) ) ;
#52340 = CARTESIAN_POINT ( 'NONE',  ( 5.719274019375991003, -21.55341960407610458, 107.7072429386476955 ) ) ;
#52341 = CARTESIAN_POINT ( 'NONE',  ( -14.29746914071037622, -8.314922557961029526, 54.16775706135235424 ) ) ;
#52342 = CARTESIAN_POINT ( 'NONE',  ( 14.34966873604960469, 8.224510206698951720, 114.1655762719810383 ) ) ;
#52343 = CARTESIAN_POINT ( 'NONE',  ( 8.314922557961029526, -14.29746914071037800, 20.41775706135234714 ) ) ;
#52344 = CARTESIAN_POINT ( 'NONE',  ( 19.03943276465977164, 0.05219959533936151252, 86.25109039468567573 ) ) ;
#52345 = CARTESIAN_POINT ( 'NONE',  ( -18.62759615963270932, 10.81492255796079327, 70.83224293864770971 ) ) ;
#52346 = CARTESIAN_POINT ( 'NONE',  ( 13.97604488694548053, -13.89961937509957401, 50.62609039468566152 ) ) ;
#52347 = DIRECTION ( 'NONE',  ( -1.000000000000000000, -0.000000000000000000, -0.000000000000000000 ) ) ;
#52348 = CARTESIAN_POINT ( 'NONE',  ( -10.72451020669898014, 18.67979575497178502, 105.4155762719810383 ) ) ;
#52349 = LINE ( 'NONE', #162523, #104880 ) ;
#52350 = CARTESIAN_POINT ( 'NONE',  ( -19.02544592524342804, 5.153800228976336051, 71.04057627198099567 ) ) ;
#52351 = CARTESIAN_POINT ( 'NONE',  ( -32.00000000000000000, -5.510910596163089556E-15, 45.00000000000000000 ) ) ;
#52352 = CARTESIAN_POINT ( 'NONE',  ( -12.06949235617739369, -12.14591786802326823, 24.37609039468567573 ) ) ;
#52353 = CARTESIAN_POINT ( 'NONE',  ( 36.81794758165437997, -5.500929263287720694, 45.34431116311555598 ) ) ;
#52355 = CARTESIAN_POINT ( 'NONE',  ( -16.55341960407611168, -4.379528057220339221, 66.45724293864768129 ) ) ;
#52354 = CARTESIAN_POINT ( 'NONE',  ( -18.67979575497178146, -10.72451020669898902, 106.6655762719810383 ) ) ;
#52356 = CARTESIAN_POINT ( 'NONE',  ( -19.05341960407611168, -5.049401038298163336, 71.45724293864766707 ) ) ;
#52357 = CARTESIAN_POINT ( 'NONE',  ( -21.52544592524334988, -5.823673210054445271, 68.95942372801901854 ) ) ;
#52359 = CARTESIAN_POINT ( 'NONE',  ( 9.474510206698729675, 16.51473224551082808, 37.08442372801899722 ) ) ;
#52358 = CARTESIAN_POINT ( 'NONE',  ( -12.14591786802326823, 12.06949235617739902, 23.12609039468567573 ) ) ;
#52360 = CARTESIAN_POINT ( 'NONE',  ( 15.80617190586769283, -15.72974639402175789, 50.62609039468568994 ) ) ;
#52361 = CARTESIAN_POINT ( 'NONE',  ( 15.72974639402176855, 15.80617190586768217, 21.87609039468567573 ) ) ;
#52362 = CARTESIAN_POINT ( 'NONE',  ( 21.53943276465977519, -0.05219959533907433946, 63.74890960531435979 ) ) ;
#52363 = CARTESIAN_POINT ( 'NONE',  ( 0.05219959533936267826, -19.03943276465977164, 110.0010903946856757 ) ) ;
#52364 = CARTESIAN_POINT ( 'NONE',  ( -16.51473224551069308, -9.474510206698971260, 41.66557627198103120 ) ) ;
#52365 = CARTESIAN_POINT ( 'NONE',  ( -19.03943276465977164, -0.05219959533935918106, 68.75109039468566152 ) ) ;
#52366 = CARTESIAN_POINT ( 'NONE',  ( -5.719274019375665041, -21.55341960407619695, 84.79275706135234714 ) ) ;
#52367 = CARTESIAN_POINT ( 'NONE',  ( 19.02544592524334988, 5.153800228976608722, 56.45942372801898301 ) ) ;
#52368 = CARTESIAN_POINT ( 'NONE',  ( -19.05341960407611168, -5.049401038298163336, 36.45724293864766707 ) ) ;
#52369 = CARTESIAN_POINT ( 'NONE',  ( 5.823673210054125526, 21.52544592524343514, 59.79057627198103120 ) ) ;
#52370 = CARTESIAN_POINT ( 'NONE',  ( 8.314922557960818139, 14.29746914071049879, 49.58224293864769550 ) ) ;
#52371 = CARTESIAN_POINT ( 'NONE',  ( 21.38418241377623019, 7.427326039334300134, 174.4773576836617224 ) ) ;
#52372 = CARTESIAN_POINT ( 'NONE',  ( -13.97604488694547697, 13.89961937509957934, 33.12609039468566863 ) ) ;
#52373 = CARTESIAN_POINT ( 'NONE',  ( -0.05219959533934338120, 16.53943276465976808, 82.50109039468568994 ) ) ;
#52374 = CARTESIAN_POINT ( 'NONE',  ( 8.224510206698953496, -14.34966873604960469, 47.91557627198102409 ) ) ;
#52375 = CARTESIAN_POINT ( 'NONE',  ( 5.719274019375673035, 21.55341960407619339, 87.29275706135236135 ) ) ;
#52376 = CARTESIAN_POINT ( 'NONE',  ( -21.55341960407619339, 5.719274019375674811, 83.54275706135234714 ) ) ;
#52377 = CARTESIAN_POINT ( 'NONE',  ( -18.67979575497178146, -10.72451020669898902, 81.66557627198103830 ) ) ;
#52378 = CARTESIAN_POINT ( 'NONE',  ( -16.51473224551069308, -9.474510206698971260, 46.66557627198102409 ) ) ;
#52379 = CARTESIAN_POINT ( 'NONE',  ( 21.52544592524334988, 5.823673210054432836, 61.45942372801901854 ) ) ;
#52380 = CARTESIAN_POINT ( 'NONE',  ( 19.03943276465977164, -0.05219959533909143690, 33.74890960531435979 ) ) ;
#52381 = ORIENTED_EDGE ( 'NONE', *, *, #81680, .F. ) ;
#52382 = CARTESIAN_POINT ( 'NONE',  ( 13.89961937509977652, -13.97604488694527269, 53.12390960531434558 ) ) ;
#52383 = CARTESIAN_POINT ( 'NONE',  ( -0.05219959533910754901, -16.53943276465976808, 112.4989096053143669 ) ) ;
#52384 = CARTESIAN_POINT ( 'NONE',  ( -9.564922557960796823, -16.46253265017161027, 102.0822429386477097 ) ) ;
#52385 = CARTESIAN_POINT ( 'NONE',  ( 16.52544592524342804, -4.483927247898539470, 53.54057627198103120 ) ) ;
#52386 = CARTESIAN_POINT ( 'NONE',  ( -0.05219959533910754901, -16.53943276465976808, 112.4989096053143669 ) ) ;
#52387 = CARTESIAN_POINT ( 'NONE',  ( 10.72451020669898902, -18.67979575497178502, 87.91557627198103830 ) ) ;
#52388 = CARTESIAN_POINT ( 'NONE',  ( 18.62759615963271287, -10.81492255796078972, 113.3322429386476955 ) ) ;
#52389 = CARTESIAN_POINT ( 'NONE',  ( 5.000000000000000000, -126.1226662136678272, 8.481152457036383652 ) ) ;
#52390 = CARTESIAN_POINT ( 'NONE',  ( -8.224510206698735004, -14.34966873604973081, 39.58442372801901143 ) ) ;
#52391 = ORIENTED_EDGE ( 'NONE', *, *, #31320, .T. ) ;
#52392 = CARTESIAN_POINT ( 'NONE',  ( -21.55341960407610458, -5.719274019375992779, 71.45724293864769550 ) ) ;
#52393 = CARTESIAN_POINT ( 'NONE',  ( -21.52544592524334988, -5.823673210054445271, 103.9594237280190185 ) ) ;
#52394 = CARTESIAN_POINT ( 'NONE',  ( -13.97604488694527625, -13.89961937509977652, 91.87390960531432427 ) ) ;
#52395 = CARTESIAN_POINT ( 'NONE',  ( 15.72974639402176855, 15.80617190586768217, 26.87609039468567218 ) ) ;
#52396 = CARTESIAN_POINT ( 'NONE',  ( -5.719274019375978568, 21.55341960407610458, 35.20724293864768839 ) ) ;
#52397 = CARTESIAN_POINT ( 'NONE',  ( 16.53943276465976808, 0.05219959533934440121, 106.2510903946856757 ) ) ;
#52399 = CARTESIAN_POINT ( 'NONE',  ( -5.719274019375665041, -21.55341960407619695, 84.79275706135234714 ) ) ;
#52398 = CARTESIAN_POINT ( 'NONE',  ( -5.719274019375665041, -21.55341960407619695, 44.79275706135234714 ) ) ;
#52400 = CARTESIAN_POINT ( 'NONE',  ( 13.89961937509957401, 13.97604488694547697, 21.87609039468566152 ) ) ;
#52401 = CARTESIAN_POINT ( 'NONE',  ( -12.06949235617739369, -12.14591786802326823, 74.37609039468568994 ) ) ;
#52402 = CARTESIAN_POINT ( 'NONE',  ( -15.80617190586768217, 15.72974639402176855, 38.12609039468567573 ) ) ;
#52403 = CARTESIAN_POINT ( 'NONE',  ( -9.474510206698964154, 16.51473224551069663, 35.41557627198102409 ) ) ;
#52404 = CARTESIAN_POINT ( 'NONE',  ( 18.62759615963255655, 10.81492255796105972, 96.66775706135234714 ) ) ;
#52405 = CARTESIAN_POINT ( 'NONE',  ( -5.049401038298153566, 19.05341960407611168, 110.2072429386476671 ) ) ;
#52406 = CARTESIAN_POINT ( 'NONE',  ( 18.67979575497178502, 10.72451020669898547, 104.1655762719810241 ) ) ;
#52408 = CARTESIAN_POINT ( 'NONE',  ( 10.72451020669898902, -18.67979575497178502, 67.91557627198102409 ) ) ;
#52407 = CARTESIAN_POINT ( 'NONE',  ( -9.164641033549692395, -36.31047332450869902, -31.46032839770261091 ) ) ;
#52410 = CARTESIAN_POINT ( 'NONE',  ( -4.483927247898539470, -16.52544592524342804, 52.29057627198102409 ) ) ;
#52409 = CARTESIAN_POINT ( 'NONE',  ( -12.14591786802326823, 12.06949235617739902, 58.12609039468568994 ) ) ;
#52411 = CARTESIAN_POINT ( 'NONE',  ( 28.79475375365586132, 2.781246896534039337E-14, 147.2656553485624045 ) ) ;
#52412 = CARTESIAN_POINT ( 'NONE',  ( 5.049401038297881783, 19.05341960407617563, 82.29275706135229029 ) ) ;
#52413 = CARTESIAN_POINT ( 'NONE',  ( -16.36317988757056696, 7.306389748694939179, 104.0978960836323211 ) ) ;
#52414 = CARTESIAN_POINT ( 'NONE',  ( -0.05219959533934338120, 16.53943276465976808, 27.50109039468567929 ) ) ;
#52415 = CARTESIAN_POINT ( 'NONE',  ( 21.52544592524344225, -5.823673210054117533, 98.54057627198105251 ) ) ;
#52416 = CARTESIAN_POINT ( 'NONE',  ( -4.379528057220328563, 16.55341960407611168, 70.20724293864769550 ) ) ;
#52417 = CARTESIAN_POINT ( 'NONE',  ( -19.02544592524342804, 5.153800228976336051, 116.0405762719810383 ) ) ;
#52418 = CARTESIAN_POINT ( 'NONE',  ( -16.55341960407617563, 4.379528057220093196, 38.54275706135234714 ) ) ;
#52419 = CARTESIAN_POINT ( 'NONE',  ( 19.02544592524343514, -5.153800228976328945, 58.54057627198102409 ) ) ;
#52421 = CARTESIAN_POINT ( 'NONE',  ( 19.02544592524334988, 5.153800228976608722, 91.45942372801900433 ) ) ;
#52420 = CARTESIAN_POINT ( 'NONE',  ( -18.67979575497193778, 10.72451020669871902, 23.33442372801901499 ) ) ;
#52422 = CARTESIAN_POINT ( 'NONE',  ( 13.89961937509977652, -13.97604488694527269, 113.1239096053143527 ) ) ;
#52423 = CARTESIAN_POINT ( 'NONE',  ( 16.46253265017160672, -9.564922557960803928, 88.33224293864769550 ) ) ;
#52424 = CARTESIAN_POINT ( 'NONE',  ( 18.67979575497178502, 10.72451020669898547, 89.16557627198102409 ) ) ;
#52425 = CARTESIAN_POINT ( 'NONE',  ( -19.02544592524342804, 5.153800228976336051, 66.04057627198103830 ) ) ;
#52426 = CARTESIAN_POINT ( 'NONE',  ( 11.74264578624799427, 36.14014761921585972, -0.5999999999999999778 ) ) ;
#52427 = CARTESIAN_POINT ( 'NONE',  ( 16.53943276465976808, -0.05219959533910856209, 68.74890960531435269 ) ) ;
#52428 = CARTESIAN_POINT ( 'NONE',  ( -16.51473224551069308, -9.474510206698971260, 101.6655762719810241 ) ) ;
#52429 = CARTESIAN_POINT ( 'NONE',  ( -31.06299995236812350, 1.355922687059702980, -50.16575868250044579 ) ) ;
#52430 = CARTESIAN_POINT ( 'NONE',  ( 9.474510206698729675, 16.51473224551082808, 77.08442372801900433 ) ) ;
#52431 = CARTESIAN_POINT ( 'NONE',  ( 5.823673210054125526, 21.52544592524343514, 89.79057627198103830 ) ) ;
#52432 = CARTESIAN_POINT ( 'NONE',  ( -9.474510206698720793, -16.51473224551083518, 44.58442372801900433 ) ) ;
#52433 = CARTESIAN_POINT ( 'NONE',  ( -21.53943276465977519, 0.05219959533907696930, 21.24890960531436690 ) ) ;
#52434 = DIRECTION ( 'NONE',  ( -0.1178549842436478201, -0.9930308165857339997, 7.149051953565419487E-31 ) ) ;
#52435 = CARTESIAN_POINT ( 'NONE',  ( -10.81492255796078084, -18.62759615963271287, 52.08224293864768839 ) ) ;
#52436 = CARTESIAN_POINT ( 'NONE',  ( -9.474510206698964154, 16.51473224551069663, 85.41557627198102409 ) ) ;
#52437 = CARTESIAN_POINT ( 'NONE',  ( 5.823673210054444382, -21.52544592524334988, 75.20942372801901854 ) ) ;
#52438 = CARTESIAN_POINT ( 'NONE',  ( -9.474510206698964154, 16.51473224551069663, 40.41557627198103120 ) ) ;
#52439 = CARTESIAN_POINT ( 'NONE',  ( 14.34966873604960469, 8.224510206698951720, 69.16557627198102409 ) ) ;
#52440 = CARTESIAN_POINT ( 'NONE',  ( -16.53943276465976808, -0.05219959533934237506, 28.75109039468567929 ) ) ;
#52441 = CARTESIAN_POINT ( 'NONE',  ( -0.05219959533937732626, 21.53943276465977519, 67.50109039468568994 ) ) ;
#52442 = ORIENTED_EDGE ( 'NONE', *, *, #11302, .T. ) ;
#52443 = LINE ( 'NONE', #86776, #107634 ) ;
#52445 = EDGE_CURVE ( 'NONE', #101229, #92045, #62760, .T. ) ;
#52444 = CARTESIAN_POINT ( 'NONE',  ( -13.97604488694547697, 13.89961937509957934, 83.12609039468564731 ) ) ;
#52446 = CARTESIAN_POINT ( 'NONE',  ( 17.50000000000000000, 5.499999999999997335, 111.7030961746582847 ) ) ;
#52447 = CARTESIAN_POINT ( 'NONE',  ( -10.72451020669898014, 18.67979575497178502, 115.4155762719810241 ) ) ;
#52448 = CARTESIAN_POINT ( 'NONE',  ( 38.00000000000000711, -12.34694845685040754, -2.849999994537626424 ) ) ;
#52449 = CARTESIAN_POINT ( 'NONE',  ( -15.80617190586768217, 15.72974639402176855, 108.1260903946856757 ) ) ;
#52450 = CARTESIAN_POINT ( 'NONE',  ( -0.05219959533909027116, -19.03943276465977164, 62.49890960531435979 ) ) ;
#52451 = CARTESIAN_POINT ( 'NONE',  ( -21.53943276465977519, -0.05219959533937600094, 113.7510903946856757 ) ) ;
#52452 = CARTESIAN_POINT ( 'NONE',  ( -12.14591786802326823, 12.06949235617739902, 108.1260903946856757 ) ) ;
#52454 = CARTESIAN_POINT ( 'NONE',  ( 10.72451020669871369, 18.67979575497193778, 77.08442372801901854 ) ) ;
#52453 = CARTESIAN_POINT ( 'NONE',  ( -19.02544592524342804, 5.153800228976336051, 96.04057627198103830 ) ) ;
#52455 = CARTESIAN_POINT ( 'NONE',  ( -36.91746825000000598, 2.428612866367529932E-14, -8.624999997268814056 ) ) ;
#52456 = CARTESIAN_POINT ( 'NONE',  ( -17.49999999999996447, -3.471454075611972723, 35.51667418855652869 ) ) ;
#52457 = CARTESIAN_POINT ( 'NONE',  ( 15.80617190586769283, -15.72974639402175789, 75.62609039468567573 ) ) ;
#52458 = CARTESIAN_POINT ( 'NONE',  ( -21.55341960407619339, 5.719274019375674811, 103.5427570613523613 ) ) ;
#52459 = CYLINDRICAL_SURFACE ( 'NONE', #70160, 0.5000000000000004441 ) ;
#52460 = CARTESIAN_POINT ( 'NONE',  ( -5.153800228976328057, -19.02544592524343514, 82.29057627198103830 ) ) ;
#52461 = CARTESIAN_POINT ( 'NONE',  ( -9.474510206698720793, -16.51473224551083518, 24.58442372801900078 ) ) ;
#52462 = CARTESIAN_POINT ( 'NONE',  ( 27.77250826529498440, -25.57832283906988025, -20.68473525701016413 ) ) ;
#52463 = CARTESIAN_POINT ( 'NONE',  ( -19.02544592524342804, 5.153800228976336051, 36.04057627198100988 ) ) ;
#52464 = CARTESIAN_POINT ( 'NONE',  ( -10.81492255796078084, -18.62759615963271287, 57.08224293864769550 ) ) ;
#52465 = CARTESIAN_POINT ( 'NONE',  ( -14.29746914071037622, -8.314922557961029526, 109.1677570613523613 ) ) ;
#52467 = CARTESIAN_POINT ( 'NONE',  ( 5.153800228976335163, 19.02544592524342804, 79.79057627198102409 ) ) ;
#52466 = CARTESIAN_POINT ( 'NONE',  ( -8.314922557960811034, -14.29746914071050412, 102.0822429386476955 ) ) ;
#52468 = CARTESIAN_POINT ( 'NONE',  ( -18.67979575497193778, 10.72451020669871902, 98.33442372801901854 ) ) ;
#52469 = CARTESIAN_POINT ( 'NONE',  ( -13.97604488694527625, -13.89961937509977652, 31.87390960531435979 ) ) ;
#52470 = CARTESIAN_POINT ( 'NONE',  ( 8.224510206698953496, -14.34966873604960469, 102.9155762719810383 ) ) ;
#52471 = CARTESIAN_POINT ( 'NONE',  ( 0.05219959533937995610, -21.53943276465977519, 50.00109039468568994 ) ) ;
#52472 = CARTESIAN_POINT ( 'NONE',  ( -18.67979575497178146, -10.72451020669898902, 81.66557627198103830 ) ) ;
#52473 = CARTESIAN_POINT ( 'NONE',  ( -5.153800228976607833, 19.02544592524334988, 47.70942372801900433 ) ) ;
#52474 = CARTESIAN_POINT ( 'NONE',  ( -26.55135571139931727, -29.92032432623640048, -6.154557619715507855 ) ) ;
#52475 = CARTESIAN_POINT ( 'NONE',  ( 19.03943276465977164, -0.05219959533909143690, 98.74890960531436690 ) ) ;
#52476 = CARTESIAN_POINT ( 'NONE',  ( -4.379528057220328563, 16.55341960407611168, 80.20724293864769550 ) ) ;
#52477 = CARTESIAN_POINT ( 'NONE',  ( -19.02544592524334988, -5.153800228976617603, 43.95942372801899012 ) ) ;
#52478 = CARTESIAN_POINT ( 'NONE',  ( 19.05341960407611168, 5.049401038298154454, 58.95724293864768129 ) ) ;
#52479 = CARTESIAN_POINT ( 'NONE',  ( -16.52544592524342804, 4.483927247898546575, 46.04057627198103830 ) ) ;
#52480 = CARTESIAN_POINT ( 'NONE',  ( -9.564922557961040184, 16.46253265017147172, 72.91775706135233293 ) ) ;
#52481 = CARTESIAN_POINT ( 'NONE',  ( 0.05219959533936267826, -19.03943276465977164, 90.00109039468567573 ) ) ;
#52482 = CARTESIAN_POINT ( 'NONE',  ( -5.719274019375978568, 21.55341960407610458, 40.20724293864769550 ) ) ;
#52483 = CARTESIAN_POINT ( 'NONE',  ( -16.53943276465976808, 0.05219959533911058130, 101.2489096053143669 ) ) ;
#52484 = CARTESIAN_POINT ( 'NONE',  ( 21.38418241377623019, 5.438282248597753110, 174.2683007571264113 ) ) ;
#52486 = CARTESIAN_POINT ( 'NONE',  ( -21.52544592524343514, 5.823673210054127303, 66.04057627198103830 ) ) ;
#52485 = CARTESIAN_POINT ( 'NONE',  ( -19.05341960407611168, -5.049401038298163336, 56.45724293864768129 ) ) ;
#52487 = CARTESIAN_POINT ( 'NONE',  ( -16.46253265017160317, 9.564922557960807481, 30.83224293864769550 ) ) ;
#52489 = CARTESIAN_POINT ( 'NONE',  ( 5.153800228976335163, 19.02544592524342804, 54.79057627198103120 ) ) ;
#52488 = CARTESIAN_POINT ( 'NONE',  ( 4.483927247898790824, -16.52544592524335698, 80.20942372801901854 ) ) ;
#52490 = CARTESIAN_POINT ( 'NONE',  ( -13.89961937509957401, -13.97604488694547875, 54.37609039468565442 ) ) ;
#52491 = CARTESIAN_POINT ( 'NONE',  ( -18.62759615963255300, -10.81492255796106328, 69.16775706135234714 ) ) ;
#52492 = CARTESIAN_POINT ( 'NONE',  ( -10.72451020669898014, 18.67979575497178502, 45.41557627198103830 ) ) ;
#52493 = CARTESIAN_POINT ( 'NONE',  ( -8.224510206698948167, 14.34966873604960824, 115.4155762719810241 ) ) ;
#52494 = CARTESIAN_POINT ( 'NONE',  ( 4.483927247898790824, -16.52544592524335698, 85.20942372801901854 ) ) ;
#52495 = CARTESIAN_POINT ( 'NONE',  ( -16.46253265017146816, -9.564922557961047289, 99.16775706135233293 ) ) ;
#52496 = CARTESIAN_POINT ( 'NONE',  ( -0.05219959533909027116, -19.03943276465977164, 27.49890960531435624 ) ) ;
#52498 = CARTESIAN_POINT ( 'NONE',  ( -18.62759615963270932, 10.81492255796079327, 60.83224293864769550 ) ) ;
#52497 = DIRECTION ( 'NONE',  ( 0.000000000000000000, 0.000000000000000000, -1.000000000000000000 ) ) ;
#52499 = CARTESIAN_POINT ( 'NONE',  ( -21.52544592524334988, -5.823673210054445271, 78.95942372801901854 ) ) ;
#52500 = CARTESIAN_POINT ( 'NONE',  ( 4.379528057220339221, -16.55341960407611168, 47.70724293864770260 ) ) ;
#52501 = CARTESIAN_POINT ( 'NONE',  ( -14.29746914071049879, 8.314922557960819915, 50.83224293864770971 ) ) ;
#52502 = CARTESIAN_POINT ( 'NONE',  ( -5.719274019375978568, 21.55341960407610458, 80.20724293864769550 ) ) ;
#52503 = CARTESIAN_POINT ( 'NONE',  ( 5.823673210054125526, 21.52544592524343514, 84.79057627198102409 ) ) ;
#52504 = CARTESIAN_POINT ( 'NONE',  ( -0.6278704076484974417, -29.03295818733088041, -49.50940399778497891 ) ) ;
#52505 = CARTESIAN_POINT ( 'NONE',  ( -18.62759615963270932, 10.81492255796079327, 35.83224293864768839 ) ) ;
#52506 = CARTESIAN_POINT ( 'NONE',  ( 16.55341960407618274, -4.379528057220086978, 66.04275706135236135 ) ) ;
#52507 = CARTESIAN_POINT ( 'NONE',  ( 8.224510206698953496, -14.34966873604960469, 82.91557627198103830 ) ) ;
#52508 = CARTESIAN_POINT ( 'NONE',  ( -13.89961937509977652, 13.97604488694528158, 30.62390960531435269 ) ) ;
#52509 = CARTESIAN_POINT ( 'NONE',  ( 35.52771690032645324, -3.099362195827463751, 38.16599597228978524 ) ) ;
#52510 = CARTESIAN_POINT ( 'NONE',  ( 0.05219959533934541429, -16.53943276465976808, 90.00109039468567573 ) ) ;
#52511 = CARTESIAN_POINT ( 'NONE',  ( -18.67979575497178146, -10.72451020669898902, 111.6655762719810525 ) ) ;
#52512 = CARTESIAN_POINT ( 'NONE',  ( -9.564922557960796823, -16.46253265017161027, 77.08224293864769550 ) ) ;
#52513 = CARTESIAN_POINT ( 'NONE',  ( -18.62759615963255300, -10.81492255796106328, 54.16775706135235424 ) ) ;
#52514 = CARTESIAN_POINT ( 'NONE',  ( -5.049401038298153566, 19.05341960407611168, 110.2072429386476671 ) ) ;
#52515 = CARTESIAN_POINT ( 'NONE',  ( -20.26331839699024329, -34.49854857074117120, -25.13492617047004174 ) ) ;
#52516 = ORIENTED_EDGE ( 'NONE', *, *, #134775, .F. ) ;
#52517 = CARTESIAN_POINT ( 'NONE',  ( 18.62759615963255655, 10.81492255796105972, 41.66775706135235424 ) ) ;
#52519 = CARTESIAN_POINT ( 'NONE',  ( -0.05219959533909027116, -19.03943276465977164, 97.49890960531436690 ) ) ;
#52518 = CARTESIAN_POINT ( 'NONE',  ( 5.153800228976335163, 19.02544592524342804, 39.79057627198100988 ) ) ;
#52520 = CARTESIAN_POINT ( 'NONE',  ( -9.474510206698720793, -16.51473224551083518, 49.58442372801899722 ) ) ;
#52521 = CARTESIAN_POINT ( 'NONE',  ( 10.72451020669871369, 18.67979575497193778, 32.08442372801901854 ) ) ;
#52522 = CARTESIAN_POINT ( 'NONE',  ( 5.049401038297881783, 19.05341960407617563, 52.29275706135234003 ) ) ;
#52523 = CARTESIAN_POINT ( 'NONE',  ( 13.97604488694527802, 13.89961937509977652, 24.37390960531435624 ) ) ;
#52524 = CARTESIAN_POINT ( 'NONE',  ( -16.53943276465976808, -0.05219959533934237506, 88.75109039468567573 ) ) ;
#52525 = CARTESIAN_POINT ( 'NONE',  ( 5.049401038297881783, 19.05341960407617563, 67.29275706135234714 ) ) ;
#52526 = CARTESIAN_POINT ( 'NONE',  ( 16.53943276465976808, 0.05219959533934440121, 101.2510903946856757 ) ) ;
#52527 = LINE ( 'NONE', #37363, #2196 ) ;
#52528 = CARTESIAN_POINT ( 'NONE',  ( 13.97604488694527802, 13.89961937509977652, 79.37390960531435269 ) ) ;
#52529 = CARTESIAN_POINT ( 'NONE',  ( -10.72451020669870658, -18.67979575497194134, 94.58442372801901854 ) ) ;
#52530 = CARTESIAN_POINT ( 'NONE',  ( 15.72974639402176855, 15.80617190586768217, 101.8760903946857042 ) ) ;
#52531 = CARTESIAN_POINT ( 'NONE',  ( -0.05219959533909027116, -19.03943276465977164, 22.49890960531436690 ) ) ;
#52532 = CARTESIAN_POINT ( 'NONE',  ( -19.02544592524342804, 5.153800228976336051, 96.04057627198103830 ) ) ;
#52533 = CARTESIAN_POINT ( 'NONE',  ( -21.53943276465977519, -0.05219959533937600094, 78.75109039468568994 ) ) ;
#52534 = CARTESIAN_POINT ( 'NONE',  ( -16.53943276465976808, -0.05219959533934237506, 18.75109039468568639 ) ) ;
#52535 = EDGE_CURVE ( 'NONE', #17032, #40299, #90750, .T. ) ;
#52536 = CARTESIAN_POINT ( 'NONE',  ( -9.474510206698964154, 16.51473224551069663, 75.41557627198103830 ) ) ;
#52537 = CARTESIAN_POINT ( 'NONE',  ( 15.80617190586746368, 15.72974639402197994, 29.37390960531435269 ) ) ;
#52538 = CARTESIAN_POINT ( 'NONE',  ( -19.02544592524342804, 5.153800228976336051, 91.04057627198100988 ) ) ;
#52539 = CARTESIAN_POINT ( 'NONE',  ( 17.58332526062524437, 7.635886036038643354, 86.57665040441534643 ) ) ;
#52540 = CARTESIAN_POINT ( 'NONE',  ( 9.474510206698971260, -16.51473224551069308, 72.91557627198102409 ) ) ;
#52541 = CARTESIAN_POINT ( 'NONE',  ( -13.97604488694527625, -13.89961937509977652, 71.87390960531433848 ) ) ;
#52542 = CARTESIAN_POINT ( 'NONE',  ( 0.05219959533934541429, -16.53943276465976808, 105.0010903946856757 ) ) ;
#52543 = CARTESIAN_POINT ( 'NONE',  ( -16.52216118717252158, 7.221426719304241182, 98.92400978952971968 ) ) ;
#52544 = CARTESIAN_POINT ( 'NONE',  ( -9.564922557961040184, 16.46253265017147172, 77.91775706135234714 ) ) ;
#52545 = CARTESIAN_POINT ( 'NONE',  ( -13.89961937509977652, 13.97604488694528158, 95.62390960531436690 ) ) ;
#52546 = CARTESIAN_POINT ( 'NONE',  ( -16.53943276465976808, 0.05219959533911058130, 81.24890960531436690 ) ) ;
#52547 = CARTESIAN_POINT ( 'NONE',  ( -5.719274019375978568, 21.55341960407610458, 50.20724293864769550 ) ) ;
#52548 = CARTESIAN_POINT ( 'NONE',  ( -10.81492255796078084, -18.62759615963271287, 22.08224293864769194 ) ) ;
#52549 = CARTESIAN_POINT ( 'NONE',  ( -8.314922557960811034, -14.29746914071050412, 112.0822429386477097 ) ) ;
#52550 = PLANE ( 'NONE',  #150037 ) ;
#52551 = CARTESIAN_POINT ( 'NONE',  ( 13.89961937509957401, 13.97604488694547697, 41.87609039468566152 ) ) ;
#52552 = CARTESIAN_POINT ( 'NONE',  ( -4.483927247898539470, -16.52544592524342804, 22.29057627198102765 ) ) ;
#52553 = CARTESIAN_POINT ( 'NONE',  ( 0.05219959533909260263, 19.03943276465977164, 104.9989096053143669 ) ) ;
#52554 = CARTESIAN_POINT ( 'NONE',  ( 18.67979575497194134, -10.72451020669871369, 60.83442372801901854 ) ) ;
#52555 = CARTESIAN_POINT ( 'NONE',  ( 10.81492255796078972, 18.62759615963270932, 59.58224293864770260 ) ) ;
#52556 = CARTESIAN_POINT ( 'NONE',  ( 5.719274019375673035, 21.55341960407619339, 37.29275706135235424 ) ) ;
#52557 = CARTESIAN_POINT ( 'NONE',  ( -21.52544592524343514, 5.823673210054127303, 86.04057627198102409 ) ) ;
#52558 = CARTESIAN_POINT ( 'NONE',  ( -21.52544592524334988, -5.823673210054445271, 38.95942372801901854 ) ) ;
#52559 = CARTESIAN_POINT ( 'NONE',  ( 12.14591786802309770, 12.06949235617756955, 114.3739096053143527 ) ) ;
#52560 = EDGE_CURVE ( 'NONE', #192038, #65708, #4730, .T. ) ;
#52561 = CARTESIAN_POINT ( 'NONE',  ( -19.02544592524334988, -5.153800228976617603, 63.95942372801899012 ) ) ;
#52562 = CARTESIAN_POINT ( 'NONE',  ( 0.05219959533909260263, 19.03943276465977164, 49.99890960531435979 ) ) ;
#52564 = CARTESIAN_POINT ( 'NONE',  ( -19.02544592524342804, 5.153800228976336051, 101.0405762719810241 ) ) ;
#52563 = CARTESIAN_POINT ( 'NONE',  ( -8.224510206698948167, 14.34966873604960824, 85.41557627198102409 ) ) ;
#52565 = CARTESIAN_POINT ( 'NONE',  ( 9.564922557960805705, 16.46253265017160317, 114.5822429386476955 ) ) ;
#52566 = CARTESIAN_POINT ( 'NONE',  ( -16.46253265017160317, 9.564922557960807481, 25.83224293864769194 ) ) ;
#52567 = CARTESIAN_POINT ( 'NONE',  ( -4.483927247898539470, -16.52544592524342804, 37.29057627198102409 ) ) ;
#52568 = CARTESIAN_POINT ( 'NONE',  ( 0.05219959533934541429, -16.53943276465976808, 105.0010903946856757 ) ) ;
#52569 = CARTESIAN_POINT ( 'NONE',  ( 9.564922557960805705, 16.46253265017160317, 49.58224293864770260 ) ) ;
#52570 = CARTESIAN_POINT ( 'NONE',  ( 12.06949235617757843, -12.14591786802309237, 113.1239096053143953 ) ) ;
#52571 = CARTESIAN_POINT ( 'NONE',  ( 0.05219959533936267826, -19.03943276465977164, 20.00109039468567218 ) ) ;
#52573 = CARTESIAN_POINT ( 'NONE',  ( -0.05219959533910754901, -16.53943276465976808, 22.49890960531436335 ) ) ;
#52572 = CARTESIAN_POINT ( 'NONE',  ( 13.97604488694527802, 13.89961937509977652, 109.3739096053143669 ) ) ;
#52574 = CARTESIAN_POINT ( 'NONE',  ( 18.62759615963255655, 10.81492255796105972, 41.66775706135235424 ) ) ;
#52575 = CARTESIAN_POINT ( 'NONE',  ( 21.98831087263036110, -5.509728484239349022, 173.5901369092267430 ) ) ;
#52576 = CARTESIAN_POINT ( 'NONE',  ( -16.55341960407617563, 4.379528057220093196, 53.54275706135234714 ) ) ;
#52577 = CARTESIAN_POINT ( 'NONE',  ( 4.379528057220339221, -16.55341960407611168, 32.70724293864770260 ) ) ;
#52578 = CARTESIAN_POINT ( 'NONE',  ( -12.06949235617739369, -12.14591786802326823, 109.3760903946857042 ) ) ;
#52579 = CARTESIAN_POINT ( 'NONE',  ( 16.53943276465976808, 0.05219959533934440121, 26.25109039468567573 ) ) ;
#52580 = CARTESIAN_POINT ( 'NONE',  ( 19.03943276465977164, -0.05219959533909143690, 43.74890960531435979 ) ) ;
#52581 = AXIS2_PLACEMENT_3D ( 'NONE', #112983, #73243, #134914 ) ;
#52582 = CARTESIAN_POINT ( 'NONE',  ( -14.29746914071049879, 8.314922557960819915, 110.8322429386476955 ) ) ;
#52583 = CARTESIAN_POINT ( 'NONE',  ( -10.72451020669870658, -18.67979575497194134, 24.58442372801901499 ) ) ;
#52584 = CARTESIAN_POINT ( 'NONE',  ( -16.51473224551069308, -9.474510206698971260, 41.66557627198103120 ) ) ;
#52585 = DIRECTION ( 'NONE',  ( 1.000000000000000000, 0.000000000000000000, 0.000000000000000000 ) ) ;
#52586 = CARTESIAN_POINT ( 'NONE',  ( -5.153800228976328057, -19.02544592524343514, 27.29057627198103120 ) ) ;
#52587 = CARTESIAN_POINT ( 'NONE',  ( 21.52544592524344225, -5.823673210054117533, 28.54057627198103120 ) ) ;
#52588 = CARTESIAN_POINT ( 'NONE',  ( -16.20579543436676317, -7.371946100355211584, 35.56520834171877254 ) ) ;
#52589 = CARTESIAN_POINT ( 'NONE',  ( -16.46253265017160317, 9.564922557960807481, 95.83224293864769550 ) ) ;
#52591 = CARTESIAN_POINT ( 'NONE',  ( -4.483927247898539470, -16.52544592524342804, 107.2905762719810525 ) ) ;
#52590 = CARTESIAN_POINT ( 'NONE',  ( -21.53943276465977519, -0.05219959533937600094, 43.75109039468568284 ) ) ;
#52592 = CARTESIAN_POINT ( 'NONE',  ( -19.03943276465977164, 0.05219959533909376836, 116.2489096053143669 ) ) ;
#52593 = CARTESIAN_POINT ( 'NONE',  ( 1.300000000000000044, -0.7216878364870318308, 1.249999999999999778 ) ) ;
#52594 = CARTESIAN_POINT ( 'NONE',  ( -4.483927247898782831, 16.52544592524335698, 82.70942372801900433 ) ) ;
#52595 = CARTESIAN_POINT ( 'NONE',  ( 21.53943276465977519, 0.05219959533937863772, 91.25109039468568994 ) ) ;
#52596 = CARTESIAN_POINT ( 'NONE',  ( -14.34966873604972548, 8.224510206698743886, 58.33442372801901143 ) ) ;
#52597 = CARTESIAN_POINT ( 'NONE',  ( 5.049401038298161559, -19.05341960407611168, 92.70724293864769550 ) ) ;
#52598 = CARTESIAN_POINT ( 'NONE',  ( -14.29746914071037622, -8.314922557961029526, 39.16775706135235424 ) ) ;
#52599 = CARTESIAN_POINT ( 'NONE',  ( -0.05219959533936034679, 19.03943276465977164, 102.5010903946856757 ) ) ;
#52600 = CARTESIAN_POINT ( 'NONE',  ( -16.53943276465976808, -0.05219959533934237506, 78.75109039468568994 ) ) ;
#52601 = CARTESIAN_POINT ( 'NONE',  ( -16.46253265017146816, -9.564922557961047289, 94.16775706135233293 ) ) ;
#52602 = CARTESIAN_POINT ( 'NONE',  ( 5.049401038298161559, -19.05341960407611168, 72.70724293864768129 ) ) ;
#52603 = CARTESIAN_POINT ( 'NONE',  ( 5.719274019375991003, -21.55341960407610458, 97.70724293864772392 ) ) ;
#52605 = CARTESIAN_POINT ( 'NONE',  ( 0.05219959533936267826, -19.03943276465977164, 100.0010903946856757 ) ) ;
#52604 = CARTESIAN_POINT ( 'NONE',  ( 16.52544592524342804, -4.483927247898539470, 103.5405762719810383 ) ) ;
#52606 = CARTESIAN_POINT ( 'NONE',  ( 14.34966873604972726, -8.224510206698740333, 75.83442372801900433 ) ) ;
#52607 = CARTESIAN_POINT ( 'NONE',  ( -16.18388926212245948, 7.379444403734574109, 44.56046848633771162 ) ) ;
#52608 = CARTESIAN_POINT ( 'NONE',  ( 16.51473224551083163, -9.474510206698727899, 65.83442372801900433 ) ) ;
#52609 = CARTESIAN_POINT ( 'NONE',  ( -8.314922557960811034, -14.29746914071050412, 32.08224293864769550 ) ) ;
#52610 = CARTESIAN_POINT ( 'NONE',  ( 16.52544592524342804, -4.483927247898539470, 88.54057627198103830 ) ) ;
#52612 = FACE_OUTER_BOUND ( 'NONE', #128988, .T. ) ;
#52611 = CARTESIAN_POINT ( 'NONE',  ( 9.564922557961047289, -16.46253265017146816, 30.41775706135232937 ) ) ;
#52613 = CARTESIAN_POINT ( 'NONE',  ( -21.55341960407619339, 5.719274019375674811, 43.54275706135235424 ) ) ;
#52614 = CARTESIAN_POINT ( 'NONE',  ( -16.46253265017146816, -9.564922557961047289, 94.16775706135233293 ) ) ;
#52615 = DIRECTION ( 'NONE',  ( 3.469446951953611033E-15, 0.000000000000000000, -1.000000000000000000 ) ) ;
#52616 = CARTESIAN_POINT ( 'NONE',  ( -0.05219959533909027116, -19.03943276465977164, 87.49890960531436690 ) ) ;
#52617 = B_SPLINE_CURVE_WITH_KNOTS ( 'NONE', 3,
 ( #104855, #56355, #72532, #74525, #119044, #73541 ),
 .UNSPECIFIED., .F., .F.,
 ( 4, 2, 4 ),
 ( 0.003989672132298145192, 0.004372778065220570172, 0.004755883998142995152 ),
 .UNSPECIFIED. ) ;
#52618 = CARTESIAN_POINT ( 'NONE',  ( 18.67979575497194134, -10.72451020669871369, 100.8344237280190185 ) ) ;
#52619 = CARTESIAN_POINT ( 'NONE',  ( -19.03943276465977164, 0.05219959533909376836, 81.24890960531436690 ) ) ;
#52620 = CARTESIAN_POINT ( 'NONE',  ( 21.55341960407610458, 5.719274019375980345, 48.95724293864770971 ) ) ;
#52621 = CARTESIAN_POINT ( 'NONE',  ( -12.14591786802309592, -12.06949235617757132, 91.87390960531436690 ) ) ;
#52622 = CARTESIAN_POINT ( 'NONE',  ( -19.05341960407611168, -5.049401038298163336, 51.45724293864770260 ) ) ;
#52623 = CARTESIAN_POINT ( 'NONE',  ( 12.14591786802309770, 12.06949235617756955, 114.3739096053143527 ) ) ;
#52624 = CARTESIAN_POINT ( 'NONE',  ( -5.719274019375665041, -21.55341960407619695, 19.79275706135235069 ) ) ;
#52625 = CARTESIAN_POINT ( 'NONE',  ( 0.05219959533937995610, -21.53943276465977519, 60.00109039468568284 ) ) ;
#52626 = CARTESIAN_POINT ( 'NONE',  ( 19.02544592524343514, -5.153800228976328945, 38.54057627198103120 ) ) ;
#52627 = CARTESIAN_POINT ( 'NONE',  ( -0.05219959533934338120, 16.53943276465976808, 72.50109039468568994 ) ) ;
#52628 = CARTESIAN_POINT ( 'NONE',  ( -15.80617190586745835, -15.72974639402198527, 111.8739096053143669 ) ) ;
#52629 = CARTESIAN_POINT ( 'NONE',  ( -5.823673210054431948, 21.52544592524334988, 27.70942372801901854 ) ) ;
#52631 = CARTESIAN_POINT ( 'NONE',  ( -13.89961937509977652, 13.97604488694528158, 70.62390960531432427 ) ) ;
#52630 = CARTESIAN_POINT ( 'NONE',  ( 19.02544592524334988, 5.153800228976608722, 51.45942372801900433 ) ) ;
#52632 = CARTESIAN_POINT ( 'NONE',  ( 13.97604488694548053, -13.89961937509957401, 35.62609039468567573 ) ) ;
#52633 = CARTESIAN_POINT ( 'NONE',  ( -18.62759615963255300, -10.81492255796106328, 69.16775706135234714 ) ) ;
#52634 = CARTESIAN_POINT ( 'NONE',  ( 5.823673210054125526, 21.52544592524343514, 74.79057627198105251 ) ) ;
#52635 = CARTESIAN_POINT ( 'NONE',  ( 0.05219959533910956823, 16.53943276465976808, 49.99890960531437401 ) ) ;
#52637 = CARTESIAN_POINT ( 'NONE',  ( -16.51473224551082808, 9.474510206698731452, 33.33442372801899722 ) ) ;
#52636 = CARTESIAN_POINT ( 'NONE',  ( 18.62759615963255655, 10.81492255796105972, 86.66775706135234714 ) ) ;
#52638 = CARTESIAN_POINT ( 'NONE',  ( 4.483927247898545687, 16.52544592524342804, 69.79057627198102409 ) ) ;
#52639 = CARTESIAN_POINT ( 'NONE',  ( -16.53943276465976808, 0.05219959533911058130, 116.2489096053143669 ) ) ;
#52640 = CARTESIAN_POINT ( 'NONE',  ( 0.05219959533936267826, -19.03943276465977164, 55.00109039468566863 ) ) ;
#52641 = CARTESIAN_POINT ( 'NONE',  ( 16.52544592524342804, -4.483927247898539470, 23.54057627198102765 ) ) ;
#52643 = EDGE_CURVE ( 'NONE', #79638, #48994, #175795, .T. ) ;
#52642 = CARTESIAN_POINT ( 'NONE',  ( 10.72451020669871369, 18.67979575497193778, 82.08442372801901854 ) ) ;
#52644 = CARTESIAN_POINT ( 'NONE',  ( -19.03943276465977164, -0.05219959533935918106, 43.75109039468566863 ) ) ;
#52645 = CARTESIAN_POINT ( 'NONE',  ( -10.72451020669898014, 18.67979575497178502, 55.41557627198102409 ) ) ;
#52646 = CARTESIAN_POINT ( 'NONE',  ( -21.55341960407619339, 5.719274019375674811, 43.54275706135235424 ) ) ;
#52647 = CARTESIAN_POINT ( 'NONE',  ( -21.52544592524343514, 5.823673210054127303, 96.04057627198102409 ) ) ;
#52648 = CARTESIAN_POINT ( 'NONE',  ( 9.474510206698729675, 16.51473224551082808, 92.08442372801900433 ) ) ;
#52649 = CARTESIAN_POINT ( 'NONE',  ( 4.379528057220092307, 16.55341960407617563, 72.29275706135236135 ) ) ;
#52651 = CARTESIAN_POINT ( 'NONE',  ( 15.80617190586746368, 15.72974639402197994, 109.3739096053143811 ) ) ;
#52650 = CARTESIAN_POINT ( 'NONE',  ( -16.02140599805581900, -17.62553472373751617, -57.13537817852984801 ) ) ;
#52653 = B_SPLINE_CURVE_WITH_KNOTS ( 'NONE', 3,
 ( #179807, #104932, #25123, #181783, #121083, #55432 ),
 .UNSPECIFIED., .F., .F.,
 ( 4, 2, 4 ),
 ( 0.003989672132298160805, 0.004372778065220584917, 0.004755883998143008162 ),
 .UNSPECIFIED. ) ;
#52652 = CARTESIAN_POINT ( 'NONE',  ( -16.52544592524342804, 4.483927247898546575, 86.04057627198102409 ) ) ;
#52654 = CARTESIAN_POINT ( 'NONE',  ( 11.40812507854754365, 35.11059874428196537, -9.724999997268813701 ) ) ;
#52655 = CARTESIAN_POINT ( 'NONE',  ( -4.483927247898782831, 16.52544592524335698, 37.70942372801900433 ) ) ;
#52656 = CARTESIAN_POINT ( 'NONE',  ( -5.719274019375978568, 21.55341960407610458, 55.20724293864770260 ) ) ;
#52657 = CARTESIAN_POINT ( 'NONE',  ( -12.14591786802326823, 12.06949235617739902, 88.12609039468570415 ) ) ;
#52658 = CARTESIAN_POINT ( 'NONE',  ( -7.500000000000000000, 0.000000000000000000, 10.00000000000000000 ) ) ;
#52659 = EDGE_CURVE ( 'NONE', #151905, #176032, #114200, .T. ) ;
#52660 = CARTESIAN_POINT ( 'NONE',  ( -4.483927247898782831, 16.52544592524335698, 72.70942372801901854 ) ) ;
#52661 = CARTESIAN_POINT ( 'NONE',  ( 15.72974639402176855, 15.80617190586768217, 41.87609039468568284 ) ) ;
#52662 = CARTESIAN_POINT ( 'NONE',  ( -15.80617190586745835, -15.72974639402198527, 56.87390960531436690 ) ) ;
#52663 = CARTESIAN_POINT ( 'NONE',  ( -14.29746914071037622, -8.314922557961029526, 89.16775706135236135 ) ) ;
#52664 = CARTESIAN_POINT ( 'NONE',  ( 10.81492255796106328, -18.62759615963255655, 75.41775706135233293 ) ) ;
#52665 = CARTESIAN_POINT ( 'NONE',  ( 15.80617190586746368, 15.72974639402197994, 49.37390960531436690 ) ) ;
#52666 = CARTESIAN_POINT ( 'NONE',  ( -5.719274019375978568, 21.55341960407610458, 35.20724293864768839 ) ) ;
#52667 = EDGE_LOOP ( 'NONE', ( #52772, #81834 ) ) ;
#52668 = CARTESIAN_POINT ( 'NONE',  ( -16.55341960407617563, 4.379528057220093196, 68.54275706135234714 ) ) ;
#52669 = CARTESIAN_POINT ( 'NONE',  ( 21.53943276465977519, -0.05219959533907433946, 28.74890960531435624 ) ) ;
#52670 = CARTESIAN_POINT ( 'NONE',  ( -5.049401038298153566, 19.05341960407611168, 105.2072429386476671 ) ) ;
#52671 = CARTESIAN_POINT ( 'NONE',  ( 4.379528057220339221, -16.55341960407611168, 22.70724293864769194 ) ) ;
#52672 = CARTESIAN_POINT ( 'NONE',  ( 9.841528761215755594, -38.18405872352758479, -31.73089324721042104 ) ) ;
#52673 = CARTESIAN_POINT ( 'NONE',  ( 8.314922557960818139, 14.29746914071049879, 114.5822429386477097 ) ) ;
#52674 = CARTESIAN_POINT ( 'NONE',  ( -15.72974639402197994, 15.80617190586746368, 45.62390960531436690 ) ) ;
#52675 = CARTESIAN_POINT ( 'NONE',  ( 19.03943276465977164, -0.05219959533909143690, 43.74890960531435979 ) ) ;
#52676 = CARTESIAN_POINT ( 'NONE',  ( -14.29746914071037622, -8.314922557961029526, 94.16775706135237556 ) ) ;
#52677 = CARTESIAN_POINT ( 'NONE',  ( 21.55341960407619695, -5.719274019375665929, 36.04275706135234714 ) ) ;
#52678 = CARTESIAN_POINT ( 'NONE',  ( -16.46253265017146816, -9.564922557961047289, 84.16775706135233293 ) ) ;
#52679 = CARTESIAN_POINT ( 'NONE',  ( -8.224510206698948167, 14.34966873604960824, 100.4155762719810241 ) ) ;
#52680 = CARTESIAN_POINT ( 'NONE',  ( 16.51473224551069308, 9.474510206698969483, 54.16557627198103120 ) ) ;
#52681 = CARTESIAN_POINT ( 'NONE',  ( -19.03943276465977164, 0.05219959533909376836, 31.24890960531435979 ) ) ;
#52682 = CARTESIAN_POINT ( 'NONE',  ( 18.22780087662125226, -5.499999999999864997, 61.01540105326109398 ) ) ;
#52683 = CARTESIAN_POINT ( 'NONE',  ( 0.05219959533909260263, 19.03943276465977164, 74.99890960531435269 ) ) ;
#52684 = CARTESIAN_POINT ( 'NONE',  ( 4.379528057220092307, 16.55341960407617563, 67.29275706135234714 ) ) ;
#52685 = CARTESIAN_POINT ( 'NONE',  ( 15.72974639402176855, 15.80617190586768217, 111.8760903946856615 ) ) ;
#52686 = CARTESIAN_POINT ( 'NONE',  ( 21.52544592524344225, -5.823673210054117533, 53.54057627198103120 ) ) ;
#52687 = CARTESIAN_POINT ( 'NONE',  ( -4.379528057220086978, -16.55341960407618274, 69.79275706135234714 ) ) ;
#52688 = CARTESIAN_POINT ( 'NONE',  ( -5.153800228976607833, 19.02544592524334988, 62.70942372801899722 ) ) ;
#52689 = CARTESIAN_POINT ( 'NONE',  ( -5.719274019375665041, -21.55341960407619695, 69.79275706135234714 ) ) ;
#52690 = CARTESIAN_POINT ( 'NONE',  ( -16.46253265017160317, 9.564922557960807481, 70.83224293864770971 ) ) ;
#52691 = CARTESIAN_POINT ( 'NONE',  ( 9.564922557960805705, 16.46253265017160317, 34.58224293864770260 ) ) ;
#52692 = CARTESIAN_POINT ( 'NONE',  ( -19.03943276465977164, -0.05219959533935918106, 58.75109039468566863 ) ) ;
#52693 = CARTESIAN_POINT ( 'NONE',  ( 5.153800228976335163, 19.02544592524342804, 114.7905762719810241 ) ) ;
#52694 = CARTESIAN_POINT ( 'NONE',  ( -9.564922557960796823, -16.46253265017161027, 102.0822429386477097 ) ) ;
#52695 = CARTESIAN_POINT ( 'NONE',  ( -12.14591786802309592, -12.06949235617757132, 51.87390960531437401 ) ) ;
#52696 = CARTESIAN_POINT ( 'NONE',  ( 10.72451020669898902, -18.67979575497178502, 42.91557627198103120 ) ) ;
#52697 = AXIS2_PLACEMENT_3D ( 'NONE', #13975, #14977, #168645 ) ;
#52698 = CARTESIAN_POINT ( 'NONE',  ( 5.049401038297881783, 19.05341960407617563, 32.29275706135233293 ) ) ;
#52699 = CYLINDRICAL_SURFACE ( 'NONE', #21807, 2.500000000000000000 ) ;
#52700 = CARTESIAN_POINT ( 'NONE',  ( 13.97604488694527802, 13.89961937509977652, 44.37390960531435269 ) ) ;
#52701 = CARTESIAN_POINT ( 'NONE',  ( -19.49671883438227127, -5.500000000000030198, 99.89279849105680853 ) ) ;
#52702 = CARTESIAN_POINT ( 'NONE',  ( -37.45873412500000654, 2.428612866367529932E-14, -1.437499995903219974 ) ) ;
#52703 = CARTESIAN_POINT ( 'NONE',  ( 12.06949235617739724, 12.14591786802326823, 76.87609039468567573 ) ) ;
#52704 = CARTESIAN_POINT ( 'NONE',  ( 5.823673210054125526, 21.52544592524343514, 99.79057627198103830 ) ) ;
#52706 = CARTESIAN_POINT ( 'NONE',  ( -3.573655867282028392E-15, 2.428612866367529932E-14, 139.9999999999999716 ) ) ;
#52705 = CARTESIAN_POINT ( 'NONE',  ( -19.03943276465977164, 0.05219959533909376836, 41.24890960531435269 ) ) ;
#52707 = CARTESIAN_POINT ( 'NONE',  ( -10.81492255796105439, 18.62759615963255655, 37.91775706135235424 ) ) ;
#52708 = CARTESIAN_POINT ( 'NONE',  ( 9.564922557961047289, -16.46253265017146816, 55.41775706135234003 ) ) ;
#52709 = CARTESIAN_POINT ( 'NONE',  ( 16.46253265017160672, -9.564922557960803928, 53.33224293864768839 ) ) ;
#52710 = CARTESIAN_POINT ( 'NONE',  ( 10.81492255796106328, -18.62759615963255655, 95.41775706135234714 ) ) ;
#52711 = CARTESIAN_POINT ( 'NONE',  ( -9.564922557960796823, -16.46253265017161027, 22.08224293864768839 ) ) ;
#52712 = CARTESIAN_POINT ( 'NONE',  ( -12.14591786802309592, -12.06949235617757132, 46.87390960531435979 ) ) ;
#52713 = CARTESIAN_POINT ( 'NONE',  ( -13.90528855463212388, 0.7844626028951359187, -60.35633530387643475 ) ) ;
#52714 = CARTESIAN_POINT ( 'NONE',  ( 15.80617190586746368, 15.72974639402197994, 44.37390960531435979 ) ) ;
#52715 = CARTESIAN_POINT ( 'NONE',  ( 1.300000000000000044, -0.7216878364870318308, -1.250000000000000000 ) ) ;
#52716 = CARTESIAN_POINT ( 'NONE',  ( -19.02544592524342804, 5.153800228976336051, 106.0405762719810241 ) ) ;
#52717 = CARTESIAN_POINT ( 'NONE',  ( 12.14591786802309770, 12.06949235617756955, 89.37390960531435269 ) ) ;
#52718 = CARTESIAN_POINT ( 'NONE',  ( 12.06949235617739724, 12.14591786802326823, 26.87609039468567218 ) ) ;
#52719 = CARTESIAN_POINT ( 'NONE',  ( -8.314922557961024197, 14.29746914071037800, 107.9177570613523471 ) ) ;
#52720 = ORIENTED_EDGE ( 'NONE', *, *, #125362, .F. ) ;
#52722 = CARTESIAN_POINT ( 'NONE',  ( -5.823673210054116645, -21.52544592524344225, 107.2905762719810525 ) ) ;
#52721 = CARTESIAN_POINT ( 'NONE',  ( 19.02544592524343514, -5.153800228976328945, 98.54057627198100988 ) ) ;
#52723 = AXIS2_PLACEMENT_3D ( 'NONE', #77432, #1579, #93588 ) ;
#52725 = CARTESIAN_POINT ( 'NONE',  ( 19.03943276465977164, -0.05219959533909143690, 103.7489096053143669 ) ) ;
#52724 = CARTESIAN_POINT ( 'NONE',  ( -4.483927247898539470, -16.52544592524342804, 32.29057627198102409 ) ) ;
#52726 = CARTESIAN_POINT ( 'NONE',  ( 16.51473224551083163, -9.474510206698727899, 90.83442372801900433 ) ) ;
#52727 = CARTESIAN_POINT ( 'NONE',  ( -21.53943276465977519, -0.05219959533937600094, 113.7510903946856757 ) ) ;
#52728 = CARTESIAN_POINT ( 'NONE',  ( 15.72974639402199770, -15.80617190586745480, 93.12390960531436690 ) ) ;
#52729 = CARTESIAN_POINT ( 'NONE',  ( 18.67979575497178502, 10.72451020669898547, 49.16557627198102409 ) ) ;
#52730 = CARTESIAN_POINT ( 'NONE',  ( -13.97604488694527625, -13.89961937509977652, 61.87390960531435979 ) ) ;
#52731 = CARTESIAN_POINT ( 'NONE',  ( 16.53943276465976808, -0.05219959533910856209, 38.74890960531435979 ) ) ;
#52732 = CARTESIAN_POINT ( 'NONE',  ( 19.02544592524343514, -5.153800228976328945, 78.54057627198099567 ) ) ;
#52733 = CARTESIAN_POINT ( 'NONE',  ( 19.25663599770057388, -5.499999999999650058, 61.49419308057201050 ) ) ;
#52734 = CARTESIAN_POINT ( 'NONE',  ( -0.05219959533936034679, 19.03943276465977164, 42.50109039468566152 ) ) ;
#52735 = CARTESIAN_POINT ( 'NONE',  ( -0.05219959533910754901, -16.53943276465976808, 92.49890960531436690 ) ) ;
#52736 = CARTESIAN_POINT ( 'NONE',  ( 5.823673210054444382, -21.52544592524334988, 25.20942372801901854 ) ) ;
#52737 = CARTESIAN_POINT ( 'NONE',  ( -27.73933785331498925, 2.428612866367529932E-14, 145.3750000027311842 ) ) ;
#52738 = CARTESIAN_POINT ( 'NONE',  ( -0.05219959533934338120, 16.53943276465976808, 112.5010903946857042 ) ) ;
#52739 = CARTESIAN_POINT ( 'NONE',  ( 0.05219959533910956823, 16.53943276465976808, 114.9989096053143669 ) ) ;
#52740 = CARTESIAN_POINT ( 'NONE',  ( 9.474510206698971260, -16.51473224551069308, 77.91557627198103830 ) ) ;
#52741 = CARTESIAN_POINT ( 'NONE',  ( -23.48298174826589602, -32.32155151706771790, -5.447842220587802764 ) ) ;
#52742 = CARTESIAN_POINT ( 'NONE',  ( 8.314922557960818139, 14.29746914071049879, 49.58224293864769550 ) ) ;
#52743 = CARTESIAN_POINT ( 'NONE',  ( 5.823673210054444382, -21.52544592524334988, 55.20942372801902565 ) ) ;
#52744 = CARTESIAN_POINT ( 'NONE',  ( 31.47295357026365892, -21.29310327861803387, -24.13113353488660096 ) ) ;
#52745 = CARTESIAN_POINT ( 'NONE',  ( -19.03943276465977164, 0.05219959533909376836, 41.24890960531435269 ) ) ;
#52746 = CARTESIAN_POINT ( 'NONE',  ( -19.02544592524342804, 5.153800228976336051, 46.04057627198101699 ) ) ;
#52747 = ORIENTED_EDGE ( 'NONE', *, *, #7790, .T. ) ;
#52748 = CARTESIAN_POINT ( 'NONE',  ( -21.55341960407619339, 5.719274019375674811, 98.54275706135234714 ) ) ;
#52749 = CARTESIAN_POINT ( 'NONE',  ( 0.05219959533934541429, -16.53943276465976808, 60.00109039468568284 ) ) ;
#52750 = CARTESIAN_POINT ( 'NONE',  ( 0.05219959533937995610, -21.53943276465977519, 85.00109039468568994 ) ) ;
#52751 = CARTESIAN_POINT ( 'NONE',  ( -15.80617190586745835, -15.72974639402198527, 26.87390960531435979 ) ) ;
#52752 = CARTESIAN_POINT ( 'NONE',  ( 0.05219959533936267826, -19.03943276465977164, 100.0010903946856757 ) ) ;
#52753 = CARTESIAN_POINT ( 'NONE',  ( -10.72451020669870658, -18.67979575497194134, 74.58442372801901854 ) ) ;
#52754 = CARTESIAN_POINT ( 'NONE',  ( 14.34966873604972726, -8.224510206698740333, 40.83442372801901854 ) ) ;
#52755 = CARTESIAN_POINT ( 'NONE',  ( 18.62759615963271287, -10.81492255796078972, 88.33224293864769550 ) ) ;
#52756 = CARTESIAN_POINT ( 'NONE',  ( 13.89961937509957401, 13.97604488694547697, 101.8760903946856331 ) ) ;
#52757 = CARTESIAN_POINT ( 'NONE',  ( -16.51473224551069308, -9.474510206698971260, 66.66557627198102409 ) ) ;
#52758 = CARTESIAN_POINT ( 'NONE',  ( 13.89961937509957401, 13.97604488694547697, 101.8760903946856331 ) ) ;
#52759 = CARTESIAN_POINT ( 'NONE',  ( -5.153800228976607833, 19.02544592524334988, 97.70942372801900433 ) ) ;
#52760 = CARTESIAN_POINT ( 'NONE',  ( 14.29746914071049879, -8.314922557960816363, 48.33224293864770260 ) ) ;
#52761 = ADVANCED_FACE ( 'NONE', ( #163738 ), #25238, .F. ) ;
#52762 = CARTESIAN_POINT ( 'NONE',  ( -5.153800228976607833, 19.02544592524334988, 72.70942372801900433 ) ) ;
#52763 = CARTESIAN_POINT ( 'NONE',  ( 12.06949235617739724, 12.14591786802326823, 66.87609039468568994 ) ) ;
#52765 = CARTESIAN_POINT ( 'NONE',  ( -13.89961937509977652, 13.97604488694528158, 40.62390960531435979 ) ) ;
#52764 = CARTESIAN_POINT ( 'NONE',  ( -18.67979575497193778, 10.72451020669871902, 23.33442372801901499 ) ) ;
#52766 = CARTESIAN_POINT ( 'NONE',  ( 19.05341960407611168, 5.049401038298154454, 58.95724293864768129 ) ) ;
#52767 = CARTESIAN_POINT ( 'NONE',  ( -16.53943276465976808, -0.05219959533934237506, 63.75109039468568284 ) ) ;
#52768 = CARTESIAN_POINT ( 'NONE',  ( 8.571926809382597767, 26.38167802310806209, 140.7750000027311899 ) ) ;
#52769 = DIRECTION ( 'NONE',  ( -0.000000000000000000, -0.000000000000000000, 1.000000000000000000 ) ) ;
#52770 = CARTESIAN_POINT ( 'NONE',  ( 9.564922557960805705, 16.46253265017160317, 99.58224293864770971 ) ) ;
#52771 = CARTESIAN_POINT ( 'NONE',  ( 16.51473224551069308, 9.474510206698969483, 29.16557627198103475 ) ) ;
#52772 = ORIENTED_EDGE ( 'NONE', *, *, #166279, .T. ) ;
#52773 = CARTESIAN_POINT ( 'NONE',  ( -13.97604488694547697, 13.89961937509957934, 108.1260903946856331 ) ) ;
#52774 = CARTESIAN_POINT ( 'NONE',  ( 21.53943276465977519, -0.05219959533907433946, 43.74890960531435979 ) ) ;
#52776 = CARTESIAN_POINT ( 'NONE',  ( 12.06949235617739724, 12.14591786802326823, 31.87609039468567929 ) ) ;
#52775 = CARTESIAN_POINT ( 'NONE',  ( -13.97604488694547697, 13.89961937509957934, 43.12609039468566152 ) ) ;
#52777 = CARTESIAN_POINT ( 'NONE',  ( 5.153800228976335163, 19.02544592524342804, 34.79057627198102409 ) ) ;
#52778 = CARTESIAN_POINT ( 'NONE',  ( -13.97604488694527625, -13.89961937509977652, 46.87390960531435979 ) ) ;
#52779 = CARTESIAN_POINT ( 'NONE',  ( 5.719274019375991003, -21.55341960407610458, 92.70724293864770971 ) ) ;
#52780 = CARTESIAN_POINT ( 'NONE',  ( 9.564922557960805705, 16.46253265017160317, 99.58224293864770971 ) ) ;
#52781 = CARTESIAN_POINT ( 'NONE',  ( -9.474510206698964154, 16.51473224551069663, 50.41557627198102409 ) ) ;
#52782 = CARTESIAN_POINT ( 'NONE',  ( 17.14385361876520264, 23.59649016807275856, 140.6750000027311387 ) ) ;
#52783 = CARTESIAN_POINT ( 'NONE',  ( 13.97604488694548053, -13.89961937509957401, 80.62609039468567573 ) ) ;
#52784 = CARTESIAN_POINT ( 'NONE',  ( -8.224510206698948167, 14.34966873604960824, 65.41557627198102409 ) ) ;
#52785 = CARTESIAN_POINT ( 'NONE',  ( 18.67979575497194134, -10.72451020669871369, 110.8344237280190043 ) ) ;
#52786 = CARTESIAN_POINT ( 'NONE',  ( 21.53943276465977519, -0.05219959533907433946, 98.74890960531438111 ) ) ;
#52787 = CARTESIAN_POINT ( 'NONE',  ( -10.72451020669870658, -18.67979575497194134, 79.58442372801903275 ) ) ;
#52788 = CARTESIAN_POINT ( 'NONE',  ( 5.719274019375673035, 21.55341960407619339, 77.29275706135234714 ) ) ;
#52789 = EDGE_CURVE ( 'NONE', #55277, #127622, #85731, .T. ) ;
#52790 = CARTESIAN_POINT ( 'NONE',  ( 19.03943276465977164, -0.05219959533909143690, 113.7489096053143669 ) ) ;
#52792 = CARTESIAN_POINT ( 'NONE',  ( 15.72974639402176855, 15.80617190586768217, 81.87609039468568994 ) ) ;
#52791 = CARTESIAN_POINT ( 'NONE',  ( -16.52544592524335698, -4.483927247898792601, 108.9594237280190185 ) ) ;
#52793 = CARTESIAN_POINT ( 'NONE',  ( -19.02544592524342804, 5.153800228976336051, 61.04057627198103120 ) ) ;
#52794 = CARTESIAN_POINT ( 'NONE',  ( -0.05219959533937732626, 21.53943276465977519, 42.50109039468567573 ) ) ;
#52795 = CARTESIAN_POINT ( 'NONE',  ( -16.46253265017160317, 9.564922557960807481, 85.83224293864769550 ) ) ;
#52796 = CARTESIAN_POINT ( 'NONE',  ( -14.34966873604960291, -8.224510206698953496, 86.66557627198102409 ) ) ;
#52797 = CARTESIAN_POINT ( 'NONE',  ( 14.34966873604960469, 8.224510206698951720, 49.16557627198102409 ) ) ;
#52798 = CARTESIAN_POINT ( 'NONE',  ( -5.823673210054116645, -21.52544592524344225, 57.29057627198103120 ) ) ;
#52799 = EDGE_CURVE ( 'NONE', #64113, #190965, #121194, .T. ) ;
#52800 = CARTESIAN_POINT ( 'NONE',  ( -13.89961937509977652, 13.97604488694528158, 55.62390960531434558 ) ) ;
#52801 = CARTESIAN_POINT ( 'NONE',  ( 10.81492255796078972, 18.62759615963270932, 74.58224293864768129 ) ) ;
#52802 = CARTESIAN_POINT ( 'NONE',  ( -9.474510206698720793, -16.51473224551083518, 64.58442372801900433 ) ) ;
#52804 = CARTESIAN_POINT ( 'NONE',  ( 14.29746914071049879, -8.314922557960816363, 73.33224293864769550 ) ) ;
#52803 = CARTESIAN_POINT ( 'NONE',  ( 19.02544592524335343, 5.153800228976608722, 26.45942372801899722 ) ) ;
#52805 = CARTESIAN_POINT ( 'NONE',  ( -18.67979575497178146, -10.72451020669898902, 56.66557627198103830 ) ) ;
#52806 = ORIENTED_EDGE ( 'NONE', *, *, #139182, .F. ) ;
#52807 = CARTESIAN_POINT ( 'NONE',  ( -17.49999999999999645, -5.500000000000000888, 120.0000000000000142 ) ) ;
#52809 = CARTESIAN_POINT ( 'NONE',  ( -22.44159573604010305, 16.30477369853692338, 143.1750000027311671 ) ) ;
#52808 = CARTESIAN_POINT ( 'NONE',  ( 0.05219959533934541429, -16.53943276465976808, 95.00109039468568994 ) ) ;
#52810 = CARTESIAN_POINT ( 'NONE',  ( -9.474510206698720793, -16.51473224551083518, 89.58442372801900433 ) ) ;
#52811 = CARTESIAN_POINT ( 'NONE',  ( -14.29746914071049879, 8.314922557960819915, 65.83224293864769550 ) ) ;
#52812 = CARTESIAN_POINT ( 'NONE',  ( -37.45873412500000654, 2.428612866367529932E-14, -10.31249999863440792 ) ) ;
#52813 = CARTESIAN_POINT ( 'NONE',  ( 5.153800228976335163, 19.02544592524342804, 59.79057627198100988 ) ) ;
#52814 = CARTESIAN_POINT ( 'NONE',  ( -14.29746914071049879, 8.314922557960819915, 55.83224293864770260 ) ) ;
#52815 = CARTESIAN_POINT ( 'NONE',  ( 0.05219959533909260263, 19.03943276465977164, 89.99890960531436690 ) ) ;
#52817 = CARTESIAN_POINT ( 'NONE',  ( 19.02544592524343514, -5.153800228976328945, 48.54057627198103120 ) ) ;
#52816 = CARTESIAN_POINT ( 'NONE',  ( -16.46253265017146816, -9.564922557961047289, 79.16775706135234714 ) ) ;
#52818 = CARTESIAN_POINT ( 'NONE',  ( -16.46253265017160317, 9.564922557960807481, 90.83224293864769550 ) ) ;
#52819 = CARTESIAN_POINT ( 'NONE',  ( -5.153800228976328057, -19.02544592524343514, 67.29057627198102409 ) ) ;
#52820 = CARTESIAN_POINT ( 'NONE',  ( -0.05219959533907301413, -21.53943276465977519, 67.49890960531436690 ) ) ;
#52821 = CARTESIAN_POINT ( 'NONE',  ( 14.29746914071037800, 8.314922557961029526, 56.66775706135235424 ) ) ;
#52822 = CARTESIAN_POINT ( 'NONE',  ( 5.000000000000000000, -139.5000000000000000, 21.82407087589996308 ) ) ;
#52823 = CARTESIAN_POINT ( 'NONE',  ( 19.05341960407611168, 5.049401038298154454, 53.95724293864770260 ) ) ;
#52824 = CARTESIAN_POINT ( 'NONE',  ( 10.72451020669898902, -18.67979575497178502, 57.91557627198103120 ) ) ;
#52825 = CARTESIAN_POINT ( 'NONE',  ( -13.89961937509957401, -13.97604488694547875, 79.37609039468567573 ) ) ;
#52826 = CARTESIAN_POINT ( 'NONE',  ( 0.05219959533910956823, 16.53943276465976808, 29.99890960531435979 ) ) ;
#52827 = CARTESIAN_POINT ( 'NONE',  ( -16.51473224551082808, 9.474510206698731452, 38.33442372801899722 ) ) ;
#52829 = CARTESIAN_POINT ( 'NONE',  ( 0.05219959533934541429, -16.53943276465976808, 100.0010903946857042 ) ) ;
#52828 = CARTESIAN_POINT ( 'NONE',  ( -16.53943276465976808, -0.05219959533934237506, 58.75109039468568994 ) ) ;
#52830 = CARTESIAN_POINT ( 'NONE',  ( 18.56453257813361901, -5.500000000000039080, 43.49000423690687711 ) ) ;
#52831 = CARTESIAN_POINT ( 'NONE',  ( 16.55341960407618274, -4.379528057220086978, 86.04275706135236135 ) ) ;
#52832 = CARTESIAN_POINT ( 'NONE',  ( -19.03943276465977164, 0.05219959533909376836, 116.2489096053143669 ) ) ;
#52833 = CARTESIAN_POINT ( 'NONE',  ( -9.474510206698964154, 16.51473224551069663, 40.41557627198103120 ) ) ;
#52834 = CARTESIAN_POINT ( 'NONE',  ( -19.03943276465977164, 0.05219959533909376836, 46.24890960531435979 ) ) ;
#52835 = CARTESIAN_POINT ( 'NONE',  ( -16.51473224551069308, -9.474510206698971260, 41.66557627198103120 ) ) ;
#52836 = CARTESIAN_POINT ( 'NONE',  ( -15.72974639402176322, -15.80617190586768395, 34.37609039468568284 ) ) ;
#52837 = CARTESIAN_POINT ( 'NONE',  ( 4.379528057220092307, 16.55341960407617563, 47.29275706135234003 ) ) ;
#52838 = CARTESIAN_POINT ( 'NONE',  ( -16.53943276465976808, -0.05219959533934237506, 113.7510903946856757 ) ) ;
#52839 = CARTESIAN_POINT ( 'NONE',  ( 16.51473224551069308, 9.474510206698969483, 24.16557627198102765 ) ) ;
#52840 = CARTESIAN_POINT ( 'NONE',  ( 13.89961937509957401, 13.97604488694547697, 21.87609039468566152 ) ) ;
#52841 = CARTESIAN_POINT ( 'NONE',  ( -19.03943276465977164, -0.05219959533935918106, 113.7510903946856757 ) ) ;
#52842 = CARTESIAN_POINT ( 'NONE',  ( 9.564922557961047289, -16.46253265017146816, 70.41775706135233293 ) ) ;
#52843 = CARTESIAN_POINT ( 'NONE',  ( -12.06949235617756955, 12.14591786802309770, 70.62390960531436690 ) ) ;
#52844 = CARTESIAN_POINT ( 'NONE',  ( 19.02544592524343514, -5.153800228976328945, 43.54057627198103120 ) ) ;
#52845 = CARTESIAN_POINT ( 'NONE',  ( -19.03943276465977164, -0.05219959533935918106, 68.75109039468566152 ) ) ;
#52846 = CARTESIAN_POINT ( 'NONE',  ( -10.81492255796105439, 18.62759615963255655, 72.91775706135234714 ) ) ;
#52847 = CARTESIAN_POINT ( 'NONE',  ( -8.314922557961024197, 14.29746914071037800, 42.91775706135235424 ) ) ;
#52848 = CARTESIAN_POINT ( 'NONE',  ( 19.53037848336980886, -5.499999999999891642, 57.35532783611445495 ) ) ;
#52849 = CARTESIAN_POINT ( 'NONE',  ( -0.05219959533907301413, -21.53943276465977519, 42.49890960531435979 ) ) ;
#52850 = CARTESIAN_POINT ( 'NONE',  ( -8.224510206698735004, -14.34966873604973081, 24.58442372801901499 ) ) ;
#52851 = CARTESIAN_POINT ( 'NONE',  ( 17.72517630440434999, -5.499999999999972466, 98.42175719257214439 ) ) ;
#52852 = CARTESIAN_POINT ( 'NONE',  ( -5.719274019375665041, -21.55341960407619695, 104.7927570613523898 ) ) ;
#52853 = CARTESIAN_POINT ( 'NONE',  ( -24.44405923433097172, 13.71792739260091132, 165.9118100595185297 ) ) ;
#52854 = CARTESIAN_POINT ( 'NONE',  ( 19.05341960407611168, 5.049401038298154454, 43.95724293864769550 ) ) ;
#52855 = CARTESIAN_POINT ( 'NONE',  ( -17.49999999999999645, 5.499999999999997335, 120.0000000000000142 ) ) ;
#52856 = CARTESIAN_POINT ( 'NONE',  ( 13.89961937509977652, -13.97604488694527269, 58.12390960531436690 ) ) ;
#52857 = CARTESIAN_POINT ( 'NONE',  ( 10.72451020669871369, 18.67979575497193778, 62.08442372801901143 ) ) ;
#52858 = CARTESIAN_POINT ( 'NONE',  ( 18.67979575497194134, -10.72451020669871369, 110.8344237280190043 ) ) ;
#52859 = CARTESIAN_POINT ( 'NONE',  ( -14.34966873604960291, -8.224510206698953496, 26.66557627198103475 ) ) ;
#52860 = CARTESIAN_POINT ( 'NONE',  ( 16.51473224551069308, 9.474510206698969483, 29.16557627198103475 ) ) ;
#52861 = CARTESIAN_POINT ( 'NONE',  ( 9.474510206698971260, -16.51473224551069308, 87.91557627198102409 ) ) ;
#52862 = CARTESIAN_POINT ( 'NONE',  ( -18.67979575497193778, 10.72451020669871902, 53.33442372801901854 ) ) ;
#52863 = CARTESIAN_POINT ( 'NONE',  ( 19.05341960407611168, 5.049401038298154454, 33.95724293864769550 ) ) ;
#52864 = VECTOR ( 'NONE', #11237, 1000.000000000000114 ) ;
#52865 = CARTESIAN_POINT ( 'NONE',  ( -5.719274019375665041, -21.55341960407619695, 69.79275706135234714 ) ) ;
#52867 = CARTESIAN_POINT ( 'NONE',  ( -9.474510206698964154, 16.51473224551069663, 110.4155762719810383 ) ) ;
#52866 = CARTESIAN_POINT ( 'NONE',  ( -9.474510206698720793, -16.51473224551083518, 89.58442372801900433 ) ) ;
#52868 = CARTESIAN_POINT ( 'NONE',  ( -14.29746914071049879, 8.314922557960819915, 115.8322429386477097 ) ) ;
#52869 = CARTESIAN_POINT ( 'NONE',  ( -5.823673210054116645, -21.52544592524344225, 112.2905762719810241 ) ) ;
#52870 = CARTESIAN_POINT ( 'NONE',  ( -19.05341960407617563, 5.049401038297882671, 33.54275706135231871 ) ) ;
#52871 = CARTESIAN_POINT ( 'NONE',  ( -12.06949235617756955, 12.14591786802309770, 115.6239096053143669 ) ) ;
#52872 = CARTESIAN_POINT ( 'NONE',  ( 19.05341960407611168, 5.049401038298154454, 58.95724293864768129 ) ) ;
#52873 = CARTESIAN_POINT ( 'NONE',  ( -19.03943276465977164, -0.05219959533935918106, 103.7510903946856757 ) ) ;
#52874 = CARTESIAN_POINT ( 'NONE',  ( -16.55341960407611168, -4.379528057220339221, 61.45724293864770260 ) ) ;
#52875 = CARTESIAN_POINT ( 'NONE',  ( 5.153800228976615827, -19.02544592524334988, 30.20942372801900433 ) ) ;
#52876 = CARTESIAN_POINT ( 'NONE',  ( -21.55341960407610458, -5.719274019375992779, 21.45724293864769550 ) ) ;
#52877 = CARTESIAN_POINT ( 'NONE',  ( 5.153800228976615827, -19.02544592524334988, 90.20942372801900433 ) ) ;
#52878 = CARTESIAN_POINT ( 'NONE',  ( 18.62759615963271287, -10.81492255796078972, 98.33224293864769550 ) ) ;
#52879 = CARTESIAN_POINT ( 'NONE',  ( -21.53943276465977519, -0.05219959533937600094, 38.75109039468567573 ) ) ;
#52880 = CARTESIAN_POINT ( 'NONE',  ( 14.29746914071037800, 8.314922557961029526, 36.66775706135234714 ) ) ;
#52882 = CARTESIAN_POINT ( 'NONE',  ( -0.05219959533937732626, 21.53943276465977519, 47.50109039468568994 ) ) ;
#52881 = CARTESIAN_POINT ( 'NONE',  ( 12.06949235617739724, 12.14591786802326823, 46.87609039468568994 ) ) ;
#52883 = CARTESIAN_POINT ( 'NONE',  ( -21.53943276465977519, 0.05219959533907696930, 56.24890960531436690 ) ) ;
#52884 = CARTESIAN_POINT ( 'NONE',  ( -19.02544592524342804, 5.153800228976336051, 36.04057627198100988 ) ) ;
#52885 = CARTESIAN_POINT ( 'NONE',  ( 3.766062262543149401E-15, -39.95556452105413570, -7.249999994537627224 ) ) ;
#52886 = CARTESIAN_POINT ( 'NONE',  ( 4.379528057220092307, 16.55341960407617563, 77.29275706135234714 ) ) ;
#52887 = CARTESIAN_POINT ( 'NONE',  ( 5.719274019375991003, -21.55341960407610458, 92.70724293864770971 ) ) ;
#52888 = CARTESIAN_POINT ( 'NONE',  ( -8.224510206698948167, 14.34966873604960824, 35.41557627198102409 ) ) ;
#52889 = CARTESIAN_POINT ( 'NONE',  ( 4.483927247898790824, -16.52544592524335698, 65.20942372801901854 ) ) ;
#52890 = CARTESIAN_POINT ( 'NONE',  ( -19.03943276465977164, -0.05219959533935918106, 98.75109039468567573 ) ) ;
#52891 = CARTESIAN_POINT ( 'NONE',  ( -10.81492255796078084, -18.62759615963271287, 92.08224293864769550 ) ) ;
#52892 = CARTESIAN_POINT ( 'NONE',  ( -16.52544592524342804, 4.483927247898546575, 26.04057627198103475 ) ) ;
#52893 = EDGE_LOOP ( 'NONE', ( #33146, #199013, #118504, #119376, #88322, #115775, #118596, #21394, #113655, #57111, #121428, #97638 ) ) ;
#52894 = CARTESIAN_POINT ( 'NONE',  ( -0.05219959533934338120, 16.53943276465976808, 72.50109039468568994 ) ) ;
#52895 = CARTESIAN_POINT ( 'NONE',  ( 26.38458505201398907, 8.641005086744664609, 167.3773361139123494 ) ) ;
#52896 = CARTESIAN_POINT ( 'NONE',  ( 5.823673210054125526, 21.52544592524343514, 69.79057627198102409 ) ) ;
#52897 = CARTESIAN_POINT ( 'NONE',  ( -14.34966873604972548, 8.224510206698743886, 103.3344237280190043 ) ) ;
#52898 = ORIENTED_EDGE ( 'NONE', *, *, #195051, .F. ) ;
#52899 = CARTESIAN_POINT ( 'NONE',  ( 18.87255363501903815, 5.499999999999949374, 88.82513748171831480 ) ) ;
#52900 = CARTESIAN_POINT ( 'NONE',  ( 5.823673210054125526, 21.52544592524343514, 104.7905762719810241 ) ) ;
#52901 = CARTESIAN_POINT ( 'NONE',  ( 15.72974639402199770, -15.80617190586745480, 108.1239096053143811 ) ) ;
#52902 = CARTESIAN_POINT ( 'NONE',  ( 0.05219959533910956823, 16.53943276465976808, 34.99890960531435979 ) ) ;
#52903 = CARTESIAN_POINT ( 'NONE',  ( 14.29746914071037800, 8.314922557961029526, 36.66775706135234714 ) ) ;
#52904 = CARTESIAN_POINT ( 'NONE',  ( 5.049401038298161559, -19.05341960407611168, 52.70724293864767418 ) ) ;
#52905 = CARTESIAN_POINT ( 'NONE',  ( -19.05341960407611168, -5.049401038298163336, 61.45724293864769550 ) ) ;
#52906 = VERTEX_POINT ( 'NONE', #72727 ) ;
#52907 = CARTESIAN_POINT ( 'NONE',  ( -9.474510206698964154, 16.51473224551069663, 110.4155762719810383 ) ) ;
#52908 = CARTESIAN_POINT ( 'NONE',  ( -9.396967334131923977, -10.08899614358906405, -62.54888902377756210 ) ) ;
#52909 = CARTESIAN_POINT ( 'NONE',  ( -13.89961937509957401, -13.97604488694547875, 109.3760903946856331 ) ) ;
#52910 = CARTESIAN_POINT ( 'NONE',  ( 0.05219959533936267826, -19.03943276465977164, 55.00109039468566863 ) ) ;
#52911 = CARTESIAN_POINT ( 'NONE',  ( 0.05219959533907565091, 21.53943276465977519, 84.99890960531436690 ) ) ;
#52912 = CARTESIAN_POINT ( 'NONE',  ( -14.34966873604972548, 8.224510206698743886, 108.3344237280190185 ) ) ;
#52913 = CARTESIAN_POINT ( 'NONE',  ( -10.81492255796078084, -18.62759615963271287, 42.08224293864769550 ) ) ;
#52915 = CARTESIAN_POINT ( 'NONE',  ( 19.03943276465977164, 0.05219959533936151252, 101.2510903946856757 ) ) ;
#52914 = CARTESIAN_POINT ( 'NONE',  ( 10.72451020669898902, -18.67979575497178502, 82.91557627198103830 ) ) ;
#52916 = CARTESIAN_POINT ( 'NONE',  ( 19.03943276465977164, -0.05219959533909143690, 113.7489096053143669 ) ) ;
#52917 = CARTESIAN_POINT ( 'NONE',  ( 15.72974639402176855, 15.80617190586768217, 81.87609039468568994 ) ) ;
#52918 = CARTESIAN_POINT ( 'NONE',  ( -19.05341960407611168, -5.049401038298163336, 71.45724293864766707 ) ) ;
#52919 = CARTESIAN_POINT ( 'NONE',  ( -19.05341960407611168, -5.049401038298163336, 21.45724293864768839 ) ) ;
#52920 = CARTESIAN_POINT ( 'NONE',  ( 16.46253265017160672, -9.564922557960803928, 73.33224293864769550 ) ) ;
#52921 = CARTESIAN_POINT ( 'NONE',  ( -8.224510206698948167, 14.34966873604960824, 90.41557627198103830 ) ) ;
#52922 = ORIENTED_EDGE ( 'NONE', *, *, #61218, .T. ) ;
#52923 = CARTESIAN_POINT ( 'NONE',  ( -5.153800228976607833, 19.02544592524334988, 102.7094237280189759 ) ) ;
#52924 = CIRCLE ( 'NONE', #101280, 27.91311885011353766 ) ;
#52925 = DIRECTION ( 'NONE',  ( -1.000000000000000000, -0.000000000000000000, -0.000000000000000000 ) ) ;
#52926 = CARTESIAN_POINT ( 'NONE',  ( -19.05341960407611168, -5.049401038298163336, 76.45724293864769550 ) ) ;
#52928 = CARTESIAN_POINT ( 'NONE',  ( 9.564922557960805705, 16.46253265017160317, 94.58224293864769550 ) ) ;
#52927 = CARTESIAN_POINT ( 'NONE',  ( -21.53943276465977519, -0.05219959533937600094, 78.75109039468568994 ) ) ;
#52929 = CARTESIAN_POINT ( 'NONE',  ( 14.29746914071037800, 8.314922557961029526, 71.66775706135234714 ) ) ;
#52930 = CARTESIAN_POINT ( 'NONE',  ( -17.31747979337950838, -6.344076630960982399, 76.37944868065184778 ) ) ;
#52931 = CARTESIAN_POINT ( 'NONE',  ( -13.97604488694547697, 13.89961937509957934, 58.12609039468566863 ) ) ;
#52932 = CARTESIAN_POINT ( 'NONE',  ( -5.153800228976607833, 19.02544592524334988, 22.70942372801899012 ) ) ;
#52933 = CARTESIAN_POINT ( 'NONE',  ( 4.619345608252475976, 6.673977169394437858, -64.16796455867367399 ) ) ;
#52934 = CARTESIAN_POINT ( 'NONE',  ( -19.03943276465977164, 0.05219959533909376836, 116.2489096053143669 ) ) ;
#52935 = CARTESIAN_POINT ( 'NONE',  ( -36.91746825000000598, 2.428612866367529932E-14, -3.124999997268813168 ) ) ;
#52936 = CARTESIAN_POINT ( 'NONE',  ( 16.55341960407611168, 4.379528057220329451, 23.95724293864769550 ) ) ;
#52937 = CARTESIAN_POINT ( 'NONE',  ( -35.59965464630457888, -2.422542088861810772, 37.88523239209964544 ) ) ;
#52938 = CARTESIAN_POINT ( 'NONE',  ( 16.52544592524335698, 4.483927247898782831, 106.4594237280190328 ) ) ;
#52939 = CARTESIAN_POINT ( 'NONE',  ( 17.05116617787824751, 6.768360034955832383, 68.84324446740802728 ) ) ;
#52940 = CARTESIAN_POINT ( 'NONE',  ( -16.52544592524335698, -4.483927247898792601, 83.95942372801900433 ) ) ;
#52941 = CARTESIAN_POINT ( 'NONE',  ( -5.823673210054431948, 21.52544592524334988, 82.70942372801900433 ) ) ;
#52942 = CARTESIAN_POINT ( 'NONE',  ( 16.51473224551083163, -9.474510206698727899, 90.83442372801900433 ) ) ;
#52943 = CARTESIAN_POINT ( 'NONE',  ( -5.049401038297874678, -19.05341960407617918, 39.79275706135232582 ) ) ;
#52944 = CARTESIAN_POINT ( 'NONE',  ( 16.46253265017160672, -9.564922557960803928, 78.33224293864769550 ) ) ;
#52945 = CARTESIAN_POINT ( 'NONE',  ( -13.89961937509977652, 13.97604488694528158, 50.62390960531435979 ) ) ;
#52946 = CARTESIAN_POINT ( 'NONE',  ( -19.46398650005389541, 5.499999999999947597, 40.18269651486372851 ) ) ;
#52947 = CARTESIAN_POINT ( 'NONE',  ( 18.67979575497178502, 10.72451020669898547, 89.16557627198102409 ) ) ;
#52948 = VECTOR ( 'NONE', #131830, 1000.000000000000114 ) ;
#52949 = CARTESIAN_POINT ( 'NONE',  ( -21.53943276465977519, 0.05219959533907696930, 51.24890960531436690 ) ) ;
#52950 = CARTESIAN_POINT ( 'NONE',  ( 16.51473224551069308, 9.474510206698969483, 49.16557627198102409 ) ) ;
#52951 = CARTESIAN_POINT ( 'NONE',  ( 16.52544592524335698, 4.483927247898782831, 61.45942372801901854 ) ) ;
#52952 = ORIENTED_EDGE ( 'NONE', *, *, #87523, .T. ) ;
#52953 = CARTESIAN_POINT ( 'NONE',  ( -18.62759615963255300, -10.81492255796106328, 44.16775706135234714 ) ) ;
#52955 = CARTESIAN_POINT ( 'NONE',  ( 36.91746824999999887, 11.99521256947799053, -7.524999997268814411 ) ) ;
#52954 = CARTESIAN_POINT ( 'NONE',  ( 8.224510206698953496, -14.34966873604960469, 62.91557627198102409 ) ) ;
#52956 = CARTESIAN_POINT ( 'NONE',  ( -16.55341960407617563, 4.379528057220093196, 43.54275706135235424 ) ) ;
#52957 = CARTESIAN_POINT ( 'NONE',  ( 8.314922557960818139, 14.29746914071049879, 104.5822429386477097 ) ) ;
#52958 = CARTESIAN_POINT ( 'NONE',  ( -5.049401038297874678, -19.05341960407617918, 49.79275706135231871 ) ) ;
#52959 = CARTESIAN_POINT ( 'NONE',  ( -8.224510206698948167, 14.34966873604960824, 60.41557627198102409 ) ) ;
#52960 = CARTESIAN_POINT ( 'NONE',  ( 0.05219959533937995610, -21.53943276465977519, 35.00109039468568284 ) ) ;
#52962 = CARTESIAN_POINT ( 'NONE',  ( -5.719274019375978568, 21.55341960407610458, 85.20724293864770971 ) ) ;
#52961 = CARTESIAN_POINT ( 'NONE',  ( 19.02544592524343514, -5.153800228976328945, 28.54057627198102409 ) ) ;
#52963 = CARTESIAN_POINT ( 'NONE',  ( 16.46253265017160672, -9.564922557960803928, 108.3322429386476955 ) ) ;
#52964 = CARTESIAN_POINT ( 'NONE',  ( -14.29746914071049879, 8.314922557960819915, 80.83224293864769550 ) ) ;
#52965 = CARTESIAN_POINT ( 'NONE',  ( 16.46253265017160672, -9.564922557960803928, 113.3322429386476955 ) ) ;
#52966 = CARTESIAN_POINT ( 'NONE',  ( 11.40812507854754365, 35.11059874428196537, -1.224999997268813479 ) ) ;
#52967 = CARTESIAN_POINT ( 'NONE',  ( -0.05219959533936034679, 19.03943276465977164, 77.50109039468566152 ) ) ;
#52968 = CARTESIAN_POINT ( 'NONE',  ( 5.823673210054444382, -21.52544592524334988, 20.20942372801900788 ) ) ;
#52969 = CARTESIAN_POINT ( 'NONE',  ( 16.51473224551069308, 9.474510206698969483, 64.16557627198102409 ) ) ;
#52970 = CARTESIAN_POINT ( 'NONE',  ( -19.05341960407617563, 5.049401038297882671, 58.54275706135234003 ) ) ;
#52971 = CARTESIAN_POINT ( 'NONE',  ( -5.153800228976328057, -19.02544592524343514, 32.29057627198102409 ) ) ;
#52972 = CARTESIAN_POINT ( 'NONE',  ( 18.67979575497194134, -10.72451020669871369, 80.83442372801901854 ) ) ;
#52973 = CARTESIAN_POINT ( 'NONE',  ( -8.314922557960811034, -14.29746914071050412, 62.08224293864769550 ) ) ;
#52974 = CARTESIAN_POINT ( 'NONE',  ( 12.14591786802309770, 12.06949235617756955, 54.37390960531435979 ) ) ;
#52975 = CARTESIAN_POINT ( 'NONE',  ( -16.51473224551069308, -9.474510206698971260, 66.66557627198102409 ) ) ;
#52976 = CARTESIAN_POINT ( 'NONE',  ( -21.52544592524343514, 5.823673210054127303, 86.04057627198102409 ) ) ;
#52977 = CARTESIAN_POINT ( 'NONE',  ( -13.89961937509977652, 13.97604488694528158, 55.62390960531434558 ) ) ;
#52978 = VERTEX_POINT ( 'NONE', #138357 ) ;
#52979 = CARTESIAN_POINT ( 'NONE',  ( -10.72451020669898014, 18.67979575497178502, 75.41557627198102409 ) ) ;
#52980 = CARTESIAN_POINT ( 'NONE',  ( -18.62759615963255300, -10.81492255796106328, 99.16775706135234714 ) ) ;
#52983 = CARTESIAN_POINT ( 'NONE',  ( -14.29746914071049879, 8.314922557960819915, 100.8322429386477097 ) ) ;
#52982 = CARTESIAN_POINT ( 'NONE',  ( -16.55341960407617563, 4.379528057220093196, 98.54275706135234714 ) ) ;
#52981 = CARTESIAN_POINT ( 'NONE',  ( -18.22780087662121673, -5.500000000000063061, 46.48459894673893444 ) ) ;
#52984 = EDGE_LOOP ( 'NONE', ( #51342, #10662, #149771 ) ) ;
#52985 = CARTESIAN_POINT ( 'NONE',  ( -19.03943276465977164, -0.05219959533935918106, 93.75109039468566152 ) ) ;
#52986 = EDGE_LOOP ( 'NONE', ( #82094, #96419, #64161, #189977 ) ) ;
#52987 = CARTESIAN_POINT ( 'NONE',  ( 18.67979575497178502, 10.72451020669898547, 109.1655762719810383 ) ) ;
#52988 = CARTESIAN_POINT ( 'NONE',  ( 13.97604488694548053, -13.89961937509957401, 55.62609039468566863 ) ) ;
#52989 = CARTESIAN_POINT ( 'NONE',  ( 12.06949235617739724, 12.14591786802326823, 96.87609039468568994 ) ) ;
#52990 = CARTESIAN_POINT ( 'NONE',  ( -9.564922557961040184, 16.46253265017147172, 27.91775706135232582 ) ) ;
#52991 = CARTESIAN_POINT ( 'NONE',  ( 5.049401038298161559, -19.05341960407611168, 102.7072429386476955 ) ) ;
#52992 = CARTESIAN_POINT ( 'NONE',  ( -21.52544592524343514, 5.823673210054127303, 61.04057627198103120 ) ) ;
#52993 = CARTESIAN_POINT ( 'NONE',  ( 9.474510206698971260, -16.51473224551069308, 22.91557627198102765 ) ) ;
#52994 = CARTESIAN_POINT ( 'NONE',  ( -0.05219959533909027116, -19.03943276465977164, 37.49890960531436690 ) ) ;
#52995 = CARTESIAN_POINT ( 'NONE',  ( -15.72974639402176322, -15.80617190586768395, 104.3760903946856899 ) ) ;
#52996 = CARTESIAN_POINT ( 'NONE',  ( 16.52544592524335698, 4.483927247898782831, 76.45942372801901854 ) ) ;
#52997 = CARTESIAN_POINT ( 'NONE',  ( -10.81492255796105439, 18.62759615963255655, 32.91775706135234714 ) ) ;
#52998 = CARTESIAN_POINT ( 'NONE',  ( 12.06949235617739724, 12.14591786802326823, 41.87609039468568284 ) ) ;
#52999 = CARTESIAN_POINT ( 'NONE',  ( -5.049401038298153566, 19.05341960407611168, 105.2072429386476671 ) ) ;
#53000 = CARTESIAN_POINT ( 'NONE',  ( 13.89961937509977652, -13.97604488694527269, 48.12390960531435979 ) ) ;
#53001 = CARTESIAN_POINT ( 'NONE',  ( 19.02544592524343514, -5.153800228976328945, 68.54057627198103830 ) ) ;
#53002 = CARTESIAN_POINT ( 'NONE',  ( 8.224510206698742110, 14.34966873604972548, 47.08442372801901854 ) ) ;
#53003 = CARTESIAN_POINT ( 'NONE',  ( 8.314922557960818139, 14.29746914071049879, 89.58224293864768129 ) ) ;
#53004 = CARTESIAN_POINT ( 'NONE',  ( -0.05219959533934338120, 16.53943276465976808, 102.5010903946856899 ) ) ;
#53005 = DIRECTION ( 'NONE',  ( 0.000000000000000000, 0.000000000000000000, 1.000000000000000000 ) ) ;
#53008 = CARTESIAN_POINT ( 'NONE',  ( -16.46253265017160317, 9.564922557960807481, 60.83224293864769550 ) ) ;
#53007 = CARTESIAN_POINT ( 'NONE',  ( 5.049401038298161559, -19.05341960407611168, 82.70724293864770971 ) ) ;
#53006 = CARTESIAN_POINT ( 'NONE',  ( -15.80617190586768217, 15.72974639402176855, 53.12609039468568284 ) ) ;
#53009 = CARTESIAN_POINT ( 'NONE',  ( 5.153800228976335163, 19.02544592524342804, 89.79057627198102409 ) ) ;
#53010 = CARTESIAN_POINT ( 'NONE',  ( 12.14591786802309770, 12.06949235617756955, 49.37390960531436690 ) ) ;
#53011 = CARTESIAN_POINT ( 'NONE',  ( -16.52544592524335698, -4.483927247898792601, 93.95942372801903275 ) ) ;
#53012 = CARTESIAN_POINT ( 'NONE',  ( 4.379528057220339221, -16.55341960407611168, 22.70724293864769194 ) ) ;
#53013 = EDGE_LOOP ( 'NONE', ( #28443, #55238, #95964, #102661 ) ) ;
#53014 = CARTESIAN_POINT ( 'NONE',  ( 0.05219959533936267826, -19.03943276465977164, 50.00109039468566863 ) ) ;
#53015 = CARTESIAN_POINT ( 'NONE',  ( -19.02544592524342804, 5.153800228976336051, 116.0405762719810383 ) ) ;
#53016 = CARTESIAN_POINT ( 'NONE',  ( 16.46253265017160672, -9.564922557960803928, 68.33224293864770971 ) ) ;
#53017 = CARTESIAN_POINT ( 'NONE',  ( -19.02544592524334988, -5.153800228976617603, 38.95942372801900433 ) ) ;
#53018 = CARTESIAN_POINT ( 'NONE',  ( 22.81625015709509441, 31.40387420917330275, -1.324999997268813123 ) ) ;
#53019 = CARTESIAN_POINT ( 'NONE',  ( 37.99999999999999289, 2.893978650043524126E-14, -2.749999994537626780 ) ) ;
#53021 = CARTESIAN_POINT ( 'NONE',  ( -4.379528057220086978, -16.55341960407618274, 69.79275706135234714 ) ) ;
#53020 = CARTESIAN_POINT ( 'NONE',  ( 19.02544592524334988, 5.153800228976608722, 86.45942372801900433 ) ) ;
#53022 = CARTESIAN_POINT ( 'NONE',  ( 17.31728774477273802, 6.344390552232390235, 91.68093348310684121 ) ) ;
#53023 = CARTESIAN_POINT ( 'NONE',  ( -16.51473224551069308, -9.474510206698971260, 91.66557627198103830 ) ) ;
#53024 = CARTESIAN_POINT ( 'NONE',  ( -10.72451020669870658, -18.67979575497194134, 34.58442372801900433 ) ) ;
#53025 = CARTESIAN_POINT ( 'NONE',  ( 16.46253265017146816, 9.564922557961045513, 81.66775706135233293 ) ) ;
#53027 = CARTESIAN_POINT ( 'NONE',  ( -19.05341960407611168, -5.049401038298163336, 51.45724293864770260 ) ) ;
#53026 = CARTESIAN_POINT ( 'NONE',  ( 17.12812012977029497, 6.668231424565951748, 88.85948759323147783 ) ) ;
#53028 = CARTESIAN_POINT ( 'NONE',  ( -19.03943276465977164, 0.05219959533909376836, 91.24890960531436690 ) ) ;
#53030 = CARTESIAN_POINT ( 'NONE',  ( 16.46253265017160672, -9.564922557960803928, 33.33224293864770260 ) ) ;
#53029 = CARTESIAN_POINT ( 'NONE',  ( 12.06949235617757843, -12.14591786802309237, 48.12390960531436690 ) ) ;
#53031 = CARTESIAN_POINT ( 'NONE',  ( -9.564922557961040184, 16.46253265017147172, 52.91775706135233293 ) ) ;
#53032 = CARTESIAN_POINT ( 'NONE',  ( 4.379528057220339221, -16.55341960407611168, 92.70724293864770971 ) ) ;
#53033 = CARTESIAN_POINT ( 'NONE',  ( -13.97604488694547697, 13.89961937509957934, 33.12609039468566863 ) ) ;
#53034 = CARTESIAN_POINT ( 'NONE',  ( 16.51473224551069308, 9.474510206698969483, 64.16557627198102409 ) ) ;
#53035 = EDGE_CURVE ( 'NONE', #115964, #89861, #197071, .T. ) ;
#53036 = CIRCLE ( 'NONE', #43397, 4.000000000000000888 ) ;
#53037 = CARTESIAN_POINT ( 'NONE',  ( -15.72974639402197994, 15.80617190586746368, 65.62390960531436690 ) ) ;
#53039 = CARTESIAN_POINT ( 'NONE',  ( 9.564922557961047289, -16.46253265017146816, 25.41775706135234003 ) ) ;
#53038 = CARTESIAN_POINT ( 'NONE',  ( -8.224510206698948167, 14.34966873604960824, 55.41557627198102409 ) ) ;
#53040 = CARTESIAN_POINT ( 'NONE',  ( -9.474510206698964154, 16.51473224551069663, 100.4155762719810241 ) ) ;
#53041 = CARTESIAN_POINT ( 'NONE',  ( 21.55341960407610458, 5.719274019375980345, 23.95724293864769550 ) ) ;
#53042 = CARTESIAN_POINT ( 'NONE',  ( 16.46253265017160672, -9.564922557960803928, 48.33224293864769550 ) ) ;
#53043 = CARTESIAN_POINT ( 'NONE',  ( 0.05219959533909260263, 19.03943276465977164, 24.99890960531435269 ) ) ;
#53044 = CARTESIAN_POINT ( 'NONE',  ( -4.483927247898539470, -16.52544592524342804, 97.29057627198105251 ) ) ;
#53045 = CARTESIAN_POINT ( 'NONE',  ( -0.05219959533907301413, -21.53943276465977519, 107.4989096053143669 ) ) ;
#53046 = CARTESIAN_POINT ( 'NONE',  ( -13.89961937509977652, 13.97604488694528158, 100.6239096053143669 ) ) ;
#53047 = CARTESIAN_POINT ( 'NONE',  ( -0.05219959533907301413, -21.53943276465977519, 107.4989096053143669 ) ) ;
#53048 = CARTESIAN_POINT ( 'NONE',  ( 16.51473224551069308, 9.474510206698969483, 99.16557627198102409 ) ) ;
#53049 = CARTESIAN_POINT ( 'NONE',  ( -8.314922557960811034, -14.29746914071050412, 112.0822429386477097 ) ) ;
#53050 = CARTESIAN_POINT ( 'NONE',  ( 21.53943276465977519, 0.05219959533937863772, 81.25109039468568994 ) ) ;
#53051 = CARTESIAN_POINT ( 'NONE',  ( 5.823673210054125526, 21.52544592524343514, 89.79057627198103830 ) ) ;
#53052 = CARTESIAN_POINT ( 'NONE',  ( 16.81555441253553695, -7.025013491695474954, 108.1368544533426501 ) ) ;
#53053 = DIRECTION ( 'NONE',  ( 0.000000000000000000, 0.000000000000000000, 1.000000000000000000 ) ) ;
#53054 = CARTESIAN_POINT ( 'NONE',  ( 17.59860650958989936, 7.585241751807028088, 59.07662985737508166 ) ) ;
#53055 = CARTESIAN_POINT ( 'NONE',  ( 16.53943276465976808, 0.05219959533934440121, 41.25109039468568284 ) ) ;
#53057 = AXIS2_PLACEMENT_3D ( 'NONE', #14245, #165964, #134636 ) ;
#53056 = CARTESIAN_POINT ( 'NONE',  ( 0.05219959533910956823, 16.53943276465976808, 104.9989096053143669 ) ) ;
#53058 = CARTESIAN_POINT ( 'NONE',  ( -17.49999999999998579, -3.850315288878773945, 110.7337086939655251 ) ) ;
#53059 = CARTESIAN_POINT ( 'NONE',  ( 16.51473224551069308, 9.474510206698969483, 54.16557627198103120 ) ) ;
#53060 = CARTESIAN_POINT ( 'NONE',  ( -4.379528057220328563, 16.55341960407611168, 90.20724293864770971 ) ) ;
#53061 = CARTESIAN_POINT ( 'NONE',  ( 15.80617190586746368, 15.72974639402197994, 39.37390960531436690 ) ) ;
#53062 = CARTESIAN_POINT ( 'NONE',  ( 12.06949235617757843, -12.14591786802309237, 63.12390960531435979 ) ) ;
#53063 = CARTESIAN_POINT ( 'NONE',  ( 16.55341960407618274, -4.379528057220086978, 21.04275706135234714 ) ) ;
#53064 = CARTESIAN_POINT ( 'NONE',  ( -5.823673210054431948, 21.52544592524334988, 77.70942372801900433 ) ) ;
#53065 = AXIS2_PLACEMENT_3D ( 'NONE', #63255, #14781, #49094 ) ;
#53066 = DIRECTION ( 'NONE',  ( -3.469446951953611033E-15, 0.000000000000000000, -1.000000000000000000 ) ) ;
#53067 = CARTESIAN_POINT ( 'NONE',  ( 14.34966873604972726, -8.224510206698740333, 95.83442372801903275 ) ) ;
#53068 = CARTESIAN_POINT ( 'NONE',  ( -8.224510206698948167, 14.34966873604960824, 45.41557627198103830 ) ) ;
#53069 = CARTESIAN_POINT ( 'NONE',  ( 9.474510206698971260, -16.51473224551069308, 32.91557627198102409 ) ) ;
#53070 = CARTESIAN_POINT ( 'NONE',  ( -9.564922557960796823, -16.46253265017161027, 87.08224293864769550 ) ) ;
#53071 = CARTESIAN_POINT ( 'NONE',  ( 5.823673210054125526, 21.52544592524343514, 94.79057627198105251 ) ) ;
#53072 = CARTESIAN_POINT ( 'NONE',  ( 14.29746914071037800, 8.314922557961029526, 26.66775706135235424 ) ) ;
#53074 = CARTESIAN_POINT ( 'NONE',  ( -21.53943276465977519, -0.05219959533937600094, 78.75109039468568994 ) ) ;
#53073 = CARTESIAN_POINT ( 'NONE',  ( -8.314922557960811034, -14.29746914071050412, 67.08224293864770971 ) ) ;
#53075 = CARTESIAN_POINT ( 'NONE',  ( -12.14591786802326823, 12.06949235617739902, 103.1260903946856757 ) ) ;
#53076 = CARTESIAN_POINT ( 'NONE',  ( 16.31925111598406630, -7.325300261831833915, 47.66424538967169156 ) ) ;
#53077 = CARTESIAN_POINT ( 'NONE',  ( -18.56101223717332260, -5.499999999999952927, 66.44978406935679516 ) ) ;
#53078 = CARTESIAN_POINT ( 'NONE',  ( -14.34966873604960291, -8.224510206698953496, 21.66557627198102409 ) ) ;
#53079 = CARTESIAN_POINT ( 'NONE',  ( -8.224510206698735004, -14.34966873604973081, 74.58442372801901854 ) ) ;
#53080 = CARTESIAN_POINT ( 'NONE',  ( 13.89961937509977652, -13.97604488694527269, 83.12390960531436690 ) ) ;
#53081 = CARTESIAN_POINT ( 'NONE',  ( -5.153800228976328057, -19.02544592524343514, 82.29057627198103830 ) ) ;
#53082 = CARTESIAN_POINT ( 'NONE',  ( 21.55341960407619695, -5.719274019375665929, 81.04275706135236135 ) ) ;
#53083 = CARTESIAN_POINT ( 'NONE',  ( -8.314922557961024197, 14.29746914071037800, 87.91775706135234714 ) ) ;
#53084 = CARTESIAN_POINT ( 'NONE',  ( 0.05219959533910956823, 16.53943276465976808, 54.99890960531435269 ) ) ;
#53085 = CARTESIAN_POINT ( 'NONE',  ( 16.46253265017160672, -9.564922557960803928, 63.33224293864769550 ) ) ;
#53086 = ORIENTED_EDGE ( 'NONE', *, *, #160165, .F. ) ;
#53087 = CARTESIAN_POINT ( 'NONE',  ( -16.52544592524335698, -4.483927247898792601, 18.95942372801901143 ) ) ;
#53088 = CARTESIAN_POINT ( 'NONE',  ( 16.52544592524342804, -4.483927247898539470, 113.5405762719810383 ) ) ;
#53089 = CARTESIAN_POINT ( 'NONE',  ( 5.049401038298161559, -19.05341960407611168, 82.70724293864770971 ) ) ;
#53091 = CARTESIAN_POINT ( 'NONE',  ( 29.86685920354754487, 21.69954338932564752, -5.424999997268813878 ) ) ;
#53090 = CARTESIAN_POINT ( 'NONE',  ( -16.53943276465976808, -0.05219959533934237506, 23.75109039468567929 ) ) ;
#53092 = CARTESIAN_POINT ( 'NONE',  ( 19.02544592524334988, 5.153800228976608722, 26.45942372801899722 ) ) ;
#53093 = CARTESIAN_POINT ( 'NONE',  ( 12.06949235617739724, 12.14591786802326823, 86.87609039468568994 ) ) ;
#53094 = CARTESIAN_POINT ( 'NONE',  ( -5.153800228976607833, 19.02544592524334988, 97.70942372801900433 ) ) ;
#53095 = CARTESIAN_POINT ( 'NONE',  ( 14.29746914071049879, -8.314922557960816363, 113.3322429386476955 ) ) ;
#53096 = CARTESIAN_POINT ( 'NONE',  ( 12.14591786802327356, -12.06949235617739191, 65.62609039468568994 ) ) ;
#53097 = CARTESIAN_POINT ( 'NONE',  ( 8.224510206698742110, 14.34966873604972548, 57.08442372801901854 ) ) ;
#53098 = DIRECTION ( 'NONE',  ( 0.000000000000000000, 0.3420201433257384349, 0.9396926207858830038 ) ) ;
#53099 = CARTESIAN_POINT ( 'NONE',  ( 16.51473224551083163, -9.474510206698727899, 50.83442372801899722 ) ) ;
#53100 = CARTESIAN_POINT ( 'NONE',  ( -18.67979575497193778, 10.72451020669871902, 98.33442372801901854 ) ) ;
#53101 = CARTESIAN_POINT ( 'NONE',  ( 16.46253265017160672, -9.564922557960803928, 28.33224293864769550 ) ) ;
#53102 = CARTESIAN_POINT ( 'NONE',  ( -5.153800228976328057, -19.02544592524343514, 82.29057627198103830 ) ) ;
#53103 = CARTESIAN_POINT ( 'NONE',  ( 4.483927247898545687, 16.52544592524342804, 69.79057627198102409 ) ) ;
#53104 = AXIS2_PLACEMENT_3D ( 'NONE', #19944, #170656, #108975 ) ;
#53105 = CARTESIAN_POINT ( 'NONE',  ( -21.52544592524334988, -5.823673210054445271, 93.95942372801903275 ) ) ;
#53106 = CARTESIAN_POINT ( 'NONE',  ( -5.153800228976607833, 19.02544592524334988, 62.70942372801899722 ) ) ;
#53107 = CARTESIAN_POINT ( 'NONE',  ( -9.474510206698720793, -16.51473224551083518, 39.58442372801899722 ) ) ;
#53108 = CARTESIAN_POINT ( 'NONE',  ( 0.05219959533907565091, 21.53943276465977519, 34.99890960531435979 ) ) ;
#53109 = CARTESIAN_POINT ( 'NONE',  ( -15.72974639402176322, -15.80617190586768395, 94.37609039468568994 ) ) ;
#53110 = CARTESIAN_POINT ( 'NONE',  ( 5.049401038298161559, -19.05341960407611168, 77.70724293864765286 ) ) ;
#53111 = CARTESIAN_POINT ( 'NONE',  ( -5.719274019375665041, -21.55341960407619695, 104.7927570613523898 ) ) ;
#53112 = CARTESIAN_POINT ( 'NONE',  ( 18.62759615963271287, -10.81492255796078972, 53.33224293864769550 ) ) ;
#53113 = CARTESIAN_POINT ( 'NONE',  ( -0.05219959533909027116, -19.03943276465977164, 97.49890960531436690 ) ) ;
#53114 = CARTESIAN_POINT ( 'NONE',  ( -19.02544592524334988, -5.153800228976617603, 78.95942372801900433 ) ) ;
#53115 = CARTESIAN_POINT ( 'NONE',  ( -5.049401038298153566, 19.05341960407611168, 105.2072429386476671 ) ) ;
#53116 = CARTESIAN_POINT ( 'NONE',  ( 16.46253265017146816, 9.564922557961045513, 101.6677570613523329 ) ) ;
#53117 = CARTESIAN_POINT ( 'NONE',  ( -16.53943276465976808, -0.05219959533934237506, 48.75109039468568284 ) ) ;
#53118 = CARTESIAN_POINT ( 'NONE',  ( 14.29746914071049879, -8.314922557960816363, 108.3322429386477097 ) ) ;
#53119 = CARTESIAN_POINT ( 'NONE',  ( 9.474510206698971260, -16.51473224551069308, 77.91557627198103830 ) ) ;
#53120 = CARTESIAN_POINT ( 'NONE',  ( 10.81492255796078972, 18.62759615963270932, 59.58224293864770260 ) ) ;
#53121 = CARTESIAN_POINT ( 'NONE',  ( 12.06949235617739724, 12.14591786802326823, 31.87609039468567929 ) ) ;
#53122 = CARTESIAN_POINT ( 'NONE',  ( -0.05219959533937732626, 21.53943276465977519, 37.50109039468568284 ) ) ;
#53123 = CARTESIAN_POINT ( 'NONE',  ( -10.72451020669870658, -18.67979575497194134, 89.58442372801901854 ) ) ;
#53124 = CARTESIAN_POINT ( 'NONE',  ( -14.29746914071037622, -8.314922557961029526, 79.16775706135234714 ) ) ;
#53125 = CARTESIAN_POINT ( 'NONE',  ( -16.51473224551069308, -9.474510206698971260, 76.66557627198103830 ) ) ;
#53126 = CARTESIAN_POINT ( 'NONE',  ( 4.379528057220339221, -16.55341960407611168, 77.70724293864770971 ) ) ;
#53127 = CARTESIAN_POINT ( 'NONE',  ( 16.53943276465976808, -0.05219959533910856209, 23.74890960531435269 ) ) ;
#53128 = CARTESIAN_POINT ( 'NONE',  ( -9.564922557961040184, 16.46253265017147172, 52.91775706135233293 ) ) ;
#53129 = CARTESIAN_POINT ( 'NONE',  ( -18.67979575497193778, 10.72451020669871902, 38.33442372801900433 ) ) ;
#53130 = CARTESIAN_POINT ( 'NONE',  ( 8.224510206698953496, -14.34966873604960469, 72.91557627198103830 ) ) ;
#53131 = CARTESIAN_POINT ( 'NONE',  ( 0.05219959533909260263, 19.03943276465977164, 114.9989096053143669 ) ) ;
#53132 = CARTESIAN_POINT ( 'NONE',  ( -4.483927247898782831, 16.52544592524335698, 102.7094237280190185 ) ) ;
#53133 = CARTESIAN_POINT ( 'NONE',  ( 15.72974639402176855, 15.80617190586768217, 71.87609039468568994 ) ) ;
#53134 = CARTESIAN_POINT ( 'NONE',  ( -12.14591786802326823, 12.06949235617739902, 43.12609039468568284 ) ) ;
#53135 = CARTESIAN_POINT ( 'NONE',  ( -21.52544592524334988, -5.823673210054445271, 43.95942372801902565 ) ) ;
#53136 = VERTEX_POINT ( 'NONE', #75682 ) ;
#53137 = CARTESIAN_POINT ( 'NONE',  ( 0.05219959533907565091, 21.53943276465977519, 114.9989096053143669 ) ) ;
#53138 = CARTESIAN_POINT ( 'NONE',  ( 8.224510206698953496, -14.34966873604960469, 97.91557627198103830 ) ) ;
#53139 = CARTESIAN_POINT ( 'NONE',  ( -21.98685479826779954, 13.98560643873834408, 165.5209445330007441 ) ) ;
#53140 = CARTESIAN_POINT ( 'NONE',  ( -14.34966873604960291, -8.224510206698953496, 51.66557627198102409 ) ) ;
#53141 = CARTESIAN_POINT ( 'NONE',  ( -8.314922557961024197, 14.29746914071037800, 92.91775706135236135 ) ) ;
#53142 = CARTESIAN_POINT ( 'NONE',  ( 19.03943276465977164, -0.05219959533909143690, 38.74890960531436690 ) ) ;
#53143 = CARTESIAN_POINT ( 'NONE',  ( 0.05219959533907565091, 21.53943276465977519, 39.99890960531436690 ) ) ;
#53144 = CARTESIAN_POINT ( 'NONE',  ( 4.483927247898545687, 16.52544592524342804, 79.79057627198102409 ) ) ;
#53145 = CARTESIAN_POINT ( 'NONE',  ( -18.62759615963270932, 10.81492255796079327, 80.83224293864769550 ) ) ;
#53146 = CARTESIAN_POINT ( 'NONE',  ( -19.03943276465977164, 0.05219959533909376836, 91.24890960531436690 ) ) ;
#53148 = CARTESIAN_POINT ( 'NONE',  ( -13.97604488694547697, 13.89961937509957934, 88.12609039468563310 ) ) ;
#53147 = CARTESIAN_POINT ( 'NONE',  ( 19.05341960407611168, 5.049401038298154454, 33.95724293864769550 ) ) ;
#53149 = CARTESIAN_POINT ( 'NONE',  ( -21.52544592524343514, 5.823673210054127303, 31.04057627198102409 ) ) ;
#53151 = CARTESIAN_POINT ( 'NONE',  ( -5.719274019375978568, 21.55341960407610458, 60.20724293864768839 ) ) ;
#53150 = CARTESIAN_POINT ( 'NONE',  ( -15.80617190586768217, 15.72974639402176855, 58.12609039468568994 ) ) ;
#53152 = CARTESIAN_POINT ( 'NONE',  ( 13.89961937509977652, -13.97604488694527269, 58.12390960531436690 ) ) ;
#53153 = CARTESIAN_POINT ( 'NONE',  ( -9.564922557960796823, -16.46253265017161027, 82.08224293864768129 ) ) ;
#53154 = EDGE_LOOP ( 'NONE', ( #186535, #91073, #10251, #113865, #177040, #156490, #48528, #174458, #39121, #20418, #9675, #28252, #88230, #166700 ) ) ;
#53155 = CARTESIAN_POINT ( 'NONE',  ( -16.53943276465976808, -0.05219959533934237506, 48.75109039468568284 ) ) ;
#53156 = CARTESIAN_POINT ( 'NONE',  ( 0.05219959533937995610, -21.53943276465977519, 30.00109039468568284 ) ) ;
#53157 = CIRCLE ( 'NONE', #166206, 38.00000000000002132 ) ;
#53158 = CARTESIAN_POINT ( 'NONE',  ( -0.05219959533937732626, 21.53943276465977519, 72.50109039468568994 ) ) ;
#53159 = CARTESIAN_POINT ( 'NONE',  ( 0.05219959533909260263, 19.03943276465977164, 114.9989096053143669 ) ) ;
#53160 = CARTESIAN_POINT ( 'NONE',  ( -15.80617190586745835, -15.72974639402198527, 91.87390960531436690 ) ) ;
#53162 = CARTESIAN_POINT ( 'NONE',  ( -14.29746914071037622, -8.314922557961029526, 69.16775706135234714 ) ) ;
#53161 = CARTESIAN_POINT ( 'NONE',  ( 15.80617190586769283, -15.72974639402175789, 25.62609039468567929 ) ) ;
#53163 = CARTESIAN_POINT ( 'NONE',  ( 10.72451020669898902, -18.67979575497178502, 57.91557627198103120 ) ) ;
#53164 = CARTESIAN_POINT ( 'NONE',  ( 19.05341960407617918, -5.049401038297876454, 21.04275706135232582 ) ) ;
#53165 = CARTESIAN_POINT ( 'NONE',  ( -0.05219959533909027116, -19.03943276465977164, 52.49890960531436690 ) ) ;
#53166 = CARTESIAN_POINT ( 'NONE',  ( 9.474510206698971260, -16.51473224551069308, 112.9155762719810383 ) ) ;
#53167 = CARTESIAN_POINT ( 'NONE',  ( 19.05341960407611168, 5.049401038298154454, 93.95724293864769550 ) ) ;
#53168 = CYLINDRICAL_SURFACE ( 'NONE', #134687, 31.90000000000003411 ) ;
#53169 = EDGE_CURVE ( 'NONE', #159210, #127511, #130599, .T. ) ;
#53170 = CARTESIAN_POINT ( 'NONE',  ( -16.46253265017146816, -9.564922557961047289, 69.16775706135233293 ) ) ;
#53171 = CARTESIAN_POINT ( 'NONE',  ( 5.823673210054125526, 21.52544592524343514, 39.79057627198103830 ) ) ;
#53172 = CARTESIAN_POINT ( 'NONE',  ( 8.224510206698953496, -14.34966873604960469, 22.91557627198102765 ) ) ;
#53173 = CARTESIAN_POINT ( 'NONE',  ( 13.97604488694548053, -13.89961937509957401, 100.6260903946856615 ) ) ;
#53174 = ADVANCED_FACE ( 'NONE', ( #120204 ), #107014, .T. ) ;
#53175 = CARTESIAN_POINT ( 'NONE',  ( 18.22780087662125226, -5.499999999999864997, 51.01540105326108687 ) ) ;
#53176 = CARTESIAN_POINT ( 'NONE',  ( 5.049401038297881783, 19.05341960407617563, 22.29275706135233648 ) ) ;
#53177 = CARTESIAN_POINT ( 'NONE',  ( 19.03943276465977164, 0.05219959533936151252, 96.25109039468567573 ) ) ;
#53179 = CARTESIAN_POINT ( 'NONE',  ( 19.02544592524334988, 5.153800228976608722, 51.45942372801900433 ) ) ;
#53178 = CARTESIAN_POINT ( 'NONE',  ( -21.52544592524343514, 5.823673210054127303, 91.04057627198103830 ) ) ;
#53180 = CARTESIAN_POINT ( 'NONE',  ( 25.78958964901895712, -10.70071173758533334, 166.5174151181484774 ) ) ;
#53181 = CARTESIAN_POINT ( 'NONE',  ( 16.51473224551069308, 9.474510206698969483, 59.16557627198102409 ) ) ;
#53182 = CARTESIAN_POINT ( 'NONE',  ( 4.483927247898545687, 16.52544592524342804, 69.79057627198102409 ) ) ;
#53183 = VECTOR ( 'NONE', #151367, 1000.000000000000000 ) ;
#53184 = CARTESIAN_POINT ( 'NONE',  ( -16.51473224551069308, -9.474510206698971260, 46.66557627198102409 ) ) ;
#53185 = CARTESIAN_POINT ( 'NONE',  ( -0.05219959533910754901, -16.53943276465976808, 57.49890960531435979 ) ) ;
#53186 = CARTESIAN_POINT ( 'NONE',  ( -0.3431728551240714742, -71.74905178543389184, -4.999999999999999112 ) ) ;
#53187 = CARTESIAN_POINT ( 'NONE',  ( 4.379528057220339221, -16.55341960407611168, 32.70724293864770260 ) ) ;
#53188 = CARTESIAN_POINT ( 'NONE',  ( -16.46253265017160317, 9.564922557960807481, 60.83224293864769550 ) ) ;
#53189 = CARTESIAN_POINT ( 'NONE',  ( 19.05341960407617918, -5.049401038297876454, 21.04275706135232582 ) ) ;
#53190 = CARTESIAN_POINT ( 'NONE',  ( 16.55341960407618274, -4.379528057220086978, 36.04275706135234714 ) ) ;
#53191 = CARTESIAN_POINT ( 'NONE',  ( -0.05219959533907301413, -21.53943276465977519, 47.49890960531435979 ) ) ;
#53193 = ORIENTED_EDGE ( 'NONE', *, *, #67401, .T. ) ;
#53192 = CARTESIAN_POINT ( 'NONE',  ( -0.05219959533937732626, 21.53943276465977519, 107.5010903946856899 ) ) ;
#53194 = CARTESIAN_POINT ( 'NONE',  ( -13.97604488694527625, -13.89961937509977652, 61.87390960531435979 ) ) ;
#53195 = CARTESIAN_POINT ( 'NONE',  ( -21.46320343559624533, 20.96320343559661481, 4.646446609406720718 ) ) ;
#53196 = CARTESIAN_POINT ( 'NONE',  ( 16.51473224551069308, 9.474510206698969483, 94.16557627198103830 ) ) ;
#53197 = CARTESIAN_POINT ( 'NONE',  ( 36.91746824999999177, 2.880721459617395097E-14, -1.624999997268813390 ) ) ;
#53198 = CARTESIAN_POINT ( 'NONE',  ( 5.719274019375673035, 21.55341960407619339, 27.29275706135234358 ) ) ;
#53199 = CARTESIAN_POINT ( 'NONE',  ( 16.52544592524342804, -4.483927247898539470, 93.54057627198103830 ) ) ;
#53201 = CARTESIAN_POINT ( 'NONE',  ( -19.05341960407611168, -5.049401038298163336, 66.45724293864769550 ) ) ;
#53200 = CARTESIAN_POINT ( 'NONE',  ( 10.81492255796078972, 18.62759615963270932, 89.58224293864768129 ) ) ;
#53202 = CARTESIAN_POINT ( 'NONE',  ( -16.51473224551069308, -9.474510206698971260, 86.66557627198102409 ) ) ;
#53203 = CARTESIAN_POINT ( 'NONE',  ( 0.05219959533907565091, 21.53943276465977519, 104.9989096053143669 ) ) ;
#53204 = ORIENTED_EDGE ( 'NONE', *, *, #147752, .F. ) ;
#53205 = CARTESIAN_POINT ( 'NONE',  ( 13.89961937509977652, -13.97604488694527269, 78.12390960531433848 ) ) ;
#53207 = CARTESIAN_POINT ( 'NONE',  ( 29.44683875480690816, -27.07775549506662927, -16.45954463943772339 ) ) ;
#53206 = CARTESIAN_POINT ( 'NONE',  ( -4.483927247898539470, -16.52544592524342804, 107.2905762719810525 ) ) ;
#53208 = CARTESIAN_POINT ( 'NONE',  ( -13.89961937509957401, -13.97604488694547875, 89.37609039468563310 ) ) ;
#53209 = CARTESIAN_POINT ( 'NONE',  ( 4.483927247898545687, 16.52544592524342804, 114.7905762719810383 ) ) ;
#53210 = CARTESIAN_POINT ( 'NONE',  ( 21.53943276465977519, 0.05219959533937863772, 66.25109039468567573 ) ) ;
#53212 = CARTESIAN_POINT ( 'NONE',  ( -21.53943276465977519, -0.05219959533937600094, 28.75109039468567929 ) ) ;
#53211 = CARTESIAN_POINT ( 'NONE',  ( -19.02544592524342804, 5.153800228976336051, 56.04057627198100988 ) ) ;
#53213 = CARTESIAN_POINT ( 'NONE',  ( 15.80617190586746368, 15.72974639402197994, 104.3739096053143669 ) ) ;
#53214 = CARTESIAN_POINT ( 'NONE',  ( 28.82186960331498327, 2.781578969918950771E-14, 143.0000000000000000 ) ) ;
#53215 = CARTESIAN_POINT ( 'NONE',  ( -19.03943276465977164, 0.05219959533909376836, 71.24890960531435269 ) ) ;
#53216 = CARTESIAN_POINT ( 'NONE',  ( 26.58496454516999563, 7.626754437231445749, 167.9682100371138915 ) ) ;
#53218 = CARTESIAN_POINT ( 'NONE',  ( 10.81492255796078972, 18.62759615963270932, 29.58224293864769905 ) ) ;
#53217 = CARTESIAN_POINT ( 'NONE',  ( -8.314922557961024197, 14.29746914071037800, 22.91775706135235069 ) ) ;
#53219 = CARTESIAN_POINT ( 'NONE',  ( 18.62759615963255655, 10.81492255796105972, 56.66775706135235424 ) ) ;
#53220 =( GEOMETRIC_REPRESENTATION_CONTEXT ( 3 ) GLOBAL_UNCERTAINTY_ASSIGNED_CONTEXT ( ( #82277 ) ) GLOBAL_UNIT_ASSIGNED_CONTEXT ( ( #175872, #80855, #4010 ) ) REPRESENTATION_CONTEXT ( 'NONE', 'WORKASPACE' ) );
#53221 = CARTESIAN_POINT ( 'NONE',  ( 5.153800228976335163, 19.02544592524342804, 114.7905762719810241 ) ) ;
#53222 =( BOUNDED_CURVE ( )  B_SPLINE_CURVE ( 3, ( #182032, #40523, #58671, #57699 ),
 .UNSPECIFIED., .F., .F. ) 
 B_SPLINE_CURVE_WITH_KNOTS ( ( 4, 4 ),
 ( 2.008945357379066543, 2.115944711806982070 ),
 .UNSPECIFIED. ) 
 CURVE ( )  GEOMETRIC_REPRESENTATION_ITEM ( )  RATIONAL_B_SPLINE_CURVE ( ( 1.000000000000000000, 0.9990461557208837329, 0.9990461557208837329, 1.000000000000000000 ) ) 
 REPRESENTATION_ITEM ( '' )  );
#53223 = CARTESIAN_POINT ( 'NONE',  ( 13.89961937509957401, 13.97604488694547697, 96.87609039468566152 ) ) ;
#53224 = CARTESIAN_POINT ( 'NONE',  ( -16.51473224551069308, -9.474510206698971260, 51.66557627198102409 ) ) ;
#53225 = CARTESIAN_POINT ( 'NONE',  ( -19.03943276465977164, 0.05219959533909376836, 71.24890960531435269 ) ) ;
#53226 = CARTESIAN_POINT ( 'NONE',  ( -8.224510206698948167, 14.34966873604960824, 95.41557627198102409 ) ) ;
#53227 = CARTESIAN_POINT ( 'NONE',  ( -9.564922557960796823, -16.46253265017161027, 102.0822429386477097 ) ) ;
#53228 = CARTESIAN_POINT ( 'NONE',  ( -16.53943276465976808, 0.05219959533911058130, 96.24890960531435269 ) ) ;
#53229 = CARTESIAN_POINT ( 'NONE',  ( 0.05219959533909260263, 19.03943276465977164, 99.99890960531436690 ) ) ;
#53231 = CARTESIAN_POINT ( 'NONE',  ( -9.474510206698964154, 16.51473224551069663, 45.41557627198103120 ) ) ;
#53230 = CARTESIAN_POINT ( 'NONE',  ( 14.29746914071049879, -8.314922557960816363, 63.33224293864770260 ) ) ;
#53232 = CARTESIAN_POINT ( 'NONE',  ( -21.53943276465977519, -0.05219959533937600094, 53.75109039468568994 ) ) ;
#53233 = CARTESIAN_POINT ( 'NONE',  ( -19.03943276465977164, -0.05219959533935918106, 93.75109039468566152 ) ) ;
#53234 = CARTESIAN_POINT ( 'NONE',  ( -16.55341960407611168, -4.379528057220339221, 46.45724293864769550 ) ) ;
#53235 = CARTESIAN_POINT ( 'NONE',  ( 10.72451020669898902, -18.67979575497178502, 107.9155762719810241 ) ) ;
#53236 = CARTESIAN_POINT ( 'NONE',  ( 18.67979575497178502, 10.72451020669898547, 49.16557627198102409 ) ) ;
#53238 = CARTESIAN_POINT ( 'NONE',  ( -16.53943276465976808, 0.05219959533911058130, 81.24890960531436690 ) ) ;
#53237 = CARTESIAN_POINT ( 'NONE',  ( 0.05219959533909260263, 19.03943276465977164, 109.9989096053143669 ) ) ;
#53239 = CARTESIAN_POINT ( 'NONE',  ( -8.906447517083053711, -27.41122689804191026, 138.6500000054623740 ) ) ;
#53240 = CARTESIAN_POINT ( 'NONE',  ( 0.05219959533909260263, 19.03943276465977164, 54.99890960531435979 ) ) ;
#53241 = CARTESIAN_POINT ( 'NONE',  ( -8.314922557960811034, -14.29746914071050412, 22.08224293864769194 ) ) ;
#53242 = CARTESIAN_POINT ( 'NONE',  ( 12.14591786802327356, -12.06949235617739191, 95.62609039468568994 ) ) ;
#53243 = CARTESIAN_POINT ( 'NONE',  ( -14.29746914071037622, -8.314922557961029526, 79.16775706135234714 ) ) ;
#53244 = CARTESIAN_POINT ( 'NONE',  ( -16.46253265017146816, -9.564922557961047289, 44.16775706135232582 ) ) ;
#53245 = CARTESIAN_POINT ( 'NONE',  ( -24.60782464877076237, -7.576768089025921249, 167.2921030401324174 ) ) ;
#53246 = CARTESIAN_POINT ( 'NONE',  ( -16.46253265017160317, 9.564922557960807481, 90.83224293864769550 ) ) ;
#53247 = CARTESIAN_POINT ( 'NONE',  ( 19.05341960407611168, 5.049401038298154454, 38.95724293864767418 ) ) ;
#53248 = EDGE_CURVE ( 'NONE', #88472, #179813, #22767, .T. ) ;
#53249 = CARTESIAN_POINT ( 'NONE',  ( 0.05219959533910956823, 16.53943276465976808, 64.99890960531435269 ) ) ;
#53250 = CARTESIAN_POINT ( 'NONE',  ( -19.02544592524342804, 5.153800228976336051, 106.0405762719810241 ) ) ;
#53251 = CARTESIAN_POINT ( 'NONE',  ( 21.55341960407610458, 5.719274019375980345, 38.95724293864768839 ) ) ;
#53252 = CARTESIAN_POINT ( 'NONE',  ( -8.224510206698948167, 14.34966873604960824, 80.41557627198103830 ) ) ;
#53253 = CARTESIAN_POINT ( 'NONE',  ( -14.29746914071037622, -8.314922557961029526, 44.16775706135234714 ) ) ;
#53254 = CARTESIAN_POINT ( 'NONE',  ( 4.483927247898545687, 16.52544592524342804, 74.79057627198105251 ) ) ;
#53255 = FACE_OUTER_BOUND ( 'NONE', #148930, .T. ) ;
#53256 = CARTESIAN_POINT ( 'NONE',  ( 19.03943276465977164, 0.05219959533936151252, 71.25109039468566152 ) ) ;
#53257 = CARTESIAN_POINT ( 'NONE',  ( 16.51473224551069308, 9.474510206698969483, 104.1655762719810241 ) ) ;
#53259 = EDGE_CURVE ( 'NONE', #128045, #198744, #45362, .T. ) ;
#53258 = CARTESIAN_POINT ( 'NONE',  ( -9.564922557961040184, 16.46253265017147172, 72.91775706135233293 ) ) ;
#53260 = CARTESIAN_POINT ( 'NONE',  ( -28.75808110634262604, -1.452795517301058048, 139.9999999999999716 ) ) ;
#53262 = CARTESIAN_POINT ( 'NONE',  ( 12.06949235617739724, 12.14591786802326823, 111.8760903946856615 ) ) ;
#53261 = CARTESIAN_POINT ( 'NONE',  ( 16.53943276465976808, 0.05219959533934440121, 31.25109039468568639 ) ) ;
#53263 = CARTESIAN_POINT ( 'NONE',  ( -19.03943276465977164, -0.05219959533935918106, 68.75109039468566152 ) ) ;
#53264 = CARTESIAN_POINT ( 'NONE',  ( -5.823673210054116645, -21.52544592524344225, 32.29057627198102409 ) ) ;
#53265 = CARTESIAN_POINT ( 'NONE',  ( 15.80617190586769283, -15.72974639402175789, 70.62609039468567573 ) ) ;
#53266 = CARTESIAN_POINT ( 'NONE',  ( 14.29746914071037800, 8.314922557961029526, 26.66775706135235424 ) ) ;
#53268 = CARTESIAN_POINT ( 'NONE',  ( 19.02544592524343514, -5.153800228976328945, 93.54057627198102409 ) ) ;
#53267 = CARTESIAN_POINT ( 'NONE',  ( 9.564922557960805705, 16.46253265017160317, 29.58224293864769550 ) ) ;
#53269 = CARTESIAN_POINT ( 'NONE',  ( 14.91565869316880288, 15.22409499613341133, -58.84910547483664089 ) ) ;
#53271 = CARTESIAN_POINT ( 'NONE',  ( 13.97604488694527802, 13.89961937509977652, 94.37390960531436690 ) ) ;
#53270 = CARTESIAN_POINT ( 'NONE',  ( -16.52544592524342804, 4.483927247898546575, 86.04057627198102409 ) ) ;
#53272 = CARTESIAN_POINT ( 'NONE',  ( 19.02544592524343514, -5.153800228976328945, 93.54057627198102409 ) ) ;
#53273 = EDGE_LOOP ( 'NONE', ( #25713, #164884, #8216, #110465, #44728, #175257, #420, #147555, #134766, #57537, #74269, #76040 ) ) ;
#53274 = CARTESIAN_POINT ( 'NONE',  ( 9.474510206698729675, 16.51473224551082808, 97.08442372801900433 ) ) ;
#53275 = CARTESIAN_POINT ( 'NONE',  ( 15.72974639402199770, -15.80617190586745480, 83.12390960531436690 ) ) ;
#53276 = CARTESIAN_POINT ( 'NONE',  ( -5.153800228976328057, -19.02544592524343514, 32.29057627198102409 ) ) ;
#53278 = CARTESIAN_POINT ( 'NONE',  ( -5.719274019375978568, 21.55341960407610458, 110.2072429386477239 ) ) ;
#53277 = CARTESIAN_POINT ( 'NONE',  ( 9.564922557961047289, -16.46253265017146816, 70.41775706135233293 ) ) ;
#53279 = CARTESIAN_POINT ( 'NONE',  ( 19.02544592524343514, -5.153800228976328945, 73.54057627198103830 ) ) ;
#53280 = CARTESIAN_POINT ( 'NONE',  ( -0.05219959533909027116, -19.03943276465977164, 102.4989096053143669 ) ) ;
#53281 = ORIENTED_EDGE ( 'NONE', *, *, #187248, .T. ) ;
#53282 = CARTESIAN_POINT ( 'NONE',  ( 15.80617190586746368, 15.72974639402197994, 109.3739096053143811 ) ) ;
#53285 = CARTESIAN_POINT ( 'NONE',  ( 16.46253265017146816, 9.564922557961045513, 66.66775706135233293 ) ) ;
#53284 = CARTESIAN_POINT ( 'NONE',  ( 16.46253265017160672, -9.564922557960803928, 83.33224293864768129 ) ) ;
#53283 = CARTESIAN_POINT ( 'NONE',  ( -12.14591786802309592, -12.06949235617757132, 106.8739096053143811 ) ) ;
#53286 = CARTESIAN_POINT ( 'NONE',  ( -5.719274019375978568, 21.55341960407610458, 90.20724293864770971 ) ) ;
#53287 = CARTESIAN_POINT ( 'NONE',  ( 18.67979575497178502, 10.72451020669898547, 69.16557627198102409 ) ) ;
#53288 = VECTOR ( 'NONE', #36079, 999.9999999999998863 ) ;
#53289 = CARTESIAN_POINT ( 'NONE',  ( 8.224510206698953496, -14.34966873604960469, 47.91557627198102409 ) ) ;
#53290 = CARTESIAN_POINT ( 'NONE',  ( 5.049401038297881783, 19.05341960407617563, 22.29275706135233648 ) ) ;
#53291 = CARTESIAN_POINT ( 'NONE',  ( -16.55341960407617563, 4.379528057220093196, 63.54275706135234003 ) ) ;
#53292 = CARTESIAN_POINT ( 'NONE',  ( 9.564922557960805705, 16.46253265017160317, 99.58224293864770971 ) ) ;
#53293 = CARTESIAN_POINT ( 'NONE',  ( -19.03943276465977164, 0.05219959533909376836, 51.24890960531436690 ) ) ;
#53294 = CARTESIAN_POINT ( 'NONE',  ( 0.05219959533937995610, -21.53943276465977519, 55.00109039468568284 ) ) ;
#53295 = CARTESIAN_POINT ( 'NONE',  ( 5.823673210054444382, -21.52544592524334988, 60.20942372801902565 ) ) ;
#53296 = CARTESIAN_POINT ( 'NONE',  ( -16.46253265017160317, 9.564922557960807481, 60.83224293864769550 ) ) ;
#53297 = CARTESIAN_POINT ( 'NONE',  ( 18.62759615963255655, 10.81492255796105972, 41.66775706135235424 ) ) ;
#53298 = CARTESIAN_POINT ( 'NONE',  ( 19.02544592524334988, 5.153800228976608722, 76.45942372801897591 ) ) ;
#53299 = CARTESIAN_POINT ( 'NONE',  ( 9.564922557961047289, -16.46253265017146816, 75.41775706135234714 ) ) ;
#53300 = CARTESIAN_POINT ( 'NONE',  ( -9.564922557960796823, -16.46253265017161027, 42.08224293864769550 ) ) ;
#53301 = CARTESIAN_POINT ( 'NONE',  ( 16.52544592524335698, 4.483927247898782831, 81.45942372801900433 ) ) ;
#53302 = CARTESIAN_POINT ( 'NONE',  ( 5.049401038298161559, -19.05341960407611168, 47.70724293864770260 ) ) ;
#53303 = CARTESIAN_POINT ( 'NONE',  ( 21.36928693577338123, -5.431965077040403322, 174.3311293403526179 ) ) ;
#53304 = CARTESIAN_POINT ( 'NONE',  ( -5.049401038298153566, 19.05341960407611168, 95.20724293864770971 ) ) ;
#53305 = CARTESIAN_POINT ( 'NONE',  ( 9.564922557960805705, 16.46253265017160317, 44.58224293864769550 ) ) ;
#53306 = AXIS2_PLACEMENT_3D ( 'NONE', #50081, #33914, #65234 ) ;
#53307 = CARTESIAN_POINT ( 'NONE',  ( -18.62759615963270932, 10.81492255796079327, 90.83224293864769550 ) ) ;
#53308 = CARTESIAN_POINT ( 'NONE',  ( -12.06949235617739369, -12.14591786802326823, 54.37609039468568994 ) ) ;
#53309 = CARTESIAN_POINT ( 'NONE',  ( 13.97604488694548053, -13.89961937509957401, 20.62609039468567573 ) ) ;
#53310 = CARTESIAN_POINT ( 'NONE',  ( 19.02544592524343514, -5.153800228976328945, 53.54057627198102409 ) ) ;
#53311 = CARTESIAN_POINT ( 'NONE',  ( 16.55341960407611168, 4.379528057220329451, 48.95724293864770971 ) ) ;
#53312 = CARTESIAN_POINT ( 'NONE',  ( -4.483927247898539470, -16.52544592524342804, 82.29057627198103830 ) ) ;
#53313 = CARTESIAN_POINT ( 'NONE',  ( -16.51473224551069308, -9.474510206698971260, 76.66557627198103830 ) ) ;
#53314 = CARTESIAN_POINT ( 'NONE',  ( 5.823673210054444382, -21.52544592524334988, 35.20942372801901854 ) ) ;
#53315 = CARTESIAN_POINT ( 'NONE',  ( -19.02544592524342804, 5.153800228976336051, 91.04057627198100988 ) ) ;
#53316 = CARTESIAN_POINT ( 'NONE',  ( 18.62759615963255655, 10.81492255796105972, 101.6677570613523613 ) ) ;
#53317 = CARTESIAN_POINT ( 'NONE',  ( -16.52544592524335698, -4.483927247898792601, 68.95942372801901854 ) ) ;
#53318 = CARTESIAN_POINT ( 'NONE',  ( 18.67979575497194134, -10.72451020669871369, 30.83442372801902209 ) ) ;
#53319 = CARTESIAN_POINT ( 'NONE',  ( -0.05219959533909027116, -19.03943276465977164, 112.4989096053143669 ) ) ;
#53320 = CARTESIAN_POINT ( 'NONE',  ( 21.55341960407610458, 5.719274019375980345, 83.95724293864770971 ) ) ;
#53321 = CARTESIAN_POINT ( 'NONE',  ( -16.53943276465976808, 0.05219959533911058130, 41.24890960531435269 ) ) ;
#53322 = CARTESIAN_POINT ( 'NONE',  ( -5.049401038298153566, 19.05341960407611168, 40.20724293864768839 ) ) ;
#53323 = CARTESIAN_POINT ( 'NONE',  ( -16.55341960407611168, -4.379528057220339221, 66.45724293864768129 ) ) ;
#53324 = CARTESIAN_POINT ( 'NONE',  ( -5.719274019375978568, 21.55341960407610458, 30.20724293864769550 ) ) ;
#53325 = CARTESIAN_POINT ( 'NONE',  ( -13.97604488694547697, 13.89961937509957934, 33.12609039468566863 ) ) ;
#53326 = CARTESIAN_POINT ( 'NONE',  ( -4.379528057220328563, 16.55341960407611168, 105.2072429386477097 ) ) ;
#53327 = CARTESIAN_POINT ( 'NONE',  ( -13.97604488694527625, -13.89961937509977652, 111.8739096053143243 ) ) ;
#53328 = ORIENTED_EDGE ( 'NONE', *, *, #35102, .F. ) ;
#53329 = CARTESIAN_POINT ( 'NONE',  ( -16.53943276465976808, -0.05219959533934237506, 58.75109039468568994 ) ) ;
#53330 = CARTESIAN_POINT ( 'NONE',  ( -19.05341960407611168, -5.049401038298163336, 51.45724293864770260 ) ) ;
#53331 = CARTESIAN_POINT ( 'NONE',  ( -4.500000000000001776, -126.1226662136678556, 8.481152457036394310 ) ) ;
#53332 = CARTESIAN_POINT ( 'NONE',  ( -4.483927247898782831, 16.52544592524335698, 87.70942372801901854 ) ) ;
#53333 = CARTESIAN_POINT ( 'NONE',  ( -19.05341960407617563, 5.049401038297882671, 113.5427570613523471 ) ) ;
#53334 = CARTESIAN_POINT ( 'NONE',  ( 5.823673210054444382, -21.52544592524334988, 75.20942372801901854 ) ) ;
#53335 = CARTESIAN_POINT ( 'NONE',  ( 19.03943276465977164, -0.05219959533909143690, 73.74890960531435269 ) ) ;
#53336 = CARTESIAN_POINT ( 'NONE',  ( -21.53943276465977519, 0.05219959533907696930, 91.24890960531436690 ) ) ;
#53337 = CARTESIAN_POINT ( 'NONE',  ( -8.224510206698735004, -14.34966873604973081, 39.58442372801901143 ) ) ;
#53339 = CARTESIAN_POINT ( 'NONE',  ( -14.34966873604960291, -8.224510206698953496, 106.6655762719810383 ) ) ;
#53338 = VECTOR ( 'NONE', #109893, 1000.000000000000000 ) ;
#53340 = CARTESIAN_POINT ( 'NONE',  ( -8.224510206698735004, -14.34966873604973081, 19.58442372801901143 ) ) ;
#53341 = CARTESIAN_POINT ( 'NONE',  ( -5.153800228976607833, 19.02544592524334988, 77.70942372801900433 ) ) ;
#53342 = CARTESIAN_POINT ( 'NONE',  ( -21.55341960407610458, -5.719274019375992779, 76.45724293864769550 ) ) ;
#53343 = CARTESIAN_POINT ( 'NONE',  ( 5.153800228976615827, -19.02544592524334988, 55.20942372801899722 ) ) ;
#53344 = CARTESIAN_POINT ( 'NONE',  ( -19.03943276465977164, 0.05219959533909376836, 111.2489096053143669 ) ) ;
#53345 = CARTESIAN_POINT ( 'NONE',  ( -18.62759615963270932, 10.81492255796079327, 85.83224293864768129 ) ) ;
#53346 = CARTESIAN_POINT ( 'NONE',  ( 17.50000000000013856, 3.417042746626917538, 27.32619603767528105 ) ) ;
#53347 = CARTESIAN_POINT ( 'NONE',  ( 19.05341960407611168, 5.049401038298154454, 63.95724293864769550 ) ) ;
#53348 = AXIS2_PLACEMENT_3D ( 'NONE', #69022, #114516, #176217 ) ;
#53349 = DIRECTION ( 'NONE',  ( 0.000000000000000000, 0.000000000000000000, -1.000000000000000000 ) ) ;
#53350 = CARTESIAN_POINT ( 'NONE',  ( 16.46253265017146816, 9.564922557961045513, 111.6677570613523329 ) ) ;
#53351 = CARTESIAN_POINT ( 'NONE',  ( 36.90807327575559071, -0.7244114042849700841, 50.46397389534120492 ) ) ;
#53352 = CARTESIAN_POINT ( 'NONE',  ( 18.67979575497194134, -10.72451020669871369, 55.83442372801901854 ) ) ;
#53354 = CARTESIAN_POINT ( 'NONE',  ( 16.55341960407611168, 4.379528057220329451, 58.95724293864770971 ) ) ;
#53353 = CARTESIAN_POINT ( 'NONE',  ( 15.80617190586746368, 15.72974639402197994, 109.3739096053143811 ) ) ;
#53355 = CARTESIAN_POINT ( 'NONE',  ( 13.97604488694527802, 13.89961937509977652, 69.37390960531436690 ) ) ;
#53356 = VECTOR ( 'NONE', #115141, 1000.000000000000000 ) ;
#53357 = CARTESIAN_POINT ( 'NONE',  ( -5.823673210054431948, 21.52544592524334988, 67.70942372801901854 ) ) ;
#53359 = CARTESIAN_POINT ( 'NONE',  ( 9.564922557961047289, -16.46253265017146816, 25.41775706135234003 ) ) ;
#53358 = CARTESIAN_POINT ( 'NONE',  ( -12.06949235617739369, -12.14591786802326823, 19.37609039468568639 ) ) ;
#53360 = CARTESIAN_POINT ( 'NONE',  ( -15.72974639402176322, -15.80617190586768395, 44.37609039468567573 ) ) ;
#53361 = CARTESIAN_POINT ( 'NONE',  ( 15.72974639402199770, -15.80617190586745480, 108.1239096053143811 ) ) ;
#53362 = CARTESIAN_POINT ( 'NONE',  ( -15.72974639402197994, 15.80617190586746368, 60.62390960531437401 ) ) ;
#53363 = CARTESIAN_POINT ( 'NONE',  ( -16.51473224551082808, 9.474510206698731452, 98.33442372801900433 ) ) ;
#53364 = CARTESIAN_POINT ( 'NONE',  ( -19.02544592524334988, -5.153800228976617603, 63.95942372801899012 ) ) ;
#53365 = CARTESIAN_POINT ( 'NONE',  ( -0.05219959533937732626, 21.53943276465977519, 87.50109039468568994 ) ) ;
#53366 = CARTESIAN_POINT ( 'NONE',  ( 5.153800228976615827, -19.02544592524334988, 55.20942372801899722 ) ) ;
#53367 = CARTESIAN_POINT ( 'NONE',  ( 16.46253265017160672, -9.564922557960803928, 28.33224293864769550 ) ) ;
#53368 = CARTESIAN_POINT ( 'NONE',  ( -18.62759615963270932, 10.81492255796079327, 60.83224293864769550 ) ) ;
#53369 = CARTESIAN_POINT ( 'NONE',  ( 14.34966873604960469, 8.224510206698951720, 54.16557627198103120 ) ) ;
#53370 = LINE ( 'NONE', #115048, #163532 ) ;
#53371 = CARTESIAN_POINT ( 'NONE',  ( -9.564922557961040184, 16.46253265017147172, 32.91775706135233293 ) ) ;
#53372 = CARTESIAN_POINT ( 'NONE',  ( -16.52544592524335698, -4.483927247898792601, 88.95942372801901854 ) ) ;
#53373 = CARTESIAN_POINT ( 'NONE',  ( 8.314922557960818139, 14.29746914071049879, 44.58224293864769550 ) ) ;
#53374 = CARTESIAN_POINT ( 'NONE',  ( 21.53943276465977519, 0.05219959533937863772, 76.25109039468568994 ) ) ;
#53375 = CARTESIAN_POINT ( 'NONE',  ( -15.72974639402176322, -15.80617190586768395, 84.37609039468570415 ) ) ;
#53376 = CARTESIAN_POINT ( 'NONE',  ( -15.72974639402197994, 15.80617190586746368, 75.62390960531439532 ) ) ;
#53377 = CARTESIAN_POINT ( 'NONE',  ( -19.03943276465977164, 0.05219959533909376836, 36.24890960531436690 ) ) ;
#53378 = CARTESIAN_POINT ( 'NONE',  ( 18.67979575497194134, -10.72451020669871369, 50.83442372801901143 ) ) ;
#53379 = CARTESIAN_POINT ( 'NONE',  ( -19.03943276465977164, 0.05219959533909376836, 31.24890960531435979 ) ) ;
#53380 = VERTEX_POINT ( 'NONE', #180911 ) ;
#53381 = CARTESIAN_POINT ( 'NONE',  ( -19.03943276465977164, 0.05219959533909376836, 51.24890960531436690 ) ) ;
#53382 = CARTESIAN_POINT ( 'NONE',  ( 0.05219959533910956823, 16.53943276465976808, 99.99890960531436690 ) ) ;
#53383 = CARTESIAN_POINT ( 'NONE',  ( 13.89961937509977652, -13.97604488694527269, 103.1239096053143527 ) ) ;
#53384 = CARTESIAN_POINT ( 'NONE',  ( 12.06949235617757843, -12.14591786802309237, 38.12390960531436690 ) ) ;
#53385 = CARTESIAN_POINT ( 'NONE',  ( 9.474510206698971260, -16.51473224551069308, 22.91557627198102765 ) ) ;
#53386 = CARTESIAN_POINT ( 'NONE',  ( 21.53943276465977519, -0.05219959533907433946, 88.74890960531436690 ) ) ;
#53387 = CARTESIAN_POINT ( 'NONE',  ( 21.53943276465977519, 0.05219959533937863772, 26.25109039468567573 ) ) ;
#53388 = CARTESIAN_POINT ( 'NONE',  ( 26.82864639204112933, -7.693045595922322732, 166.5361468217299148 ) ) ;
#53389 = CARTESIAN_POINT ( 'NONE',  ( 4.379528057220092307, 16.55341960407617563, 32.29275706135235424 ) ) ;
#53390 = ORIENTED_EDGE ( 'NONE', *, *, #82839, .F. ) ;
#53391 = CARTESIAN_POINT ( 'NONE',  ( -15.72974639402197994, 15.80617190586746368, 70.62390960531436690 ) ) ;
#53392 = CARTESIAN_POINT ( 'NONE',  ( 15.80617190586769283, -15.72974639402175789, 90.62609039468567573 ) ) ;
#53393 = CARTESIAN_POINT ( 'NONE',  ( 0.05219959533909260263, 19.03943276465977164, 94.99890960531436690 ) ) ;
#53394 = CARTESIAN_POINT ( 'NONE',  ( 0.05219959533937995610, -21.53943276465977519, 25.00109039468567218 ) ) ;
#53395 = CARTESIAN_POINT ( 'NONE',  ( -21.55341960407610458, -5.719274019375992779, 36.45724293864768839 ) ) ;
#53396 = CARTESIAN_POINT ( 'NONE',  ( -16.52544592524335698, -4.483927247898792601, 93.95942372801903275 ) ) ;
#53397 = CARTESIAN_POINT ( 'NONE',  ( 21.52544592524334988, 5.823673210054432836, 76.45942372801901854 ) ) ;
#53398 = CARTESIAN_POINT ( 'NONE',  ( -5.049401038297874678, -19.05341960407617918, 19.79275706135233293 ) ) ;
#53399 = CARTESIAN_POINT ( 'NONE',  ( 12.06949235617739724, 12.14591786802326823, 76.87609039468567573 ) ) ;
#53400 = CARTESIAN_POINT ( 'NONE',  ( -5.823673210054431948, 21.52544592524334988, 22.70942372801901499 ) ) ;
#53401 = CARTESIAN_POINT ( 'NONE',  ( -0.05219959533909027116, -19.03943276465977164, 37.49890960531436690 ) ) ;
#53402 = CARTESIAN_POINT ( 'NONE',  ( -21.52544592524334988, -5.823673210054445271, 108.9594237280190185 ) ) ;
#53403 = CARTESIAN_POINT ( 'NONE',  ( 5.049401038298161559, -19.05341960407611168, 102.7072429386476955 ) ) ;
#53404 = CARTESIAN_POINT ( 'NONE',  ( -10.72451020669898014, 18.67979575497178502, 100.4155762719810241 ) ) ;
#53406 = CARTESIAN_POINT ( 'NONE',  ( -5.823673210054116645, -21.52544592524344225, 62.29057627198102409 ) ) ;
#53405 = DIRECTION ( 'NONE',  ( 1.000000000000000000, 0.000000000000000000, 0.000000000000000000 ) ) ;
#53408 = CARTESIAN_POINT ( 'NONE',  ( 14.29746914071049879, -8.314922557960816363, 48.33224293864770260 ) ) ;
#53407 = CARTESIAN_POINT ( 'NONE',  ( 4.483927247898790824, -16.52544592524335698, 55.20942372801902565 ) ) ;
#53409 = CARTESIAN_POINT ( 'NONE',  ( -17.49999999999999645, -5.500000000000000888, 120.0000000000000142 ) ) ;
#53410 = CARTESIAN_POINT ( 'NONE',  ( -9.564922557961040184, 16.46253265017147172, 77.91775706135234714 ) ) ;
#53411 = CARTESIAN_POINT ( 'NONE',  ( -16.19135201231367205, 7.376712067591922661, 104.8131914594797252 ) ) ;
#53412 = EDGE_CURVE ( 'NONE', #123381, #135811, #44941, .T. ) ;
#53413 = CARTESIAN_POINT ( 'NONE',  ( 14.29746914071037800, 8.314922557961029526, 21.66775706135235069 ) ) ;
#53414 = CARTESIAN_POINT ( 'NONE',  ( -21.55341960407610458, -5.719274019375992779, 81.45724293864769550 ) ) ;
#53415 = CARTESIAN_POINT ( 'NONE',  ( -8.314922557960811034, -14.29746914071050412, 67.08224293864770971 ) ) ;
#53416 = CARTESIAN_POINT ( 'NONE',  ( 16.51473224551069308, 9.474510206698969483, 99.16557627198102409 ) ) ;
#53417 = CARTESIAN_POINT ( 'NONE',  ( -12.14591786802326823, 12.06949235617739902, 43.12609039468568284 ) ) ;
#53418 = CARTESIAN_POINT ( 'NONE',  ( -19.02544592524342804, 5.153800228976336051, 61.04057627198103120 ) ) ;
#53420 = CARTESIAN_POINT ( 'NONE',  ( 5.049401038297881783, 19.05341960407617563, 102.2927570613523045 ) ) ;
#53419 = CARTESIAN_POINT ( 'NONE',  ( -21.55341960407619339, 5.719274019375674811, 23.54275706135235424 ) ) ;
#53421 = CARTESIAN_POINT ( 'NONE',  ( 0.05219959533909260263, 19.03943276465977164, 99.99890960531436690 ) ) ;
#53422 = CARTESIAN_POINT ( 'NONE',  ( 16.46253265017160672, -9.564922557960803928, 93.33224293864769550 ) ) ;
#53423 = CARTESIAN_POINT ( 'NONE',  ( -10.81492255796078084, -18.62759615963271287, 87.08224293864769550 ) ) ;
#53424 = CARTESIAN_POINT ( 'NONE',  ( -19.05341960407611168, -5.049401038298163336, 41.45724293864769550 ) ) ;
#53425 = CARTESIAN_POINT ( 'NONE',  ( -16.18388926212241330, -7.379444403734409796, 60.43953151366154941 ) ) ;
#53426 = CARTESIAN_POINT ( 'NONE',  ( -16.55341960407611168, -4.379528057220339221, 71.45724293864769550 ) ) ;
#53427 = CARTESIAN_POINT ( 'NONE',  ( 19.03943276465977164, -0.05219959533909143690, 108.7489096053143527 ) ) ;
#53428 = LINE ( 'NONE', #174791, #60500 ) ;
#53429 = CARTESIAN_POINT ( 'NONE',  ( -5.049401038297874678, -19.05341960407617918, 74.79275706135231871 ) ) ;
#53430 = VECTOR ( 'NONE', #107558, 1000.000000000000000 ) ;
#53431 = CARTESIAN_POINT ( 'NONE',  ( 10.81492255796078972, 18.62759615963270932, 84.58224293864769550 ) ) ;
#53432 = CARTESIAN_POINT ( 'NONE',  ( 5.153800228976615827, -19.02544592524334988, 55.20942372801899722 ) ) ;
#53433 = CARTESIAN_POINT ( 'NONE',  ( -5.049401038298153566, 19.05341960407611168, 100.2072429386476955 ) ) ;
#53434 = PRESENTATION_STYLE_ASSIGNMENT (( #5926 ) ) ;
#53435 = CARTESIAN_POINT ( 'NONE',  ( -21.53943276465977519, 0.05219959533907696930, 41.24890960531435269 ) ) ;
#53436 = CARTESIAN_POINT ( 'NONE',  ( 9.474510206698971260, -16.51473224551069308, 87.91557627198102409 ) ) ;
#53437 = CARTESIAN_POINT ( 'NONE',  ( 10.72451020669871369, 18.67979575497193778, 67.08442372801901854 ) ) ;
#53438 = CARTESIAN_POINT ( 'NONE',  ( -5.153800228976328057, -19.02544592524343514, 37.29057627198102409 ) ) ;
#53439 = EDGE_CURVE ( 'NONE', #49688, #193619, #159741, .T. ) ;
#53440 = CARTESIAN_POINT ( 'NONE',  ( 4.379528057220339221, -16.55341960407611168, 72.70724293864769550 ) ) ;
#53441 = CARTESIAN_POINT ( 'NONE',  ( 16.55341960407618274, -4.379528057220086978, 26.04275706135235779 ) ) ;
#53442 = CARTESIAN_POINT ( 'NONE',  ( 15.80617190586769283, -15.72974639402175789, 55.62609039468568284 ) ) ;
#53443 = VERTEX_POINT ( 'NONE', #94833 ) ;
#53444 = CARTESIAN_POINT ( 'NONE',  ( -0.05219959533909027116, -19.03943276465977164, 107.4989096053143527 ) ) ;
#53445 = CARTESIAN_POINT ( 'NONE',  ( -13.89961937509957401, -13.97604488694547875, 64.37609039468567573 ) ) ;
#53446 = CARTESIAN_POINT ( 'NONE',  ( 12.99999999999999822, 0.000000000000000000, 2.055000000000000160 ) ) ;
#53447 = CARTESIAN_POINT ( 'NONE',  ( -15.80617190586768217, 15.72974639402176855, 23.12609039468567573 ) ) ;
#53448 = DIRECTION ( 'NONE',  ( 1.000000000000000000, 0.000000000000000000, 0.000000000000000000 ) ) ;
#53449 = CARTESIAN_POINT ( 'NONE',  ( -5.153800228976607833, 19.02544592524334988, 22.70942372801899012 ) ) ;
#53450 = CARTESIAN_POINT ( 'NONE',  ( -16.51473224551069308, -9.474510206698971260, 61.66557627198103120 ) ) ;
#53451 = CARTESIAN_POINT ( 'NONE',  ( 15.72974639402176855, 15.80617190586768217, 106.8760903946856899 ) ) ;
#53452 = CARTESIAN_POINT ( 'NONE',  ( -16.52544592524335698, -4.483927247898792601, 103.9594237280190185 ) ) ;
#53454 = CARTESIAN_POINT ( 'NONE',  ( -5.823673210054431948, 21.52544592524334988, 77.70942372801900433 ) ) ;
#53453 = CARTESIAN_POINT ( 'NONE',  ( -9.564922557960796823, -16.46253265017161027, 107.0822429386476955 ) ) ;
#53455 = FACE_OUTER_BOUND ( 'NONE', #170347, .T. ) ;
#53456 = CARTESIAN_POINT ( 'NONE',  ( 19.02544592524343514, -5.153800228976328945, 113.5405762719810241 ) ) ;
#53457 = CARTESIAN_POINT ( 'NONE',  ( -1.784589286804288299, -7.284589286804248331, 8.181980515339454030 ) ) ;
#53459 = CARTESIAN_POINT ( 'NONE',  ( 21.55341960407619695, -5.719274019375665929, 71.04275706135234714 ) ) ;
#53458 = CARTESIAN_POINT ( 'NONE',  ( 12.06949235617739724, 12.14591786802326823, 61.87609039468568284 ) ) ;
#53460 = CARTESIAN_POINT ( 'NONE',  ( 10.72451020669871369, 18.67979575497193778, 102.0844237280190185 ) ) ;
#53461 = CARTESIAN_POINT ( 'NONE',  ( -11.30153831258470731, -180.0000000000000000, -25.00000000000000000 ) ) ;
#53462 = CARTESIAN_POINT ( 'NONE',  ( -9.564922557960796823, -16.46253265017161027, 82.08224293864768129 ) ) ;
#53463 = CARTESIAN_POINT ( 'NONE',  ( -19.02544592524342804, 5.153800228976336051, 116.0405762719810383 ) ) ;
#53464 = DIRECTION ( 'NONE',  ( 0.000000000000000000, 0.000000000000000000, -1.000000000000000000 ) ) ;
#53465 = CARTESIAN_POINT ( 'NONE',  ( 19.03943276465977164, -0.05219959533909143690, 33.74890960531435979 ) ) ;
#53466 = CARTESIAN_POINT ( 'NONE',  ( 15.72974639402199770, -15.80617190586745480, 38.12390960531436690 ) ) ;
#53467 = CARTESIAN_POINT ( 'NONE',  ( 4.483927247898790824, -16.52544592524335698, 100.2094237280190043 ) ) ;
#53469 = CARTESIAN_POINT ( 'NONE',  ( 16.51473224551069308, 9.474510206698969483, 79.16557627198103830 ) ) ;
#53468 = CARTESIAN_POINT ( 'NONE',  ( -14.34966873604960291, -8.224510206698953496, 96.66557627198102409 ) ) ;
#53470 = CARTESIAN_POINT ( 'NONE',  ( -15.72974639402176322, -15.80617190586768395, 109.3760903946857042 ) ) ;
#53471 = CARTESIAN_POINT ( 'NONE',  ( -19.05341960407611168, -5.049401038298163336, 36.45724293864766707 ) ) ;
#53472 = CARTESIAN_POINT ( 'NONE',  ( 8.224510206698953496, -14.34966873604960469, 92.91557627198103830 ) ) ;
#53473 = CARTESIAN_POINT ( 'NONE',  ( -21.53943276465977519, -0.05219959533937600094, 48.75109039468568284 ) ) ;
#53474 = CARTESIAN_POINT ( 'NONE',  ( 21.52544592524344225, -5.823673210054117533, 88.54057627198103830 ) ) ;
#53475 = CARTESIAN_POINT ( 'NONE',  ( 19.05341960407617918, -5.049401038297876454, 46.04275706135233293 ) ) ;
#53476 = CARTESIAN_POINT ( 'NONE',  ( -13.97604488694527625, -13.89961937509977830, 46.87390960531435979 ) ) ;
#53477 = CARTESIAN_POINT ( 'NONE',  ( -19.03943276465977164, 0.05219959533909376836, 91.24890960531436690 ) ) ;
#53478 = CARTESIAN_POINT ( 'NONE',  ( -8.314922557960811034, -14.29746914071050412, 57.08224293864769550 ) ) ;
#53479 = CARTESIAN_POINT ( 'NONE',  ( -0.05219959533936034679, 19.03943276465977164, 42.50109039468566152 ) ) ;
#53480 = CARTESIAN_POINT ( 'NONE',  ( 8.224510206698953496, -14.34966873604960469, 42.91557627198103120 ) ) ;
#53481 = CARTESIAN_POINT ( 'NONE',  ( -9.564922557961040184, 16.46253265017147172, 82.91775706135233293 ) ) ;
#53482 = CARTESIAN_POINT ( 'NONE',  ( -18.22780087662123805, 5.499999999999981348, 86.01763182126894947 ) ) ;
#53483 = CARTESIAN_POINT ( 'NONE',  ( -21.52544592524343514, 5.823673210054127303, 36.04057627198102409 ) ) ;
#53484 = ADVANCED_FACE ( 'NONE', ( #110994 ), #124917, .T. ) ;
#53485 = CARTESIAN_POINT ( 'NONE',  ( 12.14591786802309770, 12.06949235617756955, 99.37390960531436690 ) ) ;
#53486 = CARTESIAN_POINT ( 'NONE',  ( -17.18269478283316332, 17.18269478283309226, -54.21489346206828230 ) ) ;
#53488 = CARTESIAN_POINT ( 'NONE',  ( -5.719274019375978568, 21.55341960407610458, 55.20724293864770260 ) ) ;
#53487 = CARTESIAN_POINT ( 'NONE',  ( 16.51473224551069308, 9.474510206698969483, 64.16557627198102409 ) ) ;
#53489 = CARTESIAN_POINT ( 'NONE',  ( -13.97604488694527625, -13.89961937509977652, 31.87390960531435979 ) ) ;
#53491 = CARTESIAN_POINT ( 'NONE',  ( 16.51473224551069308, 9.474510206698969483, 54.16557627198103120 ) ) ;
#53490 = CARTESIAN_POINT ( 'NONE',  ( 8.314922557961029526, -14.29746914071037800, 75.41775706135233293 ) ) ;
#53492 = CARTESIAN_POINT ( 'NONE',  ( 5.153800228976615827, -19.02544592524334988, 45.20942372801901143 ) ) ;
#53493 = CARTESIAN_POINT ( 'NONE',  ( -15.72974639402176322, -15.80617190586768395, 69.37609039468567573 ) ) ;
#53494 = CARTESIAN_POINT ( 'NONE',  ( -21.55341960407610458, -5.719274019375992779, 56.45724293864768839 ) ) ;
#53495 = CARTESIAN_POINT ( 'NONE',  ( 16.46253265017160672, -9.564922557960803928, 28.33224293864769550 ) ) ;
#53496 = CARTESIAN_POINT ( 'NONE',  ( -16.51473224551082808, 9.474510206698731452, 103.3344237280190043 ) ) ;
#53497 = CARTESIAN_POINT ( 'NONE',  ( 27.12243378312293274, 3.972435522077283121, 169.3718635229823235 ) ) ;
#53499 = CARTESIAN_POINT ( 'NONE',  ( -15.80617190586745835, -15.72974639402198527, 41.87390960531435979 ) ) ;
#53498 = CARTESIAN_POINT ( 'NONE',  ( 17.49999999999999645, 4.703611302595025911, 36.84949425462254169 ) ) ;
#53500 = CARTESIAN_POINT ( 'NONE',  ( -5.049401038298153566, 19.05341960407611168, 25.20724293864768484 ) ) ;
#53501 = CARTESIAN_POINT ( 'NONE',  ( -10.81492255796105439, 18.62759615963255655, 77.91775706135231871 ) ) ;
#53502 = CARTESIAN_POINT ( 'NONE',  ( 12.14591786802309770, 12.06949235617756955, 44.37390960531435979 ) ) ;
#53503 = CARTESIAN_POINT ( 'NONE',  ( 12.06949235617757843, -12.14591786802309237, 63.12390960531435979 ) ) ;
#53504 = CARTESIAN_POINT ( 'NONE',  ( 5.719274019375991003, -21.55341960407610458, 82.70724293864770971 ) ) ;
#53505 = CARTESIAN_POINT ( 'NONE',  ( -18.67979575497178146, -10.72451020669898902, 81.66557627198103830 ) ) ;
#53506 = CARTESIAN_POINT ( 'NONE',  ( 30.00000000000000000, -5.510910596163089556E-15, 45.00000000000000000 ) ) ;
#53507 = CARTESIAN_POINT ( 'NONE',  ( -10.81492255796078084, -18.62759615963271287, 27.08224293864769550 ) ) ;
#53508 = CARTESIAN_POINT ( 'NONE',  ( -16.53943276465976808, -0.05219959533934237506, 53.75109039468568994 ) ) ;
#53509 = CARTESIAN_POINT ( 'NONE',  ( 4.379528057220339221, -16.55341960407611168, 77.70724293864770971 ) ) ;
#53510 = CARTESIAN_POINT ( 'NONE',  ( 5.049401038298161559, -19.05341960407611168, 62.70724293864769550 ) ) ;
#53511 = CARTESIAN_POINT ( 'NONE',  ( -19.05341960407611168, -5.049401038298163336, 26.45724293864769550 ) ) ;
#53512 = CARTESIAN_POINT ( 'NONE',  ( 17.50000000000000000, -5.500000000000000000, 111.2176903769643559 ) ) ;
#53513 = CARTESIAN_POINT ( 'NONE',  ( -12.14591786802326823, 12.06949235617739902, 78.12609039468570415 ) ) ;
#53514 = CARTESIAN_POINT ( 'NONE',  ( 15.80617190586769283, -15.72974639402175789, 20.62609039468568639 ) ) ;
#53515 = CARTESIAN_POINT ( 'NONE',  ( 9.564922557960805705, 16.46253265017160317, 84.58224293864769550 ) ) ;
#53516 = CARTESIAN_POINT ( 'NONE',  ( -21.55341960407619339, 5.719274019375674811, 53.54275706135234714 ) ) ;
#53517 = CARTESIAN_POINT ( 'NONE',  ( 5.153800228976335163, 19.02544592524342804, 109.7905762719810099 ) ) ;
#53518 = CARTESIAN_POINT ( 'NONE',  ( -3.503282210674341979, -48.86437366581480291, -24.99999999999999289 ) ) ;
#53519 = VERTEX_POINT ( 'NONE', #139971 ) ;
#53520 = CARTESIAN_POINT ( 'NONE',  ( 0.05219959533937995610, -21.53943276465977519, 45.00109039468568284 ) ) ;
#53522 = CARTESIAN_POINT ( 'NONE',  ( 5.049401038298161559, -19.05341960407611168, 107.7072429386476955 ) ) ;
#53521 = CARTESIAN_POINT ( 'NONE',  ( 19.03943276465977164, -0.05219959533909143690, 38.74890960531436690 ) ) ;
#53523 = CARTESIAN_POINT ( 'NONE',  ( -5.049401038297874678, -19.05341960407617918, 59.79275706135231871 ) ) ;
#53524 = CARTESIAN_POINT ( 'NONE',  ( -21.53943276465977519, -0.05219959533937600094, 18.75109039468568639 ) ) ;
#53525 = CARTESIAN_POINT ( 'NONE',  ( 16.46253265017146816, 9.564922557961045513, 46.66775706135233293 ) ) ;
#53526 = CARTESIAN_POINT ( 'NONE',  ( -16.51473224551069308, -9.474510206698971260, 31.66557627198102054 ) ) ;
#53527 = CARTESIAN_POINT ( 'NONE',  ( -12.06949235617739369, -12.14591786802326823, 89.37609039468568994 ) ) ;
#53528 = CARTESIAN_POINT ( 'NONE',  ( -5.049401038297874678, -19.05341960407617918, 64.79275706135233293 ) ) ;
#53529 = CARTESIAN_POINT ( 'NONE',  ( 4.483927247898790824, -16.52544592524335698, 105.2094237280190328 ) ) ;
#53530 = CARTESIAN_POINT ( 'NONE',  ( 9.550175731184127770, 9.839468975293851116, -62.57644703671204667 ) ) ;
#53531 = CARTESIAN_POINT ( 'NONE',  ( -5.153800228976328057, -19.02544592524343514, 92.29057627198099567 ) ) ;
#53532 = AXIS2_PLACEMENT_3D ( 'NONE', #9447, #29588, #189000 ) ;
#53533 = CARTESIAN_POINT ( 'NONE',  ( 21.53943276465977519, 0.05219959533937863772, 91.25109039468568994 ) ) ;
#53534 = CARTESIAN_POINT ( 'NONE',  ( -15.80617190586768217, 15.72974639402176855, 113.1260903946856899 ) ) ;
#53535 = CARTESIAN_POINT ( 'NONE',  ( -37.99626262588769521, 12.34573411038911317, -4.102157773949822506 ) ) ;
#53536 = CARTESIAN_POINT ( 'NONE',  ( 19.02544592524343514, -5.153800228976328945, 103.5405762719809957 ) ) ;
#53537 = CARTESIAN_POINT ( 'NONE',  ( 21.52544592524334988, 5.823673210054432836, 76.45942372801901854 ) ) ;
#53538 = CARTESIAN_POINT ( 'NONE',  ( 0.05219959533936267826, -19.03943276465977164, 110.0010903946856757 ) ) ;
#53539 = CARTESIAN_POINT ( 'NONE',  ( 5.049401038298161559, -19.05341960407611168, 77.70724293864765286 ) ) ;
#53540 = CARTESIAN_POINT ( 'NONE',  ( -18.67979575497178146, -10.72451020669898902, 36.66557627198103120 ) ) ;
#53541 = CARTESIAN_POINT ( 'NONE',  ( -13.89961937509977652, 13.97604488694528158, 95.62390960531436690 ) ) ;
#53542 = DIRECTION ( 'NONE',  ( -0.000000000000000000, -0.000000000000000000, -1.000000000000000000 ) ) ;
#53543 = CARTESIAN_POINT ( 'NONE',  ( -19.02544592524342804, 5.153800228976336051, 81.04057627198103830 ) ) ;
#53544 = CARTESIAN_POINT ( 'NONE',  ( -13.97604488694527625, -13.89961937509977652, 61.87390960531435979 ) ) ;
#53545 = CARTESIAN_POINT ( 'NONE',  ( -16.53943276465976808, -0.05219959533934237506, 98.75109039468568994 ) ) ;
#53546 = CARTESIAN_POINT ( 'NONE',  ( -3.573655867282028392E-15, 2.428612866367529932E-14, 155.0000000000000000 ) ) ;
#53547 = CARTESIAN_POINT ( 'NONE',  ( -13.97604488694547697, 13.89961937509957934, 63.12609039468566152 ) ) ;
#53548 = CARTESIAN_POINT ( 'NONE',  ( -9.564922557960796823, -16.46253265017161027, 97.08224293864769550 ) ) ;
#53549 = CARTESIAN_POINT ( 'NONE',  ( 0.05219959533910956823, 16.53943276465976808, 79.99890960531435269 ) ) ;
#53550 = CARTESIAN_POINT ( 'NONE',  ( 5.719274019375991003, -21.55341960407610458, 32.70724293864770260 ) ) ;
#53551 = CARTESIAN_POINT ( 'NONE',  ( 16.46253265017160672, -9.564922557960803928, 113.3322429386476955 ) ) ;
#53552 = CARTESIAN_POINT ( 'NONE',  ( -16.53943276465976808, 0.05219959533911058130, 86.24890960531436690 ) ) ;
#53553 = LINE ( 'NONE', #9066, #124170 ) ;
#53554 = CARTESIAN_POINT ( 'NONE',  ( -16.46253265017146816, -9.564922557961047289, 44.16775706135232582 ) ) ;
#53555 = CARTESIAN_POINT ( 'NONE',  ( 8.314922557960818139, 14.29746914071049879, 29.58224293864769905 ) ) ;
#53556 = B_SPLINE_CURVE_WITH_KNOTS ( 'NONE', 3,
 ( #76565, #138240, #19866, #148960, #127029, #188736, #25631, #21863, #132780, #144194, #80533, #194467, #34049, #55938 ),
 .UNSPECIFIED., .F., .F.,
 ( 4, 2, 2, 2, 2, 2, 4 ),
 ( 1.971390914159136004E-07, 0.0002964243498305583948, 0.0005926515605697007128, 0.0008888787713088428140, 0.001185105982047984698, 0.001777560403526266515, 0.002370014825004548333 ),
 .UNSPECIFIED. ) ;
#53557 = CARTESIAN_POINT ( 'NONE',  ( 9.474510206698971260, -16.51473224551069308, 107.9155762719810383 ) ) ;
#53558 = CARTESIAN_POINT ( 'NONE',  ( 0.05219959533937995610, -21.53943276465977519, 70.00109039468568994 ) ) ;
#53559 = CARTESIAN_POINT ( 'NONE',  ( 21.52544592524344225, -5.823673210054117533, 58.54057627198103120 ) ) ;
#53560 = CARTESIAN_POINT ( 'NONE',  ( 10.72451020669871369, 18.67979575497193778, 32.08442372801901854 ) ) ;
#53561 = CARTESIAN_POINT ( 'NONE',  ( -10.72451020669898014, 18.67979575497178502, 85.41557627198102409 ) ) ;
#53562 = CARTESIAN_POINT ( 'NONE',  ( -21.53943276465977519, -0.05219959533937600094, 38.75109039468567573 ) ) ;
#53563 = CARTESIAN_POINT ( 'NONE',  ( 12.06949235617757843, -12.14591786802309237, 108.1239096053143811 ) ) ;
#53564 = CARTESIAN_POINT ( 'NONE',  ( -9.564922557961040184, 16.46253265017147172, 67.91775706135233293 ) ) ;
#53565 = CARTESIAN_POINT ( 'NONE',  ( -9.564922557960796823, -16.46253265017161027, 47.08224293864769550 ) ) ;
#53567 = CARTESIAN_POINT ( 'NONE',  ( -19.05341960407611168, -5.049401038298163336, 96.45724293864769550 ) ) ;
#53566 = CARTESIAN_POINT ( 'NONE',  ( 8.314922557960818139, 14.29746914071049879, 94.58224293864769550 ) ) ;
#53568 = CARTESIAN_POINT ( 'NONE',  ( -16.51473224551069308, -9.474510206698971260, 96.66557627198102409 ) ) ;
#53569 = CARTESIAN_POINT ( 'NONE',  ( -14.29746914071049879, 8.314922557960819915, 110.8322429386476955 ) ) ;
#53570 = CIRCLE ( 'NONE', #47239, 1.000000000000000888 ) ;
#53571 = CARTESIAN_POINT ( 'NONE',  ( -16.55341960407611168, -4.379528057220339221, 41.45724293864769550 ) ) ;
#53572 = CARTESIAN_POINT ( 'NONE',  ( 16.52544592524335698, 4.483927247898782831, 106.4594237280190328 ) ) ;
#53573 = CARTESIAN_POINT ( 'NONE',  ( 19.02544592524343514, -5.153800228976328945, 58.54057627198102409 ) ) ;
#53574 = CARTESIAN_POINT ( 'NONE',  ( -9.564922557960796823, -16.46253265017161027, 22.08224293864768839 ) ) ;
#53575 = CARTESIAN_POINT ( 'NONE',  ( 9.474510206698729675, 16.51473224551082808, 27.08442372801900433 ) ) ;
#53577 = CARTESIAN_POINT ( 'NONE',  ( 0.05219959533934541429, -16.53943276465976808, 110.0010903946856757 ) ) ;
#53576 = CARTESIAN_POINT ( 'NONE',  ( 9.564922557960805705, 16.46253265017160317, 109.5822429386476955 ) ) ;
#53578 = CARTESIAN_POINT ( 'NONE',  ( -10.81492255796105439, 18.62759615963255655, 42.91775706135235424 ) ) ;
#53579 = CARTESIAN_POINT ( 'NONE',  ( -13.97604488694527625, -13.89961937509977652, 101.8739096053143811 ) ) ;
#53580 = CARTESIAN_POINT ( 'NONE',  ( -12.06949235617739369, -12.14591786802326823, 44.37609039468567573 ) ) ;
#53581 = CARTESIAN_POINT ( 'NONE',  ( -4.483927247898782831, 16.52544592524335698, 107.7094237280190328 ) ) ;
#53582 = CARTESIAN_POINT ( 'NONE',  ( 19.05341960407611168, 5.049401038298154454, 48.95724293864768129 ) ) ;
#53583 = CARTESIAN_POINT ( 'NONE',  ( -4.483927247898782831, 16.52544592524335698, 92.70942372801901854 ) ) ;
#53584 = CARTESIAN_POINT ( 'NONE',  ( 16.53943276465976808, 0.05219959533934440121, 31.25109039468568639 ) ) ;
#53585 = EDGE_CURVE ( 'NONE', #189743, #20330, #163106, .T. ) ;
#53586 = CARTESIAN_POINT ( 'NONE',  ( -19.03943276465977164, 0.05219959533909376836, 51.24890960531436690 ) ) ;
#53587 = CARTESIAN_POINT ( 'NONE',  ( 14.29746914071049879, -8.314922557960816363, 113.3322429386476955 ) ) ;
#53588 = CARTESIAN_POINT ( 'NONE',  ( 10.81492255796106328, -18.62759615963255655, 25.41775706135235779 ) ) ;
#53589 = CARTESIAN_POINT ( 'NONE',  ( 16.46253265017160672, -9.564922557960803928, 38.33224293864768839 ) ) ;
#53590 = CARTESIAN_POINT ( 'NONE',  ( -13.97604488694527625, -13.89961937509977652, 101.8739096053143811 ) ) ;
#53591 = CARTESIAN_POINT ( 'NONE',  ( 16.51473224551069308, 9.474510206698969483, 34.16557627198102409 ) ) ;
#53592 = CARTESIAN_POINT ( 'NONE',  ( 19.05341960407611168, 5.049401038298154454, 103.9572429386476671 ) ) ;
#53593 = DIRECTION ( 'NONE',  ( 1.000000000000000000, 0.000000000000000000, 0.000000000000000000 ) ) ;
#53594 = CARTESIAN_POINT ( 'NONE',  ( 19.02544592524343514, -5.153800228976328945, 103.5405762719809957 ) ) ;
#53596 = CARTESIAN_POINT ( 'NONE',  ( -0.05219959533910754901, -16.53943276465976808, 102.4989096053143811 ) ) ;
#53595 = CARTESIAN_POINT ( 'NONE',  ( 18.62759615963255655, 10.81492255796105972, 46.66775706135234714 ) ) ;
#53597 = CARTESIAN_POINT ( 'NONE',  ( 9.474510206698971260, -16.51473224551069308, 112.9155762719810383 ) ) ;
#53598 = CARTESIAN_POINT ( 'NONE',  ( 13.97604488694548053, -13.89961937509957401, 70.62609039468567573 ) ) ;
#53599 = CARTESIAN_POINT ( 'NONE',  ( -16.55341960407617563, 4.379528057220093196, 58.54275706135235424 ) ) ;
#53600 = CARTESIAN_POINT ( 'NONE',  ( 18.67979575497194134, -10.72451020669871369, 95.83442372801903275 ) ) ;
#53601 = CARTESIAN_POINT ( 'NONE',  ( 16.53943276465976808, 0.05219959533934440121, 41.25109039468568284 ) ) ;
#53602 = CARTESIAN_POINT ( 'NONE',  ( 16.46253265017160672, -9.564922557960803928, 88.33224293864769550 ) ) ;
#53603 = CARTESIAN_POINT ( 'NONE',  ( 16.53943276465976808, 0.05219959533934440121, 31.25109039468568639 ) ) ;
#53604 = CARTESIAN_POINT ( 'NONE',  ( -5.049401038297874678, -19.05341960407617918, 104.7927570613523471 ) ) ;
#53605 = CARTESIAN_POINT ( 'NONE',  ( -12.14591786802326823, 12.06949235617739902, 78.12609039468570415 ) ) ;
#53606 = CARTESIAN_POINT ( 'NONE',  ( 13.97604488694548053, -13.89961937509957401, 90.62609039468567573 ) ) ;
#53607 = CARTESIAN_POINT ( 'NONE',  ( 16.46253265017160672, -9.564922557960803928, 73.33224293864769550 ) ) ;
#53608 = CARTESIAN_POINT ( 'NONE',  ( -5.719274019375978568, 21.55341960407610458, 100.2072429386476955 ) ) ;
#53610 = CARTESIAN_POINT ( 'NONE',  ( 19.05341960407617918, -5.049401038297876454, 86.04275706135233293 ) ) ;
#53609 = CARTESIAN_POINT ( 'NONE',  ( 8.224510206698953496, -14.34966873604960469, 92.91557627198103830 ) ) ;
#53611 = CARTESIAN_POINT ( 'NONE',  ( -14.34966873604972548, 8.224510206698743886, 78.33442372801901854 ) ) ;
#53612 = CARTESIAN_POINT ( 'NONE',  ( 21.95653654802720212, 6.613221094984321091, 171.0358100525039902 ) ) ;
#53613 = CARTESIAN_POINT ( 'NONE',  ( -9.564922557961040184, 16.46253265017147172, 72.91775706135233293 ) ) ;
#53614 = CARTESIAN_POINT ( 'NONE',  ( 8.224510206698953496, -14.34966873604960469, 32.91557627198102409 ) ) ;
#53615 = CARTESIAN_POINT ( 'NONE',  ( -4.379528057220328563, 16.55341960407611168, 100.2072429386476955 ) ) ;
#53617 = CARTESIAN_POINT ( 'NONE',  ( -13.89961937509957401, -13.97604488694547697, 44.37609039468566863 ) ) ;
#53616 = CARTESIAN_POINT ( 'NONE',  ( 5.049401038297881783, 19.05341960407617563, 32.29275706135233293 ) ) ;
#53618 = CARTESIAN_POINT ( 'NONE',  ( 5.719274019375673035, 21.55341960407619339, 27.29275706135234358 ) ) ;
#53619 = CARTESIAN_POINT ( 'NONE',  ( -37.66961640367473052, -4.999999999999976019, -15.00000000000000000 ) ) ;
#53620 = CARTESIAN_POINT ( 'NONE',  ( -9.564922557960796823, -16.46253265017161027, 72.08224293864770971 ) ) ;
#53621 = CARTESIAN_POINT ( 'NONE',  ( 5.823673210054444382, -21.52544592524334988, 95.20942372801903275 ) ) ;
#53622 = CARTESIAN_POINT ( 'NONE',  ( -16.51473224551069308, -9.474510206698971260, 76.66557627198103830 ) ) ;
#53623 = CARTESIAN_POINT ( 'NONE',  ( -10.81492255796078084, -18.62759615963271287, 47.08224293864770260 ) ) ;
#53624 = CARTESIAN_POINT ( 'NONE',  ( 16.55341960407611168, 4.379528057220329451, 73.95724293864769550 ) ) ;
#53625 = CARTESIAN_POINT ( 'NONE',  ( 5.153800228976335163, 19.02544592524342804, 54.79057627198103120 ) ) ;
#53626 = AXIS2_PLACEMENT_3D ( 'NONE', #93587, #3562, #48101 ) ;
#53627 = CARTESIAN_POINT ( 'NONE',  ( -14.34966873604960291, -8.224510206698953496, 111.6655762719810525 ) ) ;
#53628 = CARTESIAN_POINT ( 'NONE',  ( 21.52544592524334988, 5.823673210054432836, 21.45942372801901499 ) ) ;
#53629 = CARTESIAN_POINT ( 'NONE',  ( 21.55341960407619695, -5.719274019375665929, 66.04275706135236135 ) ) ;
#53630 = CARTESIAN_POINT ( 'NONE',  ( -9.564922557960796823, -16.46253265017161027, 47.08224293864769550 ) ) ;
#53631 = CARTESIAN_POINT ( 'NONE',  ( 16.55341960407618274, -4.379528057220086978, 76.04275706135237556 ) ) ;
#53632 = CARTESIAN_POINT ( 'NONE',  ( 5.823673210054125526, 21.52544592524343514, 114.7905762719810383 ) ) ;
#53633 = EDGE_LOOP ( 'NONE', ( #58742, #73803 ) ) ;
#53634 = CARTESIAN_POINT ( 'NONE',  ( -21.52544592524334988, -5.823673210054445271, 18.95942372801901143 ) ) ;
#53636 = CARTESIAN_POINT ( 'NONE',  ( 9.564922557960805705, 16.46253265017160317, 64.58224293864769550 ) ) ;
#53635 = CARTESIAN_POINT ( 'NONE',  ( 5.153800228976615827, -19.02544592524334988, 35.20942372801899722 ) ) ;
#53637 = CARTESIAN_POINT ( 'NONE',  ( 16.51473224551083163, -9.474510206698727899, 30.83442372801900433 ) ) ;
#53638 = CARTESIAN_POINT ( 'NONE',  ( 0.05219959533937995610, -21.53943276465977519, 70.00109039468568994 ) ) ;
#53639 = CARTESIAN_POINT ( 'NONE',  ( 15.80617190586746368, 15.72974639402197994, 69.37390960531436690 ) ) ;
#53640 = CARTESIAN_POINT ( 'NONE',  ( -4.379528057220328563, 16.55341960407611168, 40.20724293864769550 ) ) ;
#53642 = CARTESIAN_POINT ( 'NONE',  ( -19.03943276465977164, -0.05219959533935918106, 28.75109039468566507 ) ) ;
#53641 = CARTESIAN_POINT ( 'NONE',  ( -21.52544592524334988, -5.823673210054445271, 83.95942372801900433 ) ) ;
#53643 = CARTESIAN_POINT ( 'NONE',  ( 4.483927247898545687, 16.52544592524342804, 64.79057627198103830 ) ) ;
#53644 = CARTESIAN_POINT ( 'NONE',  ( -8.224510206698948167, 14.34966873604960824, 110.4155762719810383 ) ) ;
#53645 = CARTESIAN_POINT ( 'NONE',  ( 19.05341960407617918, -5.049401038297876454, 61.04275706135232582 ) ) ;
#53646 = CARTESIAN_POINT ( 'NONE',  ( -16.55341960407617563, 4.379528057220093196, 108.5427570613523756 ) ) ;
#53647 = CARTESIAN_POINT ( 'NONE',  ( 21.52544592524334988, 5.823673210054432836, 66.45942372801903275 ) ) ;
#53648 = CARTESIAN_POINT ( 'NONE',  ( -5.049401038298153566, 19.05341960407611168, 75.20724293864769550 ) ) ;
#53649 = CARTESIAN_POINT ( 'NONE',  ( 13.89961937509957401, 13.97604488694547697, 41.87609039468566152 ) ) ;
#53650 = CARTESIAN_POINT ( 'NONE',  ( -15.80617190586745835, -15.72974639402198527, 51.87390960531437401 ) ) ;
#53651 = B_SPLINE_CURVE_WITH_KNOTS ( 'NONE', 3,
 ( #90615, #76441, #93589, #152297, #13781, #185617, #140088, #199799, #171443, #141092, #1580, #122936, #578, #155275 ),
 .UNSPECIFIED., .F., .F.,
 ( 4, 2, 2, 2, 2, 2, 4 ),
 ( 0.000000000000000000, 0.0003275753061460234968, 0.0006551506122920469936, 0.0009827259184380704362, 0.001310301224584093987, 0.001965451836876139138, 0.002620602449168184505 ),
 .UNSPECIFIED. ) ;
#53652 = CARTESIAN_POINT ( 'NONE',  ( 18.67979575497194134, -10.72451020669871369, 50.83442372801901143 ) ) ;
#53653 = CARTESIAN_POINT ( 'NONE',  ( 10.81492255796078972, 18.62759615963270932, 104.5822429386477097 ) ) ;
#53654 = CARTESIAN_POINT ( 'NONE',  ( -5.049401038297874678, -19.05341960407617918, 99.79275706135234714 ) ) ;
#53655 = CARTESIAN_POINT ( 'NONE',  ( -16.52544592524335698, -4.483927247898792601, 68.95942372801901854 ) ) ;
#53657 = CARTESIAN_POINT ( 'NONE',  ( 5.823673210054125526, 21.52544592524343514, 109.7905762719810383 ) ) ;
#53656 = CARTESIAN_POINT ( 'NONE',  ( -30.73962218707678318, -22.33364281372842441, -5.802157773949822683 ) ) ;
#53658 = CARTESIAN_POINT ( 'NONE',  ( 12.06949235617757843, -12.14591786802309237, 93.12390960531436690 ) ) ;
#53659 = CARTESIAN_POINT ( 'NONE',  ( -17.49999999999999645, -3.565345528327900304, 30.57505513193525815 ) ) ;
#53660 = CARTESIAN_POINT ( 'NONE',  ( -16.53943276465976808, -0.05219959533934237506, 28.75109039468567929 ) ) ;
#53661 = CARTESIAN_POINT ( 'NONE',  ( 0.05219959533907565091, 21.53943276465977519, 44.99890960531435979 ) ) ;
#53662 = CARTESIAN_POINT ( 'NONE',  ( 14.29746914071037800, 8.314922557961029526, 96.66775706135234714 ) ) ;
#53663 = CARTESIAN_POINT ( 'NONE',  ( 36.67794138864803699, -4.841227315053108882, -7.999999999999994671 ) ) ;
#53664 = CARTESIAN_POINT ( 'NONE',  ( -12.14591786802326823, 12.06949235617739902, 68.12609039468567573 ) ) ;
#53665 = CARTESIAN_POINT ( 'NONE',  ( 21.55341960407619695, -5.719274019375665929, 36.04275706135234714 ) ) ;
#53666 = CARTESIAN_POINT ( 'NONE',  ( -10.72451020669898014, 18.67979575497178502, 40.41557627198103120 ) ) ;
#53667 = CARTESIAN_POINT ( 'NONE',  ( -12.06949235617739369, -12.14591786802326823, 79.37609039468567573 ) ) ;
#53668 = CARTESIAN_POINT ( 'NONE',  ( 16.51473224551069308, 9.474510206698969483, 104.1655762719810241 ) ) ;
#53669 = CARTESIAN_POINT ( 'NONE',  ( 21.53943276465977519, 0.05219959533937863772, 66.25109039468567573 ) ) ;
#53670 = CARTESIAN_POINT ( 'NONE',  ( -10.72451020669898014, 18.67979575497178502, 35.41557627198102409 ) ) ;
#53671 = CARTESIAN_POINT ( 'NONE',  ( -18.62759615963270932, 10.81492255796079327, 40.83224293864769550 ) ) ;
#53672 = VERTEX_POINT ( 'NONE', #113608 ) ;
#53673 = CARTESIAN_POINT ( 'NONE',  ( -0.05219959533936034679, 19.03943276465977164, 52.50109039468566863 ) ) ;
#53674 = CARTESIAN_POINT ( 'NONE',  ( -0.05219959533934338120, 16.53943276465976808, 62.50109039468568284 ) ) ;
#53675 = CARTESIAN_POINT ( 'NONE',  ( 15.72974639402199770, -15.80617190586745480, 33.12390960531435979 ) ) ;
#53676 = EDGE_LOOP ( 'NONE', ( #181094, #130830, #102292, #27686, #14492 ) ) ;
#53677 = EDGE_CURVE ( 'NONE', #10027, #139245, #79305, .T. ) ;
#53678 = CARTESIAN_POINT ( 'NONE',  ( -19.03943276465977164, 0.05219959533909376836, 86.24890960531436690 ) ) ;
#53679 = CARTESIAN_POINT ( 'NONE',  ( -14.29746914071049879, 8.314922557960819915, 25.83224293864769194 ) ) ;
#53680 = CYLINDRICAL_SURFACE ( 'NONE', #105355, 24.30000000000003268 ) ;
#53681 = CARTESIAN_POINT ( 'NONE',  ( -12.14591786802309592, -12.06949235617757132, 111.8739096053143669 ) ) ;
#53682 = CARTESIAN_POINT ( 'NONE',  ( 21.52544592524344225, -5.823673210054117533, 48.54057627198103120 ) ) ;
#53683 = CARTESIAN_POINT ( 'NONE',  ( -16.51473224551069308, -9.474510206698971260, 46.66557627198102409 ) ) ;
#53684 = CARTESIAN_POINT ( 'NONE',  ( 8.224510206698742110, 14.34966873604972548, 87.08442372801901854 ) ) ;
#53685 = CARTESIAN_POINT ( 'NONE',  ( 21.53943276465977519, 0.05219959533937863772, 31.25109039468568639 ) ) ;
#53686 = CARTESIAN_POINT ( 'NONE',  ( 5.049401038297881783, 19.05341960407617563, 92.29275706135234714 ) ) ;
#53687 = CARTESIAN_POINT ( 'NONE',  ( -8.224510206698948167, 14.34966873604960824, 90.41557627198103830 ) ) ;
#53688 = CARTESIAN_POINT ( 'NONE',  ( 19.05341960407611168, 5.049401038298154454, 53.95724293864770260 ) ) ;
#53689 = CARTESIAN_POINT ( 'NONE',  ( 19.02544592524343514, -5.153800228976328945, 28.54057627198102409 ) ) ;
#53690 = CARTESIAN_POINT ( 'NONE',  ( -21.55341960407619339, 5.719274019375674811, 108.5427570613523756 ) ) ;
#53691 = CARTESIAN_POINT ( 'NONE',  ( -9.564922557960796823, -16.46253265017161027, 82.08224293864768129 ) ) ;
#53692 = EDGE_CURVE ( 'NONE', #515, #85313, #130747, .T. ) ;
#53693 = CARTESIAN_POINT ( 'NONE',  ( -8.224510206698735004, -14.34966873604973081, 64.58442372801900433 ) ) ;
#53694 = CARTESIAN_POINT ( 'NONE',  ( -5.719274019375665041, -21.55341960407619695, 94.79275706135234714 ) ) ;
#53695 = CARTESIAN_POINT ( 'NONE',  ( -18.67979575497178146, -10.72451020669898902, 46.66557627198102409 ) ) ;
#53696 = CARTESIAN_POINT ( 'NONE',  ( -12.06949235617739369, -12.14591786802326823, 69.37609039468567573 ) ) ;
#53697 = CARTESIAN_POINT ( 'NONE',  ( 19.02544592524334988, 5.153800228976608722, 46.45942372801899012 ) ) ;
#53698 = CARTESIAN_POINT ( 'NONE',  ( -13.97604488694547697, 13.89961937509957934, 68.12609039468563310 ) ) ;
#53699 = VERTEX_POINT ( 'NONE', #142951 ) ;
#53700 = CARTESIAN_POINT ( 'NONE',  ( -21.52544592524334988, -5.823673210054445271, 63.95942372801901854 ) ) ;
#53701 = CARTESIAN_POINT ( 'NONE',  ( -19.03943276465977164, 0.05219959533909376836, 66.24890960531436690 ) ) ;
#53702 = CARTESIAN_POINT ( 'NONE',  ( -9.474510206698964154, 16.51473224551069663, 30.41557627198102054 ) ) ;
#53703 = CARTESIAN_POINT ( 'NONE',  ( 5.153800228976615827, -19.02544592524334988, 55.20942372801899722 ) ) ;
#53704 = CARTESIAN_POINT ( 'NONE',  ( 5.049401038298161559, -19.05341960407611168, 107.7072429386476955 ) ) ;
#53705 = CARTESIAN_POINT ( 'NONE',  ( -19.03943276465977164, 0.05219959533909376836, 96.24890960531436690 ) ) ;
#53706 = CARTESIAN_POINT ( 'NONE',  ( -16.55341960407611168, -4.379528057220339221, 51.45724293864770260 ) ) ;
#53707 = CARTESIAN_POINT ( 'NONE',  ( 18.62759615963271287, -10.81492255796078972, 43.33224293864769550 ) ) ;
#53708 = CARTESIAN_POINT ( 'NONE',  ( 21.49604614807110536, -21.49604614807103786, -64.92279855667830191 ) ) ;
#53709 = CARTESIAN_POINT ( 'NONE',  ( 16.46253265017146816, 9.564922557961045513, 21.66775706135233648 ) ) ;
#53710 =( NAMED_UNIT ( * ) SI_UNIT ( $, .STERADIAN. ) SOLID_ANGLE_UNIT ( ) );
#53711 = CARTESIAN_POINT ( 'NONE',  ( 9.474510206698971260, -16.51473224551069308, 47.91557627198102409 ) ) ;
#53712 = CARTESIAN_POINT ( 'NONE',  ( -33.70754165857147200, -5.457863348371953194, 95.70317755519533875 ) ) ;
#53713 = CARTESIAN_POINT ( 'NONE',  ( 6.906787368987876263, -36.38763403141891217, -7.999999999999998224 ) ) ;
#53714 = CARTESIAN_POINT ( 'NONE',  ( 14.29746914071037800, 8.314922557961029526, 76.66775706135234714 ) ) ;
#53715 = CARTESIAN_POINT ( 'NONE',  ( 21.55341960407610458, 5.719274019375980345, 98.95724293864770971 ) ) ;
#53716 = CARTESIAN_POINT ( 'NONE',  ( -0.05219959533910754901, -16.53943276465976808, 47.49890960531435979 ) ) ;
#53718 = CARTESIAN_POINT ( 'NONE',  ( -38.00000000000000711, -12.34694845685042708, -5.649999994537625803 ) ) ;
#53717 = CARTESIAN_POINT ( 'NONE',  ( -13.89961937509977652, 13.97604488694528158, 40.62390960531435979 ) ) ;
#53719 = CARTESIAN_POINT ( 'NONE',  ( -15.72974639402176322, -15.80617190586768395, 34.37609039468568284 ) ) ;
#53720 = CARTESIAN_POINT ( 'NONE',  ( 5.153800228976615827, -19.02544592524334988, 55.20942372801899722 ) ) ;
#53721 = CARTESIAN_POINT ( 'NONE',  ( 5.049401038298161559, -19.05341960407611168, 37.70724293864768839 ) ) ;
#53722 = CARTESIAN_POINT ( 'NONE',  ( -18.67979575497193778, 10.72451020669871902, 93.33442372801901854 ) ) ;
#53723 = CIRCLE ( 'NONE', #140742, 29.43349580481983807 ) ;
#53724 = CARTESIAN_POINT ( 'NONE',  ( -24.77450267193474076, -6.022707119490098293, 168.7078695393447560 ) ) ;
#53725 = CARTESIAN_POINT ( 'NONE',  ( -12.06949235617756955, 12.14591786802309770, 45.62390960531436690 ) ) ;
#53726 = CARTESIAN_POINT ( 'NONE',  ( 18.56101223717332971, 5.499999999999940492, 43.94978406935678095 ) ) ;
#53727 = CARTESIAN_POINT ( 'NONE',  ( -18.62759615963270932, 10.81492255796079327, 35.83224293864768839 ) ) ;
#53728 = CARTESIAN_POINT ( 'NONE',  ( 2.400000000000000799, 0.000000000000000000, 0.000000000000000000 ) ) ;
#53729 = CIRCLE ( 'NONE', #79561, 13.70000000000001528 ) ;
#53730 = CARTESIAN_POINT ( 'NONE',  ( -13.89961937509977652, 13.97604488694528158, 100.6239096053143669 ) ) ;
#53731 = CARTESIAN_POINT ( 'NONE',  ( 16.55341960407611168, 4.379528057220329451, 83.95724293864770971 ) ) ;
#53732 = CARTESIAN_POINT ( 'NONE',  ( -0.05219959533934338120, 16.53943276465976808, 27.50109039468567929 ) ) ;
#53733 = CARTESIAN_POINT ( 'NONE',  ( 12.14591786802327356, -12.06949235617739191, 110.6260903946857042 ) ) ;
#53734 = ORIENTED_EDGE ( 'NONE', *, *, #72299, .F. ) ;
#53737 = CARTESIAN_POINT ( 'NONE',  ( 15.72974639402199770, -15.80617190586745480, 98.12390960531436690 ) ) ;
#53736 = B_SPLINE_CURVE_WITH_KNOTS ( 'NONE', 3,
 ( #40758, #70095, #146933, #101409, #71093, #23595, #195458, #26602, #85242, #178283, #147942, #9428, #162099, #11437, #132760, #116594 ),
 .UNSPECIFIED., .F., .F.,
 ( 4, 2, 2, 2, 2, 2, 2, 4 ),
 ( 0.003057157445971939082, 0.003802480048122062334, 0.004175141349197131549, 0.004547802650272200764, 0.004920463951347270846, 0.005293125252422339194, 0.005665786553497409277, 0.006038447854572478492 ),
 .UNSPECIFIED. ) ;
#53735 = CARTESIAN_POINT ( 'NONE',  ( 9.474510206698971260, -16.51473224551069308, 92.91557627198103830 ) ) ;
#53739 = CARTESIAN_POINT ( 'NONE',  ( -9.564922557960796823, -16.46253265017161027, 97.08224293864769550 ) ) ;
#53738 = CARTESIAN_POINT ( 'NONE',  ( 4.483927247898545687, 16.52544592524342804, 29.79057627198102409 ) ) ;
#53740 = CARTESIAN_POINT ( 'NONE',  ( 9.564922557961047289, -16.46253265017146816, 75.41775706135234714 ) ) ;
#53741 = CARTESIAN_POINT ( 'NONE',  ( 0.05219959533937995610, -21.53943276465977519, 110.0010903946856757 ) ) ;
#53742 = CARTESIAN_POINT ( 'NONE',  ( -21.52544592524343514, 5.823673210054127303, 96.04057627198102409 ) ) ;
#53743 = CARTESIAN_POINT ( 'NONE',  ( 21.52544592524344225, -5.823673210054117533, 38.54057627198103120 ) ) ;
#53744 = CARTESIAN_POINT ( 'NONE',  ( 19.05341960407611168, 5.049401038298154454, 63.95724293864769550 ) ) ;
#53745 = CARTESIAN_POINT ( 'NONE',  ( 14.34966873604960469, 8.224510206698951720, 39.16557627198102409 ) ) ;
#53746 = CARTESIAN_POINT ( 'NONE',  ( -13.97604488694527625, -13.89961937509977652, 81.87390960531436690 ) ) ;
#53747 = ORIENTED_EDGE ( 'NONE', *, *, #12204, .F. ) ;
#53748 = CARTESIAN_POINT ( 'NONE',  ( -31.31738933903720223, -7.498949511226637554, 94.72411213025000620 ) ) ;
#53749 = CARTESIAN_POINT ( 'NONE',  ( 19.05341960407617918, -5.049401038297876454, 31.04275706135232227 ) ) ;
#53750 = CARTESIAN_POINT ( 'NONE',  ( 14.34966873604960469, 8.224510206698951720, 89.16557627198102409 ) ) ;
#53751 = CARTESIAN_POINT ( 'NONE',  ( 15.80617190586769283, -15.72974639402175789, 20.62609039468568639 ) ) ;
#53752 = CARTESIAN_POINT ( 'NONE',  ( -27.73933785331498925, -9.013057229001049109, 141.4750000027311785 ) ) ;
#53753 = CARTESIAN_POINT ( 'NONE',  ( 12.06949235617739724, 12.14591786802326823, 91.87609039468568994 ) ) ;
#53754 = CARTESIAN_POINT ( 'NONE',  ( -14.34966873604960291, -8.224510206698953496, 111.6655762719810525 ) ) ;
#53755 = CARTESIAN_POINT ( 'NONE',  ( -13.97604488694527625, -13.89961937509977652, 71.87390960531433848 ) ) ;
#53756 = CARTESIAN_POINT ( 'NONE',  ( 30.73962218707677607, -22.33364281372841376, -4.947842220587803652 ) ) ;
#53757 = CARTESIAN_POINT ( 'NONE',  ( 12.14591786802309770, 12.06949235617756955, 34.37390960531435979 ) ) ;
#53758 = CARTESIAN_POINT ( 'NONE',  ( 15.72974639402176855, 15.80617190586768217, 61.87609039468568284 ) ) ;
#53759 = CARTESIAN_POINT ( 'NONE',  ( 31.56233167169124343, -22.40491105030149299, -17.28239568967847362 ) ) ;
#53760 = CARTESIAN_POINT ( 'NONE',  ( -18.62759615963255300, -10.81492255796106328, 94.16775706135237556 ) ) ;
#53761 = CARTESIAN_POINT ( 'NONE',  ( 9.564922557960805705, 16.46253265017160317, 39.58224293864768839 ) ) ;
#53762 = CARTESIAN_POINT ( 'NONE',  ( -0.05219959533909027116, -19.03943276465977164, 57.49890960531435979 ) ) ;
#53763 = VERTEX_POINT ( 'NONE', #34793 ) ;
#53764 = CARTESIAN_POINT ( 'NONE',  ( 0.05219959533937995610, -21.53943276465977519, 95.00109039468568994 ) ) ;
#53765 = CARTESIAN_POINT ( 'NONE',  ( 0.05219959533934541429, -16.53943276465976808, 65.00109039468568994 ) ) ;
#53766 = CARTESIAN_POINT ( 'NONE',  ( 21.52544592524334988, 5.823673210054432836, 81.45942372801900433 ) ) ;
#53767 = CARTESIAN_POINT ( 'NONE',  ( 9.474510206698971260, -16.51473224551069308, 112.9155762719810383 ) ) ;
#53768 = CARTESIAN_POINT ( 'NONE',  ( -5.153800228976607833, 19.02544592524334988, 87.70942372801897591 ) ) ;
#53769 = CARTESIAN_POINT ( 'NONE',  ( 18.62759615963255655, 10.81492255796105972, 71.66775706135234714 ) ) ;
#53770 = CARTESIAN_POINT ( 'NONE',  ( 14.29746914071037800, 8.314922557961029526, 41.66775706135235424 ) ) ;
#53771 = CARTESIAN_POINT ( 'NONE',  ( 10.81492255796078972, 18.62759615963270932, 89.58224293864768129 ) ) ;
#53772 = CARTESIAN_POINT ( 'NONE',  ( 0.05219959533936267826, -19.03943276465977164, 90.00109039468567573 ) ) ;
#53773 = CARTESIAN_POINT ( 'NONE',  ( 19.05341960407611168, 5.049401038298154454, 63.95724293864769550 ) ) ;
#53774 = CARTESIAN_POINT ( 'NONE',  ( -9.564922557961040184, 16.46253265017147172, 102.9177570613523329 ) ) ;
#53775 = CARTESIAN_POINT ( 'NONE',  ( -9.474510206698720793, -16.51473224551083518, 104.5844237280190043 ) ) ;
#53776 = CARTESIAN_POINT ( 'NONE',  ( 14.34966873604960469, 8.224510206698951720, 49.16557627198102409 ) ) ;
#53777 = CARTESIAN_POINT ( 'NONE',  ( 13.89961937509957401, 13.97604488694547697, 81.87609039468564731 ) ) ;
#53778 = CARTESIAN_POINT ( 'NONE',  ( 14.34966873604972726, -8.224510206698740333, 55.83442372801901854 ) ) ;
#53779 = CARTESIAN_POINT ( 'NONE',  ( 13.89961937509977652, -13.97604488694527269, 33.12390960531434558 ) ) ;
#53780 = CARTESIAN_POINT ( 'NONE',  ( 13.97604488694527802, 13.89961937509977652, 54.37390960531435979 ) ) ;
#53781 = CARTESIAN_POINT ( 'NONE',  ( -8.224510206698735004, -14.34966873604973081, 54.58442372801901143 ) ) ;
#53782 = CARTESIAN_POINT ( 'NONE',  ( 31.79999999999968807, 4.791014396527177230E-13, 45.00000000000022027 ) ) ;
#53783 = CARTESIAN_POINT ( 'NONE',  ( -5.429308488886486681E-15, 30.30510711980690175, 141.7500000054623683 ) ) ;
#53784 = CARTESIAN_POINT ( 'NONE',  ( 5.049401038298161559, -19.05341960407611168, 107.7072429386476955 ) ) ;
#53785 = EDGE_CURVE ( 'NONE', #196359, #126376, #65127, .T. ) ;
#53786 = CARTESIAN_POINT ( 'NONE',  ( 19.02544592524343514, -5.153800228976328945, 23.54057627198102054 ) ) ;
#53787 = EDGE_LOOP ( 'NONE', ( #181125, #148460 ) ) ;
#53788 = CARTESIAN_POINT ( 'NONE',  ( -4.483927247898782831, 16.52544592524335698, 22.70942372801901499 ) ) ;
#53789 = CARTESIAN_POINT ( 'NONE',  ( 10.72451020669898902, -18.67979575497178502, 32.91557627198102409 ) ) ;
#53791 = CARTESIAN_POINT ( 'NONE',  ( 8.314922557961029526, -14.29746914071037800, 25.41775706135235779 ) ) ;
#53790 = CARTESIAN_POINT ( 'NONE',  ( -9.474510206698720793, -16.51473224551083518, 34.58442372801899722 ) ) ;
#53792 = CARTESIAN_POINT ( 'NONE',  ( 5.153800228976335163, 19.02544592524342804, 29.79057627198102409 ) ) ;
#53793 = CARTESIAN_POINT ( 'NONE',  ( 13.97604488694527802, 13.89961937509977652, 54.37390960531435979 ) ) ;
#53794 = CARTESIAN_POINT ( 'NONE',  ( 5.719274019375991003, -21.55341960407610458, 72.70724293864769550 ) ) ;
#53795 = CARTESIAN_POINT ( 'NONE',  ( -19.03943276465977164, 0.05219959533909376836, 96.24890960531436690 ) ) ;
#53796 = CARTESIAN_POINT ( 'NONE',  ( -5.049401038298153566, 19.05341960407611168, 35.20724293864768839 ) ) ;
#53797 = CARTESIAN_POINT ( 'NONE',  ( 17.14385361876520264, 23.59649016807275856, 142.6750000027311103 ) ) ;
#53798 = CARTESIAN_POINT ( 'NONE',  ( 9.564922557961047289, -16.46253265017146816, 85.41775706135233293 ) ) ;
#53799 = CARTESIAN_POINT ( 'NONE',  ( -14.29746914071049879, 8.314922557960819915, 65.83224293864769550 ) ) ;
#53800 = CARTESIAN_POINT ( 'NONE',  ( -15.72974639402197994, 15.80617190586746368, 45.62390960531436690 ) ) ;
#53801 = CARTESIAN_POINT ( 'NONE',  ( -10.81492255796105439, 18.62759615963255655, 112.9177570613523329 ) ) ;
#53802 = EDGE_CURVE ( 'NONE', #243, #44025, #127563, .T. ) ;
#53803 = CARTESIAN_POINT ( 'NONE',  ( 5.719274019375991003, -21.55341960407610458, 97.70724293864772392 ) ) ;
#53804 = CARTESIAN_POINT ( 'NONE',  ( 18.67979575497194134, -10.72451020669871369, 70.83442372801901854 ) ) ;
#53805 = CARTESIAN_POINT ( 'NONE',  ( 18.62759615963255655, 10.81492255796105972, 76.66775706135234714 ) ) ;
#53806 = CARTESIAN_POINT ( 'NONE',  ( -13.89961937509977652, 13.97604488694528158, 105.6239096053143527 ) ) ;
#53808 = CARTESIAN_POINT ( 'NONE',  ( -21.55341960407619339, 5.719274019375674811, 83.54275706135234714 ) ) ;
#53807 = CARTESIAN_POINT ( 'NONE',  ( 12.14591786802327356, -12.06949235617739191, 105.6260903946856899 ) ) ;
#53809 = CARTESIAN_POINT ( 'NONE',  ( 5.049401038298161559, -19.05341960407611168, 72.70724293864768129 ) ) ;
#53810 = CARTESIAN_POINT ( 'NONE',  ( 19.02544592524334988, 5.153800228976608722, 31.45942372801900433 ) ) ;
#53811 = CARTESIAN_POINT ( 'NONE',  ( -10.81492255796105439, 18.62759615963255655, 27.91775706135234358 ) ) ;
#53812 = CARTESIAN_POINT ( 'NONE',  ( -9.474510206698964154, 16.51473224551069663, 65.41557627198102409 ) ) ;
#53813 = CARTESIAN_POINT ( 'NONE',  ( -0.05219959533910754901, -16.53943276465976808, 87.49890960531436690 ) ) ;
#53814 = CARTESIAN_POINT ( 'NONE',  ( -0.05219959533910754901, -16.53943276465976808, 42.49890960531435979 ) ) ;
#53815 = CARTESIAN_POINT ( 'NONE',  ( -5.823673210054116645, -21.52544592524344225, 62.29057627198102409 ) ) ;
#53816 = CARTESIAN_POINT ( 'NONE',  ( -9.474510206698964154, 16.51473224551069663, 60.41557627198102409 ) ) ;
#53817 = CARTESIAN_POINT ( 'NONE',  ( -10.72451020669898014, 18.67979575497178502, 65.41557627198102409 ) ) ;
#53818 = CARTESIAN_POINT ( 'NONE',  ( -19.05341960407617563, 5.049401038297882671, 58.54275706135234003 ) ) ;
#53821 = CARTESIAN_POINT ( 'NONE',  ( 12.06949235617757843, -12.14591786802309237, 58.12390960531435979 ) ) ;
#53820 = CARTESIAN_POINT ( 'NONE',  ( -7.052343178074647945, -2.552343178074588437, 1.110912703473986074 ) ) ;
#53819 = AXIS2_PLACEMENT_3D ( 'NONE', #114699, #37867, #110716 ) ;
#53822 = CARTESIAN_POINT ( 'NONE',  ( 21.53943276465977519, -0.05219959533907433946, 38.74890960531435979 ) ) ;
#53823 = ORIENTED_EDGE ( 'NONE', *, *, #77310, .T. ) ;
#53824 = CARTESIAN_POINT ( 'NONE',  ( -17.49999999999999645, 5.499999999999997335, 105.7969038253417153 ) ) ;
#53826 = CARTESIAN_POINT ( 'NONE',  ( 22.44159573604009594, -16.30477369853687364, 140.1750000027311955 ) ) ;
#53825 = CARTESIAN_POINT ( 'NONE',  ( 8.224510206698742110, 14.34966873604972548, 92.08442372801901854 ) ) ;
#53827 = CARTESIAN_POINT ( 'NONE',  ( -5.153800228976607833, 19.02544592524334988, 87.70942372801897591 ) ) ;
#53828 = CARTESIAN_POINT ( 'NONE',  ( 0.05219959533910956823, 16.53943276465976808, 69.99890960531435269 ) ) ;
#53829 = CARTESIAN_POINT ( 'NONE',  ( -19.19724070472092237, -5.500000000000168754, 61.06193348274385357 ) ) ;
#53830 = CARTESIAN_POINT ( 'NONE',  ( -0.05219959533909027116, -19.03943276465977164, 57.49890960531435979 ) ) ;
#53831 = CARTESIAN_POINT ( 'NONE',  ( -12.14591786802309592, -12.06949235617757132, 46.87390960531435979 ) ) ;
#53832 = EDGE_CURVE ( 'NONE', #117197, #194693, #56586, .T. ) ;
#53833 = CARTESIAN_POINT ( 'NONE',  ( 5.153800228976335163, 19.02544592524342804, 84.79057627198099567 ) ) ;
#53835 = CARTESIAN_POINT ( 'NONE',  ( -19.05341960407611168, -5.049401038298163336, 51.45724293864770260 ) ) ;
#53834 = CARTESIAN_POINT ( 'NONE',  ( 13.97604488694548053, -13.89961937509957401, 80.62609039468567573 ) ) ;
#53836 = CARTESIAN_POINT ( 'NONE',  ( -10.81492255796105439, 18.62759615963255655, 52.91775706135235424 ) ) ;
#53837 = CARTESIAN_POINT ( 'NONE',  ( 16.51473224551069308, 9.474510206698969483, 89.16557627198103830 ) ) ;
#53838 = CARTESIAN_POINT ( 'NONE',  ( 5.153800228976335163, 19.02544592524342804, 29.79057627198102409 ) ) ;
#53839 = CARTESIAN_POINT ( 'NONE',  ( -13.97604488694527625, -13.89961937509977652, 76.87390960531433848 ) ) ;
#53840 = CARTESIAN_POINT ( 'NONE',  ( -18.62759615963270932, 10.81492255796079327, 50.83224293864770971 ) ) ;
#53841 = CARTESIAN_POINT ( 'NONE',  ( 13.97604488694527802, 13.89961937509977652, 44.37390960531435269 ) ) ;
#53842 = CARTESIAN_POINT ( 'NONE',  ( 15.80617190586746368, 15.72974639402197994, 59.37390960531436690 ) ) ;
#53843 = CARTESIAN_POINT ( 'NONE',  ( -19.03943276465977164, -0.05219959533935918106, 78.75109039468567573 ) ) ;
#53844 = CARTESIAN_POINT ( 'NONE',  ( -14.34966873604972548, 8.224510206698743886, 103.3344237280190043 ) ) ;
#53845 = CARTESIAN_POINT ( 'NONE',  ( 13.97604488694548053, -13.89961937509957401, 35.62609039468567573 ) ) ;
#53847 = CARTESIAN_POINT ( 'NONE',  ( -8.224510206698735004, -14.34966873604973081, 94.58442372801901854 ) ) ;
#53846 = CARTESIAN_POINT ( 'NONE',  ( 8.224510206698742110, 14.34966873604972548, 57.08442372801901854 ) ) ;
#53848 = PLANE ( 'NONE',  #101681 ) ;
#53849 = CARTESIAN_POINT ( 'NONE',  ( -0.05219959533934338120, 16.53943276465976808, 82.50109039468568994 ) ) ;
#53850 = CARTESIAN_POINT ( 'NONE',  ( -18.62759615963270932, 10.81492255796079327, 25.83224293864769194 ) ) ;
#53851 = CARTESIAN_POINT ( 'NONE',  ( -13.97604488694527625, -13.89961937509977652, 31.87390960531435979 ) ) ;
#53852 = CARTESIAN_POINT ( 'NONE',  ( -8.224510206698735004, -14.34966873604973081, 34.58442372801900433 ) ) ;
#53853 = CARTESIAN_POINT ( 'NONE',  ( -9.564922557960796823, -16.46253265017161027, 47.08224293864769550 ) ) ;
#53854 = CARTESIAN_POINT ( 'NONE',  ( -15.72974639402176322, -15.80617190586768395, 44.37609039468567573 ) ) ;
#53855 = CARTESIAN_POINT ( 'NONE',  ( -14.34966873604972548, 8.224510206698743886, 43.33442372801901143 ) ) ;
#53856 = CARTESIAN_POINT ( 'NONE',  ( -14.34966873604972548, 8.224510206698743886, 108.3344237280190185 ) ) ;
#53857 = CARTESIAN_POINT ( 'NONE',  ( 9.564922557960805705, 16.46253265017160317, 24.58224293864769194 ) ) ;
#53858 = CARTESIAN_POINT ( 'NONE',  ( -5.049401038297874678, -19.05341960407617918, 19.79275706135233293 ) ) ;
#53859 = CARTESIAN_POINT ( 'NONE',  ( 5.049401038297881783, 19.05341960407617563, 107.2927570613523187 ) ) ;
#53860 = CARTESIAN_POINT ( 'NONE',  ( -19.02544592524334988, -5.153800228976617603, 68.95942372801896170 ) ) ;
#53861 = CARTESIAN_POINT ( 'NONE',  ( -16.53943276465976808, 0.05219959533911058130, 66.24890960531436690 ) ) ;
#53862 = CARTESIAN_POINT ( 'NONE',  ( 19.05341960407611168, 5.049401038298154454, 33.95724293864769550 ) ) ;
#53864 = CARTESIAN_POINT ( 'NONE',  ( 16.18388926212238488, -7.379444403734516378, 92.06046848633846480 ) ) ;
#53863 = CARTESIAN_POINT ( 'NONE',  ( 9.564922557961047289, -16.46253265017146816, 75.41775706135234714 ) ) ;
#53865 = CARTESIAN_POINT ( 'NONE',  ( 21.53943276465977519, 0.05219959533937863772, 61.25109039468567573 ) ) ;
#53866 = CARTESIAN_POINT ( 'NONE',  ( -16.53943276465976808, -0.05219959533934237506, 38.75109039468567573 ) ) ;
#53867 = CARTESIAN_POINT ( 'NONE',  ( 18.22780087662123805, -5.499999999999976019, 73.51763182126894947 ) ) ;
#53868 = CARTESIAN_POINT ( 'NONE',  ( -21.53943276465977519, 0.05219959533907696930, 41.24890960531435269 ) ) ;
#53869 = CARTESIAN_POINT ( 'NONE',  ( -16.53943276465976808, -0.05219959533934237506, 28.75109039468567929 ) ) ;
#53870 = CARTESIAN_POINT ( 'NONE',  ( 13.97604488694527802, 13.89961937509977652, 114.3739096053143669 ) ) ;
#53871 = CARTESIAN_POINT ( 'NONE',  ( -20.93662873023604831, 11.00447265502299388, 170.1964094900432372 ) ) ;
#53872 = CARTESIAN_POINT ( 'NONE',  ( 13.89961937509977652, -13.97604488694527269, 38.12390960531436690 ) ) ;
#53873 = CARTESIAN_POINT ( 'NONE',  ( 10.81492255796106328, -18.62759615963255655, 105.4177570613523613 ) ) ;
#53874 = CARTESIAN_POINT ( 'NONE',  ( -0.05219959533909027116, -19.03943276465977164, 57.49890960531435979 ) ) ;
#53875 = CARTESIAN_POINT ( 'NONE',  ( -21.53943276465977519, -0.05219959533937600094, 63.75109039468568284 ) ) ;
#53876 = CARTESIAN_POINT ( 'NONE',  ( 15.80617190586769283, -15.72974639402175789, 100.6260903946857184 ) ) ;
#53877 = CARTESIAN_POINT ( 'NONE',  ( 16.52544592524335698, 4.483927247898782831, 111.4594237280190328 ) ) ;
#53878 = CARTESIAN_POINT ( 'NONE',  ( 19.02544592524343514, -5.153800228976328945, 28.54057627198102409 ) ) ;
#53879 = CARTESIAN_POINT ( 'NONE',  ( 16.46253265017160672, -9.564922557960803928, 88.33224293864769550 ) ) ;
#53880 = CARTESIAN_POINT ( 'NONE',  ( 10.81492255796106328, -18.62759615963255655, 55.41775706135234714 ) ) ;
#53881 = CARTESIAN_POINT ( 'NONE',  ( 13.89961937509977652, -13.97604488694527269, 33.12390960531434558 ) ) ;
#53882 = CARTESIAN_POINT ( 'NONE',  ( -21.52544592524334988, -5.823673210054445271, 58.95942372801902565 ) ) ;
#53884 = CARTESIAN_POINT ( 'NONE',  ( -19.02544592524342804, 5.153800228976336051, 101.0405762719810241 ) ) ;
#53883 = CARTESIAN_POINT ( 'NONE',  ( 9.474510206698729675, 16.51473224551082808, 97.08442372801900433 ) ) ;
#53885 = CARTESIAN_POINT ( 'NONE',  ( 16.46253265017160672, -9.564922557960803928, 23.33224293864769194 ) ) ;
#53886 = CARTESIAN_POINT ( 'NONE',  ( -21.53943276465977519, -0.05219959533937600094, 18.75109039468568639 ) ) ;
#53887 = CARTESIAN_POINT ( 'NONE',  ( 13.89961937509957401, 13.97604488694547697, 31.87609039468566863 ) ) ;
#53888 = CARTESIAN_POINT ( 'NONE',  ( -8.224510206698948167, 14.34966873604960824, 110.4155762719810383 ) ) ;
#53889 = CARTESIAN_POINT ( 'NONE',  ( -5.049401038298153566, 19.05341960407611168, 45.20724293864769550 ) ) ;
#53890 = CARTESIAN_POINT ( 'NONE',  ( 16.46253265017146816, 9.564922557961045513, 91.66775706135234714 ) ) ;
#53891 = CARTESIAN_POINT ( 'NONE',  ( 4.379528057220339221, -16.55341960407611168, 62.70724293864769550 ) ) ;
#53892 = CARTESIAN_POINT ( 'NONE',  ( 19.05341960407617918, -5.049401038297876454, 26.04275706135233293 ) ) ;
#53893 = CARTESIAN_POINT ( 'NONE',  ( 5.719274019375991003, -21.55341960407610458, 22.70724293864769194 ) ) ;
#53894 = CARTESIAN_POINT ( 'NONE',  ( 16.51473224551083163, -9.474510206698727899, 90.83442372801900433 ) ) ;
#53895 = CARTESIAN_POINT ( 'NONE',  ( 18.62759615963271287, -10.81492255796078972, 93.33224293864769550 ) ) ;
#53896 = CARTESIAN_POINT ( 'NONE',  ( -21.52544592524334988, -5.823673210054445271, 48.95942372801902565 ) ) ;
#53897 = CARTESIAN_POINT ( 'NONE',  ( -12.14591786802326823, 12.06949235617739902, 38.12609039468567573 ) ) ;
#53898 = CARTESIAN_POINT ( 'NONE',  ( 14.29746914071037800, 8.314922557961029526, 101.6677570613523613 ) ) ;
#53900 = CARTESIAN_POINT ( 'NONE',  ( -15.80617190586768217, 15.72974639402176855, 43.12609039468568284 ) ) ;
#53899 = CARTESIAN_POINT ( 'NONE',  ( 14.34966873604972726, -8.224510206698740333, 45.83442372801901854 ) ) ;
#53901 = CARTESIAN_POINT ( 'NONE',  ( -0.05219959533907301413, -21.53943276465977519, 57.49890960531435979 ) ) ;
#53902 = CARTESIAN_POINT ( 'NONE',  ( 13.89961937509977652, -13.97604488694527269, 38.12390960531436690 ) ) ;
#53903 = CARTESIAN_POINT ( 'NONE',  ( 37.99999999999999289, 2.893978650043524126E-14, -6.749999994537627224 ) ) ;
#53904 = CARTESIAN_POINT ( 'NONE',  ( -14.29746914071037622, -8.314922557961029526, 64.16775706135234714 ) ) ;
#53905 = CARTESIAN_POINT ( 'NONE',  ( -5.719274019375978568, 21.55341960407610458, 95.20724293864769550 ) ) ;
#53906 = CARTESIAN_POINT ( 'NONE',  ( -16.55341960407611168, -4.379528057220339221, 41.45724293864769550 ) ) ;
#53907 = CARTESIAN_POINT ( 'NONE',  ( 4.483927247898790824, -16.52544592524335698, 60.20942372801902565 ) ) ;
#53908 = CARTESIAN_POINT ( 'NONE',  ( -9.564922557961040184, 16.46253265017147172, 97.91775706135233293 ) ) ;
#53909 = CARTESIAN_POINT ( 'NONE',  ( 21.53943276465977519, -0.05219959533907433946, 93.74890960531436690 ) ) ;
#53910 = CARTESIAN_POINT ( 'NONE',  ( -12.06949235617756955, 12.14591786802309770, 30.62390960531436335 ) ) ;
#53911 = EDGE_LOOP ( 'NONE', ( #22303, #183775 ) ) ;
#53912 = CARTESIAN_POINT ( 'NONE',  ( 4.379528057220092307, 16.55341960407617563, 82.29275706135234714 ) ) ;
#53913 = CARTESIAN_POINT ( 'NONE',  ( 21.84611564451295962, 9.363109600221495299, 171.0247306346272751 ) ) ;
#53914 = CARTESIAN_POINT ( 'NONE',  ( 15.80617190586746368, 15.72974639402197994, 69.37390960531436690 ) ) ;
#53915 = ORIENTED_EDGE ( 'NONE', *, *, #72679, .F. ) ;
#53916 = CARTESIAN_POINT ( 'NONE',  ( -14.34966873604972548, 8.224510206698743886, 108.3344237280190185 ) ) ;
#53917 = ORIENTED_EDGE ( 'NONE', *, *, #195432, .T. ) ;
#53918 = LINE ( 'NONE', #38752, #33966 ) ;
#53919 = CARTESIAN_POINT ( 'NONE',  ( -15.72974639402197994, 15.80617190586746368, 85.62390960531436690 ) ) ;
#53920 = CARTESIAN_POINT ( 'NONE',  ( 5.823673210054125526, 21.52544592524343514, 104.7905762719810241 ) ) ;
#53921 = CARTESIAN_POINT ( 'NONE',  ( 12.14591786802309770, 12.06949235617756955, 44.37390960531435979 ) ) ;
#53922 = CARTESIAN_POINT ( 'NONE',  ( 8.314922557961029526, -14.29746914071037800, 35.41775706135234003 ) ) ;
#53923 = CARTESIAN_POINT ( 'NONE',  ( -0.05219959533909027116, -19.03943276465977164, 47.49890960531435979 ) ) ;
#53924 = CARTESIAN_POINT ( 'NONE',  ( 16.51473224551069308, 9.474510206698969483, 69.16557627198102409 ) ) ;
#53925 = CARTESIAN_POINT ( 'NONE',  ( -18.67979575497178146, -10.72451020669898902, 26.66557627198103475 ) ) ;
#53926 = CARTESIAN_POINT ( 'NONE',  ( -13.97604488694527625, -13.89961937509977652, 111.8739096053143243 ) ) ;
#53927 = CARTESIAN_POINT ( 'NONE',  ( 19.03943276465977164, 0.05219959533936151252, 106.2510903946856615 ) ) ;
#53928 = CARTESIAN_POINT ( 'NONE',  ( 9.564922557961047289, -16.46253265017146816, 45.41775706135232582 ) ) ;
#53929 = CARTESIAN_POINT ( 'NONE',  ( -21.55341960407610458, -5.719274019375992779, 91.45724293864769550 ) ) ;
#53930 = CARTESIAN_POINT ( 'NONE',  ( -14.34966873604960291, -8.224510206698953496, 26.66557627198103475 ) ) ;
#53931 = CARTESIAN_POINT ( 'NONE',  ( 18.67979575497178502, 10.72451020669898547, 44.16557627198103120 ) ) ;
#53933 = CARTESIAN_POINT ( 'NONE',  ( 5.049401038297881783, 19.05341960407617563, 112.2927570613523471 ) ) ;
#53932 = CARTESIAN_POINT ( 'NONE',  ( -10.81492255796078084, -18.62759615963271287, 87.08224293864769550 ) ) ;
#53934 = CARTESIAN_POINT ( 'NONE',  ( 5.049401038298161559, -19.05341960407611168, 102.7072429386476955 ) ) ;
#53935 = CARTESIAN_POINT ( 'NONE',  ( 10.81492255796106328, -18.62759615963255655, 75.41775706135233293 ) ) ;
#53936 = CARTESIAN_POINT ( 'NONE',  ( -0.05219959533909027116, -19.03943276465977164, 77.49890960531435269 ) ) ;
#53937 = CARTESIAN_POINT ( 'NONE',  ( -16.52544592524342804, 4.483927247898546575, 101.0405762719810383 ) ) ;
#53938 = CARTESIAN_POINT ( 'NONE',  ( 31.30058771566192988, 6.382914491190405215, 98.94581565101640308 ) ) ;
#53939 = CARTESIAN_POINT ( 'NONE',  ( -16.46253265017160317, 9.564922557960807481, 65.83224293864769550 ) ) ;
#53940 = CARTESIAN_POINT ( 'NONE',  ( -4.483927247898539470, -16.52544592524342804, 97.29057627198105251 ) ) ;
#53941 = ORIENTED_EDGE ( 'NONE', *, *, #100927, .F. ) ;
#53942 = CARTESIAN_POINT ( 'NONE',  ( -19.03943276465977164, -0.05219959533935918106, 103.7510903946856757 ) ) ;
#53943 = CARTESIAN_POINT ( 'NONE',  ( 16.29526858892876717, -7.335722546920110609, 81.70329402199794799 ) ) ;
#53944 = CARTESIAN_POINT ( 'NONE',  ( 19.03943276465977164, -0.05219959533909143690, 63.74890960531435979 ) ) ;
#53946 = CARTESIAN_POINT ( 'NONE',  ( -5.049401038298153566, 19.05341960407611168, 95.20724293864770971 ) ) ;
#53945 = CARTESIAN_POINT ( 'NONE',  ( -15.72974639402176322, -15.80617190586768395, 84.37609039468570415 ) ) ;
#53947 = CARTESIAN_POINT ( 'NONE',  ( -14.29746914071037622, -8.314922557961029526, 74.16775706135231871 ) ) ;
#53948 = CARTESIAN_POINT ( 'NONE',  ( -17.50000000000002842, -5.622605283950846911, 76.31207310596114723 ) ) ;
#53949 = CARTESIAN_POINT ( 'NONE',  ( -16.46253265017146816, -9.564922557961047289, 59.16775706135233293 ) ) ;
#53950 = CARTESIAN_POINT ( 'NONE',  ( -18.62759615963255300, -10.81492255796106328, 104.1677570613523471 ) ) ;
#53951 = CARTESIAN_POINT ( 'NONE',  ( 23.29544513554940366, -16.92513159979222337, 144.7843446568999752 ) ) ;
#53952 = CARTESIAN_POINT ( 'NONE',  ( 6.677994727576217926, 3.424326230466338661, 8.646741581399133736 ) ) ;
#53953 = CARTESIAN_POINT ( 'NONE',  ( -12.14591786802309592, -12.06949235617757132, 21.87390960531436690 ) ) ;
#53954 = ADVANCED_FACE ( 'NONE', ( #82262 ), #159750, .F. ) ;
#53955 = CARTESIAN_POINT ( 'NONE',  ( -16.46253265017146816, -9.564922557961047289, 74.16775706135234714 ) ) ;
#53956 = CARTESIAN_POINT ( 'NONE',  ( 8.224510206698742110, 14.34966873604972548, 97.08442372801904696 ) ) ;
#53957 = CARTESIAN_POINT ( 'NONE',  ( 33.33394450212942672, -22.11087592608185659, -23.55754414195986257 ) ) ;
#53958 = CARTESIAN_POINT ( 'NONE',  ( 14.29746914071037800, 8.314922557961029526, 71.66775706135234714 ) ) ;
#53959 = CARTESIAN_POINT ( 'NONE',  ( 21.52544592524334988, 5.823673210054432836, 81.45942372801900433 ) ) ;
#53960 = CARTESIAN_POINT ( 'NONE',  ( 19.05341960407617918, -5.049401038297876454, 86.04275706135233293 ) ) ;
#53961 = CARTESIAN_POINT ( 'NONE',  ( -16.51473224551082808, 9.474510206698731452, 43.33442372801900433 ) ) ;
#53962 = CARTESIAN_POINT ( 'NONE',  ( -0.05219959533909027116, -19.03943276465977164, 62.49890960531435979 ) ) ;
#53963 = CARTESIAN_POINT ( 'NONE',  ( 19.05341960407611168, 5.049401038298154454, 53.95724293864770260 ) ) ;
#53964 = ADVANCED_FACE ( 'NONE', ( #156147 ), #129763, .T. ) ;
#53965 = DIRECTION ( 'NONE',  ( -0.7071067811865463515, 0.7071067811865487940, -0.000000000000000000 ) ) ;
#53966 = CARTESIAN_POINT ( 'NONE',  ( 15.80617190586746368, 15.72974639402197994, 79.37390960531436690 ) ) ;
#53967 = CARTESIAN_POINT ( 'NONE',  ( 15.80617190586746368, 15.72974639402197994, 44.37390960531435979 ) ) ;
#53968 = CARTESIAN_POINT ( 'NONE',  ( 5.153800228976335163, 19.02544592524342804, 39.79057627198100988 ) ) ;
#53969 = CARTESIAN_POINT ( 'NONE',  ( -14.29746914071037622, -8.314922557961029526, 69.16775706135234714 ) ) ;
#53970 = UNCERTAINTY_MEASURE_WITH_UNIT (LENGTH_MEASURE( 1.000000000000000082E-05 ), #172890, 'distance_accuracy_value', 'NONE');
#53971 = ORIENTED_EDGE ( 'NONE', *, *, #80196, .F. ) ;
#53972 = CARTESIAN_POINT ( 'NONE',  ( -10.72451020669870658, -18.67979575497194134, 49.58442372801901143 ) ) ;
#53974 = CARTESIAN_POINT ( 'NONE',  ( 36.91746825000000598, -11.99521256947793546, -7.724999997268812812 ) ) ;
#53973 = CARTESIAN_POINT ( 'NONE',  ( 8.314922557960818139, 14.29746914071049879, 59.58224293864770260 ) ) ;
#53975 = CARTESIAN_POINT ( 'NONE',  ( -16.55341960407617563, 4.379528057220093196, 38.54275706135234714 ) ) ;
#53976 = CARTESIAN_POINT ( 'NONE',  ( -19.05341960407617563, 5.049401038297882671, 53.54275706135231871 ) ) ;
#53977 = AXIS2_PLACEMENT_3D ( 'NONE', #108639, #94456, #124807 ) ;
#53978 = CARTESIAN_POINT ( 'NONE',  ( 8.224510206698953496, -14.34966873604960469, 52.91557627198103830 ) ) ;
#53979 = CARTESIAN_POINT ( 'NONE',  ( 0.05219959533937995610, -21.53943276465977519, 30.00109039468568284 ) ) ;
#53981 = CARTESIAN_POINT ( 'NONE',  ( -21.52544592524343514, 5.823673210054127303, 86.04057627198102409 ) ) ;
#53980 = CARTESIAN_POINT ( 'NONE',  ( -18.22780087662123094, -5.499999999999984901, 71.48459894673891313 ) ) ;
#53982 = CARTESIAN_POINT ( 'NONE',  ( -16.51473224551069308, -9.474510206698971260, 106.6655762719810383 ) ) ;
#53983 = CARTESIAN_POINT ( 'NONE',  ( -0.05219959533910754901, -16.53943276465976808, 77.49890960531433848 ) ) ;
#53984 = CARTESIAN_POINT ( 'NONE',  ( -13.89961937509977652, 13.97604488694528158, 115.6239096053143669 ) ) ;
#53985 = CARTESIAN_POINT ( 'NONE',  ( 18.09918380851992481, 5.500000000000035527, 43.98618307335611632 ) ) ;
#53986 = CARTESIAN_POINT ( 'NONE',  ( -9.474510206698720793, -16.51473224551083518, 64.58442372801900433 ) ) ;
#53987 = CARTESIAN_POINT ( 'NONE',  ( -21.52544592524343514, 5.823673210054127303, 116.0405762719810383 ) ) ;
#53988 = CARTESIAN_POINT ( 'NONE',  ( -9.564922557960796823, -16.46253265017161027, 62.08224293864769550 ) ) ;
#53989 = CARTESIAN_POINT ( 'NONE',  ( -13.89961937509957401, -13.97604488694547875, 49.37609039468567573 ) ) ;
#53990 = CARTESIAN_POINT ( 'NONE',  ( -19.03943276465977164, 0.05219959533909376836, 26.24890960531435624 ) ) ;
#53991 = CARTESIAN_POINT ( 'NONE',  ( -0.05219959533937732626, 21.53943276465977519, 67.50109039468568994 ) ) ;
#53992 = CARTESIAN_POINT ( 'NONE',  ( -17.26172910966779384, -6.454744622555833367, 69.19353091350774321 ) ) ;
#53993 = CARTESIAN_POINT ( 'NONE',  ( -14.34966873604960291, -8.224510206698953496, 56.66557627198103830 ) ) ;
#53994 = CARTESIAN_POINT ( 'NONE',  ( 9.564922557960805705, 16.46253265017160317, 64.58224293864769550 ) ) ;
#53995 = CARTESIAN_POINT ( 'NONE',  ( -18.62759615963270932, 10.81492255796079327, 90.83224293864769550 ) ) ;
#53996 = CARTESIAN_POINT ( 'NONE',  ( -9.564922557960796823, -16.46253265017161027, 52.08224293864768839 ) ) ;
#53997 = EDGE_LOOP ( 'NONE', ( #11453, #11807, #159310, #178570 ) ) ;
#53998 = CARTESIAN_POINT ( 'NONE',  ( 10.72451020669898902, -18.67979575497178502, 82.91557627198103830 ) ) ;
#53999 = CARTESIAN_POINT ( 'NONE',  ( -21.52544592524334988, -5.823673210054445271, 103.9594237280190185 ) ) ;
#54002 = CARTESIAN_POINT ( 'NONE',  ( 12.06949235617757843, -12.14591786802309237, 88.12390960531436690 ) ) ;
#54001 = CARTESIAN_POINT ( 'NONE',  ( -4.483927247898782831, 16.52544592524335698, 92.70942372801901854 ) ) ;
#54000 = CARTESIAN_POINT ( 'NONE',  ( 19.02544592524343514, -5.153800228976328945, 28.54057627198102409 ) ) ;
#54003 = CARTESIAN_POINT ( 'NONE',  ( -5.049401038297874678, -19.05341960407617918, 94.79275706135230450 ) ) ;
#54004 = ORIENTED_EDGE ( 'NONE', *, *, #181354, .F. ) ;
#54005 = CARTESIAN_POINT ( 'NONE',  ( 5.823673210054444382, -21.52544592524334988, 20.20942372801900788 ) ) ;
#54006 = CARTESIAN_POINT ( 'NONE',  ( -5.049401038297874678, -19.05341960407617918, 44.79275706135232582 ) ) ;
#54007 = CARTESIAN_POINT ( 'NONE',  ( -16.52544592524335698, -4.483927247898792601, 98.95942372801903275 ) ) ;
#54008 = CARTESIAN_POINT ( 'NONE',  ( 0.05219959533936267826, -19.03943276465977164, 30.00109039468566863 ) ) ;
#54009 = CARTESIAN_POINT ( 'NONE',  ( 5.153800228976335163, 19.02544592524342804, 89.79057627198102409 ) ) ;
#54010 = CARTESIAN_POINT ( 'NONE',  ( 0.05219959533907565091, 21.53943276465977519, 59.99890960531436690 ) ) ;
#54011 = CARTESIAN_POINT ( 'NONE',  ( -19.25663599770058809, 5.499999999999433342, 48.99419308057196787 ) ) ;
#54012 = CARTESIAN_POINT ( 'NONE',  ( 12.14591786802309770, 12.06949235617756955, 114.3739096053143527 ) ) ;
#54013 = CARTESIAN_POINT ( 'NONE',  ( 21.53943276465977519, 0.05219959533937863772, 106.2510903946856757 ) ) ;
#54014 = CARTESIAN_POINT ( 'NONE',  ( -0.05219959533934338120, 16.53943276465976808, 77.50109039468567573 ) ) ;
#54015 = CARTESIAN_POINT ( 'NONE',  ( -21.52544592524334988, -5.823673210054445271, 33.95942372801901143 ) ) ;
#54016 = CARTESIAN_POINT ( 'NONE',  ( 14.29746914071037800, 8.314922557961029526, 31.66775706135234358 ) ) ;
#54017 = CARTESIAN_POINT ( 'NONE',  ( 13.89961937509977652, -13.97604488694527269, 103.1239096053143527 ) ) ;
#54018 = CARTESIAN_POINT ( 'NONE',  ( 0.05219959533909260263, 19.03943276465977164, 39.99890960531436690 ) ) ;
#54019 = CARTESIAN_POINT ( 'NONE',  ( -16.46253265017160317, 9.564922557960807481, 70.83224293864770971 ) ) ;
#54020 = AXIS2_PLACEMENT_3D ( 'NONE', #49223, #189731, #66369 ) ;
#54021 = CARTESIAN_POINT ( 'NONE',  ( 4.379528057220092307, 16.55341960407617563, 47.29275706135234003 ) ) ;
#54022 = CARTESIAN_POINT ( 'NONE',  ( -12.14591786802309592, -12.06949235617757132, 86.87390960531438111 ) ) ;
#54023 = CARTESIAN_POINT ( 'NONE',  ( -4.483927247898782831, 16.52544592524335698, 97.70942372801904696 ) ) ;
#54026 = CARTESIAN_POINT ( 'NONE',  ( -19.03943276465977164, 0.05219959533909376836, 61.24890960531436690 ) ) ;
#54025 = CARTESIAN_POINT ( 'NONE',  ( -13.89961937509977652, 13.97604488694528158, 80.62390960531436690 ) ) ;
#54024 = CARTESIAN_POINT ( 'NONE',  ( -5.823673210054431948, 21.52544592524334988, 57.70942372801901143 ) ) ;
#54027 = CARTESIAN_POINT ( 'NONE',  ( 13.97604488694527802, 13.89961937509977652, 99.37390960531436690 ) ) ;
#54028 = CARTESIAN_POINT ( 'NONE',  ( -16.52544592524342804, 4.483927247898546575, 41.04057627198103120 ) ) ;
#54029 = CARTESIAN_POINT ( 'NONE',  ( -14.29746914071037622, -8.314922557961029526, 99.16775706135234714 ) ) ;
#54030 = ORIENTED_EDGE ( 'NONE', *, *, #48667, .T. ) ;
#54031 = CARTESIAN_POINT ( 'NONE',  ( -9.474510206698720793, -16.51473224551083518, 44.58442372801900433 ) ) ;
#54032 = DIRECTION ( 'NONE',  ( 0.07151044867601312471, 0.9974398506828144884, 0.000000000000000000 ) ) ;
#54033 = CARTESIAN_POINT ( 'NONE',  ( 0.05219959533909260263, 19.03943276465977164, 59.99890960531436690 ) ) ;
#54034 = CARTESIAN_POINT ( 'NONE',  ( 19.03943276465977164, 0.05219959533936151252, 41.25109039468566152 ) ) ;
#54035 = CARTESIAN_POINT ( 'NONE',  ( 29.86685920354754487, 21.69954338932564752, -9.424999997268814766 ) ) ;
#54036 = CARTESIAN_POINT ( 'NONE',  ( -16.29526858892878849, -7.335722546920003140, 65.79670597800208043 ) ) ;
#54037 = CARTESIAN_POINT ( 'NONE',  ( -14.29746914071037622, -8.314922557961029526, 54.16775706135235424 ) ) ;
#54039 = CARTESIAN_POINT ( 'NONE',  ( 12.14591786802327356, -12.06949235617739191, 65.62609039468568994 ) ) ;
#54038 = CARTESIAN_POINT ( 'NONE',  ( -9.564922557961040184, 16.46253265017147172, 67.91775706135233293 ) ) ;
#54040 = CARTESIAN_POINT ( 'NONE',  ( -23.88380138457670654, 7.642903512909264840, 172.4262750319490181 ) ) ;
#54041 = CARTESIAN_POINT ( 'NONE',  ( 16.46253265017160672, -9.564922557960803928, 93.33224293864769550 ) ) ;
#54042 = CARTESIAN_POINT ( 'NONE',  ( -15.72974639402176322, -15.80617190586768395, 24.37609039468567573 ) ) ;
#54043 = CARTESIAN_POINT ( 'NONE',  ( 0.05219959533936267826, -19.03943276465977164, 75.00109039468566152 ) ) ;
#54045 = CARTESIAN_POINT ( 'NONE',  ( 19.03943276465977164, -0.05219959533909143690, 38.74890960531436690 ) ) ;
#54044 = CARTESIAN_POINT ( 'NONE',  ( 0.05219959533909260263, 19.03943276465977164, 104.9989096053143669 ) ) ;
#54046 = CARTESIAN_POINT ( 'NONE',  ( 19.03943276465977164, -0.05219959533909143690, 93.74890960531435269 ) ) ;
#54048 = CARTESIAN_POINT ( 'NONE',  ( -9.474510206698964154, 16.51473224551069663, 35.41557627198102409 ) ) ;
#54047 = CARTESIAN_POINT ( 'NONE',  ( -0.05219959533910754901, -16.53943276465976808, 42.49890960531435979 ) ) ;
#54049 = CARTESIAN_POINT ( 'NONE',  ( 19.02544592524334988, 5.153800228976608722, 46.45942372801899012 ) ) ;
#54050 = CARTESIAN_POINT ( 'NONE',  ( -12.14591786802309592, -12.06949235617757132, 91.87390960531436690 ) ) ;
#54051 = CARTESIAN_POINT ( 'NONE',  ( 0.05219959533937995610, -21.53943276465977519, 110.0010903946856757 ) ) ;
#54052 = CARTESIAN_POINT ( 'NONE',  ( 9.474510206698971260, -16.51473224551069308, 52.91557627198102409 ) ) ;
#54053 =( BOUNDED_CURVE ( )  B_SPLINE_CURVE ( 2, ( #159700, #82853, #50271, #32115, #47289, #127080, #126105, #92770, #188788, #199975, #110928 ),
 .UNSPECIFIED., .F., .F. ) 
 B_SPLINE_CURVE_WITH_KNOTS ( ( 3, 2, 2, 2, 2, 3 ),
 ( 0.9000000000000007994, 0.9200000000000007061, 0.9400000000000003908, 0.9600000000000002975, 0.9800000000000002043, 1.000000000000000000 ),
 .UNSPECIFIED. ) 
 CURVE ( )  GEOMETRIC_REPRESENTATION_ITEM ( )  RATIONAL_B_SPLINE_CURVE ( ( 0.9999999999999981126, 0.9510565162951554186, 1.000000000000000000, 0.9510565162951535312, 1.000000000000000000, 0.9510565162951535312, 1.000000000000000000, 0.9510565162951535312, 1.000000000000000000, 0.9510565162951535312, 1.000000000000000000 ) ) 
 REPRESENTATION_ITEM ( '' )  );
#54054 = CARTESIAN_POINT ( 'NONE',  ( 10.81492255796078972, 18.62759615963270932, 69.58224293864769550 ) ) ;
#54056 = CARTESIAN_POINT ( 'NONE',  ( -5.049401038297874678, -19.05341960407617918, 19.79275706135233293 ) ) ;
#54055 = CARTESIAN_POINT ( 'NONE',  ( -4.483927247898539470, -16.52544592524342804, 52.29057627198102409 ) ) ;
#54057 = CARTESIAN_POINT ( 'NONE',  ( 9.474510206698971260, -16.51473224551069308, 102.9155762719810241 ) ) ;
#54058 = CARTESIAN_POINT ( 'NONE',  ( 0.05219959533909260263, 19.03943276465977164, 109.9989096053143669 ) ) ;
#54059 = CARTESIAN_POINT ( 'NONE',  ( 0.05219959533909260263, 19.03943276465977164, 49.99890960531435979 ) ) ;
#54060 = CARTESIAN_POINT ( 'NONE',  ( -5.153800228976328057, -19.02544592524343514, 22.29057627198102765 ) ) ;
#54061 = CARTESIAN_POINT ( 'NONE',  ( -0.05219959533910754901, -16.53943276465976808, 87.49890960531436690 ) ) ;
#54062 = CARTESIAN_POINT ( 'NONE',  ( 5.823673210054125526, 21.52544592524343514, 94.79057627198105251 ) ) ;
#54063 = CARTESIAN_POINT ( 'NONE',  ( -16.51473224551069308, -9.474510206698971260, 106.6655762719810383 ) ) ;
#54064 = CARTESIAN_POINT ( 'NONE',  ( 18.67979575497178502, 10.72451020669898547, 114.1655762719810383 ) ) ;
#54065 = CARTESIAN_POINT ( 'NONE',  ( 16.46253265017160672, -9.564922557960803928, 103.3322429386476955 ) ) ;
#54066 = CARTESIAN_POINT ( 'NONE',  ( 12.06949235617757843, -12.14591786802309237, 98.12390960531436690 ) ) ;
#54067 = CARTESIAN_POINT ( 'NONE',  ( -10.72451020669870658, -18.67979575497194134, 74.58442372801901854 ) ) ;
#54068 = CARTESIAN_POINT ( 'NONE',  ( 21.52544592524344225, -5.823673210054117533, 88.54057627198103830 ) ) ;
#54069 = CARTESIAN_POINT ( 'NONE',  ( 16.21995358207305316, -7.366697692864187630, 107.4355100151216078 ) ) ;
#54070 = CARTESIAN_POINT ( 'NONE',  ( 9.474510206698971260, -16.51473224551069308, 52.91557627198102409 ) ) ;
#54071 = CARTESIAN_POINT ( 'NONE',  ( 19.26498983726238023, -5.499999999999592326, 68.05319577422007171 ) ) ;
#54072 = CARTESIAN_POINT ( 'NONE',  ( 14.34966873604972726, -8.224510206698740333, 30.83442372801902209 ) ) ;
#54073 = CARTESIAN_POINT ( 'NONE',  ( 8.314922557960818139, 14.29746914071049879, 109.5822429386476955 ) ) ;
#54074 = CARTESIAN_POINT ( 'NONE',  ( -17.50000000000000000, -3.805241302050311969, 109.6264752721740905 ) ) ;
#54075 = CARTESIAN_POINT ( 'NONE',  ( 19.02544592524343514, -5.153800228976328945, 53.54057627198102409 ) ) ;
#54076 = CARTESIAN_POINT ( 'NONE',  ( 16.55341960407611168, 4.379528057220329451, 88.95724293864769550 ) ) ;
#54077 = CARTESIAN_POINT ( 'NONE',  ( 21.52544592524344225, -5.823673210054117533, 28.54057627198103120 ) ) ;
#54078 = CARTESIAN_POINT ( 'NONE',  ( 8.314922557960818139, 14.29746914071049879, 59.58224293864770260 ) ) ;
#54079 = CARTESIAN_POINT ( 'NONE',  ( -5.153800228976607833, 19.02544592524334988, 112.7094237280190043 ) ) ;
#54080 = CARTESIAN_POINT ( 'NONE',  ( 18.62759615963255655, 10.81492255796105972, 66.66775706135234714 ) ) ;
#54081 = CARTESIAN_POINT ( 'NONE',  ( 17.58332526062528345, 7.635886036038587399, 61.57665040441535353 ) ) ;
#54082 = CARTESIAN_POINT ( 'NONE',  ( -16.51473224551069308, -9.474510206698971260, 106.6655762719810383 ) ) ;
#54083 = CARTESIAN_POINT ( 'NONE',  ( 12.14591786802327356, -12.06949235617739191, 95.62609039468568994 ) ) ;
#54084 = CARTESIAN_POINT ( 'NONE',  ( -5.153800228976328057, -19.02544592524343514, 37.29057627198102409 ) ) ;
#54085 = CARTESIAN_POINT ( 'NONE',  ( 16.51473224551069308, 9.474510206698969483, 89.16557627198103830 ) ) ;
#54086 = CARTESIAN_POINT ( 'NONE',  ( -15.72974639402197994, 15.80617190586746368, 95.62390960531436690 ) ) ;
#54087 = CARTESIAN_POINT ( 'NONE',  ( -4.483927247898782831, 16.52544592524335698, 27.70942372801901854 ) ) ;
#54089 = CARTESIAN_POINT ( 'NONE',  ( -21.53943276465977519, -0.05219959533937600094, 68.75109039468568994 ) ) ;
#54088 = CARTESIAN_POINT ( 'NONE',  ( -12.06949235617756955, 12.14591786802309770, 70.62390960531436690 ) ) ;
#54090 = CARTESIAN_POINT ( 'NONE',  ( -16.53943276465976808, -0.05219959533934237506, 103.7510903946857042 ) ) ;
#54091 = CARTESIAN_POINT ( 'NONE',  ( -23.29544513554940721, -16.92513159979223758, 140.4656553485623931 ) ) ;
#54092 = DIRECTION ( 'NONE',  ( 0.000000000000000000, 0.000000000000000000, -1.000000000000000000 ) ) ;
#54093 = CARTESIAN_POINT ( 'NONE',  ( 8.224510206698953496, -14.34966873604960469, 22.91557627198102765 ) ) ;
#54094 = CARTESIAN_POINT ( 'NONE',  ( 4.483927247898790824, -16.52544592524335698, 60.20942372801902565 ) ) ;
#54095 = CARTESIAN_POINT ( 'NONE',  ( 9.564922557960805705, 16.46253265017160317, 69.58224293864770971 ) ) ;
#54096 = CARTESIAN_POINT ( 'NONE',  ( -16.46253265017160317, 9.564922557960807481, 80.83224293864769550 ) ) ;
#54097 = CARTESIAN_POINT ( 'NONE',  ( 18.67979575497194134, -10.72451020669871369, 80.83442372801901854 ) ) ;
#54098 = CARTESIAN_POINT ( 'NONE',  ( 14.34966873604972726, -8.224510206698740333, 90.83442372801901854 ) ) ;
#54099 = CARTESIAN_POINT ( 'NONE',  ( 4.483927247898545687, 16.52544592524342804, 54.79057627198104541 ) ) ;
#54100 = CARTESIAN_POINT ( 'NONE',  ( -19.03943276465977164, 0.05219959533909376836, 66.24890960531436690 ) ) ;
#54101 = ORIENTED_EDGE ( 'NONE', *, *, #25923, .T. ) ;
#54102 = CARTESIAN_POINT ( 'NONE',  ( 9.474510206698729675, 16.51473224551082808, 107.0844237280190043 ) ) ;
#54103 = CARTESIAN_POINT ( 'NONE',  ( 4.483927247898545687, 16.52544592524342804, 109.7905762719810383 ) ) ;
#54104 = CARTESIAN_POINT ( 'NONE',  ( -13.97604488694527625, -13.89961937509977652, 76.87390960531433848 ) ) ;
#54106 = CARTESIAN_POINT ( 'NONE',  ( 29.86685920354754842, -21.69954338932559068, -5.824999997268813345 ) ) ;
#54105 = CARTESIAN_POINT ( 'NONE',  ( 16.52544592524335698, 4.483927247898782831, 21.45942372801901499 ) ) ;
#54107 = CARTESIAN_POINT ( 'NONE',  ( -21.55341960407619339, 5.719274019375674811, 113.5427570613523756 ) ) ;
#54108 = CARTESIAN_POINT ( 'NONE',  ( 16.52544592524335698, 4.483927247898782831, 86.45942372801901854 ) ) ;
#54109 = CARTESIAN_POINT ( 'NONE',  ( 13.89961937509957401, 13.97604488694547697, 86.87609039468567573 ) ) ;
#54110 = CARTESIAN_POINT ( 'NONE',  ( -9.474510206698964154, 16.51473224551069663, 25.41557627198103120 ) ) ;
#54111 = CARTESIAN_POINT ( 'NONE',  ( -12.06949235617739369, -12.14591786802326823, 64.37609039468568994 ) ) ;
#54112 = DIRECTION ( 'NONE',  ( 0.000000000000000000, -0.8283630648959183773, 0.5601916035752775302 ) ) ;
#54113 = CARTESIAN_POINT ( 'NONE',  ( -0.05219959533936034679, 19.03943276465977164, 57.50109039468566863 ) ) ;
#54114 = CARTESIAN_POINT ( 'NONE',  ( 21.52544592524334988, 5.823673210054432836, 101.4594237280190185 ) ) ;
#54115 = CARTESIAN_POINT ( 'NONE',  ( 9.564922557960805705, 16.46253265017160317, 39.58224293864768839 ) ) ;
#54116 = CARTESIAN_POINT ( 'NONE',  ( -16.51473224551069308, -9.474510206698971260, 76.66557627198103830 ) ) ;
#54117 = CARTESIAN_POINT ( 'NONE',  ( 16.52544592524342804, -4.483927247898539470, 68.54057627198103830 ) ) ;
#54118 = CIRCLE ( 'NONE', #150981, 38.00000000000000000 ) ;
#54119 = CARTESIAN_POINT ( 'NONE',  ( 5.719274019375673035, 21.55341960407619339, 87.29275706135236135 ) ) ;
#54120 = CARTESIAN_POINT ( 'NONE',  ( -13.97604488694547697, 13.89961937509957934, 53.12609039468565442 ) ) ;
#54121 = CARTESIAN_POINT ( 'NONE',  ( 5.049401038297881783, 19.05341960407617563, 42.29275706135234003 ) ) ;
#54122 = CARTESIAN_POINT ( 'NONE',  ( -5.823673210054116645, -21.52544592524344225, 42.29057627198103120 ) ) ;
#54123 = CARTESIAN_POINT ( 'NONE',  ( -21.53943276465977519, -0.05219959533937600094, 93.75109039468567573 ) ) ;
#54124 = CARTESIAN_POINT ( 'NONE',  ( 19.03943276465977164, -0.05219959533909143690, 83.74890960531436690 ) ) ;
#54125 = CARTESIAN_POINT ( 'NONE',  ( 0.05219959533937995610, -21.53943276465977519, 110.0010903946856757 ) ) ;
#54126 = CARTESIAN_POINT ( 'NONE',  ( -10.72451020669898014, 18.67979575497178502, 55.41557627198102409 ) ) ;
#54127 = CARTESIAN_POINT ( 'NONE',  ( 5.049401038298161559, -19.05341960407611168, 102.7072429386476955 ) ) ;
#54128 = CARTESIAN_POINT ( 'NONE',  ( -9.564922557961040184, 16.46253265017147172, 77.91775706135234714 ) ) ;
#54129 = CARTESIAN_POINT ( 'NONE',  ( 0.05219959533909260263, 19.03943276465977164, 99.99890960531436690 ) ) ;
#54130 = CARTESIAN_POINT ( 'NONE',  ( -5.049401038297874678, -19.05341960407617918, 94.79275706135230450 ) ) ;
#54131 = CARTESIAN_POINT ( 'NONE',  ( -8.224510206698735004, -14.34966873604973081, 39.58442372801901143 ) ) ;
#54132 = CARTESIAN_POINT ( 'NONE',  ( 16.52544592524342804, -4.483927247898539470, 108.5405762719810241 ) ) ;
#54133 = CARTESIAN_POINT ( 'NONE',  ( -13.89961937509977652, 13.97604488694528158, 70.62390960531432427 ) ) ;
#54134 = CARTESIAN_POINT ( 'NONE',  ( -0.05219959533907301413, -21.53943276465977519, 57.49890960531435979 ) ) ;
#54135 = CARTESIAN_POINT ( 'NONE',  ( 14.29746914071037800, 8.314922557961029526, 31.66775706135234358 ) ) ;
#54136 = CARTESIAN_POINT ( 'NONE',  ( -15.80617190586768217, 15.72974639402176855, 38.12609039468567573 ) ) ;
#54137 = CARTESIAN_POINT ( 'NONE',  ( 0.05219959533937995610, -21.53943276465977519, 85.00109039468568994 ) ) ;
#54138 = CARTESIAN_POINT ( 'NONE',  ( -0.05219959533934338120, 16.53943276465976808, 87.50109039468568994 ) ) ;
#54139 = CARTESIAN_POINT ( 'NONE',  ( 0.05219959533909260263, 19.03943276465977164, 69.99890960531435269 ) ) ;
#54140 = CARTESIAN_POINT ( 'NONE',  ( -14.34966873604960291, -8.224510206698953496, 76.66557627198103830 ) ) ;
#54141 = CARTESIAN_POINT ( 'NONE',  ( -12.14591786802309592, -12.06949235617757132, 21.87390960531436690 ) ) ;
#54142 = CARTESIAN_POINT ( 'NONE',  ( 19.03943276465977164, 0.05219959533936151252, 51.25109039468567573 ) ) ;
#54143 = CIRCLE ( 'NONE', #34640, 2.700000000000000622 ) ;
#54144 = CARTESIAN_POINT ( 'NONE',  ( 21.53943276465977519, 0.05219959533937863772, 36.25109039468567573 ) ) ;
#54145 = CARTESIAN_POINT ( 'NONE',  ( -8.224510206698948167, 14.34966873604960824, 85.41557627198102409 ) ) ;
#54146 = CARTESIAN_POINT ( 'NONE',  ( -9.474510206698964154, 16.51473224551069663, 100.4155762719810241 ) ) ;
#54147 = CARTESIAN_POINT ( 'NONE',  ( 12.06949235617739724, 12.14591786802326823, 101.8760903946857042 ) ) ;
#54148 = CARTESIAN_POINT ( 'NONE',  ( 18.67979575497194134, -10.72451020669871369, 65.83442372801900433 ) ) ;
#54149 = CARTESIAN_POINT ( 'NONE',  ( -14.34966873604972548, 8.224510206698743886, 48.33442372801902565 ) ) ;
#54150 = CARTESIAN_POINT ( 'NONE',  ( -15.72974639402176322, -15.80617190586768395, 34.37609039468568284 ) ) ;
#54151 = CARTESIAN_POINT ( 'NONE',  ( -14.29746914071049879, 8.314922557960819915, 65.83224293864769550 ) ) ;
#54152 = EDGE_LOOP ( 'NONE', ( #20004, #35509, #94186, #134138 ) ) ;
#54153 = CARTESIAN_POINT ( 'NONE',  ( 21.52544592524334988, 5.823673210054432836, 21.45942372801901499 ) ) ;
#54154 = CARTESIAN_POINT ( 'NONE',  ( 8.224510206698953496, -14.34966873604960469, 92.91557627198103830 ) ) ;
#54155 = CARTESIAN_POINT ( 'NONE',  ( 17.50000000000001066, -3.189878218039098989, 27.37051437428756984 ) ) ;
#54156 = CARTESIAN_POINT ( 'NONE',  ( -4.483927247898539470, -16.52544592524342804, 57.29057627198103120 ) ) ;
#54157 = CARTESIAN_POINT ( 'NONE',  ( 5.049401038298161559, -19.05341960407611168, 27.70724293864769550 ) ) ;
#54158 = CARTESIAN_POINT ( 'NONE',  ( 5.823673210054125526, 21.52544592524343514, 44.79057627198103120 ) ) ;
#54159 = CARTESIAN_POINT ( 'NONE',  ( 14.34966873604960469, 8.224510206698951720, 79.16557627198103830 ) ) ;
#54160 = AXIS2_PLACEMENT_3D ( 'NONE', #10933, #71596, #133262 ) ;
#54161 = CARTESIAN_POINT ( 'NONE',  ( -10.72451020669898014, 18.67979575497178502, 80.41557627198103830 ) ) ;
#54162 = CARTESIAN_POINT ( 'NONE',  ( 13.89961937509977652, -13.97604488694527269, 93.12390960531436690 ) ) ;
#54164 = CARTESIAN_POINT ( 'NONE',  ( 9.564922557961047289, -16.46253265017146816, 85.41775706135233293 ) ) ;
#54163 = CARTESIAN_POINT ( 'NONE',  ( -19.03943276465977164, 0.05219959533909376836, 36.24890960531436690 ) ) ;
#54166 = CARTESIAN_POINT ( 'NONE',  ( 5.719274019375991003, -21.55341960407610458, 57.70724293864770260 ) ) ;
#54165 = CARTESIAN_POINT ( 'NONE',  ( -5.719274019375665041, -21.55341960407619695, 54.79275706135235424 ) ) ;
#54167 = CARTESIAN_POINT ( 'NONE',  ( 9.564922557960805705, 16.46253265017160317, 34.58224293864770260 ) ) ;
#54168 = CARTESIAN_POINT ( 'NONE',  ( -9.474510206698964154, 16.51473224551069663, 70.41557627198102409 ) ) ;
#54169 = VERTEX_POINT ( 'NONE', #4431 ) ;
#54170 = CARTESIAN_POINT ( 'NONE',  ( 16.55341960407618274, -4.379528057220086978, 56.04275706135235424 ) ) ;
#54171 = CARTESIAN_POINT ( 'NONE',  ( 15.80617190586769283, -15.72974639402175789, 30.62609039468567929 ) ) ;
#54172 = CARTESIAN_POINT ( 'NONE',  ( 10.81492255796106328, -18.62759615963255655, 75.41775706135233293 ) ) ;
#54173 = CARTESIAN_POINT ( 'NONE',  ( -9.564922557960796823, -16.46253265017161027, 102.0822429386477097 ) ) ;
#54174 = CARTESIAN_POINT ( 'NONE',  ( 0.05219959533907565091, 21.53943276465977519, 84.99890960531436690 ) ) ;
#54176 = CARTESIAN_POINT ( 'NONE',  ( -0.05219959533934338120, 16.53943276465976808, 57.50109039468568994 ) ) ;
#54175 = CARTESIAN_POINT ( 'NONE',  ( -10.72451020669898014, 18.67979575497178502, 115.4155762719810241 ) ) ;
#54177 = CARTESIAN_POINT ( 'NONE',  ( -15.72974639402197994, 15.80617190586746368, 50.62390960531435979 ) ) ;
#54178 = CARTESIAN_POINT ( 'NONE',  ( -5.719274019375665041, -21.55341960407619695, 109.7927570613523613 ) ) ;
#54179 = CARTESIAN_POINT ( 'NONE',  ( 5.153800228976335163, 19.02544592524342804, 54.79057627198103120 ) ) ;
#54180 = CARTESIAN_POINT ( 'NONE',  ( -19.02544592524342804, 5.153800228976336051, 106.0405762719810241 ) ) ;
#54181 = CARTESIAN_POINT ( 'NONE',  ( 9.474510206698971260, -16.51473224551069308, 87.91557627198102409 ) ) ;
#54182 = CARTESIAN_POINT ( 'NONE',  ( 13.89961937509957579, 13.97604488694547520, 51.87609039468566863 ) ) ;
#54183 = CARTESIAN_POINT ( 'NONE',  ( -0.05219959533936034679, 19.03943276465977164, 62.50109039468566863 ) ) ;
#54184 = CARTESIAN_POINT ( 'NONE',  ( 21.55341960407610458, 5.719274019375980345, 38.95724293864768839 ) ) ;
#54185 = CARTESIAN_POINT ( 'NONE',  ( 4.483927247898545687, 16.52544592524342804, 24.79057627198103120 ) ) ;
#54186 = CARTESIAN_POINT ( 'NONE',  ( -5.049401038297874678, -19.05341960407617918, 104.7927570613523471 ) ) ;
#54187 = CARTESIAN_POINT ( 'NONE',  ( 19.02544592524343514, -5.153800228976328945, 23.54057627198102054 ) ) ;
#54188 = CARTESIAN_POINT ( 'NONE',  ( 13.97604488694548053, -13.89961937509957401, 25.62609039468566507 ) ) ;
#54189 = CARTESIAN_POINT ( 'NONE',  ( -5.049401038297874678, -19.05341960407617918, 99.79275706135234714 ) ) ;
#54191 = CARTESIAN_POINT ( 'NONE',  ( -9.474510206698720793, -16.51473224551083518, 64.58442372801900433 ) ) ;
#54190 = CARTESIAN_POINT ( 'NONE',  ( -21.55341960407610458, -5.719274019375992779, 76.45724293864769550 ) ) ;
#54192 = DIRECTION ( 'NONE',  ( -0.000000000000000000, 1.000000000000000000, -0.000000000000000000 ) ) ;
#54193 = CARTESIAN_POINT ( 'NONE',  ( -9.474510206698964154, 16.51473224551069663, 55.41557627198103120 ) ) ;
#54194 = CARTESIAN_POINT ( 'NONE',  ( -0.05219959533910754901, -16.53943276465976808, 67.49890960531436690 ) ) ;
#54195 = ADVANCED_FACE ( 'NONE', ( #49969 ), #125808, .T. ) ;
#54196 = CARTESIAN_POINT ( 'NONE',  ( -5.049401038298153566, 19.05341960407611168, 40.20724293864768839 ) ) ;
#54197 = CARTESIAN_POINT ( 'NONE',  ( -14.29746914071049879, 8.314922557960819915, 45.83224293864769550 ) ) ;
#54198 = CARTESIAN_POINT ( 'NONE',  ( -26.37337922943865109, -29.71119707698751000, -20.32121347158689773 ) ) ;
#54199 = CARTESIAN_POINT ( 'NONE',  ( -8.224510206698735004, -14.34966873604973081, 104.5844237280190185 ) ) ;
#54200 = CARTESIAN_POINT ( 'NONE',  ( 13.89961937509977652, -13.97604488694527269, 68.12390960531436690 ) ) ;
#54201 = CARTESIAN_POINT ( 'NONE',  ( 9.564922557961047289, -16.46253265017146816, 30.41775706135232937 ) ) ;
#54202 = CARTESIAN_POINT ( 'NONE',  ( -16.53943276465976808, -0.05219959533934237506, 33.75109039468568284 ) ) ;
#54203 = CARTESIAN_POINT ( 'NONE',  ( -10.81492255796078084, -18.62759615963271287, 57.08224293864769550 ) ) ;
#54205 = ORIENTED_EDGE ( 'NONE', *, *, #166153, .F. ) ;
#54204 = CARTESIAN_POINT ( 'NONE',  ( 5.719274019375673035, 21.55341960407619339, 107.2927570613523471 ) ) ;
#54206 = CARTESIAN_POINT ( 'NONE',  ( -9.474510206698964154, 16.51473224551069663, 60.41557627198102409 ) ) ;
#54207 = FACE_OUTER_BOUND ( 'NONE', #152882, .T. ) ;
#54208 = CARTESIAN_POINT ( 'NONE',  ( -13.89961937509977652, 13.97604488694528158, 90.62390960531432427 ) ) ;
#54209 = CARTESIAN_POINT ( 'NONE',  ( -22.81625015709510507, 31.40387420917330275, -0.9249999972688132122 ) ) ;
#54210 = CARTESIAN_POINT ( 'NONE',  ( 18.67979575497194134, -10.72451020669871369, 30.83442372801902209 ) ) ;
#54211 = CARTESIAN_POINT ( 'NONE',  ( 4.379528057220339221, -16.55341960407611168, 92.70724293864770971 ) ) ;
#54213 = CARTESIAN_POINT ( 'NONE',  ( 19.03943276465977164, -0.05219959533909143690, 63.74890960531435979 ) ) ;
#54212 = CARTESIAN_POINT ( 'NONE',  ( 18.67979575497178502, 10.72451020669898547, 84.16557627198103830 ) ) ;
#54214 = CARTESIAN_POINT ( 'NONE',  ( 9.474510206698971260, -16.51473224551069308, 67.91557627198102409 ) ) ;
#54215 = CARTESIAN_POINT ( 'NONE',  ( 21.55341960407610458, 5.719274019375980345, 103.9572429386476813 ) ) ;
#54216 = ORIENTED_EDGE ( 'NONE', *, *, #72299, .T. ) ;
#54217 = CARTESIAN_POINT ( 'NONE',  ( 13.97604488694527802, 13.89961937509977652, 79.37390960531435269 ) ) ;
#54218 = DIRECTION ( 'NONE',  ( 0.000000000000000000, 0.000000000000000000, -1.000000000000000000 ) ) ;
#54220 = CARTESIAN_POINT ( 'NONE',  ( 28.06518720328419647, -28.50306805876740412, -15.18214172726662881 ) ) ;
#54219 = CARTESIAN_POINT ( 'NONE',  ( -8.224510206698948167, 14.34966873604960824, 110.4155762719810383 ) ) ;
#54221 = CARTESIAN_POINT ( 'NONE',  ( -16.51473224551082808, 9.474510206698731452, 88.33442372801900433 ) ) ;
#54222 = CARTESIAN_POINT ( 'NONE',  ( 16.55341960407611168, 4.379528057220329451, 103.9572429386476813 ) ) ;
#54223 = CARTESIAN_POINT ( 'NONE',  ( 10.72451020669871369, 18.67979575497193778, 72.08442372801899012 ) ) ;
#54225 = CARTESIAN_POINT ( 'NONE',  ( 18.67979575497194134, -10.72451020669871369, 30.83442372801902209 ) ) ;
#54224 = CARTESIAN_POINT ( 'NONE',  ( -9.564922557960796823, -16.46253265017161027, 67.08224293864769550 ) ) ;
#54226 = CARTESIAN_POINT ( 'NONE',  ( 0.05219959533907565091, 21.53943276465977519, 114.9989096053143669 ) ) ;
#54227 = CARTESIAN_POINT ( 'NONE',  ( -28.82186960331499037, 2.428612866367529932E-14, 148.2500000054623683 ) ) ;
#54228 = CARTESIAN_POINT ( 'NONE',  ( 5.049401038298161559, -19.05341960407611168, 67.70724293864769550 ) ) ;
#54229 = CARTESIAN_POINT ( 'NONE',  ( -12.49999999999997691, -89.99999999999997158, 0.000000000000000000 ) ) ;
#54231 = CARTESIAN_POINT ( 'NONE',  ( -5.719274019375978568, 21.55341960407610458, 30.20724293864769550 ) ) ;
#54230 = CARTESIAN_POINT ( 'NONE',  ( -12.06949235617739369, -12.14591786802326823, 29.37609039468568284 ) ) ;
#54232 = CARTESIAN_POINT ( 'NONE',  ( 21.52544592524334988, 5.823673210054432836, 66.45942372801903275 ) ) ;
#54233 = CARTESIAN_POINT ( 'NONE',  ( -16.46253265017160317, 9.564922557960807481, 105.8322429386476955 ) ) ;
#54234 = CARTESIAN_POINT ( 'NONE',  ( -5.153800228976607833, 19.02544592524334988, 102.7094237280189759 ) ) ;
#54235 = CARTESIAN_POINT ( 'NONE',  ( 13.89961937509977652, -13.97604488694527269, 53.12390960531434558 ) ) ;
#54236 = CARTESIAN_POINT ( 'NONE',  ( -13.97604488694527625, -13.89961937509977652, 71.87390960531433848 ) ) ;
#54237 = CARTESIAN_POINT ( 'NONE',  ( -12.06949235617756955, 12.14591786802309770, 95.62390960531436690 ) ) ;
#54238 = CARTESIAN_POINT ( 'NONE',  ( 5.153800228976335163, 19.02544592524342804, 104.7905762719809957 ) ) ;
#54239 = CARTESIAN_POINT ( 'NONE',  ( 8.224510206698953496, -14.34966873604960469, 97.91557627198103830 ) ) ;
#54240 = CARTESIAN_POINT ( 'NONE',  ( 13.97604488694527802, 13.89961937509977652, 99.37390960531436690 ) ) ;
#54242 = CARTESIAN_POINT ( 'NONE',  ( 13.89961937509977652, -13.97604488694527269, 38.12390960531436690 ) ) ;
#54241 = CARTESIAN_POINT ( 'NONE',  ( -14.34966873604960291, -8.224510206698953496, 46.66557627198102409 ) ) ;
#54243 = CARTESIAN_POINT ( 'NONE',  ( 21.52544592524334988, 5.823673210054432836, 61.45942372801901854 ) ) ;
#54244 = CARTESIAN_POINT ( 'NONE',  ( 16.46253265017146816, 9.564922557961045513, 76.66775706135234714 ) ) ;
#54245 = CARTESIAN_POINT ( 'NONE',  ( 16.55341960407611168, 4.379528057220329451, 43.95724293864769550 ) ) ;
#54246 = CARTESIAN_POINT ( 'NONE',  ( 21.55341960407610458, 5.719274019375980345, 103.9572429386476813 ) ) ;
#54247 = CARTESIAN_POINT ( 'NONE',  ( -0.05219959533907301413, -21.53943276465977519, 42.49890960531435979 ) ) ;
#54249 = CARTESIAN_POINT ( 'NONE',  ( -0.05219959533910754901, -16.53943276465976808, 87.49890960531436690 ) ) ;
#54248 = CARTESIAN_POINT ( 'NONE',  ( -16.46253265017160317, 9.564922557960807481, 115.8322429386477097 ) ) ;
#54250 = CARTESIAN_POINT ( 'NONE',  ( -13.89961937509977652, 13.97604488694528158, 60.62390960531436690 ) ) ;
#54251 = CARTESIAN_POINT ( 'NONE',  ( 12.14591786802309770, 12.06949235617756955, 29.37390960531435269 ) ) ;
#54252 = CIRCLE ( 'NONE', #147795, 30.82560697742735556 ) ;
#54253 = CARTESIAN_POINT ( 'NONE',  ( -8.314922557961024197, 14.29746914071037800, 97.91775706135236135 ) ) ;
#54254 = CARTESIAN_POINT ( 'NONE',  ( -0.05219959533934338120, 16.53943276465976808, 77.50109039468567573 ) ) ;
#54255 = CARTESIAN_POINT ( 'NONE',  ( -13.89961937509957401, -13.97604488694547875, 34.37609039468566863 ) ) ;
#54257 = CARTESIAN_POINT ( 'NONE',  ( 19.05341960407611168, 5.049401038298154454, 108.9572429386477097 ) ) ;
#54256 = CARTESIAN_POINT ( 'NONE',  ( -24.39441179196517240, 8.562450407400056918, 166.7298547261019621 ) ) ;
#54258 = CARTESIAN_POINT ( 'NONE',  ( -19.03943276465977164, 0.05219959533909376836, 81.24890960531436690 ) ) ;
#54259 = CARTESIAN_POINT ( 'NONE',  ( -13.89961937509977652, 13.97604488694528158, 40.62390960531435979 ) ) ;
#54260 = CARTESIAN_POINT ( 'NONE',  ( 12.06949235617757843, -12.14591786802309237, 48.12390960531436690 ) ) ;
#54261 = CARTESIAN_POINT ( 'NONE',  ( 19.02544592524343514, -5.153800228976328945, 103.5405762719809957 ) ) ;
#54262 = CARTESIAN_POINT ( 'NONE',  ( -5.823673210054116645, -21.52544592524344225, 42.29057627198103120 ) ) ;
#54263 = CARTESIAN_POINT ( 'NONE',  ( -4.483927247898539470, -16.52544592524342804, 82.29057627198103830 ) ) ;
#54264 = CARTESIAN_POINT ( 'NONE',  ( -0.05219959533934338120, 16.53943276465976808, 37.50109039468568284 ) ) ;
#54265 = CARTESIAN_POINT ( 'NONE',  ( -12.06949235617756955, 12.14591786802309770, 65.62390960531436690 ) ) ;
#54266 = CARTESIAN_POINT ( 'NONE',  ( 31.20457203169702964, -1.278449583442190729, -46.64972497815392671 ) ) ;
#54267 = CARTESIAN_POINT ( 'NONE',  ( 9.564922557961047289, -16.46253265017146816, 60.41775706135233293 ) ) ;
#54268 = CARTESIAN_POINT ( 'NONE',  ( -5.049401038298153566, 19.05341960407611168, 105.2072429386476671 ) ) ;
#54269 = CARTESIAN_POINT ( 'NONE',  ( 5.153800228976615827, -19.02544592524334988, 75.20942372801896170 ) ) ;
#54270 = CARTESIAN_POINT ( 'NONE',  ( 9.564922557961047289, -16.46253265017146816, 95.41775706135233293 ) ) ;
#54272 = CARTESIAN_POINT ( 'NONE',  ( 8.314922557961029526, -14.29746914071037800, 110.4177570613523756 ) ) ;
#54271 = CARTESIAN_POINT ( 'NONE',  ( -0.05219959533936034679, 19.03943276465977164, 112.5010903946856757 ) ) ;
#54273 = CARTESIAN_POINT ( 'NONE',  ( 9.564922557961047289, -16.46253265017146816, 75.41775706135234714 ) ) ;
#54274 = CARTESIAN_POINT ( 'NONE',  ( -21.52544592524343514, 5.823673210054127303, 36.04057627198102409 ) ) ;
#54275 = CARTESIAN_POINT ( 'NONE',  ( -5.719274019375665041, -21.55341960407619695, 64.79275706135234714 ) ) ;
#54276 = CARTESIAN_POINT ( 'NONE',  ( 19.54388014595539147, 5.500000000000039080, 37.68481143343646522 ) ) ;
#54277 = CARTESIAN_POINT ( 'NONE',  ( 9.564922557961047289, -16.46253265017146816, 110.4177570613523471 ) ) ;
#54279 = CARTESIAN_POINT ( 'NONE',  ( -19.03943276465977164, 0.05219959533909376836, 76.24890960531435269 ) ) ;
#54278 = DIRECTION ( 'NONE',  ( 0.000000000000000000, 1.000000000000000000, 0.000000000000000000 ) ) ;
#54280 =( GEOMETRIC_REPRESENTATION_CONTEXT ( 3 ) GLOBAL_UNCERTAINTY_ASSIGNED_CONTEXT ( ( #191473 ) ) GLOBAL_UNIT_ASSIGNED_CONTEXT ( ( #167752, #59558, #89912 ) ) REPRESENTATION_CONTEXT ( 'NONE', 'WORKASPACE' ) );
#54281 = DIRECTION ( 'NONE',  ( 0.000000000000000000, 0.000000000000000000, -1.000000000000000000 ) ) ;
#54283 = CARTESIAN_POINT ( 'NONE',  ( -19.03943276465977164, 0.05219959533909376836, 71.24890960531435269 ) ) ;
#54282 = CARTESIAN_POINT ( 'NONE',  ( -0.05219959533910754901, -16.53943276465976808, 82.49890960531436690 ) ) ;
#54284 = CARTESIAN_POINT ( 'NONE',  ( -5.153800228976328057, -19.02544592524343514, 92.29057627198099567 ) ) ;
#54285 = ORIENTED_EDGE ( 'NONE', *, *, #6630, .T. ) ;
#54286 = CARTESIAN_POINT ( 'NONE',  ( -9.474510206698720793, -16.51473224551083518, 94.58442372801900433 ) ) ;
#54287 = CARTESIAN_POINT ( 'NONE',  ( -5.719274019375978568, 21.55341960407610458, 75.20724293864769550 ) ) ;
#54288 = CARTESIAN_POINT ( 'NONE',  ( -19.03943276465977164, 0.05219959533909376836, 36.24890960531436690 ) ) ;
#54289 = CARTESIAN_POINT ( 'NONE',  ( 16.46253265017146816, 9.564922557961045513, 76.66775706135234714 ) ) ;
#54290 = CARTESIAN_POINT ( 'NONE',  ( 19.05341960407611168, 5.049401038298154454, 68.95724293864769550 ) ) ;
#54291 = CARTESIAN_POINT ( 'NONE',  ( 19.05341960407611168, 5.049401038298154454, 88.95724293864769550 ) ) ;
#54292 = VERTEX_POINT ( 'NONE', #36768 ) ;
#54293 = CARTESIAN_POINT ( 'NONE',  ( 15.80617190586746368, 15.72974639402197994, 104.3739096053143669 ) ) ;
#54296 = CARTESIAN_POINT ( 'NONE',  ( 0.05219959533936267826, -19.03943276465977164, 65.00109039468567573 ) ) ;
#54295 = CARTESIAN_POINT ( 'NONE',  ( -9.474510206698964154, 16.51473224551069663, 80.41557627198103830 ) ) ;
#54294 = CARTESIAN_POINT ( 'NONE',  ( -14.29746914071049879, 8.314922557960819915, 95.83224293864770971 ) ) ;
#54297 = CARTESIAN_POINT ( 'NONE',  ( 18.62759615963271287, -10.81492255796078972, 93.33224293864769550 ) ) ;
#54298 = CARTESIAN_POINT ( 'NONE',  ( -10.81492255796078084, -18.62759615963271287, 67.08224293864770971 ) ) ;
#54299 = CARTESIAN_POINT ( 'NONE',  ( -4.483927247898539470, -16.52544592524342804, 42.29057627198103120 ) ) ;
#54300 = CARTESIAN_POINT ( 'NONE',  ( 0.05219959533937995610, -21.53943276465977519, 105.0010903946856757 ) ) ;
#54301 = CARTESIAN_POINT ( 'NONE',  ( 16.55341960407618274, -4.379528057220086978, 66.04275706135236135 ) ) ;
#54302 = CARTESIAN_POINT ( 'NONE',  ( 9.564922557960805705, 16.46253265017160317, 89.58224293864769550 ) ) ;
#54303 = CARTESIAN_POINT ( 'NONE',  ( 16.51473224551069308, 9.474510206698969483, 34.16557627198102409 ) ) ;
#54304 = CARTESIAN_POINT ( 'NONE',  ( 0.05219959533937995610, -21.53943276465977519, 45.00109039468568284 ) ) ;
#54305 = CARTESIAN_POINT ( 'NONE',  ( 5.719274019375673035, 21.55341960407619339, 52.29275706135236135 ) ) ;
#54306 = CARTESIAN_POINT ( 'NONE',  ( -13.89961937509977652, 13.97604488694528158, 60.62390960531436690 ) ) ;
#54307 = CARTESIAN_POINT ( 'NONE',  ( -5.823673210054431948, 21.52544592524334988, 37.70942372801900433 ) ) ;
#54308 = CARTESIAN_POINT ( 'NONE',  ( 13.97604488694548053, -13.89961937509957401, 75.62609039468564731 ) ) ;
#54309 = CARTESIAN_POINT ( 'NONE',  ( -9.564922557961040184, 16.46253265017147172, 67.91775706135233293 ) ) ;
#54310 = CARTESIAN_POINT ( 'NONE',  ( 13.97604488694527802, 13.89961937509977652, 44.37390960531435269 ) ) ;
#54311 = CARTESIAN_POINT ( 'NONE',  ( 4.379528057220092307, 16.55341960407617563, 77.29275706135234714 ) ) ;
#54312 = CARTESIAN_POINT ( 'NONE',  ( -16.46253265017160317, 9.564922557960807481, 55.83224293864769550 ) ) ;
#54313 = CARTESIAN_POINT ( 'NONE',  ( 21.84611564451239119, -8.148379233839406766, 169.4346228884785148 ) ) ;
#54314 = CARTESIAN_POINT ( 'NONE',  ( -19.02544592524342804, 5.153800228976336051, 101.0405762719810241 ) ) ;
#54315 = CARTESIAN_POINT ( 'NONE',  ( -0.05219959533909027116, -19.03943276465977164, 42.49890960531435269 ) ) ;
#54316 = CARTESIAN_POINT ( 'NONE',  ( 10.72451020669898902, -18.67979575497178502, 67.91557627198102409 ) ) ;
#54317 = CARTESIAN_POINT ( 'NONE',  ( 16.55341960407618274, -4.379528057220086978, 61.04275706135234714 ) ) ;
#54318 = CARTESIAN_POINT ( 'NONE',  ( -13.97604488694547697, 13.89961937509957934, 23.12609039468565442 ) ) ;
#54319 = CARTESIAN_POINT ( 'NONE',  ( -5.153800228976328057, -19.02544592524343514, 57.29057627198103120 ) ) ;
#54320 = CARTESIAN_POINT ( 'NONE',  ( -8.314922557960811034, -14.29746914071050412, 42.08224293864769550 ) ) ;
#54321 = CARTESIAN_POINT ( 'NONE',  ( -12.06949235617756955, 12.14591786802309770, 85.62390960531436690 ) ) ;
#54322 = CARTESIAN_POINT ( 'NONE',  ( -9.474510206698964154, 16.51473224551069663, 80.41557627198103830 ) ) ;
#54323 = CARTESIAN_POINT ( 'NONE',  ( -10.72451020669870658, -18.67979575497194134, 34.58442372801900433 ) ) ;
#54324 = CARTESIAN_POINT ( 'NONE',  ( -16.46253265017160317, 9.564922557960807481, 90.83224293864769550 ) ) ;
#54325 = CARTESIAN_POINT ( 'NONE',  ( -15.72974639402176322, -15.80617190586768395, 104.3760903946856899 ) ) ;
#54326 = CARTESIAN_POINT ( 'NONE',  ( -12.14591786802326823, 12.06949235617739902, 68.12609039468567573 ) ) ;
#54327 = EDGE_CURVE ( 'NONE', #40834, #41630, #121085, .T. ) ;
#54328 = CARTESIAN_POINT ( 'NONE',  ( -13.89961937509977652, 13.97604488694528158, 110.6239096053143243 ) ) ;
#54329 = CARTESIAN_POINT ( 'NONE',  ( 18.62759615963271287, -10.81492255796078972, 83.33224293864769550 ) ) ;
#54330 = CARTESIAN_POINT ( 'NONE',  ( 4.379528057220339221, -16.55341960407611168, 52.70724293864769550 ) ) ;
#54331 = CARTESIAN_POINT ( 'NONE',  ( 13.97604488694527802, 13.89961937509977652, 44.37390960531435269 ) ) ;
#54332 = CARTESIAN_POINT ( 'NONE',  ( 8.224510206698953496, -14.34966873604960469, 67.91557627198102409 ) ) ;
#54333 = CARTESIAN_POINT ( 'NONE',  ( 10.81492255796078972, 18.62759615963270932, 29.58224293864769905 ) ) ;
#54334 = CARTESIAN_POINT ( 'NONE',  ( -21.55341960407610458, -5.719274019375992779, 26.45724293864768839 ) ) ;
#54335 = CARTESIAN_POINT ( 'NONE',  ( 13.97604488694548053, -13.89961937509957401, 35.62609039468567573 ) ) ;
#54336 = CARTESIAN_POINT ( 'NONE',  ( 8.224510206698953496, -14.34966873604960469, 97.91557627198103830 ) ) ;
#54337 = CARTESIAN_POINT ( 'NONE',  ( 9.564922557960805705, 16.46253265017160317, 104.5822429386476955 ) ) ;
#54338 = EDGE_LOOP ( 'NONE', ( #96944, #190020, #13120, #178328 ) ) ;
#54339 = CARTESIAN_POINT ( 'NONE',  ( -8.224510206698735004, -14.34966873604973081, 59.58442372801901854 ) ) ;
#54340 = CARTESIAN_POINT ( 'NONE',  ( 19.02544592524343514, -5.153800228976328945, 48.54057627198103120 ) ) ;
#54341 = CARTESIAN_POINT ( 'NONE',  ( -17.26608964885399189, -6.138123030024978277, 21.29864325564489747 ) ) ;
#54342 = CARTESIAN_POINT ( 'NONE',  ( -19.02544592524334988, -5.153800228976617603, 58.95942372801900433 ) ) ;
#54343 = CARTESIAN_POINT ( 'NONE',  ( -14.34966873604972548, 8.224510206698743886, 98.33442372801901854 ) ) ;
#54344 = CARTESIAN_POINT ( 'NONE',  ( -16.46253265017146816, -9.564922557961047289, 94.16775706135233293 ) ) ;
#54345 = CARTESIAN_POINT ( 'NONE',  ( 15.80617190586769283, -15.72974639402175789, 65.62609039468568994 ) ) ;
#54346 = CARTESIAN_POINT ( 'NONE',  ( -16.46253265017160317, 9.564922557960807481, 80.83224293864769550 ) ) ;
#54347 = CARTESIAN_POINT ( 'NONE',  ( 18.62759615963271287, -10.81492255796078972, 93.33224293864769550 ) ) ;
#54348 = CARTESIAN_POINT ( 'NONE',  ( -13.97604488694527625, -13.89961937509977652, 21.87390960531435979 ) ) ;
#54349 = CARTESIAN_POINT ( 'NONE',  ( 19.05341960407617918, -5.049401038297876454, 76.04275706135230450 ) ) ;
#54350 = CARTESIAN_POINT ( 'NONE',  ( -5.823673210054116645, -21.52544592524344225, 77.29057627198102409 ) ) ;
#54351 = CARTESIAN_POINT ( 'NONE',  ( 16.46253265017146816, 9.564922557961045513, 41.66775706135234003 ) ) ;
#54352 = CARTESIAN_POINT ( 'NONE',  ( 19.34837522270365895, 5.499999999999788614, 98.36337684832577111 ) ) ;
#54353 = CARTESIAN_POINT ( 'NONE',  ( 15.72974639402199770, -15.80617190586745480, 88.12390960531436690 ) ) ;
#54354 = CARTESIAN_POINT ( 'NONE',  ( 17.50000000000002132, 3.345213924137314887, 27.91231376905656347 ) ) ;
#54355 = CARTESIAN_POINT ( 'NONE',  ( 9.474510206698971260, -16.51473224551069308, 67.91557627198102409 ) ) ;
#54356 = CARTESIAN_POINT ( 'NONE',  ( -11.80868324581545714, -11.80868324581525997, -59.13370768023891344 ) ) ;
#54357 = CARTESIAN_POINT ( 'NONE',  ( -5.153800228976607833, 19.02544592524334988, 112.7094237280190043 ) ) ;
#54358 = CARTESIAN_POINT ( 'NONE',  ( 36.91128768240055535, -0.3593773198236868138, 50.50000000000002842 ) ) ;
#54359 = CARTESIAN_POINT ( 'NONE',  ( 16.46253265017160672, -9.564922557960803928, 43.33224293864769550 ) ) ;
#54361 = CARTESIAN_POINT ( 'NONE',  ( -14.29746914071049879, 8.314922557960819915, 55.83224293864770260 ) ) ;
#54360 = CARTESIAN_POINT ( 'NONE',  ( -21.52544592524343514, 5.823673210054127303, 101.0405762719810383 ) ) ;
#54362 = CARTESIAN_POINT ( 'NONE',  ( 13.97604488694527802, 13.89961937509977652, 54.37390960531435979 ) ) ;
#54363 = CARTESIAN_POINT ( 'NONE',  ( 15.80617190586769283, -15.72974639402175789, 75.62609039468567573 ) ) ;
#54365 = CARTESIAN_POINT ( 'NONE',  ( 9.474510206698729675, 16.51473224551082808, 32.08442372801900433 ) ) ;
#54364 = CARTESIAN_POINT ( 'NONE',  ( 16.55341960407618274, -4.379528057220086978, 21.04275706135234714 ) ) ;
#54366 = CARTESIAN_POINT ( 'NONE',  ( 0.05219959533910956823, 16.53943276465976808, 24.99890960531435624 ) ) ;
#54367 = CARTESIAN_POINT ( 'NONE',  ( 15.72974639402176855, 15.80617190586768217, 41.87609039468568284 ) ) ;
#54368 = CARTESIAN_POINT ( 'NONE',  ( -18.62759615963270932, 10.81492255796079327, 115.8322429386477097 ) ) ;
#54369 = CARTESIAN_POINT ( 'NONE',  ( -10.81492255796078084, -18.62759615963271287, 57.08224293864769550 ) ) ;
#54370 = CARTESIAN_POINT ( 'NONE',  ( -19.05341960407617563, 5.049401038297882671, 98.54275706135233293 ) ) ;
#54371 = CARTESIAN_POINT ( 'NONE',  ( 9.474510206698729675, 16.51473224551082808, 72.08442372801900433 ) ) ;
#54372 = CARTESIAN_POINT ( 'NONE',  ( 21.52544592524334988, 5.823673210054432836, 71.45942372801901854 ) ) ;
#54373 = CARTESIAN_POINT ( 'NONE',  ( 16.46253265017146816, 9.564922557961045513, 56.66775706135233293 ) ) ;
#54374 = CARTESIAN_POINT ( 'NONE',  ( -19.02544592524342804, 5.153800228976336051, 26.04057627198103120 ) ) ;
#54375 = CARTESIAN_POINT ( 'NONE',  ( -21.52544592524343514, 5.823673210054127303, 46.04057627198103830 ) ) ;
#54376 = CARTESIAN_POINT ( 'NONE',  ( -4.483927247898539470, -16.52544592524342804, 52.29057627198102409 ) ) ;
#54377 = CARTESIAN_POINT ( 'NONE',  ( -18.22780087662122028, 5.500000000000031086, 93.51540105326107266 ) ) ;
#54378 = CARTESIAN_POINT ( 'NONE',  ( -5.719274019375665041, -21.55341960407619695, 109.7927570613523613 ) ) ;
#54379 = CARTESIAN_POINT ( 'NONE',  ( 16.52544592524335698, 4.483927247898782831, 91.45942372801901854 ) ) ;
#54380 = CARTESIAN_POINT ( 'NONE',  ( -16.55341960407611168, -4.379528057220339221, 41.45724293864769550 ) ) ;
#54381 = CARTESIAN_POINT ( 'NONE',  ( -5.823673210054431948, 21.52544592524334988, 72.70942372801901854 ) ) ;
#54382 = CARTESIAN_POINT ( 'NONE',  ( -5.719274019375665041, -21.55341960407619695, 74.79275706135234714 ) ) ;
#54383 = CARTESIAN_POINT ( 'NONE',  ( 21.53943276465977519, -0.05219959533907433946, 83.74890960531435269 ) ) ;
#54384 = CARTESIAN_POINT ( 'NONE',  ( 19.03943276465977164, -0.05219959533909143690, 38.74890960531436690 ) ) ;
#54385 = CARTESIAN_POINT ( 'NONE',  ( -5.823673210054431948, 21.52544592524334988, 62.70942372801902565 ) ) ;
#54386 = CARTESIAN_POINT ( 'NONE',  ( 5.049401038298161559, -19.05341960407611168, 32.70724293864768129 ) ) ;
#54387 = CARTESIAN_POINT ( 'NONE',  ( 19.03943276465977164, -0.05219959533909143690, 58.74890960531435979 ) ) ;
#54388 = CARTESIAN_POINT ( 'NONE',  ( 14.34966873604960469, 8.224510206698951720, 99.16557627198100988 ) ) ;
#54389 = CARTESIAN_POINT ( 'NONE',  ( -0.05219959533909027116, -19.03943276465977164, 97.49890960531436690 ) ) ;
#54390 = CARTESIAN_POINT ( 'NONE',  ( 14.34966873604960469, 8.224510206698951720, 34.16557627198102409 ) ) ;
#54391 = CARTESIAN_POINT ( 'NONE',  ( 16.46253265017160672, -9.564922557960803928, 23.33224293864769194 ) ) ;
#54392 = CARTESIAN_POINT ( 'NONE',  ( 18.62759615963271287, -10.81492255796078972, 83.33224293864769550 ) ) ;
#54393 = CARTESIAN_POINT ( 'NONE',  ( 15.72974639402176855, 15.80617190586768217, 26.87609039468567218 ) ) ;
#54394 = CARTESIAN_POINT ( 'NONE',  ( -24.49873734152895111, 24.99873734152937743, 5.353553390593269512 ) ) ;
#54395 = ADVANCED_FACE ( 'NONE', ( #189484 ), #95462, .F. ) ;
#54396 = CARTESIAN_POINT ( 'NONE',  ( -19.05341960407617563, 5.049401038297882671, 113.5427570613523471 ) ) ;
#54397 = CARTESIAN_POINT ( 'NONE',  ( 5.719274019375991003, -21.55341960407610458, 72.70724293864769550 ) ) ;
#54398 = CARTESIAN_POINT ( 'NONE',  ( -18.62759615963255300, -10.81492255796106328, 89.16775706135236135 ) ) ;
#54399 = CARTESIAN_POINT ( 'NONE',  ( 16.51473224551069308, 9.474510206698969483, 84.16557627198102409 ) ) ;
#54400 = CARTESIAN_POINT ( 'NONE',  ( 18.62759615963255655, 10.81492255796105972, 36.66775706135234714 ) ) ;
#54401 = CARTESIAN_POINT ( 'NONE',  ( -9.474510206698964154, 16.51473224551069663, 115.4155762719810241 ) ) ;
#54402 = CARTESIAN_POINT ( 'NONE',  ( -14.34966873604972548, 8.224510206698743886, 88.33442372801901854 ) ) ;
#54403 = CARTESIAN_POINT ( 'NONE',  ( 5.823673210054444382, -21.52544592524334988, 75.20942372801901854 ) ) ;
#54404 = CARTESIAN_POINT ( 'NONE',  ( 16.51473224551083163, -9.474510206698727899, 20.83442372801899722 ) ) ;
#54405 = CARTESIAN_POINT ( 'NONE',  ( -16.52544592524335698, -4.483927247898792601, 73.95942372801901854 ) ) ;
#54406 = CARTESIAN_POINT ( 'NONE',  ( 21.52544592524334988, 5.823673210054432836, 31.45942372801901854 ) ) ;
#54407 = CARTESIAN_POINT ( 'NONE',  ( 13.89961937509977652, -13.97604488694527269, 38.12390960531436690 ) ) ;
#54408 = CARTESIAN_POINT ( 'NONE',  ( 5.719274019375673035, 21.55341960407619339, 87.29275706135236135 ) ) ;
#54409 = CARTESIAN_POINT ( 'NONE',  ( 9.564922557960805705, 16.46253265017160317, 89.58224293864769550 ) ) ;
#54410 = CARTESIAN_POINT ( 'NONE',  ( 5.823673210054125526, 21.52544592524343514, 109.7905762719810383 ) ) ;
#54412 = CARTESIAN_POINT ( 'NONE',  ( -18.62759615963270932, 10.81492255796079327, 50.83224293864770971 ) ) ;
#54411 = CARTESIAN_POINT ( 'NONE',  ( 19.39720447994794483, 5.499999999999967137, 82.16317477297172900 ) ) ;
#54414 = CARTESIAN_POINT ( 'NONE',  ( -8.224510206698948167, 14.34966873604960824, 45.41557627198103830 ) ) ;
#54413 = CARTESIAN_POINT ( 'NONE',  ( 5.049401038298161559, -19.05341960407611168, 92.70724293864769550 ) ) ;
#54415 = CARTESIAN_POINT ( 'NONE',  ( -5.429308488886486681E-15, 30.30510711980690175, 145.4999999999999716 ) ) ;
#54416 = CARTESIAN_POINT ( 'NONE',  ( -9.474510206698720793, -16.51473224551083518, 79.58442372801899012 ) ) ;
#54417 =( BOUNDED_CURVE ( )  B_SPLINE_CURVE ( 2, ( #151597, #178956, #148608, #40426, #10100, #179966, #199083, #11100, #58580, #27271, #120246 ),
 .UNSPECIFIED., .F., .T. ) 
 B_SPLINE_CURVE_WITH_KNOTS ( ( 3, 2, 2, 2, 2, 3 ),
 ( 0.7000000000000001776, 0.7200000000000001954, 0.7400000000000001021, 0.7600000000000001199, 0.7800000000000000266, 0.8000000000000000444 ),
 .UNSPECIFIED. ) 
 CURVE ( )  GEOMETRIC_REPRESENTATION_ITEM ( )  RATIONAL_B_SPLINE_CURVE ( ( 0.9999999999999994449, 0.9510565162951540863, 1.000000000000000000, 0.9510565162951535312, 1.000000000000000000, 0.9510565162951535312, 1.000000000000000000, 0.9510565162951535312, 1.000000000000000000, 0.9510565162951535312, 1.000000000000000000 ) ) 
 REPRESENTATION_ITEM ( '' )  );
#54418 = AXIS2_PLACEMENT_3D ( 'NONE', #39581, #162929, #38592 ) ;
#54419 = CARTESIAN_POINT ( 'NONE',  ( 4.500000000000000888, -140.0000000000000000, 12.99999999999998224 ) ) ;
#54420 = CARTESIAN_POINT ( 'NONE',  ( -5.049401038297874678, -19.05341960407617918, 104.7927570613523471 ) ) ;
#54421 = CARTESIAN_POINT ( 'NONE',  ( 10.72451020669898902, -18.67979575497178502, 82.91557627198103830 ) ) ;
#54422 = CARTESIAN_POINT ( 'NONE',  ( 16.52544592524342804, -4.483927247898539470, 68.54057627198103830 ) ) ;
#54423 = CARTESIAN_POINT ( 'NONE',  ( -16.51473224551069308, -9.474510206698971260, 101.6655762719810241 ) ) ;
#54424 = CARTESIAN_POINT ( 'NONE',  ( -12.06949235617739369, -12.14591786802326823, 49.37609039468569705 ) ) ;
#54425 = CARTESIAN_POINT ( 'NONE',  ( -5.153800228976328057, -19.02544592524343514, 62.29057627198100988 ) ) ;
#54427 = CARTESIAN_POINT ( 'NONE',  ( 0.05219959533936267826, -19.03943276465977164, 95.00109039468567573 ) ) ;
#54426 = CARTESIAN_POINT ( 'NONE',  ( 18.62759615963255655, 10.81492255796105972, 31.66775706135234358 ) ) ;
#54428 = CARTESIAN_POINT ( 'NONE',  ( 13.97604488694527802, 13.89961937509977652, 99.37390960531436690 ) ) ;
#54429 = CARTESIAN_POINT ( 'NONE',  ( -19.05341960407611168, -5.049401038298163336, 91.45724293864766707 ) ) ;
#54430 = CARTESIAN_POINT ( 'NONE',  ( -21.53943276465977519, 0.05219959533907696930, 86.24890960531436690 ) ) ;
#54431 = CARTESIAN_POINT ( 'NONE',  ( -5.049401038298153566, 19.05341960407611168, 40.20724293864768839 ) ) ;
#54432 = CARTESIAN_POINT ( 'NONE',  ( -26.63278688795740834, 27.10001173645601114, -8.000000000000000000 ) ) ;
#54433 = CARTESIAN_POINT ( 'NONE',  ( 8.224510206698953496, -14.34966873604960469, 67.91557627198102409 ) ) ;
#54434 = CARTESIAN_POINT ( 'NONE',  ( -0.05219959533909027116, -19.03943276465977164, 107.4989096053143527 ) ) ;
#54435 = CARTESIAN_POINT ( 'NONE',  ( -28.97745891950396313, 0.4911207797137864262, -52.56957762865166472 ) ) ;
#54436 = CARTESIAN_POINT ( 'NONE',  ( 19.02544592524334988, 5.153800228976608722, 61.45942372801900433 ) ) ;
#54437 = CARTESIAN_POINT ( 'NONE',  ( -21.53943276465977519, 0.05219959533907696930, 96.24890960531435269 ) ) ;
#54438 = CARTESIAN_POINT ( 'NONE',  ( -5.153800228976607833, 19.02544592524334988, 52.70942372801900433 ) ) ;
#54439 = CARTESIAN_POINT ( 'NONE',  ( -19.05341960407611168, -5.049401038298163336, 96.45724293864769550 ) ) ;
#54440 = CARTESIAN_POINT ( 'NONE',  ( 5.719274019375991003, -21.55341960407610458, 37.70724293864769550 ) ) ;
#54441 = CARTESIAN_POINT ( 'NONE',  ( -19.05341960407611168, -5.049401038298163336, 81.45724293864769550 ) ) ;
#54442 = B_SPLINE_CURVE_WITH_KNOTS ( 'NONE', 3,
 ( #71671, #11008, #53498, #41343, #24184, #86835, #69671, #117172, #38337, #162678, #99993, #85834 ),
 .UNSPECIFIED., .F., .F.,
 ( 4, 2, 2, 2, 2, 4 ),
 ( 2.112163857337007370E-17, 0.001213821615218632025, 0.001820732422827935895, 0.002124187826632588372, 0.002275915528534913634, 0.002427643230437238463 ),
 .UNSPECIFIED. ) ;
#54443 = CARTESIAN_POINT ( 'NONE',  ( -18.62759615963255300, -10.81492255796106328, 64.16775706135234714 ) ) ;
#54444 = CARTESIAN_POINT ( 'NONE',  ( 5.153800228976335163, 19.02544592524342804, 39.79057627198100988 ) ) ;
#54445 = CARTESIAN_POINT ( 'NONE',  ( 4.483927247898545687, 16.52544592524342804, 69.79057627198102409 ) ) ;
#54446 = CARTESIAN_POINT ( 'NONE',  ( -16.51473224551082808, 9.474510206698731452, 113.3344237280190043 ) ) ;
#54447 = CARTESIAN_POINT ( 'NONE',  ( -18.67979575497193778, 10.72451020669871902, 53.33442372801901854 ) ) ;
#54448 = ORIENTED_EDGE ( 'NONE', *, *, #16286, .F. ) ;
#54449 = CARTESIAN_POINT ( 'NONE',  ( -23.49396498682886403, -16.15366880693413520, 140.0000000000000568 ) ) ;
#54450 = CARTESIAN_POINT ( 'NONE',  ( 19.02544592524334988, 5.153800228976608722, 61.45942372801900433 ) ) ;
#54451 = DIRECTION ( 'NONE',  ( -1.000000000000000000, 0.000000000000000000, 0.000000000000000000 ) ) ;
#54452 = CARTESIAN_POINT ( 'NONE',  ( -10.81492255796105439, 18.62759615963255655, 27.91775706135234358 ) ) ;
#54453 = CARTESIAN_POINT ( 'NONE',  ( -5.153800228976328057, -19.02544592524343514, 57.29057627198103120 ) ) ;
#54454 = CARTESIAN_POINT ( 'NONE',  ( 30.74264578624800137, -22.33583958711395212, -6.949999994537627401 ) ) ;
#54455 = CARTESIAN_POINT ( 'NONE',  ( -19.05341960407617563, 5.049401038297882671, 23.54275706135233648 ) ) ;
#54456 = CARTESIAN_POINT ( 'NONE',  ( 16.46253265017160672, -9.564922557960803928, 48.33224293864769550 ) ) ;
#54457 = CARTESIAN_POINT ( 'NONE',  ( 21.55341960407619695, -5.719274019375665929, 106.0427570613523471 ) ) ;
#54458 = CARTESIAN_POINT ( 'NONE',  ( -16.55341960407617563, 4.379528057220093196, 88.54275706135236135 ) ) ;
#54460 = CARTESIAN_POINT ( 'NONE',  ( -21.52544592524334988, -5.823673210054445271, 78.95942372801901854 ) ) ;
#54459 = CARTESIAN_POINT ( 'NONE',  ( -13.89961937509977652, 13.97604488694528158, 100.6239096053143669 ) ) ;
#54461 = CARTESIAN_POINT ( 'NONE',  ( -8.571926809382601320, -26.38167802310801591, 147.7750000027311899 ) ) ;
#54462 = CARTESIAN_POINT ( 'NONE',  ( -0.05219959533909027116, -19.03943276465977164, 112.4989096053143669 ) ) ;
#54463 = DIRECTION ( 'NONE',  ( -0.000000000000000000, -0.000000000000000000, 1.000000000000000000 ) ) ;
#54465 = CARTESIAN_POINT ( 'NONE',  ( -10.81492255796105439, 18.62759615963255655, 67.91775706135234714 ) ) ;
#54464 = CARTESIAN_POINT ( 'NONE',  ( -16.52544592524335698, -4.483927247898792601, 63.95942372801901854 ) ) ;
#54466 = CARTESIAN_POINT ( 'NONE',  ( 5.719274019375673035, 21.55341960407619339, 102.2927570613523613 ) ) ;
#54467 = LINE ( 'NONE', #98951, #47641 ) ;
#54468 = CARTESIAN_POINT ( 'NONE',  ( -13.89961937509977652, 13.97604488694528158, 80.62390960531436690 ) ) ;
#54469 = CARTESIAN_POINT ( 'NONE',  ( 13.89961937509977652, -13.97604488694527269, 113.1239096053143527 ) ) ;
#54470 = VERTEX_POINT ( 'NONE', #67118 ) ;
#54471 = CARTESIAN_POINT ( 'NONE',  ( 4.647474457565486646E-15, -28.90000000000004476, -52.65483682830183199 ) ) ;
#54472 = CARTESIAN_POINT ( 'NONE',  ( -9.474510206698964154, 16.51473224551069663, 45.41557627198103120 ) ) ;
#54473 = CARTESIAN_POINT ( 'NONE',  ( -0.05219959533907301413, -21.53943276465977519, 37.49890960531436690 ) ) ;
#54474 = CARTESIAN_POINT ( 'NONE',  ( -4.379528057220086978, -16.55341960407618274, 99.79275706135234714 ) ) ;
#54476 = CARTESIAN_POINT ( 'NONE',  ( -9.474510206698964154, 16.51473224551069663, 80.41557627198103830 ) ) ;
#54475 = CARTESIAN_POINT ( 'NONE',  ( 14.29746914071049879, -8.314922557960816363, 88.33224293864769550 ) ) ;
#54477 = CARTESIAN_POINT ( 'NONE',  ( 5.823673210054444382, -21.52544592524334988, 105.2094237280190328 ) ) ;
#54478 = CARTESIAN_POINT ( 'NONE',  ( -5.049401038298153566, 19.05341960407611168, 40.20724293864768839 ) ) ;
#54479 = CARTESIAN_POINT ( 'NONE',  ( 4.483927247898545687, 16.52544592524342804, 84.79057627198102409 ) ) ;
#54480 = CARTESIAN_POINT ( 'NONE',  ( -18.67979575497193778, 10.72451020669871902, 38.33442372801900433 ) ) ;
#54481 = CARTESIAN_POINT ( 'NONE',  ( -5.719274019375978568, 21.55341960407610458, 90.20724293864770971 ) ) ;
#54482 = CARTESIAN_POINT ( 'NONE',  ( -5.049401038297874678, -19.05341960407617918, 44.79275706135232582 ) ) ;
#54483 = CARTESIAN_POINT ( 'NONE',  ( -34.46971384048858766, 7.497988128173094680, 44.47943501004273514 ) ) ;
#54484 = CARTESIAN_POINT ( 'NONE',  ( 19.05341960407611168, 5.049401038298154454, 93.95724293864769550 ) ) ;
#54485 = CARTESIAN_POINT ( 'NONE',  ( -12.14591786802309592, -12.06949235617757132, 56.87390960531436690 ) ) ;
#54486 = CARTESIAN_POINT ( 'NONE',  ( 4.379528057220339221, -16.55341960407611168, 52.70724293864769550 ) ) ;
#54487 = CARTESIAN_POINT ( 'NONE',  ( -19.05341960407617563, 5.049401038297882671, 83.54275706135233293 ) ) ;
#54488 = CARTESIAN_POINT ( 'NONE',  ( -18.87580814761075132, 5.500000000000055067, 85.87172394265761000 ) ) ;
#54489 = CARTESIAN_POINT ( 'NONE',  ( 18.67979575497178502, 10.72451020669898547, 29.16557627198103120 ) ) ;
#54490 = CARTESIAN_POINT ( 'NONE',  ( 14.34966873604960469, 8.224510206698951720, 89.16557627198102409 ) ) ;
#54491 = DIRECTION ( 'NONE',  ( 0.4999999999999967248, -0.5000000000000019984, -0.7071067811865484609 ) ) ;
#54493 = CARTESIAN_POINT ( 'NONE',  ( 10.81492255796078972, 18.62759615963270932, 49.58224293864769550 ) ) ;
#54492 = CARTESIAN_POINT ( 'NONE',  ( 9.474510206698971260, -16.51473224551069308, 47.91557627198102409 ) ) ;
#54494 = CARTESIAN_POINT ( 'NONE',  ( -0.05219959533909027116, -19.03943276465977164, 32.49890960531435979 ) ) ;
#54496 = CARTESIAN_POINT ( 'NONE',  ( -19.05341960407611168, -5.049401038298163336, 66.45724293864769550 ) ) ;
#54495 = CARTESIAN_POINT ( 'NONE',  ( -12.06949235617739369, -12.14591786802326823, 84.37609039468570415 ) ) ;
#54497 = CARTESIAN_POINT ( 'NONE',  ( -16.46253265017146816, -9.564922557961047289, 34.16775706135233293 ) ) ;
#54498 = CARTESIAN_POINT ( 'NONE',  ( 21.53943276465977519, 0.05219959533937863772, 66.25109039468567573 ) ) ;
#54499 = CARTESIAN_POINT ( 'NONE',  ( 21.55341960407610458, 5.719274019375980345, 38.95724293864768839 ) ) ;
#54500 = CARTESIAN_POINT ( 'NONE',  ( 16.55341960407611168, 4.379528057220329451, 98.95724293864770971 ) ) ;
#54501 = CARTESIAN_POINT ( 'NONE',  ( 9.474510206698729675, 16.51473224551082808, 92.08442372801900433 ) ) ;
#54502 = CARTESIAN_POINT ( 'NONE',  ( 22.81625015709509441, 31.40387420917330275, -1.824999997268813345 ) ) ;
#54504 = CARTESIAN_POINT ( 'NONE',  ( -21.52544592524343514, 5.823673210054127303, 41.04057627198103120 ) ) ;
#54503 = CARTESIAN_POINT ( 'NONE',  ( -1.469699867061801779, -22.44763431097443274, -58.07555020237587939 ) ) ;
#54505 = CARTESIAN_POINT ( 'NONE',  ( 17.12812012977026654, -6.668231424566044119, 66.14051240676859322 ) ) ;
#54506 = CARTESIAN_POINT ( 'NONE',  ( 15.72974639402176855, 15.80617190586768217, 86.87609039468568994 ) ) ;
#54507 = CARTESIAN_POINT ( 'NONE',  ( 16.55341960407611168, 4.379528057220329451, 43.95724293864769550 ) ) ;
#54509 = CARTESIAN_POINT ( 'NONE',  ( -8.314922557960811034, -14.29746914071050412, 52.08224293864768839 ) ) ;
#54508 = CARTESIAN_POINT ( 'NONE',  ( 4.483927247898790824, -16.52544592524335698, 70.20942372801904696 ) ) ;
#54510 = CARTESIAN_POINT ( 'NONE',  ( 5.719274019375991003, -21.55341960407610458, 87.70724293864769550 ) ) ;
#54511 = CARTESIAN_POINT ( 'NONE',  ( 18.62759615963271287, -10.81492255796078972, 73.33224293864769550 ) ) ;
#54512 = DIRECTION ( 'NONE',  ( -0.000000000000000000, -0.000000000000000000, -1.000000000000000000 ) ) ;
#54513 = CARTESIAN_POINT ( 'NONE',  ( 5.823673210054125526, 21.52544592524343514, 29.79057627198102409 ) ) ;
#54514 = CARTESIAN_POINT ( 'NONE',  ( 0.05219959533934541429, -16.53943276465976808, 55.00109039468568284 ) ) ;
#54515 = CARTESIAN_POINT ( 'NONE',  ( -4.379528057220328563, 16.55341960407611168, 75.20724293864769550 ) ) ;
#54517 = CARTESIAN_POINT ( 'NONE',  ( 19.05341960407611168, 5.049401038298154454, 63.95724293864769550 ) ) ;
#54516 = B_SPLINE_CURVE_WITH_KNOTS ( 'NONE', 3,
 ( #113224, #174914, #115232, #101050, #178925, #69727, #148577, #176923, #100050, #85892, #159729, #37387, #40395, #116231, #161736, #23231, #128388, #146552, #177922, #114211, #131395, #190084, #25251, #36378, #193083, #21225, #144559, #54558, #6045, #67723, #163751, #175916 ),
 .UNSPECIFIED., .F., .F.,
 ( 4, 2, 2, 2, 2, 2, 2, 2, 2, 2, 2, 2, 2, 2, 2, 4 ),
 ( 2.711112516444420852E-17, 0.0003712461730037035289, 0.0007424923460073799527, 0.001113738519011056322, 0.001484984692014732800, 0.002227477038022085756, 0.002598723211025761801, 0.002969969384029437845, 0.003341215557033113889, 0.003712461730036789066, 0.004083707903040465111, 0.004454954076044140288, 0.004826200249047816332, 0.005197446422051492376, 0.005568692595055167553, 0.005939938768058842730 ),
 .UNSPECIFIED. ) ;
#54518 = CARTESIAN_POINT ( 'NONE',  ( 19.02544592524343514, -5.153800228976328945, 33.54057627198102409 ) ) ;
#54519 = CARTESIAN_POINT ( 'NONE',  ( 17.72662750342723825, 5.500000000000073719, 48.90179492283744622 ) ) ;
#54520 = CARTESIAN_POINT ( 'NONE',  ( 14.29746914071037800, 8.314922557961029526, 76.66775706135234714 ) ) ;
#54521 = CARTESIAN_POINT ( 'NONE',  ( -0.05219959533937732626, 21.53943276465977519, 22.50109039468567573 ) ) ;
#54522 = CARTESIAN_POINT ( 'NONE',  ( -19.02544592524342804, 5.153800228976336051, 71.04057627198099567 ) ) ;
#54523 = CARTESIAN_POINT ( 'NONE',  ( 15.72974639402176855, 15.80617190586768217, 51.87609039468568284 ) ) ;
#54524 = CARTESIAN_POINT ( 'NONE',  ( 0.05219959533909260263, 19.03943276465977164, 109.9989096053143669 ) ) ;
#54525 = CARTESIAN_POINT ( 'NONE',  ( -10.44694540017202478, -45.05842955090937352, -23.63933302999038588 ) ) ;
#54526 = ORIENTED_EDGE ( 'NONE', *, *, #139056, .F. ) ;
#54527 = CARTESIAN_POINT ( 'NONE',  ( -15.80617190586768217, 15.72974639402176855, 48.12609039468568284 ) ) ;
#54529 = CARTESIAN_POINT ( 'NONE',  ( 19.05341960407611168, 5.049401038298154454, 98.95724293864766707 ) ) ;
#54528 = CARTESIAN_POINT ( 'NONE',  ( 5.153800228976335163, 19.02544592524342804, 114.7905762719810241 ) ) ;
#54530 = CARTESIAN_POINT ( 'NONE',  ( -5.049401038297874678, -19.05341960407617918, 54.79275706135234003 ) ) ;
#54531 = CARTESIAN_POINT ( 'NONE',  ( -5.719274019375665041, -21.55341960407619695, 19.79275706135235069 ) ) ;
#54532 = CARTESIAN_POINT ( 'NONE',  ( 16.51473224551083163, -9.474510206698727899, 40.83442372801900433 ) ) ;
#54533 = CARTESIAN_POINT ( 'NONE',  ( -19.03943276465977164, -0.05219959533935918106, 48.75109039468566863 ) ) ;
#54534 = CARTESIAN_POINT ( 'NONE',  ( -12.06949235617739369, -12.14591786802326823, 104.3760903946856899 ) ) ;
#54535 = CARTESIAN_POINT ( 'NONE',  ( 0.000000000000000000, 0.000000000000000000, 3.799999999999999378 ) ) ;
#54536 = CARTESIAN_POINT ( 'NONE',  ( 0.05219959533909260263, 19.03943276465977164, 89.99890960531436690 ) ) ;
#54537 = CARTESIAN_POINT ( 'NONE',  ( 15.80617190586769283, -15.72974639402175789, 90.62609039468567573 ) ) ;
#54538 = CARTESIAN_POINT ( 'NONE',  ( -10.72451020669870658, -18.67979575497194134, 89.58442372801901854 ) ) ;
#54539 = CARTESIAN_POINT ( 'NONE',  ( 21.30000000000002203, -0.1123844339349802934, -56.46919128290399925 ) ) ;
#54540 = CARTESIAN_POINT ( 'NONE',  ( 5.049401038298161559, -19.05341960407611168, 107.7072429386476955 ) ) ;
#54541 = CARTESIAN_POINT ( 'NONE',  ( -15.72974639402176322, -15.80617190586768395, 74.37609039468568994 ) ) ;
#54542 = CARTESIAN_POINT ( 'NONE',  ( -19.05341960407617563, 5.049401038297882671, 108.5427570613523187 ) ) ;
#54543 = CARTESIAN_POINT ( 'NONE',  ( 5.153800228976335163, 19.02544592524342804, 74.79057627198103830 ) ) ;
#54544 = CARTESIAN_POINT ( 'NONE',  ( -10.72451020669898014, 18.67979575497178502, 25.41557627198103120 ) ) ;
#54545 = CARTESIAN_POINT ( 'NONE',  ( 9.474510206698971260, -16.51473224551069308, 92.91557627198103830 ) ) ;
#54546 = CARTESIAN_POINT ( 'NONE',  ( 5.049401038297881783, 19.05341960407617918, 87.29275706135234714 ) ) ;
#54547 = CARTESIAN_POINT ( 'NONE',  ( 19.02544592524343514, -5.153800228976328945, 73.54057627198103830 ) ) ;
#54548 = CARTESIAN_POINT ( 'NONE',  ( 16.51473224551069308, 9.474510206698969483, 69.16557627198102409 ) ) ;
#54549 = CARTESIAN_POINT ( 'NONE',  ( 21.53943276465977519, -0.05219959533907433946, 108.7489096053143669 ) ) ;
#54550 = CARTESIAN_POINT ( 'NONE',  ( 4.379528057220092307, 16.55341960407617563, 107.2927570613523471 ) ) ;
#54551 = CARTESIAN_POINT ( 'NONE',  ( -4.911121358187451425E-30, -78.67194367458512261, -13.00000000000000000 ) ) ;
#54552 = CARTESIAN_POINT ( 'NONE',  ( -9.564922557961040184, 16.46253265017147172, 52.91775706135233293 ) ) ;
#54553 = CARTESIAN_POINT ( 'NONE',  ( -19.03943276465977164, 0.05219959533909376836, 91.24890960531436690 ) ) ;
#54554 = CARTESIAN_POINT ( 'NONE',  ( -14.29746914071049879, 8.314922557960819915, 80.83224293864769550 ) ) ;
#54555 = CARTESIAN_POINT ( 'NONE',  ( 18.67979575497178502, 10.72451020669898547, 34.16557627198102409 ) ) ;
#54556 = CARTESIAN_POINT ( 'NONE',  ( 21.52544592524344225, -5.823673210054117533, 28.54057627198103120 ) ) ;
#54557 = CARTESIAN_POINT ( 'NONE',  ( -0.05219959533910754901, -16.53943276465976808, 97.49890960531436690 ) ) ;
#54558 = CARTESIAN_POINT ( 'NONE',  ( -17.40861289039004234, 6.110651285853259118, 53.62767529172569425 ) ) ;
#54559 = CARTESIAN_POINT ( 'NONE',  ( -16.46253265017146816, -9.564922557961047289, 49.16775706135233293 ) ) ;
#54560 = CARTESIAN_POINT ( 'NONE',  ( -16.53943276465976808, -0.05219959533934237506, 103.7510903946857042 ) ) ;
#54562 = EDGE_CURVE ( 'NONE', #53519, #21583, #35783, .T. ) ;
#54561 = CARTESIAN_POINT ( 'NONE',  ( 13.89961937509977652, -13.97604488694527269, 93.12390960531436690 ) ) ;
#54563 = CARTESIAN_POINT ( 'NONE',  ( -5.823673210054431948, 21.52544592524334988, 72.70942372801901854 ) ) ;
#54564 = CARTESIAN_POINT ( 'NONE',  ( -15.72974639402197994, 15.80617190586746368, 55.62390960531436690 ) ) ;
#54565 = CARTESIAN_POINT ( 'NONE',  ( -10.72451020669870658, -18.67979575497194134, 29.58442372801901854 ) ) ;
#54566 = CARTESIAN_POINT ( 'NONE',  ( 21.52544592524344225, -5.823673210054117533, 83.54057627198102409 ) ) ;
#54567 = CARTESIAN_POINT ( 'NONE',  ( 12.14591786802309770, 12.06949235617756955, 109.3739096053143811 ) ) ;
#54568 = CARTESIAN_POINT ( 'NONE',  ( -19.02544592524334988, -5.153800228976617603, 68.95942372801896170 ) ) ;
#54569 = CARTESIAN_POINT ( 'NONE',  ( 13.89961937509977652, -13.97604488694527269, 43.12390960531434558 ) ) ;
#54570 = CARTESIAN_POINT ( 'NONE',  ( -16.51473224551069308, -9.474510206698971260, 96.66557627198102409 ) ) ;
#54571 = CARTESIAN_POINT ( 'NONE',  ( 16.51473224551069308, 9.474510206698969483, 99.16557627198102409 ) ) ;
#54572 = CARTESIAN_POINT ( 'NONE',  ( 13.89961937509977652, -13.97604488694527269, 23.12390960531436335 ) ) ;
#54573 = CARTESIAN_POINT ( 'NONE',  ( -12.14591786802309592, -12.06949235617757132, 46.87390960531435979 ) ) ;
#54574 = CARTESIAN_POINT ( 'NONE',  ( 8.314922557961029526, -14.29746914071037800, 45.41775706135234003 ) ) ;
#54575 = CARTESIAN_POINT ( 'NONE',  ( 5.719274019375673035, 21.55341960407619339, 102.2927570613523613 ) ) ;
#54577 = CARTESIAN_POINT ( 'NONE',  ( -4.379528057220328563, 16.55341960407611168, 25.20724293864769550 ) ) ;
#54576 = LINE ( 'NONE', #129401, #30091 ) ;
#54578 = CARTESIAN_POINT ( 'NONE',  ( -15.80617190586768217, 15.72974639402176855, 38.12609039468567573 ) ) ;
#54579 = CARTESIAN_POINT ( 'NONE',  ( -19.02544592524342804, 5.153800228976336051, 101.0405762719810241 ) ) ;
#54580 = CARTESIAN_POINT ( 'NONE',  ( -0.05219959533934338120, 16.53943276465976808, 102.5010903946856899 ) ) ;
#54581 = CARTESIAN_POINT ( 'NONE',  ( -14.34966873604972548, 8.224510206698743886, 93.33442372801901854 ) ) ;
#54582 = CARTESIAN_POINT ( 'NONE',  ( 4.379528057220092307, 16.55341960407617563, 27.29275706135234358 ) ) ;
#54583 = CARTESIAN_POINT ( 'NONE',  ( 9.564922557960805705, 16.46253265017160317, 54.58224293864769550 ) ) ;
#54584 = CARTESIAN_POINT ( 'NONE',  ( 16.55341960407611168, 4.379528057220329451, 113.9572429386477239 ) ) ;
#54585 = CARTESIAN_POINT ( 'NONE',  ( -10.81492255796105439, 18.62759615963255655, 22.91775706135235069 ) ) ;
#54586 = CARTESIAN_POINT ( 'NONE',  ( -9.564922557960796823, -16.46253265017161027, 27.08224293864769550 ) ) ;
#54587 = CARTESIAN_POINT ( 'NONE',  ( -9.474510206698964154, 16.51473224551069663, 105.4155762719810383 ) ) ;
#54588 = CARTESIAN_POINT ( 'NONE',  ( 19.02544592524343514, -5.153800228976328945, 38.54057627198103120 ) ) ;
#54589 = CARTESIAN_POINT ( 'NONE',  ( 5.153800228976335163, 19.02544592524342804, 109.7905762719810099 ) ) ;
#54590 = CARTESIAN_POINT ( 'NONE',  ( 5.374011537017778117, -5.374011537017756801, -64.92279855667830191 ) ) ;
#54591 = CARTESIAN_POINT ( 'NONE',  ( -16.51473224551069308, -9.474510206698971260, 91.66557627198103830 ) ) ;
#54593 = CARTESIAN_POINT ( 'NONE',  ( 4.379528057220339221, -16.55341960407611168, 97.70724293864772392 ) ) ;
#54592 = CARTESIAN_POINT ( 'NONE',  ( 15.72974639402176855, 15.80617190586768217, 51.87609039468568284 ) ) ;
#54594 = CARTESIAN_POINT ( 'NONE',  ( 19.02544592524343514, -5.153800228976328945, 93.54057627198102409 ) ) ;
#54595 = CARTESIAN_POINT ( 'NONE',  ( 17.50000000000000000, -5.499999999999992895, 96.21769037696437010 ) ) ;
#54596 = CARTESIAN_POINT ( 'NONE',  ( 8.314922557961029526, -14.29746914071037800, 65.41775706135234714 ) ) ;
#54597 = CARTESIAN_POINT ( 'NONE',  ( -5.823673210054431948, 21.52544592524334988, 82.70942372801900433 ) ) ;
#54598 = CARTESIAN_POINT ( 'NONE',  ( -8.224510206698735004, -14.34966873604973081, 44.58442372801901854 ) ) ;
#54599 = CARTESIAN_POINT ( 'NONE',  ( 19.02544592524343514, -5.153800228976328945, 88.54057627198102409 ) ) ;
#54600 = CARTESIAN_POINT ( 'NONE',  ( 9.564922557961047289, -16.46253265017146816, 110.4177570613523471 ) ) ;
#54601 = CARTESIAN_POINT ( 'NONE',  ( 8.314922557961029526, -14.29746914071037800, 80.41775706135234714 ) ) ;
#54602 = CARTESIAN_POINT ( 'NONE',  ( 5.049401038297881783, 19.05341960407617563, 97.29275706135233293 ) ) ;
#54603 = CARTESIAN_POINT ( 'NONE',  ( 9.474510206698971260, -16.51473224551069308, 62.91557627198102409 ) ) ;
#54604 = CARTESIAN_POINT ( 'NONE',  ( 21.52544592524344225, -5.823673210054117533, 103.5405762719810383 ) ) ;
#54606 = CARTESIAN_POINT ( 'NONE',  ( 19.02544592524334988, 5.153800228976608722, 86.45942372801900433 ) ) ;
#54605 = CARTESIAN_POINT ( 'NONE',  ( -14.29746914071049879, 8.314922557960819915, 95.83224293864770971 ) ) ;
#54607 = CARTESIAN_POINT ( 'NONE',  ( -16.55341960407617563, 4.379528057220093196, 58.54275706135235424 ) ) ;
#54608 = CARTESIAN_POINT ( 'NONE',  ( 17.40805194822033997, -6.112264579159251809, 63.33371272510615313 ) ) ;
#54609 = CARTESIAN_POINT ( 'NONE',  ( -0.05219959533936034679, 19.03943276465977164, 57.50109039468566863 ) ) ;
#54610 = CARTESIAN_POINT ( 'NONE',  ( -16.55341960407611168, -4.379528057220339221, 31.45724293864769550 ) ) ;
#54611 = CARTESIAN_POINT ( 'NONE',  ( 16.53943276465976808, -0.05219959533910856209, 78.74890960531436690 ) ) ;
#54612 = CARTESIAN_POINT ( 'NONE',  ( -0.05219959533937732626, 21.53943276465977519, 112.5010903946857042 ) ) ;
#54613 = CARTESIAN_POINT ( 'NONE',  ( -21.55341960407619339, 5.719274019375674811, 23.54275706135235424 ) ) ;
#54614 = DIRECTION ( 'NONE',  ( 0.000000000000000000, 0.000000000000000000, -1.000000000000000000 ) ) ;
#54615 = CARTESIAN_POINT ( 'NONE',  ( -13.97604488694527625, -13.89961937509977652, 81.87390960531436690 ) ) ;
#54616 = CARTESIAN_POINT ( 'NONE',  ( -10.81492255796105439, 18.62759615963255655, 92.91775706135236135 ) ) ;
#54617 = CARTESIAN_POINT ( 'NONE',  ( -9.564922557960796823, -16.46253265017161027, 72.08224293864770971 ) ) ;
#54618 = CARTESIAN_POINT ( 'NONE',  ( 21.52544592524344225, -5.823673210054117533, 48.54057627198103120 ) ) ;
#54619 = CARTESIAN_POINT ( 'NONE',  ( -4.483927247898539470, -16.52544592524342804, 82.29057627198103830 ) ) ;
#54620 = CARTESIAN_POINT ( 'NONE',  ( 19.03943276465977164, -0.05219959533909143690, 53.74890960531436690 ) ) ;
#54621 = CARTESIAN_POINT ( 'NONE',  ( -8.224510206698948167, 14.34966873604960824, 105.4155762719810383 ) ) ;
#54622 = CARTESIAN_POINT ( 'NONE',  ( 0.05219959533937995610, -21.53943276465977519, 25.00109039468567218 ) ) ;
#54623 = CARTESIAN_POINT ( 'NONE',  ( 15.72974639402176855, 15.80617190586768217, 56.87609039468568994 ) ) ;
#54624 = CARTESIAN_POINT ( 'NONE',  ( 5.049401038298161559, -19.05341960407611168, 47.70724293864770260 ) ) ;
#54625 = ADVANCED_FACE ( 'NONE', ( #98432 ), #160128, .F. ) ;
#54626 = CARTESIAN_POINT ( 'NONE',  ( 8.224510206698742110, 14.34966873604972548, 82.08442372801901854 ) ) ;
#54627 = CARTESIAN_POINT ( 'NONE',  ( 10.81492255796078972, 18.62759615963270932, 114.5822429386477097 ) ) ;
#54628 = CARTESIAN_POINT ( 'NONE',  ( 15.80617190586746368, 15.72974639402197994, 104.3739096053143669 ) ) ;
#54630 = CARTESIAN_POINT ( 'NONE',  ( 0.05219959533909260263, 19.03943276465977164, 69.99890960531435269 ) ) ;
#54629 = CARTESIAN_POINT ( 'NONE',  ( -9.474510206698720793, -16.51473224551083518, 34.58442372801899722 ) ) ;
#54631 = CARTESIAN_POINT ( 'NONE',  ( 19.03943276465977164, 0.05219959533936151252, 36.25109039468567573 ) ) ;
#54632 = CARTESIAN_POINT ( 'NONE',  ( -10.81492255796105439, 18.62759615963255655, 67.91775706135234714 ) ) ;
#54633 = CARTESIAN_POINT ( 'NONE',  ( -5.719274019375978568, 21.55341960407610458, 50.20724293864769550 ) ) ;
#54634 = CARTESIAN_POINT ( 'NONE',  ( 4.379528057220339221, -16.55341960407611168, 42.70724293864770260 ) ) ;
#54636 = CARTESIAN_POINT ( 'NONE',  ( -9.474510206698720793, -16.51473224551083518, 19.58442372801899722 ) ) ;
#54635 = CARTESIAN_POINT ( 'NONE',  ( 5.823673210054444382, -21.52544592524334988, 85.20942372801901854 ) ) ;
#54637 = CARTESIAN_POINT ( 'NONE',  ( 8.314922557960818139, 14.29746914071049879, 54.58224293864769550 ) ) ;
#54638 = CARTESIAN_POINT ( 'NONE',  ( 16.55341960407611168, 4.379528057220329451, 108.9572429386476955 ) ) ;
#54639 = CARTESIAN_POINT ( 'NONE',  ( 19.02544592524334988, 5.153800228976608722, 61.45942372801900433 ) ) ;
#54640 = CARTESIAN_POINT ( 'NONE',  ( -16.55341960407611168, -4.379528057220339221, 21.45724293864769550 ) ) ;
#54641 = CARTESIAN_POINT ( 'NONE',  ( -5.823673210054431948, 21.52544592524334988, 62.70942372801902565 ) ) ;
#54642 = CARTESIAN_POINT ( 'NONE',  ( -0.05219959533909027116, -19.03943276465977164, 72.49890960531435269 ) ) ;
#54643 = CARTESIAN_POINT ( 'NONE',  ( 13.89961937509957401, 13.97604488694547697, 31.87609039468566863 ) ) ;
#54644 = CARTESIAN_POINT ( 'NONE',  ( 0.05219959533907565091, 21.53943276465977519, 49.99890960531437401 ) ) ;
#54645 = CARTESIAN_POINT ( 'NONE',  ( 5.823673210054444382, -21.52544592524334988, 40.20942372801901854 ) ) ;
#54646 = VECTOR ( 'NONE', #176066, 1000.000000000000000 ) ;
#54647 = CARTESIAN_POINT ( 'NONE',  ( -5.719274019375978568, 21.55341960407610458, 105.2072429386477097 ) ) ;
#54648 = CARTESIAN_POINT ( 'NONE',  ( 19.05341960407617918, -5.049401038297876454, 101.0427570613523045 ) ) ;
#54649 = CARTESIAN_POINT ( 'NONE',  ( -16.55341960407617563, 4.379528057220093196, 53.54275706135234714 ) ) ;
#54651 = CARTESIAN_POINT ( 'NONE',  ( 10.72451020669898902, -18.67979575497178502, 97.91557627198103830 ) ) ;
#54650 = CARTESIAN_POINT ( 'NONE',  ( 11.30153831258470731, -180.0000000000000000, -25.00000000000000000 ) ) ;
#54652 = CARTESIAN_POINT ( 'NONE',  ( -8.224510206698948167, 14.34966873604960824, 85.41557627198102409 ) ) ;
#54653 = CARTESIAN_POINT ( 'NONE',  ( -16.61371651742600974, -7.165104196376154810, 101.1458493000700827 ) ) ;
#54654 = CARTESIAN_POINT ( 'NONE',  ( -16.51473224551082808, 9.474510206698731452, 113.3344237280190043 ) ) ;
#54655 = CARTESIAN_POINT ( 'NONE',  ( 18.62759615963271287, -10.81492255796078972, 43.33224293864769550 ) ) ;
#54656 = CARTESIAN_POINT ( 'NONE',  ( -4.379528057220086978, -16.55341960407618274, 94.79275706135234714 ) ) ;
#54657 = DIRECTION ( 'NONE',  ( -1.000000000000000000, 0.000000000000000000, 0.000000000000000000 ) ) ;
#54658 = CARTESIAN_POINT ( 'NONE',  ( 16.55341960407618274, -4.379528057220086978, 51.04275706135234714 ) ) ;
#54659 = CARTESIAN_POINT ( 'NONE',  ( 5.719274019375673035, 21.55341960407619339, 22.29275706135235069 ) ) ;
#54660 = CARTESIAN_POINT ( 'NONE',  ( -10.81492255796078084, -18.62759615963271287, 42.08224293864769550 ) ) ;
#54661 = CARTESIAN_POINT ( 'NONE',  ( 4.483927247898790824, -16.52544592524335698, 80.20942372801901854 ) ) ;
#54662 = CARTESIAN_POINT ( 'NONE',  ( -19.03943276465977164, 0.05219959533909376836, 96.24890960531436690 ) ) ;
#54663 = CARTESIAN_POINT ( 'NONE',  ( -18.62759615963255300, -10.81492255796106328, 64.16775706135234714 ) ) ;
#54664 = CARTESIAN_POINT ( 'NONE',  ( 15.80617190586746368, 15.72974639402197994, 39.37390960531436690 ) ) ;
#54665 = CARTESIAN_POINT ( 'NONE',  ( -10.72451020669898014, 18.67979575497178502, 25.41557627198103120 ) ) ;
#54666 = ORIENTED_EDGE ( 'NONE', *, *, #23760, .T. ) ;
#54667 = CARTESIAN_POINT ( 'NONE',  ( 5.153800228976615827, -19.02544592524334988, 55.20942372801899722 ) ) ;
#54668 = CARTESIAN_POINT ( 'NONE',  ( 16.52544592524335698, 4.483927247898782831, 71.45942372801901854 ) ) ;
#54669 = CARTESIAN_POINT ( 'NONE',  ( -21.53943276465977519, 0.05219959533907696930, 36.24890960531435979 ) ) ;
#54670 = ORIENTED_EDGE ( 'NONE', *, *, #93499, .T. ) ;
#54671 = CARTESIAN_POINT ( 'NONE',  ( -19.05341960407611168, -5.049401038298163336, 81.45724293864769550 ) ) ;
#54672 = CARTESIAN_POINT ( 'NONE',  ( -12.06949235617739369, -12.14591786802326823, 109.3760903946857042 ) ) ;
#54673 = CARTESIAN_POINT ( 'NONE',  ( 6.193113236902296315, -38.78391156914228333, -32.76858701579856614 ) ) ;
#54674 = CARTESIAN_POINT ( 'NONE',  ( -4.483927247898539470, -16.52544592524342804, 112.2905762719810241 ) ) ;
#54675 = CARTESIAN_POINT ( 'NONE',  ( -15.72974639402197994, 15.80617190586746368, 50.62390960531435979 ) ) ;
#54676 = CARTESIAN_POINT ( 'NONE',  ( 0.05219959533909260263, 19.03943276465977164, 44.99890960531435979 ) ) ;
#54677 = CARTESIAN_POINT ( 'NONE',  ( 16.53943276465976808, 0.05219959533934440121, 81.25109039468568994 ) ) ;
#54678 = CARTESIAN_POINT ( 'NONE',  ( -21.53943276465977519, -0.05219959533937600094, 38.75109039468567573 ) ) ;
#54679 = CARTESIAN_POINT ( 'NONE',  ( -19.05341960407617563, 5.049401038297882671, 93.54275706135234714 ) ) ;
#54680 = CARTESIAN_POINT ( 'NONE',  ( -4.379528057220328563, 16.55341960407611168, 95.20724293864769550 ) ) ;
#54681 = CARTESIAN_POINT ( 'NONE',  ( 19.05341960407611168, 5.049401038298154454, 58.95724293864768129 ) ) ;
#54682 = CIRCLE ( 'NONE', #193541, 2.500000000000002220 ) ;
#54683 = CARTESIAN_POINT ( 'NONE',  ( 5.153800228976335163, 19.02544592524342804, 24.79057627198102765 ) ) ;
#54684 = CARTESIAN_POINT ( 'NONE',  ( -15.72974639402176322, -15.80617190586768395, 99.37609039468568994 ) ) ;
#54685 = CARTESIAN_POINT ( 'NONE',  ( -13.97604488694527625, -13.89961937509977652, 76.87390960531433848 ) ) ;
#54686 = CARTESIAN_POINT ( 'NONE',  ( -8.314922557961024197, 14.29746914071037800, 67.91775706135234714 ) ) ;
#54687 = CARTESIAN_POINT ( 'NONE',  ( 18.62759615963255655, 10.81492255796105972, 91.66775706135234714 ) ) ;
#54688 = CARTESIAN_POINT ( 'NONE',  ( -18.67979575497178146, -10.72451020669898902, 51.66557627198102409 ) ) ;
#54689 = CARTESIAN_POINT ( 'NONE',  ( 12.06949235617739724, 12.14591786802326823, 76.87609039468567573 ) ) ;
#54690 = CARTESIAN_POINT ( 'NONE',  ( -0.05219959533936034679, 19.03943276465977164, 52.50109039468566863 ) ) ;
#54691 = CARTESIAN_POINT ( 'NONE',  ( 5.153800228976615827, -19.02544592524334988, 60.20942372801899012 ) ) ;
#54692 = ORIENTED_EDGE ( 'NONE', *, *, #28742, .F. ) ;
#54693 = CARTESIAN_POINT ( 'NONE',  ( -5.719274019375665041, -21.55341960407619695, 64.79275706135234714 ) ) ;
#54694 = CARTESIAN_POINT ( 'NONE',  ( -13.97604488694527625, -13.89961937509977652, 66.87390960531436690 ) ) ;
#54695 = CARTESIAN_POINT ( 'NONE',  ( 5.153800228976335163, 19.02544592524342804, 24.79057627198102765 ) ) ;
#54696 = CARTESIAN_POINT ( 'NONE',  ( 9.564922557961047289, -16.46253265017146816, 60.41775706135233293 ) ) ;
#54697 = CARTESIAN_POINT ( 'NONE',  ( -19.03943276465977164, 0.05219959533909376836, 116.2489096053143669 ) ) ;
#54698 = CARTESIAN_POINT ( 'NONE',  ( -16.46253265017160317, 9.564922557960807481, 100.8322429386477097 ) ) ;
#54699 = CARTESIAN_POINT ( 'NONE',  ( 14.29746914071049879, -8.314922557960816363, 53.33224293864769550 ) ) ;
#54700 = CARTESIAN_POINT ( 'NONE',  ( -21.52544592524343514, 5.823673210054127303, 41.04057627198103120 ) ) ;
#54701 = CARTESIAN_POINT ( 'NONE',  ( 20.02676387111008438, 21.85243030949935061, -51.86007293692900078 ) ) ;
#54702 = CARTESIAN_POINT ( 'NONE',  ( -9.564922557961040184, 16.46253265017147172, 22.91775706135233648 ) ) ;
#54703 =( LENGTH_UNIT ( ) NAMED_UNIT ( * ) SI_UNIT ( .MILLI., .METRE. ) );
#54704 = CARTESIAN_POINT ( 'NONE',  ( 0.05219959533909260263, 19.03943276465977164, 54.99890960531435979 ) ) ;
#54705 = CARTESIAN_POINT ( 'NONE',  ( 9.564922557960805705, 16.46253265017160317, 24.58224293864769194 ) ) ;
#54706 = CARTESIAN_POINT ( 'NONE',  ( 37.99999999999999289, 12.34694845685046793, -4.899999999999999467 ) ) ;
#54707 = CARTESIAN_POINT ( 'NONE',  ( -19.63849963310777369, -31.90967075912679718, -8.000000000000000000 ) ) ;
#54708 = CARTESIAN_POINT ( 'NONE',  ( 8.224510206698742110, 14.34966873604972548, 67.08442372801901854 ) ) ;
#54709 = CARTESIAN_POINT ( 'NONE',  ( -10.72451020669898014, 18.67979575497178502, 85.41557627198102409 ) ) ;
#54710 = CARTESIAN_POINT ( 'NONE',  ( 16.53943276465976808, -0.05219959533910856209, 48.74890960531435979 ) ) ;
#54712 = DIRECTION ( 'NONE',  ( 0.000000000000000000, 0.000000000000000000, 1.000000000000000000 ) ) ;
#54711 = CARTESIAN_POINT ( 'NONE',  ( -13.97604488694527625, -13.89961937509977652, 36.87390960531436690 ) ) ;
#54713 = CARTESIAN_POINT ( 'NONE',  ( 21.52544592524334988, 5.823673210054432836, 46.45942372801901854 ) ) ;
#54714 = CARTESIAN_POINT ( 'NONE',  ( -16.46253265017146816, -9.564922557961047289, 49.16775706135233293 ) ) ;
#54715 = CARTESIAN_POINT ( 'NONE',  ( -19.05341960407611168, -5.049401038298163336, 31.45724293864769550 ) ) ;
#54716 = CARTESIAN_POINT ( 'NONE',  ( -15.72974639402176322, -15.80617190586768395, 84.37609039468570415 ) ) ;
#54717 = CARTESIAN_POINT ( 'NONE',  ( 17.50000000000000000, 5.499999999999992895, 96.70309617465829888 ) ) ;
#54718 = CARTESIAN_POINT ( 'NONE',  ( -14.29746914071049879, 8.314922557960819915, 35.83224293864768839 ) ) ;
#54719 = CARTESIAN_POINT ( 'NONE',  ( 19.20446147854529428, 5.499999999999905853, 41.88999695167679249 ) ) ;
#54720 = CARTESIAN_POINT ( 'NONE',  ( 21.55341960407610458, 5.719274019375980345, 38.95724293864768839 ) ) ;
#54721 = CARTESIAN_POINT ( 'NONE',  ( 8.571926809382597767, 26.38167802310806209, 140.2750000027311899 ) ) ;
#54722 = CARTESIAN_POINT ( 'NONE',  ( -16.46253265017160317, 9.564922557960807481, 90.83224293864769550 ) ) ;
#54723 = CARTESIAN_POINT ( 'NONE',  ( 8.314922557960818139, 14.29746914071049879, 84.58224293864769550 ) ) ;
#54724 = CARTESIAN_POINT ( 'NONE',  ( -12.14591786802326823, 12.06949235617739902, 28.12609039468568284 ) ) ;
#54725 = CARTESIAN_POINT ( 'NONE',  ( 12.06949235617739724, 12.14591786802326823, 111.8760903946856615 ) ) ;
#54726 = ORIENTED_EDGE ( 'NONE', *, *, #24668, .F. ) ;
#54727 = CARTESIAN_POINT ( 'NONE',  ( 13.97604488694527802, 13.89961937509977652, 29.37390960531435979 ) ) ;
#54728 = EDGE_CURVE ( 'NONE', #50285, #44725, #32747, .T. ) ;
#54730 = CARTESIAN_POINT ( 'NONE',  ( -5.823673210054116645, -21.52544592524344225, 92.29057627198103830 ) ) ;
#54729 = CARTESIAN_POINT ( 'NONE',  ( -5.049401038298153566, 19.05341960407611168, 80.20724293864769550 ) ) ;
#54732 = CARTESIAN_POINT ( 'NONE',  ( 16.51473224551069308, 9.474510206698969483, 104.1655762719810241 ) ) ;
#54731 = CARTESIAN_POINT ( 'NONE',  ( 0.05219959533910956823, 16.53943276465976808, 29.99890960531435979 ) ) ;
#54733 = CARTESIAN_POINT ( 'NONE',  ( 13.89961937509957401, 13.97604488694547697, 86.87609039468567573 ) ) ;
#54734 = CARTESIAN_POINT ( 'NONE',  ( 21.53943276465977519, 0.05219959533937863772, 111.2510903946856899 ) ) ;
#54735 = CARTESIAN_POINT ( 'NONE',  ( -10.81492255796078084, -18.62759615963271287, 92.08224293864769550 ) ) ;
#54736 = CARTESIAN_POINT ( 'NONE',  ( -0.05219959533907301413, -21.53943276465977519, 32.49890960531435979 ) ) ;
#54737 = CARTESIAN_POINT ( 'NONE',  ( 16.51473224551069308, 9.474510206698969483, 64.16557627198102409 ) ) ;
#54738 = CARTESIAN_POINT ( 'NONE',  ( -12.14591786802309592, -12.06949235617757132, 26.87390960531435979 ) ) ;
#54739 = CARTESIAN_POINT ( 'NONE',  ( 9.474510206698971260, -16.51473224551069308, 82.91557627198103830 ) ) ;
#54740 = ORIENTED_EDGE ( 'NONE', *, *, #55706, .F. ) ;
#54741 = CARTESIAN_POINT ( 'NONE',  ( -32.15403441185031141, -4.954129643790889048, 89.34785441345069046 ) ) ;
#54742 = CARTESIAN_POINT ( 'NONE',  ( -0.05219959533936034679, 19.03943276465977164, 22.50109039468566152 ) ) ;
#54743 = CARTESIAN_POINT ( 'NONE',  ( -4.379528057220328563, 16.55341960407611168, 90.20724293864770971 ) ) ;
#54744 = CARTESIAN_POINT ( 'NONE',  ( 15.72974639402176855, 15.80617190586768217, 21.87609039468567573 ) ) ;
#54745 = CARTESIAN_POINT ( 'NONE',  ( -17.14385361876520264, -23.59649016807271593, 145.6750000027311671 ) ) ;
#54746 = CARTESIAN_POINT ( 'NONE',  ( 18.62759615963271287, -10.81492255796078972, 68.33224293864769550 ) ) ;
#54747 = CARTESIAN_POINT ( 'NONE',  ( -14.29746914071037622, -8.314922557961029526, 89.16775706135236135 ) ) ;
#54748 = CARTESIAN_POINT ( 'NONE',  ( -13.89961937509977652, 13.97604488694528158, 25.62390960531434558 ) ) ;
#54749 = CARTESIAN_POINT ( 'NONE',  ( 13.89961937509977652, -13.97604488694527269, 78.12390960531433848 ) ) ;
#54750 = CARTESIAN_POINT ( 'NONE',  ( 18.22780087662122384, -5.500000000000022204, 71.01540105326107266 ) ) ;
#54751 = CARTESIAN_POINT ( 'NONE',  ( 23.48298174826590667, -32.32155151706770368, -5.047842220587804185 ) ) ;
#54752 = CARTESIAN_POINT ( 'NONE',  ( 16.55341960407611168, 4.379528057220329451, 33.95724293864769550 ) ) ;
#54753 = CARTESIAN_POINT ( 'NONE',  ( 18.67979575497194134, -10.72451020669871369, 65.83442372801900433 ) ) ;
#54754 = CARTESIAN_POINT ( 'NONE',  ( -5.049401038298153566, 19.05341960407611168, 115.2072429386477097 ) ) ;
#54755 = CARTESIAN_POINT ( 'NONE',  ( 18.67979575497194134, -10.72451020669871369, 100.8344237280190185 ) ) ;
#54756 = CARTESIAN_POINT ( 'NONE',  ( 9.564922557960805705, 16.46253265017160317, 44.58224293864769550 ) ) ;
#54757 = CARTESIAN_POINT ( 'NONE',  ( -19.05341960407611168, -5.049401038298163336, 51.45724293864770260 ) ) ;
#54758 = ORIENTED_EDGE ( 'NONE', *, *, #82217, .T. ) ;
#54759 = CARTESIAN_POINT ( 'NONE',  ( -18.62759615963255300, -10.81492255796106328, 94.16775706135237556 ) ) ;
#54760 = CARTESIAN_POINT ( 'NONE',  ( 12.14591786802327356, -12.06949235617739191, 55.62609039468568284 ) ) ;
#54761 = CARTESIAN_POINT ( 'NONE',  ( 18.62759615963255655, 10.81492255796105972, 86.66775706135234714 ) ) ;
#54762 = CARTESIAN_POINT ( 'NONE',  ( -21.52544592524343514, 5.823673210054127303, 26.04057627198103475 ) ) ;
#54763 = CARTESIAN_POINT ( 'NONE',  ( 5.153800228976615827, -19.02544592524334988, 100.2094237280190043 ) ) ;
#54764 = CARTESIAN_POINT ( 'NONE',  ( 15.80617190586769283, -15.72974639402175789, 50.62609039468568994 ) ) ;
#54765 = CARTESIAN_POINT ( 'NONE',  ( -14.34966873604972548, 8.224510206698743886, 33.33442372801900433 ) ) ;
#54766 = CARTESIAN_POINT ( 'NONE',  ( 21.52544592524344225, -5.823673210054117533, 88.54057627198103830 ) ) ;
#54767 = CARTESIAN_POINT ( 'NONE',  ( -9.564922557961040184, 16.46253265017147172, 87.91775706135233293 ) ) ;
#54768 = CARTESIAN_POINT ( 'NONE',  ( -19.03943276465977164, 0.05219959533909376836, 71.24890960531435269 ) ) ;
#54769 = CARTESIAN_POINT ( 'NONE',  ( 5.049401038297881783, 19.05341960407617563, 102.2927570613523045 ) ) ;
#54770 = EDGE_CURVE ( 'NONE', #177652, #26356, #175937, .T. ) ;
#54771 = CARTESIAN_POINT ( 'NONE',  ( -16.51473224551082808, 9.474510206698731452, 98.33442372801900433 ) ) ;
#54772 = CARTESIAN_POINT ( 'NONE',  ( -12.06949235617756955, 12.14591786802309770, 55.62390960531436690 ) ) ;
#54773 = CARTESIAN_POINT ( 'NONE',  ( -9.474510206698720793, -16.51473224551083518, 74.58442372801900433 ) ) ;
#54774 = CARTESIAN_POINT ( 'NONE',  ( -14.29746914071037622, -8.314922557961029526, 54.16775706135235424 ) ) ;
#54775 = CARTESIAN_POINT ( 'NONE',  ( -19.02544592524334988, -5.153800228976617603, 43.95942372801899012 ) ) ;
#54776 = CARTESIAN_POINT ( 'NONE',  ( 13.97604488694527802, 13.89961937509977652, 34.37390960531436690 ) ) ;
#54777 = CARTESIAN_POINT ( 'NONE',  ( 13.89961937509977652, -13.97604488694527269, 58.12390960531436690 ) ) ;
#54778 = CARTESIAN_POINT ( 'NONE',  ( -16.53943276465976808, -0.05219959533934237506, 53.75109039468568994 ) ) ;
#54779 = CARTESIAN_POINT ( 'NONE',  ( 27.73933785331498925, -9.013057229001033122, 142.2750000027311899 ) ) ;
#54780 = CARTESIAN_POINT ( 'NONE',  ( -23.31738231874055600, 16.94106989632528837, 140.0500000054623513 ) ) ;
#54781 = CARTESIAN_POINT ( 'NONE',  ( -19.03943276465977164, 0.05219959533909376836, 111.2489096053143669 ) ) ;
#54782 = CARTESIAN_POINT ( 'NONE',  ( -9.474510206698964154, 16.51473224551069663, 25.41557627198103120 ) ) ;
#54783 = CARTESIAN_POINT ( 'NONE',  ( 9.474510206698729675, 16.51473224551082808, 102.0844237280190043 ) ) ;
#54785 = CARTESIAN_POINT ( 'NONE',  ( -5.719274019375978568, 21.55341960407610458, 35.20724293864768839 ) ) ;
#54784 = AXIS2_PLACEMENT_3D ( 'NONE', #132148, #92596, #181659 ) ;
#54787 = CARTESIAN_POINT ( 'NONE',  ( 0.05219959533936267826, -19.03943276465977164, 110.0010903946856757 ) ) ;
#54786 = CARTESIAN_POINT ( 'NONE',  ( 5.153800228976615827, -19.02544592524334988, 35.20942372801899722 ) ) ;
#54788 = CARTESIAN_POINT ( 'NONE',  ( 16.51473224551069308, 9.474510206698969483, 29.16557627198103475 ) ) ;
#54789 = CARTESIAN_POINT ( 'NONE',  ( -19.03943276465977164, 0.05219959533909376836, 46.24890960531435979 ) ) ;
#54790 = CARTESIAN_POINT ( 'NONE',  ( 18.67979575497178502, 10.72451020669898547, 69.16557627198102409 ) ) ;
#54791 = CARTESIAN_POINT ( 'NONE',  ( 13.97604488694527802, 13.89961937509977652, 99.37390960531436690 ) ) ;
#54792 = CARTESIAN_POINT ( 'NONE',  ( 9.474510206698971260, -16.51473224551069308, 32.91557627198102409 ) ) ;
#54793 = CARTESIAN_POINT ( 'NONE',  ( -17.14385361876520264, -23.59649016807271238, 141.6750000027311387 ) ) ;
#54794 = CARTESIAN_POINT ( 'NONE',  ( 16.51473224551083163, -9.474510206698727899, 80.83442372801899012 ) ) ;
#54795 = CARTESIAN_POINT ( 'NONE',  ( 16.52544592524342804, -4.483927247898539470, 58.54057627198103120 ) ) ;
#54796 = CARTESIAN_POINT ( 'NONE',  ( 21.52544592524344225, -5.823673210054117533, 38.54057627198103120 ) ) ;
#54797 = CARTESIAN_POINT ( 'NONE',  ( 5.823673210054444382, -21.52544592524334988, 110.2094237280190185 ) ) ;
#54798 = CARTESIAN_POINT ( 'NONE',  ( -0.05219959533907301413, -21.53943276465977519, 97.49890960531436690 ) ) ;
#54799 = CARTESIAN_POINT ( 'NONE',  ( 18.67979575497194134, -10.72451020669871369, 75.83442372801900433 ) ) ;
#54800 = CARTESIAN_POINT ( 'NONE',  ( -10.81492255796105439, 18.62759615963255655, 82.91775706135234714 ) ) ;
#54801 = CARTESIAN_POINT ( 'NONE',  ( 16.46253265017160672, -9.564922557960803928, 113.3322429386476955 ) ) ;
#54803 = CARTESIAN_POINT ( 'NONE',  ( -21.52544592524334988, -5.823673210054445271, 58.95942372801902565 ) ) ;
#54802 = CARTESIAN_POINT ( 'NONE',  ( 4.379528057220092307, 16.55341960407617563, 102.2927570613523613 ) ) ;
#54804 = CARTESIAN_POINT ( 'NONE',  ( -0.05219959533909027116, -19.03943276465977164, 72.49890960531435269 ) ) ;
#54805 = CARTESIAN_POINT ( 'NONE',  ( -5.049401038297874678, -19.05341960407617918, 34.79275706135233293 ) ) ;
#54806 = CARTESIAN_POINT ( 'NONE',  ( 21.55341960407619695, -5.719274019375665929, 26.04275706135235779 ) ) ;
#54807 = CARTESIAN_POINT ( 'NONE',  ( -0.05219959533909027116, -19.03943276465977164, 67.49890960531436690 ) ) ;
#54808 = CARTESIAN_POINT ( 'NONE',  ( -4.483927247898539470, -16.52544592524342804, 82.29057627198103830 ) ) ;
#54809 = CARTESIAN_POINT ( 'NONE',  ( -12.06949235617756955, 12.14591786802309770, 50.62390960531435979 ) ) ;
#54810 = CARTESIAN_POINT ( 'NONE',  ( -18.67979575497178146, -10.72451020669898902, 51.66557627198102409 ) ) ;
#54811 = CARTESIAN_POINT ( 'NONE',  ( -19.03943276465977164, 0.05219959533909376836, 61.24890960531436690 ) ) ;
#54812 = CARTESIAN_POINT ( 'NONE',  ( 21.55341960407610458, 5.719274019375980345, 73.95724293864769550 ) ) ;
#54813 = CARTESIAN_POINT ( 'NONE',  ( 13.89961937509957401, 13.97604488694547697, 66.87609039468567573 ) ) ;
#54815 = CARTESIAN_POINT ( 'NONE',  ( 14.34966873604960469, 8.224510206698951720, 64.16557627198102409 ) ) ;
#54814 = CARTESIAN_POINT ( 'NONE',  ( -13.97604488694547520, 13.89961937509957934, 23.12609039468565797 ) ) ;
#54817 = VECTOR ( 'NONE', #141847, 1000.000000000000000 ) ;
#54816 = CARTESIAN_POINT ( 'NONE',  ( 18.67979575497178502, 10.72451020669898547, 44.16557627198103120 ) ) ;
#54818 = ORIENTED_EDGE ( 'NONE', *, *, #159341, .F. ) ;
#54819 = CARTESIAN_POINT ( 'NONE',  ( 16.52216118717206683, 7.221426719304504971, 103.5759902104699250 ) ) ;
#54821 = CARTESIAN_POINT ( 'NONE',  ( 0.9268384597861692997, 6.404133089829842973, -64.47363563910111850 ) ) ;
#54820 = CARTESIAN_POINT ( 'NONE',  ( -12.06949235617739369, -12.14591786802326823, 79.37609039468567573 ) ) ;
#54822 = CARTESIAN_POINT ( 'NONE',  ( 13.97604488694548053, -13.89961937509957401, 90.62609039468567573 ) ) ;
#54823 = EDGE_CURVE ( 'NONE', #101016, #123998, #77077, .T. ) ;
#54824 = CARTESIAN_POINT ( 'NONE',  ( -12.14591786802309592, -12.06949235617757132, 51.87390960531437401 ) ) ;
#54825 = FACE_OUTER_BOUND ( 'NONE', #133870, .T. ) ;
#54826 = CARTESIAN_POINT ( 'NONE',  ( -13.97604488694527625, -13.89961937509977652, 46.87390960531435979 ) ) ;
#54827 = CARTESIAN_POINT ( 'NONE',  ( 8.314922557960818139, 14.29746914071049879, 39.58224293864769550 ) ) ;
#54828 = CARTESIAN_POINT ( 'NONE',  ( 19.02544592524343514, -5.153800228976328945, 93.54057627198102409 ) ) ;
#54829 = CARTESIAN_POINT ( 'NONE',  ( -5.153800228976328057, -19.02544592524343514, 47.29057627198102409 ) ) ;
#54830 = CARTESIAN_POINT ( 'NONE',  ( -0.05219959533937732626, 21.53943276465977519, 57.50109039468568994 ) ) ;
#54831 = CARTESIAN_POINT ( 'NONE',  ( -19.03943276465977164, 0.05219959533909376836, 76.24890960531435269 ) ) ;
#54832 = CARTESIAN_POINT ( 'NONE',  ( -9.564922557960796823, -16.46253265017161027, 32.08224293864769550 ) ) ;
#54833 = CARTESIAN_POINT ( 'NONE',  ( 9.474510206698971260, -16.51473224551069308, 72.91557627198102409 ) ) ;
#54834 = CARTESIAN_POINT ( 'NONE',  ( 0.05219959533907565091, 21.53943276465977519, 49.99890960531437401 ) ) ;
#54835 = CARTESIAN_POINT ( 'NONE',  ( 19.03943276465977164, -0.05219959533909143690, 48.74890960531435979 ) ) ;
#54836 = CARTESIAN_POINT ( 'NONE',  ( 10.81492255796078972, 18.62759615963270932, 49.58224293864769550 ) ) ;
#54837 = CARTESIAN_POINT ( 'NONE',  ( -19.05341960407617563, 5.049401038297882671, 83.54275706135233293 ) ) ;
#54838 = CARTESIAN_POINT ( 'NONE',  ( -14.29746914071037622, -8.314922557961029526, 99.16775706135234714 ) ) ;
#54839 = CARTESIAN_POINT ( 'NONE',  ( 13.89961937509957401, 13.97604488694547697, 26.87609039468566507 ) ) ;
#54841 = CARTESIAN_POINT ( 'NONE',  ( -0.05219959533934338120, 16.53943276465976808, 77.50109039468567573 ) ) ;
#54840 = CARTESIAN_POINT ( 'NONE',  ( 16.52544592524335698, 4.483927247898782831, 51.45942372801901854 ) ) ;
#54842 = CARTESIAN_POINT ( 'NONE',  ( 7.284589286804292740, 1.784589286804177277, 1.818019484660534424 ) ) ;
#54843 = CARTESIAN_POINT ( 'NONE',  ( -16.52544592524335698, -4.483927247898792601, 68.95942372801901854 ) ) ;
#54844 = CARTESIAN_POINT ( 'NONE',  ( 10.81492255796078972, 18.62759615963270932, 29.58224293864769905 ) ) ;
#54845 = CARTESIAN_POINT ( 'NONE',  ( 16.46253265017160672, -9.564922557960803928, 28.33224293864769550 ) ) ;
#54846 = CARTESIAN_POINT ( 'NONE',  ( -16.53943276465976808, -0.05219959533934237506, 38.75109039468567573 ) ) ;
#54847 = CARTESIAN_POINT ( 'NONE',  ( -13.89961937509977652, 13.97604488694528158, 45.62390960531433848 ) ) ;
#54848 = CARTESIAN_POINT ( 'NONE',  ( -21.55341960407619339, 5.719274019375674811, 38.54275706135234714 ) ) ;
#54849 = CARTESIAN_POINT ( 'NONE',  ( 8.224510206698742110, 14.34966873604972548, 42.08442372801901854 ) ) ;
#54850 = CARTESIAN_POINT ( 'NONE',  ( 8.314922557961029526, -14.29746914071037800, 100.4177570613523471 ) ) ;
#54851 = DIRECTION ( 'NONE',  ( 0.4999999999999932276, -0.5000000000000055511, 0.7071067811865484609 ) ) ;
#54852 = CARTESIAN_POINT ( 'NONE',  ( 13.97604488694548053, -13.89961937509957401, 20.62609039468567573 ) ) ;
#54853 = CARTESIAN_POINT ( 'NONE',  ( 4.483927247898790824, -16.52544592524335698, 20.20942372801900788 ) ) ;
#54854 = CARTESIAN_POINT ( 'NONE',  ( -9.564922557961040184, 16.46253265017147172, 72.91775706135233293 ) ) ;
#54855 = CARTESIAN_POINT ( 'NONE',  ( -8.224510206698948167, 14.34966873604960824, 70.41557627198102409 ) ) ;
#54856 = CARTESIAN_POINT ( 'NONE',  ( 0.05219959533910956823, 16.53943276465976808, 114.9989096053143669 ) ) ;
#54858 = CARTESIAN_POINT ( 'NONE',  ( 16.36317988757095421, -7.306389748694852138, 56.59789608363175972 ) ) ;
#54857 = CARTESIAN_POINT ( 'NONE',  ( -16.46253265017146816, -9.564922557961047289, 59.16775706135233293 ) ) ;
#54859 = CARTESIAN_POINT ( 'NONE',  ( 5.823673210054444382, -21.52544592524334988, 60.20942372801902565 ) ) ;
#54860 = CARTESIAN_POINT ( 'NONE',  ( 8.224510206698742110, 14.34966873604972548, 22.08442372801901143 ) ) ;
#54861 = DIRECTION ( 'NONE',  ( -1.000000000000000000, 0.000000000000000000, 0.000000000000000000 ) ) ;
#54862 = CARTESIAN_POINT ( 'NONE',  ( -21.55341960407610458, -5.719274019375992779, 26.45724293864768839 ) ) ;
#54863 = CARTESIAN_POINT ( 'NONE',  ( -12.06949235617739369, -12.14591786802326823, 19.37609039468568639 ) ) ;
#54864 = LINE ( 'NONE', #117536, #8657 ) ;
#54865 = CARTESIAN_POINT ( 'NONE',  ( -19.83801684532418363, 12.12952959760495908, 169.9999999999999716 ) ) ;
#54866 = CARTESIAN_POINT ( 'NONE',  ( -19.03943276465977164, 0.05219959533909376836, 26.24890960531435624 ) ) ;
#54867 = CARTESIAN_POINT ( 'NONE',  ( 21.52544592524334988, 5.823673210054432836, 106.4594237280190328 ) ) ;
#54868 = CARTESIAN_POINT ( 'NONE',  ( -16.46253265017160317, 9.564922557960807481, 55.83224293864769550 ) ) ;
#54869 = CARTESIAN_POINT ( 'NONE',  ( 21.52544592524334988, 5.823673210054432836, 66.45942372801903275 ) ) ;
#54870 = CARTESIAN_POINT ( 'NONE',  ( -0.05219959533937732626, 21.53943276465977519, 102.5010903946856899 ) ) ;
#54871 = CARTESIAN_POINT ( 'NONE',  ( -8.314922557960811034, -14.29746914071050412, 27.08224293864769550 ) ) ;
#54872 = CARTESIAN_POINT ( 'NONE',  ( 9.564922557960805705, 16.46253265017160317, 34.58224293864770260 ) ) ;
#54873 = CARTESIAN_POINT ( 'NONE',  ( -9.564922557960796823, -16.46253265017161027, 77.08224293864769550 ) ) ;
#54874 = CARTESIAN_POINT ( 'NONE',  ( 15.80617190586769283, -15.72974639402175789, 55.62609039468568284 ) ) ;
#54875 = CARTESIAN_POINT ( 'NONE',  ( -13.97604488694527625, -13.89961937509977652, 36.87390960531436690 ) ) ;
#54876 = CARTESIAN_POINT ( 'NONE',  ( 10.81492255796106328, -18.62759615963255655, 55.41775706135234714 ) ) ;
#54878 = CARTESIAN_POINT ( 'NONE',  ( -5.153800228976328057, -19.02544592524343514, 112.2905762719810099 ) ) ;
#54877 = CARTESIAN_POINT ( 'NONE',  ( -13.97604488694547697, 13.89961937509957934, 78.12609039468567573 ) ) ;
#54879 = CARTESIAN_POINT ( 'NONE',  ( 19.02544592524343514, -5.153800228976328945, 28.54057627198102409 ) ) ;
#54880 = CARTESIAN_POINT ( 'NONE',  ( -15.72974639402197994, 15.80617190586746368, 105.6239096053143669 ) ) ;
#54881 = CARTESIAN_POINT ( 'NONE',  ( -13.89961937509957401, -13.97604488694547875, 39.37609039468566152 ) ) ;
#54882 = CARTESIAN_POINT ( 'NONE',  ( -14.34966873604960291, -8.224510206698953496, 91.66557627198103830 ) ) ;
#54883 = CARTESIAN_POINT ( 'NONE',  ( 5.153800228976335163, 19.02544592524342804, 44.79057627198103830 ) ) ;
#54884 = CARTESIAN_POINT ( 'NONE',  ( -0.05219959533936034679, 19.03943276465977164, 97.50109039468567573 ) ) ;
#54885 = CARTESIAN_POINT ( 'NONE',  ( -12.14591786802309592, -12.06949235617757132, 56.87390960531436690 ) ) ;
#54886 = CARTESIAN_POINT ( 'NONE',  ( 21.55341960407619695, -5.719274019375665929, 111.0427570613523613 ) ) ;
#54887 = CARTESIAN_POINT ( 'NONE',  ( 5.153800228976335163, 19.02544592524342804, 99.79057627198102409 ) ) ;
#54888 = CARTESIAN_POINT ( 'NONE',  ( 13.97604488694548053, -13.89961937509957401, 90.62609039468567573 ) ) ;
#54889 = CARTESIAN_POINT ( 'NONE',  ( 21.55341960407610458, 5.719274019375980345, 88.95724293864769550 ) ) ;
#54890 = CARTESIAN_POINT ( 'NONE',  ( 21.53943276465977519, 0.05219959533937863772, 41.25109039468568284 ) ) ;
#54891 = CARTESIAN_POINT ( 'NONE',  ( -14.29746914071037622, -8.314922557961029526, 44.16775706135234714 ) ) ;
#54892 = CARTESIAN_POINT ( 'NONE',  ( 8.224510206698742110, 14.34966873604972548, 107.0844237280190043 ) ) ;
#54894 = CARTESIAN_POINT ( 'NONE',  ( 10.81492255796106328, -18.62759615963255655, 50.41775706135235424 ) ) ;
#54893 = CARTESIAN_POINT ( 'NONE',  ( -16.52544592524335698, -4.483927247898792601, 43.95942372801902565 ) ) ;
#54895 = CARTESIAN_POINT ( 'NONE',  ( 18.62759615963271287, -10.81492255796078972, 38.33224293864768839 ) ) ;
#54896 = CARTESIAN_POINT ( 'NONE',  ( 0.05219959533909260263, 19.03943276465977164, 29.99890960531435979 ) ) ;
#54897 = CARTESIAN_POINT ( 'NONE',  ( -11.74264578624800670, 36.14014761921585972, -10.14999999453762669 ) ) ;
#54898 = CARTESIAN_POINT ( 'NONE',  ( 16.53943276465976808, 0.05219959533934440121, 61.25109039468567573 ) ) ;
#54899 = CARTESIAN_POINT ( 'NONE',  ( -0.05219959533907301413, -21.53943276465977519, 82.49890960531436690 ) ) ;
#54900 = CARTESIAN_POINT ( 'NONE',  ( 0.05219959533910956823, 16.53943276465976808, 39.99890960531436690 ) ) ;
#54901 = CARTESIAN_POINT ( 'NONE',  ( -12.06949235617739369, -12.14591786802326823, 64.37609039468568994 ) ) ;
#54902 = CARTESIAN_POINT ( 'NONE',  ( 5.049401038298161559, -19.05341960407611168, 62.70724293864769550 ) ) ;
#54903 = B_SPLINE_CURVE_WITH_KNOTS ( 'NONE', 3,
 ( #29944, #86884, #107753, #10059, #71719, #14774, #41392, #194088, #199791, #122929, #55550, #178917, #77425, #62242 ),
 .UNSPECIFIED., .F., .F.,
 ( 4, 2, 2, 2, 2, 2, 4 ),
 ( 1.970604704964099883E-07, 0.0003055224468752419631, 0.0006108478332799875199, 0.001221498606089477766, 0.001832149378898968121, 0.002137474765303713949, 0.002442800151708459776 ),
 .UNSPECIFIED. ) ;
#54904 = CARTESIAN_POINT ( 'NONE',  ( -13.89961937509957401, -13.97604488694547875, 94.37609039468566152 ) ) ;
#54905 = CARTESIAN_POINT ( 'NONE',  ( 21.52544592524344225, -5.823673210054117533, 83.54057627198102409 ) ) ;
#54906 = CARTESIAN_POINT ( 'NONE',  ( 8.224510206698953496, -14.34966873604960469, 32.91557627198102409 ) ) ;
#54907 = ORIENTED_EDGE ( 'NONE', *, *, #53692, .T. ) ;
#54908 = CARTESIAN_POINT ( 'NONE',  ( 23.64729612845681928, 13.72274676820423167, 169.8070494178799663 ) ) ;
#54909 = CARTESIAN_POINT ( 'NONE',  ( 18.62759615963271287, -10.81492255796078972, 68.33224293864769550 ) ) ;
#54910 = ORIENTED_EDGE ( 'NONE', *, *, #73347, .T. ) ;
#54911 = CARTESIAN_POINT ( 'NONE',  ( -8.224510206698735004, -14.34966873604973081, 109.5844237280190328 ) ) ;
#54912 = ORIENTED_EDGE ( 'NONE', *, *, #59429, .T. ) ;
#54913 = CARTESIAN_POINT ( 'NONE',  ( -9.687362902255793884, -9.687362902255632235, -64.92279855667830191 ) ) ;
#54914 = CARTESIAN_POINT ( 'NONE',  ( 18.67979575497178502, 10.72451020669898547, 94.16557627198103830 ) ) ;
#54915 = CARTESIAN_POINT ( 'NONE',  ( 21.55341960407610458, 5.719274019375980345, 103.9572429386476813 ) ) ;
#54916 = CARTESIAN_POINT ( 'NONE',  ( -16.52544592524342804, 4.483927247898546575, 26.04057627198103475 ) ) ;
#54917 = CARTESIAN_POINT ( 'NONE',  ( -8.224510206698735004, -14.34966873604973081, 39.58442372801901143 ) ) ;
#54918 = CARTESIAN_POINT ( 'NONE',  ( 13.97604488694527802, 13.89961937509977652, 29.37390960531435979 ) ) ;
#54919 = CARTESIAN_POINT ( 'NONE',  ( -16.46253265017160317, 9.564922557960807481, 65.83224293864769550 ) ) ;
#54920 = CARTESIAN_POINT ( 'NONE',  ( 28.82186960331498327, 9.364793116373570925, 149.0999999999999943 ) ) ;
#54921 = CARTESIAN_POINT ( 'NONE',  ( 18.62759615963271287, -10.81492255796078972, 23.33224293864769194 ) ) ;
#54922 = CARTESIAN_POINT ( 'NONE',  ( -69.65682714487590488, -71.74905178543390605, -25.00000000000000000 ) ) ;
#54923 = CARTESIAN_POINT ( 'NONE',  ( 19.02544592524334988, 5.153800228976608722, 101.4594237280189759 ) ) ;
#54924 = CARTESIAN_POINT ( 'NONE',  ( -9.474510206698720793, -16.51473224551083518, 34.58442372801899722 ) ) ;
#54925 = CARTESIAN_POINT ( 'NONE',  ( -5.719274019375978568, 21.55341960407610458, 95.20724293864769550 ) ) ;
#54926 = CARTESIAN_POINT ( 'NONE',  ( -16.55341960407617563, 4.379528057220093196, 113.5427570613523756 ) ) ;
#54927 = CARTESIAN_POINT ( 'NONE',  ( -5.719274019375978568, 21.55341960407610458, 45.20724293864769550 ) ) ;
#54929 = CARTESIAN_POINT ( 'NONE',  ( 19.02544592524334988, 5.153800228976608722, 111.4594237280190043 ) ) ;
#54928 = CARTESIAN_POINT ( 'NONE',  ( -10.81492255796078084, -18.62759615963271287, 82.08224293864768129 ) ) ;
#54930 = CARTESIAN_POINT ( 'NONE',  ( 19.02544592524343514, -5.153800228976328945, 98.54057627198100988 ) ) ;
#54931 = CARTESIAN_POINT ( 'NONE',  ( 21.55341960407619695, -5.719274019375665929, 76.04275706135237556 ) ) ;
#54932 = CARTESIAN_POINT ( 'NONE',  ( -19.03943276465977164, 0.05219959533909376836, 61.24890960531436690 ) ) ;
#54933 = AXIS2_PLACEMENT_3D ( 'NONE', #17276, #94099, #198316 ) ;
#54934 = CARTESIAN_POINT ( 'NONE',  ( 8.314922557960818139, 14.29746914071049879, 99.58224293864770971 ) ) ;
#54935 = CARTESIAN_POINT ( 'NONE',  ( 31.71835025711371259, 0.9887710624358057032, 102.4506977131440522 ) ) ;
#54936 = CARTESIAN_POINT ( 'NONE',  ( -19.05341960407611168, -5.049401038298163336, 66.45724293864769550 ) ) ;
#54937 = CARTESIAN_POINT ( 'NONE',  ( 14.34966873604960469, 8.224510206698951720, 94.16557627198103830 ) ) ;
#54938 = ORIENTED_EDGE ( 'NONE', *, *, #34762, .F. ) ;
#54939 = CARTESIAN_POINT ( 'NONE',  ( 16.46253265017146816, 9.564922557961045513, 96.66775706135233293 ) ) ;
#54940 = CARTESIAN_POINT ( 'NONE',  ( 16.38665767535050577, -7.295008042176161389, 82.76400864214542707 ) ) ;
#54941 = CARTESIAN_POINT ( 'NONE',  ( -0.05219959533909027116, -19.03943276465977164, 62.49890960531435979 ) ) ;
#54943 = CARTESIAN_POINT ( 'NONE',  ( 19.05341960407611168, 5.049401038298154454, 103.9572429386476671 ) ) ;
#54942 = CARTESIAN_POINT ( 'NONE',  ( -21.52544592524334988, -5.823673210054445271, 78.95942372801901854 ) ) ;
#54944 = CARTESIAN_POINT ( 'NONE',  ( -8.314922557961024197, 14.29746914071037800, 77.91775706135231871 ) ) ;
#54945 = CARTESIAN_POINT ( 'NONE',  ( -17.49999999999999645, -5.499999999999992895, 49.20309617465830598 ) ) ;
#54946 = CARTESIAN_POINT ( 'NONE',  ( 13.89961937509957401, 13.97604488694547697, 56.87609039468564731 ) ) ;
#54947 = CARTESIAN_POINT ( 'NONE',  ( -10.81492255796105439, 18.62759615963255655, 97.91775706135236135 ) ) ;
#54948 = CARTESIAN_POINT ( 'NONE',  ( 37.11214605083871021, 4.768680519348648339, 42.23634591622184331 ) ) ;
#54949 = CARTESIAN_POINT ( 'NONE',  ( 28.47622644277404191, -25.16156846422445881, -16.68312038616162241 ) ) ;
#54950 = CARTESIAN_POINT ( 'NONE',  ( -16.52544592524335698, -4.483927247898792601, 98.95942372801903275 ) ) ;
#54951 = CARTESIAN_POINT ( 'NONE',  ( 16.61636759701972466, -0.5040881997803988712, -59.17093420172795959 ) ) ;
#54952 = CARTESIAN_POINT ( 'NONE',  ( -14.34966873604972548, 8.224510206698743886, 88.33442372801901854 ) ) ;
#54953 = CARTESIAN_POINT ( 'NONE',  ( -3.573655867282028392E-15, 2.428612866367529932E-14, 167.9999999999999716 ) ) ;
#54954 = CARTESIAN_POINT ( 'NONE',  ( -14.34966873604972548, 8.224510206698743886, 63.33442372801900433 ) ) ;
#54955 = CARTESIAN_POINT ( 'NONE',  ( 18.09805431107246676, -5.500000000000095923, 68.51606229291886052 ) ) ;
#54956 = CARTESIAN_POINT ( 'NONE',  ( 18.62759615963255655, 10.81492255796105972, 76.66775706135234714 ) ) ;
#54957 = CARTESIAN_POINT ( 'NONE',  ( 19.03943276465977164, 0.05219959533936151252, 91.25109039468566152 ) ) ;
#54958 = CARTESIAN_POINT ( 'NONE',  ( -9.474510206698720793, -16.51473224551083518, 39.58442372801899722 ) ) ;
#54959 = CARTESIAN_POINT ( 'NONE',  ( -19.02544592524342804, 5.153800228976336051, 71.04057627198099567 ) ) ;
#54960 = CARTESIAN_POINT ( 'NONE',  ( -0.05219959533909027116, -19.03943276465977164, 57.49890960531435979 ) ) ;
#54961 = CYLINDRICAL_SURFACE ( 'NONE', #120780, 2.000000000000001776 ) ;
#54962 = CARTESIAN_POINT ( 'NONE',  ( -21.53943276465977519, 0.05219959533907696930, 86.24890960531436690 ) ) ;
#54963 = AXIS2_PLACEMENT_3D ( 'NONE', #192610, #12595, #72259 ) ;
#54964 = CARTESIAN_POINT ( 'NONE',  ( -21.52544592524343514, 5.823673210054127303, 36.04057627198102409 ) ) ;
#54965 = CARTESIAN_POINT ( 'NONE',  ( 19.03943276465977164, -0.05219959533909143690, 38.74890960531436690 ) ) ;
#54966 = CARTESIAN_POINT ( 'NONE',  ( -4.483927247898782831, 16.52544592524335698, 62.70942372801902565 ) ) ;
#54967 = ORIENTED_EDGE ( 'NONE', *, *, #17432, .T. ) ;
#54968 = ADVANCED_FACE ( 'NONE', ( #100447 ), #10459, .T. ) ;
#54969 = CARTESIAN_POINT ( 'NONE',  ( 10.72451020669871369, 18.67979575497193778, 27.08442372801901854 ) ) ;
#54971 = CARTESIAN_POINT ( 'NONE',  ( 11.40812507854754365, 35.11059874428196537, -7.224999997268813701 ) ) ;
#54970 = CARTESIAN_POINT ( 'NONE',  ( -16.55341960407611168, -4.379528057220339221, 66.45724293864768129 ) ) ;
#54972 = CARTESIAN_POINT ( 'NONE',  ( 14.29746914071037800, 8.314922557961029526, 26.66775706135235424 ) ) ;
#54973 = CARTESIAN_POINT ( 'NONE',  ( 9.474510206698729675, 16.51473224551082808, 52.08442372801900433 ) ) ;
#54974 = CARTESIAN_POINT ( 'NONE',  ( -0.05219959533910754901, -16.53943276465976808, 52.49890960531435979 ) ) ;
#54975 = CARTESIAN_POINT ( 'NONE',  ( -10.81492255796105439, 18.62759615963255655, 37.91775706135235424 ) ) ;
#54977 = CARTESIAN_POINT ( 'NONE',  ( -15.80617190586745835, -15.72974639402198527, 76.87390960531439532 ) ) ;
#54976 = CARTESIAN_POINT ( 'NONE',  ( 0.5042224564900709138, 16.61632169229824285, -59.17095462602203071 ) ) ;
#54978 = CARTESIAN_POINT ( 'NONE',  ( 5.049401038298161559, -19.05341960407611168, 97.70724293864766707 ) ) ;
#54979 = CARTESIAN_POINT ( 'NONE',  ( 16.52544592524342804, -4.483927247898539470, 73.54057627198102409 ) ) ;
#54980 = CARTESIAN_POINT ( 'NONE',  ( 34.32499373855911529, -22.49325299167919567, -18.44817765300317802 ) ) ;
#54981 = CARTESIAN_POINT ( 'NONE',  ( -37.32565804592077541, 3.633088190964871345, 40.85532123380856007 ) ) ;
#54982 = CARTESIAN_POINT ( 'NONE',  ( -13.97604488694547697, 13.89961937509957934, 63.12609039468566152 ) ) ;
#54983 = CARTESIAN_POINT ( 'NONE',  ( 10.72451020669898902, -18.67979575497178502, 102.9155762719810383 ) ) ;
#54984 = CARTESIAN_POINT ( 'NONE',  ( 9.474510206698971260, -16.51473224551069308, 57.91557627198103120 ) ) ;
#54985 = CARTESIAN_POINT ( 'NONE',  ( 19.05341960407617918, -5.049401038297876454, 41.04275706135233293 ) ) ;
#54986 = CARTESIAN_POINT ( 'NONE',  ( -19.05341960407611168, -5.049401038298163336, 36.45724293864766707 ) ) ;
#54987 = CARTESIAN_POINT ( 'NONE',  ( -10.81492255796105439, 18.62759615963255655, 57.91775706135234714 ) ) ;
#54988 = CARTESIAN_POINT ( 'NONE',  ( -16.81555441253552274, -7.025013491695476731, 69.36314554665744936 ) ) ;
#54989 = CARTESIAN_POINT ( 'NONE',  ( 16.52544592524342804, -4.483927247898539470, 43.54057627198103830 ) ) ;
#54990 = CARTESIAN_POINT ( 'NONE',  ( -5.153800228976328057, -19.02544592524343514, 57.29057627198103120 ) ) ;
#54991 = CARTESIAN_POINT ( 'NONE',  ( 18.67979575497178502, 10.72451020669898547, 84.16557627198103830 ) ) ;
#54992 = CARTESIAN_POINT ( 'NONE',  ( 13.89961937509977652, -13.97604488694527269, 58.12390960531436690 ) ) ;
#54993 = ORIENTED_EDGE ( 'NONE', *, *, #163633, .T. ) ;
#54994 = CARTESIAN_POINT ( 'NONE',  ( 10.72451020669898902, -18.67979575497178502, 72.91557627198103830 ) ) ;
#54995 = CARTESIAN_POINT ( 'NONE',  ( -15.80617190586768217, 15.72974639402176855, 98.12609039468570415 ) ) ;
#54998 = CARTESIAN_POINT ( 'NONE',  ( -12.14591786802309592, -12.06949235617757132, 86.87390960531438111 ) ) ;
#54997 = CARTESIAN_POINT ( 'NONE',  ( 12.14591786802327356, -12.06949235617739191, 90.62609039468567573 ) ) ;
#54996 = CARTESIAN_POINT ( 'NONE',  ( -13.89961937509977652, 13.97604488694528158, 25.62390960531434558 ) ) ;
#54999 = CARTESIAN_POINT ( 'NONE',  ( 13.89961937509957401, 13.97604488694547697, 96.87609039468566152 ) ) ;
#55000 = VERTEX_POINT ( 'NONE', #146962 ) ;
#55001 = CARTESIAN_POINT ( 'NONE',  ( 13.97604488694548053, -13.89961937509957401, 40.62609039468564731 ) ) ;
#55002 = CARTESIAN_POINT ( 'NONE',  ( 14.34966873604972726, -8.224510206698740333, 95.83442372801903275 ) ) ;
#55003 = CARTESIAN_POINT ( 'NONE',  ( -9.474510206698720793, -16.51473224551083518, 34.58442372801899722 ) ) ;
#55004 = CARTESIAN_POINT ( 'NONE',  ( -5.049401038298153566, 19.05341960407611168, 85.20724293864766707 ) ) ;
#55005 = CARTESIAN_POINT ( 'NONE',  ( 15.80617190586746368, 15.72974639402197994, 64.37390960531435269 ) ) ;
#55006 = CARTESIAN_POINT ( 'NONE',  ( -19.30190589895974185, 21.36759865781276346, 139.9999999999999716 ) ) ;
#55007 = CARTESIAN_POINT ( 'NONE',  ( 8.314922557960818139, 14.29746914071049879, 114.5822429386477097 ) ) ;
#55008 = CARTESIAN_POINT ( 'NONE',  ( -21.55341960407619339, 5.719274019375674811, 98.54275706135234714 ) ) ;
#55009 = CARTESIAN_POINT ( 'NONE',  ( -8.314922557961024197, 14.29746914071037800, 72.91775706135234714 ) ) ;
#55010 = CARTESIAN_POINT ( 'NONE',  ( -15.72974639402176322, -15.80617190586768395, 34.37609039468568284 ) ) ;
#55011 = CARTESIAN_POINT ( 'NONE',  ( -8.224510206698735004, -14.34966873604973081, 34.58442372801900433 ) ) ;
#55012 = CARTESIAN_POINT ( 'NONE',  ( 19.02544592524343514, -5.153800228976328945, 98.54057627198100988 ) ) ;
#55013 = CARTESIAN_POINT ( 'NONE',  ( -9.474510206698964154, 16.51473224551069663, 35.41557627198102409 ) ) ;
#55014 = CARTESIAN_POINT ( 'NONE',  ( -16.46253265017160317, 9.564922557960807481, 60.83224293864769550 ) ) ;
#55015 = CARTESIAN_POINT ( 'NONE',  ( -16.55341960407617563, 4.379528057220093196, 43.54275706135235424 ) ) ;
#55016 = CARTESIAN_POINT ( 'NONE',  ( 14.29746914071049879, -8.314922557960816363, 93.33224293864769550 ) ) ;
#55017 = CARTESIAN_POINT ( 'NONE',  ( -12.06949235617739369, -12.14591786802326823, 94.37609039468568994 ) ) ;
#55020 = CARTESIAN_POINT ( 'NONE',  ( -13.97604488694527625, -13.89961937509977652, 66.87390960531436690 ) ) ;
#55019 = CARTESIAN_POINT ( 'NONE',  ( -5.153800228976328057, -19.02544592524343514, 72.29057627198102409 ) ) ;
#55018 = CARTESIAN_POINT ( 'NONE',  ( -21.55341960407619339, 5.719274019375674811, 38.54275706135234714 ) ) ;
#55021 = CARTESIAN_POINT ( 'NONE',  ( 5.153800228976335163, 19.02544592524342804, 94.79057627198103830 ) ) ;
#55022 = CARTESIAN_POINT ( 'NONE',  ( -4.379528057220328563, 16.55341960407611168, 30.20724293864769550 ) ) ;
#55023 = CARTESIAN_POINT ( 'NONE',  ( -16.55341960407617563, 4.379528057220093196, 98.54275706135234714 ) ) ;
#55024 = ORIENTED_EDGE ( 'NONE', *, *, #26552, .T. ) ;
#55025 = CARTESIAN_POINT ( 'NONE',  ( 13.97604488694548053, -13.89961937509957401, 40.62609039468564731 ) ) ;
#55026 = DIRECTION ( 'NONE',  ( -0.000000000000000000, -0.000000000000000000, 1.000000000000000000 ) ) ;
#55027 = CARTESIAN_POINT ( 'NONE',  ( 19.03943276465977164, -0.05219959533909143690, 58.74890960531435979 ) ) ;
#55028 = CARTESIAN_POINT ( 'NONE',  ( 9.474510206698729675, 16.51473224551082808, 42.08442372801900433 ) ) ;
#55029 = CARTESIAN_POINT ( 'NONE',  ( 3.556970738554033499E-15, -38.81732327939057825, -4.124999997268814056 ) ) ;
#55030 = CARTESIAN_POINT ( 'NONE',  ( 19.52217212775661537, -5.499999999999910294, 72.43993709005259518 ) ) ;
#55031 = CARTESIAN_POINT ( 'NONE',  ( 14.34966873604972726, -8.224510206698740333, 45.83442372801901854 ) ) ;
#55033 = CARTESIAN_POINT ( 'NONE',  ( 16.52544592524335698, 4.483927247898782831, 61.45942372801901854 ) ) ;
#55032 = CARTESIAN_POINT ( 'NONE',  ( 16.46253265017146816, 9.564922557961045513, 76.66775706135234714 ) ) ;
#55034 = CARTESIAN_POINT ( 'NONE',  ( -11.80868324581545714, -11.80868324581525997, -59.13370768023891344 ) ) ;
#55035 = CARTESIAN_POINT ( 'NONE',  ( 13.89961937509977652, -13.97604488694527269, 93.12390960531436690 ) ) ;
#55036 = CARTESIAN_POINT ( 'NONE',  ( -10.81492255796078084, -18.62759615963271287, 107.0822429386476955 ) ) ;
#55037 = CARTESIAN_POINT ( 'NONE',  ( -13.97604488694547697, 13.89961937509957934, 73.12609039468568994 ) ) ;
#55039 = CARTESIAN_POINT ( 'NONE',  ( 16.46253265017160672, -9.564922557960803928, 28.33224293864769550 ) ) ;
#55038 = CARTESIAN_POINT ( 'NONE',  ( -19.02544592524342804, 5.153800228976336051, 101.0405762719810241 ) ) ;
#55040 = CARTESIAN_POINT ( 'NONE',  ( -9.564922557960796823, -16.46253265017161027, 72.08224293864770971 ) ) ;
#55042 = CARTESIAN_POINT ( 'NONE',  ( -16.51473224551069308, -9.474510206698971260, 36.66557627198102409 ) ) ;
#55041 = CARTESIAN_POINT ( 'NONE',  ( 12.14591786802309770, 12.06949235617756955, 54.37390960531435979 ) ) ;
#55043 = CARTESIAN_POINT ( 'NONE',  ( -9.564922557961040184, 16.46253265017147172, 57.91775706135233293 ) ) ;
#55044 = CARTESIAN_POINT ( 'NONE',  ( -14.29746914071049879, 8.314922557960819915, 85.83224293864768129 ) ) ;
#55045 = CARTESIAN_POINT ( 'NONE',  ( 21.52544592524334988, 5.823673210054432836, 106.4594237280190328 ) ) ;
#55046 = CARTESIAN_POINT ( 'NONE',  ( 19.02544592524343514, -5.153800228976328945, 53.54057627198102409 ) ) ;
#55047 = CARTESIAN_POINT ( 'NONE',  ( -21.52544592524343514, 5.823673210054127303, 56.04057627198102409 ) ) ;
#55049 = CARTESIAN_POINT ( 'NONE',  ( 16.46253265017146816, 9.564922557961045513, 21.66775706135233648 ) ) ;
#55048 = CARTESIAN_POINT ( 'NONE',  ( 16.52544592524342804, -4.483927247898539470, 53.54057627198103120 ) ) ;
#55050 = CARTESIAN_POINT ( 'NONE',  ( 5.153800228976335163, 19.02544592524342804, 109.7905762719810099 ) ) ;
#55051 = CARTESIAN_POINT ( 'NONE',  ( 5.049401038298161559, -19.05341960407611168, 102.7072429386476955 ) ) ;
#55052 = CARTESIAN_POINT ( 'NONE',  ( 5.049401038298161559, -19.05341960407611168, 37.70724293864768839 ) ) ;
#55053 = CARTESIAN_POINT ( 'NONE',  ( 5.049401038298161559, -19.05341960407611168, 27.70724293864769550 ) ) ;
#55054 = CARTESIAN_POINT ( 'NONE',  ( 16.53943276465976808, -0.05219959533910856209, 83.74890960531435269 ) ) ;
#55055 = CARTESIAN_POINT ( 'NONE',  ( -21.53943276465977519, 0.05219959533907696930, 91.24890960531436690 ) ) ;
#55056 = CARTESIAN_POINT ( 'NONE',  ( -9.474510206698964154, 16.51473224551069663, 100.4155762719810241 ) ) ;
#55057 = CARTESIAN_POINT ( 'NONE',  ( -18.62759615963270932, 10.81492255796079327, 110.8322429386476955 ) ) ;
#55058 = CARTESIAN_POINT ( 'NONE',  ( -19.02544592524342804, 5.153800228976336051, 106.0405762719810241 ) ) ;
#55059 = CARTESIAN_POINT ( 'NONE',  ( 8.314922557960818139, 14.29746914071049879, 109.5822429386476955 ) ) ;
#55060 = CARTESIAN_POINT ( 'NONE',  ( -13.97604488694527625, -13.89961937509977652, 66.87390960531436690 ) ) ;
#55061 = CARTESIAN_POINT ( 'NONE',  ( 5.719274019375991003, -21.55341960407610458, 82.70724293864770971 ) ) ;
#55062 = CARTESIAN_POINT ( 'NONE',  ( 16.18388926212238133, -7.379444403734507496, 107.0604684863384790 ) ) ;
#55063 = CARTESIAN_POINT ( 'NONE',  ( 2.500000000000000000, -1.178949249685214307, 2.042000000000002036 ) ) ;
#55065 = CARTESIAN_POINT ( 'NONE',  ( 3.181980515339539295, 6.791538853603031889, 1.110912703473986074 ) ) ;
#55064 = CARTESIAN_POINT ( 'NONE',  ( 15.80617190586746368, 15.72974639402197994, 24.37390960531435979 ) ) ;
#55066 = CARTESIAN_POINT ( 'NONE',  ( -4.379528057220086978, -16.55341960407618274, 29.79275706135234358 ) ) ;
#55067 = EDGE_CURVE ( 'NONE', #55466, #171824, #141238, .T. ) ;
#55068 = CARTESIAN_POINT ( 'NONE',  ( 0.05219959533910956823, 16.53943276465976808, 99.99890960531436690 ) ) ;
#55069 = CARTESIAN_POINT ( 'NONE',  ( -17.49999999999999289, -3.565345528327926505, 110.5750551319352866 ) ) ;
#55070 = CARTESIAN_POINT ( 'NONE',  ( -16.51473224551069308, -9.474510206698971260, 61.66557627198103120 ) ) ;
#55071 = CARTESIAN_POINT ( 'NONE',  ( 14.29746914071049879, -8.314922557960816363, 83.33224293864769550 ) ) ;
#55072 = CARTESIAN_POINT ( 'NONE',  ( -5.823673210054116645, -21.52544592524344225, 37.29057627198102409 ) ) ;
#55073 = CARTESIAN_POINT ( 'NONE',  ( -14.29746914071049879, 8.314922557960819915, 70.83224293864770971 ) ) ;
#55074 = CARTESIAN_POINT ( 'NONE',  ( 14.29746914071037800, 8.314922557961029526, 21.66775706135235069 ) ) ;
#55075 = CARTESIAN_POINT ( 'NONE',  ( -0.05219959533937732626, 21.53943276465977519, 72.50109039468568994 ) ) ;
#55076 = CARTESIAN_POINT ( 'NONE',  ( 27.73933785331498569, 2.768321779492822058E-14, 145.8750000027311842 ) ) ;
#55077 = CARTESIAN_POINT ( 'NONE',  ( 5.153800228976335163, 19.02544592524342804, 114.7905762719810241 ) ) ;
#55078 = CARTESIAN_POINT ( 'NONE',  ( -14.29746914071037622, -8.314922557961029526, 79.16775706135234714 ) ) ;
#55079 = CARTESIAN_POINT ( 'NONE',  ( -13.89961937509977652, 13.97604488694528158, 25.62390960531434558 ) ) ;
#55080 = CARTESIAN_POINT ( 'NONE',  ( -0.05219959533909027116, -19.03943276465977164, 87.49890960531436690 ) ) ;
#55081 = CARTESIAN_POINT ( 'NONE',  ( 18.62759615963271287, -10.81492255796078972, 98.33224293864769550 ) ) ;
#55082 = CARTESIAN_POINT ( 'NONE',  ( -16.55341960407617563, 4.379528057220093196, 23.54275706135235424 ) ) ;
#55084 = CARTESIAN_POINT ( 'NONE',  ( -15.72974639402176322, -15.80617190586768395, 74.37609039468568994 ) ) ;
#55083 = CARTESIAN_POINT ( 'NONE',  ( 16.52544592524342804, -4.483927247898539470, 53.54057627198103120 ) ) ;
#55085 = CARTESIAN_POINT ( 'NONE',  ( 16.52544592524335698, 4.483927247898782831, 101.4594237280190185 ) ) ;
#55086 = CARTESIAN_POINT ( 'NONE',  ( 23.64874990377914799, 15.04272038711346049, 165.8682408883346397 ) ) ;
#55087 = CARTESIAN_POINT ( 'NONE',  ( -16.31925111598456368, 7.325300261831604764, 80.16424538967254421 ) ) ;
#55088 = CARTESIAN_POINT ( 'NONE',  ( 16.55341960407618274, -4.379528057220086978, 111.0427570613523613 ) ) ;
#55089 = CARTESIAN_POINT ( 'NONE',  ( -12.06949235617739369, -12.14591786802326823, 54.37609039468568994 ) ) ;
#55090 = CARTESIAN_POINT ( 'NONE',  ( -0.05219959533909027116, -19.03943276465977164, 67.49890960531436690 ) ) ;
#55091 = CARTESIAN_POINT ( 'NONE',  ( -9.564922557960796823, -16.46253265017161027, 92.08224293864769550 ) ) ;
#55092 = CARTESIAN_POINT ( 'NONE',  ( -5.719274019375665041, -21.55341960407619695, 69.79275706135234714 ) ) ;
#55093 = EDGE_CURVE ( 'NONE', #140931, #145198, #174904, .T. ) ;
#55094 = CARTESIAN_POINT ( 'NONE',  ( 14.34966873604972726, -8.224510206698740333, 80.83442372801901854 ) ) ;
#55095 = CARTESIAN_POINT ( 'NONE',  ( 8.314922557960818139, 14.29746914071049879, 64.58224293864769550 ) ) ;
#55096 = CARTESIAN_POINT ( 'NONE',  ( 9.564922557960805705, 16.46253265017160317, 49.58224293864770260 ) ) ;
#55097 = ORIENTED_EDGE ( 'NONE', *, *, #149178, .F. ) ;
#55098 = CARTESIAN_POINT ( 'NONE',  ( -8.224510206698735004, -14.34966873604973081, 19.58442372801901143 ) ) ;
#55099 = CARTESIAN_POINT ( 'NONE',  ( 12.06949235617757843, -12.14591786802309237, 113.1239096053143953 ) ) ;
#55100 = CARTESIAN_POINT ( 'NONE',  ( -9.564922557960796823, -16.46253265017161027, 77.08224293864769550 ) ) ;
#55102 = CARTESIAN_POINT ( 'NONE',  ( 37.99999999999999289, 2.893978650043524126E-14, -7.000000000000000000 ) ) ;
#55101 = CARTESIAN_POINT ( 'NONE',  ( -19.05341960407617563, 5.049401038297882671, 98.54275706135233293 ) ) ;
#55103 = CARTESIAN_POINT ( 'NONE',  ( -18.67979575497193778, 10.72451020669871902, 108.3344237280190185 ) ) ;
#55104 = CARTESIAN_POINT ( 'NONE',  ( 8.314922557961029526, -14.29746914071037800, 75.41775706135233293 ) ) ;
#55105 = CARTESIAN_POINT ( 'NONE',  ( -9.564922557961040184, 16.46253265017147172, 92.91775706135233293 ) ) ;
#55106 = CARTESIAN_POINT ( 'NONE',  ( -5.823673210054116645, -21.52544592524344225, 57.29057627198103120 ) ) ;
#55107 = CARTESIAN_POINT ( 'NONE',  ( -8.314922557961024197, 14.29746914071037800, 67.91775706135234714 ) ) ;
#55108 = CARTESIAN_POINT ( 'NONE',  ( 0.000000000000000000, 0.000000000000000000, 0.000000000000000000 ) ) ;
#55109 = CARTESIAN_POINT ( 'NONE',  ( 19.03943276465977164, 0.05219959533936151252, 56.25109039468566863 ) ) ;
#55110 = CARTESIAN_POINT ( 'NONE',  ( -5.719274019375665041, -21.55341960407619695, 99.79275706135234714 ) ) ;
#55111 = CARTESIAN_POINT ( 'NONE',  ( -16.51473224551069308, -9.474510206698971260, 31.66557627198102054 ) ) ;
#55112 = CARTESIAN_POINT ( 'NONE',  ( 19.03943276465977164, -0.05219959533909143690, 63.74890960531435979 ) ) ;
#55113 = CARTESIAN_POINT ( 'NONE',  ( -14.34966873604960291, -8.224510206698953496, 71.66557627198100988 ) ) ;
#55114 = VECTOR ( 'NONE', #28278, 1000.000000000000000 ) ;
#55115 = CARTESIAN_POINT ( 'NONE',  ( 21.55341960407619695, -5.719274019375665929, 91.04275706135236135 ) ) ;
#55116 = CARTESIAN_POINT ( 'NONE',  ( -13.89961937509957401, -13.97604488694547875, 49.37609039468567573 ) ) ;
#55117 = CARTESIAN_POINT ( 'NONE',  ( 19.05341960407617918, -5.049401038297876454, 41.04275706135233293 ) ) ;
#55118 = CARTESIAN_POINT ( 'NONE',  ( -21.52544592524343514, 5.823673210054127303, 36.04057627198102409 ) ) ;
#55119 = CARTESIAN_POINT ( 'NONE',  ( 10.72451020669871369, 18.67979575497193778, 97.08442372801904696 ) ) ;
#55120 = CARTESIAN_POINT ( 'NONE',  ( -19.02544592524342804, 5.153800228976336051, 76.04057627198102409 ) ) ;
#55121 = CARTESIAN_POINT ( 'NONE',  ( 18.62759615963255655, 10.81492255796105972, 96.66775706135234714 ) ) ;
#55122 = CARTESIAN_POINT ( 'NONE',  ( -21.52544592524343514, 5.823673210054127303, 56.04057627198102409 ) ) ;
#55123 = CARTESIAN_POINT ( 'NONE',  ( -0.05219959533909027116, -19.03943276465977164, 87.49890960531436690 ) ) ;
#55124 = CARTESIAN_POINT ( 'NONE',  ( 13.89961937509957401, 13.97604488694547697, 76.87609039468566152 ) ) ;
#55125 = CARTESIAN_POINT ( 'NONE',  ( 16.51473224551069308, 9.474510206698969483, 94.16557627198103830 ) ) ;
#55126 = CARTESIAN_POINT ( 'NONE',  ( -13.89961937509957401, -13.97604488694547875, 99.37609039468567573 ) ) ;
#55127 = CARTESIAN_POINT ( 'NONE',  ( -14.29746914071037622, -8.314922557961029526, 49.16775706135234003 ) ) ;
#55128 = CARTESIAN_POINT ( 'NONE',  ( -0.05219959533910754901, -16.53943276465976808, 102.4989096053143811 ) ) ;
#55129 = CARTESIAN_POINT ( 'NONE',  ( 9.564922557960805705, 16.46253265017160317, 64.58224293864769550 ) ) ;
#55130 = CARTESIAN_POINT ( 'NONE',  ( -15.72974639402197994, 15.80617190586746368, 60.62390960531437401 ) ) ;
#55131 = CARTESIAN_POINT ( 'NONE',  ( -0.05219959533934338120, 16.53943276465976808, 37.50109039468568284 ) ) ;
#55132 = CARTESIAN_POINT ( 'NONE',  ( 10.72451020669871369, 18.67979575497193778, 32.08442372801901854 ) ) ;
#55133 = CARTESIAN_POINT ( 'NONE',  ( -10.72451020669870658, -18.67979575497194134, 84.58442372801903275 ) ) ;
#55134 = CARTESIAN_POINT ( 'NONE',  ( 8.224510206698742110, 14.34966873604972548, 87.08442372801901854 ) ) ;
#55135 = CARTESIAN_POINT ( 'NONE',  ( 5.153800228976335163, 19.02544592524342804, 74.79057627198103830 ) ) ;
#55136 = CARTESIAN_POINT ( 'NONE',  ( 8.224510206698953496, -14.34966873604960469, 77.91557627198102409 ) ) ;
#55137 = CARTESIAN_POINT ( 'NONE',  ( -16.53943276465976808, -0.05219959533934237506, 108.7510903946857042 ) ) ;
#55138 = CARTESIAN_POINT ( 'NONE',  ( -9.474510206698720793, -16.51473224551083518, 59.58442372801900433 ) ) ;
#55139 = CARTESIAN_POINT ( 'NONE',  ( 0.05219959533937995610, -21.53943276465977519, 25.00109039468567218 ) ) ;
#55140 = CARTESIAN_POINT ( 'NONE',  ( 14.34966873604960469, 8.224510206698951720, 79.16557627198103830 ) ) ;
#55141 = CARTESIAN_POINT ( 'NONE',  ( 19.03943276465977164, -0.05219959533909143690, 103.7489096053143669 ) ) ;
#55142 = CARTESIAN_POINT ( 'NONE',  ( 14.34966873604972726, -8.224510206698740333, 100.8344237280190185 ) ) ;
#55143 = CARTESIAN_POINT ( 'NONE',  ( -21.53943276465977519, -0.05219959533937600094, 78.75109039468568994 ) ) ;
#55144 = CARTESIAN_POINT ( 'NONE',  ( -4.379528057220086978, -16.55341960407618274, 39.79275706135235424 ) ) ;
#55145 = CARTESIAN_POINT ( 'NONE',  ( -21.53943276465977519, -0.05219959533937600094, 33.75109039468568284 ) ) ;
#55146 = CARTESIAN_POINT ( 'NONE',  ( -14.34966873604960291, -8.224510206698953496, 71.66557627198100988 ) ) ;
#55147 = ORIENTED_EDGE ( 'NONE', *, *, #92301, .T. ) ;
#55148 = CARTESIAN_POINT ( 'NONE',  ( 5.823673210054125526, 21.52544592524343514, 109.7905762719810383 ) ) ;
#55149 = CARTESIAN_POINT ( 'NONE',  ( 0.000000000000000000, -64.82615989628266107, -23.00000000000000000 ) ) ;
#55150 = CARTESIAN_POINT ( 'NONE',  ( 16.55341960407611168, 4.379528057220329451, 58.95724293864770971 ) ) ;
#55151 = CARTESIAN_POINT ( 'NONE',  ( -30.00000000000000000, -5.510910596163089556E-15, 45.00000000000000000 ) ) ;
#55152 = CARTESIAN_POINT ( 'NONE',  ( 21.55341960407610458, 5.719274019375980345, 33.95724293864769550 ) ) ;
#55153 = CARTESIAN_POINT ( 'NONE',  ( 16.52544592524342804, -4.483927247898539470, 73.54057627198102409 ) ) ;
#55154 = CARTESIAN_POINT ( 'NONE',  ( -18.62759615963270932, 10.81492255796079327, 85.83224293864768129 ) ) ;
#55155 = CARTESIAN_POINT ( 'NONE',  ( 13.89961937509977652, -13.97604488694527269, 73.12390960531436690 ) ) ;
#55157 = CARTESIAN_POINT ( 'NONE',  ( -19.05341960407617563, 5.049401038297882671, 78.54275706135233293 ) ) ;
#55156 = CARTESIAN_POINT ( 'NONE',  ( 16.46253265017160672, -9.564922557960803928, 38.33224293864768839 ) ) ;
#55159 = CARTESIAN_POINT ( 'NONE',  ( -18.67979575497178146, -10.72451020669898902, 56.66557627198103830 ) ) ;
#55158 = CARTESIAN_POINT ( 'NONE',  ( 18.62759615963255655, 10.81492255796105972, 56.66775706135235424 ) ) ;
#55160 = CARTESIAN_POINT ( 'NONE',  ( -19.02544592524342804, 5.153800228976336051, 46.04057627198101699 ) ) ;
#55161 = CARTESIAN_POINT ( 'NONE',  ( 13.89961937509977652, -13.97604488694527269, 68.12390960531436690 ) ) ;
#55162 = ORIENTED_EDGE ( 'NONE', *, *, #48777, .F. ) ;
#55163 = CARTESIAN_POINT ( 'NONE',  ( -4.483927247898782831, 16.52544592524335698, 52.70942372801902565 ) ) ;
#55164 = CARTESIAN_POINT ( 'NONE',  ( -21.53943276465977519, -0.05219959533937600094, 33.75109039468568284 ) ) ;
#55165 = CARTESIAN_POINT ( 'NONE',  ( 0.05219959533937995610, -21.53943276465977519, 60.00109039468568284 ) ) ;
#55166 = CARTESIAN_POINT ( 'NONE',  ( -13.89961937509977652, 13.97604488694528158, 110.6239096053143243 ) ) ;
#55167 = CARTESIAN_POINT ( 'NONE',  ( 15.80617190586746368, 15.72974639402197994, 84.37390960531438111 ) ) ;
#55169 = CARTESIAN_POINT ( 'NONE',  ( 14.34966873604972726, -8.224510206698740333, 50.83442372801901143 ) ) ;
#55168 = CARTESIAN_POINT ( 'NONE',  ( 21.55341960407619695, -5.719274019375665929, 21.04275706135234714 ) ) ;
#55170 = ADVANCED_FACE ( 'NONE', ( #197466 ), #198450, .F. ) ;
#55171 = CARTESIAN_POINT ( 'NONE',  ( 10.81492255796078972, 18.62759615963270932, 44.58224293864769550 ) ) ;
#55172 = CARTESIAN_POINT ( 'NONE',  ( 16.51473224551083163, -9.474510206698727899, 20.83442372801899722 ) ) ;
#55173 = CARTESIAN_POINT ( 'NONE',  ( -13.97604488694527625, -13.89961937509977652, 51.87390960531436690 ) ) ;
#55174 = CARTESIAN_POINT ( 'NONE',  ( -5.049401038298153566, 19.05341960407611168, 115.2072429386477097 ) ) ;
#55175 = B_SPLINE_CURVE_WITH_KNOTS ( 'NONE', 3,
 ( #4838, #190873, #128188, #113022, #193883, #58350, #101854, #86681, #136188, #196884, #59330, #43184, #87680, #27038, #165541, #135212, #12858, #120018, #121000, #181703, #88684, #74523, #73539, #104853, #42199, #197863, #57369, #182698, #28040, #44183, #103860, #119042 ),
 .UNSPECIFIED., .F., .F.,
 ( 4, 2, 2, 2, 2, 2, 2, 2, 2, 2, 2, 2, 2, 2, 2, 4 ),
 ( 2.711112516444420852E-17, 0.0003712461730036841758, 0.0007424923460073412466, 0.001113738519010998426, 0.001484984692014655388, 0.002227477038021976469, 0.002598723211025651212, 0.002969969384029325955, 0.003341215557033000699, 0.003712461730036675876, 0.004083707903040349751, 0.004454954076044024928, 0.004826200249047700105, 0.005197446422051375282, 0.005568692595055049592, 0.005939938768058724769 ),
 .UNSPECIFIED. ) ;
#55176 = CARTESIAN_POINT ( 'NONE',  ( -0.05219959533909027116, -19.03943276465977164, 87.49890960531436690 ) ) ;
#55177 = CARTESIAN_POINT ( 'NONE',  ( 17.50000000000005329, 3.438020150447535173, 102.9915581553581063 ) ) ;
#55178 = CARTESIAN_POINT ( 'NONE',  ( -9.474510206698720793, -16.51473224551083518, 74.58442372801900433 ) ) ;
#55179 = CARTESIAN_POINT ( 'NONE',  ( -15.72974639402197994, 15.80617190586746368, 45.62390960531436690 ) ) ;
#55180 = CARTESIAN_POINT ( 'NONE',  ( -16.53943276465976808, 0.05219959533911058130, 31.24890960531435979 ) ) ;
#55181 = CARTESIAN_POINT ( 'NONE',  ( 19.03943276465977164, 0.05219959533936151252, 91.25109039468566152 ) ) ;
#55182 = CARTESIAN_POINT ( 'NONE',  ( 5.049401038298161559, -19.05341960407611168, 22.70724293864769194 ) ) ;
#55183 = CARTESIAN_POINT ( 'NONE',  ( -0.05219959533937732626, 21.53943276465977519, 112.5010903946857042 ) ) ;
#55184 = CARTESIAN_POINT ( 'NONE',  ( -19.03943276465977164, -0.05219959533935918106, 93.75109039468566152 ) ) ;
#55185 = CARTESIAN_POINT ( 'NONE',  ( 9.564922557961047289, -16.46253265017146816, 45.41775706135232582 ) ) ;
#55186 = CARTESIAN_POINT ( 'NONE',  ( 17.40805194822032220, 6.112264579159320199, 106.6662872748939037 ) ) ;
#55187 = CARTESIAN_POINT ( 'NONE',  ( -9.474510206698964154, 16.51473224551069663, 50.41557627198102409 ) ) ;
#55188 = CARTESIAN_POINT ( 'NONE',  ( 8.314922557960818139, 14.29746914071049879, 69.58224293864769550 ) ) ;
#55189 = CARTESIAN_POINT ( 'NONE',  ( 19.05341960407611168, 5.049401038298154454, 33.95724293864769550 ) ) ;
#55190 = CARTESIAN_POINT ( 'NONE',  ( 12.14591786802309770, 12.06949235617756955, 34.37390960531435979 ) ) ;
#55191 = DIRECTION ( 'NONE',  ( -0.000000000000000000, -0.000000000000000000, 1.000000000000000000 ) ) ;
#55192 = CARTESIAN_POINT ( 'NONE',  ( 4.483927247898790824, -16.52544592524335698, 110.2094237280190185 ) ) ;
#55193 = CARTESIAN_POINT ( 'NONE',  ( -0.05219959533909027116, -19.03943276465977164, 57.49890960531435979 ) ) ;
#55194 = CARTESIAN_POINT ( 'NONE',  ( -9.474510206698720793, -16.51473224551083518, 19.58442372801899722 ) ) ;
#55195 = CARTESIAN_POINT ( 'NONE',  ( 8.314922557961029526, -14.29746914071037800, 35.41775706135234003 ) ) ;
#55196 = CARTESIAN_POINT ( 'NONE',  ( 10.72451020669898902, -18.67979575497178502, 42.91557627198103120 ) ) ;
#55198 = VERTEX_POINT ( 'NONE', #151944 ) ;
#55197 = CARTESIAN_POINT ( 'NONE',  ( -0.05219959533937732626, 21.53943276465977519, 102.5010903946856899 ) ) ;
#55199 = CARTESIAN_POINT ( 'NONE',  ( -13.97604488694527625, -13.89961937509977652, 66.87390960531436690 ) ) ;
#55200 = CARTESIAN_POINT ( 'NONE',  ( 5.049401038298161559, -19.05341960407611168, 102.7072429386476955 ) ) ;
#55201 = CARTESIAN_POINT ( 'NONE',  ( 13.97604488694527802, 13.89961937509977652, 94.37390960531436690 ) ) ;
#55202 = CARTESIAN_POINT ( 'NONE',  ( -36.91746825000000598, -11.99521256947794789, -4.524999997268813523 ) ) ;
#55203 = CARTESIAN_POINT ( 'NONE',  ( 21.52544592524334988, 5.823673210054432836, 31.45942372801901854 ) ) ;
#55204 = CARTESIAN_POINT ( 'NONE',  ( -14.29746914071049879, 8.314922557960819915, 90.83224293864769550 ) ) ;
#55206 = CARTESIAN_POINT ( 'NONE',  ( 19.02544592524343514, -5.153800228976328945, 63.54057627198103830 ) ) ;
#55205 = CARTESIAN_POINT ( 'NONE',  ( -0.05219959533907301413, -21.53943276465977519, 82.49890960531436690 ) ) ;
#55207 = CARTESIAN_POINT ( 'NONE',  ( -13.97604488694527625, -13.89961937509977652, 66.87390960531436690 ) ) ;
#55208 = CARTESIAN_POINT ( 'NONE',  ( 5.719274019375991003, -21.55341960407610458, 107.7072429386476955 ) ) ;
#55209 = ORIENTED_EDGE ( 'NONE', *, *, #149359, .T. ) ;
#55210 = CARTESIAN_POINT ( 'NONE',  ( 9.564922557960805705, 16.46253265017160317, 79.58224293864769550 ) ) ;
#55211 = FACE_OUTER_BOUND ( 'NONE', #139325, .T. ) ;
#55213 = CARTESIAN_POINT ( 'NONE',  ( -12.73749492396214578, -155.7167183371837496, -23.00000000000000000 ) ) ;
#55212 = CARTESIAN_POINT ( 'NONE',  ( 4.483927247898545687, 16.52544592524342804, 104.7905762719810241 ) ) ;
#55214 = CARTESIAN_POINT ( 'NONE',  ( -0.05219959533909027116, -19.03943276465977164, 67.49890960531436690 ) ) ;
#55215 = CARTESIAN_POINT ( 'NONE',  ( 19.03943276465977164, 0.05219959533936151252, 91.25109039468566152 ) ) ;
#55216 = CARTESIAN_POINT ( 'NONE',  ( 16.55341960407611168, 4.379528057220329451, 93.95724293864770971 ) ) ;
#55217 = CARTESIAN_POINT ( 'NONE',  ( -21.55341960407619339, 5.719274019375674811, 78.54275706135236135 ) ) ;
#55219 = CARTESIAN_POINT ( 'NONE',  ( -18.62759615963255300, -10.81492255796106328, 24.16775706135235424 ) ) ;
#55218 = CARTESIAN_POINT ( 'NONE',  ( -16.51473224551069308, -9.474510206698971260, 46.66557627198102409 ) ) ;
#55220 = CARTESIAN_POINT ( 'NONE',  ( -5.823673210054116645, -21.52544592524344225, 112.2905762719810241 ) ) ;
#55221 = CARTESIAN_POINT ( 'NONE',  ( -28.82186960331499392, -9.364793116373526516, 140.0999999999999943 ) ) ;
#55222 = CARTESIAN_POINT ( 'NONE',  ( -19.05341960407611168, -5.049401038298163336, 66.45724293864769550 ) ) ;
#55223 = CARTESIAN_POINT ( 'NONE',  ( 17.50000000000000000, 5.499999999999997335, 111.7030961746582847 ) ) ;
#55225 = CARTESIAN_POINT ( 'NONE',  ( 5.823673210054125526, 21.52544592524343514, 29.79057627198102409 ) ) ;
#55224 = CARTESIAN_POINT ( 'NONE',  ( -13.97604488694547697, 13.89961937509957934, 103.1260903946856473 ) ) ;
#55226 = CARTESIAN_POINT ( 'NONE',  ( 21.52544592524334988, 5.823673210054432836, 61.45942372801901854 ) ) ;
#55227 = CARTESIAN_POINT ( 'NONE',  ( -5.049401038298153566, 19.05341960407611168, 100.2072429386476955 ) ) ;
#55228 = CARTESIAN_POINT ( 'NONE',  ( -19.02544592524334988, -5.153800228976617603, 83.95942372801901854 ) ) ;
#55229 = CARTESIAN_POINT ( 'NONE',  ( -13.89961937509977652, 13.97604488694528158, 45.62390960531433848 ) ) ;
#55230 = CARTESIAN_POINT ( 'NONE',  ( -13.97604488694527625, -13.89961937509977652, 66.87390960531436690 ) ) ;
#55231 = CARTESIAN_POINT ( 'NONE',  ( 0.05219959533910956823, 16.53943276465976808, 74.99890960531435269 ) ) ;
#55232 = CARTESIAN_POINT ( 'NONE',  ( -5.153800228976328057, -19.02544592524343514, 97.29057627198099567 ) ) ;
#55233 = CARTESIAN_POINT ( 'NONE',  ( 14.29746914071049879, -8.314922557960816363, 98.33224293864769550 ) ) ;
#55234 = CARTESIAN_POINT ( 'NONE',  ( -5.153800228976328057, -19.02544592524343514, 102.2905762719810383 ) ) ;
#55237 = CARTESIAN_POINT ( 'NONE',  ( -5.153800228976328057, -19.02544592524343514, 22.29057627198102765 ) ) ;
#55236 =( BOUNDED_CURVE ( )  B_SPLINE_CURVE ( 3, ( #20858, #36023, #188739, #160375 ),
 .UNSPECIFIED., .F., .F. ) 
 B_SPLINE_CURVE_WITH_KNOTS ( ( 4, 4 ),
 ( 1.132647296210725907, 2.115944711806982514 ),
 .UNSPECIFIED. ) 
 CURVE ( )  GEOMETRIC_REPRESENTATION_ITEM ( )  RATIONAL_B_SPLINE_CURVE ( ( 1.000000000000000000, 0.9210371567966662010, 0.9210371567966662010, 1.000000000000000000 ) ) 
 REPRESENTATION_ITEM ( '' )  );
#55235 = CARTESIAN_POINT ( 'NONE',  ( 4.483927247898545687, 16.52544592524342804, 44.79057627198103120 ) ) ;
#55238 = ORIENTED_EDGE ( 'NONE', *, *, #112928, .T. ) ;
#55239 = CARTESIAN_POINT ( 'NONE',  ( -18.62759615963255300, -10.81492255796106328, 54.16775706135235424 ) ) ;
#55240 = CARTESIAN_POINT ( 'NONE',  ( -9.474510206698720793, -16.51473224551083518, 74.58442372801900433 ) ) ;
#55241 = CARTESIAN_POINT ( 'NONE',  ( 4.483927247898545687, 16.52544592524342804, 54.79057627198104541 ) ) ;
#55242 = CARTESIAN_POINT ( 'NONE',  ( 10.81492255796078972, 18.62759615963270932, 104.5822429386477097 ) ) ;
#55243 = CARTESIAN_POINT ( 'NONE',  ( -10.81492255796078084, -18.62759615963271287, 32.08224293864769550 ) ) ;
#55244 = CARTESIAN_POINT ( 'NONE',  ( -14.34966873604960291, -8.224510206698953496, 86.66557627198102409 ) ) ;
#55245 = CARTESIAN_POINT ( 'NONE',  ( 9.474510206698971260, -16.51473224551069308, 52.91557627198102409 ) ) ;
#55246 = CARTESIAN_POINT ( 'NONE',  ( -8.314922557960811034, -14.29746914071050412, 27.08224293864769550 ) ) ;
#55247 = CARTESIAN_POINT ( 'NONE',  ( 14.34966873604972726, -8.224510206698740333, 100.8344237280190185 ) ) ;
#55248 = CARTESIAN_POINT ( 'NONE',  ( -8.224510206698735004, -14.34966873604973081, 69.58442372801900433 ) ) ;
#55249 = CARTESIAN_POINT ( 'NONE',  ( 5.049401038297881783, 19.05341960407617563, 27.29275706135232937 ) ) ;
#55250 = CARTESIAN_POINT ( 'NONE',  ( -9.474510206698964154, 16.51473224551069663, 100.4155762719810241 ) ) ;
#55251 = CARTESIAN_POINT ( 'NONE',  ( 5.153800228976335163, 19.02544592524342804, 74.79057627198103830 ) ) ;
#55252 = CARTESIAN_POINT ( 'NONE',  ( -0.05219959533909027116, -19.03943276465977164, 42.49890960531435269 ) ) ;
#55253 = CARTESIAN_POINT ( 'NONE',  ( -8.314922557960811034, -14.29746914071050412, 47.08224293864770260 ) ) ;
#55255 = CARTESIAN_POINT ( 'NONE',  ( 9.474510206698971260, -16.51473224551069308, 102.9155762719810241 ) ) ;
#55254 = DIRECTION ( 'NONE',  ( -0.000000000000000000, -0.000000000000000000, 1.000000000000000000 ) ) ;
#55256 = CARTESIAN_POINT ( 'NONE',  ( 10.72451020669898902, -18.67979575497178502, 37.91557627198102409 ) ) ;
#55257 = CARTESIAN_POINT ( 'NONE',  ( -16.52544592524342804, 4.483927247898546575, 76.04057627198102409 ) ) ;
#55258 = CARTESIAN_POINT ( 'NONE',  ( -4.483927247898782831, 16.52544592524335698, 27.70942372801901854 ) ) ;
#55259 = CARTESIAN_POINT ( 'NONE',  ( 12.14591786802309770, 12.06949235617756955, 69.37390960531436690 ) ) ;
#55260 = CARTESIAN_POINT ( 'NONE',  ( 28.90000000000004476, 0.000000000000000000, -49.67367017693150189 ) ) ;
#55261 = CARTESIAN_POINT ( 'NONE',  ( -16.46253265017146816, -9.564922557961047289, 59.16775706135233293 ) ) ;
#55262 = CARTESIAN_POINT ( 'NONE',  ( -9.474510206698964154, 16.51473224551069663, 105.4155762719810383 ) ) ;
#55263 = CARTESIAN_POINT ( 'NONE',  ( 5.049401038297881783, 19.05341960407617563, 82.29275706135229029 ) ) ;
#55264 = DIRECTION ( 'NONE',  ( 1.000000000000000000, -2.686023446673766396E-15, 0.000000000000000000 ) ) ;
#55266 = CARTESIAN_POINT ( 'NONE',  ( -12.06949235617739369, -12.14591786802326823, 94.37609039468568994 ) ) ;
#55265 = CARTESIAN_POINT ( 'NONE',  ( -9.564922557961040184, 16.46253265017147172, 107.9177570613523471 ) ) ;
#55267 = CARTESIAN_POINT ( 'NONE',  ( 13.97604488694527802, 13.89961937509977652, 39.37390960531435269 ) ) ;
#55268 = CARTESIAN_POINT ( 'NONE',  ( -21.52544592524343514, 5.823673210054127303, 31.04057627198102409 ) ) ;
#55269 = CARTESIAN_POINT ( 'NONE',  ( -15.80617190586768217, 15.72974639402176855, 58.12609039468568994 ) ) ;
#55270 = CARTESIAN_POINT ( 'NONE',  ( -35.70266437024450568, -5.510913496957479854E-15, 37.50000000000000000 ) ) ;
#55271 = CARTESIAN_POINT ( 'NONE',  ( -0.05219959533934338120, 16.53943276465976808, 22.50109039468567573 ) ) ;
#55273 = CARTESIAN_POINT ( 'NONE',  ( 13.97604488694527802, 13.89961937509977652, 69.37390960531436690 ) ) ;
#55272 = CARTESIAN_POINT ( 'NONE',  ( 17.50000000000122924, 3.258327458701826718, 22.81645961510181664 ) ) ;
#55275 = CARTESIAN_POINT ( 'NONE',  ( -5.049401038298153566, 19.05341960407611168, 70.20724293864769550 ) ) ;
#55274 = CARTESIAN_POINT ( 'NONE',  ( -4.483927247898539470, -16.52544592524342804, 82.29057627198103830 ) ) ;
#55276 = CARTESIAN_POINT ( 'NONE',  ( 19.02544592524343514, -5.153800228976328945, 83.54057627198100988 ) ) ;
#55277 = VERTEX_POINT ( 'NONE', #105439 ) ;
#55278 = CARTESIAN_POINT ( 'NONE',  ( 16.51473224551083163, -9.474510206698727899, 85.83442372801900433 ) ) ;
#55279 = CARTESIAN_POINT ( 'NONE',  ( -0.05219959533907301413, -21.53943276465977519, 67.49890960531436690 ) ) ;
#55280 = CARTESIAN_POINT ( 'NONE',  ( 9.564922557960805705, 16.46253265017160317, 34.58224293864770260 ) ) ;
#55281 = CARTESIAN_POINT ( 'NONE',  ( 16.46253265017146816, 9.564922557961045513, 56.66775706135233293 ) ) ;
#55282 = CARTESIAN_POINT ( 'NONE',  ( -5.049401038298153566, 19.05341960407611168, 50.20724293864770260 ) ) ;
#55283 = CARTESIAN_POINT ( 'NONE',  ( -5.153800228976328057, -19.02544592524343514, 87.29057627198103830 ) ) ;
#55284 = ORIENTED_EDGE ( 'NONE', *, *, #156407, .T. ) ;
#55285 = CARTESIAN_POINT ( 'NONE',  ( -0.05219959533907301413, -21.53943276465977519, 92.49890960531436690 ) ) ;
#55288 = CARTESIAN_POINT ( 'NONE',  ( 19.05341960407617918, -5.049401038297876454, 66.04275706135233293 ) ) ;
#55287 = CARTESIAN_POINT ( 'NONE',  ( -19.05341960407611168, -5.049401038298163336, 86.45724293864769550 ) ) ;
#55286 = CARTESIAN_POINT ( 'NONE',  ( -0.05219959533910754901, -16.53943276465976808, 97.49890960531436690 ) ) ;
#55289 = CARTESIAN_POINT ( 'NONE',  ( -10.72451020669898014, 18.67979575497178502, 90.41557627198103830 ) ) ;
#55290 = CARTESIAN_POINT ( 'NONE',  ( 10.72451020669898902, -18.67979575497178502, 77.91557627198102409 ) ) ;
#55291 = CARTESIAN_POINT ( 'NONE',  ( 4.483927247898545687, 16.52544592524342804, 29.79057627198102409 ) ) ;
#55292 = CARTESIAN_POINT ( 'NONE',  ( -18.67979575497193778, 10.72451020669871902, 108.3344237280190185 ) ) ;
#55293 = CARTESIAN_POINT ( 'NONE',  ( -14.34966873604972548, 8.224510206698743886, 53.33442372801901854 ) ) ;
#55294 = CARTESIAN_POINT ( 'NONE',  ( -5.049401038298153566, 19.05341960407611168, 75.20724293864769550 ) ) ;
#55295 = CARTESIAN_POINT ( 'NONE',  ( -13.97604488694527625, -13.89961937509977652, 36.87390960531436690 ) ) ;
#55296 = CARTESIAN_POINT ( 'NONE',  ( -15.80617190586768217, 15.72974639402176855, 33.12609039468569705 ) ) ;
#55297 = CARTESIAN_POINT ( 'NONE',  ( -5.823673210054431948, 21.52544592524334988, 57.70942372801901143 ) ) ;
#55298 = CARTESIAN_POINT ( 'NONE',  ( -9.474510206698964154, 16.51473224551069663, 45.41557627198103120 ) ) ;
#55299 = CARTESIAN_POINT ( 'NONE',  ( -10.81492255796105439, 18.62759615963255655, 22.91775706135235069 ) ) ;
#55300 = CARTESIAN_POINT ( 'NONE',  ( 0.05219959533936267826, -19.03943276465977164, 70.00109039468566152 ) ) ;
#55301 = CARTESIAN_POINT ( 'NONE',  ( -16.51473224551082808, 9.474510206698731452, 78.33442372801900433 ) ) ;
#55302 = CARTESIAN_POINT ( 'NONE',  ( -9.474510206698964154, 16.51473224551069663, 30.41557627198102054 ) ) ;
#55303 = CARTESIAN_POINT ( 'NONE',  ( 0.05219959533934541429, -16.53943276465976808, 75.00109039468568994 ) ) ;
#55304 = CARTESIAN_POINT ( 'NONE',  ( -13.97604488694527625, -13.89961937509977652, 46.87390960531435979 ) ) ;
#55305 = CARTESIAN_POINT ( 'NONE',  ( 24.68411608548642988, -7.148172978124902599, 167.5704058020752996 ) ) ;
#55306 = CARTESIAN_POINT ( 'NONE',  ( 19.03943276465977164, -0.05219959533909143690, 93.74890960531435269 ) ) ;
#55307 = CARTESIAN_POINT ( 'NONE',  ( -8.224510206698948167, 14.34966873604960824, 115.4155762719810241 ) ) ;
#55308 = CARTESIAN_POINT ( 'NONE',  ( -15.80617190586745835, -15.72974639402198527, 66.87390960531436690 ) ) ;
#55309 = CARTESIAN_POINT ( 'NONE',  ( 12.14591786802327356, -12.06949235617739191, 55.62609039468568284 ) ) ;
#55310 = CARTESIAN_POINT ( 'NONE',  ( -19.03943276465977164, -0.05219959533935918106, 23.75109039468566152 ) ) ;
#55311 = ADVANCED_FACE ( 'NONE', ( #14416 ), #168100, .T. ) ;
#55312 = CARTESIAN_POINT ( 'NONE',  ( 19.03943276465977164, -0.05219959533909143690, 48.74890960531435979 ) ) ;
#55313 = CARTESIAN_POINT ( 'NONE',  ( 12.14591786802309770, 12.06949235617756955, 29.37390960531435269 ) ) ;
#55314 = CARTESIAN_POINT ( 'NONE',  ( 0.05219959533910956823, 16.53943276465976808, 69.99890960531435269 ) ) ;
#55315 = CARTESIAN_POINT ( 'NONE',  ( -16.46253265017160317, 9.564922557960807481, 75.83224293864769550 ) ) ;
#55316 = CARTESIAN_POINT ( 'NONE',  ( 21.53943276465977519, 0.05219959533937863772, 36.25109039468567573 ) ) ;
#55317 = CARTESIAN_POINT ( 'NONE',  ( -13.97604488694527625, -13.89961937509977652, 86.87390960531436690 ) ) ;
#55318 = CARTESIAN_POINT ( 'NONE',  ( -21.55341960407619339, 5.719274019375674811, 98.54275706135234714 ) ) ;
#55319 = CARTESIAN_POINT ( 'NONE',  ( 16.55341960407618274, -4.379528057220086978, 66.04275706135236135 ) ) ;
#55320 = CARTESIAN_POINT ( 'NONE',  ( 16.46253265017160672, -9.564922557960803928, 113.3322429386476955 ) ) ;
#55321 = CARTESIAN_POINT ( 'NONE',  ( -21.53943276465977519, 0.05219959533907696930, 91.24890960531436690 ) ) ;
#55322 = CARTESIAN_POINT ( 'NONE',  ( 0.05219959533910956823, 16.53943276465976808, 44.99890960531435979 ) ) ;
#55323 = CARTESIAN_POINT ( 'NONE',  ( 16.51473224551069308, 9.474510206698969483, 29.16557627198103475 ) ) ;
#55324 = CARTESIAN_POINT ( 'NONE',  ( -4.483927247898782831, 16.52544592524335698, 52.70942372801902565 ) ) ;
#55325 = CARTESIAN_POINT ( 'NONE',  ( -0.05219959533910754901, -16.53943276465976808, 72.49890960531435269 ) ) ;
#55326 = CARTESIAN_POINT ( 'NONE',  ( -19.03943276465977164, 0.05219959533909376836, 116.2489096053143669 ) ) ;
#55327 = CARTESIAN_POINT ( 'NONE',  ( -15.80617190586745835, -15.72974639402198527, 26.87390960531435979 ) ) ;
#55328 = CARTESIAN_POINT ( 'NONE',  ( -9.564922557961040184, 16.46253265017147172, 22.91775706135233648 ) ) ;
#55329 = EDGE_CURVE ( 'NONE', #196237, #6179, #184580, .T. ) ;
#55330 = CARTESIAN_POINT ( 'NONE',  ( -4.483927247898539470, -16.52544592524342804, 102.2905762719810383 ) ) ;
#55331 = CARTESIAN_POINT ( 'NONE',  ( 19.03943276465977164, -0.05219959533909143690, 103.7489096053143669 ) ) ;
#55332 = EDGE_LOOP ( 'NONE', ( #113752, #9608, #102417, #11030 ) ) ;
#55333 = CARTESIAN_POINT ( 'NONE',  ( 14.29746914071037800, 8.314922557961029526, 51.66775706135234714 ) ) ;
#55334 = CARTESIAN_POINT ( 'NONE',  ( -19.03943276465977164, 0.05219959533909376836, 56.24890960531435979 ) ) ;
#55335 = CARTESIAN_POINT ( 'NONE',  ( -16.74176944037747106, -6.099830512274460048, 20.54535278272281573 ) ) ;
#55336 = CARTESIAN_POINT ( 'NONE',  ( -5.153800228976607833, 19.02544592524334988, 52.70942372801900433 ) ) ;
#55337 = CARTESIAN_POINT ( 'NONE',  ( 8.224510206698742110, 14.34966873604972548, 92.08442372801901854 ) ) ;
#55338 = CARTESIAN_POINT ( 'NONE',  ( -16.46253265017146816, -9.564922557961047289, 99.16775706135233293 ) ) ;
#55339 = CARTESIAN_POINT ( 'NONE',  ( 21.53943276465977519, 0.05219959533937863772, 61.25109039468567573 ) ) ;
#55340 = CARTESIAN_POINT ( 'NONE',  ( -13.89961937509977652, 13.97604488694528158, 70.62390960531432427 ) ) ;
#55341 = CARTESIAN_POINT ( 'NONE',  ( -18.62759615963270932, 10.81492255796079327, 90.83224293864769550 ) ) ;
#55342 = CARTESIAN_POINT ( 'NONE',  ( -8.314922557960811034, -14.29746914071050412, 107.0822429386476955 ) ) ;
#55343 = CARTESIAN_POINT ( 'NONE',  ( 5.153800228976615827, -19.02544592524334988, 85.20942372801900433 ) ) ;
#55344 = CARTESIAN_POINT ( 'NONE',  ( 5.719274019375991003, -21.55341960407610458, 72.70724293864769550 ) ) ;
#55345 = CARTESIAN_POINT ( 'NONE',  ( -5.153800228976607833, 19.02544592524334988, 37.70942372801899722 ) ) ;
#55346 = CARTESIAN_POINT ( 'NONE',  ( -13.89961937509977652, 13.97604488694528158, 115.6239096053143669 ) ) ;
#55347 = CARTESIAN_POINT ( 'NONE',  ( -15.72974639402197994, 15.80617190586746368, 85.62390960531436690 ) ) ;
#55348 = CARTESIAN_POINT ( 'NONE',  ( -19.49149378614658090, 5.499999999999777067, 54.43757513605361709 ) ) ;
#55349 = CARTESIAN_POINT ( 'NONE',  ( 5.153800228976335163, 19.02544592524342804, 69.79057627198103830 ) ) ;
#55350 = CYLINDRICAL_SURFACE ( 'NONE', #149824, 28.79475375365586487 ) ;
#55351 = CARTESIAN_POINT ( 'NONE',  ( -16.53943276465976808, -0.05219959533934237506, 23.75109039468567929 ) ) ;
#55352 = CARTESIAN_POINT ( 'NONE',  ( 37.48574882824303245, -2.272739345372913000, 39.98829423970371977 ) ) ;
#55353 = CARTESIAN_POINT ( 'NONE',  ( 19.03943276465977164, -0.05219959533909143690, 43.74890960531435979 ) ) ;
#55354 = CARTESIAN_POINT ( 'NONE',  ( -21.53943276465977519, 0.05219959533907696930, 21.24890960531436690 ) ) ;
#55356 = CARTESIAN_POINT ( 'NONE',  ( -16.53943276465976808, 0.05219959533911058130, 46.24890960531435979 ) ) ;
#55355 = CARTESIAN_POINT ( 'NONE',  ( 10.72451020669898902, -18.67979575497178502, 107.9155762719810241 ) ) ;
#55357 = CARTESIAN_POINT ( 'NONE',  ( 10.72451020669871369, 18.67979575497193778, 72.08442372801899012 ) ) ;
#55359 = CARTESIAN_POINT ( 'NONE',  ( -13.97604488694547697, 13.89961937509957934, 23.12609039468565442 ) ) ;
#55358 = CARTESIAN_POINT ( 'NONE',  ( 12.06949235617739724, 12.14591786802326823, 26.87609039468567218 ) ) ;
#55360 = CARTESIAN_POINT ( 'NONE',  ( 4.379528057220339221, -16.55341960407611168, 27.70724293864769905 ) ) ;
#55361 = CARTESIAN_POINT ( 'NONE',  ( -10.81492255796078084, -18.62759615963271287, 112.0822429386477097 ) ) ;
#55362 = CARTESIAN_POINT ( 'NONE',  ( 8.224510206698953496, -14.34966873604960469, 52.91557627198103830 ) ) ;
#55363 = CARTESIAN_POINT ( 'NONE',  ( -13.97604488694547697, 13.89961937509957934, 98.12609039468566152 ) ) ;
#55364 = CARTESIAN_POINT ( 'NONE',  ( -13.89961937509957401, -13.97604488694547875, 69.37609039468564731 ) ) ;
#55365 = CARTESIAN_POINT ( 'NONE',  ( 5.719274019375673035, 21.55341960407619339, 72.29275706135236135 ) ) ;
#55366 = CARTESIAN_POINT ( 'NONE',  ( -13.89961937509957401, -13.97604488694547875, 59.37609039468566863 ) ) ;
#55367 = CARTESIAN_POINT ( 'NONE',  ( 16.55341960407611168, 4.379528057220329451, 113.9572429386477239 ) ) ;
#55368 = CARTESIAN_POINT ( 'NONE',  ( -21.55341960407610458, -5.719274019375992779, 46.45724293864769550 ) ) ;
#55369 = CARTESIAN_POINT ( 'NONE',  ( -4.483927247898539470, -16.52544592524342804, 47.29057627198103120 ) ) ;
#55370 = CARTESIAN_POINT ( 'NONE',  ( -19.52217212775661181, 5.499999999999920064, 94.93993709005262360 ) ) ;
#55371 = CARTESIAN_POINT ( 'NONE',  ( 18.62759615963255655, 10.81492255796105972, 106.6677570613523756 ) ) ;
#55372 = CARTESIAN_POINT ( 'NONE',  ( 16.52544592524335698, 4.483927247898782831, 86.45942372801901854 ) ) ;
#55373 = CARTESIAN_POINT ( 'NONE',  ( 14.34966873604960469, 8.224510206698951720, 34.16557627198102409 ) ) ;
#55374 = CARTESIAN_POINT ( 'NONE',  ( -18.62759615963255300, -10.81492255796106328, 79.16775706135234714 ) ) ;
#55375 = CARTESIAN_POINT ( 'NONE',  ( -21.52544592524334988, -5.823673210054445271, 83.95942372801900433 ) ) ;
#55376 = CARTESIAN_POINT ( 'NONE',  ( 15.80617190586746368, 15.72974639402197994, 79.37390960531436690 ) ) ;
#55377 = CARTESIAN_POINT ( 'NONE',  ( 5.049401038298161559, -19.05341960407611168, 32.70724293864768129 ) ) ;
#55378 = CARTESIAN_POINT ( 'NONE',  ( 18.62759615963255655, 10.81492255796105972, 56.66775706135235424 ) ) ;
#55379 = CARTESIAN_POINT ( 'NONE',  ( 9.564922557960805705, 16.46253265017160317, 39.58224293864768839 ) ) ;
#55380 = CARTESIAN_POINT ( 'NONE',  ( 5.049401038298161559, -19.05341960407611168, 57.70724293864769550 ) ) ;
#55381 = CARTESIAN_POINT ( 'NONE',  ( 16.55341960407611168, 4.379528057220329451, 93.95724293864770971 ) ) ;
#55382 = CARTESIAN_POINT ( 'NONE',  ( 16.51473224551069308, 9.474510206698969483, 94.16557627198103830 ) ) ;
#55383 = CARTESIAN_POINT ( 'NONE',  ( -12.06949235617756955, 12.14591786802309770, 35.62390960531437401 ) ) ;
#55384 = CARTESIAN_POINT ( 'NONE',  ( -12.06949235617756955, 12.14591786802309770, 110.6239096053143669 ) ) ;
#55385 = CARTESIAN_POINT ( 'NONE',  ( -18.67979575497178146, -10.72451020669898902, 86.66557627198102409 ) ) ;
#55386 = CARTESIAN_POINT ( 'NONE',  ( 5.823673210054444382, -21.52544592524334988, 20.20942372801900788 ) ) ;
#55387 = CARTESIAN_POINT ( 'NONE',  ( 27.40223502306392689, -7.751740014893113262, 163.3164180876353555 ) ) ;
#55389 = CARTESIAN_POINT ( 'NONE',  ( -16.53943276465976808, -0.05219959533934237506, 18.75109039468568639 ) ) ;
#55388 = CARTESIAN_POINT ( 'NONE',  ( 19.02544592524343514, -5.153800228976328945, 83.54057627198100988 ) ) ;
#55390 = CARTESIAN_POINT ( 'NONE',  ( -18.67979575497178146, -10.72451020669898902, 71.66557627198100988 ) ) ;
#55391 = CARTESIAN_POINT ( 'NONE',  ( -15.72974639402176322, -15.80617190586768395, 94.37609039468568994 ) ) ;
#55392 = CARTESIAN_POINT ( 'NONE',  ( -13.97604488694527625, -13.89961937509977652, 76.87390960531433848 ) ) ;
#55393 = CARTESIAN_POINT ( 'NONE',  ( -21.52544592524334988, -5.823673210054445271, 33.95942372801901143 ) ) ;
#55394 = CARTESIAN_POINT ( 'NONE',  ( 13.97604488694527802, 13.89961937509977652, 114.3739096053143669 ) ) ;
#55395 = CARTESIAN_POINT ( 'NONE',  ( -16.53943276465976808, -0.05219959533934237506, 88.75109039468567573 ) ) ;
#55396 = CARTESIAN_POINT ( 'NONE',  ( 18.67979575497194134, -10.72451020669871369, 70.83442372801901854 ) ) ;
#55397 = CARTESIAN_POINT ( 'NONE',  ( 18.62759615963255655, 10.81492255796105972, 101.6677570613523613 ) ) ;
#55398 = CARTESIAN_POINT ( 'NONE',  ( 16.53943276465976808, 0.05219959533934440121, 76.25109039468568994 ) ) ;
#55399 = CARTESIAN_POINT ( 'NONE',  ( -10.81492255796105439, 18.62759615963255655, 27.91775706135234358 ) ) ;
#55400 = CARTESIAN_POINT ( 'NONE',  ( 9.564922557960805705, 16.46253265017160317, 24.58224293864769194 ) ) ;
#55401 = CARTESIAN_POINT ( 'NONE',  ( 10.72451020669871369, 18.67979575497193778, 92.08442372801901854 ) ) ;
#55402 = CARTESIAN_POINT ( 'NONE',  ( -19.02544592524342804, 5.153800228976336051, 96.04057627198103830 ) ) ;
#55403 = CARTESIAN_POINT ( 'NONE',  ( -5.719274019375978568, 21.55341960407610458, 85.20724293864770971 ) ) ;
#55404 = CARTESIAN_POINT ( 'NONE',  ( -0.05219959533936034679, 19.03943276465977164, 62.50109039468566863 ) ) ;
#55406 = CARTESIAN_POINT ( 'NONE',  ( 5.719274019375991003, -21.55341960407610458, 47.70724293864770260 ) ) ;
#55405 = DIRECTION ( 'NONE',  ( 1.000000000000000000, 0.000000000000000000, 0.000000000000000000 ) ) ;
#55408 = CARTESIAN_POINT ( 'NONE',  ( -4.483927247898539470, -16.52544592524342804, 47.29057627198103120 ) ) ;
#55407 = CARTESIAN_POINT ( 'NONE',  ( -13.89961937509977652, 13.97604488694528158, 100.6239096053143669 ) ) ;
#55409 = CARTESIAN_POINT ( 'NONE',  ( -28.82186960331499037, 2.428612866367529932E-14, 146.0000000000000000 ) ) ;
#55410 = CARTESIAN_POINT ( 'NONE',  ( -16.51473224551082808, 9.474510206698731452, 83.33442372801899012 ) ) ;
#55411 = CARTESIAN_POINT ( 'NONE',  ( -1.499966876285938833, -15.29519331188519615, -61.92990168432673670 ) ) ;
#55412 = CARTESIAN_POINT ( 'NONE',  ( 9.474510206698729675, 16.51473224551082808, 107.0844237280190043 ) ) ;
#55413 = CARTESIAN_POINT ( 'NONE',  ( -15.72974639402197994, 15.80617190586746368, 80.62390960531438111 ) ) ;
#55414 = CARTESIAN_POINT ( 'NONE',  ( 16.53943276465976808, -0.05219959533910856209, 68.74890960531435269 ) ) ;
#55415 = CARTESIAN_POINT ( 'NONE',  ( -19.05341960407611168, -5.049401038298163336, 106.4572429386476955 ) ) ;
#55416 = CARTESIAN_POINT ( 'NONE',  ( 0.05219959533934541429, -16.53943276465976808, 45.00109039468568284 ) ) ;
#55417 = CARTESIAN_POINT ( 'NONE',  ( -16.46253265017160317, 9.564922557960807481, 55.83224293864769550 ) ) ;
#55419 = CARTESIAN_POINT ( 'NONE',  ( 19.03943276465977164, 0.05219959533936151252, 81.25109039468567573 ) ) ;
#55418 = CARTESIAN_POINT ( 'NONE',  ( -0.05219959533937732626, 21.53943276465977519, 22.50109039468567573 ) ) ;
#55420 = CARTESIAN_POINT ( 'NONE',  ( 5.049401038298161559, -19.05341960407611168, 92.70724293864769550 ) ) ;
#55421 = CARTESIAN_POINT ( 'NONE',  ( -9.474510206698964154, 16.51473224551069663, 80.41557627198103830 ) ) ;
#55422 = CARTESIAN_POINT ( 'NONE',  ( 10.72451020669898902, -18.67979575497178502, 72.91557627198103830 ) ) ;
#55423 = CARTESIAN_POINT ( 'NONE',  ( 13.97604488694527802, 13.89961937509977652, 49.37390960531434558 ) ) ;
#55424 = CARTESIAN_POINT ( 'NONE',  ( 33.56183721214949145, 15.50984559938615526, -7.999999999999996447 ) ) ;
#55425 = CARTESIAN_POINT ( 'NONE',  ( 16.53943276465976808, -0.05219959533910856209, 53.74890960531437401 ) ) ;
#55426 = CARTESIAN_POINT ( 'NONE',  ( -9.564922557960796823, -16.46253265017161027, 102.0822429386477097 ) ) ;
#55427 = CARTESIAN_POINT ( 'NONE',  ( 8.906447517083057264, -27.41122689804191026, 140.8500000054623911 ) ) ;
#55428 = CARTESIAN_POINT ( 'NONE',  ( 16.46253265017146816, 9.564922557961045513, 66.66775706135233293 ) ) ;
#55429 = CARTESIAN_POINT ( 'NONE',  ( 18.62759615963271287, -10.81492255796078972, 93.33224293864769550 ) ) ;
#55430 = CARTESIAN_POINT ( 'NONE',  ( 0.05219959533936267826, -19.03943276465977164, 55.00109039468566863 ) ) ;
#55431 = CARTESIAN_POINT ( 'NONE',  ( 9.564922557960805705, 16.46253265017160317, 104.5822429386476955 ) ) ;
#55432 = CARTESIAN_POINT ( 'NONE',  ( -17.49999999999999645, -5.499999999999992895, 74.20309617465828467 ) ) ;
#55433 = CARTESIAN_POINT ( 'NONE',  ( 15.72974639402199770, -15.80617190586745480, 43.12390960531435269 ) ) ;
#55434 = CARTESIAN_POINT ( 'NONE',  ( 13.89961937509977652, -13.97604488694527269, 73.12390960531436690 ) ) ;
#55435 = CARTESIAN_POINT ( 'NONE',  ( -21.55341960407619339, 5.719274019375674811, 63.54275706135234003 ) ) ;
#55436 = CARTESIAN_POINT ( 'NONE',  ( 13.97604488694527802, 13.89961937509977652, 39.37390960531435269 ) ) ;
#55438 = ORIENTED_EDGE ( 'NONE', *, *, #81680, .T. ) ;
#55437 = CARTESIAN_POINT ( 'NONE',  ( 8.314922557960818139, 14.29746914071049879, 69.58224293864769550 ) ) ;
#55439 = CARTESIAN_POINT ( 'NONE',  ( 8.314922557961029526, -14.29746914071037800, 20.41775706135234714 ) ) ;
#55440 = CARTESIAN_POINT ( 'NONE',  ( 10.81492255796106328, -18.62759615963255655, 55.41775706135234714 ) ) ;
#55441 = ORIENTED_EDGE ( 'NONE', *, *, #63444, .T. ) ;
#55442 = CARTESIAN_POINT ( 'NONE',  ( 5.049401038298161559, -19.05341960407611168, 112.7072429386476813 ) ) ;
#55443 = CARTESIAN_POINT ( 'NONE',  ( -5.049401038297874678, -19.05341960407617918, 64.79275706135233293 ) ) ;
#55444 = DIRECTION ( 'NONE',  ( -1.000000000000000000, 0.000000000000000000, 0.000000000000000000 ) ) ;
#55445 = CARTESIAN_POINT ( 'NONE',  ( -10.72451020669870658, -18.67979575497194134, 19.58442372801901143 ) ) ;
#55446 = CARTESIAN_POINT ( 'NONE',  ( -9.564922557960796823, -16.46253265017161027, 57.08224293864769550 ) ) ;
#55447 = CARTESIAN_POINT ( 'NONE',  ( 16.55341960407618274, -4.379528057220086978, 41.04275706135236135 ) ) ;
#55448 = CARTESIAN_POINT ( 'NONE',  ( 38.00000000000000000, 12.34694845685046616, -6.649999994537624914 ) ) ;
#55449 = CARTESIAN_POINT ( 'NONE',  ( 10.72451020669871369, 18.67979575497193778, 112.0844237280190185 ) ) ;
#55450 = CARTESIAN_POINT ( 'NONE',  ( -13.89961937509977652, 13.97604488694528158, 45.62390960531433848 ) ) ;
#55451 = CARTESIAN_POINT ( 'NONE',  ( -18.67979575497193778, 10.72451020669871902, 113.3344237280190328 ) ) ;
#55452 = CARTESIAN_POINT ( 'NONE',  ( 14.34966873604972726, -8.224510206698740333, 90.83442372801901854 ) ) ;
#55454 = CARTESIAN_POINT ( 'NONE',  ( -10.72451020669870658, -18.67979575497194134, 74.58442372801901854 ) ) ;
#55453 = CARTESIAN_POINT ( 'NONE',  ( 19.05341960407611168, 5.049401038298154454, 108.9572429386477097 ) ) ;
#55455 = CARTESIAN_POINT ( 'NONE',  ( 36.91746824999999887, 11.99521256947799053, -9.524999997268812635 ) ) ;
#55456 = DIRECTION ( 'NONE',  ( 1.000000000000000000, 0.000000000000000000, 0.000000000000000000 ) ) ;
#55457 = DIRECTION ( 'NONE',  ( 0.7071067811865483499, 0.000000000000000000, -0.7071067811865465735 ) ) ;
#55459 = CARTESIAN_POINT ( 'NONE',  ( 15.72974639402176855, 15.80617190586768217, 76.87609039468567573 ) ) ;
#55458 = CARTESIAN_POINT ( 'NONE',  ( 16.53943276465976808, 0.05219959533934440121, 51.25109039468568994 ) ) ;
#55460 = CARTESIAN_POINT ( 'NONE',  ( -0.05219959533937732626, 21.53943276465977519, 97.50109039468567573 ) ) ;
#55461 = CARTESIAN_POINT ( 'NONE',  ( -11.94368209565404548, 9.822817408786974624, -59.71171441009364145 ) ) ;
#55462 = CARTESIAN_POINT ( 'NONE',  ( -8.224510206698735004, -14.34966873604973081, 34.58442372801900433 ) ) ;
#55463 = CARTESIAN_POINT ( 'NONE',  ( -13.97604488694527625, -13.89961937509977652, 86.87390960531436690 ) ) ;
#55464 = ADVANCED_FACE ( 'NONE', ( #121589 ), #11284, .T. ) ;
#55465 = CARTESIAN_POINT ( 'NONE',  ( 9.474510206698971260, -16.51473224551069308, 107.9155762719810383 ) ) ;
#55466 = VERTEX_POINT ( 'NONE', #123565 ) ;
#55467 = CARTESIAN_POINT ( 'NONE',  ( 17.44279575226822132, 5.990770900252482711, 41.66442432485681735 ) ) ;
#55468 = CARTESIAN_POINT ( 'NONE',  ( 16.46253265017160672, -9.564922557960803928, 33.33224293864770260 ) ) ;
#55469 = CARTESIAN_POINT ( 'NONE',  ( -18.67979575497178146, -10.72451020669898902, 41.66557627198103120 ) ) ;
#55470 = CARTESIAN_POINT ( 'NONE',  ( 0.05219959533934541429, -16.53943276465976808, 105.0010903946856757 ) ) ;
#55472 = CARTESIAN_POINT ( 'NONE',  ( 9.474510206698971260, -16.51473224551069308, 72.91557627198102409 ) ) ;
#55471 = CARTESIAN_POINT ( 'NONE',  ( -12.06949235617756955, 12.14591786802309770, 80.62390960531438111 ) ) ;
#55473 = CARTESIAN_POINT ( 'NONE',  ( -10.72451020669870658, -18.67979575497194134, 99.58442372801900433 ) ) ;
#55474 = CARTESIAN_POINT ( 'NONE',  ( -8.314922557961024197, 14.29746914071037800, 22.91775706135235069 ) ) ;
#55475 = CARTESIAN_POINT ( 'NONE',  ( 12.06949235617757843, -12.14591786802309237, 83.12390960531436690 ) ) ;
#55476 = CARTESIAN_POINT ( 'NONE',  ( 18.62759615963255655, 10.81492255796105972, 46.66775706135234714 ) ) ;
#55477 = CARTESIAN_POINT ( 'NONE',  ( 21.53943276465977519, -0.05219959533907433946, 68.74890960531435269 ) ) ;
#55478 = CARTESIAN_POINT ( 'NONE',  ( 9.474510206698729675, 16.51473224551082808, 52.08442372801900433 ) ) ;
#55479 = CARTESIAN_POINT ( 'NONE',  ( -35.13534055906293929, 5.469967203781493481, 39.86293573631996168 ) ) ;
#55480 = CARTESIAN_POINT ( 'NONE',  ( -9.474510206698964154, 16.51473224551069663, 100.4155762719810241 ) ) ;
#55481 = CARTESIAN_POINT ( 'NONE',  ( -12.14591786802309592, -12.06949235617757132, 66.87390960531436690 ) ) ;
#55482 = CARTESIAN_POINT ( 'NONE',  ( 8.224510206698953496, -14.34966873604960469, 52.91557627198103830 ) ) ;
#55483 = CARTESIAN_POINT ( 'NONE',  ( -0.05219959533934338120, 16.53943276465976808, 107.5010903946856899 ) ) ;
#55484 = CARTESIAN_POINT ( 'NONE',  ( -5.153800228976607833, 19.02544592524334988, 67.70942372801900433 ) ) ;
#55485 = CARTESIAN_POINT ( 'NONE',  ( -69.65682714487590488, -71.74905178543390605, -25.00000000000000000 ) ) ;
#55486 = CARTESIAN_POINT ( 'NONE',  ( -5.049401038298153566, 19.05341960407611168, 115.2072429386477097 ) ) ;
#55487 = CARTESIAN_POINT ( 'NONE',  ( 4.379528057220339221, -16.55341960407611168, 92.70724293864770971 ) ) ;
#55488 = DIRECTION ( 'NONE',  ( -0.7071067811865483499, 0.000000000000000000, 0.7071067811865465735 ) ) ;
#55490 = CARTESIAN_POINT ( 'NONE',  ( 21.52544592524344225, -5.823673210054117533, 53.54057627198103120 ) ) ;
#55489 = CARTESIAN_POINT ( 'NONE',  ( -19.02544592524342804, 5.153800228976336051, 41.04057627198103120 ) ) ;
#55491 = CARTESIAN_POINT ( 'NONE',  ( -15.80617190586745835, -15.72974639402198527, 76.87390960531439532 ) ) ;
#55492 = CARTESIAN_POINT ( 'NONE',  ( -16.46253265017160317, 9.564922557960807481, 35.83224293864768839 ) ) ;
#55494 = CARTESIAN_POINT ( 'NONE',  ( -9.564922557960796823, -16.46253265017161027, 67.08224293864769550 ) ) ;
#55493 = CARTESIAN_POINT ( 'NONE',  ( 14.29746914071037800, 8.314922557961029526, 66.66775706135234714 ) ) ;
#55495 = CARTESIAN_POINT ( 'NONE',  ( 0.05219959533936267826, -19.03943276465977164, 35.00109039468566863 ) ) ;
#55496 = CARTESIAN_POINT ( 'NONE',  ( 21.55341960407619695, -5.719274019375665929, 51.04275706135234714 ) ) ;
#55497 = ORIENTED_EDGE ( 'NONE', *, *, #123690, .T. ) ;
#55498 = CARTESIAN_POINT ( 'NONE',  ( -0.05219959533907301413, -21.53943276465977519, 37.49890960531436690 ) ) ;
#55499 = CARTESIAN_POINT ( 'NONE',  ( 4.379528057220339221, -16.55341960407611168, 107.7072429386476955 ) ) ;
#55500 = CARTESIAN_POINT ( 'NONE',  ( 19.02544592524334988, 5.153800228976608722, 86.45942372801900433 ) ) ;
#55501 = CARTESIAN_POINT ( 'NONE',  ( -36.91746825000000598, 2.428612866367529932E-14, -3.124999997268813168 ) ) ;
#55503 = CARTESIAN_POINT ( 'NONE',  ( 15.72974639402199770, -15.80617190586745480, 53.12390960531436690 ) ) ;
#55502 = CARTESIAN_POINT ( 'NONE',  ( -0.4285070731208345807, -24.24152472029835792, -56.81472536503800796 ) ) ;
#55504 = CARTESIAN_POINT ( 'NONE',  ( 16.81555441253552274, -7.025013491695478507, 68.13685445334259327 ) ) ;
#55505 = CARTESIAN_POINT ( 'NONE',  ( 21.55341960407619695, -5.719274019375665929, 86.04275706135236135 ) ) ;
#55506 = CARTESIAN_POINT ( 'NONE',  ( 16.53943276465976808, -0.05219959533910856209, 28.74890960531435624 ) ) ;
#55508 = CARTESIAN_POINT ( 'NONE',  ( 12.14591786802309770, 12.06949235617756955, 54.37390960531435979 ) ) ;
#55507 = CARTESIAN_POINT ( 'NONE',  ( -4.483927247898782831, 16.52544592524335698, 52.70942372801902565 ) ) ;
#55509 = CARTESIAN_POINT ( 'NONE',  ( 0.05219959533907565091, 21.53943276465977519, 84.99890960531436690 ) ) ;
#55510 = CARTESIAN_POINT ( 'NONE',  ( -18.67979575497178146, -10.72451020669898902, 76.66557627198103830 ) ) ;
#55511 = DIRECTION ( 'NONE',  ( 0.000000000000000000, 0.000000000000000000, -1.000000000000000000 ) ) ;
#55513 = CARTESIAN_POINT ( 'NONE',  ( -10.81492255796078084, -18.62759615963271287, 22.08224293864769194 ) ) ;
#55512 = CARTESIAN_POINT ( 'NONE',  ( 9.564922557961047289, -16.46253265017146816, 90.41775706135234714 ) ) ;
#55514 = CARTESIAN_POINT ( 'NONE',  ( 16.46253265017160672, -9.564922557960803928, 63.33224293864769550 ) ) ;
#55515 = CARTESIAN_POINT ( 'NONE',  ( 16.46253265017160672, -9.564922557960803928, 38.33224293864768839 ) ) ;
#55516 = DIRECTION ( 'NONE',  ( 1.000000000000000000, 0.000000000000000000, 3.709348145883536076E-20 ) ) ;
#55517 = CARTESIAN_POINT ( 'NONE',  ( -12.14591786802326823, 12.06949235617739902, 88.12609039468570415 ) ) ;
#55518 = CARTESIAN_POINT ( 'NONE',  ( -10.72451020669870658, -18.67979575497194134, 19.58442372801901143 ) ) ;
#55519 = CARTESIAN_POINT ( 'NONE',  ( 9.564922557960805705, 16.46253265017160317, 69.58224293864770971 ) ) ;
#55520 = CARTESIAN_POINT ( 'NONE',  ( 0.05219959533937995610, -21.53943276465977519, 55.00109039468568284 ) ) ;
#55521 = CARTESIAN_POINT ( 'NONE',  ( -19.02544592524342804, 5.153800228976336051, 101.0405762719810241 ) ) ;
#55522 = CARTESIAN_POINT ( 'NONE',  ( -26.94323156050993617, -28.89364864972289126, -18.52709669219113309 ) ) ;
#55523 = ORIENTED_EDGE ( 'NONE', *, *, #26286, .F. ) ;
#55524 = CARTESIAN_POINT ( 'NONE',  ( 5.719274019375673035, 21.55341960407619339, 42.29275706135235424 ) ) ;
#55526 = CARTESIAN_POINT ( 'NONE',  ( 19.03943276465977164, -0.05219959533909143690, 98.74890960531436690 ) ) ;
#55525 = CARTESIAN_POINT ( 'NONE',  ( -19.02544592524342804, 5.153800228976336051, 26.04057627198103120 ) ) ;
#55527 = CARTESIAN_POINT ( 'NONE',  ( -19.03943276465977164, -0.05219959533935918106, 58.75109039468566863 ) ) ;
#55528 = CARTESIAN_POINT ( 'NONE',  ( -18.62759615963270932, 10.81492255796079327, 110.8322429386476955 ) ) ;
#55529 = CARTESIAN_POINT ( 'NONE',  ( -0.05219959533936034679, 19.03943276465977164, 47.50109039468566863 ) ) ;
#55530 = CARTESIAN_POINT ( 'NONE',  ( 9.564922557961047289, -16.46253265017146816, 45.41775706135232582 ) ) ;
#55532 = ORIENTED_EDGE ( 'NONE', *, *, #34066, .F. ) ;
#55531 = CARTESIAN_POINT ( 'NONE',  ( -16.52544592524335698, -4.483927247898792601, 103.9594237280190185 ) ) ;
#55534 = ORIENTED_EDGE ( 'NONE', *, *, #44832, .T. ) ;
#55533 = CARTESIAN_POINT ( 'NONE',  ( 11.49022483853025633, 12.06727048284061610, -61.36479237366228290 ) ) ;
#55535 = CARTESIAN_POINT ( 'NONE',  ( -9.564922557960796823, -16.46253265017161027, 72.08224293864770971 ) ) ;
#55536 = CARTESIAN_POINT ( 'NONE',  ( 15.80617190586769283, -15.72974639402175789, 75.62609039468567573 ) ) ;
#55537 = EDGE_CURVE ( 'NONE', #72076, #135352, #30228, .T. ) ;
#55538 = CARTESIAN_POINT ( 'NONE',  ( -15.72974639402176322, -15.80617190586768395, 94.37609039468568994 ) ) ;
#55539 = CARTESIAN_POINT ( 'NONE',  ( -1.313804288003784793, -8.349412516403770468, -64.09731636040746139 ) ) ;
#55540 = CARTESIAN_POINT ( 'NONE',  ( 19.05341960407611168, 5.049401038298154454, 83.95724293864766707 ) ) ;
#55541 = CARTESIAN_POINT ( 'NONE',  ( 21.53943276465977519, 0.05219959533937863772, 76.25109039468568994 ) ) ;
#55542 = CARTESIAN_POINT ( 'NONE',  ( 5.153800228976615827, -19.02544592524334988, 110.2094237280189901 ) ) ;
#55543 = CARTESIAN_POINT ( 'NONE',  ( 0.05219959533909260263, 19.03943276465977164, 69.99890960531435269 ) ) ;
#55544 = CARTESIAN_POINT ( 'NONE',  ( 13.97604488694527802, 13.89961937509977652, 114.3739096053143669 ) ) ;
#55545 = CARTESIAN_POINT ( 'NONE',  ( 0.05219959533909260263, 19.03943276465977164, 89.99890960531436690 ) ) ;
#55546 = CARTESIAN_POINT ( 'NONE',  ( -13.97604488694527625, -13.89961937509977652, 76.87390960531433848 ) ) ;
#55547 = CARTESIAN_POINT ( 'NONE',  ( 5.153800228976335163, 19.02544592524342804, 59.79057627198100988 ) ) ;
#55548 = CARTESIAN_POINT ( 'NONE',  ( 10.72451020669898902, -18.67979575497178502, 112.9155762719810383 ) ) ;
#55549 = CARTESIAN_POINT ( 'NONE',  ( -0.05219959533934338120, 16.53943276465976808, 97.50109039468567573 ) ) ;
#55550 = CARTESIAN_POINT ( 'NONE',  ( 1.455685960264199608, 15.57403722060355022, -61.81495257977202584 ) ) ;
#55551 = CARTESIAN_POINT ( 'NONE',  ( 5.153800228976615827, -19.02544592524334988, 60.20942372801899012 ) ) ;
#55552 = CARTESIAN_POINT ( 'NONE',  ( 5.049401038298161559, -19.05341960407611168, 92.70724293864769550 ) ) ;
#55553 = CARTESIAN_POINT ( 'NONE',  ( 12.14591786802309770, 12.06949235617756955, 89.37390960531435269 ) ) ;
#55554 = CARTESIAN_POINT ( 'NONE',  ( 4.483927247898545687, 16.52544592524342804, 109.7905762719810383 ) ) ;
#55555 = CARTESIAN_POINT ( 'NONE',  ( -18.67979575497178146, -10.72451020669898902, 36.66557627198103120 ) ) ;
#55556 = CARTESIAN_POINT ( 'NONE',  ( 10.72451020669898902, -18.67979575497178502, 22.91557627198102765 ) ) ;
#55557 = CARTESIAN_POINT ( 'NONE',  ( -16.53943276465976808, 0.05219959533911058130, 91.24890960531436690 ) ) ;
#55558 = DIRECTION ( 'NONE',  ( 0.000000000000000000, 0.000000000000000000, -1.000000000000000000 ) ) ;
#55559 = CARTESIAN_POINT ( 'NONE',  ( 16.51473224551083163, -9.474510206698727899, 45.83442372801900433 ) ) ;
#55560 = CARTESIAN_POINT ( 'NONE',  ( 16.53943276465976808, 0.05219959533934440121, 101.2510903946856757 ) ) ;
#55561 = CARTESIAN_POINT ( 'NONE',  ( 19.03943276465977164, -0.05219959533909143690, 93.74890960531435269 ) ) ;
#55562 = CARTESIAN_POINT ( 'NONE',  ( -5.823673210054431948, 21.52544592524334988, 67.70942372801901854 ) ) ;
#55563 = CARTESIAN_POINT ( 'NONE',  ( -5.823673210054116645, -21.52544592524344225, 42.29057627198103120 ) ) ;
#55564 = CARTESIAN_POINT ( 'NONE',  ( -5.823673210054431948, 21.52544592524334988, 27.70942372801901854 ) ) ;
#55565 = CARTESIAN_POINT ( 'NONE',  ( -15.72974639402197994, 15.80617190586746368, 85.62390960531436690 ) ) ;
#55566 = CARTESIAN_POINT ( 'NONE',  ( -0.05219959533910754901, -16.53943276465976808, 107.4989096053143669 ) ) ;
#55567 = CARTESIAN_POINT ( 'NONE',  ( 13.89961937509957401, 13.97604488694547697, 76.87609039468566152 ) ) ;
#55568 = EDGE_CURVE ( 'NONE', #42510, #150779, #198615, .T. ) ;
#55569 = CARTESIAN_POINT ( 'NONE',  ( -13.89961937509977652, 13.97604488694528158, 40.62390960531435979 ) ) ;
#55570 = CARTESIAN_POINT ( 'NONE',  ( 13.89961937509977652, -13.97604488694527269, 103.1239096053143527 ) ) ;
#55571 = CARTESIAN_POINT ( 'NONE',  ( 5.153800228976335163, 19.02544592524342804, 99.79057627198102409 ) ) ;
#55572 = CARTESIAN_POINT ( 'NONE',  ( -16.55341960407611168, -4.379528057220339221, 111.4572429386476813 ) ) ;
#55573 = CARTESIAN_POINT ( 'NONE',  ( -14.29746914071049879, 8.314922557960819915, 40.83224293864769550 ) ) ;
#55574 = CARTESIAN_POINT ( 'NONE',  ( 4.379528057220092307, 16.55341960407617563, 47.29275706135234003 ) ) ;
#55575 = CARTESIAN_POINT ( 'NONE',  ( -5.823673210054431948, 21.52544592524334988, 102.7094237280190185 ) ) ;
#55577 = CARTESIAN_POINT ( 'NONE',  ( -12.06949235617756955, 12.14591786802309770, 25.62390960531435624 ) ) ;
#55576 = DIRECTION ( 'NONE',  ( 3.491481338843133750E-15, 1.000000000000000000, -0.000000000000000000 ) ) ;
#55578 = CARTESIAN_POINT ( 'NONE',  ( 5.823673210054444382, -21.52544592524334988, 35.20942372801901854 ) ) ;
#55579 = CARTESIAN_POINT ( 'NONE',  ( -16.51473224551069308, -9.474510206698971260, 101.6655762719810241 ) ) ;
#55580 = CARTESIAN_POINT ( 'NONE',  ( 8.224510206698742110, 14.34966873604972548, 107.0844237280190043 ) ) ;
#55581 = CARTESIAN_POINT ( 'NONE',  ( 16.55341960407618274, -4.379528057220086978, 91.04275706135236135 ) ) ;
#55582 = CARTESIAN_POINT ( 'NONE',  ( -0.05219959533934338120, 16.53943276465976808, 27.50109039468567929 ) ) ;
#55583 = CARTESIAN_POINT ( 'NONE',  ( -19.05341960407611168, -5.049401038298163336, 46.45724293864768129 ) ) ;
#55584 = CARTESIAN_POINT ( 'NONE',  ( -8.314922557960811034, -14.29746914071050412, 112.0822429386477097 ) ) ;
#55585 = CARTESIAN_POINT ( 'NONE',  ( 15.72974639402176855, 15.80617190586768217, 21.87609039468567573 ) ) ;
#55586 = CARTESIAN_POINT ( 'NONE',  ( 19.02544592524343514, -5.153800228976328945, 28.54057627198102409 ) ) ;
#55587 = CARTESIAN_POINT ( 'NONE',  ( 9.474510206698971260, -16.51473224551069308, 102.9155762719810241 ) ) ;
#55588 = CARTESIAN_POINT ( 'NONE',  ( 18.62759615963255655, 10.81492255796105972, 31.66775706135234358 ) ) ;
#55589 = CARTESIAN_POINT ( 'NONE',  ( -19.02544592524342804, 5.153800228976336051, 36.04057627198100988 ) ) ;
#55590 = CARTESIAN_POINT ( 'NONE',  ( 16.51473224551069308, 9.474510206698969483, 104.1655762719810241 ) ) ;
#55591 = CARTESIAN_POINT ( 'NONE',  ( -17.05116617787824040, -6.768360034955907878, 36.34324446740804859 ) ) ;
#55592 = CARTESIAN_POINT ( 'NONE',  ( 5.153800228976335163, 19.02544592524342804, 99.79057627198102409 ) ) ;
#55594 = CARTESIAN_POINT ( 'NONE',  ( -14.34966873604960291, -8.224510206698953496, 86.66557627198102409 ) ) ;
#55593 = CARTESIAN_POINT ( 'NONE',  ( 5.823673210054444382, -21.52544592524334988, 50.20942372801901854 ) ) ;
#55595 = CARTESIAN_POINT ( 'NONE',  ( -16.46253265017160317, 9.564922557960807481, 100.8322429386477097 ) ) ;
#55596 = CARTESIAN_POINT ( 'NONE',  ( -27.89963664982370872, -6.788868650209762379, 161.9772721943246552 ) ) ;
#55598 =( BOUNDED_SURFACE ( )  B_SPLINE_SURFACE ( 3, 2, ( 
 ( #117250, #133415, #83896, #178942, #162752, #163768, #24261, #118261, #195104, #99067, #38415, #103084, #116248, #177940, #25269, #39407, #148594, #10086, #161757, #23252, #82900, #175938, #179951, #191097, #84895, #41418, #164765, #130396, #144579, #146574, #6065, #67743, #53576, #52572, #115253, #114232, #69745, #131414, #37409, #193102, #152558, #120234, #104081, #29241, #167743, #123206, #14047, #30219, #28264, #89902, #149587, #90874, #11085, #151585, #134432, #199071, #165763, #166762, #91861, #75713, #74741, #44403, #153554, #13074, #183907, #60540, #198082, #42418, #196118, #72762, #61537, #76712, #200069, #136404, #138387, #119258, #59549, #15051, #108037, #121227, #137391, #122216, #184896, #182918, #106057, #57588, #45392, #180942, #107045, #27257, #168717, #88907, #46378, #26260, #87901, #150598, #12096, #73759, #135431, #197102, #58569, #181925, #43406, #105076, #154554, #4827, #20014, #143340, #156548, #81657, #62530, #2858, #35187, #51351, #141371, #80684, #48383, #186912, #142360, #128177, #77708, #111029, #172715, #17042, #33208, #32213, #155548, #188889, #66515, #78696, #158526, #157543, #110040, #18047, #3840, #64536, #34198, #93869, #65519, #16049, #112030, #126202, #140373, #124203, #79700, #1860, #187898, #856, #95860, #185903, #49365, #31216, #139374, #169723, #92867, #63542, #171719, #125216, #50370, #127179, #47388, #94867, #173719, #96841, #19037, #189876, #109043, #170721, #163529, #147359, #54346, #82660, #116017, #101843, #175693, #144344, #194869, #25029, #129165, #177707, #52339, #160521, #192867, #84660, #86673, #37168, #36168, #99838, #98827, #22012, #161522, #148356, #97820, #9852, #191854, #6824, #5832, #117010, #70515, #115014, #146338, #190862, #23014, #159509, #53335, #7826, #85672, #40167, #71511, #133179, #100832, #176708, #69511, #24017, #131177, #39174, #83664, #8847, #21005, #55340, #162515, #145342, #67508, #132183, #68502, #193874, #113995, #178705, #130157, #113011, #174704, #38182, #56342, #118024, #165534, #58343, #27030, #137163, #90656, #41186, #88675, #167521, #183683, #180716, #74515, #45168, #44175, #106824, #152338, #197856, #26027, #59323, #168498, #119033, #87672, #138163, #29996, #72522, #120992, #195885, #103853, #136181, #28032, #91635, #42192, #179714, #43177, #150371, #11867, #104844, #153323, #102849, #14825, #135204, #73532, #149356, #60316, #13824, #120011, #89673, #134197, #166535, #164534, #196876, #151360, #29016, #76486, #10853, #182690, #57359, #105834, #181696, #12849, #75490, #198852, #121992, #122981, #199844, #50136, #188656, #156311, #94632, #63302, #17813, #48149, #61311, #80452, #47152, #46150, #142125, #169488, #18807, #157310, #65289, #109806, #30988, #172480, #79469, #49141, #107804, #64305, #92636, #170489, #124982, #19786, #33968, #158297, #154327, #141138, #2628, #108810, #186679, #62295, #185660, #3610, #173483, #31980, #81427, #184668, #171489, #111795, #15816, #187671, #34956, #125972, #77477, #110799, #95625, #96608, #139147, #32978, #140134, #126948, #624, #123962, #93636, #155321, #16810, #78460, #1626, #163298, #175463, #99607, #177478, #20772, #69276, #38947, #127944, #54115, #131955, #82428, #115789, #22781, #23786, #161287, #116781, #193639, #159276, #36934, #24797, #176473, #37947, #130943, #84429, #146106, #100604, #21781, #98597, #143113, #35942, #7590, #189646, #160290, #192633, #162286, #5596, #85436, #83432, #8614, #147127, #144116, #178472, #145109, #70287, #67276, #128934, #55111, #39939, #101608, #6592, #190635, #4592, #66285, #51121, #112780, #174473, #68271, #129922, #97588, #52110, #113767, #191622, #53101, #114780, #25801, #26794, #152104, #151126, #134969, #104612, #90419, #11632, #43935, #59088, #58116, #102622, #56110, #71287, #121749, #136926, #60081, #73299, #198613, #179486, #119786, #13588, #168259, #181470, #197623, #165301, #103625, #183441, #75255, #44926, #42948, #106582, #150130 ),
 ( #88436, #196646, #9622, #12619, #132952, #166300, #194640, #120755, #87447, #27797, #86445, #74283, #89438, #135953, #148131, #182454, #105596, #167282, #28780, #164308, #117791, #40950, #149132, #10623, #72284, #133961, #195653, #57125, #118799, #180487, #41959, #4099, #143608, #111292, #49629, #144611, #159781, #98083, #189153, #129432, #96118, #66775, #50626, #51608, #128436, #188156, #78958, #48645, #191130, #114266, #14581, #157806, #82933, #140633, #20269, #67775, #173977, #110297, #35445, #5092, #6096, #52604, #65778, #172981, #97097, #2123, #33467, #79963, #29755, #190133, #19297, #80945, #91390, #64797, #112287, #113272, #171979, #158781, #174964, #63805, #36428, #21276, #95125, #153079, #81915, #125478, #187174, #156815, #18307, #141632, #126458, #3122, #127447, #34459, #142620, #9117, #70784, #10118, #54605, #69777, #175970, #68771, #178975, #22279, #131445, #25302, #163800, #38448, #40442, #193132, #41452, #132452, #53609, #11119, #8099, #56619, #115285, #176978, #179984, #194143, #102115, #116279, #100103, #177969, #85940, #148628, #103117, #26293, #55607, #87934, #86944, #130429, #39437, #117281, #37439, #133448, #99099, #160791, #149621, #164798, #71778, #195138, #101097, #118293, #24291, #83930, #72794, #23282, #145611, #134464, #7090, #196149, #57621, #192128, #147629, #161787, #84926, #146606, #162783, #27292, #183935, #88939, #89934, #182950, #139402, #91891, #77736, #150630, #60569, #122245, #166793, #44433, #181956, #105107, #138416, #92896, #28294, #108067, #107073, #59582, #167773, #30248, #90902, #45420, #43438, #153582, #104113, #61564, #75745, #151615, #12126, #29271, #13107, #152588, #73790, #168744, #135462, #106087, #180972, #197131, #119289, #42449, #74772, #121256, #136434, #200096, #15080, #165795, #198115, #76741, #46408, #14079, #137422, #169751, #123233, #31246, #184924, #154582, #58598, #16078, #884, #199102, #120264, #144375, #51381, #78725, #65548, #1889, #110069, #142390, #34227, #36197, #125244, #185931, #49395, #186942, #171749, #111058, #113042, #47416, #97851, #141399, #156580, #32240, #66545, #20043, #64566, #95889, #140401, #172746, #109072, #173747, #157572, #127207, #48413, #35216, #170751, #4860, #19065, #33238, #155576, #80712, #94896, #3869, #93898, #188921, #17071, #50399, #124235, #63570, #62559, #18075, #79730, #126231, #2887, #143368, #96869, #187926, #112059, #158553, #189906, #81686, #128209, #174734, #159540, #21038, #82691, #147390, #175724, #8878, #194898, #68534, #37203, #87699, #56372, #22044, #70546, #145373, #53369, #85704, #177737, #179745, #130189, #129196, #192899, #191885, #115047, #54376, #118055, #190894, #41215, #84690, #99868, #98859, #9881, #163559, #7857, #39206, #83695, #116048, #52370, #146370, #100862, #178734, #133207, #102876, #132214, #164561, #193905, #160554, #69544, #55369, #67538, #25059, #114027, #5862, #26055, #6855, #162544, #24048, #131208, #117039, #40197, #176739, #86702, #38212, #161552, #148387, #23045, #71541, #101877, #14852, #197882, #119061, #122019, #167548, #198878, #57388, #13850, #180743, #120037, #12877, #169515, #183710, #107831, #42219, #90683, #152365, #196903, #74542, #11895, #135231, #168525, #123008, #58370, #138190, #137191, #89701, #59351, #72550, #75517, #134228, #136207, #103880, #45196, #88703, #151387, #76514, #60345, #121019, #29043, #153350, #182717, #106850, #30023, #44202, #165560, #27057, #195913, #184694, #199873, #46178, #105861, #61337, #150399, #91661, #31015, #149384, #10880, #73558, #28060, #166561, #181723, #43205, #104872, #49169, #189676, #156341, #126976, #110828, #111823, #188685, #48179, #139176, #108839, #51148, #174502, #77505, #17841, #143141, #652, #80481, #127973, #33997, #170520, #95653, #3639, #66312, #112809, #126002, #33007, #157341, #62322, #93666, #140164, #92665, #50165, #79499, #141168, #154353, #125012, #172512, #173511, #32009, #18836, #34984, #123992 ),
 ( #185690, #15846, #81455, #155351, #142155, #16841, #1656, #65317, #64334, #47180, #78491, #63334, #2657, #186708, #109835, #187699, #4621, #171518, #94662, #96637, #158325, #19814, #39970, #193671, #37980, #7623, #52140, #22813, #20801, #114811, #146137, #8645, #163331, #86477, #115820, #148162, #23818, #69307, #113797, #5628, #82456, #71319, #9653, #132982, #84459, #194673, #128964, #130973, #101640, #117823, #192664, #147157, #176503, #53132, #56142, #24827, #35969, #54147, #97616, #99637, #70319, #177510, #55142, #131986, #191653, #144144, #175492, #159306, #67305, #190664, #161320, #36965, #98626, #85468, #160320, #38980, #21811, #100636, #116813, #83463, #145140, #162317, #178504, #6623, #68302, #129953, #26826, #199634, #75289, #104645, #42980, #61101, #11664, #135984, #13622, #57155, #105630, #136960, #164338, #90455, #168293, #118834, #152139, #59121, #60115, #197655, #153112, #29789, #195684, #73330, #179516, #12650, #74317, #167319, #120787, #182487, #198649, #58149, #135002, #40984, #72317, #43968, #25833, #196680, #28815, #121783, #41990, #183477, #119817, #44961, #106619, #180517, #14616, #181502, #91425, #103656, #165334, #76273, #137951, #102653, #166332, #88467, #87477, #149164, #10654, #133993, #150164, #27830, #89471, #151162, #187461, #107598, #186466, #30782, #95413, #62089, #63089, #188439, #48929, #171278, #140927, #126736, #47944, #80242, #157098, #49918, #111583, #79255, #19580, #109595, #18594, #2413, #141912, #3403, #78248, #169276, #138935, #81223, #4385, #92429, #32766, #173268, #154115, #110583, #158088, #64093, #415, #125761, #33754, #96401, #142904, #156098, #124768, #172264, #15609, #123752, #170278, #122774, #65078, #94418, #17596, #184464, #155107, #34742, #45943, #185451, #77266, #46941, #108601, #31772, #93420, #16600, #139921, #1410, #146912, #84219, #39727, #116575, #82213, #160078, #86233, #163081, #23573, #36719, #143904, #69066, #5386, #113559, #145898, #37732, #101388, #128728, #189438, #52889, #190424, #175253, #114564, #54901, #50915, #24585, #144900, #21565, #35735, #70076, #85221, #68062, #99394, #67069, #176261, #112573, #6383, #161077, #38741, #193426, #178264, #7382, #147923, #53907, #159068, #129716, #130733, #127736, #8401, #174267, #66070, #97382, #20562, #22572, #192425, #191413, #115582, #177270, #51900, #131744, #98381, #83225, #100399, #162079, #28576, #167074, #75049, #57908, #179273, #182241, #27587, #58882, #117573, #74074, #40737, #180275, #73085, #29551, #43726, #135745, #136715, #90212, #42740, #104402, #105387, #88224, #103409, #9409, #102407, #12412, #55900, #165087, #120548, #197416, #72067, #151895, #26581, #198396, #166084, #87237, #44716, #41745, #13385, #148920, #10409, #59874, #89225, #121540, #149908, #133740, #183235, #150919, #106372, #168054, #91184, #11415, #134756, #132741, #71075, #194429, #196438, #164094, #25593, #195435, #119580, #56910, #118585, #181263, #1167, #63855, #31529, #17354, #94177, #16364, #107355, #60857, #76034, #172028, #48694, #33516, #93182, #110346, #122532, #78012, #125526, #18358, #139680, #32525, #185208, #123515, #95176, #187223, #156863, #62842, #152873, #154867, #79009, #124526, #140683, #2175, #46699, #199393, #169028, #14368, #137709, #30533, #186221, #184223, #92186, #45704, #153870, #15368, #47702, #77024, #138696, #178, #61846, #108361, #170039, #109352, #155856, #171034, #196014, #166660, #57490, #178839, #24157, #71645, #164663, #133312, #43305, #197002, #147494, #195001, #73657, #89803, #86808, #180842, #151485, #150497, #12976, #58468, #103980, #132319, #165659, #74640, #104973, #42319, #136306, #197981, #40307, #56479, #121124, #88804, #59451, #120135, #119159, #27157, #181826, #41318, #118157, #162651, #55474, #11994, #8985, #179847, #135329, #28161, #25166, #182819, #102978, #44301, #85808, #101983, #70653, #26159, #194011, #163664, #148494, #117144, #9985, #87800, #149486 ),
 ( #10982, #72655, #134330, #171617, #170622, #154456, #124098, #109935, #31118, #63436, #78593, #77607, #122117, #75614, #90778, #141265, #156443, #79596, #92766, #17942, #198975, #139278, #33105, #187797, #755, #16939, #184793, #123108, #2755, #94761, #64431, #62426, #126101, #169621, #140266, #185797, #125112, #1758, #61436, #152462, #183806, #105960, #167645, #13948, #15948, #29141, #137293, #93768, #60442, #47285, #45294, #108941, #186810, #106946, #168619, #32111, #46279, #155449, #30119, #91760, #153454, #48280, #14952, #76612, #138290, #199971, #107935, #5726, #83560, #127076, #175591, #145239, #34097, #160420, #38077, #188784, #21909, #129060, #84555, #36068, #111925, #7720, #112908, #69406, #81553, #67405, #6720, #50267, #37067, #68398, #95755, #130050, #99733, #173611, #191750, #190761, #53233, #52236, #22909, #161417, #65415, #143239, #131072, #98726, #176603, #114909, #82560, #144242, #146233, #128073, #4722, #49266, #142254, #113893, #157440, #66411, #110924, #172610, #35081, #18935, #189776, #80580, #3738, #96734, #158423, #51248, #19911, #174602, #97717, #159407, #20902, #118929, #86572, #70415, #195782, #134092, #89569, #180614, #196774, #194767, #56241, #115916, #57255, #177606, #117922, #100731, #165431, #132082, #133077, #58242, #42087, #41084, #10751, #119910, #179611, #150266, #26926, #164435, #8745, #162412, #39074, #27926, #43073, #166431, #102747, #104740, #85568, #25929, #181596, #74410, #87572, #103752, #71413, #9749, #151255, #12745, #192761, #149259, #54244, #72415, #88568, #11760, #73427, #135098, #148256, #23914, #193771, #147254, #55240, #116908, #178601, #40064, #101741, #163429, #24927, #77369, #152233, #139037, #47045, #109698, #171380, #169375, #76376, #517, #120886, #137056, #185551, #44068, #62189, #105728, #106717, #199734, #156199, #108702, #94517, #167415, #123853, #170381, #183574, #61200, #198746, #121881, #155211, #32867, #45059, #124870, #31872, #138053, #184560, #93526, #107696, #16700, #60211, #78350, #182585, #140024, #92530, #168391, #28911, #46041, #29886, #30883, #90551, #1513, #13718, #154219, #63190, #15709, #75384, #197750, #91524, #122872, #153211, #186569, #48042, #14716, #17699, #136076, #59217, #3501, #97479, #6480, #67168, #129812, #113657, #20660, #49028, #82314, #68160, #191511, #176362, #36819, #50020, #95513, #144004, #18693, #126836, #159165, #51010, #52988, #142012, #2514, #66170, #65177, #188542, #127832, #114666, #64194, #37835, #158187, #173372, #110683, #83322, #98485, #81319, #112671, #157199, #189538, #125861, #19677, #174363, #51998, #99495, #161175, #5485, #79356, #128825, #172363, #143002, #190524, #141027, #160178, #187561, #33853, #80340, #111685, #35833, #175351, #4480, #21668, #144999, #34842, #96497, #70176, #69165, #165188, #192523, #41845, #180375, #88323, #71175, #54006, #195536, #40835, #164192, #11519, #150013, #119678, #103512, #193527, #38839, #25690, #162176, #131844, #102508, #194526, #196538, #85322, #145998, #9509, #147014, #55001, #132839, #73189, #7481, #58008, #101491, #116670, #115680, #26683, #134860, #24684, #55998, #100497, #117676, #130832, #163180, #179373, #57010, #181361, #42840, #87335, #104505, #10509, #177368, #86333, #149021, #84319, #22672, #23674, #8499, #178361, #39825, #72171, #133846, #148020, #118683, #14469, #166186, #46800, #13481, #12511, #108459, #135845, #185309, #123614, #31631, #76131, #197514, #138797, #184323, #15471, #74175, #30637, #58982, #136817, #29647, #186319, #278, #124624, #120649, #107456, #169132, #75146, #91279, #28674, #151995, #170136, #139779, #198501, #154965, #153974, #106471, #137809, #77128, #199493, #92290, #90309, #61947, #151020, #93280, #122633, #59972, #182347, #60959, #121639, #45805, #43825, #16461, #105489, #78110, #1267, #62944, #167175, #27687, #183334, #168150, #44816, #47801, #89328, #152970, #18455, #20419, #36578, #33612, #127600, #98233 ),
 ( #2270, #142767, #175110, #191273, #81089, #82069, #188301, #126599, #21423, #159936, #83083, #65927, #6244, #173130, #143762, #189299, #128587, #5243, #64940, #155955, #125622, #67923, #109451, #94277, #34605, #144759, #17452, #97242, #129576, #50776, #187320, #112436, #66923, #171134, #32623, #4247, #49778, #174125, #79108, #110445, #140781, #96264, #172126, #63953, #157950, #48791, #141774, #35596, #190281, #95275, #158930, #51757, #156958, #113418, #80106, #3268, #111443, #19441, #133599, #70936, #26444, #103271, #68926, #146763, #11274, #179131, #180137, #10270, #86093, #147784, #87096, #131600, #8256, #52748, #145759, #55759, #99251, #69936, #102270, #40599, #115438, #117433, #193285, #118445, #9270, #130588, #88086, #85079, #195291, #192283, #53764, #56772, #132604, #163958, #54759, #177129, #25456, #194293, #149772, #148781, #41606, #116433, #178121, #176118, #71929, #37589, #39589, #160938, #164951, #38600, #101248, #72947, #134617, #162937, #114417, #22430, #24444, #84080, #7241, #100256, #161937, #23432, #155480, #95787, #62460, #33137, #16972, #17975, #94795, #154487, #42600, #12275, #157473, #80612, #181126, #124133, #49297, #104264, #186844, #34128, #140301, #73940, #1792, #109968, #172640, #18966, #32143, #139309, #63470, #165946, #197280, #196301, #185832, #58743, #57771, #47319, #119441, #31151, #78626, #156474, #135609, #125145, #79629, #27446, #171647, #187828, #120412, #141297, #48313, #2787, #64466, #89088, #110956, #184827, #92799, #150780, #126133, #46313, #107968, #93800, #169655, #15981, #77640, #788, #108974, #170655, #145271, #188815, #36098, #191783, #130084, #4753, #6752, #159438, #7753, #98757, #19943, #177638, #174633, #22941, #81584, #143270, #146267, #160450, #68431, #97750, #66442, #53265, #83591, #39105, #114942, #69437, #144272, #5759, #65446, #176635, #127108, #67435, #50298, #38110, #128103, #82591, #131105, #99765, #190792, #21941, #192793, #129092, #161450, #84587, #113924, #158454, #111955, #173644, #100761, #54275, #115948, #52266, #162443, #35113, #175624, #23944, #142289, #37098, #3769, #20933, #96765, #189807, #51279, #112940, #147285, #194797, #87601, #56270, #166461, #119940, #70444, #117953, #196803, #12776, #9781, #103781, #74441, #73456, #136108, #181625, #26957, #55269, #88600, #197784, #59250, #182618, #43105, #179644, #101772, #150296, #24957, #133108, #165461, #57284, #120919, #148287, #8775, #72448, #71443, #41113, #134123, #44103, #132110, #105761, #164464, #102777, #116938, #89599, #104773, #149287, #118958, #163459, #195812, #193803, #25958, #180644, #58271, #167447, #85598, #11792, #178631, #135129, #40094, #10781, #27958, #86604, #151287, #42119, #28944, #79394, #17737, #185588, #123890, #92565, #47078, #77403, #90585, #109732, #13751, #45093, #198779, #75419, #64232, #141064, #2550, #15744, #125897, #121916, #62222, #94555, #110721, #551, #140060, #107730, #46076, #187597, #156235, #49066, #108739, #152266, #154253, #63226, #170415, #48076, #124906, #184595, #137093, #106750, #60245, #183609, #168425, #139073, #29920, #91560, #16736, #153248, #31907, #14750, #93560, #1551, #76411, #138087, #155246, #169412, #78384, #199768, #61235, #122907, #186604, #30917, #171416, #32902, #174399, #81354, #53024, #6517, #157236, #143038, #83359, #99531, #96532, #190560, #161213, #160215, #22708, #68196, #113691, #142049, #175386, #84355, #146033, #69201, #129848, #4516, #188579, #36855, #111721, #19712, #52034, #144040, #7516, #34878, #95549, #159201, #158222, #66209, #20696, #130869, #18729, #192559, #51045, #127869, #3536, #176398, #191547, #35869, #5522, #50060, #82352, #80377, #112707, #67202, #145035, #54042, #172403, #98522, #33892, #21705, #65213, #97515, #114705, #126872, #37873, #173407, #189573, #128860, #104536, #72207, #10543, #179406, #133881, #164227, #177404, #162211, #116706, #135875, #58039, #85357, #134892, #73221, #181393 ),
 ( #23710, #57045, #118719, #163217, #40870, #178396, #101526, #196568, #89361, #24719, #166217, #103547, #56032, #25724, #26717, #87370, #180408, #39860, #88356, #100532, #119709, #195572, #86368, #8533, #149055, #148053, #41880, #147050, #165222, #70212, #150049, #42871, #11555, #131879, #117710, #27718, #151050, #12541, #74206, #197546, #115716, #9544, #38875, #193564, #55036, #71210, #132873, #194562, #102544, #32656, #45837, #109486, #152027, #92323, #124658, #140813, #30670, #170172, #137844, #76164, #171169, #186354, #47834, #15504, #155988, #122667, #93315, #77161, #78144, #154999, #14502, #105523, #75178, #17485, #59014, #43858, #184355, #94310, #167209, #46833, #79142, #311, #136850, #61979, #31665, #120681, #182380, #154008, #199525, #123645, #28706, #60006, #90342, #107488, #121673, #13513, #169166, #198535, #91311, #138831, #16495, #183368, #185342, #139812, #44850, #1300, #106506, #168183, #62978, #108493, #29679, #153003, #60993, #52779, #18486, #96293, #160968, #128619, #129607, #159967, #35627, #97272, #36608, #81117, #157980, #2303, #95304, #5276, #48821, #19472, #51788, #190312, #64970, #66958, #142797, #67953, #158960, #80135, #37619, #34634, #83115, #141805, #3298, #6275, #20450, #113448, #4278, #126629, #175141, #143793, #99281, #98265, #191303, #65958, #127629, #125654, #21454, #187351, #189329, #110474, #144792, #188330, #22462, #50806, #112464, #172156, #114448, #176149, #174156, #82101, #49809, #84110, #33642, #63984, #156988, #111474, #173159, #196333, #25485, #57801, #133632, #38631, #9301, #87127, #7271, #103302, #68955, #145789, #119472, #134647, #102299, #40629, #70967, #163988, #194323, #130618, #192314, #146795, #165975, #88118, #115469, #164981, #26476, #11308, #55791, #177158, #118477, #148812, #195324, #53794, #10302, #100288, #116465, #132635, #27477, #180168, #104294, #161966, #71959, #56804, #193316, #117462, #8288, #131632, #149802, #181155, #54790, #42630, #41637, #86124, #179161, #72978, #23462, #85109, #69966, #178154, #39619, #101278, #162968, #24474, #147815, #199286, #59767, #122426, #120441, #153766, #182134, #184118, #93077, #45600, #105282, #150808, #198289, #91080, #121435, #169933, #123410, #73970, #183128, #71, #16259, #13282, #107253, #77910, #76919, #139577, #185103, #30430, #58773, #92077, #1062, #62736, #186112, #46592, #44611, #166970, #15261, #28472, #136609, #168924, #60753, #124417, #151791, #12304, #75928, #74946, #106266, #137603, #47593, #135639, #89120, #109246, #170926, #138590, #61742, #152767, #108253, #31424, #197309, #43618, #90107, #167950, #154761, #29448, #14257, #190081, #98029, #80891, #2069, #5039, #50575, #81865, #140579, #97045, #63748, #3065, #96064, #52547, #66725, #191074, #125422, #173925, #35394, #79906, #157752, #95071, #18253, #51557, #6042, #141577, #21222, #20217, #172927, #142568, #143555, #4047, #158727, #156759, #128385, #17249, #174911, #189102, #64742, #187118, #65724, #126404, #127392, #48590, #113221, #110241, #112235, #36375, #159725, #171922, #94072, #188100, #34406, #49573, #82878, #144556, #78901, #111236, #67720, #129377, #19244, #114208, #32417, #155751, #33412, #10064, #117228, #145554, #178922, #164745, #103063, #72740, #133393, #146549, #192068, #40391, #115228, #23228, #55555, #147577, #149567, #38391, #99041, #162732, #100047, #84871, #24240, #26240, #160731, #11063, #54555, #69724, #7032, #179931, #195084, #177919, #9063, #53550, #85889, #22223, #116228, #70733, #148574, #87879, #134412, #102063, #196098, #163748, #68714, #39387, #25248, #37384, #56565, #83872, #57568, #176920, #131392, #175913, #86889, #130371, #118240, #132400, #194093, #71724, #101046, #193080, #161733, #8044, #41398, #165740, #13054, #168696, #107024, #181904, #183886, #136384, #184874, #75691, #197081, #154530, #151565, #200047, #58548, #120214, #123185, #137371, #45371, #74721, #43382, #122194, #60519, #16027, #30197 ),
 ( #14025, #182896, #199049, #167722, #180922, #27235, #105055, #139353, #61516, #88884, #138366, #76690, #46356, #29220, #150576, #91839, #153533, #15029, #12075, #108014, #73737, #89882, #44380, #833, #169700, #77685, #135410, #31193, #92845, #166738, #106036, #28242, #198061, #119238, #42397, #59527, #104060, #121205, #90853, #152538, #173694, #34174, #127155, #125193, #35162, #47365, #4802, #19013, #186889, #155524, #172689, #33183, #95835, #93845, #188863, #17019, #157519, #66491, #80659, #78672, #124178, #171694, #64511, #94842, #143315, #96817, #109020, #156522, #158502, #189854, #48359, #142335, #51328, #50346, #112988, #19989, #3815, #65493, #112005, #170699, #81632, #32188, #18022, #126178, #82637, #128154, #20980, #140348, #174681, #36146, #110013, #187873, #79675, #141346, #97798, #159487, #2833, #144320, #62507, #49341, #111003, #185880, #1836, #63518, #71244, #181425, #190839, #151082, #165256, #132908, #101562, #118754, #179440, #41915, #39894, #73254, #163253, #103581, #12573, #26750, #24755, #67484, #117746, #10579, #40906, #89394, #42903, #52315, #102579, #119742, #135908, #194595, #88389, #197579, #196601, #59046, #104568, #150083, #175671, #11587, #120712, #182412, #105555, #166251, #164263, #86402, #134924, #148087, #56066, #58072, #180443, #43892, #25758, #129142, #195607, #87404, #149089, #57080, #167241, #113973, #28739, #72240, #133917, #9578, #74239, #27751, #90376, #5809, #168216, #138862, #136883, #30704, #62010, #124691, #79175, #2335, #31697, #64016, #139843, #44883, #15535, #93346, #13546, #109518, #75212, #152061, #125685, #140846, #108525, #46864, #77193, #170204, #342, #198569, #60039, #153036, #172188, #94341, #121707, #171200, #32690, #17517, #123675, #183400, #186388, #184387, #155032, #47865, #29713, #78174, #156020, #106539, #63012, #187383, #91345, #48852, #16527, #110507, #1332, #33673, #14536, #76197, #45868, #137876, #199557, #61026, #122698, #185373, #107521, #169197, #92354, #154040, #95335, #188364, #98298, #141837, #189361, #144823, #83149, #158012, #160000, #112495, #161002, #51821, #173191, #130654, #127661, #176183, #34667, #96325, #99318, #113481, #21488, #50838, #19503, #6307, #36641, #192348, #67985, #22496, #97305, #158991, #18518, #129639, #80165, #20483, #3329, #191335, #81148, #35657, #84143, #52813, #143827, #175175, #145822, #66991, #174189, #114480, #65002, #111505, #126660, #49841, #53830, #7305, #68990, #82133, #115505, #142829, #128650, #177193, #157020, #190345, #37653, #5307, #4309, #65992, #73010, #149835, #25518, #181187, #55825, #41670, #87163, #165013, #103334, #9336, #23496, #131668, #42664, #104326, #85144, #194358, #134679, #146830, #195356, #57833, #10336, #193350, #71992, #118511, #119506, #38666, #148845, #117498, #56836, #8324, #178188, #100321, #102332, #101314, #162000, #133666, #69999, #54826, #71002, #196365, #26507, #116500, #88150, #39653, #163003, #179195, #180201, #24510, #86160, #147850, #132670, #40663, #164022, #11339, #97951, #113141, #19164, #112160, #22143, #65649, #174831, #68634, #6954, #81786, #83793, #36296, #84791, #175829, #96969, #54478, #51479, #99967, #158650, #20141, #23147, #37302, #145473, #159643, #143473, #130290, #160651, #116148, #191984, #146470, #21139, #82794, #142491, #53471, #3969, #144476, #127311, #115148, #4957, #5960, #7962, #176841, #67638, #98961, #69645, #190993, #129297, #38312, #189022, #35315, #50496, #173849, #177839, #131311, #193001, #52469, #39307, #66642, #114128, #100966, #80813, #161651, #128305, #190005, #49093, #94584, #80405, #29951, #63254, #124934, #169443, #185616, #184622, #107759, #141091, #95577, #30946, #79421, #16763, #157263, #47106, #172431, #168454, #109758, #18758, #186631, #138117, #48102, #32929, #142077, #3563, #155274, #62248, #171442, #106779, #122935, #121946, #108766, #46104, #183639, #170443, #45121, #154282, #78411, #156263, #199798, #17765 ) ),
 .UNSPECIFIED., .T., .F., .F. ) 
 B_SPLINE_SURFACE_WITH_KNOTS ( ( 4, 3, 4 ),
 ( 3, 2, 2, 2, 2, 2, 2, 2, 2, 2, 2, 2, 2, 2, 2, 2, 2, 2, 2, 2, 2, 2, 2, 2, 2, 2, 2, 2, 2, 2, 2, 2, 2, 2, 2, 2, 2, 2, 2, 2, 2, 2, 2, 2, 2, 2, 2, 2, 2, 2, 2, 2, 2, 2, 2, 2, 2, 2, 2, 2, 2, 2, 2, 2, 2, 2, 2, 2, 2, 2, 2, 2, 2, 2, 2, 2, 2, 2, 2, 2, 2, 2, 2, 2, 2, 2, 2, 2, 2, 2, 2, 2, 2, 2, 2, 2, 2, 2, 2, 2, 2, 2, 2, 2, 2, 2, 2, 2, 2, 2, 2, 2, 2, 2, 2, 2, 2, 2, 2, 2, 2, 2, 2, 2, 2, 2, 2, 2, 2, 2, 2, 2, 2, 2, 2, 2, 2, 2, 2, 2, 2, 2, 2, 2, 2, 2, 2, 2, 2, 2, 2, 2, 2, 2, 2, 2, 2, 2, 2, 2, 2, 2, 2, 2, 2, 2, 2, 2, 2, 2, 2, 2, 2, 2, 2, 2, 2, 2, 2, 2, 2, 2, 2, 2, 2, 2, 2, 2, 2, 2, 2, 2, 2, 2, 2, 2, 2, 2, 2, 2, 2, 2, 2, 2, 2, 2, 2, 2, 2, 2, 2, 2, 2, 2, 2, 2, 2, 2, 2, 2, 2, 2, 2, 2, 2, 2, 2, 2, 3 ),
 ( 0.000000000000000000, 0.5000000000000000000, 1.000000000000000000 ),
 ( 0.000000000000000000, 0.004385964912280701511, 0.008771929824561403022, 0.01315789473684210453, 0.01754385964912280604, 0.02192982456140350755, 0.02631578947368420907, 0.03070175438596491058, 0.03508771929824561209, 0.03947368421052631360, 0.04385964912280701511, 0.04824561403508771662, 0.05263157894736841813, 0.05701754385964911964, 0.06140350877192982115, 0.06578947368421052266, 0.07017543859649122417, 0.07456140350877192569, 0.07894736842105262720, 0.08333333333333332871, 0.08771929824561403022, 0.09210526315789473173, 0.09649122807017543324, 0.1008771929824561348, 0.1052631578947368363, 0.1096491228070175378, 0.1140350877192982393, 0.1184210526315789408, 0.1228070175438596423, 0.1271929824561403577, 0.1315789473684210453, 0.1359649122807017607, 0.1403508771929824483, 0.1447368421052631637, 0.1491228070175438514, 0.1535087719298245668, 0.1578947368421052544, 0.1622807017543859698, 0.1666666666666666574, 0.1710526315789473728, 0.1754385964912280604, 0.1798245614035087758, 0.1842105263157894635, 0.1885964912280701788, 0.1929824561403508665, 0.1973684210526315819, 0.2017543859649122695, 0.2061403508771929849, 0.2105263157894736725, 0.2149122807017543879, 0.2192982456140350755, 0.2236842105263157909, 0.2280701754385964786, 0.2324561403508771940, 0.2368421052631578816, 0.2412280701754385970, 0.2456140350877192846, 0.2500000000000000000, 0.2543859649122807154, 0.2587719298245614308, 0.2631578947368420907, 0.2675438596491228060, 0.2719298245614035214, 0.2763157894736842368, 0.2807017543859648967, 0.2850877192982456121, 0.2894736842105263275, 0.2938596491228070429, 0.2982456140350877027, 0.3026315789473684181, 0.3070175438596491335, 0.3114035087719298489, 0.3157894736842105088, 0.3201754385964912242, 0.3245614035087719396, 0.3289473684210526550, 0.3333333333333333148, 0.3377192982456140302, 0.3421052631578947456, 0.3464912280701754610, 0.3508771929824561209, 0.3552631578947368363, 0.3596491228070175517, 0.3640350877192982670, 0.3684210526315789269, 0.3728070175438596423, 0.3771929824561403577, 0.3815789473684210731, 0.3859649122807017330, 0.3903508771929824483, 0.3947368421052631637, 0.3991228070175438791, 0.4035087719298245390, 0.4078947368421052544, 0.4122807017543859698, 0.4166666666666666852, 0.4210526315789473450, 0.4254385964912280604, 0.4298245614035087758, 0.4342105263157894912, 0.4385964912280701511, 0.4429824561403508665, 0.4473684210526315819, 0.4517543859649122973, 0.4561403508771929571, 0.4605263157894736725, 0.4649122807017543879, 0.4692982456140351033, 0.4736842105263157632, 0.4780701754385964786, 0.4824561403508771940, 0.4868421052631579093, 0.4912280701754385692, 0.4956140350877192846, 0.5000000000000000000, 0.5043859649122807154, 0.5087719298245614308, 0.5131578947368421462, 0.5175438596491228616, 0.5219298245614034659, 0.5263157894736841813, 0.5307017543859648967, 0.5350877192982456121, 0.5394736842105263275, 0.5438596491228070429, 0.5482456140350877583, 0.5526315789473684736, 0.5570175438596490780, 0.5614035087719297934, 0.5657894736842105088, 0.5701754385964912242, 0.5745614035087719396, 0.5789473684210526550, 0.5833333333333333703, 0.5877192982456140857, 0.5921052631578946901, 0.5964912280701754055, 0.6008771929824561209, 0.6052631578947368363, 0.6096491228070175517, 0.6140350877192982670, 0.6184210526315789824, 0.6228070175438596978, 0.6271929824561403022, 0.6315789473684210176, 0.6359649122807017330, 0.6403508771929824483, 0.6447368421052631637, 0.6491228070175438791, 0.6535087719298245945, 0.6578947368421053099, 0.6622807017543859143, 0.6666666666666666297, 0.6710526315789473450, 0.6754385964912280604, 0.6798245614035087758, 0.6842105263157894912, 0.6885964912280702066, 0.6929824561403509220, 0.6973684210526315264, 0.7017543859649122417, 0.7061403508771929571, 0.7105263157894736725, 0.7149122807017543879, 0.7192982456140351033, 0.7236842105263158187, 0.7280701754385965341, 0.7324561403508771384, 0.7368421052631578538, 0.7412280701754385692, 0.7456140350877192846, 0.7500000000000000000, 0.7543859649122807154, 0.7587719298245614308, 0.7631578947368421462, 0.7675438596491228616, 0.7719298245614034659, 0.7763157894736841813, 0.7807017543859648967, 0.7850877192982456121, 0.7894736842105263275, 0.7938596491228070429, 0.7982456140350877583, 0.8026315789473684736, 0.8070175438596490780, 0.8114035087719297934, 0.8157894736842105088, 0.8201754385964912242, 0.8245614035087719396, 0.8289473684210526550, 0.8333333333333333703, 0.8377192982456140857, 0.8421052631578946901, 0.8464912280701754055, 0.8508771929824561209, 0.8552631578947368363, 0.8596491228070175517, 0.8640350877192982670, 0.8684210526315789824, 0.8728070175438596978, 0.8771929824561403022, 0.8815789473684210176, 0.8859649122807017330, 0.8903508771929824483, 0.8947368421052631637, 0.8991228070175438791, 0.9035087719298245945, 0.9078947368421053099, 0.9122807017543859143, 0.9166666666666666297, 0.9210526315789473450, 0.9254385964912280604, 0.9298245614035087758, 0.9342105263157894912, 0.9385964912280702066, 0.9429824561403509220, 0.9473684210526315264, 0.9517543859649122417, 0.9561403508771929571, 0.9605263157894736725, 0.9649122807017543879, 0.9692982456140351033, 0.9736842105263158187, 0.9780701754385965341, 0.9824561403508771384, 0.9868421052631578538, 0.9912280701754385692, 0.9956140350877192846, 1.000000000000000000 ),
 .UNSPECIFIED. ) 
 GEOMETRIC_REPRESENTATION_ITEM ( )  RATIONAL_B_SPLINE_SURFACE ( (
 ( 1.000000000000000000, 0.9659258262890683122, 1.000000000000000000, 0.9659258262890683122, 1.000000000000000000, 0.9659258262890683122, 1.000000000000000000, 0.9659258262890683122, 1.000000000000000000, 0.9659258262890683122, 1.000000000000000000, 0.9659258262890683122, 1.000000000000000000, 0.9659258262890683122, 1.000000000000000000, 0.9659258262890683122, 1.000000000000000000, 0.9659258262890683122, 1.000000000000000000, 0.9659258262890683122, 1.000000000000000000, 0.9659258262890683122, 1.000000000000000000, 0.9659258262890683122, 1.000000000000000000, 0.9659258262890683122, 1.000000000000000000, 0.9659258262890683122, 1.000000000000000000, 0.9659258262890683122, 1.000000000000000000, 0.9659258262890683122, 1.000000000000000000, 0.9659258262890683122, 1.000000000000000000, 0.9659258262890683122, 1.000000000000000000, 0.9659258262890683122, 1.000000000000000000, 0.9659258262890683122, 1.000000000000000000, 0.9659258262890683122, 1.000000000000000000, 0.9659258262890683122, 1.000000000000000000, 0.9659258262890683122, 1.000000000000000000, 0.9659258262890683122, 1.000000000000000000, 0.9659258262890683122, 1.000000000000000000, 0.9659258262890683122, 1.000000000000000000, 0.9659258262890683122, 1.000000000000000000, 0.9659258262890683122, 1.000000000000000000, 0.9659258262890683122, 1.000000000000000000, 0.9659258262890683122, 1.000000000000000000, 0.9659258262890683122, 1.000000000000000000, 0.9659258262890683122, 1.000000000000000000, 0.9659258262890683122, 1.000000000000000000, 0.9659258262890683122, 1.000000000000000000, 0.9659258262890683122, 1.000000000000000000, 0.9659258262890683122, 1.000000000000000000, 0.9659258262890683122, 1.000000000000000000, 0.9659258262890683122, 1.000000000000000000, 0.9659258262890683122, 1.000000000000000000, 0.9659258262890683122, 1.000000000000000000, 0.9659258262890683122, 1.000000000000000000, 0.9659258262890683122, 1.000000000000000000, 0.9659258262890683122, 1.000000000000000000, 0.9659258262890683122, 1.000000000000000000, 0.9659258262890683122, 1.000000000000000000, 0.9659258262890683122, 1.000000000000000000, 0.9659258262890683122, 1.000000000000000000, 0.9659258262890683122, 1.000000000000000000, 0.9659258262890683122, 1.000000000000000000, 0.9659258262890683122, 1.000000000000000000, 0.9659258262890683122, 1.000000000000000000, 0.9659258262890683122, 1.000000000000000000, 0.9659258262890683122, 1.000000000000000000, 0.9659258262890683122, 1.000000000000000000, 0.9659258262890683122, 1.000000000000000000, 0.9659258262890683122, 1.000000000000000000, 0.9659258262890683122, 1.000000000000000000, 0.9659258262890683122, 1.000000000000000000, 0.9659258262890683122, 1.000000000000000000, 0.9659258262890683122, 1.000000000000000000, 0.9659258262890683122, 1.000000000000000000, 0.9659258262890683122, 1.000000000000000000, 0.9659258262890683122, 1.000000000000000000, 0.9659258262890683122, 1.000000000000000000, 0.9659258262890683122, 1.000000000000000000, 0.9659258262890683122, 1.000000000000000000, 0.9659258262890683122, 1.000000000000000000, 0.9659258262890683122, 1.000000000000000000, 0.9659258262890683122, 1.000000000000000000, 0.9659258262890683122, 1.000000000000000000, 0.9659258262890683122, 1.000000000000000000, 0.9659258262890683122, 1.000000000000000000, 0.9659258262890683122, 1.000000000000000000, 0.9659258262890683122, 1.000000000000000000, 0.9659258262890683122, 1.000000000000000000, 0.9659258262890683122, 1.000000000000000000, 0.9659258262890683122, 1.000000000000000000, 0.9659258262890683122, 1.000000000000000000, 0.9659258262890683122, 1.000000000000000000, 0.9659258262890683122, 1.000000000000000000, 0.9659258262890683122, 1.000000000000000000, 0.9659258262890683122, 1.000000000000000000, 0.9659258262890683122, 1.000000000000000000, 0.9659258262890683122, 1.000000000000000000, 0.9659258262890683122, 1.000000000000000000, 0.9659258262890683122, 1.000000000000000000, 0.9659258262890683122, 1.000000000000000000, 0.9659258262890683122, 1.000000000000000000, 0.9659258262890683122, 1.000000000000000000, 0.9659258262890683122, 1.000000000000000000, 0.9659258262890683122, 1.000000000000000000, 0.9659258262890683122, 1.000000000000000000, 0.9659258262890683122, 1.000000000000000000, 0.9659258262890683122, 1.000000000000000000, 0.9659258262890683122, 1.000000000000000000, 0.9659258262890683122, 1.000000000000000000, 0.9659258262890683122, 1.000000000000000000, 0.9659258262890683122, 1.000000000000000000, 0.9659258262890683122, 1.000000000000000000, 0.9659258262890683122, 1.000000000000000000, 0.9659258262890683122, 1.000000000000000000, 0.9659258262890683122, 1.000000000000000000, 0.9659258262890683122, 1.000000000000000000, 0.9659258262890683122, 1.000000000000000000, 0.9659258262890683122, 1.000000000000000000, 0.9659258262890683122, 1.000000000000000000, 0.9659258262890683122, 1.000000000000000000, 0.9659258262890683122, 1.000000000000000000, 0.9659258262890683122, 1.000000000000000000, 0.9659258262890683122, 1.000000000000000000, 0.9659258262890683122, 1.000000000000000000, 0.9659258262890683122, 1.000000000000000000, 0.9659258262890683122, 1.000000000000000000, 0.9659258262890683122, 1.000000000000000000, 0.9659258262890683122, 1.000000000000000000, 0.9659258262890683122, 1.000000000000000000, 0.9659258262890683122, 1.000000000000000000, 0.9659258262890683122, 1.000000000000000000, 0.9659258262890683122, 1.000000000000000000, 0.9659258262890683122, 1.000000000000000000, 0.9659258262890683122, 1.000000000000000000, 0.9659258262890683122, 1.000000000000000000, 0.9659258262890683122, 1.000000000000000000, 0.9659258262890683122, 1.000000000000000000, 0.9659258262890683122, 1.000000000000000000, 0.9659258262890683122, 1.000000000000000000, 0.9659258262890683122, 1.000000000000000000, 0.9659258262890683122, 1.000000000000000000, 0.9659258262890683122, 1.000000000000000000, 0.9659258262890683122, 1.000000000000000000, 0.9659258262890683122, 1.000000000000000000, 0.9659258262890683122, 1.000000000000000000, 0.9659258262890683122, 1.000000000000000000, 0.9659258262890683122, 1.000000000000000000, 0.9659258262890683122, 1.000000000000000000, 0.9659258262890683122, 1.000000000000000000, 0.9659258262890683122, 1.000000000000000000, 0.9659258262890683122, 1.000000000000000000, 0.9659258262890683122, 1.000000000000000000, 0.9659258262890683122, 1.000000000000000000, 0.9659258262890683122, 1.000000000000000000, 0.9659258262890683122, 1.000000000000000000, 0.9659258262890683122, 1.000000000000000000, 0.9659258262890683122, 1.000000000000000000, 0.9659258262890683122, 1.000000000000000000, 0.9659258262890683122, 1.000000000000000000, 0.9659258262890683122, 1.000000000000000000, 0.9659258262890683122, 1.000000000000000000, 0.9659258262890683122, 1.000000000000000000, 0.9659258262890683122, 1.000000000000000000, 0.9659258262890683122, 1.000000000000000000, 0.9659258262890683122, 1.000000000000000000, 0.9659258262890683122, 1.000000000000000000, 0.9659258262890683122, 1.000000000000000000, 0.9659258262890683122, 1.000000000000000000, 0.9659258262890683122, 1.000000000000000000, 0.9659258262890683122, 1.000000000000000000, 0.9659258262890683122, 1.000000000000000000, 0.9659258262890683122, 1.000000000000000000, 0.9659258262890683122, 1.000000000000000000, 0.9659258262890683122, 1.000000000000000000, 0.9659258262890683122, 1.000000000000000000, 0.9659258262890683122, 1.000000000000000000, 0.9659258262890683122, 1.000000000000000000, 0.9659258262890683122, 1.000000000000000000, 0.9659258262890683122, 1.000000000000000000, 0.9659258262890683122, 1.000000000000000000, 0.9659258262890683122, 1.000000000000000000, 0.9659258262890683122, 1.000000000000000000, 0.9659258262890683122, 1.000000000000000000, 0.9659258262890683122, 1.000000000000000000, 0.9659258262890683122, 1.000000000000000000, 0.9659258262890683122, 1.000000000000000000, 0.9659258262890683122, 1.000000000000000000, 0.9659258262890683122, 1.000000000000000000, 0.9659258262890683122, 1.000000000000000000, 0.9659258262890683122, 1.000000000000000000, 0.9659258262890683122, 1.000000000000000000, 0.9659258262890683122, 1.000000000000000000, 0.9659258262890683122, 1.000000000000000000, 0.9659258262890683122, 1.000000000000000000, 0.9659258262890683122, 1.000000000000000000, 0.9659258262890683122, 1.000000000000000000, 0.9659258262890683122, 1.000000000000000000, 0.9659258262890683122, 1.000000000000000000, 0.9659258262890683122, 1.000000000000000000, 0.9659258262890683122, 1.000000000000000000, 0.9659258262890683122, 1.000000000000000000, 0.9659258262890683122, 1.000000000000000000, 0.9659258262890683122, 1.000000000000000000, 0.9659258262890683122, 1.000000000000000000, 0.9659258262890683122, 1.000000000000000000, 0.9659258262890683122, 1.000000000000000000, 0.9659258262890683122, 1.000000000000000000, 0.9659258262890683122, 1.000000000000000000, 0.9659258262890683122, 1.000000000000000000, 0.9659258262890683122, 1.000000000000000000, 0.9659258262890683122, 1.000000000000000000, 0.9659258262890683122, 1.000000000000000000, 0.9659258262890683122, 1.000000000000000000, 0.9659258262890683122, 1.000000000000000000, 0.9659258262890683122, 1.000000000000000000, 0.9659258262890683122, 1.000000000000000000, 0.9659258262890683122, 1.000000000000000000, 0.9659258262890683122, 1.000000000000000000, 0.9659258262890683122, 1.000000000000000000, 0.9659258262890683122, 1.000000000000000000, 0.9659258262890683122, 1.000000000000000000, 0.9659258262890683122, 1.000000000000000000, 0.9659258262890683122, 1.000000000000000000, 0.9659258262890683122, 1.000000000000000000, 0.9659258262890683122, 1.000000000000000000, 0.9659258262890683122, 1.000000000000000000, 0.9659258262890683122, 1.000000000000000000, 0.9659258262890683122, 1.000000000000000000, 0.9659258262890683122, 1.000000000000000000, 0.9659258262890683122, 1.000000000000000000, 0.9659258262890683122, 1.000000000000000000, 0.9659258262890683122, 1.000000000000000000, 0.9659258262890683122, 1.000000000000000000, 0.9659258262890683122, 1.000000000000000000, 0.9659258262890683122, 1.000000000000000000, 0.9659258262890683122, 1.000000000000000000, 0.9659258262890683122, 1.000000000000000000, 0.9659258262890683122, 1.000000000000000000, 0.9659258262890683122, 1.000000000000000000, 0.9659258262890683122, 1.000000000000000000, 0.9659258262890683122, 1.000000000000000000),
 ( 0.3333333333333333703, 0.3219752754296894559, 0.3333333333333333703, 0.3219752754296894559, 0.3333333333333333703, 0.3219752754296894559, 0.3333333333333333703, 0.3219752754296894559, 0.3333333333333333703, 0.3219752754296894559, 0.3333333333333333703, 0.3219752754296894559, 0.3333333333333333703, 0.3219752754296894559, 0.3333333333333333703, 0.3219752754296894559, 0.3333333333333333703, 0.3219752754296894559, 0.3333333333333333703, 0.3219752754296894559, 0.3333333333333333703, 0.3219752754296894559, 0.3333333333333333703, 0.3219752754296894559, 0.3333333333333333703, 0.3219752754296894559, 0.3333333333333333703, 0.3219752754296894559, 0.3333333333333333703, 0.3219752754296894559, 0.3333333333333333703, 0.3219752754296894559, 0.3333333333333333703, 0.3219752754296894559, 0.3333333333333333703, 0.3219752754296894559, 0.3333333333333333703, 0.3219752754296894559, 0.3333333333333333703, 0.3219752754296894559, 0.3333333333333333703, 0.3219752754296894559, 0.3333333333333333703, 0.3219752754296894559, 0.3333333333333333703, 0.3219752754296894559, 0.3333333333333333703, 0.3219752754296894559, 0.3333333333333333703, 0.3219752754296894559, 0.3333333333333333703, 0.3219752754296894559, 0.3333333333333333703, 0.3219752754296894559, 0.3333333333333333703, 0.3219752754296894559, 0.3333333333333333703, 0.3219752754296894559, 0.3333333333333333703, 0.3219752754296894559, 0.3333333333333333703, 0.3219752754296894559, 0.3333333333333333703, 0.3219752754296894559, 0.3333333333333333703, 0.3219752754296894559, 0.3333333333333333703, 0.3219752754296894559, 0.3333333333333333703, 0.3219752754296894559, 0.3333333333333333703, 0.3219752754296894559, 0.3333333333333333703, 0.3219752754296894559, 0.3333333333333333703, 0.3219752754296894559, 0.3333333333333333703, 0.3219752754296894559, 0.3333333333333333703, 0.3219752754296894559, 0.3333333333333333703, 0.3219752754296894559, 0.3333333333333333703, 0.3219752754296894559, 0.3333333333333333703, 0.3219752754296894559, 0.3333333333333333703, 0.3219752754296894559, 0.3333333333333333703, 0.3219752754296894559, 0.3333333333333333703, 0.3219752754296894559, 0.3333333333333333703, 0.3219752754296894559, 0.3333333333333333703, 0.3219752754296894559, 0.3333333333333333703, 0.3219752754296894559, 0.3333333333333333703, 0.3219752754296894559, 0.3333333333333333703, 0.3219752754296894559, 0.3333333333333333703, 0.3219752754296894559, 0.3333333333333333703, 0.3219752754296894559, 0.3333333333333333703, 0.3219752754296894559, 0.3333333333333333703, 0.3219752754296894559, 0.3333333333333333703, 0.3219752754296894559, 0.3333333333333333703, 0.3219752754296894559, 0.3333333333333333703, 0.3219752754296894559, 0.3333333333333333703, 0.3219752754296894559, 0.3333333333333333703, 0.3219752754296894559, 0.3333333333333333703, 0.3219752754296894559, 0.3333333333333333703, 0.3219752754296894559, 0.3333333333333333703, 0.3219752754296894559, 0.3333333333333333703, 0.3219752754296894559, 0.3333333333333333703, 0.3219752754296894559, 0.3333333333333333703, 0.3219752754296894559, 0.3333333333333333703, 0.3219752754296894559, 0.3333333333333333703, 0.3219752754296894559, 0.3333333333333333703, 0.3219752754296894559, 0.3333333333333333703, 0.3219752754296894559, 0.3333333333333333703, 0.3219752754296894559, 0.3333333333333333703, 0.3219752754296894559, 0.3333333333333333703, 0.3219752754296894559, 0.3333333333333333703, 0.3219752754296894559, 0.3333333333333333703, 0.3219752754296894559, 0.3333333333333333703, 0.3219752754296894559, 0.3333333333333333703, 0.3219752754296894559, 0.3333333333333333703, 0.3219752754296894559, 0.3333333333333333703, 0.3219752754296894559, 0.3333333333333333703, 0.3219752754296894559, 0.3333333333333333703, 0.3219752754296894559, 0.3333333333333333703, 0.3219752754296894559, 0.3333333333333333703, 0.3219752754296894559, 0.3333333333333333703, 0.3219752754296894559, 0.3333333333333333703, 0.3219752754296894559, 0.3333333333333333703, 0.3219752754296894559, 0.3333333333333333703, 0.3219752754296894559, 0.3333333333333333703, 0.3219752754296894559, 0.3333333333333333703, 0.3219752754296894559, 0.3333333333333333703, 0.3219752754296894559, 0.3333333333333333703, 0.3219752754296894559, 0.3333333333333333703, 0.3219752754296894559, 0.3333333333333333703, 0.3219752754296894559, 0.3333333333333333703, 0.3219752754296894559, 0.3333333333333333703, 0.3219752754296894559, 0.3333333333333333703, 0.3219752754296894559, 0.3333333333333333703, 0.3219752754296894559, 0.3333333333333333703, 0.3219752754296894559, 0.3333333333333333703, 0.3219752754296894559, 0.3333333333333333703, 0.3219752754296894559, 0.3333333333333333703, 0.3219752754296894559, 0.3333333333333333703, 0.3219752754296894559, 0.3333333333333333703, 0.3219752754296894559, 0.3333333333333333703, 0.3219752754296894559, 0.3333333333333333703, 0.3219752754296894559, 0.3333333333333333703, 0.3219752754296894559, 0.3333333333333333703, 0.3219752754296894559, 0.3333333333333333703, 0.3219752754296894559, 0.3333333333333333703, 0.3219752754296894559, 0.3333333333333333703, 0.3219752754296894559, 0.3333333333333333703, 0.3219752754296894559, 0.3333333333333333703, 0.3219752754296894559, 0.3333333333333333703, 0.3219752754296894559, 0.3333333333333333703, 0.3219752754296894559, 0.3333333333333333703, 0.3219752754296894559, 0.3333333333333333703, 0.3219752754296894559, 0.3333333333333333703, 0.3219752754296894559, 0.3333333333333333703, 0.3219752754296894559, 0.3333333333333333703, 0.3219752754296894559, 0.3333333333333333703, 0.3219752754296894559, 0.3333333333333333703, 0.3219752754296894559, 0.3333333333333333703, 0.3219752754296894559, 0.3333333333333333703, 0.3219752754296894559, 0.3333333333333333703, 0.3219752754296894559, 0.3333333333333333703, 0.3219752754296894559, 0.3333333333333333703, 0.3219752754296894559, 0.3333333333333333703, 0.3219752754296894559, 0.3333333333333333703, 0.3219752754296894559, 0.3333333333333333703, 0.3219752754296894559, 0.3333333333333333703, 0.3219752754296894559, 0.3333333333333333703, 0.3219752754296894559, 0.3333333333333333703, 0.3219752754296894559, 0.3333333333333333703, 0.3219752754296894559, 0.3333333333333333703, 0.3219752754296894559, 0.3333333333333333703, 0.3219752754296894559, 0.3333333333333333703, 0.3219752754296894559, 0.3333333333333333703, 0.3219752754296894559, 0.3333333333333333703, 0.3219752754296894559, 0.3333333333333333703, 0.3219752754296894559, 0.3333333333333333703, 0.3219752754296894559, 0.3333333333333333703, 0.3219752754296894559, 0.3333333333333333703, 0.3219752754296894559, 0.3333333333333333703, 0.3219752754296894559, 0.3333333333333333703, 0.3219752754296894559, 0.3333333333333333703, 0.3219752754296894559, 0.3333333333333333703, 0.3219752754296894559, 0.3333333333333333703, 0.3219752754296894559, 0.3333333333333333703, 0.3219752754296894559, 0.3333333333333333703, 0.3219752754296894559, 0.3333333333333333703, 0.3219752754296894559, 0.3333333333333333703, 0.3219752754296894559, 0.3333333333333333703, 0.3219752754296894559, 0.3333333333333333703, 0.3219752754296894559, 0.3333333333333333703, 0.3219752754296894559, 0.3333333333333333703, 0.3219752754296894559, 0.3333333333333333703, 0.3219752754296894559, 0.3333333333333333703, 0.3219752754296894559, 0.3333333333333333703, 0.3219752754296894559, 0.3333333333333333703, 0.3219752754296894559, 0.3333333333333333703, 0.3219752754296894559, 0.3333333333333333703, 0.3219752754296894559, 0.3333333333333333703, 0.3219752754296894559, 0.3333333333333333703, 0.3219752754296894559, 0.3333333333333333703, 0.3219752754296894559, 0.3333333333333333703, 0.3219752754296894559, 0.3333333333333333703, 0.3219752754296894559, 0.3333333333333333703, 0.3219752754296894559, 0.3333333333333333703, 0.3219752754296894559, 0.3333333333333333703, 0.3219752754296894559, 0.3333333333333333703, 0.3219752754296894559, 0.3333333333333333703, 0.3219752754296894559, 0.3333333333333333703, 0.3219752754296894559, 0.3333333333333333703, 0.3219752754296894559, 0.3333333333333333703, 0.3219752754296894559, 0.3333333333333333703, 0.3219752754296894559, 0.3333333333333333703, 0.3219752754296894559, 0.3333333333333333703, 0.3219752754296894559, 0.3333333333333333703, 0.3219752754296894559, 0.3333333333333333703, 0.3219752754296894559, 0.3333333333333333703, 0.3219752754296894559, 0.3333333333333333703, 0.3219752754296894559, 0.3333333333333333703, 0.3219752754296894559, 0.3333333333333333703, 0.3219752754296894559, 0.3333333333333333703, 0.3219752754296894559, 0.3333333333333333703, 0.3219752754296894559, 0.3333333333333333703, 0.3219752754296894559, 0.3333333333333333703, 0.3219752754296894559, 0.3333333333333333703, 0.3219752754296894559, 0.3333333333333333703, 0.3219752754296894559, 0.3333333333333333703, 0.3219752754296894559, 0.3333333333333333703, 0.3219752754296894559, 0.3333333333333333703, 0.3219752754296894559, 0.3333333333333333703, 0.3219752754296894559, 0.3333333333333333703, 0.3219752754296894559, 0.3333333333333333703, 0.3219752754296894559, 0.3333333333333333703, 0.3219752754296894559, 0.3333333333333333703, 0.3219752754296894559, 0.3333333333333333703, 0.3219752754296894559, 0.3333333333333333703, 0.3219752754296894559, 0.3333333333333333703, 0.3219752754296894559, 0.3333333333333333703, 0.3219752754296894559, 0.3333333333333333703, 0.3219752754296894559, 0.3333333333333333703, 0.3219752754296894559, 0.3333333333333333703, 0.3219752754296894559, 0.3333333333333333703, 0.3219752754296894559, 0.3333333333333333703, 0.3219752754296894559, 0.3333333333333333703, 0.3219752754296894559, 0.3333333333333333703, 0.3219752754296894559, 0.3333333333333333703, 0.3219752754296894559, 0.3333333333333333703, 0.3219752754296894559, 0.3333333333333333703, 0.3219752754296894559, 0.3333333333333333703, 0.3219752754296894559, 0.3333333333333333703, 0.3219752754296894559, 0.3333333333333333703, 0.3219752754296894559, 0.3333333333333333703, 0.3219752754296894559, 0.3333333333333333703, 0.3219752754296894559, 0.3333333333333333703, 0.3219752754296894559, 0.3333333333333333703, 0.3219752754296894559, 0.3333333333333333703, 0.3219752754296894559, 0.3333333333333333703, 0.3219752754296894559, 0.3333333333333333703, 0.3219752754296894559, 0.3333333333333333703, 0.3219752754296894559, 0.3333333333333333703, 0.3219752754296894559, 0.3333333333333333703, 0.3219752754296894559, 0.3333333333333333703, 0.3219752754296894559, 0.3333333333333333703, 0.3219752754296894559, 0.3333333333333333703, 0.3219752754296894559, 0.3333333333333333703, 0.3219752754296894559, 0.3333333333333333703),
 ( 0.3333333333333333703, 0.3219752754296894559, 0.3333333333333333703, 0.3219752754296894559, 0.3333333333333333703, 0.3219752754296894559, 0.3333333333333333703, 0.3219752754296894559, 0.3333333333333333703, 0.3219752754296894559, 0.3333333333333333703, 0.3219752754296894559, 0.3333333333333333703, 0.3219752754296894559, 0.3333333333333333703, 0.3219752754296894559, 0.3333333333333333703, 0.3219752754296894559, 0.3333333333333333703, 0.3219752754296894559, 0.3333333333333333703, 0.3219752754296894559, 0.3333333333333333703, 0.3219752754296894559, 0.3333333333333333703, 0.3219752754296894559, 0.3333333333333333703, 0.3219752754296894559, 0.3333333333333333703, 0.3219752754296894559, 0.3333333333333333703, 0.3219752754296894559, 0.3333333333333333703, 0.3219752754296894559, 0.3333333333333333703, 0.3219752754296894559, 0.3333333333333333703, 0.3219752754296894559, 0.3333333333333333703, 0.3219752754296894559, 0.3333333333333333703, 0.3219752754296894559, 0.3333333333333333703, 0.3219752754296894559, 0.3333333333333333703, 0.3219752754296894559, 0.3333333333333333703, 0.3219752754296894559, 0.3333333333333333703, 0.3219752754296894559, 0.3333333333333333703, 0.3219752754296894559, 0.3333333333333333703, 0.3219752754296894559, 0.3333333333333333703, 0.3219752754296894559, 0.3333333333333333703, 0.3219752754296894559, 0.3333333333333333703, 0.3219752754296894559, 0.3333333333333333703, 0.3219752754296894559, 0.3333333333333333703, 0.3219752754296894559, 0.3333333333333333703, 0.3219752754296894559, 0.3333333333333333703, 0.3219752754296894559, 0.3333333333333333703, 0.3219752754296894559, 0.3333333333333333703, 0.3219752754296894559, 0.3333333333333333703, 0.3219752754296894559, 0.3333333333333333703, 0.3219752754296894559, 0.3333333333333333703, 0.3219752754296894559, 0.3333333333333333703, 0.3219752754296894559, 0.3333333333333333703, 0.3219752754296894559, 0.3333333333333333703, 0.3219752754296894559, 0.3333333333333333703, 0.3219752754296894559, 0.3333333333333333703, 0.3219752754296894559, 0.3333333333333333703, 0.3219752754296894559, 0.3333333333333333703, 0.3219752754296894559, 0.3333333333333333703, 0.3219752754296894559, 0.3333333333333333703, 0.3219752754296894559, 0.3333333333333333703, 0.3219752754296894559, 0.3333333333333333703, 0.3219752754296894559, 0.3333333333333333703, 0.3219752754296894559, 0.3333333333333333703, 0.3219752754296894559, 0.3333333333333333703, 0.3219752754296894559, 0.3333333333333333703, 0.3219752754296894559, 0.3333333333333333703, 0.3219752754296894559, 0.3333333333333333703, 0.3219752754296894559, 0.3333333333333333703, 0.3219752754296894559, 0.3333333333333333703, 0.3219752754296894559, 0.3333333333333333703, 0.3219752754296894559, 0.3333333333333333703, 0.3219752754296894559, 0.3333333333333333703, 0.3219752754296894559, 0.3333333333333333703, 0.3219752754296894559, 0.3333333333333333703, 0.3219752754296894559, 0.3333333333333333703, 0.3219752754296894559, 0.3333333333333333703, 0.3219752754296894559, 0.3333333333333333703, 0.3219752754296894559, 0.3333333333333333703, 0.3219752754296894559, 0.3333333333333333703, 0.3219752754296894559, 0.3333333333333333703, 0.3219752754296894559, 0.3333333333333333703, 0.3219752754296894559, 0.3333333333333333703, 0.3219752754296894559, 0.3333333333333333703, 0.3219752754296894559, 0.3333333333333333703, 0.3219752754296894559, 0.3333333333333333703, 0.3219752754296894559, 0.3333333333333333703, 0.3219752754296894559, 0.3333333333333333703, 0.3219752754296894559, 0.3333333333333333703, 0.3219752754296894559, 0.3333333333333333703, 0.3219752754296894559, 0.3333333333333333703, 0.3219752754296894559, 0.3333333333333333703, 0.3219752754296894559, 0.3333333333333333703, 0.3219752754296894559, 0.3333333333333333703, 0.3219752754296894559, 0.3333333333333333703, 0.3219752754296894559, 0.3333333333333333703, 0.3219752754296894559, 0.3333333333333333703, 0.3219752754296894559, 0.3333333333333333703, 0.3219752754296894559, 0.3333333333333333703, 0.3219752754296894559, 0.3333333333333333703, 0.3219752754296894559, 0.3333333333333333703, 0.3219752754296894559, 0.3333333333333333703, 0.3219752754296894559, 0.3333333333333333703, 0.3219752754296894559, 0.3333333333333333703, 0.3219752754296894559, 0.3333333333333333703, 0.3219752754296894559, 0.3333333333333333703, 0.3219752754296894559, 0.3333333333333333703, 0.3219752754296894559, 0.3333333333333333703, 0.3219752754296894559, 0.3333333333333333703, 0.3219752754296894559, 0.3333333333333333703, 0.3219752754296894559, 0.3333333333333333703, 0.3219752754296894559, 0.3333333333333333703, 0.3219752754296894559, 0.3333333333333333703, 0.3219752754296894559, 0.3333333333333333703, 0.3219752754296894559, 0.3333333333333333703, 0.3219752754296894559, 0.3333333333333333703, 0.3219752754296894559, 0.3333333333333333703, 0.3219752754296894559, 0.3333333333333333703, 0.3219752754296894559, 0.3333333333333333703, 0.3219752754296894559, 0.3333333333333333703, 0.3219752754296894559, 0.3333333333333333703, 0.3219752754296894559, 0.3333333333333333703, 0.3219752754296894559, 0.3333333333333333703, 0.3219752754296894559, 0.3333333333333333703, 0.3219752754296894559, 0.3333333333333333703, 0.3219752754296894559, 0.3333333333333333703, 0.3219752754296894559, 0.3333333333333333703, 0.3219752754296894559, 0.3333333333333333703, 0.3219752754296894559, 0.3333333333333333703, 0.3219752754296894559, 0.3333333333333333703, 0.3219752754296894559, 0.3333333333333333703, 0.3219752754296894559, 0.3333333333333333703, 0.3219752754296894559, 0.3333333333333333703, 0.3219752754296894559, 0.3333333333333333703, 0.3219752754296894559, 0.3333333333333333703, 0.3219752754296894559, 0.3333333333333333703, 0.3219752754296894559, 0.3333333333333333703, 0.3219752754296894559, 0.3333333333333333703, 0.3219752754296894559, 0.3333333333333333703, 0.3219752754296894559, 0.3333333333333333703, 0.3219752754296894559, 0.3333333333333333703, 0.3219752754296894559, 0.3333333333333333703, 0.3219752754296894559, 0.3333333333333333703, 0.3219752754296894559, 0.3333333333333333703, 0.3219752754296894559, 0.3333333333333333703, 0.3219752754296894559, 0.3333333333333333703, 0.3219752754296894559, 0.3333333333333333703, 0.3219752754296894559, 0.3333333333333333703, 0.3219752754296894559, 0.3333333333333333703, 0.3219752754296894559, 0.3333333333333333703, 0.3219752754296894559, 0.3333333333333333703, 0.3219752754296894559, 0.3333333333333333703, 0.3219752754296894559, 0.3333333333333333703, 0.3219752754296894559, 0.3333333333333333703, 0.3219752754296894559, 0.3333333333333333703, 0.3219752754296894559, 0.3333333333333333703, 0.3219752754296894559, 0.3333333333333333703, 0.3219752754296894559, 0.3333333333333333703, 0.3219752754296894559, 0.3333333333333333703, 0.3219752754296894559, 0.3333333333333333703, 0.3219752754296894559, 0.3333333333333333703, 0.3219752754296894559, 0.3333333333333333703, 0.3219752754296894559, 0.3333333333333333703, 0.3219752754296894559, 0.3333333333333333703, 0.3219752754296894559, 0.3333333333333333703, 0.3219752754296894559, 0.3333333333333333703, 0.3219752754296894559, 0.3333333333333333703, 0.3219752754296894559, 0.3333333333333333703, 0.3219752754296894559, 0.3333333333333333703, 0.3219752754296894559, 0.3333333333333333703, 0.3219752754296894559, 0.3333333333333333703, 0.3219752754296894559, 0.3333333333333333703, 0.3219752754296894559, 0.3333333333333333703, 0.3219752754296894559, 0.3333333333333333703, 0.3219752754296894559, 0.3333333333333333703, 0.3219752754296894559, 0.3333333333333333703, 0.3219752754296894559, 0.3333333333333333703, 0.3219752754296894559, 0.3333333333333333703, 0.3219752754296894559, 0.3333333333333333703, 0.3219752754296894559, 0.3333333333333333703, 0.3219752754296894559, 0.3333333333333333703, 0.3219752754296894559, 0.3333333333333333703, 0.3219752754296894559, 0.3333333333333333703, 0.3219752754296894559, 0.3333333333333333703, 0.3219752754296894559, 0.3333333333333333703, 0.3219752754296894559, 0.3333333333333333703, 0.3219752754296894559, 0.3333333333333333703, 0.3219752754296894559, 0.3333333333333333703, 0.3219752754296894559, 0.3333333333333333703, 0.3219752754296894559, 0.3333333333333333703, 0.3219752754296894559, 0.3333333333333333703, 0.3219752754296894559, 0.3333333333333333703, 0.3219752754296894559, 0.3333333333333333703, 0.3219752754296894559, 0.3333333333333333703, 0.3219752754296894559, 0.3333333333333333703, 0.3219752754296894559, 0.3333333333333333703, 0.3219752754296894559, 0.3333333333333333703, 0.3219752754296894559, 0.3333333333333333703, 0.3219752754296894559, 0.3333333333333333703, 0.3219752754296894559, 0.3333333333333333703, 0.3219752754296894559, 0.3333333333333333703, 0.3219752754296894559, 0.3333333333333333703, 0.3219752754296894559, 0.3333333333333333703, 0.3219752754296894559, 0.3333333333333333703, 0.3219752754296894559, 0.3333333333333333703, 0.3219752754296894559, 0.3333333333333333703, 0.3219752754296894559, 0.3333333333333333703, 0.3219752754296894559, 0.3333333333333333703, 0.3219752754296894559, 0.3333333333333333703, 0.3219752754296894559, 0.3333333333333333703, 0.3219752754296894559, 0.3333333333333333703, 0.3219752754296894559, 0.3333333333333333703, 0.3219752754296894559, 0.3333333333333333703, 0.3219752754296894559, 0.3333333333333333703, 0.3219752754296894559, 0.3333333333333333703, 0.3219752754296894559, 0.3333333333333333703, 0.3219752754296894559, 0.3333333333333333703, 0.3219752754296894559, 0.3333333333333333703, 0.3219752754296894559, 0.3333333333333333703, 0.3219752754296894559, 0.3333333333333333703, 0.3219752754296894559, 0.3333333333333333703, 0.3219752754296894559, 0.3333333333333333703, 0.3219752754296894559, 0.3333333333333333703, 0.3219752754296894559, 0.3333333333333333703, 0.3219752754296894559, 0.3333333333333333703, 0.3219752754296894559, 0.3333333333333333703, 0.3219752754296894559, 0.3333333333333333703, 0.3219752754296894559, 0.3333333333333333703, 0.3219752754296894559, 0.3333333333333333703, 0.3219752754296894559, 0.3333333333333333703, 0.3219752754296894559, 0.3333333333333333703, 0.3219752754296894559, 0.3333333333333333703, 0.3219752754296894559, 0.3333333333333333703, 0.3219752754296894559, 0.3333333333333333703, 0.3219752754296894559, 0.3333333333333333703, 0.3219752754296894559, 0.3333333333333333703, 0.3219752754296894559, 0.3333333333333333703, 0.3219752754296894559, 0.3333333333333333703, 0.3219752754296894559, 0.3333333333333333703, 0.3219752754296894559, 0.3333333333333333703, 0.3219752754296894559, 0.3333333333333333703),
 ( 1.000000000000000000, 0.9659258262890683122, 1.000000000000000000, 0.9659258262890683122, 1.000000000000000000, 0.9659258262890683122, 1.000000000000000000, 0.9659258262890683122, 1.000000000000000000, 0.9659258262890683122, 1.000000000000000000, 0.9659258262890683122, 1.000000000000000000, 0.9659258262890683122, 1.000000000000000000, 0.9659258262890683122, 1.000000000000000000, 0.9659258262890683122, 1.000000000000000000, 0.9659258262890683122, 1.000000000000000000, 0.9659258262890683122, 1.000000000000000000, 0.9659258262890683122, 1.000000000000000000, 0.9659258262890683122, 1.000000000000000000, 0.9659258262890683122, 1.000000000000000000, 0.9659258262890683122, 1.000000000000000000, 0.9659258262890683122, 1.000000000000000000, 0.9659258262890683122, 1.000000000000000000, 0.9659258262890683122, 1.000000000000000000, 0.9659258262890683122, 1.000000000000000000, 0.9659258262890683122, 1.000000000000000000, 0.9659258262890683122, 1.000000000000000000, 0.9659258262890683122, 1.000000000000000000, 0.9659258262890683122, 1.000000000000000000, 0.9659258262890683122, 1.000000000000000000, 0.9659258262890683122, 1.000000000000000000, 0.9659258262890683122, 1.000000000000000000, 0.9659258262890683122, 1.000000000000000000, 0.9659258262890683122, 1.000000000000000000, 0.9659258262890683122, 1.000000000000000000, 0.9659258262890683122, 1.000000000000000000, 0.9659258262890683122, 1.000000000000000000, 0.9659258262890683122, 1.000000000000000000, 0.9659258262890683122, 1.000000000000000000, 0.9659258262890683122, 1.000000000000000000, 0.9659258262890683122, 1.000000000000000000, 0.9659258262890683122, 1.000000000000000000, 0.9659258262890683122, 1.000000000000000000, 0.9659258262890683122, 1.000000000000000000, 0.9659258262890683122, 1.000000000000000000, 0.9659258262890683122, 1.000000000000000000, 0.9659258262890683122, 1.000000000000000000, 0.9659258262890683122, 1.000000000000000000, 0.9659258262890683122, 1.000000000000000000, 0.9659258262890683122, 1.000000000000000000, 0.9659258262890683122, 1.000000000000000000, 0.9659258262890683122, 1.000000000000000000, 0.9659258262890683122, 1.000000000000000000, 0.9659258262890683122, 1.000000000000000000, 0.9659258262890683122, 1.000000000000000000, 0.9659258262890683122, 1.000000000000000000, 0.9659258262890683122, 1.000000000000000000, 0.9659258262890683122, 1.000000000000000000, 0.9659258262890683122, 1.000000000000000000, 0.9659258262890683122, 1.000000000000000000, 0.9659258262890683122, 1.000000000000000000, 0.9659258262890683122, 1.000000000000000000, 0.9659258262890683122, 1.000000000000000000, 0.9659258262890683122, 1.000000000000000000, 0.9659258262890683122, 1.000000000000000000, 0.9659258262890683122, 1.000000000000000000, 0.9659258262890683122, 1.000000000000000000, 0.9659258262890683122, 1.000000000000000000, 0.9659258262890683122, 1.000000000000000000, 0.9659258262890683122, 1.000000000000000000, 0.9659258262890683122, 1.000000000000000000, 0.9659258262890683122, 1.000000000000000000, 0.9659258262890683122, 1.000000000000000000, 0.9659258262890683122, 1.000000000000000000, 0.9659258262890683122, 1.000000000000000000, 0.9659258262890683122, 1.000000000000000000, 0.9659258262890683122, 1.000000000000000000, 0.9659258262890683122, 1.000000000000000000, 0.9659258262890683122, 1.000000000000000000, 0.9659258262890683122, 1.000000000000000000, 0.9659258262890683122, 1.000000000000000000, 0.9659258262890683122, 1.000000000000000000, 0.9659258262890683122, 1.000000000000000000, 0.9659258262890683122, 1.000000000000000000, 0.9659258262890683122, 1.000000000000000000, 0.9659258262890683122, 1.000000000000000000, 0.9659258262890683122, 1.000000000000000000, 0.9659258262890683122, 1.000000000000000000, 0.9659258262890683122, 1.000000000000000000, 0.9659258262890683122, 1.000000000000000000, 0.9659258262890683122, 1.000000000000000000, 0.9659258262890683122, 1.000000000000000000, 0.9659258262890683122, 1.000000000000000000, 0.9659258262890683122, 1.000000000000000000, 0.9659258262890683122, 1.000000000000000000, 0.9659258262890683122, 1.000000000000000000, 0.9659258262890683122, 1.000000000000000000, 0.9659258262890683122, 1.000000000000000000, 0.9659258262890683122, 1.000000000000000000, 0.9659258262890683122, 1.000000000000000000, 0.9659258262890683122, 1.000000000000000000, 0.9659258262890683122, 1.000000000000000000, 0.9659258262890683122, 1.000000000000000000, 0.9659258262890683122, 1.000000000000000000, 0.9659258262890683122, 1.000000000000000000, 0.9659258262890683122, 1.000000000000000000, 0.9659258262890683122, 1.000000000000000000, 0.9659258262890683122, 1.000000000000000000, 0.9659258262890683122, 1.000000000000000000, 0.9659258262890683122, 1.000000000000000000, 0.9659258262890683122, 1.000000000000000000, 0.9659258262890683122, 1.000000000000000000, 0.9659258262890683122, 1.000000000000000000, 0.9659258262890683122, 1.000000000000000000, 0.9659258262890683122, 1.000000000000000000, 0.9659258262890683122, 1.000000000000000000, 0.9659258262890683122, 1.000000000000000000, 0.9659258262890683122, 1.000000000000000000, 0.9659258262890683122, 1.000000000000000000, 0.9659258262890683122, 1.000000000000000000, 0.9659258262890683122, 1.000000000000000000, 0.9659258262890683122, 1.000000000000000000, 0.9659258262890683122, 1.000000000000000000, 0.9659258262890683122, 1.000000000000000000, 0.9659258262890683122, 1.000000000000000000, 0.9659258262890683122, 1.000000000000000000, 0.9659258262890683122, 1.000000000000000000, 0.9659258262890683122, 1.000000000000000000, 0.9659258262890683122, 1.000000000000000000, 0.9659258262890683122, 1.000000000000000000, 0.9659258262890683122, 1.000000000000000000, 0.9659258262890683122, 1.000000000000000000, 0.9659258262890683122, 1.000000000000000000, 0.9659258262890683122, 1.000000000000000000, 0.9659258262890683122, 1.000000000000000000, 0.9659258262890683122, 1.000000000000000000, 0.9659258262890683122, 1.000000000000000000, 0.9659258262890683122, 1.000000000000000000, 0.9659258262890683122, 1.000000000000000000, 0.9659258262890683122, 1.000000000000000000, 0.9659258262890683122, 1.000000000000000000, 0.9659258262890683122, 1.000000000000000000, 0.9659258262890683122, 1.000000000000000000, 0.9659258262890683122, 1.000000000000000000, 0.9659258262890683122, 1.000000000000000000, 0.9659258262890683122, 1.000000000000000000, 0.9659258262890683122, 1.000000000000000000, 0.9659258262890683122, 1.000000000000000000, 0.9659258262890683122, 1.000000000000000000, 0.9659258262890683122, 1.000000000000000000, 0.9659258262890683122, 1.000000000000000000, 0.9659258262890683122, 1.000000000000000000, 0.9659258262890683122, 1.000000000000000000, 0.9659258262890683122, 1.000000000000000000, 0.9659258262890683122, 1.000000000000000000, 0.9659258262890683122, 1.000000000000000000, 0.9659258262890683122, 1.000000000000000000, 0.9659258262890683122, 1.000000000000000000, 0.9659258262890683122, 1.000000000000000000, 0.9659258262890683122, 1.000000000000000000, 0.9659258262890683122, 1.000000000000000000, 0.9659258262890683122, 1.000000000000000000, 0.9659258262890683122, 1.000000000000000000, 0.9659258262890683122, 1.000000000000000000, 0.9659258262890683122, 1.000000000000000000, 0.9659258262890683122, 1.000000000000000000, 0.9659258262890683122, 1.000000000000000000, 0.9659258262890683122, 1.000000000000000000, 0.9659258262890683122, 1.000000000000000000, 0.9659258262890683122, 1.000000000000000000, 0.9659258262890683122, 1.000000000000000000, 0.9659258262890683122, 1.000000000000000000, 0.9659258262890683122, 1.000000000000000000, 0.9659258262890683122, 1.000000000000000000, 0.9659258262890683122, 1.000000000000000000, 0.9659258262890683122, 1.000000000000000000, 0.9659258262890683122, 1.000000000000000000, 0.9659258262890683122, 1.000000000000000000, 0.9659258262890683122, 1.000000000000000000, 0.9659258262890683122, 1.000000000000000000, 0.9659258262890683122, 1.000000000000000000, 0.9659258262890683122, 1.000000000000000000, 0.9659258262890683122, 1.000000000000000000, 0.9659258262890683122, 1.000000000000000000, 0.9659258262890683122, 1.000000000000000000, 0.9659258262890683122, 1.000000000000000000, 0.9659258262890683122, 1.000000000000000000, 0.9659258262890683122, 1.000000000000000000, 0.9659258262890683122, 1.000000000000000000, 0.9659258262890683122, 1.000000000000000000, 0.9659258262890683122, 1.000000000000000000, 0.9659258262890683122, 1.000000000000000000, 0.9659258262890683122, 1.000000000000000000, 0.9659258262890683122, 1.000000000000000000, 0.9659258262890683122, 1.000000000000000000, 0.9659258262890683122, 1.000000000000000000, 0.9659258262890683122, 1.000000000000000000, 0.9659258262890683122, 1.000000000000000000, 0.9659258262890683122, 1.000000000000000000, 0.9659258262890683122, 1.000000000000000000, 0.9659258262890683122, 1.000000000000000000, 0.9659258262890683122, 1.000000000000000000, 0.9659258262890683122, 1.000000000000000000, 0.9659258262890683122, 1.000000000000000000, 0.9659258262890683122, 1.000000000000000000, 0.9659258262890683122, 1.000000000000000000, 0.9659258262890683122, 1.000000000000000000, 0.9659258262890683122, 1.000000000000000000, 0.9659258262890683122, 1.000000000000000000, 0.9659258262890683122, 1.000000000000000000, 0.9659258262890683122, 1.000000000000000000, 0.9659258262890683122, 1.000000000000000000, 0.9659258262890683122, 1.000000000000000000, 0.9659258262890683122, 1.000000000000000000, 0.9659258262890683122, 1.000000000000000000, 0.9659258262890683122, 1.000000000000000000, 0.9659258262890683122, 1.000000000000000000, 0.9659258262890683122, 1.000000000000000000, 0.9659258262890683122, 1.000000000000000000, 0.9659258262890683122, 1.000000000000000000, 0.9659258262890683122, 1.000000000000000000, 0.9659258262890683122, 1.000000000000000000, 0.9659258262890683122, 1.000000000000000000, 0.9659258262890683122, 1.000000000000000000, 0.9659258262890683122, 1.000000000000000000, 0.9659258262890683122, 1.000000000000000000, 0.9659258262890683122, 1.000000000000000000, 0.9659258262890683122, 1.000000000000000000, 0.9659258262890683122, 1.000000000000000000, 0.9659258262890683122, 1.000000000000000000, 0.9659258262890683122, 1.000000000000000000, 0.9659258262890683122, 1.000000000000000000, 0.9659258262890683122, 1.000000000000000000, 0.9659258262890683122, 1.000000000000000000),
 ( 0.3333333333333333703, 0.3219752754296894559, 0.3333333333333333703, 0.3219752754296894559, 0.3333333333333333703, 0.3219752754296894559, 0.3333333333333333703, 0.3219752754296894559, 0.3333333333333333703, 0.3219752754296894559, 0.3333333333333333703, 0.3219752754296894559, 0.3333333333333333703, 0.3219752754296894559, 0.3333333333333333703, 0.3219752754296894559, 0.3333333333333333703, 0.3219752754296894559, 0.3333333333333333703, 0.3219752754296894559, 0.3333333333333333703, 0.3219752754296894559, 0.3333333333333333703, 0.3219752754296894559, 0.3333333333333333703, 0.3219752754296894559, 0.3333333333333333703, 0.3219752754296894559, 0.3333333333333333703, 0.3219752754296894559, 0.3333333333333333703, 0.3219752754296894559, 0.3333333333333333703, 0.3219752754296894559, 0.3333333333333333703, 0.3219752754296894559, 0.3333333333333333703, 0.3219752754296894559, 0.3333333333333333703, 0.3219752754296894559, 0.3333333333333333703, 0.3219752754296894559, 0.3333333333333333703, 0.3219752754296894559, 0.3333333333333333703, 0.3219752754296894559, 0.3333333333333333703, 0.3219752754296894559, 0.3333333333333333703, 0.3219752754296894559, 0.3333333333333333703, 0.3219752754296894559, 0.3333333333333333703, 0.3219752754296894559, 0.3333333333333333703, 0.3219752754296894559, 0.3333333333333333703, 0.3219752754296894559, 0.3333333333333333703, 0.3219752754296894559, 0.3333333333333333703, 0.3219752754296894559, 0.3333333333333333703, 0.3219752754296894559, 0.3333333333333333703, 0.3219752754296894559, 0.3333333333333333703, 0.3219752754296894559, 0.3333333333333333703, 0.3219752754296894559, 0.3333333333333333703, 0.3219752754296894559, 0.3333333333333333703, 0.3219752754296894559, 0.3333333333333333703, 0.3219752754296894559, 0.3333333333333333703, 0.3219752754296894559, 0.3333333333333333703, 0.3219752754296894559, 0.3333333333333333703, 0.3219752754296894559, 0.3333333333333333703, 0.3219752754296894559, 0.3333333333333333703, 0.3219752754296894559, 0.3333333333333333703, 0.3219752754296894559, 0.3333333333333333703, 0.3219752754296894559, 0.3333333333333333703, 0.3219752754296894559, 0.3333333333333333703, 0.3219752754296894559, 0.3333333333333333703, 0.3219752754296894559, 0.3333333333333333703, 0.3219752754296894559, 0.3333333333333333703, 0.3219752754296894559, 0.3333333333333333703, 0.3219752754296894559, 0.3333333333333333703, 0.3219752754296894559, 0.3333333333333333703, 0.3219752754296894559, 0.3333333333333333703, 0.3219752754296894559, 0.3333333333333333703, 0.3219752754296894559, 0.3333333333333333703, 0.3219752754296894559, 0.3333333333333333703, 0.3219752754296894559, 0.3333333333333333703, 0.3219752754296894559, 0.3333333333333333703, 0.3219752754296894559, 0.3333333333333333703, 0.3219752754296894559, 0.3333333333333333703, 0.3219752754296894559, 0.3333333333333333703, 0.3219752754296894559, 0.3333333333333333703, 0.3219752754296894559, 0.3333333333333333703, 0.3219752754296894559, 0.3333333333333333703, 0.3219752754296894559, 0.3333333333333333703, 0.3219752754296894559, 0.3333333333333333703, 0.3219752754296894559, 0.3333333333333333703, 0.3219752754296894559, 0.3333333333333333703, 0.3219752754296894559, 0.3333333333333333703, 0.3219752754296894559, 0.3333333333333333703, 0.3219752754296894559, 0.3333333333333333703, 0.3219752754296894559, 0.3333333333333333703, 0.3219752754296894559, 0.3333333333333333703, 0.3219752754296894559, 0.3333333333333333703, 0.3219752754296894559, 0.3333333333333333703, 0.3219752754296894559, 0.3333333333333333703, 0.3219752754296894559, 0.3333333333333333703, 0.3219752754296894559, 0.3333333333333333703, 0.3219752754296894559, 0.3333333333333333703, 0.3219752754296894559, 0.3333333333333333703, 0.3219752754296894559, 0.3333333333333333703, 0.3219752754296894559, 0.3333333333333333703, 0.3219752754296894559, 0.3333333333333333703, 0.3219752754296894559, 0.3333333333333333703, 0.3219752754296894559, 0.3333333333333333703, 0.3219752754296894559, 0.3333333333333333703, 0.3219752754296894559, 0.3333333333333333703, 0.3219752754296894559, 0.3333333333333333703, 0.3219752754296894559, 0.3333333333333333703, 0.3219752754296894559, 0.3333333333333333703, 0.3219752754296894559, 0.3333333333333333703, 0.3219752754296894559, 0.3333333333333333703, 0.3219752754296894559, 0.3333333333333333703, 0.3219752754296894559, 0.3333333333333333703, 0.3219752754296894559, 0.3333333333333333703, 0.3219752754296894559, 0.3333333333333333703, 0.3219752754296894559, 0.3333333333333333703, 0.3219752754296894559, 0.3333333333333333703, 0.3219752754296894559, 0.3333333333333333703, 0.3219752754296894559, 0.3333333333333333703, 0.3219752754296894559, 0.3333333333333333703, 0.3219752754296894559, 0.3333333333333333703, 0.3219752754296894559, 0.3333333333333333703, 0.3219752754296894559, 0.3333333333333333703, 0.3219752754296894559, 0.3333333333333333703, 0.3219752754296894559, 0.3333333333333333703, 0.3219752754296894559, 0.3333333333333333703, 0.3219752754296894559, 0.3333333333333333703, 0.3219752754296894559, 0.3333333333333333703, 0.3219752754296894559, 0.3333333333333333703, 0.3219752754296894559, 0.3333333333333333703, 0.3219752754296894559, 0.3333333333333333703, 0.3219752754296894559, 0.3333333333333333703, 0.3219752754296894559, 0.3333333333333333703, 0.3219752754296894559, 0.3333333333333333703, 0.3219752754296894559, 0.3333333333333333703, 0.3219752754296894559, 0.3333333333333333703, 0.3219752754296894559, 0.3333333333333333703, 0.3219752754296894559, 0.3333333333333333703, 0.3219752754296894559, 0.3333333333333333703, 0.3219752754296894559, 0.3333333333333333703, 0.3219752754296894559, 0.3333333333333333703, 0.3219752754296894559, 0.3333333333333333703, 0.3219752754296894559, 0.3333333333333333703, 0.3219752754296894559, 0.3333333333333333703, 0.3219752754296894559, 0.3333333333333333703, 0.3219752754296894559, 0.3333333333333333703, 0.3219752754296894559, 0.3333333333333333703, 0.3219752754296894559, 0.3333333333333333703, 0.3219752754296894559, 0.3333333333333333703, 0.3219752754296894559, 0.3333333333333333703, 0.3219752754296894559, 0.3333333333333333703, 0.3219752754296894559, 0.3333333333333333703, 0.3219752754296894559, 0.3333333333333333703, 0.3219752754296894559, 0.3333333333333333703, 0.3219752754296894559, 0.3333333333333333703, 0.3219752754296894559, 0.3333333333333333703, 0.3219752754296894559, 0.3333333333333333703, 0.3219752754296894559, 0.3333333333333333703, 0.3219752754296894559, 0.3333333333333333703, 0.3219752754296894559, 0.3333333333333333703, 0.3219752754296894559, 0.3333333333333333703, 0.3219752754296894559, 0.3333333333333333703, 0.3219752754296894559, 0.3333333333333333703, 0.3219752754296894559, 0.3333333333333333703, 0.3219752754296894559, 0.3333333333333333703, 0.3219752754296894559, 0.3333333333333333703, 0.3219752754296894559, 0.3333333333333333703, 0.3219752754296894559, 0.3333333333333333703, 0.3219752754296894559, 0.3333333333333333703, 0.3219752754296894559, 0.3333333333333333703, 0.3219752754296894559, 0.3333333333333333703, 0.3219752754296894559, 0.3333333333333333703, 0.3219752754296894559, 0.3333333333333333703, 0.3219752754296894559, 0.3333333333333333703, 0.3219752754296894559, 0.3333333333333333703, 0.3219752754296894559, 0.3333333333333333703, 0.3219752754296894559, 0.3333333333333333703, 0.3219752754296894559, 0.3333333333333333703, 0.3219752754296894559, 0.3333333333333333703, 0.3219752754296894559, 0.3333333333333333703, 0.3219752754296894559, 0.3333333333333333703, 0.3219752754296894559, 0.3333333333333333703, 0.3219752754296894559, 0.3333333333333333703, 0.3219752754296894559, 0.3333333333333333703, 0.3219752754296894559, 0.3333333333333333703, 0.3219752754296894559, 0.3333333333333333703, 0.3219752754296894559, 0.3333333333333333703, 0.3219752754296894559, 0.3333333333333333703, 0.3219752754296894559, 0.3333333333333333703, 0.3219752754296894559, 0.3333333333333333703, 0.3219752754296894559, 0.3333333333333333703, 0.3219752754296894559, 0.3333333333333333703, 0.3219752754296894559, 0.3333333333333333703, 0.3219752754296894559, 0.3333333333333333703, 0.3219752754296894559, 0.3333333333333333703, 0.3219752754296894559, 0.3333333333333333703, 0.3219752754296894559, 0.3333333333333333703, 0.3219752754296894559, 0.3333333333333333703, 0.3219752754296894559, 0.3333333333333333703, 0.3219752754296894559, 0.3333333333333333703, 0.3219752754296894559, 0.3333333333333333703, 0.3219752754296894559, 0.3333333333333333703, 0.3219752754296894559, 0.3333333333333333703, 0.3219752754296894559, 0.3333333333333333703, 0.3219752754296894559, 0.3333333333333333703, 0.3219752754296894559, 0.3333333333333333703, 0.3219752754296894559, 0.3333333333333333703, 0.3219752754296894559, 0.3333333333333333703, 0.3219752754296894559, 0.3333333333333333703, 0.3219752754296894559, 0.3333333333333333703, 0.3219752754296894559, 0.3333333333333333703, 0.3219752754296894559, 0.3333333333333333703, 0.3219752754296894559, 0.3333333333333333703, 0.3219752754296894559, 0.3333333333333333703, 0.3219752754296894559, 0.3333333333333333703, 0.3219752754296894559, 0.3333333333333333703, 0.3219752754296894559, 0.3333333333333333703, 0.3219752754296894559, 0.3333333333333333703, 0.3219752754296894559, 0.3333333333333333703, 0.3219752754296894559, 0.3333333333333333703, 0.3219752754296894559, 0.3333333333333333703, 0.3219752754296894559, 0.3333333333333333703, 0.3219752754296894559, 0.3333333333333333703, 0.3219752754296894559, 0.3333333333333333703, 0.3219752754296894559, 0.3333333333333333703, 0.3219752754296894559, 0.3333333333333333703, 0.3219752754296894559, 0.3333333333333333703, 0.3219752754296894559, 0.3333333333333333703, 0.3219752754296894559, 0.3333333333333333703, 0.3219752754296894559, 0.3333333333333333703, 0.3219752754296894559, 0.3333333333333333703, 0.3219752754296894559, 0.3333333333333333703, 0.3219752754296894559, 0.3333333333333333703, 0.3219752754296894559, 0.3333333333333333703, 0.3219752754296894559, 0.3333333333333333703, 0.3219752754296894559, 0.3333333333333333703, 0.3219752754296894559, 0.3333333333333333703, 0.3219752754296894559, 0.3333333333333333703, 0.3219752754296894559, 0.3333333333333333703, 0.3219752754296894559, 0.3333333333333333703, 0.3219752754296894559, 0.3333333333333333703, 0.3219752754296894559, 0.3333333333333333703, 0.3219752754296894559, 0.3333333333333333703, 0.3219752754296894559, 0.3333333333333333703, 0.3219752754296894559, 0.3333333333333333703, 0.3219752754296894559, 0.3333333333333333703, 0.3219752754296894559, 0.3333333333333333703),
 ( 0.3333333333333333703, 0.3219752754296894559, 0.3333333333333333703, 0.3219752754296894559, 0.3333333333333333703, 0.3219752754296894559, 0.3333333333333333703, 0.3219752754296894559, 0.3333333333333333703, 0.3219752754296894559, 0.3333333333333333703, 0.3219752754296894559, 0.3333333333333333703, 0.3219752754296894559, 0.3333333333333333703, 0.3219752754296894559, 0.3333333333333333703, 0.3219752754296894559, 0.3333333333333333703, 0.3219752754296894559, 0.3333333333333333703, 0.3219752754296894559, 0.3333333333333333703, 0.3219752754296894559, 0.3333333333333333703, 0.3219752754296894559, 0.3333333333333333703, 0.3219752754296894559, 0.3333333333333333703, 0.3219752754296894559, 0.3333333333333333703, 0.3219752754296894559, 0.3333333333333333703, 0.3219752754296894559, 0.3333333333333333703, 0.3219752754296894559, 0.3333333333333333703, 0.3219752754296894559, 0.3333333333333333703, 0.3219752754296894559, 0.3333333333333333703, 0.3219752754296894559, 0.3333333333333333703, 0.3219752754296894559, 0.3333333333333333703, 0.3219752754296894559, 0.3333333333333333703, 0.3219752754296894559, 0.3333333333333333703, 0.3219752754296894559, 0.3333333333333333703, 0.3219752754296894559, 0.3333333333333333703, 0.3219752754296894559, 0.3333333333333333703, 0.3219752754296894559, 0.3333333333333333703, 0.3219752754296894559, 0.3333333333333333703, 0.3219752754296894559, 0.3333333333333333703, 0.3219752754296894559, 0.3333333333333333703, 0.3219752754296894559, 0.3333333333333333703, 0.3219752754296894559, 0.3333333333333333703, 0.3219752754296894559, 0.3333333333333333703, 0.3219752754296894559, 0.3333333333333333703, 0.3219752754296894559, 0.3333333333333333703, 0.3219752754296894559, 0.3333333333333333703, 0.3219752754296894559, 0.3333333333333333703, 0.3219752754296894559, 0.3333333333333333703, 0.3219752754296894559, 0.3333333333333333703, 0.3219752754296894559, 0.3333333333333333703, 0.3219752754296894559, 0.3333333333333333703, 0.3219752754296894559, 0.3333333333333333703, 0.3219752754296894559, 0.3333333333333333703, 0.3219752754296894559, 0.3333333333333333703, 0.3219752754296894559, 0.3333333333333333703, 0.3219752754296894559, 0.3333333333333333703, 0.3219752754296894559, 0.3333333333333333703, 0.3219752754296894559, 0.3333333333333333703, 0.3219752754296894559, 0.3333333333333333703, 0.3219752754296894559, 0.3333333333333333703, 0.3219752754296894559, 0.3333333333333333703, 0.3219752754296894559, 0.3333333333333333703, 0.3219752754296894559, 0.3333333333333333703, 0.3219752754296894559, 0.3333333333333333703, 0.3219752754296894559, 0.3333333333333333703, 0.3219752754296894559, 0.3333333333333333703, 0.3219752754296894559, 0.3333333333333333703, 0.3219752754296894559, 0.3333333333333333703, 0.3219752754296894559, 0.3333333333333333703, 0.3219752754296894559, 0.3333333333333333703, 0.3219752754296894559, 0.3333333333333333703, 0.3219752754296894559, 0.3333333333333333703, 0.3219752754296894559, 0.3333333333333333703, 0.3219752754296894559, 0.3333333333333333703, 0.3219752754296894559, 0.3333333333333333703, 0.3219752754296894559, 0.3333333333333333703, 0.3219752754296894559, 0.3333333333333333703, 0.3219752754296894559, 0.3333333333333333703, 0.3219752754296894559, 0.3333333333333333703, 0.3219752754296894559, 0.3333333333333333703, 0.3219752754296894559, 0.3333333333333333703, 0.3219752754296894559, 0.3333333333333333703, 0.3219752754296894559, 0.3333333333333333703, 0.3219752754296894559, 0.3333333333333333703, 0.3219752754296894559, 0.3333333333333333703, 0.3219752754296894559, 0.3333333333333333703, 0.3219752754296894559, 0.3333333333333333703, 0.3219752754296894559, 0.3333333333333333703, 0.3219752754296894559, 0.3333333333333333703, 0.3219752754296894559, 0.3333333333333333703, 0.3219752754296894559, 0.3333333333333333703, 0.3219752754296894559, 0.3333333333333333703, 0.3219752754296894559, 0.3333333333333333703, 0.3219752754296894559, 0.3333333333333333703, 0.3219752754296894559, 0.3333333333333333703, 0.3219752754296894559, 0.3333333333333333703, 0.3219752754296894559, 0.3333333333333333703, 0.3219752754296894559, 0.3333333333333333703, 0.3219752754296894559, 0.3333333333333333703, 0.3219752754296894559, 0.3333333333333333703, 0.3219752754296894559, 0.3333333333333333703, 0.3219752754296894559, 0.3333333333333333703, 0.3219752754296894559, 0.3333333333333333703, 0.3219752754296894559, 0.3333333333333333703, 0.3219752754296894559, 0.3333333333333333703, 0.3219752754296894559, 0.3333333333333333703, 0.3219752754296894559, 0.3333333333333333703, 0.3219752754296894559, 0.3333333333333333703, 0.3219752754296894559, 0.3333333333333333703, 0.3219752754296894559, 0.3333333333333333703, 0.3219752754296894559, 0.3333333333333333703, 0.3219752754296894559, 0.3333333333333333703, 0.3219752754296894559, 0.3333333333333333703, 0.3219752754296894559, 0.3333333333333333703, 0.3219752754296894559, 0.3333333333333333703, 0.3219752754296894559, 0.3333333333333333703, 0.3219752754296894559, 0.3333333333333333703, 0.3219752754296894559, 0.3333333333333333703, 0.3219752754296894559, 0.3333333333333333703, 0.3219752754296894559, 0.3333333333333333703, 0.3219752754296894559, 0.3333333333333333703, 0.3219752754296894559, 0.3333333333333333703, 0.3219752754296894559, 0.3333333333333333703, 0.3219752754296894559, 0.3333333333333333703, 0.3219752754296894559, 0.3333333333333333703, 0.3219752754296894559, 0.3333333333333333703, 0.3219752754296894559, 0.3333333333333333703, 0.3219752754296894559, 0.3333333333333333703, 0.3219752754296894559, 0.3333333333333333703, 0.3219752754296894559, 0.3333333333333333703, 0.3219752754296894559, 0.3333333333333333703, 0.3219752754296894559, 0.3333333333333333703, 0.3219752754296894559, 0.3333333333333333703, 0.3219752754296894559, 0.3333333333333333703, 0.3219752754296894559, 0.3333333333333333703, 0.3219752754296894559, 0.3333333333333333703, 0.3219752754296894559, 0.3333333333333333703, 0.3219752754296894559, 0.3333333333333333703, 0.3219752754296894559, 0.3333333333333333703, 0.3219752754296894559, 0.3333333333333333703, 0.3219752754296894559, 0.3333333333333333703, 0.3219752754296894559, 0.3333333333333333703, 0.3219752754296894559, 0.3333333333333333703, 0.3219752754296894559, 0.3333333333333333703, 0.3219752754296894559, 0.3333333333333333703, 0.3219752754296894559, 0.3333333333333333703, 0.3219752754296894559, 0.3333333333333333703, 0.3219752754296894559, 0.3333333333333333703, 0.3219752754296894559, 0.3333333333333333703, 0.3219752754296894559, 0.3333333333333333703, 0.3219752754296894559, 0.3333333333333333703, 0.3219752754296894559, 0.3333333333333333703, 0.3219752754296894559, 0.3333333333333333703, 0.3219752754296894559, 0.3333333333333333703, 0.3219752754296894559, 0.3333333333333333703, 0.3219752754296894559, 0.3333333333333333703, 0.3219752754296894559, 0.3333333333333333703, 0.3219752754296894559, 0.3333333333333333703, 0.3219752754296894559, 0.3333333333333333703, 0.3219752754296894559, 0.3333333333333333703, 0.3219752754296894559, 0.3333333333333333703, 0.3219752754296894559, 0.3333333333333333703, 0.3219752754296894559, 0.3333333333333333703, 0.3219752754296894559, 0.3333333333333333703, 0.3219752754296894559, 0.3333333333333333703, 0.3219752754296894559, 0.3333333333333333703, 0.3219752754296894559, 0.3333333333333333703, 0.3219752754296894559, 0.3333333333333333703, 0.3219752754296894559, 0.3333333333333333703, 0.3219752754296894559, 0.3333333333333333703, 0.3219752754296894559, 0.3333333333333333703, 0.3219752754296894559, 0.3333333333333333703, 0.3219752754296894559, 0.3333333333333333703, 0.3219752754296894559, 0.3333333333333333703, 0.3219752754296894559, 0.3333333333333333703, 0.3219752754296894559, 0.3333333333333333703, 0.3219752754296894559, 0.3333333333333333703, 0.3219752754296894559, 0.3333333333333333703, 0.3219752754296894559, 0.3333333333333333703, 0.3219752754296894559, 0.3333333333333333703, 0.3219752754296894559, 0.3333333333333333703, 0.3219752754296894559, 0.3333333333333333703, 0.3219752754296894559, 0.3333333333333333703, 0.3219752754296894559, 0.3333333333333333703, 0.3219752754296894559, 0.3333333333333333703, 0.3219752754296894559, 0.3333333333333333703, 0.3219752754296894559, 0.3333333333333333703, 0.3219752754296894559, 0.3333333333333333703, 0.3219752754296894559, 0.3333333333333333703, 0.3219752754296894559, 0.3333333333333333703, 0.3219752754296894559, 0.3333333333333333703, 0.3219752754296894559, 0.3333333333333333703, 0.3219752754296894559, 0.3333333333333333703, 0.3219752754296894559, 0.3333333333333333703, 0.3219752754296894559, 0.3333333333333333703, 0.3219752754296894559, 0.3333333333333333703, 0.3219752754296894559, 0.3333333333333333703, 0.3219752754296894559, 0.3333333333333333703, 0.3219752754296894559, 0.3333333333333333703, 0.3219752754296894559, 0.3333333333333333703, 0.3219752754296894559, 0.3333333333333333703, 0.3219752754296894559, 0.3333333333333333703, 0.3219752754296894559, 0.3333333333333333703, 0.3219752754296894559, 0.3333333333333333703, 0.3219752754296894559, 0.3333333333333333703, 0.3219752754296894559, 0.3333333333333333703, 0.3219752754296894559, 0.3333333333333333703, 0.3219752754296894559, 0.3333333333333333703, 0.3219752754296894559, 0.3333333333333333703, 0.3219752754296894559, 0.3333333333333333703, 0.3219752754296894559, 0.3333333333333333703, 0.3219752754296894559, 0.3333333333333333703, 0.3219752754296894559, 0.3333333333333333703, 0.3219752754296894559, 0.3333333333333333703, 0.3219752754296894559, 0.3333333333333333703, 0.3219752754296894559, 0.3333333333333333703, 0.3219752754296894559, 0.3333333333333333703, 0.3219752754296894559, 0.3333333333333333703, 0.3219752754296894559, 0.3333333333333333703, 0.3219752754296894559, 0.3333333333333333703, 0.3219752754296894559, 0.3333333333333333703, 0.3219752754296894559, 0.3333333333333333703, 0.3219752754296894559, 0.3333333333333333703, 0.3219752754296894559, 0.3333333333333333703, 0.3219752754296894559, 0.3333333333333333703, 0.3219752754296894559, 0.3333333333333333703, 0.3219752754296894559, 0.3333333333333333703, 0.3219752754296894559, 0.3333333333333333703, 0.3219752754296894559, 0.3333333333333333703, 0.3219752754296894559, 0.3333333333333333703, 0.3219752754296894559, 0.3333333333333333703, 0.3219752754296894559, 0.3333333333333333703, 0.3219752754296894559, 0.3333333333333333703, 0.3219752754296894559, 0.3333333333333333703, 0.3219752754296894559, 0.3333333333333333703, 0.3219752754296894559, 0.3333333333333333703, 0.3219752754296894559, 0.3333333333333333703),
 ( 1.000000000000000000, 0.9659258262890683122, 1.000000000000000000, 0.9659258262890683122, 1.000000000000000000, 0.9659258262890683122, 1.000000000000000000, 0.9659258262890683122, 1.000000000000000000, 0.9659258262890683122, 1.000000000000000000, 0.9659258262890683122, 1.000000000000000000, 0.9659258262890683122, 1.000000000000000000, 0.9659258262890683122, 1.000000000000000000, 0.9659258262890683122, 1.000000000000000000, 0.9659258262890683122, 1.000000000000000000, 0.9659258262890683122, 1.000000000000000000, 0.9659258262890683122, 1.000000000000000000, 0.9659258262890683122, 1.000000000000000000, 0.9659258262890683122, 1.000000000000000000, 0.9659258262890683122, 1.000000000000000000, 0.9659258262890683122, 1.000000000000000000, 0.9659258262890683122, 1.000000000000000000, 0.9659258262890683122, 1.000000000000000000, 0.9659258262890683122, 1.000000000000000000, 0.9659258262890683122, 1.000000000000000000, 0.9659258262890683122, 1.000000000000000000, 0.9659258262890683122, 1.000000000000000000, 0.9659258262890683122, 1.000000000000000000, 0.9659258262890683122, 1.000000000000000000, 0.9659258262890683122, 1.000000000000000000, 0.9659258262890683122, 1.000000000000000000, 0.9659258262890683122, 1.000000000000000000, 0.9659258262890683122, 1.000000000000000000, 0.9659258262890683122, 1.000000000000000000, 0.9659258262890683122, 1.000000000000000000, 0.9659258262890683122, 1.000000000000000000, 0.9659258262890683122, 1.000000000000000000, 0.9659258262890683122, 1.000000000000000000, 0.9659258262890683122, 1.000000000000000000, 0.9659258262890683122, 1.000000000000000000, 0.9659258262890683122, 1.000000000000000000, 0.9659258262890683122, 1.000000000000000000, 0.9659258262890683122, 1.000000000000000000, 0.9659258262890683122, 1.000000000000000000, 0.9659258262890683122, 1.000000000000000000, 0.9659258262890683122, 1.000000000000000000, 0.9659258262890683122, 1.000000000000000000, 0.9659258262890683122, 1.000000000000000000, 0.9659258262890683122, 1.000000000000000000, 0.9659258262890683122, 1.000000000000000000, 0.9659258262890683122, 1.000000000000000000, 0.9659258262890683122, 1.000000000000000000, 0.9659258262890683122, 1.000000000000000000, 0.9659258262890683122, 1.000000000000000000, 0.9659258262890683122, 1.000000000000000000, 0.9659258262890683122, 1.000000000000000000, 0.9659258262890683122, 1.000000000000000000, 0.9659258262890683122, 1.000000000000000000, 0.9659258262890683122, 1.000000000000000000, 0.9659258262890683122, 1.000000000000000000, 0.9659258262890683122, 1.000000000000000000, 0.9659258262890683122, 1.000000000000000000, 0.9659258262890683122, 1.000000000000000000, 0.9659258262890683122, 1.000000000000000000, 0.9659258262890683122, 1.000000000000000000, 0.9659258262890683122, 1.000000000000000000, 0.9659258262890683122, 1.000000000000000000, 0.9659258262890683122, 1.000000000000000000, 0.9659258262890683122, 1.000000000000000000, 0.9659258262890683122, 1.000000000000000000, 0.9659258262890683122, 1.000000000000000000, 0.9659258262890683122, 1.000000000000000000, 0.9659258262890683122, 1.000000000000000000, 0.9659258262890683122, 1.000000000000000000, 0.9659258262890683122, 1.000000000000000000, 0.9659258262890683122, 1.000000000000000000, 0.9659258262890683122, 1.000000000000000000, 0.9659258262890683122, 1.000000000000000000, 0.9659258262890683122, 1.000000000000000000, 0.9659258262890683122, 1.000000000000000000, 0.9659258262890683122, 1.000000000000000000, 0.9659258262890683122, 1.000000000000000000, 0.9659258262890683122, 1.000000000000000000, 0.9659258262890683122, 1.000000000000000000, 0.9659258262890683122, 1.000000000000000000, 0.9659258262890683122, 1.000000000000000000, 0.9659258262890683122, 1.000000000000000000, 0.9659258262890683122, 1.000000000000000000, 0.9659258262890683122, 1.000000000000000000, 0.9659258262890683122, 1.000000000000000000, 0.9659258262890683122, 1.000000000000000000, 0.9659258262890683122, 1.000000000000000000, 0.9659258262890683122, 1.000000000000000000, 0.9659258262890683122, 1.000000000000000000, 0.9659258262890683122, 1.000000000000000000, 0.9659258262890683122, 1.000000000000000000, 0.9659258262890683122, 1.000000000000000000, 0.9659258262890683122, 1.000000000000000000, 0.9659258262890683122, 1.000000000000000000, 0.9659258262890683122, 1.000000000000000000, 0.9659258262890683122, 1.000000000000000000, 0.9659258262890683122, 1.000000000000000000, 0.9659258262890683122, 1.000000000000000000, 0.9659258262890683122, 1.000000000000000000, 0.9659258262890683122, 1.000000000000000000, 0.9659258262890683122, 1.000000000000000000, 0.9659258262890683122, 1.000000000000000000, 0.9659258262890683122, 1.000000000000000000, 0.9659258262890683122, 1.000000000000000000, 0.9659258262890683122, 1.000000000000000000, 0.9659258262890683122, 1.000000000000000000, 0.9659258262890683122, 1.000000000000000000, 0.9659258262890683122, 1.000000000000000000, 0.9659258262890683122, 1.000000000000000000, 0.9659258262890683122, 1.000000000000000000, 0.9659258262890683122, 1.000000000000000000, 0.9659258262890683122, 1.000000000000000000, 0.9659258262890683122, 1.000000000000000000, 0.9659258262890683122, 1.000000000000000000, 0.9659258262890683122, 1.000000000000000000, 0.9659258262890683122, 1.000000000000000000, 0.9659258262890683122, 1.000000000000000000, 0.9659258262890683122, 1.000000000000000000, 0.9659258262890683122, 1.000000000000000000, 0.9659258262890683122, 1.000000000000000000, 0.9659258262890683122, 1.000000000000000000, 0.9659258262890683122, 1.000000000000000000, 0.9659258262890683122, 1.000000000000000000, 0.9659258262890683122, 1.000000000000000000, 0.9659258262890683122, 1.000000000000000000, 0.9659258262890683122, 1.000000000000000000, 0.9659258262890683122, 1.000000000000000000, 0.9659258262890683122, 1.000000000000000000, 0.9659258262890683122, 1.000000000000000000, 0.9659258262890683122, 1.000000000000000000, 0.9659258262890683122, 1.000000000000000000, 0.9659258262890683122, 1.000000000000000000, 0.9659258262890683122, 1.000000000000000000, 0.9659258262890683122, 1.000000000000000000, 0.9659258262890683122, 1.000000000000000000, 0.9659258262890683122, 1.000000000000000000, 0.9659258262890683122, 1.000000000000000000, 0.9659258262890683122, 1.000000000000000000, 0.9659258262890683122, 1.000000000000000000, 0.9659258262890683122, 1.000000000000000000, 0.9659258262890683122, 1.000000000000000000, 0.9659258262890683122, 1.000000000000000000, 0.9659258262890683122, 1.000000000000000000, 0.9659258262890683122, 1.000000000000000000, 0.9659258262890683122, 1.000000000000000000, 0.9659258262890683122, 1.000000000000000000, 0.9659258262890683122, 1.000000000000000000, 0.9659258262890683122, 1.000000000000000000, 0.9659258262890683122, 1.000000000000000000, 0.9659258262890683122, 1.000000000000000000, 0.9659258262890683122, 1.000000000000000000, 0.9659258262890683122, 1.000000000000000000, 0.9659258262890683122, 1.000000000000000000, 0.9659258262890683122, 1.000000000000000000, 0.9659258262890683122, 1.000000000000000000, 0.9659258262890683122, 1.000000000000000000, 0.9659258262890683122, 1.000000000000000000, 0.9659258262890683122, 1.000000000000000000, 0.9659258262890683122, 1.000000000000000000, 0.9659258262890683122, 1.000000000000000000, 0.9659258262890683122, 1.000000000000000000, 0.9659258262890683122, 1.000000000000000000, 0.9659258262890683122, 1.000000000000000000, 0.9659258262890683122, 1.000000000000000000, 0.9659258262890683122, 1.000000000000000000, 0.9659258262890683122, 1.000000000000000000, 0.9659258262890683122, 1.000000000000000000, 0.9659258262890683122, 1.000000000000000000, 0.9659258262890683122, 1.000000000000000000, 0.9659258262890683122, 1.000000000000000000, 0.9659258262890683122, 1.000000000000000000, 0.9659258262890683122, 1.000000000000000000, 0.9659258262890683122, 1.000000000000000000, 0.9659258262890683122, 1.000000000000000000, 0.9659258262890683122, 1.000000000000000000, 0.9659258262890683122, 1.000000000000000000, 0.9659258262890683122, 1.000000000000000000, 0.9659258262890683122, 1.000000000000000000, 0.9659258262890683122, 1.000000000000000000, 0.9659258262890683122, 1.000000000000000000, 0.9659258262890683122, 1.000000000000000000, 0.9659258262890683122, 1.000000000000000000, 0.9659258262890683122, 1.000000000000000000, 0.9659258262890683122, 1.000000000000000000, 0.9659258262890683122, 1.000000000000000000, 0.9659258262890683122, 1.000000000000000000, 0.9659258262890683122, 1.000000000000000000, 0.9659258262890683122, 1.000000000000000000, 0.9659258262890683122, 1.000000000000000000, 0.9659258262890683122, 1.000000000000000000, 0.9659258262890683122, 1.000000000000000000, 0.9659258262890683122, 1.000000000000000000, 0.9659258262890683122, 1.000000000000000000, 0.9659258262890683122, 1.000000000000000000, 0.9659258262890683122, 1.000000000000000000, 0.9659258262890683122, 1.000000000000000000, 0.9659258262890683122, 1.000000000000000000, 0.9659258262890683122, 1.000000000000000000, 0.9659258262890683122, 1.000000000000000000, 0.9659258262890683122, 1.000000000000000000, 0.9659258262890683122, 1.000000000000000000, 0.9659258262890683122, 1.000000000000000000, 0.9659258262890683122, 1.000000000000000000, 0.9659258262890683122, 1.000000000000000000, 0.9659258262890683122, 1.000000000000000000, 0.9659258262890683122, 1.000000000000000000, 0.9659258262890683122, 1.000000000000000000, 0.9659258262890683122, 1.000000000000000000, 0.9659258262890683122, 1.000000000000000000, 0.9659258262890683122, 1.000000000000000000, 0.9659258262890683122, 1.000000000000000000, 0.9659258262890683122, 1.000000000000000000, 0.9659258262890683122, 1.000000000000000000, 0.9659258262890683122, 1.000000000000000000, 0.9659258262890683122, 1.000000000000000000, 0.9659258262890683122, 1.000000000000000000, 0.9659258262890683122, 1.000000000000000000, 0.9659258262890683122, 1.000000000000000000, 0.9659258262890683122, 1.000000000000000000, 0.9659258262890683122, 1.000000000000000000, 0.9659258262890683122, 1.000000000000000000, 0.9659258262890683122, 1.000000000000000000, 0.9659258262890683122, 1.000000000000000000, 0.9659258262890683122, 1.000000000000000000, 0.9659258262890683122, 1.000000000000000000, 0.9659258262890683122, 1.000000000000000000, 0.9659258262890683122, 1.000000000000000000, 0.9659258262890683122, 1.000000000000000000) ) ) 
 REPRESENTATION_ITEM ( '' )  SURFACE ( )  );
#55597 = CARTESIAN_POINT ( 'NONE',  ( 16.52544592524335698, 4.483927247898782831, 66.45942372801903275 ) ) ;
#55599 = CARTESIAN_POINT ( 'NONE',  ( 18.62759615963255655, 10.81492255796105972, 81.66775706135236135 ) ) ;
#55600 = CARTESIAN_POINT ( 'NONE',  ( 14.29746914071037800, 8.314922557961029526, 46.66775706135234714 ) ) ;
#55601 = CARTESIAN_POINT ( 'NONE',  ( 19.02544592524343514, -5.153800228976328945, 83.54057627198100988 ) ) ;
#55602 = CARTESIAN_POINT ( 'NONE',  ( 9.564922557961047289, -16.46253265017146816, 105.4177570613523471 ) ) ;
#55603 = CARTESIAN_POINT ( 'NONE',  ( 14.29746914071037800, 8.314922557961029526, 71.66775706135234714 ) ) ;
#55604 = CARTESIAN_POINT ( 'NONE',  ( 19.03943276465977164, 0.05219959533936151252, 96.25109039468567573 ) ) ;
#55605 = CARTESIAN_POINT ( 'NONE',  ( 19.02544592524343514, -5.153800228976328945, 63.54057627198103830 ) ) ;
#55606 = CARTESIAN_POINT ( 'NONE',  ( 21.52544592524344225, -5.823673210054117533, 88.54057627198103830 ) ) ;
#55608 = CARTESIAN_POINT ( 'NONE',  ( -5.153800228976607833, 19.02544592524334988, 92.70942372801901854 ) ) ;
#55607 = CARTESIAN_POINT ( 'NONE',  ( 8.314922557960818139, 14.29746914071049879, 89.58224293864768129 ) ) ;
#55609 = CARTESIAN_POINT ( 'NONE',  ( -12.14591786802326823, 12.06949235617739902, 53.12609039468568284 ) ) ;
#55610 = CARTESIAN_POINT ( 'NONE',  ( 17.13100169013303287, -6.664070546373073611, 63.26789835699851494 ) ) ;
#55611 = CARTESIAN_POINT ( 'NONE',  ( -16.51473224551082808, 9.474510206698731452, 53.33442372801900433 ) ) ;
#55612 = CARTESIAN_POINT ( 'NONE',  ( -4.483927247898539470, -16.52544592524342804, 37.29057627198102409 ) ) ;
#55613 = CARTESIAN_POINT ( 'NONE',  ( -16.52544592524342804, 4.483927247898546575, 81.04057627198102409 ) ) ;
#55615 = CARTESIAN_POINT ( 'NONE',  ( -17.05587630539706367, 6.762274262136758196, 40.74180309037283365 ) ) ;
#55614 = CARTESIAN_POINT ( 'NONE',  ( 5.719274019375673035, 21.55341960407619339, 112.2927570613523471 ) ) ;
#55616 = CARTESIAN_POINT ( 'NONE',  ( -0.05219959533937732626, 21.53943276465977519, 22.50109039468567573 ) ) ;
#55617 = DIRECTION ( 'NONE',  ( -0.000000000000000000, 1.000000000000000000, 0.000000000000000000 ) ) ;
#55618 = CARTESIAN_POINT ( 'NONE',  ( -13.89961937509977652, 13.97604488694528158, 80.62390960531436690 ) ) ;
#55619 = CARTESIAN_POINT ( 'NONE',  ( -21.55341960407619339, 5.719274019375674811, 93.54275706135234714 ) ) ;
#55620 = CARTESIAN_POINT ( 'NONE',  ( -5.153800228976328057, -19.02544592524343514, 82.29057627198103830 ) ) ;
#55621 = CARTESIAN_POINT ( 'NONE',  ( -5.823673210054116645, -21.52544592524344225, 42.29057627198103120 ) ) ;
#55622 = CARTESIAN_POINT ( 'NONE',  ( 16.52544592524342804, -4.483927247898539470, 78.54057627198103830 ) ) ;
#55623 = CARTESIAN_POINT ( 'NONE',  ( 5.049401038298161559, -19.05341960407611168, 52.70724293864767418 ) ) ;
#55624 = CARTESIAN_POINT ( 'NONE',  ( -16.52544592524342804, 4.483927247898546575, 101.0405762719810383 ) ) ;
#55625 = CARTESIAN_POINT ( 'NONE',  ( -21.52544592524334988, -5.823673210054445271, 18.95942372801901143 ) ) ;
#55626 = CARTESIAN_POINT ( 'NONE',  ( 5.719274019375673035, 21.55341960407619339, 62.29275706135236845 ) ) ;
#55627 = CARTESIAN_POINT ( 'NONE',  ( -19.03943276465977164, 0.05219959533909376836, 41.24890960531435269 ) ) ;
#55628 = CARTESIAN_POINT ( 'NONE',  ( -12.14591786802326823, 12.06949235617739902, 63.12609039468568994 ) ) ;
#55629 = CARTESIAN_POINT ( 'NONE',  ( 10.72451020669898902, -18.67979575497178502, 112.9155762719810383 ) ) ;
#55630 = CARTESIAN_POINT ( 'NONE',  ( 10.72451020669898902, -18.67979575497178502, 107.9155762719810241 ) ) ;
#55632 = CARTESIAN_POINT ( 'NONE',  ( -13.97604488694527625, -13.89961937509977652, 71.87390960531433848 ) ) ;
#55631 = CARTESIAN_POINT ( 'NONE',  ( 16.51473224551083163, -9.474510206698727899, 45.83442372801900433 ) ) ;
#55633 = CARTESIAN_POINT ( 'NONE',  ( -10.59477242850411649, -90.60836494048552936, -15.00000000000000178 ) ) ;
#55634 = CARTESIAN_POINT ( 'NONE',  ( -18.62759615963255300, -10.81492255796106328, 64.16775706135234714 ) ) ;
#55635 = CARTESIAN_POINT ( 'NONE',  ( 10.81492255796078972, 18.62759615963270932, 54.58224293864769550 ) ) ;
#55636 = CARTESIAN_POINT ( 'NONE',  ( -16.55341960407611168, -4.379528057220339221, 36.45724293864768839 ) ) ;
#55638 = CARTESIAN_POINT ( 'NONE',  ( 10.72451020669871369, 18.67979575497193778, 112.0844237280190185 ) ) ;
#55637 = CARTESIAN_POINT ( 'NONE',  ( 21.52544592524334988, 5.823673210054432836, 76.45942372801901854 ) ) ;
#55639 = CARTESIAN_POINT ( 'NONE',  ( 12.06949235617757843, -12.14591786802309237, 63.12390960531435979 ) ) ;
#55640 = CARTESIAN_POINT ( 'NONE',  ( -16.55341960407611168, -4.379528057220339221, 106.4572429386477097 ) ) ;
#55641 = CARTESIAN_POINT ( 'NONE',  ( -5.049401038297874678, -19.05341960407617918, 59.79275706135231871 ) ) ;
#55642 = CARTESIAN_POINT ( 'NONE',  ( 14.29746914071037800, 8.314922557961029526, 111.6677570613523613 ) ) ;
#55643 = CARTESIAN_POINT ( 'NONE',  ( -21.52544592524334988, -5.823673210054445271, 68.95942372801901854 ) ) ;
#55644 = CARTESIAN_POINT ( 'NONE',  ( 0.05219959533909260263, 19.03943276465977164, 54.99890960531435979 ) ) ;
#55645 = CARTESIAN_POINT ( 'NONE',  ( -13.97604488694547697, 13.89961937509957934, 38.12609039468566152 ) ) ;
#55646 = CARTESIAN_POINT ( 'NONE',  ( -5.823673210054116645, -21.52544592524344225, 37.29057627198102409 ) ) ;
#55648 = CARTESIAN_POINT ( 'NONE',  ( -18.67979575497193778, 10.72451020669871902, 38.33442372801900433 ) ) ;
#55647 = B_SPLINE_CURVE_WITH_KNOTS ( 'NONE', 3,
 ( #196056, #9025, #71686, #131353, #102023, #176882 ),
 .UNSPECIFIED., .F., .F.,
 ( 4, 2, 4 ),
 ( 0.000000000000000000, 0.0003837532665635129316, 0.0007675065331270258633 ),
 .UNSPECIFIED. ) ;
#55649 = CARTESIAN_POINT ( 'NONE',  ( 21.55341960407610458, 5.719274019375980345, 93.95724293864770971 ) ) ;
#55650 = CARTESIAN_POINT ( 'NONE',  ( -5.153800228976607833, 19.02544592524334988, 97.70942372801900433 ) ) ;
#55651 = CARTESIAN_POINT ( 'NONE',  ( -4.379528057220086978, -16.55341960407618274, 54.79275706135235424 ) ) ;
#55653 = CARTESIAN_POINT ( 'NONE',  ( 5.823673210054125526, 21.52544592524343514, 89.79057627198103830 ) ) ;
#55652 = DIRECTION ( 'NONE',  ( 0.000000000000000000, 0.000000000000000000, 1.000000000000000000 ) ) ;
#55654 = CARTESIAN_POINT ( 'NONE',  ( 16.53943276465976808, -0.05219959533910856209, 83.74890960531435269 ) ) ;
#55655 = CARTESIAN_POINT ( 'NONE',  ( 0.1381572879930670350, 31.90000000000002700, -45.64921306006599622 ) ) ;
#55656 = CARTESIAN_POINT ( 'NONE',  ( 4.483927247898790824, -16.52544592524335698, 20.20942372801900788 ) ) ;
#55657 = CARTESIAN_POINT ( 'NONE',  ( 21.52544592524344225, -5.823673210054117533, 48.54057627198103120 ) ) ;
#55658 = CARTESIAN_POINT ( 'NONE',  ( 4.483927247898790824, -16.52544592524335698, 90.20942372801903275 ) ) ;
#55659 = CARTESIAN_POINT ( 'NONE',  ( -69.65682714487590488, -71.74905178543390605, 8.936314941956774358E-29 ) ) ;
#55660 = CARTESIAN_POINT ( 'NONE',  ( 12.06949235617739724, 12.14591786802326823, 46.87609039468568994 ) ) ;
#55661 = CARTESIAN_POINT ( 'NONE',  ( -5.719274019375665041, -21.55341960407619695, 24.79275706135235779 ) ) ;
#55662 = CARTESIAN_POINT ( 'NONE',  ( 15.80617190586746368, 15.72974639402197994, 49.37390960531436690 ) ) ;
#55663 = CARTESIAN_POINT ( 'NONE',  ( -12.06949235617739369, -12.14591786802326823, 84.37609039468570415 ) ) ;
#55664 = CARTESIAN_POINT ( 'NONE',  ( -9.474510206698964154, 16.51473224551069663, 100.4155762719810241 ) ) ;
#55665 = CARTESIAN_POINT ( 'NONE',  ( 21.53943276465977519, 0.05219959533937863772, 56.25109039468568284 ) ) ;
#55666 = CARTESIAN_POINT ( 'NONE',  ( 21.53943276465977519, -0.05219959533907433946, 43.74890960531435979 ) ) ;
#55667 = CARTESIAN_POINT ( 'NONE',  ( -10.81492255796078084, -18.62759615963271287, 27.08224293864769550 ) ) ;
#55668 = ORIENTED_EDGE ( 'NONE', *, *, #37703, .T. ) ;
#55669 = CARTESIAN_POINT ( 'NONE',  ( 9.564922557961047289, -16.46253265017146816, 35.41775706135233293 ) ) ;
#55670 = CARTESIAN_POINT ( 'NONE',  ( 8.224510206698742110, 14.34966873604972548, 72.08442372801899012 ) ) ;
#55671 = CARTESIAN_POINT ( 'NONE',  ( 15.80617190586746368, 15.72974639402197994, 24.37390960531435979 ) ) ;
#55672 = ORIENTED_EDGE ( 'NONE', *, *, #91752, .F. ) ;
#55673 = CARTESIAN_POINT ( 'NONE',  ( -13.89961937509977652, 13.97604488694528158, 85.62390960531433848 ) ) ;
#55674 = CARTESIAN_POINT ( 'NONE',  ( 16.55341960407618274, -4.379528057220086978, 101.0427570613523756 ) ) ;
#55675 = CARTESIAN_POINT ( 'NONE',  ( 17.97214573761829826, 5.500000000000077272, 73.96970049038654338 ) ) ;
#55676 = CARTESIAN_POINT ( 'NONE',  ( -8.224510206698948167, 14.34966873604960824, 95.41557627198102409 ) ) ;
#55677 = CARTESIAN_POINT ( 'NONE',  ( 21.55341960407610458, 5.719274019375980345, 53.95724293864770260 ) ) ;
#55678 = CARTESIAN_POINT ( 'NONE',  ( -13.97604488694527625, -13.89961937509977652, 31.87390960531435979 ) ) ;
#55679 = CARTESIAN_POINT ( 'NONE',  ( -12.14591786802326823, 12.06949235617739902, 83.12609039468568994 ) ) ;
#55680 = CARTESIAN_POINT ( 'NONE',  ( -15.80617190586768217, 15.72974639402176855, 33.12609039468569705 ) ) ;
#55681 = CARTESIAN_POINT ( 'NONE',  ( 9.564922557961047289, -16.46253265017146816, 90.41775706135234714 ) ) ;
#55682 = CARTESIAN_POINT ( 'NONE',  ( 12.06949235617757843, -12.14591786802309237, 88.12390960531436690 ) ) ;
#55683 = CARTESIAN_POINT ( 'NONE',  ( -5.153800228976328057, -19.02544592524343514, 52.29057627198100988 ) ) ;
#55684 = CARTESIAN_POINT ( 'NONE',  ( 16.51473224551069308, 9.474510206698969483, 109.1655762719810383 ) ) ;
#55685 = CARTESIAN_POINT ( 'NONE',  ( -15.72974639402176322, -15.80617190586768395, 104.3760903946856899 ) ) ;
#55686 = CARTESIAN_POINT ( 'NONE',  ( 16.51473224551069308, 9.474510206698969483, 74.16557627198103830 ) ) ;
#55687 = CARTESIAN_POINT ( 'NONE',  ( -12.14591786802326823, 12.06949235617739902, 58.12609039468568994 ) ) ;
#55688 = CARTESIAN_POINT ( 'NONE',  ( -0.05219959533937732626, 21.53943276465977519, 92.50109039468567573 ) ) ;
#55689 = CARTESIAN_POINT ( 'NONE',  ( -8.314922557961024197, 14.29746914071037800, 67.91775706135234714 ) ) ;
#55690 = CARTESIAN_POINT ( 'NONE',  ( -19.02544592524334988, -5.153800228976617603, 53.95942372801898301 ) ) ;
#55691 = CARTESIAN_POINT ( 'NONE',  ( 5.049401038297881783, 19.05341960407617563, 62.29275706135234003 ) ) ;
#55692 = ORIENTED_EDGE ( 'NONE', *, *, #43196, .F. ) ;
#55693 = CARTESIAN_POINT ( 'NONE',  ( 5.823673210054444382, -21.52544592524334988, 65.20942372801901854 ) ) ;
#55694 = CARTESIAN_POINT ( 'NONE',  ( -19.02544592524342804, 5.153800228976336051, 71.04057627198099567 ) ) ;
#55695 = CARTESIAN_POINT ( 'NONE',  ( 9.474510206698971260, -16.51473224551069308, 22.91557627198102765 ) ) ;
#55696 = CARTESIAN_POINT ( 'NONE',  ( 16.46253265017146816, 9.564922557961045513, 56.66775706135233293 ) ) ;
#55697 = CARTESIAN_POINT ( 'NONE',  ( 13.89961937509977652, -13.97604488694527269, 113.1239096053143527 ) ) ;
#55698 = CARTESIAN_POINT ( 'NONE',  ( 16.51473224551069308, 9.474510206698969483, 84.16557627198102409 ) ) ;
#55699 = CARTESIAN_POINT ( 'NONE',  ( -12.06949235617756955, 12.14591786802309770, 35.62390960531437401 ) ) ;
#55700 = CARTESIAN_POINT ( 'NONE',  ( -21.55341960407610458, -5.719274019375992779, 46.45724293864769550 ) ) ;
#55701 = CARTESIAN_POINT ( 'NONE',  ( -8.898068258721474777, 27.38543819252877043, 141.5843446569000150 ) ) ;
#55702 = CARTESIAN_POINT ( 'NONE',  ( -10.72451020669870658, -18.67979575497194134, 109.5844237280190328 ) ) ;
#55703 = CARTESIAN_POINT ( 'NONE',  ( -17.26172910966779739, -6.454744622555842248, 79.19353091350777163 ) ) ;
#55704 = CARTESIAN_POINT ( 'NONE',  ( -19.02544592524342804, 5.153800228976336051, 36.04057627198100988 ) ) ;
#55705 = CARTESIAN_POINT ( 'NONE',  ( 5.153800228976335163, 19.02544592524342804, 29.79057627198102409 ) ) ;
#55706 = EDGE_CURVE ( 'NONE', #28823, #146440, #104934, .T. ) ;
#55707 = CARTESIAN_POINT ( 'NONE',  ( -10.41242334162750716, -12.21727042188736156, -59.44333992957475488 ) ) ;
#55708 = CARTESIAN_POINT ( 'NONE',  ( -21.53943276465977519, -0.05219959533937600094, 63.75109039468568284 ) ) ;
#55709 = CARTESIAN_POINT ( 'NONE',  ( -37.96308138437226631, -1.796937805546485301, -7.999999999999996447 ) ) ;
#55710 = CARTESIAN_POINT ( 'NONE',  ( -12.14591786802326823, 12.06949235617739902, 63.12609039468568994 ) ) ;
#55711 = CARTESIAN_POINT ( 'NONE',  ( 21.52544592524344225, -5.823673210054117533, 88.54057627198103830 ) ) ;
#55712 = CARTESIAN_POINT ( 'NONE',  ( 12.06949235617757843, -12.14591786802309237, 53.12390960531436690 ) ) ;
#55714 = CARTESIAN_POINT ( 'NONE',  ( 7.128481858827110607, -2.709097808555395392, 2.998008972631150737 ) ) ;
#55713 = CARTESIAN_POINT ( 'NONE',  ( 13.97604488694527802, 13.89961937509977652, 29.37390960531435979 ) ) ;
#55715 = CARTESIAN_POINT ( 'NONE',  ( 15.72974639402176855, 15.80617190586768217, 46.87609039468568994 ) ) ;
#55716 = CARTESIAN_POINT ( 'NONE',  ( -19.03943276465977164, -0.05219959533935918106, 53.75109039468566863 ) ) ;
#55717 = CARTESIAN_POINT ( 'NONE',  ( -13.89961937509977652, 13.97604488694528158, 35.62390960531435269 ) ) ;
#55718 = CARTESIAN_POINT ( 'NONE',  ( -5.823673210054431948, 21.52544592524334988, 82.70942372801900433 ) ) ;
#55719 = CARTESIAN_POINT ( 'NONE',  ( 16.36317988757059538, -7.306389748694917863, 31.59789608363227487 ) ) ;
#55720 = CARTESIAN_POINT ( 'NONE',  ( -8.224510206698948167, 14.34966873604960824, 40.41557627198103120 ) ) ;
#55721 = CARTESIAN_POINT ( 'NONE',  ( 36.91746824999999177, 2.880721459617395097E-14, -2.124999997268813168 ) ) ;
#55722 = CARTESIAN_POINT ( 'NONE',  ( -5.719274019375978568, 21.55341960407610458, 45.20724293864769550 ) ) ;
#55723 = CARTESIAN_POINT ( 'NONE',  ( 22.44159573604009594, -16.30477369853687364, 141.6750000027311671 ) ) ;
#55724 = CARTESIAN_POINT ( 'NONE',  ( 13.97604488694527802, 13.89961937509977652, 94.37390960531436690 ) ) ;
#55725 = CARTESIAN_POINT ( 'NONE',  ( 8.224510206698953496, -14.34966873604960469, 92.91557627198103830 ) ) ;
#55726 = CARTESIAN_POINT ( 'NONE',  ( -19.05341960407617563, 5.049401038297882671, 103.5427570613523329 ) ) ;
#55727 = CARTESIAN_POINT ( 'NONE',  ( -0.05219959533907301413, -21.53943276465977519, 67.49890960531436690 ) ) ;
#55728 = ORIENTED_EDGE ( 'NONE', *, *, #193154, .T. ) ;
#55729 = CARTESIAN_POINT ( 'NONE',  ( -5.153800228976328057, -19.02544592524343514, 37.29057627198102409 ) ) ;
#55731 = CARTESIAN_POINT ( 'NONE',  ( 21.52544592524344225, -5.823673210054117533, 88.54057627198103830 ) ) ;
#55730 = CARTESIAN_POINT ( 'NONE',  ( -19.03943276465977164, 0.05219959533909376836, 86.24890960531436690 ) ) ;
#55733 = CARTESIAN_POINT ( 'NONE',  ( 5.153800228976335163, 19.02544592524342804, 104.7905762719809957 ) ) ;
#55732 = CARTESIAN_POINT ( 'NONE',  ( -8.224510206698948167, 14.34966873604960824, 30.41557627198101699 ) ) ;
#55734 = CARTESIAN_POINT ( 'NONE',  ( 16.51473224551083163, -9.474510206698727899, 85.83442372801900433 ) ) ;
#55735 = CARTESIAN_POINT ( 'NONE',  ( -5.719274019375665041, -21.55341960407619695, 89.79275706135236135 ) ) ;
#55736 = CARTESIAN_POINT ( 'NONE',  ( -18.67979575497178146, -10.72451020669898902, 81.66557627198103830 ) ) ;
#55737 = CARTESIAN_POINT ( 'NONE',  ( 18.62759615963271287, -10.81492255796078972, 33.33224293864769550 ) ) ;
#55738 = CARTESIAN_POINT ( 'NONE',  ( 9.474510206698971260, -16.51473224551069308, 52.91557627198102409 ) ) ;
#55739 = CARTESIAN_POINT ( 'NONE',  ( -4.483927247898782831, 16.52544592524335698, 112.7094237280190328 ) ) ;
#55740 = CARTESIAN_POINT ( 'NONE',  ( -19.03943276465977164, 0.05219959533909376836, 71.24890960531435269 ) ) ;
#55741 = ORIENTED_EDGE ( 'NONE', *, *, #60543, .T. ) ;
#55742 = CARTESIAN_POINT ( 'NONE',  ( -31.23717829866982854, -7.254840157072011131, 96.91794063280337923 ) ) ;
#55743 = CARTESIAN_POINT ( 'NONE',  ( 9.474510206698729675, 16.51473224551082808, 27.08442372801900433 ) ) ;
#55744 = CARTESIAN_POINT ( 'NONE',  ( -16.52544592524342804, 4.483927247898546575, 81.04057627198102409 ) ) ;
#55745 = CARTESIAN_POINT ( 'NONE',  ( -15.72974639402176322, -15.80617190586768395, 19.37609039468568639 ) ) ;
#55746 = CARTESIAN_POINT ( 'NONE',  ( -5.359611314223446995E-15, 29.16686587814335496, 142.8750000027311842 ) ) ;
#55747 = CARTESIAN_POINT ( 'NONE',  ( -10.81492255796078084, -18.62759615963271287, 57.08224293864769550 ) ) ;
#55748 = CARTESIAN_POINT ( 'NONE',  ( 8.224510206698742110, 14.34966873604972548, 87.08442372801901854 ) ) ;
#55749 = CARTESIAN_POINT ( 'NONE',  ( 9.564922557960805705, 16.46253265017160317, 24.58224293864769194 ) ) ;
#55750 = CARTESIAN_POINT ( 'NONE',  ( 5.153800228976335163, 19.02544592524342804, 69.79057627198103830 ) ) ;
#55751 = DIRECTION ( 'NONE',  ( 1.000000000000000000, 0.000000000000000000, 3.469446951953612217E-15 ) ) ;
#55752 = CARTESIAN_POINT ( 'NONE',  ( 8.314922557960818139, 14.29746914071049879, 34.58224293864770260 ) ) ;
#55753 = CARTESIAN_POINT ( 'NONE',  ( -10.72451020669870658, -18.67979575497194134, 64.58442372801900433 ) ) ;
#55754 = CARTESIAN_POINT ( 'NONE',  ( -16.46253265017160317, 9.564922557960807481, 115.8322429386477097 ) ) ;
#55755 = CARTESIAN_POINT ( 'NONE',  ( 21.52544592524334988, 5.823673210054432836, 96.45942372801901854 ) ) ;
#55756 = CARTESIAN_POINT ( 'NONE',  ( 5.153800228976335163, 19.02544592524342804, 49.79057627198100988 ) ) ;
#55757 = CARTESIAN_POINT ( 'NONE',  ( -13.89961937509977652, 13.97604488694528158, 40.62390960531435979 ) ) ;
#55758 = ORIENTED_EDGE ( 'NONE', *, *, #9833, .F. ) ;
#55759 = CARTESIAN_POINT ( 'NONE',  ( -15.80617190586768217, 15.72974639402176855, 98.12609039468570415 ) ) ;
#55760 = CARTESIAN_POINT ( 'NONE',  ( 8.224510206698742110, 14.34966873604972548, 52.08442372801901854 ) ) ;
#55761 = CARTESIAN_POINT ( 'NONE',  ( -18.62759615963255300, -10.81492255796106328, 89.16775706135236135 ) ) ;
#55762 = CARTESIAN_POINT ( 'NONE',  ( -9.564922557960796823, -16.46253265017161027, 112.0822429386476955 ) ) ;
#55763 = CARTESIAN_POINT ( 'NONE',  ( 19.05341960407617918, -5.049401038297876454, 91.04275706135234714 ) ) ;
#55764 = CARTESIAN_POINT ( 'NONE',  ( 10.72451020669871369, 18.67979575497193778, 62.08442372801901143 ) ) ;
#55765 = CARTESIAN_POINT ( 'NONE',  ( 8.314922557961029526, -14.29746914071037800, 40.41775706135234714 ) ) ;
#55766 = CARTESIAN_POINT ( 'NONE',  ( -5.049401038297874678, -19.05341960407617918, 79.79275706135233293 ) ) ;
#55767 = CARTESIAN_POINT ( 'NONE',  ( -13.89961937509977652, 13.97604488694528158, 55.62390960531434558 ) ) ;
#55768 = CARTESIAN_POINT ( 'NONE',  ( 9.564922557961047289, -16.46253265017146816, 90.41775706135234714 ) ) ;
#55769 = CARTESIAN_POINT ( 'NONE',  ( 5.153800228976615827, -19.02544592524334988, 90.20942372801900433 ) ) ;
#55770 = CARTESIAN_POINT ( 'NONE',  ( -12.06949235617756955, 12.14591786802309770, 50.62390960531435979 ) ) ;
#55771 = CARTESIAN_POINT ( 'NONE',  ( 19.02544592524334988, 5.153800228976608722, 71.45942372801900433 ) ) ;
#55772 = CARTESIAN_POINT ( 'NONE',  ( 16.53943276465976808, 0.05219959533934440121, 66.25109039468567573 ) ) ;
#55773 = CARTESIAN_POINT ( 'NONE',  ( -13.89961937509957401, -13.97604488694547875, 19.37609039468566507 ) ) ;
#55774 = EDGE_CURVE ( 'NONE', #80486, #9032, #32574, .T. ) ;
#55775 = CARTESIAN_POINT ( 'NONE',  ( 19.02544592524343514, -5.153800228976328945, 33.54057627198102409 ) ) ;
#55776 = CARTESIAN_POINT ( 'NONE',  ( -5.153800228976328057, -19.02544592524343514, 42.29057627198101699 ) ) ;
#55777 = CARTESIAN_POINT ( 'NONE',  ( 8.224510206698742110, 14.34966873604972548, 57.08442372801901854 ) ) ;
#55778 = CARTESIAN_POINT ( 'NONE',  ( -17.14385361876520264, -23.59649016807271593, 139.6750000027311955 ) ) ;
#55779 = AXIS2_PLACEMENT_3D ( 'NONE', #92099, #135661, #136629 ) ;
#55780 = CARTESIAN_POINT ( 'NONE',  ( -23.31738231874055245, -16.94106989632524574, 140.4500000054623854 ) ) ;
#55781 = CARTESIAN_POINT ( 'NONE',  ( -5.153800228976328057, -19.02544592524343514, 112.2905762719810099 ) ) ;
#55782 = FACE_OUTER_BOUND ( 'NONE', #69865, .T. ) ;
#55783 = ORIENTED_EDGE ( 'NONE', *, *, #148801, .F. ) ;
#55784 = CARTESIAN_POINT ( 'NONE',  ( -0.05219959533936034679, 19.03943276465977164, 92.50109039468566152 ) ) ;
#55785 = EDGE_CURVE ( 'NONE', #148762, #101739, #39900, .T. ) ;
#55786 = CARTESIAN_POINT ( 'NONE',  ( 10.81492255796078972, 18.62759615963270932, 39.58224293864769550 ) ) ;
#55788 = CARTESIAN_POINT ( 'NONE',  ( 19.05341960407617918, -5.049401038297876454, 111.0427570613523329 ) ) ;
#55787 = CARTESIAN_POINT ( 'NONE',  ( 16.51473224551083163, -9.474510206698727899, 30.83442372801900433 ) ) ;
#55789 = CARTESIAN_POINT ( 'NONE',  ( 0.05219959533909260263, 19.03943276465977164, 29.99890960531435979 ) ) ;
#55790 = CARTESIAN_POINT ( 'NONE',  ( -19.05341960407611168, -5.049401038298163336, 31.45724293864769550 ) ) ;
#55791 = CARTESIAN_POINT ( 'NONE',  ( 21.53943276465977519, -0.05219959533907433946, 73.74890960531433848 ) ) ;
#55792 = CARTESIAN_POINT ( 'NONE',  ( -9.564922557960796823, -16.46253265017161027, 97.08224293864769550 ) ) ;
#55793 = CARTESIAN_POINT ( 'NONE',  ( -0.05219959533909027116, -19.03943276465977164, 42.49890960531435269 ) ) ;
#55794 = CARTESIAN_POINT ( 'NONE',  ( 8.571926809382603096, -26.38167802310801235, 143.9750000027312069 ) ) ;
#55795 = CARTESIAN_POINT ( 'NONE',  ( -5.049401038297874678, -19.05341960407617918, 84.79275706135233293 ) ) ;
#55796 = CARTESIAN_POINT ( 'NONE',  ( 16.55341960407611168, 4.379528057220329451, 48.95724293864770971 ) ) ;
#55797 = CARTESIAN_POINT ( 'NONE',  ( -0.05219959533907301413, -21.53943276465977519, 27.49890960531435269 ) ) ;
#55798 = CARTESIAN_POINT ( 'NONE',  ( 0.05219959533937995610, -21.53943276465977519, 110.0010903946856757 ) ) ;
#55799 = CARTESIAN_POINT ( 'NONE',  ( 10.81492255796078972, 18.62759615963270932, 79.58224293864769550 ) ) ;
#55800 = CARTESIAN_POINT ( 'NONE',  ( 10.81492255796106328, -18.62759615963255655, 65.41775706135234714 ) ) ;
#55801 = CARTESIAN_POINT ( 'NONE',  ( 15.80617190586769283, -15.72974639402175789, 65.62609039468568994 ) ) ;
#55802 = CARTESIAN_POINT ( 'NONE',  ( -9.474510206698964154, 16.51473224551069663, 105.4155762719810383 ) ) ;
#55804 = CARTESIAN_POINT ( 'NONE',  ( -15.72974639402176322, -15.80617190586768395, 59.37609039468568284 ) ) ;
#55803 = CARTESIAN_POINT ( 'NONE',  ( 14.29746914071037800, 8.314922557961029526, 101.6677570613523613 ) ) ;
#55805 = CARTESIAN_POINT ( 'NONE',  ( 9.564922557960805705, 16.46253265017160317, 54.58224293864769550 ) ) ;
#55806 = CARTESIAN_POINT ( 'NONE',  ( 16.46253265017146816, 9.564922557961045513, 36.66775706135233293 ) ) ;
#55807 = CARTESIAN_POINT ( 'NONE',  ( -21.55341960407619339, 5.719274019375674811, 33.54275706135234714 ) ) ;
#55808 = CARTESIAN_POINT ( 'NONE',  ( 16.51473224551069308, 9.474510206698969483, 74.16557627198103830 ) ) ;
#55809 = CARTESIAN_POINT ( 'NONE',  ( 0.05219959533910956823, 16.53943276465976808, 79.99890960531435269 ) ) ;
#55810 = CARTESIAN_POINT ( 'NONE',  ( 8.314922557960818139, 14.29746914071049879, 49.58224293864769550 ) ) ;
#55811 = CARTESIAN_POINT ( 'NONE',  ( 0.05219959533907565091, 21.53943276465977519, 59.99890960531436690 ) ) ;
#55812 = CARTESIAN_POINT ( 'NONE',  ( -16.46253265017160317, 9.564922557960807481, 55.83224293864769550 ) ) ;
#55813 = CARTESIAN_POINT ( 'NONE',  ( 0.05219959533907565091, 21.53943276465977519, 69.99890960531435269 ) ) ;
#55814 = CARTESIAN_POINT ( 'NONE',  ( 5.153800228976615827, -19.02544592524334988, 55.20942372801899722 ) ) ;
#55816 = CARTESIAN_POINT ( 'NONE',  ( -8.224510206698948167, 14.34966873604960824, 65.41557627198102409 ) ) ;
#55815 = FACE_OUTER_BOUND ( 'NONE', #73387, .T. ) ;
#55817 = CARTESIAN_POINT ( 'NONE',  ( -5.719274019375978568, 21.55341960407610458, 35.20724293864768839 ) ) ;
#55818 = ORIENTED_EDGE ( 'NONE', *, *, #57511, .F. ) ;
#55819 = DIRECTION ( 'NONE',  ( 0.000000000000000000, 0.000000000000000000, 1.000000000000000000 ) ) ;
#55821 = CARTESIAN_POINT ( 'NONE',  ( -22.44159573604009950, -16.30477369853688430, 141.5750000027311728 ) ) ;
#55820 = CARTESIAN_POINT ( 'NONE',  ( 14.34966873604972726, -8.224510206698740333, 80.83442372801901854 ) ) ;
#55822 = CARTESIAN_POINT ( 'NONE',  ( 5.153800228976615827, -19.02544592524334988, 95.20942372801897591 ) ) ;
#55823 = CARTESIAN_POINT ( 'NONE',  ( -0.05219959533910754901, -16.53943276465976808, 57.49890960531435979 ) ) ;
#55824 = CARTESIAN_POINT ( 'NONE',  ( -3.573655867282028392E-15, 2.428612866367529932E-14, 2.000000000000000000 ) ) ;
#55825 = CARTESIAN_POINT ( 'NONE',  ( 19.03943276465977164, -0.05219959533909143690, 53.74890960531436690 ) ) ;
#55826 = CARTESIAN_POINT ( 'NONE',  ( 14.29746914071049879, -8.314922557960816363, 43.33224293864769550 ) ) ;
#55827 = CARTESIAN_POINT ( 'NONE',  ( -9.474510206698964154, 16.51473224551069663, 90.41557627198103830 ) ) ;
#55828 = CARTESIAN_POINT ( 'NONE',  ( 19.03943276465977164, -0.05219959533909143690, 58.74890960531435979 ) ) ;
#55829 = CARTESIAN_POINT ( 'NONE',  ( -18.62759615963255300, -10.81492255796106328, 59.16775706135234714 ) ) ;
#55830 = CARTESIAN_POINT ( 'NONE',  ( -5.049401038298153566, 19.05341960407611168, 75.20724293864769550 ) ) ;
#55831 = CARTESIAN_POINT ( 'NONE',  ( 19.03943276465977164, -0.05219959533909143690, 23.74890960531435269 ) ) ;
#55832 = CARTESIAN_POINT ( 'NONE',  ( -19.03943276465977164, 0.05219959533909376836, 76.24890960531435269 ) ) ;
#55833 = CARTESIAN_POINT ( 'NONE',  ( -15.80617190586745835, -15.72974639402198527, 51.87390960531437401 ) ) ;
#55834 = CARTESIAN_POINT ( 'NONE',  ( 16.46253265017160672, -9.564922557960803928, 38.33224293864768839 ) ) ;
#55835 = CARTESIAN_POINT ( 'NONE',  ( 21.55341960407610458, 5.719274019375980345, 38.95724293864768839 ) ) ;
#55836 = CARTESIAN_POINT ( 'NONE',  ( -8.314922557961024197, 14.29746914071037800, 107.9177570613523471 ) ) ;
#55837 = CARTESIAN_POINT ( 'NONE',  ( 5.049401038297881783, 19.05341960407617563, 27.29275706135232937 ) ) ;
#55839 = CARTESIAN_POINT ( 'NONE',  ( 16.55341960407618274, -4.379528057220086978, 86.04275706135236135 ) ) ;
#55838 = CARTESIAN_POINT ( 'NONE',  ( 8.224510206698742110, 14.34966873604972548, 47.08442372801901854 ) ) ;
#55840 = CARTESIAN_POINT ( 'NONE',  ( -16.46253265017160317, 9.564922557960807481, 115.8322429386477097 ) ) ;
#55841 = CARTESIAN_POINT ( 'NONE',  ( 16.52544592524335698, 4.483927247898782831, 71.45942372801901854 ) ) ;
#55842 = CARTESIAN_POINT ( 'NONE',  ( 18.62759615963271287, -10.81492255796078972, 23.33224293864769194 ) ) ;
#55843 = CARTESIAN_POINT ( 'NONE',  ( -13.97604488694527625, -13.89961937509977652, 36.87390960531436690 ) ) ;
#55844 = CARTESIAN_POINT ( 'NONE',  ( -16.52544592524335698, -4.483927247898792601, 33.95942372801901143 ) ) ;
#55845 = CARTESIAN_POINT ( 'NONE',  ( 16.51473224551069308, 9.474510206698969483, 49.16557627198102409 ) ) ;
#55846 = CARTESIAN_POINT ( 'NONE',  ( 0.05219959533937995610, -21.53943276465977519, 20.00109039468568639 ) ) ;
#55847 = CARTESIAN_POINT ( 'NONE',  ( 12.14591786802327356, -12.06949235617739191, 30.62609039468567929 ) ) ;
#55848 = CARTESIAN_POINT ( 'NONE',  ( 16.52544592524335698, 4.483927247898782831, 96.45942372801901854 ) ) ;
#55849 = CARTESIAN_POINT ( 'NONE',  ( -25.77159179889071439, -6.124174026812453597, 163.0907220140216509 ) ) ;
#55850 = CARTESIAN_POINT ( 'NONE',  ( 5.823673210054444382, -21.52544592524334988, 95.20942372801903275 ) ) ;
#55851 = CARTESIAN_POINT ( 'NONE',  ( 16.46253265017146816, 9.564922557961045513, 96.66775706135233293 ) ) ;
#55852 = CARTESIAN_POINT ( 'NONE',  ( 16.46253265017146816, 9.564922557961045513, 61.66775706135234003 ) ) ;
#55853 = CARTESIAN_POINT ( 'NONE',  ( -14.29746914071049879, 8.314922557960819915, 60.83224293864769550 ) ) ;
#55854 = CARTESIAN_POINT ( 'NONE',  ( 8.314922557960818139, 14.29746914071049879, 114.5822429386477097 ) ) ;
#55856 = CARTESIAN_POINT ( 'NONE',  ( 3.766062262543149401E-15, -39.95556452105413570, -3.249999994537626780 ) ) ;
#55855 = CARTESIAN_POINT ( 'NONE',  ( -5.153800228976607833, 19.02544592524334988, 62.70942372801899722 ) ) ;
#55857 = CARTESIAN_POINT ( 'NONE',  ( 18.67979575497194134, -10.72451020669871369, 65.83442372801900433 ) ) ;
#55858 = CARTESIAN_POINT ( 'NONE',  ( -4.483927247898782831, 16.52544592524335698, 32.70942372801900433 ) ) ;
#55859 = CARTESIAN_POINT ( 'NONE',  ( -28.66795886109348501, -27.90106222674905112, -15.73198891958529622 ) ) ;
#55860 = CARTESIAN_POINT ( 'NONE',  ( 18.67979575497178502, 10.72451020669898547, 24.16557627198103120 ) ) ;
#55861 = CARTESIAN_POINT ( 'NONE',  ( 16.51473224551083163, -9.474510206698727899, 110.8344237280190043 ) ) ;
#55862 = CARTESIAN_POINT ( 'NONE',  ( -9.474510206698964154, 16.51473224551069663, 110.4155762719810383 ) ) ;
#55863 = CARTESIAN_POINT ( 'NONE',  ( -26.57611637973580443, 7.696099174151423306, 167.9177021574031983 ) ) ;
#55864 = CARTESIAN_POINT ( 'NONE',  ( 0.05219959533909260263, 19.03943276465977164, 29.99890960531435979 ) ) ;
#55865 = CARTESIAN_POINT ( 'NONE',  ( 21.53943276465977519, 0.05219959533937863772, 106.2510903946856757 ) ) ;
#55866 = CARTESIAN_POINT ( 'NONE',  ( 19.05341960407611168, 5.049401038298154454, 53.95724293864770260 ) ) ;
#55867 = CARTESIAN_POINT ( 'NONE',  ( 10.72451020669871369, 18.67979575497193778, 67.08442372801901854 ) ) ;
#55868 = CARTESIAN_POINT ( 'NONE',  ( -15.80617190586768217, 15.72974639402176855, 103.1260903946856757 ) ) ;
#55869 = CARTESIAN_POINT ( 'NONE',  ( 12.14591786802327356, -12.06949235617739191, 100.6260903946857184 ) ) ;
#55870 = CARTESIAN_POINT ( 'NONE',  ( 13.97604488694527802, 13.89961937509977652, 74.37390960531436690 ) ) ;
#55871 = CARTESIAN_POINT ( 'NONE',  ( -0.05219959533937732626, 21.53943276465977519, 52.50109039468567573 ) ) ;
#55872 = ADVANCED_FACE ( 'NONE', ( #47750 ), #80059, .F. ) ;
#55873 = B_SPLINE_CURVE_WITH_KNOTS ( 'NONE', 3,
 ( #170964, #46630, #183166, #135677, #106302, #51591 ),
 .UNSPECIFIED., .F., .F.,
 ( 4, 2, 4 ),
 ( 0.003239945802372288554, 0.003620412082092147252, 0.004000878361812005950 ),
 .UNSPECIFIED. ) ;
#55874 = CARTESIAN_POINT ( 'NONE',  ( 5.719274019375673035, 21.55341960407619339, 52.29275706135236135 ) ) ;
#55876 = CARTESIAN_POINT ( 'NONE',  ( 5.153800228976335163, 19.02544592524342804, 104.7905762719809957 ) ) ;
#55875 = CARTESIAN_POINT ( 'NONE',  ( -0.05219959533936034679, 19.03943276465977164, 82.50109039468567573 ) ) ;
#55877 = CARTESIAN_POINT ( 'NONE',  ( 12.06949235617757843, -12.14591786802309237, 113.1239096053143953 ) ) ;
#55878 = CARTESIAN_POINT ( 'NONE',  ( -21.53943276465977519, 0.05219959533907696930, 101.2489096053143669 ) ) ;
#55879 = CARTESIAN_POINT ( 'NONE',  ( -0.05219959533936034679, 19.03943276465977164, 22.50109039468566152 ) ) ;
#55880 = CARTESIAN_POINT ( 'NONE',  ( 4.483927247898545687, 16.52544592524342804, 99.79057627198103830 ) ) ;
#55881 = CARTESIAN_POINT ( 'NONE',  ( -13.97604488694527625, -13.89961937509977652, 46.87390960531435979 ) ) ;
#55882 = CARTESIAN_POINT ( 'NONE',  ( 13.97604488694548053, -13.89961937509957401, 100.6260903946856615 ) ) ;
#55883 = CARTESIAN_POINT ( 'NONE',  ( 4.379528057220339221, -16.55341960407611168, 67.70724293864769550 ) ) ;
#55884 = CARTESIAN_POINT ( 'NONE',  ( -21.55341960407619339, 5.719274019375674811, 108.5427570613523756 ) ) ;
#55885 = CARTESIAN_POINT ( 'NONE',  ( 0.05219959533909260263, 19.03943276465977164, 109.9989096053143669 ) ) ;
#55886 = CARTESIAN_POINT ( 'NONE',  ( 19.05341960407617918, -5.049401038297876454, 81.04275706135231871 ) ) ;
#55887 = CARTESIAN_POINT ( 'NONE',  ( -21.52544592524343514, 5.823673210054127303, 76.04057627198102409 ) ) ;
#55888 = CARTESIAN_POINT ( 'NONE',  ( -21.55341960407619339, 5.719274019375674811, 48.54275706135234714 ) ) ;
#55889 = CARTESIAN_POINT ( 'NONE',  ( -16.52544592524335698, -4.483927247898792601, 38.95942372801901854 ) ) ;
#55890 = CARTESIAN_POINT ( 'NONE',  ( 16.52544592524335698, 4.483927247898782831, 86.45942372801901854 ) ) ;
#55892 = CARTESIAN_POINT ( 'NONE',  ( -21.55341960407619339, 5.719274019375674811, 33.54275706135234714 ) ) ;
#55891 = CARTESIAN_POINT ( 'NONE',  ( 16.52544592524335698, 4.483927247898782831, 36.45942372801901143 ) ) ;
#55893 = CARTESIAN_POINT ( 'NONE',  ( 15.72974639402199770, -15.80617190586745480, 38.12390960531436690 ) ) ;
#55894 = CARTESIAN_POINT ( 'NONE',  ( 16.51473224551069308, 9.474510206698969483, 29.16557627198103475 ) ) ;
#55895 = CARTESIAN_POINT ( 'NONE',  ( 23.48529157249599919, 32.32473071737754111, -10.44999999453762385 ) ) ;
#55897 = AXIS2_PLACEMENT_3D ( 'NONE', #103724, #177581, #87546 ) ;
#55896 = CARTESIAN_POINT ( 'NONE',  ( -16.55341960407617563, 4.379528057220093196, 63.54275706135234003 ) ) ;
#55898 = CARTESIAN_POINT ( 'NONE',  ( -18.62759615963270932, 10.81492255796079327, 90.83224293864769550 ) ) ;
#55899 = CARTESIAN_POINT ( 'NONE',  ( 8.314922557960818139, 14.29746914071049879, 44.58224293864769550 ) ) ;
#55900 = CARTESIAN_POINT ( 'NONE',  ( 8.314922557961029526, -14.29746914071037800, 50.41775706135235424 ) ) ;
#55901 = CARTESIAN_POINT ( 'NONE',  ( -9.564922557960796823, -16.46253265017161027, 62.08224293864769550 ) ) ;
#55902 = CARTESIAN_POINT ( 'NONE',  ( -16.46253265017146816, -9.564922557961047289, 84.16775706135233293 ) ) ;
#55903 = CARTESIAN_POINT ( 'NONE',  ( -21.55341960407610458, -5.719274019375992779, 86.45724293864770971 ) ) ;
#55904 = CARTESIAN_POINT ( 'NONE',  ( 8.224510206698953496, -14.34966873604960469, 37.91557627198102409 ) ) ;
#55905 = ORIENTED_EDGE ( 'NONE', *, *, #108503, .F. ) ;
#55906 = CARTESIAN_POINT ( 'NONE',  ( 21.93180397000027781, 9.000796715316637275, 171.3297436093417900 ) ) ;
#55907 = CARTESIAN_POINT ( 'NONE',  ( -15.80617190586745835, -15.72974639402198527, 66.87390960531436690 ) ) ;
#55908 = CARTESIAN_POINT ( 'NONE',  ( 12.14591786802327356, -12.06949235617739191, 110.6260903946857042 ) ) ;
#55909 = ORIENTED_EDGE ( 'NONE', *, *, #14853, .F. ) ;
#55910 = CARTESIAN_POINT ( 'NONE',  ( 18.22780087662122739, 5.500000000000000888, 86.48236817873107896 ) ) ;
#55911 = CARTESIAN_POINT ( 'NONE',  ( -18.67979575497178146, -10.72451020669898902, 86.66557627198102409 ) ) ;
#55912 = CARTESIAN_POINT ( 'NONE',  ( 16.53943276465976808, -0.05219959533910856209, 23.74890960531435269 ) ) ;
#55913 = CARTESIAN_POINT ( 'NONE',  ( -12.06949235617739369, -12.14591786802326823, 34.37609039468568284 ) ) ;
#55914 = CARTESIAN_POINT ( 'NONE',  ( 16.51473224551069308, 9.474510206698969483, 34.16557627198102409 ) ) ;
#55915 = CARTESIAN_POINT ( 'NONE',  ( -19.05341960407611168, -5.049401038298163336, 71.45724293864766707 ) ) ;
#55916 = CARTESIAN_POINT ( 'NONE',  ( 28.82186960331498327, 2.781578969918950771E-14, 149.0000000000000000 ) ) ;
#55917 = CARTESIAN_POINT ( 'NONE',  ( -15.80617190586745835, -15.72974639402198527, 26.87390960531435979 ) ) ;
#55918 = DIRECTION ( 'NONE',  ( -1.000000000000000000, 0.000000000000000000, 0.000000000000000000 ) ) ;
#55919 = CARTESIAN_POINT ( 'NONE',  ( -4.379528057220086978, -16.55341960407618274, 99.79275706135234714 ) ) ;
#55920 = CARTESIAN_POINT ( 'NONE',  ( 5.153800228976615827, -19.02544592524334988, 110.2094237280189901 ) ) ;
#55921 = CARTESIAN_POINT ( 'NONE',  ( 16.46253265017146816, 9.564922557961045513, 31.66775706135232937 ) ) ;
#55922 = CARTESIAN_POINT ( 'NONE',  ( 10.81492255796078972, 18.62759615963270932, 94.58224293864769550 ) ) ;
#55923 = CARTESIAN_POINT ( 'NONE',  ( -4.483927247898782831, 16.52544592524335698, 112.7094237280190328 ) ) ;
#55924 = CIRCLE ( 'NONE', #168913, 39.19183588453087452 ) ;
#55925 = CARTESIAN_POINT ( 'NONE',  ( -0.05219959533907301413, -21.53943276465977519, 52.49890960531435979 ) ) ;
#55926 = CARTESIAN_POINT ( 'NONE',  ( 0.05219959533936267826, -19.03943276465977164, 110.0010903946856757 ) ) ;
#55927 = CARTESIAN_POINT ( 'NONE',  ( -9.564922557960796823, -16.46253265017161027, 107.0822429386476955 ) ) ;
#55928 = CARTESIAN_POINT ( 'NONE',  ( 15.80617190586769283, -15.72974639402175789, 60.62609039468567573 ) ) ;
#55929 = CARTESIAN_POINT ( 'NONE',  ( 19.03943276465977164, -0.05219959533909143690, 63.74890960531435979 ) ) ;
#55930 = CARTESIAN_POINT ( 'NONE',  ( 12.06949235617757843, -12.14591786802309237, 98.12390960531436690 ) ) ;
#55931 = CARTESIAN_POINT ( 'NONE',  ( 31.34393194264161053, 5.972569355670986901, 99.56318414118018723 ) ) ;
#55932 = CARTESIAN_POINT ( 'NONE',  ( -5.153800228976328057, -19.02544592524343514, 77.29057627198099567 ) ) ;
#55933 = CARTESIAN_POINT ( 'NONE',  ( -0.05219959533910754901, -16.53943276465976808, 82.49890960531436690 ) ) ;
#55934 = ORIENTED_EDGE ( 'NONE', *, *, #192965, .T. ) ;
#55935 = CARTESIAN_POINT ( 'NONE',  ( 9.474510206698729675, 16.51473224551082808, 87.08442372801900433 ) ) ;
#55936 = CARTESIAN_POINT ( 'NONE',  ( 19.34837522270366961, 5.499999999999797495, 93.36337684832579953 ) ) ;
#55937 = CARTESIAN_POINT ( 'NONE',  ( 13.89961937509977652, -13.97604488694527269, 58.12390960531436690 ) ) ;
#55938 = CARTESIAN_POINT ( 'NONE',  ( 1.500000000004064082, 7.599999999999568878, -62.20201607440122871 ) ) ;
#55940 = CARTESIAN_POINT ( 'NONE',  ( -16.46253265017160317, 9.564922557960807481, 105.8322429386476955 ) ) ;
#55939 = CARTESIAN_POINT ( 'NONE',  ( 15.72974639402176855, 15.80617190586768217, 86.87609039468568994 ) ) ;
#55941 = EDGE_CURVE ( 'NONE', #111780, #115644, #191971, .T. ) ;
#55942 = CARTESIAN_POINT ( 'NONE',  ( -4.379528057220086978, -16.55341960407618274, 64.79275706135234714 ) ) ;
#55943 = CARTESIAN_POINT ( 'NONE',  ( -21.23184647844206552, -181.1785498424364675, -15.00000000000000178 ) ) ;
#55944 = CARTESIAN_POINT ( 'NONE',  ( 5.049401038297881783, 19.05341960407617563, 42.29275706135234003 ) ) ;
#55945 = CARTESIAN_POINT ( 'NONE',  ( -0.05219959533937732626, 21.53943276465977519, 102.5010903946856899 ) ) ;
#55946 = CARTESIAN_POINT ( 'NONE',  ( 36.85386064174074505, 2.754345082724624749, 49.76404540304363167 ) ) ;
#55947 = CARTESIAN_POINT ( 'NONE',  ( -38.00000000000000711, 2.428612866367529932E-14, -6.000000000000000000 ) ) ;
#55948 = CARTESIAN_POINT ( 'NONE',  ( 12.06949235617739724, 12.14591786802326823, 101.8760903946857042 ) ) ;
#55949 = CARTESIAN_POINT ( 'NONE',  ( -34.57969012852956325, -4.582005219005604424, 50.95785156492173940 ) ) ;
#55950 = CARTESIAN_POINT ( 'NONE',  ( -0.05219959533934338120, 16.53943276465976808, 97.50109039468567573 ) ) ;
#55951 = CARTESIAN_POINT ( 'NONE',  ( 17.50000000000000000, 5.500000000000011546, 68.78230962303564411 ) ) ;
#55952 = CARTESIAN_POINT ( 'NONE',  ( 12.14591786802327356, -12.06949235617739191, 65.62609039468568994 ) ) ;
#55953 = ORIENTED_EDGE ( 'NONE', *, *, #29924, .T. ) ;
#55954 = CARTESIAN_POINT ( 'NONE',  ( -15.72974639402176322, -15.80617190586768395, 74.37609039468568994 ) ) ;
#55955 = CARTESIAN_POINT ( 'NONE',  ( 9.474510206698729675, 16.51473224551082808, 87.08442372801900433 ) ) ;
#55956 = CARTESIAN_POINT ( 'NONE',  ( -5.153800228976607833, 19.02544592524334988, 22.70942372801899012 ) ) ;
#55957 = CARTESIAN_POINT ( 'NONE',  ( 19.05341960407611168, 5.049401038298154454, 63.95724293864769550 ) ) ;
#55958 = CARTESIAN_POINT ( 'NONE',  ( 13.89961937509977652, -13.97604488694527269, 53.12390960531434558 ) ) ;
#55959 = CARTESIAN_POINT ( 'NONE',  ( -17.33350041961992360, -36.05029215572399437, -9.440814067905872520 ) ) ;
#55960 = CARTESIAN_POINT ( 'NONE',  ( -21.55341960407610458, -5.719274019375992779, 81.45724293864769550 ) ) ;
#55961 = CARTESIAN_POINT ( 'NONE',  ( 0.05219959533907565091, 21.53943276465977519, 29.99890960531435979 ) ) ;
#55962 = CARTESIAN_POINT ( 'NONE',  ( -0.05219959533909027116, -19.03943276465977164, 37.49890960531436690 ) ) ;
#55963 = CARTESIAN_POINT ( 'NONE',  ( -16.52544592524335698, -4.483927247898792601, 63.95942372801901854 ) ) ;
#55964 = EDGE_CURVE ( 'NONE', #57253, #138331, #3711, .T. ) ;
#55965 = ORIENTED_EDGE ( 'NONE', *, *, #131623, .T. ) ;
#55966 = CARTESIAN_POINT ( 'NONE',  ( 15.72974639402176855, 15.80617190586768217, 36.87609039468568994 ) ) ;
#55968 = CARTESIAN_POINT ( 'NONE',  ( 22.81625015709509441, 31.40387420917330275, -7.324999997268812457 ) ) ;
#55967 = CARTESIAN_POINT ( 'NONE',  ( 4.483927247898545687, 16.52544592524342804, 64.79057627198103830 ) ) ;
#55969 = CARTESIAN_POINT ( 'NONE',  ( 12.14591786802327356, -12.06949235617739191, 20.62609039468568639 ) ) ;
#55970 = CARTESIAN_POINT ( 'NONE',  ( 16.46253265017146816, 9.564922557961045513, 51.66775706135233293 ) ) ;
#55971 = CARTESIAN_POINT ( 'NONE',  ( -14.34966873604960291, -8.224510206698953496, 56.66557627198103830 ) ) ;
#55972 = CARTESIAN_POINT ( 'NONE',  ( -21.53943276465977519, 0.05219959533907696930, 116.2489096053143669 ) ) ;
#55974 = CARTESIAN_POINT ( 'NONE',  ( 21.55341960407610458, 5.719274019375980345, 83.95724293864770971 ) ) ;
#55973 = CARTESIAN_POINT ( 'NONE',  ( 0.7822855905564412016, 16.49570789208851807, -59.22457827466391223 ) ) ;
#55975 = CARTESIAN_POINT ( 'NONE',  ( 19.03943276465977164, -0.05219959533909143690, 88.74890960531436690 ) ) ;
#55976 = CARTESIAN_POINT ( 'NONE',  ( 16.55341960407611168, 4.379528057220329451, 58.95724293864770971 ) ) ;
#55977 = CARTESIAN_POINT ( 'NONE',  ( 29.45353567398453265, -26.40584612579220547, -18.78685418917150685 ) ) ;
#55978 = CARTESIAN_POINT ( 'NONE',  ( -36.89064505505186986, 5.462148823192606528, 44.26314855211814603 ) ) ;
#55979 = CARTESIAN_POINT ( 'NONE',  ( -9.564922557961040184, 16.46253265017147172, 72.91775706135233293 ) ) ;
#55980 = CARTESIAN_POINT ( 'NONE',  ( -18.67979575497178146, -10.72451020669898902, 111.6655762719810525 ) ) ;
#55981 = CARTESIAN_POINT ( 'NONE',  ( -19.03943276465977164, 0.05219959533909376836, 51.24890960531436690 ) ) ;
#55982 = CARTESIAN_POINT ( 'NONE',  ( 9.564922557961047289, -16.46253265017146816, 40.41775706135234003 ) ) ;
#55983 = CARTESIAN_POINT ( 'NONE',  ( -16.46253265017160317, 9.564922557960807481, 35.83224293864768839 ) ) ;
#55984 = AXIS2_PLACEMENT_3D ( 'NONE', #42291, #14925, #182789 ) ;
#55985 = CARTESIAN_POINT ( 'NONE',  ( -21.52544592524334988, -5.823673210054445271, 63.95942372801901854 ) ) ;
#55986 = CARTESIAN_POINT ( 'NONE',  ( -30.00000000000000000, -5.499999999999992895, 102.5000000000000142 ) ) ;
#55987 = CARTESIAN_POINT ( 'NONE',  ( -16.53943276465976808, 0.05219959533911058130, 41.24890960531435269 ) ) ;
#55988 = CARTESIAN_POINT ( 'NONE',  ( -19.03943276465977164, 0.05219959533909376836, 56.24890960531435979 ) ) ;
#55989 = CARTESIAN_POINT ( 'NONE',  ( -10.72451020669898014, 18.67979575497178502, 80.41557627198103830 ) ) ;
#55990 = CARTESIAN_POINT ( 'NONE',  ( 19.03943276465977164, -0.05219959533909143690, 58.74890960531435979 ) ) ;
#55991 = CARTESIAN_POINT ( 'NONE',  ( -0.05219959533907301413, -21.53943276465977519, 67.49890960531436690 ) ) ;
#55992 = CARTESIAN_POINT ( 'NONE',  ( 10.72451020669871369, 18.67979575497193778, 102.0844237280190185 ) ) ;
#55995 = CARTESIAN_POINT ( 'NONE',  ( -12.06949235617756955, 12.14591786802309770, 85.62390960531436690 ) ) ;
#55994 = CARTESIAN_POINT ( 'NONE',  ( -4.483927247898782831, 16.52544592524335698, 97.70942372801904696 ) ) ;
#55993 = CARTESIAN_POINT ( 'NONE',  ( 5.630366384172311278, -47.63986359793406677, -22.87684677291067814 ) ) ;
#55996 = CARTESIAN_POINT ( 'NONE',  ( 9.564922557961047289, -16.46253265017146816, 95.41775706135233293 ) ) ;
#55997 = EDGE_LOOP ( 'NONE', ( #119825, #193707, #29237, #30215 ) ) ;
#55998 = CARTESIAN_POINT ( 'NONE',  ( -16.51473224551082808, 9.474510206698731452, 38.33442372801899722 ) ) ;
#55999 = CARTESIAN_POINT ( 'NONE',  ( -14.34966873604972548, 8.224510206698743886, 98.33442372801901854 ) ) ;
#56000 = CARTESIAN_POINT ( 'NONE',  ( 0.05219959533936267826, -19.03943276465977164, 35.00109039468566863 ) ) ;
#56001 = CARTESIAN_POINT ( 'NONE',  ( 5.049401038298161559, -19.05341960407611168, 92.70724293864769550 ) ) ;
#56002 = CARTESIAN_POINT ( 'NONE',  ( -21.52544592524343514, 5.823673210054127303, 66.04057627198103830 ) ) ;
#56003 = CARTESIAN_POINT ( 'NONE',  ( -30.20036327792369235, -26.22857331006468229, -17.18026671435357500 ) ) ;
#56004 = CARTESIAN_POINT ( 'NONE',  ( -9.564922557960796823, -16.46253265017161027, 27.08224293864769550 ) ) ;
#56005 = CARTESIAN_POINT ( 'NONE',  ( 15.80617190586769283, -15.72974639402175789, 90.62609039468567573 ) ) ;
#56006 = CARTESIAN_POINT ( 'NONE',  ( -14.29746914071037622, -8.314922557961029526, 79.16775706135234714 ) ) ;
#56007 = CARTESIAN_POINT ( 'NONE',  ( -0.05219959533937732626, 21.53943276465977519, 27.50109039468567929 ) ) ;
#56008 = CARTESIAN_POINT ( 'NONE',  ( 16.55341960407618274, -4.379528057220086978, 26.04275706135235779 ) ) ;
#56009 = CARTESIAN_POINT ( 'NONE',  ( 13.97604488694527802, 13.89961937509977652, 109.3739096053143669 ) ) ;
#56010 = CARTESIAN_POINT ( 'NONE',  ( 19.05341960407611168, 5.049401038298154454, 33.95724293864769550 ) ) ;
#56011 = CARTESIAN_POINT ( 'NONE',  ( 19.03943276465977164, -0.05219959533909143690, 58.74890960531435979 ) ) ;
#56012 = CARTESIAN_POINT ( 'NONE',  ( -0.05219959533934338120, 16.53943276465976808, 32.50109039468568284 ) ) ;
#56013 = CARTESIAN_POINT ( 'NONE',  ( -4.483927247898539470, -16.52544592524342804, 97.29057627198105251 ) ) ;
#56014 = CARTESIAN_POINT ( 'NONE',  ( -8.224510206698735004, -14.34966873604973081, 99.58442372801900433 ) ) ;
#56017 = CARTESIAN_POINT ( 'NONE',  ( -9.564922557960796823, -16.46253265017161027, 62.08224293864769550 ) ) ;
#56016 = CARTESIAN_POINT ( 'NONE',  ( -5.153800228976328057, -19.02544592524343514, 77.29057627198099567 ) ) ;
#56015 = CARTESIAN_POINT ( 'NONE',  ( 10.72451020669871369, 18.67979575497193778, 42.08442372801901854 ) ) ;
#56018 = CARTESIAN_POINT ( 'NONE',  ( 5.049401038298161559, -19.05341960407611168, 82.70724293864770971 ) ) ;
#56019 = CARTESIAN_POINT ( 'NONE',  ( -12.14591786802309592, -12.06949235617757132, 36.87390960531435979 ) ) ;
#56020 = CARTESIAN_POINT ( 'NONE',  ( 4.483927247898790824, -16.52544592524335698, 100.2094237280190043 ) ) ;
#56021 = VERTEX_POINT ( 'NONE', #95227 ) ;
#56022 = CARTESIAN_POINT ( 'NONE',  ( 13.89961937509957401, 13.97604488694547697, 41.87609039468566152 ) ) ;
#56023 = CARTESIAN_POINT ( 'NONE',  ( -16.51473224551069308, -9.474510206698971260, 106.6655762719810383 ) ) ;
#56024 = CARTESIAN_POINT ( 'NONE',  ( -19.03943276465977164, 0.05219959533909376836, 56.24890960531435979 ) ) ;
#56025 = CARTESIAN_POINT ( 'NONE',  ( -9.474510206698720793, -16.51473224551083518, 34.58442372801899722 ) ) ;
#56026 = CARTESIAN_POINT ( 'NONE',  ( 3.556970738554033499E-15, -38.81732327939057825, -8.124999997268814056 ) ) ;
#56027 = CARTESIAN_POINT ( 'NONE',  ( -8.224510206698735004, -14.34966873604973081, 39.58442372801901143 ) ) ;
#56029 = CARTESIAN_POINT ( 'NONE',  ( 16.55341960407618274, -4.379528057220086978, 51.04275706135234714 ) ) ;
#56028 = CARTESIAN_POINT ( 'NONE',  ( -13.97604488694547697, 13.89961937509957934, 73.12609039468568994 ) ) ;
#56030 = CARTESIAN_POINT ( 'NONE',  ( 4.538945330120077948, -4.119035683228635669, -64.52788751195758721 ) ) ;
#56031 = CARTESIAN_POINT ( 'NONE',  ( 5.049401038298161559, -19.05341960407611168, 92.70724293864769550 ) ) ;
#56032 = CARTESIAN_POINT ( 'NONE',  ( 21.53943276465977519, -0.05219959533907433946, 113.7489096053143527 ) ) ;
#56033 = CARTESIAN_POINT ( 'NONE',  ( -5.153800228976607833, 19.02544592524334988, 72.70942372801900433 ) ) ;
#56035 = CARTESIAN_POINT ( 'NONE',  ( 19.03943276465977164, -0.05219959533909143690, 33.74890960531435979 ) ) ;
#56034 = CARTESIAN_POINT ( 'NONE',  ( -19.05341960407611168, -5.049401038298163336, 101.4572429386476955 ) ) ;
#56036 = CARTESIAN_POINT ( 'NONE',  ( -13.97604488694527625, -13.89961937509977652, 81.87390960531436690 ) ) ;
#56038 = CARTESIAN_POINT ( 'NONE',  ( 19.05341960407611168, 5.049401038298154454, 38.95724293864767418 ) ) ;
#56037 = CARTESIAN_POINT ( 'NONE',  ( -8.224510206698948167, 14.34966873604960824, 30.41557627198101699 ) ) ;
#56039 = CARTESIAN_POINT ( 'NONE',  ( 9.564922557961047289, -16.46253265017146816, 50.41775706135233293 ) ) ;
#56040 = CARTESIAN_POINT ( 'NONE',  ( -12.06949235617756955, 12.14591786802309770, 85.62390960531436690 ) ) ;
#56041 = CARTESIAN_POINT ( 'NONE',  ( -0.05219959533936034679, 19.03943276465977164, 22.50109039468566152 ) ) ;
#56042 = CARTESIAN_POINT ( 'NONE',  ( -19.05341960407611168, -5.049401038298163336, 46.45724293864768129 ) ) ;
#56043 = CARTESIAN_POINT ( 'NONE',  ( -10.72451020669898014, 18.67979575497178502, 50.41557627198103120 ) ) ;
#56045 = CARTESIAN_POINT ( 'NONE',  ( 21.53943276465977519, 0.05219959533937863772, 106.2510903946856757 ) ) ;
#56044 = CARTESIAN_POINT ( 'NONE',  ( -14.34966873604960291, -8.224510206698953496, 51.66557627198102409 ) ) ;
#56046 = CARTESIAN_POINT ( 'NONE',  ( 5.049401038298161559, -19.05341960407611168, 102.7072429386476955 ) ) ;
#56047 = CARTESIAN_POINT ( 'NONE',  ( -19.05341960407611168, -5.049401038298163336, 111.4572429386476671 ) ) ;
#56048 = CARTESIAN_POINT ( 'NONE',  ( 16.46253265017160672, -9.564922557960803928, 33.33224293864770260 ) ) ;
#56049 = CARTESIAN_POINT ( 'NONE',  ( -5.153800228976328057, -19.02544592524343514, 27.29057627198103120 ) ) ;
#56050 = CARTESIAN_POINT ( 'NONE',  ( -16.53943276465976808, 0.05219959533911058130, 81.24890960531436690 ) ) ;
#56051 = CARTESIAN_POINT ( 'NONE',  ( -15.80617190586745835, -15.72974639402198527, 96.87390960531436690 ) ) ;
#56052 = CARTESIAN_POINT ( 'NONE',  ( -19.02544592524342804, 5.153800228976336051, 96.04057627198103830 ) ) ;
#56053 = CARTESIAN_POINT ( 'NONE',  ( 18.62759615963271287, -10.81492255796078972, 108.3322429386477097 ) ) ;
#56054 = CARTESIAN_POINT ( 'NONE',  ( 16.51473224551069308, 9.474510206698969483, 89.16557627198103830 ) ) ;
#56056 = CARTESIAN_POINT ( 'NONE',  ( -4.379528057220328563, 16.55341960407611168, 105.2072429386477097 ) ) ;
#56055 = CARTESIAN_POINT ( 'NONE',  ( -21.36928693577339544, 5.431965077040405099, 174.3311293403526179 ) ) ;
#56057 = CARTESIAN_POINT ( 'NONE',  ( -19.05341960407611168, -5.049401038298163336, 76.45724293864769550 ) ) ;
#56058 = CARTESIAN_POINT ( 'NONE',  ( 10.81492255796078972, 18.62759615963270932, 74.58224293864768129 ) ) ;
#56059 = CARTESIAN_POINT ( 'NONE',  ( -31.33330333603525375, 7.497710212630239290, 94.47580324309011246 ) ) ;
#56060 = CARTESIAN_POINT ( 'NONE',  ( -21.82787714368444654, -6.011549001344956622, 172.1028946673681332 ) ) ;
#56062 = CARTESIAN_POINT ( 'NONE',  ( -19.97888994334923041, -34.65319547504298470, 0.000000000000000000 ) ) ;
#56061 = CARTESIAN_POINT ( 'NONE',  ( -18.62759615963270932, 10.81492255796079327, 30.83224293864770260 ) ) ;
#56063 = CARTESIAN_POINT ( 'NONE',  ( 0.05219959533934541429, -16.53943276465976808, 40.00109039468567573 ) ) ;
#56064 = CARTESIAN_POINT ( 'NONE',  ( 14.34966873604960469, 8.224510206698951720, 89.16557627198102409 ) ) ;
#56065 = CARTESIAN_POINT ( 'NONE',  ( -17.49999999999999645, -5.076555817581227537, 111.1795149204977804 ) ) ;
#56066 = CARTESIAN_POINT ( 'NONE',  ( -9.474510206698964154, 16.51473224551069663, 85.41557627198102409 ) ) ;
#56067 = CARTESIAN_POINT ( 'NONE',  ( -13.97604488694527625, -13.89961937509977652, 51.87390960531436690 ) ) ;
#56068 = CARTESIAN_POINT ( 'NONE',  ( -4.483927247898539470, -16.52544592524342804, 77.29057627198102409 ) ) ;
#56069 = AXIS2_PLACEMENT_3D ( 'NONE', #150836, #100315, #193344 ) ;
#56070 = CARTESIAN_POINT ( 'NONE',  ( -5.719274019375978568, 21.55341960407610458, 35.20724293864768839 ) ) ;
#56071 = CARTESIAN_POINT ( 'NONE',  ( -16.53943276465976808, 0.05219959533911058130, 56.24890960531436690 ) ) ;
#56072 = CARTESIAN_POINT ( 'NONE',  ( -16.51473224551082808, 9.474510206698731452, 98.33442372801900433 ) ) ;
#56073 = CARTESIAN_POINT ( 'NONE',  ( 5.823673210054444382, -21.52544592524334988, 70.20942372801904696 ) ) ;
#56074 = CARTESIAN_POINT ( 'NONE',  ( 22.44159573604009594, -16.30477369853687364, 145.6750000027311671 ) ) ;
#56075 = CARTESIAN_POINT ( 'NONE',  ( -0.05219959533907301413, -21.53943276465977519, 22.49890960531436335 ) ) ;
#56076 = CARTESIAN_POINT ( 'NONE',  ( -12.14591786802326823, 12.06949235617739902, 88.12609039468570415 ) ) ;
#56077 = CARTESIAN_POINT ( 'NONE',  ( 13.89961937509977652, -13.97604488694527269, 23.12390960531436335 ) ) ;
#56078 = CARTESIAN_POINT ( 'NONE',  ( 5.153800228976335163, 19.02544592524342804, 69.79057627198103830 ) ) ;
#56079 = CARTESIAN_POINT ( 'NONE',  ( 10.81492255796078972, 18.62759615963270932, 79.58224293864769550 ) ) ;
#56080 = CARTESIAN_POINT ( 'NONE',  ( 14.34966873604972726, -8.224510206698740333, 30.83442372801902209 ) ) ;
#56082 = CARTESIAN_POINT ( 'NONE',  ( -15.80617190586768217, 15.72974639402176855, 68.12609039468567573 ) ) ;
#56081 = CARTESIAN_POINT ( 'NONE',  ( 0.05219959533910956823, 16.53943276465976808, 54.99890960531435269 ) ) ;
#56084 = CARTESIAN_POINT ( 'NONE',  ( 13.89961937509977652, -13.97604488694527269, 113.1239096053143527 ) ) ;
#56083 = CARTESIAN_POINT ( 'NONE',  ( 12.06949235617739724, 12.14591786802326823, 91.87609039468568994 ) ) ;
#56085 = CARTESIAN_POINT ( 'NONE',  ( 25.28179187713399401, 11.97099003546684060, 166.1915553108511290 ) ) ;
#56086 = DIRECTION ( 'NONE',  ( 1.000000000000000000, 0.000000000000000000, 0.000000000000000000 ) ) ;
#56087 = CARTESIAN_POINT ( 'NONE',  ( -8.314922557961024197, 14.29746914071037800, 102.9177570613523756 ) ) ;
#56088 = CARTESIAN_POINT ( 'NONE',  ( 16.55341960407618274, -4.379528057220086978, 61.04275706135234714 ) ) ;
#56089 = CARTESIAN_POINT ( 'NONE',  ( -16.46253265017160317, 9.564922557960807481, 65.83224293864769550 ) ) ;
#56090 = CARTESIAN_POINT ( 'NONE',  ( -16.46253265017160317, 9.564922557960807481, 85.83224293864769550 ) ) ;
#56091 = CARTESIAN_POINT ( 'NONE',  ( 5.719274019375673035, 21.55341960407619339, 67.29275706135234714 ) ) ;
#56092 = CARTESIAN_POINT ( 'NONE',  ( 14.29746914071037800, 8.314922557961029526, 76.66775706135234714 ) ) ;
#56093 = CARTESIAN_POINT ( 'NONE',  ( -8.314922557960811034, -14.29746914071050412, 47.08224293864770260 ) ) ;
#56094 = CARTESIAN_POINT ( 'NONE',  ( 5.153800228976335163, 19.02544592524342804, 49.79057627198100988 ) ) ;
#56095 = CARTESIAN_POINT ( 'NONE',  ( 9.474510206698971260, -16.51473224551069308, 47.91557627198102409 ) ) ;
#56096 = VERTEX_POINT ( 'NONE', #53457 ) ;
#56097 = CARTESIAN_POINT ( 'NONE',  ( -19.05341960407617563, 5.049401038297882671, 98.54275706135233293 ) ) ;
#56098 = CARTESIAN_POINT ( 'NONE',  ( -14.29746914071049879, 8.314922557960819915, 110.8322429386476955 ) ) ;
#56099 = CARTESIAN_POINT ( 'NONE',  ( 5.153800228976335163, 19.02544592524342804, 69.79057627198103830 ) ) ;
#56101 = CARTESIAN_POINT ( 'NONE',  ( -23.48529157249600985, 32.32473071737754111, -2.299999999999999822 ) ) ;
#56100 = CARTESIAN_POINT ( 'NONE',  ( -5.049401038297874678, -19.05341960407617918, 94.79275706135230450 ) ) ;
#56102 = CARTESIAN_POINT ( 'NONE',  ( 5.823673210054444382, -21.52544592524334988, 100.2094237280190043 ) ) ;
#56103 = CARTESIAN_POINT ( 'NONE',  ( 14.29746914071037800, 8.314922557961029526, 66.66775706135234714 ) ) ;
#56104 = CARTESIAN_POINT ( 'NONE',  ( -5.049401038297874678, -19.05341960407617918, 89.79275706135230450 ) ) ;
#56105 = CARTESIAN_POINT ( 'NONE',  ( 5.719274019375991003, -21.55341960407610458, 57.70724293864770260 ) ) ;
#56106 = CARTESIAN_POINT ( 'NONE',  ( -12.14591786802326823, 12.06949235617739902, 48.12609039468568284 ) ) ;
#56107 = CARTESIAN_POINT ( 'NONE',  ( 5.000000000000000888, -140.0000000000000000, -12.99999999999999645 ) ) ;
#56108 = CARTESIAN_POINT ( 'NONE',  ( 0.05219959533936267826, -19.03943276465977164, 55.00109039468566863 ) ) ;
#56109 = CARTESIAN_POINT ( 'NONE',  ( -0.05219959533937732626, 21.53943276465977519, 97.50109039468567573 ) ) ;
#56110 = CARTESIAN_POINT ( 'NONE',  ( -9.474510206698964154, 16.51473224551069663, 25.41557627198103120 ) ) ;
#56111 = CARTESIAN_POINT ( 'NONE',  ( 16.51473224551069308, 9.474510206698969483, 64.16557627198102409 ) ) ;
#56112 = CARTESIAN_POINT ( 'NONE',  ( -16.55341960407611168, -4.379528057220339221, 56.45724293864768839 ) ) ;
#56113 = CARTESIAN_POINT ( 'NONE',  ( -10.72451020669870658, -18.67979575497194134, 89.58442372801901854 ) ) ;
#56114 = CARTESIAN_POINT ( 'NONE',  ( 5.153800228976615827, -19.02544592524334988, 45.20942372801901143 ) ) ;
#56115 = CARTESIAN_POINT ( 'NONE',  ( 16.51473224551083163, -9.474510206698727899, 25.83442372801900078 ) ) ;
#56116 = CARTESIAN_POINT ( 'NONE',  ( -10.81492255796078084, -18.62759615963271287, 22.08224293864769194 ) ) ;
#56117 = CARTESIAN_POINT ( 'NONE',  ( 5.823673210054444382, -21.52544592524334988, 100.2094237280190043 ) ) ;
#56118 = CARTESIAN_POINT ( 'NONE',  ( 19.05341960407611168, 5.049401038298154454, 73.95724293864768129 ) ) ;
#56119 = ADVANCED_FACE ( 'NONE', ( #24140 ), #48742, .F. ) ;
#56120 = CARTESIAN_POINT ( 'NONE',  ( -21.53943276465977519, -0.05219959533937600094, 93.75109039468567573 ) ) ;
#56121 = CARTESIAN_POINT ( 'NONE',  ( -5.823673210054116645, -21.52544592524344225, 52.29057627198102409 ) ) ;
#56122 = CARTESIAN_POINT ( 'NONE',  ( -5.153800228976328057, -19.02544592524343514, 77.29057627198099567 ) ) ;
#56123 = CARTESIAN_POINT ( 'NONE',  ( 16.46253265017146816, 9.564922557961045513, 71.66775706135233293 ) ) ;
#56124 = CARTESIAN_POINT ( 'NONE',  ( -0.05219959533909027116, -19.03943276465977164, 37.49890960531436690 ) ) ;
#56125 = CARTESIAN_POINT ( 'NONE',  ( 16.46253265017160672, -9.564922557960803928, 83.33224293864768129 ) ) ;
#56126 = CARTESIAN_POINT ( 'NONE',  ( -5.049401038297874678, -19.05341960407617918, 84.79275706135233293 ) ) ;
#56127 = CARTESIAN_POINT ( 'NONE',  ( -12.06949235617739369, -12.14591786802326823, 49.37609039468569705 ) ) ;
#56128 = CARTESIAN_POINT ( 'NONE',  ( -4.483927247898539470, -16.52544592524342804, 102.2905762719810383 ) ) ;
#56129 = CARTESIAN_POINT ( 'NONE',  ( -0.05219959533909027116, -19.03943276465977164, 67.49890960531436690 ) ) ;
#56130 = CARTESIAN_POINT ( 'NONE',  ( 18.67979575497178502, 10.72451020669898547, 54.16557627198103120 ) ) ;
#56131 = CARTESIAN_POINT ( 'NONE',  ( 4.379528057220092307, 16.55341960407617563, 22.29275706135235069 ) ) ;
#56132 = CARTESIAN_POINT ( 'NONE',  ( 0.05219959533937995610, -21.53943276465977519, 30.00109039468568284 ) ) ;
#56133 = CARTESIAN_POINT ( 'NONE',  ( -5.719274019375665041, -21.55341960407619695, 84.79275706135234714 ) ) ;
#56134 = CARTESIAN_POINT ( 'NONE',  ( -16.55341960407617563, 4.379528057220093196, 88.54275706135236135 ) ) ;
#56135 = CIRCLE ( 'NONE', #98071, 2.500000000000000444 ) ;
#56136 = CARTESIAN_POINT ( 'NONE',  ( 9.474510206698971260, -16.51473224551069308, 72.91557627198102409 ) ) ;
#56137 = CARTESIAN_POINT ( 'NONE',  ( 0.05219959533934541429, -16.53943276465976808, 105.0010903946856757 ) ) ;
#56138 = CARTESIAN_POINT ( 'NONE',  ( 16.51473224551083163, -9.474510206698727899, 50.83442372801899722 ) ) ;
#56139 = CARTESIAN_POINT ( 'NONE',  ( -10.72451020669870658, -18.67979575497194134, 24.58442372801901499 ) ) ;
#56140 = CARTESIAN_POINT ( 'NONE',  ( -16.52544592524342804, 4.483927247898546575, 76.04057627198102409 ) ) ;
#56141 = CARTESIAN_POINT ( 'NONE',  ( 16.46253265017160672, -9.564922557960803928, 93.33224293864769550 ) ) ;
#56142 = CARTESIAN_POINT ( 'NONE',  ( -0.05219959533934338120, 16.53943276465976808, 102.5010903946856899 ) ) ;
#56143 = CARTESIAN_POINT ( 'NONE',  ( 5.719274019375673035, 21.55341960407619339, 72.29275706135236135 ) ) ;
#56144 = CARTESIAN_POINT ( 'NONE',  ( -16.52544592524335698, -4.483927247898792601, 33.95942372801901143 ) ) ;
#56145 = CARTESIAN_POINT ( 'NONE',  ( -10.72451020669870658, -18.67979575497194134, 24.58442372801901499 ) ) ;
#56146 = CARTESIAN_POINT ( 'NONE',  ( 4.379528057220339221, -16.55341960407611168, 67.70724293864769550 ) ) ;
#56147 = ORIENTED_EDGE ( 'NONE', *, *, #197557, .T. ) ;
#56148 = CARTESIAN_POINT ( 'NONE',  ( -21.53943276465977519, 0.05219959533907696930, 101.2489096053143669 ) ) ;
#56149 = CARTESIAN_POINT ( 'NONE',  ( 14.29746914071049879, -8.314922557960816363, 58.33224293864768839 ) ) ;
#56150 = CARTESIAN_POINT ( 'NONE',  ( -9.564922557960796823, -16.46253265017161027, 32.08224293864769550 ) ) ;
#56151 = CARTESIAN_POINT ( 'NONE',  ( 18.67979575497178502, 10.72451020669898547, 29.16557627198103120 ) ) ;
#56152 = CARTESIAN_POINT ( 'NONE',  ( -10.72451020669870658, -18.67979575497194134, 44.58442372801901854 ) ) ;
#56153 = CARTESIAN_POINT ( 'NONE',  ( 12.14591786802309770, 12.06949235617756955, 59.37390960531436690 ) ) ;
#56154 = AXIS2_PLACEMENT_3D ( 'NONE', #176069, #175062, #4197 ) ;
#56155 = CARTESIAN_POINT ( 'NONE',  ( -15.80617190586745835, -15.72974639402198527, 61.87390960531436690 ) ) ;
#56156 = CARTESIAN_POINT ( 'NONE',  ( 5.153800228976335163, 19.02544592524342804, 69.79057627198103830 ) ) ;
#56158 = CARTESIAN_POINT ( 'NONE',  ( -19.03943276465977164, -0.05219959533935918106, 83.75109039468567573 ) ) ;
#56157 = CARTESIAN_POINT ( 'NONE',  ( 16.51473224551069308, 9.474510206698969483, 24.16557627198102765 ) ) ;
#56160 = CARTESIAN_POINT ( 'NONE',  ( -21.53943276465977519, 0.05219959533907696930, 56.24890960531436690 ) ) ;
#56159 = CARTESIAN_POINT ( 'NONE',  ( -21.52544592524334988, -5.823673210054445271, 53.95942372801900433 ) ) ;
#56161 = CARTESIAN_POINT ( 'NONE',  ( -5.153800228976328057, -19.02544592524343514, 42.29057627198101699 ) ) ;
#56162 = CARTESIAN_POINT ( 'NONE',  ( 16.51473224551069308, 9.474510206698969483, 69.16557627198102409 ) ) ;
#56163 = ORIENTED_EDGE ( 'NONE', *, *, #86821, .F. ) ;
#56164 = CARTESIAN_POINT ( 'NONE',  ( 8.314922557961029526, -14.29746914071037800, 50.41775706135235424 ) ) ;
#56165 = CARTESIAN_POINT ( 'NONE',  ( 15.72974639402176855, 15.80617190586768217, 36.87609039468568994 ) ) ;
#56166 = CARTESIAN_POINT ( 'NONE',  ( 15.80617190586769283, -15.72974639402175789, 60.62609039468567573 ) ) ;
#56167 = CARTESIAN_POINT ( 'NONE',  ( -13.89961937509977652, 13.97604488694528158, 105.6239096053143527 ) ) ;
#56168 = CARTESIAN_POINT ( 'NONE',  ( -21.53943276465977519, 0.05219959533907696930, 86.24890960531436690 ) ) ;
#56170 = CARTESIAN_POINT ( 'NONE',  ( 16.53943276465976808, 0.05219959533934440121, 56.25109039468568284 ) ) ;
#56169 = CARTESIAN_POINT ( 'NONE',  ( -5.823673210054431948, 21.52544592524334988, 27.70942372801901854 ) ) ;
#56171 = CARTESIAN_POINT ( 'NONE',  ( 0.05219959533907565091, 21.53943276465977519, 54.99890960531435269 ) ) ;
#56172 = CARTESIAN_POINT ( 'NONE',  ( -10.72451020669870658, -18.67979575497194134, 109.5844237280190328 ) ) ;
#56173 = CARTESIAN_POINT ( 'NONE',  ( 19.02544592524343514, -5.153800228976328945, 58.54057627198102409 ) ) ;
#56174 = CARTESIAN_POINT ( 'NONE',  ( 5.049401038298161559, -19.05341960407611168, 112.7072429386476813 ) ) ;
#56175 = CARTESIAN_POINT ( 'NONE',  ( 19.02544592524343514, -5.153800228976328945, 83.54057627198100988 ) ) ;
#56176 = CYLINDRICAL_SURFACE ( 'NONE', #2294, 28.90000000000004476 ) ;
#56177 = CARTESIAN_POINT ( 'NONE',  ( -13.89961937509957401, -13.97604488694547875, 69.37609039468564731 ) ) ;
#56178 = CARTESIAN_POINT ( 'NONE',  ( 15.72974639402199770, -15.80617190586745480, 43.12390960531435269 ) ) ;
#56179 = CARTESIAN_POINT ( 'NONE',  ( 4.483927247898545687, 16.52544592524342804, 29.79057627198102409 ) ) ;
#56180 = CARTESIAN_POINT ( 'NONE',  ( 19.03943276465977164, 0.05219959533936151252, 86.25109039468567573 ) ) ;
#56181 = CARTESIAN_POINT ( 'NONE',  ( -17.40861289039003523, 6.110651285853257342, 58.62767529172568004 ) ) ;
#56182 = CARTESIAN_POINT ( 'NONE',  ( -5.719274019375665041, -21.55341960407619695, 109.7927570613523613 ) ) ;
#56183 = CARTESIAN_POINT ( 'NONE',  ( 19.03943276465977164, 0.05219959533936151252, 81.25109039468567573 ) ) ;
#56184 = CARTESIAN_POINT ( 'NONE',  ( -19.05341960407617563, 5.049401038297882671, 43.54275706135232582 ) ) ;
#56185 = B_SPLINE_CURVE_WITH_KNOTS ( 'NONE', 3,
 ( #171048, #33529, #81985, #186237, #32538, #124540, #175032, #93196, #94191, #48707, #154881, #78026 ),
 .UNSPECIFIED., .F., .F.,
 ( 4, 2, 2, 2, 2, 4 ),
 ( 0.003927129849554285117, 0.005134622258946382710, 0.006342114668338479436, 0.007549607077730577029, 0.008153353282426625825, 0.008757099487122674622 ),
 .UNSPECIFIED. ) ;
#56186 = CARTESIAN_POINT ( 'NONE',  ( -14.92381850146897371, -15.21399023779380677, -56.46147852626893382 ) ) ;
#56187 = CARTESIAN_POINT ( 'NONE',  ( 5.049401038298161559, -19.05341960407611168, 52.70724293864767418 ) ) ;
#56188 = CARTESIAN_POINT ( 'NONE',  ( 4.483927247898545687, 16.52544592524342804, 44.79057627198103120 ) ) ;
#56189 = CARTESIAN_POINT ( 'NONE',  ( 13.89961937509977652, -13.97604488694527269, 38.12390960531436690 ) ) ;
#56190 = CARTESIAN_POINT ( 'NONE',  ( -12.14591786802309592, -12.06949235617757132, 41.87390960531435979 ) ) ;
#56191 = CARTESIAN_POINT ( 'NONE',  ( -21.61432565731197997, -33.65169730710061913, -23.91085783830776634 ) ) ;
#56192 = CARTESIAN_POINT ( 'NONE',  ( 4.379528057220092307, 16.55341960407617563, 112.2927570613523471 ) ) ;
#56193 = CARTESIAN_POINT ( 'NONE',  ( -5.153800228976328057, -19.02544592524343514, 47.29057627198102409 ) ) ;
#56194 = CARTESIAN_POINT ( 'NONE',  ( 5.153800228976615827, -19.02544592524334988, 30.20942372801900433 ) ) ;
#56195 = CARTESIAN_POINT ( 'NONE',  ( -12.14591786802326823, 12.06949235617739902, 33.12609039468569705 ) ) ;
#56196 = CARTESIAN_POINT ( 'NONE',  ( -10.72451020669898014, 18.67979575497178502, 40.41557627198103120 ) ) ;
#56198 = ORIENTED_EDGE ( 'NONE', *, *, #176051, .F. ) ;
#56197 = CARTESIAN_POINT ( 'NONE',  ( -10.81492255796105439, 18.62759615963255655, 97.91775706135236135 ) ) ;
#56199 = CARTESIAN_POINT ( 'NONE',  ( -16.51473224551069308, -9.474510206698971260, 61.66557627198103120 ) ) ;
#56200 = CARTESIAN_POINT ( 'NONE',  ( 13.89961937509977652, -13.97604488694527269, 103.1239096053143527 ) ) ;
#56201 = CARTESIAN_POINT ( 'NONE',  ( -13.89961937509977652, 13.97604488694528158, 95.62390960531436690 ) ) ;
#56202 = CARTESIAN_POINT ( 'NONE',  ( -11.40812507854754720, -35.11059874428192273, -2.224999997268813701 ) ) ;
#56203 = CARTESIAN_POINT ( 'NONE',  ( 5.823673210054444382, -21.52544592524334988, 20.20942372801900788 ) ) ;
#56204 = CARTESIAN_POINT ( 'NONE',  ( -12.06949235617756955, 12.14591786802309770, 75.62390960531439532 ) ) ;
#56206 = CARTESIAN_POINT ( 'NONE',  ( 5.153800228976335163, 19.02544592524342804, 74.79057627198103830 ) ) ;
#56205 = CARTESIAN_POINT ( 'NONE',  ( -21.52544592524343514, 5.823673210054127303, 71.04057627198103830 ) ) ;
#56207 = CARTESIAN_POINT ( 'NONE',  ( -9.474510206698964154, 16.51473224551069663, 75.41557627198103830 ) ) ;
#56208 = CARTESIAN_POINT ( 'NONE',  ( -21.52544592524343514, 5.823673210054127303, 106.0405762719810525 ) ) ;
#56209 = EDGE_CURVE ( 'NONE', #11669, #184472, #121901, .T. ) ;
#56210 = VERTEX_POINT ( 'NONE', #131296 ) ;
#56211 = CARTESIAN_POINT ( 'NONE',  ( 16.51473224551069308, 9.474510206698969483, 79.16557627198103830 ) ) ;
#56212 = CIRCLE ( 'NONE', #117546, 216.0437394197456342 ) ;
#56214 = CARTESIAN_POINT ( 'NONE',  ( -19.05341960407611168, -5.049401038298163336, 21.45724293864768839 ) ) ;
#56213 = CARTESIAN_POINT ( 'NONE',  ( -14.29746914071049879, 8.314922557960819915, 100.8322429386477097 ) ) ;
#56215 = CARTESIAN_POINT ( 'NONE',  ( 16.51473224551069308, 9.474510206698969483, 59.16557627198102409 ) ) ;
#56216 = CARTESIAN_POINT ( 'NONE',  ( 0.05219959533936267826, -19.03943276465977164, 95.00109039468567573 ) ) ;
#56217 = CARTESIAN_POINT ( 'NONE',  ( -12.14591786802309592, -12.06949235617757132, 101.8739096053143811 ) ) ;
#56218 = CARTESIAN_POINT ( 'NONE',  ( -10.81492255796105439, 18.62759615963255655, 72.91775706135234714 ) ) ;
#56220 = CARTESIAN_POINT ( 'NONE',  ( 0.05219959533907565091, 21.53943276465977519, 114.9989096053143669 ) ) ;
#56219 = CARTESIAN_POINT ( 'NONE',  ( 19.03943276465977164, -0.05219959533909143690, 43.74890960531435979 ) ) ;
#56221 = CARTESIAN_POINT ( 'NONE',  ( -8.224510206698948167, 14.34966873604960824, 105.4155762719810383 ) ) ;
#56222 = CARTESIAN_POINT ( 'NONE',  ( 28.82186960331498327, 9.364793116373570925, 143.0999999999999659 ) ) ;
#56223 = CARTESIAN_POINT ( 'NONE',  ( -13.97604488694527625, -13.89961937509977652, 76.87390960531433848 ) ) ;
#56224 = LINE ( 'NONE', #102730, #124398 ) ;
#56226 = CARTESIAN_POINT ( 'NONE',  ( -0.05219959533907301413, -21.53943276465977519, 32.49890960531435979 ) ) ;
#56225 = CARTESIAN_POINT ( 'NONE',  ( 19.02544592524334988, 5.153800228976608722, 111.4594237280190043 ) ) ;
#56227 = CARTESIAN_POINT ( 'NONE',  ( 10.81492255796106328, -18.62759615963255655, 55.41775706135234714 ) ) ;
#56228 = CARTESIAN_POINT ( 'NONE',  ( -5.049401038298153566, 19.05341960407611168, 90.20724293864766707 ) ) ;
#56229 = CARTESIAN_POINT ( 'NONE',  ( 9.474510206698729675, 16.51473224551082808, 87.08442372801900433 ) ) ;
#56230 = CARTESIAN_POINT ( 'NONE',  ( 19.02544592524343514, -5.153800228976328945, 68.54057627198103830 ) ) ;
#56231 = CARTESIAN_POINT ( 'NONE',  ( 14.29746914071049879, -8.314922557960816363, 78.33224293864770971 ) ) ;
#56232 = CARTESIAN_POINT ( 'NONE',  ( -19.05341960407611168, -5.049401038298163336, 101.4572429386476955 ) ) ;
#56233 = CARTESIAN_POINT ( 'NONE',  ( 12.06949235617757843, -12.14591786802309237, 73.12390960531436690 ) ) ;
#56234 = CARTESIAN_POINT ( 'NONE',  ( 5.049401038298161559, -19.05341960407611168, 97.70724293864766707 ) ) ;
#56235 = CIRCLE ( 'NONE', #169228, 69.99999999999998579 ) ;
#56238 = CARTESIAN_POINT ( 'NONE',  ( 19.05341960407611168, 5.049401038298154454, 33.95724293864769550 ) ) ;
#56237 = CARTESIAN_POINT ( 'NONE',  ( 0.05219959533910956823, 16.53943276465976808, 49.99890960531437401 ) ) ;
#56236 = CARTESIAN_POINT ( 'NONE',  ( -19.05341960407611168, -5.049401038298163336, 56.45724293864768129 ) ) ;
#56239 = VERTEX_POINT ( 'NONE', #111396 ) ;
#56240 = CARTESIAN_POINT ( 'NONE',  ( -18.67979575497193778, 10.72451020669871902, 63.33442372801900433 ) ) ;
#56241 = CARTESIAN_POINT ( 'NONE',  ( -9.474510206698720793, -16.51473224551083518, 84.58442372801900433 ) ) ;
#56242 = CARTESIAN_POINT ( 'NONE',  ( 8.224510206698953496, -14.34966873604960469, 52.91557627198103830 ) ) ;
#56243 = CARTESIAN_POINT ( 'NONE',  ( 15.72974639402199770, -15.80617190586745480, 98.12390960531436690 ) ) ;
#56244 = CARTESIAN_POINT ( 'NONE',  ( -21.55341960407610458, -5.719274019375992779, 36.45724293864768839 ) ) ;
#56245 = CARTESIAN_POINT ( 'NONE',  ( -0.05219959533910754901, -16.53943276465976808, 82.49890960531436690 ) ) ;
#56246 = CARTESIAN_POINT ( 'NONE',  ( 16.51473224551069308, 9.474510206698969483, 49.16557627198102409 ) ) ;
#56247 = CARTESIAN_POINT ( 'NONE',  ( -16.53943276465976808, -0.05219959533934237506, 113.7510903946856757 ) ) ;
#56248 = CARTESIAN_POINT ( 'NONE',  ( -8.314922557961024197, 14.29746914071037800, 92.91775706135236135 ) ) ;
#56249 = CARTESIAN_POINT ( 'NONE',  ( 16.55341960407618274, -4.379528057220086978, 76.04275706135237556 ) ) ;
#56250 = CARTESIAN_POINT ( 'NONE',  ( 16.51473224551083163, -9.474510206698727899, 30.83442372801900433 ) ) ;
#56251 = CARTESIAN_POINT ( 'NONE',  ( -16.51473224551069308, -9.474510206698971260, 86.66557627198102409 ) ) ;
#56252 = CARTESIAN_POINT ( 'NONE',  ( 19.02544592524343514, -5.153800228976328945, 83.54057627198100988 ) ) ;
#56253 = CARTESIAN_POINT ( 'NONE',  ( -8.224510206698735004, -14.34966873604973081, 89.58442372801901854 ) ) ;
#56254 = CARTESIAN_POINT ( 'NONE',  ( 13.89961937509977652, -13.97604488694527269, 43.12390960531434558 ) ) ;
#56255 = CARTESIAN_POINT ( 'NONE',  ( -16.55341960407611168, -4.379528057220339221, 46.45724293864769550 ) ) ;
#56256 = CARTESIAN_POINT ( 'NONE',  ( -9.474510206698964154, 16.51473224551069663, 110.4155762719810383 ) ) ;
#56257 = CARTESIAN_POINT ( 'NONE',  ( -5.719274019375978568, 21.55341960407610458, 25.20724293864769550 ) ) ;
#56258 = CARTESIAN_POINT ( 'NONE',  ( 16.52544592524342804, -4.483927247898539470, 73.54057627198102409 ) ) ;
#56259 = CARTESIAN_POINT ( 'NONE',  ( -16.53943276465976808, 0.05219959533911058130, 71.24890960531435269 ) ) ;
#56261 = VECTOR ( 'NONE', #149965, 1000.000000000000000 ) ;
#56260 = CARTESIAN_POINT ( 'NONE',  ( 18.10062525802554134, -5.500000000000022204, 86.01383468041923663 ) ) ;
#56262 = CARTESIAN_POINT ( 'NONE',  ( -9.564922557961040184, 16.46253265017147172, 57.91775706135233293 ) ) ;
#56263 = CARTESIAN_POINT ( 'NONE',  ( 16.46253265017160672, -9.564922557960803928, 98.33224293864769550 ) ) ;
#56264 = CARTESIAN_POINT ( 'NONE',  ( -19.02544592524334988, -5.153800228976617603, 78.95942372801900433 ) ) ;
#56265 = CARTESIAN_POINT ( 'NONE',  ( -8.571926809382608425, 26.38167802310805854, 148.9750000027311785 ) ) ;
#56267 = CARTESIAN_POINT ( 'NONE',  ( 8.224510206698742110, 14.34966873604972548, 92.08442372801901854 ) ) ;
#56266 = CARTESIAN_POINT ( 'NONE',  ( 16.51473224551083163, -9.474510206698727899, 105.8344237280190043 ) ) ;
#56268 = CARTESIAN_POINT ( 'NONE',  ( 16.51473224551069308, 9.474510206698969483, 34.16557627198102409 ) ) ;
#56269 = CARTESIAN_POINT ( 'NONE',  ( -5.719274019375978568, 21.55341960407610458, 40.20724293864769550 ) ) ;
#56270 = CARTESIAN_POINT ( 'NONE',  ( 21.55341960407619695, -5.719274019375665929, 61.04275706135234714 ) ) ;
#56271 = CARTESIAN_POINT ( 'NONE',  ( -16.51473224551082808, 9.474510206698731452, 113.3344237280190043 ) ) ;
#56273 = CARTESIAN_POINT ( 'NONE',  ( 19.03943276465977164, -0.05219959533909143690, 78.74890960531436690 ) ) ;
#56272 = FACE_OUTER_BOUND ( 'NONE', #20010, .T. ) ;
#56274 = CARTESIAN_POINT ( 'NONE',  ( 9.564922557960805705, 16.46253265017160317, 114.5822429386476955 ) ) ;
#56276 = CARTESIAN_POINT ( 'NONE',  ( -19.02544592524342804, 5.153800228976336051, 71.04057627198099567 ) ) ;
#56275 = CARTESIAN_POINT ( 'NONE',  ( 14.34966873604960469, 8.224510206698951720, 74.16557627198102409 ) ) ;
#56277 = CONTEXT_DEPENDENT_SHAPE_REPRESENTATION ( #157856, #171248 ) ;
#56278 = CARTESIAN_POINT ( 'NONE',  ( 19.02544592524343514, -5.153800228976328945, 88.54057627198102409 ) ) ;
#56279 = ORIENTED_EDGE ( 'NONE', *, *, #118198, .F. ) ;
#56280 = CARTESIAN_POINT ( 'NONE',  ( -13.89961937509957401, -13.97604488694547875, 89.37609039468563310 ) ) ;
#56281 = CARTESIAN_POINT ( 'NONE',  ( 21.53943276465977519, -0.05219959533907433946, 63.74890960531435979 ) ) ;
#56282 = CARTESIAN_POINT ( 'NONE',  ( -16.51473224551069308, -9.474510206698971260, 31.66557627198102054 ) ) ;
#56283 = CARTESIAN_POINT ( 'NONE',  ( 16.46253265017146816, 9.564922557961045513, 61.66775706135234003 ) ) ;
#56284 = CARTESIAN_POINT ( 'NONE',  ( 0.05219959533909260263, 19.03943276465977164, 59.99890960531436690 ) ) ;
#56285 = CARTESIAN_POINT ( 'NONE',  ( -0.05219959533909027116, -19.03943276465977164, 97.49890960531436690 ) ) ;
#56286 = ORIENTED_EDGE ( 'NONE', *, *, #175528, .T. ) ;
#56287 = CARTESIAN_POINT ( 'NONE',  ( 15.72974639402199770, -15.80617190586745480, 93.12390960531436690 ) ) ;
#56289 = CARTESIAN_POINT ( 'NONE',  ( -0.05219959533936034679, 19.03943276465977164, 52.50109039468566863 ) ) ;
#56288 = CARTESIAN_POINT ( 'NONE',  ( -16.53943276465976808, 0.05219959533911058130, 96.24890960531435269 ) ) ;
#56290 = CARTESIAN_POINT ( 'NONE',  ( -21.52544592524343514, 5.823673210054127303, 86.04057627198102409 ) ) ;
#56291 = CARTESIAN_POINT ( 'NONE',  ( 21.53943276465977519, -0.05219959533907433946, 68.74890960531435269 ) ) ;
#56292 = CARTESIAN_POINT ( 'NONE',  ( -14.34966873604960291, -8.224510206698953496, 26.66557627198103475 ) ) ;
#56293 = CARTESIAN_POINT ( 'NONE',  ( -15.72974639402176322, -15.80617190586768395, 104.3760903946856899 ) ) ;
#56294 = CARTESIAN_POINT ( 'NONE',  ( -14.34966873604972548, 8.224510206698743886, 48.33442372801902565 ) ) ;
#56295 = CARTESIAN_POINT ( 'NONE',  ( 13.89961937509977652, -13.97604488694527269, 78.12390960531433848 ) ) ;
#56296 = CARTESIAN_POINT ( 'NONE',  ( -16.46253265017160317, 9.564922557960807481, 25.83224293864769194 ) ) ;
#56297 = AXIS2_PLACEMENT_3D ( 'NONE', #177875, #98997, #40343 ) ;
#56298 = CARTESIAN_POINT ( 'NONE',  ( -15.72974639402176322, -15.80617190586768395, 44.37609039468567573 ) ) ;
#56299 = CARTESIAN_POINT ( 'NONE',  ( 21.53943276465977519, 0.05219959533937863772, 56.25109039468568284 ) ) ;
#56300 = CARTESIAN_POINT ( 'NONE',  ( -13.97604488694527625, -13.89961937509977652, 41.87390960531435979 ) ) ;
#56301 = CARTESIAN_POINT ( 'NONE',  ( -21.52544592524343514, 5.823673210054127303, 116.0405762719810383 ) ) ;
#56302 = CARTESIAN_POINT ( 'NONE',  ( 5.049401038297881783, 19.05341960407617563, 67.29275706135234714 ) ) ;
#56303 = CARTESIAN_POINT ( 'NONE',  ( -19.03943276465977164, -0.05219959533935918106, 78.75109039468567573 ) ) ;
#56304 = CARTESIAN_POINT ( 'NONE',  ( 4.379528057220092307, 16.55341960407617563, 27.29275706135234358 ) ) ;
#56305 = CARTESIAN_POINT ( 'NONE',  ( 19.02544592524343514, -5.153800228976328945, 28.54057627198102409 ) ) ;
#56306 = CARTESIAN_POINT ( 'NONE',  ( -8.314922557961024197, 14.29746914071037800, 77.91775706135231871 ) ) ;
#56307 = CARTESIAN_POINT ( 'NONE',  ( -9.474510206698964154, 16.51473224551069663, 40.41557627198103120 ) ) ;
#56308 = CARTESIAN_POINT ( 'NONE',  ( 24.72709851008550075, -6.869189314501102039, 167.7661538690260556 ) ) ;
#56309 = CARTESIAN_POINT ( 'NONE',  ( 13.97604488694527802, 13.89961937509977652, 104.3739096053143385 ) ) ;
#56310 = CARTESIAN_POINT ( 'NONE',  ( -13.89961937509977652, 13.97604488694528158, 25.62390960531434558 ) ) ;
#56311 = CARTESIAN_POINT ( 'NONE',  ( 0.05219959533907565091, 21.53943276465977519, 69.99890960531435269 ) ) ;
#56312 = CARTESIAN_POINT ( 'NONE',  ( -16.52544592524335698, -4.483927247898792601, 58.95942372801902565 ) ) ;
#56313 = CARTESIAN_POINT ( 'NONE',  ( 13.89961937509957401, 13.97604488694547697, 21.87609039468566152 ) ) ;
#56314 = ADVANCED_FACE ( 'NONE', ( #85792 ), #147478, .F. ) ;
#56315 = CARTESIAN_POINT ( 'NONE',  ( -19.02544592524342804, 5.153800228976336051, 41.04057627198103120 ) ) ;
#56316 = CARTESIAN_POINT ( 'NONE',  ( -4.483927247898539470, -16.52544592524342804, 37.29057627198102409 ) ) ;
#56317 = CARTESIAN_POINT ( 'NONE',  ( 16.53943276465976808, -0.05219959533910856209, 63.74890960531435979 ) ) ;
#56318 = CARTESIAN_POINT ( 'NONE',  ( 13.97604488694527802, 13.89961937509977652, 69.37390960531436690 ) ) ;
#56319 = CARTESIAN_POINT ( 'NONE',  ( -10.81492255796105439, 18.62759615963255655, 32.91775706135234714 ) ) ;
#56320 = CARTESIAN_POINT ( 'NONE',  ( -9.474510206698964154, 16.51473224551069663, 75.41557627198103830 ) ) ;
#56321 = CARTESIAN_POINT ( 'NONE',  ( 18.62759615963255655, 10.81492255796105972, 81.66775706135236135 ) ) ;
#56322 = CARTESIAN_POINT ( 'NONE',  ( 14.29746914071037800, 8.314922557961029526, 71.66775706135234714 ) ) ;
#56323 = CARTESIAN_POINT ( 'NONE',  ( 5.049401038298161559, -19.05341960407611168, 112.7072429386476813 ) ) ;
#56324 = EDGE_CURVE ( 'NONE', #129957, #21601, #3219, .T. ) ;
#56325 = CARTESIAN_POINT ( 'NONE',  ( -16.55341960407611168, -4.379528057220339221, 31.45724293864769550 ) ) ;
#56326 = CARTESIAN_POINT ( 'NONE',  ( 9.474510206698971260, -16.51473224551069308, 32.91557627198102409 ) ) ;
#56327 = CARTESIAN_POINT ( 'NONE',  ( 12.14591786802327356, -12.06949235617739191, 55.62609039468568284 ) ) ;
#56328 = CARTESIAN_POINT ( 'NONE',  ( -14.34966873604960291, -8.224510206698953496, 51.66557627198102409 ) ) ;
#56329 = CARTESIAN_POINT ( 'NONE',  ( -13.97604488694527625, -13.89961937509977652, 106.8739096053143669 ) ) ;
#56330 = CARTESIAN_POINT ( 'NONE',  ( 0.05219959533907565091, 21.53943276465977519, 29.99890960531435979 ) ) ;
#56331 = CARTESIAN_POINT ( 'NONE',  ( -5.823673210054431948, 21.52544592524334988, 107.7094237280190328 ) ) ;
#56332 = CARTESIAN_POINT ( 'NONE',  ( 4.483927247898545687, 16.52544592524342804, 89.79057627198103830 ) ) ;
#56333 = CARTESIAN_POINT ( 'NONE',  ( 9.474510206698971260, -16.51473224551069308, 97.91557627198102409 ) ) ;
#56334 = ORIENTED_EDGE ( 'NONE', *, *, #95040, .F. ) ;
#56335 = CARTESIAN_POINT ( 'NONE',  ( -14.29746914071037622, -8.314922557961029526, 59.16775706135234714 ) ) ;
#56336 = CARTESIAN_POINT ( 'NONE',  ( 19.05341960407611168, 5.049401038298154454, 53.95724293864770260 ) ) ;
#56337 = FACE_OUTER_BOUND ( 'NONE', #68324, .T. ) ;
#56338 = CARTESIAN_POINT ( 'NONE',  ( -16.46253265017146816, -9.564922557961047289, 44.16775706135232582 ) ) ;
#56339 = CARTESIAN_POINT ( 'NONE',  ( 14.34966873604972726, -8.224510206698740333, 85.83442372801901854 ) ) ;
#56340 = CARTESIAN_POINT ( 'NONE',  ( 9.474510206698729675, 16.51473224551082808, 97.08442372801900433 ) ) ;
#56341 = CARTESIAN_POINT ( 'NONE',  ( 21.55341960407619695, -5.719274019375665929, 66.04275706135236135 ) ) ;
#56342 = CARTESIAN_POINT ( 'NONE',  ( 9.474510206698971260, -16.51473224551069308, 67.91557627198102409 ) ) ;
#56343 = CARTESIAN_POINT ( 'NONE',  ( -10.72451020669898014, 18.67979575497178502, 95.41557627198102409 ) ) ;
#56344 = CARTESIAN_POINT ( 'NONE',  ( 4.483927247898545687, 16.52544592524342804, 104.7905762719810241 ) ) ;
#56345 = CARTESIAN_POINT ( 'NONE',  ( 13.89961937509957401, 13.97604488694547697, 71.87609039468567573 ) ) ;
#56346 = CARTESIAN_POINT ( 'NONE',  ( 5.719274019375991003, -21.55341960407610458, 67.70724293864769550 ) ) ;
#56347 = CARTESIAN_POINT ( 'NONE',  ( -19.03943276465977164, -0.05219959533935918106, 43.75109039468566863 ) ) ;
#56348 = CARTESIAN_POINT ( 'NONE',  ( -9.474510206698964154, 16.51473224551069663, 115.4155762719810241 ) ) ;
#56349 = EDGE_CURVE ( 'NONE', #177566, #17000, #143966, .T. ) ;
#56350 = CARTESIAN_POINT ( 'NONE',  ( 21.52544592524344225, -5.823673210054117533, 93.54057627198103830 ) ) ;
#56351 = CARTESIAN_POINT ( 'NONE',  ( 26.56065628307859683, -9.391201389438098346, 155.7923318601102380 ) ) ;
#56352 = CARTESIAN_POINT ( 'NONE',  ( -16.51473224551069308, -9.474510206698971260, 66.66557627198102409 ) ) ;
#56353 = CARTESIAN_POINT ( 'NONE',  ( -13.70000000000001528, 1.443387660838688656E-13, -60.44446360152740283 ) ) ;
#56354 = CARTESIAN_POINT ( 'NONE',  ( -8.314922557961024197, 14.29746914071037800, 22.91775706135235069 ) ) ;
#56355 = CARTESIAN_POINT ( 'NONE',  ( -18.09867054820431065, -5.499999999999968026, 98.98393025253585620 ) ) ;
#56356 = CARTESIAN_POINT ( 'NONE',  ( 13.89961937509977652, -13.97604488694527269, 53.12390960531434558 ) ) ;
#56357 = CARTESIAN_POINT ( 'NONE',  ( 5.153800228976335163, 19.02544592524342804, 109.7905762719810099 ) ) ;
#56359 = CARTESIAN_POINT ( 'NONE',  ( -16.53943276465976808, 0.05219959533911058130, 56.24890960531436690 ) ) ;
#56358 = CARTESIAN_POINT ( 'NONE',  ( -5.823673210054116645, -21.52544592524344225, 92.29057627198103830 ) ) ;
#56360 = CARTESIAN_POINT ( 'NONE',  ( -21.53943276465977519, -0.05219959533937600094, 73.75109039468567573 ) ) ;
#56362 = CARTESIAN_POINT ( 'NONE',  ( -5.153800228976607833, 19.02544592524334988, 22.70942372801899012 ) ) ;
#56361 = CARTESIAN_POINT ( 'NONE',  ( -14.29746914071037622, -8.314922557961029526, 24.16775706135235424 ) ) ;
#56363 = CARTESIAN_POINT ( 'NONE',  ( -16.53943276465976808, 0.05219959533911058130, 36.24890960531435979 ) ) ;
#56364 = CARTESIAN_POINT ( 'NONE',  ( -15.72974639402197994, 15.80617190586746368, 110.6239096053143669 ) ) ;
#56365 = CARTESIAN_POINT ( 'NONE',  ( 14.34966873604960469, 8.224510206698951720, 54.16557627198103120 ) ) ;
#56366 = CARTESIAN_POINT ( 'NONE',  ( 19.03943276465977164, 0.05219959533936151252, 101.2510903946856757 ) ) ;
#56367 = CARTESIAN_POINT ( 'NONE',  ( 16.46253265017146816, 9.564922557961045513, 66.66775706135233293 ) ) ;
#56368 = CARTESIAN_POINT ( 'NONE',  ( -5.823673210054431948, 21.52544592524334988, 72.70942372801901854 ) ) ;
#56369 = CARTESIAN_POINT ( 'NONE',  ( -0.05219959533936034679, 19.03943276465977164, 52.50109039468566863 ) ) ;
#56370 = CARTESIAN_POINT ( 'NONE',  ( 13.97604488694527802, 13.89961937509977652, 29.37390960531435979 ) ) ;
#56371 = CARTESIAN_POINT ( 'NONE',  ( 21.53943276465977519, -0.05219959533907433946, 38.74890960531435979 ) ) ;
#56372 = CARTESIAN_POINT ( 'NONE',  ( 0.05219959533910956823, 16.53943276465976808, 54.99890960531435269 ) ) ;
#56373 = CARTESIAN_POINT ( 'NONE',  ( -17.12812012977026654, -6.668231424566000598, 26.35948759323144941 ) ) ;
#56374 = CARTESIAN_POINT ( 'NONE',  ( 0.05219959533937995610, -21.53943276465977519, 110.0010903946856757 ) ) ;
#56375 = CARTESIAN_POINT ( 'NONE',  ( -16.55341960407617563, 4.379528057220093196, 88.54275706135236135 ) ) ;
#56376 = CARTESIAN_POINT ( 'NONE',  ( -16.55341960407611168, -4.379528057220339221, 46.45724293864769550 ) ) ;
#56377 = CARTESIAN_POINT ( 'NONE',  ( 18.67979575497194134, -10.72451020669871369, 75.83442372801900433 ) ) ;
#56378 = CARTESIAN_POINT ( 'NONE',  ( 18.67979575497194134, -10.72451020669871369, 65.83442372801900433 ) ) ;
#56379 = CARTESIAN_POINT ( 'NONE',  ( -15.80617190586745835, -15.72974639402198527, 76.87390960531439532 ) ) ;
#56380 = AXIS2_PLACEMENT_3D ( 'NONE', #15125, #185976, #32287 ) ;
#56381 = CARTESIAN_POINT ( 'NONE',  ( 13.97604488694527802, 13.89961937509977652, 44.37390960531435269 ) ) ;
#56382 = CARTESIAN_POINT ( 'NONE',  ( -0.05219959533937732626, 21.53943276465977519, 62.50109039468568284 ) ) ;
#56383 = CARTESIAN_POINT ( 'NONE',  ( -16.51473224551069308, -9.474510206698971260, 26.66557627198103120 ) ) ;
#56384 = CARTESIAN_POINT ( 'NONE',  ( -16.51473224551069308, -9.474510206698971260, 46.66557627198102409 ) ) ;
#56385 = CARTESIAN_POINT ( 'NONE',  ( 12.06949235617757843, -12.14591786802309237, 93.12390960531436690 ) ) ;
#56386 = CARTESIAN_POINT ( 'NONE',  ( -13.97604488694527625, -13.89961937509977652, 86.87390960531436690 ) ) ;
#56387 = CARTESIAN_POINT ( 'NONE',  ( -12.14591786802309592, -12.06949235617757132, 36.87390960531435979 ) ) ;
#56388 = CARTESIAN_POINT ( 'NONE',  ( 16.52544592524342804, -4.483927247898539470, 103.5405762719810383 ) ) ;
#56389 = CARTESIAN_POINT ( 'NONE',  ( -21.52544592524343514, 5.823673210054127303, 76.04057627198102409 ) ) ;
#56390 = CARTESIAN_POINT ( 'NONE',  ( 0.05219959533907565091, 21.53943276465977519, 114.9989096053143669 ) ) ;
#56391 = CARTESIAN_POINT ( 'NONE',  ( -16.11132338694247679, 14.61887724323077897, -56.15647863711519960 ) ) ;
#56393 = CARTESIAN_POINT ( 'NONE',  ( 4.379528057220092307, 16.55341960407617563, 27.29275706135234358 ) ) ;
#56392 = CARTESIAN_POINT ( 'NONE',  ( 16.46253265017160672, -9.564922557960803928, 78.33224293864769550 ) ) ;
#56394 = CARTESIAN_POINT ( 'NONE',  ( -5.823673210054116645, -21.52544592524344225, 72.29057627198102409 ) ) ;
#56395 = CIRCLE ( 'NONE', #153230, 4.324969328314201888 ) ;
#56396 = CARTESIAN_POINT ( 'NONE',  ( 5.823673210054444382, -21.52544592524334988, 100.2094237280190043 ) ) ;
#56397 = CARTESIAN_POINT ( 'NONE',  ( 16.46253265017160672, -9.564922557960803928, 78.33224293864769550 ) ) ;
#56398 = CARTESIAN_POINT ( 'NONE',  ( 15.80617190586746368, 15.72974639402197994, 109.3739096053143811 ) ) ;
#56399 = CARTESIAN_POINT ( 'NONE',  ( 19.03943276465977164, -0.05219959533909143690, 113.7489096053143669 ) ) ;
#56400 = CARTESIAN_POINT ( 'NONE',  ( 0.05219959533934541429, -16.53943276465976808, 90.00109039468567573 ) ) ;
#56401 = CARTESIAN_POINT ( 'NONE',  ( -10.72451020669870658, -18.67979575497194134, 64.58442372801900433 ) ) ;
#56402 = CARTESIAN_POINT ( 'NONE',  ( 5.719274019375673035, 21.55341960407619339, 97.29275706135234714 ) ) ;
#56403 = CARTESIAN_POINT ( 'NONE',  ( 16.55341960407618274, -4.379528057220086978, 61.04275706135234714 ) ) ;
#56404 = CARTESIAN_POINT ( 'NONE',  ( 18.62759615963255655, 10.81492255796105972, 31.66775706135234358 ) ) ;
#56405 = VECTOR ( 'NONE', #106184, 1000.000000000000000 ) ;
#56406 = CARTESIAN_POINT ( 'NONE',  ( 5.153800228976335163, 19.02544592524342804, 24.79057627198102765 ) ) ;
#56407 = CARTESIAN_POINT ( 'NONE',  ( -10.81492255796105439, 18.62759615963255655, 92.91775706135236135 ) ) ;
#56408 = CARTESIAN_POINT ( 'NONE',  ( 13.89961937509977652, -13.97604488694527269, 98.12390960531433848 ) ) ;
#56409 = CARTESIAN_POINT ( 'NONE',  ( -15.80617190586745835, -15.72974639402198527, 91.87390960531436690 ) ) ;
#56410 = CARTESIAN_POINT ( 'NONE',  ( -9.564922557961040184, 16.46253265017147172, 62.91775706135233293 ) ) ;
#56412 = CARTESIAN_POINT ( 'NONE',  ( 18.62759615963271287, -10.81492255796078972, 58.33224293864768839 ) ) ;
#56411 = CARTESIAN_POINT ( 'NONE',  ( -20.00963169948588316, -33.79917020545752848, -17.75419178524651898 ) ) ;
#56414 = CARTESIAN_POINT ( 'NONE',  ( -16.55341960407611168, -4.379528057220339221, 41.45724293864769550 ) ) ;
#56413 = CARTESIAN_POINT ( 'NONE',  ( 5.153800228976335163, 19.02544592524342804, 89.79057627198102409 ) ) ;
#56415 = CARTESIAN_POINT ( 'NONE',  ( 21.48956683882227381, 5.485153550827154945, 173.8223501052718518 ) ) ;
#56416 = CARTESIAN_POINT ( 'NONE',  ( 19.03943276465977164, 0.05219959533936151252, 76.25109039468566152 ) ) ;
#56417 = CARTESIAN_POINT ( 'NONE',  ( -1.322814319812971595, -14.46726734353923050, -62.26916108939696670 ) ) ;
#56418 = CARTESIAN_POINT ( 'NONE',  ( 5.049401038297881783, 19.05341960407617563, 112.2927570613523471 ) ) ;
#56419 = CARTESIAN_POINT ( 'NONE',  ( -18.62759615963270932, 10.81492255796079327, 85.83224293864768129 ) ) ;
#56420 = CARTESIAN_POINT ( 'NONE',  ( -8.224510206698948167, 14.34966873604960824, 60.41557627198102409 ) ) ;
#56421 = CARTESIAN_POINT ( 'NONE',  ( -12.06949235617739369, -12.14591786802326823, 24.37609039468567573 ) ) ;
#56422 = CARTESIAN_POINT ( 'NONE',  ( -9.474510206698964154, 16.51473224551069663, 50.41557627198102409 ) ) ;
#56424 = CARTESIAN_POINT ( 'NONE',  ( -16.51473224551082808, 9.474510206698731452, 83.33442372801899012 ) ) ;
#56423 = CARTESIAN_POINT ( 'NONE',  ( 21.55341960407619695, -5.719274019375665929, 21.04275706135234714 ) ) ;
#56425 = CARTESIAN_POINT ( 'NONE',  ( 19.05341960407611168, 5.049401038298154454, 93.95724293864769550 ) ) ;
#56426 =( BOUNDED_CURVE ( )  B_SPLINE_CURVE ( 2, ( #4677, #82515, #144197, #5683, #67359, #190719, #52192, #113850, #94356, #122712, #184402, #106554, #79192 ),
 .UNSPECIFIED., .F., .F. ) 
 B_SPLINE_CURVE_WITH_KNOTS ( ( 3, 2, 2, 2, 2, 2, 3 ),
 ( 0.4235287478280826967, 0.4254385964912280604, 0.4298245614035087758, 0.4342105263157894912, 0.4385964912280701511, 0.4429824561403508665, 0.4449379846255865356 ),
 .UNSPECIFIED. ) 
 CURVE ( )  GEOMETRIC_REPRESENTATION_ITEM ( )  RATIONAL_B_SPLINE_CURVE ( ( 0.9832469066685285419, 0.9851625545550100060, 1.000000000000000000, 0.9659258262890683122, 1.000000000000000000, 0.9659258262890683122, 1.000000000000000000, 0.9659258262890683122, 1.000000000000000000, 0.9659258262890683122, 1.000000000000000000, 0.9848076720550082985, 0.9831626618144002627 ) ) 
 REPRESENTATION_ITEM ( '' )  );
#56427 = CARTESIAN_POINT ( 'NONE',  ( 13.97604488694527802, 13.89961937509977652, 69.37390960531436690 ) ) ;
#56428 = CARTESIAN_POINT ( 'NONE',  ( -10.72451020669898014, 18.67979575497178502, 70.41557627198102409 ) ) ;
#56429 = CARTESIAN_POINT ( 'NONE',  ( 19.02544592524343514, -5.153800228976328945, 48.54057627198103120 ) ) ;
#56430 = CARTESIAN_POINT ( 'NONE',  ( 69.65682714487590488, -71.74905178543389184, -13.00000000000000000 ) ) ;
#56431 = CARTESIAN_POINT ( 'NONE',  ( 12.14591786802309770, 12.06949235617756955, 49.37390960531436690 ) ) ;
#56432 = CARTESIAN_POINT ( 'NONE',  ( -5.153800228976328057, -19.02544592524343514, 102.2905762719810383 ) ) ;
#56433 = CARTESIAN_POINT ( 'NONE',  ( -8.906447517083053711, -27.41122689804191026, 144.4000000000000057 ) ) ;
#56434 = CARTESIAN_POINT ( 'NONE',  ( 16.51473224551083163, -9.474510206698727899, 70.83442372801900433 ) ) ;
#56435 = CARTESIAN_POINT ( 'NONE',  ( -5.823673210054116645, -21.52544592524344225, 82.29057627198103830 ) ) ;
#56436 = CARTESIAN_POINT ( 'NONE',  ( 16.46253265017146816, 9.564922557961045513, 31.66775706135232937 ) ) ;
#56437 = CARTESIAN_POINT ( 'NONE',  ( -16.46253265017160317, 9.564922557960807481, 100.8322429386477097 ) ) ;
#56438 = CARTESIAN_POINT ( 'NONE',  ( 12.14277428280450444, -10.17741597220468108, -59.53979320017422339 ) ) ;
#56439 = CARTESIAN_POINT ( 'NONE',  ( 5.823673210054125526, 21.52544592524343514, 39.79057627198103830 ) ) ;
#56440 = AXIS2_PLACEMENT_3D ( 'NONE', #23183, #69680, #114164 ) ;
#56441 = CARTESIAN_POINT ( 'NONE',  ( -9.564922557960796823, -16.46253265017161027, 67.08224293864769550 ) ) ;
#56442 = EDGE_CURVE ( 'NONE', #164406, #148926, #14583, .T. ) ;
#56443 = CARTESIAN_POINT ( 'NONE',  ( -10.72451020669870658, -18.67979575497194134, 64.58442372801900433 ) ) ;
#56444 = CARTESIAN_POINT ( 'NONE',  ( -9.474510206698964154, 16.51473224551069663, 30.41557627198102054 ) ) ;
#56446 = ORIENTED_EDGE ( 'NONE', *, *, #102991, .F. ) ;
#56445 = CARTESIAN_POINT ( 'NONE',  ( -10.81492255796078084, -18.62759615963271287, 112.0822429386477097 ) ) ;
#56447 = CARTESIAN_POINT ( 'NONE',  ( -15.72974639402176322, -15.80617190586768395, 49.37609039468569705 ) ) ;
#56448 = ORIENTED_EDGE ( 'NONE', *, *, #40967, .T. ) ;
#56449 = CARTESIAN_POINT ( 'NONE',  ( 5.049401038298161559, -19.05341960407611168, 107.7072429386476955 ) ) ;
#56450 = CARTESIAN_POINT ( 'NONE',  ( 16.46253265017146816, 9.564922557961045513, 71.66775706135233293 ) ) ;
#56451 = CARTESIAN_POINT ( 'NONE',  ( 21.61432565731214339, -33.65169730710053386, -23.91085783830763489 ) ) ;
#56452 = CARTESIAN_POINT ( 'NONE',  ( -21.52544592524343514, 5.823673210054127303, 106.0405762719810525 ) ) ;
#56453 = CARTESIAN_POINT ( 'NONE',  ( 9.474510206698971260, -16.51473224551069308, 62.91557627198102409 ) ) ;
#56454 = CARTESIAN_POINT ( 'NONE',  ( -14.29746914071037622, -8.314922557961029526, 39.16775706135235424 ) ) ;
#56455 = CARTESIAN_POINT ( 'NONE',  ( 30.74264578624799782, 22.33583958711400541, -4.549999994537627046 ) ) ;
#56456 = CARTESIAN_POINT ( 'NONE',  ( 5.719274019375673035, 21.55341960407619339, 102.2927570613523613 ) ) ;
#56457 = CARTESIAN_POINT ( 'NONE',  ( -5.049401038298153566, 19.05341960407611168, 45.20724293864769550 ) ) ;
#56458 = CARTESIAN_POINT ( 'NONE',  ( -9.474510206698720793, -16.51473224551083518, 19.58442372801899722 ) ) ;
#56460 = CARTESIAN_POINT ( 'NONE',  ( 21.52544592524334988, 5.823673210054432836, 61.45942372801901854 ) ) ;
#56459 = CARTESIAN_POINT ( 'NONE',  ( 13.97604488694527802, 13.89961937509977652, 94.37390960531436690 ) ) ;
#56461 = CARTESIAN_POINT ( 'NONE',  ( -29.86685920354755197, -21.69954338932560134, -10.42499999726881299 ) ) ;
#56462 = CARTESIAN_POINT ( 'NONE',  ( 13.89961937509977652, -13.97604488694527269, 113.1239096053143527 ) ) ;
#56463 = CARTESIAN_POINT ( 'NONE',  ( -17.49999999999999645, 3.565345528327878544, 29.42494486806477738 ) ) ;
#56465 = CARTESIAN_POINT ( 'NONE',  ( -10.81492255796105439, 18.62759615963255655, 77.91775706135231871 ) ) ;
#56464 = CARTESIAN_POINT ( 'NONE',  ( -12.14591786802326823, 12.06949235617739902, 48.12609039468568284 ) ) ;
#56466 = CARTESIAN_POINT ( 'NONE',  ( 21.55341960407619695, -5.719274019375665929, 86.04275706135236135 ) ) ;
#56467 = CARTESIAN_POINT ( 'NONE',  ( -12.06828707866192119, 11.48863819084119342, -59.15275318406537508 ) ) ;
#56468 = CARTESIAN_POINT ( 'NONE',  ( -12.06949235617739369, -12.14591786802326823, 24.37609039468567573 ) ) ;
#56469 = CARTESIAN_POINT ( 'NONE',  ( -9.474510206698964154, 16.51473224551069663, 85.41557627198102409 ) ) ;
#56470 = CARTESIAN_POINT ( 'NONE',  ( -9.474510206698964154, 16.51473224551069663, 110.4155762719810383 ) ) ;
#56471 = CARTESIAN_POINT ( 'NONE',  ( 17.31728774477272026, 6.344390552232403557, 41.68093348310682700 ) ) ;
#56472 = CARTESIAN_POINT ( 'NONE',  ( -19.02544592524342804, 5.153800228976336051, 31.04057627198102409 ) ) ;
#56474 = EDGE_CURVE ( 'NONE', #74699, #188324, #76289, .T. ) ;
#56473 = CARTESIAN_POINT ( 'NONE',  ( 21.52544592524344225, -5.823673210054117533, 48.54057627198103120 ) ) ;
#56475 = CARTESIAN_POINT ( 'NONE',  ( -4.483927247898782831, 16.52544592524335698, 107.7094237280190328 ) ) ;
#56477 = CARTESIAN_POINT ( 'NONE',  ( 19.02544592524343514, -5.153800228976328945, 73.54057627198103830 ) ) ;
#56476 = CARTESIAN_POINT ( 'NONE',  ( -16.53943276465976808, 0.05219959533911058130, 86.24890960531436690 ) ) ;
#56478 = CARTESIAN_POINT ( 'NONE',  ( 15.80617190586769283, -15.72974639402175789, 85.62609039468568994 ) ) ;
#56479 = CARTESIAN_POINT ( 'NONE',  ( 4.483927247898790824, -16.52544592524335698, 25.20942372801901854 ) ) ;
#56480 = CARTESIAN_POINT ( 'NONE',  ( 8.314922557960818139, 14.29746914071049879, 94.58224293864769550 ) ) ;
#56481 = CARTESIAN_POINT ( 'NONE',  ( -10.72451020669870658, -18.67979575497194134, 39.58442372801901143 ) ) ;
#56482 = CARTESIAN_POINT ( 'NONE',  ( 10.72451020669898902, -18.67979575497178502, 72.91557627198103830 ) ) ;
#56483 = CARTESIAN_POINT ( 'NONE',  ( 19.02544592524334988, 5.153800228976608722, 31.45942372801900433 ) ) ;
#56484 = CARTESIAN_POINT ( 'NONE',  ( -34.51210051733097828, 7.446700168151136445, 43.98226744806001420 ) ) ;
#56485 = CARTESIAN_POINT ( 'NONE',  ( 9.474510206698971260, -16.51473224551069308, 102.9155762719810241 ) ) ;
#56486 = CARTESIAN_POINT ( 'NONE',  ( -14.34966873604960291, -8.224510206698953496, 61.66557627198103120 ) ) ;
#56487 = CARTESIAN_POINT ( 'NONE',  ( 0.05219959533910956823, 16.53943276465976808, 54.99890960531435269 ) ) ;
#56488 = CARTESIAN_POINT ( 'NONE',  ( 14.34966873604972726, -8.224510206698740333, 110.8344237280190043 ) ) ;
#56489 = CARTESIAN_POINT ( 'NONE',  ( 13.89961937509957401, 13.97604488694547697, 71.87609039468567573 ) ) ;
#56490 = CARTESIAN_POINT ( 'NONE',  ( 19.19724070472090460, 5.500000000000158096, 53.56193348274384647 ) ) ;
#56491 = CARTESIAN_POINT ( 'NONE',  ( -9.564922557960796823, -16.46253265017161027, 112.0822429386476955 ) ) ;
#56492 = CARTESIAN_POINT ( 'NONE',  ( -8.314922557960811034, -14.29746914071050412, 82.08224293864768129 ) ) ;
#56493 = DIRECTION ( 'NONE',  ( 1.000000000000000000, -1.776356839400250465E-15, 0.000000000000000000 ) ) ;
#56495 = CARTESIAN_POINT ( 'NONE',  ( -10.81492255796078084, -18.62759615963271287, 52.08224293864768839 ) ) ;
#56494 = CARTESIAN_POINT ( 'NONE',  ( 16.46253265017160672, -9.564922557960803928, 43.33224293864769550 ) ) ;
#56496 = CARTESIAN_POINT ( 'NONE',  ( 15.72974639402199770, -15.80617190586745480, 78.12390960531436690 ) ) ;
#56497 = CARTESIAN_POINT ( 'NONE',  ( 12.14591786802309770, 12.06949235617756955, 109.3739096053143811 ) ) ;
#56499 = CARTESIAN_POINT ( 'NONE',  ( 9.474510206698971260, -16.51473224551069308, 47.91557627198102409 ) ) ;
#56498 = CARTESIAN_POINT ( 'NONE',  ( 16.52544592524335698, 4.483927247898782831, 61.45942372801901854 ) ) ;
#56500 = CARTESIAN_POINT ( 'NONE',  ( -19.03943276465977164, -0.05219959533935918106, 43.75109039468566863 ) ) ;
#56501 = CIRCLE ( 'NONE', #114483, 214.0437394197456911 ) ;
#56502 = CARTESIAN_POINT ( 'NONE',  ( 21.53943276465977519, 0.05219959533937863772, 56.25109039468568284 ) ) ;
#56503 = CARTESIAN_POINT ( 'NONE',  ( -8.224510206698948167, 14.34966873604960824, 110.4155762719810383 ) ) ;
#56504 = CARTESIAN_POINT ( 'NONE',  ( 19.02544592524334988, 5.153800228976608722, 96.45942372801897591 ) ) ;
#56505 = CARTESIAN_POINT ( 'NONE',  ( 11.40812507854755253, -35.11059874428192273, -6.524999997268813523 ) ) ;
#56507 = CARTESIAN_POINT ( 'NONE',  ( -18.67979575497178146, -10.72451020669898902, 46.66557627198102409 ) ) ;
#56506 = DIRECTION ( 'NONE',  ( 1.000000000000000000, 1.776356839400250465E-15, 0.000000000000000000 ) ) ;
#56508 = CARTESIAN_POINT ( 'NONE',  ( -5.153800228976328057, -19.02544592524343514, 22.29057627198102765 ) ) ;
#56509 = CARTESIAN_POINT ( 'NONE',  ( 10.81492255796106328, -18.62759615963255655, 80.41775706135234714 ) ) ;
#56510 = CARTESIAN_POINT ( 'NONE',  ( -4.379528057220328563, 16.55341960407611168, 30.20724293864769550 ) ) ;
#56512 = CARTESIAN_POINT ( 'NONE',  ( 4.483927247898545687, 16.52544592524342804, 44.79057627198103120 ) ) ;
#56511 = CARTESIAN_POINT ( 'NONE',  ( 8.224510206698742110, 14.34966873604972548, 62.08442372801901143 ) ) ;
#56513 = CARTESIAN_POINT ( 'NONE',  ( -18.62759615963270932, 10.81492255796079327, 75.83224293864769550 ) ) ;
#56514 = CARTESIAN_POINT ( 'NONE',  ( 18.67979575497178502, 10.72451020669898547, 74.16557627198102409 ) ) ;
#56515 = CARTESIAN_POINT ( 'NONE',  ( 4.500000000000000888, -130.0000000000000000, 15.00000000000000000 ) ) ;
#56517 = CARTESIAN_POINT ( 'NONE',  ( 15.72974639402199770, -15.80617190586745480, 23.12390960531436335 ) ) ;
#56516 = CARTESIAN_POINT ( 'NONE',  ( -19.05341960407617563, 5.049401038297882671, 83.54275706135233293 ) ) ;
#56518 = CARTESIAN_POINT ( 'NONE',  ( -16.46253265017160317, 9.564922557960807481, 50.83224293864770260 ) ) ;
#56519 = CARTESIAN_POINT ( 'NONE',  ( 19.02544592524343514, -5.153800228976328945, 28.54057627198102409 ) ) ;
#56520 = FILL_AREA_STYLE_COLOUR ( '', #169409 ) ;
#56521 = DIRECTION ( 'NONE',  ( 0.000000000000000000, 0.000000000000000000, -1.000000000000000000 ) ) ;
#56522 = ORIENTED_EDGE ( 'NONE', *, *, #165511, .T. ) ;
#56524 = CARTESIAN_POINT ( 'NONE',  ( 8.314922557961029526, -14.29746914071037800, 80.41775706135234714 ) ) ;
#56523 = AXIS2_PLACEMENT_3D ( 'NONE', #173770, #132231, #81706 ) ;
#56525 = CARTESIAN_POINT ( 'NONE',  ( -21.52544592524343514, 5.823673210054127303, 106.0405762719810525 ) ) ;
#56526 = CARTESIAN_POINT ( 'NONE',  ( 9.474510206698971260, -16.51473224551069308, 67.91557627198102409 ) ) ;
#56527 = CARTESIAN_POINT ( 'NONE',  ( 18.67979575497194134, -10.72451020669871369, 35.83442372801901143 ) ) ;
#56528 = CARTESIAN_POINT ( 'NONE',  ( 9.474510206698971260, -16.51473224551069308, 102.9155762719810241 ) ) ;
#56529 = CARTESIAN_POINT ( 'NONE',  ( -26.72240360496086709, -29.37940146934014507, -20.20861161915233595 ) ) ;
#56530 = EDGE_LOOP ( 'NONE', ( #59185, #125324, #91803, #94426, #33772, #86117, #178384, #9953, #145915, #191657, #136965, #73626 ) ) ;
#56531 = CARTESIAN_POINT ( 'NONE',  ( -15.72974639402176322, -15.80617190586768395, 29.37609039468568284 ) ) ;
#56533 = CARTESIAN_POINT ( 'NONE',  ( 16.46253265017160672, -9.564922557960803928, 108.3322429386476955 ) ) ;
#56532 = CARTESIAN_POINT ( 'NONE',  ( 5.153800228976335163, 19.02544592524342804, 29.79057627198102409 ) ) ;
#56534 = CARTESIAN_POINT ( 'NONE',  ( -16.51473224551082808, 9.474510206698731452, 38.33442372801899722 ) ) ;
#56535 = CARTESIAN_POINT ( 'NONE',  ( -5.719274019375978568, 21.55341960407610458, 115.2072429386476955 ) ) ;
#56536 = CARTESIAN_POINT ( 'NONE',  ( -16.51473224551082808, 9.474510206698731452, 48.33442372801900433 ) ) ;
#56537 = CARTESIAN_POINT ( 'NONE',  ( -5.153800228976607833, 19.02544592524334988, 42.70942372801901143 ) ) ;
#56538 = CARTESIAN_POINT ( 'NONE',  ( 12.06949235617739724, 12.14591786802326823, 96.87609039468568994 ) ) ;
#56540 = ORIENTED_EDGE ( 'NONE', *, *, #35894, .F. ) ;
#56539 = DIRECTION ( 'NONE',  ( 0.000000000000000000, 0.000000000000000000, 1.000000000000000000 ) ) ;
#56541 = CARTESIAN_POINT ( 'NONE',  ( -9.474510206698964154, 16.51473224551069663, 75.41557627198103830 ) ) ;
#56542 = COLOUR_RGB ( '', 0.31764706, 0.68627451, 0.89019608) ;
#56543 = CARTESIAN_POINT ( 'NONE',  ( -10.72451020669870658, -18.67979575497194134, 79.58442372801903275 ) ) ;
#56544 = CARTESIAN_POINT ( 'NONE',  ( 18.67979575497194134, -10.72451020669871369, 90.83442372801901854 ) ) ;
#56545 = CARTESIAN_POINT ( 'NONE',  ( -1.490470117976196107, -7.405238625847243128, -64.28041130758168720 ) ) ;
#56546 = CARTESIAN_POINT ( 'NONE',  ( 5.049401038298161559, -19.05341960407611168, 92.70724293864769550 ) ) ;
#56547 = CARTESIAN_POINT ( 'NONE',  ( -21.53943276465977519, -0.05219959533937600094, 63.75109039468568284 ) ) ;
#56548 = CARTESIAN_POINT ( 'NONE',  ( 9.564922557961047289, -16.46253265017146816, 100.4177570613523329 ) ) ;
#56549 = CARTESIAN_POINT ( 'NONE',  ( -9.564922557960796823, -16.46253265017161027, 62.08224293864769550 ) ) ;
#56550 = CARTESIAN_POINT ( 'NONE',  ( -5.153800228976328057, -19.02544592524343514, 107.2905762719810383 ) ) ;
#56551 = CARTESIAN_POINT ( 'NONE',  ( 19.02544592524343514, -5.153800228976328945, 83.54057627198100988 ) ) ;
#56552 = CARTESIAN_POINT ( 'NONE',  ( -17.40805194822030799, -6.112264579159315758, 89.16628727489390371 ) ) ;
#56553 = CARTESIAN_POINT ( 'NONE',  ( 13.97604488694527802, 13.89961937509977652, 59.37390960531434558 ) ) ;
#56554 = CARTESIAN_POINT ( 'NONE',  ( 5.049401038298161559, -19.05341960407611168, 52.70724293864767418 ) ) ;
#56555 = CARTESIAN_POINT ( 'NONE',  ( -15.72974639402197994, 15.80617190586746368, 115.6239096053143669 ) ) ;
#56556 = CARTESIAN_POINT ( 'NONE',  ( -12.14591786802326823, 12.06949235617739902, 98.12609039468570415 ) ) ;
#56557 = CARTESIAN_POINT ( 'NONE',  ( 7.284589286804261654, -1.784589286804270980, 8.181980515339454030 ) ) ;
#56558 = PRESENTATION_LAYER_ASSIGNMENT (  '', '', ( #124365 ) ) ;
#56559 = DIRECTION ( 'NONE',  ( -1.000000000000000000, -0.000000000000000000, -0.000000000000000000 ) ) ;
#56560 = CARTESIAN_POINT ( 'NONE',  ( -19.03943276465977164, -0.05219959533935918106, 63.75109039468566863 ) ) ;
#56561 = CARTESIAN_POINT ( 'NONE',  ( -19.03943276465977164, 0.05219959533909376836, 76.24890960531435269 ) ) ;
#56562 = CARTESIAN_POINT ( 'NONE',  ( -16.52544592524342804, 4.483927247898546575, 66.04057627198103830 ) ) ;
#56563 = CARTESIAN_POINT ( 'NONE',  ( -4.483927247898539470, -16.52544592524342804, 107.2905762719810525 ) ) ;
#56564 = AXIS2_PLACEMENT_3D ( 'NONE', #109401, #77073, #94225 ) ;
#56565 = CARTESIAN_POINT ( 'NONE',  ( 10.81492255796078972, 18.62759615963270932, 29.58224293864769905 ) ) ;
#56566 = CARTESIAN_POINT ( 'NONE',  ( -13.97604488694527625, -13.89961937509977652, 26.87390960531434558 ) ) ;
#56567 = CARTESIAN_POINT ( 'NONE',  ( -9.474510206698964154, 16.51473224551069663, 110.4155762719810383 ) ) ;
#56568 = CARTESIAN_POINT ( 'NONE',  ( 8.224510206698953496, -14.34966873604960469, 97.91557627198103830 ) ) ;
#56569 = CARTESIAN_POINT ( 'NONE',  ( -23.48298174826589602, -32.32155151706772500, -3.702157773949823039 ) ) ;
#56570 = CARTESIAN_POINT ( 'NONE',  ( 9.564922557961047289, -16.46253265017146816, 30.41775706135232937 ) ) ;
#56571 = CARTESIAN_POINT ( 'NONE',  ( 14.29746914071037800, 8.314922557961029526, 111.6677570613523613 ) ) ;
#56572 = CARTESIAN_POINT ( 'NONE',  ( 19.03943276465977164, -0.05219959533909143690, 83.74890960531436690 ) ) ;
#56573 = CARTESIAN_POINT ( 'NONE',  ( -15.80617190586768217, 15.72974639402176855, 48.12609039468568284 ) ) ;
#56574 = CARTESIAN_POINT ( 'NONE',  ( 15.72974639402199770, -15.80617190586745480, 43.12390960531435269 ) ) ;
#56575 = CARTESIAN_POINT ( 'NONE',  ( 18.67979575497194134, -10.72451020669871369, 35.83442372801901143 ) ) ;
#56576 = CARTESIAN_POINT ( 'NONE',  ( 21.52544592524344225, -5.823673210054117533, 78.54057627198103830 ) ) ;
#56577 = CARTESIAN_POINT ( 'NONE',  ( -14.34966873604960291, -8.224510206698953496, 96.66557627198102409 ) ) ;
#56578 = CARTESIAN_POINT ( 'NONE',  ( -9.474510206698720793, -16.51473224551083518, 59.58442372801900433 ) ) ;
#56579 = CARTESIAN_POINT ( 'NONE',  ( -16.46253265017160317, 9.564922557960807481, 40.83224293864769550 ) ) ;
#56580 = CARTESIAN_POINT ( 'NONE',  ( -5.153800228976328057, -19.02544592524343514, 97.29057627198099567 ) ) ;
#56581 = CARTESIAN_POINT ( 'NONE',  ( 9.474510206698971260, -16.51473224551069308, 97.91557627198102409 ) ) ;
#56582 = CARTESIAN_POINT ( 'NONE',  ( -19.05341960407611168, -5.049401038298163336, 21.45724293864768839 ) ) ;
#56583 = CARTESIAN_POINT ( 'NONE',  ( 12.14591786802309770, 12.06949235617756955, 24.37390960531435979 ) ) ;
#56584 = CARTESIAN_POINT ( 'NONE',  ( 14.34966873604972726, -8.224510206698740333, 45.83442372801901854 ) ) ;
#56586 = CIRCLE ( 'NONE', #166302, 3.799999999999999378 ) ;
#56585 = CARTESIAN_POINT ( 'NONE',  ( 10.72451020669871369, 18.67979575497193778, 102.0844237280190185 ) ) ;
#56588 = CARTESIAN_POINT ( 'NONE',  ( -14.34966873604960291, -8.224510206698953496, 26.66557627198103475 ) ) ;
#56587 = DIRECTION ( 'NONE',  ( -1.000000000000000000, 0.000000000000000000, 0.000000000000000000 ) ) ;
#56589 = CARTESIAN_POINT ( 'NONE',  ( 15.72974639402176855, 15.80617190586768217, 31.87609039468567929 ) ) ;
#56590 = CARTESIAN_POINT ( 'NONE',  ( -9.474510206698964154, 16.51473224551069663, 40.41557627198103120 ) ) ;
#56591 = CARTESIAN_POINT ( 'NONE',  ( -14.34966873604972548, 8.224510206698743886, 38.33442372801900433 ) ) ;
#56592 = CARTESIAN_POINT ( 'NONE',  ( -4.379528057220086978, -16.55341960407618274, 109.7927570613523613 ) ) ;
#56593 = CARTESIAN_POINT ( 'NONE',  ( 8.224510206698742110, 14.34966873604972548, 97.08442372801904696 ) ) ;
#56594 = CARTESIAN_POINT ( 'NONE',  ( -0.05219959533934338120, 16.53943276465976808, 22.50109039468567573 ) ) ;
#56595 = CARTESIAN_POINT ( 'NONE',  ( -16.46253265017160317, 9.564922557960807481, 40.83224293864769550 ) ) ;
#56596 = CARTESIAN_POINT ( 'NONE',  ( -14.34966873604960291, -8.224510206698953496, 106.6655762719810383 ) ) ;
#56597 = CARTESIAN_POINT ( 'NONE',  ( -5.823673210054116645, -21.52544592524344225, 112.2905762719810241 ) ) ;
#56598 = CARTESIAN_POINT ( 'NONE',  ( 5.049401038298161559, -19.05341960407611168, 32.70724293864768129 ) ) ;
#56599 = CARTESIAN_POINT ( 'NONE',  ( 13.97604488694527802, 13.89961937509977652, 104.3739096053143385 ) ) ;
#56600 = CARTESIAN_POINT ( 'NONE',  ( -15.80617190586768217, 15.72974639402176855, 33.12609039468569705 ) ) ;
#56601 = CARTESIAN_POINT ( 'NONE',  ( 19.03943276465977164, -0.05219959533909143690, 23.74890960531435269 ) ) ;
#56602 = CARTESIAN_POINT ( 'NONE',  ( -9.474510206698964154, 16.51473224551069663, 105.4155762719810383 ) ) ;
#56603 = CARTESIAN_POINT ( 'NONE',  ( -23.29544513554940721, -16.92513159979223403, 142.1843446569000093 ) ) ;
#56604 = CARTESIAN_POINT ( 'NONE',  ( 5.049401038298161559, -19.05341960407611168, 102.7072429386476955 ) ) ;
#56606 = CARTESIAN_POINT ( 'NONE',  ( -12.14591786802309592, -12.06949235617757132, 91.87390960531436690 ) ) ;
#56605 = CARTESIAN_POINT ( 'NONE',  ( -21.55341960407619339, 5.719274019375674811, 33.54275706135234714 ) ) ;
#56607 = CARTESIAN_POINT ( 'NONE',  ( -19.05341960407611168, -5.049401038298163336, 96.45724293864769550 ) ) ;
#56608 = DIRECTION ( 'NONE',  ( -0.000000000000000000, -1.000000000000000000, -0.000000000000000000 ) ) ;
#56609 = CARTESIAN_POINT ( 'NONE',  ( -12.06949235617739369, -12.14591786802326823, 64.37609039468568994 ) ) ;
#56610 = CARTESIAN_POINT ( 'NONE',  ( -21.52544592524334988, -5.823673210054445271, 73.95942372801901854 ) ) ;
#56611 = CARTESIAN_POINT ( 'NONE',  ( 16.52544592524335698, 4.483927247898782831, 41.45942372801901143 ) ) ;
#56612 = CARTESIAN_POINT ( 'NONE',  ( -9.474510206698964154, 16.51473224551069663, 80.41557627198103830 ) ) ;
#56613 = CARTESIAN_POINT ( 'NONE',  ( -8.224510206698735004, -14.34966873604973081, 19.58442372801901143 ) ) ;
#56614 = CARTESIAN_POINT ( 'NONE',  ( -16.53943276465976808, -0.05219959533934237506, 73.75109039468567573 ) ) ;
#56615 = CARTESIAN_POINT ( 'NONE',  ( 21.53943276465977519, 0.05219959533937863772, 111.2510903946856899 ) ) ;
#56616 = CARTESIAN_POINT ( 'NONE',  ( 16.46253265017146816, 9.564922557961045513, 96.66775706135233293 ) ) ;
#56617 = CARTESIAN_POINT ( 'NONE',  ( -16.51473224551069308, -9.474510206698971260, 66.66557627198102409 ) ) ;
#56618 = CARTESIAN_POINT ( 'NONE',  ( 18.67979575497178502, 10.72451020669898547, 79.16557627198103830 ) ) ;
#56620 = CARTESIAN_POINT ( 'NONE',  ( 9.564922557961047289, -16.46253265017146816, 90.41775706135234714 ) ) ;
#56619 = CARTESIAN_POINT ( 'NONE',  ( -4.483927247898539470, -16.52544592524342804, 92.29057627198103830 ) ) ;
#56621 = CARTESIAN_POINT ( 'NONE',  ( -8.224510206698735004, -14.34966873604973081, 59.58442372801901854 ) ) ;
#56622 = CARTESIAN_POINT ( 'NONE',  ( 23.97133246043717847, 5.390759101651051211, 174.7603932261090733 ) ) ;
#56623 = CARTESIAN_POINT ( 'NONE',  ( -16.51473224551082808, 9.474510206698731452, 58.33442372801900433 ) ) ;
#56624 = CARTESIAN_POINT ( 'NONE',  ( 8.224510206698953496, -14.34966873604960469, 27.91557627198103830 ) ) ;
#56625 = CARTESIAN_POINT ( 'NONE',  ( 0.05219959533910956823, 16.53943276465976808, 79.99890960531435269 ) ) ;
#56627 = CARTESIAN_POINT ( 'NONE',  ( -4.500000000000001776, -139.6710100716628631, 12.88025745871188654 ) ) ;
#56626 = CARTESIAN_POINT ( 'NONE',  ( -19.02544592524334988, -5.153800228976617603, 23.95942372801900078 ) ) ;
#56628 = CARTESIAN_POINT ( 'NONE',  ( -15.72974639402176322, -15.80617190586768395, 29.37609039468568284 ) ) ;
#56629 = CARTESIAN_POINT ( 'NONE',  ( -13.89961937509977652, 13.97604488694528158, 100.6239096053143669 ) ) ;
#56630 = CARTESIAN_POINT ( 'NONE',  ( -13.89961937509977652, 13.97604488694528158, 75.62390960531438111 ) ) ;
#56631 = CARTESIAN_POINT ( 'NONE',  ( -15.72974639402176322, -15.80617190586768395, 99.37609039468568994 ) ) ;
#56632 = CARTESIAN_POINT ( 'NONE',  ( 16.46253265017160672, -9.564922557960803928, 73.33224293864769550 ) ) ;
#56633 = CARTESIAN_POINT ( 'NONE',  ( -10.72451020669898014, 18.67979575497178502, 35.41557627198102409 ) ) ;
#56634 = AXIS2_PLACEMENT_3D ( 'NONE', #129071, #146245, #39085 ) ;
#56635 = CARTESIAN_POINT ( 'NONE',  ( 4.379528057220339221, -16.55341960407611168, 77.70724293864770971 ) ) ;
#56636 = CARTESIAN_POINT ( 'NONE',  ( 16.46253265017160672, -9.564922557960803928, 38.33224293864768839 ) ) ;
#56637 = CARTESIAN_POINT ( 'NONE',  ( 4.379528057220339221, -16.55341960407611168, 102.7072429386476955 ) ) ;
#56638 = CARTESIAN_POINT ( 'NONE',  ( 5.719274019375991003, -21.55341960407610458, 107.7072429386476955 ) ) ;
#56639 = CARTESIAN_POINT ( 'NONE',  ( 18.62759615963255655, 10.81492255796105972, 61.66775706135235424 ) ) ;
#56640 = CARTESIAN_POINT ( 'NONE',  ( 13.97604488694527802, 13.89961937509977652, 29.37390960531435979 ) ) ;
#56641 = CARTESIAN_POINT ( 'NONE',  ( -8.224510206698735004, -14.34966873604973081, 59.58442372801901854 ) ) ;
#56642 = CARTESIAN_POINT ( 'NONE',  ( -10.81492255796078084, -18.62759615963271287, 102.0822429386476955 ) ) ;
#56643 = CARTESIAN_POINT ( 'NONE',  ( -21.53943276465977519, 0.05219959533907696930, 106.2489096053143811 ) ) ;
#56645 = CARTESIAN_POINT ( 'NONE',  ( 19.03943276465977164, -0.05219959533909143690, 58.74890960531435979 ) ) ;
#56644 = CARTESIAN_POINT ( 'NONE',  ( 19.05341960407617918, -5.049401038297876454, 36.04275706135234003 ) ) ;
#56646 = LINE ( 'NONE', #86970, #15152 ) ;
#56647 = CARTESIAN_POINT ( 'NONE',  ( -21.52544592524334988, -5.823673210054445271, 68.95942372801901854 ) ) ;
#56648 = CARTESIAN_POINT ( 'NONE',  ( -10.81492255796078084, -18.62759615963271287, 62.08224293864769550 ) ) ;
#56649 = CARTESIAN_POINT ( 'NONE',  ( -16.55341960407611168, -4.379528057220339221, 41.45724293864769550 ) ) ;
#56651 = CARTESIAN_POINT ( 'NONE',  ( -10.72451020669870658, -18.67979575497194134, 109.5844237280190328 ) ) ;
#56650 = CARTESIAN_POINT ( 'NONE',  ( -18.62759615963255300, -10.81492255796106328, 74.16775706135231871 ) ) ;
#56652 = CARTESIAN_POINT ( 'NONE',  ( -14.34966873604960291, -8.224510206698953496, 61.66557627198103120 ) ) ;
#56653 = CARTESIAN_POINT ( 'NONE',  ( -4.379528057220328563, 16.55341960407611168, 110.2072429386477239 ) ) ;
#56654 = CARTESIAN_POINT ( 'NONE',  ( -19.03943276465977164, -0.05219959533935918106, 43.75109039468566863 ) ) ;
#56655 = CARTESIAN_POINT ( 'NONE',  ( -14.29746914071037622, -8.314922557961029526, 99.16775706135234714 ) ) ;
#56656 = CARTESIAN_POINT ( 'NONE',  ( -15.80617190586768217, 15.72974639402176855, 73.12609039468567573 ) ) ;
#56657 = CARTESIAN_POINT ( 'NONE',  ( 9.564922557960805705, 16.46253265017160317, 64.58224293864769550 ) ) ;
#56658 = CARTESIAN_POINT ( 'NONE',  ( 13.97604488694548053, -13.89961937509957401, 35.62609039468567573 ) ) ;
#56659 = CARTESIAN_POINT ( 'NONE',  ( 0.05219959533907565091, 21.53943276465977519, 34.99890960531435979 ) ) ;
#56660 = CARTESIAN_POINT ( 'NONE',  ( -10.72451020669870658, -18.67979575497194134, 29.58442372801901854 ) ) ;
#56661 = CARTESIAN_POINT ( 'NONE',  ( 18.67979575497178502, 10.72451020669898547, 89.16557627198102409 ) ) ;
#56662 = CARTESIAN_POINT ( 'NONE',  ( -9.474510206698720793, -16.51473224551083518, 89.58442372801900433 ) ) ;
#56663 = CARTESIAN_POINT ( 'NONE',  ( -0.05219959533934338120, 16.53943276465976808, 52.50109039468567573 ) ) ;
#56665 = CARTESIAN_POINT ( 'NONE',  ( 18.62759615963271287, -10.81492255796078972, 93.33224293864769550 ) ) ;
#56664 = CARTESIAN_POINT ( 'NONE',  ( 5.199999999999996625, 0.000000000000000000, -2.700000000000000622 ) ) ;
#56666 = CARTESIAN_POINT ( 'NONE',  ( 0.05219959533910956823, 16.53943276465976808, 69.99890960531435269 ) ) ;
#56667 = CARTESIAN_POINT ( 'NONE',  ( -31.34482716061811303, -21.47441072263947248, -23.96158720469884074 ) ) ;
#56668 = CARTESIAN_POINT ( 'NONE',  ( 19.02544592524334988, 5.153800228976608722, 111.4594237280190043 ) ) ;
#56669 = CARTESIAN_POINT ( 'NONE',  ( 15.80617190586746368, 15.72974639402197994, 44.37390960531435979 ) ) ;
#56670 = CARTESIAN_POINT ( 'NONE',  ( 8.314922557961029526, -14.29746914071037800, 75.41775706135233293 ) ) ;
#56671 = LINE ( 'NONE', #86995, #51063 ) ;
#56672 = CARTESIAN_POINT ( 'NONE',  ( 14.29746914071037800, 8.314922557961029526, 56.66775706135235424 ) ) ;
#56673 = CARTESIAN_POINT ( 'NONE',  ( 10.81492255796106328, -18.62759615963255655, 30.41775706135234358 ) ) ;
#56674 = CARTESIAN_POINT ( 'NONE',  ( 18.67979575497178502, 10.72451020669898547, 44.16557627198103120 ) ) ;
#56675 = CARTESIAN_POINT ( 'NONE',  ( 0.05219959533934541429, -16.53943276465976808, 75.00109039468568994 ) ) ;
#56676 = CARTESIAN_POINT ( 'NONE',  ( 16.46253265017160672, -9.564922557960803928, 103.3322429386476955 ) ) ;
#56678 = CARTESIAN_POINT ( 'NONE',  ( -9.474510206698964154, 16.51473224551069663, 25.41557627198103120 ) ) ;
#56677 = CARTESIAN_POINT ( 'NONE',  ( -10.81492255796105439, 18.62759615963255655, 57.91775706135234714 ) ) ;
#56679 = CARTESIAN_POINT ( 'NONE',  ( -10.72451020669898014, 18.67979575497178502, 40.41557627198103120 ) ) ;
#56680 = CARTESIAN_POINT ( 'NONE',  ( 16.51473224551069308, 9.474510206698969483, 114.1655762719810241 ) ) ;
#56681 = VERTEX_POINT ( 'NONE', #26142 ) ;
#56682 = CARTESIAN_POINT ( 'NONE',  ( -16.51473224551082808, 9.474510206698731452, 33.33442372801899722 ) ) ;
#56683 = CARTESIAN_POINT ( 'NONE',  ( 16.52544592524335698, 4.483927247898782831, 56.45942372801902565 ) ) ;
#56684 = CARTESIAN_POINT ( 'NONE',  ( 9.564922557960805705, 16.46253265017160317, 109.5822429386476955 ) ) ;
#56685 = ORIENTED_EDGE ( 'NONE', *, *, #136297, .F. ) ;
#56686 = CARTESIAN_POINT ( 'NONE',  ( 19.02544592524343514, -5.153800228976328945, 88.54057627198102409 ) ) ;
#56687 = CARTESIAN_POINT ( 'NONE',  ( 0.05219959533934541429, -16.53943276465976808, 100.0010903946857042 ) ) ;
#56688 = CARTESIAN_POINT ( 'NONE',  ( -17.49999999999999289, 5.500000000000036415, 85.79690382534171533 ) ) ;
#56689 = CARTESIAN_POINT ( 'NONE',  ( 14.29746914071049879, -8.314922557960816363, 93.33224293864769550 ) ) ;
#56690 = CARTESIAN_POINT ( 'NONE',  ( 5.719274019375991003, -21.55341960407610458, 52.70724293864769550 ) ) ;
#56691 = CARTESIAN_POINT ( 'NONE',  ( -19.03943276465977164, 0.05219959533909376836, 36.24890960531436690 ) ) ;
#56692 = CARTESIAN_POINT ( 'NONE',  ( 16.52544592524335698, 4.483927247898782831, 76.45942372801901854 ) ) ;
#56693 = CARTESIAN_POINT ( 'NONE',  ( -21.55341960407619339, 5.719274019375674811, 23.54275706135235424 ) ) ;
#56694 = CARTESIAN_POINT ( 'NONE',  ( -19.03943276465977164, -0.05219959533935918106, 93.75109039468566152 ) ) ;
#56695 = CARTESIAN_POINT ( 'NONE',  ( 5.049401038298161559, -19.05341960407611168, 42.70724293864767418 ) ) ;
#56696 = AXIS2_PLACEMENT_3D ( 'NONE', #166900, #196262, #180097 ) ;
#56697 = CARTESIAN_POINT ( 'NONE',  ( -16.51473224551069308, -9.474510206698971260, 106.6655762719810383 ) ) ;
#56698 = CARTESIAN_POINT ( 'NONE',  ( -0.05219959533937732626, 21.53943276465977519, 102.5010903946856899 ) ) ;
#56699 = CARTESIAN_POINT ( 'NONE',  ( -16.51473224551069308, -9.474510206698971260, 81.66557627198103830 ) ) ;
#56700 = CARTESIAN_POINT ( 'NONE',  ( -16.55341960407617563, 4.379528057220093196, 58.54275706135235424 ) ) ;
#56701 = CARTESIAN_POINT ( 'NONE',  ( 18.67979575497194134, -10.72451020669871369, 90.83442372801901854 ) ) ;
#56702 = CARTESIAN_POINT ( 'NONE',  ( -19.03943276465977164, -0.05219959533935918106, 58.75109039468566863 ) ) ;
#56703 = CARTESIAN_POINT ( 'NONE',  ( -0.05219959533936034679, 19.03943276465977164, 72.50109039468566152 ) ) ;
#56704 = EDGE_LOOP ( 'NONE', ( #27445, #59215 ) ) ;
#56705 = CARTESIAN_POINT ( 'NONE',  ( 15.80617190586769283, -15.72974639402175789, 60.62609039468567573 ) ) ;
#56706 = DIRECTION ( 'NONE',  ( 0.000000000000000000, 0.000000000000000000, 1.000000000000000000 ) ) ;
#56707 = CARTESIAN_POINT ( 'NONE',  ( 16.51473224551083163, -9.474510206698727899, 60.83442372801900433 ) ) ;
#56708 = CARTESIAN_POINT ( 'NONE',  ( -5.049401038298153566, 19.05341960407611168, 105.2072429386476671 ) ) ;
#56709 = CARTESIAN_POINT ( 'NONE',  ( 13.97604488694527802, 13.89961937509977652, 79.37390960531435269 ) ) ;
#56710 = CARTESIAN_POINT ( 'NONE',  ( -8.224510206698948167, 14.34966873604960824, 40.41557627198103120 ) ) ;
#56711 = CARTESIAN_POINT ( 'NONE',  ( -18.67979575497178146, -10.72451020669898902, 31.66557627198102054 ) ) ;
#56712 = VECTOR ( 'NONE', #186081, 1000.000000000000114 ) ;
#56713 = CARTESIAN_POINT ( 'NONE',  ( 3.556970738554033499E-15, -38.81732327939057825, -2.624999997268812724 ) ) ;
#56714 = CARTESIAN_POINT ( 'NONE',  ( 17.50000000000000000, 5.499999999999992895, 56.70309617465829888 ) ) ;
#56715 = CARTESIAN_POINT ( 'NONE',  ( -18.67979575497193778, 10.72451020669871902, 113.3344237280190328 ) ) ;
#56716 = CARTESIAN_POINT ( 'NONE',  ( -27.67867608143706804, 7.698234437107397632, 161.8893175680488525 ) ) ;
#56717 = CARTESIAN_POINT ( 'NONE',  ( 9.474510206698971260, -16.51473224551069308, 32.91557627198102409 ) ) ;
#56718 = CARTESIAN_POINT ( 'NONE',  ( 5.153800228976335163, 19.02544592524342804, 24.79057627198102765 ) ) ;
#56719 = AXIS2_PLACEMENT_3D ( 'NONE', #162890, #54712, #190237 ) ;
#56720 = CARTESIAN_POINT ( 'NONE',  ( -33.98208146068709112, -4.940236926081948532, 92.55634382532309701 ) ) ;
#56721 = CARTESIAN_POINT ( 'NONE',  ( -10.81492255796105439, 18.62759615963255655, 67.91775706135234714 ) ) ;
#56722 = CARTESIAN_POINT ( 'NONE',  ( -9.776814272916249493, -36.00870872231931230, -7.999999999999998224 ) ) ;
#56723 = CARTESIAN_POINT ( 'NONE',  ( -14.29746914071037622, -8.314922557961029526, 69.16775706135234714 ) ) ;
#56725 = EDGE_CURVE ( 'NONE', #26126, #103419, #172755, .T. ) ;
#56724 = CARTESIAN_POINT ( 'NONE',  ( 21.52544592524344225, -5.823673210054117533, 83.54057627198102409 ) ) ;
#56726 = CARTESIAN_POINT ( 'NONE',  ( -16.53943276465976808, 0.05219959533911058130, 51.24890960531436690 ) ) ;
#56728 = CARTESIAN_POINT ( 'NONE',  ( 19.03943276465977164, -0.05219959533909143690, 113.7489096053143669 ) ) ;
#56727 = CARTESIAN_POINT ( 'NONE',  ( -9.474510206698964154, 16.51473224551069663, 25.41557627198103120 ) ) ;
#56729 = CARTESIAN_POINT ( 'NONE',  ( -21.53943276465977519, -0.05219959533937600094, 28.75109039468567929 ) ) ;
#56730 = CARTESIAN_POINT ( 'NONE',  ( 19.02544592524334988, 5.153800228976608722, 31.45942372801900433 ) ) ;
#56731 = CARTESIAN_POINT ( 'NONE',  ( -9.474510206698964154, 16.51473224551069663, 40.41557627198103120 ) ) ;
#56732 = CARTESIAN_POINT ( 'NONE',  ( -10.72451020669870658, -18.67979575497194134, 84.58442372801903275 ) ) ;
#56733 = DIRECTION ( 'NONE',  ( 0.000000000000000000, 0.000000000000000000, -1.000000000000000000 ) ) ;
#56734 = CARTESIAN_POINT ( 'NONE',  ( 16.52544592524342804, -4.483927247898539470, 23.54057627198102765 ) ) ;
#56735 = CARTESIAN_POINT ( 'NONE',  ( 36.91746824999999177, 11.99521256947799230, -2.024999997268813523 ) ) ;
#56736 = CARTESIAN_POINT ( 'NONE',  ( 15.72974639402199770, -15.80617190586745480, 43.12390960531435269 ) ) ;
#56737 = CARTESIAN_POINT ( 'NONE',  ( 14.34966873604960469, 8.224510206698951720, 99.16557627198100988 ) ) ;
#56738 = CARTESIAN_POINT ( 'NONE',  ( 17.41079204577542683, -36.66972510653776851, -18.74440029985508716 ) ) ;
#56739 = CARTESIAN_POINT ( 'NONE',  ( -5.049401038298153566, 19.05341960407611168, 95.20724293864770971 ) ) ;
#56740 = CARTESIAN_POINT ( 'NONE',  ( 16.55341960407611168, 4.379528057220329451, 93.95724293864770971 ) ) ;
#56741 = CARTESIAN_POINT ( 'NONE',  ( -16.46253265017146816, -9.564922557961047289, 104.1677570613523329 ) ) ;
#56742 = CARTESIAN_POINT ( 'NONE',  ( 10.81492255796078972, 18.62759615963270932, 59.58224293864770260 ) ) ;
#56743 = ORIENTED_EDGE ( 'NONE', *, *, #125362, .T. ) ;
#56744 = CARTESIAN_POINT ( 'NONE',  ( -13.97604488694527625, -13.89961937509977652, 26.87390960531434558 ) ) ;
#56746 = CARTESIAN_POINT ( 'NONE',  ( 0.05219959533907565091, 21.53943276465977519, 89.99890960531438111 ) ) ;
#56745 = CARTESIAN_POINT ( 'NONE',  ( -19.03943276465977164, 0.05219959533909376836, 81.24890960531436690 ) ) ;
#56748 = CARTESIAN_POINT ( 'NONE',  ( 16.51473224551069308, 9.474510206698969483, 84.16557627198102409 ) ) ;
#56747 = CARTESIAN_POINT ( 'NONE',  ( 12.14591786802327356, -12.06949235617739191, 110.6260903946857042 ) ) ;
#56749 = CARTESIAN_POINT ( 'NONE',  ( -0.05219959533936034679, 19.03943276465977164, 77.50109039468566152 ) ) ;
#56750 = CARTESIAN_POINT ( 'NONE',  ( -21.53943276465977519, -0.05219959533937600094, 88.75109039468567573 ) ) ;
#56751 = CARTESIAN_POINT ( 'NONE',  ( -18.67979575497178146, -10.72451020669898902, 71.66557627198100988 ) ) ;
#56752 = CARTESIAN_POINT ( 'NONE',  ( -5.823673210054116645, -21.52544592524344225, 37.29057627198102409 ) ) ;
#56753 = CARTESIAN_POINT ( 'NONE',  ( -16.46253265017160317, 9.564922557960807481, 45.83224293864769550 ) ) ;
#56754 = CARTESIAN_POINT ( 'NONE',  ( -4.483927247898782831, 16.52544592524335698, 107.7094237280190328 ) ) ;
#56755 = CARTESIAN_POINT ( 'NONE',  ( -9.474510206698964154, 16.51473224551069663, 65.41557627198102409 ) ) ;
#56756 = DIRECTION ( 'NONE',  ( -3.469446951953611033E-15, 0.000000000000000000, -1.000000000000000000 ) ) ;
#56757 = CARTESIAN_POINT ( 'NONE',  ( -13.89961937509957401, -13.97604488694547875, 24.37609039468565442 ) ) ;
#56758 = CARTESIAN_POINT ( 'NONE',  ( -4.379528057220328563, 16.55341960407611168, 70.20724293864769550 ) ) ;
#56759 = CARTESIAN_POINT ( 'NONE',  ( -15.72974639402197994, 15.80617190586746368, 115.6239096053143669 ) ) ;
#56760 = CARTESIAN_POINT ( 'NONE',  ( 27.73933785331498569, 2.768321779492822058E-14, 142.3750000027311842 ) ) ;
#56761 = CARTESIAN_POINT ( 'NONE',  ( 18.67979575497178502, 10.72451020669898547, 54.16557627198103120 ) ) ;
#56762 = CARTESIAN_POINT ( 'NONE',  ( -16.52544592524335698, -4.483927247898792601, 93.95942372801903275 ) ) ;
#56763 = CARTESIAN_POINT ( 'NONE',  ( 16.52544592524342804, -4.483927247898539470, 108.5405762719810241 ) ) ;
#56764 = CARTESIAN_POINT ( 'NONE',  ( -13.89961937509977652, 13.97604488694528158, 70.62390960531432427 ) ) ;
#56765 = CARTESIAN_POINT ( 'NONE',  ( 16.53943276465976808, -0.05219959533910856209, 28.74890960531435624 ) ) ;
#56766 = CARTESIAN_POINT ( 'NONE',  ( -15.80617190586768217, 15.72974639402176855, 53.12609039468568284 ) ) ;
#56767 = CARTESIAN_POINT ( 'NONE',  ( 19.05341960407611168, 5.049401038298154454, 103.9572429386476671 ) ) ;
#56768 = CARTESIAN_POINT ( 'NONE',  ( 5.719274019375673035, 21.55341960407619339, 77.29275706135234714 ) ) ;
#56769 = CARTESIAN_POINT ( 'NONE',  ( -19.05341960407611168, -5.049401038298163336, 31.45724293864769550 ) ) ;
#56770 = CARTESIAN_POINT ( 'NONE',  ( 19.03943276465977164, -0.05219959533909143690, 33.74890960531435979 ) ) ;
#56771 = EDGE_LOOP ( 'NONE', ( #163725, #183501, #98509 ) ) ;
#56772 = CARTESIAN_POINT ( 'NONE',  ( -5.719274019375665041, -21.55341960407619695, 94.79275706135234714 ) ) ;
#56773 = CARTESIAN_POINT ( 'NONE',  ( -16.53943276465976808, -0.05219959533934237506, 53.75109039468568994 ) ) ;
#56774 = CARTESIAN_POINT ( 'NONE',  ( -21.53943276465977519, -0.05219959533937600094, 73.75109039468567573 ) ) ;
#56775 = CARTESIAN_POINT ( 'NONE',  ( 5.153800228976335163, 19.02544592524342804, 104.7905762719809957 ) ) ;
#56776 = VERTEX_POINT ( 'NONE', #73640 ) ;
#56777 = CARTESIAN_POINT ( 'NONE',  ( -13.89961937509957401, -13.97604488694547875, 79.37609039468567573 ) ) ;
#56778 = CARTESIAN_POINT ( 'NONE',  ( 21.55341960407619695, -5.719274019375665929, 51.04275706135234714 ) ) ;
#56779 = CARTESIAN_POINT ( 'NONE',  ( 14.34966873604972726, -8.224510206698740333, 25.83442372801901499 ) ) ;
#56780 = AXIS2_PLACEMENT_3D ( 'NONE', #136920, #180482, #106576 ) ;
#56781 = CARTESIAN_POINT ( 'NONE',  ( -16.46253265017146816, -9.564922557961047289, 79.16775706135234714 ) ) ;
#56782 = CARTESIAN_POINT ( 'NONE',  ( -5.049401038298153566, 19.05341960407611168, 55.20724293864769550 ) ) ;
#56783 = CARTESIAN_POINT ( 'NONE',  ( -16.51473224551082808, 9.474510206698731452, 93.33442372801900433 ) ) ;
#56784 = CARTESIAN_POINT ( 'NONE',  ( -4.483927247898782831, 16.52544592524335698, 112.7094237280190328 ) ) ;
#56785 = CARTESIAN_POINT ( 'NONE',  ( -19.05341960407617563, 5.049401038297882671, 83.54275706135233293 ) ) ;
#56786 = CARTESIAN_POINT ( 'NONE',  ( 4.379528057220339221, -16.55341960407611168, 37.70724293864769550 ) ) ;
#56787 = CARTESIAN_POINT ( 'NONE',  ( 19.02544592524334988, 5.153800228976608722, 66.45942372801899012 ) ) ;
#56788 = CARTESIAN_POINT ( 'NONE',  ( 4.379528057220092307, 16.55341960407617563, 57.29275706135234714 ) ) ;
#56789 = CARTESIAN_POINT ( 'NONE',  ( 19.03943276465977164, 0.05219959533936151252, 21.25109039468565797 ) ) ;
#56790 = CARTESIAN_POINT ( 'NONE',  ( 19.03943276465977164, -0.05219959533909143690, 28.74890960531435624 ) ) ;
#56791 = CARTESIAN_POINT ( 'NONE',  ( 5.049401038298161559, -19.05341960407611168, 42.70724293864767418 ) ) ;
#56792 = CARTESIAN_POINT ( 'NONE',  ( 8.224510206698742110, 14.34966873604972548, 42.08442372801901854 ) ) ;
#56793 = CARTESIAN_POINT ( 'NONE',  ( -15.45904554457977653, 25.28215873741137898, 139.9235714043273617 ) ) ;
#56794 = CARTESIAN_POINT ( 'NONE',  ( 22.44159573604009594, -16.30477369853687364, 147.6750000027311671 ) ) ;
#56795 = CARTESIAN_POINT ( 'NONE',  ( -9.564922557960796823, -16.46253265017161027, 97.08224293864769550 ) ) ;
#56796 = CARTESIAN_POINT ( 'NONE',  ( -31.99364916731038022, -5.510910596163089556E-15, 47.64999999999999147 ) ) ;
#56797 = ORIENTED_EDGE ( 'NONE', *, *, #630, .T. ) ;
#56798 = CARTESIAN_POINT ( 'NONE',  ( 9.564922557961047289, -16.46253265017146816, 95.41775706135233293 ) ) ;
#56799 = CARTESIAN_POINT ( 'NONE',  ( 10.81492255796078972, 18.62759615963270932, 34.58224293864770260 ) ) ;
#56801 = CARTESIAN_POINT ( 'NONE',  ( 16.52544592524335698, 4.483927247898782831, 21.45942372801901499 ) ) ;
#56800 = CARTESIAN_POINT ( 'NONE',  ( -19.03943276465977164, -0.05219959533935918106, 33.75109039468566863 ) ) ;
#56802 = CARTESIAN_POINT ( 'NONE',  ( -16.53943276465976808, 0.05219959533911058130, 106.2489096053143811 ) ) ;
#56803 = CARTESIAN_POINT ( 'NONE',  ( 16.46253265017160672, -9.564922557960803928, 38.33224293864768839 ) ) ;
#56804 = CARTESIAN_POINT ( 'NONE',  ( -15.72974639402197994, 15.80617190586746368, 70.62390960531436690 ) ) ;
#56805 = CARTESIAN_POINT ( 'NONE',  ( -19.05341960407611168, -5.049401038298163336, 31.45724293864769550 ) ) ;
#56806 = CARTESIAN_POINT ( 'NONE',  ( -22.44159573604009950, -16.30477369853688430, 141.5750000027311728 ) ) ;
#56807 = CARTESIAN_POINT ( 'NONE',  ( -19.03943276465977164, -0.05219959533935918106, 68.75109039468566152 ) ) ;
#56808 = CARTESIAN_POINT ( 'NONE',  ( 12.06949235617757843, -12.14591786802309237, 48.12390960531436690 ) ) ;
#56809 = CARTESIAN_POINT ( 'NONE',  ( 10.81492255796078972, 18.62759615963270932, 39.58224293864769550 ) ) ;
#56810 = CARTESIAN_POINT ( 'NONE',  ( -18.67979575497193778, 10.72451020669871902, 88.33442372801901854 ) ) ;
#56811 = CARTESIAN_POINT ( 'NONE',  ( 18.67979575497178502, 10.72451020669898547, 79.16557627198103830 ) ) ;
#56812 = CARTESIAN_POINT ( 'NONE',  ( -21.55341960407619339, 5.719274019375674811, 73.54275706135234714 ) ) ;
#56813 = CARTESIAN_POINT ( 'NONE',  ( -10.72451020669870658, -18.67979575497194134, 59.58442372801901854 ) ) ;
#56814 = CARTESIAN_POINT ( 'NONE',  ( -19.05341960407611168, -5.049401038298163336, 101.4572429386476955 ) ) ;
#56816 = CARTESIAN_POINT ( 'NONE',  ( 5.719274019375673035, 21.55341960407619339, 67.29275706135234714 ) ) ;
#56815 = CARTESIAN_POINT ( 'NONE',  ( -0.05219959533934338120, 16.53943276465976808, 107.5010903946856899 ) ) ;
#56817 = CARTESIAN_POINT ( 'NONE',  ( 9.474510206698971260, -16.51473224551069308, 52.91557627198102409 ) ) ;
#56818 = CARTESIAN_POINT ( 'NONE',  ( 15.80617190586769283, -15.72974639402175789, 30.62609039468567929 ) ) ;
#56819 = CARTESIAN_POINT ( 'NONE',  ( 13.89961937509977652, -13.97604488694527269, 63.12390960531435979 ) ) ;
#56820 = CARTESIAN_POINT ( 'NONE',  ( -16.52544592524342804, 4.483927247898546575, 86.04057627198102409 ) ) ;
#56821 = CARTESIAN_POINT ( 'NONE',  ( 4.379528057220339221, -16.55341960407611168, 52.70724293864769550 ) ) ;
#56822 = CARTESIAN_POINT ( 'NONE',  ( -18.62759615963270932, 10.81492255796079327, 55.83224293864770260 ) ) ;
#56823 = CARTESIAN_POINT ( 'NONE',  ( 13.89961937509977652, -13.97604488694527269, 43.12390960531434558 ) ) ;
#56824 = CARTESIAN_POINT ( 'NONE',  ( 21.55341960407610458, 5.719274019375980345, 53.95724293864770260 ) ) ;
#56825 = CARTESIAN_POINT ( 'NONE',  ( -0.05219959533936034679, 19.03943276465977164, 57.50109039468566863 ) ) ;
#56827 = CARTESIAN_POINT ( 'NONE',  ( -4.483927247898539470, -16.52544592524342804, 62.29057627198102409 ) ) ;
#56826 = CARTESIAN_POINT ( 'NONE',  ( -19.05341960407617918, 5.049401038297883559, 23.54275706135233648 ) ) ;
#56828 = CARTESIAN_POINT ( 'NONE',  ( 5.823673210054125526, 21.52544592524343514, 39.79057627198103830 ) ) ;
#56829 = ORIENTED_EDGE ( 'NONE', *, *, #100974, .T. ) ;
#56830 = CYLINDRICAL_SURFACE ( 'NONE', #56069, 28.82186960331498682 ) ;
#56832 = CARTESIAN_POINT ( 'NONE',  ( -5.359611314223446995E-15, 29.16686587814335851, 140.8750000027311842 ) ) ;
#56831 = CARTESIAN_POINT ( 'NONE',  ( 12.06949235617739724, 12.14591786802326823, 86.87609039468568994 ) ) ;
#56833 = CARTESIAN_POINT ( 'NONE',  ( 13.97604488694548053, -13.89961937509957401, 85.62609039468568994 ) ) ;
#56834 = CARTESIAN_POINT ( 'NONE',  ( -16.55341960407611168, -4.379528057220339221, 56.45724293864768839 ) ) ;
#56835 = CARTESIAN_POINT ( 'NONE',  ( -19.49671883438228193, -5.499999999999978684, 59.89279849105680853 ) ) ;
#56836 = CARTESIAN_POINT ( 'NONE',  ( 19.03943276465977164, -0.05219959533909143690, 48.74890960531435979 ) ) ;
#56837 = CARTESIAN_POINT ( 'NONE',  ( -16.55341960407611168, -4.379528057220339221, 46.45724293864769550 ) ) ;
#56838 = CARTESIAN_POINT ( 'NONE',  ( 13.89961937509977652, -13.97604488694527269, 93.12390960531436690 ) ) ;
#56839 = CARTESIAN_POINT ( 'NONE',  ( -13.89961937509977652, 13.97604488694528158, 55.62390960531434558 ) ) ;
#56840 = CARTESIAN_POINT ( 'NONE',  ( 5.719274019375673035, 21.55341960407619339, 57.29275706135234714 ) ) ;
#56841 = CARTESIAN_POINT ( 'NONE',  ( -9.564922557960796823, -16.46253265017161027, 72.08224293864770971 ) ) ;
#56842 = CARTESIAN_POINT ( 'NONE',  ( 9.474510206698971260, -16.51473224551069308, 32.91557627198102409 ) ) ;
#56843 = CARTESIAN_POINT ( 'NONE',  ( 9.474510206698971260, -16.51473224551069308, 57.91557627198103120 ) ) ;
#56844 = CARTESIAN_POINT ( 'NONE',  ( 5.719274019375991003, -21.55341960407610458, 52.70724293864769550 ) ) ;
#56845 = CARTESIAN_POINT ( 'NONE',  ( 5.153800228976335163, 19.02544592524342804, 29.79057627198102409 ) ) ;
#56846 = CARTESIAN_POINT ( 'NONE',  ( 10.81492255796078972, 18.62759615963270932, 39.58224293864769550 ) ) ;
#56847 = CARTESIAN_POINT ( 'NONE',  ( 12.06949235617739724, 12.14591786802326823, 101.8760903946857042 ) ) ;
#56848 = EDGE_CURVE ( 'NONE', #191847, #122157, #82372, .T. ) ;
#56849 = CARTESIAN_POINT ( 'NONE',  ( -16.46253265017146816, -9.564922557961047289, 19.16775706135233293 ) ) ;
#56851 = CARTESIAN_POINT ( 'NONE',  ( 4.379528057220092307, 16.55341960407617563, 77.29275706135234714 ) ) ;
#56850 = CARTESIAN_POINT ( 'NONE',  ( 16.55341960407618274, -4.379528057220086978, 41.04275706135236135 ) ) ;
#56852 = CARTESIAN_POINT ( 'NONE',  ( 2.973862142520690366, -93.04182470242774627, -25.00000000000000000 ) ) ;
#56853 = CARTESIAN_POINT ( 'NONE',  ( -16.55341960407617563, 4.379528057220093196, 68.54275706135234714 ) ) ;
#56854 = CARTESIAN_POINT ( 'NONE',  ( -14.29746914071037622, -8.314922557961029526, 54.16775706135235424 ) ) ;
#56855 = CARTESIAN_POINT ( 'NONE',  ( 13.89961937509977652, -13.97604488694527269, 108.1239096053143669 ) ) ;
#56856 = CARTESIAN_POINT ( 'NONE',  ( -9.474510206698964154, 16.51473224551069663, 30.41557627198102054 ) ) ;
#56857 = CARTESIAN_POINT ( 'NONE',  ( 8.224510206698742110, 14.34966873604972548, 32.08442372801901854 ) ) ;
#56858 = CARTESIAN_POINT ( 'NONE',  ( -5.049401038298153566, 19.05341960407611168, 45.20724293864769550 ) ) ;
#56859 = CARTESIAN_POINT ( 'NONE',  ( 21.53943276465977519, 0.05219959533937863772, 31.25109039468568639 ) ) ;
#56860 = CARTESIAN_POINT ( 'NONE',  ( 16.52544592524335698, 4.483927247898782831, 41.45942372801901143 ) ) ;
#56861 = CARTESIAN_POINT ( 'NONE',  ( 16.53943276465976808, 0.05219959533934440121, 101.2510903946856757 ) ) ;
#56862 = CARTESIAN_POINT ( 'NONE',  ( -7.284589286804265207, -1.784589286804211916, 1.818019484660534424 ) ) ;
#56863 = CARTESIAN_POINT ( 'NONE',  ( -10.81492255796105439, 18.62759615963255655, 102.9177570613523756 ) ) ;
#56864 = CARTESIAN_POINT ( 'NONE',  ( -13.97604488694547697, 13.89961937509957934, 103.1260903946856473 ) ) ;
#56865 = CARTESIAN_POINT ( 'NONE',  ( 16.52544592524342804, -4.483927247898539470, 53.54057627198103120 ) ) ;
#56866 = CARTESIAN_POINT ( 'NONE',  ( -5.153800228976328057, -19.02544592524343514, 27.29057627198103120 ) ) ;
#56868 = CARTESIAN_POINT ( 'NONE',  ( 17.05587630539706012, -6.762274262136750203, 58.24180309037282655 ) ) ;
#56867 = CARTESIAN_POINT ( 'NONE',  ( -19.03943276465977164, -0.05219959533935918106, 58.75109039468566863 ) ) ;
#56869 = CARTESIAN_POINT ( 'NONE',  ( 21.52544592524334988, 5.823673210054432836, 61.45942372801901854 ) ) ;
#56870 = CARTESIAN_POINT ( 'NONE',  ( -12.14591786802326823, 12.06949235617739902, 28.12609039468568284 ) ) ;
#56871 = DIRECTION ( 'NONE',  ( 0.7071067811865467956, -7.406550393246786959E-15, 0.7071067811865483499 ) ) ;
#56872 = CARTESIAN_POINT ( 'NONE',  ( 10.72451020669898902, -18.67979575497178502, 27.91557627198103830 ) ) ;
#56873 = CARTESIAN_POINT ( 'NONE',  ( -19.05341960407617563, 5.049401038297882671, 113.5427570613523471 ) ) ;
#56874 = CARTESIAN_POINT ( 'NONE',  ( 23.31738231874054534, 16.94106989632529192, 147.1999999999999886 ) ) ;
#56875 = CARTESIAN_POINT ( 'NONE',  ( -25.66129429279789065, 9.008087060820807679, 171.3163768196993715 ) ) ;
#56876 = CARTESIAN_POINT ( 'NONE',  ( 16.51473224551069308, 9.474510206698969483, 24.16557627198102765 ) ) ;
#56877 = CARTESIAN_POINT ( 'NONE',  ( -5.823673210054431948, 21.52544592524334988, 102.7094237280190185 ) ) ;
#56878 = CARTESIAN_POINT ( 'NONE',  ( -19.02544592524342804, 5.153800228976336051, 46.04057627198101699 ) ) ;
#56879 = AXIS2_PLACEMENT_3D ( 'NONE', #80792, #171828, #34306 ) ;
#56880 = CARTESIAN_POINT ( 'NONE',  ( -10.81492255796105439, 18.62759615963255655, 62.91775706135236135 ) ) ;
#56881 = CARTESIAN_POINT ( 'NONE',  ( -5.719274019375665041, -21.55341960407619695, 99.79275706135234714 ) ) ;
#56882 = CARTESIAN_POINT ( 'NONE',  ( 4.379528057220092307, 16.55341960407617563, 102.2927570613523613 ) ) ;
#56883 = CARTESIAN_POINT ( 'NONE',  ( -13.89961937509977652, 13.97604488694528158, 75.62390960531438111 ) ) ;
#56884 = CARTESIAN_POINT ( 'NONE',  ( -15.72974639402176322, -15.80617190586768395, 59.37609039468568284 ) ) ;
#56885 = CARTESIAN_POINT ( 'NONE',  ( -15.72974639402176322, -15.80617190586768395, 54.37609039468568994 ) ) ;
#56887 = CARTESIAN_POINT ( 'NONE',  ( -0.05219959533909027116, -19.03943276465977164, 97.49890960531436690 ) ) ;
#56886 = CARTESIAN_POINT ( 'NONE',  ( -9.474510206698720793, -16.51473224551083518, 74.58442372801900433 ) ) ;
#56888 = CARTESIAN_POINT ( 'NONE',  ( 9.564922557960805705, 16.46253265017160317, 24.58224293864769194 ) ) ;
#56889 = CARTESIAN_POINT ( 'NONE',  ( -21.52544592524343514, 5.823673210054127303, 91.04057627198103830 ) ) ;
#56890 = CARTESIAN_POINT ( 'NONE',  ( -5.823673210054431948, 21.52544592524334988, 112.7094237280190328 ) ) ;
#56891 = CARTESIAN_POINT ( 'NONE',  ( 8.314922557960818139, 14.29746914071049879, 94.58224293864769550 ) ) ;
#56892 = CARTESIAN_POINT ( 'NONE',  ( -19.02544592524342804, 5.153800228976336051, 46.04057627198101699 ) ) ;
#56893 = CARTESIAN_POINT ( 'NONE',  ( -19.02544592524334988, -5.153800228976617603, 78.95942372801900433 ) ) ;
#56894 = CARTESIAN_POINT ( 'NONE',  ( 14.34966873604960469, 8.224510206698951720, 59.16557627198103120 ) ) ;
#56895 = CARTESIAN_POINT ( 'NONE',  ( -18.67979575497193778, 10.72451020669871902, 108.3344237280190185 ) ) ;
#56896 = CARTESIAN_POINT ( 'NONE',  ( 19.03943276465977164, -0.05219959533909143690, 108.7489096053143527 ) ) ;
#56897 = CARTESIAN_POINT ( 'NONE',  ( 9.474510206698729675, 16.51473224551082808, 77.08442372801900433 ) ) ;
#56898 = CARTESIAN_POINT ( 'NONE',  ( 15.72974639402199770, -15.80617190586745480, 73.12390960531436690 ) ) ;
#56899 = CARTESIAN_POINT ( 'NONE',  ( 21.52544592524334988, 5.823673210054432836, 26.45942372801901854 ) ) ;
#56900 = CARTESIAN_POINT ( 'NONE',  ( -16.55341960407617563, 4.379528057220093196, 23.54275706135235424 ) ) ;
#56901 = CARTESIAN_POINT ( 'NONE',  ( -12.06949235617739369, -12.14591786802326823, 99.37609039468568994 ) ) ;
#56903 = CARTESIAN_POINT ( 'NONE',  ( 5.823673210054444382, -21.52544592524334988, 35.20942372801901854 ) ) ;
#56902 = CARTESIAN_POINT ( 'NONE',  ( 16.52544592524335698, 4.483927247898782831, 41.45942372801901143 ) ) ;
#56904 = CARTESIAN_POINT ( 'NONE',  ( 10.81492255796078972, 18.62759615963270932, 44.58224293864769550 ) ) ;
#56905 = CARTESIAN_POINT ( 'NONE',  ( -9.564922557960796823, -16.46253265017161027, 37.08224293864768839 ) ) ;
#56906 = CARTESIAN_POINT ( 'NONE',  ( 29.86685920354754487, 21.69954338932564752, -1.924999997268813212 ) ) ;
#56907 = CARTESIAN_POINT ( 'NONE',  ( -0.05219959533934338120, 16.53943276465976808, 57.50109039468568994 ) ) ;
#56908 = CARTESIAN_POINT ( 'NONE',  ( -5.719274019375978568, 21.55341960407610458, 90.20724293864770971 ) ) ;
#56909 = CARTESIAN_POINT ( 'NONE',  ( -4.483927247898539470, -16.52544592524342804, 27.29057627198103120 ) ) ;
#56910 = CARTESIAN_POINT ( 'NONE',  ( -12.14591786802326823, 12.06949235617739902, 43.12609039468568284 ) ) ;
#56911 = CARTESIAN_POINT ( 'NONE',  ( -16.51473224551069308, -9.474510206698971260, 56.66557627198103120 ) ) ;
#56912 = CARTESIAN_POINT ( 'NONE',  ( -16.55341960407617563, 4.379528057220093196, 88.54275706135236135 ) ) ;
#56913 = CARTESIAN_POINT ( 'NONE',  ( -5.049401038297874678, -19.05341960407617918, 89.79275706135230450 ) ) ;
#56914 = CARTESIAN_POINT ( 'NONE',  ( 18.62759615963271287, -10.81492255796078972, 88.33224293864769550 ) ) ;
#56915 = CARTESIAN_POINT ( 'NONE',  ( -4.483927247898539470, -16.52544592524342804, 27.29057627198103120 ) ) ;
#56916 = EDGE_LOOP ( 'NONE', ( #191296, #145144, #181510, #9977, #174148 ) ) ;
#56917 = CARTESIAN_POINT ( 'NONE',  ( 21.47376810973061723, 7.452933495370294814, 174.2084625793499981 ) ) ;
#56918 = CARTESIAN_POINT ( 'NONE',  ( 0.05219959533907565091, 21.53943276465977519, 54.99890960531435269 ) ) ;
#56919 = VERTEX_POINT ( 'NONE', #149469 ) ;
#56920 = CARTESIAN_POINT ( 'NONE',  ( -4.379528057220086978, -16.55341960407618274, 104.7927570613523898 ) ) ;
#56921 = ORIENTED_EDGE ( 'NONE', *, *, #182692, .F. ) ;
#56922 = CARTESIAN_POINT ( 'NONE',  ( 18.62759615963271287, -10.81492255796078972, 33.33224293864769550 ) ) ;
#56923 = CARTESIAN_POINT ( 'NONE',  ( -15.72974639402197994, 15.80617190586746368, 90.62390960531436690 ) ) ;
#56924 = AXIS2_PLACEMENT_3D ( 'NONE', #126630, #33644, #34635 ) ;
#56925 = CARTESIAN_POINT ( 'NONE',  ( -14.34966873604960291, -8.224510206698953496, 21.66557627198102409 ) ) ;
#56926 = CARTESIAN_POINT ( 'NONE',  ( 12.14591786802327356, -12.06949235617739191, 40.62609039468567573 ) ) ;
#56927 = CARTESIAN_POINT ( 'NONE',  ( -13.89961937509977652, 13.97604488694528158, 30.62390960531435269 ) ) ;
#56928 = CARTESIAN_POINT ( 'NONE',  ( 8.224510206698742110, 14.34966873604972548, 27.08442372801901854 ) ) ;
#56929 = CARTESIAN_POINT ( 'NONE',  ( 19.03943276465977164, -0.05219959533909143690, 58.74890960531435979 ) ) ;
#56930 = ADVANCED_FACE ( 'NONE', ( #102962 ), #197964, .F. ) ;
#56931 = CARTESIAN_POINT ( 'NONE',  ( -5.359611314223446995E-15, 29.16686587814335496, 140.8750000027311842 ) ) ;
#56932 = CARTESIAN_POINT ( 'NONE',  ( 16.46253265017160672, -9.564922557960803928, 108.3322429386476955 ) ) ;
#56933 = CARTESIAN_POINT ( 'NONE',  ( 16.46253265017160672, -9.564922557960803928, 113.3322429386476955 ) ) ;
#56934 = CARTESIAN_POINT ( 'NONE',  ( 14.29746914071037800, 8.314922557961029526, 96.66775706135234714 ) ) ;
#56935 = CARTESIAN_POINT ( 'NONE',  ( 19.02544592524334988, 5.153800228976608722, 96.45942372801897591 ) ) ;
#56936 = CARTESIAN_POINT ( 'NONE',  ( -19.02544592524334988, -5.153800228976617603, 43.95942372801899012 ) ) ;
#56937 = CARTESIAN_POINT ( 'NONE',  ( 5.719274019375991003, -21.55341960407610458, 77.70724293864770971 ) ) ;
#56938 = CARTESIAN_POINT ( 'NONE',  ( -14.34966873604972548, 8.224510206698743886, 98.33442372801901854 ) ) ;
#56939 = CARTESIAN_POINT ( 'NONE',  ( -18.67979575497178146, -10.72451020669898902, 26.66557627198103475 ) ) ;
#56940 = CARTESIAN_POINT ( 'NONE',  ( 5.049401038297881783, 19.05341960407617563, 102.2927570613523045 ) ) ;
#56941 = CARTESIAN_POINT ( 'NONE',  ( 0.05219959533909260263, 19.03943276465977164, 109.9989096053143669 ) ) ;
#56942 = CARTESIAN_POINT ( 'NONE',  ( -21.52544592524334988, -5.823673210054445271, 58.95942372801902565 ) ) ;
#56943 = CARTESIAN_POINT ( 'NONE',  ( -5.153800228976328057, -19.02544592524343514, 62.29057627198100988 ) ) ;
#56944 = CARTESIAN_POINT ( 'NONE',  ( -14.29746914071049879, 8.314922557960819915, 100.8322429386477097 ) ) ;
#56945 = CARTESIAN_POINT ( 'NONE',  ( 32.00000000000000000, -1.163414459189985801E-14, 95.00000000000000000 ) ) ;
#56946 = CARTESIAN_POINT ( 'NONE',  ( 14.29746914071049879, -8.314922557960816363, 83.33224293864769550 ) ) ;
#56947 = VERTEX_POINT ( 'NONE', #44284 ) ;
#56948 = CARTESIAN_POINT ( 'NONE',  ( 13.97604488694548053, -13.89961937509957401, 85.62609039468568994 ) ) ;
#56949 = CARTESIAN_POINT ( 'NONE',  ( 19.25918095147779496, 5.499999999999526601, 91.95284276293935477 ) ) ;
#56950 = CARTESIAN_POINT ( 'NONE',  ( 16.46253265017160672, -9.564922557960803928, 63.33224293864769550 ) ) ;
#56951 = CARTESIAN_POINT ( 'NONE',  ( 16.31925111598410183, -7.325300261831686477, 72.66424538967171998 ) ) ;
#56953 = CARTESIAN_POINT ( 'NONE',  ( 19.05341960407611168, 5.049401038298154454, 83.95724293864766707 ) ) ;
#56952 = CARTESIAN_POINT ( 'NONE',  ( -5.153800228976328057, -19.02544592524343514, 77.29057627198099567 ) ) ;
#56954 = CARTESIAN_POINT ( 'NONE',  ( -12.06949235617739369, -12.14591786802326823, 69.37609039468567573 ) ) ;
#56955 = CARTESIAN_POINT ( 'NONE',  ( -21.87067081123533541, 5.494950430485542547, 173.7269556299028750 ) ) ;
#56956 = CARTESIAN_POINT ( 'NONE',  ( -5.153800228976607833, 19.02544592524334988, 37.70942372801899722 ) ) ;
#56957 = CARTESIAN_POINT ( 'NONE',  ( 36.84755799831103928, 2.910846538911452619, 49.67009533327786386 ) ) ;
#56958 = CARTESIAN_POINT ( 'NONE',  ( -5.049401038298153566, 19.05341960407611168, 110.2072429386476671 ) ) ;
#56959 = CARTESIAN_POINT ( 'NONE',  ( 8.224510206698742110, 14.34966873604972548, 107.0844237280190043 ) ) ;
#56960 = CARTESIAN_POINT ( 'NONE',  ( -34.38690502837285123, -7.455999864800775256, 45.95008414374198225 ) ) ;
#56961 = CARTESIAN_POINT ( 'NONE',  ( -4.483927247898782831, 16.52544592524335698, 97.70942372801904696 ) ) ;
#56962 = CARTESIAN_POINT ( 'NONE',  ( -16.19135201231369692, 7.376712067591784106, 29.81319145947969673 ) ) ;
#56963 = CARTESIAN_POINT ( 'NONE',  ( -4.483927247898782831, 16.52544592524335698, 72.70942372801901854 ) ) ;
#56964 = CARTESIAN_POINT ( 'NONE',  ( -4.500000000000001776, -125.7396439921083555, 8.159758652193113804 ) ) ;
#56965 = CARTESIAN_POINT ( 'NONE',  ( -0.05219959533937732626, 21.53943276465977519, 82.50109039468568994 ) ) ;
#56966 = CARTESIAN_POINT ( 'NONE',  ( -13.97604488694547697, 13.89961937509957934, 83.12609039468564731 ) ) ;
#56967 = CARTESIAN_POINT ( 'NONE',  ( 5.049401038297881783, 19.05341960407617563, 32.29275706135233293 ) ) ;
#56968 = CARTESIAN_POINT ( 'NONE',  ( -13.89961937509977652, 13.97604488694528158, 60.62390960531436690 ) ) ;
#56969 = CARTESIAN_POINT ( 'NONE',  ( 13.89961937509977652, -13.97604488694527269, 43.12390960531434558 ) ) ;
#56970 = CARTESIAN_POINT ( 'NONE',  ( -27.86273085795036408, -28.69962071417357663, 0.000000000000000000 ) ) ;
#56971 = CARTESIAN_POINT ( 'NONE',  ( -18.67979575497178146, -10.72451020669898902, 81.66557627198103830 ) ) ;
#56972 = CARTESIAN_POINT ( 'NONE',  ( 15.72974639402199770, -15.80617190586745480, 28.12390960531435979 ) ) ;
#56973 = CARTESIAN_POINT ( 'NONE',  ( 19.05341960407611168, 5.049401038298154454, 33.95724293864769550 ) ) ;
#56974 = CARTESIAN_POINT ( 'NONE',  ( 8.314922557961029526, -14.29746914071037800, 55.41775706135234714 ) ) ;
#56975 = ORIENTED_EDGE ( 'NONE', *, *, #11642, .T. ) ;
#56976 = CARTESIAN_POINT ( 'NONE',  ( 21.55341960407619695, -5.719274019375665929, 31.04275706135234714 ) ) ;
#56978 = CARTESIAN_POINT ( 'NONE',  ( 11.40812507854755253, -35.11059874428192273, -10.02499999726881441 ) ) ;
#56977 = CARTESIAN_POINT ( 'NONE',  ( -16.52544592524342804, 4.483927247898546575, 56.04057627198102409 ) ) ;
#56979 = CARTESIAN_POINT ( 'NONE',  ( 0.05219959533934541429, -16.53943276465976808, 30.00109039468568284 ) ) ;
#56980 = CARTESIAN_POINT ( 'NONE',  ( -9.564922557961040184, 16.46253265017147172, 42.91775706135234003 ) ) ;
#56981 = CARTESIAN_POINT ( 'NONE',  ( 14.34966873604960469, 8.224510206698951720, 54.16557627198103120 ) ) ;
#56982 = CARTESIAN_POINT ( 'NONE',  ( 10.81492255796106328, -18.62759615963255655, 20.41775706135234714 ) ) ;
#56984 = CARTESIAN_POINT ( 'NONE',  ( -21.55341960407610458, -5.719274019375992779, 76.45724293864769550 ) ) ;
#56983 = CARTESIAN_POINT ( 'NONE',  ( 1.221313414957698099E-14, -31.90000000000003411, -49.13275782002545355 ) ) ;
#56985 = CARTESIAN_POINT ( 'NONE',  ( 19.05341960407611168, 5.049401038298154454, 88.95724293864769550 ) ) ;
#56986 = CARTESIAN_POINT ( 'NONE',  ( -16.52544592524342804, 4.483927247898546575, 61.04057627198103120 ) ) ;
#56987 = CARTESIAN_POINT ( 'NONE',  ( -13.89961937509977652, 13.97604488694528158, 110.6239096053143243 ) ) ;
#56988 = CARTESIAN_POINT ( 'NONE',  ( 2.973862142520690366, -93.04182470242774627, -13.00000000000000000 ) ) ;
#56989 = CARTESIAN_POINT ( 'NONE',  ( 16.51473224551083163, -9.474510206698727899, 70.83442372801900433 ) ) ;
#56990 = CARTESIAN_POINT ( 'NONE',  ( 5.719274019375991003, -21.55341960407610458, 112.7072429386476955 ) ) ;
#56991 = CARTESIAN_POINT ( 'NONE',  ( -19.03943276465977164, 0.05219959533909376836, 56.24890960531435979 ) ) ;
#56992 = CARTESIAN_POINT ( 'NONE',  ( -5.049401038297874678, -19.05341960407617918, 49.79275706135231871 ) ) ;
#56993 = CARTESIAN_POINT ( 'NONE',  ( 12.06949235617757843, -12.14591786802309237, 108.1239096053143811 ) ) ;
#56994 = CARTESIAN_POINT ( 'NONE',  ( 10.81492255796106328, -18.62759615963255655, 60.41775706135235424 ) ) ;
#56995 = CARTESIAN_POINT ( 'NONE',  ( -17.31747979337951548, -6.344076630960985064, 71.37944868065186199 ) ) ;
#56996 = CARTESIAN_POINT ( 'NONE',  ( -16.55341960407611168, -4.379528057220339221, 36.45724293864768839 ) ) ;
#56997 = CARTESIAN_POINT ( 'NONE',  ( 13.97604488694527802, 13.89961937509977652, 69.37390960531436690 ) ) ;
#56998 = CARTESIAN_POINT ( 'NONE',  ( 10.81492255796078972, 18.62759615963270932, 79.58224293864769550 ) ) ;
#56999 = CARTESIAN_POINT ( 'NONE',  ( 27.73933785331498925, -9.013057229001033122, 143.7750000027311614 ) ) ;
#57000 = CARTESIAN_POINT ( 'NONE',  ( -19.02544592524342804, 5.153800228976336051, 46.04057627198101699 ) ) ;
#57001 = ORIENTED_EDGE ( 'NONE', *, *, #105079, .F. ) ;
#57002 = CARTESIAN_POINT ( 'NONE',  ( 21.55341960407610458, 5.719274019375980345, 63.95724293864770260 ) ) ;
#57003 = ORIENTED_EDGE ( 'NONE', *, *, #137018, .T. ) ;
#57004 = CARTESIAN_POINT ( 'NONE',  ( 5.823673210054444382, -21.52544592524334988, 100.2094237280190043 ) ) ;
#57007 = CARTESIAN_POINT ( 'NONE',  ( 16.55341960407611168, 4.379528057220329451, 78.95724293864769550 ) ) ;
#57006 = CARTESIAN_POINT ( 'NONE',  ( 12.06949235617739724, 12.14591786802326823, 96.87609039468568994 ) ) ;
#57005 = CARTESIAN_POINT ( 'NONE',  ( -15.49999999999999822, 5.499999999999998224, 20.00000000000000000 ) ) ;
#57008 = CARTESIAN_POINT ( 'NONE',  ( -16.46253265017160317, 9.564922557960807481, 75.83224293864769550 ) ) ;
#57009 = ORIENTED_EDGE ( 'NONE', *, *, #152340, .T. ) ;
#57010 = CARTESIAN_POINT ( 'NONE',  ( 9.474510206698729675, 16.51473224551082808, 37.08442372801899722 ) ) ;
#57011 = CARTESIAN_POINT ( 'NONE',  ( -16.52544592524335698, -4.483927247898792601, 93.95942372801903275 ) ) ;
#57012 = CARTESIAN_POINT ( 'NONE',  ( -16.51473224551082808, 9.474510206698731452, 28.33442372801900433 ) ) ;
#57013 = CARTESIAN_POINT ( 'NONE',  ( -13.89961937509977652, 13.97604488694528158, 90.62390960531432427 ) ) ;
#57014 = CARTESIAN_POINT ( 'NONE',  ( 10.81492255796078972, 18.62759615963270932, 44.58224293864769550 ) ) ;
#57015 = CARTESIAN_POINT ( 'NONE',  ( 27.12243378312305708, -3.972435522077897296, 169.3718635229811014 ) ) ;
#57016 = CARTESIAN_POINT ( 'NONE',  ( 0.05219959533909260263, 19.03943276465977164, 24.99890960531435269 ) ) ;
#57017 = CARTESIAN_POINT ( 'NONE',  ( -15.80617190586768217, 15.72974639402176855, 93.12609039468568994 ) ) ;
#57018 = CARTESIAN_POINT ( 'NONE',  ( 12.06949235617739724, 12.14591786802326823, 66.87609039468568994 ) ) ;
#57019 = CARTESIAN_POINT ( 'NONE',  ( 5.823673210054125526, 21.52544592524343514, 114.7905762719810383 ) ) ;
#57020 = CARTESIAN_POINT ( 'NONE',  ( -16.55341960407617563, 4.379528057220093196, 28.54275706135234358 ) ) ;
#57021 = CARTESIAN_POINT ( 'NONE',  ( -13.97604488694527625, -13.89961937509977652, 96.87390960531433848 ) ) ;
#57022 = CARTESIAN_POINT ( 'NONE',  ( -16.46253265017160317, 9.564922557960807481, 45.83224293864769550 ) ) ;
#57023 = CARTESIAN_POINT ( 'NONE',  ( 13.89961937509977652, -13.97604488694527269, 48.12390960531435979 ) ) ;
#57024 = AXIS2_PLACEMENT_3D ( 'NONE', #149860, #26532, #104351 ) ;
#57025 = CARTESIAN_POINT ( 'NONE',  ( 16.53943276465976808, 0.05219959533934440121, 31.25109039468568639 ) ) ;
#57026 = CARTESIAN_POINT ( 'NONE',  ( 16.52544592524342804, -4.483927247898539470, 98.54057627198105251 ) ) ;
#57027 = CARTESIAN_POINT ( 'NONE',  ( 8.314922557961029526, -14.29746914071037800, 105.4177570613523613 ) ) ;
#57030 = CARTESIAN_POINT ( 'NONE',  ( 5.049401038298161559, -19.05341960407611168, 52.70724293864767418 ) ) ;
#57029 = CARTESIAN_POINT ( 'NONE',  ( 19.05341960407611168, 5.049401038298154454, 78.95724293864769550 ) ) ;
#57028 = CARTESIAN_POINT ( 'NONE',  ( 15.72974639402176855, 15.80617190586768217, 46.87609039468568994 ) ) ;
#57031 = CARTESIAN_POINT ( 'NONE',  ( 9.474510206698971260, -16.51473224551069308, 87.91557627198102409 ) ) ;
#57032 = CARTESIAN_POINT ( 'NONE',  ( 16.52544592524342804, -4.483927247898539470, 38.54057627198103120 ) ) ;
#57033 = CARTESIAN_POINT ( 'NONE',  ( -16.52544592524335698, -4.483927247898792601, 103.9594237280190185 ) ) ;
#57034 = EDGE_LOOP ( 'NONE', ( #158185, #184469 ) ) ;
#57035 = CARTESIAN_POINT ( 'NONE',  ( -13.97604488694547697, 13.89961937509957934, 38.12609039468566152 ) ) ;
#57036 = CARTESIAN_POINT ( 'NONE',  ( -19.05341960407611168, -5.049401038298163336, 111.4572429386476671 ) ) ;
#57037 = CARTESIAN_POINT ( 'NONE',  ( 19.05341960407611168, 5.049401038298154454, 43.95724293864769550 ) ) ;
#57038 = CARTESIAN_POINT ( 'NONE',  ( 5.049401038297881783, 19.05341960407617563, 22.29275706135233648 ) ) ;
#57039 = CARTESIAN_POINT ( 'NONE',  ( -11.40812507854755609, 35.11059874428196537, -9.024999997268814411 ) ) ;
#57040 = CARTESIAN_POINT ( 'NONE',  ( -12.06949235617739369, -12.14591786802326823, 44.37609039468567573 ) ) ;
#57042 = CARTESIAN_POINT ( 'NONE',  ( 14.34966873604972726, -8.224510206698740333, 60.83442372801901854 ) ) ;
#57041 = CARTESIAN_POINT ( 'NONE',  ( -16.46253265017146816, -9.564922557961047289, 69.16775706135233293 ) ) ;
#57043 = CARTESIAN_POINT ( 'NONE',  ( 6.090539141055496763, -4.048154665053746548, -64.32606980895295123 ) ) ;
#57044 = CARTESIAN_POINT ( 'NONE',  ( 0.05219959533909260263, 19.03943276465977164, 79.99890960531436690 ) ) ;
#57045 = CARTESIAN_POINT ( 'NONE',  ( -21.52544592524343514, 5.823673210054127303, 116.0405762719810383 ) ) ;
#57046 = CARTESIAN_POINT ( 'NONE',  ( -0.05219959533936034679, 19.03943276465977164, 82.50109039468567573 ) ) ;
#57048 = CARTESIAN_POINT ( 'NONE',  ( 13.97604488694527802, 13.89961937509977652, 39.37390960531435269 ) ) ;
#57047 = CARTESIAN_POINT ( 'NONE',  ( -9.564922557960796823, -16.46253265017161027, 107.0822429386476955 ) ) ;
#57049 = CARTESIAN_POINT ( 'NONE',  ( 13.97604488694527802, 13.89961937509977652, 74.37390960531436690 ) ) ;
#57051 = CARTESIAN_POINT ( 'NONE',  ( -16.46253265017160317, 9.564922557960807481, 40.83224293864769550 ) ) ;
#57050 = CARTESIAN_POINT ( 'NONE',  ( 14.29746914071049879, -8.314922557960816363, 28.33224293864769550 ) ) ;
#57052 = CARTESIAN_POINT ( 'NONE',  ( -0.05219959533936034679, 19.03943276465977164, 47.50109039468566863 ) ) ;
#57053 = CARTESIAN_POINT ( 'NONE',  ( 12.06949235617757843, -12.14591786802309237, 73.12390960531436690 ) ) ;
#57054 = CARTESIAN_POINT ( 'NONE',  ( -21.55341960407619339, 5.719274019375674811, 113.5427570613523756 ) ) ;
#57055 = CARTESIAN_POINT ( 'NONE',  ( 9.564922557960805705, 16.46253265017160317, 54.58224293864769550 ) ) ;
#57056 = CARTESIAN_POINT ( 'NONE',  ( -21.52544592524343514, 5.823673210054127303, 46.04057627198103830 ) ) ;
#57058 = CARTESIAN_POINT ( 'NONE',  ( 21.55341960407619695, -5.719274019375665929, 101.0427570613523756 ) ) ;
#57057 = CARTESIAN_POINT ( 'NONE',  ( -4.379528057220328563, 16.55341960407611168, 60.20724293864768839 ) ) ;
#57059 = CARTESIAN_POINT ( 'NONE',  ( -16.51473224551069308, -9.474510206698971260, 91.66557627198103830 ) ) ;
#57060 = CARTESIAN_POINT ( 'NONE',  ( -19.03943276465977164, 0.05219959533909376836, 106.2489096053143669 ) ) ;
#57061 = CARTESIAN_POINT ( 'NONE',  ( -13.89961937509977652, 13.97604488694528158, 35.62390960531435269 ) ) ;
#57062 = CARTESIAN_POINT ( 'NONE',  ( 12.14591786802309770, 12.06949235617756955, 114.3739096053143527 ) ) ;
#57063 = CARTESIAN_POINT ( 'NONE',  ( 4.483927247898545687, 16.52544592524342804, 89.79057627198103830 ) ) ;
#57064 = CARTESIAN_POINT ( 'NONE',  ( 0.05219959533907565091, 21.53943276465977519, 99.99890960531436690 ) ) ;
#57065 = CARTESIAN_POINT ( 'NONE',  ( -19.03943276465977164, 0.05219959533909376836, 91.24890960531436690 ) ) ;
#57066 = CARTESIAN_POINT ( 'NONE',  ( -10.72451020669898014, 18.67979575497178502, 110.4155762719810383 ) ) ;
#57067 = CARTESIAN_POINT ( 'NONE',  ( 16.46253265017160672, -9.564922557960803928, 88.33224293864769550 ) ) ;
#57069 = CARTESIAN_POINT ( 'NONE',  ( 16.55341960407611168, 4.379528057220329451, 98.95724293864770971 ) ) ;
#57068 = CYLINDRICAL_SURFACE ( 'NONE', #65576, 40.00000000000000000 ) ;
#57071 = CARTESIAN_POINT ( 'NONE',  ( -9.564922557960796823, -16.46253265017161027, 77.08224293864769550 ) ) ;
#57070 = CIRCLE ( 'NONE', #195929, 2.649999999999999911 ) ;
#57072 = CARTESIAN_POINT ( 'NONE',  ( -21.52544592524343514, 5.823673210054127303, 76.04057627198102409 ) ) ;
#57073 = CARTESIAN_POINT ( 'NONE',  ( -5.049401038298153566, 19.05341960407611168, 115.2072429386477097 ) ) ;
#57074 = CARTESIAN_POINT ( 'NONE',  ( -8.906447517083053711, -27.41122689804191026, 146.4000000000000057 ) ) ;
#57076 = CARTESIAN_POINT ( 'NONE',  ( -2.649999999999999911, -165.0000000000000000, -15.00000000000000000 ) ) ;
#57075 = CARTESIAN_POINT ( 'NONE',  ( 18.62759615963271287, -10.81492255796078972, 23.33224293864769194 ) ) ;
#57077 = CARTESIAN_POINT ( 'NONE',  ( -4.379528057220086978, -16.55341960407618274, 39.79275706135235424 ) ) ;
#57078 = CARTESIAN_POINT ( 'NONE',  ( 8.314922557960818139, 14.29746914071049879, 94.58224293864769550 ) ) ;
#57079 = CARTESIAN_POINT ( 'NONE',  ( -17.13100169013299023, -6.664070546373153547, 94.23210164300155611 ) ) ;
#57080 = CARTESIAN_POINT ( 'NONE',  ( 19.02544592524343514, -5.153800228976328945, 83.54057627198100988 ) ) ;
#57081 = CARTESIAN_POINT ( 'NONE',  ( 16.51473224551069308, 9.474510206698969483, 44.16557627198103120 ) ) ;
#57082 = CARTESIAN_POINT ( 'NONE',  ( -16.53943276465976808, 0.05219959533911058130, 76.24890960531435269 ) ) ;
#57083 = CARTESIAN_POINT ( 'NONE',  ( -0.05219959533907301413, -21.53943276465977519, 32.49890960531435979 ) ) ;
#57084 = CARTESIAN_POINT ( 'NONE',  ( -8.314922557960811034, -14.29746914071050412, 52.08224293864768839 ) ) ;
#57085 = CARTESIAN_POINT ( 'NONE',  ( -16.46253265017146816, -9.564922557961047289, 99.16775706135233293 ) ) ;
#57086 = CARTESIAN_POINT ( 'NONE',  ( 5.823673210054444382, -21.52544592524334988, 55.20942372801902565 ) ) ;
#57087 = CARTESIAN_POINT ( 'NONE',  ( -22.44159573604010305, 16.30477369853692338, 148.6750000027311671 ) ) ;
#57088 = CARTESIAN_POINT ( 'NONE',  ( 13.97604488694527802, 13.89961937509977652, 114.3739096053143669 ) ) ;
#57089 = CARTESIAN_POINT ( 'NONE',  ( -4.379528057220086978, -16.55341960407618274, 79.79275706135236135 ) ) ;
#57090 = CARTESIAN_POINT ( 'NONE',  ( -16.46253265017160317, 9.564922557960807481, 30.83224293864769550 ) ) ;
#57091 = CARTESIAN_POINT ( 'NONE',  ( -19.05341960407611168, -5.049401038298163336, 81.45724293864769550 ) ) ;
#57092 = CARTESIAN_POINT ( 'NONE',  ( -21.55341960407610458, -5.719274019375992779, 76.45724293864769550 ) ) ;
#57093 = CARTESIAN_POINT ( 'NONE',  ( 12.06949235617739724, 12.14591786802326823, 26.87609039468567218 ) ) ;
#57095 = CARTESIAN_POINT ( 'NONE',  ( 5.719274019375673035, 21.55341960407619339, 57.29275706135234714 ) ) ;
#57094 = CARTESIAN_POINT ( 'NONE',  ( 4.483927247898545687, 16.52544592524342804, 54.79057627198104541 ) ) ;
#57096 = EDGE_CURVE ( 'NONE', #138821, #94779, #114578, .T. ) ;
#57098 = CARTESIAN_POINT ( 'NONE',  ( 10.81492255796078972, 18.62759615963270932, 24.58224293864768839 ) ) ;
#57097 = CARTESIAN_POINT ( 'NONE',  ( -0.05219959533934338120, 16.53943276465976808, 82.50109039468568994 ) ) ;
#57099 = CARTESIAN_POINT ( 'NONE',  ( -11.30153831258470731, -188.0000000000000000, -15.00000000000000000 ) ) ;
#57100 = CARTESIAN_POINT ( 'NONE',  ( -21.23184647844206197, -181.1785498424364675, -25.00000000000000000 ) ) ;
#57101 = CARTESIAN_POINT ( 'NONE',  ( 4.379528057220092307, 16.55341960407617563, 112.2927570613523471 ) ) ;
#57102 = CARTESIAN_POINT ( 'NONE',  ( -4.483927247898782831, 16.52544592524335698, 62.70942372801902565 ) ) ;
#57103 = CARTESIAN_POINT ( 'NONE',  ( 19.05341960407611168, 5.049401038298154454, 78.95724293864769550 ) ) ;
#57104 = CARTESIAN_POINT ( 'NONE',  ( 13.89961937509977652, -13.97604488694527269, 93.12390960531436690 ) ) ;
#57105 = CARTESIAN_POINT ( 'NONE',  ( 0.05219959533937995610, -21.53943276465977519, 70.00109039468568994 ) ) ;
#57106 = CARTESIAN_POINT ( 'NONE',  ( -4.483927247898782831, 16.52544592524335698, 77.70942372801900433 ) ) ;
#57107 = CARTESIAN_POINT ( 'NONE',  ( 8.314922557960818139, 14.29746914071049879, 49.58224293864769550 ) ) ;
#57108 = CARTESIAN_POINT ( 'NONE',  ( 0.05219959533909260263, 19.03943276465977164, 59.99890960531436690 ) ) ;
#57109 = CARTESIAN_POINT ( 'NONE',  ( -9.474510206698964154, 16.51473224551069663, 50.41557627198102409 ) ) ;
#57111 = ORIENTED_EDGE ( 'NONE', *, *, #141068, .F. ) ;
#57110 = CARTESIAN_POINT ( 'NONE',  ( 14.34966873604972726, -8.224510206698740333, 45.83442372801901854 ) ) ;
#57112 = CARTESIAN_POINT ( 'NONE',  ( 9.564922557961047289, -16.46253265017146816, 95.41775706135233293 ) ) ;
#57113 = CARTESIAN_POINT ( 'NONE',  ( 8.314922557960818139, 14.29746914071049879, 94.58224293864769550 ) ) ;
#57114 = CARTESIAN_POINT ( 'NONE',  ( -9.564922557960796823, -16.46253265017161027, 67.08224293864769550 ) ) ;
#57116 = CARTESIAN_POINT ( 'NONE',  ( 11.74264578624800315, -36.14014761921581709, -7.400000000000000355 ) ) ;
#57115 = CARTESIAN_POINT ( 'NONE',  ( 19.02544592524334988, 5.153800228976608722, 106.4594237280190185 ) ) ;
#57117 = CARTESIAN_POINT ( 'NONE',  ( 10.81492255796106328, -18.62759615963255655, 110.4177570613523756 ) ) ;
#57118 = CARTESIAN_POINT ( 'NONE',  ( 4.379528057220092307, 16.55341960407617563, 72.29275706135236135 ) ) ;
#57119 = CARTESIAN_POINT ( 'NONE',  ( -0.05219959533936034679, 19.03943276465977164, 97.50109039468567573 ) ) ;
#57120 = CARTESIAN_POINT ( 'NONE',  ( -10.72451020669898014, 18.67979575497178502, 60.41557627198102409 ) ) ;
#57121 = CARTESIAN_POINT ( 'NONE',  ( 16.55341960407618274, -4.379528057220086978, 51.04275706135234714 ) ) ;
#57122 = CARTESIAN_POINT ( 'NONE',  ( 11.23596569267287038, -38.39307213609681213, -14.62819055234737320 ) ) ;
#57123 = CARTESIAN_POINT ( 'NONE',  ( -19.05341960407617563, 5.049401038297882671, 58.54275706135234003 ) ) ;
#57124 = CARTESIAN_POINT ( 'NONE',  ( -16.51473224551069308, -9.474510206698971260, 91.66557627198103830 ) ) ;
#57125 = CARTESIAN_POINT ( 'NONE',  ( -12.06949235617756955, 12.14591786802309770, 110.6239096053143669 ) ) ;
#57126 = CARTESIAN_POINT ( 'NONE',  ( -16.51473224551069308, -9.474510206698971260, 66.66557627198102409 ) ) ;
#57127 = CARTESIAN_POINT ( 'NONE',  ( -0.05219959533910754901, -16.53943276465976808, 57.49890960531435979 ) ) ;
#57128 = CARTESIAN_POINT ( 'NONE',  ( 5.823673210054444382, -21.52544592524334988, 80.20942372801901854 ) ) ;
#57129 = CARTESIAN_POINT ( 'NONE',  ( -5.153800228976607833, 19.02544592524334988, 52.70942372801900433 ) ) ;
#57130 = CARTESIAN_POINT ( 'NONE',  ( -19.02544592524334988, -5.153800228976617603, 28.95942372801900433 ) ) ;
#57131 = CARTESIAN_POINT ( 'NONE',  ( -18.67979575497178146, -10.72451020669898902, 21.66557627198102409 ) ) ;
#57132 = CARTESIAN_POINT ( 'NONE',  ( -5.823673210054431948, 21.52544592524334988, 97.70942372801904696 ) ) ;
#57133 = CARTESIAN_POINT ( 'NONE',  ( 16.46253265017160672, -9.564922557960803928, 63.33224293864769550 ) ) ;
#57134 = CARTESIAN_POINT ( 'NONE',  ( 21.53943276465977519, 0.05219959533937863772, 96.25109039468568994 ) ) ;
#57135 = CARTESIAN_POINT ( 'NONE',  ( 15.80617190586746368, 15.72974639402197994, 49.37390960531436690 ) ) ;
#57136 = CARTESIAN_POINT ( 'NONE',  ( -5.049401038298153566, 19.05341960407611168, 85.20724293864766707 ) ) ;
#57137 = CARTESIAN_POINT ( 'NONE',  ( -16.51473224551082808, 9.474510206698731452, 68.33442372801900433 ) ) ;
#57138 = CARTESIAN_POINT ( 'NONE',  ( 5.153800228976335163, 19.02544592524342804, 44.79057627198103830 ) ) ;
#57139 = CARTESIAN_POINT ( 'NONE',  ( -19.02544592524342804, 5.153800228976336051, 91.04057627198100988 ) ) ;
#57140 = CARTESIAN_POINT ( 'NONE',  ( 9.474510206698729675, 16.51473224551082808, 87.08442372801900433 ) ) ;
#57141 = CARTESIAN_POINT ( 'NONE',  ( 16.55341960407618274, -4.379528057220086978, 41.04275706135236135 ) ) ;
#57142 = CARTESIAN_POINT ( 'NONE',  ( 12.06949235617757843, -12.14591786802309237, 98.12390960531436690 ) ) ;
#57143 = CARTESIAN_POINT ( 'NONE',  ( -5.153800228976328057, -19.02544592524343514, 67.29057627198102409 ) ) ;
#57144 = CARTESIAN_POINT ( 'NONE',  ( 15.72974639402199770, -15.80617190586745480, 53.12390960531436690 ) ) ;
#57145 = CARTESIAN_POINT ( 'NONE',  ( 16.46253265017146816, 9.564922557961045513, 111.6677570613523329 ) ) ;
#57146 = CARTESIAN_POINT ( 'NONE',  ( 10.72451020669871369, 18.67979575497193778, 27.08442372801901854 ) ) ;
#57147 = CARTESIAN_POINT ( 'NONE',  ( -15.80617190586768217, 15.72974639402176855, 68.12609039468567573 ) ) ;
#57148 = CARTESIAN_POINT ( 'NONE',  ( 12.14591786802327356, -12.06949235617739191, 65.62609039468568994 ) ) ;
#57149 = CARTESIAN_POINT ( 'NONE',  ( -13.97604488694527625, -13.89961937509977652, 71.87390960531433848 ) ) ;
#57150 = CARTESIAN_POINT ( 'NONE',  ( -4.483927247898782831, 16.52544592524335698, 107.7094237280190328 ) ) ;
#57151 = CARTESIAN_POINT ( 'NONE',  ( 19.05341960407617918, -5.049401038297876454, 41.04275706135233293 ) ) ;
#57152 = CARTESIAN_POINT ( 'NONE',  ( 5.719274019375673035, 21.55341960407619339, 37.29275706135235424 ) ) ;
#57153 = CARTESIAN_POINT ( 'NONE',  ( -16.55341960407611168, -4.379528057220339221, 81.45724293864769550 ) ) ;
#57154 = CARTESIAN_POINT ( 'NONE',  ( 16.46253265017160672, -9.564922557960803928, 98.33224293864769550 ) ) ;
#57155 = CARTESIAN_POINT ( 'NONE',  ( -16.52544592524335698, -4.483927247898792601, 93.95942372801903275 ) ) ;
#57156 = CARTESIAN_POINT ( 'NONE',  ( -21.55341960407619339, 5.719274019375674811, 68.54275706135234714 ) ) ;
#57157 = CARTESIAN_POINT ( 'NONE',  ( -8.314922557961024197, 14.29746914071037800, 27.91775706135234358 ) ) ;
#57158 = CARTESIAN_POINT ( 'NONE',  ( 10.81492255796106328, -18.62759615963255655, 25.41775706135235779 ) ) ;
#57159 = CARTESIAN_POINT ( 'NONE',  ( -14.34966873604960291, -8.224510206698953496, 76.66557627198103830 ) ) ;
#57160 = VERTEX_POINT ( 'NONE', #117128 ) ;
#57161 = CARTESIAN_POINT ( 'NONE',  ( -15.80617190586745835, -15.72974639402198527, 101.8739096053143811 ) ) ;
#57162 = CARTESIAN_POINT ( 'NONE',  ( -12.06949235617756955, 12.14591786802309770, 50.62390960531435979 ) ) ;
#57163 = ORIENTED_EDGE ( 'NONE', *, *, #158775, .F. ) ;
#57164 = CARTESIAN_POINT ( 'NONE',  ( 13.97604488694527802, 13.89961937509977652, 29.37390960531435979 ) ) ;
#57165 = CARTESIAN_POINT ( 'NONE',  ( 18.67979575497178502, 10.72451020669898547, 24.16557627198103120 ) ) ;
#57166 = CARTESIAN_POINT ( 'NONE',  ( -21.52544592524334988, -5.823673210054445271, 38.95942372801901854 ) ) ;
#57167 = CARTESIAN_POINT ( 'NONE',  ( -12.14591786802309592, -12.06949235617757132, 66.87390960531436690 ) ) ;
#57168 = CIRCLE ( 'NONE', #108813, 4.000000000000000888 ) ;
#57169 = CARTESIAN_POINT ( 'NONE',  ( 18.67979575497178502, 10.72451020669898547, 69.16557627198102409 ) ) ;
#57170 = CARTESIAN_POINT ( 'NONE',  ( -9.564922557960796823, -16.46253265017161027, 77.08224293864769550 ) ) ;
#57172 = CARTESIAN_POINT ( 'NONE',  ( 16.46253265017146816, 9.564922557961045513, 81.66775706135233293 ) ) ;
#57171 = CARTESIAN_POINT ( 'NONE',  ( -5.153800228976328057, -19.02544592524343514, 22.29057627198102765 ) ) ;
#57173 = EDGE_CURVE ( 'NONE', #40598, #132987, #40292, .T. ) ;
#57174 = CARTESIAN_POINT ( 'NONE',  ( 5.823673210054125526, 21.52544592524343514, 64.79057627198103830 ) ) ;
#57175 = CARTESIAN_POINT ( 'NONE',  ( -13.97604488694527625, -13.89961937509977652, 36.87390960531436690 ) ) ;
#57176 = CARTESIAN_POINT ( 'NONE',  ( -19.03943276465977164, 0.05219959533909376836, 76.24890960531435269 ) ) ;
#57177 = EDGE_LOOP ( 'NONE', ( #61642, #180884, #90308, #186342 ) ) ;
#57178 = CARTESIAN_POINT ( 'NONE',  ( 12.14591786802327356, -12.06949235617739191, 40.62609039468567573 ) ) ;
#57179 = CARTESIAN_POINT ( 'NONE',  ( -18.67979575497193778, 10.72451020669871902, 28.33442372801902209 ) ) ;
#57180 = CARTESIAN_POINT ( 'NONE',  ( -18.62759615963255300, -10.81492255796106328, 59.16775706135234714 ) ) ;
#57181 = CARTESIAN_POINT ( 'NONE',  ( 5.153800228976335163, 19.02544592524342804, 109.7905762719810099 ) ) ;
#57182 = CARTESIAN_POINT ( 'NONE',  ( 15.72974639402199770, -15.80617190586745480, 68.12390960531436690 ) ) ;
#57184 = CARTESIAN_POINT ( 'NONE',  ( -4.483927247898782831, 16.52544592524335698, 47.70942372801902565 ) ) ;
#57183 = CARTESIAN_POINT ( 'NONE',  ( 18.62759615963271287, -10.81492255796078972, 108.3322429386477097 ) ) ;
#57185 = CIRCLE ( 'NONE', #50663, 21.30000000000002913 ) ;
#57186 = CARTESIAN_POINT ( 'NONE',  ( -18.62759615963270932, 10.81492255796079327, 50.83224293864770971 ) ) ;
#57187 = CARTESIAN_POINT ( 'NONE',  ( -15.72974639402176322, -15.80617190586768395, 104.3760903946856899 ) ) ;
#57188 = CARTESIAN_POINT ( 'NONE',  ( -19.02544592524342804, 5.153800228976336051, 61.04057627198103120 ) ) ;
#57189 = CARTESIAN_POINT ( 'NONE',  ( -5.049401038298153566, 19.05341960407611168, 110.2072429386476671 ) ) ;
#57190 = CARTESIAN_POINT ( 'NONE',  ( 16.51473224551069308, 9.474510206698969483, 74.16557627198103830 ) ) ;
#57191 = APPLICATION_CONTEXT ( 'automotive_design' ) ;
#57192 = CARTESIAN_POINT ( 'NONE',  ( 17.44279575226788381, -5.990770900253884257, 88.33557567514318976 ) ) ;
#57193 = CARTESIAN_POINT ( 'NONE',  ( 5.153800228976615827, -19.02544592524334988, 65.20942372801900433 ) ) ;
#57195 = CARTESIAN_POINT ( 'NONE',  ( -10.81492255796078084, -18.62759615963271287, 47.08224293864770260 ) ) ;
#57194 = CARTESIAN_POINT ( 'NONE',  ( -10.81492255796105439, 18.62759615963255655, 112.9177570613523329 ) ) ;
#57196 = CARTESIAN_POINT ( 'NONE',  ( -8.224510206698735004, -14.34966873604973081, 99.58442372801900433 ) ) ;
#57197 = CARTESIAN_POINT ( 'NONE',  ( 19.02544592524334988, 5.153800228976608722, 86.45942372801900433 ) ) ;
#57198 = CARTESIAN_POINT ( 'NONE',  ( -17.49999999999999645, -7.500000000000000888, 120.0000000000000142 ) ) ;
#57199 = CARTESIAN_POINT ( 'NONE',  ( -13.89961937509957401, -13.97604488694547875, 24.37609039468565442 ) ) ;
#57200 = CARTESIAN_POINT ( 'NONE',  ( -19.05341960407617563, 5.049401038297882671, 78.54275706135233293 ) ) ;
#57201 = CARTESIAN_POINT ( 'NONE',  ( -5.049401038297874678, -19.05341960407617918, 44.79275706135232582 ) ) ;
#57202 = CARTESIAN_POINT ( 'NONE',  ( -16.81555441253551209, -7.025013491695503376, 44.36314554665745646 ) ) ;
#57203 = CARTESIAN_POINT ( 'NONE',  ( 16.46253265017160672, -9.564922557960803928, 38.33224293864768839 ) ) ;
#57204 = CARTESIAN_POINT ( 'NONE',  ( -4.483927247898539470, -16.52544592524342804, 52.29057627198102409 ) ) ;
#57205 = CARTESIAN_POINT ( 'NONE',  ( -13.97604488694527625, -13.89961937509977652, 36.87390960531436690 ) ) ;
#57206 = CARTESIAN_POINT ( 'NONE',  ( 14.29746914071049879, -8.314922557960816363, 38.33224293864768839 ) ) ;
#57207 = LINE ( 'NONE', #92480, #161445 ) ;
#57208 = CARTESIAN_POINT ( 'NONE',  ( -8.224510206698735004, -14.34966873604973081, 109.5844237280190328 ) ) ;
#57209 = CARTESIAN_POINT ( 'NONE',  ( 5.153800228976335163, 19.02544592524342804, 44.79057627198103830 ) ) ;
#57210 = CARTESIAN_POINT ( 'NONE',  ( 9.564922557961047289, -16.46253265017146816, 25.41775706135234003 ) ) ;
#57211 = CARTESIAN_POINT ( 'NONE',  ( 4.483927247898790824, -16.52544592524335698, 30.20942372801902565 ) ) ;
#57212 = CARTESIAN_POINT ( 'NONE',  ( 21.52544592524344225, -5.823673210054117533, 38.54057627198103120 ) ) ;
#57214 = ORIENTED_EDGE ( 'NONE', *, *, #29165, .F. ) ;
#57213 = CARTESIAN_POINT ( 'NONE',  ( -18.62759615963255300, -10.81492255796106328, 94.16775706135237556 ) ) ;
#57215 = CARTESIAN_POINT ( 'NONE',  ( 16.46253265017160672, -9.564922557960803928, 108.3322429386476955 ) ) ;
#57216 = CARTESIAN_POINT ( 'NONE',  ( 5.049401038298161559, -19.05341960407611168, 77.70724293864765286 ) ) ;
#57217 = CARTESIAN_POINT ( 'NONE',  ( -36.91746825000000598, -11.99521256947794789, -6.524999997268811747 ) ) ;
#57218 = CARTESIAN_POINT ( 'NONE',  ( 15.72974639402199770, -15.80617190586745480, 113.1239096053143953 ) ) ;
#57219 = CIRCLE ( 'NONE', #50704, 24.30000000000003268 ) ;
#57220 = CARTESIAN_POINT ( 'NONE',  ( -16.53943276465976808, 0.05219959533911058130, 86.24890960531436690 ) ) ;
#57222 = CARTESIAN_POINT ( 'NONE',  ( 9.564922557960805705, 16.46253265017160317, 69.58224293864770971 ) ) ;
#57221 = CARTESIAN_POINT ( 'NONE',  ( -10.72451020669898014, 18.67979575497178502, 75.41557627198102409 ) ) ;
#57223 = CARTESIAN_POINT ( 'NONE',  ( -16.51473224551069308, -9.474510206698971260, 71.66557627198102409 ) ) ;
#57224 = CARTESIAN_POINT ( 'NONE',  ( -21.55341960407610458, -5.719274019375992779, 101.4572429386476955 ) ) ;
#57225 = ORIENTED_EDGE ( 'NONE', *, *, #80593, .F. ) ;
#57226 = CARTESIAN_POINT ( 'NONE',  ( 0.05219959533909260263, 19.03943276465977164, 64.99890960531436690 ) ) ;
#57228 = CARTESIAN_POINT ( 'NONE',  ( 19.03943276465977164, -0.05219959533909143690, 23.74890960531435269 ) ) ;
#57227 = CARTESIAN_POINT ( 'NONE',  ( -0.05219959533910754901, -16.53943276465976808, 102.4989096053143811 ) ) ;
#57229 = CARTESIAN_POINT ( 'NONE',  ( -0.05219959533909027116, -19.03943276465977164, 57.49890960531435979 ) ) ;
#57230 = CARTESIAN_POINT ( 'NONE',  ( -13.97604488694547697, 13.89961937509957934, 78.12609039468567573 ) ) ;
#57231 = CARTESIAN_POINT ( 'NONE',  ( 8.224510206698953496, -14.34966873604960469, 97.91557627198103830 ) ) ;
#57232 = CARTESIAN_POINT ( 'NONE',  ( -15.72974639402176322, -15.80617190586768395, 64.37609039468568994 ) ) ;
#57234 = CARTESIAN_POINT ( 'NONE',  ( 5.719274019375991003, -21.55341960407610458, 112.7072429386476955 ) ) ;
#57233 = CARTESIAN_POINT ( 'NONE',  ( 5.153800228976335163, 19.02544592524342804, 49.79057627198100988 ) ) ;
#57235 = CARTESIAN_POINT ( 'NONE',  ( 0.05219959533910956823, 16.53943276465976808, 94.99890960531436690 ) ) ;
#57236 = CARTESIAN_POINT ( 'NONE',  ( 23.31738231874054534, 16.94106989632529192, 145.1999999999999886 ) ) ;
#57237 = CARTESIAN_POINT ( 'NONE',  ( -13.97604488694527625, -13.89961937509977652, 71.87390960531433848 ) ) ;
#57238 = CARTESIAN_POINT ( 'NONE',  ( 17.48847506799969409, 5.747544572773743532, 111.6730256215672199 ) ) ;
#57240 = CARTESIAN_POINT ( 'NONE',  ( -19.05341960407611168, -5.049401038298163336, 106.4572429386476955 ) ) ;
#57239 = CARTESIAN_POINT ( 'NONE',  ( 5.153800228976615827, -19.02544592524334988, 110.2094237280189901 ) ) ;
#57241 = CARTESIAN_POINT ( 'NONE',  ( -18.62759615963255300, -10.81492255796106328, 49.16775706135234003 ) ) ;
#57242 = CARTESIAN_POINT ( 'NONE',  ( -9.474510206698964154, 16.51473224551069663, 100.4155762719810241 ) ) ;
#57243 = CARTESIAN_POINT ( 'NONE',  ( 13.97604488694548053, -13.89961937509957401, 80.62609039468567573 ) ) ;
#57244 = CARTESIAN_POINT ( 'NONE',  ( -9.474510206698964154, 16.51473224551069663, 65.41557627198102409 ) ) ;
#57245 = CARTESIAN_POINT ( 'NONE',  ( -12.14591786802309592, -12.06949235617757132, 76.87390960531439532 ) ) ;
#57246 = CARTESIAN_POINT ( 'NONE',  ( -19.03943276465977164, 0.05219959533909376836, 96.24890960531436690 ) ) ;
#57247 = CARTESIAN_POINT ( 'NONE',  ( -4.379528057220328563, 16.55341960407611168, 85.20724293864770971 ) ) ;
#57248 = CARTESIAN_POINT ( 'NONE',  ( -13.97604488694527625, -13.89961937509977652, 91.87390960531432427 ) ) ;
#57249 = CARTESIAN_POINT ( 'NONE',  ( -5.153800228976607833, 19.02544592524334988, 47.70942372801900433 ) ) ;
#57252 = CARTESIAN_POINT ( 'NONE',  ( 9.474510206698971260, -16.51473224551069308, 32.91557627198102409 ) ) ;
#57251 = CARTESIAN_POINT ( 'NONE',  ( -12.14591786802309592, -12.06949235617757132, 46.87390960531435979 ) ) ;
#57250 = CARTESIAN_POINT ( 'NONE',  ( -5.049401038298153566, 19.05341960407611168, 45.20724293864769550 ) ) ;
#57253 = VERTEX_POINT ( 'NONE', #87784 ) ;
#57254 = CARTESIAN_POINT ( 'NONE',  ( 5.719274019375673035, 21.55341960407619339, 47.29275706135234003 ) ) ;
#57255 = CARTESIAN_POINT ( 'NONE',  ( -16.46253265017146816, -9.564922557961047289, 84.16775706135233293 ) ) ;
#57256 = CARTESIAN_POINT ( 'NONE',  ( -8.224510206698948167, 14.34966873604960824, 30.41557627198101699 ) ) ;
#57257 = CARTESIAN_POINT ( 'NONE',  ( -21.55341960407610458, -5.719274019375992779, 101.4572429386476955 ) ) ;
#57258 = CARTESIAN_POINT ( 'NONE',  ( 21.55341960407610458, 5.719274019375980345, 33.95724293864769550 ) ) ;
#57259 = CARTESIAN_POINT ( 'NONE',  ( 12.14591786802309770, 12.06949235617756955, 79.37390960531436690 ) ) ;
#57260 = CARTESIAN_POINT ( 'NONE',  ( -0.05219959533909027116, -19.03943276465977164, 37.49890960531436690 ) ) ;
#57261 = CARTESIAN_POINT ( 'NONE',  ( -12.06949235617739369, -12.14591786802326823, 109.3760903946857042 ) ) ;
#57262 = CARTESIAN_POINT ( 'NONE',  ( -8.314922557961024197, 14.29746914071037800, 87.91775706135234714 ) ) ;
#57263 = CARTESIAN_POINT ( 'NONE',  ( 16.53943276465976808, 0.05219959533934440121, 71.25109039468568994 ) ) ;
#57264 = CARTESIAN_POINT ( 'NONE',  ( -19.05341960407617563, 5.049401038297882671, 28.54275706135232937 ) ) ;
#57265 = CARTESIAN_POINT ( 'NONE',  ( -9.564922557960796823, -16.46253265017161027, 87.08224293864769550 ) ) ;
#57266 = CARTESIAN_POINT ( 'NONE',  ( 5.153800228976335163, 19.02544592524342804, 79.79057627198102409 ) ) ;
#57267 = CARTESIAN_POINT ( 'NONE',  ( -16.53943276465976808, -0.05219959533934237506, 73.75109039468567573 ) ) ;
#57268 = CARTESIAN_POINT ( 'NONE',  ( 19.05341960407611168, 5.049401038298154454, 33.95724293864769550 ) ) ;
#57269 = CARTESIAN_POINT ( 'NONE',  ( 14.29746914071049879, -8.314922557960816363, 48.33224293864770260 ) ) ;
#57270 = CARTESIAN_POINT ( 'NONE',  ( 13.89961937509977652, -13.97604488694527269, 98.12390960531433848 ) ) ;
#57271 = CARTESIAN_POINT ( 'NONE',  ( 18.62759615963271287, -10.81492255796078972, 33.33224293864769550 ) ) ;
#57272 = CARTESIAN_POINT ( 'NONE',  ( -12.14591786802309592, -12.06949235617757132, 66.87390960531436690 ) ) ;
#57273 = EDGE_CURVE ( 'NONE', #144758, #89112, #10964, .T. ) ;
#57274 = CARTESIAN_POINT ( 'NONE',  ( -0.05219959533910754901, -16.53943276465976808, 62.49890960531436690 ) ) ;
#57275 = CARTESIAN_POINT ( 'NONE',  ( 29.34370184275720206, -1.069973119863033784, -49.12095057784394925 ) ) ;
#57276 = CARTESIAN_POINT ( 'NONE',  ( -9.474510206698720793, -16.51473224551083518, 64.58442372801900433 ) ) ;
#57277 = CARTESIAN_POINT ( 'NONE',  ( 19.02544592524343514, -5.153800228976328945, 93.54057627198102409 ) ) ;
#57278 = CARTESIAN_POINT ( 'NONE',  ( -16.46253265017146816, -9.564922557961047289, 84.16775706135233293 ) ) ;
#57279 = CARTESIAN_POINT ( 'NONE',  ( -5.049401038297874678, -19.05341960407618274, 39.79275706135232582 ) ) ;
#57281 = CARTESIAN_POINT ( 'NONE',  ( 4.379528057220092307, 16.55341960407617563, 97.29275706135234714 ) ) ;
#57280 = CARTESIAN_POINT ( 'NONE',  ( -19.03943276465977164, -0.05219959533935918106, 113.7510903946856757 ) ) ;
#57282 = CARTESIAN_POINT ( 'NONE',  ( -19.02544592524342804, 5.153800228976336051, 46.04057627198101699 ) ) ;
#57283 = CARTESIAN_POINT ( 'NONE',  ( 5.719274019375991003, -21.55341960407610458, 27.70724293864769905 ) ) ;
#57284 = CARTESIAN_POINT ( 'NONE',  ( 15.80617190586769283, -15.72974639402175789, 55.62609039468568284 ) ) ;
#57285 = CARTESIAN_POINT ( 'NONE',  ( -16.53943276465976808, -0.05219959533934237506, 18.75109039468568639 ) ) ;
#57287 = CARTESIAN_POINT ( 'NONE',  ( -19.03943276465977164, 0.05219959533909376836, 81.24890960531436690 ) ) ;
#57286 = CARTESIAN_POINT ( 'NONE',  ( 4.999999999999999112, 5.000000000000000888, -18.00000000000000000 ) ) ;
#57288 = CARTESIAN_POINT ( 'NONE',  ( 9.474510206698971260, -16.51473224551069308, 112.9155762719810383 ) ) ;
#57290 = CARTESIAN_POINT ( 'NONE',  ( 19.02544592524343514, -5.153800228976328945, 73.54057627198103830 ) ) ;
#57289 = CARTESIAN_POINT ( 'NONE',  ( 14.29746914071049879, -8.314922557960816363, 68.33224293864769550 ) ) ;
#57291 = CARTESIAN_POINT ( 'NONE',  ( -13.89961937509977652, 13.97604488694528158, 80.62390960531436690 ) ) ;
#57292 = CARTESIAN_POINT ( 'NONE',  ( 13.97604488694548053, -13.89961937509957401, 95.62609039468563310 ) ) ;
#57293 = CARTESIAN_POINT ( 'NONE',  ( -21.52544592524343514, 5.823673210054127303, 71.04057627198103830 ) ) ;
#57294 = CARTESIAN_POINT ( 'NONE',  ( -16.46253265017160317, 9.564922557960807481, 25.83224293864769194 ) ) ;
#57295 = CARTESIAN_POINT ( 'NONE',  ( 5.049401038297881783, 19.05341960407617563, 57.29275706135231871 ) ) ;
#57296 = CARTESIAN_POINT ( 'NONE',  ( 5.049401038298161559, -19.05341960407611168, 52.70724293864767418 ) ) ;
#57297 = CARTESIAN_POINT ( 'NONE',  ( 5.153800228976335163, 19.02544592524342804, 89.79057627198102409 ) ) ;
#57298 = VERTEX_POINT ( 'NONE', #195999 ) ;
#57299 = CARTESIAN_POINT ( 'NONE',  ( -10.72451020669898014, 18.67979575497178502, 95.41557627198102409 ) ) ;
#57301 = CARTESIAN_POINT ( 'NONE',  ( -9.564922557961040184, 16.46253265017147172, 47.91775706135233293 ) ) ;
#57300 = CARTESIAN_POINT ( 'NONE',  ( 4.483927247898545687, 16.52544592524342804, 94.79057627198105251 ) ) ;
#57303 = B_SPLINE_CURVE_WITH_KNOTS ( 'NONE', 3,
 ( #162434, #196794, #195803, #42110, #56260, #192783 ),
 .UNSPECIFIED., .F., .F.,
 ( 4, 2, 4 ),
 ( 0.003239945802372255594, 0.003620412082092107353, 0.004000878361811959112 ),
 .UNSPECIFIED. ) ;
#57302 = CARTESIAN_POINT ( 'NONE',  ( -10.72451020669898014, 18.67979575497178502, 85.41557627198102409 ) ) ;
#57304 = CARTESIAN_POINT ( 'NONE',  ( -18.67979575497178146, -10.72451020669898902, 71.66557627198100988 ) ) ;
#57305 = CARTESIAN_POINT ( 'NONE',  ( 14.29746914071049879, -8.314922557960816363, 38.33224293864768839 ) ) ;
#57306 = CARTESIAN_POINT ( 'NONE',  ( -18.62759615963255300, -10.81492255796106328, 104.1677570613523471 ) ) ;
#57307 = CARTESIAN_POINT ( 'NONE',  ( 5.153800228976335163, 19.02544592524342804, 74.79057627198103830 ) ) ;
#57308 = CARTESIAN_POINT ( 'NONE',  ( 9.564922557960805705, 16.46253265017160317, 34.58224293864770260 ) ) ;
#57309 = AXIS2_PLACEMENT_3D ( 'NONE', #145004, #23679, #6485 ) ;
#57310 = CARTESIAN_POINT ( 'NONE',  ( 15.72974639402176855, 15.80617190586768217, 36.87609039468568994 ) ) ;
#57311 = CARTESIAN_POINT ( 'NONE',  ( -18.67979575497193778, 10.72451020669871902, 58.33442372801901143 ) ) ;
#57312 = CARTESIAN_POINT ( 'NONE',  ( 19.02544592524343514, -5.153800228976328945, 48.54057627198103120 ) ) ;
#57313 = CARTESIAN_POINT ( 'NONE',  ( -5.823673210054431948, 21.52544592524334988, 27.70942372801901854 ) ) ;
#57314 = CARTESIAN_POINT ( 'NONE',  ( -9.564922557961040184, 16.46253265017147172, 57.91775706135233293 ) ) ;
#57315 = CARTESIAN_POINT ( 'NONE',  ( 16.46253265017160672, -9.564922557960803928, 43.33224293864769550 ) ) ;
#57316 = CARTESIAN_POINT ( 'NONE',  ( -4.379528057220086978, -16.55341960407618274, 34.79275706135235424 ) ) ;
#57317 = CARTESIAN_POINT ( 'NONE',  ( 13.97604488694527802, 13.89961937509977652, 24.37390960531435624 ) ) ;
#57318 = CARTESIAN_POINT ( 'NONE',  ( -14.29746914071037622, -8.314922557961029526, 79.16775706135234714 ) ) ;
#57319 = CARTESIAN_POINT ( 'NONE',  ( -5.049401038298153566, 19.05341960407611168, 35.20724293864768839 ) ) ;
#57320 = CARTESIAN_POINT ( 'NONE',  ( 23.46037622755923380, -10.21219847193883368, 168.3031241911537847 ) ) ;
#57321 = CARTESIAN_POINT ( 'NONE',  ( 16.51473224551069308, 9.474510206698969483, 79.16557627198103830 ) ) ;
#57322 = CARTESIAN_POINT ( 'NONE',  ( 16.46253265017160672, -9.564922557960803928, 23.33224293864769194 ) ) ;
#57323 = CARTESIAN_POINT ( 'NONE',  ( -5.823673210054116645, -21.52544592524344225, 72.29057627198102409 ) ) ;
#57324 = CARTESIAN_POINT ( 'NONE',  ( -8.314922557961024197, 14.29746914071037800, 52.91775706135235424 ) ) ;
#57325 = CARTESIAN_POINT ( 'NONE',  ( -13.89961937509957401, -13.97604488694547875, 19.37609039468566507 ) ) ;
#57326 = CARTESIAN_POINT ( 'NONE',  ( -19.03943276465977164, 0.05219959533909376836, 36.24890960531436690 ) ) ;
#57327 = CARTESIAN_POINT ( 'NONE',  ( 4.483927247898545687, 16.52544592524342804, 34.79057627198103120 ) ) ;
#57328 = CARTESIAN_POINT ( 'NONE',  ( -16.53943276465976808, 0.05219959533911058130, 71.24890960531435269 ) ) ;
#57329 = CARTESIAN_POINT ( 'NONE',  ( 5.153800228976335163, 19.02544592524342804, 59.79057627198100988 ) ) ;
#57330 = CARTESIAN_POINT ( 'NONE',  ( -10.81492255796105439, 18.62759615963255655, 107.9177570613523471 ) ) ;
#57331 = CARTESIAN_POINT ( 'NONE',  ( 15.80617190586769283, -15.72974639402175789, 20.62609039468568639 ) ) ;
#57332 = CARTESIAN_POINT ( 'NONE',  ( 9.564922557960805705, 16.46253265017160317, 74.58224293864769550 ) ) ;
#57333 = CARTESIAN_POINT ( 'NONE',  ( -21.53943276465977519, -0.05219959533937600094, 83.75109039468568994 ) ) ;
#57334 = CARTESIAN_POINT ( 'NONE',  ( 14.34966873604972726, -8.224510206698740333, 70.83442372801901854 ) ) ;
#57335 = CARTESIAN_POINT ( 'NONE',  ( 16.55341960407618274, -4.379528057220086978, 36.04275706135234714 ) ) ;
#57337 = CARTESIAN_POINT ( 'NONE',  ( 5.049401038298161559, -19.05341960407611168, 102.7072429386476955 ) ) ;
#57336 = CARTESIAN_POINT ( 'NONE',  ( -14.29746914071049879, 8.314922557960819915, 95.83224293864770971 ) ) ;
#57338 = AXIS2_PLACEMENT_3D ( 'NONE', #95220, #153914, #15409 ) ;
#57339 = CARTESIAN_POINT ( 'NONE',  ( 16.52544592524342804, -4.483927247898539470, 28.54057627198103120 ) ) ;
#57340 = CARTESIAN_POINT ( 'NONE',  ( 9.564922557960805705, 16.46253265017160317, 34.58224293864770260 ) ) ;
#57341 = CARTESIAN_POINT ( 'NONE',  ( -16.55341960407617563, 4.379528057220093196, 48.54275706135234714 ) ) ;
#57342 = CARTESIAN_POINT ( 'NONE',  ( 8.314922557960818139, 14.29746914071049879, 59.58224293864770260 ) ) ;
#57343 = CARTESIAN_POINT ( 'NONE',  ( 16.52544592524335698, 4.483927247898782831, 96.45942372801901854 ) ) ;
#57344 = CARTESIAN_POINT ( 'NONE',  ( -5.153800228976328057, -19.02544592524343514, 112.2905762719810099 ) ) ;
#57345 = CARTESIAN_POINT ( 'NONE',  ( 21.53943276465977519, -0.05219959533907433946, 28.74890960531435624 ) ) ;
#57346 = CARTESIAN_POINT ( 'NONE',  ( 21.53943276465977519, 0.05219959533937863772, 111.2510903946856899 ) ) ;
#57347 = CARTESIAN_POINT ( 'NONE',  ( 4.483927247898545687, 16.52544592524342804, 84.79057627198102409 ) ) ;
#57348 = CARTESIAN_POINT ( 'NONE',  ( 9.564922557960805705, 16.46253265017160317, 89.58224293864769550 ) ) ;
#57349 = ORIENTED_EDGE ( 'NONE', *, *, #158665, .F. ) ;
#57350 = CARTESIAN_POINT ( 'NONE',  ( -16.53943276465976808, -0.05219959533934237506, 38.75109039468567573 ) ) ;
#57351 = CARTESIAN_POINT ( 'NONE',  ( 5.153800228976335163, 19.02544592524342804, 39.79057627198100988 ) ) ;
#57353 = CARTESIAN_POINT ( 'NONE',  ( -33.85315667487628133, 2.014031266883448522E-14, 100.5000000000010232 ) ) ;
#57352 = CARTESIAN_POINT ( 'NONE',  ( 4.483927247898790824, -16.52544592524335698, 40.20942372801901854 ) ) ;
#57354 = CARTESIAN_POINT ( 'NONE',  ( -16.51473224551082808, 9.474510206698731452, 48.33442372801900433 ) ) ;
#57355 = EDGE_CURVE ( 'NONE', #4626, #37612, #180825, .T. ) ;
#57356 = CARTESIAN_POINT ( 'NONE',  ( -19.02544592524342804, 5.153800228976336051, 51.04057627198103120 ) ) ;
#57357 = CARTESIAN_POINT ( 'NONE',  ( 14.29746914071037800, 8.314922557961029526, 86.66775706135234714 ) ) ;
#57358 = CARTESIAN_POINT ( 'NONE',  ( 13.97604488694548053, -13.89961937509957401, 90.62609039468567573 ) ) ;
#57359 = CARTESIAN_POINT ( 'NONE',  ( -19.02544592524342804, 5.153800228976336051, 56.04057627198100988 ) ) ;
#57360 = CARTESIAN_POINT ( 'NONE',  ( -0.05219959533907301413, -21.53943276465977519, 92.49890960531436690 ) ) ;
#57361 = CARTESIAN_POINT ( 'NONE',  ( 16.53943276465976808, -0.05219959533910856209, 98.74890960531438111 ) ) ;
#57362 = VECTOR ( 'NONE', #63388, 1000.000000000000000 ) ;
#57363 = EDGE_CURVE ( 'NONE', #126933, #112813, #72616, .T. ) ;
#57364 = CARTESIAN_POINT ( 'NONE',  ( -9.564922557961040184, 16.46253265017147172, 72.91775706135233293 ) ) ;
#57365 = CARTESIAN_POINT ( 'NONE',  ( -0.05219959533907301413, -21.53943276465977519, 57.49890960531435979 ) ) ;
#57366 = CARTESIAN_POINT ( 'NONE',  ( 19.05341960407617918, -5.049401038297876454, 46.04275706135233293 ) ) ;
#57367 = CARTESIAN_POINT ( 'NONE',  ( -5.153800228976328057, -19.02544592524343514, 112.2905762719810099 ) ) ;
#57368 = CARTESIAN_POINT ( 'NONE',  ( 10.81492255796078972, 18.62759615963270932, 89.58224293864768129 ) ) ;
#57369 = CARTESIAN_POINT ( 'NONE',  ( -17.31747979337949772, 6.344076630960996610, 83.62055131934816643 ) ) ;
#57370 = CARTESIAN_POINT ( 'NONE',  ( 19.03943276465977164, 0.05219959533936151252, 101.2510903946856757 ) ) ;
#57371 = CARTESIAN_POINT ( 'NONE',  ( -18.87580814761070513, 5.500000000000040856, 60.87172394265760289 ) ) ;
#57372 = CARTESIAN_POINT ( 'NONE',  ( 8.224510206698742110, 14.34966873604972548, 27.08442372801901854 ) ) ;
#57373 = CARTESIAN_POINT ( 'NONE',  ( 5.049401038298161559, -19.05341960407611168, 47.70724293864770260 ) ) ;
#57374 = CARTESIAN_POINT ( 'NONE',  ( -5.049401038298153566, 19.05341960407611168, 110.2072429386476671 ) ) ;
#57375 = CARTESIAN_POINT ( 'NONE',  ( 10.72451020669898902, -18.67979575497178502, 92.91557627198103830 ) ) ;
#57376 = CARTESIAN_POINT ( 'NONE',  ( -15.80617190586768217, 15.72974639402176855, 63.12609039468568994 ) ) ;
#57378 = CARTESIAN_POINT ( 'NONE',  ( 5.153800228976615827, -19.02544592524334988, 25.20942372801900433 ) ) ;
#57377 = CARTESIAN_POINT ( 'NONE',  ( 9.564922557961047289, -16.46253265017146816, 105.4177570613523471 ) ) ;
#57379 = CARTESIAN_POINT ( 'NONE',  ( -12.06949235617756955, 12.14591786802309770, 30.62390960531436335 ) ) ;
#57380 = CARTESIAN_POINT ( 'NONE',  ( -15.72974639402197994, 15.80617190586746368, 100.6239096053143811 ) ) ;
#57381 = CARTESIAN_POINT ( 'NONE',  ( -12.06949235617756955, 12.14591786802309770, 50.62390960531435979 ) ) ;
#57382 = CARTESIAN_POINT ( 'NONE',  ( 19.03943276465977164, 0.05219959533936151252, 91.25109039468566152 ) ) ;
#57383 = CARTESIAN_POINT ( 'NONE',  ( -19.05341960407617563, 5.049401038297882671, 53.54275706135231871 ) ) ;
#57384 = CARTESIAN_POINT ( 'NONE',  ( 18.62759615963255655, 10.81492255796105972, 76.66775706135234714 ) ) ;
#57385 = CARTESIAN_POINT ( 'NONE',  ( 19.02544592524334988, 5.153800228976608722, 46.45942372801899012 ) ) ;
#57386 = CARTESIAN_POINT ( 'NONE',  ( -12.06949235617756955, 12.14591786802309770, 115.6239096053143669 ) ) ;
#57387 = CARTESIAN_POINT ( 'NONE',  ( -15.72974639402197994, 15.80617190586746368, 45.62390960531436690 ) ) ;
#57388 = CARTESIAN_POINT ( 'NONE',  ( -12.14591786802309592, -12.06949235617757132, 41.87390960531435979 ) ) ;
#57389 = CARTESIAN_POINT ( 'NONE',  ( -0.05219959533937732626, 21.53943276465977519, 112.5010903946857042 ) ) ;
#57390 = CARTESIAN_POINT ( 'NONE',  ( 4.483927247898790824, -16.52544592524335698, 75.20942372801901854 ) ) ;
#57391 = CARTESIAN_POINT ( 'NONE',  ( 14.34966873604960469, 8.224510206698951720, 44.16557627198103120 ) ) ;
#57392 = CARTESIAN_POINT ( 'NONE',  ( 15.80617190586769283, -15.72974639402175789, 70.62609039468567573 ) ) ;
#57393 = CARTESIAN_POINT ( 'NONE',  ( -15.72974639402176322, -15.80617190586768395, 69.37609039468567573 ) ) ;
#57394 = CARTESIAN_POINT ( 'NONE',  ( 21.53943276465977519, -0.05219959533907433946, 63.74890960531435979 ) ) ;
#57395 = ORIENTED_EDGE ( 'NONE', *, *, #35688, .F. ) ;
#57396 = CARTESIAN_POINT ( 'NONE',  ( -5.153800228976328057, -19.02544592524343514, 37.29057627198102409 ) ) ;
#57397 = CARTESIAN_POINT ( 'NONE',  ( -15.80617190586768217, 15.72974639402176855, 38.12609039468567573 ) ) ;
#57398 = CARTESIAN_POINT ( 'NONE',  ( 0.05219959533910956823, 16.53943276465976808, 114.9989096053143669 ) ) ;
#57399 = CARTESIAN_POINT ( 'NONE',  ( -19.03943276465977164, 0.05219959533909376836, 41.24890960531435269 ) ) ;
#57400 = CARTESIAN_POINT ( 'NONE',  ( 14.29746914071049879, -8.314922557960816363, 88.33224293864769550 ) ) ;
#57401 = CARTESIAN_POINT ( 'NONE',  ( 5.049401038298161559, -19.05341960407611168, 82.70724293864770971 ) ) ;
#57402 = CARTESIAN_POINT ( 'NONE',  ( -4.379528057220328563, 16.55341960407611168, 45.20724293864769550 ) ) ;
#57403 = CARTESIAN_POINT ( 'NONE',  ( 8.314922557960818139, 14.29746914071049879, 94.58224293864769550 ) ) ;
#57404 = CARTESIAN_POINT ( 'NONE',  ( 18.62759615963271287, -10.81492255796078972, 63.33224293864770260 ) ) ;
#57405 = CARTESIAN_POINT ( 'NONE',  ( 18.62759615963271287, -10.81492255796078972, 103.3322429386476955 ) ) ;
#57406 = CARTESIAN_POINT ( 'NONE',  ( -17.56366054824412259, 15.66972982126927150, -54.83331888096112294 ) ) ;
#57408 = CARTESIAN_POINT ( 'NONE',  ( 0.05219959533934541429, -16.53943276465976808, 25.00109039468567218 ) ) ;
#57407 = CARTESIAN_POINT ( 'NONE',  ( 5.153800228976335163, 19.02544592524342804, 69.79057627198103830 ) ) ;
#57409 = CARTESIAN_POINT ( 'NONE',  ( 21.52544592524344225, -5.823673210054117533, 63.54057627198103830 ) ) ;
#57410 = CARTESIAN_POINT ( 'NONE',  ( -15.80617190586768217, 15.72974639402176855, 93.12609039468568994 ) ) ;
#57411 = CARTESIAN_POINT ( 'NONE',  ( 13.97604488694527802, 13.89961937509977652, 74.37390960531436690 ) ) ;
#57412 = CARTESIAN_POINT ( 'NONE',  ( 10.81492255796106328, -18.62759615963255655, 20.41775706135234714 ) ) ;
#57413 = CARTESIAN_POINT ( 'NONE',  ( 19.02544592524343514, -5.153800228976328945, 108.5405762719810383 ) ) ;
#57414 = CARTESIAN_POINT ( 'NONE',  ( -12.06949235617739369, -12.14591786802326823, 89.37609039468568994 ) ) ;
#57415 = CARTESIAN_POINT ( 'NONE',  ( -10.72451020669870658, -18.67979575497194134, 74.58442372801901854 ) ) ;
#57416 = CARTESIAN_POINT ( 'NONE',  ( -10.81492255796105439, 18.62759615963255655, 97.91775706135236135 ) ) ;
#57417 = CARTESIAN_POINT ( 'NONE',  ( -14.29746914071037622, -8.314922557961029526, 59.16775706135234714 ) ) ;
#57418 = CARTESIAN_POINT ( 'NONE',  ( -10.72451020669870658, -18.67979575497194134, 34.58442372801900433 ) ) ;
#57419 = CARTESIAN_POINT ( 'NONE',  ( 16.46253265017160672, -9.564922557960803928, 23.33224293864769194 ) ) ;
#57420 = CARTESIAN_POINT ( 'NONE',  ( 18.67979575497194134, -10.72451020669871369, 85.83442372801901854 ) ) ;
#57421 = CARTESIAN_POINT ( 'NONE',  ( -18.67979575497178146, -10.72451020669898902, 91.66557627198103830 ) ) ;
#57422 = CARTESIAN_POINT ( 'NONE',  ( 16.51473224551083163, -9.474510206698727899, 50.83442372801899722 ) ) ;
#57423 = CARTESIAN_POINT ( 'NONE',  ( -21.52544592524343514, 5.823673210054127303, 51.04057627198103120 ) ) ;
#57425 = CARTESIAN_POINT ( 'NONE',  ( 14.29746914071049879, -8.314922557960816363, 38.33224293864768839 ) ) ;
#57424 = CARTESIAN_POINT ( 'NONE',  ( -19.03943276465977164, 0.05219959533909376836, 91.24890960531436690 ) ) ;
#57426 = CARTESIAN_POINT ( 'NONE',  ( 20.48593134815244099, 11.15862823513540647, 168.1084560298344570 ) ) ;
#57427 = CARTESIAN_POINT ( 'NONE',  ( -16.51473224551082808, 9.474510206698731452, 68.33442372801900433 ) ) ;
#57428 = CARTESIAN_POINT ( 'NONE',  ( -4.500000000000001776, -120.9454340326537505, 15.08688922109887187 ) ) ;
#57429 = CARTESIAN_POINT ( 'NONE',  ( -19.03943276465977164, -0.05219959533935918106, 103.7510903946856757 ) ) ;
#57430 = CARTESIAN_POINT ( 'NONE',  ( 21.55341960407610458, 5.719274019375980345, 83.95724293864770971 ) ) ;
#57431 = CARTESIAN_POINT ( 'NONE',  ( -12.14591786802309592, -12.06949235617757132, 51.87390960531437401 ) ) ;
#57432 = CARTESIAN_POINT ( 'NONE',  ( 12.06949235617739724, 12.14591786802326823, 36.87609039468568994 ) ) ;
#57433 = CARTESIAN_POINT ( 'NONE',  ( -16.46253265017160317, 9.564922557960807481, 40.83224293864769550 ) ) ;
#57435 = CARTESIAN_POINT ( 'NONE',  ( 5.049401038297881783, 19.05341960407617563, 87.29275706135234714 ) ) ;
#57434 = CARTESIAN_POINT ( 'NONE',  ( -0.05219959533907301413, -21.53943276465977519, 112.4989096053143669 ) ) ;
#57436 = CARTESIAN_POINT ( 'NONE',  ( 5.153800228976335163, 19.02544592524342804, 89.79057627198102409 ) ) ;
#57437 = CARTESIAN_POINT ( 'NONE',  ( -19.03943276465977164, 0.05219959533909376836, 71.24890960531435269 ) ) ;
#57438 = CARTESIAN_POINT ( 'NONE',  ( 21.53943276465977519, -0.05219959533907433946, 78.74890960531436690 ) ) ;
#57439 = CARTESIAN_POINT ( 'NONE',  ( -13.89961937509977652, 13.97604488694528158, 45.62390960531433848 ) ) ;
#57440 = CARTESIAN_POINT ( 'NONE',  ( -17.96519593369847101, 33.31065106363013228, -7.999999999999994671 ) ) ;
#57441 = CARTESIAN_POINT ( 'NONE',  ( -12.14591786802309592, -12.06949235617757132, 61.87390960531436690 ) ) ;
#57442 = CARTESIAN_POINT ( 'NONE',  ( 16.46253265017160672, -9.564922557960803928, 93.33224293864769550 ) ) ;
#57443 = CARTESIAN_POINT ( 'NONE',  ( -3.573655867282028392E-15, 2.428612866367529932E-14, 150.0000000000000000 ) ) ;
#57444 = CARTESIAN_POINT ( 'NONE',  ( -5.153800228976607833, 19.02544592524334988, 67.70942372801900433 ) ) ;
#57445 = CARTESIAN_POINT ( 'NONE',  ( -10.81492255796078084, -18.62759615963271287, 77.08224293864769550 ) ) ;
#57446 = CARTESIAN_POINT ( 'NONE',  ( -13.97604488694547697, 13.89961937509957934, 38.12609039468566152 ) ) ;
#57447 = CARTESIAN_POINT ( 'NONE',  ( 13.89961937509977652, -13.97604488694527269, 98.12390960531433848 ) ) ;
#57448 = DIRECTION ( 'NONE',  ( 0.000000000000000000, -0.000000000000000000, -1.000000000000000000 ) ) ;
#57449 = CARTESIAN_POINT ( 'NONE',  ( -21.52544592524343514, 5.823673210054127303, 36.04057627198102409 ) ) ;
#57450 = CIRCLE ( 'NONE', #121938, 28.79475375365586487 ) ;
#57451 = CARTESIAN_POINT ( 'NONE',  ( 19.02544592524343514, -5.153800228976328945, 68.54057627198103830 ) ) ;
#57452 = CARTESIAN_POINT ( 'NONE',  ( -15.80617190586768217, 15.72974639402176855, 63.12609039468568994 ) ) ;
#57453 = CARTESIAN_POINT ( 'NONE',  ( -0.05219959533909027116, -19.03943276465977164, 22.49890960531436690 ) ) ;
#57455 = ORIENTED_EDGE ( 'NONE', *, *, #145117, .T. ) ;
#57454 = CARTESIAN_POINT ( 'NONE',  ( 18.62759615963271287, -10.81492255796078972, 108.3322429386477097 ) ) ;
#57456 = CARTESIAN_POINT ( 'NONE',  ( -18.62759615963255300, -10.81492255796106328, 54.16775706135235424 ) ) ;
#57457 = EDGE_LOOP ( 'NONE', ( #14194, #92671, #33820 ) ) ;
#57458 = CARTESIAN_POINT ( 'NONE',  ( -9.474510206698964154, 16.51473224551069663, 105.4155762719810383 ) ) ;
#57459 = CARTESIAN_POINT ( 'NONE',  ( 15.06137443927350361, 15.06137443927346098, -64.92279855667830191 ) ) ;
#57460 = CARTESIAN_POINT ( 'NONE',  ( 10.72451020669898902, -18.67979575497178502, 102.9155762719810383 ) ) ;
#57461 = CARTESIAN_POINT ( 'NONE',  ( -19.05341960407611168, -5.049401038298163336, 66.45724293864769550 ) ) ;
#57463 = EDGE_CURVE ( 'NONE', #199515, #106384, #49792, .T. ) ;
#57462 = CARTESIAN_POINT ( 'NONE',  ( -14.34966873604972548, 8.224510206698743886, 38.33442372801900433 ) ) ;
#57464 = CARTESIAN_POINT ( 'NONE',  ( 11.74264578624799427, 36.14014761921585972, -10.34999999453762598 ) ) ;
#57465 = CARTESIAN_POINT ( 'NONE',  ( -21.53943276465977519, -0.05219959533937600094, 103.7510903946857042 ) ) ;
#57466 = CARTESIAN_POINT ( 'NONE',  ( 9.474510206698971260, -16.51473224551069308, 42.91557627198103120 ) ) ;
#57467 = CARTESIAN_POINT ( 'NONE',  ( -5.719274019375665041, -21.55341960407619695, 99.79275706135234714 ) ) ;
#57469 = CARTESIAN_POINT ( 'NONE',  ( 18.62759615963255655, 10.81492255796105972, 61.66775706135235424 ) ) ;
#57468 = CARTESIAN_POINT ( 'NONE',  ( 5.049401038298161559, -19.05341960407611168, 82.70724293864770971 ) ) ;
#57470 = CARTESIAN_POINT ( 'NONE',  ( 17.14385361876520264, 23.59649016807275856, 148.6750000027311387 ) ) ;
#57471 = CARTESIAN_POINT ( 'NONE',  ( 9.474510206698971260, -16.51473224551069308, 107.9155762719810383 ) ) ;
#57472 = CARTESIAN_POINT ( 'NONE',  ( -17.50000000000149214, 3.254303733634584805, 30.02395893071415145 ) ) ;
#57474 = CARTESIAN_POINT ( 'NONE',  ( 0.05219959533937995610, -21.53943276465977519, 55.00109039468568284 ) ) ;
#57473 = CARTESIAN_POINT ( 'NONE',  ( 12.06949235617739724, 12.14591786802326823, 46.87609039468568994 ) ) ;
#57475 = CARTESIAN_POINT ( 'NONE',  ( -10.72451020669870658, -18.67979575497194134, 89.58442372801901854 ) ) ;
#57476 = CARTESIAN_POINT ( 'NONE',  ( -11.74387995961032516, 9.622336364422256594, -59.83536316257175258 ) ) ;
#57477 = CARTESIAN_POINT ( 'NONE',  ( 14.34966873604972726, -8.224510206698740333, 30.83442372801902209 ) ) ;
#57478 = CARTESIAN_POINT ( 'NONE',  ( 13.89961937509977652, -13.97604488694527269, 68.12390960531436690 ) ) ;
#57479 = CARTESIAN_POINT ( 'NONE',  ( -13.97604488694527625, -13.89961937509977652, 111.8739096053143243 ) ) ;
#57480 = CIRCLE ( 'NONE', #34783, 216.0437394197456342 ) ;
#57481 = ADVANCED_FACE ( 'NONE', ( #153438 ), #30749, .F. ) ;
#57482 = CARTESIAN_POINT ( 'NONE',  ( -30.00000000000000000, -5.510910596163089556E-15, 45.00000000000000000 ) ) ;
#57483 = CARTESIAN_POINT ( 'NONE',  ( 12.14591786802309770, 12.06949235617756955, 114.3739096053143527 ) ) ;
#57484 = CARTESIAN_POINT ( 'NONE',  ( 15.72974639402199770, -15.80617190586745480, 48.12390960531436690 ) ) ;
#57485 = CARTESIAN_POINT ( 'NONE',  ( 12.06949235617739724, 12.14591786802326823, 96.87609039468568994 ) ) ;
#57487 = CARTESIAN_POINT ( 'NONE',  ( 9.474510206698971260, -16.51473224551069308, 62.91557627198102409 ) ) ;
#57486 = CARTESIAN_POINT ( 'NONE',  ( 4.483927247898545687, 16.52544592524342804, 79.79057627198102409 ) ) ;
#57488 = CARTESIAN_POINT ( 'NONE',  ( -21.55341960407619339, 5.719274019375674811, 93.54275706135234714 ) ) ;
#57489 = DIRECTION ( 'NONE',  ( -0.000000000000000000, -0.000000000000000000, -1.000000000000000000 ) ) ;
#57490 = CARTESIAN_POINT ( 'NONE',  ( 14.34966873604972726, -8.224510206698740333, 30.83442372801902209 ) ) ;
#57491 = CARTESIAN_POINT ( 'NONE',  ( 16.55341960407611168, 4.379528057220329451, 83.95724293864770971 ) ) ;
#57492 = CARTESIAN_POINT ( 'NONE',  ( -10.81492255796105439, 18.62759615963255655, 37.91775706135235424 ) ) ;
#57493 = CARTESIAN_POINT ( 'NONE',  ( -21.55341960407610458, -5.719274019375992779, 71.45724293864769550 ) ) ;
#57494 = CARTESIAN_POINT ( 'NONE',  ( 13.97604488694548053, -13.89961937509957401, 35.62609039468567573 ) ) ;
#57495 = DIRECTION ( 'NONE',  ( 1.000000000000000000, 6.391086490440868450E-16, 0.000000000000000000 ) ) ;
#57496 = CARTESIAN_POINT ( 'NONE',  ( 9.474510206698971260, -16.51473224551069308, 87.91557627198102409 ) ) ;
#57497 = CARTESIAN_POINT ( 'NONE',  ( 16.55341960407611168, 4.379528057220329451, 63.95724293864770260 ) ) ;
#57498 = CARTESIAN_POINT ( 'NONE',  ( -4.483927247898539470, -16.52544592524342804, 32.29057627198102409 ) ) ;
#57499 = CARTESIAN_POINT ( 'NONE',  ( 4.483927247898790824, -16.52544592524335698, 105.2094237280190328 ) ) ;
#57500 = CARTESIAN_POINT ( 'NONE',  ( -13.89961937509957401, -13.97604488694547875, 64.37609039468567573 ) ) ;
#57501 = CARTESIAN_POINT ( 'NONE',  ( -5.153800228976607833, 19.02544592524335343, 77.70942372801900433 ) ) ;
#57502 = CARTESIAN_POINT ( 'NONE',  ( -21.53943276465977519, 0.05219959533907696930, 26.24890960531435624 ) ) ;
#57503 = CARTESIAN_POINT ( 'NONE',  ( 8.224510206698953496, -14.34966873604960469, 92.91557627198103830 ) ) ;
#57504 = LINE ( 'NONE', #73671, #112969 ) ;
#57506 = CARTESIAN_POINT ( 'NONE',  ( 10.81492255796078972, 18.62759615963270932, 44.58224293864769550 ) ) ;
#57505 = CARTESIAN_POINT ( 'NONE',  ( -13.97604488694527625, -13.89961937509977652, 41.87390960531435979 ) ) ;
#57507 = CARTESIAN_POINT ( 'NONE',  ( -21.55341960407610458, -5.719274019375992779, 66.45724293864768129 ) ) ;
#57508 = CARTESIAN_POINT ( 'NONE',  ( -14.29746914071049879, 8.314922557960819915, 110.8322429386476955 ) ) ;
#57510 = CARTESIAN_POINT ( 'NONE',  ( -16.46253265017160317, 9.564922557960807481, 50.83224293864770260 ) ) ;
#57509 = CARTESIAN_POINT ( 'NONE',  ( 16.52544592524335698, 4.483927247898782831, 71.45942372801901854 ) ) ;
#57511 = EDGE_CURVE ( 'NONE', #149477, #169869, #33088, .T. ) ;
#57512 = CARTESIAN_POINT ( 'NONE',  ( -10.72451020669870658, -18.67979575497194134, 59.58442372801901854 ) ) ;
#57513 = CARTESIAN_POINT ( 'NONE',  ( 16.53943276465976808, -0.05219959533910856209, 108.7489096053143669 ) ) ;
#57514 = CARTESIAN_POINT ( 'NONE',  ( -13.89961937509957401, -13.97604488694547875, 89.37609039468563310 ) ) ;
#57515 = CARTESIAN_POINT ( 'NONE',  ( 11.40812507854755253, -35.11059874428192273, -2.524999997268813523 ) ) ;
#57517 = CARTESIAN_POINT ( 'NONE',  ( 18.67979575497178502, 10.72451020669898547, 39.16557627198102409 ) ) ;
#57516 = CARTESIAN_POINT ( 'NONE',  ( 26.99873734152913229, -22.49873734152921045, 8.889087296526001936 ) ) ;
#57518 = CARTESIAN_POINT ( 'NONE',  ( 16.46253265017160672, -9.564922557960803928, 28.33224293864769550 ) ) ;
#57519 = CARTESIAN_POINT ( 'NONE',  ( 21.53943276465977519, 0.05219959533937863772, 76.25109039468568994 ) ) ;
#57521 = CARTESIAN_POINT ( 'NONE',  ( 16.52544592524342804, -4.483927247898539470, 48.54057627198103120 ) ) ;
#57520 = CARTESIAN_POINT ( 'NONE',  ( 16.55341960407618274, -4.379528057220086978, 61.04275706135234714 ) ) ;
#57522 = CARTESIAN_POINT ( 'NONE',  ( -18.67979575497178146, -10.72451020669898902, 66.66557627198102409 ) ) ;
#57523 = CARTESIAN_POINT ( 'NONE',  ( 21.55341960407610458, 5.719274019375980345, 68.95724293864769550 ) ) ;
#57524 = CARTESIAN_POINT ( 'NONE',  ( -21.96985492114659166, -8.492568044003455441, 171.8755390570805730 ) ) ;
#57526 = CARTESIAN_POINT ( 'NONE',  ( 18.67979575497178502, 10.72451020669898547, 24.16557627198103120 ) ) ;
#57525 = CARTESIAN_POINT ( 'NONE',  ( -19.03943276465977164, -0.05219959533935918106, 83.75109039468567573 ) ) ;
#57527 = CARTESIAN_POINT ( 'NONE',  ( 19.02544592524343514, -5.153800228976328945, 48.54057627198103120 ) ) ;
#57528 = CARTESIAN_POINT ( 'NONE',  ( -16.53943276465976808, 0.05219959533911058130, 111.2489096053143669 ) ) ;
#57529 = CARTESIAN_POINT ( 'NONE',  ( -19.05341960407611168, -5.049401038298163336, 111.4572429386476671 ) ) ;
#57530 = ORIENTED_EDGE ( 'NONE', *, *, #14301, .F. ) ;
#57531 = CARTESIAN_POINT ( 'NONE',  ( -16.52544592524335698, -4.483927247898792601, 78.95942372801901854 ) ) ;
#57532 = CARTESIAN_POINT ( 'NONE',  ( -21.55341960407610458, -5.719274019375992779, 101.4572429386476955 ) ) ;
#57533 = CARTESIAN_POINT ( 'NONE',  ( 19.02544592524343514, -5.153800228976328945, 73.54057627198103830 ) ) ;
#57534 = CARTESIAN_POINT ( 'NONE',  ( 5.823673210054444382, -21.52544592524334988, 35.20942372801901854 ) ) ;
#57535 = CARTESIAN_POINT ( 'NONE',  ( 16.46253265017160672, -9.564922557960803928, 98.33224293864769550 ) ) ;
#57536 = CARTESIAN_POINT ( 'NONE',  ( -31.90410663231274668, -24.66877891592858774, -17.57859634138819871 ) ) ;
#57537 = ORIENTED_EDGE ( 'NONE', *, *, #85994, .T. ) ;
#57538 = CARTESIAN_POINT ( 'NONE',  ( 21.55341960407619695, -5.719274019375665929, 26.04275706135235779 ) ) ;
#57540 = CARTESIAN_POINT ( 'NONE',  ( -19.03943276465977164, -0.05219959533935918106, 83.75109039468567573 ) ) ;
#57539 = CARTESIAN_POINT ( 'NONE',  ( 16.51473224551069308, 9.474510206698969483, 29.16557627198103475 ) ) ;
#57541 = CARTESIAN_POINT ( 'NONE',  ( -13.89961937509957401, -13.97604488694547875, 34.37609039468566863 ) ) ;
#57542 = CARTESIAN_POINT ( 'NONE',  ( 5.823673210054125526, 21.52544592524343514, 114.7905762719810383 ) ) ;
#57543 = CARTESIAN_POINT ( 'NONE',  ( -16.51473224551082808, 9.474510206698731452, 38.33442372801899722 ) ) ;
#57544 = CARTESIAN_POINT ( 'NONE',  ( 13.97604488694548053, -13.89961937509957401, 55.62609039468566863 ) ) ;
#57545 = CARTESIAN_POINT ( 'NONE',  ( 4.483927247898790824, -16.52544592524335698, 90.20942372801903275 ) ) ;
#57546 = CARTESIAN_POINT ( 'NONE',  ( -5.049401038298153566, 19.05341960407611168, 115.2072429386477097 ) ) ;
#57547 = CARTESIAN_POINT ( 'NONE',  ( 5.049401038298161559, -19.05341960407611168, 67.70724293864769550 ) ) ;
#57548 = CARTESIAN_POINT ( 'NONE',  ( -21.52544592524334988, -5.823673210054445271, 78.95942372801901854 ) ) ;
#57549 = CARTESIAN_POINT ( 'NONE',  ( -21.55341960407619339, 5.719274019375674811, 88.54275706135236135 ) ) ;
#57550 = CARTESIAN_POINT ( 'NONE',  ( 23.87412888849588555, -1.051486528467125758, -54.54543624665771517 ) ) ;
#57551 = CARTESIAN_POINT ( 'NONE',  ( -9.474510206698964154, 16.51473224551069663, 90.41557627198103830 ) ) ;
#57552 = CARTESIAN_POINT ( 'NONE',  ( -15.72974639402176322, -15.80617190586768395, 64.37609039468568994 ) ) ;
#57553 = CARTESIAN_POINT ( 'NONE',  ( -16.51473224551082808, 9.474510206698731452, 103.3344237280190043 ) ) ;
#57554 = CARTESIAN_POINT ( 'NONE',  ( 0.05219959533909260263, 19.03943276465977164, 59.99890960531436690 ) ) ;
#57555 = CARTESIAN_POINT ( 'NONE',  ( 16.51473224551069308, 9.474510206698969483, 114.1655762719810241 ) ) ;
#57556 = CARTESIAN_POINT ( 'NONE',  ( 19.02544592524343514, -5.153800228976328945, 73.54057627198103830 ) ) ;
#57557 = CARTESIAN_POINT ( 'NONE',  ( -17.59860650958991002, -7.585241751807008548, 76.57662985737509587 ) ) ;
#57558 = CARTESIAN_POINT ( 'NONE',  ( -13.89961937509977652, 13.97604488694528158, 70.62390960531432427 ) ) ;
#57559 = CARTESIAN_POINT ( 'NONE',  ( 13.97604488694527802, 13.89961937509977652, 54.37390960531435979 ) ) ;
#57560 = CARTESIAN_POINT ( 'NONE',  ( -21.53943276465977519, 0.05219959533907696930, 111.2489096053143669 ) ) ;
#57561 = CARTESIAN_POINT ( 'NONE',  ( 16.53943276465976808, 0.05219959533934440121, 91.25109039468568994 ) ) ;
#57562 = CARTESIAN_POINT ( 'NONE',  ( -2.500000000000000000, -165.0000000000000000, 7.000000000000003553 ) ) ;
#57563 = CARTESIAN_POINT ( 'NONE',  ( 6.100000000000006750, -2.167155344068307965E-14, -64.53213882399991519 ) ) ;
#57564 = CARTESIAN_POINT ( 'NONE',  ( -9.564922557961040184, 16.46253265017147172, 62.91775706135233293 ) ) ;
#57565 = CARTESIAN_POINT ( 'NONE',  ( -13.89961937509977652, 13.97604488694528158, 75.62390960531438111 ) ) ;
#57566 = CARTESIAN_POINT ( 'NONE',  ( -12.06949235617756955, 12.14591786802309770, 70.62390960531436690 ) ) ;
#57567 = CARTESIAN_POINT ( 'NONE',  ( -8.224510206698948167, 14.34966873604960824, 105.4155762719810383 ) ) ;
#57568 = CARTESIAN_POINT ( 'NONE',  ( 18.67979575497178502, 10.72451020669898547, 29.16557627198103120 ) ) ;
#57569 = CARTESIAN_POINT ( 'NONE',  ( 16.46253265017160672, -9.564922557960803928, 103.3322429386476955 ) ) ;
#57570 = CARTESIAN_POINT ( 'NONE',  ( 16.52544592524342804, -4.483927247898539470, 93.54057627198103830 ) ) ;
#57571 = CARTESIAN_POINT ( 'NONE',  ( 0.000000000000000000, 0.000000000000000000, -25.00000000000000000 ) ) ;
#57572 = CARTESIAN_POINT ( 'NONE',  ( 9.474510206698729675, 16.51473224551082808, 32.08442372801900433 ) ) ;
#57573 = CARTESIAN_POINT ( 'NONE',  ( -4.483927247898782831, 16.52544592524335698, 102.7094237280190185 ) ) ;
#57574 = CARTESIAN_POINT ( 'NONE',  ( 16.46253265017160672, -9.564922557960803928, 83.33224293864768129 ) ) ;
#57575 = CARTESIAN_POINT ( 'NONE',  ( -21.55341960407619339, 5.719274019375674811, 58.54275706135235424 ) ) ;
#57576 = CARTESIAN_POINT ( 'NONE',  ( 10.81492255796078972, 18.62759615963270932, 49.58224293864769550 ) ) ;
#57577 = CARTESIAN_POINT ( 'NONE',  ( 0.05219959533937995610, -21.53943276465977519, 20.00109039468568639 ) ) ;
#57578 = CARTESIAN_POINT ( 'NONE',  ( -10.81492255796078084, -18.62759615963271287, 67.08224293864770971 ) ) ;
#57579 = CARTESIAN_POINT ( 'NONE',  ( 16.52544592524342804, -4.483927247898539470, 98.54057627198105251 ) ) ;
#57580 = CARTESIAN_POINT ( 'NONE',  ( -16.51473224551082808, 9.474510206698731452, 53.33442372801900433 ) ) ;
#57581 = CARTESIAN_POINT ( 'NONE',  ( 19.05341960407611168, 5.049401038298154454, 28.95724293864769550 ) ) ;
#57582 = CARTESIAN_POINT ( 'NONE',  ( 16.46253265017160672, -9.564922557960803928, 78.33224293864769550 ) ) ;
#57583 = CARTESIAN_POINT ( 'NONE',  ( 13.89961937509977652, -13.97604488694527269, 93.12390960531436690 ) ) ;
#57584 = CARTESIAN_POINT ( 'NONE',  ( 16.46253265017160672, -9.564922557960803928, 23.33224293864769194 ) ) ;
#57585 = CARTESIAN_POINT ( 'NONE',  ( -12.14591786802309592, -12.06949235617757132, 21.87390960531436690 ) ) ;
#57586 = CARTESIAN_POINT ( 'NONE',  ( -8.224510206698735004, -14.34966873604973081, 34.58442372801900433 ) ) ;
#57587 = CARTESIAN_POINT ( 'NONE',  ( -21.52544592524334988, -5.823673210054445271, 108.9594237280190185 ) ) ;
#57588 = CARTESIAN_POINT ( 'NONE',  ( 19.02544592524343514, -5.153800228976328945, 98.54057627198100988 ) ) ;
#57589 = CARTESIAN_POINT ( 'NONE',  ( 10.72451020669871369, 18.67979575497193778, 37.08442372801901143 ) ) ;
#57590 = CARTESIAN_POINT ( 'NONE',  ( -16.51473224551069308, -9.474510206698971260, 46.66557627198102409 ) ) ;
#57591 = CARTESIAN_POINT ( 'NONE',  ( 8.224510206698742110, 14.34966873604972548, 42.08442372801901854 ) ) ;
#57592 = CARTESIAN_POINT ( 'NONE',  ( -14.34966873604972548, 8.224510206698743886, 108.3344237280190185 ) ) ;
#57593 = CARTESIAN_POINT ( 'NONE',  ( -14.29746914071037622, -8.314922557961029526, 89.16775706135236135 ) ) ;
#57594 = EDGE_CURVE ( 'NONE', #169095, #15380, #185608, .T. ) ;
#57595 = CARTESIAN_POINT ( 'NONE',  ( 16.51473224551083163, -9.474510206698727899, 105.8344237280190043 ) ) ;
#57596 = CARTESIAN_POINT ( 'NONE',  ( 19.03943276465977164, -0.05219959533909143690, 28.74890960531435624 ) ) ;
#57597 = CARTESIAN_POINT ( 'NONE',  ( -4.379528057220328563, 16.55341960407611168, 90.20724293864770971 ) ) ;
#57598 = CARTESIAN_POINT ( 'NONE',  ( -5.719274019375978568, 21.55341960407610458, 105.2072429386477097 ) ) ;
#57599 = CARTESIAN_POINT ( 'NONE',  ( 13.97604488694527802, 13.89961937509977652, 29.37390960531435979 ) ) ;
#57600 = CARTESIAN_POINT ( 'NONE',  ( 9.564922557960805705, 16.46253265017160317, 104.5822429386476955 ) ) ;
#57601 = CARTESIAN_POINT ( 'NONE',  ( -21.55341960407619339, 5.719274019375674811, 28.54275706135234358 ) ) ;
#57602 = CARTESIAN_POINT ( 'NONE',  ( -16.51473224551069308, -9.474510206698971260, 21.66557627198102765 ) ) ;
#57603 = CARTESIAN_POINT ( 'NONE',  ( 19.05341960407611168, 5.049401038298154454, 108.9572429386477097 ) ) ;
#57604 = CARTESIAN_POINT ( 'NONE',  ( -27.86473085795038429, -131.0000000000000000, -13.99999999999999822 ) ) ;
#57605 = CARTESIAN_POINT ( 'NONE',  ( 19.02544592524343514, -5.153800228976328945, 78.54057627198099567 ) ) ;
#57607 = CARTESIAN_POINT ( 'NONE',  ( 16.55341960407611168, 4.379528057220329451, 88.95724293864769550 ) ) ;
#57606 = CARTESIAN_POINT ( 'NONE',  ( -21.53943276465977519, -0.05219959533937600094, 33.75109039468568284 ) ) ;
#57608 = CARTESIAN_POINT ( 'NONE',  ( -5.153800228976328057, -19.02544592524343514, 102.2905762719810383 ) ) ;
#57609 = CARTESIAN_POINT ( 'NONE',  ( -5.153800228976607833, 19.02544592524334988, 22.70942372801899012 ) ) ;
#57610 = CARTESIAN_POINT ( 'NONE',  ( -0.05219959533934338120, 16.53943276465976808, 67.50109039468568994 ) ) ;
#57611 = CARTESIAN_POINT ( 'NONE',  ( -18.67979575497193778, 10.72451020669871902, 73.33442372801901854 ) ) ;
#57612 = AXIS2_PLACEMENT_3D ( 'NONE', #5235, #6237, #170648 ) ;
#57613 = CARTESIAN_POINT ( 'NONE',  ( 16.55341960407618274, -4.379528057220086978, 46.04275706135234714 ) ) ;
#57614 = CARTESIAN_POINT ( 'NONE',  ( -16.46253265017160317, 9.564922557960807481, 85.83224293864769550 ) ) ;
#57615 = CARTESIAN_POINT ( 'NONE',  ( 13.97604488694548053, -13.89961937509957401, 95.62609039468563310 ) ) ;
#57616 = CARTESIAN_POINT ( 'NONE',  ( -4.379528057220086978, -16.55341960407618274, 74.79275706135234714 ) ) ;
#57617 = CARTESIAN_POINT ( 'NONE',  ( 5.719274019375673035, 21.55341960407619339, 112.2927570613523471 ) ) ;
#57618 = CARTESIAN_POINT ( 'NONE',  ( 0.05219959533936267826, -19.03943276465977164, 85.00109039468567573 ) ) ;
#57619 = CARTESIAN_POINT ( 'NONE',  ( 5.153800228976335163, 19.02544592524342804, 69.79057627198103830 ) ) ;
#57620 = CARTESIAN_POINT ( 'NONE',  ( -21.52544592524343514, 5.823673210054127303, 86.04057627198102409 ) ) ;
#57622 = CARTESIAN_POINT ( 'NONE',  ( -16.51473224551082808, 9.474510206698731452, 93.33442372801900433 ) ) ;
#57621 = CARTESIAN_POINT ( 'NONE',  ( 8.314922557960818139, 14.29746914071049879, 84.58224293864769550 ) ) ;
#57623 = CARTESIAN_POINT ( 'NONE',  ( 14.29746914071037800, 8.314922557961029526, 56.66775706135235424 ) ) ;
#57624 = CARTESIAN_POINT ( 'NONE',  ( 17.50000000000002132, -5.499999999999878320, 63.29690382534172954 ) ) ;
#57626 = EDGE_CURVE ( 'NONE', #15498, #140232, #35467, .T. ) ;
#57625 = CARTESIAN_POINT ( 'NONE',  ( -9.564922557961040184, 16.46253265017147172, 57.91775706135233293 ) ) ;
#57627 = CARTESIAN_POINT ( 'NONE',  ( -4.379528057220328563, 16.55341960407611168, 25.20724293864769550 ) ) ;
#57628 = CARTESIAN_POINT ( 'NONE',  ( -4.483927247898539470, -16.52544592524342804, 77.29057627198102409 ) ) ;
#57630 = CARTESIAN_POINT ( 'NONE',  ( -16.52216118717247895, 7.221426719304377073, 38.92400978952973389 ) ) ;
#57629 = CARTESIAN_POINT ( 'NONE',  ( -5.153800228976607833, 19.02544592524334988, 22.70942372801899012 ) ) ;
#57631 = CARTESIAN_POINT ( 'NONE',  ( -18.62759615963270932, 10.81492255796079327, 115.8322429386477097 ) ) ;
#57632 =( BOUNDED_CURVE ( )  B_SPLINE_CURVE ( 2, ( #181629, #43109, #28948, #117957, #86608, #9785, #116943, #87605, #135134, #120923, #165465 ),
 .UNSPECIFIED., .F., .T. ) 
 B_SPLINE_CURVE_WITH_KNOTS ( ( 3, 2, 2, 2, 2, 3 ),
 ( 0.9000000000000000222, 0.9200000000000000400, 0.9399999999999999467, 0.9599999999999999645, 0.9799999999999999822, 1.000000000000000000 ),
 .UNSPECIFIED. ) 
 CURVE ( )  GEOMETRIC_REPRESENTATION_ITEM ( )  RATIONAL_B_SPLINE_CURVE ( ( 1.000000000000000000, 0.9510565162951535312, 1.000000000000000000, 0.9510565162951535312, 1.000000000000000000, 0.9510565162951535312, 1.000000000000000000, 0.9510565162951535312, 1.000000000000000000, 0.9510565162951535312, 1.000000000000000000 ) ) 
 REPRESENTATION_ITEM ( '' )  );
#57633 = CARTESIAN_POINT ( 'NONE',  ( 19.03943276465977164, -0.05219959533909143690, 98.74890960531436690 ) ) ;
#57634 = CARTESIAN_POINT ( 'NONE',  ( -9.564922557960796823, -16.46253265017161027, 82.08224293864768129 ) ) ;
#57635 = CARTESIAN_POINT ( 'NONE',  ( -18.62759615963255300, -10.81492255796106328, 84.16775706135234714 ) ) ;
#57636 = CARTESIAN_POINT ( 'NONE',  ( -19.05341960407611168, -5.049401038298163336, 61.45724293864769550 ) ) ;
#57637 = CARTESIAN_POINT ( 'NONE',  ( -21.52544592524343514, 5.823673210054127303, 31.04057627198102409 ) ) ;
#57638 = CARTESIAN_POINT ( 'NONE',  ( -12.06949235617756955, 12.14591786802309770, 75.62390960531439532 ) ) ;
#57639 = CARTESIAN_POINT ( 'NONE',  ( -0.05219959533909027116, -19.03943276465977164, 37.49890960531436690 ) ) ;
#57640 = CARTESIAN_POINT ( 'NONE',  ( 8.224510206698953496, -14.34966873604960469, 92.91557627198103830 ) ) ;
#57641 = CARTESIAN_POINT ( 'NONE',  ( 15.80617190586746368, 15.72974639402197994, 104.3739096053143669 ) ) ;
#57642 = CARTESIAN_POINT ( 'NONE',  ( 5.719274019375673035, 21.55341960407619339, 52.29275706135236135 ) ) ;
#57643 = CARTESIAN_POINT ( 'NONE',  ( 13.89961937509977652, -13.97604488694527269, 28.12390960531435624 ) ) ;
#57644 = CARTESIAN_POINT ( 'NONE',  ( -12.06949235617739369, -12.14591786802326823, 69.37609039468567573 ) ) ;
#57645 = CARTESIAN_POINT ( 'NONE',  ( 10.81492255796078972, 18.62759615963270932, 99.58224293864770971 ) ) ;
#57646 = CARTESIAN_POINT ( 'NONE',  ( -10.81492255796078084, -18.62759615963271287, 107.0822429386476955 ) ) ;
#57648 = CARTESIAN_POINT ( 'NONE',  ( 9.474510206698971260, -16.51473224551069308, 57.91557627198103120 ) ) ;
#57647 = CARTESIAN_POINT ( 'NONE',  ( -0.05219959533936034679, 19.03943276465977164, 37.50109039468567573 ) ) ;
#57649 = FACE_OUTER_BOUND ( 'NONE', #135011, .T. ) ;
#57650 = CARTESIAN_POINT ( 'NONE',  ( 5.823673210054444382, -21.52544592524334988, 55.20942372801902565 ) ) ;
#57651 = CARTESIAN_POINT ( 'NONE',  ( 5.823673210054125526, 21.52544592524343514, 54.79057627198104541 ) ) ;
#57652 = CARTESIAN_POINT ( 'NONE',  ( -16.55341960407611168, -4.379528057220339221, 31.45724293864769550 ) ) ;
#57654 = CARTESIAN_POINT ( 'NONE',  ( -21.55341960407619339, 5.719274019375674811, 113.5427570613523756 ) ) ;
#57653 = CARTESIAN_POINT ( 'NONE',  ( 21.55341960407619695, -5.719274019375665929, 76.04275706135237556 ) ) ;
#57655 = CARTESIAN_POINT ( 'NONE',  ( -8.314922557960811034, -14.29746914071050412, 62.08224293864769550 ) ) ;
#57656 = CARTESIAN_POINT ( 'NONE',  ( -8.314922557960811034, -14.29746914071050412, 102.0822429386476955 ) ) ;
#57657 = CARTESIAN_POINT ( 'NONE',  ( -19.05341960407617563, 5.049401038297882671, 43.54275706135232582 ) ) ;
#57658 = CARTESIAN_POINT ( 'NONE',  ( -12.06949235617739369, -12.14591786802326823, 99.37609039468568994 ) ) ;
#57659 = CARTESIAN_POINT ( 'NONE',  ( -21.53943276465977519, -0.05219959533937600094, 63.75109039468568284 ) ) ;
#57660 = CARTESIAN_POINT ( 'NONE',  ( 9.564922557960805705, 16.46253265017160317, 59.58224293864769550 ) ) ;
#57661 = CARTESIAN_POINT ( 'NONE',  ( -0.05219959533936034679, 19.03943276465977164, 32.50109039468566863 ) ) ;
#57662 = CARTESIAN_POINT ( 'NONE',  ( -21.55341960407610458, -5.719274019375992779, 36.45724293864768839 ) ) ;
#57663 = CARTESIAN_POINT ( 'NONE',  ( 15.72974639402176855, 15.80617190586768217, 36.87609039468568994 ) ) ;
#57664 = CARTESIAN_POINT ( 'NONE',  ( -5.719274019375978568, 21.55341960407610458, 90.20724293864770971 ) ) ;
#57665 = CARTESIAN_POINT ( 'NONE',  ( -16.46253265017146816, -9.564922557961047289, 89.16775706135234714 ) ) ;
#57666 = CARTESIAN_POINT ( 'NONE',  ( 16.52544592524335698, 4.483927247898782831, 56.45942372801902565 ) ) ;
#57668 = CARTESIAN_POINT ( 'NONE',  ( 10.72451020669898902, -18.67979575497178502, 87.91557627198103830 ) ) ;
#57667 = CARTESIAN_POINT ( 'NONE',  ( 17.50000000000001421, -3.190838340304443133, 37.39123124295112177 ) ) ;
#57670 = CARTESIAN_POINT ( 'NONE',  ( -8.314922557960811034, -14.29746914071050412, 72.08224293864769550 ) ) ;
#57669 = CARTESIAN_POINT ( 'NONE',  ( 4.483927247898790824, -16.52544592524335698, 80.20942372801901854 ) ) ;
#57671 = CARTESIAN_POINT ( 'NONE',  ( -17.12812012977026654, -6.668231424565994381, 101.3594875932314636 ) ) ;
#57672 = CARTESIAN_POINT ( 'NONE',  ( -12.14591786802326823, 12.06949235617739902, 28.12609039468568284 ) ) ;
#57673 = CARTESIAN_POINT ( 'NONE',  ( 15.72974639402199770, -15.80617190586745480, 33.12390960531435979 ) ) ;
#57674 = CARTESIAN_POINT ( 'NONE',  ( -8.224510206698735004, -14.34966873604973081, 74.58442372801901854 ) ) ;
#57675 = CARTESIAN_POINT ( 'NONE',  ( -13.89961937509977830, 13.97604488694528158, 95.62390960531436690 ) ) ;
#57676 = CARTESIAN_POINT ( 'NONE',  ( -4.483927247898782831, 16.52544592524335698, 57.70942372801901143 ) ) ;
#57677 = CARTESIAN_POINT ( 'NONE',  ( -21.53943276465977519, -0.05219959533937600094, 28.75109039468567929 ) ) ;
#57678 = CARTESIAN_POINT ( 'NONE',  ( -10.72451020669898014, 18.67979575497178502, 45.41557627198103830 ) ) ;
#57679 = CARTESIAN_POINT ( 'NONE',  ( 0.05219959533934541429, -16.53943276465976808, 65.00109039468568994 ) ) ;
#57680 = CARTESIAN_POINT ( 'NONE',  ( 13.97604488694527802, 13.89961937509977652, 89.37390960531436690 ) ) ;
#57682 = CARTESIAN_POINT ( 'NONE',  ( 16.51473224551069308, 9.474510206698969483, 34.16557627198102409 ) ) ;
#57681 = CARTESIAN_POINT ( 'NONE',  ( -21.55341960407619339, 5.719274019375674811, 53.54275706135234714 ) ) ;
#57683 = CARTESIAN_POINT ( 'NONE',  ( 5.823673210054125526, 21.52544592524343514, 39.79057627198103830 ) ) ;
#57684 = VERTEX_POINT ( 'NONE', #131057 ) ;
#57685 = CARTESIAN_POINT ( 'NONE',  ( 5.049401038297881783, 19.05341960407617563, 42.29275706135234003 ) ) ;
#57686 = CARTESIAN_POINT ( 'NONE',  ( -16.55341960407617563, 4.379528057220093196, 53.54275706135234714 ) ) ;
#57687 = CARTESIAN_POINT ( 'NONE',  ( -15.72974639402197994, 15.80617190586746368, 25.62390960531435624 ) ) ;
#57688 = ORIENTED_EDGE ( 'NONE', *, *, #196970, .T. ) ;
#57689 = CARTESIAN_POINT ( 'NONE',  ( 9.474510206698971260, -16.51473224551069308, 82.91557627198103830 ) ) ;
#57690 = CARTESIAN_POINT ( 'NONE',  ( -4.379528057220086978, -16.55341960407618274, 99.79275706135234714 ) ) ;
#57691 = CARTESIAN_POINT ( 'NONE',  ( -3.573655867282028392E-15, 2.428612866367529932E-14, 0.000000000000000000 ) ) ;
#57692 = CARTESIAN_POINT ( 'NONE',  ( 8.224510206698953496, -14.34966873604960469, 92.91557627198103830 ) ) ;
#57693 = CARTESIAN_POINT ( 'NONE',  ( -21.52544592524343514, 5.823673210054127303, 31.04057627198102409 ) ) ;
#57694 = CARTESIAN_POINT ( 'NONE',  ( -16.51473224551069308, -9.474510206698971260, 36.66557627198102409 ) ) ;
#57695 = CARTESIAN_POINT ( 'NONE',  ( 8.224510206698742110, 14.34966873604972548, 77.08442372801901854 ) ) ;
#57696 = CARTESIAN_POINT ( 'NONE',  ( 21.52544592524344225, -5.823673210054117533, 113.5405762719810383 ) ) ;
#57697 = CARTESIAN_POINT ( 'NONE',  ( -13.97604488694547697, 13.89961937509957934, 73.12609039468568994 ) ) ;
#57698 = CARTESIAN_POINT ( 'NONE',  ( 19.05341960407611168, 5.049401038298154454, 33.95724293864769550 ) ) ;
#57699 = CARTESIAN_POINT ( 'NONE',  ( 7.284589286804292740, 1.784589286804177277, 1.818019484660534424 ) ) ;
#57700 = CARTESIAN_POINT ( 'NONE',  ( -21.55341960407619339, 5.719274019375674811, 103.5427570613523613 ) ) ;
#57701 = CARTESIAN_POINT ( 'NONE',  ( -9.474510206698964154, 16.51473224551069663, 70.41557627198102409 ) ) ;
#57702 = CARTESIAN_POINT ( 'NONE',  ( -14.29746914071037622, -8.314922557961029526, 49.16775706135234003 ) ) ;
#57703 = CARTESIAN_POINT ( 'NONE',  ( -18.67979575497193778, 10.72451020669871902, 93.33442372801901854 ) ) ;
#57704 = CARTESIAN_POINT ( 'NONE',  ( -9.474510206698720793, -16.51473224551083518, 54.58442372801899722 ) ) ;
#57705 = CARTESIAN_POINT ( 'NONE',  ( -9.564922557961040184, 16.46253265017147172, 47.91775706135233293 ) ) ;
#57706 = ORIENTED_EDGE ( 'NONE', *, *, #82460, .F. ) ;
#57707 = CARTESIAN_POINT ( 'NONE',  ( 18.62759615963255655, 10.81492255796105972, 46.66775706135234714 ) ) ;
#57708 = EDGE_CURVE ( 'NONE', #185003, #172465, #62907, .T. ) ;
#57709 = CARTESIAN_POINT ( 'NONE',  ( -5.049401038297874678, -19.05341960407617918, 39.79275706135232582 ) ) ;
#57710 = CARTESIAN_POINT ( 'NONE',  ( -19.03943276465977164, 0.05219959533909376836, 106.2489096053143669 ) ) ;
#57711 = CARTESIAN_POINT ( 'NONE',  ( -13.89961937509977652, 13.97604488694528158, 85.62390960531433848 ) ) ;
#57712 = CARTESIAN_POINT ( 'NONE',  ( -14.34966873604960291, -8.224510206698953496, 31.66557627198102054 ) ) ;
#57713 = CARTESIAN_POINT ( 'NONE',  ( 10.72451020669898902, -18.67979575497178502, 27.91557627198103830 ) ) ;
#57714 = CARTESIAN_POINT ( 'NONE',  ( -29.86685920354755552, 21.69954338932564397, -3.324999997268813345 ) ) ;
#57715 = DIRECTION ( 'NONE',  ( 1.000000000000000000, 0.000000000000000000, 0.000000000000000000 ) ) ;
#57716 = CARTESIAN_POINT ( 'NONE',  ( 9.474510206698729675, 16.51473224551082808, 22.08442372801899722 ) ) ;
#57717 = DIRECTION ( 'NONE',  ( 0.1039620511844979306, -0.1039620511844979306, -0.9891328443778538704 ) ) ;
#57718 = CARTESIAN_POINT ( 'NONE',  ( -5.153800228976328057, -19.02544592524343514, 42.29057627198101699 ) ) ;
#57719 = CARTESIAN_POINT ( 'NONE',  ( -5.049401038298153566, 19.05341960407611168, 30.20724293864768839 ) ) ;
#57720 = CARTESIAN_POINT ( 'NONE',  ( -34.29482437030765851, -3.353353130260861015, 90.62592007927790405 ) ) ;
#57721 = CARTESIAN_POINT ( 'NONE',  ( -37.83797858686578053, -3.323448926770519840, -8.000000000000000000 ) ) ;
#57722 = CARTESIAN_POINT ( 'NONE',  ( -16.55341960407617563, 4.379528057220093196, 68.54275706135234714 ) ) ;
#57723 = CARTESIAN_POINT ( 'NONE',  ( 10.72451020669898902, -18.67979575497178502, 82.91557627198103830 ) ) ;
#57724 = CARTESIAN_POINT ( 'NONE',  ( 12.14591786802309770, 12.06949235617756955, 44.37390960531435979 ) ) ;
#57726 = CARTESIAN_POINT ( 'NONE',  ( 16.51473224551069308, 9.474510206698969483, 109.1655762719810383 ) ) ;
#57725 = CARTESIAN_POINT ( 'NONE',  ( -13.97604488694527625, -13.89961937509977652, 21.87390960531435979 ) ) ;
#57727 = CARTESIAN_POINT ( 'NONE',  ( -5.823673210054431948, 21.52544592524334988, 27.70942372801901854 ) ) ;
#57728 = CARTESIAN_POINT ( 'NONE',  ( -19.05341960407617563, 5.049401038297882671, 33.54275706135231871 ) ) ;
#57729 = CARTESIAN_POINT ( 'NONE',  ( -19.03943276465977164, 0.05219959533909376836, 36.24890960531436690 ) ) ;
#57730 = CARTESIAN_POINT ( 'NONE',  ( 15.80617190586769283, -15.72974639402175789, 80.62609039468567573 ) ) ;
#57731 = CARTESIAN_POINT ( 'NONE',  ( 17.50000000000000000, -5.624438216177593652, 33.31670344914648041 ) ) ;
#57732 = CARTESIAN_POINT ( 'NONE',  ( 8.314922557960818139, 14.29746914071049879, 29.58224293864769905 ) ) ;
#57733 = CARTESIAN_POINT ( 'NONE',  ( -5.950531402560715689E-15, 38.81732327939063509, -3.624999997268813168 ) ) ;
#57734 = CARTESIAN_POINT ( 'NONE',  ( -18.62759615963270932, 10.81492255796079327, 30.83224293864770260 ) ) ;
#57735 = CARTESIAN_POINT ( 'NONE',  ( -8.224510206698948167, 14.34966873604960824, 100.4155762719810241 ) ) ;
#57736 = CARTESIAN_POINT ( 'NONE',  ( -4.044156916725154538, -6.083257512445876536, -64.32761231701863380 ) ) ;
#57737 = CARTESIAN_POINT ( 'NONE',  ( 13.97604488694527802, 13.89961937509977652, 84.37390960531433848 ) ) ;
#57738 = CARTESIAN_POINT ( 'NONE',  ( -14.29746914071049879, 8.314922557960819915, 80.83224293864769550 ) ) ;
#57739 = CARTESIAN_POINT ( 'NONE',  ( 13.89961937509957401, 13.97604488694547697, 106.8760903946856757 ) ) ;
#57740 = CARTESIAN_POINT ( 'NONE',  ( 10.72451020669898902, -18.67979575497178502, 67.91557627198102409 ) ) ;
#57741 = ORIENTED_EDGE ( 'NONE', *, *, #61248, .F. ) ;
#57742 = CARTESIAN_POINT ( 'NONE',  ( -19.03943276465977164, 0.05219959533909376836, 26.24890960531435624 ) ) ;
#57744 = CARTESIAN_POINT ( 'NONE',  ( 10.72451020669898902, -18.67979575497178502, 92.91557627198103830 ) ) ;
#57743 = CARTESIAN_POINT ( 'NONE',  ( -5.153800228976328057, -19.02544592524343514, 82.29057627198103830 ) ) ;
#57746 = CARTESIAN_POINT ( 'NONE',  ( 9.564922557960805705, 16.46253265017160317, 84.58224293864769550 ) ) ;
#57745 = CARTESIAN_POINT ( 'NONE',  ( 4.483927247898790824, -16.52544592524335698, 100.2094237280190043 ) ) ;
#57747 = CARTESIAN_POINT ( 'NONE',  ( 9.474510206698729675, 16.51473224551082808, 87.08442372801900433 ) ) ;
#57748 = CARTESIAN_POINT ( 'NONE',  ( -18.62759615963255300, -10.81492255796106328, 89.16775706135236135 ) ) ;
#57749 = CARTESIAN_POINT ( 'NONE',  ( 0.05219959533907565091, 21.53943276465977519, 79.99890960531435269 ) ) ;
#57750 = CARTESIAN_POINT ( 'NONE',  ( 21.53943276465977519, -0.05219959533907433946, 33.74890960531436690 ) ) ;
#57751 = CARTESIAN_POINT ( 'NONE',  ( 19.05341960407611168, 5.049401038298154454, 48.95724293864768129 ) ) ;
#57752 = CARTESIAN_POINT ( 'NONE',  ( 12.06949235617757843, -12.14591786802309237, 23.12390960531436335 ) ) ;
#57753 = CARTESIAN_POINT ( 'NONE',  ( 5.153800228976335163, 19.02544592524342804, 59.79057627198100988 ) ) ;
#57754 = DIRECTION ( 'NONE',  ( -0.000000000000000000, -0.000000000000000000, -1.000000000000000000 ) ) ;
#57755 = CARTESIAN_POINT ( 'NONE',  ( 16.51473224551083163, -9.474510206698727899, 30.83442372801900433 ) ) ;
#57756 = CARTESIAN_POINT ( 'NONE',  ( -4.483927247898539470, -16.52544592524342804, 77.29057627198102409 ) ) ;
#57757 = CARTESIAN_POINT ( 'NONE',  ( 10.72451020669898902, -18.67979575497178502, 112.9155762719810383 ) ) ;
#57758 = CARTESIAN_POINT ( 'NONE',  ( -10.81492255796105439, 18.62759615963255655, 22.91775706135235069 ) ) ;
#57759 = CARTESIAN_POINT ( 'NONE',  ( 22.44159573604009239, 16.30477369853692693, 140.5750000027311728 ) ) ;
#57760 = CARTESIAN_POINT ( 'NONE',  ( -5.719274019375978568, 21.55341960407610458, 60.20724293864768839 ) ) ;
#57761 = CARTESIAN_POINT ( 'NONE',  ( 16.55341960407618274, -4.379528057220086978, 91.04275706135236135 ) ) ;
#57762 = CARTESIAN_POINT ( 'NONE',  ( -16.53943276465976808, 0.05219959533911058130, 111.2489096053143669 ) ) ;
#57763 = CARTESIAN_POINT ( 'NONE',  ( 13.97604488694527802, 13.89961937509977652, 59.37390960531434558 ) ) ;
#57764 = CARTESIAN_POINT ( 'NONE',  ( -14.29746914071049879, 8.314922557960819915, 30.83224293864770260 ) ) ;
#57765 = CARTESIAN_POINT ( 'NONE',  ( -15.72974639402176322, -15.80617190586768395, 49.37609039468569705 ) ) ;
#57766 = CARTESIAN_POINT ( 'NONE',  ( 9.564922557960805705, 16.46253265017160317, 109.5822429386476955 ) ) ;
#57767 = CARTESIAN_POINT ( 'NONE',  ( 21.52544592524334988, 5.823673210054432836, 86.45942372801901854 ) ) ;
#57768 = CARTESIAN_POINT ( 'NONE',  ( -19.03943276465977164, 0.05219959533909376836, 26.24890960531435624 ) ) ;
#57769 = CARTESIAN_POINT ( 'NONE',  ( 5.049401038298161559, -19.05341960407611168, 37.70724293864768839 ) ) ;
#57770 = ORIENTED_EDGE ( 'NONE', *, *, #146444, .F. ) ;
#57771 = CARTESIAN_POINT ( 'NONE',  ( 18.62759615963255655, 10.81492255796105972, 81.66775706135236135 ) ) ;
#57772 = CARTESIAN_POINT ( 'NONE',  ( -12.14591786802326823, 12.06949235617739902, 53.12609039468568284 ) ) ;
#57773 = CARTESIAN_POINT ( 'NONE',  ( -5.719274019375665041, -21.55341960407619695, 69.79275706135234714 ) ) ;
#57774 = CARTESIAN_POINT ( 'NONE',  ( 5.049401038298161559, -19.05341960407611168, 107.7072429386476955 ) ) ;
#57775 = CARTESIAN_POINT ( 'NONE',  ( 16.51473224551083163, -9.474510206698727899, 85.83442372801900433 ) ) ;
#57776 = CARTESIAN_POINT ( 'NONE',  ( 5.719274019375673035, 21.55341960407619339, 52.29275706135236135 ) ) ;
#57777 = CARTESIAN_POINT ( 'NONE',  ( 14.29746914071037800, 8.314922557961029526, 26.66775706135235424 ) ) ;
#57778 = CARTESIAN_POINT ( 'NONE',  ( 5.153800228976615827, -19.02544592524334988, 80.20942372801901854 ) ) ;
#57779 = CARTESIAN_POINT ( 'NONE',  ( 0.05219959533909260263, 19.03943276465977164, 49.99890960531435979 ) ) ;
#57780 = CARTESIAN_POINT ( 'NONE',  ( 9.474510206698729675, 16.51473224551082808, 82.08442372801899012 ) ) ;
#57781 = CARTESIAN_POINT ( 'NONE',  ( -16.52544592524342804, 4.483927247898546575, 31.04057627198102409 ) ) ;
#57782 = CARTESIAN_POINT ( 'NONE',  ( 13.97604488694548053, -13.89961937509957401, 90.62609039468567573 ) ) ;
#57783 = CARTESIAN_POINT ( 'NONE',  ( -12.06949235617756955, 12.14591786802309770, 35.62390960531437401 ) ) ;
#57784 = CARTESIAN_POINT ( 'NONE',  ( 5.049401038297881783, 19.05341960407617563, 62.29275706135234003 ) ) ;
#57785 = CARTESIAN_POINT ( 'NONE',  ( -14.29746914071037622, -8.314922557961029526, 44.16775706135234714 ) ) ;
#57786 = CARTESIAN_POINT ( 'NONE',  ( -16.51473224551082808, 9.474510206698731452, 23.33442372801900078 ) ) ;
#57787 = CARTESIAN_POINT ( 'NONE',  ( 16.55341960407611168, 4.379528057220329451, 113.9572429386477239 ) ) ;
#57788 = CARTESIAN_POINT ( 'NONE',  ( -19.05341960407611168, -5.049401038298163336, 36.45724293864766707 ) ) ;
#57789 = CARTESIAN_POINT ( 'NONE',  ( 16.53943276465976808, 0.05219959533934440121, 51.25109039468568994 ) ) ;
#57790 = DIRECTION ( 'NONE',  ( 1.000000000000000000, 0.000000000000000000, 0.000000000000000000 ) ) ;
#57791 = CARTESIAN_POINT ( 'NONE',  ( 23.31738231874054534, 16.94106989632529192, 139.4500000054623570 ) ) ;
#57792 = CARTESIAN_POINT ( 'NONE',  ( -5.049401038298153566, 19.05341960407611168, 95.20724293864770971 ) ) ;
#57793 = LINE ( 'NONE', #87118, #129739 ) ;
#57794 = ORIENTED_EDGE ( 'NONE', *, *, #195656, .F. ) ;
#57795 = CARTESIAN_POINT ( 'NONE',  ( 16.46253265017146816, 9.564922557961045513, 96.66775706135233293 ) ) ;
#57796 = CARTESIAN_POINT ( 'NONE',  ( 15.80617190586746368, 15.72974639402197994, 24.37390960531435979 ) ) ;
#57798 = CARTESIAN_POINT ( 'NONE',  ( 5.049401038297881783, 19.05341960407617563, 112.2927570613523471 ) ) ;
#57797 = CARTESIAN_POINT ( 'NONE',  ( -0.05219959533937732626, 21.53943276465977519, 112.5010903946857042 ) ) ;
#57799 = CARTESIAN_POINT ( 'NONE',  ( -14.34966873604960291, -8.224510206698953496, 106.6655762719810383 ) ) ;
#57800 = CARTESIAN_POINT ( 'NONE',  ( 19.05341960407611168, 5.049401038298154454, 43.95724293864769550 ) ) ;
#57801 = CARTESIAN_POINT ( 'NONE',  ( 21.55341960407610458, 5.719274019375980345, 78.95724293864769550 ) ) ;
#57802 = CARTESIAN_POINT ( 'NONE',  ( 13.89961937509977652, -13.97604488694527269, 33.12390960531434558 ) ) ;
#57803 = CARTESIAN_POINT ( 'NONE',  ( -16.51473224551082808, 9.474510206698731452, 48.33442372801900433 ) ) ;
#57804 = CARTESIAN_POINT ( 'NONE',  ( 19.03943276465977164, 0.05219959533936151252, 71.25109039468566152 ) ) ;
#57805 = CARTESIAN_POINT ( 'NONE',  ( -14.29746914071049879, 8.314922557960819915, 50.83224293864770971 ) ) ;
#57806 = CARTESIAN_POINT ( 'NONE',  ( -0.05219959533907301413, -21.53943276465977519, 32.49890960531435979 ) ) ;
#57807 = CARTESIAN_POINT ( 'NONE',  ( 5.823673210054444382, -21.52544592524334988, 95.20942372801903275 ) ) ;
#57808 = CARTESIAN_POINT ( 'NONE',  ( -21.52544592524343514, 5.823673210054127303, 81.04057627198102409 ) ) ;
#57809 = CARTESIAN_POINT ( 'NONE',  ( 21.53943276465977519, 0.05219959533937863772, 71.25109039468568994 ) ) ;
#57810 = CARTESIAN_POINT ( 'NONE',  ( 18.67979575497194134, -10.72451020669871369, 65.83442372801900433 ) ) ;
#57811 = CARTESIAN_POINT ( 'NONE',  ( -9.474510206698964154, 16.51473224551069663, 90.41557627198103830 ) ) ;
#57813 = CARTESIAN_POINT ( 'NONE',  ( -10.81492255796105439, 18.62759615963255655, 67.91775706135234714 ) ) ;
#57812 = CARTESIAN_POINT ( 'NONE',  ( 16.53943276465976808, 0.05219959533934440121, 96.25109039468568994 ) ) ;
#57814 = CARTESIAN_POINT ( 'NONE',  ( -13.89961937509977652, 13.97604488694528158, 50.62390960531435979 ) ) ;
#57815 = CARTESIAN_POINT ( 'NONE',  ( 18.62759615963255655, 10.81492255796105972, 31.66775706135234358 ) ) ;
#57816 = CARTESIAN_POINT ( 'NONE',  ( 19.02544592524343514, -5.153800228976328945, 68.54057627198103830 ) ) ;
#57817 = CARTESIAN_POINT ( 'NONE',  ( 14.34966873604960469, 8.224510206698951720, 74.16557627198102409 ) ) ;
#57818 = CARTESIAN_POINT ( 'NONE',  ( 12.14591786802309770, 12.06949235617756955, 39.37390960531436690 ) ) ;
#57819 = CARTESIAN_POINT ( 'NONE',  ( 5.823673210054125526, 21.52544592524343514, 44.79057627198103120 ) ) ;
#57820 = CARTESIAN_POINT ( 'NONE',  ( 19.02544592524343514, -5.153800228976328945, 43.54057627198103120 ) ) ;
#57821 = CARTESIAN_POINT ( 'NONE',  ( -18.62759615963270932, 10.81492255796079327, 55.83224293864770260 ) ) ;
#57822 = CARTESIAN_POINT ( 'NONE',  ( 13.89961937509957401, 13.97604488694547697, 51.87609039468566863 ) ) ;
#57824 = CARTESIAN_POINT ( 'NONE',  ( -12.06949235617756955, 12.14591786802309770, 65.62390960531436690 ) ) ;
#57823 = CARTESIAN_POINT ( 'NONE',  ( -17.26172910966778318, -6.454744622555875111, 39.19353091350778584 ) ) ;
#57825 = CARTESIAN_POINT ( 'NONE',  ( -10.81492255796078084, -18.62759615963271287, 42.08224293864769550 ) ) ;
#57826 = ORIENTED_EDGE ( 'NONE', *, *, #146342, .F. ) ;
#57827 = ORIENTED_EDGE ( 'NONE', *, *, #52445, .T. ) ;
#57828 = CARTESIAN_POINT ( 'NONE',  ( -36.91746825000000598, 2.428612866367529932E-14, -0.8749999972688132788 ) ) ;
#57829 = CARTESIAN_POINT ( 'NONE',  ( -16.53943276465976808, -0.05219959533934237506, 88.75109039468567573 ) ) ;
#57830 = CARTESIAN_POINT ( 'NONE',  ( -16.51473224551082808, 9.474510206698731452, 73.33442372801900433 ) ) ;
#57831 = CARTESIAN_POINT ( 'NONE',  ( -16.52544592524342804, 4.483927247898546575, 51.04057627198103120 ) ) ;
#57832 = CARTESIAN_POINT ( 'NONE',  ( 17.40805194822033997, -6.112264579159255362, 53.33371272510612471 ) ) ;
#57833 = CARTESIAN_POINT ( 'NONE',  ( -13.89961937509977652, 13.97604488694528158, 50.62390960531435979 ) ) ;
#57834 = CARTESIAN_POINT ( 'NONE',  ( 4.379528057220339221, -16.55341960407611168, 42.70724293864770260 ) ) ;
#57835 = CARTESIAN_POINT ( 'NONE',  ( 16.51473224551069308, 9.474510206698969483, 54.16557627198103120 ) ) ;
#57836 = CARTESIAN_POINT ( 'NONE',  ( -5.049401038298153566, 19.05341960407611168, 70.20724293864769550 ) ) ;
#57837 = CARTESIAN_POINT ( 'NONE',  ( -9.474510206698964154, 16.51473224551069663, 45.41557627198103120 ) ) ;
#57838 = CARTESIAN_POINT ( 'NONE',  ( -21.53943276465977519, -0.05219959533937600094, 43.75109039468568284 ) ) ;
#57839 = CARTESIAN_POINT ( 'NONE',  ( -19.03943276465977164, 0.05219959533909376836, 71.24890960531435269 ) ) ;
#57840 = CARTESIAN_POINT ( 'NONE',  ( 13.89961937509977652, -13.97604488694527269, 23.12390960531436335 ) ) ;
#57841 = CARTESIAN_POINT ( 'NONE',  ( -9.474510206698964154, 16.51473224551069663, 60.41557627198102409 ) ) ;
#57842 = CARTESIAN_POINT ( 'NONE',  ( 5.719274019375991003, -21.55341960407610458, 47.70724293864770260 ) ) ;
#57843 = VECTOR ( 'NONE', #37533, 1000.000000000000000 ) ;
#57844 = CARTESIAN_POINT ( 'NONE',  ( -19.05341960407611168, -5.049401038298163336, 41.45724293864769550 ) ) ;
#57845 = CARTESIAN_POINT ( 'NONE',  ( 5.719274019375991003, -21.55341960407610458, 42.70724293864770260 ) ) ;
#57846 = CARTESIAN_POINT ( 'NONE',  ( -16.53943276465976808, -0.05219959533934237506, 98.75109039468568994 ) ) ;
#57847 = CARTESIAN_POINT ( 'NONE',  ( -5.049401038297874678, -19.05341960407617918, 29.79275706135232227 ) ) ;
#57849 = CARTESIAN_POINT ( 'NONE',  ( -0.05219959533934338120, 16.53943276465976808, 82.50109039468568994 ) ) ;
#57848 = CARTESIAN_POINT ( 'NONE',  ( 0.05219959533934541429, -16.53943276465976808, 40.00109039468567573 ) ) ;
#57850 = DIRECTION ( 'NONE',  ( 0.000000000000000000, 0.4999999999999999445, 0.8660254037844387076 ) ) ;
#57851 = CARTESIAN_POINT ( 'NONE',  ( 8.314922557961029526, -14.29746914071037800, 65.41775706135234714 ) ) ;
#57852 = CARTESIAN_POINT ( 'NONE',  ( 16.53943276465976808, 0.05219959533934440121, 41.25109039468568284 ) ) ;
#57853 = CARTESIAN_POINT ( 'NONE',  ( 19.03943276465977164, -0.05219959533909143690, 108.7489096053143527 ) ) ;
#57854 = CARTESIAN_POINT ( 'NONE',  ( -12.06949235617739369, -12.14591786802326823, 39.37609039468567573 ) ) ;
#57855 = CARTESIAN_POINT ( 'NONE',  ( -13.89961937509977652, 13.97604488694528158, 30.62390960531435269 ) ) ;
#57856 = CARTESIAN_POINT ( 'NONE',  ( 21.53943276465977519, 0.05219959533937863772, 26.25109039468567573 ) ) ;
#57857 = CARTESIAN_POINT ( 'NONE',  ( 4.483927247898790824, -16.52544592524335698, 35.20942372801901854 ) ) ;
#57858 = CARTESIAN_POINT ( 'NONE',  ( -4.379528057220086978, -16.55341960407618274, 94.79275706135234714 ) ) ;
#57859 = CARTESIAN_POINT ( 'NONE',  ( 15.80617190586769283, -15.72974639402175789, 105.6260903946856899 ) ) ;
#57861 = EDGE_CURVE ( 'NONE', #104760, #66087, #191734, .T. ) ;
#57860 = CARTESIAN_POINT ( 'NONE',  ( -19.02544592524334988, -5.153800228976617603, 93.95942372801900433 ) ) ;
#57862 = CARTESIAN_POINT ( 'NONE',  ( -8.224510206698948167, 14.34966873604960824, 50.41557627198103120 ) ) ;
#57863 = CARTESIAN_POINT ( 'NONE',  ( 19.03943276465977164, -0.05219959533909143690, 23.74890960531435269 ) ) ;
#57865 = CARTESIAN_POINT ( 'NONE',  ( 16.20579543436677739, 7.371946100355113884, 78.06520834171877254 ) ) ;
#57864 = CARTESIAN_POINT ( 'NONE',  ( 9.564922557961047289, -16.46253265017146816, 60.41775706135233293 ) ) ;
#57866 = CARTESIAN_POINT ( 'NONE',  ( 15.80617190586769283, -15.72974639402175789, 60.62609039468567573 ) ) ;
#57867 = CARTESIAN_POINT ( 'NONE',  ( -0.05219959533934338120, 16.53943276465976808, 32.50109039468568284 ) ) ;
#57868 = LINE ( 'NONE', #119540, #34101 ) ;
#57869 = CARTESIAN_POINT ( 'NONE',  ( 19.05341960407611168, 5.049401038298154454, 113.9572429386477097 ) ) ;
#57870 = CARTESIAN_POINT ( 'NONE',  ( 21.52544592524344225, -5.823673210054117533, 68.54057627198103830 ) ) ;
#57871 = CARTESIAN_POINT ( 'NONE',  ( 0.05219959533936267826, -19.03943276465977164, 105.0010903946856615 ) ) ;
#57872 = CARTESIAN_POINT ( 'NONE',  ( 13.97604488694527802, 13.89961937509977652, 99.37390960531436690 ) ) ;
#57873 = CARTESIAN_POINT ( 'NONE',  ( -26.68407921138448557, 3.932373394472265193, 171.8653659962753295 ) ) ;
#57874 = CARTESIAN_POINT ( 'NONE',  ( -16.51473224551069308, -9.474510206698971260, 21.66557627198102765 ) ) ;
#57875 = CARTESIAN_POINT ( 'NONE',  ( -21.55341960407619339, 5.719274019375674811, 113.5427570613523756 ) ) ;
#57876 = CARTESIAN_POINT ( 'NONE',  ( 19.03943276465977164, -0.05219959533909143690, 38.74890960531436690 ) ) ;
#57877 = CARTESIAN_POINT ( 'NONE',  ( 21.52544592524334988, 5.823673210054432836, 56.45942372801902565 ) ) ;
#57878 = CARTESIAN_POINT ( 'NONE',  ( -5.719274019375665041, -21.55341960407619695, 104.7927570613523898 ) ) ;
#57879 = CARTESIAN_POINT ( 'NONE',  ( 16.55341960407618274, -4.379528057220086978, 106.0427570613523471 ) ) ;
#57880 = CARTESIAN_POINT ( 'NONE',  ( 9.474510206698971260, -16.51473224551069308, 77.91557627198103830 ) ) ;
#57881 = CARTESIAN_POINT ( 'NONE',  ( -5.719274019375665041, -21.55341960407619695, 44.79275706135234714 ) ) ;
#57882 = CARTESIAN_POINT ( 'NONE',  ( 0.05219959533937995610, -21.53943276465977519, 55.00109039468568284 ) ) ;
#57884 = CARTESIAN_POINT ( 'NONE',  ( 13.89961937509977652, -13.97604488694527269, 88.12390960531438111 ) ) ;
#57883 = CARTESIAN_POINT ( 'NONE',  ( -16.46253265017146816, -9.564922557961047289, 79.16775706135234714 ) ) ;
#57885 = CARTESIAN_POINT ( 'NONE',  ( 4.379528057220339221, -16.55341960407611168, 97.70724293864772392 ) ) ;
#57886 = CARTESIAN_POINT ( 'NONE',  ( -10.72451020669898014, 18.67979575497178502, 95.41557627198102409 ) ) ;
#57887 = CARTESIAN_POINT ( 'NONE',  ( -18.67979575497193778, 10.72451020669871902, 113.3344237280190328 ) ) ;
#57888 = CARTESIAN_POINT ( 'NONE',  ( -8.314922557960811034, -14.29746914071050412, 92.08224293864769550 ) ) ;
#57889 = CARTESIAN_POINT ( 'NONE',  ( -13.89961937509977652, 13.97604488694528158, 45.62390960531433848 ) ) ;
#57890 = CARTESIAN_POINT ( 'NONE',  ( -5.049401038297874678, -19.05341960407617918, 84.79275706135233293 ) ) ;
#57891 = CARTESIAN_POINT ( 'NONE',  ( -14.29746914071049879, 8.314922557960819915, 45.83224293864769550 ) ) ;
#57892 = CARTESIAN_POINT ( 'NONE',  ( 10.72451020669871369, 18.67979575497193778, 102.0844237280190185 ) ) ;
#57893 = CARTESIAN_POINT ( 'NONE',  ( 9.474510206698971260, -16.51473224551069308, 102.9155762719810241 ) ) ;
#57894 = CARTESIAN_POINT ( 'NONE',  ( -9.564922557961040184, 16.46253265017147172, 72.91775706135233293 ) ) ;
#57895 = CARTESIAN_POINT ( 'NONE',  ( -10.81492255796078084, -18.62759615963271287, 72.08224293864769550 ) ) ;
#57896 = CARTESIAN_POINT ( 'NONE',  ( 15.80617190586769283, -15.72974639402175789, 35.62609039468568994 ) ) ;
#57897 = CARTESIAN_POINT ( 'NONE',  ( 16.53943276465976808, 0.05219959533934440121, 36.25109039468567573 ) ) ;
#57898 = CARTESIAN_POINT ( 'NONE',  ( -4.379528057220086978, -16.55341960407618274, 94.79275706135234714 ) ) ;
#57900 = CARTESIAN_POINT ( 'NONE',  ( 5.823673210054444382, -21.52544592524334988, 40.20942372801901854 ) ) ;
#57899 = CARTESIAN_POINT ( 'NONE',  ( 17.48847506799967988, 5.747544572773808369, 61.67302562156719858 ) ) ;
#57901 = CARTESIAN_POINT ( 'NONE',  ( 18.67979575497178502, 10.72451020669898547, 39.16557627198102409 ) ) ;
#57902 = CARTESIAN_POINT ( 'NONE',  ( -19.05341960407611168, -5.049401038298163336, 26.45724293864769550 ) ) ;
#57903 = CARTESIAN_POINT ( 'NONE',  ( -30.74264578624800492, 22.33583958711400186, -9.949999994537627401 ) ) ;
#57904 = CARTESIAN_POINT ( 'NONE',  ( -8.314922557961024197, 14.29746914071037800, 67.91775706135234714 ) ) ;
#57905 = CARTESIAN_POINT ( 'NONE',  ( -14.34966873604960291, -8.224510206698953496, 96.66557627198102409 ) ) ;
#57906 = CARTESIAN_POINT ( 'NONE',  ( -0.05219959533907301413, -21.53943276465977519, 72.49890960531435269 ) ) ;
#57907 = CARTESIAN_POINT ( 'NONE',  ( -16.53943276465976808, 0.05219959533911058130, 31.24890960531435979 ) ) ;
#57908 = CARTESIAN_POINT ( 'NONE',  ( 4.483927247898790824, -16.52544592524335698, 55.20942372801902565 ) ) ;
#57909 = CARTESIAN_POINT ( 'NONE',  ( -19.02544592524342804, 5.153800228976336051, 61.04057627198103120 ) ) ;
#57910 = CARTESIAN_POINT ( 'NONE',  ( -4.483927247898782831, 16.52544592524335698, 97.70942372801904696 ) ) ;
#57911 = CARTESIAN_POINT ( 'NONE',  ( 5.049401038297881783, 19.05341960407617563, 82.29275706135229029 ) ) ;
#57912 = CARTESIAN_POINT ( 'NONE',  ( -15.72974639402197994, 15.80617190586746368, 90.62390960531436690 ) ) ;
#57913 = CARTESIAN_POINT ( 'NONE',  ( 8.224510206698742110, 14.34966873604972548, 112.0844237280190185 ) ) ;
#57914 = ORIENTED_EDGE ( 'NONE', *, *, #12763, .F. ) ;
#57915 = CARTESIAN_POINT ( 'NONE',  ( 5.153800228976335163, 19.02544592524342804, 114.7905762719810241 ) ) ;
#57916 = CARTESIAN_POINT ( 'NONE',  ( -10.81492255796078084, -18.62759615963271287, 57.08224293864769550 ) ) ;
#57917 = ORIENTED_EDGE ( 'NONE', *, *, #44596, .T. ) ;
#57918 = CARTESIAN_POINT ( 'NONE',  ( 12.14591786802327356, -12.06949235617739191, 90.62609039468567573 ) ) ;
#57919 = ORIENTED_EDGE ( 'NONE', *, *, #40254, .T. ) ;
#57920 = CARTESIAN_POINT ( 'NONE',  ( 15.80617190586746368, 15.72974639402197994, 34.37390960531435979 ) ) ;
#57921 = CARTESIAN_POINT ( 'NONE',  ( 17.50000000000147793, 3.254303733634550166, 107.4760410692860262 ) ) ;
#57922 = CARTESIAN_POINT ( 'NONE',  ( 21.53943276465977519, -0.05219959533907433946, 93.74890960531436690 ) ) ;
#57923 = CARTESIAN_POINT ( 'NONE',  ( 8.224510206698953496, -14.34966873604960469, 27.91557627198103830 ) ) ;
#57924 = CARTESIAN_POINT ( 'NONE',  ( 9.564922557961047289, -16.46253265017146816, 110.4177570613523471 ) ) ;
#57925 = CARTESIAN_POINT ( 'NONE',  ( 13.97604488694527802, 13.89961937509977652, 34.37390960531436690 ) ) ;
#57926 = CARTESIAN_POINT ( 'NONE',  ( -8.314922557961024197, 14.29746914071037800, 32.91775706135234714 ) ) ;
#57927 = CARTESIAN_POINT ( 'NONE',  ( -0.05219959533909027116, -19.03943276465977164, 47.49890960531435979 ) ) ;
#57928 = CARTESIAN_POINT ( 'NONE',  ( 1.993301997531345292E-15, -30.30510711980685912, 148.5000000000000000 ) ) ;
#57929 = CARTESIAN_POINT ( 'NONE',  ( 13.97604488694527802, 13.89961937509977652, 104.3739096053143385 ) ) ;
#57930 = CARTESIAN_POINT ( 'NONE',  ( 5.153800228976335163, 19.02544592524342804, 104.7905762719809957 ) ) ;
#57931 = CARTESIAN_POINT ( 'NONE',  ( 16.55341960407618274, -4.379528057220086978, 91.04275706135236135 ) ) ;
#57932 = CARTESIAN_POINT ( 'NONE',  ( 9.564922557961047289, -16.46253265017146816, 90.41775706135234714 ) ) ;
#57933 = CARTESIAN_POINT ( 'NONE',  ( -13.89961937509957401, -13.97604488694547875, 39.37609039468566152 ) ) ;
#57934 = CARTESIAN_POINT ( 'NONE',  ( -18.67979575497178146, -10.72451020669898902, 71.66557627198100988 ) ) ;
#57935 = CARTESIAN_POINT ( 'NONE',  ( -12.06949235617739369, -12.14591786802326823, 104.3760903946856899 ) ) ;
#57936 = CARTESIAN_POINT ( 'NONE',  ( -5.823673210054116645, -21.52544592524344225, 37.29057627198102409 ) ) ;
#57937 = CARTESIAN_POINT ( 'NONE',  ( -0.05219959533936034679, 19.03943276465977164, 87.50109039468567573 ) ) ;
#57938 = CARTESIAN_POINT ( 'NONE',  ( -19.05341960407611168, -5.049401038298163336, 56.45724293864768129 ) ) ;
#57939 = CARTESIAN_POINT ( 'NONE',  ( -19.02544592524342804, 5.153800228976336051, 106.0405762719810241 ) ) ;
#57940 = CARTESIAN_POINT ( 'NONE',  ( 10.81492255796106328, -18.62759615963255655, 65.41775706135234714 ) ) ;
#57941 = CARTESIAN_POINT ( 'NONE',  ( -0.05219959533909027116, -19.03943276465977164, 62.49890960531435979 ) ) ;
#57942 = CARTESIAN_POINT ( 'NONE',  ( -4.379528057220328563, 16.55341960407611168, 105.2072429386477097 ) ) ;
#57943 = CARTESIAN_POINT ( 'NONE',  ( 23.03403192006591027, -14.65170476119024912, 169.9999999999999716 ) ) ;
#57944 = CARTESIAN_POINT ( 'NONE',  ( 0.05219959533910956823, 16.53943276465976808, 79.99890960531435269 ) ) ;
#57945 = CARTESIAN_POINT ( 'NONE',  ( 21.55341960407610458, 5.719274019375980345, 68.95724293864769550 ) ) ;
#57946 = CARTESIAN_POINT ( 'NONE',  ( 5.049401038297881783, 19.05341960407617563, 87.29275706135234714 ) ) ;
#57947 = FACE_OUTER_BOUND ( 'NONE', #63952, .T. ) ;
#57948 = CARTESIAN_POINT ( 'NONE',  ( 16.51473224551069308, 9.474510206698969483, 59.16557627198102409 ) ) ;
#57949 = CARTESIAN_POINT ( 'NONE',  ( 16.88567814943194278, -6.947325034625397855, 71.20998877347402356 ) ) ;
#57951 = CARTESIAN_POINT ( 'NONE',  ( -19.05341960407611168, -5.049401038298163336, 91.45724293864766707 ) ) ;
#57950 = CARTESIAN_POINT ( 'NONE',  ( -16.51473224551069308, -9.474510206698971260, 76.66557627198103830 ) ) ;
#57952 = CARTESIAN_POINT ( 'NONE',  ( 16.53943276465976808, 0.05219959533934440121, 71.25109039468568994 ) ) ;
#57953 = CARTESIAN_POINT ( 'NONE',  ( -17.40805194822029378, -6.112264579159361055, 49.16628727489391082 ) ) ;
#57954 = CARTESIAN_POINT ( 'NONE',  ( -13.97604488694547697, 13.89961937509957934, 48.12609039468566863 ) ) ;
#57955 = CARTESIAN_POINT ( 'NONE',  ( 16.74137860779843123, 7.074371978128817240, 21.90872520115863864 ) ) ;
#57956 = CARTESIAN_POINT ( 'NONE',  ( 0.05219959533909260263, 19.03943276465977164, 104.9989096053143669 ) ) ;
#57957 = CARTESIAN_POINT ( 'NONE',  ( 16.52544592524335698, 4.483927247898782831, 106.4594237280190328 ) ) ;
#57958 = CARTESIAN_POINT ( 'NONE',  ( -34.37447276284162001, -6.948158515131154012, 47.85536288891452728 ) ) ;
#57959 = CARTESIAN_POINT ( 'NONE',  ( -14.29746914071037622, -8.314922557961029526, 99.16775706135234714 ) ) ;
#57960 = DIRECTION ( 'NONE',  ( -0.000000000000000000, -0.000000000000000000, 1.000000000000000000 ) ) ;
#57961 = CARTESIAN_POINT ( 'NONE',  ( 14.34966873604972726, -8.224510206698740333, 65.83442372801900433 ) ) ;
#57962 = FACE_OUTER_BOUND ( 'NONE', #163386, .T. ) ;
#57963 = CARTESIAN_POINT ( 'NONE',  ( -15.80617190586768217, 15.72974639402176855, 68.12609039468567573 ) ) ;
#57964 = CARTESIAN_POINT ( 'NONE',  ( 19.03943276465977164, 0.05219959533936151252, 71.25109039468566152 ) ) ;
#57965 = CARTESIAN_POINT ( 'NONE',  ( -19.03943276465977164, -0.05219959533935918106, 23.75109039468566152 ) ) ;
#57966 = CARTESIAN_POINT ( 'NONE',  ( 0.05219959533909260263, 19.03943276465977164, 59.99890960531436690 ) ) ;
#57967 = CARTESIAN_POINT ( 'NONE',  ( -5.049401038298153566, 19.05341960407611168, 40.20724293864768839 ) ) ;
#57968 = CARTESIAN_POINT ( 'NONE',  ( 17.48701582056246551, -5.762792292030415098, 23.32825582371390638 ) ) ;
#57969 = CARTESIAN_POINT ( 'NONE',  ( -15.80617190586745835, -15.72974639402198527, 86.87390960531438111 ) ) ;
#57970 = CARTESIAN_POINT ( 'NONE',  ( -10.81492255796078084, -18.62759615963271287, 37.08224293864768129 ) ) ;
#57971 = CARTESIAN_POINT ( 'NONE',  ( 0.05219959533910956823, 16.53943276465976808, 109.9989096053143527 ) ) ;
#57972 = CARTESIAN_POINT ( 'NONE',  ( -8.224510206698735004, -14.34966873604973081, 54.58442372801901143 ) ) ;
#57973 = VERTEX_POINT ( 'NONE', #54229 ) ;
#57974 = CARTESIAN_POINT ( 'NONE',  ( 21.53943276465977519, 0.05219959533937863772, 31.25109039468568639 ) ) ;
#57976 = CARTESIAN_POINT ( 'NONE',  ( -6.020228577223754586E-15, 39.95556452105416412, -8.500000000000001776 ) ) ;
#57975 = CARTESIAN_POINT ( 'NONE',  ( 12.06949235617757843, -12.14591786802309237, 58.12390960531435979 ) ) ;
#57977 = CARTESIAN_POINT ( 'NONE',  ( 16.53943276465976808, 0.05219959533934440121, 31.25109039468568639 ) ) ;
#57978 = CARTESIAN_POINT ( 'NONE',  ( 9.564922557961047289, -16.46253265017146816, 45.41775706135232582 ) ) ;
#57979 = CARTESIAN_POINT ( 'NONE',  ( -8.224510206698948167, 14.34966873604960824, 50.41557627198103120 ) ) ;
#57980 = CARTESIAN_POINT ( 'NONE',  ( -10.72451020669898014, 18.67979575497178502, 110.4155762719810383 ) ) ;
#57982 = CARTESIAN_POINT ( 'NONE',  ( 18.62759615963271287, -10.81492255796078972, 78.33224293864770971 ) ) ;
#57981 = CARTESIAN_POINT ( 'NONE',  ( 1.359207933839712945, 15.84156095272284226, -59.51388212957616730 ) ) ;
#57983 = CARTESIAN_POINT ( 'NONE',  ( -9.474510206698964154, 16.51473224551069663, 85.41557627198102409 ) ) ;
#57984 = CARTESIAN_POINT ( 'NONE',  ( 16.55341960407611168, 4.379528057220329451, 63.95724293864770260 ) ) ;
#57985 = CARTESIAN_POINT ( 'NONE',  ( 16.51473224551069308, 9.474510206698969483, 109.1655762719810383 ) ) ;
#57986 = VECTOR ( 'NONE', #58805, 1000.000000000000000 ) ;
#57987 = CARTESIAN_POINT ( 'NONE',  ( -36.95577132204472548, 5.312067825339672034, 43.56319566887930250 ) ) ;
#57988 = CARTESIAN_POINT ( 'NONE',  ( -13.97604488694547697, 13.89961937509957934, 68.12609039468563310 ) ) ;
#57989 = CARTESIAN_POINT ( 'NONE',  ( 10.81492255796078972, 18.62759615963270932, 109.5822429386476955 ) ) ;
#57990 = CARTESIAN_POINT ( 'NONE',  ( -16.46253265017160317, 9.564922557960807481, 55.83224293864769550 ) ) ;
#57991 = CARTESIAN_POINT ( 'NONE',  ( 12.06949235617757843, -12.14591786802309237, 113.1239096053143953 ) ) ;
#57992 = EDGE_CURVE ( 'NONE', #127301, #182346, #161402, .T. ) ;
#57993 = CARTESIAN_POINT ( 'NONE',  ( -21.55341960407619339, 5.719274019375674811, 68.54275706135234714 ) ) ;
#57994 = FACE_OUTER_BOUND ( 'NONE', #133947, .T. ) ;
#57995 = CARTESIAN_POINT ( 'NONE',  ( 16.52544592524342804, -4.483927247898539470, 38.54057627198103120 ) ) ;
#57996 = CARTESIAN_POINT ( 'NONE',  ( 16.51473224551069308, 9.474510206698969483, 49.16557627198102409 ) ) ;
#57997 = CARTESIAN_POINT ( 'NONE',  ( 16.46253265017160672, -9.564922557960803928, 113.3322429386476955 ) ) ;
#57998 = CARTESIAN_POINT ( 'NONE',  ( 5.823673210054125526, 21.52544592524343514, 69.79057627198102409 ) ) ;
#57999 = CARTESIAN_POINT ( 'NONE',  ( -17.14385361876520619, 23.59649016807275856, 142.5750000027312012 ) ) ;
#58000 = CARTESIAN_POINT ( 'NONE',  ( 0.05219959533909260263, 19.03943276465977164, 39.99890960531436690 ) ) ;
#58001 = CARTESIAN_POINT ( 'NONE',  ( 5.719274019375991003, -21.55341960407610458, 67.70724293864769550 ) ) ;
#58002 = CARTESIAN_POINT ( 'NONE',  ( 15.80617190586769283, -15.72974639402175789, 85.62609039468568994 ) ) ;
#58005 = CARTESIAN_POINT ( 'NONE',  ( -16.53943276465976808, 0.05219959533911058130, 86.24890960531436690 ) ) ;
#58004 = CARTESIAN_POINT ( 'NONE',  ( -4.379528057220086978, -16.55341960407618274, 84.79275706135234714 ) ) ;
#58003 = CARTESIAN_POINT ( 'NONE',  ( 6.907351198297244643, -38.20768336774872154, -23.99027881317354272 ) ) ;
#58006 = CARTESIAN_POINT ( 'NONE',  ( -16.51473224551069308, -9.474510206698971260, 71.66557627198102409 ) ) ;
#58007 = ORIENTED_EDGE ( 'NONE', *, *, #57992, .T. ) ;
#58008 = CARTESIAN_POINT ( 'NONE',  ( -5.049401038297874678, -19.05341960407617918, 39.79275706135232582 ) ) ;
#58009 = CARTESIAN_POINT ( 'NONE',  ( 4.379528057220092307, 16.55341960407617563, 92.29275706135236135 ) ) ;
#58010 = CARTESIAN_POINT ( 'NONE',  ( -5.049401038297874678, -19.05341960407617918, 19.79275706135233293 ) ) ;
#58011 = CARTESIAN_POINT ( 'NONE',  ( 9.474510206698971260, -16.51473224551069308, 92.91557627198103830 ) ) ;
#58012 = CARTESIAN_POINT ( 'NONE',  ( 15.72974639402199770, -15.80617190586745480, 43.12390960531435269 ) ) ;
#58013 = CARTESIAN_POINT ( 'NONE',  ( 21.53943276465977519, 0.05219959533937863772, 101.2510903946856757 ) ) ;
#58014 = CARTESIAN_POINT ( 'NONE',  ( 8.314922557961029526, -14.29746914071037800, 65.41775706135234714 ) ) ;
#58015 = CARTESIAN_POINT ( 'NONE',  ( -21.55341960407610458, -5.719274019375992779, 106.4572429386477097 ) ) ;
#58016 = CARTESIAN_POINT ( 'NONE',  ( 12.14591786802327356, -12.06949235617739191, 30.62609039468567929 ) ) ;
#58017 = CARTESIAN_POINT ( 'NONE',  ( 13.89961937509977652, -13.97604488694527269, 88.12390960531438111 ) ) ;
#58018 = CARTESIAN_POINT ( 'NONE',  ( -4.483927247898782831, 16.52544592524335698, 22.70942372801901499 ) ) ;
#58019 = CARTESIAN_POINT ( 'NONE',  ( -5.153800228976328057, -19.02544592524343514, 47.29057627198102409 ) ) ;
#58020 = AXIS2_PLACEMENT_3D ( 'NONE', #154566, #94881, #187911 ) ;
#58021 = CARTESIAN_POINT ( 'NONE',  ( -8.224510206698735004, -14.34966873604973081, 29.58442372801901854 ) ) ;
#58022 = CARTESIAN_POINT ( 'NONE',  ( 0.05219959533910956823, 16.53943276465976808, 84.99890960531436690 ) ) ;
#58023 = CARTESIAN_POINT ( 'NONE',  ( -16.53943276465976808, -0.05219959533934237506, 93.75109039468567573 ) ) ;
#58025 = CARTESIAN_POINT ( 'NONE',  ( 19.02544592524343514, -5.153800228976328945, 68.54057627198103830 ) ) ;
#58024 = CARTESIAN_POINT ( 'NONE',  ( 15.80617190586769283, -15.72974639402175789, 40.62609039468567573 ) ) ;
#58026 = CARTESIAN_POINT ( 'NONE',  ( -19.02544592524342804, 5.153800228976336051, 76.04057627198102409 ) ) ;
#58027 = CARTESIAN_POINT ( 'NONE',  ( -14.29746914071049879, 8.314922557960819915, 30.83224293864770260 ) ) ;
#58028 = CARTESIAN_POINT ( 'NONE',  ( 14.34966873604972726, -8.224510206698740333, 80.83442372801901854 ) ) ;
#58029 = ORIENTED_EDGE ( 'NONE', *, *, #47812, .T. ) ;
#58030 = CARTESIAN_POINT ( 'NONE',  ( 13.89961937509957401, 13.97604488694547697, 26.87609039468566507 ) ) ;
#58031 = CARTESIAN_POINT ( 'NONE',  ( 9.564922557960805705, 16.46253265017160317, 99.58224293864770971 ) ) ;
#58032 = CARTESIAN_POINT ( 'NONE',  ( 13.89961937509977652, -13.97604488694527269, 43.12390960531434558 ) ) ;
#58033 = CARTESIAN_POINT ( 'NONE',  ( -36.91746825000001309, -11.99521256947794789, -8.524999997268812635 ) ) ;
#58034 = CARTESIAN_POINT ( 'NONE',  ( 14.34966873604972726, -8.224510206698740333, 40.83442372801901854 ) ) ;
#58036 = CARTESIAN_POINT ( 'NONE',  ( -14.29746914071037622, -8.314922557961029526, 59.16775706135234714 ) ) ;
#58035 = CARTESIAN_POINT ( 'NONE',  ( 13.89961937509957401, 13.97604488694547697, 71.87609039468567573 ) ) ;
#58037 = FACE_OUTER_BOUND ( 'NONE', #10947, .T. ) ;
#58038 = CARTESIAN_POINT ( 'NONE',  ( 19.05341960407611168, 5.049401038298154454, 78.95724293864769550 ) ) ;
#58039 = CARTESIAN_POINT ( 'NONE',  ( -10.72451020669870658, -18.67979575497194134, 19.58442372801901143 ) ) ;
#58040 = CARTESIAN_POINT ( 'NONE',  ( 19.05341960407617918, -5.049401038297876454, 61.04275706135232582 ) ) ;
#58042 = CARTESIAN_POINT ( 'NONE',  ( -5.049401038298153566, 19.05341960407611168, 40.20724293864768839 ) ) ;
#58041 = CARTESIAN_POINT ( 'NONE',  ( 19.03943276465977164, -0.05219959533909143690, 103.7489096053143669 ) ) ;
#58043 = CARTESIAN_POINT ( 'NONE',  ( -5.153800228976328057, -19.02544592524343514, 77.29057627198099567 ) ) ;
#58045 = CARTESIAN_POINT ( 'NONE',  ( 5.153800228976335163, 19.02544592524342804, 29.79057627198102409 ) ) ;
#58044 = CARTESIAN_POINT ( 'NONE',  ( 12.06949235617757843, -12.14591786802309237, 33.12390960531435979 ) ) ;
#58046 = CARTESIAN_POINT ( 'NONE',  ( -0.05219959533936034679, 19.03943276465977164, 32.50109039468566863 ) ) ;
#58047 = CARTESIAN_POINT ( 'NONE',  ( -16.52544592524342804, 4.483927247898546575, 71.04057627198103830 ) ) ;
#58048 = CARTESIAN_POINT ( 'NONE',  ( -15.72974639402176322, -15.80617190586768395, 109.3760903946857042 ) ) ;
#58049 = CARTESIAN_POINT ( 'NONE',  ( -9.564922557960796823, -16.46253265017161027, 57.08224293864769550 ) ) ;
#58051 = CARTESIAN_POINT ( 'NONE',  ( -21.55341960407619339, 5.719274019375674811, 103.5427570613523613 ) ) ;
#58050 = CARTESIAN_POINT ( 'NONE',  ( -12.06949235617756955, 12.14591786802309770, 40.62390960531435269 ) ) ;
#58052 = CARTESIAN_POINT ( 'NONE',  ( 13.97604488694527802, 13.89961937509977652, 99.37390960531436690 ) ) ;
#58053 = CARTESIAN_POINT ( 'NONE',  ( 16.51473224551069308, 9.474510206698969483, 114.1655762719810241 ) ) ;
#58054 = CARTESIAN_POINT ( 'NONE',  ( 5.049401038298161559, -19.05341960407611168, 42.70724293864767418 ) ) ;
#58055 = CARTESIAN_POINT ( 'NONE',  ( 8.314922557960818139, 14.29746914071049879, 104.5822429386477097 ) ) ;
#58056 = CARTESIAN_POINT ( 'NONE',  ( -12.06949235617756955, 12.14591786802309770, 90.62390960531436690 ) ) ;
#58057 = CARTESIAN_POINT ( 'NONE',  ( -15.80617190586745835, -15.72974639402198527, 101.8739096053143811 ) ) ;
#58058 = CARTESIAN_POINT ( 'NONE',  ( -16.46253265017160317, 9.564922557960807481, 90.83224293864769550 ) ) ;
#58059 = CARTESIAN_POINT ( 'NONE',  ( 21.53943276465977519, -0.05219959533907433946, 98.74890960531438111 ) ) ;
#58060 = CARTESIAN_POINT ( 'NONE',  ( 19.03943276465977164, -0.05219959533909143690, 88.74890960531436690 ) ) ;
#58062 = CARTESIAN_POINT ( 'NONE',  ( 16.55341960407611168, 4.379528057220329451, 108.9572429386476955 ) ) ;
#58061 = CARTESIAN_POINT ( 'NONE',  ( -23.97133246043719268, 5.390759101651052099, 174.7603932261090733 ) ) ;
#58063 = CARTESIAN_POINT ( 'NONE',  ( -19.05341960407611168, -5.049401038298163336, 66.45724293864769550 ) ) ;
#58064 = CARTESIAN_POINT ( 'NONE',  ( -18.67979575497178146, -10.72451020669898902, 81.66557627198103830 ) ) ;
#58065 = EDGE_CURVE ( 'NONE', #149173, #139926, #159900, .T. ) ;
#58066 = DIRECTION ( 'NONE',  ( 0.1039620511844979306, 0.1039620511844979306, 0.9891328443778538704 ) ) ;
#58068 = DIRECTION ( 'NONE',  ( -0.000000000000000000, -0.000000000000000000, 1.000000000000000000 ) ) ;
#58067 = CARTESIAN_POINT ( 'NONE',  ( -10.72451020669898014, 18.67979575497178502, 30.41557627198101699 ) ) ;
#58069 = CARTESIAN_POINT ( 'NONE',  ( -4.483927247898782831, 16.52544592524335698, 27.70942372801901854 ) ) ;
#58070 = CARTESIAN_POINT ( 'NONE',  ( 16.52544592524342804, -4.483927247898539470, 98.54057627198105251 ) ) ;
#58071 = DIRECTION ( 'NONE',  ( 1.000000000000000000, 0.000000000000000000, 0.000000000000000000 ) ) ;
#58072 = CARTESIAN_POINT ( 'NONE',  ( -5.049401038298153566, 19.05341960407611168, 85.20724293864766707 ) ) ;
#58073 = CARTESIAN_POINT ( 'NONE',  ( -9.564922557960796823, -16.46253265017161027, 47.08224293864769550 ) ) ;
#58074 = CARTESIAN_POINT ( 'NONE',  ( -0.05219959533910754901, -16.53943276465976808, 77.49890960531433848 ) ) ;
#58075 = CARTESIAN_POINT ( 'NONE',  ( -5.049401038298153566, 19.05341960407611168, 115.2072429386477097 ) ) ;
#58076 = CARTESIAN_POINT ( 'NONE',  ( 16.55341960407611168, 4.379528057220329451, 53.95724293864770260 ) ) ;
#58077 = CARTESIAN_POINT ( 'NONE',  ( 9.474510206698729675, 16.51473224551082808, 107.0844237280190043 ) ) ;
#58078 = CARTESIAN_POINT ( 'NONE',  ( -10.81492255796105439, 18.62759615963255655, 57.91775706135234714 ) ) ;
#58079 = FACE_OUTER_BOUND ( 'NONE', #168917, .T. ) ;
#58080 = CARTESIAN_POINT ( 'NONE',  ( 5.049401038298161559, -19.05341960407611168, 97.70724293864766707 ) ) ;
#58081 = CARTESIAN_POINT ( 'NONE',  ( 14.34966873604972726, -8.224510206698740333, 80.83442372801901854 ) ) ;
#58082 = CARTESIAN_POINT ( 'NONE',  ( -13.97604488694527625, -13.89961937509977652, 31.87390960531435979 ) ) ;
#58083 = CARTESIAN_POINT ( 'NONE',  ( 16.51473224551069308, 9.474510206698969483, 79.16557627198103830 ) ) ;
#58084 = CARTESIAN_POINT ( 'NONE',  ( -21.53943276465977519, 0.05219959533907696930, 86.24890960531436690 ) ) ;
#58085 = CARTESIAN_POINT ( 'NONE',  ( 5.049401038297881783, 19.05341960407617563, 112.2927570613523471 ) ) ;
#58087 = CARTESIAN_POINT ( 'NONE',  ( 21.55341960407619695, -5.719274019375665929, 56.04275706135235424 ) ) ;
#58086 = CARTESIAN_POINT ( 'NONE',  ( 12.06949235617757843, -12.14591786802309237, 48.12390960531436690 ) ) ;
#58089 = CARTESIAN_POINT ( 'NONE',  ( -15.72974639402197994, 15.80617190586746368, 30.62390960531436335 ) ) ;
#58088 = CARTESIAN_POINT ( 'NONE',  ( 8.224510206698742110, 14.34966873604972548, 87.08442372801901854 ) ) ;
#58090 = CARTESIAN_POINT ( 'NONE',  ( -13.97604488694527625, -13.89961937509977830, 111.8739096053143527 ) ) ;
#58091 = CARTESIAN_POINT ( 'NONE',  ( -3.889087296525950421, 6.412877669190374164, 8.181980515339454030 ) ) ;
#58092 = CARTESIAN_POINT ( 'NONE',  ( -14.34966873604972548, 8.224510206698743886, 108.3344237280190185 ) ) ;
#58093 = CARTESIAN_POINT ( 'NONE',  ( 8.314922557961029526, -14.29746914071037800, 65.41775706135234714 ) ) ;
#58094 = CARTESIAN_POINT ( 'NONE',  ( -19.02544592524342804, 5.153800228976336051, 71.04057627198099567 ) ) ;
#58095 = CARTESIAN_POINT ( 'NONE',  ( -5.049401038298153566, 19.05341960407611168, 80.20724293864769550 ) ) ;
#58096 = CARTESIAN_POINT ( 'NONE',  ( -15.80617190586768217, 15.72974639402176855, 73.12609039468567573 ) ) ;
#58097 = CARTESIAN_POINT ( 'NONE',  ( -0.05219959533934338120, 16.53943276465976808, 77.50109039468567573 ) ) ;
#58098 = CARTESIAN_POINT ( 'NONE',  ( -12.14591786802309592, -12.06949235617757132, 41.87390960531435979 ) ) ;
#58099 = CARTESIAN_POINT ( 'NONE',  ( -19.02544592524342804, 5.153800228976336051, 56.04057627198100988 ) ) ;
#58100 = CARTESIAN_POINT ( 'NONE',  ( 5.049401038298161559, -19.05341960407611168, 47.70724293864770260 ) ) ;
#58102 = ORIENTED_EDGE ( 'NONE', *, *, #114142, .F. ) ;
#58101 = CARTESIAN_POINT ( 'NONE',  ( -14.34966873604972548, 8.224510206698743886, 43.33442372801901143 ) ) ;
#58103 = CARTESIAN_POINT ( 'NONE',  ( 13.89961937509957401, 13.97604488694547697, 101.8760903946856331 ) ) ;
#58104 = CARTESIAN_POINT ( 'NONE',  ( -8.314922557960811034, -14.29746914071050412, 97.08224293864770971 ) ) ;
#58105 = CARTESIAN_POINT ( 'NONE',  ( 19.02544592524343514, -5.153800228976328945, 68.54057627198103830 ) ) ;
#58107 = CARTESIAN_POINT ( 'NONE',  ( -30.74264578624800492, -22.33583958711396278, -3.799999999999999822 ) ) ;
#58106 = CARTESIAN_POINT ( 'NONE',  ( 13.89961937509957401, 13.97604488694547697, 101.8760903946856331 ) ) ;
#58108 = CARTESIAN_POINT ( 'NONE',  ( 15.72974639402176855, 15.80617190586768217, 101.8760903946857042 ) ) ;
#58109 = CARTESIAN_POINT ( 'NONE',  ( 12.14591786802327356, -12.06949235617739191, 65.62609039468568994 ) ) ;
#58110 = DIRECTION ( 'NONE',  ( -0.000000000000000000, -0.000000000000000000, -1.000000000000000000 ) ) ;
#58111 = CARTESIAN_POINT ( 'NONE',  ( 10.81492255796078972, 18.62759615963270932, 64.58224293864769550 ) ) ;
#58112 = CARTESIAN_POINT ( 'NONE',  ( -4.483927247898782831, 16.52544592524335698, 52.70942372801902565 ) ) ;
#58113 = DIRECTION ( 'NONE',  ( -8.551662891793917213E-31, 1.000000000000000000, 1.224646799147353207E-16 ) ) ;
#58114 = CARTESIAN_POINT ( 'NONE',  ( -19.02544592524334988, -5.153800228976617603, 48.95942372801900433 ) ) ;
#58115 = CARTESIAN_POINT ( 'NONE',  ( 16.51473224551069308, 9.474510206698969483, 84.16557627198102409 ) ) ;
#58116 = CARTESIAN_POINT ( 'NONE',  ( -16.46253265017160317, 9.564922557960807481, 25.83224293864769194 ) ) ;
#58117 = CARTESIAN_POINT ( 'NONE',  ( 19.05341960407611168, 5.049401038298154454, 68.95724293864769550 ) ) ;
#58118 = CARTESIAN_POINT ( 'NONE',  ( -8.224510206698948167, 14.34966873604960824, 60.41557627198102409 ) ) ;
#58119 = CARTESIAN_POINT ( 'NONE',  ( 21.53943276465977519, 0.05219959533937863772, 81.25109039468568994 ) ) ;
#58120 = CARTESIAN_POINT ( 'NONE',  ( 16.46253265017146816, 9.564922557961045513, 46.66775706135233293 ) ) ;
#58121 = CARTESIAN_POINT ( 'NONE',  ( 0.05219959533936267826, -19.03943276465977164, 30.00109039468566863 ) ) ;
#58122 = CARTESIAN_POINT ( 'NONE',  ( -5.049401038298153566, 19.05341960407611168, 50.20724293864770260 ) ) ;
#58123 = CARTESIAN_POINT ( 'NONE',  ( -5.823673210054116645, -21.52544592524344225, 22.29057627198102765 ) ) ;
#58124 = CARTESIAN_POINT ( 'NONE',  ( -10.81492255796105439, 18.62759615963255655, 77.91775706135231871 ) ) ;
#58125 = CARTESIAN_POINT ( 'NONE',  ( -13.97604488694527625, -13.89961937509977652, 66.87390960531436690 ) ) ;
#58126 = CARTESIAN_POINT ( 'NONE',  ( -15.72974639402176322, -15.80617190586768395, 89.37609039468568994 ) ) ;
#58127 = CARTESIAN_POINT ( 'NONE',  ( 10.81492255796078972, 18.62759615963270932, 39.58224293864769550 ) ) ;
#58128 = CARTESIAN_POINT ( 'NONE',  ( -5.049401038298153566, 19.05341960407611168, 90.20724293864766707 ) ) ;
#58129 = CARTESIAN_POINT ( 'NONE',  ( -0.05219959533937732626, 21.53943276465977519, 32.50109039468568284 ) ) ;
#58130 = CARTESIAN_POINT ( 'NONE',  ( -19.05341960407617563, 5.049401038297882671, 58.54275706135234003 ) ) ;
#58131 = CARTESIAN_POINT ( 'NONE',  ( 13.89961937509977652, -13.97604488694527269, 43.12390960531434558 ) ) ;
#58132 = CARTESIAN_POINT ( 'NONE',  ( 5.153800228976335163, 19.02544592524342804, 94.79057627198103830 ) ) ;
#58133 = CARTESIAN_POINT ( 'NONE',  ( -4.483927247898782831, 16.52544592524335698, 27.70942372801901854 ) ) ;
#58134 = CARTESIAN_POINT ( 'NONE',  ( -0.05219959533910754901, -16.53943276465976808, 87.49890960531436690 ) ) ;
#58135 = CARTESIAN_POINT ( 'NONE',  ( 13.97604488694527802, 13.89961937509977652, 74.37390960531436690 ) ) ;
#58136 = CARTESIAN_POINT ( 'NONE',  ( -15.80617190586745835, -15.72974639402198527, 51.87390960531437401 ) ) ;
#58137 = CIRCLE ( 'NONE', #116264, 1.610000000000000098 ) ;
#58138 = CARTESIAN_POINT ( 'NONE',  ( -16.53943276465976808, -0.05219959533934237506, 23.75109039468567929 ) ) ;
#58139 = CARTESIAN_POINT ( 'NONE',  ( -0.05219959533907301413, -21.53943276465977519, 112.4989096053143669 ) ) ;
#58140 = CARTESIAN_POINT ( 'NONE',  ( 18.67979575497194134, -10.72451020669871369, 75.83442372801900433 ) ) ;
#58141 = CARTESIAN_POINT ( 'NONE',  ( 16.52544592524335698, 4.483927247898782831, 71.45942372801901854 ) ) ;
#58142 = CARTESIAN_POINT ( 'NONE',  ( -14.29746914071037622, -8.314922557961029526, 74.16775706135231871 ) ) ;
#58143 = CARTESIAN_POINT ( 'NONE',  ( -16.46253265017160317, 9.564922557960807481, 55.83224293864769550 ) ) ;
#58144 = CARTESIAN_POINT ( 'NONE',  ( 14.29746914071037800, 8.314922557961029526, 106.6677570613523756 ) ) ;
#58145 = CARTESIAN_POINT ( 'NONE',  ( -16.51473224551082808, 9.474510206698731452, 48.33442372801900433 ) ) ;
#58146 = CARTESIAN_POINT ( 'NONE',  ( 15.72974639402176855, 15.80617190586768217, 26.87609039468567218 ) ) ;
#58147 = CARTESIAN_POINT ( 'NONE',  ( 14.29746914071049879, -8.314922557960816363, 63.33224293864770260 ) ) ;
#58148 = CARTESIAN_POINT ( 'NONE',  ( 19.05341960407611168, 5.049401038298154454, 103.9572429386476671 ) ) ;
#58149 = CARTESIAN_POINT ( 'NONE',  ( -12.06949235617739369, -12.14591786802326823, 89.37609039468568994 ) ) ;
#58150 = CARTESIAN_POINT ( 'NONE',  ( 10.81492255796106328, -18.62759615963255655, 55.41775706135234714 ) ) ;
#58151 = CARTESIAN_POINT ( 'NONE',  ( 14.34966873604972726, -8.224510206698740333, 25.83442372801901499 ) ) ;
#58152 = CARTESIAN_POINT ( 'NONE',  ( -0.05219959533937732626, 21.53943276465977519, 27.50109039468567929 ) ) ;
#58153 = CARTESIAN_POINT ( 'NONE',  ( -12.14591786802309592, -12.06949235617757132, 61.87390960531436690 ) ) ;
#58154 = ORIENTED_EDGE ( 'NONE', *, *, #59414, .F. ) ;
#58155 = CARTESIAN_POINT ( 'NONE',  ( 15.72974639402199770, -15.80617190586745480, 103.1239096053143811 ) ) ;
#58156 = CARTESIAN_POINT ( 'NONE',  ( -16.53943276465976808, 0.05219959533911058130, 41.24890960531435269 ) ) ;
#58157 = EDGE_LOOP ( 'NONE', ( #158472, #189699 ) ) ;
#58158 = CARTESIAN_POINT ( 'NONE',  ( -16.51473224551069308, -9.474510206698971260, 26.66557627198103120 ) ) ;
#58159 = CARTESIAN_POINT ( 'NONE',  ( 0.05219959533907565091, 21.53943276465977519, 29.99890960531435979 ) ) ;
#58160 = CARTESIAN_POINT ( 'NONE',  ( 15.72974639402176855, 15.80617190586768217, 31.87609039468567929 ) ) ;
#58161 = CARTESIAN_POINT ( 'NONE',  ( 0.05219959533910956823, 16.53943276465976808, 64.99890960531435269 ) ) ;
#58162 = VECTOR ( 'NONE', #83809, 1000.000000000000000 ) ;
#58163 = CARTESIAN_POINT ( 'NONE',  ( -10.72451020669898014, 18.67979575497178502, 60.41557627198102409 ) ) ;
#58164 = CARTESIAN_POINT ( 'NONE',  ( 19.02544592524343514, -5.153800228976328945, 78.54057627198099567 ) ) ;
#58166 = CARTESIAN_POINT ( 'NONE',  ( -16.51473224551082808, 9.474510206698731452, 83.33442372801899012 ) ) ;
#58165 = CARTESIAN_POINT ( 'NONE',  ( 19.02544592524343514, -5.153800228976328945, 23.54057627198102054 ) ) ;
#58167 = CARTESIAN_POINT ( 'NONE',  ( 21.53943276465977519, -0.05219959533907433946, 43.74890960531435979 ) ) ;
#58168 = CARTESIAN_POINT ( 'NONE',  ( -9.564922557960796823, -16.46253265017161027, 62.08224293864769550 ) ) ;
#58169 = EDGE_LOOP ( 'NONE', ( #121316, #48790, #158463, #157871 ) ) ;
#58170 = CARTESIAN_POINT ( 'NONE',  ( -12.06949235617739369, -12.14591786802326823, 39.37609039468567573 ) ) ;
#58171 = CARTESIAN_POINT ( 'NONE',  ( -10.81492255796078084, -18.62759615963271287, 112.0822429386477097 ) ) ;
#58172 = CARTESIAN_POINT ( 'NONE',  ( 14.29746914071049879, -8.314922557960816363, 53.33224293864769550 ) ) ;
#58173 = CARTESIAN_POINT ( 'NONE',  ( 5.049401038298161559, -19.05341960407611168, 107.7072429386476955 ) ) ;
#58174 = CARTESIAN_POINT ( 'NONE',  ( -10.72451020669898014, 18.67979575497178502, 75.41557627198102409 ) ) ;
#58176 = CARTESIAN_POINT ( 'NONE',  ( -12.06949235617739369, -12.14591786802326823, 54.37609039468568994 ) ) ;
#58175 = CARTESIAN_POINT ( 'NONE',  ( -0.05219959533907301413, -21.53943276465977519, 102.4989096053143811 ) ) ;
#58177 = CARTESIAN_POINT ( 'NONE',  ( -15.80617190586745835, -15.72974639402198527, 46.87390960531435979 ) ) ;
#58178 = CARTESIAN_POINT ( 'NONE',  ( -5.823673210054431948, 21.52544592524334988, 97.70942372801904696 ) ) ;
#58179 = CARTESIAN_POINT ( 'NONE',  ( -16.46253265017160317, 9.564922557960807481, 35.83224293864768839 ) ) ;
#58180 = CARTESIAN_POINT ( 'NONE',  ( -0.05219959533909027116, -19.03943276465977164, 102.4989096053143669 ) ) ;
#58181 = CARTESIAN_POINT ( 'NONE',  ( 9.474510206698971260, -16.51473224551069308, 72.91557627198102409 ) ) ;
#58182 = DIRECTION ( 'NONE',  ( -0.000000000000000000, 0.000000000000000000, 1.000000000000000000 ) ) ;
#58183 = CARTESIAN_POINT ( 'NONE',  ( -19.02544592524334988, -5.153800228976617603, 58.95942372801900433 ) ) ;
#58185 = CARTESIAN_POINT ( 'NONE',  ( -18.62759615963270932, 10.81492255796079327, 30.83224293864770260 ) ) ;
#58184 = CARTESIAN_POINT ( 'NONE',  ( 19.03943276465977164, 0.05219959533936151252, 21.25109039468565797 ) ) ;
#58186 = CARTESIAN_POINT ( 'NONE',  ( -16.53943276465976808, -0.05219959533934237506, 103.7510903946857042 ) ) ;
#58187 = CARTESIAN_POINT ( 'NONE',  ( -19.03943276465977164, -0.05219959533935918106, 83.75109039468567573 ) ) ;
#58188 = DIRECTION ( 'NONE',  ( -1.000000000000000000, -0.000000000000000000, -0.000000000000000000 ) ) ;
#58189 = CARTESIAN_POINT ( 'NONE',  ( 5.049401038297881783, 19.05341960407617563, 82.29275706135229029 ) ) ;
#58190 = CARTESIAN_POINT ( 'NONE',  ( -16.51473224551082808, 9.474510206698731452, 48.33442372801900433 ) ) ;
#58191 = CARTESIAN_POINT ( 'NONE',  ( -17.05587630539784882, -6.762274262135717251, 44.25819690962688213 ) ) ;
#58192 = CARTESIAN_POINT ( 'NONE',  ( 9.564922557960805705, 16.46253265017160317, 44.58224293864769550 ) ) ;
#58193 = CARTESIAN_POINT ( 'NONE',  ( 14.34966873604960469, 8.224510206698951720, 54.16557627198103120 ) ) ;
#58194 = CARTESIAN_POINT ( 'NONE',  ( 9.564922557960805705, 16.46253265017160317, 29.58224293864769550 ) ) ;
#58195 = CARTESIAN_POINT ( 'NONE',  ( 8.314922557960818139, 14.29746914071049879, 39.58224293864769550 ) ) ;
#58196 = PLANE ( 'NONE',  #29121 ) ;
#58197 = CARTESIAN_POINT ( 'NONE',  ( 0.05219959533934541429, -16.53943276465976808, 110.0010903946856757 ) ) ;
#58198 = CARTESIAN_POINT ( 'NONE',  ( -5.049401038298153566, 19.05341960407611168, 50.20724293864770260 ) ) ;
#58199 = CARTESIAN_POINT ( 'NONE',  ( 18.67979575497194134, -10.72451020669871369, 105.8344237280190328 ) ) ;
#58200 = CARTESIAN_POINT ( 'NONE',  ( 19.03943276465977164, 0.05219959533936151252, 111.2510903946856757 ) ) ;
#58201 = CARTESIAN_POINT ( 'NONE',  ( 5.823673210054125526, 21.52544592524343514, 39.79057627198103830 ) ) ;
#58202 = CARTESIAN_POINT ( 'NONE',  ( -10.81492255796105439, 18.62759615963255655, 87.91775706135234714 ) ) ;
#58203 = CARTESIAN_POINT ( 'NONE',  ( -19.02544592524342804, 5.153800228976336051, 101.0405762719810241 ) ) ;
#58204 = CARTESIAN_POINT ( 'NONE',  ( 16.51473224551069308, 9.474510206698969483, 84.16557627198102409 ) ) ;
#58205 = CARTESIAN_POINT ( 'NONE',  ( -11.40812507854754720, -35.11059874428192273, -6.224999997268812812 ) ) ;
#58206 = CARTESIAN_POINT ( 'NONE',  ( -5.719274019375978568, 21.55341960407610458, 105.2072429386477097 ) ) ;
#58207 = CARTESIAN_POINT ( 'NONE',  ( 14.34966873604960469, 8.224510206698951720, 74.16557627198102409 ) ) ;
#58208 = CARTESIAN_POINT ( 'NONE',  ( 21.52544592524344225, -5.823673210054117533, 68.54057627198103830 ) ) ;
#58209 = CARTESIAN_POINT ( 'NONE',  ( 13.97604488694527802, 13.89961937509977652, 69.37390960531436690 ) ) ;
#58210 = CARTESIAN_POINT ( 'NONE',  ( -15.72974639402197994, 15.80617190586746368, 90.62390960531436690 ) ) ;
#58211 = VERTEX_POINT ( 'NONE', #19897 ) ;
#58212 = CARTESIAN_POINT ( 'NONE',  ( 13.89961937509977652, -13.97604488694527269, 63.12390960531435979 ) ) ;
#58214 = CARTESIAN_POINT ( 'NONE',  ( 17.50000000000000000, -5.499999999999992895, 71.21769037696435589 ) ) ;
#58213 = CARTESIAN_POINT ( 'NONE',  ( -12.14591786802309592, -12.06949235617757132, 91.87390960531436690 ) ) ;
#58215 = CARTESIAN_POINT ( 'NONE',  ( 19.05341960407611168, 5.049401038298154454, 63.95724293864769550 ) ) ;
#58216 = CARTESIAN_POINT ( 'NONE',  ( -16.46253265017146816, -9.564922557961047289, 79.16775706135234714 ) ) ;
#58217 = CARTESIAN_POINT ( 'NONE',  ( 8.224510206698953496, -14.34966873604960469, 92.91557627198103830 ) ) ;
#58218 = CARTESIAN_POINT ( 'NONE',  ( 21.55341960407619695, -5.719274019375665929, 61.04275706135234714 ) ) ;
#58220 = CARTESIAN_POINT ( 'NONE',  ( 21.52544592524334988, 5.823673210054432836, 26.45942372801901854 ) ) ;
#58219 = CARTESIAN_POINT ( 'NONE',  ( 9.564922557960805705, 16.46253265017160317, 49.58224293864770260 ) ) ;
#58221 = CARTESIAN_POINT ( 'NONE',  ( 4.379528057220339221, -16.55341960407611168, 97.70724293864772392 ) ) ;
#58222 = DIRECTION ( 'NONE',  ( 0.000000000000000000, 0.000000000000000000, -1.000000000000000000 ) ) ;
#58223 = CARTESIAN_POINT ( 'NONE',  ( -9.564922557960796823, -16.46253265017161027, 62.08224293864769550 ) ) ;
#58224 = CARTESIAN_POINT ( 'NONE',  ( -11.80868324581545714, -11.80868324581525997, -64.92279855667830191 ) ) ;
#58226 = CARTESIAN_POINT ( 'NONE',  ( -21.53943276465977519, 0.05219959533907696930, 21.24890960531436690 ) ) ;
#58225 = CARTESIAN_POINT ( 'NONE',  ( 0.05219959533936267826, -19.03943276465977164, 110.0010903946856757 ) ) ;
#58227 = CARTESIAN_POINT ( 'NONE',  ( -15.80617190586768217, 15.72974639402176855, 43.12609039468568284 ) ) ;
#58228 = CARTESIAN_POINT ( 'NONE',  ( -13.89961937509977652, 13.97604488694528158, 100.6239096053143669 ) ) ;
#58229 = CARTESIAN_POINT ( 'NONE',  ( 19.05341960407617918, -5.049401038297876454, 81.04275706135231871 ) ) ;
#58230 = CARTESIAN_POINT ( 'NONE',  ( -13.97604488694527625, -13.89961937509977652, 56.87390960531434558 ) ) ;
#58231 = EDGE_CURVE ( 'NONE', #41521, #69935, #129046, .T. ) ;
#58232 = CARTESIAN_POINT ( 'NONE',  ( -14.29746914071049879, 8.314922557960819915, 85.83224293864768129 ) ) ;
#58233 = CARTESIAN_POINT ( 'NONE',  ( 19.05341960407611168, 5.049401038298154454, 88.95724293864769550 ) ) ;
#58234 = CARTESIAN_POINT ( 'NONE',  ( -8.314922557960811034, -14.29746914071050412, 72.08224293864769550 ) ) ;
#58235 = CARTESIAN_POINT ( 'NONE',  ( -5.153800228976328057, -19.02544592524343514, 87.29057627198103830 ) ) ;
#58236 = CARTESIAN_POINT ( 'NONE',  ( 19.03943276465977164, 0.05219959533936151252, 31.25109039468566863 ) ) ;
#58239 = CARTESIAN_POINT ( 'NONE',  ( 9.474510206698971260, -16.51473224551069308, 27.91557627198103120 ) ) ;
#58238 = CARTESIAN_POINT ( 'NONE',  ( 8.314922557960818139, 14.29746914071049879, 49.58224293864769550 ) ) ;
#58237 = CARTESIAN_POINT ( 'NONE',  ( 19.03943276465977164, -0.05219959533909143690, 43.74890960531435979 ) ) ;
#58240 = ORIENTED_EDGE ( 'NONE', *, *, #55774, .F. ) ;
#58241 = CARTESIAN_POINT ( 'NONE',  ( 5.823673210054444382, -21.52544592524334988, 45.20942372801901854 ) ) ;
#58242 = CARTESIAN_POINT ( 'NONE',  ( -5.153800228976607833, 19.02544592524334988, 82.70942372801897591 ) ) ;
#58243 = CARTESIAN_POINT ( 'NONE',  ( -16.55341960407611168, -4.379528057220339221, 36.45724293864768839 ) ) ;
#58244 = CARTESIAN_POINT ( 'NONE',  ( -18.62759615963270932, 10.81492255796079327, 90.83224293864769550 ) ) ;
#58245 = CARTESIAN_POINT ( 'NONE',  ( -15.72974639402197994, 15.80617190586746368, 30.62390960531436335 ) ) ;
#58246 = CARTESIAN_POINT ( 'NONE',  ( 4.483927247898545687, 16.52544592524342804, 74.79057627198105251 ) ) ;
#58247 = CARTESIAN_POINT ( 'NONE',  ( 19.03943276465977164, -0.05219959533909143690, 43.74890960531435979 ) ) ;
#58248 = CARTESIAN_POINT ( 'NONE',  ( -8.314922557961024197, 14.29746914071037800, 97.91775706135236135 ) ) ;
#58249 = CARTESIAN_POINT ( 'NONE',  ( 4.379528057220092307, 16.55341960407617563, 72.29275706135236135 ) ) ;
#58250 = CARTESIAN_POINT ( 'NONE',  ( -16.51473224551082808, 9.474510206698731452, 28.33442372801900433 ) ) ;
#58251 = CARTESIAN_POINT ( 'NONE',  ( -19.05341960407611168, -5.049401038298163336, 96.45724293864769550 ) ) ;
#58252 = CARTESIAN_POINT ( 'NONE',  ( 16.51473224551069308, 9.474510206698969483, 84.16557627198102409 ) ) ;
#58253 = CARTESIAN_POINT ( 'NONE',  ( -8.224510206698735004, -14.34966873604973081, 79.58442372801903275 ) ) ;
#58254 = CARTESIAN_POINT ( 'NONE',  ( -13.89961937509977652, 13.97604488694528158, 30.62390960531435269 ) ) ;
#58255 = CARTESIAN_POINT ( 'NONE',  ( 8.224510206698953496, -14.34966873604960469, 32.91557627198102409 ) ) ;
#58257 = CARTESIAN_POINT ( 'NONE',  ( -13.97604488694527625, -13.89961937509977652, 91.87390960531432427 ) ) ;
#58256 = CARTESIAN_POINT ( 'NONE',  ( 9.564922557960805705, 16.46253265017160317, 99.58224293864770971 ) ) ;
#58258 = CARTESIAN_POINT ( 'NONE',  ( -5.823673210054116645, -21.52544592524344225, 22.29057627198102765 ) ) ;
#58259 = CARTESIAN_POINT ( 'NONE',  ( 12.14591786802309770, 12.06949235617756955, 74.37390960531436690 ) ) ;
#58260 = CARTESIAN_POINT ( 'NONE',  ( 0.05219959533910956823, 16.53943276465976808, 69.99890960531435269 ) ) ;
#58262 = DIRECTION ( 'NONE',  ( 0.000000000000000000, -0.7071067811865483499, -0.7071067811865465735 ) ) ;
#58261 = CARTESIAN_POINT ( 'NONE',  ( -0.05219959533934338120, 16.53943276465976808, 57.50109039468568994 ) ) ;
#58263 = CARTESIAN_POINT ( 'NONE',  ( -13.89961937509957401, -13.97604488694547875, 44.37609039468566863 ) ) ;
#58264 = CARTESIAN_POINT ( 'NONE',  ( -5.049401038298153566, 19.05341960407611168, 95.20724293864770971 ) ) ;
#58265 = CARTESIAN_POINT ( 'NONE',  ( -13.89961937509957401, -13.97604488694547875, 59.37609039468566863 ) ) ;
#58266 = CARTESIAN_POINT ( 'NONE',  ( 16.51473224551083163, -9.474510206698727899, 40.83442372801900433 ) ) ;
#58268 = CARTESIAN_POINT ( 'NONE',  ( 16.55341960407618274, -4.379528057220086978, 101.0427570613523756 ) ) ;
#58267 = CARTESIAN_POINT ( 'NONE',  ( 16.55341960407618274, -4.379528057220086978, 21.04275706135234714 ) ) ;
#58269 = CARTESIAN_POINT ( 'NONE',  ( 13.89961937509977652, -13.97604488694527269, 43.12390960531434558 ) ) ;
#58270 = CARTESIAN_POINT ( 'NONE',  ( 10.72451020669898902, -18.67979575497178502, 22.91557627198102765 ) ) ;
#58271 = CARTESIAN_POINT ( 'NONE',  ( 18.67979575497194134, -10.72451020669871369, 50.83442372801901143 ) ) ;
#58272 = CARTESIAN_POINT ( 'NONE',  ( 5.049401038297881783, 19.05341960407617563, 107.2927570613523187 ) ) ;
#58274 = CARTESIAN_POINT ( 'NONE',  ( 0.05219959533909260263, 19.03943276465977164, 79.99890960531436690 ) ) ;
#58273 = DIRECTION ( 'NONE',  ( 0.000000000000000000, 0.000000000000000000, 1.000000000000000000 ) ) ;
#58275 = CARTESIAN_POINT ( 'NONE',  ( -19.05341960407611168, -5.049401038298163336, 111.4572429386476671 ) ) ;
#58277 = CARTESIAN_POINT ( 'NONE',  ( 19.03943276465977164, -0.05219959533909143690, 73.74890960531435269 ) ) ;
#58276 = CARTESIAN_POINT ( 'NONE',  ( 12.06949235617757843, -12.14591786802309237, 73.12390960531436690 ) ) ;
#58278 = CARTESIAN_POINT ( 'NONE',  ( 0.05219959533909260263, 19.03943276465977164, 69.99890960531435269 ) ) ;
#58279 = CARTESIAN_POINT ( 'NONE',  ( -19.03943276465977164, -0.05219959533935918106, 73.75109039468566152 ) ) ;
#58280 = CARTESIAN_POINT ( 'NONE',  ( -18.62759615963270932, 10.81492255796079327, 65.83224293864769550 ) ) ;
#58281 = CARTESIAN_POINT ( 'NONE',  ( -19.05341960407611168, -5.049401038298163336, 21.45724293864768839 ) ) ;
#58282 = CARTESIAN_POINT ( 'NONE',  ( -9.564922557961040184, 16.46253265017147172, 57.91775706135233293 ) ) ;
#58283 = CARTESIAN_POINT ( 'NONE',  ( 19.05341960407611168, 5.049401038298154454, 53.95724293864770260 ) ) ;
#58284 = CARTESIAN_POINT ( 'NONE',  ( 13.89961937509977652, -13.97604488694527269, 93.12390960531436690 ) ) ;
#58285 = CARTESIAN_POINT ( 'NONE',  ( 21.55341960407610458, 5.719274019375980345, 93.95724293864770971 ) ) ;
#58287 = CARTESIAN_POINT ( 'NONE',  ( -0.05219959533936034679, 19.03943276465977164, 42.50109039468566152 ) ) ;
#58286 = CARTESIAN_POINT ( 'NONE',  ( 4.483927247898545687, 16.52544592524342804, 89.79057627198103830 ) ) ;
#58288 = CARTESIAN_POINT ( 'NONE',  ( 18.67979575497178502, 10.72451020669898547, 79.16557627198103830 ) ) ;
#58289 = CARTESIAN_POINT ( 'NONE',  ( 18.67979575497178502, 10.72451020669898547, 54.16557627198103120 ) ) ;
#58290 = CARTESIAN_POINT ( 'NONE',  ( 12.06949235617757843, -12.14591786802309237, 28.12390960531435979 ) ) ;
#58291 = CARTESIAN_POINT ( 'NONE',  ( -21.55341960407619339, 5.719274019375674811, 108.5427570613523756 ) ) ;
#58292 = CARTESIAN_POINT ( 'NONE',  ( -9.564922557960796823, -16.46253265017161027, 77.08224293864769550 ) ) ;
#58293 = CARTESIAN_POINT ( 'NONE',  ( 0.05219959533909260263, 19.03943276465977164, 29.99890960531435979 ) ) ;
#58294 = CIRCLE ( 'NONE', #80781, 2.000000000000000000 ) ;
#58295 = CARTESIAN_POINT ( 'NONE',  ( -21.53943276465977519, -0.05219959533937600094, 43.75109039468568284 ) ) ;
#58296 = CARTESIAN_POINT ( 'NONE',  ( 0.05219959533937995610, -21.53943276465977519, 35.00109039468568284 ) ) ;
#58297 = CARTESIAN_POINT ( 'NONE',  ( -5.153800228976328057, -19.02544592524343514, 47.29057627198102409 ) ) ;
#58298 = CARTESIAN_POINT ( 'NONE',  ( -15.80617190586768217, 15.72974639402176855, 23.12609039468567573 ) ) ;
#58299 = EDGE_CURVE ( 'NONE', #139693, #107790, #134342, .T. ) ;
#58300 = CARTESIAN_POINT ( 'NONE',  ( 9.474510206698729675, 16.51473224551082808, 57.08442372801900433 ) ) ;
#58301 = CARTESIAN_POINT ( 'NONE',  ( -13.89961937509977652, 13.97604488694528158, 30.62390960531435269 ) ) ;
#58302 = CARTESIAN_POINT ( 'NONE',  ( -16.53943276465976808, -0.05219959533934237506, 33.75109039468568284 ) ) ;
#58303 = CARTESIAN_POINT ( 'NONE',  ( 5.049401038298161559, -19.05341960407611168, 27.70724293864769550 ) ) ;
#58304 = CARTESIAN_POINT ( 'NONE',  ( 16.55341960407618274, -4.379528057220086978, 71.04275706135234714 ) ) ;
#58305 = CARTESIAN_POINT ( 'NONE',  ( 19.03943276465977164, -0.05219959533909143690, 33.74890960531435979 ) ) ;
#58306 = CARTESIAN_POINT ( 'NONE',  ( 13.97604488694527802, 13.89961937509977652, 89.37390960531436690 ) ) ;
#58307 = CARTESIAN_POINT ( 'NONE',  ( -19.02544592524342804, 5.153800228976336051, 31.04057627198102409 ) ) ;
#58308 = CARTESIAN_POINT ( 'NONE',  ( 21.55341960407610458, 5.719274019375980345, 68.95724293864769550 ) ) ;
#58309 = CARTESIAN_POINT ( 'NONE',  ( -4.379528057220086978, -16.55341960407618274, 44.79275706135234714 ) ) ;
#58310 = CARTESIAN_POINT ( 'NONE',  ( 10.81492255796106328, -18.62759615963255655, 95.41775706135234714 ) ) ;
#58311 = CARTESIAN_POINT ( 'NONE',  ( -5.049401038298153566, 19.05341960407611168, 40.20724293864768839 ) ) ;
#58312 = CARTESIAN_POINT ( 'NONE',  ( -14.34966873604960291, -8.224510206698953496, 26.66557627198103475 ) ) ;
#58313 = CARTESIAN_POINT ( 'NONE',  ( -16.52544592524342804, 4.483927247898546575, 71.04057627198103830 ) ) ;
#58314 = CARTESIAN_POINT ( 'NONE',  ( -9.564922557960796823, -16.46253265017161027, 62.08224293864769550 ) ) ;
#58315 = CARTESIAN_POINT ( 'NONE',  ( -15.80617190586768217, 15.72974639402176855, 103.1260903946856757 ) ) ;
#58316 = CARTESIAN_POINT ( 'NONE',  ( -18.62759615963255300, -10.81492255796106328, 29.16775706135234003 ) ) ;
#58317 = CARTESIAN_POINT ( 'NONE',  ( -16.51473224551069308, -9.474510206698971260, 81.66557627198103830 ) ) ;
#58318 = CARTESIAN_POINT ( 'NONE',  ( 10.72451020669871369, 18.67979575497193778, 87.08442372801901854 ) ) ;
#58319 = CARTESIAN_POINT ( 'NONE',  ( -16.52544592524335698, -4.483927247898792601, 58.95942372801902565 ) ) ;
#58320 = CARTESIAN_POINT ( 'NONE',  ( -12.14591786802326823, 12.06949235617739902, 33.12609039468569705 ) ) ;
#58322 = CARTESIAN_POINT ( 'NONE',  ( 5.823673210054444382, -21.52544592524334988, 105.2094237280190328 ) ) ;
#58321 = CARTESIAN_POINT ( 'NONE',  ( 8.314922557960818139, 14.29746914071049879, 89.58224293864768129 ) ) ;
#58323 = CARTESIAN_POINT ( 'NONE',  ( -14.29746914071049879, 8.314922557960819915, 35.83224293864768839 ) ) ;
#58324 = CARTESIAN_POINT ( 'NONE',  ( -19.03943276465977164, 0.05219959533909376836, 31.24890960531435979 ) ) ;
#58325 = CARTESIAN_POINT ( 'NONE',  ( 14.29746914071037800, 8.314922557961029526, 51.66775706135234714 ) ) ;
#58326 = CARTESIAN_POINT ( 'NONE',  ( 16.53943276465976808, -0.05219959533910856209, 48.74890960531435979 ) ) ;
#58327 = CARTESIAN_POINT ( 'NONE',  ( -16.55341960407617563, 4.379528057220093196, 98.54275706135234714 ) ) ;
#58328 = CARTESIAN_POINT ( 'NONE',  ( -21.53943276465977519, 0.05219959533907696930, 21.24890960531436690 ) ) ;
#58329 = CARTESIAN_POINT ( 'NONE',  ( -5.823673210054116645, -21.52544592524344225, 32.29057627198102409 ) ) ;
#58330 = CARTESIAN_POINT ( 'NONE',  ( -0.05219959533937732626, 21.53943276465977519, 107.5010903946856899 ) ) ;
#58331 = CARTESIAN_POINT ( 'NONE',  ( -8.224510206698948167, 14.34966873604960824, 90.41557627198103830 ) ) ;
#58332 = CARTESIAN_POINT ( 'NONE',  ( -16.46253265017160317, 9.564922557960807481, 100.8322429386477097 ) ) ;
#58333 = ORIENTED_EDGE ( 'NONE', *, *, #197168, .F. ) ;
#58334 = CARTESIAN_POINT ( 'NONE',  ( 4.483927247898790824, -16.52544592524335698, 35.20942372801901854 ) ) ;
#58335 = CARTESIAN_POINT ( 'NONE',  ( -5.153800228976328057, -19.02544592524343514, 47.29057627198102409 ) ) ;
#58337 = CARTESIAN_POINT ( 'NONE',  ( -17.33731399503118453, -5.745198142927167240, 21.23700565386912231 ) ) ;
#58336 = CARTESIAN_POINT ( 'NONE',  ( 8.224510206698742110, 14.34966873604972548, 47.08442372801901854 ) ) ;
#58338 = CARTESIAN_POINT ( 'NONE',  ( 13.89961937509957401, 13.97604488694547697, 46.87609039468565442 ) ) ;
#58339 = CARTESIAN_POINT ( 'NONE',  ( -19.02544592524342804, 5.153800228976336051, 46.04057627198101699 ) ) ;
#58340 = CARTESIAN_POINT ( 'NONE',  ( 12.06949235617739724, 12.14591786802326823, 86.87609039468568994 ) ) ;
#58341 = CARTESIAN_POINT ( 'NONE',  ( -5.049401038297874678, -19.05341960407617918, 99.79275706135234714 ) ) ;
#58342 = CARTESIAN_POINT ( 'NONE',  ( 19.02544592524334988, 5.153800228976608722, 26.45942372801899722 ) ) ;
#58343 = CARTESIAN_POINT ( 'NONE',  ( -5.153800228976328057, -19.02544592524343514, 67.29057627198102409 ) ) ;
#58344 = CARTESIAN_POINT ( 'NONE',  ( 8.224510206698953496, -14.34966873604960469, 92.91557627198103830 ) ) ;
#58345 = CARTESIAN_POINT ( 'NONE',  ( 5.049401038297881783, 19.05341960407617563, 72.29275706135234714 ) ) ;
#58346 = CARTESIAN_POINT ( 'NONE',  ( -21.53943276465977519, 0.05219959533907696930, 61.24890960531435979 ) ) ;
#58347 = CARTESIAN_POINT ( 'NONE',  ( -5.153800228976607833, 19.02544592524334988, 42.70942372801901143 ) ) ;
#58348 = CARTESIAN_POINT ( 'NONE',  ( 19.03943276465977164, -0.05219959533909143690, 103.7489096053143669 ) ) ;
#58349 = CARTESIAN_POINT ( 'NONE',  ( -10.81492255796078084, -18.62759615963271287, 77.08224293864769550 ) ) ;
#58350 = CARTESIAN_POINT ( 'NONE',  ( -17.31728774477271671, 6.344390552232383129, 85.81906651689314458 ) ) ;
#58351 = AXIS2_PLACEMENT_3D ( 'NONE', #193468, #149956, #119624 ) ;
#58352 = CARTESIAN_POINT ( 'NONE',  ( 5.049401038297881783, 19.05341960407617563, 107.2927570613523187 ) ) ;
#58353 = CARTESIAN_POINT ( 'NONE',  ( 17.58332526062525147, 7.635886036038630920, 96.57665040441536064 ) ) ;
#58354 = CARTESIAN_POINT ( 'NONE',  ( 4.379528057220092307, 16.55341960407617563, 22.29275706135235069 ) ) ;
#58355 = CARTESIAN_POINT ( 'NONE',  ( -5.153800228976328057, -19.02544592524343514, 42.29057627198101699 ) ) ;
#58356 = CARTESIAN_POINT ( 'NONE',  ( 13.97604488694527802, 13.89961937509977652, 109.3739096053143669 ) ) ;
#58357 = CARTESIAN_POINT ( 'NONE',  ( 18.67979575497178502, 10.72451020669898547, 89.16557627198102409 ) ) ;
#58358 = CARTESIAN_POINT ( 'NONE',  ( 21.55341960407619695, -5.719274019375665929, 56.04275706135235424 ) ) ;
#58360 = CARTESIAN_POINT ( 'NONE',  ( 21.53943276465977519, 0.05219959533937863772, 111.2510903946856899 ) ) ;
#58359 = CARTESIAN_POINT ( 'NONE',  ( 19.05341960407617918, -5.049401038297876454, 106.0427570613523471 ) ) ;
#58361 = CARTESIAN_POINT ( 'NONE',  ( -14.34966873604972548, 8.224510206698743886, 108.3344237280190185 ) ) ;
#58362 = CARTESIAN_POINT ( 'NONE',  ( 5.823673210054125526, 21.52544592524343514, 94.79057627198105251 ) ) ;
#58363 = CARTESIAN_POINT ( 'NONE',  ( 4.483927247898545687, 16.52544592524342804, 49.79057627198102409 ) ) ;
#58364 = CARTESIAN_POINT ( 'NONE',  ( -19.03943276465977164, -0.05219959533935918106, 78.75109039468567573 ) ) ;
#58365 = CARTESIAN_POINT ( 'NONE',  ( -13.97604488694547697, 13.89961937509957934, 53.12609039468565442 ) ) ;
#58366 = CARTESIAN_POINT ( 'NONE',  ( 10.81492255796106328, -18.62759615963255655, 75.41775706135233293 ) ) ;
#58367 = CARTESIAN_POINT ( 'NONE',  ( 13.89961937509957401, 13.97604488694547697, 36.87609039468565442 ) ) ;
#58368 = CARTESIAN_POINT ( 'NONE',  ( -12.06949235617756955, 12.14591786802309770, 100.6239096053143811 ) ) ;
#58369 = CARTESIAN_POINT ( 'NONE',  ( 10.81492255796078972, 18.62759615963270932, 39.58224293864769550 ) ) ;
#58370 = CARTESIAN_POINT ( 'NONE',  ( 14.29746914071049879, -8.314922557960816363, 38.33224293864768839 ) ) ;
#58371 = CARTESIAN_POINT ( 'NONE',  ( -16.51473224551082808, 9.474510206698731452, 23.33442372801900078 ) ) ;
#58372 = CARTESIAN_POINT ( 'NONE',  ( -14.29746914071037622, -8.314922557961029526, 74.16775706135231871 ) ) ;
#58373 = CARTESIAN_POINT ( 'NONE',  ( -16.53943276465976808, 0.05219959533911058130, 31.24890960531435979 ) ) ;
#58374 = CARTESIAN_POINT ( 'NONE',  ( 10.72451020669871369, 18.67979575497193778, 62.08442372801901143 ) ) ;
#58375 = CARTESIAN_POINT ( 'NONE',  ( -15.80617190586768217, 15.72974639402176855, 68.12609039468567573 ) ) ;
#58376 = CARTESIAN_POINT ( 'NONE',  ( -0.05219959533907301413, -21.53943276465977519, 72.49890960531435269 ) ) ;
#58377 = ORIENTED_EDGE ( 'NONE', *, *, #114876, .T. ) ;
#58378 = CARTESIAN_POINT ( 'NONE',  ( -5.049401038298153566, 19.05341960407611168, 30.20724293864768839 ) ) ;
#58379 = CARTESIAN_POINT ( 'NONE',  ( 5.719274019375673035, 21.55341960407619339, 47.29275706135234003 ) ) ;
#58380 = CARTESIAN_POINT ( 'NONE',  ( 12.14591786802309770, 12.06949235617756955, 114.3739096053143527 ) ) ;
#58381 = CARTESIAN_POINT ( 'NONE',  ( 5.049401038298161559, -19.05341960407611168, 32.70724293864768129 ) ) ;
#58382 = CARTESIAN_POINT ( 'NONE',  ( 16.55341960407611168, 4.379528057220329451, 73.95724293864769550 ) ) ;
#58383 = CARTESIAN_POINT ( 'NONE',  ( -16.51473224551069308, -9.474510206698971260, 86.66557627198102409 ) ) ;
#58384 = CARTESIAN_POINT ( 'NONE',  ( 16.55341960407611168, 4.379528057220329451, 28.95724293864769905 ) ) ;
#58385 = CARTESIAN_POINT ( 'NONE',  ( 16.55341960407611168, 4.379528057220329451, 98.95724293864770971 ) ) ;
#58386 = CARTESIAN_POINT ( 'NONE',  ( 5.719274019375991003, -21.55341960407610458, 72.70724293864769550 ) ) ;
#58387 = CARTESIAN_POINT ( 'NONE',  ( -15.72974639402197994, 15.80617190586746368, 105.6239096053143669 ) ) ;
#58388 = CARTESIAN_POINT ( 'NONE',  ( -17.63037570847463442, 16.23105266556533621, -54.49189616393496749 ) ) ;
#58390 = CARTESIAN_POINT ( 'NONE',  ( -12.14591786802326823, 12.06949235617739902, 23.12609039468567573 ) ) ;
#58389 = CARTESIAN_POINT ( 'NONE',  ( 5.153800228976335163, 19.02544592524342804, 64.79057627198100988 ) ) ;
#58391 = CARTESIAN_POINT ( 'NONE',  ( 5.823673210054125526, 21.52544592524343514, 54.79057627198104541 ) ) ;
#58392 = CARTESIAN_POINT ( 'NONE',  ( -18.67979575497193778, 10.72451020669871902, 83.33442372801903275 ) ) ;
#58393 = CARTESIAN_POINT ( 'NONE',  ( -16.51473224551069308, -9.474510206698971260, 86.66557627198102409 ) ) ;
#58394 = EDGE_CURVE ( 'NONE', #166568, #29646, #51233, .T. ) ;
#58395 = CARTESIAN_POINT ( 'NONE',  ( -5.049401038298153566, 19.05341960407611168, 110.2072429386476671 ) ) ;
#58396 = CARTESIAN_POINT ( 'NONE',  ( 12.06949235617739724, 12.14591786802326823, 76.87609039468567573 ) ) ;
#58397 = CARTESIAN_POINT ( 'NONE',  ( -21.52544592524334988, -5.823673210054445271, 58.95942372801902565 ) ) ;
#58398 = CARTESIAN_POINT ( 'NONE',  ( 21.52544592524334988, 5.823673210054432836, 106.4594237280190328 ) ) ;
#58399 = CARTESIAN_POINT ( 'NONE',  ( -14.29746914071037622, -8.314922557961029526, 64.16775706135234714 ) ) ;
#58400 = CARTESIAN_POINT ( 'NONE',  ( -21.52544592524334988, -5.823673210054445271, 18.95942372801901143 ) ) ;
#58401 = CARTESIAN_POINT ( 'NONE',  ( 13.97604488694527802, 13.89961937509977652, 24.37390960531435624 ) ) ;
#58402 = CARTESIAN_POINT ( 'NONE',  ( 5.719274019375991003, -21.55341960407610458, 92.70724293864770971 ) ) ;
#58403 = CARTESIAN_POINT ( 'NONE',  ( -5.153800228976607833, 19.02544592524334988, 47.70942372801900433 ) ) ;
#58404 = CARTESIAN_POINT ( 'NONE',  ( 21.55341960407610458, 5.719274019375980345, 53.95724293864770260 ) ) ;
#58406 = CARTESIAN_POINT ( 'NONE',  ( -14.34966873604960291, -8.224510206698953496, 31.66557627198102054 ) ) ;
#58405 = CARTESIAN_POINT ( 'NONE',  ( 13.89961937509977652, -13.97604488694527269, 98.12390960531433848 ) ) ;
#58407 = DIRECTION ( 'NONE',  ( 0.000000000000000000, 0.000000000000000000, 1.000000000000000000 ) ) ;
#58408 = CARTESIAN_POINT ( 'NONE',  ( -18.22780087662124160, -5.499999999999927169, 78.98236817873106475 ) ) ;
#58409 = CARTESIAN_POINT ( 'NONE',  ( -0.05219959533936034679, 19.03943276465977164, 112.5010903946856757 ) ) ;
#58410 = CARTESIAN_POINT ( 'NONE',  ( 5.719274019375991003, -21.55341960407610458, 72.70724293864769550 ) ) ;
#58411 = CARTESIAN_POINT ( 'NONE',  ( -0.05219959533910754901, -16.53943276465976808, 57.49890960531435979 ) ) ;
#58412 = CARTESIAN_POINT ( 'NONE',  ( -16.53943276465976808, -0.05219959533934237506, 33.75109039468568284 ) ) ;
#58413 = CARTESIAN_POINT ( 'NONE',  ( 13.89961937509977652, -13.97604488694527269, 48.12390960531435979 ) ) ;
#58415 = CARTESIAN_POINT ( 'NONE',  ( 19.05341960407617918, -5.049401038297876454, 81.04275706135231871 ) ) ;
#58414 = CARTESIAN_POINT ( 'NONE',  ( 10.81492255796078972, 18.62759615963270932, 114.5822429386477097 ) ) ;
#58416 = CARTESIAN_POINT ( 'NONE',  ( 19.02544592524343514, -5.153800228976328945, 78.54057627198099567 ) ) ;
#58417 = CARTESIAN_POINT ( 'NONE',  ( 16.51473224551069308, 9.474510206698969483, 69.16557627198102409 ) ) ;
#58418 = CARTESIAN_POINT ( 'NONE',  ( 5.823673210054125526, 21.52544592524343514, 74.79057627198105251 ) ) ;
#58419 = CARTESIAN_POINT ( 'NONE',  ( -0.05219959533909027116, -19.03943276465977164, 32.49890960531435979 ) ) ;
#58420 = CARTESIAN_POINT ( 'NONE',  ( -9.446479005521629446, 36.53641634556310436, -7.999999999999998224 ) ) ;
#58421 = CARTESIAN_POINT ( 'NONE',  ( -14.34966873604960291, -8.224510206698953496, 56.66557627198103830 ) ) ;
#58422 = CARTESIAN_POINT ( 'NONE',  ( -13.97604488694527625, -13.89961937509977652, 96.87390960531433848 ) ) ;
#58423 = DIRECTION ( 'NONE',  ( 0.000000000000000000, 0.000000000000000000, -1.000000000000000000 ) ) ;
#58424 = CARTESIAN_POINT ( 'NONE',  ( 16.51473224551083163, -9.474510206698727899, 50.83442372801899722 ) ) ;
#58425 = CARTESIAN_POINT ( 'NONE',  ( 18.62759615963271287, -10.81492255796078972, 83.33224293864769550 ) ) ;
#58426 = CARTESIAN_POINT ( 'NONE',  ( 16.51473224551083163, -9.474510206698727899, 30.83442372801900433 ) ) ;
#58427 = CARTESIAN_POINT ( 'NONE',  ( -9.474510206698964154, 16.51473224551069663, 90.41557627198103830 ) ) ;
#58428 = FACE_BOUND ( 'NONE', #8317, .T. ) ;
#58429 = CARTESIAN_POINT ( 'NONE',  ( 18.67979575497178502, 10.72451020669898547, 29.16557627198103120 ) ) ;
#58430 = CARTESIAN_POINT ( 'NONE',  ( 13.97604488694527802, 13.89961937509977652, 79.37390960531435269 ) ) ;
#58431 = CARTESIAN_POINT ( 'NONE',  ( -5.823673210054431948, 21.52544592524334988, 47.70942372801902565 ) ) ;
#58432 = CARTESIAN_POINT ( 'NONE',  ( 19.03943276465977164, -0.05219959533909143690, 23.74890960531435269 ) ) ;
#58434 = ORIENTED_EDGE ( 'NONE', *, *, #76859, .F. ) ;
#58433 = CARTESIAN_POINT ( 'NONE',  ( -0.05219959533907301413, -21.53943276465977519, 112.4989096053143669 ) ) ;
#58435 = CARTESIAN_POINT ( 'NONE',  ( -21.53943276465977519, -0.05219959533937600094, 38.75109039468567573 ) ) ;
#58436 = VERTEX_POINT ( 'NONE', #114894 ) ;
#58437 = CARTESIAN_POINT ( 'NONE',  ( 13.97604488694527802, 13.89961937509977652, 94.37390960531436690 ) ) ;
#58438 = FACE_OUTER_BOUND ( 'NONE', #138008, .T. ) ;
#58439 = CARTESIAN_POINT ( 'NONE',  ( -15.80617190586745835, -15.72974639402198527, 101.8739096053143811 ) ) ;
#58440 = CARTESIAN_POINT ( 'NONE',  ( -5.049401038298153566, 19.05341960407611168, 60.20724293864768129 ) ) ;
#58441 = CARTESIAN_POINT ( 'NONE',  ( -19.03943276465977164, -0.05219959533935918106, 113.7510903946856757 ) ) ;
#58442 = CARTESIAN_POINT ( 'NONE',  ( -22.81625015709510507, 31.40387420917330275, -1.424999997268813212 ) ) ;
#58443 = CARTESIAN_POINT ( 'NONE',  ( 5.823673210054444382, -21.52544592524334988, 100.2094237280190043 ) ) ;
#58444 = CARTESIAN_POINT ( 'NONE',  ( -13.89961937509977652, 13.97604488694528158, 40.62390960531435979 ) ) ;
#58445 = CARTESIAN_POINT ( 'NONE',  ( 5.823673210054444382, -21.52544592524334988, 95.20942372801903275 ) ) ;
#58447 = CARTESIAN_POINT ( 'NONE',  ( 5.823673210054444382, -21.52544592524334988, 60.20942372801902565 ) ) ;
#58446 = CARTESIAN_POINT ( 'NONE',  ( 5.049401038298161559, -19.05341960407611168, 87.70724293864769550 ) ) ;
#58448 = CARTESIAN_POINT ( 'NONE',  ( 17.14385361876520264, 23.59649016807275856, 142.6750000027311103 ) ) ;
#58449 = CARTESIAN_POINT ( 'NONE',  ( 9.564922557960805705, 16.46253265017160317, 99.58224293864770971 ) ) ;
#58450 = DIRECTION ( 'NONE',  ( 0.000000000000000000, 0.000000000000000000, -1.000000000000000000 ) ) ;
#58453 = CARTESIAN_POINT ( 'NONE',  ( -18.62759615963255300, -10.81492255796106328, 64.16775706135234714 ) ) ;
#58452 = CARTESIAN_POINT ( 'NONE',  ( -16.55341960407617563, 4.379528057220093196, 63.54275706135234003 ) ) ;
#58451 = CARTESIAN_POINT ( 'NONE',  ( 12.06949235617739724, 12.14591786802326823, 51.87609039468568284 ) ) ;
#58454 = CARTESIAN_POINT ( 'NONE',  ( 21.52544592524334988, 5.823673210054432836, 91.45942372801901854 ) ) ;
#58455 = CARTESIAN_POINT ( 'NONE',  ( -10.38518860439150693, 9.278585747845273346, -60.35672204601534219 ) ) ;
#58456 = CARTESIAN_POINT ( 'NONE',  ( 12.06949235617739724, 12.14591786802326823, 26.87609039468567218 ) ) ;
#58457 = CARTESIAN_POINT ( 'NONE',  ( 19.02544592524343514, -5.153800228976328945, 78.54057627198099567 ) ) ;
#58458 = CARTESIAN_POINT ( 'NONE',  ( 5.049401038298161559, -19.05341960407611168, 97.70724293864766707 ) ) ;
#58459 = EDGE_CURVE ( 'NONE', #199067, #191847, #65400, .T. ) ;
#58460 = FACE_OUTER_BOUND ( 'NONE', #186, .T. ) ;
#58461 = CARTESIAN_POINT ( 'NONE',  ( -19.05341960407611168, -5.049401038298163336, 26.45724293864769550 ) ) ;
#58462 = CARTESIAN_POINT ( 'NONE',  ( -5.719274019375978568, 21.55341960407610458, 25.20724293864769550 ) ) ;
#58463 = CARTESIAN_POINT ( 'NONE',  ( -14.29746914071037622, -8.314922557961029526, 94.16775706135237556 ) ) ;
#58465 = CARTESIAN_POINT ( 'NONE',  ( 13.97604488694527802, 13.89961937509977652, 64.37390960531436690 ) ) ;
#58464 = CARTESIAN_POINT ( 'NONE',  ( 4.379528057220339221, -16.55341960407611168, 77.70724293864770971 ) ) ;
#58466 = CARTESIAN_POINT ( 'NONE',  ( 18.62759615963255655, 10.81492255796105972, 91.66775706135234714 ) ) ;
#58467 = CARTESIAN_POINT ( 'NONE',  ( -22.10131684062750423, 1.340157125434860985, -58.31342218742628347 ) ) ;
#58468 = CARTESIAN_POINT ( 'NONE',  ( 4.379528057220092307, 16.55341960407617563, 27.29275706135234358 ) ) ;
#58469 = CARTESIAN_POINT ( 'NONE',  ( 12.06949235617757843, -12.14591786802309237, 73.12390960531436690 ) ) ;
#58470 = CARTESIAN_POINT ( 'NONE',  ( 21.53943276465977519, 0.05219959533937863772, 36.25109039468567573 ) ) ;
#58471 = CARTESIAN_POINT ( 'NONE',  ( 18.62759615963271287, -10.81492255796078972, 68.33224293864769550 ) ) ;
#58472 = CARTESIAN_POINT ( 'NONE',  ( -16.51473224551082808, 9.474510206698731452, 43.33442372801900433 ) ) ;
#58473 = CARTESIAN_POINT ( 'NONE',  ( -37.45873412500000654, 2.428612866367529932E-14, -11.43749999590322020 ) ) ;
#58474 = CARTESIAN_POINT ( 'NONE',  ( 5.049401038298161559, -19.05341960407611168, 82.70724293864770971 ) ) ;
#58475 = CARTESIAN_POINT ( 'NONE',  ( 0.05219959533910956823, 16.53943276465976808, 44.99890960531435979 ) ) ;
#58476 = CARTESIAN_POINT ( 'NONE',  ( -16.52544592524342804, 4.483927247898546575, 36.04057627198102409 ) ) ;
#58477 = CARTESIAN_POINT ( 'NONE',  ( 4.379528057220092307, 16.55341960407617563, 112.2927570613523471 ) ) ;
#58478 = CARTESIAN_POINT ( 'NONE',  ( -9.474510206698720793, -16.51473224551083518, 64.58442372801900433 ) ) ;
#58479 = CARTESIAN_POINT ( 'NONE',  ( 19.01529144963332030, 5.500000000000157208, 53.73431955728441523 ) ) ;
#58480 = CARTESIAN_POINT ( 'NONE',  ( -5.823673210054116645, -21.52544592524344225, 22.29057627198102765 ) ) ;
#58481 = ADVANCED_FACE ( 'NONE', ( #174588 ), #36053, .F. ) ;
#58482 = CARTESIAN_POINT ( 'NONE',  ( -16.53943276465976808, 0.05219959533911058130, 86.24890960531436690 ) ) ;
#58483 = CARTESIAN_POINT ( 'NONE',  ( -18.22780087662122028, 5.500000000000031086, 58.51540105326107977 ) ) ;
#58485 = CARTESIAN_POINT ( 'NONE',  ( -5.719274019375978568, 21.55341960407610458, 40.20724293864769550 ) ) ;
#58484 = CARTESIAN_POINT ( 'NONE',  ( -9.474510206698964154, 16.51473224551069663, 35.41557627198102409 ) ) ;
#58486 = CARTESIAN_POINT ( 'NONE',  ( 10.72451020669898902, -18.67979575497178502, 62.91557627198102409 ) ) ;
#58487 = CARTESIAN_POINT ( 'NONE',  ( -16.52544592524342804, 4.483927247898546575, 116.0405762719810383 ) ) ;
#58489 = CARTESIAN_POINT ( 'NONE',  ( 19.02544592524343514, -5.153800228976328945, 48.54057627198103120 ) ) ;
#58488 = CARTESIAN_POINT ( 'NONE',  ( -4.379528057220086978, -16.55341960407618274, 64.79275706135234714 ) ) ;
#58490 = CARTESIAN_POINT ( 'NONE',  ( 15.72974639402176855, 15.80617190586768217, 51.87609039468568284 ) ) ;
#58491 = ORIENTED_EDGE ( 'NONE', *, *, #100373, .F. ) ;
#58492 = CARTESIAN_POINT ( 'NONE',  ( 12.14591786802309770, 12.06949235617756955, 99.37390960531436690 ) ) ;
#58493 = CARTESIAN_POINT ( 'NONE',  ( 5.049401038297881783, 19.05341960407617563, 92.29275706135234714 ) ) ;
#58494 = CARTESIAN_POINT ( 'NONE',  ( 11.40812507854754365, 35.11059874428196537, -7.724999997268813701 ) ) ;
#58496 = CARTESIAN_POINT ( 'NONE',  ( 5.719274019375991003, -21.55341960407610458, 27.70724293864769905 ) ) ;
#58495 = CYLINDRICAL_SURFACE ( 'NONE', #154032, 28.79475375365586487 ) ;
#58497 = CARTESIAN_POINT ( 'NONE',  ( 17.50000000000000000, -5.499999999999992895, 66.21769037696435589 ) ) ;
#58498 = CARTESIAN_POINT ( 'NONE',  ( 0.05219959533937995610, -21.53943276465977519, 65.00109039468568994 ) ) ;
#58500 = CARTESIAN_POINT ( 'NONE',  ( -8.314922557960811034, -14.29746914071050412, 42.08224293864769550 ) ) ;
#58499 = CARTESIAN_POINT ( 'NONE',  ( 0.05219959533934541429, -16.53943276465976808, 50.00109039468568994 ) ) ;
#58501 = CARTESIAN_POINT ( 'NONE',  ( -10.81492255796078084, -18.62759615963271287, 62.08224293864769550 ) ) ;
#58502 = CARTESIAN_POINT ( 'NONE',  ( 21.52544592524344225, -5.823673210054117533, 63.54057627198103830 ) ) ;
#58503 = CARTESIAN_POINT ( 'NONE',  ( -20.74379371951212647, -11.24248911466463596, 170.1280252572803988 ) ) ;
#58505 = CARTESIAN_POINT ( 'NONE',  ( 5.153800228976335163, 19.02544592524342804, 114.7905762719810241 ) ) ;
#58504 = CARTESIAN_POINT ( 'NONE',  ( -9.474510206698720793, -16.51473224551083518, 84.58442372801900433 ) ) ;
#58506 = CARTESIAN_POINT ( 'NONE',  ( 5.049401038298161559, -19.05341960407611168, 47.70724293864770260 ) ) ;
#58507 = CARTESIAN_POINT ( 'NONE',  ( 16.51473224551069308, 9.474510206698969483, 24.16557627198102765 ) ) ;
#58508 = SURFACE_SIDE_STYLE ('',( #86850 ) ) ;
#58509 = CARTESIAN_POINT ( 'NONE',  ( 16.51473224551069308, 9.474510206698969483, 109.1655762719810383 ) ) ;
#58510 = ORIENTED_EDGE ( 'NONE', *, *, #22985, .F. ) ;
#58511 = CARTESIAN_POINT ( 'NONE',  ( -4.483927247898782831, 16.52544592524335698, 72.70942372801901854 ) ) ;
#58512 = CARTESIAN_POINT ( 'NONE',  ( 15.72974639402199770, -15.80617190586745480, 98.12390960531436690 ) ) ;
#58513 = CARTESIAN_POINT ( 'NONE',  ( 0.05219959533909260263, 19.03943276465977164, 64.99890960531436690 ) ) ;
#58514 = CARTESIAN_POINT ( 'NONE',  ( -5.823673210054431948, 21.52544592524334988, 37.70942372801900433 ) ) ;
#58515 = CARTESIAN_POINT ( 'NONE',  ( 5.153800228976335163, 19.02544592524342804, 99.79057627198102409 ) ) ;
#58516 = CARTESIAN_POINT ( 'NONE',  ( -29.45353567398637651, -26.40584612579511870, -18.78685418918301409 ) ) ;
#58517 = VERTEX_POINT ( 'NONE', #11743 ) ;
#58518 = CARTESIAN_POINT ( 'NONE',  ( 15.80617190586769283, -15.72974639402175789, 35.62609039468568994 ) ) ;
#58520 = CARTESIAN_POINT ( 'NONE',  ( 19.05341960407617918, -5.049401038297876454, 91.04275706135234714 ) ) ;
#58519 = CARTESIAN_POINT ( 'NONE',  ( -5.153800228976328057, -19.02544592524343514, 22.29057627198102765 ) ) ;
#58521 = CARTESIAN_POINT ( 'NONE',  ( 13.89961937509957401, 13.97604488694547697, 36.87609039468565442 ) ) ;
#58522 = CARTESIAN_POINT ( 'NONE',  ( 18.62759615963271287, -10.81492255796078972, 98.33224293864769550 ) ) ;
#58523 = CARTESIAN_POINT ( 'NONE',  ( 9.564922557961047289, -16.46253265017146816, 30.41775706135232937 ) ) ;
#58524 = CARTESIAN_POINT ( 'NONE',  ( -0.05219959533936034679, 19.03943276465977164, 52.50109039468566863 ) ) ;
#58525 = CARTESIAN_POINT ( 'NONE',  ( -14.34966873604972548, 8.224510206698743886, 88.33442372801901854 ) ) ;
#58527 = ORIENTED_EDGE ( 'NONE', *, *, #139743, .T. ) ;
#58526 = CARTESIAN_POINT ( 'NONE',  ( 24.66673051387559568, -7.254129419879413732, 167.4978569920363043 ) ) ;
#58528 = CARTESIAN_POINT ( 'NONE',  ( -19.05341960407611168, -5.049401038298163336, 71.45724293864766707 ) ) ;
#58529 = CARTESIAN_POINT ( 'NONE',  ( 21.53943276465977519, 0.05219959533937863772, 81.25109039468568994 ) ) ;
#58530 = CARTESIAN_POINT ( 'NONE',  ( -18.67979575497193778, 10.72451020669871902, 98.33442372801901854 ) ) ;
#58531 = CARTESIAN_POINT ( 'NONE',  ( -1.197302953328902797, -6.691186640346296066, -64.41832325557876970 ) ) ;
#58532 = CARTESIAN_POINT ( 'NONE',  ( -16.46253265017160317, 9.564922557960807481, 85.83224293864769550 ) ) ;
#58533 = CARTESIAN_POINT ( 'NONE',  ( -10.81492255796105439, 18.62759615963255655, 67.91775706135234714 ) ) ;
#58534 = CARTESIAN_POINT ( 'NONE',  ( 13.97604488694548053, -13.89961937509957401, 105.6260903946856757 ) ) ;
#58535 = CARTESIAN_POINT ( 'NONE',  ( -16.51473224551069308, -9.474510206698971260, 66.66557627198102409 ) ) ;
#58536 = CARTESIAN_POINT ( 'NONE',  ( 9.564922557960805705, 16.46253265017160317, 109.5822429386476955 ) ) ;
#58537 = CARTESIAN_POINT ( 'NONE',  ( -5.049401038298153566, 19.05341960407611168, 80.20724293864769550 ) ) ;
#58538 = CARTESIAN_POINT ( 'NONE',  ( 17.50000000000003553, -3.188534218036753742, 22.34212600958745298 ) ) ;
#58539 = CARTESIAN_POINT ( 'NONE',  ( 9.474510206698971260, -16.51473224551069308, 62.91557627198102409 ) ) ;
#58540 = CARTESIAN_POINT ( 'NONE',  ( 16.51473224551069308, 9.474510206698969483, 54.16557627198103120 ) ) ;
#58541 = CARTESIAN_POINT ( 'NONE',  ( -21.52544592524334988, -5.823673210054445271, 18.95942372801901143 ) ) ;
#58542 = CARTESIAN_POINT ( 'NONE',  ( 8.224510206698742110, 14.34966873604972548, 82.08442372801901854 ) ) ;
#58543 = CARTESIAN_POINT ( 'NONE',  ( 7.214655873249300910, -1.452908486251167419, -64.31726809345072127 ) ) ;
#58544 = CARTESIAN_POINT ( 'NONE',  ( 9.564922557961047289, -16.46253265017146816, 50.41775706135233293 ) ) ;
#58545 = CARTESIAN_POINT ( 'NONE',  ( 19.05341960407611168, 5.049401038298154454, 83.95724293864766707 ) ) ;
#58546 = CARTESIAN_POINT ( 'NONE',  ( 4.379528057220339221, -16.55341960407611168, 77.70724293864770971 ) ) ;
#58547 = CARTESIAN_POINT ( 'NONE',  ( 4.483927247898545687, 16.52544592524342804, 104.7905762719810241 ) ) ;
#58548 = CARTESIAN_POINT ( 'NONE',  ( 18.62759615963271287, -10.81492255796078972, 23.33224293864769194 ) ) ;
#58549 = CARTESIAN_POINT ( 'NONE',  ( 19.05341960407611168, 5.049401038298154454, 108.9572429386477097 ) ) ;
#58550 = CARTESIAN_POINT ( 'NONE',  ( 8.314922557960818139, 14.29746914071049879, 84.58224293864769550 ) ) ;
#58551 = CARTESIAN_POINT ( 'NONE',  ( -30.73962218707678318, -22.33364281372842441, -3.802157773949823127 ) ) ;
#58552 = CARTESIAN_POINT ( 'NONE',  ( -13.89961937509957401, -13.97604488694547875, 29.37609039468565797 ) ) ;
#58553 = CARTESIAN_POINT ( 'NONE',  ( 0.05219959533934541429, -16.53943276465976808, 100.0010903946857042 ) ) ;
#58554 = CARTESIAN_POINT ( 'NONE',  ( 13.89961937509977652, -13.97604488694527269, 83.12390960531436690 ) ) ;
#58555 = CARTESIAN_POINT ( 'NONE',  ( -10.72451020669870658, -18.67979575497194134, 59.58442372801901854 ) ) ;
#58556 = CARTESIAN_POINT ( 'NONE',  ( -18.62759615963270932, 10.81492255796079327, 45.83224293864769550 ) ) ;
#58557 = CARTESIAN_POINT ( 'NONE',  ( -10.72451020669898014, 18.67979575497178502, 110.4155762719810383 ) ) ;
#58558 = CARTESIAN_POINT ( 'NONE',  ( -21.53943276465977519, 0.05219959533907696930, 76.24890960531435269 ) ) ;
#58559 = CARTESIAN_POINT ( 'NONE',  ( 12.14591786802309770, 12.06949235617756955, 94.37390960531436690 ) ) ;
#58560 = CARTESIAN_POINT ( 'NONE',  ( 19.05341960407617918, -5.049401038297876454, 61.04275706135232582 ) ) ;
#58561 = CARTESIAN_POINT ( 'NONE',  ( 16.51473224551069308, 9.474510206698969483, 29.16557627198103475 ) ) ;
#58562 = CARTESIAN_POINT ( 'NONE',  ( 19.05341960407611168, 5.049401038298154454, 88.95724293864769550 ) ) ;
#58563 = CARTESIAN_POINT ( 'NONE',  ( -5.153800228976328057, -19.02544592524343514, 77.29057627198099567 ) ) ;
#58564 = CARTESIAN_POINT ( 'NONE',  ( 12.06949235617757843, -12.14591786802309237, 98.12390960531436690 ) ) ;
#58565 = ORIENTED_EDGE ( 'NONE', *, *, #111802, .T. ) ;
#58566 = CARTESIAN_POINT ( 'NONE',  ( 16.55341960407611168, 4.379528057220329451, 33.95724293864769550 ) ) ;
#58567 = CARTESIAN_POINT ( 'NONE',  ( 0.05219959533934541429, -16.53943276465976808, 40.00109039468567573 ) ) ;
#58568 = CARTESIAN_POINT ( 'NONE',  ( 18.62759615963255655, 10.81492255796105972, 101.6677570613523613 ) ) ;
#58569 = CARTESIAN_POINT ( 'NONE',  ( -9.474510206698964154, 16.51473224551069663, 95.41557627198102409 ) ) ;
#58570 = CARTESIAN_POINT ( 'NONE',  ( 18.67979575497194134, -10.72451020669871369, 30.83442372801902209 ) ) ;
#58571 = CARTESIAN_POINT ( 'NONE',  ( -9.564922557960796823, -16.46253265017161027, 42.08224293864769550 ) ) ;
#58572 = CARTESIAN_POINT ( 'NONE',  ( -4.379528057220086978, -16.55341960407618274, 39.79275706135235424 ) ) ;
#58573 = CARTESIAN_POINT ( 'NONE',  ( -13.89961937509957401, -13.97604488694547875, 104.3760903946856757 ) ) ;
#58574 = CARTESIAN_POINT ( 'NONE',  ( 19.02544592524343514, -5.153800228976328945, 33.54057627198102409 ) ) ;
#58575 = CARTESIAN_POINT ( 'NONE',  ( 12.14591786802309770, 12.06949235617756955, 99.37390960531436690 ) ) ;
#58576 = CARTESIAN_POINT ( 'NONE',  ( 21.52544592524344225, -5.823673210054117533, 103.5405762719810383 ) ) ;
#58577 = CARTESIAN_POINT ( 'NONE',  ( 13.89961937509957401, 13.97604488694547697, 81.87609039468564731 ) ) ;
#58578 = CARTESIAN_POINT ( 'NONE',  ( -19.05341960407611168, -5.049401038298163336, 86.45724293864769550 ) ) ;
#58579 = CARTESIAN_POINT ( 'NONE',  ( -0.05219959533937732626, 21.53943276465977519, 27.50109039468567929 ) ) ;
#58580 = CARTESIAN_POINT ( 'NONE',  ( -30.73962218707678673, 22.33364281372846705, -2.202157773949823039 ) ) ;
#58581 = CARTESIAN_POINT ( 'NONE',  ( 0.05219959533909260263, 19.03943276465977164, 94.99890960531436690 ) ) ;
#58582 = FACE_OUTER_BOUND ( 'NONE', #27503, .T. ) ;
#58583 = CARTESIAN_POINT ( 'NONE',  ( 19.02544592524343514, -5.153800228976328945, 83.54057627198100988 ) ) ;
#58585 = CARTESIAN_POINT ( 'NONE',  ( 0.05219959533910956823, 16.53943276465976808, 84.99890960531436690 ) ) ;
#58584 = CARTESIAN_POINT ( 'NONE',  ( 21.53943276465977519, 0.05219959533937863772, 36.25109039468567573 ) ) ;
#58586 = CARTESIAN_POINT ( 'NONE',  ( 0.05219959533909260263, 19.03943276465977164, 99.99890960531436690 ) ) ;
#58587 = CARTESIAN_POINT ( 'NONE',  ( 19.05341960407617918, -5.049401038297876454, 31.04275706135232227 ) ) ;
#58588 = CARTESIAN_POINT ( 'NONE',  ( 14.29746914071037800, 8.314922557961029526, 46.66775706135234714 ) ) ;
#58589 = CARTESIAN_POINT ( 'NONE',  ( -0.05219959533937732626, 21.53943276465977519, 82.50109039468568994 ) ) ;
#58590 = CARTESIAN_POINT ( 'NONE',  ( 0.05219959533934541429, -16.53943276465976808, 30.00109039468568284 ) ) ;
#58591 = CARTESIAN_POINT ( 'NONE',  ( -13.89961937509977652, 13.97604488694528158, 65.62390960531436690 ) ) ;
#58592 = CARTESIAN_POINT ( 'NONE',  ( -5.153800228976607833, 19.02544592524334988, 97.70942372801900433 ) ) ;
#58593 = CARTESIAN_POINT ( 'NONE',  ( 14.29746914071037800, 8.314922557961029526, 66.66775706135234714 ) ) ;
#58594 = CARTESIAN_POINT ( 'NONE',  ( -9.474510206698720793, -16.51473224551083518, 19.58442372801899722 ) ) ;
#58595 = CARTESIAN_POINT ( 'NONE',  ( 5.153800228976615827, -19.02544592524334988, 75.20942372801896170 ) ) ;
#58596 = CARTESIAN_POINT ( 'NONE',  ( 19.03943276465977164, -0.05219959533909143690, 58.74890960531435979 ) ) ;
#58597 = CARTESIAN_POINT ( 'NONE',  ( -10.72451020669898014, 18.67979575497178502, 85.41557627198102409 ) ) ;
#58599 = CARTESIAN_POINT ( 'NONE',  ( -16.46253265017146816, -9.564922557961047289, 74.16775706135234714 ) ) ;
#58598 = CARTESIAN_POINT ( 'NONE',  ( -14.29746914071049879, 8.314922557960819915, 70.83224293864770971 ) ) ;
#58600 = CARTESIAN_POINT ( 'NONE',  ( -19.35543954521081389, -5.499999999999485745, 69.58901960356449479 ) ) ;
#58601 = CARTESIAN_POINT ( 'NONE',  ( 9.564922557961047289, -16.46253265017146816, 55.41775706135234003 ) ) ;
#58602 = CARTESIAN_POINT ( 'NONE',  ( 16.52544592524335698, 4.483927247898782831, 111.4594237280190328 ) ) ;
#58603 = CARTESIAN_POINT ( 'NONE',  ( -16.53943276465976808, 0.05219959533911058130, 76.24890960531435269 ) ) ;
#58605 = CARTESIAN_POINT ( 'NONE',  ( -5.359611314223446995E-15, 29.16686587814335496, 144.3750000027311842 ) ) ;
#58604 = CARTESIAN_POINT ( 'NONE',  ( 15.72974639402176855, 15.80617190586768217, 106.8760903946856899 ) ) ;
#58606 = CARTESIAN_POINT ( 'NONE',  ( -5.719274019375978568, 21.55341960407610458, 105.2072429386477097 ) ) ;
#58607 = CARTESIAN_POINT ( 'NONE',  ( -0.05219959533909027116, -19.03943276465977164, 102.4989096053143669 ) ) ;
#58608 = CARTESIAN_POINT ( 'NONE',  ( -19.05341960407611168, -5.049401038298163336, 66.45724293864769550 ) ) ;
#58609 = CARTESIAN_POINT ( 'NONE',  ( -5.719274019375665041, -21.55341960407619695, 79.79275706135236135 ) ) ;
#58610 = CARTESIAN_POINT ( 'NONE',  ( -9.564922557960796823, -16.46253265017161027, 57.08224293864769550 ) ) ;
#58611 = CARTESIAN_POINT ( 'NONE',  ( -13.89961937509977652, 13.97604488694528158, 40.62390960531435979 ) ) ;
#58612 = CARTESIAN_POINT ( 'NONE',  ( 5.823673210054125526, 21.52544592524343514, 24.79057627198103120 ) ) ;
#58613 = CARTESIAN_POINT ( 'NONE',  ( -4.379528057220328563, 16.55341960407611168, 70.20724293864769550 ) ) ;
#58614 = CARTESIAN_POINT ( 'NONE',  ( -19.02544592524342804, 5.153800228976336051, 41.04057627198103120 ) ) ;
#58615 = CARTESIAN_POINT ( 'NONE',  ( 16.52544592524342804, -4.483927247898539470, 98.54057627198105251 ) ) ;
#58616 = CARTESIAN_POINT ( 'NONE',  ( -15.80617190586745835, -15.72974639402198527, 111.8739096053143669 ) ) ;
#58617 = CARTESIAN_POINT ( 'NONE',  ( -5.719274019375665041, -21.55341960407619695, 49.79275706135234714 ) ) ;
#58618 = CARTESIAN_POINT ( 'NONE',  ( 13.89961937509977652, -13.97604488694527269, 33.12390960531434558 ) ) ;
#58619 = CARTESIAN_POINT ( 'NONE',  ( -16.53943276465976808, -0.05219959533934237506, 58.75109039468568994 ) ) ;
#58620 = CARTESIAN_POINT ( 'NONE',  ( -18.67979575497178146, -10.72451020669898902, 96.66557627198102409 ) ) ;
#58621 = CARTESIAN_POINT ( 'NONE',  ( 21.53943276465977519, -0.05219959533907433946, 93.74890960531436690 ) ) ;
#58623 = CARTESIAN_POINT ( 'NONE',  ( -16.46253265017160317, 9.564922557960807481, 45.83224293864769550 ) ) ;
#58622 = CARTESIAN_POINT ( 'NONE',  ( 19.02544592524334988, 5.153800228976608722, 21.45942372801899012 ) ) ;
#58624 = CARTESIAN_POINT ( 'NONE',  ( 0.2500000000000002220, 0.000000000000000000, 4.250000000000000000 ) ) ;
#58625 = CARTESIAN_POINT ( 'NONE',  ( -5.719274019375665041, -21.55341960407619695, 54.79275706135235424 ) ) ;
#58626 = EDGE_CURVE ( 'NONE', #142912, #105638, #89551, .T. ) ;
#58627 = CARTESIAN_POINT ( 'NONE',  ( -18.67979575497178146, -10.72451020669898902, 51.66557627198102409 ) ) ;
#58628 = CARTESIAN_POINT ( 'NONE',  ( 0.05219959533910956823, 16.53943276465976808, 29.99890960531435979 ) ) ;
#58630 = CARTESIAN_POINT ( 'NONE',  ( 19.05341960407617918, -5.049401038297876454, 21.04275706135232582 ) ) ;
#58629 = CARTESIAN_POINT ( 'NONE',  ( 18.67979575497194134, -10.72451020669871369, 80.83442372801901854 ) ) ;
#58631 = CARTESIAN_POINT ( 'NONE',  ( -9.564922557961040184, 16.46253265017147172, 42.91775706135234003 ) ) ;
#58632 = CARTESIAN_POINT ( 'NONE',  ( -8.224510206698735004, -14.34966873604973081, 104.5844237280190185 ) ) ;
#58633 = CARTESIAN_POINT ( 'NONE',  ( 5.719274019375673035, 21.55341960407619339, 52.29275706135236135 ) ) ;
#58634 = CARTESIAN_POINT ( 'NONE',  ( 16.46253265017160672, -9.564922557960803928, 63.33224293864769550 ) ) ;
#58635 = CARTESIAN_POINT ( 'NONE',  ( -19.03943276465977164, -0.05219959533935918106, 38.75109039468566152 ) ) ;
#58636 = CARTESIAN_POINT ( 'NONE',  ( 21.52544592524344225, -5.823673210054117533, 43.54057627198103830 ) ) ;
#58637 = CARTESIAN_POINT ( 'NONE',  ( 15.72974639402176855, 15.80617190586768217, 31.87609039468567929 ) ) ;
#58638 = CARTESIAN_POINT ( 'NONE',  ( -15.80617190586745835, -15.72974639402198527, 91.87390960531436690 ) ) ;
#58639 = CARTESIAN_POINT ( 'NONE',  ( 5.049401038297881783, 19.05341960407617563, 82.29275706135229029 ) ) ;
#58640 = CARTESIAN_POINT ( 'NONE',  ( -16.55341960407617563, 4.379528057220093196, 48.54275706135234714 ) ) ;
#58642 = CARTESIAN_POINT ( 'NONE',  ( 21.53943276465977519, -0.05219959533907433946, 98.74890960531438111 ) ) ;
#58641 = CARTESIAN_POINT ( 'NONE',  ( -4.991179326919329640, 3.920341815485290482, -62.46637012391574473 ) ) ;
#58644 = CARTESIAN_POINT ( 'NONE',  ( 4.379528057220339221, -16.55341960407611168, 72.70724293864769550 ) ) ;
#58643 = CARTESIAN_POINT ( 'NONE',  ( -0.05219959533934338120, 16.53943276465976808, 77.50109039468567573 ) ) ;
#58645 = DIRECTION ( 'NONE',  ( 0.000000000000000000, -1.224646799147353207E-16, 1.000000000000000000 ) ) ;
#58646 = CARTESIAN_POINT ( 'NONE',  ( -16.46253265017146816, -9.564922557961047289, 109.1677570613523471 ) ) ;
#58647 = CARTESIAN_POINT ( 'NONE',  ( 10.81492255796078972, 18.62759615963270932, 29.58224293864769905 ) ) ;
#58648 = DIRECTION ( 'NONE',  ( 0.000000000000000000, 1.000000000000000000, 0.000000000000000000 ) ) ;
#58649 = CARTESIAN_POINT ( 'NONE',  ( -16.52544592524335698, -4.483927247898792601, 48.95942372801902565 ) ) ;
#58650 = CARTESIAN_POINT ( 'NONE',  ( -5.823673210054431948, 21.52544592524334988, 32.70942372801900433 ) ) ;
#58651 = CARTESIAN_POINT ( 'NONE',  ( 10.72451020669898902, -18.67979575497178502, 32.91557627198102409 ) ) ;
#58652 = CARTESIAN_POINT ( 'NONE',  ( 16.55341960407618274, -4.379528057220086978, 76.04275706135237556 ) ) ;
#58653 = CARTESIAN_POINT ( 'NONE',  ( -5.049401038298153566, 19.05341960407611168, 90.20724293864766707 ) ) ;
#58655 = CARTESIAN_POINT ( 'NONE',  ( -0.05219959533909027116, -19.03943276465977164, 32.49890960531435979 ) ) ;
#58654 = CARTESIAN_POINT ( 'NONE',  ( 15.72974639402176855, 15.80617190586768217, 51.87609039468568284 ) ) ;
#58656 = CARTESIAN_POINT ( 'NONE',  ( -15.80617190586745835, -15.72974639402198527, 26.87390960531435979 ) ) ;
#58657 = CARTESIAN_POINT ( 'NONE',  ( 5.049401038297881783, 19.05341960407617563, 37.29275706135232582 ) ) ;
#58658 = CARTESIAN_POINT ( 'NONE',  ( 4.483927247898790824, -16.52544592524335698, 55.20942372801902565 ) ) ;
#58659 = CARTESIAN_POINT ( 'NONE',  ( -21.55341960407610458, -5.719274019375992779, 21.45724293864769550 ) ) ;
#58660 = CARTESIAN_POINT ( 'NONE',  ( 16.46253265017160672, -9.564922557960803928, 78.33224293864769550 ) ) ;
#58661 = CARTESIAN_POINT ( 'NONE',  ( -4.483927247898782831, 16.52544592524335698, 97.70942372801904696 ) ) ;
#58662 = CARTESIAN_POINT ( 'NONE',  ( -40.00200000000003087, -5.510910596163089556E-15, 45.00000000000000000 ) ) ;
#58663 = CARTESIAN_POINT ( 'NONE',  ( -8.224510206698948167, 14.34966873604960824, 100.4155762719810241 ) ) ;
#58664 = CARTESIAN_POINT ( 'NONE',  ( -15.72974639402197994, 15.80617190586746368, 40.62390960531435269 ) ) ;
#58665 = CARTESIAN_POINT ( 'NONE',  ( 16.51473224551069308, 9.474510206698969483, 34.16557627198102409 ) ) ;
#58666 = CARTESIAN_POINT ( 'NONE',  ( 14.29746914071037800, 8.314922557961029526, 71.66775706135234714 ) ) ;
#58667 = CARTESIAN_POINT ( 'NONE',  ( 10.72451020669898902, -18.67979575497178502, 112.9155762719810383 ) ) ;
#58668 = CARTESIAN_POINT ( 'NONE',  ( 9.564922557961047289, -16.46253265017146816, 70.41775706135233293 ) ) ;
#58669 = CARTESIAN_POINT ( 'NONE',  ( 19.02544592524343514, -5.153800228976328945, 43.54057627198103120 ) ) ;
#58670 = CARTESIAN_POINT ( 'NONE',  ( -5.719274019375978568, 21.55341960407610458, 75.20724293864769550 ) ) ;
#58671 = CARTESIAN_POINT ( 'NONE',  ( 7.220908937440039033, 2.044528755335607073, 1.589185716900142209 ) ) ;
#58672 = CARTESIAN_POINT ( 'NONE',  ( -18.62759615963255300, -10.81492255796106328, 94.16775706135237556 ) ) ;
#58673 = CARTESIAN_POINT ( 'NONE',  ( -19.02544592524342804, 5.153800228976336051, 71.04057627198099567 ) ) ;
#58674 = CARTESIAN_POINT ( 'NONE',  ( -4.379528057220086978, -16.55341960407618274, 49.79275706135234714 ) ) ;
#58675 = CARTESIAN_POINT ( 'NONE',  ( 18.67979575497194134, -10.72451020669871369, 80.83442372801901854 ) ) ;
#58676 = CARTESIAN_POINT ( 'NONE',  ( -19.05341960407617563, 5.049401038297882671, 38.54275706135233293 ) ) ;
#58677 = CARTESIAN_POINT ( 'NONE',  ( -13.89961937509957401, -13.97604488694547875, 59.37609039468566863 ) ) ;
#58678 = VERTEX_POINT ( 'NONE', #74392 ) ;
#58679 = CARTESIAN_POINT ( 'NONE',  ( -21.52544592524334988, -5.823673210054445271, 53.95942372801900433 ) ) ;
#58680 = CARTESIAN_POINT ( 'NONE',  ( -9.474510206698964154, 16.51473224551069663, 55.41557627198103120 ) ) ;
#58681 = CARTESIAN_POINT ( 'NONE',  ( -13.89961937509957401, -13.97604488694547875, 49.37609039468567573 ) ) ;
#58682 = CARTESIAN_POINT ( 'NONE',  ( 16.51473224551069308, 9.474510206698969483, 99.16557627198102409 ) ) ;
#58683 = CARTESIAN_POINT ( 'NONE',  ( 19.02544592524343514, -5.153800228976328945, 78.54057627198099567 ) ) ;
#58684 = CARTESIAN_POINT ( 'NONE',  ( 8.224510206698953496, -14.34966873604960469, 37.91557627198102409 ) ) ;
#58685 = CARTESIAN_POINT ( 'NONE',  ( -10.72451020669898014, 18.67979575497178502, 40.41557627198103120 ) ) ;
#58686 = CARTESIAN_POINT ( 'NONE',  ( 22.81625015709509441, 31.40387420917330275, -5.824999997268813345 ) ) ;
#58687 = CARTESIAN_POINT ( 'NONE',  ( -17.79613651744294600, 24.49428055684532524, 141.6843446568999809 ) ) ;
#58688 = CARTESIAN_POINT ( 'NONE',  ( -10.81492255796105439, 18.62759615963255655, 92.91775706135236135 ) ) ;
#58689 = CARTESIAN_POINT ( 'NONE',  ( -26.82864639204112578, 7.693045595922302304, 166.5361468217300569 ) ) ;
#58690 = CARTESIAN_POINT ( 'NONE',  ( 13.97604488694527802, 13.89961937509977652, 34.37390960531436690 ) ) ;
#58691 = CARTESIAN_POINT ( 'NONE',  ( -31.69676786489883469, -20.43759221091016798, -7.999999999999998224 ) ) ;
#58692 = CARTESIAN_POINT ( 'NONE',  ( 16.52544592524335698, 4.483927247898782831, 56.45942372801902565 ) ) ;
#58693 = CARTESIAN_POINT ( 'NONE',  ( 15.80617190586746368, 15.72974639402197994, 79.37390960531436690 ) ) ;
#58694 = CARTESIAN_POINT ( 'NONE',  ( -4.379528057220328563, 16.55341960407611168, 35.20724293864768839 ) ) ;
#58696 = CARTESIAN_POINT ( 'NONE',  ( 19.05341960407611168, 5.049401038298154454, 108.9572429386477097 ) ) ;
#58695 = CARTESIAN_POINT ( 'NONE',  ( -16.46253265017160317, 9.564922557960807481, 30.83224293864769550 ) ) ;
#58697 = CARTESIAN_POINT ( 'NONE',  ( -15.80617190586768217, 15.72974639402176855, 33.12609039468569705 ) ) ;
#58698 = CARTESIAN_POINT ( 'NONE',  ( -19.02544592524334988, -5.153800228976617603, 33.95942372801897591 ) ) ;
#58699 = CARTESIAN_POINT ( 'NONE',  ( 13.97604488694527802, 13.89961937509977652, 24.37390960531435624 ) ) ;
#58700 = CARTESIAN_POINT ( 'NONE',  ( 21.55341960407619695, -5.719274019375665929, 86.04275706135236135 ) ) ;
#58701 = CARTESIAN_POINT ( 'NONE',  ( 17.44279575226823908, -5.990770900252461395, 33.33557567514318976 ) ) ;
#58702 = CARTESIAN_POINT ( 'NONE',  ( 16.53943276465976808, -0.05219959533910856209, 23.74890960531435269 ) ) ;
#58703 = CARTESIAN_POINT ( 'NONE',  ( -22.81625015709510507, 31.40387420917330275, -3.424999997268813434 ) ) ;
#58704 = CARTESIAN_POINT ( 'NONE',  ( -0.05219959533907301413, -21.53943276465977519, 22.49890960531436335 ) ) ;
#58705 = CARTESIAN_POINT ( 'NONE',  ( -16.52544592524342804, 4.483927247898546575, 96.04057627198102409 ) ) ;
#58706 = CARTESIAN_POINT ( 'NONE',  ( -6.434671708797631950, -6.434671708797536027, -63.95112321872120731 ) ) ;
#58707 = CARTESIAN_POINT ( 'NONE',  ( 19.05341960407611168, 5.049401038298154454, 93.95724293864769550 ) ) ;
#58708 = CARTESIAN_POINT ( 'NONE',  ( -14.34966873604960291, -8.224510206698953496, 76.66557627198103830 ) ) ;
#58709 = CARTESIAN_POINT ( 'NONE',  ( 5.049401038297881783, 19.05341960407617563, 107.2927570613523187 ) ) ;
#58710 = CARTESIAN_POINT ( 'NONE',  ( 15.72974639402199770, -15.80617190586745480, 68.12390960531436690 ) ) ;
#58711 = ORIENTED_EDGE ( 'NONE', *, *, #39318, .F. ) ;
#58712 = EDGE_CURVE ( 'NONE', #155489, #128112, #186951, .T. ) ;
#58713 = CARTESIAN_POINT ( 'NONE',  ( -19.05341960407611168, -5.049401038298163336, 31.45724293864769550 ) ) ;
#58715 = CARTESIAN_POINT ( 'NONE',  ( -21.53943276465977519, 0.05219959533907696930, 76.24890960531435269 ) ) ;
#58714 = CARTESIAN_POINT ( 'NONE',  ( -9.474510206698964154, 16.51473224551069663, 85.41557627198102409 ) ) ;
#58717 = CARTESIAN_POINT ( 'NONE',  ( -13.89961937509977652, 13.97604488694528158, 85.62390960531433848 ) ) ;
#58716 = CARTESIAN_POINT ( 'NONE',  ( -14.34966873604972548, 8.224510206698743886, 108.3344237280190185 ) ) ;
#58718 = CARTESIAN_POINT ( 'NONE',  ( 9.474510206698729675, 16.51473224551082808, 62.08442372801899722 ) ) ;
#58719 = CARTESIAN_POINT ( 'NONE',  ( -21.52544592524334988, -5.823673210054445271, 98.95942372801903275 ) ) ;
#58720 = CARTESIAN_POINT ( 'NONE',  ( -15.80617190586745835, -15.72974639402198527, 76.87390960531439532 ) ) ;
#58721 = CARTESIAN_POINT ( 'NONE',  ( 21.53943276465977519, -0.05219959533907433946, 28.74890960531435624 ) ) ;
#58722 = CARTESIAN_POINT ( 'NONE',  ( -19.05341960407611168, -5.049401038298163336, 51.45724293864770260 ) ) ;
#58723 = CARTESIAN_POINT ( 'NONE',  ( -14.29746914071049879, 8.314922557960819915, 25.83224293864769194 ) ) ;
#58724 = CARTESIAN_POINT ( 'NONE',  ( 16.46253265017160672, -9.564922557960803928, 58.33224293864769550 ) ) ;
#58725 = CARTESIAN_POINT ( 'NONE',  ( -31.71843943275784383, -0.9850135343614436767, 102.4512077271823784 ) ) ;
#58726 = CARTESIAN_POINT ( 'NONE',  ( 0.05219959533937995610, -21.53943276465977519, 105.0010903946856757 ) ) ;
#58727 = CARTESIAN_POINT ( 'NONE',  ( -16.55341960407611168, -4.379528057220339221, 71.45724293864769550 ) ) ;
#58728 = CARTESIAN_POINT ( 'NONE',  ( -21.52544592524343514, 5.823673210054127303, 111.0405762719810525 ) ) ;
#58729 = CARTESIAN_POINT ( 'NONE',  ( 15.72974639402199770, -15.80617190586745480, 108.1239096053143811 ) ) ;
#58730 = CARTESIAN_POINT ( 'NONE',  ( -8.571926809382601320, -26.38167802310801591, 139.7750000027311899 ) ) ;
#58731 = CARTESIAN_POINT ( 'NONE',  ( -10.81492255796078084, -18.62759615963271287, 62.08224293864769550 ) ) ;
#58732 = CARTESIAN_POINT ( 'NONE',  ( 0.05219959533934541429, -16.53943276465976808, 80.00109039468568994 ) ) ;
#58733 = CARTESIAN_POINT ( 'NONE',  ( 16.52544592524342804, -4.483927247898539470, 98.54057627198105251 ) ) ;
#58734 = CARTESIAN_POINT ( 'NONE',  ( 16.51473224551069308, 9.474510206698969483, 54.16557627198103120 ) ) ;
#58735 = CARTESIAN_POINT ( 'NONE',  ( 12.14591786802327356, -12.06949235617739191, 105.6260903946856899 ) ) ;
#58736 = EDGE_CURVE ( 'NONE', #124967, #80629, #98541, .T. ) ;
#58737 = CARTESIAN_POINT ( 'NONE',  ( 18.62759615963255655, 10.81492255796105972, 46.66775706135234714 ) ) ;
#58738 = CARTESIAN_POINT ( 'NONE',  ( 5.049401038298161559, -19.05341960407611168, 112.7072429386476813 ) ) ;
#58739 = CARTESIAN_POINT ( 'NONE',  ( -10.72451020669870658, -18.67979575497194134, 84.58442372801903275 ) ) ;
#58740 = CARTESIAN_POINT ( 'NONE',  ( 19.03943276465977164, -0.05219959533909143690, 33.74890960531435979 ) ) ;
#58741 = CARTESIAN_POINT ( 'NONE',  ( 16.46253265017160672, -9.564922557960803928, 43.33224293864769550 ) ) ;
#58742 = ORIENTED_EDGE ( 'NONE', *, *, #101761, .F. ) ;
#58743 = CARTESIAN_POINT ( 'NONE',  ( 15.72974639402176855, 15.80617190586768217, 81.87609039468568994 ) ) ;
#58744 = CARTESIAN_POINT ( 'NONE',  ( -15.80617190586768217, 15.72974639402176855, 68.12609039468567573 ) ) ;
#58745 = CARTESIAN_POINT ( 'NONE',  ( -19.02544592524342804, 5.153800228976336051, 101.0405762719810241 ) ) ;
#58746 = CARTESIAN_POINT ( 'NONE',  ( -19.05341960407617563, 5.049401038297882671, 83.54275706135233293 ) ) ;
#58747 = CARTESIAN_POINT ( 'NONE',  ( -15.80617190586768217, 15.72974639402176855, 53.12609039468568284 ) ) ;
#58748 = CARTESIAN_POINT ( 'NONE',  ( -14.34966873604972548, 8.224510206698743886, 28.33442372801902209 ) ) ;
#58749 = CARTESIAN_POINT ( 'NONE',  ( 9.474510206698729675, 16.51473224551082808, 72.08442372801900433 ) ) ;
#58750 = CARTESIAN_POINT ( 'NONE',  ( 13.89961937509977652, -13.97604488694527269, 58.12390960531436690 ) ) ;
#58751 = CARTESIAN_POINT ( 'NONE',  ( 9.474510206698729675, 16.51473224551082808, 77.08442372801900433 ) ) ;
#58752 = CARTESIAN_POINT ( 'NONE',  ( 14.29746914071037800, 8.314922557961029526, 111.6677570613523613 ) ) ;
#58753 = CARTESIAN_POINT ( 'NONE',  ( -9.564922557961040184, 16.46253265017147172, 92.91775706135233293 ) ) ;
#58754 = CARTESIAN_POINT ( 'NONE',  ( 16.53943276465976808, -0.05219959533910856209, 38.74890960531435979 ) ) ;
#58755 = CARTESIAN_POINT ( 'NONE',  ( -19.03943276465977164, -0.05219959533935918106, 58.75109039468566863 ) ) ;
#58756 = CARTESIAN_POINT ( 'NONE',  ( 8.314922557961029526, -14.29746914071037800, 50.41775706135235424 ) ) ;
#58757 = CARTESIAN_POINT ( 'NONE',  ( -19.02544592524334988, -5.153800228976617603, 23.95942372801900078 ) ) ;
#58758 = CARTESIAN_POINT ( 'NONE',  ( -19.02544592524342804, 5.153800228976336051, 36.04057627198100988 ) ) ;
#58759 = CARTESIAN_POINT ( 'NONE',  ( -17.44270441346513323, -5.991230190323105553, 66.36335079264229364 ) ) ;
#58760 = CARTESIAN_POINT ( 'NONE',  ( -8.224510206698735004, -14.34966873604973081, 39.58442372801901143 ) ) ;
#58761 = DIRECTION ( 'NONE',  ( 0.000000000000000000, 0.000000000000000000, 1.000000000000000000 ) ) ;
#58763 = TOROIDAL_SURFACE ( 'NONE', #171777, 69.99999999999998579, 10.00000000000000000 ) ;
#58762 = CARTESIAN_POINT ( 'NONE',  ( -8.571926809382601320, -26.38167802310801591, 147.2750000027311899 ) ) ;
#58764 = CARTESIAN_POINT ( 'NONE',  ( -5.153800228976328057, -19.02544592524343514, 97.29057627198099567 ) ) ;
#58765 = DIRECTION ( 'NONE',  ( 1.000000000000000000, 0.000000000000000000, 0.000000000000000000 ) ) ;
#58766 = ORIENTED_EDGE ( 'NONE', *, *, #159302, .F. ) ;
#58767 = CARTESIAN_POINT ( 'NONE',  ( -16.51473224551082808, 9.474510206698731452, 103.3344237280190043 ) ) ;
#58768 = CARTESIAN_POINT ( 'NONE',  ( -16.46253265017160317, 9.564922557960807481, 115.8322429386477097 ) ) ;
#58770 = CARTESIAN_POINT ( 'NONE',  ( -19.02544592524334988, -5.153800228976617603, 98.95942372801900433 ) ) ;
#58769 = CARTESIAN_POINT ( 'NONE',  ( -21.52544592524334988, -5.823673210054445271, 108.9594237280190185 ) ) ;
#58771 = CARTESIAN_POINT ( 'NONE',  ( -16.52544592524342804, 4.483927247898546575, 116.0405762719810383 ) ) ;
#58772 = CARTESIAN_POINT ( 'NONE',  ( 13.89961937509977652, -13.97604488694527269, 43.12390960531434558 ) ) ;
#58773 = CARTESIAN_POINT ( 'NONE',  ( -10.72451020669898014, 18.67979575497178502, 60.41557627198102409 ) ) ;
#58774 = CARTESIAN_POINT ( 'NONE',  ( -16.53943276465976808, 0.05219959533911058130, 116.2489096053143669 ) ) ;
#58775 = CARTESIAN_POINT ( 'NONE',  ( 13.89961937509957579, 13.97604488694547520, 46.87609039468566152 ) ) ;
#58776 = CARTESIAN_POINT ( 'NONE',  ( 19.05341960407617918, -5.049401038297876454, 76.04275706135230450 ) ) ;
#58777 = CARTESIAN_POINT ( 'NONE',  ( 14.29746914071049879, -8.314922557960816363, 58.33224293864768839 ) ) ;
#58778 = CARTESIAN_POINT ( 'NONE',  ( 21.55341960407610458, 5.719274019375980345, 38.95724293864768839 ) ) ;
#58779 = CARTESIAN_POINT ( 'NONE',  ( 10.72451020669871369, 18.67979575497193778, 87.08442372801901854 ) ) ;
#58780 = CARTESIAN_POINT ( 'NONE',  ( 0.05219959533907565091, 21.53943276465977519, 84.99890960531436690 ) ) ;
#58781 = CARTESIAN_POINT ( 'NONE',  ( 10.81492255796106328, -18.62759615963255655, 55.41775706135234714 ) ) ;
#58782 = CARTESIAN_POINT ( 'NONE',  ( -18.62759615963255300, -10.81492255796106328, 64.16775706135234714 ) ) ;
#58783 = CARTESIAN_POINT ( 'NONE',  ( -5.153800228976328057, -19.02544592524343514, 102.2905762719810383 ) ) ;
#58785 = CARTESIAN_POINT ( 'NONE',  ( 5.719274019375673035, 21.55341960407619339, 62.29275706135236845 ) ) ;
#58784 = CARTESIAN_POINT ( 'NONE',  ( 14.29746914071037800, 8.314922557961029526, 86.66775706135234714 ) ) ;
#58786 = CARTESIAN_POINT ( 'NONE',  ( -19.03943276465977164, 0.05219959533909376836, 51.24890960531436690 ) ) ;
#58787 =( BOUNDED_SURFACE ( )  B_SPLINE_SURFACE ( 3, 2, ( 
 ( #172425, #170437, #171436, #158241, #48096, #81373, #95571, #143058, #47099, #51065, #110744, #32923, #189592, #174419, #82374, #157257, #185610, #97535, #2571, #159222, #18752, #20717, #144062, #123911, #5543, #108760, #31928, #93582, #1573, #124927, #186625, #109752, #64252, #94578, #80398, #142070, #156256, #17759, #125919, #3556, #37894, #7537, #23730, #39880, #38895, #36877, #54063, #69222, #98543, #192580, #131900, #162231, #129869, #83379, #161234, #71230, #87390, #191567, #117731, #102564, #163239, #148073, #21726, #9564, #179426, #193584, #160236, #116727, #99552, #52056, #100552, #149075, #25744, #85379, #194582, #53046, #55056, #115737, #145056, #175409, #132893, #40891, #22728, #147072, #114726, #70232, #164249, #130890, #67222, #178416, #8556, #101547, #177424, #24739, #128880, #84376, #86389, #56052, #190580, #113712, #176419, #6537, #68217, #146053, #73240, #182399, #61013, #44870, #76183, #134911, #196588, #169184, #168203, #104555, #30690, #27737, #153023, #107508, #137863, #59033, #57065, #12560, #58058, #150069, #13533, #120700, #152048, #75199, #11574, #151069, #195593, #43877, #92341, #10563, #28726, #199543, #119729, #198555, #197566, #165242, #118740, #14522, #184374, #181412, #105542, #42890, #136870, #72227, #74226, #122685, #60025, #167228, #121692, #135894, #183388, #133902, #166237, #90363, #106526, #29700, #45855, #89380, #91331, #180428, #41901, #103567, #26736, #88375, #188351, #19491, #16514, #78162, #112483, #111493, #47852, #174176, #171187, #96313, #50826, #81136, #2321, #329, #156007, #1319, #93333, #157007, #64003, #95322, #18505, #155018, #94329, #62998, #141824, #139830, #80153, #125673, #3317, #77179, #142817, #140832, #124676, #157999, #4297, #35646, #187371, #15522, #64990, #109505, #65979, #79161, #127648, #126648, #154027, #189348, #138849, #173178, #49829, #61997, #34654, #123663, #185360, #32676, #186373, #110494, #172176, #46851, #108511, #170190, #31684, #17504, #48840, #33661, #69987, #68976, #66978, #84130, #37639, #128638, #22482, #161987, #192335, #159987, #113468, #191322, #101301, #117484, #21474, #147837, #132656, #193337, #178175, #51809, #39640, #9323, #23483, #190332, #146816, #67973, #131655, #162990, #38652, #179182, #145809, #130641, #54811, #175163, #129627, #5295, #53816, #99303, #36629, #158979, #115491, #8311, #83135, #7292, #143813, #100309, #177179, #85132, #70988, #160988, #116486, #24495, #86146, #144811, #98286, #20471, #6294, #194344, #55812, #52800, #97293, #114467, #176169, #82121, #164009, #148832, #75948, #135658, #27497, #198307, #40650, #89139, #151808, #74964, #137622, #29467, #199306, #106283, #91100, #13299, #90124, #42651, #104313, #165996, #150827, #60773, #182152, #167968, #166987, #152788, #105300, #136626, #25505, #11327, #26495, #71978, #12324, #183146, #102319, #72998, #59786, #121454, #44631, #73989, #197330, #58793, #87149, #10322, #120461, #134666, #43637, #14279, #28490, #122445, #149821, #133652, #196352, #57820, #195343, #56823, #118497, #180188, #41658, #103321, #165001, #88137, #119492, #181174, #33432, #79926, #19265, #154780, #172948, #184137, #62757, #30449, #92096, #156780, #108273, #15279, #76939, #1082, #153784, #16277, #61760, #95091, #17269, #188122, #126424, #138608, #169951, #168942, #90, #32438, #110262, #78922, #125442, #186134, #48610, #80911, #77929, #2089, #141599, #47613, #49593, #46611, #140599, #170946, #65745, #31442, #155771, #34426, #18273, #111256, #93096, #139596, #142588, #3086, #124438, #4067, #109267, #96085, #45619, #157774, #94092, #123428, #63769, #187138, #185121, #171943, #64762, #107271, #160753, #143576, #21244, #190102, #83894, #66744, #145577, #129399, #99065, #50595, #100070, #6063, #51577, #176943, #23250, #69743, #191095, #189123, #22245, #36395, #161755, #67741, #84893, #7054, #127413, #131412, #112254, #38413, #53574, #173946, #68736, #130394, #158747 ),
 ( #192091, #146572, #8066, #128405, #98049, #20236, #81884, #175935, #193099, #35413, #115251, #97065, #5059, #113241, #174932, #52570, #159747, #114230, #82898, #144576, #37407, #169614, #126093, #157433, #32104, #156435, #154448, #110917, #187790, #49259, #81548, #48273, #18928, #94754, #188778, #93761, #47278, #31111, #155442, #172603, #64424, #63429, #4717, #170615, #108934, #34089, #17935, #95748, #80573, #16932, #109928, #78585, #142247, #140259, #3732, #79589, #65409, #92759, #35075, #141258, #1751, #50261, #158418, #66406, #2748, #15941, #127070, #125105, #96729, #33098, #19906, #111917, #107928, #143234, #77600, #173605, #128068, #189770, #139271, #747, #62419, #186803, #171610, #124091, #185790, #178595, #55233, #193765, #54239, #21904, #191745, #7715, #23908, #22904, #20897, #38072, #53228, #82555, #176598, #115910, #146228, #113888, #67399, #145233, #116902, #71407, #175586, #101735, #86566, #147248, #132076, #5721, #40058, #163423, #177600, #144237, #100725, #83554, #36063, #84550, #133071, #9743, #69400, #24921, #37062, #39068, #99728, #129055, #159402, #148249, #51243, #6715, #131067, #98721, #162406, #112903, #114904, #174597, #85562, #192756, #8739, #161412, #70408, #97711, #68393, #190756, #52231, #160415, #130045, #57247, #151247, #181587, #76368, #118921, #166423, #45051, #28903, #168383, #119902, #43065, #29878, #136068, #60203, #120877, #121873, #59208, #90543, #179604, #165423, #180606, #25921, #104731, #137046, #198738, #182577, #134084, #27918, #44060, #197742, #105720, #152225, #91516, #26917, #183566, #194761, #73419, #41076, #102740, #167407, #42079, #87565, #149252, #11752, #164428, #88559, #72407, #13710, #89561, #106709, #153202, #10743, #103743, #195774, #150258, #12736, #75376, #14707, #56233, #117915, #74402, #135090, #196766, #58234, #175775, #190939, #9927, #164606, #132260, #160599, #117085, #38257, #52416, #39250, #149428, #26100, #85749, #194944, #191931, #55414, #54422, #22089, #37249, #71586, #41259, #99911, #100906, #53415, #70592, #87743, #69588, #118100, #193951, #162590, #8924, #131255, #178780, #67585, #161596, #147436, #163604, #192943, #133252, #130235, #24095, #116092, #129243, #115092, #40248, #23090, #176784, #84735, #146413, #7904, #114074, #25105, #177780, #98906, #101922, #56420, #83739, #179790, #86749, #145418, #148432, #102921, #6900, #68579, #121064, #152402, #75556, #150440, #151427, #58411, #198916, #135271, #137232, #182758, #13889, #134271, #138230, #197922, #120078, #153395, #61376, #169559, #44242, #72597, #60385, #166602, #122057, #76554, #183749, #45235, #195958, #181766, #196943, #42262, #105899, #14893, #57431, #43247, #106889, #91701, #168562, #12914, #74578, #29080, #119104, #180785, #136246, #104915, #90719, #199912, #30060, #167585, #28102, #123047, #89741, #59390, #184733, #46218, #107871, #31056, #92704, #10924, #11936, #103922, #165602, #27101, #88747, #73599, #189716, #125050, #143181, #154392, #33045, #692, #62364, #127017, #78529, #185732, #47221, #171555, #124033, #186747, #32049, #65356, #187737, #158365, #96677, #108880, #140203, #139217, #170559, #2696, #188724, #19854, #95694, #174541, #141206, #49208, #111863, #93706, #48217, #109871, #1697, #157382, #173553, #15887, #172551, #3678, #63373, #64373, #155388, #18875, #34037, #80521, #128014, #94700, #50209, #126041, #35022, #156377, #16878, #77545, #17882, #142195, #110866, #79536, #51189, #81494, #4661, #66353, #112850, #36008, #133020, #192702, #84497, #55180, #97657, #146175, #8684, #132022, #194710, #86514, #56179, #163368, #148198, #131011, #178540, #101678, #71356, #22850, #7660, #117862, #39017, #24865, #69344, #40006, #159346, #68340, #193711, #9691, #147194, #99675, #161359, #115858, #20842, #67344, #54185, #129990, #177548, #179553, #100672, #162354, #6662, #82500, #191690, #53172, #70355, #116849, #144182, #5668, #129005, #23855, #37005, #85505 ),
 ( #190704, #52177, #114849, #113835, #176543, #175531, #98666, #160360, #21850, #83501, #145178, #38019, #25870, #87514, #89509, #75327, #45000, #182527, #61142, #27868, #74353, #198686, #134030, #11702, #196717, #26866, #44008, #60153, #102689, #59159, #90494, #165372, #151199, #149202, #105670, #120827, #167356, #14655, #181538, #152176, #12687, #121822, #88508, #180555, #164377, #150204, #28854, #197693, #58186, #137993, #103693, #73369, #13660, #10692, #72356, #76315, #136019, #136997, #183517, #41023, #106660, #168333, #29829, #199676, #91466, #122814, #153153, #195723, #57196, #118871, #42029, #135041, #166371, #119854, #43017, #104684, #49962, #110624, #111626, #48970, #18636, #169316, #155150, #170321, #15651, #81262, #46984, #31813, #33795, #107639, #92471, #19620, #79298, #171320, #141954, #184504, #32807, #95455, #80282, #142943, #173311, #4425, #34786, #96441, #17638, #65119, #188482, #158128, #109637, #94459, #66111, #125801, #45984, #172306, #30823, #157140, #3443, #154160, #16643, #93464, #77309, #156140, #126777, #138978, #78290, #456, #62131, #123795, #186510, #47984, #2455, #185493, #108643, #140967, #139964, #64137, #1453, #187503, #63131, #124810, #193467, #36760, #21607, #38783, #85264, #146955, #70116, #131787, #192464, #67110, #114604, #177311, #130772, #100440, #23617, #163123, #98423, #116616, #127777, #6422, #174306, #35775, #162120, #51940, #159108, #20602, #144940, #97422, #160120, #5426, #8443, #161117, #54944, #178305, #82254, #113600, #112614, #143945, #176301, #39768, #101432, #69106, #147965, #37773, #22614, #24626, #128768, #83266, #68103, #175294, #53947, #86274, #189477, #145941, #9452, #129755, #99436, #190467, #115623, #7422, #50955, #191452, #52929, #84259, #57952, #151938, #195478, #10452, #132783, #118628, #12458, #27632, #26624, #56954, #119623, #117618, #74118, #89273, #135789, #44760, #11461, #120594, #181306, #13427, #180319, #72112, #194470, #41787, #197460, #150963, #88267, #168095, #133786, #103454, #182289, #55942, #179316, #106414, #166130, #42784, #28618, #71117, #104447, #43769, #105433, #29593, #59915, #91224, #136758, #121583, #58926, #75091, #198443, #152915, #196482, #167118, #40780, #90255, #183278, #102449, #164137, #25634, #87278, #148963, #165132, #149955, #73132, #134801, #156909, #76075, #185255, #48738, #95223, #63901, #16409, #78056, #32570, #137751, #184267, #139724, #46748, #94223, #141725, #17400, #171079, #123560, #80055, #108407, #170083, #125571, #172074, #33561, #18406, #3215, #79057, #153917, #1213, #187269, #140730, #110392, #64889, #49724, #31575, #126550, #14411, #93226, #60903, #122578, #188250, #138740, #45749, #107401, #154911, #169074, #62891, #92232, #111392, #47746, #173077, #34554, #30580, #222, #199435, #15412, #124571, #96213, #77070, #155904, #61890, #186267, #109399, #2219, #50726, #128534, #113370, #143711, #163637, #118133, #19391, #178812, #9959, #133285, #132293, #127548, #144707, #98181, #189249, #83032, #25139, #55447, #20367, #174076, #51707, #164637, #180815, #82015, #10955, #195990, #56454, #65874, #81040, #102953, #57462, #86781, #112384, #71619, #190229, #142716, #193985, #42294, #119135, #40282, #87775, #5190, #148466, #6192, #35545, #97192, #26132, #134304, #175061, #117118, #66872, #194975, #157902, #159885, #72629, #179821, #101955, #41292, #21374, #149460, #4196, #36527, #158878, #67872, #105933, #107908, #166633, #60418, #90753, #185771, #28135, #183782, #74613, #89775, #151460, #12948, #136279, #62400, #61411, #197955, #124069, #121098, #46254, #728, #169594, #152436, #150471, #167618, #59424, #43278, #106922, #13922, #45268, #168595, #104947, #44275, #182792, #91734, #29114, #30095, #75589, #153430, #27131, #31092, #137268, #198951, #92740, #154428, #103954, #122091, #165633, #14928, #76588, #15922, #138264, #77580, #199947, #88778, #139252, #11966, #123082, #184768, #73631, #135301, #196974 ),
 ( #58441, #120109, #181799, #34071, #4697, #47258, #95729, #158399, #81529, #82537, #36044, #5703, #112885, #97693, #80554, #128050, #51224, #20879, #172584, #157415, #144219, #188758, #174579, #173587, #159384, #111899, #143216, #32085, #17916, #33079, #78566, #18909, #189752, #108915, #79571, #66388, #67380, #96711, #49241, #110899, #65391, #170595, #16913, #142229, #141240, #127052, #129038, #50243, #3714, #156414, #93742, #2729, #64406, #19888, #155423, #140239, #1732, #63410, #35056, #186783, #125085, #48253, #109907, #171591, #94735, #126075, #187771, #179587, #190739, #69379, #37043, #98703, #163405, #114886, #21886, #83536, #7697, #160397, #161394, #68375, #101714, #23890, #194744, #133054, #145215, #176580, #175567, #6697, #39049, #24901, #56216, #132058, #10726, #177582, #85542, #148232, #130027, #22886, #146209, #38054, #193747, #9726, #52213, #8721, #40041, #99710, #100707, #191726, #55215, #70390, #116884, #164411, #131049, #86548, #162387, #71390, #84532, #53208, #113870, #192739, #178576, #147229, #54221, #87548, #115892, #117897, #41059, #102722, #25903, #149235, #72390, #183547, #134065, #46014, #195756, #91497, #45033, #92503, #137028, #198718, #118904, #89543, #181570, #90525, #152207, #61174, #138026, #76349, #60185, #104714, #74384, #13691, #106691, #105702, #103726, #120859, #136049, #165406, #59190, #121855, #28885, #196749, #150239, #27900, #199709, #154192, #58216, #184534, #169347, #29860, #42062, #57230, #122846, #30856, #168364, #26899, #153184, #166404, #180588, #167389, #15682, #88542, #75358, #107670, #119885, #14687, #182559, #11735, #73402, #135073, #43048, #151229, #12718, #197724, #44042, #174334, #79328, #127804, #3472, #110656, #18665, #140998, #141984, #35804, #171350, #95485, #173342, #2486, #81290, #139995, #33825, #64167, #159136, #1484, #157171, #48014, #63162, #124841, #186541, #109670, #97450, #34814, #32839, #77343, #94489, #19649, #139009, #142974, #125832, #123826, #187535, #156171, #16673, #80311, #49000, #65149, #126806, #78322, #17670, #172336, #188514, #49991, #111656, #96469, #158157, #489, #4451, #66141, #189507, #50982, #112642, #62162, #185524, #47016, #108675, #170353, #31845, #93496, #155183, #162147, #100468, #36790, #86303, #117647, #147992, #69135, #67140, #22643, #68132, #160149, #23643, #130802, #85291, #146983, #21640, #161146, #129783, #8470, #144970, #70144, #192493, #131815, #143977, #9481, #7451, #191480, #163151, #71145, #179344, #53976, #82285, #193494, #176333, #132811, #145969, #194497, #54973, #20633, #55970, #5457, #178333, #116643, #40807, #39796, #101460, #128798, #37803, #52958, #177339, #38810, #102477, #24654, #190497, #51970, #114634, #84290, #113629, #175324, #115649, #98456, #83294, #6451, #99466, #89299, #28645, #58953, #26651, #180345, #57978, #168121, #184294, #88294, #14439, #199463, #59942, #72140, #87307, #106440, #60930, #90281, #56980, #13453, #134829, #148990, #135816, #45776, #122604, #182317, #91249, #149982, #151965, #150991, #118654, #133816, #29617, #137777, #196508, #197486, #11488, #167146, #164164, #166158, #76102, #75117, #120621, #105460, #27659, #136785, #25662, #119650, #43797, #121610, #12483, #152940, #73159, #198471, #74144, #10480, #181332, #183305, #42811, #104473, #44787, #103481, #195507, #41813, #165159, #31602, #33585, #17425, #48763, #30607, #34580, #94250, #16434, #49748, #157925, #65899, #79082, #169100, #110418, #62917, #96237, #32597, #19415, #156933, #107428, #81063, #92260, #64913, #18430, #127573, #172099, #95248, #153944, #124597, #154937, #63926, #125595, #142741, #111417, #173103, #80080, #78083, #47772, #187292, #141749, #140755, #77098, #155930, #109425, #138767, #2243, #3239, #126574, #170108, #123587, #1238, #4221, #189274, #93251, #15439, #248, #188275, #61917, #185281, #46773, #108432, #139751, #186292, #171104, #21401, #35569, #22407, #132580, #9245, #68902 ),
 ( #52727, #101223, #177104, #84058, #192259, #114392, #115415, #147759, #144733, #130561, #146736, #176094, #54734, #113396, #7217, #37564, #50750, #175086, #53741, #83059, #36554, #98208, #159912, #6220, #70912, #8232, #116406, #38575, #66898, #178095, #112408, #39565, #99227, #97217, #160914, #67899, #190256, #100231, #145736, #161913, #23407, #129552, #191252, #82041, #85055, #193260, #174100, #69910, #131576, #162912, #24420, #86069, #158903, #20394, #143738, #5217, #128561, #51733, #73915, #121382, #197257, #150755, #103246, #59709, #164928, #88061, #105230, #151738, #13231, #136557, #198238, #58719, #133576, #181102, #43565, #120388, #166918, #90056, #29396, #26421, #183074, #194268, #72924, #40575, #102245, #28419, #118421, #25430, #87071, #11250, #163933, #149748, #71904, #74894, #27418, #44557, #106212, #148756, #180114, #179106, #10245, #42576, #167896, #91026, #135585, #14203, #104239, #89064, #152712, #195266, #134593, #196279, #41582, #182082, #75871, #55735, #12253, #117409, #57748, #165922, #56750, #119418, #155699, #78848, #111180, #77857, #187066, #124362, #18198, #61687, #76865, #199230, #185049, #140526, #94018, #93021, #34351, #13, #46537, #48536, #60695, #45543, #172870, #32365, #186057, #95016, #137547, #47541, #110190, #171868, #96012, #126350, #157697, #3011, #188047, #170874, #79856, #141524, #19187, #62681, #109195, #122371, #2016, #184060, #63695, #107197, #168868, #33357, #30373, #125370, #138535, #139524, #108196, #156704, #123356, #64688, #17194, #49517, #92017, #153710, #15206, #169878, #31371, #154709, #16202, #1007, #142513, #22165, #36319, #7983, #5982, #69666, #130312, #80836, #193021, #3991, #38332, #192008, #39329, #83816, #145496, #65671, #97973, #128330, #37325, #98983, #131333, #84812, #23169, #6976, #51503, #21162, #160673, #53493, #52491, #50520, #67662, #82817, #112183, #129319, #68657, #175853, #143496, #96992, #174853, #146492, #100988, #4981, #54498, #116170, #176863, #189045, #127333, #177860, #162672, #115170, #173871, #99988, #113164, #35340, #114151, #158674, #20164, #161673, #81809, #66667, #190029, #191016, #159666, #144499, #166682, #198003, #195025, #196035, #10007, #27179, #121147, #26180, #74661, #150519, #57512, #165680, #87821, #88826, #182840, #118179, #42341, #120157, #149507, #28183, #86831, #180865, #11004, #105981, #148517, #104002, #56502, #71667, #133334, #179870, #41339, #44322, #181847, #89825, #12017, #40328, #151506, #24179, #12999, #72677, #70674, #134353, #103000, #163686, #73678, #119180, #135351, #58490, #9007, #164686, #197024, #55496, #43327, #136328, #85829, #104994, #59473, #147517, #132341, #194033, #117166, #178862, #102005, #25189, #95522, #138310, #50029, #97488, #173381, #126845, #76632, #35842, #199991, #61458, #81328, #127841, #189547, #112680, #174372, #34851, #106965, #157208, #19686, #96506, #143011, #66179, #5494, #123129, #159174, #167666, #49037, #13970, #75637, #4489, #91782, #198996, #60463, #184814, #137315, #110692, #45315, #51019, #3510, #20669, #82323, #122138, #153476, #152483, #183825, #18702, #144013, #67177, #111694, #190533, #80349, #65186, #128834, #168640, #172372, #33862, #14972, #158196, #52007, #29162, #188551, #90800, #142021, #30139, #160187, #116680, #131853, #55010, #87344, #54015, #163189, #100506, #194536, #37844, #52997, #175360, #161185, #178370, #70185, #69175, #10518, #176371, #22681, #24693, #36828, #21677, #149030, #8507, #162185, #71184, #113666, #23683, #86342, #148029, #72181, #102518, #133855, #179382, #164201, #147023, #56007, #117685, #195545, #38849, #85331, #98494, #39834, #83331, #101500, #145008, #6489, #9518, #68169, #25699, #129821, #40844, #191520, #193536, #114675, #99504, #84328, #132848, #146007, #7490, #130841, #192532, #115689, #177377, #118692, #91287, #41854, #27694, #42847, #88331, #167183, #199501, #180384, #89335, #152978, #137817, #106479, #58990, #120657 ),
 ( #103520, #198509, #12518, #184331, #182355, #45813, #168158, #57019, #169140, #165196, #14477, #29655, #15479, #59980, #121647, #26691, #74182, #104512, #13489, #75154, #107464, #60967, #122641, #183342, #151027, #197522, #136825, #76139, #28682, #150022, #43833, #105497, #11527, #90317, #44824, #152003, #119685, #73197, #135852, #30645, #77136, #181368, #92298, #153982, #138805, #134867, #196545, #58015, #166193, #64948, #93288, #49786, #171142, #185317, #172134, #82076, #158937, #18463, #127607, #124632, #188309, #187328, #154973, #108467, #142775, #174132, #32631, #33620, #186327, #3276, #97249, #2278, #50783, #126607, #95283, #141782, #63961, #111452, #20426, #94285, #80114, #96272, #125630, #4256, #35603, #156966, #48799, #157958, #286, #110453, #173138, #34613, #61955, #189306, #123622, #65935, #112443, #19449, #81097, #46808, #170144, #31639, #16469, #78118, #139787, #1275, #62952, #47809, #109459, #155963, #17460, #79117, #140789, #51764, #145766, #193292, #5250, #129584, #146770, #131607, #161944, #99258, #160945, #192292, #66931, #113425, #22438, #191280, #53771, #116440, #115445, #130595, #67930, #54766, #52755, #114424, #23439, #69943, #8264, #178129, #39596, #38607, #159943, #84087, #85086, #177136, #101255, #162944, #24451, #176126, #86100, #143769, #7248, #175117, #36585, #147791, #37596, #98240, #21430, #68933, #83090, #100263, #144766, #9277, #128594, #190288, #6251, #78774, #110119, #109122, #170800, #172796, #158600, #128254, #65598, #144422, #111107, #157622, #81734, #17122, #94945, #79779, #171797, #127258, #143420, #185982, #142440, #173797, #48462, #34277, #32292, #188971, #3918, #50447, #97897, #64616, #35263, #95936, #4907, #33285, #63620, #47465, #156629, #112106, #80762, #141451, #21085, #186992, #18124, #96918, #93948, #155626, #20090, #2936, #51426, #49444, #113086, #66590, #124285, #36244, #140450, #189952, #174778, #82742, #159588, #5908, #1940, #126278, #187975, #125296, #19112, #21672, #145003, #6484, #130836, #160182, #84323, #191515, #24688, #147018, #117680, #56002, #68164, #99499, #98489, #83326, #162180, #148024, #179377, #55005, #133850, #100501, #8503, #71179, #129816, #146002, #69169, #161180, #116675, #132843, #175355, #131848, #163184, #37839, #23678, #52992, #178365, #193531, #39829, #87339, #54010, #86337, #85326, #194531, #22676, #114670, #36823, #7485, #101495, #70180, #192527, #10513, #176366, #115684, #9513, #177372, #38844, #149025, #40839, #102512, #164196, #113661, #25694, #72176, #195540, #92294, #45809, #15475, #122637, #107460, #90313, #137813, #60963, #30641, #182351, #43829, #153978, #198505, #118687, #183338, #77132, #180379, #91283, #41849, #27691, #42844, #88327, #167179, #199497, #103516, #89332, #152974, #184327, #106475, #58986, #120653, #75150, #165192, #26687, #105493, #151024, #136821, #169136, #59976, #13485, #166190, #138801, #12515, #74179, #121643, #151999, #119682, #73193, #135849, #57014, #150018, #181365, #11523, #134864, #14473, #196542, #58012, #104509, #197518, #44820, #28678, #168154, #29651, #76135, #172130, #82072, #158933, #18459, #19445, #1271, #62948, #187324, #81093, #124628, #139783, #61951, #47805, #141778, #156962, #155959, #97245, #186323, #109455, #49782, #123618, #108463, #35599, #95279, #48795, #157954, #282, #110449, #111447, #34609, #20422, #189302, #185313, #65931, #50779, #33616, #142771, #4252, #174128, #125626, #80110, #46804, #3272, #170140, #126603, #31635, #93284, #96268, #154969, #171138, #32627, #16465, #64944, #127603, #78114, #94281, #112439, #17456, #173134, #2274, #63957, #188305, #79112, #140785, #68929, #114420, #23435, #70939, #146766, #100259, #52751, #9273, #176121, #37592, #54762, #101251, #162940, #86096, #147787, #8259, #83086, #130591, #193288, #69939, #116436, #39592, #179134, #99254, #132607, #143765, #22433, #85082, #25459, #192287, #51760, #175113, #36581, #160941 ),
 ( #24447, #67926, #144762, #5246, #191276, #131603, #161940, #84083, #40602, #6247, #145762, #178124, #66927, #113421, #102273, #38603, #53767, #194296, #128590, #115441, #55762, #117436, #163961, #190284, #98236, #159939, #21426, #177132, #129579, #7244, #60725, #12277, #73942, #122399, #28445, #148784, #13256, #184089, #10273, #121407, #71932, #57774, #72950, #118448, #197282, #29421, #133602, #119444, #183101, #167921, #136582, #89090, #150782, #105256, #195294, #56775, #135611, #181129, #166942, #14229, #90081, #43590, #196304, #152739, #42603, #104267, #198262, #44582, #106239, #91052, #75900, #151763, #26447, #58745, #59738, #74919, #137574, #199258, #45572, #165949, #107225, #87099, #27449, #168896, #180140, #120414, #41609, #103274, #164954, #182105, #88089, #149775, #11277, #134620, #63723, #34381, #172903, #185076, #16233, #15233, #76892, #78876, #64718, #96041, #171899, #53271, #17224, #125398, #188077, #123384, #1037, #186087, #77885, #33387, #49548, #92048, #48565, #79883, #154737, #140555, #138563, #95046, #110218, #141553, #111211, #62710, #2043, #139553, #156735, #130092, #32393, #80867, #18228, #187095, #3042, #94048, #126380, #191790, #124392, #157728, #19217, #155726, #142543, #93050, #6759, #68438, #114949, #47570, #30402, #109222, #170901, #153737, #41, #61716, #46565, #108226, #169906, #31399, #192800, #42125, #73462, #103787, #24964, #22948, #178638, #23951, #115955, #179650, #86610, #117959, #41120, #177644, #116945, #85606, #164470, #100768, #102784, #148293, #25964, #99772, #165467, #163467, #147292, #118966, #26963, #135136, #9787, #38118, #87607, #132117, #88606, #101779, #150302, #149293, #176642, #11798, #161457, #134129, #10787, #196810, #72454, #195818, #84594, #193810, #58277, #57290, #180650, #71449, #146274, #7761, #69444, #8782, #40101, #133114, #131112, #194802, #54283, #56276, #39112, #162450, #70452, #55275, #14756, #182624, #136114, #13757, #123896, #140066, #44109, #170421, #155252, #15750, #27964, #43111, #62228, #16741, #184601, #12782, #169418, #90591, #104779, #91566, #1557, #78390, #75425, #197790, #89605, #105767, #106756, #74448, #151294, #185595, #93566, #168431, #59256, #120925, #47084, #119946, #152273, #153254, #167454, #122913, #181631, #121922, #31913, #46082, #76417, #61241, #183616, #107737, #166467, #137099, #138093, #77409, #45099, #108745, #28950, #199774, #29927, #198785, #60251, #30923, #92571, #154259, #139079, #557, #187603, #21711, #20702, #128866, #143044, #79400, #190566, #160221, #52041, #111727, #109738, #65219, #110728, #2556, #66215, #173413, #4522, #127875, #64238, #3541, #172409, #51051, #49072, #189579, #34884, #112713, #186610, #113697, #50066, #33898, #5528, #175393, #83365, #96539, #124912, #174406, #18736, #36861, #188585, #98528, #35875, #63233, #145041, #48082, #82358, #97521, #171422, #159208, #144046, #32908, #80383, #94562, #67208, #156241, #158228, #17743, #141071, #125904, #95555, #126879, #19718, #157242, #81360, #142055, #193570, #147056, #37879, #131885, #71216, #101532, #69207, #22714, #100538, #10549, #26723, #130875, #57051, #41886, #102550, #114711, #129855, #149061, #103553, #132879, #99537, #56038, #177410, #191553, #178402, #88362, #165228, #162217, #84361, #176404, #192565, #161219, #55042, #8540, #146039, #116712, #194568, #163224, #54048, #7523, #23716, #72213, #6523, #115722, #118726, #68202, #164234, #38881, #53030, #133887, #85364, #117716, #70218, #179412, #39866, #24725, #86374, #148059, #9550, #40877, #25730, #87376, #195578, #180414, #104542, #58045, #92328, #123650, #120687, #121679, #135881, #153009, #46838, #152034, #316, #76170, #183375, #91318, #13519, #14508, #108498, #43864, #168189, #45842, #75184, #154014, #12547, #106512, #136856, #31670, #74213, #29686, #182386, #197552, #59020, #105529, #167215, #170177, #107494, #15509, #137850, #166223, #77166, #150055, #138836, #198541, #196575 ) ),
 .UNSPECIFIED., .T., .F., .F. ) 
 B_SPLINE_SURFACE_WITH_KNOTS ( ( 4, 3, 4 ),
 ( 3, 2, 2, 2, 2, 2, 2, 2, 2, 2, 2, 2, 2, 2, 2, 2, 2, 2, 2, 2, 2, 2, 2, 2, 2, 2, 2, 2, 2, 2, 2, 2, 2, 2, 2, 2, 2, 2, 2, 2, 2, 2, 2, 2, 2, 2, 2, 2, 2, 2, 2, 2, 2, 2, 2, 2, 2, 2, 2, 2, 2, 2, 2, 2, 2, 2, 2, 2, 2, 2, 2, 2, 2, 2, 2, 2, 2, 2, 2, 2, 2, 2, 2, 2, 2, 2, 2, 2, 2, 2, 2, 2, 2, 2, 2, 2, 2, 2, 2, 2, 2, 2, 2, 2, 2, 2, 2, 2, 2, 2, 2, 2, 2, 2, 2, 2, 2, 2, 2, 2, 2, 2, 2, 2, 2, 2, 2, 2, 2, 2, 2, 2, 2, 2, 2, 2, 2, 2, 2, 2, 2, 2, 2, 2, 2, 2, 2, 2, 2, 2, 2, 2, 2, 2, 2, 2, 2, 2, 2, 2, 2, 2, 2, 2, 2, 2, 2, 2, 2, 2, 2, 2, 2, 2, 2, 2, 2, 2, 2, 2, 2, 2, 2, 2, 2, 2, 2, 2, 2, 2, 2, 2, 2, 2, 2, 2, 2, 2, 2, 2, 2, 2, 2, 2, 2, 2, 2, 2, 2, 2, 2, 2, 2, 2, 2, 2, 2, 2, 2, 2, 2, 2, 2, 2, 2, 2, 2, 2, 3 ),
 ( 0.000000000000000000, 0.5000000000000000000, 1.000000000000000000 ),
 ( 0.000000000000000000, 0.004385964912280701511, 0.008771929824561403022, 0.01315789473684210453, 0.01754385964912280604, 0.02192982456140350755, 0.02631578947368420907, 0.03070175438596491058, 0.03508771929824561209, 0.03947368421052631360, 0.04385964912280701511, 0.04824561403508771662, 0.05263157894736841813, 0.05701754385964911964, 0.06140350877192982115, 0.06578947368421052266, 0.07017543859649122417, 0.07456140350877192569, 0.07894736842105262720, 0.08333333333333332871, 0.08771929824561403022, 0.09210526315789473173, 0.09649122807017543324, 0.1008771929824561348, 0.1052631578947368363, 0.1096491228070175378, 0.1140350877192982393, 0.1184210526315789408, 0.1228070175438596423, 0.1271929824561403577, 0.1315789473684210453, 0.1359649122807017607, 0.1403508771929824483, 0.1447368421052631637, 0.1491228070175438514, 0.1535087719298245668, 0.1578947368421052544, 0.1622807017543859698, 0.1666666666666666574, 0.1710526315789473728, 0.1754385964912280604, 0.1798245614035087758, 0.1842105263157894635, 0.1885964912280701788, 0.1929824561403508665, 0.1973684210526315819, 0.2017543859649122695, 0.2061403508771929849, 0.2105263157894736725, 0.2149122807017543879, 0.2192982456140350755, 0.2236842105263157909, 0.2280701754385964786, 0.2324561403508771940, 0.2368421052631578816, 0.2412280701754385970, 0.2456140350877192846, 0.2500000000000000000, 0.2543859649122807154, 0.2587719298245614308, 0.2631578947368420907, 0.2675438596491228060, 0.2719298245614035214, 0.2763157894736842368, 0.2807017543859648967, 0.2850877192982456121, 0.2894736842105263275, 0.2938596491228070429, 0.2982456140350877027, 0.3026315789473684181, 0.3070175438596491335, 0.3114035087719298489, 0.3157894736842105088, 0.3201754385964912242, 0.3245614035087719396, 0.3289473684210526550, 0.3333333333333333148, 0.3377192982456140302, 0.3421052631578947456, 0.3464912280701754610, 0.3508771929824561209, 0.3552631578947368363, 0.3596491228070175517, 0.3640350877192982670, 0.3684210526315789269, 0.3728070175438596423, 0.3771929824561403577, 0.3815789473684210731, 0.3859649122807017330, 0.3903508771929824483, 0.3947368421052631637, 0.3991228070175438791, 0.4035087719298245390, 0.4078947368421052544, 0.4122807017543859698, 0.4166666666666666852, 0.4210526315789473450, 0.4254385964912280604, 0.4298245614035087758, 0.4342105263157894912, 0.4385964912280701511, 0.4429824561403508665, 0.4473684210526315819, 0.4517543859649122973, 0.4561403508771929571, 0.4605263157894736725, 0.4649122807017543879, 0.4692982456140351033, 0.4736842105263157632, 0.4780701754385964786, 0.4824561403508771940, 0.4868421052631579093, 0.4912280701754385692, 0.4956140350877192846, 0.5000000000000000000, 0.5043859649122807154, 0.5087719298245614308, 0.5131578947368421462, 0.5175438596491228616, 0.5219298245614034659, 0.5263157894736841813, 0.5307017543859648967, 0.5350877192982456121, 0.5394736842105263275, 0.5438596491228070429, 0.5482456140350877583, 0.5526315789473684736, 0.5570175438596490780, 0.5614035087719297934, 0.5657894736842105088, 0.5701754385964912242, 0.5745614035087719396, 0.5789473684210526550, 0.5833333333333333703, 0.5877192982456140857, 0.5921052631578946901, 0.5964912280701754055, 0.6008771929824561209, 0.6052631578947368363, 0.6096491228070175517, 0.6140350877192982670, 0.6184210526315789824, 0.6228070175438596978, 0.6271929824561403022, 0.6315789473684210176, 0.6359649122807017330, 0.6403508771929824483, 0.6447368421052631637, 0.6491228070175438791, 0.6535087719298245945, 0.6578947368421053099, 0.6622807017543859143, 0.6666666666666666297, 0.6710526315789473450, 0.6754385964912280604, 0.6798245614035087758, 0.6842105263157894912, 0.6885964912280702066, 0.6929824561403509220, 0.6973684210526315264, 0.7017543859649122417, 0.7061403508771929571, 0.7105263157894736725, 0.7149122807017543879, 0.7192982456140351033, 0.7236842105263158187, 0.7280701754385965341, 0.7324561403508771384, 0.7368421052631578538, 0.7412280701754385692, 0.7456140350877192846, 0.7500000000000000000, 0.7543859649122807154, 0.7587719298245614308, 0.7631578947368421462, 0.7675438596491228616, 0.7719298245614034659, 0.7763157894736841813, 0.7807017543859648967, 0.7850877192982456121, 0.7894736842105263275, 0.7938596491228070429, 0.7982456140350877583, 0.8026315789473684736, 0.8070175438596490780, 0.8114035087719297934, 0.8157894736842105088, 0.8201754385964912242, 0.8245614035087719396, 0.8289473684210526550, 0.8333333333333333703, 0.8377192982456140857, 0.8421052631578946901, 0.8464912280701754055, 0.8508771929824561209, 0.8552631578947368363, 0.8596491228070175517, 0.8640350877192982670, 0.8684210526315789824, 0.8728070175438596978, 0.8771929824561403022, 0.8815789473684210176, 0.8859649122807017330, 0.8903508771929824483, 0.8947368421052631637, 0.8991228070175438791, 0.9035087719298245945, 0.9078947368421053099, 0.9122807017543859143, 0.9166666666666666297, 0.9210526315789473450, 0.9254385964912280604, 0.9298245614035087758, 0.9342105263157894912, 0.9385964912280702066, 0.9429824561403509220, 0.9473684210526315264, 0.9517543859649122417, 0.9561403508771929571, 0.9605263157894736725, 0.9649122807017543879, 0.9692982456140351033, 0.9736842105263158187, 0.9780701754385965341, 0.9824561403508771384, 0.9868421052631578538, 0.9912280701754385692, 0.9956140350877192846, 1.000000000000000000 ),
 .UNSPECIFIED. ) 
 GEOMETRIC_REPRESENTATION_ITEM ( )  RATIONAL_B_SPLINE_SURFACE ( (
 ( 1.000000000000000000, 0.9659258262890683122, 1.000000000000000000, 0.9659258262890683122, 1.000000000000000000, 0.9659258262890683122, 1.000000000000000000, 0.9659258262890683122, 1.000000000000000000, 0.9659258262890683122, 1.000000000000000000, 0.9659258262890683122, 1.000000000000000000, 0.9659258262890683122, 1.000000000000000000, 0.9659258262890683122, 1.000000000000000000, 0.9659258262890683122, 1.000000000000000000, 0.9659258262890683122, 1.000000000000000000, 0.9659258262890683122, 1.000000000000000000, 0.9659258262890683122, 1.000000000000000000, 0.9659258262890683122, 1.000000000000000000, 0.9659258262890683122, 1.000000000000000000, 0.9659258262890683122, 1.000000000000000000, 0.9659258262890683122, 1.000000000000000000, 0.9659258262890683122, 1.000000000000000000, 0.9659258262890683122, 1.000000000000000000, 0.9659258262890683122, 1.000000000000000000, 0.9659258262890683122, 1.000000000000000000, 0.9659258262890683122, 1.000000000000000000, 0.9659258262890683122, 1.000000000000000000, 0.9659258262890683122, 1.000000000000000000, 0.9659258262890683122, 1.000000000000000000, 0.9659258262890683122, 1.000000000000000000, 0.9659258262890683122, 1.000000000000000000, 0.9659258262890683122, 1.000000000000000000, 0.9659258262890683122, 1.000000000000000000, 0.9659258262890683122, 1.000000000000000000, 0.9659258262890683122, 1.000000000000000000, 0.9659258262890683122, 1.000000000000000000, 0.9659258262890683122, 1.000000000000000000, 0.9659258262890683122, 1.000000000000000000, 0.9659258262890683122, 1.000000000000000000, 0.9659258262890683122, 1.000000000000000000, 0.9659258262890683122, 1.000000000000000000, 0.9659258262890683122, 1.000000000000000000, 0.9659258262890683122, 1.000000000000000000, 0.9659258262890683122, 1.000000000000000000, 0.9659258262890683122, 1.000000000000000000, 0.9659258262890683122, 1.000000000000000000, 0.9659258262890683122, 1.000000000000000000, 0.9659258262890683122, 1.000000000000000000, 0.9659258262890683122, 1.000000000000000000, 0.9659258262890683122, 1.000000000000000000, 0.9659258262890683122, 1.000000000000000000, 0.9659258262890683122, 1.000000000000000000, 0.9659258262890683122, 1.000000000000000000, 0.9659258262890683122, 1.000000000000000000, 0.9659258262890683122, 1.000000000000000000, 0.9659258262890683122, 1.000000000000000000, 0.9659258262890683122, 1.000000000000000000, 0.9659258262890683122, 1.000000000000000000, 0.9659258262890683122, 1.000000000000000000, 0.9659258262890683122, 1.000000000000000000, 0.9659258262890683122, 1.000000000000000000, 0.9659258262890683122, 1.000000000000000000, 0.9659258262890683122, 1.000000000000000000, 0.9659258262890683122, 1.000000000000000000, 0.9659258262890683122, 1.000000000000000000, 0.9659258262890683122, 1.000000000000000000, 0.9659258262890683122, 1.000000000000000000, 0.9659258262890683122, 1.000000000000000000, 0.9659258262890683122, 1.000000000000000000, 0.9659258262890683122, 1.000000000000000000, 0.9659258262890683122, 1.000000000000000000, 0.9659258262890683122, 1.000000000000000000, 0.9659258262890683122, 1.000000000000000000, 0.9659258262890683122, 1.000000000000000000, 0.9659258262890683122, 1.000000000000000000, 0.9659258262890683122, 1.000000000000000000, 0.9659258262890683122, 1.000000000000000000, 0.9659258262890683122, 1.000000000000000000, 0.9659258262890683122, 1.000000000000000000, 0.9659258262890683122, 1.000000000000000000, 0.9659258262890683122, 1.000000000000000000, 0.9659258262890683122, 1.000000000000000000, 0.9659258262890683122, 1.000000000000000000, 0.9659258262890683122, 1.000000000000000000, 0.9659258262890683122, 1.000000000000000000, 0.9659258262890683122, 1.000000000000000000, 0.9659258262890683122, 1.000000000000000000, 0.9659258262890683122, 1.000000000000000000, 0.9659258262890683122, 1.000000000000000000, 0.9659258262890683122, 1.000000000000000000, 0.9659258262890683122, 1.000000000000000000, 0.9659258262890683122, 1.000000000000000000, 0.9659258262890683122, 1.000000000000000000, 0.9659258262890683122, 1.000000000000000000, 0.9659258262890683122, 1.000000000000000000, 0.9659258262890683122, 1.000000000000000000, 0.9659258262890683122, 1.000000000000000000, 0.9659258262890683122, 1.000000000000000000, 0.9659258262890683122, 1.000000000000000000, 0.9659258262890683122, 1.000000000000000000, 0.9659258262890683122, 1.000000000000000000, 0.9659258262890683122, 1.000000000000000000, 0.9659258262890683122, 1.000000000000000000, 0.9659258262890683122, 1.000000000000000000, 0.9659258262890683122, 1.000000000000000000, 0.9659258262890683122, 1.000000000000000000, 0.9659258262890683122, 1.000000000000000000, 0.9659258262890683122, 1.000000000000000000, 0.9659258262890683122, 1.000000000000000000, 0.9659258262890683122, 1.000000000000000000, 0.9659258262890683122, 1.000000000000000000, 0.9659258262890683122, 1.000000000000000000, 0.9659258262890683122, 1.000000000000000000, 0.9659258262890683122, 1.000000000000000000, 0.9659258262890683122, 1.000000000000000000, 0.9659258262890683122, 1.000000000000000000, 0.9659258262890683122, 1.000000000000000000, 0.9659258262890683122, 1.000000000000000000, 0.9659258262890683122, 1.000000000000000000, 0.9659258262890683122, 1.000000000000000000, 0.9659258262890683122, 1.000000000000000000, 0.9659258262890683122, 1.000000000000000000, 0.9659258262890683122, 1.000000000000000000, 0.9659258262890683122, 1.000000000000000000, 0.9659258262890683122, 1.000000000000000000, 0.9659258262890683122, 1.000000000000000000, 0.9659258262890683122, 1.000000000000000000, 0.9659258262890683122, 1.000000000000000000, 0.9659258262890683122, 1.000000000000000000, 0.9659258262890683122, 1.000000000000000000, 0.9659258262890683122, 1.000000000000000000, 0.9659258262890683122, 1.000000000000000000, 0.9659258262890683122, 1.000000000000000000, 0.9659258262890683122, 1.000000000000000000, 0.9659258262890683122, 1.000000000000000000, 0.9659258262890683122, 1.000000000000000000, 0.9659258262890683122, 1.000000000000000000, 0.9659258262890683122, 1.000000000000000000, 0.9659258262890683122, 1.000000000000000000, 0.9659258262890683122, 1.000000000000000000, 0.9659258262890683122, 1.000000000000000000, 0.9659258262890683122, 1.000000000000000000, 0.9659258262890683122, 1.000000000000000000, 0.9659258262890683122, 1.000000000000000000, 0.9659258262890683122, 1.000000000000000000, 0.9659258262890683122, 1.000000000000000000, 0.9659258262890683122, 1.000000000000000000, 0.9659258262890683122, 1.000000000000000000, 0.9659258262890683122, 1.000000000000000000, 0.9659258262890683122, 1.000000000000000000, 0.9659258262890683122, 1.000000000000000000, 0.9659258262890683122, 1.000000000000000000, 0.9659258262890683122, 1.000000000000000000, 0.9659258262890683122, 1.000000000000000000, 0.9659258262890683122, 1.000000000000000000, 0.9659258262890683122, 1.000000000000000000, 0.9659258262890683122, 1.000000000000000000, 0.9659258262890683122, 1.000000000000000000, 0.9659258262890683122, 1.000000000000000000, 0.9659258262890683122, 1.000000000000000000, 0.9659258262890683122, 1.000000000000000000, 0.9659258262890683122, 1.000000000000000000, 0.9659258262890683122, 1.000000000000000000, 0.9659258262890683122, 1.000000000000000000, 0.9659258262890683122, 1.000000000000000000, 0.9659258262890683122, 1.000000000000000000, 0.9659258262890683122, 1.000000000000000000, 0.9659258262890683122, 1.000000000000000000, 0.9659258262890683122, 1.000000000000000000, 0.9659258262890683122, 1.000000000000000000, 0.9659258262890683122, 1.000000000000000000, 0.9659258262890683122, 1.000000000000000000, 0.9659258262890683122, 1.000000000000000000, 0.9659258262890683122, 1.000000000000000000, 0.9659258262890683122, 1.000000000000000000, 0.9659258262890683122, 1.000000000000000000, 0.9659258262890683122, 1.000000000000000000, 0.9659258262890683122, 1.000000000000000000, 0.9659258262890683122, 1.000000000000000000, 0.9659258262890683122, 1.000000000000000000, 0.9659258262890683122, 1.000000000000000000, 0.9659258262890683122, 1.000000000000000000, 0.9659258262890683122, 1.000000000000000000, 0.9659258262890683122, 1.000000000000000000, 0.9659258262890683122, 1.000000000000000000, 0.9659258262890683122, 1.000000000000000000, 0.9659258262890683122, 1.000000000000000000, 0.9659258262890683122, 1.000000000000000000, 0.9659258262890683122, 1.000000000000000000, 0.9659258262890683122, 1.000000000000000000, 0.9659258262890683122, 1.000000000000000000, 0.9659258262890683122, 1.000000000000000000, 0.9659258262890683122, 1.000000000000000000, 0.9659258262890683122, 1.000000000000000000, 0.9659258262890683122, 1.000000000000000000, 0.9659258262890683122, 1.000000000000000000, 0.9659258262890683122, 1.000000000000000000, 0.9659258262890683122, 1.000000000000000000, 0.9659258262890683122, 1.000000000000000000, 0.9659258262890683122, 1.000000000000000000, 0.9659258262890683122, 1.000000000000000000, 0.9659258262890683122, 1.000000000000000000, 0.9659258262890683122, 1.000000000000000000, 0.9659258262890683122, 1.000000000000000000, 0.9659258262890683122, 1.000000000000000000, 0.9659258262890683122, 1.000000000000000000, 0.9659258262890683122, 1.000000000000000000, 0.9659258262890683122, 1.000000000000000000, 0.9659258262890683122, 1.000000000000000000, 0.9659258262890683122, 1.000000000000000000, 0.9659258262890683122, 1.000000000000000000, 0.9659258262890683122, 1.000000000000000000, 0.9659258262890683122, 1.000000000000000000, 0.9659258262890683122, 1.000000000000000000, 0.9659258262890683122, 1.000000000000000000, 0.9659258262890683122, 1.000000000000000000, 0.9659258262890683122, 1.000000000000000000, 0.9659258262890683122, 1.000000000000000000, 0.9659258262890683122, 1.000000000000000000, 0.9659258262890683122, 1.000000000000000000, 0.9659258262890683122, 1.000000000000000000, 0.9659258262890683122, 1.000000000000000000, 0.9659258262890683122, 1.000000000000000000, 0.9659258262890683122, 1.000000000000000000, 0.9659258262890683122, 1.000000000000000000, 0.9659258262890683122, 1.000000000000000000, 0.9659258262890683122, 1.000000000000000000, 0.9659258262890683122, 1.000000000000000000, 0.9659258262890683122, 1.000000000000000000, 0.9659258262890683122, 1.000000000000000000, 0.9659258262890683122, 1.000000000000000000, 0.9659258262890683122, 1.000000000000000000, 0.9659258262890683122, 1.000000000000000000),
 ( 0.3333333333333333703, 0.3219752754296894559, 0.3333333333333333703, 0.3219752754296894559, 0.3333333333333333703, 0.3219752754296894559, 0.3333333333333333703, 0.3219752754296894559, 0.3333333333333333703, 0.3219752754296894559, 0.3333333333333333703, 0.3219752754296894559, 0.3333333333333333703, 0.3219752754296894559, 0.3333333333333333703, 0.3219752754296894559, 0.3333333333333333703, 0.3219752754296894559, 0.3333333333333333703, 0.3219752754296894559, 0.3333333333333333703, 0.3219752754296894559, 0.3333333333333333703, 0.3219752754296894559, 0.3333333333333333703, 0.3219752754296894559, 0.3333333333333333703, 0.3219752754296894559, 0.3333333333333333703, 0.3219752754296894559, 0.3333333333333333703, 0.3219752754296894559, 0.3333333333333333703, 0.3219752754296894559, 0.3333333333333333703, 0.3219752754296894559, 0.3333333333333333703, 0.3219752754296894559, 0.3333333333333333703, 0.3219752754296894559, 0.3333333333333333703, 0.3219752754296894559, 0.3333333333333333703, 0.3219752754296894559, 0.3333333333333333703, 0.3219752754296894559, 0.3333333333333333703, 0.3219752754296894559, 0.3333333333333333703, 0.3219752754296894559, 0.3333333333333333703, 0.3219752754296894559, 0.3333333333333333703, 0.3219752754296894559, 0.3333333333333333703, 0.3219752754296894559, 0.3333333333333333703, 0.3219752754296894559, 0.3333333333333333703, 0.3219752754296894559, 0.3333333333333333703, 0.3219752754296894559, 0.3333333333333333703, 0.3219752754296894559, 0.3333333333333333703, 0.3219752754296894559, 0.3333333333333333703, 0.3219752754296894559, 0.3333333333333333703, 0.3219752754296894559, 0.3333333333333333703, 0.3219752754296894559, 0.3333333333333333703, 0.3219752754296894559, 0.3333333333333333703, 0.3219752754296894559, 0.3333333333333333703, 0.3219752754296894559, 0.3333333333333333703, 0.3219752754296894559, 0.3333333333333333703, 0.3219752754296894559, 0.3333333333333333703, 0.3219752754296894559, 0.3333333333333333703, 0.3219752754296894559, 0.3333333333333333703, 0.3219752754296894559, 0.3333333333333333703, 0.3219752754296894559, 0.3333333333333333703, 0.3219752754296894559, 0.3333333333333333703, 0.3219752754296894559, 0.3333333333333333703, 0.3219752754296894559, 0.3333333333333333703, 0.3219752754296894559, 0.3333333333333333703, 0.3219752754296894559, 0.3333333333333333703, 0.3219752754296894559, 0.3333333333333333703, 0.3219752754296894559, 0.3333333333333333703, 0.3219752754296894559, 0.3333333333333333703, 0.3219752754296894559, 0.3333333333333333703, 0.3219752754296894559, 0.3333333333333333703, 0.3219752754296894559, 0.3333333333333333703, 0.3219752754296894559, 0.3333333333333333703, 0.3219752754296894559, 0.3333333333333333703, 0.3219752754296894559, 0.3333333333333333703, 0.3219752754296894559, 0.3333333333333333703, 0.3219752754296894559, 0.3333333333333333703, 0.3219752754296894559, 0.3333333333333333703, 0.3219752754296894559, 0.3333333333333333703, 0.3219752754296894559, 0.3333333333333333703, 0.3219752754296894559, 0.3333333333333333703, 0.3219752754296894559, 0.3333333333333333703, 0.3219752754296894559, 0.3333333333333333703, 0.3219752754296894559, 0.3333333333333333703, 0.3219752754296894559, 0.3333333333333333703, 0.3219752754296894559, 0.3333333333333333703, 0.3219752754296894559, 0.3333333333333333703, 0.3219752754296894559, 0.3333333333333333703, 0.3219752754296894559, 0.3333333333333333703, 0.3219752754296894559, 0.3333333333333333703, 0.3219752754296894559, 0.3333333333333333703, 0.3219752754296894559, 0.3333333333333333703, 0.3219752754296894559, 0.3333333333333333703, 0.3219752754296894559, 0.3333333333333333703, 0.3219752754296894559, 0.3333333333333333703, 0.3219752754296894559, 0.3333333333333333703, 0.3219752754296894559, 0.3333333333333333703, 0.3219752754296894559, 0.3333333333333333703, 0.3219752754296894559, 0.3333333333333333703, 0.3219752754296894559, 0.3333333333333333703, 0.3219752754296894559, 0.3333333333333333703, 0.3219752754296894559, 0.3333333333333333703, 0.3219752754296894559, 0.3333333333333333703, 0.3219752754296894559, 0.3333333333333333703, 0.3219752754296894559, 0.3333333333333333703, 0.3219752754296894559, 0.3333333333333333703, 0.3219752754296894559, 0.3333333333333333703, 0.3219752754296894559, 0.3333333333333333703, 0.3219752754296894559, 0.3333333333333333703, 0.3219752754296894559, 0.3333333333333333703, 0.3219752754296894559, 0.3333333333333333703, 0.3219752754296894559, 0.3333333333333333703, 0.3219752754296894559, 0.3333333333333333703, 0.3219752754296894559, 0.3333333333333333703, 0.3219752754296894559, 0.3333333333333333703, 0.3219752754296894559, 0.3333333333333333703, 0.3219752754296894559, 0.3333333333333333703, 0.3219752754296894559, 0.3333333333333333703, 0.3219752754296894559, 0.3333333333333333703, 0.3219752754296894559, 0.3333333333333333703, 0.3219752754296894559, 0.3333333333333333703, 0.3219752754296894559, 0.3333333333333333703, 0.3219752754296894559, 0.3333333333333333703, 0.3219752754296894559, 0.3333333333333333703, 0.3219752754296894559, 0.3333333333333333703, 0.3219752754296894559, 0.3333333333333333703, 0.3219752754296894559, 0.3333333333333333703, 0.3219752754296894559, 0.3333333333333333703, 0.3219752754296894559, 0.3333333333333333703, 0.3219752754296894559, 0.3333333333333333703, 0.3219752754296894559, 0.3333333333333333703, 0.3219752754296894559, 0.3333333333333333703, 0.3219752754296894559, 0.3333333333333333703, 0.3219752754296894559, 0.3333333333333333703, 0.3219752754296894559, 0.3333333333333333703, 0.3219752754296894559, 0.3333333333333333703, 0.3219752754296894559, 0.3333333333333333703, 0.3219752754296894559, 0.3333333333333333703, 0.3219752754296894559, 0.3333333333333333703, 0.3219752754296894559, 0.3333333333333333703, 0.3219752754296894559, 0.3333333333333333703, 0.3219752754296894559, 0.3333333333333333703, 0.3219752754296894559, 0.3333333333333333703, 0.3219752754296894559, 0.3333333333333333703, 0.3219752754296894559, 0.3333333333333333703, 0.3219752754296894559, 0.3333333333333333703, 0.3219752754296894559, 0.3333333333333333703, 0.3219752754296894559, 0.3333333333333333703, 0.3219752754296894559, 0.3333333333333333703, 0.3219752754296894559, 0.3333333333333333703, 0.3219752754296894559, 0.3333333333333333703, 0.3219752754296894559, 0.3333333333333333703, 0.3219752754296894559, 0.3333333333333333703, 0.3219752754296894559, 0.3333333333333333703, 0.3219752754296894559, 0.3333333333333333703, 0.3219752754296894559, 0.3333333333333333703, 0.3219752754296894559, 0.3333333333333333703, 0.3219752754296894559, 0.3333333333333333703, 0.3219752754296894559, 0.3333333333333333703, 0.3219752754296894559, 0.3333333333333333703, 0.3219752754296894559, 0.3333333333333333703, 0.3219752754296894559, 0.3333333333333333703, 0.3219752754296894559, 0.3333333333333333703, 0.3219752754296894559, 0.3333333333333333703, 0.3219752754296894559, 0.3333333333333333703, 0.3219752754296894559, 0.3333333333333333703, 0.3219752754296894559, 0.3333333333333333703, 0.3219752754296894559, 0.3333333333333333703, 0.3219752754296894559, 0.3333333333333333703, 0.3219752754296894559, 0.3333333333333333703, 0.3219752754296894559, 0.3333333333333333703, 0.3219752754296894559, 0.3333333333333333703, 0.3219752754296894559, 0.3333333333333333703, 0.3219752754296894559, 0.3333333333333333703, 0.3219752754296894559, 0.3333333333333333703, 0.3219752754296894559, 0.3333333333333333703, 0.3219752754296894559, 0.3333333333333333703, 0.3219752754296894559, 0.3333333333333333703, 0.3219752754296894559, 0.3333333333333333703, 0.3219752754296894559, 0.3333333333333333703, 0.3219752754296894559, 0.3333333333333333703, 0.3219752754296894559, 0.3333333333333333703, 0.3219752754296894559, 0.3333333333333333703, 0.3219752754296894559, 0.3333333333333333703, 0.3219752754296894559, 0.3333333333333333703, 0.3219752754296894559, 0.3333333333333333703, 0.3219752754296894559, 0.3333333333333333703, 0.3219752754296894559, 0.3333333333333333703, 0.3219752754296894559, 0.3333333333333333703, 0.3219752754296894559, 0.3333333333333333703, 0.3219752754296894559, 0.3333333333333333703, 0.3219752754296894559, 0.3333333333333333703, 0.3219752754296894559, 0.3333333333333333703, 0.3219752754296894559, 0.3333333333333333703, 0.3219752754296894559, 0.3333333333333333703, 0.3219752754296894559, 0.3333333333333333703, 0.3219752754296894559, 0.3333333333333333703, 0.3219752754296894559, 0.3333333333333333703, 0.3219752754296894559, 0.3333333333333333703, 0.3219752754296894559, 0.3333333333333333703, 0.3219752754296894559, 0.3333333333333333703, 0.3219752754296894559, 0.3333333333333333703, 0.3219752754296894559, 0.3333333333333333703, 0.3219752754296894559, 0.3333333333333333703, 0.3219752754296894559, 0.3333333333333333703, 0.3219752754296894559, 0.3333333333333333703, 0.3219752754296894559, 0.3333333333333333703, 0.3219752754296894559, 0.3333333333333333703, 0.3219752754296894559, 0.3333333333333333703, 0.3219752754296894559, 0.3333333333333333703, 0.3219752754296894559, 0.3333333333333333703, 0.3219752754296894559, 0.3333333333333333703, 0.3219752754296894559, 0.3333333333333333703, 0.3219752754296894559, 0.3333333333333333703, 0.3219752754296894559, 0.3333333333333333703, 0.3219752754296894559, 0.3333333333333333703, 0.3219752754296894559, 0.3333333333333333703, 0.3219752754296894559, 0.3333333333333333703, 0.3219752754296894559, 0.3333333333333333703, 0.3219752754296894559, 0.3333333333333333703, 0.3219752754296894559, 0.3333333333333333703, 0.3219752754296894559, 0.3333333333333333703, 0.3219752754296894559, 0.3333333333333333703, 0.3219752754296894559, 0.3333333333333333703, 0.3219752754296894559, 0.3333333333333333703, 0.3219752754296894559, 0.3333333333333333703, 0.3219752754296894559, 0.3333333333333333703, 0.3219752754296894559, 0.3333333333333333703, 0.3219752754296894559, 0.3333333333333333703, 0.3219752754296894559, 0.3333333333333333703, 0.3219752754296894559, 0.3333333333333333703, 0.3219752754296894559, 0.3333333333333333703, 0.3219752754296894559, 0.3333333333333333703, 0.3219752754296894559, 0.3333333333333333703, 0.3219752754296894559, 0.3333333333333333703, 0.3219752754296894559, 0.3333333333333333703, 0.3219752754296894559, 0.3333333333333333703, 0.3219752754296894559, 0.3333333333333333703, 0.3219752754296894559, 0.3333333333333333703, 0.3219752754296894559, 0.3333333333333333703, 0.3219752754296894559, 0.3333333333333333703, 0.3219752754296894559, 0.3333333333333333703, 0.3219752754296894559, 0.3333333333333333703, 0.3219752754296894559, 0.3333333333333333703),
 ( 0.3333333333333333703, 0.3219752754296894559, 0.3333333333333333703, 0.3219752754296894559, 0.3333333333333333703, 0.3219752754296894559, 0.3333333333333333703, 0.3219752754296894559, 0.3333333333333333703, 0.3219752754296894559, 0.3333333333333333703, 0.3219752754296894559, 0.3333333333333333703, 0.3219752754296894559, 0.3333333333333333703, 0.3219752754296894559, 0.3333333333333333703, 0.3219752754296894559, 0.3333333333333333703, 0.3219752754296894559, 0.3333333333333333703, 0.3219752754296894559, 0.3333333333333333703, 0.3219752754296894559, 0.3333333333333333703, 0.3219752754296894559, 0.3333333333333333703, 0.3219752754296894559, 0.3333333333333333703, 0.3219752754296894559, 0.3333333333333333703, 0.3219752754296894559, 0.3333333333333333703, 0.3219752754296894559, 0.3333333333333333703, 0.3219752754296894559, 0.3333333333333333703, 0.3219752754296894559, 0.3333333333333333703, 0.3219752754296894559, 0.3333333333333333703, 0.3219752754296894559, 0.3333333333333333703, 0.3219752754296894559, 0.3333333333333333703, 0.3219752754296894559, 0.3333333333333333703, 0.3219752754296894559, 0.3333333333333333703, 0.3219752754296894559, 0.3333333333333333703, 0.3219752754296894559, 0.3333333333333333703, 0.3219752754296894559, 0.3333333333333333703, 0.3219752754296894559, 0.3333333333333333703, 0.3219752754296894559, 0.3333333333333333703, 0.3219752754296894559, 0.3333333333333333703, 0.3219752754296894559, 0.3333333333333333703, 0.3219752754296894559, 0.3333333333333333703, 0.3219752754296894559, 0.3333333333333333703, 0.3219752754296894559, 0.3333333333333333703, 0.3219752754296894559, 0.3333333333333333703, 0.3219752754296894559, 0.3333333333333333703, 0.3219752754296894559, 0.3333333333333333703, 0.3219752754296894559, 0.3333333333333333703, 0.3219752754296894559, 0.3333333333333333703, 0.3219752754296894559, 0.3333333333333333703, 0.3219752754296894559, 0.3333333333333333703, 0.3219752754296894559, 0.3333333333333333703, 0.3219752754296894559, 0.3333333333333333703, 0.3219752754296894559, 0.3333333333333333703, 0.3219752754296894559, 0.3333333333333333703, 0.3219752754296894559, 0.3333333333333333703, 0.3219752754296894559, 0.3333333333333333703, 0.3219752754296894559, 0.3333333333333333703, 0.3219752754296894559, 0.3333333333333333703, 0.3219752754296894559, 0.3333333333333333703, 0.3219752754296894559, 0.3333333333333333703, 0.3219752754296894559, 0.3333333333333333703, 0.3219752754296894559, 0.3333333333333333703, 0.3219752754296894559, 0.3333333333333333703, 0.3219752754296894559, 0.3333333333333333703, 0.3219752754296894559, 0.3333333333333333703, 0.3219752754296894559, 0.3333333333333333703, 0.3219752754296894559, 0.3333333333333333703, 0.3219752754296894559, 0.3333333333333333703, 0.3219752754296894559, 0.3333333333333333703, 0.3219752754296894559, 0.3333333333333333703, 0.3219752754296894559, 0.3333333333333333703, 0.3219752754296894559, 0.3333333333333333703, 0.3219752754296894559, 0.3333333333333333703, 0.3219752754296894559, 0.3333333333333333703, 0.3219752754296894559, 0.3333333333333333703, 0.3219752754296894559, 0.3333333333333333703, 0.3219752754296894559, 0.3333333333333333703, 0.3219752754296894559, 0.3333333333333333703, 0.3219752754296894559, 0.3333333333333333703, 0.3219752754296894559, 0.3333333333333333703, 0.3219752754296894559, 0.3333333333333333703, 0.3219752754296894559, 0.3333333333333333703, 0.3219752754296894559, 0.3333333333333333703, 0.3219752754296894559, 0.3333333333333333703, 0.3219752754296894559, 0.3333333333333333703, 0.3219752754296894559, 0.3333333333333333703, 0.3219752754296894559, 0.3333333333333333703, 0.3219752754296894559, 0.3333333333333333703, 0.3219752754296894559, 0.3333333333333333703, 0.3219752754296894559, 0.3333333333333333703, 0.3219752754296894559, 0.3333333333333333703, 0.3219752754296894559, 0.3333333333333333703, 0.3219752754296894559, 0.3333333333333333703, 0.3219752754296894559, 0.3333333333333333703, 0.3219752754296894559, 0.3333333333333333703, 0.3219752754296894559, 0.3333333333333333703, 0.3219752754296894559, 0.3333333333333333703, 0.3219752754296894559, 0.3333333333333333703, 0.3219752754296894559, 0.3333333333333333703, 0.3219752754296894559, 0.3333333333333333703, 0.3219752754296894559, 0.3333333333333333703, 0.3219752754296894559, 0.3333333333333333703, 0.3219752754296894559, 0.3333333333333333703, 0.3219752754296894559, 0.3333333333333333703, 0.3219752754296894559, 0.3333333333333333703, 0.3219752754296894559, 0.3333333333333333703, 0.3219752754296894559, 0.3333333333333333703, 0.3219752754296894559, 0.3333333333333333703, 0.3219752754296894559, 0.3333333333333333703, 0.3219752754296894559, 0.3333333333333333703, 0.3219752754296894559, 0.3333333333333333703, 0.3219752754296894559, 0.3333333333333333703, 0.3219752754296894559, 0.3333333333333333703, 0.3219752754296894559, 0.3333333333333333703, 0.3219752754296894559, 0.3333333333333333703, 0.3219752754296894559, 0.3333333333333333703, 0.3219752754296894559, 0.3333333333333333703, 0.3219752754296894559, 0.3333333333333333703, 0.3219752754296894559, 0.3333333333333333703, 0.3219752754296894559, 0.3333333333333333703, 0.3219752754296894559, 0.3333333333333333703, 0.3219752754296894559, 0.3333333333333333703, 0.3219752754296894559, 0.3333333333333333703, 0.3219752754296894559, 0.3333333333333333703, 0.3219752754296894559, 0.3333333333333333703, 0.3219752754296894559, 0.3333333333333333703, 0.3219752754296894559, 0.3333333333333333703, 0.3219752754296894559, 0.3333333333333333703, 0.3219752754296894559, 0.3333333333333333703, 0.3219752754296894559, 0.3333333333333333703, 0.3219752754296894559, 0.3333333333333333703, 0.3219752754296894559, 0.3333333333333333703, 0.3219752754296894559, 0.3333333333333333703, 0.3219752754296894559, 0.3333333333333333703, 0.3219752754296894559, 0.3333333333333333703, 0.3219752754296894559, 0.3333333333333333703, 0.3219752754296894559, 0.3333333333333333703, 0.3219752754296894559, 0.3333333333333333703, 0.3219752754296894559, 0.3333333333333333703, 0.3219752754296894559, 0.3333333333333333703, 0.3219752754296894559, 0.3333333333333333703, 0.3219752754296894559, 0.3333333333333333703, 0.3219752754296894559, 0.3333333333333333703, 0.3219752754296894559, 0.3333333333333333703, 0.3219752754296894559, 0.3333333333333333703, 0.3219752754296894559, 0.3333333333333333703, 0.3219752754296894559, 0.3333333333333333703, 0.3219752754296894559, 0.3333333333333333703, 0.3219752754296894559, 0.3333333333333333703, 0.3219752754296894559, 0.3333333333333333703, 0.3219752754296894559, 0.3333333333333333703, 0.3219752754296894559, 0.3333333333333333703, 0.3219752754296894559, 0.3333333333333333703, 0.3219752754296894559, 0.3333333333333333703, 0.3219752754296894559, 0.3333333333333333703, 0.3219752754296894559, 0.3333333333333333703, 0.3219752754296894559, 0.3333333333333333703, 0.3219752754296894559, 0.3333333333333333703, 0.3219752754296894559, 0.3333333333333333703, 0.3219752754296894559, 0.3333333333333333703, 0.3219752754296894559, 0.3333333333333333703, 0.3219752754296894559, 0.3333333333333333703, 0.3219752754296894559, 0.3333333333333333703, 0.3219752754296894559, 0.3333333333333333703, 0.3219752754296894559, 0.3333333333333333703, 0.3219752754296894559, 0.3333333333333333703, 0.3219752754296894559, 0.3333333333333333703, 0.3219752754296894559, 0.3333333333333333703, 0.3219752754296894559, 0.3333333333333333703, 0.3219752754296894559, 0.3333333333333333703, 0.3219752754296894559, 0.3333333333333333703, 0.3219752754296894559, 0.3333333333333333703, 0.3219752754296894559, 0.3333333333333333703, 0.3219752754296894559, 0.3333333333333333703, 0.3219752754296894559, 0.3333333333333333703, 0.3219752754296894559, 0.3333333333333333703, 0.3219752754296894559, 0.3333333333333333703, 0.3219752754296894559, 0.3333333333333333703, 0.3219752754296894559, 0.3333333333333333703, 0.3219752754296894559, 0.3333333333333333703, 0.3219752754296894559, 0.3333333333333333703, 0.3219752754296894559, 0.3333333333333333703, 0.3219752754296894559, 0.3333333333333333703, 0.3219752754296894559, 0.3333333333333333703, 0.3219752754296894559, 0.3333333333333333703, 0.3219752754296894559, 0.3333333333333333703, 0.3219752754296894559, 0.3333333333333333703, 0.3219752754296894559, 0.3333333333333333703, 0.3219752754296894559, 0.3333333333333333703, 0.3219752754296894559, 0.3333333333333333703, 0.3219752754296894559, 0.3333333333333333703, 0.3219752754296894559, 0.3333333333333333703, 0.3219752754296894559, 0.3333333333333333703, 0.3219752754296894559, 0.3333333333333333703, 0.3219752754296894559, 0.3333333333333333703, 0.3219752754296894559, 0.3333333333333333703, 0.3219752754296894559, 0.3333333333333333703, 0.3219752754296894559, 0.3333333333333333703, 0.3219752754296894559, 0.3333333333333333703, 0.3219752754296894559, 0.3333333333333333703, 0.3219752754296894559, 0.3333333333333333703, 0.3219752754296894559, 0.3333333333333333703, 0.3219752754296894559, 0.3333333333333333703, 0.3219752754296894559, 0.3333333333333333703, 0.3219752754296894559, 0.3333333333333333703, 0.3219752754296894559, 0.3333333333333333703, 0.3219752754296894559, 0.3333333333333333703, 0.3219752754296894559, 0.3333333333333333703, 0.3219752754296894559, 0.3333333333333333703, 0.3219752754296894559, 0.3333333333333333703, 0.3219752754296894559, 0.3333333333333333703, 0.3219752754296894559, 0.3333333333333333703, 0.3219752754296894559, 0.3333333333333333703, 0.3219752754296894559, 0.3333333333333333703, 0.3219752754296894559, 0.3333333333333333703, 0.3219752754296894559, 0.3333333333333333703, 0.3219752754296894559, 0.3333333333333333703, 0.3219752754296894559, 0.3333333333333333703, 0.3219752754296894559, 0.3333333333333333703, 0.3219752754296894559, 0.3333333333333333703, 0.3219752754296894559, 0.3333333333333333703, 0.3219752754296894559, 0.3333333333333333703, 0.3219752754296894559, 0.3333333333333333703, 0.3219752754296894559, 0.3333333333333333703, 0.3219752754296894559, 0.3333333333333333703, 0.3219752754296894559, 0.3333333333333333703, 0.3219752754296894559, 0.3333333333333333703, 0.3219752754296894559, 0.3333333333333333703, 0.3219752754296894559, 0.3333333333333333703, 0.3219752754296894559, 0.3333333333333333703, 0.3219752754296894559, 0.3333333333333333703, 0.3219752754296894559, 0.3333333333333333703, 0.3219752754296894559, 0.3333333333333333703, 0.3219752754296894559, 0.3333333333333333703, 0.3219752754296894559, 0.3333333333333333703, 0.3219752754296894559, 0.3333333333333333703, 0.3219752754296894559, 0.3333333333333333703),
 ( 1.000000000000000000, 0.9659258262890683122, 1.000000000000000000, 0.9659258262890683122, 1.000000000000000000, 0.9659258262890683122, 1.000000000000000000, 0.9659258262890683122, 1.000000000000000000, 0.9659258262890683122, 1.000000000000000000, 0.9659258262890683122, 1.000000000000000000, 0.9659258262890683122, 1.000000000000000000, 0.9659258262890683122, 1.000000000000000000, 0.9659258262890683122, 1.000000000000000000, 0.9659258262890683122, 1.000000000000000000, 0.9659258262890683122, 1.000000000000000000, 0.9659258262890683122, 1.000000000000000000, 0.9659258262890683122, 1.000000000000000000, 0.9659258262890683122, 1.000000000000000000, 0.9659258262890683122, 1.000000000000000000, 0.9659258262890683122, 1.000000000000000000, 0.9659258262890683122, 1.000000000000000000, 0.9659258262890683122, 1.000000000000000000, 0.9659258262890683122, 1.000000000000000000, 0.9659258262890683122, 1.000000000000000000, 0.9659258262890683122, 1.000000000000000000, 0.9659258262890683122, 1.000000000000000000, 0.9659258262890683122, 1.000000000000000000, 0.9659258262890683122, 1.000000000000000000, 0.9659258262890683122, 1.000000000000000000, 0.9659258262890683122, 1.000000000000000000, 0.9659258262890683122, 1.000000000000000000, 0.9659258262890683122, 1.000000000000000000, 0.9659258262890683122, 1.000000000000000000, 0.9659258262890683122, 1.000000000000000000, 0.9659258262890683122, 1.000000000000000000, 0.9659258262890683122, 1.000000000000000000, 0.9659258262890683122, 1.000000000000000000, 0.9659258262890683122, 1.000000000000000000, 0.9659258262890683122, 1.000000000000000000, 0.9659258262890683122, 1.000000000000000000, 0.9659258262890683122, 1.000000000000000000, 0.9659258262890683122, 1.000000000000000000, 0.9659258262890683122, 1.000000000000000000, 0.9659258262890683122, 1.000000000000000000, 0.9659258262890683122, 1.000000000000000000, 0.9659258262890683122, 1.000000000000000000, 0.9659258262890683122, 1.000000000000000000, 0.9659258262890683122, 1.000000000000000000, 0.9659258262890683122, 1.000000000000000000, 0.9659258262890683122, 1.000000000000000000, 0.9659258262890683122, 1.000000000000000000, 0.9659258262890683122, 1.000000000000000000, 0.9659258262890683122, 1.000000000000000000, 0.9659258262890683122, 1.000000000000000000, 0.9659258262890683122, 1.000000000000000000, 0.9659258262890683122, 1.000000000000000000, 0.9659258262890683122, 1.000000000000000000, 0.9659258262890683122, 1.000000000000000000, 0.9659258262890683122, 1.000000000000000000, 0.9659258262890683122, 1.000000000000000000, 0.9659258262890683122, 1.000000000000000000, 0.9659258262890683122, 1.000000000000000000, 0.9659258262890683122, 1.000000000000000000, 0.9659258262890683122, 1.000000000000000000, 0.9659258262890683122, 1.000000000000000000, 0.9659258262890683122, 1.000000000000000000, 0.9659258262890683122, 1.000000000000000000, 0.9659258262890683122, 1.000000000000000000, 0.9659258262890683122, 1.000000000000000000, 0.9659258262890683122, 1.000000000000000000, 0.9659258262890683122, 1.000000000000000000, 0.9659258262890683122, 1.000000000000000000, 0.9659258262890683122, 1.000000000000000000, 0.9659258262890683122, 1.000000000000000000, 0.9659258262890683122, 1.000000000000000000, 0.9659258262890683122, 1.000000000000000000, 0.9659258262890683122, 1.000000000000000000, 0.9659258262890683122, 1.000000000000000000, 0.9659258262890683122, 1.000000000000000000, 0.9659258262890683122, 1.000000000000000000, 0.9659258262890683122, 1.000000000000000000, 0.9659258262890683122, 1.000000000000000000, 0.9659258262890683122, 1.000000000000000000, 0.9659258262890683122, 1.000000000000000000, 0.9659258262890683122, 1.000000000000000000, 0.9659258262890683122, 1.000000000000000000, 0.9659258262890683122, 1.000000000000000000, 0.9659258262890683122, 1.000000000000000000, 0.9659258262890683122, 1.000000000000000000, 0.9659258262890683122, 1.000000000000000000, 0.9659258262890683122, 1.000000000000000000, 0.9659258262890683122, 1.000000000000000000, 0.9659258262890683122, 1.000000000000000000, 0.9659258262890683122, 1.000000000000000000, 0.9659258262890683122, 1.000000000000000000, 0.9659258262890683122, 1.000000000000000000, 0.9659258262890683122, 1.000000000000000000, 0.9659258262890683122, 1.000000000000000000, 0.9659258262890683122, 1.000000000000000000, 0.9659258262890683122, 1.000000000000000000, 0.9659258262890683122, 1.000000000000000000, 0.9659258262890683122, 1.000000000000000000, 0.9659258262890683122, 1.000000000000000000, 0.9659258262890683122, 1.000000000000000000, 0.9659258262890683122, 1.000000000000000000, 0.9659258262890683122, 1.000000000000000000, 0.9659258262890683122, 1.000000000000000000, 0.9659258262890683122, 1.000000000000000000, 0.9659258262890683122, 1.000000000000000000, 0.9659258262890683122, 1.000000000000000000, 0.9659258262890683122, 1.000000000000000000, 0.9659258262890683122, 1.000000000000000000, 0.9659258262890683122, 1.000000000000000000, 0.9659258262890683122, 1.000000000000000000, 0.9659258262890683122, 1.000000000000000000, 0.9659258262890683122, 1.000000000000000000, 0.9659258262890683122, 1.000000000000000000, 0.9659258262890683122, 1.000000000000000000, 0.9659258262890683122, 1.000000000000000000, 0.9659258262890683122, 1.000000000000000000, 0.9659258262890683122, 1.000000000000000000, 0.9659258262890683122, 1.000000000000000000, 0.9659258262890683122, 1.000000000000000000, 0.9659258262890683122, 1.000000000000000000, 0.9659258262890683122, 1.000000000000000000, 0.9659258262890683122, 1.000000000000000000, 0.9659258262890683122, 1.000000000000000000, 0.9659258262890683122, 1.000000000000000000, 0.9659258262890683122, 1.000000000000000000, 0.9659258262890683122, 1.000000000000000000, 0.9659258262890683122, 1.000000000000000000, 0.9659258262890683122, 1.000000000000000000, 0.9659258262890683122, 1.000000000000000000, 0.9659258262890683122, 1.000000000000000000, 0.9659258262890683122, 1.000000000000000000, 0.9659258262890683122, 1.000000000000000000, 0.9659258262890683122, 1.000000000000000000, 0.9659258262890683122, 1.000000000000000000, 0.9659258262890683122, 1.000000000000000000, 0.9659258262890683122, 1.000000000000000000, 0.9659258262890683122, 1.000000000000000000, 0.9659258262890683122, 1.000000000000000000, 0.9659258262890683122, 1.000000000000000000, 0.9659258262890683122, 1.000000000000000000, 0.9659258262890683122, 1.000000000000000000, 0.9659258262890683122, 1.000000000000000000, 0.9659258262890683122, 1.000000000000000000, 0.9659258262890683122, 1.000000000000000000, 0.9659258262890683122, 1.000000000000000000, 0.9659258262890683122, 1.000000000000000000, 0.9659258262890683122, 1.000000000000000000, 0.9659258262890683122, 1.000000000000000000, 0.9659258262890683122, 1.000000000000000000, 0.9659258262890683122, 1.000000000000000000, 0.9659258262890683122, 1.000000000000000000, 0.9659258262890683122, 1.000000000000000000, 0.9659258262890683122, 1.000000000000000000, 0.9659258262890683122, 1.000000000000000000, 0.9659258262890683122, 1.000000000000000000, 0.9659258262890683122, 1.000000000000000000, 0.9659258262890683122, 1.000000000000000000, 0.9659258262890683122, 1.000000000000000000, 0.9659258262890683122, 1.000000000000000000, 0.9659258262890683122, 1.000000000000000000, 0.9659258262890683122, 1.000000000000000000, 0.9659258262890683122, 1.000000000000000000, 0.9659258262890683122, 1.000000000000000000, 0.9659258262890683122, 1.000000000000000000, 0.9659258262890683122, 1.000000000000000000, 0.9659258262890683122, 1.000000000000000000, 0.9659258262890683122, 1.000000000000000000, 0.9659258262890683122, 1.000000000000000000, 0.9659258262890683122, 1.000000000000000000, 0.9659258262890683122, 1.000000000000000000, 0.9659258262890683122, 1.000000000000000000, 0.9659258262890683122, 1.000000000000000000, 0.9659258262890683122, 1.000000000000000000, 0.9659258262890683122, 1.000000000000000000, 0.9659258262890683122, 1.000000000000000000, 0.9659258262890683122, 1.000000000000000000, 0.9659258262890683122, 1.000000000000000000, 0.9659258262890683122, 1.000000000000000000, 0.9659258262890683122, 1.000000000000000000, 0.9659258262890683122, 1.000000000000000000, 0.9659258262890683122, 1.000000000000000000, 0.9659258262890683122, 1.000000000000000000, 0.9659258262890683122, 1.000000000000000000, 0.9659258262890683122, 1.000000000000000000, 0.9659258262890683122, 1.000000000000000000, 0.9659258262890683122, 1.000000000000000000, 0.9659258262890683122, 1.000000000000000000, 0.9659258262890683122, 1.000000000000000000, 0.9659258262890683122, 1.000000000000000000, 0.9659258262890683122, 1.000000000000000000, 0.9659258262890683122, 1.000000000000000000, 0.9659258262890683122, 1.000000000000000000, 0.9659258262890683122, 1.000000000000000000, 0.9659258262890683122, 1.000000000000000000, 0.9659258262890683122, 1.000000000000000000, 0.9659258262890683122, 1.000000000000000000, 0.9659258262890683122, 1.000000000000000000, 0.9659258262890683122, 1.000000000000000000, 0.9659258262890683122, 1.000000000000000000, 0.9659258262890683122, 1.000000000000000000, 0.9659258262890683122, 1.000000000000000000, 0.9659258262890683122, 1.000000000000000000, 0.9659258262890683122, 1.000000000000000000, 0.9659258262890683122, 1.000000000000000000, 0.9659258262890683122, 1.000000000000000000, 0.9659258262890683122, 1.000000000000000000, 0.9659258262890683122, 1.000000000000000000, 0.9659258262890683122, 1.000000000000000000, 0.9659258262890683122, 1.000000000000000000, 0.9659258262890683122, 1.000000000000000000, 0.9659258262890683122, 1.000000000000000000, 0.9659258262890683122, 1.000000000000000000, 0.9659258262890683122, 1.000000000000000000, 0.9659258262890683122, 1.000000000000000000, 0.9659258262890683122, 1.000000000000000000, 0.9659258262890683122, 1.000000000000000000, 0.9659258262890683122, 1.000000000000000000, 0.9659258262890683122, 1.000000000000000000, 0.9659258262890683122, 1.000000000000000000, 0.9659258262890683122, 1.000000000000000000, 0.9659258262890683122, 1.000000000000000000, 0.9659258262890683122, 1.000000000000000000, 0.9659258262890683122, 1.000000000000000000, 0.9659258262890683122, 1.000000000000000000, 0.9659258262890683122, 1.000000000000000000, 0.9659258262890683122, 1.000000000000000000, 0.9659258262890683122, 1.000000000000000000, 0.9659258262890683122, 1.000000000000000000),
 ( 0.3333333333333333703, 0.3219752754296894559, 0.3333333333333333703, 0.3219752754296894559, 0.3333333333333333703, 0.3219752754296894559, 0.3333333333333333703, 0.3219752754296894559, 0.3333333333333333703, 0.3219752754296894559, 0.3333333333333333703, 0.3219752754296894559, 0.3333333333333333703, 0.3219752754296894559, 0.3333333333333333703, 0.3219752754296894559, 0.3333333333333333703, 0.3219752754296894559, 0.3333333333333333703, 0.3219752754296894559, 0.3333333333333333703, 0.3219752754296894559, 0.3333333333333333703, 0.3219752754296894559, 0.3333333333333333703, 0.3219752754296894559, 0.3333333333333333703, 0.3219752754296894559, 0.3333333333333333703, 0.3219752754296894559, 0.3333333333333333703, 0.3219752754296894559, 0.3333333333333333703, 0.3219752754296894559, 0.3333333333333333703, 0.3219752754296894559, 0.3333333333333333703, 0.3219752754296894559, 0.3333333333333333703, 0.3219752754296894559, 0.3333333333333333703, 0.3219752754296894559, 0.3333333333333333703, 0.3219752754296894559, 0.3333333333333333703, 0.3219752754296894559, 0.3333333333333333703, 0.3219752754296894559, 0.3333333333333333703, 0.3219752754296894559, 0.3333333333333333703, 0.3219752754296894559, 0.3333333333333333703, 0.3219752754296894559, 0.3333333333333333703, 0.3219752754296894559, 0.3333333333333333703, 0.3219752754296894559, 0.3333333333333333703, 0.3219752754296894559, 0.3333333333333333703, 0.3219752754296894559, 0.3333333333333333703, 0.3219752754296894559, 0.3333333333333333703, 0.3219752754296894559, 0.3333333333333333703, 0.3219752754296894559, 0.3333333333333333703, 0.3219752754296894559, 0.3333333333333333703, 0.3219752754296894559, 0.3333333333333333703, 0.3219752754296894559, 0.3333333333333333703, 0.3219752754296894559, 0.3333333333333333703, 0.3219752754296894559, 0.3333333333333333703, 0.3219752754296894559, 0.3333333333333333703, 0.3219752754296894559, 0.3333333333333333703, 0.3219752754296894559, 0.3333333333333333703, 0.3219752754296894559, 0.3333333333333333703, 0.3219752754296894559, 0.3333333333333333703, 0.3219752754296894559, 0.3333333333333333703, 0.3219752754296894559, 0.3333333333333333703, 0.3219752754296894559, 0.3333333333333333703, 0.3219752754296894559, 0.3333333333333333703, 0.3219752754296894559, 0.3333333333333333703, 0.3219752754296894559, 0.3333333333333333703, 0.3219752754296894559, 0.3333333333333333703, 0.3219752754296894559, 0.3333333333333333703, 0.3219752754296894559, 0.3333333333333333703, 0.3219752754296894559, 0.3333333333333333703, 0.3219752754296894559, 0.3333333333333333703, 0.3219752754296894559, 0.3333333333333333703, 0.3219752754296894559, 0.3333333333333333703, 0.3219752754296894559, 0.3333333333333333703, 0.3219752754296894559, 0.3333333333333333703, 0.3219752754296894559, 0.3333333333333333703, 0.3219752754296894559, 0.3333333333333333703, 0.3219752754296894559, 0.3333333333333333703, 0.3219752754296894559, 0.3333333333333333703, 0.3219752754296894559, 0.3333333333333333703, 0.3219752754296894559, 0.3333333333333333703, 0.3219752754296894559, 0.3333333333333333703, 0.3219752754296894559, 0.3333333333333333703, 0.3219752754296894559, 0.3333333333333333703, 0.3219752754296894559, 0.3333333333333333703, 0.3219752754296894559, 0.3333333333333333703, 0.3219752754296894559, 0.3333333333333333703, 0.3219752754296894559, 0.3333333333333333703, 0.3219752754296894559, 0.3333333333333333703, 0.3219752754296894559, 0.3333333333333333703, 0.3219752754296894559, 0.3333333333333333703, 0.3219752754296894559, 0.3333333333333333703, 0.3219752754296894559, 0.3333333333333333703, 0.3219752754296894559, 0.3333333333333333703, 0.3219752754296894559, 0.3333333333333333703, 0.3219752754296894559, 0.3333333333333333703, 0.3219752754296894559, 0.3333333333333333703, 0.3219752754296894559, 0.3333333333333333703, 0.3219752754296894559, 0.3333333333333333703, 0.3219752754296894559, 0.3333333333333333703, 0.3219752754296894559, 0.3333333333333333703, 0.3219752754296894559, 0.3333333333333333703, 0.3219752754296894559, 0.3333333333333333703, 0.3219752754296894559, 0.3333333333333333703, 0.3219752754296894559, 0.3333333333333333703, 0.3219752754296894559, 0.3333333333333333703, 0.3219752754296894559, 0.3333333333333333703, 0.3219752754296894559, 0.3333333333333333703, 0.3219752754296894559, 0.3333333333333333703, 0.3219752754296894559, 0.3333333333333333703, 0.3219752754296894559, 0.3333333333333333703, 0.3219752754296894559, 0.3333333333333333703, 0.3219752754296894559, 0.3333333333333333703, 0.3219752754296894559, 0.3333333333333333703, 0.3219752754296894559, 0.3333333333333333703, 0.3219752754296894559, 0.3333333333333333703, 0.3219752754296894559, 0.3333333333333333703, 0.3219752754296894559, 0.3333333333333333703, 0.3219752754296894559, 0.3333333333333333703, 0.3219752754296894559, 0.3333333333333333703, 0.3219752754296894559, 0.3333333333333333703, 0.3219752754296894559, 0.3333333333333333703, 0.3219752754296894559, 0.3333333333333333703, 0.3219752754296894559, 0.3333333333333333703, 0.3219752754296894559, 0.3333333333333333703, 0.3219752754296894559, 0.3333333333333333703, 0.3219752754296894559, 0.3333333333333333703, 0.3219752754296894559, 0.3333333333333333703, 0.3219752754296894559, 0.3333333333333333703, 0.3219752754296894559, 0.3333333333333333703, 0.3219752754296894559, 0.3333333333333333703, 0.3219752754296894559, 0.3333333333333333703, 0.3219752754296894559, 0.3333333333333333703, 0.3219752754296894559, 0.3333333333333333703, 0.3219752754296894559, 0.3333333333333333703, 0.3219752754296894559, 0.3333333333333333703, 0.3219752754296894559, 0.3333333333333333703, 0.3219752754296894559, 0.3333333333333333703, 0.3219752754296894559, 0.3333333333333333703, 0.3219752754296894559, 0.3333333333333333703, 0.3219752754296894559, 0.3333333333333333703, 0.3219752754296894559, 0.3333333333333333703, 0.3219752754296894559, 0.3333333333333333703, 0.3219752754296894559, 0.3333333333333333703, 0.3219752754296894559, 0.3333333333333333703, 0.3219752754296894559, 0.3333333333333333703, 0.3219752754296894559, 0.3333333333333333703, 0.3219752754296894559, 0.3333333333333333703, 0.3219752754296894559, 0.3333333333333333703, 0.3219752754296894559, 0.3333333333333333703, 0.3219752754296894559, 0.3333333333333333703, 0.3219752754296894559, 0.3333333333333333703, 0.3219752754296894559, 0.3333333333333333703, 0.3219752754296894559, 0.3333333333333333703, 0.3219752754296894559, 0.3333333333333333703, 0.3219752754296894559, 0.3333333333333333703, 0.3219752754296894559, 0.3333333333333333703, 0.3219752754296894559, 0.3333333333333333703, 0.3219752754296894559, 0.3333333333333333703, 0.3219752754296894559, 0.3333333333333333703, 0.3219752754296894559, 0.3333333333333333703, 0.3219752754296894559, 0.3333333333333333703, 0.3219752754296894559, 0.3333333333333333703, 0.3219752754296894559, 0.3333333333333333703, 0.3219752754296894559, 0.3333333333333333703, 0.3219752754296894559, 0.3333333333333333703, 0.3219752754296894559, 0.3333333333333333703, 0.3219752754296894559, 0.3333333333333333703, 0.3219752754296894559, 0.3333333333333333703, 0.3219752754296894559, 0.3333333333333333703, 0.3219752754296894559, 0.3333333333333333703, 0.3219752754296894559, 0.3333333333333333703, 0.3219752754296894559, 0.3333333333333333703, 0.3219752754296894559, 0.3333333333333333703, 0.3219752754296894559, 0.3333333333333333703, 0.3219752754296894559, 0.3333333333333333703, 0.3219752754296894559, 0.3333333333333333703, 0.3219752754296894559, 0.3333333333333333703, 0.3219752754296894559, 0.3333333333333333703, 0.3219752754296894559, 0.3333333333333333703, 0.3219752754296894559, 0.3333333333333333703, 0.3219752754296894559, 0.3333333333333333703, 0.3219752754296894559, 0.3333333333333333703, 0.3219752754296894559, 0.3333333333333333703, 0.3219752754296894559, 0.3333333333333333703, 0.3219752754296894559, 0.3333333333333333703, 0.3219752754296894559, 0.3333333333333333703, 0.3219752754296894559, 0.3333333333333333703, 0.3219752754296894559, 0.3333333333333333703, 0.3219752754296894559, 0.3333333333333333703, 0.3219752754296894559, 0.3333333333333333703, 0.3219752754296894559, 0.3333333333333333703, 0.3219752754296894559, 0.3333333333333333703, 0.3219752754296894559, 0.3333333333333333703, 0.3219752754296894559, 0.3333333333333333703, 0.3219752754296894559, 0.3333333333333333703, 0.3219752754296894559, 0.3333333333333333703, 0.3219752754296894559, 0.3333333333333333703, 0.3219752754296894559, 0.3333333333333333703, 0.3219752754296894559, 0.3333333333333333703, 0.3219752754296894559, 0.3333333333333333703, 0.3219752754296894559, 0.3333333333333333703, 0.3219752754296894559, 0.3333333333333333703, 0.3219752754296894559, 0.3333333333333333703, 0.3219752754296894559, 0.3333333333333333703, 0.3219752754296894559, 0.3333333333333333703, 0.3219752754296894559, 0.3333333333333333703, 0.3219752754296894559, 0.3333333333333333703, 0.3219752754296894559, 0.3333333333333333703, 0.3219752754296894559, 0.3333333333333333703, 0.3219752754296894559, 0.3333333333333333703, 0.3219752754296894559, 0.3333333333333333703, 0.3219752754296894559, 0.3333333333333333703, 0.3219752754296894559, 0.3333333333333333703, 0.3219752754296894559, 0.3333333333333333703, 0.3219752754296894559, 0.3333333333333333703, 0.3219752754296894559, 0.3333333333333333703, 0.3219752754296894559, 0.3333333333333333703, 0.3219752754296894559, 0.3333333333333333703, 0.3219752754296894559, 0.3333333333333333703, 0.3219752754296894559, 0.3333333333333333703, 0.3219752754296894559, 0.3333333333333333703, 0.3219752754296894559, 0.3333333333333333703, 0.3219752754296894559, 0.3333333333333333703, 0.3219752754296894559, 0.3333333333333333703, 0.3219752754296894559, 0.3333333333333333703, 0.3219752754296894559, 0.3333333333333333703, 0.3219752754296894559, 0.3333333333333333703, 0.3219752754296894559, 0.3333333333333333703, 0.3219752754296894559, 0.3333333333333333703, 0.3219752754296894559, 0.3333333333333333703, 0.3219752754296894559, 0.3333333333333333703, 0.3219752754296894559, 0.3333333333333333703, 0.3219752754296894559, 0.3333333333333333703, 0.3219752754296894559, 0.3333333333333333703, 0.3219752754296894559, 0.3333333333333333703, 0.3219752754296894559, 0.3333333333333333703, 0.3219752754296894559, 0.3333333333333333703, 0.3219752754296894559, 0.3333333333333333703, 0.3219752754296894559, 0.3333333333333333703, 0.3219752754296894559, 0.3333333333333333703, 0.3219752754296894559, 0.3333333333333333703, 0.3219752754296894559, 0.3333333333333333703, 0.3219752754296894559, 0.3333333333333333703),
 ( 0.3333333333333333703, 0.3219752754296894559, 0.3333333333333333703, 0.3219752754296894559, 0.3333333333333333703, 0.3219752754296894559, 0.3333333333333333703, 0.3219752754296894559, 0.3333333333333333703, 0.3219752754296894559, 0.3333333333333333703, 0.3219752754296894559, 0.3333333333333333703, 0.3219752754296894559, 0.3333333333333333703, 0.3219752754296894559, 0.3333333333333333703, 0.3219752754296894559, 0.3333333333333333703, 0.3219752754296894559, 0.3333333333333333703, 0.3219752754296894559, 0.3333333333333333703, 0.3219752754296894559, 0.3333333333333333703, 0.3219752754296894559, 0.3333333333333333703, 0.3219752754296894559, 0.3333333333333333703, 0.3219752754296894559, 0.3333333333333333703, 0.3219752754296894559, 0.3333333333333333703, 0.3219752754296894559, 0.3333333333333333703, 0.3219752754296894559, 0.3333333333333333703, 0.3219752754296894559, 0.3333333333333333703, 0.3219752754296894559, 0.3333333333333333703, 0.3219752754296894559, 0.3333333333333333703, 0.3219752754296894559, 0.3333333333333333703, 0.3219752754296894559, 0.3333333333333333703, 0.3219752754296894559, 0.3333333333333333703, 0.3219752754296894559, 0.3333333333333333703, 0.3219752754296894559, 0.3333333333333333703, 0.3219752754296894559, 0.3333333333333333703, 0.3219752754296894559, 0.3333333333333333703, 0.3219752754296894559, 0.3333333333333333703, 0.3219752754296894559, 0.3333333333333333703, 0.3219752754296894559, 0.3333333333333333703, 0.3219752754296894559, 0.3333333333333333703, 0.3219752754296894559, 0.3333333333333333703, 0.3219752754296894559, 0.3333333333333333703, 0.3219752754296894559, 0.3333333333333333703, 0.3219752754296894559, 0.3333333333333333703, 0.3219752754296894559, 0.3333333333333333703, 0.3219752754296894559, 0.3333333333333333703, 0.3219752754296894559, 0.3333333333333333703, 0.3219752754296894559, 0.3333333333333333703, 0.3219752754296894559, 0.3333333333333333703, 0.3219752754296894559, 0.3333333333333333703, 0.3219752754296894559, 0.3333333333333333703, 0.3219752754296894559, 0.3333333333333333703, 0.3219752754296894559, 0.3333333333333333703, 0.3219752754296894559, 0.3333333333333333703, 0.3219752754296894559, 0.3333333333333333703, 0.3219752754296894559, 0.3333333333333333703, 0.3219752754296894559, 0.3333333333333333703, 0.3219752754296894559, 0.3333333333333333703, 0.3219752754296894559, 0.3333333333333333703, 0.3219752754296894559, 0.3333333333333333703, 0.3219752754296894559, 0.3333333333333333703, 0.3219752754296894559, 0.3333333333333333703, 0.3219752754296894559, 0.3333333333333333703, 0.3219752754296894559, 0.3333333333333333703, 0.3219752754296894559, 0.3333333333333333703, 0.3219752754296894559, 0.3333333333333333703, 0.3219752754296894559, 0.3333333333333333703, 0.3219752754296894559, 0.3333333333333333703, 0.3219752754296894559, 0.3333333333333333703, 0.3219752754296894559, 0.3333333333333333703, 0.3219752754296894559, 0.3333333333333333703, 0.3219752754296894559, 0.3333333333333333703, 0.3219752754296894559, 0.3333333333333333703, 0.3219752754296894559, 0.3333333333333333703, 0.3219752754296894559, 0.3333333333333333703, 0.3219752754296894559, 0.3333333333333333703, 0.3219752754296894559, 0.3333333333333333703, 0.3219752754296894559, 0.3333333333333333703, 0.3219752754296894559, 0.3333333333333333703, 0.3219752754296894559, 0.3333333333333333703, 0.3219752754296894559, 0.3333333333333333703, 0.3219752754296894559, 0.3333333333333333703, 0.3219752754296894559, 0.3333333333333333703, 0.3219752754296894559, 0.3333333333333333703, 0.3219752754296894559, 0.3333333333333333703, 0.3219752754296894559, 0.3333333333333333703, 0.3219752754296894559, 0.3333333333333333703, 0.3219752754296894559, 0.3333333333333333703, 0.3219752754296894559, 0.3333333333333333703, 0.3219752754296894559, 0.3333333333333333703, 0.3219752754296894559, 0.3333333333333333703, 0.3219752754296894559, 0.3333333333333333703, 0.3219752754296894559, 0.3333333333333333703, 0.3219752754296894559, 0.3333333333333333703, 0.3219752754296894559, 0.3333333333333333703, 0.3219752754296894559, 0.3333333333333333703, 0.3219752754296894559, 0.3333333333333333703, 0.3219752754296894559, 0.3333333333333333703, 0.3219752754296894559, 0.3333333333333333703, 0.3219752754296894559, 0.3333333333333333703, 0.3219752754296894559, 0.3333333333333333703, 0.3219752754296894559, 0.3333333333333333703, 0.3219752754296894559, 0.3333333333333333703, 0.3219752754296894559, 0.3333333333333333703, 0.3219752754296894559, 0.3333333333333333703, 0.3219752754296894559, 0.3333333333333333703, 0.3219752754296894559, 0.3333333333333333703, 0.3219752754296894559, 0.3333333333333333703, 0.3219752754296894559, 0.3333333333333333703, 0.3219752754296894559, 0.3333333333333333703, 0.3219752754296894559, 0.3333333333333333703, 0.3219752754296894559, 0.3333333333333333703, 0.3219752754296894559, 0.3333333333333333703, 0.3219752754296894559, 0.3333333333333333703, 0.3219752754296894559, 0.3333333333333333703, 0.3219752754296894559, 0.3333333333333333703, 0.3219752754296894559, 0.3333333333333333703, 0.3219752754296894559, 0.3333333333333333703, 0.3219752754296894559, 0.3333333333333333703, 0.3219752754296894559, 0.3333333333333333703, 0.3219752754296894559, 0.3333333333333333703, 0.3219752754296894559, 0.3333333333333333703, 0.3219752754296894559, 0.3333333333333333703, 0.3219752754296894559, 0.3333333333333333703, 0.3219752754296894559, 0.3333333333333333703, 0.3219752754296894559, 0.3333333333333333703, 0.3219752754296894559, 0.3333333333333333703, 0.3219752754296894559, 0.3333333333333333703, 0.3219752754296894559, 0.3333333333333333703, 0.3219752754296894559, 0.3333333333333333703, 0.3219752754296894559, 0.3333333333333333703, 0.3219752754296894559, 0.3333333333333333703, 0.3219752754296894559, 0.3333333333333333703, 0.3219752754296894559, 0.3333333333333333703, 0.3219752754296894559, 0.3333333333333333703, 0.3219752754296894559, 0.3333333333333333703, 0.3219752754296894559, 0.3333333333333333703, 0.3219752754296894559, 0.3333333333333333703, 0.3219752754296894559, 0.3333333333333333703, 0.3219752754296894559, 0.3333333333333333703, 0.3219752754296894559, 0.3333333333333333703, 0.3219752754296894559, 0.3333333333333333703, 0.3219752754296894559, 0.3333333333333333703, 0.3219752754296894559, 0.3333333333333333703, 0.3219752754296894559, 0.3333333333333333703, 0.3219752754296894559, 0.3333333333333333703, 0.3219752754296894559, 0.3333333333333333703, 0.3219752754296894559, 0.3333333333333333703, 0.3219752754296894559, 0.3333333333333333703, 0.3219752754296894559, 0.3333333333333333703, 0.3219752754296894559, 0.3333333333333333703, 0.3219752754296894559, 0.3333333333333333703, 0.3219752754296894559, 0.3333333333333333703, 0.3219752754296894559, 0.3333333333333333703, 0.3219752754296894559, 0.3333333333333333703, 0.3219752754296894559, 0.3333333333333333703, 0.3219752754296894559, 0.3333333333333333703, 0.3219752754296894559, 0.3333333333333333703, 0.3219752754296894559, 0.3333333333333333703, 0.3219752754296894559, 0.3333333333333333703, 0.3219752754296894559, 0.3333333333333333703, 0.3219752754296894559, 0.3333333333333333703, 0.3219752754296894559, 0.3333333333333333703, 0.3219752754296894559, 0.3333333333333333703, 0.3219752754296894559, 0.3333333333333333703, 0.3219752754296894559, 0.3333333333333333703, 0.3219752754296894559, 0.3333333333333333703, 0.3219752754296894559, 0.3333333333333333703, 0.3219752754296894559, 0.3333333333333333703, 0.3219752754296894559, 0.3333333333333333703, 0.3219752754296894559, 0.3333333333333333703, 0.3219752754296894559, 0.3333333333333333703, 0.3219752754296894559, 0.3333333333333333703, 0.3219752754296894559, 0.3333333333333333703, 0.3219752754296894559, 0.3333333333333333703, 0.3219752754296894559, 0.3333333333333333703, 0.3219752754296894559, 0.3333333333333333703, 0.3219752754296894559, 0.3333333333333333703, 0.3219752754296894559, 0.3333333333333333703, 0.3219752754296894559, 0.3333333333333333703, 0.3219752754296894559, 0.3333333333333333703, 0.3219752754296894559, 0.3333333333333333703, 0.3219752754296894559, 0.3333333333333333703, 0.3219752754296894559, 0.3333333333333333703, 0.3219752754296894559, 0.3333333333333333703, 0.3219752754296894559, 0.3333333333333333703, 0.3219752754296894559, 0.3333333333333333703, 0.3219752754296894559, 0.3333333333333333703, 0.3219752754296894559, 0.3333333333333333703, 0.3219752754296894559, 0.3333333333333333703, 0.3219752754296894559, 0.3333333333333333703, 0.3219752754296894559, 0.3333333333333333703, 0.3219752754296894559, 0.3333333333333333703, 0.3219752754296894559, 0.3333333333333333703, 0.3219752754296894559, 0.3333333333333333703, 0.3219752754296894559, 0.3333333333333333703, 0.3219752754296894559, 0.3333333333333333703, 0.3219752754296894559, 0.3333333333333333703, 0.3219752754296894559, 0.3333333333333333703, 0.3219752754296894559, 0.3333333333333333703, 0.3219752754296894559, 0.3333333333333333703, 0.3219752754296894559, 0.3333333333333333703, 0.3219752754296894559, 0.3333333333333333703, 0.3219752754296894559, 0.3333333333333333703, 0.3219752754296894559, 0.3333333333333333703, 0.3219752754296894559, 0.3333333333333333703, 0.3219752754296894559, 0.3333333333333333703, 0.3219752754296894559, 0.3333333333333333703, 0.3219752754296894559, 0.3333333333333333703, 0.3219752754296894559, 0.3333333333333333703, 0.3219752754296894559, 0.3333333333333333703, 0.3219752754296894559, 0.3333333333333333703, 0.3219752754296894559, 0.3333333333333333703, 0.3219752754296894559, 0.3333333333333333703, 0.3219752754296894559, 0.3333333333333333703, 0.3219752754296894559, 0.3333333333333333703, 0.3219752754296894559, 0.3333333333333333703, 0.3219752754296894559, 0.3333333333333333703, 0.3219752754296894559, 0.3333333333333333703, 0.3219752754296894559, 0.3333333333333333703, 0.3219752754296894559, 0.3333333333333333703, 0.3219752754296894559, 0.3333333333333333703, 0.3219752754296894559, 0.3333333333333333703, 0.3219752754296894559, 0.3333333333333333703, 0.3219752754296894559, 0.3333333333333333703, 0.3219752754296894559, 0.3333333333333333703, 0.3219752754296894559, 0.3333333333333333703, 0.3219752754296894559, 0.3333333333333333703, 0.3219752754296894559, 0.3333333333333333703, 0.3219752754296894559, 0.3333333333333333703, 0.3219752754296894559, 0.3333333333333333703, 0.3219752754296894559, 0.3333333333333333703, 0.3219752754296894559, 0.3333333333333333703, 0.3219752754296894559, 0.3333333333333333703, 0.3219752754296894559, 0.3333333333333333703, 0.3219752754296894559, 0.3333333333333333703),
 ( 1.000000000000000000, 0.9659258262890683122, 1.000000000000000000, 0.9659258262890683122, 1.000000000000000000, 0.9659258262890683122, 1.000000000000000000, 0.9659258262890683122, 1.000000000000000000, 0.9659258262890683122, 1.000000000000000000, 0.9659258262890683122, 1.000000000000000000, 0.9659258262890683122, 1.000000000000000000, 0.9659258262890683122, 1.000000000000000000, 0.9659258262890683122, 1.000000000000000000, 0.9659258262890683122, 1.000000000000000000, 0.9659258262890683122, 1.000000000000000000, 0.9659258262890683122, 1.000000000000000000, 0.9659258262890683122, 1.000000000000000000, 0.9659258262890683122, 1.000000000000000000, 0.9659258262890683122, 1.000000000000000000, 0.9659258262890683122, 1.000000000000000000, 0.9659258262890683122, 1.000000000000000000, 0.9659258262890683122, 1.000000000000000000, 0.9659258262890683122, 1.000000000000000000, 0.9659258262890683122, 1.000000000000000000, 0.9659258262890683122, 1.000000000000000000, 0.9659258262890683122, 1.000000000000000000, 0.9659258262890683122, 1.000000000000000000, 0.9659258262890683122, 1.000000000000000000, 0.9659258262890683122, 1.000000000000000000, 0.9659258262890683122, 1.000000000000000000, 0.9659258262890683122, 1.000000000000000000, 0.9659258262890683122, 1.000000000000000000, 0.9659258262890683122, 1.000000000000000000, 0.9659258262890683122, 1.000000000000000000, 0.9659258262890683122, 1.000000000000000000, 0.9659258262890683122, 1.000000000000000000, 0.9659258262890683122, 1.000000000000000000, 0.9659258262890683122, 1.000000000000000000, 0.9659258262890683122, 1.000000000000000000, 0.9659258262890683122, 1.000000000000000000, 0.9659258262890683122, 1.000000000000000000, 0.9659258262890683122, 1.000000000000000000, 0.9659258262890683122, 1.000000000000000000, 0.9659258262890683122, 1.000000000000000000, 0.9659258262890683122, 1.000000000000000000, 0.9659258262890683122, 1.000000000000000000, 0.9659258262890683122, 1.000000000000000000, 0.9659258262890683122, 1.000000000000000000, 0.9659258262890683122, 1.000000000000000000, 0.9659258262890683122, 1.000000000000000000, 0.9659258262890683122, 1.000000000000000000, 0.9659258262890683122, 1.000000000000000000, 0.9659258262890683122, 1.000000000000000000, 0.9659258262890683122, 1.000000000000000000, 0.9659258262890683122, 1.000000000000000000, 0.9659258262890683122, 1.000000000000000000, 0.9659258262890683122, 1.000000000000000000, 0.9659258262890683122, 1.000000000000000000, 0.9659258262890683122, 1.000000000000000000, 0.9659258262890683122, 1.000000000000000000, 0.9659258262890683122, 1.000000000000000000, 0.9659258262890683122, 1.000000000000000000, 0.9659258262890683122, 1.000000000000000000, 0.9659258262890683122, 1.000000000000000000, 0.9659258262890683122, 1.000000000000000000, 0.9659258262890683122, 1.000000000000000000, 0.9659258262890683122, 1.000000000000000000, 0.9659258262890683122, 1.000000000000000000, 0.9659258262890683122, 1.000000000000000000, 0.9659258262890683122, 1.000000000000000000, 0.9659258262890683122, 1.000000000000000000, 0.9659258262890683122, 1.000000000000000000, 0.9659258262890683122, 1.000000000000000000, 0.9659258262890683122, 1.000000000000000000, 0.9659258262890683122, 1.000000000000000000, 0.9659258262890683122, 1.000000000000000000, 0.9659258262890683122, 1.000000000000000000, 0.9659258262890683122, 1.000000000000000000, 0.9659258262890683122, 1.000000000000000000, 0.9659258262890683122, 1.000000000000000000, 0.9659258262890683122, 1.000000000000000000, 0.9659258262890683122, 1.000000000000000000, 0.9659258262890683122, 1.000000000000000000, 0.9659258262890683122, 1.000000000000000000, 0.9659258262890683122, 1.000000000000000000, 0.9659258262890683122, 1.000000000000000000, 0.9659258262890683122, 1.000000000000000000, 0.9659258262890683122, 1.000000000000000000, 0.9659258262890683122, 1.000000000000000000, 0.9659258262890683122, 1.000000000000000000, 0.9659258262890683122, 1.000000000000000000, 0.9659258262890683122, 1.000000000000000000, 0.9659258262890683122, 1.000000000000000000, 0.9659258262890683122, 1.000000000000000000, 0.9659258262890683122, 1.000000000000000000, 0.9659258262890683122, 1.000000000000000000, 0.9659258262890683122, 1.000000000000000000, 0.9659258262890683122, 1.000000000000000000, 0.9659258262890683122, 1.000000000000000000, 0.9659258262890683122, 1.000000000000000000, 0.9659258262890683122, 1.000000000000000000, 0.9659258262890683122, 1.000000000000000000, 0.9659258262890683122, 1.000000000000000000, 0.9659258262890683122, 1.000000000000000000, 0.9659258262890683122, 1.000000000000000000, 0.9659258262890683122, 1.000000000000000000, 0.9659258262890683122, 1.000000000000000000, 0.9659258262890683122, 1.000000000000000000, 0.9659258262890683122, 1.000000000000000000, 0.9659258262890683122, 1.000000000000000000, 0.9659258262890683122, 1.000000000000000000, 0.9659258262890683122, 1.000000000000000000, 0.9659258262890683122, 1.000000000000000000, 0.9659258262890683122, 1.000000000000000000, 0.9659258262890683122, 1.000000000000000000, 0.9659258262890683122, 1.000000000000000000, 0.9659258262890683122, 1.000000000000000000, 0.9659258262890683122, 1.000000000000000000, 0.9659258262890683122, 1.000000000000000000, 0.9659258262890683122, 1.000000000000000000, 0.9659258262890683122, 1.000000000000000000, 0.9659258262890683122, 1.000000000000000000, 0.9659258262890683122, 1.000000000000000000, 0.9659258262890683122, 1.000000000000000000, 0.9659258262890683122, 1.000000000000000000, 0.9659258262890683122, 1.000000000000000000, 0.9659258262890683122, 1.000000000000000000, 0.9659258262890683122, 1.000000000000000000, 0.9659258262890683122, 1.000000000000000000, 0.9659258262890683122, 1.000000000000000000, 0.9659258262890683122, 1.000000000000000000, 0.9659258262890683122, 1.000000000000000000, 0.9659258262890683122, 1.000000000000000000, 0.9659258262890683122, 1.000000000000000000, 0.9659258262890683122, 1.000000000000000000, 0.9659258262890683122, 1.000000000000000000, 0.9659258262890683122, 1.000000000000000000, 0.9659258262890683122, 1.000000000000000000, 0.9659258262890683122, 1.000000000000000000, 0.9659258262890683122, 1.000000000000000000, 0.9659258262890683122, 1.000000000000000000, 0.9659258262890683122, 1.000000000000000000, 0.9659258262890683122, 1.000000000000000000, 0.9659258262890683122, 1.000000000000000000, 0.9659258262890683122, 1.000000000000000000, 0.9659258262890683122, 1.000000000000000000, 0.9659258262890683122, 1.000000000000000000, 0.9659258262890683122, 1.000000000000000000, 0.9659258262890683122, 1.000000000000000000, 0.9659258262890683122, 1.000000000000000000, 0.9659258262890683122, 1.000000000000000000, 0.9659258262890683122, 1.000000000000000000, 0.9659258262890683122, 1.000000000000000000, 0.9659258262890683122, 1.000000000000000000, 0.9659258262890683122, 1.000000000000000000, 0.9659258262890683122, 1.000000000000000000, 0.9659258262890683122, 1.000000000000000000, 0.9659258262890683122, 1.000000000000000000, 0.9659258262890683122, 1.000000000000000000, 0.9659258262890683122, 1.000000000000000000, 0.9659258262890683122, 1.000000000000000000, 0.9659258262890683122, 1.000000000000000000, 0.9659258262890683122, 1.000000000000000000, 0.9659258262890683122, 1.000000000000000000, 0.9659258262890683122, 1.000000000000000000, 0.9659258262890683122, 1.000000000000000000, 0.9659258262890683122, 1.000000000000000000, 0.9659258262890683122, 1.000000000000000000, 0.9659258262890683122, 1.000000000000000000, 0.9659258262890683122, 1.000000000000000000, 0.9659258262890683122, 1.000000000000000000, 0.9659258262890683122, 1.000000000000000000, 0.9659258262890683122, 1.000000000000000000, 0.9659258262890683122, 1.000000000000000000, 0.9659258262890683122, 1.000000000000000000, 0.9659258262890683122, 1.000000000000000000, 0.9659258262890683122, 1.000000000000000000, 0.9659258262890683122, 1.000000000000000000, 0.9659258262890683122, 1.000000000000000000, 0.9659258262890683122, 1.000000000000000000, 0.9659258262890683122, 1.000000000000000000, 0.9659258262890683122, 1.000000000000000000, 0.9659258262890683122, 1.000000000000000000, 0.9659258262890683122, 1.000000000000000000, 0.9659258262890683122, 1.000000000000000000, 0.9659258262890683122, 1.000000000000000000, 0.9659258262890683122, 1.000000000000000000, 0.9659258262890683122, 1.000000000000000000, 0.9659258262890683122, 1.000000000000000000, 0.9659258262890683122, 1.000000000000000000, 0.9659258262890683122, 1.000000000000000000, 0.9659258262890683122, 1.000000000000000000, 0.9659258262890683122, 1.000000000000000000, 0.9659258262890683122, 1.000000000000000000, 0.9659258262890683122, 1.000000000000000000, 0.9659258262890683122, 1.000000000000000000, 0.9659258262890683122, 1.000000000000000000, 0.9659258262890683122, 1.000000000000000000, 0.9659258262890683122, 1.000000000000000000, 0.9659258262890683122, 1.000000000000000000, 0.9659258262890683122, 1.000000000000000000, 0.9659258262890683122, 1.000000000000000000, 0.9659258262890683122, 1.000000000000000000, 0.9659258262890683122, 1.000000000000000000, 0.9659258262890683122, 1.000000000000000000, 0.9659258262890683122, 1.000000000000000000, 0.9659258262890683122, 1.000000000000000000, 0.9659258262890683122, 1.000000000000000000, 0.9659258262890683122, 1.000000000000000000, 0.9659258262890683122, 1.000000000000000000, 0.9659258262890683122, 1.000000000000000000, 0.9659258262890683122, 1.000000000000000000, 0.9659258262890683122, 1.000000000000000000, 0.9659258262890683122, 1.000000000000000000, 0.9659258262890683122, 1.000000000000000000, 0.9659258262890683122, 1.000000000000000000, 0.9659258262890683122, 1.000000000000000000, 0.9659258262890683122, 1.000000000000000000, 0.9659258262890683122, 1.000000000000000000, 0.9659258262890683122, 1.000000000000000000, 0.9659258262890683122, 1.000000000000000000, 0.9659258262890683122, 1.000000000000000000, 0.9659258262890683122, 1.000000000000000000, 0.9659258262890683122, 1.000000000000000000, 0.9659258262890683122, 1.000000000000000000, 0.9659258262890683122, 1.000000000000000000, 0.9659258262890683122, 1.000000000000000000, 0.9659258262890683122, 1.000000000000000000, 0.9659258262890683122, 1.000000000000000000, 0.9659258262890683122, 1.000000000000000000, 0.9659258262890683122, 1.000000000000000000, 0.9659258262890683122, 1.000000000000000000) ) ) 
 REPRESENTATION_ITEM ( '' )  SURFACE ( )  );
#58788 = CARTESIAN_POINT ( 'NONE',  ( 19.02544592524343514, -5.153800228976328945, 23.54057627198102054 ) ) ;
#58789 = CARTESIAN_POINT ( 'NONE',  ( 5.049401038298161559, -19.05341960407611168, 57.70724293864769550 ) ) ;
#58790 = CARTESIAN_POINT ( 'NONE',  ( -14.34966873604960291, -8.224510206698953496, 66.66557627198102409 ) ) ;
#58791 = CARTESIAN_POINT ( 'NONE',  ( 14.34966873604960469, 8.224510206698951720, 34.16557627198102409 ) ) ;
#58792 = CARTESIAN_POINT ( 'NONE',  ( -10.72451020669898014, 18.67979575497178502, 50.41557627198103120 ) ) ;
#58793 = CARTESIAN_POINT ( 'NONE',  ( -19.02544592524342804, 5.153800228976336051, 46.04057627198101699 ) ) ;
#58794 = CARTESIAN_POINT ( 'NONE',  ( -0.05219959533907301413, -21.53943276465977519, 62.49890960531436690 ) ) ;
#58795 = CARTESIAN_POINT ( 'NONE',  ( 19.03943276465977164, 0.05219959533936151252, 46.25109039468566863 ) ) ;
#58797 = CARTESIAN_POINT ( 'NONE',  ( -16.53943276465976808, 0.05219959533911058130, 46.24890960531435979 ) ) ;
#58796 = CARTESIAN_POINT ( 'NONE',  ( 0.000000000000000000, 0.000000000000000000, -25.00000000000000000 ) ) ;
#58798 = CARTESIAN_POINT ( 'NONE',  ( -21.53943276465977519, 0.05219959533907696930, 26.24890960531435624 ) ) ;
#58799 = VERTEX_POINT ( 'NONE', #70398 ) ;
#58800 = ORIENTED_EDGE ( 'NONE', *, *, #15818, .F. ) ;
#58801 = CARTESIAN_POINT ( 'NONE',  ( -5.000000000000003553, 37.66961640367474473, -18.00000000000000355 ) ) ;
#58802 = CARTESIAN_POINT ( 'NONE',  ( 8.314922557961029526, -14.29746914071037800, 75.41775706135233293 ) ) ;
#58803 = CARTESIAN_POINT ( 'NONE',  ( 19.05341960407617918, -5.049401038297876454, 76.04275706135230450 ) ) ;
#58804 = CARTESIAN_POINT ( 'NONE',  ( 8.224510206698953496, -14.34966873604960469, 52.91557627198103830 ) ) ;
#58805 = DIRECTION ( 'NONE',  ( -0.000000000000000000, -0.000000000000000000, 1.000000000000000000 ) ) ;
#58806 = CARTESIAN_POINT ( 'NONE',  ( 14.34966873604960469, 8.224510206698951720, 24.16557627198103120 ) ) ;
#58807 = CARTESIAN_POINT ( 'NONE',  ( -19.05341960407611168, -5.049401038298163336, 51.45724293864770260 ) ) ;
#58808 = CARTESIAN_POINT ( 'NONE',  ( 13.97604488694527802, 13.89961937509977652, 69.37390960531436690 ) ) ;
#58809 = CARTESIAN_POINT ( 'NONE',  ( 13.97604488694527802, 13.89961937509977652, 34.37390960531436690 ) ) ;
#58810 = CARTESIAN_POINT ( 'NONE',  ( 21.52544592524334988, 5.823673210054432836, 51.45942372801901854 ) ) ;
#58811 = CARTESIAN_POINT ( 'NONE',  ( -19.02544592524342804, 5.153800228976336051, 76.04057627198102409 ) ) ;
#58812 = DIRECTION ( 'NONE',  ( 0.000000000000000000, 0.000000000000000000, 1.000000000000000000 ) ) ;
#58813 = CARTESIAN_POINT ( 'NONE',  ( 13.89961937509977652, -13.97604488694527269, 58.12390960531436690 ) ) ;
#58814 = EDGE_CURVE ( 'NONE', #90959, #142504, #91231, .T. ) ;
#58815 = CARTESIAN_POINT ( 'NONE',  ( 5.719274019375991003, -21.55341960407610458, 37.70724293864769550 ) ) ;
#58816 = CARTESIAN_POINT ( 'NONE',  ( 13.89961937509977652, -13.97604488694527269, 33.12390960531434558 ) ) ;
#58817 = CARTESIAN_POINT ( 'NONE',  ( 15.80617190586746368, 15.72974639402197994, 44.37390960531435979 ) ) ;
#58818 = CARTESIAN_POINT ( 'NONE',  ( -8.314922557961024197, 14.29746914071037800, 92.91775706135236135 ) ) ;
#58819 = CARTESIAN_POINT ( 'NONE',  ( 5.153800228976615827, -19.02544592524334988, 25.20942372801900433 ) ) ;
#58821 = CARTESIAN_POINT ( 'NONE',  ( 12.14591786802327356, -12.06949235617739191, 85.62609039468568994 ) ) ;
#58820 = CARTESIAN_POINT ( 'NONE',  ( -8.224510206698735004, -14.34966873604973081, 44.58442372801901854 ) ) ;
#58822 = CARTESIAN_POINT ( 'NONE',  ( 16.46253265017160672, -9.564922557960803928, 103.3322429386476955 ) ) ;
#58823 = EDGE_CURVE ( 'NONE', #141307, #91492, #56224, .T. ) ;
#58824 = CARTESIAN_POINT ( 'NONE',  ( -8.314922557961024197, 14.29746914071037800, 67.91775706135234714 ) ) ;
#58825 = CARTESIAN_POINT ( 'NONE',  ( 14.34966873604972726, -8.224510206698740333, 35.83442372801901143 ) ) ;
#58826 = CARTESIAN_POINT ( 'NONE',  ( -5.153800228976328057, -19.02544592524343514, 112.2905762719810099 ) ) ;
#58827 = CARTESIAN_POINT ( 'NONE',  ( -12.06949235617739369, -12.14591786802326823, 19.37609039468568639 ) ) ;
#58828 = CARTESIAN_POINT ( 'NONE',  ( 19.02544592524343514, -5.153800228976328945, 38.54057627198103120 ) ) ;
#58829 = CARTESIAN_POINT ( 'NONE',  ( -18.62759615963255300, -10.81492255796106328, 24.16775706135235424 ) ) ;
#58830 = CARTESIAN_POINT ( 'NONE',  ( -13.97604488694547697, 13.89961937509957934, 113.1260903946856757 ) ) ;
#58831 = CARTESIAN_POINT ( 'NONE',  ( 12.14591786802327356, -12.06949235617739191, 105.6260903946856899 ) ) ;
#58832 = CARTESIAN_POINT ( 'NONE',  ( -25.25560589046783733, -4.310829775027113620, 167.9999999999999716 ) ) ;
#58833 = CARTESIAN_POINT ( 'NONE',  ( 5.719274019375673035, 21.55341960407619339, 97.29275706135234714 ) ) ;
#58834 = CARTESIAN_POINT ( 'NONE',  ( -16.46253265017146816, -9.564922557961047289, 94.16775706135233293 ) ) ;
#58835 = CARTESIAN_POINT ( 'NONE',  ( -8.224510206698948167, 14.34966873604960824, 60.41557627198102409 ) ) ;
#58836 = CARTESIAN_POINT ( 'NONE',  ( 19.02544592524343514, -5.153800228976328945, 23.54057627198102054 ) ) ;
#58838 = CARTESIAN_POINT ( 'NONE',  ( 17.26172910966717211, -6.454744622556960465, 58.30646908649209337 ) ) ;
#58837 = CARTESIAN_POINT ( 'NONE',  ( 0.05219959533936267826, -19.03943276465977164, 65.00109039468567573 ) ) ;
#58839 = CARTESIAN_POINT ( 'NONE',  ( 10.81492255796106328, -18.62759615963255655, 55.41775706135234714 ) ) ;
#58840 = CARTESIAN_POINT ( 'NONE',  ( 8.224510206698742110, 14.34966873604972548, 32.08442372801901854 ) ) ;
#58841 = CARTESIAN_POINT ( 'NONE',  ( 22.73749492396215288, -155.7167183371838064, -25.00000000000000000 ) ) ;
#58842 = CARTESIAN_POINT ( 'NONE',  ( 5.049401038298161559, -19.05341960407611168, 112.7072429386476813 ) ) ;
#58843 = CARTESIAN_POINT ( 'NONE',  ( 21.53943276465977519, -0.05219959533907433946, 78.74890960531436690 ) ) ;
#58844 = CARTESIAN_POINT ( 'NONE',  ( -19.05341960407617563, 5.049401038297882671, 108.5427570613523187 ) ) ;
#58845 = CARTESIAN_POINT ( 'NONE',  ( -0.05219959533909027116, -19.03943276465977164, 97.49890960531436690 ) ) ;
#58846 = CARTESIAN_POINT ( 'NONE',  ( 0.2665833460779011288, -27.95491218073336270, 139.9999999999999716 ) ) ;
#58847 = CARTESIAN_POINT ( 'NONE',  ( -13.97604488694527625, -13.89961937509977652, 31.87390960531435979 ) ) ;
#58848 = CARTESIAN_POINT ( 'NONE',  ( 10.72451020669871369, 18.67979575497193778, 92.08442372801901854 ) ) ;
#58849 = CARTESIAN_POINT ( 'NONE',  ( -13.89961937509977652, 13.97604488694528158, 40.62390960531435979 ) ) ;
#58850 = CARTESIAN_POINT ( 'NONE',  ( 5.719274019375673035, 21.55341960407619339, 47.29275706135234003 ) ) ;
#58851 = CARTESIAN_POINT ( 'NONE',  ( 5.719274019375673035, 21.55341960407619339, 92.29275706135236135 ) ) ;
#58852 = CARTESIAN_POINT ( 'NONE',  ( 0.05219959533934541429, -16.53943276465976808, 100.0010903946857042 ) ) ;
#58853 = CARTESIAN_POINT ( 'NONE',  ( 16.51473224551069308, 9.474510206698969483, 84.16557627198102409 ) ) ;
#58854 = CARTESIAN_POINT ( 'NONE',  ( -21.55341960407619339, 5.719274019375674811, 38.54275706135234714 ) ) ;
#58855 = CARTESIAN_POINT ( 'NONE',  ( 21.52544592524334988, 5.823673210054432836, 41.45942372801901143 ) ) ;
#58857 = CARTESIAN_POINT ( 'NONE',  ( -0.05219959533909027116, -19.03943276465977164, 87.49890960531436690 ) ) ;
#58856 = CARTESIAN_POINT ( 'NONE',  ( 0.05219959533936267826, -19.03943276465977164, 80.00109039468567573 ) ) ;
#58858 = CARTESIAN_POINT ( 'NONE',  ( -14.29746914071049879, 8.314922557960819915, 105.8322429386476955 ) ) ;
#58859 = ADVANCED_FACE ( 'NONE', ( #104722 ), #181578, .F. ) ;
#58860 = CARTESIAN_POINT ( 'NONE',  ( -21.55341960407610458, -5.719274019375992779, 101.4572429386476955 ) ) ;
#58861 = CARTESIAN_POINT ( 'NONE',  ( 16.53943276465976808, -0.05219959533910856209, 83.74890960531435269 ) ) ;
#58862 = CARTESIAN_POINT ( 'NONE',  ( -19.05341960407617563, 5.049401038297882671, 23.54275706135233648 ) ) ;
#58863 = CARTESIAN_POINT ( 'NONE',  ( -4.379528057220328563, 16.55341960407611168, 95.20724293864769550 ) ) ;
#58864 = CARTESIAN_POINT ( 'NONE',  ( 5.153800228976335163, 19.02544592524342804, 39.79057627198100988 ) ) ;
#58865 = CARTESIAN_POINT ( 'NONE',  ( -5.153800228976607833, 19.02544592524334988, 87.70942372801897591 ) ) ;
#58866 = CARTESIAN_POINT ( 'NONE',  ( -14.34966873604960291, -8.224510206698953496, 46.66557627198102409 ) ) ;
#58867 = CARTESIAN_POINT ( 'NONE',  ( -21.55341960407619339, 5.719274019375674811, 88.54275706135236135 ) ) ;
#58868 = CARTESIAN_POINT ( 'NONE',  ( -19.03943276465977164, 0.05219959533909376836, 111.2489096053143669 ) ) ;
#58869 = CARTESIAN_POINT ( 'NONE',  ( -5.153800228976607833, 19.02544592524334988, 72.70942372801900433 ) ) ;
#58870 = CARTESIAN_POINT ( 'NONE',  ( 18.67979575497178502, 10.72451020669898547, 74.16557627198102409 ) ) ;
#58871 = CARTESIAN_POINT ( 'NONE',  ( 10.81492255796106328, -18.62759615963255655, 25.41775706135235779 ) ) ;
#58872 = CARTESIAN_POINT ( 'NONE',  ( -16.53943276465976808, -0.05219959533934237506, 28.75109039468567929 ) ) ;
#58873 = CARTESIAN_POINT ( 'NONE',  ( -12.06949235617739369, -12.14591786802326823, 94.37609039468568994 ) ) ;
#58875 = CARTESIAN_POINT ( 'NONE',  ( 21.55341960407619695, -5.719274019375665929, 41.04275706135236135 ) ) ;
#58874 = CARTESIAN_POINT ( 'NONE',  ( -16.46253265017160317, 9.564922557960807481, 25.83224293864769194 ) ) ;
#58876 = CARTESIAN_POINT ( 'NONE',  ( -4.379528057220328563, 16.55341960407611168, 115.2072429386476955 ) ) ;
#58877 = CARTESIAN_POINT ( 'NONE',  ( -38.00000000000000711, 2.428612866367529932E-14, -9.749999994537626336 ) ) ;
#58878 = CARTESIAN_POINT ( 'NONE',  ( -14.34966873604972548, 8.224510206698743886, 48.33442372801902565 ) ) ;
#58879 = CARTESIAN_POINT ( 'NONE',  ( -14.34966873604960291, -8.224510206698953496, 81.66557627198103830 ) ) ;
#58880 = CARTESIAN_POINT ( 'NONE',  ( -15.80617190586745835, -15.72974639402198527, 71.87390960531438111 ) ) ;
#58881 = CARTESIAN_POINT ( 'NONE',  ( -14.34966873604960291, -8.224510206698953496, 21.66557627198102409 ) ) ;
#58882 = CARTESIAN_POINT ( 'NONE',  ( -12.06949235617739369, -12.14591786802326823, 54.37609039468568994 ) ) ;
#58883 = CARTESIAN_POINT ( 'NONE',  ( -5.049401038298153566, 19.05341960407611168, 50.20724293864770260 ) ) ;
#58884 = CARTESIAN_POINT ( 'NONE',  ( 16.55341960407618274, -4.379528057220086978, 96.04275706135236135 ) ) ;
#58885 = CARTESIAN_POINT ( 'NONE',  ( 9.474510206698729675, 16.51473224551082808, 92.08442372801900433 ) ) ;
#58886 = CARTESIAN_POINT ( 'NONE',  ( -21.52544592524343514, 5.823673210054127303, 91.04057627198103830 ) ) ;
#58887 = CARTESIAN_POINT ( 'NONE',  ( 12.14591786802327356, -12.06949235617739191, 110.6260903946857042 ) ) ;
#58888 = ORIENTED_EDGE ( 'NONE', *, *, #29212, .T. ) ;
#58889 = CARTESIAN_POINT ( 'NONE',  ( 21.95653654802720212, 8.266568072468359674, 172.1684357517875412 ) ) ;
#58890 = CARTESIAN_POINT ( 'NONE',  ( 10.81492255796078972, 18.62759615963270932, 64.58224293864769550 ) ) ;
#58891 = ORIENTED_EDGE ( 'NONE', *, *, #101613, .F. ) ;
#58892 = CARTESIAN_POINT ( 'NONE',  ( 16.52544592524335698, 4.483927247898782831, 86.45942372801901854 ) ) ;
#58893 = ORIENTED_EDGE ( 'NONE', *, *, #20020, .T. ) ;
#58894 = CARTESIAN_POINT ( 'NONE',  ( -18.67979575497178146, -10.72451020669898902, 36.66557627198103120 ) ) ;
#58895 = CARTESIAN_POINT ( 'NONE',  ( 17.50000000000000000, 5.499999999999995559, 108.7823096230356867 ) ) ;
#58896 = CARTESIAN_POINT ( 'NONE',  ( 21.55341960407610458, 5.719274019375980345, 73.95724293864769550 ) ) ;
#58897 = CARTESIAN_POINT ( 'NONE',  ( -12.14591786802309592, -12.06949235617757132, 21.87390960531436690 ) ) ;
#58898 = CARTESIAN_POINT ( 'NONE',  ( -8.314922557961024197, 14.29746914071037800, 27.91775706135234358 ) ) ;
#58899 = CARTESIAN_POINT ( 'NONE',  ( -5.153800228976328057, -19.02544592524343514, 37.29057627198102409 ) ) ;
#58900 = CARTESIAN_POINT ( 'NONE',  ( 4.483927247898790824, -16.52544592524335698, 35.20942372801901854 ) ) ;
#58901 = CARTESIAN_POINT ( 'NONE',  ( -19.02544592524342804, 5.153800228976336051, 56.04057627198100988 ) ) ;
#58902 = CARTESIAN_POINT ( 'NONE',  ( -28.82186960331499392, 9.364793116373565596, 149.9000000000000057 ) ) ;
#58903 = CARTESIAN_POINT ( 'NONE',  ( 19.03943276465977164, -0.05219959533909143690, 103.7489096053143669 ) ) ;
#58904 = CARTESIAN_POINT ( 'NONE',  ( -19.02544592524342804, 5.153800228976336051, 101.0405762719810241 ) ) ;
#58905 = CARTESIAN_POINT ( 'NONE',  ( -4.379528057220086978, -16.55341960407618274, 84.79275706135234714 ) ) ;
#58906 = CARTESIAN_POINT ( 'NONE',  ( -9.564922557961040184, 16.46253265017147172, 92.91775706135233293 ) ) ;
#58907 = CARTESIAN_POINT ( 'NONE',  ( 16.51473224551083163, -9.474510206698727899, 40.83442372801900433 ) ) ;
#58908 = CARTESIAN_POINT ( 'NONE',  ( 5.823673210054125526, 21.52544592524343514, 79.79057627198102409 ) ) ;
#58909 = CARTESIAN_POINT ( 'NONE',  ( 8.314922557961029526, -14.29746914071037800, 95.41775706135234714 ) ) ;
#58910 = CARTESIAN_POINT ( 'NONE',  ( 21.53943276465977519, -0.05219959533907433946, 28.74890960531435624 ) ) ;
#58911 = CARTESIAN_POINT ( 'NONE',  ( 16.51473224551083163, -9.474510206698727899, 95.83442372801900433 ) ) ;
#58912 = CARTESIAN_POINT ( 'NONE',  ( 5.153800228976335163, 19.02544592524342804, 44.79057627198103830 ) ) ;
#58913 = CARTESIAN_POINT ( 'NONE',  ( -16.51473224551069308, -9.474510206698971260, 91.66557627198103830 ) ) ;
#58914 = CARTESIAN_POINT ( 'NONE',  ( -10.72451020669870658, -18.67979575497194134, 59.58442372801901854 ) ) ;
#58915 = CARTESIAN_POINT ( 'NONE',  ( -16.46253265017160317, 9.564922557960807481, 55.83224293864769550 ) ) ;
#58916 = CARTESIAN_POINT ( 'NONE',  ( -14.34966873604960291, -8.224510206698953496, 81.66557627198103830 ) ) ;
#58917 = CARTESIAN_POINT ( 'NONE',  ( -16.21995358207302118, -7.366697692864224933, 85.06448998487842061 ) ) ;
#58918 = CARTESIAN_POINT ( 'NONE',  ( 12.06949235617757843, -12.14591786802309237, 83.12390960531436690 ) ) ;
#58919 = CARTESIAN_POINT ( 'NONE',  ( 18.67979575497178502, 10.72451020669898547, 74.16557627198102409 ) ) ;
#58920 = CARTESIAN_POINT ( 'NONE',  ( 9.564922557961047289, -16.46253265017146816, 95.41775706135233293 ) ) ;
#58921 = DIRECTION ( 'NONE',  ( 0.000000000000000000, -0.8164965809277253683, 0.5773502691896268413 ) ) ;
#58922 = CARTESIAN_POINT ( 'NONE',  ( -13.97604488694547697, 13.89961937509957934, 38.12609039468566152 ) ) ;
#58923 = CARTESIAN_POINT ( 'NONE',  ( 16.29526858892906915, -7.335722546920036002, 71.70329402199735114 ) ) ;
#58925 = CARTESIAN_POINT ( 'NONE',  ( 19.02544592524343514, -5.153800228976328945, 93.54057627198102409 ) ) ;
#58924 = CARTESIAN_POINT ( 'NONE',  ( -16.46253265017160317, 9.564922557960807481, 75.83224293864769550 ) ) ;
#58926 = CARTESIAN_POINT ( 'NONE',  ( 14.29746914071037800, 8.314922557961029526, 61.66775706135235424 ) ) ;
#58927 = CARTESIAN_POINT ( 'NONE',  ( -21.62954880396024748, 5.465688001471193047, 174.0035134771795526 ) ) ;
#58928 = CARTESIAN_POINT ( 'NONE',  ( -13.97604488694547697, 13.89961937509957934, 38.12609039468566152 ) ) ;
#58929 = CARTESIAN_POINT ( 'NONE',  ( 17.06703543724471217, 6.729882984710979343, 21.75716082082560021 ) ) ;
#58930 = CARTESIAN_POINT ( 'NONE',  ( 9.564922557960805705, 16.46253265017160317, 109.5822429386476955 ) ) ;
#58931 = CARTESIAN_POINT ( 'NONE',  ( 12.06949235617739724, 12.14591786802326823, 106.8760903946856899 ) ) ;
#58932 = CARTESIAN_POINT ( 'NONE',  ( 15.57302527691884109, -1.455916144794709322, -59.63194581529845095 ) ) ;
#58933 = CARTESIAN_POINT ( 'NONE',  ( 14.34966873604972726, -8.224510206698740333, 75.83442372801900433 ) ) ;
#58934 = CYLINDRICAL_SURFACE ( 'NONE', #187032, 1.500000000000001332 ) ;
#58935 = CARTESIAN_POINT ( 'NONE',  ( -12.06949235617739369, -12.14591786802326823, 59.37609039468568284 ) ) ;
#58936 = CARTESIAN_POINT ( 'NONE',  ( 5.153800228976335163, 19.02544592524342804, 74.79057627198103830 ) ) ;
#58937 = CARTESIAN_POINT ( 'NONE',  ( -18.67979575497193778, 10.72451020669871902, 73.33442372801901854 ) ) ;
#58938 = CARTESIAN_POINT ( 'NONE',  ( 0.05219959533936267826, -19.03943276465977164, 70.00109039468566152 ) ) ;
#58939 = CARTESIAN_POINT ( 'NONE',  ( 19.03943276465977164, 0.05219959533936151252, 21.25109039468565797 ) ) ;
#58940 = CARTESIAN_POINT ( 'NONE',  ( -13.97604488694527625, -13.89961937509977652, 51.87390960531436690 ) ) ;
#58941 = CARTESIAN_POINT ( 'NONE',  ( -13.89961937509977652, 13.97604488694528158, 45.62390960531433848 ) ) ;
#58942 = DIRECTION ( 'NONE',  ( -0.000000000000000000, -0.000000000000000000, 1.000000000000000000 ) ) ;
#58943 = CARTESIAN_POINT ( 'NONE',  ( 15.80617190586746368, 15.72974639402197994, 74.37390960531436690 ) ) ;
#58944 = EDGE_CURVE ( 'NONE', #188641, #13916, #66610, .T. ) ;
#58945 = CARTESIAN_POINT ( 'NONE',  ( 5.719274019375991003, -21.55341960407610458, 32.70724293864770260 ) ) ;
#58946 = CARTESIAN_POINT ( 'NONE',  ( 14.34966873604960469, 8.224510206698951720, 114.1655762719810383 ) ) ;
#58947 = CARTESIAN_POINT ( 'NONE',  ( -16.52544592524335698, -4.483927247898792601, 53.95942372801900433 ) ) ;
#58948 = ORIENTED_EDGE ( 'NONE', *, *, #78126, .F. ) ;
#58949 = CARTESIAN_POINT ( 'NONE',  ( 5.719274019375673035, 21.55341960407619339, 37.29275706135235424 ) ) ;
#58951 = CARTESIAN_POINT ( 'NONE',  ( 30.74264578624800137, -22.33583958711395212, -3.200000000000000178 ) ) ;
#58950 = CARTESIAN_POINT ( 'NONE',  ( 8.224510206698953496, -14.34966873604960469, 47.91557627198102409 ) ) ;
#58952 = CARTESIAN_POINT ( 'NONE',  ( 16.55341960407618274, -4.379528057220086978, 26.04275706135235779 ) ) ;
#58953 = CARTESIAN_POINT ( 'NONE',  ( 19.05341960407617918, -5.049401038297876454, 46.04275706135233293 ) ) ;
#58954 = CARTESIAN_POINT ( 'NONE',  ( 4.379528057220339221, -16.55341960407611168, 47.70724293864770260 ) ) ;
#58955 = CARTESIAN_POINT ( 'NONE',  ( -18.62759615963255300, -10.81492255796106328, 24.16775706135235424 ) ) ;
#58957 = CARTESIAN_POINT ( 'NONE',  ( 18.67979575497178502, 10.72451020669898547, 79.16557627198103830 ) ) ;
#58956 = CARTESIAN_POINT ( 'NONE',  ( 9.564922557960805705, 16.46253265017160317, 99.58224293864770971 ) ) ;
#58958 = CARTESIAN_POINT ( 'NONE',  ( 5.153800228976335163, 19.02544592524342804, 89.79057627198102409 ) ) ;
#58959 = CARTESIAN_POINT ( 'NONE',  ( 12.06949235617757843, -12.14591786802309237, 63.12390960531435979 ) ) ;
#58960 = CARTESIAN_POINT ( 'NONE',  ( -16.46253265017160317, 9.564922557960807481, 105.8322429386476955 ) ) ;
#58961 = PLANE ( 'NONE',  #124739 ) ;
#58962 = CARTESIAN_POINT ( 'NONE',  ( 5.049401038297881783, 19.05341960407617563, 52.29275706135234003 ) ) ;
#58963 = CARTESIAN_POINT ( 'NONE',  ( -15.80617190586745835, -15.72974639402198527, 111.8739096053143669 ) ) ;
#58964 = CARTESIAN_POINT ( 'NONE',  ( 19.03943276465977164, -0.05219959533909143690, 48.74890960531435979 ) ) ;
#58965 = CARTESIAN_POINT ( 'NONE',  ( -14.34966873604960291, -8.224510206698953496, 106.6655762719810383 ) ) ;
#58966 = CARTESIAN_POINT ( 'NONE',  ( 21.55341960407619695, -5.719274019375665929, 51.04275706135234714 ) ) ;
#58967 = CARTESIAN_POINT ( 'NONE',  ( -8.571926809382608425, 26.38167802310805854, 148.4750000027311785 ) ) ;
#58968 = CARTESIAN_POINT ( 'NONE',  ( 4.483927247898545687, 16.52544592524342804, 34.79057627198103120 ) ) ;
#58969 = CARTESIAN_POINT ( 'NONE',  ( 13.89961937509977652, -13.97604488694527269, 43.12390960531434558 ) ) ;
#58970 = CARTESIAN_POINT ( 'NONE',  ( 9.564922557960805705, 16.46253265017160317, 104.5822429386476955 ) ) ;
#58971 = CARTESIAN_POINT ( 'NONE',  ( 15.80617190586746368, 15.72974639402197994, 79.37390960531436690 ) ) ;
#58972 = CARTESIAN_POINT ( 'NONE',  ( -17.14385361876520264, -23.59649016807271593, 143.1750000027311671 ) ) ;
#58973 = CARTESIAN_POINT ( 'NONE',  ( -13.97604488694527625, -13.89961937509977652, 46.87390960531435979 ) ) ;
#58974 = CARTESIAN_POINT ( 'NONE',  ( -21.52544592524343514, 5.823673210054127303, 71.04057627198103830 ) ) ;
#58975 = ADVANCED_FACE ( 'NONE', ( #14696 ), #167397, .F. ) ;
#58976 = CARTESIAN_POINT ( 'NONE',  ( 15.80617190586769283, -15.72974639402175789, 90.62609039468567573 ) ) ;
#58979 = CARTESIAN_POINT ( 'NONE',  ( 0.05219959533910956823, 16.53943276465976808, 69.99890960531435269 ) ) ;
#58978 = CARTESIAN_POINT ( 'NONE',  ( -8.224510206698735004, -14.34966873604973081, 79.58442372801903275 ) ) ;
#58977 = LINE ( 'NONE', #195531, #92914 ) ;
#58980 = CARTESIAN_POINT ( 'NONE',  ( 5.049401038298161559, -19.05341960407611168, 72.70724293864768129 ) ) ;
#58981 = ORIENTED_EDGE ( 'NONE', *, *, #30897, .F. ) ;
#58982 = CARTESIAN_POINT ( 'NONE',  ( -9.474510206698720793, -16.51473224551083518, 29.58442372801900433 ) ) ;
#58983 = CARTESIAN_POINT ( 'NONE',  ( -16.53943276465976808, -0.05219959533934237506, 93.75109039468567573 ) ) ;
#58984 = CARTESIAN_POINT ( 'NONE',  ( 10.72451020669871369, 18.67979575497193778, 112.0844237280190185 ) ) ;
#58985 = CARTESIAN_POINT ( 'NONE',  ( -9.564922557960796823, -16.46253265017161027, 72.08224293864770971 ) ) ;
#58986 = CARTESIAN_POINT ( 'NONE',  ( 21.53943276465977519, -0.05219959533907433946, 48.74890960531435979 ) ) ;
#58987 = CARTESIAN_POINT ( 'NONE',  ( 14.29746914071037800, 8.314922557961029526, 26.66775706135235424 ) ) ;
#58988 = CARTESIAN_POINT ( 'NONE',  ( 5.823673210054444382, -21.52544592524334988, 90.20942372801903275 ) ) ;
#58989 = CARTESIAN_POINT ( 'NONE',  ( 16.53943276465976808, 0.05219959533934440121, 56.25109039468568284 ) ) ;
#58990 = CARTESIAN_POINT ( 'NONE',  ( -21.52544592524334988, -5.823673210054445271, 18.95942372801901143 ) ) ;
#58991 = CARTESIAN_POINT ( 'NONE',  ( -16.55341960407617563, 4.379528057220093196, 23.54275706135235424 ) ) ;
#58993 = EDGE_CURVE ( 'NONE', #40993, #142912, #170492, .T. ) ;
#58992 = CARTESIAN_POINT ( 'NONE',  ( -0.05219959533909027116, -19.03943276465977164, 87.49890960531436690 ) ) ;
#58994 = CARTESIAN_POINT ( 'NONE',  ( 16.53943276465976808, 0.05219959533934440121, 31.25109039468568639 ) ) ;
#58995 = CARTESIAN_POINT ( 'NONE',  ( 0.05219959533909260263, 19.03943276465977164, 54.99890960531435979 ) ) ;
#58996 = CARTESIAN_POINT ( 'NONE',  ( 8.224510206698742110, 14.34966873604972548, 32.08442372801901854 ) ) ;
#58997 = CARTESIAN_POINT ( 'NONE',  ( 4.379528057220339221, -16.55341960407611168, 77.70724293864770971 ) ) ;
#58998 = CARTESIAN_POINT ( 'NONE',  ( -4.483927247898782831, 16.52544592524335698, 82.70942372801900433 ) ) ;
#59000 = CARTESIAN_POINT ( 'NONE',  ( 19.03943276465977164, -0.05219959533909143690, 58.74890960531435979 ) ) ;
#58999 = CARTESIAN_POINT ( 'NONE',  ( 21.52544592524334988, 5.823673210054432836, 46.45942372801901854 ) ) ;
#59001 = CARTESIAN_POINT ( 'NONE',  ( 13.89961937509977652, -13.97604488694527269, 83.12390960531436690 ) ) ;
#59002 = CARTESIAN_POINT ( 'NONE',  ( 4.379528057220092307, 16.55341960407617563, 82.29275706135234714 ) ) ;
#59003 = CARTESIAN_POINT ( 'NONE',  ( 4.500000000000000888, -139.5000000000000000, 13.35010376910484275 ) ) ;
#59004 = ORIENTED_EDGE ( 'NONE', *, *, #174899, .T. ) ;
#59005 = CARTESIAN_POINT ( 'NONE',  ( 16.51473224551083163, -9.474510206698727899, 35.83442372801899722 ) ) ;
#59006 = CARTESIAN_POINT ( 'NONE',  ( 19.03943276465977164, -0.05219959533909143690, 93.74890960531435269 ) ) ;
#59007 = CARTESIAN_POINT ( 'NONE',  ( -16.46253265017160317, 9.564922557960807481, 55.83224293864769550 ) ) ;
#59008 = CARTESIAN_POINT ( 'NONE',  ( -22.81625015709509441, -31.40387420917324590, -10.32499999726881157 ) ) ;
#59009 = CARTESIAN_POINT ( 'NONE',  ( -12.06949235617739369, -12.14591786802326823, 49.37609039468569705 ) ) ;
#59011 = CARTESIAN_POINT ( 'NONE',  ( -0.05219959533934338120, 16.53943276465976808, 57.50109039468568994 ) ) ;
#59010 = CARTESIAN_POINT ( 'NONE',  ( -9.474510206698720793, -16.51473224551083518, 64.58442372801900433 ) ) ;
#59012 = CARTESIAN_POINT ( 'NONE',  ( 6.218318179416534974, -4.125676326126586524, -64.29800624995039016 ) ) ;
#59013 = CARTESIAN_POINT ( 'NONE',  ( 5.049401038298161559, -19.05341960407611168, 77.70724293864765286 ) ) ;
#59014 = CARTESIAN_POINT ( 'NONE',  ( -18.62759615963270932, 10.81492255796079327, 100.8322429386477097 ) ) ;
#59015 = CARTESIAN_POINT ( 'NONE',  ( 16.51473224551083163, -9.474510206698727899, 60.83442372801900433 ) ) ;
#59017 = CARTESIAN_POINT ( 'NONE',  ( -9.474510206698964154, 16.51473224551069663, 25.41557627198103120 ) ) ;
#59016 = CARTESIAN_POINT ( 'NONE',  ( 16.46253265017160672, -9.564922557960803928, 88.33224293864769550 ) ) ;
#59018 = CARTESIAN_POINT ( 'NONE',  ( -16.51473224551069308, -9.474510206698971260, 81.66557627198103830 ) ) ;
#59020 = CARTESIAN_POINT ( 'NONE',  ( 19.03943276465977164, -0.05219959533909143690, 23.74890960531435269 ) ) ;
#59019 = CARTESIAN_POINT ( 'NONE',  ( 8.224510206698953496, -14.34966873604960469, 37.91557627198102409 ) ) ;
#59021 = CARTESIAN_POINT ( 'NONE',  ( -19.02544592524334988, -5.153800228976617603, 43.95942372801899012 ) ) ;
#59022 = CARTESIAN_POINT ( 'NONE',  ( 16.55341960407611168, 4.379528057220329451, 68.95724293864769550 ) ) ;
#59023 = CARTESIAN_POINT ( 'NONE',  ( -21.53943276465977519, -0.05219959533937600094, 103.7510903946857042 ) ) ;
#59024 = CARTESIAN_POINT ( 'NONE',  ( -19.02544592524342804, 5.153800228976336051, 46.04057627198101699 ) ) ;
#59026 = CARTESIAN_POINT ( 'NONE',  ( -18.67979575497193778, 10.72451020669871902, 98.33442372801901854 ) ) ;
#59025 = CARTESIAN_POINT ( 'NONE',  ( 0.05219959533910956823, 16.53943276465976808, 34.99890960531435979 ) ) ;
#59027 = CARTESIAN_POINT ( 'NONE',  ( -5.049401038298153566, 19.05341960407611168, 95.20724293864770971 ) ) ;
#59028 = CARTESIAN_POINT ( 'NONE',  ( 19.02544592524343514, -5.153800228976328945, 93.54057627198102409 ) ) ;
#59029 = CARTESIAN_POINT ( 'NONE',  ( 9.474510206698971260, -16.51473224551069308, 37.91557627198102409 ) ) ;
#59030 = CARTESIAN_POINT ( 'NONE',  ( -12.14591786802309592, -12.06949235617757132, 101.8739096053143811 ) ) ;
#59031 = CARTESIAN_POINT ( 'NONE',  ( 0.05219959533910956823, 16.53943276465976808, 69.99890960531435269 ) ) ;
#59032 = CARTESIAN_POINT ( 'NONE',  ( 21.55341960407610458, 5.719274019375980345, 88.95724293864769550 ) ) ;
#59033 = CARTESIAN_POINT ( 'NONE',  ( -19.05341960407611168, -5.049401038298163336, 91.45724293864766707 ) ) ;
#59034 = CARTESIAN_POINT ( 'NONE',  ( -10.81492255796078084, -18.62759615963271287, 92.08224293864769550 ) ) ;
#59035 = CARTESIAN_POINT ( 'NONE',  ( -9.474510206698964154, 16.51473224551069663, 90.41557627198103830 ) ) ;
#59037 = CARTESIAN_POINT ( 'NONE',  ( 16.52544592524342804, -4.483927247898539470, 88.54057627198103830 ) ) ;
#59036 = LINE ( 'NONE', #63002, #168771 ) ;
#59038 = CARTESIAN_POINT ( 'NONE',  ( -19.02544592524342804, 5.153800228976336051, 66.04057627198103830 ) ) ;
#59039 = CARTESIAN_POINT ( 'NONE',  ( 21.55341960407610458, 5.719274019375980345, 78.95724293864769550 ) ) ;
#59040 = CARTESIAN_POINT ( 'NONE',  ( 1.993301997531345686E-15, -30.30510711980685556, 146.5000000000000284 ) ) ;
#59042 = SURFACE_STYLE_USAGE ( .BOTH. , #62006 ) ;
#59041 = CARTESIAN_POINT ( 'NONE',  ( -21.52544592524343514, 5.823673210054127303, 31.04057627198102409 ) ) ;
#59043 = CARTESIAN_POINT ( 'NONE',  ( -16.46253265017146816, -9.564922557961047289, 109.1677570613523471 ) ) ;
#59044 = CARTESIAN_POINT ( 'NONE',  ( -4.483927247898539470, -16.52544592524342804, 97.29057627198105251 ) ) ;
#59045 = CARTESIAN_POINT ( 'NONE',  ( -17.26058549869092218, -6.457015423128487974, 96.37745837476067834 ) ) ;
#59046 = CARTESIAN_POINT ( 'NONE',  ( 13.89961937509977652, -13.97604488694527269, 88.12390960531438111 ) ) ;
#59047 = CARTESIAN_POINT ( 'NONE',  ( 9.474510206698971260, -16.51473224551069308, 42.91557627198103120 ) ) ;
#59048 = CARTESIAN_POINT ( 'NONE',  ( -14.34966873604960291, -8.224510206698953496, 76.66557627198103830 ) ) ;
#59049 = CARTESIAN_POINT ( 'NONE',  ( -5.049401038298153566, 19.05341960407611168, 110.2072429386476671 ) ) ;
#59050 = CARTESIAN_POINT ( 'NONE',  ( 0.05219959533910956823, 16.53943276465976808, 54.99890960531435269 ) ) ;
#59051 = CARTESIAN_POINT ( 'NONE',  ( 16.46253265017146816, 9.564922557961045513, 106.6677570613523471 ) ) ;
#59052 = CARTESIAN_POINT ( 'NONE',  ( -21.52544592524334988, -5.823673210054445271, 53.95942372801900433 ) ) ;
#59053 = CARTESIAN_POINT ( 'NONE',  ( 16.51473224551069308, 9.474510206698969483, 104.1655762719810241 ) ) ;
#59054 = CARTESIAN_POINT ( 'NONE',  ( -5.823673210054116645, -21.52544592524344225, 87.29057627198103830 ) ) ;
#59055 = CARTESIAN_POINT ( 'NONE',  ( 12.06949235617739724, 12.14591786802326823, 81.87609039468568994 ) ) ;
#59056 = CARTESIAN_POINT ( 'NONE',  ( -19.02544592524342804, 5.153800228976336051, 31.04057627198102409 ) ) ;
#59057 = CARTESIAN_POINT ( 'NONE',  ( -13.89961937509977652, 13.97604488694528158, 70.62390960531432427 ) ) ;
#59058 = CARTESIAN_POINT ( 'NONE',  ( -10.72451020669898014, 18.67979575497178502, 80.41557627198103830 ) ) ;
#59059 = CARTESIAN_POINT ( 'NONE',  ( 19.03943276465977164, 0.05219959533936151252, 111.2510903946856757 ) ) ;
#59061 = CARTESIAN_POINT ( 'NONE',  ( 5.719274019375673035, 21.55341960407619339, 62.29275706135236845 ) ) ;
#59060 = CARTESIAN_POINT ( 'NONE',  ( 14.29746914071049879, -8.314922557960816363, 53.33224293864769550 ) ) ;
#59063 = CARTESIAN_POINT ( 'NONE',  ( -21.53943276465977519, 0.05219959533907696930, 26.24890960531435624 ) ) ;
#59062 = CARTESIAN_POINT ( 'NONE',  ( 0.05219959533934541429, -16.53943276465976808, 80.00109039468568994 ) ) ;
#59064 = CARTESIAN_POINT ( 'NONE',  ( 19.05341960407611168, 5.049401038298154454, 108.9572429386476955 ) ) ;
#59065 = CARTESIAN_POINT ( 'NONE',  ( 0.000000000000000000, 0.000000000000000000, -15.00000000000000000 ) ) ;
#59066 = CARTESIAN_POINT ( 'NONE',  ( -16.53943276465976808, -0.05219959533934237506, 103.7510903946857042 ) ) ;
#59067 = CARTESIAN_POINT ( 'NONE',  ( -16.53943276465976808, -0.05219959533934237506, 43.75109039468568284 ) ) ;
#59068 = CARTESIAN_POINT ( 'NONE',  ( -13.89961937509977652, 13.97604488694528158, 60.62390960531436690 ) ) ;
#59069 = CARTESIAN_POINT ( 'NONE',  ( -9.474510206698964154, 16.51473224551069663, 80.41557627198103830 ) ) ;
#59070 = CARTESIAN_POINT ( 'NONE',  ( -16.52544592524335698, -4.483927247898792601, 73.95942372801901854 ) ) ;
#59071 = CARTESIAN_POINT ( 'NONE',  ( 4.483927247898545687, 16.52544592524342804, 49.79057627198102409 ) ) ;
#59072 = CARTESIAN_POINT ( 'NONE',  ( -16.51473224551069308, -9.474510206698971260, 56.66557627198103120 ) ) ;
#59073 = CARTESIAN_POINT ( 'NONE',  ( -0.05219959533909027116, -19.03943276465977164, 47.49890960531435979 ) ) ;
#59074 = CARTESIAN_POINT ( 'NONE',  ( 12.14591786802327356, -12.06949235617739191, 45.62609039468567573 ) ) ;
#59075 = CARTESIAN_POINT ( 'NONE',  ( 0.05219959533936267826, -19.03943276465977164, 95.00109039468567573 ) ) ;
#59076 = CARTESIAN_POINT ( 'NONE',  ( 4.379528057220339221, -16.55341960407611168, 97.70724293864772392 ) ) ;
#59077 = CARTESIAN_POINT ( 'NONE',  ( -5.153800228976328057, -19.02544592524343514, 67.29057627198102409 ) ) ;
#59079 = CARTESIAN_POINT ( 'NONE',  ( 3.766062262543149401E-15, -39.95556452105413570, -1.499999999999999778 ) ) ;
#59078 = CARTESIAN_POINT ( 'NONE',  ( 0.05219959533936267826, -19.03943276465977164, 105.0010903946856615 ) ) ;
#59080 = CARTESIAN_POINT ( 'NONE',  ( -21.55341960407619339, 5.719274019375674811, 88.54275706135236135 ) ) ;
#59081 = CARTESIAN_POINT ( 'NONE',  ( -14.29746914071037622, -8.314922557961029526, 69.16775706135234714 ) ) ;
#59082 = DIRECTION ( 'NONE',  ( -1.000000000000000000, 0.000000000000000000, 0.000000000000000000 ) ) ;
#59083 = CARTESIAN_POINT ( 'NONE',  ( 15.80617190586746368, 15.72974639402197994, 64.37390960531435269 ) ) ;
#59084 = CARTESIAN_POINT ( 'NONE',  ( 16.52544592524335698, 4.483927247898782831, 56.45942372801902565 ) ) ;
#59085 = CARTESIAN_POINT ( 'NONE',  ( -13.89961937509977830, 13.97604488694528158, 35.62390960531435979 ) ) ;
#59086 = CARTESIAN_POINT ( 'NONE',  ( -19.05341960407617563, 5.049401038297882671, 48.54275706135233293 ) ) ;
#59087 = CARTESIAN_POINT ( 'NONE',  ( 5.153800228976335163, 19.02544592524342804, 89.79057627198102409 ) ) ;
#59088 = CARTESIAN_POINT ( 'NONE',  ( -19.02544592524342804, 5.153800228976336051, 26.04057627198103120 ) ) ;
#59089 = CARTESIAN_POINT ( 'NONE',  ( 9.564922557960805705, 16.46253265017160317, 59.58224293864769550 ) ) ;
#59090 = B_SPLINE_CURVE_WITH_KNOTS ( 'NONE', 3,
 ( #73684, #139052, #532, #79374, #123868, #47060 ),
 .UNSPECIFIED., .F., .F.,
 ( 4, 2, 4 ),
 ( 0.000000000000000000, 0.0003837532665635213884, 0.0007675065331270427768 ),
 .UNSPECIFIED. ) ;
#59091 = CARTESIAN_POINT ( 'NONE',  ( -15.80617190586768217, 15.72974639402176855, 78.12609039468570415 ) ) ;
#59092 = CARTESIAN_POINT ( 'NONE',  ( -5.153800228976607833, 19.02544592524334988, 37.70942372801899722 ) ) ;
#59093 = CARTESIAN_POINT ( 'NONE',  ( -19.05341960407617563, 5.049401038297882671, 23.54275706135233648 ) ) ;
#59094 = CARTESIAN_POINT ( 'NONE',  ( 0.05219959533909260263, 19.03943276465977164, 59.99890960531436690 ) ) ;
#59095 = CARTESIAN_POINT ( 'NONE',  ( 21.53943276465977519, -0.05219959533907433946, 28.74890960531435624 ) ) ;
#59096 = CARTESIAN_POINT ( 'NONE',  ( 18.62759615963255655, 10.81492255796105972, 81.66775706135236135 ) ) ;
#59097 = CARTESIAN_POINT ( 'NONE',  ( 13.89961937509977652, -13.97604488694527269, 58.12390960531436690 ) ) ;
#59098 = TOROIDAL_SURFACE ( 'NONE', #78418, 69.99999999999998579, 10.00000000000000000 ) ;
#59099 = CARTESIAN_POINT ( 'NONE',  ( 21.52544592524334988, 5.823673210054432836, 76.45942372801901854 ) ) ;
#59100 = CARTESIAN_POINT ( 'NONE',  ( -21.52544592524343514, 5.823673210054127303, 41.04057627198103120 ) ) ;
#59101 = CARTESIAN_POINT ( 'NONE',  ( 9.564922557960805705, 16.46253265017160317, 84.58224293864769550 ) ) ;
#59102 = CARTESIAN_POINT ( 'NONE',  ( 21.53943276465977519, 0.05219959533937863772, 36.25109039468567573 ) ) ;
#59103 = CARTESIAN_POINT ( 'NONE',  ( 9.564922557961047289, -16.46253265017146816, 55.41775706135234003 ) ) ;
#59104 = CARTESIAN_POINT ( 'NONE',  ( -13.89961937509977652, 13.97604488694528158, 35.62390960531435269 ) ) ;
#59105 = CARTESIAN_POINT ( 'NONE',  ( 0.05219959533909260263, 19.03943276465977164, 84.99890960531436690 ) ) ;
#59106 = CARTESIAN_POINT ( 'NONE',  ( -8.314922557961024197, 14.29746914071037800, 22.91775706135235069 ) ) ;
#59107 = CARTESIAN_POINT ( 'NONE',  ( -8.314922557960811034, -14.29746914071050412, 92.08224293864769550 ) ) ;
#59108 = CARTESIAN_POINT ( 'NONE',  ( -19.03943276465977164, 0.05219959533909376836, 61.24890960531436690 ) ) ;
#59109 = CARTESIAN_POINT ( 'NONE',  ( 18.62759615963271287, -10.81492255796078972, 48.33224293864770260 ) ) ;
#59110 = CARTESIAN_POINT ( 'NONE',  ( -4.483927247898782831, 16.52544592524335698, 22.70942372801901499 ) ) ;
#59111 = CARTESIAN_POINT ( 'NONE',  ( -0.05219959533937732626, 21.53943276465977519, 22.50109039468567573 ) ) ;
#59112 = CARTESIAN_POINT ( 'NONE',  ( 15.72974639402176855, 15.80617190586768217, 76.87609039468567573 ) ) ;
#59113 = CARTESIAN_POINT ( 'NONE',  ( -14.34966873604972548, 8.224510206698743886, 63.33442372801900433 ) ) ;
#59114 = CARTESIAN_POINT ( 'NONE',  ( 12.06949235617739724, 12.14591786802326823, 61.87609039468568284 ) ) ;
#59115 = CARTESIAN_POINT ( 'NONE',  ( 9.564922557960805705, 16.46253265017160317, 59.58224293864769550 ) ) ;
#59116 = CARTESIAN_POINT ( 'NONE',  ( 14.29746914071037800, 8.314922557961029526, 96.66775706135234714 ) ) ;
#59117 = CARTESIAN_POINT ( 'NONE',  ( 16.51473224551083163, -9.474510206698727899, 45.83442372801900433 ) ) ;
#59118 = CARTESIAN_POINT ( 'NONE',  ( 5.823673210054125526, 21.52544592524343514, 114.7905762719810383 ) ) ;
#59119 = CARTESIAN_POINT ( 'NONE',  ( -12.14591786802309592, -12.06949235617757132, 66.87390960531436690 ) ) ;
#59120 = CARTESIAN_POINT ( 'NONE',  ( -9.474510206698964154, 16.51473224551069663, 90.41557627198103830 ) ) ;
#59121 = CARTESIAN_POINT ( 'NONE',  ( 4.379528057220092307, 16.55341960407617563, 92.29275706135236135 ) ) ;
#59122 = CARTESIAN_POINT ( 'NONE',  ( -18.67979575497193778, 10.72451020669871902, 53.33442372801901854 ) ) ;
#59123 = CARTESIAN_POINT ( 'NONE',  ( -12.14591786802326823, 12.06949235617739902, 33.12609039468569705 ) ) ;
#59124 = CARTESIAN_POINT ( 'NONE',  ( 18.62759615963255655, 10.81492255796105972, 26.66775706135235424 ) ) ;
#59125 = CARTESIAN_POINT ( 'NONE',  ( -14.29746914071049879, 8.314922557960819915, 55.83224293864770260 ) ) ;
#59126 = ORIENTED_EDGE ( 'NONE', *, *, #179989, .F. ) ;
#59127 = CARTESIAN_POINT ( 'NONE',  ( 5.823673210054125526, 21.52544592524343514, 104.7905762719810241 ) ) ;
#59128 = CARTESIAN_POINT ( 'NONE',  ( 14.34966873604960469, 8.224510206698951720, 39.16557627198102409 ) ) ;
#59129 = ORIENTED_EDGE ( 'NONE', *, *, #57861, .T. ) ;
#59130 = CARTESIAN_POINT ( 'NONE',  ( 34.57898328185100212, 4.579095689294076621, 50.94499274836910985 ) ) ;
#59131 = CARTESIAN_POINT ( 'NONE',  ( 21.52544592524344225, -5.823673210054117533, 28.54057627198103120 ) ) ;
#59132 = CARTESIAN_POINT ( 'NONE',  ( -10.72451020669870658, -18.67979575497194134, 34.58442372801900433 ) ) ;
#59133 = CARTESIAN_POINT ( 'NONE',  ( -8.224510206698948167, 14.34966873604960824, 60.41557627198102409 ) ) ;
#59134 = CARTESIAN_POINT ( 'NONE',  ( 19.05341960407611168, 5.049401038298154454, 68.95724293864769550 ) ) ;
#59136 = CARTESIAN_POINT ( 'NONE',  ( -13.97604488694547697, 13.89961937509957934, 68.12609039468563310 ) ) ;
#59135 = CARTESIAN_POINT ( 'NONE',  ( -9.564922557960796823, -16.46253265017161027, 22.08224293864768839 ) ) ;
#59137 = CARTESIAN_POINT ( 'NONE',  ( -21.52544592524343514, 5.823673210054127303, 46.04057627198103830 ) ) ;
#59138 = CARTESIAN_POINT ( 'NONE',  ( -19.02544592524342804, 5.153800228976336051, 56.04057627198100988 ) ) ;
#59139 = CARTESIAN_POINT ( 'NONE',  ( 0.05219959533934541429, -16.53943276465976808, 35.00109039468568284 ) ) ;
#59140 = CARTESIAN_POINT ( 'NONE',  ( -15.72974639402197994, 15.80617190586746368, 115.6239096053143669 ) ) ;
#59141 = CARTESIAN_POINT ( 'NONE',  ( 4.483927247898545687, 16.52544592524342804, 44.79057627198103120 ) ) ;
#59142 = ORIENTED_EDGE ( 'NONE', *, *, #188509, .F. ) ;
#59143 = CARTESIAN_POINT ( 'NONE',  ( 16.46253265017160672, -9.564922557960803928, 93.33224293864769550 ) ) ;
#59144 = CARTESIAN_POINT ( 'NONE',  ( -5.823673210054116645, -21.52544592524344225, 72.29057627198102409 ) ) ;
#59146 = CARTESIAN_POINT ( 'NONE',  ( -16.52544592524335698, -4.483927247898792601, 33.95942372801901143 ) ) ;
#59145 = CARTESIAN_POINT ( 'NONE',  ( -15.80617190586745835, -15.72974639402198527, 111.8739096053143669 ) ) ;
#59147 = CARTESIAN_POINT ( 'NONE',  ( -10.72451020669898014, 18.67979575497178502, 40.41557627198103120 ) ) ;
#59148 = CARTESIAN_POINT ( 'NONE',  ( 15.80617190586769283, -15.72974639402175789, 95.62609039468568994 ) ) ;
#59149 = CARTESIAN_POINT ( 'NONE',  ( 5.153800228976335163, 19.02544592524342804, 94.79057627198103830 ) ) ;
#59150 = CARTESIAN_POINT ( 'NONE',  ( 16.46253265017160672, -9.564922557960803928, 43.33224293864769550 ) ) ;
#59151 = CARTESIAN_POINT ( 'NONE',  ( -13.97604488694527625, -13.89961937509977652, 96.87390960531433848 ) ) ;
#59152 = CARTESIAN_POINT ( 'NONE',  ( 13.89961937509977652, -13.97604488694527269, 78.12390960531433848 ) ) ;
#59153 = AXIS2_PLACEMENT_3D ( 'NONE', #62057, #92398, #121751 ) ;
#59154 = DIRECTION ( 'NONE',  ( 0.000000000000000000, 0.000000000000000000, 1.000000000000000000 ) ) ;
#59155 = CARTESIAN_POINT ( 'NONE',  ( 16.46253265017146816, 9.564922557961045513, 61.66775706135234003 ) ) ;
#59157 = CARTESIAN_POINT ( 'NONE',  ( -10.81492255796078084, -18.62759615963271287, 37.08224293864768129 ) ) ;
#59156 = CARTESIAN_POINT ( 'NONE',  ( 10.81492255796106328, -18.62759615963255655, 110.4177570613523756 ) ) ;
#59158 = B_SPLINE_CURVE_WITH_KNOTS ( 'NONE', 3,
 ( #156602, #108088, #110090, #17092 ),
 .UNSPECIFIED., .F., .F.,
 ( 4, 4 ),
 ( 0.000000000000000000, 0.007966001190080937433 ),
 .UNSPECIFIED. ) ;
#59159 = CARTESIAN_POINT ( 'NONE',  ( -4.483927247898782831, 16.52544592524335698, 107.7094237280190328 ) ) ;
#59160 = CARTESIAN_POINT ( 'NONE',  ( 9.564922557961047289, -16.46253265017146816, 85.41775706135233293 ) ) ;
#59161 = CARTESIAN_POINT ( 'NONE',  ( -16.38665767535054840, 7.295008042176026386, 60.26400864214547681 ) ) ;
#59162 = CARTESIAN_POINT ( 'NONE',  ( -5.049401038297874678, -19.05341960407617918, 84.79275706135233293 ) ) ;
#59163 = CARTESIAN_POINT ( 'NONE',  ( -16.51473224551082808, 9.474510206698731452, 43.33442372801900433 ) ) ;
#59164 = CARTESIAN_POINT ( 'NONE',  ( 16.61371651742600264, 7.165104196376156587, 108.6458493000700543 ) ) ;
#59165 = CARTESIAN_POINT ( 'NONE',  ( -9.474510206698964154, 16.51473224551069663, 40.41557627198103120 ) ) ;
#59166 = CARTESIAN_POINT ( 'NONE',  ( -14.34966873604960291, -8.224510206698953496, 46.66557627198102409 ) ) ;
#59167 = CARTESIAN_POINT ( 'NONE',  ( -16.61371651742600264, -7.165104196376159251, 111.1458493000700116 ) ) ;
#59168 = CARTESIAN_POINT ( 'NONE',  ( -14.34966873604972548, 8.224510206698743886, 113.3344237280190328 ) ) ;
#59169 = DIRECTION ( 'NONE',  ( 0.000000000000000000, 0.000000000000000000, 1.000000000000000000 ) ) ;
#59170 = CARTESIAN_POINT ( 'NONE',  ( -4.379528057220086978, -16.55341960407618274, 89.79275706135236135 ) ) ;
#59171 = CARTESIAN_POINT ( 'NONE',  ( -9.564922557960796823, -16.46253265017161027, 47.08224293864769550 ) ) ;
#59172 = CARTESIAN_POINT ( 'NONE',  ( 5.823673210054444382, -21.52544592524334988, 110.2094237280190185 ) ) ;
#59173 = CARTESIAN_POINT ( 'NONE',  ( -16.51473224551082808, 9.474510206698731452, 113.3344237280190043 ) ) ;
#59174 = CARTESIAN_POINT ( 'NONE',  ( 21.53943276465977519, -0.05219959533907433946, 33.74890960531436690 ) ) ;
#59175 = CARTESIAN_POINT ( 'NONE',  ( 10.72451020669871369, 18.67979575497193778, 92.08442372801901854 ) ) ;
#59176 = CARTESIAN_POINT ( 'NONE',  ( 13.89961937509977652, -13.97604488694527269, 108.1239096053143669 ) ) ;
#59177 = CARTESIAN_POINT ( 'NONE',  ( -5.049401038298153566, 19.05341960407611168, 85.20724293864766707 ) ) ;
#59178 = CARTESIAN_POINT ( 'NONE',  ( -36.91746825000000598, 11.99521256947798520, -8.724999997268813701 ) ) ;
#59179 = CARTESIAN_POINT ( 'NONE',  ( 10.81492255796078972, 18.62759615963270932, 114.5822429386477097 ) ) ;
#59180 = CARTESIAN_POINT ( 'NONE',  ( 4.379528057220339221, -16.55341960407611168, 77.70724293864770971 ) ) ;
#59181 = CARTESIAN_POINT ( 'NONE',  ( -18.62759615963270932, 10.81492255796079327, 75.83224293864769550 ) ) ;
#59182 = CARTESIAN_POINT ( 'NONE',  ( 19.02544592524343514, -5.153800228976328945, 58.54057627198102409 ) ) ;
#59184 = CARTESIAN_POINT ( 'NONE',  ( 16.53943276465976808, 0.05219959533934440121, 91.25109039468568994 ) ) ;
#59183 = CARTESIAN_POINT ( 'NONE',  ( -10.81492255796078084, -18.62759615963271287, 102.0822429386476955 ) ) ;
#59185 = ORIENTED_EDGE ( 'NONE', *, *, #7692, .F. ) ;
#59186 = CARTESIAN_POINT ( 'NONE',  ( -0.05219959533909027116, -19.03943276465977164, 57.49890960531435979 ) ) ;
#59188 = CYLINDRICAL_SURFACE ( 'NONE', #36523, 1.499999999999997780 ) ;
#59187 = CARTESIAN_POINT ( 'NONE',  ( 16.53943276465976808, -0.05219959533910856209, 98.74890960531438111 ) ) ;
#59189 = CARTESIAN_POINT ( 'NONE',  ( 16.46253265017160672, -9.564922557960803928, 63.33224293864769550 ) ) ;
#59190 = CARTESIAN_POINT ( 'NONE',  ( 16.51473224551083163, -9.474510206698727899, 80.83442372801899012 ) ) ;
#59191 = CARTESIAN_POINT ( 'NONE',  ( -0.05219959533910754901, -16.53943276465976808, 87.49890960531436690 ) ) ;
#59192 = CARTESIAN_POINT ( 'NONE',  ( -21.52544592524334988, -5.823673210054445271, 63.95942372801901854 ) ) ;
#59194 = CARTESIAN_POINT ( 'NONE',  ( 18.67979575497194134, -10.72451020669871369, 25.83442372801901499 ) ) ;
#59193 = CARTESIAN_POINT ( 'NONE',  ( 16.46253265017160672, -9.564922557960803928, 48.33224293864769550 ) ) ;
#59195 = CARTESIAN_POINT ( 'NONE',  ( 0.05219959533910956823, 16.53943276465976808, 104.9989096053143669 ) ) ;
#59196 = CARTESIAN_POINT ( 'NONE',  ( 8.400629636141365708, -38.44252190851328521, -32.19688134020121595 ) ) ;
#59197 = CARTESIAN_POINT ( 'NONE',  ( 0.05219959533909260263, 19.03943276465977164, 54.99890960531435979 ) ) ;
#59198 = CARTESIAN_POINT ( 'NONE',  ( 8.906447517083050158, 27.41122689804195645, 143.6500000054623740 ) ) ;
#59200 = CARTESIAN_POINT ( 'NONE',  ( -5.823673210054116645, -21.52544592524344225, 22.29057627198102765 ) ) ;
#59199 = CARTESIAN_POINT ( 'NONE',  ( 16.46253265017146816, 9.564922557961045513, 106.6677570613523471 ) ) ;
#59201 = CARTESIAN_POINT ( 'NONE',  ( -21.53943276465977519, -0.05219959533937600094, 48.75109039468568284 ) ) ;
#59202 = CARTESIAN_POINT ( 'NONE',  ( -5.153800228976328057, -19.02544592524343514, 102.2905762719810383 ) ) ;
#59203 = CARTESIAN_POINT ( 'NONE',  ( 9.474510206698729675, 16.51473224551082808, 82.08442372801899012 ) ) ;
#59204 = CARTESIAN_POINT ( 'NONE',  ( -9.474510206698964154, 16.51473224551069663, 55.41557627198103120 ) ) ;
#59205 = CARTESIAN_POINT ( 'NONE',  ( -12.06949235617756955, 12.14591786802309770, 70.62390960531436690 ) ) ;
#59206 = CARTESIAN_POINT ( 'NONE',  ( -4.379528057220328563, 16.55341960407611168, 80.20724293864769550 ) ) ;
#59207 = CARTESIAN_POINT ( 'NONE',  ( -5.049401038298153566, 19.05341960407611168, 85.20724293864766707 ) ) ;
#59208 = CARTESIAN_POINT ( 'NONE',  ( -12.14591786802309592, -12.06949235617757132, 81.87390960531435269 ) ) ;
#59209 = CARTESIAN_POINT ( 'NONE',  ( -19.02544592524342804, 5.153800228976336051, 86.04057627198103830 ) ) ;
#59210 = EDGE_CURVE ( 'NONE', #79565, #189536, #157069, .T. ) ;
#59211 = CARTESIAN_POINT ( 'NONE',  ( 16.51473224551083163, -9.474510206698727899, 30.83442372801900433 ) ) ;
#59214 = CARTESIAN_POINT ( 'NONE',  ( 16.46253265017160672, -9.564922557960803928, 33.33224293864770260 ) ) ;
#59213 = CARTESIAN_POINT ( 'NONE',  ( -12.14591786802309592, -12.06949235617757132, 31.87390960531435979 ) ) ;
#59212 = CARTESIAN_POINT ( 'NONE',  ( -16.46253265017160317, 9.564922557960807481, 45.83224293864769550 ) ) ;
#59215 = ORIENTED_EDGE ( 'NONE', *, *, #183623, .F. ) ;
#59216 = CARTESIAN_POINT ( 'NONE',  ( -5.719274019375665041, -21.55341960407619695, 44.79275706135234714 ) ) ;
#59217 = CARTESIAN_POINT ( 'NONE',  ( 0.05219959533936267826, -19.03943276465977164, 60.00109039468566863 ) ) ;
#59218 = CARTESIAN_POINT ( 'NONE',  ( 14.29746914071049879, -8.314922557960816363, 33.33224293864769550 ) ) ;
#59219 = CARTESIAN_POINT ( 'NONE',  ( -21.53943276465977519, 0.05219959533907696930, 86.24890960531436690 ) ) ;
#59220 = CARTESIAN_POINT ( 'NONE',  ( -5.719274019375978568, 21.55341960407610458, 30.20724293864769550 ) ) ;
#59221 = CARTESIAN_POINT ( 'NONE',  ( 16.55341960407611168, 4.379528057220329451, 73.95724293864769550 ) ) ;
#59222 = CARTESIAN_POINT ( 'NONE',  ( 13.97604488694527802, 13.89961937509977652, 39.37390960531435269 ) ) ;
#59223 = CARTESIAN_POINT ( 'NONE',  ( 16.53943276465976808, 0.05219959533934440121, 101.2510903946856757 ) ) ;
#59224 = CARTESIAN_POINT ( 'NONE',  ( 16.55341960407618274, -4.379528057220086978, 51.04275706135234714 ) ) ;
#59225 = CARTESIAN_POINT ( 'NONE',  ( -5.823673210054116645, -21.52544592524344225, 42.29057627198103120 ) ) ;
#59226 = CARTESIAN_POINT ( 'NONE',  ( 0.05219959533937995610, -21.53943276465977519, 110.0010903946856757 ) ) ;
#59227 = CARTESIAN_POINT ( 'NONE',  ( 5.049401038298161559, -19.05341960407611168, 87.70724293864769550 ) ) ;
#59228 = CARTESIAN_POINT ( 'NONE',  ( -4.483927247898782831, 16.52544592524335698, 72.70942372801901854 ) ) ;
#59229 = CARTESIAN_POINT ( 'NONE',  ( 4.483927247898545687, 16.52544592524342804, 114.7905762719810383 ) ) ;
#59230 = CARTESIAN_POINT ( 'NONE',  ( -4.483927247898539470, -16.52544592524342804, 37.29057627198102409 ) ) ;
#59232 = CARTESIAN_POINT ( 'NONE',  ( -9.474510206698964154, 16.51473224551069663, 85.41557627198102409 ) ) ;
#59231 = CARTESIAN_POINT ( 'NONE',  ( 13.97604488694527802, 13.89961937509977652, 109.3739096053143669 ) ) ;
#59233 = CARTESIAN_POINT ( 'NONE',  ( -19.03943276465977164, 0.05219959533909376836, 116.2489096053143669 ) ) ;
#59234 = CARTESIAN_POINT ( 'NONE',  ( 14.29746914071049879, -8.314922557960816363, 68.33224293864769550 ) ) ;
#59235 = CIRCLE ( 'NONE', #33404, 2.649999999999992806 ) ;
#59236 = CARTESIAN_POINT ( 'NONE',  ( -16.55341960407611168, -4.379528057220339221, 51.45724293864770260 ) ) ;
#59237 = VERTEX_POINT ( 'NONE', #17679 ) ;
#59239 = CARTESIAN_POINT ( 'NONE',  ( 2.500000000000000000, -2.357898499370432610, 3.252606517456513302E-15 ) ) ;
#59238 = CARTESIAN_POINT ( 'NONE',  ( -16.52544592524335698, -4.483927247898792601, 53.95942372801900433 ) ) ;
#59240 = CARTESIAN_POINT ( 'NONE',  ( 16.46253265017146816, 9.564922557961045513, 51.66775706135233293 ) ) ;
#59241 = CARTESIAN_POINT ( 'NONE',  ( 19.05341960407611168, 5.049401038298154454, 83.95724293864766707 ) ) ;
#59242 = CARTESIAN_POINT ( 'NONE',  ( -19.02544592524334988, -5.153800228976617603, 68.95942372801896170 ) ) ;
#59243 = CARTESIAN_POINT ( 'NONE',  ( 27.73933785331498214, 9.013057229001095294, 142.4750000027311785 ) ) ;
#59244 = CARTESIAN_POINT ( 'NONE',  ( 9.564922557961047289, -16.46253265017146816, 55.41775706135234003 ) ) ;
#59246 = CARTESIAN_POINT ( 'NONE',  ( 8.314922557961029526, -14.29746914071037800, 100.4177570613523471 ) ) ;
#59245 = CARTESIAN_POINT ( 'NONE',  ( 16.46253265017146816, 9.564922557961045513, 101.6677570613523329 ) ) ;
#59247 = CARTESIAN_POINT ( 'NONE',  ( 1.784210473542230573E-15, -29.16686587814331588, 145.8750000027311273 ) ) ;
#59248 = CARTESIAN_POINT ( 'NONE',  ( 13.97604488694527802, 13.89961937509977652, 44.37390960531435269 ) ) ;
#59249 = CARTESIAN_POINT ( 'NONE',  ( 5.049401038298161559, -19.05341960407611168, 112.7072429386476813 ) ) ;
#59250 = CARTESIAN_POINT ( 'NONE',  ( -0.05219959533937732626, 21.53943276465977519, 57.50109039468568994 ) ) ;
#59251 = CARTESIAN_POINT ( 'NONE',  ( -0.05219959533936034679, 19.03943276465977164, 97.50109039468567573 ) ) ;
#59253 = CARTESIAN_POINT ( 'NONE',  ( -13.97604488694527625, -13.89961937509977652, 66.87390960531436690 ) ) ;
#59252 = DIRECTION ( 'NONE',  ( -1.000000000000000000, -0.000000000000000000, -0.000000000000000000 ) ) ;
#59254 = CARTESIAN_POINT ( 'NONE',  ( 31.90000000000003411, -9.916512055951908821E-14, -45.64921306006598201 ) ) ;
#59256 = CARTESIAN_POINT ( 'NONE',  ( 16.46253265017160672, -9.564922557960803928, 63.33224293864769550 ) ) ;
#59255 = CARTESIAN_POINT ( 'NONE',  ( 8.314922557960818139, 14.29746914071049879, 79.58224293864769550 ) ) ;
#59257 = CARTESIAN_POINT ( 'NONE',  ( -16.51473224551069308, -9.474510206698971260, 71.66557627198102409 ) ) ;
#59258 = CARTESIAN_POINT ( 'NONE',  ( 16.46253265017146816, 9.564922557961045513, 71.66775706135233293 ) ) ;
#59259 = CARTESIAN_POINT ( 'NONE',  ( 0.05219959533907565091, 21.53943276465977519, 69.99890960531435269 ) ) ;
#59260 = CARTESIAN_POINT ( 'NONE',  ( -9.564922557960796823, -16.46253265017161027, 22.08224293864768839 ) ) ;
#59261 = CARTESIAN_POINT ( 'NONE',  ( 9.474510206698729675, 16.51473224551082808, 52.08442372801900433 ) ) ;
#59262 = CARTESIAN_POINT ( 'NONE',  ( 5.153800228976335163, 19.02544592524342804, 59.79057627198100988 ) ) ;
#59263 = CARTESIAN_POINT ( 'NONE',  ( 0.05219959533909260263, 19.03943276465977164, 79.99890960531436690 ) ) ;
#59264 = CARTESIAN_POINT ( 'NONE',  ( -21.53943276465977519, 0.05219959533907696930, 91.24890960531436690 ) ) ;
#59266 = CARTESIAN_POINT ( 'NONE',  ( 0.05219959533936267826, -19.03943276465977164, 45.00109039468566863 ) ) ;
#59265 = CARTESIAN_POINT ( 'NONE',  ( 12.14591786802309770, 12.06949235617756955, 79.37390960531436690 ) ) ;
#59267 = CARTESIAN_POINT ( 'NONE',  ( -18.67979575497178146, -10.72451020669898902, 81.66557627198103830 ) ) ;
#59268 = CARTESIAN_POINT ( 'NONE',  ( 5.823673210054125526, 21.52544592524343514, 64.79057627198103830 ) ) ;
#59269 = CARTESIAN_POINT ( 'NONE',  ( 16.55341960407611168, 4.379528057220329451, 33.95724293864769550 ) ) ;
#59270 = CARTESIAN_POINT ( 'NONE',  ( 0.05219959533937995610, -21.53943276465977519, 90.00109039468567573 ) ) ;
#59271 = CARTESIAN_POINT ( 'NONE',  ( -19.02544592524342804, 5.153800228976336051, 81.04057627198103830 ) ) ;
#59272 = CARTESIAN_POINT ( 'NONE',  ( -13.89961937509977652, 13.97604488694528158, 25.62390960531434558 ) ) ;
#59273 = CARTESIAN_POINT ( 'NONE',  ( -5.719274019375665041, -21.55341960407619695, 24.79275706135235779 ) ) ;
#59274 = CARTESIAN_POINT ( 'NONE',  ( 5.823673210054444382, -21.52544592524334988, 40.20942372801901854 ) ) ;
#59275 = CARTESIAN_POINT ( 'NONE',  ( 9.474510206698971260, -16.51473224551069308, 47.91557627198102409 ) ) ;
#59276 = CARTESIAN_POINT ( 'NONE',  ( 10.81492255796106328, -18.62759615963255655, 25.41775706135235779 ) ) ;
#59277 = CARTESIAN_POINT ( 'NONE',  ( 9.564922557961047289, -16.46253265017146816, 60.41775706135233293 ) ) ;
#59278 = CARTESIAN_POINT ( 'NONE',  ( -19.05341960407611168, -5.049401038298163336, 41.45724293864769550 ) ) ;
#59279 = CARTESIAN_POINT ( 'NONE',  ( -16.53943276465976808, -0.05219959533934237506, 28.75109039468567929 ) ) ;
#59280 = CARTESIAN_POINT ( 'NONE',  ( 16.46253265017160672, -9.564922557960803928, 28.33224293864769550 ) ) ;
#59281 = CARTESIAN_POINT ( 'NONE',  ( 14.34966873604972726, -8.224510206698740333, 65.83442372801900433 ) ) ;
#59282 = CARTESIAN_POINT ( 'NONE',  ( -19.05341960407611168, -5.049401038298163336, 36.45724293864766707 ) ) ;
#59283 = B_SPLINE_CURVE_WITH_KNOTS ( 'NONE', 3,
 ( #155025, #198563, #45862, #1326, #63006, #14530, #16521, #169191, #17511, #108519 ),
 .UNSPECIFIED., .F., .F.,
 ( 4, 2, 2, 2, 4 ),
 ( 3.469446951953613804E-18, 0.0009160790699533039819, 0.001832158139906604494, 0.002748237209859905224, 0.003664316279813205519 ),
 .UNSPECIFIED. ) ;
#59284 = CARTESIAN_POINT ( 'NONE',  ( -25.55222625260941172, -11.31436996698886155, 166.3494238031455268 ) ) ;
#59285 = CARTESIAN_POINT ( 'NONE',  ( -9.474510206698964154, 16.51473224551069663, 90.41557627198103830 ) ) ;
#59286 = CARTESIAN_POINT ( 'NONE',  ( -4.379528057220328563, 16.55341960407611168, 115.2072429386476955 ) ) ;
#59287 = CARTESIAN_POINT ( 'NONE',  ( -15.72974639402197994, 15.80617190586746368, 60.62390960531437401 ) ) ;
#59288 = CARTESIAN_POINT ( 'NONE',  ( -4.483927247898782831, 16.52544592524335698, 52.70942372801902565 ) ) ;
#59289 = CARTESIAN_POINT ( 'NONE',  ( -15.72974639402176322, -15.80617190586768395, 94.37609039468568994 ) ) ;
#59290 = CARTESIAN_POINT ( 'NONE',  ( 16.51473224551069308, 9.474510206698969483, 34.16557627198102409 ) ) ;
#59291 = CARTESIAN_POINT ( 'NONE',  ( 14.29746914071049879, -8.314922557960816363, 33.33224293864769550 ) ) ;
#59292 = CARTESIAN_POINT ( 'NONE',  ( 14.29746914071049879, -8.314922557960816363, 63.33224293864770260 ) ) ;
#59293 = CARTESIAN_POINT ( 'NONE',  ( 0.05219959533909260263, 19.03943276465977164, 69.99890960531435269 ) ) ;
#59294 = CARTESIAN_POINT ( 'NONE',  ( 15.72974639402176855, 15.80617190586768217, 111.8760903946856615 ) ) ;
#59295 = CARTESIAN_POINT ( 'NONE',  ( -15.72974639402176322, -15.80617190586768395, 29.37609039468568284 ) ) ;
#59296 = CIRCLE ( 'NONE', #17293, 2.000000000000000000 ) ;
#59297 = CARTESIAN_POINT ( 'NONE',  ( 21.52544592524334988, 5.823673210054432836, 91.45942372801901854 ) ) ;
#59298 = CARTESIAN_POINT ( 'NONE',  ( 14.34966873604972726, -8.224510206698740333, 55.83442372801901854 ) ) ;
#59299 = CARTESIAN_POINT ( 'NONE',  ( 8.314922557961029526, -14.29746914071037800, 30.41775706135234358 ) ) ;
#59301 = CARTESIAN_POINT ( 'NONE',  ( 21.53943276465977519, 0.05219959533937863772, 96.25109039468568994 ) ) ;
#59300 = CARTESIAN_POINT ( 'NONE',  ( 0.05219959533910956823, 16.53943276465976808, 89.99890960531438111 ) ) ;
#59302 = CARTESIAN_POINT ( 'NONE',  ( 8.314922557960818139, 14.29746914071049879, 39.58224293864769550 ) ) ;
#59303 = CARTESIAN_POINT ( 'NONE',  ( 19.03943276465977164, -0.05219959533909143690, 23.74890960531435269 ) ) ;
#59304 = CARTESIAN_POINT ( 'NONE',  ( -12.06949235617739369, -12.14591786802326823, 59.37609039468568284 ) ) ;
#59305 = CARTESIAN_POINT ( 'NONE',  ( -12.14591786802309592, -12.06949235617757132, 56.87390960531436690 ) ) ;
#59306 = CARTESIAN_POINT ( 'NONE',  ( 14.29746914071037800, 8.314922557961029526, 106.6677570613523756 ) ) ;
#59307 = CARTESIAN_POINT ( 'NONE',  ( 10.72451020669898902, -18.67979575497178502, 22.91557627198102765 ) ) ;
#59308 = CARTESIAN_POINT ( 'NONE',  ( -9.474510206698964154, 16.51473224551069663, 115.4155762719810241 ) ) ;
#59309 = CARTESIAN_POINT ( 'NONE',  ( 13.97604488694548053, -13.89961937509957401, 20.62609039468567573 ) ) ;
#59310 = CARTESIAN_POINT ( 'NONE',  ( -14.29746914071049879, 8.314922557960819915, 85.83224293864768129 ) ) ;
#59311 = CARTESIAN_POINT ( 'NONE',  ( -9.474510206698964154, 16.51473224551069663, 95.41557627198102409 ) ) ;
#59312 = ORIENTED_EDGE ( 'NONE', *, *, #169979, .F. ) ;
#59313 = CARTESIAN_POINT ( 'NONE',  ( 16.53943276465976808, 0.05219959533934440121, 41.25109039468568284 ) ) ;
#59314 = CARTESIAN_POINT ( 'NONE',  ( -9.474510206698964154, 16.51473224551069663, 45.41557627198103120 ) ) ;
#59315 = CARTESIAN_POINT ( 'NONE',  ( -5.153800228976328057, -19.02544592524343514, 107.2905762719810383 ) ) ;
#59317 = CARTESIAN_POINT ( 'NONE',  ( 15.50000000000000355, 5.499999999999998224, 22.00000000000000711 ) ) ;
#59316 = CARTESIAN_POINT ( 'NONE',  ( -14.34966873604972548, 8.224510206698743886, 48.33442372801902565 ) ) ;
#59318 = CARTESIAN_POINT ( 'NONE',  ( 19.03943276465977164, 0.05219959533936151252, 51.25109039468567573 ) ) ;
#59319 = CARTESIAN_POINT ( 'NONE',  ( -9.564922557960796823, -16.46253265017161027, 42.08224293864769550 ) ) ;
#59320 = CARTESIAN_POINT ( 'NONE',  ( -12.14591786802326823, 12.06949235617739902, 78.12609039468570415 ) ) ;
#59321 = CARTESIAN_POINT ( 'NONE',  ( 19.03943276465977164, 0.05219959533936151252, 76.25109039468566152 ) ) ;
#59322 = CARTESIAN_POINT ( 'NONE',  ( 13.97604488694548053, -13.89961937509957401, 25.62609039468566507 ) ) ;
#59323 = CARTESIAN_POINT ( 'NONE',  ( 19.05341960407611168, 5.049401038298154454, 63.95724293864769550 ) ) ;
#59324 = CARTESIAN_POINT ( 'NONE',  ( 4.379528057220339221, -16.55341960407611168, 102.7072429386476955 ) ) ;
#59325 = CARTESIAN_POINT ( 'NONE',  ( 16.46253265017146816, 9.564922557961045513, 61.66775706135234003 ) ) ;
#59326 = CARTESIAN_POINT ( 'NONE',  ( -21.55341960407610458, -5.719274019375992779, 61.45724293864770260 ) ) ;
#59327 = CARTESIAN_POINT ( 'NONE',  ( -19.05341960407617563, 5.049401038297882671, 28.54275706135232937 ) ) ;
#59328 = CARTESIAN_POINT ( 'NONE',  ( 13.89961937509977652, -13.97604488694527269, 98.12390960531433848 ) ) ;
#59329 = CARTESIAN_POINT ( 'NONE',  ( 21.53943276465977519, -0.05219959533907433946, 78.74890960531436690 ) ) ;
#59330 = CARTESIAN_POINT ( 'NONE',  ( -16.62475595723700650, 7.163666690055240593, 85.52713351810471920 ) ) ;
#59331 = CARTESIAN_POINT ( 'NONE',  ( 5.049401038297881783, 19.05341960407617563, 97.29275706135233293 ) ) ;
#59332 = CARTESIAN_POINT ( 'NONE',  ( -11.30153831258470731, -188.0000000000000000, -15.00000000000000178 ) ) ;
#59333 = CARTESIAN_POINT ( 'NONE',  ( -8.314922557961024197, 14.29746914071037800, 32.91775706135234714 ) ) ;
#59334 = CARTESIAN_POINT ( 'NONE',  ( -5.049401038298153566, 19.05341960407611168, 40.20724293864768839 ) ) ;
#59335 = CARTESIAN_POINT ( 'NONE',  ( -9.564922557960796823, -16.46253265017161027, 107.0822429386476955 ) ) ;
#59336 = CARTESIAN_POINT ( 'NONE',  ( -18.67979575497178146, -10.72451020669898902, 96.66557627198102409 ) ) ;
#59337 = CARTESIAN_POINT ( 'NONE',  ( -15.72974639402176322, -15.80617190586768395, 54.37609039468568994 ) ) ;
#59339 = CARTESIAN_POINT ( 'NONE',  ( -18.62759615963255300, -10.81492255796106328, 109.1677570613523613 ) ) ;
#59338 = CARTESIAN_POINT ( 'NONE',  ( 9.474510206698729675, 16.51473224551082808, 107.0844237280190043 ) ) ;
#59340 = CARTESIAN_POINT ( 'NONE',  ( -14.34966873604972548, 8.224510206698743886, 113.3344237280190328 ) ) ;
#59341 = EDGE_CURVE ( 'NONE', #158898, #74699, #122128, .T. ) ;
#59342 = CARTESIAN_POINT ( 'NONE',  ( 18.67979575497178502, 10.72451020669898547, 104.1655762719810241 ) ) ;
#59343 = CARTESIAN_POINT ( 'NONE',  ( 16.53943276465976808, -0.05219959533910856209, 48.74890960531435979 ) ) ;
#59344 = CARTESIAN_POINT ( 'NONE',  ( -5.153800228976607833, 19.02544592524334988, 82.70942372801897591 ) ) ;
#59345 = ADVANCED_FACE ( 'NONE', ( #47025 ), #108683, .F. ) ;
#59346 = CARTESIAN_POINT ( 'NONE',  ( 5.049401038297881783, 19.05341960407617563, 52.29275706135234003 ) ) ;
#59347 = CARTESIAN_POINT ( 'NONE',  ( -10.81492255796105439, 18.62759615963255655, 52.91775706135235424 ) ) ;
#59348 = CARTESIAN_POINT ( 'NONE',  ( -0.05219959533936034679, 19.03943276465977164, 37.50109039468567573 ) ) ;
#59349 = CARTESIAN_POINT ( 'NONE',  ( -16.55341960407611168, -4.379528057220339221, 106.4572429386477097 ) ) ;
#59350 = CARTESIAN_POINT ( 'NONE',  ( -18.62759615963270932, 10.81492255796079327, 25.83224293864769194 ) ) ;
#59351 = CARTESIAN_POINT ( 'NONE',  ( -0.05219959533910754901, -16.53943276465976808, 37.49890960531436690 ) ) ;
#59352 = CARTESIAN_POINT ( 'NONE',  ( -21.55341960407619339, 5.719274019375674811, 103.5427570613523613 ) ) ;
#59353 = CARTESIAN_POINT ( 'NONE',  ( -8.314922557961024197, 14.29746914071037800, 77.91775706135231871 ) ) ;
#59354 = CARTESIAN_POINT ( 'NONE',  ( -14.29746914071049879, 8.314922557960819915, 30.83224293864770260 ) ) ;
#59355 = CARTESIAN_POINT ( 'NONE',  ( 0.05219959533937995610, -21.53943276465977519, 65.00109039468568994 ) ) ;
#59356 = CARTESIAN_POINT ( 'NONE',  ( -10.81492255796105439, 18.62759615963255655, 67.91775706135234714 ) ) ;
#59357 = CARTESIAN_POINT ( 'NONE',  ( 18.67979575497178502, 10.72451020669898547, 74.16557627198102409 ) ) ;
#59358 = ORIENTED_EDGE ( 'NONE', *, *, #100927, .T. ) ;
#59359 = CARTESIAN_POINT ( 'NONE',  ( 18.22780087662123805, -5.499999999999989342, 63.51763182126896368 ) ) ;
#59360 = CARTESIAN_POINT ( 'NONE',  ( -18.67979575497193778, 10.72451020669871902, 48.33442372801902565 ) ) ;
#59361 = CARTESIAN_POINT ( 'NONE',  ( -14.34966873604960291, -8.224510206698953496, 111.6655762719810525 ) ) ;
#59362 = CARTESIAN_POINT ( 'NONE',  ( 13.89961937509977652, -13.97604488694527269, 43.12390960531434558 ) ) ;
#59363 = CARTESIAN_POINT ( 'NONE',  ( 16.52544592524342804, -4.483927247898539470, 78.54057627198103830 ) ) ;
#59364 = CARTESIAN_POINT ( 'NONE',  ( -19.05341960407611168, -5.049401038298163336, 86.45724293864769550 ) ) ;
#59365 = CARTESIAN_POINT ( 'NONE',  ( -12.14591786802309592, -12.06949235617757132, 21.87390960531436690 ) ) ;
#59366 = CARTESIAN_POINT ( 'NONE',  ( 0.05219959533910956823, 16.53943276465976808, 104.9989096053143669 ) ) ;
#59367 = CARTESIAN_POINT ( 'NONE',  ( -0.05219959533907301413, -21.53943276465977519, 67.49890960531436690 ) ) ;
#59368 = CARTESIAN_POINT ( 'NONE',  ( -5.719274019375978568, 21.55341960407610458, 100.2072429386476955 ) ) ;
#59369 = DIRECTION ( 'NONE',  ( -0.000000000000000000, -0.000000000000000000, 1.000000000000000000 ) ) ;
#59371 = CARTESIAN_POINT ( 'NONE',  ( 9.474510206698729675, 16.51473224551082808, 102.0844237280190043 ) ) ;
#59370 = CARTESIAN_POINT ( 'NONE',  ( -5.049401038298153566, 19.05341960407611168, 65.20724293864765286 ) ) ;
#59372 = CARTESIAN_POINT ( 'NONE',  ( -0.05219959533907301413, -21.53943276465977519, 57.49890960531435979 ) ) ;
#59373 = CARTESIAN_POINT ( 'NONE',  ( 15.80617190586769283, -15.72974639402175789, 85.62609039468568994 ) ) ;
#59374 = CARTESIAN_POINT ( 'NONE',  ( -19.05341960407611168, -5.049401038298163336, 61.45724293864769550 ) ) ;
#59375 = AXIS2_PLACEMENT_3D ( 'NONE', #111759, #4556, #53066 ) ;
#59376 = CARTESIAN_POINT ( 'NONE',  ( 0.05219959533909260263, 19.03943276465977164, 94.99890960531436690 ) ) ;
#59377 = CARTESIAN_POINT ( 'NONE',  ( 16.52544592524335698, 4.483927247898782831, 71.45942372801901854 ) ) ;
#59378 = CARTESIAN_POINT ( 'NONE',  ( -0.05219959533937732626, 21.53943276465977519, 52.50109039468567573 ) ) ;
#59379 = CARTESIAN_POINT ( 'NONE',  ( 21.52544592524334988, 5.823673210054432836, 101.4594237280190185 ) ) ;
#59380 = CARTESIAN_POINT ( 'NONE',  ( 18.62759615963255655, 10.81492255796105972, 21.66775706135235069 ) ) ;
#59381 = CARTESIAN_POINT ( 'NONE',  ( -21.53943276465977519, 0.05219959533907696930, 76.24890960531435269 ) ) ;
#59382 = CARTESIAN_POINT ( 'NONE',  ( -13.89961937509957401, -13.97604488694547875, 44.37609039468566863 ) ) ;
#59383 = CARTESIAN_POINT ( 'NONE',  ( -18.62759615963270932, 10.81492255796079327, 40.83224293864769550 ) ) ;
#59385 = CARTESIAN_POINT ( 'NONE',  ( -4.379528057220328563, 16.55341960407611168, 35.20724293864768839 ) ) ;
#59384 = CARTESIAN_POINT ( 'NONE',  ( -5.049401038298153566, 19.05341960407611168, 85.20724293864766707 ) ) ;
#59386 = CARTESIAN_POINT ( 'NONE',  ( -16.81555441253553340, 7.025013491695480283, 65.63685445334260748 ) ) ;
#59387 = CARTESIAN_POINT ( 'NONE',  ( -19.39720447994794483, -5.500000000000082601, 79.66317477297182847 ) ) ;
#59388 = CARTESIAN_POINT ( 'NONE',  ( -13.97604488694547697, 13.89961937509957934, 93.12609039468566152 ) ) ;
#59389 = CARTESIAN_POINT ( 'NONE',  ( -10.72451020669898014, 18.67979575497178502, 65.41557627198102409 ) ) ;
#59390 = CARTESIAN_POINT ( 'NONE',  ( 8.224510206698953496, -14.34966873604960469, 47.91557627198102409 ) ) ;
#59391 = CARTESIAN_POINT ( 'NONE',  ( 12.06949235617739724, 12.14591786802326823, 26.87609039468567218 ) ) ;
#59392 = CARTESIAN_POINT ( 'NONE',  ( -19.02544592524342804, 5.153800228976336051, 46.04057627198101699 ) ) ;
#59394 = CARTESIAN_POINT ( 'NONE',  ( -16.46253265017146816, -9.564922557961047289, 89.16775706135234714 ) ) ;
#59393 = CARTESIAN_POINT ( 'NONE',  ( 5.823673210054444382, -21.52544592524334988, 20.20942372801900788 ) ) ;
#59395 = CARTESIAN_POINT ( 'NONE',  ( -9.474510206698964154, 16.51473224551069663, 80.41557627198103830 ) ) ;
#59396 = CARTESIAN_POINT ( 'NONE',  ( -14.29746914071049879, 8.314922557960819915, 85.83224293864768129 ) ) ;
#59397 = CARTESIAN_POINT ( 'NONE',  ( 13.97604488694527802, 13.89961937509977652, 74.37390960531436690 ) ) ;
#59398 = CARTESIAN_POINT ( 'NONE',  ( 15.72974639402199770, -15.80617190586745480, 73.12390960531436690 ) ) ;
#59399 = CARTESIAN_POINT ( 'NONE',  ( 5.153800228976335163, 19.02544592524342804, 29.79057627198102409 ) ) ;
#59400 = CARTESIAN_POINT ( 'NONE',  ( 1.160557336561849118, 37.56284411304923054, -8.000000000000003553 ) ) ;
#59401 = CARTESIAN_POINT ( 'NONE',  ( -0.05219959533910754901, -16.53943276465976808, 52.49890960531435979 ) ) ;
#59402 = CARTESIAN_POINT ( 'NONE',  ( 13.97604488694527802, 13.89961937509977652, 94.37390960531436690 ) ) ;
#59403 = LINE ( 'NONE', #179802, #79842 ) ;
#59404 = CARTESIAN_POINT ( 'NONE',  ( 5.049401038297881783, 19.05341960407617563, 47.29275706135231161 ) ) ;
#59405 = CARTESIAN_POINT ( 'NONE',  ( -4.483927247898782831, 16.52544592524335698, 62.70942372801902565 ) ) ;
#59406 = CARTESIAN_POINT ( 'NONE',  ( 5.719274019375991003, -21.55341960407610458, 82.70724293864770971 ) ) ;
#59407 = CARTESIAN_POINT ( 'NONE',  ( -5.153800228976607833, 19.02544592524334988, 42.70942372801901143 ) ) ;
#59408 = CARTESIAN_POINT ( 'NONE',  ( 13.89961937509977652, -13.97604488694527269, 83.12390960531436690 ) ) ;
#59409 = FACE_BOUND ( 'NONE', #161919, .T. ) ;
#59410 = CARTESIAN_POINT ( 'NONE',  ( -10.72451020669898014, 18.67979575497178502, 30.41557627198101699 ) ) ;
#59411 = CARTESIAN_POINT ( 'NONE',  ( -16.46253265017160317, 9.564922557960807481, 70.83224293864770971 ) ) ;
#59412 = CARTESIAN_POINT ( 'NONE',  ( 0.05219959533937995610, -21.53943276465977519, 50.00109039468568994 ) ) ;
#59413 = CARTESIAN_POINT ( 'NONE',  ( 13.97604488694527802, 13.89961937509977652, 29.37390960531435979 ) ) ;
#59414 = EDGE_CURVE ( 'NONE', #117112, #43523, #179280, .T. ) ;
#59417 = VERTEX_POINT ( 'NONE', #56988 ) ;
#59416 = CARTESIAN_POINT ( 'NONE',  ( -19.03943276465977164, 0.05219959533909376836, 91.24890960531436690 ) ) ;
#59415 = CARTESIAN_POINT ( 'NONE',  ( -5.719274019375978568, 21.55341960407610458, 110.2072429386477239 ) ) ;
#59418 = CARTESIAN_POINT ( 'NONE',  ( 10.81492255796106328, -18.62759615963255655, 45.41775706135234003 ) ) ;
#59419 = VERTEX_POINT ( 'NONE', #179352 ) ;
#59420 = CARTESIAN_POINT ( 'NONE',  ( -16.51473224551069308, -9.474510206698971260, 106.6655762719810383 ) ) ;
#59421 = CARTESIAN_POINT ( 'NONE',  ( -21.82762259161260232, 6.010869995788715059, 172.1044450858202026 ) ) ;
#59422 = CARTESIAN_POINT ( 'NONE',  ( -18.62759615963270932, 10.81492255796079327, 110.8322429386476955 ) ) ;
#59423 = CARTESIAN_POINT ( 'NONE',  ( 19.02544592524343514, -5.153800228976328945, 48.54057627198103120 ) ) ;
#59424 = CARTESIAN_POINT ( 'NONE',  ( 16.53943276465976808, 0.05219959533934440121, 26.25109039468567573 ) ) ;
#59425 = CARTESIAN_POINT ( 'NONE',  ( 3.556970738554033499E-15, -38.81732327939057825, -4.624999997268814056 ) ) ;
#59426 = CARTESIAN_POINT ( 'NONE',  ( 5.823673210054444382, -21.52544592524334988, 105.2094237280190328 ) ) ;
#59427 = CARTESIAN_POINT ( 'NONE',  ( 16.51473224551069308, 9.474510206698969483, 24.16557627198102765 ) ) ;
#59428 = CARTESIAN_POINT ( 'NONE',  ( 5.719274019375673035, 21.55341960407619339, 92.29275706135236135 ) ) ;
#59429 = EDGE_CURVE ( 'NONE', #54470, #118125, #117655, .T. ) ;
#59431 = CARTESIAN_POINT ( 'NONE',  ( -21.53943276465977519, -0.05219959533937600094, 63.75109039468568284 ) ) ;
#59430 = CARTESIAN_POINT ( 'NONE',  ( -5.153800228976328057, -19.02544592524343514, 92.29057627198099567 ) ) ;
#59432 = CARTESIAN_POINT ( 'NONE',  ( -27.73933785331498925, 2.428612866367529932E-14, 141.3750000027311842 ) ) ;
#59433 = CARTESIAN_POINT ( 'NONE',  ( 13.97604488694527802, 13.89961937509977652, 99.37390960531436690 ) ) ;
#59434 = DIRECTION ( 'NONE',  ( 0.000000000000000000, 0.000000000000000000, -1.000000000000000000 ) ) ;
#59437 = CARTESIAN_POINT ( 'NONE',  ( 15.72974639402176855, 15.80617190586768217, 51.87609039468568284 ) ) ;
#59436 = CARTESIAN_POINT ( 'NONE',  ( 4.379528057220092307, 16.55341960407617563, 62.29275706135236845 ) ) ;
#59435 = CARTESIAN_POINT ( 'NONE',  ( 14.34966873604972726, -8.224510206698740333, 50.83442372801901143 ) ) ;
#59438 = CARTESIAN_POINT ( 'NONE',  ( -5.823673210054431948, 21.52544592524334988, 87.70942372801901854 ) ) ;
#59439 = CARTESIAN_POINT ( 'NONE',  ( 26.53317239408746175, -7.611579847057702075, 168.2742808015845526 ) ) ;
#59440 = CARTESIAN_POINT ( 'NONE',  ( -8.224510206698735004, -14.34966873604973081, 24.58442372801901499 ) ) ;
#59441 = CARTESIAN_POINT ( 'NONE',  ( -19.03943276465977164, 0.05219959533909376836, 71.24890960531435269 ) ) ;
#59442 = CARTESIAN_POINT ( 'NONE',  ( -9.474510206698964154, 16.51473224551069663, 95.41557627198102409 ) ) ;
#59443 = CARTESIAN_POINT ( 'NONE',  ( 18.09867054820431775, 5.499999999999960032, 91.48393025253585620 ) ) ;
#59444 = CARTESIAN_POINT ( 'NONE',  ( 9.564922557960805705, 16.46253265017160317, 29.58224293864769550 ) ) ;
#59445 = CARTESIAN_POINT ( 'NONE',  ( -15.72974639402197994, 15.80617190586746368, 30.62390960531436335 ) ) ;
#59446 = CARTESIAN_POINT ( 'NONE',  ( 16.53943276465976808, 0.05219959533934440121, 91.25109039468568994 ) ) ;
#59448 = CARTESIAN_POINT ( 'NONE',  ( -5.153800228976328057, -19.02544592524343514, 72.29057627198102409 ) ) ;
#59447 = CARTESIAN_POINT ( 'NONE',  ( 14.34966873604960469, 8.224510206698951720, 74.16557627198102409 ) ) ;
#59449 = CARTESIAN_POINT ( 'NONE',  ( -15.72974639402176322, -15.80617190586768395, 94.37609039468568994 ) ) ;
#59450 = CARTESIAN_POINT ( 'NONE',  ( -19.02544592524342804, 5.153800228976336051, 116.0405762719810383 ) ) ;
#59451 = CARTESIAN_POINT ( 'NONE',  ( -8.224510206698735004, -14.34966873604973081, 24.58442372801901499 ) ) ;
#59452 = CARTESIAN_POINT ( 'NONE',  ( -14.29746914071049879, 8.314922557960819915, 80.83224293864769550 ) ) ;
#59453 = CARTESIAN_POINT ( 'NONE',  ( -21.52544592524334988, -5.823673210054445271, 33.95942372801901143 ) ) ;
#59454 = CARTESIAN_POINT ( 'NONE',  ( -15.72974639402197994, 15.80617190586746368, 70.62390960531436690 ) ) ;
#59455 = CARTESIAN_POINT ( 'NONE',  ( -9.474510206698720793, -16.51473224551083518, 39.58442372801899722 ) ) ;
#59456 = CARTESIAN_POINT ( 'NONE',  ( -28.82186960331499037, 2.428612866367529932E-14, 148.2500000054623683 ) ) ;
#59457 = CARTESIAN_POINT ( 'NONE',  ( 9.564922557960805705, 16.46253265017160317, 84.58224293864769550 ) ) ;
#59458 = CARTESIAN_POINT ( 'NONE',  ( 16.53943276465976808, -0.05219959533910856209, 43.74890960531435979 ) ) ;
#59459 = CIRCLE ( 'NONE', #56154, 10.00000000000000178 ) ;
#59460 = CARTESIAN_POINT ( 'NONE',  ( -16.53943276465976808, 0.05219959533911058130, 41.24890960531435269 ) ) ;
#59461 = CARTESIAN_POINT ( 'NONE',  ( 8.314922557961029526, -14.29746914071037800, 105.4177570613523613 ) ) ;
#59462 = CARTESIAN_POINT ( 'NONE',  ( 5.153800228976615827, -19.02544592524334988, 60.20942372801899012 ) ) ;
#59463 = CARTESIAN_POINT ( 'NONE',  ( 18.22780087662121673, 5.500000000000056843, 53.98459894673893444 ) ) ;
#59464 = CARTESIAN_POINT ( 'NONE',  ( -16.46253265017160317, 9.564922557960807481, 100.8322429386477097 ) ) ;
#59465 = CARTESIAN_POINT ( 'NONE',  ( 14.29746914071049879, -8.314922557960816363, 78.33224293864770971 ) ) ;
#59466 = FACE_OUTER_BOUND ( 'NONE', #134762, .T. ) ;
#59468 = CARTESIAN_POINT ( 'NONE',  ( 5.823673210054125526, 21.52544592524343514, 39.79057627198103830 ) ) ;
#59467 = CARTESIAN_POINT ( 'NONE',  ( -13.97604488694527625, -13.89961937509977652, 26.87390960531434558 ) ) ;
#59469 = CARTESIAN_POINT ( 'NONE',  ( -5.719274019375978568, 21.55341960407610458, 70.20724293864769550 ) ) ;
#59470 = CARTESIAN_POINT ( 'NONE',  ( -14.29746914071049879, 8.314922557960819915, 115.8322429386477097 ) ) ;
#59472 = CARTESIAN_POINT ( 'NONE',  ( 19.05341960407611168, 5.049401038298154454, 48.95724293864768129 ) ) ;
#59471 = CARTESIAN_POINT ( 'NONE',  ( -12.14591786802326823, 12.06949235617739902, 63.12609039468568994 ) ) ;
#59473 = CARTESIAN_POINT ( 'NONE',  ( 0.05219959533937995610, -21.53943276465977519, 50.00109039468568994 ) ) ;
#59474 = CARTESIAN_POINT ( 'NONE',  ( 12.14591786802309770, 12.06949235617756955, 94.37390960531436690 ) ) ;
#59475 = CARTESIAN_POINT ( 'NONE',  ( 17.26172910966779739, -6.454744622555848466, 38.30646908649224969 ) ) ;
#59476 = CARTESIAN_POINT ( 'NONE',  ( 3.556970738554034288E-15, -38.81732327939057114, -8.624999997268814056 ) ) ;
#59477 = CARTESIAN_POINT ( 'NONE',  ( -5.719274019375978568, 21.55341960407610458, 35.20724293864768839 ) ) ;
#59478 = CARTESIAN_POINT ( 'NONE',  ( 2.500000000000000000, -1.178949249685214307, 2.042000000000002036 ) ) ;
#59480 = CARTESIAN_POINT ( 'NONE',  ( 1.203566692396469184, 8.516350909510459033, -64.06484607254931518 ) ) ;
#59479 = CARTESIAN_POINT ( 'NONE',  ( 10.81492255796106328, -18.62759615963255655, 65.41775706135234714 ) ) ;
#59482 = CARTESIAN_POINT ( 'NONE',  ( -12.06949235617756955, 12.14591786802309770, 45.62390960531436690 ) ) ;
#59481 = CARTESIAN_POINT ( 'NONE',  ( 12.06949235617739724, 12.14591786802326823, 61.87609039468568284 ) ) ;
#59483 = CARTESIAN_POINT ( 'NONE',  ( -21.53943276465977519, 0.05219959533907696930, 71.24890960531435269 ) ) ;
#59484 = CARTESIAN_POINT ( 'NONE',  ( -5.823673210054116645, -21.52544592524344225, 57.29057627198103120 ) ) ;
#59485 = FACE_OUTER_BOUND ( 'NONE', #8953, .T. ) ;
#59487 = CARTESIAN_POINT ( 'NONE',  ( 21.53943276465977519, -0.05219959533907433946, 23.74890960531435269 ) ) ;
#59486 = CARTESIAN_POINT ( 'NONE',  ( 16.46253265017146816, 9.564922557961045513, 86.66775706135233293 ) ) ;
#59488 = CARTESIAN_POINT ( 'NONE',  ( 9.564922557960805705, 16.46253265017160317, 49.58224293864770260 ) ) ;
#59489 = CARTESIAN_POINT ( 'NONE',  ( 14.29746914071049879, -8.314922557960816363, 113.3322429386476955 ) ) ;
#59490 = FACE_BOUND ( 'NONE', #5824, .T. ) ;
#59491 = ORIENTED_EDGE ( 'NONE', *, *, #134324, .F. ) ;
#59492 = CARTESIAN_POINT ( 'NONE',  ( -16.55341960407617563, 4.379528057220093196, 63.54275706135234003 ) ) ;
#59493 = CARTESIAN_POINT ( 'NONE',  ( -15.72974639402197994, 15.80617190586746368, 110.6239096053143669 ) ) ;
#59494 = CARTESIAN_POINT ( 'NONE',  ( 5.049401038298161559, -19.05341960407611168, 52.70724293864767418 ) ) ;
#59495 = CARTESIAN_POINT ( 'NONE',  ( 21.55341960407619695, -5.719274019375665929, 36.04275706135234714 ) ) ;
#59496 = CARTESIAN_POINT ( 'NONE',  ( 13.97604488694527802, 13.89961937509977652, 94.37390960531436690 ) ) ;
#59497 = CARTESIAN_POINT ( 'NONE',  ( -28.71286925542075963, -27.61909494970944579, -16.96471949292295989 ) ) ;
#59498 = ORIENTED_EDGE ( 'NONE', *, *, #8310, .T. ) ;
#59499 = CARTESIAN_POINT ( 'NONE',  ( 10.81492255796106328, -18.62759615963255655, 30.41775706135234358 ) ) ;
#59501 = CARTESIAN_POINT ( 'NONE',  ( -13.89961937509957401, -13.97604488694547875, 94.37609039468566152 ) ) ;
#59500 = CARTESIAN_POINT ( 'NONE',  ( -19.02544592524342804, 5.153800228976336051, 101.0405762719810241 ) ) ;
#59502 = CARTESIAN_POINT ( 'NONE',  ( 5.153800228976615827, -19.02544592524334988, 40.20942372801898301 ) ) ;
#59503 = CARTESIAN_POINT ( 'NONE',  ( -21.52544592524343514, 5.823673210054127303, 101.0405762719810383 ) ) ;
#59504 = CARTESIAN_POINT ( 'NONE',  ( 13.89961937509957401, 13.97604488694547697, 31.87609039468566863 ) ) ;
#59505 = CARTESIAN_POINT ( 'NONE',  ( 13.97604488694548053, -13.89961937509957401, 30.62609039468566863 ) ) ;
#59506 = CARTESIAN_POINT ( 'NONE',  ( -8.314922557961024197, 14.29746914071037800, 87.91775706135234714 ) ) ;
#59507 = CARTESIAN_POINT ( 'NONE',  ( 16.46253265017160672, -9.564922557960803928, 113.3322429386476955 ) ) ;
#59508 = CARTESIAN_POINT ( 'NONE',  ( 16.46253265017160672, -9.564922557960803928, 78.33224293864769550 ) ) ;
#59509 = CARTESIAN_POINT ( 'NONE',  ( -21.55341960407619339, 5.719274019375674811, 73.54275706135234714 ) ) ;
#59510 = CARTESIAN_POINT ( 'NONE',  ( -10.72451020669870658, -18.67979575497194134, 74.58442372801901854 ) ) ;
#59511 = CARTESIAN_POINT ( 'NONE',  ( -19.05341960407611168, -5.049401038298163336, 91.45724293864766707 ) ) ;
#59512 = CARTESIAN_POINT ( 'NONE',  ( -10.81492255796105439, 18.62759615963255655, 62.91775706135236135 ) ) ;
#59513 = CARTESIAN_POINT ( 'NONE',  ( 9.564922557961047289, -16.46253265017146816, 105.4177570613523471 ) ) ;
#59514 = CARTESIAN_POINT ( 'NONE',  ( 5.049401038298161559, -19.05341960407611168, 62.70724293864769550 ) ) ;
#59515 = CARTESIAN_POINT ( 'NONE',  ( -5.153800228976328057, -19.02544592524343514, 112.2905762719810099 ) ) ;
#59516 = CARTESIAN_POINT ( 'NONE',  ( -13.89961937509977652, 13.97604488694528158, 75.62390960531438111 ) ) ;
#59517 = DIRECTION ( 'NONE',  ( 1.000000000000000000, 0.000000000000000000, 0.000000000000000000 ) ) ;
#59518 = CARTESIAN_POINT ( 'NONE',  ( -0.05219959533909027116, -19.03943276465977164, 62.49890960531435979 ) ) ;
#59519 = CARTESIAN_POINT ( 'NONE',  ( 13.97604488694527802, 13.89961937509977652, 49.37390960531434558 ) ) ;
#59520 = CARTESIAN_POINT ( 'NONE',  ( 10.72451020669898902, -18.67979575497178502, 97.91557627198103830 ) ) ;
#59521 = CARTESIAN_POINT ( 'NONE',  ( -8.314922557961024197, 14.29746914071037800, 82.91775706135234714 ) ) ;
#59522 = CARTESIAN_POINT ( 'NONE',  ( 24.93942350307308686, 7.769968609432599926, 171.2173313942149946 ) ) ;
#59523 = CARTESIAN_POINT ( 'NONE',  ( 5.049401038297881783, 19.05341960407617563, 47.29275706135231161 ) ) ;
#59524 = CARTESIAN_POINT ( 'NONE',  ( -9.474510206698964154, 16.51473224551069663, 75.41557627198103830 ) ) ;
#59525 = CARTESIAN_POINT ( 'NONE',  ( 12.06949235617757843, -12.14591786802309237, 68.12390960531436690 ) ) ;
#59526 = CARTESIAN_POINT ( 'NONE',  ( -12.14591786802309592, -12.06949235617757132, 111.8739096053143669 ) ) ;
#59527 = CARTESIAN_POINT ( 'NONE',  ( 19.05341960407611168, 5.049401038298154454, 108.9572429386477097 ) ) ;
#59528 = CARTESIAN_POINT ( 'NONE',  ( 13.89961937509977652, -13.97604488694527269, 103.1239096053143527 ) ) ;
#59529 = CARTESIAN_POINT ( 'NONE',  ( 14.34966873604960469, 8.224510206698951720, 79.16557627198103830 ) ) ;
#59530 = CARTESIAN_POINT ( 'NONE',  ( -37.99626262588766679, 2.428612866367529932E-14, -4.002157773949823749 ) ) ;
#59531 = CARTESIAN_POINT ( 'NONE',  ( 9.564922557961047289, -16.46253265017146816, 25.41775706135234003 ) ) ;
#59532 = CARTESIAN_POINT ( 'NONE',  ( -16.55341960407617563, 4.379528057220093196, 98.54275706135234714 ) ) ;
#59533 = CARTESIAN_POINT ( 'NONE',  ( -5.153800228976328057, -19.02544592524343514, 72.29057627198102409 ) ) ;
#59534 = CARTESIAN_POINT ( 'NONE',  ( 10.81492255796106328, -18.62759615963255655, 50.41775706135235424 ) ) ;
#59535 = CARTESIAN_POINT ( 'NONE',  ( 18.67979575497178502, 10.72451020669898547, 39.16557627198102409 ) ) ;
#59536 = CARTESIAN_POINT ( 'NONE',  ( 21.53943276465977519, 0.05219959533937863772, 21.25109039468567218 ) ) ;
#59537 = CARTESIAN_POINT ( 'NONE',  ( -10.72451020669898014, 18.67979575497178502, 70.41557627198102409 ) ) ;
#59538 = CARTESIAN_POINT ( 'NONE',  ( 12.14591786802309770, 12.06949235617756955, 99.37390960531436690 ) ) ;
#59539 = CARTESIAN_POINT ( 'NONE',  ( 16.46253265017146816, 9.564922557961045513, 56.66775706135233293 ) ) ;
#59540 = AXIS2_PLACEMENT_3D ( 'NONE', #155384, #58407, #181761 ) ;
#59541 = CARTESIAN_POINT ( 'NONE',  ( -19.05341960407611168, -5.049401038298163336, 36.45724293864766707 ) ) ;
#59542 = CARTESIAN_POINT ( 'NONE',  ( -19.03943276465977164, 0.05219959533909376836, 81.24890960531436690 ) ) ;
#59543 = CARTESIAN_POINT ( 'NONE',  ( 9.474510206698971260, -16.51473224551069308, 82.91557627198103830 ) ) ;
#59544 = CARTESIAN_POINT ( 'NONE',  ( -16.52544592524342804, 4.483927247898546575, 101.0405762719810383 ) ) ;
#59545 = ORIENTED_EDGE ( 'NONE', *, *, #79441, .T. ) ;
#59546 = CARTESIAN_POINT ( 'NONE',  ( -16.52544592524342804, 4.483927247898546575, 26.04057627198103475 ) ) ;
#59547 = CARTESIAN_POINT ( 'NONE',  ( 12.06949235617739724, 12.14591786802326823, 26.87609039468567218 ) ) ;
#59548 = CARTESIAN_POINT ( 'NONE',  ( -21.55341960407619339, 5.719274019375674811, 93.54275706135234714 ) ) ;
#59549 = CARTESIAN_POINT ( 'NONE',  ( -9.474510206698964154, 16.51473224551069663, 100.4155762719810241 ) ) ;
#59550 = CARTESIAN_POINT ( 'NONE',  ( -15.72974639402176322, -15.80617190586768395, 24.37609039468567573 ) ) ;
#59551 = CARTESIAN_POINT ( 'NONE',  ( -13.97604488694527625, -13.89961937509977652, 46.87390960531435979 ) ) ;
#59552 = CARTESIAN_POINT ( 'NONE',  ( -16.52544592524335698, -4.483927247898792601, 38.95942372801901854 ) ) ;
#59553 = CARTESIAN_POINT ( 'NONE',  ( 13.97604488694548053, -13.89961937509957401, 110.6260903946856615 ) ) ;
#59554 = CARTESIAN_POINT ( 'NONE',  ( 5.049401038298161559, -19.05341960407611168, 37.70724293864768839 ) ) ;
#59555 = CARTESIAN_POINT ( 'NONE',  ( -16.55341960407611168, -4.379528057220339221, 96.45724293864770971 ) ) ;
#59556 = CARTESIAN_POINT ( 'NONE',  ( 18.62759615963271287, -10.81492255796078972, 103.3322429386476955 ) ) ;
#59557 = CARTESIAN_POINT ( 'NONE',  ( -19.02544592524334988, -5.153800228976617603, 63.95942372801899012 ) ) ;
#59558 =( NAMED_UNIT ( * ) PLANE_ANGLE_UNIT ( ) SI_UNIT ( $, .RADIAN. ) );
#59559 = CARTESIAN_POINT ( 'NONE',  ( -13.89961937509977652, 13.97604488694528158, 95.62390960531436690 ) ) ;
#59560 = CARTESIAN_POINT ( 'NONE',  ( -5.719274019375665041, -21.55341960407619695, 24.79275706135235779 ) ) ;
#59561 = DIRECTION ( 'NONE',  ( 0.7071067811865467956, -2.468850131082262977E-15, -0.7071067811865483499 ) ) ;
#59562 = CARTESIAN_POINT ( 'NONE',  ( -16.46253265017160317, 9.564922557960807481, 85.83224293864769550 ) ) ;
#59563 = CIRCLE ( 'NONE', #188760, 29.43349580481983807 ) ;
#59564 = CARTESIAN_POINT ( 'NONE',  ( 17.26058549869091507, -6.457015423128544818, 111.1225416252393643 ) ) ;
#59565 = CARTESIAN_POINT ( 'NONE',  ( -19.03943276465977164, 0.05219959533909376836, 86.24890960531436690 ) ) ;
#59567 = CARTESIAN_POINT ( 'NONE',  ( 16.55341960407611168, 4.379528057220329451, 83.95724293864770971 ) ) ;
#59566 = CARTESIAN_POINT ( 'NONE',  ( -15.80617190586768217, 15.72974639402176855, 33.12609039468569705 ) ) ;
#59568 = CARTESIAN_POINT ( 'NONE',  ( -9.474510206698964154, 16.51473224551069663, 85.41557627198102409 ) ) ;
#59569 = CARTESIAN_POINT ( 'NONE',  ( -19.03943276465977164, -0.05219959533935918106, 23.75109039468566152 ) ) ;
#59571 = CARTESIAN_POINT ( 'NONE',  ( -0.05219959533936034679, 19.03943276465977164, 57.50109039468566863 ) ) ;
#59570 = CARTESIAN_POINT ( 'NONE',  ( -4.379528057220086978, -16.55341960407618274, 44.79275706135234714 ) ) ;
#59572 = CARTESIAN_POINT ( 'NONE',  ( 21.55341960407619695, -5.719274019375665929, 66.04275706135236135 ) ) ;
#59573 = CARTESIAN_POINT ( 'NONE',  ( 8.224510206698742110, 14.34966873604972548, 27.08442372801901854 ) ) ;
#59575 = EDGE_CURVE ( 'NONE', #93307, #75663, #39803, .T. ) ;
#59574 = CARTESIAN_POINT ( 'NONE',  ( 19.02544592524343514, -5.153800228976328945, 63.54057627198103830 ) ) ;
#59576 = CARTESIAN_POINT ( 'NONE',  ( -19.03943276465977164, -0.05219959533935918106, 98.75109039468567573 ) ) ;
#59577 = CARTESIAN_POINT ( 'NONE',  ( 16.55341960407618274, -4.379528057220086978, 76.04275706135237556 ) ) ;
#59578 = CARTESIAN_POINT ( 'NONE',  ( 13.89961937509957401, 13.97604488694547697, 21.87609039468566152 ) ) ;
#59579 = CARTESIAN_POINT ( 'NONE',  ( -19.05341960407617563, 5.049401038297882671, 73.54275706135233293 ) ) ;
#59580 = CARTESIAN_POINT ( 'NONE',  ( 13.97604488694527802, 13.89961937509977652, 54.37390960531435979 ) ) ;
#59581 = CARTESIAN_POINT ( 'NONE',  ( -5.823673210054116645, -21.52544592524344225, 82.29057627198103830 ) ) ;
#59583 = CARTESIAN_POINT ( 'NONE',  ( -13.89961937509957401, -13.97604488694547875, 74.37609039468566152 ) ) ;
#59582 = CARTESIAN_POINT ( 'NONE',  ( 16.55341960407611168, 4.379528057220329451, 78.95724293864769550 ) ) ;
#59584 = CARTESIAN_POINT ( 'NONE',  ( 22.55670631985092811, 22.55670631985084640, -49.13275782002545355 ) ) ;
#59585 = CARTESIAN_POINT ( 'NONE',  ( -5.049401038297874678, -19.05341960407617918, 39.79275706135232582 ) ) ;
#59586 = CARTESIAN_POINT ( 'NONE',  ( 8.314922557961029526, -14.29746914071037800, 105.4177570613523613 ) ) ;
#59587 = CARTESIAN_POINT ( 'NONE',  ( 12.06949235617757843, -12.14591786802309237, 63.12390960531435979 ) ) ;
#59589 = CARTESIAN_POINT ( 'NONE',  ( -27.73933785331498925, 9.013057229001089965, 146.7750000027312183 ) ) ;
#59588 = CARTESIAN_POINT ( 'NONE',  ( -21.52544592524334988, -5.823673210054445271, 103.9594237280190185 ) ) ;
#59590 = CARTESIAN_POINT ( 'NONE',  ( 5.823673210054125526, 21.52544592524343514, 109.7905762719810383 ) ) ;
#59591 = CARTESIAN_POINT ( 'NONE',  ( -13.89961937509977652, 13.97604488694528158, 65.62390960531436690 ) ) ;
#59592 = CARTESIAN_POINT ( 'NONE',  ( -5.719274019375665041, -21.55341960407619695, 84.79275706135234714 ) ) ;
#59593 = CARTESIAN_POINT ( 'NONE',  ( -5.153800228976328057, -19.02544592524343514, 62.29057627198100988 ) ) ;
#59594 = ORIENTED_EDGE ( 'NONE', *, *, #65973, .T. ) ;
#59595 = CARTESIAN_POINT ( 'NONE',  ( 16.55341960407611168, 4.379528057220329451, 113.9572429386477239 ) ) ;
#59596 = CARTESIAN_POINT ( 'NONE',  ( 21.52544592524344225, -5.823673210054117533, 23.54057627198102765 ) ) ;
#59597 = CARTESIAN_POINT ( 'NONE',  ( 16.52544592524342804, -4.483927247898539470, 63.54057627198103830 ) ) ;
#59598 = CARTESIAN_POINT ( 'NONE',  ( 16.51473224551069308, 9.474510206698969483, 49.16557627198102409 ) ) ;
#59599 = CARTESIAN_POINT ( 'NONE',  ( -4.483927247898539470, -16.52544592524342804, 97.29057627198105251 ) ) ;
#59600 = CIRCLE ( 'NONE', #88624, 5.500000000000032863 ) ;
#59601 = CARTESIAN_POINT ( 'NONE',  ( 21.55341960407610458, 5.719274019375980345, 113.9572429386477239 ) ) ;
#59602 = CARTESIAN_POINT ( 'NONE',  ( -10.81492255796105439, 18.62759615963255655, 42.91775706135235424 ) ) ;
#59603 = CARTESIAN_POINT ( 'NONE',  ( 16.46253265017160672, -9.564922557960803928, 33.33224293864770260 ) ) ;
#59604 = CARTESIAN_POINT ( 'NONE',  ( -12.06949235617739369, -12.14591786802326823, 64.37609039468568994 ) ) ;
#59605 = ADVANCED_FACE ( 'NONE', ( #151000 ), #164172, .T. ) ;
#59606 = CARTESIAN_POINT ( 'NONE',  ( 18.62759615963271287, -10.81492255796078972, 103.3322429386476955 ) ) ;
#59607 = CARTESIAN_POINT ( 'NONE',  ( 21.52544592524344225, -5.823673210054117533, 103.5405762719810383 ) ) ;
#59609 = CARTESIAN_POINT ( 'NONE',  ( 16.46253265017160672, -9.564922557960803928, 58.33224293864769550 ) ) ;
#59608 = CARTESIAN_POINT ( 'NONE',  ( 13.97604488694548053, -13.89961937509957401, 20.62609039468567573 ) ) ;
#59610 = CARTESIAN_POINT ( 'NONE',  ( 16.46253265017160672, -9.564922557960803928, 103.3322429386476955 ) ) ;
#59611 = CARTESIAN_POINT ( 'NONE',  ( -10.81492255796105439, 18.62759615963255655, 52.91775706135235424 ) ) ;
#59612 = CARTESIAN_POINT ( 'NONE',  ( 15.80617190586746368, 15.72974639402197994, 49.37390960531436690 ) ) ;
#59613 = CARTESIAN_POINT ( 'NONE',  ( -16.55341960407617563, 4.379528057220093196, 113.5427570613523756 ) ) ;
#59615 = CARTESIAN_POINT ( 'NONE',  ( 15.72974639402176855, 15.80617190586768217, 96.87609039468568994 ) ) ;
#59614 = CARTESIAN_POINT ( 'NONE',  ( -21.55341960407619339, 5.719274019375674811, 83.54275706135234714 ) ) ;
#59616 = CARTESIAN_POINT ( 'NONE',  ( -9.564922557961040184, 16.46253265017147172, 47.91775706135233293 ) ) ;
#59617 = CARTESIAN_POINT ( 'NONE',  ( 4.483927247898790824, -16.52544592524335698, 95.20942372801903275 ) ) ;
#59618 = CARTESIAN_POINT ( 'NONE',  ( 10.72451020669871369, 18.67979575497193778, 52.08442372801901854 ) ) ;
#59619 = CARTESIAN_POINT ( 'NONE',  ( 13.97604488694527802, 13.89961937509977652, 64.37390960531436690 ) ) ;
#59620 = CARTESIAN_POINT ( 'NONE',  ( 19.03943276465977164, 0.05219959533936151252, 21.25109039468565797 ) ) ;
#59621 = CARTESIAN_POINT ( 'NONE',  ( 21.53943276465977519, -0.05219959533907433946, 33.74890960531436690 ) ) ;
#59622 = CARTESIAN_POINT ( 'NONE',  ( 21.52544592524334988, 5.823673210054432836, 26.45942372801901854 ) ) ;
#59623 = CARTESIAN_POINT ( 'NONE',  ( -21.52544592524343514, 5.823673210054127303, 91.04057627198103830 ) ) ;
#59624 = CARTESIAN_POINT ( 'NONE',  ( -13.89961937509957401, -13.97604488694547875, 84.37609039468567573 ) ) ;
#59625 = CARTESIAN_POINT ( 'NONE',  ( 14.29746914071037800, 8.314922557961029526, 36.66775706135234714 ) ) ;
#59627 = CARTESIAN_POINT ( 'NONE',  ( 0.05219959533907565091, 21.53943276465977519, 84.99890960531436690 ) ) ;
#59626 = CARTESIAN_POINT ( 'NONE',  ( -6.863180944108042247, 5.169469635059288137, -62.01598399707661002 ) ) ;
#59629 = CARTESIAN_POINT ( 'NONE',  ( 8.224510206698953496, -14.34966873604960469, 82.91557627198103830 ) ) ;
#59628 = CARTESIAN_POINT ( 'NONE',  ( -14.29746914071037622, -8.314922557961029526, 59.16775706135234714 ) ) ;
#59630 = CARTESIAN_POINT ( 'NONE',  ( -21.51070015259078616, 19.98452092126590429, -49.12424573582180898 ) ) ;
#59631 = CARTESIAN_POINT ( 'NONE',  ( -0.05219959533936034679, 19.03943276465977164, 107.5010903946856615 ) ) ;
#59632 = CARTESIAN_POINT ( 'NONE',  ( -15.72974639402197994, 15.80617190586746368, 40.62390960531435269 ) ) ;
#59633 = CARTESIAN_POINT ( 'NONE',  ( 5.153800228976335163, 19.02544592524342804, 94.79057627198103830 ) ) ;
#59634 = CARTESIAN_POINT ( 'NONE',  ( 14.34966873604972726, -8.224510206698740333, 40.83442372801901854 ) ) ;
#59635 = CARTESIAN_POINT ( 'NONE',  ( 18.67979575497178502, 10.72451020669898547, 114.1655762719810383 ) ) ;
#59636 = CARTESIAN_POINT ( 'NONE',  ( -0.05219959533907301413, -21.53943276465977519, 27.49890960531435269 ) ) ;
#59637 = CARTESIAN_POINT ( 'NONE',  ( 14.34966873604972726, -8.224510206698740333, 65.83442372801900433 ) ) ;
#59638 = CARTESIAN_POINT ( 'NONE',  ( 16.46253265017160672, -9.564922557960803928, 88.33224293864769550 ) ) ;
#59640 = CARTESIAN_POINT ( 'NONE',  ( 16.51473224551069308, 9.474510206698969483, 29.16557627198103475 ) ) ;
#59639 = CARTESIAN_POINT ( 'NONE',  ( 15.72974639402176855, 15.80617190586768217, 56.87609039468568994 ) ) ;
#59641 = CARTESIAN_POINT ( 'NONE',  ( -21.53943276465977519, 0.05219959533907696930, 21.24890960531436690 ) ) ;
#59642 = EDGE_LOOP ( 'NONE', ( #93786, #8255, #195780, #107132 ) ) ;
#59643 = CARTESIAN_POINT ( 'NONE',  ( 13.97604488694548053, -13.89961937509957401, 45.62609039468566863 ) ) ;
#59644 = CARTESIAN_POINT ( 'NONE',  ( -8.224510206698735004, -14.34966873604973081, 54.58442372801901143 ) ) ;
#59645 = CARTESIAN_POINT ( 'NONE',  ( -9.474510206698964154, 16.51473224551069663, 110.4155762719810383 ) ) ;
#59646 = CARTESIAN_POINT ( 'NONE',  ( -19.03943276465977164, 0.05219959533909376836, 76.24890960531435269 ) ) ;
#59647 = CARTESIAN_POINT ( 'NONE',  ( 0.05219959533934541429, -16.53943276465976808, 95.00109039468568994 ) ) ;
#59648 = CARTESIAN_POINT ( 'NONE',  ( -22.80000000000002913, 2.457562174807778276E-13, -64.92279855667830191 ) ) ;
#59649 = CARTESIAN_POINT ( 'NONE',  ( 16.55341960407611168, 4.379528057220329451, 93.95724293864770971 ) ) ;
#59650 = CARTESIAN_POINT ( 'NONE',  ( 21.53943276465977519, -0.05219959533907433946, 28.74890960531435624 ) ) ;
#59651 = CARTESIAN_POINT ( 'NONE',  ( 9.474510206698971260, -16.51473224551069308, 32.91557627198102409 ) ) ;
#59652 = CARTESIAN_POINT ( 'NONE',  ( -8.314922557961024197, 14.29746914071037800, 62.91775706135236135 ) ) ;
#59653 = CARTESIAN_POINT ( 'NONE',  ( 15.72974639402176855, 15.80617190586768217, 21.87609039468567573 ) ) ;
#59654 = CARTESIAN_POINT ( 'NONE',  ( -9.564922557961040184, 16.46253265017147172, 77.91775706135234714 ) ) ;
#59655 = CARTESIAN_POINT ( 'NONE',  ( 19.05341960407611168, 5.049401038298154454, 38.95724293864767418 ) ) ;
#59656 = CARTESIAN_POINT ( 'NONE',  ( -15.80617190586745835, -15.72974639402198527, 71.87390960531438111 ) ) ;
#59657 = CARTESIAN_POINT ( 'NONE',  ( -19.02544592524342804, 5.153800228976336051, 116.0405762719810383 ) ) ;
#59658 = CARTESIAN_POINT ( 'NONE',  ( -10.81492255796105439, 18.62759615963255655, 97.91775706135236135 ) ) ;
#59659 = CARTESIAN_POINT ( 'NONE',  ( 16.46253265017160672, -9.564922557960803928, 68.33224293864770971 ) ) ;
#59660 = EDGE_CURVE ( 'NONE', #51296, #182074, #148000, .T. ) ;
#59661 = CARTESIAN_POINT ( 'NONE',  ( 14.29746914071037800, 8.314922557961029526, 46.66775706135234714 ) ) ;
#59662 = CARTESIAN_POINT ( 'NONE',  ( -19.03943276465977164, 0.05219959533909376836, 76.24890960531435269 ) ) ;
#59663 = CARTESIAN_POINT ( 'NONE',  ( -5.823673210054431948, 21.52544592524334988, 82.70942372801900433 ) ) ;
#59664 = CARTESIAN_POINT ( 'NONE',  ( -9.474510206698720793, -16.51473224551083518, 34.58442372801899722 ) ) ;
#59665 = CARTESIAN_POINT ( 'NONE',  ( -13.89961937509957401, -13.97604488694547875, 49.37609039468567573 ) ) ;
#59666 = ORIENTED_EDGE ( 'NONE', *, *, #86587, .T. ) ;
#59667 = CARTESIAN_POINT ( 'NONE',  ( 15.80617190586769283, -15.72974639402175789, 50.62609039468568994 ) ) ;
#59668 = CARTESIAN_POINT ( 'NONE',  ( -23.29544513554941076, 16.92513159979227666, 143.7843446568999752 ) ) ;
#59669 = CARTESIAN_POINT ( 'NONE',  ( 0.05219959533936267826, -19.03943276465977164, 45.00109039468566863 ) ) ;
#59670 = CARTESIAN_POINT ( 'NONE',  ( -0.05219959533909027116, -19.03943276465977164, 102.4989096053143669 ) ) ;
#59671 = CARTESIAN_POINT ( 'NONE',  ( -5.153800228976328057, -19.02544592524343514, 87.29057627198103830 ) ) ;
#59672 = CARTESIAN_POINT ( 'NONE',  ( -0.05219959533910754901, -16.53943276465976808, 37.49890960531436690 ) ) ;
#59674 = CARTESIAN_POINT ( 'NONE',  ( -21.53943276465977519, -0.05219959533937600094, 98.75109039468568994 ) ) ;
#59673 = CARTESIAN_POINT ( 'NONE',  ( -15.72974639402197994, 15.80617190586746368, 35.62390960531437401 ) ) ;
#59675 = CARTESIAN_POINT ( 'NONE',  ( -11.40812507854755609, 35.11059874428196537, -1.024999997268813301 ) ) ;
#59676 = DIRECTION ( 'NONE',  ( 1.000000000000000000, 0.000000000000000000, 0.000000000000000000 ) ) ;
#59677 = CARTESIAN_POINT ( 'NONE',  ( -21.55341960407619339, 5.719274019375674811, 93.54275706135234714 ) ) ;
#59678 = CARTESIAN_POINT ( 'NONE',  ( -27.83964505791037425, 7.578386611925740368, 161.1890226338711614 ) ) ;
#59679 = CARTESIAN_POINT ( 'NONE',  ( -5.153800228976328057, -19.02544592524343514, 32.29057627198102409 ) ) ;
#59680 = CARTESIAN_POINT ( 'NONE',  ( 16.51473224551069308, 9.474510206698969483, 109.1655762719810383 ) ) ;
#59681 = CARTESIAN_POINT ( 'NONE',  ( 33.90110335395769425, 5.206480924673163813, 93.21819085016215922 ) ) ;
#59682 = VECTOR ( 'NONE', #71017, 1000.000000000000000 ) ;
#59683 = CARTESIAN_POINT ( 'NONE',  ( 12.06949235617739724, 12.14591786802326823, 51.87609039468568284 ) ) ;
#59684 = CARTESIAN_POINT ( 'NONE',  ( -21.53943276465977519, 0.05219959533907696930, 71.24890960531435269 ) ) ;
#59685 = CARTESIAN_POINT ( 'NONE',  ( 16.55341960407611168, 4.379528057220329451, 38.95724293864768839 ) ) ;
#59687 = CARTESIAN_POINT ( 'NONE',  ( 19.02544592524343514, -5.153800228976328945, 103.5405762719809957 ) ) ;
#59686 = CARTESIAN_POINT ( 'NONE',  ( -16.51473224551069308, -9.474510206698971260, 31.66557627198102054 ) ) ;
#59688 = CARTESIAN_POINT ( 'NONE',  ( -5.719274019375665041, -21.55341960407619695, 24.79275706135235779 ) ) ;
#59689 = CARTESIAN_POINT ( 'NONE',  ( -16.51473224551082808, 9.474510206698731452, 33.33442372801899722 ) ) ;
#59690 = CARTESIAN_POINT ( 'NONE',  ( -4.379528057220328563, 16.55341960407611168, 110.2072429386477239 ) ) ;
#59691 = CARTESIAN_POINT ( 'NONE',  ( -15.80617190586768217, 15.72974639402176855, 73.12609039468567573 ) ) ;
#59692 = CARTESIAN_POINT ( 'NONE',  ( 17.48853670773246449, 5.747243402303094939, 98.83328700250008580 ) ) ;
#59693 = CARTESIAN_POINT ( 'NONE',  ( -16.53943276465976808, 0.05219959533911058130, 26.24890960531435624 ) ) ;
#59694 = CARTESIAN_POINT ( 'NONE',  ( 17.49999999999998934, 4.640572885337552300, 111.8621183545115798 ) ) ;
#59695 = CARTESIAN_POINT ( 'NONE',  ( 18.62759615963271287, -10.81492255796078972, 28.33224293864769550 ) ) ;
#59696 = CARTESIAN_POINT ( 'NONE',  ( -14.34966873604960291, -8.224510206698953496, 86.66557627198102409 ) ) ;
#59697 = CARTESIAN_POINT ( 'NONE',  ( 18.22780087662121673, 5.500000000000056843, 53.98459894673893444 ) ) ;
#59698 = CARTESIAN_POINT ( 'NONE',  ( -16.51473224551069308, -9.474510206698971260, 76.66557627198103830 ) ) ;
#59699 = CARTESIAN_POINT ( 'NONE',  ( 14.34966873604960469, 8.224510206698951720, 74.16557627198102409 ) ) ;
#59700 = CARTESIAN_POINT ( 'NONE',  ( -9.474510206698720793, -16.51473224551083518, 109.5844237280190043 ) ) ;
#59701 = CARTESIAN_POINT ( 'NONE',  ( 5.823673210054125526, 21.52544592524343514, 59.79057627198103120 ) ) ;
#59702 = ORIENTED_EDGE ( 'NONE', *, *, #166248, .T. ) ;
#59703 = CARTESIAN_POINT ( 'NONE',  ( 14.29746914071049879, -8.314922557960816363, 108.3322429386477097 ) ) ;
#59705 = CARTESIAN_POINT ( 'NONE',  ( -0.05219959533907301413, -21.53943276465977519, 72.49890960531435269 ) ) ;
#59704 = CARTESIAN_POINT ( 'NONE',  ( 19.05341960407611168, 5.049401038298154454, 68.95724293864769550 ) ) ;
#59707 = CARTESIAN_POINT ( 'NONE',  ( -19.02544592524342804, 5.153800228976336051, 86.04057627198103830 ) ) ;
#59706 = CARTESIAN_POINT ( 'NONE',  ( -0.05219959533934338120, 16.53943276465976808, 107.5010903946856899 ) ) ;
#59708 = CARTESIAN_POINT ( 'NONE',  ( 19.05341960407617918, -5.049401038297876454, 61.04275706135232582 ) ) ;
#59709 = CARTESIAN_POINT ( 'NONE',  ( 15.80617190586769283, -15.72974639402175789, 100.6260903946857184 ) ) ;
#59710 = CARTESIAN_POINT ( 'NONE',  ( 18.62759615963271287, -10.81492255796078972, 73.33224293864769550 ) ) ;
#59711 = CARTESIAN_POINT ( 'NONE',  ( 21.55341960407610458, 5.719274019375980345, 28.95724293864769905 ) ) ;
#59712 = AXIS2_PLACEMENT_3D ( 'NONE', #161996, #23492, #75707 ) ;
#59713 = CARTESIAN_POINT ( 'NONE',  ( -13.97604488694527625, -13.89961937509977652, 46.87390960531435979 ) ) ;
#59714 = CARTESIAN_POINT ( 'NONE',  ( -8.224510206698735004, -14.34966873604973081, 94.58442372801901854 ) ) ;
#59715 = CARTESIAN_POINT ( 'NONE',  ( -19.02544592524342804, 5.153800228976336051, 66.04057627198103830 ) ) ;
#59716 = CARTESIAN_POINT ( 'NONE',  ( 4.483927247898790824, -16.52544592524335698, 20.20942372801900788 ) ) ;
#59717 = CARTESIAN_POINT ( 'NONE',  ( 17.13100169013299023, 6.664070546373166870, 51.73210164300153480 ) ) ;
#59718 = CARTESIAN_POINT ( 'NONE',  ( 0.05219959533937995610, -21.53943276465977519, 110.0010903946856757 ) ) ;
#59719 = AXIS2_PLACEMENT_3D ( 'NONE', #22381, #188252, #84031 ) ;
#59720 = CARTESIAN_POINT ( 'NONE',  ( 4.483927247898545687, 16.52544592524342804, 79.79057627198102409 ) ) ;
#59721 =( BOUNDED_CURVE ( )  B_SPLINE_CURVE ( 2, ( #38213, #99869, #70547, #193906, #131209, #173402, #97510, #2545, #172398, #141059, #53019 ),
 .UNSPECIFIED., .F., .T. ) 
 B_SPLINE_CURVE_WITH_KNOTS ( ( 3, 2, 2, 2, 2, 3 ),
 ( 0.000000000000000000, 0.02000000000000000042, 0.04000000000000000083, 0.05999999999999999778, 0.08000000000000000167, 0.1000000000000000194 ),
 .UNSPECIFIED. ) 
 CURVE ( )  GEOMETRIC_REPRESENTATION_ITEM ( )  RATIONAL_B_SPLINE_CURVE ( ( 1.000000000000000000, 0.9510565162951535312, 1.000000000000000000, 0.9510565162951535312, 1.000000000000000000, 0.9510565162951535312, 1.000000000000000000, 0.9510565162951535312, 1.000000000000000000, 0.9510565162951535312, 1.000000000000000000 ) ) 
 REPRESENTATION_ITEM ( '' )  );
#59722 = CARTESIAN_POINT ( 'NONE',  ( 5.823673210054125526, 21.52544592524343514, 104.7905762719810241 ) ) ;
#59723 = CARTESIAN_POINT ( 'NONE',  ( -21.53943276465977519, 0.05219959533907696930, 106.2489096053143811 ) ) ;
#59724 = CARTESIAN_POINT ( 'NONE',  ( -6.824450432131288657, 4.979424220691202940, -64.09785073354593976 ) ) ;
#59725 = CARTESIAN_POINT ( 'NONE',  ( 21.55341960407610458, 5.719274019375980345, 58.95724293864770971 ) ) ;
#59726 = CARTESIAN_POINT ( 'NONE',  ( -4.379528057220086978, -16.55341960407618274, 84.79275706135234714 ) ) ;
#59727 = CARTESIAN_POINT ( 'NONE',  ( 8.224510206698953496, -14.34966873604960469, 107.9155762719810241 ) ) ;
#59728 = CARTESIAN_POINT ( 'NONE',  ( 5.153800228976335163, 19.02544592524342804, 64.79057627198100988 ) ) ;
#59729 = SURFACE_STYLE_FILL_AREA ( #74910 ) ;
#59730 = CARTESIAN_POINT ( 'NONE',  ( -4.379528057220086978, -16.55341960407618274, 109.7927570613523613 ) ) ;
#59731 = CARTESIAN_POINT ( 'NONE',  ( -18.67979575497193778, 10.72451020669871902, 43.33442372801901143 ) ) ;
#59732 = CARTESIAN_POINT ( 'NONE',  ( 5.049401038298161559, -19.05341960407611168, 97.70724293864766707 ) ) ;
#59733 = CARTESIAN_POINT ( 'NONE',  ( -15.72974639402176322, -15.80617190586768395, 84.37609039468570415 ) ) ;
#59734 = CARTESIAN_POINT ( 'NONE',  ( -19.03943276465977164, 0.05219959533909376836, 31.24890960531435979 ) ) ;
#59735 = CARTESIAN_POINT ( 'NONE',  ( -5.153800228976328057, -19.02544592524343514, 42.29057627198101699 ) ) ;
#59736 = EDGE_LOOP ( 'NONE', ( #50919, #61911, #60411, #198314, #132362, #8021, #90479, #66270 ) ) ;
#59737 = CARTESIAN_POINT ( 'NONE',  ( 21.52544592524334988, 5.823673210054432836, 76.45942372801901854 ) ) ;
#59738 = CARTESIAN_POINT ( 'NONE',  ( -16.46253265017160317, 9.564922557960807481, 100.8322429386477097 ) ) ;
#59739 = CARTESIAN_POINT ( 'NONE',  ( 19.05341960407617918, -5.049401038297876454, 81.04275706135231871 ) ) ;
#59740 = CARTESIAN_POINT ( 'NONE',  ( -18.62759615963255300, -10.81492255796106328, 39.16775706135235424 ) ) ;
#59741 = CARTESIAN_POINT ( 'NONE',  ( -16.52544592524335698, -4.483927247898792601, 28.95942372801902209 ) ) ;
#59742 = CARTESIAN_POINT ( 'NONE',  ( -0.05219959533936034679, 19.03943276465977164, 67.50109039468566152 ) ) ;
#59743 = CARTESIAN_POINT ( 'NONE',  ( 9.474510206698971260, -16.51473224551069308, 57.91557627198103120 ) ) ;
#59744 = CARTESIAN_POINT ( 'NONE',  ( 16.51473224551083163, -9.474510206698727899, 80.83442372801899012 ) ) ;
#59745 = AXIS2_PLACEMENT_3D ( 'NONE', #176310, #80289, #6429 ) ;
#59746 = CARTESIAN_POINT ( 'NONE',  ( -16.52544592524342804, 4.483927247898546575, 26.04057627198103475 ) ) ;
#59747 = CARTESIAN_POINT ( 'NONE',  ( 0.05219959533936267826, -19.03943276465977164, 85.00109039468567573 ) ) ;
#59748 = CARTESIAN_POINT ( 'NONE',  ( -0.05219959533910754901, -16.53943276465976808, 37.49890960531436690 ) ) ;
#59749 = CARTESIAN_POINT ( 'NONE',  ( -5.153800228976607833, 19.02544592524334988, 57.70942372801899012 ) ) ;
#59750 = CARTESIAN_POINT ( 'NONE',  ( -8.224510206698735004, -14.34966873604973081, 44.58442372801901854 ) ) ;
#59751 = CARTESIAN_POINT ( 'NONE',  ( -19.02544592524334988, -5.153800228976617603, 18.95942372801899722 ) ) ;
#59752 = CARTESIAN_POINT ( 'NONE',  ( 9.564922557960805705, 16.46253265017160317, 24.58224293864769194 ) ) ;
#59753 = CARTESIAN_POINT ( 'NONE',  ( -17.26172910966778318, -6.454744622555873335, 64.19353091350780005 ) ) ;
#59754 = CARTESIAN_POINT ( 'NONE',  ( -8.224510206698735004, -14.34966873604973081, 44.58442372801901854 ) ) ;
#59755 = CARTESIAN_POINT ( 'NONE',  ( 0.000000000000000000, 0.000000000000000000, -20.00000000000000000 ) ) ;
#59756 = EDGE_CURVE ( 'NONE', #145773, #163091, #98104, .T. ) ;
#59757 = CARTESIAN_POINT ( 'NONE',  ( 17.14385361876520264, -23.59649016807271238, 143.5750000027312012 ) ) ;
#59758 = CARTESIAN_POINT ( 'NONE',  ( 9.564922557960805705, 16.46253265017160317, 94.58224293864769550 ) ) ;
#59759 = CARTESIAN_POINT ( 'NONE',  ( -17.72560187377287022, -5.499999999999974243, 69.07814504131316369 ) ) ;
#59760 = ORIENTED_EDGE ( 'NONE', *, *, #7317, .T. ) ;
#59761 = CARTESIAN_POINT ( 'NONE',  ( 19.05341960407617918, -5.049401038297876454, 91.04275706135234714 ) ) ;
#59762 = CARTESIAN_POINT ( 'NONE',  ( 15.72974639402199770, -15.80617190586745480, 28.12390960531435979 ) ) ;
#59764 = CARTESIAN_POINT ( 'NONE',  ( 19.02544592524334988, 5.153800228976608722, 96.45942372801897591 ) ) ;
#59763 = CARTESIAN_POINT ( 'NONE',  ( 5.049401038297881783, 19.05341960407617563, 22.29275706135233648 ) ) ;
#59765 = CARTESIAN_POINT ( 'NONE',  ( -5.153800228976328057, -19.02544592524343514, 22.29057627198102765 ) ) ;
#59766 = CARTESIAN_POINT ( 'NONE',  ( 19.02544592524343514, -5.153800228976328945, 43.54057627198103120 ) ) ;
#59767 = CARTESIAN_POINT ( 'NONE',  ( -18.62759615963270932, 10.81492255796079327, 65.83224293864769550 ) ) ;
#59768 = CARTESIAN_POINT ( 'NONE',  ( 16.51473224551069308, 9.474510206698969483, 24.16557627198102765 ) ) ;
#59769 = CARTESIAN_POINT ( 'NONE',  ( -17.81289503416611097, -24.51734667627696496, 142.5500000054623513 ) ) ;
#59770 = CARTESIAN_POINT ( 'NONE',  ( 5.049401038297881783, 19.05341960407617563, 67.29275706135234714 ) ) ;
#59771 = CARTESIAN_POINT ( 'NONE',  ( -14.29746914071049879, 8.314922557960819915, 40.83224293864769550 ) ) ;
#59772 = CARTESIAN_POINT ( 'NONE',  ( 5.823673210054125526, 21.52544592524343514, 24.79057627198103120 ) ) ;
#59773 = CARTESIAN_POINT ( 'NONE',  ( 10.81492255796106328, -18.62759615963255655, 95.41775706135234714 ) ) ;
#59774 = CARTESIAN_POINT ( 'NONE',  ( 18.67979575497178502, 10.72451020669898547, 84.16557627198103830 ) ) ;
#59775 = CARTESIAN_POINT ( 'NONE',  ( 10.72451020669871369, 18.67979575497193778, 62.08442372801901143 ) ) ;
#59776 = CARTESIAN_POINT ( 'NONE',  ( -5.823673210054431948, 21.52544592524334988, 62.70942372801902565 ) ) ;
#59777 = CARTESIAN_POINT ( 'NONE',  ( -5.049401038298153566, 19.05341960407611168, 100.2072429386476955 ) ) ;
#59779 = CARTESIAN_POINT ( 'NONE',  ( -18.62759615963255300, -10.81492255796106328, 54.16775706135235424 ) ) ;
#59778 = CARTESIAN_POINT ( 'NONE',  ( 14.34966873604972726, -8.224510206698740333, 95.83442372801903275 ) ) ;
#59780 = CARTESIAN_POINT ( 'NONE',  ( -13.97604488694527625, -13.89961937509977652, 21.87390960531435979 ) ) ;
#59781 = VECTOR ( 'NONE', #18603, 1000.000000000000000 ) ;
#59782 = CARTESIAN_POINT ( 'NONE',  ( -16.52544592524342804, 4.483927247898546575, 61.04057627198103120 ) ) ;
#59783 = CARTESIAN_POINT ( 'NONE',  ( -12.06949235617756955, 12.14591786802309770, 30.62390960531436335 ) ) ;
#59784 = CARTESIAN_POINT ( 'NONE',  ( -5.823673210054116645, -21.52544592524344225, 42.29057627198103120 ) ) ;
#59785 = CARTESIAN_POINT ( 'NONE',  ( -16.51473224551069308, -9.474510206698971260, 61.66557627198103120 ) ) ;
#59786 = CARTESIAN_POINT ( 'NONE',  ( -9.564922557960796823, -16.46253265017161027, 47.08224293864769550 ) ) ;
#59787 = CARTESIAN_POINT ( 'NONE',  ( -10.81492255796078084, -18.62759615963271287, 57.08224293864769550 ) ) ;
#59788 = CARTESIAN_POINT ( 'NONE',  ( -9.474510206698720793, -16.51473224551083518, 49.58442372801899722 ) ) ;
#59790 = CARTESIAN_POINT ( 'NONE',  ( 16.53943276465976808, -0.05219959533910856209, 43.74890960531435979 ) ) ;
#59789 = CARTESIAN_POINT ( 'NONE',  ( 25.77159179889068596, 6.124174026812450045, 163.0907220140217930 ) ) ;
#59791 = CARTESIAN_POINT ( 'NONE',  ( -19.03943276465977164, 0.05219959533909376836, 116.2489096053143669 ) ) ;
#59792 = VERTEX_POINT ( 'NONE', #102485 ) ;
#59793 = VERTEX_POINT ( 'NONE', #88302 ) ;
#59794 = CARTESIAN_POINT ( 'NONE',  ( -4.379528057220086978, -16.55341960407618274, 74.79275706135234714 ) ) ;
#59795 = CARTESIAN_POINT ( 'NONE',  ( -19.03943276465977164, -0.05219959533935918106, 73.75109039468566152 ) ) ;
#59796 = CARTESIAN_POINT ( 'NONE',  ( -12.14591786802309592, -12.06949235617757132, 46.87390960531435979 ) ) ;
#59797 = DIRECTION ( 'NONE',  ( -1.000000000000000000, -0.000000000000000000, -0.000000000000000000 ) ) ;
#59798 = CARTESIAN_POINT ( 'NONE',  ( -12.14591786802309592, -12.06949235617757132, 21.87390960531436690 ) ) ;
#59799 = CARTESIAN_POINT ( 'NONE',  ( 19.05341960407611168, 5.049401038298154454, 48.95724293864768129 ) ) ;
#59800 = CARTESIAN_POINT ( 'NONE',  ( -16.46253265017160317, 9.564922557960807481, 75.83224293864769550 ) ) ;
#59801 = CARTESIAN_POINT ( 'NONE',  ( -16.46253265017160317, 9.564922557960807481, 35.83224293864768839 ) ) ;
#59802 = CARTESIAN_POINT ( 'NONE',  ( -18.62759615963255300, -10.81492255796106328, 49.16775706135234003 ) ) ;
#59803 = CARTESIAN_POINT ( 'NONE',  ( 13.89961937509977652, -13.97604488694527269, 53.12390960531434558 ) ) ;
#59804 = CARTESIAN_POINT ( 'NONE',  ( 30.00000000000000000, 5.499999999999992895, 37.50000000000000000 ) ) ;
#59805 = CARTESIAN_POINT ( 'NONE',  ( -9.564922557960796823, -16.46253265017161027, 57.08224293864769550 ) ) ;
#59806 = CARTESIAN_POINT ( 'NONE',  ( 0.05219959533907565091, 21.53943276465977519, 39.99890960531436690 ) ) ;
#59807 = CARTESIAN_POINT ( 'NONE',  ( 13.97604488694527802, 13.89961937509977652, 39.37390960531435269 ) ) ;
#59808 = CARTESIAN_POINT ( 'NONE',  ( 21.55341960407610458, 5.719274019375980345, 43.95724293864769550 ) ) ;
#59809 = CARTESIAN_POINT ( 'NONE',  ( 14.29746914071037800, 8.314922557961029526, 86.66775706135234714 ) ) ;
#59810 = CARTESIAN_POINT ( 'NONE',  ( -0.05219959533937732626, 21.53943276465977519, 107.5010903946856899 ) ) ;
#59811 = CARTESIAN_POINT ( 'NONE',  ( 8.224510206698742110, 14.34966873604972548, 62.08442372801901143 ) ) ;
#59812 = CARTESIAN_POINT ( 'NONE',  ( 19.05341960407611168, 5.049401038298154454, 108.9572429386477097 ) ) ;
#59813 = CARTESIAN_POINT ( 'NONE',  ( -8.314922557961024197, 14.29746914071037800, 52.91775706135235424 ) ) ;
#59814 = CARTESIAN_POINT ( 'NONE',  ( -8.224510206698735004, -14.34966873604973081, 34.58442372801900433 ) ) ;
#59815 = CARTESIAN_POINT ( 'NONE',  ( -5.049401038298153566, 19.05341960407611168, 110.2072429386476671 ) ) ;
#59816 = CARTESIAN_POINT ( 'NONE',  ( 16.55341960407618274, -4.379528057220086978, 21.04275706135234714 ) ) ;
#59817 = CARTESIAN_POINT ( 'NONE',  ( 13.89961937509977652, -13.97604488694527269, 38.12390960531436690 ) ) ;
#59818 = CARTESIAN_POINT ( 'NONE',  ( 18.62759615963255655, 10.81492255796105972, 26.66775706135235424 ) ) ;
#59819 = CARTESIAN_POINT ( 'NONE',  ( -8.224510206698735004, -14.34966873604973081, 19.58442372801901143 ) ) ;
#59820 = CARTESIAN_POINT ( 'NONE',  ( 16.53943276465976808, 0.05219959533934440121, 81.25109039468568994 ) ) ;
#59821 = CARTESIAN_POINT ( 'NONE',  ( -4.962140900324464532, -6.180203150055834094, 6.568406857878973604 ) ) ;
#59822 = CARTESIAN_POINT ( 'NONE',  ( 21.55341960407619695, -5.719274019375665929, 86.04275706135236135 ) ) ;
#59823 = CARTESIAN_POINT ( 'NONE',  ( 13.89961937509957401, 13.97604488694547697, 96.87609039468566152 ) ) ;
#59824 = CARTESIAN_POINT ( 'NONE',  ( -16.52544592524342804, 4.483927247898546575, 51.04057627198103120 ) ) ;
#59825 = CARTESIAN_POINT ( 'NONE',  ( 14.29746914071049879, -8.314922557960816363, 113.3322429386476955 ) ) ;
#59827 = DIRECTION ( 'NONE',  ( 0.000000000000000000, 0.000000000000000000, 1.000000000000000000 ) ) ;
#59826 = CARTESIAN_POINT ( 'NONE',  ( -16.46253265017146816, -9.564922557961047289, 44.16775706135232582 ) ) ;
#59828 = CARTESIAN_POINT ( 'NONE',  ( 10.81492255796106328, -18.62759615963255655, 45.41775706135234003 ) ) ;
#59829 = CARTESIAN_POINT ( 'NONE',  ( -13.89961937509957401, -13.97604488694547875, 104.3760903946856757 ) ) ;
#59830 = CARTESIAN_POINT ( 'NONE',  ( 16.38665767535056261, 7.295008042176082341, 82.23599135785454450 ) ) ;
#59831 = CARTESIAN_POINT ( 'NONE',  ( -19.05341960407611168, -5.049401038298163336, 111.4572429386476671 ) ) ;
#59832 = CARTESIAN_POINT ( 'NONE',  ( -21.55341960407610458, -5.719274019375992779, 66.45724293864768129 ) ) ;
#59833 = CARTESIAN_POINT ( 'NONE',  ( 19.03943276465977164, 0.05219959533936151252, 91.25109039468566152 ) ) ;
#59834 = EDGE_CURVE ( 'NONE', #4577, #98417, #70153, .T. ) ;
#59835 = CARTESIAN_POINT ( 'NONE',  ( 19.03943276465977164, -0.05219959533909143690, 103.7489096053143669 ) ) ;
#59836 = CARTESIAN_POINT ( 'NONE',  ( -21.73861122199408058, 7.688394669363296963, 173.2969830217476499 ) ) ;
#59837 = CARTESIAN_POINT ( 'NONE',  ( -4.483927247898539470, -16.52544592524342804, 102.2905762719810383 ) ) ;
#59838 = CARTESIAN_POINT ( 'NONE',  ( 18.67979575497194134, -10.72451020669871369, 90.83442372801901854 ) ) ;
#59839 = CARTESIAN_POINT ( 'NONE',  ( -5.153800228976328057, -19.02544592524343514, 47.29057627198102409 ) ) ;
#59840 = AXIS2_PLACEMENT_3D ( 'NONE', #23213, #190067, #65712 ) ;
#59841 = CARTESIAN_POINT ( 'NONE',  ( -21.52544592524334988, -5.823673210054445271, 48.95942372801902565 ) ) ;
#59842 = CARTESIAN_POINT ( 'NONE',  ( 5.823673210054444382, -21.52544592524334988, 95.20942372801903275 ) ) ;
#59843 = CARTESIAN_POINT ( 'NONE',  ( -4.483927247898782831, 16.52544592524335698, 107.7094237280190328 ) ) ;
#59844 = EDGE_CURVE ( 'NONE', #64642, #163891, #71153, .T. ) ;
#59845 = CARTESIAN_POINT ( 'NONE',  ( -5.049401038298153566, 19.05341960407611168, 65.20724293864765286 ) ) ;
#59846 = CARTESIAN_POINT ( 'NONE',  ( 18.67979575497194134, -10.72451020669871369, 40.83442372801901854 ) ) ;
#59847 = CARTESIAN_POINT ( 'NONE',  ( 10.81492255796106328, -18.62759615963255655, 45.41775706135234003 ) ) ;
#59849 = CARTESIAN_POINT ( 'NONE',  ( 19.03943276465977164, -0.05219959533909143690, 98.74890960531436690 ) ) ;
#59848 = CARTESIAN_POINT ( 'NONE',  ( 5.153800228976615827, -19.02544592524334988, 70.20942372801899012 ) ) ;
#59850 = CARTESIAN_POINT ( 'NONE',  ( -4.379528057220328563, 16.55341960407611168, 105.2072429386477097 ) ) ;
#59851 = CARTESIAN_POINT ( 'NONE',  ( -15.72974639402197994, 15.80617190586746368, 90.62390960531436690 ) ) ;
#59852 = CARTESIAN_POINT ( 'NONE',  ( 14.34966873604960469, 8.224510206698951720, 64.16557627198102409 ) ) ;
#59853 = CARTESIAN_POINT ( 'NONE',  ( -16.46253265017146816, -9.564922557961047289, 19.16775706135233293 ) ) ;
#59854 = CARTESIAN_POINT ( 'NONE',  ( -0.05219959533910754901, -16.53943276465976808, 87.49890960531436690 ) ) ;
#59855 = CARTESIAN_POINT ( 'NONE',  ( -9.474510206698964154, 16.51473224551069663, 30.41557627198102054 ) ) ;
#59856 = CARTESIAN_POINT ( 'NONE',  ( -16.46253265017146816, -9.564922557961047289, 89.16775706135234714 ) ) ;
#59857 = CARTESIAN_POINT ( 'NONE',  ( -12.14591786802309592, -12.06949235617757132, 46.87390960531435979 ) ) ;
#59858 = CARTESIAN_POINT ( 'NONE',  ( 15.72974639402176855, 15.80617190586768217, 91.87609039468568994 ) ) ;
#59859 = CARTESIAN_POINT ( 'NONE',  ( 19.02544592524343514, -5.153800228976328945, 88.54057627198102409 ) ) ;
#59860 = CARTESIAN_POINT ( 'NONE',  ( 16.51473224551083163, -9.474510206698727899, 70.83442372801900433 ) ) ;
#59861 = CARTESIAN_POINT ( 'NONE',  ( 18.62759615963271287, -10.81492255796078972, 78.33224293864770971 ) ) ;
#59862 = CARTESIAN_POINT ( 'NONE',  ( 5.823673210054444382, -21.52544592524334988, 25.20942372801901854 ) ) ;
#59863 = CARTESIAN_POINT ( 'NONE',  ( 8.224510206698742110, 14.34966873604972548, 27.08442372801901854 ) ) ;
#59864 = CARTESIAN_POINT ( 'NONE',  ( 16.55341960407618274, -4.379528057220086978, 91.04275706135236135 ) ) ;
#59866 = CARTESIAN_POINT ( 'NONE',  ( 10.81492255796106328, -18.62759615963255655, 40.41775706135234714 ) ) ;
#59865 = CARTESIAN_POINT ( 'NONE',  ( 9.564922557960805705, 16.46253265017160317, 24.58224293864769194 ) ) ;
#59867 = CARTESIAN_POINT ( 'NONE',  ( 16.51473224551069308, 9.474510206698969483, 24.16557627198102765 ) ) ;
#59868 = CARTESIAN_POINT ( 'NONE',  ( 22.81625015709510151, -31.40387420917324590, -6.424999997268812102 ) ) ;
#59869 = CARTESIAN_POINT ( 'NONE',  ( 4.483927247898790824, -16.52544592524335698, 55.20942372801902565 ) ) ;
#59870 = CARTESIAN_POINT ( 'NONE',  ( 12.14591786802309770, 12.06949235617756955, 74.37390960531436690 ) ) ;
#59871 = CARTESIAN_POINT ( 'NONE',  ( -5.719274019375978568, 21.55341960407610458, 70.20724293864769550 ) ) ;
#59872 = VECTOR ( 'NONE', #121593, 1000.000000000000000 ) ;
#59873 = CARTESIAN_POINT ( 'NONE',  ( 4.379528057220339221, -16.55341960407611168, 22.70724293864769194 ) ) ;
#59874 = CARTESIAN_POINT ( 'NONE',  ( 4.379528057220092307, 16.55341960407617563, 47.29275706135234003 ) ) ;
#59875 = CARTESIAN_POINT ( 'NONE',  ( -16.46253265017160317, 9.564922557960807481, 50.83224293864770260 ) ) ;
#59876 = CARTESIAN_POINT ( 'NONE',  ( 16.52544592524335698, 4.483927247898782831, 76.45942372801901854 ) ) ;
#59877 = CARTESIAN_POINT ( 'NONE',  ( 9.564922557961047289, -16.46253265017146816, 80.41775706135234714 ) ) ;
#59878 = CARTESIAN_POINT ( 'NONE',  ( 10.72451020669898902, -18.67979575497178502, 72.91557627198103830 ) ) ;
#59879 = CARTESIAN_POINT ( 'NONE',  ( 4.483927247898545687, 16.52544592524342804, 24.79057627198103120 ) ) ;
#59880 = ORIENTED_EDGE ( 'NONE', *, *, #56209, .T. ) ;
#59881 = CARTESIAN_POINT ( 'NONE',  ( -9.474510206698964154, 16.51473224551069663, 115.4155762719810241 ) ) ;
#59882 = CARTESIAN_POINT ( 'NONE',  ( 21.55341960407610458, 5.719274019375980345, 63.95724293864770260 ) ) ;
#59883 = ORIENTED_EDGE ( 'NONE', *, *, #193684, .T. ) ;
#59884 = CARTESIAN_POINT ( 'NONE',  ( -4.483927247898782831, 16.52544592524335698, 92.70942372801901854 ) ) ;
#59885 = VERTEX_POINT ( 'NONE', #72148 ) ;
#59886 = CARTESIAN_POINT ( 'NONE',  ( 18.62759615963271287, -10.81492255796078972, 23.33224293864769194 ) ) ;
#59887 = CARTESIAN_POINT ( 'NONE',  ( 17.49999999999998934, 3.512728167236884413, 107.2719000481888258 ) ) ;
#59888 = CARTESIAN_POINT ( 'NONE',  ( -5.719274019375978568, 21.55341960407610458, 75.20724293864769550 ) ) ;
#59889 = CARTESIAN_POINT ( 'NONE',  ( -16.55341960407617563, 4.379528057220093196, 108.5427570613523756 ) ) ;
#59890 = CARTESIAN_POINT ( 'NONE',  ( 12.14591786802327356, -12.06949235617739191, 25.62609039468567929 ) ) ;
#59891 = CARTESIAN_POINT ( 'NONE',  ( -13.97604488694527625, -13.89961937509977652, 26.87390960531434558 ) ) ;
#59892 = CARTESIAN_POINT ( 'NONE',  ( -4.483927247898782831, 16.52544592524335698, 27.70942372801901854 ) ) ;
#59893 = CARTESIAN_POINT ( 'NONE',  ( -13.89961937509977652, 13.97604488694528158, 50.62390960531435979 ) ) ;
#59894 = CARTESIAN_POINT ( 'NONE',  ( 28.82186960331498327, 2.781578969918950771E-14, 143.0000000000000000 ) ) ;
#59895 = CARTESIAN_POINT ( 'NONE',  ( 19.05341960407611168, 5.049401038298154454, 98.95724293864766707 ) ) ;
#59896 = CARTESIAN_POINT ( 'NONE',  ( 8.314922557961029526, -14.29746914071037800, 90.41775706135236135 ) ) ;
#59897 = CARTESIAN_POINT ( 'NONE',  ( 5.153800228976615827, -19.02544592524334988, 90.20942372801900433 ) ) ;
#59898 = CARTESIAN_POINT ( 'NONE',  ( -19.05341960407617563, 5.049401038297882671, 28.54275706135232937 ) ) ;
#59899 = CARTESIAN_POINT ( 'NONE',  ( -15.80617190586745835, -15.72974639402198527, 76.87390960531439532 ) ) ;
#59900 = CARTESIAN_POINT ( 'NONE',  ( -14.29746914071037622, -8.314922557961029526, 104.1677570613523471 ) ) ;
#59901 = CARTESIAN_POINT ( 'NONE',  ( -5.153800228976607833, 19.02544592524334988, 87.70942372801897591 ) ) ;
#59902 = CARTESIAN_POINT ( 'NONE',  ( -19.02544592524342804, 5.153800228976336051, 51.04057627198103120 ) ) ;
#59903 = CARTESIAN_POINT ( 'NONE',  ( -13.97604488694527625, -13.89961937509977652, 96.87390960531433848 ) ) ;
#59904 = CARTESIAN_POINT ( 'NONE',  ( -10.81492255796105439, 18.62759615963255655, 67.91775706135234714 ) ) ;
#59905 = CARTESIAN_POINT ( 'NONE',  ( -13.97604488694527625, -13.89961937509977652, 46.87390960531435979 ) ) ;
#59906 = CARTESIAN_POINT ( 'NONE',  ( -16.52216118717210236, -7.221426719304506747, 86.07599021046992505 ) ) ;
#59907 = CARTESIAN_POINT ( 'NONE',  ( -4.483927247898539470, -16.52544592524342804, 82.29057627198103830 ) ) ;
#59908 = CARTESIAN_POINT ( 'NONE',  ( 5.823673210054125526, 21.52544592524343514, 74.79057627198105251 ) ) ;
#59909 = CARTESIAN_POINT ( 'NONE',  ( -17.79613651744294600, 24.49428055684532524, 143.9656553485623647 ) ) ;
#59910 = FACE_OUTER_BOUND ( 'NONE', #65662, .T. ) ;
#59911 = CARTESIAN_POINT ( 'NONE',  ( -13.97604488694547697, 13.89961937509957934, 43.12609039468566152 ) ) ;
#59912 = CARTESIAN_POINT ( 'NONE',  ( 16.62475595723613253, -7.163666690055873865, 73.02713351810406550 ) ) ;
#59914 = CARTESIAN_POINT ( 'NONE',  ( -13.97604488694527625, -13.89961937509977652, 91.87390960531432427 ) ) ;
#59913 = CARTESIAN_POINT ( 'NONE',  ( 9.474510206698971260, -16.51473224551069308, 72.91557627198102409 ) ) ;
#59915 = CARTESIAN_POINT ( 'NONE',  ( -0.05219959533934338120, 16.53943276465976808, 62.50109039468568284 ) ) ;
#59916 = CARTESIAN_POINT ( 'NONE',  ( 19.70810511599106363, -36.80807878390139365, -19.26229262562157984 ) ) ;
#59917 = CARTESIAN_POINT ( 'NONE',  ( -9.564922557961040184, 16.46253265017147172, 27.91775706135232582 ) ) ;
#59918 = CARTESIAN_POINT ( 'NONE',  ( 36.89613260305527120, 1.429147721188409825, 50.32345767270687986 ) ) ;
#59919 = CARTESIAN_POINT ( 'NONE',  ( -19.05341960407611168, -5.049401038298163336, 106.4572429386476955 ) ) ;
#59920 = CARTESIAN_POINT ( 'NONE',  ( -16.53943276465976808, -0.05219959533934237506, 88.75109039468567573 ) ) ;
#59921 = CARTESIAN_POINT ( 'NONE',  ( -3.883669081187027139, -5.177897575765684657, -64.47298040648024653 ) ) ;
#59922 = CARTESIAN_POINT ( 'NONE',  ( 4.379528057220092307, 16.55341960407617563, 77.29275706135234714 ) ) ;
#59923 = DIRECTION ( 'NONE',  ( 1.000000000000000000, 0.000000000000000000, 0.000000000000000000 ) ) ;
#59924 = CARTESIAN_POINT ( 'NONE',  ( -0.05219959533934338120, 16.53943276465976808, 57.50109039468568994 ) ) ;
#59925 = CARTESIAN_POINT ( 'NONE',  ( -18.09867054820433907, -5.499999999999827693, 58.98393025253588462 ) ) ;
#59926 = CARTESIAN_POINT ( 'NONE',  ( 15.72974639402176855, 15.80617190586768217, 71.87609039468568994 ) ) ;
#59927 = CARTESIAN_POINT ( 'NONE',  ( 19.05341960407617918, -5.049401038297876454, 81.04275706135231871 ) ) ;
#59928 = CARTESIAN_POINT ( 'NONE',  ( 19.03943276465977164, 0.05219959533936151252, 26.25109039468566507 ) ) ;
#59929 = CIRCLE ( 'NONE', #85764, 7.999999999999998224 ) ;
#59930 = CARTESIAN_POINT ( 'NONE',  ( -9.564922557960796823, -16.46253265017161027, 47.08224293864769550 ) ) ;
#59931 = CARTESIAN_POINT ( 'NONE',  ( -16.46253265017160317, 9.564922557960807481, 45.83224293864769550 ) ) ;
#59932 = CARTESIAN_POINT ( 'NONE',  ( 16.73155767950884965, -7.079819277068864380, 23.08152769347067945 ) ) ;
#59933 = CARTESIAN_POINT ( 'NONE',  ( -21.55341960407610458, -5.719274019375992779, 61.45724293864770260 ) ) ;
#59934 = CARTESIAN_POINT ( 'NONE',  ( -0.05219959533907301413, -21.53943276465977519, 27.49890960531435269 ) ) ;
#59935 = CARTESIAN_POINT ( 'NONE',  ( 4.483927247898545687, 16.52544592524342804, 109.7905762719810383 ) ) ;
#59936 = CARTESIAN_POINT ( 'NONE',  ( 4.379528057220092307, 16.55341960407617563, 52.29275706135236135 ) ) ;
#59937 = ORIENTED_EDGE ( 'NONE', *, *, #170098, .F. ) ;
#59938 = CARTESIAN_POINT ( 'NONE',  ( -18.62759615963270932, 10.81492255796079327, 115.8322429386477097 ) ) ;
#59940 = CARTESIAN_POINT ( 'NONE',  ( -11.74264578624799782, -36.14014761921581709, -5.599999999999999645 ) ) ;
#59939 = CARTESIAN_POINT ( 'NONE',  ( 4.379528057220339221, -16.55341960407611168, 47.70724293864770260 ) ) ;
#59941 = CARTESIAN_POINT ( 'NONE',  ( -16.46253265017146816, -9.564922557961047289, 109.1677570613523471 ) ) ;
#59942 = CARTESIAN_POINT ( 'NONE',  ( -16.46253265017146816, -9.564922557961047289, 44.16775706135232582 ) ) ;
#59943 = CARTESIAN_POINT ( 'NONE',  ( -4.483927247898539470, -16.52544592524342804, 47.29057627198103120 ) ) ;
#59945 = EDGE_CURVE ( 'NONE', #136632, #150593, #88483, .T. ) ;
#59944 = CARTESIAN_POINT ( 'NONE',  ( 15.80617190586746368, 15.72974639402197994, 114.3739096053143527 ) ) ;
#59947 = CARTESIAN_POINT ( 'NONE',  ( 18.62759615963271287, -10.81492255796078972, 68.33224293864769550 ) ) ;
#59946 = CARTESIAN_POINT ( 'NONE',  ( 16.36317988757057762, 7.306389748694947173, 33.40210391636777132 ) ) ;
#59948 = CARTESIAN_POINT ( 'NONE',  ( -13.89961937509977652, 13.97604488694528158, 85.62390960531433848 ) ) ;
#59949 = CARTESIAN_POINT ( 'NONE',  ( -16.53943276465976808, 0.05219959533911058130, 61.24890960531435979 ) ) ;
#59950 = CARTESIAN_POINT ( 'NONE',  ( 9.564922557960805705, 16.46253265017160317, 104.5822429386476955 ) ) ;
#59951 = CARTESIAN_POINT ( 'NONE',  ( -36.84755799831103928, 2.910846538911445069, 49.67009533327788517 ) ) ;
#59952 = CARTESIAN_POINT ( 'NONE',  ( -9.564922557961040184, 16.46253265017147172, 52.91775706135233293 ) ) ;
#59953 = CARTESIAN_POINT ( 'NONE',  ( -0.05219959533907301413, -21.53943276465977519, 87.49890960531436690 ) ) ;
#59954 = CARTESIAN_POINT ( 'NONE',  ( 16.46253265017160672, -9.564922557960803928, 43.33224293864769550 ) ) ;
#59955 = CARTESIAN_POINT ( 'NONE',  ( 16.55341960407611168, 4.379528057220329451, 113.9572429386477239 ) ) ;
#59956 = CARTESIAN_POINT ( 'NONE',  ( 5.719274019375673035, 21.55341960407619339, 52.29275706135236135 ) ) ;
#59957 = CARTESIAN_POINT ( 'NONE',  ( 27.73933785331498214, 9.013057229001095294, 143.9750000027312069 ) ) ;
#59958 = EDGE_CURVE ( 'NONE', #43824, #40357, #115065, .T. ) ;
#59959 = CARTESIAN_POINT ( 'NONE',  ( -4.483927247898539470, -16.52544592524342804, 32.29057627198102409 ) ) ;
#59960 = CARTESIAN_POINT ( 'NONE',  ( -9.474510206698964154, 16.51473224551069663, 55.41557627198103120 ) ) ;
#59961 = CARTESIAN_POINT ( 'NONE',  ( 19.02544592524343514, -5.153800228976328945, 93.54057627198102409 ) ) ;
#59962 = CARTESIAN_POINT ( 'NONE',  ( 15.72974639402199770, -15.80617190586745480, 73.12390960531436690 ) ) ;
#59963 = CARTESIAN_POINT ( 'NONE',  ( -27.73933785331498925, 9.013057229001089965, 146.7750000027312183 ) ) ;
#59964 = CARTESIAN_POINT ( 'NONE',  ( -16.46253265017160317, 9.564922557960807481, 45.83224293864769550 ) ) ;
#59965 = CARTESIAN_POINT ( 'NONE',  ( 18.67979575497178502, 10.72451020669898547, 59.16557627198103120 ) ) ;
#59966 = CARTESIAN_POINT ( 'NONE',  ( -18.62759615963255300, -10.81492255796106328, 89.16775706135236135 ) ) ;
#59969 = CARTESIAN_POINT ( 'NONE',  ( 16.53943276465976808, -0.05219959533910856209, 63.74890960531435979 ) ) ;
#59968 = CARTESIAN_POINT ( 'NONE',  ( 12.06949235617739724, 12.14591786802326823, 76.87609039468567573 ) ) ;
#59967 = FACE_OUTER_BOUND ( 'NONE', #132662, .T. ) ;
#59970 = CARTESIAN_POINT ( 'NONE',  ( -0.05219959533909027116, -19.03943276465977164, 72.49890960531435269 ) ) ;
#59971 = ORIENTED_EDGE ( 'NONE', *, *, #79934, .F. ) ;
#59972 = CARTESIAN_POINT ( 'NONE',  ( -19.03943276465977164, -0.05219959533935918106, 23.75109039468566152 ) ) ;
#59973 = CARTESIAN_POINT ( 'NONE',  ( -8.224510206698735004, -14.34966873604973081, 94.58442372801901854 ) ) ;
#59974 = CARTESIAN_POINT ( 'NONE',  ( 0.05219959533937995610, -21.53943276465977519, 110.0010903946856757 ) ) ;
#59975 = CARTESIAN_POINT ( 'NONE',  ( 13.97604488694527802, 13.89961937509977652, 79.37390960531435269 ) ) ;
#59976 = CARTESIAN_POINT ( 'NONE',  ( -15.80617190586745835, -15.72974639402198527, 46.87390960531435979 ) ) ;
#59977 = CARTESIAN_POINT ( 'NONE',  ( 8.314922557961029526, -14.29746914071037800, 25.41775706135235779 ) ) ;
#59978 = CARTESIAN_POINT ( 'NONE',  ( -21.55341960407619339, 5.719274019375674811, 78.54275706135236135 ) ) ;
#59979 = CARTESIAN_POINT ( 'NONE',  ( 16.53943276465976808, 0.05219959533934440121, 61.25109039468567573 ) ) ;
#59980 = CARTESIAN_POINT ( 'NONE',  ( 21.52544592524344225, -5.823673210054117533, 113.5405762719810383 ) ) ;
#59981 = CARTESIAN_POINT ( 'NONE',  ( 14.34966873604972726, -8.224510206698740333, 20.83442372801901143 ) ) ;
#59982 = CARTESIAN_POINT ( 'NONE',  ( -5.153800228976328057, -19.02544592524343514, 97.29057627198099567 ) ) ;
#59983 = CARTESIAN_POINT ( 'NONE',  ( 12.14591786802327356, -12.06949235617739191, 30.62609039468567929 ) ) ;
#59984 = CARTESIAN_POINT ( 'NONE',  ( -9.564922557960796823, -16.46253265017161027, 42.08224293864769550 ) ) ;
#59985 = CARTESIAN_POINT ( 'NONE',  ( -14.34966873604972548, 8.224510206698743886, 38.33442372801900433 ) ) ;
#59986 = CARTESIAN_POINT ( 'NONE',  ( -14.34966873604960291, -8.224510206698953496, 81.66557627198103830 ) ) ;
#59987 = CARTESIAN_POINT ( 'NONE',  ( 12.14591786802327356, -12.06949235617739191, 90.62609039468567573 ) ) ;
#59989 = CARTESIAN_POINT ( 'NONE',  ( 19.05341960407611168, 5.049401038298154454, 63.95724293864769550 ) ) ;
#59988 = CARTESIAN_POINT ( 'NONE',  ( 0.05219959533937995610, -21.53943276465977519, 35.00109039468568284 ) ) ;
#59990 = CARTESIAN_POINT ( 'NONE',  ( 19.05341960407611168, 5.049401038298154454, 88.95724293864769550 ) ) ;
#59991 = CARTESIAN_POINT ( 'NONE',  ( 0.05219959533934541429, -16.53943276465976808, 85.00109039468568994 ) ) ;
#59992 = EDGE_CURVE ( 'NONE', #27205, #174275, #121618, .T. ) ;
#59994 = ORIENTED_EDGE ( 'NONE', *, *, #68507, .T. ) ;
#59993 = CARTESIAN_POINT ( 'NONE',  ( -21.36928693577339189, -5.431965077040402434, 174.3311293403526179 ) ) ;
#59995 = ORIENTED_EDGE ( 'NONE', *, *, #110091, .F. ) ;
#59996 = CARTESIAN_POINT ( 'NONE',  ( 16.46253265017146816, 9.564922557961045513, 31.66775706135232937 ) ) ;
#59997 = CARTESIAN_POINT ( 'NONE',  ( -5.049401038298153566, 19.05341960407611168, 105.2072429386476671 ) ) ;
#59998 = CARTESIAN_POINT ( 'NONE',  ( 16.46253265017160672, -9.564922557960803928, 53.33224293864768839 ) ) ;
#60000 = ORIENTED_EDGE ( 'NONE', *, *, #32834, .T. ) ;
#59999 = CARTESIAN_POINT ( 'NONE',  ( 19.03943276465977164, -0.05219959533909143690, 113.7489096053143669 ) ) ;
#60001 = CARTESIAN_POINT ( 'NONE',  ( 4.483927247898790824, -16.52544592524335698, 30.20942372801902565 ) ) ;
#60003 = CARTESIAN_POINT ( 'NONE',  ( 4.379528057220092307, 16.55341960407617563, 37.29275706135235424 ) ) ;
#60002 = CARTESIAN_POINT ( 'NONE',  ( 19.03943276465977164, 0.05219959533936151252, 56.25109039468566863 ) ) ;
#60004 = CARTESIAN_POINT ( 'NONE',  ( -9.564922557960796823, -16.46253265017161027, 107.0822429386476955 ) ) ;
#60005 = CARTESIAN_POINT ( 'NONE',  ( -16.51473224551069308, -9.474510206698971260, 76.66557627198103830 ) ) ;
#60006 = CARTESIAN_POINT ( 'NONE',  ( -5.823673210054116645, -21.52544592524344225, 97.29057627198105251 ) ) ;
#60007 = CARTESIAN_POINT ( 'NONE',  ( 5.153800228976615827, -19.02544592524334988, 65.20942372801900433 ) ) ;
#60009 = CARTESIAN_POINT ( 'NONE',  ( 17.50000000000114042, -3.530325368900714356, 21.94660113358420617 ) ) ;
#60008 = CARTESIAN_POINT ( 'NONE',  ( -9.564922557960796823, -16.46253265017161027, 92.08224293864769550 ) ) ;
#60010 = CARTESIAN_POINT ( 'NONE',  ( -13.97604488694527625, -13.89961937509977652, 66.87390960531436690 ) ) ;
#60012 = DIRECTION ( 'NONE',  ( 0.000000000000000000, 0.000000000000000000, 1.000000000000000000 ) ) ;
#60011 = CARTESIAN_POINT ( 'NONE',  ( 8.314922557960818139, 14.29746914071049879, 39.58224293864769550 ) ) ;
#60013 = CARTESIAN_POINT ( 'NONE',  ( -19.05341960407617563, 5.049401038297882671, 38.54275706135233293 ) ) ;
#60014 = CARTESIAN_POINT ( 'NONE',  ( -8.224510206698948167, 14.34966873604960824, 75.41557627198102409 ) ) ;
#60015 = CARTESIAN_POINT ( 'NONE',  ( -15.72974639402176322, -15.80617190586768395, 94.37609039468568994 ) ) ;
#60016 = CARTESIAN_POINT ( 'NONE',  ( -16.46253265017160317, 9.564922557960807481, 40.83224293864769550 ) ) ;
#60017 = CARTESIAN_POINT ( 'NONE',  ( 8.224510206698742110, 14.34966873604972548, 52.08442372801901854 ) ) ;
#60019 = CARTESIAN_POINT ( 'NONE',  ( 15.72974639402176855, 15.80617190586768217, 106.8760903946856899 ) ) ;
#60018 = CARTESIAN_POINT ( 'NONE',  ( 8.224510206698953496, -14.34966873604960469, 37.91557627198102409 ) ) ;
#60020 = CARTESIAN_POINT ( 'NONE',  ( -5.153800228976328057, -19.02544592524343514, 92.29057627198099567 ) ) ;
#60021 = CARTESIAN_POINT ( 'NONE',  ( -19.03943276465977164, 0.05219959533909376836, 96.24890960531436690 ) ) ;
#60022 = CARTESIAN_POINT ( 'NONE',  ( -0.05219959533910754901, -16.53943276465976808, 102.4989096053143811 ) ) ;
#60023 = CARTESIAN_POINT ( 'NONE',  ( -12.14591786802309592, -12.06949235617757132, 76.87390960531439532 ) ) ;
#60024 = CARTESIAN_POINT ( 'NONE',  ( -21.53943276465977519, 0.05219959533907696930, 81.24890960531436690 ) ) ;
#60025 = CARTESIAN_POINT ( 'NONE',  ( 0.05219959533909260263, 19.03943276465977164, 84.99890960531436690 ) ) ;
#60026 = CARTESIAN_POINT ( 'NONE',  ( 15.72974639402199770, -15.80617190586745480, 103.1239096053143811 ) ) ;
#60027 = CARTESIAN_POINT ( 'NONE',  ( -16.46253265017160317, 9.564922557960807481, 90.83224293864769550 ) ) ;
#60030 = CARTESIAN_POINT ( 'NONE',  ( -16.55341960407611168, -4.379528057220339221, 96.45724293864770971 ) ) ;
#60029 = CARTESIAN_POINT ( 'NONE',  ( -17.58332526062528345, -7.635886036038592728, 64.07665040441534643 ) ) ;
#60028 = TOROIDAL_SURFACE ( 'NONE', #37515, 206.0437394197456911, 8.000000000000000000 ) ;
#60031 = CARTESIAN_POINT ( 'NONE',  ( 9.474510206698971260, -16.51473224551069308, 57.91557627198103120 ) ) ;
#60032 = CARTESIAN_POINT ( 'NONE',  ( 15.80617190586746368, 15.72974639402197994, 64.37390960531435269 ) ) ;
#60033 = CARTESIAN_POINT ( 'NONE',  ( 35.00000000000000000, -0.3535533905932703447, 5.353553390593268624 ) ) ;
#60035 = CARTESIAN_POINT ( 'NONE',  ( -8.571926809382608425, 26.38167802310805854, 148.9750000027311785 ) ) ;
#60034 = CARTESIAN_POINT ( 'NONE',  ( 14.29746914071037800, 8.314922557961029526, 106.6677570613523756 ) ) ;
#60036 = CARTESIAN_POINT ( 'NONE',  ( 16.52544592524335698, 4.483927247898782831, 26.45942372801901854 ) ) ;
#60037 = CARTESIAN_POINT ( 'NONE',  ( -12.06949235617756955, 12.14591786802309770, 85.62390960531436690 ) ) ;
#60038 = DIRECTION ( 'NONE',  ( 0.000000000000000000, 0.000000000000000000, 1.000000000000000000 ) ) ;
#60039 = CARTESIAN_POINT ( 'NONE',  ( -16.46253265017160317, 9.564922557960807481, 75.83224293864769550 ) ) ;
#60040 = CARTESIAN_POINT ( 'NONE',  ( -19.02544592524342804, 5.153800228976336051, 41.04057627198103120 ) ) ;
#60041 = CARTESIAN_POINT ( 'NONE',  ( 14.34966873604960469, 8.224510206698951720, 64.16557627198102409 ) ) ;
#60042 = CARTESIAN_POINT ( 'NONE',  ( -21.55341960407610458, -5.719274019375992779, 21.45724293864769550 ) ) ;
#60043 = CARTESIAN_POINT ( 'NONE',  ( 5.153800228976615827, -19.02544592524334988, 105.2094237280190185 ) ) ;
#60044 = CARTESIAN_POINT ( 'NONE',  ( 15.72974639402176855, 15.80617190586768217, 56.87609039468568994 ) ) ;
#60045 = CARTESIAN_POINT ( 'NONE',  ( 9.474510206698971260, -16.51473224551069308, 92.91557627198103830 ) ) ;
#60046 = CARTESIAN_POINT ( 'NONE',  ( -18.62759615963270932, 10.81492255796079327, 75.83224293864769550 ) ) ;
#60047 = CARTESIAN_POINT ( 'NONE',  ( -14.34966873604972548, 8.224510206698743886, 73.33442372801901854 ) ) ;
#60048 = CARTESIAN_POINT ( 'NONE',  ( 5.049401038297881783, 19.05341960407617918, 107.2927570613523187 ) ) ;
#60049 = CARTESIAN_POINT ( 'NONE',  ( 13.97604488694527802, 13.89961937509977652, 69.37390960531436690 ) ) ;
#60050 = CARTESIAN_POINT ( 'NONE',  ( 5.719274019375991003, -21.55341960407610458, 82.70724293864770971 ) ) ;
#60051 = CARTESIAN_POINT ( 'NONE',  ( -0.05219959533936034679, 19.03943276465977164, 107.5010903946856615 ) ) ;
#60053 = CARTESIAN_POINT ( 'NONE',  ( -15.72974639402176322, -15.80617190586768395, 59.37609039468568284 ) ) ;
#60052 = CARTESIAN_POINT ( 'NONE',  ( -16.52544592524342804, 4.483927247898546575, 36.04057627198102409 ) ) ;
#60055 = CARTESIAN_POINT ( 'NONE',  ( -19.05341960407611168, -5.049401038298163336, 101.4572429386476955 ) ) ;
#60054 = CARTESIAN_POINT ( 'NONE',  ( 14.34966873604972726, -8.224510206698740333, 85.83442372801901854 ) ) ;
#60056 = CARTESIAN_POINT ( 'NONE',  ( -9.474510206698964154, 16.51473224551069663, 105.4155762719810383 ) ) ;
#60057 = CARTESIAN_POINT ( 'NONE',  ( -40.00200000000003087, -1.163414459189985801E-14, 95.00000000000000000 ) ) ;
#60058 = CARTESIAN_POINT ( 'NONE',  ( 4.483927247898790824, -16.52544592524335698, 90.20942372801903275 ) ) ;
#60059 = CARTESIAN_POINT ( 'NONE',  ( 16.52544592524335698, 4.483927247898782831, 41.45942372801901143 ) ) ;
#60060 = CARTESIAN_POINT ( 'NONE',  ( 9.474510206698971260, -16.51473224551069308, 62.91557627198102409 ) ) ;
#60061 = CARTESIAN_POINT ( 'NONE',  ( -19.02544592524342804, 5.153800228976336051, 71.04057627198099567 ) ) ;
#60062 = CARTESIAN_POINT ( 'NONE',  ( 18.67979575497194134, -10.72451020669871369, 70.83442372801901854 ) ) ;
#60063 = CARTESIAN_POINT ( 'NONE',  ( -16.55341960407617563, 4.379528057220093196, 63.54275706135234003 ) ) ;
#60064 = CARTESIAN_POINT ( 'NONE',  ( 16.52544592524342804, -4.483927247898539470, 48.54057627198103120 ) ) ;
#60065 = CARTESIAN_POINT ( 'NONE',  ( -13.89961937509977652, 13.97604488694528158, 45.62390960531433848 ) ) ;
#60066 = CARTESIAN_POINT ( 'NONE',  ( 16.51473224551069308, 9.474510206698969483, 49.16557627198102409 ) ) ;
#60067 = CARTESIAN_POINT ( 'NONE',  ( -0.05219959533934338120, 16.53943276465976808, 37.50109039468568284 ) ) ;
#60068 = CARTESIAN_POINT ( 'NONE',  ( -13.89961937509957401, -13.97604488694547875, 89.37609039468563310 ) ) ;
#60069 = CARTESIAN_POINT ( 'NONE',  ( 8.224510206698953496, -14.34966873604960469, 102.9155762719810383 ) ) ;
#60070 = CARTESIAN_POINT ( 'NONE',  ( -13.89961937509977652, 13.97604488694528158, 65.62390960531436690 ) ) ;
#60072 = CARTESIAN_POINT ( 'NONE',  ( 0.000000000000000000, 0.000000000000000000, -61.34707691135562868 ) ) ;
#60071 = CARTESIAN_POINT ( 'NONE',  ( 19.05341960407617918, -5.049401038297876454, 91.04275706135234714 ) ) ;
#60073 = CARTESIAN_POINT ( 'NONE',  ( 0.05219959533937995610, -21.53943276465977519, 95.00109039468568994 ) ) ;
#60074 = CARTESIAN_POINT ( 'NONE',  ( 12.06949235617739724, 12.14591786802326823, 71.87609039468568994 ) ) ;
#60075 = DIRECTION ( 'NONE',  ( 0.000000000000000000, 0.000000000000000000, -1.000000000000000000 ) ) ;
#60076 = CARTESIAN_POINT ( 'NONE',  ( 0.05219959533907565091, 21.53943276465977519, 49.99890960531437401 ) ) ;
#60077 = CARTESIAN_POINT ( 'NONE',  ( 16.53943276465976808, 0.05219959533934440121, 36.25109039468567573 ) ) ;
#60078 = CARTESIAN_POINT ( 'NONE',  ( -19.05341960407611168, -5.049401038298164224, 36.45724293864768129 ) ) ;
#60079 = CARTESIAN_POINT ( 'NONE',  ( -9.474510206698720793, -16.51473224551083518, 39.58442372801899722 ) ) ;
#60080 = CARTESIAN_POINT ( 'NONE',  ( -9.474510206698964154, 16.51473224551069663, 90.41557627198103830 ) ) ;
#60081 = CARTESIAN_POINT ( 'NONE',  ( 9.564922557960805705, 16.46253265017160317, 24.58224293864769194 ) ) ;
#60082 = CARTESIAN_POINT ( 'NONE',  ( -16.46253265017160317, 9.564922557960807481, 50.83224293864770260 ) ) ;
#60083 = SPHERICAL_SURFACE ( 'NONE', #91461, 0.5000000000000000000 ) ;
#60084 = CARTESIAN_POINT ( 'NONE',  ( -0.05219959533937732626, 21.53943276465977519, 77.50109039468567573 ) ) ;
#60085 = CARTESIAN_POINT ( 'NONE',  ( -10.59477242850411649, -90.60836494048552936, 0.000000000000000000 ) ) ;
#60086 = CARTESIAN_POINT ( 'NONE',  ( 5.153800228976615827, -19.02544592524334988, 35.20942372801899722 ) ) ;
#60087 = CARTESIAN_POINT ( 'NONE',  ( 19.02544592524334988, 5.153800228976608722, 26.45942372801899722 ) ) ;
#60088 = CARTESIAN_POINT ( 'NONE',  ( -4.379528057220328563, 16.55341960407611168, 55.20724293864770260 ) ) ;
#60089 = CARTESIAN_POINT ( 'NONE',  ( -19.05341960407611168, -5.049401038298163336, 61.45724293864769550 ) ) ;
#60090 = CARTESIAN_POINT ( 'NONE',  ( 10.72451020669898902, -18.67979575497178502, 27.91557627198103830 ) ) ;
#60091 = CARTESIAN_POINT ( 'NONE',  ( 10.72451020669871369, 18.67979575497193778, 77.08442372801901854 ) ) ;
#60092 = CARTESIAN_POINT ( 'NONE',  ( 19.02544592524343514, -5.153800228976328945, 68.54057627198103830 ) ) ;
#60093 = CARTESIAN_POINT ( 'NONE',  ( 18.62759615963255655, 10.81492255796105972, 76.66775706135234714 ) ) ;
#60094 = CARTESIAN_POINT ( 'NONE',  ( -5.719274019375978568, 21.55341960407610458, 35.20724293864768839 ) ) ;
#60095 = CARTESIAN_POINT ( 'NONE',  ( 18.67979575497194134, -10.72451020669871369, 35.83442372801901143 ) ) ;
#60096 = CARTESIAN_POINT ( 'NONE',  ( 19.03943276465977164, 0.05219959533936151252, 61.25109039468566863 ) ) ;
#60097 = CARTESIAN_POINT ( 'NONE',  ( -9.474510206698964154, 16.51473224551069663, 35.41557627198102409 ) ) ;
#60098 = CARTESIAN_POINT ( 'NONE',  ( 19.05341960407611168, 5.049401038298154454, 73.95724293864768129 ) ) ;
#60099 = CARTESIAN_POINT ( 'NONE',  ( -14.34966873604972548, 8.224510206698743886, 33.33442372801900433 ) ) ;
#60100 = CARTESIAN_POINT ( 'NONE',  ( -8.314922557960811034, -14.29746914071050412, 87.08224293864769550 ) ) ;
#60101 = CARTESIAN_POINT ( 'NONE',  ( 16.51473224551069308, 9.474510206698969483, 59.16557627198102409 ) ) ;
#60102 = CARTESIAN_POINT ( 'NONE',  ( -15.72974639402197994, 15.80617190586746368, 40.62390960531435269 ) ) ;
#60103 = CARTESIAN_POINT ( 'NONE',  ( 9.474510206698729675, 16.51473224551082808, 112.0844237280190043 ) ) ;
#60104 = CARTESIAN_POINT ( 'NONE',  ( 10.81492255796106328, -18.62759615963255655, 20.41775706135234714 ) ) ;
#60105 = CARTESIAN_POINT ( 'NONE',  ( 15.72974639402176855, 15.80617190586768217, 71.87609039468568994 ) ) ;
#60106 = CARTESIAN_POINT ( 'NONE',  ( 4.483927247898790824, -16.52544592524335698, 70.20942372801904696 ) ) ;
#60107 = CARTESIAN_POINT ( 'NONE',  ( -14.34966873604972548, 8.224510206698743886, 73.33442372801901854 ) ) ;
#60108 = ORIENTED_EDGE ( 'NONE', *, *, #52560, .T. ) ;
#60109 = CARTESIAN_POINT ( 'NONE',  ( -19.03943276465977164, 0.05219959533909376836, 56.24890960531435979 ) ) ;
#60110 = CARTESIAN_POINT ( 'NONE',  ( 14.29746914071037800, 8.314922557961029526, 86.66775706135234714 ) ) ;
#60111 = CARTESIAN_POINT ( 'NONE',  ( 13.97604488694548053, -13.89961937509957401, 45.62609039468566863 ) ) ;
#60112 = CARTESIAN_POINT ( 'NONE',  ( 5.719274019375673035, 21.55341960407619339, 22.29275706135235069 ) ) ;
#60113 = CARTESIAN_POINT ( 'NONE',  ( -4.483927247898539470, -16.52544592524342804, 67.29057627198103830 ) ) ;
#60114 = CARTESIAN_POINT ( 'NONE',  ( -19.02544592524342804, 5.153800228976336051, 81.04057627198103830 ) ) ;
#60115 = CARTESIAN_POINT ( 'NONE',  ( 8.224510206698742110, 14.34966873604972548, 92.08442372801901854 ) ) ;
#60116 = CARTESIAN_POINT ( 'NONE',  ( 21.53943276465977519, 0.05219959533937863772, 56.25109039468568284 ) ) ;
#60117 = CARTESIAN_POINT ( 'NONE',  ( -8.314922557961024197, 14.29746914071037800, 37.91775706135235424 ) ) ;
#60118 = CARTESIAN_POINT ( 'NONE',  ( 10.81492255796078972, 18.62759615963270932, 114.5822429386477097 ) ) ;
#60119 = CARTESIAN_POINT ( 'NONE',  ( -14.34966873604960291, -8.224510206698953496, 61.66557627198103120 ) ) ;
#60120 = EDGE_CURVE ( 'NONE', #29984, #192686, #139760, .T. ) ;
#60121 = ORIENTED_EDGE ( 'NONE', *, *, #169114, .F. ) ;
#60122 = CARTESIAN_POINT ( 'NONE',  ( 10.81492255796078972, 18.62759615963270932, 104.5822429386477097 ) ) ;
#60123 = CARTESIAN_POINT ( 'NONE',  ( -8.314922557960811034, -14.29746914071050412, 42.08224293864769550 ) ) ;
#60124 = ORIENTED_EDGE ( 'NONE', *, *, #120600, .T. ) ;
#60125 = CARTESIAN_POINT ( 'NONE',  ( 34.54575687042838439, 4.960469055748728984, 50.63070180855212499 ) ) ;
#60126 = CARTESIAN_POINT ( 'NONE',  ( 5.049401038298161559, -19.05341960407611168, 107.7072429386476955 ) ) ;
#60127 = CARTESIAN_POINT ( 'NONE',  ( 10.81492255796106328, -18.62759615963255655, 35.41775706135234003 ) ) ;
#60128 = CARTESIAN_POINT ( 'NONE',  ( -16.53943276465976808, 0.05219959533911058130, 46.24890960531435979 ) ) ;
#60129 = CARTESIAN_POINT ( 'NONE',  ( -13.89961937509977652, 13.97604488694528158, 60.62390960531436690 ) ) ;
#60130 = CARTESIAN_POINT ( 'NONE',  ( 19.03943276465977164, 0.05219959533936151252, 61.25109039468566863 ) ) ;
#60131 = CARTESIAN_POINT ( 'NONE',  ( -9.474510206698964154, 16.51473224551069663, 95.41557627198102409 ) ) ;
#60132 = CARTESIAN_POINT ( 'NONE',  ( -5.719274019375978568, 21.55341960407610458, 50.20724293864769550 ) ) ;
#60133 = CARTESIAN_POINT ( 'NONE',  ( -11.22590306719490627, -43.10241010958068841, -21.31070173013197433 ) ) ;
#60134 = CARTESIAN_POINT ( 'NONE',  ( 19.03943276465977164, -0.05219959533909143690, 58.74890960531435979 ) ) ;
#60135 = CARTESIAN_POINT ( 'NONE',  ( 14.34966873604972726, -8.224510206698740333, 30.83442372801902209 ) ) ;
#60136 = CARTESIAN_POINT ( 'NONE',  ( 18.67979575497178502, 10.72451020669898547, 109.1655762719810383 ) ) ;
#60137 = CARTESIAN_POINT ( 'NONE',  ( 4.483927247898545687, 16.52544592524342804, 49.79057627198102409 ) ) ;
#60138 = ORIENTED_EDGE ( 'NONE', *, *, #124070, .F. ) ;
#60139 = CARTESIAN_POINT ( 'NONE',  ( -13.89961937509977652, 13.97604488694528158, 90.62390960531432427 ) ) ;
#60140 = CARTESIAN_POINT ( 'NONE',  ( -5.823673210054116645, -21.52544592524344225, 67.29057627198103830 ) ) ;
#60142 = CARTESIAN_POINT ( 'NONE',  ( -14.34966873604972548, 8.224510206698743886, 38.33442372801900433 ) ) ;
#60141 = CARTESIAN_POINT ( 'NONE',  ( -15.72974639402197994, 15.80617190586746368, 105.6239096053143669 ) ) ;
#60143 = CARTESIAN_POINT ( 'NONE',  ( -18.67979575497178146, -10.72451020669898902, 31.66557627198102054 ) ) ;
#60144 = CARTESIAN_POINT ( 'NONE',  ( 18.62759615963255655, 10.81492255796105972, 101.6677570613523613 ) ) ;
#60145 = CARTESIAN_POINT ( 'NONE',  ( -19.02544592524342804, 5.153800228976336051, 106.0405762719810241 ) ) ;
#60146 = CARTESIAN_POINT ( 'NONE',  ( 16.51473224551069308, 9.474510206698969483, 39.16557627198103120 ) ) ;
#60147 = CARTESIAN_POINT ( 'NONE',  ( -9.474510206698964154, 16.51473224551069663, 100.4155762719810241 ) ) ;
#60148 = CARTESIAN_POINT ( 'NONE',  ( -13.97604488694527625, -13.89961937509977652, 81.87390960531436690 ) ) ;
#60149 = CARTESIAN_POINT ( 'NONE',  ( -4.790240017743690792, -48.14548474357629715, -22.95279619250844760 ) ) ;
#60150 = CARTESIAN_POINT ( 'NONE',  ( 19.05341960407617918, -5.049401038297876454, 61.04275706135232582 ) ) ;
#60152 = CARTESIAN_POINT ( 'NONE',  ( -18.67979575497178146, -10.72451020669898902, 36.66557627198103120 ) ) ;
#60151 = CARTESIAN_POINT ( 'NONE',  ( 19.02544592524334988, 5.153800228976608722, 21.45942372801899012 ) ) ;
#60153 = CARTESIAN_POINT ( 'NONE',  ( -12.14591786802326823, 12.06949235617739902, 108.1260903946856757 ) ) ;
#60154 = CARTESIAN_POINT ( 'NONE',  ( -19.02544592524334988, -5.153800228976617603, 78.95942372801900433 ) ) ;
#60155 = CARTESIAN_POINT ( 'NONE',  ( -16.52216118717209170, 7.221426719304504083, 58.92400978953009627 ) ) ;
#60156 = CARTESIAN_POINT ( 'NONE',  ( -9.474510206698720793, -16.51473224551083518, 79.58442372801899012 ) ) ;
#60157 = CARTESIAN_POINT ( 'NONE',  ( 19.03943276465977164, 0.05219959533936151252, 36.25109039468567573 ) ) ;
#60158 = DIRECTION ( 'NONE',  ( 0.000000000000000000, 0.000000000000000000, -1.000000000000000000 ) ) ;
#60159 = CARTESIAN_POINT ( 'NONE',  ( 5.049401038298161559, -19.05341960407611168, 37.70724293864768839 ) ) ;
#60160 = CARTESIAN_POINT ( 'NONE',  ( 14.34966873604960469, 8.224510206698951720, 49.16557627198102409 ) ) ;
#60161 = CARTESIAN_POINT ( 'NONE',  ( -17.13100169013300444, -6.664070546373134007, 109.2321016430015135 ) ) ;
#60162 = CARTESIAN_POINT ( 'NONE',  ( 8.224510206698953496, -14.34966873604960469, 32.91557627198102409 ) ) ;
#60163 = CARTESIAN_POINT ( 'NONE',  ( -17.49999999999999645, -5.500000000000000888, 22.00000000000000711 ) ) ;
#60164 = CARTESIAN_POINT ( 'NONE',  ( 8.314922557961029526, -14.29746914071037800, 100.4177570613523471 ) ) ;
#60165 = CARTESIAN_POINT ( 'NONE',  ( 16.46253265017160672, -9.564922557960803928, 48.33224293864769550 ) ) ;
#60166 = CARTESIAN_POINT ( 'NONE',  ( 21.55341960407619695, -5.719274019375665929, 111.0427570613523613 ) ) ;
#60167 = CARTESIAN_POINT ( 'NONE',  ( -5.049401038297874678, -19.05341960407617918, 109.7927570613523187 ) ) ;
#60168 = CARTESIAN_POINT ( 'NONE',  ( -18.67979575497193778, 10.72451020669871902, 98.33442372801901854 ) ) ;
#60169 = CARTESIAN_POINT ( 'NONE',  ( -9.564922557961040184, 16.46253265017147172, 67.91775706135233293 ) ) ;
#60170 = CARTESIAN_POINT ( 'NONE',  ( 5.153800228976335163, 19.02544592524342804, 94.79057627198103830 ) ) ;
#60171 = CARTESIAN_POINT ( 'NONE',  ( 13.97604488694527802, 13.89961937509977652, 89.37390960531436690 ) ) ;
#60172 = CARTESIAN_POINT ( 'NONE',  ( 36.91746824999999177, 2.880721459617395097E-14, -7.624999997268813168 ) ) ;
#60173 = CARTESIAN_POINT ( 'NONE',  ( 21.52544592524344225, -5.823673210054117533, 113.5405762719810383 ) ) ;
#60174 = AXIS2_PLACEMENT_3D ( 'NONE', #76743, #199104, #61566 ) ;
#60175 = CARTESIAN_POINT ( 'NONE',  ( -14.29746914071049879, 8.314922557960819915, 85.83224293864768129 ) ) ;
#60176 = CARTESIAN_POINT ( 'NONE',  ( 18.67979575497178502, 10.72451020669898547, 59.16557627198103120 ) ) ;
#60177 = CARTESIAN_POINT ( 'NONE',  ( 5.153800228976335163, 19.02544592524342804, 59.79057627198100988 ) ) ;
#60179 = CARTESIAN_POINT ( 'NONE',  ( -8.314922557961024197, 14.29746914071037800, 92.91775706135236135 ) ) ;
#60178 = CARTESIAN_POINT ( 'NONE',  ( 21.52544592524344225, -5.823673210054117533, 98.54057627198105251 ) ) ;
#60180 = VERTEX_POINT ( 'NONE', #170116 ) ;
#60181 = CARTESIAN_POINT ( 'NONE',  ( 19.03943276465977164, -0.05219959533909143690, 58.74890960531435979 ) ) ;
#60183 = DIRECTION ( 'NONE',  ( 0.1039620511844979306, -0.1039620511844979306, 0.9891328443778538704 ) ) ;
#60182 = CARTESIAN_POINT ( 'NONE',  ( -8.314922557960811034, -14.29746914071050412, 97.08224293864770971 ) ) ;
#60184 = CARTESIAN_POINT ( 'NONE',  ( 0.05219959533909260263, 19.03943276465977164, 44.99890960531435979 ) ) ;
#60185 = CARTESIAN_POINT ( 'NONE',  ( -9.564922557961040184, 16.46253265017147172, 82.91775706135233293 ) ) ;
#60186 = CARTESIAN_POINT ( 'NONE',  ( -16.55341960407611168, -4.379528057220339221, 81.45724293864769550 ) ) ;
#60187 = CARTESIAN_POINT ( 'NONE',  ( -21.53943276465977519, -0.05219959533937600094, 63.75109039468568284 ) ) ;
#60189 = CARTESIAN_POINT ( 'NONE',  ( 18.67979575497178502, 10.72451020669898547, 109.1655762719810383 ) ) ;
#60188 = CARTESIAN_POINT ( 'NONE',  ( -19.05341960407611168, -5.049401038298163336, 36.45724293864766707 ) ) ;
#60190 = CARTESIAN_POINT ( 'NONE',  ( -14.29746914071049879, 8.314922557960819915, 105.8322429386476955 ) ) ;
#60191 = DIRECTION ( 'NONE',  ( 0.000000000000000000, 0.000000000000000000, 1.000000000000000000 ) ) ;
#60192 = CARTESIAN_POINT ( 'NONE',  ( -13.89961937509977652, 13.97604488694528158, 60.62390960531436690 ) ) ;
#60193 = CARTESIAN_POINT ( 'NONE',  ( 19.34837522270365540, 5.499999999999731770, 48.36337684832581374 ) ) ;
#60195 = CARTESIAN_POINT ( 'NONE',  ( -9.474510206698964154, 16.51473224551069663, 110.4155762719810383 ) ) ;
#60194 = CARTESIAN_POINT ( 'NONE',  ( 9.474510206698729675, 16.51473224551082808, 97.08442372801900433 ) ) ;
#60196 = CARTESIAN_POINT ( 'NONE',  ( 5.719274019375673035, 21.55341960407619339, 47.29275706135234003 ) ) ;
#60197 = CARTESIAN_POINT ( 'NONE',  ( 9.564922557960805705, 16.46253265017160317, 84.58224293864769550 ) ) ;
#60198 = CARTESIAN_POINT ( 'NONE',  ( -19.03943276465977164, -0.05219959533935918106, 73.75109039468566152 ) ) ;
#60199 = CARTESIAN_POINT ( 'NONE',  ( -9.564922557960796823, -16.46253265017161027, 62.08224293864769550 ) ) ;
#60200 = CARTESIAN_POINT ( 'NONE',  ( -0.05219959533910754901, -16.53943276465976808, 72.49890960531435269 ) ) ;
#60201 = CARTESIAN_POINT ( 'NONE',  ( 14.34966873604960469, 8.224510206698951720, 69.16557627198102409 ) ) ;
#60202 = CARTESIAN_POINT ( 'NONE',  ( 16.51473224551069308, 9.474510206698969483, 89.16557627198103830 ) ) ;
#60203 = CARTESIAN_POINT ( 'NONE',  ( -0.05219959533910754901, -16.53943276465976808, 82.49890960531436690 ) ) ;
#60204 = CARTESIAN_POINT ( 'NONE',  ( -13.97604488694527625, -13.89961937509977652, 86.87390960531436690 ) ) ;
#60205 = CARTESIAN_POINT ( 'NONE',  ( 5.049401038297881783, 19.05341960407617563, 27.29275706135232937 ) ) ;
#60208 = CARTESIAN_POINT ( 'NONE',  ( 16.52544592524342804, -4.483927247898539470, 108.5405762719810241 ) ) ;
#60207 = CARTESIAN_POINT ( 'NONE',  ( 16.55341960407611168, 4.379528057220329451, 33.95724293864769550 ) ) ;
#60206 = CARTESIAN_POINT ( 'NONE',  ( 19.05341960407611168, 5.049401038298154454, 48.95724293864768129 ) ) ;
#60209 = VERTEX_POINT ( 'NONE', #123595 ) ;
#60210 = CARTESIAN_POINT ( 'NONE',  ( -21.53943276465977519, -0.05219959533937600094, 38.75109039468567573 ) ) ;
#60211 = CARTESIAN_POINT ( 'NONE',  ( 9.564922557961047289, -16.46253265017146816, 65.41775706135233293 ) ) ;
#60212 = CARTESIAN_POINT ( 'NONE',  ( 16.52544592524342804, -4.483927247898539470, 38.54057627198103120 ) ) ;
#60213 = CARTESIAN_POINT ( 'NONE',  ( 10.72451020669898902, -18.67979575497178502, 87.91557627198103830 ) ) ;
#60214 = CARTESIAN_POINT ( 'NONE',  ( -10.72451020669898014, 18.67979575497178502, 25.41557627198103120 ) ) ;
#60215 = CARTESIAN_POINT ( 'NONE',  ( 16.52544592524342804, -4.483927247898539470, 63.54057627198103830 ) ) ;
#60216 = CARTESIAN_POINT ( 'NONE',  ( 9.474510206698971260, -16.51473224551069308, 47.91557627198102409 ) ) ;
#60217 = CARTESIAN_POINT ( 'NONE',  ( -16.46253265017146816, -9.564922557961047289, 44.16775706135232582 ) ) ;
#60218 = CARTESIAN_POINT ( 'NONE',  ( -14.29746914071037622, -8.314922557961029526, 99.16775706135234714 ) ) ;
#60219 = CARTESIAN_POINT ( 'NONE',  ( -14.34966873604972548, 8.224510206698743886, 63.33442372801900433 ) ) ;
#60220 = CARTESIAN_POINT ( 'NONE',  ( -18.67979575497178146, -10.72451020669898902, 31.66557627198102054 ) ) ;
#60221 = CARTESIAN_POINT ( 'NONE',  ( 15.72974639402176855, 15.80617190586768217, 101.8760903946857042 ) ) ;
#60222 = CARTESIAN_POINT ( 'NONE',  ( 19.03943276465977164, -0.05219959533909143690, 88.74890960531436690 ) ) ;
#60223 = CIRCLE ( 'NONE', #8561, 31.90000000000003411 ) ;
#60224 = CARTESIAN_POINT ( 'NONE',  ( 0.05219959533934541429, -16.53943276465976808, 70.00109039468568994 ) ) ;
#60225 = CARTESIAN_POINT ( 'NONE',  ( -0.05219959533909027116, -19.03943276465977164, 22.49890960531436690 ) ) ;
#60226 = CARTESIAN_POINT ( 'NONE',  ( -0.05219959533910754901, -16.53943276465976808, 32.49890960531435979 ) ) ;
#60228 = CARTESIAN_POINT ( 'NONE',  ( -0.05219959533909027116, -19.03943276465977164, 97.49890960531436690 ) ) ;
#60227 = CARTESIAN_POINT ( 'NONE',  ( 16.51473224551069308, 9.474510206698969483, 104.1655762719810241 ) ) ;
#60229 = CARTESIAN_POINT ( 'NONE',  ( 21.53943276465977519, -0.05219959533907433946, 33.74890960531436690 ) ) ;
#60230 = CARTESIAN_POINT ( 'NONE',  ( -4.379528057220328563, 16.55341960407611168, 65.20724293864768129 ) ) ;
#60231 = CARTESIAN_POINT ( 'NONE',  ( 8.224510206698953496, -14.34966873604960469, 32.91557627198102409 ) ) ;
#60232 = CARTESIAN_POINT ( 'NONE',  ( -16.53943276465976808, 0.05219959533911058130, 46.24890960531435979 ) ) ;
#60234 = CARTESIAN_POINT ( 'NONE',  ( -9.474510206698720793, -16.51473224551083518, 59.58442372801900433 ) ) ;
#60233 = CARTESIAN_POINT ( 'NONE',  ( 12.06949235617739724, 12.14591786802326823, 51.87609039468568284 ) ) ;
#60235 = CARTESIAN_POINT ( 'NONE',  ( 5.049401038297881783, 19.05341960407617563, 52.29275706135234003 ) ) ;
#60236 = CARTESIAN_POINT ( 'NONE',  ( 9.564922557960805705, 16.46253265017160317, 89.58224293864769550 ) ) ;
#60237 = CARTESIAN_POINT ( 'NONE',  ( -19.05341960407617563, 5.049401038297882671, 68.54275706135230450 ) ) ;
#60238 = CARTESIAN_POINT ( 'NONE',  ( -8.571926809382601320, -26.38167802310801591, 143.7750000027311899 ) ) ;
#60239 = CARTESIAN_POINT ( 'NONE',  ( 5.049401038297881783, 19.05341960407617563, 62.29275706135234003 ) ) ;
#60241 = CARTESIAN_POINT ( 'NONE',  ( -16.52544592524335698, -4.483927247898792601, 83.95942372801900433 ) ) ;
#60240 = CARTESIAN_POINT ( 'NONE',  ( -19.03943276465977164, -0.05219959533935918106, 93.75109039468566152 ) ) ;
#60242 = CARTESIAN_POINT ( 'NONE',  ( -5.359611314223446995E-15, 29.16686587814335496, 142.8750000027311842 ) ) ;
#60243 = CARTESIAN_POINT ( 'NONE',  ( -9.564922557960796823, -16.46253265017161027, 32.08224293864769550 ) ) ;
#60244 = CARTESIAN_POINT ( 'NONE',  ( -21.53943276465977519, 0.05219959533907696930, 26.24890960531435624 ) ) ;
#60245 = CARTESIAN_POINT ( 'NONE',  ( 0.05219959533937995610, -21.53943276465977519, 40.00109039468567573 ) ) ;
#60246 = CARTESIAN_POINT ( 'NONE',  ( -13.97604488694547697, 13.89961937509957934, 103.1260903946856473 ) ) ;
#60248 = CARTESIAN_POINT ( 'NONE',  ( -5.153800228976328057, -19.02544592524343514, 57.29057627198103120 ) ) ;
#60247 = CARTESIAN_POINT ( 'NONE',  ( 17.50000000000000000, -3.345213924137362849, 107.0876862309434614 ) ) ;
#60249 = CARTESIAN_POINT ( 'NONE',  ( -16.51473224551069308, -9.474510206698971260, 106.6655762719810383 ) ) ;
#60251 = CARTESIAN_POINT ( 'NONE',  ( 9.474510206698971260, -16.51473224551069308, 57.91557627198103120 ) ) ;
#60250 = CARTESIAN_POINT ( 'NONE',  ( -8.314922557960811034, -14.29746914071050412, 72.08224293864769550 ) ) ;
#60252 = CARTESIAN_POINT ( 'NONE',  ( -5.049401038298153566, 19.05341960407611168, 70.20724293864769550 ) ) ;
#60253 = CARTESIAN_POINT ( 'NONE',  ( -13.89961937509957401, -13.97604488694547875, 79.37609039468567573 ) ) ;
#60254 = CARTESIAN_POINT ( 'NONE',  ( 5.823673210054125526, 21.52544592524343514, 49.79057627198102409 ) ) ;
#60255 = CARTESIAN_POINT ( 'NONE',  ( 4.483927247898545687, 16.52544592524342804, 114.7905762719810383 ) ) ;
#60256 = CARTESIAN_POINT ( 'NONE',  ( -16.46253265017146816, -9.564922557961047289, 39.16775706135234003 ) ) ;
#60257 = CARTESIAN_POINT ( 'NONE',  ( -9.564922557960796823, -16.46253265017161027, 82.08224293864768129 ) ) ;
#60258 = CARTESIAN_POINT ( 'NONE',  ( -5.719274019375978568, 21.55341960407610458, 80.20724293864769550 ) ) ;
#60260 = CARTESIAN_POINT ( 'NONE',  ( 5.049401038297881783, 19.05341960407617563, 52.29275706135234003 ) ) ;
#60259 = CARTESIAN_POINT ( 'NONE',  ( -0.05219959533910754901, -16.53943276465976808, 77.49890960531433848 ) ) ;
#60261 = CARTESIAN_POINT ( 'NONE',  ( 10.72451020669898902, -18.67979575497178502, 72.91557627198103830 ) ) ;
#60262 = CARTESIAN_POINT ( 'NONE',  ( 21.52544592524344225, -5.823673210054117533, 63.54057627198103830 ) ) ;
#60263 = CARTESIAN_POINT ( 'NONE',  ( -0.05219959533907301413, -21.53943276465977519, 37.49890960531436690 ) ) ;
#60264 = CARTESIAN_POINT ( 'NONE',  ( 5.719274019375673035, 21.55341960407619339, 87.29275706135236135 ) ) ;
#60265 = CARTESIAN_POINT ( 'NONE',  ( 16.51473224551069308, 9.474510206698969483, 64.16557627198102409 ) ) ;
#60266 = CARTESIAN_POINT ( 'NONE',  ( 16.53943276465976808, -0.05219959533910856209, 113.7489096053143527 ) ) ;
#60267 = CARTESIAN_POINT ( 'NONE',  ( 21.53943276465977519, 0.05219959533937863772, 31.25109039468568639 ) ) ;
#60268 = CARTESIAN_POINT ( 'NONE',  ( 5.823673210054444382, -21.52544592524334988, 35.20942372801901854 ) ) ;
#60269 = CARTESIAN_POINT ( 'NONE',  ( 19.03943276465977164, -0.05219959533909143690, 28.74890960531435624 ) ) ;
#60270 = CARTESIAN_POINT ( 'NONE',  ( -5.823673210054116645, -21.52544592524344225, 102.2905762719810383 ) ) ;
#60271 = CARTESIAN_POINT ( 'NONE',  ( 9.474510206698729675, 16.51473224551082808, 42.08442372801900433 ) ) ;
#60272 = CARTESIAN_POINT ( 'NONE',  ( 16.51473224551069308, 9.474510206698969483, 34.16557627198102409 ) ) ;
#60273 = CARTESIAN_POINT ( 'NONE',  ( 16.52544592524335698, 4.483927247898782831, 26.45942372801901854 ) ) ;
#60274 = CARTESIAN_POINT ( 'NONE',  ( -28.79475375365586842, 2.428612866367529932E-14, 155.0000000000000000 ) ) ;
#60275 = CARTESIAN_POINT ( 'NONE',  ( -16.53943276465976808, -0.05219959533934237506, 63.75109039468568284 ) ) ;
#60276 = CARTESIAN_POINT ( 'NONE',  ( 13.89961937509977652, -13.97604488694527269, 33.12390960531434558 ) ) ;
#60277 = CARTESIAN_POINT ( 'NONE',  ( -25.11239783071220799, -12.35465959875006092, 166.1131185557732124 ) ) ;
#60278 = CARTESIAN_POINT ( 'NONE',  ( 9.474510206698971260, -16.51473224551069308, 82.91557627198103830 ) ) ;
#60279 = CARTESIAN_POINT ( 'NONE',  ( 12.06949235617757843, -12.14591786802309237, 103.1239096053143811 ) ) ;
#60280 = CARTESIAN_POINT ( 'NONE',  ( 5.823673210054125526, 21.52544592524343514, 54.79057627198104541 ) ) ;
#60281 = CARTESIAN_POINT ( 'NONE',  ( 4.379528057220092307, 16.55341960407617563, 42.29275706135235424 ) ) ;
#60282 = CARTESIAN_POINT ( 'NONE',  ( 21.55341960407619695, -5.719274019375665929, 101.0427570613523756 ) ) ;
#60283 = CARTESIAN_POINT ( 'NONE',  ( 9.564922557960805705, 16.46253265017160317, 44.58224293864769550 ) ) ;
#60284 = CARTESIAN_POINT ( 'NONE',  ( -4.379528057220086978, -16.55341960407618274, 104.7927570613523898 ) ) ;
#60285 = CARTESIAN_POINT ( 'NONE',  ( -12.14591786802309592, -12.06949235617757132, 56.87390960531436690 ) ) ;
#60286 = CARTESIAN_POINT ( 'NONE',  ( 19.05341960407611168, 5.049401038298154454, 63.95724293864769550 ) ) ;
#60287 = CARTESIAN_POINT ( 'NONE',  ( -5.719274019375665041, -21.55341960407619695, 104.7927570613523898 ) ) ;
#60288 = CARTESIAN_POINT ( 'NONE',  ( -15.72974639402197994, 15.80617190586746368, 115.6239096053143669 ) ) ;
#60289 = CARTESIAN_POINT ( 'NONE',  ( 15.72974639402176855, 15.80617190586768217, 71.87609039468568994 ) ) ;
#60290 = CARTESIAN_POINT ( 'NONE',  ( -0.05219959533934338120, 16.53943276465976808, 52.50109039468567573 ) ) ;
#60291 = CARTESIAN_POINT ( 'NONE',  ( 16.52544592524335698, 4.483927247898782831, 26.45942372801901854 ) ) ;
#60293 = CARTESIAN_POINT ( 'NONE',  ( -18.62759615963255300, -10.81492255796106328, 94.16775706135237556 ) ) ;
#60292 = CARTESIAN_POINT ( 'NONE',  ( 8.314922557960818139, 14.29746914071049879, 79.58224293864769550 ) ) ;
#60294 = CARTESIAN_POINT ( 'NONE',  ( 0.05219959533910956823, 16.53943276465976808, 39.99890960531436690 ) ) ;
#60295 = CARTESIAN_POINT ( 'NONE',  ( -17.44279575226824974, 5.990770900252412545, 115.8355756751432182 ) ) ;
#60296 = CARTESIAN_POINT ( 'NONE',  ( -16.52544592524335698, -4.483927247898792601, 38.95942372801901854 ) ) ;
#60297 = CARTESIAN_POINT ( 'NONE',  ( 0.05219959533910956823, 16.53943276465976808, 59.99890960531436690 ) ) ;
#60298 = CARTESIAN_POINT ( 'NONE',  ( -4.483927247898782831, 16.52544592524335698, 87.70942372801901854 ) ) ;
#60299 = CARTESIAN_POINT ( 'NONE',  ( 19.02544592524343514, -5.153800228976328945, 93.54057627198102409 ) ) ;
#60300 = CARTESIAN_POINT ( 'NONE',  ( -13.97604488694527625, -13.89961937509977652, 111.8739096053143243 ) ) ;
#60301 = CARTESIAN_POINT ( 'NONE',  ( -10.81492255796105439, 18.62759615963255655, 97.91775706135236135 ) ) ;
#60302 = CARTESIAN_POINT ( 'NONE',  ( -4.483927247898782831, 16.52544592524335698, 107.7094237280190328 ) ) ;
#60303 = CARTESIAN_POINT ( 'NONE',  ( 16.53943276465976808, -0.05219959533910856209, 83.74890960531435269 ) ) ;
#60304 = CARTESIAN_POINT ( 'NONE',  ( -16.46253265017160317, 9.564922557960807481, 95.83224293864769550 ) ) ;
#60305 = VERTEX_POINT ( 'NONE', #44795 ) ;
#60306 = CARTESIAN_POINT ( 'NONE',  ( -4.379528057220086978, -16.55341960407618274, 44.79275706135234714 ) ) ;
#60307 = CARTESIAN_POINT ( 'NONE',  ( -9.564922557960796823, -16.46253265017161027, 42.08224293864769550 ) ) ;
#60308 = CARTESIAN_POINT ( 'NONE',  ( 9.474510206698971260, -16.51473224551069308, 102.9155762719810241 ) ) ;
#60310 = CARTESIAN_POINT ( 'NONE',  ( -11.40812507854754720, -35.11059874428192273, -4.224999997268813701 ) ) ;
#60309 = CARTESIAN_POINT ( 'NONE',  ( -4.379528057220086978, -16.55341960407618274, 49.79275706135234714 ) ) ;
#60311 = CARTESIAN_POINT ( 'NONE',  ( -0.05219959533936034679, 19.03943276465977164, 32.50109039468566863 ) ) ;
#60312 = CARTESIAN_POINT ( 'NONE',  ( -16.46253265017160317, 9.564922557960807481, 40.83224293864769550 ) ) ;
#60313 = CARTESIAN_POINT ( 'NONE',  ( 16.52544592524335698, 4.483927247898782831, 81.45942372801900433 ) ) ;
#60314 = CARTESIAN_POINT ( 'NONE',  ( 5.049401038297881783, 19.05341960407617563, 87.29275706135234714 ) ) ;
#60315 = CARTESIAN_POINT ( 'NONE',  ( -16.51473224551082808, 9.474510206698731452, 23.33442372801900078 ) ) ;
#60316 = CARTESIAN_POINT ( 'NONE',  ( 19.03943276465977164, -0.05219959533909143690, 58.74890960531435979 ) ) ;
#60317 = CARTESIAN_POINT ( 'NONE',  ( -8.314922557960811034, -14.29746914071050412, 97.08224293864770971 ) ) ;
#60318 = AXIS2_PLACEMENT_3D ( 'NONE', #42477, #181984, #40470 ) ;
#60319 = EDGE_CURVE ( 'NONE', #190734, #35769, #27937, .T. ) ;
#60320 = CARTESIAN_POINT ( 'NONE',  ( -19.05341960407617563, 5.049401038297882671, 63.54275706135234003 ) ) ;
#60321 = CARTESIAN_POINT ( 'NONE',  ( -15.80617190586745835, -15.72974639402198527, 61.87390960531436690 ) ) ;
#60322 = CARTESIAN_POINT ( 'NONE',  ( -9.474510206698720793, -16.51473224551083518, 29.58442372801900433 ) ) ;
#60323 = CARTESIAN_POINT ( 'NONE',  ( 5.153800228976335163, 19.02544592524342804, 104.7905762719809957 ) ) ;
#60324 = CARTESIAN_POINT ( 'NONE',  ( -18.67979575497178146, -10.72451020669898902, 71.66557627198100988 ) ) ;
#60325 = CARTESIAN_POINT ( 'NONE',  ( -13.89961937509977652, 13.97604488694528158, 105.6239096053143527 ) ) ;
#60326 = AXIS2_PLACEMENT_3D ( 'NONE', #79533, #141203, #184730 ) ;
#60327 = CARTESIAN_POINT ( 'NONE',  ( -19.03943276465977164, -0.05219959533935918106, 98.75109039468567573 ) ) ;
#60328 = CARTESIAN_POINT ( 'NONE',  ( -5.153800228976328057, -19.02544592524343514, 112.2905762719810099 ) ) ;
#60329 = CARTESIAN_POINT ( 'NONE',  ( 0.05219959533934541429, -16.53943276465976808, 25.00109039468567218 ) ) ;
#60330 = CARTESIAN_POINT ( 'NONE',  ( 19.03943276465977164, -0.05219959533909143690, 28.74890960531435624 ) ) ;
#60331 = CARTESIAN_POINT ( 'NONE',  ( 9.474510206698971260, -16.51473224551069308, 92.91557627198103830 ) ) ;
#60332 = CARTESIAN_POINT ( 'NONE',  ( -21.52544592524343514, 5.823673210054127303, 86.04057627198102409 ) ) ;
#60333 = CARTESIAN_POINT ( 'NONE',  ( 21.55341960407619695, -5.719274019375665929, 66.04275706135236135 ) ) ;
#60335 = CARTESIAN_POINT ( 'NONE',  ( -21.55341960407619339, 5.719274019375674811, 108.5427570613523756 ) ) ;
#60334 = CARTESIAN_POINT ( 'NONE',  ( -13.97604488694547697, 13.89961937509957934, 108.1260903946856331 ) ) ;
#60336 = CARTESIAN_POINT ( 'NONE',  ( 0.05219959533934541429, -16.53943276465976808, 110.0010903946856757 ) ) ;
#60337 = CARTESIAN_POINT ( 'NONE',  ( -10.81492255796078084, -18.62759615963271287, 107.0822429386476955 ) ) ;
#60338 = CARTESIAN_POINT ( 'NONE',  ( -14.29746914071049879, 8.314922557960819915, 30.83224293864770260 ) ) ;
#60339 = CARTESIAN_POINT ( 'NONE',  ( 13.97604488694548053, -13.89961937509957401, 80.62609039468567573 ) ) ;
#60340 = CARTESIAN_POINT ( 'NONE',  ( -16.51473224551082808, 9.474510206698731452, 58.33442372801900433 ) ) ;
#60341 = CARTESIAN_POINT ( 'NONE',  ( -18.62759615963255300, -10.81492255796106328, 59.16775706135234714 ) ) ;
#60342 = CARTESIAN_POINT ( 'NONE',  ( -9.474510206698720793, -16.51473224551083518, 39.58442372801899722 ) ) ;
#60343 = CARTESIAN_POINT ( 'NONE',  ( 8.314922557960818139, 14.29746914071049879, 109.5822429386476955 ) ) ;
#60344 = CARTESIAN_POINT ( 'NONE',  ( 15.80617190586746368, 15.72974639402197994, 29.37390960531435269 ) ) ;
#60345 = CARTESIAN_POINT ( 'NONE',  ( -8.224510206698948167, 14.34966873604960824, 35.41557627198102409 ) ) ;
#60346 = CARTESIAN_POINT ( 'NONE',  ( 21.53943276465977519, 0.05219959533937863772, 96.25109039468568994 ) ) ;
#60347 = CARTESIAN_POINT ( 'NONE',  ( 14.29746914071037800, 8.314922557961029526, 71.66775706135234714 ) ) ;
#60348 = CARTESIAN_POINT ( 'NONE',  ( 16.52544592524342804, -4.483927247898539470, 23.54057627198102765 ) ) ;
#60349 = CARTESIAN_POINT ( 'NONE',  ( 21.53943276465977519, 0.05219959533937863772, 61.25109039468567573 ) ) ;
#60350 = CARTESIAN_POINT ( 'NONE',  ( 21.52544592524334988, 5.823673210054432836, 71.45942372801901854 ) ) ;
#60351 = CARTESIAN_POINT ( 'NONE',  ( 0.05219959533907565091, 21.53943276465977519, 64.99890960531435269 ) ) ;
#60352 = EDGE_CURVE ( 'NONE', #33122, #171099, #24744, .T. ) ;
#60353 = VERTEX_POINT ( 'NONE', #14447 ) ;
#60354 = CARTESIAN_POINT ( 'NONE',  ( -5.153800228976328057, -19.02544592524343514, 62.29057627198102409 ) ) ;
#60355 = CARTESIAN_POINT ( 'NONE',  ( 21.55341960407619695, -5.719274019375665929, 41.04275706135236135 ) ) ;
#60356 = CARTESIAN_POINT ( 'NONE',  ( -16.51473224551069308, -9.474510206698971260, 21.66557627198102765 ) ) ;
#60357 = CARTESIAN_POINT ( 'NONE',  ( 9.474510206698971260, -16.51473224551069308, 42.91557627198103120 ) ) ;
#60358 = CARTESIAN_POINT ( 'NONE',  ( 8.224510206698953496, -14.34966873604960469, 77.91557627198102409 ) ) ;
#60359 = CARTESIAN_POINT ( 'NONE',  ( -9.474510206698964154, 16.51473224551069663, 80.41557627198103830 ) ) ;
#60360 = CARTESIAN_POINT ( 'NONE',  ( -8.314922557960811034, -14.29746914071050412, 27.08224293864769550 ) ) ;
#60361 = CARTESIAN_POINT ( 'NONE',  ( 21.53943276465977519, -0.05219959533907433946, 68.74890960531435269 ) ) ;
#60362 = VECTOR ( 'NONE', #72715, 1000.000000000000000 ) ;
#60363 = CARTESIAN_POINT ( 'NONE',  ( -21.55341960407610458, -5.719274019375992779, 106.4572429386477097 ) ) ;
#60364 = CARTESIAN_POINT ( 'NONE',  ( 5.153800228976335163, 19.02544592524342804, 104.7905762719809957 ) ) ;
#60366 = CARTESIAN_POINT ( 'NONE',  ( -19.03943276465977164, -0.05219959533935918106, 103.7510903946856757 ) ) ;
#60365 = CARTESIAN_POINT ( 'NONE',  ( 16.51473224551069308, 9.474510206698969483, 69.16557627198102409 ) ) ;
#60367 = CARTESIAN_POINT ( 'NONE',  ( 10.72451020669898902, -18.67979575497178502, 62.91557627198102409 ) ) ;
#60368 = CARTESIAN_POINT ( 'NONE',  ( 21.52544592524334988, 5.823673210054432836, 86.45942372801901854 ) ) ;
#60369 = CARTESIAN_POINT ( 'NONE',  ( -9.474510206698964154, 16.51473224551069663, 65.41557627198102409 ) ) ;
#60370 = CARTESIAN_POINT ( 'NONE',  ( -19.03943276465977164, 0.05219959533909376836, 101.2489096053143669 ) ) ;
#60371 = CARTESIAN_POINT ( 'NONE',  ( 16.53943276465976808, 0.05219959533934440121, 71.25109039468568994 ) ) ;
#60372 = CARTESIAN_POINT ( 'NONE',  ( 21.55341960407619695, -5.719274019375665929, 51.04275706135234714 ) ) ;
#60373 = CARTESIAN_POINT ( 'NONE',  ( 5.719274019375673035, 21.55341960407619339, 82.29275706135234714 ) ) ;
#60374 = CARTESIAN_POINT ( 'NONE',  ( 21.52544592524334988, 5.823673210054432836, 21.45942372801901499 ) ) ;
#60375 = CARTESIAN_POINT ( 'NONE',  ( -21.55341960407610458, -5.719274019375992779, 71.45724293864769550 ) ) ;
#60376 = CARTESIAN_POINT ( 'NONE',  ( 19.02544592524334988, 5.153800228976608722, 51.45942372801900433 ) ) ;
#60377 = CARTESIAN_POINT ( 'NONE',  ( -15.80617190586745835, -15.72974639402198527, 46.87390960531435979 ) ) ;
#60379 = CARTESIAN_POINT ( 'NONE',  ( -4.379528057220328563, 16.55341960407611168, 30.20724293864769550 ) ) ;
#60378 = CARTESIAN_POINT ( 'NONE',  ( 19.05341960407611168, 5.049401038298154454, 78.95724293864769550 ) ) ;
#60380 = CARTESIAN_POINT ( 'NONE',  ( -16.88567814943165857, 6.947325034625572826, 63.70998877347415146 ) ) ;
#60381 = CARTESIAN_POINT ( 'NONE',  ( 9.564922557960805705, 16.46253265017160317, 114.5822429386476955 ) ) ;
#60382 = CARTESIAN_POINT ( 'NONE',  ( 0.7842620108279171331, 13.90517634892589882, -60.35638352309626953 ) ) ;
#60383 = CARTESIAN_POINT ( 'NONE',  ( 0.05219959533936267826, -19.03943276465977164, 90.00109039468567573 ) ) ;
#60384 = CARTESIAN_POINT ( 'NONE',  ( -18.62759615963270932, 10.81492255796079327, 75.83224293864769550 ) ) ;
#60385 = CARTESIAN_POINT ( 'NONE',  ( 12.14591786802309770, 12.06949235617756955, 54.37390960531435979 ) ) ;
#60386 = CARTESIAN_POINT ( 'NONE',  ( 12.14591786802327356, -12.06949235617739191, 25.62609039468567929 ) ) ;
#60387 = CARTESIAN_POINT ( 'NONE',  ( -19.03943276465977164, 0.05219959533909376836, 46.24890960531435979 ) ) ;
#60389 = CARTESIAN_POINT ( 'NONE',  ( -0.05219959533936034679, 19.03943276465977164, 67.50109039468566152 ) ) ;
#60388 = CARTESIAN_POINT ( 'NONE',  ( -15.72974639402197994, 15.80617190586746368, 105.6239096053143669 ) ) ;
#60390 = CARTESIAN_POINT ( 'NONE',  ( -9.474510206698964154, 16.51473224551069663, 85.41557627198102409 ) ) ;
#60391 = CARTESIAN_POINT ( 'NONE',  ( 12.14591786802309770, 12.06949235617756955, 89.37390960531435269 ) ) ;
#60392 = CARTESIAN_POINT ( 'NONE',  ( 19.05341960407611168, 5.049401038298154454, 63.95724293864769550 ) ) ;
#60393 = CARTESIAN_POINT ( 'NONE',  ( 14.29746914071049879, -8.314922557960816363, 73.33224293864769550 ) ) ;
#60394 = CARTESIAN_POINT ( 'NONE',  ( 19.02544592524343514, -5.153800228976328945, 38.54057627198103120 ) ) ;
#60395 = CARTESIAN_POINT ( 'NONE',  ( 17.18269478283316332, -17.18269478283309226, -54.21489346206828230 ) ) ;
#60396 = CARTESIAN_POINT ( 'NONE',  ( -0.05219959533910754901, -16.53943276465976808, 42.49890960531435979 ) ) ;
#60397 = CARTESIAN_POINT ( 'NONE',  ( -5.049401038298153566, 19.05341960407611168, 85.20724293864766707 ) ) ;
#60398 = CARTESIAN_POINT ( 'NONE',  ( 9.352457526187951330E-15, -64.84118668444963873, -15.00000000000000000 ) ) ;
#60399 = CARTESIAN_POINT ( 'NONE',  ( 13.97604488694548053, -13.89961937509957401, 50.62609039468566152 ) ) ;
#60400 = CARTESIAN_POINT ( 'NONE',  ( 16.52544592524335698, 4.483927247898782831, 56.45942372801902565 ) ) ;
#60401 = CARTESIAN_POINT ( 'NONE',  ( -10.81492255796078084, -18.62759615963271287, 82.08224293864768129 ) ) ;
#60402 = CARTESIAN_POINT ( 'NONE',  ( 16.51473224551083163, -9.474510206698727899, 35.83442372801899722 ) ) ;
#60403 = CARTESIAN_POINT ( 'NONE',  ( -13.97604488694527625, -13.89961937509977652, 86.87390960531436690 ) ) ;
#60404 = CARTESIAN_POINT ( 'NONE',  ( 0.5310895872712830812, 21.39321968400172125, -58.79437919268159618 ) ) ;
#60405 = CARTESIAN_POINT ( 'NONE',  ( -10.81492255796078084, -18.62759615963271287, 22.08224293864769194 ) ) ;
#60406 = CARTESIAN_POINT ( 'NONE',  ( 13.89961937509977652, -13.97604488694527269, 58.12390960531436690 ) ) ;
#60407 = CARTESIAN_POINT ( 'NONE',  ( -10.72451020669870658, -18.67979575497194134, 49.58442372801901143 ) ) ;
#60408 = CARTESIAN_POINT ( 'NONE',  ( -13.89961937509977652, 13.97604488694528158, 30.62390960531435269 ) ) ;
#60411 = ORIENTED_EDGE ( 'NONE', *, *, #143390, .T. ) ;
#60410 = CARTESIAN_POINT ( 'NONE',  ( 0.05219959533909260263, 19.03943276465977164, 99.99890960531436690 ) ) ;
#60409 = CARTESIAN_POINT ( 'NONE',  ( -10.72451020669898014, 18.67979575497178502, 110.4155762719810383 ) ) ;
#60412 = CARTESIAN_POINT ( 'NONE',  ( -21.52544592524334988, -5.823673210054445271, 38.95942372801901854 ) ) ;
#60413 = ORIENTED_EDGE ( 'NONE', *, *, #160688, .F. ) ;
#60414 = CARTESIAN_POINT ( 'NONE',  ( -5.049401038298153566, 19.05341960407611168, 100.2072429386476955 ) ) ;
#60415 = CARTESIAN_POINT ( 'NONE',  ( -21.94595931813859124, 7.591279830614301893, 169.8931963588657368 ) ) ;
#60416 = CARTESIAN_POINT ( 'NONE',  ( -15.80617190586745835, -15.72974639402198527, 111.8739096053143669 ) ) ;
#60417 = CARTESIAN_POINT ( 'NONE',  ( 16.46253265017160672, -9.564922557960803928, 53.33224293864768839 ) ) ;
#60418 = CARTESIAN_POINT ( 'NONE',  ( 12.14591786802327356, -12.06949235617739191, 30.62609039468567929 ) ) ;
#60419 = CARTESIAN_POINT ( 'NONE',  ( -11.40812507854754720, -35.11059874428192273, -4.724999997268812812 ) ) ;
#60420 = CARTESIAN_POINT ( 'NONE',  ( 5.049401038298161559, -19.05341960407611168, 27.70724293864769550 ) ) ;
#60421 = CARTESIAN_POINT ( 'NONE',  ( -0.05219959533937732626, 21.53943276465977519, 97.50109039468567573 ) ) ;
#60423 = CARTESIAN_POINT ( 'NONE',  ( -15.72974639402176322, -15.80617190586768395, 54.37609039468568994 ) ) ;
#60422 = CARTESIAN_POINT ( 'NONE',  ( -9.564922557960796823, -16.46253265017161027, 82.08224293864768129 ) ) ;
#60424 = CARTESIAN_POINT ( 'NONE',  ( -8.571926809382608425, 26.38167802310805854, 144.9750000027312069 ) ) ;
#60425 = CARTESIAN_POINT ( 'NONE',  ( -19.02544592524342804, 5.153800228976336051, 101.0405762719810241 ) ) ;
#60426 = DIRECTION ( 'NONE',  ( 1.000000000000000000, 0.000000000000000000, 0.000000000000000000 ) ) ;
#60429 = CARTESIAN_POINT ( 'NONE',  ( -10.81492255796105439, 18.62759615963255655, 62.91775706135236135 ) ) ;
#60428 = CARTESIAN_POINT ( 'NONE',  ( 8.224510206698742110, 14.34966873604972548, 72.08442372801899012 ) ) ;
#60427 = CARTESIAN_POINT ( 'NONE',  ( -8.224510206698735004, -14.34966873604973081, 44.58442372801901854 ) ) ;
#60430 = CARTESIAN_POINT ( 'NONE',  ( 5.823673210054444382, -21.52544592524334988, 85.20942372801901854 ) ) ;
#60431 = CARTESIAN_POINT ( 'NONE',  ( 4.457937930945874427, 6.565741541539653170, -62.16217994089669929 ) ) ;
#60432 = CARTESIAN_POINT ( 'NONE',  ( 13.89961937509957401, 13.97604488694547697, 106.8760903946856757 ) ) ;
#60433 = CARTESIAN_POINT ( 'NONE',  ( 9.564922557960805705, 16.46253265017160317, 79.58224293864769550 ) ) ;
#60434 = CARTESIAN_POINT ( 'NONE',  ( -16.46253265017160317, 9.564922557960807481, 95.83224293864769550 ) ) ;
#60435 = CARTESIAN_POINT ( 'NONE',  ( 16.46253265017160672, -9.564922557960803928, 23.33224293864769194 ) ) ;
#60436 = CARTESIAN_POINT ( 'NONE',  ( 18.62759615963271287, -10.81492255796078972, 33.33224293864769550 ) ) ;
#60437 = CARTESIAN_POINT ( 'NONE',  ( -8.314922557961024197, 14.29746914071037800, 97.91775706135236135 ) ) ;
#60439 = CARTESIAN_POINT ( 'NONE',  ( -19.03943276465977164, 0.05219959533909376836, 61.24890960531436690 ) ) ;
#60438 = CARTESIAN_POINT ( 'NONE',  ( -4.483927247898539470, -16.52544592524342804, 72.29057627198102409 ) ) ;
#60440 = CARTESIAN_POINT ( 'NONE',  ( -18.62759615963255300, -10.81492255796106328, 94.16775706135237556 ) ) ;
#60441 = DIRECTION ( 'NONE',  ( 0.000000000000000000, 0.000000000000000000, 1.000000000000000000 ) ) ;
#60442 = CARTESIAN_POINT ( 'NONE',  ( -19.03943276465977164, -0.05219959533935918106, 103.7510903946856757 ) ) ;
#60443 = CARTESIAN_POINT ( 'NONE',  ( -8.314922557960811034, -14.29746914071050412, 77.08224293864769550 ) ) ;
#60444 = CARTESIAN_POINT ( 'NONE',  ( 10.72451020669871369, 18.67979575497193778, 27.08442372801901854 ) ) ;
#60445 = CARTESIAN_POINT ( 'NONE',  ( -0.05219959533907301413, -21.53943276465977519, 62.49890960531436690 ) ) ;
#60446 = CARTESIAN_POINT ( 'NONE',  ( -16.51473224551082808, 9.474510206698731452, 38.33442372801899722 ) ) ;
#60447 = CARTESIAN_POINT ( 'NONE',  ( 1.993301997531345292E-15, -30.30510711980685912, 146.7500000054623683 ) ) ;
#60448 = CARTESIAN_POINT ( 'NONE',  ( -13.97604488694527625, -13.89961937509977652, 81.87390960531436690 ) ) ;
#60449 = CARTESIAN_POINT ( 'NONE',  ( -12.06949235617756955, 12.14591786802309770, 50.62390960531435979 ) ) ;
#60450 = VECTOR ( 'NONE', #54278, 1000.000000000000000 ) ;
#60451 = CARTESIAN_POINT ( 'NONE',  ( 8.314922557960818139, 14.29746914071049879, 39.58224293864769550 ) ) ;
#60452 = CARTESIAN_POINT ( 'NONE',  ( 8.314922557961029526, -14.29746914071037800, 100.4177570613523471 ) ) ;
#60453 = CARTESIAN_POINT ( 'NONE',  ( -9.474510206698720793, -16.51473224551083518, 54.58442372801899722 ) ) ;
#60454 = CARTESIAN_POINT ( 'NONE',  ( -13.97604488694547520, 13.89961937509957934, 78.12609039468566152 ) ) ;
#60455 = CARTESIAN_POINT ( 'NONE',  ( 19.02544592524343514, -5.153800228976328945, 103.5405762719809957 ) ) ;
#60456 = CARTESIAN_POINT ( 'NONE',  ( 16.52544592524342804, -4.483927247898539470, 73.54057627198102409 ) ) ;
#60457 = CARTESIAN_POINT ( 'NONE',  ( 5.153800228976615827, -19.02544592524334988, 50.20942372801897591 ) ) ;
#60459 = CARTESIAN_POINT ( 'NONE',  ( -18.62759615963270932, 10.81492255796079327, 40.83224293864769550 ) ) ;
#60458 = CARTESIAN_POINT ( 'NONE',  ( -19.02544592524342804, 5.153800228976336051, 36.04057627198100988 ) ) ;
#60460 = CARTESIAN_POINT ( 'NONE',  ( -10.72451020669898014, 18.67979575497178502, 70.41557627198102409 ) ) ;
#60461 = CARTESIAN_POINT ( 'NONE',  ( 0.05219959533910956823, 16.53943276465976808, 109.9989096053143527 ) ) ;
#60462 = CARTESIAN_POINT ( 'NONE',  ( 4.483927247898790824, -16.52544592524335698, 55.20942372801902565 ) ) ;
#60463 = CARTESIAN_POINT ( 'NONE',  ( 18.62759615963255655, 10.81492255796105972, 41.66775706135235424 ) ) ;
#60464 = CARTESIAN_POINT ( 'NONE',  ( 0.05219959533910956823, 16.53943276465976808, 94.99890960531436690 ) ) ;
#60465 = CARTESIAN_POINT ( 'NONE',  ( 16.52216118717207749, -7.221426719304488984, 36.42400978953008206 ) ) ;
#60466 = CARTESIAN_POINT ( 'NONE',  ( 11.40812507854755253, -35.11059874428192273, -8.524999997268814411 ) ) ;
#60467 = CARTESIAN_POINT ( 'NONE',  ( -10.72451020669898014, 18.67979575497178502, 40.41557627198103120 ) ) ;
#60468 = CARTESIAN_POINT ( 'NONE',  ( 17.31747979337950483, -6.344076630960995722, 66.12055131934813801 ) ) ;
#60470 = CARTESIAN_POINT ( 'NONE',  ( -16.52544592524342804, 4.483927247898546575, 41.04057627198103120 ) ) ;
#60469 = CARTESIAN_POINT ( 'NONE',  ( -12.06949235617739369, -12.14591786802326823, 44.37609039468567573 ) ) ;
#60471 = CARTESIAN_POINT ( 'NONE',  ( -5.719274019375978568, 21.55341960407610458, 70.20724293864769550 ) ) ;
#60472 = CARTESIAN_POINT ( 'NONE',  ( -19.03943276465977164, -0.05219959533935918106, 83.75109039468567573 ) ) ;
#60473 = CARTESIAN_POINT ( 'NONE',  ( 18.62759615963271287, -10.81492255796078972, 68.33224293864769550 ) ) ;
#60474 = DIRECTION ( 'NONE',  ( 0.000000000000000000, 0.000000000000000000, -1.000000000000000000 ) ) ;
#60477 = EDGE_CURVE ( 'NONE', #147765, #189743, #154946, .T. ) ;
#60476 = CARTESIAN_POINT ( 'NONE',  ( -5.153800228976328057, -19.02544592524343514, 107.2905762719810383 ) ) ;
#60475 = CARTESIAN_POINT ( 'NONE',  ( -19.03943276465977164, 0.05219959533909376836, 41.24890960531435269 ) ) ;
#60478 = CARTESIAN_POINT ( 'NONE',  ( 16.51473224551069308, 9.474510206698969483, 44.16557627198103120 ) ) ;
#60479 = CARTESIAN_POINT ( 'NONE',  ( -14.29746914071049879, 8.314922557960819915, 115.8322429386477097 ) ) ;
#60480 = DIRECTION ( 'NONE',  ( 1.000000000000000000, 0.000000000000000000, 0.000000000000000000 ) ) ;
#60481 = CARTESIAN_POINT ( 'NONE',  ( 5.153800228976335163, 19.02544592524342804, 114.7905762719810241 ) ) ;
#60482 = VERTEX_POINT ( 'NONE', #108440 ) ;
#60483 = CARTESIAN_POINT ( 'NONE',  ( -4.483927247898782831, 16.52544592524335698, 67.70942372801901854 ) ) ;
#60484 = CARTESIAN_POINT ( 'NONE',  ( 21.52544592524344225, -5.823673210054117533, 98.54057627198105251 ) ) ;
#60485 = CARTESIAN_POINT ( 'NONE',  ( 5.153800228976335163, 19.02544592524342804, 59.79057627198100988 ) ) ;
#60486 = CARTESIAN_POINT ( 'NONE',  ( 21.55341960407619695, -5.719274019375665929, 46.04275706135234714 ) ) ;
#60487 = CARTESIAN_POINT ( 'NONE',  ( 13.97604488694527802, 13.89961937509977652, 84.37390960531433848 ) ) ;
#60488 = CARTESIAN_POINT ( 'NONE',  ( -23.29544513554941076, 16.92513159979227666, 145.7843446568999752 ) ) ;
#60489 = ORIENTED_EDGE ( 'NONE', *, *, #112510, .T. ) ;
#60490 = CARTESIAN_POINT ( 'NONE',  ( -21.52544592524334988, -5.823673210054445271, 38.95942372801901854 ) ) ;
#60492 = CARTESIAN_POINT ( 'NONE',  ( 9.564922557961047289, -16.46253265017146816, 85.41775706135233293 ) ) ;
#60491 = CARTESIAN_POINT ( 'NONE',  ( 5.153800228976335163, 19.02544592524342804, 104.7905762719809957 ) ) ;
#60493 = CARTESIAN_POINT ( 'NONE',  ( 19.05341960407617918, -5.049401038297876454, 41.04275706135233293 ) ) ;
#60494 = CARTESIAN_POINT ( 'NONE',  ( -21.53943276465977519, 0.05219959533907696930, 101.2489096053143669 ) ) ;
#60495 = CARTESIAN_POINT ( 'NONE',  ( 19.05341960407617918, -5.049401038297876454, 36.04275706135234003 ) ) ;
#60496 = CARTESIAN_POINT ( 'NONE',  ( 19.03943276465977164, 0.05219959533936151252, 36.25109039468567573 ) ) ;
#60497 = CARTESIAN_POINT ( 'NONE',  ( -14.29746914071037622, -8.314922557961029526, 89.16775706135236135 ) ) ;
#60498 = CARTESIAN_POINT ( 'NONE',  ( -0.05219959533909027116, -19.03943276465977164, 107.4989096053143527 ) ) ;
#60499 = CARTESIAN_POINT ( 'NONE',  ( -19.02544592524342804, 5.153800228976336051, 61.04057627198103120 ) ) ;
#60500 = VECTOR ( 'NONE', #127271, 1000.000000000000000 ) ;
#60501 = CARTESIAN_POINT ( 'NONE',  ( -10.81492255796105439, 18.62759615963255655, 62.91775706135236135 ) ) ;
#60502 = CARTESIAN_POINT ( 'NONE',  ( 18.62759615963255655, 10.81492255796105972, 76.66775706135234714 ) ) ;
#60503 = CARTESIAN_POINT ( 'NONE',  ( -13.89961937509977652, 13.97604488694528158, 115.6239096053143669 ) ) ;
#60504 = CARTESIAN_POINT ( 'NONE',  ( -16.46253265017160317, 9.564922557960807481, 75.83224293864769550 ) ) ;
#60505 = CARTESIAN_POINT ( 'NONE',  ( -21.55341960407619339, 5.719274019375674811, 53.54275706135234714 ) ) ;
#60506 = CARTESIAN_POINT ( 'NONE',  ( -9.474510206698720793, -16.51473224551083518, 104.5844237280190043 ) ) ;
#60507 = CARTESIAN_POINT ( 'NONE',  ( -5.153800228976328057, -19.02544592524343514, 57.29057627198103120 ) ) ;
#60508 = CARTESIAN_POINT ( 'NONE',  ( -9.474510206698964154, 16.51473224551069663, 100.4155762719810241 ) ) ;
#60509 = CARTESIAN_POINT ( 'NONE',  ( -13.89961937509977652, 13.97604488694528158, 80.62390960531436690 ) ) ;
#60510 = CARTESIAN_POINT ( 'NONE',  ( -16.51473224551069308, -9.474510206698971260, 76.66557627198103830 ) ) ;
#60511 = CARTESIAN_POINT ( 'NONE',  ( 0.05219959533909260263, 19.03943276465977164, 59.99890960531436690 ) ) ;
#60512 = CARTESIAN_POINT ( 'NONE',  ( -10.72451020669898014, 18.67979575497178502, 95.41557627198102409 ) ) ;
#60513 = CARTESIAN_POINT ( 'NONE',  ( -14.34966873604972548, 8.224510206698743886, 83.33442372801903275 ) ) ;
#60514 = CARTESIAN_POINT ( 'NONE',  ( 6.100000000000011191, -0.2000799437544851234, -64.53213882399991519 ) ) ;
#60515 = CARTESIAN_POINT ( 'NONE',  ( -19.03943276465977164, -0.05219959533935918106, 48.75109039468566863 ) ) ;
#60516 = CARTESIAN_POINT ( 'NONE',  ( 16.51473224551069308, 9.474510206698969483, 74.16557627198103830 ) ) ;
#60517 = CARTESIAN_POINT ( 'NONE',  ( 8.314922557960818139, 14.29746914071049879, 74.58224293864768129 ) ) ;
#60518 = CARTESIAN_POINT ( 'NONE',  ( -12.14591786802309592, -12.06949235617757132, 96.87390960531436690 ) ) ;
#60519 = CARTESIAN_POINT ( 'NONE',  ( -18.67979575497178146, -10.72451020669898902, 21.66557627198102409 ) ) ;
#60520 = EDGE_LOOP ( 'NONE', ( #147302, #13716, #88566, #193979, #70110 ) ) ;
#60521 = CARTESIAN_POINT ( 'NONE',  ( 5.049401038298161559, -19.05341960407611168, 102.7072429386476955 ) ) ;
#60522 = CARTESIAN_POINT ( 'NONE',  ( 5.153800228976615827, -19.02544592524334988, 30.20942372801900433 ) ) ;
#60523 = CARTESIAN_POINT ( 'NONE',  ( 14.34966873604972726, -8.224510206698740333, 95.83442372801903275 ) ) ;
#60524 = CARTESIAN_POINT ( 'NONE',  ( -16.51473224551069308, -9.474510206698971260, 76.66557627198103830 ) ) ;
#60525 = CARTESIAN_POINT ( 'NONE',  ( 21.53943276465977519, 0.05219959533937863772, 51.25109039468568994 ) ) ;
#60526 = CARTESIAN_POINT ( 'NONE',  ( 18.62759615963271287, -10.81492255796078972, 28.33224293864769550 ) ) ;
#60527 = CARTESIAN_POINT ( 'NONE',  ( 15.72974639402176855, 15.80617190586768217, 21.87609039468567573 ) ) ;
#60528 = CARTESIAN_POINT ( 'NONE',  ( 5.719274019375991003, -21.55341960407610458, 67.70724293864769550 ) ) ;
#60529 = CARTESIAN_POINT ( 'NONE',  ( 0.05219959533910956823, 16.53943276465976808, 99.99890960531436690 ) ) ;
#60530 = CARTESIAN_POINT ( 'NONE',  ( 16.51473224551083163, -9.474510206698727899, 50.83442372801899722 ) ) ;
#60531 = CARTESIAN_POINT ( 'NONE',  ( 16.51473224551069308, 9.474510206698969483, 34.16557627198102409 ) ) ;
#60532 = CARTESIAN_POINT ( 'NONE',  ( 0.05219959533909260263, 19.03943276465977164, 89.99890960531436690 ) ) ;
#60533 = CARTESIAN_POINT ( 'NONE',  ( -13.89961937509977652, 13.97604488694528158, 85.62390960531433848 ) ) ;
#60534 = CARTESIAN_POINT ( 'NONE',  ( 1.452748147864696193, 7.214060343420894306, -64.31738320500510042 ) ) ;
#60535 = CARTESIAN_POINT ( 'NONE',  ( 14.34966873604960469, 8.224510206698951720, 99.16557627198100988 ) ) ;
#60536 = ORIENTED_EDGE ( 'NONE', *, *, #121441, .T. ) ;
#60537 = CARTESIAN_POINT ( 'NONE',  ( 4.379528057220339221, -16.55341960407611168, 27.70724293864769905 ) ) ;
#60538 = CARTESIAN_POINT ( 'NONE',  ( -12.06949235617739369, -12.14591786802326823, 24.37609039468567573 ) ) ;
#60539 = CARTESIAN_POINT ( 'NONE',  ( -21.55341960407619339, 5.719274019375674811, 98.54275706135234714 ) ) ;
#60540 = CARTESIAN_POINT ( 'NONE',  ( 5.049401038298161559, -19.05341960407611168, 102.7072429386476955 ) ) ;
#60541 = CARTESIAN_POINT ( 'NONE',  ( -5.823673210054116645, -21.52544592524344225, 112.2905762719810241 ) ) ;
#60542 = CARTESIAN_POINT ( 'NONE',  ( -19.02544592524342804, 5.153800228976336051, 46.04057627198101699 ) ) ;
#60543 = EDGE_CURVE ( 'NONE', #84237, #117432, #131226, .T. ) ;
#60544 = CARTESIAN_POINT ( 'NONE',  ( 16.53943276465976808, 0.05219959533934440121, 46.25109039468567573 ) ) ;
#60545 = CARTESIAN_POINT ( 'NONE',  ( 19.05341960407617918, -5.049401038297876454, 111.0427570613523329 ) ) ;
#60546 = CARTESIAN_POINT ( 'NONE',  ( -8.224510206698948167, 14.34966873604960824, 95.41557627198102409 ) ) ;
#60547 = CARTESIAN_POINT ( 'NONE',  ( -21.52544592524343514, 5.823673210054127303, 106.0405762719810525 ) ) ;
#60548 = CARTESIAN_POINT ( 'NONE',  ( -0.05219959533936034679, 19.03943276465977164, 62.50109039468566863 ) ) ;
#60549 = CYLINDRICAL_SURFACE ( 'NONE', #112279, 0.5000000000000037748 ) ;
#60550 = CARTESIAN_POINT ( 'NONE',  ( 18.62759615963271287, -10.81492255796078972, 113.3322429386476955 ) ) ;
#60551 = DIRECTION ( 'NONE',  ( -0.000000000000000000, -0.000000000000000000, -1.000000000000000000 ) ) ;
#60552 = CARTESIAN_POINT ( 'NONE',  ( -5.049401038298153566, 19.05341960407611168, 85.20724293864766707 ) ) ;
#60553 = CARTESIAN_POINT ( 'NONE',  ( 16.61371651742598132, -7.165104196376176127, 111.3541506999299742 ) ) ;
#60554 = CARTESIAN_POINT ( 'NONE',  ( 5.049401038298161559, -19.05341960407611168, 87.70724293864769550 ) ) ;
#60556 = CARTESIAN_POINT ( 'NONE',  ( -4.483927247898539470, -16.52544592524342804, 72.29057627198102409 ) ) ;
#60555 = CARTESIAN_POINT ( 'NONE',  ( 10.72451020669871369, 18.67979575497193778, 32.08442372801901854 ) ) ;
#60557 = CARTESIAN_POINT ( 'NONE',  ( -5.153800228976328057, -19.02544592524343514, 82.29057627198103830 ) ) ;
#60559 = CARTESIAN_POINT ( 'NONE',  ( -19.05341960407617563, 5.049401038297882671, 58.54275706135234003 ) ) ;
#60558 = CARTESIAN_POINT ( 'NONE',  ( 16.55341960407618274, -4.379528057220086978, 56.04275706135235424 ) ) ;
#60560 = CARTESIAN_POINT ( 'NONE',  ( -10.72451020669870658, -18.67979575497194134, 59.58442372801901854 ) ) ;
#60561 = CARTESIAN_POINT ( 'NONE',  ( 8.224510206698742110, 14.34966873604972548, 32.08442372801901854 ) ) ;
#60562 = CARTESIAN_POINT ( 'NONE',  ( -5.049401038298153566, 19.05341960407611168, 65.20724293864765286 ) ) ;
#60563 = CARTESIAN_POINT ( 'NONE',  ( -9.474510206698720793, -16.51473224551083518, 94.58442372801900433 ) ) ;
#60564 = CARTESIAN_POINT ( 'NONE',  ( -0.05219959533934338120, 16.53943276465976808, 62.50109039468568284 ) ) ;
#60565 = CARTESIAN_POINT ( 'NONE',  ( 21.55341960407619695, -5.719274019375665929, 101.0427570613523756 ) ) ;
#60566 = CARTESIAN_POINT ( 'NONE',  ( 5.153800228976615827, -19.02544592524334988, 80.20942372801901854 ) ) ;
#60567 = CARTESIAN_POINT ( 'NONE',  ( -9.474510206698964154, 16.51473224551069663, 55.41557627198103120 ) ) ;
#60568 = CARTESIAN_POINT ( 'NONE',  ( -15.80617190586745835, -15.72974639402198527, 71.87390960531438111 ) ) ;
#60570 = CARTESIAN_POINT ( 'NONE',  ( -9.474510206698720793, -16.51473224551083518, 79.58442372801899012 ) ) ;
#60569 = CARTESIAN_POINT ( 'NONE',  ( -16.53943276465976808, 0.05219959533911058130, 81.24890960531436690 ) ) ;
#60571 = CARTESIAN_POINT ( 'NONE',  ( 17.26058549869092218, -6.457015423128527942, 61.12254162523935719 ) ) ;
#60572 = CARTESIAN_POINT ( 'NONE',  ( 5.049401038297881783, 19.05341960407617563, 42.29275706135234003 ) ) ;
#60573 = CARTESIAN_POINT ( 'NONE',  ( 16.52544592524342804, -4.483927247898539470, 23.54057627198102765 ) ) ;
#60574 = CARTESIAN_POINT ( 'NONE',  ( 16.55341960407611168, 4.379528057220329451, 68.95724293864769550 ) ) ;
#60576 = CARTESIAN_POINT ( 'NONE',  ( 1.784210473542230573E-15, -29.16686587814331588, 143.3750000027311557 ) ) ;
#60575 = CARTESIAN_POINT ( 'NONE',  ( 21.53943276465977519, 0.05219959533937863772, 96.25109039468568994 ) ) ;
#60577 = CARTESIAN_POINT ( 'NONE',  ( 0.05219959533907565091, 21.53943276465977519, 109.9989096053143527 ) ) ;
#60578 = CARTESIAN_POINT ( 'NONE',  ( 5.153800228976335163, 19.02544592524342804, 64.79057627198100988 ) ) ;
#60579 = CARTESIAN_POINT ( 'NONE',  ( -21.52544592524334988, -5.823673210054445271, 83.95942372801900433 ) ) ;
#60580 = CARTESIAN_POINT ( 'NONE',  ( -16.46253265017160317, 9.564922557960807481, 65.83224293864769550 ) ) ;
#60581 = VERTEX_POINT ( 'NONE', #76110 ) ;
#60582 = CARTESIAN_POINT ( 'NONE',  ( 0.05219959533909260263, 19.03943276465977164, 24.99890960531435269 ) ) ;
#60583 = CARTESIAN_POINT ( 'NONE',  ( 21.52544592524344225, -5.823673210054117533, 28.54057627198103120 ) ) ;
#60584 = CARTESIAN_POINT ( 'NONE',  ( -12.06949235617756955, 12.14591786802309770, 70.62390960531436690 ) ) ;
#60585 = CARTESIAN_POINT ( 'NONE',  ( -0.05219959533909027116, -19.03943276465977164, 42.49890960531435269 ) ) ;
#60586 = CARTESIAN_POINT ( 'NONE',  ( 14.29746914071049879, -8.314922557960816363, 88.33224293864769550 ) ) ;
#60587 = AXIS2_PLACEMENT_3D ( 'NONE', #165193, #88328, #150019 ) ;
#60588 = CARTESIAN_POINT ( 'NONE',  ( 10.81492255796078972, 18.62759615963270932, 114.5822429386477097 ) ) ;
#60589 = CARTESIAN_POINT ( 'NONE',  ( 5.823673210054444382, -21.52544592524334988, 55.20942372801902565 ) ) ;
#60590 = CARTESIAN_POINT ( 'NONE',  ( -9.474510206698964154, 16.51473224551069663, 25.41557627198103120 ) ) ;
#60591 = CARTESIAN_POINT ( 'NONE',  ( 16.55341960407618274, -4.379528057220086978, 56.04275706135235424 ) ) ;
#60592 = CARTESIAN_POINT ( 'NONE',  ( -5.823673210054116645, -21.52544592524344225, 97.29057627198105251 ) ) ;
#60593 = CARTESIAN_POINT ( 'NONE',  ( 5.719274019375991003, -21.55341960407610458, 92.70724293864770971 ) ) ;
#60595 = CARTESIAN_POINT ( 'NONE',  ( -9.474510206698964154, 16.51473224551069663, 55.41557627198103120 ) ) ;
#60594 = CARTESIAN_POINT ( 'NONE',  ( 16.51473224551083163, -9.474510206698727899, 25.83442372801900078 ) ) ;
#60596 = CARTESIAN_POINT ( 'NONE',  ( 13.97604488694527802, 13.89961937509977652, 104.3739096053143385 ) ) ;
#60597 = CARTESIAN_POINT ( 'NONE',  ( 10.72451020669871369, 18.67979575497193778, 62.08442372801901143 ) ) ;
#60598 = CARTESIAN_POINT ( 'NONE',  ( 10.81492255796078972, 18.62759615963270932, 44.58224293864769550 ) ) ;
#60599 = CARTESIAN_POINT ( 'NONE',  ( 8.314922557961029526, -14.29746914071037800, 110.4177570613523756 ) ) ;
#60601 = CARTESIAN_POINT ( 'NONE',  ( 15.72974639402176855, 15.80617190586768217, 101.8760903946857042 ) ) ;
#60600 = CARTESIAN_POINT ( 'NONE',  ( -21.55341960407619339, 5.719274019375674811, 58.54275706135235424 ) ) ;
#60602 = CARTESIAN_POINT ( 'NONE',  ( 19.05341960407617918, -5.049401038297876454, 46.04275706135233293 ) ) ;
#60603 = CARTESIAN_POINT ( 'NONE',  ( -12.14591786802326823, 12.06949235617739902, 103.1260903946856757 ) ) ;
#60604 = CARTESIAN_POINT ( 'NONE',  ( 18.62759615963255655, 10.81492255796105972, 56.66775706135235424 ) ) ;
#60605 = CARTESIAN_POINT ( 'NONE',  ( 16.51473224551069308, 9.474510206698969483, 44.16557627198103120 ) ) ;
#60606 = CARTESIAN_POINT ( 'NONE',  ( 5.049401038297881783, 19.05341960407617563, 22.29275706135233648 ) ) ;
#60607 = CARTESIAN_POINT ( 'NONE',  ( -5.049401038298153566, 19.05341960407611168, 115.2072429386477097 ) ) ;
#60608 = CARTESIAN_POINT ( 'NONE',  ( -18.62759615963270932, 10.81492255796079327, 110.8322429386476955 ) ) ;
#60609 = CARTESIAN_POINT ( 'NONE',  ( -18.67979575497178146, -10.72451020669898902, 71.66557627198100988 ) ) ;
#60610 = CARTESIAN_POINT ( 'NONE',  ( 4.483927247898790824, -16.52544592524335698, 40.20942372801901854 ) ) ;
#60612 = CARTESIAN_POINT ( 'NONE',  ( 21.53943276465977519, -0.05219959533907433946, 78.74890960531436690 ) ) ;
#60611 = CARTESIAN_POINT ( 'NONE',  ( 17.49999999999997868, -3.232540337672884956, 37.21909520004585659 ) ) ;
#60614 = CARTESIAN_POINT ( 'NONE',  ( 8.224510206698953496, -14.34966873604960469, 77.91557627198102409 ) ) ;
#60613 = CARTESIAN_POINT ( 'NONE',  ( 16.55341960407618274, -4.379528057220086978, 66.04275706135236135 ) ) ;
#60615 = CARTESIAN_POINT ( 'NONE',  ( -22.04836444019715458, 20.09153389842209236, -48.54295043639820051 ) ) ;
#60616 = CARTESIAN_POINT ( 'NONE',  ( 13.89961937509957401, 13.97604488694547697, 106.8760903946856757 ) ) ;
#60617 = CARTESIAN_POINT ( 'NONE',  ( -5.719274019375978568, 21.55341960407610458, 40.20724293864769550 ) ) ;
#60618 = AXIS2_PLACEMENT_3D ( 'NONE', #106066, #15059, #166772 ) ;
#60619 = DIRECTION ( 'NONE',  ( 0.000000000000000000, 0.000000000000000000, 1.000000000000000000 ) ) ;
#60620 = CARTESIAN_POINT ( 'NONE',  ( -16.53943276465976808, -0.05219959533934237506, 33.75109039468568284 ) ) ;
#60621 = CARTESIAN_POINT ( 'NONE',  ( 10.72451020669898902, -18.67979575497178502, 112.9155762719810383 ) ) ;
#60622 = CARTESIAN_POINT ( 'NONE',  ( -21.55341960407610458, -5.719274019375992779, 36.45724293864768839 ) ) ;
#60623 = CARTESIAN_POINT ( 'NONE',  ( -0.05219959533934338120, 16.53943276465976808, 72.50109039468568994 ) ) ;
#60624 = CARTESIAN_POINT ( 'NONE',  ( -5.049401038298153566, 19.05341960407611168, 80.20724293864769550 ) ) ;
#60626 = CARTESIAN_POINT ( 'NONE',  ( 9.564922557960805705, 16.46253265017160317, 34.58224293864770260 ) ) ;
#60625 = CARTESIAN_POINT ( 'NONE',  ( 21.52544592524334988, 5.823673210054432836, 46.45942372801901854 ) ) ;
#60627 = CARTESIAN_POINT ( 'NONE',  ( 21.52544592524344225, -5.823673210054117533, 23.54057627198102765 ) ) ;
#60628 = ORIENTED_EDGE ( 'NONE', *, *, #178712, .F. ) ;
#60629 = CARTESIAN_POINT ( 'NONE',  ( -13.89961937509957401, -13.97604488694547875, 24.37609039468565442 ) ) ;
#60630 = CARTESIAN_POINT ( 'NONE',  ( 14.34966873604972726, -8.224510206698740333, 50.83442372801901143 ) ) ;
#60631 = CARTESIAN_POINT ( 'NONE',  ( 13.89961937509977652, -13.97604488694527269, 98.12390960531433848 ) ) ;
#60632 = CARTESIAN_POINT ( 'NONE',  ( -21.53943276465977519, 0.05219959533907696930, 106.2489096053143811 ) ) ;
#60633 = CARTESIAN_POINT ( 'NONE',  ( -19.03943276465977164, 0.05219959533909376836, 66.24890960531436690 ) ) ;
#60634 = CARTESIAN_POINT ( 'NONE',  ( -16.79531203550650886, 7.028104445595467098, 23.74755011779560121 ) ) ;
#60635 = CARTESIAN_POINT ( 'NONE',  ( 2.285367203649865752E-16, -78.65850330665435308, -23.00000000000000000 ) ) ;
#60636 = CARTESIAN_POINT ( 'NONE',  ( 16.52544592524342804, -4.483927247898539470, 78.54057627198103830 ) ) ;
#60637 = CARTESIAN_POINT ( 'NONE',  ( -15.80617190586745835, -15.72974639402198527, 36.87390960531435979 ) ) ;
#60638 = DIRECTION ( 'NONE',  ( -0.000000000000000000, 0.7071067811865467956, 0.7071067811865483499 ) ) ;
#60639 = CARTESIAN_POINT ( 'NONE',  ( -4.483927247898782831, 16.52544592524335698, 67.70942372801901854 ) ) ;
#60640 = CARTESIAN_POINT ( 'NONE',  ( -21.52544592524334988, -5.823673210054445271, 18.95942372801901143 ) ) ;
#60641 = CARTESIAN_POINT ( 'NONE',  ( 16.46253265017146816, 9.564922557961045513, 81.66775706135233293 ) ) ;
#60642 = CARTESIAN_POINT ( 'NONE',  ( 0.05219959533909260263, 19.03943276465977164, 44.99890960531435979 ) ) ;
#60643 = CARTESIAN_POINT ( 'NONE',  ( 18.62759615963271287, -10.81492255796078972, 63.33224293864770260 ) ) ;
#60644 = CARTESIAN_POINT ( 'NONE',  ( 13.97604488694527802, 13.89961937509977652, 104.3739096053143385 ) ) ;
#60645 = CARTESIAN_POINT ( 'NONE',  ( -15.72974639402176322, -15.80617190586768395, 94.37609039468568994 ) ) ;
#60646 = CARTESIAN_POINT ( 'NONE',  ( 19.02544592524343514, -5.153800228976328945, 68.54057627198103830 ) ) ;
#60648 = B_SPLINE_CURVE_WITH_KNOTS ( 'NONE', 3,
 ( #3096, #61771, #123439, #125453, #172958, #62768, #77939, #188133, #171955, #46623, #49604, #185132, #170957, #48622, #32451, #139606, #169961, #33443, #94104, #168953 ),
 .UNSPECIFIED., .F., .F.,
 ( 4, 2, 2, 2, 2, 2, 2, 2, 2, 4 ),
 ( 3.469446951953614189E-18, 0.0004987090165372718353, 0.0009974180330745402012, 0.001246772541343170535, 0.001496127049611800869, 0.001994836066149057417, 0.002493545082686314182, 0.002742899590954942998, 0.002992254099223570947, 0.003989672132298160805 ),
 .UNSPECIFIED. ) ;
#60647 = CARTESIAN_POINT ( 'NONE',  ( -4.379528057220086978, -16.55341960407618274, 54.79275706135235424 ) ) ;
#60649 = CARTESIAN_POINT ( 'NONE',  ( -5.153800228976328057, -19.02544592524343514, 57.29057627198103120 ) ) ;
#60650 = CARTESIAN_POINT ( 'NONE',  ( 10.81492255796106328, -18.62759615963255655, 85.41775706135236135 ) ) ;
#60651 = VERTEX_POINT ( 'NONE', #169108 ) ;
#60652 = CARTESIAN_POINT ( 'NONE',  ( -9.564922557961040184, 16.46253265017147172, 37.91775706135233293 ) ) ;
#60653 = CARTESIAN_POINT ( 'NONE',  ( 13.89961937509957401, 13.97604488694547697, 46.87609039468565442 ) ) ;
#60654 = CARTESIAN_POINT ( 'NONE',  ( 15.72974639402176855, 15.80617190586768217, 51.87609039468568284 ) ) ;
#60655 = LINE ( 'NONE', #47499, #123791 ) ;
#60656 = CARTESIAN_POINT ( 'NONE',  ( 9.474510206698729675, 16.51473224551082808, 42.08442372801900433 ) ) ;
#60657 = CARTESIAN_POINT ( 'NONE',  ( -13.97604488694527625, -13.89961937509977652, 96.87390960531433848 ) ) ;
#60658 = CARTESIAN_POINT ( 'NONE',  ( 9.474510206698971260, -16.51473224551069308, 67.91557627198102409 ) ) ;
#60659 = CARTESIAN_POINT ( 'NONE',  ( 4.483927247898545687, 16.52544592524342804, 24.79057627198103120 ) ) ;
#60661 = CARTESIAN_POINT ( 'NONE',  ( -18.67979575497193778, 10.72451020669871902, 98.33442372801901854 ) ) ;
#60660 = CARTESIAN_POINT ( 'NONE',  ( -5.719274019375978568, 21.55341960407610458, 40.20724293864769550 ) ) ;
#60662 = B_SPLINE_CURVE_WITH_KNOTS ( 'NONE', 3,
 ( #121574, #91215, #197451, #26614, #42775, #15403, #167107, #75082, #27623, #169065, #198433, #88257, #44749, #58917, #149944, #153908, #43760, #77060, #46737, #59906, #184258, #61881, #152906, #183269, #120585, #199427, #28608, #119614, #73122, #123551, #138732, #182279 ),
 .UNSPECIFIED., .F., .F.,
 ( 4, 2, 2, 2, 2, 2, 2, 2, 2, 2, 2, 2, 2, 2, 2, 4 ),
 ( 5.204170427930421283E-18, 0.0003712461730036837964, 0.0007424923460073623886, 0.001113738519011040927, 0.001484984692014719573, 0.002227477038022076649, 0.002598723211025754862, 0.002969969384029433074, 0.003341215557033111287, 0.003712461730036788633, 0.004083707903040466845, 0.004454954076044144624, 0.004826200249047822403, 0.005197446422051501050, 0.005568692595055177962, 0.005939938768058855741 ),
 .UNSPECIFIED. ) ;
#60663 = CARTESIAN_POINT ( 'NONE',  ( 29.86685920354754842, -21.69954338932559068, -8.324999997268813345 ) ) ;
#60664 = CARTESIAN_POINT ( 'NONE',  ( 16.52216118717208104, 7.221426719304524511, 58.57599021046992505 ) ) ;
#60665 = CARTESIAN_POINT ( 'NONE',  ( -15.72974639402176322, -15.80617190586768395, 99.37609039468568994 ) ) ;
#60666 = CARTESIAN_POINT ( 'NONE',  ( 5.000000000000000000, -120.9454340326537505, 15.08688922109886832 ) ) ;
#60667 = CARTESIAN_POINT ( 'NONE',  ( 19.02544592524343514, -5.153800228976328945, 28.54057627198102409 ) ) ;
#60668 = CARTESIAN_POINT ( 'NONE',  ( 13.89961937509977652, -13.97604488694527269, 108.1239096053143669 ) ) ;
#60669 = CARTESIAN_POINT ( 'NONE',  ( 33.68458106784984096, 5.328653173427194467, 96.40873914273848300 ) ) ;
#60670 = CARTESIAN_POINT ( 'NONE',  ( -12.14591786802326823, 12.06949235617739902, 48.12609039468568284 ) ) ;
#60671 = CARTESIAN_POINT ( 'NONE',  ( 18.62759615963271287, -10.81492255796078972, 68.33224293864769550 ) ) ;
#60672 = CARTESIAN_POINT ( 'NONE',  ( -14.29746914071049879, 8.314922557960819915, 40.83224293864769550 ) ) ;
#60674 = CARTESIAN_POINT ( 'NONE',  ( 13.97604488694527802, 13.89961937509977652, 104.3739096053143385 ) ) ;
#60673 = CARTESIAN_POINT ( 'NONE',  ( 8.224510206698953496, -14.34966873604960469, 107.9155762719810241 ) ) ;
#60675 = CARTESIAN_POINT ( 'NONE',  ( 13.97604488694548053, -13.89961937509957401, 35.62609039468567573 ) ) ;
#60676 = CARTESIAN_POINT ( 'NONE',  ( 16.51473224551069308, 9.474510206698969483, 24.16557627198102765 ) ) ;
#60677 = CARTESIAN_POINT ( 'NONE',  ( -0.05219959533937732626, 21.53943276465977519, 67.50109039468568994 ) ) ;
#60678 = CARTESIAN_POINT ( 'NONE',  ( 5.049401038298161559, -19.05341960407611168, 112.7072429386476813 ) ) ;
#60679 = CARTESIAN_POINT ( 'NONE',  ( -4.483927247898539470, -16.52544592524342804, 32.29057627198102409 ) ) ;
#60680 = CARTESIAN_POINT ( 'NONE',  ( -16.51473224551082808, 9.474510206698731452, 68.33442372801900433 ) ) ;
#60681 = CARTESIAN_POINT ( 'NONE',  ( -10.72451020669898014, 18.67979575497178502, 25.41557627198103120 ) ) ;
#60682 = CARTESIAN_POINT ( 'NONE',  ( -14.34966873604960291, -8.224510206698953496, 91.66557627198103830 ) ) ;
#60683 = CARTESIAN_POINT ( 'NONE',  ( -19.02544592524334988, -5.153800228976617603, 63.95942372801899012 ) ) ;
#60684 = CARTESIAN_POINT ( 'NONE',  ( -5.153800228976328057, -19.02544592524343514, 77.29057627198099567 ) ) ;
#60685 = CARTESIAN_POINT ( 'NONE',  ( -12.14591786802309592, -12.06949235617757132, 81.87390960531435269 ) ) ;
#60686 = CARTESIAN_POINT ( 'NONE',  ( 16.51473224551083163, -9.474510206698727899, 90.83442372801900433 ) ) ;
#60687 = CARTESIAN_POINT ( 'NONE',  ( 10.81492255796078972, 18.62759615963270932, 44.58224293864769550 ) ) ;
#60688 = EDGE_LOOP ( 'NONE', ( #169373, #166940, #97265, #145634 ) ) ;
#60689 = CARTESIAN_POINT ( 'NONE',  ( 19.03943276465977164, -0.05219959533909143690, 23.74890960531435269 ) ) ;
#60691 = CARTESIAN_POINT ( 'NONE',  ( 21.55341960407610458, 5.719274019375980345, 78.95724293864769550 ) ) ;
#60690 = CARTESIAN_POINT ( 'NONE',  ( -0.05219959533909027116, -19.03943276465977164, 77.49890960531435269 ) ) ;
#60693 = CARTESIAN_POINT ( 'NONE',  ( -5.153800228976328057, -19.02544592524343514, 92.29057627198099567 ) ) ;
#60692 = CARTESIAN_POINT ( 'NONE',  ( -4.379528057220086978, -16.55341960407618274, 104.7927570613523898 ) ) ;
#60694 = CARTESIAN_POINT ( 'NONE',  ( -19.02544592524334988, -5.153800228976617603, 63.95942372801899012 ) ) ;
#60695 = CARTESIAN_POINT ( 'NONE',  ( -10.72451020669870658, -18.67979575497194134, 84.58442372801903275 ) ) ;
#60696 = CARTESIAN_POINT ( 'NONE',  ( 0.05219959533907565091, 21.53943276465977519, 59.99890960531436690 ) ) ;
#60697 = CARTESIAN_POINT ( 'NONE',  ( -18.62759615963270932, 10.81492255796079327, 25.83224293864769194 ) ) ;
#60698 = CARTESIAN_POINT ( 'NONE',  ( 9.474510206698971260, -16.51473224551069308, 42.91557627198103120 ) ) ;
#60699 = CARTESIAN_POINT ( 'NONE',  ( 8.314922557961029526, -14.29746914071037800, 95.41775706135234714 ) ) ;
#60700 = CARTESIAN_POINT ( 'NONE',  ( -0.05219959533909027116, -19.03943276465977164, 57.49890960531435979 ) ) ;
#60701 = CARTESIAN_POINT ( 'NONE',  ( -0.05219959533936034679, 19.03943276465977164, 112.5010903946856757 ) ) ;
#60702 = CARTESIAN_POINT ( 'NONE',  ( -18.22780087662122028, 5.500000000000031086, 83.51540105326107266 ) ) ;
#60703 = CARTESIAN_POINT ( 'NONE',  ( -0.05219959533937732626, 21.53943276465977519, 112.5010903946857042 ) ) ;
#60704 = CARTESIAN_POINT ( 'NONE',  ( -12.14591786802309592, -12.06949235617757132, 71.87390960531438111 ) ) ;
#60705 = CARTESIAN_POINT ( 'NONE',  ( 21.55341960407610458, 5.719274019375980345, 113.9572429386477239 ) ) ;
#60706 = CARTESIAN_POINT ( 'NONE',  ( -18.67979575497178146, -10.72451020669898902, 106.6655762719810383 ) ) ;
#60707 = CARTESIAN_POINT ( 'NONE',  ( 17.14385361876520264, 23.59649016807275856, 140.6750000027311387 ) ) ;
#60708 = B_SPLINE_CURVE_WITH_KNOTS ( 'NONE', 3,
 ( #132307, #104961, #72642, #88792, #118145, #58455, #179835, #163651, #182806, #117132, #119148, #103968, #9973, #86795, #57476, #55461, #193999, #166647, #134317, #150485, #41305, #56467, #181814, #196989 ),
 .UNSPECIFIED., .F., .F.,
 ( 4, 2, 2, 2, 2, 2, 2, 2, 2, 2, 2, 4 ),
 ( 2.787091051190863422E-07, 0.0003070612385125897443, 0.0006138437679200604239, 0.001227408826735005253, 0.001534191356142474739, 0.001840973885549944010, 0.002147756414957413280, 0.002454538944364882333, 0.003068104003179821741, 0.003681669061994760281, 0.004295234120809699255, 0.004908799179624637361 ),
 .UNSPECIFIED. ) ;
#60710 = ADVANCED_FACE ( 'NONE', ( #137787 ), #58961, .T. ) ;
#60709 = CARTESIAN_POINT ( 'NONE',  ( 21.53943276465977519, -0.05219959533907433946, 48.74890960531435979 ) ) ;
#60711 = CARTESIAN_POINT ( 'NONE',  ( 14.34966873604972726, -8.224510206698740333, 85.83442372801901854 ) ) ;
#60712 = CARTESIAN_POINT ( 'NONE',  ( 14.29746914071049879, -8.314922557960816363, 98.33224293864769550 ) ) ;
#60713 = CARTESIAN_POINT ( 'NONE',  ( -19.05341960407611168, -5.049401038298163336, 56.45724293864768129 ) ) ;
#60714 = SURFACE_STYLE_FILL_AREA ( #17211 ) ;
#60715 = CARTESIAN_POINT ( 'NONE',  ( -3.503282210674363295, -48.86437366581481001, -25.00000000000000000 ) ) ;
#60716 = CARTESIAN_POINT ( 'NONE',  ( -4.483927247898782831, 16.52544592524335698, 112.7094237280190328 ) ) ;
#60717 = CARTESIAN_POINT ( 'NONE',  ( -0.05219959533937732626, 21.53943276465977519, 52.50109039468567573 ) ) ;
#60718 = CARTESIAN_POINT ( 'NONE',  ( 9.474510206698971260, -16.51473224551069308, 92.91557627198103830 ) ) ;
#60719 = CARTESIAN_POINT ( 'NONE',  ( 21.52544592524334988, 5.823673210054432836, 76.45942372801901854 ) ) ;
#60720 = CARTESIAN_POINT ( 'NONE',  ( 5.000000000000000888, -130.0000000000000000, -13.99999999999999822 ) ) ;
#60721 = CARTESIAN_POINT ( 'NONE',  ( -13.89961937509977652, 13.97604488694528158, 30.62390960531435269 ) ) ;
#60722 = ORIENTED_EDGE ( 'NONE', *, *, #166964, .F. ) ;
#60723 = CARTESIAN_POINT ( 'NONE',  ( -21.55341960407619339, 5.719274019375674811, 68.54275706135234714 ) ) ;
#60724 = CARTESIAN_POINT ( 'NONE',  ( -9.564922557960796823, -16.46253265017161027, 52.08224293864768839 ) ) ;
#60725 = CARTESIAN_POINT ( 'NONE',  ( 0.05219959533909260263, 19.03943276465977164, 109.9989096053143669 ) ) ;
#60726 = CARTESIAN_POINT ( 'NONE',  ( -19.05341960407617563, 5.049401038297882671, 78.54275706135233293 ) ) ;
#60727 = CARTESIAN_POINT ( 'NONE',  ( -5.719274019375665041, -21.55341960407619695, 39.79275706135235424 ) ) ;
#60728 = CARTESIAN_POINT ( 'NONE',  ( 5.049401038297881783, 19.05341960407617563, 102.2927570613523045 ) ) ;
#60729 = CARTESIAN_POINT ( 'NONE',  ( -19.03943276465977164, -0.05219959533935918106, 78.75109039468567573 ) ) ;
#60730 = CARTESIAN_POINT ( 'NONE',  ( 13.97604488694527802, 13.89961937509977652, 34.37390960531436690 ) ) ;
#60731 = CARTESIAN_POINT ( 'NONE',  ( 0.05219959533936267826, -19.03943276465977164, 80.00109039468567573 ) ) ;
#60732 = AXIS2_PLACEMENT_3D ( 'NONE', #31292, #58648, #15128 ) ;
#60733 = CARTESIAN_POINT ( 'NONE',  ( 14.34966873604972726, -8.224510206698740333, 100.8344237280190185 ) ) ;
#60734 = CARTESIAN_POINT ( 'NONE',  ( -13.97604488694547697, 13.89961937509957934, 78.12609039468567573 ) ) ;
#60735 = CARTESIAN_POINT ( 'NONE',  ( -16.52544592524342804, 4.483927247898546575, 41.04057627198103120 ) ) ;
#60736 = CARTESIAN_POINT ( 'NONE',  ( 19.03943276465977164, 0.05219959533936151252, 61.25109039468566863 ) ) ;
#60737 = CARTESIAN_POINT ( 'NONE',  ( -5.823673210054431948, 21.52544592524334988, 107.7094237280190328 ) ) ;
#60738 = CARTESIAN_POINT ( 'NONE',  ( 13.89961937509957401, 13.97604488694547697, 26.87609039468566507 ) ) ;
#60739 = CARTESIAN_POINT ( 'NONE',  ( 16.51473224551069308, 9.474510206698969483, 29.16557627198103475 ) ) ;
#60740 = LINE ( 'NONE', #166957, #199177 ) ;
#60741 = CARTESIAN_POINT ( 'NONE',  ( -0.05219959533934338120, 16.53943276465976808, 52.50109039468567573 ) ) ;
#60742 = DIRECTION ( 'NONE',  ( -1.000000000000000000, 0.000000000000000000, 0.000000000000000000 ) ) ;
#60743 = CARTESIAN_POINT ( 'NONE',  ( -27.73933785331498925, 2.428612866367529932E-14, 144.8750000027311842 ) ) ;
#60744 = CARTESIAN_POINT ( 'NONE',  ( 9.474510206698971260, -16.51473224551069308, 97.91557627198102409 ) ) ;
#60745 = CARTESIAN_POINT ( 'NONE',  ( -17.48847506799948448, 5.747544572775424854, 100.8269743784329222 ) ) ;
#60746 = VERTEX_POINT ( 'NONE', #199471 ) ;
#60747 = CARTESIAN_POINT ( 'NONE',  ( 5.049401038297881783, 19.05341960407617563, 82.29275706135229029 ) ) ;
#60748 = CARTESIAN_POINT ( 'NONE',  ( 5.823673210054125526, 21.52544592524343514, 29.79057627198102409 ) ) ;
#60750 = CARTESIAN_POINT ( 'NONE',  ( 0.05219959533936267826, -19.03943276465977164, 100.0010903946856757 ) ) ;
#60749 = CARTESIAN_POINT ( 'NONE',  ( -5.049401038297874678, -19.05341960407617918, 19.79275706135233293 ) ) ;
#60751 = CARTESIAN_POINT ( 'NONE',  ( -8.314922557960811034, -14.29746914071050412, 112.0822429386477097 ) ) ;
#60752 = CARTESIAN_POINT ( 'NONE',  ( 5.049401038298161559, -19.05341960407611168, 27.70724293864769550 ) ) ;
#60753 = CARTESIAN_POINT ( 'NONE',  ( 10.72451020669898902, -18.67979575497178502, 57.91557627198103120 ) ) ;
#60754 = CARTESIAN_POINT ( 'NONE',  ( -15.72974639402197994, 15.80617190586746368, 45.62390960531436690 ) ) ;
#60755 = CARTESIAN_POINT ( 'NONE',  ( -5.153800228976328057, -19.02544592524343514, 27.29057627198103120 ) ) ;
#60756 = FACE_OUTER_BOUND ( 'NONE', #17600, .T. ) ;
#60757 = CARTESIAN_POINT ( 'NONE',  ( 13.97604488694548053, -13.89961937509957401, 65.62609039468567573 ) ) ;
#60759 = AXIS2_PLACEMENT_3D ( 'NONE', #111368, #33538, #83012 ) ;
#60758 = CARTESIAN_POINT ( 'NONE',  ( 16.55341960407611168, 4.379528057220329451, 33.95724293864769550 ) ) ;
#60760 = CARTESIAN_POINT ( 'NONE',  ( 19.03943276465977164, -0.05219959533909143690, 113.7489096053143669 ) ) ;
#60761 = CARTESIAN_POINT ( 'NONE',  ( -21.52544592524334988, -5.823673210054445271, 98.95942372801903275 ) ) ;
#60762 = CARTESIAN_POINT ( 'NONE',  ( -21.52544592524343514, 5.823673210054127303, 66.04057627198103830 ) ) ;
#60763 = CARTESIAN_POINT ( 'NONE',  ( 21.52544592524334988, 5.823673210054432836, 61.45942372801901854 ) ) ;
#60764 = CARTESIAN_POINT ( 'NONE',  ( -18.67979575497193778, 10.72451020669871902, 53.33442372801901854 ) ) ;
#60765 = CARTESIAN_POINT ( 'NONE',  ( 0.05219959533909260263, 19.03943276465977164, 94.99890960531436690 ) ) ;
#60767 = CARTESIAN_POINT ( 'NONE',  ( -10.81492255796105439, 18.62759615963255655, 47.91775706135234714 ) ) ;
#60766 = CARTESIAN_POINT ( 'NONE',  ( 12.06949235617739724, 12.14591786802326823, 91.87609039468568994 ) ) ;
#60768 = CARTESIAN_POINT ( 'NONE',  ( -9.564922557960796823, -16.46253265017161027, 27.08224293864769550 ) ) ;
#60769 = CARTESIAN_POINT ( 'NONE',  ( -31.68669428337296523, 6.716517432552113753, 91.65365426639641555 ) ) ;
#60770 = CARTESIAN_POINT ( 'NONE',  ( -4.379528057220328563, 16.55341960407611168, 70.20724293864769550 ) ) ;
#60771 = CARTESIAN_POINT ( 'NONE',  ( -0.05219959533910754901, -16.53943276465976808, 32.49890960531435979 ) ) ;
#60772 = CARTESIAN_POINT ( 'NONE',  ( 19.03943276465977164, -0.05219959533909143690, 63.74890960531435979 ) ) ;
#60773 = CARTESIAN_POINT ( 'NONE',  ( -5.049401038298153566, 19.05341960407611168, 50.20724293864770260 ) ) ;
#60774 = CARTESIAN_POINT ( 'NONE',  ( -21.52544592524343514, 5.823673210054127303, 61.04057627198103120 ) ) ;
#60775 = CARTESIAN_POINT ( 'NONE',  ( -16.51473224551082808, 9.474510206698731452, 38.33442372801899722 ) ) ;
#60777 = CARTESIAN_POINT ( 'NONE',  ( -8.224510206698948167, 14.34966873604960824, 45.41557627198103830 ) ) ;
#60776 = SPHERICAL_SURFACE ( 'NONE', #110757, 40.00000000000002132 ) ;
#60778 = CARTESIAN_POINT ( 'NONE',  ( -21.52544592524343514, 5.823673210054127303, 31.04057627198102409 ) ) ;
#60779 = ORIENTED_EDGE ( 'NONE', *, *, #40219, .F. ) ;
#60780 = DIRECTION ( 'NONE',  ( 0.000000000000000000, 0.000000000000000000, -1.000000000000000000 ) ) ;
#60781 = CARTESIAN_POINT ( 'NONE',  ( -4.483927247898782831, 16.52544592524335698, 67.70942372801901854 ) ) ;
#60782 = EDGE_CURVE ( 'NONE', #66675, #151273, #57070, .T. ) ;
#60783 = CARTESIAN_POINT ( 'NONE',  ( 19.03943276465977164, 0.05219959533936151252, 81.25109039468567573 ) ) ;
#60784 = CARTESIAN_POINT ( 'NONE',  ( 4.379528057220339221, -16.55341960407611168, 42.70724293864770260 ) ) ;
#60785 = CARTESIAN_POINT ( 'NONE',  ( 17.31728774477277355, -6.344390552232304969, 53.31906651689320142 ) ) ;
#60786 = CARTESIAN_POINT ( 'NONE',  ( -4.379528057220328563, 16.55341960407611168, 30.20724293864769550 ) ) ;
#60787 = CARTESIAN_POINT ( 'NONE',  ( 5.049401038298161559, -19.05341960407611168, 52.70724293864767418 ) ) ;
#60788 = CARTESIAN_POINT ( 'NONE',  ( -13.89961937509977652, 13.97604488694528158, 80.62390960531436690 ) ) ;
#60789 = CARTESIAN_POINT ( 'NONE',  ( 9.564922557960805705, 16.46253265017160317, 44.58224293864769550 ) ) ;
#60790 = CARTESIAN_POINT ( 'NONE',  ( 21.53943276465977519, 0.05219959533937863772, 46.25109039468567573 ) ) ;
#60791 = CARTESIAN_POINT ( 'NONE',  ( 13.97604488694527802, 13.89961937509977652, 54.37390960531435979 ) ) ;
#60792 = DIRECTION ( 'NONE',  ( -1.047444401652940164E-14, -1.000000000000000000, -0.000000000000000000 ) ) ;
#60793 = CARTESIAN_POINT ( 'NONE',  ( 9.474510206698971260, -16.51473224551069308, 52.91557627198102409 ) ) ;
#60794 = CARTESIAN_POINT ( 'NONE',  ( -21.55341960407610458, -5.719274019375992779, 36.45724293864768839 ) ) ;
#60795 = CARTESIAN_POINT ( 'NONE',  ( -19.02544592524342804, 5.153800228976336051, 26.04057627198103120 ) ) ;
#60796 = CARTESIAN_POINT ( 'NONE',  ( -18.67979575497178146, -10.72451020669898902, 26.66557627198103475 ) ) ;
#60797 = CARTESIAN_POINT ( 'NONE',  ( -4.379528057220086978, -16.55341960407618274, 84.79275706135234714 ) ) ;
#60798 = CARTESIAN_POINT ( 'NONE',  ( 18.62759615963255655, 10.81492255796105972, 106.6677570613523756 ) ) ;
#60799 = CARTESIAN_POINT ( 'NONE',  ( -12.14591786802326823, 12.06949235617739902, 73.12609039468567573 ) ) ;
#60800 = CARTESIAN_POINT ( 'NONE',  ( -19.03943276465977164, 0.05219959533909376836, 106.2489096053143669 ) ) ;
#60801 = CARTESIAN_POINT ( 'NONE',  ( -12.14591786802326823, 12.06949235617739902, 58.12609039468568994 ) ) ;
#60802 = CARTESIAN_POINT ( 'NONE',  ( -16.55341960407617563, 4.379528057220093196, 38.54275706135234714 ) ) ;
#60803 = CARTESIAN_POINT ( 'NONE',  ( -12.06949235617739369, -12.14591786802326823, 94.37609039468568994 ) ) ;
#60804 = CARTESIAN_POINT ( 'NONE',  ( 8.224510206698742110, 14.34966873604972548, 22.08442372801901143 ) ) ;
#60805 = CARTESIAN_POINT ( 'NONE',  ( -5.153800228976328057, -19.02544592524343514, 37.29057627198102409 ) ) ;
#60806 = CARTESIAN_POINT ( 'NONE',  ( -10.72451020669898014, 18.67979575497178502, 105.4155762719810383 ) ) ;
#60807 = CARTESIAN_POINT ( 'NONE',  ( -16.55341960407617563, 4.379528057220093196, 28.54275706135234358 ) ) ;
#60808 = CARTESIAN_POINT ( 'NONE',  ( 4.483927247898790824, -16.52544592524335698, 90.20942372801903275 ) ) ;
#60809 = LINE ( 'NONE', #94129, #92491 ) ;
#60810 = CARTESIAN_POINT ( 'NONE',  ( -21.53943276465977519, -0.05219959533937600094, 83.75109039468568994 ) ) ;
#60811 = CARTESIAN_POINT ( 'NONE',  ( -16.46253265017146816, -9.564922557961047289, 79.16775706135234714 ) ) ;
#60812 = CARTESIAN_POINT ( 'NONE',  ( -12.06949235617756955, 12.14591786802309770, 45.62390960531436690 ) ) ;
#60813 = CARTESIAN_POINT ( 'NONE',  ( -4.483927247898539470, -16.52544592524342804, 102.2905762719810383 ) ) ;
#60815 = CARTESIAN_POINT ( 'NONE',  ( 17.31747979337962207, -6.344076630960735486, 56.12055131934818775 ) ) ;
#60814 = CARTESIAN_POINT ( 'NONE',  ( -13.97604488694547697, 13.89961937509957934, 43.12609039468566152 ) ) ;
#60816 = CARTESIAN_POINT ( 'NONE',  ( 18.62759615963255655, 10.81492255796105972, 46.66775706135234714 ) ) ;
#60817 = CARTESIAN_POINT ( 'NONE',  ( 19.02544592524334988, 5.153800228976608722, 111.4594237280190043 ) ) ;
#60818 = CARTESIAN_POINT ( 'NONE',  ( 17.05116617787824396, 6.768360034955831495, 83.84324446740799885 ) ) ;
#60819 = CARTESIAN_POINT ( 'NONE',  ( -9.474510206698964154, 16.51473224551069663, 110.4155762719810383 ) ) ;
#60820 = CARTESIAN_POINT ( 'NONE',  ( -18.67979575497178146, -10.72451020669898902, 71.66557627198100988 ) ) ;
#60821 = CARTESIAN_POINT ( 'NONE',  ( 9.474510206698729675, 16.51473224551082808, 92.08442372801900433 ) ) ;
#60822 = CARTESIAN_POINT ( 'NONE',  ( -16.51473224551069308, -9.474510206698971260, 101.6655762719810241 ) ) ;
#60823 = CARTESIAN_POINT ( 'NONE',  ( -25.86526910843991800, 7.630673861713272998, 173.3900163844835163 ) ) ;
#60824 = CARTESIAN_POINT ( 'NONE',  ( -0.05219959533910754901, -16.53943276465976808, 107.4989096053143669 ) ) ;
#60825 = CARTESIAN_POINT ( 'NONE',  ( 10.81492255796106328, -18.62759615963255655, 100.4177570613523471 ) ) ;
#60826 = CARTESIAN_POINT ( 'NONE',  ( -5.049401038298153566, 19.05341960407611168, 40.20724293864768839 ) ) ;
#60827 = CARTESIAN_POINT ( 'NONE',  ( -15.72974639402176322, -15.80617190586768395, 49.37609039468569705 ) ) ;
#60828 = CARTESIAN_POINT ( 'NONE',  ( -5.823673210054431948, 21.52544592524334988, 92.70942372801901854 ) ) ;
#60829 = CARTESIAN_POINT ( 'NONE',  ( 12.14591786802327356, -12.06949235617739191, 95.62609039468568994 ) ) ;
#60830 = CARTESIAN_POINT ( 'NONE',  ( 10.81492255796106328, -18.62759615963255655, 45.41775706135234003 ) ) ;
#60831 = CARTESIAN_POINT ( 'NONE',  ( -18.62759615963255300, -10.81492255796106328, 44.16775706135234714 ) ) ;
#60833 = CARTESIAN_POINT ( 'NONE',  ( 9.474510206698971260, -16.51473224551069308, 97.91557627198102409 ) ) ;
#60832 = CARTESIAN_POINT ( 'NONE',  ( -13.89961937509957401, -13.97604488694547875, 69.37609039468564731 ) ) ;
#60834 = CARTESIAN_POINT ( 'NONE',  ( -8.314922557960811034, -14.29746914071050412, 102.0822429386476955 ) ) ;
#60835 = CARTESIAN_POINT ( 'NONE',  ( 21.55341960407610458, 5.719274019375980345, 88.95724293864769550 ) ) ;
#60836 = CARTESIAN_POINT ( 'NONE',  ( -12.14591786802309592, -12.06949235617757132, 66.87390960531436690 ) ) ;
#60837 = CARTESIAN_POINT ( 'NONE',  ( -0.05219959533937732626, 21.53943276465977519, 102.5010903946856899 ) ) ;
#60838 = CARTESIAN_POINT ( 'NONE',  ( 4.379528057220339221, -16.55341960407611168, 82.70724293864770971 ) ) ;
#60839 = CARTESIAN_POINT ( 'NONE',  ( 9.474510206698971260, -16.51473224551069308, 37.91557627198102409 ) ) ;
#60840 = CARTESIAN_POINT ( 'NONE',  ( -19.05341960407617563, 5.049401038297882671, 83.54275706135233293 ) ) ;
#60841 = CARTESIAN_POINT ( 'NONE',  ( 16.52544592524342804, -4.483927247898539470, 48.54057627198103120 ) ) ;
#60842 = CARTESIAN_POINT ( 'NONE',  ( 21.52544592524334988, 5.823673210054432836, 91.45942372801901854 ) ) ;
#60843 = CARTESIAN_POINT ( 'NONE',  ( -0.05219959533909027116, -19.03943276465977164, 97.49890960531436690 ) ) ;
#60844 = CARTESIAN_POINT ( 'NONE',  ( 9.474510206698729675, 16.51473224551082808, 67.08442372801900433 ) ) ;
#60845 = CARTESIAN_POINT ( 'NONE',  ( 15.80617190586746368, 15.72974639402197994, 59.37390960531436690 ) ) ;
#60846 = CARTESIAN_POINT ( 'NONE',  ( 10.81492255796106328, -18.62759615963255655, 35.41775706135234003 ) ) ;
#60847 = CARTESIAN_POINT ( 'NONE',  ( 12.14591786802327356, -12.06949235617739191, 25.62609039468567929 ) ) ;
#60848 = CARTESIAN_POINT ( 'NONE',  ( 14.34966873604972726, -8.224510206698740333, 85.83442372801901854 ) ) ;
#60850 = CARTESIAN_POINT ( 'NONE',  ( 21.55341960407610458, 5.719274019375980345, 113.9572429386477239 ) ) ;
#60849 = CARTESIAN_POINT ( 'NONE',  ( -16.51473224551069308, -9.474510206698971260, 21.66557627198102765 ) ) ;
#60851 = CARTESIAN_POINT ( 'NONE',  ( -16.52544592524342804, 4.483927247898546575, 111.0405762719810525 ) ) ;
#60852 = CARTESIAN_POINT ( 'NONE',  ( -36.91746825000001309, -11.99521256947794789, -9.024999997268812635 ) ) ;
#60853 = CARTESIAN_POINT ( 'NONE',  ( -16.53943276465976808, -0.05219959533934237506, 48.75109039468568284 ) ) ;
#60854 = CARTESIAN_POINT ( 'NONE',  ( 12.14591786802309770, 12.06949235617756955, 84.37390960531438111 ) ) ;
#60855 = CARTESIAN_POINT ( 'NONE',  ( -18.62759615963270932, 10.81492255796079327, 80.83224293864769550 ) ) ;
#60856 = CARTESIAN_POINT ( 'NONE',  ( -8.224510206698948167, 14.34966873604960824, 30.41557627198101699 ) ) ;
#60857 = CARTESIAN_POINT ( 'NONE',  ( 16.55341960407618274, -4.379528057220086978, 41.04275706135236135 ) ) ;
#60858 = CARTESIAN_POINT ( 'NONE',  ( -5.049401038298153566, 19.05341960407611168, 40.20724293864768839 ) ) ;
#60859 = CARTESIAN_POINT ( 'NONE',  ( 16.53943276465976808, 0.05219959533934440121, 76.25109039468568994 ) ) ;
#60860 = CARTESIAN_POINT ( 'NONE',  ( -19.05341960407617563, 5.049401038297882671, 68.54275706135230450 ) ) ;
#60861 = CARTESIAN_POINT ( 'NONE',  ( 21.53943276465977519, -0.05219959533907433946, 73.74890960531433848 ) ) ;
#60862 = CARTESIAN_POINT ( 'NONE',  ( 12.06949235617757843, -12.14591786802309237, 23.12390960531436335 ) ) ;
#60863 = EDGE_LOOP ( 'NONE', ( #58240, #18043, #101781, #150464, #91050, #34002, #161140, #78137, #100690, #187021, #140295, #88288 ) ) ;
#60864 = CARTESIAN_POINT ( 'NONE',  ( 21.81230582904511550, 7.807068725604178638, 172.9985625539982550 ) ) ;
#60865 = CARTESIAN_POINT ( 'NONE',  ( -21.53943276465977519, 0.05219959533907696930, 51.24890960531436690 ) ) ;
#60866 = VERTEX_POINT ( 'NONE', #155937 ) ;
#60867 = CARTESIAN_POINT ( 'NONE',  ( 0.05219959533934541429, -16.53943276465976808, 95.00109039468568994 ) ) ;
#60868 = ORIENTED_EDGE ( 'NONE', *, *, #20458, .T. ) ;
#60869 = CARTESIAN_POINT ( 'NONE',  ( 16.46253265017160672, -9.564922557960803928, 108.3322429386476955 ) ) ;
#60870 = CARTESIAN_POINT ( 'NONE',  ( -2.500000000000000000, -105.0000000000000000, 7.000000000000003553 ) ) ;
#60871 = CARTESIAN_POINT ( 'NONE',  ( -0.05219959533909027116, -19.03943276465977164, 42.49890960531435269 ) ) ;
#60872 = CARTESIAN_POINT ( 'NONE',  ( 5.719274019375991003, -21.55341960407610458, 72.70724293864769550 ) ) ;
#60873 = CARTESIAN_POINT ( 'NONE',  ( 14.29746914071037800, 8.314922557961029526, 101.6677570613523613 ) ) ;
#60874 = CARTESIAN_POINT ( 'NONE',  ( 15.72974639402176855, 15.80617190586768217, 61.87609039468568284 ) ) ;
#60875 = CARTESIAN_POINT ( 'NONE',  ( 14.29746914071037800, 8.314922557961029526, 21.66775706135235069 ) ) ;
#60876 = CARTESIAN_POINT ( 'NONE',  ( -4.379528057220328563, 16.55341960407611168, 110.2072429386477239 ) ) ;
#60877 = CARTESIAN_POINT ( 'NONE',  ( -4.483927247898782831, 16.52544592524335698, 22.70942372801901499 ) ) ;
#60878 = CARTESIAN_POINT ( 'NONE',  ( -16.46253265017160317, 9.564922557960807481, 55.83224293864769550 ) ) ;
#60879 = CARTESIAN_POINT ( 'NONE',  ( 16.61713888009428075, -0.5018587474792359782, -61.38171595447354179 ) ) ;
#60880 = CARTESIAN_POINT ( 'NONE',  ( -13.97604488694527625, -13.89961937509977652, 106.8739096053143669 ) ) ;
#60881 = CARTESIAN_POINT ( 'NONE',  ( 12.06949235617739724, 12.14591786802326823, 86.87609039468568994 ) ) ;
#60882 = CARTESIAN_POINT ( 'NONE',  ( -13.97604488694547697, 13.89961937509957934, 88.12609039468563310 ) ) ;
#60883 = CARTESIAN_POINT ( 'NONE',  ( 16.51473224551083163, -9.474510206698727899, 25.83442372801900078 ) ) ;
#60884 = CARTESIAN_POINT ( 'NONE',  ( 21.53943276465977519, -0.05219959533907433946, 68.74890960531435269 ) ) ;
#60885 = EDGE_CURVE ( 'NONE', #138940, #93910, #11773, .T. ) ;
#60886 = CARTESIAN_POINT ( 'NONE',  ( -0.05219959533934338120, 16.53943276465976808, 102.5010903946856899 ) ) ;
#60887 = CARTESIAN_POINT ( 'NONE',  ( 5.153800228976615827, -19.02544592524334988, 95.20942372801897591 ) ) ;
#60888 = CARTESIAN_POINT ( 'NONE',  ( -19.05341960407611168, -5.049401038298163336, 46.45724293864768129 ) ) ;
#60889 = CARTESIAN_POINT ( 'NONE',  ( -16.46253265017160317, 9.564922557960807481, 90.83224293864769550 ) ) ;
#60890 = CARTESIAN_POINT ( 'NONE',  ( 5.719274019375673035, 21.55341960407619339, 52.29275706135236135 ) ) ;
#60891 = CARTESIAN_POINT ( 'NONE',  ( 16.51473224551069308, 9.474510206698969483, 44.16557627198103120 ) ) ;
#60892 = DIRECTION ( 'NONE',  ( -0.000000000000000000, -0.000000000000000000, 1.000000000000000000 ) ) ;
#60893 = CARTESIAN_POINT ( 'NONE',  ( 5.049401038298161559, -19.05341960407611168, 112.7072429386476813 ) ) ;
#60894 = CARTESIAN_POINT ( 'NONE',  ( -12.14591786802309592, -12.06949235617757132, 61.87390960531436690 ) ) ;
#60895 = CARTESIAN_POINT ( 'NONE',  ( 18.67979575497178502, 10.72451020669898547, 79.16557627198103830 ) ) ;
#60896 = CARTESIAN_POINT ( 'NONE',  ( -18.22780087662124160, -5.499999999999927169, 73.98236817873106475 ) ) ;
#60897 =( BOUNDED_SURFACE ( )  B_SPLINE_SURFACE ( 3, 2, ( 
 ( #54697, #113362, #67864, #86034, #22371, #130525, #177069, #52693, #51699, #194231, #162875, #68866, #38540, #145700, #24383, #55697, #10207, #87034, #147721, #40536, #175054, #117370, #9208, #36518, #179067, #159875, #163896, #25392, #7182, #83024, #115381, #6184, #144698, #129519, #114357, #192222, #176062, #37529, #99192, #160880, #84022, #53704, #100196, #161878, #23372, #8195, #165882, #197220, #57710, #164889, #28380, #14163, #13194, #56708, #11209, #29357, #27379, #73878, #120349, #196241, #195227, #137509, #74857, #12215, #182044, #89025, #59670, #75831, #153670, #30335, #106174, #184022, #118381, #199190, #152674, #180075, #183035, #91976, #121342, #136519, #150716, #90987, #58682, #149710, #103207, #15167, #45504, #135548, #198200, #26383, #41544, #107159, #76826, #60657, #43527, #72884, #167857, #122330, #88022, #134553, #44518, #119380, #168830, #181063, #105192, #90018, #42538, #104201, #166879, #151701, #20872, #5696, #174571, #46494, #160390, #200179, #108155, #36037, #130019, #61648, #37035, #6690, #31331, #38047, #92982, #78810, #114879, #191718, #124321, #99703, #190732, #98696, #145207, #128043, #161387, #155661, #51217, #22878, #97686, #16163, #140489, #21879, #53202, #123316, #77817, #159376, #1977, #32328, #112878, #113863, #138497, #83529, #185009, #47501, #169837, #189744, #175559, #63657, #52205, #67372, #68368, #176573, #154667, #139486, #109157, #968, #62644, #186019, #170836, #93981, #17157, #82530, #144212, #129031, #116876, #149228, #165399, #178567, #72382, #43041, #87541, #26892, #177575, #195749, #100699, #194737, #41051, #163396, #102715, #164404, #10719, #40032, #84525, #162380, #135066, #86541, #56207, #147222, #88535, #117890, #146202, #25896, #101706, #7688, #73395, #24893, #11727, #166397, #179580, #42055, #148225, #134057, #23882, #85534, #57223, #118896, #180581, #9719, #71383, #8713, #103719, #133047, #150232, #196742, #70382, #58209, #119878, #104707, #181563, #69372, #131042, #192732, #54214, #115885, #39042, #132050, #193739, #55207, #186532, #136042, #170344, #76341, #75350, #197717, #138017, #123817, #16664, #167380, #61166, #169338, #63153, #12711, #182551, #120851, #124832, #31836, #153176, #137020, #91489, #185515, #479, #184526, #13683, #199700, #78312, #183539, #30847, #48005, #139985, #44033, #92494, #60177, #122837, #198710, #14679, #121846, #93487, #59182, #62153, #155173, #47007, #1474, #46006, #109661, #154183, #107661, #27893, #168356, #89535, #105694, #28877, #15673, #45024, #77333, #151222, #74377, #90517, #139000, #106683, #108666, #29852, #152199, #157163, #175315, #140989, #143968, #36782, #190490, #21630, #66132, #129775, #97443, #127797, #171341, #111647, #160141, #64158, #110646, #35796, #80303, #2477, #113621, #52950, #94480, #98447, #172327, #18657, #83286, #4444, #3464, #159128, #51961, #65141, #20626, #191471, #174327, #144960, #125823, #82275, #187526, #81282, #189498, #49983, #50974, #112634, #5448, #126798, #32829, #48991, #6442, #173333, #142965, #33816, #68123, #67131, #156161, #128789, #188504, #17659, #79319, #34806, #95476, #141976, #96461, #158149, #19640, #40800, #53968, #115642, #102470, #164157, #148983, #54965, #193487, #177331, #194490, #8463, #178325, #55962, #100459, #41806, #26643, #73151, #25655, #116636, #87300, #132803, #70137, #117639, #24647, #161137, #38803, #114625, #134822, #22634, #56973, #163144, #162139, #84280, #86296, #10472, #103474, #23635, #147985, #179337, #149975, #99457, #69127, #7442, #11480, #118647, #39788, #85284, #101453, #72133, #133808, #71138, #146975, #9474, #165152, #196501, #145961, #180338, #195499, #131808, #130793, #88286, #176325, #37794, #192486, #91242, #199454, #93243, #42804, #12476, #150983, #154928, #61907, #183298, #167138, #121602, #15431, #30599, #14431, #43789, #168114, #46765, #13446, #60922, #16426, #108424, #74137, #122596, #90274, #152932, #105453, #44779 ),
 ( #170100, #135809, #197479, #184285, #28637, #89291, #240, #139741, #181325, #123578, #58946, #151958, #31594, #76094, #75110, #45767, #138758, #136778, #107419, #78073, #169092, #185273, #120614, #92252, #182310, #29610, #137769, #198464, #153936, #77089, #57971, #59935, #119643, #106432, #104466, #166150, #27652, #63918, #5208, #34572, #1230, #81056, #95239, #62909, #190247, #80072, #128550, #83050, #96229, #158895, #18422, #127565, #140747, #2235, #189266, #50741, #35561, #141741, #3231, #125587, #142733, #156925, #64905, #4212, #187284, #51724, #113387, #159903, #112400, #126566, #174092, #19407, #188265, #65890, #111409, #47764, #48755, #124589, #97209, #49740, #173094, #157917, #20385, #82032, #21391, #36543, #143729, #175077, #186284, #66889, #98199, #109417, #171096, #32588, #94241, #155921, #17416, #79074, #110408, #172090, #33577, #103235, #133565, #38566, #86059, #176085, #144724, #56740, #26411, #10234, #177094, #160905, #55725, #163923, #164917, #6210, #147748, #191243, #132569, #41572, #115406, #39554, #118411, #9235, #87061, #25419, #24410, #70902, #178085, #52717, #148746, #67890, #114381, #101212, #195255, #129543, #40565, #71894, #37555, #99217, #22398, #85044, #180104, #84048, #130552, #145727, #194258, #102235, #7208, #131566, #68892, #161903, #54723, #192249, #162901, #53731, #146725, #100222, #23397, #8222, #69899, #117397, #193250, #116396, #179096, #60685, #108185, #184049, #134583, #197247, #57738, #136546, #122360, #13221, #137537, #14191, #92005, #153699, #72913, #196269, #119408, #107186, #167886, #45532, #106202, #165910, #181091, #89054, #198227, #74884, #58708, #90046, #150744, #42566, #121371, #168857, #29385, #149738, #104229, #30362, #120378, #166908, #59699, #12243, #88050, #15194, #27408, #151728, #76853, #2, #11239, #73905, #91016, #28407, #182071, #183064, #138524, #169866, #61676, #135575, #43554, #105220, #44547, #123345, #152702, #199219, #75861, #185038, #46525, #16191, #77846, #139513, #50507, #111168, #189033, #49505, #109184, #996, #32354, #141513, #18187, #2005, #33346, #94007, #62670, #64676, #112171, #172858, #93010, #47529, #65659, #63684, #110179, #156693, #155688, #31360, #173859, #34339, #48525, #79844, #125358, #96000, #35326, #190016, #66654, #142501, #20151, #154696, #96979, #158660, #124351, #19175, #128316, #157684, #80823, #187055, #127321, #95005, #186046, #170863, #51490, #81796, #171858, #3979, #17183, #78837, #143483, #113151, #4968, #2999, #140515, #126338, #188035, #133320, #56487, #116157, #21150, #162659, #71653, #145484, #69653, #86816, #177847, #117152, #55482, #54486, #39315, #7970, #82805, #194019, #36306, #144487, #131320, #163672, #97961, #70661, #40314, #67650, #195010, #129307, #115158, #148503, #25174, #160662, #174841, #24165, #132328, #178848, #161660, #159653, #191994, #84800, #5970, #193009, #101991, #191003, #85816, #52479, #100975, #147503, #68644, #8993, #38321, #114138, #175839, #37313, #9993, #130300, #98971, #22153, #83804, #6964, #53480, #176851, #99976, #23157, #146479, #137302, #76620, #199979, #59460, #164672, #105968, #14960, #88813, #12985, #30127, #121133, #60451, #198983, #197989, #182827, #151493, #26167, #122125, #179856, #87808, #74648, #106954, #41326, #13956, #183813, #10991, #138298, #72663, #58476, #91769, #168627, #103988, #118165, #167653, #75623, #45303, #104981, #102986, #135337, #28170, #149494, #136314, #196023, #120143, #153463, #134339, #57498, #119167, #44309, #181834, #12004, #89812, #90786, #180851, #42327, #165667, #27166, #150506, #166668, #152470, #43314, #29149, #73665, #197011, #127084, #46287, #107944, #169630, #80588, #141274, #18943, #79604, #139286, #31126, #62434, #171625, #48288, #32119, #63445, #124107, #92775, #94769, #142263, #2763, #123116, #77616, #95763, #93776, #140275, #186818, #185807, #61445, #3746, #64439, #78601, #109944, #155457, #126110, #65423, #19919 ),
 ( #154464, #170630, #15956, #33113, #34106, #156452, #110932, #187805, #188793, #50275, #763, #47293, #108950, #111933, #49274, #173620, #172619, #16947, #1767, #125121, #17951, #157449, #35089, #96742, #158432, #81561, #143247, #184801, #22918, #66420, #20911, #39082, #175599, #83569, #130060, #5736, #4731, #147262, #84564, #21918, #191759, #98735, #69414, #85576, #163437, #40071, #115924, #193778, #128081, #23921, #162419, #189785, #192769, #101749, #131080, #146242, #160428, #100738, #68407, #159415, #112916, #24934, #55247, #145248, #7728, #36076, #51256, #116915, #86580, #70423, #37076, #82569, #177614, #8752, #174611, #97725, #54253, #144250, #132089, #67413, #6729, #99742, #178608, #129068, #190769, #52244, #113901, #53242, #38087, #114919, #176612, #161426, #194774, #29644, #92286, #9756, #184320, #30633, #117930, #138793, #56248, #195790, #15467, #153970, #25936, #274, #199490, #45801, #169128, #180621, #61943, #134100, #106468, #148263, #91276, #164442, #44813, #77124, #71420, #179619, #87579, #152967, #133084, #41091, #57262, #122630, #107453, #102755, #72422, #118936, #168147, #149266, #10758, #14466, #76128, #137806, #60956, #104160, #85227, #114569, #38746, #120309, #84224, #72841, #166838, #182002, #83230, #134511, #161082, #162085, #176266, #53912, #37738, #135508, #98386, #165841, #197178, #150674, #43485, #23579, #89978, #57669, #146918, #128733, #69071, #105152, #21570, #68067, #196197, #99399, #160084, #73837, #13153, #51905, #58643, #129721, #22577, #28339, #8407, #145903, #119336, #12172, #7387, #181022, #151659, #42496, #190429, #144905, #27338, #6388, #100404, #88984, #130738, #113564, #175258, #36724, #192430, #191418, #52894, #115587, #177275, #184966, #137467, #78766, #108110, #74816, #154626, #168788, #136478, #63612, #153627, #1933, #156622, #169794, #32285, #91935, #926, #14122, #75789, #62600, #124278, #109114, #15123, #76785, #199147, #16120, #30290, #138456, #77776, #60613, #125287, #186984, #33278, #185974, #200137, #47458, #92938, #61606, #139444, #46450, #121302, #122288, #198158, #94937, #182994, #17115, #123275, #183977, #44477, #93940, #170793, #155619, #140443, #152632, #106132, #45463, #31287, #48455, #107117, #110112, #171790, #167816, #59628, #29315, #90945, #79772, #34270, #52409, #188964, #96910, #143412, #19105, #18117, #160592, #97889, #35256, #4900, #112099, #82734, #98898, #176777, #53407, #129236, #6893, #141442, #37242, #175766, #2929, #5901, #115085, #144415, #36237, #173789, #114068, #81727, #172789, #126271, #38249, #68571, #158593, #159581, #49438, #64608, #130228, #99904, #83732, #50440, #95929, #190932, #22081, #187968, #111099, #21078, #157614, #67578, #80755, #20082, #113079, #191923, #145411, #142432, #3911, #65591, #127251, #51419, #66582, #128247, #189944, #174771, #67138, #21638, #20631, #3470, #99464, #82283, #4449, #159134, #52956, #68130, #51968, #81288, #5455, #84288, #50980, #36788, #130801, #145967, #49989, #98454, #127802, #128796, #142972, #143975, #66139, #161144, #65147, #129781, #22641, #114632, #7449, #190495, #53975, #83292, #113627, #95483, #35802, #69133, #188512, #34812, #160147, #189505, #126804, #37801, #177338, #18663, #192492, #157169, #111654, #191478, #112640, #174332, #175322, #96467, #80309, #115648, #144968, #97448, #6449, #176331, #141982, #173340, #158155, #19647, #149981, #27658, #38809, #57977, #196507, #162146, #26650, #135815, #165158, #56979, #132810, #73158, #102476, #193493, #146982, #197485, #89298, #194496, #180344, #70143, #100467, #150990, #120620, #104472, #71144, #54972, #11487, #119649, #58952, #23642, #41812, #85290, #88293, #8469, #9480, #133815, #12482, #103480, #181331, #42810, #118653, #134828, #72139, #131814, #166157, #116642, #178332, #74143, #39795, #101459, #163150, #24653, #86302, #147991, #55969, #179343, #117646, #40806, #164163, #25661, #87306, #148989, #10479, #195506 ),
 ( #76101, #92259, #154936, #2242, #78082, #28644, #91248, #151964, #30606, #16433, #107427, #31601, #108431, #186291, #47771, #167145, #90280, #13452, #1237, #61916, #139750, #247, #59941, #75116, #183304, #153943, #169099, #152939, #184293, #44786, #136784, #15438, #62916, #123586, #109424, #198470, #121609, #106439, #124596, #185280, #171103, #46772, #168120, #29616, #14438, #77097, #138766, #137776, #45775, #199462, #60929, #170107, #32596, #93250, #43796, #122603, #94249, #155929, #17424, #79081, #140754, #182316, #63925, #105459, #142740, #50749, #19414, #190255, #6219, #84057, #160913, #36553, #114391, #125594, #144732, #83058, #48762, #113395, #22406, #51732, #143737, #81062, #159911, #189273, #80079, #33584, #145735, #176093, #4220, #66897, #156932, #187291, #37563, #7216, #191251, #157924, #141748, #98207, #67898, #110417, #172098, #128560, #95247, #175085, #18429, #96236, #20393, #99226, #21400, #129551, #52726, #5216, #3238, #158902, #64912, #126573, #188274, #49747, #111416, #173102, #34579, #65898, #127572, #112407, #174099, #35568, #97216, #82040, #57747, #54733, #27417, #118420, #26420, #72923, #55734, #89063, #86068, #179105, #165921, #163932, #146735, #70911, #88060, #181101, #192258, #8231, #87070, #9244, #162911, #40574, #41581, #150754, #164927, #115414, #178094, #38574, #117408, #103245, #194267, #180113, #195265, #134592, #102244, #116405, #25429, #39564, #196278, #100230, #149747, #119417, #11249, #42575, #148755, #68901, #56749, #10244, #130560, #132579, #104238, #161912, #69909, #133575, #101222, #23406, #53740, #177103, #85054, #131575, #193259, #24419, #147758, #71903, #44556, #76864, #93020, #106211, #12, #170873, #15205, #154708, #105229, #123355, #28418, #122370, #168867, #91025, #30372, #92016, #138534, #167895, #12252, #90055, #62680, #14202, #184059, #74893, #16201, #45542, #73914, #153709, #29395, #135584, #1006, #152711, #139523, #94017, #107196, #169877, #75870, #61686, #151737, #13230, #185048, #46536, #108195, #137546, #199229, #136556, #31370, #60694, #77856, #124361, #198237, #186056, #47540, #32364, #109194, #197256, #58718, #120387, #182081, #43564, #166917, #59708, #121381, #183073, #114150, #63694, #97972, #3990, #3010, #125369, #65670, #51502, #144498, #95015, #189044, #96991, #191014, #127332, #81808, #80835, #187065, #159664, #142512, #64687, #19186, #113162, #128329, #112182, #141523, #50519, #5981, #111179, #158673, #52490, #67661, #110189, #20163, #188046, #175851, #129318, #49516, #143495, #48535, #155698, #37324, #17193, #21161, #172869, #171867, #66666, #174852, #78847, #140525, #4980, #2015, #190028, #33356, #126349, #173870, #156703, #36318, #82816, #18197, #35338, #79854, #34350, #96011, #157695, #160672, #68655, #105734, #178861, #40327, #10006, #167421, #192006, #198752, #53492, #39328, #75390, #90557, #84811, #60217, #148516, #56500, #28917, #85828, #121887, #116169, #9006, #183580, #194032, #176862, #100987, #118178, #13724, #22164, #38331, #117165, #162671, #193020, #70673, #71666, #98982, #195024, #145495, #7981, #130311, #147516, #133333, #24177, #182591, #25188, #152239, #137062, #83815, #6975, #115169, #44075, #102003, #99987, #163685, #161672, #23168, #146490, #132340, #55495, #69665, #86830, #131332, #54497, #177859, #64201, #63197, #106723, #61206, #79363, #15715, #123859, #170387, #46047, #45065, #187568, #124877, #62195, #31878, #139043, #109705, #125868, #3508, #80347, #156206, #33860, #168397, #49035, #2521, #29892, #32874, #142019, #171387, #186576, #523, #141034, #108708, #199740, #153217, #91530, #110690, #172370, #14722, #94524, #65184, #17706, #48049, #185557, #95520, #93532, #122878, #76382, #126843, #157206, #47051, #18700, #138059, #184566, #107702, #169381, #30889, #77375, #92536, #154225, #155217, #16706, #78356, #140030, #1519, #176369, #85329, #159172, #83329, #100504, #191518, #130839, #69173, #68167 ),
 ( #81326, #128832, #162183, #177375, #174370, #147021, #37842, #146005, #192530, #175358, #8505, #5492, #98492, #70183, #145006, #66177, #190531, #7488, #23681, #111692, #127839, #6487, #52005, #82321, #160185, #161183, #188549, #84326, #34849, #97486, #158194, #36826, #22679, #113664, #99502, #114673, #54013, #115687, #173379, #96504, #50027, #35840, #19684, #21675, #20667, #52995, #38847, #144011, #143009, #4487, #189545, #51017, #112678, #67175, #129819, #41852, #88329, #10516, #150020, #11525, #58013, #164199, #131851, #9516, #182353, #133853, #103518, #194534, #135850, #165194, #193534, #73195, #25697, #55008, #120655, #72179, #43831, #116678, #151025, #89333, #178368, #119683, #28680, #181366, #134865, #87342, #166191, #195543, #86340, #39832, #90315, #105495, #149028, #196543, #163187, #101498, #167181, #13487, #197520, #57017, #148027, #42845, #12516, #152001, #24691, #104510, #71182, #27692, #132846, #102516, #26689, #56005, #74180, #58988, #117683, #179380, #40842, #118690, #180382, #94283, #136823, #44822, #79114, #154971, #16467, #186325, #140787, #168156, #172132, #29653, #15477, #48797, #63959, #60965, #33618, #124630, #32629, #2276, #61953, #95281, #92296, #185315, #156964, #170142, #152976, #77134, #155961, #187326, #198507, #14475, #93286, #138803, #169138, #46806, #47807, #75152, #171140, #121645, #184329, #106477, #123620, #109457, #284, #17458, #1273, #125628, #108465, #30643, #110451, #59978, #183340, #78116, #91285, #139785, #76137, #137815, #199499, #31637, #62950, #45811, #122639, #107462, #153980, #51762, #37594, #36583, #80112, #34611, #52753, #189304, #97247, #143767, #19447, #18461, #160943, #98238, #35601, #5248, #112441, #83088, #99256, #177134, #53769, #129582, #159941, #21428, #191278, #84085, #111449, #115443, #173136, #158935, #192289, #7246, #4254, #38605, #67928, #176123, #22436, #66929, #100261, #20424, #128592, #141780, #113423, #96270, #82074, #145764, #130593, #3274, #157956, #144764, #190286, #174130, #175115, #114422, #64946, #68931, #126605, #127605, #188307, #6249, #49784, #81095, #142773, #65933, #50781, #102275, #55764, #12279, #120416, #181131, #41611, #119446, #180142, #39594, #69941, #162942, #71934, #148786, #132609, #163963, #24449, #131605, #195297, #42605, #103276, #23437, #178127, #196306, #194298, #40604, #87101, #86098, #161942, #104269, #164956, #179136, #10275, #117438, #26449, #165951, #182107, #197284, #72952, #150784, #85084, #27451, #89092, #146768, #149777, #58747, #88091, #11279, #25461, #57776, #133604, #116438, #193290, #43592, #73944, #56778, #134622, #54764, #8261, #135613, #101253, #147789, #118451, #9275, #70941, #124394, #63725, #187097, #46567, #151765, #93052, #2045, #75902, #43, #17226, #108228, #47572, #186089, #185078, #169908, #138565, #13258, #109224, #166944, #74921, #170903, #184091, #30404, #106241, #105258, #32395, #31401, #122401, #92050, #199260, #154739, #94050, #125400, #140557, #16235, #155728, #28447, #78878, #62712, #90083, #77887, #136584, #139555, #123386, #60727, #1039, #168898, #59740, #198264, #121409, #183103, #45574, #44584, #167923, #29423, #91054, #152741, #14231, #137576, #107227, #153739, #15235, #76894, #61718, #190057, #95048, #36351, #145528, #19219, #143527, #160706, #51533, #191048, #129353, #128361, #113196, #81839, #156737, #67695, #110220, #18230, #52521, #174885, #98004, #159698, #114182, #141555, #7007, #3044, #189079, #22197, #37357, #34383, #68689, #21195, #6016, #175886, #35371, #130344, #65701, #158704, #48567, #5015, #126382, #50552, #99015, #83846, #171901, #188079, #66697, #112212, #142545, #20193, #82851, #33389, #144530, #79885, #157730, #64720, #97023, #49550, #173902, #111213, #172905, #96043, #80869, #4023, #127367, #150549, #11035, #71699, #149540, #10039, #69698, #100020, #193054, #102037, #178894, #162706, #194067, #54531, #161707, #25222, #72711, #133366, #53524 ),
 ( #134383, #115202, #23203, #196069, #195057, #56535, #103036, #57542, #84846, #88856, #146524, #132374, #165713, #180896, #177893, #12048, #41370, #119211, #42371, #40362, #73712, #9037, #163720, #192043, #86864, #131365, #55528, #104034, #27210, #176894, #116204, #118213, #117202, #85860, #148548, #164718, #38365, #87852, #8015, #101021, #39363, #179904, #26213, #24211, #147549, #70706, #139331, #75668, #29195, #185855, #93822, #154508, #15005, #92822, #153508, #13028, #43357, #136359, #45347, #122170, #106012, #137345, #198035, #105028, #168672, #16004, #76665, #197054, #151539, #169676, #167698, #14001, #60494, #59503, #135384, #77662, #138344, #152513, #183860, #90829, #200024, #810, #155502, #170677, #46334, #124155, #58522, #62483, #47341, #120188, #123162, #32165, #61492, #184850, #199025, #31172, #106999, #89856, #166712, #16995, #108996, #30173, #107990, #28216, #181878, #74694, #121178, #182872, #91816, #44353, #189830, #97773, #37121, #160474, #19966, #125168, #66466, #175646, #49320, #80635, #141321, #48336, #111978, #159460, #96789, #140324, #94819, #112963, #110980, #157496, #3792, #79652, #78649, #20956, #158478, #95810, #65469, #172665, #143292, #82613, #98780, #113947, #51302, #67458, #1814, #144294, #36121, #63493, #128128, #186867, #4778, #81608, #34151, #174656, #142312, #33160, #109991, #171671, #129116, #18989, #5784, #156497, #17999, #190815, #2810, #52290, #127132, #64488, #126155, #187851, #188838, #50323, #173670, #35137, #9801, #118980, #192816, #116962, #134143, #24978, #164484, #102798, #101793, #86624, #55290, #130110, #41134, #83616, #191806, #25978, #163481, #148307, #133128, #87621, #114966, #180663, #176659, #162465, #195832, #10801, #7778, #42139, #71463, #179664, #149307, #8797, #103800, #39127, #132133, #21965, #178653, #99789, #23966, #72470, #57304, #145294, #161475, #40115, #85621, #115970, #193825, #194819, #6777, #117973, #68456, #131128, #53287, #70467, #56291, #147308, #38136, #22964, #84612, #146291, #177658, #69461, #54298, #100782, #45110, #122923, #183628, #43123, #73476, #166479, #75436, #152284, #106767, #59268, #26976, #154269, #44120, #92581, #47093, #60262, #184611, #182637, #91577, #104791, #27978, #153266, #14767, #199785, #105779, #167466, #89617, #168442, #120937, #28961, #29938, #151306, #15760, #77419, #123905, #76428, #90602, #138104, #61253, #13768, #46092, #137110, #11812, #12795, #165480, #185604, #135149, #107747, #198796, #74460, #196822, #121933, #169428, #139091, #136126, #30933, #566, #62237, #88619, #150316, #58289, #119958, #181644, #197802, #17752, #172419, #68962, #84116, #65228, #94572, #18745, #100294, #64246, #50075, #146801, #161972, #63241, #111736, #141079, #142064, #156250, #33907, #79408, #115476, #78399, #145795, #177164, #130624, #23468, #3550, #69972, #37625, #126888, #108754, #49081, #85117, #1566, #48090, #173423, #2564, #140075, #53800, #80392, #124921, #38637, #170430, #125913, #8294, #188594, #187611, #99288, #192320, #110738, #160974, #131639, #22468, #193322, #186618, #7278, #109746, #31922, #93576, #95564, #155261, #16751, #171430, #157251, #32917, #132641, #105287, #56809, #164986, #117469, #58778, #88123, #54796, #134652, #26481, #101285, #179167, #116471, #13287, #162975, #197314, #103307, #102304, #24480, #149807, #150813, #43623, #194329, #11313, #196338, #90112, #72983, #181160, #180174, #86130, #120446, #41642, #163993, #118483, #12310, #27482, #57806, #40635, #119477, #166975, #10307, #42636, #151796, #28478, #9307, #104299, #87132, #165981, #25490, #89125, #148817, #182140, #147822, #73975, #74951, #135644, #136614, #178160, #39625, #70973, #55797, #71964, #195329, #133638, #91086, #137609, #62743, #107259, #29454, #140585, #169939, #152773, #2075, #59772, #45606, #110247, #31430, #30436, #124423, #78908, #92083, #186119, #156765, #1068, #63754, #14265, #109253, #75934, #108259, #154767, #76926 ),
 ( #77916, #153772, #121440, #187124, #138596, #125428, #79912, #93084, #155757, #15267, #47599, #199292, #60760, #170932, #32423, #94078, #78, #61748, #122432, #139583, #123416, #185109, #17255, #184124, #48596, #171929, #18259, #33418, #46599, #95077, #16265, #198295, #183133, #44617, #106270, #167955, #168930, #38397, #112241, #36381, #53557, #144562, #83878, #22229, #21228, #6048, #174917, #49579, #160737, #3072, #111242, #145560, #82884, #67726, #52553, #7038, #34412, #100053, #96070, #81871, #115235, #130377, #127399, #161739, #191080, #99047, #68720, #128391, #23234, #158733, #51563, #141584, #98035, #19250, #143562, #192075, #176926, #64748, #80897, #159732, #5045, #35400, #113227, #114214, #126410, #37390, #188106, #50581, #172933, #190088, #175919, #66731, #157760, #129384, #142574, #4053, #97051, #65730, #189108, #173932, #20223, #42403, #103069, #162738, #193086, #85895, #195089, #71730, #55561, #86896, #147583, #54561, #118246, #104066, #164751, #146555, #101053, #119244, #117235, #163754, #10070, #9069, #84878, #27241, #26246, #102069, #133400, #178928, #149573, #165747, #43389, #120220, #196104, #73744, #8051, #88890, #150582, #69730, #72747, #181910, #11069, #87885, #40398, #180928, #148580, #39393, #116234, #105061, #135416, #25254, #134418, #177925, #131398, #197087, #166745, #12081, #56572, #24246, #57574, #58554, #179937, #70739, #41404, #132406, #194099, #139358, #122199, #137376, #124184, #170704, #154535, #138372, #16032, #76695, #182902, #74726, #106041, #30203, #168701, #14031, #183891, #167727, #136390, #153538, #77690, #200052, #89888, #121211, #31199, #75696, #60524, #107029, #29225, #28248, #839, #61521, #45376, #91844, #15035, #46361, #62512, #93851, #32193, #92850, #185885, #151571, #47370, #109025, #198067, #169705, #13060, #59533, #44386, #123190, #90858, #108019, #184879, #199054, #152543, #197723, #102721, #150238, #40040, #8720, #120858, #90524, #74383, #41058, #24900, #119884, #27899, #167388, #70389, #11734, #55214, #196748, #105701, #179586, #103725, #182558, #73401, #151228, #89542, #88541, #135072, #42061, #116883, #12717, #132057, #178575, #136048, #58215, #181569, #43047, #59189, #101713, #28884, #163404, #149234, #44041, #193746, #194743, #86547, #104713, #166403, #148231, #195755, #9725, #25902, #118903, #71389, #165405, #133053, #10725, #56215, #117896, #164410, #87547, #26898, #72389, #134064, #180587, #57229, #172334, #48012, #198717, #61173, #121854, #91496, #16671, #122845, #183546, #94487, #123824, #106690, #156169, #13690, #199708, #64165, #185522, #184533, #78320, #32837, #46013, #139993, #110654, #155181, #17668, #45032, #63160, #168363, #62160, #108673, #30854, #170351, #31843, #1482, #107668, #152206, #29859, #2484, #154190, #47014, #14686, #79326, #93494, #75357, #124839, #169345, #137027, #140996, #92501, #125830, #33823, #186539, #109668, #15680, #171348, #153183, #76348, #187533, #48998, #60184, #77341, #139007, #138025, #487, #125148, #45329, #13983, #126136, #95790, #79632, #46316, #30153, #186847, #33140, #172643, #75649, #155483, #60475, #1795, #110959, #184830, #108977, #187831, #16975, #156477, #94798, #93803, #78629, #47322, #122151, #17978, #137327, #183840, #141300, #140304, #63473, #48316, #2790, #106979, #34131, #168653, #154490, #49300, #64469, #200006, #199008, #109971, #171650, #91796, #791, #153490, #31154, #124136, #14986, #170658, #76646, #15984, #138324, #61472, #123143, #107971, #32146, #77643, #169658, #185835, #92802, #139312, #62463, #3772, #66445, #127111, #5762, #130087, #53267, #65449, #128106, #188818, #67438, #191786, #82593, #6755, #83594, #161453, #97753, #51282, #7756, #115951, #176638, #37101, #114945, #175627, #35116, #50301, #158457, #129095, #144275, #189810, #159441, #19946, #111958, #190795, #38113, #98760, #18969, #173647, #99768, #112943, #36101, #52269, #81587, #157476, #22944, #160453, #174636 ) ),
 .UNSPECIFIED., .T., .F., .F. ) 
 B_SPLINE_SURFACE_WITH_KNOTS ( ( 4, 3, 4 ),
 ( 3, 2, 2, 2, 2, 2, 2, 2, 2, 2, 2, 2, 2, 2, 2, 2, 2, 2, 2, 2, 2, 2, 2, 2, 2, 2, 2, 2, 2, 2, 2, 2, 2, 2, 2, 2, 2, 2, 2, 2, 2, 2, 2, 2, 2, 2, 2, 2, 2, 2, 2, 2, 2, 2, 2, 2, 2, 2, 2, 2, 2, 2, 2, 2, 2, 2, 2, 2, 2, 2, 2, 2, 2, 2, 2, 2, 2, 2, 2, 2, 2, 2, 2, 2, 2, 2, 2, 2, 2, 2, 2, 2, 2, 2, 2, 2, 2, 2, 2, 2, 2, 2, 2, 2, 2, 2, 2, 2, 2, 2, 2, 2, 2, 2, 2, 2, 2, 2, 2, 2, 2, 2, 2, 2, 2, 2, 2, 2, 2, 2, 2, 2, 2, 2, 2, 2, 2, 2, 2, 2, 2, 2, 2, 2, 2, 2, 2, 2, 2, 2, 2, 2, 2, 2, 2, 2, 2, 2, 2, 2, 2, 2, 2, 2, 2, 2, 2, 2, 2, 2, 2, 2, 2, 2, 2, 2, 2, 2, 2, 2, 2, 2, 2, 2, 2, 2, 2, 2, 2, 2, 2, 2, 2, 2, 2, 2, 2, 2, 2, 2, 2, 2, 2, 2, 2, 2, 2, 2, 2, 2, 2, 2, 2, 2, 2, 2, 2, 2, 2, 2, 2, 2, 2, 2, 2, 2, 2, 2, 3 ),
 ( 0.000000000000000000, 0.5000000000000000000, 1.000000000000000000 ),
 ( 0.000000000000000000, 0.004385964912280701511, 0.008771929824561403022, 0.01315789473684210453, 0.01754385964912280604, 0.02192982456140350755, 0.02631578947368420907, 0.03070175438596491058, 0.03508771929824561209, 0.03947368421052631360, 0.04385964912280701511, 0.04824561403508771662, 0.05263157894736841813, 0.05701754385964911964, 0.06140350877192982115, 0.06578947368421052266, 0.07017543859649122417, 0.07456140350877192569, 0.07894736842105262720, 0.08333333333333332871, 0.08771929824561403022, 0.09210526315789473173, 0.09649122807017543324, 0.1008771929824561348, 0.1052631578947368363, 0.1096491228070175378, 0.1140350877192982393, 0.1184210526315789408, 0.1228070175438596423, 0.1271929824561403577, 0.1315789473684210453, 0.1359649122807017607, 0.1403508771929824483, 0.1447368421052631637, 0.1491228070175438514, 0.1535087719298245668, 0.1578947368421052544, 0.1622807017543859698, 0.1666666666666666574, 0.1710526315789473728, 0.1754385964912280604, 0.1798245614035087758, 0.1842105263157894635, 0.1885964912280701788, 0.1929824561403508665, 0.1973684210526315819, 0.2017543859649122695, 0.2061403508771929849, 0.2105263157894736725, 0.2149122807017543879, 0.2192982456140350755, 0.2236842105263157909, 0.2280701754385964786, 0.2324561403508771940, 0.2368421052631578816, 0.2412280701754385970, 0.2456140350877192846, 0.2500000000000000000, 0.2543859649122807154, 0.2587719298245614308, 0.2631578947368420907, 0.2675438596491228060, 0.2719298245614035214, 0.2763157894736842368, 0.2807017543859648967, 0.2850877192982456121, 0.2894736842105263275, 0.2938596491228070429, 0.2982456140350877027, 0.3026315789473684181, 0.3070175438596491335, 0.3114035087719298489, 0.3157894736842105088, 0.3201754385964912242, 0.3245614035087719396, 0.3289473684210526550, 0.3333333333333333148, 0.3377192982456140302, 0.3421052631578947456, 0.3464912280701754610, 0.3508771929824561209, 0.3552631578947368363, 0.3596491228070175517, 0.3640350877192982670, 0.3684210526315789269, 0.3728070175438596423, 0.3771929824561403577, 0.3815789473684210731, 0.3859649122807017330, 0.3903508771929824483, 0.3947368421052631637, 0.3991228070175438791, 0.4035087719298245390, 0.4078947368421052544, 0.4122807017543859698, 0.4166666666666666852, 0.4210526315789473450, 0.4254385964912280604, 0.4298245614035087758, 0.4342105263157894912, 0.4385964912280701511, 0.4429824561403508665, 0.4473684210526315819, 0.4517543859649122973, 0.4561403508771929571, 0.4605263157894736725, 0.4649122807017543879, 0.4692982456140351033, 0.4736842105263157632, 0.4780701754385964786, 0.4824561403508771940, 0.4868421052631579093, 0.4912280701754385692, 0.4956140350877192846, 0.5000000000000000000, 0.5043859649122807154, 0.5087719298245614308, 0.5131578947368421462, 0.5175438596491228616, 0.5219298245614034659, 0.5263157894736841813, 0.5307017543859648967, 0.5350877192982456121, 0.5394736842105263275, 0.5438596491228070429, 0.5482456140350877583, 0.5526315789473684736, 0.5570175438596490780, 0.5614035087719297934, 0.5657894736842105088, 0.5701754385964912242, 0.5745614035087719396, 0.5789473684210526550, 0.5833333333333333703, 0.5877192982456140857, 0.5921052631578946901, 0.5964912280701754055, 0.6008771929824561209, 0.6052631578947368363, 0.6096491228070175517, 0.6140350877192982670, 0.6184210526315789824, 0.6228070175438596978, 0.6271929824561403022, 0.6315789473684210176, 0.6359649122807017330, 0.6403508771929824483, 0.6447368421052631637, 0.6491228070175438791, 0.6535087719298245945, 0.6578947368421053099, 0.6622807017543859143, 0.6666666666666666297, 0.6710526315789473450, 0.6754385964912280604, 0.6798245614035087758, 0.6842105263157894912, 0.6885964912280702066, 0.6929824561403509220, 0.6973684210526315264, 0.7017543859649122417, 0.7061403508771929571, 0.7105263157894736725, 0.7149122807017543879, 0.7192982456140351033, 0.7236842105263158187, 0.7280701754385965341, 0.7324561403508771384, 0.7368421052631578538, 0.7412280701754385692, 0.7456140350877192846, 0.7500000000000000000, 0.7543859649122807154, 0.7587719298245614308, 0.7631578947368421462, 0.7675438596491228616, 0.7719298245614034659, 0.7763157894736841813, 0.7807017543859648967, 0.7850877192982456121, 0.7894736842105263275, 0.7938596491228070429, 0.7982456140350877583, 0.8026315789473684736, 0.8070175438596490780, 0.8114035087719297934, 0.8157894736842105088, 0.8201754385964912242, 0.8245614035087719396, 0.8289473684210526550, 0.8333333333333333703, 0.8377192982456140857, 0.8421052631578946901, 0.8464912280701754055, 0.8508771929824561209, 0.8552631578947368363, 0.8596491228070175517, 0.8640350877192982670, 0.8684210526315789824, 0.8728070175438596978, 0.8771929824561403022, 0.8815789473684210176, 0.8859649122807017330, 0.8903508771929824483, 0.8947368421052631637, 0.8991228070175438791, 0.9035087719298245945, 0.9078947368421053099, 0.9122807017543859143, 0.9166666666666666297, 0.9210526315789473450, 0.9254385964912280604, 0.9298245614035087758, 0.9342105263157894912, 0.9385964912280702066, 0.9429824561403509220, 0.9473684210526315264, 0.9517543859649122417, 0.9561403508771929571, 0.9605263157894736725, 0.9649122807017543879, 0.9692982456140351033, 0.9736842105263158187, 0.9780701754385965341, 0.9824561403508771384, 0.9868421052631578538, 0.9912280701754385692, 0.9956140350877192846, 1.000000000000000000 ),
 .UNSPECIFIED. ) 
 GEOMETRIC_REPRESENTATION_ITEM ( )  RATIONAL_B_SPLINE_SURFACE ( (
 ( 1.000000000000000000, 0.9659258262890683122, 1.000000000000000000, 0.9659258262890683122, 1.000000000000000000, 0.9659258262890683122, 1.000000000000000000, 0.9659258262890683122, 1.000000000000000000, 0.9659258262890683122, 1.000000000000000000, 0.9659258262890683122, 1.000000000000000000, 0.9659258262890683122, 1.000000000000000000, 0.9659258262890683122, 1.000000000000000000, 0.9659258262890683122, 1.000000000000000000, 0.9659258262890683122, 1.000000000000000000, 0.9659258262890683122, 1.000000000000000000, 0.9659258262890683122, 1.000000000000000000, 0.9659258262890683122, 1.000000000000000000, 0.9659258262890683122, 1.000000000000000000, 0.9659258262890683122, 1.000000000000000000, 0.9659258262890683122, 1.000000000000000000, 0.9659258262890683122, 1.000000000000000000, 0.9659258262890683122, 1.000000000000000000, 0.9659258262890683122, 1.000000000000000000, 0.9659258262890683122, 1.000000000000000000, 0.9659258262890683122, 1.000000000000000000, 0.9659258262890683122, 1.000000000000000000, 0.9659258262890683122, 1.000000000000000000, 0.9659258262890683122, 1.000000000000000000, 0.9659258262890683122, 1.000000000000000000, 0.9659258262890683122, 1.000000000000000000, 0.9659258262890683122, 1.000000000000000000, 0.9659258262890683122, 1.000000000000000000, 0.9659258262890683122, 1.000000000000000000, 0.9659258262890683122, 1.000000000000000000, 0.9659258262890683122, 1.000000000000000000, 0.9659258262890683122, 1.000000000000000000, 0.9659258262890683122, 1.000000000000000000, 0.9659258262890683122, 1.000000000000000000, 0.9659258262890683122, 1.000000000000000000, 0.9659258262890683122, 1.000000000000000000, 0.9659258262890683122, 1.000000000000000000, 0.9659258262890683122, 1.000000000000000000, 0.9659258262890683122, 1.000000000000000000, 0.9659258262890683122, 1.000000000000000000, 0.9659258262890683122, 1.000000000000000000, 0.9659258262890683122, 1.000000000000000000, 0.9659258262890683122, 1.000000000000000000, 0.9659258262890683122, 1.000000000000000000, 0.9659258262890683122, 1.000000000000000000, 0.9659258262890683122, 1.000000000000000000, 0.9659258262890683122, 1.000000000000000000, 0.9659258262890683122, 1.000000000000000000, 0.9659258262890683122, 1.000000000000000000, 0.9659258262890683122, 1.000000000000000000, 0.9659258262890683122, 1.000000000000000000, 0.9659258262890683122, 1.000000000000000000, 0.9659258262890683122, 1.000000000000000000, 0.9659258262890683122, 1.000000000000000000, 0.9659258262890683122, 1.000000000000000000, 0.9659258262890683122, 1.000000000000000000, 0.9659258262890683122, 1.000000000000000000, 0.9659258262890683122, 1.000000000000000000, 0.9659258262890683122, 1.000000000000000000, 0.9659258262890683122, 1.000000000000000000, 0.9659258262890683122, 1.000000000000000000, 0.9659258262890683122, 1.000000000000000000, 0.9659258262890683122, 1.000000000000000000, 0.9659258262890683122, 1.000000000000000000, 0.9659258262890683122, 1.000000000000000000, 0.9659258262890683122, 1.000000000000000000, 0.9659258262890683122, 1.000000000000000000, 0.9659258262890683122, 1.000000000000000000, 0.9659258262890683122, 1.000000000000000000, 0.9659258262890683122, 1.000000000000000000, 0.9659258262890683122, 1.000000000000000000, 0.9659258262890683122, 1.000000000000000000, 0.9659258262890683122, 1.000000000000000000, 0.9659258262890683122, 1.000000000000000000, 0.9659258262890683122, 1.000000000000000000, 0.9659258262890683122, 1.000000000000000000, 0.9659258262890683122, 1.000000000000000000, 0.9659258262890683122, 1.000000000000000000, 0.9659258262890683122, 1.000000000000000000, 0.9659258262890683122, 1.000000000000000000, 0.9659258262890683122, 1.000000000000000000, 0.9659258262890683122, 1.000000000000000000, 0.9659258262890683122, 1.000000000000000000, 0.9659258262890683122, 1.000000000000000000, 0.9659258262890683122, 1.000000000000000000, 0.9659258262890683122, 1.000000000000000000, 0.9659258262890683122, 1.000000000000000000, 0.9659258262890683122, 1.000000000000000000, 0.9659258262890683122, 1.000000000000000000, 0.9659258262890683122, 1.000000000000000000, 0.9659258262890683122, 1.000000000000000000, 0.9659258262890683122, 1.000000000000000000, 0.9659258262890683122, 1.000000000000000000, 0.9659258262890683122, 1.000000000000000000, 0.9659258262890683122, 1.000000000000000000, 0.9659258262890683122, 1.000000000000000000, 0.9659258262890683122, 1.000000000000000000, 0.9659258262890683122, 1.000000000000000000, 0.9659258262890683122, 1.000000000000000000, 0.9659258262890683122, 1.000000000000000000, 0.9659258262890683122, 1.000000000000000000, 0.9659258262890683122, 1.000000000000000000, 0.9659258262890683122, 1.000000000000000000, 0.9659258262890683122, 1.000000000000000000, 0.9659258262890683122, 1.000000000000000000, 0.9659258262890683122, 1.000000000000000000, 0.9659258262890683122, 1.000000000000000000, 0.9659258262890683122, 1.000000000000000000, 0.9659258262890683122, 1.000000000000000000, 0.9659258262890683122, 1.000000000000000000, 0.9659258262890683122, 1.000000000000000000, 0.9659258262890683122, 1.000000000000000000, 0.9659258262890683122, 1.000000000000000000, 0.9659258262890683122, 1.000000000000000000, 0.9659258262890683122, 1.000000000000000000, 0.9659258262890683122, 1.000000000000000000, 0.9659258262890683122, 1.000000000000000000, 0.9659258262890683122, 1.000000000000000000, 0.9659258262890683122, 1.000000000000000000, 0.9659258262890683122, 1.000000000000000000, 0.9659258262890683122, 1.000000000000000000, 0.9659258262890683122, 1.000000000000000000, 0.9659258262890683122, 1.000000000000000000, 0.9659258262890683122, 1.000000000000000000, 0.9659258262890683122, 1.000000000000000000, 0.9659258262890683122, 1.000000000000000000, 0.9659258262890683122, 1.000000000000000000, 0.9659258262890683122, 1.000000000000000000, 0.9659258262890683122, 1.000000000000000000, 0.9659258262890683122, 1.000000000000000000, 0.9659258262890683122, 1.000000000000000000, 0.9659258262890683122, 1.000000000000000000, 0.9659258262890683122, 1.000000000000000000, 0.9659258262890683122, 1.000000000000000000, 0.9659258262890683122, 1.000000000000000000, 0.9659258262890683122, 1.000000000000000000, 0.9659258262890683122, 1.000000000000000000, 0.9659258262890683122, 1.000000000000000000, 0.9659258262890683122, 1.000000000000000000, 0.9659258262890683122, 1.000000000000000000, 0.9659258262890683122, 1.000000000000000000, 0.9659258262890683122, 1.000000000000000000, 0.9659258262890683122, 1.000000000000000000, 0.9659258262890683122, 1.000000000000000000, 0.9659258262890683122, 1.000000000000000000, 0.9659258262890683122, 1.000000000000000000, 0.9659258262890683122, 1.000000000000000000, 0.9659258262890683122, 1.000000000000000000, 0.9659258262890683122, 1.000000000000000000, 0.9659258262890683122, 1.000000000000000000, 0.9659258262890683122, 1.000000000000000000, 0.9659258262890683122, 1.000000000000000000, 0.9659258262890683122, 1.000000000000000000, 0.9659258262890683122, 1.000000000000000000, 0.9659258262890683122, 1.000000000000000000, 0.9659258262890683122, 1.000000000000000000, 0.9659258262890683122, 1.000000000000000000, 0.9659258262890683122, 1.000000000000000000, 0.9659258262890683122, 1.000000000000000000, 0.9659258262890683122, 1.000000000000000000, 0.9659258262890683122, 1.000000000000000000, 0.9659258262890683122, 1.000000000000000000, 0.9659258262890683122, 1.000000000000000000, 0.9659258262890683122, 1.000000000000000000, 0.9659258262890683122, 1.000000000000000000, 0.9659258262890683122, 1.000000000000000000, 0.9659258262890683122, 1.000000000000000000, 0.9659258262890683122, 1.000000000000000000, 0.9659258262890683122, 1.000000000000000000, 0.9659258262890683122, 1.000000000000000000, 0.9659258262890683122, 1.000000000000000000, 0.9659258262890683122, 1.000000000000000000, 0.9659258262890683122, 1.000000000000000000, 0.9659258262890683122, 1.000000000000000000, 0.9659258262890683122, 1.000000000000000000, 0.9659258262890683122, 1.000000000000000000, 0.9659258262890683122, 1.000000000000000000, 0.9659258262890683122, 1.000000000000000000, 0.9659258262890683122, 1.000000000000000000, 0.9659258262890683122, 1.000000000000000000, 0.9659258262890683122, 1.000000000000000000, 0.9659258262890683122, 1.000000000000000000, 0.9659258262890683122, 1.000000000000000000, 0.9659258262890683122, 1.000000000000000000, 0.9659258262890683122, 1.000000000000000000, 0.9659258262890683122, 1.000000000000000000, 0.9659258262890683122, 1.000000000000000000, 0.9659258262890683122, 1.000000000000000000, 0.9659258262890683122, 1.000000000000000000, 0.9659258262890683122, 1.000000000000000000, 0.9659258262890683122, 1.000000000000000000, 0.9659258262890683122, 1.000000000000000000, 0.9659258262890683122, 1.000000000000000000, 0.9659258262890683122, 1.000000000000000000, 0.9659258262890683122, 1.000000000000000000, 0.9659258262890683122, 1.000000000000000000, 0.9659258262890683122, 1.000000000000000000, 0.9659258262890683122, 1.000000000000000000, 0.9659258262890683122, 1.000000000000000000, 0.9659258262890683122, 1.000000000000000000, 0.9659258262890683122, 1.000000000000000000, 0.9659258262890683122, 1.000000000000000000, 0.9659258262890683122, 1.000000000000000000, 0.9659258262890683122, 1.000000000000000000, 0.9659258262890683122, 1.000000000000000000, 0.9659258262890683122, 1.000000000000000000, 0.9659258262890683122, 1.000000000000000000, 0.9659258262890683122, 1.000000000000000000, 0.9659258262890683122, 1.000000000000000000, 0.9659258262890683122, 1.000000000000000000, 0.9659258262890683122, 1.000000000000000000, 0.9659258262890683122, 1.000000000000000000, 0.9659258262890683122, 1.000000000000000000, 0.9659258262890683122, 1.000000000000000000, 0.9659258262890683122, 1.000000000000000000, 0.9659258262890683122, 1.000000000000000000, 0.9659258262890683122, 1.000000000000000000, 0.9659258262890683122, 1.000000000000000000, 0.9659258262890683122, 1.000000000000000000, 0.9659258262890683122, 1.000000000000000000, 0.9659258262890683122, 1.000000000000000000, 0.9659258262890683122, 1.000000000000000000, 0.9659258262890683122, 1.000000000000000000, 0.9659258262890683122, 1.000000000000000000, 0.9659258262890683122, 1.000000000000000000, 0.9659258262890683122, 1.000000000000000000, 0.9659258262890683122, 1.000000000000000000, 0.9659258262890683122, 1.000000000000000000),
 ( 0.3333333333333333703, 0.3219752754296894559, 0.3333333333333333703, 0.3219752754296894559, 0.3333333333333333703, 0.3219752754296894559, 0.3333333333333333703, 0.3219752754296894559, 0.3333333333333333703, 0.3219752754296894559, 0.3333333333333333703, 0.3219752754296894559, 0.3333333333333333703, 0.3219752754296894559, 0.3333333333333333703, 0.3219752754296894559, 0.3333333333333333703, 0.3219752754296894559, 0.3333333333333333703, 0.3219752754296894559, 0.3333333333333333703, 0.3219752754296894559, 0.3333333333333333703, 0.3219752754296894559, 0.3333333333333333703, 0.3219752754296894559, 0.3333333333333333703, 0.3219752754296894559, 0.3333333333333333703, 0.3219752754296894559, 0.3333333333333333703, 0.3219752754296894559, 0.3333333333333333703, 0.3219752754296894559, 0.3333333333333333703, 0.3219752754296894559, 0.3333333333333333703, 0.3219752754296894559, 0.3333333333333333703, 0.3219752754296894559, 0.3333333333333333703, 0.3219752754296894559, 0.3333333333333333703, 0.3219752754296894559, 0.3333333333333333703, 0.3219752754296894559, 0.3333333333333333703, 0.3219752754296894559, 0.3333333333333333703, 0.3219752754296894559, 0.3333333333333333703, 0.3219752754296894559, 0.3333333333333333703, 0.3219752754296894559, 0.3333333333333333703, 0.3219752754296894559, 0.3333333333333333703, 0.3219752754296894559, 0.3333333333333333703, 0.3219752754296894559, 0.3333333333333333703, 0.3219752754296894559, 0.3333333333333333703, 0.3219752754296894559, 0.3333333333333333703, 0.3219752754296894559, 0.3333333333333333703, 0.3219752754296894559, 0.3333333333333333703, 0.3219752754296894559, 0.3333333333333333703, 0.3219752754296894559, 0.3333333333333333703, 0.3219752754296894559, 0.3333333333333333703, 0.3219752754296894559, 0.3333333333333333703, 0.3219752754296894559, 0.3333333333333333703, 0.3219752754296894559, 0.3333333333333333703, 0.3219752754296894559, 0.3333333333333333703, 0.3219752754296894559, 0.3333333333333333703, 0.3219752754296894559, 0.3333333333333333703, 0.3219752754296894559, 0.3333333333333333703, 0.3219752754296894559, 0.3333333333333333703, 0.3219752754296894559, 0.3333333333333333703, 0.3219752754296894559, 0.3333333333333333703, 0.3219752754296894559, 0.3333333333333333703, 0.3219752754296894559, 0.3333333333333333703, 0.3219752754296894559, 0.3333333333333333703, 0.3219752754296894559, 0.3333333333333333703, 0.3219752754296894559, 0.3333333333333333703, 0.3219752754296894559, 0.3333333333333333703, 0.3219752754296894559, 0.3333333333333333703, 0.3219752754296894559, 0.3333333333333333703, 0.3219752754296894559, 0.3333333333333333703, 0.3219752754296894559, 0.3333333333333333703, 0.3219752754296894559, 0.3333333333333333703, 0.3219752754296894559, 0.3333333333333333703, 0.3219752754296894559, 0.3333333333333333703, 0.3219752754296894559, 0.3333333333333333703, 0.3219752754296894559, 0.3333333333333333703, 0.3219752754296894559, 0.3333333333333333703, 0.3219752754296894559, 0.3333333333333333703, 0.3219752754296894559, 0.3333333333333333703, 0.3219752754296894559, 0.3333333333333333703, 0.3219752754296894559, 0.3333333333333333703, 0.3219752754296894559, 0.3333333333333333703, 0.3219752754296894559, 0.3333333333333333703, 0.3219752754296894559, 0.3333333333333333703, 0.3219752754296894559, 0.3333333333333333703, 0.3219752754296894559, 0.3333333333333333703, 0.3219752754296894559, 0.3333333333333333703, 0.3219752754296894559, 0.3333333333333333703, 0.3219752754296894559, 0.3333333333333333703, 0.3219752754296894559, 0.3333333333333333703, 0.3219752754296894559, 0.3333333333333333703, 0.3219752754296894559, 0.3333333333333333703, 0.3219752754296894559, 0.3333333333333333703, 0.3219752754296894559, 0.3333333333333333703, 0.3219752754296894559, 0.3333333333333333703, 0.3219752754296894559, 0.3333333333333333703, 0.3219752754296894559, 0.3333333333333333703, 0.3219752754296894559, 0.3333333333333333703, 0.3219752754296894559, 0.3333333333333333703, 0.3219752754296894559, 0.3333333333333333703, 0.3219752754296894559, 0.3333333333333333703, 0.3219752754296894559, 0.3333333333333333703, 0.3219752754296894559, 0.3333333333333333703, 0.3219752754296894559, 0.3333333333333333703, 0.3219752754296894559, 0.3333333333333333703, 0.3219752754296894559, 0.3333333333333333703, 0.3219752754296894559, 0.3333333333333333703, 0.3219752754296894559, 0.3333333333333333703, 0.3219752754296894559, 0.3333333333333333703, 0.3219752754296894559, 0.3333333333333333703, 0.3219752754296894559, 0.3333333333333333703, 0.3219752754296894559, 0.3333333333333333703, 0.3219752754296894559, 0.3333333333333333703, 0.3219752754296894559, 0.3333333333333333703, 0.3219752754296894559, 0.3333333333333333703, 0.3219752754296894559, 0.3333333333333333703, 0.3219752754296894559, 0.3333333333333333703, 0.3219752754296894559, 0.3333333333333333703, 0.3219752754296894559, 0.3333333333333333703, 0.3219752754296894559, 0.3333333333333333703, 0.3219752754296894559, 0.3333333333333333703, 0.3219752754296894559, 0.3333333333333333703, 0.3219752754296894559, 0.3333333333333333703, 0.3219752754296894559, 0.3333333333333333703, 0.3219752754296894559, 0.3333333333333333703, 0.3219752754296894559, 0.3333333333333333703, 0.3219752754296894559, 0.3333333333333333703, 0.3219752754296894559, 0.3333333333333333703, 0.3219752754296894559, 0.3333333333333333703, 0.3219752754296894559, 0.3333333333333333703, 0.3219752754296894559, 0.3333333333333333703, 0.3219752754296894559, 0.3333333333333333703, 0.3219752754296894559, 0.3333333333333333703, 0.3219752754296894559, 0.3333333333333333703, 0.3219752754296894559, 0.3333333333333333703, 0.3219752754296894559, 0.3333333333333333703, 0.3219752754296894559, 0.3333333333333333703, 0.3219752754296894559, 0.3333333333333333703, 0.3219752754296894559, 0.3333333333333333703, 0.3219752754296894559, 0.3333333333333333703, 0.3219752754296894559, 0.3333333333333333703, 0.3219752754296894559, 0.3333333333333333703, 0.3219752754296894559, 0.3333333333333333703, 0.3219752754296894559, 0.3333333333333333703, 0.3219752754296894559, 0.3333333333333333703, 0.3219752754296894559, 0.3333333333333333703, 0.3219752754296894559, 0.3333333333333333703, 0.3219752754296894559, 0.3333333333333333703, 0.3219752754296894559, 0.3333333333333333703, 0.3219752754296894559, 0.3333333333333333703, 0.3219752754296894559, 0.3333333333333333703, 0.3219752754296894559, 0.3333333333333333703, 0.3219752754296894559, 0.3333333333333333703, 0.3219752754296894559, 0.3333333333333333703, 0.3219752754296894559, 0.3333333333333333703, 0.3219752754296894559, 0.3333333333333333703, 0.3219752754296894559, 0.3333333333333333703, 0.3219752754296894559, 0.3333333333333333703, 0.3219752754296894559, 0.3333333333333333703, 0.3219752754296894559, 0.3333333333333333703, 0.3219752754296894559, 0.3333333333333333703, 0.3219752754296894559, 0.3333333333333333703, 0.3219752754296894559, 0.3333333333333333703, 0.3219752754296894559, 0.3333333333333333703, 0.3219752754296894559, 0.3333333333333333703, 0.3219752754296894559, 0.3333333333333333703, 0.3219752754296894559, 0.3333333333333333703, 0.3219752754296894559, 0.3333333333333333703, 0.3219752754296894559, 0.3333333333333333703, 0.3219752754296894559, 0.3333333333333333703, 0.3219752754296894559, 0.3333333333333333703, 0.3219752754296894559, 0.3333333333333333703, 0.3219752754296894559, 0.3333333333333333703, 0.3219752754296894559, 0.3333333333333333703, 0.3219752754296894559, 0.3333333333333333703, 0.3219752754296894559, 0.3333333333333333703, 0.3219752754296894559, 0.3333333333333333703, 0.3219752754296894559, 0.3333333333333333703, 0.3219752754296894559, 0.3333333333333333703, 0.3219752754296894559, 0.3333333333333333703, 0.3219752754296894559, 0.3333333333333333703, 0.3219752754296894559, 0.3333333333333333703, 0.3219752754296894559, 0.3333333333333333703, 0.3219752754296894559, 0.3333333333333333703, 0.3219752754296894559, 0.3333333333333333703, 0.3219752754296894559, 0.3333333333333333703, 0.3219752754296894559, 0.3333333333333333703, 0.3219752754296894559, 0.3333333333333333703, 0.3219752754296894559, 0.3333333333333333703, 0.3219752754296894559, 0.3333333333333333703, 0.3219752754296894559, 0.3333333333333333703, 0.3219752754296894559, 0.3333333333333333703, 0.3219752754296894559, 0.3333333333333333703, 0.3219752754296894559, 0.3333333333333333703, 0.3219752754296894559, 0.3333333333333333703, 0.3219752754296894559, 0.3333333333333333703, 0.3219752754296894559, 0.3333333333333333703, 0.3219752754296894559, 0.3333333333333333703, 0.3219752754296894559, 0.3333333333333333703, 0.3219752754296894559, 0.3333333333333333703, 0.3219752754296894559, 0.3333333333333333703, 0.3219752754296894559, 0.3333333333333333703, 0.3219752754296894559, 0.3333333333333333703, 0.3219752754296894559, 0.3333333333333333703, 0.3219752754296894559, 0.3333333333333333703, 0.3219752754296894559, 0.3333333333333333703, 0.3219752754296894559, 0.3333333333333333703, 0.3219752754296894559, 0.3333333333333333703, 0.3219752754296894559, 0.3333333333333333703, 0.3219752754296894559, 0.3333333333333333703, 0.3219752754296894559, 0.3333333333333333703, 0.3219752754296894559, 0.3333333333333333703, 0.3219752754296894559, 0.3333333333333333703, 0.3219752754296894559, 0.3333333333333333703, 0.3219752754296894559, 0.3333333333333333703, 0.3219752754296894559, 0.3333333333333333703, 0.3219752754296894559, 0.3333333333333333703, 0.3219752754296894559, 0.3333333333333333703, 0.3219752754296894559, 0.3333333333333333703, 0.3219752754296894559, 0.3333333333333333703, 0.3219752754296894559, 0.3333333333333333703, 0.3219752754296894559, 0.3333333333333333703, 0.3219752754296894559, 0.3333333333333333703, 0.3219752754296894559, 0.3333333333333333703, 0.3219752754296894559, 0.3333333333333333703, 0.3219752754296894559, 0.3333333333333333703, 0.3219752754296894559, 0.3333333333333333703, 0.3219752754296894559, 0.3333333333333333703, 0.3219752754296894559, 0.3333333333333333703, 0.3219752754296894559, 0.3333333333333333703, 0.3219752754296894559, 0.3333333333333333703, 0.3219752754296894559, 0.3333333333333333703, 0.3219752754296894559, 0.3333333333333333703, 0.3219752754296894559, 0.3333333333333333703, 0.3219752754296894559, 0.3333333333333333703, 0.3219752754296894559, 0.3333333333333333703, 0.3219752754296894559, 0.3333333333333333703, 0.3219752754296894559, 0.3333333333333333703, 0.3219752754296894559, 0.3333333333333333703, 0.3219752754296894559, 0.3333333333333333703, 0.3219752754296894559, 0.3333333333333333703, 0.3219752754296894559, 0.3333333333333333703),
 ( 0.3333333333333333703, 0.3219752754296894559, 0.3333333333333333703, 0.3219752754296894559, 0.3333333333333333703, 0.3219752754296894559, 0.3333333333333333703, 0.3219752754296894559, 0.3333333333333333703, 0.3219752754296894559, 0.3333333333333333703, 0.3219752754296894559, 0.3333333333333333703, 0.3219752754296894559, 0.3333333333333333703, 0.3219752754296894559, 0.3333333333333333703, 0.3219752754296894559, 0.3333333333333333703, 0.3219752754296894559, 0.3333333333333333703, 0.3219752754296894559, 0.3333333333333333703, 0.3219752754296894559, 0.3333333333333333703, 0.3219752754296894559, 0.3333333333333333703, 0.3219752754296894559, 0.3333333333333333703, 0.3219752754296894559, 0.3333333333333333703, 0.3219752754296894559, 0.3333333333333333703, 0.3219752754296894559, 0.3333333333333333703, 0.3219752754296894559, 0.3333333333333333703, 0.3219752754296894559, 0.3333333333333333703, 0.3219752754296894559, 0.3333333333333333703, 0.3219752754296894559, 0.3333333333333333703, 0.3219752754296894559, 0.3333333333333333703, 0.3219752754296894559, 0.3333333333333333703, 0.3219752754296894559, 0.3333333333333333703, 0.3219752754296894559, 0.3333333333333333703, 0.3219752754296894559, 0.3333333333333333703, 0.3219752754296894559, 0.3333333333333333703, 0.3219752754296894559, 0.3333333333333333703, 0.3219752754296894559, 0.3333333333333333703, 0.3219752754296894559, 0.3333333333333333703, 0.3219752754296894559, 0.3333333333333333703, 0.3219752754296894559, 0.3333333333333333703, 0.3219752754296894559, 0.3333333333333333703, 0.3219752754296894559, 0.3333333333333333703, 0.3219752754296894559, 0.3333333333333333703, 0.3219752754296894559, 0.3333333333333333703, 0.3219752754296894559, 0.3333333333333333703, 0.3219752754296894559, 0.3333333333333333703, 0.3219752754296894559, 0.3333333333333333703, 0.3219752754296894559, 0.3333333333333333703, 0.3219752754296894559, 0.3333333333333333703, 0.3219752754296894559, 0.3333333333333333703, 0.3219752754296894559, 0.3333333333333333703, 0.3219752754296894559, 0.3333333333333333703, 0.3219752754296894559, 0.3333333333333333703, 0.3219752754296894559, 0.3333333333333333703, 0.3219752754296894559, 0.3333333333333333703, 0.3219752754296894559, 0.3333333333333333703, 0.3219752754296894559, 0.3333333333333333703, 0.3219752754296894559, 0.3333333333333333703, 0.3219752754296894559, 0.3333333333333333703, 0.3219752754296894559, 0.3333333333333333703, 0.3219752754296894559, 0.3333333333333333703, 0.3219752754296894559, 0.3333333333333333703, 0.3219752754296894559, 0.3333333333333333703, 0.3219752754296894559, 0.3333333333333333703, 0.3219752754296894559, 0.3333333333333333703, 0.3219752754296894559, 0.3333333333333333703, 0.3219752754296894559, 0.3333333333333333703, 0.3219752754296894559, 0.3333333333333333703, 0.3219752754296894559, 0.3333333333333333703, 0.3219752754296894559, 0.3333333333333333703, 0.3219752754296894559, 0.3333333333333333703, 0.3219752754296894559, 0.3333333333333333703, 0.3219752754296894559, 0.3333333333333333703, 0.3219752754296894559, 0.3333333333333333703, 0.3219752754296894559, 0.3333333333333333703, 0.3219752754296894559, 0.3333333333333333703, 0.3219752754296894559, 0.3333333333333333703, 0.3219752754296894559, 0.3333333333333333703, 0.3219752754296894559, 0.3333333333333333703, 0.3219752754296894559, 0.3333333333333333703, 0.3219752754296894559, 0.3333333333333333703, 0.3219752754296894559, 0.3333333333333333703, 0.3219752754296894559, 0.3333333333333333703, 0.3219752754296894559, 0.3333333333333333703, 0.3219752754296894559, 0.3333333333333333703, 0.3219752754296894559, 0.3333333333333333703, 0.3219752754296894559, 0.3333333333333333703, 0.3219752754296894559, 0.3333333333333333703, 0.3219752754296894559, 0.3333333333333333703, 0.3219752754296894559, 0.3333333333333333703, 0.3219752754296894559, 0.3333333333333333703, 0.3219752754296894559, 0.3333333333333333703, 0.3219752754296894559, 0.3333333333333333703, 0.3219752754296894559, 0.3333333333333333703, 0.3219752754296894559, 0.3333333333333333703, 0.3219752754296894559, 0.3333333333333333703, 0.3219752754296894559, 0.3333333333333333703, 0.3219752754296894559, 0.3333333333333333703, 0.3219752754296894559, 0.3333333333333333703, 0.3219752754296894559, 0.3333333333333333703, 0.3219752754296894559, 0.3333333333333333703, 0.3219752754296894559, 0.3333333333333333703, 0.3219752754296894559, 0.3333333333333333703, 0.3219752754296894559, 0.3333333333333333703, 0.3219752754296894559, 0.3333333333333333703, 0.3219752754296894559, 0.3333333333333333703, 0.3219752754296894559, 0.3333333333333333703, 0.3219752754296894559, 0.3333333333333333703, 0.3219752754296894559, 0.3333333333333333703, 0.3219752754296894559, 0.3333333333333333703, 0.3219752754296894559, 0.3333333333333333703, 0.3219752754296894559, 0.3333333333333333703, 0.3219752754296894559, 0.3333333333333333703, 0.3219752754296894559, 0.3333333333333333703, 0.3219752754296894559, 0.3333333333333333703, 0.3219752754296894559, 0.3333333333333333703, 0.3219752754296894559, 0.3333333333333333703, 0.3219752754296894559, 0.3333333333333333703, 0.3219752754296894559, 0.3333333333333333703, 0.3219752754296894559, 0.3333333333333333703, 0.3219752754296894559, 0.3333333333333333703, 0.3219752754296894559, 0.3333333333333333703, 0.3219752754296894559, 0.3333333333333333703, 0.3219752754296894559, 0.3333333333333333703, 0.3219752754296894559, 0.3333333333333333703, 0.3219752754296894559, 0.3333333333333333703, 0.3219752754296894559, 0.3333333333333333703, 0.3219752754296894559, 0.3333333333333333703, 0.3219752754296894559, 0.3333333333333333703, 0.3219752754296894559, 0.3333333333333333703, 0.3219752754296894559, 0.3333333333333333703, 0.3219752754296894559, 0.3333333333333333703, 0.3219752754296894559, 0.3333333333333333703, 0.3219752754296894559, 0.3333333333333333703, 0.3219752754296894559, 0.3333333333333333703, 0.3219752754296894559, 0.3333333333333333703, 0.3219752754296894559, 0.3333333333333333703, 0.3219752754296894559, 0.3333333333333333703, 0.3219752754296894559, 0.3333333333333333703, 0.3219752754296894559, 0.3333333333333333703, 0.3219752754296894559, 0.3333333333333333703, 0.3219752754296894559, 0.3333333333333333703, 0.3219752754296894559, 0.3333333333333333703, 0.3219752754296894559, 0.3333333333333333703, 0.3219752754296894559, 0.3333333333333333703, 0.3219752754296894559, 0.3333333333333333703, 0.3219752754296894559, 0.3333333333333333703, 0.3219752754296894559, 0.3333333333333333703, 0.3219752754296894559, 0.3333333333333333703, 0.3219752754296894559, 0.3333333333333333703, 0.3219752754296894559, 0.3333333333333333703, 0.3219752754296894559, 0.3333333333333333703, 0.3219752754296894559, 0.3333333333333333703, 0.3219752754296894559, 0.3333333333333333703, 0.3219752754296894559, 0.3333333333333333703, 0.3219752754296894559, 0.3333333333333333703, 0.3219752754296894559, 0.3333333333333333703, 0.3219752754296894559, 0.3333333333333333703, 0.3219752754296894559, 0.3333333333333333703, 0.3219752754296894559, 0.3333333333333333703, 0.3219752754296894559, 0.3333333333333333703, 0.3219752754296894559, 0.3333333333333333703, 0.3219752754296894559, 0.3333333333333333703, 0.3219752754296894559, 0.3333333333333333703, 0.3219752754296894559, 0.3333333333333333703, 0.3219752754296894559, 0.3333333333333333703, 0.3219752754296894559, 0.3333333333333333703, 0.3219752754296894559, 0.3333333333333333703, 0.3219752754296894559, 0.3333333333333333703, 0.3219752754296894559, 0.3333333333333333703, 0.3219752754296894559, 0.3333333333333333703, 0.3219752754296894559, 0.3333333333333333703, 0.3219752754296894559, 0.3333333333333333703, 0.3219752754296894559, 0.3333333333333333703, 0.3219752754296894559, 0.3333333333333333703, 0.3219752754296894559, 0.3333333333333333703, 0.3219752754296894559, 0.3333333333333333703, 0.3219752754296894559, 0.3333333333333333703, 0.3219752754296894559, 0.3333333333333333703, 0.3219752754296894559, 0.3333333333333333703, 0.3219752754296894559, 0.3333333333333333703, 0.3219752754296894559, 0.3333333333333333703, 0.3219752754296894559, 0.3333333333333333703, 0.3219752754296894559, 0.3333333333333333703, 0.3219752754296894559, 0.3333333333333333703, 0.3219752754296894559, 0.3333333333333333703, 0.3219752754296894559, 0.3333333333333333703, 0.3219752754296894559, 0.3333333333333333703, 0.3219752754296894559, 0.3333333333333333703, 0.3219752754296894559, 0.3333333333333333703, 0.3219752754296894559, 0.3333333333333333703, 0.3219752754296894559, 0.3333333333333333703, 0.3219752754296894559, 0.3333333333333333703, 0.3219752754296894559, 0.3333333333333333703, 0.3219752754296894559, 0.3333333333333333703, 0.3219752754296894559, 0.3333333333333333703, 0.3219752754296894559, 0.3333333333333333703, 0.3219752754296894559, 0.3333333333333333703, 0.3219752754296894559, 0.3333333333333333703, 0.3219752754296894559, 0.3333333333333333703, 0.3219752754296894559, 0.3333333333333333703, 0.3219752754296894559, 0.3333333333333333703, 0.3219752754296894559, 0.3333333333333333703, 0.3219752754296894559, 0.3333333333333333703, 0.3219752754296894559, 0.3333333333333333703, 0.3219752754296894559, 0.3333333333333333703, 0.3219752754296894559, 0.3333333333333333703, 0.3219752754296894559, 0.3333333333333333703, 0.3219752754296894559, 0.3333333333333333703, 0.3219752754296894559, 0.3333333333333333703, 0.3219752754296894559, 0.3333333333333333703, 0.3219752754296894559, 0.3333333333333333703, 0.3219752754296894559, 0.3333333333333333703, 0.3219752754296894559, 0.3333333333333333703, 0.3219752754296894559, 0.3333333333333333703, 0.3219752754296894559, 0.3333333333333333703, 0.3219752754296894559, 0.3333333333333333703, 0.3219752754296894559, 0.3333333333333333703, 0.3219752754296894559, 0.3333333333333333703, 0.3219752754296894559, 0.3333333333333333703, 0.3219752754296894559, 0.3333333333333333703, 0.3219752754296894559, 0.3333333333333333703, 0.3219752754296894559, 0.3333333333333333703, 0.3219752754296894559, 0.3333333333333333703, 0.3219752754296894559, 0.3333333333333333703, 0.3219752754296894559, 0.3333333333333333703, 0.3219752754296894559, 0.3333333333333333703, 0.3219752754296894559, 0.3333333333333333703, 0.3219752754296894559, 0.3333333333333333703, 0.3219752754296894559, 0.3333333333333333703, 0.3219752754296894559, 0.3333333333333333703, 0.3219752754296894559, 0.3333333333333333703, 0.3219752754296894559, 0.3333333333333333703, 0.3219752754296894559, 0.3333333333333333703, 0.3219752754296894559, 0.3333333333333333703, 0.3219752754296894559, 0.3333333333333333703),
 ( 1.000000000000000000, 0.9659258262890683122, 1.000000000000000000, 0.9659258262890683122, 1.000000000000000000, 0.9659258262890683122, 1.000000000000000000, 0.9659258262890683122, 1.000000000000000000, 0.9659258262890683122, 1.000000000000000000, 0.9659258262890683122, 1.000000000000000000, 0.9659258262890683122, 1.000000000000000000, 0.9659258262890683122, 1.000000000000000000, 0.9659258262890683122, 1.000000000000000000, 0.9659258262890683122, 1.000000000000000000, 0.9659258262890683122, 1.000000000000000000, 0.9659258262890683122, 1.000000000000000000, 0.9659258262890683122, 1.000000000000000000, 0.9659258262890683122, 1.000000000000000000, 0.9659258262890683122, 1.000000000000000000, 0.9659258262890683122, 1.000000000000000000, 0.9659258262890683122, 1.000000000000000000, 0.9659258262890683122, 1.000000000000000000, 0.9659258262890683122, 1.000000000000000000, 0.9659258262890683122, 1.000000000000000000, 0.9659258262890683122, 1.000000000000000000, 0.9659258262890683122, 1.000000000000000000, 0.9659258262890683122, 1.000000000000000000, 0.9659258262890683122, 1.000000000000000000, 0.9659258262890683122, 1.000000000000000000, 0.9659258262890683122, 1.000000000000000000, 0.9659258262890683122, 1.000000000000000000, 0.9659258262890683122, 1.000000000000000000, 0.9659258262890683122, 1.000000000000000000, 0.9659258262890683122, 1.000000000000000000, 0.9659258262890683122, 1.000000000000000000, 0.9659258262890683122, 1.000000000000000000, 0.9659258262890683122, 1.000000000000000000, 0.9659258262890683122, 1.000000000000000000, 0.9659258262890683122, 1.000000000000000000, 0.9659258262890683122, 1.000000000000000000, 0.9659258262890683122, 1.000000000000000000, 0.9659258262890683122, 1.000000000000000000, 0.9659258262890683122, 1.000000000000000000, 0.9659258262890683122, 1.000000000000000000, 0.9659258262890683122, 1.000000000000000000, 0.9659258262890683122, 1.000000000000000000, 0.9659258262890683122, 1.000000000000000000, 0.9659258262890683122, 1.000000000000000000, 0.9659258262890683122, 1.000000000000000000, 0.9659258262890683122, 1.000000000000000000, 0.9659258262890683122, 1.000000000000000000, 0.9659258262890683122, 1.000000000000000000, 0.9659258262890683122, 1.000000000000000000, 0.9659258262890683122, 1.000000000000000000, 0.9659258262890683122, 1.000000000000000000, 0.9659258262890683122, 1.000000000000000000, 0.9659258262890683122, 1.000000000000000000, 0.9659258262890683122, 1.000000000000000000, 0.9659258262890683122, 1.000000000000000000, 0.9659258262890683122, 1.000000000000000000, 0.9659258262890683122, 1.000000000000000000, 0.9659258262890683122, 1.000000000000000000, 0.9659258262890683122, 1.000000000000000000, 0.9659258262890683122, 1.000000000000000000, 0.9659258262890683122, 1.000000000000000000, 0.9659258262890683122, 1.000000000000000000, 0.9659258262890683122, 1.000000000000000000, 0.9659258262890683122, 1.000000000000000000, 0.9659258262890683122, 1.000000000000000000, 0.9659258262890683122, 1.000000000000000000, 0.9659258262890683122, 1.000000000000000000, 0.9659258262890683122, 1.000000000000000000, 0.9659258262890683122, 1.000000000000000000, 0.9659258262890683122, 1.000000000000000000, 0.9659258262890683122, 1.000000000000000000, 0.9659258262890683122, 1.000000000000000000, 0.9659258262890683122, 1.000000000000000000, 0.9659258262890683122, 1.000000000000000000, 0.9659258262890683122, 1.000000000000000000, 0.9659258262890683122, 1.000000000000000000, 0.9659258262890683122, 1.000000000000000000, 0.9659258262890683122, 1.000000000000000000, 0.9659258262890683122, 1.000000000000000000, 0.9659258262890683122, 1.000000000000000000, 0.9659258262890683122, 1.000000000000000000, 0.9659258262890683122, 1.000000000000000000, 0.9659258262890683122, 1.000000000000000000, 0.9659258262890683122, 1.000000000000000000, 0.9659258262890683122, 1.000000000000000000, 0.9659258262890683122, 1.000000000000000000, 0.9659258262890683122, 1.000000000000000000, 0.9659258262890683122, 1.000000000000000000, 0.9659258262890683122, 1.000000000000000000, 0.9659258262890683122, 1.000000000000000000, 0.9659258262890683122, 1.000000000000000000, 0.9659258262890683122, 1.000000000000000000, 0.9659258262890683122, 1.000000000000000000, 0.9659258262890683122, 1.000000000000000000, 0.9659258262890683122, 1.000000000000000000, 0.9659258262890683122, 1.000000000000000000, 0.9659258262890683122, 1.000000000000000000, 0.9659258262890683122, 1.000000000000000000, 0.9659258262890683122, 1.000000000000000000, 0.9659258262890683122, 1.000000000000000000, 0.9659258262890683122, 1.000000000000000000, 0.9659258262890683122, 1.000000000000000000, 0.9659258262890683122, 1.000000000000000000, 0.9659258262890683122, 1.000000000000000000, 0.9659258262890683122, 1.000000000000000000, 0.9659258262890683122, 1.000000000000000000, 0.9659258262890683122, 1.000000000000000000, 0.9659258262890683122, 1.000000000000000000, 0.9659258262890683122, 1.000000000000000000, 0.9659258262890683122, 1.000000000000000000, 0.9659258262890683122, 1.000000000000000000, 0.9659258262890683122, 1.000000000000000000, 0.9659258262890683122, 1.000000000000000000, 0.9659258262890683122, 1.000000000000000000, 0.9659258262890683122, 1.000000000000000000, 0.9659258262890683122, 1.000000000000000000, 0.9659258262890683122, 1.000000000000000000, 0.9659258262890683122, 1.000000000000000000, 0.9659258262890683122, 1.000000000000000000, 0.9659258262890683122, 1.000000000000000000, 0.9659258262890683122, 1.000000000000000000, 0.9659258262890683122, 1.000000000000000000, 0.9659258262890683122, 1.000000000000000000, 0.9659258262890683122, 1.000000000000000000, 0.9659258262890683122, 1.000000000000000000, 0.9659258262890683122, 1.000000000000000000, 0.9659258262890683122, 1.000000000000000000, 0.9659258262890683122, 1.000000000000000000, 0.9659258262890683122, 1.000000000000000000, 0.9659258262890683122, 1.000000000000000000, 0.9659258262890683122, 1.000000000000000000, 0.9659258262890683122, 1.000000000000000000, 0.9659258262890683122, 1.000000000000000000, 0.9659258262890683122, 1.000000000000000000, 0.9659258262890683122, 1.000000000000000000, 0.9659258262890683122, 1.000000000000000000, 0.9659258262890683122, 1.000000000000000000, 0.9659258262890683122, 1.000000000000000000, 0.9659258262890683122, 1.000000000000000000, 0.9659258262890683122, 1.000000000000000000, 0.9659258262890683122, 1.000000000000000000, 0.9659258262890683122, 1.000000000000000000, 0.9659258262890683122, 1.000000000000000000, 0.9659258262890683122, 1.000000000000000000, 0.9659258262890683122, 1.000000000000000000, 0.9659258262890683122, 1.000000000000000000, 0.9659258262890683122, 1.000000000000000000, 0.9659258262890683122, 1.000000000000000000, 0.9659258262890683122, 1.000000000000000000, 0.9659258262890683122, 1.000000000000000000, 0.9659258262890683122, 1.000000000000000000, 0.9659258262890683122, 1.000000000000000000, 0.9659258262890683122, 1.000000000000000000, 0.9659258262890683122, 1.000000000000000000, 0.9659258262890683122, 1.000000000000000000, 0.9659258262890683122, 1.000000000000000000, 0.9659258262890683122, 1.000000000000000000, 0.9659258262890683122, 1.000000000000000000, 0.9659258262890683122, 1.000000000000000000, 0.9659258262890683122, 1.000000000000000000, 0.9659258262890683122, 1.000000000000000000, 0.9659258262890683122, 1.000000000000000000, 0.9659258262890683122, 1.000000000000000000, 0.9659258262890683122, 1.000000000000000000, 0.9659258262890683122, 1.000000000000000000, 0.9659258262890683122, 1.000000000000000000, 0.9659258262890683122, 1.000000000000000000, 0.9659258262890683122, 1.000000000000000000, 0.9659258262890683122, 1.000000000000000000, 0.9659258262890683122, 1.000000000000000000, 0.9659258262890683122, 1.000000000000000000, 0.9659258262890683122, 1.000000000000000000, 0.9659258262890683122, 1.000000000000000000, 0.9659258262890683122, 1.000000000000000000, 0.9659258262890683122, 1.000000000000000000, 0.9659258262890683122, 1.000000000000000000, 0.9659258262890683122, 1.000000000000000000, 0.9659258262890683122, 1.000000000000000000, 0.9659258262890683122, 1.000000000000000000, 0.9659258262890683122, 1.000000000000000000, 0.9659258262890683122, 1.000000000000000000, 0.9659258262890683122, 1.000000000000000000, 0.9659258262890683122, 1.000000000000000000, 0.9659258262890683122, 1.000000000000000000, 0.9659258262890683122, 1.000000000000000000, 0.9659258262890683122, 1.000000000000000000, 0.9659258262890683122, 1.000000000000000000, 0.9659258262890683122, 1.000000000000000000, 0.9659258262890683122, 1.000000000000000000, 0.9659258262890683122, 1.000000000000000000, 0.9659258262890683122, 1.000000000000000000, 0.9659258262890683122, 1.000000000000000000, 0.9659258262890683122, 1.000000000000000000, 0.9659258262890683122, 1.000000000000000000, 0.9659258262890683122, 1.000000000000000000, 0.9659258262890683122, 1.000000000000000000, 0.9659258262890683122, 1.000000000000000000, 0.9659258262890683122, 1.000000000000000000, 0.9659258262890683122, 1.000000000000000000, 0.9659258262890683122, 1.000000000000000000, 0.9659258262890683122, 1.000000000000000000, 0.9659258262890683122, 1.000000000000000000, 0.9659258262890683122, 1.000000000000000000, 0.9659258262890683122, 1.000000000000000000, 0.9659258262890683122, 1.000000000000000000, 0.9659258262890683122, 1.000000000000000000, 0.9659258262890683122, 1.000000000000000000, 0.9659258262890683122, 1.000000000000000000, 0.9659258262890683122, 1.000000000000000000, 0.9659258262890683122, 1.000000000000000000, 0.9659258262890683122, 1.000000000000000000, 0.9659258262890683122, 1.000000000000000000, 0.9659258262890683122, 1.000000000000000000, 0.9659258262890683122, 1.000000000000000000, 0.9659258262890683122, 1.000000000000000000, 0.9659258262890683122, 1.000000000000000000, 0.9659258262890683122, 1.000000000000000000, 0.9659258262890683122, 1.000000000000000000, 0.9659258262890683122, 1.000000000000000000, 0.9659258262890683122, 1.000000000000000000, 0.9659258262890683122, 1.000000000000000000, 0.9659258262890683122, 1.000000000000000000, 0.9659258262890683122, 1.000000000000000000, 0.9659258262890683122, 1.000000000000000000, 0.9659258262890683122, 1.000000000000000000, 0.9659258262890683122, 1.000000000000000000, 0.9659258262890683122, 1.000000000000000000, 0.9659258262890683122, 1.000000000000000000),
 ( 0.3333333333333333703, 0.3219752754296894559, 0.3333333333333333703, 0.3219752754296894559, 0.3333333333333333703, 0.3219752754296894559, 0.3333333333333333703, 0.3219752754296894559, 0.3333333333333333703, 0.3219752754296894559, 0.3333333333333333703, 0.3219752754296894559, 0.3333333333333333703, 0.3219752754296894559, 0.3333333333333333703, 0.3219752754296894559, 0.3333333333333333703, 0.3219752754296894559, 0.3333333333333333703, 0.3219752754296894559, 0.3333333333333333703, 0.3219752754296894559, 0.3333333333333333703, 0.3219752754296894559, 0.3333333333333333703, 0.3219752754296894559, 0.3333333333333333703, 0.3219752754296894559, 0.3333333333333333703, 0.3219752754296894559, 0.3333333333333333703, 0.3219752754296894559, 0.3333333333333333703, 0.3219752754296894559, 0.3333333333333333703, 0.3219752754296894559, 0.3333333333333333703, 0.3219752754296894559, 0.3333333333333333703, 0.3219752754296894559, 0.3333333333333333703, 0.3219752754296894559, 0.3333333333333333703, 0.3219752754296894559, 0.3333333333333333703, 0.3219752754296894559, 0.3333333333333333703, 0.3219752754296894559, 0.3333333333333333703, 0.3219752754296894559, 0.3333333333333333703, 0.3219752754296894559, 0.3333333333333333703, 0.3219752754296894559, 0.3333333333333333703, 0.3219752754296894559, 0.3333333333333333703, 0.3219752754296894559, 0.3333333333333333703, 0.3219752754296894559, 0.3333333333333333703, 0.3219752754296894559, 0.3333333333333333703, 0.3219752754296894559, 0.3333333333333333703, 0.3219752754296894559, 0.3333333333333333703, 0.3219752754296894559, 0.3333333333333333703, 0.3219752754296894559, 0.3333333333333333703, 0.3219752754296894559, 0.3333333333333333703, 0.3219752754296894559, 0.3333333333333333703, 0.3219752754296894559, 0.3333333333333333703, 0.3219752754296894559, 0.3333333333333333703, 0.3219752754296894559, 0.3333333333333333703, 0.3219752754296894559, 0.3333333333333333703, 0.3219752754296894559, 0.3333333333333333703, 0.3219752754296894559, 0.3333333333333333703, 0.3219752754296894559, 0.3333333333333333703, 0.3219752754296894559, 0.3333333333333333703, 0.3219752754296894559, 0.3333333333333333703, 0.3219752754296894559, 0.3333333333333333703, 0.3219752754296894559, 0.3333333333333333703, 0.3219752754296894559, 0.3333333333333333703, 0.3219752754296894559, 0.3333333333333333703, 0.3219752754296894559, 0.3333333333333333703, 0.3219752754296894559, 0.3333333333333333703, 0.3219752754296894559, 0.3333333333333333703, 0.3219752754296894559, 0.3333333333333333703, 0.3219752754296894559, 0.3333333333333333703, 0.3219752754296894559, 0.3333333333333333703, 0.3219752754296894559, 0.3333333333333333703, 0.3219752754296894559, 0.3333333333333333703, 0.3219752754296894559, 0.3333333333333333703, 0.3219752754296894559, 0.3333333333333333703, 0.3219752754296894559, 0.3333333333333333703, 0.3219752754296894559, 0.3333333333333333703, 0.3219752754296894559, 0.3333333333333333703, 0.3219752754296894559, 0.3333333333333333703, 0.3219752754296894559, 0.3333333333333333703, 0.3219752754296894559, 0.3333333333333333703, 0.3219752754296894559, 0.3333333333333333703, 0.3219752754296894559, 0.3333333333333333703, 0.3219752754296894559, 0.3333333333333333703, 0.3219752754296894559, 0.3333333333333333703, 0.3219752754296894559, 0.3333333333333333703, 0.3219752754296894559, 0.3333333333333333703, 0.3219752754296894559, 0.3333333333333333703, 0.3219752754296894559, 0.3333333333333333703, 0.3219752754296894559, 0.3333333333333333703, 0.3219752754296894559, 0.3333333333333333703, 0.3219752754296894559, 0.3333333333333333703, 0.3219752754296894559, 0.3333333333333333703, 0.3219752754296894559, 0.3333333333333333703, 0.3219752754296894559, 0.3333333333333333703, 0.3219752754296894559, 0.3333333333333333703, 0.3219752754296894559, 0.3333333333333333703, 0.3219752754296894559, 0.3333333333333333703, 0.3219752754296894559, 0.3333333333333333703, 0.3219752754296894559, 0.3333333333333333703, 0.3219752754296894559, 0.3333333333333333703, 0.3219752754296894559, 0.3333333333333333703, 0.3219752754296894559, 0.3333333333333333703, 0.3219752754296894559, 0.3333333333333333703, 0.3219752754296894559, 0.3333333333333333703, 0.3219752754296894559, 0.3333333333333333703, 0.3219752754296894559, 0.3333333333333333703, 0.3219752754296894559, 0.3333333333333333703, 0.3219752754296894559, 0.3333333333333333703, 0.3219752754296894559, 0.3333333333333333703, 0.3219752754296894559, 0.3333333333333333703, 0.3219752754296894559, 0.3333333333333333703, 0.3219752754296894559, 0.3333333333333333703, 0.3219752754296894559, 0.3333333333333333703, 0.3219752754296894559, 0.3333333333333333703, 0.3219752754296894559, 0.3333333333333333703, 0.3219752754296894559, 0.3333333333333333703, 0.3219752754296894559, 0.3333333333333333703, 0.3219752754296894559, 0.3333333333333333703, 0.3219752754296894559, 0.3333333333333333703, 0.3219752754296894559, 0.3333333333333333703, 0.3219752754296894559, 0.3333333333333333703, 0.3219752754296894559, 0.3333333333333333703, 0.3219752754296894559, 0.3333333333333333703, 0.3219752754296894559, 0.3333333333333333703, 0.3219752754296894559, 0.3333333333333333703, 0.3219752754296894559, 0.3333333333333333703, 0.3219752754296894559, 0.3333333333333333703, 0.3219752754296894559, 0.3333333333333333703, 0.3219752754296894559, 0.3333333333333333703, 0.3219752754296894559, 0.3333333333333333703, 0.3219752754296894559, 0.3333333333333333703, 0.3219752754296894559, 0.3333333333333333703, 0.3219752754296894559, 0.3333333333333333703, 0.3219752754296894559, 0.3333333333333333703, 0.3219752754296894559, 0.3333333333333333703, 0.3219752754296894559, 0.3333333333333333703, 0.3219752754296894559, 0.3333333333333333703, 0.3219752754296894559, 0.3333333333333333703, 0.3219752754296894559, 0.3333333333333333703, 0.3219752754296894559, 0.3333333333333333703, 0.3219752754296894559, 0.3333333333333333703, 0.3219752754296894559, 0.3333333333333333703, 0.3219752754296894559, 0.3333333333333333703, 0.3219752754296894559, 0.3333333333333333703, 0.3219752754296894559, 0.3333333333333333703, 0.3219752754296894559, 0.3333333333333333703, 0.3219752754296894559, 0.3333333333333333703, 0.3219752754296894559, 0.3333333333333333703, 0.3219752754296894559, 0.3333333333333333703, 0.3219752754296894559, 0.3333333333333333703, 0.3219752754296894559, 0.3333333333333333703, 0.3219752754296894559, 0.3333333333333333703, 0.3219752754296894559, 0.3333333333333333703, 0.3219752754296894559, 0.3333333333333333703, 0.3219752754296894559, 0.3333333333333333703, 0.3219752754296894559, 0.3333333333333333703, 0.3219752754296894559, 0.3333333333333333703, 0.3219752754296894559, 0.3333333333333333703, 0.3219752754296894559, 0.3333333333333333703, 0.3219752754296894559, 0.3333333333333333703, 0.3219752754296894559, 0.3333333333333333703, 0.3219752754296894559, 0.3333333333333333703, 0.3219752754296894559, 0.3333333333333333703, 0.3219752754296894559, 0.3333333333333333703, 0.3219752754296894559, 0.3333333333333333703, 0.3219752754296894559, 0.3333333333333333703, 0.3219752754296894559, 0.3333333333333333703, 0.3219752754296894559, 0.3333333333333333703, 0.3219752754296894559, 0.3333333333333333703, 0.3219752754296894559, 0.3333333333333333703, 0.3219752754296894559, 0.3333333333333333703, 0.3219752754296894559, 0.3333333333333333703, 0.3219752754296894559, 0.3333333333333333703, 0.3219752754296894559, 0.3333333333333333703, 0.3219752754296894559, 0.3333333333333333703, 0.3219752754296894559, 0.3333333333333333703, 0.3219752754296894559, 0.3333333333333333703, 0.3219752754296894559, 0.3333333333333333703, 0.3219752754296894559, 0.3333333333333333703, 0.3219752754296894559, 0.3333333333333333703, 0.3219752754296894559, 0.3333333333333333703, 0.3219752754296894559, 0.3333333333333333703, 0.3219752754296894559, 0.3333333333333333703, 0.3219752754296894559, 0.3333333333333333703, 0.3219752754296894559, 0.3333333333333333703, 0.3219752754296894559, 0.3333333333333333703, 0.3219752754296894559, 0.3333333333333333703, 0.3219752754296894559, 0.3333333333333333703, 0.3219752754296894559, 0.3333333333333333703, 0.3219752754296894559, 0.3333333333333333703, 0.3219752754296894559, 0.3333333333333333703, 0.3219752754296894559, 0.3333333333333333703, 0.3219752754296894559, 0.3333333333333333703, 0.3219752754296894559, 0.3333333333333333703, 0.3219752754296894559, 0.3333333333333333703, 0.3219752754296894559, 0.3333333333333333703, 0.3219752754296894559, 0.3333333333333333703, 0.3219752754296894559, 0.3333333333333333703, 0.3219752754296894559, 0.3333333333333333703, 0.3219752754296894559, 0.3333333333333333703, 0.3219752754296894559, 0.3333333333333333703, 0.3219752754296894559, 0.3333333333333333703, 0.3219752754296894559, 0.3333333333333333703, 0.3219752754296894559, 0.3333333333333333703, 0.3219752754296894559, 0.3333333333333333703, 0.3219752754296894559, 0.3333333333333333703, 0.3219752754296894559, 0.3333333333333333703, 0.3219752754296894559, 0.3333333333333333703, 0.3219752754296894559, 0.3333333333333333703, 0.3219752754296894559, 0.3333333333333333703, 0.3219752754296894559, 0.3333333333333333703, 0.3219752754296894559, 0.3333333333333333703, 0.3219752754296894559, 0.3333333333333333703, 0.3219752754296894559, 0.3333333333333333703, 0.3219752754296894559, 0.3333333333333333703, 0.3219752754296894559, 0.3333333333333333703, 0.3219752754296894559, 0.3333333333333333703, 0.3219752754296894559, 0.3333333333333333703, 0.3219752754296894559, 0.3333333333333333703, 0.3219752754296894559, 0.3333333333333333703, 0.3219752754296894559, 0.3333333333333333703, 0.3219752754296894559, 0.3333333333333333703, 0.3219752754296894559, 0.3333333333333333703, 0.3219752754296894559, 0.3333333333333333703, 0.3219752754296894559, 0.3333333333333333703, 0.3219752754296894559, 0.3333333333333333703, 0.3219752754296894559, 0.3333333333333333703, 0.3219752754296894559, 0.3333333333333333703, 0.3219752754296894559, 0.3333333333333333703, 0.3219752754296894559, 0.3333333333333333703, 0.3219752754296894559, 0.3333333333333333703, 0.3219752754296894559, 0.3333333333333333703, 0.3219752754296894559, 0.3333333333333333703, 0.3219752754296894559, 0.3333333333333333703, 0.3219752754296894559, 0.3333333333333333703, 0.3219752754296894559, 0.3333333333333333703, 0.3219752754296894559, 0.3333333333333333703, 0.3219752754296894559, 0.3333333333333333703, 0.3219752754296894559, 0.3333333333333333703, 0.3219752754296894559, 0.3333333333333333703, 0.3219752754296894559, 0.3333333333333333703, 0.3219752754296894559, 0.3333333333333333703),
 ( 0.3333333333333333703, 0.3219752754296894559, 0.3333333333333333703, 0.3219752754296894559, 0.3333333333333333703, 0.3219752754296894559, 0.3333333333333333703, 0.3219752754296894559, 0.3333333333333333703, 0.3219752754296894559, 0.3333333333333333703, 0.3219752754296894559, 0.3333333333333333703, 0.3219752754296894559, 0.3333333333333333703, 0.3219752754296894559, 0.3333333333333333703, 0.3219752754296894559, 0.3333333333333333703, 0.3219752754296894559, 0.3333333333333333703, 0.3219752754296894559, 0.3333333333333333703, 0.3219752754296894559, 0.3333333333333333703, 0.3219752754296894559, 0.3333333333333333703, 0.3219752754296894559, 0.3333333333333333703, 0.3219752754296894559, 0.3333333333333333703, 0.3219752754296894559, 0.3333333333333333703, 0.3219752754296894559, 0.3333333333333333703, 0.3219752754296894559, 0.3333333333333333703, 0.3219752754296894559, 0.3333333333333333703, 0.3219752754296894559, 0.3333333333333333703, 0.3219752754296894559, 0.3333333333333333703, 0.3219752754296894559, 0.3333333333333333703, 0.3219752754296894559, 0.3333333333333333703, 0.3219752754296894559, 0.3333333333333333703, 0.3219752754296894559, 0.3333333333333333703, 0.3219752754296894559, 0.3333333333333333703, 0.3219752754296894559, 0.3333333333333333703, 0.3219752754296894559, 0.3333333333333333703, 0.3219752754296894559, 0.3333333333333333703, 0.3219752754296894559, 0.3333333333333333703, 0.3219752754296894559, 0.3333333333333333703, 0.3219752754296894559, 0.3333333333333333703, 0.3219752754296894559, 0.3333333333333333703, 0.3219752754296894559, 0.3333333333333333703, 0.3219752754296894559, 0.3333333333333333703, 0.3219752754296894559, 0.3333333333333333703, 0.3219752754296894559, 0.3333333333333333703, 0.3219752754296894559, 0.3333333333333333703, 0.3219752754296894559, 0.3333333333333333703, 0.3219752754296894559, 0.3333333333333333703, 0.3219752754296894559, 0.3333333333333333703, 0.3219752754296894559, 0.3333333333333333703, 0.3219752754296894559, 0.3333333333333333703, 0.3219752754296894559, 0.3333333333333333703, 0.3219752754296894559, 0.3333333333333333703, 0.3219752754296894559, 0.3333333333333333703, 0.3219752754296894559, 0.3333333333333333703, 0.3219752754296894559, 0.3333333333333333703, 0.3219752754296894559, 0.3333333333333333703, 0.3219752754296894559, 0.3333333333333333703, 0.3219752754296894559, 0.3333333333333333703, 0.3219752754296894559, 0.3333333333333333703, 0.3219752754296894559, 0.3333333333333333703, 0.3219752754296894559, 0.3333333333333333703, 0.3219752754296894559, 0.3333333333333333703, 0.3219752754296894559, 0.3333333333333333703, 0.3219752754296894559, 0.3333333333333333703, 0.3219752754296894559, 0.3333333333333333703, 0.3219752754296894559, 0.3333333333333333703, 0.3219752754296894559, 0.3333333333333333703, 0.3219752754296894559, 0.3333333333333333703, 0.3219752754296894559, 0.3333333333333333703, 0.3219752754296894559, 0.3333333333333333703, 0.3219752754296894559, 0.3333333333333333703, 0.3219752754296894559, 0.3333333333333333703, 0.3219752754296894559, 0.3333333333333333703, 0.3219752754296894559, 0.3333333333333333703, 0.3219752754296894559, 0.3333333333333333703, 0.3219752754296894559, 0.3333333333333333703, 0.3219752754296894559, 0.3333333333333333703, 0.3219752754296894559, 0.3333333333333333703, 0.3219752754296894559, 0.3333333333333333703, 0.3219752754296894559, 0.3333333333333333703, 0.3219752754296894559, 0.3333333333333333703, 0.3219752754296894559, 0.3333333333333333703, 0.3219752754296894559, 0.3333333333333333703, 0.3219752754296894559, 0.3333333333333333703, 0.3219752754296894559, 0.3333333333333333703, 0.3219752754296894559, 0.3333333333333333703, 0.3219752754296894559, 0.3333333333333333703, 0.3219752754296894559, 0.3333333333333333703, 0.3219752754296894559, 0.3333333333333333703, 0.3219752754296894559, 0.3333333333333333703, 0.3219752754296894559, 0.3333333333333333703, 0.3219752754296894559, 0.3333333333333333703, 0.3219752754296894559, 0.3333333333333333703, 0.3219752754296894559, 0.3333333333333333703, 0.3219752754296894559, 0.3333333333333333703, 0.3219752754296894559, 0.3333333333333333703, 0.3219752754296894559, 0.3333333333333333703, 0.3219752754296894559, 0.3333333333333333703, 0.3219752754296894559, 0.3333333333333333703, 0.3219752754296894559, 0.3333333333333333703, 0.3219752754296894559, 0.3333333333333333703, 0.3219752754296894559, 0.3333333333333333703, 0.3219752754296894559, 0.3333333333333333703, 0.3219752754296894559, 0.3333333333333333703, 0.3219752754296894559, 0.3333333333333333703, 0.3219752754296894559, 0.3333333333333333703, 0.3219752754296894559, 0.3333333333333333703, 0.3219752754296894559, 0.3333333333333333703, 0.3219752754296894559, 0.3333333333333333703, 0.3219752754296894559, 0.3333333333333333703, 0.3219752754296894559, 0.3333333333333333703, 0.3219752754296894559, 0.3333333333333333703, 0.3219752754296894559, 0.3333333333333333703, 0.3219752754296894559, 0.3333333333333333703, 0.3219752754296894559, 0.3333333333333333703, 0.3219752754296894559, 0.3333333333333333703, 0.3219752754296894559, 0.3333333333333333703, 0.3219752754296894559, 0.3333333333333333703, 0.3219752754296894559, 0.3333333333333333703, 0.3219752754296894559, 0.3333333333333333703, 0.3219752754296894559, 0.3333333333333333703, 0.3219752754296894559, 0.3333333333333333703, 0.3219752754296894559, 0.3333333333333333703, 0.3219752754296894559, 0.3333333333333333703, 0.3219752754296894559, 0.3333333333333333703, 0.3219752754296894559, 0.3333333333333333703, 0.3219752754296894559, 0.3333333333333333703, 0.3219752754296894559, 0.3333333333333333703, 0.3219752754296894559, 0.3333333333333333703, 0.3219752754296894559, 0.3333333333333333703, 0.3219752754296894559, 0.3333333333333333703, 0.3219752754296894559, 0.3333333333333333703, 0.3219752754296894559, 0.3333333333333333703, 0.3219752754296894559, 0.3333333333333333703, 0.3219752754296894559, 0.3333333333333333703, 0.3219752754296894559, 0.3333333333333333703, 0.3219752754296894559, 0.3333333333333333703, 0.3219752754296894559, 0.3333333333333333703, 0.3219752754296894559, 0.3333333333333333703, 0.3219752754296894559, 0.3333333333333333703, 0.3219752754296894559, 0.3333333333333333703, 0.3219752754296894559, 0.3333333333333333703, 0.3219752754296894559, 0.3333333333333333703, 0.3219752754296894559, 0.3333333333333333703, 0.3219752754296894559, 0.3333333333333333703, 0.3219752754296894559, 0.3333333333333333703, 0.3219752754296894559, 0.3333333333333333703, 0.3219752754296894559, 0.3333333333333333703, 0.3219752754296894559, 0.3333333333333333703, 0.3219752754296894559, 0.3333333333333333703, 0.3219752754296894559, 0.3333333333333333703, 0.3219752754296894559, 0.3333333333333333703, 0.3219752754296894559, 0.3333333333333333703, 0.3219752754296894559, 0.3333333333333333703, 0.3219752754296894559, 0.3333333333333333703, 0.3219752754296894559, 0.3333333333333333703, 0.3219752754296894559, 0.3333333333333333703, 0.3219752754296894559, 0.3333333333333333703, 0.3219752754296894559, 0.3333333333333333703, 0.3219752754296894559, 0.3333333333333333703, 0.3219752754296894559, 0.3333333333333333703, 0.3219752754296894559, 0.3333333333333333703, 0.3219752754296894559, 0.3333333333333333703, 0.3219752754296894559, 0.3333333333333333703, 0.3219752754296894559, 0.3333333333333333703, 0.3219752754296894559, 0.3333333333333333703, 0.3219752754296894559, 0.3333333333333333703, 0.3219752754296894559, 0.3333333333333333703, 0.3219752754296894559, 0.3333333333333333703, 0.3219752754296894559, 0.3333333333333333703, 0.3219752754296894559, 0.3333333333333333703, 0.3219752754296894559, 0.3333333333333333703, 0.3219752754296894559, 0.3333333333333333703, 0.3219752754296894559, 0.3333333333333333703, 0.3219752754296894559, 0.3333333333333333703, 0.3219752754296894559, 0.3333333333333333703, 0.3219752754296894559, 0.3333333333333333703, 0.3219752754296894559, 0.3333333333333333703, 0.3219752754296894559, 0.3333333333333333703, 0.3219752754296894559, 0.3333333333333333703, 0.3219752754296894559, 0.3333333333333333703, 0.3219752754296894559, 0.3333333333333333703, 0.3219752754296894559, 0.3333333333333333703, 0.3219752754296894559, 0.3333333333333333703, 0.3219752754296894559, 0.3333333333333333703, 0.3219752754296894559, 0.3333333333333333703, 0.3219752754296894559, 0.3333333333333333703, 0.3219752754296894559, 0.3333333333333333703, 0.3219752754296894559, 0.3333333333333333703, 0.3219752754296894559, 0.3333333333333333703, 0.3219752754296894559, 0.3333333333333333703, 0.3219752754296894559, 0.3333333333333333703, 0.3219752754296894559, 0.3333333333333333703, 0.3219752754296894559, 0.3333333333333333703, 0.3219752754296894559, 0.3333333333333333703, 0.3219752754296894559, 0.3333333333333333703, 0.3219752754296894559, 0.3333333333333333703, 0.3219752754296894559, 0.3333333333333333703, 0.3219752754296894559, 0.3333333333333333703, 0.3219752754296894559, 0.3333333333333333703, 0.3219752754296894559, 0.3333333333333333703, 0.3219752754296894559, 0.3333333333333333703, 0.3219752754296894559, 0.3333333333333333703, 0.3219752754296894559, 0.3333333333333333703, 0.3219752754296894559, 0.3333333333333333703, 0.3219752754296894559, 0.3333333333333333703, 0.3219752754296894559, 0.3333333333333333703, 0.3219752754296894559, 0.3333333333333333703, 0.3219752754296894559, 0.3333333333333333703, 0.3219752754296894559, 0.3333333333333333703, 0.3219752754296894559, 0.3333333333333333703, 0.3219752754296894559, 0.3333333333333333703, 0.3219752754296894559, 0.3333333333333333703, 0.3219752754296894559, 0.3333333333333333703, 0.3219752754296894559, 0.3333333333333333703, 0.3219752754296894559, 0.3333333333333333703, 0.3219752754296894559, 0.3333333333333333703, 0.3219752754296894559, 0.3333333333333333703, 0.3219752754296894559, 0.3333333333333333703, 0.3219752754296894559, 0.3333333333333333703, 0.3219752754296894559, 0.3333333333333333703, 0.3219752754296894559, 0.3333333333333333703, 0.3219752754296894559, 0.3333333333333333703, 0.3219752754296894559, 0.3333333333333333703, 0.3219752754296894559, 0.3333333333333333703, 0.3219752754296894559, 0.3333333333333333703, 0.3219752754296894559, 0.3333333333333333703, 0.3219752754296894559, 0.3333333333333333703, 0.3219752754296894559, 0.3333333333333333703, 0.3219752754296894559, 0.3333333333333333703, 0.3219752754296894559, 0.3333333333333333703, 0.3219752754296894559, 0.3333333333333333703, 0.3219752754296894559, 0.3333333333333333703, 0.3219752754296894559, 0.3333333333333333703, 0.3219752754296894559, 0.3333333333333333703),
 ( 1.000000000000000000, 0.9659258262890683122, 1.000000000000000000, 0.9659258262890683122, 1.000000000000000000, 0.9659258262890683122, 1.000000000000000000, 0.9659258262890683122, 1.000000000000000000, 0.9659258262890683122, 1.000000000000000000, 0.9659258262890683122, 1.000000000000000000, 0.9659258262890683122, 1.000000000000000000, 0.9659258262890683122, 1.000000000000000000, 0.9659258262890683122, 1.000000000000000000, 0.9659258262890683122, 1.000000000000000000, 0.9659258262890683122, 1.000000000000000000, 0.9659258262890683122, 1.000000000000000000, 0.9659258262890683122, 1.000000000000000000, 0.9659258262890683122, 1.000000000000000000, 0.9659258262890683122, 1.000000000000000000, 0.9659258262890683122, 1.000000000000000000, 0.9659258262890683122, 1.000000000000000000, 0.9659258262890683122, 1.000000000000000000, 0.9659258262890683122, 1.000000000000000000, 0.9659258262890683122, 1.000000000000000000, 0.9659258262890683122, 1.000000000000000000, 0.9659258262890683122, 1.000000000000000000, 0.9659258262890683122, 1.000000000000000000, 0.9659258262890683122, 1.000000000000000000, 0.9659258262890683122, 1.000000000000000000, 0.9659258262890683122, 1.000000000000000000, 0.9659258262890683122, 1.000000000000000000, 0.9659258262890683122, 1.000000000000000000, 0.9659258262890683122, 1.000000000000000000, 0.9659258262890683122, 1.000000000000000000, 0.9659258262890683122, 1.000000000000000000, 0.9659258262890683122, 1.000000000000000000, 0.9659258262890683122, 1.000000000000000000, 0.9659258262890683122, 1.000000000000000000, 0.9659258262890683122, 1.000000000000000000, 0.9659258262890683122, 1.000000000000000000, 0.9659258262890683122, 1.000000000000000000, 0.9659258262890683122, 1.000000000000000000, 0.9659258262890683122, 1.000000000000000000, 0.9659258262890683122, 1.000000000000000000, 0.9659258262890683122, 1.000000000000000000, 0.9659258262890683122, 1.000000000000000000, 0.9659258262890683122, 1.000000000000000000, 0.9659258262890683122, 1.000000000000000000, 0.9659258262890683122, 1.000000000000000000, 0.9659258262890683122, 1.000000000000000000, 0.9659258262890683122, 1.000000000000000000, 0.9659258262890683122, 1.000000000000000000, 0.9659258262890683122, 1.000000000000000000, 0.9659258262890683122, 1.000000000000000000, 0.9659258262890683122, 1.000000000000000000, 0.9659258262890683122, 1.000000000000000000, 0.9659258262890683122, 1.000000000000000000, 0.9659258262890683122, 1.000000000000000000, 0.9659258262890683122, 1.000000000000000000, 0.9659258262890683122, 1.000000000000000000, 0.9659258262890683122, 1.000000000000000000, 0.9659258262890683122, 1.000000000000000000, 0.9659258262890683122, 1.000000000000000000, 0.9659258262890683122, 1.000000000000000000, 0.9659258262890683122, 1.000000000000000000, 0.9659258262890683122, 1.000000000000000000, 0.9659258262890683122, 1.000000000000000000, 0.9659258262890683122, 1.000000000000000000, 0.9659258262890683122, 1.000000000000000000, 0.9659258262890683122, 1.000000000000000000, 0.9659258262890683122, 1.000000000000000000, 0.9659258262890683122, 1.000000000000000000, 0.9659258262890683122, 1.000000000000000000, 0.9659258262890683122, 1.000000000000000000, 0.9659258262890683122, 1.000000000000000000, 0.9659258262890683122, 1.000000000000000000, 0.9659258262890683122, 1.000000000000000000, 0.9659258262890683122, 1.000000000000000000, 0.9659258262890683122, 1.000000000000000000, 0.9659258262890683122, 1.000000000000000000, 0.9659258262890683122, 1.000000000000000000, 0.9659258262890683122, 1.000000000000000000, 0.9659258262890683122, 1.000000000000000000, 0.9659258262890683122, 1.000000000000000000, 0.9659258262890683122, 1.000000000000000000, 0.9659258262890683122, 1.000000000000000000, 0.9659258262890683122, 1.000000000000000000, 0.9659258262890683122, 1.000000000000000000, 0.9659258262890683122, 1.000000000000000000, 0.9659258262890683122, 1.000000000000000000, 0.9659258262890683122, 1.000000000000000000, 0.9659258262890683122, 1.000000000000000000, 0.9659258262890683122, 1.000000000000000000, 0.9659258262890683122, 1.000000000000000000, 0.9659258262890683122, 1.000000000000000000, 0.9659258262890683122, 1.000000000000000000, 0.9659258262890683122, 1.000000000000000000, 0.9659258262890683122, 1.000000000000000000, 0.9659258262890683122, 1.000000000000000000, 0.9659258262890683122, 1.000000000000000000, 0.9659258262890683122, 1.000000000000000000, 0.9659258262890683122, 1.000000000000000000, 0.9659258262890683122, 1.000000000000000000, 0.9659258262890683122, 1.000000000000000000, 0.9659258262890683122, 1.000000000000000000, 0.9659258262890683122, 1.000000000000000000, 0.9659258262890683122, 1.000000000000000000, 0.9659258262890683122, 1.000000000000000000, 0.9659258262890683122, 1.000000000000000000, 0.9659258262890683122, 1.000000000000000000, 0.9659258262890683122, 1.000000000000000000, 0.9659258262890683122, 1.000000000000000000, 0.9659258262890683122, 1.000000000000000000, 0.9659258262890683122, 1.000000000000000000, 0.9659258262890683122, 1.000000000000000000, 0.9659258262890683122, 1.000000000000000000, 0.9659258262890683122, 1.000000000000000000, 0.9659258262890683122, 1.000000000000000000, 0.9659258262890683122, 1.000000000000000000, 0.9659258262890683122, 1.000000000000000000, 0.9659258262890683122, 1.000000000000000000, 0.9659258262890683122, 1.000000000000000000, 0.9659258262890683122, 1.000000000000000000, 0.9659258262890683122, 1.000000000000000000, 0.9659258262890683122, 1.000000000000000000, 0.9659258262890683122, 1.000000000000000000, 0.9659258262890683122, 1.000000000000000000, 0.9659258262890683122, 1.000000000000000000, 0.9659258262890683122, 1.000000000000000000, 0.9659258262890683122, 1.000000000000000000, 0.9659258262890683122, 1.000000000000000000, 0.9659258262890683122, 1.000000000000000000, 0.9659258262890683122, 1.000000000000000000, 0.9659258262890683122, 1.000000000000000000, 0.9659258262890683122, 1.000000000000000000, 0.9659258262890683122, 1.000000000000000000, 0.9659258262890683122, 1.000000000000000000, 0.9659258262890683122, 1.000000000000000000, 0.9659258262890683122, 1.000000000000000000, 0.9659258262890683122, 1.000000000000000000, 0.9659258262890683122, 1.000000000000000000, 0.9659258262890683122, 1.000000000000000000, 0.9659258262890683122, 1.000000000000000000, 0.9659258262890683122, 1.000000000000000000, 0.9659258262890683122, 1.000000000000000000, 0.9659258262890683122, 1.000000000000000000, 0.9659258262890683122, 1.000000000000000000, 0.9659258262890683122, 1.000000000000000000, 0.9659258262890683122, 1.000000000000000000, 0.9659258262890683122, 1.000000000000000000, 0.9659258262890683122, 1.000000000000000000, 0.9659258262890683122, 1.000000000000000000, 0.9659258262890683122, 1.000000000000000000, 0.9659258262890683122, 1.000000000000000000, 0.9659258262890683122, 1.000000000000000000, 0.9659258262890683122, 1.000000000000000000, 0.9659258262890683122, 1.000000000000000000, 0.9659258262890683122, 1.000000000000000000, 0.9659258262890683122, 1.000000000000000000, 0.9659258262890683122, 1.000000000000000000, 0.9659258262890683122, 1.000000000000000000, 0.9659258262890683122, 1.000000000000000000, 0.9659258262890683122, 1.000000000000000000, 0.9659258262890683122, 1.000000000000000000, 0.9659258262890683122, 1.000000000000000000, 0.9659258262890683122, 1.000000000000000000, 0.9659258262890683122, 1.000000000000000000, 0.9659258262890683122, 1.000000000000000000, 0.9659258262890683122, 1.000000000000000000, 0.9659258262890683122, 1.000000000000000000, 0.9659258262890683122, 1.000000000000000000, 0.9659258262890683122, 1.000000000000000000, 0.9659258262890683122, 1.000000000000000000, 0.9659258262890683122, 1.000000000000000000, 0.9659258262890683122, 1.000000000000000000, 0.9659258262890683122, 1.000000000000000000, 0.9659258262890683122, 1.000000000000000000, 0.9659258262890683122, 1.000000000000000000, 0.9659258262890683122, 1.000000000000000000, 0.9659258262890683122, 1.000000000000000000, 0.9659258262890683122, 1.000000000000000000, 0.9659258262890683122, 1.000000000000000000, 0.9659258262890683122, 1.000000000000000000, 0.9659258262890683122, 1.000000000000000000, 0.9659258262890683122, 1.000000000000000000, 0.9659258262890683122, 1.000000000000000000, 0.9659258262890683122, 1.000000000000000000, 0.9659258262890683122, 1.000000000000000000, 0.9659258262890683122, 1.000000000000000000, 0.9659258262890683122, 1.000000000000000000, 0.9659258262890683122, 1.000000000000000000, 0.9659258262890683122, 1.000000000000000000, 0.9659258262890683122, 1.000000000000000000, 0.9659258262890683122, 1.000000000000000000, 0.9659258262890683122, 1.000000000000000000, 0.9659258262890683122, 1.000000000000000000, 0.9659258262890683122, 1.000000000000000000, 0.9659258262890683122, 1.000000000000000000, 0.9659258262890683122, 1.000000000000000000, 0.9659258262890683122, 1.000000000000000000, 0.9659258262890683122, 1.000000000000000000, 0.9659258262890683122, 1.000000000000000000, 0.9659258262890683122, 1.000000000000000000, 0.9659258262890683122, 1.000000000000000000, 0.9659258262890683122, 1.000000000000000000, 0.9659258262890683122, 1.000000000000000000, 0.9659258262890683122, 1.000000000000000000, 0.9659258262890683122, 1.000000000000000000, 0.9659258262890683122, 1.000000000000000000, 0.9659258262890683122, 1.000000000000000000, 0.9659258262890683122, 1.000000000000000000, 0.9659258262890683122, 1.000000000000000000, 0.9659258262890683122, 1.000000000000000000, 0.9659258262890683122, 1.000000000000000000, 0.9659258262890683122, 1.000000000000000000, 0.9659258262890683122, 1.000000000000000000, 0.9659258262890683122, 1.000000000000000000, 0.9659258262890683122, 1.000000000000000000, 0.9659258262890683122, 1.000000000000000000, 0.9659258262890683122, 1.000000000000000000, 0.9659258262890683122, 1.000000000000000000, 0.9659258262890683122, 1.000000000000000000, 0.9659258262890683122, 1.000000000000000000, 0.9659258262890683122, 1.000000000000000000, 0.9659258262890683122, 1.000000000000000000, 0.9659258262890683122, 1.000000000000000000, 0.9659258262890683122, 1.000000000000000000, 0.9659258262890683122, 1.000000000000000000, 0.9659258262890683122, 1.000000000000000000, 0.9659258262890683122, 1.000000000000000000, 0.9659258262890683122, 1.000000000000000000, 0.9659258262890683122, 1.000000000000000000) ) ) 
 REPRESENTATION_ITEM ( '' )  SURFACE ( )  );
#60898 = CARTESIAN_POINT ( 'NONE',  ( 5.153800228976615827, -19.02544592524334988, 45.20942372801901143 ) ) ;
#60899 = CARTESIAN_POINT ( 'NONE',  ( 16.38665767534995510, -7.295008042176407415, 72.76400864214468811 ) ) ;
#60900 = VECTOR ( 'NONE', #5513, 1000.000000000000000 ) ;
#60902 = CARTESIAN_POINT ( 'NONE',  ( 5.153800228976335163, 19.02544592524342804, 84.79057627198099567 ) ) ;
#60901 = CARTESIAN_POINT ( 'NONE',  ( -5.153800228976328057, -19.02544592524343514, 62.29057627198100988 ) ) ;
#60903 = CARTESIAN_POINT ( 'NONE',  ( 0.05219959533934541429, -16.53943276465976808, 50.00109039468568994 ) ) ;
#60904 = CARTESIAN_POINT ( 'NONE',  ( 10.06251177737616054, -45.32665049860680995, -23.77652626631510913 ) ) ;
#60905 = CARTESIAN_POINT ( 'NONE',  ( -19.02544592524334988, -5.153800228976617603, 23.95942372801900078 ) ) ;
#60906 = DIRECTION ( 'NONE',  ( -0.7071067811865463515, 0.7071067811865487940, -0.000000000000000000 ) ) ;
#60907 = CARTESIAN_POINT ( 'NONE',  ( 16.55341960407618274, -4.379528057220086978, 91.04275706135236135 ) ) ;
#60908 = CARTESIAN_POINT ( 'NONE',  ( -0.8285391498303467106, -21.53159096656797544, -56.30101842015763935 ) ) ;
#60909 = CARTESIAN_POINT ( 'NONE',  ( 16.53943276465976808, 0.05219959533934440121, 81.25109039468568994 ) ) ;
#60910 = CARTESIAN_POINT ( 'NONE',  ( -16.55341960407617563, 4.379528057220093196, 58.54275706135235424 ) ) ;
#60912 = DIRECTION ( 'NONE',  ( 0.000000000000000000, 0.000000000000000000, 1.000000000000000000 ) ) ;
#60911 = CARTESIAN_POINT ( 'NONE',  ( -16.46253265017160317, 9.564922557960807481, 50.83224293864770260 ) ) ;
#60913 = CARTESIAN_POINT ( 'NONE',  ( 10.81492255796106328, -18.62759615963255655, 70.41775706135236135 ) ) ;
#60914 = CARTESIAN_POINT ( 'NONE',  ( -13.97604488694547697, 13.89961937509957934, 73.12609039468568994 ) ) ;
#60915 = CARTESIAN_POINT ( 'NONE',  ( 18.67979575497194134, -10.72451020669871369, 110.8344237280190043 ) ) ;
#60916 = CARTESIAN_POINT ( 'NONE',  ( 9.474510206698971260, -16.51473224551069308, 47.91557627198102409 ) ) ;
#60917 = CARTESIAN_POINT ( 'NONE',  ( 16.51473224551069308, 9.474510206698969483, 49.16557627198102409 ) ) ;
#60918 = DIRECTION ( 'NONE',  ( -0.000000000000000000, -0.000000000000000000, -1.000000000000000000 ) ) ;
#60919 = CARTESIAN_POINT ( 'NONE',  ( 5.823673210054125526, 21.52544592524343514, 69.79057627198102409 ) ) ;
#60920 = EDGE_CURVE ( 'NONE', #194071, #30776, #123707, .T. ) ;
#60921 = CARTESIAN_POINT ( 'NONE',  ( -5.049401038298153566, 19.05341960407611168, 110.2072429386476671 ) ) ;
#60922 = CARTESIAN_POINT ( 'NONE',  ( 9.474510206698971260, -16.51473224551069308, 22.91557627198102765 ) ) ;
#60923 = CARTESIAN_POINT ( 'NONE',  ( 4.379528057220092307, 16.55341960407617563, 57.29275706135234714 ) ) ;
#60924 = CARTESIAN_POINT ( 'NONE',  ( -8.224510206698948167, 14.34966873604960824, 30.41557627198101699 ) ) ;
#60925 = VERTEX_POINT ( 'NONE', #125602 ) ;
#60926 = CARTESIAN_POINT ( 'NONE',  ( 0.05219959533907565091, 21.53943276465977519, 114.9989096053143669 ) ) ;
#60928 = CARTESIAN_POINT ( 'NONE',  ( -30.74264578624800492, -22.33583958711396278, -5.800000000000000711 ) ) ;
#60927 = CARTESIAN_POINT ( 'NONE',  ( -0.05219959533910754901, -16.53943276465976808, 52.49890960531435979 ) ) ;
#60929 = CARTESIAN_POINT ( 'NONE',  ( -16.51473224551082808, 9.474510206698731452, 103.3344237280190043 ) ) ;
#60930 = CARTESIAN_POINT ( 'NONE',  ( -16.51473224551082808, 9.474510206698731452, 43.33442372801900433 ) ) ;
#60931 = CARTESIAN_POINT ( 'NONE',  ( 0.05219959533910956823, 16.53943276465976808, 44.99890960531435979 ) ) ;
#60932 = CARTESIAN_POINT ( 'NONE',  ( 5.823673210054125526, 21.52544592524343514, 104.7905762719810241 ) ) ;
#60934 = CARTESIAN_POINT ( 'NONE',  ( 5.823673210054125526, 21.52544592524343514, 69.79057627198102409 ) ) ;
#60933 = CARTESIAN_POINT ( 'NONE',  ( 16.18388926212241330, 7.379444403734403579, 32.93953151366154231 ) ) ;
#60935 = CARTESIAN_POINT ( 'NONE',  ( 9.564922557960805705, 16.46253265017160317, 74.58224293864769550 ) ) ;
#60936 = CARTESIAN_POINT ( 'NONE',  ( -0.05219959533910754901, -16.53943276465976808, 47.49890960531435979 ) ) ;
#60937 = CARTESIAN_POINT ( 'NONE',  ( 13.89961937509977652, -13.97604488694527269, 108.1239096053143669 ) ) ;
#60938 = DIRECTION ( 'NONE',  ( -1.000000000000000000, 0.000000000000000000, 0.000000000000000000 ) ) ;
#60939 = CARTESIAN_POINT ( 'NONE',  ( 0.05219959533936267826, -19.03943276465977164, 55.00109039468566863 ) ) ;
#60940 = CARTESIAN_POINT ( 'NONE',  ( -10.72451020669898014, 18.67979575497178502, 90.41557627198103830 ) ) ;
#60941 = CARTESIAN_POINT ( 'NONE',  ( 5.153800228976335163, 19.02544592524342804, 49.79057627198100988 ) ) ;
#60942 = CARTESIAN_POINT ( 'NONE',  ( 16.52544592524342804, -4.483927247898539470, 113.5405762719810383 ) ) ;
#60943 = CARTESIAN_POINT ( 'NONE',  ( -18.67979575497193778, 10.72451020669871902, 48.33442372801902565 ) ) ;
#60944 = CARTESIAN_POINT ( 'NONE',  ( -22.44159573604010305, 16.30477369853692338, 144.6750000027311671 ) ) ;
#60945 = CARTESIAN_POINT ( 'NONE',  ( -16.55341960407611168, -4.379528057220339221, 21.45724293864769550 ) ) ;
#60946 = CARTESIAN_POINT ( 'NONE',  ( -19.05341960407611168, -5.049401038298163336, 51.45724293864770260 ) ) ;
#60947 = CARTESIAN_POINT ( 'NONE',  ( 16.46253265017160672, -9.564922557960803928, 103.3322429386476955 ) ) ;
#60948 = CARTESIAN_POINT ( 'NONE',  ( -18.67979575497178146, -10.72451020669898902, 66.66557627198102409 ) ) ;
#60949 = CARTESIAN_POINT ( 'NONE',  ( -8.571926809382601320, -26.38167802310801591, 145.2750000027311899 ) ) ;
#60950 = CARTESIAN_POINT ( 'NONE',  ( -9.474510206698964154, 16.51473224551069663, 45.41557627198103120 ) ) ;
#60951 = CARTESIAN_POINT ( 'NONE',  ( 18.67979575497178502, 10.72451020669898547, 54.16557627198103120 ) ) ;
#60952 = ORIENTED_EDGE ( 'NONE', *, *, #106236, .T. ) ;
#60953 = CARTESIAN_POINT ( 'NONE',  ( -18.67979575497193778, 10.72451020669871902, 93.33442372801901854 ) ) ;
#60955 = CARTESIAN_POINT ( 'NONE',  ( -12.06949235617739369, -12.14591786802326823, 79.37609039468567573 ) ) ;
#60954 = CARTESIAN_POINT ( 'NONE',  ( 14.77336750280265498, -39.52550427972109048, -19.86057791183392141 ) ) ;
#60956 = CARTESIAN_POINT ( 'NONE',  ( 8.314922557961029526, -14.29746914071037800, 85.41775706135236135 ) ) ;
#60957 = CARTESIAN_POINT ( 'NONE',  ( 16.46253265017160672, -9.564922557960803928, 68.33224293864770971 ) ) ;
#60958 = ORIENTED_EDGE ( 'NONE', *, *, #68626, .F. ) ;
#60959 = CARTESIAN_POINT ( 'NONE',  ( -16.51473224551082808, 9.474510206698731452, 23.33442372801900078 ) ) ;
#60960 = CARTESIAN_POINT ( 'NONE',  ( 12.14591786802327356, -12.06949235617739191, 85.62609039468568994 ) ) ;
#60961 = CARTESIAN_POINT ( 'NONE',  ( -19.02544592524334988, -5.153800228976617603, 18.95942372801899722 ) ) ;
#60962 = CARTESIAN_POINT ( 'NONE',  ( -16.46253265017160317, 9.564922557960807481, 80.83224293864769550 ) ) ;
#60963 = CARTESIAN_POINT ( 'NONE',  ( 18.62759615963271287, -10.81492255796078972, 53.33224293864769550 ) ) ;
#60964 = CARTESIAN_POINT ( 'NONE',  ( -12.06949235617739369, -12.14591786802326823, 24.37609039468567573 ) ) ;
#60965 = CARTESIAN_POINT ( 'NONE',  ( 21.55341960407619695, -5.719274019375665929, 86.04275706135236135 ) ) ;
#60966 = CARTESIAN_POINT ( 'NONE',  ( -14.34966873604972548, 8.224510206698743886, 68.33442372801900433 ) ) ;
#60967 = CARTESIAN_POINT ( 'NONE',  ( -15.80617190586745835, -15.72974639402198527, 111.8739096053143669 ) ) ;
#60968 = CARTESIAN_POINT ( 'NONE',  ( -5.153800228976607833, 19.02544592524334988, 112.7094237280190043 ) ) ;
#60969 = CARTESIAN_POINT ( 'NONE',  ( 13.97604488694527802, 13.89961937509977652, 94.37390960531436690 ) ) ;
#60970 = CARTESIAN_POINT ( 'NONE',  ( -12.06949235617739369, -12.14591786802326823, 34.37609039468568284 ) ) ;
#60971 = CARTESIAN_POINT ( 'NONE',  ( 19.02544592524343514, -5.153800228976328945, 38.54057627198103120 ) ) ;
#60972 = CARTESIAN_POINT ( 'NONE',  ( -4.379528057220086978, -16.55341960407618274, 19.79275706135235069 ) ) ;
#60973 = CARTESIAN_POINT ( 'NONE',  ( -4.379528057220328563, 16.55341960407611168, 80.20724293864769550 ) ) ;
#60974 = CARTESIAN_POINT ( 'NONE',  ( 4.379528057220092307, 16.55341960407617563, 92.29275706135236135 ) ) ;
#60976 = CARTESIAN_POINT ( 'NONE',  ( -0.05219959533909027116, -19.03943276465977164, 62.49890960531435979 ) ) ;
#60975 = CARTESIAN_POINT ( 'NONE',  ( -15.80617190586768217, 15.72974639402176855, 33.12609039468569705 ) ) ;
#60978 = EDGE_CURVE ( 'NONE', #96409, #89861, #143745, .T. ) ;
#60977 = CARTESIAN_POINT ( 'NONE',  ( 5.049401038298161559, -19.05341960407611168, 72.70724293864768129 ) ) ;
#60979 = CARTESIAN_POINT ( 'NONE',  ( 12.14591786802327356, -12.06949235617739191, 80.62609039468567573 ) ) ;
#60981 = VERTEX_POINT ( 'NONE', #64921 ) ;
#60980 = CARTESIAN_POINT ( 'NONE',  ( -21.73861122199297924, -5.803778330637474170, 172.6157762304496828 ) ) ;
#60982 = EDGE_LOOP ( 'NONE', ( #148956, #82714, #184981 ) ) ;
#60983 = CARTESIAN_POINT ( 'NONE',  ( -5.153800228976607833, 19.02544592524334988, 27.70942372801899722 ) ) ;
#60984 = CARTESIAN_POINT ( 'NONE',  ( 16.46253265017160672, -9.564922557960803928, 33.33224293864770260 ) ) ;
#60986 = VERTEX_POINT ( 'NONE', #175092 ) ;
#60985 = CARTESIAN_POINT ( 'NONE',  ( 11.40812507854755253, -35.11059874428192273, -10.02499999726881441 ) ) ;
#60987 = CARTESIAN_POINT ( 'NONE',  ( -4.379528057220086978, -16.55341960407618274, 24.79275706135235779 ) ) ;
#60988 = AXIS2_PLACEMENT_3D ( 'NONE', #150721, #85022, #57715 ) ;
#60990 = CARTESIAN_POINT ( 'NONE',  ( -14.34966873604972548, 8.224510206698743886, 48.33442372801902565 ) ) ;
#60989 = CARTESIAN_POINT ( 'NONE',  ( 0.05219959533936267826, -19.03943276465977164, 60.00109039468566863 ) ) ;
#60991 = CARTESIAN_POINT ( 'NONE',  ( 9.564922557960805705, 16.46253265017160317, 99.58224293864770971 ) ) ;
#60992 = CARTESIAN_POINT ( 'NONE',  ( 13.97604488694527802, 13.89961937509977652, 79.37390960531435269 ) ) ;
#60993 = CARTESIAN_POINT ( 'NONE',  ( 10.72451020669898902, -18.67979575497178502, 92.91557627198103830 ) ) ;
#60994 = CARTESIAN_POINT ( 'NONE',  ( -16.51473224551082808, 9.474510206698731452, 68.33442372801900433 ) ) ;
#60996 = CARTESIAN_POINT ( 'NONE',  ( -0.05219959533909027116, -19.03943276465977164, 22.49890960531436690 ) ) ;
#60995 = CARTESIAN_POINT ( 'NONE',  ( 16.46253265017160672, -9.564922557960803928, 93.33224293864769550 ) ) ;
#60997 = APPLICATION_CONTEXT ( 'automotive_design' ) ;
#60998 = CARTESIAN_POINT ( 'NONE',  ( -9.564922557960796823, -16.46253265017161027, 57.08224293864769550 ) ) ;
#61000 = CARTESIAN_POINT ( 'NONE',  ( -17.58332526062529411, 7.635886036038502134, 70.92334959558468199 ) ) ;
#60999 = CARTESIAN_POINT ( 'NONE',  ( -16.55341960407611168, -4.379528057220339221, 26.45724293864768839 ) ) ;
#61001 = CARTESIAN_POINT ( 'NONE',  ( 13.97604488694548053, -13.89961937509957401, 35.62609039468567573 ) ) ;
#61002 = CARTESIAN_POINT ( 'NONE',  ( 8.314922557960818139, 14.29746914071049879, 69.58224293864769550 ) ) ;
#61003 = CARTESIAN_POINT ( 'NONE',  ( -18.62759615963255300, -10.81492255796106328, 94.16775706135237556 ) ) ;
#61004 = CARTESIAN_POINT ( 'NONE',  ( 5.049401038298161559, -19.05341960407611168, 42.70724293864767418 ) ) ;
#61005 = CARTESIAN_POINT ( 'NONE',  ( -14.29746914071037622, -8.314922557961029526, 54.16775706135235424 ) ) ;
#61007 = CARTESIAN_POINT ( 'NONE',  ( 5.719274019375673035, 21.55341960407619339, 87.29275706135236135 ) ) ;
#61006 = CARTESIAN_POINT ( 'NONE',  ( 16.52544592524342804, -4.483927247898539470, 38.54057627198103120 ) ) ;
#61008 = CARTESIAN_POINT ( 'NONE',  ( 19.05341960407611168, 5.049401038298154454, 98.95724293864766707 ) ) ;
#61009 = CARTESIAN_POINT ( 'NONE',  ( 19.03943276465977164, -0.05219959533909143690, 93.74890960531435269 ) ) ;
#61010 = CARTESIAN_POINT ( 'NONE',  ( 0.05219959533910956823, 16.53943276465976808, 104.9989096053143669 ) ) ;
#61011 = CARTESIAN_POINT ( 'NONE',  ( 4.379528057220339221, -16.55341960407611168, 67.70724293864769550 ) ) ;
#61012 = CARTESIAN_POINT ( 'NONE',  ( -15.72974639402197994, 15.80617190586746368, 80.62390960531438111 ) ) ;
#61013 = CARTESIAN_POINT ( 'NONE',  ( 16.51473224551069308, 9.474510206698969483, 94.16557627198103830 ) ) ;
#61014 = CARTESIAN_POINT ( 'NONE',  ( -10.72451020669898014, 18.67979575497178502, 95.41557627198102409 ) ) ;
#61015 = CARTESIAN_POINT ( 'NONE',  ( 16.46253265017146816, 9.564922557961045513, 81.66775706135233293 ) ) ;
#61017 = CARTESIAN_POINT ( 'NONE',  ( 0.05219959533910956823, 16.53943276465976808, 94.99890960531436690 ) ) ;
#61016 = CARTESIAN_POINT ( 'NONE',  ( -19.39720447994792707, -5.500000000000080824, 89.66317477297177163 ) ) ;
#61018 = CARTESIAN_POINT ( 'NONE',  ( 9.474510206698971260, -16.51473224551069308, 52.91557627198102409 ) ) ;
#61019 = CARTESIAN_POINT ( 'NONE',  ( 5.719274019375991003, -21.55341960407610458, 67.70724293864769550 ) ) ;
#61020 = CARTESIAN_POINT ( 'NONE',  ( 17.26172910966779739, -6.454744622555848466, 28.30646908649225324 ) ) ;
#61022 = CARTESIAN_POINT ( 'NONE',  ( -17.49999999999999645, 5.499999999999992895, 58.71769037696435589 ) ) ;
#61021 = CARTESIAN_POINT ( 'NONE',  ( -16.53943276465976808, 0.05219959533911058130, 21.24890960531436690 ) ) ;
#61023 = CARTESIAN_POINT ( 'NONE',  ( -14.29746914071037622, -8.314922557961029526, 19.16775706135234714 ) ) ;
#61024 = CARTESIAN_POINT ( 'NONE',  ( -14.29746914071049879, 8.314922557960819915, 85.83224293864768129 ) ) ;
#61025 = CARTESIAN_POINT ( 'NONE',  ( -16.18388926212238133, -7.379444403734540359, 95.43953151366154941 ) ) ;
#61026 = CARTESIAN_POINT ( 'NONE',  ( 13.97604488694527802, 13.89961937509977652, 69.37390960531436690 ) ) ;
#61027 = CARTESIAN_POINT ( 'NONE',  ( -19.05341960407611168, -5.049401038298163336, 31.45724293864769550 ) ) ;
#61028 = CARTESIAN_POINT ( 'NONE',  ( 8.314922557960818139, 14.29746914071049879, 69.58224293864769550 ) ) ;
#61029 = CARTESIAN_POINT ( 'NONE',  ( -18.67979575497178146, -10.72451020669898902, 21.66557627198102409 ) ) ;
#61030 = CARTESIAN_POINT ( 'NONE',  ( 0.05219959533936267826, -19.03943276465977164, 85.00109039468567573 ) ) ;
#61031 = CARTESIAN_POINT ( 'NONE',  ( -19.02544592524342804, 5.153800228976336051, 101.0405762719810241 ) ) ;
#61032 = CARTESIAN_POINT ( 'NONE',  ( -18.67979575497178146, -10.72451020669898902, 76.66557627198103830 ) ) ;
#61033 = CARTESIAN_POINT ( 'NONE',  ( -16.53943276465976808, -0.05219959533934237506, 73.75109039468567573 ) ) ;
#61034 = CARTESIAN_POINT ( 'NONE',  ( -13.97604488694547520, 13.89961937509957934, 108.1260903946856473 ) ) ;
#61035 = CARTESIAN_POINT ( 'NONE',  ( -16.51473224551069308, -9.474510206698971260, 66.66557627198102409 ) ) ;
#61036 = CARTESIAN_POINT ( 'NONE',  ( 10.81492255796078972, 18.62759615963270932, 74.58224293864768129 ) ) ;
#61037 = CARTESIAN_POINT ( 'NONE',  ( 5.049401038297881783, 19.05341960407617563, 102.2927570613523045 ) ) ;
#61039 = CARTESIAN_POINT ( 'NONE',  ( 18.67979575497194134, -10.72451020669871369, 65.83442372801900433 ) ) ;
#61038 = CARTESIAN_POINT ( 'NONE',  ( -4.483927247898539470, -16.52544592524342804, 37.29057627198102409 ) ) ;
#61040 = DIRECTION ( 'NONE',  ( -1.000000000000000000, -0.000000000000000000, 0.000000000000000000 ) ) ;
#61042 = CARTESIAN_POINT ( 'NONE',  ( -5.049401038298153566, 19.05341960407611168, 100.2072429386476955 ) ) ;
#61041 = CARTESIAN_POINT ( 'NONE',  ( 14.29746914071037800, 8.314922557961029526, 71.66775706135234714 ) ) ;
#61043 = CARTESIAN_POINT ( 'NONE',  ( 0.000000000000000000, -105.0000000000000000, 12.00000000000000355 ) ) ;
#61044 = LINE ( 'NONE', #155051, #64767 ) ;
#61045 = CARTESIAN_POINT ( 'NONE',  ( 4.379528057220092307, 16.55341960407617563, 97.29275706135234714 ) ) ;
#61046 = CARTESIAN_POINT ( 'NONE',  ( -14.34966873604972548, 8.224510206698743886, 48.33442372801902565 ) ) ;
#61047 = CARTESIAN_POINT ( 'NONE',  ( 0.05219959533909260263, 19.03943276465977164, 54.99890960531435979 ) ) ;
#61048 = CARTESIAN_POINT ( 'NONE',  ( 16.46253265017160672, -9.564922557960803928, 73.33224293864769550 ) ) ;
#61049 = CARTESIAN_POINT ( 'NONE',  ( -0.05219959533937732626, 21.53943276465977519, 72.50109039468568994 ) ) ;
#61050 = CARTESIAN_POINT ( 'NONE',  ( -8.314922557961024197, 14.29746914071037800, 62.91775706135236135 ) ) ;
#61051 = CARTESIAN_POINT ( 'NONE',  ( 4.483927247898545687, 16.52544592524342804, 34.79057627198103120 ) ) ;
#61052 = CARTESIAN_POINT ( 'NONE',  ( 9.474510206698971260, -16.51473224551069308, 37.91557627198102409 ) ) ;
#61053 = CARTESIAN_POINT ( 'NONE',  ( 5.153800228976335163, 19.02544592524342804, 34.79057627198102409 ) ) ;
#61054 = CARTESIAN_POINT ( 'NONE',  ( -4.379528057220086978, -16.55341960407618274, 29.79275706135234358 ) ) ;
#61055 = CARTESIAN_POINT ( 'NONE',  ( -19.02544592524334988, -5.153800228976617603, 78.95942372801900433 ) ) ;
#61056 = CARTESIAN_POINT ( 'NONE',  ( 16.55341960407611168, 4.379528057220329451, 93.95724293864770971 ) ) ;
#61057 = CARTESIAN_POINT ( 'NONE',  ( 9.474510206698971260, -16.51473224551069308, 57.91557627198103120 ) ) ;
#61059 = CARTESIAN_POINT ( 'NONE',  ( 38.00000000000000711, -12.34694845685040754, -9.100000000000001421 ) ) ;
#61058 = CARTESIAN_POINT ( 'NONE',  ( -5.153800228976607833, 19.02544592524334988, 82.70942372801897591 ) ) ;
#61060 = CARTESIAN_POINT ( 'NONE',  ( 21.55341960407619695, -5.719274019375665929, 86.04275706135236135 ) ) ;
#61061 = CARTESIAN_POINT ( 'NONE',  ( 12.06949235617739724, 12.14591786802326823, 56.87609039468568994 ) ) ;
#61062 = LINE ( 'NONE', #138898, #72954 ) ;
#61063 = CARTESIAN_POINT ( 'NONE',  ( 18.62759615963271287, -10.81492255796078972, 43.33224293864769550 ) ) ;
#61064 = CARTESIAN_POINT ( 'NONE',  ( -12.06949235617739369, -12.14591786802326823, 34.37609039468568284 ) ) ;
#61065 = CARTESIAN_POINT ( 'NONE',  ( -16.46253265017160317, 9.564922557960807481, 35.83224293864768839 ) ) ;
#61066 = CARTESIAN_POINT ( 'NONE',  ( -9.564922557961040184, 16.46253265017147172, 47.91775706135233293 ) ) ;
#61067 = CARTESIAN_POINT ( 'NONE',  ( 13.89961937509977652, -13.97604488694527269, 88.12390960531438111 ) ) ;
#61068 = CARTESIAN_POINT ( 'NONE',  ( -5.153800228976328057, -19.02544592524343514, 52.29057627198100988 ) ) ;
#61069 = CARTESIAN_POINT ( 'NONE',  ( -20.35785670957392668, -20.51291524300857816, -52.65483682830183199 ) ) ;
#61070 = CARTESIAN_POINT ( 'NONE',  ( -18.67979575497193778, 10.72451020669871902, 73.33442372801901854 ) ) ;
#61071 = LINE ( 'NONE', #154086, #10990 ) ;
#61072 = CARTESIAN_POINT ( 'NONE',  ( -19.02544592524334988, -5.153800228976617603, 38.95942372801900433 ) ) ;
#61073 = CARTESIAN_POINT ( 'NONE',  ( 21.52544592524334988, 5.823673210054432836, 106.4594237280190328 ) ) ;
#61074 = CARTESIAN_POINT ( 'NONE',  ( -8.314922557960811034, -14.29746914071050412, 47.08224293864770260 ) ) ;
#61075 = CARTESIAN_POINT ( 'NONE',  ( 9.474510206698971260, -16.51473224551069308, 52.91557627198102409 ) ) ;
#61076 = CARTESIAN_POINT ( 'NONE',  ( 16.46253265017160672, -9.564922557960803928, 108.3322429386476955 ) ) ;
#61077 = CARTESIAN_POINT ( 'NONE',  ( -21.55341960407619339, 5.719274019375674811, 88.54275706135236135 ) ) ;
#61078 = CARTESIAN_POINT ( 'NONE',  ( -9.474510206698964154, 16.51473224551069663, 70.41557627198102409 ) ) ;
#61079 = CARTESIAN_POINT ( 'NONE',  ( 0.05219959533937995610, -21.53943276465977519, 85.00109039468568994 ) ) ;
#61080 = CARTESIAN_POINT ( 'NONE',  ( -5.823673210054116645, -21.52544592524344225, 37.29057627198102409 ) ) ;
#61081 = CARTESIAN_POINT ( 'NONE',  ( -18.67979575497193778, 10.72451020669871902, 28.33442372801902209 ) ) ;
#61082 = CARTESIAN_POINT ( 'NONE',  ( -19.05341960407617563, 5.049401038297882671, 53.54275706135231871 ) ) ;
#61083 = CARTESIAN_POINT ( 'NONE',  ( -19.02544592524342804, 5.153800228976336051, 31.04057627198102409 ) ) ;
#61084 = CARTESIAN_POINT ( 'NONE',  ( -16.51473224551069308, -9.474510206698971260, 76.66557627198103830 ) ) ;
#61085 = EDGE_CURVE ( 'NONE', #162452, #94244, #32981, .T. ) ;
#61086 = CARTESIAN_POINT ( 'NONE',  ( -16.55341960407617563, 4.379528057220093196, 33.54275706135234714 ) ) ;
#61087 = CARTESIAN_POINT ( 'NONE',  ( -16.53943276465976808, 0.05219959533911058130, 91.24890960531436690 ) ) ;
#61088 = CARTESIAN_POINT ( 'NONE',  ( 5.153800228976335163, 19.02544592524342804, 54.79057627198103120 ) ) ;
#61089 = CARTESIAN_POINT ( 'NONE',  ( 21.52544592524344225, -5.823673210054117533, 33.54057627198102409 ) ) ;
#61090 = CARTESIAN_POINT ( 'NONE',  ( -5.153800228976607833, 19.02544592524334988, 107.7094237280189759 ) ) ;
#61091 = CARTESIAN_POINT ( 'NONE',  ( 21.53943276465977519, 0.05219959533937863772, 21.25109039468567218 ) ) ;
#61092 = CARTESIAN_POINT ( 'NONE',  ( -15.80617190586768217, 15.72974639402176855, 73.12609039468567573 ) ) ;
#61093 = CARTESIAN_POINT ( 'NONE',  ( -16.53943276465976808, -0.05219959533934237506, 68.75109039468568994 ) ) ;
#61094 = CARTESIAN_POINT ( 'NONE',  ( 12.06949235617739724, 12.14591786802326823, 71.87609039468568994 ) ) ;
#61095 = CARTESIAN_POINT ( 'NONE',  ( -16.46253265017160317, 9.564922557960807481, 60.83224293864769550 ) ) ;
#61096 = CARTESIAN_POINT ( 'NONE',  ( -4.483927247898782831, 16.52544592524335698, 92.70942372801901854 ) ) ;
#61097 = CARTESIAN_POINT ( 'NONE',  ( 16.51473224551083163, -9.474510206698727899, 35.83442372801899722 ) ) ;
#61098 = CARTESIAN_POINT ( 'NONE',  ( 5.823673210054444382, -21.52544592524334988, 20.20942372801900788 ) ) ;
#61099 = CARTESIAN_POINT ( 'NONE',  ( -16.53943276465976808, 0.05219959533911058130, 66.24890960531436690 ) ) ;
#61100 = CARTESIAN_POINT ( 'NONE',  ( 9.474510206698971260, -16.51473224551069308, 87.91557627198102409 ) ) ;
#61101 = CARTESIAN_POINT ( 'NONE',  ( -4.379528057220086978, -16.55341960407618274, 94.79275706135234714 ) ) ;
#61102 = CARTESIAN_POINT ( 'NONE',  ( -5.823673210054431948, 21.52544592524334988, 62.70942372801902565 ) ) ;
#61103 = CARTESIAN_POINT ( 'NONE',  ( 8.314922557961029526, -14.29746914071037800, 20.41775706135234714 ) ) ;
#61104 = CARTESIAN_POINT ( 'NONE',  ( -18.67979575497178146, -10.72451020669898902, 106.6655762719810383 ) ) ;
#61105 = CARTESIAN_POINT ( 'NONE',  ( 14.29746914071049879, -8.314922557960816363, 58.33224293864768839 ) ) ;
#61106 = ORIENTED_EDGE ( 'NONE', *, *, #188107, .F. ) ;
#61107 = CARTESIAN_POINT ( 'NONE',  ( -15.72974639402197994, 15.80617190586746368, 90.62390960531436690 ) ) ;
#61108 = CARTESIAN_POINT ( 'NONE',  ( -8.224510206698948167, 14.34966873604960824, 45.41557627198103830 ) ) ;
#61109 = ORIENTED_EDGE ( 'NONE', *, *, #4039, .T. ) ;
#61110 = CARTESIAN_POINT ( 'NONE',  ( 34.71410084532069362, 2.653616468751211155, 52.01918243487461524 ) ) ;
#61111 = CARTESIAN_POINT ( 'NONE',  ( -10.81492255796105439, 18.62759615963255655, 22.91775706135235069 ) ) ;
#61112 = CARTESIAN_POINT ( 'NONE',  ( -18.67979575497178146, -10.72451020669898902, 21.66557627198102409 ) ) ;
#61113 = CARTESIAN_POINT ( 'NONE',  ( 21.52544592524334988, 5.823673210054432836, 31.45942372801901854 ) ) ;
#61114 = CARTESIAN_POINT ( 'NONE',  ( -4.483927247898539470, -16.52544592524342804, 47.29057627198103120 ) ) ;
#61115 = CARTESIAN_POINT ( 'NONE',  ( 5.049401038298161559, -19.05341960407611168, 62.70724293864769550 ) ) ;
#61116 = CARTESIAN_POINT ( 'NONE',  ( 13.97604488694548053, -13.89961937509957401, 65.62609039468567573 ) ) ;
#61117 = CARTESIAN_POINT ( 'NONE',  ( -5.049401038298153566, 19.05341960407611168, 100.2072429386476955 ) ) ;
#61118 = CARTESIAN_POINT ( 'NONE',  ( 21.52544592524344225, -5.823673210054117533, 43.54057627198103830 ) ) ;
#61119 = CARTESIAN_POINT ( 'NONE',  ( -22.64239272338085485, -30.05593529206066705, -19.14955533181695202 ) ) ;
#61120 = CARTESIAN_POINT ( 'NONE',  ( -13.89961937509977652, 13.97604488694528158, 55.62390960531434558 ) ) ;
#61121 = CARTESIAN_POINT ( 'NONE',  ( -16.53943276465976808, -0.05219959533934237506, 38.75109039468567573 ) ) ;
#61122 = CARTESIAN_POINT ( 'NONE',  ( 5.049401038297881783, 19.05341960407617563, 62.29275706135234003 ) ) ;
#61123 = CARTESIAN_POINT ( 'NONE',  ( -18.62759615963255300, -10.81492255796106328, 19.16775706135234714 ) ) ;
#61124 = EDGE_CURVE ( 'NONE', #41998, #166995, #140895, .T. ) ;
#61125 = CARTESIAN_POINT ( 'NONE',  ( -0.05219959533910754901, -16.53943276465976808, 47.49890960531435979 ) ) ;
#61126 = CARTESIAN_POINT ( 'NONE',  ( 5.153800228976335163, 19.02544592524342804, 84.79057627198099567 ) ) ;
#61127 = CARTESIAN_POINT ( 'NONE',  ( 18.67979575497178502, 10.72451020669898547, 79.16557627198103830 ) ) ;
#61129 = CARTESIAN_POINT ( 'NONE',  ( -14.34966873604972548, 8.224510206698743886, 33.33442372801900433 ) ) ;
#61128 = CARTESIAN_POINT ( 'NONE',  ( 18.62759615963271287, -10.81492255796078972, 103.3322429386476955 ) ) ;
#61130 = CARTESIAN_POINT ( 'NONE',  ( 10.81492255796078972, 18.62759615963270932, 39.58224293864769550 ) ) ;
#61131 = CARTESIAN_POINT ( 'NONE',  ( 5.719274019375673035, 21.55341960407619339, 97.29275706135234714 ) ) ;
#61132 = CARTESIAN_POINT ( 'NONE',  ( 19.02544592524343514, -5.153800228976328945, 93.54057627198102409 ) ) ;
#61133 = AXIS2_PLACEMENT_3D ( 'NONE', #104325, #118510, #167981 ) ;
#61134 = CARTESIAN_POINT ( 'NONE',  ( 9.474510206698971260, -16.51473224551069308, 47.91557627198102409 ) ) ;
#61135 = CARTESIAN_POINT ( 'NONE',  ( -5.153800228976328057, -19.02544592524343514, 97.29057627198099567 ) ) ;
#61136 = CARTESIAN_POINT ( 'NONE',  ( -9.564922557960796823, -16.46253265017161027, 72.08224293864770971 ) ) ;
#61137 = CARTESIAN_POINT ( 'NONE',  ( -14.29746914071037622, -8.314922557961029526, 29.16775706135234003 ) ) ;
#61138 = CARTESIAN_POINT ( 'NONE',  ( 17.50000000000015987, 3.292511757969722286, 32.43479729789459753 ) ) ;
#61139 = CARTESIAN_POINT ( 'NONE',  ( -5.153800228976607833, 19.02544592524334988, 52.70942372801900433 ) ) ;
#61141 = CARTESIAN_POINT ( 'NONE',  ( 18.62759615963271287, -10.81492255796078972, 38.33224293864768839 ) ) ;
#61140 = CARTESIAN_POINT ( 'NONE',  ( 5.719274019375673035, 21.55341960407619339, 107.2927570613523471 ) ) ;
#61142 = CARTESIAN_POINT ( 'NONE',  ( 0.05219959533934541429, -16.53943276465976808, 110.0010903946856757 ) ) ;
#61143 = DIRECTION ( 'NONE',  ( -1.000000000000000000, 0.000000000000000000, 0.000000000000000000 ) ) ;
#61144 = CARTESIAN_POINT ( 'NONE',  ( 13.89961937509957401, 13.97604488694547697, 66.87609039468567573 ) ) ;
#61145 = CARTESIAN_POINT ( 'NONE',  ( 5.153800228976615827, -19.02544592524334988, 25.20942372801900433 ) ) ;
#61146 = CARTESIAN_POINT ( 'NONE',  ( 14.68807091101007067, -23.54891160506147330, 139.9999999999999716 ) ) ;
#61147 = CARTESIAN_POINT ( 'NONE',  ( -13.89961937509977652, 13.97604488694528158, 40.62390960531435979 ) ) ;
#61148 = CARTESIAN_POINT ( 'NONE',  ( -16.55341960407611168, -4.379528057220339221, 31.45724293864769550 ) ) ;
#61149 = CARTESIAN_POINT ( 'NONE',  ( -5.153800228976328057, -19.02544592524343514, 27.29057627198103120 ) ) ;
#61150 = CARTESIAN_POINT ( 'NONE',  ( -14.34966873604960291, -8.224510206698953496, 31.66557627198102054 ) ) ;
#61151 = DIRECTION ( 'NONE',  ( -0.000000000000000000, -0.000000000000000000, 1.000000000000000000 ) ) ;
#61152 = CARTESIAN_POINT ( 'NONE',  ( 14.34966873604972726, -8.224510206698740333, 95.83442372801903275 ) ) ;
#61153 = CARTESIAN_POINT ( 'NONE',  ( -9.474510206698964154, 16.51473224551069663, 35.41557627198102409 ) ) ;
#61154 = CARTESIAN_POINT ( 'NONE',  ( -5.719274019375665041, -21.55341960407619695, 104.7927570613523898 ) ) ;
#61155 = CARTESIAN_POINT ( 'NONE',  ( -14.29746914071037622, -8.314922557961029526, 24.16775706135235424 ) ) ;
#61157 = ORIENTED_EDGE ( 'NONE', *, *, #169870, .F. ) ;
#61156 = CARTESIAN_POINT ( 'NONE',  ( -18.67979575497193778, 10.72451020669871902, 73.33442372801901854 ) ) ;
#61158 = CARTESIAN_POINT ( 'NONE',  ( -13.89961937509957401, -13.97604488694547875, 49.37609039468567573 ) ) ;
#61159 = CARTESIAN_POINT ( 'NONE',  ( -19.05341960407611168, -5.049401038298163336, 96.45724293864769550 ) ) ;
#61160 = CARTESIAN_POINT ( 'NONE',  ( 13.97604488694527802, 13.89961937509977652, 84.37390960531433848 ) ) ;
#61161 = FACE_OUTER_BOUND ( 'NONE', #196633, .T. ) ;
#61162 = CARTESIAN_POINT ( 'NONE',  ( -21.55341960407610458, -5.719274019375992779, 106.4572429386477097 ) ) ;
#61163 = AXIS2_PLACEMENT_3D ( 'NONE', #78764, #145409, #53405 ) ;
#61164 = CARTESIAN_POINT ( 'NONE',  ( -16.55341960407611168, -4.379528057220339221, 71.45724293864769550 ) ) ;
#61165 = CARTESIAN_POINT ( 'NONE',  ( -21.55341960407610458, -5.719274019375992779, 56.45724293864768839 ) ) ;
#61166 = CARTESIAN_POINT ( 'NONE',  ( 9.564922557960805705, 16.46253265017160317, 64.58224293864769550 ) ) ;
#61168 = CARTESIAN_POINT ( 'NONE',  ( 16.55341960407618274, -4.379528057220086978, 91.04275706135236135 ) ) ;
#61167 = CARTESIAN_POINT ( 'NONE',  ( -5.823673210054116645, -21.52544592524344225, 97.29057627198105251 ) ) ;
#61169 = ORIENTED_EDGE ( 'NONE', *, *, #65499, .T. ) ;
#61170 = CARTESIAN_POINT ( 'NONE',  ( -9.564922557960796823, -16.46253265017161027, 67.08224293864769550 ) ) ;
#61172 = DIRECTION ( 'NONE',  ( -0.000000000000000000, -0.5000000000000002220, 0.8660254037844384856 ) ) ;
#61171 = CARTESIAN_POINT ( 'NONE',  ( 12.14591786802309770, 12.06949235617756955, 89.37390960531435269 ) ) ;
#61173 = CARTESIAN_POINT ( 'NONE',  ( -16.51473224551069308, -9.474510206698971260, 56.66557627198103120 ) ) ;
#61174 = CARTESIAN_POINT ( 'NONE',  ( -19.05341960407617563, 5.049401038297882671, 83.54275706135233293 ) ) ;
#61175 = CARTESIAN_POINT ( 'NONE',  ( 8.224510206698953496, -14.34966873604960469, 77.91557627198102409 ) ) ;
#61176 = CARTESIAN_POINT ( 'NONE',  ( 0.05219959533937995610, -21.53943276465977519, 55.00109039468568284 ) ) ;
#61178 = CARTESIAN_POINT ( 'NONE',  ( 10.72451020669898902, -18.67979575497178502, 102.9155762719810383 ) ) ;
#61177 = CARTESIAN_POINT ( 'NONE',  ( 9.564922557960805705, 16.46253265017160317, 29.58224293864769550 ) ) ;
#61179 = CARTESIAN_POINT ( 'NONE',  ( -12.06949235617756955, 12.14591786802309770, 85.62390960531436690 ) ) ;
#61180 = CARTESIAN_POINT ( 'NONE',  ( 6.004573588225570191, -47.77740467397576651, -24.84605846612342006 ) ) ;
#61181 = CARTESIAN_POINT ( 'NONE',  ( -16.51473224551069308, -9.474510206698971260, 56.66557627198103120 ) ) ;
#61182 = CARTESIAN_POINT ( 'NONE',  ( -11.15262245511042671, -12.20012380450693890, -61.42526006663408111 ) ) ;
#61184 = CARTESIAN_POINT ( 'NONE',  ( -16.51473224551069308, -9.474510206698971260, 106.6655762719810383 ) ) ;
#61183 = CARTESIAN_POINT ( 'NONE',  ( 19.03943276465977164, 0.05219959533936151252, 91.25109039468566152 ) ) ;
#61185 = CARTESIAN_POINT ( 'NONE',  ( -21.55341960407619339, 5.719274019375674811, 38.54275706135234714 ) ) ;
#61186 = CARTESIAN_POINT ( 'NONE',  ( -9.474510206698964154, 16.51473224551069663, 85.41557627198102409 ) ) ;
#61187 = CARTESIAN_POINT ( 'NONE',  ( -9.474510206698720793, -16.51473224551083518, 64.58442372801900433 ) ) ;
#61188 = CARTESIAN_POINT ( 'NONE',  ( -5.153800228976328057, -19.02544592524343514, 57.29057627198103120 ) ) ;
#61189 = CARTESIAN_POINT ( 'NONE',  ( 8.314922557960818139, 14.29746914071049879, 79.58224293864769550 ) ) ;
#61190 = CARTESIAN_POINT ( 'NONE',  ( 12.06949235617757843, -12.14591786802309237, 63.12390960531435979 ) ) ;
#61191 = CARTESIAN_POINT ( 'NONE',  ( 9.474510206698971260, -16.51473224551069308, 87.91557627198102409 ) ) ;
#61192 = CARTESIAN_POINT ( 'NONE',  ( 21.53943276465977519, -0.05219959533907433946, 98.74890960531438111 ) ) ;
#61193 = CARTESIAN_POINT ( 'NONE',  ( 19.03943276465977164, -0.05219959533909143690, 88.74890960531436690 ) ) ;
#61194 = CARTESIAN_POINT ( 'NONE',  ( 13.89961937509957401, 13.97604488694547697, 31.87609039468566863 ) ) ;
#61197 = CARTESIAN_POINT ( 'NONE',  ( -16.52544592524342804, 4.483927247898546575, 116.0405762719810383 ) ) ;
#61196 = CARTESIAN_POINT ( 'NONE',  ( -8.314922557960811034, -14.29746914071050412, 27.08224293864769550 ) ) ;
#61195 = CARTESIAN_POINT ( 'NONE',  ( 9.474510206698971260, -16.51473224551069308, 42.91557627198103120 ) ) ;
#61198 = ORIENTED_EDGE ( 'NONE', *, *, #183156, .F. ) ;
#61199 = CARTESIAN_POINT ( 'NONE',  ( 5.823673210054444382, -21.52544592524334988, 50.20942372801901854 ) ) ;
#61200 = CARTESIAN_POINT ( 'NONE',  ( -13.97604488694547697, 13.89961937509957934, 68.12609039468563310 ) ) ;
#61201 = CARTESIAN_POINT ( 'NONE',  ( 16.53943276465976808, -0.05219959533910856209, 33.74890960531436690 ) ) ;
#61202 = CARTESIAN_POINT ( 'NONE',  ( -18.67979575497178146, -10.72451020669898902, 86.66557627198102409 ) ) ;
#61203 = CARTESIAN_POINT ( 'NONE',  ( 0.05219959533909260263, 19.03943276465977164, 109.9989096053143669 ) ) ;
#61204 = CARTESIAN_POINT ( 'NONE',  ( -12.06949235617756955, 12.14591786802309770, 75.62390960531439532 ) ) ;
#61205 = CARTESIAN_POINT ( 'NONE',  ( -16.51473224551069308, -9.474510206698971260, 31.66557627198102054 ) ) ;
#61206 = CARTESIAN_POINT ( 'NONE',  ( -13.97604488694547697, 13.89961937509957934, 33.12609039468566863 ) ) ;
#61207 = CARTESIAN_POINT ( 'NONE',  ( -8.314922557961024197, 14.29746914071037800, 107.9177570613523471 ) ) ;
#61208 = CARTESIAN_POINT ( 'NONE',  ( -16.53943276465976808, -0.05219959533934237506, 53.75109039468568994 ) ) ;
#61209 = CARTESIAN_POINT ( 'NONE',  ( -15.72974639402197994, 15.80617190586746368, 30.62390960531436335 ) ) ;
#61210 = CARTESIAN_POINT ( 'NONE',  ( 0.05219959533937995610, -21.53943276465977519, 105.0010903946856757 ) ) ;
#61211 = CARTESIAN_POINT ( 'NONE',  ( 0.05219959533909260263, 19.03943276465977164, 74.99890960531435269 ) ) ;
#61212 = CARTESIAN_POINT ( 'NONE',  ( -4.379528057220086978, -16.55341960407618274, 74.79275706135234714 ) ) ;
#61213 = CARTESIAN_POINT ( 'NONE',  ( -19.05341960407611168, -5.049401038298163336, 21.45724293864768839 ) ) ;
#61214 = CARTESIAN_POINT ( 'NONE',  ( 12.06949235617757843, -12.14591786802309237, 28.12390960531435979 ) ) ;
#61216 = CARTESIAN_POINT ( 'NONE',  ( -19.03943276465977164, 0.05219959533909376836, 91.24890960531436690 ) ) ;
#61215 = CARTESIAN_POINT ( 'NONE',  ( -0.05219959533909027116, -19.03943276465977164, 102.4989096053143669 ) ) ;
#61218 = EDGE_CURVE ( 'NONE', #70166, #102970, #53729, .T. ) ;
#61217 = CARTESIAN_POINT ( 'NONE',  ( -5.153800228976328057, -19.02544592524343514, 107.2905762719810383 ) ) ;
#61219 = CARTESIAN_POINT ( 'NONE',  ( 12.06949235617757843, -12.14591786802309237, 63.12390960531435979 ) ) ;
#61220 = CARTESIAN_POINT ( 'NONE',  ( -14.29746914071049879, 8.314922557960819915, 30.83224293864770260 ) ) ;
#61221 = ORIENTED_EDGE ( 'NONE', *, *, #198190, .T. ) ;
#61222 = CARTESIAN_POINT ( 'NONE',  ( 16.52544592524342804, -4.483927247898539470, 48.54057627198103120 ) ) ;
#61224 = CARTESIAN_POINT ( 'NONE',  ( 9.687362902255726382, 9.687362902255699737, -62.58071313852362039 ) ) ;
#61223 = CARTESIAN_POINT ( 'NONE',  ( -8.314922557961024197, 14.29746914071037800, 42.91775706135235424 ) ) ;
#61225 = CARTESIAN_POINT ( 'NONE',  ( 0.05219959533936267826, -19.03943276465977164, 50.00109039468566863 ) ) ;
#61226 = CARTESIAN_POINT ( 'NONE',  ( -5.153800228976328057, -19.02544592524343514, 87.29057627198103830 ) ) ;
#61227 = CARTESIAN_POINT ( 'NONE',  ( -9.474510206698720793, -16.51473224551083518, 69.58442372801901854 ) ) ;
#61228 = CARTESIAN_POINT ( 'NONE',  ( 22.44159573604009594, -16.30477369853687364, 142.1750000027311671 ) ) ;
#61229 = CARTESIAN_POINT ( 'NONE',  ( -5.153800228976607833, 19.02544592524334988, 57.70942372801899012 ) ) ;
#61231 = CARTESIAN_POINT ( 'NONE',  ( -8.314922557961024197, 14.29746914071037800, 87.91775706135234714 ) ) ;
#61230 = CARTESIAN_POINT ( 'NONE',  ( 13.89961937509957401, 13.97604488694547697, 91.87609039468567573 ) ) ;
#61232 = CARTESIAN_POINT ( 'NONE',  ( -22.44159573604009950, -16.30477369853688430, 147.5750000027312012 ) ) ;
#61233 = CARTESIAN_POINT ( 'NONE',  ( 9.564922557960805705, 16.46253265017160317, 29.58224293864769550 ) ) ;
#61234 = CARTESIAN_POINT ( 'NONE',  ( -18.62759615963270932, 10.81492255796079327, 25.83224293864769194 ) ) ;
#61235 = CARTESIAN_POINT ( 'NONE',  ( 21.53943276465977519, 0.05219959533937863772, 36.25109039468567573 ) ) ;
#61236 = CARTESIAN_POINT ( 'NONE',  ( -13.89961937509957401, -13.97604488694547875, 104.3760903946856757 ) ) ;
#61238 = CARTESIAN_POINT ( 'NONE',  ( -9.474510206698964154, 16.51473224551069663, 65.41557627198102409 ) ) ;
#61237 = CARTESIAN_POINT ( 'NONE',  ( 17.50000000000000000, 5.499999999999997335, 23.78230962303566542 ) ) ;
#61239 = CARTESIAN_POINT ( 'NONE',  ( 16.46253265017160672, -9.564922557960803928, 98.33224293864769550 ) ) ;
#61241 = CARTESIAN_POINT ( 'NONE',  ( -13.89961937509977652, 13.97604488694528158, 60.62390960531436690 ) ) ;
#61240 = CARTESIAN_POINT ( 'NONE',  ( 0.05219959533910956823, 16.53943276465976808, 54.99890960531435269 ) ) ;
#61242 = CARTESIAN_POINT ( 'NONE',  ( 16.51473224551069308, 9.474510206698969483, 69.16557627198102409 ) ) ;
#61243 = CARTESIAN_POINT ( 'NONE',  ( 19.05341960407617918, -5.049401038297876454, 76.04275706135230450 ) ) ;
#61244 = CARTESIAN_POINT ( 'NONE',  ( -0.05219959533907301413, -21.53943276465977519, 57.49890960531435979 ) ) ;
#61245 = CARTESIAN_POINT ( 'NONE',  ( -4.379528057220328563, 16.55341960407611168, 115.2072429386476955 ) ) ;
#61246 = CARTESIAN_POINT ( 'NONE',  ( 16.46253265017146816, 9.564922557961045513, 41.66775706135234003 ) ) ;
#61248 = EDGE_CURVE ( 'NONE', #83484, #91305, #49415, .T. ) ;
#61247 = CARTESIAN_POINT ( 'NONE',  ( -5.049401038298153566, 19.05341960407611168, 80.20724293864769550 ) ) ;
#61249 = CARTESIAN_POINT ( 'NONE',  ( -15.72974639402197994, 15.80617190586746368, 70.62390960531436690 ) ) ;
#61251 = CARTESIAN_POINT ( 'NONE',  ( -13.89961937509957401, -13.97604488694547875, 29.37609039468565797 ) ) ;
#61250 = CARTESIAN_POINT ( 'NONE',  ( -16.53943276465976808, 0.05219959533911058130, 81.24890960531436690 ) ) ;
#61252 = CARTESIAN_POINT ( 'NONE',  ( -18.67979575497178146, -10.72451020669898902, 76.66557627198103830 ) ) ;
#61253 = CARTESIAN_POINT ( 'NONE',  ( 21.53943276465977519, -0.05219959533907433946, 58.74890960531436690 ) ) ;
#61254 = CARTESIAN_POINT ( 'NONE',  ( -5.823673210054116645, -21.52544592524344225, 37.29057627198102409 ) ) ;
#61255 = CARTESIAN_POINT ( 'NONE',  ( 15.80617190586769283, -15.72974639402175789, 95.62609039468568994 ) ) ;
#61256 = CARTESIAN_POINT ( 'NONE',  ( -19.05341960407611168, -5.049401038298163336, 61.45724293864769550 ) ) ;
#61257 = CARTESIAN_POINT ( 'NONE',  ( 0.05219959533909260263, 19.03943276465977164, 24.99890960531435269 ) ) ;
#61258 = CARTESIAN_POINT ( 'NONE',  ( 18.62759615963255655, 10.81492255796105972, 26.66775706135235424 ) ) ;
#61259 = CARTESIAN_POINT ( 'NONE',  ( -17.49999999999999645, -5.499999999999992895, 49.20309617465830598 ) ) ;
#61260 = CARTESIAN_POINT ( 'NONE',  ( -10.72451020669870658, -18.67979575497194134, 44.58442372801901854 ) ) ;
#61261 = CARTESIAN_POINT ( 'NONE',  ( 19.03943276465977164, -0.05219959533909143690, 33.74890960531435979 ) ) ;
#61262 = CARTESIAN_POINT ( 'NONE',  ( 10.81492255796078972, 18.62759615963270932, 104.5822429386477097 ) ) ;
#61263 = CARTESIAN_POINT ( 'NONE',  ( 13.89961937509957401, 13.97604488694547697, 41.87609039468566152 ) ) ;
#61264 = CARTESIAN_POINT ( 'NONE',  ( -13.97604488694527625, -13.89961937509977652, 36.87390960531436690 ) ) ;
#61265 = CARTESIAN_POINT ( 'NONE',  ( -19.24578484527059175, -180.9428398739492252, -15.00000000000000178 ) ) ;
#61266 = SURFACE_STYLE_USAGE ( .BOTH. , #2579 ) ;
#61267 = CARTESIAN_POINT ( 'NONE',  ( 0.05219959533934541429, -16.53943276465976808, 55.00109039468568284 ) ) ;
#61268 = CARTESIAN_POINT ( 'NONE',  ( 16.51473224551069308, 9.474510206698969483, 24.16557627198102765 ) ) ;
#61269 = CARTESIAN_POINT ( 'NONE',  ( -25.52568752982044842, -9.519068727187397272, 170.8917780290337873 ) ) ;
#61270 = CARTESIAN_POINT ( 'NONE',  ( -9.564922557960796823, -16.46253265017161027, 87.08224293864769550 ) ) ;
#61271 = CARTESIAN_POINT ( 'NONE',  ( -16.55341960407611168, -4.379528057220339221, 101.4572429386476955 ) ) ;
#61272 = CARTESIAN_POINT ( 'NONE',  ( 10.72451020669898902, -18.67979575497178502, 57.91557627198103120 ) ) ;
#61273 = CARTESIAN_POINT ( 'NONE',  ( -0.05219959533934338120, 16.53943276465976808, 47.50109039468568994 ) ) ;
#61274 = CARTESIAN_POINT ( 'NONE',  ( -15.80617190586768217, 15.72974639402176855, 103.1260903946856757 ) ) ;
#61275 = CARTESIAN_POINT ( 'NONE',  ( 9.564922557960805705, 16.46253265017160317, 24.58224293864769194 ) ) ;
#61276 = CARTESIAN_POINT ( 'NONE',  ( -0.05219959533910754901, -16.53943276465976808, 22.49890960531436335 ) ) ;
#61277 = CARTESIAN_POINT ( 'NONE',  ( -0.05219959533910754901, -16.53943276465976808, 57.49890960531435979 ) ) ;
#61278 = AXIS2_PLACEMENT_3D ( 'NONE', #127028, #32061, #48228 ) ;
#61279 = CARTESIAN_POINT ( 'NONE',  ( 13.89961937509977652, -13.97604488694527269, 53.12390960531434558 ) ) ;
#61280 = CARTESIAN_POINT ( 'NONE',  ( 10.81492255796106328, -18.62759615963255655, 90.41775706135236135 ) ) ;
#61281 = CARTESIAN_POINT ( 'NONE',  ( 15.80617190586769283, -15.72974639402175789, 25.62609039468567929 ) ) ;
#61282 = CARTESIAN_POINT ( 'NONE',  ( -5.719274019375665041, -21.55341960407619695, 69.79275706135234714 ) ) ;
#61283 = CARTESIAN_POINT ( 'NONE',  ( 4.483927247898790824, -16.52544592524335698, 55.20942372801902565 ) ) ;
#61284 = CARTESIAN_POINT ( 'NONE',  ( -4.483927247898782831, 16.52544592524335698, 27.70942372801901854 ) ) ;
#61286 = CARTESIAN_POINT ( 'NONE',  ( -10.81492255796105439, 18.62759615963255655, 102.9177570613523756 ) ) ;
#61285 = CARTESIAN_POINT ( 'NONE',  ( 16.53943276465976808, -0.05219959533910856209, 83.74890960531435269 ) ) ;
#61287 = CARTESIAN_POINT ( 'NONE',  ( -0.05219959533910754901, -16.53943276465976808, 22.49890960531436335 ) ) ;
#61288 = CARTESIAN_POINT ( 'NONE',  ( 0.000000000000000000, -165.0000000000000000, 7.000000000000003553 ) ) ;
#61289 = CARTESIAN_POINT ( 'NONE',  ( 8.314922557961029526, -14.29746914071037800, 45.41775706135234003 ) ) ;
#61290 = CARTESIAN_POINT ( 'NONE',  ( -16.53943276465976808, 0.05219959533911058130, 46.24890960531435979 ) ) ;
#61291 = CARTESIAN_POINT ( 'NONE',  ( -16.52544592524335698, -4.483927247898792601, 83.95942372801900433 ) ) ;
#61292 = CARTESIAN_POINT ( 'NONE',  ( 19.02544592524343514, -5.153800228976328945, 103.5405762719809957 ) ) ;
#61293 = CARTESIAN_POINT ( 'NONE',  ( -13.89961937509977652, 13.97604488694528158, 110.6239096053143243 ) ) ;
#61294 = CARTESIAN_POINT ( 'NONE',  ( -18.62759615963255300, -10.81492255796106328, 94.16775706135237556 ) ) ;
#61295 = CARTESIAN_POINT ( 'NONE',  ( 8.224510206698742110, 14.34966873604972548, 102.0844237280190185 ) ) ;
#61296 = CARTESIAN_POINT ( 'NONE',  ( 16.52544592524342804, -4.483927247898539470, 78.54057627198103830 ) ) ;
#61297 = CARTESIAN_POINT ( 'NONE',  ( -0.05219959533909027116, -19.03943276465977164, 82.49890960531436690 ) ) ;
#61298 = ORIENTED_EDGE ( 'NONE', *, *, #1307, .T. ) ;
#61299 = CARTESIAN_POINT ( 'NONE',  ( 16.53943276465976808, 0.05219959533934440121, 36.25109039468567573 ) ) ;
#61300 = CARTESIAN_POINT ( 'NONE',  ( 9.564922557960805705, 16.46253265017160317, 39.58224293864768839 ) ) ;
#61301 = CARTESIAN_POINT ( 'NONE',  ( 13.89961937509977652, -13.97604488694527269, 93.12390960531436690 ) ) ;
#61303 = CARTESIAN_POINT ( 'NONE',  ( -29.86685920354755552, 21.69954338932564397, -4.824999997268814234 ) ) ;
#61302 = CARTESIAN_POINT ( 'NONE',  ( -4.379528057220086978, -16.55341960407618274, 34.79275706135235424 ) ) ;
#61304 = CARTESIAN_POINT ( 'NONE',  ( 13.97604488694548053, -13.89961937509957401, 35.62609039468567573 ) ) ;
#61305 = CARTESIAN_POINT ( 'NONE',  ( -12.14591786802326823, 12.06949235617739902, 93.12609039468568994 ) ) ;
#61306 = CARTESIAN_POINT ( 'NONE',  ( 13.97604488694527802, 13.89961937509977652, 34.37390960531436690 ) ) ;
#61307 = CARTESIAN_POINT ( 'NONE',  ( -12.06949235617739369, -12.14591786802326823, 84.37609039468570415 ) ) ;
#61308 = CARTESIAN_POINT ( 'NONE',  ( 12.14591786802327356, -12.06949235617739191, 70.62609039468567573 ) ) ;
#61309 = CARTESIAN_POINT ( 'NONE',  ( -9.564922557961040184, 16.46253265017147172, 82.91775706135233293 ) ) ;
#61310 = CARTESIAN_POINT ( 'NONE',  ( -16.51473224551082808, 9.474510206698731452, 28.33442372801900433 ) ) ;
#61311 = CARTESIAN_POINT ( 'NONE',  ( 5.049401038298161559, -19.05341960407611168, 52.70724293864767418 ) ) ;
#61312 = CARTESIAN_POINT ( 'NONE',  ( 4.483927247898545687, 16.52544592524342804, 89.79057627198103830 ) ) ;
#61313 = CARTESIAN_POINT ( 'NONE',  ( -19.05341960407617563, 5.049401038297882671, 58.54275706135234003 ) ) ;
#61314 = CARTESIAN_POINT ( 'NONE',  ( 10.81492255796078972, 18.62759615963270932, 49.58224293864769550 ) ) ;
#61315 = CARTESIAN_POINT ( 'NONE',  ( 9.564922557961047289, -16.46253265017146816, 25.41775706135234003 ) ) ;
#61316 = CARTESIAN_POINT ( 'NONE',  ( 9.564922557960805705, 16.46253265017160317, 104.5822429386476955 ) ) ;
#61317 = CARTESIAN_POINT ( 'NONE',  ( -5.823673210054116645, -21.52544592524344225, 77.29057627198102409 ) ) ;
#61318 = CARTESIAN_POINT ( 'NONE',  ( 13.89961937509977652, -13.97604488694527269, 108.1239096053143669 ) ) ;
#61319 = CARTESIAN_POINT ( 'NONE',  ( 5.153800228976615827, -19.02544592524334988, 95.20942372801897591 ) ) ;
#61320 = ADVANCED_FACE ( 'NONE', ( #18437 ), #153893, .F. ) ;
#61321 = CARTESIAN_POINT ( 'NONE',  ( 19.05341960407617918, -5.049401038297876454, 111.0427570613523329 ) ) ;
#61322 = CARTESIAN_POINT ( 'NONE',  ( 13.97604488694527802, 13.89961937509977652, 39.37390960531435269 ) ) ;
#61323 = CARTESIAN_POINT ( 'NONE',  ( 9.564922557960805705, 16.46253265017160317, 99.58224293864770971 ) ) ;
#61324 = CARTESIAN_POINT ( 'NONE',  ( 18.62759615963271287, -10.81492255796078972, 78.33224293864770971 ) ) ;
#61325 = CARTESIAN_POINT ( 'NONE',  ( 8.314922557961029526, -14.29746914071037800, 55.41775706135234714 ) ) ;
#61326 = CARTESIAN_POINT ( 'NONE',  ( 0.05219959533937995610, -21.53943276465977519, 60.00109039468568284 ) ) ;
#61328 = CARTESIAN_POINT ( 'NONE',  ( -16.46253265017146816, -9.564922557961047289, 19.16775706135233293 ) ) ;
#61327 = CARTESIAN_POINT ( 'NONE',  ( 5.153800228976615827, -19.02544592524334988, 110.2094237280189901 ) ) ;
#61329 = CARTESIAN_POINT ( 'NONE',  ( -14.29746914071037622, -8.314922557961029526, 109.1677570613523613 ) ) ;
#61330 = CARTESIAN_POINT ( 'NONE',  ( -21.53943276465977519, 0.05219959533907696930, 106.2489096053143811 ) ) ;
#61331 = CARTESIAN_POINT ( 'NONE',  ( -12.14591786802309592, -12.06949235617757132, 41.87390960531435979 ) ) ;
#61332 = CARTESIAN_POINT ( 'NONE',  ( -16.46253265017146816, -9.564922557961047289, 79.16775706135234714 ) ) ;
#61333 = CARTESIAN_POINT ( 'NONE',  ( -0.05219959533937732626, 21.53943276465977519, 62.50109039468568284 ) ) ;
#61334 = CARTESIAN_POINT ( 'NONE',  ( -16.46253265017146816, -9.564922557961047289, 39.16775706135234003 ) ) ;
#61335 = CARTESIAN_POINT ( 'NONE',  ( 8.224510206698953496, -14.34966873604960469, 107.9155762719810241 ) ) ;
#61336 = CARTESIAN_POINT ( 'NONE',  ( 0.05219959533907565091, 21.53943276465977519, 34.99890960531435979 ) ) ;
#61337 = CARTESIAN_POINT ( 'NONE',  ( -4.483927247898539470, -16.52544592524342804, 32.29057627198102409 ) ) ;
#61338 = CARTESIAN_POINT ( 'NONE',  ( -0.05219959533937732626, 21.53943276465977519, 97.50109039468567573 ) ) ;
#61339 = CARTESIAN_POINT ( 'NONE',  ( 12.14591786802327356, -12.06949235617739191, 65.62609039468568994 ) ) ;
#61340 = CARTESIAN_POINT ( 'NONE',  ( 14.29746914071049879, -8.314922557960816363, 23.33224293864769194 ) ) ;
#61341 = CARTESIAN_POINT ( 'NONE',  ( -21.55341960407619339, 5.719274019375674811, 58.54275706135235424 ) ) ;
#61342 = CARTESIAN_POINT ( 'NONE',  ( 21.52544592524334988, 5.823673210054432836, 51.45942372801901854 ) ) ;
#61343 = ORIENTED_EDGE ( 'NONE', *, *, #46412, .F. ) ;
#61344 = CARTESIAN_POINT ( 'NONE',  ( 19.02544592524343514, -5.153800228976328945, 28.54057627198102409 ) ) ;
#61345 = CARTESIAN_POINT ( 'NONE',  ( -5.823673210054431948, 21.52544592524334988, 42.70942372801901854 ) ) ;
#61346 = CARTESIAN_POINT ( 'NONE',  ( 8.224510206698953496, -14.34966873604960469, 107.9155762719810241 ) ) ;
#61347 = CARTESIAN_POINT ( 'NONE',  ( -16.46253265017160317, 9.564922557960807481, 35.83224293864768839 ) ) ;
#61348 = CARTESIAN_POINT ( 'NONE',  ( -4.379528057220328563, 16.55341960407611168, 80.20724293864769550 ) ) ;
#61349 = CARTESIAN_POINT ( 'NONE',  ( 19.03943276465977164, -0.05219959533909143690, 73.74890960531435269 ) ) ;
#61350 = CARTESIAN_POINT ( 'NONE',  ( 8.314922557960818139, 14.29746914071049879, 24.58224293864768839 ) ) ;
#61351 = CARTESIAN_POINT ( 'NONE',  ( 21.53943276465977519, -0.05219959533907433946, 58.74890960531436690 ) ) ;
#61352 = CARTESIAN_POINT ( 'NONE',  ( 4.379528057220339221, -16.55341960407611168, 92.70724293864770971 ) ) ;
#61353 = CARTESIAN_POINT ( 'NONE',  ( 5.719274019375991003, -21.55341960407610458, 112.7072429386476955 ) ) ;
#61354 = CARTESIAN_POINT ( 'NONE',  ( -19.02544592524342804, 5.153800228976336051, 101.0405762719810241 ) ) ;
#61356 = CARTESIAN_POINT ( 'NONE',  ( -0.05219959533936034679, 19.03943276465977164, 107.5010903946856615 ) ) ;
#61355 = CARTESIAN_POINT ( 'NONE',  ( -0.05219959533909027116, -19.03943276465977164, 67.49890960531436690 ) ) ;
#61357 = CARTESIAN_POINT ( 'NONE',  ( 0.05219959533907565091, 21.53943276465977519, 59.99890960531436690 ) ) ;
#61358 = CARTESIAN_POINT ( 'NONE',  ( -21.53943276465977519, -0.05219959533937600094, 78.75109039468568994 ) ) ;
#61359 = CARTESIAN_POINT ( 'NONE',  ( -16.46253265017160317, 9.564922557960807481, 65.83224293864769550 ) ) ;
#61360 = CARTESIAN_POINT ( 'NONE',  ( -19.05341960407611168, -5.049401038298163336, 101.4572429386476955 ) ) ;
#61361 = CARTESIAN_POINT ( 'NONE',  ( 12.14591786802327356, -12.06949235617739191, 75.62609039468567573 ) ) ;
#61362 = CARTESIAN_POINT ( 'NONE',  ( -21.55341960407619339, 5.719274019375674811, 58.54275706135235424 ) ) ;
#61363 = CARTESIAN_POINT ( 'NONE',  ( 10.72451020669871369, 18.67979575497193778, 87.08442372801901854 ) ) ;
#61364 = CARTESIAN_POINT ( 'NONE',  ( -15.80617190586745835, -15.72974639402198527, 106.8739096053143811 ) ) ;
#61365 = CARTESIAN_POINT ( 'NONE',  ( -16.52544592524335698, -4.483927247898792601, 83.95942372801900433 ) ) ;
#61366 = CARTESIAN_POINT ( 'NONE',  ( -21.53943276465977519, 0.05219959533907696930, 81.24890960531436690 ) ) ;
#61367 = CARTESIAN_POINT ( 'NONE',  ( 9.564922557961047289, -16.46253265017146816, 45.41775706135232582 ) ) ;
#61368 = CARTESIAN_POINT ( 'NONE',  ( 18.62759615963271287, -10.81492255796078972, 43.33224293864769550 ) ) ;
#61370 = CARTESIAN_POINT ( 'NONE',  ( 12.06949235617757843, -12.14591786802309237, 28.12390960531435979 ) ) ;
#61369 = CARTESIAN_POINT ( 'NONE',  ( -13.97604488694527625, -13.89961937509977652, 86.87390960531436690 ) ) ;
#61371 = CARTESIAN_POINT ( 'NONE',  ( -17.05587630539787369, 6.762274262135695935, 65.74180309037313918 ) ) ;
#61372 = CARTESIAN_POINT ( 'NONE',  ( -5.153800228976328057, -19.02544592524343514, 112.2905762719810099 ) ) ;
#61373 = CARTESIAN_POINT ( 'NONE',  ( -18.39639308325438805, -5.499999999999988454, 81.48252246182198633 ) ) ;
#61374 = CARTESIAN_POINT ( 'NONE',  ( -19.03943276465977164, -0.05219959533935918106, 88.75109039468567573 ) ) ;
#61375 = CARTESIAN_POINT ( 'NONE',  ( -18.67979575497178146, -10.72451020669898902, 71.66557627198100988 ) ) ;
#61376 = CARTESIAN_POINT ( 'NONE',  ( -4.379528057220328563, 16.55341960407611168, 55.20724293864770260 ) ) ;
#61377 = CARTESIAN_POINT ( 'NONE',  ( 12.06949235617739724, 12.14591786802326823, 21.87609039468567573 ) ) ;
#61378 = CARTESIAN_POINT ( 'NONE',  ( -13.89961937509977652, 13.97604488694528158, 35.62390960531435269 ) ) ;
#61379 = CARTESIAN_POINT ( 'NONE',  ( -9.564922557961040184, 16.46253265017147172, 107.9177570613523471 ) ) ;
#61381 = CARTESIAN_POINT ( 'NONE',  ( 5.049401038297881783, 19.05341960407617563, 67.29275706135234714 ) ) ;
#61380 = CARTESIAN_POINT ( 'NONE',  ( -10.81492255796078084, -18.62759615963271287, 102.0822429386476955 ) ) ;
#61382 = CARTESIAN_POINT ( 'NONE',  ( 13.89961937509977652, -13.97604488694527269, 83.12390960531436690 ) ) ;
#61383 = CARTESIAN_POINT ( 'NONE',  ( 4.483927247898545687, 16.52544592524342804, 79.79057627198102409 ) ) ;
#61384 = CARTESIAN_POINT ( 'NONE',  ( -5.153800228976328057, -19.02544592524343514, 62.29057627198100988 ) ) ;
#61385 = CARTESIAN_POINT ( 'NONE',  ( -12.14591786802309592, -12.06949235617757132, 71.87390960531438111 ) ) ;
#61386 = CARTESIAN_POINT ( 'NONE',  ( -9.564922557960796823, -16.46253265017161027, 32.08224293864769550 ) ) ;
#61387 = CARTESIAN_POINT ( 'NONE',  ( -37.58407650405590061, -0.3597885541503507145, 39.49999999999997158 ) ) ;
#61388 = CARTESIAN_POINT ( 'NONE',  ( -12.06949235617756955, 12.14591786802309770, 40.62390960531435269 ) ) ;
#61389 = CARTESIAN_POINT ( 'NONE',  ( 19.02544592524343514, -5.153800228976328945, 93.54057627198102409 ) ) ;
#61390 = FACE_BOUND ( 'NONE', #194765, .T. ) ;
#61391 = CARTESIAN_POINT ( 'NONE',  ( -13.89961937509957401, -13.97604488694547875, 54.37609039468565442 ) ) ;
#61392 = CARTESIAN_POINT ( 'NONE',  ( -8.314922557961024197, 14.29746914071037800, 57.91775706135234714 ) ) ;
#61393 = CARTESIAN_POINT ( 'NONE',  ( 10.81492255796078972, 18.62759615963270932, 59.58224293864770260 ) ) ;
#61394 = CARTESIAN_POINT ( 'NONE',  ( -5.049401038297874678, -19.05341960407617918, 19.79275706135233293 ) ) ;
#61395 = CARTESIAN_POINT ( 'NONE',  ( -9.564922557960796823, -16.46253265017161027, 92.08224293864769550 ) ) ;
#61396 = DIRECTION ( 'NONE',  ( 1.000000000000000000, 0.000000000000000000, 0.000000000000000000 ) ) ;
#61397 = CARTESIAN_POINT ( 'NONE',  ( -5.719274019375978568, 21.55341960407610458, 30.20724293864769550 ) ) ;
#61398 = CARTESIAN_POINT ( 'NONE',  ( 9.474510206698971260, -16.51473224551069308, 62.91557627198102409 ) ) ;
#61399 = CARTESIAN_POINT ( 'NONE',  ( -10.81492255796105439, 18.62759615963255655, 52.91775706135235424 ) ) ;
#61401 = CARTESIAN_POINT ( 'NONE',  ( 16.55341960407611168, 4.379528057220329451, 103.9572429386476813 ) ) ;
#61400 = PRODUCT_DEFINITION_SHAPE ( 'NONE', 'NONE',  #48691 ) ;
#61404 = ORIENTED_EDGE ( 'NONE', *, *, #55706, .T. ) ;
#61403 = CARTESIAN_POINT ( 'NONE',  ( -19.05341960407611168, -5.049401038298163336, 101.4572429386476955 ) ) ;
#61402 = CARTESIAN_POINT ( 'NONE',  ( 21.53943276465977519, -0.05219959533907433946, 103.7489096053143669 ) ) ;
#61405 = CARTESIAN_POINT ( 'NONE',  ( -5.719274019375665041, -21.55341960407619695, 39.79275706135235424 ) ) ;
#61406 = ORIENTED_EDGE ( 'NONE', *, *, #56848, .F. ) ;
#61407 = CARTESIAN_POINT ( 'NONE',  ( -9.564922557960796823, -16.46253265017161027, 107.0822429386476955 ) ) ;
#61408 = CARTESIAN_POINT ( 'NONE',  ( -19.49401214000074489, -12.39993551617566503, 167.9999999999999716 ) ) ;
#61409 = CARTESIAN_POINT ( 'NONE',  ( 10.72451020669898902, -18.67979575497178502, 97.91557627198103830 ) ) ;
#61410 = CARTESIAN_POINT ( 'NONE',  ( 19.02544592524343514, -5.153800228976328945, 43.54057627198103120 ) ) ;
#61411 = CARTESIAN_POINT ( 'NONE',  ( -14.34966873604972548, 8.224510206698743886, 28.33442372801902209 ) ) ;
#61412 = CARTESIAN_POINT ( 'NONE',  ( -11.74264578624799782, -36.14014761921581709, -11.34999999453762776 ) ) ;
#61413 = CARTESIAN_POINT ( 'NONE',  ( 9.564922557960805705, 16.46253265017160317, 29.58224293864769550 ) ) ;
#61414 = CARTESIAN_POINT ( 'NONE',  ( 21.53943276465977519, 0.05219959533937863772, 101.2510903946856757 ) ) ;
#61416 = CARTESIAN_POINT ( 'NONE',  ( 5.823673210054444382, -21.52544592524334988, 40.20942372801901854 ) ) ;
#61415 = CARTESIAN_POINT ( 'NONE',  ( 9.564922557960805705, 16.46253265017160317, 74.58224293864769550 ) ) ;
#61417 = AXIS2_PLACEMENT_3D ( 'NONE', #182537, #195734, #42040 ) ;
#61418 = CARTESIAN_POINT ( 'NONE',  ( 17.14385361876520264, -23.59649016807271238, 144.0750000027311444 ) ) ;
#61419 = CARTESIAN_POINT ( 'NONE',  ( -5.049401038298153566, 19.05341960407611168, 100.2072429386476955 ) ) ;
#61420 = CARTESIAN_POINT ( 'NONE',  ( 18.22780087662126647, 5.499999999999818812, 61.48236817873107185 ) ) ;
#61423 = CARTESIAN_POINT ( 'NONE',  ( -5.719274019375665041, -21.55341960407619695, 59.79275706135234714 ) ) ;
#61422 = CARTESIAN_POINT ( 'NONE',  ( -16.55341960407617563, 4.379528057220093196, 73.54275706135234714 ) ) ;
#61421 = CARTESIAN_POINT ( 'NONE',  ( -12.06949235617739369, -12.14591786802326823, 34.37609039468568284 ) ) ;
#61424 = CARTESIAN_POINT ( 'NONE',  ( -10.72451020669870658, -18.67979575497194134, 79.58442372801903275 ) ) ;
#61425 = CARTESIAN_POINT ( 'NONE',  ( 11.95151397458945119, -11.66585251704126414, -59.13370768023892055 ) ) ;
#61426 = CARTESIAN_POINT ( 'NONE',  ( -13.97604488694547697, 13.89961937509957934, 108.1260903946856331 ) ) ;
#61427 = CARTESIAN_POINT ( 'NONE',  ( 19.02544592524343514, -5.153800228976328945, 73.54057627198103830 ) ) ;
#61428 = CARTESIAN_POINT ( 'NONE',  ( 19.02544592524343514, -5.153800228976328945, 103.5405762719809957 ) ) ;
#61429 = CARTESIAN_POINT ( 'NONE',  ( -4.379528057220328563, 16.55341960407611168, 110.2072429386477239 ) ) ;
#61430 = CARTESIAN_POINT ( 'NONE',  ( -21.55341960407610458, -5.719274019375992779, 26.45724293864768839 ) ) ;
#61431 = CARTESIAN_POINT ( 'NONE',  ( 16.55341960407618274, -4.379528057220086978, 96.04275706135236135 ) ) ;
#61433 = CARTESIAN_POINT ( 'NONE',  ( -19.03943276465977164, 0.05219959533909376836, 51.24890960531436690 ) ) ;
#61432 = CARTESIAN_POINT ( 'NONE',  ( 12.14591786802309770, 12.06949235617756955, 74.37390960531436690 ) ) ;
#61434 = CARTESIAN_POINT ( 'NONE',  ( -15.72974639402176322, -15.80617190586768395, 74.37609039468568994 ) ) ;
#61435 = CARTESIAN_POINT ( 'NONE',  ( 17.50000000000000355, 4.403995465277920296, 21.93328991121576621 ) ) ;
#61436 = CARTESIAN_POINT ( 'NONE',  ( 16.51473224551083163, -9.474510206698727899, 105.8344237280190043 ) ) ;
#61437 = CARTESIAN_POINT ( 'NONE',  ( 0.05219959533910956823, 16.53943276465976808, 79.99890960531435269 ) ) ;
#61438 = CARTESIAN_POINT ( 'NONE',  ( 21.55341960407619695, -5.719274019375665929, 26.04275706135235779 ) ) ;
#61439 = CARTESIAN_POINT ( 'NONE',  ( -5.719274019375978568, 21.55341960407610458, 55.20724293864770260 ) ) ;
#61440 = CARTESIAN_POINT ( 'NONE',  ( -17.31728774477274158, -6.344390552232370695, 104.1809334831068838 ) ) ;
#61441 = CARTESIAN_POINT ( 'NONE',  ( -35.70266437024450568, -5.510913496957479854E-15, 37.50000000000000000 ) ) ;
#61442 = CARTESIAN_POINT ( 'NONE',  ( 5.049401038298161559, -19.05341960407611168, 87.70724293864769550 ) ) ;
#61443 = CARTESIAN_POINT ( 'NONE',  ( 4.483927247898545687, 16.52544592524342804, 54.79057627198104541 ) ) ;
#61444 = AXIS2_PLACEMENT_3D ( 'NONE', #191114, #146590, #193116 ) ;
#61445 = CARTESIAN_POINT ( 'NONE',  ( 8.224510206698953496, -14.34966873604960469, 22.91557627198102765 ) ) ;
#61446 = CARTESIAN_POINT ( 'NONE',  ( 12.06949235617739724, 12.14591786802326823, 96.87609039468568994 ) ) ;
#61448 = ADVANCED_FACE ( 'NONE', ( #3248 ), #145743, .F. ) ;
#61447 = CARTESIAN_POINT ( 'NONE',  ( -13.89961937509957401, -13.97604488694547875, 54.37609039468565442 ) ) ;
#61449 = DIRECTION ( 'NONE',  ( -0.1178549842436472511, 0.9930308165857339997, -0.000000000000000000 ) ) ;
#61450 = CARTESIAN_POINT ( 'NONE',  ( -9.564922557960796823, -16.46253265017161027, 107.0822429386476955 ) ) ;
#61451 = CARTESIAN_POINT ( 'NONE',  ( -8.314922557960811034, -14.29746914071050412, 77.08224293864769550 ) ) ;
#61452 = CARTESIAN_POINT ( 'NONE',  ( -5.153800228976607833, 19.02544592524334988, 47.70942372801900433 ) ) ;
#61454 = CARTESIAN_POINT ( 'NONE',  ( -15.72974639402197994, 15.80617190586746368, 40.62390960531435269 ) ) ;
#61453 = CARTESIAN_POINT ( 'NONE',  ( 19.03943276465977164, -0.05219959533909143690, 33.74890960531435979 ) ) ;
#61455 = CARTESIAN_POINT ( 'NONE',  ( 21.53943276465977519, -0.05219959533907433946, 73.74890960531433848 ) ) ;
#61456 = CARTESIAN_POINT ( 'NONE',  ( 4.483927247898545687, 16.52544592524342804, 94.79057627198105251 ) ) ;
#61457 = CARTESIAN_POINT ( 'NONE',  ( -12.06949235617739369, -12.14591786802326823, 54.37609039468568994 ) ) ;
#61458 = CARTESIAN_POINT ( 'NONE',  ( 21.52544592524334988, 5.823673210054432836, 46.45942372801901854 ) ) ;
#61459 = CARTESIAN_POINT ( 'NONE',  ( -16.55341960407611168, -4.379528057220339221, 91.45724293864769550 ) ) ;
#61460 = PLANE ( 'NONE',  #64089 ) ;
#61461 = CARTESIAN_POINT ( 'NONE',  ( -16.19135201231370047, 7.376712067591785882, 49.81319145947971094 ) ) ;
#61462 = CARTESIAN_POINT ( 'NONE',  ( 5.719274019375991003, -21.55341960407610458, 32.70724293864770260 ) ) ;
#61463 = CARTESIAN_POINT ( 'NONE',  ( -5.000000000000000000, 6.123233995736766282E-16, -18.00000000000000000 ) ) ;
#61464 = CARTESIAN_POINT ( 'NONE',  ( 0.9733081508015164474, 23.94578629589191010, -57.02598899500504359 ) ) ;
#61466 = CARTESIAN_POINT ( 'NONE',  ( 0.05219959533910956823, 16.53943276465976808, 29.99890960531435979 ) ) ;
#61465 = CARTESIAN_POINT ( 'NONE',  ( -0.05219959533934338120, 16.53943276465976808, 47.50109039468568994 ) ) ;
#61467 = CARTESIAN_POINT ( 'NONE',  ( -18.62759615963270932, 10.81492255796079327, 70.83224293864770971 ) ) ;
#61468 = CARTESIAN_POINT ( 'NONE',  ( 13.89961937509957401, 13.97604488694547697, 81.87609039468564731 ) ) ;
#61469 = CARTESIAN_POINT ( 'NONE',  ( -18.62759615963270932, 10.81492255796079327, 60.83224293864769550 ) ) ;
#61470 = CARTESIAN_POINT ( 'NONE',  ( -21.59135963187072704, 7.527667041516030721, 173.8290201207856285 ) ) ;
#61471 = CARTESIAN_POINT ( 'NONE',  ( 12.14591786802327356, -12.06949235617739191, 50.62609039468568994 ) ) ;
#61473 = CARTESIAN_POINT ( 'NONE',  ( -5.049401038298153566, 19.05341960407611168, 95.20724293864770971 ) ) ;
#61472 = CARTESIAN_POINT ( 'NONE',  ( 5.049401038298161559, -19.05341960407611168, 32.70724293864768129 ) ) ;
#61474 = CARTESIAN_POINT ( 'NONE',  ( 19.02544592524343514, -5.153800228976328945, 38.54057627198103120 ) ) ;
#61475 = CARTESIAN_POINT ( 'NONE',  ( 16.55341960407611168, 4.379528057220329451, 113.9572429386477239 ) ) ;
#61476 = DIRECTION ( 'NONE',  ( 1.000000000000000000, 0.000000000000000000, 0.000000000000000000 ) ) ;
#61477 = CARTESIAN_POINT ( 'NONE',  ( 5.153800228976335163, 19.02544592524342804, 109.7905762719810099 ) ) ;
#61478 = ORIENTED_EDGE ( 'NONE', *, *, #69172, .F. ) ;
#61479 = CARTESIAN_POINT ( 'NONE',  ( 16.53943276465976808, 0.05219959533934440121, 66.25109039468567573 ) ) ;
#61480 = CARTESIAN_POINT ( 'NONE',  ( 21.53943276465977519, -0.05219959533907433946, 88.74890960531436690 ) ) ;
#61481 = CARTESIAN_POINT ( 'NONE',  ( 5.049401038298161559, -19.05341960407611168, 57.70724293864769550 ) ) ;
#61482 = CARTESIAN_POINT ( 'NONE',  ( 21.53943276465977519, 0.05219959533937863772, 31.25109039468568639 ) ) ;
#61483 = CARTESIAN_POINT ( 'NONE',  ( -13.89961937509977652, 13.97604488694528158, 80.62390960531436690 ) ) ;
#61485 = ADVANCED_FACE ( 'NONE', ( #10252 ), #177111, .F. ) ;
#61484 = CARTESIAN_POINT ( 'NONE',  ( 9.474510206698971260, -16.51473224551069308, 112.9155762719810383 ) ) ;
#61486 = VERTEX_POINT ( 'NONE', #147766 ) ;
#61487 = CARTESIAN_POINT ( 'NONE',  ( 15.72974639402176855, 15.80617190586768217, 21.87609039468567573 ) ) ;
#61490 = CARTESIAN_POINT ( 'NONE',  ( -9.474510206698720793, -16.51473224551083518, 89.58442372801900433 ) ) ;
#61489 = CARTESIAN_POINT ( 'NONE',  ( -13.89961937509977652, 13.97604488694528158, 110.6239096053143243 ) ) ;
#61488 = CARTESIAN_POINT ( 'NONE',  ( -4.379528057220328563, 16.55341960407611168, 115.2072429386476955 ) ) ;
#61491 = CARTESIAN_POINT ( 'NONE',  ( 16.51473224551083163, -9.474510206698727899, 25.83442372801900078 ) ) ;
#61492 = CARTESIAN_POINT ( 'NONE',  ( -10.81492255796078084, -18.62759615963271287, 97.08224293864770971 ) ) ;
#61493 = CARTESIAN_POINT ( 'NONE',  ( 13.89961937509957401, 13.97604488694547697, 41.87609039468566152 ) ) ;
#61494 = CARTESIAN_POINT ( 'NONE',  ( 4.483927247898790824, -16.52544592524335698, 85.20942372801901854 ) ) ;
#61495 = EDGE_CURVE ( 'NONE', #161515, #182913, #18239, .T. ) ;
#61496 = CARTESIAN_POINT ( 'NONE',  ( 16.51473224551069308, 9.474510206698969483, 109.1655762719810383 ) ) ;
#61497 = CARTESIAN_POINT ( 'NONE',  ( 16.51473224551069308, 9.474510206698969483, 64.16557627198102409 ) ) ;
#61498 = CARTESIAN_POINT ( 'NONE',  ( 21.53943276465977519, 0.05219959533937863772, 61.25109039468567573 ) ) ;
#61499 = CARTESIAN_POINT ( 'NONE',  ( -21.53943276465977519, -0.05219959533937600094, 83.75109039468568994 ) ) ;
#61500 = CARTESIAN_POINT ( 'NONE',  ( 16.46253265017160672, -9.564922557960803928, 113.3322429386476955 ) ) ;
#61501 = CARTESIAN_POINT ( 'NONE',  ( -13.97604488694527625, -13.89961937509977652, 71.87390960531433848 ) ) ;
#61502 = CARTESIAN_POINT ( 'NONE',  ( -10.81492255796105439, 18.62759615963255655, 47.91775706135234714 ) ) ;
#61503 = CARTESIAN_POINT ( 'NONE',  ( 9.474510206698729675, 16.51473224551082808, 92.08442372801900433 ) ) ;
#61504 = CARTESIAN_POINT ( 'NONE',  ( -16.46253265017160317, 9.564922557960807481, 50.83224293864770260 ) ) ;
#61505 = CARTESIAN_POINT ( 'NONE',  ( 13.89961937509977652, -13.97604488694527269, 93.12390960531436690 ) ) ;
#61506 = CARTESIAN_POINT ( 'NONE',  ( -16.46253265017160317, 9.564922557960807481, 60.83224293864769550 ) ) ;
#61507 = CARTESIAN_POINT ( 'NONE',  ( -37.99626262588766679, 2.428612866367529932E-14, -1.747842220587805251 ) ) ;
#61508 = CARTESIAN_POINT ( 'NONE',  ( 9.564922557960805705, 16.46253265017160317, 49.58224293864770260 ) ) ;
#61509 = CARTESIAN_POINT ( 'NONE',  ( -21.52544592524343514, 5.823673210054127303, 106.0405762719810525 ) ) ;
#61510 = CARTESIAN_POINT ( 'NONE',  ( 0.05219959533934541429, -16.53943276465976808, 90.00109039468567573 ) ) ;
#61511 = CARTESIAN_POINT ( 'NONE',  ( -23.84827716990724866, 9.022217638662548111, 168.8513102586128412 ) ) ;
#61512 = CARTESIAN_POINT ( 'NONE',  ( -0.05219959533936034679, 19.03943276465977164, 42.50109039468566152 ) ) ;
#61513 = CARTESIAN_POINT ( 'NONE',  ( -0.05219959533909027116, -19.03943276465977164, 67.49890960531436690 ) ) ;
#61514 = CARTESIAN_POINT ( 'NONE',  ( 0.05219959533910956823, 16.53943276465976808, 54.99890960531435269 ) ) ;
#61515 = CARTESIAN_POINT ( 'NONE',  ( -14.34966873604960291, -8.224510206698953496, 91.66557627198103830 ) ) ;
#61516 = CARTESIAN_POINT ( 'NONE',  ( 9.564922557960805705, 16.46253265017160317, 114.5822429386476955 ) ) ;
#61517 = CARTESIAN_POINT ( 'NONE',  ( 19.02544592524343514, -5.153800228976328945, 98.54057627198100988 ) ) ;
#61518 = CARTESIAN_POINT ( 'NONE',  ( -13.89961937509977652, 13.97604488694528158, 110.6239096053143243 ) ) ;
#61519 = CARTESIAN_POINT ( 'NONE',  ( -13.97604488694547697, 13.89961937509957934, 23.12609039468565442 ) ) ;
#61520 = CARTESIAN_POINT ( 'NONE',  ( 16.52544592524335698, 4.483927247898782831, 96.45942372801901854 ) ) ;
#61521 = CARTESIAN_POINT ( 'NONE',  ( -13.89961937509977652, 13.97604488694528158, 75.62390960531438111 ) ) ;
#61522 = CARTESIAN_POINT ( 'NONE',  ( -21.55341960407619339, 5.719274019375674811, 38.54275706135234714 ) ) ;
#61523 = CARTESIAN_POINT ( 'NONE',  ( -10.72451020669898014, 18.67979575497178502, 35.41557627198102409 ) ) ;
#61524 = CARTESIAN_POINT ( 'NONE',  ( -21.53943276465977519, -0.05219959533937600094, 18.75109039468568639 ) ) ;
#61525 = CARTESIAN_POINT ( 'NONE',  ( -15.72974639402197994, 15.80617190586746368, 70.62390960531436690 ) ) ;
#61526 = CARTESIAN_POINT ( 'NONE',  ( -16.52544592524342804, 4.483927247898546575, 86.04057627198102409 ) ) ;
#61527 = CARTESIAN_POINT ( 'NONE',  ( -5.153800228976607833, 19.02544592524334988, 37.70942372801899722 ) ) ;
#61528 = CARTESIAN_POINT ( 'NONE',  ( -4.483927247898539470, -16.52544592524342804, 112.2905762719810241 ) ) ;
#61529 = CARTESIAN_POINT ( 'NONE',  ( -5.153800228976328057, -19.02544592524343514, 77.29057627198099567 ) ) ;
#61530 = CARTESIAN_POINT ( 'NONE',  ( -9.564922557960796823, -16.46253265017161027, 87.08224293864769550 ) ) ;
#61531 = CARTESIAN_POINT ( 'NONE',  ( -27.73933785331498925, -9.013057229001049109, 142.9750000027312069 ) ) ;
#61532 = CARTESIAN_POINT ( 'NONE',  ( -8.224510206698948167, 14.34966873604960824, 95.41557627198102409 ) ) ;
#61533 = VERTEX_POINT ( 'NONE', #40582 ) ;
#61534 = CARTESIAN_POINT ( 'NONE',  ( -0.05219959533934338120, 16.53943276465976808, 102.5010903946856899 ) ) ;
#61535 = CARTESIAN_POINT ( 'NONE',  ( -8.224510206698735004, -14.34966873604973081, 29.58442372801901854 ) ) ;
#61536 = CARTESIAN_POINT ( 'NONE',  ( -21.52544592524334988, -5.823673210054445271, 98.95942372801903275 ) ) ;
#61537 = CARTESIAN_POINT ( 'NONE',  ( -16.51473224551069308, -9.474510206698971260, 101.6655762719810241 ) ) ;
#61538 = CARTESIAN_POINT ( 'NONE',  ( 5.719274019375673035, 21.55341960407619339, 22.29275706135235069 ) ) ;
#61539 = CARTESIAN_POINT ( 'NONE',  ( -16.46253265017160317, 9.564922557960807481, 25.83224293864769194 ) ) ;
#61540 = CARTESIAN_POINT ( 'NONE',  ( 14.34966873604972726, -8.224510206698740333, 30.83442372801902209 ) ) ;
#61541 = CARTESIAN_POINT ( 'NONE',  ( 13.89961937509957401, 13.97604488694547697, 91.87609039468567573 ) ) ;
#61542 = CARTESIAN_POINT ( 'NONE',  ( -5.719274019375978568, 21.55341960407610458, 100.2072429386476955 ) ) ;
#61543 = CARTESIAN_POINT ( 'NONE',  ( 19.03943276465977164, 0.05219959533936151252, 71.25109039468566152 ) ) ;
#61544 = CARTESIAN_POINT ( 'NONE',  ( -9.564922557960796823, -16.46253265017161027, 22.08224293864768839 ) ) ;
#61545 = CARTESIAN_POINT ( 'NONE',  ( -18.62759615963270932, 10.81492255796079327, 110.8322429386476955 ) ) ;
#61546 = CARTESIAN_POINT ( 'NONE',  ( 20.73749492396215288, -155.7167183371838064, -25.00000000000000000 ) ) ;
#61547 = CARTESIAN_POINT ( 'NONE',  ( -13.97604488694527625, -13.89961937509977652, 91.87390960531432427 ) ) ;
#61548 = CARTESIAN_POINT ( 'NONE',  ( -37.99626262588769521, 12.34573411038911317, -6.102157773949821618 ) ) ;
#61549 = CARTESIAN_POINT ( 'NONE',  ( 9.474510206698971260, -16.51473224551069308, 87.91557627198102409 ) ) ;
#61551 = CARTESIAN_POINT ( 'NONE',  ( -12.06949235617756955, 12.14591786802309770, 80.62390960531438111 ) ) ;
#61550 = CARTESIAN_POINT ( 'NONE',  ( -15.72974639402176322, -15.80617190586768395, 24.37609039468567573 ) ) ;
#61552 = CARTESIAN_POINT ( 'NONE',  ( 13.97604488694527802, 13.89961937509977652, 79.37390960531435269 ) ) ;
#61554 = CARTESIAN_POINT ( 'NONE',  ( -16.51473224551082808, 9.474510206698731452, 58.33442372801900433 ) ) ;
#61553 = CARTESIAN_POINT ( 'NONE',  ( 4.379528057220092307, 16.55341960407617563, 57.29275706135234714 ) ) ;
#61555 = CARTESIAN_POINT ( 'NONE',  ( -21.55341960407619339, 5.719274019375674811, 63.54275706135234003 ) ) ;
#61556 = CARTESIAN_POINT ( 'NONE',  ( -0.05219959533934338120, 16.53943276465976808, 22.50109039468567573 ) ) ;
#61557 = CARTESIAN_POINT ( 'NONE',  ( -5.153800228976328057, -19.02544592524343514, 62.29057627198100988 ) ) ;
#61558 = CARTESIAN_POINT ( 'NONE',  ( 16.46253265017146816, 9.564922557961045513, 91.66775706135234714 ) ) ;
#61559 = CARTESIAN_POINT ( 'NONE',  ( 4.483927247898790824, -16.52544592524335698, 50.20942372801901854 ) ) ;
#61560 = CARTESIAN_POINT ( 'NONE',  ( 15.72974639402176855, 15.80617190586768217, 91.87609039468568994 ) ) ;
#61561 = CARTESIAN_POINT ( 'NONE',  ( 19.05341960407617918, -5.049401038297876454, 76.04275706135230450 ) ) ;
#61562 = CARTESIAN_POINT ( 'NONE',  ( 16.46253265017160672, -9.564922557960803928, 48.33224293864769550 ) ) ;
#61563 = CARTESIAN_POINT ( 'NONE',  ( 21.52544592524344225, -5.823673210054117533, 68.54057627198103830 ) ) ;
#61565 = CARTESIAN_POINT ( 'NONE',  ( -5.049401038297874678, -19.05341960407617918, 79.79275706135233293 ) ) ;
#61564 = CARTESIAN_POINT ( 'NONE',  ( -4.483927247898539470, -16.52544592524342804, 77.29057627198102409 ) ) ;
#61566 = DIRECTION ( 'NONE',  ( 1.000000000000000000, 0.000000000000000000, 0.000000000000000000 ) ) ;
#61567 = CARTESIAN_POINT ( 'NONE',  ( 19.05341960407617918, -5.049401038297876454, 46.04275706135233293 ) ) ;
#61568 = CARTESIAN_POINT ( 'NONE',  ( 4.483927247898790824, -16.52544592524335698, 110.2094237280190185 ) ) ;
#61569 = CARTESIAN_POINT ( 'NONE',  ( -16.52544592524342804, 4.483927247898546575, 71.04057627198103830 ) ) ;
#61571 = CARTESIAN_POINT ( 'NONE',  ( 8.571926809382597767, 26.38167802310806209, 146.2750000027311899 ) ) ;
#61570 = CARTESIAN_POINT ( 'NONE',  ( 18.67979575497194134, -10.72451020669871369, 105.8344237280190328 ) ) ;
#61572 = CARTESIAN_POINT ( 'NONE',  ( 10.72451020669898902, -18.67979575497178502, 107.9155762719810241 ) ) ;
#61573 = CARTESIAN_POINT ( 'NONE',  ( 16.51473224551069308, 9.474510206698969483, 69.16557627198102409 ) ) ;
#61574 = CARTESIAN_POINT ( 'NONE',  ( 21.53943276465977519, 0.05219959533937863772, 81.25109039468568994 ) ) ;
#61575 = CARTESIAN_POINT ( 'NONE',  ( 5.049401038298161559, -19.05341960407611168, 62.70724293864769550 ) ) ;
#61576 = ORIENTED_EDGE ( 'NONE', *, *, #72314, .T. ) ;
#61577 = CARTESIAN_POINT ( 'NONE',  ( -16.46253265017160317, 9.564922557960807481, 25.83224293864769194 ) ) ;
#61578 = CARTESIAN_POINT ( 'NONE',  ( 16.46253265017160672, -9.564922557960803928, 113.3322429386476955 ) ) ;
#61579 = CARTESIAN_POINT ( 'NONE',  ( 16.55341960407611168, 4.379528057220329451, 68.95724293864769550 ) ) ;
#61580 = CARTESIAN_POINT ( 'NONE',  ( 9.474510206698971260, -16.51473224551069308, 32.91557627198102409 ) ) ;
#61581 = CARTESIAN_POINT ( 'NONE',  ( -12.06949235617756955, 12.14591786802309770, 80.62390960531438111 ) ) ;
#61582 = CARTESIAN_POINT ( 'NONE',  ( -15.72974639402197994, 15.80617190586746368, 100.6239096053143811 ) ) ;
#61583 = B_SPLINE_CURVE_WITH_KNOTS ( 'NONE', 3,
 ( #139467, #109137, #91958, #45486, #15146, #33300, #107141, #14146, #170816, #156643, #153651, #172809, #75813, #31309, #141466, #1956, #138479, #90969, #154648, #110133, #32308, #2950, #152656, #17137, #16143, #126291, #137491, #61630, #63635, #125311, #123298, #199171 ),
 .UNSPECIFIED., .F., .F.,
 ( 4, 2, 2, 2, 2, 2, 2, 2, 2, 2, 2, 2, 2, 2, 2, 4 ),
 ( 1.262897753262583006E-17, 0.0003712461730036916568, 0.0007424923460073706285, 0.001113738519011049600, 0.001484984692014728680, 0.002227477038022086624, 0.002598723211025759199, 0.002969969384029431773, 0.003341215557033103915, 0.003712461730036776056, 0.004083707903040449498, 0.004454954076044122073, 0.004826200249047793780, 0.005197446422051466355, 0.005568692595055138930, 0.005939938768058811505 ),
 .UNSPECIFIED. ) ;
#61584 = CARTESIAN_POINT ( 'NONE',  ( 21.55341960407619695, -5.719274019375665929, 51.04275706135234714 ) ) ;
#61585 = DIRECTION ( 'NONE',  ( -1.000000000000000000, 0.000000000000000000, 0.000000000000000000 ) ) ;
#61586 = CARTESIAN_POINT ( 'NONE',  ( -12.14591786802326823, 12.06949235617739902, 48.12609039468568284 ) ) ;
#61587 = CARTESIAN_POINT ( 'NONE',  ( 10.81492255796078972, 18.62759615963270932, 94.58224293864769550 ) ) ;
#61588 = CARTESIAN_POINT ( 'NONE',  ( 13.97604488694548053, -13.89961937509957401, 30.62609039468566863 ) ) ;
#61589 = CARTESIAN_POINT ( 'NONE',  ( -19.02544592524342804, 5.153800228976336051, 101.0405762719810241 ) ) ;
#61590 = CARTESIAN_POINT ( 'NONE',  ( 0.05219959533937995610, -21.53943276465977519, 45.00109039468568284 ) ) ;
#61591 = CARTESIAN_POINT ( 'NONE',  ( 21.52544592524344225, -5.823673210054117533, 38.54057627198103120 ) ) ;
#61592 = CARTESIAN_POINT ( 'NONE',  ( -16.53943276465976808, 0.05219959533911058130, 21.24890960531436690 ) ) ;
#61594 = CARTESIAN_POINT ( 'NONE',  ( 18.62759615963255655, 10.81492255796105972, 91.66775706135234714 ) ) ;
#61593 = CARTESIAN_POINT ( 'NONE',  ( 21.52544592524334988, 5.823673210054432836, 66.45942372801903275 ) ) ;
#61595 = CARTESIAN_POINT ( 'NONE',  ( 19.02544592524334988, 5.153800228976608722, 36.45942372801900433 ) ) ;
#61596 = CARTESIAN_POINT ( 'NONE',  ( -4.379528057220086978, -16.55341960407618274, 94.79275706135234714 ) ) ;
#61597 = CARTESIAN_POINT ( 'NONE',  ( -21.55341960407619339, 5.719274019375674811, 58.54275706135235424 ) ) ;
#61598 = CARTESIAN_POINT ( 'NONE',  ( 9.474510206698971260, -16.51473224551069308, 47.91557627198102409 ) ) ;
#61599 = CARTESIAN_POINT ( 'NONE',  ( -16.46253265017146816, -9.564922557961047289, 19.16775706135233293 ) ) ;
#61600 = CARTESIAN_POINT ( 'NONE',  ( -18.62759615963270932, 10.81492255796079327, 30.83224293864770260 ) ) ;
#61601 = CARTESIAN_POINT ( 'NONE',  ( -15.80617190586768217, 15.72974639402176855, 23.12609039468567573 ) ) ;
#61602 = CARTESIAN_POINT ( 'NONE',  ( 18.67979575497178502, 10.72451020669898547, 74.16557627198102409 ) ) ;
#61603 = CARTESIAN_POINT ( 'NONE',  ( -16.53943276465976808, -0.05219959533934237506, 38.75109039468567573 ) ) ;
#61605 = CARTESIAN_POINT ( 'NONE',  ( -18.67979575497178146, -10.72451020669898902, 76.66557627198103830 ) ) ;
#61604 = LINE ( 'NONE', #18115, #135536 ) ;
#61607 = CARTESIAN_POINT ( 'NONE',  ( 12.06949235617757843, -12.14591786802309237, 58.12390960531435979 ) ) ;
#61606 = CARTESIAN_POINT ( 'NONE',  ( -12.06949235617739369, -12.14591786802326823, 64.37609039468568994 ) ) ;
#61608 = CARTESIAN_POINT ( 'NONE',  ( 1.500000000000003553, 30.40000000000004476, -47.75060438757614634 ) ) ;
#61609 = CARTESIAN_POINT ( 'NONE',  ( 5.049401038297881783, 19.05341960407617563, 107.2927570613523187 ) ) ;
#61610 = EDGE_CURVE ( 'NONE', #68126, #133003, #155778, .T. ) ;
#61611 = CARTESIAN_POINT ( 'NONE',  ( -10.72451020669898014, 18.67979575497178502, 35.41557627198102409 ) ) ;
#61612 = DIRECTION ( 'NONE',  ( 0.000000000000000000, -0.8164965809277251463, 0.5773502691896268413 ) ) ;
#61613 = CARTESIAN_POINT ( 'NONE',  ( 8.314922557961029526, -14.29746914071037800, 45.41775706135234003 ) ) ;
#61614 = CARTESIAN_POINT ( 'NONE',  ( 0.05219959533907565091, 21.53943276465977519, 114.9989096053143669 ) ) ;
#61615 = CARTESIAN_POINT ( 'NONE',  ( 18.62759615963271287, -10.81492255796078972, 28.33224293864769550 ) ) ;
#61616 = CARTESIAN_POINT ( 'NONE',  ( -14.29746914071037622, -8.314922557961029526, 64.16775706135234714 ) ) ;
#61617 = CARTESIAN_POINT ( 'NONE',  ( -19.03943276465977164, 0.05219959533909376836, 91.24890960531436690 ) ) ;
#61619 = CARTESIAN_POINT ( 'NONE',  ( -9.564922557961040184, 16.46253265017147172, 112.9177570613523329 ) ) ;
#61618 = CARTESIAN_POINT ( 'NONE',  ( 15.72974639402176855, 15.80617190586768217, 36.87609039468568994 ) ) ;
#61620 = CARTESIAN_POINT ( 'NONE',  ( -10.81492255796078084, -18.62759615963271287, 27.08224293864769550 ) ) ;
#61621 = VERTEX_POINT ( 'NONE', #195273 ) ;
#61622 = CARTESIAN_POINT ( 'NONE',  ( -16.46253265017146816, -9.564922557961047289, 24.16775706135233648 ) ) ;
#61623 = CARTESIAN_POINT ( 'NONE',  ( 0.05219959533934541429, -16.53943276465976808, 40.00109039468567573 ) ) ;
#61624 = CARTESIAN_POINT ( 'NONE',  ( 16.46253265017160672, -9.564922557960803928, 103.3322429386476955 ) ) ;
#61625 = CARTESIAN_POINT ( 'NONE',  ( 15.72974639402199770, -15.80617190586745480, 103.1239096053143811 ) ) ;
#61626 = CARTESIAN_POINT ( 'NONE',  ( 5.049401038298161559, -19.05341960407611168, 67.70724293864769550 ) ) ;
#61627 = CYLINDRICAL_SURFACE ( 'NONE', #12202, 28.82186960331498682 ) ;
#61628 = CARTESIAN_POINT ( 'NONE',  ( -14.29746914071049879, 8.314922557960819915, 80.83224293864769550 ) ) ;
#61629 = CARTESIAN_POINT ( 'NONE',  ( -5.823673210054116645, -21.52544592524344225, 37.29057627198102409 ) ) ;
#61630 = CARTESIAN_POINT ( 'NONE',  ( -17.40861289039003523, 6.110651285853256454, 33.62767529172568004 ) ) ;
#61631 = CARTESIAN_POINT ( 'NONE',  ( -14.34966873604972548, 8.224510206698743886, 63.33442372801900433 ) ) ;
#61632 = CARTESIAN_POINT ( 'NONE',  ( 21.55341960407610458, 5.719274019375980345, 98.95724293864770971 ) ) ;
#61633 = CARTESIAN_POINT ( 'NONE',  ( 19.05341960407617918, -5.049401038297876454, 76.04275706135230450 ) ) ;
#61634 = CARTESIAN_POINT ( 'NONE',  ( 16.51473224551069308, 9.474510206698969483, 24.16557627198102765 ) ) ;
#61635 = CARTESIAN_POINT ( 'NONE',  ( -5.823673210054116645, -21.52544592524344225, 62.29057627198102409 ) ) ;
#61636 = CARTESIAN_POINT ( 'NONE',  ( 0.05219959533909260263, 19.03943276465977164, 94.99890960531436690 ) ) ;
#61637 = CARTESIAN_POINT ( 'NONE',  ( 21.53943276465977519, 0.05219959533937863772, 96.25109039468568994 ) ) ;
#61638 = CARTESIAN_POINT ( 'NONE',  ( 19.02544592524343514, -5.153800228976328945, 63.54057627198103830 ) ) ;
#61639 = CARTESIAN_POINT ( 'NONE',  ( -12.06949235617739369, -12.14591786802326823, 49.37609039468569705 ) ) ;
#61640 = CARTESIAN_POINT ( 'NONE',  ( 5.049401038298161559, -19.05341960407611168, 57.70724293864769550 ) ) ;
#61641 = CARTESIAN_POINT ( 'NONE',  ( -21.52544592524334988, -5.823673210054445271, 78.95942372801901854 ) ) ;
#61642 = ORIENTED_EDGE ( 'NONE', *, *, #170744, .F. ) ;
#61643 = CARTESIAN_POINT ( 'NONE',  ( 19.03943276465977164, 0.05219959533936151252, 36.25109039468567573 ) ) ;
#61644 = CARTESIAN_POINT ( 'NONE',  ( -16.51473224551082808, 9.474510206698731452, 53.33442372801900433 ) ) ;
#61645 = CARTESIAN_POINT ( 'NONE',  ( -10.81492255796105439, 18.62759615963255655, 52.91775706135235424 ) ) ;
#61646 = CARTESIAN_POINT ( 'NONE',  ( -28.79475375365596435, 9.355982642739093080, 143.8843446568999980 ) ) ;
#61647 = CARTESIAN_POINT ( 'NONE',  ( 16.51473224551083163, -9.474510206698727899, 40.83442372801900433 ) ) ;
#61648 = CARTESIAN_POINT ( 'NONE',  ( -19.05341960407611168, -5.049401038298163336, 91.45724293864766707 ) ) ;
#61649 = CARTESIAN_POINT ( 'NONE',  ( 9.564922557960805705, 16.46253265017160317, 64.58224293864769550 ) ) ;
#61650 = CARTESIAN_POINT ( 'NONE',  ( -12.06949235617756955, 12.14591786802309770, 25.62390960531435624 ) ) ;
#61652 = CARTESIAN_POINT ( 'NONE',  ( -15.80617190586768217, 15.72974639402176855, 93.12609039468568994 ) ) ;
#61651 = CARTESIAN_POINT ( 'NONE',  ( -19.02544592524342804, 5.153800228976336051, 116.0405762719810383 ) ) ;
#61653 = CARTESIAN_POINT ( 'NONE',  ( -5.950531402560715689E-15, 38.81732327939063509, -9.624999997268815832 ) ) ;
#61654 = CARTESIAN_POINT ( 'NONE',  ( 16.20579543436682002, 7.371946100354976217, 58.06520834171880097 ) ) ;
#61655 = CARTESIAN_POINT ( 'NONE',  ( 18.67979575497194134, -10.72451020669871369, 95.83442372801903275 ) ) ;
#61656 = CARTESIAN_POINT ( 'NONE',  ( 11.74149087413295156, -36.13659316521243881, -3.147842220587803386 ) ) ;
#61657 = CARTESIAN_POINT ( 'NONE',  ( 16.52544592524342804, -4.483927247898539470, 113.5405762719810383 ) ) ;
#61658 = CARTESIAN_POINT ( 'NONE',  ( -9.564922557960796823, -16.46253265017161027, 112.0822429386476955 ) ) ;
#61659 = CARTESIAN_POINT ( 'NONE',  ( -26.53515902489024825, -7.921333329385879196, 167.7790254135048826 ) ) ;
#61660 = CARTESIAN_POINT ( 'NONE',  ( 4.379528057220092307, 16.55341960407617563, 47.29275706135234003 ) ) ;
#61661 = CARTESIAN_POINT ( 'NONE',  ( 5.719274019375991003, -21.55341960407610458, 67.70724293864769550 ) ) ;
#61662 = CARTESIAN_POINT ( 'NONE',  ( 4.379528057220339221, -16.55341960407611168, 37.70724293864769550 ) ) ;
#61664 = CARTESIAN_POINT ( 'NONE',  ( -16.51473224551069308, -9.474510206698971260, 91.66557627198103830 ) ) ;
#61663 = CARTESIAN_POINT ( 'NONE',  ( 4.483927247898545687, 16.52544592524342804, 104.7905762719810241 ) ) ;
#61665 = CARTESIAN_POINT ( 'NONE',  ( 21.52544592524334988, 5.823673210054432836, 111.4594237280190328 ) ) ;
#61666 = CARTESIAN_POINT ( 'NONE',  ( 8.314922557960818139, 14.29746914071049879, 114.5822429386477097 ) ) ;
#61667 = CARTESIAN_POINT ( 'NONE',  ( -15.72974639402176322, -15.80617190586768395, 69.37609039468567573 ) ) ;
#61668 = CARTESIAN_POINT ( 'NONE',  ( 5.153800228976335163, 19.02544592524342804, 114.7905762719810241 ) ) ;
#61669 = CARTESIAN_POINT ( 'NONE',  ( 12.06949235617739724, 12.14591786802326823, 101.8760903946857042 ) ) ;
#61670 = CARTESIAN_POINT ( 'NONE',  ( -19.03943276465977164, -0.05219959533935918106, 68.75109039468566152 ) ) ;
#61671 = CARTESIAN_POINT ( 'NONE',  ( 32.44846625821359254, 18.14626611352247210, -7.961615373864755263 ) ) ;
#61672 = CARTESIAN_POINT ( 'NONE',  ( 21.53943276465977519, -0.05219959533907433946, 23.74890960531435269 ) ) ;
#61673 = CARTESIAN_POINT ( 'NONE',  ( -14.29746914071049879, 8.314922557960819915, 90.83224293864769550 ) ) ;
#61674 = CARTESIAN_POINT ( 'NONE',  ( 16.51473224551083163, -9.474510206698727899, 60.83442372801900433 ) ) ;
#61675 = CARTESIAN_POINT ( 'NONE',  ( -16.51473224551069308, -9.474510206698971260, 81.66557627198103830 ) ) ;
#61676 = CARTESIAN_POINT ( 'NONE',  ( -14.29746914071049879, 8.314922557960819915, 70.83224293864770971 ) ) ;
#61677 = CARTESIAN_POINT ( 'NONE',  ( -13.89961937509957401, -13.97604488694547875, 94.37609039468566152 ) ) ;
#61678 = CARTESIAN_POINT ( 'NONE',  ( -15.72974639402197994, 15.80617190586746368, 55.62390960531436690 ) ) ;
#61679 = ORIENTED_EDGE ( 'NONE', *, *, #103959, .T. ) ;
#61680 = CARTESIAN_POINT ( 'NONE',  ( -14.29746914071049879, 8.314922557960819915, 115.8322429386477097 ) ) ;
#61681 = DIRECTION ( 'NONE',  ( 0.000000000000000000, 0.000000000000000000, -1.000000000000000000 ) ) ;
#61683 = CARTESIAN_POINT ( 'NONE',  ( 15.80617190586746368, 15.72974639402197994, 79.37390960531436690 ) ) ;
#61682 = CARTESIAN_POINT ( 'NONE',  ( -16.46253265017160317, 9.564922557960807481, 75.83224293864769550 ) ) ;
#61685 = CARTESIAN_POINT ( 'NONE',  ( 13.97604488694527802, 13.89961937509977652, 74.37390960531436690 ) ) ;
#61684 = CARTESIAN_POINT ( 'NONE',  ( -14.29746914071037622, -8.314922557961029526, 94.16775706135237556 ) ) ;
#61686 = CARTESIAN_POINT ( 'NONE',  ( 19.05341960407617918, -5.049401038297876454, 66.04275706135233293 ) ) ;
#61687 = CARTESIAN_POINT ( 'NONE',  ( 15.72974639402176855, 15.80617190586768217, 86.87609039468568994 ) ) ;
#61688 = CARTESIAN_POINT ( 'NONE',  ( -18.67979575497178146, -10.72451020669898902, 56.66557627198103830 ) ) ;
#61689 = CARTESIAN_POINT ( 'NONE',  ( 5.719274019375991003, -21.55341960407610458, 22.70724293864769194 ) ) ;
#61690 = CARTESIAN_POINT ( 'NONE',  ( -19.05341960407611168, -5.049401038298163336, 41.45724293864769550 ) ) ;
#61691 = CARTESIAN_POINT ( 'NONE',  ( 12.06949235617739724, 12.14591786802326823, 106.8760903946856899 ) ) ;
#61692 = CARTESIAN_POINT ( 'NONE',  ( -19.03943276465977164, 0.05219959533909376836, 56.24890960531435979 ) ) ;
#61693 = CARTESIAN_POINT ( 'NONE',  ( 16.46253265017146816, 9.564922557961045513, 111.6677570613523329 ) ) ;
#61694 = CARTESIAN_POINT ( 'NONE',  ( 13.89961937509957579, 13.97604488694547520, 81.87609039468566152 ) ) ;
#61695 = CARTESIAN_POINT ( 'NONE',  ( 5.719274019375673035, 21.55341960407619339, 112.2927570613523471 ) ) ;
#61696 = CARTESIAN_POINT ( 'NONE',  ( -8.314922557960811034, -14.29746914071050412, 62.08224293864769550 ) ) ;
#61697 = CARTESIAN_POINT ( 'NONE',  ( 21.53943276465977519, -0.05219959533907433946, 113.7489096053143527 ) ) ;
#61698 = CARTESIAN_POINT ( 'NONE',  ( -21.53943276465977519, 0.05219959533907696930, 96.24890960531435269 ) ) ;
#61699 = CARTESIAN_POINT ( 'NONE',  ( -4.313351365237961588, 4.313351365237934942, -64.53213882399992940 ) ) ;
#61700 = CARTESIAN_POINT ( 'NONE',  ( 0.05219959533907565091, 21.53943276465977519, 49.99890960531437401 ) ) ;
#61701 = CARTESIAN_POINT ( 'NONE',  ( -8.314922557961024197, 14.29746914071037800, 82.91775706135234714 ) ) ;
#61702 = CARTESIAN_POINT ( 'NONE',  ( 16.52544592524342804, -4.483927247898539470, 93.54057627198103830 ) ) ;
#61703 = CARTESIAN_POINT ( 'NONE',  ( 13.97604488694527802, 13.89961937509977652, 64.37390960531436690 ) ) ;
#61704 = CARTESIAN_POINT ( 'NONE',  ( -15.49999999999999822, 5.499999999999997335, 22.00000000000000711 ) ) ;
#61705 = CARTESIAN_POINT ( 'NONE',  ( 16.52544592524335698, 4.483927247898782831, 106.4594237280190328 ) ) ;
#61706 = CARTESIAN_POINT ( 'NONE',  ( 10.81492255796106328, -18.62759615963255655, 35.41775706135234003 ) ) ;
#61707 = CARTESIAN_POINT ( 'NONE',  ( 9.564922557960805705, 16.46253265017160317, 99.58224293864770971 ) ) ;
#61708 = CARTESIAN_POINT ( 'NONE',  ( -5.719274019375665041, -21.55341960407619695, 69.79275706135234714 ) ) ;
#61709 = CARTESIAN_POINT ( 'NONE',  ( -9.564922557960796823, -16.46253265017161027, 22.08224293864768839 ) ) ;
#61711 = ADVANCED_FACE ( 'NONE', ( #103253 ), #130569, .T. ) ;
#61710 = CARTESIAN_POINT ( 'NONE',  ( 16.46253265017160672, -9.564922557960803928, 28.33224293864769550 ) ) ;
#61712 =( BOUNDED_SURFACE ( )  B_SPLINE_SURFACE ( 3, 2, ( 
 ( #52934, #12462, #133791, #89277, #196486, #195483, #121587, #179321, #105437, #120598, #183282, #44764, #42788, #75095, #119627, #149959, #181310, #40785, #148968, #102454, #164142, #166134, #26628, #104451, #74122, #167122, #150967, #13431, #73136, #56958, #28622, #27636, #58930, #135793, #103458, #118632, #134806, #136762, #25639, #88271, #87283, #10457, #198447, #72118, #165136, #182293, #43773, #59919, #180323, #41791, #90259, #11465, #197464, #151942, #57956, #41435, #101083, #159767, #21262, #116265, #85926, #53594, #37424, #162768, #24277, #56604, #147615, #69762, #82918, #68756, #23268, #9102, #144595, #178960, #71763, #192112, #177955, #70769, #129417, #55592, #161773, #163785, #22264, #40429, #146591, #133433, #6081, #39423, #130413, #8085, #132438, #25286, #102100, #38433, #86929, #67760, #191115, #131431, #52589, #194129, #114249, #175955, #117267, #148612, #115270, #99084, #10103, #195122, #118278, #179969, #193117, #160775, #176963, #84912, #83914, #145596, #7075, #100089, #54591, #121240, #106070, #72779, #199086, #105092, #107058, #165780, #183920, #89918, #15064, #184908, #182934, #73774, #88923, #27275, #150615, #12111, #61549, #60554, #168729, #44417, #119274, #30233, #134449, #91875, #59565, #166778, #28279, #135447, #42434, #167757, #200081, #197116, #151600, #29255, #181940, #103102, #74757, #58583, #120249, #136419, #43423, #90887, #180957, #123218, #26277, #13091, #76725, #198099, #152573, #164783, #87919, #149606, #14063, #104097, #75730, #137406, #122229, #11104, #196134, #45405, #153567, #57605, #138400, #195598, #163244, #12565, #88380, #178421, #57071, #148078, #40897, #56057, #117736, #102569, #179431, #24745, #196593, #118745, #164254, #86394, #74231, #131905, #70237, #193589, #133907, #119734, #89386, #26741, #105548, #72232, #180433, #42895, #39885, #25749, #9569, #71235, #147077, #104560, #101552, #87395, #132898, #194587, #8562, #181417, #135899, #197571, #43883, #149080, #10568, #166242, #27743, #41906, #103572, #165247, #150074, #11579, #73246, #55060, #134916, #58063, #151074, #59038, #120705, #182404, #167233, #85384, #116732, #90368, #64008, #139835, #113235, #46857, #140838, #14528, #44875, #15527, #77184, #1324, #63004, #128399, #121698, #123668, #185365, #108517, #62002, #109510, #32681, #2327, #154033, #138854, #190096, #170196, #152053, #155023, #51571, #13538, #31689, #93338, #28731, #75204, #60031, #334, #171192, #136875, #198561, #124682, #186379, #183393, #94334, #30696, #16519, #106531, #156012, #168208, #78167, #47857, #17509, #79167, #29705, #91336, #153028, #76189, #137869, #199548, #61018, #122690, #169189, #184379, #45860, #107513, #92347, #174926, #177933, #24253, #70746, #10079, #160745, #84886, #52562, #102076, #39400, #67734, #146565, #37398, #130386, #145568, #7046, #192083, #68728, #114222, #85903, #8060, #53565, #175927, #163761, #21237, #159740, #82892, #23242, #9076, #178935, #116241, #195097, #161747, #69737, #131405, #99057, #191088, #193093, #144570, #115243, #54569, #147591, #25261, #86904, #101060, #148587, #132414, #162745, #36389, #71737, #194106, #56579, #55569, #133408, #22237, #83886, #117242, #40405, #98043, #6056, #129392, #176935, #38405, #100062, #74733, #151578, #199062, #122207, #91853, #43398, #105068, #153545, #59541, #179944, #44394, #15042, #41411, #136397, #182909, #200060, #103076, #149580, #28256, #60531, #164758, #26253, #14038, #90865, #87894, #183898, #120227, #13067, #76703, #45383, #11078, #121219, #198074, #166753, #106048, #75704, #72754, #134425, #107036, #167734, #89895, #118253, #196111, #58561, #57581, #29232, #152550, #137383, #119251, #168708, #30210, #138379, #180935, #104073, #42410, #165755, #27249, #88898, #150589, #12088, #73751, #135423, #197094, #181917, #78685, #32203, #139366, #172704, #94856, #155537, #62520, #50360, #108028, #46369, #169714, #110030, #95849, #65508, #2847, #81646, #48373, #156537 ),
 ( #80673, #17031, #171708, #127169, #63531, #18036, #20003, #188879, #123197, #64525, #79690, #186902, #126192, #19027, #184887, #31207, #3829, #187888, #33198, #61528, #16040, #1849, #92858, #49355, #34188, #141360, #154545, #111018, #157533, #142349, #96831, #47378, #112019, #847, #173708, #35176, #77699, #158515, #124193, #140362, #93859, #125206, #143330, #185893, #109033, #170712, #38173, #98818, #5822, #193864, #51341, #189867, #113001, #53326, #39164, #8837, #146328, #25019, #191845, #99829, #162505, #97811, #175684, #82651, #144334, #66505, #100822, #55330, #117000, #163520, #67498, #190852, #24006, #85662, #160512, #115005, #176699, #129155, #20996, #161513, #174695, #83655, #23005, #177697, #132173, #178695, #84651, #40157, #54336, #192857, #128167, #101833, #116007, #86662, #7817, #4817, #52329, #113986, #69501, #131167, #147349, #70505, #36159, #159500, #37159, #22003, #145333, #6815, #68493, #130148, #121978, #73520, #135191, #183669, #89662, #9842, #74503, #45154, #71501, #104833, #12837, #29982, #133169, #179703, #58331, #90643, #194859, #56332, #44162, #120979, #118014, #29003, #27018, #152325, #41175, #102838, #196865, #148346, #151348, #164524, #26017, #166523, #136169, #42181, #87661, #197844, #59310, #106810, #182677, #119999, #149346, #57347, #11855, #105821, #10843, #167508, #60303, #180705, #28020, #13811, #72512, #75477, #150358, #137150, #134187, #198839, #181685, #168484, #195874, #119022, #103841, #165522, #88663, #43166, #15801, #50118, #49124, #157293, #171472, #107788, #18790, #61296, #80435, #48132, #93619, #155305, #139132, #30974, #94615, #188639, #185645, #140118, #109789, #170474, #91621, #63285, #47137, #609, #124965, #31964, #32961, #169473, #111778, #14810, #16794, #3593, #1609, #17795, #173466, #153309, #76471, #156294, #92621, #79451, #78444, #154312, #138148, #199829, #110782, #2611, #122966, #141121, #62279, #142108, #64288, #108795, #186662, #184653, #46135, #77462, #123947, #125955, #187653, #172463, #33950, #95608, #65271, #126931, #67259, #66268, #7574, #160273, #99590, #129905, #97571, #51103, #128917, #38931, #55095, #159259, #85420, #70271, #130926, #193623, #19769, #145092, #83415, #22764, #100588, #175446, #176456, #112763, #116765, #158280, #113750, #147111, #6575, #161270, #34939, #96591, #81410, #84413, #174456, #114762, #21764, #35925, #143096, #4575, #192617, #146090, #127927, #37929, #144099, #162270, #69260, #190618, #68254, #131939, #189629, #20755, #82410, #191605, #5579, #36916, #53084, #54099, #115773, #177462, #52093, #98579, #23770, #8597, #42930, #73281, #40933, #194622, #72267, #182437, #198596, #102605, #28764, #13571, #74265, #136909, #163280, #88418, #26776, #166281, #43917, #59071, #57107, #105579, #24781, #86428, #165283, #60064, #119768, #178456, #39923, #134951, #104594, #133944, #56093, #181452, #27778, #75238, #89420, #150112, #101592, #87430, #41941, #151109, #148114, #197605, #90401, #10606, #196629, #12601, #9605, #135935, #180469, #167265, #164291, #120738, #11613, #152086, #71270, #58098, #149115, #132935, #117774, #103607, #179468, #25784, #195634, #118781, #47891, #157048, #183424, #78200, #186414, #3355, #106565, #153062, #31723, #64043, #44908, #168242, #17543, #94367, #91371, #187412, #123702, #16553, #80192, #125713, #29738, #156046, #110535, #33700, #141864, #61051, #107547, #140873, #2362, #77218, #170230, #93371, #122723, #137901, #108551, #14564, #367, #155058, #79204, #48880, #172216, #1359, #95363, #171226, #109544, #76222, #18545, #32715, #121732, #139870, #199583, #169223, #184413, #63038, #124716, #45894, #30732, #92379, #154065, #15560, #138887, #62038, #185400, #46891, #99343, #115530, #190374, #51849, #100347, #6332, #126686, #191360, #162026, #188390, #21514, #129664, #146856, #49867, #96351, #175203, #7329, #111533, #173218, #161026, #37678, #34694, #130679, #67018, #160027, #23522, #69013 ),
 ( #52838, #142856, #144849, #113508, #4335, #85168, #65030, #22520, #176209, #158038, #68012, #174216, #192373, #114507, #20511, #36668, #19529, #81174, #66019, #127687, #98327, #189387, #5334, #83175, #84167, #145847, #53856, #97332, #50864, #177218, #38691, #112522, #35684, #159018, #82159, #143855, #128677, #28525, #132693, #58831, #43674, #104350, #167024, #193374, #118536, #73034, #86184, #88175, #133690, #147874, #90161, #8349, #166034, #119530, #70024, #11364, #117522, #135694, #134706, #164045, #56861, #105336, #116524, #131693, #54850, #180225, #194381, #148869, #165038, #181213, #41695, #89175, #40686, #39676, #42689, #195383, #196389, #103360, #71025, #24533, #102356, #12361, #178212, #55848, #120498, #101338, #27534, #163027, #9360, #26531, #149859, #57858, #74024, #150867, #87188, #197366, #179220, #25544, #182189, #10360, #72017, #151844, #13334, #108307, #77963, #45654, #29501, #154815, #93130, #48647, #139630, #61795, #74999, #60808, #15315, #16313, #136664, #170982, #63807, #184172, #169987, #1118, #121490, #47652, #153820, #155807, #14318, #32475, #138645, #125480, #33469, #187176, #78960, #107305, #110299, #75983, #137656, #171981, #109303, #17305, #31478, #168005, #140635, #183184, #2125, #62792, #76974, #126, #199343, #91134, #124473, #198346, #168977, #123465, #186170, #30482, #59820, #185157, #92133, #122481, #46647, #94128, #44666, #152824, #106319, #18309, #173979, #7092, #143610, #21278, #53611, #156817, #176980, #79965, #141634, #5094, #129434, #99101, #36430, #115287, #81917, #128438, #52606, #188158, #65780, #172983, #34461, #3124, #191132, #83932, #68773, #95127, #96120, #80947, #114268, #175972, #50628, #66777, #190135, #157808, #111294, #51610, #64799, #35447, #113274, #67777, #22281, #145613, #174966, #130431, #144613, #82935, #126460, #192130, #6098, #49631, #98085, #19299, #142622, #4101, #159783, #37441, #160793, #127449, #189155, #112289, #97099, #158783, #20271, #10120, #117283, #72796, #91649, #163802, #25304, #76502, #179986, #100105, #164800, #138178, #161789, #195140, #103119, #122996, #23284, #69779, #148630, #180974, #84928, #146608, #134466, #11121, #8101, #106838, #40444, #133450, #199860, #45184, #131447, #41454, #56621, #86946, #26295, #196151, #193134, #54607, #168513, #87936, #71780, #38450, #116281, #178977, #177971, #149623, #57623, #118295, #39439, #119291, #30011, #153338, #61325, #24293, #14839, #101099, #162785, #85942, #147631, #9119, #70786, #194145, #132454, #55609, #102117, #155338, #62309, #95641, #17829, #78478, #185677, #173500, #31002, #184682, #139162, #125000, #92651, #125989, #157329, #156329, #46165, #187687, #33985, #80469, #19802, #170505, #94649, #123979, #111812, #49157, #77492, #79487, #47167, #140151, #16827, #1643, #63321, #186695, #108826, #18824, #141156, #48166, #31996, #34973, #154340, #169503, #15833, #32995, #142142, #188673, #110815, #4609, #171506, #2645, #3626, #639, #109823, #93653, #64322, #107819, #65305, #96626, #158314, #143129, #172498, #126964, #50153, #81443, #66301, #176492, #37968, #67294, #144133, #114799, #112798, #6612, #99626, #100624, #55131, #178493, #7611, #39959, #177499, #115809, #189664, #163320, #38968, #9643, #146126, #101630, #113786, #5615, #161308, #22802, #162306, #23806, #24817, #20790, #84448, #69296, #130962, #192652, #68291, #85457, #86466, #53121, #54135, #148151, #147146, #51137, #8634, #127961, #174491, #70306, #131975, #35958, #97605, #159293, #193660, #116801, #82445, #128953, #190653, #52129, #175481, #36953, #129942, #98615, #160309, #21799, #83451, #145129, #191641, #196669, #135973, #28803, #194662, #117813, #13610, #197644, #119806, #150152, #105619, #121771, #58138, #181491, #106606, #12639, #132972, #59110, #168281, #56131, #27818, #120775, #153101, #179506, #102643, #42969, #75278, #40974, #164328, #167307, #43957, #25822, #136948, #73319, #166321, #29778, #198637 ),
 ( #11653, #87467, #74306, #182476, #104632, #71309, #90443, #152128, #60103, #91414, #57145, #89460, #149154, #183464, #44950, #10644, #151148, #133983, #26816, #41980, #103646, #88456, #165324, #72305, #195674, #118822, #134990, #180507, #3392, #61090, #199623, #122763, #63079, #48918, #18583, #156087, #34731, #1399, #47930, #172253, #107587, #185441, #92418, #154104, #76261, #110572, #65067, #126724, #173256, #15598, #405, #33741, #95401, #170267, #124758, #186454, #77256, #30771, #109584, #184452, #93410, #171267, #187450, #141901, #188428, #94406, #49906, #64080, #2402, #137939, #111572, #125750, #96389, #32755, #14605, #62077, #138925, #17584, #79244, #157087, #80230, #45932, #169265, #140915, #123742, #46931, #108590, #31761, #155096, #16590, #78238, #139909, #130719, #85208, #8388, #37719, #70063, #7368, #145885, #19567, #193413, #69053, #39712, #176248, #131731, #143892, #174255, #144888, #6370, #192412, #53894, #54888, #50902, #52877, #114549, #99381, #129704, #36706, #115569, #116562, #83213, #68050, #178251, #161064, #81211, #84205, #158076, #142892, #22559, #177256, #4374, #66058, #189427, #191400, #100386, #127725, #112560, #38728, #162064, #35723, #23560, #160066, #146897, #97370, #159056, #20550, #82200, #5373, #67057, #128715, #190412, #51888, #113547, #175241, #98368, #21553, #101375, #55886, #41731, #9396, #42726, #12399, #73070, #163065, #104388, #150905, #197403, #136702, #87224, #11401, #179259, #28562, #166071, #194416, #134742, #164081, #56897, #72053, #133727, #118571, #195419, #40724, #74061, #196424, #180261, #102393, #90199, #147910, #86220, #71062, #149894, #135732, #105374, #27573, #121527, #88210, #57894, #58869, #117559, #103395, #25580, #148906, #24571, #120535, #151882, #13372, #59860, #10396, #165073, #182228, #43713, #26567, #119566, #181249, #89212, #167061, #75036, #132728, #198383, #183222, #126496, #62830, #156851, #30520, #60844, #31516, #93169, #155844, #78997, #80001, #137695, #139667, #1155, #124513, #16352, #123502, #140671, #95163, #170026, #154854, #141670, #186209, #106357, #171022, #3161, #168041, #47690, #109340, #44703, #29538, #76020, #78000, #187211, #91171, #152860, #2163, #17341, #14355, #110334, #46686, #32513, #64834, #48682, #199380, #94165, #63842, #125514, #172015, #33504, #122519, #184209, #18346, #45691, #107342, #169015, #92171, #185195, #153857, #15355, #77011, #138683, #164, #61832, #108346, #83969, #23320, #174016, #98125, #65818, #115327, #191170, #80985, #159822, #50666, #143648, #158820, #20308, #5131, #81956, #127487, #99141, #21317, #66814, #189192, #177018, #34499, #173020, #96157, #36468, #22318, #192169, #129471, #8140, #175004, #82975, #145649, #142660, #128476, #112326, #35487, #49666, #7130, #38487, #100144, #146646, #97137, #190172, #68813, #130472, #51648, #144651, #6133, #113312, #4139, #67816, #157846, #52644, #114308, #160830, #161825, #84964, #176010, #69817, #37479, #188194, #53649, #111330, #19338, #149661, #134503, #101135, #27330, #133485, #135499, #194181, #12164, #118331, #43476, #13145, #105144, #58635, #86982, #166830, #55645, #117318, #89970, #88976, #197170, #11159, #147669, #120301, #162821, #181994, #87973, #195177, #56658, #179014, #70823, #196189, #28331, #25341, #180024, #72833, #10157, #131484, #103156, #148669, #40482, #164837, #71817, #57661, #9157, #151650, #54643, #41492, #193171, #26333, #119328, #116318, #178007, #39474, #181014, #132492, #42488, #104151, #102154, #24330, #85980, #150666, #165833, #163840, #73829, #183969, #1926, #139437, #30283, #123268, #171784, #182986, #33272, #136470, #184959, #199139, #15116, #31280, #47451, #46443, #155612, #107110, #106124, #109107, #200130, #919, #169787, #137460, #90938, #168780, #78759, #94931, #60606, #125281, #110105, #170786, #156616, #59620, #108103, #92931, #62593, #140436, #17107, #153620, #63605, #121293, #44470, #61599, #74808, #16112 ),
 ( #138449, #122281, #91928, #45456, #76777, #154618, #77770, #32276, #124271, #186978, #185967, #167808, #93933, #48448, #198150, #29308, #152625, #14115, #75782, #22076, #38244, #142426, #68566, #53402, #114063, #176772, #2923, #128242, #66577, #5896, #83727, #98893, #96904, #145406, #64601, #126265, #4895, #99899, #159576, #18111, #79765, #174766, #144410, #112094, #95923, #21073, #82729, #115080, #67572, #189939, #141436, #127245, #81721, #129230, #187962, #37237, #130223, #50435, #36232, #190927, #49432, #175761, #20077, #6888, #80748, #160587, #51414, #191919, #111093, #172783, #34264, #173784, #157608, #3905, #65585, #19099, #188958, #35251, #97884, #158588, #143407, #113074, #52404, #148419, #117071, #178767, #24081, #177768, #194931, #103911, #70578, #101909, #9914, #193938, #161584, #86734, #132246, #85736, #71573, #40233, #56407, #39237, #165592, #84723, #55401, #180775, #163591, #179778, #27090, #23078, #146401, #41247, #162577, #118088, #25092, #147423, #7891, #69576, #195946, #10912, #131242, #164593, #133239, #192930, #149416, #102909, #26087, #54408, #87731, #116080, #8910, #72585, #100893, #134259, #57420, #119093, #42250, #36881, #100556, #146057, #3559, #145060, #98547, #67226, #6541, #99556, #65237, #188603, #84380, #68221, #190584, #142073, #96557, #82378, #50084, #83383, #53050, #113716, #126897, #129873, #191571, #37898, #177428, #127893, #52060, #19735, #69226, #114730, #34902, #175413, #4539, #144066, #130894, #160241, #23735, #112730, #81376, #176424, #21730, #35892, #143061, #192584, #111744, #173432, #158244, #161238, #22732, #7541, #54067, #162235, #128884, #115741, #38899, #66233, #174423, #189596, #51069, #97539, #159226, #20721, #5547, #192393, #40706, #83195, #21535, #23541, #118554, #178231, #36688, #98348, #193393, #163047, #130698, #114528, #39695, #101357, #133709, #24554, #146877, #160047, #145866, #100366, #86203, #144869, #55867, #148888, #69033, #54869, #147893, #6352, #132711, #38709, #102376, #99362, #117541, #85187, #10379, #68032, #72036, #164064, #53875, #195402, #161045, #22539, #56880, #194399, #25563, #116543, #52857, #87207, #129683, #191381, #9379, #162045, #8369, #84186, #176229, #37699, #179240, #71044, #70044, #7348, #115549, #177237, #131712, #121509, #91154, #151863, #180244, #183204, #29520, #76003, #15337, #166053, #90180, #57877, #107325, #44685, #73053, #13354, #42708, #120517, #168998, #75018, #61815, #150887, #119549, #152843, #136683, #74043, #181232, #30502, #26549, #165056, #88193, #28544, #14337, #184192, #106338, #146, #167043, #198365, #137677, #134725, #12381, #104369, #27554, #41713, #199363, #60827, #89194, #59841, #168024, #135714, #122501, #45674, #197385, #92153, #153840, #58850, #196407, #76994, #149877, #182209, #138665, #103378, #11383, #43694, #105356, #35465, #173000, #111311, #185177, #158799, #34479, #5111, #141651, #97116, #109323, #139650, #110316, #171998, #96137, #157826, #20288, #16334, #18327, #79983, #3141, #95144, #2146, #19316, #173996, #48664, #33486, #81935, #64816, #46668, #49648, #143626, #108328, #126477, #188175, #123485, #170008, #154835, #156833, #65797, #31499, #93151, #80964, #142640, #77983, #189172, #125496, #4118, #1138, #127466, #62812, #50645, #112306, #124496, #186191, #47672, #171003, #32495, #187193, #94148, #155827, #17324, #78979, #140654, #63824, #115304, #23300, #145629, #66793, #38466, #22298, #114287, #100122, #7109, #8118, #144630, #25320, #190152, #68791, #178994, #176996, #193150, #86962, #128456, #148647, #131464, #6113, #146626, #192147, #67795, #51627, #113292, #24310, #177987, #174983, #69796, #175989, #194161, #54622, #83949, #161805, #163819, #36447, #21295, #98103, #102134, #116297, #130449, #84944, #39454, #101115, #147648, #99119, #159800, #162801, #53628, #85959, #9136, #129451, #82953, #160810, #70802, #191150, #52624, #117298, #37458, #132470, #55625, #40461 ),
 ( #149641, #26312, #197150, #195157, #88958, #120283, #182968, #137441, #60588, #89952, #122263, #59601, #198132, #71797, #45438, #121274, #91910, #28313, #183952, #196168, #87952, #58616, #181975, #44452, #106105, #107091, #103135, #105126, #166812, #151632, #43457, #150648, #167790, #168762, #135481, #13126, #30265, #74789, #133466, #136451, #10136, #56638, #41471, #118311, #29289, #12146, #90920, #152606, #14096, #75764, #42469, #164816, #199120, #180004, #11139, #72813, #134482, #57641, #104131, #119307, #180991, #165813, #27311, #73809, #49414, #112078, #138433, #63589, #1910, #169770, #186962, #902, #109091, #157592, #200114, #61582, #140420, #35234, #94914, #153603, #15099, #110088, #79749, #47434, #31264, #156600, #18094, #50419, #141419, #125264, #76759, #62576, #17090, #2906, #123251, #172767, #65567, #185950, #171767, #64584, #184942, #111077, #155595, #19083, #16096, #34247, #48432, #127227, #46427, #188942, #80731, #170770, #173768, #77754, #139420, #108086, #95907, #142410, #33256, #92915, #3888, #154600, #124255, #126249, #78743, #187945, #32259, #93917, #99884, #193922, #190910, #145389, #53386, #175742, #96888, #68550, #52387, #144393, #130206, #37220, #38229, #174750, #55385, #20060, #98875, #8894, #6871, #23062, #117055, #158571, #178750, #161569, #36214, #176756, #22060, #97867, #81704, #143387, #54392, #7874, #4879, #84707, #5878, #24065, #146386, #114044, #191901, #66561, #128226, #51398, #100878, #69560, #189923, #83711, #115064, #116065, #113058, #67555, #159557, #21055, #82710, #131225, #192915, #129212, #177753, #39222, #160571, #162560, #85720, #147406, #70562, #132229, #179761, #56389, #27074, #25075, #119076, #150415, #12893, #167564, #90697, #120053, #152380, #89718, #28077, #101893, #75532, #151403, #122034, #58386, #13865, #26071, #118071, #88720, #11910, #74556, #136223, #137207, #133223, #135247, #196919, #181740, #73574, #180758, #197898, #198893, #165575, #43221, #60361, #104889, #163575, #166577, #40214, #86718, #59367, #121036, #148403, #9897, #71558, #182734, #44218, #194914, #41231, #105877, #29057, #102892, #164577, #42234, #87714, #149400, #10895, #72568, #134243, #195928, #57404, #103895, #141180, #106864, #30036, #126016, #109846, #32023, #183724, #138205, #124006, #91674, #125025, #94674, #155364, #45210, #186721, #33019, #79510, #18849, #169529, #93681, #61351, #110841, #48192, #76528, #16853, #46192, #185704, #172525, #78504, #65330, #154367, #123022, #156353, #140177, #77519, #184707, #34010, #153365, #168538, #14867, #1670, #17854, #47193, #95667, #63348, #199887, #15861, #107845, #2670, #171531, #139191, #31029, #157354, #92679, #666, #62336, #64347, #187711, #49183, #80494, #3652, #170533, #142168, #108853, #19826, #97628, #4634, #66324, #188697, #161330, #22823, #112821, #83474, #114822, #174514, #146147, #7634, #82468, #175503, #36977, #127985, #143153, #113808, #111835, #5639, #98637, #99647, #54158, #177520, #6635, #38990, #176514, #37991, #50178, #162327, #84469, #8655, #145151, #100646, #35981, #189688, #160332, #21822, #69318, #130984, #23828, #81467, #68313, #129964, #191664, #53143, #67316, #192675, #85478, #52151, #115831, #147167, #126990, #173524, #34995, #96649, #158337, #51161, #159317, #20812, #144154, #128976, #190675, #12660, #131996, #193682, #166343, #42991, #39979, #135994, #72327, #165344, #28825, #74327, #55152, #73340, #26837, #195694, #135013, #27840, #116822, #178513, #197665, #196690, #118844, #70329, #24836, #10664, #101649, #11674, #181512, #42000, #163341, #58159, #119827, #89481, #105640, #56151, #180527, #148171, #59131, #104656, #86486, #103666, #132991, #182499, #120798, #25843, #43978, #194682, #117833, #90465, #151172, #167329, #150174, #9662, #152149, #71329, #179526, #88477, #134003, #57165, #40995, #102663, #164348, #87487, #149175, #62101, #170290, #92441, #13632, #185463, #169287, #61112, #46954, #154127 ),
 ( #93433, #138947, #153123, #172276, #75299, #171290, #124780, #33765, #16613, #122785, #140938, #78260, #30793, #123764, #110594, #121793, #168303, #44971, #48941, #63102, #15621, #31784, #186478, #108613, #94429, #45954, #106629, #47955, #427, #139933, #155119, #76284, #29800, #107609, #17607, #95425, #137963, #64105, #136970, #109606, #198660, #60126, #1422, #32777, #91436, #156110, #184475, #77278, #79267, #183487, #14627, #2425, #199646, #125772, #187472, #157109, #116336, #85999, #53668, #34753, #162840, #101153, #56676, #147688, #69835, #80253, #68832, #23338, #24348, #18605, #179034, #71835, #192187, #178025, #9175, #126748, #55664, #161844, #163860, #22337, #40500, #146664, #133504, #41512, #141923, #3414, #188450, #131502, #102172, #65089, #49930, #117338, #132510, #111595, #25359, #84982, #54662, #118349, #87000, #173280, #70842, #39493, #8159, #194199, #148687, #96412, #160848, #10175, #180043, #83988, #145667, #195196, #7148, #130491, #193189, #115346, #177036, #38506, #100162, #14132, #61617, #106144, #12183, #30302, #167826, #58653, #151669, #200147, #11177, #57680, #134522, #138466, #152642, #43496, #59638, #75799, #74827, #183988, #135518, #196208, #137477, #28350, #29326, #198168, #165852, #119348, #197189, #107127, #123285, #27348, #153638, #184976, #199157, #103175, #87991, #13163, #136488, #181032, #121312, #150685, #120319, #168798, #149679, #72852, #89988, #164855, #44488, #26351, #42506, #183004, #90955, #182013, #104170, #60624, #122298, #88994, #45473, #91945, #73847, #105162, #166848, #15133, #76795, #65601, #158603, #78777, #64619, #49447, #16130, #142443, #48465, #50450, #109125, #127261, #33288, #20093, #128257, #81737, #173800, #1943, #143423, #170803, #32295, #4910, #3921, #112109, #126281, #62609, #35266, #77785, #96921, #2939, #66593, #154635, #935, #139454, #46461, #95939, #186995, #187978, #19115, #18127, #188974, #140453, #124288, #80765, #171800, #111110, #141454, #93951, #185985, #63623, #108121, #169804, #155629, #31297, #92949, #47468, #17125, #125299, #156632, #94948, #110122, #79782, #172799, #34280, #157625, #36247, #174781, #176787, #71589, #131258, #189955, #51429, #146416, #116095, #83742, #67588, #192946, #54425, #86752, #177783, #99914, #113089, #98909, #53418, #39253, #97900, #8927, #101925, #22092, #7907, #100909, #159591, #85752, #191934, #193954, #52419, #70595, #38260, #163607, #21088, #25108, #117088, #145421, #148435, #114077, #175778, #9930, #147439, #55417, #69591, #5911, #178783, #82745, #40251, #162593, #115095, #161599, #37252, #129246, #24098, #144425, #6903, #23093, #132263, #68582, #190942, #84738, #130238, #160602, #166604, #73601, #74580, #10926, #91703, #56422, #11938, #122059, #182760, #72599, #153397, #194946, #14895, #197924, #134273, #12916, #58413, #195960, #133255, #118102, #90721, #44244, #179792, #136248, #42264, #60387, #59392, #88749, #181768, #135273, #28104, #41261, #137234, #102923, #121066, #89743, #120080, #105901, #152404, #164608, #196945, #13891, #43249, #167587, #26102, #87745, #104917, #149430, #29082, #75558, #151429, #57433, #198918, #183751, #45237, #168564, #119106, #106891, #180787, #30062, #103924, #165604, #27103, #150442, #16880, #3680, #171557, #158367, #47223, #154394, #187739, #109873, #170561, #77547, #65358, #123049, #61378, #184735, #125052, #110868, #80523, #17884, #96679, #63375, #33047, #34039, #169561, #108882, #15889, #139219, #138232, #172553, #95696, #62366, #94702, #64375, #124035, #157384, #18877, #32051, #186749, #48219, #694, #92706, #156379, #46220, #155390, #79538, #49210, #127019, #188726, #141208, #50211, #126043, #142197, #199914, #111865, #173555, #76556, #2698, #35024, #185734, #93708, #107873, #31058, #78531, #140205, #1699, #112852, #114851, #176545, #38021, #191692, #98668, #54187, #70357, #145180, #6664, #55182, #161361, #81496, #146177, #116851, #143183, #99677, #84499 ) ),
 .UNSPECIFIED., .T., .F., .F. ) 
 B_SPLINE_SURFACE_WITH_KNOTS ( ( 4, 3, 4 ),
 ( 3, 2, 2, 2, 2, 2, 2, 2, 2, 2, 2, 2, 2, 2, 2, 2, 2, 2, 2, 2, 2, 2, 2, 2, 2, 2, 2, 2, 2, 2, 2, 2, 2, 2, 2, 2, 2, 2, 2, 2, 2, 2, 2, 2, 2, 2, 2, 2, 2, 2, 2, 2, 2, 2, 2, 2, 2, 2, 2, 2, 2, 2, 2, 2, 2, 2, 2, 2, 2, 2, 2, 2, 2, 2, 2, 2, 2, 2, 2, 2, 2, 2, 2, 2, 2, 2, 2, 2, 2, 2, 2, 2, 2, 2, 2, 2, 2, 2, 2, 2, 2, 2, 2, 2, 2, 2, 2, 2, 2, 2, 2, 2, 2, 2, 2, 2, 2, 2, 2, 2, 2, 2, 2, 2, 2, 2, 2, 2, 2, 2, 2, 2, 2, 2, 2, 2, 2, 2, 2, 2, 2, 2, 2, 2, 2, 2, 2, 2, 2, 2, 2, 2, 2, 2, 2, 2, 2, 2, 2, 2, 2, 2, 2, 2, 2, 2, 2, 2, 2, 2, 2, 2, 2, 2, 2, 2, 2, 2, 2, 2, 2, 2, 2, 2, 2, 2, 2, 2, 2, 2, 2, 2, 2, 2, 2, 2, 2, 2, 2, 2, 2, 2, 2, 2, 2, 2, 2, 2, 2, 2, 2, 2, 2, 2, 2, 2, 2, 2, 2, 2, 2, 2, 2, 2, 2, 2, 2, 2, 3 ),
 ( 0.000000000000000000, 0.5000000000000000000, 1.000000000000000000 ),
 ( 0.000000000000000000, 0.004385964912280701511, 0.008771929824561403022, 0.01315789473684210453, 0.01754385964912280604, 0.02192982456140350755, 0.02631578947368420907, 0.03070175438596491058, 0.03508771929824561209, 0.03947368421052631360, 0.04385964912280701511, 0.04824561403508771662, 0.05263157894736841813, 0.05701754385964911964, 0.06140350877192982115, 0.06578947368421052266, 0.07017543859649122417, 0.07456140350877192569, 0.07894736842105262720, 0.08333333333333332871, 0.08771929824561403022, 0.09210526315789473173, 0.09649122807017543324, 0.1008771929824561348, 0.1052631578947368363, 0.1096491228070175378, 0.1140350877192982393, 0.1184210526315789408, 0.1228070175438596423, 0.1271929824561403577, 0.1315789473684210453, 0.1359649122807017607, 0.1403508771929824483, 0.1447368421052631637, 0.1491228070175438514, 0.1535087719298245668, 0.1578947368421052544, 0.1622807017543859698, 0.1666666666666666574, 0.1710526315789473728, 0.1754385964912280604, 0.1798245614035087758, 0.1842105263157894635, 0.1885964912280701788, 0.1929824561403508665, 0.1973684210526315819, 0.2017543859649122695, 0.2061403508771929849, 0.2105263157894736725, 0.2149122807017543879, 0.2192982456140350755, 0.2236842105263157909, 0.2280701754385964786, 0.2324561403508771940, 0.2368421052631578816, 0.2412280701754385970, 0.2456140350877192846, 0.2500000000000000000, 0.2543859649122807154, 0.2587719298245614308, 0.2631578947368420907, 0.2675438596491228060, 0.2719298245614035214, 0.2763157894736842368, 0.2807017543859648967, 0.2850877192982456121, 0.2894736842105263275, 0.2938596491228070429, 0.2982456140350877027, 0.3026315789473684181, 0.3070175438596491335, 0.3114035087719298489, 0.3157894736842105088, 0.3201754385964912242, 0.3245614035087719396, 0.3289473684210526550, 0.3333333333333333148, 0.3377192982456140302, 0.3421052631578947456, 0.3464912280701754610, 0.3508771929824561209, 0.3552631578947368363, 0.3596491228070175517, 0.3640350877192982670, 0.3684210526315789269, 0.3728070175438596423, 0.3771929824561403577, 0.3815789473684210731, 0.3859649122807017330, 0.3903508771929824483, 0.3947368421052631637, 0.3991228070175438791, 0.4035087719298245390, 0.4078947368421052544, 0.4122807017543859698, 0.4166666666666666852, 0.4210526315789473450, 0.4254385964912280604, 0.4298245614035087758, 0.4342105263157894912, 0.4385964912280701511, 0.4429824561403508665, 0.4473684210526315819, 0.4517543859649122973, 0.4561403508771929571, 0.4605263157894736725, 0.4649122807017543879, 0.4692982456140351033, 0.4736842105263157632, 0.4780701754385964786, 0.4824561403508771940, 0.4868421052631579093, 0.4912280701754385692, 0.4956140350877192846, 0.5000000000000000000, 0.5043859649122807154, 0.5087719298245614308, 0.5131578947368421462, 0.5175438596491228616, 0.5219298245614034659, 0.5263157894736841813, 0.5307017543859648967, 0.5350877192982456121, 0.5394736842105263275, 0.5438596491228070429, 0.5482456140350877583, 0.5526315789473684736, 0.5570175438596490780, 0.5614035087719297934, 0.5657894736842105088, 0.5701754385964912242, 0.5745614035087719396, 0.5789473684210526550, 0.5833333333333333703, 0.5877192982456140857, 0.5921052631578946901, 0.5964912280701754055, 0.6008771929824561209, 0.6052631578947368363, 0.6096491228070175517, 0.6140350877192982670, 0.6184210526315789824, 0.6228070175438596978, 0.6271929824561403022, 0.6315789473684210176, 0.6359649122807017330, 0.6403508771929824483, 0.6447368421052631637, 0.6491228070175438791, 0.6535087719298245945, 0.6578947368421053099, 0.6622807017543859143, 0.6666666666666666297, 0.6710526315789473450, 0.6754385964912280604, 0.6798245614035087758, 0.6842105263157894912, 0.6885964912280702066, 0.6929824561403509220, 0.6973684210526315264, 0.7017543859649122417, 0.7061403508771929571, 0.7105263157894736725, 0.7149122807017543879, 0.7192982456140351033, 0.7236842105263158187, 0.7280701754385965341, 0.7324561403508771384, 0.7368421052631578538, 0.7412280701754385692, 0.7456140350877192846, 0.7500000000000000000, 0.7543859649122807154, 0.7587719298245614308, 0.7631578947368421462, 0.7675438596491228616, 0.7719298245614034659, 0.7763157894736841813, 0.7807017543859648967, 0.7850877192982456121, 0.7894736842105263275, 0.7938596491228070429, 0.7982456140350877583, 0.8026315789473684736, 0.8070175438596490780, 0.8114035087719297934, 0.8157894736842105088, 0.8201754385964912242, 0.8245614035087719396, 0.8289473684210526550, 0.8333333333333333703, 0.8377192982456140857, 0.8421052631578946901, 0.8464912280701754055, 0.8508771929824561209, 0.8552631578947368363, 0.8596491228070175517, 0.8640350877192982670, 0.8684210526315789824, 0.8728070175438596978, 0.8771929824561403022, 0.8815789473684210176, 0.8859649122807017330, 0.8903508771929824483, 0.8947368421052631637, 0.8991228070175438791, 0.9035087719298245945, 0.9078947368421053099, 0.9122807017543859143, 0.9166666666666666297, 0.9210526315789473450, 0.9254385964912280604, 0.9298245614035087758, 0.9342105263157894912, 0.9385964912280702066, 0.9429824561403509220, 0.9473684210526315264, 0.9517543859649122417, 0.9561403508771929571, 0.9605263157894736725, 0.9649122807017543879, 0.9692982456140351033, 0.9736842105263158187, 0.9780701754385965341, 0.9824561403508771384, 0.9868421052631578538, 0.9912280701754385692, 0.9956140350877192846, 1.000000000000000000 ),
 .UNSPECIFIED. ) 
 GEOMETRIC_REPRESENTATION_ITEM ( )  RATIONAL_B_SPLINE_SURFACE ( (
 ( 1.000000000000000000, 0.9659258262890683122, 1.000000000000000000, 0.9659258262890683122, 1.000000000000000000, 0.9659258262890683122, 1.000000000000000000, 0.9659258262890683122, 1.000000000000000000, 0.9659258262890683122, 1.000000000000000000, 0.9659258262890683122, 1.000000000000000000, 0.9659258262890683122, 1.000000000000000000, 0.9659258262890683122, 1.000000000000000000, 0.9659258262890683122, 1.000000000000000000, 0.9659258262890683122, 1.000000000000000000, 0.9659258262890683122, 1.000000000000000000, 0.9659258262890683122, 1.000000000000000000, 0.9659258262890683122, 1.000000000000000000, 0.9659258262890683122, 1.000000000000000000, 0.9659258262890683122, 1.000000000000000000, 0.9659258262890683122, 1.000000000000000000, 0.9659258262890683122, 1.000000000000000000, 0.9659258262890683122, 1.000000000000000000, 0.9659258262890683122, 1.000000000000000000, 0.9659258262890683122, 1.000000000000000000, 0.9659258262890683122, 1.000000000000000000, 0.9659258262890683122, 1.000000000000000000, 0.9659258262890683122, 1.000000000000000000, 0.9659258262890683122, 1.000000000000000000, 0.9659258262890683122, 1.000000000000000000, 0.9659258262890683122, 1.000000000000000000, 0.9659258262890683122, 1.000000000000000000, 0.9659258262890683122, 1.000000000000000000, 0.9659258262890683122, 1.000000000000000000, 0.9659258262890683122, 1.000000000000000000, 0.9659258262890683122, 1.000000000000000000, 0.9659258262890683122, 1.000000000000000000, 0.9659258262890683122, 1.000000000000000000, 0.9659258262890683122, 1.000000000000000000, 0.9659258262890683122, 1.000000000000000000, 0.9659258262890683122, 1.000000000000000000, 0.9659258262890683122, 1.000000000000000000, 0.9659258262890683122, 1.000000000000000000, 0.9659258262890683122, 1.000000000000000000, 0.9659258262890683122, 1.000000000000000000, 0.9659258262890683122, 1.000000000000000000, 0.9659258262890683122, 1.000000000000000000, 0.9659258262890683122, 1.000000000000000000, 0.9659258262890683122, 1.000000000000000000, 0.9659258262890683122, 1.000000000000000000, 0.9659258262890683122, 1.000000000000000000, 0.9659258262890683122, 1.000000000000000000, 0.9659258262890683122, 1.000000000000000000, 0.9659258262890683122, 1.000000000000000000, 0.9659258262890683122, 1.000000000000000000, 0.9659258262890683122, 1.000000000000000000, 0.9659258262890683122, 1.000000000000000000, 0.9659258262890683122, 1.000000000000000000, 0.9659258262890683122, 1.000000000000000000, 0.9659258262890683122, 1.000000000000000000, 0.9659258262890683122, 1.000000000000000000, 0.9659258262890683122, 1.000000000000000000, 0.9659258262890683122, 1.000000000000000000, 0.9659258262890683122, 1.000000000000000000, 0.9659258262890683122, 1.000000000000000000, 0.9659258262890683122, 1.000000000000000000, 0.9659258262890683122, 1.000000000000000000, 0.9659258262890683122, 1.000000000000000000, 0.9659258262890683122, 1.000000000000000000, 0.9659258262890683122, 1.000000000000000000, 0.9659258262890683122, 1.000000000000000000, 0.9659258262890683122, 1.000000000000000000, 0.9659258262890683122, 1.000000000000000000, 0.9659258262890683122, 1.000000000000000000, 0.9659258262890683122, 1.000000000000000000, 0.9659258262890683122, 1.000000000000000000, 0.9659258262890683122, 1.000000000000000000, 0.9659258262890683122, 1.000000000000000000, 0.9659258262890683122, 1.000000000000000000, 0.9659258262890683122, 1.000000000000000000, 0.9659258262890683122, 1.000000000000000000, 0.9659258262890683122, 1.000000000000000000, 0.9659258262890683122, 1.000000000000000000, 0.9659258262890683122, 1.000000000000000000, 0.9659258262890683122, 1.000000000000000000, 0.9659258262890683122, 1.000000000000000000, 0.9659258262890683122, 1.000000000000000000, 0.9659258262890683122, 1.000000000000000000, 0.9659258262890683122, 1.000000000000000000, 0.9659258262890683122, 1.000000000000000000, 0.9659258262890683122, 1.000000000000000000, 0.9659258262890683122, 1.000000000000000000, 0.9659258262890683122, 1.000000000000000000, 0.9659258262890683122, 1.000000000000000000, 0.9659258262890683122, 1.000000000000000000, 0.9659258262890683122, 1.000000000000000000, 0.9659258262890683122, 1.000000000000000000, 0.9659258262890683122, 1.000000000000000000, 0.9659258262890683122, 1.000000000000000000, 0.9659258262890683122, 1.000000000000000000, 0.9659258262890683122, 1.000000000000000000, 0.9659258262890683122, 1.000000000000000000, 0.9659258262890683122, 1.000000000000000000, 0.9659258262890683122, 1.000000000000000000, 0.9659258262890683122, 1.000000000000000000, 0.9659258262890683122, 1.000000000000000000, 0.9659258262890683122, 1.000000000000000000, 0.9659258262890683122, 1.000000000000000000, 0.9659258262890683122, 1.000000000000000000, 0.9659258262890683122, 1.000000000000000000, 0.9659258262890683122, 1.000000000000000000, 0.9659258262890683122, 1.000000000000000000, 0.9659258262890683122, 1.000000000000000000, 0.9659258262890683122, 1.000000000000000000, 0.9659258262890683122, 1.000000000000000000, 0.9659258262890683122, 1.000000000000000000, 0.9659258262890683122, 1.000000000000000000, 0.9659258262890683122, 1.000000000000000000, 0.9659258262890683122, 1.000000000000000000, 0.9659258262890683122, 1.000000000000000000, 0.9659258262890683122, 1.000000000000000000, 0.9659258262890683122, 1.000000000000000000, 0.9659258262890683122, 1.000000000000000000, 0.9659258262890683122, 1.000000000000000000, 0.9659258262890683122, 1.000000000000000000, 0.9659258262890683122, 1.000000000000000000, 0.9659258262890683122, 1.000000000000000000, 0.9659258262890683122, 1.000000000000000000, 0.9659258262890683122, 1.000000000000000000, 0.9659258262890683122, 1.000000000000000000, 0.9659258262890683122, 1.000000000000000000, 0.9659258262890683122, 1.000000000000000000, 0.9659258262890683122, 1.000000000000000000, 0.9659258262890683122, 1.000000000000000000, 0.9659258262890683122, 1.000000000000000000, 0.9659258262890683122, 1.000000000000000000, 0.9659258262890683122, 1.000000000000000000, 0.9659258262890683122, 1.000000000000000000, 0.9659258262890683122, 1.000000000000000000, 0.9659258262890683122, 1.000000000000000000, 0.9659258262890683122, 1.000000000000000000, 0.9659258262890683122, 1.000000000000000000, 0.9659258262890683122, 1.000000000000000000, 0.9659258262890683122, 1.000000000000000000, 0.9659258262890683122, 1.000000000000000000, 0.9659258262890683122, 1.000000000000000000, 0.9659258262890683122, 1.000000000000000000, 0.9659258262890683122, 1.000000000000000000, 0.9659258262890683122, 1.000000000000000000, 0.9659258262890683122, 1.000000000000000000, 0.9659258262890683122, 1.000000000000000000, 0.9659258262890683122, 1.000000000000000000, 0.9659258262890683122, 1.000000000000000000, 0.9659258262890683122, 1.000000000000000000, 0.9659258262890683122, 1.000000000000000000, 0.9659258262890683122, 1.000000000000000000, 0.9659258262890683122, 1.000000000000000000, 0.9659258262890683122, 1.000000000000000000, 0.9659258262890683122, 1.000000000000000000, 0.9659258262890683122, 1.000000000000000000, 0.9659258262890683122, 1.000000000000000000, 0.9659258262890683122, 1.000000000000000000, 0.9659258262890683122, 1.000000000000000000, 0.9659258262890683122, 1.000000000000000000, 0.9659258262890683122, 1.000000000000000000, 0.9659258262890683122, 1.000000000000000000, 0.9659258262890683122, 1.000000000000000000, 0.9659258262890683122, 1.000000000000000000, 0.9659258262890683122, 1.000000000000000000, 0.9659258262890683122, 1.000000000000000000, 0.9659258262890683122, 1.000000000000000000, 0.9659258262890683122, 1.000000000000000000, 0.9659258262890683122, 1.000000000000000000, 0.9659258262890683122, 1.000000000000000000, 0.9659258262890683122, 1.000000000000000000, 0.9659258262890683122, 1.000000000000000000, 0.9659258262890683122, 1.000000000000000000, 0.9659258262890683122, 1.000000000000000000, 0.9659258262890683122, 1.000000000000000000, 0.9659258262890683122, 1.000000000000000000, 0.9659258262890683122, 1.000000000000000000, 0.9659258262890683122, 1.000000000000000000, 0.9659258262890683122, 1.000000000000000000, 0.9659258262890683122, 1.000000000000000000, 0.9659258262890683122, 1.000000000000000000, 0.9659258262890683122, 1.000000000000000000, 0.9659258262890683122, 1.000000000000000000, 0.9659258262890683122, 1.000000000000000000, 0.9659258262890683122, 1.000000000000000000, 0.9659258262890683122, 1.000000000000000000, 0.9659258262890683122, 1.000000000000000000, 0.9659258262890683122, 1.000000000000000000, 0.9659258262890683122, 1.000000000000000000, 0.9659258262890683122, 1.000000000000000000, 0.9659258262890683122, 1.000000000000000000, 0.9659258262890683122, 1.000000000000000000, 0.9659258262890683122, 1.000000000000000000, 0.9659258262890683122, 1.000000000000000000, 0.9659258262890683122, 1.000000000000000000, 0.9659258262890683122, 1.000000000000000000, 0.9659258262890683122, 1.000000000000000000, 0.9659258262890683122, 1.000000000000000000, 0.9659258262890683122, 1.000000000000000000, 0.9659258262890683122, 1.000000000000000000, 0.9659258262890683122, 1.000000000000000000, 0.9659258262890683122, 1.000000000000000000, 0.9659258262890683122, 1.000000000000000000, 0.9659258262890683122, 1.000000000000000000, 0.9659258262890683122, 1.000000000000000000, 0.9659258262890683122, 1.000000000000000000, 0.9659258262890683122, 1.000000000000000000, 0.9659258262890683122, 1.000000000000000000, 0.9659258262890683122, 1.000000000000000000, 0.9659258262890683122, 1.000000000000000000, 0.9659258262890683122, 1.000000000000000000, 0.9659258262890683122, 1.000000000000000000, 0.9659258262890683122, 1.000000000000000000, 0.9659258262890683122, 1.000000000000000000, 0.9659258262890683122, 1.000000000000000000, 0.9659258262890683122, 1.000000000000000000, 0.9659258262890683122, 1.000000000000000000, 0.9659258262890683122, 1.000000000000000000, 0.9659258262890683122, 1.000000000000000000, 0.9659258262890683122, 1.000000000000000000, 0.9659258262890683122, 1.000000000000000000, 0.9659258262890683122, 1.000000000000000000, 0.9659258262890683122, 1.000000000000000000, 0.9659258262890683122, 1.000000000000000000, 0.9659258262890683122, 1.000000000000000000, 0.9659258262890683122, 1.000000000000000000, 0.9659258262890683122, 1.000000000000000000, 0.9659258262890683122, 1.000000000000000000, 0.9659258262890683122, 1.000000000000000000),
 ( 0.3333333333333333703, 0.3219752754296894559, 0.3333333333333333703, 0.3219752754296894559, 0.3333333333333333703, 0.3219752754296894559, 0.3333333333333333703, 0.3219752754296894559, 0.3333333333333333703, 0.3219752754296894559, 0.3333333333333333703, 0.3219752754296894559, 0.3333333333333333703, 0.3219752754296894559, 0.3333333333333333703, 0.3219752754296894559, 0.3333333333333333703, 0.3219752754296894559, 0.3333333333333333703, 0.3219752754296894559, 0.3333333333333333703, 0.3219752754296894559, 0.3333333333333333703, 0.3219752754296894559, 0.3333333333333333703, 0.3219752754296894559, 0.3333333333333333703, 0.3219752754296894559, 0.3333333333333333703, 0.3219752754296894559, 0.3333333333333333703, 0.3219752754296894559, 0.3333333333333333703, 0.3219752754296894559, 0.3333333333333333703, 0.3219752754296894559, 0.3333333333333333703, 0.3219752754296894559, 0.3333333333333333703, 0.3219752754296894559, 0.3333333333333333703, 0.3219752754296894559, 0.3333333333333333703, 0.3219752754296894559, 0.3333333333333333703, 0.3219752754296894559, 0.3333333333333333703, 0.3219752754296894559, 0.3333333333333333703, 0.3219752754296894559, 0.3333333333333333703, 0.3219752754296894559, 0.3333333333333333703, 0.3219752754296894559, 0.3333333333333333703, 0.3219752754296894559, 0.3333333333333333703, 0.3219752754296894559, 0.3333333333333333703, 0.3219752754296894559, 0.3333333333333333703, 0.3219752754296894559, 0.3333333333333333703, 0.3219752754296894559, 0.3333333333333333703, 0.3219752754296894559, 0.3333333333333333703, 0.3219752754296894559, 0.3333333333333333703, 0.3219752754296894559, 0.3333333333333333703, 0.3219752754296894559, 0.3333333333333333703, 0.3219752754296894559, 0.3333333333333333703, 0.3219752754296894559, 0.3333333333333333703, 0.3219752754296894559, 0.3333333333333333703, 0.3219752754296894559, 0.3333333333333333703, 0.3219752754296894559, 0.3333333333333333703, 0.3219752754296894559, 0.3333333333333333703, 0.3219752754296894559, 0.3333333333333333703, 0.3219752754296894559, 0.3333333333333333703, 0.3219752754296894559, 0.3333333333333333703, 0.3219752754296894559, 0.3333333333333333703, 0.3219752754296894559, 0.3333333333333333703, 0.3219752754296894559, 0.3333333333333333703, 0.3219752754296894559, 0.3333333333333333703, 0.3219752754296894559, 0.3333333333333333703, 0.3219752754296894559, 0.3333333333333333703, 0.3219752754296894559, 0.3333333333333333703, 0.3219752754296894559, 0.3333333333333333703, 0.3219752754296894559, 0.3333333333333333703, 0.3219752754296894559, 0.3333333333333333703, 0.3219752754296894559, 0.3333333333333333703, 0.3219752754296894559, 0.3333333333333333703, 0.3219752754296894559, 0.3333333333333333703, 0.3219752754296894559, 0.3333333333333333703, 0.3219752754296894559, 0.3333333333333333703, 0.3219752754296894559, 0.3333333333333333703, 0.3219752754296894559, 0.3333333333333333703, 0.3219752754296894559, 0.3333333333333333703, 0.3219752754296894559, 0.3333333333333333703, 0.3219752754296894559, 0.3333333333333333703, 0.3219752754296894559, 0.3333333333333333703, 0.3219752754296894559, 0.3333333333333333703, 0.3219752754296894559, 0.3333333333333333703, 0.3219752754296894559, 0.3333333333333333703, 0.3219752754296894559, 0.3333333333333333703, 0.3219752754296894559, 0.3333333333333333703, 0.3219752754296894559, 0.3333333333333333703, 0.3219752754296894559, 0.3333333333333333703, 0.3219752754296894559, 0.3333333333333333703, 0.3219752754296894559, 0.3333333333333333703, 0.3219752754296894559, 0.3333333333333333703, 0.3219752754296894559, 0.3333333333333333703, 0.3219752754296894559, 0.3333333333333333703, 0.3219752754296894559, 0.3333333333333333703, 0.3219752754296894559, 0.3333333333333333703, 0.3219752754296894559, 0.3333333333333333703, 0.3219752754296894559, 0.3333333333333333703, 0.3219752754296894559, 0.3333333333333333703, 0.3219752754296894559, 0.3333333333333333703, 0.3219752754296894559, 0.3333333333333333703, 0.3219752754296894559, 0.3333333333333333703, 0.3219752754296894559, 0.3333333333333333703, 0.3219752754296894559, 0.3333333333333333703, 0.3219752754296894559, 0.3333333333333333703, 0.3219752754296894559, 0.3333333333333333703, 0.3219752754296894559, 0.3333333333333333703, 0.3219752754296894559, 0.3333333333333333703, 0.3219752754296894559, 0.3333333333333333703, 0.3219752754296894559, 0.3333333333333333703, 0.3219752754296894559, 0.3333333333333333703, 0.3219752754296894559, 0.3333333333333333703, 0.3219752754296894559, 0.3333333333333333703, 0.3219752754296894559, 0.3333333333333333703, 0.3219752754296894559, 0.3333333333333333703, 0.3219752754296894559, 0.3333333333333333703, 0.3219752754296894559, 0.3333333333333333703, 0.3219752754296894559, 0.3333333333333333703, 0.3219752754296894559, 0.3333333333333333703, 0.3219752754296894559, 0.3333333333333333703, 0.3219752754296894559, 0.3333333333333333703, 0.3219752754296894559, 0.3333333333333333703, 0.3219752754296894559, 0.3333333333333333703, 0.3219752754296894559, 0.3333333333333333703, 0.3219752754296894559, 0.3333333333333333703, 0.3219752754296894559, 0.3333333333333333703, 0.3219752754296894559, 0.3333333333333333703, 0.3219752754296894559, 0.3333333333333333703, 0.3219752754296894559, 0.3333333333333333703, 0.3219752754296894559, 0.3333333333333333703, 0.3219752754296894559, 0.3333333333333333703, 0.3219752754296894559, 0.3333333333333333703, 0.3219752754296894559, 0.3333333333333333703, 0.3219752754296894559, 0.3333333333333333703, 0.3219752754296894559, 0.3333333333333333703, 0.3219752754296894559, 0.3333333333333333703, 0.3219752754296894559, 0.3333333333333333703, 0.3219752754296894559, 0.3333333333333333703, 0.3219752754296894559, 0.3333333333333333703, 0.3219752754296894559, 0.3333333333333333703, 0.3219752754296894559, 0.3333333333333333703, 0.3219752754296894559, 0.3333333333333333703, 0.3219752754296894559, 0.3333333333333333703, 0.3219752754296894559, 0.3333333333333333703, 0.3219752754296894559, 0.3333333333333333703, 0.3219752754296894559, 0.3333333333333333703, 0.3219752754296894559, 0.3333333333333333703, 0.3219752754296894559, 0.3333333333333333703, 0.3219752754296894559, 0.3333333333333333703, 0.3219752754296894559, 0.3333333333333333703, 0.3219752754296894559, 0.3333333333333333703, 0.3219752754296894559, 0.3333333333333333703, 0.3219752754296894559, 0.3333333333333333703, 0.3219752754296894559, 0.3333333333333333703, 0.3219752754296894559, 0.3333333333333333703, 0.3219752754296894559, 0.3333333333333333703, 0.3219752754296894559, 0.3333333333333333703, 0.3219752754296894559, 0.3333333333333333703, 0.3219752754296894559, 0.3333333333333333703, 0.3219752754296894559, 0.3333333333333333703, 0.3219752754296894559, 0.3333333333333333703, 0.3219752754296894559, 0.3333333333333333703, 0.3219752754296894559, 0.3333333333333333703, 0.3219752754296894559, 0.3333333333333333703, 0.3219752754296894559, 0.3333333333333333703, 0.3219752754296894559, 0.3333333333333333703, 0.3219752754296894559, 0.3333333333333333703, 0.3219752754296894559, 0.3333333333333333703, 0.3219752754296894559, 0.3333333333333333703, 0.3219752754296894559, 0.3333333333333333703, 0.3219752754296894559, 0.3333333333333333703, 0.3219752754296894559, 0.3333333333333333703, 0.3219752754296894559, 0.3333333333333333703, 0.3219752754296894559, 0.3333333333333333703, 0.3219752754296894559, 0.3333333333333333703, 0.3219752754296894559, 0.3333333333333333703, 0.3219752754296894559, 0.3333333333333333703, 0.3219752754296894559, 0.3333333333333333703, 0.3219752754296894559, 0.3333333333333333703, 0.3219752754296894559, 0.3333333333333333703, 0.3219752754296894559, 0.3333333333333333703, 0.3219752754296894559, 0.3333333333333333703, 0.3219752754296894559, 0.3333333333333333703, 0.3219752754296894559, 0.3333333333333333703, 0.3219752754296894559, 0.3333333333333333703, 0.3219752754296894559, 0.3333333333333333703, 0.3219752754296894559, 0.3333333333333333703, 0.3219752754296894559, 0.3333333333333333703, 0.3219752754296894559, 0.3333333333333333703, 0.3219752754296894559, 0.3333333333333333703, 0.3219752754296894559, 0.3333333333333333703, 0.3219752754296894559, 0.3333333333333333703, 0.3219752754296894559, 0.3333333333333333703, 0.3219752754296894559, 0.3333333333333333703, 0.3219752754296894559, 0.3333333333333333703, 0.3219752754296894559, 0.3333333333333333703, 0.3219752754296894559, 0.3333333333333333703, 0.3219752754296894559, 0.3333333333333333703, 0.3219752754296894559, 0.3333333333333333703, 0.3219752754296894559, 0.3333333333333333703, 0.3219752754296894559, 0.3333333333333333703, 0.3219752754296894559, 0.3333333333333333703, 0.3219752754296894559, 0.3333333333333333703, 0.3219752754296894559, 0.3333333333333333703, 0.3219752754296894559, 0.3333333333333333703, 0.3219752754296894559, 0.3333333333333333703, 0.3219752754296894559, 0.3333333333333333703, 0.3219752754296894559, 0.3333333333333333703, 0.3219752754296894559, 0.3333333333333333703, 0.3219752754296894559, 0.3333333333333333703, 0.3219752754296894559, 0.3333333333333333703, 0.3219752754296894559, 0.3333333333333333703, 0.3219752754296894559, 0.3333333333333333703, 0.3219752754296894559, 0.3333333333333333703, 0.3219752754296894559, 0.3333333333333333703, 0.3219752754296894559, 0.3333333333333333703, 0.3219752754296894559, 0.3333333333333333703, 0.3219752754296894559, 0.3333333333333333703, 0.3219752754296894559, 0.3333333333333333703, 0.3219752754296894559, 0.3333333333333333703, 0.3219752754296894559, 0.3333333333333333703, 0.3219752754296894559, 0.3333333333333333703, 0.3219752754296894559, 0.3333333333333333703, 0.3219752754296894559, 0.3333333333333333703, 0.3219752754296894559, 0.3333333333333333703, 0.3219752754296894559, 0.3333333333333333703, 0.3219752754296894559, 0.3333333333333333703, 0.3219752754296894559, 0.3333333333333333703, 0.3219752754296894559, 0.3333333333333333703, 0.3219752754296894559, 0.3333333333333333703, 0.3219752754296894559, 0.3333333333333333703, 0.3219752754296894559, 0.3333333333333333703, 0.3219752754296894559, 0.3333333333333333703, 0.3219752754296894559, 0.3333333333333333703, 0.3219752754296894559, 0.3333333333333333703, 0.3219752754296894559, 0.3333333333333333703, 0.3219752754296894559, 0.3333333333333333703, 0.3219752754296894559, 0.3333333333333333703, 0.3219752754296894559, 0.3333333333333333703, 0.3219752754296894559, 0.3333333333333333703, 0.3219752754296894559, 0.3333333333333333703, 0.3219752754296894559, 0.3333333333333333703, 0.3219752754296894559, 0.3333333333333333703, 0.3219752754296894559, 0.3333333333333333703),
 ( 0.3333333333333333703, 0.3219752754296894559, 0.3333333333333333703, 0.3219752754296894559, 0.3333333333333333703, 0.3219752754296894559, 0.3333333333333333703, 0.3219752754296894559, 0.3333333333333333703, 0.3219752754296894559, 0.3333333333333333703, 0.3219752754296894559, 0.3333333333333333703, 0.3219752754296894559, 0.3333333333333333703, 0.3219752754296894559, 0.3333333333333333703, 0.3219752754296894559, 0.3333333333333333703, 0.3219752754296894559, 0.3333333333333333703, 0.3219752754296894559, 0.3333333333333333703, 0.3219752754296894559, 0.3333333333333333703, 0.3219752754296894559, 0.3333333333333333703, 0.3219752754296894559, 0.3333333333333333703, 0.3219752754296894559, 0.3333333333333333703, 0.3219752754296894559, 0.3333333333333333703, 0.3219752754296894559, 0.3333333333333333703, 0.3219752754296894559, 0.3333333333333333703, 0.3219752754296894559, 0.3333333333333333703, 0.3219752754296894559, 0.3333333333333333703, 0.3219752754296894559, 0.3333333333333333703, 0.3219752754296894559, 0.3333333333333333703, 0.3219752754296894559, 0.3333333333333333703, 0.3219752754296894559, 0.3333333333333333703, 0.3219752754296894559, 0.3333333333333333703, 0.3219752754296894559, 0.3333333333333333703, 0.3219752754296894559, 0.3333333333333333703, 0.3219752754296894559, 0.3333333333333333703, 0.3219752754296894559, 0.3333333333333333703, 0.3219752754296894559, 0.3333333333333333703, 0.3219752754296894559, 0.3333333333333333703, 0.3219752754296894559, 0.3333333333333333703, 0.3219752754296894559, 0.3333333333333333703, 0.3219752754296894559, 0.3333333333333333703, 0.3219752754296894559, 0.3333333333333333703, 0.3219752754296894559, 0.3333333333333333703, 0.3219752754296894559, 0.3333333333333333703, 0.3219752754296894559, 0.3333333333333333703, 0.3219752754296894559, 0.3333333333333333703, 0.3219752754296894559, 0.3333333333333333703, 0.3219752754296894559, 0.3333333333333333703, 0.3219752754296894559, 0.3333333333333333703, 0.3219752754296894559, 0.3333333333333333703, 0.3219752754296894559, 0.3333333333333333703, 0.3219752754296894559, 0.3333333333333333703, 0.3219752754296894559, 0.3333333333333333703, 0.3219752754296894559, 0.3333333333333333703, 0.3219752754296894559, 0.3333333333333333703, 0.3219752754296894559, 0.3333333333333333703, 0.3219752754296894559, 0.3333333333333333703, 0.3219752754296894559, 0.3333333333333333703, 0.3219752754296894559, 0.3333333333333333703, 0.3219752754296894559, 0.3333333333333333703, 0.3219752754296894559, 0.3333333333333333703, 0.3219752754296894559, 0.3333333333333333703, 0.3219752754296894559, 0.3333333333333333703, 0.3219752754296894559, 0.3333333333333333703, 0.3219752754296894559, 0.3333333333333333703, 0.3219752754296894559, 0.3333333333333333703, 0.3219752754296894559, 0.3333333333333333703, 0.3219752754296894559, 0.3333333333333333703, 0.3219752754296894559, 0.3333333333333333703, 0.3219752754296894559, 0.3333333333333333703, 0.3219752754296894559, 0.3333333333333333703, 0.3219752754296894559, 0.3333333333333333703, 0.3219752754296894559, 0.3333333333333333703, 0.3219752754296894559, 0.3333333333333333703, 0.3219752754296894559, 0.3333333333333333703, 0.3219752754296894559, 0.3333333333333333703, 0.3219752754296894559, 0.3333333333333333703, 0.3219752754296894559, 0.3333333333333333703, 0.3219752754296894559, 0.3333333333333333703, 0.3219752754296894559, 0.3333333333333333703, 0.3219752754296894559, 0.3333333333333333703, 0.3219752754296894559, 0.3333333333333333703, 0.3219752754296894559, 0.3333333333333333703, 0.3219752754296894559, 0.3333333333333333703, 0.3219752754296894559, 0.3333333333333333703, 0.3219752754296894559, 0.3333333333333333703, 0.3219752754296894559, 0.3333333333333333703, 0.3219752754296894559, 0.3333333333333333703, 0.3219752754296894559, 0.3333333333333333703, 0.3219752754296894559, 0.3333333333333333703, 0.3219752754296894559, 0.3333333333333333703, 0.3219752754296894559, 0.3333333333333333703, 0.3219752754296894559, 0.3333333333333333703, 0.3219752754296894559, 0.3333333333333333703, 0.3219752754296894559, 0.3333333333333333703, 0.3219752754296894559, 0.3333333333333333703, 0.3219752754296894559, 0.3333333333333333703, 0.3219752754296894559, 0.3333333333333333703, 0.3219752754296894559, 0.3333333333333333703, 0.3219752754296894559, 0.3333333333333333703, 0.3219752754296894559, 0.3333333333333333703, 0.3219752754296894559, 0.3333333333333333703, 0.3219752754296894559, 0.3333333333333333703, 0.3219752754296894559, 0.3333333333333333703, 0.3219752754296894559, 0.3333333333333333703, 0.3219752754296894559, 0.3333333333333333703, 0.3219752754296894559, 0.3333333333333333703, 0.3219752754296894559, 0.3333333333333333703, 0.3219752754296894559, 0.3333333333333333703, 0.3219752754296894559, 0.3333333333333333703, 0.3219752754296894559, 0.3333333333333333703, 0.3219752754296894559, 0.3333333333333333703, 0.3219752754296894559, 0.3333333333333333703, 0.3219752754296894559, 0.3333333333333333703, 0.3219752754296894559, 0.3333333333333333703, 0.3219752754296894559, 0.3333333333333333703, 0.3219752754296894559, 0.3333333333333333703, 0.3219752754296894559, 0.3333333333333333703, 0.3219752754296894559, 0.3333333333333333703, 0.3219752754296894559, 0.3333333333333333703, 0.3219752754296894559, 0.3333333333333333703, 0.3219752754296894559, 0.3333333333333333703, 0.3219752754296894559, 0.3333333333333333703, 0.3219752754296894559, 0.3333333333333333703, 0.3219752754296894559, 0.3333333333333333703, 0.3219752754296894559, 0.3333333333333333703, 0.3219752754296894559, 0.3333333333333333703, 0.3219752754296894559, 0.3333333333333333703, 0.3219752754296894559, 0.3333333333333333703, 0.3219752754296894559, 0.3333333333333333703, 0.3219752754296894559, 0.3333333333333333703, 0.3219752754296894559, 0.3333333333333333703, 0.3219752754296894559, 0.3333333333333333703, 0.3219752754296894559, 0.3333333333333333703, 0.3219752754296894559, 0.3333333333333333703, 0.3219752754296894559, 0.3333333333333333703, 0.3219752754296894559, 0.3333333333333333703, 0.3219752754296894559, 0.3333333333333333703, 0.3219752754296894559, 0.3333333333333333703, 0.3219752754296894559, 0.3333333333333333703, 0.3219752754296894559, 0.3333333333333333703, 0.3219752754296894559, 0.3333333333333333703, 0.3219752754296894559, 0.3333333333333333703, 0.3219752754296894559, 0.3333333333333333703, 0.3219752754296894559, 0.3333333333333333703, 0.3219752754296894559, 0.3333333333333333703, 0.3219752754296894559, 0.3333333333333333703, 0.3219752754296894559, 0.3333333333333333703, 0.3219752754296894559, 0.3333333333333333703, 0.3219752754296894559, 0.3333333333333333703, 0.3219752754296894559, 0.3333333333333333703, 0.3219752754296894559, 0.3333333333333333703, 0.3219752754296894559, 0.3333333333333333703, 0.3219752754296894559, 0.3333333333333333703, 0.3219752754296894559, 0.3333333333333333703, 0.3219752754296894559, 0.3333333333333333703, 0.3219752754296894559, 0.3333333333333333703, 0.3219752754296894559, 0.3333333333333333703, 0.3219752754296894559, 0.3333333333333333703, 0.3219752754296894559, 0.3333333333333333703, 0.3219752754296894559, 0.3333333333333333703, 0.3219752754296894559, 0.3333333333333333703, 0.3219752754296894559, 0.3333333333333333703, 0.3219752754296894559, 0.3333333333333333703, 0.3219752754296894559, 0.3333333333333333703, 0.3219752754296894559, 0.3333333333333333703, 0.3219752754296894559, 0.3333333333333333703, 0.3219752754296894559, 0.3333333333333333703, 0.3219752754296894559, 0.3333333333333333703, 0.3219752754296894559, 0.3333333333333333703, 0.3219752754296894559, 0.3333333333333333703, 0.3219752754296894559, 0.3333333333333333703, 0.3219752754296894559, 0.3333333333333333703, 0.3219752754296894559, 0.3333333333333333703, 0.3219752754296894559, 0.3333333333333333703, 0.3219752754296894559, 0.3333333333333333703, 0.3219752754296894559, 0.3333333333333333703, 0.3219752754296894559, 0.3333333333333333703, 0.3219752754296894559, 0.3333333333333333703, 0.3219752754296894559, 0.3333333333333333703, 0.3219752754296894559, 0.3333333333333333703, 0.3219752754296894559, 0.3333333333333333703, 0.3219752754296894559, 0.3333333333333333703, 0.3219752754296894559, 0.3333333333333333703, 0.3219752754296894559, 0.3333333333333333703, 0.3219752754296894559, 0.3333333333333333703, 0.3219752754296894559, 0.3333333333333333703, 0.3219752754296894559, 0.3333333333333333703, 0.3219752754296894559, 0.3333333333333333703, 0.3219752754296894559, 0.3333333333333333703, 0.3219752754296894559, 0.3333333333333333703, 0.3219752754296894559, 0.3333333333333333703, 0.3219752754296894559, 0.3333333333333333703, 0.3219752754296894559, 0.3333333333333333703, 0.3219752754296894559, 0.3333333333333333703, 0.3219752754296894559, 0.3333333333333333703, 0.3219752754296894559, 0.3333333333333333703, 0.3219752754296894559, 0.3333333333333333703, 0.3219752754296894559, 0.3333333333333333703, 0.3219752754296894559, 0.3333333333333333703, 0.3219752754296894559, 0.3333333333333333703, 0.3219752754296894559, 0.3333333333333333703, 0.3219752754296894559, 0.3333333333333333703, 0.3219752754296894559, 0.3333333333333333703, 0.3219752754296894559, 0.3333333333333333703, 0.3219752754296894559, 0.3333333333333333703, 0.3219752754296894559, 0.3333333333333333703, 0.3219752754296894559, 0.3333333333333333703, 0.3219752754296894559, 0.3333333333333333703, 0.3219752754296894559, 0.3333333333333333703, 0.3219752754296894559, 0.3333333333333333703, 0.3219752754296894559, 0.3333333333333333703, 0.3219752754296894559, 0.3333333333333333703, 0.3219752754296894559, 0.3333333333333333703, 0.3219752754296894559, 0.3333333333333333703, 0.3219752754296894559, 0.3333333333333333703, 0.3219752754296894559, 0.3333333333333333703, 0.3219752754296894559, 0.3333333333333333703, 0.3219752754296894559, 0.3333333333333333703, 0.3219752754296894559, 0.3333333333333333703, 0.3219752754296894559, 0.3333333333333333703, 0.3219752754296894559, 0.3333333333333333703, 0.3219752754296894559, 0.3333333333333333703, 0.3219752754296894559, 0.3333333333333333703, 0.3219752754296894559, 0.3333333333333333703, 0.3219752754296894559, 0.3333333333333333703, 0.3219752754296894559, 0.3333333333333333703, 0.3219752754296894559, 0.3333333333333333703, 0.3219752754296894559, 0.3333333333333333703, 0.3219752754296894559, 0.3333333333333333703, 0.3219752754296894559, 0.3333333333333333703, 0.3219752754296894559, 0.3333333333333333703, 0.3219752754296894559, 0.3333333333333333703, 0.3219752754296894559, 0.3333333333333333703, 0.3219752754296894559, 0.3333333333333333703),
 ( 1.000000000000000000, 0.9659258262890683122, 1.000000000000000000, 0.9659258262890683122, 1.000000000000000000, 0.9659258262890683122, 1.000000000000000000, 0.9659258262890683122, 1.000000000000000000, 0.9659258262890683122, 1.000000000000000000, 0.9659258262890683122, 1.000000000000000000, 0.9659258262890683122, 1.000000000000000000, 0.9659258262890683122, 1.000000000000000000, 0.9659258262890683122, 1.000000000000000000, 0.9659258262890683122, 1.000000000000000000, 0.9659258262890683122, 1.000000000000000000, 0.9659258262890683122, 1.000000000000000000, 0.9659258262890683122, 1.000000000000000000, 0.9659258262890683122, 1.000000000000000000, 0.9659258262890683122, 1.000000000000000000, 0.9659258262890683122, 1.000000000000000000, 0.9659258262890683122, 1.000000000000000000, 0.9659258262890683122, 1.000000000000000000, 0.9659258262890683122, 1.000000000000000000, 0.9659258262890683122, 1.000000000000000000, 0.9659258262890683122, 1.000000000000000000, 0.9659258262890683122, 1.000000000000000000, 0.9659258262890683122, 1.000000000000000000, 0.9659258262890683122, 1.000000000000000000, 0.9659258262890683122, 1.000000000000000000, 0.9659258262890683122, 1.000000000000000000, 0.9659258262890683122, 1.000000000000000000, 0.9659258262890683122, 1.000000000000000000, 0.9659258262890683122, 1.000000000000000000, 0.9659258262890683122, 1.000000000000000000, 0.9659258262890683122, 1.000000000000000000, 0.9659258262890683122, 1.000000000000000000, 0.9659258262890683122, 1.000000000000000000, 0.9659258262890683122, 1.000000000000000000, 0.9659258262890683122, 1.000000000000000000, 0.9659258262890683122, 1.000000000000000000, 0.9659258262890683122, 1.000000000000000000, 0.9659258262890683122, 1.000000000000000000, 0.9659258262890683122, 1.000000000000000000, 0.9659258262890683122, 1.000000000000000000, 0.9659258262890683122, 1.000000000000000000, 0.9659258262890683122, 1.000000000000000000, 0.9659258262890683122, 1.000000000000000000, 0.9659258262890683122, 1.000000000000000000, 0.9659258262890683122, 1.000000000000000000, 0.9659258262890683122, 1.000000000000000000, 0.9659258262890683122, 1.000000000000000000, 0.9659258262890683122, 1.000000000000000000, 0.9659258262890683122, 1.000000000000000000, 0.9659258262890683122, 1.000000000000000000, 0.9659258262890683122, 1.000000000000000000, 0.9659258262890683122, 1.000000000000000000, 0.9659258262890683122, 1.000000000000000000, 0.9659258262890683122, 1.000000000000000000, 0.9659258262890683122, 1.000000000000000000, 0.9659258262890683122, 1.000000000000000000, 0.9659258262890683122, 1.000000000000000000, 0.9659258262890683122, 1.000000000000000000, 0.9659258262890683122, 1.000000000000000000, 0.9659258262890683122, 1.000000000000000000, 0.9659258262890683122, 1.000000000000000000, 0.9659258262890683122, 1.000000000000000000, 0.9659258262890683122, 1.000000000000000000, 0.9659258262890683122, 1.000000000000000000, 0.9659258262890683122, 1.000000000000000000, 0.9659258262890683122, 1.000000000000000000, 0.9659258262890683122, 1.000000000000000000, 0.9659258262890683122, 1.000000000000000000, 0.9659258262890683122, 1.000000000000000000, 0.9659258262890683122, 1.000000000000000000, 0.9659258262890683122, 1.000000000000000000, 0.9659258262890683122, 1.000000000000000000, 0.9659258262890683122, 1.000000000000000000, 0.9659258262890683122, 1.000000000000000000, 0.9659258262890683122, 1.000000000000000000, 0.9659258262890683122, 1.000000000000000000, 0.9659258262890683122, 1.000000000000000000, 0.9659258262890683122, 1.000000000000000000, 0.9659258262890683122, 1.000000000000000000, 0.9659258262890683122, 1.000000000000000000, 0.9659258262890683122, 1.000000000000000000, 0.9659258262890683122, 1.000000000000000000, 0.9659258262890683122, 1.000000000000000000, 0.9659258262890683122, 1.000000000000000000, 0.9659258262890683122, 1.000000000000000000, 0.9659258262890683122, 1.000000000000000000, 0.9659258262890683122, 1.000000000000000000, 0.9659258262890683122, 1.000000000000000000, 0.9659258262890683122, 1.000000000000000000, 0.9659258262890683122, 1.000000000000000000, 0.9659258262890683122, 1.000000000000000000, 0.9659258262890683122, 1.000000000000000000, 0.9659258262890683122, 1.000000000000000000, 0.9659258262890683122, 1.000000000000000000, 0.9659258262890683122, 1.000000000000000000, 0.9659258262890683122, 1.000000000000000000, 0.9659258262890683122, 1.000000000000000000, 0.9659258262890683122, 1.000000000000000000, 0.9659258262890683122, 1.000000000000000000, 0.9659258262890683122, 1.000000000000000000, 0.9659258262890683122, 1.000000000000000000, 0.9659258262890683122, 1.000000000000000000, 0.9659258262890683122, 1.000000000000000000, 0.9659258262890683122, 1.000000000000000000, 0.9659258262890683122, 1.000000000000000000, 0.9659258262890683122, 1.000000000000000000, 0.9659258262890683122, 1.000000000000000000, 0.9659258262890683122, 1.000000000000000000, 0.9659258262890683122, 1.000000000000000000, 0.9659258262890683122, 1.000000000000000000, 0.9659258262890683122, 1.000000000000000000, 0.9659258262890683122, 1.000000000000000000, 0.9659258262890683122, 1.000000000000000000, 0.9659258262890683122, 1.000000000000000000, 0.9659258262890683122, 1.000000000000000000, 0.9659258262890683122, 1.000000000000000000, 0.9659258262890683122, 1.000000000000000000, 0.9659258262890683122, 1.000000000000000000, 0.9659258262890683122, 1.000000000000000000, 0.9659258262890683122, 1.000000000000000000, 0.9659258262890683122, 1.000000000000000000, 0.9659258262890683122, 1.000000000000000000, 0.9659258262890683122, 1.000000000000000000, 0.9659258262890683122, 1.000000000000000000, 0.9659258262890683122, 1.000000000000000000, 0.9659258262890683122, 1.000000000000000000, 0.9659258262890683122, 1.000000000000000000, 0.9659258262890683122, 1.000000000000000000, 0.9659258262890683122, 1.000000000000000000, 0.9659258262890683122, 1.000000000000000000, 0.9659258262890683122, 1.000000000000000000, 0.9659258262890683122, 1.000000000000000000, 0.9659258262890683122, 1.000000000000000000, 0.9659258262890683122, 1.000000000000000000, 0.9659258262890683122, 1.000000000000000000, 0.9659258262890683122, 1.000000000000000000, 0.9659258262890683122, 1.000000000000000000, 0.9659258262890683122, 1.000000000000000000, 0.9659258262890683122, 1.000000000000000000, 0.9659258262890683122, 1.000000000000000000, 0.9659258262890683122, 1.000000000000000000, 0.9659258262890683122, 1.000000000000000000, 0.9659258262890683122, 1.000000000000000000, 0.9659258262890683122, 1.000000000000000000, 0.9659258262890683122, 1.000000000000000000, 0.9659258262890683122, 1.000000000000000000, 0.9659258262890683122, 1.000000000000000000, 0.9659258262890683122, 1.000000000000000000, 0.9659258262890683122, 1.000000000000000000, 0.9659258262890683122, 1.000000000000000000, 0.9659258262890683122, 1.000000000000000000, 0.9659258262890683122, 1.000000000000000000, 0.9659258262890683122, 1.000000000000000000, 0.9659258262890683122, 1.000000000000000000, 0.9659258262890683122, 1.000000000000000000, 0.9659258262890683122, 1.000000000000000000, 0.9659258262890683122, 1.000000000000000000, 0.9659258262890683122, 1.000000000000000000, 0.9659258262890683122, 1.000000000000000000, 0.9659258262890683122, 1.000000000000000000, 0.9659258262890683122, 1.000000000000000000, 0.9659258262890683122, 1.000000000000000000, 0.9659258262890683122, 1.000000000000000000, 0.9659258262890683122, 1.000000000000000000, 0.9659258262890683122, 1.000000000000000000, 0.9659258262890683122, 1.000000000000000000, 0.9659258262890683122, 1.000000000000000000, 0.9659258262890683122, 1.000000000000000000, 0.9659258262890683122, 1.000000000000000000, 0.9659258262890683122, 1.000000000000000000, 0.9659258262890683122, 1.000000000000000000, 0.9659258262890683122, 1.000000000000000000, 0.9659258262890683122, 1.000000000000000000, 0.9659258262890683122, 1.000000000000000000, 0.9659258262890683122, 1.000000000000000000, 0.9659258262890683122, 1.000000000000000000, 0.9659258262890683122, 1.000000000000000000, 0.9659258262890683122, 1.000000000000000000, 0.9659258262890683122, 1.000000000000000000, 0.9659258262890683122, 1.000000000000000000, 0.9659258262890683122, 1.000000000000000000, 0.9659258262890683122, 1.000000000000000000, 0.9659258262890683122, 1.000000000000000000, 0.9659258262890683122, 1.000000000000000000, 0.9659258262890683122, 1.000000000000000000, 0.9659258262890683122, 1.000000000000000000, 0.9659258262890683122, 1.000000000000000000, 0.9659258262890683122, 1.000000000000000000, 0.9659258262890683122, 1.000000000000000000, 0.9659258262890683122, 1.000000000000000000, 0.9659258262890683122, 1.000000000000000000, 0.9659258262890683122, 1.000000000000000000, 0.9659258262890683122, 1.000000000000000000, 0.9659258262890683122, 1.000000000000000000, 0.9659258262890683122, 1.000000000000000000, 0.9659258262890683122, 1.000000000000000000, 0.9659258262890683122, 1.000000000000000000, 0.9659258262890683122, 1.000000000000000000, 0.9659258262890683122, 1.000000000000000000, 0.9659258262890683122, 1.000000000000000000, 0.9659258262890683122, 1.000000000000000000, 0.9659258262890683122, 1.000000000000000000, 0.9659258262890683122, 1.000000000000000000, 0.9659258262890683122, 1.000000000000000000, 0.9659258262890683122, 1.000000000000000000, 0.9659258262890683122, 1.000000000000000000, 0.9659258262890683122, 1.000000000000000000, 0.9659258262890683122, 1.000000000000000000, 0.9659258262890683122, 1.000000000000000000, 0.9659258262890683122, 1.000000000000000000, 0.9659258262890683122, 1.000000000000000000, 0.9659258262890683122, 1.000000000000000000, 0.9659258262890683122, 1.000000000000000000, 0.9659258262890683122, 1.000000000000000000, 0.9659258262890683122, 1.000000000000000000, 0.9659258262890683122, 1.000000000000000000, 0.9659258262890683122, 1.000000000000000000, 0.9659258262890683122, 1.000000000000000000, 0.9659258262890683122, 1.000000000000000000, 0.9659258262890683122, 1.000000000000000000, 0.9659258262890683122, 1.000000000000000000, 0.9659258262890683122, 1.000000000000000000, 0.9659258262890683122, 1.000000000000000000, 0.9659258262890683122, 1.000000000000000000, 0.9659258262890683122, 1.000000000000000000, 0.9659258262890683122, 1.000000000000000000, 0.9659258262890683122, 1.000000000000000000, 0.9659258262890683122, 1.000000000000000000),
 ( 0.3333333333333333703, 0.3219752754296894559, 0.3333333333333333703, 0.3219752754296894559, 0.3333333333333333703, 0.3219752754296894559, 0.3333333333333333703, 0.3219752754296894559, 0.3333333333333333703, 0.3219752754296894559, 0.3333333333333333703, 0.3219752754296894559, 0.3333333333333333703, 0.3219752754296894559, 0.3333333333333333703, 0.3219752754296894559, 0.3333333333333333703, 0.3219752754296894559, 0.3333333333333333703, 0.3219752754296894559, 0.3333333333333333703, 0.3219752754296894559, 0.3333333333333333703, 0.3219752754296894559, 0.3333333333333333703, 0.3219752754296894559, 0.3333333333333333703, 0.3219752754296894559, 0.3333333333333333703, 0.3219752754296894559, 0.3333333333333333703, 0.3219752754296894559, 0.3333333333333333703, 0.3219752754296894559, 0.3333333333333333703, 0.3219752754296894559, 0.3333333333333333703, 0.3219752754296894559, 0.3333333333333333703, 0.3219752754296894559, 0.3333333333333333703, 0.3219752754296894559, 0.3333333333333333703, 0.3219752754296894559, 0.3333333333333333703, 0.3219752754296894559, 0.3333333333333333703, 0.3219752754296894559, 0.3333333333333333703, 0.3219752754296894559, 0.3333333333333333703, 0.3219752754296894559, 0.3333333333333333703, 0.3219752754296894559, 0.3333333333333333703, 0.3219752754296894559, 0.3333333333333333703, 0.3219752754296894559, 0.3333333333333333703, 0.3219752754296894559, 0.3333333333333333703, 0.3219752754296894559, 0.3333333333333333703, 0.3219752754296894559, 0.3333333333333333703, 0.3219752754296894559, 0.3333333333333333703, 0.3219752754296894559, 0.3333333333333333703, 0.3219752754296894559, 0.3333333333333333703, 0.3219752754296894559, 0.3333333333333333703, 0.3219752754296894559, 0.3333333333333333703, 0.3219752754296894559, 0.3333333333333333703, 0.3219752754296894559, 0.3333333333333333703, 0.3219752754296894559, 0.3333333333333333703, 0.3219752754296894559, 0.3333333333333333703, 0.3219752754296894559, 0.3333333333333333703, 0.3219752754296894559, 0.3333333333333333703, 0.3219752754296894559, 0.3333333333333333703, 0.3219752754296894559, 0.3333333333333333703, 0.3219752754296894559, 0.3333333333333333703, 0.3219752754296894559, 0.3333333333333333703, 0.3219752754296894559, 0.3333333333333333703, 0.3219752754296894559, 0.3333333333333333703, 0.3219752754296894559, 0.3333333333333333703, 0.3219752754296894559, 0.3333333333333333703, 0.3219752754296894559, 0.3333333333333333703, 0.3219752754296894559, 0.3333333333333333703, 0.3219752754296894559, 0.3333333333333333703, 0.3219752754296894559, 0.3333333333333333703, 0.3219752754296894559, 0.3333333333333333703, 0.3219752754296894559, 0.3333333333333333703, 0.3219752754296894559, 0.3333333333333333703, 0.3219752754296894559, 0.3333333333333333703, 0.3219752754296894559, 0.3333333333333333703, 0.3219752754296894559, 0.3333333333333333703, 0.3219752754296894559, 0.3333333333333333703, 0.3219752754296894559, 0.3333333333333333703, 0.3219752754296894559, 0.3333333333333333703, 0.3219752754296894559, 0.3333333333333333703, 0.3219752754296894559, 0.3333333333333333703, 0.3219752754296894559, 0.3333333333333333703, 0.3219752754296894559, 0.3333333333333333703, 0.3219752754296894559, 0.3333333333333333703, 0.3219752754296894559, 0.3333333333333333703, 0.3219752754296894559, 0.3333333333333333703, 0.3219752754296894559, 0.3333333333333333703, 0.3219752754296894559, 0.3333333333333333703, 0.3219752754296894559, 0.3333333333333333703, 0.3219752754296894559, 0.3333333333333333703, 0.3219752754296894559, 0.3333333333333333703, 0.3219752754296894559, 0.3333333333333333703, 0.3219752754296894559, 0.3333333333333333703, 0.3219752754296894559, 0.3333333333333333703, 0.3219752754296894559, 0.3333333333333333703, 0.3219752754296894559, 0.3333333333333333703, 0.3219752754296894559, 0.3333333333333333703, 0.3219752754296894559, 0.3333333333333333703, 0.3219752754296894559, 0.3333333333333333703, 0.3219752754296894559, 0.3333333333333333703, 0.3219752754296894559, 0.3333333333333333703, 0.3219752754296894559, 0.3333333333333333703, 0.3219752754296894559, 0.3333333333333333703, 0.3219752754296894559, 0.3333333333333333703, 0.3219752754296894559, 0.3333333333333333703, 0.3219752754296894559, 0.3333333333333333703, 0.3219752754296894559, 0.3333333333333333703, 0.3219752754296894559, 0.3333333333333333703, 0.3219752754296894559, 0.3333333333333333703, 0.3219752754296894559, 0.3333333333333333703, 0.3219752754296894559, 0.3333333333333333703, 0.3219752754296894559, 0.3333333333333333703, 0.3219752754296894559, 0.3333333333333333703, 0.3219752754296894559, 0.3333333333333333703, 0.3219752754296894559, 0.3333333333333333703, 0.3219752754296894559, 0.3333333333333333703, 0.3219752754296894559, 0.3333333333333333703, 0.3219752754296894559, 0.3333333333333333703, 0.3219752754296894559, 0.3333333333333333703, 0.3219752754296894559, 0.3333333333333333703, 0.3219752754296894559, 0.3333333333333333703, 0.3219752754296894559, 0.3333333333333333703, 0.3219752754296894559, 0.3333333333333333703, 0.3219752754296894559, 0.3333333333333333703, 0.3219752754296894559, 0.3333333333333333703, 0.3219752754296894559, 0.3333333333333333703, 0.3219752754296894559, 0.3333333333333333703, 0.3219752754296894559, 0.3333333333333333703, 0.3219752754296894559, 0.3333333333333333703, 0.3219752754296894559, 0.3333333333333333703, 0.3219752754296894559, 0.3333333333333333703, 0.3219752754296894559, 0.3333333333333333703, 0.3219752754296894559, 0.3333333333333333703, 0.3219752754296894559, 0.3333333333333333703, 0.3219752754296894559, 0.3333333333333333703, 0.3219752754296894559, 0.3333333333333333703, 0.3219752754296894559, 0.3333333333333333703, 0.3219752754296894559, 0.3333333333333333703, 0.3219752754296894559, 0.3333333333333333703, 0.3219752754296894559, 0.3333333333333333703, 0.3219752754296894559, 0.3333333333333333703, 0.3219752754296894559, 0.3333333333333333703, 0.3219752754296894559, 0.3333333333333333703, 0.3219752754296894559, 0.3333333333333333703, 0.3219752754296894559, 0.3333333333333333703, 0.3219752754296894559, 0.3333333333333333703, 0.3219752754296894559, 0.3333333333333333703, 0.3219752754296894559, 0.3333333333333333703, 0.3219752754296894559, 0.3333333333333333703, 0.3219752754296894559, 0.3333333333333333703, 0.3219752754296894559, 0.3333333333333333703, 0.3219752754296894559, 0.3333333333333333703, 0.3219752754296894559, 0.3333333333333333703, 0.3219752754296894559, 0.3333333333333333703, 0.3219752754296894559, 0.3333333333333333703, 0.3219752754296894559, 0.3333333333333333703, 0.3219752754296894559, 0.3333333333333333703, 0.3219752754296894559, 0.3333333333333333703, 0.3219752754296894559, 0.3333333333333333703, 0.3219752754296894559, 0.3333333333333333703, 0.3219752754296894559, 0.3333333333333333703, 0.3219752754296894559, 0.3333333333333333703, 0.3219752754296894559, 0.3333333333333333703, 0.3219752754296894559, 0.3333333333333333703, 0.3219752754296894559, 0.3333333333333333703, 0.3219752754296894559, 0.3333333333333333703, 0.3219752754296894559, 0.3333333333333333703, 0.3219752754296894559, 0.3333333333333333703, 0.3219752754296894559, 0.3333333333333333703, 0.3219752754296894559, 0.3333333333333333703, 0.3219752754296894559, 0.3333333333333333703, 0.3219752754296894559, 0.3333333333333333703, 0.3219752754296894559, 0.3333333333333333703, 0.3219752754296894559, 0.3333333333333333703, 0.3219752754296894559, 0.3333333333333333703, 0.3219752754296894559, 0.3333333333333333703, 0.3219752754296894559, 0.3333333333333333703, 0.3219752754296894559, 0.3333333333333333703, 0.3219752754296894559, 0.3333333333333333703, 0.3219752754296894559, 0.3333333333333333703, 0.3219752754296894559, 0.3333333333333333703, 0.3219752754296894559, 0.3333333333333333703, 0.3219752754296894559, 0.3333333333333333703, 0.3219752754296894559, 0.3333333333333333703, 0.3219752754296894559, 0.3333333333333333703, 0.3219752754296894559, 0.3333333333333333703, 0.3219752754296894559, 0.3333333333333333703, 0.3219752754296894559, 0.3333333333333333703, 0.3219752754296894559, 0.3333333333333333703, 0.3219752754296894559, 0.3333333333333333703, 0.3219752754296894559, 0.3333333333333333703, 0.3219752754296894559, 0.3333333333333333703, 0.3219752754296894559, 0.3333333333333333703, 0.3219752754296894559, 0.3333333333333333703, 0.3219752754296894559, 0.3333333333333333703, 0.3219752754296894559, 0.3333333333333333703, 0.3219752754296894559, 0.3333333333333333703, 0.3219752754296894559, 0.3333333333333333703, 0.3219752754296894559, 0.3333333333333333703, 0.3219752754296894559, 0.3333333333333333703, 0.3219752754296894559, 0.3333333333333333703, 0.3219752754296894559, 0.3333333333333333703, 0.3219752754296894559, 0.3333333333333333703, 0.3219752754296894559, 0.3333333333333333703, 0.3219752754296894559, 0.3333333333333333703, 0.3219752754296894559, 0.3333333333333333703, 0.3219752754296894559, 0.3333333333333333703, 0.3219752754296894559, 0.3333333333333333703, 0.3219752754296894559, 0.3333333333333333703, 0.3219752754296894559, 0.3333333333333333703, 0.3219752754296894559, 0.3333333333333333703, 0.3219752754296894559, 0.3333333333333333703, 0.3219752754296894559, 0.3333333333333333703, 0.3219752754296894559, 0.3333333333333333703, 0.3219752754296894559, 0.3333333333333333703, 0.3219752754296894559, 0.3333333333333333703, 0.3219752754296894559, 0.3333333333333333703, 0.3219752754296894559, 0.3333333333333333703, 0.3219752754296894559, 0.3333333333333333703, 0.3219752754296894559, 0.3333333333333333703, 0.3219752754296894559, 0.3333333333333333703, 0.3219752754296894559, 0.3333333333333333703, 0.3219752754296894559, 0.3333333333333333703, 0.3219752754296894559, 0.3333333333333333703, 0.3219752754296894559, 0.3333333333333333703, 0.3219752754296894559, 0.3333333333333333703, 0.3219752754296894559, 0.3333333333333333703, 0.3219752754296894559, 0.3333333333333333703, 0.3219752754296894559, 0.3333333333333333703, 0.3219752754296894559, 0.3333333333333333703, 0.3219752754296894559, 0.3333333333333333703, 0.3219752754296894559, 0.3333333333333333703, 0.3219752754296894559, 0.3333333333333333703, 0.3219752754296894559, 0.3333333333333333703, 0.3219752754296894559, 0.3333333333333333703, 0.3219752754296894559, 0.3333333333333333703, 0.3219752754296894559, 0.3333333333333333703, 0.3219752754296894559, 0.3333333333333333703, 0.3219752754296894559, 0.3333333333333333703, 0.3219752754296894559, 0.3333333333333333703, 0.3219752754296894559, 0.3333333333333333703, 0.3219752754296894559, 0.3333333333333333703, 0.3219752754296894559, 0.3333333333333333703),
 ( 0.3333333333333333703, 0.3219752754296894559, 0.3333333333333333703, 0.3219752754296894559, 0.3333333333333333703, 0.3219752754296894559, 0.3333333333333333703, 0.3219752754296894559, 0.3333333333333333703, 0.3219752754296894559, 0.3333333333333333703, 0.3219752754296894559, 0.3333333333333333703, 0.3219752754296894559, 0.3333333333333333703, 0.3219752754296894559, 0.3333333333333333703, 0.3219752754296894559, 0.3333333333333333703, 0.3219752754296894559, 0.3333333333333333703, 0.3219752754296894559, 0.3333333333333333703, 0.3219752754296894559, 0.3333333333333333703, 0.3219752754296894559, 0.3333333333333333703, 0.3219752754296894559, 0.3333333333333333703, 0.3219752754296894559, 0.3333333333333333703, 0.3219752754296894559, 0.3333333333333333703, 0.3219752754296894559, 0.3333333333333333703, 0.3219752754296894559, 0.3333333333333333703, 0.3219752754296894559, 0.3333333333333333703, 0.3219752754296894559, 0.3333333333333333703, 0.3219752754296894559, 0.3333333333333333703, 0.3219752754296894559, 0.3333333333333333703, 0.3219752754296894559, 0.3333333333333333703, 0.3219752754296894559, 0.3333333333333333703, 0.3219752754296894559, 0.3333333333333333703, 0.3219752754296894559, 0.3333333333333333703, 0.3219752754296894559, 0.3333333333333333703, 0.3219752754296894559, 0.3333333333333333703, 0.3219752754296894559, 0.3333333333333333703, 0.3219752754296894559, 0.3333333333333333703, 0.3219752754296894559, 0.3333333333333333703, 0.3219752754296894559, 0.3333333333333333703, 0.3219752754296894559, 0.3333333333333333703, 0.3219752754296894559, 0.3333333333333333703, 0.3219752754296894559, 0.3333333333333333703, 0.3219752754296894559, 0.3333333333333333703, 0.3219752754296894559, 0.3333333333333333703, 0.3219752754296894559, 0.3333333333333333703, 0.3219752754296894559, 0.3333333333333333703, 0.3219752754296894559, 0.3333333333333333703, 0.3219752754296894559, 0.3333333333333333703, 0.3219752754296894559, 0.3333333333333333703, 0.3219752754296894559, 0.3333333333333333703, 0.3219752754296894559, 0.3333333333333333703, 0.3219752754296894559, 0.3333333333333333703, 0.3219752754296894559, 0.3333333333333333703, 0.3219752754296894559, 0.3333333333333333703, 0.3219752754296894559, 0.3333333333333333703, 0.3219752754296894559, 0.3333333333333333703, 0.3219752754296894559, 0.3333333333333333703, 0.3219752754296894559, 0.3333333333333333703, 0.3219752754296894559, 0.3333333333333333703, 0.3219752754296894559, 0.3333333333333333703, 0.3219752754296894559, 0.3333333333333333703, 0.3219752754296894559, 0.3333333333333333703, 0.3219752754296894559, 0.3333333333333333703, 0.3219752754296894559, 0.3333333333333333703, 0.3219752754296894559, 0.3333333333333333703, 0.3219752754296894559, 0.3333333333333333703, 0.3219752754296894559, 0.3333333333333333703, 0.3219752754296894559, 0.3333333333333333703, 0.3219752754296894559, 0.3333333333333333703, 0.3219752754296894559, 0.3333333333333333703, 0.3219752754296894559, 0.3333333333333333703, 0.3219752754296894559, 0.3333333333333333703, 0.3219752754296894559, 0.3333333333333333703, 0.3219752754296894559, 0.3333333333333333703, 0.3219752754296894559, 0.3333333333333333703, 0.3219752754296894559, 0.3333333333333333703, 0.3219752754296894559, 0.3333333333333333703, 0.3219752754296894559, 0.3333333333333333703, 0.3219752754296894559, 0.3333333333333333703, 0.3219752754296894559, 0.3333333333333333703, 0.3219752754296894559, 0.3333333333333333703, 0.3219752754296894559, 0.3333333333333333703, 0.3219752754296894559, 0.3333333333333333703, 0.3219752754296894559, 0.3333333333333333703, 0.3219752754296894559, 0.3333333333333333703, 0.3219752754296894559, 0.3333333333333333703, 0.3219752754296894559, 0.3333333333333333703, 0.3219752754296894559, 0.3333333333333333703, 0.3219752754296894559, 0.3333333333333333703, 0.3219752754296894559, 0.3333333333333333703, 0.3219752754296894559, 0.3333333333333333703, 0.3219752754296894559, 0.3333333333333333703, 0.3219752754296894559, 0.3333333333333333703, 0.3219752754296894559, 0.3333333333333333703, 0.3219752754296894559, 0.3333333333333333703, 0.3219752754296894559, 0.3333333333333333703, 0.3219752754296894559, 0.3333333333333333703, 0.3219752754296894559, 0.3333333333333333703, 0.3219752754296894559, 0.3333333333333333703, 0.3219752754296894559, 0.3333333333333333703, 0.3219752754296894559, 0.3333333333333333703, 0.3219752754296894559, 0.3333333333333333703, 0.3219752754296894559, 0.3333333333333333703, 0.3219752754296894559, 0.3333333333333333703, 0.3219752754296894559, 0.3333333333333333703, 0.3219752754296894559, 0.3333333333333333703, 0.3219752754296894559, 0.3333333333333333703, 0.3219752754296894559, 0.3333333333333333703, 0.3219752754296894559, 0.3333333333333333703, 0.3219752754296894559, 0.3333333333333333703, 0.3219752754296894559, 0.3333333333333333703, 0.3219752754296894559, 0.3333333333333333703, 0.3219752754296894559, 0.3333333333333333703, 0.3219752754296894559, 0.3333333333333333703, 0.3219752754296894559, 0.3333333333333333703, 0.3219752754296894559, 0.3333333333333333703, 0.3219752754296894559, 0.3333333333333333703, 0.3219752754296894559, 0.3333333333333333703, 0.3219752754296894559, 0.3333333333333333703, 0.3219752754296894559, 0.3333333333333333703, 0.3219752754296894559, 0.3333333333333333703, 0.3219752754296894559, 0.3333333333333333703, 0.3219752754296894559, 0.3333333333333333703, 0.3219752754296894559, 0.3333333333333333703, 0.3219752754296894559, 0.3333333333333333703, 0.3219752754296894559, 0.3333333333333333703, 0.3219752754296894559, 0.3333333333333333703, 0.3219752754296894559, 0.3333333333333333703, 0.3219752754296894559, 0.3333333333333333703, 0.3219752754296894559, 0.3333333333333333703, 0.3219752754296894559, 0.3333333333333333703, 0.3219752754296894559, 0.3333333333333333703, 0.3219752754296894559, 0.3333333333333333703, 0.3219752754296894559, 0.3333333333333333703, 0.3219752754296894559, 0.3333333333333333703, 0.3219752754296894559, 0.3333333333333333703, 0.3219752754296894559, 0.3333333333333333703, 0.3219752754296894559, 0.3333333333333333703, 0.3219752754296894559, 0.3333333333333333703, 0.3219752754296894559, 0.3333333333333333703, 0.3219752754296894559, 0.3333333333333333703, 0.3219752754296894559, 0.3333333333333333703, 0.3219752754296894559, 0.3333333333333333703, 0.3219752754296894559, 0.3333333333333333703, 0.3219752754296894559, 0.3333333333333333703, 0.3219752754296894559, 0.3333333333333333703, 0.3219752754296894559, 0.3333333333333333703, 0.3219752754296894559, 0.3333333333333333703, 0.3219752754296894559, 0.3333333333333333703, 0.3219752754296894559, 0.3333333333333333703, 0.3219752754296894559, 0.3333333333333333703, 0.3219752754296894559, 0.3333333333333333703, 0.3219752754296894559, 0.3333333333333333703, 0.3219752754296894559, 0.3333333333333333703, 0.3219752754296894559, 0.3333333333333333703, 0.3219752754296894559, 0.3333333333333333703, 0.3219752754296894559, 0.3333333333333333703, 0.3219752754296894559, 0.3333333333333333703, 0.3219752754296894559, 0.3333333333333333703, 0.3219752754296894559, 0.3333333333333333703, 0.3219752754296894559, 0.3333333333333333703, 0.3219752754296894559, 0.3333333333333333703, 0.3219752754296894559, 0.3333333333333333703, 0.3219752754296894559, 0.3333333333333333703, 0.3219752754296894559, 0.3333333333333333703, 0.3219752754296894559, 0.3333333333333333703, 0.3219752754296894559, 0.3333333333333333703, 0.3219752754296894559, 0.3333333333333333703, 0.3219752754296894559, 0.3333333333333333703, 0.3219752754296894559, 0.3333333333333333703, 0.3219752754296894559, 0.3333333333333333703, 0.3219752754296894559, 0.3333333333333333703, 0.3219752754296894559, 0.3333333333333333703, 0.3219752754296894559, 0.3333333333333333703, 0.3219752754296894559, 0.3333333333333333703, 0.3219752754296894559, 0.3333333333333333703, 0.3219752754296894559, 0.3333333333333333703, 0.3219752754296894559, 0.3333333333333333703, 0.3219752754296894559, 0.3333333333333333703, 0.3219752754296894559, 0.3333333333333333703, 0.3219752754296894559, 0.3333333333333333703, 0.3219752754296894559, 0.3333333333333333703, 0.3219752754296894559, 0.3333333333333333703, 0.3219752754296894559, 0.3333333333333333703, 0.3219752754296894559, 0.3333333333333333703, 0.3219752754296894559, 0.3333333333333333703, 0.3219752754296894559, 0.3333333333333333703, 0.3219752754296894559, 0.3333333333333333703, 0.3219752754296894559, 0.3333333333333333703, 0.3219752754296894559, 0.3333333333333333703, 0.3219752754296894559, 0.3333333333333333703, 0.3219752754296894559, 0.3333333333333333703, 0.3219752754296894559, 0.3333333333333333703, 0.3219752754296894559, 0.3333333333333333703, 0.3219752754296894559, 0.3333333333333333703, 0.3219752754296894559, 0.3333333333333333703, 0.3219752754296894559, 0.3333333333333333703, 0.3219752754296894559, 0.3333333333333333703, 0.3219752754296894559, 0.3333333333333333703, 0.3219752754296894559, 0.3333333333333333703, 0.3219752754296894559, 0.3333333333333333703, 0.3219752754296894559, 0.3333333333333333703, 0.3219752754296894559, 0.3333333333333333703, 0.3219752754296894559, 0.3333333333333333703, 0.3219752754296894559, 0.3333333333333333703, 0.3219752754296894559, 0.3333333333333333703, 0.3219752754296894559, 0.3333333333333333703, 0.3219752754296894559, 0.3333333333333333703, 0.3219752754296894559, 0.3333333333333333703, 0.3219752754296894559, 0.3333333333333333703, 0.3219752754296894559, 0.3333333333333333703, 0.3219752754296894559, 0.3333333333333333703, 0.3219752754296894559, 0.3333333333333333703, 0.3219752754296894559, 0.3333333333333333703, 0.3219752754296894559, 0.3333333333333333703, 0.3219752754296894559, 0.3333333333333333703, 0.3219752754296894559, 0.3333333333333333703, 0.3219752754296894559, 0.3333333333333333703, 0.3219752754296894559, 0.3333333333333333703, 0.3219752754296894559, 0.3333333333333333703, 0.3219752754296894559, 0.3333333333333333703, 0.3219752754296894559, 0.3333333333333333703, 0.3219752754296894559, 0.3333333333333333703, 0.3219752754296894559, 0.3333333333333333703, 0.3219752754296894559, 0.3333333333333333703, 0.3219752754296894559, 0.3333333333333333703, 0.3219752754296894559, 0.3333333333333333703, 0.3219752754296894559, 0.3333333333333333703, 0.3219752754296894559, 0.3333333333333333703, 0.3219752754296894559, 0.3333333333333333703, 0.3219752754296894559, 0.3333333333333333703, 0.3219752754296894559, 0.3333333333333333703, 0.3219752754296894559, 0.3333333333333333703, 0.3219752754296894559, 0.3333333333333333703, 0.3219752754296894559, 0.3333333333333333703),
 ( 1.000000000000000000, 0.9659258262890683122, 1.000000000000000000, 0.9659258262890683122, 1.000000000000000000, 0.9659258262890683122, 1.000000000000000000, 0.9659258262890683122, 1.000000000000000000, 0.9659258262890683122, 1.000000000000000000, 0.9659258262890683122, 1.000000000000000000, 0.9659258262890683122, 1.000000000000000000, 0.9659258262890683122, 1.000000000000000000, 0.9659258262890683122, 1.000000000000000000, 0.9659258262890683122, 1.000000000000000000, 0.9659258262890683122, 1.000000000000000000, 0.9659258262890683122, 1.000000000000000000, 0.9659258262890683122, 1.000000000000000000, 0.9659258262890683122, 1.000000000000000000, 0.9659258262890683122, 1.000000000000000000, 0.9659258262890683122, 1.000000000000000000, 0.9659258262890683122, 1.000000000000000000, 0.9659258262890683122, 1.000000000000000000, 0.9659258262890683122, 1.000000000000000000, 0.9659258262890683122, 1.000000000000000000, 0.9659258262890683122, 1.000000000000000000, 0.9659258262890683122, 1.000000000000000000, 0.9659258262890683122, 1.000000000000000000, 0.9659258262890683122, 1.000000000000000000, 0.9659258262890683122, 1.000000000000000000, 0.9659258262890683122, 1.000000000000000000, 0.9659258262890683122, 1.000000000000000000, 0.9659258262890683122, 1.000000000000000000, 0.9659258262890683122, 1.000000000000000000, 0.9659258262890683122, 1.000000000000000000, 0.9659258262890683122, 1.000000000000000000, 0.9659258262890683122, 1.000000000000000000, 0.9659258262890683122, 1.000000000000000000, 0.9659258262890683122, 1.000000000000000000, 0.9659258262890683122, 1.000000000000000000, 0.9659258262890683122, 1.000000000000000000, 0.9659258262890683122, 1.000000000000000000, 0.9659258262890683122, 1.000000000000000000, 0.9659258262890683122, 1.000000000000000000, 0.9659258262890683122, 1.000000000000000000, 0.9659258262890683122, 1.000000000000000000, 0.9659258262890683122, 1.000000000000000000, 0.9659258262890683122, 1.000000000000000000, 0.9659258262890683122, 1.000000000000000000, 0.9659258262890683122, 1.000000000000000000, 0.9659258262890683122, 1.000000000000000000, 0.9659258262890683122, 1.000000000000000000, 0.9659258262890683122, 1.000000000000000000, 0.9659258262890683122, 1.000000000000000000, 0.9659258262890683122, 1.000000000000000000, 0.9659258262890683122, 1.000000000000000000, 0.9659258262890683122, 1.000000000000000000, 0.9659258262890683122, 1.000000000000000000, 0.9659258262890683122, 1.000000000000000000, 0.9659258262890683122, 1.000000000000000000, 0.9659258262890683122, 1.000000000000000000, 0.9659258262890683122, 1.000000000000000000, 0.9659258262890683122, 1.000000000000000000, 0.9659258262890683122, 1.000000000000000000, 0.9659258262890683122, 1.000000000000000000, 0.9659258262890683122, 1.000000000000000000, 0.9659258262890683122, 1.000000000000000000, 0.9659258262890683122, 1.000000000000000000, 0.9659258262890683122, 1.000000000000000000, 0.9659258262890683122, 1.000000000000000000, 0.9659258262890683122, 1.000000000000000000, 0.9659258262890683122, 1.000000000000000000, 0.9659258262890683122, 1.000000000000000000, 0.9659258262890683122, 1.000000000000000000, 0.9659258262890683122, 1.000000000000000000, 0.9659258262890683122, 1.000000000000000000, 0.9659258262890683122, 1.000000000000000000, 0.9659258262890683122, 1.000000000000000000, 0.9659258262890683122, 1.000000000000000000, 0.9659258262890683122, 1.000000000000000000, 0.9659258262890683122, 1.000000000000000000, 0.9659258262890683122, 1.000000000000000000, 0.9659258262890683122, 1.000000000000000000, 0.9659258262890683122, 1.000000000000000000, 0.9659258262890683122, 1.000000000000000000, 0.9659258262890683122, 1.000000000000000000, 0.9659258262890683122, 1.000000000000000000, 0.9659258262890683122, 1.000000000000000000, 0.9659258262890683122, 1.000000000000000000, 0.9659258262890683122, 1.000000000000000000, 0.9659258262890683122, 1.000000000000000000, 0.9659258262890683122, 1.000000000000000000, 0.9659258262890683122, 1.000000000000000000, 0.9659258262890683122, 1.000000000000000000, 0.9659258262890683122, 1.000000000000000000, 0.9659258262890683122, 1.000000000000000000, 0.9659258262890683122, 1.000000000000000000, 0.9659258262890683122, 1.000000000000000000, 0.9659258262890683122, 1.000000000000000000, 0.9659258262890683122, 1.000000000000000000, 0.9659258262890683122, 1.000000000000000000, 0.9659258262890683122, 1.000000000000000000, 0.9659258262890683122, 1.000000000000000000, 0.9659258262890683122, 1.000000000000000000, 0.9659258262890683122, 1.000000000000000000, 0.9659258262890683122, 1.000000000000000000, 0.9659258262890683122, 1.000000000000000000, 0.9659258262890683122, 1.000000000000000000, 0.9659258262890683122, 1.000000000000000000, 0.9659258262890683122, 1.000000000000000000, 0.9659258262890683122, 1.000000000000000000, 0.9659258262890683122, 1.000000000000000000, 0.9659258262890683122, 1.000000000000000000, 0.9659258262890683122, 1.000000000000000000, 0.9659258262890683122, 1.000000000000000000, 0.9659258262890683122, 1.000000000000000000, 0.9659258262890683122, 1.000000000000000000, 0.9659258262890683122, 1.000000000000000000, 0.9659258262890683122, 1.000000000000000000, 0.9659258262890683122, 1.000000000000000000, 0.9659258262890683122, 1.000000000000000000, 0.9659258262890683122, 1.000000000000000000, 0.9659258262890683122, 1.000000000000000000, 0.9659258262890683122, 1.000000000000000000, 0.9659258262890683122, 1.000000000000000000, 0.9659258262890683122, 1.000000000000000000, 0.9659258262890683122, 1.000000000000000000, 0.9659258262890683122, 1.000000000000000000, 0.9659258262890683122, 1.000000000000000000, 0.9659258262890683122, 1.000000000000000000, 0.9659258262890683122, 1.000000000000000000, 0.9659258262890683122, 1.000000000000000000, 0.9659258262890683122, 1.000000000000000000, 0.9659258262890683122, 1.000000000000000000, 0.9659258262890683122, 1.000000000000000000, 0.9659258262890683122, 1.000000000000000000, 0.9659258262890683122, 1.000000000000000000, 0.9659258262890683122, 1.000000000000000000, 0.9659258262890683122, 1.000000000000000000, 0.9659258262890683122, 1.000000000000000000, 0.9659258262890683122, 1.000000000000000000, 0.9659258262890683122, 1.000000000000000000, 0.9659258262890683122, 1.000000000000000000, 0.9659258262890683122, 1.000000000000000000, 0.9659258262890683122, 1.000000000000000000, 0.9659258262890683122, 1.000000000000000000, 0.9659258262890683122, 1.000000000000000000, 0.9659258262890683122, 1.000000000000000000, 0.9659258262890683122, 1.000000000000000000, 0.9659258262890683122, 1.000000000000000000, 0.9659258262890683122, 1.000000000000000000, 0.9659258262890683122, 1.000000000000000000, 0.9659258262890683122, 1.000000000000000000, 0.9659258262890683122, 1.000000000000000000, 0.9659258262890683122, 1.000000000000000000, 0.9659258262890683122, 1.000000000000000000, 0.9659258262890683122, 1.000000000000000000, 0.9659258262890683122, 1.000000000000000000, 0.9659258262890683122, 1.000000000000000000, 0.9659258262890683122, 1.000000000000000000, 0.9659258262890683122, 1.000000000000000000, 0.9659258262890683122, 1.000000000000000000, 0.9659258262890683122, 1.000000000000000000, 0.9659258262890683122, 1.000000000000000000, 0.9659258262890683122, 1.000000000000000000, 0.9659258262890683122, 1.000000000000000000, 0.9659258262890683122, 1.000000000000000000, 0.9659258262890683122, 1.000000000000000000, 0.9659258262890683122, 1.000000000000000000, 0.9659258262890683122, 1.000000000000000000, 0.9659258262890683122, 1.000000000000000000, 0.9659258262890683122, 1.000000000000000000, 0.9659258262890683122, 1.000000000000000000, 0.9659258262890683122, 1.000000000000000000, 0.9659258262890683122, 1.000000000000000000, 0.9659258262890683122, 1.000000000000000000, 0.9659258262890683122, 1.000000000000000000, 0.9659258262890683122, 1.000000000000000000, 0.9659258262890683122, 1.000000000000000000, 0.9659258262890683122, 1.000000000000000000, 0.9659258262890683122, 1.000000000000000000, 0.9659258262890683122, 1.000000000000000000, 0.9659258262890683122, 1.000000000000000000, 0.9659258262890683122, 1.000000000000000000, 0.9659258262890683122, 1.000000000000000000, 0.9659258262890683122, 1.000000000000000000, 0.9659258262890683122, 1.000000000000000000, 0.9659258262890683122, 1.000000000000000000, 0.9659258262890683122, 1.000000000000000000, 0.9659258262890683122, 1.000000000000000000, 0.9659258262890683122, 1.000000000000000000, 0.9659258262890683122, 1.000000000000000000, 0.9659258262890683122, 1.000000000000000000, 0.9659258262890683122, 1.000000000000000000, 0.9659258262890683122, 1.000000000000000000, 0.9659258262890683122, 1.000000000000000000, 0.9659258262890683122, 1.000000000000000000, 0.9659258262890683122, 1.000000000000000000, 0.9659258262890683122, 1.000000000000000000, 0.9659258262890683122, 1.000000000000000000, 0.9659258262890683122, 1.000000000000000000, 0.9659258262890683122, 1.000000000000000000, 0.9659258262890683122, 1.000000000000000000, 0.9659258262890683122, 1.000000000000000000, 0.9659258262890683122, 1.000000000000000000, 0.9659258262890683122, 1.000000000000000000, 0.9659258262890683122, 1.000000000000000000, 0.9659258262890683122, 1.000000000000000000, 0.9659258262890683122, 1.000000000000000000, 0.9659258262890683122, 1.000000000000000000, 0.9659258262890683122, 1.000000000000000000, 0.9659258262890683122, 1.000000000000000000, 0.9659258262890683122, 1.000000000000000000, 0.9659258262890683122, 1.000000000000000000, 0.9659258262890683122, 1.000000000000000000, 0.9659258262890683122, 1.000000000000000000, 0.9659258262890683122, 1.000000000000000000, 0.9659258262890683122, 1.000000000000000000, 0.9659258262890683122, 1.000000000000000000, 0.9659258262890683122, 1.000000000000000000, 0.9659258262890683122, 1.000000000000000000, 0.9659258262890683122, 1.000000000000000000, 0.9659258262890683122, 1.000000000000000000, 0.9659258262890683122, 1.000000000000000000, 0.9659258262890683122, 1.000000000000000000, 0.9659258262890683122, 1.000000000000000000, 0.9659258262890683122, 1.000000000000000000, 0.9659258262890683122, 1.000000000000000000, 0.9659258262890683122, 1.000000000000000000, 0.9659258262890683122, 1.000000000000000000, 0.9659258262890683122, 1.000000000000000000, 0.9659258262890683122, 1.000000000000000000, 0.9659258262890683122, 1.000000000000000000) ) ) 
 REPRESENTATION_ITEM ( '' )  SURFACE ( )  );
#61713 = ORIENTED_EDGE ( 'NONE', *, *, #162564, .T. ) ;
#61714 = CARTESIAN_POINT ( 'NONE',  ( -10.72451020669870658, -18.67979575497194134, 54.58442372801901143 ) ) ;
#61715 = CARTESIAN_POINT ( 'NONE',  ( 19.05341960407611168, 5.049401038298154454, 48.95724293864768129 ) ) ;
#61716 = CARTESIAN_POINT ( 'NONE',  ( 13.97604488694527802, 13.89961937509977652, 84.37390960531433848 ) ) ;
#61717 = CARTESIAN_POINT ( 'NONE',  ( -16.51473224551082808, 9.474510206698731452, 63.33442372801900433 ) ) ;
#61718 = CARTESIAN_POINT ( 'NONE',  ( 18.67979575497194134, -10.72451020669871369, 35.83442372801901143 ) ) ;
#61719 = CARTESIAN_POINT ( 'NONE',  ( 19.02544592524334988, 5.153800228976608722, 101.4594237280189759 ) ) ;
#61720 = CARTESIAN_POINT ( 'NONE',  ( -5.049401038297874678, -19.05341960407617918, 74.79275706135231871 ) ) ;
#61721 = CARTESIAN_POINT ( 'NONE',  ( -19.05341960407611168, -5.049401038298163336, 41.45724293864769550 ) ) ;
#61722 = CARTESIAN_POINT ( 'NONE',  ( -0.05219959533936034679, 19.03943276465977164, 87.50109039468567573 ) ) ;
#61723 = CARTESIAN_POINT ( 'NONE',  ( 16.53943276465976808, 0.05219959533934440121, 111.2510903946856899 ) ) ;
#61724 = CARTESIAN_POINT ( 'NONE',  ( 5.153800228976615827, -19.02544592524334988, 80.20942372801901854 ) ) ;
#61725 = CARTESIAN_POINT ( 'NONE',  ( 8.314922557960818139, 14.29746914071049879, 29.58224293864769905 ) ) ;
#61726 = CARTESIAN_POINT ( 'NONE',  ( -9.474510206698720793, -16.51473224551083518, 54.58442372801899722 ) ) ;
#61727 = CARTESIAN_POINT ( 'NONE',  ( 10.81492255796106328, -18.62759615963255655, 100.4177570613523471 ) ) ;
#61728 = CARTESIAN_POINT ( 'NONE',  ( 0.05219959533936267826, -19.03943276465977164, 30.00109039468566863 ) ) ;
#61729 = CARTESIAN_POINT ( 'NONE',  ( 16.51473224551069308, 9.474510206698969483, 24.16557627198102765 ) ) ;
#61730 = CARTESIAN_POINT ( 'NONE',  ( -15.80617190586768217, 15.72974639402176855, 83.12609039468568994 ) ) ;
#61731 = CARTESIAN_POINT ( 'NONE',  ( 4.379528057220092307, 16.55341960407617563, 32.29275706135235424 ) ) ;
#61732 = CARTESIAN_POINT ( 'NONE',  ( 5.153800228976335163, 19.02544592524342804, 89.79057627198102409 ) ) ;
#61733 = CARTESIAN_POINT ( 'NONE',  ( -5.359611314223446995E-15, 29.16686587814335496, 144.3750000027311842 ) ) ;
#61734 = CARTESIAN_POINT ( 'NONE',  ( -19.05341960407611168, -5.049401038298163336, 76.45724293864769550 ) ) ;
#61735 = CARTESIAN_POINT ( 'NONE',  ( -17.81289503416611808, 24.51734667627700404, 141.6999999999999602 ) ) ;
#61736 = CARTESIAN_POINT ( 'NONE',  ( 9.474510206698729675, 16.51473224551082808, 82.08442372801899012 ) ) ;
#61737 = CARTESIAN_POINT ( 'NONE',  ( 5.153800228976335163, 19.02544592524342804, 114.7905762719810241 ) ) ;
#61739 = CARTESIAN_POINT ( 'NONE',  ( 13.89961937509957401, 13.97604488694547697, 101.8760903946856331 ) ) ;
#61738 = CARTESIAN_POINT ( 'NONE',  ( -15.72974639402176322, -15.80617190586768395, 109.3760903946857042 ) ) ;
#61740 = CARTESIAN_POINT ( 'NONE',  ( -16.52544592524342804, 4.483927247898546575, 96.04057627198102409 ) ) ;
#61741 = CARTESIAN_POINT ( 'NONE',  ( -16.51473224551069308, -9.474510206698971260, 21.66557627198102765 ) ) ;
#61742 = CARTESIAN_POINT ( 'NONE',  ( 0.05219959533907565091, 21.53943276465977519, 54.99890960531435269 ) ) ;
#61743 = CARTESIAN_POINT ( 'NONE',  ( -5.823673210054116645, -21.52544592524344225, 47.29057627198103120 ) ) ;
#61744 = CARTESIAN_POINT ( 'NONE',  ( 4.483927247898545687, 16.52544592524342804, 114.7905762719810383 ) ) ;
#61745 = CARTESIAN_POINT ( 'NONE',  ( 28.82186960331486958, -9.364793116373689941, 143.1500000054623740 ) ) ;
#61746 = CARTESIAN_POINT ( 'NONE',  ( 13.89961937509957401, 13.97604488694547697, 56.87609039468564731 ) ) ;
#61747 = CARTESIAN_POINT ( 'NONE',  ( 8.314922557960818139, 14.29746914071049879, 34.58224293864770260 ) ) ;
#61748 = CARTESIAN_POINT ( 'NONE',  ( 5.049401038298161559, -19.05341960407611168, 112.7072429386476813 ) ) ;
#61749 = CARTESIAN_POINT ( 'NONE',  ( 15.80617190586769283, -15.72974639402175789, 75.62609039468567573 ) ) ;
#61750 = CARTESIAN_POINT ( 'NONE',  ( -5.719274019375978568, 21.55341960407610458, 65.20724293864768129 ) ) ;
#61751 = CARTESIAN_POINT ( 'NONE',  ( 15.72974639402176855, 15.80617190586768217, 61.87609039468568284 ) ) ;
#61752 = CARTESIAN_POINT ( 'NONE',  ( 10.81492255796106328, -18.62759615963255655, 45.41775706135234003 ) ) ;
#61753 = CARTESIAN_POINT ( 'NONE',  ( 5.049401038298161559, -19.05341960407611168, 77.70724293864765286 ) ) ;
#61754 = CARTESIAN_POINT ( 'NONE',  ( -4.379528057220086978, -16.55341960407618274, 89.79275706135236135 ) ) ;
#61755 = CARTESIAN_POINT ( 'NONE',  ( -9.474510206698964154, 16.51473224551069663, 25.41557627198103120 ) ) ;
#61756 = CARTESIAN_POINT ( 'NONE',  ( -31.37700036491433053, 7.446261808816053041, 93.97872476790939800 ) ) ;
#61757 = CARTESIAN_POINT ( 'NONE',  ( -14.29746914071049879, 8.314922557960819915, 65.83224293864769550 ) ) ;
#61758 = CARTESIAN_POINT ( 'NONE',  ( -12.14591786802309592, -12.06949235617757132, 36.87390960531435979 ) ) ;
#61759 = CARTESIAN_POINT ( 'NONE',  ( -19.02544592524342804, 5.153800228976336051, 61.04057627198103120 ) ) ;
#61760 = CARTESIAN_POINT ( 'NONE',  ( 9.474510206698971260, -16.51473224551069308, 37.91557627198102409 ) ) ;
#61761 = CARTESIAN_POINT ( 'NONE',  ( -0.05219959533907301413, -21.53943276465977519, 42.49890960531435979 ) ) ;
#61762 = CARTESIAN_POINT ( 'NONE',  ( -5.049401038297874678, -19.05341960407617918, 34.79275706135233293 ) ) ;
#61764 = CARTESIAN_POINT ( 'NONE',  ( -4.379528057220328563, 16.55341960407611168, 55.20724293864770260 ) ) ;
#61763 = CARTESIAN_POINT ( 'NONE',  ( 30.00000000000000000, -5.499999999999992895, 37.50000000000000000 ) ) ;
#61765 = CARTESIAN_POINT ( 'NONE',  ( -21.55341960407610458, -5.719274019375992779, 26.45724293864768839 ) ) ;
#61766 = CARTESIAN_POINT ( 'NONE',  ( -28.32625367550113182, -10.00081768005069449, 140.0928639110588279 ) ) ;
#61767 = CARTESIAN_POINT ( 'NONE',  ( 14.29746914071037800, 8.314922557961029526, 71.66775706135234714 ) ) ;
#61768 = CARTESIAN_POINT ( 'NONE',  ( 5.153800228976615827, -19.02544592524334988, 75.20942372801896170 ) ) ;
#61769 = CARTESIAN_POINT ( 'NONE',  ( -0.05219959533910754901, -16.53943276465976808, 47.49890960531435979 ) ) ;
#61770 = VERTEX_POINT ( 'NONE', #8239 ) ;
#61771 = CARTESIAN_POINT ( 'NONE',  ( -18.39639308325438094, -5.499999999999986677, 76.48252246182195790 ) ) ;
#61772 = CARTESIAN_POINT ( 'NONE',  ( -4.379528057220328563, 16.55341960407611168, 25.20724293864769550 ) ) ;
#61773 = CARTESIAN_POINT ( 'NONE',  ( -13.97604488694527625, -13.89961937509977652, 56.87390960531434558 ) ) ;
#61774 = CARTESIAN_POINT ( 'NONE',  ( -5.153800228976328057, -19.02544592524343514, 72.29057627198102409 ) ) ;
#61775 = CARTESIAN_POINT ( 'NONE',  ( 0.05219959533909260263, 19.03943276465977164, 44.99890960531435979 ) ) ;
#61776 = CARTESIAN_POINT ( 'NONE',  ( 18.67979575497194134, -10.72451020669871369, 40.83442372801901854 ) ) ;
#61777 = CARTESIAN_POINT ( 'NONE',  ( 13.89961937509977652, -13.97604488694527269, 63.12390960531435979 ) ) ;
#61778 = DIRECTION ( 'NONE',  ( -0.000000000000000000, -0.000000000000000000, -1.000000000000000000 ) ) ;
#61779 = CARTESIAN_POINT ( 'NONE',  ( -19.02544592524342804, 5.153800228976336051, 46.04057627198101699 ) ) ;
#61780 = CARTESIAN_POINT ( 'NONE',  ( 10.81492255796078972, 18.62759615963270932, 34.58224293864770260 ) ) ;
#61782 = CARTESIAN_POINT ( 'NONE',  ( -16.51473224551069308, -9.474510206698971260, 26.66557627198103120 ) ) ;
#61781 = CARTESIAN_POINT ( 'NONE',  ( 15.72974639402176855, 15.80617190586768217, 66.87609039468568994 ) ) ;
#61783 = CARTESIAN_POINT ( 'NONE',  ( 18.67979575497178502, 10.72451020669898547, 29.16557627198103120 ) ) ;
#61784 = CARTESIAN_POINT ( 'NONE',  ( -12.14591786802326823, 12.06949235617739902, 88.12609039468570415 ) ) ;
#61785 = CARTESIAN_POINT ( 'NONE',  ( 18.62759615963255655, 10.81492255796105972, 101.6677570613523613 ) ) ;
#61786 = CARTESIAN_POINT ( 'NONE',  ( 14.29746914071037800, 8.314922557961029526, 61.66775706135235424 ) ) ;
#61787 = CARTESIAN_POINT ( 'NONE',  ( 9.474510206698971260, -16.51473224551069308, 112.9155762719810383 ) ) ;
#61788 = CARTESIAN_POINT ( 'NONE',  ( 16.52544592524335698, 4.483927247898782831, 51.45942372801901854 ) ) ;
#61789 = CARTESIAN_POINT ( 'NONE',  ( 4.379528057220092307, 16.55341960407617563, 42.29275706135235424 ) ) ;
#61790 = CARTESIAN_POINT ( 'NONE',  ( -12.14591786802326823, 12.06949235617739902, 93.12609039468568994 ) ) ;
#61791 = CARTESIAN_POINT ( 'NONE',  ( -21.53943276465977519, -0.05219959533937600094, 48.75109039468568284 ) ) ;
#61792 = CARTESIAN_POINT ( 'NONE',  ( -4.379528057220086978, -16.55341960407618274, 19.79275706135235069 ) ) ;
#61793 = CARTESIAN_POINT ( 'NONE',  ( -21.52544592524343514, 5.823673210054127303, 116.0405762719810383 ) ) ;
#61794 = CARTESIAN_POINT ( 'NONE',  ( -0.05219959533934338120, 16.53943276465976808, 22.50109039468567573 ) ) ;
#61795 = CARTESIAN_POINT ( 'NONE',  ( 12.14591786802327356, -12.06949235617739191, 90.62609039468567573 ) ) ;
#61796 = DIRECTION ( 'NONE',  ( 0.5000000000000002220, 0.4999999999999985012, -0.7071067811865483499 ) ) ;
#61797 = CARTESIAN_POINT ( 'NONE',  ( 10.72451020669871369, 18.67979575497193778, 82.08442372801901854 ) ) ;
#61798 = CARTESIAN_POINT ( 'NONE',  ( -16.46253265017146816, -9.564922557961047289, 89.16775706135234714 ) ) ;
#61799 = CARTESIAN_POINT ( 'NONE',  ( -14.29746914071049879, 8.314922557960819915, 55.83224293864770260 ) ) ;
#61800 = CARTESIAN_POINT ( 'NONE',  ( 16.55341960407611168, 4.379528057220329451, 38.95724293864768839 ) ) ;
#61801 = CARTESIAN_POINT ( 'NONE',  ( 16.52544592524342804, -4.483927247898539470, 103.5405762719810383 ) ) ;
#61803 = CARTESIAN_POINT ( 'NONE',  ( 17.72517630440436065, -5.499999999999998224, 53.42175719257213728 ) ) ;
#61802 = CARTESIAN_POINT ( 'NONE',  ( -0.05219959533936034679, 19.03943276465977164, 47.50109039468566863 ) ) ;
#61804 = CARTESIAN_POINT ( 'NONE',  ( -5.719274019375665041, -21.55341960407619695, 44.79275706135234714 ) ) ;
#61805 = CARTESIAN_POINT ( 'NONE',  ( -19.03943276465977164, -0.05219959533935918106, 113.7510903946856757 ) ) ;
#61806 = CARTESIAN_POINT ( 'NONE',  ( 1.300000000000000044, -0.7216878364870318308, 1.249999999999999778 ) ) ;
#61807 = CARTESIAN_POINT ( 'NONE',  ( -5.049401038298153566, 19.05341960407611168, 105.2072429386476671 ) ) ;
#61808 = CARTESIAN_POINT ( 'NONE',  ( -5.823673210054116645, -21.52544592524344225, 77.29057627198102409 ) ) ;
#61809 = CARTESIAN_POINT ( 'NONE',  ( -19.05341960407617563, 5.049401038297882671, 98.54275706135233293 ) ) ;
#61810 = CARTESIAN_POINT ( 'NONE',  ( 19.02544592524343514, -5.153800228976328945, 103.5405762719809957 ) ) ;
#61811 = CARTESIAN_POINT ( 'NONE',  ( 13.97604488694548053, -13.89961937509957401, 50.62609039468566152 ) ) ;
#61812 = CARTESIAN_POINT ( 'NONE',  ( -14.29746914071049879, 8.314922557960819915, 110.8322429386476955 ) ) ;
#61813 = CARTESIAN_POINT ( 'NONE',  ( -18.67979575497193778, 10.72451020669871902, 98.33442372801901854 ) ) ;
#61814 = CARTESIAN_POINT ( 'NONE',  ( 19.05341960407611168, 5.049401038298154454, 28.95724293864769550 ) ) ;
#61815 = CARTESIAN_POINT ( 'NONE',  ( -10.72451020669870658, -18.67979575497194134, 54.58442372801901143 ) ) ;
#61816 = CARTESIAN_POINT ( 'NONE',  ( 21.53943276465977519, 0.05219959533937863772, 91.25109039468568994 ) ) ;
#61817 = CARTESIAN_POINT ( 'NONE',  ( 16.53943276465976808, 0.05219959533934440121, 86.25109039468568994 ) ) ;
#61818 = CARTESIAN_POINT ( 'NONE',  ( 15.72974639402176855, 15.80617190586768217, 36.87609039468568994 ) ) ;
#61819 = CARTESIAN_POINT ( 'NONE',  ( 5.823673210054444382, -21.52544592524334988, 35.20942372801901854 ) ) ;
#61821 = CARTESIAN_POINT ( 'NONE',  ( 5.153800228976335163, 19.02544592524342804, 79.79057627198102409 ) ) ;
#61820 = CARTESIAN_POINT ( 'NONE',  ( 19.03943276465977164, 0.05219959533936151252, 66.25109039468567573 ) ) ;
#61822 = CARTESIAN_POINT ( 'NONE',  ( 8.224510206698953496, -14.34966873604960469, 102.9155762719810383 ) ) ;
#61823 = CARTESIAN_POINT ( 'NONE',  ( 5.719274019375991003, -21.55341960407610458, 77.70724293864770971 ) ) ;
#61824 = CARTESIAN_POINT ( 'NONE',  ( 12.06949235617757843, -12.14591786802309237, 63.12390960531435979 ) ) ;
#61825 = CARTESIAN_POINT ( 'NONE',  ( 5.823673210054444382, -21.52544592524334988, 110.2094237280190185 ) ) ;
#61826 = CARTESIAN_POINT ( 'NONE',  ( 4.379528057220339221, -16.55341960407611168, 87.70724293864769550 ) ) ;
#61827 = CARTESIAN_POINT ( 'NONE',  ( 9.564922557960805705, 16.46253265017160317, 39.58224293864768839 ) ) ;
#61828 = CARTESIAN_POINT ( 'NONE',  ( 16.51473224551083163, -9.474510206698727899, 65.83442372801900433 ) ) ;
#61829 = CARTESIAN_POINT ( 'NONE',  ( 0.05219959533910956823, 16.53943276465976808, 49.99890960531437401 ) ) ;
#61830 = CARTESIAN_POINT ( 'NONE',  ( 10.81492255796106328, -18.62759615963255655, 90.41775706135236135 ) ) ;
#61831 = CARTESIAN_POINT ( 'NONE',  ( -9.564922557960796823, -16.46253265017161027, 87.08224293864769550 ) ) ;
#61832 = CARTESIAN_POINT ( 'NONE',  ( 0.05219959533936267826, -19.03943276465977164, 55.00109039468566863 ) ) ;
#61833 = CARTESIAN_POINT ( 'NONE',  ( 21.52544592524344225, -5.823673210054117533, 58.54057627198103120 ) ) ;
#61834 = CARTESIAN_POINT ( 'NONE',  ( 21.55341960407610458, 5.719274019375980345, 108.9572429386476955 ) ) ;
#61835 = CARTESIAN_POINT ( 'NONE',  ( -16.53943276465976808, -0.05219959533934237506, 18.75109039468568639 ) ) ;
#61836 = CARTESIAN_POINT ( 'NONE',  ( -0.05219959533934338120, 16.53943276465976808, 77.50109039468567573 ) ) ;
#61838 = CARTESIAN_POINT ( 'NONE',  ( 15.72974639402176855, 15.80617190586768217, 26.87609039468567218 ) ) ;
#61837 = CARTESIAN_POINT ( 'NONE',  ( 18.22780087662126647, 5.499999999999818812, 56.48236817873107185 ) ) ;
#61839 = CARTESIAN_POINT ( 'NONE',  ( 19.02544592524343514, -5.153800228976328945, 23.54057627198102054 ) ) ;
#61840 = CARTESIAN_POINT ( 'NONE',  ( -29.86685920354755552, 21.69954338932564397, -5.324999997268814234 ) ) ;
#61841 = CARTESIAN_POINT ( 'NONE',  ( -12.06949235617739369, -12.14591786802326823, 44.37609039468567573 ) ) ;
#61842 = EDGE_CURVE ( 'NONE', #82818, #31542, #64110, .T. ) ;
#61843 = CARTESIAN_POINT ( 'NONE',  ( -4.483927247898539470, -16.52544592524342804, 82.29057627198103830 ) ) ;
#61844 = CARTESIAN_POINT ( 'NONE',  ( 18.67979575497178502, 10.72451020669898547, 79.16557627198103830 ) ) ;
#61845 = CARTESIAN_POINT ( 'NONE',  ( 4.379528057220092307, 16.55341960407617563, 102.2927570613523613 ) ) ;
#61846 = CARTESIAN_POINT ( 'NONE',  ( -0.05219959533934338120, 16.53943276465976808, 32.50109039468568284 ) ) ;
#61847 = CARTESIAN_POINT ( 'NONE',  ( 13.97604488694527802, 13.89961937509977652, 49.37390960531434558 ) ) ;
#61848 = CARTESIAN_POINT ( 'NONE',  ( 12.14591786802327356, -12.06949235617739191, 80.62609039468567573 ) ) ;
#61849 = CARTESIAN_POINT ( 'NONE',  ( -19.05341960407617563, 5.049401038297882671, 78.54275706135233293 ) ) ;
#61850 = CARTESIAN_POINT ( 'NONE',  ( -15.72974639402197994, 15.80617190586746368, 70.62390960531436690 ) ) ;
#61851 = CARTESIAN_POINT ( 'NONE',  ( 12.06949235617739724, 12.14591786802326823, 101.8760903946857042 ) ) ;
#61852 = CARTESIAN_POINT ( 'NONE',  ( 0.05219959533937995610, -21.53943276465977519, 85.00109039468568994 ) ) ;
#61853 = CARTESIAN_POINT ( 'NONE',  ( 10.81492255796078972, 18.62759615963270932, 64.58224293864769550 ) ) ;
#61854 = CARTESIAN_POINT ( 'NONE',  ( -0.05219959533907301413, -21.53943276465977519, 42.49890960531435979 ) ) ;
#61855 = ORIENTED_EDGE ( 'NONE', *, *, #115279, .F. ) ;
#61856 = CARTESIAN_POINT ( 'NONE',  ( 4.379528057220092307, 16.55341960407617563, 72.29275706135236135 ) ) ;
#61857 = CARTESIAN_POINT ( 'NONE',  ( -15.72974639402197994, 15.80617190586746368, 50.62390960531435979 ) ) ;
#61858 = EDGE_LOOP ( 'NONE', ( #114048, #41177, #106715, #61106 ) ) ;
#61859 = CARTESIAN_POINT ( 'NONE',  ( 10.72451020669898902, -18.67979575497178502, 22.91557627198102765 ) ) ;
#61860 = CARTESIAN_POINT ( 'NONE',  ( -19.26498983726237313, 5.499999999999801048, 75.55319577422001487 ) ) ;
#61861 = CARTESIAN_POINT ( 'NONE',  ( -0.05219959533909027116, -19.03943276465977164, 27.49890960531435624 ) ) ;
#61862 = CARTESIAN_POINT ( 'NONE',  ( -21.53943276465977519, 0.05219959533907696930, 76.24890960531435269 ) ) ;
#61863 = CARTESIAN_POINT ( 'NONE',  ( 12.14591786802327356, -12.06949235617739191, 100.6260903946857184 ) ) ;
#61864 = CARTESIAN_POINT ( 'NONE',  ( -15.80617190586768217, 15.72974639402176855, 63.12609039468568994 ) ) ;
#61865 = CARTESIAN_POINT ( 'NONE',  ( 14.29746914071037800, 8.314922557961029526, 26.66775706135235424 ) ) ;
#61866 = CARTESIAN_POINT ( 'NONE',  ( -0.05219959533910754901, -16.53943276465976808, 112.4989096053143669 ) ) ;
#61867 = CARTESIAN_POINT ( 'NONE',  ( -13.97604488694547697, 13.89961937509957934, 113.1260903946856757 ) ) ;
#61868 = CARTESIAN_POINT ( 'NONE',  ( 0.05219959533909260263, 19.03943276465977164, 34.99890960531435979 ) ) ;
#61869 = CARTESIAN_POINT ( 'NONE',  ( -8.906447517083060816, 27.41122689804195645, 143.5999999999999943 ) ) ;
#61870 = CARTESIAN_POINT ( 'NONE',  ( 13.89961937509977652, -13.97604488694527269, 103.1239096053143527 ) ) ;
#61871 = CARTESIAN_POINT ( 'NONE',  ( -16.53943276465976808, -0.05219959533934237506, 83.75109039468568994 ) ) ;
#61872 = CARTESIAN_POINT ( 'NONE',  ( 19.03943276465977164, 0.05219959533936151252, 81.25109039468567573 ) ) ;
#61873 = CARTESIAN_POINT ( 'NONE',  ( -19.02544592524334988, -5.153800228976617603, 23.95942372801900078 ) ) ;
#61874 = CARTESIAN_POINT ( 'NONE',  ( 0.05219959533907565091, 21.53943276465977519, 64.99890960531435269 ) ) ;
#61875 = CARTESIAN_POINT ( 'NONE',  ( 0.05219959533934541429, -16.53943276465976808, 90.00109039468567573 ) ) ;
#61876 = CARTESIAN_POINT ( 'NONE',  ( -19.05341960407617563, 5.049401038297882671, 88.54275706135230450 ) ) ;
#61877 = CARTESIAN_POINT ( 'NONE',  ( 19.05341960407611168, 5.049401038298154454, 48.95724293864768129 ) ) ;
#61878 = CARTESIAN_POINT ( 'NONE',  ( 0.05219959533909260263, 19.03943276465977164, 89.99890960531436690 ) ) ;
#61879 = CARTESIAN_POINT ( 'NONE',  ( 10.72451020669871369, 18.67979575497193778, 47.08442372801901854 ) ) ;
#61880 = CARTESIAN_POINT ( 'NONE',  ( -9.474510206698964154, 16.51473224551069663, 50.41557627198102409 ) ) ;
#61881 = CARTESIAN_POINT ( 'NONE',  ( -16.79531203550649110, -7.028104445595613647, 86.25244988220445919 ) ) ;
#61882 = CARTESIAN_POINT ( 'NONE',  ( -5.049401038298153566, 19.05341960407611168, 105.2072429386476671 ) ) ;
#61883 = CARTESIAN_POINT ( 'NONE',  ( -8.314922557960811034, -14.29746914071050412, 62.08224293864769550 ) ) ;
#61884 = CARTESIAN_POINT ( 'NONE',  ( 21.55341960407610458, 5.719274019375980345, 58.95724293864770971 ) ) ;
#61885 = LINE ( 'NONE', #44752, #74009 ) ;
#61886 = CARTESIAN_POINT ( 'NONE',  ( 5.049401038297881783, 19.05341960407617563, 47.29275706135231161 ) ) ;
#61887 = CARTESIAN_POINT ( 'NONE',  ( -6.938893903907228378E-15, -22.80000000000002913, -64.92279855667830191 ) ) ;
#61889 = CARTESIAN_POINT ( 'NONE',  ( -16.51473224551069308, -9.474510206698971260, 76.66557627198103830 ) ) ;
#61888 = CARTESIAN_POINT ( 'NONE',  ( -9.474510206698964154, 16.51473224551069663, 70.41557627198102409 ) ) ;
#61890 = CARTESIAN_POINT ( 'NONE',  ( 8.314922557961029526, -14.29746914071037800, 45.41775706135234003 ) ) ;
#61891 = CARTESIAN_POINT ( 'NONE',  ( -24.62642639703178205, 5.957135776930584825, 169.3344962860537635 ) ) ;
#61892 = CARTESIAN_POINT ( 'NONE',  ( 13.89961937509957401, 13.97604488694547697, 31.87609039468566863 ) ) ;
#61893 = DIRECTION ( 'NONE',  ( 1.000000000000000000, -0.000000000000000000, -0.000000000000000000 ) ) ;
#61894 = CARTESIAN_POINT ( 'NONE',  ( -16.52544592524335698, -4.483927247898792601, 88.95942372801901854 ) ) ;
#61895 = DIRECTION ( 'NONE',  ( 0.000000000000000000, 0.000000000000000000, -1.000000000000000000 ) ) ;
#61896 = CARTESIAN_POINT ( 'NONE',  ( 16.55341960407618274, -4.379528057220086978, 81.04275706135236135 ) ) ;
#61897 = CARTESIAN_POINT ( 'NONE',  ( -14.29746914071037622, -8.314922557961029526, 54.16775706135235424 ) ) ;
#61898 = CARTESIAN_POINT ( 'NONE',  ( 0.05219959533936267826, -19.03943276465977164, 25.00109039468566152 ) ) ;
#61899 = CARTESIAN_POINT ( 'NONE',  ( 0.05219959533909260263, 19.03943276465977164, 49.99890960531435979 ) ) ;
#61900 = CARTESIAN_POINT ( 'NONE',  ( 10.81492255796106328, -18.62759615963255655, 50.41775706135235424 ) ) ;
#61901 = CARTESIAN_POINT ( 'NONE',  ( -16.51473224551082808, 9.474510206698731452, 73.33442372801900433 ) ) ;
#61902 = CARTESIAN_POINT ( 'NONE',  ( 15.72974639402176855, 15.80617190586768217, 106.8760903946856899 ) ) ;
#61903 = CARTESIAN_POINT ( 'NONE',  ( 19.02544592524343514, -5.153800228976328945, 33.54057627198102409 ) ) ;
#61904 = CARTESIAN_POINT ( 'NONE',  ( -16.10093921903352765, 14.61899031675401694, -58.57166825620330286 ) ) ;
#61905 = CARTESIAN_POINT ( 'NONE',  ( 15.80617190586746368, 15.72974639402197994, 64.37390960531435269 ) ) ;
#61906 = CARTESIAN_POINT ( 'NONE',  ( 5.719274019375991003, -21.55341960407610458, 22.70724293864769194 ) ) ;
#61907 = CARTESIAN_POINT ( 'NONE',  ( -5.049401038298153566, 19.05341960407611168, 25.20724293864768484 ) ) ;
#61908 = CARTESIAN_POINT ( 'NONE',  ( -12.14591786802326823, 12.06949235617739902, 33.12609039468569705 ) ) ;
#61909 = EDGE_CURVE ( 'NONE', #11205, #31087, #34392, .T. ) ;
#61910 = CARTESIAN_POINT ( 'NONE',  ( -0.05219959533910754901, -16.53943276465976808, 32.49890960531435979 ) ) ;
#61911 = ORIENTED_EDGE ( 'NONE', *, *, #154616, .T. ) ;
#61912 = CARTESIAN_POINT ( 'NONE',  ( -10.81492255796105439, 18.62759615963255655, 22.91775706135235069 ) ) ;
#61914 = CARTESIAN_POINT ( 'NONE',  ( 38.00000000000000000, 12.34694845685046616, -4.900000000000000355 ) ) ;
#61913 = CARTESIAN_POINT ( 'NONE',  ( -14.29746914071049879, 8.314922557960819915, 45.83224293864769550 ) ) ;
#61915 = CIRCLE ( 'NONE', #7070, 16.70000000000002061 ) ;
#61916 = CARTESIAN_POINT ( 'NONE',  ( -5.049401038297874678, -19.05341960407617918, 109.7927570613523187 ) ) ;
#61917 = CARTESIAN_POINT ( 'NONE',  ( 19.03943276465977164, 0.05219959533936151252, 21.25109039468565797 ) ) ;
#61918 = CARTESIAN_POINT ( 'NONE',  ( 4.379528057220339221, -16.55341960407611168, 42.70724293864770260 ) ) ;
#61919 = CARTESIAN_POINT ( 'NONE',  ( 18.62759615963271287, -10.81492255796078972, 98.33224293864769550 ) ) ;
#61921 = CARTESIAN_POINT ( 'NONE',  ( 21.52544592524344225, -5.823673210054117533, 58.54057627198103120 ) ) ;
#61920 = CYLINDRICAL_SURFACE ( 'NONE', #176413, 31.90000000000003411 ) ;
#61922 = CARTESIAN_POINT ( 'NONE',  ( -13.97604488694527625, -13.89961937509977652, 76.87390960531433848 ) ) ;
#61923 = CARTESIAN_POINT ( 'NONE',  ( 4.483927247898545687, 16.52544592524342804, 49.79057627198102409 ) ) ;
#61924 = CARTESIAN_POINT ( 'NONE',  ( 16.46253265017160672, -9.564922557960803928, 93.33224293864769550 ) ) ;
#61925 = EDGE_CURVE ( 'NONE', #42860, #112207, #189407, .T. ) ;
#61926 = CARTESIAN_POINT ( 'NONE',  ( -17.49999999999999645, -7.500000000000000888, 118.0000000000000142 ) ) ;
#61927 = CARTESIAN_POINT ( 'NONE',  ( -5.049401038297874678, -19.05341960407617918, 54.79275706135234003 ) ) ;
#61928 = CARTESIAN_POINT ( 'NONE',  ( -21.55341960407610458, -5.719274019375992779, 91.45724293864769550 ) ) ;
#61929 = CARTESIAN_POINT ( 'NONE',  ( -16.53943276465976808, 0.05219959533911058130, 101.2489096053143669 ) ) ;
#61930 = CARTESIAN_POINT ( 'NONE',  ( 15.80617190586769283, -15.72974639402175789, 55.62609039468568284 ) ) ;
#61931 = CARTESIAN_POINT ( 'NONE',  ( 27.73933785331498925, -9.013057229001033122, 147.7750000027311899 ) ) ;
#61932 = CARTESIAN_POINT ( 'NONE',  ( 4.379528057220339221, -16.55341960407611168, 32.70724293864770260 ) ) ;
#61933 = CARTESIAN_POINT ( 'NONE',  ( 9.564922557960805705, 16.46253265017160317, 39.58224293864768839 ) ) ;
#61934 = CARTESIAN_POINT ( 'NONE',  ( 19.05341960407611168, 5.049401038298154454, 103.9572429386476671 ) ) ;
#61935 = CARTESIAN_POINT ( 'NONE',  ( -10.72451020669898014, 18.67979575497178502, 55.41557627198102409 ) ) ;
#61936 = CARTESIAN_POINT ( 'NONE',  ( -2.973862142520652174, -93.04182470242764680, -4.999999999999999112 ) ) ;
#61937 = CARTESIAN_POINT ( 'NONE',  ( -9.564922557960796823, -16.46253265017161027, 37.08224293864768839 ) ) ;
#61938 = CARTESIAN_POINT ( 'NONE',  ( 10.81492255796078972, 18.62759615963270932, 59.58224293864770260 ) ) ;
#61939 = ORIENTED_EDGE ( 'NONE', *, *, #76696, .F. ) ;
#61940 = CARTESIAN_POINT ( 'NONE',  ( -0.05219959533937732626, 21.53943276465977519, 87.50109039468568994 ) ) ;
#61942 = CARTESIAN_POINT ( 'NONE',  ( 16.55341960407618274, -4.379528057220086978, 81.04275706135236135 ) ) ;
#61941 = CARTESIAN_POINT ( 'NONE',  ( 16.00769354339547590, -38.20109431700117852, -19.33483434993953409 ) ) ;
#61943 = CARTESIAN_POINT ( 'NONE',  ( 14.34966873604972726, -8.224510206698740333, 90.83442372801901854 ) ) ;
#61944 = CARTESIAN_POINT ( 'NONE',  ( 0.05219959533909260263, 19.03943276465977164, 59.99890960531436690 ) ) ;
#61945 = CARTESIAN_POINT ( 'NONE',  ( 9.564922557960805705, 16.46253265017160317, 64.58224293864769550 ) ) ;
#61946 = ORIENTED_EDGE ( 'NONE', *, *, #171253, .F. ) ;
#61947 = CARTESIAN_POINT ( 'NONE',  ( -9.474510206698720793, -16.51473224551083518, 24.58442372801900078 ) ) ;
#61948 = CARTESIAN_POINT ( 'NONE',  ( -0.05219959533934338120, 16.53943276465976808, 77.50109039468567573 ) ) ;
#61949 = CARTESIAN_POINT ( 'NONE',  ( 19.02544592524334988, 5.153800228976608722, 21.45942372801899012 ) ) ;
#61950 = CARTESIAN_POINT ( 'NONE',  ( -16.51473224551069308, -9.474510206698971260, 76.66557627198103830 ) ) ;
#61951 = CARTESIAN_POINT ( 'NONE',  ( 18.67979575497178502, 10.72451020669898547, 39.16557627198102409 ) ) ;
#61952 = CARTESIAN_POINT ( 'NONE',  ( 8.224510206698742110, 14.34966873604972548, 27.08442372801901854 ) ) ;
#61953 = CARTESIAN_POINT ( 'NONE',  ( 0.05219959533937995610, -21.53943276465977519, 85.00109039468568994 ) ) ;
#61954 = CARTESIAN_POINT ( 'NONE',  ( -14.29746914071037622, -8.314922557961029526, 49.16775706135234003 ) ) ;
#61955 = CARTESIAN_POINT ( 'NONE',  ( -10.81492255796078084, -18.62759615963271287, 97.08224293864770971 ) ) ;
#61956 = CARTESIAN_POINT ( 'NONE',  ( 4.379528057220092307, 16.55341960407617563, 22.29275706135235069 ) ) ;
#61957 = CARTESIAN_POINT ( 'NONE',  ( 16.46253265017160672, -9.564922557960803928, 73.33224293864769550 ) ) ;
#61958 = CARTESIAN_POINT ( 'NONE',  ( -14.29746914071037622, -8.314922557961029526, 29.16775706135234003 ) ) ;
#61959 = CARTESIAN_POINT ( 'NONE',  ( 9.564922557960805705, 16.46253265017160317, 44.58224293864769550 ) ) ;
#61960 = CARTESIAN_POINT ( 'NONE',  ( 19.02544592524334988, 5.153800228976608722, 111.4594237280190043 ) ) ;
#61961 = CARTESIAN_POINT ( 'NONE',  ( 16.53943276465976808, -0.05219959533910856209, 73.74890960531433848 ) ) ;
#61962 = CARTESIAN_POINT ( 'NONE',  ( -8.314922557961024197, 14.29746914071037800, 82.91775706135234714 ) ) ;
#61964 = CARTESIAN_POINT ( 'NONE',  ( 5.153800228976335163, 19.02544592524342804, 49.79057627198100988 ) ) ;
#61963 = CARTESIAN_POINT ( 'NONE',  ( -10.72451020669870658, -18.67979575497194134, 29.58442372801901854 ) ) ;
#61965 = CARTESIAN_POINT ( 'NONE',  ( 5.153800228976335163, 19.02544592524342804, 69.79057627198103830 ) ) ;
#61966 = CARTESIAN_POINT ( 'NONE',  ( -4.379528057220086978, -16.55341960407618274, 89.79275706135236135 ) ) ;
#61968 = ORIENTED_EDGE ( 'NONE', *, *, #167140, .F. ) ;
#61967 = CARTESIAN_POINT ( 'NONE',  ( -17.72662750342728089, -5.500000000000019540, 81.40179492283745333 ) ) ;
#61969 = ORIENTED_EDGE ( 'NONE', *, *, #133785, .F. ) ;
#61970 = CARTESIAN_POINT ( 'NONE',  ( -19.03943276465977164, -0.05219959533935918106, 28.75109039468566507 ) ) ;
#61971 = CARTESIAN_POINT ( 'NONE',  ( -5.049401038298153566, 19.05341960407611168, 30.20724293864768839 ) ) ;
#61973 = ORIENTED_EDGE ( 'NONE', *, *, #43460, .F. ) ;
#61972 = CARTESIAN_POINT ( 'NONE',  ( 9.564922557960805705, 16.46253265017160317, 109.5822429386476955 ) ) ;
#61974 = CARTESIAN_POINT ( 'NONE',  ( 14.34966873604972726, -8.224510206698740333, 35.83442372801901143 ) ) ;
#61976 = CARTESIAN_POINT ( 'NONE',  ( -0.05219959533934338120, 16.53943276465976808, 47.50109039468568994 ) ) ;
#61975 = CARTESIAN_POINT ( 'NONE',  ( 13.89961937509957401, 13.97604488694547697, 51.87609039468566863 ) ) ;
#61977 = CARTESIAN_POINT ( 'NONE',  ( 19.05341960407611168, 5.049401038298154454, 108.9572429386477097 ) ) ;
#61978 = CARTESIAN_POINT ( 'NONE',  ( 0.05219959533909260263, 19.03943276465977164, 64.99890960531436690 ) ) ;
#61979 = CARTESIAN_POINT ( 'NONE',  ( 21.55341960407610458, 5.719274019375980345, 98.95724293864770971 ) ) ;
#61981 = DIRECTION ( 'NONE',  ( 0.000000000000000000, 0.000000000000000000, -1.000000000000000000 ) ) ;
#61980 = CARTESIAN_POINT ( 'NONE',  ( -13.89961937509977652, 13.97604488694528158, 90.62390960531432427 ) ) ;
#61982 = CARTESIAN_POINT ( 'NONE',  ( -16.46253265017160317, 9.564922557960807481, 65.83224293864769550 ) ) ;
#61984 = CARTESIAN_POINT ( 'NONE',  ( 13.97604488694527802, 13.89961937509977830, 69.37390960531436690 ) ) ;
#61983 = CARTESIAN_POINT ( 'NONE',  ( 16.53943276465976808, -0.05219959533910856209, 23.74890960531435269 ) ) ;
#61985 = CARTESIAN_POINT ( 'NONE',  ( -19.05341960407617563, 5.049401038297882671, 43.54275706135232582 ) ) ;
#61986 = CARTESIAN_POINT ( 'NONE',  ( 8.314922557960818139, 14.29746914071049879, 64.58224293864769550 ) ) ;
#61987 = CARTESIAN_POINT ( 'NONE',  ( -0.05219959533937732626, 21.53943276465977519, 97.50109039468567573 ) ) ;
#61988 = CARTESIAN_POINT ( 'NONE',  ( 0.05219959533909260263, 19.03943276465977164, 39.99890960531436690 ) ) ;
#61989 = CARTESIAN_POINT ( 'NONE',  ( -4.483927247898782831, 16.52544592524335698, 52.70942372801902565 ) ) ;
#61991 = CARTESIAN_POINT ( 'NONE',  ( 15.80617190586769283, -15.72974639402175789, 85.62609039468568994 ) ) ;
#61990 = CARTESIAN_POINT ( 'NONE',  ( 16.53943276465976808, -0.05219959533910856209, 38.74890960531435979 ) ) ;
#61992 = CARTESIAN_POINT ( 'NONE',  ( 9.474510206698971260, -16.51473224551069308, 82.91557627198103830 ) ) ;
#61993 = CARTESIAN_POINT ( 'NONE',  ( -16.46253265017160317, 9.564922557960807481, 90.83224293864769550 ) ) ;
#61994 = CARTESIAN_POINT ( 'NONE',  ( -12.14591786802309592, -12.06949235617757132, 111.8739096053143669 ) ) ;
#61995 = CARTESIAN_POINT ( 'NONE',  ( -4.379528057220328563, 16.55341960407611168, 80.20724293864769550 ) ) ;
#61996 = CARTESIAN_POINT ( 'NONE',  ( 18.67979575497178502, 10.72451020669898547, 84.16557627198103830 ) ) ;
#61997 = CARTESIAN_POINT ( 'NONE',  ( -19.02544592524342804, 5.153800228976336051, 71.04057627198099567 ) ) ;
#61998 = CARTESIAN_POINT ( 'NONE',  ( 5.719274019375991003, -21.55341960407610458, 102.7072429386476955 ) ) ;
#61999 = CARTESIAN_POINT ( 'NONE',  ( -13.97604488694547697, 13.89961937509957934, 78.12609039468567573 ) ) ;
#62001 = CARTESIAN_POINT ( 'NONE',  ( 12.06949235617757843, -12.14591786802309237, 88.12390960531436690 ) ) ;
#62000 = CARTESIAN_POINT ( 'NONE',  ( 18.87075004821571866, -5.499999999999894307, 46.17408112101048090 ) ) ;
#62002 = CARTESIAN_POINT ( 'NONE',  ( -19.03943276465977164, 0.05219959533909376836, 61.24890960531436690 ) ) ;
#62003 = CARTESIAN_POINT ( 'NONE',  ( -15.80617190586745835, -15.72974639402198527, 66.87390960531436690 ) ) ;
#62004 = CARTESIAN_POINT ( 'NONE',  ( -17.97058386085788229, -5.499999999999975131, 84.00390968646217971 ) ) ;
#62006 = SURFACE_SIDE_STYLE ('',( #164259 ) ) ;
#62005 = CARTESIAN_POINT ( 'NONE',  ( -12.06949235617756955, 12.14591786802309770, 25.62390960531435624 ) ) ;
#62007 = CARTESIAN_POINT ( 'NONE',  ( -19.02544592524334988, -5.153800228976617603, 108.9594237280189759 ) ) ;
#62008 = CARTESIAN_POINT ( 'NONE',  ( 8.224510206698953496, -14.34966873604960469, 87.91557627198103830 ) ) ;
#62009 = CARTESIAN_POINT ( 'NONE',  ( -19.49671883438227127, -5.500000000000027534, 94.89279849105682274 ) ) ;
#62010 = CARTESIAN_POINT ( 'NONE',  ( -9.474510206698964154, 16.51473224551069663, 80.41557627198103830 ) ) ;
#62011 = CARTESIAN_POINT ( 'NONE',  ( -5.049401038298153566, 19.05341960407611168, 30.20724293864768839 ) ) ;
#62013 = ADVANCED_FACE ( 'NONE', ( #31378 ), #151744, .F. ) ;
#62012 = CARTESIAN_POINT ( 'NONE',  ( 16.53943276465976808, -0.05219959533910856209, 73.74890960531433848 ) ) ;
#62014 = CARTESIAN_POINT ( 'NONE',  ( 10.81492255796078972, 18.62759615963270932, 24.58224293864768839 ) ) ;
#62016 = CARTESIAN_POINT ( 'NONE',  ( -16.51473224551069308, -9.474510206698971260, 76.66557627198103830 ) ) ;
#62015 = CARTESIAN_POINT ( 'NONE',  ( -16.46253265017146816, -9.564922557961047289, 94.16775706135233293 ) ) ;
#62017 = CARTESIAN_POINT ( 'NONE',  ( 9.564922557960805705, 16.46253265017160317, 84.58224293864769550 ) ) ;
#62018 = CARTESIAN_POINT ( 'NONE',  ( -5.719274019375978568, 21.55341960407610458, 70.20724293864769550 ) ) ;
#62019 = CARTESIAN_POINT ( 'NONE',  ( -0.05219959533934338120, 16.53943276465976808, 72.50109039468568994 ) ) ;
#62020 = CARTESIAN_POINT ( 'NONE',  ( 24.30000000000003268, 0.000000000000000000, -54.21489346206828230 ) ) ;
#62021 = CARTESIAN_POINT ( 'NONE',  ( -9.474510206698964154, 16.51473224551069663, 60.41557627198102409 ) ) ;
#62022 = CARTESIAN_POINT ( 'NONE',  ( 18.62759615963271287, -10.81492255796078972, 68.33224293864769550 ) ) ;
#62023 = CARTESIAN_POINT ( 'NONE',  ( 16.46253265017146816, 9.564922557961045513, 111.6677570613523329 ) ) ;
#62025 = CARTESIAN_POINT ( 'NONE',  ( -21.55341960407619339, 5.719274019375674811, 48.54275706135234714 ) ) ;
#62024 = CARTESIAN_POINT ( 'NONE',  ( 4.483927247898545687, 16.52544592524342804, 34.79057627198103120 ) ) ;
#62026 = DIRECTION ( 'NONE',  ( -0.000000000000000000, -0.000000000000000000, 1.000000000000000000 ) ) ;
#62028 = CARTESIAN_POINT ( 'NONE',  ( -19.03943276465977164, 0.05219959533909376836, 101.2489096053143669 ) ) ;
#62027 = CARTESIAN_POINT ( 'NONE',  ( -4.379528057220086978, -16.55341960407618274, 79.79275706135236135 ) ) ;
#62029 = CARTESIAN_POINT ( 'NONE',  ( -14.62203461105063873, -16.12203461105573865, -58.56003730381080175 ) ) ;
#62030 = CARTESIAN_POINT ( 'NONE',  ( 0.8851752879063210511, 31.61510582211850107, -49.48913787633048855 ) ) ;
#62031 = B_SPLINE_CURVE_WITH_KNOTS ( 'NONE', 3,
 ( #107667, #12716, #169344, #167387, #181568, #15679, #196747, #16670, #197722, #486, #119883, #77340, #185521, #74382, #27898, #47013, #170350, #28883, #108672, #44040, #43046, #105700 ),
 .UNSPECIFIED., .F., .F.,
 ( 4, 2, 2, 2, 2, 2, 2, 2, 2, 2, 4 ),
 ( 0.000000000000000000, 0.001361773908209224556, 0.002042660862313843990, 0.002723547816418463857, 0.004085321724627701857, 0.004766208678732323893, 0.005447095632836944194, 0.006808869541046241175, 0.008170643449255537288, 0.009532417357464836871, 0.01089419126567413298 ),
 .UNSPECIFIED. ) ;
#62032 = CARTESIAN_POINT ( 'NONE',  ( -16.53943276465976808, -0.05219959533934237506, 93.75109039468567573 ) ) ;
#62033 = CARTESIAN_POINT ( 'NONE',  ( -4.483927247898782831, 16.52544592524335698, 52.70942372801902565 ) ) ;
#62034 = CARTESIAN_POINT ( 'NONE',  ( 19.05341960407611168, 5.049401038298154454, 58.95724293864768129 ) ) ;
#62035 = CARTESIAN_POINT ( 'NONE',  ( 9.564922557960805705, 16.46253265017160317, 69.58224293864770971 ) ) ;
#62036 = CARTESIAN_POINT ( 'NONE',  ( -15.72974639402176322, -15.80617190586768395, 59.37609039468568284 ) ) ;
#62037 = CARTESIAN_POINT ( 'NONE',  ( -16.52544592524335698, -4.483927247898792601, 68.95942372801901854 ) ) ;
#62038 = CARTESIAN_POINT ( 'NONE',  ( -4.483927247898539470, -16.52544592524342804, 27.29057627198103120 ) ) ;
#62039 = CARTESIAN_POINT ( 'NONE',  ( -19.02544592524342804, 5.153800228976336051, 36.04057627198100988 ) ) ;
#62040 = CARTESIAN_POINT ( 'NONE',  ( -9.474510206698964154, 16.51473224551069663, 35.41557627198102409 ) ) ;
#62042 = ORIENTED_EDGE ( 'NONE', *, *, #82839, .T. ) ;
#62041 = CARTESIAN_POINT ( 'NONE',  ( -16.55341960407617563, 4.379528057220093196, 23.54275706135235424 ) ) ;
#62043 = CARTESIAN_POINT ( 'NONE',  ( 16.51473224551083163, -9.474510206698727899, 75.83442372801900433 ) ) ;
#62044 = CARTESIAN_POINT ( 'NONE',  ( -8.314922557960811034, -14.29746914071050412, 77.08224293864769550 ) ) ;
#62045 = CARTESIAN_POINT ( 'NONE',  ( -16.46253265017160317, 9.564922557960807481, 45.83224293864769550 ) ) ;
#62047 = CARTESIAN_POINT ( 'NONE',  ( -38.00000000000001421, -12.34694845685042708, -7.900000000000001243 ) ) ;
#62046 = CARTESIAN_POINT ( 'NONE',  ( 16.51473224551083163, -9.474510206698727899, 80.83442372801899012 ) ) ;
#62048 = CARTESIAN_POINT ( 'NONE',  ( -18.62759615963255300, -10.81492255796106328, 94.16775706135237556 ) ) ;
#62049 = CARTESIAN_POINT ( 'NONE',  ( -12.14591786802326823, 12.06949235617739902, 48.12609039468568284 ) ) ;
#62050 = DIRECTION ( 'NONE',  ( 7.973251674720317682E-15, -0.6427876096865524636, -0.7660444431189670222 ) ) ;
#62051 = CARTESIAN_POINT ( 'NONE',  ( -21.53943276465977519, 0.05219959533907696930, 46.24890960531435979 ) ) ;
#62052 = CARTESIAN_POINT ( 'NONE',  ( -14.34966873604972548, 8.224510206698743886, 33.33442372801900433 ) ) ;
#62053 = CARTESIAN_POINT ( 'NONE',  ( 19.02544592524343514, -5.153800228976328945, 33.54057627198102409 ) ) ;
#62054 = CARTESIAN_POINT ( 'NONE',  ( -5.049401038297874678, -19.05341960407617918, 44.79275706135232582 ) ) ;
#62055 = CARTESIAN_POINT ( 'NONE',  ( -0.05219959533909027116, -19.03943276465977164, 77.49890960531435269 ) ) ;
#62056 = CARTESIAN_POINT ( 'NONE',  ( -19.03943276465977164, 0.05219959533909376836, 46.24890960531435979 ) ) ;
#62057 = CARTESIAN_POINT ( 'NONE',  ( 0.000000000000000000, 0.000000000000000000, -61.34707691135562868 ) ) ;
#62058 = CARTESIAN_POINT ( 'NONE',  ( 5.049401038298161559, -19.05341960407611168, 72.70724293864768129 ) ) ;
#62059 = CARTESIAN_POINT ( 'NONE',  ( 22.55670631985092456, -22.55670631985084995, -64.92279855667830191 ) ) ;
#62060 = CARTESIAN_POINT ( 'NONE',  ( -13.97604488694547697, 13.89961937509957934, 33.12609039468566863 ) ) ;
#62061 = CARTESIAN_POINT ( 'NONE',  ( 10.81492255796106328, -18.62759615963255655, 105.4177570613523613 ) ) ;
#62062 = CARTESIAN_POINT ( 'NONE',  ( -4.379528057220328563, 16.55341960407611168, 40.20724293864769550 ) ) ;
#62063 = CARTESIAN_POINT ( 'NONE',  ( 9.474510206698971260, -16.51473224551069308, 37.91557627198102409 ) ) ;
#62064 = CARTESIAN_POINT ( 'NONE',  ( -19.05341960407611168, -5.049401038298163336, 106.4572429386476955 ) ) ;
#62065 = CARTESIAN_POINT ( 'NONE',  ( 10.81492255796106328, -18.62759615963255655, 85.41775706135236135 ) ) ;
#62066 = CARTESIAN_POINT ( 'NONE',  ( 5.153800228976335163, 19.02544592524342804, 54.79057627198103120 ) ) ;
#62067 = CARTESIAN_POINT ( 'NONE',  ( 21.55341960407619695, -5.719274019375665929, 86.04275706135236135 ) ) ;
#62068 = CARTESIAN_POINT ( 'NONE',  ( 21.53943276465977519, -0.05219959533907433946, 43.74890960531435979 ) ) ;
#62069 = CARTESIAN_POINT ( 'NONE',  ( 18.62759615963255655, 10.81492255796105972, 21.66775706135235069 ) ) ;
#62070 = CARTESIAN_POINT ( 'NONE',  ( 16.51473224551083163, -9.474510206698727899, 50.83442372801899722 ) ) ;
#62071 = CARTESIAN_POINT ( 'NONE',  ( -5.153800228976328057, -19.02544592524343514, 22.29057627198102765 ) ) ;
#62072 = CARTESIAN_POINT ( 'NONE',  ( -0.05219959533909027116, -19.03943276465977164, 77.49890960531435269 ) ) ;
#62073 = CARTESIAN_POINT ( 'NONE',  ( 12.14591786802327356, -12.06949235617739191, 35.62609039468568994 ) ) ;
#62074 = CARTESIAN_POINT ( 'NONE',  ( 16.53943276465976808, -0.05219959533910856209, 93.74890960531436690 ) ) ;
#62075 = CARTESIAN_POINT ( 'NONE',  ( -13.89961937509977652, 13.97604488694528158, 60.62390960531436690 ) ) ;
#62076 = CARTESIAN_POINT ( 'NONE',  ( -21.52544592524343514, 5.823673210054127303, 41.04057627198103120 ) ) ;
#62077 = CARTESIAN_POINT ( 'NONE',  ( -13.97604488694547697, 13.89961937509957934, 98.12609039468566152 ) ) ;
#62078 = CARTESIAN_POINT ( 'NONE',  ( -21.52544592524343514, 5.823673210054127303, 101.0405762719810383 ) ) ;
#62079 = CARTESIAN_POINT ( 'NONE',  ( 15.80617190586769283, -15.72974639402175789, 55.62609039468568284 ) ) ;
#62080 = CARTESIAN_POINT ( 'NONE',  ( 16.52544592524335698, 4.483927247898782831, 61.45942372801901854 ) ) ;
#62081 = CARTESIAN_POINT ( 'NONE',  ( -12.14591786802326823, 12.06949235617739902, 73.12609039468567573 ) ) ;
#62082 =( BOUNDED_CURVE ( )  B_SPLINE_CURVE ( 2, ( #167977, #1088, #155779, #152795, #78930 ),
 .UNSPECIFIED., .F., .T. ) 
 B_SPLINE_CURVE_WITH_KNOTS ( ( 3, 2, 3 ),
 ( 0.8000000000000007105, 0.8200000000000000622, 0.8250928956683720727 ),
 .UNSPECIFIED. ) 
 CURVE ( )  GEOMETRIC_REPRESENTATION_ITEM ( )  RATIONAL_B_SPLINE_CURVE ( ( 0.9999999999999983347, 0.9510565162951551965, 1.000000000000000000, 0.9875367971922273114, 0.9814209735438295112 ) ) 
 REPRESENTATION_ITEM ( '' )  );
#62083 = CARTESIAN_POINT ( 'NONE',  ( 13.89961937509977652, -13.97604488694527269, 58.12390960531436690 ) ) ;
#62084 = CARTESIAN_POINT ( 'NONE',  ( 16.53943276465976808, 0.05219959533934440121, 91.25109039468568994 ) ) ;
#62085 = EDGE_CURVE ( 'NONE', #145515, #4644, #60223, .T. ) ;
#62086 = CARTESIAN_POINT ( 'NONE',  ( 15.72974639402176855, 15.80617190586768217, 21.87609039468567573 ) ) ;
#62087 = CARTESIAN_POINT ( 'NONE',  ( -16.52544592524342804, 4.483927247898546575, 66.04057627198103830 ) ) ;
#62088 = CARTESIAN_POINT ( 'NONE',  ( -5.153800228976328057, -19.02544592524343514, 87.29057627198103830 ) ) ;
#62089 = CARTESIAN_POINT ( 'NONE',  ( 16.52544592524335698, 4.483927247898782831, 81.45942372801900433 ) ) ;
#62090 = CARTESIAN_POINT ( 'NONE',  ( -21.52544592524334988, -5.823673210054445271, 58.95942372801902565 ) ) ;
#62091 = CARTESIAN_POINT ( 'NONE',  ( -5.049401038297874678, -19.05341960407617918, 109.7927570613523187 ) ) ;
#62092 = CARTESIAN_POINT ( 'NONE',  ( -18.62759615963270932, 10.81492255796079327, 115.8322429386477097 ) ) ;
#62093 = CARTESIAN_POINT ( 'NONE',  ( 4.379528057220339221, -16.55341960407611168, 52.70724293864769550 ) ) ;
#62094 = ORIENTED_EDGE ( 'NONE', *, *, #121277, .T. ) ;
#62095 = CARTESIAN_POINT ( 'NONE',  ( 18.87075004821568314, -5.499999999999984013, 91.17408112101047379 ) ) ;
#62096 = CARTESIAN_POINT ( 'NONE',  ( 18.62759615963271287, -10.81492255796078972, 83.33224293864769550 ) ) ;
#62097 = CARTESIAN_POINT ( 'NONE',  ( 14.34966873604960469, 8.224510206698951720, 34.16557627198102409 ) ) ;
#62098 = ORIENTED_EDGE ( 'NONE', *, *, #149135, .F. ) ;
#62099 = CARTESIAN_POINT ( 'NONE',  ( 35.68624576866247367, 0.9837712456776031011, 37.56068211393102274 ) ) ;
#62100 = CARTESIAN_POINT ( 'NONE',  ( 21.55341960407610458, 5.719274019375980345, 113.9572429386477239 ) ) ;
#62101 = CARTESIAN_POINT ( 'NONE',  ( 10.72451020669898902, -18.67979575497178502, 22.91557627198102765 ) ) ;
#62102 = CARTESIAN_POINT ( 'NONE',  ( -5.823673210054431948, 21.52544592524334988, 27.70942372801901854 ) ) ;
#62103 = CARTESIAN_POINT ( 'NONE',  ( -12.06949235617756955, 12.14591786802309770, 55.62390960531436690 ) ) ;
#62104 = CARTESIAN_POINT ( 'NONE',  ( 8.224510206698742110, 14.34966873604972548, 62.08442372801901143 ) ) ;
#62105 = CARTESIAN_POINT ( 'NONE',  ( -16.46253265017160317, 9.564922557960807481, 65.83224293864769550 ) ) ;
#62106 = CARTESIAN_POINT ( 'NONE',  ( 9.474510206698729675, 16.51473224551082808, 72.08442372801900433 ) ) ;
#62107 = CARTESIAN_POINT ( 'NONE',  ( -13.89961937509977652, 13.97604488694528158, 75.62390960531438111 ) ) ;
#62108 = EDGE_CURVE ( 'NONE', #199703, #123077, #193433, .T. ) ;
#62109 = CARTESIAN_POINT ( 'NONE',  ( 5.823673210054125526, 21.52544592524343514, 49.79057627198102409 ) ) ;
#62110 = CARTESIAN_POINT ( 'NONE',  ( -8.963443992378397951, -45.12205215322087781, -22.08927284594089002 ) ) ;
#62111 = CARTESIAN_POINT ( 'NONE',  ( -19.03943276465977164, 0.05219959533909376836, 56.24890960531435979 ) ) ;
#62112 = CARTESIAN_POINT ( 'NONE',  ( -12.06949235617739369, -12.14591786802326823, 29.37609039468568284 ) ) ;
#62113 = CARTESIAN_POINT ( 'NONE',  ( 9.474510206698729675, 16.51473224551082808, 67.08442372801900433 ) ) ;
#62114 = CARTESIAN_POINT ( 'NONE',  ( -21.52544592524343514, 5.823673210054127303, 111.0405762719810525 ) ) ;
#62115 = CARTESIAN_POINT ( 'NONE',  ( -14.34966873604960291, -8.224510206698953496, 51.66557627198102409 ) ) ;
#62116 = CARTESIAN_POINT ( 'NONE',  ( -0.05219959533909027116, -19.03943276465977164, 92.49890960531436690 ) ) ;
#62117 = CARTESIAN_POINT ( 'NONE',  ( 18.62759615963271287, -10.81492255796078972, 58.33224293864768839 ) ) ;
#62119 = CARTESIAN_POINT ( 'NONE',  ( 14.34966873604972726, -8.224510206698740333, 40.83442372801901854 ) ) ;
#62118 = CARTESIAN_POINT ( 'NONE',  ( -21.55341960407610458, -5.719274019375992779, 101.4572429386476955 ) ) ;
#62120 = CARTESIAN_POINT ( 'NONE',  ( -0.05219959533907301413, -21.53943276465977519, 37.49890960531436690 ) ) ;
#62121 = CARTESIAN_POINT ( 'NONE',  ( -15.80617190586768217, 15.72974639402176855, 88.12609039468570415 ) ) ;
#62122 = CARTESIAN_POINT ( 'NONE',  ( 13.97604488694527802, 13.89961937509977652, 89.37390960531436690 ) ) ;
#62123 = CARTESIAN_POINT ( 'NONE',  ( -13.89961937509977652, 13.97604488694528158, 45.62390960531433848 ) ) ;
#62124 = CARTESIAN_POINT ( 'NONE',  ( -19.05341960407611168, -5.049401038298163336, 91.45724293864766707 ) ) ;
#62125 = CARTESIAN_POINT ( 'NONE',  ( -8.314922557960811034, -14.29746914071050412, 102.0822429386476955 ) ) ;
#62126 = CARTESIAN_POINT ( 'NONE',  ( 16.51473224551069308, 9.474510206698969483, 59.16557627198102409 ) ) ;
#62127 = CARTESIAN_POINT ( 'NONE',  ( -14.29746914071037622, -8.314922557961029526, 19.16775706135234714 ) ) ;
#62128 = CARTESIAN_POINT ( 'NONE',  ( 17.49999999999999645, 5.068104630630414498, 31.77181594659973030 ) ) ;
#62130 = CARTESIAN_POINT ( 'NONE',  ( 10.72451020669898902, -18.67979575497178502, 37.91557627198102409 ) ) ;
#62129 = CARTESIAN_POINT ( 'NONE',  ( -15.80617190586768217, 15.72974639402176855, 93.12609039468568994 ) ) ;
#62131 = CARTESIAN_POINT ( 'NONE',  ( -0.05219959533934338120, 16.53943276465976808, 87.50109039468568994 ) ) ;
#62132 = DIRECTION ( 'NONE',  ( 1.000000000000000000, 0.000000000000000000, 0.000000000000000000 ) ) ;
#62133 = CARTESIAN_POINT ( 'NONE',  ( 5.153800228976615827, -19.02544592524334988, 75.20942372801896170 ) ) ;
#62134 = CARTESIAN_POINT ( 'NONE',  ( -19.03943276465977164, -0.05219959533935918106, 33.75109039468566863 ) ) ;
#62135 = DIRECTION ( 'NONE',  ( -1.000000000000000000, 0.000000000000000000, 0.000000000000000000 ) ) ;
#62136 = CARTESIAN_POINT ( 'NONE',  ( -16.46253265017160317, 9.564922557960807481, 25.83224293864769194 ) ) ;
#62137 = CARTESIAN_POINT ( 'NONE',  ( -14.34966873604960291, -8.224510206698953496, 36.66557627198103120 ) ) ;
#62138 = CARTESIAN_POINT ( 'NONE',  ( 16.51473224551069308, 9.474510206698969483, 24.16557627198102765 ) ) ;
#62139 = CARTESIAN_POINT ( 'NONE',  ( -14.34966873604960291, -8.224510206698953496, 21.66557627198102409 ) ) ;
#62140 = CARTESIAN_POINT ( 'NONE',  ( -18.89770734986045753, -5.500000000000000888, 84.10214472496637939 ) ) ;
#62141 = CARTESIAN_POINT ( 'NONE',  ( 14.29746914071037800, 8.314922557961029526, 91.66775706135234714 ) ) ;
#62142 = CARTESIAN_POINT ( 'NONE',  ( -13.89961937509977652, 13.97604488694528158, 30.62390960531435269 ) ) ;
#62143 = CARTESIAN_POINT ( 'NONE',  ( 5.719274019375673035, 21.55341960407619339, 112.2927570613523471 ) ) ;
#62144 = CARTESIAN_POINT ( 'NONE',  ( -4.379528057220086978, -16.55341960407618274, 19.79275706135235069 ) ) ;
#62145 = CARTESIAN_POINT ( 'NONE',  ( -5.823673210054431948, 21.52544592524334988, 72.70942372801901854 ) ) ;
#62146 = CARTESIAN_POINT ( 'NONE',  ( 13.89961937509957401, 13.97604488694547697, 51.87609039468566863 ) ) ;
#62147 = CARTESIAN_POINT ( 'NONE',  ( -5.049401038298153566, 19.05341960407611168, 95.20724293864770971 ) ) ;
#62148 = CARTESIAN_POINT ( 'NONE',  ( 0.05219959533909260263, 19.03943276465977164, 69.99890960531435269 ) ) ;
#62149 = CARTESIAN_POINT ( 'NONE',  ( -19.49149378614658090, 5.499999999999783284, 39.43757513605363840 ) ) ;
#62150 = CARTESIAN_POINT ( 'NONE',  ( -10.72451020669898014, 18.67979575497178502, 100.4155762719810241 ) ) ;
#62151 = CARTESIAN_POINT ( 'NONE',  ( -14.29746914071049879, 8.314922557960819915, 60.83224293864769550 ) ) ;
#62152 = CARTESIAN_POINT ( 'NONE',  ( 5.823673210054125526, 21.52544592524343514, 54.79057627198104541 ) ) ;
#62153 = CARTESIAN_POINT ( 'NONE',  ( 16.46253265017160672, -9.564922557960803928, 58.33224293864769550 ) ) ;
#62155 = CARTESIAN_POINT ( 'NONE',  ( 8.314922557961029526, -14.29746914071037800, 75.41775706135233293 ) ) ;
#62154 = CARTESIAN_POINT ( 'NONE',  ( 21.55341960407610458, 5.719274019375980345, 88.95724293864769550 ) ) ;
#62156 = VERTEX_POINT ( 'NONE', #136563 ) ;
#62157 = CARTESIAN_POINT ( 'NONE',  ( 5.049401038298161559, -19.05341960407611168, 42.70724293864767418 ) ) ;
#62159 = CARTESIAN_POINT ( 'NONE',  ( -3.573655867282028392E-15, -12.39993551617566503, 167.9999999999999716 ) ) ;
#62158 = CARTESIAN_POINT ( 'NONE',  ( -14.34966873604960291, -8.224510206698953496, 96.66557627198102409 ) ) ;
#62160 = CARTESIAN_POINT ( 'NONE',  ( -19.05341960407611168, -5.049401038298163336, 51.45724293864770260 ) ) ;
#62161 = CARTESIAN_POINT ( 'NONE',  ( -5.049401038298153566, 19.05341960407611168, 25.20724293864768484 ) ) ;
#62162 = CARTESIAN_POINT ( 'NONE',  ( 19.02544592524334988, 5.153800228976608722, 61.45942372801900433 ) ) ;
#62163 = CARTESIAN_POINT ( 'NONE',  ( -16.55341960407611168, -4.379528057220339221, 86.45724293864770971 ) ) ;
#62164 = CARTESIAN_POINT ( 'NONE',  ( 0.05219959533937995610, -21.53943276465977519, 45.00109039468568284 ) ) ;
#62166 = CARTESIAN_POINT ( 'NONE',  ( -0.05219959533907301413, -21.53943276465977519, 107.4989096053143669 ) ) ;
#62165 = CARTESIAN_POINT ( 'NONE',  ( 13.97604488694527802, 13.89961937509977652, 39.37390960531435269 ) ) ;
#62167 = CARTESIAN_POINT ( 'NONE',  ( -16.53943276465976808, 0.05219959533911058130, 91.24890960531436690 ) ) ;
#62168 = CARTESIAN_POINT ( 'NONE',  ( 8.106210103299311243, -39.71824525391687644, -25.55638568641750297 ) ) ;
#62169 = CARTESIAN_POINT ( 'NONE',  ( 5.153800228976335163, 19.02544592524342804, 64.79057627198100988 ) ) ;
#62170 = CARTESIAN_POINT ( 'NONE',  ( -10.01072506788280414, -12.06228617636993050, -61.80095975838368361 ) ) ;
#62172 = CARTESIAN_POINT ( 'NONE',  ( -19.03943276465977164, 0.05219959533909376836, 101.2489096053143669 ) ) ;
#62171 = CARTESIAN_POINT ( 'NONE',  ( 16.51473224551083163, -9.474510206698727899, 95.83442372801900433 ) ) ;
#62173 = CARTESIAN_POINT ( 'NONE',  ( 21.52544592524334988, 5.823673210054432836, 36.45942372801901143 ) ) ;
#62174 = CARTESIAN_POINT ( 'NONE',  ( 9.564922557960805705, 16.46253265017160317, 79.58224293864769550 ) ) ;
#62175 = CARTESIAN_POINT ( 'NONE',  ( -9.564922557961040184, 16.46253265017147172, 72.91775706135233293 ) ) ;
#62176 = CARTESIAN_POINT ( 'NONE',  ( 9.474510206698971260, -16.51473224551069308, 52.91557627198102409 ) ) ;
#62177 = CARTESIAN_POINT ( 'NONE',  ( -16.52544592524342804, 4.483927247898546575, 76.04057627198102409 ) ) ;
#62178 = CARTESIAN_POINT ( 'NONE',  ( -8.224510206698948167, 14.34966873604960824, 65.41557627198102409 ) ) ;
#62179 = CARTESIAN_POINT ( 'NONE',  ( 9.564922557960805705, 16.46253265017160317, 89.58224293864769550 ) ) ;
#62180 = CARTESIAN_POINT ( 'NONE',  ( -21.55341960407610458, -5.719274019375992779, 106.4572429386477097 ) ) ;
#62181 = CARTESIAN_POINT ( 'NONE',  ( -16.46253265017160317, 9.564922557960807481, 80.83224293864769550 ) ) ;
#62182 = CARTESIAN_POINT ( 'NONE',  ( 9.474510206698729675, 16.51473224551082808, 27.08442372801900433 ) ) ;
#62185 = CARTESIAN_POINT ( 'NONE',  ( 16.53943276465976808, -0.05219959533910856209, 103.7489096053143669 ) ) ;
#62184 = CARTESIAN_POINT ( 'NONE',  ( 14.29746914071049879, -8.314922557960816363, 28.33224293864769550 ) ) ;
#62183 = CARTESIAN_POINT ( 'NONE',  ( 9.564922557960805705, 16.46253265017160317, 34.58224293864770260 ) ) ;
#62186 = CARTESIAN_POINT ( 'NONE',  ( -16.46253265017146816, -9.564922557961047289, 99.16775706135233293 ) ) ;
#62187 = EDGE_LOOP ( 'NONE', ( #71840, #180312, #45826, #113191, #148805, #131599, #73755, #119356 ) ) ;
#62188 = CARTESIAN_POINT ( 'NONE',  ( -21.52544592524334988, -5.823673210054445271, 28.95942372801902209 ) ) ;
#62189 = CARTESIAN_POINT ( 'NONE',  ( 9.564922557961047289, -16.46253265017146816, 70.41775706135233293 ) ) ;
#62190 = CARTESIAN_POINT ( 'NONE',  ( -14.29746914071049879, 8.314922557960819915, 25.83224293864769194 ) ) ;
#62191 = CARTESIAN_POINT ( 'NONE',  ( 5.719274019375991003, -21.55341960407610458, 82.70724293864770971 ) ) ;
#62192 = CARTESIAN_POINT ( 'NONE',  ( 21.53943276465977519, -0.05219959533907433946, 23.74890960531435269 ) ) ;
#62193 = CARTESIAN_POINT ( 'NONE',  ( -16.52544592524342804, 4.483927247898546575, 76.04057627198102409 ) ) ;
#62194 = CARTESIAN_POINT ( 'NONE',  ( 19.03943276465977164, -0.05219959533909143690, 23.74890960531435269 ) ) ;
#62195 = CARTESIAN_POINT ( 'NONE',  ( 19.03943276465977164, 0.05219959533936151252, 31.25109039468566863 ) ) ;
#62196 = CARTESIAN_POINT ( 'NONE',  ( 8.224510206698742110, 14.34966873604972548, 92.08442372801901854 ) ) ;
#62197 = CARTESIAN_POINT ( 'NONE',  ( -16.55341960407617563, 4.379528057220093196, 63.54275706135234003 ) ) ;
#62198 = CARTESIAN_POINT ( 'NONE',  ( 19.05341960407611168, 5.049401038298154454, 113.9572429386477097 ) ) ;
#62199 = CARTESIAN_POINT ( 'NONE',  ( 21.53943276465977519, 0.05219959533937863772, 111.2510903946856899 ) ) ;
#62200 = CARTESIAN_POINT ( 'NONE',  ( 9.474510206698971260, -16.51473224551069308, 77.91557627198103830 ) ) ;
#62201 = CARTESIAN_POINT ( 'NONE',  ( -4.379528057220086978, -16.55341960407618274, 59.79275706135234714 ) ) ;
#62202 = CARTESIAN_POINT ( 'NONE',  ( -5.049401038298153566, 19.05341960407611168, 25.20724293864768484 ) ) ;
#62203 = CARTESIAN_POINT ( 'NONE',  ( 12.14591786802309770, 12.06949235617756955, 29.37390960531435269 ) ) ;
#62204 = FACE_OUTER_BOUND ( 'NONE', #96660, .T. ) ;
#62206 = CARTESIAN_POINT ( 'NONE',  ( -16.51473224551069308, -9.474510206698971260, 81.66557627198103830 ) ) ;
#62205 = CARTESIAN_POINT ( 'NONE',  ( 19.02544592524343514, -5.153800228976328945, 103.5405762719809957 ) ) ;
#62207 = CARTESIAN_POINT ( 'NONE',  ( -19.02544592524342804, 5.153800228976336051, 111.0405762719810099 ) ) ;
#62208 = CARTESIAN_POINT ( 'NONE',  ( -12.14591786802309592, -12.06949235617757132, 56.87390960531436690 ) ) ;
#62209 = CARTESIAN_POINT ( 'NONE',  ( 14.34966873604960469, 8.224510206698951720, 34.16557627198102409 ) ) ;
#62210 = CARTESIAN_POINT ( 'NONE',  ( 16.52544592524342804, -4.483927247898539470, 53.54057627198103120 ) ) ;
#62211 = CARTESIAN_POINT ( 'NONE',  ( -12.06949235617739369, -12.14591786802326823, 44.37609039468567573 ) ) ;
#62212 = CARTESIAN_POINT ( 'NONE',  ( 19.03943276465977164, 0.05219959533936151252, 46.25109039468566863 ) ) ;
#62213 = CARTESIAN_POINT ( 'NONE',  ( -19.05341960407611168, -5.049401038298163336, 76.45724293864769550 ) ) ;
#62214 = CARTESIAN_POINT ( 'NONE',  ( 13.97604488694548053, -13.89961937509957401, 50.62609039468566152 ) ) ;
#62215 = CARTESIAN_POINT ( 'NONE',  ( 8.571926809382603096, -26.38167802310801235, 145.9750000027311785 ) ) ;
#62216 = CARTESIAN_POINT ( 'NONE',  ( 5.049401038297881783, 19.05341960407617563, 57.29275706135231871 ) ) ;
#62218 = CARTESIAN_POINT ( 'NONE',  ( 16.52544592524335698, 4.483927247898782831, 81.45942372801900433 ) ) ;
#62217 = CARTESIAN_POINT ( 'NONE',  ( -16.51473224551082808, 9.474510206698731452, 98.33442372801900433 ) ) ;
#62219 = CARTESIAN_POINT ( 'NONE',  ( -27.73933785331498925, -9.013057229001049109, 143.4750000027311785 ) ) ;
#62220 = CARTESIAN_POINT ( 'NONE',  ( -9.564922557960796823, -16.46253265017161027, 27.08224293864769550 ) ) ;
#62221 = CARTESIAN_POINT ( 'NONE',  ( 5.049401038298161559, -19.05341960407611168, 97.70724293864766707 ) ) ;
#62222 = CARTESIAN_POINT ( 'NONE',  ( -18.62759615963255300, -10.81492255796106328, 44.16775706135234714 ) ) ;
#62223 = CARTESIAN_POINT ( 'NONE',  ( -19.03943276465977164, -0.05219959533935918106, 98.75109039468567573 ) ) ;
#62225 = CARTESIAN_POINT ( 'NONE',  ( 19.05341960407611168, 5.049401038298154454, 63.95724293864769550 ) ) ;
#62224 = CARTESIAN_POINT ( 'NONE',  ( -30.74264578624800492, 22.33583958711400186, -2.200000000000000178 ) ) ;
#62226 = CARTESIAN_POINT ( 'NONE',  ( 13.97604488694527802, 13.89961937509977652, 104.3739096053143385 ) ) ;
#62228 = CARTESIAN_POINT ( 'NONE',  ( -0.05219959533909027116, -19.03943276465977164, 67.49890960531436690 ) ) ;
#62227 = CARTESIAN_POINT ( 'NONE',  ( 8.314922557960818139, 14.29746914071049879, 64.58224293864769550 ) ) ;
#62229 = CARTESIAN_POINT ( 'NONE',  ( 9.474510206698971260, -16.51473224551069308, 57.91557627198103120 ) ) ;
#62230 = CARTESIAN_POINT ( 'NONE',  ( -19.05341960407617563, 5.049401038297882671, 83.54275706135233293 ) ) ;
#62231 = CARTESIAN_POINT ( 'NONE',  ( -5.719274019375978568, 21.55341960407610458, 45.20724293864769550 ) ) ;
#62232 = CARTESIAN_POINT ( 'NONE',  ( -9.564922557961040184, 16.46253265017147172, 47.91775706135233293 ) ) ;
#62233 = CARTESIAN_POINT ( 'NONE',  ( -19.02544592524342804, 5.153800228976336051, 76.04057627198102409 ) ) ;
#62234 = CARTESIAN_POINT ( 'NONE',  ( 18.62759615963271287, -10.81492255796078972, 83.33224293864769550 ) ) ;
#62236 = CARTESIAN_POINT ( 'NONE',  ( 16.46253265017146816, 9.564922557961045513, 36.66775706135233293 ) ) ;
#62235 = CARTESIAN_POINT ( 'NONE',  ( -0.05219959533910754901, -16.53943276465976808, 82.49890960531436690 ) ) ;
#62237 = CARTESIAN_POINT ( 'NONE',  ( 5.823673210054125526, 21.52544592524343514, 54.79057627198104541 ) ) ;
#62238 = CARTESIAN_POINT ( 'NONE',  ( 18.67979575497178502, 10.72451020669898547, 44.16557627198103120 ) ) ;
#62239 = CARTESIAN_POINT ( 'NONE',  ( -19.02544592524342804, 5.153800228976336051, 66.04057627198103830 ) ) ;
#62240 = CARTESIAN_POINT ( 'NONE',  ( 16.52544592524342804, -4.483927247898539470, 108.5405762719810241 ) ) ;
#62241 = CARTESIAN_POINT ( 'NONE',  ( -5.823673210054431948, 21.52544592524334988, 27.70942372801901854 ) ) ;
#62242 = CARTESIAN_POINT ( 'NONE',  ( 1.500000000000005329, 15.20000000000001883, -61.96904110198155280 ) ) ;
#62243 = CARTESIAN_POINT ( 'NONE',  ( 0.05219959533937995610, -21.53943276465977519, 45.00109039468568284 ) ) ;
#62244 = CARTESIAN_POINT ( 'NONE',  ( 13.89961937509977652, -13.97604488694527269, 38.12390960531436690 ) ) ;
#62245 = CARTESIAN_POINT ( 'NONE',  ( -18.62759615963270932, 10.81492255796079327, 100.8322429386477097 ) ) ;
#62246 = CARTESIAN_POINT ( 'NONE',  ( -19.05341960407617563, 5.049401038297882671, 53.54275706135231871 ) ) ;
#62247 = CARTESIAN_POINT ( 'NONE',  ( 5.049401038298161559, -19.05341960407611168, 27.70724293864769550 ) ) ;
#62248 = CARTESIAN_POINT ( 'NONE',  ( 16.51473224551069308, 9.474510206698969483, 24.16557627198102765 ) ) ;
#62249 = DIRECTION ( 'NONE',  ( 0.000000000000000000, -1.000000000000000000, 0.000000000000000000 ) ) ;
#62250 = CARTESIAN_POINT ( 'NONE',  ( 4.483927247898790824, -16.52544592524335698, 60.20942372801902565 ) ) ;
#62251 = CARTESIAN_POINT ( 'NONE',  ( -19.05341960407611168, -5.049401038298163336, 21.45724293864768839 ) ) ;
#62252 = CARTESIAN_POINT ( 'NONE',  ( -26.62494319856254066, -7.396441074666470605, 168.1134502243608893 ) ) ;
#62253 = CARTESIAN_POINT ( 'NONE',  ( 16.51473224551069308, 9.474510206698969483, 69.16557627198102409 ) ) ;
#62255 = EDGE_CURVE ( 'NONE', #185826, #149684, #45550, .T. ) ;
#62254 = CARTESIAN_POINT ( 'NONE',  ( -4.483927247898539470, -16.52544592524342804, 102.2905762719810383 ) ) ;
#62256 = CIRCLE ( 'NONE', #10632, 8.000000000000000000 ) ;
#62257 = CARTESIAN_POINT ( 'NONE',  ( -5.719274019375978568, 21.55341960407610458, 65.20724293864768129 ) ) ;
#62258 = CARTESIAN_POINT ( 'NONE',  ( 0.05219959533934541429, -16.53943276465976808, 35.00109039468568284 ) ) ;
#62259 = CARTESIAN_POINT ( 'NONE',  ( 15.80617190586769283, -15.72974639402175789, 105.6260903946856899 ) ) ;
#62260 = CARTESIAN_POINT ( 'NONE',  ( -9.474510206698964154, 16.51473224551069663, 25.41557627198103120 ) ) ;
#62261 = CARTESIAN_POINT ( 'NONE',  ( 16.52544592524342804, -4.483927247898539470, 23.54057627198102765 ) ) ;
#62262 = CARTESIAN_POINT ( 'NONE',  ( 16.52544592524342804, -4.483927247898539470, 48.54057627198103120 ) ) ;
#62263 = CARTESIAN_POINT ( 'NONE',  ( 5.153800228976335163, 19.02544592524342804, 49.79057627198100988 ) ) ;
#62264 = CARTESIAN_POINT ( 'NONE',  ( 18.67979575497194134, -10.72451020669871369, 95.83442372801903275 ) ) ;
#62265 = CARTESIAN_POINT ( 'NONE',  ( 10.72451020669898902, -18.67979575497178502, 112.9155762719810383 ) ) ;
#62266 = CARTESIAN_POINT ( 'NONE',  ( 15.72974639402176855, 15.80617190586768217, 76.87609039468567573 ) ) ;
#62267 = CARTESIAN_POINT ( 'NONE',  ( -16.55341960407617563, 4.379528057220093196, 53.54275706135234714 ) ) ;
#62269 = CARTESIAN_POINT ( 'NONE',  ( 10.72451020669871369, 18.67979575497193778, 102.0844237280190185 ) ) ;
#62268 = CARTESIAN_POINT ( 'NONE',  ( -0.05219959533910754901, -16.53943276465976808, 82.49890960531436690 ) ) ;
#62270 = CARTESIAN_POINT ( 'NONE',  ( 16.55341960407618274, -4.379528057220086978, 111.0427570613523613 ) ) ;
#62271 = CARTESIAN_POINT ( 'NONE',  ( -16.62475595723700295, 7.163666690055284114, 115.5271335181047760 ) ) ;
#62272 = CARTESIAN_POINT ( 'NONE',  ( -14.34966873604972548, 8.224510206698743886, 33.33442372801900433 ) ) ;
#62273 = CARTESIAN_POINT ( 'NONE',  ( 4.379528057220339221, -16.55341960407611168, 37.70724293864769550 ) ) ;
#62274 = CARTESIAN_POINT ( 'NONE',  ( 14.34966873604972726, -8.224510206698740333, 80.83442372801901854 ) ) ;
#62275 = CARTESIAN_POINT ( 'NONE',  ( 16.51473224551069308, 9.474510206698969483, 94.16557627198103830 ) ) ;
#62276 = CARTESIAN_POINT ( 'NONE',  ( 13.97604488694527802, 13.89961937509977652, 109.3739096053143669 ) ) ;
#62277 = CARTESIAN_POINT ( 'NONE',  ( -15.80617190586768217, 15.72974639402176855, 93.12609039468568994 ) ) ;
#62278 = CARTESIAN_POINT ( 'NONE',  ( -4.379528057220086978, -16.55341960407618274, 104.7927570613523898 ) ) ;
#62279 = CARTESIAN_POINT ( 'NONE',  ( 0.05219959533910956823, 16.53943276465976808, 69.99890960531435269 ) ) ;
#62280 = CARTESIAN_POINT ( 'NONE',  ( -9.564922557960796823, -16.46253265017161027, 77.08224293864769550 ) ) ;
#62281 = VERTEX_POINT ( 'NONE', #123363 ) ;
#62282 = CARTESIAN_POINT ( 'NONE',  ( 16.55341960407618274, -4.379528057220086978, 31.04275706135234714 ) ) ;
#62283 = CARTESIAN_POINT ( 'NONE',  ( -13.89961937509977652, 13.97604488694528158, 25.62390960531434558 ) ) ;
#62284 = CARTESIAN_POINT ( 'NONE',  ( 5.049401038298161559, -19.05341960407611168, 87.70724293864769550 ) ) ;
#62286 = CARTESIAN_POINT ( 'NONE',  ( -22.81625015709509441, -31.40387420917324590, -4.324999997268812457 ) ) ;
#62285 = CARTESIAN_POINT ( 'NONE',  ( -4.483927247898782831, 16.52544592524335698, 37.70942372801900433 ) ) ;
#62287 = CARTESIAN_POINT ( 'NONE',  ( 16.46253265017146816, 9.564922557961045513, 36.66775706135233293 ) ) ;
#62288 = CARTESIAN_POINT ( 'NONE',  ( -16.55341960407617563, 4.379528057220093196, 88.54275706135236135 ) ) ;
#62290 = B_SPLINE_CURVE_WITH_KNOTS ( 'NONE', 3,
 ( #132196, #54358, #53351, #82675, #116030, #128192, #177719, #39187, #162527, #114009, #36181, #66529, #159523, #173733, #24030, #190877, #85684, #67522, #189890, #50385, #52353, #51365, #175707, #158539, #113026, #97835, #21020, #41197, #166544, #44185, #86685, #179727, #71523, #133190, #55352, #28042, #195896, #11878, #102859, #181705 ),
 .UNSPECIFIED., .F., .F.,
 ( 4, 2, 2, 2, 2, 2, 2, 2, 2, 2, 2, 2, 2, 2, 2, 2, 2, 2, 2, 4 ),
 ( 0.02146664961600480703, 0.02254346109514431332, 0.02362027257428381960, 0.02415867831385357795, 0.02469708405342333629, 0.02577389553256286339, 0.02685070701170239049, 0.02738911275127214884, 0.02792751849084190024, 0.02900432996998139265, 0.03008114144912088506, 0.03115795292826037746, 0.03223476440739986987, 0.03331157588653935880, 0.03438838736567885468, 0.03546519884481834362, 0.03600360458438808114, 0.03654201032395781867, 0.03761882180309729373, 0.03869563328223677573 ),
 .UNSPECIFIED. ) ;
#62289 = CARTESIAN_POINT ( 'NONE',  ( -19.02544592524342804, 5.153800228976336051, 31.04057627198102409 ) ) ;
#62291 = CARTESIAN_POINT ( 'NONE',  ( -16.52544592524335698, -4.483927247898792601, 73.95942372801901854 ) ) ;
#62292 = CARTESIAN_POINT ( 'NONE',  ( 12.06949235617739724, 12.14591786802326823, 66.87609039468568994 ) ) ;
#62293 = CARTESIAN_POINT ( 'NONE',  ( -13.97604488694547697, 13.89961937509957934, 83.12609039468564731 ) ) ;
#62294 = CARTESIAN_POINT ( 'NONE',  ( 9.474510206698729675, 16.51473224551082808, 32.08442372801900433 ) ) ;
#62295 = CARTESIAN_POINT ( 'NONE',  ( -9.564922557960796823, -16.46253265017161027, 47.08224293864769550 ) ) ;
#62296 = CARTESIAN_POINT ( 'NONE',  ( 0.05219959533910956823, 16.53943276465976808, 84.99890960531436690 ) ) ;
#62297 = CARTESIAN_POINT ( 'NONE',  ( 16.51473224551083163, -9.474510206698727899, 55.83442372801899722 ) ) ;
#62298 = CARTESIAN_POINT ( 'NONE',  ( -10.72451020669898014, 18.67979575497178502, 45.41557627198103830 ) ) ;
#62299 = CARTESIAN_POINT ( 'NONE',  ( -5.153800228976607833, 19.02544592524334988, 32.70942372801899722 ) ) ;
#62300 = CARTESIAN_POINT ( 'NONE',  ( -16.51473224551069308, -9.474510206698971260, 101.6655762719810241 ) ) ;
#62301 = CARTESIAN_POINT ( 'NONE',  ( -5.719274019375978568, 21.55341960407610458, 75.20724293864769550 ) ) ;
#62302 = CARTESIAN_POINT ( 'NONE',  ( 19.03943276465977164, -0.05219959533909143690, 113.7489096053143669 ) ) ;
#62303 = CARTESIAN_POINT ( 'NONE',  ( 16.51473224551083163, -9.474510206698727899, 90.83442372801900433 ) ) ;
#62304 = CARTESIAN_POINT ( 'NONE',  ( 9.564922557960805705, 16.46253265017160317, 114.5822429386476955 ) ) ;
#62305 = CARTESIAN_POINT ( 'NONE',  ( 5.153800228976615827, -19.02544592524334988, 110.2094237280189901 ) ) ;
#62306 = CARTESIAN_POINT ( 'NONE',  ( 0.05219959533909260263, 19.03943276465977164, 34.99890960531435979 ) ) ;
#62307 = CARTESIAN_POINT ( 'NONE',  ( -13.97604488694527625, -13.89961937509977652, 91.87390960531432427 ) ) ;
#62308 = CARTESIAN_POINT ( 'NONE',  ( -21.55341960407610458, -5.719274019375992779, 71.45724293864769550 ) ) ;
#62309 = CARTESIAN_POINT ( 'NONE',  ( -0.05219959533934338120, 16.53943276465976808, 52.50109039468567573 ) ) ;
#62310 = CARTESIAN_POINT ( 'NONE',  ( 15.72974639402176855, 15.80617190586768217, 41.87609039468568284 ) ) ;
#62312 = CARTESIAN_POINT ( 'NONE',  ( 0.05219959533937995610, -21.53943276465977519, 95.00109039468568994 ) ) ;
#62311 = CARTESIAN_POINT ( 'NONE',  ( -5.153800228976607833, 19.02544592524334988, 87.70942372801897591 ) ) ;
#62313 = CARTESIAN_POINT ( 'NONE',  ( 14.34966873604972726, -8.224510206698740333, 105.8344237280190328 ) ) ;
#62314 = CARTESIAN_POINT ( 'NONE',  ( 19.03943276465977164, -0.05219959533909143690, 103.7489096053143669 ) ) ;
#62315 = CARTESIAN_POINT ( 'NONE',  ( 12.14591786802309770, 12.06949235617756955, 94.37390960531436690 ) ) ;
#62316 = CARTESIAN_POINT ( 'NONE',  ( 14.29746914071049879, -8.314922557960816363, 38.33224293864768839 ) ) ;
#62317 = CARTESIAN_POINT ( 'NONE',  ( 5.049401038297881783, 19.05341960407617563, 82.29275706135229029 ) ) ;
#62318 = CARTESIAN_POINT ( 'NONE',  ( 18.62759615963255655, 10.81492255796105972, 61.66775706135235424 ) ) ;
#62319 = CARTESIAN_POINT ( 'NONE',  ( -5.153800228976607833, 19.02544592524334988, 32.70942372801899722 ) ) ;
#62320 = CARTESIAN_POINT ( 'NONE',  ( -12.06949235617756955, 12.14591786802309770, 105.6239096053143669 ) ) ;
#62321 = CARTESIAN_POINT ( 'NONE',  ( 18.67979575497178502, 10.72451020669898547, 34.16557627198102409 ) ) ;
#62322 = CARTESIAN_POINT ( 'NONE',  ( 14.34966873604960469, 8.224510206698951720, 24.16557627198103120 ) ) ;
#62323 = CARTESIAN_POINT ( 'NONE',  ( -18.62759615963255300, -10.81492255796106328, 99.16775706135234714 ) ) ;
#62324 = CARTESIAN_POINT ( 'NONE',  ( 12.06949235617739724, 12.14591786802326823, 61.87609039468568284 ) ) ;
#62325 = CARTESIAN_POINT ( 'NONE',  ( -12.14591786802309592, -12.06949235617757132, 26.87390960531435979 ) ) ;
#62326 = CARTESIAN_POINT ( 'NONE',  ( 5.719274019375673035, 21.55341960407619339, 67.29275706135234714 ) ) ;
#62327 = CARTESIAN_POINT ( 'NONE',  ( -15.72974639402176322, -15.80617190586768395, 49.37609039468569705 ) ) ;
#62328 = EDGE_LOOP ( 'NONE', ( #92976, #89479, #28260, #33012, #118927, #39501, #199514, #130455, #59312, #52331, #84253, #24649 ) ) ;
#62329 = CARTESIAN_POINT ( 'NONE',  ( -18.22780087662121673, -5.500000000000062172, 61.48459894673894155 ) ) ;
#62330 = CARTESIAN_POINT ( 'NONE',  ( 15.80617190586769283, -15.72974639402175789, 25.62609039468567929 ) ) ;
#62331 = CARTESIAN_POINT ( 'NONE',  ( -16.55341960407611168, -4.379528057220339221, 101.4572429386476955 ) ) ;
#62332 = CARTESIAN_POINT ( 'NONE',  ( 0.05219959533909260263, 19.03943276465977164, 29.99890960531435979 ) ) ;
#62333 = CARTESIAN_POINT ( 'NONE',  ( -16.55341960407611168, -4.379528057220339221, 81.45724293864769550 ) ) ;
#62334 = CARTESIAN_POINT ( 'NONE',  ( 5.049401038298161559, -19.05341960407611168, 67.70724293864769550 ) ) ;
#62335 = CARTESIAN_POINT ( 'NONE',  ( -16.52544592524342804, 4.483927247898546575, 26.04057627198103475 ) ) ;
#62336 = CARTESIAN_POINT ( 'NONE',  ( -21.55341960407610458, -5.719274019375992779, 51.45724293864770260 ) ) ;
#62337 = CARTESIAN_POINT ( 'NONE',  ( -14.29746914071049879, 8.314922557960819915, 95.83224293864770971 ) ) ;
#62338 = CARTESIAN_POINT ( 'NONE',  ( -18.62759615963270932, 10.81492255796079327, 90.83224293864769550 ) ) ;
#62339 = CARTESIAN_POINT ( 'NONE',  ( -16.51473224551069308, -9.474510206698971260, 106.6655762719810383 ) ) ;
#62341 = CARTESIAN_POINT ( 'NONE',  ( 13.89961937509957401, 13.97604488694547697, 101.8760903946856331 ) ) ;
#62340 = CARTESIAN_POINT ( 'NONE',  ( -19.02544592524342804, 5.153800228976336051, 56.04057627198100988 ) ) ;
#62342 = EDGE_CURVE ( 'NONE', #50977, #122302, #88100, .T. ) ;
#62343 = CARTESIAN_POINT ( 'NONE',  ( -18.67979575497178146, -10.72451020669898902, 46.66557627198102409 ) ) ;
#62344 = CARTESIAN_POINT ( 'NONE',  ( 21.53943276465977519, 0.05219959533937863772, 81.25109039468568994 ) ) ;
#62345 = CARTESIAN_POINT ( 'NONE',  ( 19.03943276465977164, -0.05219959533909143690, 63.74890960531435979 ) ) ;
#62346 = CARTESIAN_POINT ( 'NONE',  ( -0.05219959533909027116, -19.03943276465977164, 97.49890960531436690 ) ) ;
#62347 = CARTESIAN_POINT ( 'NONE',  ( 16.53943276465976808, 0.05219959533934440121, 76.25109039468568994 ) ) ;
#62348 = CARTESIAN_POINT ( 'NONE',  ( -15.80617190586768217, 15.72974639402176855, 58.12609039468568994 ) ) ;
#62349 = CARTESIAN_POINT ( 'NONE',  ( -15.80617190586768217, 15.72974639402176855, 93.12609039468568994 ) ) ;
#62350 = CARTESIAN_POINT ( 'NONE',  ( -21.52544592524343514, 5.823673210054127303, 106.0405762719810525 ) ) ;
#62352 = CARTESIAN_POINT ( 'NONE',  ( 16.53943276465976808, 0.05219959533934440121, 76.25109039468568994 ) ) ;
#62351 = CARTESIAN_POINT ( 'NONE',  ( 15.80617190586769283, -15.72974639402175789, 40.62609039468567573 ) ) ;
#62353 = CARTESIAN_POINT ( 'NONE',  ( -15.72974639402197994, 15.80617190586746368, 75.62390960531439532 ) ) ;
#62354 = CARTESIAN_POINT ( 'NONE',  ( 0.05219959533936267826, -19.03943276465977164, 30.00109039468566863 ) ) ;
#62355 = CARTESIAN_POINT ( 'NONE',  ( 18.67979575497178502, 10.72451020669898547, 39.16557627198102409 ) ) ;
#62357 = CARTESIAN_POINT ( 'NONE',  ( -4.483927247898539470, -16.52544592524342804, 22.29057627198102765 ) ) ;
#62356 = CARTESIAN_POINT ( 'NONE',  ( -5.153800228976328057, -19.02544592524343514, 87.29057627198103830 ) ) ;
#62358 = CARTESIAN_POINT ( 'NONE',  ( -16.21995358207306737, 7.366697692864093483, 64.93551001512160781 ) ) ;
#62360 = AXIS2_PLACEMENT_3D ( 'NONE', #131048, #9724, #193745 ) ;
#62359 = CARTESIAN_POINT ( 'NONE',  ( 13.89961937509977652, -13.97604488694527269, 108.1239096053143669 ) ) ;
#62361 = CARTESIAN_POINT ( 'NONE',  ( 17.97058386085786097, 5.500000000000042633, 81.50390968646220813 ) ) ;
#62362 = CARTESIAN_POINT ( 'NONE',  ( 19.05341960407617918, -5.049401038297876454, 101.0427570613523045 ) ) ;
#62363 = CARTESIAN_POINT ( 'NONE',  ( 21.55341960407610458, 5.719274019375980345, 73.95724293864769550 ) ) ;
#62364 = CARTESIAN_POINT ( 'NONE',  ( 16.55341960407611168, 4.379528057220329451, 43.95724293864769550 ) ) ;
#62365 = CARTESIAN_POINT ( 'NONE',  ( -0.05219959533934338120, 16.53943276465976808, 22.50109039468567573 ) ) ;
#62366 = CARTESIAN_POINT ( 'NONE',  ( -9.564922557960796823, -16.46253265017161027, 32.08224293864769550 ) ) ;
#62367 = CARTESIAN_POINT ( 'NONE',  ( -14.29746914071037622, -8.314922557961029526, 19.16775706135234714 ) ) ;
#62369 = CARTESIAN_POINT ( 'NONE',  ( -19.05341960407617563, 5.049401038297882671, 68.54275706135230450 ) ) ;
#62368 = CARTESIAN_POINT ( 'NONE',  ( -21.55341960407610458, -5.719274019375992779, 96.45724293864770971 ) ) ;
#62370 = CARTESIAN_POINT ( 'NONE',  ( -16.53943276465976808, -0.05219959533934237506, 73.75109039468567573 ) ) ;
#62371 = CARTESIAN_POINT ( 'NONE',  ( -16.51473224551069308, -9.474510206698971260, 66.66557627198102409 ) ) ;
#62372 = CARTESIAN_POINT ( 'NONE',  ( 16.52544592524342804, -4.483927247898539470, 73.54057627198102409 ) ) ;
#62373 = CARTESIAN_POINT ( 'NONE',  ( -16.51473224551069308, -9.474510206698971260, 61.66557627198103120 ) ) ;
#62374 = CARTESIAN_POINT ( 'NONE',  ( 16.53943276465976808, -0.05219959533910856209, 68.74890960531435269 ) ) ;
#62375 = CARTESIAN_POINT ( 'NONE',  ( -0.05219959533909027116, -19.03943276465977164, 37.49890960531436690 ) ) ;
#62376 = CARTESIAN_POINT ( 'NONE',  ( -37.24135263299452703, -4.142047767899336819, 41.36355589474229788 ) ) ;
#62377 = CARTESIAN_POINT ( 'NONE',  ( 8.224510206698953496, -14.34966873604960469, 42.91557627198103120 ) ) ;
#62378 = CARTESIAN_POINT ( 'NONE',  ( 9.474510206698971260, -16.51473224551069308, 72.91557627198102409 ) ) ;
#62379 = CARTESIAN_POINT ( 'NONE',  ( -28.82186960331514669, -9.364793116373306248, 144.0999999999999659 ) ) ;
#62380 = CARTESIAN_POINT ( 'NONE',  ( -19.03943276465977164, -0.05219959533935918106, 53.75109039468566863 ) ) ;
#62381 = CARTESIAN_POINT ( 'NONE',  ( -8.224510206698735004, -14.34966873604973081, 59.58442372801901854 ) ) ;
#62382 = CARTESIAN_POINT ( 'NONE',  ( 15.80617190586746368, 15.72974639402197994, 64.37390960531435269 ) ) ;
#62383 = CARTESIAN_POINT ( 'NONE',  ( -0.05219959533936034679, 19.03943276465977164, 22.50109039468566152 ) ) ;
#62384 = CARTESIAN_POINT ( 'NONE',  ( 5.049401038298161559, -19.05341960407611168, 87.70724293864769550 ) ) ;
#62385 = CARTESIAN_POINT ( 'NONE',  ( -20.15954667362742825, -22.18921734867095452, -48.35113245326059683 ) ) ;
#62386 = CARTESIAN_POINT ( 'NONE',  ( 21.53943276465977519, -0.05219959533907433946, 23.74890960531435269 ) ) ;
#62387 = CARTESIAN_POINT ( 'NONE',  ( -9.564922557960796823, -16.46253265017161027, 62.08224293864769550 ) ) ;
#62388 = CARTESIAN_POINT ( 'NONE',  ( -15.80617190586768217, 15.72974639402176855, 53.12609039468568284 ) ) ;
#62389 = CARTESIAN_POINT ( 'NONE',  ( -12.06949235617756955, 12.14591786802309770, 105.6239096053143669 ) ) ;
#62392 = ORIENTED_EDGE ( 'NONE', *, *, #157116, .F. ) ;
#62391 = CARTESIAN_POINT ( 'NONE',  ( 0.05219959533909260263, 19.03943276465977164, 94.99890960531436690 ) ) ;
#62390 = CARTESIAN_POINT ( 'NONE',  ( -21.53943276465977519, 0.05219959533907696930, 106.2489096053143811 ) ) ;
#62393 = CARTESIAN_POINT ( 'NONE',  ( -10.72451020669870658, -18.67979575497194134, 39.58442372801901143 ) ) ;
#62394 = ORIENTED_EDGE ( 'NONE', *, *, #188637, .T. ) ;
#62395 = CARTESIAN_POINT ( 'NONE',  ( -0.05219959533909027116, -19.03943276465977164, 87.49890960531436690 ) ) ;
#62396 = CIRCLE ( 'NONE', #43092, 38.00000000000000000 ) ;
#62397 = CARTESIAN_POINT ( 'NONE',  ( 19.02130022317636460, -5.499999999999792166, 83.28188669246573284 ) ) ;
#62398 = CARTESIAN_POINT ( 'NONE',  ( 10.72451020669898902, -18.67979575497178502, 87.91557627198103830 ) ) ;
#62399 = CARTESIAN_POINT ( 'NONE',  ( -16.46253265017160317, 9.564922557960807481, 50.83224293864770260 ) ) ;
#62400 = CARTESIAN_POINT ( 'NONE',  ( -16.55341960407617563, 4.379528057220093196, 28.54275706135234358 ) ) ;
#62401 = CARTESIAN_POINT ( 'NONE',  ( -36.91746825000001309, 11.99521256947798342, -1.224999997268813035 ) ) ;
#62402 = CARTESIAN_POINT ( 'NONE',  ( -16.46253265017160317, 9.564922557960807481, 25.83224293864769194 ) ) ;
#62403 = CARTESIAN_POINT ( 'NONE',  ( -18.67979575497193778, 10.72451020669871902, 83.33442372801903275 ) ) ;
#62405 = CARTESIAN_POINT ( 'NONE',  ( 15.72974639402176855, 15.80617190586768217, 46.87609039468568994 ) ) ;
#62404 = CARTESIAN_POINT ( 'NONE',  ( -5.049401038298153566, 19.05341960407611168, 75.20724293864769550 ) ) ;
#62406 = CARTESIAN_POINT ( 'NONE',  ( 0.05219959533937995610, -21.53943276465977519, 30.00109039468568284 ) ) ;
#62407 = CARTESIAN_POINT ( 'NONE',  ( -27.73933785331498925, 9.013057229001089965, 147.2750000027311614 ) ) ;
#62408 = CARTESIAN_POINT ( 'NONE',  ( -13.89961937509977652, 13.97604488694528158, 100.6239096053143669 ) ) ;
#62409 = CARTESIAN_POINT ( 'NONE',  ( -10.11138388277261946, 26.74549871207304363, 140.0000000000000000 ) ) ;
#62412 = CARTESIAN_POINT ( 'NONE',  ( -15.80617190586768217, 15.72974639402176855, 48.12609039468568284 ) ) ;
#62411 = CARTESIAN_POINT ( 'NONE',  ( -4.379528057220086978, -16.55341960407618274, 64.79275706135234714 ) ) ;
#62410 = CARTESIAN_POINT ( 'NONE',  ( -8.314922557961024197, 14.29746914071037800, 37.91775706135235424 ) ) ;
#62413 = CARTESIAN_POINT ( 'NONE',  ( 21.52544592524334988, 5.823673210054432836, 76.45942372801901854 ) ) ;
#62414 = CARTESIAN_POINT ( 'NONE',  ( 4.884302457959432076, 6.795175062723209258, -62.06722337258344169 ) ) ;
#62415 = CARTESIAN_POINT ( 'NONE',  ( 16.55341960407618274, -4.379528057220086978, 21.04275706135234714 ) ) ;
#62416 = CARTESIAN_POINT ( 'NONE',  ( 13.97604488694527802, 13.89961937509977652, 64.37390960531436690 ) ) ;
#62417 = CARTESIAN_POINT ( 'NONE',  ( 9.474510206698971260, -16.51473224551069308, 97.91557627198102409 ) ) ;
#62418 = CARTESIAN_POINT ( 'NONE',  ( -8.314922557960811034, -14.29746914071050412, 112.0822429386477097 ) ) ;
#62419 = CARTESIAN_POINT ( 'NONE',  ( 8.314922557960818139, 14.29746914071049879, 99.58224293864770971 ) ) ;
#62420 = CARTESIAN_POINT ( 'NONE',  ( 5.823673210054125526, 21.52544592524343514, 29.79057627198102409 ) ) ;
#62421 = CARTESIAN_POINT ( 'NONE',  ( 4.379528057220092307, 16.55341960407617563, 82.29275706135234714 ) ) ;
#62423 = CARTESIAN_POINT ( 'NONE',  ( -16.51473224551069308, -9.474510206698971260, 51.66557627198102409 ) ) ;
#62422 = CARTESIAN_POINT ( 'NONE',  ( -14.34966873604960291, -8.224510206698953496, 71.66557627198100988 ) ) ;
#62424 = CARTESIAN_POINT ( 'NONE',  ( 21.55341960407619695, -5.719274019375665929, 71.04275706135234714 ) ) ;
#62425 = CARTESIAN_POINT ( 'NONE',  ( 5.823673210054444382, -21.52544592524334988, 70.20942372801904696 ) ) ;
#62426 = CARTESIAN_POINT ( 'NONE',  ( 5.049401038297881783, 19.05341960407617563, 107.2927570613523187 ) ) ;
#62427 = CARTESIAN_POINT ( 'NONE',  ( 4.483927247898545687, 16.52544592524342804, 79.79057627198102409 ) ) ;
#62428 = CARTESIAN_POINT ( 'NONE',  ( 5.719274019375673035, 21.55341960407619339, 32.29275706135235424 ) ) ;
#62429 = CARTESIAN_POINT ( 'NONE',  ( -18.62759615963270932, 10.81492255796079327, 55.83224293864770260 ) ) ;
#62430 = CARTESIAN_POINT ( 'NONE',  ( -17.48853670773244318, -5.747243402303109150, 106.3332870025001284 ) ) ;
#62431 = CARTESIAN_POINT ( 'NONE',  ( -8.906447517083060816, 27.41122689804195645, 143.8500000054623911 ) ) ;
#62432 = CARTESIAN_POINT ( 'NONE',  ( 13.97604488694527802, 13.89961937509977652, 69.37390960531436690 ) ) ;
#62433 = CARTESIAN_POINT ( 'NONE',  ( 12.14591786802309770, 12.06949235617756955, 49.37390960531436690 ) ) ;
#62434 = CARTESIAN_POINT ( 'NONE',  ( -16.55341960407611168, -4.379528057220339221, 26.45724293864768839 ) ) ;
#62435 = CARTESIAN_POINT ( 'NONE',  ( 14.29746914071037800, 8.314922557961029526, 101.6677570613523613 ) ) ;
#62436 = CARTESIAN_POINT ( 'NONE',  ( -0.05219959533936034679, 19.03943276465977164, 52.50109039468566863 ) ) ;
#62437 = CARTESIAN_POINT ( 'NONE',  ( 0.05219959533909260263, 19.03943276465977164, 104.9989096053143669 ) ) ;
#62438 = CARTESIAN_POINT ( 'NONE',  ( -4.483927247898539470, -16.52544592524342804, 72.29057627198102409 ) ) ;
#62439 = CARTESIAN_POINT ( 'NONE',  ( -13.97604488694547697, 13.89961937509957934, 43.12609039468566152 ) ) ;
#62441 = CARTESIAN_POINT ( 'NONE',  ( 5.823673210054125526, 21.52544592524343514, 34.79057627198103120 ) ) ;
#62440 = CARTESIAN_POINT ( 'NONE',  ( 16.46253265017160672, -9.564922557960803928, 38.33224293864768839 ) ) ;
#62443 = ORIENTED_EDGE ( 'NONE', *, *, #75323, .T. ) ;
#62442 = CARTESIAN_POINT ( 'NONE',  ( 21.53943276465977519, -0.05219959533907433946, 53.74890960531437401 ) ) ;
#62444 = CARTESIAN_POINT ( 'NONE',  ( 0.05219959533910956823, 16.53943276465976808, 104.9989096053143669 ) ) ;
#62445 = CARTESIAN_POINT ( 'NONE',  ( -4.379528057220086978, -16.55341960407618274, 54.79275706135235424 ) ) ;
#62446 = CARTESIAN_POINT ( 'NONE',  ( -14.29746914071049879, 8.314922557960819915, 90.83224293864769550 ) ) ;
#62447 = EDGE_CURVE ( 'NONE', #30776, #61770, #182308, .T. ) ;
#62448 = CARTESIAN_POINT ( 'NONE',  ( -26.46959431505279881, -27.26463967846491698, -11.49588912907431393 ) ) ;
#62449 = CARTESIAN_POINT ( 'NONE',  ( -5.950531402560715689E-15, 38.81732327939063509, -9.624999997268815832 ) ) ;
#62450 = CARTESIAN_POINT ( 'NONE',  ( 18.62759615963271287, -10.81492255796078972, 23.33224293864769194 ) ) ;
#62451 = DIRECTION ( 'NONE',  ( 1.000000000000000000, 0.000000000000000000, 0.000000000000000000 ) ) ;
#62452 = PLANE ( 'NONE',  #89925 ) ;
#62453 = ORIENTED_EDGE ( 'NONE', *, *, #189014, .F. ) ;
#62455 = CARTESIAN_POINT ( 'NONE',  ( 12.14591786802309770, 12.06949235617756955, 24.37390960531435979 ) ) ;
#62454 = CARTESIAN_POINT ( 'NONE',  ( -12.06949235617739369, -12.14591786802326823, 39.37609039468567573 ) ) ;
#62456 = CARTESIAN_POINT ( 'NONE',  ( -21.53943276465977519, 0.05219959533907696930, 56.24890960531436690 ) ) ;
#62458 = CARTESIAN_POINT ( 'NONE',  ( -16.51473224551082808, 9.474510206698731452, 78.33442372801900433 ) ) ;
#62457 = AXIS2_PLACEMENT_3D ( 'NONE', #135298, #184765, #92737 ) ;
#62459 = CARTESIAN_POINT ( 'NONE',  ( 5.823673210054125526, 21.52544592524343514, 64.79057627198103830 ) ) ;
#62460 = CARTESIAN_POINT ( 'NONE',  ( -10.81492255796105439, 18.62759615963255655, 87.91775706135234714 ) ) ;
#62461 = CARTESIAN_POINT ( 'NONE',  ( -12.24387616833797843, 10.52174046232662619, -61.59812483265029925 ) ) ;
#62462 = CARTESIAN_POINT ( 'NONE',  ( -8.314922557961024197, 14.29746914071037800, 47.91775706135234714 ) ) ;
#62464 = CARTESIAN_POINT ( 'NONE',  ( 9.564922557960805705, 16.46253265017160317, 99.58224293864770971 ) ) ;
#62463 = CARTESIAN_POINT ( 'NONE',  ( -16.46253265017160317, 9.564922557960807481, 30.83224293864769550 ) ) ;
#62465 = CARTESIAN_POINT ( 'NONE',  ( 19.03943276465977164, -0.05219959533909143690, 38.74890960531436690 ) ) ;
#62467 = ADVANCED_FACE ( 'NONE', ( #49524 ), #113171, .T. ) ;
#62466 = CARTESIAN_POINT ( 'NONE',  ( 4.379528057220339221, -16.55341960407611168, 107.7072429386476955 ) ) ;
#62468 = DIRECTION ( 'NONE',  ( 1.000000000000000000, 0.000000000000000000, 0.000000000000000000 ) ) ;
#62469 = CARTESIAN_POINT ( 'NONE',  ( 13.97604488694527802, 13.89961937509977652, 99.37390960531436690 ) ) ;
#62470 = ORIENTED_EDGE ( 'NONE', *, *, #142804, .F. ) ;
#62471 = CARTESIAN_POINT ( 'NONE',  ( 0.05219959533934541429, -16.53943276465976808, 70.00109039468568994 ) ) ;
#62472 = CARTESIAN_POINT ( 'NONE',  ( -5.823673210054116645, -21.52544592524344225, 92.29057627198103830 ) ) ;
#62473 = CARTESIAN_POINT ( 'NONE',  ( 13.89961937509977652, -13.97604488694527269, 53.12390960531434558 ) ) ;
#62474 = CARTESIAN_POINT ( 'NONE',  ( 10.72451020669871369, 18.67979575497193778, 22.08442372801901143 ) ) ;
#62475 = CARTESIAN_POINT ( 'NONE',  ( -9.474510206698964154, 16.51473224551069663, 85.41557627198102409 ) ) ;
#62476 = CARTESIAN_POINT ( 'NONE',  ( -34.32499373855440439, -22.49325299168063452, -18.44817765300819445 ) ) ;
#62477 = ORIENTED_EDGE ( 'NONE', *, *, #129099, .F. ) ;
#62478 = CARTESIAN_POINT ( 'NONE',  ( 21.55341960407610458, 5.719274019375980345, 113.9572429386477239 ) ) ;
#62481 = CARTESIAN_POINT ( 'NONE',  ( 16.51473224551083163, -9.474510206698727899, 70.83442372801900433 ) ) ;
#62480 = CARTESIAN_POINT ( 'NONE',  ( 19.03943276465977164, -0.05219959533909143690, 103.7489096053143669 ) ) ;
#62479 = CARTESIAN_POINT ( 'NONE',  ( -19.03943276465977164, 0.05219959533909376836, 26.24890960531435624 ) ) ;
#62482 = CARTESIAN_POINT ( 'NONE',  ( -5.153800228976607833, 19.02544592524334988, 27.70942372801899722 ) ) ;
#62483 = CARTESIAN_POINT ( 'NONE',  ( 15.72974639402199770, -15.80617190586745480, 98.12390960531436690 ) ) ;
#62484 = CARTESIAN_POINT ( 'NONE',  ( 19.05341960407617918, -5.049401038297876454, 41.04275706135233293 ) ) ;
#62485 = CARTESIAN_POINT ( 'NONE',  ( 4.483927247898790824, -16.52544592524335698, 75.20942372801901854 ) ) ;
#62487 = ORIENTED_EDGE ( 'NONE', *, *, #116810, .T. ) ;
#62486 = CARTESIAN_POINT ( 'NONE',  ( 16.51473224551069308, 9.474510206698969483, 104.1655762719810241 ) ) ;
#62488 = CARTESIAN_POINT ( 'NONE',  ( 13.89961937509977652, -13.97604488694527269, 63.12390960531435979 ) ) ;
#62489 = CARTESIAN_POINT ( 'NONE',  ( -10.72451020669870658, -18.67979575497194134, 59.58442372801901854 ) ) ;
#62490 = CARTESIAN_POINT ( 'NONE',  ( 10.81492255796106328, -18.62759615963255655, 80.41775706135234714 ) ) ;
#62491 = CARTESIAN_POINT ( 'NONE',  ( 5.049401038298161559, -19.05341960407611168, 77.70724293864765286 ) ) ;
#62492 = CARTESIAN_POINT ( 'NONE',  ( -0.05219959533937732626, 21.53943276465977519, 42.50109039468567573 ) ) ;
#62493 = CARTESIAN_POINT ( 'NONE',  ( -0.05219959533936034679, 19.03943276465977164, 92.50109039468566152 ) ) ;
#62494 = CARTESIAN_POINT ( 'NONE',  ( -13.97604488694527625, -13.89961937509977652, 46.87390960531435979 ) ) ;
#62495 = CARTESIAN_POINT ( 'NONE',  ( 5.153800228976335163, 19.02544592524342804, 99.79057627198102409 ) ) ;
#62496 = CARTESIAN_POINT ( 'NONE',  ( -19.02544592524342804, 5.153800228976336051, 66.04057627198103830 ) ) ;
#62497 = CARTESIAN_POINT ( 'NONE',  ( -19.03943276465977164, 0.05219959533909376836, 111.2489096053143669 ) ) ;
#62499 = ADVANCED_FACE ( 'NONE', ( #18204 ), #66706, .F. ) ;
#62498 = CARTESIAN_POINT ( 'NONE',  ( -5.049401038298153566, 19.05341960407611168, 50.20724293864770260 ) ) ;
#62500 = CARTESIAN_POINT ( 'NONE',  ( 10.72451020669898902, -18.67979575497178502, 102.9155762719810383 ) ) ;
#62501 = CARTESIAN_POINT ( 'NONE',  ( 12.14591786802327356, -12.06949235617739191, 80.62609039468567573 ) ) ;
#62502 = CARTESIAN_POINT ( 'NONE',  ( -24.86035471869041302, 4.680034064337904809, 169.8578160361100799 ) ) ;
#62503 = CARTESIAN_POINT ( 'NONE',  ( -13.97604488694547697, 13.89961937509957934, 38.12609039468566152 ) ) ;
#62504 = CARTESIAN_POINT ( 'NONE',  ( 16.51473224551069308, 9.474510206698969483, 64.16557627198102409 ) ) ;
#62505 = CARTESIAN_POINT ( 'NONE',  ( 12.06949235617757843, -12.14591786802309237, 58.12390960531435979 ) ) ;
#62506 = CARTESIAN_POINT ( 'NONE',  ( 12.06949235617757843, -12.14591786802309237, 98.12390960531436690 ) ) ;
#62507 = CARTESIAN_POINT ( 'NONE',  ( -16.46253265017160317, 9.564922557960807481, 95.83224293864769550 ) ) ;
#62508 = CARTESIAN_POINT ( 'NONE',  ( -19.03943276465977164, 0.05219959533909376836, 86.24890960531436690 ) ) ;
#62509 = CARTESIAN_POINT ( 'NONE',  ( 13.97604488694527802, 13.89961937509977652, 104.3739096053143385 ) ) ;
#62510 = CARTESIAN_POINT ( 'NONE',  ( -0.05219959533937732626, 21.53943276465977519, 107.5010903946856899 ) ) ;
#62511 = CARTESIAN_POINT ( 'NONE',  ( -16.53943276465976808, -0.05219959533934237506, 93.75109039468567573 ) ) ;
#62512 = CARTESIAN_POINT ( 'NONE',  ( 9.564922557960805705, 16.46253265017160317, 74.58224293864769550 ) ) ;
#62513 = CARTESIAN_POINT ( 'NONE',  ( -18.67979575497193778, 10.72451020669871902, 33.33442372801900433 ) ) ;
#62514 = CARTESIAN_POINT ( 'NONE',  ( -21.53943276465977519, 0.05219959533907696930, 36.24890960531435979 ) ) ;
#62515 = CARTESIAN_POINT ( 'NONE',  ( -10.81492255796078084, -18.62759615963271287, 102.0822429386476955 ) ) ;
#62516 = CARTESIAN_POINT ( 'NONE',  ( 14.34966873604960469, 8.224510206698951720, 59.16557627198103120 ) ) ;
#62517 = CARTESIAN_POINT ( 'NONE',  ( 19.03943276465977164, -0.05219959533909143690, 48.74890960531435979 ) ) ;
#62518 = CARTESIAN_POINT ( 'NONE',  ( 8.314922557960818139, 14.29746914071049879, 84.58224293864769550 ) ) ;
#62519 = CARTESIAN_POINT ( 'NONE',  ( -5.049401038297874678, -19.05341960407617918, 44.79275706135232582 ) ) ;
#62520 = CARTESIAN_POINT ( 'NONE',  ( 19.02544592524343514, -5.153800228976328945, 23.54057627198102054 ) ) ;
#62521 = CARTESIAN_POINT ( 'NONE',  ( -4.379528057220086978, -16.55341960407618274, 69.79275706135234714 ) ) ;
#62522 = CARTESIAN_POINT ( 'NONE',  ( -5.153800228976328057, -19.02544592524343514, 87.29057627198103830 ) ) ;
#62523 = CARTESIAN_POINT ( 'NONE',  ( 17.14385361876520264, 23.59649016807275856, 144.1750000027311671 ) ) ;
#62524 = CARTESIAN_POINT ( 'NONE',  ( 8.314922557960818139, 14.29746914071049879, 104.5822429386477097 ) ) ;
#62525 = CARTESIAN_POINT ( 'NONE',  ( 5.823673210054125526, 21.52544592524343514, 39.79057627198103830 ) ) ;
#62526 = EDGE_LOOP ( 'NONE', ( #85864, #50307, #158845, #194292, #76344, #136549, #199692, #6762 ) ) ;
#62527 = CARTESIAN_POINT ( 'NONE',  ( 16.52544592524335698, 4.483927247898782831, 106.4594237280190328 ) ) ;
#62528 = CARTESIAN_POINT ( 'NONE',  ( 8.224510206698742110, 14.34966873604972548, 32.08442372801901854 ) ) ;
#62529 = CARTESIAN_POINT ( 'NONE',  ( -18.67979575497193778, 10.72451020669871902, 88.33442372801901854 ) ) ;
#62530 = CARTESIAN_POINT ( 'NONE',  ( 16.46253265017160672, -9.564922557960803928, 93.33224293864769550 ) ) ;
#62531 = CARTESIAN_POINT ( 'NONE',  ( -18.62759615963270932, 10.81492255796079327, 115.8322429386477097 ) ) ;
#62532 = CARTESIAN_POINT ( 'NONE',  ( 9.564922557960805705, 16.46253265017160317, 24.58224293864769194 ) ) ;
#62533 = CARTESIAN_POINT ( 'NONE',  ( 0.05219959533934541429, -16.53943276465976808, 30.00109039468568284 ) ) ;
#62534 = CARTESIAN_POINT ( 'NONE',  ( 19.03943276465977164, 0.05219959533936151252, 91.25109039468566152 ) ) ;
#62535 = AXIS2_PLACEMENT_3D ( 'NONE', #12539, #180406, #193562 ) ;
#62536 = CARTESIAN_POINT ( 'NONE',  ( -21.52544592524343514, 5.823673210054127303, 86.04057627198102409 ) ) ;
#62537 = CARTESIAN_POINT ( 'NONE',  ( -9.564922557961040184, 16.46253265017147172, 67.91775706135233293 ) ) ;
#62538 = CARTESIAN_POINT ( 'NONE',  ( -5.153800228976328057, -19.02544592524343514, 22.29057627198102765 ) ) ;
#62539 = CARTESIAN_POINT ( 'NONE',  ( 15.72974639402176855, 15.80617190586768217, 21.87609039468567573 ) ) ;
#62540 = CARTESIAN_POINT ( 'NONE',  ( -9.564922557960796823, -16.46253265017161027, 72.08224293864770971 ) ) ;
#62541 = CARTESIAN_POINT ( 'NONE',  ( -19.03943276465977164, 0.05219959533909376836, 96.24890960531436690 ) ) ;
#62542 = CARTESIAN_POINT ( 'NONE',  ( 4.379528057220092307, 16.55341960407617563, 27.29275706135234358 ) ) ;
#62543 = CARTESIAN_POINT ( 'NONE',  ( -23.48298174826590667, 32.32155151706776053, -6.302157773949822683 ) ) ;
#62544 = CARTESIAN_POINT ( 'NONE',  ( -13.89961937509957401, -13.97604488694547875, 59.37609039468566863 ) ) ;
#62546 = CARTESIAN_POINT ( 'NONE',  ( 14.34966873604960469, 8.224510206698951720, 79.16557627198103830 ) ) ;
#62545 = CARTESIAN_POINT ( 'NONE',  ( -21.53943276465977519, -0.05219959533937600094, 18.75109039468568639 ) ) ;
#62547 = CARTESIAN_POINT ( 'NONE',  ( 19.02544592524343514, -5.153800228976328945, 88.54057627198102409 ) ) ;
#62549 = CARTESIAN_POINT ( 'NONE',  ( -5.049401038297874678, -19.05341960407617918, 54.79275706135234003 ) ) ;
#62548 = CARTESIAN_POINT ( 'NONE',  ( 14.34966873604972726, -8.224510206698740333, 50.83442372801901143 ) ) ;
#62550 = CARTESIAN_POINT ( 'NONE',  ( -10.72451020669870658, -18.67979575497194134, 69.58442372801900433 ) ) ;
#62551 = CARTESIAN_POINT ( 'NONE',  ( 16.53943276465976808, 0.05219959533934440121, 31.25109039468568639 ) ) ;
#62552 = CARTESIAN_POINT ( 'NONE',  ( 19.03943276465977164, -0.05219959533909143690, 73.74890960531435269 ) ) ;
#62553 = CARTESIAN_POINT ( 'NONE',  ( 13.89961937509957401, 13.97604488694547697, 81.87609039468564731 ) ) ;
#62554 = CARTESIAN_POINT ( 'NONE',  ( 14.34966873604972726, -8.224510206698740333, 55.83442372801901854 ) ) ;
#62555 = CARTESIAN_POINT ( 'NONE',  ( 18.62759615963255655, 10.81492255796105972, 91.66775706135234714 ) ) ;
#62556 = CARTESIAN_POINT ( 'NONE',  ( 9.474510206698729675, 16.51473224551082808, 67.08442372801900433 ) ) ;
#62557 = CARTESIAN_POINT ( 'NONE',  ( -5.049401038298153566, 19.05341960407611168, 50.20724293864770260 ) ) ;
#62558 = CARTESIAN_POINT ( 'NONE',  ( -18.62759615963270932, 10.81492255796079327, 70.83224293864770971 ) ) ;
#62560 = CARTESIAN_POINT ( 'NONE',  ( 16.51473224551083163, -9.474510206698727899, 80.83442372801899012 ) ) ;
#62559 = CARTESIAN_POINT ( 'NONE',  ( 0.05219959533910956823, 16.53943276465976808, 59.99890960531436690 ) ) ;
#62561 = CARTESIAN_POINT ( 'NONE',  ( 16.20579543436675962, -7.371946100355160958, 61.93479165828127009 ) ) ;
#62562 = CARTESIAN_POINT ( 'NONE',  ( -13.97604488694547697, 13.89961937509957934, 43.12609039468566152 ) ) ;
#62563 = CARTESIAN_POINT ( 'NONE',  ( -12.06949235617739369, -12.14591786802326823, 104.3760903946856899 ) ) ;
#62564 = CARTESIAN_POINT ( 'NONE',  ( -16.52544592524342804, 4.483927247898546575, 66.04057627198103830 ) ) ;
#62566 = CARTESIAN_POINT ( 'NONE',  ( -8.571926809382608425, 26.38167802310805854, 148.4750000027311785 ) ) ;
#62565 = CARTESIAN_POINT ( 'NONE',  ( -18.62759615963255300, -10.81492255796106328, 99.16775706135234714 ) ) ;
#62567 = CARTESIAN_POINT ( 'NONE',  ( 15.80617190586746368, 15.72974639402197994, 99.37390960531436690 ) ) ;
#62568 = CARTESIAN_POINT ( 'NONE',  ( 13.97604488694527802, 13.89961937509977652, 59.37390960531434558 ) ) ;
#62569 = CARTESIAN_POINT ( 'NONE',  ( 21.52544592524334988, 5.823673210054432836, 76.45942372801901854 ) ) ;
#62570 = CARTESIAN_POINT ( 'NONE',  ( 13.89961937509977652, -13.97604488694527269, 48.12390960531435979 ) ) ;
#62571 = CARTESIAN_POINT ( 'NONE',  ( -13.97604488694527625, -13.89961937509977652, 26.87390960531434558 ) ) ;
#62572 = CARTESIAN_POINT ( 'NONE',  ( -19.05341960407611168, -5.049401038298163336, 111.4572429386476671 ) ) ;
#62573 = CARTESIAN_POINT ( 'NONE',  ( -16.53943276465976808, 0.05219959533911058130, 66.24890960531436690 ) ) ;
#62574 = CARTESIAN_POINT ( 'NONE',  ( 19.03943276465977164, -0.05219959533909143690, 23.74890960531435269 ) ) ;
#62575 = CARTESIAN_POINT ( 'NONE',  ( -4.379528057220328563, 16.55341960407611168, 85.20724293864770971 ) ) ;
#62576 = CARTESIAN_POINT ( 'NONE',  ( -5.823673210054116645, -21.52544592524344225, 97.29057627198105251 ) ) ;
#62577 = EDGE_CURVE ( 'NONE', #58799, #11425, #15054, .T. ) ;
#62578 = CARTESIAN_POINT ( 'NONE',  ( 18.62759615963255655, 10.81492255796105972, 36.66775706135234714 ) ) ;
#62579 = CARTESIAN_POINT ( 'NONE',  ( 27.88129983271663903, -6.733757357602863536, 162.1517353552116560 ) ) ;
#62580 = CARTESIAN_POINT ( 'NONE',  ( -16.53943276465976808, -0.05219959533934237506, 53.75109039468568994 ) ) ;
#62581 = CARTESIAN_POINT ( 'NONE',  ( -21.52544592524343514, 5.823673210054127303, 81.04057627198102409 ) ) ;
#62582 = CARTESIAN_POINT ( 'NONE',  ( -13.97604488694547697, 13.89961937509957934, 28.12609039468565797 ) ) ;
#62583 = CARTESIAN_POINT ( 'NONE',  ( 16.46253265017160672, -9.564922557960803928, 108.3322429386476955 ) ) ;
#62584 = CARTESIAN_POINT ( 'NONE',  ( -5.823673210054431948, 21.52544592524334988, 42.70942372801901854 ) ) ;
#62585 = CARTESIAN_POINT ( 'NONE',  ( -21.53943276465977519, 0.05219959533907696930, 46.24890960531435979 ) ) ;
#62586 = CARTESIAN_POINT ( 'NONE',  ( 8.224510206698953496, -14.34966873604960469, 22.91557627198102765 ) ) ;
#62588 = CARTESIAN_POINT ( 'NONE',  ( 21.55341960407619695, -5.719274019375665929, 96.04275706135236135 ) ) ;
#62587 = CARTESIAN_POINT ( 'NONE',  ( 21.55341960407619695, -5.719274019375665929, 66.04275706135236135 ) ) ;
#62589 = CARTESIAN_POINT ( 'NONE',  ( -13.97604488694547697, 13.89961937509957934, 33.12609039468566863 ) ) ;
#62590 = CARTESIAN_POINT ( 'NONE',  ( 4.379528057220092307, 16.55341960407617563, 92.29275706135236135 ) ) ;
#62591 = CARTESIAN_POINT ( 'NONE',  ( -15.72974639402176322, -15.80617190586768395, 54.37609039468568994 ) ) ;
#62592 = CARTESIAN_POINT ( 'NONE',  ( -16.51473224551069308, -9.474510206698971260, 51.66557627198102409 ) ) ;
#62593 = CARTESIAN_POINT ( 'NONE',  ( 13.97604488694548053, -13.89961937509957401, 20.62609039468567573 ) ) ;
#62594 = CARTESIAN_POINT ( 'NONE',  ( -10.81492255796078084, -18.62759615963271287, 27.08224293864769550 ) ) ;
#62595 = CARTESIAN_POINT ( 'NONE',  ( -21.55341960407619339, 5.719274019375674811, 23.54275706135235424 ) ) ;
#62596 = CARTESIAN_POINT ( 'NONE',  ( -5.719274019375978568, 21.55341960407610458, 75.20724293864769550 ) ) ;
#62597 = CARTESIAN_POINT ( 'NONE',  ( -14.34966873604972548, 8.224510206698743886, 38.33442372801900433 ) ) ;
#62599 = CARTESIAN_POINT ( 'NONE',  ( 21.55341960407610458, 5.719274019375980345, 73.95724293864769550 ) ) ;
#62598 = CARTESIAN_POINT ( 'NONE',  ( -193.3062444957834884, -155.7167183371838064, -25.00000000000000000 ) ) ;
#62601 = CARTESIAN_POINT ( 'NONE',  ( -16.52544592524342804, 4.483927247898546575, 66.04057627198103830 ) ) ;
#62600 = CARTESIAN_POINT ( 'NONE',  ( -12.14591786802326823, 12.06949235617739902, 68.12609039468567573 ) ) ;
#62602 = CARTESIAN_POINT ( 'NONE',  ( -27.12243378312308195, -3.972435522077939929, 169.3718635229810729 ) ) ;
#62603 = CARTESIAN_POINT ( 'NONE',  ( -19.03943276465977164, -0.05219959533935918106, 98.75109039468567573 ) ) ;
#62604 = CARTESIAN_POINT ( 'NONE',  ( -23.87412888849583936, 1.051486528467328041, -54.54543624665774360 ) ) ;
#62605 = CARTESIAN_POINT ( 'NONE',  ( -8.224510206698735004, -14.34966873604973081, 39.58442372801901143 ) ) ;
#62606 = CARTESIAN_POINT ( 'NONE',  ( -15.72974639402197994, 15.80617190586746368, 105.6239096053143669 ) ) ;
#62607 = CARTESIAN_POINT ( 'NONE',  ( -21.55341960407610458, -5.719274019375992779, 26.45724293864768839 ) ) ;
#62608 = CARTESIAN_POINT ( 'NONE',  ( 0.05219959533934541429, -16.53943276465976808, 60.00109039468568284 ) ) ;
#62609 = CARTESIAN_POINT ( 'NONE',  ( 13.89961937509977652, -13.97604488694527269, 73.12390960531436690 ) ) ;
#62611 = CARTESIAN_POINT ( 'NONE',  ( -0.05219959533934338120, 16.53943276465976808, 22.50109039468567573 ) ) ;
#62610 = CARTESIAN_POINT ( 'NONE',  ( 18.67979575497194134, -10.72451020669871369, 40.83442372801901854 ) ) ;
#62612 = EDGE_CURVE ( 'NONE', #118125, #8593, #5354, .T. ) ;
#62613 = CARTESIAN_POINT ( 'NONE',  ( -21.52544592524343514, 5.823673210054127303, 31.04057627198102409 ) ) ;
#62614 = CARTESIAN_POINT ( 'NONE',  ( -16.51473224551082808, 9.474510206698731452, 23.33442372801900078 ) ) ;
#62615 = CARTESIAN_POINT ( 'NONE',  ( 14.29746914071037800, 8.314922557961029526, 41.66775706135235424 ) ) ;
#62616 = CARTESIAN_POINT ( 'NONE',  ( -13.97604488694527625, -13.89961937509977652, 106.8739096053143669 ) ) ;
#62617 = CARTESIAN_POINT ( 'NONE',  ( -18.67979575497178146, -10.72451020669898902, 96.66557627198102409 ) ) ;
#62618 = CARTESIAN_POINT ( 'NONE',  ( 13.97604488694527802, 13.89961937509977652, 69.37390960531436690 ) ) ;
#62619 = CARTESIAN_POINT ( 'NONE',  ( -17.44279575226823198, 5.990770900252464060, 25.83557567514319686 ) ) ;
#62620 = CARTESIAN_POINT ( 'NONE',  ( 8.314922557960818139, 14.29746914071049879, 84.58224293864769550 ) ) ;
#62621 = CARTESIAN_POINT ( 'NONE',  ( -9.564922557960796823, -16.46253265017161027, 112.0822429386476955 ) ) ;
#62622 = DIRECTION ( 'NONE',  ( 0.000000000000000000, 0.000000000000000000, 1.000000000000000000 ) ) ;
#62623 = CARTESIAN_POINT ( 'NONE',  ( -12.14591786802326823, 12.06949235617739902, 68.12609039468567573 ) ) ;
#62624 = CARTESIAN_POINT ( 'NONE',  ( 15.80617190586746368, 15.72974639402197994, 109.3739096053143811 ) ) ;
#62625 = CARTESIAN_POINT ( 'NONE',  ( -13.97604488694547697, 13.89961937509957934, 68.12609039468563310 ) ) ;
#62627 = EDGE_CURVE ( 'NONE', #87358, #84042, #144207, .T. ) ;
#62626 = CARTESIAN_POINT ( 'NONE',  ( -5.823673210054116645, -21.52544592524344225, 27.29057627198103120 ) ) ;
#62628 = CARTESIAN_POINT ( 'NONE',  ( 9.564922557960805705, 16.46253265017160317, 24.58224293864769194 ) ) ;
#62629 = CARTESIAN_POINT ( 'NONE',  ( 21.55341960407610458, 5.719274019375980345, 73.95724293864769550 ) ) ;
#62630 = VECTOR ( 'NONE', #92032, 1000.000000000000000 ) ;
#62631 = CARTESIAN_POINT ( 'NONE',  ( -0.05219959533909027116, -19.03943276465977164, 102.4989096053143669 ) ) ;
#62632 = CARTESIAN_POINT ( 'NONE',  ( 5.823673210054444382, -21.52544592524334988, 90.20942372801903275 ) ) ;
#62633 = CARTESIAN_POINT ( 'NONE',  ( 19.02544592524343514, -5.153800228976328945, 48.54057627198103120 ) ) ;
#62634 = CARTESIAN_POINT ( 'NONE',  ( 16.55341960407611168, 4.379528057220329451, 88.95724293864769550 ) ) ;
#62635 = CARTESIAN_POINT ( 'NONE',  ( -16.53943276465976808, -0.05219959533934237506, 38.75109039468567573 ) ) ;
#62636 = CARTESIAN_POINT ( 'NONE',  ( 19.05341960407611168, 5.049401038298154454, 58.95724293864768129 ) ) ;
#62637 = CARTESIAN_POINT ( 'NONE',  ( -18.62759615963255300, -10.81492255796106328, 74.16775706135231871 ) ) ;
#62638 = ORIENTED_EDGE ( 'NONE', *, *, #135320, .F. ) ;
#62639 = CARTESIAN_POINT ( 'NONE',  ( 0.05219959533936267826, -19.03943276465977164, 45.00109039468566863 ) ) ;
#62640 = CARTESIAN_POINT ( 'NONE',  ( 19.05341960407617918, -5.049401038297876454, 41.04275706135233293 ) ) ;
#62641 = CARTESIAN_POINT ( 'NONE',  ( -5.823673210054431948, 21.52544592524334988, 42.70942372801901854 ) ) ;
#62642 = CARTESIAN_POINT ( 'NONE',  ( -6.404810000729013630, 0.9277198534073001213, -62.44539631020982284 ) ) ;
#62643 = CARTESIAN_POINT ( 'NONE',  ( 19.03943276465977164, 0.05219959533936151252, 26.25109039468566507 ) ) ;
#62644 = CARTESIAN_POINT ( 'NONE',  ( -16.51473224551069308, -9.474510206698971260, 81.66557627198103830 ) ) ;
#62645 = CARTESIAN_POINT ( 'NONE',  ( 5.049401038298161559, -19.05341960407611168, 72.70724293864768129 ) ) ;
#62646 = CARTESIAN_POINT ( 'NONE',  ( -14.29746914071049879, 8.314922557960819915, 25.83224293864769194 ) ) ;
#62648 = CARTESIAN_POINT ( 'NONE',  ( 10.72451020669871369, 18.67979575497193778, 82.08442372801901854 ) ) ;
#62647 = CARTESIAN_POINT ( 'NONE',  ( -15.80617190586745835, -15.72974639402198527, 26.87390960531435979 ) ) ;
#62649 = CARTESIAN_POINT ( 'NONE',  ( 36.91746824999999177, 2.880721459617395097E-14, -1.624999997268813390 ) ) ;
#62650 = CARTESIAN_POINT ( 'NONE',  ( -3.573655867282028392E-15, 2.428612866367529932E-14, 165.8682408883346397 ) ) ;
#62651 = CARTESIAN_POINT ( 'NONE',  ( 18.67979575497194134, -10.72451020669871369, 100.8344237280190185 ) ) ;
#62652 = CARTESIAN_POINT ( 'NONE',  ( -3.573655867282028392E-15, 2.428612866367529932E-14, 165.8682408883346397 ) ) ;
#62653 = CARTESIAN_POINT ( 'NONE',  ( 16.51473224551069308, 9.474510206698969483, 114.1655762719810241 ) ) ;
#62654 = CARTESIAN_POINT ( 'NONE',  ( -25.79025989231046623, -10.69883710965550527, 166.5180000355201742 ) ) ;
#62655 = CARTESIAN_POINT ( 'NONE',  ( -8.224510206698735004, -14.34966873604973081, 49.58442372801901143 ) ) ;
#62656 = CARTESIAN_POINT ( 'NONE',  ( -21.53943276465977519, 0.05219959533907696930, 76.24890960531435269 ) ) ;
#62657 = CARTESIAN_POINT ( 'NONE',  ( 8.224510206698953496, -14.34966873604960469, 27.91557627198103830 ) ) ;
#62659 = CARTESIAN_POINT ( 'NONE',  ( 9.474510206698971260, -16.51473224551069308, 97.91557627198102409 ) ) ;
#62658 = CARTESIAN_POINT ( 'NONE',  ( -16.51473224551069308, -9.474510206698971260, 21.66557627198102765 ) ) ;
#62660 = CARTESIAN_POINT ( 'NONE',  ( -13.89961937509957401, -13.97604488694547875, 19.37609039468566507 ) ) ;
#62661 = CARTESIAN_POINT ( 'NONE',  ( -5.153800228976328057, -19.02544592524343514, 22.29057627198102765 ) ) ;
#62662 = CARTESIAN_POINT ( 'NONE',  ( -15.72974639402176322, -15.80617190586768395, 64.37609039468568994 ) ) ;
#62663 = CARTESIAN_POINT ( 'NONE',  ( 16.53943276465976808, 0.05219959533934440121, 111.2510903946856899 ) ) ;
#62664 = CARTESIAN_POINT ( 'NONE',  ( 5.153800228976615827, -19.02544592524334988, 65.20942372801900433 ) ) ;
#62665 = CARTESIAN_POINT ( 'NONE',  ( -11.40812507854755609, 35.11059874428196537, -7.524999997268813523 ) ) ;
#62666 = CARTESIAN_POINT ( 'NONE',  ( -16.51473224551069308, -9.474510206698971260, 106.6655762719810383 ) ) ;
#62667 = CARTESIAN_POINT ( 'NONE',  ( 8.314922557960818139, 14.29746914071049879, 89.58224293864768129 ) ) ;
#62668 = CARTESIAN_POINT ( 'NONE',  ( -19.05341960407617563, 5.049401038297882671, 58.54275706135234003 ) ) ;
#62669 = CARTESIAN_POINT ( 'NONE',  ( -16.46253265017160317, 9.564922557960807481, 75.83224293864769550 ) ) ;
#62670 = CARTESIAN_POINT ( 'NONE',  ( -8.224510206698948167, 14.34966873604960824, 65.41557627198102409 ) ) ;
#62671 = CARTESIAN_POINT ( 'NONE',  ( -5.049401038297874678, -19.05341960407617918, 94.79275706135230450 ) ) ;
#62672 = CARTESIAN_POINT ( 'NONE',  ( 5.823673210054125526, 21.52544592524343514, 54.79057627198104541 ) ) ;
#62673 = ORIENTED_EDGE ( 'NONE', *, *, #85633, .F. ) ;
#62674 = CARTESIAN_POINT ( 'NONE',  ( -16.53943276465976808, 0.05219959533911058130, 116.2489096053143669 ) ) ;
#62675 = CARTESIAN_POINT ( 'NONE',  ( -17.48847506799968343, -5.747544572773811034, 29.17302562156720924 ) ) ;
#62677 = CARTESIAN_POINT ( 'NONE',  ( -10.72451020669898014, 18.67979575497178502, 80.41557627198103830 ) ) ;
#62676 = CARTESIAN_POINT ( 'NONE',  ( -0.05219959533909027116, -19.03943276465977164, 72.49890960531435269 ) ) ;
#62679 = CARTESIAN_POINT ( 'NONE',  ( 9.474510206698971260, -16.51473224551069308, 77.91557627198103830 ) ) ;
#62678 = CARTESIAN_POINT ( 'NONE',  ( 8.224510206698742110, 14.34966873604972548, 97.08442372801904696 ) ) ;
#62680 = CARTESIAN_POINT ( 'NONE',  ( -9.474510206698720793, -16.51473224551083518, 69.58442372801901854 ) ) ;
#62681 = CARTESIAN_POINT ( 'NONE',  ( 15.80617190586769283, -15.72974639402175789, 80.62609039468567573 ) ) ;
#62682 = CARTESIAN_POINT ( 'NONE',  ( -21.53943276465977519, 0.05219959533907696930, 61.24890960531435979 ) ) ;
#62683 = CARTESIAN_POINT ( 'NONE',  ( -15.72974639402197994, 15.80617190586746368, 30.62390960531436335 ) ) ;
#62684 = CARTESIAN_POINT ( 'NONE',  ( -16.51473224551069308, -9.474510206698971260, 41.66557627198103120 ) ) ;
#62685 = CARTESIAN_POINT ( 'NONE',  ( 8.224510206698742110, 14.34966873604972548, 107.0844237280190043 ) ) ;
#62686 = CARTESIAN_POINT ( 'NONE',  ( -16.51473224551069308, -9.474510206698971260, 51.66557627198102409 ) ) ;
#62687 = CARTESIAN_POINT ( 'NONE',  ( 8.314922557961029526, -14.29746914071037800, 20.41775706135234714 ) ) ;
#62688 = DIRECTION ( 'NONE',  ( -1.000000000000000000, -0.000000000000000000, -0.000000000000000000 ) ) ;
#62689 = CARTESIAN_POINT ( 'NONE',  ( -21.53943276465977519, -0.05219959533937600094, 108.7510903946857042 ) ) ;
#62690 = CARTESIAN_POINT ( 'NONE',  ( -4.379528057220328563, 16.55341960407611168, 55.20724293864770260 ) ) ;
#62691 = CARTESIAN_POINT ( 'NONE',  ( 18.67979575497178502, 10.72451020669898547, 99.16557627198100988 ) ) ;
#62692 = CARTESIAN_POINT ( 'NONE',  ( -18.62759615963270932, 10.81492255796079327, 105.8322429386476955 ) ) ;
#62693 = CARTESIAN_POINT ( 'NONE',  ( 17.79613651744293534, 24.49428055684532524, 149.2843446569000037 ) ) ;
#62694 = CARTESIAN_POINT ( 'NONE',  ( 0.05219959533907565091, 21.53943276465977519, 44.99890960531435979 ) ) ;
#62695 = CARTESIAN_POINT ( 'NONE',  ( 16.55341960407618274, -4.379528057220086978, 86.04275706135236135 ) ) ;
#62696 = CARTESIAN_POINT ( 'NONE',  ( -14.29746914071049879, 8.314922557960819915, 90.83224293864769550 ) ) ;
#62697 = CARTESIAN_POINT ( 'NONE',  ( -16.46253265017160317, 9.564922557960807481, 45.83224293864769550 ) ) ;
#62698 = CARTESIAN_POINT ( 'NONE',  ( -4.908066780550751851, -48.27782543269305648, -24.94981842180952825 ) ) ;
#62699 = CARTESIAN_POINT ( 'NONE',  ( -14.34966873604972548, 8.224510206698743886, 103.3344237280190043 ) ) ;
#62700 = CARTESIAN_POINT ( 'NONE',  ( 0.05219959533937995610, -21.53943276465977519, 35.00109039468568284 ) ) ;
#62701 = CARTESIAN_POINT ( 'NONE',  ( -19.03943276465977164, 0.05219959533909376836, 96.24890960531436690 ) ) ;
#62702 = CARTESIAN_POINT ( 'NONE',  ( 10.72451020669871369, 18.67979575497193778, 72.08442372801899012 ) ) ;
#62703 = DIRECTION ( 'NONE',  ( 1.000000000000000000, 0.000000000000000000, 0.000000000000000000 ) ) ;
#62704 = CARTESIAN_POINT ( 'NONE',  ( 13.89961937509977652, -13.97604488694527269, 28.12390960531435624 ) ) ;
#62705 = VECTOR ( 'NONE', #34208, 1000.000000000000000 ) ;
#62706 = ORIENTED_EDGE ( 'NONE', *, *, #81519, .T. ) ;
#62707 = CARTESIAN_POINT ( 'NONE',  ( 18.62759615963255655, 10.81492255796105972, 61.66775706135235424 ) ) ;
#62709 = CARTESIAN_POINT ( 'NONE',  ( 9.564922557960805705, 16.46253265017160317, 114.5822429386476955 ) ) ;
#62708 = CARTESIAN_POINT ( 'NONE',  ( 9.564922557960805705, 16.46253265017160317, 54.58224293864769550 ) ) ;
#62710 = CARTESIAN_POINT ( 'NONE',  ( -5.049401038298153566, 19.05341960407611168, 90.20724293864766707 ) ) ;
#62711 = CARTESIAN_POINT ( 'NONE',  ( 19.03943276465977164, 0.05219959533936151252, 71.25109039468566152 ) ) ;
#62712 = CARTESIAN_POINT ( 'NONE',  ( 21.55341960407619695, -5.719274019375665929, 41.04275706135236135 ) ) ;
#62713 = CARTESIAN_POINT ( 'NONE',  ( -13.89961937509957401, -13.97604488694547875, 104.3760903946856757 ) ) ;
#62714 = CARTESIAN_POINT ( 'NONE',  ( -16.51473224551082808, 9.474510206698731452, 58.33442372801900433 ) ) ;
#62715 = CARTESIAN_POINT ( 'NONE',  ( 19.03943276465977164, -0.05219959533909143690, 38.74890960531436690 ) ) ;
#62716 = CARTESIAN_POINT ( 'NONE',  ( -16.55341960407617563, 4.379528057220093196, 103.5427570613523613 ) ) ;
#62717 = CARTESIAN_POINT ( 'NONE',  ( 19.02544592524334988, 5.153800228976608722, 71.45942372801900433 ) ) ;
#62718 = CARTESIAN_POINT ( 'NONE',  ( -4.379528057220328563, 16.55341960407611168, 30.20724293864769550 ) ) ;
#62719 = CARTESIAN_POINT ( 'NONE',  ( -16.51473224551082808, 9.474510206698731452, 53.33442372801900433 ) ) ;
#62720 = CARTESIAN_POINT ( 'NONE',  ( -18.67979575497193778, 10.72451020669871902, 108.3344237280190185 ) ) ;
#62721 = CARTESIAN_POINT ( 'NONE',  ( -13.89961937509957401, -13.97604488694547875, 24.37609039468565442 ) ) ;
#62722 = CARTESIAN_POINT ( 'NONE',  ( -16.46253265017160317, 9.564922557960807481, 25.83224293864769194 ) ) ;
#62723 = CARTESIAN_POINT ( 'NONE',  ( -21.55341960407619339, 5.719274019375674811, 88.54275706135236135 ) ) ;
#62724 = CARTESIAN_POINT ( 'NONE',  ( 0.05219959533934541429, -16.53943276465976808, 35.00109039468568284 ) ) ;
#62725 = AXIS2_PLACEMENT_3D ( 'NONE', #59755, #11295, #184106 ) ;
#62726 = CARTESIAN_POINT ( 'NONE',  ( 9.474510206698971260, -16.51473224551069308, 92.91557627198103830 ) ) ;
#62727 = CARTESIAN_POINT ( 'NONE',  ( -17.14385361876520264, -23.59649016807271593, 141.1750000027311671 ) ) ;
#62728 = CARTESIAN_POINT ( 'NONE',  ( 9.564922557960805705, 16.46253265017160317, 79.58224293864769550 ) ) ;
#62729 = CARTESIAN_POINT ( 'NONE',  ( -16.81555441253467009, 7.025013491696203261, 100.6368544533421101 ) ) ;
#62730 = AXIS2_PLACEMENT_3D ( 'NONE', #168455, #124935, #186632 ) ;
#62731 = CARTESIAN_POINT ( 'NONE',  ( -19.03943276465977164, -0.05219959533935918106, 78.75109039468567573 ) ) ;
#62732 = CARTESIAN_POINT ( 'NONE',  ( 5.049401038298161559, -19.05341960407611168, 107.7072429386476955 ) ) ;
#62733 = CARTESIAN_POINT ( 'NONE',  ( 5.823673210054444382, -21.52544592524334988, 100.2094237280190043 ) ) ;
#62734 = CARTESIAN_POINT ( 'NONE',  ( -16.55341960407611168, -4.379528057220339221, 101.4572429386476955 ) ) ;
#62735 = CARTESIAN_POINT ( 'NONE',  ( 19.05341960407611168, 5.049401038298154454, 28.95724293864769550 ) ) ;
#62736 = CARTESIAN_POINT ( 'NONE',  ( 5.823673210054125526, 21.52544592524343514, 59.79057627198103120 ) ) ;
#62737 =( GEOMETRIC_REPRESENTATION_CONTEXT ( 3 ) GLOBAL_UNCERTAINTY_ASSIGNED_CONTEXT ( ( #130795 ) ) GLOBAL_UNIT_ASSIGNED_CONTEXT ( ( #151754, #106229, #163949 ) ) REPRESENTATION_CONTEXT ( 'NONE', 'WORKASPACE' ) );
#62738 = CARTESIAN_POINT ( 'NONE',  ( -10.72451020669898014, 18.67979575497178502, 40.41557627198103120 ) ) ;
#62739 = CARTESIAN_POINT ( 'NONE',  ( 16.46253265017160672, -9.564922557960803928, 23.33224293864769194 ) ) ;
#62740 = CARTESIAN_POINT ( 'NONE',  ( 0.000000000000000000, 0.000000000000000000, -59.13370768023891344 ) ) ;
#62741 = CARTESIAN_POINT ( 'NONE',  ( -19.05341960407617563, 5.049401038297882671, 58.54275706135234003 ) ) ;
#62742 = CARTESIAN_POINT ( 'NONE',  ( -8.224510206698948167, 14.34966873604960824, 40.41557627198103120 ) ) ;
#62743 = CARTESIAN_POINT ( 'NONE',  ( -21.53943276465977519, 0.05219959533907696930, 26.24890960531435624 ) ) ;
#62744 = CARTESIAN_POINT ( 'NONE',  ( -10.81492255796105439, 18.62759615963255655, 82.91775706135234714 ) ) ;
#62745 = CARTESIAN_POINT ( 'NONE',  ( -21.52544592524343514, 5.823673210054127303, 71.04057627198103830 ) ) ;
#62746 = CARTESIAN_POINT ( 'NONE',  ( -15.80617190586768217, 15.72974639402176855, 63.12609039468568994 ) ) ;
#62747 = CARTESIAN_POINT ( 'NONE',  ( -15.72974639402197994, 15.80617190586746368, 95.62390960531436690 ) ) ;
#62748 = CARTESIAN_POINT ( 'NONE',  ( 15.80617190586769283, -15.72974639402175789, 55.62609039468568284 ) ) ;
#62749 = CARTESIAN_POINT ( 'NONE',  ( -9.564922557960796823, -16.46253265017161027, 22.08224293864768839 ) ) ;
#62750 = CARTESIAN_POINT ( 'NONE',  ( -9.564922557960796823, -16.46253265017161027, 87.08224293864769550 ) ) ;
#62751 = CARTESIAN_POINT ( 'NONE',  ( 8.314922557961029526, -14.29746914071037800, 80.41775706135234714 ) ) ;
#62752 = CARTESIAN_POINT ( 'NONE',  ( 16.52544592524342804, -4.483927247898539470, 108.5405762719810241 ) ) ;
#62753 = CARTESIAN_POINT ( 'NONE',  ( -31.91717023173582746, 5.953136853522615013, 90.41250038490913710 ) ) ;
#62754 = CARTESIAN_POINT ( 'NONE',  ( 0.05219959533910956823, 16.53943276465976808, 54.99890960531435269 ) ) ;
#62755 = CARTESIAN_POINT ( 'NONE',  ( -0.05219959533934338120, 16.53943276465976808, 107.5010903946856899 ) ) ;
#62756 = CARTESIAN_POINT ( 'NONE',  ( -13.89961937509977652, 13.97604488694528158, 70.62390960531432427 ) ) ;
#62757 = CARTESIAN_POINT ( 'NONE',  ( 0.05219959533909260263, 19.03943276465977164, 39.99890960531436690 ) ) ;
#62758 = CARTESIAN_POINT ( 'NONE',  ( 21.52544592524344225, -5.823673210054117533, 43.54057627198103830 ) ) ;
#62760 = CIRCLE ( 'NONE', #1425, 61.99999999999998579 ) ;
#62759 = CARTESIAN_POINT ( 'NONE',  ( -16.46253265017146816, -9.564922557961047289, 44.16775706135232582 ) ) ;
#62762 = CARTESIAN_POINT ( 'NONE',  ( -8.314922557960811034, -14.29746914071050412, 47.08224293864770260 ) ) ;
#62761 = DIRECTION ( 'NONE',  ( -0.3041824702427698979, 0.9526137857479317628, 7.149051953565419487E-31 ) ) ;
#62763 = CARTESIAN_POINT ( 'NONE',  ( 5.719274019375991003, -21.55341960407610458, 32.70724293864770260 ) ) ;
#62764 = CARTESIAN_POINT ( 'NONE',  ( 4.500000000000000888, -126.1226662136678272, 8.481152457036388981 ) ) ;
#62765 = CARTESIAN_POINT ( 'NONE',  ( 4.379528057220092307, 16.55341960407617563, 67.29275706135234714 ) ) ;
#62766 = CARTESIAN_POINT ( 'NONE',  ( -19.05341960407617563, 5.049401038297882671, 58.54275706135234003 ) ) ;
#62767 = CARTESIAN_POINT ( 'NONE',  ( -4.483927247898539470, -16.52544592524342804, 42.29057627198103120 ) ) ;
#62768 = CARTESIAN_POINT ( 'NONE',  ( -19.19724070472092592, -5.500000000000081712, 76.06193348274379673 ) ) ;
#62769 = CARTESIAN_POINT ( 'NONE',  ( -12.14591786802309592, -12.06949235617757132, 26.87390960531435979 ) ) ;
#62770 = CARTESIAN_POINT ( 'NONE',  ( -16.51473224551069308, -9.474510206698971260, 41.66557627198103120 ) ) ;
#62771 = CARTESIAN_POINT ( 'NONE',  ( -0.05219959533909027116, -19.03943276465977164, 62.49890960531435979 ) ) ;
#62772 = CARTESIAN_POINT ( 'NONE',  ( -13.97604488694527625, -13.89961937509977652, 26.87390960531434558 ) ) ;
#62773 = CARTESIAN_POINT ( 'NONE',  ( 18.62759615963255655, 10.81492255796105972, 36.66775706135234714 ) ) ;
#62774 = CARTESIAN_POINT ( 'NONE',  ( 13.89961937509977652, -13.97604488694527269, 58.12390960531436690 ) ) ;
#62775 = LINE ( 'NONE', #121474, #200166 ) ;
#62776 = CARTESIAN_POINT ( 'NONE',  ( -13.89961937509977652, 13.97604488694528158, 50.62390960531435979 ) ) ;
#62777 = CARTESIAN_POINT ( 'NONE',  ( -0.05219959533907301413, -21.53943276465977519, 42.49890960531435979 ) ) ;
#62779 = CARTESIAN_POINT ( 'NONE',  ( 19.05341960407611168, 5.049401038298154454, 28.95724293864769550 ) ) ;
#62778 = CARTESIAN_POINT ( 'NONE',  ( -0.05219959533937732626, 21.53943276465977519, 57.50109039468568994 ) ) ;
#62780 = CARTESIAN_POINT ( 'NONE',  ( 21.53943276465977519, -0.05219959533907433946, 23.74890960531435269 ) ) ;
#62781 = CARTESIAN_POINT ( 'NONE',  ( 16.52544592524335698, 4.483927247898782831, 91.45942372801901854 ) ) ;
#62782 = CARTESIAN_POINT ( 'NONE',  ( 21.52544592524334988, 5.823673210054432836, 106.4594237280190328 ) ) ;
#62783 = CARTESIAN_POINT ( 'NONE',  ( 8.314922557961029526, -14.29746914071037800, 65.41775706135234714 ) ) ;
#62784 = CARTESIAN_POINT ( 'NONE',  ( 9.474510206698971260, -16.51473224551069308, 107.9155762719810383 ) ) ;
#62785 = CARTESIAN_POINT ( 'NONE',  ( 0.05219959533934541429, -16.53943276465976808, 50.00109039468568994 ) ) ;
#62786 = CARTESIAN_POINT ( 'NONE',  ( 14.29746914071037800, 8.314922557961029526, 31.66775706135234358 ) ) ;
#62787 = CARTESIAN_POINT ( 'NONE',  ( 8.314922557961029526, -14.29746914071037800, 90.41775706135236135 ) ) ;
#62788 = CARTESIAN_POINT ( 'NONE',  ( 18.62759615963255655, 10.81492255796105972, 56.66775706135235424 ) ) ;
#62789 = CARTESIAN_POINT ( 'NONE',  ( 16.53943276465976808, 0.05219959533934440121, 26.25109039468567573 ) ) ;
#62790 = CARTESIAN_POINT ( 'NONE',  ( 5.823673210054125526, 21.52544592524343514, 104.7905762719810241 ) ) ;
#62791 = CARTESIAN_POINT ( 'NONE',  ( 8.314922557961029526, -14.29746914071037800, 20.41775706135234714 ) ) ;
#62792 = CARTESIAN_POINT ( 'NONE',  ( -16.55341960407617563, 4.379528057220093196, 83.54275706135234714 ) ) ;
#62793 = CARTESIAN_POINT ( 'NONE',  ( 22.49873734152911453, -26.99873734152921045, 1.110912703473986074 ) ) ;
#62794 = CARTESIAN_POINT ( 'NONE',  ( -15.72974639402176322, -15.80617190586768395, 89.37609039468568994 ) ) ;
#62795 = CARTESIAN_POINT ( 'NONE',  ( 13.89961937509957401, 13.97604488694547697, 86.87609039468567573 ) ) ;
#62796 = CARTESIAN_POINT ( 'NONE',  ( 4.379528057220339221, -16.55341960407611168, 42.70724293864770260 ) ) ;
#62797 = CARTESIAN_POINT ( 'NONE',  ( -8.314922557960811034, -14.29746914071050412, 37.08224293864768129 ) ) ;
#62798 = CARTESIAN_POINT ( 'NONE',  ( 16.55341960407611168, 4.379528057220329451, 103.9572429386476813 ) ) ;
#62800 = CARTESIAN_POINT ( 'NONE',  ( 17.50000000000000000, -5.499999999999992895, 56.21769037696436300 ) ) ;
#62799 = CARTESIAN_POINT ( 'NONE',  ( -19.02544592524334988, -5.153800228976617603, 48.95942372801900433 ) ) ;
#62801 = CARTESIAN_POINT ( 'NONE',  ( -21.52544592524334988, -5.823673210054445271, 53.95942372801900433 ) ) ;
#62802 = CARTESIAN_POINT ( 'NONE',  ( 5.049401038297881783, 19.05341960407617563, 112.2927570613523471 ) ) ;
#62803 = DIRECTION ( 'NONE',  ( 0.000000000000000000, 0.000000000000000000, -1.000000000000000000 ) ) ;
#62804 = CARTESIAN_POINT ( 'NONE',  ( -5.049401038298153566, 19.05341960407611168, 100.2072429386476955 ) ) ;
#62805 = CARTESIAN_POINT ( 'NONE',  ( -21.53943276465977519, 0.05219959533907696930, 56.24890960531436690 ) ) ;
#62806 = CARTESIAN_POINT ( 'NONE',  ( 19.02544592524334988, 5.153800228976608722, 96.45942372801897591 ) ) ;
#62807 = CARTESIAN_POINT ( 'NONE',  ( 19.02544592524343514, -5.153800228976328945, 88.54057627198102409 ) ) ;
#62808 = CARTESIAN_POINT ( 'NONE',  ( -0.05219959533907301413, -21.53943276465977519, 62.49890960531436690 ) ) ;
#62809 = CARTESIAN_POINT ( 'NONE',  ( 0.05219959533910956823, 16.53943276465976808, 109.9989096053143527 ) ) ;
#62810 = CARTESIAN_POINT ( 'NONE',  ( -19.03943276465977164, 0.05219959533909376836, 71.24890960531435269 ) ) ;
#62811 = CARTESIAN_POINT ( 'NONE',  ( 16.46253265017160672, -9.564922557960803928, 28.33224293864769550 ) ) ;
#62812 = CARTESIAN_POINT ( 'NONE',  ( 0.05219959533937995610, -21.53943276465977519, 35.00109039468568284 ) ) ;
#62813 = CARTESIAN_POINT ( 'NONE',  ( -21.53943276465977519, -0.05219959533937600094, 83.75109039468568994 ) ) ;
#62814 = CARTESIAN_POINT ( 'NONE',  ( 16.55341960407618274, -4.379528057220086978, 91.04275706135236135 ) ) ;
#62815 = CARTESIAN_POINT ( 'NONE',  ( 21.52544592524334988, 5.823673210054432836, 36.45942372801901143 ) ) ;
#62816 = CARTESIAN_POINT ( 'NONE',  ( -21.52544592524334988, -5.823673210054445271, 43.95942372801902565 ) ) ;
#62818 = CARTESIAN_POINT ( 'NONE',  ( 13.89961937509977652, -13.97604488694527269, 73.12390960531436690 ) ) ;
#62817 = CARTESIAN_POINT ( 'NONE',  ( -19.03943276465977164, -0.05219959533935918106, 68.75109039468566152 ) ) ;
#62819 = CARTESIAN_POINT ( 'NONE',  ( -18.62759615963255300, -10.81492255796106328, 89.16775706135236135 ) ) ;
#62820 = CIRCLE ( 'NONE', #175852, 38.00000000000000000 ) ;
#62821 = CARTESIAN_POINT ( 'NONE',  ( 5.719274019375991003, -21.55341960407610458, 82.70724293864770971 ) ) ;
#62822 = CARTESIAN_POINT ( 'NONE',  ( 12.14591786802309770, 12.06949235617756955, 59.37390960531436690 ) ) ;
#62823 = CARTESIAN_POINT ( 'NONE',  ( -15.72974639402176322, -15.80617190586768395, 104.3760903946856899 ) ) ;
#62824 = CARTESIAN_POINT ( 'NONE',  ( 12.14591786802309770, 12.06949235617756955, 84.37390960531438111 ) ) ;
#62825 = CARTESIAN_POINT ( 'NONE',  ( -5.153800228976328057, -19.02544592524343514, 42.29057627198101699 ) ) ;
#62826 = CARTESIAN_POINT ( 'NONE',  ( -5.049401038297874678, -19.05341960407617918, 64.79275706135233293 ) ) ;
#62827 = CARTESIAN_POINT ( 'NONE',  ( 0.05219959533910956823, 16.53943276465976808, 29.99890960531435979 ) ) ;
#62828 = CARTESIAN_POINT ( 'NONE',  ( -21.55341960407619339, 5.719274019375674811, 98.54275706135234714 ) ) ;
#62829 = CARTESIAN_POINT ( 'NONE',  ( 9.474510206698971260, -16.51473224551069308, 87.91557627198102409 ) ) ;
#62830 = CARTESIAN_POINT ( 'NONE',  ( -5.153800228976607833, 19.02544592524334988, 67.70942372801900433 ) ) ;
#62831 = CARTESIAN_POINT ( 'NONE',  ( -10.81492255796078084, -18.62759615963271287, 67.08224293864770971 ) ) ;
#62832 = CARTESIAN_POINT ( 'NONE',  ( -15.72974639402176322, -15.80617190586768395, 19.37609039468568639 ) ) ;
#62833 = CARTESIAN_POINT ( 'NONE',  ( 16.51473224551083163, -9.474510206698727899, 105.8344237280190043 ) ) ;
#62834 = CARTESIAN_POINT ( 'NONE',  ( 4.483927247898790824, -16.52544592524335698, 85.20942372801901854 ) ) ;
#62836 = CARTESIAN_POINT ( 'NONE',  ( -15.72974639402176322, -15.80617190586768395, 24.37609039468567573 ) ) ;
#62835 = LINE ( 'NONE', #124519, #116020 ) ;
#62837 = CARTESIAN_POINT ( 'NONE',  ( 4.483927247898545687, 16.52544592524342804, 99.79057627198103830 ) ) ;
#62838 = CARTESIAN_POINT ( 'NONE',  ( -36.91746825000001309, 11.99521256947798342, -5.224999997268811924 ) ) ;
#62839 = CARTESIAN_POINT ( 'NONE',  ( -4.379528057220086978, -16.55341960407618274, 54.79275706135235424 ) ) ;
#62840 = CARTESIAN_POINT ( 'NONE',  ( -21.55341960407610458, -5.719274019375992779, 61.45724293864770260 ) ) ;
#62841 = CARTESIAN_POINT ( 'NONE',  ( -4.483927247898782831, 16.52544592524335698, 107.7094237280190328 ) ) ;
#62842 = CARTESIAN_POINT ( 'NONE',  ( 4.379528057220092307, 16.55341960407617563, 37.29275706135235424 ) ) ;
#62843 = CARTESIAN_POINT ( 'NONE',  ( -16.46253265017160317, 9.564922557960807481, 25.83224293864769194 ) ) ;
#62844 = CARTESIAN_POINT ( 'NONE',  ( -12.06949235617739369, -12.14591786802326823, 79.37609039468567573 ) ) ;
#62845 = CARTESIAN_POINT ( 'NONE',  ( 9.564922557961047289, -16.46253265017146816, 70.41775706135233293 ) ) ;
#62846 = CARTESIAN_POINT ( 'NONE',  ( 0.05219959533907565091, 21.53943276465977519, 74.99890960531435269 ) ) ;
#62847 = CARTESIAN_POINT ( 'NONE',  ( 8.224510206698742110, 14.34966873604972548, 102.0844237280190185 ) ) ;
#62848 = CARTESIAN_POINT ( 'NONE',  ( -5.719274019375665041, -21.55341960407619695, 79.79275706135236135 ) ) ;
#62849 = EDGE_CURVE ( 'NONE', #173655, #193677, #82860, .T. ) ;
#62850 = CIRCLE ( 'NONE', #117721, 1.249999999999999778 ) ;
#62851 = CARTESIAN_POINT ( 'NONE',  ( 18.67979575497178502, 10.72451020669898547, 64.16557627198102409 ) ) ;
#62852 = CARTESIAN_POINT ( 'NONE',  ( -15.72974639402197994, 15.80617190586746368, 50.62390960531435979 ) ) ;
#62853 = ORIENTED_EDGE ( 'NONE', *, *, #38977, .T. ) ;
#62854 = CARTESIAN_POINT ( 'NONE',  ( 8.314922557961029526, -14.29746914071037800, 80.41775706135234714 ) ) ;
#62855 = CARTESIAN_POINT ( 'NONE',  ( 21.55341960407610458, 5.719274019375980345, 43.95724293864769550 ) ) ;
#62856 = ORIENTED_EDGE ( 'NONE', *, *, #119131, .T. ) ;
#62857 = CARTESIAN_POINT ( 'NONE',  ( 5.719274019375991003, -21.55341960407610458, 22.70724293864769194 ) ) ;
#62858 = DIRECTION ( 'NONE',  ( 0.000000000000000000, 1.000000000000000000, 0.000000000000000000 ) ) ;
#62859 = CARTESIAN_POINT ( 'NONE',  ( 13.89961937509977652, -13.97604488694527269, 28.12390960531435624 ) ) ;
#62860 = CARTESIAN_POINT ( 'NONE',  ( -15.80617190586745835, -15.72974639402198527, 71.87390960531438111 ) ) ;
#62861 = CARTESIAN_POINT ( 'NONE',  ( 16.53943276465976808, 0.05219959533934440121, 101.2510903946856757 ) ) ;
#62862 = CARTESIAN_POINT ( 'NONE',  ( -18.62759615963255300, -10.81492255796106328, 49.16775706135234003 ) ) ;
#62863 = CARTESIAN_POINT ( 'NONE',  ( -16.46253265017146816, -9.564922557961047289, 104.1677570613523329 ) ) ;
#62864 = CARTESIAN_POINT ( 'NONE',  ( -8.314922557960811034, -14.29746914071050412, 112.0822429386477097 ) ) ;
#62865 = CARTESIAN_POINT ( 'NONE',  ( -19.02544592524334988, -5.153800228976617603, 108.9594237280189759 ) ) ;
#62866 = CARTESIAN_POINT ( 'NONE',  ( 13.97604488694527802, 13.89961937509977652, 44.37390960531435269 ) ) ;
#62867 = CARTESIAN_POINT ( 'NONE',  ( 28.82186960331499392, -9.364793116373510529, 142.9000000000000057 ) ) ;
#62868 = CARTESIAN_POINT ( 'NONE',  ( 5.049401038298161559, -19.05341960407611168, 92.70724293864769550 ) ) ;
#62869 = VECTOR ( 'NONE', #175537, 1000.000000000000000 ) ;
#62870 = CARTESIAN_POINT ( 'NONE',  ( -8.224510206698735004, -14.34966873604973081, 69.58442372801900433 ) ) ;
#62871 = CARTESIAN_POINT ( 'NONE',  ( 5.049401038297881783, 19.05341960407617563, 82.29275706135229029 ) ) ;
#62872 = CARTESIAN_POINT ( 'NONE',  ( -5.049401038297874678, -19.05341960407617918, 29.79275706135232227 ) ) ;
#62873 = CARTESIAN_POINT ( 'NONE',  ( 21.52544592524344225, -5.823673210054117533, 58.54057627198103120 ) ) ;
#62874 = CARTESIAN_POINT ( 'NONE',  ( 12.06949235617739724, 12.14591786802326823, 86.87609039468568994 ) ) ;
#62875 = CARTESIAN_POINT ( 'NONE',  ( 19.03943276465977164, 0.05219959533936151252, 81.25109039468567573 ) ) ;
#62876 = CARTESIAN_POINT ( 'NONE',  ( -5.049401038298153566, 19.05341960407611168, 35.20724293864768839 ) ) ;
#62878 = TOROIDAL_SURFACE ( 'NONE', #88590, 2.700000000000000622, 0.2000000000000000111 ) ;
#62877 = CARTESIAN_POINT ( 'NONE',  ( 16.51473224551069308, 9.474510206698969483, 84.16557627198102409 ) ) ;
#62879 = CARTESIAN_POINT ( 'NONE',  ( -18.62759615963255300, -10.81492255796106328, 49.16775706135234003 ) ) ;
#62880 = CARTESIAN_POINT ( 'NONE',  ( 19.03943276465977164, -0.05219959533909143690, 53.74890960531436690 ) ) ;
#62881 = CARTESIAN_POINT ( 'NONE',  ( 26.79623349963120660, -5.044589688426930785, 170.2051123914326070 ) ) ;
#62882 = CARTESIAN_POINT ( 'NONE',  ( -16.51473224551069308, -9.474510206698971260, 111.6655762719810383 ) ) ;
#62883 = CARTESIAN_POINT ( 'NONE',  ( -4.483927247898539470, -16.52544592524342804, 67.29057627198103830 ) ) ;
#62884 = CARTESIAN_POINT ( 'NONE',  ( 5.823673210054125526, 21.52544592524343514, 54.79057627198104541 ) ) ;
#62885 = CARTESIAN_POINT ( 'NONE',  ( 18.22780087662122739, 5.500000000000000888, 81.48236817873103632 ) ) ;
#62886 = AXIS2_PLACEMENT_3D ( 'NONE', #169662, #91800, #62468 ) ;
#62887 = CARTESIAN_POINT ( 'NONE',  ( -9.564922557961040184, 16.46253265017147172, 47.91775706135233293 ) ) ;
#62888 = CARTESIAN_POINT ( 'NONE',  ( 21.65274598442062626, -9.891030456500306656, 170.6639841963363438 ) ) ;
#62890 = CARTESIAN_POINT ( 'NONE',  ( -19.03943276465977164, 0.05219959533909376836, 71.24890960531435269 ) ) ;
#62889 = CARTESIAN_POINT ( 'NONE',  ( 13.89961937509977652, -13.97604488694527269, 58.12390960531436690 ) ) ;
#62891 = CARTESIAN_POINT ( 'NONE',  ( -14.34966873604972548, 8.224510206698743886, 48.33442372801902565 ) ) ;
#62892 = DIRECTION ( 'NONE',  ( 0.000000000000000000, 0.000000000000000000, 1.000000000000000000 ) ) ;
#62893 = CARTESIAN_POINT ( 'NONE',  ( -16.55341960407617563, 4.379528057220093196, 83.54275706135234714 ) ) ;
#62894 = DIRECTION ( 'NONE',  ( 5.392603844284257652E-33, -1.000000000000000000, 0.000000000000000000 ) ) ;
#62895 = CARTESIAN_POINT ( 'NONE',  ( 0.05219959533934541429, -16.53943276465976808, 80.00109039468568994 ) ) ;
#62896 =( BOUNDED_CURVE ( )  B_SPLINE_CURVE ( 2, ( #99335, #69005, #5325, #80184, #141856, #65022, #98318, #126678, #128668, #174207, #188382 ),
 .UNSPECIFIED., .F., .F. ) 
 B_SPLINE_CURVE_WITH_KNOTS ( ( 3, 2, 2, 2, 2, 3 ),
 ( 0.000000000000000000, 0.02000000000000001776, 0.04000000000000003553, 0.06000000000000005329, 0.08000000000000007105, 0.1000000000000000888 ),
 .UNSPECIFIED. ) 
 CURVE ( )  GEOMETRIC_REPRESENTATION_ITEM ( )  RATIONAL_B_SPLINE_CURVE ( ( 1.000000000000000000, 0.9510565162951535312, 1.000000000000000000, 0.9510565162951535312, 1.000000000000000000, 0.9510565162951535312, 1.000000000000000000, 0.9510565162951535312, 1.000000000000000000, 0.9510565162951533091, 1.000000000000000222 ) ) 
 REPRESENTATION_ITEM ( '' )  );
#62897 = CARTESIAN_POINT ( 'NONE',  ( 4.483927247898790824, -16.52544592524335698, 50.20942372801901854 ) ) ;
#62898 = CARTESIAN_POINT ( 'NONE',  ( 0.05219959533936267826, -19.03943276465977164, 30.00109039468566863 ) ) ;
#62900 = FACE_OUTER_BOUND ( 'NONE', #146917, .T. ) ;
#62899 = CARTESIAN_POINT ( 'NONE',  ( 19.05341960407611168, 5.049401038298154454, 58.95724293864768129 ) ) ;
#62901 = CARTESIAN_POINT ( 'NONE',  ( 21.52544592524334988, 5.823673210054432836, 51.45942372801901854 ) ) ;
#62902 = CARTESIAN_POINT ( 'NONE',  ( 5.049401038297881783, 19.05341960407617563, 62.29275706135234003 ) ) ;
#62903 = CARTESIAN_POINT ( 'NONE',  ( -10.72451020669870658, -18.67979575497194134, 104.5844237280190185 ) ) ;
#62904 = CARTESIAN_POINT ( 'NONE',  ( 9.564922557960805705, 16.46253265017160317, 34.58224293864770260 ) ) ;
#62905 = CARTESIAN_POINT ( 'NONE',  ( -17.18269478283316332, 17.18269478283309226, -56.77278709839600879 ) ) ;
#62906 = CARTESIAN_POINT ( 'NONE',  ( -21.53943276465977519, 0.05219959533907696930, 71.24890960531435269 ) ) ;
#62907 = CIRCLE ( 'NONE', #27456, 4.324969328314201888 ) ;
#62908 = CARTESIAN_POINT ( 'NONE',  ( -0.05219959533907301413, -21.53943276465977519, 22.49890960531436335 ) ) ;
#62909 = CARTESIAN_POINT ( 'NONE',  ( -4.483927247898539470, -16.52544592524342804, 107.2905762719810525 ) ) ;
#62910 = CARTESIAN_POINT ( 'NONE',  ( 0.05219959533934541429, -16.53943276465976808, 35.00109039468568284 ) ) ;
#62911 = CARTESIAN_POINT ( 'NONE',  ( -16.52544592524342804, 4.483927247898546575, 36.04057627198102409 ) ) ;
#62912 = ORIENTED_EDGE ( 'NONE', *, *, #89293, .F. ) ;
#62913 = CARTESIAN_POINT ( 'NONE',  ( 21.53943276465977519, 0.05219959533937863772, 21.25109039468567218 ) ) ;
#62915 = LINE ( 'NONE', #49746, #139856 ) ;
#62914 = CARTESIAN_POINT ( 'NONE',  ( 14.29746914071049879, -8.314922557960816363, 38.33224293864768839 ) ) ;
#62916 = CARTESIAN_POINT ( 'NONE',  ( 9.474510206698729675, 16.51473224551082808, 107.0844237280190043 ) ) ;
#62917 = CARTESIAN_POINT ( 'NONE',  ( 5.153800228976615827, -19.02544592524334988, 30.20942372801900433 ) ) ;
#62918 = CARTESIAN_POINT ( 'NONE',  ( 12.14591786802309770, 12.06949235617756955, 29.37390960531435269 ) ) ;
#62919 = CARTESIAN_POINT ( 'NONE',  ( -18.67979575497178146, -10.72451020669898902, 96.66557627198102409 ) ) ;
#62921 = CARTESIAN_POINT ( 'NONE',  ( -15.80617190586745835, -15.72974639402198527, 61.87390960531436690 ) ) ;
#62920 = CARTESIAN_POINT ( 'NONE',  ( 17.31728774477272381, 6.344390552232406222, 31.68093348310680568 ) ) ;
#62922 = CARTESIAN_POINT ( 'NONE',  ( -16.51473224551069308, -9.474510206698971260, 71.66557627198102409 ) ) ;
#62923 = CARTESIAN_POINT ( 'NONE',  ( -12.14591786802309592, -12.06949235617757132, 46.87390960531435979 ) ) ;
#62924 = CARTESIAN_POINT ( 'NONE',  ( 9.564922557960805705, 16.46253265017160317, 89.58224293864769550 ) ) ;
#62925 = DIRECTION ( 'NONE',  ( -0.000000000000000000, -0.000000000000000000, -1.000000000000000000 ) ) ;
#62926 = CARTESIAN_POINT ( 'NONE',  ( 9.474510206698729675, 16.51473224551082808, 57.08442372801900433 ) ) ;
#62927 = CARTESIAN_POINT ( 'NONE',  ( 5.823673210054125526, 21.52544592524343514, 94.79057627198105251 ) ) ;
#62928 = CARTESIAN_POINT ( 'NONE',  ( -16.52544592524342804, 4.483927247898546575, 96.04057627198102409 ) ) ;
#62929 = CARTESIAN_POINT ( 'NONE',  ( 18.67979575497194134, -10.72451020669871369, 40.83442372801901854 ) ) ;
#62930 = CARTESIAN_POINT ( 'NONE',  ( -17.14385361876520619, 23.59649016807275856, 140.5750000027311728 ) ) ;
#62931 = CARTESIAN_POINT ( 'NONE',  ( -0.05219959533910754901, -16.53943276465976808, 27.49890960531435269 ) ) ;
#62932 = CARTESIAN_POINT ( 'NONE',  ( 19.03943276465977164, -0.05219959533909143690, 38.74890960531436690 ) ) ;
#62933 = CARTESIAN_POINT ( 'NONE',  ( -19.02544592524342804, 5.153800228976336051, 96.04057627198103830 ) ) ;
#62934 = CARTESIAN_POINT ( 'NONE',  ( -21.52544592524343514, 5.823673210054127303, 66.04057627198103830 ) ) ;
#62935 = CARTESIAN_POINT ( 'NONE',  ( -18.87580814761071935, 5.500000000000041744, 45.87172394265761710 ) ) ;
#62936 = CARTESIAN_POINT ( 'NONE',  ( 9.474510206698971260, -16.51473224551069308, 27.91557627198103120 ) ) ;
#62937 = CARTESIAN_POINT ( 'NONE',  ( -18.62759615963270932, 10.81492255796079327, 55.83224293864770260 ) ) ;
#62938 = CARTESIAN_POINT ( 'NONE',  ( 0.05219959533937995610, -21.53943276465977519, 70.00109039468568994 ) ) ;
#62940 = CARTESIAN_POINT ( 'NONE',  ( 14.29746914071037800, 8.314922557961029526, 71.66775706135234714 ) ) ;
#62939 = CARTESIAN_POINT ( 'NONE',  ( 20.37447694478314730, -32.07477979233135557, -24.11443027216501278 ) ) ;
#62941 = CARTESIAN_POINT ( 'NONE',  ( -0.05219959533909027116, -19.03943276465977164, 62.49890960531435979 ) ) ;
#62942 = CARTESIAN_POINT ( 'NONE',  ( 16.51473224551069308, 9.474510206698969483, 59.16557627198102409 ) ) ;
#62943 = EDGE_LOOP ( 'NONE', ( #188880, #13305, #88527, #30306 ) ) ;
#62944 = CARTESIAN_POINT ( 'NONE',  ( 16.46253265017146816, 9.564922557961045513, 21.66775706135233648 ) ) ;
#62945 = CARTESIAN_POINT ( 'NONE',  ( -12.14591786802326823, 12.06949235617739902, 78.12609039468570415 ) ) ;
#62946 = CARTESIAN_POINT ( 'NONE',  ( -21.52544592524334988, -5.823673210054445271, 93.95942372801903275 ) ) ;
#62947 = CARTESIAN_POINT ( 'NONE',  ( -16.51473224551069308, -9.474510206698971260, 71.66557627198102409 ) ) ;
#62948 = CARTESIAN_POINT ( 'NONE',  ( -5.719274019375978568, 21.55341960407610458, 40.20724293864769550 ) ) ;
#62949 = CARTESIAN_POINT ( 'NONE',  ( 19.03943276465977164, 0.05219959533936151252, 106.2510903946856615 ) ) ;
#62950 = CARTESIAN_POINT ( 'NONE',  ( 18.62759615963255655, 10.81492255796105972, 76.66775706135234714 ) ) ;
#62951 = CARTESIAN_POINT ( 'NONE',  ( -16.53943276465976808, -0.05219959533934237506, 53.75109039468568994 ) ) ;
#62952 = CARTESIAN_POINT ( 'NONE',  ( 18.67979575497178502, 10.72451020669898547, 94.16557627198103830 ) ) ;
#62953 = CARTESIAN_POINT ( 'NONE',  ( 13.89961937509957401, 13.97604488694547697, 111.8760903946856757 ) ) ;
#62954 = CARTESIAN_POINT ( 'NONE',  ( 19.03943276465977164, -0.05219959533909143690, 78.74890960531436690 ) ) ;
#62955 = CARTESIAN_POINT ( 'NONE',  ( 8.314922557961029526, -14.29746914071037800, 20.41775706135234714 ) ) ;
#62956 = CARTESIAN_POINT ( 'NONE',  ( -19.05341960407611168, -5.049401038298163336, 41.45724293864769550 ) ) ;
#62957 = CARTESIAN_POINT ( 'NONE',  ( -13.89961937509957401, -13.97604488694547875, 109.3760903946856331 ) ) ;
#62958 = CARTESIAN_POINT ( 'NONE',  ( 14.34966873604960469, 8.224510206698951720, 69.16557627198102409 ) ) ;
#62959 = CARTESIAN_POINT ( 'NONE',  ( 14.34966873604972726, -8.224510206698740333, 70.83442372801901854 ) ) ;
#62961 = CARTESIAN_POINT ( 'NONE',  ( -19.02544592524342804, 5.153800228976336051, 56.04057627198100988 ) ) ;
#62960 = CARTESIAN_POINT ( 'NONE',  ( 15.72974639402176855, 15.80617190586768217, 26.87609039468567218 ) ) ;
#62962 = CARTESIAN_POINT ( 'NONE',  ( -5.049401038298153566, 19.05341960407611168, 65.20724293864765286 ) ) ;
#62963 = CARTESIAN_POINT ( 'NONE',  ( -14.34966873604972548, 8.224510206698743886, 73.33442372801901854 ) ) ;
#62964 = AXIS2_PLACEMENT_3D ( 'NONE', #49087, #112726, #173429 ) ;
#62966 = ORIENTED_EDGE ( 'NONE', *, *, #123454, .F. ) ;
#62965 = CARTESIAN_POINT ( 'NONE',  ( -18.22780087662123094, -5.499999999999984901, 81.48459894673892734 ) ) ;
#62967 = VERTEX_POINT ( 'NONE', #129327 ) ;
#62968 = CARTESIAN_POINT ( 'NONE',  ( 13.97604488694548053, -13.89961937509957401, 20.62609039468567573 ) ) ;
#62969 = CARTESIAN_POINT ( 'NONE',  ( 9.564922557960805705, 16.46253265017160317, 39.58224293864768839 ) ) ;
#62971 = ORIENTED_EDGE ( 'NONE', *, *, #116692, .F. ) ;
#62970 = FACE_OUTER_BOUND ( 'NONE', #21958, .T. ) ;
#62972 = CARTESIAN_POINT ( 'NONE',  ( -12.06949235617739369, -12.14591786802326823, 29.37609039468568284 ) ) ;
#62974 = CARTESIAN_POINT ( 'NONE',  ( 4.379528057220092307, 16.55341960407617563, 42.29275706135235424 ) ) ;
#62973 = CARTESIAN_POINT ( 'NONE',  ( -9.474510206698720793, -16.51473224551083518, 54.58442372801899722 ) ) ;
#62975 = CARTESIAN_POINT ( 'NONE',  ( 16.46253265017160672, -9.564922557960803928, 43.33224293864769550 ) ) ;
#62976 = CARTESIAN_POINT ( 'NONE',  ( -19.03943276465977164, 0.05219959533909376836, 106.2489096053143669 ) ) ;
#62977 = CARTESIAN_POINT ( 'NONE',  ( 19.05341960407611168, 5.049401038298154454, 58.95724293864768129 ) ) ;
#62978 = CARTESIAN_POINT ( 'NONE',  ( 21.53943276465977519, -0.05219959533907433946, 93.74890960531436690 ) ) ;
#62980 = CARTESIAN_POINT ( 'NONE',  ( -5.049401038298153566, 19.05341960407611168, 25.20724293864768484 ) ) ;
#62979 = CARTESIAN_POINT ( 'NONE',  ( -9.474510206698964154, 16.51473224551069663, 95.41557627198102409 ) ) ;
#62981 = EDGE_CURVE ( 'NONE', #68796, #89992, #73811, .T. ) ;
#62982 = CARTESIAN_POINT ( 'NONE',  ( -0.05219959533909027116, -19.03943276465977164, 62.49890960531435979 ) ) ;
#62984 = CARTESIAN_POINT ( 'NONE',  ( -8.571926809382601320, -26.38167802310801591, 147.7750000027311899 ) ) ;
#62983 = CARTESIAN_POINT ( 'NONE',  ( -4.483927247898782831, 16.52544592524335698, 112.7094237280190328 ) ) ;
#62985 = CARTESIAN_POINT ( 'NONE',  ( 19.05341960407617918, -5.049401038297876454, 96.04275706135231871 ) ) ;
#62986 = CARTESIAN_POINT ( 'NONE',  ( 19.03943276465977164, 0.05219959533936151252, 26.25109039468566507 ) ) ;
#62987 = AXIS2_PLACEMENT_3D ( 'NONE', #162562, #7876, #97869 ) ;
#62988 = CARTESIAN_POINT ( 'NONE',  ( -8.224510206698948167, 14.34966873604960824, 55.41557627198102409 ) ) ;
#62989 = CARTESIAN_POINT ( 'NONE',  ( 5.823673210054444382, -21.52544592524334988, 95.20942372801903275 ) ) ;
#62990 = CARTESIAN_POINT ( 'NONE',  ( -16.46253265017160317, 9.564922557960807481, 45.83224293864769550 ) ) ;
#62992 = CARTESIAN_POINT ( 'NONE',  ( -18.62759615963255300, -10.81492255796106328, 84.16775706135234714 ) ) ;
#62991 = CARTESIAN_POINT ( 'NONE',  ( 4.379528057220339221, -16.55341960407611168, 22.70724293864769194 ) ) ;
#62993 = CARTESIAN_POINT ( 'NONE',  ( 16.46253265017160672, -9.564922557960803928, 83.33224293864768129 ) ) ;
#62994 = CARTESIAN_POINT ( 'NONE',  ( -0.05219959533909027116, -19.03943276465977164, 92.49890960531436690 ) ) ;
#62995 = CARTESIAN_POINT ( 'NONE',  ( 12.14591786802309770, 12.06949235617756955, 89.37390960531435269 ) ) ;
#62996 = CARTESIAN_POINT ( 'NONE',  ( -16.55341960407611168, -4.379528057220339221, 71.45724293864769550 ) ) ;
#62997 = CARTESIAN_POINT ( 'NONE',  ( 0.05219959533907565091, 21.53943276465977519, 79.99890960531435269 ) ) ;
#62998 = CARTESIAN_POINT ( 'NONE',  ( -19.05341960407611168, -5.049401038298163336, 76.45724293864769550 ) ) ;
#62999 = CARTESIAN_POINT ( 'NONE',  ( 21.55341960407610458, 5.719274019375980345, 78.95724293864769550 ) ) ;
#63000 = VECTOR ( 'NONE', #51444, 1000.000000000000000 ) ;
#63001 = CARTESIAN_POINT ( 'NONE',  ( -16.46253265017146816, -9.564922557961047289, 84.16775706135233293 ) ) ;
#63003 = CARTESIAN_POINT ( 'NONE',  ( -16.52544592524342804, 4.483927247898546575, 96.04057627198102409 ) ) ;
#63002 = CARTESIAN_POINT ( 'NONE',  ( -17.49999999999999645, -5.500000000000000888, 120.0000000000000142 ) ) ;
#63004 = CARTESIAN_POINT ( 'NONE',  ( -0.05219959533909027116, -19.03943276465977164, 62.49890960531435979 ) ) ;
#63005 = CARTESIAN_POINT ( 'NONE',  ( -10.81492255796078084, -18.62759615963271287, 62.08224293864769550 ) ) ;
#63006 = CARTESIAN_POINT ( 'NONE',  ( -25.82491430096448681, -7.758527484246124040, 169.9682266581730232 ) ) ;
#63008 = DIRECTION ( 'NONE',  ( 0.000000000000000000, 0.000000000000000000, -1.000000000000000000 ) ) ;
#63007 = CARTESIAN_POINT ( 'NONE',  ( 16.53943276465976808, 0.05219959533934440121, 111.2510903946856899 ) ) ;
#63009 = CARTESIAN_POINT ( 'NONE',  ( 5.153800228976615827, -19.02544592524334988, 110.2094237280189901 ) ) ;
#63010 = CARTESIAN_POINT ( 'NONE',  ( -16.55341960407611168, -4.379528057220339221, 86.45724293864770971 ) ) ;
#63011 = CARTESIAN_POINT ( 'NONE',  ( 8.516083024820106928, -1.203758653825250269, -62.01440738234568073 ) ) ;
#63012 = CARTESIAN_POINT ( 'NONE',  ( -9.564922557960796823, -16.46253265017161027, 72.08224293864770971 ) ) ;
#63013 = CARTESIAN_POINT ( 'NONE',  ( 0.05219959533909260263, 19.03943276465977164, 34.99890960531435979 ) ) ;
#63014 = CARTESIAN_POINT ( 'NONE',  ( -16.53943276465976808, 0.05219959533911058130, 71.24890960531435269 ) ) ;
#63015 = CARTESIAN_POINT ( 'NONE',  ( -13.89961937509977652, 13.97604488694528158, 100.6239096053143669 ) ) ;
#63017 = CARTESIAN_POINT ( 'NONE',  ( 5.153800228976335163, 19.02544592524342804, 79.79057627198102409 ) ) ;
#63016 = CARTESIAN_POINT ( 'NONE',  ( -5.049401038297874678, -19.05341960407617918, 94.79275706135230450 ) ) ;
#63018 = CARTESIAN_POINT ( 'NONE',  ( 16.51473224551069308, 9.474510206698969483, 89.16557627198103830 ) ) ;
#63019 = CARTESIAN_POINT ( 'NONE',  ( -5.719274019375978568, 21.55341960407610458, 75.20724293864769550 ) ) ;
#63020 = CARTESIAN_POINT ( 'NONE',  ( -16.53943276465976808, -0.05219959533934237506, 68.75109039468568994 ) ) ;
#63021 = CIRCLE ( 'NONE', #172735, 4.999999999999998224 ) ;
#63022 = CARTESIAN_POINT ( 'NONE',  ( -16.31925111598408051, 7.325300261831769078, 95.16424538967171998 ) ) ;
#63023 = CARTESIAN_POINT ( 'NONE',  ( -13.97604488694527625, -13.89961937509977652, 61.87390960531435979 ) ) ;
#63024 = CARTESIAN_POINT ( 'NONE',  ( 5.823673210054125526, 21.52544592524343514, 69.79057627198102409 ) ) ;
#63025 = CARTESIAN_POINT ( 'NONE',  ( 13.97604488694548053, -13.89961937509957401, 100.6260903946856615 ) ) ;
#63027 = CARTESIAN_POINT ( 'NONE',  ( -10.81492255796105439, 18.62759615963255655, 42.91775706135235424 ) ) ;
#63026 = CARTESIAN_POINT ( 'NONE',  ( -12.14591786802309592, -12.06949235617757132, 31.87390960531435979 ) ) ;
#63028 = CARTESIAN_POINT ( 'NONE',  ( 34.52594549653173317, 2.428612888752089207E-14, 89.49999999999897682 ) ) ;
#63030 = CARTESIAN_POINT ( 'NONE',  ( -9.474510206698964154, 16.51473224551069663, 100.4155762719810241 ) ) ;
#63029 = CARTESIAN_POINT ( 'NONE',  ( 8.314922557961029526, -14.29746914071037800, 70.41775706135236135 ) ) ;
#63031 = CARTESIAN_POINT ( 'NONE',  ( 19.02544592524343514, -5.153800228976328945, 108.5405762719810383 ) ) ;
#63032 = CARTESIAN_POINT ( 'NONE',  ( 12.14591786802327356, -12.06949235617739191, 90.62609039468567573 ) ) ;
#63033 = CARTESIAN_POINT ( 'NONE',  ( -4.379528057220086978, -16.55341960407618274, 44.79275706135234714 ) ) ;
#63034 = CARTESIAN_POINT ( 'NONE',  ( 9.564922557960805705, 16.46253265017160317, 59.58224293864769550 ) ) ;
#63035 = CARTESIAN_POINT ( 'NONE',  ( 0.05219959533909260263, 19.03943276465977164, 64.99890960531436690 ) ) ;
#63036 = CARTESIAN_POINT ( 'NONE',  ( 21.52544592524334988, 5.823673210054432836, 51.45942372801901854 ) ) ;
#63037 = CARTESIAN_POINT ( 'NONE',  ( 4.379528057220092307, 16.55341960407617563, 67.29275706135234714 ) ) ;
#63038 = CARTESIAN_POINT ( 'NONE',  ( 16.55341960407611168, 4.379528057220329451, 28.95724293864769905 ) ) ;
#63039 = CARTESIAN_POINT ( 'NONE',  ( -5.049401038298153566, 19.05341960407611168, 35.20724293864768839 ) ) ;
#63040 = CARTESIAN_POINT ( 'NONE',  ( 16.46253265017160672, -9.564922557960803928, 28.33224293864769550 ) ) ;
#63041 = CARTESIAN_POINT ( 'NONE',  ( 12.06949235617739724, 12.14591786802326823, 21.87609039468567573 ) ) ;
#63042 = CARTESIAN_POINT ( 'NONE',  ( 9.474510206698729675, 16.51473224551082808, 87.08442372801900433 ) ) ;
#63043 = CARTESIAN_POINT ( 'NONE',  ( -14.29746914071049879, 8.314922557960819915, 80.83224293864769550 ) ) ;
#63044 = CARTESIAN_POINT ( 'NONE',  ( -5.153800228976328057, -19.02544592524343514, 52.29057627198100988 ) ) ;
#63046 = DIRECTION ( 'NONE',  ( 0.7071067811865466846, -7.406550393246786959E-15, 0.7071067811865484609 ) ) ;
#63045 = CARTESIAN_POINT ( 'NONE',  ( -19.05341960407617563, 5.049401038297882671, 88.54275706135230450 ) ) ;
#63047 = CARTESIAN_POINT ( 'NONE',  ( 0.05219959533937995610, -21.53943276465977519, 90.00109039468567573 ) ) ;
#63048 = CARTESIAN_POINT ( 'NONE',  ( 14.29746914071037800, 8.314922557961029526, 51.66775706135234714 ) ) ;
#63049 = LINE ( 'NONE', #17555, #37403 ) ;
#63050 = CARTESIAN_POINT ( 'NONE',  ( -18.67979575497178146, -10.72451020669898902, 46.66557627198102409 ) ) ;
#63051 = CARTESIAN_POINT ( 'NONE',  ( -12.06949235617739369, -12.14591786802326823, 44.37609039468567573 ) ) ;
#63052 = CARTESIAN_POINT ( 'NONE',  ( 9.474510206698971260, -16.51473224551069308, 37.91557627198102409 ) ) ;
#63053 = CARTESIAN_POINT ( 'NONE',  ( 13.89961937509957401, 13.97604488694547697, 31.87609039468566863 ) ) ;
#63054 = CARTESIAN_POINT ( 'NONE',  ( -0.05219959533909027116, -19.03943276465977164, 72.49890960531435269 ) ) ;
#63055 = CARTESIAN_POINT ( 'NONE',  ( 9.687362902255724606, 9.687362902255701513, -60.44446360152740993 ) ) ;
#63056 = CARTESIAN_POINT ( 'NONE',  ( -5.049401038298153566, 19.05341960407611168, 55.20724293864769550 ) ) ;
#63057 = CARTESIAN_POINT ( 'NONE',  ( -17.49999999999999645, 5.499999999999997335, 120.0000000000000142 ) ) ;
#63058 = CARTESIAN_POINT ( 'NONE',  ( 13.97604488694527802, 13.89961937509977652, 69.37390960531436690 ) ) ;
#63059 = CARTESIAN_POINT ( 'NONE',  ( -18.89770734986051082, -5.499999999999912959, 54.10214472496640070 ) ) ;
#63060 = PRODUCT_DEFINITION_SHAPE ( 'NONE', 'NONE',  #200203 ) ;
#63061 = EDGE_CURVE ( 'NONE', #3830, #179309, #134724, .T. ) ;
#63062 = CARTESIAN_POINT ( 'NONE',  ( 9.474510206698729675, 16.51473224551082808, 37.08442372801899722 ) ) ;
#63063 = CARTESIAN_POINT ( 'NONE',  ( -5.719274019375665041, -21.55341960407619695, 104.7927570613523898 ) ) ;
#63064 = CARTESIAN_POINT ( 'NONE',  ( 14.29746914071049879, -8.314922557960816363, 38.33224293864768839 ) ) ;
#63065 = CARTESIAN_POINT ( 'NONE',  ( -16.51473224551069308, -9.474510206698971260, 46.66557627198102409 ) ) ;
#63066 = CARTESIAN_POINT ( 'NONE',  ( 5.153800228976335163, 19.02544592524342804, 104.7905762719809957 ) ) ;
#63067 = CARTESIAN_POINT ( 'NONE',  ( 5.823673210054444382, -21.52544592524334988, 75.20942372801901854 ) ) ;
#63068 = CARTESIAN_POINT ( 'NONE',  ( -13.89961937509977652, 13.97604488694528158, 50.62390960531435979 ) ) ;
#63069 = CARTESIAN_POINT ( 'NONE',  ( 5.823673210054444382, -21.52544592524334988, 85.20942372801901854 ) ) ;
#63070 = CARTESIAN_POINT ( 'NONE',  ( 0.05219959533907565091, 21.53943276465977519, 29.99890960531435979 ) ) ;
#63071 = CARTESIAN_POINT ( 'NONE',  ( 16.46253265017160672, -9.564922557960803928, 33.33224293864770260 ) ) ;
#63072 = CARTESIAN_POINT ( 'NONE',  ( -21.52544592524334988, -5.823673210054445271, 28.95942372801902209 ) ) ;
#63073 = CARTESIAN_POINT ( 'NONE',  ( -9.474510206698720793, -16.51473224551083518, 54.58442372801899722 ) ) ;
#63074 = CARTESIAN_POINT ( 'NONE',  ( 19.03943276465977164, -0.05219959533909143690, 28.74890960531435624 ) ) ;
#63075 = CARTESIAN_POINT ( 'NONE',  ( -13.89961937509977652, 13.97604488694528158, 75.62390960531438111 ) ) ;
#63076 = CARTESIAN_POINT ( 'NONE',  ( -16.46253265017146816, -9.564922557961047289, 109.1677570613523471 ) ) ;
#63077 = CARTESIAN_POINT ( 'NONE',  ( 4.483927247898545687, 16.52544592524342804, 74.79057627198105251 ) ) ;
#63078 = CARTESIAN_POINT ( 'NONE',  ( -5.719274019375978568, 21.55341960407610458, 40.20724293864769550 ) ) ;
#63079 = CARTESIAN_POINT ( 'NONE',  ( 9.474510206698729675, 16.51473224551082808, 107.0844237280190043 ) ) ;
#63080 = CARTESIAN_POINT ( 'NONE',  ( 15.80617190586746368, 15.72974639402197994, 99.37390960531436690 ) ) ;
#63081 = CARTESIAN_POINT ( 'NONE',  ( -21.52544592524334988, -5.823673210054445271, 63.95942372801901854 ) ) ;
#63082 = CARTESIAN_POINT ( 'NONE',  ( 12.06949235617739724, 12.14591786802326823, 51.87609039468568284 ) ) ;
#63083 = CARTESIAN_POINT ( 'NONE',  ( -4.379528057220086978, -16.55341960407618274, 54.79275706135235424 ) ) ;
#63084 = CARTESIAN_POINT ( 'NONE',  ( 9.564922557960805705, 16.46253265017160317, 54.58224293864769550 ) ) ;
#63085 = CARTESIAN_POINT ( 'NONE',  ( -14.34966873604972548, 8.224510206698743886, 83.33442372801903275 ) ) ;
#63086 = CARTESIAN_POINT ( 'NONE',  ( -15.72974639402197994, 15.80617190586746368, 110.6239096053143669 ) ) ;
#63087 = CARTESIAN_POINT ( 'NONE',  ( -16.55341960407611168, -4.379528057220339221, 56.45724293864768839 ) ) ;
#63088 = CARTESIAN_POINT ( 'NONE',  ( 16.51473224551069308, 9.474510206698969483, 84.16557627198102409 ) ) ;
#63089 = CARTESIAN_POINT ( 'NONE',  ( 16.53943276465976808, 0.05219959533934440121, 81.25109039468568994 ) ) ;
#63090 = CARTESIAN_POINT ( 'NONE',  ( 18.67979575497194134, -10.72451020669871369, 45.83442372801901854 ) ) ;
#63091 = CARTESIAN_POINT ( 'NONE',  ( 5.049401038297881783, 19.05341960407617563, 107.2927570613523187 ) ) ;
#63092 = CARTESIAN_POINT ( 'NONE',  ( 15.80617190586746368, 15.72974639402197994, 109.3739096053143811 ) ) ;
#63093 = CARTESIAN_POINT ( 'NONE',  ( 16.55341960407611168, 4.379528057220329451, 48.95724293864770971 ) ) ;
#63094 = ORIENTED_EDGE ( 'NONE', *, *, #90349, .F. ) ;
#63095 = CARTESIAN_POINT ( 'NONE',  ( -16.52216118717208815, 7.221426719304501418, 68.92400978953010338 ) ) ;
#63096 = CARTESIAN_POINT ( 'NONE',  ( 21.55341960407610458, 5.719274019375980345, 93.95724293864770971 ) ) ;
#63097 = CARTESIAN_POINT ( 'NONE',  ( -0.05219959533934338120, 16.53943276465976808, 112.5010903946857042 ) ) ;
#63098 = ORIENTED_EDGE ( 'NONE', *, *, #95584, .F. ) ;
#63099 = CARTESIAN_POINT ( 'NONE',  ( -17.44270441346512968, -5.991230190323104665, 56.36335079264227943 ) ) ;
#63100 = CARTESIAN_POINT ( 'NONE',  ( 10.72451020669871369, 18.67979575497193778, 22.08442372801901143 ) ) ;
#63101 = AXIS2_PLACEMENT_3D ( 'NONE', #177276, #147929, #71081 ) ;
#63102 = CARTESIAN_POINT ( 'NONE',  ( -5.153800228976328057, -19.02544592524343514, 112.2905762719810099 ) ) ;
#63103 = CARTESIAN_POINT ( 'NONE',  ( -0.05219959533937732626, 21.53943276465977519, 22.50109039468567573 ) ) ;
#63104 = CARTESIAN_POINT ( 'NONE',  ( -4.379528057220328563, 16.55341960407611168, 55.20724293864770260 ) ) ;
#63105 = CARTESIAN_POINT ( 'NONE',  ( -8.224510206698735004, -14.34966873604973081, 64.58442372801900433 ) ) ;
#63106 = CARTESIAN_POINT ( 'NONE',  ( -5.153800228976328057, -19.02544592524343514, 67.29057627198102409 ) ) ;
#63107 = CARTESIAN_POINT ( 'NONE',  ( 9.564922557961047289, -16.46253265017146816, 65.41775706135233293 ) ) ;
#63108 = CARTESIAN_POINT ( 'NONE',  ( 16.51473224551069308, 9.474510206698969483, 74.16557627198103830 ) ) ;
#63109 = CARTESIAN_POINT ( 'NONE',  ( -5.719274019375978568, 21.55341960407610458, 30.20724293864769550 ) ) ;
#63110 = CARTESIAN_POINT ( 'NONE',  ( -19.25015247713983868, -32.77362114220466083, -25.12817986194701803 ) ) ;
#63111 = CARTESIAN_POINT ( 'NONE',  ( 19.02544592524343514, -5.153800228976328945, 48.54057627198103120 ) ) ;
#63112 = CARTESIAN_POINT ( 'NONE',  ( 16.55341960407618274, -4.379528057220086978, 21.04275706135234714 ) ) ;
#63113 = CARTESIAN_POINT ( 'NONE',  ( -16.46253265017146816, -9.564922557961047289, 59.16775706135233293 ) ) ;
#63114 = CARTESIAN_POINT ( 'NONE',  ( 5.719274019375991003, -21.55341960407610458, 102.7072429386476955 ) ) ;
#63115 = CARTESIAN_POINT ( 'NONE',  ( 4.483927247898545687, 16.52544592524342804, 34.79057627198103120 ) ) ;
#63116 = CARTESIAN_POINT ( 'NONE',  ( -5.049401038298153566, 19.05341960407611168, 95.20724293864770971 ) ) ;
#63117 = CARTESIAN_POINT ( 'NONE',  ( -21.52544592524343514, 5.823673210054127303, 61.04057627198103120 ) ) ;
#63119 = CARTESIAN_POINT ( 'NONE',  ( 8.314922557961029526, -14.29746914071037800, 20.41775706135234714 ) ) ;
#63118 = CARTESIAN_POINT ( 'NONE',  ( 21.55341960407610458, 5.719274019375980345, 88.95724293864769550 ) ) ;
#63120 = CARTESIAN_POINT ( 'NONE',  ( -15.72974639402197994, 15.80617190586746368, 30.62390960531436335 ) ) ;
#63121 = CARTESIAN_POINT ( 'NONE',  ( 21.53943276465977519, 0.05219959533937863772, 91.25109039468568994 ) ) ;
#63122 = CARTESIAN_POINT ( 'NONE',  ( 0.05219959533909260263, 19.03943276465977164, 89.99890960531436690 ) ) ;
#63123 = CARTESIAN_POINT ( 'NONE',  ( -9.474510206698964154, 16.51473224551069663, 25.41557627198103120 ) ) ;
#63124 = CARTESIAN_POINT ( 'NONE',  ( 16.46253265017160672, -9.564922557960803928, 83.33224293864768129 ) ) ;
#63125 = CARTESIAN_POINT ( 'NONE',  ( 16.53943276465976808, -0.05219959533910856209, 103.7489096053143669 ) ) ;
#63126 = CARTESIAN_POINT ( 'NONE',  ( -5.153800228976328057, -19.02544592524343514, 62.29057627198100988 ) ) ;
#63127 = CARTESIAN_POINT ( 'NONE',  ( 8.224510206698742110, 14.34966873604972548, 22.08442372801901143 ) ) ;
#63128 = CARTESIAN_POINT ( 'NONE',  ( 17.26058549869104652, -6.457015423128285470, 86.12254162523935008 ) ) ;
#63130 = CARTESIAN_POINT ( 'NONE',  ( 13.89961937509977652, -13.97604488694527269, 108.1239096053143669 ) ) ;
#63129 = CARTESIAN_POINT ( 'NONE',  ( 21.55341960407619695, -5.719274019375665929, 96.04275706135236135 ) ) ;
#63131 = CARTESIAN_POINT ( 'NONE',  ( 0.05219959533934541429, -16.53943276465976808, 85.00109039468568994 ) ) ;
#63132 = CARTESIAN_POINT ( 'NONE',  ( 20.43538597629128262, -20.43538597629122222, -49.67367017693150189 ) ) ;
#63133 = CARTESIAN_POINT ( 'NONE',  ( 13.97604488694548053, -13.89961937509957401, 70.62609039468567573 ) ) ;
#63134 = CARTESIAN_POINT ( 'NONE',  ( 9.474510206698729675, 16.51473224551082808, 27.08442372801900433 ) ) ;
#63135 = CARTESIAN_POINT ( 'NONE',  ( 4.175862767829956468, 6.297097159419585033, -64.28037419727766633 ) ) ;
#63136 = CARTESIAN_POINT ( 'NONE',  ( 16.51473224551069308, 9.474510206698969483, 29.16557627198103475 ) ) ;
#63137 = CARTESIAN_POINT ( 'NONE',  ( 12.06949235617757843, -12.14591786802309237, 33.12390960531435979 ) ) ;
#63138 = CARTESIAN_POINT ( 'NONE',  ( -17.31747979337946575, -6.344076630961068552, 111.3794486806518194 ) ) ;
#63139 = CARTESIAN_POINT ( 'NONE',  ( 8.224510206698953496, -14.34966873604960469, 27.91557627198103830 ) ) ;
#63140 = CARTESIAN_POINT ( 'NONE',  ( 22.99604614807110181, -21.49604614807104142, -49.67998909148434450 ) ) ;
#63141 = CARTESIAN_POINT ( 'NONE',  ( 16.55341960407618274, -4.379528057220086978, 101.0427570613523756 ) ) ;
#63142 = CARTESIAN_POINT ( 'NONE',  ( 0.05219959533909260263, 19.03943276465977164, 39.99890960531436690 ) ) ;
#63143 = CARTESIAN_POINT ( 'NONE',  ( 10.81492255796106328, -18.62759615963255655, 90.41775706135236135 ) ) ;
#63144 = CARTESIAN_POINT ( 'NONE',  ( -16.51473224551082808, 9.474510206698731452, 98.33442372801900433 ) ) ;
#63145 = CARTESIAN_POINT ( 'NONE',  ( -18.62759615963255300, -10.81492255796106328, 84.16775706135234714 ) ) ;
#63146 = CARTESIAN_POINT ( 'NONE',  ( 9.564922557961047289, -16.46253265017146816, 50.41775706135233293 ) ) ;
#63147 = CARTESIAN_POINT ( 'NONE',  ( 16.46253265017160672, -9.564922557960803928, 98.33224293864769550 ) ) ;
#63148 = CARTESIAN_POINT ( 'NONE',  ( -0.05219959533909027116, -19.03943276465977164, 67.49890960531436690 ) ) ;
#63149 = CARTESIAN_POINT ( 'NONE',  ( 17.49999999999999645, 5.500000000000007994, 73.78230962303568674 ) ) ;
#63150 = AXIS2_PLACEMENT_3D ( 'NONE', #4034, #189090, #50563 ) ;
#63151 = CARTESIAN_POINT ( 'NONE',  ( 4.379528057220339221, -16.55341960407611168, 72.70724293864769550 ) ) ;
#63152 = CARTESIAN_POINT ( 'NONE',  ( 10.81492255796078972, 18.62759615963270932, 64.58224293864769550 ) ) ;
#63153 = CARTESIAN_POINT ( 'NONE',  ( 16.51473224551069308, 9.474510206698969483, 64.16557627198102409 ) ) ;
#63155 = CARTESIAN_POINT ( 'NONE',  ( -14.34966873604972548, 8.224510206698743886, 73.33442372801901854 ) ) ;
#63154 = CARTESIAN_POINT ( 'NONE',  ( -18.67979575497178146, -10.72451020669898902, 86.66557627198102409 ) ) ;
#63156 = ORIENTED_EDGE ( 'NONE', *, *, #125997, .F. ) ;
#63157 = CARTESIAN_POINT ( 'NONE',  ( 5.153800228976335163, 19.02544592524342804, 49.79057627198100988 ) ) ;
#63159 = CARTESIAN_POINT ( 'NONE',  ( -36.91746825000000598, 2.428612866367529932E-14, -4.624999997268814056 ) ) ;
#63158 = CARTESIAN_POINT ( 'NONE',  ( -12.06949235617756955, 12.14591786802309770, 85.62390960531436690 ) ) ;
#63160 = CARTESIAN_POINT ( 'NONE',  ( -13.97604488694527625, -13.89961937509977652, 51.87390960531436690 ) ) ;
#63161 = CARTESIAN_POINT ( 'NONE',  ( -14.29746914071049879, 8.314922557960819915, 115.8322429386477097 ) ) ;
#63162 = CARTESIAN_POINT ( 'NONE',  ( -19.03943276465977164, -0.05219959533935918106, 68.75109039468566152 ) ) ;
#63163 = CARTESIAN_POINT ( 'NONE',  ( 8.314922557960818139, 14.29746914071049879, 79.58224293864769550 ) ) ;
#63164 = CARTESIAN_POINT ( 'NONE',  ( 0.05219959533937995610, -21.53943276465977519, 40.00109039468567573 ) ) ;
#63166 = CARTESIAN_POINT ( 'NONE',  ( 21.53943276465977519, -0.05219959533907433946, 103.7489096053143669 ) ) ;
#63165 = CARTESIAN_POINT ( 'NONE',  ( 9.564922557960805705, 16.46253265017160317, 34.58224293864770260 ) ) ;
#63167 = CARTESIAN_POINT ( 'NONE',  ( -9.474510206698964154, 16.51473224551069663, 110.4155762719810383 ) ) ;
#63168 = CARTESIAN_POINT ( 'NONE',  ( 0.05219959533910956823, 16.53943276465976808, 84.99890960531436690 ) ) ;
#63169 = CARTESIAN_POINT ( 'NONE',  ( 26.41049836824324260, -29.67629096701676161, -20.30943395415963693 ) ) ;
#63170 = CARTESIAN_POINT ( 'NONE',  ( -9.474510206698964154, 16.51473224551069663, 45.41557627198103120 ) ) ;
#63171 = DIRECTION ( 'NONE',  ( 1.000000000000000000, -0.000000000000000000, -0.000000000000000000 ) ) ;
#63173 = CARTESIAN_POINT ( 'NONE',  ( -0.05219959533909027116, -19.03943276465977164, 92.49890960531436690 ) ) ;
#63172 = CARTESIAN_POINT ( 'NONE',  ( 19.02544592524334988, 5.153800228976608722, 91.45942372801900433 ) ) ;
#63174 = CARTESIAN_POINT ( 'NONE',  ( -5.719274019375665041, -21.55341960407619695, 34.79275706135235424 ) ) ;
#63175 = CARTESIAN_POINT ( 'NONE',  ( 13.89961937509977652, -13.97604488694527269, 78.12390960531433848 ) ) ;
#63176 = CARTESIAN_POINT ( 'NONE',  ( 13.97604488694548053, -13.89961937509957401, 75.62609039468564731 ) ) ;
#63177 = CARTESIAN_POINT ( 'NONE',  ( 9.474510206698971260, -16.51473224551069308, 42.91557627198103120 ) ) ;
#63178 = CARTESIAN_POINT ( 'NONE',  ( -4.379528057220328563, 16.55341960407611168, 70.20724293864769550 ) ) ;
#63179 = CARTESIAN_POINT ( 'NONE',  ( 12.06949235617757843, -12.14591786802309237, 68.12390960531436690 ) ) ;
#63180 = CARTESIAN_POINT ( 'NONE',  ( -19.05341960407611168, -5.049401038298163336, 76.45724293864769550 ) ) ;
#63181 = CARTESIAN_POINT ( 'NONE',  ( -5.719274019375978568, 21.55341960407610458, 100.2072429386476955 ) ) ;
#63182 = CARTESIAN_POINT ( 'NONE',  ( 9.564922557960805705, 16.46253265017160317, 74.58224293864769550 ) ) ;
#63183 = CARTESIAN_POINT ( 'NONE',  ( 9.474510206698729675, 16.51473224551082808, 22.08442372801899722 ) ) ;
#63186 = CARTESIAN_POINT ( 'NONE',  ( -16.55341960407611168, -4.379528057220339221, 106.4572429386477097 ) ) ;
#63185 = CARTESIAN_POINT ( 'NONE',  ( -12.14591786802309592, -12.06949235617757132, 26.87390960531435979 ) ) ;
#63184 = CARTESIAN_POINT ( 'NONE',  ( 13.89961937509977652, -13.97604488694527269, 38.12390960531436690 ) ) ;
#63187 = CARTESIAN_POINT ( 'NONE',  ( 0.05219959533936267826, -19.03943276465977164, 100.0010903946856757 ) ) ;
#63188 = EDGE_LOOP ( 'NONE', ( #25422, #9251, #31653, #170640 ) ) ;
#63189 = CARTESIAN_POINT ( 'NONE',  ( 15.80617190586769283, -15.72974639402175789, 25.62609039468567929 ) ) ;
#63190 = CARTESIAN_POINT ( 'NONE',  ( -0.05219959533936034679, 19.03943276465977164, 62.50109039468566863 ) ) ;
#63191 = CARTESIAN_POINT ( 'NONE',  ( 4.379528057220092307, 16.55341960407617563, 112.2927570613523471 ) ) ;
#63192 = CARTESIAN_POINT ( 'NONE',  ( 10.72451020669898902, -18.67979575497178502, 67.91557627198102409 ) ) ;
#63193 = CARTESIAN_POINT ( 'NONE',  ( 9.564922557960805705, 16.46253265017160317, 109.5822429386476955 ) ) ;
#63194 = CARTESIAN_POINT ( 'NONE',  ( -12.14591786802309592, -12.06949235617757132, 61.87390960531436690 ) ) ;
#63195 = CARTESIAN_POINT ( 'NONE',  ( 16.51473224551069308, 9.474510206698969483, 29.16557627198103475 ) ) ;
#63196 = CARTESIAN_POINT ( 'NONE',  ( 5.153800228976335163, 19.02544592524342804, 44.79057627198103830 ) ) ;
#63197 = CARTESIAN_POINT ( 'NONE',  ( -19.05341960407617563, 5.049401038297882671, 33.54275706135231871 ) ) ;
#63198 = CARTESIAN_POINT ( 'NONE',  ( -8.224510206698735004, -14.34966873604973081, 94.58442372801901854 ) ) ;
#63199 = CARTESIAN_POINT ( 'NONE',  ( -4.483927247898782831, 16.52544592524335698, 62.70942372801902565 ) ) ;
#63200 = CARTESIAN_POINT ( 'NONE',  ( -21.52544592524343514, 5.823673210054127303, 26.04057627198103475 ) ) ;
#63201 = CARTESIAN_POINT ( 'NONE',  ( 10.72451020669871369, 18.67979575497193778, 107.0844237280190043 ) ) ;
#63202 = CARTESIAN_POINT ( 'NONE',  ( 19.03943276465977164, -0.05219959533909143690, 78.74890960531436690 ) ) ;
#63203 = VECTOR ( 'NONE', #14890, 1000.000000000000000 ) ;
#63204 = CARTESIAN_POINT ( 'NONE',  ( -12.14591786802326823, 12.06949235617739902, 63.12609039468568994 ) ) ;
#63205 = CARTESIAN_POINT ( 'NONE',  ( 12.06949235617757843, -12.14591786802309237, 108.1239096053143811 ) ) ;
#63206 = CARTESIAN_POINT ( 'NONE',  ( -12.14591786802326823, 12.06949235617739902, 113.1260903946856899 ) ) ;
#63207 = DIRECTION ( 'NONE',  ( -7.709882115452472644E-15, 0.000000000000000000, 1.000000000000000000 ) ) ;
#63210 = CARTESIAN_POINT ( 'NONE',  ( -13.89961937509977652, 13.97604488694528158, 75.62390960531438111 ) ) ;
#63209 = CARTESIAN_POINT ( 'NONE',  ( -0.05219959533909027116, -19.03943276465977164, 87.49890960531436690 ) ) ;
#63208 = CARTESIAN_POINT ( 'NONE',  ( 18.62759615963255655, 10.81492255796105972, 71.66775706135234714 ) ) ;
#63211 = CARTESIAN_POINT ( 'NONE',  ( -16.51473224551069308, -9.474510206698971260, 106.6655762719810383 ) ) ;
#63212 = CARTESIAN_POINT ( 'NONE',  ( 8.314922557960818139, 14.29746914071049879, 59.58224293864770260 ) ) ;
#63213 = CARTESIAN_POINT ( 'NONE',  ( 12.14591786802309770, 12.06949235617756955, 24.37390960531435979 ) ) ;
#63214 = CARTESIAN_POINT ( 'NONE',  ( -0.05219959533910754901, -16.53943276465976808, 47.49890960531435979 ) ) ;
#63216 = CARTESIAN_POINT ( 'NONE',  ( -18.22780087662121673, -5.500000000000063061, 66.48459894673892734 ) ) ;
#63215 = CARTESIAN_POINT ( 'NONE',  ( -16.55341960407617563, 4.379528057220093196, 38.54275706135234714 ) ) ;
#63217 = CARTESIAN_POINT ( 'NONE',  ( -5.153800228976607833, 19.02544592524334988, 37.70942372801899722 ) ) ;
#63218 = CARTESIAN_POINT ( 'NONE',  ( -13.97604488694527625, -13.89961937509977652, 76.87390960531433848 ) ) ;
#63219 = CARTESIAN_POINT ( 'NONE',  ( -0.05219959533936034679, 19.03943276465977164, 47.50109039468566863 ) ) ;
#63220 = CARTESIAN_POINT ( 'NONE',  ( -0.05219959533936034679, 19.03943276465977164, 57.50109039468566863 ) ) ;
#63222 = CARTESIAN_POINT ( 'NONE',  ( 12.14591786802327356, -12.06949235617739191, 80.62609039468567573 ) ) ;
#63221 = CARTESIAN_POINT ( 'NONE',  ( 0.05219959533936267826, -19.03943276465977164, 100.0010903946856757 ) ) ;
#63223 = CARTESIAN_POINT ( 'NONE',  ( 27.73933785331498569, 2.768321779492822058E-14, 148.3750000027311842 ) ) ;
#63224 = CARTESIAN_POINT ( 'NONE',  ( -16.46253265017160317, 9.564922557960807481, 30.83224293864769550 ) ) ;
#63225 = CARTESIAN_POINT ( 'NONE',  ( 5.153800228976335163, 19.02544592524342804, 109.7905762719810099 ) ) ;
#63226 = CARTESIAN_POINT ( 'NONE',  ( 21.52544592524334988, 5.823673210054432836, 41.45942372801901143 ) ) ;
#63227 = CARTESIAN_POINT ( 'NONE',  ( -5.153800228976607833, 19.02544592524334988, 92.70942372801901854 ) ) ;
#63229 = CARTESIAN_POINT ( 'NONE',  ( 19.03943276465977164, -0.05219959533909143690, 63.74890960531435979 ) ) ;
#63228 = CARTESIAN_POINT ( 'NONE',  ( -23.48529157249600985, 32.32473071737754111, -2.299999999999998934 ) ) ;
#63230 = EDGE_CURVE ( 'NONE', #109664, #165524, #54442, .T. ) ;
#63231 = CARTESIAN_POINT ( 'NONE',  ( 19.03943276465977164, -0.05219959533909143690, 98.74890960531436690 ) ) ;
#63233 = CARTESIAN_POINT ( 'NONE',  ( 13.89961937509977652, -13.97604488694527269, 48.12390960531435979 ) ) ;
#63232 = CARTESIAN_POINT ( 'NONE',  ( 4.483927247898545687, 16.52544592524342804, 54.79057627198104541 ) ) ;
#63234 = CARTESIAN_POINT ( 'NONE',  ( -5.153800228976328057, -19.02544592524343514, 67.29057627198102409 ) ) ;
#63235 = CARTESIAN_POINT ( 'NONE',  ( -19.03943276465977164, -0.05219959533935918106, 58.75109039468566863 ) ) ;
#63236 = CARTESIAN_POINT ( 'NONE',  ( 9.564922557961047289, -16.46253265017146816, 40.41775706135234003 ) ) ;
#63237 = CARTESIAN_POINT ( 'NONE',  ( 13.97604488694527802, 13.89961937509977652, 84.37390960531433848 ) ) ;
#63238 = CARTESIAN_POINT ( 'NONE',  ( -21.55341960407610458, -5.719274019375992779, 81.45724293864769550 ) ) ;
#63240 = CARTESIAN_POINT ( 'NONE',  ( 19.03943276465977164, 0.05219959533936151252, 41.25109039468566152 ) ) ;
#63239 = CARTESIAN_POINT ( 'NONE',  ( -16.55341960407611168, -4.379528057220339221, 81.45724293864769550 ) ) ;
#63241 = CARTESIAN_POINT ( 'NONE',  ( -18.62759615963270932, 10.81492255796079327, 50.83224293864770971 ) ) ;
#63242 = CIRCLE ( 'NONE', #195651, 7.500000000000000000 ) ;
#63243 = CARTESIAN_POINT ( 'NONE',  ( 21.55341960407610458, 5.719274019375980345, 33.95724293864769550 ) ) ;
#63244 = CARTESIAN_POINT ( 'NONE',  ( 9.564922557960805705, 16.46253265017160317, 64.58224293864769550 ) ) ;
#63245 = CARTESIAN_POINT ( 'NONE',  ( 13.89961937509977652, -13.97604488694527269, 58.12390960531436690 ) ) ;
#63246 = CARTESIAN_POINT ( 'NONE',  ( -16.53943276465976808, 0.05219959533911058130, 111.2489096053143669 ) ) ;
#63247 = CARTESIAN_POINT ( 'NONE',  ( 18.67979575497194134, -10.72451020669871369, 20.83442372801901143 ) ) ;
#63248 = CYLINDRICAL_SURFACE ( 'NONE', #53306, 7.500000000000000000 ) ;
#63249 = CARTESIAN_POINT ( 'NONE',  ( 21.52544592524334988, 5.823673210054432836, 31.45942372801901854 ) ) ;
#63250 = CARTESIAN_POINT ( 'NONE',  ( 13.97604488694527802, 13.89961937509977652, 29.37390960531435979 ) ) ;
#63251 = CARTESIAN_POINT ( 'NONE',  ( -10.81492255796078084, -18.62759615963271287, 102.0822429386476955 ) ) ;
#63252 = CARTESIAN_POINT ( 'NONE',  ( 5.049401038297881783, 19.05341960407617563, 42.29275706135234003 ) ) ;
#63253 = LINE ( 'NONE', #124933, #140791 ) ;
#63254 = CARTESIAN_POINT ( 'NONE',  ( 16.51473224551069308, 9.474510206698969483, 29.16557627198103475 ) ) ;
#63255 = CARTESIAN_POINT ( 'NONE',  ( 30.00000000000000000, -1.163414459189985801E-14, 95.00000000000000000 ) ) ;
#63256 = CARTESIAN_POINT ( 'NONE',  ( 14.29746914071037800, 8.314922557961029526, 61.66775706135235424 ) ) ;
#63257 = CARTESIAN_POINT ( 'NONE',  ( -16.53943276465976808, 0.05219959533911058130, 116.2489096053143669 ) ) ;
#63258 = CARTESIAN_POINT ( 'NONE',  ( 33.83559363775140838, -1.430799499857053680, 100.3228003899268401 ) ) ;
#63259 = CARTESIAN_POINT ( 'NONE',  ( -16.51473224551069308, -9.474510206698971260, 66.66557627198102409 ) ) ;
#63260 = CARTESIAN_POINT ( 'NONE',  ( 16.53943276465976808, -0.05219959533910856209, 108.7489096053143669 ) ) ;
#63261 = CARTESIAN_POINT ( 'NONE',  ( 0.05219959533907565091, 21.53943276465977519, 59.99890960531436690 ) ) ;
#63262 = CARTESIAN_POINT ( 'NONE',  ( 0.05219959533910956823, 16.53943276465976808, 74.99890960531435269 ) ) ;
#63263 = CARTESIAN_POINT ( 'NONE',  ( -16.55341960407617563, 4.379528057220093196, 28.54275706135234358 ) ) ;
#63264 = CARTESIAN_POINT ( 'NONE',  ( 21.53943276465977519, 0.05219959533937863772, 86.25109039468568994 ) ) ;
#63265 = CARTESIAN_POINT ( 'NONE',  ( -19.02544592524342804, 5.153800228976336051, 26.04057627198103120 ) ) ;
#63266 = CARTESIAN_POINT ( 'NONE',  ( 16.53943276465976808, -0.05219959533910856209, 23.74890960531435269 ) ) ;
#63267 = CARTESIAN_POINT ( 'NONE',  ( 16.52544592524342804, -4.483927247898539470, 58.54057627198103120 ) ) ;
#63268 = CARTESIAN_POINT ( 'NONE',  ( -19.02544592524342804, 5.153800228976336051, 51.04057627198103120 ) ) ;
#63269 = CARTESIAN_POINT ( 'NONE',  ( 15.80617190586769283, -15.72974639402175789, 100.6260903946857184 ) ) ;
#63270 = CARTESIAN_POINT ( 'NONE',  ( -5.823673210054116645, -21.52544592524344225, 107.2905762719810525 ) ) ;
#63271 =( BOUNDED_SURFACE ( )  B_SPLINE_SURFACE ( 3, 2, ( 
 ( #191487, #148998, #71152, #53984, #6458, #132818, #190504, #23650, #194504, #68139, #39802, #87314, #128805, #192500, #52965, #129790, #37812, #176340, #101467, #69142, #99473, #161153, #22650, #84297, #100475, #115657, #146990, #56987, #105467, #167153, #106447, #150998, #120628, #75124, #57985, #165166, #104481, #28652, #151972, #60937, #134836, #136792, #89306, #137785, #91256, #14446, #153951, #12490, #41820, #152947, #58960, #74151, #90288, #198478, #166165, #149989, #59950, #13460, #169107, #121617, #76109, #135823, #197493, #195514, #183312, #118661, #182325, #180352, #43804, #44794, #11495, #103488, #168128, #26659, #29624, #199470, #122611, #184301, #88301, #45783, #73166, #196515, #119657, #107435, #30614, #92267, #72147, #133823, #181339, #42818, #27666, #97223, #187298, #126580, #94256, #32603, #48770, #156939, #109432, #81069, #112414, #79088, #49755, #172105, #33591, #47779, #15447, #95254, #2249, #50756, #61924, #123594, #140761, #65906, #185288, #3245, #174106, #18436, #31609, #80086, #188281, #189280, #35575, #110424, #155936, #141755, #255, #16441, #62924, #142747, #77105, #63932, #111423, #64919, #173109, #171112, #138774, #34586, #125601, #46780, #108439, #170115, #96243, #127579, #93259, #157931, #154944, #19421, #78090, #4227, #139758, #1245, #124604, #186299, #17431, #23412, #143744, #159917, #6225, #179112, #54739, #84063, #66904, #116411, #20400, #53746, #193265, #36559, #85060, #178100, #39570, #22412, #83064, #190262, #67904, #82049, #146742, #99232, #132585, #9250, #175091, #52732, #130567, #40580, #129557, #5223, #192264, #115420, #101228, #37569, #7222, #161918, #144738, #51739, #191257, #177109, #38580, #147764, #21406, #8237, #176099, #24425, #162917, #86074, #158909, #160919, #128567, #70917, #145741, #68907, #100236, #69915, #114398, #98214, #131581, #194273, #55740, #117414, #113401, #104244, #165927, #25435, #166923, #87076, #27424, #10250, #150760, #91031, #164933, #26426, #195271, #41587, #28424, #151743, #71909, #105235, #90061, #180119, #44562, #133581, #121387, #59715, #167901, #12258, #56755, #74899, #120393, #13236, #118426, #136562, #103251, #72929, #89069, #122376, #198243, #102250, #135590, #88066, #183079, #149753, #73920, #163938, #11256, #148761, #106217, #134598, #152717, #184065, #29401, #14208, #196284, #57753, #119423, #75876, #197262, #181107, #42581, #137552, #58724, #199235, #43570, #182087, #60700, #37081, #190774, #168873, #52249, #18, #61692, #51261, #185054, #93026, #47546, #108202, #1012, #169883, #35095, #98740, #31376, #113906, #96747, #160433, #30378, #83574, #159420, #145253, #5742, #158437, #124368, #82574, #62686, #123361, #19924, #92023, #186063, #81566, #20916, #175604, #21923, #128086, #6734, #36081, #138540, #111938, #189790, #107203, #67418, #153715, #143252, #68412, #154714, #16207, #46542, #77862, #112921, #97730, #15211, #174616, #144255, #139529, #130065, #76870, #129073, #45548, #173625, #4736, #66425, #164448, #9762, #41097, #99748, #56254, #161432, #162425, #55252, #11775, #25942, #191764, #73439, #23926, #133090, #39088, #116920, #54259, #87585, #163442, #117936, #102761, #84570, #165443, #22924, #53247, #149272, #24939, #179625, #115930, #10764, #176618, #134106, #148270, #177620, #146248, #101754, #85581, #114925, #132094, #7734, #72428, #178613, #193783, #71426, #195796, #147267, #69420, #194780, #57268, #88580, #118942, #180627, #40076, #86586, #38093, #42099, #131086, #103764, #192775, #100744, #8757, #70428, #150278, #26938, #58254, #152246, #91537, #46054, #92544, #181608, #153224, #151267, #104753, #119922, #170394, #185564, #108716, #121894, #47058, #27939, #168404, #530, #16713, #106730, #107709, #13731, #75397, #29899, #76390, #28924, #62202, #31885, #198759, #169388, #14729, #138066, #167428, #135110, #199747, #183587, #93539, #43086, #166443, #60225, #155224, #89581, #122885, #196786, #61213, #12757 ),
 ( #74422, #184573, #136088, #123866, #197762, #15722, #30896, #59229, #44083, #120898, #154232, #45072, #182598, #105741, #90564, #137069, #77382, #139050, #48056, #19692, #67183, #20675, #1526, #82330, #32882, #94532, #81334, #17714, #125876, #80356, #141043, #33870, #2529, #65193, #128840, #64209, #144020, #126852, #190539, #63205, #113672, #189553, #175366, #140037, #109712, #78363, #127848, #124885, #52013, #98500, #159180, #112686, #186583, #187576, #171395, #143017, #188558, #156214, #79372, #5501, #142028, #97494, #4495, #49044, #66186, #36834, #160194, #110699, #172379, #95529, #157216, #51025, #18709, #3517, #50037, #111701, #173387, #34857, #96512, #158202, #174378, #35848, #70192, #10524, #145014, #57026, #132854, #118699, #179388, #131859, #100512, #56013, #38855, #176377, #8514, #6495, #162191, #193543, #194542, #149036, #72187, #101506, #133861, #9524, #114682, #85337, #163196, #83337, #40851, #68175, #55016, #195552, #84334, #146013, #37851, #161191, #86349, #71190, #129827, #24700, #117691, #99510, #164207, #191526, #102525, #25705, #87350, #116686, #53003, #180390, #39840, #41861, #22687, #148035, #7496, #192539, #147030, #103527, #21684, #69181, #130847, #54022, #115695, #177384, #178376, #23689, #137824, #136832, #29661, #14483, #58022, #138812, #134874, #46814, #76145, #198515, #91293, #27700, #199507, #150028, #107470, #121654, #89342, #119691, #75160, #135858, #59986, #196551, #152984, #181375, #152009, #13495, #42853, #60973, #183348, #122648, #73203, #184337, #104518, #197528, #28688, #185324, #45819, #165202, #26697, #58997, #106486, #12524, #90324, #151034, #169147, #44830, #30651, #92305, #166199, #292, #74189, #88337, #153988, #168164, #15485, #120663, #77142, #11534, #61961, #123628, #182361, #43839, #105504, #167190, #141787, #139793, #173143, #1282, #95288, #170152, #78124, #108473, #157963, #154980, #97254, #128599, #189311, #142780, #93294, #17467, #62958, #34618, #18469, #124639, #16475, #35609, #110458, #127612, #49791, #186334, #111457, #158942, #50789, #31645, #112448, #47816, #109465, #96277, #171149, #155969, #172139, #32637, #63967, #94291, #156972, #20431, #79123, #174137, #80119, #82082, #140796, #143774, #19455, #5255, #65941, #3282, #187334, #4261, #125637, #2285, #64953, #48804, #33625, #126612, #81102, #66937, #190293, #188314, #102281, #39601, #144771, #115451, #193297, #113430, #9282, #175122, #100268, #40611, #114430, #176131, #6256, #191285, #116446, #101260, #159948, #54772, #162950, #129589, #194304, #21435, #70947, #132617, #117444, #85091, #146776, #86105, #130601, #161949, #178134, #37601, #67936, #84093, #8269, #131613, #163969, #99264, #24456, #68938, #179143, #55770, #25467, #133611, #192297, #83096, #87107, #38612, #53776, #69948, #147797, #145771, #52760, #148793, #10283, #71941, #51770, #36590, #177141, #23444, #98246, #160950, #22443, #7253, #103283, #195305, #104276, #180150, #92058, #106248, #118458, #12287, #151772, #167930, #152748, #41618, #13265, #11287, #164963, #26456, #30411, #45581, #168905, #182114, #107234, #88098, #28454, #60735, #76901, #166951, #29430, #73952, #135620, #90090, #136591, #89100, #122408, #153747, #58754, #91061, #74928, #198271, #27459, #56786, #59748, #43600, #15242, #149784, #72960, #120423, #134629, #196314, #183110, #57783, #121418, #119453, #44592, #14238, #181138, #42612, #75910, #197291, #137584, #165958, #150791, #105265, #199267, #184098, #63730, #46574, #96048, #50, #33394, #172910, #16241, #64725, #34388, #157735, #2051, #62718, #169915, #47577, #61725, #126387, #78883, #112217, #189084, #154745, #32400, #110225, #158709, #186095, #123393, #111218, #138572, #20198, #170908, #79890, #109229, #125405, #1045, #19224, #171906, #3049, #188084, #31407, #173907, #108235, #185085, #49555, #95053, #80874, #124401, #142550, #93058, #4028, #156742, #94055, #77893, #48572, #155733, #18236, #139561 ),
 ( #17231, #140562, #65706, #141560, #187102, #127372, #50557, #35376, #97028, #23208, #51538, #84851, #70709, #24214, #5020, #85863, #36356, #98008, #146528, #21200, #129358, #83851, #144535, #37362, #6021, #68694, #132377, #67700, #147552, #130349, #194070, #66702, #117205, #193057, #178897, #39366, #192048, #160711, #116207, #99020, #159703, #53529, #128366, #22202, #115207, #54534, #9040, #55531, #161712, #40365, #69701, #174890, #145533, #8019, #143532, #101024, #190062, #176899, #102040, #191053, #52526, #82856, #114187, #131368, #177896, #113201, #162709, #163723, #175891, #81844, #7012, #38370, #100025, #90832, #73715, #195060, #198038, #43360, #74697, #133369, #89859, #56538, #196072, #88859, #45350, #10042, #134386, #118216, #151542, #135387, #179907, #41373, #152516, #27213, #44356, #166715, #103039, #28219, #14004, #167701, #148551, #29198, #164721, #26216, #13031, #87855, #72714, #150552, #149543, #180899, #11038, #12051, #75671, #57545, #137348, #197057, #199028, #71702, #60497, #136362, #122173, #182875, #58525, #104037, #59506, #42374, #119214, #120191, #165716, #181881, #105031, #121181, #183863, #107002, #106015, #25225, #86867, #61494, #32167, #109993, #30175, #126157, #91818, #16997, #157499, #31174, #92824, #123164, #107992, #33162, #18001, #76667, #171673, #156499, #46336, #110982, #138346, #187853, #49322, #34153, #78651, #200026, #141323, #186869, #79654, #184852, #94821, #169678, #139333, #93824, #188841, #2812, #168675, #50326, #812, #64490, #16006, #155504, #154510, #172667, #140326, #95813, #18992, #77664, #142315, #62485, #153510, #80638, #1816, #3795, #124157, #65472, #15007, #127135, #125170, #185857, #47343, #63495, #108998, #48338, #170679, #176662, #143295, #98783, #173673, #81611, #111981, #161478, #158481, #100785, #132136, #192819, #146294, #145297, #7781, #190818, #160477, #114969, #97776, #4781, #144297, #68459, #191809, #162468, #174659, #38139, #129119, #177661, #131131, #54301, #193828, #52293, #66469, #115973, #21968, #113950, #130113, #99792, #5787, #189833, #22967, #53291, #8800, #84615, #39130, #175649, #37124, #35140, #69465, #96792, #83619, #19969, #128131, #20959, #51305, #70470, #23969, #112966, #6780, #85625, #147311, #36124, #159463, #82616, #67461, #163484, #178656, #77171, #154019, #138841, #136861, #15514, #24981, #183380, #169176, #123655, #121684, #137855, #90354, #28717, #44862, #29692, #102801, #30681, #321, #75189, #61005, #106517, #168195, #164487, #55293, #91323, #198547, #61989, #101797, #86627, #60017, #116965, #148310, #199535, #40118, #184366, #152039, #45847, #92333, #9804, #71466, #122677, #153014, #133131, #179667, #14514, #76175, #194822, #56294, #107500, #13524, #117977, #41137, #55574, #27255, #180940, #131411, #117248, #177938, #11083, #56584, #39405, #54574, #88905, #164763, #120232, #197100, #162750, #40410, #118259, #166760, #194111, #193098, #179949, #8065, #178940, #148592, #102082, #150596, #42416, #116246, #163766, #101065, #72759, #41416, #24258, #73757, #134430, #58567, #104079, #87899, #85909, #149585, #135429, #12094, #69742, #181923, #147596, #9081, #196116, #70751, #25266, #10084, #132419, #86909, #71742, #133413, #43404, #195102, #105074, #103082, #28262, #26258, #146571, #57586, #119256, #165761, #138385, #168715, #124201, #107043, #44401, #76710, #74739, #30217, #200067, #62528, #17040, #140371, #169721, #1858, #77706, #182916, #153552, #31214, #151583, #47386, #13072, #61535, #78694, #152556, #14045, #106055, #29239, #154552, #139372, #198080, #92865, #854, #167741, #32211, #59547, #109041, #170719, #155546, #123204, #121225, #185901, #108035, #93867, #90872, #16047, #75711, #60538, #15049, #110038, #63540, #89900, #171717, #122214, #125214, #137389, #184894, #199069, #186910, #46376, #48381, #136402, #183905, #45390, #91859, #115012, #144342, #4825, #97818, #95858, #5830, #18045, #175691, #189874, #157541 ),
 ( #66513, #53333, #80682, #79698, #128175, #51349, #67506, #112028, #81655, #36166, #19035, #126200, #65517, #113009, #174702, #22010, #142358, #159507, #50368, #98825, #52337, #37166, #33206, #173717, #2856, #113993, #20012, #35185, #21003, #82658, #127177, #111027, #129163, #190860, #130155, #160519, #83662, #96839, #158524, #156546, #145340, #141369, #143338, #64534, #94865, #3838, #187896, #191852, #6822, #49363, #68500, #172713, #34196, #188887, #23012, #133177, #192865, #146336, #161520, #11865, #27028, #150369, #163527, #88673, #69509, #9850, #42191, #58341, #148354, #87670, #55338, #193872, #71509, #118022, #70513, #103851, #73530, #40165, #10852, #194867, #56340, #8845, #176706, #179712, #25027, #135202, #84658, #7824, #101841, #196874, #131175, #164532, #38180, #41184, #54344, #102847, #149355, #99836, #116015, #26025, #117008, #72521, #177705, #39172, #24015, #100830, #134196, #86671, #195884, #162513, #132181, #57358, #119032, #85670, #180715, #165532, #147357, #178703, #44173, #151358, #92634, #199842, #622, #138161, #93634, #170487, #153321, #60314, #184666, #104842, #120990, #167519, #140132, #15814, #45166, #183681, #1623, #152336, #76484, #154325, #197854, #46148, #77475, #139145, #106822, #105832, #12847, #62293, #61309, #123960, #122979, #155319, #31978, #136179, #13822, #91633, #120009, #29014, #166533, #14823, #107802, #185658, #198850, #168496, #169486, #90654, #74513, #75488, #30986, #47150, #108808, #182688, #16808, #137161, #78458, #181694, #43175, #28030, #121990, #89671, #59321, #29994, #65287, #19784, #189644, #157308, #141136, #66283, #4590, #160288, #51119, #67274, #126946, #188654, #186677, #127942, #48147, #50133, #171487, #63300, #172478, #109804, #21779, #174471, #32976, #80450, #81425, #35940, #20770, #94630, #143111, #79467, #156309, #17810, #98594, #113765, #36932, #111793, #175461, #2626, #96606, #128932, #145107, #34954, #97586, #142123, #3608, #158295, #112778, #18805, #190633, #83430, #173481, #159274, #82425, #144114, #95623, #124980, #5594, #52108, #64303, #125970, #187669, #49139, #110797, #33965, #194638, #41957, #148129, #22779, #9620, #117789, #180485, #103623, #132950, #102620, #40948, #70285, #130940, #37945, #179483, #86443, #87445, #24795, #165299, #57123, #84427, #100602, #178470, #26792, #54113, #191620, #39937, #101606, #164306, #85434, #55109, #71285, #192631, #99605, #38945, #163295, #56108, #195650, #69274, #25799, #23784, #72282, #149130, #10621, #88434, #147125, #176471, #133959, #193637, #8612, #118797, #6590, #162284, #146104, #68269, #129920, #53099, #114777, #161285, #131953, #116779, #7588, #115787, #177476, #13586, #58114, #150128, #59086, #134967, #46907, #61066, #73297, #167280, #106580, #122738, #107562, #196644, #168257, #166298, #119784, #181468, #185416, #382, #123719, #136924, #62054, #42946, #183439, #15575, #31739, #121747, #184429, #28778, #90417, #44924, #91388, #43932, #77233, #108567, #75253, #45909, #29753, #153077, #182452, #11629, #14579, #198611, #170245, #104610, #27794, #60079, #89436, #151124, #137916, #12617, #76237, #74281, #199599, #169240, #135951, #197621, #30746, #152102, #92394, #120753, #105594, #154081, #138902, #189402, #18560, #157063, #113524, #125728, #49883, #127702, #171241, #78215, #190389, #4350, #16568, #110550, #111548, #66035, #50879, #139885, #173233, #109560, #63053, #1374, #128692, #143870, #67033, #80208, #5349, #186430, #126701, #159033, #175218, #65045, #112537, #172231, #33716, #188405, #34709, #187427, #20526, #51864, #141879, #174231, #96366, #158054, #48895, #93387, #19544, #3370, #155073, #124732, #47906, #81189, #32730, #94382, #142871, #156061, #35700, #17559, #97347, #82174, #79219, #140888, #2378, #95378, #64058, #21529, #37693, #86940, #59578, #135458, #164794, #103113, #121252, #71774, #196145, #73786, #114523, #165791, #197127, #58594, #26289, #163796, #68027, #12122 ),
 ( #120260, #118289, #87930, #42445, #25298, #129678, #133444, #57617, #119285, #28290, #102111, #104109, #56615, #105103, #181952, #43434, #36683, #179980, #6347, #166789, #149617, #41448, #180968, #27288, #195134, #176224, #88934, #150626, #136430, #89930, #151611, #11115, #72790, #160042, #13103, #83190, #134460, #144864, #98343, #148624, #74768, #198111, #191376, #52852, #10114, #46404, #124231, #44429, #140397, #106083, #31242, #171745, #45416, #107069, #75741, #122241, #47412, #32236, #90898, #185927, #170747, #60565, #125240, #152584, #1885, #63566, #48409, #92892, #14074, #155572, #880, #93894, #137418, #109068, #199098, #153578, #108063, #2883, #17067, #182946, #64562, #15076, #78721, #30244, #169747, #168740, #186938, #154578, #110065, #33234, #183931, #156576, #91887, #167769, #94892, #16074, #18071, #76736, #79726, #29267, #141395, #139398, #138412, #200092, #77732, #61560, #62555, #123229, #184920, #157568, #113038, #187922, #95885, #126227, #49391, #35212, #128205, #96865, #6851, #160550, #111054, #158549, #19061, #190890, #36193, #80708, #53365, #114023, #176735, #22040, #67534, #142386, #129192, #115043, #68530, #172742, #130185, #3865, #65544, #52366, #127203, #173743, #189902, #188917, #81682, #50395, #174730, #38208, #112055, #191881, #97847, #99864, #34223, #161548, #37199, #23041, #83691, #159536, #4856, #145369, #143364, #20039, #21034, #66541, #51377, #82687, #98855, #84686, #144371, #146366, #7853, #5858, #175720, #100858, #134224, #179741, #162540, #196899, #57384, #120033, #103876, #10876, #39202, #72546, #58366, #11891, #192895, #73554, #24044, #85700, #195909, #8874, #117035, #71537, #132210, #25055, #193901, #56368, #181719, #55365, #135227, #118051, #43201, #54372, #104868, #180739, #166557, #27053, #41211, #148383, #165556, #86698, #147386, #102872, #116044, #9877, #164557, #42215, #28056, #89697, #149380, #151383, #119057, #70542, #133203, #88699, #131204, #150395, #177733, #26051, #69540, #178730, #40192, #101873, #163555, #194894, #87695, #121015, #15842, #648, #90679, #155347, #182713, #32005, #170516, #78487, #61333, #44198, #185686, #31011, #62318, #105857, #77501, #167544, #183706, #76510, #33003, #47176, #12873, #94657, #45192, #154349, #60341, #138186, #75513, #108835, #184690, #139171, #123988, #29039, #186704, #152361, #74538, #93662, #46174, #16836, #137187, #140160, #197878, #1652, #169511, #198874, #13846, #123004, #106846, #107827, #122015, #63330, #168521, #199869, #136203, #30019, #59347, #91657, #153346, #14848, #92661, #125008, #48175, #109831, #171514, #49165, #129950, #125998, #37977, #67302, #127969, #20798, #18832, #128961, #141164, #98623, #112806, #80477, #110824, #66309, #126973, #189673, #187695, #82453, #172506, #143138, #17837, #33993, #156337, #79495, #65313, #158322, #188681, #36962, #190661, #2653, #50161, #95649, #144141, #51145, #157337, #83459, #5624, #6620, #52137, #97613, #142151, #159303, #145137, #160317, #64330, #21808, #3635, #111820, #113794, #173508, #34981, #19811, #96634, #81452, #4617, #174499, #68299, #35966, #191650, #175489, #53129, #114808, #176500, #10651, #196677, #57152, #148159, #178501, #133990, #116809, #54144, #86474, #84456, #39967, #9650, #72313, #26823, #150160, #179513, #11661, #87474, #192661, #163328, #40981, #161316, #118831, #22810, #71316, #88464, #162314, #23815, #115817, #38976, #164335, #149161, #7620, #102650, #195681, #177507, #41987, #69304, #180514, #103653, #165331, #132979, #130970, #73327, #117820, #134999, #100633, #25830, #85465, #70316, #24824, #119814, #58146, #99634, #181499, #131983, #146134, #147154, #194669, #8642, #193668, #55139, #101637, #56139, #90452, #44958, #105627, #45940, #75286, #199631, #122771, #31769, #167316, #107595, #60112, #108598, #62086, #185448, #124765, #183474, #12647, #123749, #29786, #106616, #61098, #169273, #136957, #120784, #30779, #184461, #139918, #92426 ),
 ( #166329, #121780, #154112, #15606, #412, #89468, #77263, #59118, #74314, #27826, #78245, #93417, #16597, #91422, #155104, #135981, #76270, #170275, #42977, #14613, #138932, #168290, #153109, #137948, #46938, #198646, #1407, #63086, #104642, #151159, #197652, #182484, #43965, #28812, #152136, #13619, #21563, #32763, #94415, #49915, #36717, #156095, #174265, #83223, #127734, #2410, #189436, #97380, #160076, #144898, #19577, #126733, #50913, #171275, #187458, #33751, #6381, #82211, #111580, #173265, #68060, #18591, #142901, #20560, #64090, #112571, #143902, #5384, #34739, #110580, #17593, #159066, #66068, #67067, #4383, #186463, #98379, #125758, #80239, #158085, #47941, #95410, #157095, #96398, #48926, #128726, #81220, #35733, #190422, #79252, #109592, #140924, #172261, #51898, #113557, #175251, #141909, #3400, #65075, #188436, #86231, #53905, #22570, #39725, #100397, #163079, #161075, #194427, #84217, #116573, #191411, #99392, #129714, #52887, #38739, #131742, #162077, #10407, #164092, #114562, #23571, #145896, #55898, #101386, #7380, #56908, #117571, #180273, #25591, #71073, #69064, #132739, #118583, #72065, #176259, #133738, #130731, #192423, #179271, #115580, #177268, #9407, #24583, #103407, #85219, #178262, #41743, #146910, #195433, #147921, #165085, #37730, #26579, #40735, #88222, #87235, #102405, #8399, #148918, #70074, #193424, #149906, #54899, #11413, #183233, #45702, #176, #123513, #152871, #185206, #60855, #166082, #136713, #14366, #134754, #30531, #196436, #121538, #61844, #135743, #197414, #27585, #12410, #137707, #122530, #181261, #76031, #184221, #150917, #15366, #42738, #92184, #153868, #138694, #44714, #104400, #107353, #91182, #169026, #89223, #199391, #74072, #43724, #198394, #93180, #77022, #73083, #154865, #105385, #46697, #57906, #108358, #29549, #58880, #120546, #106370, #167072, #168052, #182239, #170037, #28574, #59871, #119578, #90210, #151893, #13383, #75047, #31527, #125524, #97148, #50679, #1165, #187221, #47700, #80995, #126506, #109350, #143660, #4149, #66825, #112337, #157857, #186219, #19347, #5143, #158831, #139678, #20319, #171032, #32523, #142670, #155854, #63853, #96167, #188204, #190184, #79007, #3171, #128489, #140681, #81968, #64844, #51659, #62840, #113323, #127497, #175015, #174027, #49676, #95174, #35498, #33514, #94175, #111340, #124524, #156861, #173031, #189202, #36480, #98136, #65828, #16362, #78010, #17352, #80011, #2173, #48692, #110344, #172026, #34509, #18356, #141680, #22330, #52656, #99152, #24341, #9168, #67827, #162832, #147680, #37490, #102165, #129483, #179025, #117331, #25352, #8151, #191181, #132503, #178018, #70835, #114319, #85991, #176021, #130483, #23331, #180035, #194192, #159834, #41504, #192180, #101146, #7141, #84975, #83981, #55657, #131495, #40493, #163851, #160841, #133497, #145660, #21328, #86993, #193182, #148680, #68824, #10168, #146657, #161837, #116329, #71828, #53661, #115339, #195189, #56669, #118342, #82986, #144662, #69828, #54655, #6146, #177029, #38499, #39486, #100155, #103168, #12176, #87984, #200141, #14126, #26344, #120313, #59632, #75793, #60617, #149672, #121306, #119340, #72846, #11170, #138460, #153632, #76789, #89982, #15127, #196201, #136482, #168792, #184970, #74820, #137471, #182007, #43489, #198162, #44481, #197182, #30295, #61611, #166842, #199151, #182998, #106137, #135512, #164848, #167820, #151663, #123279, #134515, #57673, #28344, #181026, #42500, #90949, #104164, #29319, #165846, #152636, #122292, #27342, #88988, #183982, #105156, #45467, #150679, #73841, #58647, #13157, #107121, #91939, #112836, #69332, #81481, #5654, #83489, #127003, #175517, #145166, #6650, #174528, #173540, #80508, #21836, #128992, #129978, #67330, #22838, #99662, #65343, #143168, #20828, #130998, #96664, #31291, #82484, #144168, #68328, #128001, #4648, #46455, #142181, #52165, #66339, #190690, #113822, #38007, #111850 ),
 ( #84485, #160347, #146162, #191678, #97642, #189703, #53159, #51176, #3665, #35995, #92942, #159331, #36992, #114837, #176531, #161347, #98653, #7648, #108114, #188711, #169798, #157368, #18862, #50194, #35009, #158351, #19840, #55166, #116837, #85493, #132010, #57181, #42015, #100660, #195709, #180541, #70343, #135028, #162342, #11689, #150191, #58173, #41010, #23843, #165359, #10678, #103680, #147181, #118858, #8670, #163356, #56167, #12673, #26853, #192690, #74340, #24852, #134017, #39994, #117848, #178527, #88494, #164362, #73355, #196703, #193697, #166357, #101666, #54173, #119840, #25857, #181525, #86501, #43004, #177535, #104671, #149189, #148185, #9679, #102677, #71344, #87501, #133007, #27855, #194698, #179541, #115846, #72343, #39005, #89495, #151185, #137978, #44985, #16628, #170305, #120813, #106645, #167342, #441, #45968, #28839, #63116, #123779, #186493, #31798, #77292, #105654, #138963, #124795, #78275, #59143, #139948, #90480, #152162, #62116, #75312, #183502, #15635, #107622, #109621, #198672, #122799, #47969, #60139, #169300, #108627, #171305, #32791, #185478, #94444, #46968, #13645, #199660, #93447, #197678, #155134, #182513, #184489, #156124, #121806, #168317, #136983, #29814, #1438, #17623, #43992, #136006, #91450, #153138, #14640, #76300, #61126, #30806, #92455, #154143, #187488, #159092, #127761, #97405, #125786, #174289, #48954, #65103, #34769, #83249, #20586, #79282, #144924, #188464, #112597, #3427, #96426, #18619, #82238, #4409, #35759, #143928, #172290, #160103, #110607, #140952, #5410, #66094, #67093, #80266, #128752, #33779, #51924, #189461, #126761, #95439, #50939, #49946, #190449, #157123, #113584, #141936, #142928, #64121, #111610, #2439, #158112, #175278, #36743, #98407, #173295, #19604, #21590, #81246, #91099, #124437, #169950, #152787, #187137, #47612, #110261, #94091, #1081, #29466, #62756, #48609, #2088, #183145, #63768, #14278, #75947, #186133, #199305, #107270, #139595, #31441, #33431, #122444, #46610, #171942, #184136, #125441, #108272, #95090, #44630, #156779, #170945, #18272, #17268, #93095, #138607, #155770, #76938, #137621, #154779, #106282, #89, #60772, #16276, #30448, #77928, #45618, #109266, #168941, #32437, #121453, #92095, #59785, #167967, #153783, #61759, #15278, #140598, #78921, #123427, #185120, #79925, #141598, #113240, #34425, #130393, #191094, #53573, #37406, #144575, #172947, #6062, #192090, #145576, #126423, #7053, #157773, #19264, #67740, #142587, #50594, #82897, #174931, #176942, #65744, #190101, #115250, #127412, #68735, #51576, #38412, #188121, #100069, #114229, #161754, #160752, #36394, #81883, #99064, #20235, #80910, #98048, #49592, #143575, #159746, #175934, #23249, #84892, #129398, #3085, #52569, #96084, #66743, #22244, #64761, #83893, #111255, #21243, #4066, #189122, #112253, #173945, #35412, #97064, #158746, #5058, #128404, #57282, #163457, #116936, #132108, #182616, #197782, #120917, #134121, #59248, #40092, #180642, #12774, #28942, #118956, #58269, #25956, #164462, #42117, #88598, #41111, #74439, #44101, #10779, #181623, #103779, #165458, #179641, #147283, #26955, #195810, #105759, #193800, #55267, #72446, #167445, #178629, #135127, #8773, #150294, #24955, #11790, #119938, #70442, #136106, #101770, #73454, #86602, #196801, #148285, #43103, #104771, #9779, #166459, #71441, #27956, #133106, #194795, #56268, #117951, #102775, #89597, #151284, #87599, #149285, #109730, #77401, #32900, #60243, #171414, #48074, #156233, #139071, #121914, #63224, #108736, #140058, #198777, #155244, #183607, #61233, #154251, #110719, #124904, #90583, #172401, #122904, #31905, #138085, #15742, #153246, #186602, #62220, #16734, #1549, #45091, #64230, #106748, #152264, #94552, #123888, #78382, #14748, #17735, #75417, #79392, #47076, #76409, #168423, #549, #184593, #185586, #29918, #141062, #91558, #170413, #13749, #199766, #137090, #46074, #107728 ) ),
 .UNSPECIFIED., .T., .F., .T. ) 
 B_SPLINE_SURFACE_WITH_KNOTS ( ( 4, 3, 4 ),
 ( 3, 2, 2, 2, 2, 2, 2, 2, 2, 2, 2, 2, 2, 2, 2, 2, 2, 2, 2, 2, 2, 2, 2, 2, 2, 2, 2, 2, 2, 2, 2, 2, 2, 2, 2, 2, 2, 2, 2, 2, 2, 2, 2, 2, 2, 2, 2, 2, 2, 2, 2, 2, 2, 2, 2, 2, 2, 2, 2, 2, 2, 2, 2, 2, 2, 2, 2, 2, 2, 2, 2, 2, 2, 2, 2, 2, 2, 2, 2, 2, 2, 2, 2, 2, 2, 2, 2, 2, 2, 2, 2, 2, 2, 2, 2, 2, 2, 2, 2, 2, 2, 2, 2, 2, 2, 2, 2, 2, 2, 2, 2, 2, 2, 2, 2, 2, 2, 2, 2, 2, 2, 2, 2, 2, 2, 2, 2, 2, 2, 2, 2, 2, 2, 2, 2, 2, 2, 2, 2, 2, 2, 2, 2, 2, 2, 2, 2, 2, 2, 2, 2, 2, 2, 2, 2, 2, 2, 2, 2, 2, 2, 2, 2, 2, 2, 2, 2, 2, 2, 2, 2, 2, 2, 2, 2, 2, 2, 2, 2, 2, 2, 2, 2, 2, 2, 2, 2, 2, 2, 2, 2, 2, 2, 2, 2, 2, 2, 2, 2, 2, 2, 2, 2, 2, 2, 2, 2, 2, 2, 2, 2, 2, 2, 2, 2, 2, 2, 2, 2, 2, 2, 2, 2, 2, 2, 2, 2, 2, 3 ),
 ( 0.000000000000000000, 0.5000000000000000000, 1.000000000000000000 ),
 ( 0.000000000000000000, 0.004385964912280701511, 0.008771929824561403022, 0.01315789473684210453, 0.01754385964912280604, 0.02192982456140350755, 0.02631578947368420907, 0.03070175438596491058, 0.03508771929824561209, 0.03947368421052631360, 0.04385964912280701511, 0.04824561403508771662, 0.05263157894736841813, 0.05701754385964911964, 0.06140350877192982115, 0.06578947368421052266, 0.07017543859649122417, 0.07456140350877192569, 0.07894736842105262720, 0.08333333333333332871, 0.08771929824561403022, 0.09210526315789473173, 0.09649122807017543324, 0.1008771929824561348, 0.1052631578947368363, 0.1096491228070175378, 0.1140350877192982393, 0.1184210526315789408, 0.1228070175438596423, 0.1271929824561403577, 0.1315789473684210453, 0.1359649122807017607, 0.1403508771929824483, 0.1447368421052631637, 0.1491228070175438514, 0.1535087719298245668, 0.1578947368421052544, 0.1622807017543859698, 0.1666666666666666574, 0.1710526315789473728, 0.1754385964912280604, 0.1798245614035087758, 0.1842105263157894635, 0.1885964912280701788, 0.1929824561403508665, 0.1973684210526315819, 0.2017543859649122695, 0.2061403508771929849, 0.2105263157894736725, 0.2149122807017543879, 0.2192982456140350755, 0.2236842105263157909, 0.2280701754385964786, 0.2324561403508771940, 0.2368421052631578816, 0.2412280701754385970, 0.2456140350877192846, 0.2500000000000000000, 0.2543859649122807154, 0.2587719298245614308, 0.2631578947368420907, 0.2675438596491228060, 0.2719298245614035214, 0.2763157894736842368, 0.2807017543859648967, 0.2850877192982456121, 0.2894736842105263275, 0.2938596491228070429, 0.2982456140350877027, 0.3026315789473684181, 0.3070175438596491335, 0.3114035087719298489, 0.3157894736842105088, 0.3201754385964912242, 0.3245614035087719396, 0.3289473684210526550, 0.3333333333333333148, 0.3377192982456140302, 0.3421052631578947456, 0.3464912280701754610, 0.3508771929824561209, 0.3552631578947368363, 0.3596491228070175517, 0.3640350877192982670, 0.3684210526315789269, 0.3728070175438596423, 0.3771929824561403577, 0.3815789473684210731, 0.3859649122807017330, 0.3903508771929824483, 0.3947368421052631637, 0.3991228070175438791, 0.4035087719298245390, 0.4078947368421052544, 0.4122807017543859698, 0.4166666666666666852, 0.4210526315789473450, 0.4254385964912280604, 0.4298245614035087758, 0.4342105263157894912, 0.4385964912280701511, 0.4429824561403508665, 0.4473684210526315819, 0.4517543859649122973, 0.4561403508771929571, 0.4605263157894736725, 0.4649122807017543879, 0.4692982456140351033, 0.4736842105263157632, 0.4780701754385964786, 0.4824561403508771940, 0.4868421052631579093, 0.4912280701754385692, 0.4956140350877192846, 0.5000000000000000000, 0.5043859649122807154, 0.5087719298245614308, 0.5131578947368421462, 0.5175438596491228616, 0.5219298245614034659, 0.5263157894736841813, 0.5307017543859648967, 0.5350877192982456121, 0.5394736842105263275, 0.5438596491228070429, 0.5482456140350877583, 0.5526315789473684736, 0.5570175438596490780, 0.5614035087719297934, 0.5657894736842105088, 0.5701754385964912242, 0.5745614035087719396, 0.5789473684210526550, 0.5833333333333333703, 0.5877192982456140857, 0.5921052631578946901, 0.5964912280701754055, 0.6008771929824561209, 0.6052631578947368363, 0.6096491228070175517, 0.6140350877192982670, 0.6184210526315789824, 0.6228070175438596978, 0.6271929824561403022, 0.6315789473684210176, 0.6359649122807017330, 0.6403508771929824483, 0.6447368421052631637, 0.6491228070175438791, 0.6535087719298245945, 0.6578947368421053099, 0.6622807017543859143, 0.6666666666666666297, 0.6710526315789473450, 0.6754385964912280604, 0.6798245614035087758, 0.6842105263157894912, 0.6885964912280702066, 0.6929824561403509220, 0.6973684210526315264, 0.7017543859649122417, 0.7061403508771929571, 0.7105263157894736725, 0.7149122807017543879, 0.7192982456140351033, 0.7236842105263158187, 0.7280701754385965341, 0.7324561403508771384, 0.7368421052631578538, 0.7412280701754385692, 0.7456140350877192846, 0.7500000000000000000, 0.7543859649122807154, 0.7587719298245614308, 0.7631578947368421462, 0.7675438596491228616, 0.7719298245614034659, 0.7763157894736841813, 0.7807017543859648967, 0.7850877192982456121, 0.7894736842105263275, 0.7938596491228070429, 0.7982456140350877583, 0.8026315789473684736, 0.8070175438596490780, 0.8114035087719297934, 0.8157894736842105088, 0.8201754385964912242, 0.8245614035087719396, 0.8289473684210526550, 0.8333333333333333703, 0.8377192982456140857, 0.8421052631578946901, 0.8464912280701754055, 0.8508771929824561209, 0.8552631578947368363, 0.8596491228070175517, 0.8640350877192982670, 0.8684210526315789824, 0.8728070175438596978, 0.8771929824561403022, 0.8815789473684210176, 0.8859649122807017330, 0.8903508771929824483, 0.8947368421052631637, 0.8991228070175438791, 0.9035087719298245945, 0.9078947368421053099, 0.9122807017543859143, 0.9166666666666666297, 0.9210526315789473450, 0.9254385964912280604, 0.9298245614035087758, 0.9342105263157894912, 0.9385964912280702066, 0.9429824561403509220, 0.9473684210526315264, 0.9517543859649122417, 0.9561403508771929571, 0.9605263157894736725, 0.9649122807017543879, 0.9692982456140351033, 0.9736842105263158187, 0.9780701754385965341, 0.9824561403508771384, 0.9868421052631578538, 0.9912280701754385692, 0.9956140350877192846, 1.000000000000000000 ),
 .UNSPECIFIED. ) 
 GEOMETRIC_REPRESENTATION_ITEM ( )  RATIONAL_B_SPLINE_SURFACE ( (
 ( 1.000000000000000000, 0.9659258262890683122, 1.000000000000000000, 0.9659258262890683122, 1.000000000000000000, 0.9659258262890683122, 1.000000000000000000, 0.9659258262890683122, 1.000000000000000000, 0.9659258262890683122, 1.000000000000000000, 0.9659258262890683122, 1.000000000000000000, 0.9659258262890683122, 1.000000000000000000, 0.9659258262890683122, 1.000000000000000000, 0.9659258262890683122, 1.000000000000000000, 0.9659258262890683122, 1.000000000000000000, 0.9659258262890683122, 1.000000000000000000, 0.9659258262890683122, 1.000000000000000000, 0.9659258262890683122, 1.000000000000000000, 0.9659258262890683122, 1.000000000000000000, 0.9659258262890683122, 1.000000000000000000, 0.9659258262890683122, 1.000000000000000000, 0.9659258262890683122, 1.000000000000000000, 0.9659258262890683122, 1.000000000000000000, 0.9659258262890683122, 1.000000000000000000, 0.9659258262890683122, 1.000000000000000000, 0.9659258262890683122, 1.000000000000000000, 0.9659258262890683122, 1.000000000000000000, 0.9659258262890683122, 1.000000000000000000, 0.9659258262890683122, 1.000000000000000000, 0.9659258262890683122, 1.000000000000000000, 0.9659258262890683122, 1.000000000000000000, 0.9659258262890683122, 1.000000000000000000, 0.9659258262890683122, 1.000000000000000000, 0.9659258262890683122, 1.000000000000000000, 0.9659258262890683122, 1.000000000000000000, 0.9659258262890683122, 1.000000000000000000, 0.9659258262890683122, 1.000000000000000000, 0.9659258262890683122, 1.000000000000000000, 0.9659258262890683122, 1.000000000000000000, 0.9659258262890683122, 1.000000000000000000, 0.9659258262890683122, 1.000000000000000000, 0.9659258262890683122, 1.000000000000000000, 0.9659258262890683122, 1.000000000000000000, 0.9659258262890683122, 1.000000000000000000, 0.9659258262890683122, 1.000000000000000000, 0.9659258262890683122, 1.000000000000000000, 0.9659258262890683122, 1.000000000000000000, 0.9659258262890683122, 1.000000000000000000, 0.9659258262890683122, 1.000000000000000000, 0.9659258262890683122, 1.000000000000000000, 0.9659258262890683122, 1.000000000000000000, 0.9659258262890683122, 1.000000000000000000, 0.9659258262890683122, 1.000000000000000000, 0.9659258262890683122, 1.000000000000000000, 0.9659258262890683122, 1.000000000000000000, 0.9659258262890683122, 1.000000000000000000, 0.9659258262890683122, 1.000000000000000000, 0.9659258262890683122, 1.000000000000000000, 0.9659258262890683122, 1.000000000000000000, 0.9659258262890683122, 1.000000000000000000, 0.9659258262890683122, 1.000000000000000000, 0.9659258262890683122, 1.000000000000000000, 0.9659258262890683122, 1.000000000000000000, 0.9659258262890683122, 1.000000000000000000, 0.9659258262890683122, 1.000000000000000000, 0.9659258262890683122, 1.000000000000000000, 0.9659258262890683122, 1.000000000000000000, 0.9659258262890683122, 1.000000000000000000, 0.9659258262890683122, 1.000000000000000000, 0.9659258262890683122, 1.000000000000000000, 0.9659258262890683122, 1.000000000000000000, 0.9659258262890683122, 1.000000000000000000, 0.9659258262890683122, 1.000000000000000000, 0.9659258262890683122, 1.000000000000000000, 0.9659258262890683122, 1.000000000000000000, 0.9659258262890683122, 1.000000000000000000, 0.9659258262890683122, 1.000000000000000000, 0.9659258262890683122, 1.000000000000000000, 0.9659258262890683122, 1.000000000000000000, 0.9659258262890683122, 1.000000000000000000, 0.9659258262890683122, 1.000000000000000000, 0.9659258262890683122, 1.000000000000000000, 0.9659258262890683122, 1.000000000000000000, 0.9659258262890683122, 1.000000000000000000, 0.9659258262890683122, 1.000000000000000000, 0.9659258262890683122, 1.000000000000000000, 0.9659258262890683122, 1.000000000000000000, 0.9659258262890683122, 1.000000000000000000, 0.9659258262890683122, 1.000000000000000000, 0.9659258262890683122, 1.000000000000000000, 0.9659258262890683122, 1.000000000000000000, 0.9659258262890683122, 1.000000000000000000, 0.9659258262890683122, 1.000000000000000000, 0.9659258262890683122, 1.000000000000000000, 0.9659258262890683122, 1.000000000000000000, 0.9659258262890683122, 1.000000000000000000, 0.9659258262890683122, 1.000000000000000000, 0.9659258262890683122, 1.000000000000000000, 0.9659258262890683122, 1.000000000000000000, 0.9659258262890683122, 1.000000000000000000, 0.9659258262890683122, 1.000000000000000000, 0.9659258262890683122, 1.000000000000000000, 0.9659258262890683122, 1.000000000000000000, 0.9659258262890683122, 1.000000000000000000, 0.9659258262890683122, 1.000000000000000000, 0.9659258262890683122, 1.000000000000000000, 0.9659258262890683122, 1.000000000000000000, 0.9659258262890683122, 1.000000000000000000, 0.9659258262890683122, 1.000000000000000000, 0.9659258262890683122, 1.000000000000000000, 0.9659258262890683122, 1.000000000000000000, 0.9659258262890683122, 1.000000000000000000, 0.9659258262890683122, 1.000000000000000000, 0.9659258262890683122, 1.000000000000000000, 0.9659258262890683122, 1.000000000000000000, 0.9659258262890683122, 1.000000000000000000, 0.9659258262890683122, 1.000000000000000000, 0.9659258262890683122, 1.000000000000000000, 0.9659258262890683122, 1.000000000000000000, 0.9659258262890683122, 1.000000000000000000, 0.9659258262890683122, 1.000000000000000000, 0.9659258262890683122, 1.000000000000000000, 0.9659258262890683122, 1.000000000000000000, 0.9659258262890683122, 1.000000000000000000, 0.9659258262890683122, 1.000000000000000000, 0.9659258262890683122, 1.000000000000000000, 0.9659258262890683122, 1.000000000000000000, 0.9659258262890683122, 1.000000000000000000, 0.9659258262890683122, 1.000000000000000000, 0.9659258262890683122, 1.000000000000000000, 0.9659258262890683122, 1.000000000000000000, 0.9659258262890683122, 1.000000000000000000, 0.9659258262890683122, 1.000000000000000000, 0.9659258262890683122, 1.000000000000000000, 0.9659258262890683122, 1.000000000000000000, 0.9659258262890683122, 1.000000000000000000, 0.9659258262890683122, 1.000000000000000000, 0.9659258262890683122, 1.000000000000000000, 0.9659258262890683122, 1.000000000000000000, 0.9659258262890683122, 1.000000000000000000, 0.9659258262890683122, 1.000000000000000000, 0.9659258262890683122, 1.000000000000000000, 0.9659258262890683122, 1.000000000000000000, 0.9659258262890683122, 1.000000000000000000, 0.9659258262890683122, 1.000000000000000000, 0.9659258262890683122, 1.000000000000000000, 0.9659258262890683122, 1.000000000000000000, 0.9659258262890683122, 1.000000000000000000, 0.9659258262890683122, 1.000000000000000000, 0.9659258262890683122, 1.000000000000000000, 0.9659258262890683122, 1.000000000000000000, 0.9659258262890683122, 1.000000000000000000, 0.9659258262890683122, 1.000000000000000000, 0.9659258262890683122, 1.000000000000000000, 0.9659258262890683122, 1.000000000000000000, 0.9659258262890683122, 1.000000000000000000, 0.9659258262890683122, 1.000000000000000000, 0.9659258262890683122, 1.000000000000000000, 0.9659258262890683122, 1.000000000000000000, 0.9659258262890683122, 1.000000000000000000, 0.9659258262890683122, 1.000000000000000000, 0.9659258262890683122, 1.000000000000000000, 0.9659258262890683122, 1.000000000000000000, 0.9659258262890683122, 1.000000000000000000, 0.9659258262890683122, 1.000000000000000000, 0.9659258262890683122, 1.000000000000000000, 0.9659258262890683122, 1.000000000000000000, 0.9659258262890683122, 1.000000000000000000, 0.9659258262890683122, 1.000000000000000000, 0.9659258262890683122, 1.000000000000000000, 0.9659258262890683122, 1.000000000000000000, 0.9659258262890683122, 1.000000000000000000, 0.9659258262890683122, 1.000000000000000000, 0.9659258262890683122, 1.000000000000000000, 0.9659258262890683122, 1.000000000000000000, 0.9659258262890683122, 1.000000000000000000, 0.9659258262890683122, 1.000000000000000000, 0.9659258262890683122, 1.000000000000000000, 0.9659258262890683122, 1.000000000000000000, 0.9659258262890683122, 1.000000000000000000, 0.9659258262890683122, 1.000000000000000000, 0.9659258262890683122, 1.000000000000000000, 0.9659258262890683122, 1.000000000000000000, 0.9659258262890683122, 1.000000000000000000, 0.9659258262890683122, 1.000000000000000000, 0.9659258262890683122, 1.000000000000000000, 0.9659258262890683122, 1.000000000000000000, 0.9659258262890683122, 1.000000000000000000, 0.9659258262890683122, 1.000000000000000000, 0.9659258262890683122, 1.000000000000000000, 0.9659258262890683122, 1.000000000000000000, 0.9659258262890683122, 1.000000000000000000, 0.9659258262890683122, 1.000000000000000000, 0.9659258262890683122, 1.000000000000000000, 0.9659258262890683122, 1.000000000000000000, 0.9659258262890683122, 1.000000000000000000, 0.9659258262890683122, 1.000000000000000000, 0.9659258262890683122, 1.000000000000000000, 0.9659258262890683122, 1.000000000000000000, 0.9659258262890683122, 1.000000000000000000, 0.9659258262890683122, 1.000000000000000000, 0.9659258262890683122, 1.000000000000000000, 0.9659258262890683122, 1.000000000000000000, 0.9659258262890683122, 1.000000000000000000, 0.9659258262890683122, 1.000000000000000000, 0.9659258262890683122, 1.000000000000000000, 0.9659258262890683122, 1.000000000000000000, 0.9659258262890683122, 1.000000000000000000, 0.9659258262890683122, 1.000000000000000000, 0.9659258262890683122, 1.000000000000000000, 0.9659258262890683122, 1.000000000000000000, 0.9659258262890683122, 1.000000000000000000, 0.9659258262890683122, 1.000000000000000000, 0.9659258262890683122, 1.000000000000000000, 0.9659258262890683122, 1.000000000000000000, 0.9659258262890683122, 1.000000000000000000, 0.9659258262890683122, 1.000000000000000000, 0.9659258262890683122, 1.000000000000000000, 0.9659258262890683122, 1.000000000000000000, 0.9659258262890683122, 1.000000000000000000, 0.9659258262890683122, 1.000000000000000000, 0.9659258262890683122, 1.000000000000000000, 0.9659258262890683122, 1.000000000000000000, 0.9659258262890683122, 1.000000000000000000, 0.9659258262890683122, 1.000000000000000000, 0.9659258262890683122, 1.000000000000000000, 0.9659258262890683122, 1.000000000000000000, 0.9659258262890683122, 1.000000000000000000, 0.9659258262890683122, 1.000000000000000000, 0.9659258262890683122, 1.000000000000000000, 0.9659258262890683122, 1.000000000000000000, 0.9659258262890683122, 1.000000000000000000, 0.9659258262890683122, 1.000000000000000000),
 ( 0.3333333333333333703, 0.3219752754296894559, 0.3333333333333333703, 0.3219752754296894559, 0.3333333333333333703, 0.3219752754296894559, 0.3333333333333333703, 0.3219752754296894559, 0.3333333333333333703, 0.3219752754296894559, 0.3333333333333333703, 0.3219752754296894559, 0.3333333333333333703, 0.3219752754296894559, 0.3333333333333333703, 0.3219752754296894559, 0.3333333333333333703, 0.3219752754296894559, 0.3333333333333333703, 0.3219752754296894559, 0.3333333333333333703, 0.3219752754296894559, 0.3333333333333333703, 0.3219752754296894559, 0.3333333333333333703, 0.3219752754296894559, 0.3333333333333333703, 0.3219752754296894559, 0.3333333333333333703, 0.3219752754296894559, 0.3333333333333333703, 0.3219752754296894559, 0.3333333333333333703, 0.3219752754296894559, 0.3333333333333333703, 0.3219752754296894559, 0.3333333333333333703, 0.3219752754296894559, 0.3333333333333333703, 0.3219752754296894559, 0.3333333333333333703, 0.3219752754296894559, 0.3333333333333333703, 0.3219752754296894559, 0.3333333333333333703, 0.3219752754296894559, 0.3333333333333333703, 0.3219752754296894559, 0.3333333333333333703, 0.3219752754296894559, 0.3333333333333333703, 0.3219752754296894559, 0.3333333333333333703, 0.3219752754296894559, 0.3333333333333333703, 0.3219752754296894559, 0.3333333333333333703, 0.3219752754296894559, 0.3333333333333333703, 0.3219752754296894559, 0.3333333333333333703, 0.3219752754296894559, 0.3333333333333333703, 0.3219752754296894559, 0.3333333333333333703, 0.3219752754296894559, 0.3333333333333333703, 0.3219752754296894559, 0.3333333333333333703, 0.3219752754296894559, 0.3333333333333333703, 0.3219752754296894559, 0.3333333333333333703, 0.3219752754296894559, 0.3333333333333333703, 0.3219752754296894559, 0.3333333333333333703, 0.3219752754296894559, 0.3333333333333333703, 0.3219752754296894559, 0.3333333333333333703, 0.3219752754296894559, 0.3333333333333333703, 0.3219752754296894559, 0.3333333333333333703, 0.3219752754296894559, 0.3333333333333333703, 0.3219752754296894559, 0.3333333333333333703, 0.3219752754296894559, 0.3333333333333333703, 0.3219752754296894559, 0.3333333333333333703, 0.3219752754296894559, 0.3333333333333333703, 0.3219752754296894559, 0.3333333333333333703, 0.3219752754296894559, 0.3333333333333333703, 0.3219752754296894559, 0.3333333333333333703, 0.3219752754296894559, 0.3333333333333333703, 0.3219752754296894559, 0.3333333333333333703, 0.3219752754296894559, 0.3333333333333333703, 0.3219752754296894559, 0.3333333333333333703, 0.3219752754296894559, 0.3333333333333333703, 0.3219752754296894559, 0.3333333333333333703, 0.3219752754296894559, 0.3333333333333333703, 0.3219752754296894559, 0.3333333333333333703, 0.3219752754296894559, 0.3333333333333333703, 0.3219752754296894559, 0.3333333333333333703, 0.3219752754296894559, 0.3333333333333333703, 0.3219752754296894559, 0.3333333333333333703, 0.3219752754296894559, 0.3333333333333333703, 0.3219752754296894559, 0.3333333333333333703, 0.3219752754296894559, 0.3333333333333333703, 0.3219752754296894559, 0.3333333333333333703, 0.3219752754296894559, 0.3333333333333333703, 0.3219752754296894559, 0.3333333333333333703, 0.3219752754296894559, 0.3333333333333333703, 0.3219752754296894559, 0.3333333333333333703, 0.3219752754296894559, 0.3333333333333333703, 0.3219752754296894559, 0.3333333333333333703, 0.3219752754296894559, 0.3333333333333333703, 0.3219752754296894559, 0.3333333333333333703, 0.3219752754296894559, 0.3333333333333333703, 0.3219752754296894559, 0.3333333333333333703, 0.3219752754296894559, 0.3333333333333333703, 0.3219752754296894559, 0.3333333333333333703, 0.3219752754296894559, 0.3333333333333333703, 0.3219752754296894559, 0.3333333333333333703, 0.3219752754296894559, 0.3333333333333333703, 0.3219752754296894559, 0.3333333333333333703, 0.3219752754296894559, 0.3333333333333333703, 0.3219752754296894559, 0.3333333333333333703, 0.3219752754296894559, 0.3333333333333333703, 0.3219752754296894559, 0.3333333333333333703, 0.3219752754296894559, 0.3333333333333333703, 0.3219752754296894559, 0.3333333333333333703, 0.3219752754296894559, 0.3333333333333333703, 0.3219752754296894559, 0.3333333333333333703, 0.3219752754296894559, 0.3333333333333333703, 0.3219752754296894559, 0.3333333333333333703, 0.3219752754296894559, 0.3333333333333333703, 0.3219752754296894559, 0.3333333333333333703, 0.3219752754296894559, 0.3333333333333333703, 0.3219752754296894559, 0.3333333333333333703, 0.3219752754296894559, 0.3333333333333333703, 0.3219752754296894559, 0.3333333333333333703, 0.3219752754296894559, 0.3333333333333333703, 0.3219752754296894559, 0.3333333333333333703, 0.3219752754296894559, 0.3333333333333333703, 0.3219752754296894559, 0.3333333333333333703, 0.3219752754296894559, 0.3333333333333333703, 0.3219752754296894559, 0.3333333333333333703, 0.3219752754296894559, 0.3333333333333333703, 0.3219752754296894559, 0.3333333333333333703, 0.3219752754296894559, 0.3333333333333333703, 0.3219752754296894559, 0.3333333333333333703, 0.3219752754296894559, 0.3333333333333333703, 0.3219752754296894559, 0.3333333333333333703, 0.3219752754296894559, 0.3333333333333333703, 0.3219752754296894559, 0.3333333333333333703, 0.3219752754296894559, 0.3333333333333333703, 0.3219752754296894559, 0.3333333333333333703, 0.3219752754296894559, 0.3333333333333333703, 0.3219752754296894559, 0.3333333333333333703, 0.3219752754296894559, 0.3333333333333333703, 0.3219752754296894559, 0.3333333333333333703, 0.3219752754296894559, 0.3333333333333333703, 0.3219752754296894559, 0.3333333333333333703, 0.3219752754296894559, 0.3333333333333333703, 0.3219752754296894559, 0.3333333333333333703, 0.3219752754296894559, 0.3333333333333333703, 0.3219752754296894559, 0.3333333333333333703, 0.3219752754296894559, 0.3333333333333333703, 0.3219752754296894559, 0.3333333333333333703, 0.3219752754296894559, 0.3333333333333333703, 0.3219752754296894559, 0.3333333333333333703, 0.3219752754296894559, 0.3333333333333333703, 0.3219752754296894559, 0.3333333333333333703, 0.3219752754296894559, 0.3333333333333333703, 0.3219752754296894559, 0.3333333333333333703, 0.3219752754296894559, 0.3333333333333333703, 0.3219752754296894559, 0.3333333333333333703, 0.3219752754296894559, 0.3333333333333333703, 0.3219752754296894559, 0.3333333333333333703, 0.3219752754296894559, 0.3333333333333333703, 0.3219752754296894559, 0.3333333333333333703, 0.3219752754296894559, 0.3333333333333333703, 0.3219752754296894559, 0.3333333333333333703, 0.3219752754296894559, 0.3333333333333333703, 0.3219752754296894559, 0.3333333333333333703, 0.3219752754296894559, 0.3333333333333333703, 0.3219752754296894559, 0.3333333333333333703, 0.3219752754296894559, 0.3333333333333333703, 0.3219752754296894559, 0.3333333333333333703, 0.3219752754296894559, 0.3333333333333333703, 0.3219752754296894559, 0.3333333333333333703, 0.3219752754296894559, 0.3333333333333333703, 0.3219752754296894559, 0.3333333333333333703, 0.3219752754296894559, 0.3333333333333333703, 0.3219752754296894559, 0.3333333333333333703, 0.3219752754296894559, 0.3333333333333333703, 0.3219752754296894559, 0.3333333333333333703, 0.3219752754296894559, 0.3333333333333333703, 0.3219752754296894559, 0.3333333333333333703, 0.3219752754296894559, 0.3333333333333333703, 0.3219752754296894559, 0.3333333333333333703, 0.3219752754296894559, 0.3333333333333333703, 0.3219752754296894559, 0.3333333333333333703, 0.3219752754296894559, 0.3333333333333333703, 0.3219752754296894559, 0.3333333333333333703, 0.3219752754296894559, 0.3333333333333333703, 0.3219752754296894559, 0.3333333333333333703, 0.3219752754296894559, 0.3333333333333333703, 0.3219752754296894559, 0.3333333333333333703, 0.3219752754296894559, 0.3333333333333333703, 0.3219752754296894559, 0.3333333333333333703, 0.3219752754296894559, 0.3333333333333333703, 0.3219752754296894559, 0.3333333333333333703, 0.3219752754296894559, 0.3333333333333333703, 0.3219752754296894559, 0.3333333333333333703, 0.3219752754296894559, 0.3333333333333333703, 0.3219752754296894559, 0.3333333333333333703, 0.3219752754296894559, 0.3333333333333333703, 0.3219752754296894559, 0.3333333333333333703, 0.3219752754296894559, 0.3333333333333333703, 0.3219752754296894559, 0.3333333333333333703, 0.3219752754296894559, 0.3333333333333333703, 0.3219752754296894559, 0.3333333333333333703, 0.3219752754296894559, 0.3333333333333333703, 0.3219752754296894559, 0.3333333333333333703, 0.3219752754296894559, 0.3333333333333333703, 0.3219752754296894559, 0.3333333333333333703, 0.3219752754296894559, 0.3333333333333333703, 0.3219752754296894559, 0.3333333333333333703, 0.3219752754296894559, 0.3333333333333333703, 0.3219752754296894559, 0.3333333333333333703, 0.3219752754296894559, 0.3333333333333333703, 0.3219752754296894559, 0.3333333333333333703, 0.3219752754296894559, 0.3333333333333333703, 0.3219752754296894559, 0.3333333333333333703, 0.3219752754296894559, 0.3333333333333333703, 0.3219752754296894559, 0.3333333333333333703, 0.3219752754296894559, 0.3333333333333333703, 0.3219752754296894559, 0.3333333333333333703, 0.3219752754296894559, 0.3333333333333333703, 0.3219752754296894559, 0.3333333333333333703, 0.3219752754296894559, 0.3333333333333333703, 0.3219752754296894559, 0.3333333333333333703, 0.3219752754296894559, 0.3333333333333333703, 0.3219752754296894559, 0.3333333333333333703, 0.3219752754296894559, 0.3333333333333333703, 0.3219752754296894559, 0.3333333333333333703, 0.3219752754296894559, 0.3333333333333333703, 0.3219752754296894559, 0.3333333333333333703, 0.3219752754296894559, 0.3333333333333333703, 0.3219752754296894559, 0.3333333333333333703, 0.3219752754296894559, 0.3333333333333333703, 0.3219752754296894559, 0.3333333333333333703, 0.3219752754296894559, 0.3333333333333333703, 0.3219752754296894559, 0.3333333333333333703, 0.3219752754296894559, 0.3333333333333333703, 0.3219752754296894559, 0.3333333333333333703, 0.3219752754296894559, 0.3333333333333333703, 0.3219752754296894559, 0.3333333333333333703, 0.3219752754296894559, 0.3333333333333333703, 0.3219752754296894559, 0.3333333333333333703, 0.3219752754296894559, 0.3333333333333333703, 0.3219752754296894559, 0.3333333333333333703, 0.3219752754296894559, 0.3333333333333333703, 0.3219752754296894559, 0.3333333333333333703, 0.3219752754296894559, 0.3333333333333333703, 0.3219752754296894559, 0.3333333333333333703, 0.3219752754296894559, 0.3333333333333333703, 0.3219752754296894559, 0.3333333333333333703, 0.3219752754296894559, 0.3333333333333333703, 0.3219752754296894559, 0.3333333333333333703),
 ( 0.3333333333333333703, 0.3219752754296894559, 0.3333333333333333703, 0.3219752754296894559, 0.3333333333333333703, 0.3219752754296894559, 0.3333333333333333703, 0.3219752754296894559, 0.3333333333333333703, 0.3219752754296894559, 0.3333333333333333703, 0.3219752754296894559, 0.3333333333333333703, 0.3219752754296894559, 0.3333333333333333703, 0.3219752754296894559, 0.3333333333333333703, 0.3219752754296894559, 0.3333333333333333703, 0.3219752754296894559, 0.3333333333333333703, 0.3219752754296894559, 0.3333333333333333703, 0.3219752754296894559, 0.3333333333333333703, 0.3219752754296894559, 0.3333333333333333703, 0.3219752754296894559, 0.3333333333333333703, 0.3219752754296894559, 0.3333333333333333703, 0.3219752754296894559, 0.3333333333333333703, 0.3219752754296894559, 0.3333333333333333703, 0.3219752754296894559, 0.3333333333333333703, 0.3219752754296894559, 0.3333333333333333703, 0.3219752754296894559, 0.3333333333333333703, 0.3219752754296894559, 0.3333333333333333703, 0.3219752754296894559, 0.3333333333333333703, 0.3219752754296894559, 0.3333333333333333703, 0.3219752754296894559, 0.3333333333333333703, 0.3219752754296894559, 0.3333333333333333703, 0.3219752754296894559, 0.3333333333333333703, 0.3219752754296894559, 0.3333333333333333703, 0.3219752754296894559, 0.3333333333333333703, 0.3219752754296894559, 0.3333333333333333703, 0.3219752754296894559, 0.3333333333333333703, 0.3219752754296894559, 0.3333333333333333703, 0.3219752754296894559, 0.3333333333333333703, 0.3219752754296894559, 0.3333333333333333703, 0.3219752754296894559, 0.3333333333333333703, 0.3219752754296894559, 0.3333333333333333703, 0.3219752754296894559, 0.3333333333333333703, 0.3219752754296894559, 0.3333333333333333703, 0.3219752754296894559, 0.3333333333333333703, 0.3219752754296894559, 0.3333333333333333703, 0.3219752754296894559, 0.3333333333333333703, 0.3219752754296894559, 0.3333333333333333703, 0.3219752754296894559, 0.3333333333333333703, 0.3219752754296894559, 0.3333333333333333703, 0.3219752754296894559, 0.3333333333333333703, 0.3219752754296894559, 0.3333333333333333703, 0.3219752754296894559, 0.3333333333333333703, 0.3219752754296894559, 0.3333333333333333703, 0.3219752754296894559, 0.3333333333333333703, 0.3219752754296894559, 0.3333333333333333703, 0.3219752754296894559, 0.3333333333333333703, 0.3219752754296894559, 0.3333333333333333703, 0.3219752754296894559, 0.3333333333333333703, 0.3219752754296894559, 0.3333333333333333703, 0.3219752754296894559, 0.3333333333333333703, 0.3219752754296894559, 0.3333333333333333703, 0.3219752754296894559, 0.3333333333333333703, 0.3219752754296894559, 0.3333333333333333703, 0.3219752754296894559, 0.3333333333333333703, 0.3219752754296894559, 0.3333333333333333703, 0.3219752754296894559, 0.3333333333333333703, 0.3219752754296894559, 0.3333333333333333703, 0.3219752754296894559, 0.3333333333333333703, 0.3219752754296894559, 0.3333333333333333703, 0.3219752754296894559, 0.3333333333333333703, 0.3219752754296894559, 0.3333333333333333703, 0.3219752754296894559, 0.3333333333333333703, 0.3219752754296894559, 0.3333333333333333703, 0.3219752754296894559, 0.3333333333333333703, 0.3219752754296894559, 0.3333333333333333703, 0.3219752754296894559, 0.3333333333333333703, 0.3219752754296894559, 0.3333333333333333703, 0.3219752754296894559, 0.3333333333333333703, 0.3219752754296894559, 0.3333333333333333703, 0.3219752754296894559, 0.3333333333333333703, 0.3219752754296894559, 0.3333333333333333703, 0.3219752754296894559, 0.3333333333333333703, 0.3219752754296894559, 0.3333333333333333703, 0.3219752754296894559, 0.3333333333333333703, 0.3219752754296894559, 0.3333333333333333703, 0.3219752754296894559, 0.3333333333333333703, 0.3219752754296894559, 0.3333333333333333703, 0.3219752754296894559, 0.3333333333333333703, 0.3219752754296894559, 0.3333333333333333703, 0.3219752754296894559, 0.3333333333333333703, 0.3219752754296894559, 0.3333333333333333703, 0.3219752754296894559, 0.3333333333333333703, 0.3219752754296894559, 0.3333333333333333703, 0.3219752754296894559, 0.3333333333333333703, 0.3219752754296894559, 0.3333333333333333703, 0.3219752754296894559, 0.3333333333333333703, 0.3219752754296894559, 0.3333333333333333703, 0.3219752754296894559, 0.3333333333333333703, 0.3219752754296894559, 0.3333333333333333703, 0.3219752754296894559, 0.3333333333333333703, 0.3219752754296894559, 0.3333333333333333703, 0.3219752754296894559, 0.3333333333333333703, 0.3219752754296894559, 0.3333333333333333703, 0.3219752754296894559, 0.3333333333333333703, 0.3219752754296894559, 0.3333333333333333703, 0.3219752754296894559, 0.3333333333333333703, 0.3219752754296894559, 0.3333333333333333703, 0.3219752754296894559, 0.3333333333333333703, 0.3219752754296894559, 0.3333333333333333703, 0.3219752754296894559, 0.3333333333333333703, 0.3219752754296894559, 0.3333333333333333703, 0.3219752754296894559, 0.3333333333333333703, 0.3219752754296894559, 0.3333333333333333703, 0.3219752754296894559, 0.3333333333333333703, 0.3219752754296894559, 0.3333333333333333703, 0.3219752754296894559, 0.3333333333333333703, 0.3219752754296894559, 0.3333333333333333703, 0.3219752754296894559, 0.3333333333333333703, 0.3219752754296894559, 0.3333333333333333703, 0.3219752754296894559, 0.3333333333333333703, 0.3219752754296894559, 0.3333333333333333703, 0.3219752754296894559, 0.3333333333333333703, 0.3219752754296894559, 0.3333333333333333703, 0.3219752754296894559, 0.3333333333333333703, 0.3219752754296894559, 0.3333333333333333703, 0.3219752754296894559, 0.3333333333333333703, 0.3219752754296894559, 0.3333333333333333703, 0.3219752754296894559, 0.3333333333333333703, 0.3219752754296894559, 0.3333333333333333703, 0.3219752754296894559, 0.3333333333333333703, 0.3219752754296894559, 0.3333333333333333703, 0.3219752754296894559, 0.3333333333333333703, 0.3219752754296894559, 0.3333333333333333703, 0.3219752754296894559, 0.3333333333333333703, 0.3219752754296894559, 0.3333333333333333703, 0.3219752754296894559, 0.3333333333333333703, 0.3219752754296894559, 0.3333333333333333703, 0.3219752754296894559, 0.3333333333333333703, 0.3219752754296894559, 0.3333333333333333703, 0.3219752754296894559, 0.3333333333333333703, 0.3219752754296894559, 0.3333333333333333703, 0.3219752754296894559, 0.3333333333333333703, 0.3219752754296894559, 0.3333333333333333703, 0.3219752754296894559, 0.3333333333333333703, 0.3219752754296894559, 0.3333333333333333703, 0.3219752754296894559, 0.3333333333333333703, 0.3219752754296894559, 0.3333333333333333703, 0.3219752754296894559, 0.3333333333333333703, 0.3219752754296894559, 0.3333333333333333703, 0.3219752754296894559, 0.3333333333333333703, 0.3219752754296894559, 0.3333333333333333703, 0.3219752754296894559, 0.3333333333333333703, 0.3219752754296894559, 0.3333333333333333703, 0.3219752754296894559, 0.3333333333333333703, 0.3219752754296894559, 0.3333333333333333703, 0.3219752754296894559, 0.3333333333333333703, 0.3219752754296894559, 0.3333333333333333703, 0.3219752754296894559, 0.3333333333333333703, 0.3219752754296894559, 0.3333333333333333703, 0.3219752754296894559, 0.3333333333333333703, 0.3219752754296894559, 0.3333333333333333703, 0.3219752754296894559, 0.3333333333333333703, 0.3219752754296894559, 0.3333333333333333703, 0.3219752754296894559, 0.3333333333333333703, 0.3219752754296894559, 0.3333333333333333703, 0.3219752754296894559, 0.3333333333333333703, 0.3219752754296894559, 0.3333333333333333703, 0.3219752754296894559, 0.3333333333333333703, 0.3219752754296894559, 0.3333333333333333703, 0.3219752754296894559, 0.3333333333333333703, 0.3219752754296894559, 0.3333333333333333703, 0.3219752754296894559, 0.3333333333333333703, 0.3219752754296894559, 0.3333333333333333703, 0.3219752754296894559, 0.3333333333333333703, 0.3219752754296894559, 0.3333333333333333703, 0.3219752754296894559, 0.3333333333333333703, 0.3219752754296894559, 0.3333333333333333703, 0.3219752754296894559, 0.3333333333333333703, 0.3219752754296894559, 0.3333333333333333703, 0.3219752754296894559, 0.3333333333333333703, 0.3219752754296894559, 0.3333333333333333703, 0.3219752754296894559, 0.3333333333333333703, 0.3219752754296894559, 0.3333333333333333703, 0.3219752754296894559, 0.3333333333333333703, 0.3219752754296894559, 0.3333333333333333703, 0.3219752754296894559, 0.3333333333333333703, 0.3219752754296894559, 0.3333333333333333703, 0.3219752754296894559, 0.3333333333333333703, 0.3219752754296894559, 0.3333333333333333703, 0.3219752754296894559, 0.3333333333333333703, 0.3219752754296894559, 0.3333333333333333703, 0.3219752754296894559, 0.3333333333333333703, 0.3219752754296894559, 0.3333333333333333703, 0.3219752754296894559, 0.3333333333333333703, 0.3219752754296894559, 0.3333333333333333703, 0.3219752754296894559, 0.3333333333333333703, 0.3219752754296894559, 0.3333333333333333703, 0.3219752754296894559, 0.3333333333333333703, 0.3219752754296894559, 0.3333333333333333703, 0.3219752754296894559, 0.3333333333333333703, 0.3219752754296894559, 0.3333333333333333703, 0.3219752754296894559, 0.3333333333333333703, 0.3219752754296894559, 0.3333333333333333703, 0.3219752754296894559, 0.3333333333333333703, 0.3219752754296894559, 0.3333333333333333703, 0.3219752754296894559, 0.3333333333333333703, 0.3219752754296894559, 0.3333333333333333703, 0.3219752754296894559, 0.3333333333333333703, 0.3219752754296894559, 0.3333333333333333703, 0.3219752754296894559, 0.3333333333333333703, 0.3219752754296894559, 0.3333333333333333703, 0.3219752754296894559, 0.3333333333333333703, 0.3219752754296894559, 0.3333333333333333703, 0.3219752754296894559, 0.3333333333333333703, 0.3219752754296894559, 0.3333333333333333703, 0.3219752754296894559, 0.3333333333333333703, 0.3219752754296894559, 0.3333333333333333703, 0.3219752754296894559, 0.3333333333333333703, 0.3219752754296894559, 0.3333333333333333703, 0.3219752754296894559, 0.3333333333333333703, 0.3219752754296894559, 0.3333333333333333703, 0.3219752754296894559, 0.3333333333333333703, 0.3219752754296894559, 0.3333333333333333703, 0.3219752754296894559, 0.3333333333333333703, 0.3219752754296894559, 0.3333333333333333703, 0.3219752754296894559, 0.3333333333333333703, 0.3219752754296894559, 0.3333333333333333703, 0.3219752754296894559, 0.3333333333333333703, 0.3219752754296894559, 0.3333333333333333703, 0.3219752754296894559, 0.3333333333333333703, 0.3219752754296894559, 0.3333333333333333703, 0.3219752754296894559, 0.3333333333333333703, 0.3219752754296894559, 0.3333333333333333703, 0.3219752754296894559, 0.3333333333333333703),
 ( 1.000000000000000000, 0.9659258262890683122, 1.000000000000000000, 0.9659258262890683122, 1.000000000000000000, 0.9659258262890683122, 1.000000000000000000, 0.9659258262890683122, 1.000000000000000000, 0.9659258262890683122, 1.000000000000000000, 0.9659258262890683122, 1.000000000000000000, 0.9659258262890683122, 1.000000000000000000, 0.9659258262890683122, 1.000000000000000000, 0.9659258262890683122, 1.000000000000000000, 0.9659258262890683122, 1.000000000000000000, 0.9659258262890683122, 1.000000000000000000, 0.9659258262890683122, 1.000000000000000000, 0.9659258262890683122, 1.000000000000000000, 0.9659258262890683122, 1.000000000000000000, 0.9659258262890683122, 1.000000000000000000, 0.9659258262890683122, 1.000000000000000000, 0.9659258262890683122, 1.000000000000000000, 0.9659258262890683122, 1.000000000000000000, 0.9659258262890683122, 1.000000000000000000, 0.9659258262890683122, 1.000000000000000000, 0.9659258262890683122, 1.000000000000000000, 0.9659258262890683122, 1.000000000000000000, 0.9659258262890683122, 1.000000000000000000, 0.9659258262890683122, 1.000000000000000000, 0.9659258262890683122, 1.000000000000000000, 0.9659258262890683122, 1.000000000000000000, 0.9659258262890683122, 1.000000000000000000, 0.9659258262890683122, 1.000000000000000000, 0.9659258262890683122, 1.000000000000000000, 0.9659258262890683122, 1.000000000000000000, 0.9659258262890683122, 1.000000000000000000, 0.9659258262890683122, 1.000000000000000000, 0.9659258262890683122, 1.000000000000000000, 0.9659258262890683122, 1.000000000000000000, 0.9659258262890683122, 1.000000000000000000, 0.9659258262890683122, 1.000000000000000000, 0.9659258262890683122, 1.000000000000000000, 0.9659258262890683122, 1.000000000000000000, 0.9659258262890683122, 1.000000000000000000, 0.9659258262890683122, 1.000000000000000000, 0.9659258262890683122, 1.000000000000000000, 0.9659258262890683122, 1.000000000000000000, 0.9659258262890683122, 1.000000000000000000, 0.9659258262890683122, 1.000000000000000000, 0.9659258262890683122, 1.000000000000000000, 0.9659258262890683122, 1.000000000000000000, 0.9659258262890683122, 1.000000000000000000, 0.9659258262890683122, 1.000000000000000000, 0.9659258262890683122, 1.000000000000000000, 0.9659258262890683122, 1.000000000000000000, 0.9659258262890683122, 1.000000000000000000, 0.9659258262890683122, 1.000000000000000000, 0.9659258262890683122, 1.000000000000000000, 0.9659258262890683122, 1.000000000000000000, 0.9659258262890683122, 1.000000000000000000, 0.9659258262890683122, 1.000000000000000000, 0.9659258262890683122, 1.000000000000000000, 0.9659258262890683122, 1.000000000000000000, 0.9659258262890683122, 1.000000000000000000, 0.9659258262890683122, 1.000000000000000000, 0.9659258262890683122, 1.000000000000000000, 0.9659258262890683122, 1.000000000000000000, 0.9659258262890683122, 1.000000000000000000, 0.9659258262890683122, 1.000000000000000000, 0.9659258262890683122, 1.000000000000000000, 0.9659258262890683122, 1.000000000000000000, 0.9659258262890683122, 1.000000000000000000, 0.9659258262890683122, 1.000000000000000000, 0.9659258262890683122, 1.000000000000000000, 0.9659258262890683122, 1.000000000000000000, 0.9659258262890683122, 1.000000000000000000, 0.9659258262890683122, 1.000000000000000000, 0.9659258262890683122, 1.000000000000000000, 0.9659258262890683122, 1.000000000000000000, 0.9659258262890683122, 1.000000000000000000, 0.9659258262890683122, 1.000000000000000000, 0.9659258262890683122, 1.000000000000000000, 0.9659258262890683122, 1.000000000000000000, 0.9659258262890683122, 1.000000000000000000, 0.9659258262890683122, 1.000000000000000000, 0.9659258262890683122, 1.000000000000000000, 0.9659258262890683122, 1.000000000000000000, 0.9659258262890683122, 1.000000000000000000, 0.9659258262890683122, 1.000000000000000000, 0.9659258262890683122, 1.000000000000000000, 0.9659258262890683122, 1.000000000000000000, 0.9659258262890683122, 1.000000000000000000, 0.9659258262890683122, 1.000000000000000000, 0.9659258262890683122, 1.000000000000000000, 0.9659258262890683122, 1.000000000000000000, 0.9659258262890683122, 1.000000000000000000, 0.9659258262890683122, 1.000000000000000000, 0.9659258262890683122, 1.000000000000000000, 0.9659258262890683122, 1.000000000000000000, 0.9659258262890683122, 1.000000000000000000, 0.9659258262890683122, 1.000000000000000000, 0.9659258262890683122, 1.000000000000000000, 0.9659258262890683122, 1.000000000000000000, 0.9659258262890683122, 1.000000000000000000, 0.9659258262890683122, 1.000000000000000000, 0.9659258262890683122, 1.000000000000000000, 0.9659258262890683122, 1.000000000000000000, 0.9659258262890683122, 1.000000000000000000, 0.9659258262890683122, 1.000000000000000000, 0.9659258262890683122, 1.000000000000000000, 0.9659258262890683122, 1.000000000000000000, 0.9659258262890683122, 1.000000000000000000, 0.9659258262890683122, 1.000000000000000000, 0.9659258262890683122, 1.000000000000000000, 0.9659258262890683122, 1.000000000000000000, 0.9659258262890683122, 1.000000000000000000, 0.9659258262890683122, 1.000000000000000000, 0.9659258262890683122, 1.000000000000000000, 0.9659258262890683122, 1.000000000000000000, 0.9659258262890683122, 1.000000000000000000, 0.9659258262890683122, 1.000000000000000000, 0.9659258262890683122, 1.000000000000000000, 0.9659258262890683122, 1.000000000000000000, 0.9659258262890683122, 1.000000000000000000, 0.9659258262890683122, 1.000000000000000000, 0.9659258262890683122, 1.000000000000000000, 0.9659258262890683122, 1.000000000000000000, 0.9659258262890683122, 1.000000000000000000, 0.9659258262890683122, 1.000000000000000000, 0.9659258262890683122, 1.000000000000000000, 0.9659258262890683122, 1.000000000000000000, 0.9659258262890683122, 1.000000000000000000, 0.9659258262890683122, 1.000000000000000000, 0.9659258262890683122, 1.000000000000000000, 0.9659258262890683122, 1.000000000000000000, 0.9659258262890683122, 1.000000000000000000, 0.9659258262890683122, 1.000000000000000000, 0.9659258262890683122, 1.000000000000000000, 0.9659258262890683122, 1.000000000000000000, 0.9659258262890683122, 1.000000000000000000, 0.9659258262890683122, 1.000000000000000000, 0.9659258262890683122, 1.000000000000000000, 0.9659258262890683122, 1.000000000000000000, 0.9659258262890683122, 1.000000000000000000, 0.9659258262890683122, 1.000000000000000000, 0.9659258262890683122, 1.000000000000000000, 0.9659258262890683122, 1.000000000000000000, 0.9659258262890683122, 1.000000000000000000, 0.9659258262890683122, 1.000000000000000000, 0.9659258262890683122, 1.000000000000000000, 0.9659258262890683122, 1.000000000000000000, 0.9659258262890683122, 1.000000000000000000, 0.9659258262890683122, 1.000000000000000000, 0.9659258262890683122, 1.000000000000000000, 0.9659258262890683122, 1.000000000000000000, 0.9659258262890683122, 1.000000000000000000, 0.9659258262890683122, 1.000000000000000000, 0.9659258262890683122, 1.000000000000000000, 0.9659258262890683122, 1.000000000000000000, 0.9659258262890683122, 1.000000000000000000, 0.9659258262890683122, 1.000000000000000000, 0.9659258262890683122, 1.000000000000000000, 0.9659258262890683122, 1.000000000000000000, 0.9659258262890683122, 1.000000000000000000, 0.9659258262890683122, 1.000000000000000000, 0.9659258262890683122, 1.000000000000000000, 0.9659258262890683122, 1.000000000000000000, 0.9659258262890683122, 1.000000000000000000, 0.9659258262890683122, 1.000000000000000000, 0.9659258262890683122, 1.000000000000000000, 0.9659258262890683122, 1.000000000000000000, 0.9659258262890683122, 1.000000000000000000, 0.9659258262890683122, 1.000000000000000000, 0.9659258262890683122, 1.000000000000000000, 0.9659258262890683122, 1.000000000000000000, 0.9659258262890683122, 1.000000000000000000, 0.9659258262890683122, 1.000000000000000000, 0.9659258262890683122, 1.000000000000000000, 0.9659258262890683122, 1.000000000000000000, 0.9659258262890683122, 1.000000000000000000, 0.9659258262890683122, 1.000000000000000000, 0.9659258262890683122, 1.000000000000000000, 0.9659258262890683122, 1.000000000000000000, 0.9659258262890683122, 1.000000000000000000, 0.9659258262890683122, 1.000000000000000000, 0.9659258262890683122, 1.000000000000000000, 0.9659258262890683122, 1.000000000000000000, 0.9659258262890683122, 1.000000000000000000, 0.9659258262890683122, 1.000000000000000000, 0.9659258262890683122, 1.000000000000000000, 0.9659258262890683122, 1.000000000000000000, 0.9659258262890683122, 1.000000000000000000, 0.9659258262890683122, 1.000000000000000000, 0.9659258262890683122, 1.000000000000000000, 0.9659258262890683122, 1.000000000000000000, 0.9659258262890683122, 1.000000000000000000, 0.9659258262890683122, 1.000000000000000000, 0.9659258262890683122, 1.000000000000000000, 0.9659258262890683122, 1.000000000000000000, 0.9659258262890683122, 1.000000000000000000, 0.9659258262890683122, 1.000000000000000000, 0.9659258262890683122, 1.000000000000000000, 0.9659258262890683122, 1.000000000000000000, 0.9659258262890683122, 1.000000000000000000, 0.9659258262890683122, 1.000000000000000000, 0.9659258262890683122, 1.000000000000000000, 0.9659258262890683122, 1.000000000000000000, 0.9659258262890683122, 1.000000000000000000, 0.9659258262890683122, 1.000000000000000000, 0.9659258262890683122, 1.000000000000000000, 0.9659258262890683122, 1.000000000000000000, 0.9659258262890683122, 1.000000000000000000, 0.9659258262890683122, 1.000000000000000000, 0.9659258262890683122, 1.000000000000000000, 0.9659258262890683122, 1.000000000000000000, 0.9659258262890683122, 1.000000000000000000, 0.9659258262890683122, 1.000000000000000000, 0.9659258262890683122, 1.000000000000000000, 0.9659258262890683122, 1.000000000000000000, 0.9659258262890683122, 1.000000000000000000, 0.9659258262890683122, 1.000000000000000000, 0.9659258262890683122, 1.000000000000000000, 0.9659258262890683122, 1.000000000000000000, 0.9659258262890683122, 1.000000000000000000, 0.9659258262890683122, 1.000000000000000000, 0.9659258262890683122, 1.000000000000000000, 0.9659258262890683122, 1.000000000000000000, 0.9659258262890683122, 1.000000000000000000, 0.9659258262890683122, 1.000000000000000000, 0.9659258262890683122, 1.000000000000000000, 0.9659258262890683122, 1.000000000000000000, 0.9659258262890683122, 1.000000000000000000, 0.9659258262890683122, 1.000000000000000000),
 ( 0.3333333333333333703, 0.3219752754296894559, 0.3333333333333333703, 0.3219752754296894559, 0.3333333333333333703, 0.3219752754296894559, 0.3333333333333333703, 0.3219752754296894559, 0.3333333333333333703, 0.3219752754296894559, 0.3333333333333333703, 0.3219752754296894559, 0.3333333333333333703, 0.3219752754296894559, 0.3333333333333333703, 0.3219752754296894559, 0.3333333333333333703, 0.3219752754296894559, 0.3333333333333333703, 0.3219752754296894559, 0.3333333333333333703, 0.3219752754296894559, 0.3333333333333333703, 0.3219752754296894559, 0.3333333333333333703, 0.3219752754296894559, 0.3333333333333333703, 0.3219752754296894559, 0.3333333333333333703, 0.3219752754296894559, 0.3333333333333333703, 0.3219752754296894559, 0.3333333333333333703, 0.3219752754296894559, 0.3333333333333333703, 0.3219752754296894559, 0.3333333333333333703, 0.3219752754296894559, 0.3333333333333333703, 0.3219752754296894559, 0.3333333333333333703, 0.3219752754296894559, 0.3333333333333333703, 0.3219752754296894559, 0.3333333333333333703, 0.3219752754296894559, 0.3333333333333333703, 0.3219752754296894559, 0.3333333333333333703, 0.3219752754296894559, 0.3333333333333333703, 0.3219752754296894559, 0.3333333333333333703, 0.3219752754296894559, 0.3333333333333333703, 0.3219752754296894559, 0.3333333333333333703, 0.3219752754296894559, 0.3333333333333333703, 0.3219752754296894559, 0.3333333333333333703, 0.3219752754296894559, 0.3333333333333333703, 0.3219752754296894559, 0.3333333333333333703, 0.3219752754296894559, 0.3333333333333333703, 0.3219752754296894559, 0.3333333333333333703, 0.3219752754296894559, 0.3333333333333333703, 0.3219752754296894559, 0.3333333333333333703, 0.3219752754296894559, 0.3333333333333333703, 0.3219752754296894559, 0.3333333333333333703, 0.3219752754296894559, 0.3333333333333333703, 0.3219752754296894559, 0.3333333333333333703, 0.3219752754296894559, 0.3333333333333333703, 0.3219752754296894559, 0.3333333333333333703, 0.3219752754296894559, 0.3333333333333333703, 0.3219752754296894559, 0.3333333333333333703, 0.3219752754296894559, 0.3333333333333333703, 0.3219752754296894559, 0.3333333333333333703, 0.3219752754296894559, 0.3333333333333333703, 0.3219752754296894559, 0.3333333333333333703, 0.3219752754296894559, 0.3333333333333333703, 0.3219752754296894559, 0.3333333333333333703, 0.3219752754296894559, 0.3333333333333333703, 0.3219752754296894559, 0.3333333333333333703, 0.3219752754296894559, 0.3333333333333333703, 0.3219752754296894559, 0.3333333333333333703, 0.3219752754296894559, 0.3333333333333333703, 0.3219752754296894559, 0.3333333333333333703, 0.3219752754296894559, 0.3333333333333333703, 0.3219752754296894559, 0.3333333333333333703, 0.3219752754296894559, 0.3333333333333333703, 0.3219752754296894559, 0.3333333333333333703, 0.3219752754296894559, 0.3333333333333333703, 0.3219752754296894559, 0.3333333333333333703, 0.3219752754296894559, 0.3333333333333333703, 0.3219752754296894559, 0.3333333333333333703, 0.3219752754296894559, 0.3333333333333333703, 0.3219752754296894559, 0.3333333333333333703, 0.3219752754296894559, 0.3333333333333333703, 0.3219752754296894559, 0.3333333333333333703, 0.3219752754296894559, 0.3333333333333333703, 0.3219752754296894559, 0.3333333333333333703, 0.3219752754296894559, 0.3333333333333333703, 0.3219752754296894559, 0.3333333333333333703, 0.3219752754296894559, 0.3333333333333333703, 0.3219752754296894559, 0.3333333333333333703, 0.3219752754296894559, 0.3333333333333333703, 0.3219752754296894559, 0.3333333333333333703, 0.3219752754296894559, 0.3333333333333333703, 0.3219752754296894559, 0.3333333333333333703, 0.3219752754296894559, 0.3333333333333333703, 0.3219752754296894559, 0.3333333333333333703, 0.3219752754296894559, 0.3333333333333333703, 0.3219752754296894559, 0.3333333333333333703, 0.3219752754296894559, 0.3333333333333333703, 0.3219752754296894559, 0.3333333333333333703, 0.3219752754296894559, 0.3333333333333333703, 0.3219752754296894559, 0.3333333333333333703, 0.3219752754296894559, 0.3333333333333333703, 0.3219752754296894559, 0.3333333333333333703, 0.3219752754296894559, 0.3333333333333333703, 0.3219752754296894559, 0.3333333333333333703, 0.3219752754296894559, 0.3333333333333333703, 0.3219752754296894559, 0.3333333333333333703, 0.3219752754296894559, 0.3333333333333333703, 0.3219752754296894559, 0.3333333333333333703, 0.3219752754296894559, 0.3333333333333333703, 0.3219752754296894559, 0.3333333333333333703, 0.3219752754296894559, 0.3333333333333333703, 0.3219752754296894559, 0.3333333333333333703, 0.3219752754296894559, 0.3333333333333333703, 0.3219752754296894559, 0.3333333333333333703, 0.3219752754296894559, 0.3333333333333333703, 0.3219752754296894559, 0.3333333333333333703, 0.3219752754296894559, 0.3333333333333333703, 0.3219752754296894559, 0.3333333333333333703, 0.3219752754296894559, 0.3333333333333333703, 0.3219752754296894559, 0.3333333333333333703, 0.3219752754296894559, 0.3333333333333333703, 0.3219752754296894559, 0.3333333333333333703, 0.3219752754296894559, 0.3333333333333333703, 0.3219752754296894559, 0.3333333333333333703, 0.3219752754296894559, 0.3333333333333333703, 0.3219752754296894559, 0.3333333333333333703, 0.3219752754296894559, 0.3333333333333333703, 0.3219752754296894559, 0.3333333333333333703, 0.3219752754296894559, 0.3333333333333333703, 0.3219752754296894559, 0.3333333333333333703, 0.3219752754296894559, 0.3333333333333333703, 0.3219752754296894559, 0.3333333333333333703, 0.3219752754296894559, 0.3333333333333333703, 0.3219752754296894559, 0.3333333333333333703, 0.3219752754296894559, 0.3333333333333333703, 0.3219752754296894559, 0.3333333333333333703, 0.3219752754296894559, 0.3333333333333333703, 0.3219752754296894559, 0.3333333333333333703, 0.3219752754296894559, 0.3333333333333333703, 0.3219752754296894559, 0.3333333333333333703, 0.3219752754296894559, 0.3333333333333333703, 0.3219752754296894559, 0.3333333333333333703, 0.3219752754296894559, 0.3333333333333333703, 0.3219752754296894559, 0.3333333333333333703, 0.3219752754296894559, 0.3333333333333333703, 0.3219752754296894559, 0.3333333333333333703, 0.3219752754296894559, 0.3333333333333333703, 0.3219752754296894559, 0.3333333333333333703, 0.3219752754296894559, 0.3333333333333333703, 0.3219752754296894559, 0.3333333333333333703, 0.3219752754296894559, 0.3333333333333333703, 0.3219752754296894559, 0.3333333333333333703, 0.3219752754296894559, 0.3333333333333333703, 0.3219752754296894559, 0.3333333333333333703, 0.3219752754296894559, 0.3333333333333333703, 0.3219752754296894559, 0.3333333333333333703, 0.3219752754296894559, 0.3333333333333333703, 0.3219752754296894559, 0.3333333333333333703, 0.3219752754296894559, 0.3333333333333333703, 0.3219752754296894559, 0.3333333333333333703, 0.3219752754296894559, 0.3333333333333333703, 0.3219752754296894559, 0.3333333333333333703, 0.3219752754296894559, 0.3333333333333333703, 0.3219752754296894559, 0.3333333333333333703, 0.3219752754296894559, 0.3333333333333333703, 0.3219752754296894559, 0.3333333333333333703, 0.3219752754296894559, 0.3333333333333333703, 0.3219752754296894559, 0.3333333333333333703, 0.3219752754296894559, 0.3333333333333333703, 0.3219752754296894559, 0.3333333333333333703, 0.3219752754296894559, 0.3333333333333333703, 0.3219752754296894559, 0.3333333333333333703, 0.3219752754296894559, 0.3333333333333333703, 0.3219752754296894559, 0.3333333333333333703, 0.3219752754296894559, 0.3333333333333333703, 0.3219752754296894559, 0.3333333333333333703, 0.3219752754296894559, 0.3333333333333333703, 0.3219752754296894559, 0.3333333333333333703, 0.3219752754296894559, 0.3333333333333333703, 0.3219752754296894559, 0.3333333333333333703, 0.3219752754296894559, 0.3333333333333333703, 0.3219752754296894559, 0.3333333333333333703, 0.3219752754296894559, 0.3333333333333333703, 0.3219752754296894559, 0.3333333333333333703, 0.3219752754296894559, 0.3333333333333333703, 0.3219752754296894559, 0.3333333333333333703, 0.3219752754296894559, 0.3333333333333333703, 0.3219752754296894559, 0.3333333333333333703, 0.3219752754296894559, 0.3333333333333333703, 0.3219752754296894559, 0.3333333333333333703, 0.3219752754296894559, 0.3333333333333333703, 0.3219752754296894559, 0.3333333333333333703, 0.3219752754296894559, 0.3333333333333333703, 0.3219752754296894559, 0.3333333333333333703, 0.3219752754296894559, 0.3333333333333333703, 0.3219752754296894559, 0.3333333333333333703, 0.3219752754296894559, 0.3333333333333333703, 0.3219752754296894559, 0.3333333333333333703, 0.3219752754296894559, 0.3333333333333333703, 0.3219752754296894559, 0.3333333333333333703, 0.3219752754296894559, 0.3333333333333333703, 0.3219752754296894559, 0.3333333333333333703, 0.3219752754296894559, 0.3333333333333333703, 0.3219752754296894559, 0.3333333333333333703, 0.3219752754296894559, 0.3333333333333333703, 0.3219752754296894559, 0.3333333333333333703, 0.3219752754296894559, 0.3333333333333333703, 0.3219752754296894559, 0.3333333333333333703, 0.3219752754296894559, 0.3333333333333333703, 0.3219752754296894559, 0.3333333333333333703, 0.3219752754296894559, 0.3333333333333333703, 0.3219752754296894559, 0.3333333333333333703, 0.3219752754296894559, 0.3333333333333333703, 0.3219752754296894559, 0.3333333333333333703, 0.3219752754296894559, 0.3333333333333333703, 0.3219752754296894559, 0.3333333333333333703, 0.3219752754296894559, 0.3333333333333333703, 0.3219752754296894559, 0.3333333333333333703, 0.3219752754296894559, 0.3333333333333333703, 0.3219752754296894559, 0.3333333333333333703, 0.3219752754296894559, 0.3333333333333333703, 0.3219752754296894559, 0.3333333333333333703, 0.3219752754296894559, 0.3333333333333333703, 0.3219752754296894559, 0.3333333333333333703, 0.3219752754296894559, 0.3333333333333333703, 0.3219752754296894559, 0.3333333333333333703, 0.3219752754296894559, 0.3333333333333333703, 0.3219752754296894559, 0.3333333333333333703, 0.3219752754296894559, 0.3333333333333333703, 0.3219752754296894559, 0.3333333333333333703, 0.3219752754296894559, 0.3333333333333333703, 0.3219752754296894559, 0.3333333333333333703, 0.3219752754296894559, 0.3333333333333333703, 0.3219752754296894559, 0.3333333333333333703, 0.3219752754296894559, 0.3333333333333333703, 0.3219752754296894559, 0.3333333333333333703, 0.3219752754296894559, 0.3333333333333333703, 0.3219752754296894559, 0.3333333333333333703, 0.3219752754296894559, 0.3333333333333333703, 0.3219752754296894559, 0.3333333333333333703, 0.3219752754296894559, 0.3333333333333333703, 0.3219752754296894559, 0.3333333333333333703),
 ( 0.3333333333333333703, 0.3219752754296894559, 0.3333333333333333703, 0.3219752754296894559, 0.3333333333333333703, 0.3219752754296894559, 0.3333333333333333703, 0.3219752754296894559, 0.3333333333333333703, 0.3219752754296894559, 0.3333333333333333703, 0.3219752754296894559, 0.3333333333333333703, 0.3219752754296894559, 0.3333333333333333703, 0.3219752754296894559, 0.3333333333333333703, 0.3219752754296894559, 0.3333333333333333703, 0.3219752754296894559, 0.3333333333333333703, 0.3219752754296894559, 0.3333333333333333703, 0.3219752754296894559, 0.3333333333333333703, 0.3219752754296894559, 0.3333333333333333703, 0.3219752754296894559, 0.3333333333333333703, 0.3219752754296894559, 0.3333333333333333703, 0.3219752754296894559, 0.3333333333333333703, 0.3219752754296894559, 0.3333333333333333703, 0.3219752754296894559, 0.3333333333333333703, 0.3219752754296894559, 0.3333333333333333703, 0.3219752754296894559, 0.3333333333333333703, 0.3219752754296894559, 0.3333333333333333703, 0.3219752754296894559, 0.3333333333333333703, 0.3219752754296894559, 0.3333333333333333703, 0.3219752754296894559, 0.3333333333333333703, 0.3219752754296894559, 0.3333333333333333703, 0.3219752754296894559, 0.3333333333333333703, 0.3219752754296894559, 0.3333333333333333703, 0.3219752754296894559, 0.3333333333333333703, 0.3219752754296894559, 0.3333333333333333703, 0.3219752754296894559, 0.3333333333333333703, 0.3219752754296894559, 0.3333333333333333703, 0.3219752754296894559, 0.3333333333333333703, 0.3219752754296894559, 0.3333333333333333703, 0.3219752754296894559, 0.3333333333333333703, 0.3219752754296894559, 0.3333333333333333703, 0.3219752754296894559, 0.3333333333333333703, 0.3219752754296894559, 0.3333333333333333703, 0.3219752754296894559, 0.3333333333333333703, 0.3219752754296894559, 0.3333333333333333703, 0.3219752754296894559, 0.3333333333333333703, 0.3219752754296894559, 0.3333333333333333703, 0.3219752754296894559, 0.3333333333333333703, 0.3219752754296894559, 0.3333333333333333703, 0.3219752754296894559, 0.3333333333333333703, 0.3219752754296894559, 0.3333333333333333703, 0.3219752754296894559, 0.3333333333333333703, 0.3219752754296894559, 0.3333333333333333703, 0.3219752754296894559, 0.3333333333333333703, 0.3219752754296894559, 0.3333333333333333703, 0.3219752754296894559, 0.3333333333333333703, 0.3219752754296894559, 0.3333333333333333703, 0.3219752754296894559, 0.3333333333333333703, 0.3219752754296894559, 0.3333333333333333703, 0.3219752754296894559, 0.3333333333333333703, 0.3219752754296894559, 0.3333333333333333703, 0.3219752754296894559, 0.3333333333333333703, 0.3219752754296894559, 0.3333333333333333703, 0.3219752754296894559, 0.3333333333333333703, 0.3219752754296894559, 0.3333333333333333703, 0.3219752754296894559, 0.3333333333333333703, 0.3219752754296894559, 0.3333333333333333703, 0.3219752754296894559, 0.3333333333333333703, 0.3219752754296894559, 0.3333333333333333703, 0.3219752754296894559, 0.3333333333333333703, 0.3219752754296894559, 0.3333333333333333703, 0.3219752754296894559, 0.3333333333333333703, 0.3219752754296894559, 0.3333333333333333703, 0.3219752754296894559, 0.3333333333333333703, 0.3219752754296894559, 0.3333333333333333703, 0.3219752754296894559, 0.3333333333333333703, 0.3219752754296894559, 0.3333333333333333703, 0.3219752754296894559, 0.3333333333333333703, 0.3219752754296894559, 0.3333333333333333703, 0.3219752754296894559, 0.3333333333333333703, 0.3219752754296894559, 0.3333333333333333703, 0.3219752754296894559, 0.3333333333333333703, 0.3219752754296894559, 0.3333333333333333703, 0.3219752754296894559, 0.3333333333333333703, 0.3219752754296894559, 0.3333333333333333703, 0.3219752754296894559, 0.3333333333333333703, 0.3219752754296894559, 0.3333333333333333703, 0.3219752754296894559, 0.3333333333333333703, 0.3219752754296894559, 0.3333333333333333703, 0.3219752754296894559, 0.3333333333333333703, 0.3219752754296894559, 0.3333333333333333703, 0.3219752754296894559, 0.3333333333333333703, 0.3219752754296894559, 0.3333333333333333703, 0.3219752754296894559, 0.3333333333333333703, 0.3219752754296894559, 0.3333333333333333703, 0.3219752754296894559, 0.3333333333333333703, 0.3219752754296894559, 0.3333333333333333703, 0.3219752754296894559, 0.3333333333333333703, 0.3219752754296894559, 0.3333333333333333703, 0.3219752754296894559, 0.3333333333333333703, 0.3219752754296894559, 0.3333333333333333703, 0.3219752754296894559, 0.3333333333333333703, 0.3219752754296894559, 0.3333333333333333703, 0.3219752754296894559, 0.3333333333333333703, 0.3219752754296894559, 0.3333333333333333703, 0.3219752754296894559, 0.3333333333333333703, 0.3219752754296894559, 0.3333333333333333703, 0.3219752754296894559, 0.3333333333333333703, 0.3219752754296894559, 0.3333333333333333703, 0.3219752754296894559, 0.3333333333333333703, 0.3219752754296894559, 0.3333333333333333703, 0.3219752754296894559, 0.3333333333333333703, 0.3219752754296894559, 0.3333333333333333703, 0.3219752754296894559, 0.3333333333333333703, 0.3219752754296894559, 0.3333333333333333703, 0.3219752754296894559, 0.3333333333333333703, 0.3219752754296894559, 0.3333333333333333703, 0.3219752754296894559, 0.3333333333333333703, 0.3219752754296894559, 0.3333333333333333703, 0.3219752754296894559, 0.3333333333333333703, 0.3219752754296894559, 0.3333333333333333703, 0.3219752754296894559, 0.3333333333333333703, 0.3219752754296894559, 0.3333333333333333703, 0.3219752754296894559, 0.3333333333333333703, 0.3219752754296894559, 0.3333333333333333703, 0.3219752754296894559, 0.3333333333333333703, 0.3219752754296894559, 0.3333333333333333703, 0.3219752754296894559, 0.3333333333333333703, 0.3219752754296894559, 0.3333333333333333703, 0.3219752754296894559, 0.3333333333333333703, 0.3219752754296894559, 0.3333333333333333703, 0.3219752754296894559, 0.3333333333333333703, 0.3219752754296894559, 0.3333333333333333703, 0.3219752754296894559, 0.3333333333333333703, 0.3219752754296894559, 0.3333333333333333703, 0.3219752754296894559, 0.3333333333333333703, 0.3219752754296894559, 0.3333333333333333703, 0.3219752754296894559, 0.3333333333333333703, 0.3219752754296894559, 0.3333333333333333703, 0.3219752754296894559, 0.3333333333333333703, 0.3219752754296894559, 0.3333333333333333703, 0.3219752754296894559, 0.3333333333333333703, 0.3219752754296894559, 0.3333333333333333703, 0.3219752754296894559, 0.3333333333333333703, 0.3219752754296894559, 0.3333333333333333703, 0.3219752754296894559, 0.3333333333333333703, 0.3219752754296894559, 0.3333333333333333703, 0.3219752754296894559, 0.3333333333333333703, 0.3219752754296894559, 0.3333333333333333703, 0.3219752754296894559, 0.3333333333333333703, 0.3219752754296894559, 0.3333333333333333703, 0.3219752754296894559, 0.3333333333333333703, 0.3219752754296894559, 0.3333333333333333703, 0.3219752754296894559, 0.3333333333333333703, 0.3219752754296894559, 0.3333333333333333703, 0.3219752754296894559, 0.3333333333333333703, 0.3219752754296894559, 0.3333333333333333703, 0.3219752754296894559, 0.3333333333333333703, 0.3219752754296894559, 0.3333333333333333703, 0.3219752754296894559, 0.3333333333333333703, 0.3219752754296894559, 0.3333333333333333703, 0.3219752754296894559, 0.3333333333333333703, 0.3219752754296894559, 0.3333333333333333703, 0.3219752754296894559, 0.3333333333333333703, 0.3219752754296894559, 0.3333333333333333703, 0.3219752754296894559, 0.3333333333333333703, 0.3219752754296894559, 0.3333333333333333703, 0.3219752754296894559, 0.3333333333333333703, 0.3219752754296894559, 0.3333333333333333703, 0.3219752754296894559, 0.3333333333333333703, 0.3219752754296894559, 0.3333333333333333703, 0.3219752754296894559, 0.3333333333333333703, 0.3219752754296894559, 0.3333333333333333703, 0.3219752754296894559, 0.3333333333333333703, 0.3219752754296894559, 0.3333333333333333703, 0.3219752754296894559, 0.3333333333333333703, 0.3219752754296894559, 0.3333333333333333703, 0.3219752754296894559, 0.3333333333333333703, 0.3219752754296894559, 0.3333333333333333703, 0.3219752754296894559, 0.3333333333333333703, 0.3219752754296894559, 0.3333333333333333703, 0.3219752754296894559, 0.3333333333333333703, 0.3219752754296894559, 0.3333333333333333703, 0.3219752754296894559, 0.3333333333333333703, 0.3219752754296894559, 0.3333333333333333703, 0.3219752754296894559, 0.3333333333333333703, 0.3219752754296894559, 0.3333333333333333703, 0.3219752754296894559, 0.3333333333333333703, 0.3219752754296894559, 0.3333333333333333703, 0.3219752754296894559, 0.3333333333333333703, 0.3219752754296894559, 0.3333333333333333703, 0.3219752754296894559, 0.3333333333333333703, 0.3219752754296894559, 0.3333333333333333703, 0.3219752754296894559, 0.3333333333333333703, 0.3219752754296894559, 0.3333333333333333703, 0.3219752754296894559, 0.3333333333333333703, 0.3219752754296894559, 0.3333333333333333703, 0.3219752754296894559, 0.3333333333333333703, 0.3219752754296894559, 0.3333333333333333703, 0.3219752754296894559, 0.3333333333333333703, 0.3219752754296894559, 0.3333333333333333703, 0.3219752754296894559, 0.3333333333333333703, 0.3219752754296894559, 0.3333333333333333703, 0.3219752754296894559, 0.3333333333333333703, 0.3219752754296894559, 0.3333333333333333703, 0.3219752754296894559, 0.3333333333333333703, 0.3219752754296894559, 0.3333333333333333703, 0.3219752754296894559, 0.3333333333333333703, 0.3219752754296894559, 0.3333333333333333703, 0.3219752754296894559, 0.3333333333333333703, 0.3219752754296894559, 0.3333333333333333703, 0.3219752754296894559, 0.3333333333333333703, 0.3219752754296894559, 0.3333333333333333703, 0.3219752754296894559, 0.3333333333333333703, 0.3219752754296894559, 0.3333333333333333703, 0.3219752754296894559, 0.3333333333333333703, 0.3219752754296894559, 0.3333333333333333703, 0.3219752754296894559, 0.3333333333333333703, 0.3219752754296894559, 0.3333333333333333703, 0.3219752754296894559, 0.3333333333333333703, 0.3219752754296894559, 0.3333333333333333703, 0.3219752754296894559, 0.3333333333333333703, 0.3219752754296894559, 0.3333333333333333703, 0.3219752754296894559, 0.3333333333333333703, 0.3219752754296894559, 0.3333333333333333703, 0.3219752754296894559, 0.3333333333333333703, 0.3219752754296894559, 0.3333333333333333703, 0.3219752754296894559, 0.3333333333333333703, 0.3219752754296894559, 0.3333333333333333703, 0.3219752754296894559, 0.3333333333333333703, 0.3219752754296894559, 0.3333333333333333703, 0.3219752754296894559, 0.3333333333333333703, 0.3219752754296894559, 0.3333333333333333703, 0.3219752754296894559, 0.3333333333333333703),
 ( 1.000000000000000000, 0.9659258262890683122, 1.000000000000000000, 0.9659258262890683122, 1.000000000000000000, 0.9659258262890683122, 1.000000000000000000, 0.9659258262890683122, 1.000000000000000000, 0.9659258262890683122, 1.000000000000000000, 0.9659258262890683122, 1.000000000000000000, 0.9659258262890683122, 1.000000000000000000, 0.9659258262890683122, 1.000000000000000000, 0.9659258262890683122, 1.000000000000000000, 0.9659258262890683122, 1.000000000000000000, 0.9659258262890683122, 1.000000000000000000, 0.9659258262890683122, 1.000000000000000000, 0.9659258262890683122, 1.000000000000000000, 0.9659258262890683122, 1.000000000000000000, 0.9659258262890683122, 1.000000000000000000, 0.9659258262890683122, 1.000000000000000000, 0.9659258262890683122, 1.000000000000000000, 0.9659258262890683122, 1.000000000000000000, 0.9659258262890683122, 1.000000000000000000, 0.9659258262890683122, 1.000000000000000000, 0.9659258262890683122, 1.000000000000000000, 0.9659258262890683122, 1.000000000000000000, 0.9659258262890683122, 1.000000000000000000, 0.9659258262890683122, 1.000000000000000000, 0.9659258262890683122, 1.000000000000000000, 0.9659258262890683122, 1.000000000000000000, 0.9659258262890683122, 1.000000000000000000, 0.9659258262890683122, 1.000000000000000000, 0.9659258262890683122, 1.000000000000000000, 0.9659258262890683122, 1.000000000000000000, 0.9659258262890683122, 1.000000000000000000, 0.9659258262890683122, 1.000000000000000000, 0.9659258262890683122, 1.000000000000000000, 0.9659258262890683122, 1.000000000000000000, 0.9659258262890683122, 1.000000000000000000, 0.9659258262890683122, 1.000000000000000000, 0.9659258262890683122, 1.000000000000000000, 0.9659258262890683122, 1.000000000000000000, 0.9659258262890683122, 1.000000000000000000, 0.9659258262890683122, 1.000000000000000000, 0.9659258262890683122, 1.000000000000000000, 0.9659258262890683122, 1.000000000000000000, 0.9659258262890683122, 1.000000000000000000, 0.9659258262890683122, 1.000000000000000000, 0.9659258262890683122, 1.000000000000000000, 0.9659258262890683122, 1.000000000000000000, 0.9659258262890683122, 1.000000000000000000, 0.9659258262890683122, 1.000000000000000000, 0.9659258262890683122, 1.000000000000000000, 0.9659258262890683122, 1.000000000000000000, 0.9659258262890683122, 1.000000000000000000, 0.9659258262890683122, 1.000000000000000000, 0.9659258262890683122, 1.000000000000000000, 0.9659258262890683122, 1.000000000000000000, 0.9659258262890683122, 1.000000000000000000, 0.9659258262890683122, 1.000000000000000000, 0.9659258262890683122, 1.000000000000000000, 0.9659258262890683122, 1.000000000000000000, 0.9659258262890683122, 1.000000000000000000, 0.9659258262890683122, 1.000000000000000000, 0.9659258262890683122, 1.000000000000000000, 0.9659258262890683122, 1.000000000000000000, 0.9659258262890683122, 1.000000000000000000, 0.9659258262890683122, 1.000000000000000000, 0.9659258262890683122, 1.000000000000000000, 0.9659258262890683122, 1.000000000000000000, 0.9659258262890683122, 1.000000000000000000, 0.9659258262890683122, 1.000000000000000000, 0.9659258262890683122, 1.000000000000000000, 0.9659258262890683122, 1.000000000000000000, 0.9659258262890683122, 1.000000000000000000, 0.9659258262890683122, 1.000000000000000000, 0.9659258262890683122, 1.000000000000000000, 0.9659258262890683122, 1.000000000000000000, 0.9659258262890683122, 1.000000000000000000, 0.9659258262890683122, 1.000000000000000000, 0.9659258262890683122, 1.000000000000000000, 0.9659258262890683122, 1.000000000000000000, 0.9659258262890683122, 1.000000000000000000, 0.9659258262890683122, 1.000000000000000000, 0.9659258262890683122, 1.000000000000000000, 0.9659258262890683122, 1.000000000000000000, 0.9659258262890683122, 1.000000000000000000, 0.9659258262890683122, 1.000000000000000000, 0.9659258262890683122, 1.000000000000000000, 0.9659258262890683122, 1.000000000000000000, 0.9659258262890683122, 1.000000000000000000, 0.9659258262890683122, 1.000000000000000000, 0.9659258262890683122, 1.000000000000000000, 0.9659258262890683122, 1.000000000000000000, 0.9659258262890683122, 1.000000000000000000, 0.9659258262890683122, 1.000000000000000000, 0.9659258262890683122, 1.000000000000000000, 0.9659258262890683122, 1.000000000000000000, 0.9659258262890683122, 1.000000000000000000, 0.9659258262890683122, 1.000000000000000000, 0.9659258262890683122, 1.000000000000000000, 0.9659258262890683122, 1.000000000000000000, 0.9659258262890683122, 1.000000000000000000, 0.9659258262890683122, 1.000000000000000000, 0.9659258262890683122, 1.000000000000000000, 0.9659258262890683122, 1.000000000000000000, 0.9659258262890683122, 1.000000000000000000, 0.9659258262890683122, 1.000000000000000000, 0.9659258262890683122, 1.000000000000000000, 0.9659258262890683122, 1.000000000000000000, 0.9659258262890683122, 1.000000000000000000, 0.9659258262890683122, 1.000000000000000000, 0.9659258262890683122, 1.000000000000000000, 0.9659258262890683122, 1.000000000000000000, 0.9659258262890683122, 1.000000000000000000, 0.9659258262890683122, 1.000000000000000000, 0.9659258262890683122, 1.000000000000000000, 0.9659258262890683122, 1.000000000000000000, 0.9659258262890683122, 1.000000000000000000, 0.9659258262890683122, 1.000000000000000000, 0.9659258262890683122, 1.000000000000000000, 0.9659258262890683122, 1.000000000000000000, 0.9659258262890683122, 1.000000000000000000, 0.9659258262890683122, 1.000000000000000000, 0.9659258262890683122, 1.000000000000000000, 0.9659258262890683122, 1.000000000000000000, 0.9659258262890683122, 1.000000000000000000, 0.9659258262890683122, 1.000000000000000000, 0.9659258262890683122, 1.000000000000000000, 0.9659258262890683122, 1.000000000000000000, 0.9659258262890683122, 1.000000000000000000, 0.9659258262890683122, 1.000000000000000000, 0.9659258262890683122, 1.000000000000000000, 0.9659258262890683122, 1.000000000000000000, 0.9659258262890683122, 1.000000000000000000, 0.9659258262890683122, 1.000000000000000000, 0.9659258262890683122, 1.000000000000000000, 0.9659258262890683122, 1.000000000000000000, 0.9659258262890683122, 1.000000000000000000, 0.9659258262890683122, 1.000000000000000000, 0.9659258262890683122, 1.000000000000000000, 0.9659258262890683122, 1.000000000000000000, 0.9659258262890683122, 1.000000000000000000, 0.9659258262890683122, 1.000000000000000000, 0.9659258262890683122, 1.000000000000000000, 0.9659258262890683122, 1.000000000000000000, 0.9659258262890683122, 1.000000000000000000, 0.9659258262890683122, 1.000000000000000000, 0.9659258262890683122, 1.000000000000000000, 0.9659258262890683122, 1.000000000000000000, 0.9659258262890683122, 1.000000000000000000, 0.9659258262890683122, 1.000000000000000000, 0.9659258262890683122, 1.000000000000000000, 0.9659258262890683122, 1.000000000000000000, 0.9659258262890683122, 1.000000000000000000, 0.9659258262890683122, 1.000000000000000000, 0.9659258262890683122, 1.000000000000000000, 0.9659258262890683122, 1.000000000000000000, 0.9659258262890683122, 1.000000000000000000, 0.9659258262890683122, 1.000000000000000000, 0.9659258262890683122, 1.000000000000000000, 0.9659258262890683122, 1.000000000000000000, 0.9659258262890683122, 1.000000000000000000, 0.9659258262890683122, 1.000000000000000000, 0.9659258262890683122, 1.000000000000000000, 0.9659258262890683122, 1.000000000000000000, 0.9659258262890683122, 1.000000000000000000, 0.9659258262890683122, 1.000000000000000000, 0.9659258262890683122, 1.000000000000000000, 0.9659258262890683122, 1.000000000000000000, 0.9659258262890683122, 1.000000000000000000, 0.9659258262890683122, 1.000000000000000000, 0.9659258262890683122, 1.000000000000000000, 0.9659258262890683122, 1.000000000000000000, 0.9659258262890683122, 1.000000000000000000, 0.9659258262890683122, 1.000000000000000000, 0.9659258262890683122, 1.000000000000000000, 0.9659258262890683122, 1.000000000000000000, 0.9659258262890683122, 1.000000000000000000, 0.9659258262890683122, 1.000000000000000000, 0.9659258262890683122, 1.000000000000000000, 0.9659258262890683122, 1.000000000000000000, 0.9659258262890683122, 1.000000000000000000, 0.9659258262890683122, 1.000000000000000000, 0.9659258262890683122, 1.000000000000000000, 0.9659258262890683122, 1.000000000000000000, 0.9659258262890683122, 1.000000000000000000, 0.9659258262890683122, 1.000000000000000000, 0.9659258262890683122, 1.000000000000000000, 0.9659258262890683122, 1.000000000000000000, 0.9659258262890683122, 1.000000000000000000, 0.9659258262890683122, 1.000000000000000000, 0.9659258262890683122, 1.000000000000000000, 0.9659258262890683122, 1.000000000000000000, 0.9659258262890683122, 1.000000000000000000, 0.9659258262890683122, 1.000000000000000000, 0.9659258262890683122, 1.000000000000000000, 0.9659258262890683122, 1.000000000000000000, 0.9659258262890683122, 1.000000000000000000, 0.9659258262890683122, 1.000000000000000000, 0.9659258262890683122, 1.000000000000000000, 0.9659258262890683122, 1.000000000000000000, 0.9659258262890683122, 1.000000000000000000, 0.9659258262890683122, 1.000000000000000000, 0.9659258262890683122, 1.000000000000000000, 0.9659258262890683122, 1.000000000000000000, 0.9659258262890683122, 1.000000000000000000, 0.9659258262890683122, 1.000000000000000000, 0.9659258262890683122, 1.000000000000000000, 0.9659258262890683122, 1.000000000000000000, 0.9659258262890683122, 1.000000000000000000, 0.9659258262890683122, 1.000000000000000000, 0.9659258262890683122, 1.000000000000000000, 0.9659258262890683122, 1.000000000000000000, 0.9659258262890683122, 1.000000000000000000, 0.9659258262890683122, 1.000000000000000000, 0.9659258262890683122, 1.000000000000000000, 0.9659258262890683122, 1.000000000000000000, 0.9659258262890683122, 1.000000000000000000, 0.9659258262890683122, 1.000000000000000000, 0.9659258262890683122, 1.000000000000000000, 0.9659258262890683122, 1.000000000000000000, 0.9659258262890683122, 1.000000000000000000, 0.9659258262890683122, 1.000000000000000000, 0.9659258262890683122, 1.000000000000000000, 0.9659258262890683122, 1.000000000000000000, 0.9659258262890683122, 1.000000000000000000, 0.9659258262890683122, 1.000000000000000000, 0.9659258262890683122, 1.000000000000000000, 0.9659258262890683122, 1.000000000000000000, 0.9659258262890683122, 1.000000000000000000, 0.9659258262890683122, 1.000000000000000000) ) ) 
 REPRESENTATION_ITEM ( '' )  SURFACE ( )  );
#63272 = CARTESIAN_POINT ( 'NONE',  ( 21.53943276465977519, 0.05219959533937863772, 71.25109039468568994 ) ) ;
#63273 = CARTESIAN_POINT ( 'NONE',  ( -16.52544592524335698, -4.483927247898792601, 38.95942372801901854 ) ) ;
#63275 = CARTESIAN_POINT ( 'NONE',  ( -15.80617190586768217, 15.72974639402176855, 88.12609039468570415 ) ) ;
#63274 = CARTESIAN_POINT ( 'NONE',  ( 16.53943276465976808, -0.05219959533910856209, 73.74890960531433848 ) ) ;
#63276 = CARTESIAN_POINT ( 'NONE',  ( 8.224510206698742110, 14.34966873604972548, 112.0844237280190185 ) ) ;
#63277 = PLANE ( 'NONE',  #114653 ) ;
#63278 = CARTESIAN_POINT ( 'NONE',  ( -4.379528057220086978, -16.55341960407618274, 39.79275706135235424 ) ) ;
#63279 = CARTESIAN_POINT ( 'NONE',  ( 16.52544592524342804, -4.483927247898539470, 43.54057627198103830 ) ) ;
#63280 = CARTESIAN_POINT ( 'NONE',  ( -4.379528057220086978, -16.55341960407618274, 89.79275706135236135 ) ) ;
#63281 = CARTESIAN_POINT ( 'NONE',  ( -5.153800228976328057, -19.02544592524343514, 97.29057627198099567 ) ) ;
#63282 = CARTESIAN_POINT ( 'NONE',  ( 19.03943276465977164, -0.05219959533909143690, 113.7489096053143669 ) ) ;
#63283 = CARTESIAN_POINT ( 'NONE',  ( 21.55341960407619695, -5.719274019375665929, 101.0427570613523756 ) ) ;
#63284 = CARTESIAN_POINT ( 'NONE',  ( 14.29746914071037800, 8.314922557961029526, 106.6677570613523756 ) ) ;
#63285 = CARTESIAN_POINT ( 'NONE',  ( -12.06949235617756955, 12.14591786802309770, 75.62390960531439532 ) ) ;
#63286 = CARTESIAN_POINT ( 'NONE',  ( -19.02544592524342804, 5.153800228976336051, 81.04057627198103830 ) ) ;
#63287 = VERTEX_POINT ( 'NONE', #98990 ) ;
#63288 = CARTESIAN_POINT ( 'NONE',  ( -14.34966873604972548, 8.224510206698743886, 23.33442372801901499 ) ) ;
#63289 = CARTESIAN_POINT ( 'NONE',  ( 16.46253265017160672, -9.564922557960803928, 33.33224293864770260 ) ) ;
#63290 = CARTESIAN_POINT ( 'NONE',  ( 9.474510206698971260, -16.51473224551069308, 87.91557627198102409 ) ) ;
#63292 = CARTESIAN_POINT ( 'NONE',  ( -36.91746825000001309, 11.99521256947798342, -4.724999997268811924 ) ) ;
#63291 = CARTESIAN_POINT ( 'NONE',  ( 4.483927247898790824, -16.52544592524335698, 35.20942372801901854 ) ) ;
#63293 = CARTESIAN_POINT ( 'NONE',  ( 5.049401038297881783, 19.05341960407617563, 37.29275706135232582 ) ) ;
#63294 = CARTESIAN_POINT ( 'NONE',  ( -14.34966873604972548, 8.224510206698743886, 98.33442372801901854 ) ) ;
#63295 = CARTESIAN_POINT ( 'NONE',  ( -19.02544592524334988, -5.153800228976617603, 108.9594237280189759 ) ) ;
#63296 = CARTESIAN_POINT ( 'NONE',  ( -5.153800228976328057, -19.02544592524343514, 32.29057627198102409 ) ) ;
#63297 = CARTESIAN_POINT ( 'NONE',  ( -8.224510206698735004, -14.34966873604973081, 79.58442372801903275 ) ) ;
#63298 = CARTESIAN_POINT ( 'NONE',  ( 16.53943276465976808, 0.05219959533934440121, 66.25109039468567573 ) ) ;
#63299 = CARTESIAN_POINT ( 'NONE',  ( -16.51473224551069308, -9.474510206698971260, 36.66557627198102409 ) ) ;
#63300 = CARTESIAN_POINT ( 'NONE',  ( 5.049401038297881783, 19.05341960407617563, 72.29275706135234714 ) ) ;
#63301 = CARTESIAN_POINT ( 'NONE',  ( -10.81492255796105439, 18.62759615963255655, 107.9177570613523471 ) ) ;
#63302 = CARTESIAN_POINT ( 'NONE',  ( 16.46253265017160672, -9.564922557960803928, 53.33224293864768839 ) ) ;
#63303 = CIRCLE ( 'NONE', #176320, 10.00000000000000000 ) ;
#63304 = CARTESIAN_POINT ( 'NONE',  ( -5.049401038298153566, 19.05341960407611168, 95.20724293864770971 ) ) ;
#63305 = CARTESIAN_POINT ( 'NONE',  ( 4.379528057220339221, -16.55341960407611168, 87.70724293864769550 ) ) ;
#63306 = EDGE_CURVE ( 'NONE', #133509, #191474, #57219, .T. ) ;
#63307 = CARTESIAN_POINT ( 'NONE',  ( -16.51473224551082808, 9.474510206698731452, 53.33442372801900433 ) ) ;
#63308 = CARTESIAN_POINT ( 'NONE',  ( 21.55341960407610458, 5.719274019375980345, 53.95724293864770260 ) ) ;
#63309 = CARTESIAN_POINT ( 'NONE',  ( -19.03943276465977164, -0.05219959533935918106, 28.75109039468566507 ) ) ;
#63310 = CARTESIAN_POINT ( 'NONE',  ( -5.049401038298153566, 19.05341960407611168, 85.20724293864766707 ) ) ;
#63311 = CARTESIAN_POINT ( 'NONE',  ( 5.153800228976615827, -19.02544592524334988, 20.20942372801899722 ) ) ;
#63312 = CARTESIAN_POINT ( 'NONE',  ( 18.67979575497178502, 10.72451020669898547, 64.16557627198102409 ) ) ;
#63313 = CARTESIAN_POINT ( 'NONE',  ( -5.153800228976328057, -19.02544592524343514, 107.2905762719810383 ) ) ;
#63314 = CARTESIAN_POINT ( 'NONE',  ( -16.51473224551082808, 9.474510206698731452, 83.33442372801899012 ) ) ;
#63315 = CARTESIAN_POINT ( 'NONE',  ( 0.05219959533909260263, 19.03943276465977164, 114.9989096053143669 ) ) ;
#63316 = CARTESIAN_POINT ( 'NONE',  ( 9.474510206698729675, 16.51473224551082808, 112.0844237280190043 ) ) ;
#63317 = CARTESIAN_POINT ( 'NONE',  ( 9.474510206698971260, -16.51473224551069308, 27.91557627198103120 ) ) ;
#63318 = CARTESIAN_POINT ( 'NONE',  ( 16.51473224551069308, 9.474510206698969483, 99.16557627198102409 ) ) ;
#63320 = B_SPLINE_CURVE_WITH_KNOTS ( 'NONE', 3,
 ( #158459, #84592, #53269, #52271, #51284, #114947, #162448, #7759, #69442, #177642, #39110, #146272, #100766, #85604, #175629, #19948, #132115, #82595, #8780, #143275, #144277, #113929, #40099, #27962 ),
 .UNSPECIFIED., .F., .F.,
 ( 4, 2, 2, 2, 2, 2, 2, 2, 2, 2, 2, 4 ),
 ( 2.784816138770050137E-07, 0.0003261688173017064543, 0.0006520591529895358339, 0.0009779494886773747002, 0.001303839824365213458, 0.001955620495740909189, 0.002607401167116605353, 0.003259181838492301083, 0.003910962509867992910, 0.004562743181243684304, 0.004888633516931526098, 0.005214523852619367891 ),
 .UNSPECIFIED. ) ;
#63319 = CARTESIAN_POINT ( 'NONE',  ( 18.67979575497178502, 10.72451020669898547, 79.16557627198103830 ) ) ;
#63321 = CARTESIAN_POINT ( 'NONE',  ( 16.53943276465976808, 0.05219959533934440121, 46.25109039468567573 ) ) ;
#63322 = CARTESIAN_POINT ( 'NONE',  ( 18.67979575497194134, -10.72451020669871369, 40.83442372801901854 ) ) ;
#63324 = CARTESIAN_POINT ( 'NONE',  ( -0.05219959533937732626, 21.53943276465977519, 92.50109039468567573 ) ) ;
#63323 = CARTESIAN_POINT ( 'NONE',  ( 19.02544592524334988, 5.153800228976608722, 86.45942372801900433 ) ) ;
#63325 = CARTESIAN_POINT ( 'NONE',  ( 16.52544592524335698, 4.483927247898782831, 91.45942372801901854 ) ) ;
#63326 = CARTESIAN_POINT ( 'NONE',  ( 5.049401038298161559, -19.05341960407611168, 102.7072429386476955 ) ) ;
#63327 = CARTESIAN_POINT ( 'NONE',  ( 8.314922557960818139, 14.29746914071049879, 84.58224293864769550 ) ) ;
#63328 = CARTESIAN_POINT ( 'NONE',  ( -0.05219959533910754901, -16.53943276465976808, 37.49890960531436690 ) ) ;
#63329 = CARTESIAN_POINT ( 'NONE',  ( 16.46253265017146816, 9.564922557961045513, 66.66775706135233293 ) ) ;
#63330 = CARTESIAN_POINT ( 'NONE',  ( -21.52544592524334988, -5.823673210054445271, 53.95942372801900433 ) ) ;
#63331 = CARTESIAN_POINT ( 'NONE',  ( 16.46253265017146816, 9.564922557961045513, 21.66775706135233648 ) ) ;
#63332 = CARTESIAN_POINT ( 'NONE',  ( -12.14591786802309592, -12.06949235617757132, 91.87390960531436690 ) ) ;
#63333 = CARTESIAN_POINT ( 'NONE',  ( 10.81492255796078972, 18.62759615963270932, 34.58224293864770260 ) ) ;
#63334 = CARTESIAN_POINT ( 'NONE',  ( 16.52544592524335698, 4.483927247898782831, 111.4594237280190328 ) ) ;
#63336 = CARTESIAN_POINT ( 'NONE',  ( -10.72451020669870658, -18.67979575497194134, 94.58442372801901854 ) ) ;
#63335 = B_SPLINE_CURVE_WITH_KNOTS ( 'NONE', 3,
 ( #159851, #116347, #177047, #67842, #114335, #194210, #133516, #8170, #147699, #52672, #146675, #193200, #115357, #54673, #178036, #162852 ),
 .UNSPECIFIED., .F., .F.,
 ( 4, 2, 2, 2, 2, 2, 2, 4 ),
 ( 0.02152764489805616965, 0.02408704820948082137, 0.02664645152090547309, 0.03176525814375479040, 0.03432466145517944905, 0.03560436311089177491, 0.03688406476660410077, 0.04200287138945340421 ),
 .UNSPECIFIED. ) ;
#63337 = CARTESIAN_POINT ( 'NONE',  ( -8.314922557961024197, 14.29746914071037800, 62.91775706135236135 ) ) ;
#63338 = CARTESIAN_POINT ( 'NONE',  ( 14.34966873604972726, -8.224510206698740333, 110.8344237280190043 ) ) ;
#63339 = CARTESIAN_POINT ( 'NONE',  ( 5.719274019375673035, 21.55341960407619339, 52.29275706135236135 ) ) ;
#63340 = CARTESIAN_POINT ( 'NONE',  ( -5.719274019375665041, -21.55341960407619695, 54.79275706135235424 ) ) ;
#63341 = VERTEX_POINT ( 'NONE', #147524 ) ;
#63342 = CARTESIAN_POINT ( 'NONE',  ( 15.80617190586769283, -15.72974639402175789, 30.62609039468567929 ) ) ;
#63343 = CARTESIAN_POINT ( 'NONE',  ( 14.34966873604960469, 8.224510206698951720, 109.1655762719810383 ) ) ;
#63344 = CARTESIAN_POINT ( 'NONE',  ( -16.46253265017160317, 9.564922557960807481, 30.83224293864769550 ) ) ;
#63345 = CARTESIAN_POINT ( 'NONE',  ( 8.224510206698953496, -14.34966873604960469, 67.91557627198102409 ) ) ;
#63346 = CARTESIAN_POINT ( 'NONE',  ( -16.46253265017160317, 9.564922557960807481, 65.83224293864769550 ) ) ;
#63347 = CARTESIAN_POINT ( 'NONE',  ( 4.483927247898790824, -16.52544592524335698, 110.2094237280190185 ) ) ;
#63348 = CARTESIAN_POINT ( 'NONE',  ( 21.53943276465977519, -0.05219959533907433946, 53.74890960531437401 ) ) ;
#63349 = CARTESIAN_POINT ( 'NONE',  ( -4.379528057220328563, 16.55341960407611168, 95.20724293864769550 ) ) ;
#63350 = CARTESIAN_POINT ( 'NONE',  ( 21.53943276465977519, -0.05219959533907433946, 98.74890960531438111 ) ) ;
#63351 = CARTESIAN_POINT ( 'NONE',  ( -19.02544592524342804, 5.153800228976336051, 106.0405762719810241 ) ) ;
#63353 = CARTESIAN_POINT ( 'NONE',  ( -16.46253265017146816, -9.564922557961047289, 109.1677570613523471 ) ) ;
#63352 = CARTESIAN_POINT ( 'NONE',  ( 5.049401038298161559, -19.05341960407611168, 47.70724293864770260 ) ) ;
#63354 = CARTESIAN_POINT ( 'NONE',  ( -15.72974639402197994, 15.80617190586746368, 50.62390960531435979 ) ) ;
#63355 = CARTESIAN_POINT ( 'NONE',  ( -5.719274019375665041, -21.55341960407619695, 69.79275706135234714 ) ) ;
#63356 = CARTESIAN_POINT ( 'NONE',  ( -5.049401038298153566, 19.05341960407611168, 70.20724293864769550 ) ) ;
#63357 = CARTESIAN_POINT ( 'NONE',  ( 13.89961937509977652, -13.97604488694527269, 98.12390960531433848 ) ) ;
#63358 = CARTESIAN_POINT ( 'NONE',  ( 14.34966873604972726, -8.224510206698740333, 65.83442372801900433 ) ) ;
#63359 = CARTESIAN_POINT ( 'NONE',  ( 5.719274019375673035, 21.55341960407619339, 47.29275706135234003 ) ) ;
#63360 = CARTESIAN_POINT ( 'NONE',  ( 21.53943276465977519, 0.05219959533937863772, 81.25109039468568994 ) ) ;
#63361 = CARTESIAN_POINT ( 'NONE',  ( 10.72451020669898902, -18.67979575497178502, 92.91557627198103830 ) ) ;
#63363 = CARTESIAN_POINT ( 'NONE',  ( -8.224510206698735004, -14.34966873604973081, 84.58442372801903275 ) ) ;
#63362 = CARTESIAN_POINT ( 'NONE',  ( -21.53943276465977519, -0.05219959533937600094, 38.75109039468567573 ) ) ;
#63364 = CARTESIAN_POINT ( 'NONE',  ( 0.05219959533907565091, 21.53943276465977519, 74.99890960531435269 ) ) ;
#63365 = CARTESIAN_POINT ( 'NONE',  ( 19.02544592524334988, 5.153800228976608722, 31.45942372801900433 ) ) ;
#63367 = CARTESIAN_POINT ( 'NONE',  ( 16.55341960407611168, 4.379528057220329451, 23.95724293864769550 ) ) ;
#63366 = CARTESIAN_POINT ( 'NONE',  ( -5.153800228976328057, -19.02544592524343514, 82.29057627198103830 ) ) ;
#63368 = CARTESIAN_POINT ( 'NONE',  ( -17.49999999999999645, -3.189878218039172264, 105.1294856257125758 ) ) ;
#63369 = CARTESIAN_POINT ( 'NONE',  ( 9.474510206698971260, -16.51473224551069308, 97.91557627198102409 ) ) ;
#63370 = CARTESIAN_POINT ( 'NONE',  ( 0.000000000000000000, 0.000000000000000000, 0.000000000000000000 ) ) ;
#63371 = CARTESIAN_POINT ( 'NONE',  ( 5.153800228976615827, -19.02544592524334988, 75.20942372801896170 ) ) ;
#63372 = CARTESIAN_POINT ( 'NONE',  ( 15.72974639402199770, -15.80617190586745480, 58.12390960531435979 ) ) ;
#63373 = CARTESIAN_POINT ( 'NONE',  ( -12.14591786802309592, -12.06949235617757132, 36.87390960531435979 ) ) ;
#63374 = CARTESIAN_POINT ( 'NONE',  ( -9.474510206698720793, -16.51473224551083518, 109.5844237280190043 ) ) ;
#63375 = CARTESIAN_POINT ( 'NONE',  ( 16.51473224551069308, 9.474510206698969483, 34.16557627198102409 ) ) ;
#63376 = CARTESIAN_POINT ( 'NONE',  ( -16.53943276465976808, -0.05219959533934237506, 18.75109039468568639 ) ) ;
#63378 = CARTESIAN_POINT ( 'NONE',  ( -5.153800228976607833, 19.02544592524334988, 67.70942372801900433 ) ) ;
#63377 = CARTESIAN_POINT ( 'NONE',  ( -18.67979575497178146, -10.72451020669898902, 96.66557627198102409 ) ) ;
#63379 = CARTESIAN_POINT ( 'NONE',  ( -8.314922557961024197, 14.29746914071037800, 82.91775706135234714 ) ) ;
#63380 = CARTESIAN_POINT ( 'NONE',  ( 13.89961937509977652, -13.97604488694527269, 63.12390960531435979 ) ) ;
#63381 = CARTESIAN_POINT ( 'NONE',  ( 0.05219959533910956823, 16.53943276465976808, 74.99890960531435269 ) ) ;
#63382 = CARTESIAN_POINT ( 'NONE',  ( -9.564922557960796823, -16.46253265017161027, 62.08224293864769550 ) ) ;
#63383 = CARTESIAN_POINT ( 'NONE',  ( 16.52544592524342804, -4.483927247898539470, 73.54057627198102409 ) ) ;
#63384 = CARTESIAN_POINT ( 'NONE',  ( 9.564922557960805705, 16.46253265017160317, 24.58224293864769194 ) ) ;
#63385 = CARTESIAN_POINT ( 'NONE',  ( -37.52651979737520094, -1.772832052285354010, 39.78107084225509738 ) ) ;
#63386 = CARTESIAN_POINT ( 'NONE',  ( -16.52544592524342804, 4.483927247898546575, 36.04057627198102409 ) ) ;
#63387 = CARTESIAN_POINT ( 'NONE',  ( 19.05341960407611168, 5.049401038298154454, 78.95724293864769550 ) ) ;
#63388 = DIRECTION ( 'NONE',  ( 0.000000000000000000, 0.000000000000000000, -1.000000000000000000 ) ) ;
#63389 = CARTESIAN_POINT ( 'NONE',  ( 5.153800228976615827, -19.02544592524334988, 35.20942372801899722 ) ) ;
#63390 = CARTESIAN_POINT ( 'NONE',  ( 12.14591786802327356, -12.06949235617739191, 55.62609039468568284 ) ) ;
#63391 = CARTESIAN_POINT ( 'NONE',  ( -15.80617190586745835, -15.72974639402198527, 66.87390960531436690 ) ) ;
#63392 = CARTESIAN_POINT ( 'NONE',  ( 10.72451020669871369, 18.67979575497193778, 112.0844237280190185 ) ) ;
#63393 = CARTESIAN_POINT ( 'NONE',  ( -16.51473224551069308, -9.474510206698971260, 71.66557627198102409 ) ) ;
#63394 = CARTESIAN_POINT ( 'NONE',  ( -22.48049813892993143, -22.63291450077185019, -45.64921306006597490 ) ) ;
#63395 = CARTESIAN_POINT ( 'NONE',  ( -21.55341960407610458, -5.719274019375992779, 21.45724293864769550 ) ) ;
#63396 = CARTESIAN_POINT ( 'NONE',  ( 5.049401038298161559, -19.05341960407611168, 62.70724293864769550 ) ) ;
#63397 = CARTESIAN_POINT ( 'NONE',  ( 18.67979575497194134, -10.72451020669871369, 35.83442372801901143 ) ) ;
#63398 = CARTESIAN_POINT ( 'NONE',  ( 16.52544592524342804, -4.483927247898539470, 103.5405762719810383 ) ) ;
#63401 = ORIENTED_EDGE ( 'NONE', *, *, #170744, .T. ) ;
#63400 = CARTESIAN_POINT ( 'NONE',  ( -13.89961937509977652, 13.97604488694528158, 95.62390960531436690 ) ) ;
#63399 = CARTESIAN_POINT ( 'NONE',  ( -21.52544592524343514, 5.823673210054127303, 106.0405762719810525 ) ) ;
#63402 = CARTESIAN_POINT ( 'NONE',  ( -18.67979575497193778, 10.72451020669871902, 28.33442372801902209 ) ) ;
#63403 = EDGE_LOOP ( 'NONE', ( #100641, #65175, #20997, #81111 ) ) ;
#63404 = CARTESIAN_POINT ( 'NONE',  ( 9.474510206698971260, -16.51473224551069308, 82.91557627198103830 ) ) ;
#63405 = ADVANCED_FACE ( 'NONE', ( #175859 ), #23174, .T. ) ;
#63406 = B_SPLINE_CURVE_WITH_KNOTS ( 'NONE', 3,
 ( #85740, #113077, #6891, #100897, #81725, #22079 ),
 .UNSPECIFIED., .F., .F.,
 ( 4, 2, 4 ),
 ( 3.469446951953613804E-18, 0.0003837532665554152424, 0.0007675065331108270154 ),
 .UNSPECIFIED. ) ;
#63407 = DIRECTION ( 'NONE',  ( -1.000000000000000000, -0.000000000000000000, -0.000000000000000000 ) ) ;
#63408 = CARTESIAN_POINT ( 'NONE',  ( -5.823673210054116645, -21.52544592524344225, 97.29057627198105251 ) ) ;
#63409 = CARTESIAN_POINT ( 'NONE',  ( 5.153800228976335163, 19.02544592524342804, 44.79057627198103830 ) ) ;
#63410 = CARTESIAN_POINT ( 'NONE',  ( 13.89961937509957401, 13.97604488694547697, 101.8760903946856331 ) ) ;
#63411 = CARTESIAN_POINT ( 'NONE',  ( -11.40812507854754720, -35.11059874428192273, -8.724999997268813701 ) ) ;
#63412 = CARTESIAN_POINT ( 'NONE',  ( 16.46253265017160672, -9.564922557960803928, 23.33224293864769194 ) ) ;
#63413 = CARTESIAN_POINT ( 'NONE',  ( -5.719274019375665041, -21.55341960407619695, 79.79275706135236135 ) ) ;
#63415 = CARTESIAN_POINT ( 'NONE',  ( 5.719274019375673035, 21.55341960407619339, 52.29275706135236135 ) ) ;
#63414 = CARTESIAN_POINT ( 'NONE',  ( -19.02544592524342804, 5.153800228976336051, 81.04057627198103830 ) ) ;
#63416 = CARTESIAN_POINT ( 'NONE',  ( 21.55341960407619695, -5.719274019375665929, 31.04275706135234714 ) ) ;
#63417 = CARTESIAN_POINT ( 'NONE',  ( -17.81289503416611808, 24.51734667627700404, 149.6999999999999602 ) ) ;
#63418 = CARTESIAN_POINT ( 'NONE',  ( 0.05219959533909260263, 19.03943276465977164, 89.99890960531436690 ) ) ;
#63419 = CARTESIAN_POINT ( 'NONE',  ( 18.56399227203345248, 5.499999999999818812, 61.47830131249903474 ) ) ;
#63422 = CARTESIAN_POINT ( 'NONE',  ( -15.72974639402176322, -15.80617190586768395, 39.37609039468567573 ) ) ;
#63421 = CARTESIAN_POINT ( 'NONE',  ( 15.80617190586746368, 15.72974639402197994, 49.37390960531436690 ) ) ;
#63420 = CARTESIAN_POINT ( 'NONE',  ( -12.14591786802326823, 12.06949235617739902, 38.12609039468567573 ) ) ;
#63423 = CARTESIAN_POINT ( 'NONE',  ( -15.80617190586768217, 15.72974639402176855, 73.12609039468567573 ) ) ;
#63424 = DIRECTION ( 'NONE',  ( 0.000000000000000000, 0.8660254037844380415, -0.5000000000000012212 ) ) ;
#63425 = CARTESIAN_POINT ( 'NONE',  ( -19.05341960407617563, 5.049401038297882671, 108.5427570613523187 ) ) ;
#63426 = CARTESIAN_POINT ( 'NONE',  ( -13.89961937509977652, 13.97604488694528158, 55.62390960531434558 ) ) ;
#63427 = CARTESIAN_POINT ( 'NONE',  ( -16.46253265017160317, 9.564922557960807481, 80.83224293864769550 ) ) ;
#63428 = CARTESIAN_POINT ( 'NONE',  ( 16.52544592524342804, -4.483927247898539470, 108.5405762719810241 ) ) ;
#63429 = CARTESIAN_POINT ( 'NONE',  ( 4.379528057220339221, -16.55341960407611168, 107.7072429386476955 ) ) ;
#63430 = CARTESIAN_POINT ( 'NONE',  ( -13.97604488694527625, -13.89961937509977652, 111.8739096053143243 ) ) ;
#63431 = CARTESIAN_POINT ( 'NONE',  ( -12.06949235617739369, -12.14591786802326823, 84.37609039468570415 ) ) ;
#63433 = CARTESIAN_POINT ( 'NONE',  ( -5.049401038298153566, 19.05341960407611168, 60.20724293864768129 ) ) ;
#63432 = CARTESIAN_POINT ( 'NONE',  ( -16.55341960407611168, -4.379528057220339221, 76.45724293864769550 ) ) ;
#63434 = CARTESIAN_POINT ( 'NONE',  ( -0.05219959533937732626, 21.53943276465977519, 82.50109039468568994 ) ) ;
#63435 = CARTESIAN_POINT ( 'NONE',  ( 21.53943276465977519, 0.05219959533937863772, 66.25109039468567573 ) ) ;
#63436 = CARTESIAN_POINT ( 'NONE',  ( 13.89961937509957401, 13.97604488694547697, 111.8760903946856757 ) ) ;
#63437 = CARTESIAN_POINT ( 'NONE',  ( -14.34966873604960291, -8.224510206698953496, 61.66557627198103120 ) ) ;
#63438 = CARTESIAN_POINT ( 'NONE',  ( 10.81492255796106328, -18.62759615963255655, 25.41775706135235779 ) ) ;
#63439 = CARTESIAN_POINT ( 'NONE',  ( 0.05219959533907565091, 21.53943276465977519, 64.99890960531435269 ) ) ;
#63440 = CARTESIAN_POINT ( 'NONE',  ( -17.49999999999999645, -5.500000000000000888, 104.2030961746582847 ) ) ;
#63441 = CARTESIAN_POINT ( 'NONE',  ( -17.81289503416611097, -24.51734667627696496, 144.5500000054623513 ) ) ;
#63442 = CARTESIAN_POINT ( 'NONE',  ( 0.05219959533909260263, 19.03943276465977164, 69.99890960531435269 ) ) ;
#63443 = CARTESIAN_POINT ( 'NONE',  ( 0.05219959533910956823, 16.53943276465976808, 39.99890960531436690 ) ) ;
#63444 = EDGE_CURVE ( 'NONE', #188934, #102970, #149511, .T. ) ;
#63445 = CARTESIAN_POINT ( 'NONE',  ( -12.06949235617756955, 12.14591786802309770, 25.62390960531435624 ) ) ;
#63446 = CARTESIAN_POINT ( 'NONE',  ( -8.314922557961024197, 14.29746914071037800, 92.91775706135236135 ) ) ;
#63447 = CARTESIAN_POINT ( 'NONE',  ( 19.05341960407617918, -5.049401038297876454, 56.04275706135234714 ) ) ;
#63448 = CARTESIAN_POINT ( 'NONE',  ( 17.12812012977023812, 6.668231424566063659, 48.85948759323144941 ) ) ;
#63449 = CARTESIAN_POINT ( 'NONE',  ( -19.02544592524342804, 5.153800228976336051, 106.0405762719810241 ) ) ;
#63450 = CARTESIAN_POINT ( 'NONE',  ( 0.05219959533910956823, 16.53943276465976808, 79.99890960531435269 ) ) ;
#63451 = CARTESIAN_POINT ( 'NONE',  ( -16.46253265017146816, -9.564922557961047289, 44.16775706135232582 ) ) ;
#63453 = CARTESIAN_POINT ( 'NONE',  ( 19.05341960407611168, 5.049401038298154454, 113.9572429386477097 ) ) ;
#63452 = CARTESIAN_POINT ( 'NONE',  ( 17.50000000000000000, -5.500000000000000888, 103.2969038253417153 ) ) ;
#63455 = VERTEX_POINT ( 'NONE', #133338 ) ;
#63454 = CARTESIAN_POINT ( 'NONE',  ( 0.05219959533907565091, 21.53943276465977519, 59.99890960531436690 ) ) ;
#63456 = CARTESIAN_POINT ( 'NONE',  ( -0.05219959533910754901, -16.53943276465976808, 102.4989096053143811 ) ) ;
#63457 = CARTESIAN_POINT ( 'NONE',  ( 16.52544592524335698, 4.483927247898782831, 56.45942372801902565 ) ) ;
#63458 = CARTESIAN_POINT ( 'NONE',  ( 14.29746914071049879, -8.314922557960816363, 93.33224293864769550 ) ) ;
#63459 = CARTESIAN_POINT ( 'NONE',  ( -28.79475375365586842, 2.428612866367529932E-14, 143.9843446568999923 ) ) ;
#63460 = CARTESIAN_POINT ( 'NONE',  ( -16.18388926212241685, 7.379444403734378710, 49.56046848633847191 ) ) ;
#63461 = CARTESIAN_POINT ( 'NONE',  ( 19.03943276465977164, -0.05219959533909143690, 113.7489096053143669 ) ) ;
#63462 = CARTESIAN_POINT ( 'NONE',  ( 11.40812507854755253, -35.11059874428192273, -6.524999997268813523 ) ) ;
#63463 = CARTESIAN_POINT ( 'NONE',  ( 1.227931366032057224E-14, 24.30000000000003268, -56.77278709839600879 ) ) ;
#63464 = ORIENTED_EDGE ( 'NONE', *, *, #192158, .F. ) ;
#63466 = CARTESIAN_POINT ( 'NONE',  ( -12.06949235617756955, 12.14591786802309770, 35.62390960531437401 ) ) ;
#63465 = CARTESIAN_POINT ( 'NONE',  ( 8.224510206698742110, 14.34966873604972548, 42.08442372801901854 ) ) ;
#63467 = CARTESIAN_POINT ( 'NONE',  ( -10.72451020669898014, 18.67979575497178502, 60.41557627198102409 ) ) ;
#63468 = CARTESIAN_POINT ( 'NONE',  ( -9.474510206698720793, -16.51473224551083518, 89.58442372801900433 ) ) ;
#63469 = CARTESIAN_POINT ( 'NONE',  ( 0.05219959533907565091, 21.53943276465977519, 49.99890960531437401 ) ) ;
#63470 = CARTESIAN_POINT ( 'NONE',  ( -10.81492255796105439, 18.62759615963255655, 82.91775706135234714 ) ) ;
#63471 = CARTESIAN_POINT ( 'NONE',  ( 13.29753078558972668, -35.33598341332321269, -29.59763579011271517 ) ) ;
#63472 = CARTESIAN_POINT ( 'NONE',  ( -0.05219959533934338120, 16.53943276465976808, 32.50109039468568284 ) ) ;
#63474 = CARTESIAN_POINT ( 'NONE',  ( -13.89961937509977652, 13.97604488694528158, 105.6239096053143527 ) ) ;
#63473 = CARTESIAN_POINT ( 'NONE',  ( -0.05219959533909027116, -19.03943276465977164, 37.49890960531436690 ) ) ;
#63475 = CARTESIAN_POINT ( 'NONE',  ( 16.46253265017160672, -9.564922557960803928, 38.33224293864768839 ) ) ;
#63476 = CARTESIAN_POINT ( 'NONE',  ( 12.14591786802309770, 12.06949235617756955, 104.3739096053143669 ) ) ;
#63477 = CARTESIAN_POINT ( 'NONE',  ( -9.474510206698964154, 16.51473224551069663, 100.4155762719810241 ) ) ;
#63478 = ORIENTED_EDGE ( 'NONE', *, *, #15614, .F. ) ;
#63479 = CARTESIAN_POINT ( 'NONE',  ( 16.55341960407618274, -4.379528057220086978, 51.04275706135234714 ) ) ;
#63480 = CARTESIAN_POINT ( 'NONE',  ( 21.52544592524344225, -5.823673210054117533, 88.54057627198103830 ) ) ;
#63481 = CARTESIAN_POINT ( 'NONE',  ( 0.05219959533909260263, 19.03943276465977164, 59.99890960531436690 ) ) ;
#63482 = CARTESIAN_POINT ( 'NONE',  ( 18.62759615963255655, 10.81492255796105972, 21.66775706135235069 ) ) ;
#63483 = CARTESIAN_POINT ( 'NONE',  ( -13.97604488694527625, -13.89961937509977652, 81.87390960531436690 ) ) ;
#63484 = CARTESIAN_POINT ( 'NONE',  ( -4.429638872090642462E-30, -165.0000000000000000, -13.00000000000000000 ) ) ;
#63485 = EDGE_LOOP ( 'NONE', ( #181791, #118149, #177869, #29107 ) ) ;
#63486 = CARTESIAN_POINT ( 'NONE',  ( -12.06949235617739369, -12.14591786802326823, 44.37609039468567573 ) ) ;
#63487 = CARTESIAN_POINT ( 'NONE',  ( -5.719274019375665041, -21.55341960407619695, 24.79275706135235779 ) ) ;
#63490 = CARTESIAN_POINT ( 'NONE',  ( -9.564922557961040184, 16.46253265017147172, 77.91775706135234714 ) ) ;
#63489 = CARTESIAN_POINT ( 'NONE',  ( -5.153800228976328057, -19.02544592524343514, 102.2905762719810383 ) ) ;
#63488 = CARTESIAN_POINT ( 'NONE',  ( 9.474510206698971260, -16.51473224551069308, 22.91557627198102765 ) ) ;
#63491 = ADVANCED_FACE ( 'NONE', ( #134357 ), #164690, .T. ) ;
#63492 = CARTESIAN_POINT ( 'NONE',  ( -16.51473224551082808, 9.474510206698731452, 33.33442372801899722 ) ) ;
#63493 = CARTESIAN_POINT ( 'NONE',  ( -15.72974639402197994, 15.80617190586746368, 85.62390960531436690 ) ) ;
#63494 = CARTESIAN_POINT ( 'NONE',  ( 19.02544592524334988, 5.153800228976608722, 41.45942372801900433 ) ) ;
#63495 = CARTESIAN_POINT ( 'NONE',  ( -4.483927247898782831, 16.52544592524335698, 72.70942372801901854 ) ) ;
#63497 = VERTEX_POINT ( 'NONE', #40334 ) ;
#63496 = CARTESIAN_POINT ( 'NONE',  ( -5.153800228976328057, -19.02544592524343514, 112.2905762719810099 ) ) ;
#63498 = CARTESIAN_POINT ( 'NONE',  ( -13.89961937509977652, 13.97604488694528158, 60.62390960531436690 ) ) ;
#63499 = VECTOR ( 'NONE', #107306, 1000.000000000000000 ) ;
#63500 = CARTESIAN_POINT ( 'NONE',  ( -10.81492255796105439, 18.62759615963255655, 67.91775706135234714 ) ) ;
#63501 = CARTESIAN_POINT ( 'NONE',  ( 15.80617190586769283, -15.72974639402175789, 85.62609039468568994 ) ) ;
#63502 = CARTESIAN_POINT ( 'NONE',  ( -19.02544592524342804, 5.153800228976336051, 71.04057627198099567 ) ) ;
#63503 = CARTESIAN_POINT ( 'NONE',  ( 18.62759615963255655, 10.81492255796105972, 46.66775706135234714 ) ) ;
#63504 = CARTESIAN_POINT ( 'NONE',  ( 16.51473224551083163, -9.474510206698727899, 85.83442372801900433 ) ) ;
#63505 = ADVANCED_FACE ( 'NONE', ( #161678 ), #177865, .T. ) ;
#63506 = CARTESIAN_POINT ( 'NONE',  ( 5.153800228976335163, 19.02544592524342804, 54.79057627198103120 ) ) ;
#63507 = CARTESIAN_POINT ( 'NONE',  ( 16.46253265017160672, -9.564922557960803928, 103.3322429386476955 ) ) ;
#63508 = CARTESIAN_POINT ( 'NONE',  ( -19.03943276465977164, 0.05219959533909376836, 61.24890960531436690 ) ) ;
#63509 = CARTESIAN_POINT ( 'NONE',  ( -5.153800228976328057, -19.02544592524343514, 112.2905762719810099 ) ) ;
#63510 = CARTESIAN_POINT ( 'NONE',  ( -9.474510206698964154, 16.51473224551069663, 45.41557627198103120 ) ) ;
#63511 = CARTESIAN_POINT ( 'NONE',  ( -15.80617190586745835, -15.72974639402198527, 101.8739096053143811 ) ) ;
#63512 = CARTESIAN_POINT ( 'NONE',  ( -0.05219959533934338120, 16.53943276465976808, 77.50109039468567573 ) ) ;
#63513 = CARTESIAN_POINT ( 'NONE',  ( -24.17640770809925854, 7.553848413212390867, 169.9412368235690565 ) ) ;
#63514 = CARTESIAN_POINT ( 'NONE',  ( 19.05341960407617918, -5.049401038297876454, 36.04275706135234003 ) ) ;
#63515 = CARTESIAN_POINT ( 'NONE',  ( -9.474510206698964154, 16.51473224551069663, 70.41557627198102409 ) ) ;
#63516 = CARTESIAN_POINT ( 'NONE',  ( -12.14591786802309592, -12.06949235617757132, 61.87390960531436690 ) ) ;
#63517 = CARTESIAN_POINT ( 'NONE',  ( 14.34966873604960469, 8.224510206698951720, 99.16557627198100988 ) ) ;
#63518 = CARTESIAN_POINT ( 'NONE',  ( 5.153800228976335163, 19.02544592524342804, 94.79057627198103830 ) ) ;
#63519 = CARTESIAN_POINT ( 'NONE',  ( 16.46253265017160672, -9.564922557960803928, 88.33224293864769550 ) ) ;
#63520 = CARTESIAN_POINT ( 'NONE',  ( -16.51473224551069308, -9.474510206698971260, 101.6655762719810241 ) ) ;
#63521 = CARTESIAN_POINT ( 'NONE',  ( -5.049401038297874678, -19.05341960407617918, 19.79275706135233293 ) ) ;
#63522 = CARTESIAN_POINT ( 'NONE',  ( 8.314922557961029526, -14.29746914071037800, 95.41775706135234714 ) ) ;
#63523 = CARTESIAN_POINT ( 'NONE',  ( 5.719274019375673035, 21.55341960407619339, 37.29275706135235424 ) ) ;
#63524 = CARTESIAN_POINT ( 'NONE',  ( -10.72451020669898014, 18.67979575497178502, 30.41557627198101699 ) ) ;
#63525 = CARTESIAN_POINT ( 'NONE',  ( -18.67979575497178146, -10.72451020669898902, 106.6655762719810383 ) ) ;
#63526 = CARTESIAN_POINT ( 'NONE',  ( -4.379528057220328563, 16.55341960407611168, 60.20724293864768839 ) ) ;
#63527 = CARTESIAN_POINT ( 'NONE',  ( 5.153800228976335163, 19.02544592524342804, 49.79057627198100988 ) ) ;
#63528 = CARTESIAN_POINT ( 'NONE',  ( 4.483927247898545687, 16.52544592524342804, 84.79057627198102409 ) ) ;
#63529 = CARTESIAN_POINT ( 'NONE',  ( 15.80617190586746368, 15.72974639402197994, 39.37390960531436690 ) ) ;
#63530 = CARTESIAN_POINT ( 'NONE',  ( -19.03943276465977164, -0.05219959533935918106, 38.75109039468566152 ) ) ;
#63531 = CARTESIAN_POINT ( 'NONE',  ( -8.224510206698948167, 14.34966873604960824, 115.4155762719810241 ) ) ;
#63532 = ORIENTED_EDGE ( 'NONE', *, *, #55093, .T. ) ;
#63533 = CARTESIAN_POINT ( 'NONE',  ( 4.483927247898790824, -16.52544592524335698, 65.20942372801901854 ) ) ;
#63534 = CARTESIAN_POINT ( 'NONE',  ( 0.05219959533909260263, 19.03943276465977164, 64.99890960531436690 ) ) ;
#63535 = CARTESIAN_POINT ( 'NONE',  ( -8.571926809382608425, 26.38167802310805854, 146.4750000027311785 ) ) ;
#63536 = CARTESIAN_POINT ( 'NONE',  ( -16.53943276465976808, 0.05219959533911058130, 86.24890960531436690 ) ) ;
#63537 = CARTESIAN_POINT ( 'NONE',  ( -5.719274019375978568, 21.55341960407610458, 35.20724293864768839 ) ) ;
#63538 = ORIENTED_EDGE ( 'NONE', *, *, #67479, .T. ) ;
#63539 = CARTESIAN_POINT ( 'NONE',  ( 8.314922557961029526, -14.29746914071037800, 105.4177570613523613 ) ) ;
#63540 = CARTESIAN_POINT ( 'NONE',  ( -16.53943276465976808, -0.05219959533934237506, 23.75109039468567929 ) ) ;
#63541 = CARTESIAN_POINT ( 'NONE',  ( -15.80617190586768217, 15.72974639402176855, 98.12609039468570415 ) ) ;
#63542 = CARTESIAN_POINT ( 'NONE',  ( 19.05341960407611168, 5.049401038298154454, 83.95724293864766707 ) ) ;
#63543 = CARTESIAN_POINT ( 'NONE',  ( 21.55341960407610458, 5.719274019375980345, 113.9572429386477239 ) ) ;
#63544 = CARTESIAN_POINT ( 'NONE',  ( 5.153800228976335163, 19.02544592524342804, 29.79057627198102409 ) ) ;
#63545 = CARTESIAN_POINT ( 'NONE',  ( 16.53943276465976808, 0.05219959533934440121, 36.25109039468567573 ) ) ;
#63546 = CARTESIAN_POINT ( 'NONE',  ( -16.46253265017146816, -9.564922557961047289, 89.16775706135234714 ) ) ;
#63547 = CARTESIAN_POINT ( 'NONE',  ( -15.80617190586745835, -15.72974639402198527, 91.87390960531436690 ) ) ;
#63548 = CARTESIAN_POINT ( 'NONE',  ( 9.564922557961047289, -16.46253265017146816, 65.41775706135233293 ) ) ;
#63549 = DIRECTION ( 'NONE',  ( 0.000000000000000000, -0.7660444431189771253, 0.6427876096865404731 ) ) ;
#63550 = CARTESIAN_POINT ( 'NONE',  ( 18.67979575497178502, 10.72451020669898547, 114.1655762719810383 ) ) ;
#63551 = CARTESIAN_POINT ( 'NONE',  ( 0.000000000000000000, 0.000000000000000000, 120.0000000000000142 ) ) ;
#63552 = CARTESIAN_POINT ( 'NONE',  ( 5.049401038298161559, -19.05341960407611168, 77.70724293864765286 ) ) ;
#63553 = CARTESIAN_POINT ( 'NONE',  ( 12.06949235617739724, 12.14591786802326823, 31.87609039468567929 ) ) ;
#63554 = CARTESIAN_POINT ( 'NONE',  ( 17.34328899321214124, -36.04909658921342697, -9.447446616692788623 ) ) ;
#63555 = CARTESIAN_POINT ( 'NONE',  ( -9.564922557961040184, 16.46253265017147172, 57.91775706135233293 ) ) ;
#63557 = CARTESIAN_POINT ( 'NONE',  ( 16.55341960407611168, 4.379528057220329451, 78.95724293864769550 ) ) ;
#63556 = CARTESIAN_POINT ( 'NONE',  ( -18.62759615963255300, -10.81492255796106328, 19.16775706135234714 ) ) ;
#63558 = CARTESIAN_POINT ( 'NONE',  ( 19.03943276465977164, -0.05219959533909143690, 78.74890960531436690 ) ) ;
#63560 = CARTESIAN_POINT ( 'NONE',  ( 0.05219959533936267826, -19.03943276465977164, 40.00109039468566152 ) ) ;
#63559 = CARTESIAN_POINT ( 'NONE',  ( 8.314922557961029526, -14.29746914071037800, 40.41775706135234714 ) ) ;
#63561 = CARTESIAN_POINT ( 'NONE',  ( 15.72974639402176855, 15.80617190586768217, 66.87609039468568994 ) ) ;
#63562 = CARTESIAN_POINT ( 'NONE',  ( -13.89961937509957401, -13.97604488694547875, 104.3760903946856757 ) ) ;
#63563 = CARTESIAN_POINT ( 'NONE',  ( 0.05219959533909260263, 19.03943276465977164, 54.99890960531435979 ) ) ;
#63564 = CARTESIAN_POINT ( 'NONE',  ( -16.51473224551082808, 9.474510206698731452, 83.33442372801899012 ) ) ;
#63565 = CARTESIAN_POINT ( 'NONE',  ( 12.14591786802327356, -12.06949235617739191, 55.62609039468568284 ) ) ;
#63566 = CARTESIAN_POINT ( 'NONE',  ( 5.823673210054444382, -21.52544592524334988, 100.2094237280190043 ) ) ;
#63567 = CARTESIAN_POINT ( 'NONE',  ( -13.97604488694547697, 13.89961937509957934, 73.12609039468568994 ) ) ;
#63568 = CARTESIAN_POINT ( 'NONE',  ( 19.05341960407611168, 5.049401038298154454, 53.95724293864770260 ) ) ;
#63569 = CARTESIAN_POINT ( 'NONE',  ( -21.55341960407610458, -5.719274019375992779, 66.45724293864768129 ) ) ;
#63571 = CARTESIAN_POINT ( 'NONE',  ( -16.51473224551082808, 9.474510206698731452, 63.33442372801900433 ) ) ;
#63570 = CARTESIAN_POINT ( 'NONE',  ( -4.379528057220328563, 16.55341960407611168, 60.20724293864768839 ) ) ;
#63572 = CARTESIAN_POINT ( 'NONE',  ( -17.26172910966780094, -6.454744622555795175, 24.19353091350776452 ) ) ;
#63573 = CARTESIAN_POINT ( 'NONE',  ( -13.89961937509957401, -13.97604488694547875, 49.37609039468567573 ) ) ;
#63574 = CARTESIAN_POINT ( 'NONE',  ( -14.34966873604972548, 8.224510206698743886, 98.33442372801901854 ) ) ;
#63575 = CARTESIAN_POINT ( 'NONE',  ( 8.224510206698953496, -14.34966873604960469, 62.91557627198102409 ) ) ;
#63577 = CARTESIAN_POINT ( 'NONE',  ( 1.784210473542230573E-15, -29.16686587814331588, 139.3750000027311842 ) ) ;
#63576 = CARTESIAN_POINT ( 'NONE',  ( -5.719274019375665041, -21.55341960407619695, 94.79275706135234714 ) ) ;
#63578 = CARTESIAN_POINT ( 'NONE',  ( 10.81492255796078972, 18.62759615963270932, 89.58224293864768129 ) ) ;
#63579 = CARTESIAN_POINT ( 'NONE',  ( -19.05341960407611168, -5.049401038298163336, 56.45724293864768129 ) ) ;
#63580 = CARTESIAN_POINT ( 'NONE',  ( -21.55341960407619339, 5.719274019375674811, 73.54275706135234714 ) ) ;
#63581 = CARTESIAN_POINT ( 'NONE',  ( -9.564922557960796823, -16.46253265017161027, 52.08224293864768839 ) ) ;
#63582 = VERTEX_POINT ( 'NONE', #87825 ) ;
#63583 = CARTESIAN_POINT ( 'NONE',  ( 5.049401038298161559, -19.05341960407611168, 62.70724293864769550 ) ) ;
#63584 = CARTESIAN_POINT ( 'NONE',  ( 19.03943276465977164, -0.05219959533909143690, 23.74890960531435269 ) ) ;
#63585 = CARTESIAN_POINT ( 'NONE',  ( -19.03943276465977164, 0.05219959533909376836, 116.2489096053143669 ) ) ;
#63586 = CARTESIAN_POINT ( 'NONE',  ( -4.483927247898539470, -16.52544592524342804, 57.29057627198103120 ) ) ;
#63587 = CARTESIAN_POINT ( 'NONE',  ( -5.049401038298153566, 19.05341960407611168, 25.20724293864768484 ) ) ;
#63588 = CARTESIAN_POINT ( 'NONE',  ( 4.483927247898545687, 16.52544592524342804, 89.79057627198103830 ) ) ;
#63589 = CARTESIAN_POINT ( 'NONE',  ( -5.823673210054116645, -21.52544592524344225, 102.2905762719810383 ) ) ;
#63590 = CARTESIAN_POINT ( 'NONE',  ( 21.55341960407619695, -5.719274019375665929, 31.04275706135234714 ) ) ;
#63591 = CARTESIAN_POINT ( 'NONE',  ( 1.197484662147158874, 6.691433960895806443, -62.38716993895737062 ) ) ;
#63592 = CARTESIAN_POINT ( 'NONE',  ( -8.224510206698735004, -14.34966873604973081, 44.58442372801901854 ) ) ;
#63593 = CARTESIAN_POINT ( 'NONE',  ( 21.52544592524344225, -5.823673210054117533, 78.54057627198103830 ) ) ;
#63594 = CARTESIAN_POINT ( 'NONE',  ( -21.55341960407619339, 5.719274019375674811, 103.5427570613523613 ) ) ;
#63595 = CARTESIAN_POINT ( 'NONE',  ( 9.564922557960805705, 16.46253265017160317, 109.5822429386476955 ) ) ;
#63596 = CARTESIAN_POINT ( 'NONE',  ( -5.719274019375665041, -21.55341960407619695, 49.79275706135234714 ) ) ;
#63597 = CARTESIAN_POINT ( 'NONE',  ( 10.81492255796078972, 18.62759615963270932, 39.58224293864769550 ) ) ;
#63598 = CARTESIAN_POINT ( 'NONE',  ( -8.224510206698735004, -14.34966873604973081, 99.58442372801900433 ) ) ;
#63600 = CARTESIAN_POINT ( 'NONE',  ( -10.81492255796105439, 18.62759615963255655, 97.91775706135236135 ) ) ;
#63599 = CARTESIAN_POINT ( 'NONE',  ( 21.52544592524334988, 5.823673210054432836, 61.45942372801901854 ) ) ;
#63601 = CARTESIAN_POINT ( 'NONE',  ( 9.474510206698729675, 16.51473224551082808, 37.08442372801899722 ) ) ;
#63602 = CARTESIAN_POINT ( 'NONE',  ( -8.224510206698735004, -14.34966873604973081, 84.58442372801903275 ) ) ;
#63603 = CARTESIAN_POINT ( 'NONE',  ( -0.05219959533937732626, 21.53943276465977519, 47.50109039468568994 ) ) ;
#63604 = CARTESIAN_POINT ( 'NONE',  ( 19.05341960407611168, 5.049401038298154454, 48.95724293864768129 ) ) ;
#63605 = CARTESIAN_POINT ( 'NONE',  ( -5.049401038297874678, -19.05341960407617918, 19.79275706135233293 ) ) ;
#63606 = CARTESIAN_POINT ( 'NONE',  ( 18.62759615963271287, -10.81492255796078972, 23.33224293864769194 ) ) ;
#63607 = CARTESIAN_POINT ( 'NONE',  ( -21.53943276465977519, 0.05219959533907696930, 111.2489096053143669 ) ) ;
#63608 = CARTESIAN_POINT ( 'NONE',  ( 21.55341960407610458, 5.719274019375980345, 78.95724293864769550 ) ) ;
#63609 = CARTESIAN_POINT ( 'NONE',  ( 14.34966873604972726, -8.224510206698740333, 35.83442372801901143 ) ) ;
#63611 = CARTESIAN_POINT ( 'NONE',  ( -5.823673210054116645, -21.52544592524344225, 82.29057627198103830 ) ) ;
#63610 = CARTESIAN_POINT ( 'NONE',  ( -18.22780087662121673, -5.500000000000063061, 61.48459894673894155 ) ) ;
#63613 = CARTESIAN_POINT ( 'NONE',  ( 4.379528057220339221, -16.55341960407611168, 62.70724293864769550 ) ) ;
#63612 = CARTESIAN_POINT ( 'NONE',  ( 4.483927247898790824, -16.52544592524335698, 70.20942372801904696 ) ) ;
#63614 = CARTESIAN_POINT ( 'NONE',  ( 24.69864206457978639, 7.736332803992567619, 171.5373547058828763 ) ) ;
#63615 = CARTESIAN_POINT ( 'NONE',  ( 5.049401038297881783, 19.05341960407617563, 97.29275706135233293 ) ) ;
#63616 = CARTESIAN_POINT ( 'NONE',  ( 31.99364916731006048, 4.791014396527177230E-13, 45.00000000000022027 ) ) ;
#63617 = ADVANCED_FACE ( 'NONE', ( #26185 ), #118184, .F. ) ;
#63618 = CARTESIAN_POINT ( 'NONE',  ( -12.06949235617739369, -12.14591786802326823, 39.37609039468567573 ) ) ;
#63619 = CARTESIAN_POINT ( 'NONE',  ( 21.55341960407610458, 5.719274019375980345, 113.9572429386477239 ) ) ;
#63620 = CARTESIAN_POINT ( 'NONE',  ( 10.81492255796078972, 18.62759615963270932, 74.58224293864768129 ) ) ;
#63621 = CARTESIAN_POINT ( 'NONE',  ( 19.02544592524343514, -5.153800228976328945, 113.5405762719810241 ) ) ;
#63622 = CARTESIAN_POINT ( 'NONE',  ( -0.05219959533934338120, 16.53943276465976808, 57.50109039468568994 ) ) ;
#63623 = CARTESIAN_POINT ( 'NONE',  ( 13.89961937509977652, -13.97604488694527269, 68.12390960531436690 ) ) ;
#63625 = CARTESIAN_POINT ( 'NONE',  ( -13.97604488694547697, 13.89961937509957934, 108.1260903946856331 ) ) ;
#63624 = CARTESIAN_POINT ( 'NONE',  ( 5.719274019375673035, 21.55341960407619339, 42.29275706135235424 ) ) ;
#63626 = CARTESIAN_POINT ( 'NONE',  ( 0.05219959533909260263, 19.03943276465977164, 114.9989096053143669 ) ) ;
#63627 = CARTESIAN_POINT ( 'NONE',  ( 19.05341960407617918, -5.049401038297876454, 31.04275706135232227 ) ) ;
#63628 = CARTESIAN_POINT ( 'NONE',  ( -14.29746914071037622, -8.314922557961029526, 44.16775706135234714 ) ) ;
#63629 = CARTESIAN_POINT ( 'NONE',  ( 9.474510206698971260, -16.51473224551069308, 97.91557627198102409 ) ) ;
#63630 = CARTESIAN_POINT ( 'NONE',  ( 5.823673210054125526, 21.52544592524343514, 109.7905762719810383 ) ) ;
#63631 = CARTESIAN_POINT ( 'NONE',  ( -9.564922557960796823, -16.46253265017161027, 57.08224293864769550 ) ) ;
#63632 = CARTESIAN_POINT ( 'NONE',  ( -16.62475595723696031, 7.163666690055234376, 25.52713351810466591 ) ) ;
#63633 = CARTESIAN_POINT ( 'NONE',  ( 0.05219959533910956823, 16.53943276465976808, 84.99890960531436690 ) ) ;
#63634 = CARTESIAN_POINT ( 'NONE',  ( -19.02544592524342804, 5.153800228976336051, 111.0405762719810099 ) ) ;
#63635 = CARTESIAN_POINT ( 'NONE',  ( -17.44270441346513678, 5.991230190323086013, 33.63664920735774189 ) ) ;
#63636 = CARTESIAN_POINT ( 'NONE',  ( 10.72451020669898902, -18.67979575497178502, 97.91557627198103830 ) ) ;
#63637 = CARTESIAN_POINT ( 'NONE',  ( -0.05219959533936034679, 19.03943276465977164, 62.50109039468566863 ) ) ;
#63638 = CARTESIAN_POINT ( 'NONE',  ( -5.719274019375978568, 21.55341960407610458, 30.20724293864769550 ) ) ;
#63639 = CARTESIAN_POINT ( 'NONE',  ( -13.97604488694527625, -13.89961937509977652, 21.87390960531435979 ) ) ;
#63640 = CARTESIAN_POINT ( 'NONE',  ( 21.53943276465977519, -0.05219959533907433946, 58.74890960531436690 ) ) ;
#63641 = CONICAL_SURFACE ( 'NONE', #47486, 40.00000000000002132, 0.06108652381980166773 ) ;
#63642 = CARTESIAN_POINT ( 'NONE',  ( -16.46253265017160317, 9.564922557960807481, 100.8322429386477097 ) ) ;
#63643 = CARTESIAN_POINT ( 'NONE',  ( -5.719274019375665041, -21.55341960407619695, 74.79275706135234714 ) ) ;
#63644 = CARTESIAN_POINT ( 'NONE',  ( -9.474510206698964154, 16.51473224551069663, 50.41557627198102409 ) ) ;
#63645 = CARTESIAN_POINT ( 'NONE',  ( 16.52544592524342804, -4.483927247898539470, 83.54057627198102409 ) ) ;
#63646 = CARTESIAN_POINT ( 'NONE',  ( 0.05219959533934541429, -16.53943276465976808, 30.00109039468568284 ) ) ;
#63647 = CARTESIAN_POINT ( 'NONE',  ( 19.03943276465977164, -0.05219959533909143690, 58.74890960531435979 ) ) ;
#63648 = CARTESIAN_POINT ( 'NONE',  ( 5.823673210054444382, -21.52544592524334988, 65.20942372801901854 ) ) ;
#63649 = EDGE_LOOP ( 'NONE', ( #119590, #37646, #82480, #150835 ) ) ;
#63650 = CARTESIAN_POINT ( 'NONE',  ( -0.05219959533936034679, 19.03943276465977164, 22.50109039468566152 ) ) ;
#63651 = EDGE_CURVE ( 'NONE', #174040, #151167, #144348, .T. ) ;
#63652 = CARTESIAN_POINT ( 'NONE',  ( 13.97604488694548053, -13.89961937509957401, 40.62609039468564731 ) ) ;
#63653 = CARTESIAN_POINT ( 'NONE',  ( -17.50000000000002132, -5.499999999999948486, 91.28230962303565832 ) ) ;
#63654 = CARTESIAN_POINT ( 'NONE',  ( 15.72974639402176855, 15.80617190586768217, 31.87609039468567929 ) ) ;
#63655 = CARTESIAN_POINT ( 'NONE',  ( -18.22780087662121673, -5.500000000000063061, 46.48459894673893444 ) ) ;
#63656 = CARTESIAN_POINT ( 'NONE',  ( -16.51473224551082808, 9.474510206698731452, 33.33442372801899722 ) ) ;
#63657 = CARTESIAN_POINT ( 'NONE',  ( 19.02544592524343514, -5.153800228976328945, 83.54057627198100988 ) ) ;
#63658 = CARTESIAN_POINT ( 'NONE',  ( 5.049401038298161559, -19.05341960407611168, 67.70724293864769550 ) ) ;
#63659 = CARTESIAN_POINT ( 'NONE',  ( 16.52544592524342804, -4.483927247898539470, 23.54057627198102765 ) ) ;
#63661 = CARTESIAN_POINT ( 'NONE',  ( -5.719274019375665041, -21.55341960407619695, 84.79275706135234714 ) ) ;
#63660 = CARTESIAN_POINT ( 'NONE',  ( -0.05219959533909027116, -19.03943276465977164, 112.4989096053143669 ) ) ;
#63662 = CARTESIAN_POINT ( 'NONE',  ( 36.91746824999999887, 11.99521256947799053, -8.024999997268814411 ) ) ;
#63663 = DIRECTION ( 'NONE',  ( 0.000000000000000000, 0.000000000000000000, -1.000000000000000000 ) ) ;
#63664 = CARTESIAN_POINT ( 'NONE',  ( 5.823673210054444382, -21.52544592524334988, 90.20942372801903275 ) ) ;
#63665 = CARTESIAN_POINT ( 'NONE',  ( 23.94686256013573100, -0.9720251121415568463, -57.02522261278120652 ) ) ;
#63666 = CARTESIAN_POINT ( 'NONE',  ( 9.564922557960805705, 16.46253265017160317, 104.5822429386476955 ) ) ;
#63667 = CARTESIAN_POINT ( 'NONE',  ( 34.48736576873178450, 1.429538131128955669, 89.67663809442005629 ) ) ;
#63668 = CARTESIAN_POINT ( 'NONE',  ( -5.823673210054116645, -21.52544592524344225, 67.29057627198103830 ) ) ;
#63669 = CARTESIAN_POINT ( 'NONE',  ( -16.55341960407617563, 4.379528057220093196, 113.5427570613523756 ) ) ;
#63671 = CARTESIAN_POINT ( 'NONE',  ( 13.97604488694527802, 13.89961937509977652, 89.37390960531436690 ) ) ;
#63670 = CARTESIAN_POINT ( 'NONE',  ( -8.224510206698948167, 14.34966873604960824, 110.4155762719810383 ) ) ;
#63672 = CARTESIAN_POINT ( 'NONE',  ( -19.02544592524334988, -5.153800228976617603, 18.95942372801899722 ) ) ;
#63673 = CARTESIAN_POINT ( 'NONE',  ( -14.29746914071049879, 8.314922557960819915, 100.8322429386477097 ) ) ;
#63674 = CARTESIAN_POINT ( 'NONE',  ( 5.719274019375673035, 21.55341960407619339, 62.29275706135236845 ) ) ;
#63675 = DIRECTION ( 'NONE',  ( -1.000000000000000000, -0.000000000000000000, -0.000000000000000000 ) ) ;
#63676 = CARTESIAN_POINT ( 'NONE',  ( -4.379528057220086978, -16.55341960407618274, 104.7927570613523898 ) ) ;
#63677 = CARTESIAN_POINT ( 'NONE',  ( -9.564922557961040184, 16.46253265017147172, 62.91775706135233293 ) ) ;
#63678 = CARTESIAN_POINT ( 'NONE',  ( -29.86685920354755197, -21.69954338932560134, -6.924999997268813878 ) ) ;
#63679 = CARTESIAN_POINT ( 'NONE',  ( 16.46253265017160672, -9.564922557960803928, 103.3322429386476955 ) ) ;
#63680 = CARTESIAN_POINT ( 'NONE',  ( 8.314922557960818139, 14.29746914071049879, 79.58224293864769550 ) ) ;
#63681 = CARTESIAN_POINT ( 'NONE',  ( -9.474510206698720793, -16.51473224551083518, 59.58442372801900433 ) ) ;
#63682 = CIRCLE ( 'NONE', #86347, 9.100000000000001421 ) ;
#63683 = CARTESIAN_POINT ( 'NONE',  ( 19.03943276465977164, -0.05219959533909143690, 63.74890960531435979 ) ) ;
#63684 = CARTESIAN_POINT ( 'NONE',  ( 16.55341960407611168, 4.379528057220329451, 63.95724293864770260 ) ) ;
#63685 = CARTESIAN_POINT ( 'NONE',  ( 19.02544592524334988, 5.153800228976608722, 96.45942372801897591 ) ) ;
#63686 = CARTESIAN_POINT ( 'NONE',  ( -10.81492255796078084, -18.62759615963271287, 47.08224293864770260 ) ) ;
#63687 = ORIENTED_EDGE ( 'NONE', *, *, #197919, .F. ) ;
#63688 = CARTESIAN_POINT ( 'NONE',  ( 4.483927247898545687, 16.52544592524342804, 114.7905762719810383 ) ) ;
#63689 = CARTESIAN_POINT ( 'NONE',  ( -17.31747979337949772, -6.344076630961024144, 31.37944868065185844 ) ) ;
#63691 = CARTESIAN_POINT ( 'NONE',  ( -5.719274019375978568, 21.55341960407610458, 65.20724293864768129 ) ) ;
#63690 = CARTESIAN_POINT ( 'NONE',  ( 13.97604488694527802, 13.89961937509977652, 74.37390960531436690 ) ) ;
#63693 = CARTESIAN_POINT ( 'NONE',  ( 5.153800228976335163, 19.02544592524342804, 74.79057627198103830 ) ) ;
#63692 = CARTESIAN_POINT ( 'NONE',  ( 16.55341960407618274, -4.379528057220086978, 86.04275706135236135 ) ) ;
#63694 = CARTESIAN_POINT ( 'NONE',  ( 5.153800228976615827, -19.02544592524334988, 60.20942372801899012 ) ) ;
#63695 = CARTESIAN_POINT ( 'NONE',  ( -10.72451020669870658, -18.67979575497194134, 79.58442372801903275 ) ) ;
#63696 = CARTESIAN_POINT ( 'NONE',  ( 21.52544592524344225, -5.823673210054117533, 58.54057627198103120 ) ) ;
#63697 = CARTESIAN_POINT ( 'NONE',  ( -5.153800228976328057, -19.02544592524343514, 107.2905762719810383 ) ) ;
#63698 = CARTESIAN_POINT ( 'NONE',  ( 19.05341960407611168, 5.049401038298154454, 33.95724293864769550 ) ) ;
#63699 = CARTESIAN_POINT ( 'NONE',  ( -14.29746914071037622, -8.314922557961029526, 104.1677570613523471 ) ) ;
#63700 = CARTESIAN_POINT ( 'NONE',  ( 12.06949235617739724, 12.14591786802326823, 21.87609039468567573 ) ) ;
#63701 = CARTESIAN_POINT ( 'NONE',  ( 17.50000000000000000, -5.500000000000000888, 43.29690382534172244 ) ) ;
#63702 = CARTESIAN_POINT ( 'NONE',  ( -5.719274019375665041, -21.55341960407619695, 99.79275706135234714 ) ) ;
#63703 = CARTESIAN_POINT ( 'NONE',  ( 14.29746914071049879, -8.314922557960816363, 63.33224293864770260 ) ) ;
#63704 = CARTESIAN_POINT ( 'NONE',  ( 12.14591786802309770, 12.06949235617756955, 69.37390960531436690 ) ) ;
#63705 = CARTESIAN_POINT ( 'NONE',  ( 18.67979575497178502, 10.72451020669898547, 94.16557627198103830 ) ) ;
#63706 = CARTESIAN_POINT ( 'NONE',  ( -21.52544592524343514, 5.823673210054127303, 86.04057627198102409 ) ) ;
#63707 = CARTESIAN_POINT ( 'NONE',  ( -0.6194686979411263561, -31.77050690183225257, -45.83912112027729080 ) ) ;
#63708 = CARTESIAN_POINT ( 'NONE',  ( 18.62759615963271287, -10.81492255796078972, 48.33224293864770260 ) ) ;
#63709 = CARTESIAN_POINT ( 'NONE',  ( 16.53943276465976808, 0.05219959533934440121, 61.25109039468567573 ) ) ;
#63710 = CARTESIAN_POINT ( 'NONE',  ( -8.224510206698948167, 14.34966873604960824, 90.41557627198103830 ) ) ;
#63711 = CARTESIAN_POINT ( 'NONE',  ( -19.02544592524342804, 5.153800228976336051, 51.04057627198103120 ) ) ;
#63712 = CARTESIAN_POINT ( 'NONE',  ( 34.37447276284161291, -6.948158515131153123, 47.85536288891451306 ) ) ;
#63713 = CARTESIAN_POINT ( 'NONE',  ( -12.06949235617739369, -12.14591786802326823, 99.37609039468568994 ) ) ;
#63714 = CARTESIAN_POINT ( 'NONE',  ( 21.52544592524334988, 5.823673210054432836, 31.45942372801901854 ) ) ;
#63715 = CARTESIAN_POINT ( 'NONE',  ( -9.564922557960796823, -16.46253265017161027, 97.08224293864769550 ) ) ;
#63716 = CARTESIAN_POINT ( 'NONE',  ( 10.72451020669871369, 18.67979575497193778, 67.08442372801901854 ) ) ;
#63717 = CARTESIAN_POINT ( 'NONE',  ( -16.51473224551069308, -9.474510206698971260, 21.66557627198102765 ) ) ;
#63718 = CARTESIAN_POINT ( 'NONE',  ( 19.05341960407611168, 5.049401038298154454, 23.95724293864769194 ) ) ;
#63719 = ORIENTED_EDGE ( 'NONE', *, *, #36310, .F. ) ;
#63720 = CARTESIAN_POINT ( 'NONE',  ( -5.719274019375665041, -21.55341960407619695, 59.79275706135234714 ) ) ;
#63722 = CARTESIAN_POINT ( 'NONE',  ( 19.05341960407611168, 5.049401038298154454, 23.95724293864769194 ) ) ;
#63721 = CARTESIAN_POINT ( 'NONE',  ( 9.564922557960805705, 16.46253265017160317, 49.58224293864770260 ) ) ;
#63723 = CARTESIAN_POINT ( 'NONE',  ( -16.51473224551069308, -9.474510206698971260, 96.66557627198102409 ) ) ;
#63724 = CARTESIAN_POINT ( 'NONE',  ( 9.564922557961047289, -16.46253265017146816, 70.41775706135233293 ) ) ;
#63725 = CARTESIAN_POINT ( 'NONE',  ( -21.53943276465977519, -0.05219959533937600094, 48.75109039468568284 ) ) ;
#63726 = CARTESIAN_POINT ( 'NONE',  ( 16.51473224551083163, -9.474510206698727899, 60.83442372801900433 ) ) ;
#63727 = CARTESIAN_POINT ( 'NONE',  ( -13.97604488694527625, -13.89961937509977652, 36.87390960531436690 ) ) ;
#63728 = CARTESIAN_POINT ( 'NONE',  ( -16.55341960407617563, 4.379528057220093196, 108.5427570613523756 ) ) ;
#63729 = CARTESIAN_POINT ( 'NONE',  ( -0.05219959533936034679, 19.03943276465977164, 77.50109039468566152 ) ) ;
#63730 = CARTESIAN_POINT ( 'NONE',  ( -0.05219959533910754901, -16.53943276465976808, 32.49890960531435979 ) ) ;
#63731 = CARTESIAN_POINT ( 'NONE',  ( -16.46253265017146816, -9.564922557961047289, 54.16775706135234003 ) ) ;
#63732 = CARTESIAN_POINT ( 'NONE',  ( -13.97604488694527625, -13.89961937509977652, 96.87390960531433848 ) ) ;
#63733 = CARTESIAN_POINT ( 'NONE',  ( 18.62759615963255655, 10.81492255796105972, 106.6677570613523756 ) ) ;
#63734 = CARTESIAN_POINT ( 'NONE',  ( 19.05341960407617918, -5.049401038297876454, 26.04275706135233293 ) ) ;
#63735 = CARTESIAN_POINT ( 'NONE',  ( 13.97604488694527802, 13.89961937509977652, 34.37390960531436690 ) ) ;
#63736 = CARTESIAN_POINT ( 'NONE',  ( -0.05219959533937732626, 21.53943276465977519, 87.50109039468568994 ) ) ;
#63737 = CARTESIAN_POINT ( 'NONE',  ( -4.483927247898782831, 16.52544592524335698, 37.70942372801900433 ) ) ;
#63738 = EDGE_CURVE ( 'NONE', #42359, #93735, #27984, .T. ) ;
#63739 = CARTESIAN_POINT ( 'NONE',  ( -9.564922557960796823, -16.46253265017161027, 92.08224293864769550 ) ) ;
#63740 = CARTESIAN_POINT ( 'NONE',  ( -27.73933785331498925, -9.013057229001049109, 138.9750000027311785 ) ) ;
#63741 = CARTESIAN_POINT ( 'NONE',  ( 16.46253265017160672, -9.564922557960803928, 73.33224293864769550 ) ) ;
#63742 = CARTESIAN_POINT ( 'NONE',  ( -28.82186960331499037, 2.428612866367529932E-14, 142.0000000000000000 ) ) ;
#63743 = CARTESIAN_POINT ( 'NONE',  ( 9.564922557961047289, -16.46253265017146816, 90.41775706135234714 ) ) ;
#63744 = CARTESIAN_POINT ( 'NONE',  ( 9.474510206698971260, -16.51473224551069308, 102.9155762719810241 ) ) ;
#63745 = CARTESIAN_POINT ( 'NONE',  ( 10.72451020669871369, 18.67979575497193778, 97.08442372801904696 ) ) ;
#63746 = CARTESIAN_POINT ( 'NONE',  ( -0.05219959533910754901, -16.53943276465976808, 102.4989096053143811 ) ) ;
#63747 = CARTESIAN_POINT ( 'NONE',  ( 16.51473224551069308, 9.474510206698969483, 24.16557627198102765 ) ) ;
#63748 = CARTESIAN_POINT ( 'NONE',  ( -18.62759615963270932, 10.81492255796079327, 50.83224293864770971 ) ) ;
#63749 = CARTESIAN_POINT ( 'NONE',  ( -15.72974639402197994, 15.80617190586746368, 30.62390960531436335 ) ) ;
#63750 = CARTESIAN_POINT ( 'NONE',  ( 12.06949235617757843, -12.14591786802309237, 108.1239096053143811 ) ) ;
#63751 = CARTESIAN_POINT ( 'NONE',  ( -0.6707077324887361636, -8.945340038113741343, -61.92615459704094860 ) ) ;
#63752 = CARTESIAN_POINT ( 'NONE',  ( -16.51473224551082808, 9.474510206698731452, 58.33442372801900433 ) ) ;
#63753 = CARTESIAN_POINT ( 'NONE',  ( -16.53943276465976808, 0.05219959533911058130, 41.24890960531435269 ) ) ;
#63754 = CARTESIAN_POINT ( 'NONE',  ( -0.05219959533907301413, -21.53943276465977519, 22.49890960531436335 ) ) ;
#63755 = CARTESIAN_POINT ( 'NONE',  ( 21.52544592524334988, 5.823673210054432836, 86.45942372801901854 ) ) ;
#63756 = CARTESIAN_POINT ( 'NONE',  ( -0.05219959533907301413, -21.53943276465977519, 77.49890960531433848 ) ) ;
